#130574 = CARTESIAN_POINT ( 'NONE',  ( 15.72974639402176855, 15.80617190586768217, 26.87609039468567218 ) ) ;
#130575 = CARTESIAN_POINT ( 'NONE',  ( 22.44159573604009594, -16.30477369853687364, 142.1750000027311671 ) ) ;
#130576 = CARTESIAN_POINT ( 'NONE',  ( 8.224510206698742110, 14.34966873604972548, 107.0844237280190043 ) ) ;
#130577 = CARTESIAN_POINT ( 'NONE',  ( 16.55341960407611168, 4.379528057220329451, 113.9572429386477239 ) ) ;
#130578 = CARTESIAN_POINT ( 'NONE',  ( -19.02544592524342804, 5.153800228976336051, 76.04057627198102409 ) ) ;
#130579 = CARTESIAN_POINT ( 'NONE',  ( 16.20063489777861676, -7.373262058553140541, 22.00000000000000711 ) ) ;
#130580 = CARTESIAN_POINT ( 'NONE',  ( 37.99999999999999289, 12.34694845685046793, -10.64999999453762669 ) ) ;
#130581 = CARTESIAN_POINT ( 'NONE',  ( -16.52544592524342804, 4.483927247898546575, 31.04057627198102409 ) ) ;
#130582 = CARTESIAN_POINT ( 'NONE',  ( 21.53943276465977519, 0.05219959533937863772, 56.25109039468568284 ) ) ;
#130583 = CARTESIAN_POINT ( 'NONE',  ( 27.29882810768421919, -25.71095057349885948, -18.52182797988482221 ) ) ;
#130584 = CARTESIAN_POINT ( 'NONE',  ( -10.81492255796105439, 18.62759615963255655, 87.91775706135234714 ) ) ;
#130585 = CARTESIAN_POINT ( 'NONE',  ( -5.049401038298153566, 19.05341960407611168, 50.20724293864770260 ) ) ;
#130586 = CARTESIAN_POINT ( 'NONE',  ( -16.46253265017160317, 9.564922557960807481, 50.83224293864770260 ) ) ;
#130587 = ORIENTED_EDGE ( 'NONE', *, *, #181371, .F. ) ;
#130588 = CARTESIAN_POINT ( 'NONE',  ( 21.55341960407619695, -5.719274019375665929, 96.04275706135236135 ) ) ;
#130589 = CARTESIAN_POINT ( 'NONE',  ( 14.34966873604972726, -8.224510206698740333, 60.83442372801901854 ) ) ;
#130590 = CARTESIAN_POINT ( 'NONE',  ( -21.52544592524334988, -5.823673210054445271, 88.95942372801901854 ) ) ;
#130591 = CARTESIAN_POINT ( 'NONE',  ( 10.81492255796078972, 18.62759615963270932, 24.58224293864768839 ) ) ;
#130592 = CARTESIAN_POINT ( 'NONE',  ( 5.153800228976615827, -19.02544592524334988, 95.20942372801897591 ) ) ;
#130593 = CARTESIAN_POINT ( 'NONE',  ( 21.53943276465977519, 0.05219959533937863772, 66.25109039468567573 ) ) ;
#130594 = CARTESIAN_POINT ( 'NONE',  ( 4.483927247898790824, -16.52544592524335698, 35.20942372801901854 ) ) ;
#130595 = CARTESIAN_POINT ( 'NONE',  ( 21.55341960407610458, 5.719274019375980345, 88.95724293864769550 ) ) ;
#130596 = CARTESIAN_POINT ( 'NONE',  ( 13.97604488694548053, -13.89961937509957401, 80.62609039468567573 ) ) ;
#130597 = CARTESIAN_POINT ( 'NONE',  ( 13.97604488694527802, 13.89961937509977652, 64.37390960531436690 ) ) ;
#130598 = CARTESIAN_POINT ( 'NONE',  ( -9.564922557961040184, 16.46253265017147172, 97.91775706135233293 ) ) ;
#130599 = CIRCLE ( 'NONE', #182456, 40.00000000000002132 ) ;
#130600 = CARTESIAN_POINT ( 'NONE',  ( 5.049401038297881783, 19.05341960407617563, 107.2927570613523187 ) ) ;
#130601 = CARTESIAN_POINT ( 'NONE',  ( 14.29746914071049879, -8.314922557960816363, 53.33224293864769550 ) ) ;
#130602 = EDGE_CURVE ( 'NONE', #166806, #126933, #67622, .T. ) ;
#130603 = CARTESIAN_POINT ( 'NONE',  ( 16.51473224551083163, -9.474510206698727899, 75.83442372801900433 ) ) ;
#130604 = CARTESIAN_POINT ( 'NONE',  ( 4.483927247898790824, -16.52544592524335698, 65.20942372801901854 ) ) ;
#130605 = CARTESIAN_POINT ( 'NONE',  ( -13.89961937509977652, 13.97604488694528158, 35.62390960531435269 ) ) ;
#130606 = CARTESIAN_POINT ( 'NONE',  ( -0.05219959533909027116, -19.03943276465977164, 57.49890960531435979 ) ) ;
#130607 = CARTESIAN_POINT ( 'NONE',  ( 16.55341960407618274, -4.379528057220086978, 56.04275706135235424 ) ) ;
#130608 = CARTESIAN_POINT ( 'NONE',  ( -22.44159573604010305, 16.30477369853692338, 148.6750000027311671 ) ) ;
#130609 = CARTESIAN_POINT ( 'NONE',  ( -5.049401038298153566, 19.05341960407611168, 110.2072429386476671 ) ) ;
#130610 = CARTESIAN_POINT ( 'NONE',  ( 19.05341960407611168, 5.049401038298154454, 23.95724293864769194 ) ) ;
#130611 = ORIENTED_EDGE ( 'NONE', *, *, #18566, .T. ) ;
#130612 = CARTESIAN_POINT ( 'NONE',  ( 13.89961937509957401, 13.97604488694547697, 106.8760903946856757 ) ) ;
#130613 = CARTESIAN_POINT ( 'NONE',  ( -10.81492255796078084, -18.62759615963271287, 42.08224293864769550 ) ) ;
#130615 = CARTESIAN_POINT ( 'NONE',  ( -14.34966873604972548, 8.224510206698743886, 28.33442372801902209 ) ) ;
#130614 = CARTESIAN_POINT ( 'NONE',  ( 9.564922557961047289, -16.46253265017146816, 35.41775706135233293 ) ) ;
#130616 = CARTESIAN_POINT ( 'NONE',  ( 19.03943276465977164, -0.05219959533909143690, 23.74890960531435269 ) ) ;
#130617 = CARTESIAN_POINT ( 'NONE',  ( -9.474510206698964154, 16.51473224551069663, 45.41557627198103120 ) ) ;
#130618 = CARTESIAN_POINT ( 'NONE',  ( -15.72974639402197994, 15.80617190586746368, 75.62390960531439532 ) ) ;
#130619 = CARTESIAN_POINT ( 'NONE',  ( -16.51473224551069308, -9.474510206698971260, 101.6655762719810241 ) ) ;
#130620 = CARTESIAN_POINT ( 'NONE',  ( 19.05341960407611168, 5.049401038298154454, 53.95724293864770260 ) ) ;
#130621 = CARTESIAN_POINT ( 'NONE',  ( 27.73933785331498925, -9.013057229001034898, 144.2750000027311899 ) ) ;
#130622 = CARTESIAN_POINT ( 'NONE',  ( 5.153800228976615827, -19.02544592524334988, 80.20942372801901854 ) ) ;
#130623 = CARTESIAN_POINT ( 'NONE',  ( -16.52544592524342804, 4.483927247898546575, 71.04057627198103830 ) ) ;
#130624 = CARTESIAN_POINT ( 'NONE',  ( 21.52544592524344225, -5.823673210054117533, 48.54057627198103120 ) ) ;
#130625 = CARTESIAN_POINT ( 'NONE',  ( -18.62759615963255300, -10.81492255796106328, 109.1677570613523613 ) ) ;
#130626 = CARTESIAN_POINT ( 'NONE',  ( -5.823673210054116645, -21.52544592524344225, 97.29057627198105251 ) ) ;
#130627 = CARTESIAN_POINT ( 'NONE',  ( -10.72451020669870658, -18.67979575497194134, 69.58442372801900433 ) ) ;
#130628 = B_SPLINE_CURVE_WITH_KNOTS ( 'NONE', 3,
 ( #73957, #130862, #29435, #105270, #91066, #182119, #59753, #122414, #137589, #38870, #90095, #131873, #199272, #12292, #167936, #70206, #152753, #54036, #121423, #14243, #106253, #197296, #75915, #151777, #115710, #74933, #193558, #177398, #58759, #183115, #120428, #136596 ),
 .UNSPECIFIED., .F., .F.,
 ( 4, 2, 2, 2, 2, 2, 2, 2, 2, 2, 2, 2, 2, 2, 2, 4 ),
 ( 2.969368287472575283E-17, 0.0003712461730036904100, 0.0007424923460073511129, 0.001113738519011011653, 0.001484984692014672519, 0.002227477038022000321, 0.002598723211025682003, 0.002969969384029364119, 0.003341215557033045368, 0.003712461730036727917, 0.004083707903040409599, 0.004454954076044090848, 0.004826200249047772964, 0.005197446422051455080, 0.005568692595055137196, 0.005939938768058818444 ),
 .UNSPECIFIED. ) ;
#130629 = CARTESIAN_POINT ( 'NONE',  ( -21.52544592524334988, -5.823673210054445271, 78.95942372801901854 ) ) ;
#130630 = ADVANCED_FACE ( 'NONE', ( #74976 ), #73009, .F. ) ;
#130631 = CARTESIAN_POINT ( 'NONE',  ( 16.51473224551069308, 9.474510206698969483, 114.1655762719810241 ) ) ;
#130633 = CARTESIAN_POINT ( 'NONE',  ( 15.72974639402176855, 15.80617190586768217, 71.87609039468568994 ) ) ;
#130632 = CARTESIAN_POINT ( 'NONE',  ( -0.05219959533934338120, 16.53943276465976808, 112.5010903946857042 ) ) ;
#130634 = CARTESIAN_POINT ( 'NONE',  ( -19.03943276465977164, 0.05219959533909376836, 66.24890960531436690 ) ) ;
#130635 = CARTESIAN_POINT ( 'NONE',  ( -21.53943276465977519, -0.05219959533937600094, 28.75109039468567929 ) ) ;
#130636 = CARTESIAN_POINT ( 'NONE',  ( -5.049401038298153566, 19.05341960407611168, 65.20724293864765286 ) ) ;
#130637 = CARTESIAN_POINT ( 'NONE',  ( 12.14591786802309770, 12.06949235617756955, 74.37390960531436690 ) ) ;
#130638 = CARTESIAN_POINT ( 'NONE',  ( 12.06949235617757843, -12.14591786802309237, 43.12390960531435269 ) ) ;
#130639 = CARTESIAN_POINT ( 'NONE',  ( 15.72974639402199770, -15.80617190586745480, 53.12390960531436690 ) ) ;
#130640 = EDGE_CURVE ( 'NONE', #12139, #197947, #149834, .T. ) ;
#130641 = CARTESIAN_POINT ( 'NONE',  ( -19.05341960407611168, -5.049401038298163336, 61.45724293864769550 ) ) ;
#130642 = CARTESIAN_POINT ( 'NONE',  ( 21.55341960407610458, 5.719274019375980345, 68.95724293864769550 ) ) ;
#130643 = CARTESIAN_POINT ( 'NONE',  ( 19.05341960407617918, -5.049401038297876454, 66.04275706135233293 ) ) ;
#130645 = CARTESIAN_POINT ( 'NONE',  ( 4.483927247898545687, 16.52544592524342804, 64.79057627198103830 ) ) ;
#130644 = CARTESIAN_POINT ( 'NONE',  ( -16.46253265017146816, -9.564922557961047289, 19.16775706135233293 ) ) ;
#130646 = CARTESIAN_POINT ( 'NONE',  ( 18.62759615963271287, -10.81492255796078972, 43.33224293864769550 ) ) ;
#130647 = VERTEX_POINT ( 'NONE', #75959 ) ;
#130648 = LINE ( 'NONE', #126654, #133424 ) ;
#130650 = CARTESIAN_POINT ( 'NONE',  ( 27.73933785331498569, 2.768321779492822058E-14, 140.3750000027311842 ) ) ;
#130649 = CARTESIAN_POINT ( 'NONE',  ( 16.52544592524335698, 4.483927247898782831, 96.45942372801901854 ) ) ;
#130651 = CARTESIAN_POINT ( 'NONE',  ( -13.89961937509957401, -13.97604488694547875, 84.37609039468567573 ) ) ;
#130652 = CARTESIAN_POINT ( 'NONE',  ( 12.06949235617757843, -12.14591786802309237, 73.12390960531436690 ) ) ;
#130653 = CARTESIAN_POINT ( 'NONE',  ( -5.000000000000000000, -130.0000000000000000, 13.99999999999999822 ) ) ;
#130654 = CARTESIAN_POINT ( 'NONE',  ( -5.049401038298153566, 19.05341960407611168, 65.20724293864765286 ) ) ;
#130655 = CARTESIAN_POINT ( 'NONE',  ( -14.34966873604960291, -8.224510206698953496, 51.66557627198102409 ) ) ;
#130656 = CARTESIAN_POINT ( 'NONE',  ( -5.153800228976328057, -19.02544592524343514, 82.29057627198103830 ) ) ;
#130657 = AXIS2_PLACEMENT_3D ( 'NONE', #105058, #167724, #103066 ) ;
#130659 = CARTESIAN_POINT ( 'NONE',  ( 0.05219959533909260263, 19.03943276465977164, 49.99890960531435979 ) ) ;
#130658 = CARTESIAN_POINT ( 'NONE',  ( 13.97604488694548053, -13.89961937509957401, 75.62609039468564731 ) ) ;
#130660 = CARTESIAN_POINT ( 'NONE',  ( -9.474510206698964154, 16.51473224551069663, 80.41557627198103830 ) ) ;
#130661 = CARTESIAN_POINT ( 'NONE',  ( -16.51473224551069308, -9.474510206698971260, 21.66557627198102765 ) ) ;
#130662 = CARTESIAN_POINT ( 'NONE',  ( -19.05341960407611168, -5.049401038298163336, 66.45724293864769550 ) ) ;
#130663 = CARTESIAN_POINT ( 'NONE',  ( -21.53943276465977519, 0.05219959533907696930, 56.24890960531436690 ) ) ;
#130664 = CARTESIAN_POINT ( 'NONE',  ( -16.46253265017160317, 9.564922557960807481, 45.83224293864769550 ) ) ;
#130665 = CARTESIAN_POINT ( 'NONE',  ( 21.52544592524344225, -5.823673210054117533, 53.54057627198103120 ) ) ;
#130666 = CARTESIAN_POINT ( 'NONE',  ( 9.564922557961047289, -16.46253265017146816, 80.41775706135234714 ) ) ;
#130667 = CARTESIAN_POINT ( 'NONE',  ( -8.314922557961024197, 14.29746914071037800, 102.9177570613523756 ) ) ;
#130668 = CARTESIAN_POINT ( 'NONE',  ( 9.474510206698729675, 16.51473224551082808, 42.08442372801900433 ) ) ;
#130670 = CARTESIAN_POINT ( 'NONE',  ( -16.53943276465976808, -0.05219959533934237506, 98.75109039468568994 ) ) ;
#130669 = CARTESIAN_POINT ( 'NONE',  ( -0.05219959533934338120, 16.53943276465976808, 57.50109039468568994 ) ) ;
#130671 = CARTESIAN_POINT ( 'NONE',  ( 18.39443945427631277, -5.499999999999984013, 41.01745347608650860 ) ) ;
#130672 = CARTESIAN_POINT ( 'NONE',  ( 14.29746914071037800, 8.314922557961029526, 76.66775706135234714 ) ) ;
#130673 = CARTESIAN_POINT ( 'NONE',  ( -5.719274019375978568, 21.55341960407610458, 30.20724293864769550 ) ) ;
#130674 = CARTESIAN_POINT ( 'NONE',  ( -19.05341960407611168, -5.049401038298163336, 31.45724293864769550 ) ) ;
#130675 = CARTESIAN_POINT ( 'NONE',  ( -16.53943276465976808, -0.05219959533934237506, 33.75109039468568284 ) ) ;
#130676 = CARTESIAN_POINT ( 'NONE',  ( 9.564922557960805705, 16.46253265017160317, 44.58224293864769550 ) ) ;
#130677 = CARTESIAN_POINT ( 'NONE',  ( -18.67979575497193778, 10.72451020669871902, 43.33442372801901143 ) ) ;
#130678 = CARTESIAN_POINT ( 'NONE',  ( -16.52544592524335698, -4.483927247898792601, 43.95942372801902565 ) ) ;
#130679 = CARTESIAN_POINT ( 'NONE',  ( -8.314922557960811034, -14.29746914071050412, 22.08224293864769194 ) ) ;
#130680 = CARTESIAN_POINT ( 'NONE',  ( 5.153800228976335163, 19.02544592524342804, 24.79057627198102765 ) ) ;
#130681 = CARTESIAN_POINT ( 'NONE',  ( 16.46253265017146816, 9.564922557961045513, 21.66775706135233648 ) ) ;
#130682 = CARTESIAN_POINT ( 'NONE',  ( 13.97604488694548053, -13.89961937509957401, 110.6260903946856615 ) ) ;
#130683 = CARTESIAN_POINT ( 'NONE',  ( -9.564922557961040184, 16.46253265017147172, 67.91775706135233293 ) ) ;
#130684 = CARTESIAN_POINT ( 'NONE',  ( 14.34966873604960469, 8.224510206698951720, 69.16557627198102409 ) ) ;
#130685 = CARTESIAN_POINT ( 'NONE',  ( 5.049401038298161559, -19.05341960407611168, 42.70724293864767418 ) ) ;
#130687 = DIRECTION ( 'NONE',  ( 0.000000000000000000, 0.7071067811865466846, 0.7071067811865484609 ) ) ;
#130686 = CARTESIAN_POINT ( 'NONE',  ( 13.97604488694548053, -13.89961937509957401, 80.62609039468567573 ) ) ;
#130688 = CARTESIAN_POINT ( 'NONE',  ( 21.53943276465977519, 0.05219959533937863772, 66.25109039468567573 ) ) ;
#130689 = CARTESIAN_POINT ( 'NONE',  ( 16.52544592524335698, 4.483927247898782831, 46.45942372801901854 ) ) ;
#130690 = CARTESIAN_POINT ( 'NONE',  ( 19.52837319214028255, -5.499999999999890754, 57.10471352585541638 ) ) ;
#130691 = CARTESIAN_POINT ( 'NONE',  ( -21.55341960407610458, -5.719274019375992779, 31.45724293864769550 ) ) ;
#130692 = CARTESIAN_POINT ( 'NONE',  ( 16.53943276465976808, 0.05219959533934440121, 26.25109039468567573 ) ) ;
#130693 = CARTESIAN_POINT ( 'NONE',  ( -27.19095269391954517, -8.032454009542490780, 149.5864051666458181 ) ) ;
#130694 = CARTESIAN_POINT ( 'NONE',  ( -21.97054992548845576, 8.562709642470919036, 171.7904333278019351 ) ) ;
#130695 = CARTESIAN_POINT ( 'NONE',  ( 19.03943276465977164, -0.05219959533909143690, 43.74890960531435979 ) ) ;
#130696 = CARTESIAN_POINT ( 'NONE',  ( -0.05219959533937732626, 21.53943276465977519, 107.5010903946856899 ) ) ;
#130697 = CARTESIAN_POINT ( 'NONE',  ( -13.89961937509977652, 13.97604488694528158, 50.62390960531435979 ) ) ;
#130698 = CARTESIAN_POINT ( 'NONE',  ( -10.72451020669870658, -18.67979575497194134, 69.58442372801900433 ) ) ;
#130699 = CARTESIAN_POINT ( 'NONE',  ( 21.52544592524334988, 5.823673210054432836, 106.4594237280190328 ) ) ;
#130700 = CARTESIAN_POINT ( 'NONE',  ( -16.55341960407617563, 4.379528057220093196, 113.5427570613523756 ) ) ;
#130701 = CARTESIAN_POINT ( 'NONE',  ( -13.89961937509977652, 13.97604488694528158, 35.62390960531435269 ) ) ;
#130702 = CARTESIAN_POINT ( 'NONE',  ( -19.05341960407611168, -5.049401038298163336, 86.45724293864769550 ) ) ;
#130703 = CARTESIAN_POINT ( 'NONE',  ( 21.52544592524334988, 5.823673210054432836, 51.45942372801901854 ) ) ;
#130704 = CARTESIAN_POINT ( 'NONE',  ( -9.564922557960796823, -16.46253265017161027, 32.08224293864769550 ) ) ;
#130705 = B_SPLINE_CURVE_WITH_KNOTS ( 'NONE', 3,
 ( #130478, #191176, #98131, #176016, #128483, #178013, #7136, #131490, #66820, #52650, #192175, #175010, #177024, #117324, #36474, #39480 ),
 .UNSPECIFIED., .F., .F.,
 ( 4, 2, 2, 2, 2, 2, 2, 4 ),
 ( 0.001218919368246023033, 0.002217820489337911892, 0.002717271049883857731, 0.003216721610429803570, 0.003716172170975749409, 0.004215622731521694380, 0.004715073292067640219, 0.005214523852613586058 ),
 .UNSPECIFIED. ) ;
#130706 = CARTESIAN_POINT ( 'NONE',  ( -18.67979575497193778, 10.72451020669871902, 48.33442372801902565 ) ) ;
#130708 = CARTESIAN_POINT ( 'NONE',  ( -5.153800228976328057, -19.02544592524343514, 107.2905762719810383 ) ) ;
#130707 = CARTESIAN_POINT ( 'NONE',  ( -16.46253265017146816, -9.564922557961047289, 94.16775706135233293 ) ) ;
#130709 = CARTESIAN_POINT ( 'NONE',  ( 19.05341960407611168, 5.049401038298154454, 23.95724293864769194 ) ) ;
#130710 = CARTESIAN_POINT ( 'NONE',  ( -21.52544592524343514, 5.823673210054127303, 111.0405762719810525 ) ) ;
#130711 = CARTESIAN_POINT ( 'NONE',  ( 16.46253265017146816, 9.564922557961045513, 31.66775706135232937 ) ) ;
#130712 = CARTESIAN_POINT ( 'NONE',  ( 16.52544592524342804, -4.483927247898539470, 113.5405762719810383 ) ) ;
#130713 = CARTESIAN_POINT ( 'NONE',  ( -0.05219959533909027116, -19.03943276465977164, 62.49890960531435979 ) ) ;
#130715 = AXIS2_PLACEMENT_3D ( 'NONE', #60072, #2371, #48888 ) ;
#130714 = CARTESIAN_POINT ( 'NONE',  ( 13.89961937509957401, 13.97604488694547697, 91.87609039468567573 ) ) ;
#130716 = CARTESIAN_POINT ( 'NONE',  ( -4.379528057220328563, 16.55341960407611168, 65.20724293864768129 ) ) ;
#130717 = CARTESIAN_POINT ( 'NONE',  ( 5.049401038297881783, 19.05341960407617563, 27.29275706135232937 ) ) ;
#130718 = CARTESIAN_POINT ( 'NONE',  ( 5.049401038298161559, -19.05341960407611168, 112.7072429386476813 ) ) ;
#130719 = CARTESIAN_POINT ( 'NONE',  ( -9.474510206698720793, -16.51473224551083518, 94.58442372801900433 ) ) ;
#130720 = CARTESIAN_POINT ( 'NONE',  ( -21.53943276465977519, 0.05219959533907696930, 91.24890960531436690 ) ) ;
#130721 = CIRCLE ( 'NONE', #121057, 7.500000000000000000 ) ;
#130722 = CARTESIAN_POINT ( 'NONE',  ( 15.80617190586769283, -15.72974639402175789, 45.62609039468567573 ) ) ;
#130723 = CARTESIAN_POINT ( 'NONE',  ( -4.483927247898782831, 16.52544592524335698, 42.70942372801901854 ) ) ;
#130724 = CARTESIAN_POINT ( 'NONE',  ( -0.05219959533934338120, 16.53943276465976808, 102.5010903946856899 ) ) ;
#130726 = CARTESIAN_POINT ( 'NONE',  ( -10.72451020669870658, -18.67979575497194134, 49.58442372801901143 ) ) ;
#130725 = CARTESIAN_POINT ( 'NONE',  ( 4.483927247898790824, -16.52544592524335698, 45.20942372801901854 ) ) ;
#130727 = CARTESIAN_POINT ( 'NONE',  ( -21.55341960407610458, -5.719274019375992779, 51.45724293864770260 ) ) ;
#130728 = CARTESIAN_POINT ( 'NONE',  ( 13.89961937509977652, -13.97604488694527269, 28.12390960531435624 ) ) ;
#130729 = CARTESIAN_POINT ( 'NONE',  ( 38.00000000000000000, 12.34694845685046616, -6.649999994537624914 ) ) ;
#130730 = CARTESIAN_POINT ( 'NONE',  ( 0.05219959533934541429, -16.53943276465976808, 60.00109039468568284 ) ) ;
#130731 = CARTESIAN_POINT ( 'NONE',  ( 10.72451020669898902, -18.67979575497178502, 87.91557627198103830 ) ) ;
#130732 = CARTESIAN_POINT ( 'NONE',  ( 4.483927247898545687, 16.52544592524342804, 39.79057627198103830 ) ) ;
#130733 = CARTESIAN_POINT ( 'NONE',  ( -8.224510206698735004, -14.34966873604973081, 59.58442372801901854 ) ) ;
#130734 = CARTESIAN_POINT ( 'NONE',  ( -19.05341960407617563, 5.049401038297882671, 103.5427570613523329 ) ) ;
#130735 = CARTESIAN_POINT ( 'NONE',  ( 5.719274019375991003, -21.55341960407610458, 97.70724293864772392 ) ) ;
#130736 = CARTESIAN_POINT ( 'NONE',  ( 16.53943276465976808, -0.05219959533910856209, 33.74890960531436690 ) ) ;
#130737 = EDGE_LOOP ( 'NONE', ( #165681, #38569, #71952, #45156 ) ) ;
#130738 = CARTESIAN_POINT ( 'NONE',  ( -16.53943276465976808, -0.05219959533934237506, 73.75109039468567573 ) ) ;
#130739 = CARTESIAN_POINT ( 'NONE',  ( 23.03403192006594224, 14.65170476119024201, 169.9999999999999716 ) ) ;
#130740 = CARTESIAN_POINT ( 'NONE',  ( -18.62759615963270932, 10.81492255796079327, 70.83224293864770971 ) ) ;
#130741 = CARTESIAN_POINT ( 'NONE',  ( 16.52544592524335698, 4.483927247898782831, 101.4594237280190185 ) ) ;
#130742 = ORIENTED_EDGE ( 'NONE', *, *, #170510, .F. ) ;
#130743 = CARTESIAN_POINT ( 'NONE',  ( 19.20446147854527297, 5.499999999999894307, 86.88999695167679249 ) ) ;
#130744 = CARTESIAN_POINT ( 'NONE',  ( 21.55341960407610458, 5.719274019375980345, 93.95724293864770971 ) ) ;
#130745 = CARTESIAN_POINT ( 'NONE',  ( -18.62759615963270932, 10.81492255796079327, 105.8322429386476955 ) ) ;
#130746 = CARTESIAN_POINT ( 'NONE',  ( 12.14591786802309770, 12.06949235617756955, 39.37390960531436690 ) ) ;
#130748 = CARTESIAN_POINT ( 'NONE',  ( -14.29746914071037622, -8.314922557961029526, 39.16775706135235424 ) ) ;
#130747 = CIRCLE ( 'NONE', #108085, 4.000000000000000888 ) ;
#130749 = CARTESIAN_POINT ( 'NONE',  ( -19.05341960407611168, -5.049401038298163336, 46.45724293864768129 ) ) ;
#130750 = CARTESIAN_POINT ( 'NONE',  ( 19.03943276465977164, -0.05219959533909143690, 63.74890960531435979 ) ) ;
#130751 = CARTESIAN_POINT ( 'NONE',  ( 13.97604488694527802, 13.89961937509977652, 114.3739096053143669 ) ) ;
#130752 = CARTESIAN_POINT ( 'NONE',  ( -9.474510206698964154, 16.51473224551069663, 115.4155762719810241 ) ) ;
#130753 = CARTESIAN_POINT ( 'NONE',  ( -9.564922557961040184, 16.46253265017147172, 102.9177570613523329 ) ) ;
#130754 = CARTESIAN_POINT ( 'NONE',  ( -19.02544592524334988, -5.153800228976617603, 48.95942372801900433 ) ) ;
#130755 = CARTESIAN_POINT ( 'NONE',  ( 18.67979575497178502, 10.72451020669898547, 94.16557627198103830 ) ) ;
#130756 = CARTESIAN_POINT ( 'NONE',  ( -12.06949235617756955, 12.14591786802309770, 25.62390960531435624 ) ) ;
#130757 = CARTESIAN_POINT ( 'NONE',  ( 10.72451020669898902, -18.67979575497178502, 42.91557627198103120 ) ) ;
#130759 = CARTESIAN_POINT ( 'NONE',  ( -5.049401038297874678, -19.05341960407617918, 109.7927570613523187 ) ) ;
#130758 = CARTESIAN_POINT ( 'NONE',  ( 18.67979575497178502, 10.72451020669898547, 84.16557627198103830 ) ) ;
#130760 = CARTESIAN_POINT ( 'NONE',  ( -5.049401038298153566, 19.05341960407611168, 105.2072429386476671 ) ) ;
#130761 = CARTESIAN_POINT ( 'NONE',  ( 5.823673210054444382, -21.52544592524334988, 75.20942372801901854 ) ) ;
#130762 = CARTESIAN_POINT ( 'NONE',  ( 13.89961937509977652, -13.97604488694527269, 68.12390960531436690 ) ) ;
#130763 = DIRECTION ( 'NONE',  ( 0.000000000000000000, 0.000000000000000000, -1.000000000000000000 ) ) ;
#130764 = CARTESIAN_POINT ( 'NONE',  ( -5.049401038298153566, 19.05341960407611168, 70.20724293864769550 ) ) ;
#130765 = CARTESIAN_POINT ( 'NONE',  ( -8.224510206698948167, 14.34966873604960824, 85.41557627198102409 ) ) ;
#130766 = EDGE_LOOP ( 'NONE', ( #117109, #95511, #184232 ) ) ;
#130767 = CARTESIAN_POINT ( 'NONE',  ( -9.474510206698720793, -16.51473224551083518, 104.5844237280190043 ) ) ;
#130768 = CARTESIAN_POINT ( 'NONE',  ( 16.18388926212238488, -7.379444403734519931, 82.06046848633847901 ) ) ;
#130769 = CARTESIAN_POINT ( 'NONE',  ( 19.05341960407611168, 5.049401038298154454, 68.95724293864769550 ) ) ;
#130771 = CARTESIAN_POINT ( 'NONE',  ( -9.564922557960796823, -16.46253265017161027, 97.08224293864769550 ) ) ;
#130770 = CARTESIAN_POINT ( 'NONE',  ( -5.719274019375665041, -21.55341960407619695, 84.79275706135234714 ) ) ;
#130772 = CARTESIAN_POINT ( 'NONE',  ( 8.224510206698742110, 14.34966873604972548, 82.08442372801901854 ) ) ;
#130773 = CARTESIAN_POINT ( 'NONE',  ( -31.90000000000003411, 3.219216299777112361E-13, -45.64921306006598201 ) ) ;
#130774 = CARTESIAN_POINT ( 'NONE',  ( -5.153800228976607833, 19.02544592524334988, 62.70942372801899722 ) ) ;
#130775 = CARTESIAN_POINT ( 'NONE',  ( -15.72974639402176322, -15.80617190586768395, 94.37609039468568994 ) ) ;
#130776 = DIRECTION ( 'NONE',  ( 1.000000000000000000, 0.000000000000000000, 0.000000000000000000 ) ) ;
#130777 = LINE ( 'NONE', #113605, #198340 ) ;
#130778 = CARTESIAN_POINT ( 'NONE',  ( -11.40812507854755609, 35.11059874428196537, -5.524999997268813523 ) ) ;
#130779 = CARTESIAN_POINT ( 'NONE',  ( -4.379528057220086978, -16.55341960407618274, 109.7927570613523613 ) ) ;
#130780 = CARTESIAN_POINT ( 'NONE',  ( 0.05219959533936267826, -19.03943276465977164, 75.00109039468566152 ) ) ;
#130781 = CARTESIAN_POINT ( 'NONE',  ( 0.05219959533934541429, -16.53943276465976808, 90.00109039468567573 ) ) ;
#130782 = CARTESIAN_POINT ( 'NONE',  ( -0.3535533905929095222, 35.00000000000000000, 4.646446609406721606 ) ) ;
#130783 = CARTESIAN_POINT ( 'NONE',  ( -12.14591786802326823, 12.06949235617739902, 73.12609039468567573 ) ) ;
#130784 = CARTESIAN_POINT ( 'NONE',  ( 5.719274019375673035, 21.55341960407619339, 82.29275706135234714 ) ) ;
#130785 = CARTESIAN_POINT ( 'NONE',  ( 19.03943276465977164, 0.05219959533936151252, 86.25109039468567573 ) ) ;
#130786 = CARTESIAN_POINT ( 'NONE',  ( -19.05341960407617563, 5.049401038297882671, 33.54275706135231871 ) ) ;
#130787 = AXIS2_PLACEMENT_3D ( 'NONE', #5395, #20571, #124778 ) ;
#130788 = CARTESIAN_POINT ( 'NONE',  ( -19.03943276465977164, 0.05219959533909376836, 66.24890960531436690 ) ) ;
#130789 = CARTESIAN_POINT ( 'NONE',  ( -5.049401038298153566, 19.05341960407611168, 55.20724293864769550 ) ) ;
#130790 = CARTESIAN_POINT ( 'NONE',  ( -16.51473224551069308, -9.474510206698971260, 86.66557627198102409 ) ) ;
#130791 = CARTESIAN_POINT ( 'NONE',  ( 10.72451020669898902, -18.67979575497178502, 82.91557627198103830 ) ) ;
#130792 = CARTESIAN_POINT ( 'NONE',  ( -18.62759615963270932, 10.81492255796079327, 50.83224293864770971 ) ) ;
#130793 = CARTESIAN_POINT ( 'NONE',  ( 5.049401038298161559, -19.05341960407611168, 27.70724293864769550 ) ) ;
#130794 = CARTESIAN_POINT ( 'NONE',  ( 4.483927247898790824, -16.52544592524335698, 70.20942372801904696 ) ) ;
#130795 = UNCERTAINTY_MEASURE_WITH_UNIT (LENGTH_MEASURE( 1.000000000000000082E-05 ), #151754, 'distance_accuracy_value', 'NONE');
#130796 = VERTEX_POINT ( 'NONE', #196364 ) ;
#130797 = CARTESIAN_POINT ( 'NONE',  ( 18.67979575497194134, -10.72451020669871369, 45.83442372801901854 ) ) ;
#130798 = CONICAL_SURFACE ( 'NONE', #43654, 2.500000000000002220, 1.029744258676656754 ) ;
#130800 = CARTESIAN_POINT ( 'NONE',  ( -38.00000000000000711, 2.428612866367529932E-14, -2.000000000000000000 ) ) ;
#130799 = CARTESIAN_POINT ( 'NONE',  ( -8.224510206698948167, 14.34966873604960824, 60.41557627198102409 ) ) ;
#130801 = CARTESIAN_POINT ( 'NONE',  ( 12.06949235617739724, 12.14591786802326823, 41.87609039468568284 ) ) ;
#130802 = CARTESIAN_POINT ( 'NONE',  ( 5.049401038297881783, 19.05341960407617563, 57.29275706135231871 ) ) ;
#130803 = CARTESIAN_POINT ( 'NONE',  ( 16.55341960407611168, 4.379528057220329451, 53.95724293864770260 ) ) ;
#130804 = CARTESIAN_POINT ( 'NONE',  ( 18.62759615963255655, 10.81492255796105972, 36.66775706135234714 ) ) ;
#130806 = CARTESIAN_POINT ( 'NONE',  ( 5.719274019375991003, -21.55341960407610458, 87.70724293864769550 ) ) ;
#130805 = DIRECTION ( 'NONE',  ( 1.000000000000000000, 0.000000000000000000, -0.000000000000000000 ) ) ;
#130807 = CARTESIAN_POINT ( 'NONE',  ( 19.02544592524343514, -5.153800228976328945, 103.5405762719809957 ) ) ;
#130808 = CARTESIAN_POINT ( 'NONE',  ( 0.05219959533910956823, 16.53943276465976808, 79.99890960531435269 ) ) ;
#130809 = CARTESIAN_POINT ( 'NONE',  ( 29.21837264310193305, -26.94013878454481414, -20.44914777673364981 ) ) ;
#130810 = CARTESIAN_POINT ( 'NONE',  ( -29.86685920354755197, -21.69954338932560134, -6.424999997268812990 ) ) ;
#130811 = CARTESIAN_POINT ( 'NONE',  ( 16.46253265017146816, 9.564922557961045513, 66.66775706135233293 ) ) ;
#130812 = CARTESIAN_POINT ( 'NONE',  ( -21.53943276465977519, -0.05219959533937600094, 18.75109039468568639 ) ) ;
#130813 = CARTESIAN_POINT ( 'NONE',  ( -0.05219959533909027116, -19.03943276465977164, 57.49890960531435979 ) ) ;
#130814 = CARTESIAN_POINT ( 'NONE',  ( 19.03943276465977164, 0.05219959533936151252, 61.25109039468566863 ) ) ;
#130815 = CARTESIAN_POINT ( 'NONE',  ( 9.474510206698971260, -16.51473224551069308, 27.91557627198103120 ) ) ;
#130816 = CARTESIAN_POINT ( 'NONE',  ( 5.823673210054444382, -21.52544592524334988, 70.20942372801904696 ) ) ;
#130817 = CARTESIAN_POINT ( 'NONE',  ( -16.21995358207302829, -7.366697692864232039, 70.06448998487846325 ) ) ;
#130818 = CARTESIAN_POINT ( 'NONE',  ( -12.14591786802309592, -12.06949235617757132, 51.87390960531437401 ) ) ;
#130819 = CARTESIAN_POINT ( 'NONE',  ( -5.049401038298153566, 19.05341960407611168, 60.20724293864768129 ) ) ;
#130820 = CARTESIAN_POINT ( 'NONE',  ( -21.53943276465977519, 0.05219959533907696930, 91.24890960531436690 ) ) ;
#130821 = CARTESIAN_POINT ( 'NONE',  ( 9.474510206698971260, -16.51473224551069308, 52.91557627198102409 ) ) ;
#130822 = ORIENTED_EDGE ( 'NONE', *, *, #94296, .T. ) ;
#130823 = CARTESIAN_POINT ( 'NONE',  ( 5.823673210054125526, 21.52544592524343514, 79.79057627198102409 ) ) ;
#130824 = EDGE_LOOP ( 'NONE', ( #111963, #178898, #57395, #35131 ) ) ;
#130825 = CARTESIAN_POINT ( 'NONE',  ( -18.67979575497193778, 10.72451020669871902, 103.3344237280190043 ) ) ;
#130828 = CARTESIAN_POINT ( 'NONE',  ( 14.34966873604960469, 8.224510206698951720, 94.16557627198103830 ) ) ;
#130827 = CARTESIAN_POINT ( 'NONE',  ( -16.52544592524335698, -4.483927247898792601, 93.95942372801903275 ) ) ;
#130826 = CARTESIAN_POINT ( 'NONE',  ( 9.474510206698971260, -16.51473224551069308, 22.91557627198102765 ) ) ;
#130829 = CARTESIAN_POINT ( 'NONE',  ( -9.564922557961040184, 16.46253265017147172, 97.91775706135233293 ) ) ;
#130830 = ORIENTED_EDGE ( 'NONE', *, *, #131641, .F. ) ;
#130831 = CARTESIAN_POINT ( 'NONE',  ( 10.72451020669871369, 18.67979575497193778, 22.08442372801901143 ) ) ;
#130832 = CARTESIAN_POINT ( 'NONE',  ( -5.153800228976607833, 19.02544592524334988, 37.70942372801899722 ) ) ;
#130833 = CARTESIAN_POINT ( 'NONE',  ( -14.34966873604972548, 8.224510206698743886, 103.3344237280190043 ) ) ;
#130834 = CARTESIAN_POINT ( 'NONE',  ( -16.46253265017146816, -9.564922557961047289, 29.16775706135232937 ) ) ;
#130835 = CARTESIAN_POINT ( 'NONE',  ( -9.564922557960796823, -16.46253265017161027, 92.08224293864769550 ) ) ;
#130836 = CARTESIAN_POINT ( 'NONE',  ( -0.05219959533907301413, -21.53943276465977519, 67.49890960531436690 ) ) ;
#130837 = CARTESIAN_POINT ( 'NONE',  ( -19.01533133064921088, 5.499999999999432454, 48.76586590595736226 ) ) ;
#130838 = CARTESIAN_POINT ( 'NONE',  ( -19.05341960407611168, -5.049401038298163336, 21.45724293864768839 ) ) ;
#130839 = CARTESIAN_POINT ( 'NONE',  ( -16.46253265017146816, -9.564922557961047289, 19.16775706135233293 ) ) ;
#130840 = CARTESIAN_POINT ( 'NONE',  ( 16.55341960407618274, -4.379528057220086978, 81.04275706135236135 ) ) ;
#130841 = CARTESIAN_POINT ( 'NONE',  ( -0.05219959533937732626, 21.53943276465977519, 22.50109039468567573 ) ) ;
#130842 = CARTESIAN_POINT ( 'NONE',  ( -14.29746914071037622, -8.314922557961029526, 29.16775706135234003 ) ) ;
#130843 = CARTESIAN_POINT ( 'NONE',  ( 5.049401038298161559, -19.05341960407611168, 107.7072429386476955 ) ) ;
#130844 = CARTESIAN_POINT ( 'NONE',  ( -13.89961937509977652, 13.97604488694528158, 40.62390960531435979 ) ) ;
#130845 = CARTESIAN_POINT ( 'NONE',  ( -5.049401038298153566, 19.05341960407611168, 70.20724293864769550 ) ) ;
#130846 = CARTESIAN_POINT ( 'NONE',  ( 8.314922557961029526, -14.29746914071037800, 45.41775706135234003 ) ) ;
#130847 = CARTESIAN_POINT ( 'NONE',  ( -8.314922557960811034, -14.29746914071050412, 87.08224293864769550 ) ) ;
#130848 = CARTESIAN_POINT ( 'NONE',  ( 16.55341960407618274, -4.379528057220086978, 96.04275706135236135 ) ) ;
#130851 = CARTESIAN_POINT ( 'NONE',  ( -13.89961937509977652, 13.97604488694528158, 70.62390960531432427 ) ) ;
#130850 = CARTESIAN_POINT ( 'NONE',  ( -19.03943276465977164, 0.05219959533909376836, 76.24890960531435269 ) ) ;
#130849 = CARTESIAN_POINT ( 'NONE',  ( -15.80617190586768217, 15.72974639402176855, 58.12609039468568994 ) ) ;
#130852 = CARTESIAN_POINT ( 'NONE',  ( -19.02544592524342804, 5.153800228976336051, 101.0405762719810241 ) ) ;
#130853 = CARTESIAN_POINT ( 'NONE',  ( -16.55341960407611168, -4.379528057220339221, 46.45724293864769550 ) ) ;
#130854 = CARTESIAN_POINT ( 'NONE',  ( -4.379528057220086978, -16.55341960407618274, 94.79275706135234714 ) ) ;
#130855 = ORIENTED_EDGE ( 'NONE', *, *, #37807, .T. ) ;
#130856 = CARTESIAN_POINT ( 'NONE',  ( 13.89961937509957401, 13.97604488694547697, 46.87609039468565442 ) ) ;
#130858 = AXIS2_PLACEMENT_3D ( 'NONE', #103367, #149866, #150874 ) ;
#130857 = CARTESIAN_POINT ( 'NONE',  ( 9.564922557960805705, 16.46253265017160317, 114.5822429386476955 ) ) ;
#130859 = CARTESIAN_POINT ( 'NONE',  ( -9.564922557960796823, -16.46253265017161027, 62.08224293864769550 ) ) ;
#130860 = CARTESIAN_POINT ( 'NONE',  ( 0.05219959533936267826, -19.03943276465977164, 45.00109039468566863 ) ) ;
#130861 = CARTESIAN_POINT ( 'NONE',  ( -29.86685920354755197, -21.69954338932560134, -8.424999997268812990 ) ) ;
#130862 = CARTESIAN_POINT ( 'NONE',  ( -17.49999999999998934, -5.624438216177606087, 64.18329655085355512 ) ) ;
#130863 = CARTESIAN_POINT ( 'NONE',  ( -14.29746914071037622, -8.314922557961029526, 59.16775706135234714 ) ) ;
#130864 = VECTOR ( 'NONE', #97426, 1000.000000000000000 ) ;
#130866 = CARTESIAN_POINT ( 'NONE',  ( 12.06949235617739724, 12.14591786802326823, 71.87609039468568994 ) ) ;
#130865 = CARTESIAN_POINT ( 'NONE',  ( 0.05219959533936267826, -19.03943276465977164, 70.00109039468566152 ) ) ;
#130867 = CARTESIAN_POINT ( 'NONE',  ( 17.40805194822030799, 6.112264579159338851, 91.66628727489390371 ) ) ;
#130868 = CARTESIAN_POINT ( 'NONE',  ( 16.51473224551069308, 9.474510206698969483, 84.16557627198102409 ) ) ;
#130869 = CARTESIAN_POINT ( 'NONE',  ( -5.823673210054431948, 21.52544592524334988, 27.70942372801901854 ) ) ;
#130870 = CARTESIAN_POINT ( 'NONE',  ( -0.05219959533936034679, 19.03943276465977164, 77.50109039468566152 ) ) ;
#130872 = CARTESIAN_POINT ( 'NONE',  ( 16.51473224551069308, 9.474510206698969483, 39.16557627198103120 ) ) ;
#130871 = CARTESIAN_POINT ( 'NONE',  ( -16.51473224551069308, -9.474510206698971260, 106.6655762719810383 ) ) ;
#130873 = CARTESIAN_POINT ( 'NONE',  ( 9.564922557960805705, 16.46253265017160317, 94.58224293864769550 ) ) ;
#130875 = CARTESIAN_POINT ( 'NONE',  ( -19.02544592524342804, 5.153800228976336051, 41.04057627198103120 ) ) ;
#130874 = CARTESIAN_POINT ( 'NONE',  ( 8.224510206698953496, -14.34966873604960469, 47.91557627198102409 ) ) ;
#130876 = CARTESIAN_POINT ( 'NONE',  ( 9.564922557961047289, -16.46253265017146816, 45.41775706135232582 ) ) ;
#130877 = CARTESIAN_POINT ( 'NONE',  ( 14.34966873604960469, 8.224510206698951720, 94.16557627198103830 ) ) ;
#130878 = CARTESIAN_POINT ( 'NONE',  ( 18.67979575497194134, -10.72451020669871369, 110.8344237280190043 ) ) ;
#130879 = CARTESIAN_POINT ( 'NONE',  ( 19.05341960407611168, 5.049401038298154454, 53.95724293864770260 ) ) ;
#130880 = ADVANCED_FACE ( 'NONE', ( #121467, #148844 ), #103333, .T. ) ;
#130881 = CARTESIAN_POINT ( 'NONE',  ( 21.53943276465977519, -0.05219959533907433946, 58.74890960531436690 ) ) ;
#130883 = CARTESIAN_POINT ( 'NONE',  ( 16.51473224551083163, -9.474510206698727899, 20.83442372801899722 ) ) ;
#130882 = CARTESIAN_POINT ( 'NONE',  ( 14.34966873604960469, 8.224510206698951720, 49.16557627198102409 ) ) ;
#130884 = CARTESIAN_POINT ( 'NONE',  ( -5.049401038298153566, 19.05341960407611168, 105.2072429386476671 ) ) ;
#130885 = CARTESIAN_POINT ( 'NONE',  ( -5.049401038298153566, 19.05341960407611168, 110.2072429386476671 ) ) ;
#130886 = CARTESIAN_POINT ( 'NONE',  ( 5.049401038298161559, -19.05341960407611168, 52.70724293864767418 ) ) ;
#130887 = CARTESIAN_POINT ( 'NONE',  ( -13.89961937509977652, 13.97604488694528158, 25.62390960531434558 ) ) ;
#130888 = CARTESIAN_POINT ( 'NONE',  ( -14.34966873604960291, -8.224510206698953496, 91.66557627198103830 ) ) ;
#130889 = CARTESIAN_POINT ( 'NONE',  ( -5.719274019375978568, 21.55341960407610458, 100.2072429386476955 ) ) ;
#130890 = CARTESIAN_POINT ( 'NONE',  ( 13.89961937509977652, -13.97604488694527269, 98.12390960531433848 ) ) ;
#130891 = CARTESIAN_POINT ( 'NONE',  ( -10.72451020669870658, -18.67979575497194134, 19.58442372801901143 ) ) ;
#130892 = CARTESIAN_POINT ( 'NONE',  ( 5.153800228976335163, 19.02544592524342804, 109.7905762719810099 ) ) ;
#130893 = CARTESIAN_POINT ( 'NONE',  ( 16.51473224551069308, 9.474510206698969483, 24.16557627198102765 ) ) ;
#130894 = CARTESIAN_POINT ( 'NONE',  ( -10.81492255796105439, 18.62759615963255655, 77.91775706135231871 ) ) ;
#130895 = CARTESIAN_POINT ( 'NONE',  ( -21.53943276465977519, 0.05219959533907696930, 91.24890960531436690 ) ) ;
#130896 = CARTESIAN_POINT ( 'NONE',  ( 17.50000000000000355, -5.624438216177586547, 108.3167034491464591 ) ) ;
#130897 = DIRECTION ( 'NONE',  ( -0.000000000000000000, -0.000000000000000000, 1.000000000000000000 ) ) ;
#130898 = CARTESIAN_POINT ( 'NONE',  ( 31.49504140153652898, -1.029908246020218687, -49.63772645510939441 ) ) ;
#130899 = CARTESIAN_POINT ( 'NONE',  ( -14.34966873604972548, 8.224510206698743886, 33.33442372801900433 ) ) ;
#130900 = CARTESIAN_POINT ( 'NONE',  ( 14.34966873604960469, 8.224510206698951720, 104.1655762719810241 ) ) ;
#130901 = CARTESIAN_POINT ( 'NONE',  ( 28.82186960331498327, 2.781578969918950771E-14, 143.2500000054623683 ) ) ;
#130902 = CARTESIAN_POINT ( 'NONE',  ( -9.474510206698964154, 16.51473224551069663, 55.41557627198103120 ) ) ;
#130903 = CARTESIAN_POINT ( 'NONE',  ( 12.14591786802309770, 12.06949235617756955, 89.37390960531435269 ) ) ;
#130904 = CARTESIAN_POINT ( 'NONE',  ( 21.55341960407610458, 5.719274019375980345, 28.95724293864769905 ) ) ;
#130905 = CARTESIAN_POINT ( 'NONE',  ( 0.05219959533910956823, 16.53943276465976808, 59.99890960531436690 ) ) ;
#130906 = CARTESIAN_POINT ( 'NONE',  ( 16.51473224551083163, -9.474510206698727899, 110.8344237280190043 ) ) ;
#130907 = CARTESIAN_POINT ( 'NONE',  ( 15.72974639402176855, 15.80617190586768217, 66.87609039468568994 ) ) ;
#130908 = CARTESIAN_POINT ( 'NONE',  ( 16.29526858892876362, -7.335722546920109721, 76.70329402199793378 ) ) ;
#130909 = CARTESIAN_POINT ( 'NONE',  ( 16.46253265017160672, -9.564922557960803928, 108.3322429386476955 ) ) ;
#130910 = CARTESIAN_POINT ( 'NONE',  ( 14.29746914071037800, 8.314922557961029526, 96.66775706135234714 ) ) ;
#130911 = CARTESIAN_POINT ( 'NONE',  ( -19.03943276465977164, 0.05219959533909376836, 41.24890960531435269 ) ) ;
#130912 = CARTESIAN_POINT ( 'NONE',  ( 9.564922557960805705, 16.46253265017160317, 84.58224293864769550 ) ) ;
#130913 = CARTESIAN_POINT ( 'NONE',  ( -10.81492255796078084, -18.62759615963271287, 92.08224293864769550 ) ) ;
#130914 = CARTESIAN_POINT ( 'NONE',  ( 12.14591786802327356, -12.06949235617739191, 30.62609039468567929 ) ) ;
#130916 = CARTESIAN_POINT ( 'NONE',  ( 5.719274019375673035, 21.55341960407619339, 67.29275706135234714 ) ) ;
#130915 = CARTESIAN_POINT ( 'NONE',  ( 0.05219959533910956823, 16.53943276465976808, 59.99890960531436690 ) ) ;
#130917 = CARTESIAN_POINT ( 'NONE',  ( 16.55341960407618274, -4.379528057220086978, 101.0427570613523756 ) ) ;
#130918 = CARTESIAN_POINT ( 'NONE',  ( 16.19135201231369692, 7.376712067591807198, 27.68680854052031393 ) ) ;
#130919 = CARTESIAN_POINT ( 'NONE',  ( -17.49999999999999645, 5.624438216177592764, 80.81670344914644488 ) ) ;
#130920 = CARTESIAN_POINT ( 'NONE',  ( -16.52544592524342804, 4.483927247898546575, 31.04057627198102409 ) ) ;
#130921 = CARTESIAN_POINT ( 'NONE',  ( -4.483927247898782831, 16.52544592524335698, 67.70942372801901854 ) ) ;
#130922 = CARTESIAN_POINT ( 'NONE',  ( 5.153800228976335163, 19.02544592524342804, 74.79057627198103830 ) ) ;
#130923 = CARTESIAN_POINT ( 'NONE',  ( -16.51473224551069308, -9.474510206698971260, 91.66557627198103830 ) ) ;
#130924 = CARTESIAN_POINT ( 'NONE',  ( 15.72974639402176855, 15.80617190586768217, 91.87609039468568994 ) ) ;
#130925 = CARTESIAN_POINT ( 'NONE',  ( -16.53943276465976808, -0.05219959533934237506, 83.75109039468568994 ) ) ;
#130926 = CARTESIAN_POINT ( 'NONE',  ( 16.53943276465976808, -0.05219959533910856209, 63.74890960531435979 ) ) ;
#130927 = CARTESIAN_POINT ( 'NONE',  ( 9.564922557960805705, 16.46253265017160317, 74.58224293864769550 ) ) ;
#130928 = ORIENTED_EDGE ( 'NONE', *, *, #183592, .T. ) ;
#130929 = CARTESIAN_POINT ( 'NONE',  ( -5.153800228976607833, 19.02544592524334988, 112.7094237280190043 ) ) ;
#130930 = CARTESIAN_POINT ( 'NONE',  ( 0.05219959533910956823, 16.53943276465976808, 109.9989096053143527 ) ) ;
#130931 = CARTESIAN_POINT ( 'NONE',  ( -0.05219959533909027116, -19.03943276465977164, 77.49890960531435269 ) ) ;
#130933 = CARTESIAN_POINT ( 'NONE',  ( -11.40812507854755609, 35.11059874428196537, -7.024999997268813523 ) ) ;
#130932 = CARTESIAN_POINT ( 'NONE',  ( -9.564922557961040184, 16.46253265017147172, 107.9177570613523471 ) ) ;
#130934 = CARTESIAN_POINT ( 'NONE',  ( 13.97604488694548053, -13.89961937509957401, 20.62609039468567573 ) ) ;
#130935 = CARTESIAN_POINT ( 'NONE',  ( -12.06949235617739369, -12.14591786802326823, 79.37609039468567573 ) ) ;
#130936 = CARTESIAN_POINT ( 'NONE',  ( 5.049401038297881783, 19.05341960407617563, 87.29275706135234714 ) ) ;
#130937 = CARTESIAN_POINT ( 'NONE',  ( 14.34966873604960469, 8.224510206698951720, 109.1655762719810383 ) ) ;
#130938 = CARTESIAN_POINT ( 'NONE',  ( -16.55341960407617563, 4.379528057220093196, 68.54275706135234714 ) ) ;
#130939 = CARTESIAN_POINT ( 'NONE',  ( -7.656827144875921753, -71.74905178543390605, -4.999999999999999112 ) ) ;
#130940 = CARTESIAN_POINT ( 'NONE',  ( 0.05219959533936267826, -19.03943276465977164, 60.00109039468566863 ) ) ;
#130941 = AXIS2_PLACEMENT_3D ( 'NONE', #110309, #2136, #80957 ) ;
#130942 = CARTESIAN_POINT ( 'NONE',  ( 18.67979575497194134, -10.72451020669871369, 95.83442372801903275 ) ) ;
#130943 = CARTESIAN_POINT ( 'NONE',  ( -16.51473224551069308, -9.474510206698971260, 36.66557627198102409 ) ) ;
#130944 = CARTESIAN_POINT ( 'NONE',  ( -9.564922557960796823, -16.46253265017161027, 77.08224293864769550 ) ) ;
#130945 = CARTESIAN_POINT ( 'NONE',  ( -16.55341960407611168, -4.379528057220339221, 76.45724293864769550 ) ) ;
#130946 = CARTESIAN_POINT ( 'NONE',  ( -21.53943276465977519, -0.05219959533937600094, 83.75109039468568994 ) ) ;
#130947 = CARTESIAN_POINT ( 'NONE',  ( 16.46253265017146816, 9.564922557961045513, 61.66775706135234003 ) ) ;
#130948 = CARTESIAN_POINT ( 'NONE',  ( 19.03943276465977164, 0.05219959533936151252, 46.25109039468566863 ) ) ;
#130949 = CARTESIAN_POINT ( 'NONE',  ( -18.62759615963270932, 10.81492255796079327, 35.83224293864768839 ) ) ;
#130950 = CARTESIAN_POINT ( 'NONE',  ( 18.67979575497194134, -10.72451020669871369, 95.83442372801903275 ) ) ;
#130951 = CARTESIAN_POINT ( 'NONE',  ( -5.153800228976328057, -19.02544592524343514, 82.29057627198103830 ) ) ;
#130952 = CARTESIAN_POINT ( 'NONE',  ( 18.62759615963255655, 10.81492255796105972, 106.6677570613523756 ) ) ;
#130953 = CARTESIAN_POINT ( 'NONE',  ( -18.62759615963270932, 10.81492255796079327, 45.83224293864769550 ) ) ;
#130954 = CARTESIAN_POINT ( 'NONE',  ( -19.02544592524342804, 5.153800228976336051, 101.0405762719810241 ) ) ;
#130955 = CARTESIAN_POINT ( 'NONE',  ( -16.46253265017146816, -9.564922557961047289, 69.16775706135233293 ) ) ;
#130956 = CARTESIAN_POINT ( 'NONE',  ( -16.46253265017160317, 9.564922557960807481, 100.8322429386477097 ) ) ;
#130957 = CARTESIAN_POINT ( 'NONE',  ( -19.02544592524334988, -5.153800228976617603, 93.95942372801900433 ) ) ;
#130958 = CARTESIAN_POINT ( 'NONE',  ( 16.52544592524335698, 4.483927247898782831, 46.45942372801901854 ) ) ;
#130959 = CARTESIAN_POINT ( 'NONE',  ( -14.34966873604960291, -8.224510206698953496, 96.66557627198102409 ) ) ;
#130960 = CARTESIAN_POINT ( 'NONE',  ( 19.03943276465977164, -0.05219959533909143690, 83.74890960531436690 ) ) ;
#130961 = CARTESIAN_POINT ( 'NONE',  ( 21.53943276465977519, -0.05219959533907433946, 58.74890960531436690 ) ) ;
#130962 = CARTESIAN_POINT ( 'NONE',  ( -8.314922557961024197, 14.29746914071037800, 32.91775706135234714 ) ) ;
#130963 = CARTESIAN_POINT ( 'NONE',  ( 15.80617190586769283, -15.72974639402175789, 30.62609039468567929 ) ) ;
#130964 = CARTESIAN_POINT ( 'NONE',  ( -21.53943276465977519, -0.05219959533937600094, 88.75109039468567573 ) ) ;
#130965 = CARTESIAN_POINT ( 'NONE',  ( 16.55341960407618274, -4.379528057220086978, 81.04275706135236135 ) ) ;
#130966 = CARTESIAN_POINT ( 'NONE',  ( 19.03943276465977164, -0.05219959533909143690, 73.74890960531435269 ) ) ;
#130967 = CARTESIAN_POINT ( 'NONE',  ( -16.55341960407611168, -4.379528057220339221, 81.45724293864769550 ) ) ;
#130968 = CARTESIAN_POINT ( 'NONE',  ( -12.06949235617739369, -12.14591786802326823, 109.3760903946857042 ) ) ;
#130969 = CARTESIAN_POINT ( 'NONE',  ( 16.46253265017146816, 9.564922557961045513, 51.66775706135233293 ) ) ;
#130970 = CARTESIAN_POINT ( 'NONE',  ( -21.52544592524334988, -5.823673210054445271, 28.95942372801902209 ) ) ;
#130971 = CARTESIAN_POINT ( 'NONE',  ( 12.14591786802309770, 12.06949235617756955, 84.37390960531438111 ) ) ;
#130972 = CARTESIAN_POINT ( 'NONE',  ( 5.153800228976335163, 19.02544592524342804, 104.7905762719809957 ) ) ;
#130973 = CARTESIAN_POINT ( 'NONE',  ( -16.52544592524335698, -4.483927247898792601, 103.9594237280190185 ) ) ;
#130974 = CARTESIAN_POINT ( 'NONE',  ( 21.53943276465977519, 0.05219959533937863772, 76.25109039468568994 ) ) ;
#130975 = CARTESIAN_POINT ( 'NONE',  ( 8.314922557961029526, -14.29746914071037800, 50.41775706135235424 ) ) ;
#130976 = CARTESIAN_POINT ( 'NONE',  ( 10.72451020669871369, 18.67979575497193778, 47.08442372801901854 ) ) ;
#130977 = CARTESIAN_POINT ( 'NONE',  ( -16.53943276465976808, 0.05219959533911058130, 66.24890960531436690 ) ) ;
#130978 = ORIENTED_EDGE ( 'NONE', *, *, #4625, .F. ) ;
#130979 = CARTESIAN_POINT ( 'NONE',  ( 15.80617190586746368, 15.72974639402197994, 114.3739096053143527 ) ) ;
#130980 = CARTESIAN_POINT ( 'NONE',  ( -14.34966873604960291, -8.224510206698953496, 91.66557627198103830 ) ) ;
#130981 = CARTESIAN_POINT ( 'NONE',  ( 17.50000000000001776, -3.565345528327878100, 26.92494486806473120 ) ) ;
#130982 = CARTESIAN_POINT ( 'NONE',  ( 14.34966873604960469, 8.224510206698951720, 59.16557627198103120 ) ) ;
#130983 = CARTESIAN_POINT ( 'NONE',  ( -9.474510206698964154, 16.51473224551069663, 25.41557627198103120 ) ) ;
#130984 = CARTESIAN_POINT ( 'NONE',  ( -21.53943276465977519, 0.05219959533907696930, 41.24890960531435269 ) ) ;
#130985 = CARTESIAN_POINT ( 'NONE',  ( -12.14591786802309592, -12.06949235617757132, 81.87390960531435269 ) ) ;
#130986 = CARTESIAN_POINT ( 'NONE',  ( 18.62759615963271287, -10.81492255796078972, 78.33224293864770971 ) ) ;
#130987 = CARTESIAN_POINT ( 'NONE',  ( 16.51473224551069308, 9.474510206698969483, 84.16557627198102409 ) ) ;
#130989 = CARTESIAN_POINT ( 'NONE',  ( 5.153800228976615827, -19.02544592524334988, 85.20942372801900433 ) ) ;
#130988 = CARTESIAN_POINT ( 'NONE',  ( 5.049401038298161559, -19.05341960407611168, 37.70724293864768839 ) ) ;
#130991 = CARTESIAN_POINT ( 'NONE',  ( 5.719274019375991003, -21.55341960407610458, 67.70724293864769550 ) ) ;
#130990 = CARTESIAN_POINT ( 'NONE',  ( 0.05219959533937995610, -21.53943276465977519, 55.00109039468568284 ) ) ;
#130992 = CARTESIAN_POINT ( 'NONE',  ( -9.474510206698964154, 16.51473224551069663, 35.41557627198102409 ) ) ;
#130993 = CARTESIAN_POINT ( 'NONE',  ( -0.05219959533909027116, -19.03943276465977164, 77.49890960531435269 ) ) ;
#130994 = ORIENTED_EDGE ( 'NONE', *, *, #110091, .T. ) ;
#130995 = CARTESIAN_POINT ( 'NONE',  ( 16.55341960407618274, -4.379528057220086978, 46.04275706135234714 ) ) ;
#130996 = CARTESIAN_POINT ( 'NONE',  ( 15.72974639402176855, 15.80617190586768217, 31.87609039468567929 ) ) ;
#130997 = CARTESIAN_POINT ( 'NONE',  ( 21.52544592524334988, 5.823673210054432836, 76.45942372801901854 ) ) ;
#130998 = CARTESIAN_POINT ( 'NONE',  ( 15.80617190586746368, 15.72974639402197994, 24.37390960531435979 ) ) ;
#130999 = CARTESIAN_POINT ( 'NONE',  ( -15.72974639402197994, 15.80617190586746368, 90.62390960531436690 ) ) ;
#131001 = CARTESIAN_POINT ( 'NONE',  ( -16.55341960407617563, 4.379528057220093196, 48.54275706135234714 ) ) ;
#131000 = CARTESIAN_POINT ( 'NONE',  ( -21.53943276465977519, -0.05219959533937600094, 18.75109039468568639 ) ) ;
#131002 = CARTESIAN_POINT ( 'NONE',  ( -15.80617190586745835, -15.72974639402198527, 51.87390960531437401 ) ) ;
#131003 = CARTESIAN_POINT ( 'NONE',  ( -19.03943276465977164, -0.05219959533935918106, 23.75109039468566152 ) ) ;
#131004 = CARTESIAN_POINT ( 'NONE',  ( 19.03943276465977164, -0.05219959533909143690, 58.74890960531435979 ) ) ;
#131005 = CARTESIAN_POINT ( 'NONE',  ( -0.05219959533909027116, -19.03943276465977164, 112.4989096053143669 ) ) ;
#131006 = CARTESIAN_POINT ( 'NONE',  ( 16.51473224551069308, 9.474510206698969483, 89.16557627198103830 ) ) ;
#131007 = CARTESIAN_POINT ( 'NONE',  ( 9.474510206698729675, 16.51473224551082808, 52.08442372801900433 ) ) ;
#131008 = EDGE_CURVE ( 'NONE', #165007, #21338, #188507, .T. ) ;
#131009 = CARTESIAN_POINT ( 'NONE',  ( -9.564922557961040184, 16.46253265017147172, 62.91775706135233293 ) ) ;
#131010 = CARTESIAN_POINT ( 'NONE',  ( -5.823673210054116645, -21.52544592524344225, 42.29057627198103120 ) ) ;
#131011 = CARTESIAN_POINT ( 'NONE',  ( 14.34966873604960469, 8.224510206698951720, 29.16557627198103120 ) ) ;
#131012 = CARTESIAN_POINT ( 'NONE',  ( -9.564922557961040184, 16.46253265017147172, 97.91775706135233293 ) ) ;
#131013 = EDGE_CURVE ( 'NONE', #127046, #164406, #155783, .T. ) ;
#131014 = DIRECTION ( 'NONE',  ( 1.000000000000000000, 0.000000000000000000, 0.000000000000000000 ) ) ;
#131015 = CARTESIAN_POINT ( 'NONE',  ( 19.03943276465977164, 0.05219959533936151252, 21.25109039468565797 ) ) ;
#131016 = CARTESIAN_POINT ( 'NONE',  ( 16.51473224551083163, -9.474510206698727899, 100.8344237280190043 ) ) ;
#131018 = CARTESIAN_POINT ( 'NONE',  ( -16.51473224551082808, 9.474510206698731452, 53.33442372801900433 ) ) ;
#131017 = CARTESIAN_POINT ( 'NONE',  ( -21.55341960407610458, -5.719274019375992779, 86.45724293864770971 ) ) ;
#131019 = B_SPLINE_CURVE_WITH_KNOTS ( 'NONE', 3,
 ( #106154, #149691, #167836, #122309 ),
 .UNSPECIFIED., .F., .F.,
 ( 4, 4 ),
 ( 0.000000000000000000, 0.007966001190080656408 ),
 .UNSPECIFIED. ) ;
#131020 = CARTESIAN_POINT ( 'NONE',  ( 26.00011078373264795, -10.07146799416501359, 166.7325096689061752 ) ) ;
#131021 = CARTESIAN_POINT ( 'NONE',  ( -16.51473224551069308, -9.474510206698971260, 56.66557627198103120 ) ) ;
#131022 = CARTESIAN_POINT ( 'NONE',  ( -12.14591786802309592, -12.06949235617757132, 66.87390960531436690 ) ) ;
#131023 = CARTESIAN_POINT ( 'NONE',  ( -5.153800228976328057, -19.02544592524343514, 37.29057627198102409 ) ) ;
#131024 = CARTESIAN_POINT ( 'NONE',  ( -12.14591786802309592, -12.06949235617757132, 36.87390960531435979 ) ) ;
#131025 = FACE_OUTER_BOUND ( 'NONE', #7505, .T. ) ;
#131026 = CARTESIAN_POINT ( 'NONE',  ( -16.53943276465976808, -0.05219959533934237506, 103.7510903946857042 ) ) ;
#131027 = CARTESIAN_POINT ( 'NONE',  ( -13.89961937509977652, 13.97604488694528158, 65.62390960531436690 ) ) ;
#131028 = CARTESIAN_POINT ( 'NONE',  ( -13.97604488694547697, 13.89961937509957934, 23.12609039468565442 ) ) ;
#131029 = CARTESIAN_POINT ( 'NONE',  ( -4.379528057220086978, -16.55341960407618274, 39.79275706135235424 ) ) ;
#131030 = CARTESIAN_POINT ( 'NONE',  ( -5.719274019375978568, 21.55341960407610458, 55.20724293864770260 ) ) ;
#131032 = EDGE_LOOP ( 'NONE', ( #123245, #160459, #5632, #18952 ) ) ;
#131031 = CARTESIAN_POINT ( 'NONE',  ( -15.72974639402176322, -15.80617190586768395, 109.3760903946857042 ) ) ;
#131033 = CARTESIAN_POINT ( 'NONE',  ( -19.02544592524342804, 5.153800228976336051, 61.04057627198103120 ) ) ;
#131034 = CARTESIAN_POINT ( 'NONE',  ( 16.51473224551069308, 9.474510206698969483, 114.1655762719810241 ) ) ;
#131035 = CARTESIAN_POINT ( 'NONE',  ( -9.564922557960796823, -16.46253265017161027, 97.08224293864769550 ) ) ;
#131036 = CARTESIAN_POINT ( 'NONE',  ( 11.40812507854755253, -35.11059874428192273, -2.024999997268813079 ) ) ;
#131037 = CARTESIAN_POINT ( 'NONE',  ( 21.55341960407619695, -5.719274019375665929, 21.04275706135234714 ) ) ;
#131038 = VECTOR ( 'NONE', #83261, 1000.000000000000114 ) ;
#131039 = CARTESIAN_POINT ( 'NONE',  ( 14.34966873604960469, 8.224510206698951720, 94.16557627198103830 ) ) ;
#131041 = CARTESIAN_POINT ( 'NONE',  ( 9.564922557960805705, 16.46253265017160317, 64.58224293864769550 ) ) ;
#131040 = CARTESIAN_POINT ( 'NONE',  ( 10.81492255796078972, 18.62759615963270932, 94.58224293864769550 ) ) ;
#131042 = CARTESIAN_POINT ( 'NONE',  ( 16.46253265017160672, -9.564922557960803928, 68.33224293864770971 ) ) ;
#131043 = CARTESIAN_POINT ( 'NONE',  ( 15.80617190586746368, 15.72974639402197994, 104.3739096053143669 ) ) ;
#131044 = VERTEX_POINT ( 'NONE', #101 ) ;
#131045 = CARTESIAN_POINT ( 'NONE',  ( -0.05219959533909027116, -19.03943276465977164, 72.49890960531435269 ) ) ;
#131046 = CARTESIAN_POINT ( 'NONE',  ( 18.22780087662123805, -5.499999999999976019, 98.51763182126896368 ) ) ;
#131048 = CARTESIAN_POINT ( 'NONE',  ( 0.000000000000000000, 0.000000000000000000, -61.89430850415821794 ) ) ;
#131047 = CARTESIAN_POINT ( 'NONE',  ( -16.55341960407611168, -4.379528057220339221, 101.4572429386476955 ) ) ;
#131049 = CARTESIAN_POINT ( 'NONE',  ( 9.564922557961047289, -16.46253265017146816, 90.41775706135234714 ) ) ;
#131050 = CARTESIAN_POINT ( 'NONE',  ( -14.29746914071049879, 8.314922557960819915, 100.8322429386477097 ) ) ;
#131051 = CARTESIAN_POINT ( 'NONE',  ( 5.719274019375673035, 21.55341960407619339, 77.29275706135234714 ) ) ;
#131053 = CARTESIAN_POINT ( 'NONE',  ( 18.62759615963255655, 10.81492255796105972, 31.66775706135234358 ) ) ;
#131052 = CARTESIAN_POINT ( 'NONE',  ( 19.05341960407611168, 5.049401038298154454, 58.95724293864768129 ) ) ;
#131054 = CARTESIAN_POINT ( 'NONE',  ( 0.05219959533907565091, 21.53943276465977519, 109.9989096053143527 ) ) ;
#131055 = CARTESIAN_POINT ( 'NONE',  ( -28.82186960331499392, -9.364793116373526516, 142.0999999999999659 ) ) ;
#131056 = CARTESIAN_POINT ( 'NONE',  ( 5.049401038298161559, -19.05341960407611168, 72.70724293864768129 ) ) ;
#131057 = CARTESIAN_POINT ( 'NONE',  ( 21.30000000000002913, -7.567280135845077329E-14, -58.85720012050612837 ) ) ;
#131059 = CARTESIAN_POINT ( 'NONE',  ( 0.05219959533907565091, 21.53943276465977519, 24.99890960531435624 ) ) ;
#131058 = CARTESIAN_POINT ( 'NONE',  ( -16.53943276465976808, -0.05219959533934237506, 23.75109039468567929 ) ) ;
#131060 = CARTESIAN_POINT ( 'NONE',  ( -18.62759615963255300, -10.81492255796106328, 69.16775706135234714 ) ) ;
#131061 = CARTESIAN_POINT ( 'NONE',  ( 9.564922557960805705, 16.46253265017160317, 104.5822429386476955 ) ) ;
#131062 = CARTESIAN_POINT ( 'NONE',  ( -13.97604488694547697, 13.89961937509957934, 98.12609039468566152 ) ) ;
#131063 = CARTESIAN_POINT ( 'NONE',  ( 0.05219959533909260263, 19.03943276465977164, 44.99890960531435979 ) ) ;
#131064 = CARTESIAN_POINT ( 'NONE',  ( -19.03943276465977164, 0.05219959533909376836, 76.24890960531435269 ) ) ;
#131065 = CARTESIAN_POINT ( 'NONE',  ( 8.314922557960818139, 14.29746914071049879, 94.58224293864769550 ) ) ;
#131066 = CARTESIAN_POINT ( 'NONE',  ( -9.474510206698964154, 16.51473224551069663, 100.4155762719810241 ) ) ;
#131067 = CARTESIAN_POINT ( 'NONE',  ( 16.53943276465976808, -0.05219959533910856209, 88.74890960531436690 ) ) ;
#131068 = CARTESIAN_POINT ( 'NONE',  ( 13.97604488694527802, 13.89961937509977652, 104.3739096053143385 ) ) ;
#131070 = CARTESIAN_POINT ( 'NONE',  ( -0.05219959533909027116, -19.03943276465977164, 42.49890960531435269 ) ) ;
#131069 = CARTESIAN_POINT ( 'NONE',  ( 14.34966873604960469, 8.224510206698951720, 49.16557627198102409 ) ) ;
#131071 = CARTESIAN_POINT ( 'NONE',  ( -21.52544592524334988, -5.823673210054445271, 58.95942372801902565 ) ) ;
#131072 = CARTESIAN_POINT ( 'NONE',  ( -0.05219959533936034679, 19.03943276465977164, 92.50109039468566152 ) ) ;
#131073 = CARTESIAN_POINT ( 'NONE',  ( 12.14591786802309770, 12.06949235617756955, 49.37390960531436690 ) ) ;
#131074 = CARTESIAN_POINT ( 'NONE',  ( -10.81492255796078084, -18.62759615963271287, 102.0822429386476955 ) ) ;
#131075 = CARTESIAN_POINT ( 'NONE',  ( 10.72451020669898902, -18.67979575497178502, 42.91557627198103120 ) ) ;
#131077 = CARTESIAN_POINT ( 'NONE',  ( 8.224510206698953496, -14.34966873604960469, 82.91557627198103830 ) ) ;
#131076 = CARTESIAN_POINT ( 'NONE',  ( 9.474510206698971260, -16.51473224551069308, 107.9155762719810383 ) ) ;
#131078 = CARTESIAN_POINT ( 'NONE',  ( -5.049401038298153566, 19.05341960407611168, 60.20724293864768129 ) ) ;
#131079 = CARTESIAN_POINT ( 'NONE',  ( 4.483927247898545687, 16.52544592524342804, 29.79057627198102409 ) ) ;
#131080 = CARTESIAN_POINT ( 'NONE',  ( -0.05219959533934338120, 16.53943276465976808, 102.5010903946856899 ) ) ;
#131081 = CARTESIAN_POINT ( 'NONE',  ( -8.314922557961024197, 14.29746914071037800, 87.91775706135234714 ) ) ;
#131082 = CARTESIAN_POINT ( 'NONE',  ( 0.05219959533936267826, -19.03943276465977164, 35.00109039468566863 ) ) ;
#131084 = CARTESIAN_POINT ( 'NONE',  ( 19.05341960407611168, 5.049401038298154454, 103.9572429386476671 ) ) ;
#131083 = CARTESIAN_POINT ( 'NONE',  ( -24.79445753310783473, -6.337991946471490223, 168.1742925226654393 ) ) ;
#131085 = CARTESIAN_POINT ( 'NONE',  ( 16.46253265017160672, -9.564922557960803928, 73.33224293864769550 ) ) ;
#131086 = CARTESIAN_POINT ( 'NONE',  ( -5.153800228976328057, -19.02544592524343514, 32.29057627198102409 ) ) ;
#131087 = EDGE_CURVE ( 'NONE', #179813, #123998, #60648, .T. ) ;
#131088 = CARTESIAN_POINT ( 'NONE',  ( 16.55341960407611168, 4.379528057220329451, 53.95724293864770260 ) ) ;
#131090 = CARTESIAN_POINT ( 'NONE',  ( 19.05341960407611168, 5.049401038298154454, 108.9572429386477097 ) ) ;
#131089 = CARTESIAN_POINT ( 'NONE',  ( 16.46253265017160672, -9.564922557960803928, 113.3322429386476955 ) ) ;
#131091 = CARTESIAN_POINT ( 'NONE',  ( 15.80617190586746368, 15.72974639402197994, 44.37390960531435979 ) ) ;
#131092 = CARTESIAN_POINT ( 'NONE',  ( 12.06949235617757843, -12.14591786802309237, 88.12390960531436690 ) ) ;
#131093 = CARTESIAN_POINT ( 'NONE',  ( -4.379528057220086978, -16.55341960407618274, 34.79275706135235424 ) ) ;
#131094 = CARTESIAN_POINT ( 'NONE',  ( 14.34966873604960469, 8.224510206698951720, 59.16557627198103120 ) ) ;
#131095 = CARTESIAN_POINT ( 'NONE',  ( -4.000000000000000888, -165.0000000000000000, -23.00000000000000000 ) ) ;
#131096 = CARTESIAN_POINT ( 'NONE',  ( 16.51473224551083163, -9.474510206698727899, 70.83442372801900433 ) ) ;
#131097 = CARTESIAN_POINT ( 'NONE',  ( 19.02544592524343514, -5.153800228976328945, 108.5405762719810383 ) ) ;
#131099 = ADVANCED_FACE ( 'NONE', ( #93106 ), #185404, .F. ) ;
#131098 = CARTESIAN_POINT ( 'NONE',  ( 5.153800228976615827, -19.02544592524334988, 80.20942372801901854 ) ) ;
#131100 = CARTESIAN_POINT ( 'NONE',  ( 8.571926809382603096, -26.38167802310801235, 147.9750000027311785 ) ) ;
#131102 = CARTESIAN_POINT ( 'NONE',  ( -4.483927247898782831, 16.52544592524335698, 102.7094237280190185 ) ) ;
#131101 = CARTESIAN_POINT ( 'NONE',  ( -14.29746914071037622, -8.314922557961029526, 29.16775706135234003 ) ) ;
#131103 = CARTESIAN_POINT ( 'NONE',  ( -5.049401038297874678, -19.05341960407617918, 69.79275706135233293 ) ) ;
#131104 = CARTESIAN_POINT ( 'NONE',  ( -5.719274019375978568, 21.55341960407610458, 30.20724293864769550 ) ) ;
#131105 = CARTESIAN_POINT ( 'NONE',  ( -0.05219959533937732626, 21.53943276465977519, 67.50109039468568994 ) ) ;
#131106 = CARTESIAN_POINT ( 'NONE',  ( -23.46037622756033869, -10.21219847193828123, 168.3031241911537847 ) ) ;
#131107 = CARTESIAN_POINT ( 'NONE',  ( 16.51473224551083163, -9.474510206698727899, 110.8344237280190043 ) ) ;
#131109 = CARTESIAN_POINT ( 'NONE',  ( -19.02544592524342804, 5.153800228976336051, 71.04057627198099567 ) ) ;
#131108 = LINE ( 'NONE', #192796, #60450 ) ;
#131110 = CARTESIAN_POINT ( 'NONE',  ( -5.049401038298153566, 19.05341960407611168, 25.20724293864768484 ) ) ;
#131112 = CARTESIAN_POINT ( 'NONE',  ( -16.51473224551069308, -9.474510206698971260, 71.66557627198102409 ) ) ;
#131111 = CARTESIAN_POINT ( 'NONE',  ( -12.14591786802309592, -12.06949235617757132, 81.87390960531435269 ) ) ;
#131113 = CARTESIAN_POINT ( 'NONE',  ( 0.05219959533909260263, 19.03943276465977164, 89.99890960531436690 ) ) ;
#131114 = ORIENTED_EDGE ( 'NONE', *, *, #40503, .T. ) ;
#131115 = CARTESIAN_POINT ( 'NONE',  ( 13.89961937509957401, 13.97604488694547697, 86.87609039468567573 ) ) ;
#131116 = CARTESIAN_POINT ( 'NONE',  ( -18.62759615963270932, 10.81492255796079327, 75.83224293864769550 ) ) ;
#131117 = CARTESIAN_POINT ( 'NONE',  ( 19.02544592524343514, -5.153800228976328945, 28.54057627198102409 ) ) ;
#131119 = CARTESIAN_POINT ( 'NONE',  ( 21.55341960407610458, 5.719274019375980345, 108.9572429386476955 ) ) ;
#131118 = CARTESIAN_POINT ( 'NONE',  ( 19.05341960407617918, -5.049401038297876454, 66.04275706135233293 ) ) ;
#131120 = CARTESIAN_POINT ( 'NONE',  ( -5.153800228976328057, -19.02544592524343514, 67.29057627198102409 ) ) ;
#131121 = CARTESIAN_POINT ( 'NONE',  ( -9.474510206698964154, 16.51473224551069663, 105.4155762719810383 ) ) ;
#131122 = EDGE_LOOP ( 'NONE', ( #77575, #145782, #113357, #112669 ) ) ;
#131123 = CARTESIAN_POINT ( 'NONE',  ( 21.53943276465977519, -0.05219959533907433946, 98.74890960531438111 ) ) ;
#131126 = CARTESIAN_POINT ( 'NONE',  ( 13.89961937509957401, 13.97604488694547697, 66.87609039468567573 ) ) ;
#131125 = CARTESIAN_POINT ( 'NONE',  ( 5.153800228976335163, 19.02544592524342804, 84.79057627198099567 ) ) ;
#131124 = CARTESIAN_POINT ( 'NONE',  ( 16.53943276465976808, -0.05219959533910856209, 98.74890960531438111 ) ) ;
#131127 = CARTESIAN_POINT ( 'NONE',  ( 18.62759615963271287, -10.81492255796078972, 83.33224293864769550 ) ) ;
#131128 = CARTESIAN_POINT ( 'NONE',  ( 15.80617190586746368, 15.72974639402197994, 69.37390960531436690 ) ) ;
#131129 = CARTESIAN_POINT ( 'NONE',  ( -14.29746914071049879, 8.314922557960819915, 40.83224293864769550 ) ) ;
#131130 = CARTESIAN_POINT ( 'NONE',  ( 10.72451020669871369, 18.67979575497193778, 107.0844237280190043 ) ) ;
#131132 = AXIS2_PLACEMENT_3D ( 'NONE', #6543, #82380, #7543 ) ;
#131131 = CARTESIAN_POINT ( 'NONE',  ( 16.53943276465976808, 0.05219959533934440121, 66.25109039468567573 ) ) ;
#131133 = CARTESIAN_POINT ( 'NONE',  ( -19.02544592524342804, 5.153800228976336051, 96.04057627198103830 ) ) ;
#131134 = CARTESIAN_POINT ( 'NONE',  ( 19.02544592524343514, -5.153800228976328945, 33.54057627198102409 ) ) ;
#131135 = CARTESIAN_POINT ( 'NONE',  ( 21.53943276465977519, 0.05219959533937863772, 36.25109039468567573 ) ) ;
#131136 = CARTESIAN_POINT ( 'NONE',  ( 18.67979575497194134, -10.72451020669871369, 55.83442372801901854 ) ) ;
#131137 = CARTESIAN_POINT ( 'NONE',  ( -19.03943276465977164, 0.05219959533909376836, 61.24890960531436690 ) ) ;
#131138 = CARTESIAN_POINT ( 'NONE',  ( -18.67979575497193778, 10.72451020669871902, 33.33442372801900433 ) ) ;
#131139 = CARTESIAN_POINT ( 'NONE',  ( -9.474510206698720793, -16.51473224551083518, 79.58442372801899012 ) ) ;
#131140 = CARTESIAN_POINT ( 'NONE',  ( -19.02544592524334988, -5.153800228976617603, 73.95942372801900433 ) ) ;
#131141 = CARTESIAN_POINT ( 'NONE',  ( 16.46253265017160672, -9.564922557960803928, 43.33224293864769550 ) ) ;
#131142 = CARTESIAN_POINT ( 'NONE',  ( 12.14591786802327356, -12.06949235617739191, 90.62609039468567573 ) ) ;
#131143 = CARTESIAN_POINT ( 'NONE',  ( -19.05341960407611168, -5.049401038298163336, 51.45724293864770260 ) ) ;
#131144 = DIRECTION ( 'NONE',  ( 0.5150380749100522682, 1.049727191138620051E-16, 0.8571673007021134438 ) ) ;
#131145 = CARTESIAN_POINT ( 'NONE',  ( -16.46253265017160317, 9.564922557960807481, 95.83224293864769550 ) ) ;
#131146 = CARTESIAN_POINT ( 'NONE',  ( 16.51473224551069308, 9.474510206698969483, 44.16557627198103120 ) ) ;
#131147 = CARTESIAN_POINT ( 'NONE',  ( -5.719274019375978568, 21.55341960407610458, 70.20724293864769550 ) ) ;
#131148 = CARTESIAN_POINT ( 'NONE',  ( 12.14591786802327356, -12.06949235617739191, 60.62609039468567573 ) ) ;
#131149 = CARTESIAN_POINT ( 'NONE',  ( -15.80617190586768217, 15.72974639402176855, 113.1260903946856899 ) ) ;
#131150 = CARTESIAN_POINT ( 'NONE',  ( -16.51473224551069308, -9.474510206698971260, 56.66557627198103120 ) ) ;
#131151 = CARTESIAN_POINT ( 'NONE',  ( -4.379528057220328563, 16.55341960407611168, 40.20724293864769550 ) ) ;
#131152 = CARTESIAN_POINT ( 'NONE',  ( -0.05219959533910754901, -16.53943276465976808, 77.49890960531433848 ) ) ;
#131153 = CARTESIAN_POINT ( 'NONE',  ( 0.05219959533909260263, 19.03943276465977164, 79.99890960531436690 ) ) ;
#131154 = CARTESIAN_POINT ( 'NONE',  ( -5.823673210054431948, 21.52544592524334988, 37.70942372801900433 ) ) ;
#131155 = CARTESIAN_POINT ( 'NONE',  ( -9.564922557960796823, -16.46253265017161027, 92.08224293864769550 ) ) ;
#131156 = CARTESIAN_POINT ( 'NONE',  ( -18.67979575497193778, 10.72451020669871902, 103.3344237280190043 ) ) ;
#131157 = CARTESIAN_POINT ( 'NONE',  ( -4.483927247898782831, 16.52544592524335698, 62.70942372801902565 ) ) ;
#131158 = CARTESIAN_POINT ( 'NONE',  ( 5.719274019375673035, 21.55341960407619339, 32.29275706135235424 ) ) ;
#131159 = CARTESIAN_POINT ( 'NONE',  ( -5.153800228976328057, -19.02544592524343514, 102.2905762719810383 ) ) ;
#131160 = CARTESIAN_POINT ( 'NONE',  ( 21.53943276465977519, -0.05219959533907433946, 83.74890960531435269 ) ) ;
#131161 = CARTESIAN_POINT ( 'NONE',  ( -4.483927247898539470, -16.52544592524342804, 52.29057627198102409 ) ) ;
#131162 = CARTESIAN_POINT ( 'NONE',  ( -13.89961937509977652, 13.97604488694528158, 45.62390960531433848 ) ) ;
#131163 = CARTESIAN_POINT ( 'NONE',  ( 4.379528057220339221, -16.55341960407611168, 62.70724293864769550 ) ) ;
#131164 = CARTESIAN_POINT ( 'NONE',  ( 5.719274019375991003, -21.55341960407610458, 32.70724293864770260 ) ) ;
#131165 = CARTESIAN_POINT ( 'NONE',  ( 10.72451020669898902, -18.67979575497178502, 27.91557627198103830 ) ) ;
#131166 = CARTESIAN_POINT ( 'NONE',  ( 19.03943276465977164, 0.05219959533936151252, 26.25109039468566507 ) ) ;
#131167 = CARTESIAN_POINT ( 'NONE',  ( -12.06949235617756955, 12.14591786802309770, 95.62390960531436690 ) ) ;
#131168 = CARTESIAN_POINT ( 'NONE',  ( -13.89961937509977652, 13.97604488694528158, 105.6239096053143527 ) ) ;
#131169 = ORIENTED_EDGE ( 'NONE', *, *, #137592, .T. ) ;
#131170 = CARTESIAN_POINT ( 'NONE',  ( -12.14591786802326823, 12.06949235617739902, 53.12609039468568284 ) ) ;
#131171 = CARTESIAN_POINT ( 'NONE',  ( 19.03943276465977164, -0.05219959533909143690, 48.74890960531435979 ) ) ;
#131172 = CARTESIAN_POINT ( 'NONE',  ( -16.75229466661211930, -6.775384016297254952, 21.10007927763472679 ) ) ;
#131173 = CARTESIAN_POINT ( 'NONE',  ( 13.97604488694548053, -13.89961937509957401, 60.62609039468564731 ) ) ;
#131174 = CARTESIAN_POINT ( 'NONE',  ( 4.483927247898790824, -16.52544592524335698, 100.2094237280190043 ) ) ;
#131175 = CARTESIAN_POINT ( 'NONE',  ( 0.05219959533936267826, -19.03943276465977164, 95.00109039468567573 ) ) ;
#131176 = CARTESIAN_POINT ( 'NONE',  ( 0.05219959533937995610, -21.53943276465977519, 65.00109039468568994 ) ) ;
#131177 = CARTESIAN_POINT ( 'NONE',  ( -16.51473224551069308, -9.474510206698971260, 71.66557627198102409 ) ) ;
#131178 = CARTESIAN_POINT ( 'NONE',  ( 0.05219959533907565091, 21.53943276465977519, 89.99890960531438111 ) ) ;
#131179 = CARTESIAN_POINT ( 'NONE',  ( -4.483927247898782831, 16.52544592524335698, 47.70942372801902565 ) ) ;
#131180 = CARTESIAN_POINT ( 'NONE',  ( -8.314922557960811034, -14.29746914071050412, 112.0822429386477097 ) ) ;
#131181 = CARTESIAN_POINT ( 'NONE',  ( -13.97604488694547697, 13.89961937509957934, 78.12609039468567573 ) ) ;
#131182 = CARTESIAN_POINT ( 'NONE',  ( -5.823673210054116645, -21.52544592524344225, 72.29057627198102409 ) ) ;
#131183 = CARTESIAN_POINT ( 'NONE',  ( 5.153800228976615827, -19.02544592524334988, 45.20942372801901143 ) ) ;
#131184 = CARTESIAN_POINT ( 'NONE',  ( 13.97604488694527802, 13.89961937509977652, 114.3739096053143669 ) ) ;
#131185 = CARTESIAN_POINT ( 'NONE',  ( 21.55341960407610458, 5.719274019375980345, 88.95724293864769550 ) ) ;
#131186 = CARTESIAN_POINT ( 'NONE',  ( 17.50000000000001421, 3.189878218039106983, 27.62948562571252964 ) ) ;
#131187 = CARTESIAN_POINT ( 'NONE',  ( -13.89961937509977652, 13.97604488694528158, 70.62390960531432427 ) ) ;
#131188 = CARTESIAN_POINT ( 'NONE',  ( -11.69745301899430956, -11.91991347263640222, -59.13370768023892055 ) ) ;
#131189 = CARTESIAN_POINT ( 'NONE',  ( -19.05341960407617563, 5.049401038297882671, 113.5427570613523471 ) ) ;
#131190 = CARTESIAN_POINT ( 'NONE',  ( 23.27014042476076838, 11.64952740454485713, 165.7333935355015342 ) ) ;
#131191 = CARTESIAN_POINT ( 'NONE',  ( -9.474510206698964154, 16.51473224551069663, 50.41557627198102409 ) ) ;
#131193 = CARTESIAN_POINT ( 'NONE',  ( 12.14591786802309770, 12.06949235617756955, 54.37390960531435979 ) ) ;
#131192 = CARTESIAN_POINT ( 'NONE',  ( 5.823673210054125526, 21.52544592524343514, 104.7905762719810241 ) ) ;
#131194 = CARTESIAN_POINT ( 'NONE',  ( 5.049401038298161559, -19.05341960407611168, 52.70724293864767418 ) ) ;
#131195 = CARTESIAN_POINT ( 'NONE',  ( -10.81492255796105439, 18.62759615963255655, 72.91775706135234714 ) ) ;
#131197 = CARTESIAN_POINT ( 'NONE',  ( 0.05219959533936267826, -19.03943276465977164, 25.00109039468566152 ) ) ;
#131196 = CARTESIAN_POINT ( 'NONE',  ( -16.51473224551082808, 9.474510206698731452, 113.3344237280190043 ) ) ;
#131198 = CARTESIAN_POINT ( 'NONE',  ( -8.224510206698948167, 14.34966873604960824, 25.41557627198103120 ) ) ;
#131199 = CARTESIAN_POINT ( 'NONE',  ( -10.72451020669870658, -18.67979575497194134, 44.58442372801901854 ) ) ;
#131200 = CARTESIAN_POINT ( 'NONE',  ( -5.823673210054431948, 21.52544592524334988, 22.70942372801901499 ) ) ;
#131201 = CARTESIAN_POINT ( 'NONE',  ( 5.823673210054125526, 21.52544592524343514, 59.79057627198103120 ) ) ;
#131202 = CARTESIAN_POINT ( 'NONE',  ( -16.46253265017146816, -9.564922557961047289, 94.16775706135233293 ) ) ;
#131203 = CARTESIAN_POINT ( 'NONE',  ( 5.049401038297881783, 19.05341960407617563, 62.29275706135234003 ) ) ;
#131204 = CARTESIAN_POINT ( 'NONE',  ( 18.62759615963255655, 10.81492255796105972, 66.66775706135234714 ) ) ;
#131205 = CARTESIAN_POINT ( 'NONE',  ( -5.153800228976607833, 19.02544592524334988, 52.70942372801900433 ) ) ;
#131206 = CARTESIAN_POINT ( 'NONE',  ( -16.52544592524342804, 4.483927247898546575, 116.0405762719810383 ) ) ;
#131207 = CARTESIAN_POINT ( 'NONE',  ( -0.05219959533907301413, -21.53943276465977519, 52.49890960531435979 ) ) ;
#131208 = CARTESIAN_POINT ( 'NONE',  ( -8.224510206698948167, 14.34966873604960824, 45.41557627198103830 ) ) ;
#131209 = CARTESIAN_POINT ( 'NONE',  ( -11.74264578624800670, 36.14014761921585972, -2.149999994537626691 ) ) ;
#131210 = CARTESIAN_POINT ( 'NONE',  ( -10.72451020669870658, -18.67979575497194134, 109.5844237280190328 ) ) ;
#131211 = CARTESIAN_POINT ( 'NONE',  ( 12.14591786802327356, -12.06949235617739191, 85.62609039468568994 ) ) ;
#131212 = CARTESIAN_POINT ( 'NONE',  ( 12.06949235617757843, -12.14591786802309237, 38.12390960531436690 ) ) ;
#131213 = CARTESIAN_POINT ( 'NONE',  ( 15.80617190586769283, -15.72974639402175789, 75.62609039468567573 ) ) ;
#131214 = CARTESIAN_POINT ( 'NONE',  ( 5.823673210054444382, -21.52544592524334988, 75.20942372801901854 ) ) ;
#131215 = CARTESIAN_POINT ( 'NONE',  ( 21.55341960407610458, 5.719274019375980345, 83.95724293864770971 ) ) ;
#131216 = CARTESIAN_POINT ( 'NONE',  ( 13.97604488694527802, 13.89961937509977652, 34.37390960531436690 ) ) ;
#131217 = CARTESIAN_POINT ( 'NONE',  ( -10.72451020669870658, -18.67979575497194134, 59.58442372801901854 ) ) ;
#131218 = CARTESIAN_POINT ( 'NONE',  ( 5.049401038298161559, -19.05341960407611168, 42.70724293864767418 ) ) ;
#131219 = CARTESIAN_POINT ( 'NONE',  ( 13.97604488694527802, 13.89961937509977652, 54.37390960531435979 ) ) ;
#131220 = CARTESIAN_POINT ( 'NONE',  ( 16.55341960407611168, 4.379528057220329451, 98.95724293864770971 ) ) ;
#131221 = CARTESIAN_POINT ( 'NONE',  ( 9.474510206698971260, -16.51473224551069308, 97.91557627198102409 ) ) ;
#131222 = AXIS2_PLACEMENT_3D ( 'NONE', #41329, #102989, #89815 ) ;
#131223 = CARTESIAN_POINT ( 'NONE',  ( 12.14591786802309770, 12.06949235617756955, 34.37390960531435979 ) ) ;
#131224 = CARTESIAN_POINT ( 'NONE',  ( 8.224510206698953496, -14.34966873604960469, 107.9155762719810241 ) ) ;
#131225 = CARTESIAN_POINT ( 'NONE',  ( 21.52544592524344225, -5.823673210054117533, 78.54057627198103830 ) ) ;
#131226 = CIRCLE ( 'NONE', #2054, 10.00000000000000000 ) ;
#131227 = CARTESIAN_POINT ( 'NONE',  ( -21.55341960407619339, 5.719274019375674811, 23.54275706135235424 ) ) ;
#131228 = CARTESIAN_POINT ( 'NONE',  ( 27.83964505791056254, -7.578386611925591154, 161.1890226338703940 ) ) ;
#131229 = CARTESIAN_POINT ( 'NONE',  ( 8.314922557961029526, -14.29746914071037800, 25.41775706135235779 ) ) ;
#131230 = CARTESIAN_POINT ( 'NONE',  ( 18.67979575497178502, 10.72451020669898547, 74.16557627198102409 ) ) ;
#131231 = CARTESIAN_POINT ( 'NONE',  ( -21.53943276465977519, -0.05219959533937600094, 93.75109039468567573 ) ) ;
#131232 = B_SPLINE_CURVE_WITH_KNOTS ( 'NONE', 3,
 ( #54595, #115274, #85930, #129421, #71767, #131435 ),
 .UNSPECIFIED., .F., .F.,
 ( 4, 2, 4 ),
 ( 0.003239945802372248222, 0.003620412082092099547, 0.004000878361811951306 ),
 .UNSPECIFIED. ) ;
#131233 = CARTESIAN_POINT ( 'NONE',  ( -9.474510206698964154, 16.51473224551069663, 85.41557627198102409 ) ) ;
#131234 = CARTESIAN_POINT ( 'NONE',  ( -18.62759615963255300, -10.81492255796106328, 24.16775706135235424 ) ) ;
#131235 = CARTESIAN_POINT ( 'NONE',  ( 5.049401038298161559, -19.05341960407611168, 112.7072429386476813 ) ) ;
#131236 = CARTESIAN_POINT ( 'NONE',  ( -8.224510206698735004, -14.34966873604973081, 94.58442372801901854 ) ) ;
#131237 = CARTESIAN_POINT ( 'NONE',  ( 18.62759615963255655, 10.81492255796105972, 76.66775706135234714 ) ) ;
#131238 = CARTESIAN_POINT ( 'NONE',  ( 19.02544592524334988, 5.153800228976608722, 21.45942372801899012 ) ) ;
#131239 = CARTESIAN_POINT ( 'NONE',  ( 4.483927247898790824, -16.52544592524335698, 70.20942372801904696 ) ) ;
#131240 = CARTESIAN_POINT ( 'NONE',  ( 15.72974639402176855, 15.80617190586768217, 31.87609039468567929 ) ) ;
#131241 = CARTESIAN_POINT ( 'NONE',  ( 16.46253265017160672, -9.564922557960803928, 33.33224293864770260 ) ) ;
#131242 = CARTESIAN_POINT ( 'NONE',  ( -21.53943276465977519, -0.05219959533937600094, 88.75109039468567573 ) ) ;
#131243 = CARTESIAN_POINT ( 'NONE',  ( -19.05341960407611168, -5.049401038298163336, 91.45724293864766707 ) ) ;
#131244 = CARTESIAN_POINT ( 'NONE',  ( 0.05219959533907565091, 21.53943276465977519, 104.9989096053143669 ) ) ;
#131246 = CARTESIAN_POINT ( 'NONE',  ( 21.55341960407610458, 5.719274019375980345, 58.95724293864770971 ) ) ;
#131245 = CARTESIAN_POINT ( 'NONE',  ( 19.34837522270368027, 5.499999999999741540, 83.36337684832578532 ) ) ;
#131248 = CARTESIAN_POINT ( 'NONE',  ( 4.379528057220339221, -16.55341960407611168, 47.70724293864770260 ) ) ;
#131247 = CARTESIAN_POINT ( 'NONE',  ( 13.89961937509977652, -13.97604488694527269, 93.12390960531436690 ) ) ;
#131249 = PLANE ( 'NONE',  #153204 ) ;
#131250 = CARTESIAN_POINT ( 'NONE',  ( -0.05219959533936034679, 19.03943276465977164, 82.50109039468567573 ) ) ;
#131251 = CARTESIAN_POINT ( 'NONE',  ( -16.18388926212237777, 7.379444403734522595, 104.5604684863385216 ) ) ;
#131252 = EDGE_CURVE ( 'NONE', #22005, #114833, #18284, .T. ) ;
#131253 = CARTESIAN_POINT ( 'NONE',  ( 9.564922557961047289, -16.46253265017146816, 105.4177570613523471 ) ) ;
#131254 = CARTESIAN_POINT ( 'NONE',  ( -10.72451020669898014, 18.67979575497178502, 80.41557627198103830 ) ) ;
#131255 = CARTESIAN_POINT ( 'NONE',  ( -8.224510206698948167, 14.34966873604960824, 65.41557627198102409 ) ) ;
#131256 = CARTESIAN_POINT ( 'NONE',  ( -13.89961937509977652, 13.97604488694528158, 100.6239096053143669 ) ) ;
#131257 = CARTESIAN_POINT ( 'NONE',  ( -14.34966873604972548, 8.224510206698743886, 38.33442372801900433 ) ) ;
#131258 = CARTESIAN_POINT ( 'NONE',  ( 19.05341960407611168, 5.049401038298154454, 63.95724293864769550 ) ) ;
#131260 = CARTESIAN_POINT ( 'NONE',  ( -0.05219959533936034679, 19.03943276465977164, 97.50109039468567573 ) ) ;
#131259 = CARTESIAN_POINT ( 'NONE',  ( 21.52544592524334988, 5.823673210054432836, 26.45942372801901854 ) ) ;
#131261 = CARTESIAN_POINT ( 'NONE',  ( -19.02544592524342804, 5.153800228976336051, 101.0405762719810241 ) ) ;
#131262 = CARTESIAN_POINT ( 'NONE',  ( -19.03943276465977164, 0.05219959533909376836, 86.24890960531436690 ) ) ;
#131263 = CARTESIAN_POINT ( 'NONE',  ( -5.719274019375978568, 21.55341960407610458, 90.20724293864770971 ) ) ;
#131264 = CARTESIAN_POINT ( 'NONE',  ( -9.474510206698964154, 16.51473224551069663, 40.41557627198103120 ) ) ;
#131265 = CARTESIAN_POINT ( 'NONE',  ( -16.29526858892878494, -7.335722546920003140, 60.79670597800208753 ) ) ;
#131266 = CARTESIAN_POINT ( 'NONE',  ( -16.52544592524342804, 4.483927247898546575, 71.04057627198103830 ) ) ;
#131267 = CARTESIAN_POINT ( 'NONE',  ( 5.049401038298161559, -19.05341960407611168, 102.7072429386476955 ) ) ;
#131268 = CARTESIAN_POINT ( 'NONE',  ( -18.09805431107247031, 5.500000000000101252, 61.01606229291886763 ) ) ;
#131269 = CARTESIAN_POINT ( 'NONE',  ( -9.474510206698720793, -16.51473224551083518, 59.58442372801900433 ) ) ;
#131270 = CARTESIAN_POINT ( 'NONE',  ( 15.72974639402199770, -15.80617190586745480, 93.12390960531436690 ) ) ;
#131271 = CARTESIAN_POINT ( 'NONE',  ( 5.049401038297881783, 19.05341960407617563, 52.29275706135234003 ) ) ;
#131272 = CARTESIAN_POINT ( 'NONE',  ( -0.05219959533909027116, -19.03943276465977164, 97.49890960531436690 ) ) ;
#131273 = CARTESIAN_POINT ( 'NONE',  ( 5.719274019375991003, -21.55341960407610458, 47.70724293864770260 ) ) ;
#131274 = CARTESIAN_POINT ( 'NONE',  ( -13.97604488694527625, -13.89961937509977652, 91.87390960531432427 ) ) ;
#131275 = CARTESIAN_POINT ( 'NONE',  ( -10.72451020669870658, -18.67979575497194134, 69.58442372801900433 ) ) ;
#131276 = CARTESIAN_POINT ( 'NONE',  ( -19.03943276465977164, 0.05219959533909376836, 41.24890960531435269 ) ) ;
#131277 = ADVANCED_FACE ( 'NONE', ( #154791 ), #16289, .T. ) ;
#131278 = CARTESIAN_POINT ( 'NONE',  ( -8.224510206698948167, 14.34966873604960824, 75.41557627198102409 ) ) ;
#131279 = CARTESIAN_POINT ( 'NONE',  ( -8.224510206698735004, -14.34966873604973081, 24.58442372801901499 ) ) ;
#131280 = CARTESIAN_POINT ( 'NONE',  ( 5.823673210054444382, -21.52544592524334988, 50.20942372801901854 ) ) ;
#131281 = EDGE_LOOP ( 'NONE', ( #95856, #195692, #44066, #22869 ) ) ;
#131282 = CARTESIAN_POINT ( 'NONE',  ( 19.02544592524343514, -5.153800228976328945, 113.5405762719810241 ) ) ;
#131283 = CARTESIAN_POINT ( 'NONE',  ( 9.564922557961047289, -16.46253265017146816, 65.41775706135233293 ) ) ;
#131284 = CARTESIAN_POINT ( 'NONE',  ( -12.73749492396214578, -155.7167183371837496, -13.00000000000000000 ) ) ;
#131285 = CARTESIAN_POINT ( 'NONE',  ( 5.823673210054444382, -21.52544592524334988, 20.20942372801900788 ) ) ;
#131286 = CARTESIAN_POINT ( 'NONE',  ( -19.03943276465977164, 0.05219959533909376836, 56.24890960531435979 ) ) ;
#131287 = CARTESIAN_POINT ( 'NONE',  ( -30.74264578624800492, -22.33583958711396278, -7.549999994537627934 ) ) ;
#131288 = CARTESIAN_POINT ( 'NONE',  ( -16.51473224551082808, 9.474510206698731452, 23.33442372801900078 ) ) ;
#131289 = CARTESIAN_POINT ( 'NONE',  ( -5.049401038298153566, 19.05341960407611168, 55.20724293864769550 ) ) ;
#131290 = CARTESIAN_POINT ( 'NONE',  ( -18.67979575497193778, 10.72451020669871902, 108.3344237280190185 ) ) ;
#131291 = CARTESIAN_POINT ( 'NONE',  ( 0.05219959533934541429, -16.53943276465976808, 100.0010903946857042 ) ) ;
#131293 = CARTESIAN_POINT ( 'NONE',  ( 5.719274019375673035, 21.55341960407619339, 72.29275706135236135 ) ) ;
#131292 = CARTESIAN_POINT ( 'NONE',  ( -9.564922557960796823, -16.46253265017161027, 102.0822429386477097 ) ) ;
#131294 = CARTESIAN_POINT ( 'NONE',  ( 1.784210473542230573E-15, -29.16686587814331588, 147.8750000027311273 ) ) ;
#131295 = CARTESIAN_POINT ( 'NONE',  ( 16.51473224551069308, 9.474510206698969483, 114.1655762719810241 ) ) ;
#131296 = CARTESIAN_POINT ( 'NONE',  ( -17.49999999999999645, -5.499999999999992895, 94.20309617465827046 ) ) ;
#131298 = CARTESIAN_POINT ( 'NONE',  ( 10.81492255796106328, -18.62759615963255655, 75.41775706135233293 ) ) ;
#131297 = CARTESIAN_POINT ( 'NONE',  ( -4.379528057220086978, -16.55341960407618274, 59.79275706135234714 ) ) ;
#131299 = CARTESIAN_POINT ( 'NONE',  ( -15.80617190586768217, 15.72974639402176855, 103.1260903946856757 ) ) ;
#131300 = CARTESIAN_POINT ( 'NONE',  ( 11.45643923738960446, -4.999999999999992895, -18.00000000000000000 ) ) ;
#131301 = CARTESIAN_POINT ( 'NONE',  ( -19.02544592524342804, 5.153800228976336051, 81.04057627198103830 ) ) ;
#131302 = CARTESIAN_POINT ( 'NONE',  ( -5.049401038298153566, 19.05341960407611168, 105.2072429386476671 ) ) ;
#131303 = ORIENTED_EDGE ( 'NONE', *, *, #126809, .T. ) ;
#131304 = CARTESIAN_POINT ( 'NONE',  ( 16.52216118717209170, 7.221426719304526287, 43.57599021046996057 ) ) ;
#131305 = CARTESIAN_POINT ( 'NONE',  ( -5.049401038298153566, 19.05341960407611168, 45.20724293864769550 ) ) ;
#131306 = CARTESIAN_POINT ( 'NONE',  ( 5.719274019375991003, -21.55341960407610458, 47.70724293864770260 ) ) ;
#131307 = CARTESIAN_POINT ( 'NONE',  ( 14.29746914071037800, 8.314922557961029526, 111.6677570613523613 ) ) ;
#131309 = CARTESIAN_POINT ( 'NONE',  ( 5.153800228976335163, 19.02544592524342804, 84.79057627198099567 ) ) ;
#131308 = CARTESIAN_POINT ( 'NONE',  ( 16.55341960407611168, 4.379528057220329451, 83.95724293864770971 ) ) ;
#131310 = CARTESIAN_POINT ( 'NONE',  ( 21.53943276465977519, 0.05219959533937863772, 101.2510903946856757 ) ) ;
#131311 = CARTESIAN_POINT ( 'NONE',  ( -5.153800228976328057, -19.02544592524343514, 32.29057627198102409 ) ) ;
#131312 = CARTESIAN_POINT ( 'NONE',  ( -16.52544592524342804, 4.483927247898546575, 86.04057627198102409 ) ) ;
#131313 = CARTESIAN_POINT ( 'NONE',  ( -21.52544592524334988, -5.823673210054445271, 43.95942372801902565 ) ) ;
#131314 = CARTESIAN_POINT ( 'NONE',  ( 18.67979575497178502, 10.72451020669898547, 89.16557627198102409 ) ) ;
#131315 = CARTESIAN_POINT ( 'NONE',  ( 0.05219959533936267826, -19.03943276465977164, 45.00109039468566863 ) ) ;
#131316 = CARTESIAN_POINT ( 'NONE',  ( -34.40392893854400569, 6.519971432731296979, 48.73974290947565891 ) ) ;
#131317 = CARTESIAN_POINT ( 'NONE',  ( 5.153800228976335163, 19.02544592524342804, 89.79057627198102409 ) ) ;
#131318 = CARTESIAN_POINT ( 'NONE',  ( 14.34966873604960469, 8.224510206698951720, 64.16557627198102409 ) ) ;
#131319 = AXIS2_PLACEMENT_3D ( 'NONE', #134490, #165822, #24318 ) ;
#131320 = CARTESIAN_POINT ( 'NONE',  ( -16.53943276465976808, 0.05219959533911058130, 51.24890960531436690 ) ) ;
#131321 = CARTESIAN_POINT ( 'NONE',  ( -16.46253265017146816, -9.564922557961047289, 84.16775706135233293 ) ) ;
#131322 = CARTESIAN_POINT ( 'NONE',  ( -3.573655867282028392E-15, 2.428612866367529932E-14, 139.9999999999999716 ) ) ;
#131323 = CARTESIAN_POINT ( 'NONE',  ( -5.719274019375978568, 21.55341960407610458, 25.20724293864769550 ) ) ;
#131324 = EDGE_CURVE ( 'NONE', #16960, #99783, #120134, .T. ) ;
#131325 = CARTESIAN_POINT ( 'NONE',  ( -4.483927247898539470, -16.52544592524342804, 92.29057627198103830 ) ) ;
#131326 = CARTESIAN_POINT ( 'NONE',  ( -69.65682714487590488, -71.74905178543390605, -15.00000000000000000 ) ) ;
#131328 = CARTESIAN_POINT ( 'NONE',  ( -21.55341960407610458, -5.719274019375992779, 51.45724293864770260 ) ) ;
#131327 = CARTESIAN_POINT ( 'NONE',  ( 9.564922557960805705, 16.46253265017160317, 49.58224293864770260 ) ) ;
#131329 = CARTESIAN_POINT ( 'NONE',  ( -5.049401038298153566, 19.05341960407611168, 30.20724293864768839 ) ) ;
#131331 = CARTESIAN_POINT ( 'NONE',  ( -16.51473224551069308, -9.474510206698971260, 61.66557627198103120 ) ) ;
#131330 = CARTESIAN_POINT ( 'NONE',  ( -14.34966873604972548, 8.224510206698743886, 73.33442372801901854 ) ) ;
#131332 = CARTESIAN_POINT ( 'NONE',  ( -13.89961937509957401, -13.97604488694547875, 34.37609039468566863 ) ) ;
#131333 = CARTESIAN_POINT ( 'NONE',  ( 18.67979575497194134, -10.72451020669871369, 70.83442372801901854 ) ) ;
#131334 = CARTESIAN_POINT ( 'NONE',  ( 18.62759615963271287, -10.81492255796078972, 38.33224293864768839 ) ) ;
#131335 = CARTESIAN_POINT ( 'NONE',  ( 16.46253265017160672, -9.564922557960803928, 23.33224293864769194 ) ) ;
#131336 = CARTESIAN_POINT ( 'NONE',  ( 13.89961937509957401, 13.97604488694547697, 96.87609039468566152 ) ) ;
#131337 = CARTESIAN_POINT ( 'NONE',  ( -36.91746825000000598, 2.428612866367529932E-14, -5.124999997268813168 ) ) ;
#131339 = CARTESIAN_POINT ( 'NONE',  ( -0.05219959533907301413, -21.53943276465977519, 42.49890960531435979 ) ) ;
#131338 = CARTESIAN_POINT ( 'NONE',  ( -1.500431131851305500, -22.62413958104530920, -57.95367621771161737 ) ) ;
#131340 = CARTESIAN_POINT ( 'NONE',  ( 16.51473224551069308, 9.474510206698969483, 24.16557627198102765 ) ) ;
#131341 = CARTESIAN_POINT ( 'NONE',  ( -15.80617190586768217, 15.72974639402176855, 78.12609039468570415 ) ) ;
#131342 = CARTESIAN_POINT ( 'NONE',  ( -14.34966873604960291, -8.224510206698953496, 46.66557627198102409 ) ) ;
#131344 = CARTESIAN_POINT ( 'NONE',  ( 16.52544592524342804, -4.483927247898539470, 53.54057627198103120 ) ) ;
#131343 = CARTESIAN_POINT ( 'NONE',  ( -4.379528057220086978, -16.55341960407618274, 74.79275706135234714 ) ) ;
#131345 = CARTESIAN_POINT ( 'NONE',  ( 21.52544592524344225, -5.823673210054117533, 78.54057627198103830 ) ) ;
#131346 = CARTESIAN_POINT ( 'NONE',  ( 0.05219959533907565091, 21.53943276465977519, 74.99890960531435269 ) ) ;
#131347 = CARTESIAN_POINT ( 'NONE',  ( -28.47622644277399928, -25.16156846422451920, -16.68312038616162951 ) ) ;
#131348 = CARTESIAN_POINT ( 'NONE',  ( -10.81492255796078084, -18.62759615963271287, 37.08224293864768129 ) ) ;
#131349 = CARTESIAN_POINT ( 'NONE',  ( -0.05219959533934338120, 16.53943276465976808, 47.50109039468568994 ) ) ;
#131350 = CARTESIAN_POINT ( 'NONE',  ( 16.52544592524342804, -4.483927247898539470, 78.54057627198103830 ) ) ;
#131351 = CARTESIAN_POINT ( 'NONE',  ( 16.46253265017160672, -9.564922557960803928, 68.33224293864770971 ) ) ;
#131352 = CARTESIAN_POINT ( 'NONE',  ( -16.51473224551069308, -9.474510206698971260, 31.66557627198102054 ) ) ;
#131353 = CARTESIAN_POINT ( 'NONE',  ( -17.72517630440434289, 5.499999999999977796, 75.92175719257211597 ) ) ;
#131354 = CARTESIAN_POINT ( 'NONE',  ( 12.06949235617739724, 12.14591786802326823, 76.87609039468567573 ) ) ;
#131355 = CARTESIAN_POINT ( 'NONE',  ( 15.80617190586746368, 15.72974639402197994, 114.3739096053143527 ) ) ;
#131356 = CARTESIAN_POINT ( 'NONE',  ( -16.51473224551069308, -9.474510206698971260, 66.66557627198102409 ) ) ;
#131357 = CARTESIAN_POINT ( 'NONE',  ( -5.823673210054431948, 21.52544592524334988, 52.70942372801902565 ) ) ;
#131358 = CARTESIAN_POINT ( 'NONE',  ( -0.05219959533909027116, -19.03943276465977164, 112.4989096053143669 ) ) ;
#131359 = CARTESIAN_POINT ( 'NONE',  ( -8.543935154431821388, -46.31530851242288804, -24.25021605108518941 ) ) ;
#131360 = ORIENTED_EDGE ( 'NONE', *, *, #60782, .F. ) ;
#131361 = CARTESIAN_POINT ( 'NONE',  ( 0.05219959533937995610, -21.53943276465977519, 50.00109039468568994 ) ) ;
#131363 = CARTESIAN_POINT ( 'NONE',  ( 16.46253265017160672, -9.564922557960803928, 103.3322429386476955 ) ) ;
#131362 = CARTESIAN_POINT ( 'NONE',  ( -9.474510206698964154, 16.51473224551069663, 115.4155762719810241 ) ) ;
#131364 = CARTESIAN_POINT ( 'NONE',  ( 0.05219959533936267826, -19.03943276465977164, 55.00109039468566863 ) ) ;
#131365 = CARTESIAN_POINT ( 'NONE',  ( -21.52544592524343514, 5.823673210054127303, 111.0405762719810525 ) ) ;
#131366 = CARTESIAN_POINT ( 'NONE',  ( -9.564922557961040184, 16.46253265017147172, 42.91775706135234003 ) ) ;
#131367 = CARTESIAN_POINT ( 'NONE',  ( -19.03943276465977164, -0.05219959533935918106, 68.75109039468566152 ) ) ;
#131368 = CARTESIAN_POINT ( 'NONE',  ( 12.14591786802327356, -12.06949235617739191, 100.6260903946857184 ) ) ;
#131370 = ORIENTED_EDGE ( 'NONE', *, *, #42762, .T. ) ;
#131369 = CARTESIAN_POINT ( 'NONE',  ( 30.00000000000000000, -5.510910596163089556E-15, 42.49999999999999289 ) ) ;
#131371 = CARTESIAN_POINT ( 'NONE',  ( 16.51473224551069308, 9.474510206698969483, 84.16557627198102409 ) ) ;
#131372 = CIRCLE ( 'NONE', #199217, 61.99999999999998579 ) ;
#131373 = CARTESIAN_POINT ( 'NONE',  ( 18.62759615963255655, 10.81492255796105972, 91.66775706135234714 ) ) ;
#131374 = CARTESIAN_POINT ( 'NONE',  ( 10.81492255796106328, -18.62759615963255655, 90.41775706135236135 ) ) ;
#131375 = CARTESIAN_POINT ( 'NONE',  ( 21.31291730435230747, -0.2247805922399771505, -56.45983593933052447 ) ) ;
#131376 = CARTESIAN_POINT ( 'NONE',  ( -5.153800228976328057, -19.02544592524343514, 107.2905762719810383 ) ) ;
#131377 = CARTESIAN_POINT ( 'NONE',  ( 5.823673210054444382, -21.52544592524334988, 75.20942372801901854 ) ) ;
#131378 = CARTESIAN_POINT ( 'NONE',  ( -19.03943276465977164, -0.05219959533935918106, 108.7510903946856615 ) ) ;
#131379 = CARTESIAN_POINT ( 'NONE',  ( -19.05341960407611168, -5.049401038298163336, 81.45724293864769550 ) ) ;
#131380 = CARTESIAN_POINT ( 'NONE',  ( -5.823673210054116645, -21.52544592524344225, 27.29057627198103120 ) ) ;
#131381 = CARTESIAN_POINT ( 'NONE',  ( 19.02544592524343514, -5.153800228976328945, 98.54057627198100988 ) ) ;
#131382 = CARTESIAN_POINT ( 'NONE',  ( -17.05116617787826527, -6.768360034955815507, 91.34324446740806991 ) ) ;
#131383 = CARTESIAN_POINT ( 'NONE',  ( 13.97604488694527802, 13.89961937509977652, 79.37390960531435269 ) ) ;
#131384 = CARTESIAN_POINT ( 'NONE',  ( -19.05341960407611168, -5.049401038298163336, 66.45724293864769550 ) ) ;
#131385 = CARTESIAN_POINT ( 'NONE',  ( 0.05219959533907565091, 21.53943276465977519, 109.9989096053143527 ) ) ;
#131386 = CARTESIAN_POINT ( 'NONE',  ( -8.314922557961024197, 14.29746914071037800, 97.91775706135236135 ) ) ;
#131387 = FACE_OUTER_BOUND ( 'NONE', #40329, .T. ) ;
#131388 = CARTESIAN_POINT ( 'NONE',  ( -5.153800228976607833, 19.02544592524334988, 52.70942372801900433 ) ) ;
#131389 = CARTESIAN_POINT ( 'NONE',  ( -13.97604488694527625, -13.89961937509977652, 96.87390960531433848 ) ) ;
#131390 = CARTESIAN_POINT ( 'NONE',  ( -8.314922557960811034, -14.29746914071050412, 87.08224293864769550 ) ) ;
#131391 = B_SPLINE_CURVE_WITH_KNOTS ( 'NONE', 3,
 ( #44873, #27741, #89383, #182402, #169187, #12563, #14526, #74229, #75202, #106529, #168206, #76187, #199546, #61016, #144814, #156010, #17507, #173182, #159991, #79165 ),
 .UNSPECIFIED., .F., .F.,
 ( 4, 2, 2, 2, 2, 2, 2, 2, 2, 4 ),
 ( 0.000000000000000000, 0.0004987090165372591501, 0.0009974180330745183003, 0.001246772541343151670, 0.001496127049611785040, 0.001994836066149047443, 0.002493545082686309412, 0.002742899590954942565, 0.002992254099223575717, 0.003989672132298185958 ),
 .UNSPECIFIED. ) ;
#131392 = CARTESIAN_POINT ( 'NONE',  ( 21.53943276465977519, -0.05219959533907433946, 28.74890960531435624 ) ) ;
#131393 = CARTESIAN_POINT ( 'NONE',  ( -9.564922557960796823, -16.46253265017161027, 112.0822429386476955 ) ) ;
#131394 = CARTESIAN_POINT ( 'NONE',  ( -16.55341960407611168, -4.379528057220339221, 96.45724293864770971 ) ) ;
#131395 = CARTESIAN_POINT ( 'NONE',  ( -16.61371651742604172, 7.165104196376022472, 53.85415069992998127 ) ) ;
#131396 = CARTESIAN_POINT ( 'NONE',  ( 19.05341960407617918, -5.049401038297876454, 41.04275706135233293 ) ) ;
#131397 = CARTESIAN_POINT ( 'NONE',  ( -16.53943276465976808, -0.05219959533934237506, 108.7510903946857042 ) ) ;
#131398 = CARTESIAN_POINT ( 'NONE',  ( 9.564922557960805705, 16.46253265017160317, 84.58224293864769550 ) ) ;
#131399 = CARTESIAN_POINT ( 'NONE',  ( 21.53943276465977519, 0.05219959533937863772, 71.25109039468568994 ) ) ;
#131400 = CARTESIAN_POINT ( 'NONE',  ( -21.53943276465977519, 0.05219959533907696930, 51.24890960531436690 ) ) ;
#131401 = CARTESIAN_POINT ( 'NONE',  ( -15.72974639402176322, -15.80617190586768395, 34.37609039468568284 ) ) ;
#131402 = CARTESIAN_POINT ( 'NONE',  ( 21.53943276465977519, -0.05219959533907433946, 88.74890960531436690 ) ) ;
#131403 = CARTESIAN_POINT ( 'NONE',  ( 8.314922557960818139, 14.29746914071049879, 114.5822429386477097 ) ) ;
#131404 = CARTESIAN_POINT ( 'NONE',  ( -19.05341960407617563, 5.049401038297882671, 68.54275706135230450 ) ) ;
#131405 = CARTESIAN_POINT ( 'NONE',  ( 13.97604488694527802, 13.89961937509977652, 44.37390960531435269 ) ) ;
#131406 =( BOUNDED_SURFACE ( )  B_SPLINE_SURFACE ( 3, 2, ( 
 ( #39061, #142242, #20892, #96724, #173600, #129050, #18922, #53221, #130039, #127065, #191738, #190751, #21898, #6709, #38066, #143229, #189765, #114898, #82550, #83548, #176592, #80567, #36057, #99722, #144232, #37056, #51237, #97706, #5716, #175579, #4712, #65404, #84544, #3727, #174592, #145227, #66401, #67393, #128063, #52225, #35069, #146221, #161406, #22898, #188773, #112898, #50256, #68387, #98715, #111912, #54233, #158412, #7709, #69393, #115904, #160409, #131061, #192750, #177594, #157428, #19901, #81542, #193759, #133066, #102734, #164423, #178588, #59202, #23902, #179599, #89555, #150253, #40052, #120871, #25916, #58228, #57242, #55227, #181582, #182571, #103738, #117910, #104726, #74396, #101729, #88554, #165418, #9738, #27912, #26911, #135085, #163417, #11747, #196761, #119897, #87560, #24913, #132070, #162399, #134079, #10738, #73414, #43060, #194756, #116896, #166418, #149247, #151241, #195768, #86560, #118916, #180600, #12730, #41071, #42074, #136061, #85556, #100719, #147241, #8733, #72402, #197736, #70402, #148244, #71402, #56228, #183559, #155196, #47029, #106703, #125844, #185536, #44054, #105714, #502, #170365, #138039, #121867, #108687, #31857, #141011, #93510, #154204, #167401, #153196, #107682, #123838, #79341, #61186, #28897, #13703, #124854, #60197, #90537, #122858, #16685, #75370, #17683, #186554, #30869, #156184, #152219, #199720, #168376, #184546, #137040, #29872, #91509, #2498, #1497, #109683, #78335, #45045, #171364, #198731, #32852, #62174, #46026, #14700, #140008, #48026, #76362, #169359, #63175, #92515, #94502, #64179, #15694, #77355, #139022, #112655, #67151, #81302, #127816, #174346, #143988, #34826, #95497, #114646, #110668, #4464, #51982, #173355, #97462, #96481, #159148, #65161, #176344, #68143, #21652, #172348, #158169, #18677, #113640, #20644, #80323, #84301, #128809, #188526, #35816, #142986, #50003, #37816, #33837, #157183, #141996, #82297, #83305, #3484, #190508, #126820, #19661, #144982, #111668, #99477, #36802, #66153, #189521, #49013, #6462, #50994, #5469, #175335, #98467, #160161, #129794, #161158, #69146, #191491, #187546, #52969, #22654, #145980, #7462, #8481, #133827, #72151, #27670, #118665, #40818, #53988, #39806, #194508, #10491, #166169, #148003, #192504, #100479, #11499, #146994, #115661, #9493, #195518, #162158, #104485, #73170, #117658, #42822, #12494, #24665, #54984, #86314, #130813, #193507, #116653, #89310, #88305, #196519, #56991, #70156, #57990, #23654, #119661, #87318, #132822, #178344, #177351, #180356, #181343, #151003, #71156, #179355, #149002, #41825, #163162, #38821, #103492, #85302, #134840, #165170, #131826, #101472, #55981, #26663, #102488, #164175, #25673, #149993, #75128, #60941, #168132, #136796, #65667, #120632, #58964, #182329, #122616, #111176, #90292, #77109, #13464, #121621, #172866, #105471, #127329, #126346, #151976, #198482, #135827, #34347, #76113, #92271, #183316, #64684, #96008, #197497, #138779, #260, #184306, #45787, #59954, #44798, #107439, #43808, #152951, #169111, #49513, #3987, #189041, #153955, #50516, #188043, #157692, #167157, #30618, #106453, #19183, #28657, #137790, #29628, #15451, #80832, #142509, #74156, #112179, #35335, #91260, #173867, #96988, #158670, #14450, #199474, #159661, #193017, #145492, #6972, #55492, #161669, #81805, #146487, #117162, #143492, #176859, #84808, #102000, #4977, #22161, #21158, #36315, #192003, #66663, #116166, #54494, #190025, #177856, #53489, #7978, #69662, #100984, #5978, #52487, #39325, #68652, #131329, #162668, #128326, #98979, #24174, #130308, #99984, #114147, #160669, #115166, #38328, #67658, #51499, #147513, #113159, #37321, #85825, #129315, #23165, #191011, #9003, #97969, #83812, #70670, #132337, #175848, #174849, #194029, #82813, #178858, #40324, #20160, #144495, #149504, #73675, #41336, #90796, #44319, #198000, #148513, #72673, #195021, #28180, #135347 ),
 ( #197021, #58487, #59470, #42338, #43324, #13967, #10003, #183823, #122136, #71663, #120154, #12014, #25185, #118175, #136325, #181844, #86827, #11001, #182837, #121143, #45313, #104991, #163682, #133330, #166679, #89822, #57508, #102997, #151503, #12995, #60461, #74658, #105978, #56497, #134350, #27176, #167663, #198993, #180862, #179866, #164683, #29159, #26177, #87818, #103999, #152480, #196032, #137312, #75634, #150516, #119177, #165677, #88823, #31138, #62444, #188803, #169642, #92786, #65433, #64450, #172627, #186830, #123127, #34115, #76630, #95773, #63456, #108961, #154474, #168637, #33123, #157459, #3756, #774, #155467, #125132, #48298, #139296, #106963, #109955, #199989, #124118, #170641, #32129, #184812, #127094, #30137, #185818, #18953, #156461, #46298, #91780, #93787, #94780, #153474, #16958, #15967, #78612, #140286, #171634, #14970, #17960, #138308, #61456, #1777, #79615, #141284, #142274, #107955, #77627, #2774, #126120, #187815, #47305, #49284, #110942, #80598, #85586, #111943, #6739, #114930, #132098, #35100, #52254, #189795, #66430, #21928, #173630, #146253, #22929, #19930, #84575, #83579, #176623, #99753, #131092, #36086, #82579, #7739, #175610, #38098, #69425, #96752, #129078, #192780, #37086, #130070, #144260, #190779, #98745, #68417, #97736, #158442, #177625, #81571, #67423, #161437, #159425, #160438, #20921, #145258, #128091, #39093, #54263, #115935, #143257, #5747, #4741, #100749, #191769, #51266, #147272, #53252, #112926, #162430, #113911, #174621, #23931, #8763, #70432, #50286, #42105, #27945, #9767, #196791, #133095, #41101, #89586, #24944, #182603, #43091, #71431, #194785, #55257, #151272, #195800, #11780, #102766, #181613, #12762, #116925, #58259, #119928, #103769, #165448, #56258, #117941, #180632, #178618, #72435, #26943, #166448, #120904, #44088, #73444, #105747, #104759, #74427, #40081, #88585, #25947, #136093, #75403, #135115, #193788, #101759, #150284, #197768, #87590, #179630, #59234, #167433, #90569, #28929, #152251, #163447, #164453, #57272, #13736, #86592, #10769, #148275, #149276, #134111, #118947, #60230, #15728, #16721, #106735, #110706, #17721, #123872, #49051, #18716, #30902, #61219, #92549, #137075, #199752, #122890, #95536, #94540, #2536, #78370, #153231, #64217, #168409, #125883, #93546, #139057, #184578, #198764, #63212, #187583, #33877, #154238, #185571, #155231, #140044, #169394, #121899, #1534, #29904, #77388, #536, #62208, #14734, #157223, #183593, #47064, #172387, #186591, #76395, #45077, #108724, #156221, #124892, #91542, #79379, #138071, #48063, #170401, #141050, #46059, #107714, #109719, #171402, #31892, #32889, #145021, #114689, #158209, #6502, #176384, #37858, #144027, #4502, #111708, #142036, #113679, #190546, #53010, #161199, #112693, #173394, #99517, #5509, #68182, #175373, #143024, #36841, #98506, #22694, #159187, #160201, #130853, #65200, #100518, #38862, #126859, #52020, #128847, #3524, #34864, #84341, #21691, #188565, #127856, #146020, #69187, #50045, #96519, #19699, #83345, #7503, #81341, #129834, #66193, #189560, #192545, #51032, #54028, #191533, #174385, #35855, #97501, #115701, #82337, #177390, #20682, #162197, #80363, #67190, #57032, #118705, #164214, #25711, #39846, #116693, #87356, #147036, #56019, #149042, #165208, #196556, #119697, #133867, #181380, #41867, #180396, #85343, #102531, #71196, #103533, #8520, #117697, #148041, #10530, #72194, #195558, #23695, #26703, #70198, #163202, #88343, #150035, #11541, #131865, #193549, #132860, #58027, #73209, #134880, #55022, #42858, #101512, #104523, #178382, #86355, #166204, #27706, #24706, #194549, #89348, #9530, #179394, #40857, #65843, #100172, #177046, #174045, #38516, #176037, #68842, #53679, #84993, #190199, #36496, #161854, #129497, #130501, #23348, #127513, #83001, #146674, #191196, #83998, #98150, #144676, #52671, #160857, #51677, #112354, #131513, #189217, #21343, #192197 ),
 ( #35514, #101163, #145677, #5158, #114334, #159850, #66841, #37505, #7159, #4165, #115356, #162851, #97162, #99167, #22347, #8169, #39503, #24358, #143677, #69845, #193199, #54672, #86009, #116346, #50696, #178035, #158847, #20335, #81984, #128504, #113339, #175031, #6161, #67841, #163871, #119358, #9186, #43505, #120327, #117348, #182022, #181042, #12193, #197198, #28359, #133515, #180054, #105171, #72863, #73858, #166857, #70851, #26362, #89997, #134533, #27358, #41523, #88002, #196220, #104180, #195207, #55674, #74835, #132520, #164867, #135527, #56687, #57690, #118361, #42517, #25370, #136497, #151679, #13172, #194209, #103186, #179044, #58661, #165862, #40512, #44497, #89004, #148698, #150695, #149690, #10186, #198177, #102183, #87012, #71846, #59647, #121321, #11188, #183013, #106153, #167835, #29336, #147698, #99803, #7793, #34162, #159475, #97786, #110992, #3804, #21978, #20969, #172677, #96805, #68469, #6790, #131142, #190828, #49331, #95823, #5798, #175660, #143304, #127144, #52304, #113961, #146304, #37134, #82626, #157508, #158491, #112976, #129130, #84626, #66480, #19002, #80648, #130124, #65482, #142324, #67471, #81621, #188851, #98794, #50335, #4790, #51315, #174669, #111992, #69476, #173682, #128142, #38149, #160488, #35149, #19978, #36134, #191821, #83630, #189842, #53301, #144308, #145307, #114980, #176673, #22977, #161489, #180677, #195845, #101808, #119971, #57318, #26989, #70480, #118994, #88634, #150330, #56306, #116975, #23980, #54311, #25991, #102813, #165493, #73490, #24994, #85636, #11825, #117988, #42153, #87634, #55303, #149320, #10814, #135163, #71477, #134157, #133142, #72484, #43136, #151319, #177672, #164498, #41150, #115983, #147323, #196836, #103813, #39140, #40130, #58304, #181657, #74475, #104805, #192830, #100795, #166494, #27992, #86638, #132146, #89631, #12808, #162478, #8811, #193839, #178667, #163496, #179678, #148321, #9816, #194833, #197816, #105793, #16765, #152298, #59281, #14782, #15774, #167479, #109760, #78413, #122937, #48104, #17766, #29953, #60275, #91591, #136140, #198810, #121948, #94586, #93590, #1581, #77433, #13782, #63256, #28974, #124936, #92594, #138119, #183641, #120951, #62250, #186633, #32931, #153281, #184624, #154284, #168456, #123919, #182650, #199800, #45123, #46106, #169445, #139105, #44134, #185618, #156265, #90616, #30947, #579, #47108, #171444, #75449, #137123, #108767, #61267, #107760, #106781, #170445, #76442, #31936, #155276, #140089, #35898, #144071, #161243, #64260, #81382, #18760, #95579, #51074, #141093, #175418, #52065, #49095, #113722, #112735, #5552, #128889, #160246, #65243, #111750, #36886, #4545, #67231, #98552, #2580, #158251, #21735, #66239, #159231, #173438, #19741, #127899, #97544, #126903, #187625, #6546, #125926, #96563, #190589, #188609, #189601, #50090, #174428, #157264, #68225, #83388, #145065, #110752, #34907, #172433, #129878, #20726, #33922, #176429, #82383, #80407, #191577, #143067, #142079, #53055, #3565, #114735, #37903, #99561, #79422, #56063, #57077, #101558, #164260, #163250, #102576, #73251, #181422, #7546, #132904, #71241, #84385, #177433, #195604, #194592, #146062, #70243, #41912, #180440, #104565, #25755, #22737, #69232, #179437, #149086, #116737, #100561, #87401, #10574, #119739, #72237, #117742, #130899, #131911, #86399, #133913, #118751, #178427, #24752, #148084, #40903, #193595, #192589, #150079, #54072, #39891, #103578, #8568, #165253, #55066, #26747, #162241, #11584, #88385, #134921, #115746, #9575, #38904, #196598, #58069, #23741, #42900, #85390, #147084, #153033, #60036, #167238, #155028, #12570, #93343, #75209, #46861, #91342, #182409, #169194, #105552, #13543, #108522, #170201, #16524, #76194, #43888, #28736, #27748, #339, #168213, #184384, #136880, #154037, #123672, #89391, #30701, #92351, #14533, #137873, #90373, #152058, #199553, #151079, #44880, #61023, #138859, #78171 ),
 ( #74236, #106536, #45865, #135905, #139840, #31694, #122695, #1329, #47862, #121703, #198566, #183397, #166247, #29710, #107518, #124688, #185370, #63009, #15532, #77189, #186384, #197576, #59043, #62007, #120709, #172185, #171197, #35654, #36638, #6304, #3326, #158009, #65988, #127658, #141834, #191332, #189358, #2332, #64999, #111502, #173188, #187380, #67982, #32686, #188360, #98295, #158988, #48849, #129636, #110503, #159997, #190342, #143823, #94338, #18515, #140843, #174186, #19500, #64013, #109515, #50835, #33670, #96322, #126657, #95332, #21484, #156017, #83146, #80162, #51818, #34664, #125682, #112492, #157017, #49838, #113478, #175172, #144820, #81145, #142826, #4306, #17514, #5304, #97302, #20480, #82130, #66988, #128647, #79172, #55822, #117495, #101311, #163000, #192345, #68987, #39650, #37650, #131665, #24506, #25515, #180198, #103331, #132666, #165010, #102329, #40660, #114477, #86157, #85142, #164019, #176180, #54822, #161997, #147847, #9333, #194355, #52810, #179192, #11336, #145819, #70999, #87160, #148842, #88146, #73007, #53827, #10332, #178185, #71989, #149832, #133663, #99314, #195353, #134676, #160999, #56833, #118508, #22493, #84140, #116497, #115502, #130651, #41667, #7302, #26504, #177189, #38663, #100318, #23493, #146827, #8321, #69997, #193347, #28500, #153793, #121464, #60783, #15288, #119503, #74974, #76947, #183157, #75957, #90134, #136636, #44641, #152797, #43647, #104323, #123436, #181184, #13308, #122454, #182163, #106293, #105311, #167979, #151819, #120471, #198318, #77937, #58803, #166998, #154788, #138617, #61768, #137631, #12334, #185129, #166007, #46620, #14289, #59795, #29477, #57830, #184147, #108281, #93104, #91108, #199316, #45628, #107280, #168951, #196362, #30457, #89149, #92105, #99, #169959, #73998, #16287, #42661, #31451, #27508, #150838, #135668, #197340, #141607, #97074, #96094, #32448, #20244, #162511, #142596, #156789, #143585, #116013, #17278, #127423, #4076, #48620, #69507, #65753, #173954, #78932, #189131, #35421, #158755, #3094, #63779, #170955, #1090, #172956, #49602, #112262, #81892, #171953, #94102, #5068, #110271, #19273, #155781, #111265, #34434, #157783, #131173, #18282, #80920, #79937, #50603, #192863, #100828, #124447, #54342, #188130, #62766, #140608, #177703, #39170, #186143, #187147, #24012, #139604, #47622, #109276, #2098, #125451, #33441, #95100, #64771, #126433, #88670, #27025, #182685, #73527, #195881, #8843, #194865, #149352, #165529, #120987, #102844, #147355, #55336, #166530, #101838, #70511, #164529, #150366, #117006, #59318, #28027, #72518, #197851, #167516, #87667, #103848, #133175, #135198, #43172, #132179, #11862, #196871, #134193, #57354, #25025, #163525, #119029, #193870, #26022, #180712, #58338, #12844, #136176, #120006, #44170, #181691, #104839, #178701, #42188, #118020, #89668, #40163, #10849, #56338, #151355, #74510, #105829, #85668, #86669, #148352, #9848, #71507, #179709, #41181, #64296, #187661, #168492, #1617, #154320, #15809, #125963, #170482, #90651, #155313, #49132, #152333, #185653, #93628, #110790, #13819, #30981, #29990, #45162, #617, #75485, #124973, #63293, #198847, #186670, #62287, #16802, #78452, #109797, #14818, #61304, #48140, #77470, #140126, #171480, #137158, #107797, #32969, #139140, #108803, #122974, #169481, #123955, #47145, #76479, #60311, #156302, #121987, #46143, #94623, #138156, #31972, #199837, #17803, #106818, #79460, #141129, #2619, #183677, #184661, #91629, #29011, #153317, #92629, #69268, #52101, #173474, #159267, #66276, #34947, #161278, #18798, #99598, #81418, #53092, #97579, #188647, #175454, #111786, #19777, #114770, #176464, #22773, #82418, #50126, #96599, #33958, #6583, #20763, #127935, #158288, #84421, #80443, #146098, #143104, #37937, #144107, #4583, #36925, #189637, #51112, #7582, #130934, #192625, #5587, #112771, #174464, #95616, #68262, #35933, #190626, #67267 ),
 ( #145100, #54107, #172471, #113758, #157301, #21772, #160281, #142116, #128925, #98587, #83423, #3601, #129913, #191613, #65280, #126939, #57117, #115781, #41951, #74275, #8606, #10615, #72276, #133953, #151119, #135945, #55103, #88428, #40942, #102614, #12611, #118791, #177470, #103617, #197615, #38939, #195644, #180480, #100596, #162278, #117783, #116773, #131947, #87439, #23778, #11623, #150122, #85428, #73291, #149124, #165293, #26786, #196639, #101600, #148123, #134961, #164300, #58108, #119778, #147119, #194632, #181462, #25793, #42940, #9614, #56102, #104604, #166292, #163288, #70279, #27788, #193631, #132944, #89430, #24789, #178464, #86437, #39931, #71279, #179477, #139879, #93381, #43926, #168251, #90411, #123713, #169234, #152096, #156056, #138896, #60073, #185410, #153071, #136918, #62048, #376, #17553, #46901, #30740, #182446, #29747, #122732, #108561, #94376, #76231, #120747, #28773, #1368, #75247, #105588, #137911, #170239, #13580, #32724, #63047, #45903, #171235, #140882, #14573, #183433, #199593, #59080, #121741, #44918, #79213, #16562, #124726, #31733, #198605, #186424, #106574, #47900, #15569, #61060, #91382, #167274, #155067, #109554, #184423, #107556, #92388, #77227, #78209, #154075, #84176, #20520, #95372, #34703, #4344, #66029, #80202, #161035, #125722, #81183, #191370, #51858, #141873, #22529, #127696, #160036, #159027, #157057, #83184, #2372, #5343, #19538, #6341, #176218, #3364, #190383, #67027, #111542, #129672, #128686, #36677, #65039, #113518, #98337, #21523, #189396, #126695, #33710, #64052, #35694, #112531, #175212, #144858, #96360, #18554, #68021, #173227, #82168, #188399, #174225, #97341, #143864, #52846, #142865, #114517, #50873, #37687, #99352, #187421, #48889, #110544, #172225, #49877, #158048, #118544, #194390, #7338, #193383, #165046, #103368, #27542, #87197, #145856, #69023, #102365, #10369, #180234, #23531, #72026, #41703, #26539, #9369, #70033, #177227, #130688, #179229, #55857, #88183, #149867, #178221, #38699, #11372, #116533, #25553, #100356, #117531, #40695, #164054, #73042, #24543, #148878, #86193, #133699, #196397, #104358, #192382, #195391, #56869, #53865, #162035, #134714, #57866, #115539, #54859, #119538, #181221, #85177, #42697, #146866, #8358, #166042, #131702, #39685, #101347, #163036, #147883, #71034, #132701, #199351, #12369, #198354, #152832, #168987, #124483, #106327, #150875, #58839, #169996, #105344, #74032, #168013, #30491, #120506, #62801, #31487, #75991, #1127, #170991, #183192, #13343, #44674, #89183, #151852, #75007, #47661, #46657, #154824, #92142, #167031, #16322, #182197, #77972, #45663, #91143, #136672, #135703, #15324, #139639, #186179, #29509, #137664, #107314, #153829, #121498, #197374, #76983, #43682, #14326, #60816, #122490, #28533, #109312, #90169, #184181, #59828, #138654, #135, #61804, #123474, #108316, #185166, #93139, #113282, #52613, #35456, #49639, #36437, #6103, #110307, #20279, #97107, #141642, #159790, #34469, #171989, #48655, #4109, #94137, #128445, #5101, #2134, #66783, #65788, #158790, #81925, #174973, #18317, #64807, #190141, #157817, #143617, #51617, #155816, #111302, #98092, #19307, #112297, #126468, #172991, #80955, #189163, #79974, #140644, #21285, #17314, #96128, #82942, #3132, #142630, #188166, #127457, #33477, #144620, #67784, #129441, #78969, #50635, #63814, #191140, #173987, #125487, #114275, #32484, #95135, #187184, #156824, #176987, #164807, #22288, #103126, #84935, #56628, #101106, #192137, #178984, #115294, #23291, #118302, #179994, #26302, #85949, #53618, #38457, #37447, #10127, #177978, #194152, #146616, #163809, #133457, #99108, #40451, #102125, #24301, #147638, #100112, #161796, #162792, #160800, #54613, #9127, #148637, #87942, #149630, #55616, #11128, #25311, #86953, #83939, #70793, #8108, #71787, #145620, #39446, #69786, #132461, #117290, #195147, #175979, #131454, #41461, #72803, #134473 ),
 ( #7099, #196158, #57631, #68781, #130438, #193141, #116288, #197139, #45428, #15088, #153590, #182958, #43446, #150638, #180981, #152596, #29279, #91899, #200104, #151623, #12134, #76749, #89942, #199110, #73798, #90911, #14087, #75753, #138424, #198123, #60577, #59590, #122253, #169759, #77744, #104121, #137430, #167781, #42457, #135471, #61572, #183943, #165803, #166801, #123241, #184932, #892, #107081, #119298, #27300, #168753, #30256, #13116, #58606, #46417, #108075, #16086, #31254, #92904, #88947, #28302, #44441, #154590, #139410, #136442, #120272, #181964, #105115, #74780, #121264, #106095, #111066, #156588, #110077, #143375, #49403, #174741, #144382, #18083, #186950, #79738, #62567, #125252, #48421, #21045, #20050, #128216, #142399, #78733, #189913, #32248, #51388, #19073, #64574, #171757, #124244, #188930, #113049, #159547, #141407, #172754, #80721, #3878, #94904, #185939, #65557, #155584, #2895, #126239, #187934, #140409, #82698, #47424, #34235, #36204, #112068, #1898, #109080, #95897, #81693, #127216, #17079, #4867, #170759, #50408, #157580, #66552, #97858, #63578, #173756, #35224, #33246, #93906, #96877, #158560, #192906, #38219, #193912, #67545, #7864, #115054, #116055, #39213, #40204, #114034, #99875, #84697, #98866, #100869, #162551, #24055, #41222, #164568, #145380, #178741, #131215, #54383, #102883, #147397, #129203, #132220, #26062, #190901, #85711, #70553, #87705, #52377, #69551, #6862, #22051, #177744, #175731, #101884, #163566, #37210, #25066, #8885, #55376, #117046, #86709, #191892, #161559, #148394, #9888, #71548, #133214, #160561, #146377, #194905, #56379, #118062, #23052, #179752, #5869, #83702, #53376, #68541, #130196, #176746, #166567, #13856, #135237, #59357, #196909, #121026, #27063, #79249, #32760, #186459, #134234, #58376, #180749, #75523, #182723, #42225, #48923, #29049, #150405, #136213, #43211, #11901, #140920, #195919, #2407, #120043, #94411, #74548, #165566, #152371, #88709, #181730, #156092, #17589, #64086, #44208, #73564, #104878, #10886, #47935, #151393, #167554, #28067, #137198, #109589, #72557, #198884, #60351, #197888, #105867, #89707, #12883, #90689, #57394, #122025, #171272, #125755, #187455, #110577, #172258, #33746, #149390, #103886, #119067, #128721, #5379, #68056, #176255, #127730, #126730, #129710, #66063, #175247, #188433, #67063, #190418, #51894, #191406, #174261, #36712, #35729, #98374, #145892, #53901, #80235, #113553, #143898, #157092, #49911, #52883, #160072, #18588, #142897, #114557, #37726, #177263, #21559, #95406, #141906, #83219, #144894, #189432, #173261, #6376, #99388, #192419, #161071, #22566, #3397, #4379, #159062, #84212, #130727, #112566, #65072, #111577, #7375, #34736, #96394, #69060, #115576, #50908, #97376, #158081, #82206, #19572, #81216, #20556, #39719, #147917, #104395, #178258, #101382, #42733, #103402, #149901, #148913, #131738, #11408, #146905, #73077, #25587, #194423, #116569, #38735, #56904, #134749, #100393, #71069, #102401, #10403, #72060, #9403, #162071, #133734, #193420, #132735, #117566, #179266, #163073, #23567, #8395, #40731, #181256, #165080, #24578, #85215, #164088, #196431, #118578, #86227, #57901, #70070, #26574, #87231, #54895, #55893, #119573, #195427, #180268, #41738, #88217, #83862, #53540, #97038, #145544, #115217, #176910, #82868, #143544, #38381, #142560, #98018, #100037, #144546, #99031, #113212, #159713, #6031, #175902, #66715, #127383, #146538, #4038, #36366, #7022, #5030, #129368, #128376, #191064, #158718, #8032, #161723, #23218, #65716, #190072, #50567, #68704, #52537, #112227, #116217, #160721, #20208, #67710, #174901, #81854, #69713, #189094, #131380, #51548, #84861, #114197, #35386, #22213, #21211, #37373, #193068, #54544, #177908, #130360, #192058, #39376, #80883, #101035, #19235, #173917, #10052, #150564, #120202, #85877, #165727, #27223, #11049, #72725, #102051, #178909, #149554, #147565 ),
 ( #24226, #164732, #71712, #134398, #196085, #197069, #70720, #195070, #41385, #55544, #57555, #119225, #180909, #198049, #121192, #163736, #135398, #87866, #42384, #59515, #104047, #9050, #88871, #182885, #132388, #12063, #73725, #44368, #194081, #26226, #25236, #40377, #58536, #117216, #181892, #43370, #86877, #105042, #166726, #28230, #89870, #151552, #148561, #56550, #13042, #74709, #136372, #162720, #133380, #179918, #118227, #103050, #183875, #93833, #109009, #15018, #33172, #170688, #140335, #45360, #32177, #1825, #63507, #169688, #30186, #137359, #167712, #139342, #16016, #78660, #186878, #138355, #199038, #125182, #76679, #185868, #60508, #77673, #821, #62495, #48348, #184862, #47354, #46345, #155513, #156509, #64500, #90842, #124166, #154519, #29208, #122183, #110002, #17008, #152527, #153521, #171683, #94831, #187862, #18010, #106025, #14014, #79664, #141335, #200037, #107012, #2822, #126167, #75680, #168685, #91828, #61505, #123174, #31183, #108002, #92834, #189366, #4314, #20489, #127666, #128655, #51826, #52818, #126665, #50843, #97310, #111510, #113486, #175180, #36646, #53837, #177199, #158017, #191340, #143832, #5312, #115511, #160005, #80171, #144828, #38672, #141843, #98305, #83154, #100327, #3334, #82138, #19508, #34672, #190350, #65008, #114486, #176189, #188369, #37658, #21493, #6312, #67990, #99323, #65997, #112500, #161007, #66996, #129644, #22501, #49846, #158996, #84148, #145827, #7310, #174194, #68995, #130660, #192353, #173196, #18524, #96330, #35662, #81153, #142835, #71997, #147855, #133671, #39658, #89157, #42671, #196371, #146836, #71007, #193355, #26512, #195362, #54831, #58811, #41675, #163008, #148850, #55830, #24515, #150846, #8329, #12342, #132675, #104332, #87169, #178193, #165019, #101319, #9342, #166016, #27516, #74006, #56841, #86165, #194363, #23502, #57839, #164027, #180206, #117503, #149841, #119512, #85150, #88156, #11345, #10341, #118516, #179200, #40668, #103339, #70004, #102337, #73016, #134685, #135676, #197348, #181193, #120480, #182171, #43657, #131674, #162006, #116505, #25523, #91116, #107288, #14298, #15296, #138626, #139612, #13316, #137639, #184155, #198327, #107, #61777, #123445, #140616, #63787, #44649, #77945, #30465, #92113, #2106, #46629, #167006, #31460, #125459, #28508, #185138, #169967, #187156, #90142, #168959, #106301, #121473, #76956, #151827, #1098, #62774, #74982, #124455, #108289, #93112, #154797, #186151, #152806, #199326, #47630, #153802, #16295, #109285, #136644, #45636, #170963, #32457, #94110, #60791, #155789, #17286, #78940, #75966, #105319, #59803, #122462, #183165, #167987, #29485, #160769, #130408, #142604, #172964, #4083, #48628, #111273, #34442, #7069, #6076, #114243, #128419, #64780, #175950, #18290, #37419, #5075, #50610, #96101, #110280, #174946, #99079, #145591, #65761, #97081, #66758, #190115, #80927, #171961, #51590, #141615, #127430, #112269, #173961, #126441, #68751, #33449, #189138, #22259, #98063, #188139, #95108, #35428, #67754, #113255, #3102, #129412, #156797, #36408, #158762, #52584, #83908, #49610, #159762, #21257, #157790, #79945, #82912, #144590, #19280, #191109, #20253, #81899, #143592, #116259, #23263, #53589, #25280, #102094, #164777, #72773, #24271, #84907, #26271, #162762, #71757, #146586, #163779, #86923, #148605, #87913, #70763, #133427, #132431, #195115, #42429, #150609, #176958, #10097, #40423, #115265, #8080, #149600, #56598, #38427, #39418, #11097, #134443, #73768, #118272, #192106, #100083, #179962, #41429, #85920, #69756, #103095, #196128, #88917, #57599, #119268, #161768, #101077, #55586, #147608, #12105, #180951, #131426, #193112, #104091, #54586, #177950, #9096, #194123, #117261, #165774, #27268, #178953, #93877, #137400, #92874, #91869, #28273, #16057, #155555, #138395, #152568, #139381, #109051, #13085, #123213, #200076, #44412, #62538, #61544, #169730, #74750, #184903, #31225 ) ),
 .UNSPECIFIED., .T., .F., .T. ) 
 B_SPLINE_SURFACE_WITH_KNOTS ( ( 4, 3, 4 ),
 ( 3, 2, 2, 2, 2, 2, 2, 2, 2, 2, 2, 2, 2, 2, 2, 2, 2, 2, 2, 2, 2, 2, 2, 2, 2, 2, 2, 2, 2, 2, 2, 2, 2, 2, 2, 2, 2, 2, 2, 2, 2, 2, 2, 2, 2, 2, 2, 2, 2, 2, 2, 2, 2, 2, 2, 2, 2, 2, 2, 2, 2, 2, 2, 2, 2, 2, 2, 2, 2, 2, 2, 2, 2, 2, 2, 2, 2, 2, 2, 2, 2, 2, 2, 2, 2, 2, 2, 2, 2, 2, 2, 2, 2, 2, 2, 2, 2, 2, 2, 2, 2, 2, 2, 2, 2, 2, 2, 2, 2, 2, 2, 2, 2, 2, 2, 2, 2, 2, 2, 2, 2, 2, 2, 2, 2, 2, 2, 2, 2, 2, 2, 2, 2, 2, 2, 2, 2, 2, 2, 2, 2, 2, 2, 2, 2, 2, 2, 2, 2, 2, 2, 2, 2, 2, 2, 2, 2, 2, 2, 2, 2, 2, 2, 2, 2, 2, 2, 2, 2, 2, 2, 2, 2, 2, 2, 2, 2, 2, 2, 2, 2, 2, 2, 2, 2, 2, 2, 2, 2, 2, 2, 2, 2, 2, 2, 2, 2, 2, 2, 2, 2, 2, 2, 2, 2, 2, 2, 2, 2, 2, 2, 2, 2, 2, 2, 2, 2, 2, 2, 2, 2, 2, 2, 2, 2, 2, 2, 2, 3 ),
 ( 0.000000000000000000, 0.5000000000000000000, 1.000000000000000000 ),
 ( 0.000000000000000000, 0.004385964912280701511, 0.008771929824561403022, 0.01315789473684210453, 0.01754385964912280604, 0.02192982456140350755, 0.02631578947368420907, 0.03070175438596491058, 0.03508771929824561209, 0.03947368421052631360, 0.04385964912280701511, 0.04824561403508771662, 0.05263157894736841813, 0.05701754385964911964, 0.06140350877192982115, 0.06578947368421052266, 0.07017543859649122417, 0.07456140350877192569, 0.07894736842105262720, 0.08333333333333332871, 0.08771929824561403022, 0.09210526315789473173, 0.09649122807017543324, 0.1008771929824561348, 0.1052631578947368363, 0.1096491228070175378, 0.1140350877192982393, 0.1184210526315789408, 0.1228070175438596423, 0.1271929824561403577, 0.1315789473684210453, 0.1359649122807017607, 0.1403508771929824483, 0.1447368421052631637, 0.1491228070175438514, 0.1535087719298245668, 0.1578947368421052544, 0.1622807017543859698, 0.1666666666666666574, 0.1710526315789473728, 0.1754385964912280604, 0.1798245614035087758, 0.1842105263157894635, 0.1885964912280701788, 0.1929824561403508665, 0.1973684210526315819, 0.2017543859649122695, 0.2061403508771929849, 0.2105263157894736725, 0.2149122807017543879, 0.2192982456140350755, 0.2236842105263157909, 0.2280701754385964786, 0.2324561403508771940, 0.2368421052631578816, 0.2412280701754385970, 0.2456140350877192846, 0.2500000000000000000, 0.2543859649122807154, 0.2587719298245614308, 0.2631578947368420907, 0.2675438596491228060, 0.2719298245614035214, 0.2763157894736842368, 0.2807017543859648967, 0.2850877192982456121, 0.2894736842105263275, 0.2938596491228070429, 0.2982456140350877027, 0.3026315789473684181, 0.3070175438596491335, 0.3114035087719298489, 0.3157894736842105088, 0.3201754385964912242, 0.3245614035087719396, 0.3289473684210526550, 0.3333333333333333148, 0.3377192982456140302, 0.3421052631578947456, 0.3464912280701754610, 0.3508771929824561209, 0.3552631578947368363, 0.3596491228070175517, 0.3640350877192982670, 0.3684210526315789269, 0.3728070175438596423, 0.3771929824561403577, 0.3815789473684210731, 0.3859649122807017330, 0.3903508771929824483, 0.3947368421052631637, 0.3991228070175438791, 0.4035087719298245390, 0.4078947368421052544, 0.4122807017543859698, 0.4166666666666666852, 0.4210526315789473450, 0.4254385964912280604, 0.4298245614035087758, 0.4342105263157894912, 0.4385964912280701511, 0.4429824561403508665, 0.4473684210526315819, 0.4517543859649122973, 0.4561403508771929571, 0.4605263157894736725, 0.4649122807017543879, 0.4692982456140351033, 0.4736842105263157632, 0.4780701754385964786, 0.4824561403508771940, 0.4868421052631579093, 0.4912280701754385692, 0.4956140350877192846, 0.5000000000000000000, 0.5043859649122807154, 0.5087719298245614308, 0.5131578947368421462, 0.5175438596491228616, 0.5219298245614034659, 0.5263157894736841813, 0.5307017543859648967, 0.5350877192982456121, 0.5394736842105263275, 0.5438596491228070429, 0.5482456140350877583, 0.5526315789473684736, 0.5570175438596490780, 0.5614035087719297934, 0.5657894736842105088, 0.5701754385964912242, 0.5745614035087719396, 0.5789473684210526550, 0.5833333333333333703, 0.5877192982456140857, 0.5921052631578946901, 0.5964912280701754055, 0.6008771929824561209, 0.6052631578947368363, 0.6096491228070175517, 0.6140350877192982670, 0.6184210526315789824, 0.6228070175438596978, 0.6271929824561403022, 0.6315789473684210176, 0.6359649122807017330, 0.6403508771929824483, 0.6447368421052631637, 0.6491228070175438791, 0.6535087719298245945, 0.6578947368421053099, 0.6622807017543859143, 0.6666666666666666297, 0.6710526315789473450, 0.6754385964912280604, 0.6798245614035087758, 0.6842105263157894912, 0.6885964912280702066, 0.6929824561403509220, 0.6973684210526315264, 0.7017543859649122417, 0.7061403508771929571, 0.7105263157894736725, 0.7149122807017543879, 0.7192982456140351033, 0.7236842105263158187, 0.7280701754385965341, 0.7324561403508771384, 0.7368421052631578538, 0.7412280701754385692, 0.7456140350877192846, 0.7500000000000000000, 0.7543859649122807154, 0.7587719298245614308, 0.7631578947368421462, 0.7675438596491228616, 0.7719298245614034659, 0.7763157894736841813, 0.7807017543859648967, 0.7850877192982456121, 0.7894736842105263275, 0.7938596491228070429, 0.7982456140350877583, 0.8026315789473684736, 0.8070175438596490780, 0.8114035087719297934, 0.8157894736842105088, 0.8201754385964912242, 0.8245614035087719396, 0.8289473684210526550, 0.8333333333333333703, 0.8377192982456140857, 0.8421052631578946901, 0.8464912280701754055, 0.8508771929824561209, 0.8552631578947368363, 0.8596491228070175517, 0.8640350877192982670, 0.8684210526315789824, 0.8728070175438596978, 0.8771929824561403022, 0.8815789473684210176, 0.8859649122807017330, 0.8903508771929824483, 0.8947368421052631637, 0.8991228070175438791, 0.9035087719298245945, 0.9078947368421053099, 0.9122807017543859143, 0.9166666666666666297, 0.9210526315789473450, 0.9254385964912280604, 0.9298245614035087758, 0.9342105263157894912, 0.9385964912280702066, 0.9429824561403509220, 0.9473684210526315264, 0.9517543859649122417, 0.9561403508771929571, 0.9605263157894736725, 0.9649122807017543879, 0.9692982456140351033, 0.9736842105263158187, 0.9780701754385965341, 0.9824561403508771384, 0.9868421052631578538, 0.9912280701754385692, 0.9956140350877192846, 1.000000000000000000 ),
 .UNSPECIFIED. ) 
 GEOMETRIC_REPRESENTATION_ITEM ( )  RATIONAL_B_SPLINE_SURFACE ( (
 ( 1.000000000000000000, 0.9659258262890683122, 1.000000000000000000, 0.9659258262890683122, 1.000000000000000000, 0.9659258262890683122, 1.000000000000000000, 0.9659258262890683122, 1.000000000000000000, 0.9659258262890683122, 1.000000000000000000, 0.9659258262890683122, 1.000000000000000000, 0.9659258262890683122, 1.000000000000000000, 0.9659258262890683122, 1.000000000000000000, 0.9659258262890683122, 1.000000000000000000, 0.9659258262890683122, 1.000000000000000000, 0.9659258262890683122, 1.000000000000000000, 0.9659258262890683122, 1.000000000000000000, 0.9659258262890683122, 1.000000000000000000, 0.9659258262890683122, 1.000000000000000000, 0.9659258262890683122, 1.000000000000000000, 0.9659258262890683122, 1.000000000000000000, 0.9659258262890683122, 1.000000000000000000, 0.9659258262890683122, 1.000000000000000000, 0.9659258262890683122, 1.000000000000000000, 0.9659258262890683122, 1.000000000000000000, 0.9659258262890683122, 1.000000000000000000, 0.9659258262890683122, 1.000000000000000000, 0.9659258262890683122, 1.000000000000000000, 0.9659258262890683122, 1.000000000000000000, 0.9659258262890683122, 1.000000000000000000, 0.9659258262890683122, 1.000000000000000000, 0.9659258262890683122, 1.000000000000000000, 0.9659258262890683122, 1.000000000000000000, 0.9659258262890683122, 1.000000000000000000, 0.9659258262890683122, 1.000000000000000000, 0.9659258262890683122, 1.000000000000000000, 0.9659258262890683122, 1.000000000000000000, 0.9659258262890683122, 1.000000000000000000, 0.9659258262890683122, 1.000000000000000000, 0.9659258262890683122, 1.000000000000000000, 0.9659258262890683122, 1.000000000000000000, 0.9659258262890683122, 1.000000000000000000, 0.9659258262890683122, 1.000000000000000000, 0.9659258262890683122, 1.000000000000000000, 0.9659258262890683122, 1.000000000000000000, 0.9659258262890683122, 1.000000000000000000, 0.9659258262890683122, 1.000000000000000000, 0.9659258262890683122, 1.000000000000000000, 0.9659258262890683122, 1.000000000000000000, 0.9659258262890683122, 1.000000000000000000, 0.9659258262890683122, 1.000000000000000000, 0.9659258262890683122, 1.000000000000000000, 0.9659258262890683122, 1.000000000000000000, 0.9659258262890683122, 1.000000000000000000, 0.9659258262890683122, 1.000000000000000000, 0.9659258262890683122, 1.000000000000000000, 0.9659258262890683122, 1.000000000000000000, 0.9659258262890683122, 1.000000000000000000, 0.9659258262890683122, 1.000000000000000000, 0.9659258262890683122, 1.000000000000000000, 0.9659258262890683122, 1.000000000000000000, 0.9659258262890683122, 1.000000000000000000, 0.9659258262890683122, 1.000000000000000000, 0.9659258262890683122, 1.000000000000000000, 0.9659258262890683122, 1.000000000000000000, 0.9659258262890683122, 1.000000000000000000, 0.9659258262890683122, 1.000000000000000000, 0.9659258262890683122, 1.000000000000000000, 0.9659258262890683122, 1.000000000000000000, 0.9659258262890683122, 1.000000000000000000, 0.9659258262890683122, 1.000000000000000000, 0.9659258262890683122, 1.000000000000000000, 0.9659258262890683122, 1.000000000000000000, 0.9659258262890683122, 1.000000000000000000, 0.9659258262890683122, 1.000000000000000000, 0.9659258262890683122, 1.000000000000000000, 0.9659258262890683122, 1.000000000000000000, 0.9659258262890683122, 1.000000000000000000, 0.9659258262890683122, 1.000000000000000000, 0.9659258262890683122, 1.000000000000000000, 0.9659258262890683122, 1.000000000000000000, 0.9659258262890683122, 1.000000000000000000, 0.9659258262890683122, 1.000000000000000000, 0.9659258262890683122, 1.000000000000000000, 0.9659258262890683122, 1.000000000000000000, 0.9659258262890683122, 1.000000000000000000, 0.9659258262890683122, 1.000000000000000000, 0.9659258262890683122, 1.000000000000000000, 0.9659258262890683122, 1.000000000000000000, 0.9659258262890683122, 1.000000000000000000, 0.9659258262890683122, 1.000000000000000000, 0.9659258262890683122, 1.000000000000000000, 0.9659258262890683122, 1.000000000000000000, 0.9659258262890683122, 1.000000000000000000, 0.9659258262890683122, 1.000000000000000000, 0.9659258262890683122, 1.000000000000000000, 0.9659258262890683122, 1.000000000000000000, 0.9659258262890683122, 1.000000000000000000, 0.9659258262890683122, 1.000000000000000000, 0.9659258262890683122, 1.000000000000000000, 0.9659258262890683122, 1.000000000000000000, 0.9659258262890683122, 1.000000000000000000, 0.9659258262890683122, 1.000000000000000000, 0.9659258262890683122, 1.000000000000000000, 0.9659258262890683122, 1.000000000000000000, 0.9659258262890683122, 1.000000000000000000, 0.9659258262890683122, 1.000000000000000000, 0.9659258262890683122, 1.000000000000000000, 0.9659258262890683122, 1.000000000000000000, 0.9659258262890683122, 1.000000000000000000, 0.9659258262890683122, 1.000000000000000000, 0.9659258262890683122, 1.000000000000000000, 0.9659258262890683122, 1.000000000000000000, 0.9659258262890683122, 1.000000000000000000, 0.9659258262890683122, 1.000000000000000000, 0.9659258262890683122, 1.000000000000000000, 0.9659258262890683122, 1.000000000000000000, 0.9659258262890683122, 1.000000000000000000, 0.9659258262890683122, 1.000000000000000000, 0.9659258262890683122, 1.000000000000000000, 0.9659258262890683122, 1.000000000000000000, 0.9659258262890683122, 1.000000000000000000, 0.9659258262890683122, 1.000000000000000000, 0.9659258262890683122, 1.000000000000000000, 0.9659258262890683122, 1.000000000000000000, 0.9659258262890683122, 1.000000000000000000, 0.9659258262890683122, 1.000000000000000000, 0.9659258262890683122, 1.000000000000000000, 0.9659258262890683122, 1.000000000000000000, 0.9659258262890683122, 1.000000000000000000, 0.9659258262890683122, 1.000000000000000000, 0.9659258262890683122, 1.000000000000000000, 0.9659258262890683122, 1.000000000000000000, 0.9659258262890683122, 1.000000000000000000, 0.9659258262890683122, 1.000000000000000000, 0.9659258262890683122, 1.000000000000000000, 0.9659258262890683122, 1.000000000000000000, 0.9659258262890683122, 1.000000000000000000, 0.9659258262890683122, 1.000000000000000000, 0.9659258262890683122, 1.000000000000000000, 0.9659258262890683122, 1.000000000000000000, 0.9659258262890683122, 1.000000000000000000, 0.9659258262890683122, 1.000000000000000000, 0.9659258262890683122, 1.000000000000000000, 0.9659258262890683122, 1.000000000000000000, 0.9659258262890683122, 1.000000000000000000, 0.9659258262890683122, 1.000000000000000000, 0.9659258262890683122, 1.000000000000000000, 0.9659258262890683122, 1.000000000000000000, 0.9659258262890683122, 1.000000000000000000, 0.9659258262890683122, 1.000000000000000000, 0.9659258262890683122, 1.000000000000000000, 0.9659258262890683122, 1.000000000000000000, 0.9659258262890683122, 1.000000000000000000, 0.9659258262890683122, 1.000000000000000000, 0.9659258262890683122, 1.000000000000000000, 0.9659258262890683122, 1.000000000000000000, 0.9659258262890683122, 1.000000000000000000, 0.9659258262890683122, 1.000000000000000000, 0.9659258262890683122, 1.000000000000000000, 0.9659258262890683122, 1.000000000000000000, 0.9659258262890683122, 1.000000000000000000, 0.9659258262890683122, 1.000000000000000000, 0.9659258262890683122, 1.000000000000000000, 0.9659258262890683122, 1.000000000000000000, 0.9659258262890683122, 1.000000000000000000, 0.9659258262890683122, 1.000000000000000000, 0.9659258262890683122, 1.000000000000000000, 0.9659258262890683122, 1.000000000000000000, 0.9659258262890683122, 1.000000000000000000, 0.9659258262890683122, 1.000000000000000000, 0.9659258262890683122, 1.000000000000000000, 0.9659258262890683122, 1.000000000000000000, 0.9659258262890683122, 1.000000000000000000, 0.9659258262890683122, 1.000000000000000000, 0.9659258262890683122, 1.000000000000000000, 0.9659258262890683122, 1.000000000000000000, 0.9659258262890683122, 1.000000000000000000, 0.9659258262890683122, 1.000000000000000000, 0.9659258262890683122, 1.000000000000000000, 0.9659258262890683122, 1.000000000000000000, 0.9659258262890683122, 1.000000000000000000, 0.9659258262890683122, 1.000000000000000000, 0.9659258262890683122, 1.000000000000000000, 0.9659258262890683122, 1.000000000000000000, 0.9659258262890683122, 1.000000000000000000, 0.9659258262890683122, 1.000000000000000000, 0.9659258262890683122, 1.000000000000000000, 0.9659258262890683122, 1.000000000000000000, 0.9659258262890683122, 1.000000000000000000, 0.9659258262890683122, 1.000000000000000000, 0.9659258262890683122, 1.000000000000000000, 0.9659258262890683122, 1.000000000000000000, 0.9659258262890683122, 1.000000000000000000, 0.9659258262890683122, 1.000000000000000000, 0.9659258262890683122, 1.000000000000000000, 0.9659258262890683122, 1.000000000000000000, 0.9659258262890683122, 1.000000000000000000, 0.9659258262890683122, 1.000000000000000000, 0.9659258262890683122, 1.000000000000000000, 0.9659258262890683122, 1.000000000000000000, 0.9659258262890683122, 1.000000000000000000, 0.9659258262890683122, 1.000000000000000000, 0.9659258262890683122, 1.000000000000000000, 0.9659258262890683122, 1.000000000000000000, 0.9659258262890683122, 1.000000000000000000, 0.9659258262890683122, 1.000000000000000000, 0.9659258262890683122, 1.000000000000000000, 0.9659258262890683122, 1.000000000000000000, 0.9659258262890683122, 1.000000000000000000, 0.9659258262890683122, 1.000000000000000000, 0.9659258262890683122, 1.000000000000000000, 0.9659258262890683122, 1.000000000000000000, 0.9659258262890683122, 1.000000000000000000, 0.9659258262890683122, 1.000000000000000000, 0.9659258262890683122, 1.000000000000000000, 0.9659258262890683122, 1.000000000000000000, 0.9659258262890683122, 1.000000000000000000, 0.9659258262890683122, 1.000000000000000000, 0.9659258262890683122, 1.000000000000000000, 0.9659258262890683122, 1.000000000000000000, 0.9659258262890683122, 1.000000000000000000, 0.9659258262890683122, 1.000000000000000000, 0.9659258262890683122, 1.000000000000000000, 0.9659258262890683122, 1.000000000000000000, 0.9659258262890683122, 1.000000000000000000, 0.9659258262890683122, 1.000000000000000000, 0.9659258262890683122, 1.000000000000000000, 0.9659258262890683122, 1.000000000000000000, 0.9659258262890683122, 1.000000000000000000, 0.9659258262890683122, 1.000000000000000000, 0.9659258262890683122, 1.000000000000000000, 0.9659258262890683122, 1.000000000000000000),
 ( 0.3333333333333333703, 0.3219752754296894559, 0.3333333333333333703, 0.3219752754296894559, 0.3333333333333333703, 0.3219752754296894559, 0.3333333333333333703, 0.3219752754296894559, 0.3333333333333333703, 0.3219752754296894559, 0.3333333333333333703, 0.3219752754296894559, 0.3333333333333333703, 0.3219752754296894559, 0.3333333333333333703, 0.3219752754296894559, 0.3333333333333333703, 0.3219752754296894559, 0.3333333333333333703, 0.3219752754296894559, 0.3333333333333333703, 0.3219752754296894559, 0.3333333333333333703, 0.3219752754296894559, 0.3333333333333333703, 0.3219752754296894559, 0.3333333333333333703, 0.3219752754296894559, 0.3333333333333333703, 0.3219752754296894559, 0.3333333333333333703, 0.3219752754296894559, 0.3333333333333333703, 0.3219752754296894559, 0.3333333333333333703, 0.3219752754296894559, 0.3333333333333333703, 0.3219752754296894559, 0.3333333333333333703, 0.3219752754296894559, 0.3333333333333333703, 0.3219752754296894559, 0.3333333333333333703, 0.3219752754296894559, 0.3333333333333333703, 0.3219752754296894559, 0.3333333333333333703, 0.3219752754296894559, 0.3333333333333333703, 0.3219752754296894559, 0.3333333333333333703, 0.3219752754296894559, 0.3333333333333333703, 0.3219752754296894559, 0.3333333333333333703, 0.3219752754296894559, 0.3333333333333333703, 0.3219752754296894559, 0.3333333333333333703, 0.3219752754296894559, 0.3333333333333333703, 0.3219752754296894559, 0.3333333333333333703, 0.3219752754296894559, 0.3333333333333333703, 0.3219752754296894559, 0.3333333333333333703, 0.3219752754296894559, 0.3333333333333333703, 0.3219752754296894559, 0.3333333333333333703, 0.3219752754296894559, 0.3333333333333333703, 0.3219752754296894559, 0.3333333333333333703, 0.3219752754296894559, 0.3333333333333333703, 0.3219752754296894559, 0.3333333333333333703, 0.3219752754296894559, 0.3333333333333333703, 0.3219752754296894559, 0.3333333333333333703, 0.3219752754296894559, 0.3333333333333333703, 0.3219752754296894559, 0.3333333333333333703, 0.3219752754296894559, 0.3333333333333333703, 0.3219752754296894559, 0.3333333333333333703, 0.3219752754296894559, 0.3333333333333333703, 0.3219752754296894559, 0.3333333333333333703, 0.3219752754296894559, 0.3333333333333333703, 0.3219752754296894559, 0.3333333333333333703, 0.3219752754296894559, 0.3333333333333333703, 0.3219752754296894559, 0.3333333333333333703, 0.3219752754296894559, 0.3333333333333333703, 0.3219752754296894559, 0.3333333333333333703, 0.3219752754296894559, 0.3333333333333333703, 0.3219752754296894559, 0.3333333333333333703, 0.3219752754296894559, 0.3333333333333333703, 0.3219752754296894559, 0.3333333333333333703, 0.3219752754296894559, 0.3333333333333333703, 0.3219752754296894559, 0.3333333333333333703, 0.3219752754296894559, 0.3333333333333333703, 0.3219752754296894559, 0.3333333333333333703, 0.3219752754296894559, 0.3333333333333333703, 0.3219752754296894559, 0.3333333333333333703, 0.3219752754296894559, 0.3333333333333333703, 0.3219752754296894559, 0.3333333333333333703, 0.3219752754296894559, 0.3333333333333333703, 0.3219752754296894559, 0.3333333333333333703, 0.3219752754296894559, 0.3333333333333333703, 0.3219752754296894559, 0.3333333333333333703, 0.3219752754296894559, 0.3333333333333333703, 0.3219752754296894559, 0.3333333333333333703, 0.3219752754296894559, 0.3333333333333333703, 0.3219752754296894559, 0.3333333333333333703, 0.3219752754296894559, 0.3333333333333333703, 0.3219752754296894559, 0.3333333333333333703, 0.3219752754296894559, 0.3333333333333333703, 0.3219752754296894559, 0.3333333333333333703, 0.3219752754296894559, 0.3333333333333333703, 0.3219752754296894559, 0.3333333333333333703, 0.3219752754296894559, 0.3333333333333333703, 0.3219752754296894559, 0.3333333333333333703, 0.3219752754296894559, 0.3333333333333333703, 0.3219752754296894559, 0.3333333333333333703, 0.3219752754296894559, 0.3333333333333333703, 0.3219752754296894559, 0.3333333333333333703, 0.3219752754296894559, 0.3333333333333333703, 0.3219752754296894559, 0.3333333333333333703, 0.3219752754296894559, 0.3333333333333333703, 0.3219752754296894559, 0.3333333333333333703, 0.3219752754296894559, 0.3333333333333333703, 0.3219752754296894559, 0.3333333333333333703, 0.3219752754296894559, 0.3333333333333333703, 0.3219752754296894559, 0.3333333333333333703, 0.3219752754296894559, 0.3333333333333333703, 0.3219752754296894559, 0.3333333333333333703, 0.3219752754296894559, 0.3333333333333333703, 0.3219752754296894559, 0.3333333333333333703, 0.3219752754296894559, 0.3333333333333333703, 0.3219752754296894559, 0.3333333333333333703, 0.3219752754296894559, 0.3333333333333333703, 0.3219752754296894559, 0.3333333333333333703, 0.3219752754296894559, 0.3333333333333333703, 0.3219752754296894559, 0.3333333333333333703, 0.3219752754296894559, 0.3333333333333333703, 0.3219752754296894559, 0.3333333333333333703, 0.3219752754296894559, 0.3333333333333333703, 0.3219752754296894559, 0.3333333333333333703, 0.3219752754296894559, 0.3333333333333333703, 0.3219752754296894559, 0.3333333333333333703, 0.3219752754296894559, 0.3333333333333333703, 0.3219752754296894559, 0.3333333333333333703, 0.3219752754296894559, 0.3333333333333333703, 0.3219752754296894559, 0.3333333333333333703, 0.3219752754296894559, 0.3333333333333333703, 0.3219752754296894559, 0.3333333333333333703, 0.3219752754296894559, 0.3333333333333333703, 0.3219752754296894559, 0.3333333333333333703, 0.3219752754296894559, 0.3333333333333333703, 0.3219752754296894559, 0.3333333333333333703, 0.3219752754296894559, 0.3333333333333333703, 0.3219752754296894559, 0.3333333333333333703, 0.3219752754296894559, 0.3333333333333333703, 0.3219752754296894559, 0.3333333333333333703, 0.3219752754296894559, 0.3333333333333333703, 0.3219752754296894559, 0.3333333333333333703, 0.3219752754296894559, 0.3333333333333333703, 0.3219752754296894559, 0.3333333333333333703, 0.3219752754296894559, 0.3333333333333333703, 0.3219752754296894559, 0.3333333333333333703, 0.3219752754296894559, 0.3333333333333333703, 0.3219752754296894559, 0.3333333333333333703, 0.3219752754296894559, 0.3333333333333333703, 0.3219752754296894559, 0.3333333333333333703, 0.3219752754296894559, 0.3333333333333333703, 0.3219752754296894559, 0.3333333333333333703, 0.3219752754296894559, 0.3333333333333333703, 0.3219752754296894559, 0.3333333333333333703, 0.3219752754296894559, 0.3333333333333333703, 0.3219752754296894559, 0.3333333333333333703, 0.3219752754296894559, 0.3333333333333333703, 0.3219752754296894559, 0.3333333333333333703, 0.3219752754296894559, 0.3333333333333333703, 0.3219752754296894559, 0.3333333333333333703, 0.3219752754296894559, 0.3333333333333333703, 0.3219752754296894559, 0.3333333333333333703, 0.3219752754296894559, 0.3333333333333333703, 0.3219752754296894559, 0.3333333333333333703, 0.3219752754296894559, 0.3333333333333333703, 0.3219752754296894559, 0.3333333333333333703, 0.3219752754296894559, 0.3333333333333333703, 0.3219752754296894559, 0.3333333333333333703, 0.3219752754296894559, 0.3333333333333333703, 0.3219752754296894559, 0.3333333333333333703, 0.3219752754296894559, 0.3333333333333333703, 0.3219752754296894559, 0.3333333333333333703, 0.3219752754296894559, 0.3333333333333333703, 0.3219752754296894559, 0.3333333333333333703, 0.3219752754296894559, 0.3333333333333333703, 0.3219752754296894559, 0.3333333333333333703, 0.3219752754296894559, 0.3333333333333333703, 0.3219752754296894559, 0.3333333333333333703, 0.3219752754296894559, 0.3333333333333333703, 0.3219752754296894559, 0.3333333333333333703, 0.3219752754296894559, 0.3333333333333333703, 0.3219752754296894559, 0.3333333333333333703, 0.3219752754296894559, 0.3333333333333333703, 0.3219752754296894559, 0.3333333333333333703, 0.3219752754296894559, 0.3333333333333333703, 0.3219752754296894559, 0.3333333333333333703, 0.3219752754296894559, 0.3333333333333333703, 0.3219752754296894559, 0.3333333333333333703, 0.3219752754296894559, 0.3333333333333333703, 0.3219752754296894559, 0.3333333333333333703, 0.3219752754296894559, 0.3333333333333333703, 0.3219752754296894559, 0.3333333333333333703, 0.3219752754296894559, 0.3333333333333333703, 0.3219752754296894559, 0.3333333333333333703, 0.3219752754296894559, 0.3333333333333333703, 0.3219752754296894559, 0.3333333333333333703, 0.3219752754296894559, 0.3333333333333333703, 0.3219752754296894559, 0.3333333333333333703, 0.3219752754296894559, 0.3333333333333333703, 0.3219752754296894559, 0.3333333333333333703, 0.3219752754296894559, 0.3333333333333333703, 0.3219752754296894559, 0.3333333333333333703, 0.3219752754296894559, 0.3333333333333333703, 0.3219752754296894559, 0.3333333333333333703, 0.3219752754296894559, 0.3333333333333333703, 0.3219752754296894559, 0.3333333333333333703, 0.3219752754296894559, 0.3333333333333333703, 0.3219752754296894559, 0.3333333333333333703, 0.3219752754296894559, 0.3333333333333333703, 0.3219752754296894559, 0.3333333333333333703, 0.3219752754296894559, 0.3333333333333333703, 0.3219752754296894559, 0.3333333333333333703, 0.3219752754296894559, 0.3333333333333333703, 0.3219752754296894559, 0.3333333333333333703, 0.3219752754296894559, 0.3333333333333333703, 0.3219752754296894559, 0.3333333333333333703, 0.3219752754296894559, 0.3333333333333333703, 0.3219752754296894559, 0.3333333333333333703, 0.3219752754296894559, 0.3333333333333333703, 0.3219752754296894559, 0.3333333333333333703, 0.3219752754296894559, 0.3333333333333333703, 0.3219752754296894559, 0.3333333333333333703, 0.3219752754296894559, 0.3333333333333333703, 0.3219752754296894559, 0.3333333333333333703, 0.3219752754296894559, 0.3333333333333333703, 0.3219752754296894559, 0.3333333333333333703, 0.3219752754296894559, 0.3333333333333333703, 0.3219752754296894559, 0.3333333333333333703, 0.3219752754296894559, 0.3333333333333333703, 0.3219752754296894559, 0.3333333333333333703, 0.3219752754296894559, 0.3333333333333333703, 0.3219752754296894559, 0.3333333333333333703, 0.3219752754296894559, 0.3333333333333333703, 0.3219752754296894559, 0.3333333333333333703, 0.3219752754296894559, 0.3333333333333333703, 0.3219752754296894559, 0.3333333333333333703, 0.3219752754296894559, 0.3333333333333333703, 0.3219752754296894559, 0.3333333333333333703, 0.3219752754296894559, 0.3333333333333333703, 0.3219752754296894559, 0.3333333333333333703, 0.3219752754296894559, 0.3333333333333333703, 0.3219752754296894559, 0.3333333333333333703, 0.3219752754296894559, 0.3333333333333333703, 0.3219752754296894559, 0.3333333333333333703, 0.3219752754296894559, 0.3333333333333333703),
 ( 0.3333333333333333703, 0.3219752754296894559, 0.3333333333333333703, 0.3219752754296894559, 0.3333333333333333703, 0.3219752754296894559, 0.3333333333333333703, 0.3219752754296894559, 0.3333333333333333703, 0.3219752754296894559, 0.3333333333333333703, 0.3219752754296894559, 0.3333333333333333703, 0.3219752754296894559, 0.3333333333333333703, 0.3219752754296894559, 0.3333333333333333703, 0.3219752754296894559, 0.3333333333333333703, 0.3219752754296894559, 0.3333333333333333703, 0.3219752754296894559, 0.3333333333333333703, 0.3219752754296894559, 0.3333333333333333703, 0.3219752754296894559, 0.3333333333333333703, 0.3219752754296894559, 0.3333333333333333703, 0.3219752754296894559, 0.3333333333333333703, 0.3219752754296894559, 0.3333333333333333703, 0.3219752754296894559, 0.3333333333333333703, 0.3219752754296894559, 0.3333333333333333703, 0.3219752754296894559, 0.3333333333333333703, 0.3219752754296894559, 0.3333333333333333703, 0.3219752754296894559, 0.3333333333333333703, 0.3219752754296894559, 0.3333333333333333703, 0.3219752754296894559, 0.3333333333333333703, 0.3219752754296894559, 0.3333333333333333703, 0.3219752754296894559, 0.3333333333333333703, 0.3219752754296894559, 0.3333333333333333703, 0.3219752754296894559, 0.3333333333333333703, 0.3219752754296894559, 0.3333333333333333703, 0.3219752754296894559, 0.3333333333333333703, 0.3219752754296894559, 0.3333333333333333703, 0.3219752754296894559, 0.3333333333333333703, 0.3219752754296894559, 0.3333333333333333703, 0.3219752754296894559, 0.3333333333333333703, 0.3219752754296894559, 0.3333333333333333703, 0.3219752754296894559, 0.3333333333333333703, 0.3219752754296894559, 0.3333333333333333703, 0.3219752754296894559, 0.3333333333333333703, 0.3219752754296894559, 0.3333333333333333703, 0.3219752754296894559, 0.3333333333333333703, 0.3219752754296894559, 0.3333333333333333703, 0.3219752754296894559, 0.3333333333333333703, 0.3219752754296894559, 0.3333333333333333703, 0.3219752754296894559, 0.3333333333333333703, 0.3219752754296894559, 0.3333333333333333703, 0.3219752754296894559, 0.3333333333333333703, 0.3219752754296894559, 0.3333333333333333703, 0.3219752754296894559, 0.3333333333333333703, 0.3219752754296894559, 0.3333333333333333703, 0.3219752754296894559, 0.3333333333333333703, 0.3219752754296894559, 0.3333333333333333703, 0.3219752754296894559, 0.3333333333333333703, 0.3219752754296894559, 0.3333333333333333703, 0.3219752754296894559, 0.3333333333333333703, 0.3219752754296894559, 0.3333333333333333703, 0.3219752754296894559, 0.3333333333333333703, 0.3219752754296894559, 0.3333333333333333703, 0.3219752754296894559, 0.3333333333333333703, 0.3219752754296894559, 0.3333333333333333703, 0.3219752754296894559, 0.3333333333333333703, 0.3219752754296894559, 0.3333333333333333703, 0.3219752754296894559, 0.3333333333333333703, 0.3219752754296894559, 0.3333333333333333703, 0.3219752754296894559, 0.3333333333333333703, 0.3219752754296894559, 0.3333333333333333703, 0.3219752754296894559, 0.3333333333333333703, 0.3219752754296894559, 0.3333333333333333703, 0.3219752754296894559, 0.3333333333333333703, 0.3219752754296894559, 0.3333333333333333703, 0.3219752754296894559, 0.3333333333333333703, 0.3219752754296894559, 0.3333333333333333703, 0.3219752754296894559, 0.3333333333333333703, 0.3219752754296894559, 0.3333333333333333703, 0.3219752754296894559, 0.3333333333333333703, 0.3219752754296894559, 0.3333333333333333703, 0.3219752754296894559, 0.3333333333333333703, 0.3219752754296894559, 0.3333333333333333703, 0.3219752754296894559, 0.3333333333333333703, 0.3219752754296894559, 0.3333333333333333703, 0.3219752754296894559, 0.3333333333333333703, 0.3219752754296894559, 0.3333333333333333703, 0.3219752754296894559, 0.3333333333333333703, 0.3219752754296894559, 0.3333333333333333703, 0.3219752754296894559, 0.3333333333333333703, 0.3219752754296894559, 0.3333333333333333703, 0.3219752754296894559, 0.3333333333333333703, 0.3219752754296894559, 0.3333333333333333703, 0.3219752754296894559, 0.3333333333333333703, 0.3219752754296894559, 0.3333333333333333703, 0.3219752754296894559, 0.3333333333333333703, 0.3219752754296894559, 0.3333333333333333703, 0.3219752754296894559, 0.3333333333333333703, 0.3219752754296894559, 0.3333333333333333703, 0.3219752754296894559, 0.3333333333333333703, 0.3219752754296894559, 0.3333333333333333703, 0.3219752754296894559, 0.3333333333333333703, 0.3219752754296894559, 0.3333333333333333703, 0.3219752754296894559, 0.3333333333333333703, 0.3219752754296894559, 0.3333333333333333703, 0.3219752754296894559, 0.3333333333333333703, 0.3219752754296894559, 0.3333333333333333703, 0.3219752754296894559, 0.3333333333333333703, 0.3219752754296894559, 0.3333333333333333703, 0.3219752754296894559, 0.3333333333333333703, 0.3219752754296894559, 0.3333333333333333703, 0.3219752754296894559, 0.3333333333333333703, 0.3219752754296894559, 0.3333333333333333703, 0.3219752754296894559, 0.3333333333333333703, 0.3219752754296894559, 0.3333333333333333703, 0.3219752754296894559, 0.3333333333333333703, 0.3219752754296894559, 0.3333333333333333703, 0.3219752754296894559, 0.3333333333333333703, 0.3219752754296894559, 0.3333333333333333703, 0.3219752754296894559, 0.3333333333333333703, 0.3219752754296894559, 0.3333333333333333703, 0.3219752754296894559, 0.3333333333333333703, 0.3219752754296894559, 0.3333333333333333703, 0.3219752754296894559, 0.3333333333333333703, 0.3219752754296894559, 0.3333333333333333703, 0.3219752754296894559, 0.3333333333333333703, 0.3219752754296894559, 0.3333333333333333703, 0.3219752754296894559, 0.3333333333333333703, 0.3219752754296894559, 0.3333333333333333703, 0.3219752754296894559, 0.3333333333333333703, 0.3219752754296894559, 0.3333333333333333703, 0.3219752754296894559, 0.3333333333333333703, 0.3219752754296894559, 0.3333333333333333703, 0.3219752754296894559, 0.3333333333333333703, 0.3219752754296894559, 0.3333333333333333703, 0.3219752754296894559, 0.3333333333333333703, 0.3219752754296894559, 0.3333333333333333703, 0.3219752754296894559, 0.3333333333333333703, 0.3219752754296894559, 0.3333333333333333703, 0.3219752754296894559, 0.3333333333333333703, 0.3219752754296894559, 0.3333333333333333703, 0.3219752754296894559, 0.3333333333333333703, 0.3219752754296894559, 0.3333333333333333703, 0.3219752754296894559, 0.3333333333333333703, 0.3219752754296894559, 0.3333333333333333703, 0.3219752754296894559, 0.3333333333333333703, 0.3219752754296894559, 0.3333333333333333703, 0.3219752754296894559, 0.3333333333333333703, 0.3219752754296894559, 0.3333333333333333703, 0.3219752754296894559, 0.3333333333333333703, 0.3219752754296894559, 0.3333333333333333703, 0.3219752754296894559, 0.3333333333333333703, 0.3219752754296894559, 0.3333333333333333703, 0.3219752754296894559, 0.3333333333333333703, 0.3219752754296894559, 0.3333333333333333703, 0.3219752754296894559, 0.3333333333333333703, 0.3219752754296894559, 0.3333333333333333703, 0.3219752754296894559, 0.3333333333333333703, 0.3219752754296894559, 0.3333333333333333703, 0.3219752754296894559, 0.3333333333333333703, 0.3219752754296894559, 0.3333333333333333703, 0.3219752754296894559, 0.3333333333333333703, 0.3219752754296894559, 0.3333333333333333703, 0.3219752754296894559, 0.3333333333333333703, 0.3219752754296894559, 0.3333333333333333703, 0.3219752754296894559, 0.3333333333333333703, 0.3219752754296894559, 0.3333333333333333703, 0.3219752754296894559, 0.3333333333333333703, 0.3219752754296894559, 0.3333333333333333703, 0.3219752754296894559, 0.3333333333333333703, 0.3219752754296894559, 0.3333333333333333703, 0.3219752754296894559, 0.3333333333333333703, 0.3219752754296894559, 0.3333333333333333703, 0.3219752754296894559, 0.3333333333333333703, 0.3219752754296894559, 0.3333333333333333703, 0.3219752754296894559, 0.3333333333333333703, 0.3219752754296894559, 0.3333333333333333703, 0.3219752754296894559, 0.3333333333333333703, 0.3219752754296894559, 0.3333333333333333703, 0.3219752754296894559, 0.3333333333333333703, 0.3219752754296894559, 0.3333333333333333703, 0.3219752754296894559, 0.3333333333333333703, 0.3219752754296894559, 0.3333333333333333703, 0.3219752754296894559, 0.3333333333333333703, 0.3219752754296894559, 0.3333333333333333703, 0.3219752754296894559, 0.3333333333333333703, 0.3219752754296894559, 0.3333333333333333703, 0.3219752754296894559, 0.3333333333333333703, 0.3219752754296894559, 0.3333333333333333703, 0.3219752754296894559, 0.3333333333333333703, 0.3219752754296894559, 0.3333333333333333703, 0.3219752754296894559, 0.3333333333333333703, 0.3219752754296894559, 0.3333333333333333703, 0.3219752754296894559, 0.3333333333333333703, 0.3219752754296894559, 0.3333333333333333703, 0.3219752754296894559, 0.3333333333333333703, 0.3219752754296894559, 0.3333333333333333703, 0.3219752754296894559, 0.3333333333333333703, 0.3219752754296894559, 0.3333333333333333703, 0.3219752754296894559, 0.3333333333333333703, 0.3219752754296894559, 0.3333333333333333703, 0.3219752754296894559, 0.3333333333333333703, 0.3219752754296894559, 0.3333333333333333703, 0.3219752754296894559, 0.3333333333333333703, 0.3219752754296894559, 0.3333333333333333703, 0.3219752754296894559, 0.3333333333333333703, 0.3219752754296894559, 0.3333333333333333703, 0.3219752754296894559, 0.3333333333333333703, 0.3219752754296894559, 0.3333333333333333703, 0.3219752754296894559, 0.3333333333333333703, 0.3219752754296894559, 0.3333333333333333703, 0.3219752754296894559, 0.3333333333333333703, 0.3219752754296894559, 0.3333333333333333703, 0.3219752754296894559, 0.3333333333333333703, 0.3219752754296894559, 0.3333333333333333703, 0.3219752754296894559, 0.3333333333333333703, 0.3219752754296894559, 0.3333333333333333703, 0.3219752754296894559, 0.3333333333333333703, 0.3219752754296894559, 0.3333333333333333703, 0.3219752754296894559, 0.3333333333333333703, 0.3219752754296894559, 0.3333333333333333703, 0.3219752754296894559, 0.3333333333333333703, 0.3219752754296894559, 0.3333333333333333703, 0.3219752754296894559, 0.3333333333333333703, 0.3219752754296894559, 0.3333333333333333703, 0.3219752754296894559, 0.3333333333333333703, 0.3219752754296894559, 0.3333333333333333703, 0.3219752754296894559, 0.3333333333333333703, 0.3219752754296894559, 0.3333333333333333703, 0.3219752754296894559, 0.3333333333333333703, 0.3219752754296894559, 0.3333333333333333703, 0.3219752754296894559, 0.3333333333333333703, 0.3219752754296894559, 0.3333333333333333703, 0.3219752754296894559, 0.3333333333333333703, 0.3219752754296894559, 0.3333333333333333703),
 ( 1.000000000000000000, 0.9659258262890683122, 1.000000000000000000, 0.9659258262890683122, 1.000000000000000000, 0.9659258262890683122, 1.000000000000000000, 0.9659258262890683122, 1.000000000000000000, 0.9659258262890683122, 1.000000000000000000, 0.9659258262890683122, 1.000000000000000000, 0.9659258262890683122, 1.000000000000000000, 0.9659258262890683122, 1.000000000000000000, 0.9659258262890683122, 1.000000000000000000, 0.9659258262890683122, 1.000000000000000000, 0.9659258262890683122, 1.000000000000000000, 0.9659258262890683122, 1.000000000000000000, 0.9659258262890683122, 1.000000000000000000, 0.9659258262890683122, 1.000000000000000000, 0.9659258262890683122, 1.000000000000000000, 0.9659258262890683122, 1.000000000000000000, 0.9659258262890683122, 1.000000000000000000, 0.9659258262890683122, 1.000000000000000000, 0.9659258262890683122, 1.000000000000000000, 0.9659258262890683122, 1.000000000000000000, 0.9659258262890683122, 1.000000000000000000, 0.9659258262890683122, 1.000000000000000000, 0.9659258262890683122, 1.000000000000000000, 0.9659258262890683122, 1.000000000000000000, 0.9659258262890683122, 1.000000000000000000, 0.9659258262890683122, 1.000000000000000000, 0.9659258262890683122, 1.000000000000000000, 0.9659258262890683122, 1.000000000000000000, 0.9659258262890683122, 1.000000000000000000, 0.9659258262890683122, 1.000000000000000000, 0.9659258262890683122, 1.000000000000000000, 0.9659258262890683122, 1.000000000000000000, 0.9659258262890683122, 1.000000000000000000, 0.9659258262890683122, 1.000000000000000000, 0.9659258262890683122, 1.000000000000000000, 0.9659258262890683122, 1.000000000000000000, 0.9659258262890683122, 1.000000000000000000, 0.9659258262890683122, 1.000000000000000000, 0.9659258262890683122, 1.000000000000000000, 0.9659258262890683122, 1.000000000000000000, 0.9659258262890683122, 1.000000000000000000, 0.9659258262890683122, 1.000000000000000000, 0.9659258262890683122, 1.000000000000000000, 0.9659258262890683122, 1.000000000000000000, 0.9659258262890683122, 1.000000000000000000, 0.9659258262890683122, 1.000000000000000000, 0.9659258262890683122, 1.000000000000000000, 0.9659258262890683122, 1.000000000000000000, 0.9659258262890683122, 1.000000000000000000, 0.9659258262890683122, 1.000000000000000000, 0.9659258262890683122, 1.000000000000000000, 0.9659258262890683122, 1.000000000000000000, 0.9659258262890683122, 1.000000000000000000, 0.9659258262890683122, 1.000000000000000000, 0.9659258262890683122, 1.000000000000000000, 0.9659258262890683122, 1.000000000000000000, 0.9659258262890683122, 1.000000000000000000, 0.9659258262890683122, 1.000000000000000000, 0.9659258262890683122, 1.000000000000000000, 0.9659258262890683122, 1.000000000000000000, 0.9659258262890683122, 1.000000000000000000, 0.9659258262890683122, 1.000000000000000000, 0.9659258262890683122, 1.000000000000000000, 0.9659258262890683122, 1.000000000000000000, 0.9659258262890683122, 1.000000000000000000, 0.9659258262890683122, 1.000000000000000000, 0.9659258262890683122, 1.000000000000000000, 0.9659258262890683122, 1.000000000000000000, 0.9659258262890683122, 1.000000000000000000, 0.9659258262890683122, 1.000000000000000000, 0.9659258262890683122, 1.000000000000000000, 0.9659258262890683122, 1.000000000000000000, 0.9659258262890683122, 1.000000000000000000, 0.9659258262890683122, 1.000000000000000000, 0.9659258262890683122, 1.000000000000000000, 0.9659258262890683122, 1.000000000000000000, 0.9659258262890683122, 1.000000000000000000, 0.9659258262890683122, 1.000000000000000000, 0.9659258262890683122, 1.000000000000000000, 0.9659258262890683122, 1.000000000000000000, 0.9659258262890683122, 1.000000000000000000, 0.9659258262890683122, 1.000000000000000000, 0.9659258262890683122, 1.000000000000000000, 0.9659258262890683122, 1.000000000000000000, 0.9659258262890683122, 1.000000000000000000, 0.9659258262890683122, 1.000000000000000000, 0.9659258262890683122, 1.000000000000000000, 0.9659258262890683122, 1.000000000000000000, 0.9659258262890683122, 1.000000000000000000, 0.9659258262890683122, 1.000000000000000000, 0.9659258262890683122, 1.000000000000000000, 0.9659258262890683122, 1.000000000000000000, 0.9659258262890683122, 1.000000000000000000, 0.9659258262890683122, 1.000000000000000000, 0.9659258262890683122, 1.000000000000000000, 0.9659258262890683122, 1.000000000000000000, 0.9659258262890683122, 1.000000000000000000, 0.9659258262890683122, 1.000000000000000000, 0.9659258262890683122, 1.000000000000000000, 0.9659258262890683122, 1.000000000000000000, 0.9659258262890683122, 1.000000000000000000, 0.9659258262890683122, 1.000000000000000000, 0.9659258262890683122, 1.000000000000000000, 0.9659258262890683122, 1.000000000000000000, 0.9659258262890683122, 1.000000000000000000, 0.9659258262890683122, 1.000000000000000000, 0.9659258262890683122, 1.000000000000000000, 0.9659258262890683122, 1.000000000000000000, 0.9659258262890683122, 1.000000000000000000, 0.9659258262890683122, 1.000000000000000000, 0.9659258262890683122, 1.000000000000000000, 0.9659258262890683122, 1.000000000000000000, 0.9659258262890683122, 1.000000000000000000, 0.9659258262890683122, 1.000000000000000000, 0.9659258262890683122, 1.000000000000000000, 0.9659258262890683122, 1.000000000000000000, 0.9659258262890683122, 1.000000000000000000, 0.9659258262890683122, 1.000000000000000000, 0.9659258262890683122, 1.000000000000000000, 0.9659258262890683122, 1.000000000000000000, 0.9659258262890683122, 1.000000000000000000, 0.9659258262890683122, 1.000000000000000000, 0.9659258262890683122, 1.000000000000000000, 0.9659258262890683122, 1.000000000000000000, 0.9659258262890683122, 1.000000000000000000, 0.9659258262890683122, 1.000000000000000000, 0.9659258262890683122, 1.000000000000000000, 0.9659258262890683122, 1.000000000000000000, 0.9659258262890683122, 1.000000000000000000, 0.9659258262890683122, 1.000000000000000000, 0.9659258262890683122, 1.000000000000000000, 0.9659258262890683122, 1.000000000000000000, 0.9659258262890683122, 1.000000000000000000, 0.9659258262890683122, 1.000000000000000000, 0.9659258262890683122, 1.000000000000000000, 0.9659258262890683122, 1.000000000000000000, 0.9659258262890683122, 1.000000000000000000, 0.9659258262890683122, 1.000000000000000000, 0.9659258262890683122, 1.000000000000000000, 0.9659258262890683122, 1.000000000000000000, 0.9659258262890683122, 1.000000000000000000, 0.9659258262890683122, 1.000000000000000000, 0.9659258262890683122, 1.000000000000000000, 0.9659258262890683122, 1.000000000000000000, 0.9659258262890683122, 1.000000000000000000, 0.9659258262890683122, 1.000000000000000000, 0.9659258262890683122, 1.000000000000000000, 0.9659258262890683122, 1.000000000000000000, 0.9659258262890683122, 1.000000000000000000, 0.9659258262890683122, 1.000000000000000000, 0.9659258262890683122, 1.000000000000000000, 0.9659258262890683122, 1.000000000000000000, 0.9659258262890683122, 1.000000000000000000, 0.9659258262890683122, 1.000000000000000000, 0.9659258262890683122, 1.000000000000000000, 0.9659258262890683122, 1.000000000000000000, 0.9659258262890683122, 1.000000000000000000, 0.9659258262890683122, 1.000000000000000000, 0.9659258262890683122, 1.000000000000000000, 0.9659258262890683122, 1.000000000000000000, 0.9659258262890683122, 1.000000000000000000, 0.9659258262890683122, 1.000000000000000000, 0.9659258262890683122, 1.000000000000000000, 0.9659258262890683122, 1.000000000000000000, 0.9659258262890683122, 1.000000000000000000, 0.9659258262890683122, 1.000000000000000000, 0.9659258262890683122, 1.000000000000000000, 0.9659258262890683122, 1.000000000000000000, 0.9659258262890683122, 1.000000000000000000, 0.9659258262890683122, 1.000000000000000000, 0.9659258262890683122, 1.000000000000000000, 0.9659258262890683122, 1.000000000000000000, 0.9659258262890683122, 1.000000000000000000, 0.9659258262890683122, 1.000000000000000000, 0.9659258262890683122, 1.000000000000000000, 0.9659258262890683122, 1.000000000000000000, 0.9659258262890683122, 1.000000000000000000, 0.9659258262890683122, 1.000000000000000000, 0.9659258262890683122, 1.000000000000000000, 0.9659258262890683122, 1.000000000000000000, 0.9659258262890683122, 1.000000000000000000, 0.9659258262890683122, 1.000000000000000000, 0.9659258262890683122, 1.000000000000000000, 0.9659258262890683122, 1.000000000000000000, 0.9659258262890683122, 1.000000000000000000, 0.9659258262890683122, 1.000000000000000000, 0.9659258262890683122, 1.000000000000000000, 0.9659258262890683122, 1.000000000000000000, 0.9659258262890683122, 1.000000000000000000, 0.9659258262890683122, 1.000000000000000000, 0.9659258262890683122, 1.000000000000000000, 0.9659258262890683122, 1.000000000000000000, 0.9659258262890683122, 1.000000000000000000, 0.9659258262890683122, 1.000000000000000000, 0.9659258262890683122, 1.000000000000000000, 0.9659258262890683122, 1.000000000000000000, 0.9659258262890683122, 1.000000000000000000, 0.9659258262890683122, 1.000000000000000000, 0.9659258262890683122, 1.000000000000000000, 0.9659258262890683122, 1.000000000000000000, 0.9659258262890683122, 1.000000000000000000, 0.9659258262890683122, 1.000000000000000000, 0.9659258262890683122, 1.000000000000000000, 0.9659258262890683122, 1.000000000000000000, 0.9659258262890683122, 1.000000000000000000, 0.9659258262890683122, 1.000000000000000000, 0.9659258262890683122, 1.000000000000000000, 0.9659258262890683122, 1.000000000000000000, 0.9659258262890683122, 1.000000000000000000, 0.9659258262890683122, 1.000000000000000000, 0.9659258262890683122, 1.000000000000000000, 0.9659258262890683122, 1.000000000000000000, 0.9659258262890683122, 1.000000000000000000, 0.9659258262890683122, 1.000000000000000000, 0.9659258262890683122, 1.000000000000000000, 0.9659258262890683122, 1.000000000000000000, 0.9659258262890683122, 1.000000000000000000, 0.9659258262890683122, 1.000000000000000000, 0.9659258262890683122, 1.000000000000000000, 0.9659258262890683122, 1.000000000000000000, 0.9659258262890683122, 1.000000000000000000, 0.9659258262890683122, 1.000000000000000000, 0.9659258262890683122, 1.000000000000000000, 0.9659258262890683122, 1.000000000000000000, 0.9659258262890683122, 1.000000000000000000, 0.9659258262890683122, 1.000000000000000000, 0.9659258262890683122, 1.000000000000000000, 0.9659258262890683122, 1.000000000000000000),
 ( 0.3333333333333333703, 0.3219752754296894559, 0.3333333333333333703, 0.3219752754296894559, 0.3333333333333333703, 0.3219752754296894559, 0.3333333333333333703, 0.3219752754296894559, 0.3333333333333333703, 0.3219752754296894559, 0.3333333333333333703, 0.3219752754296894559, 0.3333333333333333703, 0.3219752754296894559, 0.3333333333333333703, 0.3219752754296894559, 0.3333333333333333703, 0.3219752754296894559, 0.3333333333333333703, 0.3219752754296894559, 0.3333333333333333703, 0.3219752754296894559, 0.3333333333333333703, 0.3219752754296894559, 0.3333333333333333703, 0.3219752754296894559, 0.3333333333333333703, 0.3219752754296894559, 0.3333333333333333703, 0.3219752754296894559, 0.3333333333333333703, 0.3219752754296894559, 0.3333333333333333703, 0.3219752754296894559, 0.3333333333333333703, 0.3219752754296894559, 0.3333333333333333703, 0.3219752754296894559, 0.3333333333333333703, 0.3219752754296894559, 0.3333333333333333703, 0.3219752754296894559, 0.3333333333333333703, 0.3219752754296894559, 0.3333333333333333703, 0.3219752754296894559, 0.3333333333333333703, 0.3219752754296894559, 0.3333333333333333703, 0.3219752754296894559, 0.3333333333333333703, 0.3219752754296894559, 0.3333333333333333703, 0.3219752754296894559, 0.3333333333333333703, 0.3219752754296894559, 0.3333333333333333703, 0.3219752754296894559, 0.3333333333333333703, 0.3219752754296894559, 0.3333333333333333703, 0.3219752754296894559, 0.3333333333333333703, 0.3219752754296894559, 0.3333333333333333703, 0.3219752754296894559, 0.3333333333333333703, 0.3219752754296894559, 0.3333333333333333703, 0.3219752754296894559, 0.3333333333333333703, 0.3219752754296894559, 0.3333333333333333703, 0.3219752754296894559, 0.3333333333333333703, 0.3219752754296894559, 0.3333333333333333703, 0.3219752754296894559, 0.3333333333333333703, 0.3219752754296894559, 0.3333333333333333703, 0.3219752754296894559, 0.3333333333333333703, 0.3219752754296894559, 0.3333333333333333703, 0.3219752754296894559, 0.3333333333333333703, 0.3219752754296894559, 0.3333333333333333703, 0.3219752754296894559, 0.3333333333333333703, 0.3219752754296894559, 0.3333333333333333703, 0.3219752754296894559, 0.3333333333333333703, 0.3219752754296894559, 0.3333333333333333703, 0.3219752754296894559, 0.3333333333333333703, 0.3219752754296894559, 0.3333333333333333703, 0.3219752754296894559, 0.3333333333333333703, 0.3219752754296894559, 0.3333333333333333703, 0.3219752754296894559, 0.3333333333333333703, 0.3219752754296894559, 0.3333333333333333703, 0.3219752754296894559, 0.3333333333333333703, 0.3219752754296894559, 0.3333333333333333703, 0.3219752754296894559, 0.3333333333333333703, 0.3219752754296894559, 0.3333333333333333703, 0.3219752754296894559, 0.3333333333333333703, 0.3219752754296894559, 0.3333333333333333703, 0.3219752754296894559, 0.3333333333333333703, 0.3219752754296894559, 0.3333333333333333703, 0.3219752754296894559, 0.3333333333333333703, 0.3219752754296894559, 0.3333333333333333703, 0.3219752754296894559, 0.3333333333333333703, 0.3219752754296894559, 0.3333333333333333703, 0.3219752754296894559, 0.3333333333333333703, 0.3219752754296894559, 0.3333333333333333703, 0.3219752754296894559, 0.3333333333333333703, 0.3219752754296894559, 0.3333333333333333703, 0.3219752754296894559, 0.3333333333333333703, 0.3219752754296894559, 0.3333333333333333703, 0.3219752754296894559, 0.3333333333333333703, 0.3219752754296894559, 0.3333333333333333703, 0.3219752754296894559, 0.3333333333333333703, 0.3219752754296894559, 0.3333333333333333703, 0.3219752754296894559, 0.3333333333333333703, 0.3219752754296894559, 0.3333333333333333703, 0.3219752754296894559, 0.3333333333333333703, 0.3219752754296894559, 0.3333333333333333703, 0.3219752754296894559, 0.3333333333333333703, 0.3219752754296894559, 0.3333333333333333703, 0.3219752754296894559, 0.3333333333333333703, 0.3219752754296894559, 0.3333333333333333703, 0.3219752754296894559, 0.3333333333333333703, 0.3219752754296894559, 0.3333333333333333703, 0.3219752754296894559, 0.3333333333333333703, 0.3219752754296894559, 0.3333333333333333703, 0.3219752754296894559, 0.3333333333333333703, 0.3219752754296894559, 0.3333333333333333703, 0.3219752754296894559, 0.3333333333333333703, 0.3219752754296894559, 0.3333333333333333703, 0.3219752754296894559, 0.3333333333333333703, 0.3219752754296894559, 0.3333333333333333703, 0.3219752754296894559, 0.3333333333333333703, 0.3219752754296894559, 0.3333333333333333703, 0.3219752754296894559, 0.3333333333333333703, 0.3219752754296894559, 0.3333333333333333703, 0.3219752754296894559, 0.3333333333333333703, 0.3219752754296894559, 0.3333333333333333703, 0.3219752754296894559, 0.3333333333333333703, 0.3219752754296894559, 0.3333333333333333703, 0.3219752754296894559, 0.3333333333333333703, 0.3219752754296894559, 0.3333333333333333703, 0.3219752754296894559, 0.3333333333333333703, 0.3219752754296894559, 0.3333333333333333703, 0.3219752754296894559, 0.3333333333333333703, 0.3219752754296894559, 0.3333333333333333703, 0.3219752754296894559, 0.3333333333333333703, 0.3219752754296894559, 0.3333333333333333703, 0.3219752754296894559, 0.3333333333333333703, 0.3219752754296894559, 0.3333333333333333703, 0.3219752754296894559, 0.3333333333333333703, 0.3219752754296894559, 0.3333333333333333703, 0.3219752754296894559, 0.3333333333333333703, 0.3219752754296894559, 0.3333333333333333703, 0.3219752754296894559, 0.3333333333333333703, 0.3219752754296894559, 0.3333333333333333703, 0.3219752754296894559, 0.3333333333333333703, 0.3219752754296894559, 0.3333333333333333703, 0.3219752754296894559, 0.3333333333333333703, 0.3219752754296894559, 0.3333333333333333703, 0.3219752754296894559, 0.3333333333333333703, 0.3219752754296894559, 0.3333333333333333703, 0.3219752754296894559, 0.3333333333333333703, 0.3219752754296894559, 0.3333333333333333703, 0.3219752754296894559, 0.3333333333333333703, 0.3219752754296894559, 0.3333333333333333703, 0.3219752754296894559, 0.3333333333333333703, 0.3219752754296894559, 0.3333333333333333703, 0.3219752754296894559, 0.3333333333333333703, 0.3219752754296894559, 0.3333333333333333703, 0.3219752754296894559, 0.3333333333333333703, 0.3219752754296894559, 0.3333333333333333703, 0.3219752754296894559, 0.3333333333333333703, 0.3219752754296894559, 0.3333333333333333703, 0.3219752754296894559, 0.3333333333333333703, 0.3219752754296894559, 0.3333333333333333703, 0.3219752754296894559, 0.3333333333333333703, 0.3219752754296894559, 0.3333333333333333703, 0.3219752754296894559, 0.3333333333333333703, 0.3219752754296894559, 0.3333333333333333703, 0.3219752754296894559, 0.3333333333333333703, 0.3219752754296894559, 0.3333333333333333703, 0.3219752754296894559, 0.3333333333333333703, 0.3219752754296894559, 0.3333333333333333703, 0.3219752754296894559, 0.3333333333333333703, 0.3219752754296894559, 0.3333333333333333703, 0.3219752754296894559, 0.3333333333333333703, 0.3219752754296894559, 0.3333333333333333703, 0.3219752754296894559, 0.3333333333333333703, 0.3219752754296894559, 0.3333333333333333703, 0.3219752754296894559, 0.3333333333333333703, 0.3219752754296894559, 0.3333333333333333703, 0.3219752754296894559, 0.3333333333333333703, 0.3219752754296894559, 0.3333333333333333703, 0.3219752754296894559, 0.3333333333333333703, 0.3219752754296894559, 0.3333333333333333703, 0.3219752754296894559, 0.3333333333333333703, 0.3219752754296894559, 0.3333333333333333703, 0.3219752754296894559, 0.3333333333333333703, 0.3219752754296894559, 0.3333333333333333703, 0.3219752754296894559, 0.3333333333333333703, 0.3219752754296894559, 0.3333333333333333703, 0.3219752754296894559, 0.3333333333333333703, 0.3219752754296894559, 0.3333333333333333703, 0.3219752754296894559, 0.3333333333333333703, 0.3219752754296894559, 0.3333333333333333703, 0.3219752754296894559, 0.3333333333333333703, 0.3219752754296894559, 0.3333333333333333703, 0.3219752754296894559, 0.3333333333333333703, 0.3219752754296894559, 0.3333333333333333703, 0.3219752754296894559, 0.3333333333333333703, 0.3219752754296894559, 0.3333333333333333703, 0.3219752754296894559, 0.3333333333333333703, 0.3219752754296894559, 0.3333333333333333703, 0.3219752754296894559, 0.3333333333333333703, 0.3219752754296894559, 0.3333333333333333703, 0.3219752754296894559, 0.3333333333333333703, 0.3219752754296894559, 0.3333333333333333703, 0.3219752754296894559, 0.3333333333333333703, 0.3219752754296894559, 0.3333333333333333703, 0.3219752754296894559, 0.3333333333333333703, 0.3219752754296894559, 0.3333333333333333703, 0.3219752754296894559, 0.3333333333333333703, 0.3219752754296894559, 0.3333333333333333703, 0.3219752754296894559, 0.3333333333333333703, 0.3219752754296894559, 0.3333333333333333703, 0.3219752754296894559, 0.3333333333333333703, 0.3219752754296894559, 0.3333333333333333703, 0.3219752754296894559, 0.3333333333333333703, 0.3219752754296894559, 0.3333333333333333703, 0.3219752754296894559, 0.3333333333333333703, 0.3219752754296894559, 0.3333333333333333703, 0.3219752754296894559, 0.3333333333333333703, 0.3219752754296894559, 0.3333333333333333703, 0.3219752754296894559, 0.3333333333333333703, 0.3219752754296894559, 0.3333333333333333703, 0.3219752754296894559, 0.3333333333333333703, 0.3219752754296894559, 0.3333333333333333703, 0.3219752754296894559, 0.3333333333333333703, 0.3219752754296894559, 0.3333333333333333703, 0.3219752754296894559, 0.3333333333333333703, 0.3219752754296894559, 0.3333333333333333703, 0.3219752754296894559, 0.3333333333333333703, 0.3219752754296894559, 0.3333333333333333703, 0.3219752754296894559, 0.3333333333333333703, 0.3219752754296894559, 0.3333333333333333703, 0.3219752754296894559, 0.3333333333333333703, 0.3219752754296894559, 0.3333333333333333703, 0.3219752754296894559, 0.3333333333333333703, 0.3219752754296894559, 0.3333333333333333703, 0.3219752754296894559, 0.3333333333333333703, 0.3219752754296894559, 0.3333333333333333703, 0.3219752754296894559, 0.3333333333333333703, 0.3219752754296894559, 0.3333333333333333703, 0.3219752754296894559, 0.3333333333333333703, 0.3219752754296894559, 0.3333333333333333703, 0.3219752754296894559, 0.3333333333333333703, 0.3219752754296894559, 0.3333333333333333703, 0.3219752754296894559, 0.3333333333333333703, 0.3219752754296894559, 0.3333333333333333703, 0.3219752754296894559, 0.3333333333333333703, 0.3219752754296894559, 0.3333333333333333703, 0.3219752754296894559, 0.3333333333333333703, 0.3219752754296894559, 0.3333333333333333703, 0.3219752754296894559, 0.3333333333333333703, 0.3219752754296894559, 0.3333333333333333703),
 ( 0.3333333333333333703, 0.3219752754296894559, 0.3333333333333333703, 0.3219752754296894559, 0.3333333333333333703, 0.3219752754296894559, 0.3333333333333333703, 0.3219752754296894559, 0.3333333333333333703, 0.3219752754296894559, 0.3333333333333333703, 0.3219752754296894559, 0.3333333333333333703, 0.3219752754296894559, 0.3333333333333333703, 0.3219752754296894559, 0.3333333333333333703, 0.3219752754296894559, 0.3333333333333333703, 0.3219752754296894559, 0.3333333333333333703, 0.3219752754296894559, 0.3333333333333333703, 0.3219752754296894559, 0.3333333333333333703, 0.3219752754296894559, 0.3333333333333333703, 0.3219752754296894559, 0.3333333333333333703, 0.3219752754296894559, 0.3333333333333333703, 0.3219752754296894559, 0.3333333333333333703, 0.3219752754296894559, 0.3333333333333333703, 0.3219752754296894559, 0.3333333333333333703, 0.3219752754296894559, 0.3333333333333333703, 0.3219752754296894559, 0.3333333333333333703, 0.3219752754296894559, 0.3333333333333333703, 0.3219752754296894559, 0.3333333333333333703, 0.3219752754296894559, 0.3333333333333333703, 0.3219752754296894559, 0.3333333333333333703, 0.3219752754296894559, 0.3333333333333333703, 0.3219752754296894559, 0.3333333333333333703, 0.3219752754296894559, 0.3333333333333333703, 0.3219752754296894559, 0.3333333333333333703, 0.3219752754296894559, 0.3333333333333333703, 0.3219752754296894559, 0.3333333333333333703, 0.3219752754296894559, 0.3333333333333333703, 0.3219752754296894559, 0.3333333333333333703, 0.3219752754296894559, 0.3333333333333333703, 0.3219752754296894559, 0.3333333333333333703, 0.3219752754296894559, 0.3333333333333333703, 0.3219752754296894559, 0.3333333333333333703, 0.3219752754296894559, 0.3333333333333333703, 0.3219752754296894559, 0.3333333333333333703, 0.3219752754296894559, 0.3333333333333333703, 0.3219752754296894559, 0.3333333333333333703, 0.3219752754296894559, 0.3333333333333333703, 0.3219752754296894559, 0.3333333333333333703, 0.3219752754296894559, 0.3333333333333333703, 0.3219752754296894559, 0.3333333333333333703, 0.3219752754296894559, 0.3333333333333333703, 0.3219752754296894559, 0.3333333333333333703, 0.3219752754296894559, 0.3333333333333333703, 0.3219752754296894559, 0.3333333333333333703, 0.3219752754296894559, 0.3333333333333333703, 0.3219752754296894559, 0.3333333333333333703, 0.3219752754296894559, 0.3333333333333333703, 0.3219752754296894559, 0.3333333333333333703, 0.3219752754296894559, 0.3333333333333333703, 0.3219752754296894559, 0.3333333333333333703, 0.3219752754296894559, 0.3333333333333333703, 0.3219752754296894559, 0.3333333333333333703, 0.3219752754296894559, 0.3333333333333333703, 0.3219752754296894559, 0.3333333333333333703, 0.3219752754296894559, 0.3333333333333333703, 0.3219752754296894559, 0.3333333333333333703, 0.3219752754296894559, 0.3333333333333333703, 0.3219752754296894559, 0.3333333333333333703, 0.3219752754296894559, 0.3333333333333333703, 0.3219752754296894559, 0.3333333333333333703, 0.3219752754296894559, 0.3333333333333333703, 0.3219752754296894559, 0.3333333333333333703, 0.3219752754296894559, 0.3333333333333333703, 0.3219752754296894559, 0.3333333333333333703, 0.3219752754296894559, 0.3333333333333333703, 0.3219752754296894559, 0.3333333333333333703, 0.3219752754296894559, 0.3333333333333333703, 0.3219752754296894559, 0.3333333333333333703, 0.3219752754296894559, 0.3333333333333333703, 0.3219752754296894559, 0.3333333333333333703, 0.3219752754296894559, 0.3333333333333333703, 0.3219752754296894559, 0.3333333333333333703, 0.3219752754296894559, 0.3333333333333333703, 0.3219752754296894559, 0.3333333333333333703, 0.3219752754296894559, 0.3333333333333333703, 0.3219752754296894559, 0.3333333333333333703, 0.3219752754296894559, 0.3333333333333333703, 0.3219752754296894559, 0.3333333333333333703, 0.3219752754296894559, 0.3333333333333333703, 0.3219752754296894559, 0.3333333333333333703, 0.3219752754296894559, 0.3333333333333333703, 0.3219752754296894559, 0.3333333333333333703, 0.3219752754296894559, 0.3333333333333333703, 0.3219752754296894559, 0.3333333333333333703, 0.3219752754296894559, 0.3333333333333333703, 0.3219752754296894559, 0.3333333333333333703, 0.3219752754296894559, 0.3333333333333333703, 0.3219752754296894559, 0.3333333333333333703, 0.3219752754296894559, 0.3333333333333333703, 0.3219752754296894559, 0.3333333333333333703, 0.3219752754296894559, 0.3333333333333333703, 0.3219752754296894559, 0.3333333333333333703, 0.3219752754296894559, 0.3333333333333333703, 0.3219752754296894559, 0.3333333333333333703, 0.3219752754296894559, 0.3333333333333333703, 0.3219752754296894559, 0.3333333333333333703, 0.3219752754296894559, 0.3333333333333333703, 0.3219752754296894559, 0.3333333333333333703, 0.3219752754296894559, 0.3333333333333333703, 0.3219752754296894559, 0.3333333333333333703, 0.3219752754296894559, 0.3333333333333333703, 0.3219752754296894559, 0.3333333333333333703, 0.3219752754296894559, 0.3333333333333333703, 0.3219752754296894559, 0.3333333333333333703, 0.3219752754296894559, 0.3333333333333333703, 0.3219752754296894559, 0.3333333333333333703, 0.3219752754296894559, 0.3333333333333333703, 0.3219752754296894559, 0.3333333333333333703, 0.3219752754296894559, 0.3333333333333333703, 0.3219752754296894559, 0.3333333333333333703, 0.3219752754296894559, 0.3333333333333333703, 0.3219752754296894559, 0.3333333333333333703, 0.3219752754296894559, 0.3333333333333333703, 0.3219752754296894559, 0.3333333333333333703, 0.3219752754296894559, 0.3333333333333333703, 0.3219752754296894559, 0.3333333333333333703, 0.3219752754296894559, 0.3333333333333333703, 0.3219752754296894559, 0.3333333333333333703, 0.3219752754296894559, 0.3333333333333333703, 0.3219752754296894559, 0.3333333333333333703, 0.3219752754296894559, 0.3333333333333333703, 0.3219752754296894559, 0.3333333333333333703, 0.3219752754296894559, 0.3333333333333333703, 0.3219752754296894559, 0.3333333333333333703, 0.3219752754296894559, 0.3333333333333333703, 0.3219752754296894559, 0.3333333333333333703, 0.3219752754296894559, 0.3333333333333333703, 0.3219752754296894559, 0.3333333333333333703, 0.3219752754296894559, 0.3333333333333333703, 0.3219752754296894559, 0.3333333333333333703, 0.3219752754296894559, 0.3333333333333333703, 0.3219752754296894559, 0.3333333333333333703, 0.3219752754296894559, 0.3333333333333333703, 0.3219752754296894559, 0.3333333333333333703, 0.3219752754296894559, 0.3333333333333333703, 0.3219752754296894559, 0.3333333333333333703, 0.3219752754296894559, 0.3333333333333333703, 0.3219752754296894559, 0.3333333333333333703, 0.3219752754296894559, 0.3333333333333333703, 0.3219752754296894559, 0.3333333333333333703, 0.3219752754296894559, 0.3333333333333333703, 0.3219752754296894559, 0.3333333333333333703, 0.3219752754296894559, 0.3333333333333333703, 0.3219752754296894559, 0.3333333333333333703, 0.3219752754296894559, 0.3333333333333333703, 0.3219752754296894559, 0.3333333333333333703, 0.3219752754296894559, 0.3333333333333333703, 0.3219752754296894559, 0.3333333333333333703, 0.3219752754296894559, 0.3333333333333333703, 0.3219752754296894559, 0.3333333333333333703, 0.3219752754296894559, 0.3333333333333333703, 0.3219752754296894559, 0.3333333333333333703, 0.3219752754296894559, 0.3333333333333333703, 0.3219752754296894559, 0.3333333333333333703, 0.3219752754296894559, 0.3333333333333333703, 0.3219752754296894559, 0.3333333333333333703, 0.3219752754296894559, 0.3333333333333333703, 0.3219752754296894559, 0.3333333333333333703, 0.3219752754296894559, 0.3333333333333333703, 0.3219752754296894559, 0.3333333333333333703, 0.3219752754296894559, 0.3333333333333333703, 0.3219752754296894559, 0.3333333333333333703, 0.3219752754296894559, 0.3333333333333333703, 0.3219752754296894559, 0.3333333333333333703, 0.3219752754296894559, 0.3333333333333333703, 0.3219752754296894559, 0.3333333333333333703, 0.3219752754296894559, 0.3333333333333333703, 0.3219752754296894559, 0.3333333333333333703, 0.3219752754296894559, 0.3333333333333333703, 0.3219752754296894559, 0.3333333333333333703, 0.3219752754296894559, 0.3333333333333333703, 0.3219752754296894559, 0.3333333333333333703, 0.3219752754296894559, 0.3333333333333333703, 0.3219752754296894559, 0.3333333333333333703, 0.3219752754296894559, 0.3333333333333333703, 0.3219752754296894559, 0.3333333333333333703, 0.3219752754296894559, 0.3333333333333333703, 0.3219752754296894559, 0.3333333333333333703, 0.3219752754296894559, 0.3333333333333333703, 0.3219752754296894559, 0.3333333333333333703, 0.3219752754296894559, 0.3333333333333333703, 0.3219752754296894559, 0.3333333333333333703, 0.3219752754296894559, 0.3333333333333333703, 0.3219752754296894559, 0.3333333333333333703, 0.3219752754296894559, 0.3333333333333333703, 0.3219752754296894559, 0.3333333333333333703, 0.3219752754296894559, 0.3333333333333333703, 0.3219752754296894559, 0.3333333333333333703, 0.3219752754296894559, 0.3333333333333333703, 0.3219752754296894559, 0.3333333333333333703, 0.3219752754296894559, 0.3333333333333333703, 0.3219752754296894559, 0.3333333333333333703, 0.3219752754296894559, 0.3333333333333333703, 0.3219752754296894559, 0.3333333333333333703, 0.3219752754296894559, 0.3333333333333333703, 0.3219752754296894559, 0.3333333333333333703, 0.3219752754296894559, 0.3333333333333333703, 0.3219752754296894559, 0.3333333333333333703, 0.3219752754296894559, 0.3333333333333333703, 0.3219752754296894559, 0.3333333333333333703, 0.3219752754296894559, 0.3333333333333333703, 0.3219752754296894559, 0.3333333333333333703, 0.3219752754296894559, 0.3333333333333333703, 0.3219752754296894559, 0.3333333333333333703, 0.3219752754296894559, 0.3333333333333333703, 0.3219752754296894559, 0.3333333333333333703, 0.3219752754296894559, 0.3333333333333333703, 0.3219752754296894559, 0.3333333333333333703, 0.3219752754296894559, 0.3333333333333333703, 0.3219752754296894559, 0.3333333333333333703, 0.3219752754296894559, 0.3333333333333333703, 0.3219752754296894559, 0.3333333333333333703, 0.3219752754296894559, 0.3333333333333333703, 0.3219752754296894559, 0.3333333333333333703, 0.3219752754296894559, 0.3333333333333333703, 0.3219752754296894559, 0.3333333333333333703, 0.3219752754296894559, 0.3333333333333333703, 0.3219752754296894559, 0.3333333333333333703, 0.3219752754296894559, 0.3333333333333333703, 0.3219752754296894559, 0.3333333333333333703, 0.3219752754296894559, 0.3333333333333333703, 0.3219752754296894559, 0.3333333333333333703, 0.3219752754296894559, 0.3333333333333333703, 0.3219752754296894559, 0.3333333333333333703),
 ( 1.000000000000000000, 0.9659258262890683122, 1.000000000000000000, 0.9659258262890683122, 1.000000000000000000, 0.9659258262890683122, 1.000000000000000000, 0.9659258262890683122, 1.000000000000000000, 0.9659258262890683122, 1.000000000000000000, 0.9659258262890683122, 1.000000000000000000, 0.9659258262890683122, 1.000000000000000000, 0.9659258262890683122, 1.000000000000000000, 0.9659258262890683122, 1.000000000000000000, 0.9659258262890683122, 1.000000000000000000, 0.9659258262890683122, 1.000000000000000000, 0.9659258262890683122, 1.000000000000000000, 0.9659258262890683122, 1.000000000000000000, 0.9659258262890683122, 1.000000000000000000, 0.9659258262890683122, 1.000000000000000000, 0.9659258262890683122, 1.000000000000000000, 0.9659258262890683122, 1.000000000000000000, 0.9659258262890683122, 1.000000000000000000, 0.9659258262890683122, 1.000000000000000000, 0.9659258262890683122, 1.000000000000000000, 0.9659258262890683122, 1.000000000000000000, 0.9659258262890683122, 1.000000000000000000, 0.9659258262890683122, 1.000000000000000000, 0.9659258262890683122, 1.000000000000000000, 0.9659258262890683122, 1.000000000000000000, 0.9659258262890683122, 1.000000000000000000, 0.9659258262890683122, 1.000000000000000000, 0.9659258262890683122, 1.000000000000000000, 0.9659258262890683122, 1.000000000000000000, 0.9659258262890683122, 1.000000000000000000, 0.9659258262890683122, 1.000000000000000000, 0.9659258262890683122, 1.000000000000000000, 0.9659258262890683122, 1.000000000000000000, 0.9659258262890683122, 1.000000000000000000, 0.9659258262890683122, 1.000000000000000000, 0.9659258262890683122, 1.000000000000000000, 0.9659258262890683122, 1.000000000000000000, 0.9659258262890683122, 1.000000000000000000, 0.9659258262890683122, 1.000000000000000000, 0.9659258262890683122, 1.000000000000000000, 0.9659258262890683122, 1.000000000000000000, 0.9659258262890683122, 1.000000000000000000, 0.9659258262890683122, 1.000000000000000000, 0.9659258262890683122, 1.000000000000000000, 0.9659258262890683122, 1.000000000000000000, 0.9659258262890683122, 1.000000000000000000, 0.9659258262890683122, 1.000000000000000000, 0.9659258262890683122, 1.000000000000000000, 0.9659258262890683122, 1.000000000000000000, 0.9659258262890683122, 1.000000000000000000, 0.9659258262890683122, 1.000000000000000000, 0.9659258262890683122, 1.000000000000000000, 0.9659258262890683122, 1.000000000000000000, 0.9659258262890683122, 1.000000000000000000, 0.9659258262890683122, 1.000000000000000000, 0.9659258262890683122, 1.000000000000000000, 0.9659258262890683122, 1.000000000000000000, 0.9659258262890683122, 1.000000000000000000, 0.9659258262890683122, 1.000000000000000000, 0.9659258262890683122, 1.000000000000000000, 0.9659258262890683122, 1.000000000000000000, 0.9659258262890683122, 1.000000000000000000, 0.9659258262890683122, 1.000000000000000000, 0.9659258262890683122, 1.000000000000000000, 0.9659258262890683122, 1.000000000000000000, 0.9659258262890683122, 1.000000000000000000, 0.9659258262890683122, 1.000000000000000000, 0.9659258262890683122, 1.000000000000000000, 0.9659258262890683122, 1.000000000000000000, 0.9659258262890683122, 1.000000000000000000, 0.9659258262890683122, 1.000000000000000000, 0.9659258262890683122, 1.000000000000000000, 0.9659258262890683122, 1.000000000000000000, 0.9659258262890683122, 1.000000000000000000, 0.9659258262890683122, 1.000000000000000000, 0.9659258262890683122, 1.000000000000000000, 0.9659258262890683122, 1.000000000000000000, 0.9659258262890683122, 1.000000000000000000, 0.9659258262890683122, 1.000000000000000000, 0.9659258262890683122, 1.000000000000000000, 0.9659258262890683122, 1.000000000000000000, 0.9659258262890683122, 1.000000000000000000, 0.9659258262890683122, 1.000000000000000000, 0.9659258262890683122, 1.000000000000000000, 0.9659258262890683122, 1.000000000000000000, 0.9659258262890683122, 1.000000000000000000, 0.9659258262890683122, 1.000000000000000000, 0.9659258262890683122, 1.000000000000000000, 0.9659258262890683122, 1.000000000000000000, 0.9659258262890683122, 1.000000000000000000, 0.9659258262890683122, 1.000000000000000000, 0.9659258262890683122, 1.000000000000000000, 0.9659258262890683122, 1.000000000000000000, 0.9659258262890683122, 1.000000000000000000, 0.9659258262890683122, 1.000000000000000000, 0.9659258262890683122, 1.000000000000000000, 0.9659258262890683122, 1.000000000000000000, 0.9659258262890683122, 1.000000000000000000, 0.9659258262890683122, 1.000000000000000000, 0.9659258262890683122, 1.000000000000000000, 0.9659258262890683122, 1.000000000000000000, 0.9659258262890683122, 1.000000000000000000, 0.9659258262890683122, 1.000000000000000000, 0.9659258262890683122, 1.000000000000000000, 0.9659258262890683122, 1.000000000000000000, 0.9659258262890683122, 1.000000000000000000, 0.9659258262890683122, 1.000000000000000000, 0.9659258262890683122, 1.000000000000000000, 0.9659258262890683122, 1.000000000000000000, 0.9659258262890683122, 1.000000000000000000, 0.9659258262890683122, 1.000000000000000000, 0.9659258262890683122, 1.000000000000000000, 0.9659258262890683122, 1.000000000000000000, 0.9659258262890683122, 1.000000000000000000, 0.9659258262890683122, 1.000000000000000000, 0.9659258262890683122, 1.000000000000000000, 0.9659258262890683122, 1.000000000000000000, 0.9659258262890683122, 1.000000000000000000, 0.9659258262890683122, 1.000000000000000000, 0.9659258262890683122, 1.000000000000000000, 0.9659258262890683122, 1.000000000000000000, 0.9659258262890683122, 1.000000000000000000, 0.9659258262890683122, 1.000000000000000000, 0.9659258262890683122, 1.000000000000000000, 0.9659258262890683122, 1.000000000000000000, 0.9659258262890683122, 1.000000000000000000, 0.9659258262890683122, 1.000000000000000000, 0.9659258262890683122, 1.000000000000000000, 0.9659258262890683122, 1.000000000000000000, 0.9659258262890683122, 1.000000000000000000, 0.9659258262890683122, 1.000000000000000000, 0.9659258262890683122, 1.000000000000000000, 0.9659258262890683122, 1.000000000000000000, 0.9659258262890683122, 1.000000000000000000, 0.9659258262890683122, 1.000000000000000000, 0.9659258262890683122, 1.000000000000000000, 0.9659258262890683122, 1.000000000000000000, 0.9659258262890683122, 1.000000000000000000, 0.9659258262890683122, 1.000000000000000000, 0.9659258262890683122, 1.000000000000000000, 0.9659258262890683122, 1.000000000000000000, 0.9659258262890683122, 1.000000000000000000, 0.9659258262890683122, 1.000000000000000000, 0.9659258262890683122, 1.000000000000000000, 0.9659258262890683122, 1.000000000000000000, 0.9659258262890683122, 1.000000000000000000, 0.9659258262890683122, 1.000000000000000000, 0.9659258262890683122, 1.000000000000000000, 0.9659258262890683122, 1.000000000000000000, 0.9659258262890683122, 1.000000000000000000, 0.9659258262890683122, 1.000000000000000000, 0.9659258262890683122, 1.000000000000000000, 0.9659258262890683122, 1.000000000000000000, 0.9659258262890683122, 1.000000000000000000, 0.9659258262890683122, 1.000000000000000000, 0.9659258262890683122, 1.000000000000000000, 0.9659258262890683122, 1.000000000000000000, 0.9659258262890683122, 1.000000000000000000, 0.9659258262890683122, 1.000000000000000000, 0.9659258262890683122, 1.000000000000000000, 0.9659258262890683122, 1.000000000000000000, 0.9659258262890683122, 1.000000000000000000, 0.9659258262890683122, 1.000000000000000000, 0.9659258262890683122, 1.000000000000000000, 0.9659258262890683122, 1.000000000000000000, 0.9659258262890683122, 1.000000000000000000, 0.9659258262890683122, 1.000000000000000000, 0.9659258262890683122, 1.000000000000000000, 0.9659258262890683122, 1.000000000000000000, 0.9659258262890683122, 1.000000000000000000, 0.9659258262890683122, 1.000000000000000000, 0.9659258262890683122, 1.000000000000000000, 0.9659258262890683122, 1.000000000000000000, 0.9659258262890683122, 1.000000000000000000, 0.9659258262890683122, 1.000000000000000000, 0.9659258262890683122, 1.000000000000000000, 0.9659258262890683122, 1.000000000000000000, 0.9659258262890683122, 1.000000000000000000, 0.9659258262890683122, 1.000000000000000000, 0.9659258262890683122, 1.000000000000000000, 0.9659258262890683122, 1.000000000000000000, 0.9659258262890683122, 1.000000000000000000, 0.9659258262890683122, 1.000000000000000000, 0.9659258262890683122, 1.000000000000000000, 0.9659258262890683122, 1.000000000000000000, 0.9659258262890683122, 1.000000000000000000, 0.9659258262890683122, 1.000000000000000000, 0.9659258262890683122, 1.000000000000000000, 0.9659258262890683122, 1.000000000000000000, 0.9659258262890683122, 1.000000000000000000, 0.9659258262890683122, 1.000000000000000000, 0.9659258262890683122, 1.000000000000000000, 0.9659258262890683122, 1.000000000000000000, 0.9659258262890683122, 1.000000000000000000, 0.9659258262890683122, 1.000000000000000000, 0.9659258262890683122, 1.000000000000000000, 0.9659258262890683122, 1.000000000000000000, 0.9659258262890683122, 1.000000000000000000, 0.9659258262890683122, 1.000000000000000000, 0.9659258262890683122, 1.000000000000000000, 0.9659258262890683122, 1.000000000000000000, 0.9659258262890683122, 1.000000000000000000, 0.9659258262890683122, 1.000000000000000000, 0.9659258262890683122, 1.000000000000000000, 0.9659258262890683122, 1.000000000000000000, 0.9659258262890683122, 1.000000000000000000, 0.9659258262890683122, 1.000000000000000000, 0.9659258262890683122, 1.000000000000000000, 0.9659258262890683122, 1.000000000000000000, 0.9659258262890683122, 1.000000000000000000, 0.9659258262890683122, 1.000000000000000000, 0.9659258262890683122, 1.000000000000000000, 0.9659258262890683122, 1.000000000000000000, 0.9659258262890683122, 1.000000000000000000, 0.9659258262890683122, 1.000000000000000000, 0.9659258262890683122, 1.000000000000000000, 0.9659258262890683122, 1.000000000000000000, 0.9659258262890683122, 1.000000000000000000, 0.9659258262890683122, 1.000000000000000000, 0.9659258262890683122, 1.000000000000000000, 0.9659258262890683122, 1.000000000000000000, 0.9659258262890683122, 1.000000000000000000, 0.9659258262890683122, 1.000000000000000000, 0.9659258262890683122, 1.000000000000000000, 0.9659258262890683122, 1.000000000000000000, 0.9659258262890683122, 1.000000000000000000, 0.9659258262890683122, 1.000000000000000000, 0.9659258262890683122, 1.000000000000000000) ) ) 
 REPRESENTATION_ITEM ( '' )  SURFACE ( )  );
#131407 = CARTESIAN_POINT ( 'NONE',  ( -9.474510206698964154, 16.51473224551069663, 100.4155762719810241 ) ) ;
#131408 = CARTESIAN_POINT ( 'NONE',  ( -19.03943276465977164, 0.05219959533909376836, 96.24890960531436690 ) ) ;
#131409 = CARTESIAN_POINT ( 'NONE',  ( 16.53943276465976808, -0.05219959533910856209, 108.7489096053143669 ) ) ;
#131410 = CARTESIAN_POINT ( 'NONE',  ( -12.06949235617756955, 12.14591786802309770, 45.62390960531436690 ) ) ;
#131411 = CARTESIAN_POINT ( 'NONE',  ( 14.29746914071037800, 8.314922557961029526, 46.66775706135234714 ) ) ;
#131412 = CARTESIAN_POINT ( 'NONE',  ( 5.049401038298161559, -19.05341960407611168, 22.70724293864769194 ) ) ;
#131413 = CARTESIAN_POINT ( 'NONE',  ( 5.823673210054444382, -21.52544592524334988, 100.2094237280190043 ) ) ;
#131415 = CARTESIAN_POINT ( 'NONE',  ( -8.224510206698735004, -14.34966873604973081, 109.5844237280190328 ) ) ;
#131414 = CARTESIAN_POINT ( 'NONE',  ( 19.02544592524343514, -5.153800228976328945, 108.5405762719810383 ) ) ;
#131416 = CARTESIAN_POINT ( 'NONE',  ( -0.05219959533937732626, 21.53943276465977519, 32.50109039468568284 ) ) ;
#131417 = CARTESIAN_POINT ( 'NONE',  ( -9.564922557960796823, -16.46253265017161027, 107.0822429386476955 ) ) ;
#131418 = CARTESIAN_POINT ( 'NONE',  ( 8.314922557961029526, -14.29746914071037800, 40.41775706135234714 ) ) ;
#131419 = CARTESIAN_POINT ( 'NONE',  ( 8.314922557961029526, -14.29746914071037800, 110.4177570613523756 ) ) ;
#131420 = CARTESIAN_POINT ( 'NONE',  ( 12.06949235617739724, 12.14591786802326823, 86.87609039468568994 ) ) ;
#131421 = CARTESIAN_POINT ( 'NONE',  ( 8.314922557961029526, -14.29746914071037800, 30.41775706135234358 ) ) ;
#131422 = EDGE_CURVE ( 'NONE', #90572, #185765, #46278, .T. ) ;
#131423 = CARTESIAN_POINT ( 'NONE',  ( 16.46253265017160672, -9.564922557960803928, 53.33224293864768839 ) ) ;
#131424 = CARTESIAN_POINT ( 'NONE',  ( 0.05219959533910956823, 16.53943276465976808, 109.9989096053143527 ) ) ;
#131425 = CARTESIAN_POINT ( 'NONE',  ( -18.67979575497178146, -10.72451020669898902, 111.6655762719810525 ) ) ;
#131426 = CARTESIAN_POINT ( 'NONE',  ( 5.049401038298161559, -19.05341960407611168, 27.70724293864769550 ) ) ;
#131427 = CARTESIAN_POINT ( 'NONE',  ( -19.05341960407611168, -5.049401038298163336, 101.4572429386476955 ) ) ;
#131428 = CARTESIAN_POINT ( 'NONE',  ( 16.46253265017160672, -9.564922557960803928, 38.33224293864768839 ) ) ;
#131429 = CARTESIAN_POINT ( 'NONE',  ( -16.46253265017160317, 9.564922557960807481, 105.8322429386476955 ) ) ;
#131430 = CARTESIAN_POINT ( 'NONE',  ( -17.50000000000000711, -5.624438216177558125, 34.18329655085356933 ) ) ;
#131431 = CARTESIAN_POINT ( 'NONE',  ( -19.02544592524342804, 5.153800228976336051, 96.04057627198103830 ) ) ;
#131433 = CARTESIAN_POINT ( 'NONE',  ( 12.14591786802309770, 12.06949235617756955, 94.37390960531436690 ) ) ;
#131432 = CARTESIAN_POINT ( 'NONE',  ( -0.05219959533937732626, 21.53943276465977519, 42.50109039468567573 ) ) ;
#131434 = CARTESIAN_POINT ( 'NONE',  ( -16.46253265017160317, 9.564922557960807481, 110.8322429386476955 ) ) ;
#131435 = CARTESIAN_POINT ( 'NONE',  ( 18.22780087662122384, -5.500000000000022204, 96.01540105326108687 ) ) ;
#131436 = CARTESIAN_POINT ( 'NONE',  ( 14.34966873604972726, -8.224510206698740333, 60.83442372801901854 ) ) ;
#131437 = CARTESIAN_POINT ( 'NONE',  ( -0.05219959533937732626, 21.53943276465977519, 72.50109039468568994 ) ) ;
#131438 = CARTESIAN_POINT ( 'NONE',  ( 16.55341960407618274, -4.379528057220086978, 41.04275706135236135 ) ) ;
#131439 = CARTESIAN_POINT ( 'NONE',  ( -16.46253265017160317, 9.564922557960807481, 75.83224293864769550 ) ) ;
#131440 = CARTESIAN_POINT ( 'NONE',  ( -19.02544592524334988, -5.153800228976617603, 108.9594237280189759 ) ) ;
#131441 = CARTESIAN_POINT ( 'NONE',  ( -12.06949235617739369, -12.14591786802326823, 89.37609039468568994 ) ) ;
#131442 = CARTESIAN_POINT ( 'NONE',  ( -13.89961937509957401, -13.97604488694547875, 89.37609039468563310 ) ) ;
#131443 = CARTESIAN_POINT ( 'NONE',  ( 16.46253265017160672, -9.564922557960803928, 58.33224293864769550 ) ) ;
#131444 = CARTESIAN_POINT ( 'NONE',  ( 10.81492255796078972, 18.62759615963270932, 94.58224293864769550 ) ) ;
#131446 = CARTESIAN_POINT ( 'NONE',  ( 16.46253265017146816, 9.564922557961045513, 91.66775706135234714 ) ) ;
#131445 = CARTESIAN_POINT ( 'NONE',  ( 8.314922557960818139, 14.29746914071049879, 94.58224293864769550 ) ) ;
#131447 = CARTESIAN_POINT ( 'NONE',  ( 0.05219959533934541429, -16.53943276465976808, 60.00109039468568284 ) ) ;
#131448 = CARTESIAN_POINT ( 'NONE',  ( 24.81886791266634162, 6.075537473402705224, 168.3989613422507432 ) ) ;
#131449 = CARTESIAN_POINT ( 'NONE',  ( -19.05341960407617563, 5.049401038297882671, 73.54275706135233293 ) ) ;
#131450 = CARTESIAN_POINT ( 'NONE',  ( -16.55341960407611168, -4.379528057220339221, 36.45724293864768839 ) ) ;
#131451 = CARTESIAN_POINT ( 'NONE',  ( 14.29746914071049879, -8.314922557960816363, 78.33224293864770971 ) ) ;
#131453 = CARTESIAN_POINT ( 'NONE',  ( -17.44270441346522560, 5.991230190322816895, 38.63664920735773478 ) ) ;
#131452 = CARTESIAN_POINT ( 'NONE',  ( -13.97604488694547697, 13.89961937509957934, 23.12609039468565442 ) ) ;
#131454 = CARTESIAN_POINT ( 'NONE',  ( -15.72974639402176322, -15.80617190586768395, 19.37609039468568639 ) ) ;
#131455 = CARTESIAN_POINT ( 'NONE',  ( 5.153800228976335163, 19.02544592524342804, 114.7905762719810241 ) ) ;
#131456 = CARTESIAN_POINT ( 'NONE',  ( -16.51473224551069308, -9.474510206698971260, 81.66557627198103830 ) ) ;
#131457 = CARTESIAN_POINT ( 'NONE',  ( -10.81492255796105439, 18.62759615963255655, 97.91775706135236135 ) ) ;
#131458 = CARTESIAN_POINT ( 'NONE',  ( -19.02544592524342804, 5.153800228976336051, 81.04057627198103830 ) ) ;
#131459 = CARTESIAN_POINT ( 'NONE',  ( 0.05219959533907565091, 21.53943276465977519, 39.99890960531436690 ) ) ;
#131460 = CARTESIAN_POINT ( 'NONE',  ( 14.34966873604960469, 8.224510206698951720, 79.16557627198103830 ) ) ;
#131461 = CARTESIAN_POINT ( 'NONE',  ( 0.05219959533909260263, 19.03943276465977164, 54.99890960531435979 ) ) ;
#131462 = CARTESIAN_POINT ( 'NONE',  ( -4.483927247898539470, -16.52544592524342804, 112.2905762719810241 ) ) ;
#131463 = VECTOR ( 'NONE', #49543, 1000.000000000000000 ) ;
#131464 = CARTESIAN_POINT ( 'NONE',  ( -5.823673210054431948, 21.52544592524334988, 27.70942372801901854 ) ) ;
#131465 = CARTESIAN_POINT ( 'NONE',  ( -0.05219959533937732626, 21.53943276465977519, 67.50109039468568994 ) ) ;
#131466 = CARTESIAN_POINT ( 'NONE',  ( -19.02544592524342804, 5.153800228976336051, 46.04057627198101699 ) ) ;
#131467 = CARTESIAN_POINT ( 'NONE',  ( 16.53943276465976808, 0.05219959533934440121, 71.25109039468568994 ) ) ;
#131468 = CARTESIAN_POINT ( 'NONE',  ( -18.62759615963270932, 10.81492255796079327, 110.8322429386476955 ) ) ;
#131469 = CARTESIAN_POINT ( 'NONE',  ( 5.719274019375991003, -21.55341960407610458, 112.7072429386476955 ) ) ;
#131471 = CARTESIAN_POINT ( 'NONE',  ( 0.05219959533909260263, 19.03943276465977164, 59.99890960531436690 ) ) ;
#131470 = CARTESIAN_POINT ( 'NONE',  ( -16.46253265017146816, -9.564922557961047289, 44.16775706135232582 ) ) ;
#131472 = CARTESIAN_POINT ( 'NONE',  ( 19.03943276465977164, 0.05219959533936151252, 31.25109039468566863 ) ) ;
#131473 = CARTESIAN_POINT ( 'NONE',  ( -18.67979575497193778, 10.72451020669871902, 68.33442372801900433 ) ) ;
#131474 = CARTESIAN_POINT ( 'NONE',  ( 15.72974639402199770, -15.80617190586745480, 68.12390960531436690 ) ) ;
#131475 = CARTESIAN_POINT ( 'NONE',  ( 4.379528057220339221, -16.55341960407611168, 32.70724293864770260 ) ) ;
#131477 = CARTESIAN_POINT ( 'NONE',  ( -10.81492255796105439, 18.62759615963255655, 107.9177570613523471 ) ) ;
#131476 = CARTESIAN_POINT ( 'NONE',  ( 0.05219959533937995610, -21.53943276465977519, 85.00109039468568994 ) ) ;
#131478 = CARTESIAN_POINT ( 'NONE',  ( 4.483927247898545687, 16.52544592524342804, 54.79057627198104541 ) ) ;
#131479 = CARTESIAN_POINT ( 'NONE',  ( -0.05219959533910754901, -16.53943276465976808, 102.4989096053143811 ) ) ;
#131480 = CARTESIAN_POINT ( 'NONE',  ( -5.049401038297874678, -19.05341960407617918, 54.79275706135234003 ) ) ;
#131481 = CARTESIAN_POINT ( 'NONE',  ( 8.224510206698953496, -14.34966873604960469, 22.91557627198102765 ) ) ;
#131482 = CARTESIAN_POINT ( 'NONE',  ( -10.81492255796105439, 18.62759615963255655, 62.91775706135236135 ) ) ;
#131483 = CARTESIAN_POINT ( 'NONE',  ( 16.46253265017160672, -9.564922557960803928, 73.33224293864769550 ) ) ;
#131484 = CARTESIAN_POINT ( 'NONE',  ( -19.03943276465977164, -0.05219959533935918106, 33.75109039468566863 ) ) ;
#131485 = CARTESIAN_POINT ( 'NONE',  ( 21.52544592524344225, -5.823673210054117533, 53.54057627198103120 ) ) ;
#131486 = CARTESIAN_POINT ( 'NONE',  ( 10.81492255796106328, -18.62759615963255655, 40.41775706135234714 ) ) ;
#131487 = CARTESIAN_POINT ( 'NONE',  ( 21.52544592524344225, -5.823673210054117533, 98.54057627198105251 ) ) ;
#131488 = CARTESIAN_POINT ( 'NONE',  ( 0.05219959533936267826, -19.03943276465977164, 95.00109039468567573 ) ) ;
#131489 = CARTESIAN_POINT ( 'NONE',  ( -14.29746914071037622, -8.314922557961029526, 69.16775706135234714 ) ) ;
#131491 = CARTESIAN_POINT ( 'NONE',  ( 5.823673210054125526, 21.52544592524343514, 99.79057627198103830 ) ) ;
#131490 = CARTESIAN_POINT ( 'NONE',  ( -15.60300394477387265, -17.53633401217249954, -57.38906433430459231 ) ) ;
#131492 = CARTESIAN_POINT ( 'NONE',  ( -14.34966873604960291, -8.224510206698953496, 86.66557627198102409 ) ) ;
#131493 = CARTESIAN_POINT ( 'NONE',  ( -27.77250826529492755, -25.57832283906995130, -20.68473525701014992 ) ) ;
#131494 = CARTESIAN_POINT ( 'NONE',  ( -16.55341960407617563, 4.379528057220093196, 28.54275706135234358 ) ) ;
#131495 = CARTESIAN_POINT ( 'NONE',  ( 18.62759615963271287, -10.81492255796078972, 48.33224293864770260 ) ) ;
#131496 = CARTESIAN_POINT ( 'NONE',  ( -14.29746914071037622, -8.314922557961029526, 94.16775706135237556 ) ) ;
#131497 = CARTESIAN_POINT ( 'NONE',  ( -16.51473224551069308, -9.474510206698971260, 21.66557627198102765 ) ) ;
#131498 = CARTESIAN_POINT ( 'NONE',  ( 12.06949235617739724, 12.14591786802326823, 56.87609039468568994 ) ) ;
#131499 = CARTESIAN_POINT ( 'NONE',  ( -15.80617190586768217, 15.72974639402176855, 28.12609039468568284 ) ) ;
#131500 = CARTESIAN_POINT ( 'NONE',  ( 5.719274019375991003, -21.55341960407610458, 47.70724293864770260 ) ) ;
#131501 = CARTESIAN_POINT ( 'NONE',  ( 4.483927247898790824, -16.52544592524335698, 85.20942372801901854 ) ) ;
#131502 = CARTESIAN_POINT ( 'NONE',  ( 13.89961937509977652, -13.97604488694527269, 98.12390960531433848 ) ) ;
#131503 = CARTESIAN_POINT ( 'NONE',  ( -10.81492255796105439, 18.62759615963255655, 72.91775706135234714 ) ) ;
#131504 = CARTESIAN_POINT ( 'NONE',  ( 5.823673210054125526, 21.52544592524343514, 44.79057627198103120 ) ) ;
#131505 = CARTESIAN_POINT ( 'NONE',  ( -15.72974639402197994, 15.80617190586746368, 25.62390960531435624 ) ) ;
#131506 = VERTEX_POINT ( 'NONE', #121123 ) ;
#131507 = CARTESIAN_POINT ( 'NONE',  ( 13.89961937509957401, 13.97604488694547697, 56.87609039468564731 ) ) ;
#131508 = CARTESIAN_POINT ( 'NONE',  ( -16.52544592524335698, -4.483927247898792601, 63.95942372801901854 ) ) ;
#131509 = CARTESIAN_POINT ( 'NONE',  ( -5.719274019375978568, 21.55341960407610458, 35.20724293864768839 ) ) ;
#131510 = ORIENTED_EDGE ( 'NONE', *, *, #199827, .T. ) ;
#131511 = EDGE_CURVE ( 'NONE', #159561, #168063, #106491, .T. ) ;
#131512 = CARTESIAN_POINT ( 'NONE',  ( -19.02544592524342804, 5.153800228976336051, 86.04057627198103830 ) ) ;
#131513 = CARTESIAN_POINT ( 'NONE',  ( -12.14591786802309592, -12.06949235617757132, 21.87390960531436690 ) ) ;
#131514 = CARTESIAN_POINT ( 'NONE',  ( -17.72560187377287022, -5.499999999999976019, 79.07814504131323474 ) ) ;
#131515 = CARTESIAN_POINT ( 'NONE',  ( 0.05219959533910956823, 16.53943276465976808, 104.9989096053143669 ) ) ;
#131516 = CARTESIAN_POINT ( 'NONE',  ( -10.81492255796078084, -18.62759615963271287, 42.08224293864769550 ) ) ;
#131517 = CARTESIAN_POINT ( 'NONE',  ( -13.89961937509977652, 13.97604488694528158, 50.62390960531435979 ) ) ;
#131518 = CARTESIAN_POINT ( 'NONE',  ( -12.14591786802326823, 12.06949235617739902, 78.12609039468570415 ) ) ;
#131519 = CARTESIAN_POINT ( 'NONE',  ( -0.05219959533937732626, 21.53943276465977519, 27.50109039468567929 ) ) ;
#131520 = CARTESIAN_POINT ( 'NONE',  ( 16.46253265017146816, 9.564922557961045513, 86.66775706135233293 ) ) ;
#131521 = CARTESIAN_POINT ( 'NONE',  ( 8.224510206698953496, -14.34966873604960469, 87.91557627198103830 ) ) ;
#131522 = CARTESIAN_POINT ( 'NONE',  ( 19.03943276465977164, -0.05219959533909143690, 58.74890960531435979 ) ) ;
#131523 = AXIS2_PLACEMENT_3D ( 'NONE', #48868, #199571, #15549 ) ;
#131524 = CARTESIAN_POINT ( 'NONE',  ( 5.049401038298161559, -19.05341960407611168, 27.70724293864769550 ) ) ;
#131525 = CARTESIAN_POINT ( 'NONE',  ( 21.52544592524334988, 5.823673210054432836, 101.4594237280190185 ) ) ;
#131526 = CARTESIAN_POINT ( 'NONE',  ( 16.46253265017160672, -9.564922557960803928, 83.33224293864768129 ) ) ;
#131527 = ADVANCED_FACE ( 'NONE', ( #198974 ), #138289, .F. ) ;
#131528 = CARTESIAN_POINT ( 'NONE',  ( -14.29746914071037622, -8.314922557961029526, 69.16775706135234714 ) ) ;
#131529 = CARTESIAN_POINT ( 'NONE',  ( -21.52544592524334988, -5.823673210054445271, 93.95942372801903275 ) ) ;
#131530 = CARTESIAN_POINT ( 'NONE',  ( -10.72451020669898014, 18.67979575497178502, 45.41557627198103830 ) ) ;
#131531 = CARTESIAN_POINT ( 'NONE',  ( -8.224510206698735004, -14.34966873604973081, 79.58442372801903275 ) ) ;
#131532 = CARTESIAN_POINT ( 'NONE',  ( 5.049401038297881783, 19.05341960407617563, 47.29275706135231161 ) ) ;
#131533 = CARTESIAN_POINT ( 'NONE',  ( 13.97604488694548053, -13.89961937509957401, 60.62609039468564731 ) ) ;
#131534 = ORIENTED_EDGE ( 'NONE', *, *, #27507, .F. ) ;
#131535 = CARTESIAN_POINT ( 'NONE',  ( -0.05219959533937732626, 21.53943276465977519, 67.50109039468568994 ) ) ;
#131536 = CARTESIAN_POINT ( 'NONE',  ( -9.564922557960796823, -16.46253265017161027, 62.08224293864769550 ) ) ;
#131537 = CARTESIAN_POINT ( 'NONE',  ( -18.22780087662123805, 5.499999999999981348, 91.01763182126894947 ) ) ;
#131538 = CARTESIAN_POINT ( 'NONE',  ( -13.97604488694547697, 13.89961937509957934, 63.12609039468566152 ) ) ;
#131539 = DIRECTION ( 'NONE',  ( 0.000000000000000000, 0.000000000000000000, -1.000000000000000000 ) ) ;
#131540 = CARTESIAN_POINT ( 'NONE',  ( -16.46253265017160317, 9.564922557960807481, 90.83224293864769550 ) ) ;
#131541 = CARTESIAN_POINT ( 'NONE',  ( -12.14591786802309592, -12.06949235617757132, 46.87390960531435979 ) ) ;
#131542 = CARTESIAN_POINT ( 'NONE',  ( 21.55341960407610458, 5.719274019375980345, 48.95724293864770971 ) ) ;
#131543 = DIRECTION ( 'NONE',  ( 0.000000000000000000, 0.000000000000000000, -1.000000000000000000 ) ) ;
#131544 = CARTESIAN_POINT ( 'NONE',  ( 21.53943276465977519, 0.05219959533937863772, 111.2510903946856899 ) ) ;
#131545 = CARTESIAN_POINT ( 'NONE',  ( -17.50000000000001421, -5.622605283950846911, 81.31207310596113302 ) ) ;
#131546 = CARTESIAN_POINT ( 'NONE',  ( -9.474510206698964154, 16.51473224551069663, 55.41557627198103120 ) ) ;
#131547 = CARTESIAN_POINT ( 'NONE',  ( 16.46253265017160672, -9.564922557960803928, 28.33224293864769550 ) ) ;
#131548 = CARTESIAN_POINT ( 'NONE',  ( -9.248023074035629065, -10.74802307403544077, -60.25555373585994090 ) ) ;
#131549 = CARTESIAN_POINT ( 'NONE',  ( -11.74149087413294623, -36.13659316521243881, -1.602157773949822950 ) ) ;
#131550 = CARTESIAN_POINT ( 'NONE',  ( -12.14591786802326823, 12.06949235617739902, 68.12609039468567573 ) ) ;
#131551 = CARTESIAN_POINT ( 'NONE',  ( -21.53943276465977519, 0.05219959533907696930, 86.24890960531436690 ) ) ;
#131552 = CARTESIAN_POINT ( 'NONE',  ( 4.483927247898545687, 16.52544592524342804, 59.79057627198103120 ) ) ;
#131554 = CARTESIAN_POINT ( 'NONE',  ( -19.02544592524342804, 5.153800228976336051, 116.0405762719810383 ) ) ;
#131553 = CARTESIAN_POINT ( 'NONE',  ( -13.89961937509977652, 13.97604488694528158, 45.62390960531433848 ) ) ;
#131555 = CARTESIAN_POINT ( 'NONE',  ( -5.719274019375665041, -21.55341960407619695, 34.79275706135235424 ) ) ;
#131556 = CARTESIAN_POINT ( 'NONE',  ( -9.474510206698720793, -16.51473224551083518, 54.58442372801899722 ) ) ;
#131557 = CARTESIAN_POINT ( 'NONE',  ( -0.05219959533909027116, -19.03943276465977164, 37.49890960531436690 ) ) ;
#131558 = CARTESIAN_POINT ( 'NONE',  ( -21.55341960407619339, 5.719274019375674811, 93.54275706135234714 ) ) ;
#131559 = CARTESIAN_POINT ( 'NONE',  ( -23.84755066337005758, -5.771293611162919390, 171.0999092862842303 ) ) ;
#131560 = ORIENTED_EDGE ( 'NONE', *, *, #67045, .F. ) ;
#131561 = CARTESIAN_POINT ( 'NONE',  ( 12.14591786802309770, 12.06949235617756955, 44.37390960531435979 ) ) ;
#131562 = CARTESIAN_POINT ( 'NONE',  ( -14.30620887846971279, 1.220661533321985903, -60.18359034246770989 ) ) ;
#131563 = CARTESIAN_POINT ( 'NONE',  ( -5.823673210054116645, -21.52544592524344225, 42.29057627198103120 ) ) ;
#131564 = FACE_OUTER_BOUND ( 'NONE', #96641, .T. ) ;
#131565 = CARTESIAN_POINT ( 'NONE',  ( -19.02544592524342804, 5.153800228976336051, 91.04057627198100988 ) ) ;
#131566 = CARTESIAN_POINT ( 'NONE',  ( -4.379528057220328563, 16.55341960407611168, 85.20724293864770971 ) ) ;
#131567 = CARTESIAN_POINT ( 'NONE',  ( 14.29746914071037800, 8.314922557961029526, 21.66775706135235069 ) ) ;
#131568 = CARTESIAN_POINT ( 'NONE',  ( 14.29746914071037800, 8.314922557961029526, 111.6677570613523613 ) ) ;
#131569 = VERTEX_POINT ( 'NONE', #122116 ) ;
#131570 = CARTESIAN_POINT ( 'NONE',  ( 16.51473224551069308, 9.474510206698969483, 44.16557627198103120 ) ) ;
#131572 = CARTESIAN_POINT ( 'NONE',  ( -10.72451020669898014, 18.67979575497178502, 85.41557627198102409 ) ) ;
#131571 = CARTESIAN_POINT ( 'NONE',  ( -19.03943276465977164, 0.05219959533909376836, 91.24890960531436690 ) ) ;
#131574 = CARTESIAN_POINT ( 'NONE',  ( 9.564922557960805705, 16.46253265017160317, 99.58224293864770971 ) ) ;
#131573 = CARTESIAN_POINT ( 'NONE',  ( -12.14591786802309592, -12.06949235617757132, 31.87390960531435979 ) ) ;
#131575 = CARTESIAN_POINT ( 'NONE',  ( -5.049401038297874678, -19.05341960407617918, 74.79275706135231871 ) ) ;
#131576 = CARTESIAN_POINT ( 'NONE',  ( -21.53943276465977519, -0.05219959533937600094, 103.7510903946857042 ) ) ;
#131577 = CARTESIAN_POINT ( 'NONE',  ( -15.72974639402197994, 15.80617190586746368, 95.62390960531436690 ) ) ;
#131578 = CARTESIAN_POINT ( 'NONE',  ( -0.05219959533907301413, -21.53943276465977519, 37.49890960531436690 ) ) ;
#131579 = CARTESIAN_POINT ( 'NONE',  ( -5.153800228976328057, -19.02544592524343514, 67.29057627198102409 ) ) ;
#131580 = CARTESIAN_POINT ( 'NONE',  ( -14.29746914071037622, -8.314922557961029526, 109.1677570613523613 ) ) ;
#131581 = CARTESIAN_POINT ( 'NONE',  ( -16.51473224551069308, -9.474510206698971260, 71.66557627198102409 ) ) ;
#131582 = EDGE_LOOP ( 'NONE', ( #68840, #67801 ) ) ;
#131583 = CARTESIAN_POINT ( 'NONE',  ( -193.3062444957834884, -155.7167183371838064, -15.00000000000000000 ) ) ;
#131584 = CARTESIAN_POINT ( 'NONE',  ( -9.564922557961040184, 16.46253265017147172, 22.91775706135233648 ) ) ;
#131585 = CARTESIAN_POINT ( 'NONE',  ( -14.29746914071049879, 8.314922557960819915, 85.83224293864768129 ) ) ;
#131586 = CARTESIAN_POINT ( 'NONE',  ( 10.72451020669871369, 18.67979575497193778, 22.08442372801901143 ) ) ;
#131587 = CARTESIAN_POINT ( 'NONE',  ( -5.359611314223446995E-15, 29.16686587814335496, 146.8750000027311273 ) ) ;
#131588 = CARTESIAN_POINT ( 'NONE',  ( 21.53943276465977519, -0.05219959533907433946, 68.74890960531435269 ) ) ;
#131589 = CARTESIAN_POINT ( 'NONE',  ( 4.379528057220092307, 16.55341960407617563, 97.29275706135234714 ) ) ;
#131590 = CARTESIAN_POINT ( 'NONE',  ( 19.02544592524343514, -5.153800228976328945, 23.54057627198102054 ) ) ;
#131591 = CARTESIAN_POINT ( 'NONE',  ( -0.05219959533909027116, -19.03943276465977164, 72.49890960531435269 ) ) ;
#131592 = CARTESIAN_POINT ( 'NONE',  ( 37.99999999999999289, 2.893978650043524126E-14, -10.74999999453762811 ) ) ;
#131593 = CARTESIAN_POINT ( 'NONE',  ( -16.55341960407611168, -4.379528057220339221, 36.45724293864768839 ) ) ;
#131594 = CARTESIAN_POINT ( 'NONE',  ( 18.62759615963255655, 10.81492255796105972, 66.66775706135234714 ) ) ;
#131595 = CARTESIAN_POINT ( 'NONE',  ( -13.97604488694527625, -13.89961937509977652, 106.8739096053143669 ) ) ;
#131596 = CARTESIAN_POINT ( 'NONE',  ( 10.81492255796106328, -18.62759615963255655, 90.41775706135236135 ) ) ;
#131597 = CARTESIAN_POINT ( 'NONE',  ( -19.02544592524342804, 5.153800228976336051, 41.04057627198103120 ) ) ;
#131598 = CARTESIAN_POINT ( 'NONE',  ( 16.46253265017160672, -9.564922557960803928, 48.33224293864769550 ) ) ;
#131599 = ORIENTED_EDGE ( 'NONE', *, *, #137500, .T. ) ;
#131600 = CARTESIAN_POINT ( 'NONE',  ( -21.52544592524334988, -5.823673210054445271, 98.95942372801903275 ) ) ;
#131601 = CARTESIAN_POINT ( 'NONE',  ( -0.05219959533934338120, 16.53943276465976808, 62.50109039468568284 ) ) ;
#131602 = CARTESIAN_POINT ( 'NONE',  ( -15.80617190586768217, 15.72974639402176855, 88.12609039468570415 ) ) ;
#131603 = CARTESIAN_POINT ( 'NONE',  ( -5.049401038298153566, 19.05341960407611168, 115.2072429386477097 ) ) ;
#131604 = CARTESIAN_POINT ( 'NONE',  ( 19.03943276465977164, 0.05219959533936151252, 91.25109039468566152 ) ) ;
#131605 = CARTESIAN_POINT ( 'NONE',  ( -21.52544592524334988, -5.823673210054445271, 58.95942372801902565 ) ) ;
#131606 = CARTESIAN_POINT ( 'NONE',  ( 0.05219959533934541429, -16.53943276465976808, 40.00109039468567573 ) ) ;
#131607 = CARTESIAN_POINT ( 'NONE',  ( -21.55341960407610458, -5.719274019375992779, 91.45724293864769550 ) ) ;
#131608 = CARTESIAN_POINT ( 'NONE',  ( 19.03943276465977164, 0.05219959533936151252, 86.25109039468567573 ) ) ;
#131609 = CARTESIAN_POINT ( 'NONE',  ( 0.05219959533909260263, 19.03943276465977164, 59.99890960531436690 ) ) ;
#131610 = CARTESIAN_POINT ( 'NONE',  ( -13.89961937509957401, -13.97604488694547875, 94.37609039468566152 ) ) ;
#131611 = CIRCLE ( 'NONE', #8944, 2.649999999999992806 ) ;
#131612 = CARTESIAN_POINT ( 'NONE',  ( -13.97604488694547697, 13.89961937509957934, 103.1260903946856473 ) ) ;
#131613 = CARTESIAN_POINT ( 'NONE',  ( -12.14591786802309592, -12.06949235617757132, 51.87390960531437401 ) ) ;
#131614 = CARTESIAN_POINT ( 'NONE',  ( -16.46253265017146816, -9.564922557961047289, 79.16775706135234714 ) ) ;
#131615 = CARTESIAN_POINT ( 'NONE',  ( 8.224510206698742110, 14.34966873604972548, 67.08442372801901854 ) ) ;
#131616 = CARTESIAN_POINT ( 'NONE',  ( -16.46253265017146816, -9.564922557961047289, 44.16775706135232582 ) ) ;
#131617 = CARTESIAN_POINT ( 'NONE',  ( -9.564922557960796823, -16.46253265017161027, 42.08224293864769550 ) ) ;
#131618 = CARTESIAN_POINT ( 'NONE',  ( -19.05341960407611168, -5.049401038298163336, 51.45724293864770260 ) ) ;
#131619 = CARTESIAN_POINT ( 'NONE',  ( 16.52544592524335698, 4.483927247898782831, 61.45942372801901854 ) ) ;
#131620 = DIRECTION ( 'NONE',  ( 0.000000000000000000, -0.7071067811865466846, 0.7071067811865484609 ) ) ;
#131621 = CARTESIAN_POINT ( 'NONE',  ( -8.906447517083053711, -27.41122689804191026, 140.6500000054623740 ) ) ;
#131622 = CARTESIAN_POINT ( 'NONE',  ( -5.049401038298153566, 19.05341960407611168, 105.2072429386476671 ) ) ;
#131623 = EDGE_CURVE ( 'NONE', #131044, #69189, #47565, .T. ) ;
#131624 = CARTESIAN_POINT ( 'NONE',  ( -9.564922557960796823, -16.46253265017161027, 22.08224293864768839 ) ) ;
#131625 = ORIENTED_EDGE ( 'NONE', *, *, #192484, .F. ) ;
#131626 = CARTESIAN_POINT ( 'NONE',  ( -19.05341960407617563, 5.049401038297882671, 98.54275706135233293 ) ) ;
#131627 = CARTESIAN_POINT ( 'NONE',  ( -18.67979575497178146, -10.72451020669898902, 36.66557627198103120 ) ) ;
#131629 = CARTESIAN_POINT ( 'NONE',  ( 8.224510206698742110, 14.34966873604972548, 22.08442372801901143 ) ) ;
#131628 = CARTESIAN_POINT ( 'NONE',  ( -13.97604488694547697, 13.89961937509957934, 28.12609039468565797 ) ) ;
#131630 = CARTESIAN_POINT ( 'NONE',  ( 19.02544592524343514, -5.153800228976328945, 33.54057627198102409 ) ) ;
#131631 = CARTESIAN_POINT ( 'NONE',  ( 5.153800228976335163, 19.02544592524342804, 44.79057627198103830 ) ) ;
#131632 = CARTESIAN_POINT ( 'NONE',  ( 5.823673210054125526, 21.52544592524343514, 69.79057627198102409 ) ) ;
#131633 = CARTESIAN_POINT ( 'NONE',  ( -19.05341960407611168, -5.049401038298163336, 101.4572429386476955 ) ) ;
#131634 = CARTESIAN_POINT ( 'NONE',  ( 16.51473224551069308, 9.474510206698969483, 34.16557627198102409 ) ) ;
#131635 = CARTESIAN_POINT ( 'NONE',  ( 27.73933785331498925, -9.013057229001034898, 142.2750000027311899 ) ) ;
#131636 = CARTESIAN_POINT ( 'NONE',  ( 0.05219959533936267826, -19.03943276465977164, 90.00109039468567573 ) ) ;
#131638 = VECTOR ( 'NONE', #199198, 1000.000000000000000 ) ;
#131637 = CARTESIAN_POINT ( 'NONE',  ( 4.379528057220339221, -16.55341960407611168, 52.70724293864769550 ) ) ;
#131639 = CARTESIAN_POINT ( 'NONE',  ( 10.72451020669898902, -18.67979575497178502, 42.91557627198103120 ) ) ;
#131640 = CARTESIAN_POINT ( 'NONE',  ( -5.823673210054431948, 21.52544592524334988, 107.7094237280190328 ) ) ;
#131641 = EDGE_CURVE ( 'NONE', #150038, #140047, #24508, .T. ) ;
#131642 = CARTESIAN_POINT ( 'NONE',  ( -18.62759615963270932, 10.81492255796079327, 95.83224293864770971 ) ) ;
#131643 = CARTESIAN_POINT ( 'NONE',  ( 21.53943276465977519, 0.05219959533937863772, 66.25109039468567573 ) ) ;
#131644 = CARTESIAN_POINT ( 'NONE',  ( -0.05219959533937732626, 21.53943276465977519, 72.50109039468568994 ) ) ;
#131645 = CARTESIAN_POINT ( 'NONE',  ( 9.474510206698971260, -16.51473224551069308, 112.9155762719810383 ) ) ;
#131647 = CARTESIAN_POINT ( 'NONE',  ( 21.52544592524334988, 5.823673210054432836, 66.45942372801903275 ) ) ;
#131646 = CARTESIAN_POINT ( 'NONE',  ( -16.55341960407617563, 4.379528057220093196, 108.5427570613523756 ) ) ;
#131648 = CARTESIAN_POINT ( 'NONE',  ( 9.474510206698971260, -16.51473224551069308, 62.91557627198102409 ) ) ;
#131649 = CARTESIAN_POINT ( 'NONE',  ( 13.89961937509957401, 13.97604488694547697, 31.87609039468566863 ) ) ;
#131650 = CARTESIAN_POINT ( 'NONE',  ( -15.72974639402176322, -15.80617190586768395, 29.37609039468568284 ) ) ;
#131651 = CARTESIAN_POINT ( 'NONE',  ( 19.05341960407611168, 5.049401038298154454, 68.95724293864769550 ) ) ;
#131652 = CARTESIAN_POINT ( 'NONE',  ( -4.379528057220328563, 16.55341960407611168, 85.20724293864770971 ) ) ;
#131653 = CARTESIAN_POINT ( 'NONE',  ( -14.34966873604960291, -8.224510206698953496, 41.66557627198103120 ) ) ;
#131654 = CARTESIAN_POINT ( 'NONE',  ( -18.67979575497178146, -10.72451020669898902, 56.66557627198103830 ) ) ;
#131655 = CARTESIAN_POINT ( 'NONE',  ( -0.05219959533909027116, -19.03943276465977164, 62.49890960531435979 ) ) ;
#131656 = CARTESIAN_POINT ( 'NONE',  ( -5.823673210054116645, -21.52544592524344225, 67.29057627198103830 ) ) ;
#131657 = CARTESIAN_POINT ( 'NONE',  ( 19.03943276465977164, 0.05219959533936151252, 66.25109039468567573 ) ) ;
#131659 = CARTESIAN_POINT ( 'NONE',  ( -0.05219959533910754901, -16.53943276465976808, 57.49890960531435979 ) ) ;
#131658 = CARTESIAN_POINT ( 'NONE',  ( 13.89961937509957579, 13.97604488694547520, 26.87609039468566507 ) ) ;
#131660 = CARTESIAN_POINT ( 'NONE',  ( -21.53943276465977519, 0.05219959533907696930, 36.24890960531435979 ) ) ;
#131661 = ORIENTED_EDGE ( 'NONE', *, *, #76859, .T. ) ;
#131662 = FACE_OUTER_BOUND ( 'NONE', #3002, .T. ) ;
#131664 = CARTESIAN_POINT ( 'NONE',  ( -27.73933785331498925, 2.428612866367529932E-14, 141.3750000027311842 ) ) ;
#131663 = CARTESIAN_POINT ( 'NONE',  ( 12.06949235617739724, 12.14591786802326823, 81.87609039468568994 ) ) ;
#131665 = CARTESIAN_POINT ( 'NONE',  ( -19.05341960407617563, 5.049401038297882671, 93.54275706135234714 ) ) ;
#131666 = CARTESIAN_POINT ( 'NONE',  ( -16.52544592524342804, 4.483927247898546575, 61.04057627198103120 ) ) ;
#131667 = CARTESIAN_POINT ( 'NONE',  ( 4.500000000000000888, -130.0000000000000000, 13.99999999999999822 ) ) ;
#131668 = CARTESIAN_POINT ( 'NONE',  ( -5.153800228976328057, -19.02544592524343514, 52.29057627198100988 ) ) ;
#131669 = CARTESIAN_POINT ( 'NONE',  ( 16.53943276465976808, -0.05219959533910856209, 43.74890960531435979 ) ) ;
#131670 = EDGE_CURVE ( 'NONE', #93910, #194492, #46561, .T. ) ;
#131671 = CARTESIAN_POINT ( 'NONE',  ( -9.564922557960796823, -16.46253265017161027, 87.08224293864769550 ) ) ;
#131672 = CARTESIAN_POINT ( 'NONE',  ( -13.97604488694527625, -13.89961937509977652, 46.87390960531435979 ) ) ;
#131673 = CARTESIAN_POINT ( 'NONE',  ( 10.72451020669871369, 18.67979575497193778, 62.08442372801901143 ) ) ;
#131674 = CARTESIAN_POINT ( 'NONE',  ( -19.03943276465977164, 0.05219959533909376836, 66.24890960531436690 ) ) ;
#131675 = CARTESIAN_POINT ( 'NONE',  ( -19.03943276465977164, 0.05219959533909376836, 21.24890960531436335 ) ) ;
#131676 = CARTESIAN_POINT ( 'NONE',  ( 19.02544592524343514, -5.153800228976328945, 78.54057627198099567 ) ) ;
#131677 = CARTESIAN_POINT ( 'NONE',  ( -5.823673210054116645, -21.52544592524344225, 47.29057627198103120 ) ) ;
#131678 = CARTESIAN_POINT ( 'NONE',  ( -13.97604488694527625, -13.89961937509977652, 51.87390960531436690 ) ) ;
#131679 = CARTESIAN_POINT ( 'NONE',  ( 21.55341960407610458, 5.719274019375980345, 58.95724293864770971 ) ) ;
#131680 = CARTESIAN_POINT ( 'NONE',  ( -19.05341960407617563, 5.049401038297882671, 78.54275706135233293 ) ) ;
#131681 = CARTESIAN_POINT ( 'NONE',  ( -16.52544592524335698, -4.483927247898792601, 103.9594237280190185 ) ) ;
#131682 = CARTESIAN_POINT ( 'NONE',  ( -5.153800228976607833, 19.02544592524334988, 27.70942372801899722 ) ) ;
#131684 = CARTESIAN_POINT ( 'NONE',  ( 14.34966873604972726, -8.224510206698740333, 85.83442372801901854 ) ) ;
#131683 = CARTESIAN_POINT ( 'NONE',  ( 4.483927247898790824, -16.52544592524335698, 65.20942372801901854 ) ) ;
#131685 = CARTESIAN_POINT ( 'NONE',  ( -17.97182807773871716, 5.500000000000050626, 68.53038844047289047 ) ) ;
#131686 = CARTESIAN_POINT ( 'NONE',  ( 0.05219959533934541429, -16.53943276465976808, 65.00109039468568994 ) ) ;
#131687 = CARTESIAN_POINT ( 'NONE',  ( -15.72974639402197994, 15.80617190586746368, 30.62390960531436335 ) ) ;
#131688 = CARTESIAN_POINT ( 'NONE',  ( 19.02544592524343514, -5.153800228976328945, 38.54057627198103120 ) ) ;
#131689 = CARTESIAN_POINT ( 'NONE',  ( -16.55341960407617563, 4.379528057220093196, 38.54275706135234714 ) ) ;
#131690 = CARTESIAN_POINT ( 'NONE',  ( 19.03943276465977164, -0.05219959533909143690, 48.74890960531435979 ) ) ;
#131691 = CARTESIAN_POINT ( 'NONE',  ( 15.80617190586769283, -15.72974639402175789, 40.62609039468567573 ) ) ;
#131692 = CARTESIAN_POINT ( 'NONE',  ( 4.379528057220092307, 16.55341960407617563, 32.29275706135235424 ) ) ;
#131693 = CARTESIAN_POINT ( 'NONE',  ( 12.14591786802327356, -12.06949235617739191, 100.6260903946857184 ) ) ;
#131694 = CARTESIAN_POINT ( 'NONE',  ( -28.79475375365586842, 2.428612866367529932E-14, 141.9843446568999923 ) ) ;
#131695 = CARTESIAN_POINT ( 'NONE',  ( -0.05219959533936034679, 19.03943276465977164, 22.50109039468566152 ) ) ;
#131696 = CARTESIAN_POINT ( 'NONE',  ( 19.02544592524334988, 5.153800228976608722, 106.4594237280190185 ) ) ;
#131697 = CARTESIAN_POINT ( 'NONE',  ( -9.474510206698720793, -16.51473224551083518, 64.58442372801900433 ) ) ;
#131698 = CARTESIAN_POINT ( 'NONE',  ( -4.483927247898539470, -16.52544592524342804, 72.29057627198102409 ) ) ;
#131699 = CARTESIAN_POINT ( 'NONE',  ( -9.564922557960796823, -16.46253265017161027, 22.08224293864768839 ) ) ;
#131701 = DIRECTION ( 'NONE',  ( 0.000000000000000000, 1.000000000000000000, -4.336808689942013299E-16 ) ) ;
#131700 = CARTESIAN_POINT ( 'NONE',  ( 16.46253265017146816, 9.564922557961045513, 61.66775706135234003 ) ) ;
#131702 = CARTESIAN_POINT ( 'NONE',  ( -21.55341960407619339, 5.719274019375674811, 58.54275706135235424 ) ) ;
#131703 = CARTESIAN_POINT ( 'NONE',  ( 0.05219959533934541429, -16.53943276465976808, 40.00109039468567573 ) ) ;
#131704 = CARTESIAN_POINT ( 'NONE',  ( -30.20036327792369235, -26.22857331006468229, -17.18026671435357500 ) ) ;
#131705 = CARTESIAN_POINT ( 'NONE',  ( -10.81492255796078084, -18.62759615963271287, 27.08224293864769550 ) ) ;
#131706 = CARTESIAN_POINT ( 'NONE',  ( -9.564922557961040184, 16.46253265017147172, 102.9177570613523329 ) ) ;
#131707 = LINE ( 'NONE', #114522, #121652 ) ;
#131708 = CARTESIAN_POINT ( 'NONE',  ( -25.41223161463592106, 11.66315983254869693, 166.2610598689586254 ) ) ;
#131709 = CARTESIAN_POINT ( 'NONE',  ( -9.564922557960796823, -16.46253265017161027, 27.08224293864769550 ) ) ;
#131710 = CARTESIAN_POINT ( 'NONE',  ( -21.52544592524334988, -5.823673210054445271, 103.9594237280190185 ) ) ;
#131711 = CARTESIAN_POINT ( 'NONE',  ( 5.049401038298161559, -19.05341960407611168, 52.70724293864767418 ) ) ;
#131712 = CARTESIAN_POINT ( 'NONE',  ( -21.53943276465977519, -0.05219959533937600094, 58.75109039468568994 ) ) ;
#131713 = CARTESIAN_POINT ( 'NONE',  ( 21.53943276465977519, 0.05219959533937863772, 96.25109039468568994 ) ) ;
#131714 = CARTESIAN_POINT ( 'NONE',  ( 12.06949235617757843, -12.14591786802309237, 23.12390960531436335 ) ) ;
#131715 = CARTESIAN_POINT ( 'NONE',  ( -9.474510206698964154, 16.51473224551069663, 35.41557627198102409 ) ) ;
#131716 = CARTESIAN_POINT ( 'NONE',  ( -19.02544592524342804, 5.153800228976336051, 76.04057627198102409 ) ) ;
#131717 = CARTESIAN_POINT ( 'NONE',  ( -10.81492255796105439, 18.62759615963255655, 57.91775706135234714 ) ) ;
#131718 = CARTESIAN_POINT ( 'NONE',  ( 13.89961937509977652, -13.97604488694527269, 43.12390960531434558 ) ) ;
#131719 = CARTESIAN_POINT ( 'NONE',  ( 10.72451020669871369, 18.67979575497193778, 57.08442372801901854 ) ) ;
#131721 = CARTESIAN_POINT ( 'NONE',  ( 19.02544592524343514, -5.153800228976328945, 108.5405762719810383 ) ) ;
#131720 = CARTESIAN_POINT ( 'NONE',  ( -19.05341960407617563, 5.049401038297882671, 78.54275706135233293 ) ) ;
#131722 = CARTESIAN_POINT ( 'NONE',  ( -19.02544592524342804, 5.153800228976336051, 26.04057627198103120 ) ) ;
#131723 = CARTESIAN_POINT ( 'NONE',  ( -18.67979575497178146, -10.72451020669898902, 111.6655762719810525 ) ) ;
#131724 = CARTESIAN_POINT ( 'NONE',  ( 16.51473224551083163, -9.474510206698727899, 40.83442372801900433 ) ) ;
#131725 = CARTESIAN_POINT ( 'NONE',  ( -12.14591786802309592, -12.06949235617757132, 96.87390960531436690 ) ) ;
#131726 = CARTESIAN_POINT ( 'NONE',  ( 9.564922557960805705, 16.46253265017160317, 54.58224293864769550 ) ) ;
#131727 = CARTESIAN_POINT ( 'NONE',  ( 0.05219959533936267826, -19.03943276465977164, 100.0010903946856757 ) ) ;
#131728 = CARTESIAN_POINT ( 'NONE',  ( -8.314922557960811034, -14.29746914071050412, 62.08224293864769550 ) ) ;
#131729 = CARTESIAN_POINT ( 'NONE',  ( -5.823673210054431948, 21.52544592524334988, 112.7094237280190328 ) ) ;
#131730 = CARTESIAN_POINT ( 'NONE',  ( -5.049401038298153566, 19.05341960407611168, 100.2072429386476955 ) ) ;
#131731 = CARTESIAN_POINT ( 'NONE',  ( 9.474510206698729675, 16.51473224551082808, 92.08442372801900433 ) ) ;
#131732 = CARTESIAN_POINT ( 'NONE',  ( -5.719274019375978568, 21.55341960407610458, 90.20724293864770971 ) ) ;
#131733 = CARTESIAN_POINT ( 'NONE',  ( -5.823673210054431948, 21.52544592524334988, 42.70942372801901854 ) ) ;
#131734 = CARTESIAN_POINT ( 'NONE',  ( -16.55341960407617563, 4.379528057220093196, 43.54275706135235424 ) ) ;
#131735 = CARTESIAN_POINT ( 'NONE',  ( -12.14591786802326823, 12.06949235617739902, 108.1260903946856757 ) ) ;
#131737 = CARTESIAN_POINT ( 'NONE',  ( -5.823673210054431948, 21.52544592524334988, 42.70942372801901854 ) ) ;
#131736 = CARTESIAN_POINT ( 'NONE',  ( 0.05219959533934541429, -16.53943276465976808, 40.00109039468567573 ) ) ;
#131738 = CARTESIAN_POINT ( 'NONE',  ( -21.53943276465977519, 0.05219959533907696930, 46.24890960531435979 ) ) ;
#131739 = CARTESIAN_POINT ( 'NONE',  ( -0.05219959533909027116, -19.03943276465977164, 32.49890960531435979 ) ) ;
#131740 = CARTESIAN_POINT ( 'NONE',  ( -38.00000000000001421, 12.34694845685046438, -5.849999994537627757 ) ) ;
#131741 = CARTESIAN_POINT ( 'NONE',  ( -12.14591786802326823, 12.06949235617739902, 68.12609039468567573 ) ) ;
#131742 = CARTESIAN_POINT ( 'NONE',  ( -5.823673210054116645, -21.52544592524344225, 92.29057627198103830 ) ) ;
#131743 = CARTESIAN_POINT ( 'NONE',  ( 16.52544592524342804, -4.483927247898539470, 43.54057627198103830 ) ) ;
#131744 = CARTESIAN_POINT ( 'NONE',  ( 12.06949235617739724, 12.14591786802326823, 56.87609039468568994 ) ) ;
#131745 = CARTESIAN_POINT ( 'NONE',  ( -5.153800228976328057, -19.02544592524343514, 62.29057627198100988 ) ) ;
#131746 = CARTESIAN_POINT ( 'NONE',  ( 9.564922557961047289, -16.46253265017146816, 95.41775706135233293 ) ) ;
#131747 = CARTESIAN_POINT ( 'NONE',  ( -10.72451020669898014, 18.67979575497178502, 90.41557627198103830 ) ) ;
#131748 = CARTESIAN_POINT ( 'NONE',  ( -16.52544592524342804, 4.483927247898546575, 31.04057627198102409 ) ) ;
#131749 = ORIENTED_EDGE ( 'NONE', *, *, #6444, .F. ) ;
#131750 = CARTESIAN_POINT ( 'NONE',  ( 26.13941622279051558, 9.616497135380347672, 166.9083969906205311 ) ) ;
#131751 = CARTESIAN_POINT ( 'NONE',  ( 21.53943276465977519, -0.05219959533907433946, 68.74890960531435269 ) ) ;
#131752 = VERTEX_POINT ( 'NONE', #166659 ) ;
#131753 = CARTESIAN_POINT ( 'NONE',  ( -16.53943276465976808, -0.05219959533934237506, 108.7510903946857042 ) ) ;
#131754 = EDGE_LOOP ( 'NONE', ( #176701, #114815, #82996 ) ) ;
#131755 = CARTESIAN_POINT ( 'NONE',  ( 17.50000000000000711, -4.703611302593163401, 103.1505057453771030 ) ) ;
#131756 = CARTESIAN_POINT ( 'NONE',  ( 15.80617190586746368, 15.72974639402197994, 89.37390960531435269 ) ) ;
#131757 = CARTESIAN_POINT ( 'NONE',  ( 15.80617190586746368, 15.72974639402197994, 114.3739096053143527 ) ) ;
#131758 = CARTESIAN_POINT ( 'NONE',  ( 4.483927247898545687, 16.52544592524342804, 24.79057627198103120 ) ) ;
#131759 = CARTESIAN_POINT ( 'NONE',  ( -14.34966873604972548, 8.224510206698743886, 28.33442372801902209 ) ) ;
#131760 = CARTESIAN_POINT ( 'NONE',  ( 19.03943276465977164, -0.05219959533909143690, 38.74890960531436690 ) ) ;
#131761 = CARTESIAN_POINT ( 'NONE',  ( 19.05341960407611168, 5.049401038298154454, 68.95724293864769550 ) ) ;
#131762 = CARTESIAN_POINT ( 'NONE',  ( -22.44159573604009950, -16.30477369853688430, 139.5750000027311728 ) ) ;
#131763 = CARTESIAN_POINT ( 'NONE',  ( 15.72974639402199770, -15.80617190586745480, 28.12390960531435979 ) ) ;
#131764 = CARTESIAN_POINT ( 'NONE',  ( -9.248023074035627289, -10.55727144485873126, -62.45740887555399468 ) ) ;
#131765 = CARTESIAN_POINT ( 'NONE',  ( 5.049401038297881783, 19.05341960407617563, 102.2927570613523045 ) ) ;
#131766 = CARTESIAN_POINT ( 'NONE',  ( -13.97604488694547697, 13.89961937509957934, 43.12609039468566152 ) ) ;
#131767 = CARTESIAN_POINT ( 'NONE',  ( -10.72451020669898014, 18.67979575497178502, 85.41557627198102409 ) ) ;
#131768 = CARTESIAN_POINT ( 'NONE',  ( -12.06949235617739369, -12.14591786802326823, 109.3760903946857042 ) ) ;
#131769 = CARTESIAN_POINT ( 'NONE',  ( -18.67979575497178146, -10.72451020669898902, 51.66557627198102409 ) ) ;
#131771 = CARTESIAN_POINT ( 'NONE',  ( 19.02544592524334988, 5.153800228976608722, 101.4594237280189759 ) ) ;
#131770 = CARTESIAN_POINT ( 'NONE',  ( -5.719274019375978568, 21.55341960407610458, 80.20724293864769550 ) ) ;
#131772 = CARTESIAN_POINT ( 'NONE',  ( 19.03943276465977164, -0.05219959533909143690, 98.74890960531436690 ) ) ;
#131773 = CARTESIAN_POINT ( 'NONE',  ( -18.62759615963255300, -10.81492255796106328, 74.16775706135231871 ) ) ;
#131774 = CARTESIAN_POINT ( 'NONE',  ( 5.153800228976335163, 19.02544592524342804, 79.79057627198102409 ) ) ;
#131775 = CARTESIAN_POINT ( 'NONE',  ( -0.05219959533910754901, -16.53943276465976808, 97.49890960531436690 ) ) ;
#131776 = CARTESIAN_POINT ( 'NONE',  ( 31.72709406046301339, 0.4964181571218307387, 102.5000000000000284 ) ) ;
#131777 = CARTESIAN_POINT ( 'NONE',  ( 19.03943276465977164, -0.05219959533909143690, 68.74890960531436690 ) ) ;
#131778 = CARTESIAN_POINT ( 'NONE',  ( 4.379528057220339221, -16.55341960407611168, 97.70724293864772392 ) ) ;
#131779 = ORIENTED_EDGE ( 'NONE', *, *, #27507, .T. ) ;
#131780 = CARTESIAN_POINT ( 'NONE',  ( 5.153800228976615827, -19.02544592524334988, 90.20942372801900433 ) ) ;
#131781 =( BOUNDED_CURVE ( )  B_SPLINE_CURVE ( 3, ( #80990, #80006, #142665, #4144 ),
 .UNSPECIFIED., .F., .T. ) 
 B_SPLINE_CURVE_WITH_KNOTS ( ( 4, 4 ),
 ( 2.008945357379066987, 2.115944711806982070 ),
 .UNSPECIFIED. ) 
 CURVE ( )  GEOMETRIC_REPRESENTATION_ITEM ( )  RATIONAL_B_SPLINE_CURVE ( ( 1.000000000000000000, 0.9990461557208837329, 0.9990461557208837329, 1.000000000000000000 ) ) 
 REPRESENTATION_ITEM ( '' )  );
#131782 = CARTESIAN_POINT ( 'NONE',  ( 1.300000000000000044, -1.443375672974063884, -3.691112476943992763E-18 ) ) ;
#131783 = CARTESIAN_POINT ( 'NONE',  ( 19.05341960407611168, 5.049401038298154454, 63.95724293864769550 ) ) ;
#131784 = CIRCLE ( 'NONE', #41310, 28.79475375365586487 ) ;
#131786 = CARTESIAN_POINT ( 'NONE',  ( 16.51473224551069308, 9.474510206698969483, 104.1655762719810241 ) ) ;
#131785 = CARTESIAN_POINT ( 'NONE',  ( -21.53943276465977519, -0.05219959533937600094, 83.75109039468568994 ) ) ;
#131787 = CARTESIAN_POINT ( 'NONE',  ( -12.14591786802326823, 12.06949235617739902, 83.12609039468568994 ) ) ;
#131788 = CARTESIAN_POINT ( 'NONE',  ( -29.87692619418718110, 1.408284774589867894, -48.43935853184042628 ) ) ;
#131789 = CARTESIAN_POINT ( 'NONE',  ( 19.03943276465977164, 0.05219959533936151252, 56.25109039468566863 ) ) ;
#131790 = CARTESIAN_POINT ( 'NONE',  ( -10.72451020669870658, -18.67979575497194134, 99.58442372801900433 ) ) ;
#131791 = CARTESIAN_POINT ( 'NONE',  ( 37.24189295061466964, 4.138848244557342682, 41.36027101465354150 ) ) ;
#131792 = CARTESIAN_POINT ( 'NONE',  ( 6.551653823223136719, 3.660253528765625486, 8.410814283099844246 ) ) ;
#131793 = CARTESIAN_POINT ( 'NONE',  ( 14.34966873604972726, -8.224510206698740333, 105.8344237280190328 ) ) ;
#131794 = ADVANCED_FACE ( 'NONE', ( #74639 ), #82738, .T. ) ;
#131795 = CARTESIAN_POINT ( 'NONE',  ( 16.64782025964803225, -0.4052355915353793581, -59.15693706287429876 ) ) ;
#131796 = CARTESIAN_POINT ( 'NONE',  ( -4.379528057220086978, -16.55341960407618274, 94.79275706135234714 ) ) ;
#131797 = DIRECTION ( 'NONE',  ( 0.000000000000000000, 0.000000000000000000, 1.000000000000000000 ) ) ;
#131798 = CARTESIAN_POINT ( 'NONE',  ( -16.52544592524335698, -4.483927247898792601, 73.95942372801901854 ) ) ;
#131799 = DIRECTION ( 'NONE',  ( -5.204170427930421283E-16, 0.000000000000000000, -1.000000000000000000 ) ) ;
#131800 = CARTESIAN_POINT ( 'NONE',  ( 21.55341960407619695, -5.719274019375665929, 81.04275706135236135 ) ) ;
#131801 = CARTESIAN_POINT ( 'NONE',  ( 0.05219959533936267826, -19.03943276465977164, 85.00109039468567573 ) ) ;
#131802 = CARTESIAN_POINT ( 'NONE',  ( 16.51473224551083163, -9.474510206698727899, 45.83442372801900433 ) ) ;
#131803 = CARTESIAN_POINT ( 'NONE',  ( 9.474510206698971260, -16.51473224551069308, 67.91557627198102409 ) ) ;
#131804 = CARTESIAN_POINT ( 'NONE',  ( -13.97604488694527625, -13.89961937509977652, 61.87390960531435979 ) ) ;
#131805 = DIRECTION ( 'NONE',  ( -0.000000000000000000, -0.000000000000000000, 1.000000000000000000 ) ) ;
#131806 = CARTESIAN_POINT ( 'NONE',  ( -21.52544592524343514, 5.823673210054127303, 76.04057627198102409 ) ) ;
#131807 = CARTESIAN_POINT ( 'NONE',  ( -21.52544592524343514, 5.823673210054127303, 41.04057627198103120 ) ) ;
#131808 = CARTESIAN_POINT ( 'NONE',  ( 9.474510206698971260, -16.51473224551069308, 27.91557627198103120 ) ) ;
#131809 = CARTESIAN_POINT ( 'NONE',  ( -4.379528057220086978, -16.55341960407618274, 64.79275706135234714 ) ) ;
#131810 = EDGE_LOOP ( 'NONE', ( #17474, #141367, #104940, #158105 ) ) ;
#131811 = CARTESIAN_POINT ( 'NONE',  ( 5.823673210054444382, -21.52544592524334988, 30.20942372801902565 ) ) ;
#131813 = CARTESIAN_POINT ( 'NONE',  ( 37.99999999999999289, 2.893978650043524126E-14, -1.000000000000000000 ) ) ;
#131812 = CARTESIAN_POINT ( 'NONE',  ( -14.29746914071049879, 8.314922557960819915, 70.83224293864770971 ) ) ;
#131814 = CARTESIAN_POINT ( 'NONE',  ( -8.314922557961024197, 14.29746914071037800, 22.91775706135235069 ) ) ;
#131815 = CARTESIAN_POINT ( 'NONE',  ( 5.153800228976615827, -19.02544592524334988, 55.20942372801899722 ) ) ;
#131816 = CARTESIAN_POINT ( 'NONE',  ( 4.483927247898545687, 16.52544592524342804, 54.79057627198104541 ) ) ;
#131817 = CARTESIAN_POINT ( 'NONE',  ( 21.55341960407619695, -5.719274019375665929, 26.04275706135235779 ) ) ;
#131819 = CARTESIAN_POINT ( 'NONE',  ( -21.53943276465977519, 0.05219959533907696930, 71.24890960531435269 ) ) ;
#131818 = DIRECTION ( 'NONE',  ( 1.000000000000000000, 0.000000000000000000, 0.000000000000000000 ) ) ;
#131820 = CARTESIAN_POINT ( 'NONE',  ( 5.153800228976335163, 19.02544592524342804, 99.79057627198102409 ) ) ;
#131821 = CARTESIAN_POINT ( 'NONE',  ( -16.52544592524342804, 4.483927247898546575, 81.04057627198102409 ) ) ;
#131822 = CARTESIAN_POINT ( 'NONE',  ( 29.51469970000643883, -26.64072072720820472, -20.60124869737700948 ) ) ;
#131823 = CARTESIAN_POINT ( 'NONE',  ( 36.91746824999999887, -11.99521256947793546, -7.724999997268813701 ) ) ;
#131824 = CARTESIAN_POINT ( 'NONE',  ( 16.51473224551083163, -9.474510206698727899, 65.83442372801900433 ) ) ;
#131825 = CARTESIAN_POINT ( 'NONE',  ( 10.81492255796106328, -18.62759615963255655, 25.41775706135235779 ) ) ;
#131826 = CARTESIAN_POINT ( 'NONE',  ( -16.51473224551069308, -9.474510206698971260, 51.66557627198102409 ) ) ;
#131827 = CARTESIAN_POINT ( 'NONE',  ( 19.02544592524334988, 5.153800228976608722, 41.45942372801900433 ) ) ;
#131828 = CARTESIAN_POINT ( 'NONE',  ( -16.46253265017160317, 9.564922557960807481, 25.83224293864769194 ) ) ;
#131829 = CARTESIAN_POINT ( 'NONE',  ( -15.80617190586768217, 15.72974639402176855, 58.12609039468568994 ) ) ;
#131830 = DIRECTION ( 'NONE',  ( -0.1039620511844979306, 0.1039620511844979306, -0.9891328443778538704 ) ) ;
#131831 = CARTESIAN_POINT ( 'NONE',  ( 16.53943276465976808, -0.05219959533910856209, 43.74890960531435979 ) ) ;
#131832 = CARTESIAN_POINT ( 'NONE',  ( 16.51473224551069308, 9.474510206698969483, 64.16557627198102409 ) ) ;
#131833 = CARTESIAN_POINT ( 'NONE',  ( 0.05219959533907565091, 21.53943276465977519, 84.99890960531436690 ) ) ;
#131834 = CARTESIAN_POINT ( 'NONE',  ( -19.02544592524342804, 5.153800228976336051, 61.04057627198103120 ) ) ;
#131835 = ORIENTED_EDGE ( 'NONE', *, *, #153999, .T. ) ;
#131836 = CARTESIAN_POINT ( 'NONE',  ( 10.81492255796078972, 18.62759615963270932, 69.58224293864769550 ) ) ;
#131837 = CARTESIAN_POINT ( 'NONE',  ( -21.53943276465977519, -0.05219959533937600094, 103.7510903946857042 ) ) ;
#131840 = CARTESIAN_POINT ( 'NONE',  ( 14.29746914071049879, -8.314922557960816363, 88.33224293864769550 ) ) ;
#131839 = CARTESIAN_POINT ( 'NONE',  ( 16.55341960407618274, -4.379528057220086978, 91.04275706135236135 ) ) ;
#131838 = CARTESIAN_POINT ( 'NONE',  ( -9.474510206698964154, 16.51473224551069663, 25.41557627198103120 ) ) ;
#131841 = CARTESIAN_POINT ( 'NONE',  ( 16.51473224551083163, -9.474510206698727899, 90.83442372801900433 ) ) ;
#131842 = ORIENTED_EDGE ( 'NONE', *, *, #172113, .T. ) ;
#131843 = CARTESIAN_POINT ( 'NONE',  ( 15.80617190586746368, 15.72974639402197994, 114.3739096053143527 ) ) ;
#131844 = CARTESIAN_POINT ( 'NONE',  ( 5.049401038297881783, 19.05341960407617563, 42.29275706135234003 ) ) ;
#131845 = CARTESIAN_POINT ( 'NONE',  ( 16.52544592524335698, 4.483927247898782831, 96.45942372801901854 ) ) ;
#131846 = CARTESIAN_POINT ( 'NONE',  ( -13.97604488694547697, 13.89961937509957934, 33.12609039468566863 ) ) ;
#131847 = CARTESIAN_POINT ( 'NONE',  ( -0.05219959533909027116, -19.03943276465977164, 87.49890960531436690 ) ) ;
#131848 = CARTESIAN_POINT ( 'NONE',  ( -15.80617190586745835, -15.72974639402198527, 61.87390960531436690 ) ) ;
#131849 = CARTESIAN_POINT ( 'NONE',  ( 5.049401038298161559, -19.05341960407611168, 22.70724293864769194 ) ) ;
#131850 = CARTESIAN_POINT ( 'NONE',  ( -0.05219959533910754901, -16.53943276465976808, 112.4989096053143669 ) ) ;
#131851 = CARTESIAN_POINT ( 'NONE',  ( 18.67979575497194134, -10.72451020669871369, 100.8344237280190185 ) ) ;
#131852 = CARTESIAN_POINT ( 'NONE',  ( 0.05219959533934541429, -16.53943276465976808, 75.00109039468568994 ) ) ;
#131853 = CARTESIAN_POINT ( 'NONE',  ( -10.72451020669870658, -18.67979575497194134, 34.58442372801900433 ) ) ;
#131854 = CARTESIAN_POINT ( 'NONE',  ( 8.224510206698742110, 14.34966873604972548, 32.08442372801901854 ) ) ;
#131855 = CARTESIAN_POINT ( 'NONE',  ( 9.474510206698971260, -16.51473224551069308, 102.9155762719810241 ) ) ;
#131856 = CARTESIAN_POINT ( 'NONE',  ( -13.89961937509977652, 13.97604488694528158, 35.62390960531435269 ) ) ;
#131857 = CARTESIAN_POINT ( 'NONE',  ( -19.02544592524342804, 5.153800228976336051, 61.04057627198103120 ) ) ;
#131858 = CARTESIAN_POINT ( 'NONE',  ( -4.483927247898782831, 16.52544592524335698, 52.70942372801902565 ) ) ;
#131859 = CARTESIAN_POINT ( 'NONE',  ( 4.379528057220339221, -16.55341960407611168, 97.70724293864772392 ) ) ;
#131860 = CARTESIAN_POINT ( 'NONE',  ( -4.379528057220086978, -16.55341960407618274, 94.79275706135234714 ) ) ;
#131863 = CARTESIAN_POINT ( 'NONE',  ( -16.51473224551069308, -9.474510206698971260, 66.66557627198102409 ) ) ;
#131862 = CARTESIAN_POINT ( 'NONE',  ( -5.049401038298153566, 19.05341960407611168, 80.20724293864769550 ) ) ;
#131861 = CARTESIAN_POINT ( 'NONE',  ( -18.62759615963255300, -10.81492255796106328, 44.16775706135234714 ) ) ;
#131864 = CARTESIAN_POINT ( 'NONE',  ( -16.46253265017160317, 9.564922557960807481, 100.8322429386477097 ) ) ;
#131865 = CARTESIAN_POINT ( 'NONE',  ( -16.55341960407611168, -4.379528057220339221, 31.45724293864769550 ) ) ;
#131866 = CARTESIAN_POINT ( 'NONE',  ( -0.05219959533934338120, 16.53943276465976808, 97.50109039468567573 ) ) ;
#131867 = ORIENTED_EDGE ( 'NONE', *, *, #181095, .T. ) ;
#131868 = CARTESIAN_POINT ( 'NONE',  ( -16.51473224551082808, 9.474510206698731452, 43.33442372801900433 ) ) ;
#131869 = CARTESIAN_POINT ( 'NONE',  ( 16.46253265017160672, -9.564922557960803928, 108.3322429386476955 ) ) ;
#131870 = CARTESIAN_POINT ( 'NONE',  ( 9.474510206698971260, -16.51473224551069308, 62.91557627198102409 ) ) ;
#131871 = CARTESIAN_POINT ( 'NONE',  ( -13.89961937509957401, -13.97604488694547875, 44.37609039468566863 ) ) ;
#131872 = CARTESIAN_POINT ( 'NONE',  ( -22.81625015709509441, -31.40387420917324590, -6.324999997268815122 ) ) ;
#131873 = CARTESIAN_POINT ( 'NONE',  ( -16.38665767535052353, -7.295008042176046814, 64.73599135785458714 ) ) ;
#131874 = CARTESIAN_POINT ( 'NONE',  ( -0.05219959533934338120, 16.53943276465976808, 42.50109039468567573 ) ) ;
#131876 = CARTESIAN_POINT ( 'NONE',  ( -8.314922557961024197, 14.29746914071037800, 52.91775706135235424 ) ) ;
#131875 = CARTESIAN_POINT ( 'NONE',  ( 0.05219959533936267826, -19.03943276465977164, 65.00109039468567573 ) ) ;
#131877 = CARTESIAN_POINT ( 'NONE',  ( -5.049401038298153566, 19.05341960407611168, 115.2072429386477097 ) ) ;
#131878 = CARTESIAN_POINT ( 'NONE',  ( -19.02544592524342804, 5.153800228976336051, 96.04057627198103830 ) ) ;
#131879 = CARTESIAN_POINT ( 'NONE',  ( 15.80617190586746368, 15.72974639402197994, 109.3739096053143811 ) ) ;
#131880 = CARTESIAN_POINT ( 'NONE',  ( 13.97604488694548053, -13.89961937509957401, 75.62609039468564731 ) ) ;
#131882 = CARTESIAN_POINT ( 'NONE',  ( 19.03943276465977164, -0.05219959533909143690, 28.74890960531435624 ) ) ;
#131881 = CARTESIAN_POINT ( 'NONE',  ( -5.153800228976328057, -19.02544592524343514, 102.2905762719810383 ) ) ;
#131883 = CARTESIAN_POINT ( 'NONE',  ( 19.02544592524343514, -5.153800228976328945, 78.54057627198099567 ) ) ;
#131885 = CARTESIAN_POINT ( 'NONE',  ( 5.049401038298161559, -19.05341960407611168, 42.70724293864767418 ) ) ;
#131884 = CARTESIAN_POINT ( 'NONE',  ( -0.05219959533910754901, -16.53943276465976808, 52.49890960531435979 ) ) ;
#131886 = CARTESIAN_POINT ( 'NONE',  ( 19.02544592524334988, 5.153800228976608722, 51.45942372801900433 ) ) ;
#131887 = B_SPLINE_CURVE_WITH_KNOTS ( 'NONE', 3,
 ( #183120, #88110, #148804, #26468, #11299, #72970, #15253, #139571 ),
 .UNSPECIFIED., .F., .F.,
 ( 4, 2, 2, 4 ),
 ( 0.002324770996991016962, 0.005594641632892926458, 0.007229576950843881640, 0.008864512268794836822 ),
 .UNSPECIFIED. ) ;
#131888 = CARTESIAN_POINT ( 'NONE',  ( 8.224510206698953496, -14.34966873604960469, 87.91557627198103830 ) ) ;
#131889 = CARTESIAN_POINT ( 'NONE',  ( 15.72974639402176855, 15.80617190586768217, 106.8760903946856899 ) ) ;
#131890 = CARTESIAN_POINT ( 'NONE',  ( -5.049401038298153566, 19.05341960407611168, 55.20724293864769550 ) ) ;
#131891 = CARTESIAN_POINT ( 'NONE',  ( -10.72451020669898014, 18.67979575497178502, 55.41557627198102409 ) ) ;
#131893 = CARTESIAN_POINT ( 'NONE',  ( -13.97604488694547697, 13.89961937509957934, 23.12609039468565442 ) ) ;
#131892 = CARTESIAN_POINT ( 'NONE',  ( -4.483927247898539470, -16.52544592524342804, 47.29057627198103120 ) ) ;
#131894 = CARTESIAN_POINT ( 'NONE',  ( 9.564922557960805705, 16.46253265017160317, 104.5822429386476955 ) ) ;
#131895 = CARTESIAN_POINT ( 'NONE',  ( 16.46253265017160672, -9.564922557960803928, 103.3322429386476955 ) ) ;
#131896 = CARTESIAN_POINT ( 'NONE',  ( -9.474510206698964154, 16.51473224551069663, 35.41557627198102409 ) ) ;
#131897 = CARTESIAN_POINT ( 'NONE',  ( -13.97604488694527625, -13.89961937509977652, 31.87390960531435979 ) ) ;
#131898 = CARTESIAN_POINT ( 'NONE',  ( 8.224510206698953496, -14.34966873604960469, 87.91557627198103830 ) ) ;
#131899 = CARTESIAN_POINT ( 'NONE',  ( -18.67979575497178146, -10.72451020669898902, 91.66557627198103830 ) ) ;
#131900 = CARTESIAN_POINT ( 'NONE',  ( -16.46253265017160317, 9.564922557960807481, 105.8322429386476955 ) ) ;
#131901 = CARTESIAN_POINT ( 'NONE',  ( -18.67979575497178146, -10.72451020669898902, 106.6655762719810383 ) ) ;
#131902 = CARTESIAN_POINT ( 'NONE',  ( 13.89961937509977652, -13.97604488694527269, 98.12390960531433848 ) ) ;
#131904 = CARTESIAN_POINT ( 'NONE',  ( 4.483927247898545687, 16.52544592524342804, 104.7905762719810241 ) ) ;
#131903 = FACE_OUTER_BOUND ( 'NONE', #102673, .T. ) ;
#131905 = CARTESIAN_POINT ( 'NONE',  ( 13.97604488694527802, 13.89961937509977652, 74.37390960531436690 ) ) ;
#131906 = CARTESIAN_POINT ( 'NONE',  ( -21.53943276465977519, 0.05219959533907696930, 86.24890960531436690 ) ) ;
#131907 = CARTESIAN_POINT ( 'NONE',  ( 17.50000000000001066, -5.622605283950885990, 106.1879268940388954 ) ) ;
#131908 = CARTESIAN_POINT ( 'NONE',  ( -21.97143472835162825, -7.273127645264535701, 170.2116391040481176 ) ) ;
#131910 = CARTESIAN_POINT ( 'NONE',  ( 19.49149378614658090, -5.499999999999772626, 66.93757513605362419 ) ) ;
#131909 = CARTESIAN_POINT ( 'NONE',  ( -15.72974639402197994, 15.80617190586746368, 25.62390960531435624 ) ) ;
#131911 = CARTESIAN_POINT ( 'NONE',  ( -12.14591786802326823, 12.06949235617739902, 33.12609039468569705 ) ) ;
#131912 = CARTESIAN_POINT ( 'NONE',  ( -16.53943276465976808, 0.05219959533911058130, 101.2489096053143669 ) ) ;
#131913 = CARTESIAN_POINT ( 'NONE',  ( 18.39443945427642291, -5.499999999999867661, 51.01745347608655123 ) ) ;
#131914 = CARTESIAN_POINT ( 'NONE',  ( -0.05219959533909027116, -19.03943276465977164, 52.49890960531436690 ) ) ;
#131915 = CARTESIAN_POINT ( 'NONE',  ( -4.379528057220328563, 16.55341960407611168, 75.20724293864769550 ) ) ;
#131916 = CARTESIAN_POINT ( 'NONE',  ( -18.67979575497178146, -10.72451020669898902, 26.66557627198103475 ) ) ;
#131917 = CARTESIAN_POINT ( 'NONE',  ( -16.52544592524342804, 4.483927247898546575, 66.04057627198103830 ) ) ;
#131918 = CARTESIAN_POINT ( 'NONE',  ( -16.53943276465976808, -0.05219959533934237506, 23.75109039468567929 ) ) ;
#131919 = CARTESIAN_POINT ( 'NONE',  ( -21.55341960407619339, 5.719274019375674811, 78.54275706135236135 ) ) ;
#131920 = CARTESIAN_POINT ( 'NONE',  ( 17.26058549869092573, -6.457015423128476428, 76.12254162523932166 ) ) ;
#131921 = CARTESIAN_POINT ( 'NONE',  ( 5.719274019375991003, -21.55341960407610458, 22.70724293864769194 ) ) ;
#131922 = CARTESIAN_POINT ( 'NONE',  ( 8.314922557961029526, -14.29746914071037800, 80.41775706135234714 ) ) ;
#131923 = CARTESIAN_POINT ( 'NONE',  ( 16.46253265017160672, -9.564922557960803928, 43.33224293864769550 ) ) ;
#131924 = CARTESIAN_POINT ( 'NONE',  ( -0.05219959533909027116, -19.03943276465977164, 92.49890960531436690 ) ) ;
#131925 = CARTESIAN_POINT ( 'NONE',  ( -18.67979575497178146, -10.72451020669898902, 96.66557627198102409 ) ) ;
#131926 = CARTESIAN_POINT ( 'NONE',  ( 16.52544592524335698, 4.483927247898782831, 21.45942372801901499 ) ) ;
#131928 = CARTESIAN_POINT ( 'NONE',  ( 18.67979575497194134, -10.72451020669871369, 70.83442372801901854 ) ) ;
#131927 = CARTESIAN_POINT ( 'NONE',  ( -8.314922557960811034, -14.29746914071050412, 57.08224293864769550 ) ) ;
#131929 = AXIS2_PLACEMENT_3D ( 'NONE', #108728, #74430, #136097 ) ;
#131930 = CARTESIAN_POINT ( 'NONE',  ( 4.379528057220092307, 16.55341960407617563, 102.2927570613523613 ) ) ;
#131931 = CARTESIAN_POINT ( 'NONE',  ( 24.84792715949108199, 12.91290060751520130, 166.0205615092970106 ) ) ;
#131932 = FACE_OUTER_BOUND ( 'NONE', #181273, .T. ) ;
#131933 = CARTESIAN_POINT ( 'NONE',  ( -16.55341960407611168, -4.379528057220339221, 21.45724293864769550 ) ) ;
#131934 = CARTESIAN_POINT ( 'NONE',  ( -14.34966873604972548, 8.224510206698743886, 63.33442372801900433 ) ) ;
#131935 = CARTESIAN_POINT ( 'NONE',  ( -9.474510206698964154, 16.51473224551069663, 75.41557627198103830 ) ) ;
#131936 = CARTESIAN_POINT ( 'NONE',  ( -13.97604488694527625, -13.89961937509977652, 81.87390960531436690 ) ) ;
#131937 = CARTESIAN_POINT ( 'NONE',  ( 21.53943276465977519, 0.05219959533937863772, 66.25109039468567573 ) ) ;
#131938 = CARTESIAN_POINT ( 'NONE',  ( 16.53943276465976808, 0.05219959533934440121, 71.25109039468568994 ) ) ;
#131939 = CARTESIAN_POINT ( 'NONE',  ( -16.55341960407611168, -4.379528057220339221, 56.45724293864768839 ) ) ;
#131940 = CARTESIAN_POINT ( 'NONE',  ( 0.05219959533909260263, 19.03943276465977164, 49.99890960531435979 ) ) ;
#131941 = ORIENTED_EDGE ( 'NONE', *, *, #57594, .T. ) ;
#131942 = CARTESIAN_POINT ( 'NONE',  ( -0.05219959533936034679, 19.03943276465977164, 102.5010903946856757 ) ) ;
#131943 = CARTESIAN_POINT ( 'NONE',  ( -16.52544592524342804, 4.483927247898546575, 106.0405762719810525 ) ) ;
#131944 = CARTESIAN_POINT ( 'NONE',  ( 9.564922557960805705, 16.46253265017160317, 84.58224293864769550 ) ) ;
#131946 = CARTESIAN_POINT ( 'NONE',  ( 30.74264578624799782, 22.33583958711400541, -4.800000000000000711 ) ) ;
#131945 = CARTESIAN_POINT ( 'NONE',  ( 8.314922557961029526, -14.29746914071037800, 20.41775706135234714 ) ) ;
#131947 = CARTESIAN_POINT ( 'NONE',  ( 0.05219959533937995610, -21.53943276465977519, 105.0010903946856757 ) ) ;
#131948 = CARTESIAN_POINT ( 'NONE',  ( 4.483927247898790824, -16.52544592524335698, 75.20942372801901854 ) ) ;
#131949 = CARTESIAN_POINT ( 'NONE',  ( -0.05219959533936034679, 19.03943276465977164, 92.50109039468566152 ) ) ;
#131950 = CARTESIAN_POINT ( 'NONE',  ( 10.72451020669898902, -18.67979575497178502, 57.91557627198103120 ) ) ;
#131951 = CARTESIAN_POINT ( 'NONE',  ( -16.52544592524335698, -4.483927247898792601, 68.95942372801901854 ) ) ;
#131952 = CARTESIAN_POINT ( 'NONE',  ( -31.74999999999995737, 0.000000000000000000, 2.500000000000000444 ) ) ;
#131953 = CARTESIAN_POINT ( 'NONE',  ( 5.153800228976615827, -19.02544592524334988, 50.20942372801897591 ) ) ;
#131954 = CARTESIAN_POINT ( 'NONE',  ( -18.67979575497193778, 10.72451020669871902, 93.33442372801901854 ) ) ;
#131955 = CARTESIAN_POINT ( 'NONE',  ( 13.97604488694527802, 13.89961937509977652, 39.37390960531435269 ) ) ;
#131956 = CARTESIAN_POINT ( 'NONE',  ( 9.474510206698971260, -16.51473224551069308, 77.91557627198103830 ) ) ;
#131957 = CARTESIAN_POINT ( 'NONE',  ( -12.06949235617756955, 12.14591786802309770, 70.62390960531436690 ) ) ;
#131958 = CARTESIAN_POINT ( 'NONE',  ( 10.81492255796106328, -18.62759615963255655, 90.41775706135236135 ) ) ;
#131959 = CARTESIAN_POINT ( 'NONE',  ( 13.89961937509957401, 13.97604488694547697, 51.87609039468566863 ) ) ;
#131960 = CARTESIAN_POINT ( 'NONE',  ( 19.02544592524334988, 5.153800228976608722, 36.45942372801900433 ) ) ;
#131961 = CARTESIAN_POINT ( 'NONE',  ( 21.53943276465977519, -0.05219959533907433946, 38.74890960531435979 ) ) ;
#131962 = CARTESIAN_POINT ( 'NONE',  ( -18.67979575497193778, 10.72451020669871902, 98.33442372801901854 ) ) ;
#131963 = CARTESIAN_POINT ( 'NONE',  ( 19.03943276465977164, -0.05219959533909143690, 78.74890960531436690 ) ) ;
#131964 = CARTESIAN_POINT ( 'NONE',  ( 10.72451020669871369, 18.67979575497193778, 97.08442372801904696 ) ) ;
#131965 = CARTESIAN_POINT ( 'NONE',  ( -0.05219959533907301413, -21.53943276465977519, 52.49890960531435979 ) ) ;
#131967 = B_SPLINE_CURVE_WITH_KNOTS ( 'NONE', 3,
 ( #128697, #51869, #173239, #113529, #66040, #127707, #16573, #172236, #157070, #18565, #34714, #175223, #50884, #174236, #35705, #159038, #196523, #102494, #195522, #101476 ),
 .UNSPECIFIED., .F., .F.,
 ( 4, 2, 2, 2, 2, 2, 2, 2, 2, 4 ),
 ( 0.004000878361811991205, 0.004499404418915995893, 0.004997930476019999714, 0.005496456533124003535, 0.005994982590228008223, 0.006244245618780010568, 0.006493508647332012912, 0.006992034704436012396, 0.007490560761540013615, 0.007989086818644013099 ),
 .UNSPECIFIED. ) ;
#131966 = CARTESIAN_POINT ( 'NONE',  ( 5.153800228976335163, 19.02544592524342804, 89.79057627198102409 ) ) ;
#131968 = CARTESIAN_POINT ( 'NONE',  ( -9.474510206698720793, -16.51473224551083518, 79.58442372801899012 ) ) ;
#131969 = CARTESIAN_POINT ( 'NONE',  ( 16.46253265017160672, -9.564922557960803928, 93.33224293864769550 ) ) ;
#131970 = CARTESIAN_POINT ( 'NONE',  ( 13.97604488694548053, -13.89961937509957401, 90.62609039468567573 ) ) ;
#131971 = CARTESIAN_POINT ( 'NONE',  ( 16.53943276465976808, 0.05219959533934440121, 36.25109039468567573 ) ) ;
#131972 = CARTESIAN_POINT ( 'NONE',  ( -14.29746914071049879, 8.314922557960819915, 95.83224293864770971 ) ) ;
#131973 = CARTESIAN_POINT ( 'NONE',  ( 9.564922557960805705, 16.46253265017160317, 69.58224293864770971 ) ) ;
#131974 = CARTESIAN_POINT ( 'NONE',  ( -21.52544592524343514, 5.823673210054127303, 66.04057627198103830 ) ) ;
#131975 = CARTESIAN_POINT ( 'NONE',  ( 0.05219959533934541429, -16.53943276465976808, 30.00109039468568284 ) ) ;
#131976 = CARTESIAN_POINT ( 'NONE',  ( 15.72974639402176855, 15.80617190586768217, 36.87609039468568994 ) ) ;
#131977 = CARTESIAN_POINT ( 'NONE',  ( -15.80617190586768217, 15.72974639402176855, 88.12609039468570415 ) ) ;
#131978 = CARTESIAN_POINT ( 'NONE',  ( -8.314922557961024197, 14.29746914071037800, 82.91775706135234714 ) ) ;
#131979 = CARTESIAN_POINT ( 'NONE',  ( 13.89961937509977652, -13.97604488694527269, 68.12390960531436690 ) ) ;
#131980 = CARTESIAN_POINT ( 'NONE',  ( 16.53943276465976808, -0.05219959533910856209, 78.74890960531436690 ) ) ;
#131981 = CARTESIAN_POINT ( 'NONE',  ( 16.52544592524335698, 4.483927247898782831, 96.45942372801901854 ) ) ;
#131982 = CARTESIAN_POINT ( 'NONE',  ( -5.049401038297874678, -19.05341960407617918, 59.79275706135231871 ) ) ;
#131983 = CARTESIAN_POINT ( 'NONE',  ( 21.53943276465977519, 0.05219959533937863772, 26.25109039468567573 ) ) ;
#131984 = CARTESIAN_POINT ( 'NONE',  ( 16.55341960407611168, 4.379528057220329451, 78.95724293864769550 ) ) ;
#131985 = CARTESIAN_POINT ( 'NONE',  ( -5.049401038298153566, 19.05341960407611168, 95.20724293864770971 ) ) ;
#131986 = CARTESIAN_POINT ( 'NONE',  ( 12.14591786802327356, -12.06949235617739191, 100.6260903946857184 ) ) ;
#131987 = CARTESIAN_POINT ( 'NONE',  ( 15.80617190586769283, -15.72974639402175789, 75.62609039468567573 ) ) ;
#131988 = CARTESIAN_POINT ( 'NONE',  ( 8.314922557961029526, -14.29746914071037800, 45.41775706135234003 ) ) ;
#131989 = CARTESIAN_POINT ( 'NONE',  ( -5.823673210054431948, 21.52544592524334988, 27.70942372801901854 ) ) ;
#131990 = CARTESIAN_POINT ( 'NONE',  ( -4.483927247898539470, -16.52544592524342804, 67.29057627198103830 ) ) ;
#131991 = ORIENTED_EDGE ( 'NONE', *, *, #121465, .F. ) ;
#131992 = CARTESIAN_POINT ( 'NONE',  ( 5.719274019375991003, -21.55341960407610458, 112.7072429386476955 ) ) ;
#131993 = DIRECTION ( 'NONE',  ( 1.000000000000000000, 0.000000000000000000, 3.709348145883536076E-20 ) ) ;
#131994 = CARTESIAN_POINT ( 'NONE',  ( -12.06949235617756955, 12.14591786802309770, 55.62390960531436690 ) ) ;
#131995 = CARTESIAN_POINT ( 'NONE',  ( -13.97604488694527625, -13.89961937509977652, 21.87390960531435979 ) ) ;
#131996 = CARTESIAN_POINT ( 'NONE',  ( -21.52544592524343514, 5.823673210054127303, 36.04057627198102409 ) ) ;
#131997 = CARTESIAN_POINT ( 'NONE',  ( 8.224510206698953496, -14.34966873604960469, 77.91557627198102409 ) ) ;
#131998 = CARTESIAN_POINT ( 'NONE',  ( 18.67979575497178502, 10.72451020669898547, 79.16557627198103830 ) ) ;
#131999 = CARTESIAN_POINT ( 'NONE',  ( 16.46253265017160672, -9.564922557960803928, 73.33224293864769550 ) ) ;
#132001 = CARTESIAN_POINT ( 'NONE',  ( 13.89961937509957401, 13.97604488694547697, 81.87609039468564731 ) ) ;
#132000 = CARTESIAN_POINT ( 'NONE',  ( -19.02544592524342804, 5.153800228976336051, 36.04057627198100988 ) ) ;
#132003 = CARTESIAN_POINT ( 'NONE',  ( 18.67979575497178502, 10.72451020669898547, 59.16557627198103120 ) ) ;
#132002 = CARTESIAN_POINT ( 'NONE',  ( -21.55341960407619339, 5.719274019375674811, 53.54275706135234714 ) ) ;
#132004 = CARTESIAN_POINT ( 'NONE',  ( 9.564922557960805705, 16.46253265017160317, 44.58224293864769550 ) ) ;
#132005 = CARTESIAN_POINT ( 'NONE',  ( 16.46253265017160672, -9.564922557960803928, 78.33224293864769550 ) ) ;
#132006 = ORIENTED_EDGE ( 'NONE', *, *, #199554, .F. ) ;
#132007 = CARTESIAN_POINT ( 'NONE',  ( -8.224510206698735004, -14.34966873604973081, 49.58442372801901143 ) ) ;
#132008 = CARTESIAN_POINT ( 'NONE',  ( 5.823673210054444382, -21.52544592524334988, 25.20942372801901854 ) ) ;
#132009 = CARTESIAN_POINT ( 'NONE',  ( -21.53943276465977519, -0.05219959533937600094, 58.75109039468568994 ) ) ;
#132010 = CARTESIAN_POINT ( 'NONE',  ( 0.05219959533909260263, 19.03943276465977164, 109.9989096053143669 ) ) ;
#132011 = CARTESIAN_POINT ( 'NONE',  ( 10.72451020669898902, -18.67979575497178502, 87.91557627198103830 ) ) ;
#132013 = CARTESIAN_POINT ( 'NONE',  ( 8.314922557961029526, -14.29746914071037800, 55.41775706135234714 ) ) ;
#132012 = CARTESIAN_POINT ( 'NONE',  ( 18.62759615963255655, 10.81492255796105972, 21.66775706135235069 ) ) ;
#132014 = CARTESIAN_POINT ( 'NONE',  ( 21.53943276465977519, -0.05219959533907433946, 48.74890960531435979 ) ) ;
#132015 = CARTESIAN_POINT ( 'NONE',  ( -21.55341960407619339, 5.719274019375674811, 113.5427570613523756 ) ) ;
#132016 = CARTESIAN_POINT ( 'NONE',  ( 13.97604488694527802, 13.89961937509977652, 59.37390960531434558 ) ) ;
#132017 = CARTESIAN_POINT ( 'NONE',  ( 19.05341960407611168, 5.049401038298154454, 108.9572429386477097 ) ) ;
#132018 = CARTESIAN_POINT ( 'NONE',  ( -19.05341960407611168, -5.049401038298163336, 86.45724293864769550 ) ) ;
#132019 = CARTESIAN_POINT ( 'NONE',  ( 16.46253265017146816, 9.564922557961045513, 51.66775706135233293 ) ) ;
#132020 = CARTESIAN_POINT ( 'NONE',  ( -5.049401038297874678, -19.05341960407617918, 69.79275706135233293 ) ) ;
#132021 = CARTESIAN_POINT ( 'NONE',  ( -10.72451020669898014, 18.67979575497178502, 45.41557627198103830 ) ) ;
#132022 = CARTESIAN_POINT ( 'NONE',  ( -8.224510206698948167, 14.34966873604960824, 30.41557627198101699 ) ) ;
#132023 = CARTESIAN_POINT ( 'NONE',  ( 19.05341960407617918, -5.049401038297876454, 81.04275706135231871 ) ) ;
#132024 = CARTESIAN_POINT ( 'NONE',  ( 0.000000000000000000, 0.000000000000000000, -10.00000000000000000 ) ) ;
#132025 = CARTESIAN_POINT ( 'NONE',  ( 21.55341960407619695, -5.719274019375665929, 111.0427570613523613 ) ) ;
#132026 = CARTESIAN_POINT ( 'NONE',  ( 5.153800228976615827, -19.02544592524334988, 95.20942372801897591 ) ) ;
#132027 = CARTESIAN_POINT ( 'NONE',  ( -5.153800228976607833, 19.02544592524334988, 47.70942372801900433 ) ) ;
#132028 = LINE ( 'NONE', #129997, #140377 ) ;
#132029 = CARTESIAN_POINT ( 'NONE',  ( -19.05341960407611168, -5.049401038298163336, 51.45724293864770260 ) ) ;
#132030 = CARTESIAN_POINT ( 'NONE',  ( 16.53943276465976808, -0.05219959533910856209, 68.74890960531435269 ) ) ;
#132031 = EDGE_CURVE ( 'NONE', #60180, #167889, #144744, .T. ) ;
#132032 = CARTESIAN_POINT ( 'NONE',  ( -19.02544592524342804, 5.153800228976336051, 31.04057627198102409 ) ) ;
#132033 = CARTESIAN_POINT ( 'NONE',  ( -4.483927247898539470, -16.52544592524342804, 37.29057627198102409 ) ) ;
#132034 = CARTESIAN_POINT ( 'NONE',  ( -33.40031027765337512, -22.02106105253704982, -24.45416078184958764 ) ) ;
#132035 = CARTESIAN_POINT ( 'NONE',  ( -0.05219959533934338120, 16.53943276465976808, 102.5010903946856899 ) ) ;
#132036 = CARTESIAN_POINT ( 'NONE',  ( 0.05219959533909260263, 19.03943276465977164, 64.99890960531436690 ) ) ;
#132037 = CARTESIAN_POINT ( 'NONE',  ( 5.153800228976615827, -19.02544592524334988, 20.20942372801899722 ) ) ;
#132038 = CARTESIAN_POINT ( 'NONE',  ( -0.05219959533934338120, 16.53943276465976808, 27.50109039468567929 ) ) ;
#132039 = CARTESIAN_POINT ( 'NONE',  ( 21.53943276465977519, -0.05219959533907433946, 48.74890960531435979 ) ) ;
#132041 = ORIENTED_EDGE ( 'NONE', *, *, #482, .F. ) ;
#132040 = CARTESIAN_POINT ( 'NONE',  ( -21.52544592524334988, -5.823673210054445271, 103.9594237280190185 ) ) ;
#132042 = CARTESIAN_POINT ( 'NONE',  ( 5.153800228976335163, 19.02544592524342804, 59.79057627198100988 ) ) ;
#132043 = CARTESIAN_POINT ( 'NONE',  ( 0.05219959533909260263, 19.03943276465977164, 109.9989096053143669 ) ) ;
#132044 = CARTESIAN_POINT ( 'NONE',  ( 9.564922557960805705, 16.46253265017160317, 99.58224293864770971 ) ) ;
#132045 = CARTESIAN_POINT ( 'NONE',  ( 11.40812507854755253, -35.11059874428192273, -4.024999997268814411 ) ) ;
#132046 = CARTESIAN_POINT ( 'NONE',  ( 10.81492255796106328, -18.62759615963255655, 20.41775706135234714 ) ) ;
#132047 = CARTESIAN_POINT ( 'NONE',  ( -8.224510206698948167, 14.34966873604960824, 90.41557627198103830 ) ) ;
#132049 = CARTESIAN_POINT ( 'NONE',  ( -9.564922557960796823, -16.46253265017161027, 62.08224293864769550 ) ) ;
#132048 = CARTESIAN_POINT ( 'NONE',  ( 5.719274019375991003, -21.55341960407610458, 82.70724293864770971 ) ) ;
#132050 = CARTESIAN_POINT ( 'NONE',  ( -5.153800228976328057, -19.02544592524343514, 67.29057627198102409 ) ) ;
#132051 = CARTESIAN_POINT ( 'NONE',  ( -21.52544592524334988, -5.823673210054445271, 18.95942372801901143 ) ) ;
#132052 = ORIENTED_EDGE ( 'NONE', *, *, #165213, .T. ) ;
#132053 = CARTESIAN_POINT ( 'NONE',  ( 16.46253265017160672, -9.564922557960803928, 68.33224293864770971 ) ) ;
#132054 = CARTESIAN_POINT ( 'NONE',  ( -37.45873412500000654, 2.428612866367529932E-14, -1.437499995903219974 ) ) ;
#132056 = FACE_OUTER_BOUND ( 'NONE', #93194, .T. ) ;
#132055 = CARTESIAN_POINT ( 'NONE',  ( -0.05219959533910754901, -16.53943276465976808, 107.4989096053143669 ) ) ;
#132057 = CARTESIAN_POINT ( 'NONE',  ( 9.564922557960805705, 16.46253265017160317, 64.58224293864769550 ) ) ;
#132058 = CARTESIAN_POINT ( 'NONE',  ( -5.049401038297874678, -19.05341960407617918, 94.79275706135230450 ) ) ;
#132059 = CARTESIAN_POINT ( 'NONE',  ( 16.53943276465976808, -0.05219959533910856209, 98.74890960531438111 ) ) ;
#132060 = CARTESIAN_POINT ( 'NONE',  ( -18.67979575497193778, 10.72451020669871902, 78.33442372801901854 ) ) ;
#132062 = CARTESIAN_POINT ( 'NONE',  ( -10.72451020669870658, -18.67979575497194134, 29.58442372801901854 ) ) ;
#132061 = CARTESIAN_POINT ( 'NONE',  ( 16.51473224551069308, 9.474510206698969483, 54.16557627198103120 ) ) ;
#132063 = CARTESIAN_POINT ( 'NONE',  ( -5.823673210054116645, -21.52544592524344225, 107.2905762719810525 ) ) ;
#132064 = CARTESIAN_POINT ( 'NONE',  ( 17.81289503416611453, -24.51734667627695785, 140.6999999999999602 ) ) ;
#132065 = CARTESIAN_POINT ( 'NONE',  ( -16.51473224551069308, -9.474510206698971260, 66.66557627198102409 ) ) ;
#132066 = CARTESIAN_POINT ( 'NONE',  ( -17.81289503416611097, -24.51734667627696496, 138.5500000054623229 ) ) ;
#132068 = CARTESIAN_POINT ( 'NONE',  ( -21.52544592524343514, 5.823673210054127303, 31.04057627198102409 ) ) ;
#132067 = CARTESIAN_POINT ( 'NONE',  ( -19.02544592524334988, -5.153800228976617603, 103.9594237280190043 ) ) ;
#132069 = CARTESIAN_POINT ( 'NONE',  ( 5.823673210054444382, -21.52544592524334988, 65.20942372801901854 ) ) ;
#132070 = CARTESIAN_POINT ( 'NONE',  ( -19.02544592524342804, 5.153800228976336051, 96.04057627198103830 ) ) ;
#132071 = CARTESIAN_POINT ( 'NONE',  ( 19.03943276465977164, 0.05219959533936151252, 86.25109039468567573 ) ) ;
#132072 = CARTESIAN_POINT ( 'NONE',  ( 16.46253265017160672, -9.564922557960803928, 48.33224293864769550 ) ) ;
#132073 = CARTESIAN_POINT ( 'NONE',  ( 9.474510206698971260, -16.51473224551069308, 77.91557627198103830 ) ) ;
#132074 = CARTESIAN_POINT ( 'NONE',  ( 8.224510206698953496, -14.34966873604960469, 82.91557627198103830 ) ) ;
#132075 = CARTESIAN_POINT ( 'NONE',  ( 9.564922557960805705, 16.46253265017160317, 99.58224293864770971 ) ) ;
#132076 = CARTESIAN_POINT ( 'NONE',  ( 14.29746914071049879, -8.314922557960816363, 93.33224293864769550 ) ) ;
#132077 = CARTESIAN_POINT ( 'NONE',  ( -16.46253265017160317, 9.564922557960807481, 95.83224293864769550 ) ) ;
#132079 = CARTESIAN_POINT ( 'NONE',  ( -13.89961937509977652, 13.97604488694528158, 25.62390960531434558 ) ) ;
#132078 = CARTESIAN_POINT ( 'NONE',  ( -0.05219959533910754901, -16.53943276465976808, 37.49890960531436690 ) ) ;
#132080 = ORIENTED_EDGE ( 'NONE', *, *, #99048, .F. ) ;
#132081 = CARTESIAN_POINT ( 'NONE',  ( 18.67979575497194134, -10.72451020669871369, 55.83442372801901854 ) ) ;
#132082 = CARTESIAN_POINT ( 'NONE',  ( -13.97604488694547697, 13.89961937509957934, 83.12609039468564731 ) ) ;
#132083 = CARTESIAN_POINT ( 'NONE',  ( 16.53943276465976808, -0.05219959533910856209, 43.74890960531435979 ) ) ;
#132084 = CARTESIAN_POINT ( 'NONE',  ( 5.823673210054125526, 21.52544592524343514, 94.79057627198105251 ) ) ;
#132085 = CARTESIAN_POINT ( 'NONE',  ( -0.05219959533907301413, -21.53943276465977519, 32.49890960531435979 ) ) ;
#132086 = CARTESIAN_POINT ( 'NONE',  ( 12.14591786802309770, 12.06949235617756955, 89.37390960531435269 ) ) ;
#132087 = CARTESIAN_POINT ( 'NONE',  ( 16.51473224551069308, 9.474510206698969483, 59.16557627198102409 ) ) ;
#132088 = CARTESIAN_POINT ( 'NONE',  ( -14.29746914071049879, 8.314922557960819915, 25.83224293864769194 ) ) ;
#132089 = CARTESIAN_POINT ( 'NONE',  ( -0.05219959533934338120, 16.53943276465976808, 97.50109039468567573 ) ) ;
#132090 = CARTESIAN_POINT ( 'NONE',  ( 12.06949235617739724, 12.14591786802326823, 71.87609039468568994 ) ) ;
#132091 = CARTESIAN_POINT ( 'NONE',  ( 0.05219959533936267826, -19.03943276465977164, 25.00109039468566152 ) ) ;
#132092 = CARTESIAN_POINT ( 'NONE',  ( -13.97604488694527625, -13.89961937509977652, 101.8739096053143811 ) ) ;
#132093 = CARTESIAN_POINT ( 'NONE',  ( -13.97604488694527625, -13.89961937509977652, 71.87390960531433848 ) ) ;
#132094 = CARTESIAN_POINT ( 'NONE',  ( -19.02544592524342804, 5.153800228976336051, 36.04057627198100988 ) ) ;
#132095 = CARTESIAN_POINT ( 'NONE',  ( -4.483927247898539470, -16.52544592524342804, 47.29057627198103120 ) ) ;
#132096 = CARTESIAN_POINT ( 'NONE',  ( 16.51473224551069308, 9.474510206698969483, 109.1655762719810383 ) ) ;
#132097 = CARTESIAN_POINT ( 'NONE',  ( 15.72974639402199770, -15.80617190586745480, 38.12390960531436690 ) ) ;
#132098 = CARTESIAN_POINT ( 'NONE',  ( -16.52544592524342804, 4.483927247898546575, 91.04057627198103830 ) ) ;
#132099 = CARTESIAN_POINT ( 'NONE',  ( -8.224510206698735004, -14.34966873604973081, 24.58442372801901499 ) ) ;
#132100 = CARTESIAN_POINT ( 'NONE',  ( -16.53943276465976808, 0.05219959533911058130, 66.24890960531436690 ) ) ;
#132101 = CARTESIAN_POINT ( 'NONE',  ( 28.90000000000002700, -0.1353689087803565394, -49.67367017693150189 ) ) ;
#132102 = CARTESIAN_POINT ( 'NONE',  ( 9.474510206698729675, 16.51473224551082808, 67.08442372801900433 ) ) ;
#132103 = CARTESIAN_POINT ( 'NONE',  ( 19.03943276465977164, -0.05219959533909143690, 108.7489096053143527 ) ) ;
#132104 = CARTESIAN_POINT ( 'NONE',  ( -9.474510206698720793, -16.51473224551083518, 84.58442372801900433 ) ) ;
#132105 = CARTESIAN_POINT ( 'NONE',  ( -8.571926809382601320, -26.38167802310801591, 147.7750000027311899 ) ) ;
#132107 = CARTESIAN_POINT ( 'NONE',  ( 12.14591786802327356, -12.06949235617739191, 110.6260903946857042 ) ) ;
#132106 = CARTESIAN_POINT ( 'NONE',  ( -19.02544592524334988, -5.153800228976617603, 108.9594237280189759 ) ) ;
#132108 = CARTESIAN_POINT ( 'NONE',  ( -9.474510206698964154, 16.51473224551069663, 45.41557627198103120 ) ) ;
#132109 = CARTESIAN_POINT ( 'NONE',  ( 21.53943276465977519, -0.05219959533907433946, 33.74890960531436690 ) ) ;
#132110 = CARTESIAN_POINT ( 'NONE',  ( -21.53943276465977519, -0.05219959533937600094, 53.75109039468568994 ) ) ;
#132111 = CARTESIAN_POINT ( 'NONE',  ( 19.15291303114474886, 5.500000000000047962, 38.60837706366875466 ) ) ;
#132112 = CARTESIAN_POINT ( 'NONE',  ( 8.314922557961029526, -14.29746914071037800, 25.41775706135235779 ) ) ;
#132114 = CARTESIAN_POINT ( 'NONE',  ( 5.153800228976335163, 19.02544592524342804, 69.79057627198103830 ) ) ;
#132113 = CARTESIAN_POINT ( 'NONE',  ( 17.50000000000000355, 3.201899417648170321, 22.70706107622752512 ) ) ;
#132115 = CARTESIAN_POINT ( 'NONE',  ( 15.85590801997753552, 17.61085972261885502, -57.22569728324523197 ) ) ;
#132117 = CARTESIAN_POINT ( 'NONE',  ( -13.97604488694527625, -13.89961937509977652, 76.87390960531433848 ) ) ;
#132116 = CARTESIAN_POINT ( 'NONE',  ( 16.55341960407611168, 4.379528057220329451, 83.95724293864770971 ) ) ;
#132118 = CARTESIAN_POINT ( 'NONE',  ( 9.474510206698971260, -16.51473224551069308, 87.91557627198102409 ) ) ;
#132119 = ORIENTED_EDGE ( 'NONE', *, *, #109656, .F. ) ;
#132120 = CARTESIAN_POINT ( 'NONE',  ( -13.89961937509957401, -13.97604488694547875, 94.37609039468566152 ) ) ;
#132121 = CARTESIAN_POINT ( 'NONE',  ( 0.05219959533907565091, 21.53943276465977519, 64.99890960531435269 ) ) ;
#132122 = CARTESIAN_POINT ( 'NONE',  ( 19.05341960407611168, 5.049401038298154454, 23.95724293864769194 ) ) ;
#132123 = CARTESIAN_POINT ( 'NONE',  ( -5.153800228976607833, 19.02544592524334988, 62.70942372801899722 ) ) ;
#132124 = CARTESIAN_POINT ( 'NONE',  ( -13.89961937509977652, 13.97604488694528158, 50.62390960531435979 ) ) ;
#132125 = CARTESIAN_POINT ( 'NONE',  ( -9.564922557960796823, -16.46253265017161027, 97.08224293864769550 ) ) ;
#132126 = ORIENTED_EDGE ( 'NONE', *, *, #192515, .T. ) ;
#132127 = CARTESIAN_POINT ( 'NONE',  ( -18.62759615963270932, 10.81492255796079327, 85.83224293864768129 ) ) ;
#132130 = CARTESIAN_POINT ( 'NONE',  ( -16.51473224551082808, 9.474510206698731452, 58.33442372801900433 ) ) ;
#132129 = CARTESIAN_POINT ( 'NONE',  ( -19.03943276465977164, 0.05219959533909376836, 86.24890960531436690 ) ) ;
#132128 = CARTESIAN_POINT ( 'NONE',  ( -8.314922557960811034, -14.29746914071050412, 87.08224293864769550 ) ) ;
#132132 = B_SPLINE_CURVE_WITH_KNOTS ( 'NONE', 3,
 ( #140050, #44092, #167436, #12766, #47068, #43095 ),
 .UNSPECIFIED., .F., .F.,
 ( 4, 2, 4 ),
 ( 0.007228050697041446017, 0.007608510107494925040, 0.007988969517948404930 ),
 .UNSPECIFIED. ) ;
#132131 = CARTESIAN_POINT ( 'NONE',  ( -18.62759615963270932, 10.81492255796079327, 90.83224293864769550 ) ) ;
#132133 = CARTESIAN_POINT ( 'NONE',  ( 10.72451020669898902, -18.67979575497178502, 72.91557627198103830 ) ) ;
#132134 = CARTESIAN_POINT ( 'NONE',  ( 16.55341960407611168, 4.379528057220329451, 38.95724293864768839 ) ) ;
#132135 = CARTESIAN_POINT ( 'NONE',  ( -10.81492255796105439, 18.62759615963255655, 97.91775706135236135 ) ) ;
#132136 = CARTESIAN_POINT ( 'NONE',  ( 0.05219959533934541429, -16.53943276465976808, 70.00109039468568994 ) ) ;
#132137 = CARTESIAN_POINT ( 'NONE',  ( -19.05341960407611168, -5.049401038298163336, 76.45724293864769550 ) ) ;
#132138 = CARTESIAN_POINT ( 'NONE',  ( 9.474510206698971260, -16.51473224551069308, 27.91557627198103120 ) ) ;
#132139 = CARTESIAN_POINT ( 'NONE',  ( -21.55341960407619339, 5.719274019375674811, 33.54275706135234714 ) ) ;
#132140 = CARTESIAN_POINT ( 'NONE',  ( -21.55341960407619339, 5.719274019375674811, 58.54275706135235424 ) ) ;
#132141 = CARTESIAN_POINT ( 'NONE',  ( 5.153800228976335163, 19.02544592524342804, 44.79057627198103830 ) ) ;
#132142 = CARTESIAN_POINT ( 'NONE',  ( -18.62759615963255300, -10.81492255796106328, 24.16775706135235424 ) ) ;
#132143 = CARTESIAN_POINT ( 'NONE',  ( -19.02544592524334988, -5.153800228976617603, 73.95942372801900433 ) ) ;
#132144 = CARTESIAN_POINT ( 'NONE',  ( 5.049401038297881783, 19.05341960407617563, 72.29275706135234714 ) ) ;
#132145 = CARTESIAN_POINT ( 'NONE',  ( -5.049401038298153566, 19.05341960407611168, 25.20724293864768484 ) ) ;
#132146 = CARTESIAN_POINT ( 'NONE',  ( -14.29746914071037622, -8.314922557961029526, 69.16775706135234714 ) ) ;
#132147 = CARTESIAN_POINT ( 'NONE',  ( -0.05219959533909027116, -19.03943276465977164, 47.49890960531435979 ) ) ;
#132148 = CARTESIAN_POINT ( 'NONE',  ( -69.65682714487590488, -71.74905178543390605, -4.999999999999999112 ) ) ;
#132149 = CARTESIAN_POINT ( 'NONE',  ( -19.03943276465977164, 0.05219959533909376836, 96.24890960531436690 ) ) ;
#132150 = CARTESIAN_POINT ( 'NONE',  ( 16.46253265017160672, -9.564922557960803928, 38.33224293864768839 ) ) ;
#132151 = CARTESIAN_POINT ( 'NONE',  ( -10.81492255796078084, -18.62759615963271287, 67.08224293864770971 ) ) ;
#132152 = CARTESIAN_POINT ( 'NONE',  ( 16.55341960407618274, -4.379528057220086978, 56.04275706135235424 ) ) ;
#132153 = CARTESIAN_POINT ( 'NONE',  ( -21.55341960407619339, 5.719274019375674811, 108.5427570613523756 ) ) ;
#132154 = CARTESIAN_POINT ( 'NONE',  ( -19.03943276465977164, 0.05219959533909376836, 51.24890960531436690 ) ) ;
#132155 = CARTESIAN_POINT ( 'NONE',  ( -16.52544592524342804, 4.483927247898546575, 26.04057627198103475 ) ) ;
#132156 = CARTESIAN_POINT ( 'NONE',  ( -8.224510206698948167, 14.34966873604960824, 70.41557627198102409 ) ) ;
#132157 = CIRCLE ( 'NONE', #25528, 0.5000000000000004441 ) ;
#132158 = CARTESIAN_POINT ( 'NONE',  ( -5.049401038298153566, 19.05341960407611168, 75.20724293864769550 ) ) ;
#132159 = CARTESIAN_POINT ( 'NONE',  ( -21.53943276465977519, -0.05219959533937600094, 33.75109039468568284 ) ) ;
#132160 = CARTESIAN_POINT ( 'NONE',  ( -9.564922557960796823, -16.46253265017161027, 97.08224293864769550 ) ) ;
#132161 = CARTESIAN_POINT ( 'NONE',  ( 18.62759615963255655, 10.81492255796105972, 96.66775706135234714 ) ) ;
#132162 = CARTESIAN_POINT ( 'NONE',  ( 8.224510206698742110, 14.34966873604972548, 67.08442372801901854 ) ) ;
#132163 = EDGE_CURVE ( 'NONE', #132746, #142969, #185860, .T. ) ;
#132164 = CARTESIAN_POINT ( 'NONE',  ( 13.97604488694527802, 13.89961937509977652, 109.3739096053143669 ) ) ;
#132165 = CARTESIAN_POINT ( 'NONE',  ( 18.62759615963271287, -10.81492255796078972, 93.33224293864769550 ) ) ;
#132166 = CARTESIAN_POINT ( 'NONE',  ( -16.53943276465976808, 0.05219959533911058130, 51.24890960531436690 ) ) ;
#132167 = CARTESIAN_POINT ( 'NONE',  ( 5.153800228976335163, 19.02544592524342804, 29.79057627198102409 ) ) ;
#132168 = CARTESIAN_POINT ( 'NONE',  ( 4.379528057220092307, 16.55341960407617563, 57.29275706135234714 ) ) ;
#132169 = CARTESIAN_POINT ( 'NONE',  ( -12.14591786802309592, -12.06949235617757132, 61.87390960531436690 ) ) ;
#132170 = CARTESIAN_POINT ( 'NONE',  ( -16.51473224551069308, -9.474510206698971260, 111.6655762719810383 ) ) ;
#132171 = CARTESIAN_POINT ( 'NONE',  ( -5.823673210054116645, -21.52544592524344225, 37.29057627198102409 ) ) ;
#132172 = CARTESIAN_POINT ( 'NONE',  ( 19.02544592524334988, 5.153800228976608722, 26.45942372801899722 ) ) ;
#132173 = CARTESIAN_POINT ( 'NONE',  ( 16.53943276465976808, -0.05219959533910856209, 98.74890960531438111 ) ) ;
#132174 = CARTESIAN_POINT ( 'NONE',  ( 13.89961937509977652, -13.97604488694527269, 108.1239096053143669 ) ) ;
#132175 = ORIENTED_EDGE ( 'NONE', *, *, #56209, .F. ) ;
#132176 = CARTESIAN_POINT ( 'NONE',  ( -0.05219959533934338120, 16.53943276465976808, 57.50109039468568994 ) ) ;
#132177 = CARTESIAN_POINT ( 'NONE',  ( -0.05219959533909027116, -19.03943276465977164, 57.49890960531435979 ) ) ;
#132178 = DIRECTION ( 'NONE',  ( -1.734723475976805517E-15, 0.3420201433256828127, 0.9396926207859033209 ) ) ;
#132179 = CARTESIAN_POINT ( 'NONE',  ( -16.46253265017146816, -9.564922557961047289, 49.16775706135233293 ) ) ;
#132180 = CARTESIAN_POINT ( 'NONE',  ( -16.52544592524335698, -4.483927247898792601, 98.95942372801903275 ) ) ;
#132181 = CARTESIAN_POINT ( 'NONE',  ( 16.51473224551083163, -9.474510206698727899, 90.83442372801900433 ) ) ;
#132182 = CARTESIAN_POINT ( 'NONE',  ( 18.62759615963255655, 10.81492255796105972, 61.66775706135235424 ) ) ;
#132183 = CARTESIAN_POINT ( 'NONE',  ( 5.153800228976335163, 19.02544592524342804, 69.79057627198103830 ) ) ;
#132184 = CARTESIAN_POINT ( 'NONE',  ( -10.72451020669898014, 18.67979575497178502, 90.41557627198103830 ) ) ;
#132185 = CARTESIAN_POINT ( 'NONE',  ( 8.314922557960818139, 14.29746914071049879, 109.5822429386476955 ) ) ;
#132186 = AXIS2_PLACEMENT_3D ( 'NONE', #38494, #100150, #101141 ) ;
#132187 = CARTESIAN_POINT ( 'NONE',  ( 16.51473224551083163, -9.474510206698727899, 85.83442372801900433 ) ) ;
#132188 = CARTESIAN_POINT ( 'NONE',  ( 18.62759615963271287, -10.81492255796078972, 83.33224293864769550 ) ) ;
#132189 = CARTESIAN_POINT ( 'NONE',  ( -9.564922557961040184, 16.46253265017147172, 37.91775706135233293 ) ) ;
#132190 = DIRECTION ( 'NONE',  ( -1.000000000000000000, -0.000000000000000000, -0.000000000000000000 ) ) ;
#132191 = CARTESIAN_POINT ( 'NONE',  ( -18.67979575497178146, -10.72451020669898902, 86.66557627198102409 ) ) ;
#132192 = CARTESIAN_POINT ( 'NONE',  ( -19.35633801406906684, 5.499999999999777955, 54.13373818172763663 ) ) ;
#132193 = CARTESIAN_POINT ( 'NONE',  ( -16.46253265017160317, 9.564922557960807481, 70.83224293864770971 ) ) ;
#132194 = CARTESIAN_POINT ( 'NONE',  ( -26.46959431505279881, -27.26463967846491698, -11.49588912907431393 ) ) ;
#132195 = CARTESIAN_POINT ( 'NONE',  ( 16.55341960407618274, -4.379528057220086978, 26.04275706135235779 ) ) ;
#132196 = CARTESIAN_POINT ( 'NONE',  ( 36.91128768240056246, 2.428612879436746321E-14, 50.50000000000002842 ) ) ;
#132197 = CARTESIAN_POINT ( 'NONE',  ( 13.89961937509977652, -13.97604488694527269, 48.12390960531435979 ) ) ;
#132198 = CARTESIAN_POINT ( 'NONE',  ( 5.049401038298161559, -19.05341960407611168, 107.7072429386476955 ) ) ;
#132200 = CARTESIAN_POINT ( 'NONE',  ( -12.06949235617756955, 12.14591786802309770, 45.62390960531436690 ) ) ;
#132199 = CARTESIAN_POINT ( 'NONE',  ( 21.55341960407610458, 5.719274019375980345, 108.9572429386476955 ) ) ;
#132201 = CARTESIAN_POINT ( 'NONE',  ( 10.72451020669871369, 18.67979575497193778, 77.08442372801901854 ) ) ;
#132203 = CARTESIAN_POINT ( 'NONE',  ( -19.03943276465977164, -0.05219959533935918106, 23.75109039468566152 ) ) ;
#132202 = CARTESIAN_POINT ( 'NONE',  ( -12.06949235617739369, -12.14591786802326823, 29.37609039468568284 ) ) ;
#132204 = CARTESIAN_POINT ( 'NONE',  ( 8.224510206698953496, -14.34966873604960469, 32.91557627198102409 ) ) ;
#132205 = CARTESIAN_POINT ( 'NONE',  ( -10.81492255796105439, 18.62759615963255655, 32.91775706135234714 ) ) ;
#132206 = CARTESIAN_POINT ( 'NONE',  ( -21.53943276465977519, 0.05219959533907696930, 116.2489096053143669 ) ) ;
#132207 = CARTESIAN_POINT ( 'NONE',  ( 14.34966873604960469, 8.224510206698951720, 44.16557627198103120 ) ) ;
#132208 = CARTESIAN_POINT ( 'NONE',  ( -19.03943276465977164, -0.05219959533935918106, 98.75109039468567573 ) ) ;
#132209 = CARTESIAN_POINT ( 'NONE',  ( 13.89961937509957401, 13.97604488694547697, 71.87609039468567573 ) ) ;
#132210 = CARTESIAN_POINT ( 'NONE',  ( -18.67979575497193778, 10.72451020669871902, 73.33442372801901854 ) ) ;
#132211 = CARTESIAN_POINT ( 'NONE',  ( 9.564922557961047289, -16.46253265017146816, 55.41775706135234003 ) ) ;
#132212 = CARTESIAN_POINT ( 'NONE',  ( -19.03943276465977164, 0.05219959533909376836, 26.24890960531435624 ) ) ;
#132213 = CARTESIAN_POINT ( 'NONE',  ( 15.72974639402199770, -15.80617190586745480, 48.12390960531436690 ) ) ;
#132214 = CARTESIAN_POINT ( 'NONE',  ( 14.29746914071049879, -8.314922557960816363, 48.33224293864770260 ) ) ;
#132215 = CARTESIAN_POINT ( 'NONE',  ( 5.049401038297881783, 19.05341960407617563, 22.29275706135233648 ) ) ;
#132216 = CARTESIAN_POINT ( 'NONE',  ( 16.53943276465976808, 0.05219959533934440121, 81.25109039468568994 ) ) ;
#132217 = CARTESIAN_POINT ( 'NONE',  ( 12.14591786802309770, 12.06949235617756955, 34.37390960531435979 ) ) ;
#132218 = CARTESIAN_POINT ( 'NONE',  ( 5.719274019375673035, 21.55341960407619339, 82.29275706135234714 ) ) ;
#132219 = CARTESIAN_POINT ( 'NONE',  ( -5.823673210054431948, 21.52544592524334988, 77.70942372801900433 ) ) ;
#132220 = CARTESIAN_POINT ( 'NONE',  ( 10.72451020669898902, -18.67979575497178502, 82.91557627198103830 ) ) ;
#132221 = CARTESIAN_POINT ( 'NONE',  ( -5.153800228976328057, -19.02544592524343514, 32.29057627198102409 ) ) ;
#132222 = CARTESIAN_POINT ( 'NONE',  ( -10.81492255796105439, 18.62759615963255655, 62.91775706135236135 ) ) ;
#132223 = CARTESIAN_POINT ( 'NONE',  ( 9.474510206698971260, -16.51473224551069308, 42.91557627198103120 ) ) ;
#132224 = CARTESIAN_POINT ( 'NONE',  ( -19.05341960407611168, -5.049401038298163336, 56.45724293864768129 ) ) ;
#132225 = CARTESIAN_POINT ( 'NONE',  ( -16.53943276465976808, 0.05219959533911058130, 86.24890960531436690 ) ) ;
#132226 = CARTESIAN_POINT ( 'NONE',  ( 16.46253265017160672, -9.564922557960803928, 98.33224293864769550 ) ) ;
#132227 = CARTESIAN_POINT ( 'NONE',  ( -8.314922557960811034, -14.29746914071050412, 37.08224293864768129 ) ) ;
#132228 = CARTESIAN_POINT ( 'NONE',  ( -16.53943276465976808, 0.05219959533911058130, 111.2489096053143669 ) ) ;
#132229 = CARTESIAN_POINT ( 'NONE',  ( -21.55341960407610458, -5.719274019375992779, 76.45724293864769550 ) ) ;
#132230 = CARTESIAN_POINT ( 'NONE',  ( -21.53943276465977519, -0.05219959533937600094, 28.75109039468567929 ) ) ;
#132231 = DIRECTION ( 'NONE',  ( 0.000000000000000000, 0.000000000000000000, -1.000000000000000000 ) ) ;
#132232 = EDGE_CURVE ( 'NONE', #89057, #18224, #38376, .T. ) ;
#132234 = CARTESIAN_POINT ( 'NONE',  ( 16.55341960407618274, -4.379528057220086978, 26.04275706135235779 ) ) ;
#132233 = CARTESIAN_POINT ( 'NONE',  ( -13.89961937509977652, 13.97604488694528158, 75.62390960531438111 ) ) ;
#132235 = CARTESIAN_POINT ( 'NONE',  ( 10.72451020669898902, -18.67979575497178502, 72.91557627198103830 ) ) ;
#132236 = CARTESIAN_POINT ( 'NONE',  ( 21.52544592524334988, 5.823673210054432836, 96.45942372801901854 ) ) ;
#132237 = CARTESIAN_POINT ( 'NONE',  ( -9.474510206698964154, 16.51473224551069663, 80.41557627198103830 ) ) ;
#132238 = CARTESIAN_POINT ( 'NONE',  ( 5.823673210054444382, -21.52544592524334988, 35.20942372801901854 ) ) ;
#132239 = CARTESIAN_POINT ( 'NONE',  ( 15.72974639402199770, -15.80617190586745480, 23.12390960531436335 ) ) ;
#132240 = CARTESIAN_POINT ( 'NONE',  ( -12.06949235617739369, -12.14591786802326823, 84.37609039468570415 ) ) ;
#132241 = CARTESIAN_POINT ( 'NONE',  ( -10.72451020669870658, -18.67979575497194134, 69.58442372801900433 ) ) ;
#132242 = CARTESIAN_POINT ( 'NONE',  ( -21.52544592524334988, -5.823673210054445271, 103.9594237280190185 ) ) ;
#132243 = CARTESIAN_POINT ( 'NONE',  ( 4.379528057220092307, 16.55341960407617563, 77.29275706135234714 ) ) ;
#132244 = CARTESIAN_POINT ( 'NONE',  ( -10.81492255796105439, 18.62759615963255655, 22.91775706135235069 ) ) ;
#132245 = CARTESIAN_POINT ( 'NONE',  ( -13.89961937509977652, 13.97604488694528158, 25.62390960531434558 ) ) ;
#132246 = CARTESIAN_POINT ( 'NONE',  ( -21.53943276465977519, -0.05219959533937600094, 93.75109039468567573 ) ) ;
#132247 = CARTESIAN_POINT ( 'NONE',  ( -0.05219959533909027116, -19.03943276465977164, 87.49890960531436690 ) ) ;
#132249 = CARTESIAN_POINT ( 'NONE',  ( 21.55341960407610458, 5.719274019375980345, 93.95724293864770971 ) ) ;
#132248 = B_SPLINE_CURVE_WITH_KNOTS ( 'NONE', 3,
 ( #7935, #69618, #179818, #39280, #102950, #100937, #101952, #9956, #194972, #164634, #11963, #73628, #198948, #60415, #106919, #12945, #151457, #59421, #165630, #27128, #150468, #72626 ),
 .UNSPECIFIED., .F., .F.,
 ( 4, 2, 2, 2, 2, 2, 2, 2, 2, 2, 4 ),
 ( 0.000000000000000000, 0.001361773908209231061, 0.002042660862313851362, 0.002723547816418472097, 0.004085321724627708796, 0.004766208678732329965, 0.005447095632836950266, 0.006808869541046243777, 0.008170643449255537288, 0.009532417357464831667, 0.01089419126567412605 ),
 .UNSPECIFIED. ) ;
#132250 = CARTESIAN_POINT ( 'NONE',  ( 19.05341960407617918, -5.049401038297876454, 61.04275706135232582 ) ) ;
#132252 = CARTESIAN_POINT ( 'NONE',  ( -15.80617190586745835, -15.72974639402198527, 51.87390960531437401 ) ) ;
#132251 = CARTESIAN_POINT ( 'NONE',  ( 18.39639308325437028, 5.500000000000035527, 83.98252246182197212 ) ) ;
#132254 = CARTESIAN_POINT ( 'NONE',  ( 8.314922557960818139, 14.29746914071049879, 54.58224293864769550 ) ) ;
#132253 = CARTESIAN_POINT ( 'NONE',  ( -0.05219959533909027116, -19.03943276465977164, 92.49890960531436690 ) ) ;
#132255 = CARTESIAN_POINT ( 'NONE',  ( -28.82186960331489445, 9.364793116373697046, 145.8999999999999773 ) ) ;
#132256 = CARTESIAN_POINT ( 'NONE',  ( 19.05341960407617918, -5.049401038297876454, 81.04275706135231871 ) ) ;
#132257 = LINE ( 'NONE', #54419, #76495 ) ;
#132258 = CARTESIAN_POINT ( 'NONE',  ( 13.89961937509957401, 13.97604488694547697, 101.8760903946856331 ) ) ;
#132259 = CARTESIAN_POINT ( 'NONE',  ( -21.55341960407610458, -5.719274019375992779, 86.45724293864770971 ) ) ;
#132260 = CARTESIAN_POINT ( 'NONE',  ( -16.52544592524342804, 4.483927247898546575, 71.04057627198103830 ) ) ;
#132261 = CARTESIAN_POINT ( 'NONE',  ( 16.46253265017160672, -9.564922557960803928, 103.3322429386476955 ) ) ;
#132262 = CARTESIAN_POINT ( 'NONE',  ( -12.14591786802326823, 12.06949235617739902, 48.12609039468568284 ) ) ;
#132263 = CARTESIAN_POINT ( 'NONE',  ( 5.049401038298161559, -19.05341960407611168, 52.70724293864767418 ) ) ;
#132265 = CARTESIAN_POINT ( 'NONE',  ( -13.97604488694547697, 13.89961937509957934, 83.12609039468564731 ) ) ;
#132264 = CARTESIAN_POINT ( 'NONE',  ( -5.823673210054431948, 21.52544592524334988, 22.70942372801901499 ) ) ;
#132266 = CARTESIAN_POINT ( 'NONE',  ( 16.46253265017160672, -9.564922557960803928, 93.33224293864769550 ) ) ;
#132267 = CARTESIAN_POINT ( 'NONE',  ( 9.474510206698971260, -16.51473224551069308, 72.91557627198102409 ) ) ;
#132268 = CARTESIAN_POINT ( 'NONE',  ( -15.72974639402197994, 15.80617190586746368, 80.62390960531438111 ) ) ;
#132269 = CARTESIAN_POINT ( 'NONE',  ( 19.02544592524343514, -5.153800228976328945, 43.54057627198103120 ) ) ;
#132270 = CARTESIAN_POINT ( 'NONE',  ( 30.62874253898671384, 20.86932501997322476, -8.000000000000003553 ) ) ;
#132271 = CARTESIAN_POINT ( 'NONE',  ( 16.52544592524342804, -4.483927247898539470, 53.54057627198103120 ) ) ;
#132272 = CARTESIAN_POINT ( 'NONE',  ( -19.03943276465977164, 0.05219959533909376836, 106.2489096053143669 ) ) ;
#132273 = DIRECTION ( 'NONE',  ( -1.000000000000000000, 0.000000000000000000, 0.000000000000000000 ) ) ;
#132274 = CARTESIAN_POINT ( 'NONE',  ( 13.97604488694548053, -13.89961937509957401, 70.62609039468567573 ) ) ;
#132275 = CARTESIAN_POINT ( 'NONE',  ( 0.05219959533907565091, 21.53943276465977519, 89.99890960531438111 ) ) ;
#132276 = CARTESIAN_POINT ( 'NONE',  ( -19.02544592524334988, -5.153800228976617603, 48.95942372801900433 ) ) ;
#132277 = CARTESIAN_POINT ( 'NONE',  ( 5.153800228976335163, 19.02544592524342804, 94.79057627198103830 ) ) ;
#132278 = CARTESIAN_POINT ( 'NONE',  ( 7.992609269207028790E-30, -165.0000000000000000, -15.00000000000000000 ) ) ;
#132279 = CARTESIAN_POINT ( 'NONE',  ( -15.80617190586745835, -15.72974639402198527, 41.87390960531435979 ) ) ;
#132280 = CARTESIAN_POINT ( 'NONE',  ( 19.03943276465977164, -0.05219959533909143690, 78.74890960531436690 ) ) ;
#132281 = CARTESIAN_POINT ( 'NONE',  ( 21.53943276465977519, 0.05219959533937863772, 71.25109039468568994 ) ) ;
#132282 = CARTESIAN_POINT ( 'NONE',  ( 9.564922557960805705, 16.46253265017160317, 39.58224293864768839 ) ) ;
#132284 = ORIENTED_EDGE ( 'NONE', *, *, #143733, .F. ) ;
#132283 = CARTESIAN_POINT ( 'NONE',  ( 16.52544592524342804, -4.483927247898539470, 73.54057627198102409 ) ) ;
#132285 = CARTESIAN_POINT ( 'NONE',  ( 12.06949235617739724, 12.14591786802326823, 26.87609039468567218 ) ) ;
#132286 = CARTESIAN_POINT ( 'NONE',  ( -10.81492255796105439, 18.62759615963255655, 57.91775706135234714 ) ) ;
#132287 = ORIENTED_EDGE ( 'NONE', *, *, #70955, .F. ) ;
#132288 = CARTESIAN_POINT ( 'NONE',  ( -28.67965155328242233, -2.583289564940497218, 139.9999999999999716 ) ) ;
#132289 = CARTESIAN_POINT ( 'NONE',  ( 13.97604488694548053, -13.89961937509957401, 70.62609039468567573 ) ) ;
#132290 = DIRECTION ( 'NONE',  ( 0.000000000000000000, 0.000000000000000000, 1.000000000000000000 ) ) ;
#132291 = CARTESIAN_POINT ( 'NONE',  ( 10.81492255796106328, -18.62759615963255655, 25.41775706135235779 ) ) ;
#132292 = CARTESIAN_POINT ( 'NONE',  ( 5.153800228976335163, 19.02544592524342804, 59.79057627198100988 ) ) ;
#132293 = CARTESIAN_POINT ( 'NONE',  ( -0.05219959533934338120, 16.53943276465976808, 42.50109039468567573 ) ) ;
#132294 = CARTESIAN_POINT ( 'NONE',  ( 38.00000000000000000, 12.34694845685046616, -8.649999994537624914 ) ) ;
#132295 = CARTESIAN_POINT ( 'NONE',  ( -9.564922557961040184, 16.46253265017147172, 22.91775706135233648 ) ) ;
#132296 = CARTESIAN_POINT ( 'NONE',  ( -13.97604488694527625, -13.89961937509977652, 41.87390960531435979 ) ) ;
#132297 = CARTESIAN_POINT ( 'NONE',  ( 5.823673210054444382, -21.52544592524334988, 110.2094237280190185 ) ) ;
#132298 = CARTESIAN_POINT ( 'NONE',  ( 16.52544592524335698, 4.483927247898782831, 96.45942372801901854 ) ) ;
#132300 = CARTESIAN_POINT ( 'NONE',  ( -21.55341960407619339, 5.719274019375674811, 68.54275706135234714 ) ) ;
#132299 = CARTESIAN_POINT ( 'NONE',  ( -16.46253265017160317, 9.564922557960807481, 105.8322429386476955 ) ) ;
#132301 = CARTESIAN_POINT ( 'NONE',  ( -36.91746825000000598, 2.428612866367529932E-14, -10.62499999726881406 ) ) ;
#132302 = CARTESIAN_POINT ( 'NONE',  ( -19.03943276465977164, 0.05219959533909376836, 111.2489096053143669 ) ) ;
#132303 = DIRECTION ( 'NONE',  ( 0.000000000000000000, 0.000000000000000000, -1.000000000000000000 ) ) ;
#132305 = CARTESIAN_POINT ( 'NONE',  ( 5.823673210054444382, -21.52544592524334988, 70.20942372801904696 ) ) ;
#132304 = CARTESIAN_POINT ( 'NONE',  ( -8.224510206698735004, -14.34966873604973081, 54.58442372801901143 ) ) ;
#132306 = CARTESIAN_POINT ( 'NONE',  ( -15.72974639402176322, -15.80617190586768395, 99.37609039468568994 ) ) ;
#132307 = CARTESIAN_POINT ( 'NONE',  ( -9.687362902255733488, 9.687362902255692632, -60.44446360152740993 ) ) ;
#132308 = CARTESIAN_POINT ( 'NONE',  ( 16.52544592524335698, 4.483927247898782831, 31.45942372801901854 ) ) ;
#132309 = CARTESIAN_POINT ( 'NONE',  ( 19.03943276465977164, -0.05219959533909143690, 83.74890960531436690 ) ) ;
#132310 = CARTESIAN_POINT ( 'NONE',  ( 19.05341960407611168, 5.049401038298154454, 108.9572429386477097 ) ) ;
#132311 = ORIENTED_EDGE ( 'NONE', *, *, #140339, .F. ) ;
#132312 = CARTESIAN_POINT ( 'NONE',  ( 16.21995358207306026, 7.366697692864113911, 42.56448998487845614 ) ) ;
#132313 = CARTESIAN_POINT ( 'NONE',  ( 19.05341960407611168, 5.049401038298154454, 33.95724293864769550 ) ) ;
#132314 = CARTESIAN_POINT ( 'NONE',  ( 18.62759615963271287, -10.81492255796078972, 48.33224293864770260 ) ) ;
#132315 = CARTESIAN_POINT ( 'NONE',  ( -16.55341960407617563, 4.379528057220093196, 108.5427570613523756 ) ) ;
#132317 = CARTESIAN_POINT ( 'NONE',  ( -19.02544592524342804, 5.153800228976336051, 66.04057627198103830 ) ) ;
#132316 = CARTESIAN_POINT ( 'NONE',  ( 14.34966873604960469, 8.224510206698951720, 89.16557627198102409 ) ) ;
#132318 = CARTESIAN_POINT ( 'NONE',  ( 5.823673210054444382, -21.52544592524334988, 100.2094237280190043 ) ) ;
#132319 = CARTESIAN_POINT ( 'NONE',  ( 12.06949235617739724, 12.14591786802326823, 26.87609039468567218 ) ) ;
#132320 = CARTESIAN_POINT ( 'NONE',  ( -12.06949235617756955, 12.14591786802309770, 85.62390960531436690 ) ) ;
#132321 = CARTESIAN_POINT ( 'NONE',  ( 5.823673210054444382, -21.52544592524334988, 35.20942372801901854 ) ) ;
#132322 = CARTESIAN_POINT ( 'NONE',  ( 15.80617190586746368, 15.72974639402197994, 69.37390960531436690 ) ) ;
#132323 = CARTESIAN_POINT ( 'NONE',  ( 19.02544592524334988, 5.153800228976608722, 56.45942372801898301 ) ) ;
#132324 = CARTESIAN_POINT ( 'NONE',  ( -34.67272174748971736, 7.108278434163710635, 42.55803597338269384 ) ) ;
#132325 = CARTESIAN_POINT ( 'NONE',  ( 5.049401038298161559, -19.05341960407611168, 102.7072429386476955 ) ) ;
#132326 = CARTESIAN_POINT ( 'NONE',  ( 4.483927247898545687, 16.52544592524342804, 69.79057627198102409 ) ) ;
#132327 = CIRCLE ( 'NONE', #35466, 3.799999999999999378 ) ;
#132328 = CARTESIAN_POINT ( 'NONE',  ( 14.29746914071049879, -8.314922557960816363, 48.33224293864770260 ) ) ;
#132329 = CARTESIAN_POINT ( 'NONE',  ( -4.483927247898782831, 16.52544592524335698, 112.7094237280190328 ) ) ;
#132330 = CARTESIAN_POINT ( 'NONE',  ( 9.474510206698729675, 16.51473224551082808, 72.08442372801900433 ) ) ;
#132331 = CARTESIAN_POINT ( 'NONE',  ( -19.26498983726237313, 5.499999999999802824, 85.55319577422001487 ) ) ;
#132332 = CARTESIAN_POINT ( 'NONE',  ( 21.55341960407610458, 5.719274019375980345, 23.95724293864769550 ) ) ;
#132333 = CARTESIAN_POINT ( 'NONE',  ( -14.34966873604960291, -8.224510206698953496, 86.66557627198102409 ) ) ;
#132334 = DIRECTION ( 'NONE',  ( -0.000000000000000000, -0.000000000000000000, 1.000000000000000000 ) ) ;
#132336 = CARTESIAN_POINT ( 'NONE',  ( -15.80617190586745835, -15.72974639402198527, 51.87390960531437401 ) ) ;
#132335 = CARTESIAN_POINT ( 'NONE',  ( -19.03943276465977164, 0.05219959533909376836, 51.24890960531436690 ) ) ;
#132337 = CARTESIAN_POINT ( 'NONE',  ( -5.049401038298153566, 19.05341960407611168, 25.20724293864768484 ) ) ;
#132339 = CARTESIAN_POINT ( 'NONE',  ( 19.05341960407611168, 5.049401038298154454, 58.95724293864768129 ) ) ;
#132338 = CARTESIAN_POINT ( 'NONE',  ( -0.05219959533934338120, 16.53943276465976808, 67.50109039468568994 ) ) ;
#132340 = CARTESIAN_POINT ( 'NONE',  ( 5.153800228976615827, -19.02544592524334988, 35.20942372801899722 ) ) ;
#132341 = CARTESIAN_POINT ( 'NONE',  ( -10.72451020669870658, -18.67979575497194134, 49.58442372801901143 ) ) ;
#132342 = CARTESIAN_POINT ( 'NONE',  ( 5.719274019375991003, -21.55341960407610458, 42.70724293864770260 ) ) ;
#132343 = CARTESIAN_POINT ( 'NONE',  ( 14.34966873604960469, 8.224510206698951720, 99.16557627198100988 ) ) ;
#132344 = CARTESIAN_POINT ( 'NONE',  ( -19.02544592524334988, -5.153800228976617603, 93.95942372801900433 ) ) ;
#132345 = CARTESIAN_POINT ( 'NONE',  ( 36.91746824999999177, 2.880721459617395097E-14, -6.124999997268813168 ) ) ;
#132347 = CARTESIAN_POINT ( 'NONE',  ( -15.80617190586745835, -15.72974639402198527, 46.87390960531435979 ) ) ;
#132346 = CARTESIAN_POINT ( 'NONE',  ( -40.00200000000003087, -1.163414459189985801E-14, 95.00000000000000000 ) ) ;
#132348 = CARTESIAN_POINT ( 'NONE',  ( -13.89961937509977652, 13.97604488694528158, 25.62390960531434558 ) ) ;
#132349 = CARTESIAN_POINT ( 'NONE',  ( -15.80617190586768217, 15.72974639402176855, 88.12609039468570415 ) ) ;
#132350 = CARTESIAN_POINT ( 'NONE',  ( 16.52544592524342804, -4.483927247898539470, 48.54057627198103120 ) ) ;
#132352 = CARTESIAN_POINT ( 'NONE',  ( 16.55341960407611168, 4.379528057220329451, 53.95724293864770260 ) ) ;
#132351 = CARTESIAN_POINT ( 'NONE',  ( -14.29746914071037622, -8.314922557961029526, 59.16775706135234714 ) ) ;
#132353 = CARTESIAN_POINT ( 'NONE',  ( 15.72974639402199770, -15.80617190586745480, 83.12390960531436690 ) ) ;
#132354 = CARTESIAN_POINT ( 'NONE',  ( -10.72451020669898014, 18.67979575497178502, 70.41557627198102409 ) ) ;
#132355 = DIRECTION ( 'NONE',  ( 1.000000000000000000, 0.000000000000000000, 3.709348145883536076E-20 ) ) ;
#132357 = CARTESIAN_POINT ( 'NONE',  ( -15.80617190586745835, -15.72974639402198527, 21.87390960531436690 ) ) ;
#132356 = CARTESIAN_POINT ( 'NONE',  ( 13.89961937509957401, 13.97604488694547697, 86.87609039468567573 ) ) ;
#132358 = EDGE_CURVE ( 'NONE', #19818, #31363, #82020, .T. ) ;
#132359 = CARTESIAN_POINT ( 'NONE',  ( 19.02544592524343514, -5.153800228976328945, 63.54057627198103830 ) ) ;
#132360 = CARTESIAN_POINT ( 'NONE',  ( 19.05341960407611168, 5.049401038298154454, 28.95724293864769550 ) ) ;
#132361 = CARTESIAN_POINT ( 'NONE',  ( 17.49999999999999289, 5.500000000000006217, 48.78230962303565121 ) ) ;
#132362 = ORIENTED_EDGE ( 'NONE', *, *, #98398, .T. ) ;
#132363 = CARTESIAN_POINT ( 'NONE',  ( -16.55341960407617563, 4.379528057220093196, 88.54275706135236135 ) ) ;
#132364 = CARTESIAN_POINT ( 'NONE',  ( -15.80617190586768217, 15.72974639402176855, 23.12609039468567573 ) ) ;
#132365 = CARTESIAN_POINT ( 'NONE',  ( 16.46253265017160672, -9.564922557960803928, 63.33224293864769550 ) ) ;
#132366 = CARTESIAN_POINT ( 'NONE',  ( 5.823673210054444382, -21.52544592524334988, 50.20942372801901854 ) ) ;
#132367 = CARTESIAN_POINT ( 'NONE',  ( -5.153800228976328057, -19.02544592524343514, 102.2905762719810383 ) ) ;
#132368 = CARTESIAN_POINT ( 'NONE',  ( -23.77862661291642610, -32.55609251395267734, -17.57696395782127752 ) ) ;
#132369 = ORIENTED_EDGE ( 'NONE', *, *, #52560, .F. ) ;
#132370 = CARTESIAN_POINT ( 'NONE',  ( -5.823673210054431948, 21.52544592524334988, 42.70942372801901854 ) ) ;
#132372 = CARTESIAN_POINT ( 'NONE',  ( 19.02544592524343514, -5.153800228976328945, 108.5405762719810383 ) ) ;
#132371 = CARTESIAN_POINT ( 'NONE',  ( -19.05341960407611168, -5.049401038298163336, 21.45724293864768839 ) ) ;
#132373 = CARTESIAN_POINT ( 'NONE',  ( -16.46253265017146816, -9.564922557961047289, 54.16775706135234003 ) ) ;
#132374 = CARTESIAN_POINT ( 'NONE',  ( 21.55341960407610458, 5.719274019375980345, 113.9572429386477239 ) ) ;
#132375 = CARTESIAN_POINT ( 'NONE',  ( -19.03943276465977164, -0.05219959533935918106, 43.75109039468566863 ) ) ;
#132376 = CARTESIAN_POINT ( 'NONE',  ( 13.97604488694548053, -13.89961937509957401, 45.62609039468566863 ) ) ;
#132377 = CARTESIAN_POINT ( 'NONE',  ( -14.34966873604972548, 8.224510206698743886, 108.3344237280190185 ) ) ;
#132379 = VERTEX_POINT ( 'NONE', #161718 ) ;
#132378 = CARTESIAN_POINT ( 'NONE',  ( 9.455153793104345894, 11.51446144058595422, -62.12179458070791327 ) ) ;
#132380 = CARTESIAN_POINT ( 'NONE',  ( 9.474510206698971260, -16.51473224551069308, 72.91557627198102409 ) ) ;
#132381 = CARTESIAN_POINT ( 'NONE',  ( -5.823673210054431948, 21.52544592524334988, 77.70942372801900433 ) ) ;
#132382 = CARTESIAN_POINT ( 'NONE',  ( 21.53943276465977519, 0.05219959533937863772, 91.25109039468568994 ) ) ;
#132383 = CARTESIAN_POINT ( 'NONE',  ( -1.203296689329353519, -8.516692751257727068, -64.06477955746662190 ) ) ;
#132384 = CARTESIAN_POINT ( 'NONE',  ( -5.049401038298153566, 19.05341960407611168, 85.20724293864766707 ) ) ;
#132385 = CARTESIAN_POINT ( 'NONE',  ( 10.72451020669871369, 18.67979575497193778, 82.08442372801901854 ) ) ;
#132386 = CARTESIAN_POINT ( 'NONE',  ( -0.05219959533936034679, 19.03943276465977164, 112.5010903946856757 ) ) ;
#132387 = CARTESIAN_POINT ( 'NONE',  ( 0.05219959533909260263, 19.03943276465977164, 74.99890960531435269 ) ) ;
#132388 = CARTESIAN_POINT ( 'NONE',  ( -19.03943276465977164, 0.05219959533909376836, 111.2489096053143669 ) ) ;
#132389 = CARTESIAN_POINT ( 'NONE',  ( 16.51473224551069308, 9.474510206698969483, 89.16557627198103830 ) ) ;
#132390 = DIRECTION ( 'NONE',  ( 1.000000000000000000, 0.000000000000000000, 0.000000000000000000 ) ) ;
#132391 = CARTESIAN_POINT ( 'NONE',  ( -5.153800228976328057, -19.02544592524343514, 82.29057627198103830 ) ) ;
#132392 = CARTESIAN_POINT ( 'NONE',  ( 19.02544592524343514, -5.153800228976328945, 63.54057627198103830 ) ) ;
#132393 = CARTESIAN_POINT ( 'NONE',  ( -15.80617190586745835, -15.72974639402198527, 106.8739096053143811 ) ) ;
#132394 = CARTESIAN_POINT ( 'NONE',  ( -14.34966873604972548, 8.224510206698743886, 98.33442372801901854 ) ) ;
#132395 = CARTESIAN_POINT ( 'NONE',  ( 0.000000000000000000, -105.0000000000000000, 5.497848452431111532 ) ) ;
#132396 = CARTESIAN_POINT ( 'NONE',  ( 19.02544592524334988, 5.153800228976608722, 51.45942372801900433 ) ) ;
#132397 = CARTESIAN_POINT ( 'NONE',  ( 19.02544592524343514, -5.153800228976328945, 93.54057627198102409 ) ) ;
#132398 = CARTESIAN_POINT ( 'NONE',  ( -8.224510206698948167, 14.34966873604960824, 85.41557627198102409 ) ) ;
#132399 = CARTESIAN_POINT ( 'NONE',  ( 13.97604488694527802, 13.89961937509977652, 24.37390960531435624 ) ) ;
#132400 = CARTESIAN_POINT ( 'NONE',  ( 5.719274019375991003, -21.55341960407610458, 27.70724293864769905 ) ) ;
#132401 = CARTESIAN_POINT ( 'NONE',  ( 18.62759615963271287, -10.81492255796078972, 23.33224293864769194 ) ) ;
#132402 = CARTESIAN_POINT ( 'NONE',  ( -4.379528057220328563, 16.55341960407611168, 95.20724293864769550 ) ) ;
#132403 = CARTESIAN_POINT ( 'NONE',  ( -3.573655867282028392E-15, 2.428612866367529932E-14, 167.9999999999999716 ) ) ;
#132404 = CARTESIAN_POINT ( 'NONE',  ( -19.03943276465977164, -0.05219959533935918106, 48.75109039468566863 ) ) ;
#132405 = CARTESIAN_POINT ( 'NONE',  ( 4.379528057220092307, 16.55341960407617563, 102.2927570613523613 ) ) ;
#132407 = EDGE_CURVE ( 'NONE', #171657, #65708, #98186, .T. ) ;
#132406 = CARTESIAN_POINT ( 'NONE',  ( -5.153800228976328057, -19.02544592524343514, 82.29057627198103830 ) ) ;
#132408 = CARTESIAN_POINT ( 'NONE',  ( -18.67979575497193778, 10.72451020669871902, 63.33442372801900433 ) ) ;
#132409 = CARTESIAN_POINT ( 'NONE',  ( 0.05219959533907565091, 21.53943276465977519, 44.99890960531435979 ) ) ;
#132410 = CARTESIAN_POINT ( 'NONE',  ( 18.62759615963255655, 10.81492255796105972, 36.66775706135234714 ) ) ;
#132411 = CARTESIAN_POINT ( 'NONE',  ( 0.05219959533907565091, 21.53943276465977519, 79.99890960531435269 ) ) ;
#132412 = CARTESIAN_POINT ( 'NONE',  ( 16.55341960407611168, 4.379528057220329451, 103.9572429386476813 ) ) ;
#132413 = CARTESIAN_POINT ( 'NONE',  ( 13.89961937509957401, 13.97604488694547697, 71.87609039468567573 ) ) ;
#132414 = CARTESIAN_POINT ( 'NONE',  ( -13.97604488694527625, -13.89961937509977652, 41.87390960531435979 ) ) ;
#132415 = CARTESIAN_POINT ( 'NONE',  ( 5.049401038298161559, -19.05341960407611168, 92.70724293864769550 ) ) ;
#132416 = CARTESIAN_POINT ( 'NONE',  ( -19.03943276465977164, 0.05219959533909376836, 101.2489096053143669 ) ) ;
#132417 = CARTESIAN_POINT ( 'NONE',  ( -9.564922557960796823, -16.46253265017161027, 22.08224293864768839 ) ) ;
#132418 = CARTESIAN_POINT ( 'NONE',  ( 4.379528057220339221, -16.55341960407611168, 42.70724293864770260 ) ) ;
#132419 = CARTESIAN_POINT ( 'NONE',  ( 12.06949235617739724, 12.14591786802326823, 36.87609039468568994 ) ) ;
#132420 = CARTESIAN_POINT ( 'NONE',  ( -10.81492255796105439, 18.62759615963255655, 112.9177570613523329 ) ) ;
#132422 = CARTESIAN_POINT ( 'NONE',  ( -16.55341960407611168, -4.379528057220339221, 21.45724293864769550 ) ) ;
#132421 = DIRECTION ( 'NONE',  ( 0.000000000000000000, 1.000000000000000000, 0.000000000000000000 ) ) ;
#132423 = CARTESIAN_POINT ( 'NONE',  ( -18.62759615963255300, -10.81492255796106328, 34.16775706135234714 ) ) ;
#132424 = CARTESIAN_POINT ( 'NONE',  ( 5.049401038298161559, -19.05341960407611168, 102.7072429386476955 ) ) ;
#132425 = CARTESIAN_POINT ( 'NONE',  ( -12.14591786802326823, 12.06949235617739902, 108.1260903946856757 ) ) ;
#132426 = CARTESIAN_POINT ( 'NONE',  ( 4.379528057220092307, 16.55341960407617563, 97.29275706135234714 ) ) ;
#132427 = CARTESIAN_POINT ( 'NONE',  ( 4.483927247898790824, -16.52544592524335698, 25.20942372801901854 ) ) ;
#132428 = CARTESIAN_POINT ( 'NONE',  ( 19.05341960407611168, 5.049401038298154454, 53.95724293864770260 ) ) ;
#132429 = CARTESIAN_POINT ( 'NONE',  ( -4.379528057220328563, 16.55341960407611168, 105.2072429386477097 ) ) ;
#132430 = CARTESIAN_POINT ( 'NONE',  ( 18.62759615963255655, 10.81492255796105972, 21.66775706135235069 ) ) ;
#132431 = CARTESIAN_POINT ( 'NONE',  ( 5.153800228976335163, 19.02544592524342804, 34.79057627198102409 ) ) ;
#132432 = CARTESIAN_POINT ( 'NONE',  ( 19.03943276465977164, -0.05219959533909143690, 108.7489096053143527 ) ) ;
#132433 = CARTESIAN_POINT ( 'NONE',  ( -18.67979575497193778, 10.72451020669871902, 38.33442372801900433 ) ) ;
#132434 = CARTESIAN_POINT ( 'NONE',  ( 19.03943276465977164, -0.05219959533909143690, 28.74890960531435624 ) ) ;
#132435 = CARTESIAN_POINT ( 'NONE',  ( -13.97604488694527625, -13.89961937509977652, 106.8739096053143669 ) ) ;
#132436 = CARTESIAN_POINT ( 'NONE',  ( -16.36317988757060604, -7.306389748694898323, 35.90210391636776421 ) ) ;
#132437 = AXIS2_PLACEMENT_3D ( 'NONE', #44639, #140606, #107278 ) ;
#132438 = CARTESIAN_POINT ( 'NONE',  ( -0.05219959533909027116, -19.03943276465977164, 97.49890960531436690 ) ) ;
#132440 = CARTESIAN_POINT ( 'NONE',  ( 12.06949235617757843, -12.14591786802309237, 88.12390960531436690 ) ) ;
#132439 = CARTESIAN_POINT ( 'NONE',  ( -21.52544592524334988, -5.823673210054445271, 48.95942372801902565 ) ) ;
#132441 = CARTESIAN_POINT ( 'NONE',  ( 19.05341960407611168, 5.049401038298154454, 98.95724293864766707 ) ) ;
#132442 = CARTESIAN_POINT ( 'NONE',  ( -27.95311704539973974, -7.352561457324001459, 160.8984504615040976 ) ) ;
#132443 = CARTESIAN_POINT ( 'NONE',  ( 12.06949235617739724, 12.14591786802326823, 66.87609039468568994 ) ) ;
#132444 = CARTESIAN_POINT ( 'NONE',  ( -21.52544592524334988, -5.823673210054445271, 78.95942372801901854 ) ) ;
#132445 = CARTESIAN_POINT ( 'NONE',  ( 14.34966873604972726, -8.224510206698740333, 35.83442372801901143 ) ) ;
#132446 = CARTESIAN_POINT ( 'NONE',  ( -13.97604488694527625, -13.89961937509977652, 76.87390960531433848 ) ) ;
#132447 = CARTESIAN_POINT ( 'NONE',  ( -12.06949235617739369, -12.14591786802326823, 19.37609039468568639 ) ) ;
#132448 = CARTESIAN_POINT ( 'NONE',  ( 12.06949235617739724, 12.14591786802326823, 71.87609039468568994 ) ) ;
#132449 = CARTESIAN_POINT ( 'NONE',  ( -19.05341960407617563, 5.049401038297882671, 88.54275706135230450 ) ) ;
#132450 = CARTESIAN_POINT ( 'NONE',  ( 5.153800228976335163, 19.02544592524342804, 64.79057627198100988 ) ) ;
#132451 = CARTESIAN_POINT ( 'NONE',  ( -18.62759615963270932, 10.81492255796079327, 90.83224293864769550 ) ) ;
#132453 = CARTESIAN_POINT ( 'NONE',  ( -16.46253265017146816, -9.564922557961047289, 94.16775706135233293 ) ) ;
#132452 = CARTESIAN_POINT ( 'NONE',  ( 12.06949235617757843, -12.14591786802309237, 93.12390960531436690 ) ) ;
#132454 = CARTESIAN_POINT ( 'NONE',  ( -14.34966873604972548, 8.224510206698743886, 53.33442372801901854 ) ) ;
#132455 = CARTESIAN_POINT ( 'NONE',  ( -19.48894818550246200, 5.499999999999919176, 80.10307310435239003 ) ) ;
#132456 = CARTESIAN_POINT ( 'NONE',  ( -5.153800228976607833, 19.02544592524334988, 62.70942372801899722 ) ) ;
#132457 = CARTESIAN_POINT ( 'NONE',  ( -12.06949235617756955, 12.14591786802309770, 35.62390960531437401 ) ) ;
#132458 = CARTESIAN_POINT ( 'NONE',  ( 16.53943276465976808, -0.05219959533910856209, 73.74890960531433848 ) ) ;
#132460 = CARTESIAN_POINT ( 'NONE',  ( -17.05116617787847844, 6.768360034955528626, 38.65675553259191588 ) ) ;
#132459 = CARTESIAN_POINT ( 'NONE',  ( 19.02544592524334988, 5.153800228976608722, 21.45942372801899012 ) ) ;
#132461 = CARTESIAN_POINT ( 'NONE',  ( 5.823673210054444382, -21.52544592524334988, 20.20942372801900788 ) ) ;
#132462 = CARTESIAN_POINT ( 'NONE',  ( -69.65682714487590488, -71.74905178543390605, 8.936314941956774358E-29 ) ) ;
#132463 = CARTESIAN_POINT ( 'NONE',  ( -19.03943276465977164, 0.05219959533909376836, 76.24890960531435269 ) ) ;
#132464 = CARTESIAN_POINT ( 'NONE',  ( 5.823673210054444382, -21.52544592524334988, 100.2094237280190043 ) ) ;
#132465 = CARTESIAN_POINT ( 'NONE',  ( -9.474510206698964154, 16.51473224551069663, 80.41557627198103830 ) ) ;
#132466 = CARTESIAN_POINT ( 'NONE',  ( 15.72974639402199770, -15.80617190586745480, 43.12390960531435269 ) ) ;
#132467 = CARTESIAN_POINT ( 'NONE',  ( -14.34966873604960291, -8.224510206698953496, 76.66557627198103830 ) ) ;
#132468 = CARTESIAN_POINT ( 'NONE',  ( 19.02544592524343514, -5.153800228976328945, 53.54057627198102409 ) ) ;
#132469 = CARTESIAN_POINT ( 'NONE',  ( 0.05219959533910956823, 16.53943276465976808, 109.9989096053143527 ) ) ;
#132470 = CARTESIAN_POINT ( 'NONE',  ( -18.62759615963255300, -10.81492255796106328, 19.16775706135234714 ) ) ;
#132471 = AXIS2_PLACEMENT_3D ( 'NONE', #77211, #185393, #78193 ) ;
#132472 = CARTESIAN_POINT ( 'NONE',  ( 21.52544592524334988, 5.823673210054432836, 66.45942372801903275 ) ) ;
#132473 = CARTESIAN_POINT ( 'NONE',  ( -19.05341960407611168, -5.049401038298163336, 46.45724293864768129 ) ) ;
#132474 = EDGE_CURVE ( 'NONE', #106381, #23056, #27032, .T. ) ;
#132475 = CARTESIAN_POINT ( 'NONE',  ( -16.55341960407617563, 4.379528057220093196, 63.54275706135234003 ) ) ;
#132476 = CARTESIAN_POINT ( 'NONE',  ( -5.823673210054431948, 21.52544592524334988, 22.70942372801901499 ) ) ;
#132477 = CARTESIAN_POINT ( 'NONE',  ( -18.62759615963255300, -10.81492255796106328, 19.16775706135234714 ) ) ;
#132479 = CARTESIAN_POINT ( 'NONE',  ( 16.51473224551069308, 9.474510206698969483, 69.16557627198102409 ) ) ;
#132478 = CARTESIAN_POINT ( 'NONE',  ( -5.049401038297874678, -19.05341960407617918, 44.79275706135232582 ) ) ;
#132480 = CARTESIAN_POINT ( 'NONE',  ( -18.22780087662119541, 5.500000000000102141, 41.01763182126894236 ) ) ;
#132481 = CARTESIAN_POINT ( 'NONE',  ( 0.05219959533937995610, -21.53943276465977519, 65.00109039468568994 ) ) ;
#132482 = CARTESIAN_POINT ( 'NONE',  ( -10.81492255796078084, -18.62759615963271287, 57.08224293864769550 ) ) ;
#132483 = CARTESIAN_POINT ( 'NONE',  ( -14.29746914071049879, 8.314922557960819915, 35.83224293864768839 ) ) ;
#132485 = CARTESIAN_POINT ( 'NONE',  ( 13.89961937509957401, 13.97604488694547697, 21.87609039468566152 ) ) ;
#132484 = CARTESIAN_POINT ( 'NONE',  ( -10.81492255796105439, 18.62759615963255655, 72.91775706135234714 ) ) ;
#132486 = CARTESIAN_POINT ( 'NONE',  ( 14.29746914071049879, -8.314922557960816363, 63.33224293864770260 ) ) ;
#132487 = CARTESIAN_POINT ( 'NONE',  ( -12.06949235617756955, 12.14591786802309770, 110.6239096053143669 ) ) ;
#132488 = CARTESIAN_POINT ( 'NONE',  ( -16.51473224551082808, 9.474510206698731452, 63.33442372801900433 ) ) ;
#132489 = CARTESIAN_POINT ( 'NONE',  ( 14.29746914071049879, -8.314922557960816363, 28.33224293864769550 ) ) ;
#132490 = CARTESIAN_POINT ( 'NONE',  ( 5.719274019375673035, 21.55341960407619339, 72.29275706135236135 ) ) ;
#132491 = CARTESIAN_POINT ( 'NONE',  ( -13.97604488694527625, -13.89961937509977652, 76.87390960531433848 ) ) ;
#132492 = CARTESIAN_POINT ( 'NONE',  ( 0.05219959533936267826, -19.03943276465977164, 30.00109039468566863 ) ) ;
#132493 = CARTESIAN_POINT ( 'NONE',  ( -18.67979575497178146, -10.72451020669898902, 41.66557627198103120 ) ) ;
#132494 = CARTESIAN_POINT ( 'NONE',  ( 18.67979575497194134, -10.72451020669871369, 30.83442372801902209 ) ) ;
#132495 = CARTESIAN_POINT ( 'NONE',  ( 15.72974639402199770, -15.80617190586745480, 93.12390960531436690 ) ) ;
#132496 = CARTESIAN_POINT ( 'NONE',  ( -5.153800228976607833, 19.02544592524334988, 102.7094237280189759 ) ) ;
#132497 = CARTESIAN_POINT ( 'NONE',  ( 16.52544592524335698, 4.483927247898782831, 51.45942372801901854 ) ) ;
#132499 = CARTESIAN_POINT ( 'NONE',  ( 15.72974639402199770, -15.80617190586745480, 93.12390960531436690 ) ) ;
#132498 = DIRECTION ( 'NONE',  ( 0.000000000000000000, 0.000000000000000000, 1.000000000000000000 ) ) ;
#132500 = CARTESIAN_POINT ( 'NONE',  ( 14.29746914071049879, -8.314922557960816363, 93.33224293864769550 ) ) ;
#132501 = CARTESIAN_POINT ( 'NONE',  ( -26.42731554605150635, -26.90581007260913537, -20.33945912742373707 ) ) ;
#132502 = CARTESIAN_POINT ( 'NONE',  ( 16.46253265017146816, 9.564922557961045513, 111.6677570613523329 ) ) ;
#132503 = CARTESIAN_POINT ( 'NONE',  ( -10.81492255796078084, -18.62759615963271287, 52.08224293864768839 ) ) ;
#132504 = CARTESIAN_POINT ( 'NONE',  ( 16.52544592524335698, 4.483927247898782831, 96.45942372801901854 ) ) ;
#132505 = CARTESIAN_POINT ( 'NONE',  ( 13.89961937509977652, -13.97604488694527269, 23.12390960531436335 ) ) ;
#132506 = CARTESIAN_POINT ( 'NONE',  ( 4.379528057220092307, 16.55341960407617563, 47.29275706135234003 ) ) ;
#132507 = CARTESIAN_POINT ( 'NONE',  ( -0.05219959533937732626, 21.53943276465977519, 27.50109039468567929 ) ) ;
#132508 = CARTESIAN_POINT ( 'NONE',  ( 18.62759615963271287, -10.81492255796078972, 48.33224293864770260 ) ) ;
#132509 = CARTESIAN_POINT ( 'NONE',  ( 16.52544592524335698, 4.483927247898782831, 86.45942372801901854 ) ) ;
#132510 = CARTESIAN_POINT ( 'NONE',  ( -9.564922557960796823, -16.46253265017161027, 97.08224293864769550 ) ) ;
#132511 = CARTESIAN_POINT ( 'NONE',  ( -15.80617190586768217, 15.72974639402176855, 68.12609039468567573 ) ) ;
#132512 = CARTESIAN_POINT ( 'NONE',  ( 15.72974639402199770, -15.80617190586745480, 43.12390960531435269 ) ) ;
#132513 = CARTESIAN_POINT ( 'NONE',  ( 13.89961937509977652, -13.97604488694527269, 113.1239096053143527 ) ) ;
#132514 = VERTEX_POINT ( 'NONE', #81850 ) ;
#132515 = CARTESIAN_POINT ( 'NONE',  ( -5.153800228976607833, 19.02544592524334988, 52.70942372801900433 ) ) ;
#132516 = CARTESIAN_POINT ( 'NONE',  ( -14.29746914071037622, -8.314922557961029526, 69.16775706135234714 ) ) ;
#132517 = CARTESIAN_POINT ( 'NONE',  ( -19.02544592524342804, 5.153800228976336051, 116.0405762719810383 ) ) ;
#132518 = ORIENTED_EDGE ( 'NONE', *, *, #48174, .F. ) ;
#132519 = CARTESIAN_POINT ( 'NONE',  ( 16.51473224551069308, 9.474510206698969483, 89.16557627198103830 ) ) ;
#132520 = CARTESIAN_POINT ( 'NONE',  ( 12.14591786802327356, -12.06949235617739191, 100.6260903946857184 ) ) ;
#132521 = CARTESIAN_POINT ( 'NONE',  ( 7.284589286804261654, -1.784589286804270980, 8.181980515339454030 ) ) ;
#132522 = CARTESIAN_POINT ( 'NONE',  ( 16.52544592524342804, -4.483927247898539470, 98.54057627198105251 ) ) ;
#132523 = CARTESIAN_POINT ( 'NONE',  ( -18.62759615963270932, 10.81492255796079327, 50.83224293864770971 ) ) ;
#132524 = CARTESIAN_POINT ( 'NONE',  ( 13.97604488694527802, 13.89961937509977652, 34.37390960531436690 ) ) ;
#132525 = CARTESIAN_POINT ( 'NONE',  ( 16.53943276465976808, 0.05219959533934440121, 71.25109039468568994 ) ) ;
#132526 = CARTESIAN_POINT ( 'NONE',  ( -15.72974639402176322, -15.80617190586768395, 34.37609039468568284 ) ) ;
#132527 = CARTESIAN_POINT ( 'NONE',  ( 19.02544592524334988, 5.153800228976608722, 86.45942372801900433 ) ) ;
#132528 = CARTESIAN_POINT ( 'NONE',  ( -14.34966873604960291, -8.224510206698953496, 91.66557627198103830 ) ) ;
#132529 = CARTESIAN_POINT ( 'NONE',  ( -16.46253265017160317, 9.564922557960807481, 55.83224293864769550 ) ) ;
#132530 = CARTESIAN_POINT ( 'NONE',  ( 0.05219959533909260263, 19.03943276465977164, 114.9989096053143669 ) ) ;
#132531 = CARTESIAN_POINT ( 'NONE',  ( -21.52544592524334988, -5.823673210054445271, 108.9594237280190185 ) ) ;
#132532 = CARTESIAN_POINT ( 'NONE',  ( -0.05219959533909027116, -19.03943276465977164, 77.49890960531435269 ) ) ;
#132533 = CARTESIAN_POINT ( 'NONE',  ( -16.53943276465976808, -0.05219959533934237506, 58.75109039468568994 ) ) ;
#132534 = CARTESIAN_POINT ( 'NONE',  ( -21.53943276465977519, -0.05219959533937600094, 98.75109039468568994 ) ) ;
#132535 = CARTESIAN_POINT ( 'NONE',  ( 8.314922557961029526, -14.29746914071037800, 75.41775706135233293 ) ) ;
#132536 = CARTESIAN_POINT ( 'NONE',  ( 0.05219959533936267826, -19.03943276465977164, 55.00109039468566863 ) ) ;
#132537 = CARTESIAN_POINT ( 'NONE',  ( -5.153800228976607833, 19.02544592524334988, 72.70942372801900433 ) ) ;
#132538 = ORIENTED_EDGE ( 'NONE', *, *, #73698, .T. ) ;
#132539 = CARTESIAN_POINT ( 'NONE',  ( -5.719274019375665041, -21.55341960407619695, 59.79275706135234714 ) ) ;
#132540 = CARTESIAN_POINT ( 'NONE',  ( 16.46253265017160672, -9.564922557960803928, 68.33224293864770971 ) ) ;
#132541 = DIRECTION ( 'NONE',  ( -0.000000000000000000, -0.000000000000000000, -1.000000000000000000 ) ) ;
#132542 = CARTESIAN_POINT ( 'NONE',  ( 0.05219959533936267826, -19.03943276465977164, 65.00109039468567573 ) ) ;
#132543 = CARTESIAN_POINT ( 'NONE',  ( 19.05341960407611168, 5.049401038298154454, 88.95724293864769550 ) ) ;
#132544 = CARTESIAN_POINT ( 'NONE',  ( -4.483927247898539470, -16.52544592524342804, 42.29057627198103120 ) ) ;
#132545 = CARTESIAN_POINT ( 'NONE',  ( 21.55341960407610458, 5.719274019375980345, 53.95724293864770260 ) ) ;
#132546 = CARTESIAN_POINT ( 'NONE',  ( 8.898068258721464119, 27.38543819252877398, 141.3843446568999980 ) ) ;
#132547 = B_SPLINE_CURVE_WITH_KNOTS ( 'NONE', 3,
 ( #71604, #90738, #43264, #167604, #74597, #70611, #133270, #194961, #56438, #118119, #164623, #78550 ),
 .UNSPECIFIED., .F., .F.,
 ( 4, 2, 2, 2, 2, 4 ),
 ( 2.787091001330594030E-07, 0.0009290869694426631643, 0.001857895229785193293, 0.002786703490127723313, 0.003251107620298992334, 0.003715511750470261790 ),
 .UNSPECIFIED. ) ;
#132548 = CARTESIAN_POINT ( 'NONE',  ( 19.02544592524334988, 5.153800228976608722, 21.45942372801899012 ) ) ;
#132549 = CARTESIAN_POINT ( 'NONE',  ( -17.44270441346519007, -5.991230190322953675, 81.36335079264232206 ) ) ;
#132550 = CARTESIAN_POINT ( 'NONE',  ( -19.03943276465977164, 0.05219959533909376836, 36.24890960531436690 ) ) ;
#132551 = CARTESIAN_POINT ( 'NONE',  ( 13.89961937509977652, -13.97604488694527269, 28.12390960531435624 ) ) ;
#132552 = CARTESIAN_POINT ( 'NONE',  ( -18.09805431107249518, 5.499999999999980460, 81.01606229291886052 ) ) ;
#132553 = CARTESIAN_POINT ( 'NONE',  ( 21.53943276465977519, 0.05219959533937863772, 66.25109039468567573 ) ) ;
#132554 = CARTESIAN_POINT ( 'NONE',  ( -23.64874990377911956, -15.04272038711346582, 165.8682408883346397 ) ) ;
#132555 = CARTESIAN_POINT ( 'NONE',  ( -4.483927247898782831, 16.52544592524335698, 62.70942372801902565 ) ) ;
#132556 = CARTESIAN_POINT ( 'NONE',  ( 15.80617190586746368, 15.72974639402197994, 84.37390960531438111 ) ) ;
#132557 = CARTESIAN_POINT ( 'NONE',  ( -8.314922557960811034, -14.29746914071050412, 57.08224293864769550 ) ) ;
#132558 = CARTESIAN_POINT ( 'NONE',  ( 19.02544592524343514, -5.153800228976328945, 33.54057627198102409 ) ) ;
#132559 = CARTESIAN_POINT ( 'NONE',  ( -5.719274019375665041, -21.55341960407619695, 44.79275706135234714 ) ) ;
#132560 = CARTESIAN_POINT ( 'NONE',  ( -9.474510206698720793, -16.51473224551083518, 44.58442372801900433 ) ) ;
#132561 = CARTESIAN_POINT ( 'NONE',  ( 9.474510206698971260, -16.51473224551069308, 27.91557627198103120 ) ) ;
#132562 = CARTESIAN_POINT ( 'NONE',  ( 5.823673210054444382, -21.52544592524334988, 85.20942372801901854 ) ) ;
#132563 = CARTESIAN_POINT ( 'NONE',  ( 16.18388926212238488, 7.379444403734537694, 97.93953151366152099 ) ) ;
#132564 = CARTESIAN_POINT ( 'NONE',  ( -8.314922557960811034, -14.29746914071050412, 37.08224293864768129 ) ) ;
#132565 = CARTESIAN_POINT ( 'NONE',  ( 17.50000000000000711, 3.237210098469639696, 112.7876301262046894 ) ) ;
#132566 = CARTESIAN_POINT ( 'NONE',  ( -0.05219959533907301413, -21.53943276465977519, 47.49890960531435979 ) ) ;
#132567 = CARTESIAN_POINT ( 'NONE',  ( 27.73933785331498925, -9.013057229001034898, 141.7750000027311899 ) ) ;
#132568 = CARTESIAN_POINT ( 'NONE',  ( 9.564922557960805705, 16.46253265017160317, 89.58224293864769550 ) ) ;
#132569 = CARTESIAN_POINT ( 'NONE',  ( -14.34966873604960291, -8.224510206698953496, 91.66557627198103830 ) ) ;
#132570 = CARTESIAN_POINT ( 'NONE',  ( 4.483927247898790824, -16.52544592524335698, 30.20942372801902565 ) ) ;
#132571 = CARTESIAN_POINT ( 'NONE',  ( -5.719274019375978568, 21.55341960407610458, 60.20724293864768839 ) ) ;
#132572 = VERTEX_POINT ( 'NONE', #99026 ) ;
#132573 = CARTESIAN_POINT ( 'NONE',  ( -13.97604488694527625, -13.89961937509977652, 31.87390960531435979 ) ) ;
#132574 = EDGE_CURVE ( 'NONE', #31363, #171664, #134200, .T. ) ;
#132576 = CARTESIAN_POINT ( 'NONE',  ( 21.52544592524344225, -5.823673210054117533, 83.54057627198102409 ) ) ;
#132575 = CARTESIAN_POINT ( 'NONE',  ( 13.97604488694527802, 13.89961937509977652, 79.37390960531435269 ) ) ;
#132578 = CARTESIAN_POINT ( 'NONE',  ( -13.89961937509977652, 13.97604488694528158, 95.62390960531436690 ) ) ;
#132577 = CARTESIAN_POINT ( 'NONE',  ( -8.314922557960811034, -14.29746914071050412, 32.08224293864769550 ) ) ;
#132579 = CARTESIAN_POINT ( 'NONE',  ( 13.89961937509957401, 13.97604488694547697, 76.87609039468566152 ) ) ;
#132580 = CARTESIAN_POINT ( 'NONE',  ( -16.46253265017146816, -9.564922557961047289, 19.16775706135233293 ) ) ;
#132581 = CARTESIAN_POINT ( 'NONE',  ( -0.05219959533907301413, -21.53943276465977519, 82.49890960531436690 ) ) ;
#132582 = CARTESIAN_POINT ( 'NONE',  ( -0.05219959533907301413, -21.53943276465977519, 42.49890960531435979 ) ) ;
#132583 = CARTESIAN_POINT ( 'NONE',  ( -13.97604488694527625, -13.89961937509977652, 51.87390960531436690 ) ) ;
#132584 = CARTESIAN_POINT ( 'NONE',  ( -14.34966873604972548, 8.224510206698743886, 113.3344237280190328 ) ) ;
#132585 = CARTESIAN_POINT ( 'NONE',  ( 16.51473224551069308, 9.474510206698969483, 79.16557627198103830 ) ) ;
#132586 = ORIENTED_EDGE ( 'NONE', *, *, #13873, .F. ) ;
#132587 = CARTESIAN_POINT ( 'NONE',  ( -19.02544592524334988, -5.153800228976617603, 28.95942372801900433 ) ) ;
#132588 = CARTESIAN_POINT ( 'NONE',  ( 12.06949235617757843, -12.14591786802309237, 83.12390960531436690 ) ) ;
#132589 = CARTESIAN_POINT ( 'NONE',  ( 10.81492255796106328, -18.62759615963255655, 30.41775706135234358 ) ) ;
#132590 = CARTESIAN_POINT ( 'NONE',  ( 17.14385361876520264, -23.59649016807271238, 144.0750000027311444 ) ) ;
#132591 = CARTESIAN_POINT ( 'NONE',  ( 10.81492255796078972, 18.62759615963270932, 64.58224293864769550 ) ) ;
#132592 = CARTESIAN_POINT ( 'NONE',  ( 4.379528057220092307, 16.55341960407617563, 87.29275706135236135 ) ) ;
#132593 = CARTESIAN_POINT ( 'NONE',  ( 0.05219959533909260263, 19.03943276465977164, 24.99890960531435269 ) ) ;
#132594 = CARTESIAN_POINT ( 'NONE',  ( -19.03943276465977164, 0.05219959533909376836, 76.24890960531435269 ) ) ;
#132595 = CARTESIAN_POINT ( 'NONE',  ( -19.03943276465977164, 0.05219959533909376836, 21.24890960531436335 ) ) ;
#132596 = CARTESIAN_POINT ( 'NONE',  ( 12.06949235617757843, -12.14591786802309237, 28.12390960531435979 ) ) ;
#132597 = CARTESIAN_POINT ( 'NONE',  ( 21.53943276465977519, 0.05219959533937863772, 61.25109039468567573 ) ) ;
#132598 = CARTESIAN_POINT ( 'NONE',  ( -19.02544592524342804, 5.153800228976336051, 111.0405762719810099 ) ) ;
#132599 = CARTESIAN_POINT ( 'NONE',  ( 5.823673210054444382, -21.52544592524334988, 95.20942372801903275 ) ) ;
#132600 = CARTESIAN_POINT ( 'NONE',  ( 16.51473224551069308, 9.474510206698969483, 39.16557627198103120 ) ) ;
#132601 = CARTESIAN_POINT ( 'NONE',  ( 9.474510206698971260, -16.51473224551069308, 42.91557627198103120 ) ) ;
#132602 =( BOUNDED_CURVE ( )  B_SPLINE_CURVE ( 2, ( #83749, #112116, #96928, #19122, #68589, #97907, #52426, #81744, #22099, #143431, #65608 ),
 .UNSPECIFIED., .F., .F. ) 
 B_SPLINE_CURVE_WITH_KNOTS ( ( 3, 2, 2, 2, 2, 3 ),
 ( 0.000000000000000000, 0.02000000000000000042, 0.04000000000000000083, 0.05999999999999999778, 0.08000000000000000167, 0.1000000000000000194 ),
 .UNSPECIFIED. ) 
 CURVE ( )  GEOMETRIC_REPRESENTATION_ITEM ( )  RATIONAL_B_SPLINE_CURVE ( ( 1.000000000000000000, 0.9510565162951535312, 1.000000000000000000, 0.9510565162951535312, 1.000000000000000000, 0.9510565162951535312, 1.000000000000000000, 0.9510565162951535312, 1.000000000000000000, 0.9510565162951535312, 1.000000000000000000 ) ) 
 REPRESENTATION_ITEM ( '' )  );
#132603 = VERTEX_POINT ( 'NONE', #20204 ) ;
#132604 = CARTESIAN_POINT ( 'NONE',  ( -10.72451020669870658, -18.67979575497194134, 94.58442372801901854 ) ) ;
#132605 = CARTESIAN_POINT ( 'NONE',  ( 12.14591786802327356, -12.06949235617739191, 60.62609039468567573 ) ) ;
#132606 = CARTESIAN_POINT ( 'NONE',  ( 21.55341960407619695, -5.719274019375665929, 81.04275706135236135 ) ) ;
#132607 = CARTESIAN_POINT ( 'NONE',  ( 15.72974639402199770, -15.80617190586745480, 23.12390960531436335 ) ) ;
#132608 = CARTESIAN_POINT ( 'NONE',  ( -19.05341960407617563, 5.049401038297882671, 93.54275706135234714 ) ) ;
#132609 = CARTESIAN_POINT ( 'NONE',  ( -10.72451020669870658, -18.67979575497194134, 59.58442372801901854 ) ) ;
#132610 = CARTESIAN_POINT ( 'NONE',  ( 16.55341960407618274, -4.379528057220086978, 36.04275706135234714 ) ) ;
#132611 = CARTESIAN_POINT ( 'NONE',  ( -0.05219959533936034679, 19.03943276465977164, 87.50109039468567573 ) ) ;
#132612 = CARTESIAN_POINT ( 'NONE',  ( -19.05341960407611168, -5.049401038298163336, 56.45724293864768129 ) ) ;
#132613 = CARTESIAN_POINT ( 'NONE',  ( 19.03943276465977164, 0.05219959533936151252, 96.25109039468567573 ) ) ;
#132614 = EDGE_CURVE ( 'NONE', #144758, #2854, #172855, .T. ) ;
#132615 = VECTOR ( 'NONE', #26276, 1000.000000000000000 ) ;
#132616 = CARTESIAN_POINT ( 'NONE',  ( -5.153800228976607833, 19.02544592524334988, 87.70942372801897591 ) ) ;
#132617 = CARTESIAN_POINT ( 'NONE',  ( 12.14591786802309770, 12.06949235617756955, 54.37390960531435979 ) ) ;
#132618 = CARTESIAN_POINT ( 'NONE',  ( -16.51473224551082808, 9.474510206698731452, 73.33442372801900433 ) ) ;
#132619 = CARTESIAN_POINT ( 'NONE',  ( -12.06949235617739369, -12.14591786802326823, 54.37609039468568994 ) ) ;
#132620 = CARTESIAN_POINT ( 'NONE',  ( 19.05341960407617918, -5.049401038297876454, 21.04275706135232582 ) ) ;
#132621 = CARTESIAN_POINT ( 'NONE',  ( 19.05341960407611168, 5.049401038298154454, 33.95724293864769550 ) ) ;
#132622 = CARTESIAN_POINT ( 'NONE',  ( 19.05341960407611168, 5.049401038298154454, 43.95724293864769550 ) ) ;
#132623 = CARTESIAN_POINT ( 'NONE',  ( 4.379528057220092307, 16.55341960407617563, 57.29275706135234714 ) ) ;
#132624 = CARTESIAN_POINT ( 'NONE',  ( 22.44159573604009239, 16.30477369853692693, 142.5750000027311728 ) ) ;
#132625 = CARTESIAN_POINT ( 'NONE',  ( 22.44159573604009239, 16.30477369853692693, 148.0750000027312012 ) ) ;
#132626 = CARTESIAN_POINT ( 'NONE',  ( -0.05219959533909027116, -19.03943276465977164, 102.4989096053143669 ) ) ;
#132627 = LINE ( 'NONE', #119463, #184630 ) ;
#132628 = VERTEX_POINT ( 'NONE', #83857 ) ;
#132629 = CARTESIAN_POINT ( 'NONE',  ( 19.03943276465977164, 0.05219959533936151252, 101.2510903946856757 ) ) ;
#132630 = CARTESIAN_POINT ( 'NONE',  ( 5.719274019375991003, -21.55341960407610458, 32.70724293864770260 ) ) ;
#132632 = CARTESIAN_POINT ( 'NONE',  ( 16.46253265017146816, 9.564922557961045513, 111.6677570613523329 ) ) ;
#132631 = CARTESIAN_POINT ( 'NONE',  ( 19.05341960407617918, -5.049401038297876454, 31.04275706135232227 ) ) ;
#132633 = CARTESIAN_POINT ( 'NONE',  ( -19.02544592524342804, 5.153800228976336051, 36.04057627198100988 ) ) ;
#132634 = CARTESIAN_POINT ( 'NONE',  ( -0.05219959533909027116, -19.03943276465977164, 37.49890960531436690 ) ) ;
#132635 = CARTESIAN_POINT ( 'NONE',  ( -15.80617190586745835, -15.72974639402198527, 71.87390960531438111 ) ) ;
#132636 = CARTESIAN_POINT ( 'NONE',  ( -0.05219959533909027116, -19.03943276465977164, 102.4989096053143669 ) ) ;
#132637 = CARTESIAN_POINT ( 'NONE',  ( -9.564922557960796823, -16.46253265017161027, 32.08224293864769550 ) ) ;
#132638 = CARTESIAN_POINT ( 'NONE',  ( -5.359611314223446995E-15, 29.16686587814335851, 142.8750000027311842 ) ) ;
#132639 = CARTESIAN_POINT ( 'NONE',  ( 5.049401038297881783, 19.05341960407617563, 87.29275706135234714 ) ) ;
#132640 = CARTESIAN_POINT ( 'NONE',  ( 14.29746914071049879, -8.314922557960816363, 48.33224293864770260 ) ) ;
#132641 = CARTESIAN_POINT ( 'NONE',  ( 0.05219959533907565091, 21.53943276465977519, 39.99890960531436690 ) ) ;
#132642 = CARTESIAN_POINT ( 'NONE',  ( -10.81492255796105439, 18.62759615963255655, 102.9177570613523756 ) ) ;
#132643 = CARTESIAN_POINT ( 'NONE',  ( 18.67979575497178502, 10.72451020669898547, 99.16557627198100988 ) ) ;
#132644 = CARTESIAN_POINT ( 'NONE',  ( 15.72974639402176855, 15.80617190586768217, 76.87609039468567573 ) ) ;
#132645 = CARTESIAN_POINT ( 'NONE',  ( -5.719274019375665041, -21.55341960407619695, 74.79275706135234714 ) ) ;
#132646 = CARTESIAN_POINT ( 'NONE',  ( 13.97604488694527802, 13.89961937509977652, 109.3739096053143669 ) ) ;
#132648 = CARTESIAN_POINT ( 'NONE',  ( 5.823673210054444382, -21.52544592524334988, 65.20942372801901854 ) ) ;
#132647 = CARTESIAN_POINT ( 'NONE',  ( 16.55341960407618274, -4.379528057220086978, 111.0427570613523613 ) ) ;
#132649 = CARTESIAN_POINT ( 'NONE',  ( 19.03943276465977164, -0.05219959533909143690, 58.74890960531435979 ) ) ;
#132650 = CARTESIAN_POINT ( 'NONE',  ( 5.049401038297881783, 19.05341960407617563, 37.29275706135232582 ) ) ;
#132651 = CARTESIAN_POINT ( 'NONE',  ( -0.05219959533937732626, 21.53943276465977519, 32.50109039468568284 ) ) ;
#132652 = CARTESIAN_POINT ( 'NONE',  ( -9.564922557960796823, -16.46253265017161027, 67.08224293864769550 ) ) ;
#132653 = CARTESIAN_POINT ( 'NONE',  ( -12.06949235617756955, 12.14591786802309770, 85.62390960531436690 ) ) ;
#132654 = CARTESIAN_POINT ( 'NONE',  ( -8.314922557960811034, -14.29746914071050412, 52.08224293864768839 ) ) ;
#132655 = CARTESIAN_POINT ( 'NONE',  ( -21.55341960407610458, -5.719274019375992779, 61.45724293864770260 ) ) ;
#132656 = CARTESIAN_POINT ( 'NONE',  ( 9.564922557960805705, 16.46253265017160317, 64.58224293864769550 ) ) ;
#132657 = CARTESIAN_POINT ( 'NONE',  ( 10.72451020669898902, -18.67979575497178502, 77.91557627198102409 ) ) ;
#132658 = CARTESIAN_POINT ( 'NONE',  ( 19.02544592524334988, 5.153800228976608722, 56.45942372801898301 ) ) ;
#132660 = CARTESIAN_POINT ( 'NONE',  ( 16.52544592524342804, -4.483927247898539470, 58.54057627198103120 ) ) ;
#132659 = DIRECTION ( 'NONE',  ( 0.000000000000000000, 0.000000000000000000, 1.000000000000000000 ) ) ;
#132661 = CARTESIAN_POINT ( 'NONE',  ( -15.72974639402197994, 15.80617190586746368, 35.62390960531437401 ) ) ;
#132662 = EDGE_LOOP ( 'NONE', ( #135631, #187655, #72170, #96705, #178806, #107422 ) ) ;
#132663 = CARTESIAN_POINT ( 'NONE',  ( 16.21995358207305316, 7.366697692864181413, 102.5644899848784348 ) ) ;
#132665 = CARTESIAN_POINT ( 'NONE',  ( 8.571926809382603096, -26.38167802310801235, 147.4750000027311785 ) ) ;
#132664 = CARTESIAN_POINT ( 'NONE',  ( 0.05219959533934541429, -16.53943276465976808, 85.00109039468568994 ) ) ;
#132666 = CARTESIAN_POINT ( 'NONE',  ( -0.05219959533936034679, 19.03943276465977164, 92.50109039468566152 ) ) ;
#132667 = ADVANCED_FACE ( 'NONE', ( #145538 ), #174895, .F. ) ;
#132668 = CARTESIAN_POINT ( 'NONE',  ( -14.34966873604960291, -8.224510206698953496, 56.66557627198103830 ) ) ;
#132669 = DIRECTION ( 'NONE',  ( 1.000000000000000000, 0.000000000000000000, 0.000000000000000000 ) ) ;
#132670 = CARTESIAN_POINT ( 'NONE',  ( 16.51473224551069308, 9.474510206698969483, 44.16557627198103120 ) ) ;
#132671 = CARTESIAN_POINT ( 'NONE',  ( 0.05219959533910956823, 16.53943276465976808, 44.99890960531435979 ) ) ;
#132672 = CARTESIAN_POINT ( 'NONE',  ( 13.97604488694527802, 13.89961937509977652, 84.37390960531433848 ) ) ;
#132673 = CARTESIAN_POINT ( 'NONE',  ( -16.46253265017160317, 9.564922557960807481, 50.83224293864770260 ) ) ;
#132674 = CARTESIAN_POINT ( 'NONE',  ( 15.80617190586769283, -15.72974639402175789, 55.62609039468568284 ) ) ;
#132675 = CARTESIAN_POINT ( 'NONE',  ( 16.51473224551069308, 9.474510206698969483, 74.16557627198103830 ) ) ;
#132676 = CARTESIAN_POINT ( 'NONE',  ( 13.97604488694527802, 13.89961937509977652, 24.37390960531435624 ) ) ;
#132677 = CARTESIAN_POINT ( 'NONE',  ( -19.05341960407611168, -5.049401038298163336, 71.45724293864766707 ) ) ;
#132678 = CARTESIAN_POINT ( 'NONE',  ( 18.67979575497178502, 10.72451020669898547, 44.16557627198103120 ) ) ;
#132679 = CARTESIAN_POINT ( 'NONE',  ( -13.89961937509977652, 13.97604488694528158, 40.62390960531435979 ) ) ;
#132680 = CARTESIAN_POINT ( 'NONE',  ( 18.62759615963271287, -10.81492255796078972, 38.33224293864768839 ) ) ;
#132681 = CARTESIAN_POINT ( 'NONE',  ( 8.224510206698742110, 14.34966873604972548, 107.0844237280190043 ) ) ;
#132682 = CARTESIAN_POINT ( 'NONE',  ( -13.89961937509957401, -13.97604488694547875, 29.37609039468565797 ) ) ;
#132684 = CARTESIAN_POINT ( 'NONE',  ( 14.34966873604972726, -8.224510206698740333, 80.83442372801901854 ) ) ;
#132683 = CARTESIAN_POINT ( 'NONE',  ( 8.314922557961029526, -14.29746914071037800, 45.41775706135234003 ) ) ;
#132685 = CARTESIAN_POINT ( 'NONE',  ( -19.02544592524342804, 5.153800228976336051, 116.0405762719810383 ) ) ;
#132686 = CARTESIAN_POINT ( 'NONE',  ( -8.314922557961024197, 14.29746914071037800, 62.91775706135236135 ) ) ;
#132687 = CARTESIAN_POINT ( 'NONE',  ( 21.55341960407610458, 5.719274019375980345, 28.95724293864769905 ) ) ;
#132688 = CARTESIAN_POINT ( 'NONE',  ( -5.049401038298153566, 19.05341960407611168, 30.20724293864768839 ) ) ;
#132689 = CARTESIAN_POINT ( 'NONE',  ( 16.55341960407618274, -4.379528057220086978, 36.04275706135234714 ) ) ;
#132690 = CARTESIAN_POINT ( 'NONE',  ( -9.474510206698964154, 16.51473224551069663, 45.41557627198103120 ) ) ;
#132691 = CARTESIAN_POINT ( 'NONE',  ( 10.81492255796106328, -18.62759615963255655, 20.41775706135234714 ) ) ;
#132692 = CARTESIAN_POINT ( 'NONE',  ( -12.14591786802326823, 12.06949235617739902, 33.12609039468569705 ) ) ;
#132693 = CARTESIAN_POINT ( 'NONE',  ( 14.34966873604972726, -8.224510206698740333, 105.8344237280190328 ) ) ;
#132694 = CARTESIAN_POINT ( 'NONE',  ( 5.719274019375673035, 21.55341960407619339, 107.2927570613523471 ) ) ;
#132695 = CARTESIAN_POINT ( 'NONE',  ( 5.049401038297881783, 19.05341960407617563, 102.2927570613523045 ) ) ;
#132696 = CARTESIAN_POINT ( 'NONE',  ( 9.474510206698729675, 16.51473224551082808, 52.08442372801900433 ) ) ;
#132697 = CARTESIAN_POINT ( 'NONE',  ( 16.55341960407611168, 4.379528057220329451, 73.95724293864769550 ) ) ;
#132698 = CARTESIAN_POINT ( 'NONE',  ( -8.224510206698948167, 14.34966873604960824, 115.4155762719810241 ) ) ;
#132700 = CARTESIAN_POINT ( 'NONE',  ( -23.48529157249599919, -32.32473071737749848, -3.449999994537626957 ) ) ;
#132699 = CARTESIAN_POINT ( 'NONE',  ( 5.153800228976615827, -19.02544592524334988, 55.20942372801899722 ) ) ;
#132701 = CARTESIAN_POINT ( 'NONE',  ( 5.719274019375673035, 21.55341960407619339, 57.29275706135234714 ) ) ;
#132702 = CARTESIAN_POINT ( 'NONE',  ( 14.34966873604972726, -8.224510206698740333, 30.83442372801902209 ) ) ;
#132703 = CARTESIAN_POINT ( 'NONE',  ( 19.49149378614658090, -5.499999999999769074, 56.93757513605362419 ) ) ;
#132704 = CARTESIAN_POINT ( 'NONE',  ( 15.72974639402199770, -15.80617190586745480, 28.12390960531435979 ) ) ;
#132705 = CARTESIAN_POINT ( 'NONE',  ( -5.049401038297874678, -19.05341960407617918, 109.7927570613523187 ) ) ;
#132706 = CARTESIAN_POINT ( 'NONE',  ( -1.022580077288041090E-15, -16.70000000000002061, -64.92279855667830191 ) ) ;
#132707 = CARTESIAN_POINT ( 'NONE',  ( -26.45594755429569034, 8.318738267476192050, 167.5492909577866385 ) ) ;
#132708 = CARTESIAN_POINT ( 'NONE',  ( 4.483927247898545687, 16.52544592524342804, 114.7905762719810383 ) ) ;
#132709 = CARTESIAN_POINT ( 'NONE',  ( 18.67979575497194134, -10.72451020669871369, 110.8344237280190043 ) ) ;
#132710 = CARTESIAN_POINT ( 'NONE',  ( -9.474510206698964154, 16.51473224551069663, 60.41557627198102409 ) ) ;
#132711 = CARTESIAN_POINT ( 'NONE',  ( 18.67979575497194134, -10.72451020669871369, 65.83442372801900433 ) ) ;
#132712 = CARTESIAN_POINT ( 'NONE',  ( 0.05219959533937995610, -21.53943276465977519, 100.0010903946857042 ) ) ;
#132713 = CARTESIAN_POINT ( 'NONE',  ( -14.34966873604972548, 8.224510206698743886, 98.33442372801901854 ) ) ;
#132714 = CARTESIAN_POINT ( 'NONE',  ( 19.02544592524343514, -5.153800228976328945, 73.54057627198103830 ) ) ;
#132715 = CARTESIAN_POINT ( 'NONE',  ( -5.823673210054431948, 21.52544592524334988, 52.70942372801902565 ) ) ;
#132716 = CARTESIAN_POINT ( 'NONE',  ( -18.67979575497193778, 10.72451020669871902, 53.33442372801901854 ) ) ;
#132718 = CARTESIAN_POINT ( 'NONE',  ( 16.51473224551069308, 9.474510206698969483, 109.1655762719810383 ) ) ;
#132717 = CARTESIAN_POINT ( 'NONE',  ( -13.89961937509957401, -13.97604488694547875, 84.37609039468567573 ) ) ;
#132719 = CARTESIAN_POINT ( 'NONE',  ( -19.03943276465977164, 0.05219959533909376836, 21.24890960531436335 ) ) ;
#132720 = CARTESIAN_POINT ( 'NONE',  ( 10.81492255796078972, 18.62759615963270932, 99.58224293864770971 ) ) ;
#132721 = CARTESIAN_POINT ( 'NONE',  ( -0.05219959533936034679, 19.03943276465977164, 27.50109039468566507 ) ) ;
#132722 = CARTESIAN_POINT ( 'NONE',  ( 14.34966873604960469, 8.224510206698951720, 99.16557627198100988 ) ) ;
#132723 = CARTESIAN_POINT ( 'NONE',  ( 5.049401038298161559, -19.05341960407611168, 47.70724293864770260 ) ) ;
#132724 = CARTESIAN_POINT ( 'NONE',  ( -0.05219959533936034679, 19.03943276465977164, 102.5010903946856757 ) ) ;
#132725 = CARTESIAN_POINT ( 'NONE',  ( 16.55341960407611168, 4.379528057220329451, 63.95724293864770260 ) ) ;
#132726 = CARTESIAN_POINT ( 'NONE',  ( -21.52544592524334988, -5.823673210054445271, 103.9594237280190185 ) ) ;
#132727 = CARTESIAN_POINT ( 'NONE',  ( 19.05341960407611168, 5.049401038298154454, 108.9572429386477097 ) ) ;
#132728 = CARTESIAN_POINT ( 'NONE',  ( -19.05341960407617563, 5.049401038297882671, 68.54275706135230450 ) ) ;
#132729 = CARTESIAN_POINT ( 'NONE',  ( -5.719274019375978568, 21.55341960407610458, 80.20724293864769550 ) ) ;
#132730 = CARTESIAN_POINT ( 'NONE',  ( -15.72974639402176322, -15.80617190586768395, 39.37609039468567573 ) ) ;
#132731 = CARTESIAN_POINT ( 'NONE',  ( 8.224510206698742110, 14.34966873604972548, 42.08442372801901854 ) ) ;
#132732 = CARTESIAN_POINT ( 'NONE',  ( -12.14591786802326823, 12.06949235617739902, 93.12609039468568994 ) ) ;
#132734 = CARTESIAN_POINT ( 'NONE',  ( 18.62759615963255655, 10.81492255796105972, 31.66775706135234358 ) ) ;
#132733 = CARTESIAN_POINT ( 'NONE',  ( 4.379528057220092307, 16.55341960407617563, 37.29275706135235424 ) ) ;
#132735 = CARTESIAN_POINT ( 'NONE',  ( -5.823673210054116645, -21.52544592524344225, 42.29057627198103120 ) ) ;
#132736 = CARTESIAN_POINT ( 'NONE',  ( 5.049401038298161559, -19.05341960407611168, 37.70724293864768839 ) ) ;
#132737 = CARTESIAN_POINT ( 'NONE',  ( 11.74264578624799427, 36.14014761921585972, -8.349999994537625980 ) ) ;
#132738 = CARTESIAN_POINT ( 'NONE',  ( 14.34966873604972726, -8.224510206698740333, 55.83442372801901854 ) ) ;
#132739 = CARTESIAN_POINT ( 'NONE',  ( 21.55341960407610458, 5.719274019375980345, 88.95724293864769550 ) ) ;
#132740 = CARTESIAN_POINT ( 'NONE',  ( -16.53943276465976808, 0.05219959533911058130, 36.24890960531435979 ) ) ;
#132741 = CARTESIAN_POINT ( 'NONE',  ( -4.379528057220086978, -16.55341960407618274, 44.79275706135234714 ) ) ;
#132742 = CARTESIAN_POINT ( 'NONE',  ( 5.153800228976335163, 19.02544592524342804, 59.79057627198100988 ) ) ;
#132743 = CARTESIAN_POINT ( 'NONE',  ( -16.46253265017146816, -9.564922557961047289, 89.16775706135234714 ) ) ;
#132744 = CARTESIAN_POINT ( 'NONE',  ( -18.62759615963270932, 10.81492255796079327, 80.83224293864769550 ) ) ;
#132745 = CARTESIAN_POINT ( 'NONE',  ( 4.379528057220339221, -16.55341960407611168, 32.70724293864770260 ) ) ;
#132746 = VERTEX_POINT ( 'NONE', #68699 ) ;
#132747 = CARTESIAN_POINT ( 'NONE',  ( 24.95262708931866058, 12.69764001896744432, 166.0532406165024497 ) ) ;
#132748 = CARTESIAN_POINT ( 'NONE',  ( -18.67979575497178146, -10.72451020669898902, 56.66557627198103830 ) ) ;
#132749 = ORIENTED_EDGE ( 'NONE', *, *, #196169, .F. ) ;
#132750 = CARTESIAN_POINT ( 'NONE',  ( 16.55341960407618274, -4.379528057220086978, 106.0427570613523471 ) ) ;
#132751 = EDGE_LOOP ( 'NONE', ( #174095, #152500, #43611, #69328, #13189, #24677 ) ) ;
#132752 = CARTESIAN_POINT ( 'NONE',  ( 19.49671883438228193, 5.499999999999968026, 87.39279849105679432 ) ) ;
#132753 = CARTESIAN_POINT ( 'NONE',  ( -10.72451020669898014, 18.67979575497178502, 85.41557627198102409 ) ) ;
#132754 = CARTESIAN_POINT ( 'NONE',  ( 16.52544592524342804, -4.483927247898539470, 28.54057627198103120 ) ) ;
#132755 = CARTESIAN_POINT ( 'NONE',  ( -14.34966873604972548, 8.224510206698743886, 38.33442372801900433 ) ) ;
#132756 = CARTESIAN_POINT ( 'NONE',  ( 13.97604488694527802, 13.89961937509977652, 39.37390960531435269 ) ) ;
#132757 = CARTESIAN_POINT ( 'NONE',  ( 13.97604488694527802, 13.89961937509977652, 64.37390960531436690 ) ) ;
#132758 = CARTESIAN_POINT ( 'NONE',  ( 8.906447517083050158, 27.41122689804195645, 149.4000000000000057 ) ) ;
#132759 = CARTESIAN_POINT ( 'NONE',  ( -16.46253265017160317, 9.564922557960807481, 115.8322429386477097 ) ) ;
#132760 = CARTESIAN_POINT ( 'NONE',  ( 0.1264748200299367631, 28.90000000000004832, -52.65483682830182488 ) ) ;
#132761 = CARTESIAN_POINT ( 'NONE',  ( -12.06949235617739369, -12.14591786802326823, 99.37609039468568994 ) ) ;
#132762 = CARTESIAN_POINT ( 'NONE',  ( 19.02544592524334988, 5.153800228976608722, 106.4594237280190185 ) ) ;
#132763 = CARTESIAN_POINT ( 'NONE',  ( 9.474510206698729675, 16.51473224551082808, 32.08442372801900433 ) ) ;
#132764 = CARTESIAN_POINT ( 'NONE',  ( 10.72451020669898902, -18.67979575497178502, 82.91557627198103830 ) ) ;
#132765 = CARTESIAN_POINT ( 'NONE',  ( 8.224510206698953496, -14.34966873604960469, 22.91557627198102765 ) ) ;
#132766 = CARTESIAN_POINT ( 'NONE',  ( 10.81492255796078972, 18.62759615963270932, 44.58224293864769550 ) ) ;
#132768 = CARTESIAN_POINT ( 'NONE',  ( 16.51473224551083163, -9.474510206698727899, 110.8344237280190043 ) ) ;
#132767 = CARTESIAN_POINT ( 'NONE',  ( 15.80617190586746368, 15.72974639402197994, 69.37390960531436690 ) ) ;
#132769 = CARTESIAN_POINT ( 'NONE',  ( -5.049401038298153566, 19.05341960407611168, 110.2072429386476671 ) ) ;
#132770 = CARTESIAN_POINT ( 'NONE',  ( -18.67979575497193778, 10.72451020669871902, 63.33442372801900433 ) ) ;
#132771 = CARTESIAN_POINT ( 'NONE',  ( 13.97604488694527802, 13.89961937509977652, 54.37390960531435979 ) ) ;
#132772 = CARTESIAN_POINT ( 'NONE',  ( -16.53943276465976808, 0.05219959533911058130, 96.24890960531435269 ) ) ;
#132773 = CARTESIAN_POINT ( 'NONE',  ( 32.42786921226272767, 3.325810949901237379, 88.27324663263311777 ) ) ;
#132774 = CARTESIAN_POINT ( 'NONE',  ( 16.51473224551069308, 9.474510206698969483, 69.16557627198102409 ) ) ;
#132775 = CARTESIAN_POINT ( 'NONE',  ( 12.14591786802309770, 12.06949235617756955, 79.37390960531436690 ) ) ;
#132776 = ORIENTED_EDGE ( 'NONE', *, *, #118723, .T. ) ;
#132777 = CARTESIAN_POINT ( 'NONE',  ( -19.05341960407617563, 5.049401038297882671, 93.54275706135234714 ) ) ;
#132778 = DIRECTION ( 'NONE',  ( -0.000000000000000000, -0.000000000000000000, -1.000000000000000000 ) ) ;
#132779 = CARTESIAN_POINT ( 'NONE',  ( 16.51473224551069308, 9.474510206698969483, 54.16557627198103120 ) ) ;
#132780 = CARTESIAN_POINT ( 'NONE',  ( 0.9976825729257744468, 8.724364686941823877, -61.97160884975856732 ) ) ;
#132782 = CARTESIAN_POINT ( 'NONE',  ( 5.153800228976335163, 19.02544592524342804, 104.7905762719809957 ) ) ;
#132781 = CARTESIAN_POINT ( 'NONE',  ( 21.52544592524334988, 5.823673210054432836, 86.45942372801901854 ) ) ;
#132783 = CARTESIAN_POINT ( 'NONE',  ( 8.314922557961029526, -14.29746914071037800, 70.41775706135236135 ) ) ;
#132784 = DIRECTION ( 'NONE',  ( -0.7071067811865561215, -0.7071067811865389130, -0.000000000000000000 ) ) ;
#132785 = CARTESIAN_POINT ( 'NONE',  ( 5.049401038297881783, 19.05341960407617563, 47.29275706135231161 ) ) ;
#132786 = CARTESIAN_POINT ( 'NONE',  ( -10.72451020669870658, -18.67979575497194134, 104.5844237280190185 ) ) ;
#132787 = CARTESIAN_POINT ( 'NONE',  ( 36.77234560139675779, 5.215770478161304347, 46.75454185840154508 ) ) ;
#132788 = CARTESIAN_POINT ( 'NONE',  ( -19.05341960407611168, -5.049401038298163336, 21.45724293864768839 ) ) ;
#132789 = CARTESIAN_POINT ( 'NONE',  ( -8.314922557961024197, 14.29746914071037800, 102.9177570613523756 ) ) ;
#132790 = DIRECTION ( 'NONE',  ( 1.000000000000000000, 0.000000000000000000, 0.000000000000000000 ) ) ;
#132791 = CARTESIAN_POINT ( 'NONE',  ( -8.314922557961024197, 14.29746914071037800, 97.91775706135236135 ) ) ;
#132792 = CARTESIAN_POINT ( 'NONE',  ( -28.79475375365501932, 9.355982642740395150, 146.1656553485623249 ) ) ;
#132793 = CARTESIAN_POINT ( 'NONE',  ( -14.29746914071037622, -8.314922557961029526, 74.16775706135231871 ) ) ;
#132794 = CARTESIAN_POINT ( 'NONE',  ( 17.60728821186566506, -5.500000000000022204, 68.36690927743006796 ) ) ;
#132795 = CARTESIAN_POINT ( 'NONE',  ( 15.80617190586769283, -15.72974639402175789, 75.62609039468567573 ) ) ;
#132796 = CARTESIAN_POINT ( 'NONE',  ( -9.474510206698720793, -16.51473224551083518, 94.58442372801900433 ) ) ;
#132797 = CARTESIAN_POINT ( 'NONE',  ( 19.02544592524334988, 5.153800228976608722, 21.45942372801899012 ) ) ;
#132798 = CARTESIAN_POINT ( 'NONE',  ( -9.474510206698964154, 16.51473224551069663, 65.41557627198102409 ) ) ;
#132799 = CARTESIAN_POINT ( 'NONE',  ( 5.049401038298161559, -19.05341960407611168, 62.70724293864769550 ) ) ;
#132800 = CARTESIAN_POINT ( 'NONE',  ( -19.11512514549023578, -35.13775691452683247, -7.538968404279507318 ) ) ;
#132801 = CARTESIAN_POINT ( 'NONE',  ( 18.62759615963271287, -10.81492255796078972, 83.33224293864769550 ) ) ;
#132802 = CARTESIAN_POINT ( 'NONE',  ( -21.52544592524343514, 5.823673210054127303, 31.04057627198102409 ) ) ;
#132803 = CARTESIAN_POINT ( 'NONE',  ( -16.46253265017160317, 9.564922557960807481, 35.83224293864768839 ) ) ;
#132804 = CARTESIAN_POINT ( 'NONE',  ( 12.14591786802327356, -12.06949235617739191, 65.62609039468568994 ) ) ;
#132805 = ORIENTED_EDGE ( 'NONE', *, *, #184390, .F. ) ;
#132806 = ADVANCED_FACE ( 'NONE', ( #130354 ), #107880, .T. ) ;
#132807 = CARTESIAN_POINT ( 'NONE',  ( -18.67979575497193778, 10.72451020669871902, 33.33442372801900433 ) ) ;
#132809 = CARTESIAN_POINT ( 'NONE',  ( -11.40812507854755609, 35.11059874428196537, -7.024999997268813523 ) ) ;
#132808 = CARTESIAN_POINT ( 'NONE',  ( 14.29746914071049879, -8.314922557960816363, 63.33224293864770260 ) ) ;
#132810 = CARTESIAN_POINT ( 'NONE',  ( -4.379528057220086978, -16.55341960407618274, 29.79275706135234358 ) ) ;
#132811 = CARTESIAN_POINT ( 'NONE',  ( -5.153800228976607833, 19.02544592524334988, 52.70942372801900433 ) ) ;
#132812 = CARTESIAN_POINT ( 'NONE',  ( -14.34966873604960291, -8.224510206698953496, 61.66557627198103120 ) ) ;
#132813 = CARTESIAN_POINT ( 'NONE',  ( 10.81492255796078972, 18.62759615963270932, 114.5822429386477097 ) ) ;
#132815 = CARTESIAN_POINT ( 'NONE',  ( -10.81492255796078084, -18.62759615963271287, 72.08224293864769550 ) ) ;
#132814 = CARTESIAN_POINT ( 'NONE',  ( -18.22780087662123805, 5.499999999999981348, 101.0176318212689495 ) ) ;
#132816 = CARTESIAN_POINT ( 'NONE',  ( 19.05341960407611168, 5.049401038298154454, 93.95724293864769550 ) ) ;
#132817 = CARTESIAN_POINT ( 'NONE',  ( 4.483927247898545687, 16.52544592524342804, 64.79057627198103830 ) ) ;
#132818 = CARTESIAN_POINT ( 'NONE',  ( -5.049401038298153566, 19.05341960407611168, 115.2072429386477097 ) ) ;
#132819 = DIRECTION ( 'NONE',  ( 0.06104853953485701173, 0.000000000000000000, -0.9981347984218670311 ) ) ;
#132820 = CARTESIAN_POINT ( 'NONE',  ( -5.153800228976607833, 19.02544592524334988, 62.70942372801899722 ) ) ;
#132821 = CARTESIAN_POINT ( 'NONE',  ( 21.52544592524344225, -5.823673210054117533, 113.5405762719810383 ) ) ;
#132822 = CARTESIAN_POINT ( 'NONE',  ( 0.05219959533909260263, 19.03943276465977164, 54.99890960531435979 ) ) ;
#132823 = CARTESIAN_POINT ( 'NONE',  ( -16.51473224551082808, 9.474510206698731452, 43.33442372801900433 ) ) ;
#132824 = CARTESIAN_POINT ( 'NONE',  ( -5.049401038298153566, 19.05341960407611168, 35.20724293864768839 ) ) ;
#132825 = CARTESIAN_POINT ( 'NONE',  ( -21.55341960407619339, 5.719274019375674811, 63.54275706135234003 ) ) ;
#132826 = CARTESIAN_POINT ( 'NONE',  ( -17.49999999999999645, -5.499999999999992895, 69.20309617465828467 ) ) ;
#132827 = CARTESIAN_POINT ( 'NONE',  ( -14.34966873604960291, -8.224510206698953496, 36.66557627198103120 ) ) ;
#132828 = CARTESIAN_POINT ( 'NONE',  ( -9.564922557960796823, -16.46253265017161027, 57.08224293864769550 ) ) ;
#132829 = CARTESIAN_POINT ( 'NONE',  ( -15.80617190586745835, -15.72974639402198527, 71.87390960531438111 ) ) ;
#132830 = CARTESIAN_POINT ( 'NONE',  ( 9.564922557960805705, 16.46253265017160317, 59.58224293864769550 ) ) ;
#132831 = ORIENTED_EDGE ( 'NONE', *, *, #11291, .T. ) ;
#132832 = CARTESIAN_POINT ( 'NONE',  ( 10.72451020669898902, -18.67979575497178502, 67.91557627198102409 ) ) ;
#132833 = CARTESIAN_POINT ( 'NONE',  ( 15.72974639402176855, 15.80617190586768217, 101.8760903946857042 ) ) ;
#132836 = CARTESIAN_POINT ( 'NONE',  ( 12.14591786802309770, 12.06949235617756955, 89.37390960531435269 ) ) ;
#132835 = CARTESIAN_POINT ( 'NONE',  ( -4.379528057220086978, -16.55341960407618274, 99.79275706135234714 ) ) ;
#132834 = LINE ( 'NONE', #103507, #76758 ) ;
#132837 = CARTESIAN_POINT ( 'NONE',  ( -9.474510206698720793, -16.51473224551083518, 89.58442372801900433 ) ) ;
#132838 = EDGE_LOOP ( 'NONE', ( #131991, #131360 ) ) ;
#132839 = CARTESIAN_POINT ( 'NONE',  ( 9.564922557961047289, -16.46253265017146816, 40.41775706135234003 ) ) ;
#132840 = CARTESIAN_POINT ( 'NONE',  ( -4.483927247898782831, 16.52544592524335698, 107.7094237280190328 ) ) ;
#132841 = CARTESIAN_POINT ( 'NONE',  ( -19.05341960407617563, 5.049401038297882671, 28.54275706135232937 ) ) ;
#132842 = CARTESIAN_POINT ( 'NONE',  ( 9.564922557960805705, 16.46253265017160317, 94.58224293864769550 ) ) ;
#132843 = CARTESIAN_POINT ( 'NONE',  ( -5.823673210054116645, -21.52544592524344225, 62.29057627198102409 ) ) ;
#132844 = CARTESIAN_POINT ( 'NONE',  ( -18.22780087662119541, 5.500000000000102141, 51.01763182126894947 ) ) ;
#132845 = CARTESIAN_POINT ( 'NONE',  ( -19.03943276465977164, 0.05219959533909376836, 21.24890960531436335 ) ) ;
#132846 = CARTESIAN_POINT ( 'NONE',  ( 21.53943276465977519, 0.05219959533937863772, 91.25109039468568994 ) ) ;
#132847 = CARTESIAN_POINT ( 'NONE',  ( 8.224510206698742110, 14.34966873604972548, 82.08442372801901854 ) ) ;
#132848 = CARTESIAN_POINT ( 'NONE',  ( -15.80617190586768217, 15.72974639402176855, 23.12609039468567573 ) ) ;
#132849 = CARTESIAN_POINT ( 'NONE',  ( 0.05219959533934541429, -16.53943276465976808, 35.00109039468568284 ) ) ;
#132850 = CARTESIAN_POINT ( 'NONE',  ( 9.564922557960805705, 16.46253265017160317, 109.5822429386476955 ) ) ;
#132851 = CARTESIAN_POINT ( 'NONE',  ( 16.51473224551069308, 9.474510206698969483, 34.16557627198102409 ) ) ;
#132852 = CARTESIAN_POINT ( 'NONE',  ( 19.02544592524343514, -5.153800228976328945, 58.54057627198102409 ) ) ;
#132853 = CARTESIAN_POINT ( 'NONE',  ( -16.55341960407617563, 4.379528057220093196, 33.54275706135234714 ) ) ;
#132854 = CARTESIAN_POINT ( 'NONE',  ( 14.29746914071049879, -8.314922557960816363, 98.33224293864769550 ) ) ;
#132855 = CARTESIAN_POINT ( 'NONE',  ( -12.14591786802326823, 12.06949235617739902, 103.1260903946856757 ) ) ;
#132858 = CARTESIAN_POINT ( 'NONE',  ( 0.05219959533909260263, 19.03943276465977164, 69.99890960531435269 ) ) ;
#132857 = CARTESIAN_POINT ( 'NONE',  ( -9.564922557960796823, -16.46253265017161027, 82.08224293864768129 ) ) ;
#132856 = CARTESIAN_POINT ( 'NONE',  ( 0.05219959533937995610, -21.53943276465977519, 45.00109039468568284 ) ) ;
#132859 = CARTESIAN_POINT ( 'NONE',  ( -16.51473224551069308, -9.474510206698971260, 86.66557627198102409 ) ) ;
#132860 = CARTESIAN_POINT ( 'NONE',  ( -16.52544592524342804, 4.483927247898546575, 31.04057627198102409 ) ) ;
#132861 = CARTESIAN_POINT ( 'NONE',  ( 16.55341960407618274, -4.379528057220086978, 96.04275706135236135 ) ) ;
#132862 = ORIENTED_EDGE ( 'NONE', *, *, #18488, .F. ) ;
#132863 = CARTESIAN_POINT ( 'NONE',  ( -19.02544592524334988, -5.153800228976617603, 38.95942372801900433 ) ) ;
#132864 = CARTESIAN_POINT ( 'NONE',  ( -9.564922557960796823, -16.46253265017161027, 107.0822429386476955 ) ) ;
#132865 = CARTESIAN_POINT ( 'NONE',  ( -19.05341960407611168, -5.049401038298163336, 56.45724293864768129 ) ) ;
#132866 = CARTESIAN_POINT ( 'NONE',  ( -19.05341960407617563, 5.049401038297882671, 43.54275706135232582 ) ) ;
#132867 = CARTESIAN_POINT ( 'NONE',  ( -29.86685920354755552, 21.69954338932564397, -8.824999997268815122 ) ) ;
#132868 = CARTESIAN_POINT ( 'NONE',  ( 4.483927247898790824, -16.52544592524335698, 40.20942372801901854 ) ) ;
#132870 = CARTESIAN_POINT ( 'NONE',  ( 14.29746914071037800, 8.314922557961029526, 51.66775706135234714 ) ) ;
#132869 = CARTESIAN_POINT ( 'NONE',  ( 19.05341960407617918, -5.049401038297876454, 76.04275706135230450 ) ) ;
#132871 = CARTESIAN_POINT ( 'NONE',  ( 16.51473224551069308, 9.474510206698969483, 114.1655762719810241 ) ) ;
#132872 = CARTESIAN_POINT ( 'NONE',  ( -19.05341960407611168, -5.049401038298163336, 86.45724293864769550 ) ) ;
#132873 = CARTESIAN_POINT ( 'NONE',  ( -18.67979575497178146, -10.72451020669898902, 106.6655762719810383 ) ) ;
#132874 = CARTESIAN_POINT ( 'NONE',  ( 19.03943276465977164, 0.05219959533936151252, 81.25109039468567573 ) ) ;
#132876 = CARTESIAN_POINT ( 'NONE',  ( -5.153800228976328057, -19.02544592524343514, 37.29057627198102409 ) ) ;
#132875 = CARTESIAN_POINT ( 'NONE',  ( -19.02544592524342804, 5.153800228976336051, 106.0405762719810241 ) ) ;
#132877 = CARTESIAN_POINT ( 'NONE',  ( 19.02544592524343514, -5.153800228976328945, 83.54057627198100988 ) ) ;
#132879 = CARTESIAN_POINT ( 'NONE',  ( 13.97604488694527802, 13.89961937509977652, 39.37390960531435269 ) ) ;
#132878 = CARTESIAN_POINT ( 'NONE',  ( -12.14591786802309592, -12.06949235617757132, 31.87390960531435979 ) ) ;
#132880 = CARTESIAN_POINT ( 'NONE',  ( 16.46253265017146816, 9.564922557961045513, 56.66775706135233293 ) ) ;
#132881 = CARTESIAN_POINT ( 'NONE',  ( 16.52544592524342804, -4.483927247898539470, 93.54057627198103830 ) ) ;
#132882 = CARTESIAN_POINT ( 'NONE',  ( 10.81492255796106328, -18.62759615963255655, 105.4177570613523613 ) ) ;
#132883 = CARTESIAN_POINT ( 'NONE',  ( -13.97604488694527625, -13.89961937509977652, 46.87390960531435979 ) ) ;
#132884 = CARTESIAN_POINT ( 'NONE',  ( -5.719274019375978568, 21.55341960407610458, 45.20724293864769550 ) ) ;
#132886 = CARTESIAN_POINT ( 'NONE',  ( -18.62759615963255300, -10.81492255796106328, 99.16775706135234714 ) ) ;
#132885 = CARTESIAN_POINT ( 'NONE',  ( 16.55341960407611168, 4.379528057220329451, 53.95724293864770260 ) ) ;
#132887 = CARTESIAN_POINT ( 'NONE',  ( -13.89961937509977652, 13.97604488694528158, 110.6239096053143243 ) ) ;
#132888 = CARTESIAN_POINT ( 'NONE',  ( 16.51473224551069308, 9.474510206698969483, 104.1655762719810241 ) ) ;
#132889 = CARTESIAN_POINT ( 'NONE',  ( 16.51473224551069308, 9.474510206698969483, 34.16557627198102409 ) ) ;
#132890 = CARTESIAN_POINT ( 'NONE',  ( 9.564922557960805705, 16.46253265017160317, 29.58224293864769550 ) ) ;
#132891 = CARTESIAN_POINT ( 'NONE',  ( -14.34966873604960291, -8.224510206698953496, 81.66557627198103830 ) ) ;
#132892 = CARTESIAN_POINT ( 'NONE',  ( -21.52544592524343514, 5.823673210054127303, 96.04057627198102409 ) ) ;
#132893 = CARTESIAN_POINT ( 'NONE',  ( 9.564922557960805705, 16.46253265017160317, 99.58224293864770971 ) ) ;
#132894 = CARTESIAN_POINT ( 'NONE',  ( -5.823673210054116645, -21.52544592524344225, 112.2905762719810241 ) ) ;
#132895 = CARTESIAN_POINT ( 'NONE',  ( 5.049401038298161559, -19.05341960407611168, 87.70724293864769550 ) ) ;
#132897 = CARTESIAN_POINT ( 'NONE',  ( -4.483927247898539470, -16.52544592524342804, 97.29057627198105251 ) ) ;
#132896 = CARTESIAN_POINT ( 'NONE',  ( 17.50000000000000000, 5.499999999999997335, 120.0000000000000142 ) ) ;
#132898 = CARTESIAN_POINT ( 'NONE',  ( -9.474510206698964154, 16.51473224551069663, 70.41557627198102409 ) ) ;
#132899 = CARTESIAN_POINT ( 'NONE',  ( -10.72451020669898014, 18.67979575497178502, 75.41557627198102409 ) ) ;
#132900 = CARTESIAN_POINT ( 'NONE',  ( -31.25711108810729755, 6.845500155895384076, 98.07395821223767030 ) ) ;
#132901 = CARTESIAN_POINT ( 'NONE',  ( -21.38418241377623374, -5.438282248597753110, 174.2683007571264113 ) ) ;
#132903 = PLANE ( 'NONE',  #33738 ) ;
#132902 = CARTESIAN_POINT ( 'NONE',  ( 21.52544592524344225, -5.823673210054117533, 33.54057627198102409 ) ) ;
#132904 = CARTESIAN_POINT ( 'NONE',  ( -12.14591786802326823, 12.06949235617739902, 38.12609039468567573 ) ) ;
#132905 = EDGE_CURVE ( 'NONE', #94779, #138821, #159548, .T. ) ;
#132906 = CARTESIAN_POINT ( 'NONE',  ( 4.483927247898545687, 16.52544592524342804, 94.79057627198105251 ) ) ;
#132907 = CARTESIAN_POINT ( 'NONE',  ( -17.50000000000000355, -3.189878218039142954, 110.1294856257124337 ) ) ;
#132908 = CARTESIAN_POINT ( 'NONE',  ( 19.02544592524343514, -5.153800228976328945, 93.54057627198102409 ) ) ;
#132909 = CARTESIAN_POINT ( 'NONE',  ( -19.02544592524342804, 5.153800228976336051, 51.04057627198103120 ) ) ;
#132910 = CARTESIAN_POINT ( 'NONE',  ( 16.52544592524342804, -4.483927247898539470, 83.54057627198102409 ) ) ;
#132911 = CARTESIAN_POINT ( 'NONE',  ( 15.80617190586746368, 15.72974639402197994, 34.37390960531435979 ) ) ;
#132912 = CARTESIAN_POINT ( 'NONE',  ( -16.55341960407611168, -4.379528057220339221, 51.45724293864770260 ) ) ;
#132913 = CARTESIAN_POINT ( 'NONE',  ( 8.314922557961029526, -14.29746914071037800, 25.41775706135235779 ) ) ;
#132914 = CARTESIAN_POINT ( 'NONE',  ( -21.53943276465977519, -0.05219959533937600094, 73.75109039468567573 ) ) ;
#132915 = CARTESIAN_POINT ( 'NONE',  ( -8.571926809382601320, -26.38167802310801591, 145.2750000027311899 ) ) ;
#132916 = CARTESIAN_POINT ( 'NONE',  ( -0.05219959533909027116, -19.03943276465977164, 112.4989096053143669 ) ) ;
#132917 = CARTESIAN_POINT ( 'NONE',  ( -16.55341960407617563, 4.379528057220093196, 83.54275706135234714 ) ) ;
#132918 = CARTESIAN_POINT ( 'NONE',  ( -16.46253265017160317, 9.564922557960807481, 25.83224293864769194 ) ) ;
#132919 = CARTESIAN_POINT ( 'NONE',  ( 19.05341960407611168, 5.049401038298154454, 78.95724293864769550 ) ) ;
#132920 = CARTESIAN_POINT ( 'NONE',  ( -15.80617190586745835, -15.72974639402198527, 81.87390960531435269 ) ) ;
#132921 = CARTESIAN_POINT ( 'NONE',  ( 8.224510206698742110, 14.34966873604972548, 32.08442372801901854 ) ) ;
#132923 = CARTESIAN_POINT ( 'NONE',  ( -10.81492255796105439, 18.62759615963255655, 72.91775706135234714 ) ) ;
#132922 = CARTESIAN_POINT ( 'NONE',  ( -8.224510206698948167, 14.34966873604960824, 55.41557627198102409 ) ) ;
#132925 = CARTESIAN_POINT ( 'NONE',  ( 16.46253265017160672, -9.564922557960803928, 113.3322429386476955 ) ) ;
#132924 = CARTESIAN_POINT ( 'NONE',  ( -8.314922557961024197, 14.29746914071037800, 92.91775706135236135 ) ) ;
#132926 = CARTESIAN_POINT ( 'NONE',  ( 17.05116617787826172, 6.768360034955700044, 28.84324446740803083 ) ) ;
#132927 = CARTESIAN_POINT ( 'NONE',  ( -24.95432927374998755, -4.974562764236790002, 190.0000000000000000 ) ) ;
#132928 = CARTESIAN_POINT ( 'NONE',  ( 8.224510206698742110, 14.34966873604972548, 102.0844237280190185 ) ) ;
#132929 = CARTESIAN_POINT ( 'NONE',  ( -4.379528057220086978, -16.55341960407618274, 59.79275706135234714 ) ) ;
#132930 = CARTESIAN_POINT ( 'NONE',  ( -19.03943276465977164, 0.05219959533909376836, 66.24890960531436690 ) ) ;
#132931 = CARTESIAN_POINT ( 'NONE',  ( -16.46253265017160317, 9.564922557960807481, 90.83224293864769550 ) ) ;
#132932 = CARTESIAN_POINT ( 'NONE',  ( -21.53943276465977519, -0.05219959533937600094, 73.75109039468567573 ) ) ;
#132933 = EDGE_CURVE ( 'NONE', #122157, #64689, #82470, .T. ) ;
#132934 = CARTESIAN_POINT ( 'NONE',  ( -14.34966873604972548, 8.224510206698743886, 78.33442372801901854 ) ) ;
#132935 = CARTESIAN_POINT ( 'NONE',  ( -16.55341960407611168, -4.379528057220339221, 41.45724293864769550 ) ) ;
#132936 = CARTESIAN_POINT ( 'NONE',  ( -16.46253265017160317, 9.564922557960807481, 50.83224293864770260 ) ) ;
#132937 = CARTESIAN_POINT ( 'NONE',  ( 16.46253265017160672, -9.564922557960803928, 48.33224293864769550 ) ) ;
#132938 = ORIENTED_EDGE ( 'NONE', *, *, #19810, .T. ) ;
#132939 = CARTESIAN_POINT ( 'NONE',  ( 5.049401038297881783, 19.05341960407617563, 112.2927570613523471 ) ) ;
#132940 = CARTESIAN_POINT ( 'NONE',  ( -16.52544592524342804, 4.483927247898546575, 111.0405762719810525 ) ) ;
#132941 = CARTESIAN_POINT ( 'NONE',  ( -16.51473224551069308, -9.474510206698971260, 66.66557627198102409 ) ) ;
#132943 = CARTESIAN_POINT ( 'NONE',  ( -23.48529157249599919, -32.32473071737750558, -1.699999999999999734 ) ) ;
#132942 = CARTESIAN_POINT ( 'NONE',  ( 9.474510206698729675, 16.51473224551082808, 97.08442372801900433 ) ) ;
#132944 = CARTESIAN_POINT ( 'NONE',  ( -21.53943276465977519, -0.05219959533937600094, 98.75109039468568994 ) ) ;
#132945 = CARTESIAN_POINT ( 'NONE',  ( 0.05219959533934541429, -16.53943276465976808, 70.00109039468568994 ) ) ;
#132946 = CARTESIAN_POINT ( 'NONE',  ( -9.474510206698720793, -16.51473224551083518, 94.58442372801900433 ) ) ;
#132947 = CARTESIAN_POINT ( 'NONE',  ( -15.72974639402197994, 15.80617190586746368, 60.62390960531437401 ) ) ;
#132948 = CARTESIAN_POINT ( 'NONE',  ( -8.314922557961024197, 14.29746914071037800, 57.91775706135234714 ) ) ;
#132949 = DIRECTION ( 'NONE',  ( 1.000000000000000000, 0.000000000000000000, 0.000000000000000000 ) ) ;
#132950 = CARTESIAN_POINT ( 'NONE',  ( 16.51473224551083163, -9.474510206698727899, 60.83442372801900433 ) ) ;
#132951 = CARTESIAN_POINT ( 'NONE',  ( -18.67979575497193778, 10.72451020669871902, 103.3344237280190043 ) ) ;
#132952 = CARTESIAN_POINT ( 'NONE',  ( -8.224510206698948167, 14.34966873604960824, 115.4155762719810241 ) ) ;
#132953 = CARTESIAN_POINT ( 'NONE',  ( -9.474510206698964154, 16.51473224551069663, 65.41557627198102409 ) ) ;
#132954 = CARTESIAN_POINT ( 'NONE',  ( 8.314922557960818139, 14.29746914071049879, 59.58224293864770260 ) ) ;
#132955 = CARTESIAN_POINT ( 'NONE',  ( 15.80617190586769283, -15.72974639402175789, 90.62609039468567573 ) ) ;
#132956 = CARTESIAN_POINT ( 'NONE',  ( -0.05219959533936034679, 19.03943276465977164, 42.50109039468566152 ) ) ;
#132957 = CARTESIAN_POINT ( 'NONE',  ( 16.46253265017146816, 9.564922557961045513, 21.66775706135233648 ) ) ;
#132958 = CARTESIAN_POINT ( 'NONE',  ( 18.62759615963271287, -10.81492255796078972, 23.33224293864769194 ) ) ;
#132959 = CARTESIAN_POINT ( 'NONE',  ( 10.81492255796106328, -18.62759615963255655, 95.41775706135234714 ) ) ;
#132960 = CARTESIAN_POINT ( 'NONE',  ( -9.474510206698964154, 16.51473224551069663, 75.41557627198103830 ) ) ;
#132961 = CARTESIAN_POINT ( 'NONE',  ( 0.05219959533937995610, -21.53943276465977519, 90.00109039468567573 ) ) ;
#132962 = CARTESIAN_POINT ( 'NONE',  ( -15.72974639402197994, 15.80617190586746368, 50.62390960531435979 ) ) ;
#132963 = CARTESIAN_POINT ( 'NONE',  ( 19.02544592524343514, -5.153800228976328945, 83.54057627198100988 ) ) ;
#132964 = CARTESIAN_POINT ( 'NONE',  ( 16.46253265017146816, 9.564922557961045513, 76.66775706135234714 ) ) ;
#132965 = CARTESIAN_POINT ( 'NONE',  ( 13.97604488694527802, 13.89961937509977652, 39.37390960531435269 ) ) ;
#132966 = CARTESIAN_POINT ( 'NONE',  ( 13.97604488694527802, 13.89961937509977652, 94.37390960531436690 ) ) ;
#132967 = CARTESIAN_POINT ( 'NONE',  ( 16.46253265017146816, 9.564922557961045513, 86.66775706135233293 ) ) ;
#132968 = CARTESIAN_POINT ( 'NONE',  ( -12.14591786802326823, 12.06949235617739902, 43.12609039468568284 ) ) ;
#132969 = CARTESIAN_POINT ( 'NONE',  ( 16.53943276465976808, -0.05219959533910856209, 108.7489096053143669 ) ) ;
#132970 = CARTESIAN_POINT ( 'NONE',  ( 9.474510206698971260, -16.51473224551069308, 67.91557627198102409 ) ) ;
#132971 = CARTESIAN_POINT ( 'NONE',  ( 15.80617190586746368, 15.72974639402197994, 44.37390960531435979 ) ) ;
#132972 = CARTESIAN_POINT ( 'NONE',  ( -8.314922557961024197, 14.29746914071037800, 22.91775706135235069 ) ) ;
#132973 = CARTESIAN_POINT ( 'NONE',  ( -10.81492255796105439, 18.62759615963255655, 32.91775706135234714 ) ) ;
#132974 = CARTESIAN_POINT ( 'NONE',  ( 5.719274019375673035, 21.55341960407619339, 87.29275706135236135 ) ) ;
#132975 = CARTESIAN_POINT ( 'NONE',  ( -0.05219959533934338120, 16.53943276465976808, 82.50109039468568994 ) ) ;
#132976 = CARTESIAN_POINT ( 'NONE',  ( -5.049401038298153566, 19.05341960407611168, 75.20724293864769550 ) ) ;
#132977 = CARTESIAN_POINT ( 'NONE',  ( 16.52544592524335698, 4.483927247898782831, 106.4594237280190328 ) ) ;
#132978 = CARTESIAN_POINT ( 'NONE',  ( 13.89961937509957401, 13.97604488694547697, 51.87609039468566863 ) ) ;
#132979 = CARTESIAN_POINT ( 'NONE',  ( -18.62759615963255300, -10.81492255796106328, 29.16775706135234003 ) ) ;
#132980 = CARTESIAN_POINT ( 'NONE',  ( -0.05219959533910754901, -16.53943276465976808, 77.49890960531433848 ) ) ;
#132981 = CARTESIAN_POINT ( 'NONE',  ( 16.51473224551069308, 9.474510206698969483, 94.16557627198103830 ) ) ;
#132982 = CARTESIAN_POINT ( 'NONE',  ( -4.379528057220086978, -16.55341960407618274, 104.7927570613523898 ) ) ;
#132983 = CARTESIAN_POINT ( 'NONE',  ( 5.719274019375673035, 21.55341960407619339, 77.29275706135234714 ) ) ;
#132984 = CARTESIAN_POINT ( 'NONE',  ( 16.55341960407618274, -4.379528057220086978, 36.04275706135234714 ) ) ;
#132985 = CARTESIAN_POINT ( 'NONE',  ( -18.67979575497193778, 10.72451020669871902, 28.33442372801902209 ) ) ;
#132986 = CARTESIAN_POINT ( 'NONE',  ( 16.52544592524342804, -4.483927247898539470, 68.54057627198103830 ) ) ;
#132987 = VERTEX_POINT ( 'NONE', #71707 ) ;
#132988 = CARTESIAN_POINT ( 'NONE',  ( 5.719274019375991003, -21.55341960407610458, 102.7072429386476955 ) ) ;
#132989 = CARTESIAN_POINT ( 'NONE',  ( 16.53943276465976808, -0.05219959533910856209, 53.74890960531437401 ) ) ;
#132990 = CARTESIAN_POINT ( 'NONE',  ( 13.89961937509977652, -13.97604488694527269, 23.12390960531436335 ) ) ;
#132991 = CARTESIAN_POINT ( 'NONE',  ( 5.719274019375991003, -21.55341960407610458, 27.70724293864769905 ) ) ;
#132992 = CARTESIAN_POINT ( 'NONE',  ( 18.62759615963255655, 10.81492255796105972, 51.66775706135234714 ) ) ;
#132993 = CARTESIAN_POINT ( 'NONE',  ( 8.224510206698953496, -14.34966873604960469, 67.91557627198102409 ) ) ;
#132994 = CARTESIAN_POINT ( 'NONE',  ( 21.53943276465977519, -0.05219959533907433946, 73.74890960531433848 ) ) ;
#132995 = CARTESIAN_POINT ( 'NONE',  ( -5.153800228976328057, -19.02544592524343514, 72.29057627198102409 ) ) ;
#132997 = CARTESIAN_POINT ( 'NONE',  ( -5.049401038297874678, -19.05341960407617918, 74.79275706135231871 ) ) ;
#132996 = CARTESIAN_POINT ( 'NONE',  ( -19.05341960407611168, -5.049401038298163336, 26.45724293864769550 ) ) ;
#132999 = CARTESIAN_POINT ( 'NONE',  ( -0.05219959533907301413, -21.53943276465977519, 62.49890960531436690 ) ) ;
#132998 = CARTESIAN_POINT ( 'NONE',  ( -5.719274019375665041, -21.55341960407619695, 59.79275706135234714 ) ) ;
#133000 = B_SPLINE_CURVE_WITH_KNOTS ( 'NONE', 3,
 ( #106020, #123169, #158235, #89865, #66222, #167707 ),
 .UNSPECIFIED., .F., .F.,
 ( 4, 2, 4 ),
 ( 0.003989672132298083609, 0.004372778065220518998, 0.004755883998142954386 ),
 .UNSPECIFIED. ) ;
#133001 = CARTESIAN_POINT ( 'NONE',  ( -5.049401038298153566, 19.05341960407611168, 40.20724293864768839 ) ) ;
#133002 = CARTESIAN_POINT ( 'NONE',  ( -13.89961937509977652, 13.97604488694528158, 70.62390960531432427 ) ) ;
#133003 = VERTEX_POINT ( 'NONE', #165722 ) ;
#133004 = CARTESIAN_POINT ( 'NONE',  ( 4.483927247898790824, -16.52544592524335698, 45.20942372801901854 ) ) ;
#133005 = CARTESIAN_POINT ( 'NONE',  ( -18.62759615963255300, -10.81492255796106328, 34.16775706135234714 ) ) ;
#133006 = CARTESIAN_POINT ( 'NONE',  ( -15.72974639402176322, -15.80617190586768395, 59.37609039468568284 ) ) ;
#133007 = CARTESIAN_POINT ( 'NONE',  ( 16.51473224551069308, 9.474510206698969483, 99.16557627198102409 ) ) ;
#133008 = CARTESIAN_POINT ( 'NONE',  ( -5.823673210054116645, -21.52544592524344225, 82.29057627198103830 ) ) ;
#133010 = CARTESIAN_POINT ( 'NONE',  ( 14.29746914071037800, 8.314922557961029526, 46.66775706135234714 ) ) ;
#133009 = CARTESIAN_POINT ( 'NONE',  ( -0.05219959533937732626, 21.53943276465977519, 22.50109039468567573 ) ) ;
#133011 = EDGE_CURVE ( 'NONE', #100403, #116458, #29523, .T. ) ;
#133012 = CARTESIAN_POINT ( 'NONE',  ( 0.05219959533907565091, 21.53943276465977519, 49.99890960531437401 ) ) ;
#133013 = CARTESIAN_POINT ( 'NONE',  ( 18.67979575497194134, -10.72451020669871369, 110.8344237280190043 ) ) ;
#133014 = CARTESIAN_POINT ( 'NONE',  ( 13.89961937509977652, -13.97604488694527269, 53.12390960531434558 ) ) ;
#133015 = CARTESIAN_POINT ( 'NONE',  ( -9.474510206698964154, 16.51473224551069663, 110.4155762719810383 ) ) ;
#133016 = CARTESIAN_POINT ( 'NONE',  ( 16.51473224551069308, 9.474510206698969483, 84.16557627198102409 ) ) ;
#133017 = CARTESIAN_POINT ( 'NONE',  ( 0.000000000000000000, 0.000000000000000000, -64.92279855667830191 ) ) ;
#133018 = CARTESIAN_POINT ( 'NONE',  ( 16.46253265017146816, 9.564922557961045513, 71.66775706135233293 ) ) ;
#133019 = CARTESIAN_POINT ( 'NONE',  ( 10.81492255796078972, 18.62759615963270932, 44.58224293864769550 ) ) ;
#133020 = CARTESIAN_POINT ( 'NONE',  ( -12.14591786802309592, -12.06949235617757132, 31.87390960531435979 ) ) ;
#133021 = CARTESIAN_POINT ( 'NONE',  ( -0.05219959533936034679, 19.03943276465977164, 87.50109039468567573 ) ) ;
#133022 = CARTESIAN_POINT ( 'NONE',  ( -17.44279575226822843, 5.990770900252466724, 60.83557567514318265 ) ) ;
#133023 = CARTESIAN_POINT ( 'NONE',  ( 5.719274019375673035, 21.55341960407619339, 112.2927570613523471 ) ) ;
#133024 = CARTESIAN_POINT ( 'NONE',  ( 16.46253265017146816, 9.564922557961045513, 81.66775706135233293 ) ) ;
#133025 = CARTESIAN_POINT ( 'NONE',  ( -5.049401038297874678, -19.05341960407617918, 49.79275706135231871 ) ) ;
#133026 = CARTESIAN_POINT ( 'NONE',  ( -15.06137443927361019, -15.06137443927335440, -56.46919128290398504 ) ) ;
#133027 = CARTESIAN_POINT ( 'NONE',  ( 5.049401038298161559, -19.05341960407611168, 57.70724293864769550 ) ) ;
#133028 = CARTESIAN_POINT ( 'NONE',  ( 14.29746914071049879, -8.314922557960816363, 48.33224293864770260 ) ) ;
#133029 = CARTESIAN_POINT ( 'NONE',  ( 5.153800228976335163, 19.02544592524342804, 34.79057627198102409 ) ) ;
#133030 = CARTESIAN_POINT ( 'NONE',  ( -8.314922557960811034, -14.29746914071050412, 42.08224293864769550 ) ) ;
#133031 = FACE_OUTER_BOUND ( 'NONE', #198500, .T. ) ;
#133032 = CARTESIAN_POINT ( 'NONE',  ( 16.52544592524335698, 4.483927247898782831, 111.4594237280190328 ) ) ;
#133033 = CARTESIAN_POINT ( 'NONE',  ( 9.564922557960805705, 16.46253265017160317, 44.58224293864769550 ) ) ;
#133034 = CARTESIAN_POINT ( 'NONE',  ( -19.03943276465977164, -0.05219959533935918106, 23.75109039468566152 ) ) ;
#133035 = CARTESIAN_POINT ( 'NONE',  ( -12.06949235617739369, -12.14591786802326823, 39.37609039468567573 ) ) ;
#133036 = CARTESIAN_POINT ( 'NONE',  ( 15.72974639402199770, -15.80617190586745480, 33.12390960531435979 ) ) ;
#133038 = ORIENTED_EDGE ( 'NONE', *, *, #43155, .F. ) ;
#133037 = CARTESIAN_POINT ( 'NONE',  ( 0.05219959533937995610, -21.53943276465977519, 90.00109039468567573 ) ) ;
#133039 = CARTESIAN_POINT ( 'NONE',  ( 0.05219959533909260263, 19.03943276465977164, 59.99890960531436690 ) ) ;
#133040 = CARTESIAN_POINT ( 'NONE',  ( -9.564922557960796823, -16.46253265017161027, 107.0822429386476955 ) ) ;
#133041 = CARTESIAN_POINT ( 'NONE',  ( 19.02544592524343514, -5.153800228976328945, 98.54057627198100988 ) ) ;
#133042 = CARTESIAN_POINT ( 'NONE',  ( -22.81625015709510507, 31.40387420917330275, -2.924999997268813434 ) ) ;
#133043 = CARTESIAN_POINT ( 'NONE',  ( 21.53943276465977519, 0.05219959533937863772, 26.25109039468567573 ) ) ;
#133044 = CARTESIAN_POINT ( 'NONE',  ( 8.224510206698953496, -14.34966873604960469, 82.91557627198103830 ) ) ;
#133046 = CARTESIAN_POINT ( 'NONE',  ( -9.474510206698964154, 16.51473224551069663, 70.41557627198102409 ) ) ;
#133045 = CARTESIAN_POINT ( 'NONE',  ( 10.72451020669898902, -18.67979575497178502, 72.91557627198103830 ) ) ;
#133047 = CARTESIAN_POINT ( 'NONE',  ( -5.049401038298153566, 19.05341960407611168, 70.20724293864769550 ) ) ;
#133048 = CARTESIAN_POINT ( 'NONE',  ( 5.823673210054125526, 21.52544592524343514, 109.7905762719810383 ) ) ;
#133049 = ORIENTED_EDGE ( 'NONE', *, *, #110780, .F. ) ;
#133050 = CARTESIAN_POINT ( 'NONE',  ( 13.97604488694527802, 13.89961937509977652, 69.37390960531436690 ) ) ;
#133052 = CARTESIAN_POINT ( 'NONE',  ( 2.973862142520697471, -93.04182470242776049, -15.00000000000000178 ) ) ;
#133051 = CARTESIAN_POINT ( 'NONE',  ( 12.06949235617757843, -12.14591786802309237, 103.1239096053143811 ) ) ;
#133053 = CARTESIAN_POINT ( 'NONE',  ( 9.564922557960805705, 16.46253265017160317, 59.58224293864769550 ) ) ;
#133054 = CARTESIAN_POINT ( 'NONE',  ( 19.02544592524334988, 5.153800228976608722, 96.45942372801897591 ) ) ;
#133055 = CARTESIAN_POINT ( 'NONE',  ( 12.06949235617757843, -12.14591786802309237, 103.1239096053143811 ) ) ;
#133056 = CARTESIAN_POINT ( 'NONE',  ( -5.719274019375665041, -21.55341960407619695, 74.79275706135234714 ) ) ;
#133058 = CARTESIAN_POINT ( 'NONE',  ( -15.72974639402176322, -15.80617190586768395, 24.37609039468567573 ) ) ;
#133057 = CARTESIAN_POINT ( 'NONE',  ( -19.03943276465977164, 0.05219959533909376836, 46.24890960531435979 ) ) ;
#133059 = CARTESIAN_POINT ( 'NONE',  ( -16.52544592524342804, 4.483927247898546575, 96.04057627198102409 ) ) ;
#133060 = CARTESIAN_POINT ( 'NONE',  ( -28.82186960331499392, 9.364793116373565596, 143.9000000000000057 ) ) ;
#133061 = CARTESIAN_POINT ( 'NONE',  ( 16.46253265017160672, -9.564922557960803928, 78.33224293864769550 ) ) ;
#133062 = CARTESIAN_POINT ( 'NONE',  ( 16.20579543436677739, 7.371946100355099674, 113.0652083417187441 ) ) ;
#133064 = CARTESIAN_POINT ( 'NONE',  ( 21.55341960407610458, 5.719274019375980345, 33.95724293864769550 ) ) ;
#133063 = CARTESIAN_POINT ( 'NONE',  ( -12.06949235617739369, -12.14591786802326823, 19.37609039468568639 ) ) ;
#133065 = CARTESIAN_POINT ( 'NONE',  ( 15.80617190586769283, -15.72974639402175789, 50.62609039468568994 ) ) ;
#133066 = CARTESIAN_POINT ( 'NONE',  ( 13.89961937509977652, -13.97604488694527269, 103.1239096053143527 ) ) ;
#133067 = CARTESIAN_POINT ( 'NONE',  ( -13.89961937509957401, -13.97604488694547875, 79.37609039468567573 ) ) ;
#133068 = CARTESIAN_POINT ( 'NONE',  ( -16.51473224551069308, -9.474510206698971260, 71.66557627198102409 ) ) ;
#133069 = CARTESIAN_POINT ( 'NONE',  ( -4.483927247898539470, -16.52544592524342804, 82.29057627198103830 ) ) ;
#133070 = CARTESIAN_POINT ( 'NONE',  ( -16.46253265017160317, 9.564922557960807481, 100.8322429386477097 ) ) ;
#133071 = CARTESIAN_POINT ( 'NONE',  ( -16.53943276465976808, 0.05219959533911058130, 91.24890960531436690 ) ) ;
#133072 = CARTESIAN_POINT ( 'NONE',  ( 5.049401038298161559, -19.05341960407611168, 92.70724293864769550 ) ) ;
#133074 = CARTESIAN_POINT ( 'NONE',  ( -19.05341960407611168, -5.049401038298163336, 31.45724293864769550 ) ) ;
#133073 = CARTESIAN_POINT ( 'NONE',  ( 16.52544592524342804, -4.483927247898539470, 43.54057627198103830 ) ) ;
#133075 = ORIENTED_EDGE ( 'NONE', *, *, #165138, .T. ) ;
#133076 = CARTESIAN_POINT ( 'NONE',  ( -10.81492255796105439, 18.62759615963255655, 57.91775706135234714 ) ) ;
#133077 = CARTESIAN_POINT ( 'NONE',  ( -9.564922557961040184, 16.46253265017147172, 82.91775706135233293 ) ) ;
#133078 = CARTESIAN_POINT ( 'NONE',  ( 16.52544592524342804, -4.483927247898539470, 43.54057627198103830 ) ) ;
#133079 = CARTESIAN_POINT ( 'NONE',  ( 21.52544592524344225, -5.823673210054117533, 98.54057627198105251 ) ) ;
#133080 = CARTESIAN_POINT ( 'NONE',  ( 18.62759615963271287, -10.81492255796078972, 33.33224293864769550 ) ) ;
#133081 = CARTESIAN_POINT ( 'NONE',  ( -8.314922557960811034, -14.29746914071050412, 87.08224293864769550 ) ) ;
#133082 = CARTESIAN_POINT ( 'NONE',  ( 19.05341960407611168, 5.049401038298154454, 53.95724293864770260 ) ) ;
#133083 = CARTESIAN_POINT ( 'NONE',  ( -12.14591786802309592, -12.06949235617757132, 21.87390960531436690 ) ) ;
#133084 = CARTESIAN_POINT ( 'NONE',  ( -14.34966873604972548, 8.224510206698743886, 88.33442372801901854 ) ) ;
#133085 = CARTESIAN_POINT ( 'NONE',  ( -16.52544592524335698, -4.483927247898792601, 73.95942372801901854 ) ) ;
#133086 = CARTESIAN_POINT ( 'NONE',  ( -9.474510206698720793, -16.51473224551083518, 19.58442372801899722 ) ) ;
#133087 = CARTESIAN_POINT ( 'NONE',  ( 19.02544592524343514, -5.153800228976328945, 88.54057627198102409 ) ) ;
#133088 = CARTESIAN_POINT ( 'NONE',  ( -9.564922557960796823, -16.46253265017161027, 82.08224293864768129 ) ) ;
#133089 = CARTESIAN_POINT ( 'NONE',  ( 16.52544592524335698, 4.483927247898782831, 91.45942372801901854 ) ) ;
#133090 = CARTESIAN_POINT ( 'NONE',  ( -19.03943276465977164, 0.05219959533909376836, 41.24890960531435269 ) ) ;
#133091 = CARTESIAN_POINT ( 'NONE',  ( 12.14591786802309770, 12.06949235617756955, 54.37390960531435979 ) ) ;
#133093 = CARTESIAN_POINT ( 'NONE',  ( 16.46253265017160672, -9.564922557960803928, 103.3322429386476955 ) ) ;
#133092 = DIRECTION ( 'NONE',  ( -7.855351589328939542E-15, 0.000000000000000000, 1.000000000000000000 ) ) ;
#133094 = CARTESIAN_POINT ( 'NONE',  ( -15.72974639402197994, 15.80617190586746368, 35.62390960531437401 ) ) ;
#133095 = CARTESIAN_POINT ( 'NONE',  ( 4.379528057220339221, -16.55341960407611168, 77.70724293864770971 ) ) ;
#133096 = CARTESIAN_POINT ( 'NONE',  ( 16.55341960407618274, -4.379528057220086978, 31.04275706135234714 ) ) ;
#133097 = ORIENTED_EDGE ( 'NONE', *, *, #133150, .F. ) ;
#133098 = CARTESIAN_POINT ( 'NONE',  ( 8.314922557960818139, 14.29746914071049879, 59.58224293864770260 ) ) ;
#133099 = CARTESIAN_POINT ( 'NONE',  ( 0.000000000000000000, -0.7216878364870318308, -1.250000000000000000 ) ) ;
#133100 = CARTESIAN_POINT ( 'NONE',  ( -5.153800228976607833, 19.02544592524334988, 57.70942372801899012 ) ) ;
#133101 = CARTESIAN_POINT ( 'NONE',  ( -5.049401038298153566, 19.05341960407611168, 100.2072429386476955 ) ) ;
#133102 = CARTESIAN_POINT ( 'NONE',  ( -5.049401038297874678, -19.05341960407617918, 74.79275706135231871 ) ) ;
#133103 = CARTESIAN_POINT ( 'NONE',  ( -22.44159573604009950, -16.30477369853688430, 147.5750000027312012 ) ) ;
#133105 = CARTESIAN_POINT ( 'NONE',  ( 16.53943276465976808, 0.05219959533934440121, 101.2510903946856757 ) ) ;
#133104 = CARTESIAN_POINT ( 'NONE',  ( 19.02544592524334988, 5.153800228976608722, 106.4594237280190185 ) ) ;
#133106 = CARTESIAN_POINT ( 'NONE',  ( 9.564922557960805705, 16.46253265017160317, 34.58224293864770260 ) ) ;
#133107 = CARTESIAN_POINT ( 'NONE',  ( 18.67979575497178502, 10.72451020669898547, 29.16557627198103120 ) ) ;
#133108 = CARTESIAN_POINT ( 'NONE',  ( 21.55341960407619695, -5.719274019375665929, 56.04275706135235424 ) ) ;
#133109 = CARTESIAN_POINT ( 'NONE',  ( -19.05341960407617563, 5.049401038297882671, 113.5427570613523471 ) ) ;
#133111 = CARTESIAN_POINT ( 'NONE',  ( -16.51473224551069308, -9.474510206698971260, 76.66557627198103830 ) ) ;
#133110 = LINE ( 'NONE', #11794, #163818 ) ;
#133112 = CARTESIAN_POINT ( 'NONE',  ( 27.86273085795036408, -28.69962071417356242, -25.00000000000000000 ) ) ;
#133114 = CARTESIAN_POINT ( 'NONE',  ( -13.97604488694527625, -13.89961937509977652, 71.87390960531433848 ) ) ;
#133113 = CARTESIAN_POINT ( 'NONE',  ( 16.53943276465976808, -0.05219959533910856209, 68.74890960531435269 ) ) ;
#133115 = CARTESIAN_POINT ( 'NONE',  ( -9.564922557960796823, -16.46253265017161027, 92.08224293864769550 ) ) ;
#133116 = ORIENTED_EDGE ( 'NONE', *, *, #93518, .F. ) ;
#133117 = CARTESIAN_POINT ( 'NONE',  ( 19.05341960407617918, -5.049401038297876454, 96.04275706135231871 ) ) ;
#133118 = CARTESIAN_POINT ( 'NONE',  ( 21.55341960407610458, 5.719274019375980345, 63.95724293864770260 ) ) ;
#133119 = CARTESIAN_POINT ( 'NONE',  ( -9.474510206698964154, 16.51473224551069663, 35.41557627198102409 ) ) ;
#133120 = CARTESIAN_POINT ( 'NONE',  ( -13.97604488694547697, 13.89961937509957934, 63.12609039468566152 ) ) ;
#133121 = CARTESIAN_POINT ( 'NONE',  ( -16.46253265017160317, 9.564922557960807481, 60.83224293864769550 ) ) ;
#133122 = CARTESIAN_POINT ( 'NONE',  ( 19.03943276465977164, -0.05219959533909143690, 88.74890960531436690 ) ) ;
#133123 = VERTEX_POINT ( 'NONE', #73720 ) ;
#133124 = CARTESIAN_POINT ( 'NONE',  ( -21.53943276465977519, 0.05219959533907696930, 96.24890960531435269 ) ) ;
#133126 = CARTESIAN_POINT ( 'NONE',  ( -19.05341960407617563, 5.049401038297882671, 53.54275706135231871 ) ) ;
#133125 = CARTESIAN_POINT ( 'NONE',  ( 16.55341960407611168, 4.379528057220329451, 93.95724293864770971 ) ) ;
#133127 = CARTESIAN_POINT ( 'NONE',  ( 0.05219959533907565091, 21.53943276465977519, 94.99890960531436690 ) ) ;
#133128 = CARTESIAN_POINT ( 'NONE',  ( -21.53943276465977519, 0.05219959533907696930, 76.24890960531435269 ) ) ;
#133129 = CARTESIAN_POINT ( 'NONE',  ( -12.14591786802309592, -12.06949235617757132, 31.87390960531435979 ) ) ;
#133130 = CARTESIAN_POINT ( 'NONE',  ( 18.67979575497194134, -10.72451020669871369, 105.8344237280190328 ) ) ;
#133131 = CARTESIAN_POINT ( 'NONE',  ( -12.06949235617739369, -12.14591786802326823, 49.37609039468569705 ) ) ;
#133132 = CARTESIAN_POINT ( 'NONE',  ( -13.97604488694527625, -13.89961937509977652, 81.87390960531436690 ) ) ;
#133133 = CARTESIAN_POINT ( 'NONE',  ( -19.02544592524342804, 5.153800228976336051, 26.04057627198103120 ) ) ;
#133134 = CARTESIAN_POINT ( 'NONE',  ( -10.81492255796105439, 18.62759615963255655, 37.91775706135235424 ) ) ;
#133135 = CARTESIAN_POINT ( 'NONE',  ( 10.81492255796106328, -18.62759615963255655, 60.41775706135235424 ) ) ;
#133136 = CARTESIAN_POINT ( 'NONE',  ( 0.05219959533909260263, 19.03943276465977164, 44.99890960531435979 ) ) ;
#133137 = CARTESIAN_POINT ( 'NONE',  ( -18.62759615963255300, -10.81492255796106328, 19.16775706135234714 ) ) ;
#133138 = CARTESIAN_POINT ( 'NONE',  ( -5.153800228976607833, 19.02544592524334988, 67.70942372801900433 ) ) ;
#133139 = CARTESIAN_POINT ( 'NONE',  ( 5.049401038297881783, 19.05341960407617563, 77.29275706135231871 ) ) ;
#133140 = CARTESIAN_POINT ( 'NONE',  ( -14.34966873604972548, 8.224510206698743886, 28.33442372801902209 ) ) ;
#133141 = CARTESIAN_POINT ( 'NONE',  ( -5.049401038298153566, 19.05341960407611168, 30.20724293864768839 ) ) ;
#133142 = CARTESIAN_POINT ( 'NONE',  ( -16.53943276465976808, -0.05219959533934237506, 73.75109039468567573 ) ) ;
#133143 = CARTESIAN_POINT ( 'NONE',  ( 13.97604488694527802, 13.89961937509977652, 44.37390960531435269 ) ) ;
#133144 = CARTESIAN_POINT ( 'NONE',  ( 24.51266705573319626, -8.027923408435217567, 167.0300397585817791 ) ) ;
#133145 = CARTESIAN_POINT ( 'NONE',  ( 5.153800228976335163, 19.02544592524342804, 104.7905762719809957 ) ) ;
#133146 = CARTESIAN_POINT ( 'NONE',  ( -19.05341960407611168, -5.049401038298163336, 31.45724293864769550 ) ) ;
#133147 = CARTESIAN_POINT ( 'NONE',  ( -21.52544592524343514, 5.823673210054127303, 71.04057627198103830 ) ) ;
#133148 = CARTESIAN_POINT ( 'NONE',  ( -12.06949235617739369, -12.14591786802326823, 59.37609039468568284 ) ) ;
#133149 = CARTESIAN_POINT ( 'NONE',  ( -21.53943276465977519, -0.05219959533937600094, 108.7510903946857042 ) ) ;
#133150 = EDGE_CURVE ( 'NONE', #112132, #86619, #143815, .T. ) ;
#133151 = CARTESIAN_POINT ( 'NONE',  ( -0.05219959533909027116, -19.03943276465977164, 42.49890960531435269 ) ) ;
#133152 = CARTESIAN_POINT ( 'NONE',  ( -12.06949235617756955, 12.14591786802309770, 25.62390960531435624 ) ) ;
#133153 = CARTESIAN_POINT ( 'NONE',  ( -8.314922557960811034, -14.29746914071050412, 62.08224293864769550 ) ) ;
#133154 = CARTESIAN_POINT ( 'NONE',  ( 19.02544592524343514, -5.153800228976328945, 68.54057627198103830 ) ) ;
#133155 = CARTESIAN_POINT ( 'NONE',  ( 18.62759615963255655, 10.81492255796105972, 41.66775706135235424 ) ) ;
#133156 = CARTESIAN_POINT ( 'NONE',  ( -13.97604488694527625, -13.89961937509977652, 81.87390960531436690 ) ) ;
#133157 = CARTESIAN_POINT ( 'NONE',  ( 15.80617190586769283, -15.72974639402175789, 85.62609039468568994 ) ) ;
#133158 = CARTESIAN_POINT ( 'NONE',  ( -14.29746914071037622, -8.314922557961029526, 69.16775706135234714 ) ) ;
#133159 = CARTESIAN_POINT ( 'NONE',  ( -5.049401038298153566, 19.05341960407611168, 105.2072429386476671 ) ) ;
#133160 = CARTESIAN_POINT ( 'NONE',  ( -16.52544592524342804, 4.483927247898546575, 46.04057627198103830 ) ) ;
#133161 = CARTESIAN_POINT ( 'NONE',  ( -16.51473224551069308, -9.474510206698971260, 21.66557627198102765 ) ) ;
#133162 = CARTESIAN_POINT ( 'NONE',  ( -14.29746914071037622, -8.314922557961029526, 49.16775706135234003 ) ) ;
#133163 = CARTESIAN_POINT ( 'NONE',  ( -8.224510206698948167, 14.34966873604960824, 60.41557627198102409 ) ) ;
#133164 = B_SPLINE_CURVE_WITH_KNOTS ( 'NONE', 3,
 ( #52371, #128210, #67539, #17073, #36198, #174735, #140403, #4861, #81687, #126233, #189907, #48415, #51382, #80714, #171751, #125246, #129197, #49397, #173749, #78727, #110071, #64568 ),
 .UNSPECIFIED., .F., .F.,
 ( 4, 2, 2, 2, 2, 2, 2, 2, 2, 2, 4 ),
 ( 0.000000000000000000, 0.001027542925581743189, 0.002055085851163486379, 0.002568857313954357648, 0.003082628776745229785, 0.004110171702327031738, 0.004623943165117908212, 0.005137714627908783818, 0.006165257553490564521, 0.007192800479072345224, 0.008220343404654125927 ),
 .UNSPECIFIED. ) ;
#133165 = CARTESIAN_POINT ( 'NONE',  ( -5.823673210054116645, -21.52544592524344225, 22.29057627198102765 ) ) ;
#133166 = CARTESIAN_POINT ( 'NONE',  ( -10.81492255796078084, -18.62759615963271287, 27.08224293864769550 ) ) ;
#133167 = CARTESIAN_POINT ( 'NONE',  ( 21.55341960407619695, -5.719274019375665929, 111.0427570613523613 ) ) ;
#133168 = EDGE_CURVE ( 'NONE', #62156, #193436, #25231, .T. ) ;
#133169 = CARTESIAN_POINT ( 'NONE',  ( -14.29746914071049879, 8.314922557960819915, 90.83224293864769550 ) ) ;
#133170 = CARTESIAN_POINT ( 'NONE',  ( -19.02544592524342804, 5.153800228976336051, 101.0405762719810241 ) ) ;
#133171 = VERTEX_POINT ( 'NONE', #87861 ) ;
#133172 = CARTESIAN_POINT ( 'NONE',  ( 4.483927247898790824, -16.52544592524335698, 60.20942372801902565 ) ) ;
#133173 = CARTESIAN_POINT ( 'NONE',  ( -5.049401038298153566, 19.05341960407611168, 55.20724293864769550 ) ) ;
#133174 = SURFACE_STYLE_FILL_AREA ( #90650 ) ;
#133175 = CARTESIAN_POINT ( 'NONE',  ( -5.049401038297874678, -19.05341960407617918, 49.79275706135231871 ) ) ;
#133176 = CARTESIAN_POINT ( 'NONE',  ( 14.34966873604972726, -8.224510206698740333, 80.83442372801901854 ) ) ;
#133177 = CARTESIAN_POINT ( 'NONE',  ( 5.049401038297881783, 19.05341960407617563, 102.2927570613523045 ) ) ;
#133178 = CARTESIAN_POINT ( 'NONE',  ( -21.53943276465977519, -0.05219959533937600094, 63.75109039468568284 ) ) ;
#133179 = CARTESIAN_POINT ( 'NONE',  ( 5.049401038298161559, -19.05341960407611168, 72.70724293864768129 ) ) ;
#133180 = CARTESIAN_POINT ( 'NONE',  ( 15.80617190586746368, 15.72974639402197994, 89.37390960531435269 ) ) ;
#133181 = CARTESIAN_POINT ( 'NONE',  ( 16.52544592524342804, -4.483927247898539470, 103.5405762719810383 ) ) ;
#133182 = CARTESIAN_POINT ( 'NONE',  ( -13.97604488694547697, 13.89961937509957934, 73.12609039468568994 ) ) ;
#133183 = CARTESIAN_POINT ( 'NONE',  ( 15.80617190586746368, 15.72974639402197994, 69.37390960531436690 ) ) ;
#133184 = CARTESIAN_POINT ( 'NONE',  ( 16.51473224551083163, -9.474510206698727899, 35.83442372801899722 ) ) ;
#133185 = CARTESIAN_POINT ( 'NONE',  ( -5.823673210054116645, -21.52544592524344225, 92.29057627198103830 ) ) ;
#133186 = CARTESIAN_POINT ( 'NONE',  ( 18.22780087662125226, -5.499999999999864997, 51.01540105326108687 ) ) ;
#133187 = CARTESIAN_POINT ( 'NONE',  ( -13.89961937509977652, 13.97604488694528158, 60.62390960531436690 ) ) ;
#133188 = LINE ( 'NONE', #76243, #195009 ) ;
#133189 = CARTESIAN_POINT ( 'NONE',  ( 5.153800228976615827, -19.02544592524334988, 110.2094237280189901 ) ) ;
#133190 = CARTESIAN_POINT ( 'NONE',  ( 37.47059448506524149, -2.437326220201137872, 40.06626038917661958 ) ) ;
#133191 = CARTESIAN_POINT ( 'NONE',  ( 19.02544592524343514, -5.153800228976328945, 53.54057627198102409 ) ) ;
#133192 = CARTESIAN_POINT ( 'NONE',  ( -13.89961937509977652, 13.97604488694528158, 105.6239096053143527 ) ) ;
#133194 = CARTESIAN_POINT ( 'NONE',  ( -4.379528057220328563, 16.55341960407611168, 45.20724293864769550 ) ) ;
#133193 = CARTESIAN_POINT ( 'NONE',  ( 5.823673210054125526, 21.52544592524343514, 84.79057627198102409 ) ) ;
#133195 = CARTESIAN_POINT ( 'NONE',  ( 21.55341960407619695, -5.719274019375665929, 76.04275706135237556 ) ) ;
#133197 = CARTESIAN_POINT ( 'NONE',  ( -9.474510206698720793, -16.51473224551083518, 24.58442372801900078 ) ) ;
#133196 = CARTESIAN_POINT ( 'NONE',  ( 8.314922557961029526, -14.29746914071037800, 25.41775706135235779 ) ) ;
#133198 = CARTESIAN_POINT ( 'NONE',  ( 16.52544592524342804, -4.483927247898539470, 28.54057627198103120 ) ) ;
#133199 = CARTESIAN_POINT ( 'NONE',  ( 10.81492255796078972, 18.62759615963270932, 109.5822429386476955 ) ) ;
#133200 = CARTESIAN_POINT ( 'NONE',  ( 14.29746914071049879, -8.314922557960816363, 48.33224293864770260 ) ) ;
#133201 = CARTESIAN_POINT ( 'NONE',  ( -19.02544592524334988, -5.153800228976617603, 98.95942372801900433 ) ) ;
#133202 = CARTESIAN_POINT ( 'NONE',  ( -5.153800228976607833, 19.02544592524334988, 72.70942372801900433 ) ) ;
#133203 = CARTESIAN_POINT ( 'NONE',  ( 10.72451020669871369, 18.67979575497193778, 67.08442372801901854 ) ) ;
#133204 = CARTESIAN_POINT ( 'NONE',  ( 5.049401038297881783, 19.05341960407617563, 57.29275706135231871 ) ) ;
#133205 = CARTESIAN_POINT ( 'NONE',  ( 9.564922557960805705, 16.46253265017160317, 29.58224293864769550 ) ) ;
#133206 = CARTESIAN_POINT ( 'NONE',  ( -5.719274019375978568, 21.55341960407610458, 45.20724293864769550 ) ) ;
#133207 = CARTESIAN_POINT ( 'NONE',  ( 16.53943276465976808, -0.05219959533910856209, 48.74890960531435979 ) ) ;
#133208 = CARTESIAN_POINT ( 'NONE',  ( -18.39635199886970440, 5.499999999999980460, 96.01967076360006104 ) ) ;
#133209 = CARTESIAN_POINT ( 'NONE',  ( 0.05219959533936267826, -19.03943276465977164, 20.00109039468567218 ) ) ;
#133210 = CARTESIAN_POINT ( 'NONE',  ( 16.55341960407618274, -4.379528057220086978, 86.04275706135236135 ) ) ;
#133211 = CARTESIAN_POINT ( 'NONE',  ( 4.483927247898545687, 16.52544592524342804, 44.79057627198103120 ) ) ;
#133212 = CARTESIAN_POINT ( 'NONE',  ( -5.719274019375665041, -21.55341960407619695, 74.79275706135234714 ) ) ;
#133213 = CARTESIAN_POINT ( 'NONE',  ( -21.55341960407619339, 5.719274019375674811, 73.54275706135234714 ) ) ;
#133214 = CARTESIAN_POINT ( 'NONE',  ( 5.719274019375991003, -21.55341960407610458, 77.70724293864770971 ) ) ;
#133215 = CARTESIAN_POINT ( 'NONE',  ( -19.03943276465977164, 0.05219959533909376836, 41.24890960531435269 ) ) ;
#133216 = CARTESIAN_POINT ( 'NONE',  ( -0.05219959533937732626, 21.53943276465977519, 52.50109039468567573 ) ) ;
#133217 = CARTESIAN_POINT ( 'NONE',  ( 16.46253265017160672, -9.564922557960803928, 33.33224293864770260 ) ) ;
#133218 = CARTESIAN_POINT ( 'NONE',  ( -9.564922557960796823, -16.46253265017161027, 47.08224293864769550 ) ) ;
#133219 = CARTESIAN_POINT ( 'NONE',  ( 14.29746914071049879, -8.314922557960816363, 93.33224293864769550 ) ) ;
#133220 = CARTESIAN_POINT ( 'NONE',  ( -19.05341960407611168, -5.049401038298163336, 81.45724293864769550 ) ) ;
#133221 = CARTESIAN_POINT ( 'NONE',  ( 0.05219959533910956823, 16.53943276465976808, 39.99890960531436690 ) ) ;
#133222 = CARTESIAN_POINT ( 'NONE',  ( 16.52544592524342804, -4.483927247898539470, 98.54057627198105251 ) ) ;
#133223 = CARTESIAN_POINT ( 'NONE',  ( -18.62759615963270932, 10.81492255796079327, 70.83224293864770971 ) ) ;
#133224 = CARTESIAN_POINT ( 'NONE',  ( -15.72974639402176322, -15.80617190586768395, 24.37609039468567573 ) ) ;
#133225 = CYLINDRICAL_SURFACE ( 'NONE', #18142, 1.500000000000001332 ) ;
#133227 = CARTESIAN_POINT ( 'NONE',  ( 8.314922557961029526, -14.29746914071037800, 30.41775706135234358 ) ) ;
#133226 = CARTESIAN_POINT ( 'NONE',  ( 5.049401038298161559, -19.05341960407611168, 82.70724293864770971 ) ) ;
#133228 = CARTESIAN_POINT ( 'NONE',  ( -10.72451020669898014, 18.67979575497178502, 75.41557627198102409 ) ) ;
#133229 = CARTESIAN_POINT ( 'NONE',  ( -5.823673210054431948, 21.52544592524334988, 92.70942372801901854 ) ) ;
#133230 = CARTESIAN_POINT ( 'NONE',  ( 19.02544592524343514, -5.153800228976328945, 83.54057627198100988 ) ) ;
#133231 = CARTESIAN_POINT ( 'NONE',  ( -18.62759615963270932, 10.81492255796079327, 110.8322429386476955 ) ) ;
#133232 = CARTESIAN_POINT ( 'NONE',  ( 13.97604488694527802, 13.89961937509977652, 109.3739096053143669 ) ) ;
#133233 = CARTESIAN_POINT ( 'NONE',  ( -12.06949235617739369, -12.14591786802326823, 94.37609039468568994 ) ) ;
#133234 = CARTESIAN_POINT ( 'NONE',  ( 21.55341960407619695, -5.719274019375665929, 76.04275706135237556 ) ) ;
#133235 = CARTESIAN_POINT ( 'NONE',  ( -21.53943276465977519, -0.05219959533937600094, 93.75109039468567573 ) ) ;
#133236 = CARTESIAN_POINT ( 'NONE',  ( -8.314922557961024197, 14.29746914071037800, 62.91775706135236135 ) ) ;
#133237 = CARTESIAN_POINT ( 'NONE',  ( 21.52544592524334988, 5.823673210054432836, 26.45942372801901854 ) ) ;
#133238 = CARTESIAN_POINT ( 'NONE',  ( 13.97604488694527802, 13.89961937509977652, 114.3739096053143669 ) ) ;
#133239 = CARTESIAN_POINT ( 'NONE',  ( -18.67979575497193778, 10.72451020669871902, 88.33442372801901854 ) ) ;
#133240 = CARTESIAN_POINT ( 'NONE',  ( -0.05219959533909027116, -19.03943276465977164, 97.49890960531436690 ) ) ;
#133241 = CARTESIAN_POINT ( 'NONE',  ( -15.72974639402197994, 15.80617190586746368, 95.62390960531436690 ) ) ;
#133242 = CARTESIAN_POINT ( 'NONE',  ( -19.05341960407617563, 5.049401038297882671, 58.54275706135234003 ) ) ;
#133244 = CARTESIAN_POINT ( 'NONE',  ( 21.53943276465977519, -0.05219959533907433946, 58.74890960531436690 ) ) ;
#133243 = CARTESIAN_POINT ( 'NONE',  ( -21.74014569710914202, -31.09693755439675300, -22.87366378656648536 ) ) ;
#133246 = CARTESIAN_POINT ( 'NONE',  ( 8.314922557960818139, 14.29746914071049879, 34.58224293864770260 ) ) ;
#133245 = CARTESIAN_POINT ( 'NONE',  ( 16.46253265017160672, -9.564922557960803928, 88.33224293864769550 ) ) ;
#133247 = CARTESIAN_POINT ( 'NONE',  ( 28.82186960331511827, 9.364793116373395065, 145.0999999999999943 ) ) ;
#133248 = CARTESIAN_POINT ( 'NONE',  ( 5.049401038297881783, 19.05341960407617563, 77.29275706135231871 ) ) ;
#133249 = DIRECTION ( 'NONE',  ( -0.000000000000000000, -0.9396926207859095381, 0.3420201433256656043 ) ) ;
#133250 = CARTESIAN_POINT ( 'NONE',  ( -13.97604488694547697, 13.89961937509957934, 113.1260903946856757 ) ) ;
#133251 = CARTESIAN_POINT ( 'NONE',  ( -15.80617190586745835, -15.72974639402198527, 86.87390960531438111 ) ) ;
#133252 = CARTESIAN_POINT ( 'NONE',  ( 16.55341960407611168, 4.379528057220329451, 63.95724293864770260 ) ) ;
#133253 = CARTESIAN_POINT ( 'NONE',  ( -5.049401038298153566, 19.05341960407611168, 95.20724293864770971 ) ) ;
#133254 = CARTESIAN_POINT ( 'NONE',  ( 16.53943276465976808, 0.05219959533934440121, 26.25109039468567573 ) ) ;
#133255 = CARTESIAN_POINT ( 'NONE',  ( 5.049401038298161559, -19.05341960407611168, 47.70724293864770260 ) ) ;
#133257 = CARTESIAN_POINT ( 'NONE',  ( 16.51473224551083163, -9.474510206698727899, 85.83442372801900433 ) ) ;
#133256 = CARTESIAN_POINT ( 'NONE',  ( -21.55341960407610458, -5.719274019375992779, 111.4572429386476813 ) ) ;
#133258 = CARTESIAN_POINT ( 'NONE',  ( -16.51473224551069308, -9.474510206698971260, 96.66557627198102409 ) ) ;
#133259 = CARTESIAN_POINT ( 'NONE',  ( -5.049401038298153566, 19.05341960407611168, 75.20724293864769550 ) ) ;
#133260 = CARTESIAN_POINT ( 'NONE',  ( -18.62759615963270932, 10.81492255796079327, 70.83224293864770971 ) ) ;
#133261 = CARTESIAN_POINT ( 'NONE',  ( 0.05219959533909260263, 19.03943276465977164, 49.99890960531435979 ) ) ;
#133262 = DIRECTION ( 'NONE',  ( 1.000000000000000000, 0.000000000000000000, 0.000000000000000000 ) ) ;
#133263 = CARTESIAN_POINT ( 'NONE',  ( 4.483927247898545687, 16.52544592524342804, 49.79057627198102409 ) ) ;
#133264 = CARTESIAN_POINT ( 'NONE',  ( 19.05341960407611168, 5.049401038298154454, 98.95724293864766707 ) ) ;
#133265 = CARTESIAN_POINT ( 'NONE',  ( -37.99626262588766679, 2.428612866367529932E-14, 6.432029388270255055E-14 ) ) ;
#133266 = CARTESIAN_POINT ( 'NONE',  ( -16.51473224551082808, 9.474510206698731452, 68.33442372801900433 ) ) ;
#133267 = CARTESIAN_POINT ( 'NONE',  ( 21.52544592524344225, -5.823673210054117533, 83.54057627198102409 ) ) ;
#133268 = CARTESIAN_POINT ( 'NONE',  ( -16.46253265017146816, -9.564922557961047289, 54.16775706135234003 ) ) ;
#133269 = CARTESIAN_POINT ( 'NONE',  ( -0.05219959533909027116, -19.03943276465977164, 102.4989096053143669 ) ) ;
#133270 = CARTESIAN_POINT ( 'NONE',  ( 11.84747491945383224, -9.688819730466811109, -59.78303737067794543 ) ) ;
#133271 = CARTESIAN_POINT ( 'NONE',  ( 21.52544592524344225, -5.823673210054117533, 43.54057627198103830 ) ) ;
#133272 = CARTESIAN_POINT ( 'NONE',  ( -0.05219959533909027116, -19.03943276465977164, 67.49890960531436690 ) ) ;
#133273 = CARTESIAN_POINT ( 'NONE',  ( 15.72974639402176855, 15.80617190586768217, 71.87609039468568994 ) ) ;
#133274 = CARTESIAN_POINT ( 'NONE',  ( 16.52544592524342804, -4.483927247898539470, 113.5405762719810383 ) ) ;
#133276 = ORIENTED_EDGE ( 'NONE', *, *, #73153, .T. ) ;
#133275 = CARTESIAN_POINT ( 'NONE',  ( 5.719274019375673035, 21.55341960407619339, 22.29275706135235069 ) ) ;
#133277 = CARTESIAN_POINT ( 'NONE',  ( 18.67979575497194134, -10.72451020669871369, 50.83442372801901143 ) ) ;
#133278 = ORIENTED_EDGE ( 'NONE', *, *, #11460, .T. ) ;
#133279 = CARTESIAN_POINT ( 'NONE',  ( -16.46253265017160317, 9.564922557960807481, 110.8322429386476955 ) ) ;
#133280 = CARTESIAN_POINT ( 'NONE',  ( 16.51473224551083163, -9.474510206698727899, 65.83442372801900433 ) ) ;
#133281 = AXIS2_PLACEMENT_3D ( 'NONE', #90127, #197333, #107274 ) ;
#133282 = CARTESIAN_POINT ( 'NONE',  ( 23.36741966814239646, -32.36690354120208468, -22.32433735814155540 ) ) ;
#133283 = CARTESIAN_POINT ( 'NONE',  ( 10.72451020669898902, -18.67979575497178502, 107.9155762719810241 ) ) ;
#133284 = CARTESIAN_POINT ( 'NONE',  ( -19.02544592524342804, 5.153800228976336051, 66.04057627198103830 ) ) ;
#133285 = CARTESIAN_POINT ( 'NONE',  ( -4.483927247898782831, 16.52544592524335698, 42.70942372801901854 ) ) ;
#133286 = CARTESIAN_POINT ( 'NONE',  ( 3.766062262543149401E-15, -39.95556452105413570, -9.249999994537628112 ) ) ;
#133287 = CARTESIAN_POINT ( 'NONE',  ( -0.05219959533937732626, 21.53943276465977519, 102.5010903946856899 ) ) ;
#133288 = CARTESIAN_POINT ( 'NONE',  ( -9.564922557960796823, -16.46253265017161027, 37.08224293864768839 ) ) ;
#133289 = CARTESIAN_POINT ( 'NONE',  ( 13.97604488694548053, -13.89961937509957401, 20.62609039468567573 ) ) ;
#133290 = CARTESIAN_POINT ( 'NONE',  ( 4.483927247898790824, -16.52544592524335698, 85.20942372801901854 ) ) ;
#133292 = CARTESIAN_POINT ( 'NONE',  ( -21.52544592524334988, -5.823673210054445271, 53.95942372801900433 ) ) ;
#133291 = CARTESIAN_POINT ( 'NONE',  ( -5.049401038298153566, 19.05341960407611168, 95.20724293864770971 ) ) ;
#133293 = CARTESIAN_POINT ( 'NONE',  ( 6.874011537017776341, -5.374011537017756801, -61.98469907122333922 ) ) ;
#133294 = CARTESIAN_POINT ( 'NONE',  ( -16.46253265017160317, 9.564922557960807481, 115.8322429386477097 ) ) ;
#133295 = CARTESIAN_POINT ( 'NONE',  ( 17.72560187377285601, 5.500000000000048850, 46.57814504131322053 ) ) ;
#133297 = CARTESIAN_POINT ( 'NONE',  ( 0.05219959533937995610, -21.53943276465977519, 70.00109039468568994 ) ) ;
#133296 = CARTESIAN_POINT ( 'NONE',  ( -16.53943276465976808, -0.05219959533934237506, 48.75109039468568284 ) ) ;
#133298 = CARTESIAN_POINT ( 'NONE',  ( -21.52544592524334988, -5.823673210054445271, 93.95942372801903275 ) ) ;
#133299 = CARTESIAN_POINT ( 'NONE',  ( -4.500000000000000888, -126.1226662136678272, 8.481152457036387204 ) ) ;
#133300 = CARTESIAN_POINT ( 'NONE',  ( 8.314922557961029526, -14.29746914071037800, 25.41775706135235779 ) ) ;
#133301 = CARTESIAN_POINT ( 'NONE',  ( -19.02544592524342804, 5.153800228976336051, 91.04057627198100988 ) ) ;
#133302 = EDGE_CURVE ( 'NONE', #34377, #90572, #124042, .T. ) ;
#133303 = CARTESIAN_POINT ( 'NONE',  ( 16.51473224551069308, 9.474510206698969483, 109.1655762719810383 ) ) ;
#133304 = ORIENTED_EDGE ( 'NONE', *, *, #31820, .T. ) ;
#133305 = CARTESIAN_POINT ( 'NONE',  ( 17.50000000000000355, 5.622605283950885990, 43.81207310596114013 ) ) ;
#133306 = CARTESIAN_POINT ( 'NONE',  ( -4.379528057220328563, 16.55341960407611168, 115.2072429386476955 ) ) ;
#133307 = CARTESIAN_POINT ( 'NONE',  ( 10.72451020669898902, -18.67979575497178502, 42.91557627198103120 ) ) ;
#133308 = CARTESIAN_POINT ( 'NONE',  ( -12.06949235617739369, -12.14591786802326823, 109.3760903946857042 ) ) ;
#133310 = CARTESIAN_POINT ( 'NONE',  ( 9.564922557960805705, 16.46253265017160317, 64.58224293864769550 ) ) ;
#133309 = CARTESIAN_POINT ( 'NONE',  ( -14.29746914071049879, 8.314922557960819915, 85.83224293864768129 ) ) ;
#133311 = CARTESIAN_POINT ( 'NONE',  ( 21.53943276465977519, 0.05219959533937863772, 86.25109039468568994 ) ) ;
#133312 = CARTESIAN_POINT ( 'NONE',  ( -4.379528057220086978, -16.55341960407618274, 29.79275706135234358 ) ) ;
#133313 = CARTESIAN_POINT ( 'NONE',  ( 12.14591786802309770, 12.06949235617756955, 84.37390960531438111 ) ) ;
#133314 = CARTESIAN_POINT ( 'NONE',  ( -21.55341960407619339, 5.719274019375674811, 38.54275706135234714 ) ) ;
#133315 = CARTESIAN_POINT ( 'NONE',  ( 21.52544592524344225, -5.823673210054117533, 73.54057627198102409 ) ) ;
#133316 = CARTESIAN_POINT ( 'NONE',  ( 13.89961937509957401, 13.97604488694547697, 31.87609039468566863 ) ) ;
#133317 = CARTESIAN_POINT ( 'NONE',  ( -34.37178856895487655, 7.314363934749350094, 46.67665261413968381 ) ) ;
#133318 = CARTESIAN_POINT ( 'NONE',  ( 16.46253265017160672, -9.564922557960803928, 98.33224293864769550 ) ) ;
#133319 = CARTESIAN_POINT ( 'NONE',  ( 12.14591786802309770, 12.06949235617756955, 64.37390960531435269 ) ) ;
#133320 = CARTESIAN_POINT ( 'NONE',  ( -4.379528057220328563, 16.55341960407611168, 55.20724293864770260 ) ) ;
#133321 = CARTESIAN_POINT ( 'NONE',  ( 16.52544592524335698, 4.483927247898782831, 111.4594237280190328 ) ) ;
#133322 = CARTESIAN_POINT ( 'NONE',  ( -19.02544592524334988, -5.153800228976617603, 63.95942372801899012 ) ) ;
#133323 = CARTESIAN_POINT ( 'NONE',  ( 18.22780087662126647, 5.499999999999818812, 51.48236817873107896 ) ) ;
#133324 = CARTESIAN_POINT ( 'NONE',  ( -5.153800228976328057, -19.02544592524343514, 112.2905762719810099 ) ) ;
#133325 = CARTESIAN_POINT ( 'NONE',  ( -0.05219959533910754901, -16.53943276465976808, 82.49890960531436690 ) ) ;
#133326 = CARTESIAN_POINT ( 'NONE',  ( 19.48255537605750831, -5.500000000000005329, 37.64712184717532750 ) ) ;
#133328 = CARTESIAN_POINT ( 'NONE',  ( 21.52544592524344225, -5.823673210054117533, 48.54057627198103120 ) ) ;
#133327 = CARTESIAN_POINT ( 'NONE',  ( 19.03943276465977164, -0.05219959533909143690, 48.74890960531435979 ) ) ;
#133329 = CARTESIAN_POINT ( 'NONE',  ( 0.05219959533907565091, 21.53943276465977519, 84.99890960531436690 ) ) ;
#133330 = CARTESIAN_POINT ( 'NONE',  ( -16.55341960407611168, -4.379528057220339221, 111.4572429386476813 ) ) ;
#133332 = CARTESIAN_POINT ( 'NONE',  ( -13.97604488694527625, -13.89961937509977652, 51.87390960531436690 ) ) ;
#133331 = CARTESIAN_POINT ( 'NONE',  ( 16.53943276465976808, 0.05219959533934440121, 71.25109039468568994 ) ) ;
#133333 = CARTESIAN_POINT ( 'NONE',  ( -19.05341960407617563, 5.049401038297882671, 38.54275706135233293 ) ) ;
#133334 = CARTESIAN_POINT ( 'NONE',  ( 18.67979575497194134, -10.72451020669871369, 55.83442372801901854 ) ) ;
#133335 = CARTESIAN_POINT ( 'NONE',  ( -14.29746914071049879, 8.314922557960819915, 105.8322429386476955 ) ) ;
#133336 = CARTESIAN_POINT ( 'NONE',  ( 9.474510206698729675, 16.51473224551082808, 97.08442372801900433 ) ) ;
#133337 = CARTESIAN_POINT ( 'NONE',  ( 29.86685920354754842, -21.69954338932559068, -2.324999997268813345 ) ) ;
#133339 = CARTESIAN_POINT ( 'NONE',  ( -21.52544592524343514, 5.823673210054127303, 46.04057627198103830 ) ) ;
#133338 = CARTESIAN_POINT ( 'NONE',  ( -18.22780087662123094, -5.499999999999984901, 91.48459894673894155 ) ) ;
#133340 = CARTESIAN_POINT ( 'NONE',  ( 19.05341960407611168, 5.049401038298154454, 23.95724293864769194 ) ) ;
#133341 = CARTESIAN_POINT ( 'NONE',  ( -18.67979575497193778, 10.72451020669871902, 83.33442372801903275 ) ) ;
#133342 = CARTESIAN_POINT ( 'NONE',  ( -8.314922557960811034, -14.29746914071050412, 37.08224293864768129 ) ) ;
#133344 = CARTESIAN_POINT ( 'NONE',  ( -0.05219959533910754901, -16.53943276465976808, 37.49890960531436690 ) ) ;
#133343 = CARTESIAN_POINT ( 'NONE',  ( 4.379528057220092307, 16.55341960407617563, 52.29275706135236135 ) ) ;
#133345 = CARTESIAN_POINT ( 'NONE',  ( -5.719274019375978568, 21.55341960407610458, 75.20724293864769550 ) ) ;
#133346 = CARTESIAN_POINT ( 'NONE',  ( -10.81492255796078084, -18.62759615963271287, 82.08224293864768129 ) ) ;
#133347 = CARTESIAN_POINT ( 'NONE',  ( -9.687362902255733488, 9.687362902255692632, -65.00100000000003320 ) ) ;
#133349 = CARTESIAN_POINT ( 'NONE',  ( 16.51473224551069308, 9.474510206698969483, 109.1655762719810383 ) ) ;
#133348 = CARTESIAN_POINT ( 'NONE',  ( -13.97604488694547697, 13.89961937509957934, 88.12609039468563310 ) ) ;
#133350 = CARTESIAN_POINT ( 'NONE',  ( 13.89961937509977652, -13.97604488694527269, 43.12390960531434558 ) ) ;
#133351 = CARTESIAN_POINT ( 'NONE',  ( 19.05341960407611168, 5.049401038298154454, 33.95724293864769550 ) ) ;
#133352 = CARTESIAN_POINT ( 'NONE',  ( 0.000000000000000000, 0.000000000000000000, 0.000000000000000000 ) ) ;
#133353 = FACE_OUTER_BOUND ( 'NONE', #158864, .T. ) ;
#133354 = ORIENTED_EDGE ( 'NONE', *, *, #112928, .F. ) ;
#133355 = CARTESIAN_POINT ( 'NONE',  ( 8.314922557961029526, -14.29746914071037800, 85.41775706135236135 ) ) ;
#133356 = CARTESIAN_POINT ( 'NONE',  ( 0.05219959533907565091, 21.53943276465977519, 109.9989096053143527 ) ) ;
#133357 = CARTESIAN_POINT ( 'NONE',  ( -13.89961937509977652, 13.97604488694528158, 75.62390960531438111 ) ) ;
#133358 = CARTESIAN_POINT ( 'NONE',  ( -10.72451020669870658, -18.67979575497194134, 44.58442372801901854 ) ) ;
#133359 = CARTESIAN_POINT ( 'NONE',  ( 13.89961937509977652, -13.97604488694527269, 98.12390960531433848 ) ) ;
#133360 = CARTESIAN_POINT ( 'NONE',  ( -29.18329815487601664, -27.17471096552342402, -17.01306446741856249 ) ) ;
#133361 = VERTEX_POINT ( 'NONE', #179913 ) ;
#133362 = CARTESIAN_POINT ( 'NONE',  ( 18.62759615963255655, 10.81492255796105972, 31.66775706135234358 ) ) ;
#133364 = CARTESIAN_POINT ( 'NONE',  ( -19.03943276465977164, 0.05219959533909376836, 101.2489096053143669 ) ) ;
#133363 = CARTESIAN_POINT ( 'NONE',  ( 19.03943276465977164, -0.05219959533909143690, 113.7489096053143669 ) ) ;
#133365 = CARTESIAN_POINT ( 'NONE',  ( 0.05219959533936267826, -19.03943276465977164, 35.00109039468566863 ) ) ;
#133366 = CARTESIAN_POINT ( 'NONE',  ( -21.52544592524334988, -5.823673210054445271, 18.95942372801901143 ) ) ;
#133367 = CARTESIAN_POINT ( 'NONE',  ( 19.03943276465977164, 0.05219959533936151252, 41.25109039468566152 ) ) ;
#133368 = CARTESIAN_POINT ( 'NONE',  ( 19.05341960407617918, -5.049401038297876454, 46.04275706135233293 ) ) ;
#133369 = CARTESIAN_POINT ( 'NONE',  ( 4.379528057220092307, 16.55341960407617563, 97.29275706135234714 ) ) ;
#133371 = EDGE_LOOP ( 'NONE', ( #59937, #141744, #8522, #10295 ) ) ;
#133370 = CARTESIAN_POINT ( 'NONE',  ( -28.79475375365571210, -9.355982642739411048, 146.0843446569000434 ) ) ;
#133372 = CARTESIAN_POINT ( 'NONE',  ( -19.03943276465977164, 0.05219959533909376836, 71.24890960531435269 ) ) ;
#133373 = CARTESIAN_POINT ( 'NONE',  ( -18.62759615963255300, -10.81492255796106328, 74.16775706135231871 ) ) ;
#133374 = CARTESIAN_POINT ( 'NONE',  ( -18.62759615963255300, -10.81492255796106328, 89.16775706135236135 ) ) ;
#133375 = LINE ( 'NONE', #150559, #11532 ) ;
#133376 = CARTESIAN_POINT ( 'NONE',  ( 9.474510206698971260, -16.51473224551069308, 82.91557627198103830 ) ) ;
#133377 = CARTESIAN_POINT ( 'NONE',  ( -21.53943276465977519, -0.05219959533937600094, 68.75109039468568994 ) ) ;
#133378 = CARTESIAN_POINT ( 'NONE',  ( -13.97604488694547697, 13.89961937509957934, 98.12609039468566152 ) ) ;
#133379 = CARTESIAN_POINT ( 'NONE',  ( -19.05341960407611168, -5.049401038298163336, 66.45724293864769550 ) ) ;
#133380 = CARTESIAN_POINT ( 'NONE',  ( -19.03943276465977164, 0.05219959533909376836, 106.2489096053143669 ) ) ;
#133381 = CARTESIAN_POINT ( 'NONE',  ( 0.05219959533909260263, 19.03943276465977164, 84.99890960531436690 ) ) ;
#133382 = CARTESIAN_POINT ( 'NONE',  ( -17.49999999999999645, -5.499999999999992895, 89.20309617465829888 ) ) ;
#133383 = CARTESIAN_POINT ( 'NONE',  ( -0.05219959533909027116, -19.03943276465977164, 67.49890960531436690 ) ) ;
#133384 = CARTESIAN_POINT ( 'NONE',  ( 19.03943276465977164, -0.05219959533909143690, 53.74890960531436690 ) ) ;
#133385 = CARTESIAN_POINT ( 'NONE',  ( -21.52544592524343514, 5.823673210054127303, 116.0405762719810383 ) ) ;
#133386 = CARTESIAN_POINT ( 'NONE',  ( -14.29746914071037622, -8.314922557961029526, 99.16775706135234714 ) ) ;
#133387 = FACE_OUTER_BOUND ( 'NONE', #119908, .T. ) ;
#133388 = DIRECTION ( 'NONE',  ( 1.000000000000000000, 0.000000000000000000, 0.000000000000000000 ) ) ;
#133389 = CARTESIAN_POINT ( 'NONE',  ( 16.46253265017146816, 9.564922557961045513, 56.66775706135233293 ) ) ;
#133390 = CARTESIAN_POINT ( 'NONE',  ( -13.89961937509977652, 13.97604488694528158, 85.62390960531433848 ) ) ;
#133391 = CARTESIAN_POINT ( 'NONE',  ( -14.34966873604960291, -8.224510206698953496, 66.66557627198102409 ) ) ;
#133392 = CARTESIAN_POINT ( 'NONE',  ( -0.05219959533910754901, -16.53943276465976808, 102.4989096053143811 ) ) ;
#133393 = CARTESIAN_POINT ( 'NONE',  ( 10.72451020669898902, -18.67979575497178502, 37.91557627198102409 ) ) ;
#133394 = CARTESIAN_POINT ( 'NONE',  ( 15.80617190586746368, 15.72974639402197994, 29.37390960531435269 ) ) ;
#133395 = AXIS2_PLACEMENT_3D ( 'NONE', #70388, #101712, #116882 ) ;
#133396 = CARTESIAN_POINT ( 'NONE',  ( 16.52544592524342804, -4.483927247898539470, 98.54057627198105251 ) ) ;
#133397 = CARTESIAN_POINT ( 'NONE',  ( -3.181980515339573046, -29.99999999999998934, 1.110912703473986074 ) ) ;
#133398 = CARTESIAN_POINT ( 'NONE',  ( -5.049401038297874678, -19.05341960407617918, 24.79275706135233648 ) ) ;
#133399 = CARTESIAN_POINT ( 'NONE',  ( 12.14591786802327356, -12.06949235617739191, 110.6260903946857042 ) ) ;
#133400 = CARTESIAN_POINT ( 'NONE',  ( 0.05219959533909260263, 19.03943276465977164, 89.99890960531436690 ) ) ;
#133401 = CARTESIAN_POINT ( 'NONE',  ( -18.67979575497193778, 10.72451020669871902, 58.33442372801901143 ) ) ;
#133402 = CARTESIAN_POINT ( 'NONE',  ( 5.823673210054125526, 21.52544592524343514, 49.79057627198102409 ) ) ;
#133403 = CARTESIAN_POINT ( 'NONE',  ( 5.719274019375673035, 21.55341960407619339, 27.29275706135234358 ) ) ;
#133404 = CARTESIAN_POINT ( 'NONE',  ( 18.62759615963271287, -10.81492255796078972, 78.33224293864770971 ) ) ;
#133405 = CARTESIAN_POINT ( 'NONE',  ( 8.224510206698953496, -14.34966873604960469, 97.91557627198103830 ) ) ;
#133406 = CARTESIAN_POINT ( 'NONE',  ( 9.474510206698729675, 16.51473224551082808, 62.08442372801899722 ) ) ;
#133407 = EDGE_CURVE ( 'NONE', #94299, #124967, #133375, .T. ) ;
#133408 = CARTESIAN_POINT ( 'NONE',  ( -9.474510206698964154, 16.51473224551069663, 40.41557627198103120 ) ) ;
#133409 = CARTESIAN_POINT ( 'NONE',  ( -0.05219959533909027116, -19.03943276465977164, 92.49890960531436690 ) ) ;
#133410 = CARTESIAN_POINT ( 'NONE',  ( -19.05341960407611168, -5.049401038298163336, 101.4572429386476955 ) ) ;
#133411 = CARTESIAN_POINT ( 'NONE',  ( -14.34966873604960291, -8.224510206698953496, 111.6655762719810525 ) ) ;
#133412 = CARTESIAN_POINT ( 'NONE',  ( -16.53943276465976808, 0.05219959533911058130, 41.24890960531435269 ) ) ;
#133413 = CARTESIAN_POINT ( 'NONE',  ( 16.53943276465976808, 0.05219959533934440121, 36.25109039468567573 ) ) ;
#133414 = CARTESIAN_POINT ( 'NONE',  ( -18.67979575497193778, 10.72451020669871902, 103.3344237280190043 ) ) ;
#133416 = CARTESIAN_POINT ( 'NONE',  ( -8.314922557961024197, 14.29746914071037800, 112.9177570613523329 ) ) ;
#133415 = CARTESIAN_POINT ( 'NONE',  ( -19.02544592524342804, 5.153800228976336051, 116.0405762719810383 ) ) ;
#133417 = CARTESIAN_POINT ( 'NONE',  ( -15.72974639402176322, -15.80617190586768395, 39.37609039468567573 ) ) ;
#133418 = CARTESIAN_POINT ( 'NONE',  ( -13.97604488694527625, -13.89961937509977652, 106.8739096053143669 ) ) ;
#133419 = CARTESIAN_POINT ( 'NONE',  ( -14.29746914071037622, -8.314922557961029526, 39.16775706135235424 ) ) ;
#133420 = CARTESIAN_POINT ( 'NONE',  ( -16.55341960407617563, 4.379528057220093196, 113.5427570613523756 ) ) ;
#133421 = CARTESIAN_POINT ( 'NONE',  ( 14.29746914071037800, 8.314922557961029526, 96.66775706135234714 ) ) ;
#133422 = CARTESIAN_POINT ( 'NONE',  ( 4.483927247898790824, -16.52544592524335698, 30.20942372801902565 ) ) ;
#133423 = CARTESIAN_POINT ( 'NONE',  ( -13.89961937509977652, 13.97604488694528158, 35.62390960531435269 ) ) ;
#133424 = VECTOR ( 'NONE', #114474, 1000.000000000000000 ) ;
#133425 = CARTESIAN_POINT ( 'NONE',  ( 4.379528057220339221, -16.55341960407611168, 107.7072429386476955 ) ) ;
#133426 = CARTESIAN_POINT ( 'NONE',  ( -0.05219959533907301413, -21.53943276465977519, 112.4989096053143669 ) ) ;
#133427 = CARTESIAN_POINT ( 'NONE',  ( 0.05219959533909260263, 19.03943276465977164, 34.99890960531435979 ) ) ;
#133428 = CARTESIAN_POINT ( 'NONE',  ( 5.153800228976335163, 19.02544592524342804, 104.7905762719809957 ) ) ;
#133429 = CARTESIAN_POINT ( 'NONE',  ( 5.719274019375673035, 21.55341960407619339, 32.29275706135235424 ) ) ;
#133430 = CARTESIAN_POINT ( 'NONE',  ( -16.46253265017160317, 9.564922557960807481, 25.83224293864769194 ) ) ;
#133431 = CARTESIAN_POINT ( 'NONE',  ( -0.05219959533909027116, -19.03943276465977164, 102.4989096053143669 ) ) ;
#133432 = CARTESIAN_POINT ( 'NONE',  ( 17.05587630539789146, -6.762274262135674618, 113.2418030903731534 ) ) ;
#133433 = CARTESIAN_POINT ( 'NONE',  ( 19.02544592524343514, -5.153800228976328945, 98.54057627198100988 ) ) ;
#133435 = CARTESIAN_POINT ( 'NONE',  ( -0.05219959533910754901, -16.53943276465976808, 92.49890960531436690 ) ) ;
#133434 = CARTESIAN_POINT ( 'NONE',  ( 10.72451020669871369, 18.67979575497193778, 47.08442372801901854 ) ) ;
#133436 = CARTESIAN_POINT ( 'NONE',  ( 9.474510206698971260, -16.51473224551069308, 102.9155762719810241 ) ) ;
#133437 = CARTESIAN_POINT ( 'NONE',  ( -27.67912082739735524, -7.698001346388012145, 161.8872396492397741 ) ) ;
#133438 = CARTESIAN_POINT ( 'NONE',  ( 8.224510206698742110, 14.34966873604972548, 62.08442372801901143 ) ) ;
#133439 = CARTESIAN_POINT ( 'NONE',  ( -5.719274019375665041, -21.55341960407619695, 84.79275706135234714 ) ) ;
#133440 = CARTESIAN_POINT ( 'NONE',  ( 12.06949235617739724, 12.14591786802326823, 46.87609039468568994 ) ) ;
#133441 = CARTESIAN_POINT ( 'NONE',  ( 19.03943276465977164, -0.05219959533909143690, 78.74890960531436690 ) ) ;
#133442 = CARTESIAN_POINT ( 'NONE',  ( -14.29746914071037622, -8.314922557961029526, 19.16775706135234714 ) ) ;
#133443 = CARTESIAN_POINT ( 'NONE',  ( -12.06949235617739369, -12.14591786802326823, 64.37609039468568994 ) ) ;
#133444 = CARTESIAN_POINT ( 'NONE',  ( -0.05219959533937732626, 21.53943276465977519, 112.5010903946857042 ) ) ;
#133445 = CARTESIAN_POINT ( 'NONE',  ( 5.049401038297881783, 19.05341960407617563, 87.29275706135234714 ) ) ;
#133446 = CARTESIAN_POINT ( 'NONE',  ( -5.153800228976328057, -19.02544592524343514, 57.29057627198103120 ) ) ;
#133447 = CARTESIAN_POINT ( 'NONE',  ( 5.823673210054125526, 21.52544592524343514, 79.79057627198102409 ) ) ;
#133449 = CARTESIAN_POINT ( 'NONE',  ( 5.153800228976615827, -19.02544592524334988, 95.20942372801897591 ) ) ;
#133448 = CARTESIAN_POINT ( 'NONE',  ( 12.06949235617757843, -12.14591786802309237, 88.12390960531436690 ) ) ;
#133450 = CARTESIAN_POINT ( 'NONE',  ( 12.14591786802327356, -12.06949235617739191, 60.62609039468567573 ) ) ;
#133451 = CARTESIAN_POINT ( 'NONE',  ( 21.94905633995363559, 7.481063542984161430, 170.0146117665088923 ) ) ;
#133452 = CARTESIAN_POINT ( 'NONE',  ( -16.51473224551082808, 9.474510206698731452, 63.33442372801900433 ) ) ;
#133453 = CARTESIAN_POINT ( 'NONE',  ( -16.52544592524342804, 4.483927247898546575, 36.04057627198102409 ) ) ;
#133454 = CARTESIAN_POINT ( 'NONE',  ( -16.52544592524342804, 4.483927247898546575, 76.04057627198102409 ) ) ;
#133456 = CARTESIAN_POINT ( 'NONE',  ( -17.48853670773248226, 5.747243402302952830, 38.66671299749993551 ) ) ;
#133455 = CARTESIAN_POINT ( 'NONE',  ( -13.89961937509957401, -13.97604488694547875, 19.37609039468566507 ) ) ;
#133457 = CARTESIAN_POINT ( 'NONE',  ( 15.80617190586769283, -15.72974639402175789, 25.62609039468567929 ) ) ;
#133458 = CARTESIAN_POINT ( 'NONE',  ( 9.564922557960805705, 16.46253265017160317, 104.5822429386476955 ) ) ;
#133459 = CARTESIAN_POINT ( 'NONE',  ( -19.05341960407611168, -5.049401038298163336, 76.45724293864769550 ) ) ;
#133460 = CARTESIAN_POINT ( 'NONE',  ( -5.823673210054431948, 21.52544592524334988, 92.70942372801901854 ) ) ;
#133461 = CARTESIAN_POINT ( 'NONE',  ( -16.46253265017160317, 9.564922557960807481, 75.83224293864769550 ) ) ;
#133462 = CARTESIAN_POINT ( 'NONE',  ( 10.72451020669898902, -18.67979575497178502, 37.91557627198102409 ) ) ;
#133463 = CARTESIAN_POINT ( 'NONE',  ( 8.314922557960818139, 14.29746914071049879, 74.58224293864768129 ) ) ;
#133464 = CARTESIAN_POINT ( 'NONE',  ( 19.02544592524343514, -5.153800228976328945, 38.54057627198103120 ) ) ;
#133465 = CARTESIAN_POINT ( 'NONE',  ( -14.34966873604960291, -8.224510206698953496, 91.66557627198103830 ) ) ;
#133466 = CARTESIAN_POINT ( 'NONE',  ( 18.62759615963271287, -10.81492255796078972, 108.3322429386477097 ) ) ;
#133467 = CARTESIAN_POINT ( 'NONE',  ( 15.72974639402176855, 15.80617190586768217, 61.87609039468568284 ) ) ;
#133468 = CARTESIAN_POINT ( 'NONE',  ( -0.05219959533909027116, -19.03943276465977164, 27.49890960531435624 ) ) ;
#133469 = CARTESIAN_POINT ( 'NONE',  ( 12.14591786802327356, -12.06949235617739191, 65.62609039468568994 ) ) ;
#133470 = CARTESIAN_POINT ( 'NONE',  ( 5.823673210054444382, -21.52544592524334988, 20.20942372801900788 ) ) ;
#133471 = CARTESIAN_POINT ( 'NONE',  ( -15.80617190586745835, -15.72974639402198527, 106.8739096053143811 ) ) ;
#133473 = CARTESIAN_POINT ( 'NONE',  ( 16.46253265017160672, -9.564922557960803928, 48.33224293864769550 ) ) ;
#133472 = CARTESIAN_POINT ( 'NONE',  ( -16.46253265017146816, -9.564922557961047289, 39.16775706135234003 ) ) ;
#133474 = CARTESIAN_POINT ( 'NONE',  ( -18.62759615963255300, -10.81492255796106328, 74.16775706135231871 ) ) ;
#133475 = CARTESIAN_POINT ( 'NONE',  ( -18.62759615963270932, 10.81492255796079327, 60.83224293864769550 ) ) ;
#133476 = CARTESIAN_POINT ( 'NONE',  ( -12.14591786802309592, -12.06949235617757132, 31.87390960531435979 ) ) ;
#133478 = CARTESIAN_POINT ( 'NONE',  ( 16.46253265017146816, 9.564922557961045513, 21.66775706135233648 ) ) ;
#133477 = CARTESIAN_POINT ( 'NONE',  ( 18.62759615963255655, 10.81492255796105972, 81.66775706135236135 ) ) ;
#133479 = CARTESIAN_POINT ( 'NONE',  ( 14.29746914071049879, -8.314922557960816363, 53.33224293864769550 ) ) ;
#133480 = CARTESIAN_POINT ( 'NONE',  ( -16.53943276465976808, 0.05219959533911058130, 106.2489096053143811 ) ) ;
#133481 = CARTESIAN_POINT ( 'NONE',  ( 19.03943276465977164, 0.05219959533936151252, 46.25109039468566863 ) ) ;
#133482 = CARTESIAN_POINT ( 'NONE',  ( 14.34966873604972726, -8.224510206698740333, 95.83442372801903275 ) ) ;
#133483 = CARTESIAN_POINT ( 'NONE',  ( 15.80617190586769283, -15.72974639402175789, 65.62609039468568994 ) ) ;
#133484 = CARTESIAN_POINT ( 'NONE',  ( -13.89961937509977652, 13.97604488694528158, 65.62390960531436690 ) ) ;
#133485 = CARTESIAN_POINT ( 'NONE',  ( 9.564922557961047289, -16.46253265017146816, 40.41775706135234003 ) ) ;
#133486 = CARTESIAN_POINT ( 'NONE',  ( 15.72974639402199770, -15.80617190586745480, 33.12390960531435979 ) ) ;
#133487 = CARTESIAN_POINT ( 'NONE',  ( 10.72451020669871369, 18.67979575497193778, 37.08442372801901143 ) ) ;
#133488 = CARTESIAN_POINT ( 'NONE',  ( 18.62759615963271287, -10.81492255796078972, 93.33224293864769550 ) ) ;
#133489 = CARTESIAN_POINT ( 'NONE',  ( -5.049401038297874678, -19.05341960407617918, 84.79275706135233293 ) ) ;
#133490 = CARTESIAN_POINT ( 'NONE',  ( -12.14591786802326823, 12.06949235617739902, 48.12609039468568284 ) ) ;
#133492 = CARTESIAN_POINT ( 'NONE',  ( -15.80617190586745835, -15.72974639402198527, 96.87390960531436690 ) ) ;
#133491 = CARTESIAN_POINT ( 'NONE',  ( -4.625078002628085549, 4.070616889113791714, -62.49731305256337066 ) ) ;
#133493 = CARTESIAN_POINT ( 'NONE',  ( -8.224510206698948167, 14.34966873604960824, 70.41557627198102409 ) ) ;
#133494 = CARTESIAN_POINT ( 'NONE',  ( -19.96964676835922248, -32.33678545050552344, -24.48363814647542114 ) ) ;
#133495 = CARTESIAN_POINT ( 'NONE',  ( 4.379528057220092307, 16.55341960407617563, 27.29275706135234358 ) ) ;
#133496 = CIRCLE ( 'NONE', #72154, 16.70000000000002061 ) ;
#133497 = CARTESIAN_POINT ( 'NONE',  ( -0.05219959533907301413, -21.53943276465977519, 47.49890960531435979 ) ) ;
#133498 = CARTESIAN_POINT ( 'NONE',  ( 14.29746914071037800, 8.314922557961029526, 76.66775706135234714 ) ) ;
#133499 = FACE_OUTER_BOUND ( 'NONE', #144288, .T. ) ;
#133500 = CARTESIAN_POINT ( 'NONE',  ( -8.314922557961024197, 14.29746914071037800, 57.91775706135234714 ) ) ;
#133501 = CARTESIAN_POINT ( 'NONE',  ( 15.72974639402176855, 15.80617190586768217, 26.87609039468567218 ) ) ;
#133502 = CARTESIAN_POINT ( 'NONE',  ( 15.80617190586746368, 15.72974639402197994, 44.37390960531435979 ) ) ;
#133503 = CARTESIAN_POINT ( 'NONE',  ( -0.05219959533934338120, 16.53943276465976808, 77.50109039468567573 ) ) ;
#133504 = CARTESIAN_POINT ( 'NONE',  ( 16.51473224551069308, 9.474510206698969483, 99.16557627198102409 ) ) ;
#133506 = CARTESIAN_POINT ( 'NONE',  ( 13.97604488694527802, 13.89961937509977652, 29.37390960531435979 ) ) ;
#133505 = CARTESIAN_POINT ( 'NONE',  ( -18.62759615963255300, -10.81492255796106328, 59.16775706135234714 ) ) ;
#133507 = CARTESIAN_POINT ( 'NONE',  ( -21.52544592524343514, 5.823673210054127303, 36.04057627198102409 ) ) ;
#133508 = CARTESIAN_POINT ( 'NONE',  ( -13.89961937509977652, 13.97604488694528158, 110.6239096053143243 ) ) ;
#133509 = VERTEX_POINT ( 'NONE', #85871 ) ;
#133510 = CARTESIAN_POINT ( 'NONE',  ( 19.02544592524334988, 5.153800228976608722, 36.45942372801900433 ) ) ;
#133511 = CARTESIAN_POINT ( 'NONE',  ( -16.53943276465976808, -0.05219959533934237506, 53.75109039468568994 ) ) ;
#133512 = CARTESIAN_POINT ( 'NONE',  ( 0.05219959533909260263, 19.03943276465977164, 109.9989096053143669 ) ) ;
#133513 = EDGE_LOOP ( 'NONE', ( #53390, #122661, #36845, #161378 ) ) ;
#133514 = CARTESIAN_POINT ( 'NONE',  ( -19.05341960407611168, -5.049401038298163336, 86.45724293864769550 ) ) ;
#133515 = CARTESIAN_POINT ( 'NONE',  ( -12.06949235617739369, -12.14591786802326823, 104.3760903946856899 ) ) ;
#133516 = CARTESIAN_POINT ( 'NONE',  ( 13.99740082693655019, -37.19577201402442057, -29.83961662117126323 ) ) ;
#133517 = CARTESIAN_POINT ( 'NONE',  ( -4.379528057220328563, 16.55341960407611168, 90.20724293864770971 ) ) ;
#133518 = CARTESIAN_POINT ( 'NONE',  ( 15.80617190586746368, 15.72974639402197994, 49.37390960531436690 ) ) ;
#133519 = CARTESIAN_POINT ( 'NONE',  ( -19.05341960407611168, -5.049401038298163336, 31.45724293864769550 ) ) ;
#133520 = CARTESIAN_POINT ( 'NONE',  ( -12.14591786802326823, 12.06949235617739902, 73.12609039468567573 ) ) ;
#133521 = CARTESIAN_POINT ( 'NONE',  ( 21.55341960407619695, -5.719274019375665929, 26.04275706135235779 ) ) ;
#133522 = CARTESIAN_POINT ( 'NONE',  ( 19.05341960407617918, -5.049401038297876454, 96.04275706135231871 ) ) ;
#133523 = CARTESIAN_POINT ( 'NONE',  ( -16.51473224551069308, -9.474510206698971260, 46.66557627198102409 ) ) ;
#133524 = CARTESIAN_POINT ( 'NONE',  ( -9.564922557960796823, -16.46253265017161027, 107.0822429386476955 ) ) ;
#133525 = CARTESIAN_POINT ( 'NONE',  ( 15.80617190586769283, -15.72974639402175789, 105.6260903946856899 ) ) ;
#133526 = CARTESIAN_POINT ( 'NONE',  ( 5.153800228976335163, 19.02544592524342804, 84.79057627198099567 ) ) ;
#133527 = CARTESIAN_POINT ( 'NONE',  ( 12.06949235617739724, 12.14591786802326823, 56.87609039468568994 ) ) ;
#133528 = CARTESIAN_POINT ( 'NONE',  ( -10.81492255796105439, 18.62759615963255655, 97.91775706135236135 ) ) ;
#133529 = CARTESIAN_POINT ( 'NONE',  ( -13.89961937509957401, -13.97604488694547875, 49.37609039468567573 ) ) ;
#133530 = CARTESIAN_POINT ( 'NONE',  ( -9.474510206698720793, -16.51473224551083518, 69.58442372801901854 ) ) ;
#133531 = ORIENTED_EDGE ( 'NONE', *, *, #160688, .T. ) ;
#133532 = CARTESIAN_POINT ( 'NONE',  ( 10.72451020669871369, 18.67979575497193778, 67.08442372801901854 ) ) ;
#133533 = DIRECTION ( 'NONE',  ( 0.000000000000000000, 0.000000000000000000, -1.000000000000000000 ) ) ;
#133534 = CARTESIAN_POINT ( 'NONE',  ( -13.89961937509957401, -13.97604488694547875, 54.37609039468565442 ) ) ;
#133535 = CARTESIAN_POINT ( 'NONE',  ( 4.999999999999997335, 0.000000000000000000, 0.000000000000000000 ) ) ;
#133536 = CARTESIAN_POINT ( 'NONE',  ( 19.05341960407611168, 5.049401038298154454, 83.95724293864766707 ) ) ;
#133537 = CARTESIAN_POINT ( 'NONE',  ( 16.55341960407611168, 4.379528057220329451, 43.95724293864769550 ) ) ;
#133538 = CARTESIAN_POINT ( 'NONE',  ( 21.52544592524344225, -5.823673210054117533, 33.54057627198102409 ) ) ;
#133539 = CARTESIAN_POINT ( 'NONE',  ( 17.49999999999999645, 5.624438216177602534, 56.68329655085356933 ) ) ;
#133540 =( BOUNDED_CURVE ( )  B_SPLINE_CURVE ( 2, ( #173236, #33719, #159036, #68030, #99360, #7346, #161043, #112540, #176227, #5352, #114526, #81192, #67036 ),
 .UNSPECIFIED., .F., .T. ) 
 B_SPLINE_CURVE_WITH_KNOTS ( ( 3, 2, 2, 2, 2, 2, 3 ),
 ( 0.5814234846701880066, 0.5833333333333333703, 0.5877192982456140857, 0.5921052631578946901, 0.5964912280701754055, 0.6008771929824561209, 0.6028327214676918455 ),
 .UNSPECIFIED. ) 
 CURVE ( )  GEOMETRIC_REPRESENTATION_ITEM ( )  RATIONAL_B_SPLINE_CURVE ( ( 0.9832469066685285419, 0.9851625545550100060, 1.000000000000000000, 0.9659258262890683122, 1.000000000000000000, 0.9659258262890683122, 1.000000000000000000, 0.9659258262890683122, 1.000000000000000000, 0.9659258262890683122, 1.000000000000000000, 0.9848076720550078544, 0.9831626618144001517 ) ) 
 REPRESENTATION_ITEM ( '' )  );
#133541 = CARTESIAN_POINT ( 'NONE',  ( -21.53943276465977519, -0.05219959533937600094, 113.7510903946856757 ) ) ;
#133542 = CARTESIAN_POINT ( 'NONE',  ( -27.94119071623633843, 7.398115196984048403, 160.8979257793639590 ) ) ;
#133543 = CARTESIAN_POINT ( 'NONE',  ( -16.46253265017160317, 9.564922557960807481, 40.83224293864769550 ) ) ;
#133544 = CARTESIAN_POINT ( 'NONE',  ( -17.58332526062529411, 7.635886036038502134, 85.92334959558466778 ) ) ;
#133545 = EDGE_CURVE ( 'NONE', #153939, #79638, #121184, .T. ) ;
#133546 = CARTESIAN_POINT ( 'NONE',  ( -18.22780087662123805, 5.499999999999981348, 81.01763182126896368 ) ) ;
#133547 = CARTESIAN_POINT ( 'NONE',  ( 21.52544592524334988, 5.823673210054432836, 66.45942372801903275 ) ) ;
#133548 = CARTESIAN_POINT ( 'NONE',  ( -30.34862450090452057, -22.29628711642643779, -7.999999999999994671 ) ) ;
#133549 = CARTESIAN_POINT ( 'NONE',  ( -14.34966873604972548, 8.224510206698743886, 63.33442372801900433 ) ) ;
#133550 = CARTESIAN_POINT ( 'NONE',  ( 18.67979575497178502, 10.72451020669898547, 84.16557627198103830 ) ) ;
#133551 = CARTESIAN_POINT ( 'NONE',  ( 16.52544592524342804, -4.483927247898539470, 53.54057627198103120 ) ) ;
#133553 = CARTESIAN_POINT ( 'NONE',  ( -13.97604488694527625, -13.89961937509977652, 106.8739096053143669 ) ) ;
#133552 = CARTESIAN_POINT ( 'NONE',  ( 16.46253265017160672, -9.564922557960803928, 23.33224293864769194 ) ) ;
#133554 = CARTESIAN_POINT ( 'NONE',  ( 18.62759615963255655, 10.81492255796105972, 31.66775706135234358 ) ) ;
#133555 = CARTESIAN_POINT ( 'NONE',  ( -19.02544592524334988, -5.153800228976617603, 53.95942372801898301 ) ) ;
#133556 = CARTESIAN_POINT ( 'NONE',  ( 16.51473224551069308, 9.474510206698969483, 39.16557627198103120 ) ) ;
#133557 = CARTESIAN_POINT ( 'NONE',  ( 15.72974639402176855, 15.80617190586768217, 81.87609039468568994 ) ) ;
#133558 = CARTESIAN_POINT ( 'NONE',  ( 16.18388926212234580, -7.379444403734662927, 32.06046848633847901 ) ) ;
#133559 = CARTESIAN_POINT ( 'NONE',  ( 16.53943276465976808, -0.05219959533910856209, 28.74890960531435624 ) ) ;
#133560 = CARTESIAN_POINT ( 'NONE',  ( 17.50000000000148148, 3.254303733634527074, 112.4760410692860830 ) ) ;
#133561 = CARTESIAN_POINT ( 'NONE',  ( -18.62759615963270932, 10.81492255796079327, 45.83224293864769550 ) ) ;
#133562 = CARTESIAN_POINT ( 'NONE',  ( 16.52544592524342804, -4.483927247898539470, 103.5405762719810383 ) ) ;
#133563 = CARTESIAN_POINT ( 'NONE',  ( 8.898962301217535398, -0.7565710328820663966, -63.99033069988504963 ) ) ;
#133564 = CARTESIAN_POINT ( 'NONE',  ( 9.474510206698971260, -16.51473224551069308, 87.91557627198102409 ) ) ;
#133565 = CARTESIAN_POINT ( 'NONE',  ( 0.05219959533910956823, 16.53943276465976808, 94.99890960531436690 ) ) ;
#133566 = CARTESIAN_POINT ( 'NONE',  ( 16.51473224551083163, -9.474510206698727899, 105.8344237280190043 ) ) ;
#133567 = CARTESIAN_POINT ( 'NONE',  ( -5.719274019375978568, 21.55341960407610458, 65.20724293864768129 ) ) ;
#133568 = VERTEX_POINT ( 'NONE', #149549 ) ;
#133569 = CARTESIAN_POINT ( 'NONE',  ( 19.03943276465977164, -0.05219959533909143690, 28.74890960531435624 ) ) ;
#133571 = CARTESIAN_POINT ( 'NONE',  ( 21.53943276465977519, -0.05219959533907433946, 93.74890960531436690 ) ) ;
#133570 = CARTESIAN_POINT ( 'NONE',  ( -0.05219959533909027116, -19.03943276465977164, 87.49890960531436690 ) ) ;
#133572 = CIRCLE ( 'NONE', #81856, 10.00000000000000000 ) ;
#133574 = CARTESIAN_POINT ( 'NONE',  ( 9.474510206698971260, -16.51473224551069308, 102.9155762719810241 ) ) ;
#133573 = CARTESIAN_POINT ( 'NONE',  ( 12.06949235617739724, 12.14591786802326823, 106.8760903946856899 ) ) ;
#133575 = CARTESIAN_POINT ( 'NONE',  ( 19.05341960407617918, -5.049401038297876454, 76.04275706135230450 ) ) ;
#133576 = CARTESIAN_POINT ( 'NONE',  ( -21.53943276465977519, -0.05219959533937600094, 98.75109039468568994 ) ) ;
#133577 = CARTESIAN_POINT ( 'NONE',  ( 18.67979575497178502, 10.72451020669898547, 74.16557627198102409 ) ) ;
#133578 = CARTESIAN_POINT ( 'NONE',  ( 21.53943276465977519, -0.05219959533907433946, 43.74890960531435979 ) ) ;
#133579 = CARTESIAN_POINT ( 'NONE',  ( -19.03943276465977164, 0.05219959533909376836, 56.24890960531435979 ) ) ;
#133580 = CARTESIAN_POINT ( 'NONE',  ( -8.224510206698735004, -14.34966873604973081, 109.5844237280190328 ) ) ;
#133581 = CARTESIAN_POINT ( 'NONE',  ( -19.05341960407611168, -5.049401038298163336, 66.45724293864769550 ) ) ;
#133582 = ORIENTED_EDGE ( 'NONE', *, *, #126480, .T. ) ;
#133583 = CARTESIAN_POINT ( 'NONE',  ( -31.24012740013092326, -7.112679799535561287, 97.39185870086456021 ) ) ;
#133584 = CARTESIAN_POINT ( 'NONE',  ( 16.51473224551083163, -9.474510206698727899, 25.83442372801900078 ) ) ;
#133585 = CARTESIAN_POINT ( 'NONE',  ( 16.52544592524342804, -4.483927247898539470, 78.54057627198103830 ) ) ;
#133586 = CARTESIAN_POINT ( 'NONE',  ( -21.52544592524343514, 5.823673210054127303, 116.0405762719810383 ) ) ;
#133587 = CARTESIAN_POINT ( 'NONE',  ( -22.44159573604010305, 16.30477369853692338, 141.1750000027311671 ) ) ;
#133588 = CARTESIAN_POINT ( 'NONE',  ( -18.67979575497178146, -10.72451020669898902, 56.66557627198103830 ) ) ;
#133589 = CARTESIAN_POINT ( 'NONE',  ( -8.224510206698735004, -14.34966873604973081, 94.58442372801901854 ) ) ;
#133590 = CARTESIAN_POINT ( 'NONE',  ( 4.483927247898545687, 16.52544592524342804, 109.7905762719810383 ) ) ;
#133591 = CARTESIAN_POINT ( 'NONE',  ( 13.89961937509977652, -13.97604488694527269, 73.12390960531436690 ) ) ;
#133592 = CARTESIAN_POINT ( 'NONE',  ( -14.34966873604960291, -8.224510206698953496, 31.66557627198102054 ) ) ;
#133593 = CARTESIAN_POINT ( 'NONE',  ( -0.05219959533937732626, 21.53943276465977519, 42.50109039468567573 ) ) ;
#133594 = CARTESIAN_POINT ( 'NONE',  ( -19.02544592524342804, 5.153800228976336051, 106.0405762719810241 ) ) ;
#133595 = CARTESIAN_POINT ( 'NONE',  ( 5.823673210054444382, -21.52544592524334988, 80.20942372801901854 ) ) ;
#133596 = CARTESIAN_POINT ( 'NONE',  ( 5.049401038298161559, -19.05341960407611168, 27.70724293864769550 ) ) ;
#133597 = CARTESIAN_POINT ( 'NONE',  ( -0.05219959533909027116, -19.03943276465977164, 32.49890960531435979 ) ) ;
#133598 = ORIENTED_EDGE ( 'NONE', *, *, #2819, .F. ) ;
#133599 = CARTESIAN_POINT ( 'NONE',  ( 18.62759615963255655, 10.81492255796105972, 101.6677570613523613 ) ) ;
#133600 = CARTESIAN_POINT ( 'NONE',  ( 14.34966873604972726, -8.224510206698740333, 45.83442372801901854 ) ) ;
#133601 = CARTESIAN_POINT ( 'NONE',  ( -15.72974639402176322, -15.80617190586768395, 74.37609039468568994 ) ) ;
#133602 = CARTESIAN_POINT ( 'NONE',  ( -16.51473224551069308, -9.474510206698971260, 106.6655762719810383 ) ) ;
#133603 = CARTESIAN_POINT ( 'NONE',  ( 19.05341960407617918, -5.049401038297876454, 76.04275706135230450 ) ) ;
#133604 = CARTESIAN_POINT ( 'NONE',  ( 10.72451020669871369, 18.67979575497193778, 52.08442372801901854 ) ) ;
#133605 = CARTESIAN_POINT ( 'NONE',  ( 4.483927247898790824, -16.52544592524335698, 25.20942372801901854 ) ) ;
#133606 = CARTESIAN_POINT ( 'NONE',  ( -9.474510206698720793, -16.51473224551083518, 79.58442372801899012 ) ) ;
#133607 = CARTESIAN_POINT ( 'NONE',  ( -13.97604488694527625, -13.89961937509977652, 46.87390960531435979 ) ) ;
#133608 = CARTESIAN_POINT ( 'NONE',  ( 9.564922557961047289, -16.46253265017146816, 100.4177570613523329 ) ) ;
#133609 = CARTESIAN_POINT ( 'NONE',  ( -16.55341960407617563, 4.379528057220093196, 113.5427570613523756 ) ) ;
#133610 = CARTESIAN_POINT ( 'NONE',  ( 16.51473224551083163, -9.474510206698727899, 90.83442372801900433 ) ) ;
#133611 = CARTESIAN_POINT ( 'NONE',  ( -4.379528057220328563, 16.55341960407611168, 50.20724293864769550 ) ) ;
#133612 = CARTESIAN_POINT ( 'NONE',  ( 13.97604488694548053, -13.89961937509957401, 60.62609039468564731 ) ) ;
#133613 = CARTESIAN_POINT ( 'NONE',  ( -14.29746914071037622, -8.314922557961029526, 64.16775706135234714 ) ) ;
#133614 = CARTESIAN_POINT ( 'NONE',  ( -18.67979575497193778, 10.72451020669871902, 113.3344237280190328 ) ) ;
#133615 = EDGE_CURVE ( 'NONE', #48307, #106382, #171681, .T. ) ;
#133616 = CARTESIAN_POINT ( 'NONE',  ( -19.03943276465977164, 0.05219959533909376836, 21.24890960531436335 ) ) ;
#133617 = CARTESIAN_POINT ( 'NONE',  ( -9.564922557960796823, -16.46253265017161027, 47.08224293864769550 ) ) ;
#133618 = CARTESIAN_POINT ( 'NONE',  ( 0.05219959533934541429, -16.53943276465976808, 55.00109039468568284 ) ) ;
#133619 = DIRECTION ( 'NONE',  ( 0.000000000000000000, 0.000000000000000000, 1.000000000000000000 ) ) ;
#133620 = CARTESIAN_POINT ( 'NONE',  ( -8.906447517083060816, 27.41122689804195645, 139.8500000054623911 ) ) ;
#133621 = CARTESIAN_POINT ( 'NONE',  ( -5.153800228976328057, -19.02544592524343514, 87.29057627198103830 ) ) ;
#133622 = CARTESIAN_POINT ( 'NONE',  ( 17.50000000000000000, 5.499999999999997335, 120.0000000000000142 ) ) ;
#133623 = EDGE_CURVE ( 'NONE', #77704, #156506, #195550, .T. ) ;
#133624 = ORIENTED_EDGE ( 'NONE', *, *, #56474, .T. ) ;
#133625 = CARTESIAN_POINT ( 'NONE',  ( 19.05341960407617918, -5.049401038297876454, 101.0427570613523045 ) ) ;
#133626 = ADVANCED_FACE ( 'NONE', ( #111735 ), #163194, .F. ) ;
#133627 = CARTESIAN_POINT ( 'NONE',  ( -21.55341960407610458, -5.719274019375992779, 36.45724293864768839 ) ) ;
#133629 = CARTESIAN_POINT ( 'NONE',  ( 16.51473224551083163, -9.474510206698727899, 110.8344237280190043 ) ) ;
#133628 = CARTESIAN_POINT ( 'NONE',  ( 16.46253265017146816, 9.564922557961045513, 36.66775706135233293 ) ) ;
#133630 = CARTESIAN_POINT ( 'NONE',  ( -16.55341960407611168, -4.379528057220339221, 111.4572429386476813 ) ) ;
#133631 = CARTESIAN_POINT ( 'NONE',  ( -5.153800228976328057, -19.02544592524343514, 42.29057627198101699 ) ) ;
#133632 = CARTESIAN_POINT ( 'NONE',  ( 21.53943276465977519, -0.05219959533907433946, 78.74890960531436690 ) ) ;
#133633 = AXIS2_PLACEMENT_3D ( 'NONE', #70133, #131805, #193484 ) ;
#133634 = CARTESIAN_POINT ( 'NONE',  ( -9.474510206698964154, 16.51473224551069663, 30.41557627198102054 ) ) ;
#133635 = CARTESIAN_POINT ( 'NONE',  ( 8.571926809382603096, -26.38167802310801235, 141.9750000027312069 ) ) ;
#133636 = CARTESIAN_POINT ( 'NONE',  ( 19.02544592524334988, 5.153800228976608722, 86.45942372801900433 ) ) ;
#133637 = CARTESIAN_POINT ( 'NONE',  ( 12.06949235617757843, -12.14591786802309237, 53.12390960531436690 ) ) ;
#133638 = CARTESIAN_POINT ( 'NONE',  ( -15.80617190586745835, -15.72974639402198527, 26.87390960531435979 ) ) ;
#133639 = CARTESIAN_POINT ( 'NONE',  ( -15.72974639402176322, -15.80617190586768395, 94.37609039468568994 ) ) ;
#133640 = CARTESIAN_POINT ( 'NONE',  ( 10.72451020669898902, -18.67979575497178502, 82.91557627198103830 ) ) ;
#133641 = CARTESIAN_POINT ( 'NONE',  ( 10.72451020669871369, 18.67979575497193778, 77.08442372801901854 ) ) ;
#133642 = CARTESIAN_POINT ( 'NONE',  ( 0.05219959533937995610, -21.53943276465977519, 60.00109039468568284 ) ) ;
#133643 = CARTESIAN_POINT ( 'NONE',  ( 5.153800228976335163, 19.02544592524342804, 99.79057627198102409 ) ) ;
#133645 = CARTESIAN_POINT ( 'NONE',  ( -21.52544592524334988, -5.823673210054445271, 63.95942372801901854 ) ) ;
#133644 = CARTESIAN_POINT ( 'NONE',  ( -4.483927247898782831, 16.52544592524335698, 112.7094237280190328 ) ) ;
#133646 = CARTESIAN_POINT ( 'NONE',  ( 19.05341960407611168, 5.049401038298154454, 53.95724293864770260 ) ) ;
#133647 = CARTESIAN_POINT ( 'NONE',  ( -18.67979575497193778, 10.72451020669871902, 33.33442372801900433 ) ) ;
#133648 = CARTESIAN_POINT ( 'NONE',  ( 19.05341960407611168, 5.049401038298154454, 63.95724293864769550 ) ) ;
#133649 = CARTESIAN_POINT ( 'NONE',  ( 16.52544592524342804, -4.483927247898539470, 83.54057627198102409 ) ) ;
#133650 = CARTESIAN_POINT ( 'NONE',  ( -14.29746914071049879, 8.314922557960819915, 45.83224293864769550 ) ) ;
#133651 = CARTESIAN_POINT ( 'NONE',  ( 10.72451020669898902, -18.67979575497178502, 62.91557627198102409 ) ) ;
#133652 = CARTESIAN_POINT ( 'NONE',  ( 19.05341960407611168, 5.049401038298154454, 43.95724293864769550 ) ) ;
#133653 = CARTESIAN_POINT ( 'NONE',  ( -5.719274019375978568, 21.55341960407610458, 65.20724293864768129 ) ) ;
#133655 = VECTOR ( 'NONE', #101002, 1000.000000000000000 ) ;
#133654 = CARTESIAN_POINT ( 'NONE',  ( -19.05341960407617563, 5.049401038297882671, 48.54275706135233293 ) ) ;
#133657 = CARTESIAN_POINT ( 'NONE',  ( -0.05219959533910754901, -16.53943276465976808, 62.49890960531436690 ) ) ;
#133656 = CARTESIAN_POINT ( 'NONE',  ( 9.564922557961047289, -16.46253265017146816, 20.41775706135233293 ) ) ;
#133658 = CARTESIAN_POINT ( 'NONE',  ( -10.72451020669898014, 18.67979575497178502, 40.41557627198103120 ) ) ;
#133659 = ORIENTED_EDGE ( 'NONE', *, *, #182855, .T. ) ;
#133660 = LINE ( 'NONE', #9330, #143212 ) ;
#133662 = CARTESIAN_POINT ( 'NONE',  ( 1.490379145827383622, 7.404560491896994279, -64.28054250939490544 ) ) ;
#133661 = CARTESIAN_POINT ( 'NONE',  ( -8.224510206698735004, -14.34966873604973081, 84.58442372801903275 ) ) ;
#133663 = CARTESIAN_POINT ( 'NONE',  ( 16.46253265017146816, 9.564922557961045513, 86.66775706135233293 ) ) ;
#133664 = CARTESIAN_POINT ( 'NONE',  ( 14.29746914071049879, -8.314922557960816363, 58.33224293864768839 ) ) ;
#133665 = CARTESIAN_POINT ( 'NONE',  ( -19.20446147854528718, -5.499999999999910294, 59.38999695167679960 ) ) ;
#133666 = CARTESIAN_POINT ( 'NONE',  ( -5.153800228976328057, -19.02544592524343514, 47.29057627198102409 ) ) ;
#133667 = CARTESIAN_POINT ( 'NONE',  ( 8.314922557960818139, 14.29746914071049879, 44.58224293864769550 ) ) ;
#133668 = CARTESIAN_POINT ( 'NONE',  ( -16.46253265017160317, 9.564922557960807481, 85.83224293864769550 ) ) ;
#133669 = CARTESIAN_POINT ( 'NONE',  ( 9.564922557960805705, 16.46253265017160317, 54.58224293864769550 ) ) ;
#133670 = CARTESIAN_POINT ( 'NONE',  ( -0.05219959533937732626, 21.53943276465977519, 62.50109039468568284 ) ) ;
#133671 = CARTESIAN_POINT ( 'NONE',  ( 16.46253265017160672, -9.564922557960803928, 78.33224293864769550 ) ) ;
#133672 = CARTESIAN_POINT ( 'NONE',  ( 16.51473224551069308, 9.474510206698969483, 24.16557627198102765 ) ) ;
#133673 = CARTESIAN_POINT ( 'NONE',  ( -13.89961937509977652, 13.97604488694528158, 65.62390960531436690 ) ) ;
#133674 = CARTESIAN_POINT ( 'NONE',  ( 15.72974639402199770, -15.80617190586745480, 43.12390960531435269 ) ) ;
#133675 = CARTESIAN_POINT ( 'NONE',  ( -5.049401038298153566, 19.05341960407611168, 30.20724293864768839 ) ) ;
#133676 = CARTESIAN_POINT ( 'NONE',  ( 5.823673210054125526, 21.52544592524343514, 39.79057627198103830 ) ) ;
#133677 = CARTESIAN_POINT ( 'NONE',  ( 4.379528057220092307, 16.55341960407617563, 102.2927570613523613 ) ) ;
#133678 = CARTESIAN_POINT ( 'NONE',  ( -13.89961937509957401, -13.97604488694547875, 24.37609039468565442 ) ) ;
#133680 = CARTESIAN_POINT ( 'NONE',  ( -12.14591786802326823, 12.06949235617739902, 78.12609039468570415 ) ) ;
#133679 = CARTESIAN_POINT ( 'NONE',  ( 16.52544592524335698, 4.483927247898782831, 41.45942372801901143 ) ) ;
#133681 = DIRECTION ( 'NONE',  ( -0.000000000000000000, -0.000000000000000000, 1.000000000000000000 ) ) ;
#133682 = CARTESIAN_POINT ( 'NONE',  ( 8.314922557961029526, -14.29746914071037800, 70.41775706135236135 ) ) ;
#133683 = CARTESIAN_POINT ( 'NONE',  ( -16.52544592524335698, -4.483927247898792601, 53.95942372801900433 ) ) ;
#133684 = CARTESIAN_POINT ( 'NONE',  ( 19.05341960407611168, 5.049401038298154454, 103.9572429386476671 ) ) ;
#133685 = CARTESIAN_POINT ( 'NONE',  ( -16.46253265017160317, 9.564922557960807481, 30.83224293864769550 ) ) ;
#133686 = CARTESIAN_POINT ( 'NONE',  ( -0.05219959533934338120, 16.53943276465976808, 32.50109039468568284 ) ) ;
#133687 = CARTESIAN_POINT ( 'NONE',  ( 13.97604488694527802, 13.89961937509977652, 49.37390960531434558 ) ) ;
#133688 = CARTESIAN_POINT ( 'NONE',  ( 5.719274019375673035, 21.55341960407619339, 27.29275706135234358 ) ) ;
#133689 = CARTESIAN_POINT ( 'NONE',  ( -14.34966873604972548, 8.224510206698743886, 38.33442372801900433 ) ) ;
#133690 = CARTESIAN_POINT ( 'NONE',  ( -16.53943276465976808, -0.05219959533934237506, 103.7510903946857042 ) ) ;
#133691 = PLANE ( 'NONE',  #150704 ) ;
#133692 = CARTESIAN_POINT ( 'NONE',  ( 10.81492255796106328, -18.62759615963255655, 105.4177570613523613 ) ) ;
#133693 = CARTESIAN_POINT ( 'NONE',  ( 9.474510206698729675, 16.51473224551082808, 92.08442372801900433 ) ) ;
#133694 = CARTESIAN_POINT ( 'NONE',  ( -16.46253265017146816, -9.564922557961047289, 59.16775706135233293 ) ) ;
#133695 = CARTESIAN_POINT ( 'NONE',  ( -4.379528057220328563, 16.55341960407611168, 60.20724293864768839 ) ) ;
#133696 = CARTESIAN_POINT ( 'NONE',  ( -9.474510206698964154, 16.51473224551069663, 30.41557627198102054 ) ) ;
#133698 = CARTESIAN_POINT ( 'NONE',  ( 38.00000000000000000, -12.34694845685040754, -2.849999994537626424 ) ) ;
#133697 = CARTESIAN_POINT ( 'NONE',  ( 5.049401038297881783, 19.05341960407617563, 67.29275706135234714 ) ) ;
#133699 = CARTESIAN_POINT ( 'NONE',  ( -0.05219959533937732626, 21.53943276465977519, 62.50109039468568284 ) ) ;
#133700 = CARTESIAN_POINT ( 'NONE',  ( 16.53943276465976808, 0.05219959533934440121, 31.25109039468568639 ) ) ;
#133701 = CARTESIAN_POINT ( 'NONE',  ( 17.50000000000000000, 5.499999999999992895, 81.70309617465829888 ) ) ;
#133702 = CARTESIAN_POINT ( 'NONE',  ( -5.049401038298153566, 19.05341960407611168, 115.2072429386477097 ) ) ;
#133703 = CARTESIAN_POINT ( 'NONE',  ( 19.05341960407617918, -5.049401038297876454, 111.0427570613523329 ) ) ;
#133704 = DIRECTION ( 'NONE',  ( -0.000000000000000000, -0.000000000000000000, 1.000000000000000000 ) ) ;
#133705 = CARTESIAN_POINT ( 'NONE',  ( -20.56371838171435584, 11.43208494587337043, 170.0924998638764976 ) ) ;
#133706 = CARTESIAN_POINT ( 'NONE',  ( 13.97604488694527802, 13.89961937509977652, 24.37390960531435624 ) ) ;
#133707 = CARTESIAN_POINT ( 'NONE',  ( 10.72451020669871369, 18.67979575497193778, 107.0844237280190043 ) ) ;
#133708 = CARTESIAN_POINT ( 'NONE',  ( -0.05219959533909027116, -19.03943276465977164, 42.49890960531435269 ) ) ;
#133709 = CARTESIAN_POINT ( 'NONE',  ( -21.53943276465977519, -0.05219959533937600094, 68.75109039468568994 ) ) ;
#133710 = CARTESIAN_POINT ( 'NONE',  ( 21.55341960407619695, -5.719274019375665929, 106.0427570613523471 ) ) ;
#133711 = CARTESIAN_POINT ( 'NONE',  ( -16.53943276465976808, -0.05219959533934237506, 103.7510903946857042 ) ) ;
#133712 = CARTESIAN_POINT ( 'NONE',  ( 19.05341960407611168, 5.049401038298154454, 78.95724293864769550 ) ) ;
#133713 = CARTESIAN_POINT ( 'NONE',  ( -21.55341960407619339, 5.719274019375674811, 53.54275706135234714 ) ) ;
#133714 = ADVANCED_FACE ( 'NONE', ( #127882 ), #108327, .T. ) ;
#133715 = CARTESIAN_POINT ( 'NONE',  ( -21.52544592524334988, -5.823673210054445271, 53.95942372801900433 ) ) ;
#133717 = CARTESIAN_POINT ( 'NONE',  ( 5.049401038298161559, -19.05341960407611168, 107.7072429386476955 ) ) ;
#133716 = CARTESIAN_POINT ( 'NONE',  ( 19.02544592524334988, 5.153800228976608722, 76.45942372801897591 ) ) ;
#133718 = CARTESIAN_POINT ( 'NONE',  ( 13.89961937509977652, -13.97604488694527269, 28.12390960531435624 ) ) ;
#133719 = CARTESIAN_POINT ( 'NONE',  ( -5.719274019375978568, 21.55341960407610458, 95.20724293864769550 ) ) ;
#133720 = CARTESIAN_POINT ( 'NONE',  ( -21.53943276465977519, -0.05219959533937600094, 113.7510903946856757 ) ) ;
#133721 = CARTESIAN_POINT ( 'NONE',  ( -8.314922557960811034, -14.29746914071050412, 97.08224293864770971 ) ) ;
#133722 = CARTESIAN_POINT ( 'NONE',  ( 19.03943276465977164, -0.05219959533909143690, 48.74890960531435979 ) ) ;
#133723 = CARTESIAN_POINT ( 'NONE',  ( 9.564922557961047289, -16.46253265017146816, 80.41775706135234714 ) ) ;
#133724 = CARTESIAN_POINT ( 'NONE',  ( -8.224510206698948167, 14.34966873604960824, 65.41557627198102409 ) ) ;
#133725 = CARTESIAN_POINT ( 'NONE',  ( -19.03943276465977164, -0.05219959533935918106, 18.75109039468567218 ) ) ;
#133726 = CARTESIAN_POINT ( 'NONE',  ( -19.05341960407611168, -5.049401038298163336, 106.4572429386476955 ) ) ;
#133727 = CARTESIAN_POINT ( 'NONE',  ( 16.46253265017146816, 9.564922557961045513, 76.66775706135234714 ) ) ;
#133728 = CARTESIAN_POINT ( 'NONE',  ( 10.81492255796078972, 18.62759615963270932, 74.58224293864768129 ) ) ;
#133729 = CARTESIAN_POINT ( 'NONE',  ( -10.81492255796105439, 18.62759615963255655, 32.91775706135234714 ) ) ;
#133730 = CARTESIAN_POINT ( 'NONE',  ( 8.314922557961029526, -14.29746914071037800, 30.41775706135234358 ) ) ;
#133731 = CARTESIAN_POINT ( 'NONE',  ( 4.379528057220092307, 16.55341960407617563, 87.29275706135236135 ) ) ;
#133733 = CARTESIAN_POINT ( 'NONE',  ( -10.72451020669870658, -18.67979575497194134, 34.58442372801900433 ) ) ;
#133732 = CARTESIAN_POINT ( 'NONE',  ( -4.379528057220086978, -16.55341960407618274, 44.79275706135234714 ) ) ;
#133734 = CARTESIAN_POINT ( 'NONE',  ( 5.719274019375991003, -21.55341960407610458, 42.70724293864770260 ) ) ;
#133735 = CARTESIAN_POINT ( 'NONE',  ( -9.474510206698964154, 16.51473224551069663, 30.41557627198102054 ) ) ;
#133736 = CARTESIAN_POINT ( 'NONE',  ( -38.00000000000001421, -12.34694845685042708, -7.649999994537626691 ) ) ;
#133737 = CARTESIAN_POINT ( 'NONE',  ( -16.53943276465976808, -0.05219959533934237506, 58.75109039468568994 ) ) ;
#133738 = CARTESIAN_POINT ( 'NONE',  ( 15.72974639402199770, -15.80617190586745480, 88.12390960531436690 ) ) ;
#133739 = CARTESIAN_POINT ( 'NONE',  ( 4.379528057220339221, -16.55341960407611168, 42.70724293864770260 ) ) ;
#133740 = CARTESIAN_POINT ( 'NONE',  ( 16.52544592524335698, 4.483927247898782831, 46.45942372801901854 ) ) ;
#133741 = CARTESIAN_POINT ( 'NONE',  ( 0.05219959533909260263, 19.03943276465977164, 64.99890960531436690 ) ) ;
#133742 = CARTESIAN_POINT ( 'NONE',  ( -16.52544592524335698, -4.483927247898792601, 98.95942372801903275 ) ) ;
#133743 = CARTESIAN_POINT ( 'NONE',  ( 9.564922557961047289, -16.46253265017146816, 90.41775706135234714 ) ) ;
#133744 = CARTESIAN_POINT ( 'NONE',  ( -5.823673210054116645, -21.52544592524344225, 87.29057627198103830 ) ) ;
#133745 = CARTESIAN_POINT ( 'NONE',  ( 14.29746914071049879, -8.314922557960816363, 33.33224293864769550 ) ) ;
#133746 = ORIENTED_EDGE ( 'NONE', *, *, #132163, .T. ) ;
#133747 = CARTESIAN_POINT ( 'NONE',  ( 9.100000000000001421, 0.000000000000000000, -63.95112321872120731 ) ) ;
#133748 = VECTOR ( 'NONE', #92107, 1000.000000000000000 ) ;
#133749 = CARTESIAN_POINT ( 'NONE',  ( 18.62759615963271287, -10.81492255796078972, 58.33224293864768839 ) ) ;
#133750 = ORIENTED_EDGE ( 'NONE', *, *, #6380, .T. ) ;
#133751 = CARTESIAN_POINT ( 'NONE',  ( 4.379528057220092307, 16.55341960407617563, 107.2927570613523471 ) ) ;
#133752 = VERTEX_POINT ( 'NONE', #168680 ) ;
#133753 = CARTESIAN_POINT ( 'NONE',  ( -5.719274019375978568, 21.55341960407610458, 30.20724293864769550 ) ) ;
#133754 = CARTESIAN_POINT ( 'NONE',  ( -38.00000000000000711, 2.428612866367529932E-14, -4.000000000000000000 ) ) ;
#133755 = CARTESIAN_POINT ( 'NONE',  ( 5.719274019375991003, -21.55341960407610458, 92.70724293864770971 ) ) ;
#133756 = CARTESIAN_POINT ( 'NONE',  ( 12.06949235617739724, 12.14591786802326823, 111.8760903946856615 ) ) ;
#133757 = CARTESIAN_POINT ( 'NONE',  ( -16.55341960407617563, 4.379528057220093196, 38.54275706135234714 ) ) ;
#133758 = CARTESIAN_POINT ( 'NONE',  ( 19.02544592524343514, -5.153800228976328945, 28.54057627198102409 ) ) ;
#133759 = CARTESIAN_POINT ( 'NONE',  ( 16.52544592524335698, 4.483927247898782831, 31.45942372801901854 ) ) ;
#133760 = CARTESIAN_POINT ( 'NONE',  ( 19.03943276465977164, -0.05219959533909143690, 53.74890960531436690 ) ) ;
#133761 = CARTESIAN_POINT ( 'NONE',  ( -8.906447517083060816, 27.41122689804195645, 147.5999999999999943 ) ) ;
#133762 = CARTESIAN_POINT ( 'NONE',  ( 13.97604488694527802, 13.89961937509977652, 109.3739096053143669 ) ) ;
#133763 = CARTESIAN_POINT ( 'NONE',  ( 19.03943276465977164, -0.05219959533909143690, 113.7489096053143669 ) ) ;
#133764 = CARTESIAN_POINT ( 'NONE',  ( 12.14591786802327356, -12.06949235617739191, 100.6260903946857184 ) ) ;
#133765 = CARTESIAN_POINT ( 'NONE',  ( 5.049401038297881783, 19.05341960407617563, 87.29275706135234714 ) ) ;
#133766 = CARTESIAN_POINT ( 'NONE',  ( 13.89961937509957401, 13.97604488694547697, 36.87609039468565442 ) ) ;
#133767 = CARTESIAN_POINT ( 'NONE',  ( 21.53943276465977519, -0.05219959533907433946, 88.74890960531436690 ) ) ;
#133768 = CARTESIAN_POINT ( 'NONE',  ( 0.05219959533934541429, -16.53943276465976808, 100.0010903946857042 ) ) ;
#133769 = CARTESIAN_POINT ( 'NONE',  ( -18.67979575497178146, -10.72451020669898902, 31.66557627198102054 ) ) ;
#133770 = CARTESIAN_POINT ( 'NONE',  ( -0.05219959533936034679, 19.03943276465977164, 102.5010903946856757 ) ) ;
#133772 = AXIS2_PLACEMENT_3D ( 'NONE', #120605, #105444, #13437 ) ;
#133771 = CARTESIAN_POINT ( 'NONE',  ( -13.97604488694527625, -13.89961937509977652, 106.8739096053143669 ) ) ;
#133773 = CARTESIAN_POINT ( 'NONE',  ( -18.62759615963255300, -10.81492255796106328, 59.16775706135234714 ) ) ;
#133774 = CARTESIAN_POINT ( 'NONE',  ( -5.153800228976328057, -19.02544592524343514, 57.29057627198103120 ) ) ;
#133775 = CARTESIAN_POINT ( 'NONE',  ( -4.379528057220328563, 16.55341960407611168, 95.20724293864769550 ) ) ;
#133776 = CARTESIAN_POINT ( 'NONE',  ( 32.33351994418282516, 3.967450966133691193, 88.63067128610951784 ) ) ;
#133777 = CARTESIAN_POINT ( 'NONE',  ( -14.34966873604960291, -8.224510206698953496, 71.66557627198100988 ) ) ;
#133778 = ORIENTED_EDGE ( 'NONE', *, *, #103351, .T. ) ;
#133779 = CARTESIAN_POINT ( 'NONE',  ( -0.05219959533936034679, 19.03943276465977164, 87.50109039468567573 ) ) ;
#133780 = DIRECTION ( 'NONE',  ( 0.000000000000000000, 0.000000000000000000, 1.000000000000000000 ) ) ;
#133781 = CARTESIAN_POINT ( 'NONE',  ( -5.049401038298153566, 19.05341960407611168, 65.20724293864765286 ) ) ;
#133782 = CARTESIAN_POINT ( 'NONE',  ( 10.20000000000000107, 0.000000000000000000, 1.610000000000000098 ) ) ;
#133784 = CARTESIAN_POINT ( 'NONE',  ( 19.05341960407611168, 5.049401038298154454, 88.95724293864769550 ) ) ;
#133783 = CARTESIAN_POINT ( 'NONE',  ( 16.51473224551069308, 9.474510206698969483, 79.16557627198103830 ) ) ;
#133785 = EDGE_CURVE ( 'NONE', #29612, #120193, #7751, .T. ) ;
#133786 = CARTESIAN_POINT ( 'NONE',  ( 8.314922557961029526, -14.29746914071037800, 65.41775706135234714 ) ) ;
#133787 = CARTESIAN_POINT ( 'NONE',  ( -16.21995358207306381, -7.366697692864125457, 50.06448998487844904 ) ) ;
#133788 = CARTESIAN_POINT ( 'NONE',  ( -9.474510206698720793, -16.51473224551083518, 44.58442372801900433 ) ) ;
#133789 = CARTESIAN_POINT ( 'NONE',  ( 21.53943276465977519, 0.05219959533937863772, 101.2510903946856757 ) ) ;
#133790 = CARTESIAN_POINT ( 'NONE',  ( 17.51956405198879807, -15.55922825390971731, -57.41917273836692459 ) ) ;
#133791 = CARTESIAN_POINT ( 'NONE',  ( -16.46253265017160317, 9.564922557960807481, 115.8322429386477097 ) ) ;
#133792 = CARTESIAN_POINT ( 'NONE',  ( 16.55341960407618274, -4.379528057220086978, 96.04275706135236135 ) ) ;
#133793 = CARTESIAN_POINT ( 'NONE',  ( 15.92681084339661268, -1.315686079477300874, -59.47631410104522587 ) ) ;
#133794 = CARTESIAN_POINT ( 'NONE',  ( 12.06949235617739724, 12.14591786802326823, 91.87609039468568994 ) ) ;
#133795 = CARTESIAN_POINT ( 'NONE',  ( -17.44279575226823198, 5.990770900252466724, 30.83557567514319331 ) ) ;
#133796 =( BOUNDED_CURVE ( )  B_SPLINE_CURVE ( 2, ( #164806, #134472, #163808, #179993, #100111, #68780, #42456, #130437, #192136, #53617, #176986, #41460, #117289 ),
 .UNSPECIFIED., .F., .T. ) 
 B_SPLINE_CURVE_WITH_KNOTS ( ( 3, 2, 2, 2, 2, 2, 3 ),
 ( 0.7130024320386090242, 0.7149122807017543879, 0.7192982456140351033, 0.7236842105263158187, 0.7280701754385965341, 0.7324561403508771384, 0.7344116688361128631 ),
 .UNSPECIFIED. ) 
 CURVE ( )  GEOMETRIC_REPRESENTATION_ITEM ( )  RATIONAL_B_SPLINE_CURVE ( ( 0.9832469066685285419, 0.9851625545550100060, 1.000000000000000000, 0.9659258262890683122, 1.000000000000000000, 0.9659258262890683122, 1.000000000000000000, 0.9659258262890683122, 1.000000000000000000, 0.9659258262890683122, 1.000000000000000000, 0.9848076720550078544, 0.9831626618144001517 ) ) 
 REPRESENTATION_ITEM ( '' )  );
#133797 = CARTESIAN_POINT ( 'NONE',  ( 16.52544592524335698, 4.483927247898782831, 66.45942372801903275 ) ) ;
#133798 = CARTESIAN_POINT ( 'NONE',  ( -17.60691670004651499, -5.500000000000069278, 59.13333313366439370 ) ) ;
#133799 = CARTESIAN_POINT ( 'NONE',  ( 5.719274019375673035, 21.55341960407619339, 87.29275706135236135 ) ) ;
#133800 = CARTESIAN_POINT ( 'NONE',  ( -19.05341960407617563, 5.049401038297882671, 93.54275706135234714 ) ) ;
#133801 = CARTESIAN_POINT ( 'NONE',  ( 13.97604488694548053, -13.89961937509957401, 30.62609039468566863 ) ) ;
#133802 = CARTESIAN_POINT ( 'NONE',  ( 13.97604488694527802, 13.89961937509977652, 64.37390960531436690 ) ) ;
#133803 = CARTESIAN_POINT ( 'NONE',  ( -9.474510206698964154, 16.51473224551069663, 45.41557627198103120 ) ) ;
#133804 = CARTESIAN_POINT ( 'NONE',  ( -3.503282210674349528, -48.86437366581481001, -23.00000000000000000 ) ) ;
#133805 = CARTESIAN_POINT ( 'NONE',  ( 10.72451020669898902, -18.67979575497178502, 77.91557627198102409 ) ) ;
#133806 = AXIS2_PLACEMENT_3D ( 'NONE', #33632, #97261, #191293 ) ;
#133807 = CARTESIAN_POINT ( 'NONE',  ( 21.55341960407610458, 5.719274019375980345, 33.95724293864769550 ) ) ;
#133808 = CARTESIAN_POINT ( 'NONE',  ( 5.153800228976335163, 19.02544592524342804, 29.79057627198102409 ) ) ;
#133809 = CARTESIAN_POINT ( 'NONE',  ( 16.55341960407618274, -4.379528057220086978, 56.04275706135235424 ) ) ;
#133810 = EDGE_CURVE ( 'NONE', #46248, #10418, #133000, .T. ) ;
#133811 = VERTEX_POINT ( 'NONE', #50074 ) ;
#133812 = CARTESIAN_POINT ( 'NONE',  ( 0.05219959533937995610, -21.53943276465977519, 30.00109039468568284 ) ) ;
#133814 = CARTESIAN_POINT ( 'NONE',  ( 36.91746824999999177, 2.880721459617395097E-14, -9.624999997268814056 ) ) ;
#133813 = CARTESIAN_POINT ( 'NONE',  ( -8.314922557960811034, -14.29746914071050412, 57.08224293864769550 ) ) ;
#133815 = CARTESIAN_POINT ( 'NONE',  ( -8.224510206698735004, -14.34966873604973081, 24.58442372801901499 ) ) ;
#133816 = CARTESIAN_POINT ( 'NONE',  ( 5.153800228976615827, -19.02544592524334988, 40.20942372801898301 ) ) ;
#133817 = CARTESIAN_POINT ( 'NONE',  ( 16.53943276465976808, -0.05219959533910856209, 58.74890960531436690 ) ) ;
#133818 = CARTESIAN_POINT ( 'NONE',  ( 21.53943276465977519, -0.05219959533907433946, 113.7489096053143527 ) ) ;
#133820 = CARTESIAN_POINT ( 'NONE',  ( -21.53943276465977519, 0.05219959533907696930, 76.24890960531435269 ) ) ;
#133819 = FACE_OUTER_BOUND ( 'NONE', #25478, .T. ) ;
#133821 = CARTESIAN_POINT ( 'NONE',  ( -5.049401038298153566, 19.05341960407611168, 90.20724293864766707 ) ) ;
#133822 = CARTESIAN_POINT ( 'NONE',  ( -8.314922557960811034, -14.29746914071050412, 67.08224293864770971 ) ) ;
#133823 = CARTESIAN_POINT ( 'NONE',  ( 13.89961937509977652, -13.97604488694527269, 98.12390960531433848 ) ) ;
#133824 = CARTESIAN_POINT ( 'NONE',  ( -37.58407650405590061, 0.3600258186295099971, 39.49999999999997868 ) ) ;
#133825 = CARTESIAN_POINT ( 'NONE',  ( 0.05219959533936267826, -19.03943276465977164, 70.00109039468566152 ) ) ;
#133826 = CARTESIAN_POINT ( 'NONE',  ( -0.05219959533907301413, -21.53943276465977519, 107.4989096053143669 ) ) ;
#133827 = CARTESIAN_POINT ( 'NONE',  ( 13.89961937509977652, -13.97604488694527269, 63.12390960531435979 ) ) ;
#133828 = CARTESIAN_POINT ( 'NONE',  ( -19.02544592524334988, -5.153800228976617603, 48.95942372801900433 ) ) ;
#133829 = CARTESIAN_POINT ( 'NONE',  ( 16.52544592524342804, -4.483927247898539470, 108.5405762719810241 ) ) ;
#133830 = CARTESIAN_POINT ( 'NONE',  ( 15.80617190586769283, -15.72974639402175789, 65.62609039468568994 ) ) ;
#133831 = CARTESIAN_POINT ( 'NONE',  ( -17.05116617787826172, -6.768360034955815507, 71.34324446740799885 ) ) ;
#133832 = CARTESIAN_POINT ( 'NONE',  ( 16.55341960407611168, 4.379528057220329451, 43.95724293864769550 ) ) ;
#133833 = CARTESIAN_POINT ( 'NONE',  ( -9.564922557960796823, -16.46253265017161027, 62.08224293864769550 ) ) ;
#133834 = CARTESIAN_POINT ( 'NONE',  ( -21.55341960407610458, -5.719274019375992779, 76.45724293864769550 ) ) ;
#133835 = CARTESIAN_POINT ( 'NONE',  ( 27.73933785331498569, 2.768321779492822058E-14, 145.8750000027311842 ) ) ;
#133836 = CARTESIAN_POINT ( 'NONE',  ( -5.049401038298153566, 19.05341960407611168, 55.20724293864769550 ) ) ;
#133837 = ORIENTED_EDGE ( 'NONE', *, *, #110611, .T. ) ;
#133838 = CARTESIAN_POINT ( 'NONE',  ( -10.81492255796078084, -18.62759615963271287, 67.08224293864770971 ) ) ;
#133839 = ORIENTED_EDGE ( 'NONE', *, *, #172288, .F. ) ;
#133840 = CARTESIAN_POINT ( 'NONE',  ( -10.81492255796105439, 18.62759615963255655, 102.9177570613523756 ) ) ;
#133843 = CARTESIAN_POINT ( 'NONE',  ( 4.379528057220339221, -16.55341960407611168, 87.70724293864769550 ) ) ;
#133842 = CARTESIAN_POINT ( 'NONE',  ( 12.14591786802327356, -12.06949235617739191, 95.62609039468568994 ) ) ;
#133841 = CARTESIAN_POINT ( 'NONE',  ( 17.60779699588839975, 5.500000000000012434, 53.84981316670104690 ) ) ;
#133844 = CARTESIAN_POINT ( 'NONE',  ( 0.05219959533909260263, 19.03943276465977164, 64.99890960531436690 ) ) ;
#133845 = EDGE_LOOP ( 'NONE', ( #135751, #74080, #183067, #28587 ) ) ;
#133846 = CARTESIAN_POINT ( 'NONE',  ( -19.03943276465977164, -0.05219959533935918106, 33.75109039468566863 ) ) ;
#133847 = CARTESIAN_POINT ( 'NONE',  ( -8.224510206698735004, -14.34966873604973081, 84.58442372801903275 ) ) ;
#133848 = CARTESIAN_POINT ( 'NONE',  ( -16.51473224551082808, 9.474510206698731452, 33.33442372801899722 ) ) ;
#133849 = CARTESIAN_POINT ( 'NONE',  ( 16.51473224551069308, 9.474510206698969483, 94.16557627198103830 ) ) ;
#133850 = CARTESIAN_POINT ( 'NONE',  ( 18.67979575497178502, 10.72451020669898547, 64.16557627198102409 ) ) ;
#133851 = DIRECTION ( 'NONE',  ( -1.000000000000000000, 0.000000000000000000, 0.000000000000000000 ) ) ;
#133852 = CARTESIAN_POINT ( 'NONE',  ( -5.153800228976328057, -19.02544592524343514, 22.29057627198102765 ) ) ;
#133853 = CARTESIAN_POINT ( 'NONE',  ( 5.823673210054444382, -21.52544592524334988, 100.2094237280190043 ) ) ;
#133854 = CARTESIAN_POINT ( 'NONE',  ( 16.52544592524335698, 4.483927247898782831, 61.45942372801901854 ) ) ;
#133855 = CARTESIAN_POINT ( 'NONE',  ( -18.67979575497193778, 10.72451020669871902, 28.33442372801902209 ) ) ;
#133856 = CARTESIAN_POINT ( 'NONE',  ( -0.05219959533934338120, 16.53943276465976808, 32.50109039468568284 ) ) ;
#133857 = CARTESIAN_POINT ( 'NONE',  ( -9.474510206698964154, 16.51473224551069663, 95.41557627198102409 ) ) ;
#133858 = CARTESIAN_POINT ( 'NONE',  ( -9.474510206698964154, 16.51473224551069663, 40.41557627198103120 ) ) ;
#133859 = CARTESIAN_POINT ( 'NONE',  ( 5.049401038298161559, -19.05341960407611168, 52.70724293864767418 ) ) ;
#133860 = CARTESIAN_POINT ( 'NONE',  ( -14.29746914071037622, -8.314922557961029526, 34.16775706135234714 ) ) ;
#133861 = CARTESIAN_POINT ( 'NONE',  ( 0.05219959533910956823, 16.53943276465976808, 94.99890960531436690 ) ) ;
#133862 = CARTESIAN_POINT ( 'NONE',  ( 4.379528057220092307, 16.55341960407617563, 107.2927570613523471 ) ) ;
#133865 = CARTESIAN_POINT ( 'NONE',  ( 13.97604488694527802, 13.89961937509977652, 49.37390960531434558 ) ) ;
#133864 = CARTESIAN_POINT ( 'NONE',  ( 13.89961937509977652, -13.97604488694527269, 78.12390960531433848 ) ) ;
#133863 = CARTESIAN_POINT ( 'NONE',  ( -5.719274019375665041, -21.55341960407619695, 49.79275706135234714 ) ) ;
#133866 = CARTESIAN_POINT ( 'NONE',  ( 5.153800228976335163, 19.02544592524342804, 84.79057627198099567 ) ) ;
#133867 = CARTESIAN_POINT ( 'NONE',  ( -14.29746914071049879, 8.314922557960819915, 35.83224293864768839 ) ) ;
#133868 = CARTESIAN_POINT ( 'NONE',  ( 8.314922557961029526, -14.29746914071037800, 95.41775706135234714 ) ) ;
#133869 = AXIS2_PLACEMENT_3D ( 'NONE', #165978, #167952, #122429 ) ;
#133870 = EDGE_LOOP ( 'NONE', ( #92317, #28128 ) ) ;
#133871 = CARTESIAN_POINT ( 'NONE',  ( 16.46253265017146816, 9.564922557961045513, 41.66775706135234003 ) ) ;
#133872 = CARTESIAN_POINT ( 'NONE',  ( 19.03943276465977164, -0.05219959533909143690, 113.7489096053143669 ) ) ;
#133873 = CARTESIAN_POINT ( 'NONE',  ( -5.049401038298153566, 19.05341960407611168, 50.20724293864770260 ) ) ;
#133874 = CARTESIAN_POINT ( 'NONE',  ( -9.474510206698720793, -16.51473224551083518, 19.58442372801899722 ) ) ;
#133875 = CARTESIAN_POINT ( 'NONE',  ( 29.86685920354754487, 21.69954338932564752, -7.424999997268813878 ) ) ;
#133876 = CARTESIAN_POINT ( 'NONE',  ( 8.224510206698742110, 14.34966873604972548, 37.08442372801901143 ) ) ;
#133878 = CARTESIAN_POINT ( 'NONE',  ( 16.55341960407618274, -4.379528057220086978, 61.04275706135234714 ) ) ;
#133877 = CARTESIAN_POINT ( 'NONE',  ( -9.564922557961040184, 16.46253265017147172, 72.91775706135233293 ) ) ;
#133879 = CARTESIAN_POINT ( 'NONE',  ( 5.153800228976335163, 19.02544592524342804, 114.7905762719810241 ) ) ;
#133880 = CARTESIAN_POINT ( 'NONE',  ( -13.97604488694527625, -13.89961937509977652, 76.87390960531433848 ) ) ;
#133881 = CARTESIAN_POINT ( 'NONE',  ( 18.67979575497194134, -10.72451020669871369, 20.83442372801901143 ) ) ;
#133882 = CARTESIAN_POINT ( 'NONE',  ( 19.05341960407617918, -5.049401038297876454, 81.04275706135231871 ) ) ;
#133884 = CARTESIAN_POINT ( 'NONE',  ( 9.564922557960805705, 16.46253265017160317, 29.58224293864769550 ) ) ;
#133883 = CARTESIAN_POINT ( 'NONE',  ( 16.51473224551069308, 9.474510206698969483, 109.1655762719810383 ) ) ;
#133885 = CARTESIAN_POINT ( 'NONE',  ( 9.564922557960805705, 16.46253265017160317, 74.58224293864769550 ) ) ;
#133887 = CARTESIAN_POINT ( 'NONE',  ( 13.89961937509977652, -13.97604488694527269, 33.12390960531434558 ) ) ;
#133886 = CARTESIAN_POINT ( 'NONE',  ( 16.52544592524342804, -4.483927247898539470, 28.54057627198103120 ) ) ;
#133888 = CARTESIAN_POINT ( 'NONE',  ( -5.153800228976607833, 19.02544592524334988, 52.70942372801900433 ) ) ;
#133889 = CARTESIAN_POINT ( 'NONE',  ( 14.29746914071049879, -8.314922557960816363, 78.33224293864770971 ) ) ;
#133890 = CARTESIAN_POINT ( 'NONE',  ( -9.474510206698720793, -16.51473224551083518, 19.58442372801899722 ) ) ;
#133891 = CARTESIAN_POINT ( 'NONE',  ( -13.97604488694527625, -13.89961937509977652, 56.87390960531434558 ) ) ;
#133892 = AXIS2_PLACEMENT_3D ( 'NONE', #16873, #153388, #170554 ) ;
#133893 = CARTESIAN_POINT ( 'NONE',  ( -0.05219959533907301413, -21.53943276465977519, 47.49890960531435979 ) ) ;
#133895 = CARTESIAN_POINT ( 'NONE',  ( 10.81492255796106328, -18.62759615963255655, 100.4177570613523471 ) ) ;
#133894 = CARTESIAN_POINT ( 'NONE',  ( -16.52544592524342804, 4.483927247898546575, 51.04057627198103120 ) ) ;
#133896 = CARTESIAN_POINT ( 'NONE',  ( -19.05341960407611168, -5.049401038298163336, 96.45724293864769550 ) ) ;
#133897 = CARTESIAN_POINT ( 'NONE',  ( 9.564922557960805705, 16.46253265017160317, 109.5822429386476955 ) ) ;
#133898 = CARTESIAN_POINT ( 'NONE',  ( 16.46253265017160672, -9.564922557960803928, 38.33224293864768839 ) ) ;
#133899 = CARTESIAN_POINT ( 'NONE',  ( 4.483927247898545687, 16.52544592524342804, 114.7905762719810383 ) ) ;
#133900 = CARTESIAN_POINT ( 'NONE',  ( 16.55341960407611168, 4.379528057220329451, 93.95724293864770971 ) ) ;
#133901 = CARTESIAN_POINT ( 'NONE',  ( -15.72974639402197994, 15.80617190586746368, 100.6239096053143811 ) ) ;
#133902 = CARTESIAN_POINT ( 'NONE',  ( 19.05341960407611168, 5.049401038298154454, 83.95724293864766707 ) ) ;
#133903 = CARTESIAN_POINT ( 'NONE',  ( -21.53943276465977519, -0.05219959533937600094, 18.75109039468568639 ) ) ;
#133904 = CARTESIAN_POINT ( 'NONE',  ( -19.03943276465977164, 0.05219959533909376836, 91.24890960531436690 ) ) ;
#133906 = CARTESIAN_POINT ( 'NONE',  ( 16.55341960407611168, 4.379528057220329451, 103.9572429386476813 ) ) ;
#133905 = FACE_OUTER_BOUND ( 'NONE', #11242, .T. ) ;
#133907 = CARTESIAN_POINT ( 'NONE',  ( 19.03943276465977164, -0.05219959533909143690, 73.74890960531435269 ) ) ;
#133908 = CARTESIAN_POINT ( 'NONE',  ( -21.53943276465977519, 0.05219959533907696930, 76.24890960531435269 ) ) ;
#133909 = CARTESIAN_POINT ( 'NONE',  ( -13.89961937509977652, 13.97604488694528158, 115.6239096053143669 ) ) ;
#133910 = DIRECTION ( 'NONE',  ( 1.000000000000000000, -0.000000000000000000, -0.000000000000000000 ) ) ;
#133912 = CARTESIAN_POINT ( 'NONE',  ( 18.22780087662119897, -5.500000000000096811, 68.51763182126893525 ) ) ;
#133911 = CARTESIAN_POINT ( 'NONE',  ( 18.62759615963271287, -10.81492255796078972, 33.33224293864769550 ) ) ;
#133913 = CARTESIAN_POINT ( 'NONE',  ( -4.483927247898782831, 16.52544592524335698, 32.70942372801900433 ) ) ;
#133915 =( GEOMETRIC_REPRESENTATION_CONTEXT ( 3 ) GLOBAL_UNCERTAINTY_ASSIGNED_CONTEXT ( ( #100462 ) ) GLOBAL_UNIT_ASSIGNED_CONTEXT ( ( #126467, #81924, #157816 ) ) REPRESENTATION_CONTEXT ( 'NONE', 'WORKASPACE' ) );
#133914 = CARTESIAN_POINT ( 'NONE',  ( -12.14591786802309592, -12.06949235617757132, 91.87390960531436690 ) ) ;
#133916 = CARTESIAN_POINT ( 'NONE',  ( -17.50000000000001066, -3.471454075611646317, 110.5166741885564505 ) ) ;
#133917 = CARTESIAN_POINT ( 'NONE',  ( -0.05219959533909027116, -19.03943276465977164, 82.49890960531436690 ) ) ;
#133918 = CARTESIAN_POINT ( 'NONE',  ( 5.049401038298161559, -19.05341960407611168, 42.70724293864767418 ) ) ;
#133919 = CARTESIAN_POINT ( 'NONE',  ( 16.52544592524342804, -4.483927247898539470, 78.54057627198103830 ) ) ;
#133920 = CARTESIAN_POINT ( 'NONE',  ( -0.05219959533907301413, -21.53943276465977519, 37.49890960531436690 ) ) ;
#133921 = CARTESIAN_POINT ( 'NONE',  ( -0.05219959533910754901, -16.53943276465976808, 57.49890960531435979 ) ) ;
#133922 = CARTESIAN_POINT ( 'NONE',  ( 13.97604488694548053, -13.89961937509957401, 105.6260903946856757 ) ) ;
#133923 = CARTESIAN_POINT ( 'NONE',  ( 15.80617190586769283, -15.72974639402175789, 65.62609039468568994 ) ) ;
#133924 = AXIS2_PLACEMENT_3D ( 'NONE', #12807, #151318, #163495 ) ;
#133925 = CARTESIAN_POINT ( 'NONE',  ( -8.571926809382608425, 26.38167802310805854, 148.4750000027311785 ) ) ;
#133926 = CARTESIAN_POINT ( 'NONE',  ( -5.049401038298153566, 19.05341960407611168, 115.2072429386477097 ) ) ;
#133927 = CARTESIAN_POINT ( 'NONE',  ( 12.14591786802327356, -12.06949235617739191, 85.62609039468568994 ) ) ;
#133928 = CARTESIAN_POINT ( 'NONE',  ( -17.31728774477212340, 6.344390552233681646, 95.81906651689308774 ) ) ;
#133929 = CARTESIAN_POINT ( 'NONE',  ( -0.05219959533909027116, -19.03943276465977164, 72.49890960531435269 ) ) ;
#133930 = CARTESIAN_POINT ( 'NONE',  ( 5.719274019375991003, -21.55341960407610458, 77.70724293864770971 ) ) ;
#133931 = CARTESIAN_POINT ( 'NONE',  ( -4.483927247898782831, 16.52544592524335698, 22.70942372801901499 ) ) ;
#133933 = CARTESIAN_POINT ( 'NONE',  ( -21.52544592524334988, -5.823673210054445271, 58.95942372801902565 ) ) ;
#133932 = CARTESIAN_POINT ( 'NONE',  ( -16.53943276465976808, 0.05219959533911058130, 51.24890960531436690 ) ) ;
#133935 = CARTESIAN_POINT ( 'NONE',  ( 18.67979575497178502, 10.72451020669898547, 24.16557627198103120 ) ) ;
#133934 = CARTESIAN_POINT ( 'NONE',  ( -16.52544592524335698, -4.483927247898792601, 83.95942372801900433 ) ) ;
#133936 = CARTESIAN_POINT ( 'NONE',  ( -13.89961937509977830, 13.97604488694528158, 115.6239096053143669 ) ) ;
#133937 = CARTESIAN_POINT ( 'NONE',  ( -17.48847506799967633, 5.747544572773789717, 80.82697437843280852 ) ) ;
#133938 = CARTESIAN_POINT ( 'NONE',  ( 16.55341960407618274, -4.379528057220086978, 101.0427570613523756 ) ) ;
#133939 = CARTESIAN_POINT ( 'NONE',  ( -8.224510206698735004, -14.34966873604973081, 54.58442372801901143 ) ) ;
#133940 = CARTESIAN_POINT ( 'NONE',  ( 16.46253265017160672, -9.564922557960803928, 78.33224293864769550 ) ) ;
#133941 = CARTESIAN_POINT ( 'NONE',  ( -19.02544592524342804, 5.153800228976336051, 91.04057627198100988 ) ) ;
#133942 = CARTESIAN_POINT ( 'NONE',  ( 5.719274019375673035, 21.55341960407619339, 77.29275706135234714 ) ) ;
#133943 = CARTESIAN_POINT ( 'NONE',  ( 16.52544592524335698, 4.483927247898782831, 71.45942372801901854 ) ) ;
#133944 = CARTESIAN_POINT ( 'NONE',  ( -4.483927247898539470, -16.52544592524342804, 47.29057627198103120 ) ) ;
#133945 = CARTESIAN_POINT ( 'NONE',  ( 19.02544592524343514, -5.153800228976328945, 48.54057627198103120 ) ) ;
#133946 = CARTESIAN_POINT ( 'NONE',  ( -13.97604488694527625, -13.89961937509977652, 41.87390960531435979 ) ) ;
#133947 = EDGE_LOOP ( 'NONE', ( #85536, #98649, #22489, #10532 ) ) ;
#133948 = CARTESIAN_POINT ( 'NONE',  ( 5.153800228976615827, -19.02544592524334988, 90.20942372801900433 ) ) ;
#133949 = CARTESIAN_POINT ( 'NONE',  ( 12.06949235617757843, -12.14591786802309237, 103.1239096053143811 ) ) ;
#133950 = CARTESIAN_POINT ( 'NONE',  ( -19.03943276465977164, 0.05219959533909376836, 61.24890960531436690 ) ) ;
#133952 = CARTESIAN_POINT ( 'NONE',  ( -11.74264578624800670, 36.14014761921585972, -4.400000000000000355 ) ) ;
#133951 = CARTESIAN_POINT ( 'NONE',  ( 5.049401038297881783, 19.05341960407617563, 107.2927570613523187 ) ) ;
#133953 = CARTESIAN_POINT ( 'NONE',  ( -21.52544592524334988, -5.823673210054445271, 108.9594237280190185 ) ) ;
#133954 = CARTESIAN_POINT ( 'NONE',  ( -4.379528057220086978, -16.55341960407618274, 69.79275706135234714 ) ) ;
#133955 = CARTESIAN_POINT ( 'NONE',  ( -19.05341960407617563, 5.049401038297882671, 93.54275706135234714 ) ) ;
#133956 = CARTESIAN_POINT ( 'NONE',  ( 15.80617190586746368, 15.72974639402197994, 59.37390960531436690 ) ) ;
#133957 = CARTESIAN_POINT ( 'NONE',  ( 16.55341960407618274, -4.379528057220086978, 56.04275706135235424 ) ) ;
#133958 = CARTESIAN_POINT ( 'NONE',  ( 4.500000000000000888, -139.5000000000000000, 21.32407087589995953 ) ) ;
#133959 = CARTESIAN_POINT ( 'NONE',  ( -5.153800228976607833, 19.02544592524334988, 52.70942372801900433 ) ) ;
#133960 = CARTESIAN_POINT ( 'NONE',  ( 0.05219959533909260263, 19.03943276465977164, 84.99890960531436690 ) ) ;
#133961 = CARTESIAN_POINT ( 'NONE',  ( -16.52544592524342804, 4.483927247898546575, 111.0405762719810525 ) ) ;
#133962 = CARTESIAN_POINT ( 'NONE',  ( -9.564922557960796823, -16.46253265017161027, 62.08224293864769550 ) ) ;
#133963 = CARTESIAN_POINT ( 'NONE',  ( -14.34966873604960291, -8.224510206698953496, 56.66557627198103830 ) ) ;
#133964 = AXIS2_PLACEMENT_3D ( 'NONE', #177822, #38297, #125575 ) ;
#133965 = CARTESIAN_POINT ( 'NONE',  ( -18.62759615963255300, -10.81492255796106328, 94.16775706135237556 ) ) ;
#133966 = CARTESIAN_POINT ( 'NONE',  ( -16.51473224551082808, 9.474510206698731452, 48.33442372801900433 ) ) ;
#133967 = CARTESIAN_POINT ( 'NONE',  ( -0.05219959533936034679, 19.03943276465977164, 27.50109039468566507 ) ) ;
#133968 = CARTESIAN_POINT ( 'NONE',  ( 21.52544592524344225, -5.823673210054117533, 23.54057627198102765 ) ) ;
#133969 = CARTESIAN_POINT ( 'NONE',  ( -21.55341960407619339, 5.719274019375674811, 93.54275706135234714 ) ) ;
#133970 = CARTESIAN_POINT ( 'NONE',  ( 16.46253265017160672, -9.564922557960803928, 78.33224293864769550 ) ) ;
#133971 = ADVANCED_FACE ( 'NONE', ( #184857 ), #189586, .F. ) ;
#133972 = CARTESIAN_POINT ( 'NONE',  ( -5.719274019375665041, -21.55341960407619695, 99.79275706135234714 ) ) ;
#133973 = CARTESIAN_POINT ( 'NONE',  ( -21.53943276465977519, 0.05219959533907696930, 46.24890960531435979 ) ) ;
#133974 = CARTESIAN_POINT ( 'NONE',  ( 5.153800228976335163, 19.02544592524342804, 84.79057627198099567 ) ) ;
#133975 = CARTESIAN_POINT ( 'NONE',  ( -0.05219959533936034679, 19.03943276465977164, 67.50109039468566152 ) ) ;
#133976 = CARTESIAN_POINT ( 'NONE',  ( -9.564922557960796823, -16.46253265017161027, 37.08224293864768839 ) ) ;
#133977 = CARTESIAN_POINT ( 'NONE',  ( 19.03943276465977164, -0.05219959533909143690, 93.74890960531435269 ) ) ;
#133978 = CARTESIAN_POINT ( 'NONE',  ( -9.564922557961040184, 16.46253265017147172, 87.91775706135233293 ) ) ;
#133979 = CARTESIAN_POINT ( 'NONE',  ( -16.52544592524335698, -4.483927247898792601, 43.95942372801902565 ) ) ;
#133980 = CARTESIAN_POINT ( 'NONE',  ( 14.34966873604960469, 8.224510206698951720, 99.16557627198100988 ) ) ;
#133981 = CARTESIAN_POINT ( 'NONE',  ( 19.02544592524343514, -5.153800228976328945, 68.54057627198103830 ) ) ;
#133982 = CARTESIAN_POINT ( 'NONE',  ( 10.81492255796078972, 18.62759615963270932, 54.58224293864769550 ) ) ;
#133983 = CARTESIAN_POINT ( 'NONE',  ( 5.153800228976615827, -19.02544592524334988, 110.2094237280189901 ) ) ;
#133984 = CARTESIAN_POINT ( 'NONE',  ( 5.823673210054125526, 21.52544592524343514, 114.7905762719810383 ) ) ;
#133985 = CARTESIAN_POINT ( 'NONE',  ( 18.62759615963255655, 10.81492255796105972, 71.66775706135234714 ) ) ;
#133986 = CARTESIAN_POINT ( 'NONE',  ( -8.314922557961024197, 14.29746914071037800, 77.91775706135231871 ) ) ;
#133987 = CARTESIAN_POINT ( 'NONE',  ( -9.564922557960796823, -16.46253265017161027, 72.08224293864770971 ) ) ;
#133988 = CARTESIAN_POINT ( 'NONE',  ( -0.05219959533934338120, 16.53943276465976808, 107.5010903946856899 ) ) ;
#133989 = CARTESIAN_POINT ( 'NONE',  ( -13.89961937509957401, -13.97604488694547875, 39.37609039468566152 ) ) ;
#133990 = CARTESIAN_POINT ( 'NONE',  ( 18.62759615963255655, 10.81492255796105972, 36.66775706135234714 ) ) ;
#133991 = CARTESIAN_POINT ( 'NONE',  ( -0.05219959533910754901, -16.53943276465976808, 82.49890960531436690 ) ) ;
#133992 = CARTESIAN_POINT ( 'NONE',  ( -19.03943276465977164, 0.05219959533909376836, 101.2489096053143669 ) ) ;
#133993 = CARTESIAN_POINT ( 'NONE',  ( -16.55341960407617563, 4.379528057220093196, 83.54275706135234714 ) ) ;
#133994 = CARTESIAN_POINT ( 'NONE',  ( 21.55341960407619695, -5.719274019375665929, 76.04275706135237556 ) ) ;
#133995 = CARTESIAN_POINT ( 'NONE',  ( -16.52544592524335698, -4.483927247898792601, 28.95942372801902209 ) ) ;
#133996 = CARTESIAN_POINT ( 'NONE',  ( 21.52544592524334988, 5.823673210054432836, 26.45942372801901854 ) ) ;
#133997 = CARTESIAN_POINT ( 'NONE',  ( 16.53943276465976808, -0.05219959533910856209, 73.74890960531433848 ) ) ;
#133998 = ORIENTED_EDGE ( 'NONE', *, *, #72679, .T. ) ;
#133999 = CARTESIAN_POINT ( 'NONE',  ( 5.823673210054125526, 21.52544592524343514, 94.79057627198105251 ) ) ;
#134000 = CARTESIAN_POINT ( 'NONE',  ( 0.05219959533910956823, 16.53943276465976808, 54.99890960531435269 ) ) ;
#134001 = ORIENTED_EDGE ( 'NONE', *, *, #195051, .T. ) ;
#134002 = CARTESIAN_POINT ( 'NONE',  ( -13.97604488694527625, -13.89961937509977652, 31.87390960531435979 ) ) ;
#134003 = CARTESIAN_POINT ( 'NONE',  ( 15.80617190586746368, 15.72974639402197994, 24.37390960531435979 ) ) ;
#134004 = CARTESIAN_POINT ( 'NONE',  ( 10.81492255796106328, -18.62759615963255655, 40.41775706135234714 ) ) ;
#134005 = CARTESIAN_POINT ( 'NONE',  ( 12.14591786802309770, 12.06949235617756955, 69.37390960531436690 ) ) ;
#134006 = CARTESIAN_POINT ( 'NONE',  ( -10.81492255796078084, -18.62759615963271287, 72.08224293864769550 ) ) ;
#134007 = CARTESIAN_POINT ( 'NONE',  ( 5.049401038298161559, -19.05341960407611168, 77.70724293864765286 ) ) ;
#134009 = CARTESIAN_POINT ( 'NONE',  ( 19.03943276465977164, 0.05219959533936151252, 76.25109039468566152 ) ) ;
#134008 = CARTESIAN_POINT ( 'NONE',  ( 9.564922557960805705, 16.46253265017160317, 24.58224293864769194 ) ) ;
#134010 = CARTESIAN_POINT ( 'NONE',  ( -18.62759615963270932, 10.81492255796079327, 60.83224293864769550 ) ) ;
#134011 = CARTESIAN_POINT ( 'NONE',  ( 9.474510206698971260, -16.51473224551069308, 37.91557627198102409 ) ) ;
#134012 = CARTESIAN_POINT ( 'NONE',  ( -13.97604488694527625, -13.89961937509977652, 66.87390960531436690 ) ) ;
#134013 = ORIENTED_EDGE ( 'NONE', *, *, #193512, .F. ) ;
#134014 = CARTESIAN_POINT ( 'NONE',  ( 12.14591786802327356, -12.06949235617739191, 50.62609039468568994 ) ) ;
#134015 = CARTESIAN_POINT ( 'NONE',  ( 18.67979575497194134, -10.72451020669871369, 25.83442372801901499 ) ) ;
#134016 = CARTESIAN_POINT ( 'NONE',  ( -21.52544592524334988, -5.823673210054445271, 53.95942372801900433 ) ) ;
#134017 = CARTESIAN_POINT ( 'NONE',  ( 13.97604488694527802, 13.89961937509977652, 104.3739096053143385 ) ) ;
#134018 = CARTESIAN_POINT ( 'NONE',  ( 15.80617190586746368, 15.72974639402197994, 69.37390960531436690 ) ) ;
#134020 = CARTESIAN_POINT ( 'NONE',  ( -16.53943276465976808, -0.05219959533934237506, 48.75109039468568284 ) ) ;
#134019 = CARTESIAN_POINT ( 'NONE',  ( 21.52544592524344225, -5.823673210054117533, 113.5405762719810383 ) ) ;
#134021 = CARTESIAN_POINT ( 'NONE',  ( 15.72974639402199770, -15.80617190586745480, 48.12390960531436690 ) ) ;
#134022 = CARTESIAN_POINT ( 'NONE',  ( 18.67979575497194134, -10.72451020669871369, 105.8344237280190328 ) ) ;
#134023 = CARTESIAN_POINT ( 'NONE',  ( 9.474510206698971260, -16.51473224551069308, 57.91557627198103120 ) ) ;
#134024 = CARTESIAN_POINT ( 'NONE',  ( -193.3062444957834884, -155.7167183371838064, -15.00000000000000000 ) ) ;
#134025 = CARTESIAN_POINT ( 'NONE',  ( 13.97604488694527802, 13.89961937509977652, 74.37390960531436690 ) ) ;
#134026 = CARTESIAN_POINT ( 'NONE',  ( -23.23284429171610910, -30.31406682163553867, -16.83429831496585649 ) ) ;
#134027 = CARTESIAN_POINT ( 'NONE',  ( -5.049401038297874678, -19.05341960407617918, 64.79275706135233293 ) ) ;
#134029 = CARTESIAN_POINT ( 'NONE',  ( -5.719274019375978568, 21.55341960407610458, 40.20724293864769550 ) ) ;
#134028 = CARTESIAN_POINT ( 'NONE',  ( 16.51473224551083163, -9.474510206698727899, 20.83442372801899722 ) ) ;
#134030 = CARTESIAN_POINT ( 'NONE',  ( -14.29746914071037622, -8.314922557961029526, 109.1677570613523613 ) ) ;
#134031 = CARTESIAN_POINT ( 'NONE',  ( -16.51473224551082808, 9.474510206698731452, 83.33442372801899012 ) ) ;
#134032 = CARTESIAN_POINT ( 'NONE',  ( -17.31728774477273802, 6.344390552232390235, 60.81906651689319432 ) ) ;
#134033 = CARTESIAN_POINT ( 'NONE',  ( 19.02544592524334988, 5.153800228976608722, 26.45942372801899722 ) ) ;
#134034 = CARTESIAN_POINT ( 'NONE',  ( -19.03943276465977164, -0.05219959533935918106, 78.75109039468567573 ) ) ;
#134035 = CARTESIAN_POINT ( 'NONE',  ( 5.049401038297881783, 19.05341960407617563, 47.29275706135231161 ) ) ;
#134036 = CARTESIAN_POINT ( 'NONE',  ( -17.44279575226823198, -5.990770900252489817, 44.16442432485681735 ) ) ;
#134037 = CARTESIAN_POINT ( 'NONE',  ( 5.153800228976335163, 19.02544592524342804, 39.79057627198100988 ) ) ;
#134038 = CARTESIAN_POINT ( 'NONE',  ( -8.314922557960811034, -14.29746914071050412, 52.08224293864768839 ) ) ;
#134039 = CARTESIAN_POINT ( 'NONE',  ( -19.02544592524342804, 5.153800228976336051, 36.04057627198100988 ) ) ;
#134040 = CARTESIAN_POINT ( 'NONE',  ( 4.483927247898545687, 16.52544592524342804, 44.79057627198103120 ) ) ;
#134041 = CARTESIAN_POINT ( 'NONE',  ( 7.052343178074679031, 2.552343178074557350, 1.110912703473986074 ) ) ;
#134042 = CARTESIAN_POINT ( 'NONE',  ( -14.34966873604972548, 8.224510206698743886, 108.3344237280190185 ) ) ;
#134043 = CARTESIAN_POINT ( 'NONE',  ( 19.02544592524343514, -5.153800228976328945, 48.54057627198103120 ) ) ;
#134044 = CARTESIAN_POINT ( 'NONE',  ( -5.153800228976607833, 19.02544592524334988, 27.70942372801899722 ) ) ;
#134045 = CARTESIAN_POINT ( 'NONE',  ( 12.14591786802327356, -12.06949235617739191, 30.62609039468567929 ) ) ;
#134046 = CARTESIAN_POINT ( 'NONE',  ( 15.80617190586746368, 15.72974639402197994, 39.37390960531436690 ) ) ;
#134048 = VERTEX_POINT ( 'NONE', #3549 ) ;
#134047 = CARTESIAN_POINT ( 'NONE',  ( -10.72451020669870658, -18.67979575497194134, 94.58442372801901854 ) ) ;
#134049 = CARTESIAN_POINT ( 'NONE',  ( -16.46253265017160317, 9.564922557960807481, 110.8322429386476955 ) ) ;
#134050 = CARTESIAN_POINT ( 'NONE',  ( 9.564922557960805705, 16.46253265017160317, 94.58224293864769550 ) ) ;
#134051 = CARTESIAN_POINT ( 'NONE',  ( -11.40812507854754720, -35.11059874428192273, -10.22499999726881548 ) ) ;
#134052 = CARTESIAN_POINT ( 'NONE',  ( 15.72974639402199770, -15.80617190586745480, 103.1239096053143811 ) ) ;
#134053 = AXIS2_PLACEMENT_3D ( 'NONE', #191766, #99750, #38095 ) ;
#134054 = CARTESIAN_POINT ( 'NONE',  ( 16.52544592524342804, -4.483927247898539470, 73.54057627198102409 ) ) ;
#134056 = CARTESIAN_POINT ( 'NONE',  ( -16.46253265017160317, 9.564922557960807481, 65.83224293864769550 ) ) ;
#134055 = CARTESIAN_POINT ( 'NONE',  ( 18.62759615963271287, -10.81492255796078972, 78.33224293864770971 ) ) ;
#134057 = CARTESIAN_POINT ( 'NONE',  ( -5.153800228976328057, -19.02544592524343514, 72.29057627198102409 ) ) ;
#134058 = CARTESIAN_POINT ( 'NONE',  ( 21.55341960407610458, 5.719274019375980345, 98.95724293864770971 ) ) ;
#134059 = EDGE_CURVE ( 'NONE', #152327, #125536, #96548, .T. ) ;
#134060 = ORIENTED_EDGE ( 'NONE', *, *, #78948, .T. ) ;
#134061 = CARTESIAN_POINT ( 'NONE',  ( -9.564922557960796823, -16.46253265017161027, 62.08224293864769550 ) ) ;
#134063 = CARTESIAN_POINT ( 'NONE',  ( -19.05341960407611168, -5.049401038298163336, 26.45724293864769550 ) ) ;
#134062 = CARTESIAN_POINT ( 'NONE',  ( -8.314922557960811034, -14.29746914071050412, 112.0822429386477097 ) ) ;
#134064 = CARTESIAN_POINT ( 'NONE',  ( 9.474510206698971260, -16.51473224551069308, 57.91557627198103120 ) ) ;
#134065 = CARTESIAN_POINT ( 'NONE',  ( 19.03943276465977164, 0.05219959533936151252, 86.25109039468567573 ) ) ;
#134066 = AXIS2_PLACEMENT_3D ( 'NONE', #44169, #42187, #167515 ) ;
#134067 = CARTESIAN_POINT ( 'NONE',  ( -12.06949235617756955, 12.14591786802309770, 100.6239096053143811 ) ) ;
#134068 = CARTESIAN_POINT ( 'NONE',  ( -18.67979575497193778, 10.72451020669871902, 53.33442372801901854 ) ) ;
#134070 = CARTESIAN_POINT ( 'NONE',  ( 10.72451020669898902, -18.67979575497178502, 112.9155762719810383 ) ) ;
#134069 = CARTESIAN_POINT ( 'NONE',  ( 13.89961937509977652, -13.97604488694527269, 48.12390960531435979 ) ) ;
#134071 = CARTESIAN_POINT ( 'NONE',  ( -8.224510206698948167, 14.34966873604960824, 95.41557627198102409 ) ) ;
#134072 = CARTESIAN_POINT ( 'NONE',  ( -8.906447517083053711, -27.41122689804191026, 140.4000000000000057 ) ) ;
#134073 = CARTESIAN_POINT ( 'NONE',  ( -9.564922557960796823, -16.46253265017161027, 77.08224293864769550 ) ) ;
#134074 = DIRECTION ( 'NONE',  ( -0.000000000000000000, -0.000000000000000000, 1.000000000000000000 ) ) ;
#134076 = CARTESIAN_POINT ( 'NONE',  ( 0.05219959533907565091, 21.53943276465977519, 29.99890960531435979 ) ) ;
#134075 = CARTESIAN_POINT ( 'NONE',  ( -8.224510206698735004, -14.34966873604973081, 19.58442372801901143 ) ) ;
#134077 = CARTESIAN_POINT ( 'NONE',  ( 10.72451020669871369, 18.67979575497193778, 52.08442372801901854 ) ) ;
#134078 = PRODUCT_DEFINITION_FORMATION_WITH_SPECIFIED_SOURCE ( 'ANY', '', #14587, .NOT_KNOWN. ) ;
#134079 = CARTESIAN_POINT ( 'NONE',  ( -13.89961937509977652, 13.97604488694528158, 95.62390960531436690 ) ) ;
#134080 = CARTESIAN_POINT ( 'NONE',  ( 13.89961937509957401, 13.97604488694547697, 86.87609039468567573 ) ) ;
#134081 = CARTESIAN_POINT ( 'NONE',  ( -16.46253265017160317, 9.564922557960807481, 65.83224293864769550 ) ) ;
#134082 = CARTESIAN_POINT ( 'NONE',  ( 0.05219959533910956823, 16.53943276465976808, 84.99890960531436690 ) ) ;
#134083 = CARTESIAN_POINT ( 'NONE',  ( 19.03943276465977164, -0.05219959533909143690, 108.7489096053143527 ) ) ;
#134084 = CARTESIAN_POINT ( 'NONE',  ( 4.483927247898545687, 16.52544592524342804, 79.79057627198102409 ) ) ;
#134085 = CARTESIAN_POINT ( 'NONE',  ( 9.474510206698971260, -16.51473224551069308, 92.91557627198103830 ) ) ;
#134086 = CARTESIAN_POINT ( 'NONE',  ( 16.51473224551083163, -9.474510206698727899, 40.83442372801900433 ) ) ;
#134089 = CARTESIAN_POINT ( 'NONE',  ( -19.03943276465977164, 0.05219959533909376836, 31.24890960531435979 ) ) ;
#134088 = CARTESIAN_POINT ( 'NONE',  ( 12.14591786802309770, 12.06949235617756955, 39.37390960531436690 ) ) ;
#134087 = CARTESIAN_POINT ( 'NONE',  ( -19.03943276465977164, 0.05219959533909376836, 46.24890960531435979 ) ) ;
#134090 = EDGE_LOOP ( 'NONE', ( #171895, #135117, #12655 ) ) ;
#134091 = CARTESIAN_POINT ( 'NONE',  ( -5.719274019375665041, -21.55341960407619695, 39.79275706135235424 ) ) ;
#134092 = CARTESIAN_POINT ( 'NONE',  ( 13.97604488694548053, -13.89961937509957401, 85.62609039468568994 ) ) ;
#134093 = CARTESIAN_POINT ( 'NONE',  ( 16.53943276465976808, -0.05219959533910856209, 53.74890960531437401 ) ) ;
#134094 = CARTESIAN_POINT ( 'NONE',  ( -21.52544592524343514, 5.823673210054127303, 106.0405762719810525 ) ) ;
#134095 = CARTESIAN_POINT ( 'NONE',  ( -21.53943276465977519, 0.05219959533907696930, 36.24890960531435979 ) ) ;
#134096 = CARTESIAN_POINT ( 'NONE',  ( 4.483927247898545687, 16.52544592524342804, 79.79057627198102409 ) ) ;
#134097 = CARTESIAN_POINT ( 'NONE',  ( 16.51473224551069308, 9.474510206698969483, 44.16557627198103120 ) ) ;
#134098 = CARTESIAN_POINT ( 'NONE',  ( -12.14591786802326823, 12.06949235617739902, 113.1260903946856899 ) ) ;
#134099 = VECTOR ( 'NONE', #41067, 1000.000000000000000 ) ;
#134100 = CARTESIAN_POINT ( 'NONE',  ( 12.14591786802327356, -12.06949235617739191, 90.62609039468567573 ) ) ;
#134101 = CARTESIAN_POINT ( 'NONE',  ( 16.52544592524335698, 4.483927247898782831, 76.45942372801901854 ) ) ;
#134102 = CARTESIAN_POINT ( 'NONE',  ( 5.153800228976615827, -19.02544592524334988, 30.20942372801900433 ) ) ;
#134103 = CARTESIAN_POINT ( 'NONE',  ( 19.05341960407611168, 5.049401038298154454, 88.95724293864769550 ) ) ;
#134104 = CARTESIAN_POINT ( 'NONE',  ( -13.89961937509977652, 13.97604488694528158, 75.62390960531438111 ) ) ;
#134105 = CARTESIAN_POINT ( 'NONE',  ( 8.224510206698742110, 14.34966873604972548, 72.08442372801899012 ) ) ;
#134106 = CARTESIAN_POINT ( 'NONE',  ( -0.05219959533909027116, -19.03943276465977164, 37.49890960531436690 ) ) ;
#134107 = CARTESIAN_POINT ( 'NONE',  ( 0.05219959533910956823, 16.53943276465976808, 49.99890960531437401 ) ) ;
#134109 = CARTESIAN_POINT ( 'NONE',  ( 19.02544592524343514, -5.153800228976328945, 98.54057627198100988 ) ) ;
#134108 = DIRECTION ( 'NONE',  ( -1.000000000000000000, 0.000000000000000000, 0.000000000000000000 ) ) ;
#134110 = CARTESIAN_POINT ( 'NONE',  ( -10.72451020669898014, 18.67979575497178502, 30.41557627198101699 ) ) ;
#134111 = CARTESIAN_POINT ( 'NONE',  ( -12.06949235617756955, 12.14591786802309770, 65.62390960531436690 ) ) ;
#134112 = ORIENTED_EDGE ( 'NONE', *, *, #66266, .F. ) ;
#134113 = CARTESIAN_POINT ( 'NONE',  ( -16.52544592524342804, 4.483927247898546575, 66.04057627198103830 ) ) ;
#134114 = CARTESIAN_POINT ( 'NONE',  ( 30.59399807301411656, -1.495846735942621297, -47.49088840515945265 ) ) ;
#134115 = CARTESIAN_POINT ( 'NONE',  ( -9.564922557961040184, 16.46253265017147172, 67.91775706135233293 ) ) ;
#134116 = CARTESIAN_POINT ( 'NONE',  ( 5.049401038298161559, -19.05341960407611168, 87.70724293864769550 ) ) ;
#134117 = CARTESIAN_POINT ( 'NONE',  ( -9.474510206698720793, -16.51473224551083518, 74.58442372801900433 ) ) ;
#134118 = CARTESIAN_POINT ( 'NONE',  ( -18.22780087662123805, -5.499999999999968026, 93.98236817873105053 ) ) ;
#134120 = CARTESIAN_POINT ( 'NONE',  ( 0.05219959533934541429, -16.53943276465976808, 100.0010903946857042 ) ) ;
#134119 = CARTESIAN_POINT ( 'NONE',  ( -4.379528057220086978, -16.55341960407618274, 19.79275706135235069 ) ) ;
#134121 = CARTESIAN_POINT ( 'NONE',  ( 9.564922557960805705, 16.46253265017160317, 44.58224293864769550 ) ) ;
#134122 = CARTESIAN_POINT ( 'NONE',  ( 21.52544592524344225, -5.823673210054117533, 28.54057627198103120 ) ) ;
#134123 = CARTESIAN_POINT ( 'NONE',  ( -18.62759615963255300, -10.81492255796106328, 54.16775706135235424 ) ) ;
#134124 = CARTESIAN_POINT ( 'NONE',  ( -4.483927247898782831, 16.52544592524335698, 22.70942372801901499 ) ) ;
#134126 = CARTESIAN_POINT ( 'NONE',  ( 0.05219959533909260263, 19.03943276465977164, 74.99890960531435269 ) ) ;
#134125 = CARTESIAN_POINT ( 'NONE',  ( -18.22780087662126647, -5.499999999999827693, 53.98236817873107185 ) ) ;
#134127 = CARTESIAN_POINT ( 'NONE',  ( -5.153800228976328057, -19.02544592524343514, 112.2905762719810099 ) ) ;
#134129 = CARTESIAN_POINT ( 'NONE',  ( -5.049401038298153566, 19.05341960407611168, 75.20724293864769550 ) ) ;
#134128 = CARTESIAN_POINT ( 'NONE',  ( -16.53943276465976808, 0.05219959533911058130, 76.24890960531435269 ) ) ;
#134130 = CARTESIAN_POINT ( 'NONE',  ( 0.05219959533909260263, 19.03943276465977164, 79.99890960531436690 ) ) ;
#134131 = ORIENTED_EDGE ( 'NONE', *, *, #122987, .F. ) ;
#134132 = CARTESIAN_POINT ( 'NONE',  ( 13.97604488694548053, -13.89961937509957401, 85.62609039468568994 ) ) ;
#134133 = CARTESIAN_POINT ( 'NONE',  ( -10.72451020669898014, 18.67979575497178502, 65.41557627198102409 ) ) ;
#134134 = CARTESIAN_POINT ( 'NONE',  ( 5.049401038298161559, -19.05341960407611168, 27.70724293864769550 ) ) ;
#134135 = CARTESIAN_POINT ( 'NONE',  ( 16.51473224551083163, -9.474510206698727899, 60.83442372801900433 ) ) ;
#134136 = CARTESIAN_POINT ( 'NONE',  ( 9.564922557960805705, 16.46253265017160317, 59.58224293864769550 ) ) ;
#134137 = CARTESIAN_POINT ( 'NONE',  ( -16.51473224551069308, -9.474510206698971260, 96.66557627198102409 ) ) ;
#134138 = ORIENTED_EDGE ( 'NONE', *, *, #121277, .F. ) ;
#134139 = CARTESIAN_POINT ( 'NONE',  ( -15.72974639402197994, 15.80617190586746368, 85.62390960531436690 ) ) ;
#134141 = CARTESIAN_POINT ( 'NONE',  ( 16.46253265017146816, 9.564922557961045513, 51.66775706135233293 ) ) ;
#134140 = CARTESIAN_POINT ( 'NONE',  ( -8.314922557960811034, -14.29746914071050412, 97.08224293864770971 ) ) ;
#134142 = CARTESIAN_POINT ( 'NONE',  ( -5.719274019375978568, 21.55341960407610458, 85.20724293864770971 ) ) ;
#134143 = CARTESIAN_POINT ( 'NONE',  ( 18.67979575497178502, 10.72451020669898547, 79.16557627198103830 ) ) ;
#134144 = VECTOR ( 'NONE', #96410, 1000.000000000000000 ) ;
#134145 = CARTESIAN_POINT ( 'NONE',  ( 16.53943276465976808, -0.05219959533910856209, 38.74890960531435979 ) ) ;
#134146 = CARTESIAN_POINT ( 'NONE',  ( -15.80617190586768217, 15.72974639402176855, 108.1260903946856757 ) ) ;
#134147 = CARTESIAN_POINT ( 'NONE',  ( 19.05341960407611168, 5.049401038298154454, 73.95724293864768129 ) ) ;
#134148 = CARTESIAN_POINT ( 'NONE',  ( -19.02544592524342804, 5.153800228976336051, 36.04057627198100988 ) ) ;
#134149 = CARTESIAN_POINT ( 'NONE',  ( 15.80617190586769283, -15.72974639402175789, 45.62609039468567573 ) ) ;
#134150 = CARTESIAN_POINT ( 'NONE',  ( 18.67979575497194134, -10.72451020669871369, 50.83442372801901143 ) ) ;
#134151 = CARTESIAN_POINT ( 'NONE',  ( 0.05219959533909260263, 19.03943276465977164, 49.99890960531435979 ) ) ;
#134152 = CARTESIAN_POINT ( 'NONE',  ( 5.719274019375673035, 21.55341960407619339, 22.29275706135235069 ) ) ;
#134153 = CARTESIAN_POINT ( 'NONE',  ( -9.474510206698720793, -16.51473224551083518, 54.58442372801899722 ) ) ;
#134154 = CARTESIAN_POINT ( 'NONE',  ( -9.564922557960796823, -16.46253265017161027, 42.08224293864769550 ) ) ;
#134155 = CARTESIAN_POINT ( 'NONE',  ( -14.34966873604972548, 8.224510206698743886, 23.33442372801901499 ) ) ;
#134156 = CARTESIAN_POINT ( 'NONE',  ( -0.05219959533909027116, -19.03943276465977164, 22.49890960531436690 ) ) ;
#134157 = CARTESIAN_POINT ( 'NONE',  ( -16.52544592524335698, -4.483927247898792601, 73.95942372801901854 ) ) ;
#134158 = CARTESIAN_POINT ( 'NONE',  ( -13.89961937509977652, 13.97604488694528158, 40.62390960531435979 ) ) ;
#134159 = CARTESIAN_POINT ( 'NONE',  ( 21.70479006154308621, -8.695791278452025708, 169.0563666577075423 ) ) ;
#134160 = CARTESIAN_POINT ( 'NONE',  ( -5.049401038298153566, 19.05341960407611168, 80.20724293864769550 ) ) ;
#134161 = CARTESIAN_POINT ( 'NONE',  ( -13.97604488694527625, -13.89961937509977652, 31.87390960531435979 ) ) ;
#134162 = CARTESIAN_POINT ( 'NONE',  ( 10.81492255796078972, 18.62759615963270932, 74.58224293864768129 ) ) ;
#134163 = CARTESIAN_POINT ( 'NONE',  ( -12.14591786802326823, 12.06949235617739902, 43.12609039468568284 ) ) ;
#134164 = CARTESIAN_POINT ( 'NONE',  ( -21.53943276465977519, -0.05219959533937600094, 113.7510903946856757 ) ) ;
#134165 = ADVANCED_FACE ( 'NONE', ( #65227 ), #136367, .F. ) ;
#134166 = CARTESIAN_POINT ( 'NONE',  ( 19.02544592524343514, -5.153800228976328945, 33.54057627198102409 ) ) ;
#134167 = CARTESIAN_POINT ( 'NONE',  ( -8.224510206698948167, 14.34966873604960824, 25.41557627198103120 ) ) ;
#134168 = CARTESIAN_POINT ( 'NONE',  ( 4.483927247898545687, 16.52544592524342804, 69.79057627198102409 ) ) ;
#134169 = CARTESIAN_POINT ( 'NONE',  ( 9.564922557960805705, 16.46253265017160317, 69.58224293864770971 ) ) ;
#134170 = CARTESIAN_POINT ( 'NONE',  ( -21.55341960407619339, 5.719274019375674811, 108.5427570613523756 ) ) ;
#134171 = CARTESIAN_POINT ( 'NONE',  ( -10.81492255796105439, 18.62759615963255655, 27.91775706135234358 ) ) ;
#134172 = CARTESIAN_POINT ( 'NONE',  ( -5.049401038298153566, 19.05341960407611168, 75.20724293864769550 ) ) ;
#134173 = CARTESIAN_POINT ( 'NONE',  ( -21.52544592524334988, -5.823673210054445271, 88.95942372801901854 ) ) ;
#134174 = CARTESIAN_POINT ( 'NONE',  ( 14.29746914071037800, 8.314922557961029526, 66.66775706135234714 ) ) ;
#134175 = CARTESIAN_POINT ( 'NONE',  ( 0.05219959533934541429, -16.53943276465976808, 35.00109039468568284 ) ) ;
#134177 = CARTESIAN_POINT ( 'NONE',  ( 9.474510206698971260, -16.51473224551069308, 102.9155762719810241 ) ) ;
#134176 = CARTESIAN_POINT ( 'NONE',  ( -14.34966873604960291, -8.224510206698953496, 91.66557627198103830 ) ) ;
#134178 = ADVANCED_FACE ( 'NONE', ( #90837 ), #47937, .T. ) ;
#134179 = CARTESIAN_POINT ( 'NONE',  ( 14.34966873604960469, 8.224510206698951720, 34.16557627198102409 ) ) ;
#134180 = CARTESIAN_POINT ( 'NONE',  ( -13.89961937509977652, 13.97604488694528158, 25.62390960531434558 ) ) ;
#134181 = CARTESIAN_POINT ( 'NONE',  ( -16.53943276465976808, -0.05219959533934237506, 48.75109039468568284 ) ) ;
#134182 = CARTESIAN_POINT ( 'NONE',  ( 0.05219959533910956823, 16.53943276465976808, 49.99890960531437401 ) ) ;
#134183 = CARTESIAN_POINT ( 'NONE',  ( -12.14591786802326823, 12.06949235617739902, 98.12609039468570415 ) ) ;
#134184 = CARTESIAN_POINT ( 'NONE',  ( -16.46253265017160317, 9.564922557960807481, 115.8322429386477097 ) ) ;
#134185 = CARTESIAN_POINT ( 'NONE',  ( -5.719274019375978568, 21.55341960407610458, 30.20724293864769550 ) ) ;
#134186 = CARTESIAN_POINT ( 'NONE',  ( 5.823673210054444382, -21.52544592524334988, 110.2094237280190185 ) ) ;
#134187 = CARTESIAN_POINT ( 'NONE',  ( -8.314922557960811034, -14.29746914071050412, 82.08224293864768129 ) ) ;
#134188 = CARTESIAN_POINT ( 'NONE',  ( 0.05219959533909260263, 19.03943276465977164, 89.99890960531436690 ) ) ;
#134189 = ORIENTED_EDGE ( 'NONE', *, *, #69472, .F. ) ;
#134190 = CARTESIAN_POINT ( 'NONE',  ( -8.224510206698735004, -14.34966873604973081, 39.58442372801901143 ) ) ;
#134191 = CARTESIAN_POINT ( 'NONE',  ( 0.05219959533909260263, 19.03943276465977164, 39.99890960531436690 ) ) ;
#134192 = CARTESIAN_POINT ( 'NONE',  ( -17.33423593373957772, -5.611347464745015223, 21.19882084351016971 ) ) ;
#134193 = CARTESIAN_POINT ( 'NONE',  ( -19.05341960407617563, 5.049401038297882671, 48.54275706135233293 ) ) ;
#134194 = CARTESIAN_POINT ( 'NONE',  ( 5.049401038298161559, -19.05341960407611168, 42.70724293864767418 ) ) ;
#134195 = CARTESIAN_POINT ( 'NONE',  ( -14.29746914071037622, -8.314922557961029526, 74.16775706135231871 ) ) ;
#134196 = CARTESIAN_POINT ( 'NONE',  ( 16.46253265017146816, 9.564922557961045513, 91.66775706135234714 ) ) ;
#134197 = CARTESIAN_POINT ( 'NONE',  ( 9.474510206698971260, -16.51473224551069308, 57.91557627198103120 ) ) ;
#134198 = CARTESIAN_POINT ( 'NONE',  ( 10.72451020669898902, -18.67979575497178502, 87.91557627198103830 ) ) ;
#134200 = CIRCLE ( 'NONE', #34012, 40.00000000000000000 ) ;
#134199 = CARTESIAN_POINT ( 'NONE',  ( -16.55341960407611168, -4.379528057220339221, 96.45724293864770971 ) ) ;
#134201 = CARTESIAN_POINT ( 'NONE',  ( -9.564922557961040184, 16.46253265017147172, 67.91775706135233293 ) ) ;
#134202 = CARTESIAN_POINT ( 'NONE',  ( 0.05219959533907565091, 21.53943276465977519, 59.99890960531436690 ) ) ;
#134203 = CARTESIAN_POINT ( 'NONE',  ( 16.46253265017146816, 9.564922557961045513, 46.66775706135233293 ) ) ;
#134204 = CARTESIAN_POINT ( 'NONE',  ( 5.049401038298161559, -19.05341960407611168, 112.7072429386476813 ) ) ;
#134205 = EDGE_CURVE ( 'NONE', #75891, #66692, #96803, .T. ) ;
#134206 = CARTESIAN_POINT ( 'NONE',  ( -10.81492255796078084, -18.62759615963271287, 92.08224293864769550 ) ) ;
#134207 = CARTESIAN_POINT ( 'NONE',  ( -18.56453257813361191, 5.500000000000043521, 55.99000423690686290 ) ) ;
#134208 = CARTESIAN_POINT ( 'NONE',  ( -9.474510206698720793, -16.51473224551083518, 104.5844237280190043 ) ) ;
#134209 = CARTESIAN_POINT ( 'NONE',  ( -18.39443945427639449, 5.500000000000033751, 58.51745347608655123 ) ) ;
#134210 = CARTESIAN_POINT ( 'NONE',  ( -14.29746914071037622, -8.314922557961029526, 29.16775706135234003 ) ) ;
#134211 = CARTESIAN_POINT ( 'NONE',  ( -16.46253265017160317, 9.564922557960807481, 45.83224293864769550 ) ) ;
#134212 = CARTESIAN_POINT ( 'NONE',  ( 13.89961937509977652, -13.97604488694527269, 113.1239096053143527 ) ) ;
#134213 = CARTESIAN_POINT ( 'NONE',  ( 21.53943276465977519, -0.05219959533907433946, 83.74890960531435269 ) ) ;
#134214 = VECTOR ( 'NONE', #154731, 1000.000000000000000 ) ;
#134215 = CARTESIAN_POINT ( 'NONE',  ( -15.72974639402176322, -15.80617190586768395, 64.37609039468568994 ) ) ;
#134217 = CARTESIAN_POINT ( 'NONE',  ( -13.97604488694547697, 13.89961937509957934, 33.12609039468566863 ) ) ;
#134216 = CARTESIAN_POINT ( 'NONE',  ( 9.564922557961047289, -16.46253265017146816, 110.4177570613523471 ) ) ;
#134218 = CARTESIAN_POINT ( 'NONE',  ( -14.29746914071049879, 8.314922557960819915, 35.83224293864768839 ) ) ;
#134219 = CARTESIAN_POINT ( 'NONE',  ( 10.72451020669898902, -18.67979575497178502, 97.91557627198103830 ) ) ;
#134220 = CARTESIAN_POINT ( 'NONE',  ( -16.53943276465976808, 0.05219959533911058130, 51.24890960531436690 ) ) ;
#134221 = CARTESIAN_POINT ( 'NONE',  ( 0.05219959533936267826, -19.03943276465977164, 100.0010903946856757 ) ) ;
#134222 = CARTESIAN_POINT ( 'NONE',  ( 16.51473224551083163, -9.474510206698727899, 55.83442372801899722 ) ) ;
#134223 = CONICAL_SURFACE ( 'NONE', #49752, 2.041999999999999815, 1.047197551196591858 ) ;
#134224 = CARTESIAN_POINT ( 'NONE',  ( -0.05219959533937732626, 21.53943276465977519, 77.50109039468567573 ) ) ;
#134225 = CARTESIAN_POINT ( 'NONE',  ( 0.05219959533936267826, -19.03943276465977164, 45.00109039468566863 ) ) ;
#134226 = CARTESIAN_POINT ( 'NONE',  ( -19.05341960407611168, -5.049401038298163336, 21.45724293864768839 ) ) ;
#134227 = CARTESIAN_POINT ( 'NONE',  ( 21.52544592524344225, -5.823673210054117533, 43.54057627198103830 ) ) ;
#134228 = CARTESIAN_POINT ( 'NONE',  ( -12.14591786802309592, -12.06949235617757132, 36.87390960531435979 ) ) ;
#134229 = CARTESIAN_POINT ( 'NONE',  ( -21.55341960407619339, 5.719274019375674811, 113.5427570613523756 ) ) ;
#134230 = CARTESIAN_POINT ( 'NONE',  ( 8.314922557961029526, -14.29746914071037800, 70.41775706135236135 ) ) ;
#134231 = CARTESIAN_POINT ( 'NONE',  ( -14.29746914071049879, 8.314922557960819915, 40.83224293864769550 ) ) ;
#134232 = CARTESIAN_POINT ( 'NONE',  ( 21.52544592524334988, 5.823673210054432836, 71.45942372801901854 ) ) ;
#134233 = CARTESIAN_POINT ( 'NONE',  ( -18.62759615963255300, -10.81492255796106328, 64.16775706135234714 ) ) ;
#134234 = CARTESIAN_POINT ( 'NONE',  ( 5.719274019375991003, -21.55341960407610458, 72.70724293864769550 ) ) ;
#134235 = CARTESIAN_POINT ( 'NONE',  ( 13.89961937509977652, -13.97604488694527269, 43.12390960531434558 ) ) ;
#134236 = CARTESIAN_POINT ( 'NONE',  ( -0.05219959533937732626, 21.53943276465977519, 47.50109039468568994 ) ) ;
#134237 = CARTESIAN_POINT ( 'NONE',  ( -16.52544592524342804, 4.483927247898546575, 116.0405762719810383 ) ) ;
#134238 = CARTESIAN_POINT ( 'NONE',  ( -9.474510206698964154, 16.51473224551069663, 40.41557627198103120 ) ) ;
#134239 = CARTESIAN_POINT ( 'NONE',  ( 16.55341960407611168, 4.379528057220329451, 88.95724293864769550 ) ) ;
#134240 = CARTESIAN_POINT ( 'NONE',  ( 19.03943276465977164, -0.05219959533909143690, 78.74890960531436690 ) ) ;
#134241 = CARTESIAN_POINT ( 'NONE',  ( -12.14591786802309592, -12.06949235617757132, 46.87390960531435979 ) ) ;
#134242 = CARTESIAN_POINT ( 'NONE',  ( 0.05219959533910956823, 16.53943276465976808, 94.99890960531436690 ) ) ;
#134243 = CARTESIAN_POINT ( 'NONE',  ( 21.53943276465977519, -0.05219959533907433946, 63.74890960531435979 ) ) ;
#134244 = CARTESIAN_POINT ( 'NONE',  ( -5.719274019375978568, 21.55341960407610458, 110.2072429386477239 ) ) ;
#134245 = CARTESIAN_POINT ( 'NONE',  ( -9.564922557960796823, -16.46253265017161027, 112.0822429386476955 ) ) ;
#134247 = CARTESIAN_POINT ( 'NONE',  ( -4.379528057220086978, -16.55341960407618274, 24.79275706135235779 ) ) ;
#134246 = CARTESIAN_POINT ( 'NONE',  ( 9.564922557960805705, 16.46253265017160317, 59.58224293864769550 ) ) ;
#134248 = CARTESIAN_POINT ( 'NONE',  ( -18.67979575497178146, -10.72451020669898902, 61.66557627198103120 ) ) ;
#134249 = CARTESIAN_POINT ( 'NONE',  ( -15.80617190586768217, 15.72974639402176855, 98.12609039468570415 ) ) ;
#134250 = CARTESIAN_POINT ( 'NONE',  ( 0.05219959533909260263, 19.03943276465977164, 74.99890960531435269 ) ) ;
#134251 = CARTESIAN_POINT ( 'NONE',  ( 18.62759615963255655, 10.81492255796105972, 21.66775706135235069 ) ) ;
#134252 = CARTESIAN_POINT ( 'NONE',  ( 19.03943276465977164, -0.05219959533909143690, 108.7489096053143527 ) ) ;
#134253 = CARTESIAN_POINT ( 'NONE',  ( -8.224510206698735004, -14.34966873604973081, 89.58442372801901854 ) ) ;
#134254 = CARTESIAN_POINT ( 'NONE',  ( 18.62759615963255655, 10.81492255796105972, 66.66775706135234714 ) ) ;
#134255 = CARTESIAN_POINT ( 'NONE',  ( 5.823673210054444382, -21.52544592524334988, 105.2094237280190328 ) ) ;
#134256 = CARTESIAN_POINT ( 'NONE',  ( 12.14591786802327356, -12.06949235617739191, 60.62609039468567573 ) ) ;
#134257 = CARTESIAN_POINT ( 'NONE',  ( 18.62759615963255655, 10.81492255796105972, 26.66775706135235424 ) ) ;
#134258 = CARTESIAN_POINT ( 'NONE',  ( -19.03943276465977164, 0.05219959533909376836, 111.2489096053143669 ) ) ;
#134259 = CARTESIAN_POINT ( 'NONE',  ( 21.55341960407619695, -5.719274019375665929, 86.04275706135236135 ) ) ;
#134260 = CARTESIAN_POINT ( 'NONE',  ( 9.474510206698971260, -16.51473224551069308, 92.91557627198103830 ) ) ;
#134261 = CARTESIAN_POINT ( 'NONE',  ( 10.72451020669898902, -18.67979575497178502, 87.91557627198103830 ) ) ;
#134262 = CARTESIAN_POINT ( 'NONE',  ( -0.05219959533936034679, 19.03943276465977164, 52.50109039468566863 ) ) ;
#134263 = CARTESIAN_POINT ( 'NONE',  ( -15.72974639402197994, 15.80617190586746368, 55.62390960531436690 ) ) ;
#134265 = CARTESIAN_POINT ( 'NONE',  ( -8.314922557960811034, -14.29746914071050412, 42.08224293864769550 ) ) ;
#134264 = CARTESIAN_POINT ( 'NONE',  ( 16.51473224551069308, 9.474510206698969483, 94.16557627198103830 ) ) ;
#134266 = CARTESIAN_POINT ( 'NONE',  ( 21.27717364736664152, 9.815017990598704500, 168.4818444780604523 ) ) ;
#134267 = CARTESIAN_POINT ( 'NONE',  ( 13.89961937509957401, 13.97604488694547697, 61.87609039468566863 ) ) ;
#134268 = CARTESIAN_POINT ( 'NONE',  ( 8.388830574159379737E-16, 13.70000000000001528, -60.44446360152740283 ) ) ;
#134269 = CARTESIAN_POINT ( 'NONE',  ( 0.05219959533936267826, -19.03943276465977164, 105.0010903946856615 ) ) ;
#134270 = CARTESIAN_POINT ( 'NONE',  ( 18.67979575497178502, 10.72451020669898547, 89.16557627198102409 ) ) ;
#134271 = CARTESIAN_POINT ( 'NONE',  ( -16.53943276465976808, 0.05219959533911058130, 56.24890960531436690 ) ) ;
#134272 = CARTESIAN_POINT ( 'NONE',  ( -16.52544592524335698, -4.483927247898792601, 33.95942372801901143 ) ) ;
#134273 = CARTESIAN_POINT ( 'NONE',  ( 19.02544592524343514, -5.153800228976328945, 48.54057627198103120 ) ) ;
#134275 = CARTESIAN_POINT ( 'NONE',  ( 5.153800228976615827, -19.02544592524334988, 90.20942372801900433 ) ) ;
#134274 = CARTESIAN_POINT ( 'NONE',  ( -15.72974639402176322, -15.80617190586768395, 19.37609039468568639 ) ) ;
#134276 = CARTESIAN_POINT ( 'NONE',  ( -19.02544592524342804, 5.153800228976336051, 91.04057627198100988 ) ) ;
#134277 = CARTESIAN_POINT ( 'NONE',  ( -19.02544592524342804, 5.153800228976336051, 81.04057627198103830 ) ) ;
#134278 = CARTESIAN_POINT ( 'NONE',  ( 10.72451020669898902, -18.67979575497178502, 82.91557627198103830 ) ) ;
#134279 = CARTESIAN_POINT ( 'NONE',  ( -13.97604488694527625, -13.89961937509977652, 46.87390960531435979 ) ) ;
#134280 = CARTESIAN_POINT ( 'NONE',  ( 8.704215515294519534, 36.44267296588056837, -7.999999999999996447 ) ) ;
#134281 = CARTESIAN_POINT ( 'NONE',  ( 4.483927247898545687, 16.52544592524342804, 59.79057627198103120 ) ) ;
#134282 = CARTESIAN_POINT ( 'NONE',  ( 9.474510206698971260, -16.51473224551069308, 92.91557627198103830 ) ) ;
#134283 = CARTESIAN_POINT ( 'NONE',  ( -32.00000000000000000, -5.510910596163089556E-15, 45.00000000000000000 ) ) ;
#134284 = CARTESIAN_POINT ( 'NONE',  ( -5.153800228976607833, 19.02544592524334988, 62.70942372801899722 ) ) ;
#134285 = AXIS2_PLACEMENT_3D ( 'NONE', #40697, #23533, #54861 ) ;
#134286 = CARTESIAN_POINT ( 'NONE',  ( -10.81492255796078084, -18.62759615963271287, 72.08224293864769550 ) ) ;
#134287 = CARTESIAN_POINT ( 'NONE',  ( -19.03943276465977164, -0.05219959533935918106, 33.75109039468566863 ) ) ;
#134288 = CARTESIAN_POINT ( 'NONE',  ( 9.564922557960805705, 16.46253265017160317, 99.58224293864770971 ) ) ;
#134289 = LINE ( 'NONE', #119121, #4830 ) ;
#134290 = CARTESIAN_POINT ( 'NONE',  ( 18.62759615963271287, -10.81492255796078972, 38.33224293864768839 ) ) ;
#134291 = CARTESIAN_POINT ( 'NONE',  ( 19.02544592524343514, -5.153800228976328945, 73.54057627198103830 ) ) ;
#134292 = EDGE_CURVE ( 'NONE', #87243, #185765, #40522, .T. ) ;
#134293 = CARTESIAN_POINT ( 'NONE',  ( -15.72974639402176322, -15.80617190586768395, 59.37609039468568284 ) ) ;
#134294 = CARTESIAN_POINT ( 'NONE',  ( -5.049401038298153566, 19.05341960407611168, 30.20724293864768839 ) ) ;
#134296 = ORIENTED_EDGE ( 'NONE', *, *, #80939, .F. ) ;
#134295 = CARTESIAN_POINT ( 'NONE',  ( -5.823673210054116645, -21.52544592524344225, 112.2905762719810241 ) ) ;
#134297 = CARTESIAN_POINT ( 'NONE',  ( -18.67979575497193778, 10.72451020669871902, 48.33442372801902565 ) ) ;
#134298 = VERTEX_POINT ( 'NONE', #86053 ) ;
#134299 = CARTESIAN_POINT ( 'NONE',  ( -19.02544592524342804, 5.153800228976336051, 96.04057627198103830 ) ) ;
#134300 = CARTESIAN_POINT ( 'NONE',  ( 9.474510206698729675, 16.51473224551082808, 72.08442372801900433 ) ) ;
#134301 = DIRECTION ( 'NONE',  ( -0.000000000000000000, -0.000000000000000000, 1.000000000000000000 ) ) ;
#134302 = CARTESIAN_POINT ( 'NONE',  ( 21.52544592524344225, -5.823673210054117533, 103.5405762719810383 ) ) ;
#134303 = CARTESIAN_POINT ( 'NONE',  ( -19.05341960407611168, -5.049401038298163336, 56.45724293864768129 ) ) ;
#134304 = CARTESIAN_POINT ( 'NONE',  ( -4.379528057220086978, -16.55341960407618274, 34.79275706135235424 ) ) ;
#134305 = CARTESIAN_POINT ( 'NONE',  ( -30.74264578624800492, 22.33583958711400186, -5.949999994537626513 ) ) ;
#134306 = CARTESIAN_POINT ( 'NONE',  ( 10.72451020669871369, 18.67979575497193778, 97.08442372801904696 ) ) ;
#134307 = CARTESIAN_POINT ( 'NONE',  ( 19.02544592524343514, -5.153800228976328945, 48.54057627198103120 ) ) ;
#134308 = CARTESIAN_POINT ( 'NONE',  ( -5.719274019375665041, -21.55341960407619695, 104.7927570613523898 ) ) ;
#134310 = CARTESIAN_POINT ( 'NONE',  ( 21.55341960407619695, -5.719274019375665929, 61.04275706135234714 ) ) ;
#134309 = CARTESIAN_POINT ( 'NONE',  ( 9.564922557960805705, 16.46253265017160317, 94.58224293864769550 ) ) ;
#134311 = CARTESIAN_POINT ( 'NONE',  ( 6.218960876731467913, -4.126125163602036849, -62.26018854728523166 ) ) ;
#134312 = CARTESIAN_POINT ( 'NONE',  ( -9.474510206698964154, 16.51473224551069663, 110.4155762719810383 ) ) ;
#134313 = DIRECTION ( 'NONE',  ( -1.000000000000000000, -0.000000000000000000, -0.000000000000000000 ) ) ;
#134315 = CARTESIAN_POINT ( 'NONE',  ( 15.72974639402176855, 15.80617190586768217, 66.87609039468568994 ) ) ;
#134314 = CARTESIAN_POINT ( 'NONE',  ( -16.55341960407617563, 4.379528057220093196, 48.54275706135234714 ) ) ;
#134316 = CARTESIAN_POINT ( 'NONE',  ( -0.05219959533937732626, 21.53943276465977519, 92.50109039468567573 ) ) ;
#134317 = CARTESIAN_POINT ( 'NONE',  ( -12.24338688535747721, 10.51869806896807802, -59.40202214942380721 ) ) ;
#134318 = CARTESIAN_POINT ( 'NONE',  ( 16.52544592524335698, 4.483927247898782831, 21.45942372801901499 ) ) ;
#134319 = CARTESIAN_POINT ( 'NONE',  ( 9.564922557960805705, 16.46253265017160317, 69.58224293864770971 ) ) ;
#134320 = CARTESIAN_POINT ( 'NONE',  ( -13.97604488694527625, -13.89961937509977652, 106.8739096053143669 ) ) ;
#134321 = CARTESIAN_POINT ( 'NONE',  ( -1.366177905283608052, -29.77433414031402137, -51.67655205196554391 ) ) ;
#134322 = CARTESIAN_POINT ( 'NONE',  ( 5.153800228976335163, 19.02544592524342804, 24.79057627198102765 ) ) ;
#134324 = EDGE_CURVE ( 'NONE', #135096, #59793, #169152, .T. ) ;
#134323 = CARTESIAN_POINT ( 'NONE',  ( 21.55341960407610458, 5.719274019375980345, 48.95724293864770971 ) ) ;
#134325 = CARTESIAN_POINT ( 'NONE',  ( -16.52544592524335698, -4.483927247898792601, 98.95942372801903275 ) ) ;
#134327 = CARTESIAN_POINT ( 'NONE',  ( 19.02544592524343514, -5.153800228976328945, 63.54057627198103830 ) ) ;
#134326 = CARTESIAN_POINT ( 'NONE',  ( -16.55341960407611168, -4.379528057220339221, 81.45724293864769550 ) ) ;
#134328 = CARTESIAN_POINT ( 'NONE',  ( 0.05219959533937995610, -21.53943276465977519, 85.00109039468568994 ) ) ;
#134329 = CARTESIAN_POINT ( 'NONE',  ( -24.24152472029835792, 0.4285070731210879891, -56.81472536503801507 ) ) ;
#134330 = CARTESIAN_POINT ( 'NONE',  ( -16.51473224551082808, 9.474510206698731452, 113.3344237280190043 ) ) ;
#134331 = CARTESIAN_POINT ( 'NONE',  ( 14.29746914071049879, -8.314922557960816363, 93.33224293864769550 ) ) ;
#134332 = CARTESIAN_POINT ( 'NONE',  ( -15.80617190586768217, 15.72974639402176855, 38.12609039468567573 ) ) ;
#134333 = CARTESIAN_POINT ( 'NONE',  ( -5.823673210054116645, -21.52544592524344225, 72.29057627198102409 ) ) ;
#134334 = CARTESIAN_POINT ( 'NONE',  ( 13.97604488694548053, -13.89961937509957401, 40.62609039468564731 ) ) ;
#134335 = DIRECTION ( 'NONE',  ( -0.8660254037844391517, -0.000000000000000000, -0.4999999999999991673 ) ) ;
#134336 = CARTESIAN_POINT ( 'NONE',  ( 16.51473224551069308, 9.474510206698969483, 89.16557627198103830 ) ) ;
#134337 = CARTESIAN_POINT ( 'NONE',  ( -16.55341960407611168, -4.379528057220339221, 66.45724293864768129 ) ) ;
#134338 = EDGE_CURVE ( 'NONE', #184472, #70081, #144778, .T. ) ;
#134339 = CARTESIAN_POINT ( 'NONE',  ( -0.05219959533910754901, -16.53943276465976808, 32.49890960531435979 ) ) ;
#134340 = CARTESIAN_POINT ( 'NONE',  ( 14.34966873604972726, -8.224510206698740333, 105.8344237280190328 ) ) ;
#134341 = CARTESIAN_POINT ( 'NONE',  ( -5.049401038297874678, -19.05341960407617918, 69.79275706135233293 ) ) ;
#134342 = B_SPLINE_CURVE_WITH_KNOTS ( 'NONE', 3,
 ( #53216, #188768, #7705, #20888, #113878, #177590, #143225, #142238, #190747, #189761, #144228, #68383, #176588, #3723, #159393, #99718, #52221, #98711, #66397, #130035, #38062, #4707, #192746, #115900, #18918, #22894, #39057, #128059 ),
 .UNSPECIFIED., .F., .F.,
 ( 4, 2, 2, 2, 2, 2, 2, 2, 2, 2, 2, 2, 2, 4 ),
 ( 0.000000000000000000, 0.002181393419099474963, 0.004362786838198949926, 0.005453483547748686974, 0.006544180257298424890, 0.006816854434685860019, 0.007089528612073295148, 0.007225865700767011846, 0.007294034245113868893, 0.007362202789460725941, 0.007498539878154482537, 0.007634876966848239133, 0.008180225321623478887, 0.008725573676398716907 ),
 .UNSPECIFIED. ) ;
#134343 = FACE_OUTER_BOUND ( 'NONE', #97415, .T. ) ;
#134344 = CARTESIAN_POINT ( 'NONE',  ( -18.67979575497178146, -10.72451020669898902, 26.66557627198103475 ) ) ;
#134345 = CARTESIAN_POINT ( 'NONE',  ( 4.483927247898545687, 16.52544592524342804, 89.79057627198103830 ) ) ;
#134346 = CYLINDRICAL_SURFACE ( 'NONE', #169059, 37.99626262588765968 ) ;
#134348 = CARTESIAN_POINT ( 'NONE',  ( -15.80617190586745835, -15.72974639402198527, 46.87390960531435979 ) ) ;
#134347 = CARTESIAN_POINT ( 'NONE',  ( 5.049401038298161559, -19.05341960407611168, 47.70724293864770260 ) ) ;
#134349 = CARTESIAN_POINT ( 'NONE',  ( 0.05219959533907565091, 21.53943276465977519, 69.99890960531435269 ) ) ;
#134350 = CARTESIAN_POINT ( 'NONE',  ( 14.34966873604960469, 8.224510206698951720, 109.1655762719810383 ) ) ;
#134352 = CARTESIAN_POINT ( 'NONE',  ( -19.05341960407611168, -5.049401038298163336, 41.45724293864769550 ) ) ;
#134351 = CARTESIAN_POINT ( 'NONE',  ( -8.224510206698735004, -14.34966873604973081, 59.58442372801901854 ) ) ;
#134353 = CARTESIAN_POINT ( 'NONE',  ( -15.80617190586768217, 15.72974639402176855, 53.12609039468568284 ) ) ;
#134354 = CARTESIAN_POINT ( 'NONE',  ( -12.06949235617756955, 12.14591786802309770, 105.6239096053143669 ) ) ;
#134355 = CARTESIAN_POINT ( 'NONE',  ( 16.46253265017146816, 9.564922557961045513, 91.66775706135234714 ) ) ;
#134356 = CARTESIAN_POINT ( 'NONE',  ( -22.81625015709510507, 31.40387420917330275, -3.424999997268813434 ) ) ;
#134358 = CARTESIAN_POINT ( 'NONE',  ( 18.67979575497178502, 10.72451020669898547, 49.16557627198102409 ) ) ;
#134357 = FACE_OUTER_BOUND ( 'NONE', #107369, .T. ) ;
#134359 = CARTESIAN_POINT ( 'NONE',  ( 16.19135201231363297, -7.376712067592068323, 67.31319145947966831 ) ) ;
#134360 = CARTESIAN_POINT ( 'NONE',  ( 21.53943276465977519, 0.05219959533937863772, 71.25109039468568994 ) ) ;
#134362 = CARTESIAN_POINT ( 'NONE',  ( -14.34966873604960291, -8.224510206698953496, 36.66557627198103120 ) ) ;
#134361 = CARTESIAN_POINT ( 'NONE',  ( -14.34966873604972548, 8.224510206698743886, 53.33442372801901854 ) ) ;
#134363 = CARTESIAN_POINT ( 'NONE',  ( 15.80617190586746368, 15.72974639402197994, 74.37390960531436690 ) ) ;
#134364 = CARTESIAN_POINT ( 'NONE',  ( 15.80617190586746368, 15.72974639402197994, 69.37390960531436690 ) ) ;
#134365 = CARTESIAN_POINT ( 'NONE',  ( 30.57569798415968876, -22.56501773984572168, -20.05394705607442063 ) ) ;
#134367 = CARTESIAN_POINT ( 'NONE',  ( -13.97604488694527625, -13.89961937509977652, 111.8739096053143243 ) ) ;
#134366 = CARTESIAN_POINT ( 'NONE',  ( 9.564922557961047289, -16.46253265017146816, 85.41775706135233293 ) ) ;
#134368 = CARTESIAN_POINT ( 'NONE',  ( 16.51473224551069308, 9.474510206698969483, 54.16557627198103120 ) ) ;
#134369 = CARTESIAN_POINT ( 'NONE',  ( -19.03943276465977164, 0.05219959533909376836, 21.24890960531436335 ) ) ;
#134370 = DIRECTION ( 'NONE',  ( -1.000000000000000000, 0.000000000000000000, 0.000000000000000000 ) ) ;
#134371 = ORIENTED_EDGE ( 'NONE', *, *, #29683, .F. ) ;
#134372 = CARTESIAN_POINT ( 'NONE',  ( 14.29746914071037800, 8.314922557961029526, 86.66775706135234714 ) ) ;
#134373 = CARTESIAN_POINT ( 'NONE',  ( 15.80617190586746368, 15.72974639402197994, 104.3739096053143669 ) ) ;
#134374 = CARTESIAN_POINT ( 'NONE',  ( -9.564922557960796823, -16.46253265017161027, 72.08224293864770971 ) ) ;
#134375 = CARTESIAN_POINT ( 'NONE',  ( -5.823673210054431948, 21.52544592524334988, 42.70942372801901854 ) ) ;
#134376 = CARTESIAN_POINT ( 'NONE',  ( 9.564922557960805705, 16.46253265017160317, 99.58224293864770971 ) ) ;
#134377 = CARTESIAN_POINT ( 'NONE',  ( -30.85002141292116917, -24.92539791875024946, -19.32025355658407761 ) ) ;
#134378 = ORIENTED_EDGE ( 'NONE', *, *, #130602, .T. ) ;
#134379 = CARTESIAN_POINT ( 'NONE',  ( 18.67979575497194134, -10.72451020669871369, 25.83442372801901499 ) ) ;
#134381 = CARTESIAN_POINT ( 'NONE',  ( 13.89961937509957401, 13.97604488694547697, 86.87609039468567573 ) ) ;
#134380 = CARTESIAN_POINT ( 'NONE',  ( -16.51473224551069308, -9.474510206698971260, 21.66557627198102765 ) ) ;
#134382 = CARTESIAN_POINT ( 'NONE',  ( -9.564922557961040184, 16.46253265017147172, 37.91775706135233293 ) ) ;
#134383 = CARTESIAN_POINT ( 'NONE',  ( -21.53943276465977519, 0.05219959533907696930, 116.2489096053143669 ) ) ;
#134384 = CARTESIAN_POINT ( 'NONE',  ( 19.02544592524334988, 5.153800228976608722, 36.45942372801900433 ) ) ;
#134385 = CARTESIAN_POINT ( 'NONE',  ( -19.02544592524334988, -5.153800228976617603, 43.95942372801899012 ) ) ;
#134386 = CARTESIAN_POINT ( 'NONE',  ( 14.34966873604972726, -8.224510206698740333, 95.83442372801903275 ) ) ;
#134388 = ORIENTED_EDGE ( 'NONE', *, *, #95674, .F. ) ;
#134387 = CARTESIAN_POINT ( 'NONE',  ( 19.05341960407611168, 5.049401038298154454, 113.9572429386477097 ) ) ;
#134389 = CARTESIAN_POINT ( 'NONE',  ( 13.89961937509977652, -13.97604488694527269, 68.12390960531436690 ) ) ;
#134390 = AXIS2_PLACEMENT_3D ( 'NONE', #162621, #115121, #54451 ) ;
#134391 = CARTESIAN_POINT ( 'NONE',  ( 0.05219959533937995610, -21.53943276465977519, 75.00109039468568994 ) ) ;
#134392 = CARTESIAN_POINT ( 'NONE',  ( -21.53943276465977519, -0.05219959533937600094, 98.75109039468568994 ) ) ;
#134393 = CARTESIAN_POINT ( 'NONE',  ( -0.3916721525565259876, -9.051314012904525086, -63.96062167512636876 ) ) ;
#134394 = CARTESIAN_POINT ( 'NONE',  ( 16.51473224551069308, 9.474510206698969483, 84.16557627198102409 ) ) ;
#134395 = CARTESIAN_POINT ( 'NONE',  ( -18.67979575497193778, 10.72451020669871902, 58.33442372801901143 ) ) ;
#134396 = CARTESIAN_POINT ( 'NONE',  ( 0.05219959533936267826, -19.03943276465977164, 95.00109039468567573 ) ) ;
#134397 = CARTESIAN_POINT ( 'NONE',  ( 13.97604488694527802, 13.89961937509977652, 64.37390960531436690 ) ) ;
#134398 = CARTESIAN_POINT ( 'NONE',  ( -13.89961937509977652, 13.97604488694528158, 115.6239096053143669 ) ) ;
#134399 = CARTESIAN_POINT ( 'NONE',  ( 13.97604488694527802, 13.89961937509977652, 74.37390960531436690 ) ) ;
#134400 = DIRECTION ( 'NONE',  ( -3.720488476448336339E-46, 1.000000000000000000, 7.149051953565418611E-31 ) ) ;
#134401 = CARTESIAN_POINT ( 'NONE',  ( 13.89961937509977652, -13.97604488694527269, 68.12390960531436690 ) ) ;
#134402 = CARTESIAN_POINT ( 'NONE',  ( -5.049401038298153566, 19.05341960407611168, 55.20724293864769550 ) ) ;
#134403 = CARTESIAN_POINT ( 'NONE',  ( 5.823673210054125526, 21.52544592524343514, 114.7905762719810383 ) ) ;
#134404 = CARTESIAN_POINT ( 'NONE',  ( -16.53943276465976808, -0.05219959533934237506, 83.75109039468568994 ) ) ;
#134405 = CARTESIAN_POINT ( 'NONE',  ( 7.052343178074640839, -2.552343178074650609, 8.889087296526001936 ) ) ;
#134406 = DIRECTION ( 'NONE',  ( -1.000000000000000000, -0.000000000000000000, -0.000000000000000000 ) ) ;
#134407 = CARTESIAN_POINT ( 'NONE',  ( 9.474510206698729675, 16.51473224551082808, 57.08442372801900433 ) ) ;
#134408 = B_SPLINE_CURVE_WITH_KNOTS ( 'NONE', 3,
 ( #179575, #41045, #102710, #195743, #42050, #103714, #27888, #89530, #165394, #26887, #88530, #151218 ),
 .UNSPECIFIED., .F., .F.,
 ( 4, 2, 2, 2, 2, 4 ),
 ( -6.183812803946990913E-05, 0.002421080454147832121, 0.004903999036335133718, 0.006145458327428788420, 0.007386917618522443121, 0.009869836200709747320 ),
 .UNSPECIFIED. ) ;
#134409 = CARTESIAN_POINT ( 'NONE',  ( -16.51473224551069308, -9.474510206698971260, 76.66557627198103830 ) ) ;
#134410 = CARTESIAN_POINT ( 'NONE',  ( -0.05219959533910754901, -16.53943276465976808, 67.49890960531436690 ) ) ;
#134411 = CARTESIAN_POINT ( 'NONE',  ( 14.29746914071049879, -8.314922557960816363, 103.3322429386476955 ) ) ;
#134412 = CARTESIAN_POINT ( 'NONE',  ( -21.53943276465977519, 0.05219959533907696930, 31.24890960531435979 ) ) ;
#134413 = CARTESIAN_POINT ( 'NONE',  ( -9.564922557960796823, -16.46253265017161027, 107.0822429386476955 ) ) ;
#134414 = CARTESIAN_POINT ( 'NONE',  ( 8.314922557960818139, 14.29746914071049879, 94.58224293864769550 ) ) ;
#134415 = CARTESIAN_POINT ( 'NONE',  ( -37.99626262588762415, -12.34573411038919311, -3.902157773949822772 ) ) ;
#134416 = CARTESIAN_POINT ( 'NONE',  ( 13.89961937509957401, 13.97604488694547697, 36.87609039468565442 ) ) ;
#134417 = CARTESIAN_POINT ( 'NONE',  ( -12.14591786802326823, 12.06949235617739902, 103.1260903946856757 ) ) ;
#134418 = CARTESIAN_POINT ( 'NONE',  ( 0.05219959533909260263, 19.03943276465977164, 84.99890960531436690 ) ) ;
#134419 = CARTESIAN_POINT ( 'NONE',  ( 18.62759615963255655, 10.81492255796105972, 56.66775706135235424 ) ) ;
#134420 = CARTESIAN_POINT ( 'NONE',  ( 21.55341960407610458, 5.719274019375980345, 43.95724293864769550 ) ) ;
#134421 = CARTESIAN_POINT ( 'NONE',  ( -21.55341960407610458, -5.719274019375992779, 111.4572429386476813 ) ) ;
#134422 = CARTESIAN_POINT ( 'NONE',  ( 10.72451020669898902, -18.67979575497178502, 72.91557627198103830 ) ) ;
#134423 = CARTESIAN_POINT ( 'NONE',  ( -4.379528057220328563, 16.55341960407611168, 90.20724293864770971 ) ) ;
#134424 = CARTESIAN_POINT ( 'NONE',  ( -13.97604488694547697, 13.89961937509957934, 63.12609039468566152 ) ) ;
#134425 = CARTESIAN_POINT ( 'NONE',  ( -9.474510206698964154, 16.51473224551069663, 30.41557627198102054 ) ) ;
#134426 = CARTESIAN_POINT ( 'NONE',  ( 0.05219959533909260263, 19.03943276465977164, 99.99890960531436690 ) ) ;
#134427 = CARTESIAN_POINT ( 'NONE',  ( -19.03943276465977164, 0.05219959533909376836, 91.24890960531436690 ) ) ;
#134428 = CARTESIAN_POINT ( 'NONE',  ( 12.06949235617757843, -12.14591786802309237, 108.1239096053143811 ) ) ;
#134429 = CARTESIAN_POINT ( 'NONE',  ( 14.34966873604960469, 8.224510206698951720, 24.16557627198103120 ) ) ;
#134430 = CARTESIAN_POINT ( 'NONE',  ( 4.483927247898790824, -16.52544592524335698, 40.20942372801901854 ) ) ;
#134431 = CARTESIAN_POINT ( 'NONE',  ( -15.80617190586768217, 15.72974639402176855, 113.1260903946856899 ) ) ;
#134433 = CARTESIAN_POINT ( 'NONE',  ( 16.52544592524342804, -4.483927247898539470, 28.54057627198103120 ) ) ;
#134432 = CARTESIAN_POINT ( 'NONE',  ( 0.05219959533909260263, 19.03943276465977164, 104.9989096053143669 ) ) ;
#134434 = CARTESIAN_POINT ( 'NONE',  ( -18.67979575497193778, 10.72451020669871902, 33.33442372801900433 ) ) ;
#134435 = CARTESIAN_POINT ( 'NONE',  ( 16.51473224551069308, 9.474510206698969483, 44.16557627198103120 ) ) ;
#134436 = CARTESIAN_POINT ( 'NONE',  ( -4.379528057220086978, -16.55341960407618274, 44.79275706135234714 ) ) ;
#134437 = CARTESIAN_POINT ( 'NONE',  ( 4.483927247898790824, -16.52544592524335698, 110.2094237280190185 ) ) ;
#134438 = CARTESIAN_POINT ( 'NONE',  ( 12.14591786802327356, -12.06949235617739191, 95.62609039468568994 ) ) ;
#134439 = CARTESIAN_POINT ( 'NONE',  ( -16.52544592524335698, -4.483927247898792601, 18.95942372801901143 ) ) ;
#134440 = CARTESIAN_POINT ( 'NONE',  ( 19.05341960407611168, 5.049401038298154454, 28.95724293864769550 ) ) ;
#134441 = CARTESIAN_POINT ( 'NONE',  ( -8.224510206698948167, 14.34966873604960824, 90.41557627198103830 ) ) ;
#134442 = CARTESIAN_POINT ( 'NONE',  ( 5.719274019375991003, -21.55341960407610458, 107.7072429386476955 ) ) ;
#134443 = CARTESIAN_POINT ( 'NONE',  ( -13.97604488694527625, -13.89961937509977652, 31.87390960531435979 ) ) ;
#134444 = CARTESIAN_POINT ( 'NONE',  ( -19.03943276465977164, 0.05219959533909376836, 101.2489096053143669 ) ) ;
#134445 = CARTESIAN_POINT ( 'NONE',  ( -5.823673210054431948, 21.52544592524334988, 37.70942372801900433 ) ) ;
#134446 = DIRECTION ( 'NONE',  ( -0.000000000000000000, -0.000000000000000000, 1.000000000000000000 ) ) ;
#134447 = CARTESIAN_POINT ( 'NONE',  ( -13.89961937509977652, 13.97604488694528158, 105.6239096053143527 ) ) ;
#134448 = CARTESIAN_POINT ( 'NONE',  ( 16.38665767535056261, -7.295008042176093888, 112.7640086421455123 ) ) ;
#134449 = CARTESIAN_POINT ( 'NONE',  ( -16.51473224551069308, -9.474510206698971260, 86.66557627198102409 ) ) ;
#134451 = CARTESIAN_POINT ( 'NONE',  ( 16.55341960407611168, 4.379528057220329451, 93.95724293864770971 ) ) ;
#134450 = CARTESIAN_POINT ( 'NONE',  ( -21.53943276465977519, -0.05219959533937600094, 28.75109039468567929 ) ) ;
#134452 = CARTESIAN_POINT ( 'NONE',  ( -5.153800228976328057, -19.02544592524343514, 92.29057627198099567 ) ) ;
#134453 = CARTESIAN_POINT ( 'NONE',  ( -16.51473224551082808, 9.474510206698731452, 28.33442372801900433 ) ) ;
#134454 = CARTESIAN_POINT ( 'NONE',  ( -14.29746914071037622, -8.314922557961029526, 59.16775706135234714 ) ) ;
#134455 = CARTESIAN_POINT ( 'NONE',  ( -21.55341960407619339, 5.719274019375674811, 73.54275706135234714 ) ) ;
#134456 = CARTESIAN_POINT ( 'NONE',  ( -14.34966873604972548, 8.224510206698743886, 38.33442372801900433 ) ) ;
#134457 = CARTESIAN_POINT ( 'NONE',  ( -16.51473224551069308, -9.474510206698971260, 76.66557627198103830 ) ) ;
#134458 = CARTESIAN_POINT ( 'NONE',  ( 13.97604488694548053, -13.89961937509957401, 100.6260903946856615 ) ) ;
#134459 = CARTESIAN_POINT ( 'NONE',  ( -8.314922557961024197, 14.29746914071037800, 62.91775706135236135 ) ) ;
#134460 = CARTESIAN_POINT ( 'NONE',  ( 21.53943276465977519, 0.05219959533937863772, 106.2510903946856757 ) ) ;
#134461 = CARTESIAN_POINT ( 'NONE',  ( 16.46253265017146816, 9.564922557961045513, 86.66775706135233293 ) ) ;
#134462 = CARTESIAN_POINT ( 'NONE',  ( -9.564922557960796823, -16.46253265017161027, 67.08224293864769550 ) ) ;
#134463 = CARTESIAN_POINT ( 'NONE',  ( 5.719274019375991003, -21.55341960407610458, 87.70724293864769550 ) ) ;
#134465 = CARTESIAN_POINT ( 'NONE',  ( 13.89961937509957401, 13.97604488694547697, 86.87609039468567573 ) ) ;
#134464 = CARTESIAN_POINT ( 'NONE',  ( -4.379528057220328563, 16.55341960407611168, 85.20724293864770971 ) ) ;
#134466 = CARTESIAN_POINT ( 'NONE',  ( 14.29746914071037800, 8.314922557961029526, 61.66775706135235424 ) ) ;
#134467 = CARTESIAN_POINT ( 'NONE',  ( -18.22780087662122028, 5.500000000000031086, 78.51540105326107266 ) ) ;
#134468 = CARTESIAN_POINT ( 'NONE',  ( -19.03943276465977164, -0.05219959533935918106, 53.75109039468566863 ) ) ;
#134469 = CARTESIAN_POINT ( 'NONE',  ( -16.55341960407611168, -4.379528057220339221, 21.45724293864769550 ) ) ;
#134470 = CARTESIAN_POINT ( 'NONE',  ( -0.05219959533910754901, -16.53943276465976808, 82.49890960531436690 ) ) ;
#134472 = CARTESIAN_POINT ( 'NONE',  ( 17.59860650958994555, -7.585241751806880650, 45.92337014262493966 ) ) ;
#134471 = CARTESIAN_POINT ( 'NONE',  ( 9.564922557961047289, -16.46253265017146816, 20.41775706135233293 ) ) ;
#134473 = CARTESIAN_POINT ( 'NONE',  ( -21.53943276465977519, -0.05219959533937600094, 18.75109039468568639 ) ) ;
#134474 = CARTESIAN_POINT ( 'NONE',  ( -16.51473224551069308, -9.474510206698971260, 101.6655762719810241 ) ) ;
#134475 = CARTESIAN_POINT ( 'NONE',  ( 0.05219959533909260263, 19.03943276465977164, 74.99890960531435269 ) ) ;
#134476 = CARTESIAN_POINT ( 'NONE',  ( -21.55341960407619339, 5.719274019375674811, 88.54275706135236135 ) ) ;
#134477 = CARTESIAN_POINT ( 'NONE',  ( 19.03943276465977164, -0.05219959533909143690, 58.74890960531435979 ) ) ;
#134478 = CARTESIAN_POINT ( 'NONE',  ( 15.80617190586746368, 15.72974639402197994, 29.37390960531435269 ) ) ;
#134479 = CARTESIAN_POINT ( 'NONE',  ( -12.06949235617756955, 12.14591786802309770, 80.62390960531438111 ) ) ;
#134480 = CARTESIAN_POINT ( 'NONE',  ( 19.05341960407611168, 5.049401038298154454, 38.95724293864767418 ) ) ;
#134481 = CARTESIAN_POINT ( 'NONE',  ( -4.379528057220328563, 16.55341960407611168, 95.20724293864769550 ) ) ;
#134482 = CARTESIAN_POINT ( 'NONE',  ( 10.81492255796078972, 18.62759615963270932, 104.5822429386477097 ) ) ;
#134483 = CARTESIAN_POINT ( 'NONE',  ( 0.05219959533937995610, -21.53943276465977519, 65.00109039468568994 ) ) ;
#134484 = CARTESIAN_POINT ( 'NONE',  ( -19.05341960407611168, -5.049401038298163336, 26.45724293864769550 ) ) ;
#134485 = CARTESIAN_POINT ( 'NONE',  ( 8.224510206698742110, 14.34966873604972548, 62.08442372801901143 ) ) ;
#134486 = CARTESIAN_POINT ( 'NONE',  ( -21.53943276465977519, 0.05219959533907696930, 101.2489096053143669 ) ) ;
#134487 = CARTESIAN_POINT ( 'NONE',  ( -18.67979575497178146, -10.72451020669898902, 111.6655762719810525 ) ) ;
#134489 = CARTESIAN_POINT ( 'NONE',  ( -0.05219959533909027116, -19.03943276465977164, 47.49890960531435979 ) ) ;
#134488 = CARTESIAN_POINT ( 'NONE',  ( 9.564922557961047289, -16.46253265017146816, 40.41775706135234003 ) ) ;
#134490 = CARTESIAN_POINT ( 'NONE',  ( -3.573655867282028392E-15, 2.428612866367529932E-14, -23.00000000000000000 ) ) ;
#134491 = CARTESIAN_POINT ( 'NONE',  ( -21.52544592524334988, -5.823673210054445271, 53.95942372801900433 ) ) ;
#134492 = CARTESIAN_POINT ( 'NONE',  ( -5.719274019375978568, 21.55341960407610458, 60.20724293864768839 ) ) ;
#134493 = CARTESIAN_POINT ( 'NONE',  ( 14.29746914071049879, -8.314922557960816363, 38.33224293864768839 ) ) ;
#134495 = CARTESIAN_POINT ( 'NONE',  ( 21.52544592524334988, 5.823673210054432836, 111.4594237280190328 ) ) ;
#134494 = CARTESIAN_POINT ( 'NONE',  ( 10.72451020669871369, 18.67979575497193778, 72.08442372801899012 ) ) ;
#134496 = CARTESIAN_POINT ( 'NONE',  ( 16.52544592524342804, -4.483927247898539470, 63.54057627198103830 ) ) ;
#134498 = B_SPLINE_CURVE_WITH_KNOTS ( 'NONE', 3,
 ( #158059, #124740, #189408, #95383, #97352, #17565 ),
 .UNSPECIFIED., .F., .F.,
 ( 4, 2, 4 ),
 ( 3.469446951953614189E-18, 0.0003837532665635036075, 0.0007675065331270037455 ),
 .UNSPECIFIED. ) ;
#134497 = CARTESIAN_POINT ( 'NONE',  ( 8.314922557960818139, 14.29746914071049879, 104.5822429386477097 ) ) ;
#134499 = CARTESIAN_POINT ( 'NONE',  ( 19.05341960407617918, -5.049401038297876454, 41.04275706135233293 ) ) ;
#134500 = CARTESIAN_POINT ( 'NONE',  ( 14.29746914071037800, 8.314922557961029526, 96.66775706135234714 ) ) ;
#134501 = CARTESIAN_POINT ( 'NONE',  ( 10.72451020669871369, 18.67979575497193778, 67.08442372801901854 ) ) ;
#134502 = CARTESIAN_POINT ( 'NONE',  ( 9.564922557960805705, 16.46253265017160317, 54.58224293864769550 ) ) ;
#134503 = CARTESIAN_POINT ( 'NONE',  ( 19.05341960407617918, -5.049401038297876454, 41.04275706135233293 ) ) ;
#134504 = CARTESIAN_POINT ( 'NONE',  ( 15.72974639402199770, -15.80617190586745480, 43.12390960531435269 ) ) ;
#134505 = CARTESIAN_POINT ( 'NONE',  ( 21.53943276465977519, 0.05219959533937863772, 31.25109039468568639 ) ) ;
#134506 = CARTESIAN_POINT ( 'NONE',  ( -15.80617190586745835, -15.72974639402198527, 81.87390960531435269 ) ) ;
#134507 = CARTESIAN_POINT ( 'NONE',  ( 9.564922557961047289, -16.46253265017146816, 85.41775706135233293 ) ) ;
#134508 = CARTESIAN_POINT ( 'NONE',  ( 16.55341960407618274, -4.379528057220086978, 51.04275706135234714 ) ) ;
#134510 = CARTESIAN_POINT ( 'NONE',  ( -21.52544592524343514, 5.823673210054127303, 91.04057627198103830 ) ) ;
#134509 = CARTESIAN_POINT ( 'NONE',  ( 38.00000000000002842, 12.34694845685041109, -6.899999999999999467 ) ) ;
#134512 = CARTESIAN_POINT ( 'NONE',  ( 12.14591786802309770, 12.06949235617756955, 74.37390960531436690 ) ) ;
#134511 = CARTESIAN_POINT ( 'NONE',  ( -12.14591786802326823, 12.06949235617739902, 83.12609039468568994 ) ) ;
#134513 = CARTESIAN_POINT ( 'NONE',  ( -17.48853670773243607, -5.747243402303094051, 101.3332870025000574 ) ) ;
#134514 = CARTESIAN_POINT ( 'NONE',  ( -0.05219959533934338120, 16.53943276465976808, 22.50109039468567573 ) ) ;
#134515 = CARTESIAN_POINT ( 'NONE',  ( 18.62759615963271287, -10.81492255796078972, 33.33224293864769550 ) ) ;
#134516 = CARTESIAN_POINT ( 'NONE',  ( 8.224510206698742110, 14.34966873604972548, 82.08442372801901854 ) ) ;
#134517 = FACE_OUTER_BOUND ( 'NONE', #129580, .T. ) ;
#134518 = CARTESIAN_POINT ( 'NONE',  ( 4.379528057220092307, 16.55341960407617563, 52.29275706135236135 ) ) ;
#134519 = CARTESIAN_POINT ( 'NONE',  ( -18.67979575497193778, 10.72451020669871902, 33.33442372801900433 ) ) ;
#134520 = CARTESIAN_POINT ( 'NONE',  ( 5.719274019375991003, -21.55341960407610458, 42.70724293864770260 ) ) ;
#134521 = CARTESIAN_POINT ( 'NONE',  ( -8.224510206698735004, -14.34966873604973081, 69.58442372801900433 ) ) ;
#134522 = CARTESIAN_POINT ( 'NONE',  ( 16.51473224551069308, 9.474510206698969483, 89.16557627198103830 ) ) ;
#134524 = CARTESIAN_POINT ( 'NONE',  ( 9.564922557960805705, 16.46253265017160317, 29.58224293864769550 ) ) ;
#134523 = CARTESIAN_POINT ( 'NONE',  ( -10.72451020669870658, -18.67979575497194134, 54.58442372801901143 ) ) ;
#134525 = CARTESIAN_POINT ( 'NONE',  ( -5.719274019375978568, 21.55341960407610458, 35.20724293864768839 ) ) ;
#134526 = CARTESIAN_POINT ( 'NONE',  ( -19.03943276465977164, 0.05219959533909376836, 116.2489096053143669 ) ) ;
#134527 = EDGE_LOOP ( 'NONE', ( #98698, #166739, #152372, #9796 ) ) ;
#134528 = CARTESIAN_POINT ( 'NONE',  ( -19.03943276465977164, -0.05219959533935918106, 38.75109039468566152 ) ) ;
#134529 = CARTESIAN_POINT ( 'NONE',  ( 8.314922557961029526, -14.29746914071037800, 55.41775706135234714 ) ) ;
#134530 = CARTESIAN_POINT ( 'NONE',  ( 9.474510206698971260, -16.51473224551069308, 107.9155762719810383 ) ) ;
#134531 = ORIENTED_EDGE ( 'NONE', *, *, #186207, .T. ) ;
#134532 = CARTESIAN_POINT ( 'NONE',  ( -9.564922557960796823, -16.46253265017161027, 82.08224293864768129 ) ) ;
#134533 = CARTESIAN_POINT ( 'NONE',  ( -0.05219959533934338120, 16.53943276465976808, 102.5010903946856899 ) ) ;
#134534 = CARTESIAN_POINT ( 'NONE',  ( -14.29746914071049879, 8.314922557960819915, 95.83224293864770971 ) ) ;
#134535 = CARTESIAN_POINT ( 'NONE',  ( 5.719274019375991003, -21.55341960407610458, 32.70724293864770260 ) ) ;
#134536 = CARTESIAN_POINT ( 'NONE',  ( 13.89961937509977652, -13.97604488694527269, 33.12390960531434558 ) ) ;
#134537 = CARTESIAN_POINT ( 'NONE',  ( -8.224510206698735004, -14.34966873604973081, 79.58442372801903275 ) ) ;
#134538 = CARTESIAN_POINT ( 'NONE',  ( 21.52544592524334988, 5.823673210054432836, 21.45942372801901499 ) ) ;
#134539 = CARTESIAN_POINT ( 'NONE',  ( 9.564922557961047289, -16.46253265017146816, 80.41775706135234714 ) ) ;
#134540 = CARTESIAN_POINT ( 'NONE',  ( 13.97604488694527802, 13.89961937509977652, 34.37390960531436690 ) ) ;
#134541 = CONICAL_SURFACE ( 'NONE', #173181, 28.85599147140294107, 0.1745329251994333364 ) ;
#134542 = CARTESIAN_POINT ( 'NONE',  ( 5.823673210054444382, -21.52544592524334988, 105.2094237280190328 ) ) ;
#134543 = CARTESIAN_POINT ( 'NONE',  ( -13.97604488694527625, -13.89961937509977652, 61.87390960531435979 ) ) ;
#134544 = CARTESIAN_POINT ( 'NONE',  ( 16.52544592524335698, 4.483927247898782831, 51.45942372801901854 ) ) ;
#134545 = CARTESIAN_POINT ( 'NONE',  ( 21.53943276465977519, 0.05219959533937863772, 86.25109039468568994 ) ) ;
#134546 = CARTESIAN_POINT ( 'NONE',  ( 9.474510206698729675, 16.51473224551082808, 47.08442372801900433 ) ) ;
#134547 = CARTESIAN_POINT ( 'NONE',  ( -19.05341960407617563, 5.049401038297882671, 58.54275706135234003 ) ) ;
#134548 = ORIENTED_EDGE ( 'NONE', *, *, #139988, .F. ) ;
#134549 = CARTESIAN_POINT ( 'NONE',  ( 15.80617190586769283, -15.72974639402175789, 55.62609039468568284 ) ) ;
#134550 = DIRECTION ( 'NONE',  ( -1.000000000000000000, -5.267352820763006950E-15, 0.000000000000000000 ) ) ;
#134552 = B_SPLINE_CURVE_WITH_KNOTS ( 'NONE', 3,
 ( #172578, #54955, #126069, #174570, #132794, #20871 ),
 .UNSPECIFIED., .F., .F.,
 ( 4, 2, 4 ),
 ( 0.000000000000000000, 0.0003837532665635039327, 0.0007675065331270078655 ),
 .UNSPECIFIED. ) ;
#134551 = CARTESIAN_POINT ( 'NONE',  ( 5.153800228976615827, -19.02544592524334988, 40.20942372801898301 ) ) ;
#134553 = CARTESIAN_POINT ( 'NONE',  ( -13.89961937509977652, 13.97604488694528158, 95.62390960531436690 ) ) ;
#134554 = CARTESIAN_POINT ( 'NONE',  ( -0.05219959533909027116, -19.03943276465977164, 77.49890960531435269 ) ) ;
#134555 = CARTESIAN_POINT ( 'NONE',  ( -12.14591786802309592, -12.06949235617757132, 31.87390960531435979 ) ) ;
#134556 = CARTESIAN_POINT ( 'NONE',  ( 21.53943276465977519, -0.05219959533907433946, 28.74890960531435624 ) ) ;
#134557 = CARTESIAN_POINT ( 'NONE',  ( 29.86685920354754842, -21.69954338932559068, -2.324999997268813345 ) ) ;
#134558 = CARTESIAN_POINT ( 'NONE',  ( 20.56805782000754590, 22.68575836265089762, -50.73663675503807013 ) ) ;
#134559 = CARTESIAN_POINT ( 'NONE',  ( -0.05219959533937732626, 21.53943276465977519, 112.5010903946857042 ) ) ;
#134560 = DIRECTION ( 'NONE',  ( -1.000000000000000000, -0.000000000000000000, -0.000000000000000000 ) ) ;
#134561 = CARTESIAN_POINT ( 'NONE',  ( -19.02544592524342804, 5.153800228976336051, 41.04057627198103120 ) ) ;
#134562 = CARTESIAN_POINT ( 'NONE',  ( 19.02544592524343514, -5.153800228976328945, 28.54057627198102409 ) ) ;
#134563 = CARTESIAN_POINT ( 'NONE',  ( -10.00792592295668548, -12.06067447007310101, -59.61799893849534016 ) ) ;
#134564 = CARTESIAN_POINT ( 'NONE',  ( -5.271334918318021145, -36.86995875308960535, -7.999999999999994671 ) ) ;
#134565 = CARTESIAN_POINT ( 'NONE',  ( 12.06949235617739724, 12.14591786802326823, 61.87609039468568284 ) ) ;
#134567 = EDGE_CURVE ( 'NONE', #141307, #46822, #120371, .T. ) ;
#134566 = CARTESIAN_POINT ( 'NONE',  ( 18.62759615963271287, -10.81492255796078972, 83.33224293864769550 ) ) ;
#134568 = CARTESIAN_POINT ( 'NONE',  ( -4.483927247898539470, -16.52544592524342804, 57.29057627198103120 ) ) ;
#134570 = CARTESIAN_POINT ( 'NONE',  ( -19.03943276465977164, 0.05219959533909376836, 111.2489096053143669 ) ) ;
#134569 = CARTESIAN_POINT ( 'NONE',  ( 19.02544592524343514, -5.153800228976328945, 28.54057627198102409 ) ) ;
#134571 = CARTESIAN_POINT ( 'NONE',  ( -15.72974639402176322, -15.80617190586768395, 29.37609039468568284 ) ) ;
#134572 = CARTESIAN_POINT ( 'NONE',  ( 13.97604488694548053, -13.89961937509957401, 40.62609039468564731 ) ) ;
#134573 = CARTESIAN_POINT ( 'NONE',  ( 9.474510206698971260, -16.51473224551069308, 37.91557627198102409 ) ) ;
#134574 = CARTESIAN_POINT ( 'NONE',  ( -10.81492255796105439, 18.62759615963255655, 87.91775706135234714 ) ) ;
#134575 = CARTESIAN_POINT ( 'NONE',  ( 16.61371651742598132, -7.165104196376269385, 31.35415069992996706 ) ) ;
#134576 = CARTESIAN_POINT ( 'NONE',  ( -4.483927247898539470, -16.52544592524342804, 22.29057627198102765 ) ) ;
#134577 = CARTESIAN_POINT ( 'NONE',  ( -36.91746825000000598, 11.99521256947798520, -3.224999997268813257 ) ) ;
#134578 = CARTESIAN_POINT ( 'NONE',  ( -18.67979575497178146, -10.72451020669898902, 26.66557627198103475 ) ) ;
#134579 = CARTESIAN_POINT ( 'NONE',  ( 12.14591786802309770, 12.06949235617756955, 104.3739096053143669 ) ) ;
#134580 = CARTESIAN_POINT ( 'NONE',  ( 8.343164238912780917, -45.63112023308525522, -22.26988597240829293 ) ) ;
#134581 = AXIS2_PLACEMENT_3D ( 'NONE', #125841, #170361, #30865 ) ;
#134582 = CARTESIAN_POINT ( 'NONE',  ( 19.02544592524343514, -5.153800228976328945, 93.54057627198102409 ) ) ;
#134583 = CARTESIAN_POINT ( 'NONE',  ( -16.53943276465976808, 0.05219959533911058130, 81.24890960531436690 ) ) ;
#134584 = CARTESIAN_POINT ( 'NONE',  ( 19.05341960407617918, -5.049401038297876454, 101.0427570613523045 ) ) ;
#134585 = CARTESIAN_POINT ( 'NONE',  ( 18.62759615963271287, -10.81492255796078972, 68.33224293864769550 ) ) ;
#134586 = EDGE_LOOP ( 'NONE', ( #170526, #66616, #157534, #121661 ) ) ;
#134587 = CARTESIAN_POINT ( 'NONE',  ( -5.153800228976328057, -19.02544592524343514, 27.29057627198103120 ) ) ;
#134589 = CARTESIAN_POINT ( 'NONE',  ( 15.72974639402199770, -15.80617190586745480, 93.12390960531436690 ) ) ;
#134588 = CARTESIAN_POINT ( 'NONE',  ( -16.46253265017160317, 9.564922557960807481, 90.83224293864769550 ) ) ;
#134591 = CARTESIAN_POINT ( 'NONE',  ( -0.05219959533909027116, -19.03943276465977164, 87.49890960531436690 ) ) ;
#134590 = CARTESIAN_POINT ( 'NONE',  ( 12.06949235617739724, 12.14591786802326823, 111.8760903946856615 ) ) ;
#134592 = CARTESIAN_POINT ( 'NONE',  ( 5.153800228976615827, -19.02544592524334988, 80.20942372801901854 ) ) ;
#134593 = CARTESIAN_POINT ( 'NONE',  ( 18.67979575497194134, -10.72451020669871369, 90.83442372801901854 ) ) ;
#134594 = CARTESIAN_POINT ( 'NONE',  ( -5.823673210054116645, -21.52544592524344225, 82.29057627198103830 ) ) ;
#134595 = CARTESIAN_POINT ( 'NONE',  ( 10.81492255796078972, 18.62759615963270932, 34.58224293864770260 ) ) ;
#134596 = CARTESIAN_POINT ( 'NONE',  ( 0.05219959533909260263, 19.03943276465977164, 49.99890960531435979 ) ) ;
#134597 = CARTESIAN_POINT ( 'NONE',  ( -16.52544592524342804, 4.483927247898546575, 26.04057627198103475 ) ) ;
#134598 = CARTESIAN_POINT ( 'NONE',  ( -19.02544592524342804, 5.153800228976336051, 61.04057627198103120 ) ) ;
#134599 = CARTESIAN_POINT ( 'NONE',  ( -69.65682714487590488, -71.74905178543390605, -15.00000000000000178 ) ) ;
#134600 = CARTESIAN_POINT ( 'NONE',  ( 5.153800228976615827, -19.02544592524334988, 25.20942372801900433 ) ) ;
#134601 = CARTESIAN_POINT ( 'NONE',  ( -4.483927247898539470, -16.52544592524342804, 67.29057627198103830 ) ) ;
#134602 = CARTESIAN_POINT ( 'NONE',  ( 21.52544592524344225, -5.823673210054117533, 113.5405762719810383 ) ) ;
#134603 = CARTESIAN_POINT ( 'NONE',  ( -6.875025434611812258, 5.563988007711742512, -64.01045944195826110 ) ) ;
#134604 = CARTESIAN_POINT ( 'NONE',  ( -5.719274019375978568, 21.55341960407610458, 55.20724293864770260 ) ) ;
#134605 = CARTESIAN_POINT ( 'NONE',  ( -12.14591786802326823, 12.06949235617739902, 93.12609039468568994 ) ) ;
#134606 = CARTESIAN_POINT ( 'NONE',  ( -12.14591786802309592, -12.06949235617757132, 106.8739096053143811 ) ) ;
#134607 = CARTESIAN_POINT ( 'NONE',  ( -16.46253265017160317, 9.564922557960807481, 65.83224293864769550 ) ) ;
#134608 =( NAMED_UNIT ( * ) PLANE_ANGLE_UNIT ( ) SI_UNIT ( $, .RADIAN. ) );
#134609 = CARTESIAN_POINT ( 'NONE',  ( -4.379528057220328563, 16.55341960407611168, 35.20724293864768839 ) ) ;
#134610 = ORIENTED_EDGE ( 'NONE', *, *, #43224, .F. ) ;
#134611 = CARTESIAN_POINT ( 'NONE',  ( 21.52544592524334988, 5.823673210054432836, 46.45942372801901854 ) ) ;
#134612 = CARTESIAN_POINT ( 'NONE',  ( 5.153800228976335163, 19.02544592524342804, 109.7905762719810099 ) ) ;
#134613 = CARTESIAN_POINT ( 'NONE',  ( -5.719274019375665041, -21.55341960407619695, 79.79275706135236135 ) ) ;
#134614 = CARTESIAN_POINT ( 'NONE',  ( -0.05219959533909027116, -19.03943276465977164, 27.49890960531435624 ) ) ;
#134615 = CARTESIAN_POINT ( 'NONE',  ( 19.03943276465977164, -0.05219959533909143690, 38.74890960531436690 ) ) ;
#134616 = ORIENTED_EDGE ( 'NONE', *, *, #145209, .T. ) ;
#134617 = CARTESIAN_POINT ( 'NONE',  ( 10.81492255796106328, -18.62759615963255655, 90.41775706135236135 ) ) ;
#134618 = CARTESIAN_POINT ( 'NONE',  ( -12.06949235617739369, -12.14591786802326823, 44.37609039468567573 ) ) ;
#134619 = CARTESIAN_POINT ( 'NONE',  ( 18.67979575497194134, -10.72451020669871369, 70.83442372801901854 ) ) ;
#134620 = CARTESIAN_POINT ( 'NONE',  ( -13.97604488694527625, -13.89961937509977652, 96.87390960531433848 ) ) ;
#134621 = CARTESIAN_POINT ( 'NONE',  ( 13.89961937509957401, 13.97604488694547697, 86.87609039468567573 ) ) ;
#134622 = CARTESIAN_POINT ( 'NONE',  ( 18.67979575497194134, -10.72451020669871369, 50.83442372801901143 ) ) ;
#134623 = CARTESIAN_POINT ( 'NONE',  ( -14.34966873604972548, 8.224510206698743886, 23.33442372801901499 ) ) ;
#134624 = CARTESIAN_POINT ( 'NONE',  ( 9.564922557961047289, -16.46253265017146816, 85.41775706135233293 ) ) ;
#134625 = CARTESIAN_POINT ( 'NONE',  ( 9.474510206698971260, -16.51473224551069308, 52.91557627198102409 ) ) ;
#134626 = CARTESIAN_POINT ( 'NONE',  ( -16.51473224551082808, 9.474510206698731452, 83.33442372801899012 ) ) ;
#134627 = CARTESIAN_POINT ( 'NONE',  ( -16.53943276465976808, 0.05219959533911058130, 21.24890960531436690 ) ) ;
#134628 = CARTESIAN_POINT ( 'NONE',  ( 0.05219959533936267826, -19.03943276465977164, 90.00109039468567573 ) ) ;
#134629 = CARTESIAN_POINT ( 'NONE',  ( -16.53943276465976808, 0.05219959533911058130, 36.24890960531435979 ) ) ;
#134630 = CARTESIAN_POINT ( 'NONE',  ( 13.97604488694548053, -13.89961937509957401, 65.62609039468567573 ) ) ;
#134631 = CARTESIAN_POINT ( 'NONE',  ( 12.14591786802327356, -12.06949235617739191, 45.62609039468567573 ) ) ;
#134632 = CARTESIAN_POINT ( 'NONE',  ( 13.97604488694548053, -13.89961937509957401, 25.62609039468566507 ) ) ;
#134633 = CARTESIAN_POINT ( 'NONE',  ( 8.314922557960818139, 14.29746914071049879, 114.5822429386477097 ) ) ;
#134634 = CARTESIAN_POINT ( 'NONE',  ( 5.153800228976335163, 19.02544592524342804, 39.79057627198100988 ) ) ;
#134635 = CARTESIAN_POINT ( 'NONE',  ( 8.224510206698742110, 14.34966873604972548, 52.08442372801901854 ) ) ;
#134636 = DIRECTION ( 'NONE',  ( 0.000000000000000000, 0.000000000000000000, -1.000000000000000000 ) ) ;
#134637 = CARTESIAN_POINT ( 'NONE',  ( 1.993301997531345292E-15, -30.30510711980685912, 140.7500000054623683 ) ) ;
#134638 = CARTESIAN_POINT ( 'NONE',  ( -19.03943276465977164, 0.05219959533909376836, 86.24890960531436690 ) ) ;
#134639 = CYLINDRICAL_SURFACE ( 'NONE', #584, 1.500000000000001332 ) ;
#134640 = ORIENTED_EDGE ( 'NONE', *, *, #59992, .F. ) ;
#134641 = CARTESIAN_POINT ( 'NONE',  ( -13.97604488694547697, 13.89961937509957934, 93.12609039468566152 ) ) ;
#134642 = CARTESIAN_POINT ( 'NONE',  ( -15.72974639402197994, 15.80617190586746368, 25.62390960531435624 ) ) ;
#134644 = CARTESIAN_POINT ( 'NONE',  ( -9.474510206698720793, -16.51473224551083518, 104.5844237280190043 ) ) ;
#134643 = CARTESIAN_POINT ( 'NONE',  ( 19.05341960407617918, -5.049401038297876454, 36.04275706135234003 ) ) ;
#134645 = CARTESIAN_POINT ( 'NONE',  ( -12.14591786802309592, -12.06949235617757132, 106.8739096053143811 ) ) ;
#134646 = CARTESIAN_POINT ( 'NONE',  ( 19.02544592524343514, -5.153800228976328945, 33.54057627198102409 ) ) ;
#134647 = CARTESIAN_POINT ( 'NONE',  ( -15.80617190586745835, -15.72974639402198527, 76.87390960531439532 ) ) ;
#134648 = CARTESIAN_POINT ( 'NONE',  ( -19.03943276465977164, 0.05219959533909376836, 36.24890960531436690 ) ) ;
#134649 = DIRECTION ( 'NONE',  ( 1.000000000000000000, -0.000000000000000000, -0.000000000000000000 ) ) ;
#134650 = CARTESIAN_POINT ( 'NONE',  ( 9.564922557961047289, -16.46253265017146816, 70.41775706135233293 ) ) ;
#134651 = CARTESIAN_POINT ( 'NONE',  ( 8.224510206698953496, -14.34966873604960469, 57.91557627198103120 ) ) ;
#134652 = CARTESIAN_POINT ( 'NONE',  ( 18.62759615963271287, -10.81492255796078972, 38.33224293864768839 ) ) ;
#134653 = CARTESIAN_POINT ( 'NONE',  ( -15.72974639402176322, -15.80617190586768395, 89.37609039468568994 ) ) ;
#134654 = CARTESIAN_POINT ( 'NONE',  ( 21.53943276465977519, -0.05219959533907433946, 78.74890960531436690 ) ) ;
#134655 = CARTESIAN_POINT ( 'NONE',  ( -18.67979575497193778, 10.72451020669871902, 73.33442372801901854 ) ) ;
#134656 = CARTESIAN_POINT ( 'NONE',  ( 18.67979575497194134, -10.72451020669871369, 60.83442372801901854 ) ) ;
#134657 = CARTESIAN_POINT ( 'NONE',  ( 13.97604488694527802, 13.89961937509977652, 94.37390960531436690 ) ) ;
#134659 = CARTESIAN_POINT ( 'NONE',  ( -18.62759615963255300, -10.81492255796106328, 59.16775706135234714 ) ) ;
#134658 = CARTESIAN_POINT ( 'NONE',  ( -12.06949235617739369, -12.14591786802326823, 99.37609039468568994 ) ) ;
#134660 = CARTESIAN_POINT ( 'NONE',  ( -13.89961937509977652, 13.97604488694528158, 55.62390960531434558 ) ) ;
#134661 = CARTESIAN_POINT ( 'NONE',  ( -21.52544592524334988, -5.823673210054445271, 33.95942372801901143 ) ) ;
#134662 = CARTESIAN_POINT ( 'NONE',  ( 13.97604488694527802, 13.89961937509977652, 69.37390960531436690 ) ) ;
#134663 = CARTESIAN_POINT ( 'NONE',  ( 0.05219959533910956823, 16.53943276465976808, 69.99890960531435269 ) ) ;
#134664 = CARTESIAN_POINT ( 'NONE',  ( -4.379528057220328563, 16.55341960407611168, 40.20724293864769550 ) ) ;
#134665 = CARTESIAN_POINT ( 'NONE',  ( 5.823673210054125526, 21.52544592524343514, 49.79057627198102409 ) ) ;
#134666 = CARTESIAN_POINT ( 'NONE',  ( -5.049401038298153566, 19.05341960407611168, 45.20724293864769550 ) ) ;
#134667 = CARTESIAN_POINT ( 'NONE',  ( 21.55341960407610458, 5.719274019375980345, 63.95724293864770260 ) ) ;
#134668 = CARTESIAN_POINT ( 'NONE',  ( 0.05219959533936267826, -19.03943276465977164, 55.00109039468566863 ) ) ;
#134671 = CARTESIAN_POINT ( 'NONE',  ( 8.224510206698953496, -14.34966873604960469, 67.91557627198102409 ) ) ;
#134670 = FACE_OUTER_BOUND ( 'NONE', #181969, .T. ) ;
#134669 = AXIS2_PLACEMENT_3D ( 'NONE', #104609, #10620, #117788 ) ;
#134672 = CARTESIAN_POINT ( 'NONE',  ( -15.80617190586745835, -15.72974639402198527, 36.87390960531435979 ) ) ;
#134673 = EDGE_LOOP ( 'NONE', ( #148696, #138619, #128220, #189824 ) ) ;
#134674 = LINE ( 'NONE', #57828, #26944 ) ;
#134675 = CARTESIAN_POINT ( 'NONE',  ( 0.05219959533934541429, -16.53943276465976808, 90.00109039468567573 ) ) ;
#134676 = CARTESIAN_POINT ( 'NONE',  ( 19.05341960407617918, -5.049401038297876454, 86.04275706135233293 ) ) ;
#134677 = CARTESIAN_POINT ( 'NONE',  ( 8.224510206698953496, -14.34966873604960469, 57.91557627198103120 ) ) ;
#134678 = CARTESIAN_POINT ( 'NONE',  ( 17.50000000000002132, -5.624438216177543026, 53.31670344914648041 ) ) ;
#134679 = CARTESIAN_POINT ( 'NONE',  ( -19.03943276465977164, 0.05219959533909376836, 51.24890960531436690 ) ) ;
#134680 = CARTESIAN_POINT ( 'NONE',  ( -14.29746914071049879, 8.314922557960819915, 35.83224293864768839 ) ) ;
#134681 = CARTESIAN_POINT ( 'NONE',  ( -13.89961937509977652, 13.97604488694528158, 50.62390960531435979 ) ) ;
#134682 = CARTESIAN_POINT ( 'NONE',  ( -9.474510206698964154, 16.51473224551069663, 70.41557627198102409 ) ) ;
#134683 = CARTESIAN_POINT ( 'NONE',  ( 19.03943276465977164, -0.05219959533909143690, 38.74890960531436690 ) ) ;
#134684 = CARTESIAN_POINT ( 'NONE',  ( 0.05219959533937995610, -21.53943276465977519, 50.00109039468568994 ) ) ;
#134685 = CARTESIAN_POINT ( 'NONE',  ( 5.049401038298161559, -19.05341960407611168, 67.70724293864769550 ) ) ;
#134686 = CARTESIAN_POINT ( 'NONE',  ( 5.153800228976335163, 19.02544592524342804, 24.79057627198102765 ) ) ;
#134687 = AXIS2_PLACEMENT_3D ( 'NONE', #24861, #39014, #161356 ) ;
#134688 = CARTESIAN_POINT ( 'NONE',  ( -19.02544592524342804, 5.153800228976336051, 56.04057627198100988 ) ) ;
#134689 = CARTESIAN_POINT ( 'NONE',  ( -15.72974639402197994, 15.80617190586746368, 45.62390960531436690 ) ) ;
#134690 = CARTESIAN_POINT ( 'NONE',  ( -19.02544592524342804, 5.153800228976336051, 41.04057627198103120 ) ) ;
#134691 = CARTESIAN_POINT ( 'NONE',  ( -15.72974639402197994, 15.80617190586746368, 45.62390960531436690 ) ) ;
#134692 = ADVANCED_FACE ( 'NONE', ( #75853 ), #137529, .T. ) ;
#134693 = CARTESIAN_POINT ( 'NONE',  ( -8.224510206698735004, -14.34966873604973081, 99.58442372801900433 ) ) ;
#134694 = EDGE_CURVE ( 'NONE', #42057, #120796, #102228, .T. ) ;
#134695 = CARTESIAN_POINT ( 'NONE',  ( 19.03943276465977164, 0.05219959533936151252, 21.25109039468565797 ) ) ;
#134697 = CARTESIAN_POINT ( 'NONE',  ( -14.29746914071037622, -8.314922557961029526, 79.16775706135234714 ) ) ;
#134696 = CARTESIAN_POINT ( 'NONE',  ( -16.55341960407617563, 4.379528057220093196, 43.54275706135235424 ) ) ;
#134698 = DIRECTION ( 'NONE',  ( 0.000000000000000000, 0.8660254037844387076, -0.4999999999999999445 ) ) ;
#134699 = CARTESIAN_POINT ( 'NONE',  ( -0.05219959533934338120, 16.53943276465976808, 67.50109039468568994 ) ) ;
#134700 = CARTESIAN_POINT ( 'NONE',  ( 16.53943276465976808, 0.05219959533934440121, 51.25109039468568994 ) ) ;
#134701 = CARTESIAN_POINT ( 'NONE',  ( 0.05219959533909260263, 19.03943276465977164, 104.9989096053143669 ) ) ;
#134702 = CARTESIAN_POINT ( 'NONE',  ( 14.29746914071037800, 8.314922557961029526, 41.66775706135235424 ) ) ;
#134703 = CARTESIAN_POINT ( 'NONE',  ( -5.049401038298153566, 19.05341960407611168, 35.20724293864768839 ) ) ;
#134704 = CARTESIAN_POINT ( 'NONE',  ( 21.52544592524334988, 5.823673210054432836, 31.45942372801901854 ) ) ;
#134705 = CARTESIAN_POINT ( 'NONE',  ( -8.224510206698735004, -14.34966873604973081, 34.58442372801900433 ) ) ;
#134706 = CARTESIAN_POINT ( 'NONE',  ( 14.29746914071037800, 8.314922557961029526, 101.6677570613523613 ) ) ;
#134707 = CARTESIAN_POINT ( 'NONE',  ( -17.97214573761834799, -5.500000000000021316, 71.46970049038654338 ) ) ;
#134708 = CARTESIAN_POINT ( 'NONE',  ( 21.52544592524334988, 5.823673210054432836, 106.4594237280190328 ) ) ;
#134709 = CARTESIAN_POINT ( 'NONE',  ( 9.564922557961047289, -16.46253265017146816, 100.4177570613523329 ) ) ;
#134710 = CARTESIAN_POINT ( 'NONE',  ( 8.224510206698953496, -14.34966873604960469, 62.91557627198102409 ) ) ;
#134711 = CARTESIAN_POINT ( 'NONE',  ( 9.474510206698971260, -16.51473224551069308, 22.91557627198102765 ) ) ;
#134713 = CARTESIAN_POINT ( 'NONE',  ( 17.50000000000001066, 5.622605283950888655, 78.81207310596111881 ) ) ;
#134712 = CARTESIAN_POINT ( 'NONE',  ( 19.03943276465977164, 0.05219959533936151252, 56.25109039468566863 ) ) ;
#134714 = CARTESIAN_POINT ( 'NONE',  ( 18.67979575497194134, -10.72451020669871369, 60.83442372801901854 ) ) ;
#134715 = CARTESIAN_POINT ( 'NONE',  ( -14.29746914071037622, -8.314922557961029526, 29.16775706135234003 ) ) ;
#134716 = CARTESIAN_POINT ( 'NONE',  ( 17.50000000000000000, 5.500000000000013323, 63.78230962303565832 ) ) ;
#134717 = CARTESIAN_POINT ( 'NONE',  ( 5.719274019375991003, -21.55341960407610458, 27.70724293864769905 ) ) ;
#134718 = CARTESIAN_POINT ( 'NONE',  ( 13.97604488694548053, -13.89961937509957401, 105.6260903946856757 ) ) ;
#134719 = CARTESIAN_POINT ( 'NONE',  ( 17.81289503416610742, 24.51734667627700404, 147.2999999999999545 ) ) ;
#134720 = CARTESIAN_POINT ( 'NONE',  ( 10.65970682939788716, -25.60940286011448919, 139.9999999999999716 ) ) ;
#134721 = CARTESIAN_POINT ( 'NONE',  ( -5.049401038298153566, 19.05341960407611168, 25.20724293864768484 ) ) ;
#134722 = CARTESIAN_POINT ( 'NONE',  ( 10.72451020669871369, 18.67979575497193778, 102.0844237280190185 ) ) ;
#134723 = CARTESIAN_POINT ( 'NONE',  ( -13.97604488694527625, -13.89961937509977652, 41.87390960531435979 ) ) ;
#134725 = CARTESIAN_POINT ( 'NONE',  ( 15.80617190586769283, -15.72974639402175789, 50.62609039468568994 ) ) ;
#134724 = CIRCLE ( 'NONE', #166906, 2.000000000000001776 ) ;
#134726 = CARTESIAN_POINT ( 'NONE',  ( 5.719274019375673035, 21.55341960407619339, 97.29275706135234714 ) ) ;
#134727 = CARTESIAN_POINT ( 'NONE',  ( -14.29746914071037622, -8.314922557961029526, 99.16775706135234714 ) ) ;
#134728 = CARTESIAN_POINT ( 'NONE',  ( 19.05341960407611168, 5.049401038298154454, 83.95724293864766707 ) ) ;
#134729 = CARTESIAN_POINT ( 'NONE',  ( -15.80617190586768217, 15.72974639402176855, 48.12609039468568284 ) ) ;
#134730 = CARTESIAN_POINT ( 'NONE',  ( -18.62759615963255300, -10.81492255796106328, 49.16775706135234003 ) ) ;
#134732 = CARTESIAN_POINT ( 'NONE',  ( -13.89961937509977652, 13.97604488694528158, 90.62390960531432427 ) ) ;
#134731 = CARTESIAN_POINT ( 'NONE',  ( -9.564922557961040184, 16.46253265017147172, 77.91775706135234714 ) ) ;
#134733 = CARTESIAN_POINT ( 'NONE',  ( -12.06949235617756955, 12.14591786802309770, 100.6239096053143811 ) ) ;
#134734 = CARTESIAN_POINT ( 'NONE',  ( -5.719274019375978568, 21.55341960407610458, 100.2072429386476955 ) ) ;
#134735 = CARTESIAN_POINT ( 'NONE',  ( 19.05341960407617918, -5.049401038297876454, 21.04275706135232582 ) ) ;
#134736 = CARTESIAN_POINT ( 'NONE',  ( 14.34966873604960469, 8.224510206698951720, 94.16557627198103830 ) ) ;
#134737 = CARTESIAN_POINT ( 'NONE',  ( -9.564922557960796823, -16.46253265017161027, 47.08224293864769550 ) ) ;
#134738 = CARTESIAN_POINT ( 'NONE',  ( 0.05219959533936267826, -19.03943276465977164, 80.00109039468567573 ) ) ;
#134739 = CARTESIAN_POINT ( 'NONE',  ( 16.52544592524342804, -4.483927247898539470, 43.54057627198103830 ) ) ;
#134740 = CARTESIAN_POINT ( 'NONE',  ( -5.049401038297874678, -19.05341960407617918, 19.79275706135233293 ) ) ;
#134741 = CARTESIAN_POINT ( 'NONE',  ( 13.89961937509977652, -13.97604488694527269, 108.1239096053143669 ) ) ;
#134742 = CARTESIAN_POINT ( 'NONE',  ( -0.05219959533936034679, 19.03943276465977164, 77.50109039468566152 ) ) ;
#134743 = CARTESIAN_POINT ( 'NONE',  ( -21.55341960407610458, -5.719274019375992779, 81.45724293864769550 ) ) ;
#134744 = CARTESIAN_POINT ( 'NONE',  ( 21.52544592524334988, 5.823673210054432836, 36.45942372801901143 ) ) ;
#134745 = CARTESIAN_POINT ( 'NONE',  ( -4.379528057220086978, -16.55341960407618274, 29.79275706135234358 ) ) ;
#134746 = CARTESIAN_POINT ( 'NONE',  ( 12.06949235617739724, 12.14591786802326823, 86.87609039468568994 ) ) ;
#134748 = CARTESIAN_POINT ( 'NONE',  ( 5.823673210054444382, -21.52544592524334988, 30.20942372801902565 ) ) ;
#134747 = CARTESIAN_POINT ( 'NONE',  ( 17.50000000000000000, 5.499999999999992895, 61.70309617465829177 ) ) ;
#134749 = CARTESIAN_POINT ( 'NONE',  ( 15.80617190586746368, 15.72974639402197994, 44.37390960531435979 ) ) ;
#134750 = CARTESIAN_POINT ( 'NONE',  ( 9.474510206698971260, -16.51473224551069308, 27.91557627198103120 ) ) ;
#134751 = CARTESIAN_POINT ( 'NONE',  ( 30.74264578624799782, 22.33583958711400541, -8.549999994537627046 ) ) ;
#134752 = CARTESIAN_POINT ( 'NONE',  ( 8.224510206698742110, 14.34966873604972548, 57.08442372801901854 ) ) ;
#134753 = CARTESIAN_POINT ( 'NONE',  ( 4.379528057220339221, -16.55341960407611168, 92.70724293864770971 ) ) ;
#134754 = CARTESIAN_POINT ( 'NONE',  ( 0.05219959533907565091, 21.53943276465977519, 79.99890960531435269 ) ) ;
#134755 = CARTESIAN_POINT ( 'NONE',  ( 14.29746914071037800, 8.314922557961029526, 111.6677570613523613 ) ) ;
#134756 = CARTESIAN_POINT ( 'NONE',  ( 0.05219959533934541429, -16.53943276465976808, 45.00109039468568284 ) ) ;
#134757 = CARTESIAN_POINT ( 'NONE',  ( -13.89961937509977652, 13.97604488694528158, 55.62390960531434558 ) ) ;
#134758 = CARTESIAN_POINT ( 'NONE',  ( 12.06949235617739724, 12.14591786802326823, 86.87609039468568994 ) ) ;
#134759 = CARTESIAN_POINT ( 'NONE',  ( -19.02544592524334988, -5.153800228976617603, 83.95942372801901854 ) ) ;
#134760 = CARTESIAN_POINT ( 'NONE',  ( 10.81492255796078972, 18.62759615963270932, 84.58224293864769550 ) ) ;
#134761 = CARTESIAN_POINT ( 'NONE',  ( 12.14591786802327356, -12.06949235617739191, 105.6260903946856899 ) ) ;
#134762 = EDGE_LOOP ( 'NONE', ( #181848, #13033, #163134, #62098 ) ) ;
#134763 = DIRECTION ( 'NONE',  ( -0.000000000000000000, -0.000000000000000000, 1.000000000000000000 ) ) ;
#134764 = CARTESIAN_POINT ( 'NONE',  ( 5.823673210054125526, 21.52544592524343514, 59.79057627198103120 ) ) ;
#134765 = CARTESIAN_POINT ( 'NONE',  ( 16.53943276465976808, 0.05219959533934440121, 96.25109039468568994 ) ) ;
#134766 = ORIENTED_EDGE ( 'NONE', *, *, #177434, .T. ) ;
#134767 = CARTESIAN_POINT ( 'NONE',  ( -21.53943276465977519, 0.05219959533907696930, 31.24890960531435979 ) ) ;
#134768 = CARTESIAN_POINT ( 'NONE',  ( -19.48894818550246200, 5.499999999999919176, 75.10307310435239003 ) ) ;
#134769 = CARTESIAN_POINT ( 'NONE',  ( 21.53943276465977519, -0.05219959533907433946, 83.74890960531435269 ) ) ;
#134770 = CARTESIAN_POINT ( 'NONE',  ( -0.05219959533910754901, -16.53943276465976808, 27.49890960531435269 ) ) ;
#134771 = CARTESIAN_POINT ( 'NONE',  ( 8.314922557961029526, -14.29746914071037800, 20.41775706135234714 ) ) ;
#134772 = CARTESIAN_POINT ( 'NONE',  ( -5.153800228976328057, -19.02544592524343514, 32.29057627198102409 ) ) ;
#134773 = CARTESIAN_POINT ( 'NONE',  ( -16.53943276465976808, -0.05219959533934237506, 23.75109039468567929 ) ) ;
#134774 = CARTESIAN_POINT ( 'NONE',  ( -13.97604488694527625, -13.89961937509977652, 51.87390960531436690 ) ) ;
#134775 = EDGE_CURVE ( 'NONE', #105306, #104760, #30844, .T. ) ;
#134776 = CARTESIAN_POINT ( 'NONE',  ( 17.14385361876520264, 23.59649016807275856, 140.6750000027311387 ) ) ;
#134777 = CARTESIAN_POINT ( 'NONE',  ( -5.049401038298153566, 19.05341960407611168, 105.2072429386476671 ) ) ;
#134778 = CARTESIAN_POINT ( 'NONE',  ( 9.564922557960805705, 16.46253265017160317, 109.5822429386476955 ) ) ;
#134779 = CARTESIAN_POINT ( 'NONE',  ( 16.52544592524335698, 4.483927247898782831, 86.45942372801901854 ) ) ;
#134780 = CARTESIAN_POINT ( 'NONE',  ( 9.474510206698729675, 16.51473224551082808, 97.08442372801900433 ) ) ;
#134781 = CARTESIAN_POINT ( 'NONE',  ( -19.05341960407617563, 5.049401038297882671, 33.54275706135231871 ) ) ;
#134782 = CARTESIAN_POINT ( 'NONE',  ( -15.72974639402197994, 15.80617190586746368, 75.62390960531439532 ) ) ;
#134783 = CARTESIAN_POINT ( 'NONE',  ( 16.53943276465976808, 0.05219959533934440121, 106.2510903946856757 ) ) ;
#134784 = CARTESIAN_POINT ( 'NONE',  ( -18.67979575497178146, -10.72451020669898902, 36.66557627198103120 ) ) ;
#134785 = CARTESIAN_POINT ( 'NONE',  ( -13.97604488694547697, 13.89961937509957934, 93.12609039468566152 ) ) ;
#134786 = CARTESIAN_POINT ( 'NONE',  ( 13.89961937509977652, -13.97604488694527269, 53.12390960531434558 ) ) ;
#134787 = CARTESIAN_POINT ( 'NONE',  ( -19.05341960407611168, -5.049401038298163336, 101.4572429386476955 ) ) ;
#134788 = CARTESIAN_POINT ( 'NONE',  ( 15.80617190586769283, -15.72974639402175789, 65.62609039468568994 ) ) ;
#134789 = CARTESIAN_POINT ( 'NONE',  ( -16.51473224551069308, -9.474510206698971260, 66.66557627198102409 ) ) ;
#134790 = CARTESIAN_POINT ( 'NONE',  ( 16.55341960407611168, 4.379528057220329451, 93.95724293864770971 ) ) ;
#134791 = DIRECTION ( 'NONE',  ( 1.000000000000000000, 0.000000000000000000, 0.000000000000000000 ) ) ;
#134792 = CARTESIAN_POINT ( 'NONE',  ( -12.06949235617756955, 12.14591786802309770, 75.62390960531439532 ) ) ;
#134793 = CARTESIAN_POINT ( 'NONE',  ( -5.719274019375978568, 21.55341960407610458, 80.20724293864769550 ) ) ;
#134794 = EDGE_LOOP ( 'NONE', ( #119411, #144739, #188824, #33527, #121546, #132586, #196744, #129110 ) ) ;
#134795 = CARTESIAN_POINT ( 'NONE',  ( 16.51473224551083163, -9.474510206698727899, 85.83442372801900433 ) ) ;
#134796 = CARTESIAN_POINT ( 'NONE',  ( 16.52216118717209881, -7.221426719304498754, 81.42400978953010338 ) ) ;
#134797 = CARTESIAN_POINT ( 'NONE',  ( 0.05219959533909260263, 19.03943276465977164, 64.99890960531436690 ) ) ;
#134798 = CARTESIAN_POINT ( 'NONE',  ( 17.31728774477215183, -6.344390552233685199, 73.31906651689308774 ) ) ;
#134800 = CARTESIAN_POINT ( 'NONE',  ( 9.474510206698971260, -16.51473224551069308, 82.91557627198103830 ) ) ;
#134799 = CARTESIAN_POINT ( 'NONE',  ( -19.05341960407611168, -5.049401038298163336, 81.45724293864769550 ) ) ;
#134801 = CARTESIAN_POINT ( 'NONE',  ( -12.14591786802326823, 12.06949235617739902, 58.12609039468568994 ) ) ;
#134802 = EDGE_CURVE ( 'NONE', #38745, #146788, #79610, .T. ) ;
#134803 = CARTESIAN_POINT ( 'NONE',  ( -16.18388926212241330, -7.379444403734411573, 50.43953151366153520 ) ) ;
#134804 = CARTESIAN_POINT ( 'NONE',  ( -5.049401038297874678, -19.05341960407617918, 39.79275706135232582 ) ) ;
#134805 = CARTESIAN_POINT ( 'NONE',  ( 17.31245056299218632, 6.303547735381235917, 21.68954763021610432 ) ) ;
#134806 = CARTESIAN_POINT ( 'NONE',  ( 19.03943276465977164, -0.05219959533909143690, 108.7489096053143527 ) ) ;
#134807 = CARTESIAN_POINT ( 'NONE',  ( -14.34966873604972548, 8.224510206698743886, 103.3344237280190043 ) ) ;
#134808 = CARTESIAN_POINT ( 'NONE',  ( -34.75592306271660448, -1.707766843171850679, 52.30709029423474021 ) ) ;
#134809 = CARTESIAN_POINT ( 'NONE',  ( -16.52544592524335698, -4.483927247898792601, 93.95942372801903275 ) ) ;
#134810 = CARTESIAN_POINT ( 'NONE',  ( -17.49999999999999645, 5.499999999999992006, 28.71769037696435234 ) ) ;
#134811 = CARTESIAN_POINT ( 'NONE',  ( 16.52544592524335698, 4.483927247898782831, 71.45942372801901854 ) ) ;
#134812 = CARTESIAN_POINT ( 'NONE',  ( 13.97604488694527802, 13.89961937509977830, 74.37390960531436690 ) ) ;
#134813 = CARTESIAN_POINT ( 'NONE',  ( -18.62759615963255300, -10.81492255796106328, 64.16775706135234714 ) ) ;
#134814 = CARTESIAN_POINT ( 'NONE',  ( 19.05341960407617918, -5.049401038297876454, 76.04275706135230450 ) ) ;
#134815 = CARTESIAN_POINT ( 'NONE',  ( -9.564922557961040184, 16.46253265017147172, 32.91775706135233293 ) ) ;
#134816 = CARTESIAN_POINT ( 'NONE',  ( -19.05341960407611168, -5.049401038298163336, 66.45724293864769550 ) ) ;
#134817 = CARTESIAN_POINT ( 'NONE',  ( 13.89961937509977652, -13.97604488694527269, 48.12390960531435979 ) ) ;
#134818 = CARTESIAN_POINT ( 'NONE',  ( -19.29520783494825409, -35.03893545922181119, -7.263628290518377106 ) ) ;
#134819 = CARTESIAN_POINT ( 'NONE',  ( -18.62759615963270932, 10.81492255796079327, 80.83224293864769550 ) ) ;
#134820 = AXIS2_PLACEMENT_3D ( 'NONE', #27960, #59252, #182620 ) ;
#134821 = CARTESIAN_POINT ( 'NONE',  ( -18.62759615963270932, 10.81492255796079327, 35.83224293864768839 ) ) ;
#134822 = CARTESIAN_POINT ( 'NONE',  ( 13.97604488694527802, 13.89961937509977652, 34.37390960531436690 ) ) ;
#134823 = CARTESIAN_POINT ( 'NONE',  ( -16.55341960407617563, 4.379528057220093196, 48.54275706135234714 ) ) ;
#134824 = VERTEX_POINT ( 'NONE', #117391 ) ;
#134825 = CARTESIAN_POINT ( 'NONE',  ( 15.80617190586769283, -15.72974639402175789, 35.62609039468568994 ) ) ;
#134827 = CARTESIAN_POINT ( 'NONE',  ( -23.48529157249600985, 32.32473071737754111, -8.300000000000000711 ) ) ;
#134826 = CARTESIAN_POINT ( 'NONE',  ( -12.06949235617756955, 12.14591786802309770, 50.62390960531435979 ) ) ;
#134828 = CARTESIAN_POINT ( 'NONE',  ( -14.34966873604972548, 8.224510206698743886, 23.33442372801901499 ) ) ;
#134829 = CARTESIAN_POINT ( 'NONE',  ( -0.05219959533936034679, 19.03943276465977164, 42.50109039468566152 ) ) ;
#134830 = CARTESIAN_POINT ( 'NONE',  ( -16.53943276465976808, 0.05219959533911058130, 61.24890960531435979 ) ) ;
#134831 = CARTESIAN_POINT ( 'NONE',  ( -18.67979575497193778, 10.72451020669871902, 23.33442372801901499 ) ) ;
#134833 = CARTESIAN_POINT ( 'NONE',  ( 18.62759615963271287, -10.81492255796078972, 73.33224293864769550 ) ) ;
#134832 = CARTESIAN_POINT ( 'NONE',  ( 1.151390856322186851, 16.16634691005189595, -59.37054012757567278 ) ) ;
#134834 = CARTESIAN_POINT ( 'NONE',  ( -0.05219959533909027116, -19.03943276465977164, 87.49890960531436690 ) ) ;
#134835 = CARTESIAN_POINT ( 'NONE',  ( -12.06949235617756955, 12.14591786802309770, 65.62390960531436690 ) ) ;
#134836 = CARTESIAN_POINT ( 'NONE',  ( 9.474510206698971260, -16.51473224551069308, 107.9155762719810383 ) ) ;
#134837 = CARTESIAN_POINT ( 'NONE',  ( 14.18669005401828187, -34.08280046153741694, -8.000000000000001776 ) ) ;
#134838 = CARTESIAN_POINT ( 'NONE',  ( -13.97604488694547697, 13.89961937509957934, 73.12609039468568994 ) ) ;
#134839 = CARTESIAN_POINT ( 'NONE',  ( -21.52544592524343514, 5.823673210054127303, 111.0405762719810525 ) ) ;
#134840 = CARTESIAN_POINT ( 'NONE',  ( -9.564922557960796823, -16.46253265017161027, 52.08224293864768839 ) ) ;
#134841 = CARTESIAN_POINT ( 'NONE',  ( -19.05341960407617563, 5.049401038297882671, 43.54275706135232582 ) ) ;
#134842 = CARTESIAN_POINT ( 'NONE',  ( 4.483927247898545687, 16.52544592524342804, 114.7905762719810383 ) ) ;
#134843 = CARTESIAN_POINT ( 'NONE',  ( -10.72451020669870658, -18.67979575497194134, 64.58442372801900433 ) ) ;
#134844 = AXIS2_PLACEMENT_3D ( 'NONE', #62652, #125338, #76834 ) ;
#134845 = CARTESIAN_POINT ( 'NONE',  ( -16.52216118717210591, -7.221426719304506747, 71.07599021046993926 ) ) ;
#134846 = CARTESIAN_POINT ( 'NONE',  ( -8.314922557960811034, -14.29746914071050412, 42.08224293864769550 ) ) ;
#134847 = CARTESIAN_POINT ( 'NONE',  ( -16.46253265017160317, 9.564922557960807481, 50.83224293864770260 ) ) ;
#134848 = CARTESIAN_POINT ( 'NONE',  ( 19.20446147854523389, 5.500000000000086153, 71.88999695167674986 ) ) ;
#134849 = CARTESIAN_POINT ( 'NONE',  ( -5.719274019375978568, 21.55341960407610458, 80.20724293864769550 ) ) ;
#134850 = CARTESIAN_POINT ( 'NONE',  ( 17.14385361876520264, 23.59649016807275856, 146.1750000027311387 ) ) ;
#134851 = CARTESIAN_POINT ( 'NONE',  ( 0.05219959533909260263, 19.03943276465977164, 44.99890960531435979 ) ) ;
#134852 = CARTESIAN_POINT ( 'NONE',  ( -0.05219959533907301413, -21.53943276465977519, 62.49890960531436690 ) ) ;
#134853 = EDGE_LOOP ( 'NONE', ( #123877, #26379, #54912, #125957 ) ) ;
#134854 = CARTESIAN_POINT ( 'NONE',  ( 18.67979575497194134, -10.72451020669871369, 80.83442372801901854 ) ) ;
#134857 = CARTESIAN_POINT ( 'NONE',  ( 12.14591786802309770, 12.06949235617756955, 84.37390960531438111 ) ) ;
#134856 = CARTESIAN_POINT ( 'NONE',  ( 16.53943276465976808, 0.05219959533934440121, 86.25109039468568994 ) ) ;
#134855 = DIRECTION ( 'NONE',  ( 1.000000000000000000, 0.000000000000000000, 0.000000000000000000 ) ) ;
#134858 = CARTESIAN_POINT ( 'NONE',  ( 16.46253265017160672, -9.564922557960803928, 73.33224293864769550 ) ) ;
#134859 = EDGE_LOOP ( 'NONE', ( #103503, #190433, #46709, #70200 ) ) ;
#134860 = CARTESIAN_POINT ( 'NONE',  ( -19.03943276465977164, -0.05219959533935918106, 38.75109039468566152 ) ) ;
#134861 = CARTESIAN_POINT ( 'NONE',  ( 12.06949235617739724, 12.14591786802326823, 81.87609039468568994 ) ) ;
#134862 = CARTESIAN_POINT ( 'NONE',  ( -13.97604488694547697, 13.89961937509957934, 23.12609039468565442 ) ) ;
#134863 = CARTESIAN_POINT ( 'NONE',  ( 9.474510206698971260, -16.51473224551069308, 82.91557627198103830 ) ) ;
#134864 = CARTESIAN_POINT ( 'NONE',  ( 21.53943276465977519, -0.05219959533907433946, 43.74890960531435979 ) ) ;
#134865 = CARTESIAN_POINT ( 'NONE',  ( 21.53943276465977519, 0.05219959533937863772, 96.25109039468568994 ) ) ;
#134866 = CARTESIAN_POINT ( 'NONE',  ( -12.14591786802326823, 12.06949235617739902, 58.12609039468568994 ) ) ;
#134867 = CARTESIAN_POINT ( 'NONE',  ( -15.80617190586745835, -15.72974639402198527, 106.8739096053143811 ) ) ;
#134868 = CARTESIAN_POINT ( 'NONE',  ( -16.53943276465976808, -0.05219959533934237506, 33.75109039468568284 ) ) ;
#134869 = CARTESIAN_POINT ( 'NONE',  ( 19.05341960407611168, 5.049401038298154454, 88.95724293864769550 ) ) ;
#134870 = CARTESIAN_POINT ( 'NONE',  ( 16.46253265017160672, -9.564922557960803928, 43.33224293864769550 ) ) ;
#134871 = CARTESIAN_POINT ( 'NONE',  ( -19.02544592524342804, 5.153800228976336051, 51.04057627198103120 ) ) ;
#134872 = CIRCLE ( 'NONE', #89532, 28.79475375365586487 ) ;
#134873 = CARTESIAN_POINT ( 'NONE',  ( -14.34966873604972548, 8.224510206698743886, 28.33442372801902209 ) ) ;
#134874 = CARTESIAN_POINT ( 'NONE',  ( 8.314922557960818139, 14.29746914071049879, 84.58224293864769550 ) ) ;
#134875 = CARTESIAN_POINT ( 'NONE',  ( 0.05219959533934541429, -16.53943276465976808, 90.00109039468567573 ) ) ;
#134878 = CARTESIAN_POINT ( 'NONE',  ( -9.474510206698964154, 16.51473224551069663, 55.41557627198103120 ) ) ;
#134877 = CARTESIAN_POINT ( 'NONE',  ( -5.049401038298153566, 19.05341960407611168, 70.20724293864769550 ) ) ;
#134876 = CARTESIAN_POINT ( 'NONE',  ( -10.81492255796105439, 18.62759615963255655, 47.91775706135234714 ) ) ;
#134879 = CARTESIAN_POINT ( 'NONE',  ( -19.03943276465977164, 0.05219959533909376836, 76.24890960531435269 ) ) ;
#134880 = CARTESIAN_POINT ( 'NONE',  ( -8.224510206698948167, 14.34966873604960824, 30.41557627198101699 ) ) ;
#134881 = CARTESIAN_POINT ( 'NONE',  ( 0.05219959533934541429, -16.53943276465976808, 90.00109039468567573 ) ) ;
#134882 = ORIENTED_EDGE ( 'NONE', *, *, #120075, .T. ) ;
#134883 = CARTESIAN_POINT ( 'NONE',  ( -5.049401038297874678, -19.05341960407617918, 29.79275706135232227 ) ) ;
#134884 = CARTESIAN_POINT ( 'NONE',  ( 13.97604488694527802, 13.89961937509977652, 104.3739096053143385 ) ) ;
#134885 = CARTESIAN_POINT ( 'NONE',  ( 19.03943276465977164, -0.05219959533909143690, 43.74890960531435979 ) ) ;
#134886 = CARTESIAN_POINT ( 'NONE',  ( -5.950531402560715689E-15, 38.81732327939063509, -7.124999997268814944 ) ) ;
#134887 = CARTESIAN_POINT ( 'NONE',  ( 16.55341960407618274, -4.379528057220086978, 41.04275706135236135 ) ) ;
#134889 = CARTESIAN_POINT ( 'NONE',  ( -16.52544592524335698, -4.483927247898792601, 58.95942372801902565 ) ) ;
#134888 = CARTESIAN_POINT ( 'NONE',  ( 5.049401038297881783, 19.05341960407617563, 72.29275706135234714 ) ) ;
#134890 = CARTESIAN_POINT ( 'NONE',  ( 6.874011537017777229, -5.225174246120010579, -64.05724122177205970 ) ) ;
#134891 = CARTESIAN_POINT ( 'NONE',  ( 16.46253265017160672, -9.564922557960803928, 83.33224293864768129 ) ) ;
#134892 = CARTESIAN_POINT ( 'NONE',  ( -18.62759615963255300, -10.81492255796106328, 19.16775706135234714 ) ) ;
#134893 = CARTESIAN_POINT ( 'NONE',  ( -9.564922557961040184, 16.46253265017147172, 62.91775706135233293 ) ) ;
#134895 = CARTESIAN_POINT ( 'NONE',  ( -13.97604488694527625, -13.89961937509977652, 36.87390960531436690 ) ) ;
#134894 = CARTESIAN_POINT ( 'NONE',  ( -19.05341960407611168, -5.049401038298163336, 111.4572429386476671 ) ) ;
#134896 = CARTESIAN_POINT ( 'NONE',  ( -19.02544592524342804, 5.153800228976336051, 81.04057627198103830 ) ) ;
#134898 = CARTESIAN_POINT ( 'NONE',  ( -13.89961937509977830, 13.97604488694528158, 70.62390960531435269 ) ) ;
#134897 = CARTESIAN_POINT ( 'NONE',  ( -0.05219959533910754901, -16.53943276465976808, 37.49890960531436690 ) ) ;
#134899 = CARTESIAN_POINT ( 'NONE',  ( -16.46253265017146816, -9.564922557961047289, 34.16775706135233293 ) ) ;
#134900 = CARTESIAN_POINT ( 'NONE',  ( -16.55341960407611168, -4.379528057220339221, 71.45724293864769550 ) ) ;
#134901 = CARTESIAN_POINT ( 'NONE',  ( -5.719274019375665041, -21.55341960407619695, 109.7927570613523613 ) ) ;
#134902 = CARTESIAN_POINT ( 'NONE',  ( 19.03943276465977164, -0.05219959533909143690, 53.74890960531436690 ) ) ;
#134904 = CARTESIAN_POINT ( 'NONE',  ( -10.72451020669870658, -18.67979575497194134, 104.5844237280190185 ) ) ;
#134903 = CARTESIAN_POINT ( 'NONE',  ( -12.06949235617756955, 12.14591786802309770, 35.62390960531437401 ) ) ;
#134905 = CARTESIAN_POINT ( 'NONE',  ( 13.89961937509977652, -13.97604488694527269, 93.12390960531436690 ) ) ;
#134906 = CARTESIAN_POINT ( 'NONE',  ( -13.89961937509977652, 13.97604488694528158, 105.6239096053143527 ) ) ;
#134907 = CARTESIAN_POINT ( 'NONE',  ( -9.564922557960796823, -16.46253265017161027, 42.08224293864769550 ) ) ;
#134908 = CARTESIAN_POINT ( 'NONE',  ( -12.06949235617756955, 12.14591786802309770, 110.6239096053143669 ) ) ;
#134909 = CARTESIAN_POINT ( 'NONE',  ( 8.224510206698953496, -14.34966873604960469, 92.91557627198103830 ) ) ;
#134910 = CARTESIAN_POINT ( 'NONE',  ( -21.55341960407610458, -5.719274019375992779, 101.4572429386476955 ) ) ;
#134911 = CARTESIAN_POINT ( 'NONE',  ( 19.02544592524343514, -5.153800228976328945, 93.54057627198102409 ) ) ;
#134912 = CARTESIAN_POINT ( 'NONE',  ( -18.67979575497178146, -10.72451020669898902, 96.66557627198102409 ) ) ;
#134913 = CARTESIAN_POINT ( 'NONE',  ( -13.97604488694527625, -13.89961937509977652, 91.87390960531432427 ) ) ;
#134915 = CARTESIAN_POINT ( 'NONE',  ( 14.34966873604960469, 8.224510206698951720, 104.1655762719810241 ) ) ;
#134914 = DIRECTION ( 'NONE',  ( 1.000000000000000000, 0.000000000000000000, 0.000000000000000000 ) ) ;
#134916 = CARTESIAN_POINT ( 'NONE',  ( -16.51473224551069308, -9.474510206698971260, 66.66557627198102409 ) ) ;
#134917 = CARTESIAN_POINT ( 'NONE',  ( 21.55341960407610458, 5.719274019375980345, 83.95724293864770971 ) ) ;
#134918 = DIRECTION ( 'NONE',  ( 0.000000000000000000, 0.000000000000000000, 1.000000000000000000 ) ) ;
#134920 = CARTESIAN_POINT ( 'NONE',  ( 17.50000000000000000, 5.499999999999997335, 120.0000000000000142 ) ) ;
#134919 = CARTESIAN_POINT ( 'NONE',  ( 10.72451020669898902, -18.67979575497178502, 32.91557627198102409 ) ) ;
#134921 = CARTESIAN_POINT ( 'NONE',  ( -16.53943276465976808, -0.05219959533934237506, 28.75109039468567929 ) ) ;
#134922 = CARTESIAN_POINT ( 'NONE',  ( 12.14591786802309770, 12.06949235617756955, 99.37390960531436690 ) ) ;
#134923 = CARTESIAN_POINT ( 'NONE',  ( 0.000000000000000000, 0.000000000000000000, -61.89430850415821794 ) ) ;
#134924 = CARTESIAN_POINT ( 'NONE',  ( -16.46253265017160317, 9.564922557960807481, 85.83224293864769550 ) ) ;
#134925 = CARTESIAN_POINT ( 'NONE',  ( 0.05219959533909260263, 19.03943276465977164, 44.99890960531435979 ) ) ;
#134926 = CARTESIAN_POINT ( 'NONE',  ( 16.55341960407611168, 4.379528057220329451, 78.95724293864769550 ) ) ;
#134927 = CARTESIAN_POINT ( 'NONE',  ( -5.719274019375978568, 21.55341960407610458, 25.20724293864769550 ) ) ;
#134928 = CARTESIAN_POINT ( 'NONE',  ( -16.52544592524342804, 4.483927247898546575, 56.04057627198102409 ) ) ;
#134929 = CARTESIAN_POINT ( 'NONE',  ( 9.564922557961047289, -16.46253265017146816, 105.4177570613523471 ) ) ;
#134930 = CARTESIAN_POINT ( 'NONE',  ( -0.05219959533937732626, 21.53943276465977519, 57.50109039468568994 ) ) ;
#134931 = CYLINDRICAL_SURFACE ( 'NONE', #172389, 40.00000000000000711 ) ;
#134932 = CARTESIAN_POINT ( 'NONE',  ( 0.05219959533909260263, 19.03943276465977164, 99.99890960531436690 ) ) ;
#134933 = CARTESIAN_POINT ( 'NONE',  ( 16.53943276465976808, 0.05219959533934440121, 81.25109039468568994 ) ) ;
#134934 = CARTESIAN_POINT ( 'NONE',  ( -17.13100169013222640, 6.664070546374242454, 95.76789835699824494 ) ) ;
#134935 = CARTESIAN_POINT ( 'NONE',  ( -16.51473224551069308, -9.474510206698971260, 76.66557627198103830 ) ) ;
#134936 = CARTESIAN_POINT ( 'NONE',  ( -5.823673210054116645, -21.52544592524344225, 87.29057627198103830 ) ) ;
#134937 = CARTESIAN_POINT ( 'NONE',  ( 16.51473224551083163, -9.474510206698727899, 105.8344237280190043 ) ) ;
#134939 = CARTESIAN_POINT ( 'NONE',  ( 21.55341960407619695, -5.719274019375665929, 61.04275706135234714 ) ) ;
#134938 = CARTESIAN_POINT ( 'NONE',  ( -12.14591786802309592, -12.06949235617757132, 51.87390960531437401 ) ) ;
#134940 = EDGE_CURVE ( 'NONE', #60353, #185073, #40559, .T. ) ;
#134942 = CARTESIAN_POINT ( 'NONE',  ( -9.474510206698964154, 16.51473224551069663, 115.4155762719810241 ) ) ;
#134941 = CARTESIAN_POINT ( 'NONE',  ( 8.224510206698742110, 14.34966873604972548, 82.08442372801901854 ) ) ;
#134943 = CARTESIAN_POINT ( 'NONE',  ( 16.46253265017160672, -9.564922557960803928, 113.3322429386476955 ) ) ;
#134944 = DIRECTION ( 'NONE',  ( -1.000000000000000000, 0.000000000000000000, -0.000000000000000000 ) ) ;
#134945 = CARTESIAN_POINT ( 'NONE',  ( 12.14591786802327356, -12.06949235617739191, 110.6260903946857042 ) ) ;
#134946 = CARTESIAN_POINT ( 'NONE',  ( -8.224510206698735004, -14.34966873604973081, 64.58442372801900433 ) ) ;
#134947 = CARTESIAN_POINT ( 'NONE',  ( 19.05341960407611168, 5.049401038298154454, 68.95724293864769550 ) ) ;
#134948 = CARTESIAN_POINT ( 'NONE',  ( -13.89961937509977652, 13.97604488694528158, 70.62390960531432427 ) ) ;
#134949 = CARTESIAN_POINT ( 'NONE',  ( -5.823673210054431948, 21.52544592524334988, 72.70942372801901854 ) ) ;
#134950 = CARTESIAN_POINT ( 'NONE',  ( -8.224510206698735004, -14.34966873604973081, 79.58442372801903275 ) ) ;
#134951 = CARTESIAN_POINT ( 'NONE',  ( 4.379528057220339221, -16.55341960407611168, 47.70724293864770260 ) ) ;
#134952 = CARTESIAN_POINT ( 'NONE',  ( -9.474510206698964154, 16.51473224551069663, 60.41557627198102409 ) ) ;
#134953 = CARTESIAN_POINT ( 'NONE',  ( 0.05219959533909260263, 19.03943276465977164, 49.99890960531435979 ) ) ;
#134955 = ORIENTED_EDGE ( 'NONE', *, *, #115825, .F. ) ;
#134954 = CARTESIAN_POINT ( 'NONE',  ( -14.34966873604972548, 8.224510206698743886, 48.33442372801902565 ) ) ;
#134956 = CARTESIAN_POINT ( 'NONE',  ( -13.89961937509957401, -13.97604488694547875, 99.37609039468567573 ) ) ;
#134957 = CARTESIAN_POINT ( 'NONE',  ( -16.52544592524342804, 4.483927247898546575, 101.0405762719810383 ) ) ;
#134958 = CARTESIAN_POINT ( 'NONE',  ( -13.89961937509977652, 13.97604488694528158, 70.62390960531432427 ) ) ;
#134960 = CARTESIAN_POINT ( 'NONE',  ( 37.99999999999999289, 2.893978650043524126E-14, -3.000000000000000000 ) ) ;
#134959 = CARTESIAN_POINT ( 'NONE',  ( -19.03943276465977164, -0.05219959533935918106, 103.7510903946856757 ) ) ;
#134961 = CARTESIAN_POINT ( 'NONE',  ( 5.719274019375673035, 21.55341960407619339, 102.2927570613523613 ) ) ;
#134962 = CARTESIAN_POINT ( 'NONE',  ( -16.55341960407617563, 4.379528057220093196, 73.54275706135234714 ) ) ;
#134963 = CARTESIAN_POINT ( 'NONE',  ( 4.500000000000000888, -125.7396439921083555, 8.159758652193113804 ) ) ;
#134964 = CARTESIAN_POINT ( 'NONE',  ( 15.72974639402199770, -15.80617190586745480, 68.12390960531436690 ) ) ;
#134965 = CARTESIAN_POINT ( 'NONE',  ( -14.34966873604972548, 8.224510206698743886, 58.33442372801901143 ) ) ;
#134966 = DIRECTION ( 'NONE',  ( 1.000000000000000000, 0.000000000000000000, 0.000000000000000000 ) ) ;
#134967 = CARTESIAN_POINT ( 'NONE',  ( -16.51473224551082808, 9.474510206698731452, 48.33442372801900433 ) ) ;
#134968 = CARTESIAN_POINT ( 'NONE',  ( -19.02544592524342804, 5.153800228976336051, 86.04057627198103830 ) ) ;
#134969 = CARTESIAN_POINT ( 'NONE',  ( -9.564922557960796823, -16.46253265017161027, 27.08224293864769550 ) ) ;
#134970 = CARTESIAN_POINT ( 'NONE',  ( -0.05219959533909027116, -19.03943276465977164, 67.49890960531436690 ) ) ;
#134971 = CARTESIAN_POINT ( 'NONE',  ( 0.05219959533910956823, 16.53943276465976808, 59.99890960531436690 ) ) ;
#134972 = AXIS2_PLACEMENT_3D ( 'NONE', #8493, #191505, #128819 ) ;
#134973 = CARTESIAN_POINT ( 'NONE',  ( -0.05219959533937732626, 21.53943276465977519, 72.50109039468568994 ) ) ;
#134974 = CARTESIAN_POINT ( 'NONE',  ( 19.05341960407617918, -5.049401038297876454, 41.04275706135233293 ) ) ;
#134975 = CARTESIAN_POINT ( 'NONE',  ( 9.474510206698729675, 16.51473224551082808, 32.08442372801900433 ) ) ;
#134976 = CARTESIAN_POINT ( 'NONE',  ( -13.89961937509977652, 13.97604488694528158, 50.62390960531435979 ) ) ;
#134977 = CARTESIAN_POINT ( 'NONE',  ( 18.62759615963271287, -10.81492255796078972, 28.33224293864769550 ) ) ;
#134978 = CARTESIAN_POINT ( 'NONE',  ( 18.62759615963255655, 10.81492255796105972, 101.6677570613523613 ) ) ;
#134979 = CARTESIAN_POINT ( 'NONE',  ( 0.05219959533909260263, 19.03943276465977164, 64.99890960531436690 ) ) ;
#134980 = CARTESIAN_POINT ( 'NONE',  ( -18.62759615963255300, -10.81492255796106328, 94.16775706135237556 ) ) ;
#134981 = CARTESIAN_POINT ( 'NONE',  ( 15.72974639402199770, -15.80617190586745480, 33.12390960531435979 ) ) ;
#134982 = CARTESIAN_POINT ( 'NONE',  ( -9.474510206698964154, 16.51473224551069663, 80.41557627198103830 ) ) ;
#134983 = CARTESIAN_POINT ( 'NONE',  ( -5.153800228976607833, 19.02544592524334988, 62.70942372801899722 ) ) ;
#134984 = CARTESIAN_POINT ( 'NONE',  ( 19.02544592524343514, -5.153800228976328945, 43.54057627198103120 ) ) ;
#134985 = CARTESIAN_POINT ( 'NONE',  ( 0.05219959533909260263, 19.03943276465977164, 89.99890960531436690 ) ) ;
#134986 = CARTESIAN_POINT ( 'NONE',  ( 8.314922557961029526, -14.29746914071037800, 30.41775706135234358 ) ) ;
#134987 = CARTESIAN_POINT ( 'NONE',  ( -14.34966873604960291, -8.224510206698953496, 91.66557627198103830 ) ) ;
#134988 = CARTESIAN_POINT ( 'NONE',  ( -19.05341960407611168, -5.049401038298163336, 76.45724293864769550 ) ) ;
#134989 = CARTESIAN_POINT ( 'NONE',  ( -5.719274019375978568, 21.55341960407610458, 50.20724293864769550 ) ) ;
#134990 = CARTESIAN_POINT ( 'NONE',  ( -16.51473224551082808, 9.474510206698731452, 108.3344237280190043 ) ) ;
#134991 = CARTESIAN_POINT ( 'NONE',  ( 15.72974639402199770, -15.80617190586745480, 113.1239096053143953 ) ) ;
#134992 = CARTESIAN_POINT ( 'NONE',  ( -15.72974639402176322, -15.80617190586768395, 64.37609039468568994 ) ) ;
#134993 = CARTESIAN_POINT ( 'NONE',  ( -8.224510206698735004, -14.34966873604973081, 69.58442372801900433 ) ) ;
#134994 = CARTESIAN_POINT ( 'NONE',  ( 4.483927247898790824, -16.52544592524335698, 65.20942372801901854 ) ) ;
#134995 = CARTESIAN_POINT ( 'NONE',  ( -19.02544592524342804, 5.153800228976336051, 56.04057627198100988 ) ) ;
#134996 = CARTESIAN_POINT ( 'NONE',  ( -4.483927247898782831, 16.52544592524335698, 97.70942372801904696 ) ) ;
#134997 = CARTESIAN_POINT ( 'NONE',  ( -16.46253265017146816, -9.564922557961047289, 44.16775706135232582 ) ) ;
#134998 = AXIS2_PLACEMENT_3D ( 'NONE', #22132, #84780, #113130 ) ;
#134999 = CARTESIAN_POINT ( 'NONE',  ( -18.67979575497193778, 10.72451020669871902, 28.33442372801902209 ) ) ;
#135000 = CARTESIAN_POINT ( 'NONE',  ( -12.14591786802309592, -12.06949235617757132, 61.87390960531436690 ) ) ;
#135001 = CARTESIAN_POINT ( 'NONE',  ( 9.564922557960805705, 16.46253265017160317, 104.5822429386476955 ) ) ;
#135002 = CARTESIAN_POINT ( 'NONE',  ( -14.29746914071037622, -8.314922557961029526, 89.16775706135236135 ) ) ;
#135003 = CARTESIAN_POINT ( 'NONE',  ( -5.823673210054431948, 21.52544592524334988, 72.70942372801901854 ) ) ;
#135004 = CARTESIAN_POINT ( 'NONE',  ( 12.14591786802327356, -12.06949235617739191, 30.62609039468567929 ) ) ;
#135005 = CARTESIAN_POINT ( 'NONE',  ( -18.62759615963255300, -10.81492255796106328, 29.16775706135234003 ) ) ;
#135006 = CARTESIAN_POINT ( 'NONE',  ( 16.52544592524342804, -4.483927247898539470, 63.54057627198103830 ) ) ;
#135007 = ORIENTED_EDGE ( 'NONE', *, *, #187359, .T. ) ;
#135008 =( BOUNDED_SURFACE ( )  B_SPLINE_SURFACE ( 1, 2, ( 
 ( #150637, #89941, #138423, #170758, #62566, #14086, #139409, #154589, #182957, #137429, #29278, #151622, #200103, #15087, #135470, #891, #167780, #109079, #122252, #124243, #181963, #59589, #32247, #76748, #197138, #13115, #61571, #123240, #185938, #44440, #47423, #184931, #43445, #46416, #121263, #153589, #106094, #12133, #16085, #73797, #90910, #45427, #108074, #199109, #105114, #58605, #92903, #120271, #152595, #183942, #136441, #169758, #166800, #75752, #28301, #60576, #107080, #74779, #168752, #198122, #30255, #91898, #31253, #77743, #18082, #156587, #96875, #49402, #2894, #93905, #48420, #187933, #112066, #80719, #188928, #155583, #111065, #17078, #186949, #110076, #50406, #79737, #141406, #64573, #171756, #140408, #157579, #173754, #126238, #35222, #172753, #65555, #34234, #78732, #1897, #63577, #95896, #33245, #125251, #19072, #127214 ),
 ( #142397, #94903, #3876, #50795, #14747, #45090, #15741, #29917, #1547, #199765, #63223, #123887, #74438, #189318, #76408, #91557, #97260, #30914, #61232, #158948, #137088, #46073, #124903, #108735, #140057, #136105, #169408, #197781, #28941, #13748, #78381, #106747, #153244, #168422, #75416, #59247, #77400, #112454, #138084, #16733, #107727, #170412, #121913, #120916, #155243, #174143, #122903, #44100, #182615, #90582, #92562, #167444, #152263, #35615, #184592, #154250, #139070, #548, #105758, #62219, #185585, #47075, #31904, #198776, #93557, #60242, #183606, #20437, #132624, #82088, #99270, #54779, #102288, #23451, #85098, #5263, #176138, #51777, #143781, #159955, #8277, #40618, #194312, #84099, #9289, #24463, #52768, #7259, #160957, #21443, #69955, #146784, #66945, #70954, #37607, #179150, #192303, #55778, #113437, #129596, #128607 ) ),
 .UNSPECIFIED., .F., .F., .T. ) 
 B_SPLINE_SURFACE_WITH_KNOTS ( ( 2, 2 ),
 ( 3, 2, 2, 2, 2, 2, 2, 2, 2, 2, 2, 2, 2, 2, 2, 2, 2, 2, 2, 2, 2, 2, 2, 2, 2, 2, 2, 2, 2, 2, 2, 2, 2, 2, 2, 2, 2, 2, 2, 2, 2, 2, 2, 2, 2, 2, 2, 2, 2, 2, 3 ),
 ( 0.000000000000000000, 1.000000000000000000 ),
 ( 0.000000000000000000, 0.02000000000000000042, 0.04000000000000000083, 0.05999999999999999778, 0.08000000000000000167, 0.1000000000000000056, 0.1199999999999999956, 0.1400000000000000133, 0.1600000000000000033, 0.1799999999999999933, 0.2000000000000000111, 0.2200000000000000011, 0.2399999999999999911, 0.2600000000000000089, 0.2800000000000000266, 0.2999999999999999889, 0.3200000000000000067, 0.3400000000000000244, 0.3599999999999999867, 0.3800000000000000044, 0.4000000000000000222, 0.4199999999999999845, 0.4400000000000000022, 0.4600000000000000200, 0.4799999999999999822, 0.5000000000000000000, 0.5200000000000000178, 0.5400000000000000355, 0.5600000000000000533, 0.5799999999999999600, 0.5999999999999999778, 0.6199999999999999956, 0.6400000000000000133, 0.6600000000000000311, 0.6800000000000000488, 0.6999999999999999556, 0.7199999999999999734, 0.7399999999999999911, 0.7600000000000000089, 0.7800000000000000266, 0.8000000000000000444, 0.8199999999999999512, 0.8399999999999999689, 0.8599999999999999867, 0.8800000000000000044, 0.9000000000000000222, 0.9200000000000000400, 0.9399999999999999467, 0.9599999999999999645, 0.9799999999999999822, 1.000000000000000000 ),
 .UNSPECIFIED. ) 
 GEOMETRIC_REPRESENTATION_ITEM ( )  RATIONAL_B_SPLINE_SURFACE ( (
 ( 1.000000000000000000, 0.9510565162951535312, 1.000000000000000000, 0.9510565162951535312, 1.000000000000000000, 0.9510565162951535312, 1.000000000000000000, 0.9510565162951535312, 1.000000000000000000, 0.9510565162951535312, 1.000000000000000000, 0.9510565162951535312, 1.000000000000000000, 0.9510565162951535312, 1.000000000000000000, 0.9510565162951535312, 1.000000000000000000, 0.9510565162951535312, 1.000000000000000000, 0.9510565162951535312, 1.000000000000000000, 0.9510565162951535312, 1.000000000000000000, 0.9510565162951535312, 1.000000000000000000, 0.9510565162951535312, 1.000000000000000000, 0.9510565162951535312, 1.000000000000000000, 0.9510565162951535312, 1.000000000000000000, 0.9510565162951535312, 1.000000000000000000, 0.9510565162951535312, 1.000000000000000000, 0.9510565162951535312, 1.000000000000000000, 0.9510565162951535312, 1.000000000000000000, 0.9510565162951535312, 1.000000000000000000, 0.9510565162951535312, 1.000000000000000000, 0.9510565162951535312, 1.000000000000000000, 0.9510565162951535312, 1.000000000000000000, 0.9510565162951535312, 1.000000000000000000, 0.9510565162951535312, 1.000000000000000000, 0.9510565162951535312, 1.000000000000000000, 0.9510565162951535312, 1.000000000000000000, 0.9510565162951535312, 1.000000000000000000, 0.9510565162951535312, 1.000000000000000000, 0.9510565162951535312, 1.000000000000000000, 0.9510565162951535312, 1.000000000000000000, 0.9510565162951535312, 1.000000000000000000, 0.9510565162951535312, 1.000000000000000000, 0.9510565162951535312, 1.000000000000000000, 0.9510565162951535312, 1.000000000000000000, 0.9510565162951535312, 1.000000000000000000, 0.9510565162951535312, 1.000000000000000000, 0.9510565162951535312, 1.000000000000000000, 0.9510565162951535312, 1.000000000000000000, 0.9510565162951535312, 1.000000000000000000, 0.9510565162951535312, 1.000000000000000000, 0.9510565162951535312, 1.000000000000000000, 0.9510565162951535312, 1.000000000000000000, 0.9510565162951535312, 1.000000000000000000, 0.9510565162951535312, 1.000000000000000000, 0.9510565162951535312, 1.000000000000000000, 0.9510565162951535312, 1.000000000000000000, 0.9510565162951535312, 1.000000000000000000, 0.9510565162951535312, 1.000000000000000000, 0.9510565162951535312, 1.000000000000000000),
 ( 1.000000000000000000, 0.9510565162951535312, 1.000000000000000000, 0.9510565162951535312, 1.000000000000000000, 0.9510565162951535312, 1.000000000000000000, 0.9510565162951535312, 1.000000000000000000, 0.9510565162951535312, 1.000000000000000000, 0.9510565162951535312, 1.000000000000000000, 0.9510565162951535312, 1.000000000000000000, 0.9510565162951535312, 1.000000000000000000, 0.9510565162951535312, 1.000000000000000000, 0.9510565162951535312, 1.000000000000000000, 0.9510565162951535312, 1.000000000000000000, 0.9510565162951535312, 1.000000000000000000, 0.9510565162951535312, 1.000000000000000000, 0.9510565162951535312, 1.000000000000000000, 0.9510565162951535312, 1.000000000000000000, 0.9510565162951535312, 1.000000000000000000, 0.9510565162951535312, 1.000000000000000000, 0.9510565162951535312, 1.000000000000000000, 0.9510565162951535312, 1.000000000000000000, 0.9510565162951535312, 1.000000000000000000, 0.9510565162951535312, 1.000000000000000000, 0.9510565162951535312, 1.000000000000000000, 0.9510565162951535312, 1.000000000000000000, 0.9510565162951535312, 1.000000000000000000, 0.9510565162951535312, 1.000000000000000000, 0.9510565162951535312, 1.000000000000000000, 0.9510565162951535312, 1.000000000000000000, 0.9510565162951535312, 1.000000000000000000, 0.9510565162951535312, 1.000000000000000000, 0.9510565162951535312, 1.000000000000000000, 0.9510565162951535312, 1.000000000000000000, 0.9510565162951535312, 1.000000000000000000, 0.9510565162951535312, 1.000000000000000000, 0.9510565162951535312, 1.000000000000000000, 0.9510565162951535312, 1.000000000000000000, 0.9510565162951535312, 1.000000000000000000, 0.9510565162951535312, 1.000000000000000000, 0.9510565162951535312, 1.000000000000000000, 0.9510565162951535312, 1.000000000000000000, 0.9510565162951535312, 1.000000000000000000, 0.9510565162951535312, 1.000000000000000000, 0.9510565162951535312, 1.000000000000000000, 0.9510565162951535312, 1.000000000000000000, 0.9510565162951535312, 1.000000000000000000, 0.9510565162951535312, 1.000000000000000000, 0.9510565162951535312, 1.000000000000000000, 0.9510565162951535312, 1.000000000000000000, 0.9510565162951535312, 1.000000000000000000, 0.9510565162951535312, 1.000000000000000000, 0.9510565162951535312, 1.000000000000000000) ) ) 
 REPRESENTATION_ITEM ( '' )  SURFACE ( )  );
#135009 = CARTESIAN_POINT ( 'NONE',  ( -10.72451020669898014, 18.67979575497178502, 105.4155762719810383 ) ) ;
#135010 = CARTESIAN_POINT ( 'NONE',  ( -12.14591786802309592, -12.06949235617757132, 41.87390960531435979 ) ) ;
#135011 = EDGE_LOOP ( 'NONE', ( #11961, #22607, #130103, #104738 ) ) ;
#135012 = CARTESIAN_POINT ( 'NONE',  ( 5.049401038298161559, -19.05341960407611168, 22.70724293864769194 ) ) ;
#135013 = CARTESIAN_POINT ( 'NONE',  ( 15.72974639402199770, -15.80617190586745480, 33.12390960531435979 ) ) ;
#135014 = CARTESIAN_POINT ( 'NONE',  ( -10.72451020669870658, -18.67979575497194134, 39.58442372801901143 ) ) ;
#135015 = CARTESIAN_POINT ( 'NONE',  ( -4.379528057220328563, 16.55341960407611168, 65.20724293864768129 ) ) ;
#135016 = CARTESIAN_POINT ( 'NONE',  ( 18.62759615963271287, -10.81492255796078972, 68.33224293864769550 ) ) ;
#135017 = CARTESIAN_POINT ( 'NONE',  ( 0.05219959533909260263, 19.03943276465977164, 69.99890960531435269 ) ) ;
#135019 = CARTESIAN_POINT ( 'NONE',  ( 19.05341960407617918, -5.049401038297876454, 81.04275706135231871 ) ) ;
#135018 = CARTESIAN_POINT ( 'NONE',  ( -9.474510206698964154, 16.51473224551069663, 30.41557627198102054 ) ) ;
#135020 = EDGE_CURVE ( 'NONE', #108375, #136724, #42559, .T. ) ;
#135021 = CARTESIAN_POINT ( 'NONE',  ( 18.67979575497178502, 10.72451020669898547, 44.16557627198103120 ) ) ;
#135022 = CARTESIAN_POINT ( 'NONE',  ( 13.97604488694527802, 13.89961937509977652, 39.37390960531435269 ) ) ;
#135023 = CARTESIAN_POINT ( 'NONE',  ( 19.02544592524343514, -5.153800228976328945, 68.54057627198103830 ) ) ;
#135024 = VERTEX_POINT ( 'NONE', #118403 ) ;
#135025 = CARTESIAN_POINT ( 'NONE',  ( 14.34966873604972726, -8.224510206698740333, 40.83442372801901854 ) ) ;
#135026 = CARTESIAN_POINT ( 'NONE',  ( 5.719274019375673035, 21.55341960407619339, 22.29275706135235069 ) ) ;
#135027 = CARTESIAN_POINT ( 'NONE',  ( -14.34966873604960291, -8.224510206698953496, 41.66557627198103120 ) ) ;
#135028 = CARTESIAN_POINT ( 'NONE',  ( 19.02544592524343514, -5.153800228976328945, 108.5405762719810383 ) ) ;
#135029 = CARTESIAN_POINT ( 'NONE',  ( -21.52544592524343514, 5.823673210054127303, 76.04057627198102409 ) ) ;
#135031 = CARTESIAN_POINT ( 'NONE',  ( 4.379528057220092307, 16.55341960407617563, 52.29275706135236135 ) ) ;
#135030 = CARTESIAN_POINT ( 'NONE',  ( 18.67979575497178502, 10.72451020669898547, 104.1655762719810241 ) ) ;
#135032 = CARTESIAN_POINT ( 'NONE',  ( -5.823673210054116645, -21.52544592524344225, 47.29057627198103120 ) ) ;
#135033 = CARTESIAN_POINT ( 'NONE',  ( -10.81492255796105439, 18.62759615963255655, 97.91775706135236135 ) ) ;
#135034 = CARTESIAN_POINT ( 'NONE',  ( 13.89961937509977652, -13.97604488694527269, 43.12390960531434558 ) ) ;
#135035 = CARTESIAN_POINT ( 'NONE',  ( 13.89961937509977652, -13.97604488694527269, 103.1239096053143527 ) ) ;
#135036 = CARTESIAN_POINT ( 'NONE',  ( 0.05219959533909260263, 19.03943276465977164, 69.99890960531435269 ) ) ;
#135037 = CARTESIAN_POINT ( 'NONE',  ( -15.49673173449292563, -38.75597260390001964, -19.54956558032594671 ) ) ;
#135038 = CARTESIAN_POINT ( 'NONE',  ( -5.049401038297874678, -19.05341960407617918, 59.79275706135231871 ) ) ;
#135040 = CARTESIAN_POINT ( 'NONE',  ( 21.53943276465977519, -0.05219959533907433946, 33.74890960531436690 ) ) ;
#135039 = CARTESIAN_POINT ( 'NONE',  ( -15.72974639402176322, -15.80617190586768395, 109.3760903946857042 ) ) ;
#135041 = CARTESIAN_POINT ( 'NONE',  ( -16.52544592524335698, -4.483927247898792601, 98.95942372801903275 ) ) ;
#135042 = CARTESIAN_POINT ( 'NONE',  ( -16.46253265017146816, -9.564922557961047289, 84.16775706135233293 ) ) ;
#135043 = CARTESIAN_POINT ( 'NONE',  ( -14.76659222988139675, -15.47206428619941398, -58.80197253718059613 ) ) ;
#135044 = CARTESIAN_POINT ( 'NONE',  ( 13.89961937509977652, -13.97604488694527269, 103.1239096053143527 ) ) ;
#135045 = CARTESIAN_POINT ( 'NONE',  ( -9.564922557961040184, 16.46253265017147172, 82.91775706135233293 ) ) ;
#135046 = CARTESIAN_POINT ( 'NONE',  ( -16.46253265017146816, -9.564922557961047289, 49.16775706135233293 ) ) ;
#135047 = CARTESIAN_POINT ( 'NONE',  ( -17.13100169013299023, -6.664070546373169535, 44.23210164300152059 ) ) ;
#135048 = CARTESIAN_POINT ( 'NONE',  ( 5.049401038298161559, -19.05341960407611168, 47.70724293864770260 ) ) ;
#135049 = CARTESIAN_POINT ( 'NONE',  ( -16.55341960407611168, -4.379528057220339221, 51.45724293864770260 ) ) ;
#135050 = CARTESIAN_POINT ( 'NONE',  ( 13.97604488694527802, 13.89961937509977652, 39.37390960531435269 ) ) ;
#135051 = CARTESIAN_POINT ( 'NONE',  ( -4.379528057220328563, 16.55341960407611168, 45.20724293864769550 ) ) ;
#135052 = DIRECTION ( 'NONE',  ( -0.8660254037844391517, 0.000000000000000000, 0.4999999999999989453 ) ) ;
#135053 = CARTESIAN_POINT ( 'NONE',  ( 0.05219959533934541429, -16.53943276465976808, 105.0010903946856757 ) ) ;
#135054 = CARTESIAN_POINT ( 'NONE',  ( -19.02544592524342804, 5.153800228976336051, 51.04057627198103120 ) ) ;
#135055 = CARTESIAN_POINT ( 'NONE',  ( 10.72451020669871369, 18.67979575497193778, 107.0844237280190043 ) ) ;
#135056 = CARTESIAN_POINT ( 'NONE',  ( -14.34966873604972548, 8.224510206698743886, 38.33442372801900433 ) ) ;
#135057 = CARTESIAN_POINT ( 'NONE',  ( 0.05219959533907565091, 21.53943276465977519, 39.99890960531436690 ) ) ;
#135059 = ORIENTED_EDGE ( 'NONE', *, *, #124207, .F. ) ;
#135058 = CARTESIAN_POINT ( 'NONE',  ( -5.823673210054431948, 21.52544592524334988, 97.70942372801904696 ) ) ;
#135060 = CARTESIAN_POINT ( 'NONE',  ( -19.03943276465977164, 0.05219959533909376836, 111.2489096053143669 ) ) ;
#135061 = CARTESIAN_POINT ( 'NONE',  ( 19.05341960407611168, 5.049401038298154454, 83.95724293864766707 ) ) ;
#135062 = CARTESIAN_POINT ( 'NONE',  ( 36.91746824999999887, -11.99521256947793546, -7.724999997268813701 ) ) ;
#135063 = CARTESIAN_POINT ( 'NONE',  ( 5.719274019375991003, -21.55341960407610458, 107.7072429386476955 ) ) ;
#135064 = CARTESIAN_POINT ( 'NONE',  ( 0.05219959533910956823, 16.53943276465976808, 74.99890960531435269 ) ) ;
#135065 = CARTESIAN_POINT ( 'NONE',  ( -10.81492255796078084, -18.62759615963271287, 72.08224293864769550 ) ) ;
#135066 = CARTESIAN_POINT ( 'NONE',  ( -16.46253265017160317, 9.564922557960807481, 75.83224293864769550 ) ) ;
#135067 = CARTESIAN_POINT ( 'NONE',  ( 5.719274019375991003, -21.55341960407610458, 92.70724293864770971 ) ) ;
#135068 = EDGE_LOOP ( 'NONE', ( #44209, #161081, #5242 ) ) ;
#135069 = CARTESIAN_POINT ( 'NONE',  ( -16.51473224551069308, -9.474510206698971260, 66.66557627198102409 ) ) ;
#135071 = CARTESIAN_POINT ( 'NONE',  ( 13.97604488694527802, 13.89961937509977652, 24.37390960531435624 ) ) ;
#135070 = CARTESIAN_POINT ( 'NONE',  ( 4.379528057220339221, -16.55341960407611168, 92.70724293864770971 ) ) ;
#135072 = CARTESIAN_POINT ( 'NONE',  ( -9.474510206698964154, 16.51473224551069663, 65.41557627198102409 ) ) ;
#135073 = CARTESIAN_POINT ( 'NONE',  ( -13.89961937509957401, -13.97604488694547875, 74.37609039468566152 ) ) ;
#135074 = CARTESIAN_POINT ( 'NONE',  ( -14.34966873604960291, -8.224510206698953496, 96.66557627198102409 ) ) ;
#135075 = CARTESIAN_POINT ( 'NONE',  ( 18.67979575497194134, -10.72451020669871369, 60.83442372801901854 ) ) ;
#135077 = CARTESIAN_POINT ( 'NONE',  ( 21.55341960407610458, 5.719274019375980345, 113.9572429386477239 ) ) ;
#135076 = CARTESIAN_POINT ( 'NONE',  ( 5.049401038298161559, -19.05341960407611168, 52.70724293864767418 ) ) ;
#135078 = CARTESIAN_POINT ( 'NONE',  ( -4.483927247898539470, -16.52544592524342804, 97.29057627198105251 ) ) ;
#135079 = CARTESIAN_POINT ( 'NONE',  ( -8.906447517083060816, 27.41122689804195645, 147.8500000054623627 ) ) ;
#135080 = CARTESIAN_POINT ( 'NONE',  ( 19.05341960407611168, 5.049401038298154454, 58.95724293864768129 ) ) ;
#135081 = CARTESIAN_POINT ( 'NONE',  ( -28.82186960331499037, 2.428612866367529932E-14, 138.2500000054623683 ) ) ;
#135083 = CARTESIAN_POINT ( 'NONE',  ( -13.97604488694527625, -13.89961937509977652, 111.8739096053143243 ) ) ;
#135082 = CARTESIAN_POINT ( 'NONE',  ( -19.05341960407617563, 5.049401038297882671, 108.5427570613523187 ) ) ;
#135084 = CARTESIAN_POINT ( 'NONE',  ( -18.67979575497193778, 10.72451020669871902, 43.33442372801901143 ) ) ;
#135085 = CARTESIAN_POINT ( 'NONE',  ( -0.05219959533909027116, -19.03943276465977164, 97.49890960531436690 ) ) ;
#135086 = CARTESIAN_POINT ( 'NONE',  ( 5.153800228976615827, -19.02544592524334988, 85.20942372801900433 ) ) ;
#135087 = CARTESIAN_POINT ( 'NONE',  ( 16.51473224551069308, 9.474510206698969483, 59.16557627198102409 ) ) ;
#135088 = CARTESIAN_POINT ( 'NONE',  ( -4.379528057220328563, 16.55341960407611168, 75.20724293864769550 ) ) ;
#135089 = CARTESIAN_POINT ( 'NONE',  ( 5.049401038298161559, -19.05341960407611168, 92.70724293864769550 ) ) ;
#135090 = CARTESIAN_POINT ( 'NONE',  ( -0.05219959533910754901, -16.53943276465976808, 72.49890960531435269 ) ) ;
#135091 = CARTESIAN_POINT ( 'NONE',  ( 16.46253265017160672, -9.564922557960803928, 78.33224293864769550 ) ) ;
#135092 = CARTESIAN_POINT ( 'NONE',  ( 16.46253265017146816, 9.564922557961045513, 31.66775706135232937 ) ) ;
#135095 = CARTESIAN_POINT ( 'NONE',  ( 13.89961937509977652, -13.97604488694527269, 23.12390960531436335 ) ) ;
#135094 = CARTESIAN_POINT ( 'NONE',  ( -4.483927247898539470, -16.52544592524342804, 42.29057627198103120 ) ) ;
#135093 = CARTESIAN_POINT ( 'NONE',  ( -9.474510206698964154, 16.51473224551069663, 55.41557627198103120 ) ) ;
#135096 = VERTEX_POINT ( 'NONE', #103228 ) ;
#135097 = CARTESIAN_POINT ( 'NONE',  ( 21.52544592524334988, 5.823673210054432836, 41.45942372801901143 ) ) ;
#135098 = CARTESIAN_POINT ( 'NONE',  ( 13.97604488694548053, -13.89961937509957401, 75.62609039468564731 ) ) ;
#135099 = CARTESIAN_POINT ( 'NONE',  ( 0.05219959533910956823, 16.53943276465976808, 29.99890960531435979 ) ) ;
#135100 = CARTESIAN_POINT ( 'NONE',  ( -5.719274019375978568, 21.55341960407610458, 105.2072429386477097 ) ) ;
#135101 = CARTESIAN_POINT ( 'NONE',  ( 15.80617190586746368, 15.72974639402197994, 39.37390960531436690 ) ) ;
#135102 = CARTESIAN_POINT ( 'NONE',  ( 14.34966873604960469, 8.224510206698951720, 69.16557627198102409 ) ) ;
#135103 = CARTESIAN_POINT ( 'NONE',  ( -9.564922557960796823, -16.46253265017161027, 47.08224293864769550 ) ) ;
#135104 = CARTESIAN_POINT ( 'NONE',  ( 14.34966873604972726, -8.224510206698740333, 100.8344237280190185 ) ) ;
#135105 = CARTESIAN_POINT ( 'NONE',  ( -12.06949235617739369, -12.14591786802326823, 64.37609039468568994 ) ) ;
#135106 = CARTESIAN_POINT ( 'NONE',  ( -19.03943276465977164, -0.05219959533935918106, 23.75109039468566152 ) ) ;
#135107 = CARTESIAN_POINT ( 'NONE',  ( 19.03943276465977164, -0.05219959533909143690, 98.74890960531436690 ) ) ;
#135108 = CARTESIAN_POINT ( 'NONE',  ( -16.51473224551069308, -9.474510206698971260, 81.66557627198103830 ) ) ;
#135109 = CARTESIAN_POINT ( 'NONE',  ( -16.55341960407617563, 4.379528057220093196, 68.54275706135234714 ) ) ;
#135110 = CARTESIAN_POINT ( 'NONE',  ( 19.03943276465977164, -0.05219959533909143690, 23.74890960531435269 ) ) ;
#135111 = CARTESIAN_POINT ( 'NONE',  ( -12.14591786802309592, -12.06949235617757132, 46.87390960531435979 ) ) ;
#135113 = CARTESIAN_POINT ( 'NONE',  ( -9.564922557960796823, -16.46253265017161027, 87.08224293864769550 ) ) ;
#135112 = CARTESIAN_POINT ( 'NONE',  ( -16.51473224551069308, -9.474510206698971260, 101.6655762719810241 ) ) ;
#135114 = CARTESIAN_POINT ( 'NONE',  ( 0.05219959533907565091, 21.53943276465977519, 24.99890960531435624 ) ) ;
#135115 = CARTESIAN_POINT ( 'NONE',  ( 4.483927247898545687, 16.52544592524342804, 69.79057627198102409 ) ) ;
#135116 = EDGE_CURVE ( 'NONE', #163891, #54169, #164910, .T. ) ;
#135117 = ORIENTED_EDGE ( 'NONE', *, *, #45131, .F. ) ;
#135118 = CARTESIAN_POINT ( 'NONE',  ( 14.34966873604960469, 8.224510206698951720, 69.16557627198102409 ) ) ;
#135120 = CARTESIAN_POINT ( 'NONE',  ( 31.88110949919180470, -0.2682394567895525772, -45.67705988491094615 ) ) ;
#135119 = CARTESIAN_POINT ( 'NONE',  ( 16.55341960407618274, -4.379528057220086978, 56.04275706135235424 ) ) ;
#135121 = CARTESIAN_POINT ( 'NONE',  ( 16.46253265017146816, 9.564922557961045513, 61.66775706135234003 ) ) ;
#135122 = CARTESIAN_POINT ( 'NONE',  ( 19.02544592524343514, -5.153800228976328945, 83.54057627198100988 ) ) ;
#135123 = CARTESIAN_POINT ( 'NONE',  ( 0.05219959533936267826, -19.03943276465977164, 60.00109039468566863 ) ) ;
#135124 = CARTESIAN_POINT ( 'NONE',  ( -27.73933785331498925, 9.013057229001089965, 149.2750000027311330 ) ) ;
#135126 = CARTESIAN_POINT ( 'NONE',  ( -14.29746914071037622, -8.314922557961029526, 94.16775706135237556 ) ) ;
#135125 = CARTESIAN_POINT ( 'NONE',  ( 16.46253265017146816, 9.564922557961045513, 111.6677570613523329 ) ) ;
#135127 = CARTESIAN_POINT ( 'NONE',  ( 19.02544592524343514, -5.153800228976328945, 38.54057627198103120 ) ) ;
#135128 = CARTESIAN_POINT ( 'NONE',  ( 21.55341960407610458, 5.719274019375980345, 23.95724293864769550 ) ) ;
#135129 = CARTESIAN_POINT ( 'NONE',  ( -5.719274019375665041, -21.55341960407619695, 49.79275706135234714 ) ) ;
#135130 = CARTESIAN_POINT ( 'NONE',  ( -16.46253265017146816, -9.564922557961047289, 109.1677570613523471 ) ) ;
#135132 = CARTESIAN_POINT ( 'NONE',  ( -13.89961937509977652, 13.97604488694528158, 80.62390960531436690 ) ) ;
#135131 = LINE ( 'NONE', #57286, #108949 ) ;
#135133 = AXIS2_PLACEMENT_3D ( 'NONE', #27949, #155236, #540 ) ;
#135134 = CARTESIAN_POINT ( 'NONE',  ( -30.73962218707678673, 22.33364281372846705, -0.2021577739498228998 ) ) ;
#135136 = CARTESIAN_POINT ( 'NONE',  ( 5.049401038298161559, -19.05341960407611168, 77.70724293864765286 ) ) ;
#135135 = CARTESIAN_POINT ( 'NONE',  ( 4.483927247898545687, 16.52544592524342804, 74.79057627198105251 ) ) ;
#135137 = CARTESIAN_POINT ( 'NONE',  ( 5.049401038298161559, -19.05341960407611168, 72.70724293864768129 ) ) ;
#135138 = CARTESIAN_POINT ( 'NONE',  ( -5.049401038297874678, -19.05341960407617918, 74.79275706135231871 ) ) ;
#135139 = CARTESIAN_POINT ( 'NONE',  ( 10.72451020669898902, -18.67979575497178502, 62.91557627198102409 ) ) ;
#135140 = CARTESIAN_POINT ( 'NONE',  ( -16.55341960407611168, -4.379528057220339221, 111.4572429386476813 ) ) ;
#135141 = CARTESIAN_POINT ( 'NONE',  ( -5.049401038297874678, -19.05341960407617918, 54.79275706135234003 ) ) ;
#135142 = CARTESIAN_POINT ( 'NONE',  ( -19.03943276465977164, 0.05219959533909376836, 51.24890960531436690 ) ) ;
#135143 = CARTESIAN_POINT ( 'NONE',  ( -5.049401038298153566, 19.05341960407611168, 90.20724293864766707 ) ) ;
#135144 = VERTEX_POINT ( 'NONE', #165903 ) ;
#135145 = CARTESIAN_POINT ( 'NONE',  ( 21.52544592524344225, -5.823673210054117533, 83.54057627198102409 ) ) ;
#135147 = CARTESIAN_POINT ( 'NONE',  ( 13.89961937509957401, 13.97604488694547697, 41.87609039468566152 ) ) ;
#135146 = CARTESIAN_POINT ( 'NONE',  ( 0.05219959533910956823, 16.53943276465976808, 89.99890960531438111 ) ) ;
#135148 = CARTESIAN_POINT ( 'NONE',  ( -5.719274019375978568, 21.55341960407610458, 80.20724293864769550 ) ) ;
#135149 = CARTESIAN_POINT ( 'NONE',  ( -10.81492255796078084, -18.62759615963271287, 57.08224293864769550 ) ) ;
#135150 = CARTESIAN_POINT ( 'NONE',  ( -12.06949235617756955, 12.14591786802309770, 35.62390960531437401 ) ) ;
#135151 = CARTESIAN_POINT ( 'NONE',  ( 21.55341960407619695, -5.719274019375665929, 101.0427570613523756 ) ) ;
#135152 = CARTESIAN_POINT ( 'NONE',  ( 9.474510206698971260, -16.51473224551069308, 77.91557627198103830 ) ) ;
#135153 = CARTESIAN_POINT ( 'NONE',  ( -0.05219959533909027116, -19.03943276465977164, 37.49890960531436690 ) ) ;
#135154 = CARTESIAN_POINT ( 'NONE',  ( 5.719274019375673035, 21.55341960407619339, 42.29275706135235424 ) ) ;
#135155 = CARTESIAN_POINT ( 'NONE',  ( 18.67979575497194134, -10.72451020669871369, 35.83442372801901143 ) ) ;
#135156 = CARTESIAN_POINT ( 'NONE',  ( -5.049401038298153566, 19.05341960407611168, 50.20724293864770260 ) ) ;
#135157 = CARTESIAN_POINT ( 'NONE',  ( -5.823673210054431948, 21.52544592524334988, 22.70942372801901499 ) ) ;
#135158 = CARTESIAN_POINT ( 'NONE',  ( 0.05219959533936267826, -19.03943276465977164, 65.00109039468567573 ) ) ;
#135160 = CARTESIAN_POINT ( 'NONE',  ( 16.46253265017160672, -9.564922557960803928, 33.33224293864770260 ) ) ;
#135159 = B_SPLINE_CURVE_WITH_KNOTS ( 'NONE', 3,
 ( #65593, #4902, #98900, #145413, #50442, #96912, #6895, #68573, #20084, #173791, #158595, #143414 ),
 .UNSPECIFIED., .F., .F.,
 ( 4, 2, 2, 2, 2, 4 ),
 ( 0.002244533994399153676, 0.002800305961463194111, 0.003078191944995206306, 0.003356077928527217633, 0.003911849895591248093, 0.004467621862655278553 ),
 .UNSPECIFIED. ) ;
#135161 = CARTESIAN_POINT ( 'NONE',  ( 16.53943276465976808, 0.05219959533934440121, 31.25109039468568639 ) ) ;
#135162 = CARTESIAN_POINT ( 'NONE',  ( 19.05341960407611168, 5.049401038298154454, 28.95724293864769550 ) ) ;
#135163 = CARTESIAN_POINT ( 'NONE',  ( -12.06949235617739369, -12.14591786802326823, 74.37609039468568994 ) ) ;
#135164 = CARTESIAN_POINT ( 'NONE',  ( 0.05219959533909260263, 19.03943276465977164, 39.99890960531436690 ) ) ;
#135165 = CARTESIAN_POINT ( 'NONE',  ( -24.54404792736193386, -12.06373989673657654, 169.8487138613016896 ) ) ;
#135166 = CARTESIAN_POINT ( 'NONE',  ( -16.46253265017160317, 9.564922557960807481, 90.83224293864769550 ) ) ;
#135167 = CARTESIAN_POINT ( 'NONE',  ( -13.89961937509977652, 13.97604488694528158, 30.62390960531435269 ) ) ;
#135168 = CARTESIAN_POINT ( 'NONE',  ( -21.55341960407610458, -5.719274019375992779, 71.45724293864769550 ) ) ;
#135169 = CARTESIAN_POINT ( 'NONE',  ( -16.53943276465976808, -0.05219959533934237506, 53.75109039468568994 ) ) ;
#135170 = CARTESIAN_POINT ( 'NONE',  ( 21.52544592524334988, 5.823673210054432836, 96.45942372801901854 ) ) ;
#135171 = CARTESIAN_POINT ( 'NONE',  ( 9.474510206698971260, -16.51473224551069308, 42.91557627198103120 ) ) ;
#135172 = CARTESIAN_POINT ( 'NONE',  ( -4.379528057220328563, 16.55341960407611168, 35.20724293864768839 ) ) ;
#135173 = CARTESIAN_POINT ( 'NONE',  ( 8.314922557960818139, 14.29746914071049879, 74.58224293864768129 ) ) ;
#135174 = CARTESIAN_POINT ( 'NONE',  ( 19.05341960407611168, 5.049401038298154454, 68.95724293864769550 ) ) ;
#135175 = CARTESIAN_POINT ( 'NONE',  ( 5.153800228976615827, -19.02544592524334988, 20.20942372801899722 ) ) ;
#135176 = CARTESIAN_POINT ( 'NONE',  ( 10.72451020669871369, 18.67979575497193778, 22.08442372801901143 ) ) ;
#135177 = CARTESIAN_POINT ( 'NONE',  ( 19.02544592524343514, -5.153800228976328945, 83.54057627198100988 ) ) ;
#135178 = CARTESIAN_POINT ( 'NONE',  ( -10.72451020669870658, -18.67979575497194134, 89.58442372801901854 ) ) ;
#135179 = CARTESIAN_POINT ( 'NONE',  ( 4.379528057220092307, 16.55341960407617563, 47.29275706135234003 ) ) ;
#135180 = CARTESIAN_POINT ( 'NONE',  ( -4.379528057220086978, -16.55341960407618274, 24.79275706135235779 ) ) ;
#135182 = CARTESIAN_POINT ( 'NONE',  ( 10.72451020669871369, 18.67979575497193778, 97.08442372801904696 ) ) ;
#135181 = CARTESIAN_POINT ( 'NONE',  ( -0.05219959533910754901, -16.53943276465976808, 92.49890960531436690 ) ) ;
#135183 = CARTESIAN_POINT ( 'NONE',  ( 4.483927247898545687, 16.52544592524342804, 34.79057627198103120 ) ) ;
#135184 = CARTESIAN_POINT ( 'NONE',  ( -16.46253265017160317, 9.564922557960807481, 25.83224293864769194 ) ) ;
#135185 = CARTESIAN_POINT ( 'NONE',  ( -8.314922557961024197, 14.29746914071037800, 57.91775706135234714 ) ) ;
#135186 = CARTESIAN_POINT ( 'NONE',  ( -4.483927247898539470, -16.52544592524342804, 52.29057627198102409 ) ) ;
#135187 = CARTESIAN_POINT ( 'NONE',  ( 16.55341960407618274, -4.379528057220086978, 96.04275706135236135 ) ) ;
#135188 = CARTESIAN_POINT ( 'NONE',  ( -10.81492255796078084, -18.62759615963271287, 22.08224293864769194 ) ) ;
#135189 = CARTESIAN_POINT ( 'NONE',  ( 5.719274019375991003, -21.55341960407610458, 37.70724293864769550 ) ) ;
#135190 = CARTESIAN_POINT ( 'NONE',  ( 15.72974639402176855, 15.80617190586768217, 111.8760903946856615 ) ) ;
#135191 = CARTESIAN_POINT ( 'NONE',  ( 8.224510206698953496, -14.34966873604960469, 92.91557627198103830 ) ) ;
#135192 = CARTESIAN_POINT ( 'NONE',  ( 5.049401038298161559, -19.05341960407611168, 92.70724293864769550 ) ) ;
#135193 = ORIENTED_EDGE ( 'NONE', *, *, #38432, .F. ) ;
#135194 = CARTESIAN_POINT ( 'NONE',  ( -8.314922557961024197, 14.29746914071037800, 37.91775706135235424 ) ) ;
#135195 = CARTESIAN_POINT ( 'NONE',  ( -16.46253265017160317, 9.564922557960807481, 35.83224293864768839 ) ) ;
#135197 = DIRECTION ( 'NONE',  ( -1.000000000000000000, -0.000000000000000000, -0.000000000000000000 ) ) ;
#135196 = CARTESIAN_POINT ( 'NONE',  ( 16.55341960407618274, -4.379528057220086978, 46.04275706135234714 ) ) ;
#135198 = CARTESIAN_POINT ( 'NONE',  ( -9.474510206698720793, -16.51473224551083518, 49.58442372801899722 ) ) ;
#135199 = EDGE_CURVE ( 'NONE', #42057, #76374, #176171, .T. ) ;
#135200 = CARTESIAN_POINT ( 'NONE',  ( -13.89961937509977652, 13.97604488694528158, 40.62390960531435979 ) ) ;
#135201 = CARTESIAN_POINT ( 'NONE',  ( 4.483927247898790824, -16.52544592524335698, 85.20942372801901854 ) ) ;
#135202 = CARTESIAN_POINT ( 'NONE',  ( 19.05341960407617918, -5.049401038297876454, 96.04275706135231871 ) ) ;
#135203 = CARTESIAN_POINT ( 'NONE',  ( 19.02544592524334988, 5.153800228976608722, 31.45942372801900433 ) ) ;
#135204 = CARTESIAN_POINT ( 'NONE',  ( 13.97604488694527802, 13.89961937509977652, 59.37390960531434558 ) ) ;
#135205 = CARTESIAN_POINT ( 'NONE',  ( 14.29746914071049879, -8.314922557960816363, 93.33224293864769550 ) ) ;
#135206 = EDGE_CURVE ( 'NONE', #160176, #161389, #56235, .T. ) ;
#135207 = CARTESIAN_POINT ( 'NONE',  ( -5.049401038297874678, -19.05341960407617918, 64.79275706135233293 ) ) ;
#135208 = CARTESIAN_POINT ( 'NONE',  ( 10.81492255796078972, 18.62759615963270932, 64.58224293864769550 ) ) ;
#135209 = CARTESIAN_POINT ( 'NONE',  ( -5.049401038297874678, -19.05341960407617918, 34.79275706135233293 ) ) ;
#135210 = CARTESIAN_POINT ( 'NONE',  ( -13.89961937509977652, 13.97604488694528158, 100.6239096053143669 ) ) ;
#135211 = CARTESIAN_POINT ( 'NONE',  ( -15.80617190586745835, -15.72974639402198527, 86.87390960531438111 ) ) ;
#135212 = CARTESIAN_POINT ( 'NONE',  ( -16.18388926212237777, 7.379444403734523483, 84.56046848633847901 ) ) ;
#135213 = CARTESIAN_POINT ( 'NONE',  ( -0.05219959533936034679, 19.03943276465977164, 97.50109039468567573 ) ) ;
#135214 = CARTESIAN_POINT ( 'NONE',  ( -18.22780087662122028, 5.500000000000031086, 98.51540105326105845 ) ) ;
#135215 = CARTESIAN_POINT ( 'NONE',  ( -14.29746914071037622, -8.314922557961029526, 24.16775706135235424 ) ) ;
#135216 = CARTESIAN_POINT ( 'NONE',  ( -9.474510206698964154, 16.51473224551069663, 45.41557627198103120 ) ) ;
#135217 = CARTESIAN_POINT ( 'NONE',  ( 19.03943276465977164, -0.05219959533909143690, 113.7489096053143669 ) ) ;
#135218 = CARTESIAN_POINT ( 'NONE',  ( 21.52544592524344225, -5.823673210054117533, 93.54057627198103830 ) ) ;
#135219 = CARTESIAN_POINT ( 'NONE',  ( -15.72974639402176322, -15.80617190586768395, 59.37609039468568284 ) ) ;
#135221 = CARTESIAN_POINT ( 'NONE',  ( -10.81492255796105439, 18.62759615963255655, 112.9177570613523329 ) ) ;
#135220 = CARTESIAN_POINT ( 'NONE',  ( 16.46253265017146816, 9.564922557961045513, 111.6677570613523329 ) ) ;
#135222 = CARTESIAN_POINT ( 'NONE',  ( -4.483927247898539470, -16.52544592524342804, 22.29057627198102765 ) ) ;
#135223 = CARTESIAN_POINT ( 'NONE',  ( 21.53943276465977519, -0.05219959533907433946, 103.7489096053143669 ) ) ;
#135224 = CARTESIAN_POINT ( 'NONE',  ( 0.05219959533910956823, 16.53943276465976808, 49.99890960531437401 ) ) ;
#135225 = CARTESIAN_POINT ( 'NONE',  ( -0.05219959533936034679, 19.03943276465977164, 82.50109039468567573 ) ) ;
#135226 = CARTESIAN_POINT ( 'NONE',  ( 19.03943276465977164, 0.05219959533936151252, 51.25109039468567573 ) ) ;
#135227 = CARTESIAN_POINT ( 'NONE',  ( 10.72451020669871369, 18.67979575497193778, 72.08442372801899012 ) ) ;
#135228 = CARTESIAN_POINT ( 'NONE',  ( -16.51473224551082808, 9.474510206698731452, 33.33442372801899722 ) ) ;
#135229 = CARTESIAN_POINT ( 'NONE',  ( 5.153800228976335163, 19.02544592524342804, 24.79057627198102765 ) ) ;
#135230 = CARTESIAN_POINT ( 'NONE',  ( -15.72974639402197994, 15.80617190586746368, 40.62390960531435269 ) ) ;
#135231 = CARTESIAN_POINT ( 'NONE',  ( 16.55341960407611168, 4.379528057220329451, 38.95724293864768839 ) ) ;
#135232 = CARTESIAN_POINT ( 'NONE',  ( 21.53943276465977519, 0.05219959533937863772, 106.2510903946856757 ) ) ;
#135233 = CARTESIAN_POINT ( 'NONE',  ( 4.379528057220092307, 16.55341960407617563, 77.29275706135234714 ) ) ;
#135234 = CARTESIAN_POINT ( 'NONE',  ( 8.314922557960818139, 14.29746914071049879, 24.58224293864768839 ) ) ;
#135235 = CARTESIAN_POINT ( 'NONE',  ( -21.52544592524334988, -5.823673210054445271, 63.95942372801901854 ) ) ;
#135236 = CARTESIAN_POINT ( 'NONE',  ( 5.719274019375673035, 21.55341960407619339, 72.29275706135236135 ) ) ;
#135237 = CARTESIAN_POINT ( 'NONE',  ( 15.80617190586746368, 15.72974639402197994, 74.37390960531436690 ) ) ;
#135238 = ORIENTED_EDGE ( 'NONE', *, *, #57626, .T. ) ;
#135239 = CARTESIAN_POINT ( 'NONE',  ( -0.05219959533909027116, -19.03943276465977164, 22.49890960531436690 ) ) ;
#135240 = CARTESIAN_POINT ( 'NONE',  ( -10.72451020669870658, -18.67979575497194134, 49.58442372801901143 ) ) ;
#135241 = CARTESIAN_POINT ( 'NONE',  ( -0.05219959533909027116, -19.03943276465977164, 27.49890960531435624 ) ) ;
#135242 = CARTESIAN_POINT ( 'NONE',  ( 5.049401038298161559, -19.05341960407611168, 42.70724293864767418 ) ) ;
#135243 = CARTESIAN_POINT ( 'NONE',  ( -14.29746914071049879, 8.314922557960819915, 90.83224293864769550 ) ) ;
#135244 = CARTESIAN_POINT ( 'NONE',  ( 5.049401038298161559, -19.05341960407611168, 87.70724293864769550 ) ) ;
#135245 = CARTESIAN_POINT ( 'NONE',  ( 4.483927247898545687, 16.52544592524342804, 29.79057627198102409 ) ) ;
#135246 = CARTESIAN_POINT ( 'NONE',  ( -8.224510206698948167, 14.34966873604960824, 100.4155762719810241 ) ) ;
#135247 = CARTESIAN_POINT ( 'NONE',  ( -15.72974639402197994, 15.80617190586746368, 70.62390960531436690 ) ) ;
#135248 = CARTESIAN_POINT ( 'NONE',  ( -5.823673210054116645, -21.52544592524344225, 102.2905762719810383 ) ) ;
#135249 = CARTESIAN_POINT ( 'NONE',  ( -13.97604488694527625, -13.89961937509977652, 111.8739096053143243 ) ) ;
#135251 = CARTESIAN_POINT ( 'NONE',  ( -16.52544592524335698, -4.483927247898792601, 23.95942372801901143 ) ) ;
#135250 = CARTESIAN_POINT ( 'NONE',  ( 0.05219959533909260263, 19.03943276465977164, 64.99890960531436690 ) ) ;
#135252 = CARTESIAN_POINT ( 'NONE',  ( 10.72451020669898902, -18.67979575497178502, 57.91557627198103120 ) ) ;
#135253 = CARTESIAN_POINT ( 'NONE',  ( 21.53943276465977519, 0.05219959533937863772, 86.25109039468568994 ) ) ;
#135254 = CARTESIAN_POINT ( 'NONE',  ( 5.049401038298161559, -19.05341960407611168, 77.70724293864765286 ) ) ;
#135255 = CARTESIAN_POINT ( 'NONE',  ( -5.049401038298153566, 19.05341960407611168, 115.2072429386477097 ) ) ;
#135256 = CARTESIAN_POINT ( 'NONE',  ( 14.29746914071037800, 8.314922557961029526, 81.66775706135236135 ) ) ;
#135257 = CARTESIAN_POINT ( 'NONE',  ( 5.823673210054444382, -21.52544592524334988, 60.20942372801902565 ) ) ;
#135258 = CARTESIAN_POINT ( 'NONE',  ( 10.81492255796106328, -18.62759615963255655, 95.41775706135234714 ) ) ;
#135259 = CARTESIAN_POINT ( 'NONE',  ( 14.29746914071037800, 8.314922557961029526, 61.66775706135235424 ) ) ;
#135260 = CARTESIAN_POINT ( 'NONE',  ( 21.55341960407610458, 5.719274019375980345, 108.9572429386476955 ) ) ;
#135261 = CARTESIAN_POINT ( 'NONE',  ( -0.05219959533909027116, -19.03943276465977164, 22.49890960531436690 ) ) ;
#135262 = VERTEX_POINT ( 'NONE', #154688 ) ;
#135263 = CARTESIAN_POINT ( 'NONE',  ( 21.53943276465977519, -0.05219959533907433946, 93.74890960531436690 ) ) ;
#135264 = CARTESIAN_POINT ( 'NONE',  ( 9.474510206698729675, 16.51473224551082808, 52.08442372801900433 ) ) ;
#135265 = CARTESIAN_POINT ( 'NONE',  ( -15.80617190586745835, -15.72974639402198527, 56.87390960531436690 ) ) ;
#135267 = CARTESIAN_POINT ( 'NONE',  ( -4.483927247898539470, -16.52544592524342804, 32.29057627198102409 ) ) ;
#135266 = CARTESIAN_POINT ( 'NONE',  ( -5.049401038298153566, 19.05341960407611168, 95.20724293864770971 ) ) ;
#135268 = CARTESIAN_POINT ( 'NONE',  ( 37.99999999999999289, 2.428612866367529932E-14, -24.99999999999997868 ) ) ;
#135269 = CARTESIAN_POINT ( 'NONE',  ( 9.564922557961047289, -16.46253265017146816, 110.4177570613523471 ) ) ;
#135270 = CARTESIAN_POINT ( 'NONE',  ( 10.81492255796078972, 18.62759615963270932, 74.58224293864768129 ) ) ;
#135271 = CARTESIAN_POINT ( 'NONE',  ( -8.314922557960811034, -14.29746914071050412, 57.08224293864769550 ) ) ;
#135272 = CARTESIAN_POINT ( 'NONE',  ( -8.314922557961024197, 14.29746914071037800, 27.91775706135234358 ) ) ;
#135273 = CARTESIAN_POINT ( 'NONE',  ( -9.474510206698964154, 16.51473224551069663, 45.41557627198103120 ) ) ;
#135275 = CARTESIAN_POINT ( 'NONE',  ( 16.46253265017146816, 9.564922557961045513, 81.66775706135233293 ) ) ;
#135274 = CARTESIAN_POINT ( 'NONE',  ( -15.72974639402197994, 15.80617190586746368, 115.6239096053143669 ) ) ;
#135276 = CARTESIAN_POINT ( 'NONE',  ( 9.564922557960805705, 16.46253265017160317, 79.58224293864769550 ) ) ;
#135277 = CARTESIAN_POINT ( 'NONE',  ( 16.51473224551069308, 9.474510206698969483, 79.16557627198103830 ) ) ;
#135278 = CARTESIAN_POINT ( 'NONE',  ( 18.67979575497178502, 10.72451020669898547, 79.16557627198103830 ) ) ;
#135279 = CARTESIAN_POINT ( 'NONE',  ( -19.02544592524342804, 5.153800228976336051, 36.04057627198100988 ) ) ;
#135280 = DIRECTION ( 'NONE',  ( -1.000000000000000000, 0.000000000000000000, 0.000000000000000000 ) ) ;
#135281 = CARTESIAN_POINT ( 'NONE',  ( 12.06949235617757843, -12.14591786802309237, 53.12390960531436690 ) ) ;
#135282 = CARTESIAN_POINT ( 'NONE',  ( 19.03943276465977164, -0.05219959533909143690, 83.74890960531436690 ) ) ;
#135283 = DIRECTION ( 'NONE',  ( 1.000000000000000000, -0.000000000000000000, -0.000000000000000000 ) ) ;
#135284 = CARTESIAN_POINT ( 'NONE',  ( 19.03943276465977164, 0.05219959533936151252, 71.25109039468566152 ) ) ;
#135285 = CARTESIAN_POINT ( 'NONE',  ( -15.80617190586745835, -15.72974639402198527, 76.87390960531439532 ) ) ;
#135286 = CARTESIAN_POINT ( 'NONE',  ( 9.564922557961047289, -16.46253265017146816, 40.41775706135234003 ) ) ;
#135287 = CARTESIAN_POINT ( 'NONE',  ( 13.97604488694527802, 13.89961937509977652, 84.37390960531433848 ) ) ;
#135288 = DIRECTION ( 'NONE',  ( -0.000000000000000000, -0.000000000000000000, 1.000000000000000000 ) ) ;
#135289 = CARTESIAN_POINT ( 'NONE',  ( 5.719274019375991003, -21.55341960407610458, 32.70724293864770260 ) ) ;
#135290 = CARTESIAN_POINT ( 'NONE',  ( 16.46253265017160672, -9.564922557960803928, 78.33224293864769550 ) ) ;
#135291 = CARTESIAN_POINT ( 'NONE',  ( 10.81492255796106328, -18.62759615963255655, 50.41775706135235424 ) ) ;
#135292 = CARTESIAN_POINT ( 'NONE',  ( -19.05341960407611168, -5.049401038298163336, 26.45724293864769550 ) ) ;
#135294 = ORIENTED_EDGE ( 'NONE', *, *, #40745, .T. ) ;
#135293 = CARTESIAN_POINT ( 'NONE',  ( 21.52544592524344225, -5.823673210054117533, 113.5405762719810383 ) ) ;
#135295 = CARTESIAN_POINT ( 'NONE',  ( -21.52544592524334988, -5.823673210054445271, 43.95942372801902565 ) ) ;
#135296 = ORIENTED_EDGE ( 'NONE', *, *, #102991, .T. ) ;
#135297 = CARTESIAN_POINT ( 'NONE',  ( -19.02544592524342804, 5.153800228976336051, 106.0405762719810241 ) ) ;
#135298 = CARTESIAN_POINT ( 'NONE',  ( -30.00000000000000000, 40.00100000000004741, 37.49999999999999289 ) ) ;
#135299 = CARTESIAN_POINT ( 'NONE',  ( 10.81492255796078972, 18.62759615963270932, 109.5822429386476955 ) ) ;
#135300 = CARTESIAN_POINT ( 'NONE',  ( -13.97604488694527625, -13.89961937509977652, 61.87390960531435979 ) ) ;
#135302 = EDGE_CURVE ( 'NONE', #132379, #88260, #144383, .T. ) ;
#135301 = CARTESIAN_POINT ( 'NONE',  ( -16.52544592524335698, -4.483927247898792601, 18.95942372801901143 ) ) ;
#135303 = CARTESIAN_POINT ( 'NONE',  ( 37.99999999999999289, 2.893978650043524126E-14, -6.749999994537627224 ) ) ;
#135304 = CARTESIAN_POINT ( 'NONE',  ( -21.52544592524334988, -5.823673210054445271, 103.9594237280190185 ) ) ;
#135305 = CARTESIAN_POINT ( 'NONE',  ( 9.564922557960805705, 16.46253265017160317, 44.58224293864769550 ) ) ;
#135306 = CARTESIAN_POINT ( 'NONE',  ( 10.72451020669871369, 18.67979575497193778, 97.08442372801904696 ) ) ;
#135308 = CARTESIAN_POINT ( 'NONE',  ( 10.81492255796106328, -18.62759615963255655, 60.41775706135235424 ) ) ;
#135307 = CARTESIAN_POINT ( 'NONE',  ( -5.049401038298153566, 19.05341960407611168, 90.20724293864766707 ) ) ;
#135309 = CARTESIAN_POINT ( 'NONE',  ( -17.14385361876520264, -23.59649016807271593, 143.6750000027311671 ) ) ;
#135310 = CARTESIAN_POINT ( 'NONE',  ( -5.153800228976328057, -19.02544592524343514, 97.29057627198099567 ) ) ;
#135311 = CARTESIAN_POINT ( 'NONE',  ( -24.49873734152895111, 24.99873734152937743, 5.353553390593268624 ) ) ;
#135314 = CARTESIAN_POINT ( 'NONE',  ( 21.53943276465977519, 0.05219959533937863772, 61.25109039468567573 ) ) ;
#135313 = CARTESIAN_POINT ( 'NONE',  ( -16.52544592524335698, -4.483927247898792601, 63.95942372801901854 ) ) ;
#135312 = CARTESIAN_POINT ( 'NONE',  ( 16.55341960407618274, -4.379528057220086978, 56.04275706135235424 ) ) ;
#135315 = CARTESIAN_POINT ( 'NONE',  ( -21.53943276465977519, -0.05219959533937600094, 83.75109039468568994 ) ) ;
#135316 = CARTESIAN_POINT ( 'NONE',  ( 31.79999999999968807, 4.791014396527177230E-13, 45.00000000000022027 ) ) ;
#135317 = CARTESIAN_POINT ( 'NONE',  ( 8.224510206698742110, 14.34966873604972548, 27.08442372801901854 ) ) ;
#135318 = CARTESIAN_POINT ( 'NONE',  ( 16.51473224551069308, 9.474510206698969483, 74.16557627198103830 ) ) ;
#135319 = CARTESIAN_POINT ( 'NONE',  ( -16.46253265017160317, 9.564922557960807481, 100.8322429386477097 ) ) ;
#135320 = EDGE_CURVE ( 'NONE', #15137, #114628, #171850, .T. ) ;
#135321 = CARTESIAN_POINT ( 'NONE',  ( 16.79531203550650176, 7.028104445595485750, 43.75244988220443787 ) ) ;
#135322 = CARTESIAN_POINT ( 'NONE',  ( 5.153800228976335163, 19.02544592524342804, 29.79057627198102409 ) ) ;
#135323 = CARTESIAN_POINT ( 'NONE',  ( -15.72974639402197994, 15.80617190586746368, 40.62390960531435269 ) ) ;
#135324 = CARTESIAN_POINT ( 'NONE',  ( -16.53943276465976808, -0.05219959533934237506, 88.75109039468567573 ) ) ;
#135326 = CARTESIAN_POINT ( 'NONE',  ( -16.51473224551069308, -9.474510206698971260, 61.66557627198103120 ) ) ;
#135325 = CARTESIAN_POINT ( 'NONE',  ( 8.314922557960818139, 14.29746914071049879, 89.58224293864768129 ) ) ;
#135327 = CARTESIAN_POINT ( 'NONE',  ( -15.80617190586768217, 15.72974639402176855, 88.12609039468570415 ) ) ;
#135328 = CARTESIAN_POINT ( 'NONE',  ( -24.28797299941338039, 0.2180554607495331365, -56.78142080721297447 ) ) ;
#135329 = CARTESIAN_POINT ( 'NONE',  ( 8.224510206698742110, 14.34966873604972548, 22.08442372801901143 ) ) ;
#135330 = CARTESIAN_POINT ( 'NONE',  ( 12.14591786802309770, 12.06949235617756955, 79.37390960531436690 ) ) ;
#135331 = CARTESIAN_POINT ( 'NONE',  ( -10.81492255796105439, 18.62759615963255655, 47.91775706135234714 ) ) ;
#135332 = CARTESIAN_POINT ( 'NONE',  ( -15.80617190586745835, -15.72974639402198527, 71.87390960531438111 ) ) ;
#135333 = CARTESIAN_POINT ( 'NONE',  ( -13.89961937509957401, -13.97604488694547875, 34.37609039468566863 ) ) ;
#135334 = CARTESIAN_POINT ( 'NONE',  ( 18.22780087662121673, 5.500000000000056843, 43.98459894673892734 ) ) ;
#135335 = CARTESIAN_POINT ( 'NONE',  ( -9.564922557960796823, -16.46253265017161027, 77.08224293864769550 ) ) ;
#135336 = CARTESIAN_POINT ( 'NONE',  ( -8.224510206698948167, 14.34966873604960824, 45.41557627198103830 ) ) ;
#135337 = CARTESIAN_POINT ( 'NONE',  ( 16.55341960407611168, 4.379528057220329451, 33.95724293864769550 ) ) ;
#135338 = CARTESIAN_POINT ( 'NONE',  ( -16.53943276465976808, 0.05219959533911058130, 21.24890960531436690 ) ) ;
#135339 = CARTESIAN_POINT ( 'NONE',  ( 19.02544592524334988, 5.153800228976608722, 66.45942372801899012 ) ) ;
#135340 = CARTESIAN_POINT ( 'NONE',  ( 18.87255363501902394, 5.499999999999941380, 53.82513748171829349 ) ) ;
#135341 = CARTESIAN_POINT ( 'NONE',  ( 15.80617190586746368, 15.72974639402197994, 29.37390960531435269 ) ) ;
#135342 = CARTESIAN_POINT ( 'NONE',  ( 16.55341960407611168, 4.379528057220329451, 93.95724293864770971 ) ) ;
#135343 = DIRECTION ( 'NONE',  ( 0.000000000000000000, 0.000000000000000000, -1.000000000000000000 ) ) ;
#135345 = CARTESIAN_POINT ( 'NONE',  ( -18.62759615963270932, 10.81492255796079327, 30.83224293864770260 ) ) ;
#135344 = CARTESIAN_POINT ( 'NONE',  ( 13.97604488694527802, 13.89961937509977652, 39.37390960531435269 ) ) ;
#135346 = CARTESIAN_POINT ( 'NONE',  ( 5.719274019375991003, -21.55341960407610458, 62.70724293864769550 ) ) ;
#135347 = CARTESIAN_POINT ( 'NONE',  ( -19.03943276465977164, 0.05219959533909376836, 21.24890960531436335 ) ) ;
#135349 = CARTESIAN_POINT ( 'NONE',  ( 5.049401038298161559, -19.05341960407611168, 52.70724293864767418 ) ) ;
#135348 = CARTESIAN_POINT ( 'NONE',  ( -14.29746914071037622, -8.314922557961029526, 69.16775706135234714 ) ) ;
#135350 = EDGE_CURVE ( 'NONE', #80087, #165429, #168850, .T. ) ;
#135351 = CARTESIAN_POINT ( 'NONE',  ( 10.72451020669871369, 18.67979575497193778, 52.08442372801901854 ) ) ;
#135352 = VERTEX_POINT ( 'NONE', #184042 ) ;
#135353 = CARTESIAN_POINT ( 'NONE',  ( -12.14591786802309592, -12.06949235617757132, 101.8739096053143811 ) ) ;
#135354 = CARTESIAN_POINT ( 'NONE',  ( 9.564922557961047289, -16.46253265017146816, 90.41775706135234714 ) ) ;
#135355 = CARTESIAN_POINT ( 'NONE',  ( -36.91746825000000598, -11.99521256947794789, -5.024999997268813523 ) ) ;
#135357 = CARTESIAN_POINT ( 'NONE',  ( -15.80617190586745835, -15.72974639402198527, 36.87390960531435979 ) ) ;
#135356 = LINE ( 'NONE', #124887, #170195 ) ;
#135358 = CARTESIAN_POINT ( 'NONE',  ( 17.49999999999998934, -5.500000000000023981, 78.29690382534170112 ) ) ;
#135359 = CARTESIAN_POINT ( 'NONE',  ( -21.55341960407619339, 5.719274019375674811, 73.54275706135234714 ) ) ;
#135360 = VECTOR ( 'NONE', #33556, 1000.000000000000000 ) ;
#135362 = CARTESIAN_POINT ( 'NONE',  ( -0.05219959533910754901, -16.53943276465976808, 42.49890960531435979 ) ) ;
#135361 = CARTESIAN_POINT ( 'NONE',  ( 4.483927247898790824, -16.52544592524335698, 50.20942372801901854 ) ) ;
#135363 = CARTESIAN_POINT ( 'NONE',  ( 21.53943276465977519, -0.05219959533907433946, 68.74890960531435269 ) ) ;
#135364 = CARTESIAN_POINT ( 'NONE',  ( -15.80617190586745835, -15.72974639402198527, 66.87390960531436690 ) ) ;
#135365 = CARTESIAN_POINT ( 'NONE',  ( -21.81018892176227553, -9.477090470496813523, 170.9397748289982246 ) ) ;
#135367 = CARTESIAN_POINT ( 'NONE',  ( -18.62759615963270932, 10.81492255796079327, 25.83224293864769194 ) ) ;
#135366 = CARTESIAN_POINT ( 'NONE',  ( -13.97604488694547697, 13.89961937509957934, 83.12609039468564731 ) ) ;
#135368 = CARTESIAN_POINT ( 'NONE',  ( 9.474510206698971260, -16.51473224551069308, 47.91557627198102409 ) ) ;
#135369 = CARTESIAN_POINT ( 'NONE',  ( 8.314922557960818139, 14.29746914071049879, 109.5822429386476955 ) ) ;
#135370 =( NAMED_UNIT ( * ) SI_UNIT ( $, .STERADIAN. ) SOLID_ANGLE_UNIT ( ) );
#135371 = CARTESIAN_POINT ( 'NONE',  ( -19.02544592524342804, 5.153800228976336051, 116.0405762719810383 ) ) ;
#135372 = EDGE_LOOP ( 'NONE', ( #184079, #73182 ) ) ;
#135373 = CARTESIAN_POINT ( 'NONE',  ( 12.06949235617739724, 12.14591786802326823, 71.87609039468568994 ) ) ;
#135374 = CARTESIAN_POINT ( 'NONE',  ( 10.72451020669898902, -18.67979575497178502, 102.9155762719810383 ) ) ;
#135375 = CARTESIAN_POINT ( 'NONE',  ( -13.97604488694527625, -13.89961937509977652, 66.87390960531436690 ) ) ;
#135376 = CARTESIAN_POINT ( 'NONE',  ( -15.72974639402176322, -15.80617190586768395, 39.37609039468567573 ) ) ;
#135377 = CARTESIAN_POINT ( 'NONE',  ( -13.97604488694527625, -13.89961937509977652, 101.8739096053143811 ) ) ;
#135378 = CARTESIAN_POINT ( 'NONE',  ( -26.35664240927071944, -29.91691629194321322, -17.00538226201434711 ) ) ;
#135379 = EDGE_LOOP ( 'NONE', ( #169124, #165287 ) ) ;
#135380 = CARTESIAN_POINT ( 'NONE',  ( 5.719274019375673035, 21.55341960407619339, 32.29275706135235424 ) ) ;
#135382 = CARTESIAN_POINT ( 'NONE',  ( -19.05341960407617563, 5.049401038297882671, 93.54275706135234714 ) ) ;
#135381 = CARTESIAN_POINT ( 'NONE',  ( 5.153800228976335163, 19.02544592524342804, 24.79057627198102765 ) ) ;
#135383 = CARTESIAN_POINT ( 'NONE',  ( 9.474510206698729675, 16.51473224551082808, 47.08442372801900433 ) ) ;
#135384 = CARTESIAN_POINT ( 'NONE',  ( -18.62759615963270932, 10.81492255796079327, 100.8322429386477097 ) ) ;
#135385 = CARTESIAN_POINT ( 'NONE',  ( 5.049401038297881783, 19.05341960407617563, 37.29275706135232582 ) ) ;
#135386 = CARTESIAN_POINT ( 'NONE',  ( 19.03943276465977164, 0.05219959533936151252, 46.25109039468566863 ) ) ;
#135387 = CARTESIAN_POINT ( 'NONE',  ( 4.483927247898790824, -16.52544592524335698, 95.20942372801903275 ) ) ;
#135389 = EDGE_LOOP ( 'NONE', ( #90331, #68836, #102269, #58711 ) ) ;
#135388 = CARTESIAN_POINT ( 'NONE',  ( -16.46253265017160317, 9.564922557960807481, 115.8322429386477097 ) ) ;
#135390 = CARTESIAN_POINT ( 'NONE',  ( -5.153800228976328057, -19.02544592524343514, 67.29057627198102409 ) ) ;
#135391 = CARTESIAN_POINT ( 'NONE',  ( -0.05219959533937732626, 21.53943276465977519, 82.50109039468568994 ) ) ;
#135392 = CARTESIAN_POINT ( 'NONE',  ( 15.80617190586769283, -15.72974639402175789, 90.62609039468567573 ) ) ;
#135393 = CARTESIAN_POINT ( 'NONE',  ( -1.351053078614605107, -6.941067294099600105, -64.37011660792194334 ) ) ;
#135394 = CARTESIAN_POINT ( 'NONE',  ( 9.564922557960805705, 16.46253265017160317, 89.58224293864769550 ) ) ;
#135395 = CARTESIAN_POINT ( 'NONE',  ( 5.823673210054444382, -21.52544592524334988, 60.20942372801902565 ) ) ;
#135396 = CARTESIAN_POINT ( 'NONE',  ( 9.474510206698729675, 16.51473224551082808, 107.0844237280190043 ) ) ;
#135397 = CARTESIAN_POINT ( 'NONE',  ( -13.97604488694527625, -13.89961937509977652, 61.87390960531435979 ) ) ;
#135398 = CARTESIAN_POINT ( 'NONE',  ( 9.474510206698971260, -16.51473224551069308, 112.9155762719810383 ) ) ;
#135399 = CARTESIAN_POINT ( 'NONE',  ( 13.97604488694527802, 13.89961937509977652, 84.37390960531433848 ) ) ;
#135400 = CARTESIAN_POINT ( 'NONE',  ( -17.44270441346520073, -5.991230190322948346, 91.36335079264229364 ) ) ;
#135401 = CARTESIAN_POINT ( 'NONE',  ( 13.97604488694527802, 13.89961937509977652, 64.37390960531436690 ) ) ;
#135402 = CARTESIAN_POINT ( 'NONE',  ( -19.02544592524342804, 5.153800228976336051, 46.04057627198101699 ) ) ;
#135403 = CARTESIAN_POINT ( 'NONE',  ( -10.72451020669898014, 18.67979575497178502, 110.4155762719810383 ) ) ;
#135404 = CARTESIAN_POINT ( 'NONE',  ( -12.14591786802326823, 12.06949235617739902, 88.12609039468570415 ) ) ;
#135405 = FACE_OUTER_BOUND ( 'NONE', #159261, .T. ) ;
#135406 = CARTESIAN_POINT ( 'NONE',  ( -16.46253265017146816, -9.564922557961047289, 49.16775706135233293 ) ) ;
#135407 = CARTESIAN_POINT ( 'NONE',  ( 13.89961937509977652, -13.97604488694527269, 73.12390960531436690 ) ) ;
#135408 = CARTESIAN_POINT ( 'NONE',  ( -12.06949235617756955, 12.14591786802309770, 65.62390960531436690 ) ) ;
#135409 = CARTESIAN_POINT ( 'NONE',  ( -14.34966873604960291, -8.224510206698953496, 106.6655762719810383 ) ) ;
#135410 = CARTESIAN_POINT ( 'NONE',  ( -16.46253265017160317, 9.564922557960807481, 110.8322429386476955 ) ) ;
#135411 = CARTESIAN_POINT ( 'NONE',  ( -13.97604488694527625, -13.89961937509977652, 111.8739096053143243 ) ) ;
#135412 = CARTESIAN_POINT ( 'NONE',  ( -14.29746914071049879, 8.314922557960819915, 75.83224293864769550 ) ) ;
#135413 = CARTESIAN_POINT ( 'NONE',  ( 19.97888994334924817, -34.65319547504296338, -7.500000000000000000 ) ) ;
#135414 = CARTESIAN_POINT ( 'NONE',  ( -16.46253265017146816, -9.564922557961047289, 29.16775706135232937 ) ) ;
#135415 = CARTESIAN_POINT ( 'NONE',  ( 12.14591786802327356, -12.06949235617739191, 100.6260903946857184 ) ) ;
#135416 = CARTESIAN_POINT ( 'NONE',  ( -9.474510206698964154, 16.51473224551069663, 85.41557627198102409 ) ) ;
#135417 = CARTESIAN_POINT ( 'NONE',  ( 10.81492255796106328, -18.62759615963255655, 55.41775706135234714 ) ) ;
#135418 = CARTESIAN_POINT ( 'NONE',  ( -21.55341960407610458, -5.719274019375992779, 46.45724293864769550 ) ) ;
#135419 = CARTESIAN_POINT ( 'NONE',  ( -21.53943276465977519, 0.05219959533907696930, 111.2489096053143669 ) ) ;
#135420 = CARTESIAN_POINT ( 'NONE',  ( 21.52544592524344225, -5.823673210054117533, 63.54057627198103830 ) ) ;
#135421 = CARTESIAN_POINT ( 'NONE',  ( 8.314922557960818139, 14.29746914071049879, 94.58224293864769550 ) ) ;
#135422 = CARTESIAN_POINT ( 'NONE',  ( -16.51473224551082808, 9.474510206698731452, 58.33442372801900433 ) ) ;
#135423 = CARTESIAN_POINT ( 'NONE',  ( -9.474510206698964154, 16.51473224551069663, 25.41557627198103120 ) ) ;
#135424 = CARTESIAN_POINT ( 'NONE',  ( 9.564922557960805705, 16.46253265017160317, 84.58224293864769550 ) ) ;
#135425 = CARTESIAN_POINT ( 'NONE',  ( 19.03943276465977164, -0.05219959533909143690, 83.74890960531436690 ) ) ;
#135426 = CARTESIAN_POINT ( 'NONE',  ( -8.314922557960811034, -14.29746914071050412, 107.0822429386476955 ) ) ;
#135427 = ORIENTED_EDGE ( 'NONE', *, *, #172537, .F. ) ;
#135428 = CARTESIAN_POINT ( 'NONE',  ( -8.224510206698948167, 14.34966873604960824, 30.41557627198101699 ) ) ;
#135429 = CARTESIAN_POINT ( 'NONE',  ( -16.52544592524335698, -4.483927247898792601, 38.95942372801901854 ) ) ;
#135430 = CARTESIAN_POINT ( 'NONE',  ( 0.05219959533937995610, -21.53943276465977519, 105.0010903946856757 ) ) ;
#135431 = CARTESIAN_POINT ( 'NONE',  ( -16.46253265017160317, 9.564922557960807481, 95.83224293864769550 ) ) ;
#135432 = CARTESIAN_POINT ( 'NONE',  ( -5.719274019375665041, -21.55341960407619695, 34.79275706135235424 ) ) ;
#135433 = CARTESIAN_POINT ( 'NONE',  ( 9.564922557960805705, 16.46253265017160317, 49.58224293864770260 ) ) ;
#135434 = CARTESIAN_POINT ( 'NONE',  ( 8.314922557961029526, -14.29746914071037800, 45.41775706135234003 ) ) ;
#135435 = EDGE_CURVE ( 'NONE', #84987, #171876, #62850, .T. ) ;
#135436 = CARTESIAN_POINT ( 'NONE',  ( -13.97604488694547697, 13.89961937509957934, 108.1260903946856331 ) ) ;
#135437 = CARTESIAN_POINT ( 'NONE',  ( 0.05219959533909260263, 19.03943276465977164, 39.99890960531436690 ) ) ;
#135438 = CARTESIAN_POINT ( 'NONE',  ( 4.379528057220339221, -16.55341960407611168, 97.70724293864772392 ) ) ;
#135439 = CARTESIAN_POINT ( 'NONE',  ( 18.67979575497178502, 10.72451020669898547, 99.16557627198100988 ) ) ;
#135440 = CARTESIAN_POINT ( 'NONE',  ( -5.153800228976607833, 19.02544592524334988, 77.70942372801900433 ) ) ;
#135441 = FILL_AREA_STYLE ('',( #182929 ) ) ;
#135442 = CARTESIAN_POINT ( 'NONE',  ( 16.51473224551069308, 9.474510206698969483, 89.16557627198103830 ) ) ;
#135443 = CARTESIAN_POINT ( 'NONE',  ( 18.67979575497194134, -10.72451020669871369, 35.83442372801901143 ) ) ;
#135444 = CARTESIAN_POINT ( 'NONE',  ( -19.03943276465977164, 0.05219959533909376836, 21.24890960531436335 ) ) ;
#135445 = CARTESIAN_POINT ( 'NONE',  ( -16.51473224551069308, -9.474510206698971260, 91.66557627198103830 ) ) ;
#135446 = CARTESIAN_POINT ( 'NONE',  ( 17.31728774477275223, -6.344390552232368030, 113.3190665168932014 ) ) ;
#135447 = CARTESIAN_POINT ( 'NONE',  ( -13.89961937509977652, 13.97604488694528158, 85.62390960531433848 ) ) ;
#135449 = CARTESIAN_POINT ( 'NONE',  ( -4.379528057220328563, 16.55341960407611168, 85.20724293864770971 ) ) ;
#135448 = CARTESIAN_POINT ( 'NONE',  ( -18.62759615963255300, -10.81492255796106328, 34.16775706135234714 ) ) ;
#135450 = CARTESIAN_POINT ( 'NONE',  ( -13.97604488694527625, -13.89961937509977652, 96.87390960531433848 ) ) ;
#135451 = CARTESIAN_POINT ( 'NONE',  ( -21.55341960407619339, 5.719274019375674811, 113.5427570613523756 ) ) ;
#135452 = CARTESIAN_POINT ( 'NONE',  ( 12.06949235617739724, 12.14591786802326823, 51.87609039468568284 ) ) ;
#135453 = CARTESIAN_POINT ( 'NONE',  ( -18.62759615963255300, -10.81492255796106328, 74.16775706135231871 ) ) ;
#135454 = CARTESIAN_POINT ( 'NONE',  ( -16.55341960407617563, 4.379528057220093196, 28.54275706135234358 ) ) ;
#135455 = CARTESIAN_POINT ( 'NONE',  ( -19.03943276465977164, 0.05219959533909376836, 66.24890960531436690 ) ) ;
#135456 = CARTESIAN_POINT ( 'NONE',  ( 13.97604488694548053, -13.89961937509957401, 90.62609039468567573 ) ) ;
#135457 = CARTESIAN_POINT ( 'NONE',  ( -16.52544592524335698, -4.483927247898792601, 68.95942372801901854 ) ) ;
#135458 = CARTESIAN_POINT ( 'NONE',  ( 16.46253265017146816, 9.564922557961045513, 21.66775706135233648 ) ) ;
#135459 = CARTESIAN_POINT ( 'NONE',  ( 9.474510206698729675, 16.51473224551082808, 82.08442372801899012 ) ) ;
#135460 = CARTESIAN_POINT ( 'NONE',  ( 19.05341960407611168, 5.049401038298154454, 58.95724293864768129 ) ) ;
#135461 = CARTESIAN_POINT ( 'NONE',  ( 15.80617190586746368, 15.72974639402197994, 89.37390960531435269 ) ) ;
#135463 = CARTESIAN_POINT ( 'NONE',  ( -19.03943276465977164, -0.05219959533935918106, 78.75109039468567573 ) ) ;
#135462 = CARTESIAN_POINT ( 'NONE',  ( -8.224510206698948167, 14.34966873604960824, 75.41557627198102409 ) ) ;
#135464 = CARTESIAN_POINT ( 'NONE',  ( -17.49999999999999645, -5.499999999999992895, 74.20309617465828467 ) ) ;
#135466 = ADVANCED_FACE ( 'NONE', ( #16183 ), #28473, .T. ) ;
#135465 = CARTESIAN_POINT ( 'NONE',  ( 19.03943276465977164, 0.05219959533936151252, 51.25109039468567573 ) ) ;
#135467 = CARTESIAN_POINT ( 'NONE',  ( 8.314922557960818139, 14.29746914071049879, 24.58224293864768839 ) ) ;
#135468 = CARTESIAN_POINT ( 'NONE',  ( -14.34966873604960291, -8.224510206698953496, 81.66557627198103830 ) ) ;
#135470 = CARTESIAN_POINT ( 'NONE',  ( 8.571926809382603096, -26.38167802310801235, 147.4750000027311785 ) ) ;
#135469 = CARTESIAN_POINT ( 'NONE',  ( -15.80617190586768217, 15.72974639402176855, 113.1260903946856899 ) ) ;
#135471 = CARTESIAN_POINT ( 'NONE',  ( 15.72974639402199770, -15.80617190586745480, 108.1239096053143811 ) ) ;
#135472 = CARTESIAN_POINT ( 'NONE',  ( -9.474510206698964154, 16.51473224551069663, 100.4155762719810241 ) ) ;
#135473 = CARTESIAN_POINT ( 'NONE',  ( 13.89961937509977652, -13.97604488694527269, 68.12390960531436690 ) ) ;
#135474 = CARTESIAN_POINT ( 'NONE',  ( -15.72974639402176322, -15.80617190586768395, 79.37609039468567573 ) ) ;
#135475 = CARTESIAN_POINT ( 'NONE',  ( -19.05341960407611168, -5.049401038298163336, 66.45724293864769550 ) ) ;
#135476 = CARTESIAN_POINT ( 'NONE',  ( -16.46253265017160317, 9.564922557960807481, 35.83224293864768839 ) ) ;
#135477 = CARTESIAN_POINT ( 'NONE',  ( -5.719274019375978568, 21.55341960407610458, 25.20724293864769550 ) ) ;
#135478 = CARTESIAN_POINT ( 'NONE',  ( -14.29746914071049879, 8.314922557960819915, 85.83224293864768129 ) ) ;
#135479 = CARTESIAN_POINT ( 'NONE',  ( 5.153800228976335163, 19.02544592524342804, 44.79057627198103830 ) ) ;
#135480 = CARTESIAN_POINT ( 'NONE',  ( -12.14591786802309592, -12.06949235617757132, 101.8739096053143811 ) ) ;
#135481 = CARTESIAN_POINT ( 'NONE',  ( 18.67979575497178502, 10.72451020669898547, 109.1655762719810383 ) ) ;
#135482 = CARTESIAN_POINT ( 'NONE',  ( -10.72451020669870658, -18.67979575497194134, 44.58442372801901854 ) ) ;
#135483 = CARTESIAN_POINT ( 'NONE',  ( 16.51473224551069308, 9.474510206698969483, 34.16557627198102409 ) ) ;
#135484 = CARTESIAN_POINT ( 'NONE',  ( 4.483927247898790824, -16.52544592524335698, 70.20942372801904696 ) ) ;
#135485 = CARTESIAN_POINT ( 'NONE',  ( -15.80617190586745835, -15.72974639402198527, 96.87390960531436690 ) ) ;
#135486 = CARTESIAN_POINT ( 'NONE',  ( -21.52544592524343514, 5.823673210054127303, 96.04057627198102409 ) ) ;
#135488 = CARTESIAN_POINT ( 'NONE',  ( 19.02544592524343514, -5.153800228976328945, 58.54057627198102409 ) ) ;
#135487 = CARTESIAN_POINT ( 'NONE',  ( -19.02544592524334988, -5.153800228976617603, 23.95942372801900078 ) ) ;
#135489 = CARTESIAN_POINT ( 'NONE',  ( -17.97161686094258215, 5.499999999999976019, 40.99637206859248550 ) ) ;
#135490 = CARTESIAN_POINT ( 'NONE',  ( -10.72451020669870658, -18.67979575497194134, 59.58442372801901854 ) ) ;
#135491 = CARTESIAN_POINT ( 'NONE',  ( -15.72974639402197994, 15.80617190586746368, 60.62390960531437401 ) ) ;
#135492 = CARTESIAN_POINT ( 'NONE',  ( 0.05219959533910956823, 16.53943276465976808, 24.99890960531435624 ) ) ;
#135494 = CARTESIAN_POINT ( 'NONE',  ( 9.474510206698729675, 16.51473224551082808, 22.08442372801899722 ) ) ;
#135493 = CARTESIAN_POINT ( 'NONE',  ( -21.55341960407619339, 5.719274019375674811, 73.54275706135234714 ) ) ;
#135495 = CARTESIAN_POINT ( 'NONE',  ( 5.049401038297881783, 19.05341960407617563, 47.29275706135231161 ) ) ;
#135496 = CARTESIAN_POINT ( 'NONE',  ( 16.53943276465976808, 0.05219959533934440121, 96.25109039468568994 ) ) ;
#135497 = CARTESIAN_POINT ( 'NONE',  ( -10.81492255796105439, 18.62759615963255655, 52.91775706135235424 ) ) ;
#135498 = CARTESIAN_POINT ( 'NONE',  ( 9.474510206698971260, -16.51473224551069308, 52.91557627198102409 ) ) ;
#135499 = CARTESIAN_POINT ( 'NONE',  ( 5.153800228976615827, -19.02544592524334988, 40.20942372801898301 ) ) ;
#135500 = CARTESIAN_POINT ( 'NONE',  ( -5.719274019375978568, 21.55341960407610458, 35.20724293864768839 ) ) ;
#135501 = CARTESIAN_POINT ( 'NONE',  ( -21.53943276465977519, -0.05219959533937600094, 33.75109039468568284 ) ) ;
#135502 = VECTOR ( 'NONE', #114479, 999.9999999999998863 ) ;
#135503 = CARTESIAN_POINT ( 'NONE',  ( -21.52544592524343514, 5.823673210054127303, 86.04057627198102409 ) ) ;
#135504 = CARTESIAN_POINT ( 'NONE',  ( -5.153800228976607833, 19.02544592524334988, 82.70942372801897591 ) ) ;
#135505 = CARTESIAN_POINT ( 'NONE',  ( 14.34966873604972726, -8.224510206698740333, 50.83442372801901143 ) ) ;
#135507 = CARTESIAN_POINT ( 'NONE',  ( 0.05219959533907565091, 21.53943276465977519, 94.99890960531436690 ) ) ;
#135506 = CARTESIAN_POINT ( 'NONE',  ( -6.875118674992797274, 5.563226388833924396, -61.95704554880759218 ) ) ;
#135509 = CARTESIAN_POINT ( 'NONE',  ( -8.224510206698948167, 14.34966873604960824, 80.41557627198103830 ) ) ;
#135508 = CARTESIAN_POINT ( 'NONE',  ( 12.06949235617739724, 12.14591786802326823, 81.87609039468568994 ) ) ;
#135510 = DIRECTION ( 'NONE',  ( 0.5000000000000037748, 0.4999999999999950595, 0.7071067811865484609 ) ) ;
#135511 = CARTESIAN_POINT ( 'NONE',  ( 13.89961937509957401, 13.97604488694547697, 101.8760903946856331 ) ) ;
#135512 = CARTESIAN_POINT ( 'NONE',  ( 15.80617190586746368, 15.72974639402197994, 34.37390960531435979 ) ) ;
#135513 = CARTESIAN_POINT ( 'NONE',  ( -18.22780087662123805, 5.499999999999981348, 96.01763182126897789 ) ) ;
#135514 = CARTESIAN_POINT ( 'NONE',  ( -8.224510206698735004, -14.34966873604973081, 49.58442372801901143 ) ) ;
#135515 = CARTESIAN_POINT ( 'NONE',  ( -15.80617190586768217, 15.72974639402176855, 33.12609039468569705 ) ) ;
#135516 = CARTESIAN_POINT ( 'NONE',  ( 21.52544592524344225, -5.823673210054117533, 33.54057627198102409 ) ) ;
#135517 = CARTESIAN_POINT ( 'NONE',  ( -16.55341960407617563, 4.379528057220093196, 68.54275706135234714 ) ) ;
#135518 = CARTESIAN_POINT ( 'NONE',  ( -0.05219959533909027116, -19.03943276465977164, 87.49890960531436690 ) ) ;
#135520 = CARTESIAN_POINT ( 'NONE',  ( 13.89961937509977652, -13.97604488694527269, 28.12390960531435624 ) ) ;
#135519 = CARTESIAN_POINT ( 'NONE',  ( -15.80617190586768217, 15.72974639402176855, 58.12609039468568994 ) ) ;
#135521 = CARTESIAN_POINT ( 'NONE',  ( 5.719274019375991003, -21.55341960407610458, 27.70724293864769905 ) ) ;
#135522 = ORIENTED_EDGE ( 'NONE', *, *, #74471, .T. ) ;
#135523 = CARTESIAN_POINT ( 'NONE',  ( 13.89961937509957401, 13.97604488694547697, 36.87609039468565442 ) ) ;
#135524 = CARTESIAN_POINT ( 'NONE',  ( 8.224510206698742110, 14.34966873604972548, 57.08442372801901854 ) ) ;
#135525 = CARTESIAN_POINT ( 'NONE',  ( 5.823673210054125526, 21.52544592524343514, 24.79057627198103120 ) ) ;
#135526 = CARTESIAN_POINT ( 'NONE',  ( 19.05341960407611168, 5.049401038298154454, 68.95724293864769550 ) ) ;
#135527 = CARTESIAN_POINT ( 'NONE',  ( 4.483927247898790824, -16.52544592524335698, 100.2094237280190043 ) ) ;
#135528 = CYLINDRICAL_SURFACE ( 'NONE', #153839, 7.500000000000000000 ) ;
#135529 = CARTESIAN_POINT ( 'NONE',  ( -14.34966873604960291, -8.224510206698953496, 96.66557627198102409 ) ) ;
#135530 = CARTESIAN_POINT ( 'NONE',  ( 0.05219959533907565091, 21.53943276465977519, 34.99890960531435979 ) ) ;
#135531 = CARTESIAN_POINT ( 'NONE',  ( -13.97604488694527625, -13.89961937509977652, 36.87390960531436690 ) ) ;
#135532 = CARTESIAN_POINT ( 'NONE',  ( -8.224510206698735004, -14.34966873604973081, 74.58442372801901854 ) ) ;
#135533 = CARTESIAN_POINT ( 'NONE',  ( -5.719274019375665041, -21.55341960407619695, 19.79275706135235069 ) ) ;
#135534 = CARTESIAN_POINT ( 'NONE',  ( -16.46253265017146816, -9.564922557961047289, 74.16775706135234714 ) ) ;
#135535 = CARTESIAN_POINT ( 'NONE',  ( 13.89961937509977652, -13.97604488694527269, 43.12390960531434558 ) ) ;
#135536 = VECTOR ( 'NONE', #65589, 1000.000000000000000 ) ;
#135537 = CARTESIAN_POINT ( 'NONE',  ( -13.89961937509977652, 13.97604488694528158, 110.6239096053143243 ) ) ;
#135538 = CARTESIAN_POINT ( 'NONE',  ( 5.719274019375673035, 21.55341960407619339, 97.29275706135234714 ) ) ;
#135539 = CARTESIAN_POINT ( 'NONE',  ( 19.02544592524343514, -5.153800228976328945, 58.54057627198102409 ) ) ;
#135540 = CARTESIAN_POINT ( 'NONE',  ( -12.14591786802326823, 12.06949235617739902, 53.12609039468568284 ) ) ;
#135541 = CARTESIAN_POINT ( 'NONE',  ( -21.52544592524334988, -5.823673210054445271, 83.95942372801900433 ) ) ;
#135542 = CARTESIAN_POINT ( 'NONE',  ( 19.05341960407617918, -5.049401038297876454, 36.04275706135234003 ) ) ;
#135543 = CARTESIAN_POINT ( 'NONE',  ( 0.05219959533936267826, -19.03943276465977164, 55.00109039468566863 ) ) ;
#135544 = CARTESIAN_POINT ( 'NONE',  ( -21.55341960407619339, 5.719274019375674811, 53.54275706135234714 ) ) ;
#135545 = EDGE_CURVE ( 'NONE', #91305, #199831, #49110, .T. ) ;
#135546 = CARTESIAN_POINT ( 'NONE',  ( -5.049401038298153566, 19.05341960407611168, 25.20724293864768484 ) ) ;
#135547 = CARTESIAN_POINT ( 'NONE',  ( 19.05341960407617918, -5.049401038297876454, 51.04275706135231871 ) ) ;
#135548 = CARTESIAN_POINT ( 'NONE',  ( 13.89961937509977652, -13.97604488694527269, 98.12390960531433848 ) ) ;
#135549 = CARTESIAN_POINT ( 'NONE',  ( 16.51473224551069308, 9.474510206698969483, 79.16557627198103830 ) ) ;
#135550 = CARTESIAN_POINT ( 'NONE',  ( 14.29746914071049879, -8.314922557960816363, 38.33224293864768839 ) ) ;
#135551 = CARTESIAN_POINT ( 'NONE',  ( -21.55341960407610458, -5.719274019375992779, 36.45724293864768839 ) ) ;
#135552 = CARTESIAN_POINT ( 'NONE',  ( -11.40812507854754720, -35.11059874428192273, -4.724999997268812812 ) ) ;
#135553 = CARTESIAN_POINT ( 'NONE',  ( 28.79475375365586132, 2.781246896534039337E-14, 140.9843446568999923 ) ) ;
#135554 = CARTESIAN_POINT ( 'NONE',  ( 10.81492255796106328, -18.62759615963255655, 95.41775706135234714 ) ) ;
#135555 = CARTESIAN_POINT ( 'NONE',  ( -27.89903062892789620, 7.496893268503697527, 160.9845644947731387 ) ) ;
#135556 = CARTESIAN_POINT ( 'NONE',  ( 19.03943276465977164, -0.05219959533909143690, 38.74890960531436690 ) ) ;
#135557 = FACE_OUTER_BOUND ( 'NONE', #181040, .T. ) ;
#135558 = CARTESIAN_POINT ( 'NONE',  ( 0.05219959533934541429, -16.53943276465976808, 65.00109039468568994 ) ) ;
#135559 = EDGE_CURVE ( 'NONE', #164346, #138197, #53036, .T. ) ;
#135560 = CARTESIAN_POINT ( 'NONE',  ( -5.823673210054116645, -21.52544592524344225, 77.29057627198102409 ) ) ;
#135561 = CARTESIAN_POINT ( 'NONE',  ( 12.06949235617757843, -12.14591786802309237, 38.12390960531436690 ) ) ;
#135563 = CARTESIAN_POINT ( 'NONE',  ( 13.89961937509977652, -13.97604488694527269, 108.1239096053143669 ) ) ;
#135562 = CARTESIAN_POINT ( 'NONE',  ( -9.474510206698964154, 16.51473224551069663, 30.41557627198102054 ) ) ;
#135564 = CARTESIAN_POINT ( 'NONE',  ( -21.53943276465977519, -0.05219959533937600094, 23.75109039468567929 ) ) ;
#135565 = CARTESIAN_POINT ( 'NONE',  ( -9.474510206698720793, -16.51473224551083518, 29.58442372801900433 ) ) ;
#135566 = CARTESIAN_POINT ( 'NONE',  ( -19.03943276465977164, 0.05219959533909376836, 21.24890960531436335 ) ) ;
#135567 = CARTESIAN_POINT ( 'NONE',  ( 21.53943276465977519, 0.05219959533937863772, 81.25109039468568994 ) ) ;
#135568 = DIRECTION ( 'NONE',  ( 1.000000000000000000, 0.000000000000000000, 0.000000000000000000 ) ) ;
#135569 = CARTESIAN_POINT ( 'NONE',  ( -14.34966873604960291, -8.224510206698953496, 21.66557627198102409 ) ) ;
#135570 = CARTESIAN_POINT ( 'NONE',  ( -22.81625015709510507, 31.40387420917330275, -1.424999997268813212 ) ) ;
#135571 = CARTESIAN_POINT ( 'NONE',  ( 10.72451020669898902, -18.67979575497178502, 22.91557627198102765 ) ) ;
#135572 = CARTESIAN_POINT ( 'NONE',  ( -0.05219959533910754901, -16.53943276465976808, 102.4989096053143811 ) ) ;
#135573 = CARTESIAN_POINT ( 'NONE',  ( 21.25171708481321176, -32.43382446246057071, -17.33145006470355654 ) ) ;
#135574 = CARTESIAN_POINT ( 'NONE',  ( 0.05219959533909260263, 19.03943276465977164, 84.99890960531436690 ) ) ;
#135575 = CARTESIAN_POINT ( 'NONE',  ( -12.06949235617756955, 12.14591786802309770, 70.62390960531436690 ) ) ;
#135576 = CARTESIAN_POINT ( 'NONE',  ( -9.474510206698720793, -16.51473224551083518, 99.58442372801900433 ) ) ;
#135577 = CARTESIAN_POINT ( 'NONE',  ( -5.823673210054116645, -21.52544592524344225, 62.29057627198102409 ) ) ;
#135578 = ORIENTED_EDGE ( 'NONE', *, *, #184713, .F. ) ;
#135579 = CARTESIAN_POINT ( 'NONE',  ( 19.02544592524343514, -5.153800228976328945, 33.54057627198102409 ) ) ;
#135581 = CARTESIAN_POINT ( 'NONE',  ( -18.67979575497178146, -10.72451020669898902, 86.66557627198102409 ) ) ;
#135580 = CARTESIAN_POINT ( 'NONE',  ( -16.51473224551069308, -9.474510206698971260, 91.66557627198103830 ) ) ;
#135583 = CARTESIAN_POINT ( 'NONE',  ( -19.02544592524342804, 5.153800228976336051, 81.04057627198103830 ) ) ;
#135582 = CARTESIAN_POINT ( 'NONE',  ( -16.52544592524335698, -4.483927247898792601, 98.95942372801903275 ) ) ;
#135584 = CARTESIAN_POINT ( 'NONE',  ( -5.153800228976607833, 19.02544592524334988, 67.70942372801900433 ) ) ;
#135585 = CARTESIAN_POINT ( 'NONE',  ( 10.72451020669871369, 18.67979575497193778, 92.08442372801901854 ) ) ;
#135586 = CARTESIAN_POINT ( 'NONE',  ( -18.62759615963270932, 10.81492255796079327, 70.83224293864770971 ) ) ;
#135587 = CARTESIAN_POINT ( 'NONE',  ( 21.55341960407610458, 5.719274019375980345, 38.95724293864768839 ) ) ;
#135588 = CARTESIAN_POINT ( 'NONE',  ( -16.51473224551069308, -9.474510206698971260, 56.66557627198103120 ) ) ;
#135589 = CARTESIAN_POINT ( 'NONE',  ( -14.34966873604960291, -8.224510206698953496, 21.66557627198102409 ) ) ;
#135590 = CARTESIAN_POINT ( 'NONE',  ( 9.474510206698971260, -16.51473224551069308, 62.91557627198102409 ) ) ;
#135591 = CARTESIAN_POINT ( 'NONE',  ( 17.50000000000000000, 5.624438216177601646, 51.68329655085358354 ) ) ;
#135592 = CARTESIAN_POINT ( 'NONE',  ( 18.67979575497194134, -10.72451020669871369, 105.8344237280190328 ) ) ;
#135593 = CARTESIAN_POINT ( 'NONE',  ( -14.29746914071049879, 8.314922557960819915, 75.83224293864769550 ) ) ;
#135594 = CARTESIAN_POINT ( 'NONE',  ( 15.72974639402199770, -15.80617190586745480, 108.1239096053143811 ) ) ;
#135595 = CARTESIAN_POINT ( 'NONE',  ( -15.72974639402197994, 15.80617190586746368, 105.6239096053143669 ) ) ;
#135596 = CARTESIAN_POINT ( 'NONE',  ( 0.000000000000000000, 0.000000000000000000, -10.00000000000000000 ) ) ;
#135597 = CARTESIAN_POINT ( 'NONE',  ( 15.80617190586746368, 15.72974639402197994, 64.37390960531435269 ) ) ;
#135598 = CARTESIAN_POINT ( 'NONE',  ( 8.314922557961029526, -14.29746914071037800, 85.41775706135236135 ) ) ;
#135599 = CARTESIAN_POINT ( 'NONE',  ( -16.52544592524342804, 4.483927247898546575, 106.0405762719810525 ) ) ;
#135600 = CARTESIAN_POINT ( 'NONE',  ( -9.474510206698964154, 16.51473224551069663, 65.41557627198102409 ) ) ;
#135601 = FILL_AREA_STYLE_COLOUR ( '', #136953 ) ;
#135602 = CARTESIAN_POINT ( 'NONE',  ( -4.379528057220086978, -16.55341960407618274, 104.7927570613523898 ) ) ;
#135603 = CARTESIAN_POINT ( 'NONE',  ( -21.53943276465977519, -0.05219959533937600094, 48.75109039468568284 ) ) ;
#135604 = CARTESIAN_POINT ( 'NONE',  ( 16.46253265017160672, -9.564922557960803928, 103.3322429386476955 ) ) ;
#135605 = CARTESIAN_POINT ( 'NONE',  ( 18.67979575497194134, -10.72451020669871369, 85.83442372801901854 ) ) ;
#135606 = CARTESIAN_POINT ( 'NONE',  ( -9.474510206698964154, 16.51473224551069663, 25.41557627198103120 ) ) ;
#135607 = CARTESIAN_POINT ( 'NONE',  ( -13.97604488694527625, -13.89961937509977652, 36.87390960531436690 ) ) ;
#135608 = ORIENTED_EDGE ( 'NONE', *, *, #53169, .F. ) ;
#135609 = CARTESIAN_POINT ( 'NONE',  ( 10.81492255796106328, -18.62759615963255655, 80.41775706135234714 ) ) ;
#135610 = CARTESIAN_POINT ( 'NONE',  ( -15.80617190586768217, 15.72974639402176855, 73.12609039468567573 ) ) ;
#135611 = CARTESIAN_POINT ( 'NONE',  ( 9.564922557960805705, 16.46253265017160317, 104.5822429386476955 ) ) ;
#135612 = CARTESIAN_POINT ( 'NONE',  ( 9.474510206698729675, 16.51473224551082808, 77.08442372801900433 ) ) ;
#135613 = CARTESIAN_POINT ( 'NONE',  ( 5.823673210054444382, -21.52544592524334988, 50.20942372801901854 ) ) ;
#135614 = CARTESIAN_POINT ( 'NONE',  ( -12.06949235617739369, -12.14591786802326823, 24.37609039468567573 ) ) ;
#135615 = CARTESIAN_POINT ( 'NONE',  ( -13.89961937509957401, -13.97604488694547875, 74.37609039468566152 ) ) ;
#135616 = CARTESIAN_POINT ( 'NONE',  ( 16.46253265017160672, -9.564922557960803928, 48.33224293864769550 ) ) ;
#135617 = CARTESIAN_POINT ( 'NONE',  ( -0.05219959533936034679, 19.03943276465977164, 77.50109039468566152 ) ) ;
#135618 = CARTESIAN_POINT ( 'NONE',  ( 0.05219959533910956823, 16.53943276465976808, 24.99890960531435624 ) ) ;
#135619 = CARTESIAN_POINT ( 'NONE',  ( 0.05219959533936267826, -19.03943276465977164, 95.00109039468567573 ) ) ;
#135620 = CARTESIAN_POINT ( 'NONE',  ( 0.05219959533910956823, 16.53943276465976808, 39.99890960531436690 ) ) ;
#135621 = CARTESIAN_POINT ( 'NONE',  ( -13.89961937509957401, -13.97604488694547875, 64.37609039468567573 ) ) ;
#135622 = CARTESIAN_POINT ( 'NONE',  ( -8.314922557961024197, 14.29746914071037800, 42.91775706135235424 ) ) ;
#135623 = CARTESIAN_POINT ( 'NONE',  ( 5.049401038297881783, 19.05341960407617563, 27.29275706135232937 ) ) ;
#135624 = CARTESIAN_POINT ( 'NONE',  ( -9.564922557960796823, -16.46253265017161027, 37.08224293864768839 ) ) ;
#135625 = CARTESIAN_POINT ( 'NONE',  ( -17.59860650958989936, -7.585241751807033417, 66.57662985737508166 ) ) ;
#135626 = CARTESIAN_POINT ( 'NONE',  ( 16.55341960407618274, -4.379528057220086978, 46.04275706135234714 ) ) ;
#135627 = FACE_OUTER_BOUND ( 'NONE', #104835, .T. ) ;
#135628 = CARTESIAN_POINT ( 'NONE',  ( 22.44159573604009594, -16.30477369853687364, 141.6750000027311671 ) ) ;
#135629 = CARTESIAN_POINT ( 'NONE',  ( -16.46253265017160317, 9.564922557960807481, 95.83224293864769550 ) ) ;
#135630 = CARTESIAN_POINT ( 'NONE',  ( -17.58332526062526213, -7.635886036038624702, 84.07665040441537485 ) ) ;
#135631 = ORIENTED_EDGE ( 'NONE', *, *, #101975, .T. ) ;
#135632 = CARTESIAN_POINT ( 'NONE',  ( 0.05219959533936267826, -19.03943276465977164, 95.00109039468567573 ) ) ;
#135634 = CARTESIAN_POINT ( 'NONE',  ( -15.80617190586745835, -15.72974639402198527, 21.87390960531436690 ) ) ;
#135633 = CIRCLE ( 'NONE', #132437, 2.700000000000001066 ) ;
#135636 = CARTESIAN_POINT ( 'NONE',  ( 13.89961937509957401, 13.97604488694547697, 106.8760903946856757 ) ) ;
#135635 = CARTESIAN_POINT ( 'NONE',  ( 21.53943276465977519, 0.05219959533937863772, 111.2510903946856899 ) ) ;
#135637 = CARTESIAN_POINT ( 'NONE',  ( -16.51473224551069308, -9.474510206698971260, 21.66557627198102765 ) ) ;
#135638 = CARTESIAN_POINT ( 'NONE',  ( -5.153800228976328057, -19.02544592524343514, 37.29057627198102409 ) ) ;
#135639 = CARTESIAN_POINT ( 'NONE',  ( -21.52544592524343514, 5.823673210054127303, 56.04057627198102409 ) ) ;
#135640 = CARTESIAN_POINT ( 'NONE',  ( -13.89961937509977652, 13.97604488694528158, 35.62390960531435269 ) ) ;
#135641 = CARTESIAN_POINT ( 'NONE',  ( 1.993301997531345686E-15, -30.30510711980685556, 142.7500000054623683 ) ) ;
#135642 = CARTESIAN_POINT ( 'NONE',  ( -19.05341960407617563, 5.049401038297882671, 68.54275706135230450 ) ) ;
#135643 = CARTESIAN_POINT ( 'NONE',  ( -16.53943276465976808, 0.05219959533911058130, 56.24890960531436690 ) ) ;
#135644 = CARTESIAN_POINT ( 'NONE',  ( 21.52544592524344225, -5.823673210054117533, 28.54057627198103120 ) ) ;
#135645 = CARTESIAN_POINT ( 'NONE',  ( -21.55341960407619339, 5.719274019375674811, 93.54275706135234714 ) ) ;
#135646 = CARTESIAN_POINT ( 'NONE',  ( 21.53943276465977519, -0.05219959533907433946, 83.74890960531435269 ) ) ;
#135647 = CARTESIAN_POINT ( 'NONE',  ( 21.55341960407619695, -5.719274019375665929, 61.04275706135234714 ) ) ;
#135648 = CARTESIAN_POINT ( 'NONE',  ( 0.05219959533937995610, -21.53943276465977519, 70.00109039468568994 ) ) ;
#135649 = CARTESIAN_POINT ( 'NONE',  ( -19.02544592524342804, 5.153800228976336051, 96.04057627198103830 ) ) ;
#135651 = CARTESIAN_POINT ( 'NONE',  ( -10.72451020669870658, -18.67979575497194134, 64.58442372801900433 ) ) ;
#135650 = CARTESIAN_POINT ( 'NONE',  ( -16.52544592524335698, -4.483927247898792601, 88.95942372801901854 ) ) ;
#135652 = CARTESIAN_POINT ( 'NONE',  ( 19.03943276465977164, -0.05219959533909143690, 53.74890960531436690 ) ) ;
#135653 = CARTESIAN_POINT ( 'NONE',  ( -9.564922557960796823, -16.46253265017161027, 22.08224293864768839 ) ) ;
#135654 = CARTESIAN_POINT ( 'NONE',  ( 16.51473224551069308, 9.474510206698969483, 49.16557627198102409 ) ) ;
#135655 = CARTESIAN_POINT ( 'NONE',  ( 16.52544592524342804, -4.483927247898539470, 68.54057627198103830 ) ) ;
#135656 = CARTESIAN_POINT ( 'NONE',  ( 16.53943276465976808, -0.05219959533910856209, 33.74890960531436690 ) ) ;
#135657 = CARTESIAN_POINT ( 'NONE',  ( 21.53943276465977519, -0.05219959533907433946, 48.74890960531435979 ) ) ;
#135658 = CARTESIAN_POINT ( 'NONE',  ( 19.05341960407611168, 5.049401038298154454, 53.95724293864770260 ) ) ;
#135659 = CARTESIAN_POINT ( 'NONE',  ( 10.81492255796078972, 18.62759615963270932, 59.58224293864770260 ) ) ;
#135660 = CARTESIAN_POINT ( 'NONE',  ( -9.564922557961040184, 16.46253265017147172, 47.91775706135233293 ) ) ;
#135662 = CARTESIAN_POINT ( 'NONE',  ( 16.55341960407611168, 4.379528057220329451, 53.95724293864770260 ) ) ;
#135661 = DIRECTION ( 'NONE',  ( -0.000000000000000000, -0.000000000000000000, 1.000000000000000000 ) ) ;
#135663 = CARTESIAN_POINT ( 'NONE',  ( -0.05219959533907301413, -21.53943276465977519, 27.49890960531435269 ) ) ;
#135664 = ORIENTED_EDGE ( 'NONE', *, *, #95255, .T. ) ;
#135665 = EDGE_LOOP ( 'NONE', ( #171162, #131625, #152428, #28022 ) ) ;
#135666 = CARTESIAN_POINT ( 'NONE',  ( 17.26058549869091152, 6.457015423128542153, 103.8774583747606783 ) ) ;
#135667 = CARTESIAN_POINT ( 'NONE',  ( 12.14591786802327356, -12.06949235617739191, 65.62609039468568994 ) ) ;
#135668 = CARTESIAN_POINT ( 'NONE',  ( -19.02544592524334988, -5.153800228976617603, 68.95942372801896170 ) ) ;
#135669 = CARTESIAN_POINT ( 'NONE',  ( -8.224510206698948167, 14.34966873604960824, 55.41557627198102409 ) ) ;
#135670 = DIRECTION ( 'NONE',  ( 0.000000000000000000, 0.000000000000000000, 1.000000000000000000 ) ) ;
#135671 = CARTESIAN_POINT ( 'NONE',  ( -14.29746914071049879, 8.314922557960819915, 40.83224293864769550 ) ) ;
#135672 = CARTESIAN_POINT ( 'NONE',  ( 5.049401038298161559, -19.05341960407611168, 47.70724293864770260 ) ) ;
#135673 = CARTESIAN_POINT ( 'NONE',  ( 9.564922557960805705, 16.46253265017160317, 69.58224293864770971 ) ) ;
#135674 = CARTESIAN_POINT ( 'NONE',  ( -19.02544592524342804, 5.153800228976336051, 41.04057627198103120 ) ) ;
#135675 = CARTESIAN_POINT ( 'NONE',  ( 15.72974639402176855, 15.80617190586768217, 41.87609039468568284 ) ) ;
#135676 = CARTESIAN_POINT ( 'NONE',  ( -0.05219959533909027116, -19.03943276465977164, 67.49890960531436690 ) ) ;
#135677 = CARTESIAN_POINT ( 'NONE',  ( 17.97182807773871005, -5.500000000000040856, 81.03038844047284783 ) ) ;
#135678 = CARTESIAN_POINT ( 'NONE',  ( -5.153800228976328057, -19.02544592524343514, 57.29057627198103120 ) ) ;
#135679 = CARTESIAN_POINT ( 'NONE',  ( 15.80617190586746368, 15.72974639402197994, 39.37390960531436690 ) ) ;
#135680 = CARTESIAN_POINT ( 'NONE',  ( 16.46253265017160672, -9.564922557960803928, 33.33224293864770260 ) ) ;
#135681 = CARTESIAN_POINT ( 'NONE',  ( 15.72974639402199770, -15.80617190586745480, 43.12390960531435269 ) ) ;
#135682 = CARTESIAN_POINT ( 'NONE',  ( 12.14591786802327356, -12.06949235617739191, 95.62609039468568994 ) ) ;
#135683 = CARTESIAN_POINT ( 'NONE',  ( 19.05341960407617918, -5.049401038297876454, 21.04275706135232582 ) ) ;
#135685 = CARTESIAN_POINT ( 'NONE',  ( 12.14591786802327356, -12.06949235617739191, 75.62609039468567573 ) ) ;
#135684 = CARTESIAN_POINT ( 'NONE',  ( -0.05219959533934338120, 16.53943276465976808, 52.50109039468567573 ) ) ;
#135686 = CARTESIAN_POINT ( 'NONE',  ( 5.153800228976335163, 19.02544592524342804, 104.7905762719809957 ) ) ;
#135687 = CARTESIAN_POINT ( 'NONE',  ( -12.14591786802326823, 12.06949235617739902, 68.12609039468567573 ) ) ;
#135688 = CARTESIAN_POINT ( 'NONE',  ( -4.379528057220086978, -16.55341960407618274, 44.79275706135234714 ) ) ;
#135689 = CARTESIAN_POINT ( 'NONE',  ( 5.153800228976335163, 19.02544592524342804, 109.7905762719810099 ) ) ;
#135690 = CARTESIAN_POINT ( 'NONE',  ( 12.14591786802327356, -12.06949235617739191, 20.62609039468568639 ) ) ;
#135691 = CARTESIAN_POINT ( 'NONE',  ( 5.153800228976335163, 19.02544592524342804, 34.79057627198102409 ) ) ;
#135692 = CARTESIAN_POINT ( 'NONE',  ( 15.80617190586769283, -15.72974639402175789, 30.62609039468567929 ) ) ;
#135693 = CARTESIAN_POINT ( 'NONE',  ( -8.314922557961024197, 14.29746914071037800, 32.91775706135234714 ) ) ;
#135694 = CARTESIAN_POINT ( 'NONE',  ( 12.06949235617739724, 12.14591786802326823, 101.8760903946857042 ) ) ;
#135695 = CARTESIAN_POINT ( 'NONE',  ( 27.29906736325804673, 2.428612866367529932E-14, 169.9999999999999716 ) ) ;
#135696 = CARTESIAN_POINT ( 'NONE',  ( -10.81492255796105439, 18.62759615963255655, 97.91775706135236135 ) ) ;
#135698 = ADVANCED_FACE ( 'NONE', ( #98377 ), #165095, .T. ) ;
#135697 = CARTESIAN_POINT ( 'NONE',  ( -9.474510206698720793, -16.51473224551083518, 94.58442372801900433 ) ) ;
#135699 = CARTESIAN_POINT ( 'NONE',  ( 4.379528057220339221, -16.55341960407611168, 62.70724293864769550 ) ) ;
#135700 = CARTESIAN_POINT ( 'NONE',  ( -16.46253265017160317, 9.564922557960807481, 30.83224293864769550 ) ) ;
#135702 = CARTESIAN_POINT ( 'NONE',  ( 17.50000000001358202, -5.500000000000038192, 58.29690382535058291 ) ) ;
#135701 = CARTESIAN_POINT ( 'NONE',  ( 9.564922557961047289, -16.46253265017146816, 55.41775706135234003 ) ) ;
#135703 = CARTESIAN_POINT ( 'NONE',  ( -15.72974639402176322, -15.80617190586768395, 49.37609039468569705 ) ) ;
#135704 = CARTESIAN_POINT ( 'NONE',  ( 14.29746914071037800, 8.314922557961029526, 31.66775706135234358 ) ) ;
#135705 = CARTESIAN_POINT ( 'NONE',  ( 17.13100169013299734, 6.664070546373167758, 81.73210164300149927 ) ) ;
#135706 = CARTESIAN_POINT ( 'NONE',  ( 13.89961937509977652, -13.97604488694527269, 113.1239096053143527 ) ) ;
#135707 = CARTESIAN_POINT ( 'NONE',  ( -15.72974639402197994, 15.80617190586746368, 75.62390960531439532 ) ) ;
#135708 = CARTESIAN_POINT ( 'NONE',  ( -13.97604488694547697, 13.89961937509957934, 113.1260903946856757 ) ) ;
#135709 = CARTESIAN_POINT ( 'NONE',  ( -19.05341960407611168, -5.049401038298163336, 106.4572429386476955 ) ) ;
#135710 = CARTESIAN_POINT ( 'NONE',  ( -10.24465944170948895, -26.23679381505269959, 139.9999999999999716 ) ) ;
#135711 = CARTESIAN_POINT ( 'NONE',  ( 9.474510206698971260, -16.51473224551069308, 22.91557627198102765 ) ) ;
#135712 = CARTESIAN_POINT ( 'NONE',  ( -10.81492255796105439, 18.62759615963255655, 87.91775706135234714 ) ) ;
#135713 = CARTESIAN_POINT ( 'NONE',  ( 19.02544592524343514, -5.153800228976328945, 43.54057627198103120 ) ) ;
#135714 = CARTESIAN_POINT ( 'NONE',  ( -21.55341960407619339, 5.719274019375674811, 48.54275706135234714 ) ) ;
#135715 = CARTESIAN_POINT ( 'NONE',  ( -18.67979575497193778, 10.72451020669871902, 88.33442372801901854 ) ) ;
#135716 = CARTESIAN_POINT ( 'NONE',  ( 8.314922557961029526, -14.29746914071037800, 100.4177570613523471 ) ) ;
#135717 = CARTESIAN_POINT ( 'NONE',  ( -19.03943276465977164, 0.05219959533909376836, 81.24890960531436690 ) ) ;
#135718 = CARTESIAN_POINT ( 'NONE',  ( 21.53943276465977519, 0.05219959533937863772, 46.25109039468567573 ) ) ;
#135719 = CARTESIAN_POINT ( 'NONE',  ( 10.72451020669871369, 18.67979575497193778, 37.08442372801901143 ) ) ;
#135721 = CARTESIAN_POINT ( 'NONE',  ( -5.049401038298153566, 19.05341960407611168, 90.20724293864766707 ) ) ;
#135720 = CARTESIAN_POINT ( 'NONE',  ( -19.02544592524334988, -5.153800228976617603, 73.95942372801900433 ) ) ;
#135722 = CARTESIAN_POINT ( 'NONE',  ( -8.224510206698948167, 14.34966873604960824, 110.4155762719810383 ) ) ;
#135723 = CARTESIAN_POINT ( 'NONE',  ( 18.62759615963271287, -10.81492255796078972, 93.33224293864769550 ) ) ;
#135724 = CARTESIAN_POINT ( 'NONE',  ( 12.14591786802309770, 12.06949235617756955, 79.37390960531436690 ) ) ;
#135725 = CARTESIAN_POINT ( 'NONE',  ( 5.049401038297881783, 19.05341960407617563, 22.29275706135233648 ) ) ;
#135726 = CARTESIAN_POINT ( 'NONE',  ( -14.29746914071049879, 8.314922557960819915, 95.83224293864770971 ) ) ;
#135727 = CARTESIAN_POINT ( 'NONE',  ( -9.564922557960796823, -16.46253265017161027, 52.08224293864768839 ) ) ;
#135728 = CARTESIAN_POINT ( 'NONE',  ( 19.03943276465977164, 0.05219959533936151252, 86.25109039468567573 ) ) ;
#135729 = CARTESIAN_POINT ( 'NONE',  ( -16.52544592524342804, 4.483927247898546575, 46.04057627198103830 ) ) ;
#135730 = CARTESIAN_POINT ( 'NONE',  ( 5.719274019375673035, 21.55341960407619339, 112.2927570613523471 ) ) ;
#135731 = CARTESIAN_POINT ( 'NONE',  ( 19.02544592524343514, -5.153800228976328945, 108.5405762719810383 ) ) ;
#135732 = CARTESIAN_POINT ( 'NONE',  ( -19.02544592524334988, -5.153800228976617603, 73.95942372801900433 ) ) ;
#135733 = CARTESIAN_POINT ( 'NONE',  ( -0.05219959533907301413, -21.53943276465977519, 77.49890960531433848 ) ) ;
#135734 = CARTESIAN_POINT ( 'NONE',  ( 5.823673210054444382, -21.52544592524334988, 35.20942372801901854 ) ) ;
#135735 = CARTESIAN_POINT ( 'NONE',  ( -16.55341960407617563, 4.379528057220093196, 33.54275706135234714 ) ) ;
#135736 = CARTESIAN_POINT ( 'NONE',  ( -8.314922557961024197, 14.29746914071037800, 97.91775706135236135 ) ) ;
#135738 = CARTESIAN_POINT ( 'NONE',  ( -21.53943276465977519, -0.05219959533937600094, 38.75109039468567573 ) ) ;
#135737 = CARTESIAN_POINT ( 'NONE',  ( -9.564922557960796823, -16.46253265017161027, 22.08224293864768839 ) ) ;
#135739 = CARTESIAN_POINT ( 'NONE',  ( -19.02544592524342804, 5.153800228976336051, 26.04057627198103120 ) ) ;
#135740 = CARTESIAN_POINT ( 'NONE',  ( 36.91746825000000598, -11.99521256947793546, -2.224999997268813701 ) ) ;
#135741 = CARTESIAN_POINT ( 'NONE',  ( 0.05219959533934541429, -16.53943276465976808, 50.00109039468568994 ) ) ;
#135742 = CARTESIAN_POINT ( 'NONE',  ( 16.55341960407611168, 4.379528057220329451, 83.95724293864770971 ) ) ;
#135743 = CARTESIAN_POINT ( 'NONE',  ( 21.55341960407610458, 5.719274019375980345, 78.95724293864769550 ) ) ;
#135744 = CARTESIAN_POINT ( 'NONE',  ( -4.483927247898539470, -16.52544592524342804, 22.29057627198102765 ) ) ;
#135745 = CARTESIAN_POINT ( 'NONE',  ( -4.483927247898782831, 16.52544592524335698, 52.70942372801902565 ) ) ;
#135746 = CARTESIAN_POINT ( 'NONE',  ( 16.51473224551069308, 9.474510206698969483, 44.16557627198103120 ) ) ;
#135747 = CARTESIAN_POINT ( 'NONE',  ( -14.34966873604972548, 8.224510206698743886, 93.33442372801901854 ) ) ;
#135748 = CARTESIAN_POINT ( 'NONE',  ( 13.89961937509957401, 13.97604488694547697, 86.87609039468567573 ) ) ;
#135749 = CARTESIAN_POINT ( 'NONE',  ( -21.55341960407610458, -5.719274019375992779, 81.45724293864769550 ) ) ;
#135750 = CARTESIAN_POINT ( 'NONE',  ( -8.314922557961024197, 14.29746914071037800, 112.9177570613523329 ) ) ;
#135751 = ORIENTED_EDGE ( 'NONE', *, *, #142962, .F. ) ;
#135752 = CARTESIAN_POINT ( 'NONE',  ( 9.474510206698971260, -16.51473224551069308, 112.9155762719810383 ) ) ;
#135753 = CARTESIAN_POINT ( 'NONE',  ( -5.823673210054116645, -21.52544592524344225, 67.29057627198103830 ) ) ;
#135754 = ORIENTED_EDGE ( 'NONE', *, *, #41891, .T. ) ;
#135755 = CARTESIAN_POINT ( 'NONE',  ( 8.314922557961029526, -14.29746914071037800, 95.41775706135234714 ) ) ;
#135756 = ORIENTED_EDGE ( 'NONE', *, *, #109880, .T. ) ;
#135757 = CARTESIAN_POINT ( 'NONE',  ( 21.53943276465977519, -0.05219959533907433946, 33.74890960531436690 ) ) ;
#135758 = CARTESIAN_POINT ( 'NONE',  ( 17.50000000000014566, 3.417042746626903771, 107.3261960376752455 ) ) ;
#135759 = CARTESIAN_POINT ( 'NONE',  ( 21.55341960407610458, 5.719274019375980345, 78.95724293864769550 ) ) ;
#135760 = CARTESIAN_POINT ( 'NONE',  ( 8.224510206698953496, -14.34966873604960469, 22.91557627198102765 ) ) ;
#135761 = CARTESIAN_POINT ( 'NONE',  ( 9.474510206698729675, 16.51473224551082808, 112.0844237280190043 ) ) ;
#135762 = CARTESIAN_POINT ( 'NONE',  ( -19.02544592524342804, 5.153800228976336051, 31.04057627198102409 ) ) ;
#135763 = CARTESIAN_POINT ( 'NONE',  ( -4.379528057220086978, -16.55341960407618274, 29.79275706135234358 ) ) ;
#135764 = CARTESIAN_POINT ( 'NONE',  ( -9.564922557960796823, -16.46253265017161027, 52.08224293864768839 ) ) ;
#135765 = CARTESIAN_POINT ( 'NONE',  ( 22.44159573604009594, -16.30477369853687364, 140.1750000027311955 ) ) ;
#135766 = CARTESIAN_POINT ( 'NONE',  ( -13.97604488694527625, -13.89961937509977652, 106.8739096053143669 ) ) ;
#135767 = CARTESIAN_POINT ( 'NONE',  ( -16.51473224551069308, -9.474510206698971260, 101.6655762719810241 ) ) ;
#135768 = CARTESIAN_POINT ( 'NONE',  ( 4.379528057220092307, 16.55341960407617563, 87.29275706135236135 ) ) ;
#135769 = CARTESIAN_POINT ( 'NONE',  ( 19.03943276465977164, 0.05219959533936151252, 86.25109039468567573 ) ) ;
#135770 = CARTESIAN_POINT ( 'NONE',  ( 19.05341960407617918, -5.049401038297876454, 31.04275706135232227 ) ) ;
#135771 = CARTESIAN_POINT ( 'NONE',  ( -18.62759615963270932, 10.81492255796079327, 80.83224293864769550 ) ) ;
#135772 = CARTESIAN_POINT ( 'NONE',  ( 14.29746914071037800, 8.314922557961029526, 96.66775706135234714 ) ) ;
#135773 = CARTESIAN_POINT ( 'NONE',  ( -10.81492255796078084, -18.62759615963271287, 32.08224293864769550 ) ) ;
#135774 = CARTESIAN_POINT ( 'NONE',  ( -19.02544592524334988, -5.153800228976617603, 98.95942372801900433 ) ) ;
#135775 = CARTESIAN_POINT ( 'NONE',  ( -5.049401038298153566, 19.05341960407611168, 45.20724293864769550 ) ) ;
#135776 = CARTESIAN_POINT ( 'NONE',  ( 13.89961937509977652, -13.97604488694527269, 93.12390960531436690 ) ) ;
#135777 = CARTESIAN_POINT ( 'NONE',  ( 21.55341960407619695, -5.719274019375665929, 66.04275706135236135 ) ) ;
#135778 = CARTESIAN_POINT ( 'NONE',  ( 9.564922557960805705, 16.46253265017160317, 54.58224293864769550 ) ) ;
#135779 = CARTESIAN_POINT ( 'NONE',  ( -16.52544592524342804, 4.483927247898546575, 106.0405762719810525 ) ) ;
#135780 = CARTESIAN_POINT ( 'NONE',  ( 20.14845677604719754, -11.85354687992394496, 170.0217845860066745 ) ) ;
#135781 = CARTESIAN_POINT ( 'NONE',  ( 4.379528057220339221, -16.55341960407611168, 82.70724293864770971 ) ) ;
#135782 = CARTESIAN_POINT ( 'NONE',  ( 0.05219959533907565091, 21.53943276465977519, 79.99890960531435269 ) ) ;
#135783 = CARTESIAN_POINT ( 'NONE',  ( 13.97604488694548053, -13.89961937509957401, 90.62609039468567573 ) ) ;
#135784 = CARTESIAN_POINT ( 'NONE',  ( 16.36317988757059894, -7.306389748694929409, 81.59789608363225000 ) ) ;
#135785 = CARTESIAN_POINT ( 'NONE',  ( 13.97604488694548053, -13.89961937509957401, 40.62609039468564731 ) ) ;
#135786 = CARTESIAN_POINT ( 'NONE',  ( 17.48847506799950224, -5.747544572775296068, 73.32697437843290800 ) ) ;
#135788 = CARTESIAN_POINT ( 'NONE',  ( -13.89961937509977652, 13.97604488694528158, 85.62390960531433848 ) ) ;
#135787 = CARTESIAN_POINT ( 'NONE',  ( -19.05341960407611168, -5.049401038298163336, 76.45724293864769550 ) ) ;
#135789 = CARTESIAN_POINT ( 'NONE',  ( -14.34966873604972548, 8.224510206698743886, 68.33442372801900433 ) ) ;
#135790 = CARTESIAN_POINT ( 'NONE',  ( -10.74802307403555268, 10.74802307403551715, -65.00100000000003320 ) ) ;
#135791 = CARTESIAN_POINT ( 'NONE',  ( 13.89961937509957401, 13.97604488694547697, 46.87609039468565442 ) ) ;
#135792 = CARTESIAN_POINT ( 'NONE',  ( 16.22700747346227246, -14.59405422056926938, -58.52327065384329075 ) ) ;
#135793 = CARTESIAN_POINT ( 'NONE',  ( 13.97604488694527802, 13.89961937509977652, 109.3739096053143669 ) ) ;
#135794 = CARTESIAN_POINT ( 'NONE',  ( -12.06949235617739369, -12.14591786802326823, 99.37609039468568994 ) ) ;
#135795 = CARTESIAN_POINT ( 'NONE',  ( -0.9928668394654698304, -21.65895526037597563, -56.20821996642036567 ) ) ;
#135796 = CARTESIAN_POINT ( 'NONE',  ( 16.55341960407618274, -4.379528057220086978, 76.04275706135237556 ) ) ;
#135797 = CYLINDRICAL_SURFACE ( 'NONE', #77156, 2.500000000000000000 ) ;
#135798 = CARTESIAN_POINT ( 'NONE',  ( -4.379528057220086978, -16.55341960407618274, 59.79275706135234714 ) ) ;
#135799 = CARTESIAN_POINT ( 'NONE',  ( -18.22780087662124160, -5.499999999999927169, 78.98236817873106475 ) ) ;
#135800 = CARTESIAN_POINT ( 'NONE',  ( -21.53943276465977519, -0.05219959533937600094, 68.75109039468568994 ) ) ;
#135801 = CARTESIAN_POINT ( 'NONE',  ( 9.564922557961047289, -16.46253265017146816, 70.41775706135233293 ) ) ;
#135802 = CARTESIAN_POINT ( 'NONE',  ( 5.049401038297881783, 19.05341960407617563, 22.29275706135233648 ) ) ;
#135803 = CARTESIAN_POINT ( 'NONE',  ( 19.02544592524343514, -5.153800228976328945, 53.54057627198102409 ) ) ;
#135804 = CARTESIAN_POINT ( 'NONE',  ( -9.474510206698964154, 16.51473224551069663, 40.41557627198103120 ) ) ;
#135805 = DIRECTION ( 'NONE',  ( 0.000000000000000000, 0.000000000000000000, -1.000000000000000000 ) ) ;
#135806 = CARTESIAN_POINT ( 'NONE',  ( 15.72974639402199770, -15.80617190586745480, 73.12390960531436690 ) ) ;
#135807 = CIRCLE ( 'NONE', #16283, 10.00000000000000000 ) ;
#135808 = CARTESIAN_POINT ( 'NONE',  ( -15.80617190586745835, -15.72974639402198527, 36.87390960531435979 ) ) ;
#135809 = CARTESIAN_POINT ( 'NONE',  ( -16.52544592524342804, 4.483927247898546575, 116.0405762719810383 ) ) ;
#135810 = CARTESIAN_POINT ( 'NONE',  ( -16.53943276465976808, -0.05219959533934237506, 48.75109039468568284 ) ) ;
#135811 = VERTEX_POINT ( 'NONE', #111338 ) ;
#135812 = CARTESIAN_POINT ( 'NONE',  ( -5.823673210054431948, 21.52544592524334988, 32.70942372801900433 ) ) ;
#135814 = CARTESIAN_POINT ( 'NONE',  ( 23.48529157249599919, 32.32473071737754111, -4.699999999999999289 ) ) ;
#135813 = CARTESIAN_POINT ( 'NONE',  ( 12.06949235617757843, -12.14591786802309237, 48.12390960531436690 ) ) ;
#135815 = CARTESIAN_POINT ( 'NONE',  ( 8.314922557961029526, -14.29746914071037800, 30.41775706135234358 ) ) ;
#135816 = CARTESIAN_POINT ( 'NONE',  ( 9.474510206698729675, 16.51473224551082808, 42.08442372801900433 ) ) ;
#135817 = CARTESIAN_POINT ( 'NONE',  ( 16.55341960407611168, 4.379528057220329451, 43.95724293864769550 ) ) ;
#135818 = CARTESIAN_POINT ( 'NONE',  ( -21.52544592524334988, -5.823673210054445271, 18.95942372801901143 ) ) ;
#135820 = CARTESIAN_POINT ( 'NONE',  ( 21.53943276465977519, -0.05219959533907433946, 73.74890960531433848 ) ) ;
#135819 = CARTESIAN_POINT ( 'NONE',  ( -9.474510206698964154, 16.51473224551069663, 100.4155762719810241 ) ) ;
#135821 = CARTESIAN_POINT ( 'NONE',  ( 0.05219959533909260263, 19.03943276465977164, 89.99890960531436690 ) ) ;
#135822 = CARTESIAN_POINT ( 'NONE',  ( -16.52544592524342804, 4.483927247898546575, 66.04057627198103830 ) ) ;
#135823 = CARTESIAN_POINT ( 'NONE',  ( 19.02544592524343514, -5.153800228976328945, 103.5405762719809957 ) ) ;
#135824 = DIRECTION ( 'NONE',  ( 0.000000000000000000, -0.4999999999999998890, 0.8660254037844387076 ) ) ;
#135825 = CARTESIAN_POINT ( 'NONE',  ( -9.564922557961040184, 16.46253265017147172, 57.91775706135233293 ) ) ;
#135826 = CARTESIAN_POINT ( 'NONE',  ( -18.62759615963270932, 10.81492255796079327, 100.8322429386477097 ) ) ;
#135827 = CARTESIAN_POINT ( 'NONE',  ( -16.46253265017160317, 9.564922557960807481, 45.83224293864769550 ) ) ;
#135828 = CARTESIAN_POINT ( 'NONE',  ( -0.05219959533909027116, -19.03943276465977164, 22.49890960531436690 ) ) ;
#135829 = ADVANCED_FACE ( 'NONE', ( #112335 ), #35496, .F. ) ;
#135830 = CARTESIAN_POINT ( 'NONE',  ( 15.72974639402176855, 15.80617190586768217, 51.87609039468568284 ) ) ;
#135831 = CARTESIAN_POINT ( 'NONE',  ( -27.73933785331498925, 2.428612866367529932E-14, 148.8750000027311842 ) ) ;
#135832 = CARTESIAN_POINT ( 'NONE',  ( -8.224510206698948167, 14.34966873604960824, 35.41557627198102409 ) ) ;
#135833 = CARTESIAN_POINT ( 'NONE',  ( 9.564922557960805705, 16.46253265017160317, 44.58224293864769550 ) ) ;
#135834 = CARTESIAN_POINT ( 'NONE',  ( 9.474510206698971260, -16.51473224551069308, 97.91557627198102409 ) ) ;
#135835 = CARTESIAN_POINT ( 'NONE',  ( -15.72974639402197994, 15.80617190586746368, 75.62390960531439532 ) ) ;
#135836 = CARTESIAN_POINT ( 'NONE',  ( -17.14385361876520619, 23.59649016807275856, 146.5750000027311444 ) ) ;
#135837 = CARTESIAN_POINT ( 'NONE',  ( 19.03943276465977164, -0.05219959533909143690, 48.74890960531435979 ) ) ;
#135838 = CARTESIAN_POINT ( 'NONE',  ( 5.719274019375991003, -21.55341960407610458, 72.70724293864769550 ) ) ;
#135839 = CARTESIAN_POINT ( 'NONE',  ( 10.81492255796106328, -18.62759615963255655, 90.41775706135236135 ) ) ;
#135842 = CARTESIAN_POINT ( 'NONE',  ( -0.05219959533910754901, -16.53943276465976808, 67.49890960531436690 ) ) ;
#135841 = CARTESIAN_POINT ( 'NONE',  ( 12.14591786802327356, -12.06949235617739191, 80.62609039468567573 ) ) ;
#135840 = DIRECTION ( 'NONE',  ( 0.000000000000000000, -0.8164965809277234809, -0.5773502691896292838 ) ) ;
#135843 = CARTESIAN_POINT ( 'NONE',  ( -9.564922557960796823, -16.46253265017161027, 67.08224293864769550 ) ) ;
#135844 = ORIENTED_EDGE ( 'NONE', *, *, #64962, .F. ) ;
#135845 = CARTESIAN_POINT ( 'NONE',  ( 13.89961937509957401, 13.97604488694547697, 31.87609039468566863 ) ) ;
#135846 = CARTESIAN_POINT ( 'NONE',  ( 14.34966873604972726, -8.224510206698740333, 90.83442372801901854 ) ) ;
#135847 = CARTESIAN_POINT ( 'NONE',  ( -10.72451020669870658, -18.67979575497194134, 109.5844237280190328 ) ) ;
#135848 = CARTESIAN_POINT ( 'NONE',  ( -9.564922557960796823, -16.46253265017161027, 82.08224293864768129 ) ) ;
#135849 = CARTESIAN_POINT ( 'NONE',  ( 5.823673210054125526, 21.52544592524343514, 44.79057627198103120 ) ) ;
#135850 = CARTESIAN_POINT ( 'NONE',  ( -10.72451020669870658, -18.67979575497194134, 99.58442372801900433 ) ) ;
#135851 = CARTESIAN_POINT ( 'NONE',  ( 0.05219959533934541429, -16.53943276465976808, 65.00109039468568994 ) ) ;
#135852 = CARTESIAN_POINT ( 'NONE',  ( 18.62759615963271287, -10.81492255796078972, 108.3322429386477097 ) ) ;
#135853 = CARTESIAN_POINT ( 'NONE',  ( 13.97604488694548053, -13.89961937509957401, 110.6260903946856615 ) ) ;
#135854 = CARTESIAN_POINT ( 'NONE',  ( 19.03943276465977164, -0.05219959533909143690, 88.74890960531436690 ) ) ;
#135855 = CARTESIAN_POINT ( 'NONE',  ( 16.52544592524335698, 4.483927247898782831, 31.45942372801901854 ) ) ;
#135856 = CARTESIAN_POINT ( 'NONE',  ( -16.46253265017160317, 9.564922557960807481, 50.83224293864770260 ) ) ;
#135857 = CARTESIAN_POINT ( 'NONE',  ( 16.55341960407618274, -4.379528057220086978, 36.04275706135234714 ) ) ;
#135858 = CARTESIAN_POINT ( 'NONE',  ( -12.14591786802309592, -12.06949235617757132, 81.87390960531435269 ) ) ;
#135859 = CARTESIAN_POINT ( 'NONE',  ( -14.29746914071037622, -8.314922557961029526, 89.16775706135236135 ) ) ;
#135861 = CARTESIAN_POINT ( 'NONE',  ( 16.51473224551069308, 9.474510206698969483, 59.16557627198102409 ) ) ;
#135860 = CARTESIAN_POINT ( 'NONE',  ( -10.72451020669870658, -18.67979575497194134, 39.58442372801901143 ) ) ;
#135862 = CARTESIAN_POINT ( 'NONE',  ( 19.05341960407611168, 5.049401038298154454, 78.95724293864769550 ) ) ;
#135863 = CARTESIAN_POINT ( 'NONE',  ( -16.55341960407617563, 4.379528057220093196, 88.54275706135236135 ) ) ;
#135864 = DIRECTION ( 'NONE',  ( -1.000000000000000000, -0.000000000000000000, -0.000000000000000000 ) ) ;
#135865 = EDGE_LOOP ( 'NONE', ( #138257, #133582, #120183, #102533 ) ) ;
#135866 = CARTESIAN_POINT ( 'NONE',  ( 5.049401038297881783, 19.05341960407617563, 37.29275706135232582 ) ) ;
#135867 = CARTESIAN_POINT ( 'NONE',  ( -19.05341960407611168, -5.049401038298163336, 101.4572429386476955 ) ) ;
#135868 = CARTESIAN_POINT ( 'NONE',  ( -19.03943276465977164, 0.05219959533909376836, 51.24890960531436690 ) ) ;
#135869 = CARTESIAN_POINT ( 'NONE',  ( 5.153800228976335163, 19.02544592524342804, 109.7905762719810099 ) ) ;
#135870 = CARTESIAN_POINT ( 'NONE',  ( -16.53943276465976808, -0.05219959533934237506, 48.75109039468568284 ) ) ;
#135872 = CARTESIAN_POINT ( 'NONE',  ( -12.06949235617739369, -12.14591786802326823, 59.37609039468568284 ) ) ;
#135871 = CARTESIAN_POINT ( 'NONE',  ( -9.474510206698720793, -16.51473224551083518, 59.58442372801900433 ) ) ;
#135873 = CARTESIAN_POINT ( 'NONE',  ( 5.686924398124309832, -3.878244659966709307, -64.40439148883940845 ) ) ;
#135874 = CARTESIAN_POINT ( 'NONE',  ( -16.46253265017160317, 9.564922557960807481, 80.83224293864769550 ) ) ;
#135875 = CARTESIAN_POINT ( 'NONE',  ( -5.719274019375665041, -21.55341960407619695, 19.79275706135235069 ) ) ;
#135876 = CARTESIAN_POINT ( 'NONE',  ( -19.02544592524334988, -5.153800228976617603, 68.95942372801896170 ) ) ;
#135878 = CARTESIAN_POINT ( 'NONE',  ( -13.97604488694527625, -13.89961937509977652, 26.87390960531434558 ) ) ;
#135877 = CARTESIAN_POINT ( 'NONE',  ( 13.97604488694527802, 13.89961937509977652, 89.37390960531436690 ) ) ;
#135879 = CARTESIAN_POINT ( 'NONE',  ( 9.474510206698971260, -16.51473224551069308, 72.91557627198102409 ) ) ;
#135881 = CARTESIAN_POINT ( 'NONE',  ( 19.03943276465977164, -0.05219959533909143690, 28.74890960531435624 ) ) ;
#135880 = CARTESIAN_POINT ( 'NONE',  ( -14.29746914071049879, 8.314922557960819915, 30.83224293864770260 ) ) ;
#135882 = CARTESIAN_POINT ( 'NONE',  ( 16.51473224551083163, -9.474510206698727899, 40.83442372801900433 ) ) ;
#135883 = CARTESIAN_POINT ( 'NONE',  ( 12.14591786802309770, 12.06949235617756955, 69.37390960531436690 ) ) ;
#135884 = CARTESIAN_POINT ( 'NONE',  ( -15.72974639402176322, -15.80617190586768395, 99.37609039468568994 ) ) ;
#135885 = CARTESIAN_POINT ( 'NONE',  ( 13.97604488694527802, 13.89961937509977652, 39.37390960531435269 ) ) ;
#135887 = CARTESIAN_POINT ( 'NONE',  ( -21.55341960407619339, 5.719274019375674811, 98.54275706135234714 ) ) ;
#135886 = CARTESIAN_POINT ( 'NONE',  ( 4.483927247898545687, 16.52544592524342804, 44.79057627198103120 ) ) ;
#135888 = CARTESIAN_POINT ( 'NONE',  ( -9.564922557960796823, -16.46253265017161027, 97.08224293864769550 ) ) ;
#135889 = CARTESIAN_POINT ( 'NONE',  ( -5.049401038298153566, 19.05341960407611168, 90.20724293864766707 ) ) ;
#135890 = CARTESIAN_POINT ( 'NONE',  ( 5.153800228976335163, 19.02544592524342804, 39.79057627198100988 ) ) ;
#135891 = CARTESIAN_POINT ( 'NONE',  ( -16.52544592524342804, 4.483927247898546575, 106.0405762719810525 ) ) ;
#135892 = CARTESIAN_POINT ( 'NONE',  ( -8.314922557960811034, -14.29746914071050412, 72.08224293864769550 ) ) ;
#135893 = CARTESIAN_POINT ( 'NONE',  ( 21.55341960407610458, 5.719274019375980345, 83.95724293864770971 ) ) ;
#135894 = CARTESIAN_POINT ( 'NONE',  ( 13.97604488694527802, 13.89961937509977652, 84.37390960531433848 ) ) ;
#135895 = CARTESIAN_POINT ( 'NONE',  ( 18.62759615963271287, -10.81492255796078972, 93.33224293864769550 ) ) ;
#135896 = CARTESIAN_POINT ( 'NONE',  ( 13.97604488694527802, 13.89961937509977652, 89.37390960531436690 ) ) ;
#135898 = CARTESIAN_POINT ( 'NONE',  ( 4.483927247898545687, 16.52544592524342804, 89.79057627198103830 ) ) ;
#135897 = CARTESIAN_POINT ( 'NONE',  ( 17.50000000001358202, -5.500000000000038192, 88.29690382535061133 ) ) ;
#135899 = CARTESIAN_POINT ( 'NONE',  ( 9.564922557960805705, 16.46253265017160317, 69.58224293864770971 ) ) ;
#135900 = CARTESIAN_POINT ( 'NONE',  ( 18.67979575497178502, 10.72451020669898547, 79.16557627198103830 ) ) ;
#135901 = EDGE_CURVE ( 'NONE', #167324, #197337, #26645, .T. ) ;
#135902 = CYLINDRICAL_SURFACE ( 'NONE', #85051, 7.500000000000007105 ) ;
#135904 = CARTESIAN_POINT ( 'NONE',  ( 19.35633801406907750, -5.499999999999773515, 66.63373818172765084 ) ) ;
#135903 = CARTESIAN_POINT ( 'NONE',  ( 21.53943276465977519, -0.05219959533907433946, 33.74890960531436690 ) ) ;
#135905 = CARTESIAN_POINT ( 'NONE',  ( -13.97604488694547697, 13.89961937509957934, 113.1260903946856757 ) ) ;
#135906 = CARTESIAN_POINT ( 'NONE',  ( 16.55341960407611168, 4.379528057220329451, 93.95724293864770971 ) ) ;
#135907 = CARTESIAN_POINT ( 'NONE',  ( -17.05116617787827238, -6.768360034955764881, 96.34324446740805570 ) ) ;
#135908 = CARTESIAN_POINT ( 'NONE',  ( 16.51473224551069308, 9.474510206698969483, 89.16557627198103830 ) ) ;
#135909 = CARTESIAN_POINT ( 'NONE',  ( -5.153800228976328057, -19.02544592524343514, 52.29057627198100988 ) ) ;
#135910 = CARTESIAN_POINT ( 'NONE',  ( -12.14591786802309592, -12.06949235617757132, 81.87390960531435269 ) ) ;
#135911 = CARTESIAN_POINT ( 'NONE',  ( -19.02544592524342804, 5.153800228976336051, 111.0405762719810099 ) ) ;
#135912 = CARTESIAN_POINT ( 'NONE',  ( -8.224510206698948167, 14.34966873604960824, 55.41557627198102409 ) ) ;
#135913 = CARTESIAN_POINT ( 'NONE',  ( -13.97604488694547697, 13.89961937509957934, 108.1260903946856331 ) ) ;
#135914 = CARTESIAN_POINT ( 'NONE',  ( 0.05219959533937995610, -21.53943276465977519, 55.00109039468568284 ) ) ;
#135915 = CARTESIAN_POINT ( 'NONE',  ( 27.73933785331498569, 9.013057229001093518, 145.9750000027311785 ) ) ;
#135916 = CARTESIAN_POINT ( 'NONE',  ( 19.03943276465977164, -0.05219959533909143690, 93.74890960531435269 ) ) ;
#135917 = CARTESIAN_POINT ( 'NONE',  ( -0.05219959533907301413, -21.53943276465977519, 92.49890960531436690 ) ) ;
#135918 = CARTESIAN_POINT ( 'NONE',  ( -16.52544592524335698, -4.483927247898792601, 83.95942372801900433 ) ) ;
#135919 = CARTESIAN_POINT ( 'NONE',  ( 9.564922557960805705, 16.46253265017160317, 24.58224293864769194 ) ) ;
#135920 = CARTESIAN_POINT ( 'NONE',  ( -13.89961937509977652, 13.97604488694528158, 80.62390960531436690 ) ) ;
#135921 = CARTESIAN_POINT ( 'NONE',  ( 5.823673210054125526, 21.52544592524343514, 84.79057627198102409 ) ) ;
#135922 =( BOUNDED_CURVE ( )  B_SPLINE_CURVE ( 3, ( #125489, #142633, #187186, #19309 ),
 .UNSPECIFIED., .F., .F. ) 
 B_SPLINE_CURVE_WITH_KNOTS ( ( 4, 4 ),
 ( 1.025647941782811046, 2.008945357379067431 ),
 .UNSPECIFIED. ) 
 CURVE ( )  GEOMETRIC_REPRESENTATION_ITEM ( )  RATIONAL_B_SPLINE_CURVE ( ( 1.000000000000000000, 0.9210371567966664230, 0.9210371567966664230, 1.000000000000000000 ) ) 
 REPRESENTATION_ITEM ( '' )  );
#135923 = CARTESIAN_POINT ( 'NONE',  ( -19.02544592524334988, -5.153800228976617603, 103.9594237280190043 ) ) ;
#135925 = CARTESIAN_POINT ( 'NONE',  ( 10.81492255796106328, -18.62759615963255655, 65.41775706135234714 ) ) ;
#135924 = CARTESIAN_POINT ( 'NONE',  ( -4.483927247898539470, -16.52544592524342804, 47.29057627198103120 ) ) ;
#135927 = CARTESIAN_POINT ( 'NONE',  ( 19.05341960407611168, 5.049401038298154454, 113.9572429386477097 ) ) ;
#135926 = CARTESIAN_POINT ( 'NONE',  ( 4.379528057220092307, 16.55341960407617563, 92.29275706135236135 ) ) ;
#135928 = CARTESIAN_POINT ( 'NONE',  ( 16.51473224551069308, 9.474510206698969483, 109.1655762719810383 ) ) ;
#135929 = CARTESIAN_POINT ( 'NONE',  ( -16.29526858892876717, 7.335722546920118603, 79.20329402199793378 ) ) ;
#135930 = CARTESIAN_POINT ( 'NONE',  ( -4.483927247898782831, 16.52544592524335698, 102.7094237280190185 ) ) ;
#135931 = CARTESIAN_POINT ( 'NONE',  ( -14.34966873604972548, 8.224510206698743886, 53.33442372801901854 ) ) ;
#135932 = CARTESIAN_POINT ( 'NONE',  ( -19.03943276465977164, 0.05219959533909376836, 61.24890960531436690 ) ) ;
#135933 = CARTESIAN_POINT ( 'NONE',  ( 19.02544592524343514, -5.153800228976328945, 73.54057627198103830 ) ) ;
#135934 = CARTESIAN_POINT ( 'NONE',  ( 0.05219959533934541429, -16.53943276465976808, 80.00109039468568994 ) ) ;
#135935 = CARTESIAN_POINT ( 'NONE',  ( 16.52544592524342804, -4.483927247898539470, 43.54057627198103830 ) ) ;
#135936 = CARTESIAN_POINT ( 'NONE',  ( 13.97604488694527802, 13.89961937509977652, 54.37390960531435979 ) ) ;
#135937 = CARTESIAN_POINT ( 'NONE',  ( -9.564922557960796823, -16.46253265017161027, 47.08224293864769550 ) ) ;
#135939 = VERTEX_POINT ( 'NONE', #143657 ) ;
#135938 = CARTESIAN_POINT ( 'NONE',  ( -8.314922557961024197, 14.29746914071037800, 47.91775706135234714 ) ) ;
#135940 = CARTESIAN_POINT ( 'NONE',  ( 19.02544592524334988, 5.153800228976608722, 91.45942372801900433 ) ) ;
#135941 = CARTESIAN_POINT ( 'NONE',  ( 14.29746914071049879, -8.314922557960816363, 93.33224293864769550 ) ) ;
#135942 = CARTESIAN_POINT ( 'NONE',  ( 9.474510206698971260, -16.51473224551069308, 67.91557627198102409 ) ) ;
#135944 = CARTESIAN_POINT ( 'NONE',  ( 30.74264578624799782, 22.33583958711400541, -6.800000000000000711 ) ) ;
#135943 = CARTESIAN_POINT ( 'NONE',  ( -9.474510206698720793, -16.51473224551083518, 104.5844237280190043 ) ) ;
#135945 = CARTESIAN_POINT ( 'NONE',  ( -21.55341960407619339, 5.719274019375674811, 108.5427570613523756 ) ) ;
#135946 = CARTESIAN_POINT ( 'NONE',  ( 16.55341960407618274, -4.379528057220086978, 71.04275706135234714 ) ) ;
#135947 = CARTESIAN_POINT ( 'NONE',  ( 30.00000000000000000, -5.499999999999992895, 102.5000000000000142 ) ) ;
#135948 = CARTESIAN_POINT ( 'NONE',  ( 0.05219959533907565091, 21.53943276465977519, 59.99890960531436690 ) ) ;
#135949 = CARTESIAN_POINT ( 'NONE',  ( -16.55341960407617563, 4.379528057220093196, 58.54275706135235424 ) ) ;
#135950 = CARTESIAN_POINT ( 'NONE',  ( -19.05341960407611168, -5.049401038298164224, 31.45724293864769905 ) ) ;
#135951 = CARTESIAN_POINT ( 'NONE',  ( -5.153800228976607833, 19.02544592524334988, 37.70942372801899722 ) ) ;
#135952 = CARTESIAN_POINT ( 'NONE',  ( -0.05219959533909027116, -19.03943276465977164, 92.49890960531436690 ) ) ;
#135953 = CARTESIAN_POINT ( 'NONE',  ( 16.52544592524342804, -4.483927247898539470, 113.5405762719810383 ) ) ;
#135954 = CARTESIAN_POINT ( 'NONE',  ( -16.51473224551069308, -9.474510206698971260, 61.66557627198103120 ) ) ;
#135955 = CARTESIAN_POINT ( 'NONE',  ( -10.81492255796105439, 18.62759615963255655, 82.91775706135234714 ) ) ;
#135956 = CARTESIAN_POINT ( 'NONE',  ( -16.51473224551082808, 9.474510206698731452, 38.33442372801899722 ) ) ;
#135957 = CARTESIAN_POINT ( 'NONE',  ( -0.05219959533936034679, 19.03943276465977164, 32.50109039468566863 ) ) ;
#135958 = CARTESIAN_POINT ( 'NONE',  ( -16.46253265017160317, 9.564922557960807481, 55.83224293864769550 ) ) ;
#135959 = CARTESIAN_POINT ( 'NONE',  ( 5.823673210054125526, 21.52544592524343514, 29.79057627198102409 ) ) ;
#135960 = CARTESIAN_POINT ( 'NONE',  ( 10.72451020669871369, 18.67979575497193778, 82.08442372801901854 ) ) ;
#135961 = CARTESIAN_POINT ( 'NONE',  ( -13.89961937509977652, 13.97604488694528158, 60.62390960531436690 ) ) ;
#135962 = CARTESIAN_POINT ( 'NONE',  ( -5.823673210054431948, 21.52544592524334988, 92.70942372801901854 ) ) ;
#135963 = CARTESIAN_POINT ( 'NONE',  ( -15.80617190586745835, -15.72974639402198527, 41.87390960531435979 ) ) ;
#135964 = CARTESIAN_POINT ( 'NONE',  ( -13.97604488694527625, -13.89961937509977652, 81.87390960531436690 ) ) ;
#135965 = CARTESIAN_POINT ( 'NONE',  ( 0.05219959533937995610, -21.53943276465977519, 40.00109039468567573 ) ) ;
#135966 = CARTESIAN_POINT ( 'NONE',  ( 16.51473224551083163, -9.474510206698727899, 55.83442372801899722 ) ) ;
#135967 = CARTESIAN_POINT ( 'NONE',  ( -16.46253265017160317, 9.564922557960807481, 35.83224293864768839 ) ) ;
#135968 = CARTESIAN_POINT ( 'NONE',  ( -16.46253265017160317, 9.564922557960807481, 85.83224293864769550 ) ) ;
#135969 = CARTESIAN_POINT ( 'NONE',  ( -12.14591786802326823, 12.06949235617739902, 23.12609039468567573 ) ) ;
#135970 = CARTESIAN_POINT ( 'NONE',  ( 14.34966873604960469, 8.224510206698951720, 94.16557627198103830 ) ) ;
#135971 = CARTESIAN_POINT ( 'NONE',  ( -19.02544592524342804, 5.153800228976336051, 71.04057627198099567 ) ) ;
#135972 = CARTESIAN_POINT ( 'NONE',  ( -5.823673210054116645, -21.52544592524344225, 47.29057627198103120 ) ) ;
#135973 = CARTESIAN_POINT ( 'NONE',  ( 14.34966873604972726, -8.224510206698740333, 25.83442372801901499 ) ) ;
#135974 = CARTESIAN_POINT ( 'NONE',  ( 5.719274019375991003, -21.55341960407610458, 112.7072429386476955 ) ) ;
#135975 = CARTESIAN_POINT ( 'NONE',  ( 21.55341960407619695, -5.719274019375665929, 76.04275706135237556 ) ) ;
#135976 = CARTESIAN_POINT ( 'NONE',  ( -8.314922557961024197, 14.29746914071037800, 72.91775706135234714 ) ) ;
#135977 = CARTESIAN_POINT ( 'NONE',  ( 4.379528057220092307, 16.55341960407617563, 62.29275706135236845 ) ) ;
#135978 = CARTESIAN_POINT ( 'NONE',  ( -19.05341960407611168, -5.049401038298163336, 66.45724293864769550 ) ) ;
#135979 = CARTESIAN_POINT ( 'NONE',  ( -12.06949235617739369, -12.14591786802326823, 99.37609039468568994 ) ) ;
#135980 = CARTESIAN_POINT ( 'NONE',  ( 5.049401038297881783, 19.05341960407617563, 47.29275706135231161 ) ) ;
#135981 = CARTESIAN_POINT ( 'NONE',  ( 15.72974639402199770, -15.80617190586745480, 113.1239096053143953 ) ) ;
#135982 = CARTESIAN_POINT ( 'NONE',  ( -4.379528057220328563, 16.55341960407611168, 60.20724293864768839 ) ) ;
#135983 = CARTESIAN_POINT ( 'NONE',  ( 5.049401038298161559, -19.05341960407611168, 92.70724293864769550 ) ) ;
#135984 = CARTESIAN_POINT ( 'NONE',  ( -12.06949235617739369, -12.14591786802326823, 94.37609039468568994 ) ) ;
#135985 = CARTESIAN_POINT ( 'NONE',  ( 21.52544592524334988, 5.823673210054432836, 56.45942372801902565 ) ) ;
#135986 = CARTESIAN_POINT ( 'NONE',  ( -4.379528057220086978, -16.55341960407618274, 29.79275706135234358 ) ) ;
#135987 = CARTESIAN_POINT ( 'NONE',  ( -21.55341960407619339, 5.719274019375674811, 33.54275706135234714 ) ) ;
#135988 = CARTESIAN_POINT ( 'NONE',  ( -8.314922557960811034, -14.29746914071050412, 62.08224293864769550 ) ) ;
#135989 = VERTEX_POINT ( 'NONE', #50675 ) ;
#135990 = CARTESIAN_POINT ( 'NONE',  ( -21.52544592524343514, 5.823673210054127303, 101.0405762719810383 ) ) ;
#135991 = CARTESIAN_POINT ( 'NONE',  ( -12.14591786802309592, -12.06949235617757132, 36.87390960531435979 ) ) ;
#135992 = ORIENTED_EDGE ( 'NONE', *, *, #20851, .F. ) ;
#135993 = DIRECTION ( 'NONE',  ( 0.8164965809277261455, 0.000000000000000000, 0.5773502691896257311 ) ) ;
#135994 = CARTESIAN_POINT ( 'NONE',  ( 0.05219959533907565091, 21.53943276465977519, 34.99890960531435979 ) ) ;
#135995 = CARTESIAN_POINT ( 'NONE',  ( -10.81492255796105439, 18.62759615963255655, 37.91775706135235424 ) ) ;
#135996 = CARTESIAN_POINT ( 'NONE',  ( -16.52544592524342804, 4.483927247898546575, 61.04057627198103120 ) ) ;
#135997 = CARTESIAN_POINT ( 'NONE',  ( -5.823673210054116645, -21.52544592524344225, 67.29057627198103830 ) ) ;
#135998 = CARTESIAN_POINT ( 'NONE',  ( -9.474510206698964154, 16.51473224551069663, 70.41557627198102409 ) ) ;
#136000 = CARTESIAN_POINT ( 'NONE',  ( -16.46253265017146816, -9.564922557961047289, 69.16775706135233293 ) ) ;
#135999 = CARTESIAN_POINT ( 'NONE',  ( -5.049401038298153566, 19.05341960407611168, 30.20724293864768839 ) ) ;
#136001 = CARTESIAN_POINT ( 'NONE',  ( -18.67979575497178146, -10.72451020669898902, 46.66557627198102409 ) ) ;
#136002 = CARTESIAN_POINT ( 'NONE',  ( 5.153800228976335163, 19.02544592524342804, 59.79057627198100988 ) ) ;
#136003 = CARTESIAN_POINT ( 'NONE',  ( 12.06949235617739724, 12.14591786802326823, 41.87609039468568284 ) ) ;
#136004 = CARTESIAN_POINT ( 'NONE',  ( 18.67979575497194134, -10.72451020669871369, 20.83442372801901143 ) ) ;
#136005 = CARTESIAN_POINT ( 'NONE',  ( 16.55341960407611168, 4.379528057220329451, 53.95724293864770260 ) ) ;
#136006 = CARTESIAN_POINT ( 'NONE',  ( -16.46253265017160317, 9.564922557960807481, 85.83224293864769550 ) ) ;
#136007 = CARTESIAN_POINT ( 'NONE',  ( -10.81492255796078084, -18.62759615963271287, 77.08224293864769550 ) ) ;
#136009 = CARTESIAN_POINT ( 'NONE',  ( -12.14591786802326823, 12.06949235617739902, 38.12609039468567573 ) ) ;
#136008 = CARTESIAN_POINT ( 'NONE',  ( -18.62759615963270932, 10.81492255796079327, 110.8322429386476955 ) ) ;
#136010 = CARTESIAN_POINT ( 'NONE',  ( -10.81492255796078084, -18.62759615963271287, 37.08224293864768129 ) ) ;
#136011 = CARTESIAN_POINT ( 'NONE',  ( -18.67979575497193778, 10.72451020669871902, 98.33442372801901854 ) ) ;
#136012 = CARTESIAN_POINT ( 'NONE',  ( 13.89961937509977652, -13.97604488694527269, 48.12390960531435979 ) ) ;
#136013 = CARTESIAN_POINT ( 'NONE',  ( -9.564922557960796823, -16.46253265017161027, 102.0822429386477097 ) ) ;
#136014 = CARTESIAN_POINT ( 'NONE',  ( -19.02544592524342804, 5.153800228976336051, 76.04057627198102409 ) ) ;
#136015 = CARTESIAN_POINT ( 'NONE',  ( -25.80819889657188781, -27.69677943096050043, -16.54815200935615493 ) ) ;
#136016 = CARTESIAN_POINT ( 'NONE',  ( 19.02544592524334988, 5.153800228976608722, 51.45942372801900433 ) ) ;
#136018 = CARTESIAN_POINT ( 'NONE',  ( 10.81492255796078972, 18.62759615963270932, 29.58224293864769905 ) ) ;
#136017 = CARTESIAN_POINT ( 'NONE',  ( 21.53943276465977519, 0.05219959533937863772, 106.2510903946856757 ) ) ;
#136019 = CARTESIAN_POINT ( 'NONE',  ( 8.224510206698742110, 14.34966873604972548, 102.0844237280190185 ) ) ;
#136020 = CARTESIAN_POINT ( 'NONE',  ( -5.049401038297874678, -19.05341960407617918, 89.79275706135230450 ) ) ;
#136021 = CARTESIAN_POINT ( 'NONE',  ( -16.81555441253552274, 7.025013491695479395, 60.63685445334257906 ) ) ;
#136022 = CARTESIAN_POINT ( 'NONE',  ( 5.153800228976615827, -19.02544592524334988, 90.20942372801900433 ) ) ;
#136023 = CARTESIAN_POINT ( 'NONE',  ( 0.05219959533936267826, -19.03943276465977164, 50.00109039468566863 ) ) ;
#136024 = CARTESIAN_POINT ( 'NONE',  ( -16.21995358207306026, -7.366697692864121016, 45.06448998487843483 ) ) ;
#136025 = CARTESIAN_POINT ( 'NONE',  ( 19.03943276465977164, -0.05219959533909143690, 38.74890960531436690 ) ) ;
#136026 = CARTESIAN_POINT ( 'NONE',  ( 0.05219959533910956823, 16.53943276465976808, 54.99890960531435269 ) ) ;
#136027 = CARTESIAN_POINT ( 'NONE',  ( 5.153800228976335163, 19.02544592524342804, 24.79057627198102765 ) ) ;
#136028 = CARTESIAN_POINT ( 'NONE',  ( 14.29746914071049879, -8.314922557960816363, 23.33224293864769194 ) ) ;
#136029 = DIRECTION ( 'NONE',  ( -1.000000000000000000, -0.000000000000000000, -0.000000000000000000 ) ) ;
#136030 = CARTESIAN_POINT ( 'NONE',  ( 8.314922557961029526, -14.29746914071037800, 90.41775706135236135 ) ) ;
#136031 = CARTESIAN_POINT ( 'NONE',  ( -13.89961937509977652, 13.97604488694528158, 50.62390960531435979 ) ) ;
#136032 = CARTESIAN_POINT ( 'NONE',  ( -10.81492255796105439, 18.62759615963255655, 102.9177570613523756 ) ) ;
#136033 = CARTESIAN_POINT ( 'NONE',  ( 14.29746914071037800, 8.314922557961029526, 21.66775706135235069 ) ) ;
#136034 = CARTESIAN_POINT ( 'NONE',  ( 15.80617190586746368, 15.72974639402197994, 34.37390960531435979 ) ) ;
#136035 = CARTESIAN_POINT ( 'NONE',  ( -21.53943276465977519, -0.05219959533937600094, 93.75109039468567573 ) ) ;
#136036 = CARTESIAN_POINT ( 'NONE',  ( 16.46253265017160672, -9.564922557960803928, 103.3322429386476955 ) ) ;
#136037 = CARTESIAN_POINT ( 'NONE',  ( 19.05341960407611168, 5.049401038298154454, 88.95724293864769550 ) ) ;
#136038 = CARTESIAN_POINT ( 'NONE',  ( -22.81625015709509441, -31.40387420917324590, -10.32499999726881157 ) ) ;
#136039 = CARTESIAN_POINT ( 'NONE',  ( 21.53943276465977519, -0.05219959533907433946, 103.7489096053143669 ) ) ;
#136040 = CARTESIAN_POINT ( 'NONE',  ( 16.53943276465976808, -0.05219959533910856209, 78.74890960531436690 ) ) ;
#136041 = CARTESIAN_POINT ( 'NONE',  ( 5.823673210054125526, 21.52544592524343514, 79.79057627198102409 ) ) ;
#136042 = CARTESIAN_POINT ( 'NONE',  ( -19.05341960407611168, -5.049401038298163336, 66.45724293864769550 ) ) ;
#136043 = CARTESIAN_POINT ( 'NONE',  ( 21.52544592524344225, -5.823673210054117533, 103.5405762719810383 ) ) ;
#136044 = EDGE_LOOP ( 'NONE', ( #151224, #164713, #1807, #91019, #104598, #5394, #131842, #123527 ) ) ;
#136045 = CARTESIAN_POINT ( 'NONE',  ( 19.03943276465977164, -0.05219959533909143690, 63.74890960531435979 ) ) ;
#136047 = CYLINDRICAL_SURFACE ( 'NONE', #17061, 1.499999999999997780 ) ;
#136046 = CARTESIAN_POINT ( 'NONE',  ( 16.55341960407611168, 4.379528057220329451, 88.95724293864769550 ) ) ;
#136048 = CARTESIAN_POINT ( 'NONE',  ( 16.51473224551069308, 9.474510206698969483, 64.16557627198102409 ) ) ;
#136049 = CARTESIAN_POINT ( 'NONE',  ( 19.03943276465977164, 0.05219959533936151252, 81.25109039468567573 ) ) ;
#136050 = CARTESIAN_POINT ( 'NONE',  ( -8.224510206698948167, 14.34966873604960824, 90.41557627198103830 ) ) ;
#136051 = CARTESIAN_POINT ( 'NONE',  ( -18.67979575497193778, 10.72451020669871902, 58.33442372801901143 ) ) ;
#136053 = CARTESIAN_POINT ( 'NONE',  ( 5.823673210054444382, -21.52544592524334988, 25.20942372801901854 ) ) ;
#136052 = CARTESIAN_POINT ( 'NONE',  ( -19.05341960407611168, -5.049401038298163336, 51.45724293864770260 ) ) ;
#136054 = CARTESIAN_POINT ( 'NONE',  ( 14.34966873604960469, 8.224510206698951720, 99.16557627198100988 ) ) ;
#136055 = CARTESIAN_POINT ( 'NONE',  ( 0.000000000000000000, -5.500000000000000888, 118.0000000000000142 ) ) ;
#136056 = CARTESIAN_POINT ( 'NONE',  ( -16.51473224551069308, -9.474510206698971260, 61.66557627198103120 ) ) ;
#136057 = DIRECTION ( 'NONE',  ( 0.000000000000000000, -1.734723475976807489E-15, 1.000000000000000000 ) ) ;
#136059 = CARTESIAN_POINT ( 'NONE',  ( 19.05341960407611168, 5.049401038298154454, 113.9572429386477097 ) ) ;
#136058 = CARTESIAN_POINT ( 'NONE',  ( 13.97604488694548053, -13.89961937509957401, 110.6260903946856615 ) ) ;
#136060 = CARTESIAN_POINT ( 'NONE',  ( -21.55341960407619339, 5.719274019375674811, 53.54275706135234714 ) ) ;
#136061 = CARTESIAN_POINT ( 'NONE',  ( -5.153800228976328057, -19.02544592524343514, 92.29057627198099567 ) ) ;
#136062 = CARTESIAN_POINT ( 'NONE',  ( 5.049401038297881783, 19.05341960407617563, 82.29275706135229029 ) ) ;
#136063 = CARTESIAN_POINT ( 'NONE',  ( 9.474510206698971260, -16.51473224551069308, 62.91557627198102409 ) ) ;
#136064 = EDGE_CURVE ( 'NONE', #129907, #115190, #6143, .T. ) ;
#136065 = CARTESIAN_POINT ( 'NONE',  ( -16.55341960407611168, -4.379528057220339221, 76.45724293864769550 ) ) ;
#136066 = CARTESIAN_POINT ( 'NONE',  ( -16.53943276465976808, 0.05219959533911058130, 86.24890960531436690 ) ) ;
#136067 = CARTESIAN_POINT ( 'NONE',  ( -13.97604488694527625, -13.89961937509977652, 86.87390960531436690 ) ) ;
#136068 = CARTESIAN_POINT ( 'NONE',  ( 4.379528057220339221, -16.55341960407611168, 82.70724293864770971 ) ) ;
#136069 = CARTESIAN_POINT ( 'NONE',  ( 5.049401038298161559, -19.05341960407611168, 82.70724293864770971 ) ) ;
#136070 = CARTESIAN_POINT ( 'NONE',  ( 13.97604488694548053, -13.89961937509957401, 25.62609039468566507 ) ) ;
#136073 = CARTESIAN_POINT ( 'NONE',  ( -16.51473224551069308, -9.474510206698971260, 31.66557627198102054 ) ) ;
#136072 = CARTESIAN_POINT ( 'NONE',  ( 12.14591786802309770, 12.06949235617756955, 24.37390960531435979 ) ) ;
#136071 = CARTESIAN_POINT ( 'NONE',  ( -0.05219959533909027116, -19.03943276465977164, 52.49890960531436690 ) ) ;
#136074 = ORIENTED_EDGE ( 'NONE', *, *, #96295, .T. ) ;
#136075 = CARTESIAN_POINT ( 'NONE',  ( 21.53943276465977519, 0.05219959533937863772, 46.25109039468567573 ) ) ;
#136076 = CARTESIAN_POINT ( 'NONE',  ( 5.153800228976615827, -19.02544592524334988, 60.20942372801899012 ) ) ;
#136077 = CARTESIAN_POINT ( 'NONE',  ( 16.53943276465976808, -0.05219959533910856209, 38.74890960531435979 ) ) ;
#136078 = CARTESIAN_POINT ( 'NONE',  ( -15.72974639402197994, 15.80617190586746368, 90.62390960531436690 ) ) ;
#136079 = CARTESIAN_POINT ( 'NONE',  ( -18.62759615963270932, 10.81492255796079327, 30.83224293864770260 ) ) ;
#136080 = CARTESIAN_POINT ( 'NONE',  ( -14.29746914071049879, 8.314922557960819915, 70.83224293864770971 ) ) ;
#136081 = CARTESIAN_POINT ( 'NONE',  ( -9.474510206698964154, 16.51473224551069663, 40.41557627198103120 ) ) ;
#136082 = CARTESIAN_POINT ( 'NONE',  ( 16.53943276465976808, 0.05219959533934440121, 96.25109039468568994 ) ) ;
#136083 = CARTESIAN_POINT ( 'NONE',  ( -12.14591786802326823, 12.06949235617739902, 73.12609039468567573 ) ) ;
#136084 = CARTESIAN_POINT ( 'NONE',  ( -15.80617190586745835, -15.72974639402198527, 31.87390960531435979 ) ) ;
#136085 = CARTESIAN_POINT ( 'NONE',  ( -0.05219959533936034679, 19.03943276465977164, 32.50109039468566863 ) ) ;
#136086 = CARTESIAN_POINT ( 'NONE',  ( -19.03943276465977164, 0.05219959533909376836, 91.24890960531436690 ) ) ;
#136087 = CARTESIAN_POINT ( 'NONE',  ( -12.06949235617739369, -12.14591786802326823, 74.37609039468568994 ) ) ;
#136088 = CARTESIAN_POINT ( 'NONE',  ( -14.29746914071049879, 8.314922557960819915, 115.8322429386477097 ) ) ;
#136089 = CARTESIAN_POINT ( 'NONE',  ( 16.55341960407611168, 4.379528057220329451, 33.95724293864769550 ) ) ;
#136091 = CARTESIAN_POINT ( 'NONE',  ( -16.51473224551069308, -9.474510206698971260, 86.66557627198102409 ) ) ;
#136090 = CARTESIAN_POINT ( 'NONE',  ( -9.474510206698964154, 16.51473224551069663, 100.4155762719810241 ) ) ;
#136092 = CARTESIAN_POINT ( 'NONE',  ( -15.80617190586745835, -15.72974639402198527, 26.87390960531435979 ) ) ;
#136093 = CARTESIAN_POINT ( 'NONE',  ( -4.379528057220328563, 16.55341960407611168, 70.20724293864769550 ) ) ;
#136094 = EDGE_LOOP ( 'NONE', ( #109478, #49470, #157584, #175686, #35349, #184558, #114952, #23873, #3836, #65623, #93046, #19137, #160113, #130210, #136780, #23823, #94303, #188215, #12940, #28354, #168177, #186232, #165856, #181507, #68982, #185332, #103476, #25898, #60413, #157197, #25599, #71922, #41540, #108371, #181180, #804, #132287, #143522, #134112, #197042, #14921, #126620, #119677, #193519, #199020, #151527, #132175, #113184, #147059, #185460, #147486, #176387, #175513, #194967, #166096, #5581 ) ) ;
#136095 = CARTESIAN_POINT ( 'NONE',  ( 16.53943276465976808, -0.05219959533910856209, 53.74890960531437401 ) ) ;
#136097 = DIRECTION ( 'NONE',  ( -1.000000000000000000, 0.000000000000000000, 0.000000000000000000 ) ) ;
#136096 = CARTESIAN_POINT ( 'NONE',  ( -8.314922557961024197, 14.29746914071037800, 52.91775706135235424 ) ) ;
#136098 = CARTESIAN_POINT ( 'NONE',  ( 5.153800228976615827, -19.02544592524334988, 50.20942372801897591 ) ) ;
#136099 = CARTESIAN_POINT ( 'NONE',  ( -19.02544592524342804, 5.153800228976336051, 86.04057627198103830 ) ) ;
#136100 = CARTESIAN_POINT ( 'NONE',  ( -16.51473224551082808, 9.474510206698731452, 68.33442372801900433 ) ) ;
#136101 = CARTESIAN_POINT ( 'NONE',  ( -5.359611314223446995E-15, 29.16686587814335496, 144.8750000027311557 ) ) ;
#136102 = CARTESIAN_POINT ( 'NONE',  ( 5.153800228976615827, -19.02544592524334988, 60.20942372801899012 ) ) ;
#136104 = CARTESIAN_POINT ( 'NONE',  ( -4.379528057220086978, -16.55341960407618274, 89.79275706135236135 ) ) ;
#136103 = CARTESIAN_POINT ( 'NONE',  ( 5.049401038297881783, 19.05341960407617563, 112.2927570613523471 ) ) ;
#136105 = CARTESIAN_POINT ( 'NONE',  ( -5.359611314223446995E-15, 29.16686587814335496, 146.8750000027311273 ) ) ;
#136106 = CARTESIAN_POINT ( 'NONE',  ( -9.564922557960796823, -16.46253265017161027, 37.08224293864768839 ) ) ;
#136107 = CARTESIAN_POINT ( 'NONE',  ( -15.80617190586745835, -15.72974639402198527, 21.87390960531436690 ) ) ;
#136108 = CARTESIAN_POINT ( 'NONE',  ( -21.53943276465977519, -0.05219959533937600094, 58.75109039468568994 ) ) ;
#136109 = CARTESIAN_POINT ( 'NONE',  ( -5.153800228976607833, 19.02544592524334988, 97.70942372801900433 ) ) ;
#136111 = CARTESIAN_POINT ( 'NONE',  ( 19.02544592524343514, -5.153800228976328945, 63.54057627198103830 ) ) ;
#136110 = CARTESIAN_POINT ( 'NONE',  ( 19.49401214000076621, 12.39993551617566681, 167.9999999999999716 ) ) ;
#136112 = CARTESIAN_POINT ( 'NONE',  ( 5.153800228976335163, 19.02544592524342804, 114.7905762719810241 ) ) ;
#136114 = CARTESIAN_POINT ( 'NONE',  ( 9.564922557960805705, 16.46253265017160317, 69.58224293864770971 ) ) ;
#136113 = CARTESIAN_POINT ( 'NONE',  ( -16.52544592524342804, 4.483927247898546575, 76.04057627198102409 ) ) ;
#136115 = CARTESIAN_POINT ( 'NONE',  ( -19.03943276465977164, 0.05219959533909376836, 71.24890960531435269 ) ) ;
#136116 = CARTESIAN_POINT ( 'NONE',  ( -13.97604488694547697, 13.89961937509957934, 78.12609039468567573 ) ) ;
#136117 = CARTESIAN_POINT ( 'NONE',  ( -10.72451020669898014, 18.67979575497178502, 70.41557627198102409 ) ) ;
#136118 = CARTESIAN_POINT ( 'NONE',  ( 8.314922557960818139, 14.29746914071049879, 109.5822429386476955 ) ) ;
#136119 = CARTESIAN_POINT ( 'NONE',  ( 13.97604488694548053, -13.89961937509957401, 60.62609039468564731 ) ) ;
#136120 = CARTESIAN_POINT ( 'NONE',  ( -19.02544592524342804, 5.153800228976336051, 51.04057627198103120 ) ) ;
#136121 = CARTESIAN_POINT ( 'NONE',  ( -13.97604488694527625, -13.89961937509977652, 81.87390960531436690 ) ) ;
#136122 = CARTESIAN_POINT ( 'NONE',  ( -10.81492255796078084, -18.62759615963271287, 92.08224293864769550 ) ) ;
#136124 = CARTESIAN_POINT ( 'NONE',  ( 13.89961937509957401, 13.97604488694547697, 46.87609039468565442 ) ) ;
#136123 = CARTESIAN_POINT ( 'NONE',  ( 14.29746914071049879, -8.314922557960816363, 83.33224293864769550 ) ) ;
#136125 = CARTESIAN_POINT ( 'NONE',  ( -5.823673210054116645, -21.52544592524344225, 82.29057627198103830 ) ) ;
#136126 = CARTESIAN_POINT ( 'NONE',  ( -10.72451020669898014, 18.67979575497178502, 55.41557627198102409 ) ) ;
#136127 = CARTESIAN_POINT ( 'NONE',  ( -12.14591786802309592, -12.06949235617757132, 36.87390960531435979 ) ) ;
#136128 = CARTESIAN_POINT ( 'NONE',  ( 5.823673210054444382, -21.52544592524334988, 90.20942372801903275 ) ) ;
#136129 = CARTESIAN_POINT ( 'NONE',  ( 9.564922557960805705, 16.46253265017160317, 84.58224293864769550 ) ) ;
#136130 = CARTESIAN_POINT ( 'NONE',  ( 12.06949235617757843, -12.14591786802309237, 113.1239096053143953 ) ) ;
#136131 = CARTESIAN_POINT ( 'NONE',  ( 15.72974639402176855, 15.80617190586768217, 26.87609039468567218 ) ) ;
#136132 = CARTESIAN_POINT ( 'NONE',  ( 21.55341960407619695, -5.719274019375665929, 41.04275706135236135 ) ) ;
#136133 = CARTESIAN_POINT ( 'NONE',  ( -16.46253265017160317, 9.564922557960807481, 45.83224293864769550 ) ) ;
#136134 = CARTESIAN_POINT ( 'NONE',  ( 21.55341960407619695, -5.719274019375665929, 26.04275706135235779 ) ) ;
#136135 = EDGE_CURVE ( 'NONE', #99274, #91848, #130453, .T. ) ;
#136136 = CARTESIAN_POINT ( 'NONE',  ( 16.51473224551083163, -9.474510206698727899, 60.83442372801900433 ) ) ;
#136137 = CARTESIAN_POINT ( 'NONE',  ( -13.97604488694527625, -13.89961937509977652, 41.87390960531435979 ) ) ;
#136138 = CARTESIAN_POINT ( 'NONE',  ( 4.379528057220092307, 16.55341960407617563, 32.29275706135235424 ) ) ;
#136139 = CARTESIAN_POINT ( 'NONE',  ( -13.89961937509977652, 13.97604488694528158, 30.62390960531435269 ) ) ;
#136140 = CARTESIAN_POINT ( 'NONE',  ( -14.34966873604972548, 8.224510206698743886, 63.33442372801900433 ) ) ;
#136141 = CARTESIAN_POINT ( 'NONE',  ( 19.05341960407611168, 5.049401038298154454, 38.95724293864767418 ) ) ;
#136142 = CARTESIAN_POINT ( 'NONE',  ( -20.56371838171433097, -11.43208494587363688, 170.0924998638764691 ) ) ;
#136143 = CARTESIAN_POINT ( 'NONE',  ( -5.049401038298153566, 19.05341960407611168, 85.20724293864766707 ) ) ;
#136144 = CARTESIAN_POINT ( 'NONE',  ( -9.564922557960796823, -16.46253265017161027, 27.08224293864769550 ) ) ;
#136145 = CARTESIAN_POINT ( 'NONE',  ( 18.62759615963271287, -10.81492255796078972, 58.33224293864768839 ) ) ;
#136146 = CARTESIAN_POINT ( 'NONE',  ( 14.34966873604972726, -8.224510206698740333, 45.83442372801901854 ) ) ;
#136147 = CARTESIAN_POINT ( 'NONE',  ( 18.67979575497194134, -10.72451020669871369, 95.83442372801903275 ) ) ;
#136148 = CARTESIAN_POINT ( 'NONE',  ( 13.89961937509977652, -13.97604488694527269, 43.12390960531434558 ) ) ;
#136149 = EDGE_CURVE ( 'NONE', #13391, #20566, #19460, .T. ) ;
#136150 = CARTESIAN_POINT ( 'NONE',  ( 0.05219959533910956823, 16.53943276465976808, 29.99890960531435979 ) ) ;
#136151 = CARTESIAN_POINT ( 'NONE',  ( -12.06949235617756955, 12.14591786802309770, 65.62390960531436690 ) ) ;
#136152 = CARTESIAN_POINT ( 'NONE',  ( 5.049401038298161559, -19.05341960407611168, 62.70724293864769550 ) ) ;
#136153 = CARTESIAN_POINT ( 'NONE',  ( 13.97604488694548053, -13.89961937509957401, 20.62609039468567573 ) ) ;
#136154 = CARTESIAN_POINT ( 'NONE',  ( -15.72974639402176322, -15.80617190586768395, 24.37609039468567573 ) ) ;
#136155 = CARTESIAN_POINT ( 'NONE',  ( 19.02544592524343514, -5.153800228976328945, 78.54057627198099567 ) ) ;
#136156 = CARTESIAN_POINT ( 'NONE',  ( 18.62759615963255655, 10.81492255796105972, 86.66775706135234714 ) ) ;
#136157 = CARTESIAN_POINT ( 'NONE',  ( -12.06949235617739369, -12.14591786802326823, 49.37609039468569705 ) ) ;
#136158 = CARTESIAN_POINT ( 'NONE',  ( 0.05219959533934541429, -16.53943276465976808, 25.00109039468567218 ) ) ;
#136160 = CARTESIAN_POINT ( 'NONE',  ( 15.80617190586769283, -15.72974639402175789, 95.62609039468568994 ) ) ;
#136159 = CARTESIAN_POINT ( 'NONE',  ( 12.06949235617757843, -12.14591786802309237, 98.12390960531436690 ) ) ;
#136161 = CARTESIAN_POINT ( 'NONE',  ( -0.05219959533910754901, -16.53943276465976808, 32.49890960531435979 ) ) ;
#136162 = CARTESIAN_POINT ( 'NONE',  ( 16.46253265017160672, -9.564922557960803928, 33.33224293864770260 ) ) ;
#136163 = CARTESIAN_POINT ( 'NONE',  ( -8.314922557961024197, 14.29746914071037800, 47.91775706135234714 ) ) ;
#136164 = CARTESIAN_POINT ( 'NONE',  ( -8.314922557960811034, -14.29746914071050412, 57.08224293864769550 ) ) ;
#136165 = CARTESIAN_POINT ( 'NONE',  ( 12.14591786802327356, -12.06949235617739191, 100.6260903946857184 ) ) ;
#136166 = CARTESIAN_POINT ( 'NONE',  ( -19.02544592524342804, 5.153800228976336051, 111.0405762719810099 ) ) ;
#136167 = CARTESIAN_POINT ( 'NONE',  ( 9.474510206698971260, -16.51473224551069308, 107.9155762719810383 ) ) ;
#136168 = CARTESIAN_POINT ( 'NONE',  ( -19.03943276465977164, -0.05219959533935918106, 23.75109039468566152 ) ) ;
#136169 = CARTESIAN_POINT ( 'NONE',  ( -14.34966873604960291, -8.224510206698953496, 86.66557627198102409 ) ) ;
#136170 = CARTESIAN_POINT ( 'NONE',  ( -16.51473224551069308, -9.474510206698971260, 101.6655762719810241 ) ) ;
#136171 = ORIENTED_EDGE ( 'NONE', *, *, #63061, .F. ) ;
#136172 = CARTESIAN_POINT ( 'NONE',  ( -14.29746914071037622, -8.314922557961029526, 39.16775706135235424 ) ) ;
#136173 = CARTESIAN_POINT ( 'NONE',  ( -9.474510206698964154, 16.51473224551069663, 35.41557627198102409 ) ) ;
#136175 = DIRECTION ( 'NONE',  ( 1.000000000000000000, -4.336808689942017120E-17, 0.000000000000000000 ) ) ;
#136174 = CARTESIAN_POINT ( 'NONE',  ( -16.55341960407617563, 4.379528057220093196, 48.54275706135234714 ) ) ;
#136176 = CARTESIAN_POINT ( 'NONE',  ( 19.02544592524334988, 5.153800228976608722, 46.45942372801899012 ) ) ;
#136177 = CARTESIAN_POINT ( 'NONE',  ( -13.89961937509977652, 13.97604488694528158, 50.62390960531435979 ) ) ;
#136178 = CARTESIAN_POINT ( 'NONE',  ( 16.55341960407618274, -4.379528057220086978, 81.04275706135236135 ) ) ;
#136179 = CARTESIAN_POINT ( 'NONE',  ( 13.89961937509957401, 13.97604488694547697, 81.87609039468564731 ) ) ;
#136180 = CARTESIAN_POINT ( 'NONE',  ( -9.474510206698720793, -16.51473224551083518, 29.58442372801900433 ) ) ;
#136181 = CARTESIAN_POINT ( 'NONE',  ( -13.97604488694527625, -13.89961937509977652, 61.87390960531435979 ) ) ;
#136182 = CARTESIAN_POINT ( 'NONE',  ( -12.14591786802309592, -12.06949235617757132, 101.8739096053143811 ) ) ;
#136183 = CARTESIAN_POINT ( 'NONE',  ( 19.03943276465977164, 0.05219959533936151252, 66.25109039468567573 ) ) ;
#136184 = CARTESIAN_POINT ( 'NONE',  ( 21.52544592524344225, -5.823673210054117533, 63.54057627198103830 ) ) ;
#136185 = CARTESIAN_POINT ( 'NONE',  ( -9.474510206698720793, -16.51473224551083518, 24.58442372801900078 ) ) ;
#136186 = CARTESIAN_POINT ( 'NONE',  ( -16.46253265017160317, 9.564922557960807481, 105.8322429386476955 ) ) ;
#136187 = CARTESIAN_POINT ( 'NONE',  ( -18.67979575497178146, -10.72451020669898902, 81.66557627198103830 ) ) ;
#136188 = CARTESIAN_POINT ( 'NONE',  ( -17.05587630539787014, 6.762274262135701264, 85.74180309037315340 ) ) ;
#136189 = CARTESIAN_POINT ( 'NONE',  ( -5.049401038297874678, -19.05341960407617918, 99.79275706135234714 ) ) ;
#136190 = CARTESIAN_POINT ( 'NONE',  ( -17.59860650958993844, 7.585241751806885979, 98.42337014262494677 ) ) ;
#136191 = CARTESIAN_POINT ( 'NONE',  ( 4.379528057220092307, 16.55341960407617563, 32.29275706135235424 ) ) ;
#136192 = CARTESIAN_POINT ( 'NONE',  ( 5.049401038298161559, -19.05341960407611168, 32.70724293864768129 ) ) ;
#136193 = CARTESIAN_POINT ( 'NONE',  ( -5.153800228976328057, -19.02544592524343514, 107.2905762719810383 ) ) ;
#136194 = CARTESIAN_POINT ( 'NONE',  ( -21.53943276465977519, 0.05219959533907696930, 96.24890960531435269 ) ) ;
#136195 = CARTESIAN_POINT ( 'NONE',  ( -0.05219959533937732626, 21.53943276465977519, 62.50109039468568284 ) ) ;
#136197 = CARTESIAN_POINT ( 'NONE',  ( -15.80617190586768217, 15.72974639402176855, 113.1260903946856899 ) ) ;
#136196 = CARTESIAN_POINT ( 'NONE',  ( 5.049401038297881783, 19.05341960407617563, 107.2927570613523187 ) ) ;
#136198 = CARTESIAN_POINT ( 'NONE',  ( -14.34966873604972548, 8.224510206698743886, 103.3344237280190043 ) ) ;
#136199 = CARTESIAN_POINT ( 'NONE',  ( -21.55341960407610458, -5.719274019375992779, 106.4572429386477097 ) ) ;
#136200 = CARTESIAN_POINT ( 'NONE',  ( 4.379528057220339221, -16.55341960407611168, 47.70724293864770260 ) ) ;
#136201 = CARTESIAN_POINT ( 'NONE',  ( 5.049401038297881783, 19.05341960407617563, 87.29275706135234714 ) ) ;
#136202 = CARTESIAN_POINT ( 'NONE',  ( -9.474510206698720793, -16.51473224551083518, 54.58442372801899722 ) ) ;
#136203 = CARTESIAN_POINT ( 'NONE',  ( -18.67979575497193778, 10.72451020669871902, 53.33442372801901854 ) ) ;
#136204 = CARTESIAN_POINT ( 'NONE',  ( 19.03943276465977164, 0.05219959533936151252, 46.25109039468566863 ) ) ;
#136205 = CARTESIAN_POINT ( 'NONE',  ( 8.314922557960818139, 14.29746914071049879, 104.5822429386477097 ) ) ;
#136206 = CARTESIAN_POINT ( 'NONE',  ( 10.81492255796078972, 18.62759615963270932, 24.58224293864768839 ) ) ;
#136207 = CARTESIAN_POINT ( 'NONE',  ( -14.34966873604960291, -8.224510206698953496, 36.66557627198103120 ) ) ;
#136208 = CARTESIAN_POINT ( 'NONE',  ( 21.52544592524334988, 5.823673210054432836, 101.4594237280190185 ) ) ;
#136209 = CARTESIAN_POINT ( 'NONE',  ( 8.314922557961029526, -14.29746914071037800, 75.41775706135233293 ) ) ;
#136210 = CARTESIAN_POINT ( 'NONE',  ( -0.05219959533910754901, -16.53943276465976808, 22.49890960531436335 ) ) ;
#136211 = CARTESIAN_POINT ( 'NONE',  ( 18.62759615963255655, 10.81492255796105972, 56.66775706135235424 ) ) ;
#136212 = CARTESIAN_POINT ( 'NONE',  ( -5.823673210054431948, 21.52544592524334988, 62.70942372801902565 ) ) ;
#136213 = CARTESIAN_POINT ( 'NONE',  ( -18.62759615963270932, 10.81492255796079327, 70.83224293864770971 ) ) ;
#136214 = VERTEX_POINT ( 'NONE', #101144 ) ;
#136215 = CARTESIAN_POINT ( 'NONE',  ( 5.153800228976335163, 19.02544592524342804, 29.79057627198102409 ) ) ;
#136216 = CARTESIAN_POINT ( 'NONE',  ( -18.62759615963255300, -10.81492255796106328, 44.16775706135234714 ) ) ;
#136217 = CARTESIAN_POINT ( 'NONE',  ( -8.224510206698948167, 14.34966873604960824, 115.4155762719810241 ) ) ;
#136218 = CARTESIAN_POINT ( 'NONE',  ( -5.049401038298153566, 19.05341960407611168, 45.20724293864769550 ) ) ;
#136219 = CARTESIAN_POINT ( 'NONE',  ( 16.53943276465976808, -0.05219959533910856209, 78.74890960531436690 ) ) ;
#136220 = CARTESIAN_POINT ( 'NONE',  ( -19.02544592524342804, 5.153800228976336051, 86.04057627198103830 ) ) ;
#136221 = CARTESIAN_POINT ( 'NONE',  ( -14.34966873604972548, 8.224510206698743886, 113.3344237280190328 ) ) ;
#136222 = CARTESIAN_POINT ( 'NONE',  ( -12.14591786802309592, -12.06949235617757132, 96.87390960531436690 ) ) ;
#136223 = CARTESIAN_POINT ( 'NONE',  ( -21.53943276465977519, 0.05219959533907696930, 71.24890960531435269 ) ) ;
#136224 = CARTESIAN_POINT ( 'NONE',  ( -15.80617190586745835, -15.72974639402198527, 111.8739096053143669 ) ) ;
#136225 = CARTESIAN_POINT ( 'NONE',  ( 9.474510206698971260, -16.51473224551069308, 112.9155762719810383 ) ) ;
#136227 = CARTESIAN_POINT ( 'NONE',  ( 19.05341960407617918, -5.049401038297876454, 101.0427570613523045 ) ) ;
#136226 = CARTESIAN_POINT ( 'NONE',  ( -19.02544592524342804, 5.153800228976336051, 66.04057627198103830 ) ) ;
#136228 = CARTESIAN_POINT ( 'NONE',  ( -21.52544592524343514, 5.823673210054127303, 61.04057627198103120 ) ) ;
#136229 = CARTESIAN_POINT ( 'NONE',  ( -21.52544592524334988, -5.823673210054445271, 83.95942372801900433 ) ) ;
#136230 = CARTESIAN_POINT ( 'NONE',  ( 5.049401038298161559, -19.05341960407611168, 62.70724293864769550 ) ) ;
#136231 = EDGE_CURVE ( 'NONE', #37612, #89057, #166092, .T. ) ;
#136232 = CARTESIAN_POINT ( 'NONE',  ( -19.05341960407611168, -5.049401038298163336, 96.45724293864769550 ) ) ;
#136233 = CARTESIAN_POINT ( 'NONE',  ( 4.483927247898790824, -16.52544592524335698, 80.20942372801901854 ) ) ;
#136234 = CARTESIAN_POINT ( 'NONE',  ( -10.81492255796105439, 18.62759615963255655, 57.91775706135234714 ) ) ;
#136235 = CARTESIAN_POINT ( 'NONE',  ( -10.81492255796105439, 18.62759615963255655, 102.9177570613523756 ) ) ;
#136236 = CARTESIAN_POINT ( 'NONE',  ( 18.62759615963271287, -10.81492255796078972, 113.3322429386476955 ) ) ;
#136237 = CARTESIAN_POINT ( 'NONE',  ( -21.53943276465977519, 0.05219959533907696930, 86.24890960531436690 ) ) ;
#136238 = CARTESIAN_POINT ( 'NONE',  ( 16.46253265017146816, 9.564922557961045513, 51.66775706135233293 ) ) ;
#136239 = CARTESIAN_POINT ( 'NONE',  ( -21.55341960407610458, -5.719274019375992779, 46.45724293864769550 ) ) ;
#136241 = CARTESIAN_POINT ( 'NONE',  ( -16.52544592524342804, 4.483927247898546575, 31.04057627198102409 ) ) ;
#136240 = CARTESIAN_POINT ( 'NONE',  ( -5.049401038298153566, 19.05341960407611168, 80.20724293864769550 ) ) ;
#136242 = PLANE ( 'NONE',  #27248 ) ;
#136243 = CARTESIAN_POINT ( 'NONE',  ( -18.56101223717333326, -5.500000000000065725, 81.44978406935680937 ) ) ;
#136244 = CARTESIAN_POINT ( 'NONE',  ( 16.51473224551083163, -9.474510206698727899, 95.83442372801900433 ) ) ;
#136245 = CARTESIAN_POINT ( 'NONE',  ( -21.52544592524343514, 5.823673210054127303, 66.04057627198103830 ) ) ;
#136246 = CARTESIAN_POINT ( 'NONE',  ( 4.483927247898545687, 16.52544592524342804, 49.79057627198102409 ) ) ;
#136247 = CARTESIAN_POINT ( 'NONE',  ( 16.53943276465976808, 0.05219959533934440121, 31.25109039468568639 ) ) ;
#136248 = CARTESIAN_POINT ( 'NONE',  ( -16.51473224551069308, -9.474510206698971260, 46.66557627198102409 ) ) ;
#136250 = CARTESIAN_POINT ( 'NONE',  ( 0.05219959533936267826, -19.03943276465977164, 85.00109039468567573 ) ) ;
#136249 = CARTESIAN_POINT ( 'NONE',  ( 10.72451020669898902, -18.67979575497178502, 107.9155762719810241 ) ) ;
#136251 = CARTESIAN_POINT ( 'NONE',  ( -9.474510206698964154, 16.51473224551069663, 75.41557627198103830 ) ) ;
#136252 = CARTESIAN_POINT ( 'NONE',  ( -16.52544592524342804, 4.483927247898546575, 86.04057627198102409 ) ) ;
#136253 = CARTESIAN_POINT ( 'NONE',  ( -13.89961937509977652, 13.97604488694528158, 80.62390960531436690 ) ) ;
#136254 = CARTESIAN_POINT ( 'NONE',  ( -0.05219959533907301413, -21.53943276465977519, 77.49890960531433848 ) ) ;
#136255 = CARTESIAN_POINT ( 'NONE',  ( 9.474510206698971260, -16.51473224551069308, 27.91557627198103120 ) ) ;
#136256 = CARTESIAN_POINT ( 'NONE',  ( 12.34766581223309245, 35.29190279822739740, -8.000000000000007105 ) ) ;
#136257 = CARTESIAN_POINT ( 'NONE',  ( 14.34966873604960469, 8.224510206698951720, 54.16557627198103120 ) ) ;
#136258 = CARTESIAN_POINT ( 'NONE',  ( -13.97604488694527625, -13.89961937509977652, 91.87390960531432427 ) ) ;
#136259 = CARTESIAN_POINT ( 'NONE',  ( 25.62086810090348976, 2.428612866367529932E-14, 167.9999999999999716 ) ) ;
#136260 = CARTESIAN_POINT ( 'NONE',  ( -16.46253265017146816, -9.564922557961047289, 49.16775706135233293 ) ) ;
#136261 = CARTESIAN_POINT ( 'NONE',  ( -8.224510206698735004, -14.34966873604973081, 54.58442372801901143 ) ) ;
#136262 = CARTESIAN_POINT ( 'NONE',  ( -18.67979575497178146, -10.72451020669898902, 76.66557627198103830 ) ) ;
#136263 = CARTESIAN_POINT ( 'NONE',  ( -9.564922557961040184, 16.46253265017147172, 37.91775706135233293 ) ) ;
#136264 = CARTESIAN_POINT ( 'NONE',  ( 9.564922557960805705, 16.46253265017160317, 84.58224293864769550 ) ) ;
#136265 = CARTESIAN_POINT ( 'NONE',  ( -17.49999999999999645, 3.209263204892610410, 114.7619682560627297 ) ) ;
#136266 = CARTESIAN_POINT ( 'NONE',  ( 21.52544592524344225, -5.823673210054117533, 23.54057627198102765 ) ) ;
#136267 = CARTESIAN_POINT ( 'NONE',  ( -9.564922557960796823, -16.46253265017161027, 72.08224293864770971 ) ) ;
#136268 = CARTESIAN_POINT ( 'NONE',  ( -18.62759615963255300, -10.81492255796106328, 49.16775706135234003 ) ) ;
#136269 = CARTESIAN_POINT ( 'NONE',  ( 16.51473224551069308, 9.474510206698969483, 24.16557627198102765 ) ) ;
#136272 = ORIENTED_EDGE ( 'NONE', *, *, #57708, .T. ) ;
#136271 = CARTESIAN_POINT ( 'NONE',  ( 16.46253265017160672, -9.564922557960803928, 93.33224293864769550 ) ) ;
#136270 = CARTESIAN_POINT ( 'NONE',  ( -18.62759615963270932, 10.81492255796079327, 110.8322429386476955 ) ) ;
#136273 = CARTESIAN_POINT ( 'NONE',  ( -5.823673210054431948, 21.52544592524334988, 42.70942372801901854 ) ) ;
#136274 = ORIENTED_EDGE ( 'NONE', *, *, #108101, .T. ) ;
#136275 = CARTESIAN_POINT ( 'NONE',  ( 13.97604488694527802, 13.89961937509977652, 99.37390960531436690 ) ) ;
#136276 = CARTESIAN_POINT ( 'NONE',  ( 16.51473224551069308, 9.474510206698969483, 89.16557627198103830 ) ) ;
#136277 = CARTESIAN_POINT ( 'NONE',  ( 10.72451020669898902, -18.67979575497178502, 112.9155762719810383 ) ) ;
#136278 = CARTESIAN_POINT ( 'NONE',  ( 13.89961937509977652, -13.97604488694527269, 48.12390960531435979 ) ) ;
#136279 = CARTESIAN_POINT ( 'NONE',  ( -16.53943276465976808, -0.05219959533934237506, 28.75109039468567929 ) ) ;
#136280 = CARTESIAN_POINT ( 'NONE',  ( 22.81625015709510151, -31.40387420917324590, -4.424999997268812990 ) ) ;
#136281 = CARTESIAN_POINT ( 'NONE',  ( -10.72451020669870658, -18.67979575497194134, 99.58442372801900433 ) ) ;
#136282 = CARTESIAN_POINT ( 'NONE',  ( -9.564922557960796823, -16.46253265017161027, 32.08224293864769550 ) ) ;
#136283 = CARTESIAN_POINT ( 'NONE',  ( -5.823673210054431948, 21.52544592524334988, 92.70942372801901854 ) ) ;
#136285 = CARTESIAN_POINT ( 'NONE',  ( 10.72451020669871369, 18.67979575497193778, 62.08442372801901143 ) ) ;
#136284 = CARTESIAN_POINT ( 'NONE',  ( 16.51473224551069308, 9.474510206698969483, 89.16557627198103830 ) ) ;
#136286 = CARTESIAN_POINT ( 'NONE',  ( -22.44159573604009950, -16.30477369853688430, 141.5750000027311728 ) ) ;
#136287 = CARTESIAN_POINT ( 'NONE',  ( -9.474510206698964154, 16.51473224551069663, 105.4155762719810383 ) ) ;
#136288 = CARTESIAN_POINT ( 'NONE',  ( 15.50000000000000178, -5.500000000000000888, 22.00000000000000711 ) ) ;
#136291 = CARTESIAN_POINT ( 'NONE',  ( 21.55341960407619695, -5.719274019375665929, 56.04275706135235424 ) ) ;
#136290 = CARTESIAN_POINT ( 'NONE',  ( 16.52544592524335698, 4.483927247898782831, 71.45942372801901854 ) ) ;
#136289 = CARTESIAN_POINT ( 'NONE',  ( 14.29746914071037800, 8.314922557961029526, 51.66775706135234714 ) ) ;
#136292 = CARTESIAN_POINT ( 'NONE',  ( 5.719274019375673035, 21.55341960407619339, 92.29275706135236135 ) ) ;
#136293 = CARTESIAN_POINT ( 'NONE',  ( -18.22780087662124160, -5.499999999999927169, 68.98236817873106475 ) ) ;
#136294 = CARTESIAN_POINT ( 'NONE',  ( -16.53943276465976808, -0.05219959533934237506, 28.75109039468567929 ) ) ;
#136295 = CARTESIAN_POINT ( 'NONE',  ( 5.049401038298161559, -19.05341960407611168, 72.70724293864768129 ) ) ;
#136296 = CARTESIAN_POINT ( 'NONE',  ( -19.02544592524342804, 5.153800228976336051, 96.04057627198103830 ) ) ;
#136297 = EDGE_CURVE ( 'NONE', #186567, #24637, #180996, .T. ) ;
#136298 = LINE ( 'NONE', #78327, #118042 ) ;
#136299 = CARTESIAN_POINT ( 'NONE',  ( -9.564922557960796823, -16.46253265017161027, 22.08224293864768839 ) ) ;
#136300 = CARTESIAN_POINT ( 'NONE',  ( 15.80617190586746368, 15.72974639402197994, 24.37390960531435979 ) ) ;
#136301 = CARTESIAN_POINT ( 'NONE',  ( -12.06949235617739369, -12.14591786802326823, 89.37609039468568994 ) ) ;
#136303 = CARTESIAN_POINT ( 'NONE',  ( 16.46253265017160672, -9.564922557960803928, 68.33224293864770971 ) ) ;
#136302 = CARTESIAN_POINT ( 'NONE',  ( -14.34966873604960291, -8.224510206698953496, 76.66557627198103830 ) ) ;
#136304 = CARTESIAN_POINT ( 'NONE',  ( 5.719274019375673035, 21.55341960407619339, 97.29275706135234714 ) ) ;
#136305 = DIRECTION ( 'NONE',  ( 1.000000000000000000, 0.000000000000000000, 0.000000000000000000 ) ) ;
#136306 = CARTESIAN_POINT ( 'NONE',  ( 14.34966873604972726, -8.224510206698740333, 25.83442372801901499 ) ) ;
#136307 = CARTESIAN_POINT ( 'NONE',  ( 12.14591786802309770, 12.06949235617756955, 69.37390960531436690 ) ) ;
#136308 = CARTESIAN_POINT ( 'NONE',  ( 0.05219959533937995610, -21.53943276465977519, 25.00109039468567218 ) ) ;
#136309 = CARTESIAN_POINT ( 'NONE',  ( 0.05219959533907565091, 21.53943276465977519, 79.99890960531435269 ) ) ;
#136310 = CARTESIAN_POINT ( 'NONE',  ( -19.05341960407617563, 5.049401038297882671, 38.54275706135233293 ) ) ;
#136311 = CARTESIAN_POINT ( 'NONE',  ( -23.31738231874055245, -16.94106989632524574, 144.4500000054623854 ) ) ;
#136312 = CARTESIAN_POINT ( 'NONE',  ( 9.474510206698971260, -16.51473224551069308, 82.91557627198103830 ) ) ;
#136313 = CARTESIAN_POINT ( 'NONE',  ( -16.53943276465976808, 0.05219959533911058130, 46.24890960531435979 ) ) ;
#136314 = CARTESIAN_POINT ( 'NONE',  ( 14.29746914071049879, -8.314922557960816363, 33.33224293864769550 ) ) ;
#136315 = CARTESIAN_POINT ( 'NONE',  ( -12.14591786802326823, 12.06949235617739902, 113.1260903946856899 ) ) ;
#136316 = CARTESIAN_POINT ( 'NONE',  ( 16.51473224551083163, -9.474510206698727899, 60.83442372801900433 ) ) ;
#136317 = CARTESIAN_POINT ( 'NONE',  ( 19.35543954521082455, 5.499999999999579892, 52.08901960356453742 ) ) ;
#136318 = CARTESIAN_POINT ( 'NONE',  ( -13.89961937509977652, 13.97604488694528158, 110.6239096053143243 ) ) ;
#136319 = EDGE_CURVE ( 'NONE', #182913, #191214, #169368, .T. ) ;
#136320 = CARTESIAN_POINT ( 'NONE',  ( -4.379528057220328563, 16.55341960407611168, 75.20724293864769550 ) ) ;
#136321 = CARTESIAN_POINT ( 'NONE',  ( -1.221313414957698099E-14, 31.90000000000003411, -49.13275782002545355 ) ) ;
#136323 = CARTESIAN_POINT ( 'NONE',  ( -21.55341960407610458, -5.719274019375992779, 41.45724293864769550 ) ) ;
#136322 = CARTESIAN_POINT ( 'NONE',  ( -19.03943276465977164, 0.05219959533909376836, 31.24890960531435979 ) ) ;
#136324 = CARTESIAN_POINT ( 'NONE',  ( -0.05219959533907301413, -21.53943276465977519, 67.49890960531436690 ) ) ;
#136325 = CARTESIAN_POINT ( 'NONE',  ( 14.29746914071049879, -8.314922557960816363, 113.3322429386476955 ) ) ;
#136327 = CARTESIAN_POINT ( 'NONE',  ( 19.02544592524343514, -5.153800228976328945, 53.54057627198102409 ) ) ;
#136326 = CARTESIAN_POINT ( 'NONE',  ( 14.29746914071037800, 8.314922557961029526, 61.66775706135235424 ) ) ;
#136328 = CARTESIAN_POINT ( 'NONE',  ( 15.80617190586769283, -15.72974639402175789, 50.62609039468568994 ) ) ;
#136329 = ORIENTED_EDGE ( 'NONE', *, *, #70955, .T. ) ;
#136330 = CARTESIAN_POINT ( 'NONE',  ( -8.224510206698948167, 14.34966873604960824, 95.41557627198102409 ) ) ;
#136331 = CARTESIAN_POINT ( 'NONE',  ( -17.50000000001356781, 5.500000000000039968, 40.79690382535057580 ) ) ;
#136332 = CARTESIAN_POINT ( 'NONE',  ( -17.49999999999999645, 5.624438216177593652, 50.81670344914645909 ) ) ;
#136333 = CARTESIAN_POINT ( 'NONE',  ( 21.55341960407610458, 5.719274019375980345, 38.95724293864768839 ) ) ;
#136334 = CARTESIAN_POINT ( 'NONE',  ( 22.73749492396215288, -155.7167183371838064, -15.00000000000000000 ) ) ;
#136336 = DIRECTION ( 'NONE',  ( 0.000000000000000000, 0.000000000000000000, -1.000000000000000000 ) ) ;
#136335 = CARTESIAN_POINT ( 'NONE',  ( -21.52544592524334988, -5.823673210054445271, 73.95942372801901854 ) ) ;
#136338 = CARTESIAN_POINT ( 'NONE',  ( 8.224510206698953496, -14.34966873604960469, 37.91557627198102409 ) ) ;
#136337 = CARTESIAN_POINT ( 'NONE',  ( 14.29746914071037800, 8.314922557961029526, 61.66775706135235424 ) ) ;
#136339 = CARTESIAN_POINT ( 'NONE',  ( 5.823673210054125526, 21.52544592524343514, 74.79057627198105251 ) ) ;
#136340 = CARTESIAN_POINT ( 'NONE',  ( 15.72974639402199770, -15.80617190586745480, 58.12390960531435979 ) ) ;
#136341 = CARTESIAN_POINT ( 'NONE',  ( -21.83923006935332367, -7.858462611068593340, 172.8812894384829519 ) ) ;
#136343 = CARTESIAN_POINT ( 'NONE',  ( 19.02544592524343514, -5.153800228976328945, 113.5405762719810241 ) ) ;
#136342 = CARTESIAN_POINT ( 'NONE',  ( -19.02544592524334988, -5.153800228976617603, 78.95942372801900433 ) ) ;
#136344 = CARTESIAN_POINT ( 'NONE',  ( 9.564922557960805705, 16.46253265017160317, 54.58224293864769550 ) ) ;
#136345 = CARTESIAN_POINT ( 'NONE',  ( -9.564922557960796823, -16.46253265017161027, 22.08224293864768839 ) ) ;
#136346 = LINE ( 'NONE', #105998, #18609 ) ;
#136347 = ORIENTED_EDGE ( 'NONE', *, *, #157667, .F. ) ;
#136348 = CARTESIAN_POINT ( 'NONE',  ( -16.53943276465976808, -0.05219959533934237506, 63.75109039468568284 ) ) ;
#136349 = CARTESIAN_POINT ( 'NONE',  ( -15.80617190586745835, -15.72974639402198527, 101.8739096053143811 ) ) ;
#136350 = CARTESIAN_POINT ( 'NONE',  ( -19.02544592524342804, 5.153800228976336051, 51.04057627198103120 ) ) ;
#136351 = CARTESIAN_POINT ( 'NONE',  ( 21.55341960407619695, -5.719274019375665929, 41.04275706135236135 ) ) ;
#136352 = CARTESIAN_POINT ( 'NONE',  ( -16.46253265017160317, 9.564922557960807481, 95.83224293864769550 ) ) ;
#136353 = CARTESIAN_POINT ( 'NONE',  ( -31.83877234781512655, -24.10177343596587107, -22.51708424455619451 ) ) ;
#136354 = ORIENTED_EDGE ( 'NONE', *, *, #26797, .F. ) ;
#136355 = CARTESIAN_POINT ( 'NONE',  ( -10.72451020669870658, -18.67979575497194134, 29.58442372801901854 ) ) ;
#136357 = CARTESIAN_POINT ( 'NONE',  ( -16.46253265017146816, -9.564922557961047289, 84.16775706135233293 ) ) ;
#136356 = CARTESIAN_POINT ( 'NONE',  ( -19.03943276465977164, 0.05219959533909376836, 106.2489096053143669 ) ) ;
#136358 = CARTESIAN_POINT ( 'NONE',  ( 16.46253265017146816, 9.564922557961045513, 41.66775706135234003 ) ) ;
#136359 = CARTESIAN_POINT ( 'NONE',  ( 15.80617190586746368, 15.72974639402197994, 104.3739096053143669 ) ) ;
#136360 = CARTESIAN_POINT ( 'NONE',  ( 16.51473224551083163, -9.474510206698727899, 35.83442372801899722 ) ) ;
#136361 = CARTESIAN_POINT ( 'NONE',  ( 5.153800228976615827, -19.02544592524334988, 40.20942372801898301 ) ) ;
#136362 = CARTESIAN_POINT ( 'NONE',  ( -16.52544592524335698, -4.483927247898792601, 88.95942372801901854 ) ) ;
#136363 = FACE_OUTER_BOUND ( 'NONE', #102840, .T. ) ;
#136364 = CARTESIAN_POINT ( 'NONE',  ( -19.03943276465977164, 0.05219959533909376836, 66.24890960531436690 ) ) ;
#136365 = CARTESIAN_POINT ( 'NONE',  ( -18.67979575497193778, 10.72451020669871902, 78.33442372801901854 ) ) ;
#136366 = CARTESIAN_POINT ( 'NONE',  ( 5.823673210054444382, -21.52544592524334988, 75.20942372801901854 ) ) ;
#136367 = PLANE ( 'NONE',  #127650 ) ;
#136368 = CARTESIAN_POINT ( 'NONE',  ( 5.049401038298161559, -19.05341960407611168, 87.70724293864769550 ) ) ;
#136369 = CARTESIAN_POINT ( 'NONE',  ( 18.67979575497194134, -10.72451020669871369, 65.83442372801900433 ) ) ;
#136370 = CARTESIAN_POINT ( 'NONE',  ( -19.05341960407617563, 5.049401038297882671, 98.54275706135233293 ) ) ;
#136371 = CARTESIAN_POINT ( 'NONE',  ( -9.564922557960796823, -16.46253265017161027, 67.08224293864769550 ) ) ;
#136372 = CARTESIAN_POINT ( 'NONE',  ( -16.51473224551069308, -9.474510206698971260, 106.6655762719810383 ) ) ;
#136373 = CARTESIAN_POINT ( 'NONE',  ( -16.46253265017160317, 9.564922557960807481, 75.83224293864769550 ) ) ;
#136374 = DIRECTION ( 'NONE',  ( -1.000000000000000000, 6.391086490440866478E-16, 0.000000000000000000 ) ) ;
#136375 = CARTESIAN_POINT ( 'NONE',  ( -13.97604488694527625, -13.89961937509977652, 71.87390960531433848 ) ) ;
#136376 = CARTESIAN_POINT ( 'NONE',  ( -19.05341960407611168, -5.049401038298163336, 51.45724293864770260 ) ) ;
#136377 = CARTESIAN_POINT ( 'NONE',  ( -21.52544592524343514, 5.823673210054127303, 101.0405762719810383 ) ) ;
#136378 = CARTESIAN_POINT ( 'NONE',  ( 14.34966873604972726, -8.224510206698740333, 80.83442372801901854 ) ) ;
#136379 = CARTESIAN_POINT ( 'NONE',  ( -15.49999999999999822, 5.499999999999998224, 22.00000000000000000 ) ) ;
#136380 = CARTESIAN_POINT ( 'NONE',  ( 19.02544592524334988, 5.153800228976608722, 41.45942372801900433 ) ) ;
#136381 = CARTESIAN_POINT ( 'NONE',  ( 16.51473224551069308, 9.474510206698969483, 79.16557627198103830 ) ) ;
#136382 = CARTESIAN_POINT ( 'NONE',  ( 0.05219959533910956823, 16.53943276465976808, 74.99890960531435269 ) ) ;
#136383 = CARTESIAN_POINT ( 'NONE',  ( 12.14591786802309770, 12.06949235617756955, 114.3739096053143527 ) ) ;
#136384 = CARTESIAN_POINT ( 'NONE',  ( 5.823673210054125526, 21.52544592524343514, 24.79057627198103120 ) ) ;
#136385 = CARTESIAN_POINT ( 'NONE',  ( -19.02544592524342804, 5.153800228976336051, 101.0405762719810241 ) ) ;
#136386 = CARTESIAN_POINT ( 'NONE',  ( -14.29746914071049879, 8.314922557960819915, 80.83224293864769550 ) ) ;
#136387 = CARTESIAN_POINT ( 'NONE',  ( -11.74149087413294623, -36.13659316521243881, -3.602157773949823394 ) ) ;
#136388 = CARTESIAN_POINT ( 'NONE',  ( 13.97604488694548053, -13.89961937509957401, 25.62609039468566507 ) ) ;
#136389 = CARTESIAN_POINT ( 'NONE',  ( -8.314922557961024197, 14.29746914071037800, 97.91775706135236135 ) ) ;
#136390 = CARTESIAN_POINT ( 'NONE',  ( 16.46253265017160672, -9.564922557960803928, 78.33224293864769550 ) ) ;
#136391 = CARTESIAN_POINT ( 'NONE',  ( 15.80617190586769283, -15.72974639402175789, 50.62609039468568994 ) ) ;
#136392 = CARTESIAN_POINT ( 'NONE',  ( 15.80617190586746368, 15.72974639402197994, 39.37390960531436690 ) ) ;
#136393 = CARTESIAN_POINT ( 'NONE',  ( 18.62759615963271287, -10.81492255796078972, 113.3322429386476955 ) ) ;
#136394 = CARTESIAN_POINT ( 'NONE',  ( 18.62759615963271287, -10.81492255796078972, 73.33224293864769550 ) ) ;
#136395 = CARTESIAN_POINT ( 'NONE',  ( 16.52544592524342804, -4.483927247898539470, 93.54057627198103830 ) ) ;
#136396 = CARTESIAN_POINT ( 'NONE',  ( 13.89961937509957401, 13.97604488694547697, 61.87609039468566863 ) ) ;
#136397 = CARTESIAN_POINT ( 'NONE',  ( -9.474510206698964154, 16.51473224551069663, 35.41557627198102409 ) ) ;
#136398 = CARTESIAN_POINT ( 'NONE',  ( 13.97604488694527802, 13.89961937509977652, 79.37390960531435269 ) ) ;
#136399 = CARTESIAN_POINT ( 'NONE',  ( 5.049401038298161559, -19.05341960407611168, 82.70724293864770971 ) ) ;
#136400 = CARTESIAN_POINT ( 'NONE',  ( 14.29746914071049879, -8.314922557960816363, 98.33224293864769550 ) ) ;
#136401 = CARTESIAN_POINT ( 'NONE',  ( 8.224510206698953496, -14.34966873604960469, 27.91557627198103830 ) ) ;
#136402 = CARTESIAN_POINT ( 'NONE',  ( 16.52544592524335698, 4.483927247898782831, 21.45942372801901499 ) ) ;
#136403 = CARTESIAN_POINT ( 'NONE',  ( -10.81492255796105439, 18.62759615963255655, 97.91775706135236135 ) ) ;
#136404 = CARTESIAN_POINT ( 'NONE',  ( -19.02544592524342804, 5.153800228976336051, 101.0405762719810241 ) ) ;
#136405 = CARTESIAN_POINT ( 'NONE',  ( 21.52544592524344225, -5.823673210054117533, 113.5405762719810383 ) ) ;
#136406 = CARTESIAN_POINT ( 'NONE',  ( -16.51473224551069308, -9.474510206698971260, 41.66557627198103120 ) ) ;
#136407 = CARTESIAN_POINT ( 'NONE',  ( -16.52544592524335698, -4.483927247898792601, 43.95942372801902565 ) ) ;
#136408 = CARTESIAN_POINT ( 'NONE',  ( -19.05341960407617563, 5.049401038297882671, 103.5427570613523329 ) ) ;
#136409 = CARTESIAN_POINT ( 'NONE',  ( -5.153800228976328057, -19.02544592524343514, 37.29057627198102409 ) ) ;
#136410 = CARTESIAN_POINT ( 'NONE',  ( 16.53943276465976808, -0.05219959533910856209, 98.74890960531438111 ) ) ;
#136411 = CARTESIAN_POINT ( 'NONE',  ( 15.72974639402199770, -15.80617190586745480, 103.1239096053143811 ) ) ;
#136412 = CARTESIAN_POINT ( 'NONE',  ( 19.02544592524334988, 5.153800228976608722, 66.45942372801899012 ) ) ;
#136413 = CARTESIAN_POINT ( 'NONE',  ( -17.60691670004651499, -5.500000000000069278, 64.13333313366436528 ) ) ;
#136414 = CARTESIAN_POINT ( 'NONE',  ( 5.153800228976335163, 19.02544592524342804, 94.79057627198103830 ) ) ;
#136415 = CARTESIAN_POINT ( 'NONE',  ( 18.62759615963255655, 10.81492255796105972, 21.66775706135235069 ) ) ;
#136416 = DIRECTION ( 'NONE',  ( 0.000000000000000000, 0.000000000000000000, -1.000000000000000000 ) ) ;
#136417 = CARTESIAN_POINT ( 'NONE',  ( -19.05341960407611168, -5.049401038298163336, 86.45724293864769550 ) ) ;
#136418 = CARTESIAN_POINT ( 'NONE',  ( 17.05116617787824396, -6.768360034955819060, 111.1567555325920011 ) ) ;
#136419 = CARTESIAN_POINT ( 'NONE',  ( 13.89961937509977652, -13.97604488694527269, 83.12390960531436690 ) ) ;
#136421 = CARTESIAN_POINT ( 'NONE',  ( 16.53943276465976808, -0.05219959533910856209, 78.74890960531436690 ) ) ;
#136420 = CARTESIAN_POINT ( 'NONE',  ( -15.80617190586768217, 15.72974639402176855, 38.12609039468567573 ) ) ;
#136422 = CARTESIAN_POINT ( 'NONE',  ( -19.02544592524342804, 5.153800228976336051, 86.04057627198103830 ) ) ;
#136423 = CARTESIAN_POINT ( 'NONE',  ( 9.564922557961047289, -16.46253265017146816, 25.41775706135234003 ) ) ;
#136424 = CARTESIAN_POINT ( 'NONE',  ( 14.34966873604972726, -8.224510206698740333, 55.83442372801901854 ) ) ;
#136425 = CARTESIAN_POINT ( 'NONE',  ( 21.53943276465977519, 0.05219959533937863772, 71.25109039468568994 ) ) ;
#136426 = CARTESIAN_POINT ( 'NONE',  ( 16.52544592524335698, 4.483927247898782831, 21.45942372801901499 ) ) ;
#136427 = CARTESIAN_POINT ( 'NONE',  ( 9.564922557960805705, 16.46253265017160317, 64.58224293864769550 ) ) ;
#136428 = CARTESIAN_POINT ( 'NONE',  ( -5.049401038297874678, -19.05341960407617918, 94.79275706135230450 ) ) ;
#136429 = CARTESIAN_POINT ( 'NONE',  ( 14.34966873604972726, -8.224510206698740333, 65.83442372801900433 ) ) ;
#136430 = CARTESIAN_POINT ( 'NONE',  ( -10.81492255796105439, 18.62759615963255655, 107.9177570613523471 ) ) ;
#136431 = CARTESIAN_POINT ( 'NONE',  ( -19.03943276465977164, -0.05219959533935918106, 73.75109039468566152 ) ) ;
#136432 = CARTESIAN_POINT ( 'NONE',  ( 13.89961937509977652, -13.97604488694527269, 53.12390960531434558 ) ) ;
#136433 = CARTESIAN_POINT ( 'NONE',  ( 0.05219959533907565091, 21.53943276465977519, 79.99890960531435269 ) ) ;
#136435 = CARTESIAN_POINT ( 'NONE',  ( 13.89961937509957401, 13.97604488694547697, 81.87609039468564731 ) ) ;
#136434 = CARTESIAN_POINT ( 'NONE',  ( 16.53943276465976808, -0.05219959533910856209, 73.74890960531433848 ) ) ;
#136436 = CARTESIAN_POINT ( 'NONE',  ( -2.500000000000000000, 3.061616997868383141E-16, -65.00100000000003320 ) ) ;
#136437 = CARTESIAN_POINT ( 'NONE',  ( -9.474510206698720793, -16.51473224551083518, 44.58442372801900433 ) ) ;
#136438 = CARTESIAN_POINT ( 'NONE',  ( 16.53943276465976808, 0.05219959533934440121, 106.2510903946856757 ) ) ;
#136439 = CARTESIAN_POINT ( 'NONE',  ( 14.29746914071049879, -8.314922557960816363, 63.33224293864770260 ) ) ;
#136441 = CARTESIAN_POINT ( 'NONE',  ( 27.73933785331498569, 2.768321779492822058E-14, 143.8750000027311842 ) ) ;
#136440 = CARTESIAN_POINT ( 'NONE',  ( -0.05219959533937732626, 21.53943276465977519, 97.50109039468567573 ) ) ;
#136442 = CARTESIAN_POINT ( 'NONE',  ( 10.72451020669898902, -18.67979575497178502, 102.9155762719810383 ) ) ;
#136443 = CARTESIAN_POINT ( 'NONE',  ( -13.89961937509977652, 13.97604488694528158, 60.62390960531436690 ) ) ;
#136444 = CARTESIAN_POINT ( 'NONE',  ( -10.81492255796105439, 18.62759615963255655, 77.91775706135231871 ) ) ;
#136445 = CARTESIAN_POINT ( 'NONE',  ( -0.05219959533909027116, -19.03943276465977164, 67.49890960531436690 ) ) ;
#136446 = CARTESIAN_POINT ( 'NONE',  ( -5.049401038298153566, 19.05341960407611168, 25.20724293864768484 ) ) ;
#136447 = CARTESIAN_POINT ( 'NONE',  ( -15.72974639402197994, 15.80617190586746368, 25.62390960531435624 ) ) ;
#136448 = CARTESIAN_POINT ( 'NONE',  ( 4.483927247898545687, 16.52544592524342804, 64.79057627198103830 ) ) ;
#136449 = CARTESIAN_POINT ( 'NONE',  ( 19.03943276465977164, -0.05219959533909143690, 38.74890960531436690 ) ) ;
#136450 = CARTESIAN_POINT ( 'NONE',  ( 16.53943276465976808, -0.05219959533910856209, 93.74890960531436690 ) ) ;
#136451 = CARTESIAN_POINT ( 'NONE',  ( 15.72974639402199770, -15.80617190586745480, 108.1239096053143811 ) ) ;
#136452 = CARTESIAN_POINT ( 'NONE',  ( -18.67979575497193778, 10.72451020669871902, 53.33442372801901854 ) ) ;
#136453 = CARTESIAN_POINT ( 'NONE',  ( 16.46253265017160672, -9.564922557960803928, 28.33224293864769550 ) ) ;
#136454 = CARTESIAN_POINT ( 'NONE',  ( -14.29746914071037622, -8.314922557961029526, 69.16775706135234714 ) ) ;
#136455 = CARTESIAN_POINT ( 'NONE',  ( -21.53943276465977519, 0.05219959533907696930, 106.2489096053143811 ) ) ;
#136456 = CARTESIAN_POINT ( 'NONE',  ( -18.67979575497178146, -10.72451020669898902, 101.6655762719810383 ) ) ;
#136458 = CARTESIAN_POINT ( 'NONE',  ( -13.89961937509977652, 13.97604488694528158, 55.62390960531434558 ) ) ;
#136457 = CARTESIAN_POINT ( 'NONE',  ( -9.474510206698720793, -16.51473224551083518, 24.58442372801900078 ) ) ;
#136459 = CARTESIAN_POINT ( 'NONE',  ( -18.10062525802553424, 5.500000000000031086, 83.51383468041922242 ) ) ;
#136460 = CARTESIAN_POINT ( 'NONE',  ( -15.72974639402176322, -15.80617190586768395, 54.37609039468568994 ) ) ;
#136461 = EDGE_CURVE ( 'NONE', #89236, #140310, #147320, .T. ) ;
#136462 = CARTESIAN_POINT ( 'NONE',  ( -15.72974639402197994, 15.80617190586746368, 50.62390960531435979 ) ) ;
#136463 = CARTESIAN_POINT ( 'NONE',  ( 4.379528057220339221, -16.55341960407611168, 22.70724293864769194 ) ) ;
#136465 = CARTESIAN_POINT ( 'NONE',  ( 18.62759615963255655, 10.81492255796105972, 101.6677570613523613 ) ) ;
#136464 = CARTESIAN_POINT ( 'NONE',  ( 21.53943276465977519, 0.05219959533937863772, 76.25109039468568994 ) ) ;
#136466 = CARTESIAN_POINT ( 'NONE',  ( 16.46253265017146816, 9.564922557961045513, 46.66775706135233293 ) ) ;
#136467 = CARTESIAN_POINT ( 'NONE',  ( 0.05219959533934541429, -16.53943276465976808, 105.0010903946856757 ) ) ;
#136468 = CARTESIAN_POINT ( 'NONE',  ( -5.719274019375665041, -21.55341960407619695, 59.79275706135234714 ) ) ;
#136469 = CARTESIAN_POINT ( 'NONE',  ( 0.05219959533909260263, 19.03943276465977164, 64.99890960531436690 ) ) ;
#136470 = CARTESIAN_POINT ( 'NONE',  ( 19.03943276465977164, 0.05219959533936151252, 26.25109039468566507 ) ) ;
#136471 = CARTESIAN_POINT ( 'NONE',  ( -10.72451020669898014, 18.67979575497178502, 40.41557627198103120 ) ) ;
#136472 = CARTESIAN_POINT ( 'NONE',  ( 15.72974639402176855, 15.80617190586768217, 26.87609039468567218 ) ) ;
#136473 = CARTESIAN_POINT ( 'NONE',  ( 21.52544592524344225, -5.823673210054117533, 83.54057627198102409 ) ) ;
#136474 = CARTESIAN_POINT ( 'NONE',  ( -19.02544592524334988, -5.153800228976617603, 88.95942372801897591 ) ) ;
#136475 = CARTESIAN_POINT ( 'NONE',  ( -16.52544592524335698, -4.483927247898792601, 53.95942372801900433 ) ) ;
#136477 = CARTESIAN_POINT ( 'NONE',  ( 5.719274019375991003, -21.55341960407610458, 82.70724293864770971 ) ) ;
#136476 = CARTESIAN_POINT ( 'NONE',  ( 18.22780087662121673, 5.500000000000056843, 63.98459894673894155 ) ) ;
#136479 = CARTESIAN_POINT ( 'NONE',  ( 4.379528057220339221, -16.55341960407611168, 77.70724293864770971 ) ) ;
#136478 = CARTESIAN_POINT ( 'NONE',  ( 8.314922557961029526, -14.29746914071037800, 70.41775706135236135 ) ) ;
#136480 = CARTESIAN_POINT ( 'NONE',  ( -20.85937581585705658, 20.13181022538182674, -49.56857446948050949 ) ) ;
#136481 = CARTESIAN_POINT ( 'NONE',  ( -13.97604488694547697, 13.89961937509957934, 98.12609039468566152 ) ) ;
#136482 = CARTESIAN_POINT ( 'NONE',  ( 5.719274019375991003, -21.55341960407610458, 37.70724293864769550 ) ) ;
#136483 = CARTESIAN_POINT ( 'NONE',  ( -17.58332526062529411, 7.635886036038502134, 95.92334959558468199 ) ) ;
#136484 = CARTESIAN_POINT ( 'NONE',  ( 14.29746914071037800, 8.314922557961029526, 41.66775706135235424 ) ) ;
#136485 = CARTESIAN_POINT ( 'NONE',  ( 5.719274019375991003, -21.55341960407610458, 107.7072429386476955 ) ) ;
#136486 = CARTESIAN_POINT ( 'NONE',  ( 21.52544592524344225, -5.823673210054117533, 38.54057627198103120 ) ) ;
#136487 = CARTESIAN_POINT ( 'NONE',  ( 16.55341960407618274, -4.379528057220086978, 66.04275706135236135 ) ) ;
#136488 = CARTESIAN_POINT ( 'NONE',  ( 19.03943276465977164, -0.05219959533909143690, 83.74890960531436690 ) ) ;
#136490 = CARTESIAN_POINT ( 'NONE',  ( -16.51473224551069308, -9.474510206698971260, 31.66557627198102054 ) ) ;
#136489 = CARTESIAN_POINT ( 'NONE',  ( 15.80617190586769283, -15.72974639402175789, 50.62609039468568994 ) ) ;
#136491 = CARTESIAN_POINT ( 'NONE',  ( -18.67979575497178146, -10.72451020669898902, 21.66557627198102409 ) ) ;
#136492 = ORIENTED_EDGE ( 'NONE', *, *, #122945, .T. ) ;
#136493 = CARTESIAN_POINT ( 'NONE',  ( 5.153800228976615827, -19.02544592524334988, 40.20942372801898301 ) ) ;
#136494 = CARTESIAN_POINT ( 'NONE',  ( 4.379528057220092307, 16.55341960407617563, 47.29275706135234003 ) ) ;
#136495 = CARTESIAN_POINT ( 'NONE',  ( -16.46253265017160317, 9.564922557960807481, 110.8322429386476955 ) ) ;
#136496 = CARTESIAN_POINT ( 'NONE',  ( 9.474510206698971260, -16.51473224551069308, 72.91557627198102409 ) ) ;
#136497 = CARTESIAN_POINT ( 'NONE',  ( -16.52544592524335698, -4.483927247898792601, 98.95942372801903275 ) ) ;
#136498 = DIRECTION ( 'NONE',  ( -1.000000000000000000, 0.000000000000000000, 0.000000000000000000 ) ) ;
#136499 = CARTESIAN_POINT ( 'NONE',  ( 4.483927247898545687, 16.52544592524342804, 99.79057627198103830 ) ) ;
#136500 = CARTESIAN_POINT ( 'NONE',  ( 18.67979575497178502, 10.72451020669898547, 29.16557627198103120 ) ) ;
#136501 = CARTESIAN_POINT ( 'NONE',  ( 5.153800228976335163, 19.02544592524342804, 29.79057627198102409 ) ) ;
#136502 = CARTESIAN_POINT ( 'NONE',  ( -16.55341960407617563, 4.379528057220093196, 63.54275706135234003 ) ) ;
#136503 = CARTESIAN_POINT ( 'NONE',  ( 10.81492255796078972, 18.62759615963270932, 114.5822429386477097 ) ) ;
#136504 = CARTESIAN_POINT ( 'NONE',  ( 13.89961937509957401, 13.97604488694547697, 81.87609039468564731 ) ) ;
#136505 = CARTESIAN_POINT ( 'NONE',  ( -5.049401038298153566, 19.05341960407611168, 45.20724293864769550 ) ) ;
#136506 = CARTESIAN_POINT ( 'NONE',  ( -0.05219959533907301413, -21.53943276465977519, 67.49890960531436690 ) ) ;
#136507 = CARTESIAN_POINT ( 'NONE',  ( 19.05341960407611168, 5.049401038298154454, 108.9572429386477097 ) ) ;
#136508 = CARTESIAN_POINT ( 'NONE',  ( 5.719274019375673035, 21.55341960407619339, 87.29275706135236135 ) ) ;
#136509 = CARTESIAN_POINT ( 'NONE',  ( 0.05219959533909260263, 19.03943276465977164, 69.99890960531435269 ) ) ;
#136510 = CARTESIAN_POINT ( 'NONE',  ( 8.314922557961029526, -14.29746914071037800, 50.41775706135235424 ) ) ;
#136511 = CARTESIAN_POINT ( 'NONE',  ( -19.03943276465977164, 0.05219959533909376836, 66.24890960531436690 ) ) ;
#136512 = CARTESIAN_POINT ( 'NONE',  ( 21.52544592524334988, 5.823673210054432836, 81.45942372801900433 ) ) ;
#136513 = CARTESIAN_POINT ( 'NONE',  ( 0.05219959533936267826, -19.03943276465977164, 35.00109039468566863 ) ) ;
#136514 = CARTESIAN_POINT ( 'NONE',  ( -19.03943276465977164, -0.05219959533935918106, 53.75109039468566863 ) ) ;
#136515 = ORIENTED_EDGE ( 'NONE', *, *, #137830, .F. ) ;
#136516 = CARTESIAN_POINT ( 'NONE',  ( 15.80617190586769283, -15.72974639402175789, 45.62609039468567573 ) ) ;
#136517 = DIRECTION ( 'NONE',  ( 1.186620743768021534E-15, -0.9396926207859040980, 0.3420201433256805368 ) ) ;
#136518 = CARTESIAN_POINT ( 'NONE',  ( -5.049401038297874678, -19.05341960407617918, 49.79275706135231871 ) ) ;
#136519 = CARTESIAN_POINT ( 'NONE',  ( 5.153800228976335163, 19.02544592524342804, 99.79057627198102409 ) ) ;
#136520 = CARTESIAN_POINT ( 'NONE',  ( 16.46253265017160672, -9.564922557960803928, 83.33224293864768129 ) ) ;
#136521 = CARTESIAN_POINT ( 'NONE',  ( 12.14591786802309770, 12.06949235617756955, 34.37390960531435979 ) ) ;
#136522 = CARTESIAN_POINT ( 'NONE',  ( -10.81492255796078084, -18.62759615963271287, 32.08224293864769550 ) ) ;
#136523 = CARTESIAN_POINT ( 'NONE',  ( -36.91746825000001309, 11.99521256947798342, -0.7249999972688133676 ) ) ;
#136524 = CYLINDRICAL_SURFACE ( 'NONE', #170841, 38.00000000000000000 ) ;
#136525 = CARTESIAN_POINT ( 'NONE',  ( -10.72451020669870658, -18.67979575497194134, 94.58442372801901854 ) ) ;
#136526 = CARTESIAN_POINT ( 'NONE',  ( -27.94727395831376882, 6.976223361892389896, 161.4607800657733492 ) ) ;
#136527 = CARTESIAN_POINT ( 'NONE',  ( 5.049401038298161559, -19.05341960407611168, 32.70724293864768129 ) ) ;
#136528 = CARTESIAN_POINT ( 'NONE',  ( 0.05219959533909260263, 19.03943276465977164, 109.9989096053143669 ) ) ;
#136529 = DIRECTION ( 'NONE',  ( 1.000000000000000000, -0.000000000000000000, -0.000000000000000000 ) ) ;
#136530 = CARTESIAN_POINT ( 'NONE',  ( -14.34966873604972548, 8.224510206698743886, 48.33442372801902565 ) ) ;
#136531 = CARTESIAN_POINT ( 'NONE',  ( -18.62759615963270932, 10.81492255796079327, 75.83224293864769550 ) ) ;
#136532 = CARTESIAN_POINT ( 'NONE',  ( 16.53943276465976808, -0.05219959533910856209, 33.74890960531436690 ) ) ;
#136534 = CARTESIAN_POINT ( 'NONE',  ( 5.049401038298161559, -19.05341960407611168, 107.7072429386476955 ) ) ;
#136533 = CARTESIAN_POINT ( 'NONE',  ( -19.02544592524342804, 5.153800228976336051, 26.04057627198103120 ) ) ;
#136535 = CARTESIAN_POINT ( 'NONE',  ( 15.72974639402176855, 15.80617190586768217, 26.87609039468567218 ) ) ;
#136536 = CARTESIAN_POINT ( 'NONE',  ( 19.05341960407617918, -5.049401038297876454, 41.04275706135233293 ) ) ;
#136537 = CARTESIAN_POINT ( 'NONE',  ( -8.224510206698948167, 14.34966873604960824, 110.4155762719810383 ) ) ;
#136538 = CARTESIAN_POINT ( 'NONE',  ( -0.05219959533937732626, 21.53943276465977519, 87.50109039468568994 ) ) ;
#136539 = CARTESIAN_POINT ( 'NONE',  ( 17.31747979337950483, -6.344076630960993946, 31.12055131934817354 ) ) ;
#136540 = CARTESIAN_POINT ( 'NONE',  ( -12.14591786802309592, -12.06949235617757132, 26.87390960531435979 ) ) ;
#136541 = PLANE ( 'NONE',  #194989 ) ;
#136542 = CARTESIAN_POINT ( 'NONE',  ( -15.80617190586745835, -15.72974639402198527, 31.87390960531435979 ) ) ;
#136543 = CARTESIAN_POINT ( 'NONE',  ( -16.53943276465976808, 0.05219959533911058130, 91.24890960531436690 ) ) ;
#136544 = DIRECTION ( 'NONE',  ( -1.000000000000000000, 0.000000000000000000, 0.000000000000000000 ) ) ;
#136545 = CARTESIAN_POINT ( 'NONE',  ( -19.02544592524342804, 5.153800228976336051, 76.04057627198102409 ) ) ;
#136546 = CARTESIAN_POINT ( 'NONE',  ( -12.06949235617756955, 12.14591786802309770, 80.62390960531438111 ) ) ;
#136547 = CARTESIAN_POINT ( 'NONE',  ( 5.049401038297881783, 19.05341960407617563, 112.2927570613523471 ) ) ;
#136548 = CARTESIAN_POINT ( 'NONE',  ( -10.72451020669898014, 18.67979575497178502, 60.41557627198102409 ) ) ;
#136549 = ORIENTED_EDGE ( 'NONE', *, *, #181095, .F. ) ;
#136550 = EDGE_CURVE ( 'NONE', #26587, #80788, #127361, .T. ) ;
#136551 = CARTESIAN_POINT ( 'NONE',  ( -5.049401038298153566, 19.05341960407611168, 35.20724293864768839 ) ) ;
#136553 = CARTESIAN_POINT ( 'NONE',  ( 10.81492255796078972, 18.62759615963270932, 69.58224293864769550 ) ) ;
#136552 = CARTESIAN_POINT ( 'NONE',  ( -5.049401038298153566, 19.05341960407611168, 70.20724293864769550 ) ) ;
#136555 = CARTESIAN_POINT ( 'NONE',  ( 5.049401038298161559, -19.05341960407611168, 82.70724293864770971 ) ) ;
#136554 = CARTESIAN_POINT ( 'NONE',  ( 14.34966873604972726, -8.224510206698740333, 105.8344237280190328 ) ) ;
#136556 = CARTESIAN_POINT ( 'NONE',  ( -13.89961937509957401, -13.97604488694547875, 64.37609039468567573 ) ) ;
#136557 = CARTESIAN_POINT ( 'NONE',  ( -15.72974639402176322, -15.80617190586768395, 99.37609039468568994 ) ) ;
#136558 = CARTESIAN_POINT ( 'NONE',  ( -10.81492255796078084, -18.62759615963271287, 77.08224293864769550 ) ) ;
#136559 = CARTESIAN_POINT ( 'NONE',  ( -15.80617190586745835, -15.72974639402198527, 21.87390960531436690 ) ) ;
#136560 = CARTESIAN_POINT ( 'NONE',  ( 9.564922557960805705, 16.46253265017160317, 49.58224293864770260 ) ) ;
#136561 = CARTESIAN_POINT ( 'NONE',  ( 8.224510206698742110, 14.34966873604972548, 97.08442372801904696 ) ) ;
#136562 = CARTESIAN_POINT ( 'NONE',  ( 13.97604488694527802, 13.89961937509977652, 64.37390960531436690 ) ) ;
#136563 = CARTESIAN_POINT ( 'NONE',  ( 27.05641397906351386, 3.631740835637567333, 169.9999999999999716 ) ) ;
#136564 = CARTESIAN_POINT ( 'NONE',  ( -21.55341960407619339, 5.719274019375674811, 103.5427570613523613 ) ) ;
#136565 = CARTESIAN_POINT ( 'NONE',  ( -12.14591786802309592, -12.06949235617757132, 66.87390960531436690 ) ) ;
#136566 = VECTOR ( 'NONE', #160960, 1000.000000000000000 ) ;
#136567 = CARTESIAN_POINT ( 'NONE',  ( -21.55341960407610458, -5.719274019375992779, 111.4572429386476813 ) ) ;
#136568 = CARTESIAN_POINT ( 'NONE',  ( 15.72974639402199770, -15.80617190586745480, 98.12390960531436690 ) ) ;
#136569 = LINE ( 'NONE', #150766, #62630 ) ;
#136570 = CARTESIAN_POINT ( 'NONE',  ( -15.80617190586745835, -15.72974639402198527, 61.87390960531436690 ) ) ;
#136571 = CARTESIAN_POINT ( 'NONE',  ( -4.379528057220086978, -16.55341960407618274, 79.79275706135236135 ) ) ;
#136572 = CARTESIAN_POINT ( 'NONE',  ( -4.379528057220328563, 16.55341960407611168, 100.2072429386476955 ) ) ;
#136573 = CARTESIAN_POINT ( 'NONE',  ( 13.89961937509977652, -13.97604488694527269, 58.12390960531436690 ) ) ;
#136574 = CARTESIAN_POINT ( 'NONE',  ( 16.52544592524335698, 4.483927247898782831, 111.4594237280190328 ) ) ;
#136575 = CARTESIAN_POINT ( 'NONE',  ( 5.719274019375673035, 21.55341960407619339, 47.29275706135234003 ) ) ;
#136576 = CARTESIAN_POINT ( 'NONE',  ( -19.05341960407611168, -5.049401038298163336, 96.45724293864769550 ) ) ;
#136577 = CARTESIAN_POINT ( 'NONE',  ( -0.05219959533937732626, 21.53943276465977519, 77.50109039468567573 ) ) ;
#136578 = CARTESIAN_POINT ( 'NONE',  ( 13.97604488694527802, 13.89961937509977652, 24.37390960531435624 ) ) ;
#136579 = CARTESIAN_POINT ( 'NONE',  ( 13.97604488694527802, 13.89961937509977652, 34.37390960531436690 ) ) ;
#136580 = ORIENTED_EDGE ( 'NONE', *, *, #117330, .T. ) ;
#136581 = CARTESIAN_POINT ( 'NONE',  ( -10.81492255796105439, 18.62759615963255655, 77.91775706135231871 ) ) ;
#136582 = CARTESIAN_POINT ( 'NONE',  ( -16.46253265017160317, 9.564922557960807481, 105.8322429386476955 ) ) ;
#136583 = CARTESIAN_POINT ( 'NONE',  ( 13.97604488694548053, -13.89961937509957401, 85.62609039468568994 ) ) ;
#136584 = CARTESIAN_POINT ( 'NONE',  ( 10.81492255796106328, -18.62759615963255655, 40.41775706135234714 ) ) ;
#136585 = CARTESIAN_POINT ( 'NONE',  ( 0.05219959533934541429, -16.53943276465976808, 20.00109039468568639 ) ) ;
#136586 = CARTESIAN_POINT ( 'NONE',  ( -16.51473224551082808, 9.474510206698731452, 68.33442372801900433 ) ) ;
#136587 = CARTESIAN_POINT ( 'NONE',  ( 16.46253265017160672, -9.564922557960803928, 53.33224293864768839 ) ) ;
#136588 = CARTESIAN_POINT ( 'NONE',  ( -19.05341960407617563, 5.049401038297882671, 83.54275706135233293 ) ) ;
#136589 = CARTESIAN_POINT ( 'NONE',  ( 0.05219959533910956823, 16.53943276465976808, 29.99890960531435979 ) ) ;
#136590 = CARTESIAN_POINT ( 'NONE',  ( 9.564922557961047289, -16.46253265017146816, 85.41775706135233293 ) ) ;
#136591 = CARTESIAN_POINT ( 'NONE',  ( 8.314922557960818139, 14.29746914071049879, 39.58224293864769550 ) ) ;
#136592 = CARTESIAN_POINT ( 'NONE',  ( 0.05219959533936267826, -19.03943276465977164, 60.00109039468566863 ) ) ;
#136593 = CARTESIAN_POINT ( 'NONE',  ( 12.06949235617739724, 12.14591786802326823, 46.87609039468568994 ) ) ;
#136594 = CARTESIAN_POINT ( 'NONE',  ( 9.474510206698729675, 16.51473224551082808, 27.08442372801900433 ) ) ;
#136595 = CARTESIAN_POINT ( 'NONE',  ( 19.03943276465977164, -0.05219959533909143690, 38.74890960531436690 ) ) ;
#136596 = CARTESIAN_POINT ( 'NONE',  ( -17.50000000000000355, -5.500000000000022204, 66.28230962303567253 ) ) ;
#136597 = CARTESIAN_POINT ( 'NONE',  ( 4.379528057220092307, 16.55341960407617563, 47.29275706135234003 ) ) ;
#136598 = FACE_OUTER_BOUND ( 'NONE', #37861, .T. ) ;
#136599 = CARTESIAN_POINT ( 'NONE',  ( 8.571926809382597767, 26.38167802310806209, 144.2750000027311899 ) ) ;
#136600 = CARTESIAN_POINT ( 'NONE',  ( 13.89961937509977652, -13.97604488694527269, 93.12390960531436690 ) ) ;
#136601 = CARTESIAN_POINT ( 'NONE',  ( -18.22780087662124160, -5.499999999999927169, 68.98236817873106475 ) ) ;
#136602 = ORIENTED_EDGE ( 'NONE', *, *, #85875, .F. ) ;
#136603 = CARTESIAN_POINT ( 'NONE',  ( -16.51473224551082808, 9.474510206698731452, 88.33442372801900433 ) ) ;
#136604 = CARTESIAN_POINT ( 'NONE',  ( 18.62759615963271287, -10.81492255796078972, 23.33224293864769194 ) ) ;
#136606 = CARTESIAN_POINT ( 'NONE',  ( -5.153800228976607833, 19.02544592524334988, 102.7094237280189759 ) ) ;
#136605 = CARTESIAN_POINT ( 'NONE',  ( -13.97604488694547697, 13.89961937509957934, 23.12609039468565442 ) ) ;
#136607 = CARTESIAN_POINT ( 'NONE',  ( -19.05341960407611168, -5.049401038298163336, 21.45724293864768839 ) ) ;
#136608 = CARTESIAN_POINT ( 'NONE',  ( -19.05341960407611168, -5.049401038298163336, 36.45724293864766707 ) ) ;
#136609 = CARTESIAN_POINT ( 'NONE',  ( 18.62759615963271287, -10.81492255796078972, 58.33224293864768839 ) ) ;
#136610 = CARTESIAN_POINT ( 'NONE',  ( -5.153800228976328057, -19.02544592524343514, 22.29057627198102765 ) ) ;
#136611 = CARTESIAN_POINT ( 'NONE',  ( 18.22780087662121673, 5.500000000000056843, 78.98459894673892734 ) ) ;
#136612 = CARTESIAN_POINT ( 'NONE',  ( 5.049401038297881783, 19.05341960407617563, 72.29275706135234714 ) ) ;
#136613 = CARTESIAN_POINT ( 'NONE',  ( 0.05219959533910956823, 16.53943276465976808, 34.99890960531435979 ) ) ;
#136614 = CARTESIAN_POINT ( 'NONE',  ( 18.62759615963271287, -10.81492255796078972, 28.33224293864769550 ) ) ;
#136615 = CARTESIAN_POINT ( 'NONE',  ( -18.67979575497193778, 10.72451020669871902, 98.33442372801901854 ) ) ;
#136616 = CARTESIAN_POINT ( 'NONE',  ( -10.81492255796078084, -18.62759615963271287, 87.08224293864769550 ) ) ;
#136617 = CARTESIAN_POINT ( 'NONE',  ( 5.719274019375673035, 21.55341960407619339, 52.29275706135236135 ) ) ;
#136618 = CARTESIAN_POINT ( 'NONE',  ( 10.72451020669871369, 18.67979575497193778, 67.08442372801901854 ) ) ;
#136619 = CARTESIAN_POINT ( 'NONE',  ( -5.049401038298153566, 19.05341960407611168, 95.20724293864770971 ) ) ;
#136621 = CARTESIAN_POINT ( 'NONE',  ( 5.823673210054444382, -21.52544592524334988, 55.20942372801902565 ) ) ;
#136620 = CARTESIAN_POINT ( 'NONE',  ( 16.52544592524335698, 4.483927247898782831, 91.45942372801901854 ) ) ;
#136622 = CARTESIAN_POINT ( 'NONE',  ( 16.55341960407611168, 4.379528057220329451, 113.9572429386477239 ) ) ;
#136623 = CARTESIAN_POINT ( 'NONE',  ( -16.53943276465976808, 0.05219959533911058130, 61.24890960531435979 ) ) ;
#136624 = CARTESIAN_POINT ( 'NONE',  ( -16.55341960407611168, -4.379528057220339221, 36.45724293864768839 ) ) ;
#136625 = CARTESIAN_POINT ( 'NONE',  ( 5.719274019375991003, -21.55341960407610458, 37.70724293864769550 ) ) ;
#136626 = CARTESIAN_POINT ( 'NONE',  ( 19.05341960407611168, 5.049401038298154454, 48.95724293864768129 ) ) ;
#136627 = CARTESIAN_POINT ( 'NONE',  ( 21.53943276465977519, -0.05219959533907433946, 53.74890960531437401 ) ) ;
#136628 = CARTESIAN_POINT ( 'NONE',  ( 5.153800228976615827, -19.02544592524334988, 45.20942372801901143 ) ) ;
#136630 = CARTESIAN_POINT ( 'NONE',  ( -16.53943276465976808, 0.05219959533911058130, 51.24890960531436690 ) ) ;
#136629 = DIRECTION ( 'NONE',  ( 1.000000000000000000, 0.000000000000000000, 0.000000000000000000 ) ) ;
#136631 = CARTESIAN_POINT ( 'NONE',  ( 15.72974639402199770, -15.80617190586745480, 33.12390960531435979 ) ) ;
#136632 = VERTEX_POINT ( 'NONE', #14124 ) ;
#136633 = ORIENTED_EDGE ( 'NONE', *, *, #185965, .F. ) ;
#136634 = CARTESIAN_POINT ( 'NONE',  ( -22.00000000000000000, -5.510910596163089556E-15, 45.00000000000000000 ) ) ;
#136635 = CARTESIAN_POINT ( 'NONE',  ( 4.379528057220092307, 16.55341960407617563, 72.29275706135236135 ) ) ;
#136636 = CARTESIAN_POINT ( 'NONE',  ( -9.474510206698720793, -16.51473224551083518, 79.58442372801899012 ) ) ;
#136637 = CARTESIAN_POINT ( 'NONE',  ( 12.14591786802309770, 12.06949235617756955, 44.37390960531435979 ) ) ;
#136638 = CARTESIAN_POINT ( 'NONE',  ( 8.673617379884035472E-16, 0.000000000000000000, 0.000000000000000000 ) ) ;
#136639 = CARTESIAN_POINT ( 'NONE',  ( -0.05219959533910754901, -16.53943276465976808, 32.49890960531435979 ) ) ;
#136640 = CARTESIAN_POINT ( 'NONE',  ( 13.89961937509977652, -13.97604488694527269, 53.12390960531434558 ) ) ;
#136641 = CARTESIAN_POINT ( 'NONE',  ( 13.97604488694527802, 13.89961937509977652, 79.37390960531435269 ) ) ;
#136642 = CARTESIAN_POINT ( 'NONE',  ( -0.05219959533909027116, -19.03943276465977164, 42.49890960531435269 ) ) ;
#136643 = CARTESIAN_POINT ( 'NONE',  ( 18.62759615963255655, 10.81492255796105972, 46.66775706135234714 ) ) ;
#136644 = CARTESIAN_POINT ( 'NONE',  ( -9.474510206698964154, 16.51473224551069663, 55.41557627198103120 ) ) ;
#136645 = DIRECTION ( 'NONE',  ( -1.000000000000000000, 0.000000000000000000, 0.000000000000000000 ) ) ;
#136646 = CARTESIAN_POINT ( 'NONE',  ( 19.03943276465977164, -0.05219959533909143690, 58.74890960531435979 ) ) ;
#136647 = EDGE_CURVE ( 'NONE', #24637, #44838, #166674, .T. ) ;
#136648 = CARTESIAN_POINT ( 'NONE',  ( 15.80617190586746368, 15.72974639402197994, 34.37390960531435979 ) ) ;
#136649 = CARTESIAN_POINT ( 'NONE',  ( -9.564922557960796823, -16.46253265017161027, 42.08224293864769550 ) ) ;
#136650 = CARTESIAN_POINT ( 'NONE',  ( -21.53943276465977519, 0.05219959533907696930, 46.24890960531435979 ) ) ;
#136651 = AXIS2_PLACEMENT_3D ( 'NONE', #1729, #63407, #186780 ) ;
#136652 = CARTESIAN_POINT ( 'NONE',  ( 8.224510206698742110, 14.34966873604972548, 87.08442372801901854 ) ) ;
#136653 = CARTESIAN_POINT ( 'NONE',  ( 10.72451020669871369, 18.67979575497193778, 112.0844237280190185 ) ) ;
#136654 = CARTESIAN_POINT ( 'NONE',  ( -4.483927247898782831, 16.52544592524335698, 62.70942372801902565 ) ) ;
#136655 = CARTESIAN_POINT ( 'NONE',  ( -5.153800228976328057, -19.02544592524343514, 102.2905762719810383 ) ) ;
#136656 = EDGE_CURVE ( 'NONE', #146461, #119499, #91852, .T. ) ;
#136657 = CARTESIAN_POINT ( 'NONE',  ( 0.05219959533934541429, -16.53943276465976808, 55.00109039468568284 ) ) ;
#136658 = CARTESIAN_POINT ( 'NONE',  ( -12.14591786802326823, 12.06949235617739902, 43.12609039468568284 ) ) ;
#136659 = CARTESIAN_POINT ( 'NONE',  ( 19.03943276465977164, -0.05219959533909143690, 113.7489096053143669 ) ) ;
#136660 = CARTESIAN_POINT ( 'NONE',  ( -14.29746914071037622, -8.314922557961029526, 29.16775706135234003 ) ) ;
#136661 = CARTESIAN_POINT ( 'NONE',  ( -5.049401038298153566, 19.05341960407611168, 40.20724293864768839 ) ) ;
#136662 = CARTESIAN_POINT ( 'NONE',  ( 15.72974639402176855, 15.80617190586768217, 26.87609039468567218 ) ) ;
#136663 = CARTESIAN_POINT ( 'NONE',  ( 19.03943276465977164, 0.05219959533936151252, 111.2510903946856757 ) ) ;
#136664 = CARTESIAN_POINT ( 'NONE',  ( -8.224510206698735004, -14.34966873604973081, 89.58442372801901854 ) ) ;
#136665 = CARTESIAN_POINT ( 'NONE',  ( -3.573655867282028392E-15, 2.428612866367529932E-14, 0.000000000000000000 ) ) ;
#136666 = CARTESIAN_POINT ( 'NONE',  ( -15.80617190586768217, 15.72974639402176855, 98.12609039468570415 ) ) ;
#136667 = CARTESIAN_POINT ( 'NONE',  ( -13.89961937509957401, -13.97604488694547875, 94.37609039468566152 ) ) ;
#136668 = CARTESIAN_POINT ( 'NONE',  ( -16.53943276465976808, 0.05219959533911058130, 51.24890960531436690 ) ) ;
#136669 = CARTESIAN_POINT ( 'NONE',  ( 4.379528057220339221, -16.55341960407611168, 102.7072429386476955 ) ) ;
#136671 = CARTESIAN_POINT ( 'NONE',  ( -6.615299585309108110, 1.135848680322218751, -64.43295106733367561 ) ) ;
#136670 = CARTESIAN_POINT ( 'NONE',  ( 5.153800228976615827, -19.02544592524334988, 45.20942372801901143 ) ) ;
#136672 = CARTESIAN_POINT ( 'NONE',  ( -10.72451020669870658, -18.67979575497194134, 49.58442372801901143 ) ) ;
#136673 = CARTESIAN_POINT ( 'NONE',  ( -0.05219959533936034679, 19.03943276465977164, 107.5010903946856615 ) ) ;
#136674 = CARTESIAN_POINT ( 'NONE',  ( -17.49999999999999645, 5.499999999999992895, 63.71769037696435589 ) ) ;
#136675 = CARTESIAN_POINT ( 'NONE',  ( 16.51473224551069308, 9.474510206698969483, 104.1655762719810241 ) ) ;
#136676 = CARTESIAN_POINT ( 'NONE',  ( -15.80617190586745835, -15.72974639402198527, 71.87390960531438111 ) ) ;
#136677 = CARTESIAN_POINT ( 'NONE',  ( 9.564922557961047289, -16.46253265017146816, 95.41775706135233293 ) ) ;
#136678 = CARTESIAN_POINT ( 'NONE',  ( 9.564922557960805705, 16.46253265017160317, 109.5822429386476955 ) ) ;
#136679 = CARTESIAN_POINT ( 'NONE',  ( -26.79623349963135581, 5.044589688426436069, 170.2051123914324080 ) ) ;
#136680 = CARTESIAN_POINT ( 'NONE',  ( 4.379528057220339221, -16.55341960407611168, 102.7072429386476955 ) ) ;
#136681 = CARTESIAN_POINT ( 'NONE',  ( -18.62759615963255300, -10.81492255796106328, 94.16775706135237556 ) ) ;
#136682 = CARTESIAN_POINT ( 'NONE',  ( 5.153800228976335163, 19.02544592524342804, 39.79057627198100988 ) ) ;
#136683 = CARTESIAN_POINT ( 'NONE',  ( -21.53943276465977519, -0.05219959533937600094, 53.75109039468568994 ) ) ;
#136684 = CARTESIAN_POINT ( 'NONE',  ( 10.72451020669871369, 18.67979575497193778, 92.08442372801901854 ) ) ;
#136685 = CARTESIAN_POINT ( 'NONE',  ( -8.224510206698735004, -14.34966873604973081, 109.5844237280190328 ) ) ;
#136686 = CARTESIAN_POINT ( 'NONE',  ( -16.51473224551069308, -9.474510206698971260, 61.66557627198103120 ) ) ;
#136687 = CARTESIAN_POINT ( 'NONE',  ( -10.81492255796105439, 18.62759615963255655, 37.91775706135235424 ) ) ;
#136688 = CARTESIAN_POINT ( 'NONE',  ( -10.72451020669870658, -18.67979575497194134, 44.58442372801901854 ) ) ;
#136690 = CARTESIAN_POINT ( 'NONE',  ( 5.153800228976335163, 19.02544592524342804, 94.79057627198103830 ) ) ;
#136689 = CARTESIAN_POINT ( 'NONE',  ( 0.05219959533936267826, -19.03943276465977164, 70.00109039468566152 ) ) ;
#136691 = CARTESIAN_POINT ( 'NONE',  ( 0.05219959533910956823, 16.53943276465976808, 104.9989096053143669 ) ) ;
#136692 = EDGE_CURVE ( 'NONE', #69503, #42366, #84623, .T. ) ;
#136693 = CARTESIAN_POINT ( 'NONE',  ( 10.81492255796078972, 18.62759615963270932, 94.58224293864769550 ) ) ;
#136694 = CARTESIAN_POINT ( 'NONE',  ( 14.34966873604960469, 8.224510206698951720, 69.16557627198102409 ) ) ;
#136695 = CARTESIAN_POINT ( 'NONE',  ( -16.51473224551082808, 9.474510206698731452, 23.33442372801900078 ) ) ;
#136696 = CARTESIAN_POINT ( 'NONE',  ( -12.14591786802309592, -12.06949235617757132, 86.87390960531438111 ) ) ;
#136697 = CARTESIAN_POINT ( 'NONE',  ( 19.03943276465977164, -0.05219959533909143690, 38.74890960531436690 ) ) ;
#136698 = CARTESIAN_POINT ( 'NONE',  ( 0.05219959533936267826, -19.03943276465977164, 90.00109039468567573 ) ) ;
#136699 = CARTESIAN_POINT ( 'NONE',  ( -12.14591786802309592, -12.06949235617757132, 51.87390960531437401 ) ) ;
#136700 = CARTESIAN_POINT ( 'NONE',  ( -18.67979575497193778, 10.72451020669871902, 93.33442372801901854 ) ) ;
#136701 = CARTESIAN_POINT ( 'NONE',  ( 5.049401038298161559, -19.05341960407611168, 87.70724293864769550 ) ) ;
#136702 = CARTESIAN_POINT ( 'NONE',  ( -19.02544592524334988, -5.153800228976617603, 78.95942372801900433 ) ) ;
#136703 = CARTESIAN_POINT ( 'NONE',  ( -5.719274019375978568, 21.55341960407610458, 75.20724293864769550 ) ) ;
#136704 = CARTESIAN_POINT ( 'NONE',  ( 21.53943276465977519, 0.05219959533937863772, 26.25109039468567573 ) ) ;
#136705 = CARTESIAN_POINT ( 'NONE',  ( -4.379528057220086978, -16.55341960407618274, 34.79275706135235424 ) ) ;
#136706 = CARTESIAN_POINT ( 'NONE',  ( -16.52544592524335698, -4.483927247898792601, 88.95942372801901854 ) ) ;
#136708 = CARTESIAN_POINT ( 'NONE',  ( -21.52544592524334988, -5.823673210054445271, 38.95942372801901854 ) ) ;
#136707 = CARTESIAN_POINT ( 'NONE',  ( -16.51473224551069308, -9.474510206698971260, 26.66557627198103120 ) ) ;
#136709 = CARTESIAN_POINT ( 'NONE',  ( 19.03943276465977164, -0.05219959533909143690, 23.74890960531435269 ) ) ;
#136710 = CARTESIAN_POINT ( 'NONE',  ( 23.48529157249600630, -32.32473071737749137, -9.049999994537627046 ) ) ;
#136711 = CARTESIAN_POINT ( 'NONE',  ( 0.05219959533934541429, -16.53943276465976808, 55.00109039468568284 ) ) ;
#136712 = CARTESIAN_POINT ( 'NONE',  ( 8.314922557960818139, 14.29746914071049879, 74.58224293864768129 ) ) ;
#136713 = CARTESIAN_POINT ( 'NONE',  ( -10.72451020669898014, 18.67979575497178502, 80.41557627198103830 ) ) ;
#136714 = CARTESIAN_POINT ( 'NONE',  ( 12.06949235617757843, -12.14591786802309237, 28.12390960531435979 ) ) ;
#136715 = CARTESIAN_POINT ( 'NONE',  ( -0.05219959533934338120, 16.53943276465976808, 52.50109039468567573 ) ) ;
#136716 = CARTESIAN_POINT ( 'NONE',  ( -13.97604488694527625, -13.89961937509977652, 41.87390960531435979 ) ) ;
#136717 = CARTESIAN_POINT ( 'NONE',  ( -14.34966873604972548, 8.224510206698743886, 98.33442372801901854 ) ) ;
#136718 = CARTESIAN_POINT ( 'NONE',  ( 13.97604488694548053, -13.89961937509957401, 80.62609039468567573 ) ) ;
#136719 = CARTESIAN_POINT ( 'NONE',  ( 18.62759615963271287, -10.81492255796078972, 78.33224293864770971 ) ) ;
#136720 = CARTESIAN_POINT ( 'NONE',  ( 14.34966873604972726, -8.224510206698740333, 110.8344237280190043 ) ) ;
#136721 = EDGE_LOOP ( 'NONE', ( #71273, #131661, #94857, #121268 ) ) ;
#136722 = CARTESIAN_POINT ( 'NONE',  ( 0.000000000000000000, 0.000000000000000000, -62.50719930893269805 ) ) ;
#136723 = CARTESIAN_POINT ( 'NONE',  ( 18.67979575497178502, 10.72451020669898547, 59.16557627198103120 ) ) ;
#136724 = VERTEX_POINT ( 'NONE', #89980 ) ;
#136725 = CARTESIAN_POINT ( 'NONE',  ( 16.53943276465976808, 0.05219959533934440121, 86.25109039468568994 ) ) ;
#136726 = ORIENTED_EDGE ( 'NONE', *, *, #160293, .F. ) ;
#136727 = CARTESIAN_POINT ( 'NONE',  ( -5.153800228976328057, -19.02544592524343514, 107.2905762719810383 ) ) ;
#136728 = CARTESIAN_POINT ( 'NONE',  ( 17.49999999999999289, 4.640572885337564735, 106.8621183545116082 ) ) ;
#136729 = CARTESIAN_POINT ( 'NONE',  ( 18.67979575497178502, 10.72451020669898547, 79.16557627198103830 ) ) ;
#136730 = CARTESIAN_POINT ( 'NONE',  ( -8.224510206698735004, -14.34966873604973081, 109.5844237280190328 ) ) ;
#136731 = CARTESIAN_POINT ( 'NONE',  ( -19.05341960407617563, 5.049401038297882671, 113.5427570613523471 ) ) ;
#136732 = CARTESIAN_POINT ( 'NONE',  ( 0.05219959533909260263, 19.03943276465977164, 24.99890960531435269 ) ) ;
#136733 = CARTESIAN_POINT ( 'NONE',  ( 16.53943276465976808, 0.05219959533934440121, 26.25109039468567573 ) ) ;
#136734 = CARTESIAN_POINT ( 'NONE',  ( -13.97604488694527625, -13.89961937509977652, 56.87390960531434558 ) ) ;
#136735 = CARTESIAN_POINT ( 'NONE',  ( 8.906447517083057264, -27.41122689804191026, 140.5999999999999943 ) ) ;
#136736 = CARTESIAN_POINT ( 'NONE',  ( 19.02544592524343514, -5.153800228976328945, 103.5405762719809957 ) ) ;
#136737 = CARTESIAN_POINT ( 'NONE',  ( -14.34966873604972548, 8.224510206698743886, 93.33442372801901854 ) ) ;
#136738 = CARTESIAN_POINT ( 'NONE',  ( 13.89961937509957401, 13.97604488694547697, 96.87609039468566152 ) ) ;
#136739 = CARTESIAN_POINT ( 'NONE',  ( -16.51473224551082808, 9.474510206698731452, 23.33442372801900078 ) ) ;
#136740 = CARTESIAN_POINT ( 'NONE',  ( 15.80617190586746368, 15.72974639402197994, 79.37390960531436690 ) ) ;
#136741 = CARTESIAN_POINT ( 'NONE',  ( 16.52544592524335698, 4.483927247898782831, 106.4594237280190328 ) ) ;
#136742 = VECTOR ( 'NONE', #133910, 1000.000000000000000 ) ;
#136743 = CARTESIAN_POINT ( 'NONE',  ( -19.02544592524334988, -5.153800228976617603, 93.95942372801900433 ) ) ;
#136744 = CARTESIAN_POINT ( 'NONE',  ( -9.474510206698964154, 16.51473224551069663, 55.41557627198103120 ) ) ;
#136745 = CARTESIAN_POINT ( 'NONE',  ( -0.05219959533909027116, -19.03943276465977164, 92.49890960531436690 ) ) ;
#136746 = CARTESIAN_POINT ( 'NONE',  ( 21.52544592524334988, 5.823673210054432836, 56.45942372801902565 ) ) ;
#136747 = CARTESIAN_POINT ( 'NONE',  ( 19.05341960407611168, 5.049401038298154454, 63.95724293864769550 ) ) ;
#136748 = CARTESIAN_POINT ( 'NONE',  ( -0.05219959533910754901, -16.53943276465976808, 92.49890960531436690 ) ) ;
#136749 = CARTESIAN_POINT ( 'NONE',  ( 24.95262708931878493, -12.69764001896723116, 166.0532406165022508 ) ) ;
#136750 = CARTESIAN_POINT ( 'NONE',  ( -16.55341960407611168, -4.379528057220339221, 76.45724293864769550 ) ) ;
#136751 = CARTESIAN_POINT ( 'NONE',  ( -15.72974639402197994, 15.80617190586746368, 80.62390960531438111 ) ) ;
#136752 = CARTESIAN_POINT ( 'NONE',  ( -28.79475375365586842, 2.428612866367529932E-14, 144.2656553485623760 ) ) ;
#136753 = CARTESIAN_POINT ( 'NONE',  ( 16.61371651742602396, -7.165104196376141488, 81.35415069992998838 ) ) ;
#136754 = CARTESIAN_POINT ( 'NONE',  ( 19.05341960407617918, -5.049401038297876454, 46.04275706135233293 ) ) ;
#136755 = CARTESIAN_POINT ( 'NONE',  ( 17.26172910966714724, -6.454744622557085698, 73.30646908649207205 ) ) ;
#136757 = CARTESIAN_POINT ( 'NONE',  ( -19.02544592524342804, 5.153800228976336051, 86.04057627198103830 ) ) ;
#136756 = CARTESIAN_POINT ( 'NONE',  ( 16.51473224551069308, 9.474510206698969483, 74.16557627198103830 ) ) ;
#136758 = CARTESIAN_POINT ( 'NONE',  ( 8.224510206698742110, 14.34966873604972548, 62.08442372801901143 ) ) ;
#136759 = CARTESIAN_POINT ( 'NONE',  ( 18.70878831527338093, -37.83292004501380035, -19.76830273372893387 ) ) ;
#136760 = CARTESIAN_POINT ( 'NONE',  ( -16.46253265017146816, -9.564922557961047289, 49.16775706135233293 ) ) ;
#136761 = DIRECTION ( 'NONE',  ( 0.000000000000000000, 0.000000000000000000, -1.000000000000000000 ) ) ;
#136762 = CARTESIAN_POINT ( 'NONE',  ( 19.02544592524343514, -5.153800228976328945, 108.5405762719810383 ) ) ;
#136763 = CARTESIAN_POINT ( 'NONE',  ( 14.29746914071037800, 8.314922557961029526, 86.66775706135234714 ) ) ;
#136764 = CARTESIAN_POINT ( 'NONE',  ( -0.4379334789936237260, -21.36119649488922789, -56.42482690868973094 ) ) ;
#136765 = CARTESIAN_POINT ( 'NONE',  ( -14.29746914071037622, -8.314922557961029526, 74.16775706135231871 ) ) ;
#136766 = DIRECTION ( 'NONE',  ( 0.000000000000000000, -1.000000000000000000, 0.000000000000000000 ) ) ;
#136767 = CARTESIAN_POINT ( 'NONE',  ( 12.14591786802327356, -12.06949235617739191, 55.62609039468568284 ) ) ;
#136768 = CARTESIAN_POINT ( 'NONE',  ( -16.46253265017160317, 9.564922557960807481, 75.83224293864769550 ) ) ;
#136769 = CARTESIAN_POINT ( 'NONE',  ( 21.53943276465977519, 0.05219959533937863772, 61.25109039468567573 ) ) ;
#136770 = CARTESIAN_POINT ( 'NONE',  ( -9.474510206698720793, -16.51473224551083518, 79.58442372801899012 ) ) ;
#136771 = CARTESIAN_POINT ( 'NONE',  ( 5.153800228976615827, -19.02544592524334988, 20.20942372801899722 ) ) ;
#136772 = CARTESIAN_POINT ( 'NONE',  ( -5.049401038298153566, 19.05341960407611168, 50.20724293864770260 ) ) ;
#136773 = CARTESIAN_POINT ( 'NONE',  ( 5.153800228976335163, 19.02544592524342804, 44.79057627198103830 ) ) ;
#136774 = CARTESIAN_POINT ( 'NONE',  ( 16.62544781628812274, 7.153289815129877383, 22.00000000000000000 ) ) ;
#136775 = CARTESIAN_POINT ( 'NONE',  ( 5.719274019375991003, -21.55341960407610458, 62.70724293864769550 ) ) ;
#136776 = EDGE_CURVE ( 'NONE', #31087, #46062, #2631, .T. ) ;
#136777 = CARTESIAN_POINT ( 'NONE',  ( 19.05341960407611168, 5.049401038298154454, 113.9572429386477097 ) ) ;
#136778 = CARTESIAN_POINT ( 'NONE',  ( 4.379528057220339221, -16.55341960407611168, 112.7072429386476955 ) ) ;
#136779 = CARTESIAN_POINT ( 'NONE',  ( -14.29746914071037622, -8.314922557961029526, 54.16775706135235424 ) ) ;
#136780 = ORIENTED_EDGE ( 'NONE', *, *, #87285, .F. ) ;
#136781 = CARTESIAN_POINT ( 'NONE',  ( -21.53943276465977519, -0.05219959533937600094, 23.75109039468567929 ) ) ;
#136783 = CARTESIAN_POINT ( 'NONE',  ( 37.99999999999999289, 2.893978650043524126E-14, -5.000000000000000000 ) ) ;
#136782 = CARTESIAN_POINT ( 'NONE',  ( -16.53943276465976808, 0.05219959533911058130, 51.24890960531436690 ) ) ;
#136784 = CARTESIAN_POINT ( 'NONE',  ( -0.05219959533936034679, 19.03943276465977164, 107.5010903946856615 ) ) ;
#136785 = CARTESIAN_POINT ( 'NONE',  ( 5.049401038297881783, 19.05341960407617563, 37.29275706135232582 ) ) ;
#136786 = CARTESIAN_POINT ( 'NONE',  ( 12.14591786802309770, 12.06949235617756955, 39.37390960531436690 ) ) ;
#136787 = CARTESIAN_POINT ( 'NONE',  ( -10.81492255796105439, 18.62759615963255655, 22.91775706135235069 ) ) ;
#136789 = CARTESIAN_POINT ( 'NONE',  ( 10.72451020669898902, -18.67979575497178502, 57.91557627198103120 ) ) ;
#136788 = CARTESIAN_POINT ( 'NONE',  ( 17.12812012977024878, 6.668231424566067211, 33.85948759323144941 ) ) ;
#136790 = CARTESIAN_POINT ( 'NONE',  ( 19.02544592524343514, -5.153800228976328945, 93.54057627198102409 ) ) ;
#136791 = CARTESIAN_POINT ( 'NONE',  ( -16.53943276465976808, 0.05219959533911058130, 56.24890960531436690 ) ) ;
#136792 = CARTESIAN_POINT ( 'NONE',  ( 5.049401038298161559, -19.05341960407611168, 107.7072429386476955 ) ) ;
#136793 = CARTESIAN_POINT ( 'NONE',  ( -36.81592377195798349, 3.639597414954541144, 49.13916779353752418 ) ) ;
#136794 = CARTESIAN_POINT ( 'NONE',  ( -19.03943276465977164, -0.05219959533935918106, 48.75109039468566863 ) ) ;
#136795 = CARTESIAN_POINT ( 'NONE',  ( -18.67979575497178146, -10.72451020669898902, 91.66557627198103830 ) ) ;
#136796 = CARTESIAN_POINT ( 'NONE',  ( 13.97604488694527802, 13.89961937509977652, 49.37390960531434558 ) ) ;
#136797 = B_SPLINE_CURVE_WITH_KNOTS ( 'NONE', 3,
 ( #81462, #92675, #32019, #66319, #187706, #49178, #46188, #154363 ),
 .UNSPECIFIED., .F., .F.,
 ( 4, 2, 2, 4 ),
 ( 2.110382192020081086E-17, 0.002784256700436093385, 0.005568513400872164218, 0.01113702680174430762 ),
 .UNSPECIFIED. ) ;
#136798 = CARTESIAN_POINT ( 'NONE',  ( -4.379528057220328563, 16.55341960407611168, 110.2072429386477239 ) ) ;
#136799 = VECTOR ( 'NONE', #48988, 1000.000000000000000 ) ;
#136800 = CARTESIAN_POINT ( 'NONE',  ( 5.823673210054444382, -21.52544592524334988, 45.20942372801901854 ) ) ;
#136801 = DIRECTION ( 'NONE',  ( 1.000000000000000000, 0.000000000000000000, 0.000000000000000000 ) ) ;
#136802 = CARTESIAN_POINT ( 'NONE',  ( 14.34966873604960469, 8.224510206698951720, 24.16557627198103120 ) ) ;
#136803 = CARTESIAN_POINT ( 'NONE',  ( -16.46253265017160317, 9.564922557960807481, 55.83224293864769550 ) ) ;
#136804 = CARTESIAN_POINT ( 'NONE',  ( 19.05341960407611168, 5.049401038298154454, 93.95724293864769550 ) ) ;
#136805 = CARTESIAN_POINT ( 'NONE',  ( 5.719274019375991003, -21.55341960407610458, 72.70724293864769550 ) ) ;
#136806 = CARTESIAN_POINT ( 'NONE',  ( 8.571926809382603096, -26.38167802310801235, 141.4750000027312069 ) ) ;
#136807 = CARTESIAN_POINT ( 'NONE',  ( 5.153800228976335163, 19.02544592524342804, 49.79057627198100988 ) ) ;
#136808 = CARTESIAN_POINT ( 'NONE',  ( 21.52544592524344225, -5.823673210054117533, 48.54057627198103120 ) ) ;
#136809 = ADVANCED_FACE ( 'NONE', ( #124280, #151661 ), #13155, .T. ) ;
#136810 = ORIENTED_EDGE ( 'NONE', *, *, #53259, .T. ) ;
#136811 = CARTESIAN_POINT ( 'NONE',  ( -15.72974639402176322, -15.80617190586768395, 89.37609039468568994 ) ) ;
#136814 = CARTESIAN_POINT ( 'NONE',  ( 12.14591786802309770, 12.06949235617756955, 64.37390960531435269 ) ) ;
#136813 = CARTESIAN_POINT ( 'NONE',  ( 14.29746914071037800, 8.314922557961029526, 76.66775706135234714 ) ) ;
#136812 = CARTESIAN_POINT ( 'NONE',  ( 2.662494480112517437, -37.13692398601924793, -32.60000000000000142 ) ) ;
#136815 = CARTESIAN_POINT ( 'NONE',  ( 9.564922557960805705, 16.46253265017160317, 74.58224293864769550 ) ) ;
#136816 = ORIENTED_EDGE ( 'NONE', *, *, #131324, .T. ) ;
#136817 = CARTESIAN_POINT ( 'NONE',  ( -13.89961937509957401, -13.97604488694547875, 29.37609039468565797 ) ) ;
#136818 = CARTESIAN_POINT ( 'NONE',  ( -14.29746914071037622, -8.314922557961029526, 89.16775706135236135 ) ) ;
#136819 = CARTESIAN_POINT ( 'NONE',  ( 10.81492255796106328, -18.62759615963255655, 110.4177570613523756 ) ) ;
#136820 = CARTESIAN_POINT ( 'NONE',  ( -5.049401038298153566, 19.05341960407611168, 75.20724293864769550 ) ) ;
#136821 = CARTESIAN_POINT ( 'NONE',  ( -5.823673210054116645, -21.52544592524344225, 47.29057627198103120 ) ) ;
#136822 = CARTESIAN_POINT ( 'NONE',  ( -16.55341960407617563, 4.379528057220093196, 28.54275706135234358 ) ) ;
#136823 = CARTESIAN_POINT ( 'NONE',  ( -21.53943276465977519, -0.05219959533937600094, 88.75109039468567573 ) ) ;
#136824 = CARTESIAN_POINT ( 'NONE',  ( -16.55341960407617563, 4.379528057220093196, 68.54275706135234714 ) ) ;
#136825 = CARTESIAN_POINT ( 'NONE',  ( -18.62759615963270932, 10.81492255796079327, 110.8322429386476955 ) ) ;
#136826 = CARTESIAN_POINT ( 'NONE',  ( 19.03943276465977164, 0.05219959533936151252, 111.2510903946856757 ) ) ;
#136828 = EDGE_CURVE ( 'NONE', #107664, #60981, #120806, .T. ) ;
#136827 = CARTESIAN_POINT ( 'NONE',  ( -9.474510206698964154, 16.51473224551069663, 85.41557627198102409 ) ) ;
#136829 = CARTESIAN_POINT ( 'NONE',  ( -14.34966873604972548, 8.224510206698743886, 33.33442372801900433 ) ) ;
#136830 = CARTESIAN_POINT ( 'NONE',  ( 16.51473224551069308, 9.474510206698969483, 59.16557627198102409 ) ) ;
#136831 = CARTESIAN_POINT ( 'NONE',  ( 12.14591786802327356, -12.06949235617739191, 30.62609039468567929 ) ) ;
#136832 = CARTESIAN_POINT ( 'NONE',  ( -12.06949235617756955, 12.14591786802309770, 85.62390960531436690 ) ) ;
#136833 = CARTESIAN_POINT ( 'NONE',  ( -8.224510206698735004, -14.34966873604973081, 89.58442372801901854 ) ) ;
#136835 = CARTESIAN_POINT ( 'NONE',  ( 13.97604488694527802, 13.89961937509977652, 69.37390960531436690 ) ) ;
#136834 = CARTESIAN_POINT ( 'NONE',  ( -5.719274019375665041, -21.55341960407619695, 24.79275706135235779 ) ) ;
#136836 = CARTESIAN_POINT ( 'NONE',  ( 19.03943276465977164, -0.05219959533909143690, 78.74890960531436690 ) ) ;
#136837 = CARTESIAN_POINT ( 'NONE',  ( -0.05219959533934338120, 16.53943276465976808, 87.50109039468568994 ) ) ;
#136839 = ORIENTED_EDGE ( 'NONE', *, *, #95776, .F. ) ;
#136838 = CARTESIAN_POINT ( 'NONE',  ( -24.66578506923897152, -3.377805382906099219, 172.1149105766467926 ) ) ;
#136840 = ORIENTED_EDGE ( 'NONE', *, *, #37272, .F. ) ;
#136841 = CARTESIAN_POINT ( 'NONE',  ( 5.153800228976615827, -19.02544592524334988, 30.20942372801900433 ) ) ;
#136842 = CARTESIAN_POINT ( 'NONE',  ( 9.564922557960805705, 16.46253265017160317, 104.5822429386476955 ) ) ;
#136843 = CARTESIAN_POINT ( 'NONE',  ( -19.03943276465977164, 0.05219959533909376836, 46.24890960531435979 ) ) ;
#136844 = CARTESIAN_POINT ( 'NONE',  ( 16.51473224551069308, 9.474510206698969483, 114.1655762719810241 ) ) ;
#136845 = CARTESIAN_POINT ( 'NONE',  ( 12.06949235617739724, 12.14591786802326823, 31.87609039468567929 ) ) ;
#136847 = CARTESIAN_POINT ( 'NONE',  ( -14.29746914071037622, -8.314922557961029526, 39.16775706135235424 ) ) ;
#136846 = CARTESIAN_POINT ( 'NONE',  ( -16.46253265017146816, -9.564922557961047289, 54.16775706135234003 ) ) ;
#136848 = CARTESIAN_POINT ( 'NONE',  ( -16.51473224551069308, -9.474510206698971260, 111.6655762719810383 ) ) ;
#136849 = CARTESIAN_POINT ( 'NONE',  ( 19.02544592524343514, -5.153800228976328945, 78.54057627198099567 ) ) ;
#136850 = CARTESIAN_POINT ( 'NONE',  ( 18.67979575497178502, 10.72451020669898547, 99.16557627198100988 ) ) ;
#136851 = CARTESIAN_POINT ( 'NONE',  ( -5.049401038297874678, -19.05341960407617918, 69.79275706135233293 ) ) ;
#136853 = CARTESIAN_POINT ( 'NONE',  ( 17.49809244619821413, -3.610541912967066835, 21.90429107297349987 ) ) ;
#136852 = CARTESIAN_POINT ( 'NONE',  ( -19.05341960407611168, -5.049401038298163336, 86.45724293864769550 ) ) ;
#136854 = CARTESIAN_POINT ( 'NONE',  ( 5.049401038298161559, -19.05341960407611168, 67.70724293864769550 ) ) ;
#136856 = CARTESIAN_POINT ( 'NONE',  ( 0.05219959533909260263, 19.03943276465977164, 24.99890960531435269 ) ) ;
#136855 = CARTESIAN_POINT ( 'NONE',  ( -8.224510206698948167, 14.34966873604960824, 35.41557627198102409 ) ) ;
#136857 = CARTESIAN_POINT ( 'NONE',  ( -0.05219959533936034679, 19.03943276465977164, 37.50109039468567573 ) ) ;
#136858 = CARTESIAN_POINT ( 'NONE',  ( 12.06949235617757843, -12.14591786802309237, 78.12390960531436690 ) ) ;
#136859 = CARTESIAN_POINT ( 'NONE',  ( 15.80617190586769283, -15.72974639402175789, 95.62609039468568994 ) ) ;
#136860 = CARTESIAN_POINT ( 'NONE',  ( 19.02544592524343514, -5.153800228976328945, 33.54057627198102409 ) ) ;
#136861 = CARTESIAN_POINT ( 'NONE',  ( -0.05219959533934338120, 16.53943276465976808, 57.50109039468568994 ) ) ;
#136863 = CARTESIAN_POINT ( 'NONE',  ( 18.67979575497194134, -10.72451020669871369, 100.8344237280190185 ) ) ;
#136862 = CARTESIAN_POINT ( 'NONE',  ( -4.483927247898539470, -16.52544592524342804, 42.29057627198103120 ) ) ;
#136864 = CARTESIAN_POINT ( 'NONE',  ( -19.05341960407611168, -5.049401038298163336, 91.45724293864766707 ) ) ;
#136865 = CARTESIAN_POINT ( 'NONE',  ( -19.02544592524342804, 5.153800228976336051, 96.04057627198103830 ) ) ;
#136866 = CARTESIAN_POINT ( 'NONE',  ( 0.05219959533909260263, 19.03943276465977164, 24.99890960531435269 ) ) ;
#136867 = CARTESIAN_POINT ( 'NONE',  ( 14.29746914071049879, -8.314922557960816363, 103.3322429386476955 ) ) ;
#136868 = CARTESIAN_POINT ( 'NONE',  ( 0.05219959533910956823, 16.53943276465976808, 79.99890960531435269 ) ) ;
#136869 = CARTESIAN_POINT ( 'NONE',  ( 21.55341960407610458, 5.719274019375980345, 78.95724293864769550 ) ) ;
#136870 = CARTESIAN_POINT ( 'NONE',  ( -16.46253265017160317, 9.564922557960807481, 85.83224293864769550 ) ) ;
#136871 = CARTESIAN_POINT ( 'NONE',  ( 5.823673210054125526, 21.52544592524343514, 99.79057627198103830 ) ) ;
#136872 = CARTESIAN_POINT ( 'NONE',  ( -13.97604488694527625, -13.89961937509977652, 86.87390960531436690 ) ) ;
#136874 = CARTESIAN_POINT ( 'NONE',  ( -12.14591786802309592, -12.06949235617757132, 86.87390960531438111 ) ) ;
#136873 = DIRECTION ( 'NONE',  ( -0.000000000000000000, -0.000000000000000000, 1.000000000000000000 ) ) ;
#136875 = CARTESIAN_POINT ( 'NONE',  ( -5.153800228976328057, -19.02544592524343514, 57.29057627198103120 ) ) ;
#136876 = CARTESIAN_POINT ( 'NONE',  ( -21.55341960407610458, -5.719274019375992779, 71.45724293864769550 ) ) ;
#136877 = FACE_OUTER_BOUND ( 'NONE', #14624, .T. ) ;
#136879 = CARTESIAN_POINT ( 'NONE',  ( -22.44159573604010305, 16.30477369853692338, 149.1750000027311671 ) ) ;
#136878 = CARTESIAN_POINT ( 'NONE',  ( 8.314922557960818139, 14.29746914071049879, 24.58224293864768839 ) ) ;
#136880 = CARTESIAN_POINT ( 'NONE',  ( 12.06949235617739724, 12.14591786802326823, 21.87609039468567573 ) ) ;
#136881 = CARTESIAN_POINT ( 'NONE',  ( 4.379528057220339221, -16.55341960407611168, 77.70724293864770971 ) ) ;
#136882 = CARTESIAN_POINT ( 'NONE',  ( -17.44270441346516165, -5.991230190323025617, 96.36335079264230785 ) ) ;
#136883 = CARTESIAN_POINT ( 'NONE',  ( -16.46253265017160317, 9.564922557960807481, 80.83224293864769550 ) ) ;
#136884 = CARTESIAN_POINT ( 'NONE',  ( 0.05219959533909260263, 19.03943276465977164, 49.99890960531435979 ) ) ;
#136885 = CARTESIAN_POINT ( 'NONE',  ( -16.55341960407611168, -4.379528057220339221, 66.45724293864768129 ) ) ;
#136886 = AXIS2_PLACEMENT_3D ( 'NONE', #182833, #44315, #56493 ) ;
#136887 = CARTESIAN_POINT ( 'NONE',  ( -19.03943276465977164, 0.05219959533909376836, 111.2489096053143669 ) ) ;
#136888 = CARTESIAN_POINT ( 'NONE',  ( -19.03943276465977164, -0.05219959533935918106, 98.75109039468567573 ) ) ;
#136889 = CARTESIAN_POINT ( 'NONE',  ( 5.719274019375673035, 21.55341960407619339, 57.29275706135234714 ) ) ;
#136890 = CARTESIAN_POINT ( 'NONE',  ( -5.049401038298153566, 19.05341960407611168, 105.2072429386476671 ) ) ;
#136891 = CARTESIAN_POINT ( 'NONE',  ( 21.55341960407610458, 5.719274019375980345, 78.95724293864769550 ) ) ;
#136892 = CARTESIAN_POINT ( 'NONE',  ( 8.224510206698742110, 14.34966873604972548, 67.08442372801901854 ) ) ;
#136893 = CARTESIAN_POINT ( 'NONE',  ( 5.153800228976335163, 19.02544592524342804, 29.79057627198102409 ) ) ;
#136894 = CARTESIAN_POINT ( 'NONE',  ( -16.46253265017160317, 9.564922557960807481, 75.83224293864769550 ) ) ;
#136895 = CARTESIAN_POINT ( 'NONE',  ( 21.53943276465977519, -0.05219959533907433946, 83.74890960531435269 ) ) ;
#136896 = CARTESIAN_POINT ( 'NONE',  ( -13.97604488694547697, 13.89961937509957934, 113.1260903946856757 ) ) ;
#136898 = CARTESIAN_POINT ( 'NONE',  ( 0.05219959533937995610, -21.53943276465977519, 60.00109039468568284 ) ) ;
#136897 = CARTESIAN_POINT ( 'NONE',  ( -16.53943276465976808, 0.05219959533911058130, 41.24890960531435269 ) ) ;
#136900 = CARTESIAN_POINT ( 'NONE',  ( -9.564922557960796823, -16.46253265017161027, 102.0822429386477097 ) ) ;
#136899 = CARTESIAN_POINT ( 'NONE',  ( 16.52544592524335698, 4.483927247898782831, 91.45942372801901854 ) ) ;
#136901 = CARTESIAN_POINT ( 'NONE',  ( -16.51473224551069308, -9.474510206698971260, 106.6655762719810383 ) ) ;
#136902 = CARTESIAN_POINT ( 'NONE',  ( 0.7993202289070840960, 31.67416946171545433, -49.41566550377648070 ) ) ;
#136903 = CARTESIAN_POINT ( 'NONE',  ( 16.52544592524335698, 4.483927247898782831, 91.45942372801901854 ) ) ;
#136904 = CARTESIAN_POINT ( 'NONE',  ( -14.29746914071037622, -8.314922557961029526, 49.16775706135234003 ) ) ;
#136905 = CARTESIAN_POINT ( 'NONE',  ( -13.89961937509977652, 13.97604488694528158, 55.62390960531434558 ) ) ;
#136906 = CARTESIAN_POINT ( 'NONE',  ( 16.46253265017160672, -9.564922557960803928, 68.33224293864770971 ) ) ;
#136907 = CARTESIAN_POINT ( 'NONE',  ( 10.81492255796106328, -18.62759615963255655, 65.41775706135234714 ) ) ;
#136908 = CARTESIAN_POINT ( 'NONE',  ( 8.314922557961029526, -14.29746914071037800, 65.41775706135234714 ) ) ;
#136909 = CARTESIAN_POINT ( 'NONE',  ( -16.52544592524342804, 4.483927247898546575, 51.04057627198103120 ) ) ;
#136910 = CARTESIAN_POINT ( 'NONE',  ( -9.474510206698964154, 16.51473224551069663, 45.41557627198103120 ) ) ;
#136911 = CARTESIAN_POINT ( 'NONE',  ( -9.564922557960796823, -16.46253265017161027, 52.08224293864768839 ) ) ;
#136912 = CARTESIAN_POINT ( 'NONE',  ( 12.06949235617739724, 12.14591786802326823, 46.87609039468568994 ) ) ;
#136913 = CARTESIAN_POINT ( 'NONE',  ( -16.51473224551082808, 9.474510206698731452, 93.33442372801900433 ) ) ;
#136914 = CARTESIAN_POINT ( 'NONE',  ( -14.29746914071049879, 8.314922557960819915, 90.83224293864769550 ) ) ;
#136915 = CARTESIAN_POINT ( 'NONE',  ( -19.02544592524342804, 5.153800228976336051, 66.04057627198103830 ) ) ;
#136917 = CARTESIAN_POINT ( 'NONE',  ( 30.00000000000000000, 5.499999999999992895, 102.5000000000000142 ) ) ;
#136916 = CARTESIAN_POINT ( 'NONE',  ( -19.02544592524334988, -5.153800228976617603, 103.9594237280190043 ) ) ;
#136918 = CARTESIAN_POINT ( 'NONE',  ( -15.72974639402176322, -15.80617190586768395, 94.37609039468568994 ) ) ;
#136919 = CARTESIAN_POINT ( 'NONE',  ( 8.224510206698742110, 14.34966873604972548, 67.08442372801901854 ) ) ;
#136920 = CARTESIAN_POINT ( 'NONE',  ( -28.28060372831499336, 2.428612866367529932E-14, 139.6875000013656063 ) ) ;
#136921 = CARTESIAN_POINT ( 'NONE',  ( 5.719274019375991003, -21.55341960407610458, 52.70724293864769550 ) ) ;
#136922 = CARTESIAN_POINT ( 'NONE',  ( -16.53943276465976808, -0.05219959533934237506, 48.75109039468568284 ) ) ;
#136923 = CARTESIAN_POINT ( 'NONE',  ( -19.53037848336980886, 5.499999999999899636, 69.85532783611442653 ) ) ;
#136924 = CARTESIAN_POINT ( 'NONE',  ( 0.05219959533936267826, -19.03943276465977164, 45.00109039468566863 ) ) ;
#136925 = CARTESIAN_POINT ( 'NONE',  ( -19.03943276465977164, 0.05219959533909376836, 96.24890960531436690 ) ) ;
#136926 = CARTESIAN_POINT ( 'NONE',  ( 5.153800228976335163, 19.02544592524342804, 24.79057627198102765 ) ) ;
#136927 = CARTESIAN_POINT ( 'NONE',  ( -19.02544592524342804, 5.153800228976336051, 46.04057627198101699 ) ) ;
#136928 = DIRECTION ( 'NONE',  ( 1.000000000000000000, -0.000000000000000000, -0.000000000000000000 ) ) ;
#136929 = CARTESIAN_POINT ( 'NONE',  ( -5.719274019375665041, -21.55341960407619695, 74.79275706135234714 ) ) ;
#136930 = CARTESIAN_POINT ( 'NONE',  ( -3.573655867282028392E-15, 2.428612866367529932E-14, 155.0000000000000000 ) ) ;
#136931 = CARTESIAN_POINT ( 'NONE',  ( -19.02544592524334988, -5.153800228976617603, 28.95942372801900433 ) ) ;
#136932 = CARTESIAN_POINT ( 'NONE',  ( -0.05219959533936034679, 19.03943276465977164, 22.50109039468566152 ) ) ;
#136933 = CARTESIAN_POINT ( 'NONE',  ( 0.05219959533910956823, 16.53943276465976808, 54.99890960531435269 ) ) ;
#136934 = CARTESIAN_POINT ( 'NONE',  ( -13.89961937509977652, 13.97604488694528158, 55.62390960531434558 ) ) ;
#136935 = CARTESIAN_POINT ( 'NONE',  ( 10.72451020669898902, -18.67979575497178502, 22.91557627198102765 ) ) ;
#136936 = CARTESIAN_POINT ( 'NONE',  ( 18.67979575497194134, -10.72451020669871369, 80.83442372801901854 ) ) ;
#136937 = CARTESIAN_POINT ( 'NONE',  ( -5.153800228976328057, -19.02544592524343514, 62.29057627198100988 ) ) ;
#136938 = CARTESIAN_POINT ( 'NONE',  ( 10.81492255796106328, -18.62759615963255655, 75.41775706135233293 ) ) ;
#136939 = CARTESIAN_POINT ( 'NONE',  ( -18.62759615963270932, 10.81492255796079327, 30.83224293864770260 ) ) ;
#136940 = CARTESIAN_POINT ( 'NONE',  ( 18.62759615963255655, 10.81492255796105972, 36.66775706135234714 ) ) ;
#136941 = CARTESIAN_POINT ( 'NONE',  ( -5.153800228976607833, 19.02544592524334988, 67.70942372801900433 ) ) ;
#136942 = CARTESIAN_POINT ( 'NONE',  ( 13.97604488694527802, 13.89961937509977652, 44.37390960531435269 ) ) ;
#136943 = CARTESIAN_POINT ( 'NONE',  ( -9.564922557960796823, -16.46253265017161027, 82.08224293864768129 ) ) ;
#136944 = CARTESIAN_POINT ( 'NONE',  ( -12.06949235617739369, -12.14591786802326823, 34.37609039468568284 ) ) ;
#136945 = CARTESIAN_POINT ( 'NONE',  ( 16.53943276465976808, -0.05219959533910856209, 88.74890960531436690 ) ) ;
#136946 = CARTESIAN_POINT ( 'NONE',  ( 13.97604488694527802, 13.89961937509977652, 54.37390960531435979 ) ) ;
#136947 = CARTESIAN_POINT ( 'NONE',  ( -10.72451020669898014, 18.67979575497178502, 45.41557627198103830 ) ) ;
#136948 = CARTESIAN_POINT ( 'NONE',  ( -8.224510206698735004, -14.34966873604973081, 19.58442372801901143 ) ) ;
#136949 = CARTESIAN_POINT ( 'NONE',  ( 5.719274019375673035, 21.55341960407619339, 22.29275706135235069 ) ) ;
#136950 = CARTESIAN_POINT ( 'NONE',  ( 10.72451020669871369, 18.67979575497193778, 72.08442372801899012 ) ) ;
#136951 = CARTESIAN_POINT ( 'NONE',  ( -12.14591786802326823, 12.06949235617739902, 73.12609039468567573 ) ) ;
#136952 = CARTESIAN_POINT ( 'NONE',  ( -8.224510206698735004, -14.34966873604973081, 74.58442372801901854 ) ) ;
#136953 = COLOUR_RGB ( '', 0.66274510, 0.83137255, 0.94901961) ;
#136954 = CARTESIAN_POINT ( 'NONE',  ( 0.05219959533909260263, 19.03943276465977164, 54.99890960531435979 ) ) ;
#136955 = CARTESIAN_POINT ( 'NONE',  ( -12.14591786802326823, 12.06949235617739902, 88.12609039468570415 ) ) ;
#136956 = CARTESIAN_POINT ( 'NONE',  ( 16.51473224551083163, -9.474510206698727899, 40.83442372801900433 ) ) ;
#136957 = CARTESIAN_POINT ( 'NONE',  ( -5.719274019375665041, -21.55341960407619695, 19.79275706135235069 ) ) ;
#136958 = CARTESIAN_POINT ( 'NONE',  ( 14.34966873604960469, 8.224510206698951720, 59.16557627198103120 ) ) ;
#136959 = CARTESIAN_POINT ( 'NONE',  ( -16.51473224551069308, -9.474510206698971260, 81.66557627198103830 ) ) ;
#136960 = CARTESIAN_POINT ( 'NONE',  ( -16.55341960407617563, 4.379528057220093196, 93.54275706135234714 ) ) ;
#136961 = CARTESIAN_POINT ( 'NONE',  ( 18.62759615963255655, 10.81492255796105972, 61.66775706135235424 ) ) ;
#136962 = CARTESIAN_POINT ( 'NONE',  ( -12.14591786802326823, 12.06949235617739902, 38.12609039468567573 ) ) ;
#136963 = CARTESIAN_POINT ( 'NONE',  ( -10.72451020669898014, 18.67979575497178502, 105.4155762719810383 ) ) ;
#136964 = CARTESIAN_POINT ( 'NONE',  ( -4.483927247898539470, -16.52544592524342804, 62.29057627198102409 ) ) ;
#136965 = ORIENTED_EDGE ( 'NONE', *, *, #32058, .T. ) ;
#136966 = CARTESIAN_POINT ( 'NONE',  ( 21.53943276465977519, -0.05219959533907433946, 103.7489096053143669 ) ) ;
#136967 = CARTESIAN_POINT ( 'NONE',  ( 12.06949235617757843, -12.14591786802309237, 38.12390960531436690 ) ) ;
#136968 = ORIENTED_EDGE ( 'NONE', *, *, #132232, .T. ) ;
#136969 = CARTESIAN_POINT ( 'NONE',  ( 34.61352925372422362, 7.251504142776767026, 43.02394063628852194 ) ) ;
#136970 = CARTESIAN_POINT ( 'NONE',  ( 16.46253265017160672, -9.564922557960803928, 108.3322429386476955 ) ) ;
#136971 = CARTESIAN_POINT ( 'NONE',  ( -21.53943276465977519, -0.05219959533937600094, 38.75109039468567573 ) ) ;
#136972 = CARTESIAN_POINT ( 'NONE',  ( -16.55341960407611168, -4.379528057220339221, 71.45724293864769550 ) ) ;
#136973 = VECTOR ( 'NONE', #191866, 1000.000000000000000 ) ;
#136974 = CARTESIAN_POINT ( 'NONE',  ( 19.02544592524343514, -5.153800228976328945, 63.54057627198103830 ) ) ;
#136975 = CARTESIAN_POINT ( 'NONE',  ( 16.46253265017146816, 9.564922557961045513, 61.66775706135234003 ) ) ;
#136976 = CARTESIAN_POINT ( 'NONE',  ( 21.52544592524344225, -5.823673210054117533, 53.54057627198103120 ) ) ;
#136977 = CARTESIAN_POINT ( 'NONE',  ( -14.93382465614873666, -34.77343615282673994, -28.53315611748318759 ) ) ;
#136978 = CARTESIAN_POINT ( 'NONE',  ( -0.05219959533909027116, -19.03943276465977164, 57.49890960531435979 ) ) ;
#136979 = CARTESIAN_POINT ( 'NONE',  ( 4.483927247898790824, -16.52544592524335698, 40.20942372801901854 ) ) ;
#136980 = CARTESIAN_POINT ( 'NONE',  ( -18.67979575497193778, 10.72451020669871902, 23.33442372801901499 ) ) ;
#136981 = CARTESIAN_POINT ( 'NONE',  ( -16.55341960407611168, -4.379528057220339221, 51.45724293864770260 ) ) ;
#136982 = ORIENTED_EDGE ( 'NONE', *, *, #143563, .T. ) ;
#136983 = CARTESIAN_POINT ( 'NONE',  ( -13.97604488694527625, -13.89961937509977652, 86.87390960531436690 ) ) ;
#136984 = CARTESIAN_POINT ( 'NONE',  ( 21.53943276465977519, -0.05219959533907433946, 68.74890960531435269 ) ) ;
#136986 = CARTESIAN_POINT ( 'NONE',  ( -16.53943276465976808, -0.05219959533934237506, 38.75109039468567573 ) ) ;
#136985 = CARTESIAN_POINT ( 'NONE',  ( -21.53943276465977519, 0.05219959533907696930, 111.2489096053143669 ) ) ;
#136987 = CARTESIAN_POINT ( 'NONE',  ( -10.81492255796078084, -18.62759615963271287, 32.08224293864769550 ) ) ;
#136988 = CARTESIAN_POINT ( 'NONE',  ( -21.53943276465977519, -0.05219959533937600094, 103.7510903946857042 ) ) ;
#136989 = CARTESIAN_POINT ( 'NONE',  ( -5.153800228976328057, -19.02544592524343514, 102.2905762719810383 ) ) ;
#136990 = CARTESIAN_POINT ( 'NONE',  ( -19.05341960407611168, -5.049401038298163336, 46.45724293864768129 ) ) ;
#136991 = CARTESIAN_POINT ( 'NONE',  ( 5.049401038298161559, -19.05341960407611168, 92.70724293864769550 ) ) ;
#136992 = CARTESIAN_POINT ( 'NONE',  ( -9.474510206698964154, 16.51473224551069663, 75.41557627198103830 ) ) ;
#136993 = CARTESIAN_POINT ( 'NONE',  ( -7.776400214313161641, -46.08030136692367051, -22.42299576004354833 ) ) ;
#136994 = CARTESIAN_POINT ( 'NONE',  ( -19.02544592524334988, -5.153800228976617603, 53.95942372801898301 ) ) ;
#136996 = CARTESIAN_POINT ( 'NONE',  ( 18.67979575497178502, 10.72451020669898547, 29.16557627198103120 ) ) ;
#136995 = CARTESIAN_POINT ( 'NONE',  ( -21.55341960407619339, 5.719274019375674811, 108.5427570613523756 ) ) ;
#136997 = CARTESIAN_POINT ( 'NONE',  ( 12.06949235617739724, 12.14591786802326823, 101.8760903946857042 ) ) ;
#136998 = CARTESIAN_POINT ( 'NONE',  ( -9.564922557961040184, 16.46253265017147172, 72.91775706135233293 ) ) ;
#136999 = AXIS2_PLACEMENT_3D ( 'NONE', #145946, #8448, #163128 ) ;
#137000 = CARTESIAN_POINT ( 'NONE',  ( 17.59860650958989936, 7.585241751807028088, 39.07662985737508166 ) ) ;
#137001 = CARTESIAN_POINT ( 'NONE',  ( -0.05219959533936034679, 19.03943276465977164, 82.50109039468567573 ) ) ;
#137002 = CARTESIAN_POINT ( 'NONE',  ( -13.89961937509957401, -13.97604488694547875, 34.37609039468566863 ) ) ;
#137003 = CARTESIAN_POINT ( 'NONE',  ( 13.97604488694527802, 13.89961937509977652, 39.37390960531435269 ) ) ;
#137004 = CARTESIAN_POINT ( 'NONE',  ( 12.14591786802309770, 12.06949235617756955, 44.37390960531435979 ) ) ;
#137005 = CARTESIAN_POINT ( 'NONE',  ( -17.44279575226825685, -5.990770900252416098, 109.1644243248568387 ) ) ;
#137006 = CARTESIAN_POINT ( 'NONE',  ( 8.314922557960818139, 14.29746914071049879, 29.58224293864769905 ) ) ;
#137007 = CARTESIAN_POINT ( 'NONE',  ( 6.874011537017776341, -5.374011537017756801, -61.98469907122333922 ) ) ;
#137008 = CARTESIAN_POINT ( 'NONE',  ( -14.34966873604972548, 8.224510206698743886, 88.33442372801901854 ) ) ;
#137009 = CARTESIAN_POINT ( 'NONE',  ( 5.153800228976335163, 19.02544592524342804, 54.79057627198103120 ) ) ;
#137010 = CARTESIAN_POINT ( 'NONE',  ( 15.72974639402176855, 15.80617190586768217, 106.8760903946856899 ) ) ;
#137011 = CARTESIAN_POINT ( 'NONE',  ( -8.314922557961024197, 14.29746914071037800, 22.91775706135235069 ) ) ;
#137012 = CARTESIAN_POINT ( 'NONE',  ( 18.67979575497194134, -10.72451020669871369, 90.83442372801901854 ) ) ;
#137013 = CARTESIAN_POINT ( 'NONE',  ( -19.02544592524342804, 5.153800228976336051, 91.04057627198100988 ) ) ;
#137014 = CARTESIAN_POINT ( 'NONE',  ( -19.05341960407611168, -5.049401038298163336, 86.45724293864769550 ) ) ;
#137015 = CARTESIAN_POINT ( 'NONE',  ( 36.91746824999999177, 11.99521256947799230, -5.524999997268812635 ) ) ;
#137016 = CARTESIAN_POINT ( 'NONE',  ( -10.72451020669898014, 18.67979575497178502, 105.4155762719810383 ) ) ;
#137018 = EDGE_CURVE ( 'NONE', #171133, #130796, #159583, .T. ) ;
#137017 = CARTESIAN_POINT ( 'NONE',  ( -16.55341960407611168, -4.379528057220339221, 81.45724293864769550 ) ) ;
#137019 = CARTESIAN_POINT ( 'NONE',  ( -0.05219959533907301413, -21.53943276465977519, 72.49890960531435269 ) ) ;
#137020 = CARTESIAN_POINT ( 'NONE',  ( 5.049401038298161559, -19.05341960407611168, 62.70724293864769550 ) ) ;
#137022 = CARTESIAN_POINT ( 'NONE',  ( 12.14591786802327356, -12.06949235617739191, 85.62609039468568994 ) ) ;
#137021 = CARTESIAN_POINT ( 'NONE',  ( -10.81492255796078084, -18.62759615963271287, 97.08224293864770971 ) ) ;
#137023 = ORIENTED_EDGE ( 'NONE', *, *, #66474, .T. ) ;
#137024 = CARTESIAN_POINT ( 'NONE',  ( 16.46253265017160672, -9.564922557960803928, 58.33224293864769550 ) ) ;
#137026 = LINE ( 'NONE', #198716, #175387 ) ;
#137025 = CARTESIAN_POINT ( 'NONE',  ( -16.52544592524342804, 4.483927247898546575, 86.04057627198102409 ) ) ;
#137027 = CARTESIAN_POINT ( 'NONE',  ( 5.049401038298161559, -19.05341960407611168, 47.70724293864770260 ) ) ;
#137028 = CARTESIAN_POINT ( 'NONE',  ( 0.05219959533936267826, -19.03943276465977164, 85.00109039468567573 ) ) ;
#137029 = CARTESIAN_POINT ( 'NONE',  ( -16.53943276465976808, 0.05219959533911058130, 86.24890960531436690 ) ) ;
#137030 = CARTESIAN_POINT ( 'NONE',  ( 15.72974639402176855, 15.80617190586768217, 61.87609039468568284 ) ) ;
#137032 = CARTESIAN_POINT ( 'NONE',  ( 18.67979575497178502, 10.72451020669898547, 99.16557627198100988 ) ) ;
#137031 = CARTESIAN_POINT ( 'NONE',  ( -0.05219959533909027116, -19.03943276465977164, 32.49890960531435979 ) ) ;
#137033 = CARTESIAN_POINT ( 'NONE',  ( -4.483927247898539470, -16.52544592524342804, 102.2905762719810383 ) ) ;
#137034 = CARTESIAN_POINT ( 'NONE',  ( 13.59403193627403539, -42.61206874333516481, -22.32444481402548675 ) ) ;
#137035 = CARTESIAN_POINT ( 'NONE',  ( 19.03943276465977164, -0.05219959533909143690, 63.74890960531435979 ) ) ;
#137036 = CARTESIAN_POINT ( 'NONE',  ( 17.40861289039003879, 6.110651285853319514, 113.8723247082744052 ) ) ;
#137038 = CARTESIAN_POINT ( 'NONE',  ( -13.97604488694527625, -13.89961937509977652, 106.8739096053143669 ) ) ;
#137037 = CARTESIAN_POINT ( 'NONE',  ( 19.02544592524334988, 5.153800228976608722, 101.4594237280189759 ) ) ;
#137039 = CARTESIAN_POINT ( 'NONE',  ( -21.52544592524334988, -5.823673210054445271, 43.95942372801902565 ) ) ;
#137040 = CARTESIAN_POINT ( 'NONE',  ( -13.97604488694527625, -13.89961937509977652, 81.87390960531436690 ) ) ;
#137041 = CARTESIAN_POINT ( 'NONE',  ( -0.05219959533936034679, 19.03943276465977164, 72.50109039468566152 ) ) ;
#137042 = CARTESIAN_POINT ( 'NONE',  ( 19.02544592524343514, -5.153800228976328945, 63.54057627198103830 ) ) ;
#137043 = CARTESIAN_POINT ( 'NONE',  ( 14.29746914071049879, -8.314922557960816363, 73.33224293864769550 ) ) ;
#137044 = CARTESIAN_POINT ( 'NONE',  ( -8.314922557960811034, -14.29746914071050412, 67.08224293864770971 ) ) ;
#137045 = CARTESIAN_POINT ( 'NONE',  ( 13.97604488694527802, 13.89961937509977652, 84.37390960531433848 ) ) ;
#137046 = CARTESIAN_POINT ( 'NONE',  ( -8.224510206698948167, 14.34966873604960824, 80.41557627198103830 ) ) ;
#137047 = CARTESIAN_POINT ( 'NONE',  ( -16.51473224551069308, -9.474510206698971260, 86.66557627198102409 ) ) ;
#137048 = EDGE_CURVE ( 'NONE', #176832, #106856, #97891, .T. ) ;
#137049 = AXIS2_PLACEMENT_3D ( 'NONE', #94878, #122226, #30230 ) ;
#137050 = CARTESIAN_POINT ( 'NONE',  ( -13.89961937509957401, -13.97604488694547875, 29.37609039468565797 ) ) ;
#137053 = CARTESIAN_POINT ( 'NONE',  ( 8.224510206698953496, -14.34966873604960469, 112.9155762719810383 ) ) ;
#137052 = CARTESIAN_POINT ( 'NONE',  ( -14.34966873604960291, -8.224510206698953496, 26.66557627198103475 ) ) ;
#137051 = CARTESIAN_POINT ( 'NONE',  ( -16.51473224551069308, -9.474510206698971260, 46.66557627198102409 ) ) ;
#137054 = ORIENTED_EDGE ( 'NONE', *, *, #79191, .T. ) ;
#137055 = CARTESIAN_POINT ( 'NONE',  ( -15.72974639402176322, -15.80617190586768395, 39.37609039468567573 ) ) ;
#137056 = CARTESIAN_POINT ( 'NONE',  ( 19.05341960407617918, -5.049401038297876454, 71.04275706135234714 ) ) ;
#137057 = CARTESIAN_POINT ( 'NONE',  ( 14.29746914071049879, -8.314922557960816363, 38.33224293864768839 ) ) ;
#137058 = CARTESIAN_POINT ( 'NONE',  ( 0.05219959533907565091, 21.53943276465977519, 79.99890960531435269 ) ) ;
#137059 = CARTESIAN_POINT ( 'NONE',  ( -5.823673210054116645, -21.52544592524344225, 22.29057627198102765 ) ) ;
#137060 = CARTESIAN_POINT ( 'NONE',  ( 8.314922557960818139, 14.29746914071049879, 74.58224293864768129 ) ) ;
#137061 = CARTESIAN_POINT ( 'NONE',  ( 9.564922557960805705, 16.46253265017160317, 39.58224293864768839 ) ) ;
#137062 = CARTESIAN_POINT ( 'NONE',  ( -0.05219959533936034679, 19.03943276465977164, 37.50109039468567573 ) ) ;
#137063 = CARTESIAN_POINT ( 'NONE',  ( 14.29746914071037800, 8.314922557961029526, 101.6677570613523613 ) ) ;
#137064 = CARTESIAN_POINT ( 'NONE',  ( 14.34966873604972726, -8.224510206698740333, 60.83442372801901854 ) ) ;
#137065 = CARTESIAN_POINT ( 'NONE',  ( -10.72451020669898014, 18.67979575497178502, 35.41557627198102409 ) ) ;
#137066 = CARTESIAN_POINT ( 'NONE',  ( 5.719274019375673035, 21.55341960407619339, 102.2927570613523613 ) ) ;
#137067 = CARTESIAN_POINT ( 'NONE',  ( -19.05341960407611168, -5.049401038298163336, 91.45724293864766707 ) ) ;
#137068 = CARTESIAN_POINT ( 'NONE',  ( 16.55341960407618274, -4.379528057220086978, 76.04275706135237556 ) ) ;
#137069 = CARTESIAN_POINT ( 'NONE',  ( 12.06949235617757843, -12.14591786802309237, 113.1239096053143953 ) ) ;
#137070 = CARTESIAN_POINT ( 'NONE',  ( 14.34966873604960469, 8.224510206698951720, 29.16557627198103120 ) ) ;
#137072 = CARTESIAN_POINT ( 'NONE',  ( -16.46253265017160317, 9.564922557960807481, 85.83224293864769550 ) ) ;
#137071 = CARTESIAN_POINT ( 'NONE',  ( -16.46253265017160317, 9.564922557960807481, 110.8322429386476955 ) ) ;
#137073 = CARTESIAN_POINT ( 'NONE',  ( -19.02544592524342804, 5.153800228976336051, 116.0405762719810383 ) ) ;
#137074 = AXIS2_PLACEMENT_3D ( 'NONE', #128444, #99107, #4108 ) ;
#137075 = CARTESIAN_POINT ( 'NONE',  ( 4.379528057220339221, -16.55341960407611168, 62.70724293864769550 ) ) ;
#137076 = CARTESIAN_POINT ( 'NONE',  ( -16.53943276465976808, 0.05219959533911058130, 36.24890960531435979 ) ) ;
#137077 = CARTESIAN_POINT ( 'NONE',  ( 4.483927247898545687, 16.52544592524342804, 54.79057627198104541 ) ) ;
#137080 = VECTOR ( 'NONE', #90589, 1000.000000000000000 ) ;
#137079 = CARTESIAN_POINT ( 'NONE',  ( -13.89961937509957401, -13.97604488694547697, 59.37609039468566863 ) ) ;
#137078 = CARTESIAN_POINT ( 'NONE',  ( -12.14591786802326823, 12.06949235617739902, 53.12609039468568284 ) ) ;
#137081 = CARTESIAN_POINT ( 'NONE',  ( 9.564922557961047289, -16.46253265017146816, 50.41775706135233293 ) ) ;
#137082 = CARTESIAN_POINT ( 'NONE',  ( 9.564922557960805705, 16.46253265017160317, 94.58224293864769550 ) ) ;
#137083 = CARTESIAN_POINT ( 'NONE',  ( 16.46253265017146816, 9.564922557961045513, 71.66775706135233293 ) ) ;
#137084 = CARTESIAN_POINT ( 'NONE',  ( -27.73933785331498925, 9.013057229001089965, 141.2750000027311614 ) ) ;
#137085 = CARTESIAN_POINT ( 'NONE',  ( 13.97604488694548053, -13.89961937509957401, 50.62609039468566152 ) ) ;
#137087 = CARTESIAN_POINT ( 'NONE',  ( -0.05219959533934338120, 16.53943276465976808, 97.50109039468567573 ) ) ;
#137086 = CARTESIAN_POINT ( 'NONE',  ( -19.02544592524334988, -5.153800228976617603, 93.95942372801900433 ) ) ;
#137088 = CARTESIAN_POINT ( 'NONE',  ( -27.73933785331498925, 2.428612866367529932E-14, 147.3750000027311842 ) ) ;
#137090 = CARTESIAN_POINT ( 'NONE',  ( -16.51473224551069308, -9.474510206698971260, 21.66557627198102765 ) ) ;
#137089 = COLOUR_RGB ( '', 0.08235294, 0.09019608, 0.10196078) ;
#137091 =( BOUNDED_CURVE ( )  B_SPLINE_CURVE ( 2, ( #35838, #70181, #143007, #128830, #55006 ),
 .UNSPECIFIED., .F., .T. ) 
 B_SPLINE_CURVE_WITH_KNOTS ( ( 3, 2, 3 ),
 ( 0.8000000000000035971, 0.8200000000000008393, 0.8266400941232673327 ),
 .UNSPECIFIED. ) 
 CURVE ( )  GEOMETRIC_REPRESENTATION_ITEM ( )  RATIONAL_B_SPLINE_CURVE ( ( 0.9999999999999913403, 0.9510565162951621909, 1.000000000000000000, 0.9837505330739607645, 0.9782908651321036153 ) ) 
 REPRESENTATION_ITEM ( '' )  );
#137092 = CARTESIAN_POINT ( 'NONE',  ( 13.89961937509977652, -13.97604488694527269, 113.1239096053143527 ) ) ;
#137093 = CARTESIAN_POINT ( 'NONE',  ( 10.81492255796106328, -18.62759615963255655, 40.41775706135234714 ) ) ;
#137094 = CARTESIAN_POINT ( 'NONE',  ( 13.97604488694548053, -13.89961937509957401, 105.6260903946856757 ) ) ;
#137096 = CARTESIAN_POINT ( 'NONE',  ( 0.05219959533909260263, 19.03943276465977164, 54.99890960531435979 ) ) ;
#137095 = CARTESIAN_POINT ( 'NONE',  ( 17.50000000000147793, -3.254303733634592799, 107.5239589307140591 ) ) ;
#137097 = CARTESIAN_POINT ( 'NONE',  ( 0.05219959533909260263, 19.03943276465977164, 99.99890960531436690 ) ) ;
#137099 = CARTESIAN_POINT ( 'NONE',  ( 5.153800228976335163, 19.02544592524342804, 59.79057627198100988 ) ) ;
#137098 = CARTESIAN_POINT ( 'NONE',  ( -4.379528057220328563, 16.55341960407611168, 75.20724293864769550 ) ) ;
#137100 = CARTESIAN_POINT ( 'NONE',  ( -16.46253265017160317, 9.564922557960807481, 75.83224293864769550 ) ) ;
#137101 = CARTESIAN_POINT ( 'NONE',  ( 5.153800228976615827, -19.02544592524334988, 80.20942372801901854 ) ) ;
#137102 = CARTESIAN_POINT ( 'NONE',  ( -21.52544592524343514, 5.823673210054127303, 51.04057627198103120 ) ) ;
#137103 = CARTESIAN_POINT ( 'NONE',  ( 12.06949235617757843, -12.14591786802309237, 108.1239096053143811 ) ) ;
#137104 = CARTESIAN_POINT ( 'NONE',  ( -13.89961937509957401, -13.97604488694547875, 49.37609039468567573 ) ) ;
#137105 = CARTESIAN_POINT ( 'NONE',  ( 13.89961937509977652, -13.97604488694527269, 73.12390960531436690 ) ) ;
#137106 = CARTESIAN_POINT ( 'NONE',  ( -10.81492255796078084, -18.62759615963271287, 72.08224293864769550 ) ) ;
#137108 = CARTESIAN_POINT ( 'NONE',  ( -5.049401038297874678, -19.05341960407617918, 54.79275706135234003 ) ) ;
#137107 = CARTESIAN_POINT ( 'NONE',  ( -8.224510206698948167, 14.34966873604960824, 80.41557627198103830 ) ) ;
#137109 = CARTESIAN_POINT ( 'NONE',  ( 15.80617190586746368, 15.72974639402197994, 74.37390960531436690 ) ) ;
#137110 = CARTESIAN_POINT ( 'NONE',  ( 15.72974639402199770, -15.80617190586745480, 58.12390960531435979 ) ) ;
#137111 = CARTESIAN_POINT ( 'NONE',  ( -21.52544592524343514, 5.823673210054127303, 46.04057627198103830 ) ) ;
#137112 = CARTESIAN_POINT ( 'NONE',  ( 10.81492255796106328, -18.62759615963255655, 90.41775706135236135 ) ) ;
#137113 = CARTESIAN_POINT ( 'NONE',  ( 16.51473224551069308, 9.474510206698969483, 69.16557627198102409 ) ) ;
#137114 = CARTESIAN_POINT ( 'NONE',  ( 16.51473224551069308, 9.474510206698969483, 24.16557627198102765 ) ) ;
#137115 = CIRCLE ( 'NONE', #179141, 5.000000000000000000 ) ;
#137116 = CARTESIAN_POINT ( 'NONE',  ( 21.55341960407619695, -5.719274019375665929, 21.04275706135234714 ) ) ;
#137117 = CARTESIAN_POINT ( 'NONE',  ( -21.53943276465977519, -0.05219959533937600094, 38.75109039468567573 ) ) ;
#137118 = CARTESIAN_POINT ( 'NONE',  ( 9.564922557960805705, 16.46253265017160317, 29.58224293864769550 ) ) ;
#137119 = CARTESIAN_POINT ( 'NONE',  ( -15.80617190586745835, -15.72974639402198527, 106.8739096053143811 ) ) ;
#137120 = CARTESIAN_POINT ( 'NONE',  ( 16.51473224551083163, -9.474510206698727899, 55.83442372801899722 ) ) ;
#137121 = CARTESIAN_POINT ( 'NONE',  ( 9.564922557960805705, 16.46253265017160317, 34.58224293864770260 ) ) ;
#137122 = CARTESIAN_POINT ( 'NONE',  ( 14.34966873604972726, -8.224510206698740333, 25.83442372801901499 ) ) ;
#137123 = CARTESIAN_POINT ( 'NONE',  ( 8.314922557961029526, -14.29746914071037800, 55.41775706135234714 ) ) ;
#137124 = CARTESIAN_POINT ( 'NONE',  ( 16.51473224551069308, 9.474510206698969483, 34.16557627198102409 ) ) ;
#137125 = CARTESIAN_POINT ( 'NONE',  ( -21.97054992548789087, -8.562709642470920812, 171.7904333278019351 ) ) ;
#137126 = CARTESIAN_POINT ( 'NONE',  ( 16.51473224551069308, 9.474510206698969483, 89.16557627198103830 ) ) ;
#137127 = CARTESIAN_POINT ( 'NONE',  ( 12.14591786802309770, 12.06949235617756955, 104.3739096053143669 ) ) ;
#137128 = CARTESIAN_POINT ( 'NONE',  ( -18.62759615963270932, 10.81492255796079327, 60.83224293864769550 ) ) ;
#137129 = CARTESIAN_POINT ( 'NONE',  ( 16.55341960407618274, -4.379528057220086978, 46.04275706135234714 ) ) ;
#137130 = CARTESIAN_POINT ( 'NONE',  ( -15.72974639402176322, -15.80617190586768395, 99.37609039468568994 ) ) ;
#137131 = CARTESIAN_POINT ( 'NONE',  ( -16.51473224551069308, -9.474510206698971260, 41.66557627198103120 ) ) ;
#137132 = CARTESIAN_POINT ( 'NONE',  ( 4.483927247898790824, -16.52544592524335698, 105.2094237280190328 ) ) ;
#137133 = CARTESIAN_POINT ( 'NONE',  ( 8.224510206698953496, -14.34966873604960469, 57.91557627198103120 ) ) ;
#137134 = CARTESIAN_POINT ( 'NONE',  ( 0.05219959533909260263, 19.03943276465977164, 64.99890960531436690 ) ) ;
#137135 = CARTESIAN_POINT ( 'NONE',  ( 15.72974639402176855, 15.80617190586768217, 106.8760903946856899 ) ) ;
#137136 = CARTESIAN_POINT ( 'NONE',  ( 18.62759615963255655, 10.81492255796105972, 21.66775706135235069 ) ) ;
#137137 = CARTESIAN_POINT ( 'NONE',  ( 5.823673210054444382, -21.52544592524334988, 80.20942372801901854 ) ) ;
#137138 = CARTESIAN_POINT ( 'NONE',  ( 16.53943276465976808, 0.05219959533934440121, 46.25109039468567573 ) ) ;
#137139 = CARTESIAN_POINT ( 'NONE',  ( -16.53943276465976808, -0.05219959533934237506, 33.75109039468568284 ) ) ;
#137141 = CARTESIAN_POINT ( 'NONE',  ( 21.55341960407619695, -5.719274019375665929, 106.0427570613523471 ) ) ;
#137140 = CARTESIAN_POINT ( 'NONE',  ( 14.34966873604960469, 8.224510206698951720, 74.16557627198102409 ) ) ;
#137142 = CARTESIAN_POINT ( 'NONE',  ( -8.224510206698948167, 14.34966873604960824, 30.41557627198101699 ) ) ;
#137143 = CARTESIAN_POINT ( 'NONE',  ( -16.18388926212238133, 7.379444403734517266, 114.5604684863385359 ) ) ;
#137144 = CARTESIAN_POINT ( 'NONE',  ( 14.34966873604972726, -8.224510206698740333, 40.83442372801901854 ) ) ;
#137145 = CARTESIAN_POINT ( 'NONE',  ( 8.224510206698953496, -14.34966873604960469, 52.91557627198103830 ) ) ;
#137146 = CARTESIAN_POINT ( 'NONE',  ( 12.06949235617739724, 12.14591786802326823, 91.87609039468568994 ) ) ;
#137147 = CARTESIAN_POINT ( 'NONE',  ( -0.05219959533909027116, -19.03943276465977164, 97.49890960531436690 ) ) ;
#137148 = CARTESIAN_POINT ( 'NONE',  ( 0.05219959533907565091, 21.53943276465977519, 24.99890960531435624 ) ) ;
#137149 = CARTESIAN_POINT ( 'NONE',  ( -21.52544592524334988, -5.823673210054445271, 98.95942372801903275 ) ) ;
#137150 = CARTESIAN_POINT ( 'NONE',  ( -4.483927247898539470, -16.52544592524342804, 82.29057627198103830 ) ) ;
#137151 = CARTESIAN_POINT ( 'NONE',  ( 19.02544592524343514, -5.153800228976328945, 98.54057627198100988 ) ) ;
#137152 = ORIENTED_EDGE ( 'NONE', *, *, #188131, .F. ) ;
#137153 = CARTESIAN_POINT ( 'NONE',  ( 8.314922557961029526, -14.29746914071037800, 35.41775706135234003 ) ) ;
#137154 = CARTESIAN_POINT ( 'NONE',  ( 19.03943276465977164, -0.05219959533909143690, 38.74890960531436690 ) ) ;
#137155 = CARTESIAN_POINT ( 'NONE',  ( -19.05341960407611168, -5.049401038298163336, 106.4572429386476955 ) ) ;
#137157 = CARTESIAN_POINT ( 'NONE',  ( 18.09873248133752810, 5.499999999999960032, 101.4839295033382882 ) ) ;
#137156 = CARTESIAN_POINT ( 'NONE',  ( 12.14591786802327356, -12.06949235617739191, 40.62609039468567573 ) ) ;
#137158 = CARTESIAN_POINT ( 'NONE',  ( -9.474510206698720793, -16.51473224551083518, 34.58442372801899722 ) ) ;
#137159 = CARTESIAN_POINT ( 'NONE',  ( -5.049401038298153566, 19.05341960407611168, 45.20724293864769550 ) ) ;
#137160 = CARTESIAN_POINT ( 'NONE',  ( -16.55341960407617563, 4.379528057220093196, 78.54275706135236135 ) ) ;
#137161 = CARTESIAN_POINT ( 'NONE',  ( -5.153800228976607833, 19.02544592524334988, 77.70942372801900433 ) ) ;
#137162 = CARTESIAN_POINT ( 'NONE',  ( 9.564922557961047289, -16.46253265017146816, 25.41775706135234003 ) ) ;
#137163 = CARTESIAN_POINT ( 'NONE',  ( -13.97604488694527625, -13.89961937509977652, 66.87390960531436690 ) ) ;
#137164 = CARTESIAN_POINT ( 'NONE',  ( -4.483927247898539470, -16.52544592524342804, 102.2905762719810383 ) ) ;
#137165 = CARTESIAN_POINT ( 'NONE',  ( 0.05219959533936267826, -19.03943276465977164, 65.00109039468567573 ) ) ;
#137166 = CARTESIAN_POINT ( 'NONE',  ( 21.52544592524344225, -5.823673210054117533, 58.54057627198103120 ) ) ;
#137167 = CARTESIAN_POINT ( 'NONE',  ( -0.05219959533936034679, 19.03943276465977164, 32.50109039468566863 ) ) ;
#137168 = CARTESIAN_POINT ( 'NONE',  ( 13.89961937509977652, -13.97604488694527269, 108.1239096053143669 ) ) ;
#137169 = CONICAL_SURFACE ( 'NONE', #20826, 2.500000000000002220, 1.029744260000000189 ) ;
#137170 = CARTESIAN_POINT ( 'NONE',  ( -10.81492255796078084, -18.62759615963271287, 72.08224293864769550 ) ) ;
#137171 = CARTESIAN_POINT ( 'NONE',  ( -16.51473224551069308, -9.474510206698971260, 106.6655762719810383 ) ) ;
#137172 = CARTESIAN_POINT ( 'NONE',  ( 16.51473224551083163, -9.474510206698727899, 95.83442372801900433 ) ) ;
#137173 = CARTESIAN_POINT ( 'NONE',  ( -9.474510206698964154, 16.51473224551069663, 110.4155762719810383 ) ) ;
#137174 = CARTESIAN_POINT ( 'NONE',  ( 16.52544592524335698, 4.483927247898782831, 21.45942372801901499 ) ) ;
#137175 = CARTESIAN_POINT ( 'NONE',  ( 19.02544592524343514, -5.153800228976328945, 33.54057627198102409 ) ) ;
#137176 = CARTESIAN_POINT ( 'NONE',  ( 16.46253265017160672, -9.564922557960803928, 93.33224293864769550 ) ) ;
#137177 = CARTESIAN_POINT ( 'NONE',  ( -5.719274019375978568, 21.55341960407610458, 95.20724293864769550 ) ) ;
#137178 = CARTESIAN_POINT ( 'NONE',  ( 10.81492255796106328, -18.62759615963255655, 60.41775706135235424 ) ) ;
#137180 = CARTESIAN_POINT ( 'NONE',  ( -5.823673210054431948, 21.52544592524334988, 112.7094237280190328 ) ) ;
#137179 = CARTESIAN_POINT ( 'NONE',  ( -0.05219959533936034679, 19.03943276465977164, 102.5010903946856757 ) ) ;
#137181 = CARTESIAN_POINT ( 'NONE',  ( 12.06949235617739724, 12.14591786802326823, 111.8760903946856615 ) ) ;
#137182 = CARTESIAN_POINT ( 'NONE',  ( -10.72451020669898014, 18.67979575497178502, 100.4155762719810241 ) ) ;
#137183 = CARTESIAN_POINT ( 'NONE',  ( -16.52544592524342804, 4.483927247898546575, 36.04057627198102409 ) ) ;
#137184 = CARTESIAN_POINT ( 'NONE',  ( 19.03943276465977164, 0.05219959533936151252, 86.25109039468567573 ) ) ;
#137185 = EDGE_CURVE ( 'NONE', #90049, #109599, #185741, .T. ) ;
#137186 = CARTESIAN_POINT ( 'NONE',  ( 5.049401038297881783, 19.05341960407617563, 57.29275706135231871 ) ) ;
#137187 = CARTESIAN_POINT ( 'NONE',  ( 21.53943276465977519, 0.05219959533937863772, 56.25109039468568284 ) ) ;
#137188 = CARTESIAN_POINT ( 'NONE',  ( 9.564922557961047289, -16.46253265017146816, 40.41775706135234003 ) ) ;
#137189 = CARTESIAN_POINT ( 'NONE',  ( 16.55341960407611168, 4.379528057220329451, 103.9572429386476813 ) ) ;
#137190 = CARTESIAN_POINT ( 'NONE',  ( 18.62759615963271287, -10.81492255796078972, 33.33224293864769550 ) ) ;
#137192 = EDGE_CURVE ( 'NONE', #93735, #145198, #188966, .T. ) ;
#137191 = CARTESIAN_POINT ( 'NONE',  ( 8.224510206698953496, -14.34966873604960469, 37.91557627198102409 ) ) ;
#137193 = CARTESIAN_POINT ( 'NONE',  ( 15.72974639402176855, 15.80617190586768217, 96.87609039468568994 ) ) ;
#137194 = CARTESIAN_POINT ( 'NONE',  ( -16.52544592524335698, -4.483927247898792601, 68.95942372801901854 ) ) ;
#137195 = CARTESIAN_POINT ( 'NONE',  ( 16.52544592524342804, -4.483927247898539470, 28.54057627198103120 ) ) ;
#137196 = CARTESIAN_POINT ( 'NONE',  ( 15.72974639402176855, 15.80617190586768217, 61.87609039468568284 ) ) ;
#137197 = CARTESIAN_POINT ( 'NONE',  ( -21.53943276465977519, -0.05219959533937600094, 68.75109039468568994 ) ) ;
#137198 = CARTESIAN_POINT ( 'NONE',  ( -18.62759615963270932, 10.81492255796079327, 65.83224293864769550 ) ) ;
#137199 = ORIENTED_EDGE ( 'NONE', *, *, #79032, .T. ) ;
#137200 = CARTESIAN_POINT ( 'NONE',  ( 5.049401038298161559, -19.05341960407611168, 22.70724293864769194 ) ) ;
#137201 = CARTESIAN_POINT ( 'NONE',  ( -15.80617190586768217, 15.72974639402176855, 43.12609039468568284 ) ) ;
#137202 = CARTESIAN_POINT ( 'NONE',  ( 4.483927247898545687, 16.52544592524342804, 114.7905762719810383 ) ) ;
#137203 = CARTESIAN_POINT ( 'NONE',  ( 16.46253265017160672, -9.564922557960803928, 33.33224293864770260 ) ) ;
#137204 = CARTESIAN_POINT ( 'NONE',  ( -8.224510206698948167, 14.34966873604960824, 85.41557627198102409 ) ) ;
#137205 = CARTESIAN_POINT ( 'NONE',  ( -19.02544592524342804, 5.153800228976336051, 81.04057627198103830 ) ) ;
#137206 = CARTESIAN_POINT ( 'NONE',  ( 16.53943276465976808, -0.05219959533910856209, 28.74890960531435624 ) ) ;
#137207 = CARTESIAN_POINT ( 'NONE',  ( -21.52544592524343514, 5.823673210054127303, 71.04057627198103830 ) ) ;
#137208 = CARTESIAN_POINT ( 'NONE',  ( -0.05219959533907301413, -21.53943276465977519, 107.4989096053143669 ) ) ;
#137209 = CARTESIAN_POINT ( 'NONE',  ( -5.153800228976328057, -19.02544592524343514, 112.2905762719810099 ) ) ;
#137211 = CARTESIAN_POINT ( 'NONE',  ( 5.153800228976615827, -19.02544592524334988, 105.2094237280190185 ) ) ;
#137210 = CARTESIAN_POINT ( 'NONE',  ( -19.05341960407611168, -5.049401038298163336, 71.45724293864766707 ) ) ;
#137212 = CARTESIAN_POINT ( 'NONE',  ( 21.55341960407610458, 5.719274019375980345, 63.95724293864770260 ) ) ;
#137213 = CARTESIAN_POINT ( 'NONE',  ( 21.55341960407619695, -5.719274019375665929, 76.04275706135237556 ) ) ;
#137214 = CARTESIAN_POINT ( 'NONE',  ( -13.89961937509977652, 13.97604488694528158, 60.62390960531436690 ) ) ;
#137215 = CARTESIAN_POINT ( 'NONE',  ( -9.474510206698964154, 16.51473224551069663, 100.4155762719810241 ) ) ;
#137216 = CARTESIAN_POINT ( 'NONE',  ( 8.224510206698742110, 14.34966873604972548, 77.08442372801901854 ) ) ;
#137217 = CARTESIAN_POINT ( 'NONE',  ( 15.72974639402176855, 15.80617190586768217, 51.87609039468568284 ) ) ;
#137218 = CARTESIAN_POINT ( 'NONE',  ( -0.05219959533937732626, 21.53943276465977519, 82.50109039468568994 ) ) ;
#137219 = CARTESIAN_POINT ( 'NONE',  ( -5.719274019375978568, 21.55341960407610458, 115.2072429386476955 ) ) ;
#137220 = COLOUR_RGB ( '', 0.31764706, 0.68627451, 0.89019608) ;
#137221 = CARTESIAN_POINT ( 'NONE',  ( -5.823673210054116645, -21.52544592524344225, 72.29057627198102409 ) ) ;
#137222 = CARTESIAN_POINT ( 'NONE',  ( -13.89961937509957401, -13.97604488694547875, 49.37609039468567573 ) ) ;
#137223 = CARTESIAN_POINT ( 'NONE',  ( -18.62759615963270932, 10.81492255796079327, 35.83224293864768839 ) ) ;
#137224 = VECTOR ( 'NONE', #111630, 1000.000000000000000 ) ;
#137226 = CARTESIAN_POINT ( 'NONE',  ( -0.05219959533910754901, -16.53943276465976808, 32.49890960531435979 ) ) ;
#137225 = CARTESIAN_POINT ( 'NONE',  ( 5.153800228976335163, 19.02544592524342804, 84.79057627198099567 ) ) ;
#137227 = FACE_OUTER_BOUND ( 'NONE', #25368, .T. ) ;
#137228 = AXIS2_PLACEMENT_3D ( 'NONE', #138329, #108982, #125152 ) ;
#137229 = DIRECTION ( 'NONE',  ( -0.000000000000000000, -0.000000000000000000, 1.000000000000000000 ) ) ;
#137230 = CARTESIAN_POINT ( 'NONE',  ( 19.05341960407617918, -5.049401038297876454, 91.04275706135234714 ) ) ;
#137231 = CARTESIAN_POINT ( 'NONE',  ( -5.719274019375978568, 21.55341960407610458, 65.20724293864768129 ) ) ;
#137232 = CARTESIAN_POINT ( 'NONE',  ( -12.14591786802309592, -12.06949235617757132, 56.87390960531436690 ) ) ;
#137233 = CARTESIAN_POINT ( 'NONE',  ( -4.483927247898782831, 16.52544592524335698, 32.70942372801900433 ) ) ;
#137234 = CARTESIAN_POINT ( 'NONE',  ( 5.153800228976335163, 19.02544592524342804, 44.79057627198103830 ) ) ;
#137236 = CARTESIAN_POINT ( 'NONE',  ( -16.51473224551082808, 9.474510206698731452, 68.33442372801900433 ) ) ;
#137235 = CARTESIAN_POINT ( 'NONE',  ( -18.62759615963270932, 10.81492255796079327, 100.8322429386477097 ) ) ;
#137237 = CARTESIAN_POINT ( 'NONE',  ( -9.564922557960796823, -16.46253265017161027, 87.08224293864769550 ) ) ;
#137238 = CARTESIAN_POINT ( 'NONE',  ( 4.483927247898545687, 16.52544592524342804, 89.79057627198103830 ) ) ;
#137239 = CARTESIAN_POINT ( 'NONE',  ( -19.03943276465977164, 0.05219959533909376836, 61.24890960531436690 ) ) ;
#137240 = CARTESIAN_POINT ( 'NONE',  ( -8.224510206698948167, 14.34966873604960824, 70.41557627198102409 ) ) ;
#137241 = CARTESIAN_POINT ( 'NONE',  ( 19.05341960407611168, 5.049401038298154454, 38.95724293864767418 ) ) ;
#137242 = CARTESIAN_POINT ( 'NONE',  ( -17.10208260729133301, -5.355177916403385474, 20.80190055885774569 ) ) ;
#137243 = CARTESIAN_POINT ( 'NONE',  ( 14.34966873604960469, 8.224510206698951720, 44.16557627198103120 ) ) ;
#137244 = CARTESIAN_POINT ( 'NONE',  ( -19.03943276465977164, 0.05219959533909376836, 86.24890960531436690 ) ) ;
#137245 = FACE_BOUND ( 'NONE', #53676, .T. ) ;
#137246 = CARTESIAN_POINT ( 'NONE',  ( -16.51473224551082808, 9.474510206698731452, 53.33442372801900433 ) ) ;
#137247 = CARTESIAN_POINT ( 'NONE',  ( -12.06949235617739369, -12.14591786802326823, 59.37609039468568284 ) ) ;
#137248 = CARTESIAN_POINT ( 'NONE',  ( -21.55341960407610458, -5.719274019375992779, 81.45724293864769550 ) ) ;
#137249 = CARTESIAN_POINT ( 'NONE',  ( 19.05341960407617918, -5.049401038297876454, 41.04275706135233293 ) ) ;
#137250 = CARTESIAN_POINT ( 'NONE',  ( -19.05341960407611168, -5.049401038298163336, 91.45724293864766707 ) ) ;
#137251 = CARTESIAN_POINT ( 'NONE',  ( -19.99604614807126524, -21.49604614807087799, -49.12629558063592583 ) ) ;
#137252 = CARTESIAN_POINT ( 'NONE',  ( 15.72974639402199770, -15.80617190586745480, 33.12390960531435979 ) ) ;
#137253 = AXIS2_PLACEMENT_3D ( 'NONE', #162127, #179323, #23623 ) ;
#137254 = CARTESIAN_POINT ( 'NONE',  ( 19.05341960407611168, 5.049401038298154454, 58.95724293864768129 ) ) ;
#137255 = CARTESIAN_POINT ( 'NONE',  ( 15.72974639402176855, 15.80617190586768217, 51.87609039468568284 ) ) ;
#137257 = CARTESIAN_POINT ( 'NONE',  ( 12.14591786802309770, 12.06949235617756955, 114.3739096053143527 ) ) ;
#137256 = PRODUCT_DEFINITION_SHAPE ( 'NONE', 'NONE',  #189524 ) ;
#137258 = ADVANCED_FACE ( 'NONE', ( #35258 ), #34272, .F. ) ;
#137261 = ORIENTED_EDGE ( 'NONE', *, *, #14195, .T. ) ;
#137260 = CARTESIAN_POINT ( 'NONE',  ( -13.97604488694527625, -13.89961937509977652, 96.87390960531433848 ) ) ;
#137259 = CARTESIAN_POINT ( 'NONE',  ( -21.55341960407610458, -5.719274019375992779, 111.4572429386476813 ) ) ;
#137262 = CARTESIAN_POINT ( 'NONE',  ( -21.55341960407619339, 5.719274019375674811, 43.54275706135235424 ) ) ;
#137263 = ORIENTED_EDGE ( 'NONE', *, *, #110504, .T. ) ;
#137264 = CARTESIAN_POINT ( 'NONE',  ( -5.153800228976328057, -19.02544592524343514, 102.2905762719810383 ) ) ;
#137265 = DIRECTION ( 'NONE',  ( -1.000000000000000000, -0.000000000000000000, -0.000000000000000000 ) ) ;
#137266 = CARTESIAN_POINT ( 'NONE',  ( 21.53943276465977519, -0.05219959533907433946, 108.7489096053143669 ) ) ;
#137267 = CARTESIAN_POINT ( 'NONE',  ( -9.474510206698964154, 16.51473224551069663, 50.41557627198102409 ) ) ;
#137268 = CARTESIAN_POINT ( 'NONE',  ( -8.314922557961024197, 14.29746914071037800, 22.91775706135235069 ) ) ;
#137269 = CARTESIAN_POINT ( 'NONE',  ( 36.91746825000000598, -11.99521256947793546, -4.224999997268812812 ) ) ;
#137270 = CARTESIAN_POINT ( 'NONE',  ( -15.80617190586768217, 15.72974639402176855, 98.12609039468570415 ) ) ;
#137271 = CARTESIAN_POINT ( 'NONE',  ( -13.89961937509977652, 13.97604488694528158, 30.62390960531435269 ) ) ;
#137272 = CARTESIAN_POINT ( 'NONE',  ( -15.72974639402176322, -15.80617190586768395, 94.37609039468568994 ) ) ;
#137274 = CARTESIAN_POINT ( 'NONE',  ( 18.67979575497194134, -10.72451020669871369, 65.83442372801900433 ) ) ;
#137273 = CARTESIAN_POINT ( 'NONE',  ( 19.05341960407611168, 5.049401038298154454, 93.95724293864769550 ) ) ;
#137275 = CARTESIAN_POINT ( 'NONE',  ( -8.571926809382601320, -26.38167802310801591, 143.7750000027311899 ) ) ;
#137276 = CARTESIAN_POINT ( 'NONE',  ( 19.05341960407611168, 5.049401038298154454, 93.95724293864769550 ) ) ;
#137277 = CARTESIAN_POINT ( 'NONE',  ( 18.87255363501903105, 5.499999999999943157, 63.82513748171827928 ) ) ;
#137280 = CARTESIAN_POINT ( 'NONE',  ( -15.80617190586768217, 15.72974639402176855, 53.12609039468568284 ) ) ;
#137279 = CARTESIAN_POINT ( 'NONE',  ( 16.53943276465976808, 0.05219959533934440121, 66.25109039468567573 ) ) ;
#137278 = CARTESIAN_POINT ( 'NONE',  ( 14.34966873604972726, -8.224510206698740333, 40.83442372801901854 ) ) ;
#137281 = CARTESIAN_POINT ( 'NONE',  ( -18.67979575497193778, 10.72451020669871902, 93.33442372801901854 ) ) ;
#137282 = CARTESIAN_POINT ( 'NONE',  ( -17.49999999999999645, -5.500000000000000888, 39.20309617465829177 ) ) ;
#137283 = CARTESIAN_POINT ( 'NONE',  ( -0.05219959533936034679, 19.03943276465977164, 112.5010903946856757 ) ) ;
#137284 = CARTESIAN_POINT ( 'NONE',  ( 9.564922557960805705, 16.46253265017160317, 74.58224293864769550 ) ) ;
#137285 = CARTESIAN_POINT ( 'NONE',  ( -19.05341960407611168, -5.049401038298163336, 101.4572429386476955 ) ) ;
#137286 = CARTESIAN_POINT ( 'NONE',  ( 13.97604488694527802, 13.89961937509977652, 24.37390960531435624 ) ) ;
#137287 = CARTESIAN_POINT ( 'NONE',  ( 21.52544592524344225, -5.823673210054117533, 23.54057627198102765 ) ) ;
#137288 = CARTESIAN_POINT ( 'NONE',  ( -0.05219959533934338120, 16.53943276465976808, 92.50109039468567573 ) ) ;
#137290 = CARTESIAN_POINT ( 'NONE',  ( 5.153800228976335163, 19.02544592524342804, 54.79057627198103120 ) ) ;
#137289 = CARTESIAN_POINT ( 'NONE',  ( 14.34966873604960469, 8.224510206698951720, 64.16557627198102409 ) ) ;
#137291 = CARTESIAN_POINT ( 'NONE',  ( -15.72974639402176322, -15.80617190586768395, 89.37609039468568994 ) ) ;
#137292 = CARTESIAN_POINT ( 'NONE',  ( 17.50000000000000000, 4.189786006557876696, 22.00000000000000711 ) ) ;
#137293 = CARTESIAN_POINT ( 'NONE',  ( -16.46253265017146816, -9.564922557961047289, 104.1677570613523329 ) ) ;
#137294 = CARTESIAN_POINT ( 'NONE',  ( 14.34966873604960469, 8.224510206698951720, 79.16557627198103830 ) ) ;
#137295 = CARTESIAN_POINT ( 'NONE',  ( -10.72451020669870658, -18.67979575497194134, 29.58442372801901854 ) ) ;
#137296 = CARTESIAN_POINT ( 'NONE',  ( -15.72974639402197994, 15.80617190586746368, 65.62390960531436690 ) ) ;
#137298 = CARTESIAN_POINT ( 'NONE',  ( 5.153800228976615827, -19.02544592524334988, 40.20942372801898301 ) ) ;
#137297 = AXIS2_PLACEMENT_3D ( 'NONE', #143678, #109366, #127514 ) ;
#137299 = CARTESIAN_POINT ( 'NONE',  ( -23.31738231874055600, 16.94106989632528837, 144.0500000054623513 ) ) ;
#137300 = CARTESIAN_POINT ( 'NONE',  ( -5.153800228976328057, -19.02544592524343514, 82.29057627198103830 ) ) ;
#137301 = CARTESIAN_POINT ( 'NONE',  ( -16.55341960407611168, -4.379528057220339221, 51.45724293864770260 ) ) ;
#137302 = CARTESIAN_POINT ( 'NONE',  ( -12.14591786802309592, -12.06949235617757132, 41.87390960531435979 ) ) ;
#137303 = CARTESIAN_POINT ( 'NONE',  ( -16.55341960407617563, 4.379528057220093196, 98.54275706135234714 ) ) ;
#137304 = CARTESIAN_POINT ( 'NONE',  ( -19.03943276465977164, -0.05219959533935918106, 48.75109039468566863 ) ) ;
#137305 = CARTESIAN_POINT ( 'NONE',  ( 18.56399227203345959, 5.499999999999819700, 51.47830131249905605 ) ) ;
#137306 = CARTESIAN_POINT ( 'NONE',  ( 13.97604488694527802, 13.89961937509977652, 99.37390960531436690 ) ) ;
#137307 = CARTESIAN_POINT ( 'NONE',  ( 4.483927247898545687, 16.52544592524342804, 74.79057627198105251 ) ) ;
#137308 = CARTESIAN_POINT ( 'NONE',  ( 16.51473224551083163, -9.474510206698727899, 45.83442372801900433 ) ) ;
#137310 = CARTESIAN_POINT ( 'NONE',  ( -18.62759615963270932, 10.81492255796079327, 35.83224293864768839 ) ) ;
#137309 = CARTESIAN_POINT ( 'NONE',  ( -9.474510206698964154, 16.51473224551069663, 30.41557627198102054 ) ) ;
#137311 = CARTESIAN_POINT ( 'NONE',  ( 15.80617190586746368, 15.72974639402197994, 69.37390960531436690 ) ) ;
#137312 = CARTESIAN_POINT ( 'NONE',  ( -16.55341960407611168, -4.379528057220339221, 106.4572429386477097 ) ) ;
#137314 = CARTESIAN_POINT ( 'NONE',  ( 19.03943276465977164, -0.05219959533909143690, 53.74890960531436690 ) ) ;
#137313 = CARTESIAN_POINT ( 'NONE',  ( -16.53943276465976808, -0.05219959533934237506, 53.75109039468568994 ) ) ;
#137315 = CARTESIAN_POINT ( 'NONE',  ( 21.53943276465977519, 0.05219959533937863772, 41.25109039468568284 ) ) ;
#137316 = CARTESIAN_POINT ( 'NONE',  ( 16.55341960407611168, 4.379528057220329451, 93.95724293864770971 ) ) ;
#137317 = DIRECTION ( 'NONE',  ( 0.000000000000000000, -1.000000000000000000, 0.000000000000000000 ) ) ;
#137318 = CARTESIAN_POINT ( 'NONE',  ( 36.91746824999999177, 11.99521256947799230, -8.024999997268814411 ) ) ;
#137319 = CARTESIAN_POINT ( 'NONE',  ( 21.52544592524344225, -5.823673210054117533, 28.54057627198103120 ) ) ;
#137320 = CARTESIAN_POINT ( 'NONE',  ( 17.40861289039004944, -6.110651285853255565, 66.12767529172569425 ) ) ;
#137321 = CARTESIAN_POINT ( 'NONE',  ( 1.242190437790102076, 23.66305621013599136, -57.22677643647746493 ) ) ;
#137323 = CARTESIAN_POINT ( 'NONE',  ( -14.29746914071049879, 8.314922557960819915, 45.83224293864769550 ) ) ;
#137322 = CARTESIAN_POINT ( 'NONE',  ( 14.29746914071037800, 8.314922557961029526, 46.66775706135234714 ) ) ;
#137324 = CARTESIAN_POINT ( 'NONE',  ( -10.81492255796078084, -18.62759615963271287, 67.08224293864770971 ) ) ;
#137325 = CARTESIAN_POINT ( 'NONE',  ( -21.52544592524343514, 5.823673210054127303, 56.04057627198102409 ) ) ;
#137326 = CARTESIAN_POINT ( 'NONE',  ( -20.02446474427092937, -11.96320450740733676, 170.0134183209140133 ) ) ;
#137328 = CARTESIAN_POINT ( 'NONE',  ( -5.049401038298153566, 19.05341960407611168, 105.2072429386476671 ) ) ;
#137327 = CARTESIAN_POINT ( 'NONE',  ( 16.46253265017160672, -9.564922557960803928, 38.33224293864768839 ) ) ;
#137329 = CARTESIAN_POINT ( 'NONE',  ( -5.049401038298153566, 19.05341960407611168, 50.20724293864770260 ) ) ;
#137330 = CARTESIAN_POINT ( 'NONE',  ( -19.05341960407611168, -5.049401038298163336, 21.45724293864768839 ) ) ;
#137331 = DIRECTION ( 'NONE',  ( 5.551115123125774690E-17, 9.714451465470120961E-17, -1.000000000000000000 ) ) ;
#137332 = CARTESIAN_POINT ( 'NONE',  ( 16.51473224551069308, 9.474510206698969483, 114.1655762719810241 ) ) ;
#137333 = ORIENTED_EDGE ( 'NONE', *, *, #176321, .T. ) ;
#137334 = CARTESIAN_POINT ( 'NONE',  ( -12.14591786802326823, 12.06949235617739902, 68.12609039468567573 ) ) ;
#137335 = CARTESIAN_POINT ( 'NONE',  ( 5.823673210054125526, 21.52544592524343514, 99.79057627198103830 ) ) ;
#137336 = CARTESIAN_POINT ( 'NONE',  ( -5.153800228976328057, -19.02544592524343514, 57.29057627198103120 ) ) ;
#137337 = CARTESIAN_POINT ( 'NONE',  ( 18.67979575497194134, -10.72451020669871369, 45.83442372801901854 ) ) ;
#137338 = CARTESIAN_POINT ( 'NONE',  ( -5.153800228976328057, -19.02544592524343514, 87.29057627198103830 ) ) ;
#137339 = CARTESIAN_POINT ( 'NONE',  ( 13.97604488694527802, 13.89961937509977652, 114.3739096053143669 ) ) ;
#137340 = ORIENTED_EDGE ( 'NONE', *, *, #98904, .T. ) ;
#137341 = CARTESIAN_POINT ( 'NONE',  ( -21.53943276465977519, -0.05219959533937600094, 28.75109039468567929 ) ) ;
#137343 = CARTESIAN_POINT ( 'NONE',  ( 19.03943276465977164, 0.05219959533936151252, 86.25109039468567573 ) ) ;
#137342 = CARTESIAN_POINT ( 'NONE',  ( -19.05341960407611168, -5.049401038298163336, 111.4572429386476671 ) ) ;
#137344 = CARTESIAN_POINT ( 'NONE',  ( 16.51473224551083163, -9.474510206698727899, 40.83442372801900433 ) ) ;
#137345 = CARTESIAN_POINT ( 'NONE',  ( 21.52544592524344225, -5.823673210054117533, 103.5405762719810383 ) ) ;
#137346 = CARTESIAN_POINT ( 'NONE',  ( -13.97604488694547697, 13.89961937509957934, 38.12609039468566152 ) ) ;
#137347 = CARTESIAN_POINT ( 'NONE',  ( 0.05219959533936267826, -19.03943276465977164, 35.00109039468566863 ) ) ;
#137348 = CARTESIAN_POINT ( 'NONE',  ( 0.05219959533934541429, -16.53943276465976808, 90.00109039468567573 ) ) ;
#137349 = CARTESIAN_POINT ( 'NONE',  ( 23.29544513554940366, -16.92513159979222337, 146.7843446569000037 ) ) ;
#137350 = CARTESIAN_POINT ( 'NONE',  ( 0.05219959533909260263, 19.03943276465977164, 54.99890960531435979 ) ) ;
#137351 = AXIS2_PLACEMENT_3D ( 'NONE', #72654, #149485, #103979 ) ;
#137352 = CARTESIAN_POINT ( 'NONE',  ( -15.80617190586768217, 15.72974639402176855, 63.12609039468568994 ) ) ;
#137353 = CARTESIAN_POINT ( 'NONE',  ( 18.62759615963255655, 10.81492255796105972, 81.66775706135236135 ) ) ;
#137354 = DIRECTION ( 'NONE',  ( 0.000000000000000000, -0.7071067811865483499, -0.7071067811865465735 ) ) ;
#137355 = CARTESIAN_POINT ( 'NONE',  ( -0.05219959533909027116, -19.03943276465977164, 72.49890960531435269 ) ) ;
#137356 = CARTESIAN_POINT ( 'NONE',  ( 5.823673210054444382, -21.52544592524334988, 65.20942372801901854 ) ) ;
#137357 = CARTESIAN_POINT ( 'NONE',  ( 0.05219959533936267826, -19.03943276465977164, 105.0010903946856615 ) ) ;
#137358 = CARTESIAN_POINT ( 'NONE',  ( 19.02544592524343514, -5.153800228976328945, 58.54057627198102409 ) ) ;
#137359 = CARTESIAN_POINT ( 'NONE',  ( 5.049401038298161559, -19.05341960407611168, 102.7072429386476955 ) ) ;
#137360 = CARTESIAN_POINT ( 'NONE',  ( -0.05219959533909027116, -19.03943276465977164, 77.49890960531435269 ) ) ;
#137361 = DIRECTION ( 'NONE',  ( -1.000000000000000000, 0.000000000000000000, 0.000000000000000000 ) ) ;
#137362 = CARTESIAN_POINT ( 'NONE',  ( -9.474510206698964154, 16.51473224551069663, 60.41557627198102409 ) ) ;
#137363 = CARTESIAN_POINT ( 'NONE',  ( 21.53943276465977519, -0.05219959533907433946, 93.74890960531436690 ) ) ;
#137364 = CARTESIAN_POINT ( 'NONE',  ( -8.314922557961024197, 14.29746914071037800, 92.91775706135236135 ) ) ;
#137365 = CARTESIAN_POINT ( 'NONE',  ( 7.405238625847253786, -1.490470117976223863, -64.28041130758167299 ) ) ;
#137366 = CARTESIAN_POINT ( 'NONE',  ( 13.89961937509957401, 13.97604488694547697, 41.87609039468566152 ) ) ;
#137367 = CARTESIAN_POINT ( 'NONE',  ( 16.51473224551069308, 9.474510206698969483, 84.16557627198102409 ) ) ;
#137368 = CARTESIAN_POINT ( 'NONE',  ( 12.14591786802309770, 12.06949235617756955, 69.37390960531436690 ) ) ;
#137369 = CARTESIAN_POINT ( 'NONE',  ( 8.224510206698953496, -14.34966873604960469, 107.9155762719810241 ) ) ;
#137370 = AXIS2_PLACEMENT_3D ( 'NONE', #172896, #96035, #157722 ) ;
#137371 = CARTESIAN_POINT ( 'NONE',  ( 5.719274019375991003, -21.55341960407610458, 22.70724293864769194 ) ) ;
#137372 = CARTESIAN_POINT ( 'NONE',  ( -0.05219959533909027116, -19.03943276465977164, 102.4989096053143669 ) ) ;
#137373 = CARTESIAN_POINT ( 'NONE',  ( 30.00000000000000711, -5.510910596163089556E-15, 45.00000000000000000 ) ) ;
#137374 = CARTESIAN_POINT ( 'NONE',  ( 0.05219959533936267826, -19.03943276465977164, 25.00109039468566152 ) ) ;
#137375 = CARTESIAN_POINT ( 'NONE',  ( 8.224510206698742110, 14.34966873604972548, 92.08442372801901854 ) ) ;
#137376 = CARTESIAN_POINT ( 'NONE',  ( -19.05341960407611168, -5.049401038298163336, 81.45724293864769550 ) ) ;
#137377 = CARTESIAN_POINT ( 'NONE',  ( 15.72974639402176855, 15.80617190586768217, 51.87609039468568284 ) ) ;
#137378 = CARTESIAN_POINT ( 'NONE',  ( 18.62759615963271287, -10.81492255796078972, 33.33224293864769550 ) ) ;
#137379 = CARTESIAN_POINT ( 'NONE',  ( 5.823673210054444382, -21.52544592524334988, 25.20942372801901854 ) ) ;
#137380 = CARTESIAN_POINT ( 'NONE',  ( -18.67979575497178146, -10.72451020669898902, 66.66557627198102409 ) ) ;
#137381 = CARTESIAN_POINT ( 'NONE',  ( -4.379528057220328563, 16.55341960407611168, 100.2072429386476955 ) ) ;
#137382 = CARTESIAN_POINT ( 'NONE',  ( -5.153800228976607833, 19.02544592524334988, 52.70942372801900433 ) ) ;
#137383 = CARTESIAN_POINT ( 'NONE',  ( 16.46253265017160672, -9.564922557960803928, 28.33224293864769550 ) ) ;
#137384 = CARTESIAN_POINT ( 'NONE',  ( -13.97604488694527625, -13.89961937509977652, 86.87390960531436690 ) ) ;
#137385 = CARTESIAN_POINT ( 'NONE',  ( -0.05219959533909027116, -19.03943276465977164, 82.49890960531436690 ) ) ;
#137386 = CARTESIAN_POINT ( 'NONE',  ( 16.53943276465976808, -0.05219959533910856209, 98.74890960531438111 ) ) ;
#137387 = ORIENTED_EDGE ( 'NONE', *, *, #21229, .T. ) ;
#137388 = CARTESIAN_POINT ( 'NONE',  ( -12.14591786802309592, -12.06949235617757132, 31.87390960531435979 ) ) ;
#137389 = CARTESIAN_POINT ( 'NONE',  ( -4.483927247898782831, 16.52544592524335698, 22.70942372801901499 ) ) ;
#137390 = CARTESIAN_POINT ( 'NONE',  ( -21.53943276465977519, -0.05219959533937600094, 88.75109039468567573 ) ) ;
#137391 = CARTESIAN_POINT ( 'NONE',  ( 9.564922557960805705, 16.46253265017160317, 99.58224293864770971 ) ) ;
#137392 = CARTESIAN_POINT ( 'NONE',  ( -18.62759615963255300, -10.81492255796106328, 24.16775706135235424 ) ) ;
#137393 = CARTESIAN_POINT ( 'NONE',  ( 13.89961937509977652, -13.97604488694527269, 48.12390960531435979 ) ) ;
#137394 = CARTESIAN_POINT ( 'NONE',  ( -16.53943276465976808, -0.05219959533934237506, 38.75109039468567573 ) ) ;
#137395 = CARTESIAN_POINT ( 'NONE',  ( -19.02544592524334988, -5.153800228976617603, 103.9594237280190043 ) ) ;
#137396 = CARTESIAN_POINT ( 'NONE',  ( -19.02544592524342804, 5.153800228976336051, 31.04057627198102409 ) ) ;
#137397 = CARTESIAN_POINT ( 'NONE',  ( 0.05219959533910956823, 16.53943276465976808, 99.99890960531436690 ) ) ;
#137398 = CARTESIAN_POINT ( 'NONE',  ( 18.62759615963271287, -10.81492255796078972, 108.3322429386477097 ) ) ;
#137399 = CARTESIAN_POINT ( 'NONE',  ( 9.474510206698729675, 16.51473224551082808, 62.08442372801899722 ) ) ;
#137400 = CARTESIAN_POINT ( 'NONE',  ( -5.049401038298153566, 19.05341960407611168, 25.20724293864768484 ) ) ;
#137401 = CARTESIAN_POINT ( 'NONE',  ( 5.823673210054444382, -21.52544592524334988, 20.20942372801900788 ) ) ;
#137402 = CARTESIAN_POINT ( 'NONE',  ( 1.022580077288041090E-15, 16.70000000000002061, -65.00100000000003320 ) ) ;
#137403 = CARTESIAN_POINT ( 'NONE',  ( -13.89961937509977652, 13.97604488694528158, 85.62390960531433848 ) ) ;
#137404 = CARTESIAN_POINT ( 'NONE',  ( 16.88567814943161594, -6.947325034625701612, 111.2099887734741799 ) ) ;
#137405 = B_SPLINE_CURVE_WITH_KNOTS ( 'NONE', 3,
 ( #198691, #105675, #9697, #183521, #41029, #73375 ),
 .UNSPECIFIED., .F., .F.,
 ( 4, 2, 4 ),
 ( 0.003989672132298154733, 0.004372778065220565835, 0.004755883998142976937 ),
 .UNSPECIFIED. ) ;
#137406 = CARTESIAN_POINT ( 'NONE',  ( 5.153800228976335163, 19.02544592524342804, 79.79057627198102409 ) ) ;
#137408 = CARTESIAN_POINT ( 'NONE',  ( -16.52544592524342804, 4.483927247898546575, 76.04057627198102409 ) ) ;
#137407 = CARTESIAN_POINT ( 'NONE',  ( 10.81492255796106328, -18.62759615963255655, 35.41775706135234003 ) ) ;
#137409 = CARTESIAN_POINT ( 'NONE',  ( 13.97604488694527802, 13.89961937509977652, 89.37390960531436690 ) ) ;
#137411 = CARTESIAN_POINT ( 'NONE',  ( 13.97604488694548053, -13.89961937509957401, 50.62609039468566152 ) ) ;
#137410 = CARTESIAN_POINT ( 'NONE',  ( 16.55341960407618274, -4.379528057220086978, 51.04275706135234714 ) ) ;
#137412 = CARTESIAN_POINT ( 'NONE',  ( 0.05219959533937995610, -21.53943276465977519, 70.00109039468568994 ) ) ;
#137413 = CARTESIAN_POINT ( 'NONE',  ( 16.53943276465976808, 0.05219959533934440121, 26.25109039468567573 ) ) ;
#137415 = ADVANCED_FACE ( 'NONE', ( #129238 ), #144417, .F. ) ;
#137414 = CARTESIAN_POINT ( 'NONE',  ( -16.46253265017160317, 9.564922557960807481, 70.83224293864770971 ) ) ;
#137416 = CARTESIAN_POINT ( 'NONE',  ( -9.564922557961040184, 16.46253265017147172, 92.91775706135233293 ) ) ;
#137417 = CARTESIAN_POINT ( 'NONE',  ( 0.05219959533934541429, -16.53943276465976808, 55.00109039468568284 ) ) ;
#137418 = CARTESIAN_POINT ( 'NONE',  ( -21.53943276465977519, -0.05219959533937600094, 98.75109039468568994 ) ) ;
#137419 = CARTESIAN_POINT ( 'NONE',  ( 19.02544592524334988, 5.153800228976608722, 86.45942372801900433 ) ) ;
#137420 = CARTESIAN_POINT ( 'NONE',  ( 16.51473224551069308, 9.474510206698969483, 49.16557627198102409 ) ) ;
#137421 = CARTESIAN_POINT ( 'NONE',  ( 18.62759615963271287, -10.81492255796078972, 73.33224293864769550 ) ) ;
#137423 = CARTESIAN_POINT ( 'NONE',  ( 19.02544592524334988, 5.153800228976608722, 71.45942372801900433 ) ) ;
#137422 = CARTESIAN_POINT ( 'NONE',  ( -8.314922557960811034, -14.29746914071050412, 72.08224293864769550 ) ) ;
#137424 = CARTESIAN_POINT ( 'NONE',  ( 17.48853670773246805, -5.747243402303059412, 61.16671299749989288 ) ) ;
#137425 = CARTESIAN_POINT ( 'NONE',  ( -16.46253265017146816, -9.564922557961047289, 44.16775706135232582 ) ) ;
#137426 = CARTESIAN_POINT ( 'NONE',  ( 16.55341960407611168, 4.379528057220329451, 23.95724293864769550 ) ) ;
#137427 = CARTESIAN_POINT ( 'NONE',  ( -8.224510206698948167, 14.34966873604960824, 70.41557627198102409 ) ) ;
#137429 = CARTESIAN_POINT ( 'NONE',  ( 27.73933785331498214, 9.013057229001095294, 147.9750000027311501 ) ) ;
#137428 = CARTESIAN_POINT ( 'NONE',  ( 21.52544592524334988, 5.823673210054432836, 96.45942372801901854 ) ) ;
#137430 = CARTESIAN_POINT ( 'NONE',  ( 21.53943276465977519, -0.05219959533907433946, 108.7489096053143669 ) ) ;
#137431 = CARTESIAN_POINT ( 'NONE',  ( -19.03943276465977164, 0.05219959533909376836, 71.24890960531435269 ) ) ;
#137432 = CARTESIAN_POINT ( 'NONE',  ( 10.81492255796106328, -18.62759615963255655, 85.41775706135236135 ) ) ;
#137433 = CARTESIAN_POINT ( 'NONE',  ( 13.89961937509977652, -13.97604488694527269, 63.12390960531435979 ) ) ;
#137434 = ORIENTED_EDGE ( 'NONE', *, *, #47812, .F. ) ;
#137435 = CARTESIAN_POINT ( 'NONE',  ( -19.02544592524342804, 5.153800228976336051, 26.04057627198103120 ) ) ;
#137436 = CARTESIAN_POINT ( 'NONE',  ( -21.55341960407610458, -5.719274019375992779, 36.45724293864768839 ) ) ;
#137437 = VECTOR ( 'NONE', #137, 1000.000000000000000 ) ;
#137438 = CARTESIAN_POINT ( 'NONE',  ( -0.05219959533910754901, -16.53943276465976808, 72.49890960531435269 ) ) ;
#137439 = CARTESIAN_POINT ( 'NONE',  ( 5.049401038298161559, -19.05341960407611168, 42.70724293864767418 ) ) ;
#137440 = CARTESIAN_POINT ( 'NONE',  ( 12.06949235617757843, -12.14591786802309237, 93.12390960531436690 ) ) ;
#137441 = CARTESIAN_POINT ( 'NONE',  ( 5.823673210054125526, 21.52544592524343514, 114.7905762719810383 ) ) ;
#137442 = CARTESIAN_POINT ( 'NONE',  ( -10.81492255796105439, 18.62759615963255655, 52.91775706135235424 ) ) ;
#137443 = CARTESIAN_POINT ( 'NONE',  ( -5.049401038298153566, 19.05341960407611168, 35.20724293864768839 ) ) ;
#137444 = CARTESIAN_POINT ( 'NONE',  ( -4.483927247898782831, 16.52544592524335698, 47.70942372801902565 ) ) ;
#137445 = EDGE_CURVE ( 'NONE', #138583, #196688, #68207, .T. ) ;
#137446 = CARTESIAN_POINT ( 'NONE',  ( 15.72974639402199770, -15.80617190586745480, 98.12390960531436690 ) ) ;
#137447 = CARTESIAN_POINT ( 'NONE',  ( 21.55341960407610458, 5.719274019375980345, 103.9572429386476813 ) ) ;
#137449 = CARTESIAN_POINT ( 'NONE',  ( 5.153800228976335163, 19.02544592524342804, 49.79057627198100988 ) ) ;
#137448 = CARTESIAN_POINT ( 'NONE',  ( 19.02544592524334988, 5.153800228976608722, 26.45942372801899722 ) ) ;
#137450 = CARTESIAN_POINT ( 'NONE',  ( 0.05219959533909260263, 19.03943276465977164, 104.9989096053143669 ) ) ;
#137451 = CARTESIAN_POINT ( 'NONE',  ( 21.55341960407619695, -5.719274019375665929, 56.04275706135235424 ) ) ;
#137452 = CARTESIAN_POINT ( 'NONE',  ( 0.05219959533907565091, 21.53943276465977519, 49.99890960531437401 ) ) ;
#137453 = CARTESIAN_POINT ( 'NONE',  ( 16.53943276465976808, 0.05219959533934440121, 111.2510903946856899 ) ) ;
#137455 = CARTESIAN_POINT ( 'NONE',  ( 10.81492255796106328, -18.62759615963255655, 95.41775706135234714 ) ) ;
#137454 = CARTESIAN_POINT ( 'NONE',  ( 15.80617190586769283, -15.72974639402175789, 65.62609039468568994 ) ) ;
#137456 = CARTESIAN_POINT ( 'NONE',  ( 5.153800228976615827, -19.02544592524334988, 50.20942372801897591 ) ) ;
#137457 = CARTESIAN_POINT ( 'NONE',  ( 14.29746914071037800, 8.314922557961029526, 106.6677570613523756 ) ) ;
#137458 = CARTESIAN_POINT ( 'NONE',  ( 18.62759615963255655, 10.81492255796105972, 61.66775706135235424 ) ) ;
#137459 = CARTESIAN_POINT ( 'NONE',  ( -19.02544592524342804, 5.153800228976336051, 56.04057627198100988 ) ) ;
#137460 = CARTESIAN_POINT ( 'NONE',  ( -16.51473224551082808, 9.474510206698731452, 23.33442372801900078 ) ) ;
#137461 = CARTESIAN_POINT ( 'NONE',  ( 5.719274019375991003, -21.55341960407610458, 22.70724293864769194 ) ) ;
#137462 = CARTESIAN_POINT ( 'NONE',  ( 15.80617190586769283, -15.72974639402175789, 20.62609039468568639 ) ) ;
#137463 = CARTESIAN_POINT ( 'NONE',  ( -0.05219959533907301413, -21.53943276465977519, 72.49890960531435269 ) ) ;
#137464 = CARTESIAN_POINT ( 'NONE',  ( 16.53943276465976808, 0.05219959533934440121, 46.25109039468567573 ) ) ;
#137466 = CARTESIAN_POINT ( 'NONE',  ( 21.55341960407610458, 5.719274019375980345, 83.95724293864770971 ) ) ;
#137465 = LINE ( 'NONE', #41499, #106339 ) ;
#137468 = CARTESIAN_POINT ( 'NONE',  ( 16.55341960407611168, 4.379528057220329451, 73.95724293864769550 ) ) ;
#137467 = CARTESIAN_POINT ( 'NONE',  ( 14.29746914071037800, 8.314922557961029526, 71.66775706135234714 ) ) ;
#137469 = CARTESIAN_POINT ( 'NONE',  ( 1.285635531079530436, 29.62244251375079784, -48.76710130854527137 ) ) ;
#137470 = CARTESIAN_POINT ( 'NONE',  ( -9.564922557961040184, 16.46253265017147172, 102.9177570613523329 ) ) ;
#137471 = CARTESIAN_POINT ( 'NONE',  ( -15.80617190586745835, -15.72974639402198527, 36.87390960531435979 ) ) ;
#137472 = CARTESIAN_POINT ( 'NONE',  ( 16.51473224551069308, 9.474510206698969483, 94.16557627198103830 ) ) ;
#137473 = CARTESIAN_POINT ( 'NONE',  ( -4.379528057220086978, -16.55341960407618274, 34.79275706135235424 ) ) ;
#137474 = CARTESIAN_POINT ( 'NONE',  ( -5.719274019375978568, 21.55341960407610458, 105.2072429386477097 ) ) ;
#137475 = CARTESIAN_POINT ( 'NONE',  ( 10.72451020669898902, -18.67979575497178502, 37.91557627198102409 ) ) ;
#137476 = CARTESIAN_POINT ( 'NONE',  ( -16.55341960407617563, 4.379528057220093196, 73.54275706135234714 ) ) ;
#137477 = CARTESIAN_POINT ( 'NONE',  ( -9.564922557960796823, -16.46253265017161027, 87.08224293864769550 ) ) ;
#137479 = CARTESIAN_POINT ( 'NONE',  ( 9.474510206698971260, -16.51473224551069308, 22.91557627198102765 ) ) ;
#137478 = CARTESIAN_POINT ( 'NONE',  ( -0.05219959533937732626, 21.53943276465977519, 37.50109039468568284 ) ) ;
#137480 = CARTESIAN_POINT ( 'NONE',  ( 0.05219959533907565091, 21.53943276465977519, 24.99890960531435624 ) ) ;
#137481 = EDGE_LOOP ( 'NONE', ( #55668, #37985, #61968, #39791 ) ) ;
#137482 = CARTESIAN_POINT ( 'NONE',  ( 16.51473224551083163, -9.474510206698727899, 25.83442372801900078 ) ) ;
#137483 = CARTESIAN_POINT ( 'NONE',  ( -14.29746914071037622, -8.314922557961029526, 54.16775706135235424 ) ) ;
#137484 = CARTESIAN_POINT ( 'NONE',  ( -19.02544592524342804, 5.153800228976336051, 106.0405762719810241 ) ) ;
#137485 = CARTESIAN_POINT ( 'NONE',  ( -5.823673210054116645, -21.52544592524344225, 97.29057627198105251 ) ) ;
#137486 = CARTESIAN_POINT ( 'NONE',  ( 19.02544592524343514, -5.153800228976328945, 73.54057627198103830 ) ) ;
#137487 = CARTESIAN_POINT ( 'NONE',  ( -3.874011537017815421, -5.374011537017722162, -62.41807096325323556 ) ) ;
#137488 = CARTESIAN_POINT ( 'NONE',  ( -6.856101608890801443E-16, -71.74905178543389184, -22.99263613531268291 ) ) ;
#137489 = CARTESIAN_POINT ( 'NONE',  ( 8.224510206698953496, -14.34966873604960469, 87.91557627198103830 ) ) ;
#137490 = CARTESIAN_POINT ( 'NONE',  ( -15.72974639402197994, 15.80617190586746368, 30.62390960531436335 ) ) ;
#137491 = CARTESIAN_POINT ( 'NONE',  ( -17.31747979337949417, 6.344076630960994834, 33.62055131934815932 ) ) ;
#137492 = CARTESIAN_POINT ( 'NONE',  ( 14.34966873604972726, -8.224510206698740333, 65.83442372801900433 ) ) ;
#137493 = CARTESIAN_POINT ( 'NONE',  ( 15.72974639402199770, -15.80617190586745480, 113.1239096053143953 ) ) ;
#137494 = CARTESIAN_POINT ( 'NONE',  ( -9.564922557961040184, 16.46253265017147172, 72.91775706135233293 ) ) ;
#137495 = CARTESIAN_POINT ( 'NONE',  ( 16.51473224551069308, 9.474510206698969483, 44.16557627198103120 ) ) ;
#137496 = CARTESIAN_POINT ( 'NONE',  ( 21.53943276465977519, -0.05219959533907433946, 63.74890960531435979 ) ) ;
#137497 = CARTESIAN_POINT ( 'NONE',  ( 5.153800228976335163, 19.02544592524342804, 99.79057627198102409 ) ) ;
#137498 = CARTESIAN_POINT ( 'NONE',  ( 21.55341960407619695, -5.719274019375665929, 91.04275706135236135 ) ) ;
#137499 = CARTESIAN_POINT ( 'NONE',  ( 9.564922557960805705, 16.46253265017160317, 69.58224293864770971 ) ) ;
#137500 = EDGE_CURVE ( 'NONE', #62281, #123348, #135159, .T. ) ;
#137501 = CARTESIAN_POINT ( 'NONE',  ( -16.52544592524335698, -4.483927247898792601, 43.95942372801902565 ) ) ;
#137502 = CARTESIAN_POINT ( 'NONE',  ( -19.02544592524342804, 5.153800228976336051, 61.04057627198103120 ) ) ;
#137503 = CARTESIAN_POINT ( 'NONE',  ( -15.72974639402176322, -15.80617190586768395, 74.37609039468568994 ) ) ;
#137504 = CARTESIAN_POINT ( 'NONE',  ( 19.03943276465977164, 0.05219959533936151252, 41.25109039468566152 ) ) ;
#137505 = CARTESIAN_POINT ( 'NONE',  ( -16.51473224551082808, 9.474510206698731452, 48.33442372801900433 ) ) ;
#137506 = CARTESIAN_POINT ( 'NONE',  ( -21.53943276465977519, -0.05219959533937600094, 48.75109039468568284 ) ) ;
#137507 = CARTESIAN_POINT ( 'NONE',  ( -18.56101223717332971, -5.499999999999953815, 46.44978406935678805 ) ) ;
#137508 = CARTESIAN_POINT ( 'NONE',  ( 5.049401038297881783, 19.05341960407617563, 47.29275706135231161 ) ) ;
#137509 = CARTESIAN_POINT ( 'NONE',  ( 19.02544592524343514, -5.153800228976328945, 103.5405762719809957 ) ) ;
#137510 = CARTESIAN_POINT ( 'NONE',  ( 16.51473224551069308, 9.474510206698969483, 69.16557627198102409 ) ) ;
#137511 = CARTESIAN_POINT ( 'NONE',  ( -16.53943276465976808, -0.05219959533934237506, 113.7510903946856757 ) ) ;
#137513 = CARTESIAN_POINT ( 'NONE',  ( 18.67979575497194134, -10.72451020669871369, 100.8344237280190185 ) ) ;
#137512 = CARTESIAN_POINT ( 'NONE',  ( 21.52544592524344225, -5.823673210054117533, 28.54057627198103120 ) ) ;
#137514 = CARTESIAN_POINT ( 'NONE',  ( -36.91746825000001309, -11.99521256947794789, -2.524999997268813523 ) ) ;
#137515 = CARTESIAN_POINT ( 'NONE',  ( 16.21995358207306026, 7.366697692864117464, 57.56448998487844904 ) ) ;
#137516 = CARTESIAN_POINT ( 'NONE',  ( -18.62759615963255300, -10.81492255796106328, 99.16775706135234714 ) ) ;
#137517 = CARTESIAN_POINT ( 'NONE',  ( 9.100000000000001421, 0.000000000000000000, -61.89430850415821794 ) ) ;
#137518 = CARTESIAN_POINT ( 'NONE',  ( 5.153800228976335163, 19.02544592524342804, 24.79057627198102765 ) ) ;
#137519 = CARTESIAN_POINT ( 'NONE',  ( 19.05341960407611168, 5.049401038298154454, 108.9572429386477097 ) ) ;
#137520 = CARTESIAN_POINT ( 'NONE',  ( 34.25194412823101686, 3.632597792548375448, 90.85486465461555383 ) ) ;
#137521 = CARTESIAN_POINT ( 'NONE',  ( 4.379528057220092307, 16.55341960407617563, 52.29275706135236135 ) ) ;
#137522 = CARTESIAN_POINT ( 'NONE',  ( 21.53943276465977519, -0.05219959533907433946, 73.74890960531433848 ) ) ;
#137523 = CARTESIAN_POINT ( 'NONE',  ( 14.29746914071049879, -8.314922557960816363, 43.33224293864769550 ) ) ;
#137525 = CARTESIAN_POINT ( 'NONE',  ( 5.153800228976335163, 19.02544592524342804, 104.7905762719809957 ) ) ;
#137524 = CARTESIAN_POINT ( 'NONE',  ( -16.52544592524342804, 4.483927247898546575, 111.0405762719810525 ) ) ;
#137526 = CARTESIAN_POINT ( 'NONE',  ( 9.474510206698729675, 16.51473224551082808, 37.08442372801899722 ) ) ;
#137527 = CARTESIAN_POINT ( 'NONE',  ( -16.53943276465976808, 0.05219959533911058130, 111.2489096053143669 ) ) ;
#137528 = CARTESIAN_POINT ( 'NONE',  ( -18.62759615963255300, -10.81492255796106328, 74.16775706135231871 ) ) ;
#137529 = CYLINDRICAL_SURFACE ( 'NONE', #4965, 28.90000000000004476 ) ;
#137530 = CARTESIAN_POINT ( 'NONE',  ( -16.55341960407611168, -4.379528057220339221, 31.45724293864769550 ) ) ;
#137531 = CARTESIAN_POINT ( 'NONE',  ( -17.59860650958993844, 7.585241751806885979, 68.42337014262493256 ) ) ;
#137532 = CARTESIAN_POINT ( 'NONE',  ( 18.67979575497178502, 10.72451020669898547, 29.16557627198103120 ) ) ;
#137533 = CARTESIAN_POINT ( 'NONE',  ( 16.53943276465976808, -0.05219959533910856209, 83.74890960531435269 ) ) ;
#137535 = CARTESIAN_POINT ( 'NONE',  ( -5.362406601429247743, -6.881127002625603062, -64.03737582163388709 ) ) ;
#137534 = AXIS2_PLACEMENT_3D ( 'NONE', #88262, #132778, #194465 ) ;
#137536 = CARTESIAN_POINT ( 'NONE',  ( 16.51473224551069308, 9.474510206698969483, 74.16557627198103830 ) ) ;
#137537 = CARTESIAN_POINT ( 'NONE',  ( 0.05219959533910956823, 16.53943276465976808, 79.99890960531435269 ) ) ;
#137538 = CARTESIAN_POINT ( 'NONE',  ( 5.153800228976615827, -19.02544592524334988, 110.2094237280189901 ) ) ;
#137539 = CARTESIAN_POINT ( 'NONE',  ( -18.62759615963270932, 10.81492255796079327, 50.83224293864770971 ) ) ;
#137540 = ORIENTED_EDGE ( 'NONE', *, *, #103145, .F. ) ;
#137541 = CARTESIAN_POINT ( 'NONE',  ( -9.474510206698964154, 16.51473224551069663, 25.41557627198103120 ) ) ;
#137543 = CARTESIAN_POINT ( 'NONE',  ( -18.67979575497178146, -10.72451020669898902, 71.66557627198100988 ) ) ;
#137542 = CARTESIAN_POINT ( 'NONE',  ( -9.474510206698964154, 16.51473224551069663, 75.41557627198103830 ) ) ;
#137545 = CARTESIAN_POINT ( 'NONE',  ( -19.02544592524342804, 5.153800228976336051, 91.04057627198100988 ) ) ;
#137544 = CARTESIAN_POINT ( 'NONE',  ( 8.314922557961029526, -14.29746914071037800, 100.4177570613523471 ) ) ;
#137546 = CARTESIAN_POINT ( 'NONE',  ( -5.049401038297874678, -19.05341960407617918, 64.79275706135233293 ) ) ;
#137547 = CARTESIAN_POINT ( 'NONE',  ( -18.67979575497193778, 10.72451020669871902, 83.33442372801903275 ) ) ;
#137548 = CARTESIAN_POINT ( 'NONE',  ( 5.719274019375991003, -21.55341960407610458, 62.70724293864769550 ) ) ;
#137549 = CARTESIAN_POINT ( 'NONE',  ( -10.72451020669898014, 18.67979575497178502, 25.41557627198103120 ) ) ;
#137550 = CARTESIAN_POINT ( 'NONE',  ( 16.46253265017160672, -9.564922557960803928, 43.33224293864769550 ) ) ;
#137551 = CARTESIAN_POINT ( 'NONE',  ( 14.29746914071037800, 8.314922557961029526, 96.66775706135234714 ) ) ;
#137552 = CARTESIAN_POINT ( 'NONE',  ( 19.02544592524343514, -5.153800228976328945, 58.54057627198102409 ) ) ;
#137553 = CARTESIAN_POINT ( 'NONE',  ( -16.53943276465976808, -0.05219959533934237506, 28.75109039468567929 ) ) ;
#137554 = CARTESIAN_POINT ( 'NONE',  ( 18.22780087662122739, 5.500000000000000888, 81.48236817873103632 ) ) ;
#137555 = CARTESIAN_POINT ( 'NONE',  ( 16.51473224551083163, -9.474510206698727899, 20.83442372801899722 ) ) ;
#137556 = CARTESIAN_POINT ( 'NONE',  ( 16.53943276465976808, -0.05219959533910856209, 68.74890960531435269 ) ) ;
#137557 = CARTESIAN_POINT ( 'NONE',  ( 21.55341960407610458, 5.719274019375980345, 108.9572429386476955 ) ) ;
#137558 = CARTESIAN_POINT ( 'NONE',  ( -18.67979575497178146, -10.72451020669898902, 101.6655762719810383 ) ) ;
#137559 = DIRECTION ( 'NONE',  ( 0.000000000000000000, 0.000000000000000000, 1.000000000000000000 ) ) ;
#137560 = CARTESIAN_POINT ( 'NONE',  ( 10.81492255796078972, 18.62759615963270932, 39.58224293864769550 ) ) ;
#137561 = CARTESIAN_POINT ( 'NONE',  ( 8.224510206698742110, 14.34966873604972548, 82.08442372801901854 ) ) ;
#137562 = CARTESIAN_POINT ( 'NONE',  ( 12.14591786802309770, 12.06949235617756955, 99.37390960531436690 ) ) ;
#137563 = CARTESIAN_POINT ( 'NONE',  ( -19.03943276465977164, 0.05219959533909376836, 56.24890960531435979 ) ) ;
#137564 = LINE ( 'NONE', #138553, #167284 ) ;
#137565 = CARTESIAN_POINT ( 'NONE',  ( 12.06949235617739724, 12.14591786802326823, 111.8760903946856615 ) ) ;
#137566 = VERTEX_POINT ( 'NONE', #81729 ) ;
#137567 = CARTESIAN_POINT ( 'NONE',  ( 21.52544592524334988, 5.823673210054432836, 41.45942372801901143 ) ) ;
#137568 = CARTESIAN_POINT ( 'NONE',  ( 16.51473224551069308, 9.474510206698969483, 94.16557627198103830 ) ) ;
#137569 = CARTESIAN_POINT ( 'NONE',  ( -21.53943276465977519, -0.05219959533937600094, 83.75109039468568994 ) ) ;
#137570 = CARTESIAN_POINT ( 'NONE',  ( -9.564922557960796823, -16.46253265017161027, 32.08224293864769550 ) ) ;
#137571 = CARTESIAN_POINT ( 'NONE',  ( 13.89961937509977652, -13.97604488694527269, 23.12390960531436335 ) ) ;
#137572 = VERTEX_POINT ( 'NONE', #130230 ) ;
#137573 = CARTESIAN_POINT ( 'NONE',  ( 5.823673210054444382, -21.52544592524334988, 75.20942372801901854 ) ) ;
#137574 = CARTESIAN_POINT ( 'NONE',  ( -9.474510206698964154, 16.51473224551069663, 100.4155762719810241 ) ) ;
#137575 = CARTESIAN_POINT ( 'NONE',  ( 16.46253265017146816, 9.564922557961045513, 86.66775706135233293 ) ) ;
#137576 = CARTESIAN_POINT ( 'NONE',  ( 15.72974639402176855, 15.80617190586768217, 36.87609039468568994 ) ) ;
#137577 = CARTESIAN_POINT ( 'NONE',  ( -16.51473224551082808, 9.474510206698731452, 113.3344237280190043 ) ) ;
#137578 = VECTOR ( 'NONE', #194022, 1000.000000000000114 ) ;
#137579 = CARTESIAN_POINT ( 'NONE',  ( -19.03943276465977164, -0.05219959533935918106, 73.75109039468566152 ) ) ;
#137580 = CARTESIAN_POINT ( 'NONE',  ( -5.153800228976328057, -19.02544592524343514, 42.29057627198101699 ) ) ;
#137581 = CARTESIAN_POINT ( 'NONE',  ( 5.049401038297881783, 19.05341960407617563, 77.29275706135231871 ) ) ;
#137582 = CARTESIAN_POINT ( 'NONE',  ( 8.224510206698953496, -14.34966873604960469, 22.91557627198102765 ) ) ;
#137583 = CARTESIAN_POINT ( 'NONE',  ( -16.46253265017146816, -9.564922557961047289, 79.16775706135234714 ) ) ;
#137584 = CARTESIAN_POINT ( 'NONE',  ( 16.53943276465976808, -0.05219959533910856209, 33.74890960531436690 ) ) ;
#137585 = CARTESIAN_POINT ( 'NONE',  ( 0.05219959533936267826, -19.03943276465977164, 65.00109039468567573 ) ) ;
#137586 = CARTESIAN_POINT ( 'NONE',  ( -21.55341960407619339, 5.719274019375674811, 108.5427570613523756 ) ) ;
#137587 = CARTESIAN_POINT ( 'NONE',  ( -5.049401038297874678, -19.05341960407617918, 29.79275706135232227 ) ) ;
#137588 = CARTESIAN_POINT ( 'NONE',  ( 13.89961937509977652, -13.97604488694527269, 28.12390960531435624 ) ) ;
#137589 = CARTESIAN_POINT ( 'NONE',  ( -17.05587630539784527, -6.762274262135712810, 64.25819690962687503 ) ) ;
#137590 = CARTESIAN_POINT ( 'NONE',  ( -14.34966873604972548, 8.224510206698743886, 48.33442372801902565 ) ) ;
#137591 = CARTESIAN_POINT ( 'NONE',  ( -17.49999999999999645, 5.499999999999992895, 120.0000000000000142 ) ) ;
#137592 = EDGE_CURVE ( 'NONE', #92102, #170830, #191925, .T. ) ;
#137593 = CARTESIAN_POINT ( 'NONE',  ( -27.73933785331498925, 9.013057229001089965, 144.7750000027311614 ) ) ;
#137594 = CARTESIAN_POINT ( 'NONE',  ( 5.049401038298161559, -19.05341960407611168, 87.70724293864769550 ) ) ;
#137595 = CARTESIAN_POINT ( 'NONE',  ( 11.30153831258470731, -188.0000000000000000, -1.787262988391354872E-28 ) ) ;
#137596 = VERTEX_POINT ( 'NONE', #171792 ) ;
#137597 = CARTESIAN_POINT ( 'NONE',  ( 16.51473224551083163, -9.474510206698727899, 90.83442372801900433 ) ) ;
#137598 = CARTESIAN_POINT ( 'NONE',  ( -13.89961937509977652, 13.97604488694528158, 115.6239096053143669 ) ) ;
#137600 = CARTESIAN_POINT ( 'NONE',  ( 9.474510206698729675, 16.51473224551082808, 97.08442372801900433 ) ) ;
#137599 = CARTESIAN_POINT ( 'NONE',  ( 5.153800228976615827, -19.02544592524334988, 20.20942372801899722 ) ) ;
#137601 = CARTESIAN_POINT ( 'NONE',  ( -8.314922557960811034, -14.29746914071050412, 107.0822429386476955 ) ) ;
#137602 = CARTESIAN_POINT ( 'NONE',  ( 16.46253265017160672, -9.564922557960803928, 28.33224293864769550 ) ) ;
#137603 = CARTESIAN_POINT ( 'NONE',  ( -21.55341960407610458, -5.719274019375992779, 56.45724293864768839 ) ) ;
#137604 = CARTESIAN_POINT ( 'NONE',  ( 18.67979575497178502, 10.72451020669898547, 49.16557627198102409 ) ) ;
#137605 = CARTESIAN_POINT ( 'NONE',  ( -9.474510206698964154, 16.51473224551069663, 25.41557627198103120 ) ) ;
#137606 = CARTESIAN_POINT ( 'NONE',  ( 17.85839625232364014, -22.61300660583702538, 140.0884876851766876 ) ) ;
#137607 = CARTESIAN_POINT ( 'NONE',  ( -19.05341960407617563, 5.049401038297882671, 73.54275706135233293 ) ) ;
#137608 = CARTESIAN_POINT ( 'NONE',  ( 12.14591786802309770, 12.06949235617756955, 34.37390960531435979 ) ) ;
#137609 = CARTESIAN_POINT ( 'NONE',  ( -21.55341960407610458, -5.719274019375992779, 26.45724293864768839 ) ) ;
#137610 = CARTESIAN_POINT ( 'NONE',  ( -5.823673210054431948, 21.52544592524334988, 87.70942372801901854 ) ) ;
#137611 = CARTESIAN_POINT ( 'NONE',  ( -5.823673210054116645, -21.52544592524344225, 82.29057627198103830 ) ) ;
#137612 = CARTESIAN_POINT ( 'NONE',  ( -10.72451020669870658, -18.67979575497194134, 54.58442372801901143 ) ) ;
#137613 = CARTESIAN_POINT ( 'NONE',  ( -10.72451020669870658, -18.67979575497194134, 69.58442372801900433 ) ) ;
#137614 = CARTESIAN_POINT ( 'NONE',  ( -19.03943276465977164, 0.05219959533909376836, 101.2489096053143669 ) ) ;
#137616 = CARTESIAN_POINT ( 'NONE',  ( -18.67979575497193778, 10.72451020669871902, 53.33442372801901854 ) ) ;
#137615 = CARTESIAN_POINT ( 'NONE',  ( -4.483927247898782831, 16.52544592524335698, 92.70942372801901854 ) ) ;
#137617 = CARTESIAN_POINT ( 'NONE',  ( 4.483927247898545687, 16.52544592524342804, 114.7905762719810383 ) ) ;
#137618 = CARTESIAN_POINT ( 'NONE',  ( -32.53418548917481701, 2.421649558188280427, 87.88477275112326481 ) ) ;
#137619 = CARTESIAN_POINT ( 'NONE',  ( -0.05219959533910754901, -16.53943276465976808, 72.49890960531435269 ) ) ;
#137620 = CARTESIAN_POINT ( 'NONE',  ( 16.53943276465976808, -0.05219959533910856209, 38.74890960531435979 ) ) ;
#137621 = CARTESIAN_POINT ( 'NONE',  ( 9.564922557960805705, 16.46253265017160317, 64.58224293864769550 ) ) ;
#137622 = CARTESIAN_POINT ( 'NONE',  ( -0.05219959533909027116, -19.03943276465977164, 52.49890960531436690 ) ) ;
#137623 = CARTESIAN_POINT ( 'NONE',  ( 18.62759615963271287, -10.81492255796078972, 63.33224293864770260 ) ) ;
#137624 = CARTESIAN_POINT ( 'NONE',  ( -5.049401038297874678, -19.05341960407617918, 39.79275706135232582 ) ) ;
#137626 = CARTESIAN_POINT ( 'NONE',  ( -8.224510206698948167, 14.34966873604960824, 55.41557627198102409 ) ) ;
#137625 = CARTESIAN_POINT ( 'NONE',  ( 22.71484980649369945, -22.39856283320808217, -49.13275782002545355 ) ) ;
#137627 = CARTESIAN_POINT ( 'NONE',  ( 21.55341960407610458, 5.719274019375980345, 23.95724293864769550 ) ) ;
#137628 = ORIENTED_EDGE ( 'NONE', *, *, #1893, .T. ) ;
#137629 = DIRECTION ( 'NONE',  ( 0.000000000000000000, 0.4999999999999991118, -0.8660254037844391517 ) ) ;
#137630 = CARTESIAN_POINT ( 'NONE',  ( -16.55341960407617563, 4.379528057220093196, 68.54275706135234714 ) ) ;
#137631 = CARTESIAN_POINT ( 'NONE',  ( 0.05219959533936267826, -19.03943276465977164, 75.00109039468566152 ) ) ;
#137632 = CARTESIAN_POINT ( 'NONE',  ( -14.34966873604960291, -8.224510206698953496, 46.66557627198102409 ) ) ;
#137633 = DIRECTION ( 'NONE',  ( 1.000000000000000000, 0.000000000000000000, -0.000000000000000000 ) ) ;
#137634 = CARTESIAN_POINT ( 'NONE',  ( -14.34966873604960291, -8.224510206698953496, 26.66557627198103475 ) ) ;
#137635 = CARTESIAN_POINT ( 'NONE',  ( 19.03943276465977164, -0.05219959533909143690, 53.74890960531436690 ) ) ;
#137636 = CARTESIAN_POINT ( 'NONE',  ( -5.153800228976328057, -19.02544592524343514, 77.29057627198099567 ) ) ;
#137637 = CARTESIAN_POINT ( 'NONE',  ( -13.89961937509977652, 13.97604488694528158, 45.62390960531433848 ) ) ;
#137638 = CARTESIAN_POINT ( 'NONE',  ( -18.62759615963255300, -10.81492255796106328, 44.16775706135234714 ) ) ;
#137639 = CARTESIAN_POINT ( 'NONE',  ( 19.05341960407611168, 5.049401038298154454, 63.95724293864769550 ) ) ;
#137640 = DIRECTION ( 'NONE',  ( 0.000000000000000000, 0.000000000000000000, -1.000000000000000000 ) ) ;
#137641 = CARTESIAN_POINT ( 'NONE',  ( 13.97604488694527802, 13.89961937509977652, 64.37390960531436690 ) ) ;
#137642 = CARTESIAN_POINT ( 'NONE',  ( -5.823673210054116645, -21.52544592524344225, 42.29057627198103120 ) ) ;
#137643 = CARTESIAN_POINT ( 'NONE',  ( 16.51473224551069308, 9.474510206698969483, 24.16557627198102765 ) ) ;
#137644 = CARTESIAN_POINT ( 'NONE',  ( -10.81492255796078084, -18.62759615963271287, 32.08224293864769550 ) ) ;
#137645 = CARTESIAN_POINT ( 'NONE',  ( -16.55341960407617563, 4.379528057220093196, 93.54275706135234714 ) ) ;
#137646 = CARTESIAN_POINT ( 'NONE',  ( -5.719274019375665041, -21.55341960407619695, 109.7927570613523613 ) ) ;
#137647 = CARTESIAN_POINT ( 'NONE',  ( 12.06949235617739724, 12.14591786802326823, 71.87609039468568994 ) ) ;
#137648 = CARTESIAN_POINT ( 'NONE',  ( -5.153800228976328057, -19.02544592524343514, 112.2905762719810099 ) ) ;
#137649 = CARTESIAN_POINT ( 'NONE',  ( -4.379528057220086978, -16.55341960407618274, 59.79275706135234714 ) ) ;
#137650 = CARTESIAN_POINT ( 'NONE',  ( 8.314922557961029526, -14.29746914071037800, 45.41775706135234003 ) ) ;
#137651 = CARTESIAN_POINT ( 'NONE',  ( -5.153800228976328057, -19.02544592524343514, 107.2905762719810383 ) ) ;
#137652 = CARTESIAN_POINT ( 'NONE',  ( -12.14591786802326823, 12.06949235617739902, 23.12609039468567573 ) ) ;
#137653 = CARTESIAN_POINT ( 'NONE',  ( 5.153800228976335163, 19.02544592524342804, 39.79057627198100988 ) ) ;
#137654 = CARTESIAN_POINT ( 'NONE',  ( 18.67979575497178502, 10.72451020669898547, 109.1655762719810383 ) ) ;
#137655 = CARTESIAN_POINT ( 'NONE',  ( -16.53943276465976808, -0.05219959533934237506, 18.75109039468568639 ) ) ;
#137656 = CARTESIAN_POINT ( 'NONE',  ( 8.314922557961029526, -14.29746914071037800, 85.41775706135236135 ) ) ;
#137657 = CARTESIAN_POINT ( 'NONE',  ( -17.31728774477213051, 6.344390552233684311, 45.81906651689308063 ) ) ;
#137658 = CARTESIAN_POINT ( 'NONE',  ( 10.81492255796106328, -18.62759615963255655, 85.41775706135236135 ) ) ;
#137659 = CARTESIAN_POINT ( 'NONE',  ( -13.97604488694547697, 13.89961937509957934, 88.12609039468563310 ) ) ;
#137660 = CARTESIAN_POINT ( 'NONE',  ( 16.53943276465976808, -0.05219959533910856209, 48.74890960531435979 ) ) ;
#137661 = CARTESIAN_POINT ( 'NONE',  ( 12.14591786802309770, 12.06949235617756955, 104.3739096053143669 ) ) ;
#137663 = PLANE ( 'NONE',  #166405 ) ;
#137662 = CARTESIAN_POINT ( 'NONE',  ( -9.564922557961040184, 16.46253265017147172, 42.91775706135234003 ) ) ;
#137664 = CARTESIAN_POINT ( 'NONE',  ( -18.67979575497193778, 10.72451020669871902, 48.33442372801902565 ) ) ;
#137665 = CARTESIAN_POINT ( 'NONE',  ( -19.02544592524334988, -5.153800228976617603, 103.9594237280190043 ) ) ;
#137666 = CARTESIAN_POINT ( 'NONE',  ( 16.19135201231366494, 7.376712067591956412, 82.68680854052030327 ) ) ;
#137667 = CARTESIAN_POINT ( 'NONE',  ( -19.03943276465977164, 0.05219959533909376836, 101.2489096053143669 ) ) ;
#137668 = CARTESIAN_POINT ( 'NONE',  ( 10.81492255796078972, 18.62759615963270932, 74.58224293864768129 ) ) ;
#137669 = CARTESIAN_POINT ( 'NONE',  ( 19.02544592524334988, 5.153800228976608722, 101.4594237280189759 ) ) ;
#137670 = EDGE_CURVE ( 'NONE', #188934, #113441, #197812, .T. ) ;
#137671 = CARTESIAN_POINT ( 'NONE',  ( 13.97604488694527802, 13.89961937509977652, 104.3739096053143385 ) ) ;
#137672 = CARTESIAN_POINT ( 'NONE',  ( 9.564922557961047289, -16.46253265017146816, 50.41775706135233293 ) ) ;
#137673 = CARTESIAN_POINT ( 'NONE',  ( -14.29746914071049879, 8.314922557960819915, 100.8322429386477097 ) ) ;
#137674 = CARTESIAN_POINT ( 'NONE',  ( -21.53943276465977519, -0.05219959533937600094, 88.75109039468567573 ) ) ;
#137675 = CARTESIAN_POINT ( 'NONE',  ( -5.049401038298153566, 19.05341960407611168, 45.20724293864769550 ) ) ;
#137676 = CIRCLE ( 'NONE', #50504, 0.5000000000000004441 ) ;
#137677 = CARTESIAN_POINT ( 'NONE',  ( 18.67979575497194134, -10.72451020669871369, 50.83442372801901143 ) ) ;
#137678 = CARTESIAN_POINT ( 'NONE',  ( -18.62759615963255300, -10.81492255796106328, 89.16775706135236135 ) ) ;
#137679 = CARTESIAN_POINT ( 'NONE',  ( 0.05219959533934541429, -16.53943276465976808, 85.00109039468568994 ) ) ;
#137680 = EDGE_CURVE ( 'NONE', #83313, #16981, #41254, .T. ) ;
#137681 = CARTESIAN_POINT ( 'NONE',  ( 5.823673210054444382, -21.52544592524334988, 40.20942372801901854 ) ) ;
#137682 = CARTESIAN_POINT ( 'NONE',  ( -0.05219959533937732626, 21.53943276465977519, 42.50109039468567573 ) ) ;
#137684 = CARTESIAN_POINT ( 'NONE',  ( -16.51473224551069308, -9.474510206698971260, 96.66557627198102409 ) ) ;
#137683 = CARTESIAN_POINT ( 'NONE',  ( -19.05341960407617563, 5.049401038297882671, 63.54275706135234003 ) ) ;
#137685 = CARTESIAN_POINT ( 'NONE',  ( 16.52544592524342804, -4.483927247898539470, 103.5405762719810383 ) ) ;
#137686 = CARTESIAN_POINT ( 'NONE',  ( -15.80617190586745835, -15.72974639402198527, 81.87390960531435269 ) ) ;
#137687 = CARTESIAN_POINT ( 'NONE',  ( 14.29746914071049879, -8.314922557960816363, 68.33224293864769550 ) ) ;
#137688 = CARTESIAN_POINT ( 'NONE',  ( -10.72451020669870658, -18.67979575497194134, 109.5844237280190328 ) ) ;
#137689 = CARTESIAN_POINT ( 'NONE',  ( 14.29746914071049879, -8.314922557960816363, 78.33224293864770971 ) ) ;
#137690 = CARTESIAN_POINT ( 'NONE',  ( -16.51473224551069308, -9.474510206698971260, 36.66557627198102409 ) ) ;
#137691 = CARTESIAN_POINT ( 'NONE',  ( 19.05341960407617918, -5.049401038297876454, 91.04275706135234714 ) ) ;
#137692 = CARTESIAN_POINT ( 'NONE',  ( 14.34966873604960469, 8.224510206698951720, 49.16557627198102409 ) ) ;
#137693 = CARTESIAN_POINT ( 'NONE',  ( -15.72974639402176322, -15.80617190586768395, 89.37609039468568994 ) ) ;
#137694 = CARTESIAN_POINT ( 'NONE',  ( -13.89961937509977652, 13.97604488694528158, 85.62390960531433848 ) ) ;
#137695 = CARTESIAN_POINT ( 'NONE',  ( 16.51473224551083163, -9.474510206698727899, 65.83442372801900433 ) ) ;
#137696 = CARTESIAN_POINT ( 'NONE',  ( -5.719274019375978568, 21.55341960407610458, 60.20724293864768839 ) ) ;
#137697 = CARTESIAN_POINT ( 'NONE',  ( -15.80617190586768217, 15.72974639402176855, 28.12609039468568284 ) ) ;
#137698 = CARTESIAN_POINT ( 'NONE',  ( 12.06949235617739724, 12.14591786802326823, 26.87609039468567218 ) ) ;
#137699 = CARTESIAN_POINT ( 'NONE',  ( 16.53943276465976808, 0.05219959533934440121, 81.25109039468568994 ) ) ;
#137701 = CARTESIAN_POINT ( 'NONE',  ( -21.52544592524334988, -5.823673210054445271, 18.95942372801901143 ) ) ;
#137700 = CARTESIAN_POINT ( 'NONE',  ( 16.51473224551069308, 9.474510206698969483, 29.16557627198103475 ) ) ;
#137702 = CARTESIAN_POINT ( 'NONE',  ( -16.55341960407611168, -4.379528057220339221, 111.4572429386476813 ) ) ;
#137703 = CARTESIAN_POINT ( 'NONE',  ( 3.556970738554033499E-15, -38.81732327939057825, -8.624999997268814056 ) ) ;
#137704 = CARTESIAN_POINT ( 'NONE',  ( -14.29746914071037622, -8.314922557961029526, 54.16775706135235424 ) ) ;
#137705 = B_SPLINE_CURVE_WITH_KNOTS ( 'NONE', 3,
 ( #162881, #51705, #129525, #160886, #145706, #36525, #55703, #143708, #68872, #147727, #146704, #98179, #117376, #130531, #9214, #115387, #113368, #70881, #179073, #100202, #192229, #177075, #23378, #83030, #38546, #144704, #85024, #159883, #132549, #194237, #131545, #5188 ),
 .UNSPECIFIED., .F., .F.,
 ( 4, 2, 2, 2, 2, 2, 2, 2, 2, 2, 2, 2, 2, 2, 2, 4 ),
 ( 4.336808689942017736E-18, 0.0003712461730036830374, 0.0007424923460073617381, 0.001113738519011040493, 0.001484984692014719139, 0.002227477038022076649, 0.002598723211025741418, 0.002969969384029406186, 0.003341215557033070955, 0.003712461730036735724, 0.004083707903040400058, 0.004454954076044064827, 0.004826200249047730463, 0.005197446422051395232, 0.005568692595055060000, 0.005939938768058724769 ),
 .UNSPECIFIED. ) ;
#137706 = CARTESIAN_POINT ( 'NONE',  ( 12.14591786802309770, 12.06949235617756955, 79.37390960531436690 ) ) ;
#137707 = CARTESIAN_POINT ( 'NONE',  ( 15.72974639402199770, -15.80617190586745480, 78.12390960531436690 ) ) ;
#137708 = CARTESIAN_POINT ( 'NONE',  ( 16.53943276465976808, -0.05219959533910856209, 23.74890960531435269 ) ) ;
#137709 = CARTESIAN_POINT ( 'NONE',  ( 0.05219959533934541429, -16.53943276465976808, 35.00109039468568284 ) ) ;
#137710 = CARTESIAN_POINT ( 'NONE',  ( -13.89961937509977652, 13.97604488694528158, 40.62390960531435979 ) ) ;
#137711 = CARTESIAN_POINT ( 'NONE',  ( -16.55341960407617563, 4.379528057220093196, 78.54275706135236135 ) ) ;
#137712 = CARTESIAN_POINT ( 'NONE',  ( 16.46253265017146816, 9.564922557961045513, 71.66775706135233293 ) ) ;
#137713 = CARTESIAN_POINT ( 'NONE',  ( -18.62759615963270932, 10.81492255796079327, 65.83224293864769550 ) ) ;
#137714 = CARTESIAN_POINT ( 'NONE',  ( -12.14591786802309592, -12.06949235617757132, 21.87390960531436690 ) ) ;
#137715 = ORIENTED_EDGE ( 'NONE', *, *, #70168, .F. ) ;
#137716 = CARTESIAN_POINT ( 'NONE',  ( 26.68407921138447847, 3.932373394472265193, 171.8653659962753295 ) ) ;
#137717 = CARTESIAN_POINT ( 'NONE',  ( 21.52544592524344225, -5.823673210054117533, 43.54057627198103830 ) ) ;
#137718 = ORIENTED_EDGE ( 'NONE', *, *, #187478, .T. ) ;
#137719 = ORIENTED_EDGE ( 'NONE', *, *, #55537, .F. ) ;
#137720 = CARTESIAN_POINT ( 'NONE',  ( -14.29746914071037622, -8.314922557961029526, 89.16775706135236135 ) ) ;
#137721 = VERTEX_POINT ( 'NONE', #180781 ) ;
#137722 = CARTESIAN_POINT ( 'NONE',  ( 16.46253265017160672, -9.564922557960803928, 113.3322429386476955 ) ) ;
#137723 = CARTESIAN_POINT ( 'NONE',  ( -38.00000000000000711, 2.428612866367529932E-14, -1.749999994537626558 ) ) ;
#137724 = CARTESIAN_POINT ( 'NONE',  ( 21.53943276465977519, -0.05219959533907433946, 78.74890960531436690 ) ) ;
#137725 = CARTESIAN_POINT ( 'NONE',  ( -16.53943276465976808, -0.05219959533934237506, 108.7510903946857042 ) ) ;
#137726 = CARTESIAN_POINT ( 'NONE',  ( 18.67979575497194134, -10.72451020669871369, 65.83442372801900433 ) ) ;
#137727 = CARTESIAN_POINT ( 'NONE',  ( -4.379528057220086978, -16.55341960407618274, 24.79275706135235779 ) ) ;
#137728 = CARTESIAN_POINT ( 'NONE',  ( -12.06949235617756955, 12.14591786802309770, 110.6239096053143669 ) ) ;
#137729 = CARTESIAN_POINT ( 'NONE',  ( -12.14591786802326823, 12.06949235617739902, 23.12609039468567573 ) ) ;
#137730 = CARTESIAN_POINT ( 'NONE',  ( 16.51473224551069308, 9.474510206698969483, 59.16557627198102409 ) ) ;
#137731 = CARTESIAN_POINT ( 'NONE',  ( -17.81289503416611808, 24.51734667627700404, 141.6999999999999602 ) ) ;
#137732 = CARTESIAN_POINT ( 'NONE',  ( 16.46253265017160672, -9.564922557960803928, 108.3322429386476955 ) ) ;
#137733 = CARTESIAN_POINT ( 'NONE',  ( -14.29746914071037622, -8.314922557961029526, 94.16775706135237556 ) ) ;
#137734 = CARTESIAN_POINT ( 'NONE',  ( 0.05219959533936267826, -19.03943276465977164, 90.00109039468567573 ) ) ;
#137735 = CARTESIAN_POINT ( 'NONE',  ( -21.55341960407619339, 5.719274019375674811, 113.5427570613523756 ) ) ;
#137736 = CARTESIAN_POINT ( 'NONE',  ( 18.67979575497178502, 10.72451020669898547, 69.16557627198102409 ) ) ;
#137737 = CARTESIAN_POINT ( 'NONE',  ( 8.314922557961029526, -14.29746914071037800, 105.4177570613523613 ) ) ;
#137738 = CARTESIAN_POINT ( 'NONE',  ( -9.474510206698720793, -16.51473224551083518, 94.58442372801900433 ) ) ;
#137739 = CARTESIAN_POINT ( 'NONE',  ( -0.05219959533909027116, -19.03943276465977164, 52.49890960531436690 ) ) ;
#137740 = CARTESIAN_POINT ( 'NONE',  ( -0.05219959533909027116, -19.03943276465977164, 97.49890960531436690 ) ) ;
#137741 = CARTESIAN_POINT ( 'NONE',  ( 18.62759615963255655, 10.81492255796105972, 46.66775706135234714 ) ) ;
#137742 = CARTESIAN_POINT ( 'NONE',  ( 0.05219959533909260263, 19.03943276465977164, 44.99890960531435979 ) ) ;
#137743 = DIRECTION ( 'NONE',  ( -1.000000000000000000, 0.000000000000000000, 5.204170427930421283E-16 ) ) ;
#137744 = CARTESIAN_POINT ( 'NONE',  ( 16.52544592524342804, -4.483927247898539470, 58.54057627198103120 ) ) ;
#137745 = CARTESIAN_POINT ( 'NONE',  ( 10.72451020669898902, -18.67979575497178502, 72.91557627198103830 ) ) ;
#137746 = CARTESIAN_POINT ( 'NONE',  ( -4.500000000000001776, -120.9970989573719038, 14.58956564881029827 ) ) ;
#137747 = CARTESIAN_POINT ( 'NONE',  ( 5.049401038297881783, 19.05341960407617563, 37.29275706135232582 ) ) ;
#137748 = DIRECTION ( 'NONE',  ( -0.7071067811865492381, 0.000000000000000000, 0.7071067811865457964 ) ) ;
#137750 = CARTESIAN_POINT ( 'NONE',  ( 16.46253265017160672, -9.564922557960803928, 88.33224293864769550 ) ) ;
#137749 = CARTESIAN_POINT ( 'NONE',  ( 19.02544592524343514, -5.153800228976328945, 73.54057627198103830 ) ) ;
#137751 = CARTESIAN_POINT ( 'NONE',  ( 16.55341960407618274, -4.379528057220086978, 56.04275706135235424 ) ) ;
#137752 = CARTESIAN_POINT ( 'NONE',  ( -23.31738231874055600, 16.94106989632528837, 143.7999999999999829 ) ) ;
#137753 = CARTESIAN_POINT ( 'NONE',  ( 19.02544592524334988, 5.153800228976608722, 31.45942372801900433 ) ) ;
#137754 = DIRECTION ( 'NONE',  ( -0.000000000000000000, -0.000000000000000000, -1.000000000000000000 ) ) ;
#137755 = CARTESIAN_POINT ( 'NONE',  ( 16.53943276465976808, 0.05219959533934440121, 91.25109039468568994 ) ) ;
#137756 = CARTESIAN_POINT ( 'NONE',  ( -19.99999999999998224, -190.0000000000000000, -15.00000000000000000 ) ) ;
#137757 = CARTESIAN_POINT ( 'NONE',  ( 16.53943276465976808, 0.05219959533934440121, 86.25109039468568994 ) ) ;
#137758 = CARTESIAN_POINT ( 'NONE',  ( -12.06949235617739369, -12.14591786802326823, 54.37609039468568994 ) ) ;
#137760 = DIRECTION ( 'NONE',  ( 0.000000000000000000, -1.000000000000000000, 0.000000000000000000 ) ) ;
#137759 = CARTESIAN_POINT ( 'NONE',  ( -19.05341960407611168, -5.049401038298163336, 61.45724293864769550 ) ) ;
#137761 = CARTESIAN_POINT ( 'NONE',  ( -5.823673210054431948, 21.52544592524334988, 62.70942372801902565 ) ) ;
#137762 = CARTESIAN_POINT ( 'NONE',  ( 16.51473224551083163, -9.474510206698727899, 75.83442372801900433 ) ) ;
#137763 = CARTESIAN_POINT ( 'NONE',  ( -16.46253265017146816, -9.564922557961047289, 19.16775706135233293 ) ) ;
#137764 = CARTESIAN_POINT ( 'NONE',  ( 0.05219959533909260263, 19.03943276465977164, 49.99890960531435979 ) ) ;
#137765 = CARTESIAN_POINT ( 'NONE',  ( -5.153800228976328057, -19.02544592524343514, 37.29057627198102409 ) ) ;
#137766 = CARTESIAN_POINT ( 'NONE',  ( 19.24578484527059175, -180.9428398739492820, -25.00000000000000000 ) ) ;
#137767 = CARTESIAN_POINT ( 'NONE',  ( 18.62759615963271287, -10.81492255796078972, 68.33224293864769550 ) ) ;
#137768 = CARTESIAN_POINT ( 'NONE',  ( -9.474510206698964154, 16.51473224551069663, 110.4155762719810383 ) ) ;
#137769 = CARTESIAN_POINT ( 'NONE',  ( -14.29746914071049879, 8.314922557960819915, 110.8322429386476955 ) ) ;
#137770 = CARTESIAN_POINT ( 'NONE',  ( -4.379528057220086978, -16.55341960407618274, 44.79275706135234714 ) ) ;
#137771 = CARTESIAN_POINT ( 'NONE',  ( -12.06949235617756955, 12.14591786802309770, 30.62390960531436335 ) ) ;
#137772 = ORIENTED_EDGE ( 'NONE', *, *, #57273, .F. ) ;
#137773 = CARTESIAN_POINT ( 'NONE',  ( 15.80617190586746368, 15.72974639402197994, 109.3739096053143811 ) ) ;
#137775 = CARTESIAN_POINT ( 'NONE',  ( 3.766062262543149401E-15, -39.95556452105413570, -3.499999999999999556 ) ) ;
#137774 = CARTESIAN_POINT ( 'NONE',  ( 16.55341960407611168, 4.379528057220329451, 58.95724293864770971 ) ) ;
#137776 = CARTESIAN_POINT ( 'NONE',  ( -19.02544592524334988, -5.153800228976617603, 103.9594237280190043 ) ) ;
#137777 = CARTESIAN_POINT ( 'NONE',  ( -5.049401038297874678, -19.05341960407617918, 39.79275706135232582 ) ) ;
#137778 = CARTESIAN_POINT ( 'NONE',  ( -12.06949235617756955, 12.14591786802309770, 50.62390960531435979 ) ) ;
#137780 = EDGE_CURVE ( 'NONE', #38003, #59237, #163075, .T. ) ;
#137779 = CARTESIAN_POINT ( 'NONE',  ( -5.719274019375978568, 21.55341960407610458, 105.2072429386477097 ) ) ;
#137782 = CARTESIAN_POINT ( 'NONE',  ( 18.67979575497178502, 10.72451020669898547, 59.16557627198103120 ) ) ;
#137781 = CARTESIAN_POINT ( 'NONE',  ( 17.40861289039003879, 6.110651285853275994, 33.87232470827431996 ) ) ;
#137783 = CARTESIAN_POINT ( 'NONE',  ( 9.474510206698971260, -16.51473224551069308, 72.91557627198102409 ) ) ;
#137784 = CARTESIAN_POINT ( 'NONE',  ( 14.29746914071049879, -8.314922557960816363, 48.33224293864770260 ) ) ;
#137785 = CARTESIAN_POINT ( 'NONE',  ( -5.153800228976328057, -19.02544592524343514, 107.2905762719810383 ) ) ;
#137786 = B_SPLINE_CURVE_WITH_KNOTS ( 'NONE', 3,
 ( #146826, #10331, #133662, #60534, #116495, #183901, #148841, #100317, #195352, #54821, #71987, #178184, #115501, #90868 ),
 .UNSPECIFIED., .F., .F.,
 ( 4, 2, 2, 2, 2, 2, 4 ),
 ( 0.002367542108447648688, 0.002663271933649134175, 0.002959001758850619661, 0.003254731584052104713, 0.003550461409253590200, 0.004141921059656562473, 0.004733380710059535181 ),
 .UNSPECIFIED. ) ;
#137787 = FACE_OUTER_BOUND ( 'NONE', #168713, .T. ) ;
#137788 = CARTESIAN_POINT ( 'NONE',  ( 5.153800228976615827, -19.02544592524334988, 55.20942372801899722 ) ) ;
#137789 = CARTESIAN_POINT ( 'NONE',  ( 5.719274019375991003, -21.55341960407610458, 92.70724293864770971 ) ) ;
#137790 = CARTESIAN_POINT ( 'NONE',  ( 9.564922557960805705, 16.46253265017160317, 39.58224293864768839 ) ) ;
#137791 = CARTESIAN_POINT ( 'NONE',  ( -16.52544592524342804, 4.483927247898546575, 116.0405762719810383 ) ) ;
#137792 = CARTESIAN_POINT ( 'NONE',  ( 10.81492255796106328, -18.62759615963255655, 50.41775706135235424 ) ) ;
#137793 = CARTESIAN_POINT ( 'NONE',  ( -22.44159573604009950, -16.30477369853688430, 145.0750000027311728 ) ) ;
#137794 = ADVANCED_FACE ( 'NONE', ( #115087 ), #131249, .T. ) ;
#137795 = CARTESIAN_POINT ( 'NONE',  ( 14.29746914071049879, -8.314922557960816363, 33.33224293864769550 ) ) ;
#137796 = CARTESIAN_POINT ( 'NONE',  ( 9.474510206698971260, -16.51473224551069308, 47.91557627198102409 ) ) ;
#137797 = CARTESIAN_POINT ( 'NONE',  ( 5.153800228976335163, 19.02544592524342804, 104.7905762719809957 ) ) ;
#137798 = CARTESIAN_POINT ( 'NONE',  ( -15.72974639402197994, 15.80617190586746368, 65.62390960531436690 ) ) ;
#137799 = CARTESIAN_POINT ( 'NONE',  ( 17.14385361876520264, -23.59649016807271238, 141.5750000027312012 ) ) ;
#137800 = CARTESIAN_POINT ( 'NONE',  ( -19.03943276465977164, 0.05219959533909376836, 46.24890960531435979 ) ) ;
#137801 = CARTESIAN_POINT ( 'NONE',  ( -10.72451020669898014, 18.67979575497178502, 50.41557627198103120 ) ) ;
#137802 = CARTESIAN_POINT ( 'NONE',  ( 18.62759615963255655, 10.81492255796105972, 81.66775706135236135 ) ) ;
#137805 = CARTESIAN_POINT ( 'NONE',  ( -14.29746914071049879, 8.314922557960819915, 70.83224293864770971 ) ) ;
#137804 = CARTESIAN_POINT ( 'NONE',  ( -14.29746914071037622, -8.314922557961029526, 84.16775706135234714 ) ) ;
#137803 = CARTESIAN_POINT ( 'NONE',  ( 12.88217944815845684, -35.43691452638582717, -29.79217952741381836 ) ) ;
#137806 = CARTESIAN_POINT ( 'NONE',  ( 12.14591786802327356, -12.06949235617739191, 85.62609039468568994 ) ) ;
#137807 = CARTESIAN_POINT ( 'NONE',  ( 0.05219959533909260263, 19.03943276465977164, 74.99890960531435269 ) ) ;
#137808 = VERTEX_POINT ( 'NONE', #73595 ) ;
#137809 = CARTESIAN_POINT ( 'NONE',  ( 13.97604488694548053, -13.89961937509957401, 25.62609039468566507 ) ) ;
#137810 = CARTESIAN_POINT ( 'NONE',  ( -0.05219959533934338120, 16.53943276465976808, 92.50109039468567573 ) ) ;
#137811 = CARTESIAN_POINT ( 'NONE',  ( -21.53943276465977519, -0.05219959533937600094, 113.7510903946856757 ) ) ;
#137812 = CARTESIAN_POINT ( 'NONE',  ( 16.46253265017160672, -9.564922557960803928, 78.33224293864769550 ) ) ;
#137813 = CARTESIAN_POINT ( 'NONE',  ( 21.52544592524344225, -5.823673210054117533, 53.54057627198103120 ) ) ;
#137814 = CARTESIAN_POINT ( 'NONE',  ( 16.53943276465976808, 0.05219959533934440121, 26.25109039468567573 ) ) ;
#137815 = CARTESIAN_POINT ( 'NONE',  ( 5.719274019375673035, 21.55341960407619339, 77.29275706135234714 ) ) ;
#137816 = CARTESIAN_POINT ( 'NONE',  ( 4.379528057220092307, 16.55341960407617563, 67.29275706135234714 ) ) ;
#137817 = CARTESIAN_POINT ( 'NONE',  ( -15.72974639402176322, -15.80617190586768395, 19.37609039468568639 ) ) ;
#137818 = CARTESIAN_POINT ( 'NONE',  ( 16.46253265017146816, 9.564922557961045513, 111.6677570613523329 ) ) ;
#137819 = CARTESIAN_POINT ( 'NONE',  ( -19.05341960407611168, -5.049401038298163336, 96.45724293864769550 ) ) ;
#137820 = CARTESIAN_POINT ( 'NONE',  ( 14.29746914071037800, 8.314922557961029526, 26.66775706135235424 ) ) ;
#137821 = CARTESIAN_POINT ( 'NONE',  ( -0.05219959533909027116, -19.03943276465977164, 37.49890960531436690 ) ) ;
#137822 = AXIS2_PLACEMENT_3D ( 'NONE', #43605, #13270, #192553 ) ;
#137823 = CARTESIAN_POINT ( 'NONE',  ( 16.52544592524335698, 4.483927247898782831, 21.45942372801901499 ) ) ;
#137824 = CARTESIAN_POINT ( 'NONE',  ( -14.29746914071049879, 8.314922557960819915, 85.83224293864768129 ) ) ;
#137825 = CARTESIAN_POINT ( 'NONE',  ( 16.53943276465976808, 0.05219959533934440121, 91.25109039468568994 ) ) ;
#137827 = CARTESIAN_POINT ( 'NONE',  ( 16.46253265017160672, -9.564922557960803928, 68.33224293864770971 ) ) ;
#137826 = CARTESIAN_POINT ( 'NONE',  ( 5.719274019375673035, 21.55341960407619339, 27.29275706135234358 ) ) ;
#137828 = CARTESIAN_POINT ( 'NONE',  ( -13.97604488694527625, -13.89961937509977652, 71.87390960531433848 ) ) ;
#137829 = CARTESIAN_POINT ( 'NONE',  ( -4.379528057220086978, -16.55341960407618274, 84.79275706135234714 ) ) ;
#137830 = EDGE_CURVE ( 'NONE', #123524, #146762, #8918, .T. ) ;
#137832 = ORIENTED_EDGE ( 'NONE', *, *, #113277, .F. ) ;
#137831 = CARTESIAN_POINT ( 'NONE',  ( -21.93180397000192272, -7.641141194970263228, 169.8616410530808878 ) ) ;
#137833 = VERTEX_POINT ( 'NONE', #87738 ) ;
#137834 = CARTESIAN_POINT ( 'NONE',  ( 9.564922557961047289, -16.46253265017146816, 30.41775706135232937 ) ) ;
#137835 = AXIS2_PLACEMENT_3D ( 'NONE', #92701, #1694, #18872 ) ;
#137836 = CARTESIAN_POINT ( 'NONE',  ( 13.89961937509977652, -13.97604488694527269, 48.12390960531435979 ) ) ;
#137838 = ORIENTED_EDGE ( 'NONE', *, *, #143824, .F. ) ;
#137837 = CARTESIAN_POINT ( 'NONE',  ( -5.049401038298153566, 19.05341960407611168, 110.2072429386476671 ) ) ;
#137839 = CARTESIAN_POINT ( 'NONE',  ( -8.224510206698735004, -14.34966873604973081, 24.58442372801901499 ) ) ;
#137841 = CARTESIAN_POINT ( 'NONE',  ( -8.224510206698735004, -14.34966873604973081, 44.58442372801901854 ) ) ;
#137840 = CARTESIAN_POINT ( 'NONE',  ( 13.89961937509957401, 13.97604488694547697, 56.87609039468564731 ) ) ;
#137842 = CARTESIAN_POINT ( 'NONE',  ( 5.153800228976335163, 19.02544592524342804, 99.79057627198102409 ) ) ;
#137843 = CARTESIAN_POINT ( 'NONE',  ( 19.03943276465977164, -0.05219959533909143690, 78.74890960531436690 ) ) ;
#137844 = CARTESIAN_POINT ( 'NONE',  ( 18.67979575497178502, 10.72451020669898547, 104.1655762719810241 ) ) ;
#137845 = CARTESIAN_POINT ( 'NONE',  ( 9.474510206698729675, 16.51473224551082808, 67.08442372801900433 ) ) ;
#137847 = CARTESIAN_POINT ( 'NONE',  ( -9.564922557960796823, -16.46253265017161027, 22.08224293864768839 ) ) ;
#137846 = CARTESIAN_POINT ( 'NONE',  ( 9.474510206698971260, -16.51473224551069308, 92.91557627198103830 ) ) ;
#137848 = CARTESIAN_POINT ( 'NONE',  ( 0.05219959533909260263, 19.03943276465977164, 64.99890960531436690 ) ) ;
#137850 = CARTESIAN_POINT ( 'NONE',  ( -0.05219959533909027116, -19.03943276465977164, 22.49890960531436690 ) ) ;
#137849 = CARTESIAN_POINT ( 'NONE',  ( 4.379528057220339221, -16.55341960407611168, 22.70724293864769194 ) ) ;
#137851 = CARTESIAN_POINT ( 'NONE',  ( -13.97604488694547697, 13.89961937509957934, 43.12609039468566152 ) ) ;
#137852 = CARTESIAN_POINT ( 'NONE',  ( 12.14591786802309770, 12.06949235617756955, 74.37390960531436690 ) ) ;
#137853 = CARTESIAN_POINT ( 'NONE',  ( -10.81492255796105439, 18.62759615963255655, 92.91775706135236135 ) ) ;
#137854 = CARTESIAN_POINT ( 'NONE',  ( -13.89961937509977652, 13.97604488694528158, 40.62390960531435979 ) ) ;
#137855 = CARTESIAN_POINT ( 'NONE',  ( 16.55341960407618274, -4.379528057220086978, 56.04275706135235424 ) ) ;
#137857 = CARTESIAN_POINT ( 'NONE',  ( -0.05219959533937732626, 21.53943276465977519, 87.50109039468568994 ) ) ;
#137856 = CARTESIAN_POINT ( 'NONE',  ( 8.314922557960818139, 14.29746914071049879, 44.58224293864769550 ) ) ;
#137858 = CARTESIAN_POINT ( 'NONE',  ( -5.153800228976328057, -19.02544592524343514, 97.29057627198099567 ) ) ;
#137859 = CARTESIAN_POINT ( 'NONE',  ( 16.46253265017160672, -9.564922557960803928, 93.33224293864769550 ) ) ;
#137860 = CARTESIAN_POINT ( 'NONE',  ( -4.483927247898539470, -16.52544592524342804, 107.2905762719810525 ) ) ;
#137861 = CARTESIAN_POINT ( 'NONE',  ( 12.06949235617757843, -12.14591786802309237, 68.12390960531436690 ) ) ;
#137862 = CARTESIAN_POINT ( 'NONE',  ( 5.823673210054125526, 21.52544592524343514, 89.79057627198103830 ) ) ;
#137863 = CARTESIAN_POINT ( 'NONE',  ( -16.51473224551069308, -9.474510206698971260, 91.66557627198103830 ) ) ;
#137864 = CARTESIAN_POINT ( 'NONE',  ( -15.80617190586745835, -15.72974639402198527, 96.87390960531436690 ) ) ;
#137865 = CARTESIAN_POINT ( 'NONE',  ( -16.51473224551082808, 9.474510206698731452, 73.33442372801900433 ) ) ;
#137867 = CARTESIAN_POINT ( 'NONE',  ( 0.05219959533910956823, 16.53943276465976808, 84.99890960531436690 ) ) ;
#137866 = DIRECTION ( 'NONE',  ( -0.000000000000000000, 0.7071067811865483499, 0.7071067811865467956 ) ) ;
#137869 = CARTESIAN_POINT ( 'NONE',  ( 16.46253265017160672, -9.564922557960803928, 53.33224293864768839 ) ) ;
#137868 = AXIS2_PLACEMENT_3D ( 'NONE', #128367, #190063, #175892 ) ;
#137870 = CARTESIAN_POINT ( 'NONE',  ( 0.05219959533907565091, 21.53943276465977519, 69.99890960531435269 ) ) ;
#137871 = CARTESIAN_POINT ( 'NONE',  ( 17.31728774477274158, -6.344390552232384906, 28.31906651689320142 ) ) ;
#137872 = CARTESIAN_POINT ( 'NONE',  ( 4.483927247898545687, 16.52544592524342804, 24.79057627198103120 ) ) ;
#137873 = CARTESIAN_POINT ( 'NONE',  ( 8.314922557961029526, -14.29746914071037800, 20.41775706135234714 ) ) ;
#137874 = CARTESIAN_POINT ( 'NONE',  ( -4.483927247898539470, -16.52544592524342804, 87.29057627198103830 ) ) ;
#137875 = CARTESIAN_POINT ( 'NONE',  ( -17.31747979337947285, -6.344076630961057006, 96.37944868065184778 ) ) ;
#137876 = CARTESIAN_POINT ( 'NONE',  ( 5.153800228976335163, 19.02544592524342804, 69.79057627198103830 ) ) ;
#137877 = CARTESIAN_POINT ( 'NONE',  ( -19.02544592524342804, 5.153800228976336051, 36.04057627198100988 ) ) ;
#137878 = CARTESIAN_POINT ( 'NONE',  ( -12.06949235617756955, 12.14591786802309770, 65.62390960531436690 ) ) ;
#137879 = CARTESIAN_POINT ( 'NONE',  ( -18.62759615963270932, 10.81492255796079327, 25.83224293864769194 ) ) ;
#137880 = CARTESIAN_POINT ( 'NONE',  ( 5.153800228976615827, -19.02544592524334988, 90.20942372801900433 ) ) ;
#137881 = CARTESIAN_POINT ( 'NONE',  ( 5.049401038298161559, -19.05341960407611168, 102.7072429386476955 ) ) ;
#137882 = CARTESIAN_POINT ( 'NONE',  ( -15.80617190586745835, -15.72974639402198527, 71.87390960531438111 ) ) ;
#137883 = CARTESIAN_POINT ( 'NONE',  ( -14.34966873604972548, 8.224510206698743886, 68.33442372801900433 ) ) ;
#137884 = CARTESIAN_POINT ( 'NONE',  ( 13.89961937509957579, 13.97604488694547520, 106.8760903946856615 ) ) ;
#137885 = CARTESIAN_POINT ( 'NONE',  ( -9.474510206698964154, 16.51473224551069663, 65.41557627198102409 ) ) ;
#137886 = CARTESIAN_POINT ( 'NONE',  ( -15.80617190586745835, -15.72974639402198527, 71.87390960531438111 ) ) ;
#137887 = CARTESIAN_POINT ( 'NONE',  ( -5.153800228976607833, 19.02544592524334988, 107.7094237280189759 ) ) ;
#137889 = CARTESIAN_POINT ( 'NONE',  ( -21.55341960407619339, 5.719274019375674811, 58.54275706135235424 ) ) ;
#137888 = CARTESIAN_POINT ( 'NONE',  ( 8.314922557960818139, 14.29746914071049879, 39.58224293864769550 ) ) ;
#137890 = CARTESIAN_POINT ( 'NONE',  ( 17.81289503416611453, -24.51734667627695785, 144.9500000054623854 ) ) ;
#137892 = CARTESIAN_POINT ( 'NONE',  ( -13.89961937509977652, 13.97604488694528158, 100.6239096053143669 ) ) ;
#137891 = CARTESIAN_POINT ( 'NONE',  ( -14.34966873604972548, 8.224510206698743886, 78.33442372801901854 ) ) ;
#137893 = CARTESIAN_POINT ( 'NONE',  ( -13.89961937509977830, 13.97604488694528158, 105.6239096053143527 ) ) ;
#137894 = CARTESIAN_POINT ( 'NONE',  ( -16.61371651742601685, 7.165104196376145040, 78.85415069992998838 ) ) ;
#137895 = CARTESIAN_POINT ( 'NONE',  ( -12.14591786802326823, 12.06949235617739902, 98.12609039468570415 ) ) ;
#137896 = CARTESIAN_POINT ( 'NONE',  ( 12.14591786802327356, -12.06949235617739191, 40.62609039468567573 ) ) ;
#137897 = CARTESIAN_POINT ( 'NONE',  ( 0.05219959533909260263, 19.03943276465977164, 59.99890960531436690 ) ) ;
#137898 = CARTESIAN_POINT ( 'NONE',  ( -5.153800228976328057, -19.02544592524343514, 72.29057627198102409 ) ) ;
#137899 = CARTESIAN_POINT ( 'NONE',  ( 21.53943276465977519, 0.05219959533937863772, 66.25109039468567573 ) ) ;
#137900 = CARTESIAN_POINT ( 'NONE',  ( -4.379528057220086978, -16.55341960407618274, 59.79275706135234714 ) ) ;
#137901 = CARTESIAN_POINT ( 'NONE',  ( 12.06949235617757843, -12.14591786802309237, 33.12390960531435979 ) ) ;
#137902 = CARTESIAN_POINT ( 'NONE',  ( 19.03943276465977164, -0.05219959533909143690, 38.74890960531436690 ) ) ;
#137903 = CARTESIAN_POINT ( 'NONE',  ( -16.46253265017160317, 9.564922557960807481, 35.83224293864768839 ) ) ;
#137904 = CARTESIAN_POINT ( 'NONE',  ( 12.06949235617739724, 12.14591786802326823, 31.87609039468567929 ) ) ;
#137906 = CARTESIAN_POINT ( 'NONE',  ( -16.46253265017146816, -9.564922557961047289, 99.16775706135233293 ) ) ;
#137905 =( BOUNDED_CURVE ( )  B_SPLINE_CURVE ( 2, ( #79899, #51550, #174903, #141570, #64735, #98021, #159716, #21213, #126397, #188093, #191066 ),
 .UNSPECIFIED., .F., .T. ) 
 B_SPLINE_CURVE_WITH_KNOTS ( ( 3, 2, 2, 2, 2, 3 ),
 ( 0.7000000000000001776, 0.7200000000000001954, 0.7400000000000001021, 0.7600000000000001199, 0.7800000000000000266, 0.8000000000000000444 ),
 .UNSPECIFIED. ) 
 CURVE ( )  GEOMETRIC_REPRESENTATION_ITEM ( )  RATIONAL_B_SPLINE_CURVE ( ( 0.9999999999999994449, 0.9510565162951540863, 1.000000000000000000, 0.9510565162951535312, 1.000000000000000000, 0.9510565162951535312, 1.000000000000000000, 0.9510565162951535312, 1.000000000000000000, 0.9510565162951535312, 1.000000000000000000 ) ) 
 REPRESENTATION_ITEM ( '' )  );
#137907 = CARTESIAN_POINT ( 'NONE',  ( -16.53943276465976808, 0.05219959533911058130, 96.24890960531435269 ) ) ;
#137908 = CARTESIAN_POINT ( 'NONE',  ( 13.97604488694527802, 13.89961937509977652, 54.37390960531435979 ) ) ;
#137910 = CARTESIAN_POINT ( 'NONE',  ( -38.00000000000000711, 2.428612866367529932E-14, -10.00000000000000000 ) ) ;
#137909 = CARTESIAN_POINT ( 'NONE',  ( -19.03943276465977164, -0.05219959533935918106, 83.75109039468567573 ) ) ;
#137911 = CARTESIAN_POINT ( 'NONE',  ( 18.67979575497194134, -10.72451020669871369, 90.83442372801901854 ) ) ;
#137912 = CARTESIAN_POINT ( 'NONE',  ( 0.05219959533934541429, -16.53943276465976808, 60.00109039468568284 ) ) ;
#137913 = SPHERICAL_SURFACE ( 'NONE', #8263, 0.5000000000000000000 ) ;
#137914 = CARTESIAN_POINT ( 'NONE',  ( -5.719274019375978568, 21.55341960407610458, 45.20724293864769550 ) ) ;
#137915 = CARTESIAN_POINT ( 'NONE',  ( -4.379528057220086978, -16.55341960407618274, 34.79275706135235424 ) ) ;
#137916 = CARTESIAN_POINT ( 'NONE',  ( -19.02544592524334988, -5.153800228976617603, 38.95942372801900433 ) ) ;
#137917 = CARTESIAN_POINT ( 'NONE',  ( -13.89961937509977652, 13.97604488694528158, 95.62390960531436690 ) ) ;
#137918 = CARTESIAN_POINT ( 'NONE',  ( -13.89961937509977652, 13.97604488694528158, 50.62390960531435979 ) ) ;
#137919 = CARTESIAN_POINT ( 'NONE',  ( -21.74947994262150175, -22.98248435370785714, -49.47049204653305310 ) ) ;
#137920 = CARTESIAN_POINT ( 'NONE',  ( -21.55341960407619339, 5.719274019375674811, 78.54275706135236135 ) ) ;
#137921 = CARTESIAN_POINT ( 'NONE',  ( 0.000000000000000000, -1.443375672974063884, -3.691112476943992763E-18 ) ) ;
#137922 = CARTESIAN_POINT ( 'NONE',  ( 5.049401038297881783, 19.05341960407617563, 27.29275706135232937 ) ) ;
#137923 = CARTESIAN_POINT ( 'NONE',  ( -15.80617190586768217, 15.72974639402176855, 108.1260903946856757 ) ) ;
#137924 = CARTESIAN_POINT ( 'NONE',  ( -4.483927247898539470, -16.52544592524342804, 47.29057627198103120 ) ) ;
#137925 = CARTESIAN_POINT ( 'NONE',  ( -19.02544592524342804, 5.153800228976336051, 61.04057627198103120 ) ) ;
#137926 = CARTESIAN_POINT ( 'NONE',  ( -5.049401038298153566, 19.05341960407611168, 110.2072429386476671 ) ) ;
#137927 = CARTESIAN_POINT ( 'NONE',  ( -18.67979575497193778, 10.72451020669871902, 78.33442372801901854 ) ) ;
#137928 = CARTESIAN_POINT ( 'NONE',  ( 5.153800228976335163, 19.02544592524342804, 69.79057627198103830 ) ) ;
#137929 = CARTESIAN_POINT ( 'NONE',  ( -18.67979575497193778, 10.72451020669871902, 73.33442372801901854 ) ) ;
#137930 = CARTESIAN_POINT ( 'NONE',  ( 21.52544592524344225, -5.823673210054117533, 43.54057627198103830 ) ) ;
#137931 = CARTESIAN_POINT ( 'NONE',  ( -18.62759615963255300, -10.81492255796106328, 24.16775706135235424 ) ) ;
#137932 = CARTESIAN_POINT ( 'NONE',  ( -9.564922557961040184, 16.46253265017147172, 62.91775706135233293 ) ) ;
#137933 = CARTESIAN_POINT ( 'NONE',  ( 16.46253265017160672, -9.564922557960803928, 33.33224293864770260 ) ) ;
#137934 = CARTESIAN_POINT ( 'NONE',  ( -0.05219959533909027116, -19.03943276465977164, 72.49890960531435269 ) ) ;
#137935 = CARTESIAN_POINT ( 'NONE',  ( -4.379528057220086978, -16.55341960407618274, 24.79275706135235779 ) ) ;
#137936 = CARTESIAN_POINT ( 'NONE',  ( 12.06949235617757843, -12.14591786802309237, 88.12390960531436690 ) ) ;
#137937 = CARTESIAN_POINT ( 'NONE',  ( 9.564922557960805705, 16.46253265017160317, 54.58224293864769550 ) ) ;
#137938 = CARTESIAN_POINT ( 'NONE',  ( 15.80617190586746368, 15.72974639402197994, 39.37390960531436690 ) ) ;
#137939 = CARTESIAN_POINT ( 'NONE',  ( -13.89961937509957401, -13.97604488694547875, 99.37609039468567573 ) ) ;
#137940 = CARTESIAN_POINT ( 'NONE',  ( -15.80617190586768217, 15.72974639402176855, 23.12609039468567573 ) ) ;
#137941 = CARTESIAN_POINT ( 'NONE',  ( -18.62759615963255300, -10.81492255796106328, 74.16775706135231871 ) ) ;
#137942 = CARTESIAN_POINT ( 'NONE',  ( -8.224510206698735004, -14.34966873604973081, 74.58442372801901854 ) ) ;
#137943 = CARTESIAN_POINT ( 'NONE',  ( 4.379528057220092307, 16.55341960407617563, 67.29275706135234714 ) ) ;
#137944 = ORIENTED_EDGE ( 'NONE', *, *, #115458, .T. ) ;
#137945 = CARTESIAN_POINT ( 'NONE',  ( 5.049401038298161559, -19.05341960407611168, 62.70724293864769550 ) ) ;
#137946 = CARTESIAN_POINT ( 'NONE',  ( -12.06949235617739369, -12.14591786802326823, 84.37609039468570415 ) ) ;
#137947 = CARTESIAN_POINT ( 'NONE',  ( -16.51473224551082808, 9.474510206698731452, 43.33442372801900433 ) ) ;
#137948 = CARTESIAN_POINT ( 'NONE',  ( -21.55341960407610458, -5.719274019375992779, 111.4572429386476813 ) ) ;
#137949 = CARTESIAN_POINT ( 'NONE',  ( 8.314922557960818139, 14.29746914071049879, 69.58224293864769550 ) ) ;
#137950 = CARTESIAN_POINT ( 'NONE',  ( 9.564922557960805705, 16.46253265017160317, 89.58224293864769550 ) ) ;
#137951 = CARTESIAN_POINT ( 'NONE',  ( 0.05219959533934541429, -16.53943276465976808, 85.00109039468568994 ) ) ;
#137952 = CARTESIAN_POINT ( 'NONE',  ( -18.62759615963255300, -10.81492255796106328, 59.16775706135234714 ) ) ;
#137953 = CARTESIAN_POINT ( 'NONE',  ( 5.049401038297881783, 19.05341960407617563, 112.2927570613523471 ) ) ;
#137954 = CARTESIAN_POINT ( 'NONE',  ( -5.719274019375978568, 21.55341960407610458, 115.2072429386476955 ) ) ;
#137955 = CARTESIAN_POINT ( 'NONE',  ( 8.314922557960818139, 14.29746914071049879, 54.58224293864769550 ) ) ;
#137956 = EDGE_CURVE ( 'NONE', #101739, #172658, #106109, .T. ) ;
#137957 = ORIENTED_EDGE ( 'NONE', *, *, #118820, .F. ) ;
#137958 = CARTESIAN_POINT ( 'NONE',  ( -5.823673210054116645, -21.52544592524344225, 92.29057627198103830 ) ) ;
#137959 = CARTESIAN_POINT ( 'NONE',  ( -8.224510206698948167, 14.34966873604960824, 40.41557627198103120 ) ) ;
#137960 = VERTEX_POINT ( 'NONE', #195953 ) ;
#137961 = PLANE ( 'NONE',  #108269 ) ;
#137962 = CARTESIAN_POINT ( 'NONE',  ( -21.53943276465977519, -0.05219959533937600094, 23.75109039468567929 ) ) ;
#137963 = CARTESIAN_POINT ( 'NONE',  ( 19.03943276465977164, -0.05219959533909143690, 108.7489096053143527 ) ) ;
#137964 = CARTESIAN_POINT ( 'NONE',  ( 15.80617190586769283, -15.72974639402175789, 30.62609039468567929 ) ) ;
#137965 = CARTESIAN_POINT ( 'NONE',  ( 12.06949235617757843, -12.14591786802309237, 58.12390960531435979 ) ) ;
#137966 = AXIS2_PLACEMENT_3D ( 'NONE', #133535, #193223, #98173 ) ;
#137967 = CARTESIAN_POINT ( 'NONE',  ( -19.03943276465977164, 0.05219959533909376836, 56.24890960531435979 ) ) ;
#137968 = CARTESIAN_POINT ( 'NONE',  ( -9.564922557961040184, 16.46253265017147172, 62.91775706135233293 ) ) ;
#137969 = CARTESIAN_POINT ( 'NONE',  ( 13.97604488694527802, 13.89961937509977652, 89.37390960531436690 ) ) ;
#137970 = CARTESIAN_POINT ( 'NONE',  ( 0.05219959533907565091, 21.53943276465977519, 44.99890960531435979 ) ) ;
#137971 = CARTESIAN_POINT ( 'NONE',  ( -23.65597376185835898, -29.51279439667934668, -21.31698521574488225 ) ) ;
#137972 = CARTESIAN_POINT ( 'NONE',  ( -5.049401038298153566, 19.05341960407611168, 65.20724293864765286 ) ) ;
#137973 = CARTESIAN_POINT ( 'NONE',  ( -12.14591786802326823, 12.06949235617739902, 43.12609039468568284 ) ) ;
#137974 = CARTESIAN_POINT ( 'NONE',  ( 19.05341960407617918, -5.049401038297876454, 66.04275706135233293 ) ) ;
#137975 = CARTESIAN_POINT ( 'NONE',  ( -5.719274019375978568, 21.55341960407610458, 110.2072429386477239 ) ) ;
#137976 = CARTESIAN_POINT ( 'NONE',  ( 16.55341960407611168, 4.379528057220329451, 48.95724293864770971 ) ) ;
#137977 = ORIENTED_EDGE ( 'NONE', *, *, #20816, .T. ) ;
#137978 = CARTESIAN_POINT ( 'NONE',  ( -5.153800228976328057, -19.02544592524343514, 97.29057627198099567 ) ) ;
#137979 = CARTESIAN_POINT ( 'NONE',  ( 21.53943276465977519, -0.05219959533907433946, 73.74890960531433848 ) ) ;
#137981 = CARTESIAN_POINT ( 'NONE',  ( 12.14591786802327356, -12.06949235617739191, 35.62609039468568994 ) ) ;
#137980 = CARTESIAN_POINT ( 'NONE',  ( 21.53943276465977519, -0.05219959533907433946, 103.7489096053143669 ) ) ;
#137982 = CARTESIAN_POINT ( 'NONE',  ( -21.55341960407610458, -5.719274019375992779, 31.45724293864769550 ) ) ;
#137983 = CARTESIAN_POINT ( 'NONE',  ( -21.55341960407619339, 5.719274019375674811, 98.54275706135234714 ) ) ;
#137984 = CARTESIAN_POINT ( 'NONE',  ( -16.51473224551069308, -9.474510206698971260, 91.66557627198103830 ) ) ;
#137985 = CARTESIAN_POINT ( 'NONE',  ( -13.89961937509977652, 13.97604488694528158, 40.62390960531435979 ) ) ;
#137986 = CARTESIAN_POINT ( 'NONE',  ( 13.97604488694527802, 13.89961937509977652, 99.37390960531436690 ) ) ;
#137987 = CARTESIAN_POINT ( 'NONE',  ( -16.51473224551069308, -9.474510206698971260, 71.66557627198102409 ) ) ;
#137988 = CARTESIAN_POINT ( 'NONE',  ( 4.483927247898790824, -16.52544592524335698, 20.20942372801900788 ) ) ;
#137989 = CARTESIAN_POINT ( 'NONE',  ( 0.05219959533936267826, -19.03943276465977164, 55.00109039468566863 ) ) ;
#137990 = AXIS2_PLACEMENT_3D ( 'NONE', #181070, #120357, #90996 ) ;
#137992 = CARTESIAN_POINT ( 'NONE',  ( -21.53943276465977519, 0.05219959533907696930, 31.24890960531435979 ) ) ;
#137991 = CARTESIAN_POINT ( 'NONE',  ( -21.52544592524334988, -5.823673210054445271, 108.9594237280190185 ) ) ;
#137993 = CARTESIAN_POINT ( 'NONE',  ( -16.55341960407617563, 4.379528057220093196, 103.5427570613523613 ) ) ;
#137994 = CARTESIAN_POINT ( 'NONE',  ( 20.85174543112844603, -20.13817253549177977, -49.56969272635731727 ) ) ;
#137995 = CARTESIAN_POINT ( 'NONE',  ( -19.02544592524334988, -5.153800228976617603, 73.95942372801900433 ) ) ;
#137996 = CARTESIAN_POINT ( 'NONE',  ( 9.564922557961047289, -16.46253265017146816, 35.41775706135233293 ) ) ;
#137997 = CARTESIAN_POINT ( 'NONE',  ( 24.07993927064490336, -13.88935938516710777, 140.0000000000000853 ) ) ;
#137998 = CARTESIAN_POINT ( 'NONE',  ( -9.474510206698964154, 16.51473224551069663, 45.41557627198103120 ) ) ;
#137999 = CARTESIAN_POINT ( 'NONE',  ( -16.53943276465976808, 0.05219959533911058130, 41.24890960531435269 ) ) ;
#138000 = CARTESIAN_POINT ( 'NONE',  ( -0.05219959533909027116, -19.03943276465977164, 22.49890960531436690 ) ) ;
#138001 = CARTESIAN_POINT ( 'NONE',  ( -0.05219959533910754901, -16.53943276465976808, 32.49890960531435979 ) ) ;
#138002 = LINE ( 'NONE', #153163, #145266 ) ;
#138003 = CARTESIAN_POINT ( 'NONE',  ( 0.05219959533934541429, -16.53943276465976808, 100.0010903946857042 ) ) ;
#138004 = CARTESIAN_POINT ( 'NONE',  ( -19.05341960407611168, -5.049401038298163336, 36.45724293864766707 ) ) ;
#138005 = CARTESIAN_POINT ( 'NONE',  ( 5.719274019375673035, 21.55341960407619339, 107.2927570613523471 ) ) ;
#138006 = CARTESIAN_POINT ( 'NONE',  ( -19.03943276465977164, -0.05219959533935918106, 113.7510903946856757 ) ) ;
#138008 = EDGE_LOOP ( 'NONE', ( #100237, #84415, #157411, #115586 ) ) ;
#138007 = CARTESIAN_POINT ( 'NONE',  ( -21.53943276465977519, -0.05219959533937600094, 83.75109039468568994 ) ) ;
#138009 = CARTESIAN_POINT ( 'NONE',  ( 19.02544592524334988, 5.153800228976608722, 56.45942372801898301 ) ) ;
#138010 = CARTESIAN_POINT ( 'NONE',  ( 13.97604488694527802, 13.89961937509977652, 94.37390960531436690 ) ) ;
#138011 = CARTESIAN_POINT ( 'NONE',  ( -0.05219959533909027116, -19.03943276465977164, 82.49890960531436690 ) ) ;
#138012 = CARTESIAN_POINT ( 'NONE',  ( -11.40812507854755609, 35.11059874428196537, -7.024999997268813523 ) ) ;
#138013 = CARTESIAN_POINT ( 'NONE',  ( 21.53943276465977519, -0.05219959533907433946, 108.7489096053143669 ) ) ;
#138014 = AXIS2_PLACEMENT_3D ( 'NONE', #171215, #138876, #45883 ) ;
#138015 = CARTESIAN_POINT ( 'NONE',  ( -16.52544592524342804, 4.483927247898546575, 66.04057627198103830 ) ) ;
#138016 = CARTESIAN_POINT ( 'NONE',  ( -0.05219959533907301413, -21.53943276465977519, 67.49890960531436690 ) ) ;
#138017 = CARTESIAN_POINT ( 'NONE',  ( -9.474510206698964154, 16.51473224551069663, 65.41557627198102409 ) ) ;
#138019 = CARTESIAN_POINT ( 'NONE',  ( 16.53943276465976808, 0.05219959533934440121, 96.25109039468568994 ) ) ;
#138018 = CARTESIAN_POINT ( 'NONE',  ( -5.823673210054116645, -21.52544592524344225, 92.29057627198103830 ) ) ;
#138021 = VERTEX_POINT ( 'NONE', #165598 ) ;
#138020 = B_SPLINE_CURVE_WITH_KNOTS ( 'NONE', 3,
 ( #86159, #40662, #37652, #22495, #145821, #53829, #38665, #100320, #161999, #89151, #195355, #44643, #56835, #90136, #10335, #150840, #133665, #183159, #165012, #12336 ),
 .UNSPECIFIED., .F., .F.,
 ( 4, 2, 2, 2, 2, 2, 2, 2, 2, 4 ),
 ( 0.000000000000000000, 0.0004987090165372568733, 0.0009974180330745137466, 0.001246772541343134973, 0.001496127049611756417, 0.001994836066149022289, 0.002493545082686287728, 0.002742899590954930421, 0.002992254099223572682, 0.003989672132298142590 ),
 .UNSPECIFIED. ) ;
#138022 = CARTESIAN_POINT ( 'NONE',  ( -16.51473224551069308, -9.474510206698971260, 56.66557627198103120 ) ) ;
#138024 = DIRECTION ( 'NONE',  ( -0.000000000000000000, -0.000000000000000000, -1.000000000000000000 ) ) ;
#138023 = CARTESIAN_POINT ( 'NONE',  ( 8.224510206698953496, -14.34966873604960469, 97.91557627198103830 ) ) ;
#138025 = CARTESIAN_POINT ( 'NONE',  ( 13.97604488694527802, 13.89961937509977652, 44.37390960531435269 ) ) ;
#138026 = CARTESIAN_POINT ( 'NONE',  ( -16.51473224551082808, 9.474510206698731452, 83.33442372801899012 ) ) ;
#138027 = CARTESIAN_POINT ( 'NONE',  ( 14.29746914071049879, -8.314922557960816363, 78.33224293864770971 ) ) ;
#138028 = CARTESIAN_POINT ( 'NONE',  ( -0.05219959533937732626, 21.53943276465977519, 62.50109039468568284 ) ) ;
#138030 = CARTESIAN_POINT ( 'NONE',  ( 10.81492255796078972, 18.62759615963270932, 104.5822429386477097 ) ) ;
#138029 = CARTESIAN_POINT ( 'NONE',  ( -9.474510206698964154, 16.51473224551069663, 30.41557627198102054 ) ) ;
#138031 = CARTESIAN_POINT ( 'NONE',  ( -14.34966873604960291, -8.224510206698953496, 86.66557627198102409 ) ) ;
#138032 = CARTESIAN_POINT ( 'NONE',  ( -40.00200000000003087, -4.592425496802575156E-15, 52.50000000000000000 ) ) ;
#138033 = B_SPLINE_CURVE_WITH_KNOTS ( 'NONE', 3,
 ( #40097, #24960, #26959, #88602, #119942, #164466, #25960 ),
 .UNSPECIFIED., .F., .F.,
 ( 4, 3, 4 ),
 ( -4.508036450095025827E-05, 0.000000000000000000, 0.006877813788783031929 ),
 .UNSPECIFIED. ) ;
#138034 = CARTESIAN_POINT ( 'NONE',  ( 13.97604488694527802, 13.89961937509977652, 59.37390960531434558 ) ) ;
#138035 = CARTESIAN_POINT ( 'NONE',  ( 19.52851543214741881, 5.500000000000026645, 47.89357721762581122 ) ) ;
#138037 = CARTESIAN_POINT ( 'NONE',  ( -19.03943276465977164, 0.05219959533909376836, 111.2489096053143669 ) ) ;
#138036 = CARTESIAN_POINT ( 'NONE',  ( 5.153800228976615827, -19.02544592524334988, 95.20942372801897591 ) ) ;
#138038 = CARTESIAN_POINT ( 'NONE',  ( -15.72974639402176322, -15.80617190586768395, 34.37609039468568284 ) ) ;
#138039 = CARTESIAN_POINT ( 'NONE',  ( 9.474510206698971260, -16.51473224551069308, 87.91557627198102409 ) ) ;
#138040 = CARTESIAN_POINT ( 'NONE',  ( -13.97604488694547697, 13.89961937509957934, 73.12609039468568994 ) ) ;
#138041 = CARTESIAN_POINT ( 'NONE',  ( 16.46253265017160672, -9.564922557960803928, 63.33224293864769550 ) ) ;
#138042 = CARTESIAN_POINT ( 'NONE',  ( -16.53943276465976808, 0.05219959533911058130, 76.24890960531435269 ) ) ;
#138043 = CARTESIAN_POINT ( 'NONE',  ( 16.52544592524342804, -4.483927247898539470, 63.54057627198103830 ) ) ;
#138044 = CARTESIAN_POINT ( 'NONE',  ( -0.05219959533909027116, -19.03943276465977164, 92.49890960531436690 ) ) ;
#138045 = CARTESIAN_POINT ( 'NONE',  ( 10.72451020669898902, -18.67979575497178502, 102.9155762719810383 ) ) ;
#138046 = CARTESIAN_POINT ( 'NONE',  ( 16.46253265017160672, -9.564922557960803928, 88.33224293864769550 ) ) ;
#138047 = CARTESIAN_POINT ( 'NONE',  ( -19.05341960407617563, 5.049401038297882671, 33.54275706135231871 ) ) ;
#138050 = CARTESIAN_POINT ( 'NONE',  ( 12.14591786802309770, 12.06949235617756955, 104.3739096053143669 ) ) ;
#138049 = CARTESIAN_POINT ( 'NONE',  ( 4.483927247898545687, 16.52544592524342804, 34.79057627198103120 ) ) ;
#138048 = CARTESIAN_POINT ( 'NONE',  ( -16.46253265017160317, 9.564922557960807481, 30.83224293864769550 ) ) ;
#138051 = ORIENTED_EDGE ( 'NONE', *, *, #135206, .F. ) ;
#138052 = CARTESIAN_POINT ( 'NONE',  ( -10.81492255796105439, 18.62759615963255655, 37.91775706135235424 ) ) ;
#138053 = CARTESIAN_POINT ( 'NONE',  ( 19.02544592524334988, 5.153800228976608722, 66.45942372801899012 ) ) ;
#138054 = CARTESIAN_POINT ( 'NONE',  ( 4.483927247898545687, 16.52544592524342804, 34.79057627198103120 ) ) ;
#138055 = CARTESIAN_POINT ( 'NONE',  ( 21.55341960407610458, 5.719274019375980345, 88.95724293864769550 ) ) ;
#138056 = CARTESIAN_POINT ( 'NONE',  ( -9.474510206698964154, 16.51473224551069663, 110.4155762719810383 ) ) ;
#138057 = CARTESIAN_POINT ( 'NONE',  ( 0.05219959533910956823, 16.53943276465976808, 69.99890960531435269 ) ) ;
#138058 = CARTESIAN_POINT ( 'NONE',  ( -0.05219959533909027116, -19.03943276465977164, 27.49890960531435624 ) ) ;
#138059 = CARTESIAN_POINT ( 'NONE',  ( -13.97604488694547697, 13.89961937509957934, 23.12609039468565442 ) ) ;
#138060 = CARTESIAN_POINT ( 'NONE',  ( 12.06949235617739724, 12.14591786802326823, 96.87609039468568994 ) ) ;
#138061 = CARTESIAN_POINT ( 'NONE',  ( -16.53943276465976808, -0.05219959533934237506, 58.75109039468568994 ) ) ;
#138062 = CARTESIAN_POINT ( 'NONE',  ( 10.72451020669898902, -18.67979575497178502, 37.91557627198102409 ) ) ;
#138063 = CARTESIAN_POINT ( 'NONE',  ( 21.52544592524334988, 5.823673210054432836, 101.4594237280190185 ) ) ;
#138064 = CARTESIAN_POINT ( 'NONE',  ( 13.89961937509977652, -13.97604488694527269, 78.12390960531433848 ) ) ;
#138065 = CARTESIAN_POINT ( 'NONE',  ( -12.06949235617739369, -12.14591786802326823, 79.37609039468567573 ) ) ;
#138066 = CARTESIAN_POINT ( 'NONE',  ( 16.51473224551069308, 9.474510206698969483, 24.16557627198102765 ) ) ;
#138067 = CARTESIAN_POINT ( 'NONE',  ( 14.34966873604960469, 8.224510206698951720, 34.16557627198102409 ) ) ;
#138069 = CARTESIAN_POINT ( 'NONE',  ( -13.89961937509977652, 13.97604488694528158, 90.62390960531432427 ) ) ;
#138068 = CARTESIAN_POINT ( 'NONE',  ( 19.03943276465977164, -0.05219959533909143690, 103.7489096053143669 ) ) ;
#138070 = CARTESIAN_POINT ( 'NONE',  ( 21.53943276465977519, -0.05219959533907433946, 28.74890960531435624 ) ) ;
#138071 = CARTESIAN_POINT ( 'NONE',  ( 16.55341960407611168, 4.379528057220329451, 53.95724293864770260 ) ) ;
#138072 = CARTESIAN_POINT ( 'NONE',  ( -4.379528057220328563, 16.55341960407611168, 35.20724293864768839 ) ) ;
#138073 = ORIENTED_EDGE ( 'NONE', *, *, #145930, .T. ) ;
#138074 = CARTESIAN_POINT ( 'NONE',  ( -4.379528057220328563, 16.55341960407611168, 50.20724293864769550 ) ) ;
#138076 = DIRECTION ( 'NONE',  ( 0.000000000000000000, -0.7071067811865466846, 0.7071067811865484609 ) ) ;
#138075 = CARTESIAN_POINT ( 'NONE',  ( -16.52544592524335698, -4.483927247898792601, 43.95942372801902565 ) ) ;
#138077 = CARTESIAN_POINT ( 'NONE',  ( -9.474510206698720793, -16.51473224551083518, 54.58442372801899722 ) ) ;
#138078 = CARTESIAN_POINT ( 'NONE',  ( 19.05341960407611168, 5.049401038298154454, 88.95724293864769550 ) ) ;
#138079 = CARTESIAN_POINT ( 'NONE',  ( 13.97604488694548053, -13.89961937509957401, 60.62609039468564731 ) ) ;
#138080 = CARTESIAN_POINT ( 'NONE',  ( 22.44159573604009594, -16.30477369853687364, 146.1750000027311671 ) ) ;
#138081 = CARTESIAN_POINT ( 'NONE',  ( 19.02544592524334988, 5.153800228976608722, 61.45942372801900433 ) ) ;
#138083 = CARTESIAN_POINT ( 'NONE',  ( -14.29746914071037622, -8.314922557961029526, 84.16775706135234714 ) ) ;
#138082 = CARTESIAN_POINT ( 'NONE',  ( 5.153800228976615827, -19.02544592524334988, 95.20942372801897591 ) ) ;
#138084 = CARTESIAN_POINT ( 'NONE',  ( -22.44159573604009950, -16.30477369853688430, 145.5750000027311728 ) ) ;
#138085 = CARTESIAN_POINT ( 'NONE',  ( 9.474510206698971260, -16.51473224551069308, 27.91557627198103120 ) ) ;
#138086 = CARTESIAN_POINT ( 'NONE',  ( 18.62759615963271287, -10.81492255796078972, 23.33224293864769194 ) ) ;
#138087 = CARTESIAN_POINT ( 'NONE',  ( 5.719274019375673035, 21.55341960407619339, 37.29275706135235424 ) ) ;
#138088 = CARTESIAN_POINT ( 'NONE',  ( 5.153800228976615827, -19.02544592524334988, 110.2094237280189901 ) ) ;
#138090 = CARTESIAN_POINT ( 'NONE',  ( 16.46253265017160672, -9.564922557960803928, 63.33224293864769550 ) ) ;
#138089 = CARTESIAN_POINT ( 'NONE',  ( 17.50000000000001066, 3.604700896430133472, 23.09746379124990767 ) ) ;
#138091 = CARTESIAN_POINT ( 'NONE',  ( -13.97604488694527625, -13.89961937509977652, 106.8739096053143669 ) ) ;
#138093 = CARTESIAN_POINT ( 'NONE',  ( 9.564922557960805705, 16.46253265017160317, 59.58224293864769550 ) ) ;
#138092 = CARTESIAN_POINT ( 'NONE',  ( -14.29746914071049879, 8.314922557960819915, 55.83224293864770260 ) ) ;
#138094 = CARTESIAN_POINT ( 'NONE',  ( 19.02544592524343514, -5.153800228976328945, 73.54057627198103830 ) ) ;
#138095 = CARTESIAN_POINT ( 'NONE',  ( -0.05219959533936034679, 19.03943276465977164, 77.50109039468566152 ) ) ;
#138096 = CARTESIAN_POINT ( 'NONE',  ( 10.81492255796078972, 18.62759615963270932, 54.58224293864769550 ) ) ;
#138097 = CARTESIAN_POINT ( 'NONE',  ( -14.29746914071049879, 8.314922557960819915, 110.8322429386476955 ) ) ;
#138098 = CARTESIAN_POINT ( 'NONE',  ( -16.51473224551082808, 9.474510206698731452, 48.33442372801900433 ) ) ;
#138099 = CARTESIAN_POINT ( 'NONE',  ( -5.049401038298153566, 19.05341960407611168, 85.20724293864766707 ) ) ;
#138100 = CARTESIAN_POINT ( 'NONE',  ( -21.52544592524343514, 5.823673210054127303, 71.04057627198103830 ) ) ;
#138102 = CARTESIAN_POINT ( 'NONE',  ( 5.153800228976615827, -19.02544592524334988, 30.20942372801900433 ) ) ;
#138101 = CARTESIAN_POINT ( 'NONE',  ( 14.34966873604960469, 8.224510206698951720, 79.16557627198103830 ) ) ;
#138103 = CARTESIAN_POINT ( 'NONE',  ( -15.80617190586745835, -15.72974639402198527, 71.87390960531438111 ) ) ;
#138104 = CARTESIAN_POINT ( 'NONE',  ( 21.55341960407610458, 5.719274019375980345, 58.95724293864770971 ) ) ;
#138105 = CARTESIAN_POINT ( 'NONE',  ( 5.719274019375991003, -21.55341960407610458, 42.70724293864770260 ) ) ;
#138106 = CARTESIAN_POINT ( 'NONE',  ( 5.823673210054444382, -21.52544592524334988, 85.20942372801901854 ) ) ;
#138107 = CARTESIAN_POINT ( 'NONE',  ( -9.564922557960796823, -16.46253265017161027, 62.08224293864769550 ) ) ;
#138108 = CARTESIAN_POINT ( 'NONE',  ( 0.05219959533910956823, 16.53943276465976808, 114.9989096053143669 ) ) ;
#138109 = AXIS2_PLACEMENT_3D ( 'NONE', #90304, #9504, #150008 ) ;
#138110 = CARTESIAN_POINT ( 'NONE',  ( -10.81492255796105439, 18.62759615963255655, 27.91775706135234358 ) ) ;
#138111 = FACE_OUTER_BOUND ( 'NONE', #156050, .T. ) ;
#138112 = CARTESIAN_POINT ( 'NONE',  ( 15.72974639402176855, 15.80617190586768217, 36.87609039468568994 ) ) ;
#138113 = CARTESIAN_POINT ( 'NONE',  ( 5.153800228976335163, 19.02544592524342804, 34.79057627198102409 ) ) ;
#138114 = CARTESIAN_POINT ( 'NONE',  ( 15.72974639402199770, -15.80617190586745480, 103.1239096053143811 ) ) ;
#138115 = CARTESIAN_POINT ( 'NONE',  ( -13.89961937509957401, -13.97604488694547875, 44.37609039468566863 ) ) ;
#138116 = CARTESIAN_POINT ( 'NONE',  ( 0.05219959533909260263, 19.03943276465977164, 39.99890960531436690 ) ) ;
#138117 = CARTESIAN_POINT ( 'NONE',  ( -9.474510206698964154, 16.51473224551069663, 25.41557627198103120 ) ) ;
#138118 = CARTESIAN_POINT ( 'NONE',  ( -3.573655867282028392E-15, 2.428612866367529932E-14, -24.99999999999997868 ) ) ;
#138119 = CARTESIAN_POINT ( 'NONE',  ( 14.34966873604972726, -8.224510206698740333, 60.83442372801901854 ) ) ;
#138120 = CARTESIAN_POINT ( 'NONE',  ( -5.153800228976328057, -19.02544592524343514, 27.29057627198103120 ) ) ;
#138121 = CARTESIAN_POINT ( 'NONE',  ( -23.35043118190795042, -14.19381810412062883, 169.8796877288296798 ) ) ;
#138122 = CARTESIAN_POINT ( 'NONE',  ( -19.02544592524342804, 5.153800228976336051, 91.04057627198100988 ) ) ;
#138123 = CARTESIAN_POINT ( 'NONE',  ( 14.34966873604960469, 8.224510206698951720, 104.1655762719810241 ) ) ;
#138124 = CARTESIAN_POINT ( 'NONE',  ( 21.52544592524344225, -5.823673210054117533, 58.54057627198103120 ) ) ;
#138125 = CARTESIAN_POINT ( 'NONE',  ( 12.14591786802327356, -12.06949235617739191, 45.62609039468567573 ) ) ;
#138126 = CARTESIAN_POINT ( 'NONE',  ( 0.05219959533937995610, -21.53943276465977519, 95.00109039468568994 ) ) ;
#138127 = CARTESIAN_POINT ( 'NONE',  ( -9.564922557960796823, -16.46253265017161027, 27.08224293864769550 ) ) ;
#138128 = CARTESIAN_POINT ( 'NONE',  ( 12.06949235617757843, -12.14591786802309237, 23.12390960531436335 ) ) ;
#138129 = CARTESIAN_POINT ( 'NONE',  ( 14.34966873604960469, 8.224510206698951720, 59.16557627198103120 ) ) ;
#138130 = CARTESIAN_POINT ( 'NONE',  ( -9.474510206698964154, 16.51473224551069663, 55.41557627198103120 ) ) ;
#138131 = CARTESIAN_POINT ( 'NONE',  ( -19.02544592524334988, -5.153800228976617603, 18.95942372801899722 ) ) ;
#138132 = CARTESIAN_POINT ( 'NONE',  ( 10.72451020669871369, 18.67979575497193778, 27.08442372801901854 ) ) ;
#138133 = CARTESIAN_POINT ( 'NONE',  ( 0.05219959533937995610, -21.53943276465977519, 75.00109039468568994 ) ) ;
#138134 = CARTESIAN_POINT ( 'NONE',  ( -0.05219959533934338120, 16.53943276465976808, 57.50109039468568994 ) ) ;
#138135 = CARTESIAN_POINT ( 'NONE',  ( -14.34966873604972548, 8.224510206698743886, 28.33442372801902209 ) ) ;
#138137 = CARTESIAN_POINT ( 'NONE',  ( -15.80617190586768217, 15.72974639402176855, 93.12609039468568994 ) ) ;
#138136 = CARTESIAN_POINT ( 'NONE',  ( 4.379528057220339221, -16.55341960407611168, 82.70724293864770971 ) ) ;
#138138 = AXIS2_PLACEMENT_3D ( 'NONE', #42307, #43293, #197969 ) ;
#138139 = CARTESIAN_POINT ( 'NONE',  ( -8.224510206698948167, 14.34966873604960824, 25.41557627198103120 ) ) ;
#138140 = CARTESIAN_POINT ( 'NONE',  ( -17.49999999999999645, 5.499999999999996447, 113.7176903769643417 ) ) ;
#138141 = CARTESIAN_POINT ( 'NONE',  ( 12.06949235617739724, 12.14591786802326823, 36.87609039468568994 ) ) ;
#138142 = CARTESIAN_POINT ( 'NONE',  ( 16.52544592524342804, -4.483927247898539470, 38.54057627198103120 ) ) ;
#138143 = CARTESIAN_POINT ( 'NONE',  ( -12.14591786802326823, 12.06949235617739902, 88.12609039468570415 ) ) ;
#138144 = CARTESIAN_POINT ( 'NONE',  ( 5.049401038298161559, -19.05341960407611168, 97.70724293864766707 ) ) ;
#138145 = CARTESIAN_POINT ( 'NONE',  ( 13.97604488694527802, 13.89961937509977652, 114.3739096053143669 ) ) ;
#138146 = CARTESIAN_POINT ( 'NONE',  ( 18.67979575497194134, -10.72451020669871369, 95.83442372801903275 ) ) ;
#138147 = CARTESIAN_POINT ( 'NONE',  ( -4.483927247898782831, 16.52544592524335698, 97.70942372801904696 ) ) ;
#138148 = CARTESIAN_POINT ( 'NONE',  ( -16.53943276465976808, 0.05219959533911058130, 71.24890960531435269 ) ) ;
#138149 = CARTESIAN_POINT ( 'NONE',  ( -16.46253265017160317, 9.564922557960807481, 85.83224293864769550 ) ) ;
#138150 = ORIENTED_EDGE ( 'NONE', *, *, #85603, .F. ) ;
#138151 = CARTESIAN_POINT ( 'NONE',  ( 4.483927247898790824, -16.52544592524335698, 40.20942372801901854 ) ) ;
#138152 = CARTESIAN_POINT ( 'NONE',  ( 16.51473224551069308, 9.474510206698969483, 44.16557627198103120 ) ) ;
#138153 = CARTESIAN_POINT ( 'NONE',  ( -0.05219959533909027116, -19.03943276465977164, 97.49890960531436690 ) ) ;
#138155 = CARTESIAN_POINT ( 'NONE',  ( -36.91746825000000598, 2.428612866367529932E-14, -4.624999997268814056 ) ) ;
#138154 = CARTESIAN_POINT ( 'NONE',  ( -14.29746914071037622, -8.314922557961029526, 34.16775706135234714 ) ) ;
#138156 = CARTESIAN_POINT ( 'NONE',  ( 19.02544592524334988, 5.153800228976608722, 31.45942372801900433 ) ) ;
#138157 = CARTESIAN_POINT ( 'NONE',  ( -0.05219959533934338120, 16.53943276465976808, 92.50109039468567573 ) ) ;
#138158 = CARTESIAN_POINT ( 'NONE',  ( 13.89961937509977652, -13.97604488694527269, 38.12390960531436690 ) ) ;
#138159 = CARTESIAN_POINT ( 'NONE',  ( 8.314922557961029526, -14.29746914071037800, 85.41775706135236135 ) ) ;
#138160 = CARTESIAN_POINT ( 'NONE',  ( 16.55341960407618274, -4.379528057220086978, 66.04275706135236135 ) ) ;
#138161 = CARTESIAN_POINT ( 'NONE',  ( -13.97604488694547697, 13.89961937509957934, 88.12609039468563310 ) ) ;
#138162 = CARTESIAN_POINT ( 'NONE',  ( -16.46253265017146816, -9.564922557961047289, 29.16775706135232937 ) ) ;
#138163 = CARTESIAN_POINT ( 'NONE',  ( 13.89961937509977652, -13.97604488694527269, 63.12390960531435979 ) ) ;
#138164 = CARTESIAN_POINT ( 'NONE',  ( -14.34966873604960291, -8.224510206698953496, 86.66557627198102409 ) ) ;
#138165 = EDGE_CURVE ( 'NONE', #115190, #22576, #103994, .T. ) ;
#138166 = CARTESIAN_POINT ( 'NONE',  ( 19.03943276465977164, 0.05219959533936151252, 56.25109039468566863 ) ) ;
#138167 = CARTESIAN_POINT ( 'NONE',  ( -21.55341960407610458, -5.719274019375992779, 56.45724293864768839 ) ) ;
#138168 = CARTESIAN_POINT ( 'NONE',  ( 16.46253265017146816, 9.564922557961045513, 21.66775706135233648 ) ) ;
#138169 = CARTESIAN_POINT ( 'NONE',  ( 9.474510206698971260, -16.51473224551069308, 107.9155762719810383 ) ) ;
#138170 = CARTESIAN_POINT ( 'NONE',  ( 21.52544592524344225, -5.823673210054117533, 83.54057627198102409 ) ) ;
#138171 = CARTESIAN_POINT ( 'NONE',  ( 19.05341960407611168, 5.049401038298154454, 103.9572429386476671 ) ) ;
#138172 = CARTESIAN_POINT ( 'NONE',  ( 9.474510206698729675, 16.51473224551082808, 97.08442372801900433 ) ) ;
#138173 = CARTESIAN_POINT ( 'NONE',  ( -9.564922557960796823, -16.46253265017161027, 112.0822429386476955 ) ) ;
#138174 = CARTESIAN_POINT ( 'NONE',  ( -13.97604488694547697, 13.89961937509957934, 108.1260903946856331 ) ) ;
#138175 = CARTESIAN_POINT ( 'NONE',  ( 19.03943276465977164, -0.05219959533909143690, 33.74890960531435979 ) ) ;
#138176 = CARTESIAN_POINT ( 'NONE',  ( -5.153800228976328057, -19.02544592524343514, 102.2905762719810383 ) ) ;
#138177 = CARTESIAN_POINT ( 'NONE',  ( -0.05219959533907301413, -21.53943276465977519, 82.49890960531436690 ) ) ;
#138178 = CARTESIAN_POINT ( 'NONE',  ( -16.52544592524335698, -4.483927247898792601, 63.95942372801901854 ) ) ;
#138179 = CARTESIAN_POINT ( 'NONE',  ( 21.53943276465977519, 0.05219959533937863772, 66.25109039468567573 ) ) ;
#138181 = CARTESIAN_POINT ( 'NONE',  ( 10.72451020669871369, 18.67979575497193778, 112.0844237280190185 ) ) ;
#138180 = CARTESIAN_POINT ( 'NONE',  ( 0.05219959533936267826, -19.03943276465977164, 100.0010903946856757 ) ) ;
#138182 = CARTESIAN_POINT ( 'NONE',  ( -12.14591786802309592, -12.06949235617757132, 21.87390960531436690 ) ) ;
#138183 = CARTESIAN_POINT ( 'NONE',  ( 10.72451020669898902, -18.67979575497178502, 102.9155762719810383 ) ) ;
#138184 = CARTESIAN_POINT ( 'NONE',  ( -12.06949235617756955, 12.14591786802309770, 35.62390960531437401 ) ) ;
#138185 = CARTESIAN_POINT ( 'NONE',  ( 13.89961937509957401, 13.97604488694547697, 76.87609039468566152 ) ) ;
#138186 = CARTESIAN_POINT ( 'NONE',  ( -21.52544592524334988, -5.823673210054445271, 58.95942372801902565 ) ) ;
#138187 = CARTESIAN_POINT ( 'NONE',  ( 5.153800228976615827, -19.02544592524334988, 35.20942372801899722 ) ) ;
#138188 = CARTESIAN_POINT ( 'NONE',  ( -16.55341960407611168, -4.379528057220339221, 101.4572429386476955 ) ) ;
#138189 = CARTESIAN_POINT ( 'NONE',  ( -21.52544592524343514, 5.823673210054127303, 26.04057627198103475 ) ) ;
#138190 = CARTESIAN_POINT ( 'NONE',  ( 12.06949235617757843, -12.14591786802309237, 38.12390960531436690 ) ) ;
#138191 = CARTESIAN_POINT ( 'NONE',  ( 5.719274019375673035, 21.55341960407619339, 97.29275706135234714 ) ) ;
#138192 = CARTESIAN_POINT ( 'NONE',  ( -0.05219959533934338120, 16.53943276465976808, 72.50109039468568994 ) ) ;
#138193 = CARTESIAN_POINT ( 'NONE',  ( 4.379528057220339221, -16.55341960407611168, 32.70724293864770260 ) ) ;
#138194 = CARTESIAN_POINT ( 'NONE',  ( -18.67979575497193778, 10.72451020669871902, 58.33442372801901143 ) ) ;
#138195 = CARTESIAN_POINT ( 'NONE',  ( 10.72451020669871369, 18.67979575497193778, 52.08442372801901854 ) ) ;
#138196 = ADVANCED_FACE ( 'NONE', ( #104911 ), #199907, .F. ) ;
#138197 = VERTEX_POINT ( 'NONE', #107866 ) ;
#138198 = CARTESIAN_POINT ( 'NONE',  ( 19.05341960407611168, 5.049401038298154454, 23.95724293864769194 ) ) ;
#138199 = CARTESIAN_POINT ( 'NONE',  ( -18.62759615963255300, -10.81492255796106328, 49.16775706135234003 ) ) ;
#138200 = CARTESIAN_POINT ( 'NONE',  ( 19.03943276465977164, -0.05219959533909143690, 23.74890960531435269 ) ) ;
#138201 = CARTESIAN_POINT ( 'NONE',  ( 16.46253265017160672, -9.564922557960803928, 38.33224293864768839 ) ) ;
#138202 = CARTESIAN_POINT ( 'NONE',  ( 4.483927247898545687, 16.52544592524342804, 84.79057627198102409 ) ) ;
#138203 = CARTESIAN_POINT ( 'NONE',  ( 5.153800228976335163, 19.02544592524342804, 74.79057627198103830 ) ) ;
#138204 = CARTESIAN_POINT ( 'NONE',  ( 8.224510206698953496, -14.34966873604960469, 27.91557627198103830 ) ) ;
#138205 = CARTESIAN_POINT ( 'NONE',  ( -21.55341960407610458, -5.719274019375992779, 61.45724293864770260 ) ) ;
#138206 = CARTESIAN_POINT ( 'NONE',  ( 16.52544592524342804, -4.483927247898539470, 93.54057627198103830 ) ) ;
#138207 = CARTESIAN_POINT ( 'NONE',  ( -18.62759615963270932, 10.81492255796079327, 105.8322429386476955 ) ) ;
#138208 = CARTESIAN_POINT ( 'NONE',  ( 16.46253265017160672, -9.564922557960803928, 103.3322429386476955 ) ) ;
#138210 = CARTESIAN_POINT ( 'NONE',  ( -9.474510206698720793, -16.51473224551083518, 99.58442372801900433 ) ) ;
#138209 = CARTESIAN_POINT ( 'NONE',  ( -13.97604488694527625, -13.89961937509977652, 71.87390960531433848 ) ) ;
#138211 = CARTESIAN_POINT ( 'NONE',  ( -10.72451020669898014, 18.67979575497178502, 55.41557627198102409 ) ) ;
#138212 = CARTESIAN_POINT ( 'NONE',  ( -0.05219959533937732626, 21.53943276465977519, 77.50109039468567573 ) ) ;
#138213 = CARTESIAN_POINT ( 'NONE',  ( 0.05219959533909260263, 19.03943276465977164, 69.99890960531435269 ) ) ;
#138214 = CARTESIAN_POINT ( 'NONE',  ( 9.564922557960805705, 16.46253265017160317, 104.5822429386476955 ) ) ;
#138215 = CARTESIAN_POINT ( 'NONE',  ( -0.05219959533934338120, 16.53943276465976808, 72.50109039468568994 ) ) ;
#138216 = CARTESIAN_POINT ( 'NONE',  ( -5.719274019375665041, -21.55341960407619695, 54.79275706135235424 ) ) ;
#138217 = CARTESIAN_POINT ( 'NONE',  ( 21.52544592524334988, 5.823673210054432836, 81.45942372801900433 ) ) ;
#138218 = CARTESIAN_POINT ( 'NONE',  ( 5.719274019375991003, -21.55341960407610458, 107.7072429386476955 ) ) ;
#138219 = CARTESIAN_POINT ( 'NONE',  ( -4.483927247898782831, 16.52544592524335698, 72.70942372801901854 ) ) ;
#138220 = CARTESIAN_POINT ( 'NONE',  ( 0.05219959533907565091, 21.53943276465977519, 69.99890960531435269 ) ) ;
#138221 = CARTESIAN_POINT ( 'NONE',  ( -5.049401038297874678, -19.05341960407617918, 44.79275706135232582 ) ) ;
#138222 = CARTESIAN_POINT ( 'NONE',  ( 10.72451020669898902, -18.67979575497178502, 37.91557627198102409 ) ) ;
#138224 = CARTESIAN_POINT ( 'NONE',  ( -14.34966873604972548, 8.224510206698743886, 113.3344237280190328 ) ) ;
#138223 = CARTESIAN_POINT ( 'NONE',  ( -19.02544592524342804, 5.153800228976336051, 86.04057627198103830 ) ) ;
#138225 = CARTESIAN_POINT ( 'NONE',  ( -17.40861289039003168, 6.110651285853254677, 63.62767529172569425 ) ) ;
#138226 = CARTESIAN_POINT ( 'NONE',  ( 19.02544592524343514, -5.153800228976328945, 113.5405762719810241 ) ) ;
#138227 = LINE ( 'NONE', #89738, #70145 ) ;
#138228 = CARTESIAN_POINT ( 'NONE',  ( -16.46253265017146816, -9.564922557961047289, 89.16775706135234714 ) ) ;
#138229 = CARTESIAN_POINT ( 'NONE',  ( -15.80617190586745835, -15.72974639402198527, 71.87390960531438111 ) ) ;
#138230 = CARTESIAN_POINT ( 'NONE',  ( -16.52544592524342804, 4.483927247898546575, 56.04057627198102409 ) ) ;
#138231 = CARTESIAN_POINT ( 'NONE',  ( -5.049401038297874678, -19.05341960407617918, 109.7927570613523187 ) ) ;
#138232 = CARTESIAN_POINT ( 'NONE',  ( 5.049401038298161559, -19.05341960407611168, 32.70724293864768129 ) ) ;
#138234 = CARTESIAN_POINT ( 'NONE',  ( -19.03943276465977164, -0.05219959533935918106, 73.75109039468566152 ) ) ;
#138233 = CARTESIAN_POINT ( 'NONE',  ( -21.52544592524343514, 5.823673210054127303, 96.04057627198102409 ) ) ;
#138235 = CARTESIAN_POINT ( 'NONE',  ( 9.474510206698971260, -16.51473224551069308, 77.91557627198103830 ) ) ;
#138236 = CARTESIAN_POINT ( 'NONE',  ( -16.55341960407611168, -4.379528057220339221, 81.45724293864769550 ) ) ;
#138237 = CARTESIAN_POINT ( 'NONE',  ( -0.05219959533909027116, -19.03943276465977164, 57.49890960531435979 ) ) ;
#138238 = CARTESIAN_POINT ( 'NONE',  ( -12.06949235617756955, 12.14591786802309770, 60.62390960531437401 ) ) ;
#138239 = CARTESIAN_POINT ( 'NONE',  ( 5.049401038298161559, -19.05341960407611168, 27.70724293864769550 ) ) ;
#138240 = CARTESIAN_POINT ( 'NONE',  ( 0.1001742010324345455, 9.100000000000003197, -61.89430850415824636 ) ) ;
#138241 = CARTESIAN_POINT ( 'NONE',  ( 4.483927247898545687, 16.52544592524342804, 44.79057627198103120 ) ) ;
#138242 = CARTESIAN_POINT ( 'NONE',  ( 16.51473224551069308, 9.474510206698969483, 89.16557627198103830 ) ) ;
#138243 = CARTESIAN_POINT ( 'NONE',  ( -9.656827144875922642, -71.74905178543390605, 0.000000000000000000 ) ) ;
#138244 = CARTESIAN_POINT ( 'NONE',  ( -5.153800228976607833, 19.02544592524334988, 47.70942372801900433 ) ) ;
#138245 = CARTESIAN_POINT ( 'NONE',  ( -4.483927247898782831, 16.52544592524335698, 57.70942372801901143 ) ) ;
#138246 = CARTESIAN_POINT ( 'NONE',  ( -10.72451020669898014, 18.67979575497178502, 60.41557627198102409 ) ) ;
#138247 = CARTESIAN_POINT ( 'NONE',  ( -0.05219959533937732626, 21.53943276465977519, 112.5010903946857042 ) ) ;
#138248 = CARTESIAN_POINT ( 'NONE',  ( -13.89961937509977652, 13.97604488694528158, 90.62390960531432427 ) ) ;
#138249 = CARTESIAN_POINT ( 'NONE',  ( -21.88302055210221297, -22.95674879174745087, -45.93240442770092358 ) ) ;
#138250 = CARTESIAN_POINT ( 'NONE',  ( -0.05219959533907301413, -21.53943276465977519, 27.49890960531435269 ) ) ;
#138251 = AXIS2_PLACEMENT_3D ( 'NONE', #167821, #105157, #29320 ) ;
#138252 = CARTESIAN_POINT ( 'NONE',  ( -16.46253265017160317, 9.564922557960807481, 55.83224293864769550 ) ) ;
#138253 = CARTESIAN_POINT ( 'NONE',  ( 10.81492255796106328, -18.62759615963255655, 45.41775706135234003 ) ) ;
#138254 = CARTESIAN_POINT ( 'NONE',  ( 0.05219959533910956823, 16.53943276465976808, 104.9989096053143669 ) ) ;
#138257 = ORIENTED_EDGE ( 'NONE', *, *, #106636, .F. ) ;
#138256 = CARTESIAN_POINT ( 'NONE',  ( -5.049401038298153566, 19.05341960407611168, 100.2072429386476955 ) ) ;
#138255 = CARTESIAN_POINT ( 'NONE',  ( 15.72974639402199770, -15.80617190586745480, 98.12390960531436690 ) ) ;
#138258 = CARTESIAN_POINT ( 'NONE',  ( -10.72451020669870658, -18.67979575497194134, 44.58442372801901854 ) ) ;
#138259 = ORIENTED_EDGE ( 'NONE', *, *, #5261, .T. ) ;
#138260 = CARTESIAN_POINT ( 'NONE',  ( -16.46253265017160317, 9.564922557960807481, 95.83224293864769550 ) ) ;
#138261 = LINE ( 'NONE', #28132, #69705 ) ;
#138262 = CARTESIAN_POINT ( 'NONE',  ( -10.81492255796078084, -18.62759615963271287, 92.08224293864769550 ) ) ;
#138263 = CARTESIAN_POINT ( 'NONE',  ( 16.51473224551069308, 9.474510206698969483, 44.16557627198103120 ) ) ;
#138264 = CARTESIAN_POINT ( 'NONE',  ( 14.34966873604972726, -8.224510206698740333, 20.83442372801901143 ) ) ;
#138265 = CARTESIAN_POINT ( 'NONE',  ( -38.00000000000000711, 2.428612866367529932E-14, -11.74999999453762634 ) ) ;
#138266 = CARTESIAN_POINT ( 'NONE',  ( 9.474510206698971260, -16.51473224551069308, 22.91557627198102765 ) ) ;
#138267 = CARTESIAN_POINT ( 'NONE',  ( -21.55341960407619339, 5.719274019375674811, 103.5427570613523613 ) ) ;
#138269 = CARTESIAN_POINT ( 'NONE',  ( 18.67979575497194134, -10.72451020669871369, 50.83442372801901143 ) ) ;
#138268 = CARTESIAN_POINT ( 'NONE',  ( -13.89961937509977652, 13.97604488694528158, 75.62390960531438111 ) ) ;
#138270 = CARTESIAN_POINT ( 'NONE',  ( 17.14385361876520264, 23.59649016807275856, 144.6750000027311671 ) ) ;
#138271 = CARTESIAN_POINT ( 'NONE',  ( 13.89961937509977652, -13.97604488694527269, 93.12390960531436690 ) ) ;
#138272 = CARTESIAN_POINT ( 'NONE',  ( 19.35543954521082455, 5.499999999999579892, 62.08901960356454452 ) ) ;
#138275 = CARTESIAN_POINT ( 'NONE',  ( -18.67979575497193778, 10.72451020669871902, 63.33442372801900433 ) ) ;
#138274 = CARTESIAN_POINT ( 'NONE',  ( -4.483927247898782831, 16.52544592524335698, 67.70942372801901854 ) ) ;
#138273 = CARTESIAN_POINT ( 'NONE',  ( 14.34966873604972726, -8.224510206698740333, 35.83442372801901143 ) ) ;
#138276 = CARTESIAN_POINT ( 'NONE',  ( 21.53943276465977519, 0.05219959533937863772, 81.25109039468568994 ) ) ;
#138277 = CARTESIAN_POINT ( 'NONE',  ( 12.24802307403557577, -10.74802307403608737, -59.32879157176802920 ) ) ;
#138278 =( BOUNDED_SURFACE ( )  B_SPLINE_SURFACE ( 3, 2, ( 
 ( #41765, #22591, #115601, #69085, #130752, #99414, #25612, #24605, #148941, #177290, #10431, #72089, #133763, #161096, #56933, #103430, #165109, #149930, #84239, #129734, #192444, #53926, #100418, #45729, #201, #123540, #152894, #183257, #92211, #170064, #184247, #14390, #134778, #30559, #196460, #31554, #90234, #107381, #137732, #93206, #154891, #27609, #76056, #181284, #199416, #60880, #150941, #42761, #169053, #122557, #15392, #138720, #121562, #104424, #153896, #57930, #77049, #108387, #119601, #166107, #43748, #136736, #73108, #61870, #89249, #12435, #105411, #74097, #185233, #46724, #135767, #197438, #44738, #58904, #120570, #182264, #167095, #28596, #151917, #13406, #106394, #75070, #198418, #59895, #168076, #29573, #91204, #140709, #109376, #126531, #187247, #63880, #124550, #143688, #139705, #17378, #66853, #175043, #33539, #142696, #172052, #173058, #36508, #1192, #188230, #64869, #78036, #171058, #189229, #49703, #34535, #157883, #158858, #62868, #186247, #97173, #3196, #18385, #96194, #4176, #110370, #94201, #19372, #81021, #113351, #65854, #98162, #5170, #47725, #111369, #127525, #32548, #80036, #155881, #50707, #112365, #79034, #2199, #174056, #48717, #190210, #35525, #20346, #81995, #125551, #128515, #51689, #16389, #95202, #156889, #141705, #133526, #146686, #10197, #25381, #39515, #176050, #87023, #131526, #70864, #38528, #177058, #193211, #101175, #53691, #148709, #56699, #115369, #8182, #116358, #178047, #192209, #41534, #162863, #69858, #195218, #6173, #67853, #23360, #71857, #129508, #147711, #118372, #9198, #37518, #180066, #132532, #159863, #21356, #54685, #40525, #83013, #24371, #100184, #85005, #84011, #144688, #191208, #52683, #99180, #161866, #194221, #55686, #160869, #86022, #117360, #179056, #102196, #145689, #114346, #68854, #22359, #163884, #7171, #130513, #103198, #26373, #58673, #120339, #88013, #57701, #153659, #136509, #198189, #137499, #182034, #90009, #14154, #199180, #60646, #59659, #149701, #107149, #43517, #122320, #105183, #119370, #151693, #11199, #166870, #13183, #75821, #30324, #15155, #183026, #74846, #184012, #200169, #45494, #44509, #164878, #168819, #72875, #61638, #28371, #91966, #167848, #123306, #184999, #181053, #106165, #134543, #29348, #90977, #42528, #196232, #76816, #152664, #138487, #104191, #121333, #165873, #27369, #89016, #150707, #12206, #73869, #135539, #197210, #110141, #66612, #19133, #46483, #128276, #78798, #108143, #142461, #80784, #16153, #3939, #18148, #111129, #95960, #139476, #20111, #77807, #169827, #157644, #79802, #172818, #109145, #125319, #127279, #171820, #126299, #170824, #957, #156652, #17145, #93970, #154657, #173819, #31319, #47489, #96940, #4929, #63644, #34298, #1964, #143443, #140476, #188992, #65619, #92971, #155650, #62633, #50468, #141474, #124309, #186007, #35284, #48486, #112128, #2958, #187015, #64637, #158621, #33308, #32317, #94968, #187996, #49466, #81755, #129267, #37271, #162613, #40272, #82764, #175798, #67606, #190961, #51448, #24118, #191953, #7927, #98929, #177803, #9949, #71608, #144445, #131276, #97919, #192964, #39272, #52438, #159612, #85771, #54444, #132282, #55436, #38279, #21109, #147458, #113109, #116114, #25129, #174799, #5930, #160620, #53438, #189973, #8947, #36265, #114096, #22111, #83761, #70615, #193974, #145441, #117107, #161619, #100929, #178802, #6923, #163626, #68601, #130257, #101945, #23113, #86771, #115113, #176807, #148454, #99933, #69611, #84758, #146436, #43268, #103943, #180806, #41281, #60408, #56444, #134294, #183772, #91724, #150462, #59413, #88769, #30083, #165623, #13913, #167608, #118123, #42285, #164627, #197944, #104937, #26121, #102943, #122081, #135292, #152425, #89765, #27122, #151450, #90742, #196964, #87764, #11957, #73622, #149449, #136269, #72619, #58432, #105923, #45258, #10945, #119125, #195980, #57453, #194965, #29104, #120099, #12937, #181787, #121088 ),
 ( #106912, #168585, #74602, #166623, #75579, #153420, #44265, #182782, #179811, #137257, #28125, #14917, #198941, #133274, #141229, #48242, #2720, #126065, #169584, #50233, #46243, #158389, #187762, #109897, #64397, #139242, #155413, #157406, #1722, #156402, #717, #31082, #186772, #47248, #124059, #184758, #3702, #199937, #77570, #127041, #35046, #93732, #49232, #32075, #173577, #110890, #154418, #172575, #34061, #95720, #140229, #62389, #107897, #185760, #138254, #18899, #16903, #17906, #76578, #61401, #78554, #63398, #123072, #92729, #188748, #171581, #33069, #80545, #125075, #94724, #142219, #65381, #79562, #96700, #15912, #111888, #108905, #170584, #174567, #192728, #68365, #38044, #161384, #162377, #81518, #189740, #100696, #6687, #21876, #176570, #146199, #113860, #97682, #22875, #84522, #116873, #7685, #178564, #8710, #128039, #130016, #69369, #4686, #83526, #51213, #191715, #131039, #159371, #112874, #53199, #190729, #193736, #115882, #54211, #177572, #66378, #99700, #114875, #39039, #36033, #37031, #70379, #55204, #23879, #132047, #85531, #147219, #20868, #40029, #101703, #19878, #98693, #160387, #143205, #82526, #175556, #144208, #5693, #145204, #67369, #129028, #52202, #195746, #104705, #57220, #28875, #60175, #118893, #11725, #119876, #181561, #180578, #45022, #43039, #150229, #198708, #9716, #71380, #26889, #13681, #133044, #151220, #152197, #12709, #41048, #121844, #74375, #137017, #183537, #196740, #44031, #163393, #166395, #42052, #88532, #87538, #24890, #86538, #75348, #105692, #136040, #167378, #197715, #102712, #89533, #59180, #120849, #73393, #149225, #194734, #72379, #148222, #182549, #103716, #27891, #56204, #117887, #165396, #135064, #179577, #164401, #25893, #58207, #90515, #10716, #134054, #93485, #17657, #140987, #63151, #65139, #91487, #16662, #155171, #168354, #61164, #79317, #78310, #124830, #48003, #48989, #29850, #76339, #187524, #139983, #108664, #186530, #32827, #477, #184524, #109659, #171339, #3462, #94478, #126796, #95474, #14677, #1472, #156159, #153174, #170342, #138015, #2475, #64156, #46004, #199698, #125820, #77331, #80301, #110644, #172325, #33814, #122835, #157161, #18655, #141974, #107659, #123815, #188502, #106681, #169336, #30845, #92492, #154181, #15671, #138998, #62151, #185513, #47005, #31834, #24397, #131552, #69883, #86046, #194245, #146712, #118396, #149724, #8208, #101198, #9222, #70889, #85031, #134568, #132557, #39539, #88036, #99204, #160892, #116382, #103221, #22384, #40552, #41558, #102221, #130538, #11225, #163910, #26397, #72899, #147735, #133551, #49981, #55712, #193237, #178072, #177081, #111645, #173331, #164903, #195242, #25406, #56726, #87048, #192236, #179083, #148733, #10221, #162888, #38552, #84034, #161889, #37540, #71881, #54710, #117384, #145713, #7194, #180090, #68878, #53716, #115393, #100209, #23385, #29371, #30349, #74870, #183049, #107173, #91991, #152688, #154682, #181077, #106188, #44533, #57724, #150729, #168844, #167872, #14177, #137523, #138511, #119394, #165896, #76840, #91002, #198213, #75847, #122347, #90032, #73891, #199205, #60672, #92996, #184036, #16177, #185024, #104215, #45519, #153685, #42552, #59685, #27394, #15181, #153389, #135561, #89039, #61662, #166893, #169851, #123331, #46511, #108170, #12229, #31345, #77832, #196255, #197233, #13207, #58694, #120364, #182057, #43540, #105206, #28393, #151714, #136532, #121356, #50492, #187041, #157671, #96965, #2983, #109170, #33332, #18172, #155674, #142487, #78823, #48511, #112156, #190001, #32340, #125343, #17169, #140501, #982, #173845, #141499, #19160, #110165, #127307, #35311, #34325, #62657, #143469, #79829, #158645, #156678, #93993, #126324, #124336, #64662, #49493, #20137, #66638, #51475, #80808, #111155, #81782, #36291, #4953, #3965, #186032, #128301, #47514, #97947, #188021, #113137, #65645, #159639, #21135, #1990, #189018, #170849, #174827, #139499 ),
 ( #172844, #63669, #95986, #171844, #94992, #24153, #176837, #148490, #179843, #38308, #131307, #39303, #100962, #115144, #164659, #162647, #69641, #118153, #129293, #190989, #146466, #133308, #52465, #70649, #71641, #132315, #160647, #41314, #194007, #56475, #102974, #116144, #163659, #82790, #85804, #99963, #7958, #6950, #144472, #5956, #194997, #25162, #55470, #86804, #117140, #22139, #8981, #178835, #40303, #192997, #68630, #114123, #191980, #67634, #101979, #23143, #147490, #175825, #9981, #37298, #98957, #83789, #145469, #130286, #161647, #53467, #84787, #54474, #177835, #180837, #167640, #134325, #29136, #13943, #103975, #196010, #60437, #90773, #168614, #91755, #74635, #57485, #198970, #87796, #152457, #61431, #149481, #119155, #196996, #89798, #46274, #122112, #26154, #107930, #58463, #10977, #183801, #45289, #42314, #106941, #197976, #75609, #137288, #165654, #199966, #27152, #72650, #30114, #59446, #153449, #88799, #104968, #14947, #151480, #105955, #150492, #11989, #136301, #120130, #73652, #135324, #76607, #181821, #43300, #138285, #184788, #166655, #123103, #28156, #12971, #121119, #182813, #44296, #154450, #93763, #77602, #64426, #171612, #139273, #15943, #142249, #63431, #95750, #156438, #32106, #17937, #34092, #125107, #750, #16934, #1753, #62421, #141260, #185792, #155444, #110919, #65411, #124093, #170617, #47280, #108936, #31113, #172605, #186805, #79591, #78588, #126095, #157435, #94756, #92761, #18930, #48275, #80575, #140261, #109930, #33100, #2750, #187792, #49261, #3734, #127072, #188780, #50263, #111920, #173607, #35077, #169616, #106610, #136952, #198641, #58142, #167311, #409, #123746, #60107, #62081, #15602, #29782, #166325, #77260, #121775, #61094, #28807, #90447, #183468, #91418, #43961, #138929, #46935, #105623, #44954, #168285, #153105, #182480, #31765, #14609, #76265, #185445, #196673, #119810, #13615, #108594, #181495, #137943, #170271, #199627, #27822, #150156, #122767, #11657, #73323, #184456, #30775, #134994, #45936, #152132, #75282, #74310, #42973, #104636, #89464, #92422, #107591, #154108, #169269, #151153, #12643, #135977, #197648, #59114, #120779, #124762, #2406, #155100, #81215, #33745, #34735, #93414, #16594, #48922, #110576, #78242, #47934, #143896, #126729, #188432, #127729, #172257, #80234, #4378, #189431, #49910, #51892, #139913, #3396, #141905, #1404, #109588, #66062, #65071, #111576, #96393, #35727, #63083, #186458, #174259, #173260, #95405, #158080, #19571, #187454, #171271, #142896, #50906, #190416, #112564, #113551, #82204, #32759, #97374, #159060, #94410, #157091, #156091, #20554, #5377, #17588, #79248, #67061, #64085, #128719, #175245, #140919, #125754, #18587, #87229, #10401, #23565, #148911, #102399, #116567, #52881, #164086, #8393, #147915, #115574, #53899, #70068, #178256, #130725, #25585, #133732, #192417, #85213, #193418, #54893, #69058, #118576, #39717, #146903, #72058, #83217, #144892, #100391, #195425, #6374, #24576, #56902, #86225, #114555, #36710, #9401, #98372, #160070, #131736, #117564, #21557, #101380, #177261, #162069, #161069, #68054, #129708, #191404, #179264, #71067, #40729, #132733, #176253, #163071, #194421, #55891, #37724, #22564, #99386, #145890, #84210, #7373, #38733, #199504, #27697, #60970, #46811, #121650, #89338, #152006, #136829, #74185, #122644, #197525, #105500, #30648, #108470, #151030, #43836, #135855, #58994, #119688, #92302, #59983, #76142, #167186, #45816, #153985, #152981, #181372, #61958, #198512, #15482, #75157, #12521, #44827, #42850, #183345, #168161, #77139, #185320, #170148, #137820, #29658, #138808, #154976, #169143, #184334, #104515, #289, #166196, #16472, #106482, #123625, #107467, #78121, #139790, #120660, #31642, #182358, #93291, #58018, #28685, #90320, #13492, #91290, #14480, #111455, #20429, #98243, #112446, #142778, #62955, #158940, #124636, #159946, #18466, #174135, #65938, #21433, #83093 ),
 ( #35606, #186330, #127610, #36588, #47813, #171145, #172137, #64951, #1278, #97252, #109462, #32634, #33623, #94288, #82079, #143772, #155966, #5253, #173141, #189309, #50786, #17463, #175120, #79120, #140793, #66934, #34616, #128597, #63964, #80117, #190291, #126610, #81100, #125634, #2281, #96275, #95286, #48802, #187331, #51767, #110456, #156970, #113428, #141785, #3279, #188312, #49789, #157961, #19452, #4259, #179140, #129587, #53774, #176129, #9280, #54769, #37599, #52758, #71938, #146773, #163967, #86103, #114427, #147794, #133608, #8267, #99261, #38610, #23442, #160948, #70945, #84090, #192295, #117442, #195301, #22441, #130598, #145769, #7251, #6254, #40609, #69946, #162947, #115448, #132613, #102279, #39599, #67933, #148790, #85089, #25465, #161947, #68936, #131610, #191283, #193295, #116443, #87105, #56783, #118455, #180146, #178132, #10279, #164960, #194302, #101258, #24454, #177139, #26453, #41615, #103280, #144769, #55768, #100266, #122405, #165955, #14235, #184095, #45578, #151769, #12283, #119450, #197288, #149781, #75906, #28451, #61722, #138569, #104273, #182111, #43596, #11283, #42609, #47, #121414, #183107, #107231, #166948, #74925, #199264, #168902, #44588, #46571, #72957, #198268, #136588, #134626, #27455, #196310, #123390, #30408, #106245, #57780, #92054, #90087, #153744, #105262, #89097, #59744, #181135, #13262, #167927, #60731, #15239, #185082, #29427, #91058, #76898, #110969, #172653, #152745, #150788, #88095, #73948, #135617, #137581, #58751, #120420, #54289, #115961, #188828, #175636, #142302, #37110, #21954, #111968, #3782, #68445, #98769, #176649, #99779, #82603, #65459, #6766, #95800, #160463, #69451, #157486, #127122, #4768, #97763, #34141, #130099, #18979, #80625, #66455, #50312, #191796, #53277, #173660, #114956, #5773, #83604, #145283, #35127, #7768, #96779, #158468, #38125, #67448, #161464, #19956, #112953, #22954, #159450, #113937, #84602, #146281, #81598, #131118, #192807, #143282, #20946, #128117, #189820, #51292, #174646, #36111, #144284, #129106, #190805, #52279, #71455, #133120, #100773, #132123, #27970, #10793, #72461, #11804, #56283, #164476, #88611, #73468, #134135, #136119, #162456, #87613, #25970, #40107, #42131, #194809, #43116, #195824, #118972, #119951, #39117, #147299, #58282, #149299, #179656, #57295, #103792, #117965, #55281, #180655, #165472, #74453, #26968, #197795, #166472, #85612, #150307, #135141, #23957, #41126, #8788, #196815, #181636, #116952, #70458, #104784, #148299, #151299, #89610, #12788, #59261, #193816, #177649, #178644, #101785, #163473, #102790, #24970, #86616, #9793, #171425, #186613, #561, #137104, #48085, #92576, #31917, #199779, #138098, #154264, #62232, #14761, #109741, #17747, #76422, #169423, #77414, #139084, #153259, #2559, #123900, #107742, #156245, #167459, #28955, #184606, #32912, #90596, #108749, #94566, #170425, #198790, #79403, #93571, #141074, #120930, #15755, #1561, #182629, #185599, #61246, #46087, #45104, #44114, #105772, #152278, #63236, #155256, #122918, #13762, #75430, #30928, #60256, #121927, #47088, #183621, #106761, #16745, #78394, #140070, #124915, #168436, #29932, #91571, #129858, #161223, #158230, #112715, #20705, #82361, #96542, #146042, #144050, #51053, #99541, #110731, #172413, #127877, #114715, #33901, #52045, #53033, #113701, #142058, #22717, #175397, #37883, #84365, #97523, #145045, #64241, #67211, #81362, #189581, #188588, #125908, #187606, #176407, #6526, #36865, #68205, #98531, #3544, #190569, #160224, #21715, #174408, #50069, #95558, #173417, #49075, #83368, #4524, #157245, #18739, #80386, #19720, #143046, #65222, #126882, #111730, #159211, #5532, #191556, #66217, #35877, #34887, #128869, #164237, #166226, #192568, #117719, #56041, #70221, #72216, #24728, #73230, #25733, #149064, #150058, #69210, #177413, #88365, #194571, #9553, #87379, #133890, #101535, #85367, #10552, #195582 ),
 ( #180417, #57054, #27727, #89370, #162220, #118729, #115726, #41889, #103556, #147061, #38884, #165231, #26726, #196578, #130878, #42880, #11564, #102553, #54051, #134901, #86377, #58048, #148062, #23719, #179415, #100541, #71219, #40880, #119718, #181402, #104545, #7526, #8543, #131889, #193573, #55045, #116716, #178405, #39869, #163228, #132882, #168193, #123653, #15512, #171178, #32666, #105532, #92331, #59023, #154017, #138839, #28715, #120690, #185351, #77169, #93324, #16505, #199533, #182389, #46842, #12550, #319, #186363, #74216, #43867, #121682, #14512, #151059, #108501, #135884, #197555, #183378, #167218, #170181, #31675, #90352, #155008, #122675, #61987, #78153, #152037, #124667, #13522, #75187, #139821, #184364, #1310, #136859, #29690, #62989, #76173, #30679, #198545, #60015, #61003, #44860, #106515, #91321, #47843, #153012, #137853, #109496, #45845, #107498, #169174, #3306, #63992, #21462, #175149, #128627, #79151, #64979, #125663, #158968, #4286, #187361, #2311, #83124, #96302, #113456, #35635, #48830, #97280, #144800, #157988, #110483, #188339, #173167, #172166, #20460, #33651, #141813, #66967, #6283, #95312, #80143, #156997, #18495, #155997, #190320, #142806, #51797, #140822, #126637, #49818, #82110, #65967, #111482, #34643, #67961, #19479, #36617, #143801, #81125, #5284, #129616, #127637, #189337, #50815, #112472, #174165, #98274, #159975, #191311, #52787, #114456, #176158, #94319, #17493, #115479, #99291, #71967, #86133, #26484, #160977, #72986, #133641, #132644, #22471, #41645, #116474, #195332, #54799, #192323, #24483, #84119, #178163, #147825, #10310, #164990, #88126, #117472, #9311, #56812, #134655, #148820, #179170, #145798, #118486, #7281, #196341, #39628, #180177, #102307, #57809, #119480, #53804, #40638, #68965, #163996, #25493, #177167, #130627, #103310, #87136, #149810, #11316, #70976, #38640, #37628, #100297, #161975, #23471, #85120, #146804, #8297, #101288, #69975, #131643, #193325, #162978, #194332, #55800, #76930, #153775, #150816, #15270, #152776, #45610, #30439, #73978, #154771, #12313, #62746, #92086, #14268, #107262, #43627, #59775, #61751, #106273, #60763, #105290, #135647, #91089, #151799, #28481, #89128, #108262, #104302, #182143, #31433, #139586, #198298, #16268, #90115, #197317, #169942, #123419, #29457, #93087, #165985, #77919, #138599, #75937, #27485, #185112, #121444, #81, #183136, #58781, #167958, #120450, #44620, #137612, #46602, #1071, #181163, #122435, #199296, #42640, #166978, #13290, #184127, #74954, #136617, #168933, #82887, #141587, #97054, #189111, #144565, #6051, #78911, #65734, #32427, #127402, #112244, #2078, #94081, #158737, #50584, #66734, #190091, #172936, #155760, #20226, #186122, #173935, #159735, #47602, #17258, #95080, #188110, #124426, #81874, #109256, #170935, #156768, #140588, #143566, #5048, #63757, #128394, #96074, #35403, #51566, #125431, #98038, #187127, #48599, #113230, #157763, #174920, #110251, #3075, #36384, #49582, #4056, #171932, #33421, #34415, #18262, #79915, #64751, #21232, #126413, #111245, #19253, #80900, #142577, #41407, #176930, #37393, #195092, #148583, #102072, #52556, #38400, #99051, #132410, #177928, #160740, #175922, #56575, #69733, #86899, #9072, #22232, #70742, #118249, #131401, #83881, #161742, #146559, #145563, #194102, #7041, #115238, #40401, #179940, #68723, #53560, #130380, #192078, #129387, #163757, #191083, #100056, #103072, #101056, #162741, #25257, #8054, #54565, #178931, #10074, #24249, #26249, #114217, #39396, #116237, #23237, #55564, #84881, #133403, #85898, #117238, #71733, #193089, #147586, #164754, #87889, #149576, #67729, #137379, #105064, #88893, #14034, #152546, #108022, #199058, #169709, #200055, #119247, #121215, #75699, #196107, #74729, #180931, #182905, #60527, #150585, #42406, #59536, #181913, #184882, #107032, #122202, #168704, #57577, #167730, #198070, #44389, #104069, #28251, #61524 ),
 ( #166748, #76699, #31202, #89891, #106044, #29228, #90861, #43393, #92853, #183894, #45379, #46364, #165751, #27244, #136393, #123193, #12084, #30206, #11072, #91847, #73747, #72750, #153541, #134421, #135419, #15038, #138375, #197090, #58557, #151574, #120223, #13063, #36153, #128161, #4810, #96825, #3823, #35170, #188871, #32197, #80667, #50354, #112013, #18030, #78679, #185888, #63525, #16035, #142343, #94850, #189861, #66498, #170707, #48367, #110023, #65502, #126186, #19021, #17026, #33191, #158509, #79684, #34182, #140355, #47373, #64519, #125200, #1843, #62515, #81640, #77693, #155531, #51335, #112995, #171702, #174689, #186896, #124187, #143323, #19996, #173702, #139361, #156531, #109028, #127163, #187882, #93854, #141354, #154539, #2841, #842, #95843, #49349, #157527, #111011, #172697, #67492, #191839, #176693, #113980, #100814, #37152, #145327, #70497, #151092, #190846, #83649, #175678, #98812, #159494, #132165, #146322, #89403, #20989, #135917, #193856, #192850, #82644, #101825, #38167, #55321, #114999, #52323, #84645, #144327, #99822, #7811, #116992, #27760, #12583, #177689, #69495, #178687, #197588, #8829, #39157, #5816, #40148, #129149, #59054, #161507, #166261, #162497, #120721, #182420, #160506, #23997, #21996, #85654, #147341, #6809, #68487, #74248, #97805, #130142, #53320, #131160, #22999, #54329, #116000, #170211, #79183, #105562, #13553, #14543, #107527, #64023, #16534, #43899, #125693, #76203, #167248, #139850, #78181, #75219, #1339, #15541, #108532, #93353, #136891, #17524, #198577, #28747, #155039, #140853, #2342, #77199, #124698, #90383, #46872, #61032, #169204, #168222, #152068, #60046, #94348, #186395, #63019, #47872, #109525, #121713, #31704, #171207, #32697, #30711, #29719, #183406, #153043, #44889, #156027, #184394, #106546, #91351, #137882, #199563, #122704, #45874, #92360, #154046, #138868, #348, #62018, #123682, #185381, #98307, #21495, #143834, #145829, #172196, #97312, #35664, #49848, #51829, #4316, #52820, #5314, #128657, #129646, #48860, #157028, #67993, #174196, #189368, #66998, #113488, #81155, #65010, #190352, #175182, #84150, #36649, #37660, #160007, #80173, #50845, #83156, #110515, #144830, #33681, #7312, #65999, #6314, #191342, #68997, #187392, #141845, #114489, #95343, #176191, #99325, #126667, #18526, #161009, #22503, #3336, #188371, #158998, #111512, #173198, #34674, #96332, #158019, #19510, #142837, #127668, #112502, #20491, #82140, #130663, #150850, #163011, #192357, #26515, #103343, #100330, #165022, #102341, #195365, #180209, #23505, #104335, #162009, #12345, #41678, #164030, #56844, #193358, #9345, #11348, #55833, #88159, #85153, #166019, #146839, #53840, #149844, #25527, #118520, #54834, #71010, #73019, #117506, #10344, #116508, #8332, #40671, #101322, #178196, #38675, #57842, #115514, #131677, #181197, #89160, #147859, #27519, #39661, #70008, #119515, #134689, #196374, #177202, #24518, #86169, #42674, #87172, #132678, #194366, #179203, #148853, #72000, #133674, #43660, #15299, #62777, #137642, #105322, #167990, #152809, #90145, #76959, #13319, #121476, #46632, #124458, #167010, #59806, #151830, #74985, #135679, #108292, #122465, #186154, #197351, #109288, #169971, #168962, #58815, #77948, #14302, #31463, #91120, #28511, #60794, #120483, #75969, #184158, #93115, #1101, #47634, #153805, #170966, #61780, #136648, #199329, #138629, #182174, #154800, #198330, #32460, #45639, #16298, #110, #94113, #155792, #183169, #123448, #44652, #185141, #139615, #106304, #29487, #74008, #107291, #30468, #92117, #65764, #187159, #190118, #78943, #143595, #52587, #140619, #48631, #188142, #80931, #37422, #51593, #17289, #99082, #49613, #2109, #113258, #174950, #110283, #36412, #189140, #81902, #97084, #141618, #171964, #127433, #111276, #64783, #125463, #144593, #63790, #18293, #67757, #175953, #34445, #191113, #126444, #33452, #6079, #98066, #159765 ),
 ( #172967, #96104, #95111, #156800, #129415, #50613, #112272, #21260, #157793, #4086, #128422, #82915, #173964, #79948, #3106, #35431, #158767, #19283, #5078, #142607, #114247, #20256, #66761, #103100, #22262, #130411, #41433, #147613, #162765, #117265, #86927, #54589, #38430, #163783, #102098, #57603, #148609, #164781, #24275, #85924, #83911, #25284, #145594, #9100, #68754, #132435, #10101, #100086, #192110, #70767, #131429, #134447, #56602, #71761, #118276, #7073, #178957, #194127, #55590, #53592, #177953, #11101, #196132, #40427, #72777, #26275, #133431, #176961, #87917, #195119, #179967, #39421, #101080, #149604, #119272, #116262, #180955, #42432, #160772, #115268, #161771, #23266, #193115, #84910, #146589, #8083, #69760, #150613, #12109, #167755, #154564, #73772, #91872, #92877, #153565, #181938, #62541, #27272, #108048, #182932, #138398, #121238, #58581, #90885, #88921, #44415, #14060, #76722, #31228, #16060, #183918, #77718, #15062, #197114, #29253, #45403, #165778, #61547, #135445, #124215, #106069, #200079, #168727, #185913, #104095, #120247, #107056, #43420, #30231, #123216, #105090, #166776, #184906, #46390, #169733, #139384, #152571, #28277, #866, #89916, #151598, #13089, #74754, #136417, #198097, #75727, #59562, #137403, #199084, #60552, #122227, #109054, #143351, #20026, #17052, #81668, #19048, #112042, #96852, #140383, #21016, #78707, #129176, #158536, #80695, #173730, #110051, #126213, #128189, #172727, #127190, #171731, #1871, #157555, #18058, #94879, #155558, #174715, #170731, #48394, #97832, #5843, #64548, #82672, #156559, #63552, #36179, #189887, #4839, #32222, #79713, #125226, #35199, #142372, #186924, #33219, #159520, #49378, #66526, #188901, #141382, #50382, #144356, #111041, #2870, #187909, #34209, #95872, #51362, #3851, #65530, #113023, #67519, #47398, #93880, #145353, #6835, #52350, #132193, #131187, #86682, #114006, #71520, #55349, #116027, #194878, #38192, #175704, #193884, #117019, #98839, #178714, #54355, #24027, #8857, #22023, #9861, #160534, #56352, #70524, #177716, #85681, #68514, #23025, #40176, #69522, #100842, #191865, #83675, #192877, #176719, #53347, #37180, #163539, #130168, #115026, #148366, #190874, #101855, #99848, #147368, #39184, #161532, #84670, #146349, #162524, #25039, #133187, #7836, #81331, #2525, #79367, #98497, #173384, #190536, #112683, #141038, #174375, #160190, #34854, #64205, #65189, #50032, #187572, #35845, #110695, #18705, #144016, #21680, #125872, #157211, #49040, #172375, #32878, #5497, #19689, #83334, #94528, #6492, #67180, #66182, #156210, #175363, #111697, #128837, #188554, #33865, #158199, #17710, #96509, #143014, #52010, #145011, #68172, #51022, #129824, #159177, #95525, #4492, #97491, #80352, #113669, #142024, #191523, #127844, #36831, #20672, #53000, #171391, #3513, #82326, #126848, #189550, #102521, #192535, #84331, #149033, #179385, #57022, #180387, #163192, #146010, #87347, #176374, #40847, #150025, #37847, #7493, #85334, #178373, #134870, #10521, #114678, #11530, #99507, #69178, #147026, #39837, #196548, #72184, #161188, #22684, #8510, #130844, #133858, #195548, #54018, #118695, #86345, #164204, #25702, #115692, #88334, #177380, #38852, #41857, #148032, #103524, #100509, #193539, #165199, #101503, #194539, #162188, #23686, #24696, #70188, #131856, #55013, #26694, #116683, #9521, #73200, #71187, #132851, #56010, #117688, #25524, #165020, #8330, #56842, #26513, #88157, #194364, #54832, #162007, #39659, #192354, #118517, #71008, #104333, #181194, #146837, #24516, #86166, #53838, #85151, #42672, #164028, #87170, #149842, #9343, #117504, #41676, #11346, #148851, #89158, #115512, #40669, #179201, #193356, #195363, #147856, #196372, #10342, #71998, #73017, #177200, #100328, #134686, #102338, #132676, #133672, #180207, #55831, #70005, #103340, #57840, #27517, #119513, #166017, #150847, #12343, #38673, #130661, #23503, #131675 ) ),
 .UNSPECIFIED., .T., .F., .F. ) 
 B_SPLINE_SURFACE_WITH_KNOTS ( ( 4, 3, 4 ),
 ( 3, 2, 2, 2, 2, 2, 2, 2, 2, 2, 2, 2, 2, 2, 2, 2, 2, 2, 2, 2, 2, 2, 2, 2, 2, 2, 2, 2, 2, 2, 2, 2, 2, 2, 2, 2, 2, 2, 2, 2, 2, 2, 2, 2, 2, 2, 2, 2, 2, 2, 2, 2, 2, 2, 2, 2, 2, 2, 2, 2, 2, 2, 2, 2, 2, 2, 2, 2, 2, 2, 2, 2, 2, 2, 2, 2, 2, 2, 2, 2, 2, 2, 2, 2, 2, 2, 2, 2, 2, 2, 2, 2, 2, 2, 2, 2, 2, 2, 2, 2, 2, 2, 2, 2, 2, 2, 2, 2, 2, 2, 2, 2, 2, 2, 2, 2, 2, 2, 2, 2, 2, 2, 2, 2, 2, 2, 2, 2, 2, 2, 2, 2, 2, 2, 2, 2, 2, 2, 2, 2, 2, 2, 2, 2, 2, 2, 2, 2, 2, 2, 2, 2, 2, 2, 2, 2, 2, 2, 2, 2, 2, 2, 2, 2, 2, 2, 2, 2, 2, 2, 2, 2, 2, 2, 2, 2, 2, 2, 2, 2, 2, 2, 2, 2, 2, 2, 2, 2, 2, 2, 2, 2, 2, 2, 2, 2, 2, 2, 2, 2, 2, 2, 2, 2, 2, 2, 2, 2, 2, 2, 2, 2, 2, 2, 2, 2, 2, 2, 2, 2, 2, 2, 2, 2, 2, 2, 2, 2, 3 ),
 ( 0.000000000000000000, 0.5000000000000000000, 1.000000000000000000 ),
 ( 0.000000000000000000, 0.004385964912280701511, 0.008771929824561403022, 0.01315789473684210453, 0.01754385964912280604, 0.02192982456140350755, 0.02631578947368420907, 0.03070175438596491058, 0.03508771929824561209, 0.03947368421052631360, 0.04385964912280701511, 0.04824561403508771662, 0.05263157894736841813, 0.05701754385964911964, 0.06140350877192982115, 0.06578947368421052266, 0.07017543859649122417, 0.07456140350877192569, 0.07894736842105262720, 0.08333333333333332871, 0.08771929824561403022, 0.09210526315789473173, 0.09649122807017543324, 0.1008771929824561348, 0.1052631578947368363, 0.1096491228070175378, 0.1140350877192982393, 0.1184210526315789408, 0.1228070175438596423, 0.1271929824561403577, 0.1315789473684210453, 0.1359649122807017607, 0.1403508771929824483, 0.1447368421052631637, 0.1491228070175438514, 0.1535087719298245668, 0.1578947368421052544, 0.1622807017543859698, 0.1666666666666666574, 0.1710526315789473728, 0.1754385964912280604, 0.1798245614035087758, 0.1842105263157894635, 0.1885964912280701788, 0.1929824561403508665, 0.1973684210526315819, 0.2017543859649122695, 0.2061403508771929849, 0.2105263157894736725, 0.2149122807017543879, 0.2192982456140350755, 0.2236842105263157909, 0.2280701754385964786, 0.2324561403508771940, 0.2368421052631578816, 0.2412280701754385970, 0.2456140350877192846, 0.2500000000000000000, 0.2543859649122807154, 0.2587719298245614308, 0.2631578947368420907, 0.2675438596491228060, 0.2719298245614035214, 0.2763157894736842368, 0.2807017543859648967, 0.2850877192982456121, 0.2894736842105263275, 0.2938596491228070429, 0.2982456140350877027, 0.3026315789473684181, 0.3070175438596491335, 0.3114035087719298489, 0.3157894736842105088, 0.3201754385964912242, 0.3245614035087719396, 0.3289473684210526550, 0.3333333333333333148, 0.3377192982456140302, 0.3421052631578947456, 0.3464912280701754610, 0.3508771929824561209, 0.3552631578947368363, 0.3596491228070175517, 0.3640350877192982670, 0.3684210526315789269, 0.3728070175438596423, 0.3771929824561403577, 0.3815789473684210731, 0.3859649122807017330, 0.3903508771929824483, 0.3947368421052631637, 0.3991228070175438791, 0.4035087719298245390, 0.4078947368421052544, 0.4122807017543859698, 0.4166666666666666852, 0.4210526315789473450, 0.4254385964912280604, 0.4298245614035087758, 0.4342105263157894912, 0.4385964912280701511, 0.4429824561403508665, 0.4473684210526315819, 0.4517543859649122973, 0.4561403508771929571, 0.4605263157894736725, 0.4649122807017543879, 0.4692982456140351033, 0.4736842105263157632, 0.4780701754385964786, 0.4824561403508771940, 0.4868421052631579093, 0.4912280701754385692, 0.4956140350877192846, 0.5000000000000000000, 0.5043859649122807154, 0.5087719298245614308, 0.5131578947368421462, 0.5175438596491228616, 0.5219298245614034659, 0.5263157894736841813, 0.5307017543859648967, 0.5350877192982456121, 0.5394736842105263275, 0.5438596491228070429, 0.5482456140350877583, 0.5526315789473684736, 0.5570175438596490780, 0.5614035087719297934, 0.5657894736842105088, 0.5701754385964912242, 0.5745614035087719396, 0.5789473684210526550, 0.5833333333333333703, 0.5877192982456140857, 0.5921052631578946901, 0.5964912280701754055, 0.6008771929824561209, 0.6052631578947368363, 0.6096491228070175517, 0.6140350877192982670, 0.6184210526315789824, 0.6228070175438596978, 0.6271929824561403022, 0.6315789473684210176, 0.6359649122807017330, 0.6403508771929824483, 0.6447368421052631637, 0.6491228070175438791, 0.6535087719298245945, 0.6578947368421053099, 0.6622807017543859143, 0.6666666666666666297, 0.6710526315789473450, 0.6754385964912280604, 0.6798245614035087758, 0.6842105263157894912, 0.6885964912280702066, 0.6929824561403509220, 0.6973684210526315264, 0.7017543859649122417, 0.7061403508771929571, 0.7105263157894736725, 0.7149122807017543879, 0.7192982456140351033, 0.7236842105263158187, 0.7280701754385965341, 0.7324561403508771384, 0.7368421052631578538, 0.7412280701754385692, 0.7456140350877192846, 0.7500000000000000000, 0.7543859649122807154, 0.7587719298245614308, 0.7631578947368421462, 0.7675438596491228616, 0.7719298245614034659, 0.7763157894736841813, 0.7807017543859648967, 0.7850877192982456121, 0.7894736842105263275, 0.7938596491228070429, 0.7982456140350877583, 0.8026315789473684736, 0.8070175438596490780, 0.8114035087719297934, 0.8157894736842105088, 0.8201754385964912242, 0.8245614035087719396, 0.8289473684210526550, 0.8333333333333333703, 0.8377192982456140857, 0.8421052631578946901, 0.8464912280701754055, 0.8508771929824561209, 0.8552631578947368363, 0.8596491228070175517, 0.8640350877192982670, 0.8684210526315789824, 0.8728070175438596978, 0.8771929824561403022, 0.8815789473684210176, 0.8859649122807017330, 0.8903508771929824483, 0.8947368421052631637, 0.8991228070175438791, 0.9035087719298245945, 0.9078947368421053099, 0.9122807017543859143, 0.9166666666666666297, 0.9210526315789473450, 0.9254385964912280604, 0.9298245614035087758, 0.9342105263157894912, 0.9385964912280702066, 0.9429824561403509220, 0.9473684210526315264, 0.9517543859649122417, 0.9561403508771929571, 0.9605263157894736725, 0.9649122807017543879, 0.9692982456140351033, 0.9736842105263158187, 0.9780701754385965341, 0.9824561403508771384, 0.9868421052631578538, 0.9912280701754385692, 0.9956140350877192846, 1.000000000000000000 ),
 .UNSPECIFIED. ) 
 GEOMETRIC_REPRESENTATION_ITEM ( )  RATIONAL_B_SPLINE_SURFACE ( (
 ( 1.000000000000000000, 0.9659258262890683122, 1.000000000000000000, 0.9659258262890683122, 1.000000000000000000, 0.9659258262890683122, 1.000000000000000000, 0.9659258262890683122, 1.000000000000000000, 0.9659258262890683122, 1.000000000000000000, 0.9659258262890683122, 1.000000000000000000, 0.9659258262890683122, 1.000000000000000000, 0.9659258262890683122, 1.000000000000000000, 0.9659258262890683122, 1.000000000000000000, 0.9659258262890683122, 1.000000000000000000, 0.9659258262890683122, 1.000000000000000000, 0.9659258262890683122, 1.000000000000000000, 0.9659258262890683122, 1.000000000000000000, 0.9659258262890683122, 1.000000000000000000, 0.9659258262890683122, 1.000000000000000000, 0.9659258262890683122, 1.000000000000000000, 0.9659258262890683122, 1.000000000000000000, 0.9659258262890683122, 1.000000000000000000, 0.9659258262890683122, 1.000000000000000000, 0.9659258262890683122, 1.000000000000000000, 0.9659258262890683122, 1.000000000000000000, 0.9659258262890683122, 1.000000000000000000, 0.9659258262890683122, 1.000000000000000000, 0.9659258262890683122, 1.000000000000000000, 0.9659258262890683122, 1.000000000000000000, 0.9659258262890683122, 1.000000000000000000, 0.9659258262890683122, 1.000000000000000000, 0.9659258262890683122, 1.000000000000000000, 0.9659258262890683122, 1.000000000000000000, 0.9659258262890683122, 1.000000000000000000, 0.9659258262890683122, 1.000000000000000000, 0.9659258262890683122, 1.000000000000000000, 0.9659258262890683122, 1.000000000000000000, 0.9659258262890683122, 1.000000000000000000, 0.9659258262890683122, 1.000000000000000000, 0.9659258262890683122, 1.000000000000000000, 0.9659258262890683122, 1.000000000000000000, 0.9659258262890683122, 1.000000000000000000, 0.9659258262890683122, 1.000000000000000000, 0.9659258262890683122, 1.000000000000000000, 0.9659258262890683122, 1.000000000000000000, 0.9659258262890683122, 1.000000000000000000, 0.9659258262890683122, 1.000000000000000000, 0.9659258262890683122, 1.000000000000000000, 0.9659258262890683122, 1.000000000000000000, 0.9659258262890683122, 1.000000000000000000, 0.9659258262890683122, 1.000000000000000000, 0.9659258262890683122, 1.000000000000000000, 0.9659258262890683122, 1.000000000000000000, 0.9659258262890683122, 1.000000000000000000, 0.9659258262890683122, 1.000000000000000000, 0.9659258262890683122, 1.000000000000000000, 0.9659258262890683122, 1.000000000000000000, 0.9659258262890683122, 1.000000000000000000, 0.9659258262890683122, 1.000000000000000000, 0.9659258262890683122, 1.000000000000000000, 0.9659258262890683122, 1.000000000000000000, 0.9659258262890683122, 1.000000000000000000, 0.9659258262890683122, 1.000000000000000000, 0.9659258262890683122, 1.000000000000000000, 0.9659258262890683122, 1.000000000000000000, 0.9659258262890683122, 1.000000000000000000, 0.9659258262890683122, 1.000000000000000000, 0.9659258262890683122, 1.000000000000000000, 0.9659258262890683122, 1.000000000000000000, 0.9659258262890683122, 1.000000000000000000, 0.9659258262890683122, 1.000000000000000000, 0.9659258262890683122, 1.000000000000000000, 0.9659258262890683122, 1.000000000000000000, 0.9659258262890683122, 1.000000000000000000, 0.9659258262890683122, 1.000000000000000000, 0.9659258262890683122, 1.000000000000000000, 0.9659258262890683122, 1.000000000000000000, 0.9659258262890683122, 1.000000000000000000, 0.9659258262890683122, 1.000000000000000000, 0.9659258262890683122, 1.000000000000000000, 0.9659258262890683122, 1.000000000000000000, 0.9659258262890683122, 1.000000000000000000, 0.9659258262890683122, 1.000000000000000000, 0.9659258262890683122, 1.000000000000000000, 0.9659258262890683122, 1.000000000000000000, 0.9659258262890683122, 1.000000000000000000, 0.9659258262890683122, 1.000000000000000000, 0.9659258262890683122, 1.000000000000000000, 0.9659258262890683122, 1.000000000000000000, 0.9659258262890683122, 1.000000000000000000, 0.9659258262890683122, 1.000000000000000000, 0.9659258262890683122, 1.000000000000000000, 0.9659258262890683122, 1.000000000000000000, 0.9659258262890683122, 1.000000000000000000, 0.9659258262890683122, 1.000000000000000000, 0.9659258262890683122, 1.000000000000000000, 0.9659258262890683122, 1.000000000000000000, 0.9659258262890683122, 1.000000000000000000, 0.9659258262890683122, 1.000000000000000000, 0.9659258262890683122, 1.000000000000000000, 0.9659258262890683122, 1.000000000000000000, 0.9659258262890683122, 1.000000000000000000, 0.9659258262890683122, 1.000000000000000000, 0.9659258262890683122, 1.000000000000000000, 0.9659258262890683122, 1.000000000000000000, 0.9659258262890683122, 1.000000000000000000, 0.9659258262890683122, 1.000000000000000000, 0.9659258262890683122, 1.000000000000000000, 0.9659258262890683122, 1.000000000000000000, 0.9659258262890683122, 1.000000000000000000, 0.9659258262890683122, 1.000000000000000000, 0.9659258262890683122, 1.000000000000000000, 0.9659258262890683122, 1.000000000000000000, 0.9659258262890683122, 1.000000000000000000, 0.9659258262890683122, 1.000000000000000000, 0.9659258262890683122, 1.000000000000000000, 0.9659258262890683122, 1.000000000000000000, 0.9659258262890683122, 1.000000000000000000, 0.9659258262890683122, 1.000000000000000000, 0.9659258262890683122, 1.000000000000000000, 0.9659258262890683122, 1.000000000000000000, 0.9659258262890683122, 1.000000000000000000, 0.9659258262890683122, 1.000000000000000000, 0.9659258262890683122, 1.000000000000000000, 0.9659258262890683122, 1.000000000000000000, 0.9659258262890683122, 1.000000000000000000, 0.9659258262890683122, 1.000000000000000000, 0.9659258262890683122, 1.000000000000000000, 0.9659258262890683122, 1.000000000000000000, 0.9659258262890683122, 1.000000000000000000, 0.9659258262890683122, 1.000000000000000000, 0.9659258262890683122, 1.000000000000000000, 0.9659258262890683122, 1.000000000000000000, 0.9659258262890683122, 1.000000000000000000, 0.9659258262890683122, 1.000000000000000000, 0.9659258262890683122, 1.000000000000000000, 0.9659258262890683122, 1.000000000000000000, 0.9659258262890683122, 1.000000000000000000, 0.9659258262890683122, 1.000000000000000000, 0.9659258262890683122, 1.000000000000000000, 0.9659258262890683122, 1.000000000000000000, 0.9659258262890683122, 1.000000000000000000, 0.9659258262890683122, 1.000000000000000000, 0.9659258262890683122, 1.000000000000000000, 0.9659258262890683122, 1.000000000000000000, 0.9659258262890683122, 1.000000000000000000, 0.9659258262890683122, 1.000000000000000000, 0.9659258262890683122, 1.000000000000000000, 0.9659258262890683122, 1.000000000000000000, 0.9659258262890683122, 1.000000000000000000, 0.9659258262890683122, 1.000000000000000000, 0.9659258262890683122, 1.000000000000000000, 0.9659258262890683122, 1.000000000000000000, 0.9659258262890683122, 1.000000000000000000, 0.9659258262890683122, 1.000000000000000000, 0.9659258262890683122, 1.000000000000000000, 0.9659258262890683122, 1.000000000000000000, 0.9659258262890683122, 1.000000000000000000, 0.9659258262890683122, 1.000000000000000000, 0.9659258262890683122, 1.000000000000000000, 0.9659258262890683122, 1.000000000000000000, 0.9659258262890683122, 1.000000000000000000, 0.9659258262890683122, 1.000000000000000000, 0.9659258262890683122, 1.000000000000000000, 0.9659258262890683122, 1.000000000000000000, 0.9659258262890683122, 1.000000000000000000, 0.9659258262890683122, 1.000000000000000000, 0.9659258262890683122, 1.000000000000000000, 0.9659258262890683122, 1.000000000000000000, 0.9659258262890683122, 1.000000000000000000, 0.9659258262890683122, 1.000000000000000000, 0.9659258262890683122, 1.000000000000000000, 0.9659258262890683122, 1.000000000000000000, 0.9659258262890683122, 1.000000000000000000, 0.9659258262890683122, 1.000000000000000000, 0.9659258262890683122, 1.000000000000000000, 0.9659258262890683122, 1.000000000000000000, 0.9659258262890683122, 1.000000000000000000, 0.9659258262890683122, 1.000000000000000000, 0.9659258262890683122, 1.000000000000000000, 0.9659258262890683122, 1.000000000000000000, 0.9659258262890683122, 1.000000000000000000, 0.9659258262890683122, 1.000000000000000000, 0.9659258262890683122, 1.000000000000000000, 0.9659258262890683122, 1.000000000000000000, 0.9659258262890683122, 1.000000000000000000, 0.9659258262890683122, 1.000000000000000000, 0.9659258262890683122, 1.000000000000000000, 0.9659258262890683122, 1.000000000000000000, 0.9659258262890683122, 1.000000000000000000, 0.9659258262890683122, 1.000000000000000000, 0.9659258262890683122, 1.000000000000000000, 0.9659258262890683122, 1.000000000000000000, 0.9659258262890683122, 1.000000000000000000, 0.9659258262890683122, 1.000000000000000000, 0.9659258262890683122, 1.000000000000000000, 0.9659258262890683122, 1.000000000000000000, 0.9659258262890683122, 1.000000000000000000, 0.9659258262890683122, 1.000000000000000000, 0.9659258262890683122, 1.000000000000000000, 0.9659258262890683122, 1.000000000000000000, 0.9659258262890683122, 1.000000000000000000, 0.9659258262890683122, 1.000000000000000000, 0.9659258262890683122, 1.000000000000000000, 0.9659258262890683122, 1.000000000000000000, 0.9659258262890683122, 1.000000000000000000, 0.9659258262890683122, 1.000000000000000000, 0.9659258262890683122, 1.000000000000000000, 0.9659258262890683122, 1.000000000000000000, 0.9659258262890683122, 1.000000000000000000, 0.9659258262890683122, 1.000000000000000000, 0.9659258262890683122, 1.000000000000000000, 0.9659258262890683122, 1.000000000000000000, 0.9659258262890683122, 1.000000000000000000, 0.9659258262890683122, 1.000000000000000000, 0.9659258262890683122, 1.000000000000000000, 0.9659258262890683122, 1.000000000000000000, 0.9659258262890683122, 1.000000000000000000, 0.9659258262890683122, 1.000000000000000000, 0.9659258262890683122, 1.000000000000000000, 0.9659258262890683122, 1.000000000000000000, 0.9659258262890683122, 1.000000000000000000, 0.9659258262890683122, 1.000000000000000000, 0.9659258262890683122, 1.000000000000000000, 0.9659258262890683122, 1.000000000000000000, 0.9659258262890683122, 1.000000000000000000, 0.9659258262890683122, 1.000000000000000000, 0.9659258262890683122, 1.000000000000000000, 0.9659258262890683122, 1.000000000000000000, 0.9659258262890683122, 1.000000000000000000, 0.9659258262890683122, 1.000000000000000000, 0.9659258262890683122, 1.000000000000000000),
 ( 0.3333333333333333703, 0.3219752754296894559, 0.3333333333333333703, 0.3219752754296894559, 0.3333333333333333703, 0.3219752754296894559, 0.3333333333333333703, 0.3219752754296894559, 0.3333333333333333703, 0.3219752754296894559, 0.3333333333333333703, 0.3219752754296894559, 0.3333333333333333703, 0.3219752754296894559, 0.3333333333333333703, 0.3219752754296894559, 0.3333333333333333703, 0.3219752754296894559, 0.3333333333333333703, 0.3219752754296894559, 0.3333333333333333703, 0.3219752754296894559, 0.3333333333333333703, 0.3219752754296894559, 0.3333333333333333703, 0.3219752754296894559, 0.3333333333333333703, 0.3219752754296894559, 0.3333333333333333703, 0.3219752754296894559, 0.3333333333333333703, 0.3219752754296894559, 0.3333333333333333703, 0.3219752754296894559, 0.3333333333333333703, 0.3219752754296894559, 0.3333333333333333703, 0.3219752754296894559, 0.3333333333333333703, 0.3219752754296894559, 0.3333333333333333703, 0.3219752754296894559, 0.3333333333333333703, 0.3219752754296894559, 0.3333333333333333703, 0.3219752754296894559, 0.3333333333333333703, 0.3219752754296894559, 0.3333333333333333703, 0.3219752754296894559, 0.3333333333333333703, 0.3219752754296894559, 0.3333333333333333703, 0.3219752754296894559, 0.3333333333333333703, 0.3219752754296894559, 0.3333333333333333703, 0.3219752754296894559, 0.3333333333333333703, 0.3219752754296894559, 0.3333333333333333703, 0.3219752754296894559, 0.3333333333333333703, 0.3219752754296894559, 0.3333333333333333703, 0.3219752754296894559, 0.3333333333333333703, 0.3219752754296894559, 0.3333333333333333703, 0.3219752754296894559, 0.3333333333333333703, 0.3219752754296894559, 0.3333333333333333703, 0.3219752754296894559, 0.3333333333333333703, 0.3219752754296894559, 0.3333333333333333703, 0.3219752754296894559, 0.3333333333333333703, 0.3219752754296894559, 0.3333333333333333703, 0.3219752754296894559, 0.3333333333333333703, 0.3219752754296894559, 0.3333333333333333703, 0.3219752754296894559, 0.3333333333333333703, 0.3219752754296894559, 0.3333333333333333703, 0.3219752754296894559, 0.3333333333333333703, 0.3219752754296894559, 0.3333333333333333703, 0.3219752754296894559, 0.3333333333333333703, 0.3219752754296894559, 0.3333333333333333703, 0.3219752754296894559, 0.3333333333333333703, 0.3219752754296894559, 0.3333333333333333703, 0.3219752754296894559, 0.3333333333333333703, 0.3219752754296894559, 0.3333333333333333703, 0.3219752754296894559, 0.3333333333333333703, 0.3219752754296894559, 0.3333333333333333703, 0.3219752754296894559, 0.3333333333333333703, 0.3219752754296894559, 0.3333333333333333703, 0.3219752754296894559, 0.3333333333333333703, 0.3219752754296894559, 0.3333333333333333703, 0.3219752754296894559, 0.3333333333333333703, 0.3219752754296894559, 0.3333333333333333703, 0.3219752754296894559, 0.3333333333333333703, 0.3219752754296894559, 0.3333333333333333703, 0.3219752754296894559, 0.3333333333333333703, 0.3219752754296894559, 0.3333333333333333703, 0.3219752754296894559, 0.3333333333333333703, 0.3219752754296894559, 0.3333333333333333703, 0.3219752754296894559, 0.3333333333333333703, 0.3219752754296894559, 0.3333333333333333703, 0.3219752754296894559, 0.3333333333333333703, 0.3219752754296894559, 0.3333333333333333703, 0.3219752754296894559, 0.3333333333333333703, 0.3219752754296894559, 0.3333333333333333703, 0.3219752754296894559, 0.3333333333333333703, 0.3219752754296894559, 0.3333333333333333703, 0.3219752754296894559, 0.3333333333333333703, 0.3219752754296894559, 0.3333333333333333703, 0.3219752754296894559, 0.3333333333333333703, 0.3219752754296894559, 0.3333333333333333703, 0.3219752754296894559, 0.3333333333333333703, 0.3219752754296894559, 0.3333333333333333703, 0.3219752754296894559, 0.3333333333333333703, 0.3219752754296894559, 0.3333333333333333703, 0.3219752754296894559, 0.3333333333333333703, 0.3219752754296894559, 0.3333333333333333703, 0.3219752754296894559, 0.3333333333333333703, 0.3219752754296894559, 0.3333333333333333703, 0.3219752754296894559, 0.3333333333333333703, 0.3219752754296894559, 0.3333333333333333703, 0.3219752754296894559, 0.3333333333333333703, 0.3219752754296894559, 0.3333333333333333703, 0.3219752754296894559, 0.3333333333333333703, 0.3219752754296894559, 0.3333333333333333703, 0.3219752754296894559, 0.3333333333333333703, 0.3219752754296894559, 0.3333333333333333703, 0.3219752754296894559, 0.3333333333333333703, 0.3219752754296894559, 0.3333333333333333703, 0.3219752754296894559, 0.3333333333333333703, 0.3219752754296894559, 0.3333333333333333703, 0.3219752754296894559, 0.3333333333333333703, 0.3219752754296894559, 0.3333333333333333703, 0.3219752754296894559, 0.3333333333333333703, 0.3219752754296894559, 0.3333333333333333703, 0.3219752754296894559, 0.3333333333333333703, 0.3219752754296894559, 0.3333333333333333703, 0.3219752754296894559, 0.3333333333333333703, 0.3219752754296894559, 0.3333333333333333703, 0.3219752754296894559, 0.3333333333333333703, 0.3219752754296894559, 0.3333333333333333703, 0.3219752754296894559, 0.3333333333333333703, 0.3219752754296894559, 0.3333333333333333703, 0.3219752754296894559, 0.3333333333333333703, 0.3219752754296894559, 0.3333333333333333703, 0.3219752754296894559, 0.3333333333333333703, 0.3219752754296894559, 0.3333333333333333703, 0.3219752754296894559, 0.3333333333333333703, 0.3219752754296894559, 0.3333333333333333703, 0.3219752754296894559, 0.3333333333333333703, 0.3219752754296894559, 0.3333333333333333703, 0.3219752754296894559, 0.3333333333333333703, 0.3219752754296894559, 0.3333333333333333703, 0.3219752754296894559, 0.3333333333333333703, 0.3219752754296894559, 0.3333333333333333703, 0.3219752754296894559, 0.3333333333333333703, 0.3219752754296894559, 0.3333333333333333703, 0.3219752754296894559, 0.3333333333333333703, 0.3219752754296894559, 0.3333333333333333703, 0.3219752754296894559, 0.3333333333333333703, 0.3219752754296894559, 0.3333333333333333703, 0.3219752754296894559, 0.3333333333333333703, 0.3219752754296894559, 0.3333333333333333703, 0.3219752754296894559, 0.3333333333333333703, 0.3219752754296894559, 0.3333333333333333703, 0.3219752754296894559, 0.3333333333333333703, 0.3219752754296894559, 0.3333333333333333703, 0.3219752754296894559, 0.3333333333333333703, 0.3219752754296894559, 0.3333333333333333703, 0.3219752754296894559, 0.3333333333333333703, 0.3219752754296894559, 0.3333333333333333703, 0.3219752754296894559, 0.3333333333333333703, 0.3219752754296894559, 0.3333333333333333703, 0.3219752754296894559, 0.3333333333333333703, 0.3219752754296894559, 0.3333333333333333703, 0.3219752754296894559, 0.3333333333333333703, 0.3219752754296894559, 0.3333333333333333703, 0.3219752754296894559, 0.3333333333333333703, 0.3219752754296894559, 0.3333333333333333703, 0.3219752754296894559, 0.3333333333333333703, 0.3219752754296894559, 0.3333333333333333703, 0.3219752754296894559, 0.3333333333333333703, 0.3219752754296894559, 0.3333333333333333703, 0.3219752754296894559, 0.3333333333333333703, 0.3219752754296894559, 0.3333333333333333703, 0.3219752754296894559, 0.3333333333333333703, 0.3219752754296894559, 0.3333333333333333703, 0.3219752754296894559, 0.3333333333333333703, 0.3219752754296894559, 0.3333333333333333703, 0.3219752754296894559, 0.3333333333333333703, 0.3219752754296894559, 0.3333333333333333703, 0.3219752754296894559, 0.3333333333333333703, 0.3219752754296894559, 0.3333333333333333703, 0.3219752754296894559, 0.3333333333333333703, 0.3219752754296894559, 0.3333333333333333703, 0.3219752754296894559, 0.3333333333333333703, 0.3219752754296894559, 0.3333333333333333703, 0.3219752754296894559, 0.3333333333333333703, 0.3219752754296894559, 0.3333333333333333703, 0.3219752754296894559, 0.3333333333333333703, 0.3219752754296894559, 0.3333333333333333703, 0.3219752754296894559, 0.3333333333333333703, 0.3219752754296894559, 0.3333333333333333703, 0.3219752754296894559, 0.3333333333333333703, 0.3219752754296894559, 0.3333333333333333703, 0.3219752754296894559, 0.3333333333333333703, 0.3219752754296894559, 0.3333333333333333703, 0.3219752754296894559, 0.3333333333333333703, 0.3219752754296894559, 0.3333333333333333703, 0.3219752754296894559, 0.3333333333333333703, 0.3219752754296894559, 0.3333333333333333703, 0.3219752754296894559, 0.3333333333333333703, 0.3219752754296894559, 0.3333333333333333703, 0.3219752754296894559, 0.3333333333333333703, 0.3219752754296894559, 0.3333333333333333703, 0.3219752754296894559, 0.3333333333333333703, 0.3219752754296894559, 0.3333333333333333703, 0.3219752754296894559, 0.3333333333333333703, 0.3219752754296894559, 0.3333333333333333703, 0.3219752754296894559, 0.3333333333333333703, 0.3219752754296894559, 0.3333333333333333703, 0.3219752754296894559, 0.3333333333333333703, 0.3219752754296894559, 0.3333333333333333703, 0.3219752754296894559, 0.3333333333333333703, 0.3219752754296894559, 0.3333333333333333703, 0.3219752754296894559, 0.3333333333333333703, 0.3219752754296894559, 0.3333333333333333703, 0.3219752754296894559, 0.3333333333333333703, 0.3219752754296894559, 0.3333333333333333703, 0.3219752754296894559, 0.3333333333333333703, 0.3219752754296894559, 0.3333333333333333703, 0.3219752754296894559, 0.3333333333333333703, 0.3219752754296894559, 0.3333333333333333703, 0.3219752754296894559, 0.3333333333333333703, 0.3219752754296894559, 0.3333333333333333703, 0.3219752754296894559, 0.3333333333333333703, 0.3219752754296894559, 0.3333333333333333703, 0.3219752754296894559, 0.3333333333333333703, 0.3219752754296894559, 0.3333333333333333703, 0.3219752754296894559, 0.3333333333333333703, 0.3219752754296894559, 0.3333333333333333703, 0.3219752754296894559, 0.3333333333333333703, 0.3219752754296894559, 0.3333333333333333703, 0.3219752754296894559, 0.3333333333333333703, 0.3219752754296894559, 0.3333333333333333703, 0.3219752754296894559, 0.3333333333333333703, 0.3219752754296894559, 0.3333333333333333703, 0.3219752754296894559, 0.3333333333333333703, 0.3219752754296894559, 0.3333333333333333703, 0.3219752754296894559, 0.3333333333333333703, 0.3219752754296894559, 0.3333333333333333703, 0.3219752754296894559, 0.3333333333333333703, 0.3219752754296894559, 0.3333333333333333703, 0.3219752754296894559, 0.3333333333333333703, 0.3219752754296894559, 0.3333333333333333703, 0.3219752754296894559, 0.3333333333333333703, 0.3219752754296894559, 0.3333333333333333703, 0.3219752754296894559, 0.3333333333333333703, 0.3219752754296894559, 0.3333333333333333703, 0.3219752754296894559, 0.3333333333333333703, 0.3219752754296894559, 0.3333333333333333703),
 ( 0.3333333333333333703, 0.3219752754296894559, 0.3333333333333333703, 0.3219752754296894559, 0.3333333333333333703, 0.3219752754296894559, 0.3333333333333333703, 0.3219752754296894559, 0.3333333333333333703, 0.3219752754296894559, 0.3333333333333333703, 0.3219752754296894559, 0.3333333333333333703, 0.3219752754296894559, 0.3333333333333333703, 0.3219752754296894559, 0.3333333333333333703, 0.3219752754296894559, 0.3333333333333333703, 0.3219752754296894559, 0.3333333333333333703, 0.3219752754296894559, 0.3333333333333333703, 0.3219752754296894559, 0.3333333333333333703, 0.3219752754296894559, 0.3333333333333333703, 0.3219752754296894559, 0.3333333333333333703, 0.3219752754296894559, 0.3333333333333333703, 0.3219752754296894559, 0.3333333333333333703, 0.3219752754296894559, 0.3333333333333333703, 0.3219752754296894559, 0.3333333333333333703, 0.3219752754296894559, 0.3333333333333333703, 0.3219752754296894559, 0.3333333333333333703, 0.3219752754296894559, 0.3333333333333333703, 0.3219752754296894559, 0.3333333333333333703, 0.3219752754296894559, 0.3333333333333333703, 0.3219752754296894559, 0.3333333333333333703, 0.3219752754296894559, 0.3333333333333333703, 0.3219752754296894559, 0.3333333333333333703, 0.3219752754296894559, 0.3333333333333333703, 0.3219752754296894559, 0.3333333333333333703, 0.3219752754296894559, 0.3333333333333333703, 0.3219752754296894559, 0.3333333333333333703, 0.3219752754296894559, 0.3333333333333333703, 0.3219752754296894559, 0.3333333333333333703, 0.3219752754296894559, 0.3333333333333333703, 0.3219752754296894559, 0.3333333333333333703, 0.3219752754296894559, 0.3333333333333333703, 0.3219752754296894559, 0.3333333333333333703, 0.3219752754296894559, 0.3333333333333333703, 0.3219752754296894559, 0.3333333333333333703, 0.3219752754296894559, 0.3333333333333333703, 0.3219752754296894559, 0.3333333333333333703, 0.3219752754296894559, 0.3333333333333333703, 0.3219752754296894559, 0.3333333333333333703, 0.3219752754296894559, 0.3333333333333333703, 0.3219752754296894559, 0.3333333333333333703, 0.3219752754296894559, 0.3333333333333333703, 0.3219752754296894559, 0.3333333333333333703, 0.3219752754296894559, 0.3333333333333333703, 0.3219752754296894559, 0.3333333333333333703, 0.3219752754296894559, 0.3333333333333333703, 0.3219752754296894559, 0.3333333333333333703, 0.3219752754296894559, 0.3333333333333333703, 0.3219752754296894559, 0.3333333333333333703, 0.3219752754296894559, 0.3333333333333333703, 0.3219752754296894559, 0.3333333333333333703, 0.3219752754296894559, 0.3333333333333333703, 0.3219752754296894559, 0.3333333333333333703, 0.3219752754296894559, 0.3333333333333333703, 0.3219752754296894559, 0.3333333333333333703, 0.3219752754296894559, 0.3333333333333333703, 0.3219752754296894559, 0.3333333333333333703, 0.3219752754296894559, 0.3333333333333333703, 0.3219752754296894559, 0.3333333333333333703, 0.3219752754296894559, 0.3333333333333333703, 0.3219752754296894559, 0.3333333333333333703, 0.3219752754296894559, 0.3333333333333333703, 0.3219752754296894559, 0.3333333333333333703, 0.3219752754296894559, 0.3333333333333333703, 0.3219752754296894559, 0.3333333333333333703, 0.3219752754296894559, 0.3333333333333333703, 0.3219752754296894559, 0.3333333333333333703, 0.3219752754296894559, 0.3333333333333333703, 0.3219752754296894559, 0.3333333333333333703, 0.3219752754296894559, 0.3333333333333333703, 0.3219752754296894559, 0.3333333333333333703, 0.3219752754296894559, 0.3333333333333333703, 0.3219752754296894559, 0.3333333333333333703, 0.3219752754296894559, 0.3333333333333333703, 0.3219752754296894559, 0.3333333333333333703, 0.3219752754296894559, 0.3333333333333333703, 0.3219752754296894559, 0.3333333333333333703, 0.3219752754296894559, 0.3333333333333333703, 0.3219752754296894559, 0.3333333333333333703, 0.3219752754296894559, 0.3333333333333333703, 0.3219752754296894559, 0.3333333333333333703, 0.3219752754296894559, 0.3333333333333333703, 0.3219752754296894559, 0.3333333333333333703, 0.3219752754296894559, 0.3333333333333333703, 0.3219752754296894559, 0.3333333333333333703, 0.3219752754296894559, 0.3333333333333333703, 0.3219752754296894559, 0.3333333333333333703, 0.3219752754296894559, 0.3333333333333333703, 0.3219752754296894559, 0.3333333333333333703, 0.3219752754296894559, 0.3333333333333333703, 0.3219752754296894559, 0.3333333333333333703, 0.3219752754296894559, 0.3333333333333333703, 0.3219752754296894559, 0.3333333333333333703, 0.3219752754296894559, 0.3333333333333333703, 0.3219752754296894559, 0.3333333333333333703, 0.3219752754296894559, 0.3333333333333333703, 0.3219752754296894559, 0.3333333333333333703, 0.3219752754296894559, 0.3333333333333333703, 0.3219752754296894559, 0.3333333333333333703, 0.3219752754296894559, 0.3333333333333333703, 0.3219752754296894559, 0.3333333333333333703, 0.3219752754296894559, 0.3333333333333333703, 0.3219752754296894559, 0.3333333333333333703, 0.3219752754296894559, 0.3333333333333333703, 0.3219752754296894559, 0.3333333333333333703, 0.3219752754296894559, 0.3333333333333333703, 0.3219752754296894559, 0.3333333333333333703, 0.3219752754296894559, 0.3333333333333333703, 0.3219752754296894559, 0.3333333333333333703, 0.3219752754296894559, 0.3333333333333333703, 0.3219752754296894559, 0.3333333333333333703, 0.3219752754296894559, 0.3333333333333333703, 0.3219752754296894559, 0.3333333333333333703, 0.3219752754296894559, 0.3333333333333333703, 0.3219752754296894559, 0.3333333333333333703, 0.3219752754296894559, 0.3333333333333333703, 0.3219752754296894559, 0.3333333333333333703, 0.3219752754296894559, 0.3333333333333333703, 0.3219752754296894559, 0.3333333333333333703, 0.3219752754296894559, 0.3333333333333333703, 0.3219752754296894559, 0.3333333333333333703, 0.3219752754296894559, 0.3333333333333333703, 0.3219752754296894559, 0.3333333333333333703, 0.3219752754296894559, 0.3333333333333333703, 0.3219752754296894559, 0.3333333333333333703, 0.3219752754296894559, 0.3333333333333333703, 0.3219752754296894559, 0.3333333333333333703, 0.3219752754296894559, 0.3333333333333333703, 0.3219752754296894559, 0.3333333333333333703, 0.3219752754296894559, 0.3333333333333333703, 0.3219752754296894559, 0.3333333333333333703, 0.3219752754296894559, 0.3333333333333333703, 0.3219752754296894559, 0.3333333333333333703, 0.3219752754296894559, 0.3333333333333333703, 0.3219752754296894559, 0.3333333333333333703, 0.3219752754296894559, 0.3333333333333333703, 0.3219752754296894559, 0.3333333333333333703, 0.3219752754296894559, 0.3333333333333333703, 0.3219752754296894559, 0.3333333333333333703, 0.3219752754296894559, 0.3333333333333333703, 0.3219752754296894559, 0.3333333333333333703, 0.3219752754296894559, 0.3333333333333333703, 0.3219752754296894559, 0.3333333333333333703, 0.3219752754296894559, 0.3333333333333333703, 0.3219752754296894559, 0.3333333333333333703, 0.3219752754296894559, 0.3333333333333333703, 0.3219752754296894559, 0.3333333333333333703, 0.3219752754296894559, 0.3333333333333333703, 0.3219752754296894559, 0.3333333333333333703, 0.3219752754296894559, 0.3333333333333333703, 0.3219752754296894559, 0.3333333333333333703, 0.3219752754296894559, 0.3333333333333333703, 0.3219752754296894559, 0.3333333333333333703, 0.3219752754296894559, 0.3333333333333333703, 0.3219752754296894559, 0.3333333333333333703, 0.3219752754296894559, 0.3333333333333333703, 0.3219752754296894559, 0.3333333333333333703, 0.3219752754296894559, 0.3333333333333333703, 0.3219752754296894559, 0.3333333333333333703, 0.3219752754296894559, 0.3333333333333333703, 0.3219752754296894559, 0.3333333333333333703, 0.3219752754296894559, 0.3333333333333333703, 0.3219752754296894559, 0.3333333333333333703, 0.3219752754296894559, 0.3333333333333333703, 0.3219752754296894559, 0.3333333333333333703, 0.3219752754296894559, 0.3333333333333333703, 0.3219752754296894559, 0.3333333333333333703, 0.3219752754296894559, 0.3333333333333333703, 0.3219752754296894559, 0.3333333333333333703, 0.3219752754296894559, 0.3333333333333333703, 0.3219752754296894559, 0.3333333333333333703, 0.3219752754296894559, 0.3333333333333333703, 0.3219752754296894559, 0.3333333333333333703, 0.3219752754296894559, 0.3333333333333333703, 0.3219752754296894559, 0.3333333333333333703, 0.3219752754296894559, 0.3333333333333333703, 0.3219752754296894559, 0.3333333333333333703, 0.3219752754296894559, 0.3333333333333333703, 0.3219752754296894559, 0.3333333333333333703, 0.3219752754296894559, 0.3333333333333333703, 0.3219752754296894559, 0.3333333333333333703, 0.3219752754296894559, 0.3333333333333333703, 0.3219752754296894559, 0.3333333333333333703, 0.3219752754296894559, 0.3333333333333333703, 0.3219752754296894559, 0.3333333333333333703, 0.3219752754296894559, 0.3333333333333333703, 0.3219752754296894559, 0.3333333333333333703, 0.3219752754296894559, 0.3333333333333333703, 0.3219752754296894559, 0.3333333333333333703, 0.3219752754296894559, 0.3333333333333333703, 0.3219752754296894559, 0.3333333333333333703, 0.3219752754296894559, 0.3333333333333333703, 0.3219752754296894559, 0.3333333333333333703, 0.3219752754296894559, 0.3333333333333333703, 0.3219752754296894559, 0.3333333333333333703, 0.3219752754296894559, 0.3333333333333333703, 0.3219752754296894559, 0.3333333333333333703, 0.3219752754296894559, 0.3333333333333333703, 0.3219752754296894559, 0.3333333333333333703, 0.3219752754296894559, 0.3333333333333333703, 0.3219752754296894559, 0.3333333333333333703, 0.3219752754296894559, 0.3333333333333333703, 0.3219752754296894559, 0.3333333333333333703, 0.3219752754296894559, 0.3333333333333333703, 0.3219752754296894559, 0.3333333333333333703, 0.3219752754296894559, 0.3333333333333333703, 0.3219752754296894559, 0.3333333333333333703, 0.3219752754296894559, 0.3333333333333333703, 0.3219752754296894559, 0.3333333333333333703, 0.3219752754296894559, 0.3333333333333333703, 0.3219752754296894559, 0.3333333333333333703, 0.3219752754296894559, 0.3333333333333333703, 0.3219752754296894559, 0.3333333333333333703, 0.3219752754296894559, 0.3333333333333333703, 0.3219752754296894559, 0.3333333333333333703, 0.3219752754296894559, 0.3333333333333333703, 0.3219752754296894559, 0.3333333333333333703, 0.3219752754296894559, 0.3333333333333333703, 0.3219752754296894559, 0.3333333333333333703, 0.3219752754296894559, 0.3333333333333333703, 0.3219752754296894559, 0.3333333333333333703, 0.3219752754296894559, 0.3333333333333333703, 0.3219752754296894559, 0.3333333333333333703, 0.3219752754296894559, 0.3333333333333333703, 0.3219752754296894559, 0.3333333333333333703),
 ( 1.000000000000000000, 0.9659258262890683122, 1.000000000000000000, 0.9659258262890683122, 1.000000000000000000, 0.9659258262890683122, 1.000000000000000000, 0.9659258262890683122, 1.000000000000000000, 0.9659258262890683122, 1.000000000000000000, 0.9659258262890683122, 1.000000000000000000, 0.9659258262890683122, 1.000000000000000000, 0.9659258262890683122, 1.000000000000000000, 0.9659258262890683122, 1.000000000000000000, 0.9659258262890683122, 1.000000000000000000, 0.9659258262890683122, 1.000000000000000000, 0.9659258262890683122, 1.000000000000000000, 0.9659258262890683122, 1.000000000000000000, 0.9659258262890683122, 1.000000000000000000, 0.9659258262890683122, 1.000000000000000000, 0.9659258262890683122, 1.000000000000000000, 0.9659258262890683122, 1.000000000000000000, 0.9659258262890683122, 1.000000000000000000, 0.9659258262890683122, 1.000000000000000000, 0.9659258262890683122, 1.000000000000000000, 0.9659258262890683122, 1.000000000000000000, 0.9659258262890683122, 1.000000000000000000, 0.9659258262890683122, 1.000000000000000000, 0.9659258262890683122, 1.000000000000000000, 0.9659258262890683122, 1.000000000000000000, 0.9659258262890683122, 1.000000000000000000, 0.9659258262890683122, 1.000000000000000000, 0.9659258262890683122, 1.000000000000000000, 0.9659258262890683122, 1.000000000000000000, 0.9659258262890683122, 1.000000000000000000, 0.9659258262890683122, 1.000000000000000000, 0.9659258262890683122, 1.000000000000000000, 0.9659258262890683122, 1.000000000000000000, 0.9659258262890683122, 1.000000000000000000, 0.9659258262890683122, 1.000000000000000000, 0.9659258262890683122, 1.000000000000000000, 0.9659258262890683122, 1.000000000000000000, 0.9659258262890683122, 1.000000000000000000, 0.9659258262890683122, 1.000000000000000000, 0.9659258262890683122, 1.000000000000000000, 0.9659258262890683122, 1.000000000000000000, 0.9659258262890683122, 1.000000000000000000, 0.9659258262890683122, 1.000000000000000000, 0.9659258262890683122, 1.000000000000000000, 0.9659258262890683122, 1.000000000000000000, 0.9659258262890683122, 1.000000000000000000, 0.9659258262890683122, 1.000000000000000000, 0.9659258262890683122, 1.000000000000000000, 0.9659258262890683122, 1.000000000000000000, 0.9659258262890683122, 1.000000000000000000, 0.9659258262890683122, 1.000000000000000000, 0.9659258262890683122, 1.000000000000000000, 0.9659258262890683122, 1.000000000000000000, 0.9659258262890683122, 1.000000000000000000, 0.9659258262890683122, 1.000000000000000000, 0.9659258262890683122, 1.000000000000000000, 0.9659258262890683122, 1.000000000000000000, 0.9659258262890683122, 1.000000000000000000, 0.9659258262890683122, 1.000000000000000000, 0.9659258262890683122, 1.000000000000000000, 0.9659258262890683122, 1.000000000000000000, 0.9659258262890683122, 1.000000000000000000, 0.9659258262890683122, 1.000000000000000000, 0.9659258262890683122, 1.000000000000000000, 0.9659258262890683122, 1.000000000000000000, 0.9659258262890683122, 1.000000000000000000, 0.9659258262890683122, 1.000000000000000000, 0.9659258262890683122, 1.000000000000000000, 0.9659258262890683122, 1.000000000000000000, 0.9659258262890683122, 1.000000000000000000, 0.9659258262890683122, 1.000000000000000000, 0.9659258262890683122, 1.000000000000000000, 0.9659258262890683122, 1.000000000000000000, 0.9659258262890683122, 1.000000000000000000, 0.9659258262890683122, 1.000000000000000000, 0.9659258262890683122, 1.000000000000000000, 0.9659258262890683122, 1.000000000000000000, 0.9659258262890683122, 1.000000000000000000, 0.9659258262890683122, 1.000000000000000000, 0.9659258262890683122, 1.000000000000000000, 0.9659258262890683122, 1.000000000000000000, 0.9659258262890683122, 1.000000000000000000, 0.9659258262890683122, 1.000000000000000000, 0.9659258262890683122, 1.000000000000000000, 0.9659258262890683122, 1.000000000000000000, 0.9659258262890683122, 1.000000000000000000, 0.9659258262890683122, 1.000000000000000000, 0.9659258262890683122, 1.000000000000000000, 0.9659258262890683122, 1.000000000000000000, 0.9659258262890683122, 1.000000000000000000, 0.9659258262890683122, 1.000000000000000000, 0.9659258262890683122, 1.000000000000000000, 0.9659258262890683122, 1.000000000000000000, 0.9659258262890683122, 1.000000000000000000, 0.9659258262890683122, 1.000000000000000000, 0.9659258262890683122, 1.000000000000000000, 0.9659258262890683122, 1.000000000000000000, 0.9659258262890683122, 1.000000000000000000, 0.9659258262890683122, 1.000000000000000000, 0.9659258262890683122, 1.000000000000000000, 0.9659258262890683122, 1.000000000000000000, 0.9659258262890683122, 1.000000000000000000, 0.9659258262890683122, 1.000000000000000000, 0.9659258262890683122, 1.000000000000000000, 0.9659258262890683122, 1.000000000000000000, 0.9659258262890683122, 1.000000000000000000, 0.9659258262890683122, 1.000000000000000000, 0.9659258262890683122, 1.000000000000000000, 0.9659258262890683122, 1.000000000000000000, 0.9659258262890683122, 1.000000000000000000, 0.9659258262890683122, 1.000000000000000000, 0.9659258262890683122, 1.000000000000000000, 0.9659258262890683122, 1.000000000000000000, 0.9659258262890683122, 1.000000000000000000, 0.9659258262890683122, 1.000000000000000000, 0.9659258262890683122, 1.000000000000000000, 0.9659258262890683122, 1.000000000000000000, 0.9659258262890683122, 1.000000000000000000, 0.9659258262890683122, 1.000000000000000000, 0.9659258262890683122, 1.000000000000000000, 0.9659258262890683122, 1.000000000000000000, 0.9659258262890683122, 1.000000000000000000, 0.9659258262890683122, 1.000000000000000000, 0.9659258262890683122, 1.000000000000000000, 0.9659258262890683122, 1.000000000000000000, 0.9659258262890683122, 1.000000000000000000, 0.9659258262890683122, 1.000000000000000000, 0.9659258262890683122, 1.000000000000000000, 0.9659258262890683122, 1.000000000000000000, 0.9659258262890683122, 1.000000000000000000, 0.9659258262890683122, 1.000000000000000000, 0.9659258262890683122, 1.000000000000000000, 0.9659258262890683122, 1.000000000000000000, 0.9659258262890683122, 1.000000000000000000, 0.9659258262890683122, 1.000000000000000000, 0.9659258262890683122, 1.000000000000000000, 0.9659258262890683122, 1.000000000000000000, 0.9659258262890683122, 1.000000000000000000, 0.9659258262890683122, 1.000000000000000000, 0.9659258262890683122, 1.000000000000000000, 0.9659258262890683122, 1.000000000000000000, 0.9659258262890683122, 1.000000000000000000, 0.9659258262890683122, 1.000000000000000000, 0.9659258262890683122, 1.000000000000000000, 0.9659258262890683122, 1.000000000000000000, 0.9659258262890683122, 1.000000000000000000, 0.9659258262890683122, 1.000000000000000000, 0.9659258262890683122, 1.000000000000000000, 0.9659258262890683122, 1.000000000000000000, 0.9659258262890683122, 1.000000000000000000, 0.9659258262890683122, 1.000000000000000000, 0.9659258262890683122, 1.000000000000000000, 0.9659258262890683122, 1.000000000000000000, 0.9659258262890683122, 1.000000000000000000, 0.9659258262890683122, 1.000000000000000000, 0.9659258262890683122, 1.000000000000000000, 0.9659258262890683122, 1.000000000000000000, 0.9659258262890683122, 1.000000000000000000, 0.9659258262890683122, 1.000000000000000000, 0.9659258262890683122, 1.000000000000000000, 0.9659258262890683122, 1.000000000000000000, 0.9659258262890683122, 1.000000000000000000, 0.9659258262890683122, 1.000000000000000000, 0.9659258262890683122, 1.000000000000000000, 0.9659258262890683122, 1.000000000000000000, 0.9659258262890683122, 1.000000000000000000, 0.9659258262890683122, 1.000000000000000000, 0.9659258262890683122, 1.000000000000000000, 0.9659258262890683122, 1.000000000000000000, 0.9659258262890683122, 1.000000000000000000, 0.9659258262890683122, 1.000000000000000000, 0.9659258262890683122, 1.000000000000000000, 0.9659258262890683122, 1.000000000000000000, 0.9659258262890683122, 1.000000000000000000, 0.9659258262890683122, 1.000000000000000000, 0.9659258262890683122, 1.000000000000000000, 0.9659258262890683122, 1.000000000000000000, 0.9659258262890683122, 1.000000000000000000, 0.9659258262890683122, 1.000000000000000000, 0.9659258262890683122, 1.000000000000000000, 0.9659258262890683122, 1.000000000000000000, 0.9659258262890683122, 1.000000000000000000, 0.9659258262890683122, 1.000000000000000000, 0.9659258262890683122, 1.000000000000000000, 0.9659258262890683122, 1.000000000000000000, 0.9659258262890683122, 1.000000000000000000, 0.9659258262890683122, 1.000000000000000000, 0.9659258262890683122, 1.000000000000000000, 0.9659258262890683122, 1.000000000000000000, 0.9659258262890683122, 1.000000000000000000, 0.9659258262890683122, 1.000000000000000000, 0.9659258262890683122, 1.000000000000000000, 0.9659258262890683122, 1.000000000000000000, 0.9659258262890683122, 1.000000000000000000, 0.9659258262890683122, 1.000000000000000000, 0.9659258262890683122, 1.000000000000000000, 0.9659258262890683122, 1.000000000000000000, 0.9659258262890683122, 1.000000000000000000, 0.9659258262890683122, 1.000000000000000000, 0.9659258262890683122, 1.000000000000000000, 0.9659258262890683122, 1.000000000000000000, 0.9659258262890683122, 1.000000000000000000, 0.9659258262890683122, 1.000000000000000000, 0.9659258262890683122, 1.000000000000000000, 0.9659258262890683122, 1.000000000000000000, 0.9659258262890683122, 1.000000000000000000, 0.9659258262890683122, 1.000000000000000000, 0.9659258262890683122, 1.000000000000000000, 0.9659258262890683122, 1.000000000000000000, 0.9659258262890683122, 1.000000000000000000, 0.9659258262890683122, 1.000000000000000000, 0.9659258262890683122, 1.000000000000000000, 0.9659258262890683122, 1.000000000000000000, 0.9659258262890683122, 1.000000000000000000, 0.9659258262890683122, 1.000000000000000000, 0.9659258262890683122, 1.000000000000000000, 0.9659258262890683122, 1.000000000000000000, 0.9659258262890683122, 1.000000000000000000, 0.9659258262890683122, 1.000000000000000000, 0.9659258262890683122, 1.000000000000000000, 0.9659258262890683122, 1.000000000000000000, 0.9659258262890683122, 1.000000000000000000, 0.9659258262890683122, 1.000000000000000000, 0.9659258262890683122, 1.000000000000000000, 0.9659258262890683122, 1.000000000000000000, 0.9659258262890683122, 1.000000000000000000, 0.9659258262890683122, 1.000000000000000000, 0.9659258262890683122, 1.000000000000000000),
 ( 0.3333333333333333703, 0.3219752754296894559, 0.3333333333333333703, 0.3219752754296894559, 0.3333333333333333703, 0.3219752754296894559, 0.3333333333333333703, 0.3219752754296894559, 0.3333333333333333703, 0.3219752754296894559, 0.3333333333333333703, 0.3219752754296894559, 0.3333333333333333703, 0.3219752754296894559, 0.3333333333333333703, 0.3219752754296894559, 0.3333333333333333703, 0.3219752754296894559, 0.3333333333333333703, 0.3219752754296894559, 0.3333333333333333703, 0.3219752754296894559, 0.3333333333333333703, 0.3219752754296894559, 0.3333333333333333703, 0.3219752754296894559, 0.3333333333333333703, 0.3219752754296894559, 0.3333333333333333703, 0.3219752754296894559, 0.3333333333333333703, 0.3219752754296894559, 0.3333333333333333703, 0.3219752754296894559, 0.3333333333333333703, 0.3219752754296894559, 0.3333333333333333703, 0.3219752754296894559, 0.3333333333333333703, 0.3219752754296894559, 0.3333333333333333703, 0.3219752754296894559, 0.3333333333333333703, 0.3219752754296894559, 0.3333333333333333703, 0.3219752754296894559, 0.3333333333333333703, 0.3219752754296894559, 0.3333333333333333703, 0.3219752754296894559, 0.3333333333333333703, 0.3219752754296894559, 0.3333333333333333703, 0.3219752754296894559, 0.3333333333333333703, 0.3219752754296894559, 0.3333333333333333703, 0.3219752754296894559, 0.3333333333333333703, 0.3219752754296894559, 0.3333333333333333703, 0.3219752754296894559, 0.3333333333333333703, 0.3219752754296894559, 0.3333333333333333703, 0.3219752754296894559, 0.3333333333333333703, 0.3219752754296894559, 0.3333333333333333703, 0.3219752754296894559, 0.3333333333333333703, 0.3219752754296894559, 0.3333333333333333703, 0.3219752754296894559, 0.3333333333333333703, 0.3219752754296894559, 0.3333333333333333703, 0.3219752754296894559, 0.3333333333333333703, 0.3219752754296894559, 0.3333333333333333703, 0.3219752754296894559, 0.3333333333333333703, 0.3219752754296894559, 0.3333333333333333703, 0.3219752754296894559, 0.3333333333333333703, 0.3219752754296894559, 0.3333333333333333703, 0.3219752754296894559, 0.3333333333333333703, 0.3219752754296894559, 0.3333333333333333703, 0.3219752754296894559, 0.3333333333333333703, 0.3219752754296894559, 0.3333333333333333703, 0.3219752754296894559, 0.3333333333333333703, 0.3219752754296894559, 0.3333333333333333703, 0.3219752754296894559, 0.3333333333333333703, 0.3219752754296894559, 0.3333333333333333703, 0.3219752754296894559, 0.3333333333333333703, 0.3219752754296894559, 0.3333333333333333703, 0.3219752754296894559, 0.3333333333333333703, 0.3219752754296894559, 0.3333333333333333703, 0.3219752754296894559, 0.3333333333333333703, 0.3219752754296894559, 0.3333333333333333703, 0.3219752754296894559, 0.3333333333333333703, 0.3219752754296894559, 0.3333333333333333703, 0.3219752754296894559, 0.3333333333333333703, 0.3219752754296894559, 0.3333333333333333703, 0.3219752754296894559, 0.3333333333333333703, 0.3219752754296894559, 0.3333333333333333703, 0.3219752754296894559, 0.3333333333333333703, 0.3219752754296894559, 0.3333333333333333703, 0.3219752754296894559, 0.3333333333333333703, 0.3219752754296894559, 0.3333333333333333703, 0.3219752754296894559, 0.3333333333333333703, 0.3219752754296894559, 0.3333333333333333703, 0.3219752754296894559, 0.3333333333333333703, 0.3219752754296894559, 0.3333333333333333703, 0.3219752754296894559, 0.3333333333333333703, 0.3219752754296894559, 0.3333333333333333703, 0.3219752754296894559, 0.3333333333333333703, 0.3219752754296894559, 0.3333333333333333703, 0.3219752754296894559, 0.3333333333333333703, 0.3219752754296894559, 0.3333333333333333703, 0.3219752754296894559, 0.3333333333333333703, 0.3219752754296894559, 0.3333333333333333703, 0.3219752754296894559, 0.3333333333333333703, 0.3219752754296894559, 0.3333333333333333703, 0.3219752754296894559, 0.3333333333333333703, 0.3219752754296894559, 0.3333333333333333703, 0.3219752754296894559, 0.3333333333333333703, 0.3219752754296894559, 0.3333333333333333703, 0.3219752754296894559, 0.3333333333333333703, 0.3219752754296894559, 0.3333333333333333703, 0.3219752754296894559, 0.3333333333333333703, 0.3219752754296894559, 0.3333333333333333703, 0.3219752754296894559, 0.3333333333333333703, 0.3219752754296894559, 0.3333333333333333703, 0.3219752754296894559, 0.3333333333333333703, 0.3219752754296894559, 0.3333333333333333703, 0.3219752754296894559, 0.3333333333333333703, 0.3219752754296894559, 0.3333333333333333703, 0.3219752754296894559, 0.3333333333333333703, 0.3219752754296894559, 0.3333333333333333703, 0.3219752754296894559, 0.3333333333333333703, 0.3219752754296894559, 0.3333333333333333703, 0.3219752754296894559, 0.3333333333333333703, 0.3219752754296894559, 0.3333333333333333703, 0.3219752754296894559, 0.3333333333333333703, 0.3219752754296894559, 0.3333333333333333703, 0.3219752754296894559, 0.3333333333333333703, 0.3219752754296894559, 0.3333333333333333703, 0.3219752754296894559, 0.3333333333333333703, 0.3219752754296894559, 0.3333333333333333703, 0.3219752754296894559, 0.3333333333333333703, 0.3219752754296894559, 0.3333333333333333703, 0.3219752754296894559, 0.3333333333333333703, 0.3219752754296894559, 0.3333333333333333703, 0.3219752754296894559, 0.3333333333333333703, 0.3219752754296894559, 0.3333333333333333703, 0.3219752754296894559, 0.3333333333333333703, 0.3219752754296894559, 0.3333333333333333703, 0.3219752754296894559, 0.3333333333333333703, 0.3219752754296894559, 0.3333333333333333703, 0.3219752754296894559, 0.3333333333333333703, 0.3219752754296894559, 0.3333333333333333703, 0.3219752754296894559, 0.3333333333333333703, 0.3219752754296894559, 0.3333333333333333703, 0.3219752754296894559, 0.3333333333333333703, 0.3219752754296894559, 0.3333333333333333703, 0.3219752754296894559, 0.3333333333333333703, 0.3219752754296894559, 0.3333333333333333703, 0.3219752754296894559, 0.3333333333333333703, 0.3219752754296894559, 0.3333333333333333703, 0.3219752754296894559, 0.3333333333333333703, 0.3219752754296894559, 0.3333333333333333703, 0.3219752754296894559, 0.3333333333333333703, 0.3219752754296894559, 0.3333333333333333703, 0.3219752754296894559, 0.3333333333333333703, 0.3219752754296894559, 0.3333333333333333703, 0.3219752754296894559, 0.3333333333333333703, 0.3219752754296894559, 0.3333333333333333703, 0.3219752754296894559, 0.3333333333333333703, 0.3219752754296894559, 0.3333333333333333703, 0.3219752754296894559, 0.3333333333333333703, 0.3219752754296894559, 0.3333333333333333703, 0.3219752754296894559, 0.3333333333333333703, 0.3219752754296894559, 0.3333333333333333703, 0.3219752754296894559, 0.3333333333333333703, 0.3219752754296894559, 0.3333333333333333703, 0.3219752754296894559, 0.3333333333333333703, 0.3219752754296894559, 0.3333333333333333703, 0.3219752754296894559, 0.3333333333333333703, 0.3219752754296894559, 0.3333333333333333703, 0.3219752754296894559, 0.3333333333333333703, 0.3219752754296894559, 0.3333333333333333703, 0.3219752754296894559, 0.3333333333333333703, 0.3219752754296894559, 0.3333333333333333703, 0.3219752754296894559, 0.3333333333333333703, 0.3219752754296894559, 0.3333333333333333703, 0.3219752754296894559, 0.3333333333333333703, 0.3219752754296894559, 0.3333333333333333703, 0.3219752754296894559, 0.3333333333333333703, 0.3219752754296894559, 0.3333333333333333703, 0.3219752754296894559, 0.3333333333333333703, 0.3219752754296894559, 0.3333333333333333703, 0.3219752754296894559, 0.3333333333333333703, 0.3219752754296894559, 0.3333333333333333703, 0.3219752754296894559, 0.3333333333333333703, 0.3219752754296894559, 0.3333333333333333703, 0.3219752754296894559, 0.3333333333333333703, 0.3219752754296894559, 0.3333333333333333703, 0.3219752754296894559, 0.3333333333333333703, 0.3219752754296894559, 0.3333333333333333703, 0.3219752754296894559, 0.3333333333333333703, 0.3219752754296894559, 0.3333333333333333703, 0.3219752754296894559, 0.3333333333333333703, 0.3219752754296894559, 0.3333333333333333703, 0.3219752754296894559, 0.3333333333333333703, 0.3219752754296894559, 0.3333333333333333703, 0.3219752754296894559, 0.3333333333333333703, 0.3219752754296894559, 0.3333333333333333703, 0.3219752754296894559, 0.3333333333333333703, 0.3219752754296894559, 0.3333333333333333703, 0.3219752754296894559, 0.3333333333333333703, 0.3219752754296894559, 0.3333333333333333703, 0.3219752754296894559, 0.3333333333333333703, 0.3219752754296894559, 0.3333333333333333703, 0.3219752754296894559, 0.3333333333333333703, 0.3219752754296894559, 0.3333333333333333703, 0.3219752754296894559, 0.3333333333333333703, 0.3219752754296894559, 0.3333333333333333703, 0.3219752754296894559, 0.3333333333333333703, 0.3219752754296894559, 0.3333333333333333703, 0.3219752754296894559, 0.3333333333333333703, 0.3219752754296894559, 0.3333333333333333703, 0.3219752754296894559, 0.3333333333333333703, 0.3219752754296894559, 0.3333333333333333703, 0.3219752754296894559, 0.3333333333333333703, 0.3219752754296894559, 0.3333333333333333703, 0.3219752754296894559, 0.3333333333333333703, 0.3219752754296894559, 0.3333333333333333703, 0.3219752754296894559, 0.3333333333333333703, 0.3219752754296894559, 0.3333333333333333703, 0.3219752754296894559, 0.3333333333333333703, 0.3219752754296894559, 0.3333333333333333703, 0.3219752754296894559, 0.3333333333333333703, 0.3219752754296894559, 0.3333333333333333703, 0.3219752754296894559, 0.3333333333333333703, 0.3219752754296894559, 0.3333333333333333703, 0.3219752754296894559, 0.3333333333333333703, 0.3219752754296894559, 0.3333333333333333703, 0.3219752754296894559, 0.3333333333333333703, 0.3219752754296894559, 0.3333333333333333703, 0.3219752754296894559, 0.3333333333333333703, 0.3219752754296894559, 0.3333333333333333703, 0.3219752754296894559, 0.3333333333333333703, 0.3219752754296894559, 0.3333333333333333703, 0.3219752754296894559, 0.3333333333333333703, 0.3219752754296894559, 0.3333333333333333703, 0.3219752754296894559, 0.3333333333333333703, 0.3219752754296894559, 0.3333333333333333703, 0.3219752754296894559, 0.3333333333333333703, 0.3219752754296894559, 0.3333333333333333703, 0.3219752754296894559, 0.3333333333333333703, 0.3219752754296894559, 0.3333333333333333703, 0.3219752754296894559, 0.3333333333333333703, 0.3219752754296894559, 0.3333333333333333703, 0.3219752754296894559, 0.3333333333333333703, 0.3219752754296894559, 0.3333333333333333703, 0.3219752754296894559, 0.3333333333333333703, 0.3219752754296894559, 0.3333333333333333703, 0.3219752754296894559, 0.3333333333333333703, 0.3219752754296894559, 0.3333333333333333703),
 ( 0.3333333333333333703, 0.3219752754296894559, 0.3333333333333333703, 0.3219752754296894559, 0.3333333333333333703, 0.3219752754296894559, 0.3333333333333333703, 0.3219752754296894559, 0.3333333333333333703, 0.3219752754296894559, 0.3333333333333333703, 0.3219752754296894559, 0.3333333333333333703, 0.3219752754296894559, 0.3333333333333333703, 0.3219752754296894559, 0.3333333333333333703, 0.3219752754296894559, 0.3333333333333333703, 0.3219752754296894559, 0.3333333333333333703, 0.3219752754296894559, 0.3333333333333333703, 0.3219752754296894559, 0.3333333333333333703, 0.3219752754296894559, 0.3333333333333333703, 0.3219752754296894559, 0.3333333333333333703, 0.3219752754296894559, 0.3333333333333333703, 0.3219752754296894559, 0.3333333333333333703, 0.3219752754296894559, 0.3333333333333333703, 0.3219752754296894559, 0.3333333333333333703, 0.3219752754296894559, 0.3333333333333333703, 0.3219752754296894559, 0.3333333333333333703, 0.3219752754296894559, 0.3333333333333333703, 0.3219752754296894559, 0.3333333333333333703, 0.3219752754296894559, 0.3333333333333333703, 0.3219752754296894559, 0.3333333333333333703, 0.3219752754296894559, 0.3333333333333333703, 0.3219752754296894559, 0.3333333333333333703, 0.3219752754296894559, 0.3333333333333333703, 0.3219752754296894559, 0.3333333333333333703, 0.3219752754296894559, 0.3333333333333333703, 0.3219752754296894559, 0.3333333333333333703, 0.3219752754296894559, 0.3333333333333333703, 0.3219752754296894559, 0.3333333333333333703, 0.3219752754296894559, 0.3333333333333333703, 0.3219752754296894559, 0.3333333333333333703, 0.3219752754296894559, 0.3333333333333333703, 0.3219752754296894559, 0.3333333333333333703, 0.3219752754296894559, 0.3333333333333333703, 0.3219752754296894559, 0.3333333333333333703, 0.3219752754296894559, 0.3333333333333333703, 0.3219752754296894559, 0.3333333333333333703, 0.3219752754296894559, 0.3333333333333333703, 0.3219752754296894559, 0.3333333333333333703, 0.3219752754296894559, 0.3333333333333333703, 0.3219752754296894559, 0.3333333333333333703, 0.3219752754296894559, 0.3333333333333333703, 0.3219752754296894559, 0.3333333333333333703, 0.3219752754296894559, 0.3333333333333333703, 0.3219752754296894559, 0.3333333333333333703, 0.3219752754296894559, 0.3333333333333333703, 0.3219752754296894559, 0.3333333333333333703, 0.3219752754296894559, 0.3333333333333333703, 0.3219752754296894559, 0.3333333333333333703, 0.3219752754296894559, 0.3333333333333333703, 0.3219752754296894559, 0.3333333333333333703, 0.3219752754296894559, 0.3333333333333333703, 0.3219752754296894559, 0.3333333333333333703, 0.3219752754296894559, 0.3333333333333333703, 0.3219752754296894559, 0.3333333333333333703, 0.3219752754296894559, 0.3333333333333333703, 0.3219752754296894559, 0.3333333333333333703, 0.3219752754296894559, 0.3333333333333333703, 0.3219752754296894559, 0.3333333333333333703, 0.3219752754296894559, 0.3333333333333333703, 0.3219752754296894559, 0.3333333333333333703, 0.3219752754296894559, 0.3333333333333333703, 0.3219752754296894559, 0.3333333333333333703, 0.3219752754296894559, 0.3333333333333333703, 0.3219752754296894559, 0.3333333333333333703, 0.3219752754296894559, 0.3333333333333333703, 0.3219752754296894559, 0.3333333333333333703, 0.3219752754296894559, 0.3333333333333333703, 0.3219752754296894559, 0.3333333333333333703, 0.3219752754296894559, 0.3333333333333333703, 0.3219752754296894559, 0.3333333333333333703, 0.3219752754296894559, 0.3333333333333333703, 0.3219752754296894559, 0.3333333333333333703, 0.3219752754296894559, 0.3333333333333333703, 0.3219752754296894559, 0.3333333333333333703, 0.3219752754296894559, 0.3333333333333333703, 0.3219752754296894559, 0.3333333333333333703, 0.3219752754296894559, 0.3333333333333333703, 0.3219752754296894559, 0.3333333333333333703, 0.3219752754296894559, 0.3333333333333333703, 0.3219752754296894559, 0.3333333333333333703, 0.3219752754296894559, 0.3333333333333333703, 0.3219752754296894559, 0.3333333333333333703, 0.3219752754296894559, 0.3333333333333333703, 0.3219752754296894559, 0.3333333333333333703, 0.3219752754296894559, 0.3333333333333333703, 0.3219752754296894559, 0.3333333333333333703, 0.3219752754296894559, 0.3333333333333333703, 0.3219752754296894559, 0.3333333333333333703, 0.3219752754296894559, 0.3333333333333333703, 0.3219752754296894559, 0.3333333333333333703, 0.3219752754296894559, 0.3333333333333333703, 0.3219752754296894559, 0.3333333333333333703, 0.3219752754296894559, 0.3333333333333333703, 0.3219752754296894559, 0.3333333333333333703, 0.3219752754296894559, 0.3333333333333333703, 0.3219752754296894559, 0.3333333333333333703, 0.3219752754296894559, 0.3333333333333333703, 0.3219752754296894559, 0.3333333333333333703, 0.3219752754296894559, 0.3333333333333333703, 0.3219752754296894559, 0.3333333333333333703, 0.3219752754296894559, 0.3333333333333333703, 0.3219752754296894559, 0.3333333333333333703, 0.3219752754296894559, 0.3333333333333333703, 0.3219752754296894559, 0.3333333333333333703, 0.3219752754296894559, 0.3333333333333333703, 0.3219752754296894559, 0.3333333333333333703, 0.3219752754296894559, 0.3333333333333333703, 0.3219752754296894559, 0.3333333333333333703, 0.3219752754296894559, 0.3333333333333333703, 0.3219752754296894559, 0.3333333333333333703, 0.3219752754296894559, 0.3333333333333333703, 0.3219752754296894559, 0.3333333333333333703, 0.3219752754296894559, 0.3333333333333333703, 0.3219752754296894559, 0.3333333333333333703, 0.3219752754296894559, 0.3333333333333333703, 0.3219752754296894559, 0.3333333333333333703, 0.3219752754296894559, 0.3333333333333333703, 0.3219752754296894559, 0.3333333333333333703, 0.3219752754296894559, 0.3333333333333333703, 0.3219752754296894559, 0.3333333333333333703, 0.3219752754296894559, 0.3333333333333333703, 0.3219752754296894559, 0.3333333333333333703, 0.3219752754296894559, 0.3333333333333333703, 0.3219752754296894559, 0.3333333333333333703, 0.3219752754296894559, 0.3333333333333333703, 0.3219752754296894559, 0.3333333333333333703, 0.3219752754296894559, 0.3333333333333333703, 0.3219752754296894559, 0.3333333333333333703, 0.3219752754296894559, 0.3333333333333333703, 0.3219752754296894559, 0.3333333333333333703, 0.3219752754296894559, 0.3333333333333333703, 0.3219752754296894559, 0.3333333333333333703, 0.3219752754296894559, 0.3333333333333333703, 0.3219752754296894559, 0.3333333333333333703, 0.3219752754296894559, 0.3333333333333333703, 0.3219752754296894559, 0.3333333333333333703, 0.3219752754296894559, 0.3333333333333333703, 0.3219752754296894559, 0.3333333333333333703, 0.3219752754296894559, 0.3333333333333333703, 0.3219752754296894559, 0.3333333333333333703, 0.3219752754296894559, 0.3333333333333333703, 0.3219752754296894559, 0.3333333333333333703, 0.3219752754296894559, 0.3333333333333333703, 0.3219752754296894559, 0.3333333333333333703, 0.3219752754296894559, 0.3333333333333333703, 0.3219752754296894559, 0.3333333333333333703, 0.3219752754296894559, 0.3333333333333333703, 0.3219752754296894559, 0.3333333333333333703, 0.3219752754296894559, 0.3333333333333333703, 0.3219752754296894559, 0.3333333333333333703, 0.3219752754296894559, 0.3333333333333333703, 0.3219752754296894559, 0.3333333333333333703, 0.3219752754296894559, 0.3333333333333333703, 0.3219752754296894559, 0.3333333333333333703, 0.3219752754296894559, 0.3333333333333333703, 0.3219752754296894559, 0.3333333333333333703, 0.3219752754296894559, 0.3333333333333333703, 0.3219752754296894559, 0.3333333333333333703, 0.3219752754296894559, 0.3333333333333333703, 0.3219752754296894559, 0.3333333333333333703, 0.3219752754296894559, 0.3333333333333333703, 0.3219752754296894559, 0.3333333333333333703, 0.3219752754296894559, 0.3333333333333333703, 0.3219752754296894559, 0.3333333333333333703, 0.3219752754296894559, 0.3333333333333333703, 0.3219752754296894559, 0.3333333333333333703, 0.3219752754296894559, 0.3333333333333333703, 0.3219752754296894559, 0.3333333333333333703, 0.3219752754296894559, 0.3333333333333333703, 0.3219752754296894559, 0.3333333333333333703, 0.3219752754296894559, 0.3333333333333333703, 0.3219752754296894559, 0.3333333333333333703, 0.3219752754296894559, 0.3333333333333333703, 0.3219752754296894559, 0.3333333333333333703, 0.3219752754296894559, 0.3333333333333333703, 0.3219752754296894559, 0.3333333333333333703, 0.3219752754296894559, 0.3333333333333333703, 0.3219752754296894559, 0.3333333333333333703, 0.3219752754296894559, 0.3333333333333333703, 0.3219752754296894559, 0.3333333333333333703, 0.3219752754296894559, 0.3333333333333333703, 0.3219752754296894559, 0.3333333333333333703, 0.3219752754296894559, 0.3333333333333333703, 0.3219752754296894559, 0.3333333333333333703, 0.3219752754296894559, 0.3333333333333333703, 0.3219752754296894559, 0.3333333333333333703, 0.3219752754296894559, 0.3333333333333333703, 0.3219752754296894559, 0.3333333333333333703, 0.3219752754296894559, 0.3333333333333333703, 0.3219752754296894559, 0.3333333333333333703, 0.3219752754296894559, 0.3333333333333333703, 0.3219752754296894559, 0.3333333333333333703, 0.3219752754296894559, 0.3333333333333333703, 0.3219752754296894559, 0.3333333333333333703, 0.3219752754296894559, 0.3333333333333333703, 0.3219752754296894559, 0.3333333333333333703, 0.3219752754296894559, 0.3333333333333333703, 0.3219752754296894559, 0.3333333333333333703, 0.3219752754296894559, 0.3333333333333333703, 0.3219752754296894559, 0.3333333333333333703, 0.3219752754296894559, 0.3333333333333333703, 0.3219752754296894559, 0.3333333333333333703, 0.3219752754296894559, 0.3333333333333333703, 0.3219752754296894559, 0.3333333333333333703, 0.3219752754296894559, 0.3333333333333333703, 0.3219752754296894559, 0.3333333333333333703, 0.3219752754296894559, 0.3333333333333333703, 0.3219752754296894559, 0.3333333333333333703, 0.3219752754296894559, 0.3333333333333333703, 0.3219752754296894559, 0.3333333333333333703, 0.3219752754296894559, 0.3333333333333333703, 0.3219752754296894559, 0.3333333333333333703, 0.3219752754296894559, 0.3333333333333333703, 0.3219752754296894559, 0.3333333333333333703, 0.3219752754296894559, 0.3333333333333333703, 0.3219752754296894559, 0.3333333333333333703, 0.3219752754296894559, 0.3333333333333333703, 0.3219752754296894559, 0.3333333333333333703, 0.3219752754296894559, 0.3333333333333333703, 0.3219752754296894559, 0.3333333333333333703, 0.3219752754296894559, 0.3333333333333333703, 0.3219752754296894559, 0.3333333333333333703, 0.3219752754296894559, 0.3333333333333333703, 0.3219752754296894559, 0.3333333333333333703),
 ( 1.000000000000000000, 0.9659258262890683122, 1.000000000000000000, 0.9659258262890683122, 1.000000000000000000, 0.9659258262890683122, 1.000000000000000000, 0.9659258262890683122, 1.000000000000000000, 0.9659258262890683122, 1.000000000000000000, 0.9659258262890683122, 1.000000000000000000, 0.9659258262890683122, 1.000000000000000000, 0.9659258262890683122, 1.000000000000000000, 0.9659258262890683122, 1.000000000000000000, 0.9659258262890683122, 1.000000000000000000, 0.9659258262890683122, 1.000000000000000000, 0.9659258262890683122, 1.000000000000000000, 0.9659258262890683122, 1.000000000000000000, 0.9659258262890683122, 1.000000000000000000, 0.9659258262890683122, 1.000000000000000000, 0.9659258262890683122, 1.000000000000000000, 0.9659258262890683122, 1.000000000000000000, 0.9659258262890683122, 1.000000000000000000, 0.9659258262890683122, 1.000000000000000000, 0.9659258262890683122, 1.000000000000000000, 0.9659258262890683122, 1.000000000000000000, 0.9659258262890683122, 1.000000000000000000, 0.9659258262890683122, 1.000000000000000000, 0.9659258262890683122, 1.000000000000000000, 0.9659258262890683122, 1.000000000000000000, 0.9659258262890683122, 1.000000000000000000, 0.9659258262890683122, 1.000000000000000000, 0.9659258262890683122, 1.000000000000000000, 0.9659258262890683122, 1.000000000000000000, 0.9659258262890683122, 1.000000000000000000, 0.9659258262890683122, 1.000000000000000000, 0.9659258262890683122, 1.000000000000000000, 0.9659258262890683122, 1.000000000000000000, 0.9659258262890683122, 1.000000000000000000, 0.9659258262890683122, 1.000000000000000000, 0.9659258262890683122, 1.000000000000000000, 0.9659258262890683122, 1.000000000000000000, 0.9659258262890683122, 1.000000000000000000, 0.9659258262890683122, 1.000000000000000000, 0.9659258262890683122, 1.000000000000000000, 0.9659258262890683122, 1.000000000000000000, 0.9659258262890683122, 1.000000000000000000, 0.9659258262890683122, 1.000000000000000000, 0.9659258262890683122, 1.000000000000000000, 0.9659258262890683122, 1.000000000000000000, 0.9659258262890683122, 1.000000000000000000, 0.9659258262890683122, 1.000000000000000000, 0.9659258262890683122, 1.000000000000000000, 0.9659258262890683122, 1.000000000000000000, 0.9659258262890683122, 1.000000000000000000, 0.9659258262890683122, 1.000000000000000000, 0.9659258262890683122, 1.000000000000000000, 0.9659258262890683122, 1.000000000000000000, 0.9659258262890683122, 1.000000000000000000, 0.9659258262890683122, 1.000000000000000000, 0.9659258262890683122, 1.000000000000000000, 0.9659258262890683122, 1.000000000000000000, 0.9659258262890683122, 1.000000000000000000, 0.9659258262890683122, 1.000000000000000000, 0.9659258262890683122, 1.000000000000000000, 0.9659258262890683122, 1.000000000000000000, 0.9659258262890683122, 1.000000000000000000, 0.9659258262890683122, 1.000000000000000000, 0.9659258262890683122, 1.000000000000000000, 0.9659258262890683122, 1.000000000000000000, 0.9659258262890683122, 1.000000000000000000, 0.9659258262890683122, 1.000000000000000000, 0.9659258262890683122, 1.000000000000000000, 0.9659258262890683122, 1.000000000000000000, 0.9659258262890683122, 1.000000000000000000, 0.9659258262890683122, 1.000000000000000000, 0.9659258262890683122, 1.000000000000000000, 0.9659258262890683122, 1.000000000000000000, 0.9659258262890683122, 1.000000000000000000, 0.9659258262890683122, 1.000000000000000000, 0.9659258262890683122, 1.000000000000000000, 0.9659258262890683122, 1.000000000000000000, 0.9659258262890683122, 1.000000000000000000, 0.9659258262890683122, 1.000000000000000000, 0.9659258262890683122, 1.000000000000000000, 0.9659258262890683122, 1.000000000000000000, 0.9659258262890683122, 1.000000000000000000, 0.9659258262890683122, 1.000000000000000000, 0.9659258262890683122, 1.000000000000000000, 0.9659258262890683122, 1.000000000000000000, 0.9659258262890683122, 1.000000000000000000, 0.9659258262890683122, 1.000000000000000000, 0.9659258262890683122, 1.000000000000000000, 0.9659258262890683122, 1.000000000000000000, 0.9659258262890683122, 1.000000000000000000, 0.9659258262890683122, 1.000000000000000000, 0.9659258262890683122, 1.000000000000000000, 0.9659258262890683122, 1.000000000000000000, 0.9659258262890683122, 1.000000000000000000, 0.9659258262890683122, 1.000000000000000000, 0.9659258262890683122, 1.000000000000000000, 0.9659258262890683122, 1.000000000000000000, 0.9659258262890683122, 1.000000000000000000, 0.9659258262890683122, 1.000000000000000000, 0.9659258262890683122, 1.000000000000000000, 0.9659258262890683122, 1.000000000000000000, 0.9659258262890683122, 1.000000000000000000, 0.9659258262890683122, 1.000000000000000000, 0.9659258262890683122, 1.000000000000000000, 0.9659258262890683122, 1.000000000000000000, 0.9659258262890683122, 1.000000000000000000, 0.9659258262890683122, 1.000000000000000000, 0.9659258262890683122, 1.000000000000000000, 0.9659258262890683122, 1.000000000000000000, 0.9659258262890683122, 1.000000000000000000, 0.9659258262890683122, 1.000000000000000000, 0.9659258262890683122, 1.000000000000000000, 0.9659258262890683122, 1.000000000000000000, 0.9659258262890683122, 1.000000000000000000, 0.9659258262890683122, 1.000000000000000000, 0.9659258262890683122, 1.000000000000000000, 0.9659258262890683122, 1.000000000000000000, 0.9659258262890683122, 1.000000000000000000, 0.9659258262890683122, 1.000000000000000000, 0.9659258262890683122, 1.000000000000000000, 0.9659258262890683122, 1.000000000000000000, 0.9659258262890683122, 1.000000000000000000, 0.9659258262890683122, 1.000000000000000000, 0.9659258262890683122, 1.000000000000000000, 0.9659258262890683122, 1.000000000000000000, 0.9659258262890683122, 1.000000000000000000, 0.9659258262890683122, 1.000000000000000000, 0.9659258262890683122, 1.000000000000000000, 0.9659258262890683122, 1.000000000000000000, 0.9659258262890683122, 1.000000000000000000, 0.9659258262890683122, 1.000000000000000000, 0.9659258262890683122, 1.000000000000000000, 0.9659258262890683122, 1.000000000000000000, 0.9659258262890683122, 1.000000000000000000, 0.9659258262890683122, 1.000000000000000000, 0.9659258262890683122, 1.000000000000000000, 0.9659258262890683122, 1.000000000000000000, 0.9659258262890683122, 1.000000000000000000, 0.9659258262890683122, 1.000000000000000000, 0.9659258262890683122, 1.000000000000000000, 0.9659258262890683122, 1.000000000000000000, 0.9659258262890683122, 1.000000000000000000, 0.9659258262890683122, 1.000000000000000000, 0.9659258262890683122, 1.000000000000000000, 0.9659258262890683122, 1.000000000000000000, 0.9659258262890683122, 1.000000000000000000, 0.9659258262890683122, 1.000000000000000000, 0.9659258262890683122, 1.000000000000000000, 0.9659258262890683122, 1.000000000000000000, 0.9659258262890683122, 1.000000000000000000, 0.9659258262890683122, 1.000000000000000000, 0.9659258262890683122, 1.000000000000000000, 0.9659258262890683122, 1.000000000000000000, 0.9659258262890683122, 1.000000000000000000, 0.9659258262890683122, 1.000000000000000000, 0.9659258262890683122, 1.000000000000000000, 0.9659258262890683122, 1.000000000000000000, 0.9659258262890683122, 1.000000000000000000, 0.9659258262890683122, 1.000000000000000000, 0.9659258262890683122, 1.000000000000000000, 0.9659258262890683122, 1.000000000000000000, 0.9659258262890683122, 1.000000000000000000, 0.9659258262890683122, 1.000000000000000000, 0.9659258262890683122, 1.000000000000000000, 0.9659258262890683122, 1.000000000000000000, 0.9659258262890683122, 1.000000000000000000, 0.9659258262890683122, 1.000000000000000000, 0.9659258262890683122, 1.000000000000000000, 0.9659258262890683122, 1.000000000000000000, 0.9659258262890683122, 1.000000000000000000, 0.9659258262890683122, 1.000000000000000000, 0.9659258262890683122, 1.000000000000000000, 0.9659258262890683122, 1.000000000000000000, 0.9659258262890683122, 1.000000000000000000, 0.9659258262890683122, 1.000000000000000000, 0.9659258262890683122, 1.000000000000000000, 0.9659258262890683122, 1.000000000000000000, 0.9659258262890683122, 1.000000000000000000, 0.9659258262890683122, 1.000000000000000000, 0.9659258262890683122, 1.000000000000000000, 0.9659258262890683122, 1.000000000000000000, 0.9659258262890683122, 1.000000000000000000, 0.9659258262890683122, 1.000000000000000000, 0.9659258262890683122, 1.000000000000000000, 0.9659258262890683122, 1.000000000000000000, 0.9659258262890683122, 1.000000000000000000, 0.9659258262890683122, 1.000000000000000000, 0.9659258262890683122, 1.000000000000000000, 0.9659258262890683122, 1.000000000000000000, 0.9659258262890683122, 1.000000000000000000, 0.9659258262890683122, 1.000000000000000000, 0.9659258262890683122, 1.000000000000000000, 0.9659258262890683122, 1.000000000000000000, 0.9659258262890683122, 1.000000000000000000, 0.9659258262890683122, 1.000000000000000000, 0.9659258262890683122, 1.000000000000000000, 0.9659258262890683122, 1.000000000000000000, 0.9659258262890683122, 1.000000000000000000, 0.9659258262890683122, 1.000000000000000000, 0.9659258262890683122, 1.000000000000000000, 0.9659258262890683122, 1.000000000000000000, 0.9659258262890683122, 1.000000000000000000, 0.9659258262890683122, 1.000000000000000000, 0.9659258262890683122, 1.000000000000000000, 0.9659258262890683122, 1.000000000000000000, 0.9659258262890683122, 1.000000000000000000, 0.9659258262890683122, 1.000000000000000000, 0.9659258262890683122, 1.000000000000000000, 0.9659258262890683122, 1.000000000000000000, 0.9659258262890683122, 1.000000000000000000, 0.9659258262890683122, 1.000000000000000000, 0.9659258262890683122, 1.000000000000000000, 0.9659258262890683122, 1.000000000000000000, 0.9659258262890683122, 1.000000000000000000, 0.9659258262890683122, 1.000000000000000000, 0.9659258262890683122, 1.000000000000000000, 0.9659258262890683122, 1.000000000000000000, 0.9659258262890683122, 1.000000000000000000, 0.9659258262890683122, 1.000000000000000000, 0.9659258262890683122, 1.000000000000000000, 0.9659258262890683122, 1.000000000000000000, 0.9659258262890683122, 1.000000000000000000, 0.9659258262890683122, 1.000000000000000000, 0.9659258262890683122, 1.000000000000000000, 0.9659258262890683122, 1.000000000000000000, 0.9659258262890683122, 1.000000000000000000, 0.9659258262890683122, 1.000000000000000000, 0.9659258262890683122, 1.000000000000000000) ) ) 
 REPRESENTATION_ITEM ( '' )  SURFACE ( )  );
#138279 = CARTESIAN_POINT ( 'NONE',  ( -16.46253265017146816, -9.564922557961047289, 104.1677570613523329 ) ) ;
#138280 = CARTESIAN_POINT ( 'NONE',  ( 5.153800228976335163, 19.02544592524342804, 69.79057627198103830 ) ) ;
#138281 = CARTESIAN_POINT ( 'NONE',  ( -9.564922557960796823, -16.46253265017161027, 97.08224293864769550 ) ) ;
#138282 = VECTOR ( 'NONE', #160441, 1000.000000000000000 ) ;
#138283 = CARTESIAN_POINT ( 'NONE',  ( -14.34966873604960291, -8.224510206698953496, 106.6655762719810383 ) ) ;
#138284 = CARTESIAN_POINT ( 'NONE',  ( -21.53943276465977519, 0.05219959533907696930, 36.24890960531435979 ) ) ;
#138285 = CARTESIAN_POINT ( 'NONE',  ( -8.314922557961024197, 14.29746914071037800, 87.91775706135234714 ) ) ;
#138287 = CARTESIAN_POINT ( 'NONE',  ( -9.474510206698964154, 16.51473224551069663, 55.41557627198103120 ) ) ;
#138286 = CARTESIAN_POINT ( 'NONE',  ( 16.53943276465976808, -0.05219959533910856209, 73.74890960531433848 ) ) ;
#138288 = CARTESIAN_POINT ( 'NONE',  ( -0.05219959533937732626, 21.53943276465977519, 77.50109039468567573 ) ) ;
#138289 = CYLINDRICAL_SURFACE ( 'NONE', #117580, 59.99999999999998579 ) ;
#138290 = CARTESIAN_POINT ( 'NONE',  ( 9.564922557961047289, -16.46253265017146816, 100.4177570613523329 ) ) ;
#138291 = CARTESIAN_POINT ( 'NONE',  ( 16.55341960407611168, 4.379528057220329451, 78.95724293864769550 ) ) ;
#138292 = CARTESIAN_POINT ( 'NONE',  ( 15.80617190586769283, -15.72974639402175789, 30.62609039468567929 ) ) ;
#138293 = CARTESIAN_POINT ( 'NONE',  ( -15.72974639402197994, 15.80617190586746368, 55.62390960531436690 ) ) ;
#138294 = CARTESIAN_POINT ( 'NONE',  ( -17.26172910966779739, -6.454744622555836919, 104.1935309135077574 ) ) ;
#138295 = CARTESIAN_POINT ( 'NONE',  ( 8.906447517083050158, 27.41122689804195645, 145.6500000054623740 ) ) ;
#138296 = CARTESIAN_POINT ( 'NONE',  ( -9.564922557960796823, -16.46253265017161027, 87.08224293864769550 ) ) ;
#138297 = CARTESIAN_POINT ( 'NONE',  ( 14.34966873604960469, 8.224510206698951720, 49.16557627198102409 ) ) ;
#138298 = CARTESIAN_POINT ( 'NONE',  ( -16.55341960407611168, -4.379528057220339221, 36.45724293864768839 ) ) ;
#138299 = CARTESIAN_POINT ( 'NONE',  ( -14.29746914071037622, -8.314922557961029526, 99.16775706135234714 ) ) ;
#138300 = CARTESIAN_POINT ( 'NONE',  ( 13.89961937509957401, 13.97604488694547697, 46.87609039468565442 ) ) ;
#138301 = CARTESIAN_POINT ( 'NONE',  ( 16.20579543436682002, 7.371946100354975329, 48.06520834171878676 ) ) ;
#138302 = CARTESIAN_POINT ( 'NONE',  ( 19.02544592524343514, -5.153800228976328945, 108.5405762719810383 ) ) ;
#138303 = CARTESIAN_POINT ( 'NONE',  ( -0.05219959533910754901, -16.53943276465976808, 77.49890960531433848 ) ) ;
#138304 = CARTESIAN_POINT ( 'NONE',  ( -9.564922557961040184, 16.46253265017147172, 37.91775706135233293 ) ) ;
#138306 = CARTESIAN_POINT ( 'NONE',  ( 21.53943276465977519, -0.05219959533907433946, 33.74890960531436690 ) ) ;
#138305 = CARTESIAN_POINT ( 'NONE',  ( 19.05341960407611168, 5.049401038298154454, 33.95724293864769550 ) ) ;
#138307 = CARTESIAN_POINT ( 'NONE',  ( -18.62759615963270932, 10.81492255796079327, 60.83224293864769550 ) ) ;
#138308 = CARTESIAN_POINT ( 'NONE',  ( 0.05219959533910956823, 16.53943276465976808, 94.99890960531436690 ) ) ;
#138309 = CARTESIAN_POINT ( 'NONE',  ( 16.55341960407618274, -4.379528057220086978, 56.04275706135235424 ) ) ;
#138310 = CARTESIAN_POINT ( 'NONE',  ( -15.80617190586768217, 15.72974639402176855, 48.12609039468568284 ) ) ;
#138311 = CARTESIAN_POINT ( 'NONE',  ( 4.483927247898545687, 16.52544592524342804, 89.79057627198103830 ) ) ;
#138312 = CARTESIAN_POINT ( 'NONE',  ( 17.40861289039004944, -6.110651285853252901, 36.12767529172568715 ) ) ;
#138313 = CARTESIAN_POINT ( 'NONE',  ( -17.40861289039003523, 6.110651285853255565, 48.62767529172570136 ) ) ;
#138314 = CARTESIAN_POINT ( 'NONE',  ( 0.05219959533907565091, 21.53943276465977519, 29.99890960531435979 ) ) ;
#138315 = CARTESIAN_POINT ( 'NONE',  ( -17.49999999999999645, 5.499999999999992895, 63.71769037696435589 ) ) ;
#138316 = CARTESIAN_POINT ( 'NONE',  ( -23.48298174826589602, -32.32155151706771790, -7.447842220587802764 ) ) ;
#138318 = CARTESIAN_POINT ( 'NONE',  ( -12.14591786802309592, -12.06949235617757132, 31.87390960531435979 ) ) ;
#138317 = CARTESIAN_POINT ( 'NONE',  ( -4.379528057220086978, -16.55341960407618274, 39.79275706135235424 ) ) ;
#138319 = CARTESIAN_POINT ( 'NONE',  ( -21.55341960407610458, -5.719274019375992779, 66.45724293864768129 ) ) ;
#138320 = CARTESIAN_POINT ( 'NONE',  ( -16.51473224551082808, 9.474510206698731452, 83.33442372801899012 ) ) ;
#138321 = CARTESIAN_POINT ( 'NONE',  ( 5.719274019375991003, -21.55341960407610458, 62.70724293864769550 ) ) ;
#138322 = CARTESIAN_POINT ( 'NONE',  ( -20.51334883519573182, 11.49142661404780696, 170.0774692710818101 ) ) ;
#138323 = CARTESIAN_POINT ( 'NONE',  ( -14.34966873604972548, 8.224510206698743886, 53.33442372801901854 ) ) ;
#138326 = EDGE_CURVE ( 'NONE', #190734, #45261, #32044, .T. ) ;
#138325 = CARTESIAN_POINT ( 'NONE',  ( -19.02544592524342804, 5.153800228976336051, 106.0405762719810241 ) ) ;
#138324 = CARTESIAN_POINT ( 'NONE',  ( 9.474510206698971260, -16.51473224551069308, 32.91557627198102409 ) ) ;
#138327 = CARTESIAN_POINT ( 'NONE',  ( -5.153800228976328057, -19.02544592524343514, 42.29057627198101699 ) ) ;
#138328 = CARTESIAN_POINT ( 'NONE',  ( -16.46253265017160317, 9.564922557960807481, 25.83224293864769194 ) ) ;
#138329 = CARTESIAN_POINT ( 'NONE',  ( 0.000000000000000000, 0.000000000000000000, 0.000000000000000000 ) ) ;
#138330 = CARTESIAN_POINT ( 'NONE',  ( 13.97604488694527802, 13.89961937509977652, 114.3739096053143669 ) ) ;
#138331 = VERTEX_POINT ( 'NONE', #91696 ) ;
#138332 = CARTESIAN_POINT ( 'NONE',  ( 16.55341960407618274, -4.379528057220086978, 76.04275706135237556 ) ) ;
#138333 = CARTESIAN_POINT ( 'NONE',  ( 21.55341960407610458, 5.719274019375980345, 88.95724293864769550 ) ) ;
#138334 = CARTESIAN_POINT ( 'NONE',  ( 16.51473224551069308, 9.474510206698969483, 59.16557627198102409 ) ) ;
#138335 = CARTESIAN_POINT ( 'NONE',  ( 5.823673210054444382, -21.52544592524334988, 30.20942372801902565 ) ) ;
#138336 = CARTESIAN_POINT ( 'NONE',  ( -19.02544592524342804, 5.153800228976336051, 86.04057627198103830 ) ) ;
#138337 = CARTESIAN_POINT ( 'NONE',  ( 13.89961937509977652, -13.97604488694527269, 113.1239096053143527 ) ) ;
#138338 = EDGE_LOOP ( 'NONE', ( #196444, #69455, #85866, #95256 ) ) ;
#138339 = CARTESIAN_POINT ( 'NONE',  ( -21.53943276465977519, -0.05219959533937600094, 18.75109039468568639 ) ) ;
#138342 = CARTESIAN_POINT ( 'NONE',  ( 16.46253265017146816, 9.564922557961045513, 91.66775706135234714 ) ) ;
#138341 = CARTESIAN_POINT ( 'NONE',  ( 0.05219959533909260263, 19.03943276465977164, 104.9989096053143669 ) ) ;
#138340 = CARTESIAN_POINT ( 'NONE',  ( -8.224510206698948167, 14.34966873604960824, 115.4155762719810241 ) ) ;
#138343 = CARTESIAN_POINT ( 'NONE',  ( 5.049401038297881783, 19.05341960407617563, 27.29275706135232937 ) ) ;
#138344 = CARTESIAN_POINT ( 'NONE',  ( -10.72451020669898014, 18.67979575497178502, 100.4155762719810241 ) ) ;
#138345 = CARTESIAN_POINT ( 'NONE',  ( 9.564922557961047289, -16.46253265017146816, 30.41775706135232937 ) ) ;
#138346 = CARTESIAN_POINT ( 'NONE',  ( 16.53943276465976808, 0.05219959533934440121, 81.25109039468568994 ) ) ;
#138347 = CARTESIAN_POINT ( 'NONE',  ( -0.05219959533909027116, -19.03943276465977164, 112.4989096053143669 ) ) ;
#138348 = CARTESIAN_POINT ( 'NONE',  ( 19.05341960407611168, 5.049401038298154454, 53.95724293864770260 ) ) ;
#138349 = CARTESIAN_POINT ( 'NONE',  ( 18.67979575497194134, -10.72451020669871369, 70.83442372801901854 ) ) ;
#138350 = CARTESIAN_POINT ( 'NONE',  ( 21.55341960407619695, -5.719274019375665929, 86.04275706135236135 ) ) ;
#138351 = CARTESIAN_POINT ( 'NONE',  ( 5.049401038298161559, -19.05341960407611168, 72.70724293864768129 ) ) ;
#138352 = CARTESIAN_POINT ( 'NONE',  ( 15.72974639402176855, 15.80617190586768217, 46.87609039468568994 ) ) ;
#138353 = CARTESIAN_POINT ( 'NONE',  ( 5.153800228976615827, -19.02544592524334988, 90.20942372801900433 ) ) ;
#138354 = CARTESIAN_POINT ( 'NONE',  ( -19.03943276465977164, 0.05219959533909376836, 46.24890960531435979 ) ) ;
#138355 = CARTESIAN_POINT ( 'NONE',  ( -19.05341960407611168, -5.049401038298163336, 101.4572429386476955 ) ) ;
#138356 = CARTESIAN_POINT ( 'NONE',  ( -13.97604488694527625, -13.89961937509977652, 71.87390960531433848 ) ) ;
#138357 = CARTESIAN_POINT ( 'NONE',  ( 16.70000000000002061, 0.000000000000000000, -61.34707691135562868 ) ) ;
#138358 = CARTESIAN_POINT ( 'NONE',  ( 13.97604488694527802, 13.89961937509977652, 49.37390960531434558 ) ) ;
#138359 = CARTESIAN_POINT ( 'NONE',  ( 21.55341960407610458, 5.719274019375980345, 98.95724293864770971 ) ) ;
#138360 = CARTESIAN_POINT ( 'NONE',  ( -16.55341960407617563, 4.379528057220093196, 93.54275706135234714 ) ) ;
#138361 = CARTESIAN_POINT ( 'NONE',  ( -24.10884208241213500, 5.471882726981272427, 173.8287385965644489 ) ) ;
#138362 = CARTESIAN_POINT ( 'NONE',  ( 19.03943276465977164, 0.05219959533936151252, 51.25109039468567573 ) ) ;
#138363 = CARTESIAN_POINT ( 'NONE',  ( -19.03943276465977164, 0.05219959533909376836, 66.24890960531436690 ) ) ;
#138364 = CARTESIAN_POINT ( 'NONE',  ( -12.06949235617756955, 12.14591786802309770, 60.62390960531437401 ) ) ;
#138365 = CARTESIAN_POINT ( 'NONE',  ( 8.224510206698953496, -14.34966873604960469, 92.91557627198103830 ) ) ;
#138366 = CARTESIAN_POINT ( 'NONE',  ( 16.51473224551069308, 9.474510206698969483, 114.1655762719810241 ) ) ;
#138367 = CARTESIAN_POINT ( 'NONE',  ( -0.05219959533909027116, -19.03943276465977164, 87.49890960531436690 ) ) ;
#138368 = CARTESIAN_POINT ( 'NONE',  ( 5.049401038298161559, -19.05341960407611168, 112.7072429386476813 ) ) ;
#138369 = APPLICATION_CONTEXT ( 'automotive_design' ) ;
#138370 = CARTESIAN_POINT ( 'NONE',  ( -5.823673210054431948, 21.52544592524334988, 112.7094237280190328 ) ) ;
#138371 = CARTESIAN_POINT ( 'NONE',  ( 16.52544592524335698, 4.483927247898782831, 86.45942372801901854 ) ) ;
#138372 = CARTESIAN_POINT ( 'NONE',  ( -13.89961937509977652, 13.97604488694528158, 80.62390960531436690 ) ) ;
#138373 = CARTESIAN_POINT ( 'NONE',  ( 21.53943276465977519, 0.05219959533937863772, 46.25109039468567573 ) ) ;
#138374 = CARTESIAN_POINT ( 'NONE',  ( -15.80617190586745835, -15.72974639402198527, 26.87390960531435979 ) ) ;
#138375 = CARTESIAN_POINT ( 'NONE',  ( -18.62759615963270932, 10.81492255796079327, 110.8322429386476955 ) ) ;
#138376 = CARTESIAN_POINT ( 'NONE',  ( 5.823673210054125526, 21.52544592524343514, 64.79057627198103830 ) ) ;
#138377 = CARTESIAN_POINT ( 'NONE',  ( -12.06949235617756955, 12.14591786802309770, 85.62390960531436690 ) ) ;
#138378 = CARTESIAN_POINT ( 'NONE',  ( 13.89961937509957401, 13.97604488694547697, 46.87609039468565442 ) ) ;
#138379 = CARTESIAN_POINT ( 'NONE',  ( -0.05219959533909027116, -19.03943276465977164, 27.49890960531435624 ) ) ;
#138380 = CARTESIAN_POINT ( 'NONE',  ( 13.97604488694527802, 13.89961937509977652, 84.37390960531433848 ) ) ;
#138381 = CARTESIAN_POINT ( 'NONE',  ( -19.03943276465977164, 0.05219959533909376836, 76.24890960531435269 ) ) ;
#138382 = CARTESIAN_POINT ( 'NONE',  ( -27.73933785331498925, 2.428612866367529932E-14, 140.8750000027311842 ) ) ;
#138383 = CARTESIAN_POINT ( 'NONE',  ( -4.379528057220328563, 16.55341960407611168, 100.2072429386476955 ) ) ;
#138384 = CARTESIAN_POINT ( 'NONE',  ( -8.314922557961024197, 14.29746914071037800, 107.9177570613523471 ) ) ;
#138385 = CARTESIAN_POINT ( 'NONE',  ( -16.52544592524335698, -4.483927247898792601, 33.95942372801901143 ) ) ;
#138386 = CARTESIAN_POINT ( 'NONE',  ( 5.719274019375673035, 21.55341960407619339, 87.29275706135236135 ) ) ;
#138387 = CARTESIAN_POINT ( 'NONE',  ( -16.46253265017160317, 9.564922557960807481, 100.8322429386477097 ) ) ;
#138388 = CARTESIAN_POINT ( 'NONE',  ( -18.67979575497193778, 10.72451020669871902, 23.33442372801901499 ) ) ;
#138389 = CARTESIAN_POINT ( 'NONE',  ( -9.564922557960796823, -16.46253265017161027, 47.08224293864769550 ) ) ;
#138390 = ADVANCED_FACE ( 'NONE', ( #77540, #105895 ), #136242, .T. ) ;
#138391 = CARTESIAN_POINT ( 'NONE',  ( -0.05219959533934338120, 16.53943276465976808, 27.50109039468567929 ) ) ;
#138392 = CARTESIAN_POINT ( 'NONE',  ( -16.51473224551082808, 9.474510206698731452, 108.3344237280190043 ) ) ;
#138393 = CARTESIAN_POINT ( 'NONE',  ( 18.62759615963271287, -10.81492255796078972, 98.33224293864769550 ) ) ;
#138394 = CARTESIAN_POINT ( 'NONE',  ( -0.05219959533936034679, 19.03943276465977164, 67.50109039468566152 ) ) ;
#138395 = CARTESIAN_POINT ( 'NONE',  ( 19.05341960407611168, 5.049401038298154454, 23.95724293864769194 ) ) ;
#138396 = CARTESIAN_POINT ( 'NONE',  ( -21.52544592524343514, 5.823673210054127303, 111.0405762719810525 ) ) ;
#138397 = CARTESIAN_POINT ( 'NONE',  ( 17.81289503416610742, 24.51734667627700404, 141.5500000054623513 ) ) ;
#138398 = CARTESIAN_POINT ( 'NONE',  ( -9.474510206698964154, 16.51473224551069663, 95.41557627198102409 ) ) ;
#138399 = CARTESIAN_POINT ( 'NONE',  ( -17.50000000001358202, 5.499999999999951150, 100.7969038253505687 ) ) ;
#138400 = CARTESIAN_POINT ( 'NONE',  ( 16.46253265017160672, -9.564922557960803928, 78.33224293864769550 ) ) ;
#138402 = CARTESIAN_POINT ( 'NONE',  ( 14.34966873604960469, 8.224510206698951720, 84.16557627198103830 ) ) ;
#138401 = CARTESIAN_POINT ( 'NONE',  ( 15.72974639402176855, 15.80617190586768217, 26.87609039468567218 ) ) ;
#138403 = CARTESIAN_POINT ( 'NONE',  ( -9.474510206698964154, 16.51473224551069663, 80.41557627198103830 ) ) ;
#138405 = CARTESIAN_POINT ( 'NONE',  ( 9.564922557961047289, -16.46253265017146816, 60.41775706135233293 ) ) ;
#138404 = CARTESIAN_POINT ( 'NONE',  ( 16.53943276465976808, 0.05219959533934440121, 51.25109039468568994 ) ) ;
#138406 = CARTESIAN_POINT ( 'NONE',  ( 18.67979575497194134, -10.72451020669871369, 70.83442372801901854 ) ) ;
#138407 = VECTOR ( 'NONE', #79385, 1000.000000000000000 ) ;
#138408 = CARTESIAN_POINT ( 'NONE',  ( -8.314922557961024197, 14.29746914071037800, 22.91775706135235069 ) ) ;
#138409 = CARTESIAN_POINT ( 'NONE',  ( 9.474510206698971260, -16.51473224551069308, 62.91557627198102409 ) ) ;
#138410 = CARTESIAN_POINT ( 'NONE',  ( 0.05219959533936267826, -19.03943276465977164, 90.00109039468567573 ) ) ;
#138411 = CARTESIAN_POINT ( 'NONE',  ( 16.55341960407618274, -4.379528057220086978, 51.04275706135234714 ) ) ;
#138412 = CARTESIAN_POINT ( 'NONE',  ( -0.05219959533937732626, 21.53943276465977519, 92.50109039468567573 ) ) ;
#138413 = CARTESIAN_POINT ( 'NONE',  ( -9.564922557961040184, 16.46253265017147172, 77.91775706135234714 ) ) ;
#138414 = CARTESIAN_POINT ( 'NONE',  ( 5.153800228976335163, 19.02544592524342804, 54.79057627198103120 ) ) ;
#138415 = CARTESIAN_POINT ( 'NONE',  ( 5.823673210054125526, 21.52544592524343514, 69.79057627198102409 ) ) ;
#138417 = CARTESIAN_POINT ( 'NONE',  ( -16.46253265017146816, -9.564922557961047289, 84.16775706135233293 ) ) ;
#138416 = CARTESIAN_POINT ( 'NONE',  ( 0.05219959533910956823, 16.53943276465976808, 79.99890960531435269 ) ) ;
#138418 = CARTESIAN_POINT ( 'NONE',  ( 16.38665767535056617, -7.295008042175987306, 62.76400864214551234 ) ) ;
#138419 = CARTESIAN_POINT ( 'NONE',  ( -16.46253265017146816, -9.564922557961047289, 49.16775706135233293 ) ) ;
#138420 = CARTESIAN_POINT ( 'NONE',  ( -12.14591786802326823, 12.06949235617739902, 113.1260903946856899 ) ) ;
#138421 = CARTESIAN_POINT ( 'NONE',  ( -14.34966873604960291, -8.224510206698953496, 61.66557627198103120 ) ) ;
#138423 = CARTESIAN_POINT ( 'NONE',  ( -22.44159573604010305, 16.30477369853692338, 148.6750000027311671 ) ) ;
#138422 = CARTESIAN_POINT ( 'NONE',  ( -21.53943276465977519, -0.05219959533937600094, 108.7510903946857042 ) ) ;
#138424 = CARTESIAN_POINT ( 'NONE',  ( -10.72451020669898014, 18.67979575497178502, 110.4155762719810383 ) ) ;
#138425 = CARTESIAN_POINT ( 'NONE',  ( -16.51473224551069308, -9.474510206698971260, 66.66557627198102409 ) ) ;
#138426 = CARTESIAN_POINT ( 'NONE',  ( -0.05219959533937732626, 21.53943276465977519, 82.50109039468568994 ) ) ;
#138427 = CARTESIAN_POINT ( 'NONE',  ( 19.03943276465977164, -0.05219959533909143690, 68.74890960531436690 ) ) ;
#138428 = CARTESIAN_POINT ( 'NONE',  ( -5.049401038298153566, 19.05341960407611168, 30.20724293864768839 ) ) ;
#138429 = CARTESIAN_POINT ( 'NONE',  ( -21.53943276465977519, 0.05219959533907696930, 31.24890960531435979 ) ) ;
#138430 = CARTESIAN_POINT ( 'NONE',  ( -8.224510206698948167, 14.34966873604960824, 70.41557627198102409 ) ) ;
#138431 = CARTESIAN_POINT ( 'NONE',  ( -13.89961937509977652, 13.97604488694528158, 25.62390960531434558 ) ) ;
#138432 = CARTESIAN_POINT ( 'NONE',  ( 0.05219959533910956823, 16.53943276465976808, 89.99890960531438111 ) ) ;
#138433 = CARTESIAN_POINT ( 'NONE',  ( -0.05219959533907301413, -21.53943276465977519, 102.4989096053143811 ) ) ;
#138434 = CARTESIAN_POINT ( 'NONE',  ( -15.72974639402176322, -15.80617190586768395, 54.37609039468568994 ) ) ;
#138435 = CARTESIAN_POINT ( 'NONE',  ( -17.81289503416611808, 24.51734667627700404, 149.6999999999999602 ) ) ;
#138436 = CARTESIAN_POINT ( 'NONE',  ( 12.14591786802327356, -12.06949235617739191, 55.62609039468568284 ) ) ;
#138437 = CARTESIAN_POINT ( 'NONE',  ( -10.81492255796078084, -18.62759615963271287, 102.0822429386476955 ) ) ;
#138438 = CARTESIAN_POINT ( 'NONE',  ( -16.51473224551082808, 9.474510206698731452, 23.33442372801900078 ) ) ;
#138439 = CARTESIAN_POINT ( 'NONE',  ( -19.05341960407611168, -5.049401038298163336, 101.4572429386476955 ) ) ;
#138440 = CARTESIAN_POINT ( 'NONE',  ( -18.62759615963255300, -10.81492255796106328, 59.16775706135234714 ) ) ;
#138441 = CARTESIAN_POINT ( 'NONE',  ( 5.823673210054125526, 21.52544592524343514, 39.79057627198103830 ) ) ;
#138442 = CARTESIAN_POINT ( 'NONE',  ( 16.55341960407618274, -4.379528057220086978, 111.0427570613523613 ) ) ;
#138444 = CARTESIAN_POINT ( 'NONE',  ( 15.72974639402176855, 15.80617190586768217, 91.87609039468568994 ) ) ;
#138443 = CARTESIAN_POINT ( 'NONE',  ( -21.52544592524334988, -5.823673210054445271, 63.95942372801901854 ) ) ;
#138445 = CARTESIAN_POINT ( 'NONE',  ( -19.05341960407617563, 5.049401038297882671, 28.54275706135232937 ) ) ;
#138446 = CARTESIAN_POINT ( 'NONE',  ( 14.34966873604972726, -8.224510206698740333, 90.83442372801901854 ) ) ;
#138447 = CARTESIAN_POINT ( 'NONE',  ( -21.55341960407619339, 5.719274019375674811, 53.54275706135234714 ) ) ;
#138448 = CARTESIAN_POINT ( 'NONE',  ( 13.89961937509977652, -13.97604488694527269, 43.12390960531434558 ) ) ;
#138449 = CARTESIAN_POINT ( 'NONE',  ( -21.53943276465977519, -0.05219959533937600094, 113.7510903946856757 ) ) ;
#138450 = CARTESIAN_POINT ( 'NONE',  ( 15.80617190586746368, 15.72974639402197994, 29.37390960531435269 ) ) ;
#138451 = CARTESIAN_POINT ( 'NONE',  ( 0.05219959533907565091, 21.53943276465977519, 109.9989096053143527 ) ) ;
#138452 = CARTESIAN_POINT ( 'NONE',  ( 21.53943276465977519, -0.05219959533907433946, 68.74890960531435269 ) ) ;
#138453 = CARTESIAN_POINT ( 'NONE',  ( -12.06949235617739369, -12.14591786802326823, 39.37609039468567573 ) ) ;
#138455 = CARTESIAN_POINT ( 'NONE',  ( -10.72451020669898014, 18.67979575497178502, 85.41557627198102409 ) ) ;
#138454 = CARTESIAN_POINT ( 'NONE',  ( -18.09918380851992836, -5.500000000000039968, 61.48618307335612343 ) ) ;
#138457 = CARTESIAN_POINT ( 'NONE',  ( 16.52544592524342804, -4.483927247898539470, 68.54057627198103830 ) ) ;
#138456 = CARTESIAN_POINT ( 'NONE',  ( 16.52544592524335698, 4.483927247898782831, 66.45942372801903275 ) ) ;
#138458 = CARTESIAN_POINT ( 'NONE',  ( -27.18966431762779834, -4.276553394869433866, 168.7322077152509507 ) ) ;
#138459 = CARTESIAN_POINT ( 'NONE',  ( -9.564922557961040184, 16.46253265017147172, 107.9177570613523471 ) ) ;
#138460 = CARTESIAN_POINT ( 'NONE',  ( 21.55341960407610458, 5.719274019375980345, 38.95724293864768839 ) ) ;
#138461 = CARTESIAN_POINT ( 'NONE',  ( -5.049401038298153566, 19.05341960407611168, 95.20724293864769550 ) ) ;
#138462 = CARTESIAN_POINT ( 'NONE',  ( -14.34966873604972548, 8.224510206698743886, 43.33442372801901143 ) ) ;
#138463 = CARTESIAN_POINT ( 'NONE',  ( 10.81492255796078972, 18.62759615963270932, 109.5822429386476955 ) ) ;
#138464 = CARTESIAN_POINT ( 'NONE',  ( 10.81492255796078972, 18.62759615963270932, 34.58224293864770260 ) ) ;
#138465 = CARTESIAN_POINT ( 'NONE',  ( -8.224510206698735004, -14.34966873604973081, 54.58442372801901143 ) ) ;
#138466 = CARTESIAN_POINT ( 'NONE',  ( 19.05341960407611168, 5.049401038298154454, 88.95724293864769550 ) ) ;
#138468 = CARTESIAN_POINT ( 'NONE',  ( 14.34966873604972726, -8.224510206698740333, 20.83442372801901143 ) ) ;
#138467 = CARTESIAN_POINT ( 'NONE',  ( -10.81492255796105439, 18.62759615963255655, 47.91775706135234714 ) ) ;
#138469 = CARTESIAN_POINT ( 'NONE',  ( -5.719274019375978568, 21.55341960407610458, 25.20724293864769550 ) ) ;
#138470 = ORIENTED_EDGE ( 'NONE', *, *, #181979, .T. ) ;
#138471 = CARTESIAN_POINT ( 'NONE',  ( 16.46253265017146816, 9.564922557961045513, 26.66775706135234003 ) ) ;
#138472 = CARTESIAN_POINT ( 'NONE',  ( 12.14591786802327356, -12.06949235617739191, 40.62609039468567573 ) ) ;
#138473 = CARTESIAN_POINT ( 'NONE',  ( 13.89961937509977652, -13.97604488694527269, 103.1239096053143527 ) ) ;
#138474 = CARTESIAN_POINT ( 'NONE',  ( -10.81492255796078084, -18.62759615963271287, 107.0822429386476955 ) ) ;
#138475 = CARTESIAN_POINT ( 'NONE',  ( 5.049401038298161559, -19.05341960407611168, 77.70724293864765286 ) ) ;
#138476 = DIRECTION ( 'NONE',  ( -1.000000000000000000, -0.000000000000000000, -0.000000000000000000 ) ) ;
#138477 = CARTESIAN_POINT ( 'NONE',  ( -12.06949235617756955, 12.14591786802309770, 80.62390960531438111 ) ) ;
#138478 = CARTESIAN_POINT ( 'NONE',  ( -0.05219959533907301413, -21.53943276465977519, 37.49890960531436690 ) ) ;
#138479 = CARTESIAN_POINT ( 'NONE',  ( -16.20579543436675252, 7.371946100355235565, 34.43479165828124877 ) ) ;
#138480 = CARTESIAN_POINT ( 'NONE',  ( -8.224510206698735004, -14.34966873604973081, 64.58442372801900433 ) ) ;
#138481 = CARTESIAN_POINT ( 'NONE',  ( 10.81492255796078972, 18.62759615963270932, 99.58224293864770971 ) ) ;
#138482 = CARTESIAN_POINT ( 'NONE',  ( 9.474510206698729675, 16.51473224551082808, 77.08442372801900433 ) ) ;
#138483 = CARTESIAN_POINT ( 'NONE',  ( -5.153800228976328057, -19.02544592524343514, 27.29057627198103120 ) ) ;
#138484 = CARTESIAN_POINT ( 'NONE',  ( 18.67979575497178502, 10.72451020669898547, 64.16557627198102409 ) ) ;
#138485 = CARTESIAN_POINT ( 'NONE',  ( -16.46253265017160317, 9.564922557960807481, 95.83224293864769550 ) ) ;
#138486 = CARTESIAN_POINT ( 'NONE',  ( 10.81492255796106328, -18.62759615963255655, 95.41775706135234714 ) ) ;
#138487 = CARTESIAN_POINT ( 'NONE',  ( -9.474510206698964154, 16.51473224551069663, 60.41557627198102409 ) ) ;
#138488 = CARTESIAN_POINT ( 'NONE',  ( 16.53943276465976808, 0.05219959533934440121, 51.25109039468568994 ) ) ;
#138489 = CARTESIAN_POINT ( 'NONE',  ( 19.02544592524343514, -5.153800228976328945, 53.54057627198102409 ) ) ;
#138490 = CARTESIAN_POINT ( 'NONE',  ( 18.62759615963255655, 10.81492255796105972, 76.66775706135234714 ) ) ;
#138491 = ORIENTED_EDGE ( 'NONE', *, *, #13540, .F. ) ;
#138492 = CARTESIAN_POINT ( 'NONE',  ( -9.564922557961040184, 16.46253265017147172, 32.91775706135233293 ) ) ;
#138493 = CARTESIAN_POINT ( 'NONE',  ( 13.89961937509957401, 13.97604488694547697, 56.87609039468564731 ) ) ;
#138494 = CARTESIAN_POINT ( 'NONE',  ( 21.55341960407619695, -5.719274019375665929, 51.04275706135234714 ) ) ;
#138495 = CARTESIAN_POINT ( 'NONE',  ( -9.051216217265920960, 0.3920586954752999786, -61.90435651123958394 ) ) ;
#138496 = CARTESIAN_POINT ( 'NONE',  ( 19.05341960407617918, -5.049401038297876454, 41.04275706135233293 ) ) ;
#138497 = CARTESIAN_POINT ( 'NONE',  ( 0.05219959533909260263, 19.03943276465977164, 84.99890960531436690 ) ) ;
#138498 = CARTESIAN_POINT ( 'NONE',  ( -9.564922557960796823, -16.46253265017161027, 72.08224293864770971 ) ) ;
#138499 = CARTESIAN_POINT ( 'NONE',  ( 12.06949235617757843, -12.14591786802309237, 28.12390960531435979 ) ) ;
#138501 = CARTESIAN_POINT ( 'NONE',  ( -0.05219959533937732626, 21.53943276465977519, 92.50109039468567573 ) ) ;
#138500 = CARTESIAN_POINT ( 'NONE',  ( 5.823673210054125526, 21.52544592524343514, 24.79057627198103120 ) ) ;
#138502 = VECTOR ( 'NONE', #101087, 1000.000000000000000 ) ;
#138503 = CARTESIAN_POINT ( 'NONE',  ( -36.91746825000001309, 11.99521256947798342, -9.224999997268813701 ) ) ;
#138504 = CARTESIAN_POINT ( 'NONE',  ( 5.000000000000000888, -130.0000000000000000, -12.99999999999999822 ) ) ;
#138505 = CARTESIAN_POINT ( 'NONE',  ( 15.72974639402176855, 15.80617190586768217, 96.87609039468568994 ) ) ;
#138506 = CARTESIAN_POINT ( 'NONE',  ( 19.05341960407611168, 5.049401038298154454, 23.95724293864769194 ) ) ;
#138507 = CARTESIAN_POINT ( 'NONE',  ( 19.05341960407611168, 5.049401038298154454, 113.9572429386477097 ) ) ;
#138508 = CARTESIAN_POINT ( 'NONE',  ( 33.78659134798514430, 2.758747016945830133, 99.77194732211482631 ) ) ;
#138509 = CARTESIAN_POINT ( 'NONE',  ( -12.06949235617739369, -12.14591786802326823, 49.37609039468569705 ) ) ;
#138510 = CARTESIAN_POINT ( 'NONE',  ( -10.72451020669898014, 18.67979575497178502, 75.41557627198102409 ) ) ;
#138511 = CARTESIAN_POINT ( 'NONE',  ( 12.06949235617757843, -12.14591786802309237, 43.12390960531435269 ) ) ;
#138513 = CARTESIAN_POINT ( 'NONE',  ( -5.153800228976328057, -19.02544592524343514, 92.29057627198099567 ) ) ;
#138512 = CARTESIAN_POINT ( 'NONE',  ( 14.34966873604960469, 8.224510206698951720, 114.1655762719810383 ) ) ;
#138514 = CARTESIAN_POINT ( 'NONE',  ( -5.049401038297874678, -19.05341960407617918, 34.79275706135233293 ) ) ;
#138515 = CARTESIAN_POINT ( 'NONE',  ( 4.379528057220339221, -16.55341960407611168, 112.7072429386476955 ) ) ;
#138516 = CARTESIAN_POINT ( 'NONE',  ( 0.05219959533937995610, -21.53943276465977519, 75.00109039468568994 ) ) ;
#138517 = CARTESIAN_POINT ( 'NONE',  ( -19.03943276465977164, 0.05219959533909376836, 116.2489096053143669 ) ) ;
#138518 = CARTESIAN_POINT ( 'NONE',  ( 8.314922557961029526, -14.29746914071037800, 110.4177570613523756 ) ) ;
#138519 = CARTESIAN_POINT ( 'NONE',  ( 36.91746824999999887, -11.99521256947793546, -6.224999997268814589 ) ) ;
#138520 = CARTESIAN_POINT ( 'NONE',  ( -21.55341960407610458, -5.719274019375992779, 26.45724293864768839 ) ) ;
#138521 = CARTESIAN_POINT ( 'NONE',  ( -12.14591786802309592, -12.06949235617757132, 91.87390960531436690 ) ) ;
#138522 = CARTESIAN_POINT ( 'NONE',  ( -5.049401038297874678, -19.05341960407617918, 59.79275706135231871 ) ) ;
#138523 = CARTESIAN_POINT ( 'NONE',  ( 13.97604488694527802, 13.89961937509977652, 74.37390960531436690 ) ) ;
#138524 = CARTESIAN_POINT ( 'NONE',  ( -16.53943276465976808, 0.05219959533911058130, 71.24890960531435269 ) ) ;
#138525 = CARTESIAN_POINT ( 'NONE',  ( -19.05341960407617563, 5.049401038297882671, 88.54275706135230450 ) ) ;
#138526 = CARTESIAN_POINT ( 'NONE',  ( 0.05219959533907565091, 21.53943276465977519, 54.99890960531435269 ) ) ;
#138527 = ORIENTED_EDGE ( 'NONE', *, *, #86587, .F. ) ;
#138528 = CARTESIAN_POINT ( 'NONE',  ( 0.05219959533910956823, 16.53943276465976808, 114.9989096053143669 ) ) ;
#138529 = CARTESIAN_POINT ( 'NONE',  ( -3.573655867282025236E-15, -180.0000000000000000, -13.00000000000000000 ) ) ;
#138531 = CARTESIAN_POINT ( 'NONE',  ( -5.719274019375978568, 21.55341960407610458, 75.20724293864769550 ) ) ;
#138530 = CARTESIAN_POINT ( 'NONE',  ( -19.02544592524342804, 5.153800228976336051, 66.04057627198103830 ) ) ;
#138533 = CARTESIAN_POINT ( 'NONE',  ( 19.05341960407611168, 5.049401038298154454, 88.95724293864769550 ) ) ;
#138532 = CARTESIAN_POINT ( 'NONE',  ( 0.05219959533934541429, -16.53943276465976808, 90.00109039468567573 ) ) ;
#138534 = CARTESIAN_POINT ( 'NONE',  ( 9.564922557961047289, -16.46253265017146816, 70.41775706135233293 ) ) ;
#138535 = CARTESIAN_POINT ( 'NONE',  ( -18.67979575497193778, 10.72451020669871902, 78.33442372801901854 ) ) ;
#138536 = CARTESIAN_POINT ( 'NONE',  ( -10.81492255796078084, -18.62759615963271287, 57.08224293864769550 ) ) ;
#138537 = CARTESIAN_POINT ( 'NONE',  ( -18.67979575497178146, -10.72451020669898902, 26.66557627198103475 ) ) ;
#138538 = CARTESIAN_POINT ( 'NONE',  ( 9.564922557960805705, 16.46253265017160317, 34.58224293864770260 ) ) ;
#138539 = CARTESIAN_POINT ( 'NONE',  ( -12.14591786802326823, 12.06949235617739902, 98.12609039468570415 ) ) ;
#138540 = CARTESIAN_POINT ( 'NONE',  ( 16.51473224551069308, 9.474510206698969483, 49.16557627198102409 ) ) ;
#138541 = CARTESIAN_POINT ( 'NONE',  ( -14.29746914071037622, -8.314922557961029526, 24.16775706135235424 ) ) ;
#138542 = CARTESIAN_POINT ( 'NONE',  ( 17.50000000000000000, 5.499999999999992895, 51.70309617465830598 ) ) ;
#138543 = CARTESIAN_POINT ( 'NONE',  ( -19.03943276465977164, -0.05219959533935918106, 18.75109039468567218 ) ) ;
#138544 = CARTESIAN_POINT ( 'NONE',  ( -16.55341960407611168, -4.379528057220339221, 56.45724293864768839 ) ) ;
#138545 = CARTESIAN_POINT ( 'NONE',  ( -21.55341960407610458, -5.719274019375992779, 106.4572429386477097 ) ) ;
#138546 = CARTESIAN_POINT ( 'NONE',  ( 10.72451020669898902, -18.67979575497178502, 97.91557627198103830 ) ) ;
#138547 = CARTESIAN_POINT ( 'NONE',  ( -6.502961151143344942, 4.381597987324907351, -64.22400872216478263 ) ) ;
#138549 = EDGE_CURVE ( 'NONE', #17000, #88586, #13884, .T. ) ;
#138548 = CARTESIAN_POINT ( 'NONE',  ( 18.62759615963271287, -10.81492255796078972, 43.33224293864769550 ) ) ;
#138550 = CARTESIAN_POINT ( 'NONE',  ( -4.379528057220086978, -16.55341960407618274, 74.79275706135234714 ) ) ;
#138551 = CARTESIAN_POINT ( 'NONE',  ( 4.483927247898545687, 16.52544592524342804, 89.79057627198103830 ) ) ;
#138552 = CARTESIAN_POINT ( 'NONE',  ( -19.05341960407611168, -5.049401038298163336, 61.45724293864769550 ) ) ;
#138553 = CARTESIAN_POINT ( 'NONE',  ( 22.49873734152911453, -26.99873734152921045, 1.110912703473986074 ) ) ;
#138554 = CARTESIAN_POINT ( 'NONE',  ( -0.05219959533934338120, 16.53943276465976808, 107.5010903946856899 ) ) ;
#138555 = CARTESIAN_POINT ( 'NONE',  ( 18.67979575497194134, -10.72451020669871369, 35.83442372801901143 ) ) ;
#138556 = CARTESIAN_POINT ( 'NONE',  ( -9.564922557960796823, -16.46253265017161027, 92.08224293864769550 ) ) ;
#138557 = CARTESIAN_POINT ( 'NONE',  ( 21.53943276465977519, 0.05219959533937863772, 71.25109039468568994 ) ) ;
#138558 = FACE_OUTER_BOUND ( 'NONE', #81593, .T. ) ;
#138559 = LINE ( 'NONE', #37, #176804 ) ;
#138560 = ORIENTED_EDGE ( 'NONE', *, *, #72464, .F. ) ;
#138561 = CARTESIAN_POINT ( 'NONE',  ( -15.72974639402176322, -15.80617190586768395, 59.37609039468568284 ) ) ;
#138562 = CARTESIAN_POINT ( 'NONE',  ( -16.46253265017160317, 9.564922557960807481, 55.83224293864769550 ) ) ;
#138563 = CARTESIAN_POINT ( 'NONE',  ( -19.03943276465977164, 0.05219959533909376836, 91.24890960531436690 ) ) ;
#138564 = CARTESIAN_POINT ( 'NONE',  ( -19.03943276465977164, -0.05219959533935918106, 63.75109039468566863 ) ) ;
#138565 = CARTESIAN_POINT ( 'NONE',  ( 18.67979575497194134, -10.72451020669871369, 45.83442372801901854 ) ) ;
#138566 = CARTESIAN_POINT ( 'NONE',  ( -9.474510206698720793, -16.51473224551083518, 104.5844237280190043 ) ) ;
#138567 = CARTESIAN_POINT ( 'NONE',  ( 9.564922557961047289, -16.46253265017146816, 70.41775706135233293 ) ) ;
#138568 = CARTESIAN_POINT ( 'NONE',  ( 16.51473224551069308, 9.474510206698969483, 39.16557627198103120 ) ) ;
#138569 = CARTESIAN_POINT ( 'NONE',  ( 5.049401038297881783, 19.05341960407617563, 87.29275706135234714 ) ) ;
#138570 = CARTESIAN_POINT ( 'NONE',  ( -14.29746914071037622, -8.314922557961029526, 99.16775706135234714 ) ) ;
#138571 = CARTESIAN_POINT ( 'NONE',  ( 9.474510206698729675, 16.51473224551082808, 72.08442372801900433 ) ) ;
#138572 = CARTESIAN_POINT ( 'NONE',  ( -8.314922557960811034, -14.29746914071050412, 27.08224293864769550 ) ) ;
#138573 = CARTESIAN_POINT ( 'NONE',  ( -13.97604488694547697, 13.89961937509957934, 48.12609039468566863 ) ) ;
#138574 = CARTESIAN_POINT ( 'NONE',  ( -18.62759615963255300, -10.81492255796106328, 109.1677570613523613 ) ) ;
#138575 = CARTESIAN_POINT ( 'NONE',  ( -9.474510206698720793, -16.51473224551083518, 24.58442372801900078 ) ) ;
#138576 = CARTESIAN_POINT ( 'NONE',  ( 0.05219959533909260263, 19.03943276465977164, 34.99890960531435979 ) ) ;
#138577 = CARTESIAN_POINT ( 'NONE',  ( 15.80617190586769283, -15.72974639402175789, 85.62609039468568994 ) ) ;
#138578 = CARTESIAN_POINT ( 'NONE',  ( -0.05219959533934338120, 16.53943276465976808, 42.50109039468567573 ) ) ;
#138579 = CARTESIAN_POINT ( 'NONE',  ( 13.97604488694527802, 13.89961937509977652, 99.37390960531436690 ) ) ;
#138580 = CARTESIAN_POINT ( 'NONE',  ( 22.44159573604009594, -16.30477369853687364, 145.6750000027311671 ) ) ;
#138581 = CARTESIAN_POINT ( 'NONE',  ( -5.049401038298153566, 19.05341960407611168, 80.20724293864769550 ) ) ;
#138582 = CARTESIAN_POINT ( 'NONE',  ( -17.60728821187772297, 5.500000000000019540, 95.86690927743606494 ) ) ;
#138583 = VERTEX_POINT ( 'NONE', #75551 ) ;
#138584 = CARTESIAN_POINT ( 'NONE',  ( -19.03943276465977164, -0.05219959533935918106, 88.75109039468567573 ) ) ;
#138585 = CARTESIAN_POINT ( 'NONE',  ( -19.03943276465977164, 0.05219959533909376836, 116.2489096053143669 ) ) ;
#138587 = CARTESIAN_POINT ( 'NONE',  ( -16.51473224551082808, 9.474510206698731452, 103.3344237280190043 ) ) ;
#138586 = CARTESIAN_POINT ( 'NONE',  ( -5.719274019375665041, -21.55341960407619695, 109.7927570613523613 ) ) ;
#138588 = CARTESIAN_POINT ( 'NONE',  ( 8.224510206698953496, -14.34966873604960469, 97.91557627198103830 ) ) ;
#138589 = CARTESIAN_POINT ( 'NONE',  ( 19.03943276465977164, -0.05219959533909143690, 28.74890960531435624 ) ) ;
#138590 = CARTESIAN_POINT ( 'NONE',  ( -5.719274019375978568, 21.55341960407610458, 55.20724293864770260 ) ) ;
#138591 = CARTESIAN_POINT ( 'NONE',  ( 18.62759615963271287, -10.81492255796078972, 48.33224293864770260 ) ) ;
#138592 = CARTESIAN_POINT ( 'NONE',  ( 0.05219959533910956823, 16.53943276465976808, 114.9989096053143669 ) ) ;
#138593 = DIRECTION ( 'NONE',  ( 0.000000000000000000, 0.000000000000000000, -1.000000000000000000 ) ) ;
#138594 = CARTESIAN_POINT ( 'NONE',  ( -0.05219959533936034679, 19.03943276465977164, 72.50109039468566152 ) ) ;
#138595 = CARTESIAN_POINT ( 'NONE',  ( -12.06949235617756955, 12.14591786802309770, 45.62390960531436690 ) ) ;
#138596 = CARTESIAN_POINT ( 'NONE',  ( -9.474510206698964154, 16.51473224551069663, 115.4155762719810241 ) ) ;
#138597 = CARTESIAN_POINT ( 'NONE',  ( 21.55341960407619695, -5.719274019375665929, 76.04275706135237556 ) ) ;
#138598 = CARTESIAN_POINT ( 'NONE',  ( -21.53943276465977519, 0.05219959533907696930, 66.24890960531436690 ) ) ;
#138599 = CARTESIAN_POINT ( 'NONE',  ( 15.72974639402176855, 15.80617190586768217, 56.87609039468568994 ) ) ;
#138600 = CARTESIAN_POINT ( 'NONE',  ( 21.55341960407619695, -5.719274019375665929, 46.04275706135234714 ) ) ;
#138601 = CARTESIAN_POINT ( 'NONE',  ( 9.564922557960805705, 16.46253265017160317, 79.58224293864769550 ) ) ;
#138602 = CARTESIAN_POINT ( 'NONE',  ( 4.483927247898790824, -16.52544592524335698, 90.20942372801903275 ) ) ;
#138603 = CARTESIAN_POINT ( 'NONE',  ( 5.049401038298161559, -19.05341960407611168, 27.70724293864769550 ) ) ;
#138604 = CARTESIAN_POINT ( 'NONE',  ( -31.24009710442677701, 7.113574878955727598, 97.38907943302068304 ) ) ;
#138605 = CARTESIAN_POINT ( 'NONE',  ( 0.05219959533910956823, 16.53943276465976808, 64.99890960531435269 ) ) ;
#138606 = CARTESIAN_POINT ( 'NONE',  ( 4.483927247898545687, 16.52544592524342804, 29.79057627198102409 ) ) ;
#138607 = CARTESIAN_POINT ( 'NONE',  ( -5.049401038298153566, 19.05341960407611168, 65.20724293864765286 ) ) ;
#138608 = CARTESIAN_POINT ( 'NONE',  ( -13.97604488694527625, -13.89961937509977652, 36.87390960531436690 ) ) ;
#138609 = CARTESIAN_POINT ( 'NONE',  ( 18.62759615963271287, -10.81492255796078972, 48.33224293864770260 ) ) ;
#138610 = CARTESIAN_POINT ( 'NONE',  ( -0.05219959533936034679, 19.03943276465977164, 32.50109039468566863 ) ) ;
#138612 = CARTESIAN_POINT ( 'NONE',  ( 14.29746914071049879, -8.314922557960816363, 48.33224293864770260 ) ) ;
#138611 = CARTESIAN_POINT ( 'NONE',  ( 9.809999999999998721, 0.000000000000000000, 0.000000000000000000 ) ) ;
#138613 = CARTESIAN_POINT ( 'NONE',  ( -0.05219959533907301413, -21.53943276465977519, 32.49890960531435979 ) ) ;
#138614 = LINE ( 'NONE', #123434, #25846 ) ;
#138615 = CARTESIAN_POINT ( 'NONE',  ( -14.29746914071037622, -8.314922557961029526, 74.16775706135231871 ) ) ;
#138616 = ADVANCED_FACE ( 'NONE', ( #93701 ), #108874, .T. ) ;
#138617 = CARTESIAN_POINT ( 'NONE',  ( 9.564922557961047289, -16.46253265017146816, 75.41775706135234714 ) ) ;
#138618 = CARTESIAN_POINT ( 'NONE',  ( -8.224510206698948167, 14.34966873604960824, 45.41557627198103830 ) ) ;
#138619 = ORIENTED_EDGE ( 'NONE', *, *, #9338, .T. ) ;
#138620 = CARTESIAN_POINT ( 'NONE',  ( 17.50000000000006040, -5.622605283950772304, 51.18792689403892382 ) ) ;
#138621 = CARTESIAN_POINT ( 'NONE',  ( -8.314922557960811034, -14.29746914071050412, 32.08224293864769550 ) ) ;
#138622 = CARTESIAN_POINT ( 'NONE',  ( 19.02544592524343514, -5.153800228976328945, 48.54057627198103120 ) ) ;
#138623 = CARTESIAN_POINT ( 'NONE',  ( 13.97604488694527802, 13.89961937509977652, 74.37390960531436690 ) ) ;
#138624 = CARTESIAN_POINT ( 'NONE',  ( -9.474510206698964154, 16.51473224551069663, 40.41557627198103120 ) ) ;
#138625 = CARTESIAN_POINT ( 'NONE',  ( 21.53943276465977519, 0.05219959533937863772, 41.25109039468568284 ) ) ;
#138626 = CARTESIAN_POINT ( 'NONE',  ( 9.564922557960805705, 16.46253265017160317, 64.58224293864769550 ) ) ;
#138627 = CARTESIAN_POINT ( 'NONE',  ( -24.95432927374998044, 3.806786798636383917, 190.0000000000000000 ) ) ;
#138628 = CARTESIAN_POINT ( 'NONE',  ( 9.474510206698971260, -16.51473224551069308, 47.91557627198102409 ) ) ;
#138629 = CARTESIAN_POINT ( 'NONE',  ( 21.55341960407610458, 5.719274019375980345, 33.95724293864769550 ) ) ;
#138630 = AXIS2_PLACEMENT_3D ( 'NONE', #77192, #122697, #150082 ) ;
#138632 = CARTESIAN_POINT ( 'NONE',  ( 19.03943276465977164, -0.05219959533909143690, 28.74890960531435624 ) ) ;
#138631 = CARTESIAN_POINT ( 'NONE',  ( 21.55341960407619695, -5.719274019375665929, 76.04275706135237556 ) ) ;
#138633 = CARTESIAN_POINT ( 'NONE',  ( 18.62759615963271287, -10.81492255796078972, 33.33224293864769550 ) ) ;
#138634 = CARTESIAN_POINT ( 'NONE',  ( 0.05219959533934541429, -16.53943276465976808, 95.00109039468568994 ) ) ;
#138635 = CARTESIAN_POINT ( 'NONE',  ( -18.62759615963255300, -10.81492255796106328, 99.16775706135234714 ) ) ;
#138636 = CARTESIAN_POINT ( 'NONE',  ( -14.29746914071037622, -8.314922557961029526, 64.16775706135234714 ) ) ;
#138637 = CARTESIAN_POINT ( 'NONE',  ( 5.049401038298161559, -19.05341960407611168, 107.7072429386476955 ) ) ;
#138638 = CARTESIAN_POINT ( 'NONE',  ( -4.483927247898782831, 16.52544592524335698, 52.70942372801902565 ) ) ;
#138639 = CARTESIAN_POINT ( 'NONE',  ( 8.314922557961029526, -14.29746914071037800, 40.41775706135234714 ) ) ;
#138640 = CARTESIAN_POINT ( 'NONE',  ( -16.53943276465976808, -0.05219959533934237506, 93.75109039468567573 ) ) ;
#138641 = CARTESIAN_POINT ( 'NONE',  ( 21.52544592524334988, 5.823673210054432836, 56.45942372801902565 ) ) ;
#138642 = CARTESIAN_POINT ( 'NONE',  ( -14.34966873604972548, 8.224510206698743886, 23.33442372801901499 ) ) ;
#138643 = CARTESIAN_POINT ( 'NONE',  ( 21.53943276465977519, -0.05219959533907433946, 113.7489096053143527 ) ) ;
#138644 = CARTESIAN_POINT ( 'NONE',  ( -0.05219959533934338120, 16.53943276465976808, 27.50109039468567929 ) ) ;
#138645 = CARTESIAN_POINT ( 'NONE',  ( 8.224510206698742110, 14.34966873604972548, 87.08442372801901854 ) ) ;
#138646 = CARTESIAN_POINT ( 'NONE',  ( -16.81555441253465943, 7.025013491696272538, 45.63685445334211011 ) ) ;
#138647 = CARTESIAN_POINT ( 'NONE',  ( 21.53943276465977519, 0.05219959533937863772, 81.25109039468568994 ) ) ;
#138648 = CARTESIAN_POINT ( 'NONE',  ( -5.049401038297874678, -19.05341960407617918, 79.79275706135233293 ) ) ;
#138649 = CARTESIAN_POINT ( 'NONE',  ( 12.06949235617757843, -12.14591786802309237, 58.12390960531435979 ) ) ;
#138650 = CARTESIAN_POINT ( 'NONE',  ( 16.52544592524342804, -4.483927247898539470, 43.54057627198103830 ) ) ;
#138651 = CARTESIAN_POINT ( 'NONE',  ( 12.06949235617757843, -12.14591786802309237, 113.1239096053143953 ) ) ;
#138653 = CARTESIAN_POINT ( 'NONE',  ( -19.03943276465977164, 0.05219959533909376836, 21.24890960531436335 ) ) ;
#138652 = CARTESIAN_POINT ( 'NONE',  ( -19.02544592524334988, -5.153800228976617603, 53.95942372801898301 ) ) ;
#138654 = CARTESIAN_POINT ( 'NONE',  ( 5.823673210054444382, -21.52544592524334988, 45.20942372801901854 ) ) ;
#138655 = CARTESIAN_POINT ( 'NONE',  ( 13.89961937509957401, 13.97604488694547697, 106.8760903946856757 ) ) ;
#138656 = LINE ( 'NONE', #32486, #137437 ) ;
#138657 = CARTESIAN_POINT ( 'NONE',  ( -16.51473224551069308, -9.474510206698971260, 106.6655762719810383 ) ) ;
#138658 = CARTESIAN_POINT ( 'NONE',  ( 21.52544592524344225, -5.823673210054117533, 73.54057627198102409 ) ) ;
#138659 = CARTESIAN_POINT ( 'NONE',  ( -16.51473224551082808, 9.474510206698731452, 98.33442372801900433 ) ) ;
#138660 = CARTESIAN_POINT ( 'NONE',  ( -19.03943276465977164, 0.05219959533909376836, 106.2489096053143669 ) ) ;
#138661 = CARTESIAN_POINT ( 'NONE',  ( -20.73749492396214933, -155.7167183371837496, -4.999999999999999112 ) ) ;
#138662 = CARTESIAN_POINT ( 'NONE',  ( -0.05219959533910754901, -16.53943276465976808, 102.4989096053143811 ) ) ;
#138663 = CARTESIAN_POINT ( 'NONE',  ( -18.62759615963255300, -10.81492255796106328, 99.16775706135234714 ) ) ;
#138664 = CARTESIAN_POINT ( 'NONE',  ( 13.97604488694527802, 13.89961937509977652, 24.37390960531435624 ) ) ;
#138665 = CARTESIAN_POINT ( 'NONE',  ( 21.53943276465977519, 0.05219959533937863772, 46.25109039468567573 ) ) ;
#138666 = VECTOR ( 'NONE', #97887, 1000.000000000000000 ) ;
#138667 = CARTESIAN_POINT ( 'NONE',  ( -5.823673210054431948, 21.52544592524334988, 87.70942372801901854 ) ) ;
#138668 = CARTESIAN_POINT ( 'NONE',  ( -0.05219959533934338120, 16.53943276465976808, 87.50109039468568994 ) ) ;
#138669 = CARTESIAN_POINT ( 'NONE',  ( 10.72451020669871369, 18.67979575497193778, 42.08442372801901854 ) ) ;
#138670 = CARTESIAN_POINT ( 'NONE',  ( -0.05219959533937732626, 21.53943276465977519, 37.50109039468568284 ) ) ;
#138672 = CARTESIAN_POINT ( 'NONE',  ( -5.153800228976328057, -19.02544592524343514, 97.29057627198099567 ) ) ;
#138671 = CARTESIAN_POINT ( 'NONE',  ( -5.153800228976607833, 19.02544592524334988, 72.70942372801900433 ) ) ;
#138673 = CARTESIAN_POINT ( 'NONE',  ( 4.379528057220339221, -16.55341960407611168, 107.7072429386476955 ) ) ;
#138674 = CARTESIAN_POINT ( 'NONE',  ( 21.53943276465977519, -0.05219959533907433946, 88.74890960531436690 ) ) ;
#138675 = CARTESIAN_POINT ( 'NONE',  ( -16.55341960407611168, -4.379528057220339221, 66.45724293864768129 ) ) ;
#138676 = CARTESIAN_POINT ( 'NONE',  ( -0.05219959533937732626, 21.53943276465977519, 97.50109039468567573 ) ) ;
#138677 = CARTESIAN_POINT ( 'NONE',  ( 0.05219959533910956823, 16.53943276465976808, 79.99890960531435269 ) ) ;
#138678 = CARTESIAN_POINT ( 'NONE',  ( -0.05219959533909027116, -19.03943276465977164, 32.49890960531435979 ) ) ;
#138679 = CARTESIAN_POINT ( 'NONE',  ( 19.05341960407617918, -5.049401038297876454, 66.04275706135233293 ) ) ;
#138680 = CARTESIAN_POINT ( 'NONE',  ( 14.29746914071049879, -8.314922557960816363, 53.33224293864769550 ) ) ;
#138681 = CARTESIAN_POINT ( 'NONE',  ( 5.823673210054444382, -21.52544592524334988, 90.20942372801903275 ) ) ;
#138682 = CARTESIAN_POINT ( 'NONE',  ( 5.153800228976335163, 19.02544592524342804, 89.79057627198102409 ) ) ;
#138683 = CARTESIAN_POINT ( 'NONE',  ( 9.564922557961047289, -16.46253265017146816, 55.41775706135234003 ) ) ;
#138684 = CARTESIAN_POINT ( 'NONE',  ( 21.55341960407610458, 5.719274019375980345, 58.95724293864770971 ) ) ;
#138685 = CARTESIAN_POINT ( 'NONE',  ( 15.80617190586746368, 15.72974639402197994, 109.3739096053143811 ) ) ;
#138686 = CARTESIAN_POINT ( 'NONE',  ( 16.46253265017146816, 9.564922557961045513, 111.6677570613523329 ) ) ;
#138687 = CARTESIAN_POINT ( 'NONE',  ( -14.29746914071037622, -8.314922557961029526, 84.16775706135234714 ) ) ;
#138689 = CARTESIAN_POINT ( 'NONE',  ( 5.823673210054444382, -21.52544592524334988, 20.20942372801900788 ) ) ;
#138688 = CARTESIAN_POINT ( 'NONE',  ( 19.03943276465977164, -0.05219959533909143690, 28.74890960531435624 ) ) ;
#138690 = CARTESIAN_POINT ( 'NONE',  ( -16.53943276465976808, 0.05219959533911058130, 111.2489096053143669 ) ) ;
#138691 = CARTESIAN_POINT ( 'NONE',  ( -5.950531402560715689E-15, 38.81732327939063509, -5.624999997268812280 ) ) ;
#138692 = CARTESIAN_POINT ( 'NONE',  ( 12.06949235617739724, 12.14591786802326823, 46.87609039468568994 ) ) ;
#138693 = CARTESIAN_POINT ( 'NONE',  ( 0.05219959533910956823, 16.53943276465976808, 79.99890960531435269 ) ) ;
#138694 = CARTESIAN_POINT ( 'NONE',  ( -21.52544592524343514, 5.823673210054127303, 76.04057627198102409 ) ) ;
#138695 = CARTESIAN_POINT ( 'NONE',  ( -12.14591786802326823, 12.06949235617739902, 113.1260903946856899 ) ) ;
#138696 = CARTESIAN_POINT ( 'NONE',  ( -8.314922557961024197, 14.29746914071037800, 32.91775706135234714 ) ) ;
#138697 = CARTESIAN_POINT ( 'NONE',  ( 19.05341960407611168, 5.049401038298154454, 38.95724293864767418 ) ) ;
#138698 = CARTESIAN_POINT ( 'NONE',  ( 0.05219959533934541429, -16.53943276465976808, 85.00109039468568994 ) ) ;
#138699 = CARTESIAN_POINT ( 'NONE',  ( -16.46253265017146816, -9.564922557961047289, 74.16775706135234714 ) ) ;
#138700 = CARTESIAN_POINT ( 'NONE',  ( -10.72451020669898014, 18.67979575497178502, 65.41557627198102409 ) ) ;
#138701 = CARTESIAN_POINT ( 'NONE',  ( -12.14591786802326823, 12.06949235617739902, 113.1260903946856899 ) ) ;
#138702 = ORIENTED_EDGE ( 'NONE', *, *, #148381, .F. ) ;
#138703 = CARTESIAN_POINT ( 'NONE',  ( 5.823673210054444382, -21.52544592524334988, 85.20942372801901854 ) ) ;
#138704 = CARTESIAN_POINT ( 'NONE',  ( 21.52544592524344225, -5.823673210054117533, 48.54057627198103120 ) ) ;
#138705 = ORIENTED_EDGE ( 'NONE', *, *, #114259, .F. ) ;
#138706 = CARTESIAN_POINT ( 'NONE',  ( 8.224510206698742110, 14.34966873604972548, 87.08442372801901854 ) ) ;
#138707 = CARTESIAN_POINT ( 'NONE',  ( 5.719274019375991003, -21.55341960407610458, 47.70724293864770260 ) ) ;
#138708 = ORIENTED_EDGE ( 'NONE', *, *, #125504, .F. ) ;
#138709 = CARTESIAN_POINT ( 'NONE',  ( -5.049401038298153566, 19.05341960407611168, 115.2072429386477097 ) ) ;
#138710 = CARTESIAN_POINT ( 'NONE',  ( -18.56197773271726703, 5.500000000000080824, 73.55066217314454491 ) ) ;
#138711 = CARTESIAN_POINT ( 'NONE',  ( 16.46253265017160672, -9.564922557960803928, 28.33224293864769550 ) ) ;
#138712 = CARTESIAN_POINT ( 'NONE',  ( 18.62759615963271287, -10.81492255796078972, 78.33224293864770971 ) ) ;
#138713 = CARTESIAN_POINT ( 'NONE',  ( 14.34966873604972726, -8.224510206698740333, 100.8344237280190185 ) ) ;
#138714 = CARTESIAN_POINT ( 'NONE',  ( -10.81492255796105439, 18.62759615963255655, 62.91775706135236135 ) ) ;
#138715 = CARTESIAN_POINT ( 'NONE',  ( -4.483927247898782831, 16.52544592524335698, 22.70942372801901499 ) ) ;
#138716 = CARTESIAN_POINT ( 'NONE',  ( 8.314922557960818139, 14.29746914071049879, 114.5822429386477097 ) ) ;
#138717 = CARTESIAN_POINT ( 'NONE',  ( 13.97604488694548053, -13.89961937509957401, 105.6260903946856757 ) ) ;
#138718 = CARTESIAN_POINT ( 'NONE',  ( -9.474510206698964154, 16.51473224551069663, 35.41557627198102409 ) ) ;
#138719 = CARTESIAN_POINT ( 'NONE',  ( -17.81289503416611097, -24.51734667627696496, 144.2999999999999829 ) ) ;
#138720 = CARTESIAN_POINT ( 'NONE',  ( -13.89961937509977652, 13.97604488694528158, 105.6239096053143527 ) ) ;
#138721 = CARTESIAN_POINT ( 'NONE',  ( -16.52544592524335698, -4.483927247898792601, 88.95942372801901854 ) ) ;
#138722 = CARTESIAN_POINT ( 'NONE',  ( 0.05219959533936267826, -19.03943276465977164, 80.00109039468567573 ) ) ;
#138723 = CARTESIAN_POINT ( 'NONE',  ( -13.97604488694547697, 13.89961937509957934, 23.12609039468565442 ) ) ;
#138724 = CARTESIAN_POINT ( 'NONE',  ( -21.53943276465977519, 0.05219959533907696930, 66.24890960531436690 ) ) ;
#138725 = ADVANCED_FACE ( 'NONE', ( #137227 ), #183743, .T. ) ;
#138726 = CARTESIAN_POINT ( 'NONE',  ( -16.55341960407617563, 4.379528057220093196, 83.54275706135234714 ) ) ;
#138727 = CARTESIAN_POINT ( 'NONE',  ( -19.02544592524334988, -5.153800228976617603, 88.95942372801897591 ) ) ;
#138728 = CARTESIAN_POINT ( 'NONE',  ( -19.03943276465977164, 0.05219959533909376836, 46.24890960531435979 ) ) ;
#138729 = CARTESIAN_POINT ( 'NONE',  ( -19.02544592524342804, 5.153800228976336051, 86.04057627198103830 ) ) ;
#138730 = CARTESIAN_POINT ( 'NONE',  ( -18.67979575497193778, 10.72451020669871902, 48.33442372801902565 ) ) ;
#138731 = CARTESIAN_POINT ( 'NONE',  ( -9.564922557960796823, -16.46253265017161027, 42.08224293864769550 ) ) ;
#138732 = CARTESIAN_POINT ( 'NONE',  ( -17.50000000000001421, -5.622605283950843358, 86.31207310596114723 ) ) ;
#138733 = CARTESIAN_POINT ( 'NONE',  ( 0.05219959533909260263, 19.03943276465977164, 114.9989096053143669 ) ) ;
#138734 = CARTESIAN_POINT ( 'NONE',  ( 12.14591786802309770, 12.06949235617756955, 59.37390960531436690 ) ) ;
#138735 = CARTESIAN_POINT ( 'NONE',  ( -18.67979575497178146, -10.72451020669898902, 76.66557627198103830 ) ) ;
#138736 = CARTESIAN_POINT ( 'NONE',  ( -13.89961937509957401, -13.97604488694547875, 49.37609039468567573 ) ) ;
#138737 = CARTESIAN_POINT ( 'NONE',  ( 19.49401214000073779, -12.39993551617566503, 169.9999999999999716 ) ) ;
#138739 = CARTESIAN_POINT ( 'NONE',  ( 16.51473224551069308, 9.474510206698969483, 69.16557627198102409 ) ) ;
#138738 = CARTESIAN_POINT ( 'NONE',  ( 19.05341960407611168, 5.049401038298154454, 63.95724293864769550 ) ) ;
#138740 = CARTESIAN_POINT ( 'NONE',  ( -12.06949235617739369, -12.14591786802326823, 49.37609039468569705 ) ) ;
#138741 = DIRECTION ( 'NONE',  ( 1.000000000000000000, 0.000000000000000000, 0.000000000000000000 ) ) ;
#138742 = CARTESIAN_POINT ( 'NONE',  ( -9.564922557961040184, 16.46253265017147172, 32.91775706135233293 ) ) ;
#138743 = CARTESIAN_POINT ( 'NONE',  ( -17.49999999999999645, 5.624438216177580330, 110.8167034491464449 ) ) ;
#138744 = CARTESIAN_POINT ( 'NONE',  ( 0.05219959533934541429, -16.53943276465976808, 85.00109039468568994 ) ) ;
#138745 = CARTESIAN_POINT ( 'NONE',  ( 13.70000000000001528, 0.000000000000000000, -60.44446360152740283 ) ) ;
#138746 = CARTESIAN_POINT ( 'NONE',  ( -14.34966873604972548, 8.224510206698743886, 83.33442372801903275 ) ) ;
#138747 = CARTESIAN_POINT ( 'NONE',  ( 4.379528057220092307, 16.55341960407617563, 52.29275706135236135 ) ) ;
#138748 = CARTESIAN_POINT ( 'NONE',  ( -10.81492255796105439, 18.62759615963255655, 112.9177570613523329 ) ) ;
#138750 = FACE_BOUND ( 'NONE', #150116, .T. ) ;
#138749 = CARTESIAN_POINT ( 'NONE',  ( 5.049401038298161559, -19.05341960407611168, 57.70724293864769550 ) ) ;
#138751 = CARTESIAN_POINT ( 'NONE',  ( 15.80617190586769283, -15.72974639402175789, 70.62609039468567573 ) ) ;
#138752 = CARTESIAN_POINT ( 'NONE',  ( 19.03943276465977164, 0.05219959533936151252, 76.25109039468566152 ) ) ;
#138753 = CARTESIAN_POINT ( 'NONE',  ( -21.53943276465977519, -0.05219959533937600094, 113.7510903946856757 ) ) ;
#138754 = CARTESIAN_POINT ( 'NONE',  ( 9.564922557960805705, 16.46253265017160317, 29.58224293864769550 ) ) ;
#138755 = CARTESIAN_POINT ( 'NONE',  ( -17.41603567004575837, 15.34147874640864906, -57.57865799245708871 ) ) ;
#138756 = CARTESIAN_POINT ( 'NONE',  ( -18.67979575497178146, -10.72451020669898902, 61.66557627198103120 ) ) ;
#138757 = CARTESIAN_POINT ( 'NONE',  ( 21.53943276465977519, -0.05219959533907433946, 23.74890960531435269 ) ) ;
#138758 = CARTESIAN_POINT ( 'NONE',  ( 8.224510206698953496, -14.34966873604960469, 112.9155762719810383 ) ) ;
#138759 = CARTESIAN_POINT ( 'NONE',  ( 8.314922557961029526, -14.29746914071037800, 35.41775706135234003 ) ) ;
#138760 = CARTESIAN_POINT ( 'NONE',  ( 4.483927247898545687, 16.52544592524342804, 24.79057627198103120 ) ) ;
#138761 = VERTEX_POINT ( 'NONE', #45230 ) ;
#138762 = B_SPLINE_CURVE_WITH_KNOTS ( 'NONE', 3,
 ( #98292, #128644, #97299, #20477, #82127, #190339, #51815, #191329, #87157, #27505, #161994, #73996, #117492, #132663, #8318, #42659, #196360, #40657, #10329, #54819, #25512, #194351, #116493, #41665, #180195, #135666, #26502, #104321, #102326, #164016, #23490, #103329 ),
 .UNSPECIFIED., .F., .F.,
 ( 4, 2, 2, 2, 2, 2, 2, 2, 2, 2, 2, 2, 2, 2, 2, 4 ),
 ( 1.430489624538199204E-17, 0.0003712461730036792969, 0.0007424923460073442824, 0.001113738519011009268, 0.001484984692014674253, 0.002227477038022005959, 0.002598723211025686340, 0.002969969384029366288, 0.003341215557033046235, 0.003712461730036726616, 0.004083707903040406130, 0.004454954076044086511, 0.004826200249047766025, 0.005197446422051446406, 0.005568692595055126787, 0.005939938768058806301 ),
 .UNSPECIFIED. ) ;
#138763 = CARTESIAN_POINT ( 'NONE',  ( 10.72451020669898902, -18.67979575497178502, 112.9155762719810383 ) ) ;
#138765 = CARTESIAN_POINT ( 'NONE',  ( -11.74264578624799782, -36.14014761921581709, -7.599999999999999645 ) ) ;
#138764 = CARTESIAN_POINT ( 'NONE',  ( 12.06949235617757843, -12.14591786802309237, 38.12390960531436690 ) ) ;
#138766 = CARTESIAN_POINT ( 'NONE',  ( -16.46253265017146816, -9.564922557961047289, 104.1677570613523329 ) ) ;
#138767 = CARTESIAN_POINT ( 'NONE',  ( -19.02544592524334988, -5.153800228976617603, 23.95942372801900078 ) ) ;
#138768 = CARTESIAN_POINT ( 'NONE',  ( -14.34966873604960291, -8.224510206698953496, 46.66557627198102409 ) ) ;
#138769 = CARTESIAN_POINT ( 'NONE',  ( 15.80617190586746368, 15.72974639402197994, 99.37390960531436690 ) ) ;
#138771 = CARTESIAN_POINT ( 'NONE',  ( 5.823673210054125526, 21.52544592524343514, 59.79057627198103120 ) ) ;
#138770 = CARTESIAN_POINT ( 'NONE',  ( -28.82186960331499037, 2.428612866367529932E-14, 139.9999999999999716 ) ) ;
#138772 = CARTESIAN_POINT ( 'NONE',  ( -13.97604488694527625, -13.89961937509977652, 71.87390960531433848 ) ) ;
#138773 = CARTESIAN_POINT ( 'NONE',  ( -8.224510206698948167, 14.34966873604960824, 50.41557627198103120 ) ) ;
#138774 = CARTESIAN_POINT ( 'NONE',  ( 9.474510206698971260, -16.51473224551069308, 87.91557627198102409 ) ) ;
#138775 = AXIS2_PLACEMENT_3D ( 'NONE', #136634, #106291, #76945 ) ;
#138776 = CARTESIAN_POINT ( 'NONE',  ( -36.77035430826401097, 5.154579508995667858, 46.92692430510570034 ) ) ;
#138777 = CARTESIAN_POINT ( 'NONE',  ( -16.51473224551082808, 9.474510206698731452, 53.33442372801900433 ) ) ;
#138778 = CARTESIAN_POINT ( 'NONE',  ( 21.52544592524344225, -5.823673210054117533, 88.54057627198103830 ) ) ;
#138779 = CARTESIAN_POINT ( 'NONE',  ( 16.51473224551069308, 9.474510206698969483, 44.16557627198103120 ) ) ;
#138780 = CARTESIAN_POINT ( 'NONE',  ( -8.224510206698948167, 14.34966873604960824, 105.4155762719810383 ) ) ;
#138781 = CARTESIAN_POINT ( 'NONE',  ( 5.719274019375673035, 21.55341960407619339, 57.29275706135234714 ) ) ;
#138782 = DIRECTION ( 'NONE',  ( -0.000000000000000000, -0.000000000000000000, 1.000000000000000000 ) ) ;
#138783 = CARTESIAN_POINT ( 'NONE',  ( -4.483927247898539470, -16.52544592524342804, 27.29057627198103120 ) ) ;
#138784 = CARTESIAN_POINT ( 'NONE',  ( -5.153800228976328057, -19.02544592524343514, 52.29057627198100988 ) ) ;
#138785 = CARTESIAN_POINT ( 'NONE',  ( -13.97604488694527625, -13.89961937509977652, 101.8739096053143811 ) ) ;
#138786 = CARTESIAN_POINT ( 'NONE',  ( -21.55341960407610458, -5.719274019375992779, 66.45724293864768129 ) ) ;
#138787 = CARTESIAN_POINT ( 'NONE',  ( -0.05219959533936034679, 19.03943276465977164, 92.50109039468566152 ) ) ;
#138788 = CARTESIAN_POINT ( 'NONE',  ( -16.51473224551069308, -9.474510206698971260, 46.66557627198102409 ) ) ;
#138789 = CARTESIAN_POINT ( 'NONE',  ( -0.05219959533907301413, -21.53943276465977519, 52.49890960531435979 ) ) ;
#138790 = CARTESIAN_POINT ( 'NONE',  ( 5.719274019375673035, 21.55341960407619339, 82.29275706135234714 ) ) ;
#138792 = CARTESIAN_POINT ( 'NONE',  ( 14.34966873604972726, -8.224510206698740333, 85.83442372801901854 ) ) ;
#138791 = CARTESIAN_POINT ( 'NONE',  ( 17.48462780208548750, -33.70920939566803298, -26.63509803227954720 ) ) ;
#138793 = CARTESIAN_POINT ( 'NONE',  ( -12.14591786802326823, 12.06949235617739902, 93.12609039468568994 ) ) ;
#138794 = CARTESIAN_POINT ( 'NONE',  ( -19.05341960407611168, -5.049401038298163336, 56.45724293864768129 ) ) ;
#138795 = CARTESIAN_POINT ( 'NONE',  ( 9.474510206698971260, -16.51473224551069308, 67.91557627198102409 ) ) ;
#138796 = ORIENTED_EDGE ( 'NONE', *, *, #96295, .F. ) ;
#138797 = CARTESIAN_POINT ( 'NONE',  ( 13.97604488694548053, -13.89961937509957401, 30.62609039468566863 ) ) ;
#138798 = CARTESIAN_POINT ( 'NONE',  ( -16.53943276465976808, -0.05219959533934237506, 78.75109039468568994 ) ) ;
#138799 = CARTESIAN_POINT ( 'NONE',  ( -21.53943276465977519, -0.05219959533937600094, 108.7510903946857042 ) ) ;
#138800 = CARTESIAN_POINT ( 'NONE',  ( -13.97604488694527625, -13.89961937509977652, 71.87390960531433848 ) ) ;
#138801 = CARTESIAN_POINT ( 'NONE',  ( -21.53943276465977519, 0.05219959533907696930, 46.24890960531435979 ) ) ;
#138802 = CARTESIAN_POINT ( 'NONE',  ( 16.52544592524335698, 4.483927247898782831, 26.45942372801901854 ) ) ;
#138803 = CARTESIAN_POINT ( 'NONE',  ( 5.719274019375673035, 21.55341960407619339, 82.29275706135234714 ) ) ;
#138804 = CARTESIAN_POINT ( 'NONE',  ( -16.52544592524335698, -4.483927247898792601, 43.95942372801902565 ) ) ;
#138805 = CARTESIAN_POINT ( 'NONE',  ( -10.81492255796078084, -18.62759615963271287, 107.0822429386476955 ) ) ;
#138806 = CARTESIAN_POINT ( 'NONE',  ( 16.55341960407618274, -4.379528057220086978, 21.04275706135234714 ) ) ;
#138807 = CARTESIAN_POINT ( 'NONE',  ( 9.474510206698971260, -16.51473224551069308, 82.91557627198103830 ) ) ;
#138808 = CARTESIAN_POINT ( 'NONE',  ( 16.53943276465976808, 0.05219959533934440121, 26.25109039468567573 ) ) ;
#138809 = CARTESIAN_POINT ( 'NONE',  ( 16.51473224551069308, 9.474510206698969483, 39.16557627198103120 ) ) ;
#138810 = AXIS2_PLACEMENT_3D ( 'NONE', #5975, #39322, #116163 ) ;
#138811 = CARTESIAN_POINT ( 'NONE',  ( -12.06949235617739369, -12.14591786802326823, 19.37609039468568639 ) ) ;
#138812 = CARTESIAN_POINT ( 'NONE',  ( 4.483927247898545687, 16.52544592524342804, 84.79057627198102409 ) ) ;
#138813 = CARTESIAN_POINT ( 'NONE',  ( -16.53943276465976808, -0.05219959533934237506, 88.75109039468567573 ) ) ;
#138815 = CARTESIAN_POINT ( 'NONE',  ( 9.564922557960805705, 16.46253265017160317, 59.58224293864769550 ) ) ;
#138814 = CARTESIAN_POINT ( 'NONE',  ( -18.67979575497193778, 10.72451020669871902, 28.33442372801902209 ) ) ;
#138817 = EDGE_CURVE ( 'NONE', #172040, #39588, #86890, .T. ) ;
#138816 = CARTESIAN_POINT ( 'NONE',  ( 16.46253265017160672, -9.564922557960803928, 63.33224293864769550 ) ) ;
#138818 = CARTESIAN_POINT ( 'NONE',  ( -8.314922557961024197, 14.29746914071037800, 87.91775706135234714 ) ) ;
#138820 = ORIENTED_EDGE ( 'NONE', *, *, #79148, .F. ) ;
#138819 = DIRECTION ( 'NONE',  ( 0.000000000000000000, 0.000000000000000000, -1.000000000000000000 ) ) ;
#138821 = VERTEX_POINT ( 'NONE', #66347 ) ;
#138822 = CARTESIAN_POINT ( 'NONE',  ( -13.89961937509957401, -13.97604488694547875, 29.37609039468565797 ) ) ;
#138823 = CARTESIAN_POINT ( 'NONE',  ( -19.02544592524342804, 5.153800228976336051, 31.04057627198102409 ) ) ;
#138825 = VERTEX_POINT ( 'NONE', #156373 ) ;
#138824 = CARTESIAN_POINT ( 'NONE',  ( -13.89961937509977652, 13.97604488694528158, 110.6239096053143243 ) ) ;
#138826 = CARTESIAN_POINT ( 'NONE',  ( -14.34966873604972548, 8.224510206698743886, 33.33442372801900433 ) ) ;
#138828 = CARTESIAN_POINT ( 'NONE',  ( 4.483927247898790824, -16.52544592524335698, 45.20942372801901854 ) ) ;
#138827 = CARTESIAN_POINT ( 'NONE',  ( 13.89961937509957401, 13.97604488694547697, 61.87609039468566863 ) ) ;
#138829 = CARTESIAN_POINT ( 'NONE',  ( 19.05341960407611168, 5.049401038298154454, 103.9572429386476671 ) ) ;
#138830 = CARTESIAN_POINT ( 'NONE',  ( 16.46253265017160672, -9.564922557960803928, 68.33224293864770971 ) ) ;
#138831 = CARTESIAN_POINT ( 'NONE',  ( -15.72974639402197994, 15.80617190586746368, 95.62390960531436690 ) ) ;
#138833 = FACE_OUTER_BOUND ( 'NONE', #32389, .T. ) ;
#138832 = CARTESIAN_POINT ( 'NONE',  ( -19.03943276465977164, 0.05219959533909376836, 91.24890960531436690 ) ) ;
#138834 = CARTESIAN_POINT ( 'NONE',  ( 16.51473224551069308, 9.474510206698969483, 69.16557627198102409 ) ) ;
#138836 = CARTESIAN_POINT ( 'NONE',  ( -16.51473224551069308, -9.474510206698971260, 21.66557627198102765 ) ) ;
#138835 = CARTESIAN_POINT ( 'NONE',  ( 12.06949235617739724, 12.14591786802326823, 111.8760903946856615 ) ) ;
#138837 = CARTESIAN_POINT ( 'NONE',  ( 19.03943276465977164, 0.05219959533936151252, 36.25109039468567573 ) ) ;
#138838 = CARTESIAN_POINT ( 'NONE',  ( -12.06949235617756955, 12.14591786802309770, 60.62390960531437401 ) ) ;
#138839 = CARTESIAN_POINT ( 'NONE',  ( -18.67979575497193778, 10.72451020669871902, 103.3344237280190043 ) ) ;
#138840 = CARTESIAN_POINT ( 'NONE',  ( -9.474510206698964154, 16.51473224551069663, 40.41557627198103120 ) ) ;
#138841 = CARTESIAN_POINT ( 'NONE',  ( -4.483927247898782831, 16.52544592524335698, 57.70942372801901143 ) ) ;
#138843 = CARTESIAN_POINT ( 'NONE',  ( 0.05219959533937995610, -21.53943276465977519, 90.00109039468567573 ) ) ;
#138842 = CARTESIAN_POINT ( 'NONE',  ( -16.52544592524342804, 4.483927247898546575, 36.04057627198102409 ) ) ;
#138844 = CARTESIAN_POINT ( 'NONE',  ( 9.564922557960805705, 16.46253265017160317, 84.58224293864769550 ) ) ;
#138845 = CARTESIAN_POINT ( 'NONE',  ( 0.05219959533909260263, 19.03943276465977164, 99.99890960531436690 ) ) ;
#138846 = CARTESIAN_POINT ( 'NONE',  ( 8.224510206698953496, -14.34966873604960469, 107.9155762719810241 ) ) ;
#138847 = CARTESIAN_POINT ( 'NONE',  ( 12.06949235617757843, -12.14591786802309237, 78.12390960531436690 ) ) ;
#138848 = CARTESIAN_POINT ( 'NONE',  ( 5.823673210054125526, 21.52544592524343514, 84.79057627198102409 ) ) ;
#138849 = CARTESIAN_POINT ( 'NONE',  ( -16.51473224551069308, -9.474510206698971260, 71.66557627198102409 ) ) ;
#138850 = CARTESIAN_POINT ( 'NONE',  ( 18.67979575497178502, 10.72451020669898547, 99.16557627198100988 ) ) ;
#138851 = CARTESIAN_POINT ( 'NONE',  ( 13.89961937509957401, 13.97604488694547697, 71.87609039468567573 ) ) ;
#138853 = CARTESIAN_POINT ( 'NONE',  ( 14.34966873604960469, 8.224510206698951720, 94.16557627198103830 ) ) ;
#138852 = CARTESIAN_POINT ( 'NONE',  ( 19.26498983726237668, -5.499999999999590550, 48.05319577422005040 ) ) ;
#138854 = CARTESIAN_POINT ( 'NONE',  ( -5.049401038298153566, 19.05341960407611168, 60.20724293864768129 ) ) ;
#138855 = CARTESIAN_POINT ( 'NONE',  ( 10.72451020669898902, -18.67979575497178502, 67.91557627198102409 ) ) ;
#138856 = CARTESIAN_POINT ( 'NONE',  ( -18.22780087662124160, -5.499999999999927169, 83.98236817873107896 ) ) ;
#138858 = DIRECTION ( 'NONE',  ( 1.000000000000000000, 0.000000000000000000, 0.000000000000000000 ) ) ;
#138857 = CARTESIAN_POINT ( 'NONE',  ( -14.34966873604960291, -8.224510206698953496, 21.66557627198102409 ) ) ;
#138859 = CARTESIAN_POINT ( 'NONE',  ( -16.52544592524335698, -4.483927247898792601, 18.95942372801901143 ) ) ;
#138860 = CARTESIAN_POINT ( 'NONE',  ( 8.224510206698953496, -14.34966873604960469, 77.91557627198102409 ) ) ;
#138861 = CARTESIAN_POINT ( 'NONE',  ( -19.49190055781012276, -5.500000000000019540, 95.56116087098779133 ) ) ;
#138862 = CARTESIAN_POINT ( 'NONE',  ( -19.02544592524342804, 5.153800228976336051, 81.04057627198103830 ) ) ;
#138863 = CARTESIAN_POINT ( 'NONE',  ( 5.049401038298161559, -19.05341960407611168, 32.70724293864768129 ) ) ;
#138864 = CARTESIAN_POINT ( 'NONE',  ( -16.53943276465976808, 0.05219959533911058130, 66.24890960531436690 ) ) ;
#138865 = CARTESIAN_POINT ( 'NONE',  ( 21.55341960407610458, 5.719274019375980345, 23.95724293864769550 ) ) ;
#138866 = CARTESIAN_POINT ( 'NONE',  ( 16.46253265017146816, 9.564922557961045513, 86.66775706135233293 ) ) ;
#138867 = CARTESIAN_POINT ( 'NONE',  ( -19.05341960407611168, -5.049401038298163336, 96.45724293864769550 ) ) ;
#138868 = CARTESIAN_POINT ( 'NONE',  ( -15.72974639402197994, 15.80617190586746368, 70.62390960531436690 ) ) ;
#138869 = CARTESIAN_POINT ( 'NONE',  ( -8.314922557961024197, 14.29746914071037800, 72.91775706135234714 ) ) ;
#138870 = CARTESIAN_POINT ( 'NONE',  ( -0.05219959533936034679, 19.03943276465977164, 112.5010903946856757 ) ) ;
#138871 = CARTESIAN_POINT ( 'NONE',  ( -5.153800228976328057, -19.02544592524343514, 57.29057627198103120 ) ) ;
#138872 = CARTESIAN_POINT ( 'NONE',  ( 15.80617190586746368, 15.72974639402197994, 74.37390960531436690 ) ) ;
#138873 = CARTESIAN_POINT ( 'NONE',  ( 19.05341960407617918, -5.049401038297876454, 111.0427570613523329 ) ) ;
#138875 = CARTESIAN_POINT ( 'NONE',  ( 5.719274019375673035, 21.55341960407619339, 47.29275706135234003 ) ) ;
#138874 = CARTESIAN_POINT ( 'NONE',  ( -12.14591786802309592, -12.06949235617757132, 36.87390960531435979 ) ) ;
#138876 = DIRECTION ( 'NONE',  ( -0.000000000000000000, -0.000000000000000000, 1.000000000000000000 ) ) ;
#138878 = CARTESIAN_POINT ( 'NONE',  ( 19.03943276465977164, -0.05219959533909143690, 103.7489096053143669 ) ) ;
#138877 = CARTESIAN_POINT ( 'NONE',  ( -14.29746914071037622, -8.314922557961029526, 74.16775706135231871 ) ) ;
#138879 = DIRECTION ( 'NONE',  ( -1.000000000000000000, 0.000000000000000000, 0.000000000000000000 ) ) ;
#138880 = CARTESIAN_POINT ( 'NONE',  ( -16.88567814943162659, 6.947325034625691842, 78.70998877347415146 ) ) ;
#138881 = CARTESIAN_POINT ( 'NONE',  ( 16.55341960407618274, -4.379528057220086978, 91.04275706135236135 ) ) ;
#138882 = CARTESIAN_POINT ( 'NONE',  ( 8.224510206698742110, 14.34966873604972548, 52.08442372801901854 ) ) ;
#138883 = CARTESIAN_POINT ( 'NONE',  ( 13.89961937509977652, -13.97604488694527269, 63.12390960531435979 ) ) ;
#138884 = CARTESIAN_POINT ( 'NONE',  ( 16.46253265017160672, -9.564922557960803928, 78.33224293864769550 ) ) ;
#138885 = CARTESIAN_POINT ( 'NONE',  ( 5.823673210054444382, -21.52544592524334988, 55.20942372801902565 ) ) ;
#138886 = CARTESIAN_POINT ( 'NONE',  ( 12.14591786802327356, -12.06949235617739191, 65.62609039468568994 ) ) ;
#138887 = CARTESIAN_POINT ( 'NONE',  ( -0.05219959533910754901, -16.53943276465976808, 27.49890960531435269 ) ) ;
#138888 = CARTESIAN_POINT ( 'NONE',  ( 13.89961937509977652, -13.97604488694527269, 43.12390960531434558 ) ) ;
#138889 = CARTESIAN_POINT ( 'NONE',  ( -9.564922557960796823, -16.46253265017161027, 37.08224293864768839 ) ) ;
#138890 = CARTESIAN_POINT ( 'NONE',  ( -0.05219959533934338120, 16.53943276465976808, 27.50109039468567929 ) ) ;
#138891 = CARTESIAN_POINT ( 'NONE',  ( -16.51473224551082808, 9.474510206698731452, 78.33442372801900433 ) ) ;
#138892 = CARTESIAN_POINT ( 'NONE',  ( 16.55341960407611168, 4.379528057220329451, 83.95724293864770971 ) ) ;
#138893 = CARTESIAN_POINT ( 'NONE',  ( 5.049401038298161559, -19.05341960407611168, 57.70724293864769550 ) ) ;
#138895 = CARTESIAN_POINT ( 'NONE',  ( 23.29544513554940366, -16.92513159979222337, 148.7843446569000037 ) ) ;
#138894 = CARTESIAN_POINT ( 'NONE',  ( 9.564922557961047289, -16.46253265017146816, 90.41775706135234714 ) ) ;
#138896 = CARTESIAN_POINT ( 'NONE',  ( 5.823673210054444382, -21.52544592524334988, 95.20942372801903275 ) ) ;
#138897 = CARTESIAN_POINT ( 'NONE',  ( -16.55341960407617563, 4.379528057220093196, 48.54275706135234714 ) ) ;
#138898 = CARTESIAN_POINT ( 'NONE',  ( 0.3535533905936371069, 34.99999999999999289, 5.353553390593268624 ) ) ;
#138899 = CARTESIAN_POINT ( 'NONE',  ( 15.72974639402199770, -15.80617190586745480, 53.12390960531436690 ) ) ;
#138900 = CARTESIAN_POINT ( 'NONE',  ( -16.55341960407617563, 4.379528057220093196, 33.54275706135234714 ) ) ;
#138901 = CARTESIAN_POINT ( 'NONE',  ( 16.46253265017160672, -9.564922557960803928, 33.33224293864770260 ) ) ;
#138902 = CARTESIAN_POINT ( 'NONE',  ( 19.05341960407617918, -5.049401038297876454, 36.04275706135234003 ) ) ;
#138903 = CARTESIAN_POINT ( 'NONE',  ( -13.97604488694527625, -13.89961937509977652, 76.87390960531433848 ) ) ;
#138904 = CARTESIAN_POINT ( 'NONE',  ( -13.97604488694527625, -13.89961937509977652, 46.87390960531435979 ) ) ;
#138905 = CARTESIAN_POINT ( 'NONE',  ( -18.22780087662123805, 5.499999999999981348, 81.01763182126896368 ) ) ;
#138906 = CARTESIAN_POINT ( 'NONE',  ( 0.05219959533909260263, 19.03943276465977164, 74.99890960531435269 ) ) ;
#138907 = CARTESIAN_POINT ( 'NONE',  ( 5.153800228976615827, -19.02544592524334988, 30.20942372801900433 ) ) ;
#138908 = CARTESIAN_POINT ( 'NONE',  ( 19.03943276465977164, 0.05219959533936151252, 21.25109039468565797 ) ) ;
#138909 = CARTESIAN_POINT ( 'NONE',  ( -12.14591786802309592, -12.06949235617757132, 41.87390960531435979 ) ) ;
#138910 = CARTESIAN_POINT ( 'NONE',  ( 16.46253265017160672, -9.564922557960803928, 38.33224293864768839 ) ) ;
#138911 = CARTESIAN_POINT ( 'NONE',  ( 13.97604488694527802, 13.89961937509977652, 109.3739096053143669 ) ) ;
#138912 = CARTESIAN_POINT ( 'NONE',  ( -10.72451020669870658, -18.67979575497194134, 84.58442372801903275 ) ) ;
#138913 = CARTESIAN_POINT ( 'NONE',  ( -9.564922557960796823, -16.46253265017161027, 57.08224293864769550 ) ) ;
#138914 = CARTESIAN_POINT ( 'NONE',  ( -10.81492255796105439, 18.62759615963255655, 77.91775706135231871 ) ) ;
#138915 = CARTESIAN_POINT ( 'NONE',  ( -10.72451020669898014, 18.67979575497178502, 40.41557627198103120 ) ) ;
#138916 = CARTESIAN_POINT ( 'NONE',  ( 15.80617190586769283, -15.72974639402175789, 25.62609039468567929 ) ) ;
#138917 = CARTESIAN_POINT ( 'NONE',  ( -19.02544592524334988, -5.153800228976617603, 48.95942372801900433 ) ) ;
#138918 = CARTESIAN_POINT ( 'NONE',  ( 5.049401038298161559, -19.05341960407611168, 22.70724293864769194 ) ) ;
#138919 = CARTESIAN_POINT ( 'NONE',  ( 5.049401038298161559, -19.05341960407611168, 82.70724293864770971 ) ) ;
#138920 = CARTESIAN_POINT ( 'NONE',  ( 14.34966873604972726, -8.224510206698740333, 35.83442372801901143 ) ) ;
#138921 = CARTESIAN_POINT ( 'NONE',  ( -16.52544592524342804, 4.483927247898546575, 91.04057627198103830 ) ) ;
#138922 = CARTESIAN_POINT ( 'NONE',  ( -19.05341960407611168, -5.049401038298163336, 61.45724293864769550 ) ) ;
#138923 = CARTESIAN_POINT ( 'NONE',  ( 21.53943276465977519, -0.05219959533907433946, 38.74890960531435979 ) ) ;
#138924 = AXIS2_PLACEMENT_3D ( 'NONE', #85273, #131797, #144950 ) ;
#138925 = CARTESIAN_POINT ( 'NONE',  ( -9.564922557961040184, 16.46253265017147172, 97.91775706135233293 ) ) ;
#138926 = CARTESIAN_POINT ( 'NONE',  ( 18.67979575497178502, 10.72451020669898547, 104.1655762719810241 ) ) ;
#138927 = CARTESIAN_POINT ( 'NONE',  ( -10.72451020669870658, -18.67979575497194134, 54.58442372801901143 ) ) ;
#138928 = CARTESIAN_POINT ( 'NONE',  ( 8.314922557961029526, -14.29746914071037800, 70.41775706135236135 ) ) ;
#138929 = CARTESIAN_POINT ( 'NONE',  ( 12.14591786802327356, -12.06949235617739191, 70.62609039468567573 ) ) ;
#138930 = CARTESIAN_POINT ( 'NONE',  ( 16.51473224551069308, 9.474510206698969483, 59.16557627198102409 ) ) ;
#138931 = CARTESIAN_POINT ( 'NONE',  ( 8.224510206698742110, 14.34966873604972548, 87.08442372801901854 ) ) ;
#138932 = CARTESIAN_POINT ( 'NONE',  ( -10.81492255796078084, -18.62759615963271287, 112.0822429386477097 ) ) ;
#138933 = CARTESIAN_POINT ( 'NONE',  ( 8.224510206698953496, -14.34966873604960469, 67.91557627198102409 ) ) ;
#138934 = CARTESIAN_POINT ( 'NONE',  ( -19.03943276465977164, 0.05219959533909376836, 91.24890960531436690 ) ) ;
#138935 = CARTESIAN_POINT ( 'NONE',  ( 8.224510206698742110, 14.34966873604972548, 77.08442372801901854 ) ) ;
#138936 = CARTESIAN_POINT ( 'NONE',  ( -15.80617190586768217, 15.72974639402176855, 63.12609039468568994 ) ) ;
#138937 = CARTESIAN_POINT ( 'NONE',  ( -14.29746914071037622, -8.314922557961029526, 24.16775706135235424 ) ) ;
#138938 = CARTESIAN_POINT ( 'NONE',  ( 21.52544592524344225, -5.823673210054117533, 108.5405762719810241 ) ) ;
#138939 = CARTESIAN_POINT ( 'NONE',  ( -0.05219959533910754901, -16.53943276465976808, 57.49890960531435979 ) ) ;
#138940 = VERTEX_POINT ( 'NONE', #109866 ) ;
#138941 = CARTESIAN_POINT ( 'NONE',  ( -16.18388926212238133, 7.379444403734531477, 74.56046848633853585 ) ) ;
#138942 = CARTESIAN_POINT ( 'NONE',  ( 0.05219959533907565091, 21.53943276465977519, 84.99890960531436690 ) ) ;
#138943 = CARTESIAN_POINT ( 'NONE',  ( 8.314922557960818139, 14.29746914071049879, 34.58224293864770260 ) ) ;
#138944 = ORIENTED_EDGE ( 'NONE', *, *, #166279, .F. ) ;
#138945 = CARTESIAN_POINT ( 'NONE',  ( 34.74703179323498148, 1.946018278951714198, 52.24735473369668171 ) ) ;
#138946 = CARTESIAN_POINT ( 'NONE',  ( -21.52544592524334988, -5.823673210054445271, 18.95942372801901143 ) ) ;
#138947 = CARTESIAN_POINT ( 'NONE',  ( -19.02544592524342804, 5.153800228976336051, 116.0405762719810383 ) ) ;
#138948 = CARTESIAN_POINT ( 'NONE',  ( 21.53943276465977519, 0.05219959533937863772, 21.25109039468567218 ) ) ;
#138949 = CARTESIAN_POINT ( 'NONE',  ( 16.52544592524342804, -4.483927247898539470, 53.54057627198103120 ) ) ;
#138950 = CARTESIAN_POINT ( 'NONE',  ( 4.379528057220092307, 16.55341960407617563, 57.29275706135234714 ) ) ;
#138951 = CIRCLE ( 'NONE', #184143, 2.000000000000001776 ) ;
#138952 = CARTESIAN_POINT ( 'NONE',  ( 0.05219959533909260263, 19.03943276465977164, 59.99890960531436690 ) ) ;
#138953 = CARTESIAN_POINT ( 'NONE',  ( -0.05219959533936034679, 19.03943276465977164, 67.50109039468566152 ) ) ;
#138954 = CARTESIAN_POINT ( 'NONE',  ( -19.05341960407611168, -5.049401038298163336, 76.45724293864769550 ) ) ;
#138955 = CARTESIAN_POINT ( 'NONE',  ( -15.80617190586745835, -15.72974639402198527, 41.87390960531435979 ) ) ;
#138956 = CARTESIAN_POINT ( 'NONE',  ( -8.122171662652368340, -45.80197342711005604, -22.32604245071853555 ) ) ;
#138957 = CARTESIAN_POINT ( 'NONE',  ( 16.51473224551069308, 9.474510206698969483, 64.16557627198102409 ) ) ;
#138958 = CARTESIAN_POINT ( 'NONE',  ( -12.06949235617739369, -12.14591786802326823, 24.37609039468567573 ) ) ;
#138959 = CARTESIAN_POINT ( 'NONE',  ( -9.474510206698720793, -16.51473224551083518, 69.58442372801901854 ) ) ;
#138960 = CARTESIAN_POINT ( 'NONE',  ( -21.52544592524343514, 5.823673210054127303, 116.0405762719810383 ) ) ;
#138961 = EDGE_CURVE ( 'NONE', #141234, #61486, #173822, .T. ) ;
#138962 = CARTESIAN_POINT ( 'NONE',  ( -4.483927247898539470, -16.52544592524342804, 52.29057627198102409 ) ) ;
#138963 = CARTESIAN_POINT ( 'NONE',  ( 19.05341960407611168, 5.049401038298154454, 93.95724293864769550 ) ) ;
#138964 = CARTESIAN_POINT ( 'NONE',  ( 18.67979575497178502, 10.72451020669898547, 59.16557627198103120 ) ) ;
#138966 = CARTESIAN_POINT ( 'NONE',  ( -4.379528057220086978, -16.55341960407618274, 34.79275706135235424 ) ) ;
#138965 = CARTESIAN_POINT ( 'NONE',  ( 15.72974639402199770, -15.80617190586745480, 93.12390960531436690 ) ) ;
#138967 = CARTESIAN_POINT ( 'NONE',  ( -10.72451020669898014, 18.67979575497178502, 30.41557627198101699 ) ) ;
#138968 = CARTESIAN_POINT ( 'NONE',  ( 5.823673210054444382, -21.52544592524334988, 90.20942372801903275 ) ) ;
#138969 = CARTESIAN_POINT ( 'NONE',  ( 9.474510206698971260, -16.51473224551069308, 82.91557627198103830 ) ) ;
#138970 = CARTESIAN_POINT ( 'NONE',  ( 13.97604488694527802, 13.89961937509977652, 39.37390960531435269 ) ) ;
#138971 = CARTESIAN_POINT ( 'NONE',  ( 16.46253265017160672, -9.564922557960803928, 98.33224293864769550 ) ) ;
#138972 = CARTESIAN_POINT ( 'NONE',  ( 16.55341960407611168, 4.379528057220329451, 103.9572429386476813 ) ) ;
#138973 = CARTESIAN_POINT ( 'NONE',  ( -9.474510206698964154, 16.51473224551069663, 60.41557627198102409 ) ) ;
#138974 = CARTESIAN_POINT ( 'NONE',  ( 12.14591786802327356, -12.06949235617739191, 25.62609039468567929 ) ) ;
#138975 = CARTESIAN_POINT ( 'NONE',  ( 17.50000000000003197, 4.049696124445839374, 33.31960329334057747 ) ) ;
#138977 = CARTESIAN_POINT ( 'NONE',  ( 15.72974639402199770, -15.80617190586745480, 28.12390960531435979 ) ) ;
#138976 = CARTESIAN_POINT ( 'NONE',  ( 15.80617190586769283, -15.72974639402175789, 100.6260903946857184 ) ) ;
#138978 = CARTESIAN_POINT ( 'NONE',  ( -12.14591786802326823, 12.06949235617739902, 88.12609039468570415 ) ) ;
#138979 = CARTESIAN_POINT ( 'NONE',  ( 37.99999999999999289, 2.893978650043524126E-14, -9.000000000000001776 ) ) ;
#138980 = CARTESIAN_POINT ( 'NONE',  ( -19.02544592524334988, -5.153800228976617603, 63.95942372801899012 ) ) ;
#138981 = CARTESIAN_POINT ( 'NONE',  ( -16.46253265017146816, -9.564922557961047289, 34.16775706135233293 ) ) ;
#138982 = CARTESIAN_POINT ( 'NONE',  ( 26.33251596241889914, 8.908286433081562095, 140.0000000000000000 ) ) ;
#138983 = CARTESIAN_POINT ( 'NONE',  ( 19.03943276465977164, -0.05219959533909143690, 28.74890960531435624 ) ) ;
#138984 = CARTESIAN_POINT ( 'NONE',  ( -12.14591786802309592, -12.06949235617757132, 41.87390960531435979 ) ) ;
#138985 = CARTESIAN_POINT ( 'NONE',  ( -16.20579543436677383, -7.371946100355105003, 110.5652083417187157 ) ) ;
#138986 = CARTESIAN_POINT ( 'NONE',  ( -4.483927247898539470, -16.52544592524342804, 27.29057627198103120 ) ) ;
#138987 = CARTESIAN_POINT ( 'NONE',  ( 17.50000000000000000, 5.499999999999992895, 66.70309617465828467 ) ) ;
#138988 = CARTESIAN_POINT ( 'NONE',  ( 4.379528057220092307, 16.55341960407617563, 97.29275706135234714 ) ) ;
#138989 = CARTESIAN_POINT ( 'NONE',  ( -9.564922557960796823, -16.46253265017161027, 32.08224293864769550 ) ) ;
#138990 = CARTESIAN_POINT ( 'NONE',  ( 5.823673210054444382, -21.52544592524334988, 105.2094237280190328 ) ) ;
#138991 = CARTESIAN_POINT ( 'NONE',  ( 16.53943276465976808, 0.05219959533934440121, 26.25109039468567573 ) ) ;
#138992 = CARTESIAN_POINT ( 'NONE',  ( -15.72974639402176322, -15.80617190586768395, 74.37609039468568994 ) ) ;
#138993 = CARTESIAN_POINT ( 'NONE',  ( 16.51473224551083163, -9.474510206698727899, 55.83442372801899722 ) ) ;
#138994 = CARTESIAN_POINT ( 'NONE',  ( 0.05219959533909260263, 19.03943276465977164, 94.99890960531436690 ) ) ;
#138995 = CARTESIAN_POINT ( 'NONE',  ( -16.51473224551069308, -9.474510206698971260, 71.66557627198102409 ) ) ;
#138996 = CARTESIAN_POINT ( 'NONE',  ( -19.25663599770061296, 5.499999999999452882, 38.99419308057201050 ) ) ;
#138997 = CARTESIAN_POINT ( 'NONE',  ( 15.72974639402199770, -15.80617190586745480, 93.12390960531436690 ) ) ;
#138998 = CARTESIAN_POINT ( 'NONE',  ( -16.52544592524342804, 4.483927247898546575, 61.04057627198103120 ) ) ;
#138999 = CARTESIAN_POINT ( 'NONE',  ( -15.72974639402197994, 15.80617190586746368, 55.62390960531436690 ) ) ;
#139000 = CARTESIAN_POINT ( 'NONE',  ( 13.97604488694527802, 13.89961937509977652, 54.37390960531435979 ) ) ;
#139002 = CARTESIAN_POINT ( 'NONE',  ( 8.224510206698742110, 14.34966873604972548, 77.08442372801901854 ) ) ;
#139001 = CARTESIAN_POINT ( 'NONE',  ( 18.67979575497178502, 10.72451020669898547, 89.16557627198102409 ) ) ;
#139003 = VERTEX_POINT ( 'NONE', #128009 ) ;
#139004 = CARTESIAN_POINT ( 'NONE',  ( -0.05219959533909027116, -19.03943276465977164, 42.49890960531435269 ) ) ;
#139006 = DIRECTION ( 'NONE',  ( 0.000000000000000000, 0.000000000000000000, 1.000000000000000000 ) ) ;
#139005 = CARTESIAN_POINT ( 'NONE',  ( 8.224510206698953496, -14.34966873604960469, 87.91557627198103830 ) ) ;
#139007 = CARTESIAN_POINT ( 'NONE',  ( 9.564922557960805705, 16.46253265017160317, 44.58224293864769550 ) ) ;
#139008 = CARTESIAN_POINT ( 'NONE',  ( -4.379528057220328563, 16.55341960407611168, 115.2072429386476955 ) ) ;
#139009 = CARTESIAN_POINT ( 'NONE',  ( 16.46253265017146816, 9.564922557961045513, 66.66775706135233293 ) ) ;
#139010 = CARTESIAN_POINT ( 'NONE',  ( -4.379528057220328563, 16.55341960407611168, 90.20724293864770971 ) ) ;
#139011 = CARTESIAN_POINT ( 'NONE',  ( 18.67979575497194134, -10.72451020669871369, 50.83442372801901143 ) ) ;
#139013 = CARTESIAN_POINT ( 'NONE',  ( 10.81492255796078972, 18.62759615963270932, 109.5822429386476955 ) ) ;
#139012 = CARTESIAN_POINT ( 'NONE',  ( -9.474510206698964154, 16.51473224551069663, 35.41557627198102409 ) ) ;
#139014 = B_SPLINE_CURVE_WITH_KNOTS ( 'NONE', 3,
 ( #144720, #7204, #53726, #19404, #66885, #146721, #190243, #161899, #158891, #68888, #176081, #20381, #96225, #82028, #67886, #37550, #54719, #51720, #6206, #130548 ),
 .UNSPECIFIED., .F., .F.,
 ( 4, 2, 2, 2, 2, 2, 2, 2, 2, 4 ),
 ( 0.000000000000000000, 0.0004987090165372665227, 0.0009974180330745330454, 0.001246772541343162946, 0.001496127049611792846, 0.001994836066149056984, 0.002493545082686320687, 0.002742899590954941264, 0.002992254099223561406, 0.003989672132298042843 ),
 .UNSPECIFIED. ) ;
#139015 = CARTESIAN_POINT ( 'NONE',  ( 16.55341960407611168, 4.379528057220329451, 83.95724293864770971 ) ) ;
#139016 = CARTESIAN_POINT ( 'NONE',  ( 17.72662750342728444, 5.499999999999958256, 93.90179492283741070 ) ) ;
#139017 = CARTESIAN_POINT ( 'NONE',  ( -5.049401038298153566, 19.05341960407611168, 65.20724293864765286 ) ) ;
#139018 = CARTESIAN_POINT ( 'NONE',  ( -11.57166747000293228, -12.01093693996313405, -61.35735997286332122 ) ) ;
#139020 = CARTESIAN_POINT ( 'NONE',  ( -0.05219959533909027116, -19.03943276465977164, 97.49890960531436690 ) ) ;
#139019 = CARTESIAN_POINT ( 'NONE',  ( -19.05341960407617563, 5.049401038297882671, 93.54275706135234714 ) ) ;
#139021 = CARTESIAN_POINT ( 'NONE',  ( 18.67979575497194134, -10.72451020669871369, 40.83442372801901854 ) ) ;
#139022 = CARTESIAN_POINT ( 'NONE',  ( -13.97604488694527625, -13.89961937509977652, 76.87390960531433848 ) ) ;
#139023 = CARTESIAN_POINT ( 'NONE',  ( 13.97604488694548053, -13.89961937509957401, 65.62609039468567573 ) ) ;
#139024 = CARTESIAN_POINT ( 'NONE',  ( -9.474510206698964154, 16.51473224551069663, 60.41557627198102409 ) ) ;
#139025 = CARTESIAN_POINT ( 'NONE',  ( 8.224510206698953496, -14.34966873604960469, 77.91557627198102409 ) ) ;
#139026 = B_SPLINE_CURVE_WITH_KNOTS ( 'NONE', 3,
 ( #154304, #186654, #48124, #171464, #15793, #2602 ),
 .UNSPECIFIED., .F., .F.,
 ( 4, 2, 4 ),
 ( 0.003239945802372271207, 0.003620412082092145951, 0.004000878361812020695 ),
 .UNSPECIFIED. ) ;
#139027 = CARTESIAN_POINT ( 'NONE',  ( -14.34966873604960291, -8.224510206698953496, 66.66557627198102409 ) ) ;
#139028 = CARTESIAN_POINT ( 'NONE',  ( -19.05341960407611168, -5.049401038298163336, 91.45724293864766707 ) ) ;
#139029 = CARTESIAN_POINT ( 'NONE',  ( 0.05219959533907565091, 21.53943276465977519, 94.99890960531436690 ) ) ;
#139030 = CARTESIAN_POINT ( 'NONE',  ( -19.03943276465977164, 0.05219959533909376836, 81.24890960531436690 ) ) ;
#139031 = CARTESIAN_POINT ( 'NONE',  ( 19.02544592524334988, 5.153800228976608722, 36.45942372801900433 ) ) ;
#139034 = CARTESIAN_POINT ( 'NONE',  ( 8.314922557960818139, 14.29746914071049879, 104.5822429386477097 ) ) ;
#139033 = CARTESIAN_POINT ( 'NONE',  ( 16.52544592524342804, -4.483927247898539470, 33.54057627198102409 ) ) ;
#139032 = CARTESIAN_POINT ( 'NONE',  ( -13.89961937509977652, 13.97604488694528158, 30.62390960531435269 ) ) ;
#139035 = ORIENTED_EDGE ( 'NONE', *, *, #77093, .T. ) ;
#139036 = CARTESIAN_POINT ( 'NONE',  ( -5.823673210054431948, 21.52544592524334988, 32.70942372801900433 ) ) ;
#139037 = CARTESIAN_POINT ( 'NONE',  ( -5.153800228976607833, 19.02544592524334988, 72.70942372801900433 ) ) ;
#139038 = CARTESIAN_POINT ( 'NONE',  ( 4.379528057220339221, -16.55341960407611168, 27.70724293864769905 ) ) ;
#139039 = CARTESIAN_POINT ( 'NONE',  ( 15.72974639402199770, -15.80617190586745480, 83.12390960531436690 ) ) ;
#139040 = CARTESIAN_POINT ( 'NONE',  ( -21.53943276465977519, 0.05219959533907696930, 21.24890960531436690 ) ) ;
#139041 = CARTESIAN_POINT ( 'NONE',  ( -12.06949235617756955, 12.14591786802309770, 65.62390960531436690 ) ) ;
#139042 = CARTESIAN_POINT ( 'NONE',  ( 19.05341960407611168, 5.049401038298154454, 23.95724293864769194 ) ) ;
#139043 = CARTESIAN_POINT ( 'NONE',  ( 16.51473224551083163, -9.474510206698727899, 30.83442372801900433 ) ) ;
#139044 = CARTESIAN_POINT ( 'NONE',  ( -4.379528057220086978, -16.55341960407618274, 99.79275706135234714 ) ) ;
#139045 = CARTESIAN_POINT ( 'NONE',  ( 4.379528057220092307, 16.55341960407617563, 52.29275706135236135 ) ) ;
#139046 = CARTESIAN_POINT ( 'NONE',  ( 0.05219959533907565091, 21.53943276465977519, 24.99890960531435624 ) ) ;
#139047 = CARTESIAN_POINT ( 'NONE',  ( 21.55341960407619695, -5.719274019375665929, 106.0427570613523471 ) ) ;
#139048 = CARTESIAN_POINT ( 'NONE',  ( 19.05341960407611168, 5.049401038298154454, 78.95724293864769550 ) ) ;
#139049 = CARTESIAN_POINT ( 'NONE',  ( -8.224510206698735004, -14.34966873604973081, 64.58442372801900433 ) ) ;
#139050 = CARTESIAN_POINT ( 'NONE',  ( 4.379528057220339221, -16.55341960407611168, 112.7072429386476955 ) ) ;
#139051 = CARTESIAN_POINT ( 'NONE',  ( -12.06949235617756955, 12.14591786802309770, 35.62390960531437401 ) ) ;
#139052 = CARTESIAN_POINT ( 'NONE',  ( -18.09805431107249873, 5.499999999999980460, 71.01606229291884631 ) ) ;
#139054 = CARTESIAN_POINT ( 'NONE',  ( 19.02544592524343514, -5.153800228976328945, 93.54057627198102409 ) ) ;
#139053 = CARTESIAN_POINT ( 'NONE',  ( -5.049401038298153566, 19.05341960407611168, 110.2072429386476671 ) ) ;
#139056 = EDGE_CURVE ( 'NONE', #27352, #166707, #78871, .T. ) ;
#139055 = CARTESIAN_POINT ( 'NONE',  ( -19.03943276465977164, 0.05219959533909376836, 111.2489096053143669 ) ) ;
#139057 = CARTESIAN_POINT ( 'NONE',  ( -4.379528057220328563, 16.55341960407611168, 60.20724293864768839 ) ) ;
#139058 = CARTESIAN_POINT ( 'NONE',  ( 12.14591786802309770, 12.06949235617756955, 34.37390960531435979 ) ) ;
#139059 = CARTESIAN_POINT ( 'NONE',  ( -4.379528057220328563, 16.55341960407611168, 55.20724293864770260 ) ) ;
#139060 = ORIENTED_EDGE ( 'NONE', *, *, #3105, .T. ) ;
#139062 = CARTESIAN_POINT ( 'NONE',  ( 17.59860650958997397, -7.585241751806833577, 60.92337014262493966 ) ) ;
#139061 = CARTESIAN_POINT ( 'NONE',  ( 0.05219959533934541429, -16.53943276465976808, 45.00109039468568284 ) ) ;
#139063 = CARTESIAN_POINT ( 'NONE',  ( 0.05219959533936267826, -19.03943276465977164, 55.00109039468566863 ) ) ;
#139064 = CARTESIAN_POINT ( 'NONE',  ( -13.97604488694527625, -13.89961937509977652, 81.87390960531436690 ) ) ;
#139065 = CARTESIAN_POINT ( 'NONE',  ( 19.03943276465977164, 0.05219959533936151252, 71.25109039468566152 ) ) ;
#139066 = CARTESIAN_POINT ( 'NONE',  ( -22.44159573604010305, 16.30477369853692338, 143.1750000027311671 ) ) ;
#139067 = CARTESIAN_POINT ( 'NONE',  ( 16.51473224551083163, -9.474510206698727899, 60.83442372801900433 ) ) ;
#139069 = CARTESIAN_POINT ( 'NONE',  ( 4.483927247898790824, -16.52544592524335698, 85.20942372801901854 ) ) ;
#139068 = CARTESIAN_POINT ( 'NONE',  ( -5.049401038297874678, -19.05341960407617918, 104.7927570613523471 ) ) ;
#139070 = CARTESIAN_POINT ( 'NONE',  ( -8.571926809382601320, -26.38167802310801591, 143.7750000027311899 ) ) ;
#139071 = CARTESIAN_POINT ( 'NONE',  ( -19.03943276465977164, 0.05219959533909376836, 31.24890960531435979 ) ) ;
#139072 = CARTESIAN_POINT ( 'NONE',  ( 13.89961937509977652, -13.97604488694527269, 98.12390960531433848 ) ) ;
#139073 = CARTESIAN_POINT ( 'NONE',  ( -15.72974639402176322, -15.80617190586768395, 39.37609039468567573 ) ) ;
#139074 = CARTESIAN_POINT ( 'NONE',  ( 13.89961937509957401, 13.97604488694547697, 101.8760903946856331 ) ) ;
#139076 = CARTESIAN_POINT ( 'NONE',  ( 13.89961937509977652, -13.97604488694527269, 58.12390960531436690 ) ) ;
#139075 = CARTESIAN_POINT ( 'NONE',  ( 17.50000000000000711, 4.873317850230757031, 23.61681730595545758 ) ) ;
#139077 = CARTESIAN_POINT ( 'NONE',  ( -9.474510206698964154, 16.51473224551069663, 105.4155762719810383 ) ) ;
#139079 = CARTESIAN_POINT ( 'NONE',  ( -9.564922557960796823, -16.46253265017161027, 57.08224293864769550 ) ) ;
#139078 = CARTESIAN_POINT ( 'NONE',  ( -16.53943276465976808, 0.05219959533911058130, 61.24890960531435979 ) ) ;
#139080 = CARTESIAN_POINT ( 'NONE',  ( 16.46253265017160672, -9.564922557960803928, 63.33224293864769550 ) ) ;
#139081 = CARTESIAN_POINT ( 'NONE',  ( 5.049401038297881783, 19.05341960407617563, 82.29275706135229029 ) ) ;
#139082 = CARTESIAN_POINT ( 'NONE',  ( -18.62759615963270932, 10.81492255796079327, 45.83224293864769550 ) ) ;
#139083 = CARTESIAN_POINT ( 'NONE',  ( -0.05219959533909027116, -19.03943276465977164, 22.49890960531436690 ) ) ;
#139084 = CARTESIAN_POINT ( 'NONE',  ( 19.02544592524334988, 5.153800228976608722, 46.45942372801899012 ) ) ;
#139086 = EDGE_CURVE ( 'NONE', #161460, #130499, #5662, .T. ) ;
#139085 = CARTESIAN_POINT ( 'NONE',  ( 13.97604488694527802, 13.89961937509977652, 79.37390960531435269 ) ) ;
#139087 =( BOUNDED_CURVE ( )  B_SPLINE_CURVE ( 2, ( #176636, #144273, #163460, #128104, #145272, #193804, #115949, #5760, #24958, #66443, #4754 ),
 .UNSPECIFIED., .F., .F. ) 
 B_SPLINE_CURVE_WITH_KNOTS ( ( 3, 2, 2, 2, 2, 3 ),
 ( 0.1000000000000000888, 0.1200000000000000927, 0.1400000000000001243, 0.1600000000000001421, 0.1800000000000001321, 0.2000000000000001776 ),
 .UNSPECIFIED. ) 
 CURVE ( )  GEOMETRIC_REPRESENTATION_ITEM ( )  RATIONAL_B_SPLINE_CURVE ( ( 0.9999999999999997780, 0.9510565162951537532, 1.000000000000000000, 0.9510565162951535312, 1.000000000000000000, 0.9510565162951535312, 1.000000000000000000, 0.9510565162951535312, 1.000000000000000000, 0.9510565162951530871, 1.000000000000000444 ) ) 
 REPRESENTATION_ITEM ( '' )  );
#139088 = CARTESIAN_POINT ( 'NONE',  ( -21.52544592524343514, 5.823673210054127303, 81.04057627198102409 ) ) ;
#139090 = CARTESIAN_POINT ( 'NONE',  ( -0.05219959533936034679, 19.03943276465977164, 32.50109039468566863 ) ) ;
#139089 = CARTESIAN_POINT ( 'NONE',  ( 16.52544592524342804, -4.483927247898539470, 78.54057627198103830 ) ) ;
#139091 = CARTESIAN_POINT ( 'NONE',  ( -15.72974639402197994, 15.80617190586746368, 55.62390960531436690 ) ) ;
#139092 = CARTESIAN_POINT ( 'NONE',  ( 21.52544592524344225, -5.823673210054117533, 43.54057627198103830 ) ) ;
#139093 = CARTESIAN_POINT ( 'NONE',  ( 21.53943276465977519, 0.05219959533937863772, 91.25109039468568994 ) ) ;
#139094 = CARTESIAN_POINT ( 'NONE',  ( -9.474510206698964154, 16.51473224551069663, 70.41557627198102409 ) ) ;
#139095 = CARTESIAN_POINT ( 'NONE',  ( -4.379528057220328563, 16.55341960407611168, 110.2072429386477239 ) ) ;
#139096 = CARTESIAN_POINT ( 'NONE',  ( 18.67979575497194134, -10.72451020669871369, 30.83442372801902209 ) ) ;
#139097 = CARTESIAN_POINT ( 'NONE',  ( -19.25918095147780917, -5.499999999999586997, 39.45284276293936188 ) ) ;
#139098 = CARTESIAN_POINT ( 'NONE',  ( -5.719274019375665041, -21.55341960407619695, 39.79275706135235424 ) ) ;
#139099 = CARTESIAN_POINT ( 'NONE',  ( 16.46253265017160672, -9.564922557960803928, 33.33224293864770260 ) ) ;
#139100 = CARTESIAN_POINT ( 'NONE',  ( -18.67979575497178146, -10.72451020669898902, 101.6655762719810383 ) ) ;
#139101 = CARTESIAN_POINT ( 'NONE',  ( -13.89961937509957401, -13.97604488694547875, 49.37609039468567573 ) ) ;
#139102 = CARTESIAN_POINT ( 'NONE',  ( 4.999999999999997335, 5.204748896376250699E-16, -4.250000000000000000 ) ) ;
#139103 = CARTESIAN_POINT ( 'NONE',  ( 18.39443945427639449, -5.500000000000023093, 76.01745347608652992 ) ) ;
#139104 = DIRECTION ( 'NONE',  ( 0.000000000000000000, 0.000000000000000000, 1.000000000000000000 ) ) ;
#139105 = CARTESIAN_POINT ( 'NONE',  ( -0.05219959533934338120, 16.53943276465976808, 57.50109039468568994 ) ) ;
#139106 = CARTESIAN_POINT ( 'NONE',  ( -0.05219959533909027116, -19.03943276465977164, 22.49890960531436690 ) ) ;
#139107 = CARTESIAN_POINT ( 'NONE',  ( -26.57611637973506546, -7.696099174151179056, 167.9177021574075468 ) ) ;
#139108 = CARTESIAN_POINT ( 'NONE',  ( -5.153800228976328057, -19.02544592524343514, 72.29057627198102409 ) ) ;
#139109 = CARTESIAN_POINT ( 'NONE',  ( 8.314922557960818139, 14.29746914071049879, 104.5822429386477097 ) ) ;
#139110 = CARTESIAN_POINT ( 'NONE',  ( -10.72451020669898014, 18.67979575497178502, 60.41557627198102409 ) ) ;
#139111 = CARTESIAN_POINT ( 'NONE',  ( -16.55341960407617563, 4.379528057220093196, 33.54275706135234714 ) ) ;
#139112 = CARTESIAN_POINT ( 'NONE',  ( 10.72451020669871369, 18.67979575497193778, 97.08442372801904696 ) ) ;
#139113 = FACE_OUTER_BOUND ( 'NONE', #134859, .T. ) ;
#139114 = CARTESIAN_POINT ( 'NONE',  ( 8.224510206698742110, 14.34966873604972548, 107.0844237280190043 ) ) ;
#139115 = CARTESIAN_POINT ( 'NONE',  ( 16.55341960407611168, 4.379528057220329451, 48.95724293864770971 ) ) ;
#139116 = CARTESIAN_POINT ( 'NONE',  ( 0.05219959533909260263, 19.03943276465977164, 54.99890960531435979 ) ) ;
#139117 = CARTESIAN_POINT ( 'NONE',  ( 0.05219959533937995610, -21.53943276465977519, 95.00109039468568994 ) ) ;
#139118 = CARTESIAN_POINT ( 'NONE',  ( -0.05219959533907301413, -21.53943276465977519, 112.4989096053143669 ) ) ;
#139119 = CARTESIAN_POINT ( 'NONE',  ( 21.53943276465977519, 0.05219959533937863772, 66.25109039468567573 ) ) ;
#139120 = CARTESIAN_POINT ( 'NONE',  ( -12.06949235617739369, -12.14591786802326823, 54.37609039468568994 ) ) ;
#139122 = CARTESIAN_POINT ( 'NONE',  ( 15.80617190586769283, -15.72974639402175789, 105.6260903946856899 ) ) ;
#139121 = CARTESIAN_POINT ( 'NONE',  ( -4.379528057220328563, 16.55341960407611168, 80.20724293864769550 ) ) ;
#139123 = CARTESIAN_POINT ( 'NONE',  ( 4.483927247898545687, 16.52544592524342804, 24.79057627198103120 ) ) ;
#139124 = CARTESIAN_POINT ( 'NONE',  ( -8.898068258721469448, -27.38543819252872069, 140.6656553485623817 ) ) ;
#139125 = CARTESIAN_POINT ( 'NONE',  ( -16.55341960407617563, 4.379528057220093196, 33.54275706135234714 ) ) ;
#139126 = CARTESIAN_POINT ( 'NONE',  ( -16.52544592524342804, 4.483927247898546575, 41.04057627198103120 ) ) ;
#139127 = CARTESIAN_POINT ( 'NONE',  ( 16.52544592524335698, 4.483927247898782831, 81.45942372801900433 ) ) ;
#139128 = CARTESIAN_POINT ( 'NONE',  ( -19.02544592524342804, 5.153800228976336051, 96.04057627198103830 ) ) ;
#139129 = CARTESIAN_POINT ( 'NONE',  ( -19.05341960407611168, -5.049401038298163336, 111.4572429386476671 ) ) ;
#139130 = CARTESIAN_POINT ( 'NONE',  ( 18.62759615963255655, 10.81492255796105972, 96.66775706135234714 ) ) ;
#139131 = CARTESIAN_POINT ( 'NONE',  ( -12.06949235617739369, -12.14591786802326823, 104.3760903946856899 ) ) ;
#139132 = CARTESIAN_POINT ( 'NONE',  ( -0.05219959533910754901, -16.53943276465976808, 77.49890960531433848 ) ) ;
#139133 = CARTESIAN_POINT ( 'NONE',  ( -16.51473224551069308, -9.474510206698971260, 76.66557627198103830 ) ) ;
#139134 = ORIENTED_EDGE ( 'NONE', *, *, #189500, .F. ) ;
#139135 = CARTESIAN_POINT ( 'NONE',  ( 0.05219959533934541429, -16.53943276465976808, 30.00109039468568284 ) ) ;
#139136 = CARTESIAN_POINT ( 'NONE',  ( -19.02544592524342804, 5.153800228976336051, 26.04057627198103120 ) ) ;
#139137 = CARTESIAN_POINT ( 'NONE',  ( 16.46253265017160672, -9.564922557960803928, 88.33224293864769550 ) ) ;
#139139 = CARTESIAN_POINT ( 'NONE',  ( 18.09918380851992481, 5.500000000000035527, 68.98618307335613054 ) ) ;
#139138 = CARTESIAN_POINT ( 'NONE',  ( -16.55341960407617563, 4.379528057220093196, 38.54275706135234714 ) ) ;
#139140 = CARTESIAN_POINT ( 'NONE',  ( -19.02544592524334988, -5.153800228976617603, 33.95942372801897591 ) ) ;
#139141 = CARTESIAN_POINT ( 'NONE',  ( -4.483927247898782831, 16.52544592524335698, 97.70942372801904696 ) ) ;
#139142 = CARTESIAN_POINT ( 'NONE',  ( -19.05341960407611168, -5.049401038298163336, 31.45724293864769550 ) ) ;
#139143 = CARTESIAN_POINT ( 'NONE',  ( -12.06949235617739369, -12.14591786802326823, 74.37609039468568994 ) ) ;
#139144 = CARTESIAN_POINT ( 'NONE',  ( 8.224510206698742110, 14.34966873604972548, 62.08442372801901143 ) ) ;
#139145 = CARTESIAN_POINT ( 'NONE',  ( -19.02544592524334988, -5.153800228976617603, 83.95942372801901854 ) ) ;
#139146 = CARTESIAN_POINT ( 'NONE',  ( -5.049401038297874678, -19.05341960407617918, 29.79275706135232227 ) ) ;
#139147 = CARTESIAN_POINT ( 'NONE',  ( 19.02544592524343514, -5.153800228976328945, 43.54057627198103120 ) ) ;
#139148 = CARTESIAN_POINT ( 'NONE',  ( -4.379528057220328563, 16.55341960407611168, 85.20724293864770971 ) ) ;
#139149 = CARTESIAN_POINT ( 'NONE',  ( 9.564922557961047289, -16.46253265017146816, 50.41775706135233293 ) ) ;
#139150 = CARTESIAN_POINT ( 'NONE',  ( 18.62759615963271287, -10.81492255796078972, 48.33224293864770260 ) ) ;
#139151 = CARTESIAN_POINT ( 'NONE',  ( -19.02544592524334988, -5.153800228976617603, 33.95942372801897591 ) ) ;
#139152 = CARTESIAN_POINT ( 'NONE',  ( 19.05341960407611168, 5.049401038298154454, 98.95724293864766707 ) ) ;
#139153 = CARTESIAN_POINT ( 'NONE',  ( -18.67979575497178146, -10.72451020669898902, 76.66557627198103830 ) ) ;
#139154 = FACE_OUTER_BOUND ( 'NONE', #89946, .T. ) ;
#139155 = CARTESIAN_POINT ( 'NONE',  ( -16.51473224551082808, 9.474510206698731452, 93.33442372801900433 ) ) ;
#139156 = CARTESIAN_POINT ( 'NONE',  ( -2.044528755335720316, -7.220908937440006170, 8.410814283099840694 ) ) ;
#139157 = EDGE_CURVE ( 'NONE', #91492, #147765, #24122, .T. ) ;
#139158 = CARTESIAN_POINT ( 'NONE',  ( 16.46253265017146816, 9.564922557961045513, 111.6677570613523329 ) ) ;
#139159 = CARTESIAN_POINT ( 'NONE',  ( 5.153800228976335163, 19.02544592524342804, 39.79057627198100988 ) ) ;
#139160 = CARTESIAN_POINT ( 'NONE',  ( -9.564922557960796823, -16.46253265017161027, 102.0822429386477097 ) ) ;
#139161 = CARTESIAN_POINT ( 'NONE',  ( -15.80617190586745835, -15.72974639402198527, 71.87390960531438111 ) ) ;
#139162 = CARTESIAN_POINT ( 'NONE',  ( 14.34966873604972726, -8.224510206698740333, 50.83442372801901143 ) ) ;
#139163 = CARTESIAN_POINT ( 'NONE',  ( -21.55341960407619339, 5.719274019375674811, 43.54275706135235424 ) ) ;
#139165 = CARTESIAN_POINT ( 'NONE',  ( -15.80617190586768217, 15.72974639402176855, 108.1260903946856757 ) ) ;
#139164 = CARTESIAN_POINT ( 'NONE',  ( -5.049401038297874678, -19.05341960407617918, 94.79275706135230450 ) ) ;
#139166 = CARTESIAN_POINT ( 'NONE',  ( 16.55341960407618274, -4.379528057220086978, 106.0427570613523471 ) ) ;
#139167 = CARTESIAN_POINT ( 'NONE',  ( 5.153800228976335163, 19.02544592524342804, 99.79057627198102409 ) ) ;
#139168 = CARTESIAN_POINT ( 'NONE',  ( 8.224510206698953496, -14.34966873604960469, 92.91557627198103830 ) ) ;
#139169 = CARTESIAN_POINT ( 'NONE',  ( 14.34966873604960469, 8.224510206698951720, 39.16557627198102409 ) ) ;
#139170 = CARTESIAN_POINT ( 'NONE',  ( 16.46253265017146816, 9.564922557961045513, 86.66775706135233293 ) ) ;
#139171 = CARTESIAN_POINT ( 'NONE',  ( -15.80617190586768217, 15.72974639402176855, 58.12609039468568994 ) ) ;
#139173 = ADVANCED_FACE ( 'NONE', ( #80516 ), #113830, .T. ) ;
#139172 = CARTESIAN_POINT ( 'NONE',  ( 9.474510206698729675, 16.51473224551082808, 32.08442372801900433 ) ) ;
#139174 = CARTESIAN_POINT ( 'NONE',  ( -16.55341960407611168, -4.379528057220339221, 111.4572429386476813 ) ) ;
#139175 = CARTESIAN_POINT ( 'NONE',  ( -5.719274019375978568, 21.55341960407610458, 25.20724293864769550 ) ) ;
#139176 = CARTESIAN_POINT ( 'NONE',  ( 12.06949235617757843, -12.14591786802309237, 28.12390960531435979 ) ) ;
#139177 = CARTESIAN_POINT ( 'NONE',  ( 0.05219959533937995610, -21.53943276465977519, 105.0010903946856757 ) ) ;
#139178 = CARTESIAN_POINT ( 'NONE',  ( 12.06949235617739724, 12.14591786802326823, 56.87609039468568994 ) ) ;
#139179 = CARTESIAN_POINT ( 'NONE',  ( 16.55341960407611168, 4.379528057220329451, 28.95724293864769905 ) ) ;
#139180 = CARTESIAN_POINT ( 'NONE',  ( -0.05219959533937732626, 21.53943276465977519, 57.50109039468568994 ) ) ;
#139182 = EDGE_CURVE ( 'NONE', #45563, #89527, #66023, .T. ) ;
#139181 = CARTESIAN_POINT ( 'NONE',  ( 15.72974639402176855, 15.80617190586768217, 51.87609039468568284 ) ) ;
#139183 = EDGE_LOOP ( 'NONE', ( #135294, #41309, #121667, #68605, #164343, #116610, #56975, #110468 ) ) ;
#139184 = CARTESIAN_POINT ( 'NONE',  ( -17.59860650958989936, -7.585241751807033417, 61.57662985737508876 ) ) ;
#139185 = CARTESIAN_POINT ( 'NONE',  ( 21.52544592524334988, 5.823673210054432836, 26.45942372801901854 ) ) ;
#139186 = CARTESIAN_POINT ( 'NONE',  ( -4.483927247898539470, -16.52544592524342804, 102.2905762719810383 ) ) ;
#139187 = CARTESIAN_POINT ( 'NONE',  ( 19.03943276465977164, -0.05219959533909143690, 23.74890960531435269 ) ) ;
#139188 = CARTESIAN_POINT ( 'NONE',  ( -12.06949235617756955, 12.14591786802309770, 85.62390960531436690 ) ) ;
#139189 = CARTESIAN_POINT ( 'NONE',  ( 13.89961937509977652, -13.97604488694527269, 68.12390960531436690 ) ) ;
#139190 = CARTESIAN_POINT ( 'NONE',  ( -12.06949235617756955, 12.14591786802309770, 25.62390960531435624 ) ) ;
#139191 = CARTESIAN_POINT ( 'NONE',  ( -0.05219959533907301413, -21.53943276465977519, 52.49890960531435979 ) ) ;
#139192 = CARTESIAN_POINT ( 'NONE',  ( -16.53943276465976808, 0.05219959533911058130, 91.24890960531436690 ) ) ;
#139193 = CARTESIAN_POINT ( 'NONE',  ( -5.823673210054116645, -21.52544592524344225, 92.29057627198103830 ) ) ;
#139194 = CARTESIAN_POINT ( 'NONE',  ( 0.05219959533909260263, 19.03943276465977164, 104.9989096053143669 ) ) ;
#139196 = CARTESIAN_POINT ( 'NONE',  ( 9.474510206698729675, 16.51473224551082808, 112.0844237280190043 ) ) ;
#139195 = CARTESIAN_POINT ( 'NONE',  ( -5.153800228976328057, -19.02544592524343514, 47.29057627198102409 ) ) ;
#139197 = CARTESIAN_POINT ( 'NONE',  ( -5.823673210054116645, -21.52544592524344225, 42.29057627198103120 ) ) ;
#139198 = CARTESIAN_POINT ( 'NONE',  ( 18.62759615963255655, 10.81492255796105972, 76.66775706135234714 ) ) ;
#139199 = CARTESIAN_POINT ( 'NONE',  ( 19.05341960407611168, 5.049401038298154454, 63.95724293864769550 ) ) ;
#139200 = CARTESIAN_POINT ( 'NONE',  ( -19.02544592524342804, 5.153800228976336051, 101.0405762719810241 ) ) ;
#139201 = CARTESIAN_POINT ( 'NONE',  ( 16.55341960407618274, -4.379528057220086978, 81.04275706135236135 ) ) ;
#139202 = CARTESIAN_POINT ( 'NONE',  ( -0.05219959533937732626, 21.53943276465977519, 62.50109039468568284 ) ) ;
#139203 = CARTESIAN_POINT ( 'NONE',  ( 15.80617190586769283, -15.72974639402175789, 90.62609039468567573 ) ) ;
#139204 = CARTESIAN_POINT ( 'NONE',  ( -5.719274019375978568, 21.55341960407610458, 110.2072429386477239 ) ) ;
#139206 = CARTESIAN_POINT ( 'NONE',  ( -12.06949235617739369, -12.14591786802326823, 84.37609039468570415 ) ) ;
#139205 = CARTESIAN_POINT ( 'NONE',  ( -18.62759615963255300, -10.81492255796106328, 39.16775706135235424 ) ) ;
#139207 = CARTESIAN_POINT ( 'NONE',  ( -10.72451020669898014, 18.67979575497178502, 80.41557627198103830 ) ) ;
#139208 = CARTESIAN_POINT ( 'NONE',  ( -13.89961937509957401, -13.97604488694547875, 34.37609039468566863 ) ) ;
#139209 = CARTESIAN_POINT ( 'NONE',  ( 21.53943276465977519, -0.05219959533907433946, 43.74890960531435979 ) ) ;
#139211 = CARTESIAN_POINT ( 'NONE',  ( -14.29746914071049879, 8.314922557960819915, 25.83224293864769194 ) ) ;
#139210 = CARTESIAN_POINT ( 'NONE',  ( 16.46253265017160672, -9.564922557960803928, 83.33224293864768129 ) ) ;
#139212 = CARTESIAN_POINT ( 'NONE',  ( -17.48847506799968343, 5.747544572773785276, 65.82697437843285115 ) ) ;
#139213 = CARTESIAN_POINT ( 'NONE',  ( -0.05219959533909027116, -19.03943276465977164, 107.4989096053143527 ) ) ;
#139214 = CARTESIAN_POINT ( 'NONE',  ( -3.573655867282028392E-15, 2.428612866367529932E-14, 139.9999999999999716 ) ) ;
#139215 = CARTESIAN_POINT ( 'NONE',  ( 9.474510206698729675, 16.51473224551082808, 97.08442372801900433 ) ) ;
#139216 = CARTESIAN_POINT ( 'NONE',  ( 0.05219959533907565091, 21.53943276465977519, 69.99890960531435269 ) ) ;
#139217 = CARTESIAN_POINT ( 'NONE',  ( -14.29746914071049879, 8.314922557960819915, 40.83224293864769550 ) ) ;
#139218 = CARTESIAN_POINT ( 'NONE',  ( 5.049401038297881783, 19.05341960407617563, 112.2927570613523471 ) ) ;
#139219 = CARTESIAN_POINT ( 'NONE',  ( 9.474510206698971260, -16.51473224551069308, 32.91557627198102409 ) ) ;
#139220 = CARTESIAN_POINT ( 'NONE',  ( 5.049401038297881783, 19.05341960407617563, 107.2927570613523187 ) ) ;
#139222 = CARTESIAN_POINT ( 'NONE',  ( 0.05219959533936267826, -19.03943276465977164, 65.00109039468567573 ) ) ;
#139221 = CARTESIAN_POINT ( 'NONE',  ( -21.52544592524343514, 5.823673210054127303, 101.0405762719810383 ) ) ;
#139223 = CARTESIAN_POINT ( 'NONE',  ( 14.29746914071037800, 8.314922557961029526, 76.66775706135234714 ) ) ;
#139224 = CARTESIAN_POINT ( 'NONE',  ( -19.03943276465977164, 0.05219959533909376836, 81.24890960531436690 ) ) ;
#139225 = CARTESIAN_POINT ( 'NONE',  ( 16.53943276465976808, -0.05219959533910856209, 78.74890960531436690 ) ) ;
#139226 = CARTESIAN_POINT ( 'NONE',  ( -5.153800228976328057, -19.02544592524343514, 67.29057627198102409 ) ) ;
#139227 = CARTESIAN_POINT ( 'NONE',  ( 8.314922557960818139, 14.29746914071049879, 69.58224293864769550 ) ) ;
#139228 = CARTESIAN_POINT ( 'NONE',  ( -19.05341960407611168, -5.049401038298163336, 31.45724293864769550 ) ) ;
#139229 = CARTESIAN_POINT ( 'NONE',  ( -36.89003987753539349, -5.463308683677073674, 44.27017301194418764 ) ) ;
#139230 = CARTESIAN_POINT ( 'NONE',  ( -14.29746914071049879, 8.314922557960819915, 40.83224293864769550 ) ) ;
#139231 = CARTESIAN_POINT ( 'NONE',  ( 13.89961937509977652, -13.97604488694527269, 78.12390960531433848 ) ) ;
#139232 = CARTESIAN_POINT ( 'NONE',  ( 9.310586156219267749E-15, -64.87124026077280803, -14.99999901254159873 ) ) ;
#139233 = CARTESIAN_POINT ( 'NONE',  ( 19.05341960407617918, -5.049401038297876454, 46.04275706135233293 ) ) ;
#139234 = CARTESIAN_POINT ( 'NONE',  ( 14.34966873604972726, -8.224510206698740333, 60.83442372801901854 ) ) ;
#139235 = CARTESIAN_POINT ( 'NONE',  ( 5.719274019375991003, -21.55341960407610458, 57.70724293864770260 ) ) ;
#139236 = CARTESIAN_POINT ( 'NONE',  ( -16.51473224551082808, 9.474510206698731452, 23.33442372801900078 ) ) ;
#139237 = CARTESIAN_POINT ( 'NONE',  ( -5.049401038298153566, 19.05341960407611168, 90.20724293864766707 ) ) ;
#139238 = DIRECTION ( 'NONE',  ( 0.000000000000000000, 0.000000000000000000, 1.000000000000000000 ) ) ;
#139239 = CARTESIAN_POINT ( 'NONE',  ( -21.55341960407610458, -5.719274019375992779, 26.45724293864768839 ) ) ;
#139240 = CARTESIAN_POINT ( 'NONE',  ( -16.46253265017160317, 9.564922557960807481, 60.83224293864769550 ) ) ;
#139241 = CARTESIAN_POINT ( 'NONE',  ( 18.62759615963255655, 10.81492255796105972, 56.66775706135235424 ) ) ;
#139242 = CARTESIAN_POINT ( 'NONE',  ( -16.52544592524342804, 4.483927247898546575, 111.0405762719810525 ) ) ;
#139245 = VERTEX_POINT ( 'NONE', #187732 ) ;
#139244 = CARTESIAN_POINT ( 'NONE',  ( 9.474510206698971260, -16.51473224551069308, 92.91557627198103830 ) ) ;
#139243 = CARTESIAN_POINT ( 'NONE',  ( 21.55341960407610458, 5.719274019375980345, 103.9572429386476813 ) ) ;
#139246 = CARTESIAN_POINT ( 'NONE',  ( 0.05219959533937995610, -21.53943276465977519, 40.00109039468567573 ) ) ;
#139247 = VERTEX_POINT ( 'NONE', #125045 ) ;
#139248 = CARTESIAN_POINT ( 'NONE',  ( -13.89961937509977652, 13.97604488694528158, 90.62390960531432427 ) ) ;
#139249 = CARTESIAN_POINT ( 'NONE',  ( 18.56197773271728479, -5.500000000000079048, 81.05066217314454491 ) ) ;
#139250 = CARTESIAN_POINT ( 'NONE',  ( 18.62759615963271287, -10.81492255796078972, 88.33224293864769550 ) ) ;
#139251 = CARTESIAN_POINT ( 'NONE',  ( -19.02544592524342804, 5.153800228976336051, 51.04057627198103120 ) ) ;
#139252 = CARTESIAN_POINT ( 'NONE',  ( 0.05219959533934541429, -16.53943276465976808, 20.00109039468568639 ) ) ;
#139253 = CARTESIAN_POINT ( 'NONE',  ( 3.766062262543149401E-15, -39.95556452105413570, -11.24999999453762278 ) ) ;
#139254 = CARTESIAN_POINT ( 'NONE',  ( -9.474510206698964154, 16.51473224551069663, 30.41557627198102054 ) ) ;
#139255 = CARTESIAN_POINT ( 'NONE',  ( -21.53943276465977519, -0.05219959533937600094, 83.75109039468568994 ) ) ;
#139257 = CARTESIAN_POINT ( 'NONE',  ( -15.80617190586768217, 15.72974639402176855, 48.12609039468568284 ) ) ;
#139256 = CARTESIAN_POINT ( 'NONE',  ( -5.153800228976328057, -19.02544592524343514, 72.29057627198102409 ) ) ;
#139258 = CARTESIAN_POINT ( 'NONE',  ( 0.05219959533937995610, -21.53943276465977519, 25.00109039468567218 ) ) ;
#139259 = CARTESIAN_POINT ( 'NONE',  ( 8.571926809382597767, 26.38167802310806209, 142.7750000027311899 ) ) ;
#139260 = CARTESIAN_POINT ( 'NONE',  ( 9.474510206698971260, -16.51473224551069308, 92.91557627198103830 ) ) ;
#139261 = CARTESIAN_POINT ( 'NONE',  ( 18.22780087662121673, 5.500000000000056843, 63.98459894673894155 ) ) ;
#139264 = CARTESIAN_POINT ( 'NONE',  ( 0.05219959533937995610, -21.53943276465977519, 45.00109039468568284 ) ) ;
#139263 = CARTESIAN_POINT ( 'NONE',  ( 14.29746914071037800, 8.314922557961029526, 66.66775706135234714 ) ) ;
#139262 = CARTESIAN_POINT ( 'NONE',  ( -12.14591786802326823, 12.06949235617739902, 33.12609039468569705 ) ) ;
#139265 = CARTESIAN_POINT ( 'NONE',  ( 18.67979575497194134, -10.72451020669871369, 80.83442372801901854 ) ) ;
#139266 = CARTESIAN_POINT ( 'NONE',  ( 2.500000000000000000, 2.357898499370431722, -2.818925648462311528E-15 ) ) ;
#139267 = CARTESIAN_POINT ( 'NONE',  ( 9.564922557961047289, -16.46253265017146816, 110.4177570613523471 ) ) ;
#139268 = CARTESIAN_POINT ( 'NONE',  ( -5.049401038298153566, 19.05341960407611168, 60.20724293864768129 ) ) ;
#139269 = CARTESIAN_POINT ( 'NONE',  ( 19.05341960407611168, 5.049401038298154454, 98.95724293864766707 ) ) ;
#139270 = CARTESIAN_POINT ( 'NONE',  ( 4.379528057220339221, -16.55341960407611168, 112.7072429386476955 ) ) ;
#139271 = CARTESIAN_POINT ( 'NONE',  ( 0.05219959533910956823, 16.53943276465976808, 99.99890960531436690 ) ) ;
#139272 = CARTESIAN_POINT ( 'NONE',  ( 15.72974639402199770, -15.80617190586745480, 33.12390960531435979 ) ) ;
#139273 = CARTESIAN_POINT ( 'NONE',  ( 0.05219959533934541429, -16.53943276465976808, 85.00109039468568994 ) ) ;
#139275 = CARTESIAN_POINT ( 'NONE',  ( 9.564922557960805705, 16.46253265017160317, 59.58224293864769550 ) ) ;
#139274 = CARTESIAN_POINT ( 'NONE',  ( 14.34966873604960469, 8.224510206698951720, 69.16557627198102409 ) ) ;
#139276 = CARTESIAN_POINT ( 'NONE',  ( -5.823673210054431948, 21.52544592524334988, 72.70942372801901854 ) ) ;
#139277 = CARTESIAN_POINT ( 'NONE',  ( 21.53943276465977519, 0.05219959533937863772, 71.25109039468568994 ) ) ;
#139278 = CARTESIAN_POINT ( 'NONE',  ( -13.89961937509957401, -13.97604488694547875, 109.3760903946856331 ) ) ;
#139279 = CARTESIAN_POINT ( 'NONE',  ( -12.14591786802309592, -12.06949235617757132, 71.87390960531438111 ) ) ;
#139280 = CARTESIAN_POINT ( 'NONE',  ( -18.67979575497193778, 10.72451020669871902, 23.33442372801901499 ) ) ;
#139281 = CARTESIAN_POINT ( 'NONE',  ( -21.52544592524343514, 5.823673210054127303, 56.04057627198102409 ) ) ;
#139282 = CARTESIAN_POINT ( 'NONE',  ( -17.40861289039000326, -6.110651285853326620, 106.3723247082743057 ) ) ;
#139283 = CARTESIAN_POINT ( 'NONE',  ( 8.906447517083057264, -27.41122689804191026, 146.8500000054623627 ) ) ;
#139284 = CARTESIAN_POINT ( 'NONE',  ( 9.564922557960805705, 16.46253265017160317, 74.58224293864769550 ) ) ;
#139285 = CARTESIAN_POINT ( 'NONE',  ( 4.379528057220339221, -16.55341960407611168, 52.70724293864769550 ) ) ;
#139286 = CARTESIAN_POINT ( 'NONE',  ( -12.14591786802309592, -12.06949235617757132, 26.87390960531435979 ) ) ;
#139287 = CARTESIAN_POINT ( 'NONE',  ( 16.55341960407618274, -4.379528057220086978, 91.04275706135236135 ) ) ;
#139288 = CARTESIAN_POINT ( 'NONE',  ( -19.05341960407617563, 5.049401038297882671, 53.54275706135231871 ) ) ;
#139289 = CARTESIAN_POINT ( 'NONE',  ( -23.84689744903970876, -10.26551614244695720, 166.0764362378396868 ) ) ;
#139290 = CARTESIAN_POINT ( 'NONE',  ( -19.05341960407611168, -5.049401038298163336, 106.4572429386476955 ) ) ;
#139291 = CARTESIAN_POINT ( 'NONE',  ( 8.314922557960818139, 14.29746914071049879, 79.58224293864769550 ) ) ;
#139292 = CARTESIAN_POINT ( 'NONE',  ( -13.89961937509957401, -13.97604488694547875, 44.37609039468566863 ) ) ;
#139294 = CARTESIAN_POINT ( 'NONE',  ( 21.52544592524344225, -5.823673210054117533, 33.54057627198102409 ) ) ;
#139293 = CARTESIAN_POINT ( 'NONE',  ( -5.049401038298153566, 19.05341960407611168, 35.20724293864768839 ) ) ;
#139295 = CARTESIAN_POINT ( 'NONE',  ( 0.05219959533907565091, 21.53943276465977519, 54.99890960531435269 ) ) ;
#139296 = CARTESIAN_POINT ( 'NONE',  ( -4.379528057220328563, 16.55341960407611168, 100.2072429386476955 ) ) ;
#139297 = CARTESIAN_POINT ( 'NONE',  ( 8.224510206698742110, 14.34966873604972548, 57.08442372801901854 ) ) ;
#139298 = CARTESIAN_POINT ( 'NONE',  ( 16.52544592524342804, -4.483927247898539470, 93.54057627198103830 ) ) ;
#139299 = CARTESIAN_POINT ( 'NONE',  ( -38.00000000000000711, 2.893978650043524126E-14, -25.00000000000000000 ) ) ;
#139300 = CARTESIAN_POINT ( 'NONE',  ( -17.05587630539785948, 6.762274262135695047, 50.74180309037313208 ) ) ;
#139301 = CARTESIAN_POINT ( 'NONE',  ( -15.80617190586745835, -15.72974639402198527, 31.87390960531435979 ) ) ;
#139302 = LINE ( 'NONE', #136334, #42917 ) ;
#139303 = CARTESIAN_POINT ( 'NONE',  ( 17.81289503416611453, -24.51734667627695785, 142.6999999999999886 ) ) ;
#139305 = CARTESIAN_POINT ( 'NONE',  ( -14.29746914071049879, 8.314922557960819915, 25.83224293864769194 ) ) ;
#139304 = CARTESIAN_POINT ( 'NONE',  ( 16.52544592524335698, 4.483927247898782831, 41.45942372801901143 ) ) ;
#139306 = CARTESIAN_POINT ( 'NONE',  ( 10.72451020669898902, -18.67979575497178502, 52.91557627198103830 ) ) ;
#139307 = CARTESIAN_POINT ( 'NONE',  ( 13.89961937509957401, 13.97604488694547697, 86.87609039468567573 ) ) ;
#139308 = CARTESIAN_POINT ( 'NONE',  ( 21.53943276465977519, -0.05219959533907433946, 58.74890960531436690 ) ) ;
#139309 = CARTESIAN_POINT ( 'NONE',  ( -15.80617190586768217, 15.72974639402176855, 83.12609039468568994 ) ) ;
#139310 = CARTESIAN_POINT ( 'NONE',  ( -9.760382078682885876, 9.614343725828547349, -62.58071313852360618 ) ) ;
#139311 = CARTESIAN_POINT ( 'NONE',  ( 8.224510206698742110, 14.34966873604972548, 42.08442372801901854 ) ) ;
#139313 = CARTESIAN_POINT ( 'NONE',  ( 19.02544592524343514, -5.153800228976328945, 103.5405762719809957 ) ) ;
#139312 = CARTESIAN_POINT ( 'NONE',  ( -19.02544592524342804, 5.153800228976336051, 31.04057627198102409 ) ) ;
#139314 = CARTESIAN_POINT ( 'NONE',  ( -9.474510206698964154, 16.51473224551069663, 30.41557627198102054 ) ) ;
#139315 = CARTESIAN_POINT ( 'NONE',  ( -8.224510206698948167, 14.34966873604960824, 95.41557627198102409 ) ) ;
#139316 = DIRECTION ( 'NONE',  ( -1.000000000000000000, 0.000000000000000000, 0.000000000000000000 ) ) ;
#139317 = EDGE_LOOP ( 'NONE', ( #114960, #57225, #159935, #157687, #5156 ) ) ;
#139318 = CARTESIAN_POINT ( 'NONE',  ( 12.14591786802327356, -12.06949235617739191, 75.62609039468567573 ) ) ;
#139319 = CARTESIAN_POINT ( 'NONE',  ( 5.823673210054125526, 21.52544592524343514, 89.79057627198103830 ) ) ;
#139320 = CARTESIAN_POINT ( 'NONE',  ( -19.05341960407611168, -5.049401038298163336, 56.45724293864768129 ) ) ;
#139321 = CARTESIAN_POINT ( 'NONE',  ( 5.719274019375673035, 21.55341960407619339, 22.29275706135235069 ) ) ;
#139322 = CARTESIAN_POINT ( 'NONE',  ( -9.564922557960796823, -16.46253265017161027, 87.08224293864769550 ) ) ;
#139324 = ADVANCED_FACE ( 'NONE', ( #48212 ), #49203, .F. ) ;
#139323 = PLANE ( 'NONE',  #157313 ) ;
#139325 = EDGE_LOOP ( 'NONE', ( #49777, #40827, #10502, #121460 ) ) ;
#139326 = CARTESIAN_POINT ( 'NONE',  ( 10.81492255796106328, -18.62759615963255655, 25.41775706135235779 ) ) ;
#139329 = CARTESIAN_POINT ( 'NONE',  ( 13.97604488694548053, -13.89961937509957401, 75.62609039468564731 ) ) ;
#139328 = CARTESIAN_POINT ( 'NONE',  ( -5.153800228976328057, -19.02544592524343514, 107.2905762719810383 ) ) ;
#139327 = CARTESIAN_POINT ( 'NONE',  ( -13.89961937509977652, 13.97604488694528158, 30.62390960531435269 ) ) ;
#139330 = CARTESIAN_POINT ( 'NONE',  ( -5.153800228976607833, 19.02544592524334988, 32.70942372801899722 ) ) ;
#139331 = CARTESIAN_POINT ( 'NONE',  ( -18.67979575497178146, -10.72451020669898902, 106.6655762719810383 ) ) ;
#139332 = CARTESIAN_POINT ( 'NONE',  ( 5.153800228976615827, -19.02544592524334988, 35.20942372801899722 ) ) ;
#139333 = CARTESIAN_POINT ( 'NONE',  ( -16.53943276465976808, -0.05219959533934237506, 78.75109039468568994 ) ) ;
#139334 = CARTESIAN_POINT ( 'NONE',  ( 19.05341960407611168, 5.049401038298154454, 103.9572429386476671 ) ) ;
#139335 = CARTESIAN_POINT ( 'NONE',  ( 9.474510206698971260, -16.51473224551069308, 52.91557627198102409 ) ) ;
#139336 = CARTESIAN_POINT ( 'NONE',  ( -5.719274019375665041, -21.55341960407619695, 59.79275706135234714 ) ) ;
#139337 = CARTESIAN_POINT ( 'NONE',  ( 21.53943276465977519, 0.05219959533937863772, 76.25109039468568994 ) ) ;
#139338 = CARTESIAN_POINT ( 'NONE',  ( 19.05341960407611168, 5.049401038298154454, 68.95724293864769550 ) ) ;
#139339 = CARTESIAN_POINT ( 'NONE',  ( 18.67979575497194134, -10.72451020669871369, 50.83442372801901143 ) ) ;
#139340 = CARTESIAN_POINT ( 'NONE',  ( -16.51473224551082808, 9.474510206698731452, 88.33442372801900433 ) ) ;
#139341 = CARTESIAN_POINT ( 'NONE',  ( 9.474510206698971260, -16.51473224551069308, 47.91557627198102409 ) ) ;
#139342 = CARTESIAN_POINT ( 'NONE',  ( -5.153800228976328057, -19.02544592524343514, 102.2905762719810383 ) ) ;
#139343 = CARTESIAN_POINT ( 'NONE',  ( -5.153800228976328057, -19.02544592524343514, 62.29057627198100988 ) ) ;
#139344 = CARTESIAN_POINT ( 'NONE',  ( 5.153800228976335163, 19.02544592524342804, 109.7905762719810099 ) ) ;
#139345 = CARTESIAN_POINT ( 'NONE',  ( -5.049401038298153566, 19.05341960407611168, 55.20724293864769550 ) ) ;
#139346 = CARTESIAN_POINT ( 'NONE',  ( -10.72451020669898014, 18.67979575497178502, 100.4155762719810241 ) ) ;
#139347 = CARTESIAN_POINT ( 'NONE',  ( 4.379528057220092307, 16.55341960407617563, 77.29275706135234714 ) ) ;
#139348 = CARTESIAN_POINT ( 'NONE',  ( -23.19706360625338704, 11.80427776162510689, 165.7059442611694067 ) ) ;
#139349 = CARTESIAN_POINT ( 'NONE',  ( 9.564922557961047289, -16.46253265017146816, 40.41775706135234003 ) ) ;
#139350 = CARTESIAN_POINT ( 'NONE',  ( 13.97604488694527802, 13.89961937509977652, 64.37390960531436690 ) ) ;
#139351 = CARTESIAN_POINT ( 'NONE',  ( -14.29746914071049879, 8.314922557960819915, 60.83224293864769550 ) ) ;
#139352 = CARTESIAN_POINT ( 'NONE',  ( 8.314922557960818139, 14.29746914071049879, 89.58224293864768129 ) ) ;
#139353 = CARTESIAN_POINT ( 'NONE',  ( 5.153800228976335163, 19.02544592524342804, 114.7905762719810241 ) ) ;
#139354 = CARTESIAN_POINT ( 'NONE',  ( -9.564922557960796823, -16.46253265017161027, 87.08224293864769550 ) ) ;
#139355 = CARTESIAN_POINT ( 'NONE',  ( 9.564922557960805705, 16.46253265017160317, 109.5822429386476955 ) ) ;
#139356 = CARTESIAN_POINT ( 'NONE',  ( 10.72451020669871369, 18.67979575497193778, 107.0844237280190043 ) ) ;
#139357 = CARTESIAN_POINT ( 'NONE',  ( 12.06949235617739724, 12.14591786802326823, 91.87609039468568994 ) ) ;
#139358 = CARTESIAN_POINT ( 'NONE',  ( -13.97604488694527625, -13.89961937509977652, 81.87390960531436690 ) ) ;
#139359 = CARTESIAN_POINT ( 'NONE',  ( -21.53943276465977519, -0.05219959533937600094, 33.75109039468568284 ) ) ;
#139360 = CARTESIAN_POINT ( 'NONE',  ( -15.72974639402197994, 15.80617190586746368, 35.62390960531437401 ) ) ;
#139361 = CARTESIAN_POINT ( 'NONE',  ( 15.80617190586746368, 15.72974639402197994, 99.37390960531436690 ) ) ;
#139362 = CARTESIAN_POINT ( 'NONE',  ( 0.05219959533910956823, 16.53943276465976808, 59.99890960531436690 ) ) ;
#139363 = CARTESIAN_POINT ( 'NONE',  ( 5.049401038298161559, -19.05341960407611168, 52.70724293864767418 ) ) ;
#139364 = CARTESIAN_POINT ( 'NONE',  ( 0.05219959533910956823, 16.53943276465976808, 84.99890960531436690 ) ) ;
#139365 = CARTESIAN_POINT ( 'NONE',  ( -9.474510206698720793, -16.51473224551083518, 39.58442372801899722 ) ) ;
#139366 = CARTESIAN_POINT ( 'NONE',  ( 13.97604488694527802, 13.89961937509977652, 24.37390960531435624 ) ) ;
#139367 = CARTESIAN_POINT ( 'NONE',  ( 4.379528057220092307, 16.55341960407617563, 67.29275706135234714 ) ) ;
#139368 = CARTESIAN_POINT ( 'NONE',  ( -5.049401038298153566, 19.05341960407611168, 75.20724293864769550 ) ) ;
#139369 = CARTESIAN_POINT ( 'NONE',  ( -17.14385361876520975, 23.59649016807275856, 144.5750000027311728 ) ) ;
#139370 = CARTESIAN_POINT ( 'NONE',  ( 4.379528057220339221, -16.55341960407611168, 102.7072429386476955 ) ) ;
#139371 = CARTESIAN_POINT ( 'NONE',  ( 16.55341960407618274, -4.379528057220086978, 101.0427570613523756 ) ) ;
#139372 = CARTESIAN_POINT ( 'NONE',  ( -12.14591786802326823, 12.06949235617739902, 28.12609039468568284 ) ) ;
#139373 = CARTESIAN_POINT ( 'NONE',  ( -5.719274019375665041, -21.55341960407619695, 89.79275706135236135 ) ) ;
#139374 = CARTESIAN_POINT ( 'NONE',  ( 9.564922557960805705, 16.46253265017160317, 84.58224293864769550 ) ) ;
#139375 = CARTESIAN_POINT ( 'NONE',  ( -18.62759615963255300, -10.81492255796106328, 19.16775706135234714 ) ) ;
#139376 = CARTESIAN_POINT ( 'NONE',  ( -13.97604488694527625, -13.89961937509977652, 36.87390960531436690 ) ) ;
#139377 = CARTESIAN_POINT ( 'NONE',  ( 4.483927247898790824, -16.52544592524335698, 25.20942372801901854 ) ) ;
#139378 = CARTESIAN_POINT ( 'NONE',  ( 13.97604488694548053, -13.89961937509957401, 95.62609039468563310 ) ) ;
#139379 = CARTESIAN_POINT ( 'NONE',  ( 15.80617190586746368, 15.72974639402197994, 94.37390960531436690 ) ) ;
#139380 = CARTESIAN_POINT ( 'NONE',  ( 16.46253265017146816, 9.564922557961045513, 66.66775706135233293 ) ) ;
#139381 = CARTESIAN_POINT ( 'NONE',  ( 19.02544592524343514, -5.153800228976328945, 23.54057627198102054 ) ) ;
#139382 = CARTESIAN_POINT ( 'NONE',  ( 21.55341960407619695, -5.719274019375665929, 26.04275706135235779 ) ) ;
#139383 = CARTESIAN_POINT ( 'NONE',  ( -32.09281931051391012, -20.34824190692417289, -24.99999999999999289 ) ) ;
#139384 = CARTESIAN_POINT ( 'NONE',  ( 13.89961937509977652, -13.97604488694527269, 88.12390960531438111 ) ) ;
#139385 = CARTESIAN_POINT ( 'NONE',  ( 4.379528057220092307, 16.55341960407617563, 47.29275706135234003 ) ) ;
#139386 = CARTESIAN_POINT ( 'NONE',  ( -3.573655867282028392E-15, 2.428612866367529932E-14, 165.5209445330007441 ) ) ;
#139387 = CARTESIAN_POINT ( 'NONE',  ( -19.02544592524334988, -5.153800228976617603, 53.95942372801898301 ) ) ;
#139389 = CARTESIAN_POINT ( 'NONE',  ( 8.314922557960818139, 14.29746914071049879, 74.58224293864768129 ) ) ;
#139388 = CARTESIAN_POINT ( 'NONE',  ( -10.72451020669870658, -18.67979575497194134, 19.58442372801901143 ) ) ;
#139390 = CARTESIAN_POINT ( 'NONE',  ( 5.153800228976335163, 19.02544592524342804, 89.79057627198102409 ) ) ;
#139392 = CARTESIAN_POINT ( 'NONE',  ( 16.51473224551083163, -9.474510206698727899, 60.83442372801900433 ) ) ;
#139391 = CARTESIAN_POINT ( 'NONE',  ( 16.52544592524335698, 4.483927247898782831, 56.45942372801902565 ) ) ;
#139393 = CARTESIAN_POINT ( 'NONE',  ( 15.72974639402176855, 15.80617190586768217, 71.87609039468568994 ) ) ;
#139394 = CARTESIAN_POINT ( 'NONE',  ( -12.14591786802326823, 12.06949235617739902, 28.12609039468568284 ) ) ;
#139395 = CARTESIAN_POINT ( 'NONE',  ( 9.564922557960805705, 16.46253265017160317, 69.58224293864770971 ) ) ;
#139396 = CARTESIAN_POINT ( 'NONE',  ( -19.03943276465977164, -0.05219959533935918106, 78.75109039468567573 ) ) ;
#139397 = CARTESIAN_POINT ( 'NONE',  ( -4.379528057220086978, -16.55341960407618274, 59.79275706135234714 ) ) ;
#139398 = CARTESIAN_POINT ( 'NONE',  ( -5.823673210054431948, 21.52544592524334988, 92.70942372801901854 ) ) ;
#139399 = CARTESIAN_POINT ( 'NONE',  ( -19.02544592524334988, -5.153800228976617603, 68.95942372801896170 ) ) ;
#139400 = CARTESIAN_POINT ( 'NONE',  ( 9.564922557960805705, 16.46253265017160317, 54.58224293864769550 ) ) ;
#139401 = CARTESIAN_POINT ( 'NONE',  ( -10.81492255796078084, -18.62759615963271287, 72.08224293864769550 ) ) ;
#139403 = CARTESIAN_POINT ( 'NONE',  ( 9.564922557961047289, -16.46253265017146816, 80.41775706135234714 ) ) ;
#139402 = CARTESIAN_POINT ( 'NONE',  ( -8.314922557960811034, -14.29746914071050412, 82.08224293864768129 ) ) ;
#139404 = CARTESIAN_POINT ( 'NONE',  ( -19.49671883438224640, -5.500000000000076383, 69.89279849105676590 ) ) ;
#139405 = CARTESIAN_POINT ( 'NONE',  ( -13.89961937509957401, -13.97604488694547875, 44.37609039468566863 ) ) ;
#139406 = CARTESIAN_POINT ( 'NONE',  ( -12.14591786802326823, 12.06949235617739902, 103.1260903946856757 ) ) ;
#139407 = CARTESIAN_POINT ( 'NONE',  ( 8.224510206698953496, -14.34966873604960469, 67.91557627198102409 ) ) ;
#139409 = CARTESIAN_POINT ( 'NONE',  ( 8.571926809382597767, 26.38167802310806209, 148.2750000027311899 ) ) ;
#139408 = CARTESIAN_POINT ( 'NONE',  ( -15.72974639402176322, -15.80617190586768395, 104.3760903946856899 ) ) ;
#139410 = CARTESIAN_POINT ( 'NONE',  ( 15.72974639402199770, -15.80617190586745480, 103.1239096053143811 ) ) ;
#139411 = CARTESIAN_POINT ( 'NONE',  ( 16.51473224551069308, 9.474510206698969483, 64.16557627198102409 ) ) ;
#139412 = CARTESIAN_POINT ( 'NONE',  ( -21.53943276465977519, -0.05219959533937600094, 73.75109039468567573 ) ) ;
#139413 = CARTESIAN_POINT ( 'NONE',  ( 0.05219959533909260263, 19.03943276465977164, 54.99890960531435979 ) ) ;
#139414 = ORIENTED_EDGE ( 'NONE', *, *, #5777, .T. ) ;
#139415 = CARTESIAN_POINT ( 'NONE',  ( -5.153800228976328057, -19.02544592524343514, 22.29057627198102765 ) ) ;
#139416 = CARTESIAN_POINT ( 'NONE',  ( 9.474510206698971260, -16.51473224551069308, 112.9155762719810383 ) ) ;
#139417 = CARTESIAN_POINT ( 'NONE',  ( -16.55341960407611168, -4.379528057220339221, 66.45724293864768129 ) ) ;
#139418 = CARTESIAN_POINT ( 'NONE',  ( 16.51473224551069308, 9.474510206698969483, 24.16557627198102765 ) ) ;
#139419 = CARTESIAN_POINT ( 'NONE',  ( -12.06949235617756955, 12.14591786802309770, 90.62390960531436690 ) ) ;
#139420 = CARTESIAN_POINT ( 'NONE',  ( -0.05219959533907301413, -21.53943276465977519, 92.49890960531436690 ) ) ;
#139421 = CARTESIAN_POINT ( 'NONE',  ( 21.55341960407619695, -5.719274019375665929, 36.04275706135234714 ) ) ;
#139422 = CARTESIAN_POINT ( 'NONE',  ( -5.429308488886486681E-15, 30.30510711980690175, 149.5000000000000000 ) ) ;
#139423 = CARTESIAN_POINT ( 'NONE',  ( 0.05219959533934541429, -16.53943276465976808, 50.00109039468568994 ) ) ;
#139424 = CARTESIAN_POINT ( 'NONE',  ( -15.72974639402197994, 15.80617190586746368, 100.6239096053143811 ) ) ;
#139425 = CARTESIAN_POINT ( 'NONE',  ( -13.89961937509957401, -13.97604488694547875, 29.37609039468565797 ) ) ;
#139426 = CARTESIAN_POINT ( 'NONE',  ( 5.153800228976335163, 19.02544592524342804, 109.7905762719810099 ) ) ;
#139427 = CARTESIAN_POINT ( 'NONE',  ( -0.05219959533937732626, 21.53943276465977519, 47.50109039468568994 ) ) ;
#139428 = CARTESIAN_POINT ( 'NONE',  ( -10.72451020669898014, 18.67979575497178502, 45.41557627198103830 ) ) ;
#139429 = CARTESIAN_POINT ( 'NONE',  ( -4.483927247898539470, -16.52544592524342804, 27.29057627198103120 ) ) ;
#139430 = CIRCLE ( 'NONE', #10292, 7.500000000000000000 ) ;
#139432 = CARTESIAN_POINT ( 'NONE',  ( -10.81492255796105439, 18.62759615963255655, 102.9177570613523756 ) ) ;
#139431 = CARTESIAN_POINT ( 'NONE',  ( 15.80617190586769283, -15.72974639402175789, 60.62609039468567573 ) ) ;
#139433 = CARTESIAN_POINT ( 'NONE',  ( 13.97604488694548053, -13.89961937509957401, 30.62609039468566863 ) ) ;
#139434 = CARTESIAN_POINT ( 'NONE',  ( -8.314922557961024197, 14.29746914071037800, 92.91775706135236135 ) ) ;
#139435 = CARTESIAN_POINT ( 'NONE',  ( 18.67979575497194134, -10.72451020669871369, 50.83442372801901143 ) ) ;
#139436 = CARTESIAN_POINT ( 'NONE',  ( 16.51473224551069308, 9.474510206698969483, 49.16557627198102409 ) ) ;
#139437 = CARTESIAN_POINT ( 'NONE',  ( -0.05219959533936034679, 19.03943276465977164, 27.50109039468566507 ) ) ;
#139438 = CARTESIAN_POINT ( 'NONE',  ( 0.05219959533907565091, 21.53943276465977519, 24.99890960531435624 ) ) ;
#139439 = CARTESIAN_POINT ( 'NONE',  ( -18.62759615963255300, -10.81492255796106328, 24.16775706135235424 ) ) ;
#139440 = CARTESIAN_POINT ( 'NONE',  ( 15.80617190586746368, 15.72974639402197994, 74.37390960531436690 ) ) ;
#139441 = CARTESIAN_POINT ( 'NONE',  ( 8.314922557961029526, -14.29746914071037800, 40.41775706135234714 ) ) ;
#139443 = CARTESIAN_POINT ( 'NONE',  ( -15.72974639402197994, 15.80617190586746368, 75.62390960531439532 ) ) ;
#139442 = CYLINDRICAL_SURFACE ( 'NONE', #122502, 216.0437394197456342 ) ;
#139445 = CARTESIAN_POINT ( 'NONE',  ( 14.34966873604960469, 8.224510206698951720, 59.16557627198103120 ) ) ;
#139444 = CARTESIAN_POINT ( 'NONE',  ( -14.29746914071037622, -8.314922557961029526, 64.16775706135234714 ) ) ;
#139446 = CARTESIAN_POINT ( 'NONE',  ( 1.236971479055096745, 29.54649313627097840, -48.86402641782576239 ) ) ;
#139447 = CARTESIAN_POINT ( 'NONE',  ( -13.89961937509957401, -13.97604488694547875, 109.3760903946856331 ) ) ;
#139448 =( BOUNDED_CURVE ( )  B_SPLINE_CURVE ( 2, ( #34657, #143817, #65982, #128641, #66981, #64993, #140836, #96316, #6297, #2324, #64006, #158002, #21478, #125676, #97296, #67976, #50829, #187374, #112486, #20474, #83138, #19494, #80156, #142820, #48843, #174179, #110497, #81139, #171190, #172179, #109508, #32679, #18508, #111496, #141827, #190335, #51812, #94332, #3320, #82124, #36632, #33664, #113471, #189352, #175166, #127652, #129630, #191325, #95326, #126651, #157011, #4300, #158982, #98289, #188354, #49832, #87152, #131658, #146819, #52803, #145812, #115494, #176173, #39643, #177182, #161990, #101304, #41661, #37643, #88140, #193340, #8314, #22485, #56826, #10325, #54814, #24498, #68979, #162993, #99306, #116489, #147840, #160991, #149825, #178178, #148835, #9326, #71981, #133656, #69990, #84133, #86150, #11330, #7295, #130644, #70991, #103324 ),
 .UNSPECIFIED., .F., .F. ) 
 B_SPLINE_CURVE_WITH_KNOTS ( ( 3, 2, 2, 2, 2, 2, 2, 2, 2, 2, 2, 2, 2, 2, 2, 2, 2, 2, 2, 2, 2, 2, 2, 2, 2, 2, 2, 2, 2, 2, 2, 2, 2, 2, 2, 2, 2, 2, 2, 2, 2, 2, 2, 2, 2, 2, 2, 2, 3 ),
 ( 0.7919498004596616791, 0.7938596491228070429, 0.7982456140350877583, 0.8026315789473684736, 0.8070175438596490780, 0.8114035087719297934, 0.8157894736842105088, 0.8201754385964912242, 0.8245614035087719396, 0.8289473684210526550, 0.8333333333333333703, 0.8377192982456140857, 0.8421052631578946901, 0.8464912280701754055, 0.8508771929824561209, 0.8552631578947368363, 0.8596491228070175517, 0.8640350877192982670, 0.8684210526315789824, 0.8728070175438596978, 0.8771929824561403022, 0.8815789473684210176, 0.8859649122807017330, 0.8903508771929824483, 0.8947368421052631637, 0.8991228070175438791, 0.9035087719298245945, 0.9078947368421053099, 0.9122807017543859143, 0.9166666666666666297, 0.9210526315789473450, 0.9254385964912280604, 0.9298245614035087758, 0.9342105263157894912, 0.9385964912280702066, 0.9429824561403509220, 0.9473684210526315264, 0.9517543859649122417, 0.9561403508771929571, 0.9605263157894736725, 0.9649122807017543879, 0.9692982456140351033, 0.9736842105263158187, 0.9780701754385965341, 0.9824561403508771384, 0.9868421052631578538, 0.9912280701754385692, 0.9956140350877192846, 1.000000000000000000 ),
 .UNSPECIFIED. ) 
 CURVE ( )  GEOMETRIC_REPRESENTATION_ITEM ( )  RATIONAL_B_SPLINE_CURVE ( ( 0.9832469066685285419, 0.9851625545550100060, 1.000000000000000000, 0.9659258262890683122, 1.000000000000000000, 0.9659258262890683122, 1.000000000000000000, 0.9659258262890683122, 1.000000000000000000, 0.9659258262890683122, 1.000000000000000000, 0.9659258262890683122, 1.000000000000000000, 0.9659258262890683122, 1.000000000000000000, 0.9659258262890683122, 1.000000000000000000, 0.9659258262890683122, 1.000000000000000000, 0.9659258262890683122, 1.000000000000000000, 0.9659258262890683122, 1.000000000000000000, 0.9659258262890683122, 1.000000000000000000, 0.9659258262890683122, 1.000000000000000000, 0.9659258262890683122, 1.000000000000000000, 0.9659258262890683122, 1.000000000000000000, 0.9659258262890683122, 1.000000000000000000, 0.9659258262890683122, 1.000000000000000000, 0.9659258262890683122, 1.000000000000000000, 0.9659258262890683122, 1.000000000000000000, 0.9659258262890683122, 1.000000000000000000, 0.9659258262890683122, 1.000000000000000000, 0.9659258262890683122, 1.000000000000000000, 0.9659258262890683122, 1.000000000000000000, 0.9659258262890683122, 1.000000000000000000, 0.9659258262890683122, 1.000000000000000000, 0.9659258262890683122, 1.000000000000000000, 0.9659258262890683122, 1.000000000000000000, 0.9659258262890683122, 1.000000000000000000, 0.9659258262890683122, 1.000000000000000000, 0.9659258262890683122, 1.000000000000000000, 0.9659258262890683122, 1.000000000000000000, 0.9659258262890683122, 1.000000000000000000, 0.9659258262890683122, 1.000000000000000000, 0.9659258262890683122, 1.000000000000000000, 0.9659258262890683122, 1.000000000000000000, 0.9659258262890683122, 1.000000000000000000, 0.9659258262890683122, 1.000000000000000000, 0.9659258262890683122, 1.000000000000000000, 0.9659258262890683122, 1.000000000000000000, 0.9659258262890683122, 1.000000000000000000, 0.9659258262890683122, 1.000000000000000000, 0.9659258262890683122, 1.000000000000000000, 0.9659258262890683122, 1.000000000000000000, 0.9659258262890683122, 1.000000000000000000, 0.9659258262890683122, 1.000000000000000000, 0.9659258262890683122, 1.000000000000000000, 0.9659258262890683122, 1.000000000000000000, 0.9659258262890683122, 1.000000000000000000 ) ) 
 REPRESENTATION_ITEM ( '' )  );
#139449 = CARTESIAN_POINT ( 'NONE',  ( 6.835670873143622650, -5.764277696854612998, -61.93353089080586216 ) ) ;
#139450 = CARTESIAN_POINT ( 'NONE',  ( -14.34966873604972548, 8.224510206698743886, 38.33442372801900433 ) ) ;
#139451 = CARTESIAN_POINT ( 'NONE',  ( -5.823673210054116645, -21.52544592524344225, 112.2905762719810241 ) ) ;
#139452 = CARTESIAN_POINT ( 'NONE',  ( 5.719274019375991003, -21.55341960407610458, 32.70724293864770260 ) ) ;
#139453 = CARTESIAN_POINT ( 'NONE',  ( 16.53943276465976808, 0.05219959533934440121, 51.25109039468568994 ) ) ;
#139454 = CARTESIAN_POINT ( 'NONE',  ( -19.05341960407611168, -5.049401038298163336, 71.45724293864766707 ) ) ;
#139456 = CARTESIAN_POINT ( 'NONE',  ( 8.224510206698742110, 14.34966873604972548, 22.08442372801901143 ) ) ;
#139455 = CARTESIAN_POINT ( 'NONE',  ( -10.81492255796105439, 18.62759615963255655, 42.91775706135235424 ) ) ;
#139457 = CARTESIAN_POINT ( 'NONE',  ( 21.53943276465977519, -0.05219959533907433946, 23.74890960531435269 ) ) ;
#139458 = ORIENTED_EDGE ( 'NONE', *, *, #176553, .F. ) ;
#139459 = CARTESIAN_POINT ( 'NONE',  ( -5.153800228976607833, 19.02544592524334988, 27.70942372801899722 ) ) ;
#139460 = CARTESIAN_POINT ( 'NONE',  ( -8.224510206698735004, -14.34966873604973081, 44.58442372801901854 ) ) ;
#139461 = CARTESIAN_POINT ( 'NONE',  ( -19.03943276465977164, 0.05219959533909376836, 106.2489096053143669 ) ) ;
#139462 = CARTESIAN_POINT ( 'NONE',  ( -10.81492255796078084, -18.62759615963271287, 97.08224293864770971 ) ) ;
#139463 = CARTESIAN_POINT ( 'NONE',  ( 16.51473224551069308, 9.474510206698969483, 69.16557627198102409 ) ) ;
#139464 = CARTESIAN_POINT ( 'NONE',  ( -3.949974356353050720, -4.892573799038928861, -62.47626111183155473 ) ) ;
#139465 = CARTESIAN_POINT ( 'NONE',  ( 12.14591786802309770, 12.06949235617756955, 79.37390960531436690 ) ) ;
#139466 = CARTESIAN_POINT ( 'NONE',  ( -13.97604488694527625, -13.89961937509977652, 111.8739096053143243 ) ) ;
#139467 = CARTESIAN_POINT ( 'NONE',  ( -17.49999999999999645, 5.499999999999997335, 35.79690382534171533 ) ) ;
#139468 = CARTESIAN_POINT ( 'NONE',  ( 0.05219959533934541429, -16.53943276465976808, 60.00109039468568284 ) ) ;
#139469 = CARTESIAN_POINT ( 'NONE',  ( -15.80617190586745835, -15.72974639402198527, 101.8739096053143811 ) ) ;
#139470 = CARTESIAN_POINT ( 'NONE',  ( -9.564922557961040184, 16.46253265017147172, 57.91775706135233293 ) ) ;
#139471 = CARTESIAN_POINT ( 'NONE',  ( -10.81492255796078084, -18.62759615963271287, 27.08224293864769550 ) ) ;
#139472 = CARTESIAN_POINT ( 'NONE',  ( 5.153800228976335163, 19.02544592524342804, 29.79057627198102409 ) ) ;
#139473 = CARTESIAN_POINT ( 'NONE',  ( 5.719274019375991003, -21.55341960407610458, 72.70724293864769550 ) ) ;
#139474 = CARTESIAN_POINT ( 'NONE',  ( -13.89961937509977652, 13.97604488694528158, 105.6239096053143527 ) ) ;
#139475 = CARTESIAN_POINT ( 'NONE',  ( 15.72974639402176855, 15.80617190586768217, 91.87609039468568994 ) ) ;
#139476 = CARTESIAN_POINT ( 'NONE',  ( -5.049401038298153566, 19.05341960407611168, 55.20724293864769550 ) ) ;
#139477 = CARTESIAN_POINT ( 'NONE',  ( 14.29746914071037800, 8.314922557961029526, 31.66775706135234358 ) ) ;
#139478 = CARTESIAN_POINT ( 'NONE',  ( -5.049401038298153566, 19.05341960407611168, 55.20724293864769550 ) ) ;
#139479 = CARTESIAN_POINT ( 'NONE',  ( -10.72451020669870658, -18.67979575497194134, 74.58442372801901854 ) ) ;
#139480 = EDGE_LOOP ( 'NONE', ( #131835, #176527, #187889, #23584, #103180, #120554, #70384, #11133, #189269, #106205, #61946, #164015 ) ) ;
#139481 = CARTESIAN_POINT ( 'NONE',  ( 9.564922557961047289, -16.46253265017146816, 40.41775706135234003 ) ) ;
#139482 = CARTESIAN_POINT ( 'NONE',  ( -5.049401038297874678, -19.05341960407617918, 44.79275706135232582 ) ) ;
#139483 = CARTESIAN_POINT ( 'NONE',  ( 21.53943276465977519, 0.05219959533937863772, 41.25109039468568284 ) ) ;
#139484 = CARTESIAN_POINT ( 'NONE',  ( 8.898068258721464119, 27.38543819252877398, 143.3843446568999980 ) ) ;
#139485 = CARTESIAN_POINT ( 'NONE',  ( 9.474510206698729675, 16.51473224551082808, 37.08442372801899722 ) ) ;
#139486 = CARTESIAN_POINT ( 'NONE',  ( -5.153800228976328057, -19.02544592524343514, 82.29057627198103830 ) ) ;
#139487 = CARTESIAN_POINT ( 'NONE',  ( -9.474510206698964154, 16.51473224551069663, 75.41557627198103830 ) ) ;
#139488 = CARTESIAN_POINT ( 'NONE',  ( 12.14591786802309770, 12.06949235617756955, 24.37390960531435979 ) ) ;
#139490 = CARTESIAN_POINT ( 'NONE',  ( -18.67979575497193778, 10.72451020669871902, 83.33442372801903275 ) ) ;
#139489 = CARTESIAN_POINT ( 'NONE',  ( -19.05341960407611168, -5.049401038298163336, 111.4572429386476671 ) ) ;
#139491 = CARTESIAN_POINT ( 'NONE',  ( 36.91746825000000598, -11.99521256947793546, -1.724999997268813479 ) ) ;
#139492 = CARTESIAN_POINT ( 'NONE',  ( 17.48847506799968343, 5.747544572773806593, 56.67302562156723411 ) ) ;
#139493 = CARTESIAN_POINT ( 'NONE',  ( -15.80617190586768217, 15.72974639402176855, 98.12609039468570415 ) ) ;
#139494 = CARTESIAN_POINT ( 'NONE',  ( 24.30000000000003268, 0.000000000000000000, -56.77278709839600879 ) ) ;
#139495 = CARTESIAN_POINT ( 'NONE',  ( -5.049401038298153566, 19.05341960407611168, 115.2072429386477097 ) ) ;
#139496 = DIRECTION ( 'NONE',  ( -0.5150380737757255245, 1.049727191973305394E-16, -0.8571673013836856869 ) ) ;
#139497 = CARTESIAN_POINT ( 'NONE',  ( -16.52544592524335698, -4.483927247898792601, 53.95942372801900433 ) ) ;
#139498 = CARTESIAN_POINT ( 'NONE',  ( -21.52544592524343514, 5.823673210054127303, 76.04057627198102409 ) ) ;
#139499 = CARTESIAN_POINT ( 'NONE',  ( -16.53943276465976808, 0.05219959533911058130, 21.24890960531436690 ) ) ;
#139501 = CARTESIAN_POINT ( 'NONE',  ( 19.03943276465977164, -0.05219959533909143690, 88.74890960531436690 ) ) ;
#139500 = CARTESIAN_POINT ( 'NONE',  ( 0.05219959533910956823, 16.53943276465976808, 114.9989096053143669 ) ) ;
#139502 = CARTESIAN_POINT ( 'NONE',  ( -5.153800228976607833, 19.02544592524334988, 22.70942372801899012 ) ) ;
#139503 = CARTESIAN_POINT ( 'NONE',  ( 19.02544592524343514, -5.153800228976328945, 23.54057627198102054 ) ) ;
#139504 = CARTESIAN_POINT ( 'NONE',  ( 18.67979575497194134, -10.72451020669871369, 65.83442372801900433 ) ) ;
#139505 = CARTESIAN_POINT ( 'NONE',  ( 18.46320343559671429, 23.96320343559620625, 8.181980515339455806 ) ) ;
#139506 = CARTESIAN_POINT ( 'NONE',  ( -8.224510206698735004, -14.34966873604973081, 109.5844237280190328 ) ) ;
#139507 = CARTESIAN_POINT ( 'NONE',  ( 19.03943276465977164, 0.05219959533936151252, 66.25109039468567573 ) ) ;
#139508 = CARTESIAN_POINT ( 'NONE',  ( -36.91746825000000598, 2.428612866367529932E-14, -7.124999997268813168 ) ) ;
#139509 = CARTESIAN_POINT ( 'NONE',  ( -19.03943276465977164, 0.05219959533909376836, 106.2489096053143669 ) ) ;
#139510 = CARTESIAN_POINT ( 'NONE',  ( 12.06949235617757843, -12.14591786802309237, 88.12390960531436690 ) ) ;
#139511 = CARTESIAN_POINT ( 'NONE',  ( 16.46253265017146816, 9.564922557961045513, 51.66775706135233293 ) ) ;
#139512 = CARTESIAN_POINT ( 'NONE',  ( 19.03943276465977164, -0.05219959533909143690, 78.74890960531436690 ) ) ;
#139513 = CARTESIAN_POINT ( 'NONE',  ( 12.06949235617757843, -12.14591786802309237, 68.12390960531436690 ) ) ;
#139514 = CARTESIAN_POINT ( 'NONE',  ( -16.51473224551082808, 9.474510206698731452, 88.33442372801900433 ) ) ;
#139515 = CARTESIAN_POINT ( 'NONE',  ( 15.72974639402199770, -15.80617190586745480, 53.12390960531436690 ) ) ;
#139516 = ORIENTED_EDGE ( 'NONE', *, *, #10280, .T. ) ;
#139517 = CARTESIAN_POINT ( 'NONE',  ( 12.14591786802309770, 12.06949235617756955, 109.3739096053143811 ) ) ;
#139518 = CARTESIAN_POINT ( 'NONE',  ( 0.05219959533936267826, -19.03943276465977164, 100.0010903946856757 ) ) ;
#139520 = CARTESIAN_POINT ( 'NONE',  ( -10.72451020669898014, 18.67979575497178502, 70.41557627198102409 ) ) ;
#139519 = CARTESIAN_POINT ( 'NONE',  ( -19.03943276465977164, 0.05219959533909376836, 76.24890960531435269 ) ) ;
#139522 = CARTESIAN_POINT ( 'NONE',  ( -9.564922557960796823, -16.46253265017161027, 72.08224293864770971 ) ) ;
#139521 = CARTESIAN_POINT ( 'NONE',  ( -0.05219959533934338120, 16.53943276465976808, 92.50109039468567573 ) ) ;
#139523 = CARTESIAN_POINT ( 'NONE',  ( 9.474510206698729675, 16.51473224551082808, 67.08442372801900433 ) ) ;
#139524 = CARTESIAN_POINT ( 'NONE',  ( -15.80617190586768217, 15.72974639402176855, 78.12609039468570415 ) ) ;
#139525 = CARTESIAN_POINT ( 'NONE',  ( -0.05219959533907301413, -21.53943276465977519, 67.49890960531436690 ) ) ;
#139526 = CARTESIAN_POINT ( 'NONE',  ( 21.53943276465977519, -0.05219959533907433946, 23.74890960531435269 ) ) ;
#139527 = CARTESIAN_POINT ( 'NONE',  ( -9.564922557960796823, -16.46253265017161027, 32.08224293864769550 ) ) ;
#139528 = CARTESIAN_POINT ( 'NONE',  ( -0.05219959533934338120, 16.53943276465976808, 97.50109039468567573 ) ) ;
#139529 = CARTESIAN_POINT ( 'NONE',  ( -13.89961937509977652, 13.97604488694528158, 45.62390960531433848 ) ) ;
#139530 = CARTESIAN_POINT ( 'NONE',  ( -4.379528057220086978, -16.55341960407618274, 19.79275706135235069 ) ) ;
#139531 = CARTESIAN_POINT ( 'NONE',  ( -31.43434485161624536, -5.140865793513094140, 100.4663950908259409 ) ) ;
#139532 = CARTESIAN_POINT ( 'NONE',  ( 15.72974639402176855, 15.80617190586768217, 111.8760903946856615 ) ) ;
#139533 = CARTESIAN_POINT ( 'NONE',  ( 0.05219959533910956823, 16.53943276465976808, 64.99890960531435269 ) ) ;
#139534 = CARTESIAN_POINT ( 'NONE',  ( 10.81492255796078972, 18.62759615963270932, 99.58224293864770971 ) ) ;
#139535 = CARTESIAN_POINT ( 'NONE',  ( 15.80617190586746368, 15.72974639402197994, 104.3739096053143669 ) ) ;
#139536 = CARTESIAN_POINT ( 'NONE',  ( 16.19135201231366494, -7.376712067591922661, 97.31319145947975358 ) ) ;
#139537 = CARTESIAN_POINT ( 'NONE',  ( -21.55341960407610458, -5.719274019375992779, 51.45724293864770260 ) ) ;
#139538 = CARTESIAN_POINT ( 'NONE',  ( -14.34966873604972548, 8.224510206698743886, 83.33442372801903275 ) ) ;
#139539 = CARTESIAN_POINT ( 'NONE',  ( 16.55341960407611168, 4.379528057220329451, 88.95724293864769550 ) ) ;
#139540 = CARTESIAN_POINT ( 'NONE',  ( 19.03943276465977164, -0.05219959533909143690, 48.74890960531435979 ) ) ;
#139541 = CARTESIAN_POINT ( 'NONE',  ( -29.09442113371788352, -27.25731168736310295, -16.99878707713624948 ) ) ;
#139542 = CARTESIAN_POINT ( 'NONE',  ( -16.55341960407617563, 4.379528057220093196, 103.5427570613523613 ) ) ;
#139543 = CARTESIAN_POINT ( 'NONE',  ( -5.823673210054431948, 21.52544592524334988, 27.70942372801901854 ) ) ;
#139544 = CARTESIAN_POINT ( 'NONE',  ( 16.46253265017160672, -9.564922557960803928, 98.33224293864769550 ) ) ;
#139545 = CARTESIAN_POINT ( 'NONE',  ( -21.52544592524334988, -5.823673210054445271, 68.95942372801901854 ) ) ;
#139546 = CYLINDRICAL_SURFACE ( 'NONE', #169699, 214.0437394197456911 ) ;
#139548 = EDGE_CURVE ( 'NONE', #97924, #142920, #75703, .T. ) ;
#139547 = CARTESIAN_POINT ( 'NONE',  ( 16.51473224551069308, 9.474510206698969483, 29.16557627198103475 ) ) ;
#139549 = ORIENTED_EDGE ( 'NONE', *, *, #102120, .F. ) ;
#139550 = CARTESIAN_POINT ( 'NONE',  ( -0.05219959533937732626, 21.53943276465977519, 57.50109039468568994 ) ) ;
#139552 = CARTESIAN_POINT ( 'NONE',  ( 0.05219959533909260263, 19.03943276465977164, 24.99890960531435269 ) ) ;
#139551 = CARTESIAN_POINT ( 'NONE',  ( -5.049401038298153566, 19.05341960407611168, 45.20724293864769550 ) ) ;
#139553 = CARTESIAN_POINT ( 'NONE',  ( 5.153800228976335163, 19.02544592524342804, 89.79057627198102409 ) ) ;
#139554 = CARTESIAN_POINT ( 'NONE',  ( 5.153800228976615827, -19.02544592524334988, 70.20942372801899012 ) ) ;
#139555 = CARTESIAN_POINT ( 'NONE',  ( 5.823673210054444382, -21.52544592524334988, 40.20942372801901854 ) ) ;
#139556 = CARTESIAN_POINT ( 'NONE',  ( -0.05219959533936034679, 19.03943276465977164, 107.5010903946856615 ) ) ;
#139557 = CARTESIAN_POINT ( 'NONE',  ( 13.97604488694548053, -13.89961937509957401, 75.62609039468564731 ) ) ;
#139558 = CARTESIAN_POINT ( 'NONE',  ( -9.564922557960796823, -16.46253265017161027, 32.08224293864769550 ) ) ;
#139559 = CARTESIAN_POINT ( 'NONE',  ( -8.314922557961024197, 14.29746914071037800, 102.9177570613523756 ) ) ;
#139560 = CARTESIAN_POINT ( 'NONE',  ( 5.153800228976615827, -19.02544592524334988, 75.20942372801896170 ) ) ;
#139561 = CARTESIAN_POINT ( 'NONE',  ( -16.53943276465976808, 0.05219959533911058130, 21.24890960531436690 ) ) ;
#139562 = CARTESIAN_POINT ( 'NONE',  ( 16.46253265017146816, 9.564922557961045513, 56.66775706135233293 ) ) ;
#139563 = CARTESIAN_POINT ( 'NONE',  ( 15.72974639402176855, 15.80617190586768217, 106.8760903946856899 ) ) ;
#139564 = CARTESIAN_POINT ( 'NONE',  ( 19.05341960407617918, -5.049401038297876454, 31.04275706135232227 ) ) ;
#139565 = CARTESIAN_POINT ( 'NONE',  ( -13.97604488694527625, -13.89961937509977652, 31.87390960531435979 ) ) ;
#139566 = CARTESIAN_POINT ( 'NONE',  ( 10.81492255796106328, -18.62759615963255655, 95.41775706135234714 ) ) ;
#139567 = CARTESIAN_POINT ( 'NONE',  ( 8.224510206698742110, 14.34966873604972548, 27.08442372801901854 ) ) ;
#139568 = CARTESIAN_POINT ( 'NONE',  ( -16.46253265017160317, 9.564922557960807481, 90.83224293864769550 ) ) ;
#139569 = CARTESIAN_POINT ( 'NONE',  ( -8.571926809382601320, -26.38167802310801591, 141.2750000027311899 ) ) ;
#139570 = CARTESIAN_POINT ( 'NONE',  ( 5.153800228976335163, 19.02544592524342804, 74.79057627198103830 ) ) ;
#139571 = CARTESIAN_POINT ( 'NONE',  ( 17.50000000000001066, -3.242565516153302241, 102.5000000000090807 ) ) ;
#139572 = CARTESIAN_POINT ( 'NONE',  ( -9.474510206698720793, -16.51473224551083518, 89.58442372801900433 ) ) ;
#139573 = CARTESIAN_POINT ( 'NONE',  ( -16.51473224551069308, -9.474510206698971260, 111.6655762719810383 ) ) ;
#139574 = CARTESIAN_POINT ( 'NONE',  ( 9.564922557961047289, -16.46253265017146816, 20.41775706135233293 ) ) ;
#139575 = CARTESIAN_POINT ( 'NONE',  ( -12.14591786802309592, -12.06949235617757132, 91.87390960531436690 ) ) ;
#139576 = CARTESIAN_POINT ( 'NONE',  ( 22.78714015946003002, -11.73760554535578748, 167.9671921004704700 ) ) ;
#139577 = CARTESIAN_POINT ( 'NONE',  ( -21.52544592524343514, 5.823673210054127303, 61.04057627198103120 ) ) ;
#139578 = CARTESIAN_POINT ( 'NONE',  ( -0.05219959533907301413, -21.53943276465977519, 32.49890960531435979 ) ) ;
#139579 = CARTESIAN_POINT ( 'NONE',  ( 16.51473224551069308, 9.474510206698969483, 29.16557627198103475 ) ) ;
#139580 = CARTESIAN_POINT ( 'NONE',  ( -3.573655867282028392E-15, 2.428612866367529932E-14, -25.00000000000000000 ) ) ;
#139581 = CARTESIAN_POINT ( 'NONE',  ( -5.049401038297874678, -19.05341960407617918, 59.79275706135231871 ) ) ;
#139582 = CARTESIAN_POINT ( 'NONE',  ( -4.483927247898539470, -16.52544592524342804, 42.29057627198103120 ) ) ;
#139583 = CARTESIAN_POINT ( 'NONE',  ( -5.153800228976328057, -19.02544592524343514, 112.2905762719810099 ) ) ;
#139584 = CARTESIAN_POINT ( 'NONE',  ( -5.719274019375665041, -21.55341960407619695, 74.79275706135234714 ) ) ;
#139585 = CARTESIAN_POINT ( 'NONE',  ( -10.81492255796078084, -18.62759615963271287, 77.08224293864769550 ) ) ;
#139586 = CARTESIAN_POINT ( 'NONE',  ( -18.62759615963255300, -10.81492255796106328, 59.16775706135234714 ) ) ;
#139587 = CARTESIAN_POINT ( 'NONE',  ( 10.72451020669898902, -18.67979575497178502, 97.91557627198103830 ) ) ;
#139588 = CARTESIAN_POINT ( 'NONE',  ( 0.05219959533937995610, -21.53943276465977519, 55.00109039468568284 ) ) ;
#139589 = CARTESIAN_POINT ( 'NONE',  ( -9.564922557960796823, -16.46253265017161027, 77.08224293864769550 ) ) ;
#139590 = CARTESIAN_POINT ( 'NONE',  ( 8.314922557961029526, -14.29746914071037800, 85.41775706135236135 ) ) ;
#139591 = CARTESIAN_POINT ( 'NONE',  ( -5.153800228976328057, -19.02544592524343514, 22.29057627198102765 ) ) ;
#139592 = CARTESIAN_POINT ( 'NONE',  ( -31.76179951907201371, 6.484602924383671585, 91.22381659560100786 ) ) ;
#139593 = CARTESIAN_POINT ( 'NONE',  ( -4.379528057220328563, 16.55341960407611168, 60.20724293864768839 ) ) ;
#139594 = CARTESIAN_POINT ( 'NONE',  ( -4.483927247898539470, -16.52544592524342804, 22.29057627198102765 ) ) ;
#139595 = CARTESIAN_POINT ( 'NONE',  ( 19.02544592524343514, -5.153800228976328945, 68.54057627198103830 ) ) ;
#139596 = CARTESIAN_POINT ( 'NONE',  ( -19.05341960407611168, -5.049401038298163336, 31.45724293864769550 ) ) ;
#139597 = CARTESIAN_POINT ( 'NONE',  ( 21.53943276465977519, -0.05219959533907433946, 43.74890960531435979 ) ) ;
#139598 = CARTESIAN_POINT ( 'NONE',  ( 5.153800228976615827, -19.02544592524334988, 40.20942372801898301 ) ) ;
#139600 = CARTESIAN_POINT ( 'NONE',  ( -14.34966873604960291, -8.224510206698953496, 51.66557627198102409 ) ) ;
#139599 = CARTESIAN_POINT ( 'NONE',  ( -18.22780087662123094, -5.499999999999984901, 86.48459894673892734 ) ) ;
#139601 = CARTESIAN_POINT ( 'NONE',  ( -5.823673210054116645, -21.52544592524344225, 32.29057627198102409 ) ) ;
#139602 = CARTESIAN_POINT ( 'NONE',  ( -3.573655867282028392E-15, 2.428612866367529932E-14, 155.0000000000000000 ) ) ;
#139603 = CARTESIAN_POINT ( 'NONE',  ( -8.314922557961024197, 14.29746914071037800, 77.91775706135231871 ) ) ;
#139604 = CARTESIAN_POINT ( 'NONE',  ( 9.474510206698729675, 16.51473224551082808, 57.08442372801900433 ) ) ;
#139605 = CARTESIAN_POINT ( 'NONE',  ( 12.06949235617757843, -12.14591786802309237, 38.12390960531436690 ) ) ;
#139606 = CARTESIAN_POINT ( 'NONE',  ( -19.25918095147780562, -5.499999999999489297, 74.45284276293934056 ) ) ;
#139607 = CARTESIAN_POINT ( 'NONE',  ( 8.224510206698953496, -14.34966873604960469, 22.91557627198102765 ) ) ;
#139608 = CARTESIAN_POINT ( 'NONE',  ( 5.153800228976335163, 19.02544592524342804, 44.79057627198103830 ) ) ;
#139609 = CARTESIAN_POINT ( 'NONE',  ( -13.89961937509977652, 13.97604488694528158, 65.62390960531436690 ) ) ;
#139610 = CARTESIAN_POINT ( 'NONE',  ( 19.02544592524343514, -5.153800228976328945, 23.54057627198102054 ) ) ;
#139611 = CARTESIAN_POINT ( 'NONE',  ( 15.72974639402176855, 15.80617190586768217, 26.87609039468567218 ) ) ;
#139612 = CARTESIAN_POINT ( 'NONE',  ( 13.97604488694527802, 13.89961937509977652, 64.37390960531436690 ) ) ;
#139613 = FACE_OUTER_BOUND ( 'NONE', #154876, .T. ) ;
#139614 = CARTESIAN_POINT ( 'NONE',  ( -19.03943276465977164, 0.05219959533909376836, 41.24890960531435269 ) ) ;
#139615 = CARTESIAN_POINT ( 'NONE',  ( -21.52544592524343514, 5.823673210054127303, 31.04057627198102409 ) ) ;
#139617 = CARTESIAN_POINT ( 'NONE',  ( -14.29746914071049879, 8.314922557960819915, 115.8322429386477097 ) ) ;
#139616 = CARTESIAN_POINT ( 'NONE',  ( -21.52544592524334988, -5.823673210054445271, 58.95942372801902565 ) ) ;
#139618 = CARTESIAN_POINT ( 'NONE',  ( 21.53943276465977519, -0.05219959533907433946, 33.74890960531436690 ) ) ;
#139619 = CARTESIAN_POINT ( 'NONE',  ( -0.05219959533934338120, 16.53943276465976808, 87.50109039468568994 ) ) ;
#139620 = CARTESIAN_POINT ( 'NONE',  ( 5.823673210054444382, -21.52544592524334988, 110.2094237280190185 ) ) ;
#139621 = CARTESIAN_POINT ( 'NONE',  ( 16.53943276465976808, 0.05219959533934440121, 66.25109039468567573 ) ) ;
#139622 = CARTESIAN_POINT ( 'NONE',  ( -16.46253265017160317, 9.564922557960807481, 110.8322429386476955 ) ) ;
#139623 = CARTESIAN_POINT ( 'NONE',  ( -0.05219959533934338120, 16.53943276465976808, 52.50109039468567573 ) ) ;
#139624 = CARTESIAN_POINT ( 'NONE',  ( 16.55341960407618274, -4.379528057220086978, 41.04275706135236135 ) ) ;
#139625 = CARTESIAN_POINT ( 'NONE',  ( 12.14591786802327356, -12.06949235617739191, 90.62609039468567573 ) ) ;
#139626 = CARTESIAN_POINT ( 'NONE',  ( 0.05219959533937995610, -21.53943276465977519, 50.00109039468568994 ) ) ;
#139627 = CARTESIAN_POINT ( 'NONE',  ( -16.51473224551082808, 9.474510206698731452, 113.3344237280190043 ) ) ;
#139628 = CARTESIAN_POINT ( 'NONE',  ( -5.719274019375978568, 21.55341960407610458, 105.2072429386477097 ) ) ;
#139629 = CARTESIAN_POINT ( 'NONE',  ( 12.14591786802327356, -12.06949235617739191, 20.62609039468568639 ) ) ;
#139630 = CARTESIAN_POINT ( 'NONE',  ( 14.34966873604972726, -8.224510206698740333, 90.83442372801901854 ) ) ;
#139631 = CARTESIAN_POINT ( 'NONE',  ( -38.00000000000000711, 12.34694845685046438, -3.849999994537626424 ) ) ;
#139632 = CARTESIAN_POINT ( 'NONE',  ( 18.67979575497194134, -10.72451020669871369, 90.83442372801901854 ) ) ;
#139633 = CARTESIAN_POINT ( 'NONE',  ( -19.03943276465977164, -0.05219959533935918106, 88.75109039468567573 ) ) ;
#139634 = CARTESIAN_POINT ( 'NONE',  ( 14.29746914071049879, -8.314922557960816363, 63.33224293864770260 ) ) ;
#139635 = CARTESIAN_POINT ( 'NONE',  ( -0.05219959533910754901, -16.53943276465976808, 37.49890960531436690 ) ) ;
#139636 = CARTESIAN_POINT ( 'NONE',  ( 16.52544592524342804, -4.483927247898539470, 113.5405762719810383 ) ) ;
#139638 = SURFACE_STYLE_USAGE ( .BOTH. , #77971 ) ;
#139637 = CARTESIAN_POINT ( 'NONE',  ( 13.97604488694548053, -13.89961937509957401, 50.62609039468566152 ) ) ;
#139639 = CARTESIAN_POINT ( 'NONE',  ( -21.52544592524334988, -5.823673210054445271, 48.95942372801902565 ) ) ;
#139640 = CARTESIAN_POINT ( 'NONE',  ( 9.474510206698729675, 16.51473224551082808, 107.0844237280190043 ) ) ;
#139641 = DIRECTION ( 'NONE',  ( 0.000000000000000000, 0.000000000000000000, 1.000000000000000000 ) ) ;
#139642 = CARTESIAN_POINT ( 'NONE',  ( -13.97604488694527625, -13.89961937509977652, 106.8739096053143669 ) ) ;
#139643 = CARTESIAN_POINT ( 'NONE',  ( 10.81492255796078972, 18.62759615963270932, 69.58224293864769550 ) ) ;
#139644 = CARTESIAN_POINT ( 'NONE',  ( -0.05219959533936034679, 19.03943276465977164, 92.50109039468566152 ) ) ;
#139645 = CARTESIAN_POINT ( 'NONE',  ( -19.05341960407611168, -5.049401038298163336, 86.45724293864769550 ) ) ;
#139646 = CARTESIAN_POINT ( 'NONE',  ( -15.72974639402197994, 15.80617190586746368, 60.62390960531437401 ) ) ;
#139647 = CARTESIAN_POINT ( 'NONE',  ( -16.55341960407611168, -4.379528057220339221, 101.4572429386476955 ) ) ;
#139648 = CARTESIAN_POINT ( 'NONE',  ( -5.153800228976328057, -19.02544592524343514, 67.29057627198102409 ) ) ;
#139649 = CARTESIAN_POINT ( 'NONE',  ( -16.51473224551069308, -9.474510206698971260, 31.66557627198102054 ) ) ;
#139650 = CARTESIAN_POINT ( 'NONE',  ( -15.80617190586768217, 15.72974639402176855, 43.12609039468568284 ) ) ;
#139651 = CARTESIAN_POINT ( 'NONE',  ( -21.52544592524334988, -5.823673210054445271, 83.95942372801900433 ) ) ;
#139652 = CARTESIAN_POINT ( 'NONE',  ( 16.55341960407618274, -4.379528057220086978, 96.04275706135236135 ) ) ;
#139653 = CARTESIAN_POINT ( 'NONE',  ( 5.823673210054444382, -21.52544592524334988, 35.20942372801901854 ) ) ;
#139654 = CARTESIAN_POINT ( 'NONE',  ( 10.72451020669871369, 18.67979575497193778, 42.08442372801901854 ) ) ;
#139656 = CARTESIAN_POINT ( 'NONE',  ( 19.02544592524343514, -5.153800228976328945, 78.54057627198099567 ) ) ;
#139655 = CARTESIAN_POINT ( 'NONE',  ( -19.03943276465977164, -0.05219959533935918106, 63.75109039468566863 ) ) ;
#139657 = CARTESIAN_POINT ( 'NONE',  ( -21.52544592524334988, -5.823673210054445271, 83.95942372801900433 ) ) ;
#139658 = CARTESIAN_POINT ( 'NONE',  ( 10.81492255796078972, 18.62759615963270932, 84.58224293864769550 ) ) ;
#139659 = CARTESIAN_POINT ( 'NONE',  ( 0.05219959533910956823, 16.53943276465976808, 69.99890960531435269 ) ) ;
#139660 = CARTESIAN_POINT ( 'NONE',  ( 21.55341960407619695, -5.719274019375665929, 106.0427570613523471 ) ) ;
#139661 = CARTESIAN_POINT ( 'NONE',  ( -12.06949235617756955, 12.14591786802309770, 90.62390960531436690 ) ) ;
#139662 = CARTESIAN_POINT ( 'NONE',  ( 19.02544592524343514, -5.153800228976328945, 33.54057627198102409 ) ) ;
#139663 = CARTESIAN_POINT ( 'NONE',  ( -19.03943276465977164, -0.05219959533935918106, 68.75109039468566152 ) ) ;
#139664 = CARTESIAN_POINT ( 'NONE',  ( -14.34966873604960291, -8.224510206698953496, 36.66557627198103120 ) ) ;
#139665 = CARTESIAN_POINT ( 'NONE',  ( 15.80617190586769283, -15.72974639402175789, 100.6260903946857184 ) ) ;
#139666 = CARTESIAN_POINT ( 'NONE',  ( -9.474510206698964154, 16.51473224551069663, 90.41557627198103830 ) ) ;
#139667 = CARTESIAN_POINT ( 'NONE',  ( 13.97604488694548053, -13.89961937509957401, 65.62609039468567573 ) ) ;
#139668 = CARTESIAN_POINT ( 'NONE',  ( -15.80617190586745835, -15.72974639402198527, 61.87390960531436690 ) ) ;
#139669 = CARTESIAN_POINT ( 'NONE',  ( 15.80617190586769283, -15.72974639402175789, 20.62609039468568639 ) ) ;
#139670 = CARTESIAN_POINT ( 'NONE',  ( 19.03943276465977164, 0.05219959533936151252, 106.2510903946856615 ) ) ;
#139671 = CARTESIAN_POINT ( 'NONE',  ( -16.53943276465976808, -0.05219959533934237506, 78.75109039468568994 ) ) ;
#139673 = CARTESIAN_POINT ( 'NONE',  ( 18.62759615963255655, 10.81492255796105972, 26.66775706135235424 ) ) ;
#139672 = CARTESIAN_POINT ( 'NONE',  ( 16.88567814943165146, 6.947325034625595030, 63.79001122652589117 ) ) ;
#139674 = CARTESIAN_POINT ( 'NONE',  ( -4.483927247898539470, -16.52544592524342804, 102.2905762719810383 ) ) ;
#139675 = CARTESIAN_POINT ( 'NONE',  ( 36.91746824999999177, 2.880721459617395097E-14, -6.124999997268813168 ) ) ;
#139676 = CARTESIAN_POINT ( 'NONE',  ( -16.55341960407617563, 4.379528057220093196, 43.54275706135235424 ) ) ;
#139677 = ADVANCED_FACE ( 'NONE', ( #178534 ), #128198, .T. ) ;
#139678 = CARTESIAN_POINT ( 'NONE',  ( 0.05219959533907565091, 21.53943276465977519, 64.99890960531435269 ) ) ;
#139679 = CARTESIAN_POINT ( 'NONE',  ( -16.52544592524335698, -4.483927247898792601, 98.95942372801903275 ) ) ;
#139680 = CARTESIAN_POINT ( 'NONE',  ( -16.53943276465976808, -0.05219959533934237506, 38.75109039468567573 ) ) ;
#139681 = CARTESIAN_POINT ( 'NONE',  ( 19.02544592524343514, -5.153800228976328945, 48.54057627198103120 ) ) ;
#139682 = CARTESIAN_POINT ( 'NONE',  ( -4.483927247898782831, 16.52544592524335698, 82.70942372801900433 ) ) ;
#139683 = CARTESIAN_POINT ( 'NONE',  ( -13.97604488694547697, 13.89961937509957934, 78.12609039468567573 ) ) ;
#139684 = EDGE_CURVE ( 'NONE', #46374, #189055, #54417, .T. ) ;
#139685 = CARTESIAN_POINT ( 'NONE',  ( -21.53943276465977519, 0.05219959533907696930, 66.24890960531436690 ) ) ;
#139686 = CARTESIAN_POINT ( 'NONE',  ( 14.29746914071037800, 8.314922557961029526, 91.66775706135234714 ) ) ;
#139687 = CARTESIAN_POINT ( 'NONE',  ( -21.55341960407619339, 5.719274019375674811, 83.54275706135234714 ) ) ;
#139688 = CARTESIAN_POINT ( 'NONE',  ( 0.05219959533907565091, 21.53943276465977519, 69.99890960531435269 ) ) ;
#139689 = CARTESIAN_POINT ( 'NONE',  ( 21.53943276465977519, -0.05219959533907433946, 53.74890960531437401 ) ) ;
#139690 = ORIENTED_EDGE ( 'NONE', *, *, #158172, .T. ) ;
#139691 = CARTESIAN_POINT ( 'NONE',  ( 14.29746914071037800, 8.314922557961029526, 76.66775706135234714 ) ) ;
#139692 = CARTESIAN_POINT ( 'NONE',  ( 0.05219959533907565091, 21.53943276465977519, 44.99890960531435979 ) ) ;
#139693 = VERTEX_POINT ( 'NONE', #121237 ) ;
#139694 = CARTESIAN_POINT ( 'NONE',  ( -5.049401038298153566, 19.05341960407611168, 110.2072429386476671 ) ) ;
#139695 = CARTESIAN_POINT ( 'NONE',  ( -18.46320343559621691, 23.96320343559658994, 1.818019484660534424 ) ) ;
#139696 = CARTESIAN_POINT ( 'NONE',  ( 9.474510206698971260, -16.51473224551069308, 22.91557627198102765 ) ) ;
#139697 = CARTESIAN_POINT ( 'NONE',  ( -10.81492255796078084, -18.62759615963271287, 72.08224293864769550 ) ) ;
#139698 = CARTESIAN_POINT ( 'NONE',  ( -14.29746914071037622, -8.314922557961029526, 99.16775706135234714 ) ) ;
#139699 = CARTESIAN_POINT ( 'NONE',  ( 15.72974639402176855, 15.80617190586768217, 51.87609039468568284 ) ) ;
#139700 = CARTESIAN_POINT ( 'NONE',  ( 19.05341960407617918, -5.049401038297876454, 106.0427570613523471 ) ) ;
#139701 = CARTESIAN_POINT ( 'NONE',  ( 14.29746914071049879, -8.314922557960816363, 113.3322429386476955 ) ) ;
#139702 = CARTESIAN_POINT ( 'NONE',  ( 5.153800228976615827, -19.02544592524334988, 105.2094237280190185 ) ) ;
#139703 = CARTESIAN_POINT ( 'NONE',  ( -19.02544592524342804, 5.153800228976336051, 46.04057627198101699 ) ) ;
#139704 = CARTESIAN_POINT ( 'NONE',  ( -28.82186960331499392, -9.364793116373526516, 144.0999999999999659 ) ) ;
#139705 = CARTESIAN_POINT ( 'NONE',  ( -16.51473224551069308, -9.474510206698971260, 96.66557627198102409 ) ) ;
#139706 = CARTESIAN_POINT ( 'NONE',  ( 12.14591786802327356, -12.06949235617739191, 80.62609039468567573 ) ) ;
#139707 = CARTESIAN_POINT ( 'NONE',  ( 19.05341960407617918, -5.049401038297876454, 76.04275706135230450 ) ) ;
#139708 = CARTESIAN_POINT ( 'NONE',  ( 13.97604488694548053, -13.89961937509957401, 20.62609039468567573 ) ) ;
#139709 = CARTESIAN_POINT ( 'NONE',  ( 21.55341960407610458, 5.719274019375980345, 63.95724293864770260 ) ) ;
#139710 = CARTESIAN_POINT ( 'NONE',  ( 4.379528057220092307, 16.55341960407617563, 82.29275706135234714 ) ) ;
#139711 = CARTESIAN_POINT ( 'NONE',  ( 16.46253265017146816, 9.564922557961045513, 81.66775706135233293 ) ) ;
#139712 = CARTESIAN_POINT ( 'NONE',  ( 16.46253265017160672, -9.564922557960803928, 33.33224293864770260 ) ) ;
#139713 = CARTESIAN_POINT ( 'NONE',  ( -5.049401038298153566, 19.05341960407611168, 90.20724293864766707 ) ) ;
#139714 = CARTESIAN_POINT ( 'NONE',  ( 5.823673210054444382, -21.52544592524334988, 45.20942372801901854 ) ) ;
#139715 = CARTESIAN_POINT ( 'NONE',  ( 16.51473224551069308, 9.474510206698969483, 49.16557627198102409 ) ) ;
#139716 = CARTESIAN_POINT ( 'NONE',  ( 26.26139018963107219, -3.005588016160671838, 174.9127113745526287 ) ) ;
#139717 = CARTESIAN_POINT ( 'NONE',  ( 19.03943276465977164, -0.05219959533909143690, 113.7489096053143669 ) ) ;
#139718 = CARTESIAN_POINT ( 'NONE',  ( 12.06949235617757843, -12.14591786802309237, 58.12390960531435979 ) ) ;
#139719 = CARTESIAN_POINT ( 'NONE',  ( 0.05219959533907565091, 21.53943276465977519, 59.99890960531436690 ) ) ;
#139720 = DIRECTION ( 'NONE',  ( 0.000000000000000000, 1.000000000000000000, 0.000000000000000000 ) ) ;
#139721 = CARTESIAN_POINT ( 'NONE',  ( -5.153800228976607833, 19.02544592524334988, 47.70942372801900433 ) ) ;
#139723 = CARTESIAN_POINT ( 'NONE',  ( 9.474510206698971260, -16.51473224551069308, 77.91557627198103830 ) ) ;
#139722 = CARTESIAN_POINT ( 'NONE',  ( 13.97604488694527802, 13.89961937509977652, 59.37390960531434558 ) ) ;
#139724 = CARTESIAN_POINT ( 'NONE',  ( 12.14591786802327356, -12.06949235617739191, 55.62609039468568284 ) ) ;
#139725 = CARTESIAN_POINT ( 'NONE',  ( -17.81289503416611808, 24.51734667627700404, 143.6999999999999886 ) ) ;
#139726 = CARTESIAN_POINT ( 'NONE',  ( 28.82186960331498327, 2.781578969918950771E-14, 145.2500000054623683 ) ) ;
#139727 = CARTESIAN_POINT ( 'NONE',  ( -8.314922557961024197, 14.29746914071037800, 87.91775706135234714 ) ) ;
#139728 = CARTESIAN_POINT ( 'NONE',  ( -4.072063699643443613, -4.622657777628663922, -64.52289142388788434 ) ) ;
#139729 = CARTESIAN_POINT ( 'NONE',  ( 16.52544592524335698, 4.483927247898782831, 76.45942372801901854 ) ) ;
#139730 = CARTESIAN_POINT ( 'NONE',  ( 14.34966873604972726, -8.224510206698740333, 50.83442372801901143 ) ) ;
#139731 = CARTESIAN_POINT ( 'NONE',  ( 13.89961937509957401, 13.97604488694547697, 26.87609039468566507 ) ) ;
#139733 = DIRECTION ( 'NONE',  ( -1.000000000000000000, 0.000000000000000000, -0.000000000000000000 ) ) ;
#139732 = CARTESIAN_POINT ( 'NONE',  ( 19.02544592524343514, -5.153800228976328945, 58.54057627198102409 ) ) ;
#139734 = CARTESIAN_POINT ( 'NONE',  ( 10.72451020669871369, 18.67979575497193778, 52.08442372801901854 ) ) ;
#139735 = CARTESIAN_POINT ( 'NONE',  ( -0.05219959533936034679, 19.03943276465977164, 67.50109039468566152 ) ) ;
#139736 = CARTESIAN_POINT ( 'NONE',  ( 5.719274019375673035, 21.55341960407619339, 112.2927570613523471 ) ) ;
#139737 = CARTESIAN_POINT ( 'NONE',  ( 16.51473224551069308, 9.474510206698969483, 24.16557627198102765 ) ) ;
#139738 = CARTESIAN_POINT ( 'NONE',  ( -17.60164288208769889, 16.44579809102482670, -56.93377352129066082 ) ) ;
#139739 = CARTESIAN_POINT ( 'NONE',  ( -10.81492255796078084, -18.62759615963271287, 67.08224293864770971 ) ) ;
#139740 = CARTESIAN_POINT ( 'NONE',  ( -10.81492255796078084, -18.62759615963271287, 22.08224293864769194 ) ) ;
#139741 = CARTESIAN_POINT ( 'NONE',  ( 4.483927247898545687, 16.52544592524342804, 114.7905762719810383 ) ) ;
#139742 = CARTESIAN_POINT ( 'NONE',  ( -14.34966873604972548, 8.224510206698743886, 38.33442372801900433 ) ) ;
#139743 = EDGE_CURVE ( 'NONE', #149545, #45716, #140212, .T. ) ;
#139744 = CARTESIAN_POINT ( 'NONE',  ( -14.34966873604960291, -8.224510206698953496, 36.66557627198103120 ) ) ;
#139745 = ORIENTED_EDGE ( 'NONE', *, *, #166522, .T. ) ;
#139746 = CARTESIAN_POINT ( 'NONE',  ( 10.81492255796078972, 18.62759615963270932, 114.5822429386477097 ) ) ;
#139747 = AXIS2_PLACEMENT_3D ( 'NONE', #185124, #152791, #91103 ) ;
#139749 = CARTESIAN_POINT ( 'NONE',  ( -19.03943276465977164, 0.05219959533909376836, 116.2489096053143669 ) ) ;
#139748 = CARTESIAN_POINT ( 'NONE',  ( 16.55341960407611168, 4.379528057220329451, 43.95724293864769550 ) ) ;
#139750 = CARTESIAN_POINT ( 'NONE',  ( -9.474510206698720793, -16.51473224551083518, 109.5844237280190043 ) ) ;
#139751 = CARTESIAN_POINT ( 'NONE',  ( 9.564922557961047289, -16.46253265017146816, 20.41775706135233293 ) ) ;
#139752 = CARTESIAN_POINT ( 'NONE',  ( -0.05219959533910754901, -16.53943276465976808, 27.49890960531435269 ) ) ;
#139753 = CARTESIAN_POINT ( 'NONE',  ( -15.80617190586745835, -15.72974639402198527, 96.87390960531436690 ) ) ;
#139755 = CARTESIAN_POINT ( 'NONE',  ( -5.719274019375978568, 21.55341960407610458, 60.20724293864768839 ) ) ;
#139754 = CARTESIAN_POINT ( 'NONE',  ( 17.05587630539785593, 6.762274262135710146, 31.75819690962688924 ) ) ;
#139756 = CARTESIAN_POINT ( 'NONE',  ( -13.89961937509977652, 13.97604488694528158, 80.62390960531436690 ) ) ;
#139757 = CARTESIAN_POINT ( 'NONE',  ( 12.14591786802309770, 12.06949235617756955, 54.37390960531435979 ) ) ;
#139758 = CARTESIAN_POINT ( 'NONE',  ( 0.05219959533909260263, 19.03943276465977164, 84.99890960531436690 ) ) ;
#139759 = EDGE_CURVE ( 'NONE', #178146, #85226, #105089, .T. ) ;
#139760 = LINE ( 'NONE', #61926, #160386 ) ;
#139761 = CARTESIAN_POINT ( 'NONE',  ( 16.51473224551083163, -9.474510206698727899, 50.83442372801899722 ) ) ;
#139762 = CARTESIAN_POINT ( 'NONE',  ( 0.05219959533907565091, 21.53943276465977519, 94.99890960531436690 ) ) ;
#139763 = CARTESIAN_POINT ( 'NONE',  ( 16.52544592524342804, -4.483927247898539470, 98.54057627198105251 ) ) ;
#139764 = CARTESIAN_POINT ( 'NONE',  ( 21.52544592524334988, 5.823673210054432836, 56.45942372801902565 ) ) ;
#139765 = CARTESIAN_POINT ( 'NONE',  ( -17.14385361876520264, -23.59649016807271593, 143.1750000027311671 ) ) ;
#139766 = CARTESIAN_POINT ( 'NONE',  ( 8.314922557960818139, 14.29746914071049879, 29.58224293864769905 ) ) ;
#139767 = CARTESIAN_POINT ( 'NONE',  ( -16.46253265017160317, 9.564922557960807481, 35.83224293864768839 ) ) ;
#139768 = CARTESIAN_POINT ( 'NONE',  ( -0.05219959533909027116, -19.03943276465977164, 97.49890960531436690 ) ) ;
#139769 = CARTESIAN_POINT ( 'NONE',  ( -15.72974639402197994, 15.80617190586746368, 60.62390960531437401 ) ) ;
#139770 = CARTESIAN_POINT ( 'NONE',  ( -18.39443945427639449, 5.500000000000030198, 43.51745347608652281 ) ) ;
#139771 = CARTESIAN_POINT ( 'NONE',  ( 5.049401038298161559, -19.05341960407611168, 32.70724293864768129 ) ) ;
#139772 = CARTESIAN_POINT ( 'NONE',  ( -10.81492255796078084, -18.62759615963271287, 47.08224293864770260 ) ) ;
#139773 = CARTESIAN_POINT ( 'NONE',  ( -15.72974639402176322, -15.80617190586768395, 79.37609039468567573 ) ) ;
#139775 = CARTESIAN_POINT ( 'NONE',  ( 8.314922557961029526, -14.29746914071037800, 70.41775706135236135 ) ) ;
#139774 = CARTESIAN_POINT ( 'NONE',  ( 14.93382465614801902, -34.77343615282724443, -28.53315611748132241 ) ) ;
#139776 = CARTESIAN_POINT ( 'NONE',  ( 5.153800228976335163, 19.02544592524342804, 59.79057627198100988 ) ) ;
#139777 = CARTESIAN_POINT ( 'NONE',  ( 5.153800228976335163, 19.02544592524342804, 59.79057627198100988 ) ) ;
#139778 = VERTEX_POINT ( 'NONE', #164780 ) ;
#139779 = CARTESIAN_POINT ( 'NONE',  ( 16.46253265017146816, 9.564922557961045513, 26.66775706135234003 ) ) ;
#139780 = CARTESIAN_POINT ( 'NONE',  ( 12.06949235617739724, 12.14591786802326823, 76.87609039468567573 ) ) ;
#139781 = CARTESIAN_POINT ( 'NONE',  ( -18.62759615963255300, -10.81492255796106328, 94.16775706135237556 ) ) ;
#139782 = CARTESIAN_POINT ( 'NONE',  ( 13.97604488694527802, 13.89961937509977652, 74.37390960531436690 ) ) ;
#139783 = CARTESIAN_POINT ( 'NONE',  ( 15.80617190586746368, 15.72974639402197994, 39.37390960531436690 ) ) ;
#139784 = CARTESIAN_POINT ( 'NONE',  ( -9.474510206698720793, -16.51473224551083518, 109.5844237280190043 ) ) ;
#139785 = CARTESIAN_POINT ( 'NONE',  ( -5.823673210054431948, 21.52544592524334988, 77.70942372801900433 ) ) ;
#139786 = CARTESIAN_POINT ( 'NONE',  ( -12.06949235617739369, -12.14591786802326823, 49.37609039468569705 ) ) ;
#139787 = CARTESIAN_POINT ( 'NONE',  ( 10.81492255796078972, 18.62759615963270932, 94.58224293864769550 ) ) ;
#139788 = CARTESIAN_POINT ( 'NONE',  ( -4.379528057220086978, -16.55341960407618274, 19.79275706135235069 ) ) ;
#139789 = CARTESIAN_POINT ( 'NONE',  ( -5.153800228976328057, -19.02544592524343514, 82.29057627198103830 ) ) ;
#139790 = CARTESIAN_POINT ( 'NONE',  ( -16.53943276465976808, -0.05219959533934237506, 23.75109039468567929 ) ) ;
#139791 = CARTESIAN_POINT ( 'NONE',  ( -16.46253265017160317, 9.564922557960807481, 45.83224293864769550 ) ) ;
#139792 = CARTESIAN_POINT ( 'NONE',  ( -9.474510206698720793, -16.51473224551083518, 109.5844237280190043 ) ) ;
#139793 = CARTESIAN_POINT ( 'NONE',  ( -4.483927247898539470, -16.52544592524342804, 72.29057627198102409 ) ) ;
#139794 = CARTESIAN_POINT ( 'NONE',  ( 16.53943276465976808, 0.05219959533934440121, 71.25109039468568994 ) ) ;
#139796 = CARTESIAN_POINT ( 'NONE',  ( 19.02544592524343514, -5.153800228976328945, 53.54057627198102409 ) ) ;
#139795 = CARTESIAN_POINT ( 'NONE',  ( 10.72451020669871369, 18.67979575497193778, 27.08442372801901854 ) ) ;
#139797 = CARTESIAN_POINT ( 'NONE',  ( 19.05341960407611168, 5.049401038298154454, 68.95724293864769550 ) ) ;
#139798 = CARTESIAN_POINT ( 'NONE',  ( -0.05219959533934338120, 16.53943276465976808, 77.50109039468567573 ) ) ;
#139800 = ORIENTED_EDGE ( 'NONE', *, *, #53832, .F. ) ;
#139799 = CARTESIAN_POINT ( 'NONE',  ( -18.09918380851993902, -5.499999999999988454, 81.48618307335611632 ) ) ;
#139801 = ORIENTED_EDGE ( 'NONE', *, *, #132614, .T. ) ;
#139802 = CARTESIAN_POINT ( 'NONE',  ( 21.53943276465977519, 0.05219959533937863772, 111.2510903946856899 ) ) ;
#139803 = CARTESIAN_POINT ( 'NONE',  ( 5.049401038298161559, -19.05341960407611168, 42.70724293864767418 ) ) ;
#139805 = VERTEX_POINT ( 'NONE', #198096 ) ;
#139804 = CARTESIAN_POINT ( 'NONE',  ( 3.556970738554033499E-15, -38.81732327939057825, -10.12499999726881228 ) ) ;
#139806 = CARTESIAN_POINT ( 'NONE',  ( 4.379528057220092307, 16.55341960407617563, 32.29275706135235424 ) ) ;
#139808 = CARTESIAN_POINT ( 'NONE',  ( -12.14591786802326823, 12.06949235617739902, 38.12609039468567573 ) ) ;
#139807 = CARTESIAN_POINT ( 'NONE',  ( -16.46253265017146816, -9.564922557961047289, 64.16775706135233293 ) ) ;
#139809 = CARTESIAN_POINT ( 'NONE',  ( 16.51473224551069308, 9.474510206698969483, 39.16557627198103120 ) ) ;
#139810 = CARTESIAN_POINT ( 'NONE',  ( -5.153800228976328057, -19.02544592524343514, 112.2905762719810099 ) ) ;
#139811 = CARTESIAN_POINT ( 'NONE',  ( 9.564922557960805705, 16.46253265017160317, 59.58224293864769550 ) ) ;
#139812 = CARTESIAN_POINT ( 'NONE',  ( 5.823673210054125526, 21.52544592524343514, 94.79057627198105251 ) ) ;
#139814 = CARTESIAN_POINT ( 'NONE',  ( -19.03943276465977164, 0.05219959533909376836, 21.24890960531436335 ) ) ;
#139813 = CARTESIAN_POINT ( 'NONE',  ( 19.05341960407611168, 5.049401038298154454, 88.95724293864769550 ) ) ;
#139815 =( REPRESENTATION_RELATIONSHIP ('NONE','NONE', #154205, #31381 ) REPRESENTATION_RELATIONSHIP_WITH_TRANSFORMATION ( #34135 )SHAPE_REPRESENTATION_RELATIONSHIP( ) );
#139816 = CARTESIAN_POINT ( 'NONE',  ( 16.51473224551069308, 9.474510206698969483, 59.16557627198102409 ) ) ;
#139817 = CARTESIAN_POINT ( 'NONE',  ( -16.53943276465976808, 0.05219959533911058130, 21.24890960531436690 ) ) ;
#139818 = CARTESIAN_POINT ( 'NONE',  ( 19.03943276465977164, 0.05219959533936151252, 101.2510903946856757 ) ) ;
#139819 = CARTESIAN_POINT ( 'NONE',  ( -9.564922557961040184, 16.46253265017147172, 22.91775706135233648 ) ) ;
#139820 = CARTESIAN_POINT ( 'NONE',  ( -12.06949235617756955, 12.14591786802309770, 55.62390960531436690 ) ) ;
#139821 = CARTESIAN_POINT ( 'NONE',  ( 21.53943276465977519, 0.05219959533937863772, 96.25109039468568994 ) ) ;
#139822 = CARTESIAN_POINT ( 'NONE',  ( -5.049401038298153566, 19.05341960407611168, 45.20724293864769550 ) ) ;
#139824 = CARTESIAN_POINT ( 'NONE',  ( -10.72451020669870658, -18.67979575497194134, 84.58442372801903275 ) ) ;
#139823 = CARTESIAN_POINT ( 'NONE',  ( -8.224510206698948167, 14.34966873604960824, 30.41557627198101699 ) ) ;
#139825 = CARTESIAN_POINT ( 'NONE',  ( -5.049401038298153566, 19.05341960407611168, 80.20724293864769550 ) ) ;
#139826 = CARTESIAN_POINT ( 'NONE',  ( 13.97604488694527802, 13.89961937509977652, 94.37390960531436690 ) ) ;
#139827 = CARTESIAN_POINT ( 'NONE',  ( -8.224510206698948167, 14.34966873604960824, 95.41557627198102409 ) ) ;
#139828 = CARTESIAN_POINT ( 'NONE',  ( -0.05219959533910754901, -16.53943276465976808, 72.49890960531435269 ) ) ;
#139829 = CARTESIAN_POINT ( 'NONE',  ( -21.52544592524343514, 5.823673210054127303, 81.04057627198102409 ) ) ;
#139830 = CARTESIAN_POINT ( 'NONE',  ( -19.02544592524342804, 5.153800228976336051, 76.04057627198102409 ) ) ;
#139831 = CARTESIAN_POINT ( 'NONE',  ( 15.80617190586746368, 15.72974639402197994, 79.37390960531436690 ) ) ;
#139832 = CARTESIAN_POINT ( 'NONE',  ( -13.89961937509957401, -13.97604488694547875, 74.37609039468566152 ) ) ;
#139834 = CARTESIAN_POINT ( 'NONE',  ( -8.314922557960811034, -14.29746914071050412, 92.08224293864769550 ) ) ;
#139833 = DIRECTION ( 'NONE',  ( 0.7071067811865483499, 0.000000000000000000, -0.7071067811865465735 ) ) ;
#139835 = CARTESIAN_POINT ( 'NONE',  ( 13.97604488694527802, 13.89961937509977652, 64.37390960531436690 ) ) ;
#139836 = CARTESIAN_POINT ( 'NONE',  ( 21.53943276465977519, -0.05219959533907433946, 68.74890960531435269 ) ) ;
#139837 = CARTESIAN_POINT ( 'NONE',  ( -28.82186960331499037, 2.428612866367529932E-14, 146.0000000000000000 ) ) ;
#139839 = CARTESIAN_POINT ( 'NONE',  ( -69.65682714487590488, -71.74905178543390605, -15.00000000000000178 ) ) ;
#139838 = CARTESIAN_POINT ( 'NONE',  ( 12.14591786802309770, 12.06949235617756955, 24.37390960531435979 ) ) ;
#139840 = CARTESIAN_POINT ( 'NONE',  ( -9.564922557961040184, 16.46253265017147172, 112.9177570613523329 ) ) ;
#139841 = CARTESIAN_POINT ( 'NONE',  ( 12.06949235617757843, -12.14591786802309237, 83.12390960531436690 ) ) ;
#139842 = CARTESIAN_POINT ( 'NONE',  ( 9.100000000000001421, 0.000000000000000000, -61.89430850415821794 ) ) ;
#139843 = CARTESIAN_POINT ( 'NONE',  ( 16.51473224551069308, 9.474510206698969483, 79.16557627198103830 ) ) ;
#139844 = CARTESIAN_POINT ( 'NONE',  ( -9.564922557960796823, -16.46253265017161027, 27.08224293864769550 ) ) ;
#139845 = CARTESIAN_POINT ( 'NONE',  ( 8.224510206698953496, -14.34966873604960469, 62.91557627198102409 ) ) ;
#139846 = CARTESIAN_POINT ( 'NONE',  ( -0.05219959533909027116, -19.03943276465977164, 102.4989096053143669 ) ) ;
#139848 = CARTESIAN_POINT ( 'NONE',  ( 0.05219959533909260263, 19.03943276465977164, 84.99890960531436690 ) ) ;
#139847 = CARTESIAN_POINT ( 'NONE',  ( 16.46253265017146816, 9.564922557961045513, 91.66775706135234714 ) ) ;
#139849 = CARTESIAN_POINT ( 'NONE',  ( 16.46253265017160672, -9.564922557960803928, 88.33224293864769550 ) ) ;
#139850 = CARTESIAN_POINT ( 'NONE',  ( -10.72451020669898014, 18.67979575497178502, 80.41557627198103830 ) ) ;
#139851 = CARTESIAN_POINT ( 'NONE',  ( -16.55341960407617563, 4.379528057220093196, 68.54275706135234714 ) ) ;
#139852 = CARTESIAN_POINT ( 'NONE',  ( -16.52216118717250737, 7.221426719304233188, 93.92400978952976232 ) ) ;
#139853 = CARTESIAN_POINT ( 'NONE',  ( -5.153800228976328057, -19.02544592524343514, 67.29057627198102409 ) ) ;
#139854 = CARTESIAN_POINT ( 'NONE',  ( -5.823673210054116645, -21.52544592524344225, 67.29057627198103830 ) ) ;
#139855 = CARTESIAN_POINT ( 'NONE',  ( 19.03943276465977164, 0.05219959533936151252, 96.25109039468567573 ) ) ;
#139856 = VECTOR ( 'NONE', #140753, 1000.000000000000000 ) ;
#139858 = CARTESIAN_POINT ( 'NONE',  ( -5.719274019375665041, -21.55341960407619695, 49.79275706135234714 ) ) ;
#139857 = CARTESIAN_POINT ( 'NONE',  ( -8.314922557960811034, -14.29746914071050412, 32.08224293864769550 ) ) ;
#139859 = CARTESIAN_POINT ( 'NONE',  ( 18.09918380851992126, 5.500000000000036415, 83.98618307335611632 ) ) ;
#139861 = CARTESIAN_POINT ( 'NONE',  ( -16.51473224551069308, -9.474510206698971260, 101.6655762719810241 ) ) ;
#139860 = CARTESIAN_POINT ( 'NONE',  ( -12.14591786802326823, 12.06949235617739902, 78.12609039468570415 ) ) ;
#139862 = CARTESIAN_POINT ( 'NONE',  ( -0.05219959533909027116, -19.03943276465977164, 107.4989096053143527 ) ) ;
#139863 = CARTESIAN_POINT ( 'NONE',  ( 15.06137443927350361, 15.06137443927346098, -56.46919128290398504 ) ) ;
#139864 = CARTESIAN_POINT ( 'NONE',  ( -8.224510206698735004, -14.34966873604973081, 94.58442372801901854 ) ) ;
#139865 = CARTESIAN_POINT ( 'NONE',  ( 4.379528057220092307, 16.55341960407617563, 42.29275706135235424 ) ) ;
#139866 = CARTESIAN_POINT ( 'NONE',  ( -9.564922557960796823, -16.46253265017161027, 62.08224293864769550 ) ) ;
#139867 = CARTESIAN_POINT ( 'NONE',  ( -19.03943276465977164, 0.05219959533909376836, 66.24890960531436690 ) ) ;
#139868 = CARTESIAN_POINT ( 'NONE',  ( -21.52544592524334988, -5.823673210054445271, 48.95942372801902565 ) ) ;
#139869 = CARTESIAN_POINT ( 'NONE',  ( -14.29746914071037622, -8.314922557961029526, 69.16775706135234714 ) ) ;
#139870 = CARTESIAN_POINT ( 'NONE',  ( 4.483927247898545687, 16.52544592524342804, 29.79057627198102409 ) ) ;
#139871 = CARTESIAN_POINT ( 'NONE',  ( 0.05219959533909260263, 19.03943276465977164, 44.99890960531435979 ) ) ;
#139872 = CARTESIAN_POINT ( 'NONE',  ( 19.03943276465977164, -0.05219959533909143690, 28.74890960531435624 ) ) ;
#139873 = CARTESIAN_POINT ( 'NONE',  ( 8.224510206698742110, 14.34966873604972548, 22.08442372801901143 ) ) ;
#139874 = CARTESIAN_POINT ( 'NONE',  ( 13.89961937509957401, 13.97604488694547697, 76.87609039468566152 ) ) ;
#139875 = CARTESIAN_POINT ( 'NONE',  ( 16.55341960407611168, 4.379528057220329451, 88.95724293864769550 ) ) ;
#139876 = CARTESIAN_POINT ( 'NONE',  ( -19.05341960407611168, -5.049401038298163336, 56.45724293864768129 ) ) ;
#139878 = DIRECTION ( 'NONE',  ( 0.000000000000000000, 1.000000000000000000, 0.000000000000000000 ) ) ;
#139877 = CARTESIAN_POINT ( 'NONE',  ( 19.05341960407617918, -5.049401038297876454, 86.04275706135233293 ) ) ;
#139879 = CARTESIAN_POINT ( 'NONE',  ( 10.72451020669871369, 18.67979575497193778, 97.08442372801904696 ) ) ;
#139880 = CARTESIAN_POINT ( 'NONE',  ( -4.483927247898782831, 16.52544592524335698, 52.70942372801902565 ) ) ;
#139881 = CARTESIAN_POINT ( 'NONE',  ( 17.50000000000000000, -5.499999999999992895, 81.21769037696435589 ) ) ;
#139882 = CARTESIAN_POINT ( 'NONE',  ( -5.719274019375978568, 21.55341960407610458, 50.20724293864769550 ) ) ;
#139883 = CARTESIAN_POINT ( 'NONE',  ( 16.53943276465976808, 0.05219959533934440121, 46.25109039468567573 ) ) ;
#139884 = CARTESIAN_POINT ( 'NONE',  ( -13.97604488694527625, -13.89961937509977830, 36.87390960531436690 ) ) ;
#139885 = CARTESIAN_POINT ( 'NONE',  ( -0.05219959533936034679, 19.03943276465977164, 32.50109039468566863 ) ) ;
#139886 = CARTESIAN_POINT ( 'NONE',  ( 19.05341960407611168, 5.049401038298154454, 73.95724293864768129 ) ) ;
#139887 = CARTESIAN_POINT ( 'NONE',  ( -30.74264578624800492, -22.33583958711396278, -7.800000000000000711 ) ) ;
#139888 = CARTESIAN_POINT ( 'NONE',  ( -19.05341960407611168, -5.049401038298163336, 46.45724293864768129 ) ) ;
#139889 = CARTESIAN_POINT ( 'NONE',  ( -19.99604614807123326, -21.65269601533040245, -52.04364612718746486 ) ) ;
#139890 = CARTESIAN_POINT ( 'NONE',  ( -13.89961937509977652, 13.97604488694528158, 70.62390960531432427 ) ) ;
#139891 = CARTESIAN_POINT ( 'NONE',  ( 17.50000000000001066, -4.658240926743199672, 111.4447041781679957 ) ) ;
#139892 = CARTESIAN_POINT ( 'NONE',  ( 9.474510206698729675, 16.51473224551082808, 32.08442372801900433 ) ) ;
#139893 = CARTESIAN_POINT ( 'NONE',  ( -21.55341960407619339, 5.719274019375674811, 103.5427570613523613 ) ) ;
#139894 = CARTESIAN_POINT ( 'NONE',  ( 16.55341960407611168, 4.379528057220329451, 33.95724293864769550 ) ) ;
#139895 = CARTESIAN_POINT ( 'NONE',  ( 16.51473224551069308, 9.474510206698969483, 44.16557627198103120 ) ) ;
#139896 = CARTESIAN_POINT ( 'NONE',  ( 13.89961937509977652, -13.97604488694527269, 108.1239096053143669 ) ) ;
#139897 = CARTESIAN_POINT ( 'NONE',  ( 5.719274019375673035, 21.55341960407619339, 67.29275706135234714 ) ) ;
#139898 = CARTESIAN_POINT ( 'NONE',  ( -16.51473224551069308, -9.474510206698971260, 46.66557627198102409 ) ) ;
#139899 = CIRCLE ( 'NONE', #156076, 214.0437394197456342 ) ;
#139900 = CARTESIAN_POINT ( 'NONE',  ( 0.05219959533937995610, -21.53943276465977519, 75.00109039468568994 ) ) ;
#139901 = CARTESIAN_POINT ( 'NONE',  ( 21.55341960407610458, 5.719274019375980345, 28.95724293864769905 ) ) ;
#139902 = CARTESIAN_POINT ( 'NONE',  ( 5.719274019375673035, 21.55341960407619339, 32.29275706135235424 ) ) ;
#139903 = CARTESIAN_POINT ( 'NONE',  ( -0.05219959533936034679, 19.03943276465977164, 52.50109039468566863 ) ) ;
#139904 = CARTESIAN_POINT ( 'NONE',  ( -16.51473224551069308, -9.474510206698971260, 31.66557627198102054 ) ) ;
#139905 = CARTESIAN_POINT ( 'NONE',  ( 16.51473224551069308, 9.474510206698969483, 79.16557627198103830 ) ) ;
#139906 = CARTESIAN_POINT ( 'NONE',  ( 0.05219959533936267826, -19.03943276465977164, 110.0010903946856757 ) ) ;
#139907 = CARTESIAN_POINT ( 'NONE',  ( -8.314922557960811034, -14.29746914071050412, 77.08224293864769550 ) ) ;
#139908 = CARTESIAN_POINT ( 'NONE',  ( 18.62759615963271287, -10.81492255796078972, 38.33224293864768839 ) ) ;
#139909 = CARTESIAN_POINT ( 'NONE',  ( -5.049401038297874678, -19.05341960407617918, 94.79275706135230450 ) ) ;
#139910 = CARTESIAN_POINT ( 'NONE',  ( 5.719274019375991003, -21.55341960407610458, 102.7072429386476955 ) ) ;
#139911 = CARTESIAN_POINT ( 'NONE',  ( 15.80617190586769283, -15.72974639402175789, 60.62609039468567573 ) ) ;
#139912 = CARTESIAN_POINT ( 'NONE',  ( -4.379528057220086978, -16.55341960407618274, 59.79275706135234714 ) ) ;
#139913 = CARTESIAN_POINT ( 'NONE',  ( 12.06949235617739724, 12.14591786802326823, 56.87609039468568994 ) ) ;
#139914 = ORIENTED_EDGE ( 'NONE', *, *, #68656, .T. ) ;
#139915 = CARTESIAN_POINT ( 'NONE',  ( 19.03943276465977164, -0.05219959533909143690, 43.74890960531435979 ) ) ;
#139916 = CARTESIAN_POINT ( 'NONE',  ( -16.55341960407617563, 4.379528057220093196, 83.54275706135234714 ) ) ;
#139917 = EDGE_CURVE ( 'NONE', #141361, #51904, #14059, .T. ) ;
#139918 = CARTESIAN_POINT ( 'NONE',  ( -21.52544592524334988, -5.823673210054445271, 18.95942372801901143 ) ) ;
#139919 = CARTESIAN_POINT ( 'NONE',  ( -4.483927247898539470, -16.52544592524342804, 47.29057627198103120 ) ) ;
#139920 = CARTESIAN_POINT ( 'NONE',  ( -13.97604488694527625, -13.89961937509977652, 81.87390960531436690 ) ) ;
#139921 = CARTESIAN_POINT ( 'NONE',  ( -8.224510206698735004, -14.34966873604973081, 69.58442372801900433 ) ) ;
#139922 = CARTESIAN_POINT ( 'NONE',  ( -21.52544592524334988, -5.823673210054445271, 48.95942372801902565 ) ) ;
#139923 = CARTESIAN_POINT ( 'NONE',  ( -14.34966873604972548, 8.224510206698743886, 23.33442372801901499 ) ) ;
#139924 = CARTESIAN_POINT ( 'NONE',  ( -21.55341960407610458, -5.719274019375992779, 111.4572429386476813 ) ) ;
#139925 = CARTESIAN_POINT ( 'NONE',  ( 0.05219959533910956823, 16.53943276465976808, 49.99890960531437401 ) ) ;
#139926 = VERTEX_POINT ( 'NONE', #75726 ) ;
#139927 = CARTESIAN_POINT ( 'NONE',  ( -17.44270441346519362, 5.991230190322974103, 73.63664920735772057 ) ) ;
#139928 = CARTESIAN_POINT ( 'NONE',  ( -21.53943276465977519, 0.05219959533907696930, 81.24890960531436690 ) ) ;
#139929 = CARTESIAN_POINT ( 'NONE',  ( -4.483927247898782831, 16.52544592524335698, 112.7094237280190328 ) ) ;
#139930 = ORIENTED_EDGE ( 'NONE', *, *, #13078, .T. ) ;
#139931 = FACE_BOUND ( 'NONE', #52667, .T. ) ;
#139932 = CARTESIAN_POINT ( 'NONE',  ( -15.80617190586768217, 15.72974639402176855, 23.12609039468567573 ) ) ;
#139933 = CARTESIAN_POINT ( 'NONE',  ( -5.049401038298153566, 19.05341960407611168, 110.2072429386476671 ) ) ;
#139934 = CARTESIAN_POINT ( 'NONE',  ( 5.823673210054444382, -21.52544592524334988, 20.20942372801900788 ) ) ;
#139935 = CARTESIAN_POINT ( 'NONE',  ( -14.29746914071049879, 8.314922557960819915, 50.83224293864770971 ) ) ;
#139936 = CARTESIAN_POINT ( 'NONE',  ( -14.34966873604972548, 8.224510206698743886, 63.33442372801900433 ) ) ;
#139937 = CARTESIAN_POINT ( 'NONE',  ( -5.049401038298153566, 19.05341960407611168, 65.20724293864765286 ) ) ;
#139938 = CARTESIAN_POINT ( 'NONE',  ( 13.89961937509957401, 13.97604488694547697, 71.87609039468567573 ) ) ;
#139939 = CARTESIAN_POINT ( 'NONE',  ( 13.97604488694527802, 13.89961937509977652, 74.37390960531436690 ) ) ;
#139940 = EDGE_CURVE ( 'NONE', #23953, #63287, #11224, .T. ) ;
#139941 = CARTESIAN_POINT ( 'NONE',  ( -21.53943276465977519, 0.05219959533907696930, 41.24890960531435269 ) ) ;
#139942 = CARTESIAN_POINT ( 'NONE',  ( -14.16830335033896660, -40.16376294012538040, -20.11902964094489121 ) ) ;
#139943 = CARTESIAN_POINT ( 'NONE',  ( 13.89961937509977652, -13.97604488694527269, 63.12390960531435979 ) ) ;
#139944 = CARTESIAN_POINT ( 'NONE',  ( 16.52544592524335698, 4.483927247898782831, 21.45942372801901499 ) ) ;
#139945 = CARTESIAN_POINT ( 'NONE',  ( -19.03943276465977164, -0.05219959533935918106, 63.75109039468566863 ) ) ;
#139946 = CARTESIAN_POINT ( 'NONE',  ( 5.719274019375991003, -21.55341960407610458, 107.7072429386476955 ) ) ;
#139947 = CARTESIAN_POINT ( 'NONE',  ( 16.53943276465976808, -0.05219959533910856209, 38.74890960531435979 ) ) ;
#139948 = CARTESIAN_POINT ( 'NONE',  ( 13.89961937509977652, -13.97604488694527269, 93.12390960531436690 ) ) ;
#139949 = CARTESIAN_POINT ( 'NONE',  ( -18.62759615963270932, 10.81492255796079327, 60.83224293864769550 ) ) ;
#139951 = CARTESIAN_POINT ( 'NONE',  ( -8.224510206698735004, -14.34966873604973081, 39.58442372801901143 ) ) ;
#139950 = CARTESIAN_POINT ( 'NONE',  ( -5.719274019375978568, 21.55341960407610458, 90.20724293864770971 ) ) ;
#139952 = CARTESIAN_POINT ( 'NONE',  ( -18.62759615963270932, 10.81492255796079327, 30.83224293864770260 ) ) ;
#139953 = CARTESIAN_POINT ( 'NONE',  ( 15.80617190586769283, -15.72974639402175789, 85.62609039468568994 ) ) ;
#139954 = CARTESIAN_POINT ( 'NONE',  ( -9.564922557960796823, -16.46253265017161027, 82.08224293864768129 ) ) ;
#139955 = CARTESIAN_POINT ( 'NONE',  ( -19.02544592524342804, 5.153800228976336051, 26.04057627198103120 ) ) ;
#139956 = CARTESIAN_POINT ( 'NONE',  ( -19.05341960407611168, -5.049401038298163336, 86.45724293864769550 ) ) ;
#139957 = CARTESIAN_POINT ( 'NONE',  ( 16.53943276465976808, -0.05219959533910856209, 108.7489096053143669 ) ) ;
#139958 = CARTESIAN_POINT ( 'NONE',  ( 9.564922557960805705, 16.46253265017160317, 64.58224293864769550 ) ) ;
#139959 = CARTESIAN_POINT ( 'NONE',  ( 19.02544592524334988, 5.153800228976608722, 111.4594237280190043 ) ) ;
#139960 = CIRCLE ( 'NONE', #13980, 2.500000000000000444 ) ;
#139961 = CARTESIAN_POINT ( 'NONE',  ( 17.58332526062528345, 7.635886036038587399, 41.57665040441534643 ) ) ;
#139963 = CARTESIAN_POINT ( 'NONE',  ( 10.81492255796078972, 18.62759615963270932, 24.58224293864768839 ) ) ;
#139962 = CARTESIAN_POINT ( 'NONE',  ( -15.72974639402176322, -15.80617190586768395, 94.37609039468568994 ) ) ;
#139964 = CARTESIAN_POINT ( 'NONE',  ( 14.34966873604972726, -8.224510206698740333, 85.83442372801901854 ) ) ;
#139965 = DIRECTION ( 'NONE',  ( 1.000000000000000000, 0.000000000000000000, 0.000000000000000000 ) ) ;
#139966 = CARTESIAN_POINT ( 'NONE',  ( 5.049401038297881783, 19.05341960407617563, 67.29275706135234714 ) ) ;
#139967 = CARTESIAN_POINT ( 'NONE',  ( -16.46253265017146816, -9.564922557961047289, 29.16775706135232937 ) ) ;
#139968 = CARTESIAN_POINT ( 'NONE',  ( 3.873560230149206252, 5.283393095647500814, -64.45999282322711110 ) ) ;
#139969 = CARTESIAN_POINT ( 'NONE',  ( 13.97604488694527802, 13.89961937509977652, 24.37390960531435624 ) ) ;
#139970 = CARTESIAN_POINT ( 'NONE',  ( -8.224510206698948167, 14.34966873604960824, 30.41557627198101699 ) ) ;
#139971 = CARTESIAN_POINT ( 'NONE',  ( -31.90000000000003411, 3.219216299777112361E-13, -49.13275782002545355 ) ) ;
#139972 = CARTESIAN_POINT ( 'NONE',  ( -16.55341960407611168, -4.379528057220339221, 26.45724293864768839 ) ) ;
#139973 = DIRECTION ( 'NONE',  ( 0.000000000000000000, 0.000000000000000000, -1.000000000000000000 ) ) ;
#139974 = CARTESIAN_POINT ( 'NONE',  ( 16.53943276465976808, 0.05219959533934440121, 96.25109039468568994 ) ) ;
#139975 = CARTESIAN_POINT ( 'NONE',  ( -19.03943276465977164, 0.05219959533909376836, 41.24890960531435269 ) ) ;
#139976 = CARTESIAN_POINT ( 'NONE',  ( 10.72451020669871369, 18.67979575497193778, 97.08442372801904696 ) ) ;
#139977 = CARTESIAN_POINT ( 'NONE',  ( -9.564922557961040184, 16.46253265017147172, 102.9177570613523329 ) ) ;
#139978 = CARTESIAN_POINT ( 'NONE',  ( -5.719274019375665041, -21.55341960407619695, 84.79275706135234714 ) ) ;
#139979 = CARTESIAN_POINT ( 'NONE',  ( -19.05341960407617563, 5.049401038297882671, 58.54275706135234003 ) ) ;
#139980 = CARTESIAN_POINT ( 'NONE',  ( -9.564922557960796823, -16.46253265017161027, 87.08224293864769550 ) ) ;
#139981 = CARTESIAN_POINT ( 'NONE',  ( 13.89961937509977652, -13.97604488694527269, 68.12390960531436690 ) ) ;
#139982 = DIRECTION ( 'NONE',  ( -1.000000000000000000, 0.000000000000000000, 0.000000000000000000 ) ) ;
#139983 = CARTESIAN_POINT ( 'NONE',  ( 8.314922557960818139, 14.29746914071049879, 69.58224293864769550 ) ) ;
#139984 = CARTESIAN_POINT ( 'NONE',  ( 5.719274019375991003, -21.55341960407610458, 57.70724293864770260 ) ) ;
#139985 = CARTESIAN_POINT ( 'NONE',  ( -9.474510206698964154, 16.51473224551069663, 60.41557627198102409 ) ) ;
#139987 = CARTESIAN_POINT ( 'NONE',  ( -0.05219959533934338120, 16.53943276465976808, 72.50109039468568994 ) ) ;
#139986 = CARTESIAN_POINT ( 'NONE',  ( 5.823673210054125526, 21.52544592524343514, 84.79057627198102409 ) ) ;
#139988 = EDGE_CURVE ( 'NONE', #126376, #154964, #149603, .T. ) ;
#139989 = VERTEX_POINT ( 'NONE', #196131 ) ;
#139990 = CARTESIAN_POINT ( 'NONE',  ( -19.05341960407611168, -5.049401038298163336, 51.45724293864770260 ) ) ;
#139992 = CARTESIAN_POINT ( 'NONE',  ( -11.40812507854755609, 35.11059874428196537, -1.024999997268813301 ) ) ;
#139991 = CARTESIAN_POINT ( 'NONE',  ( -12.06949235617756955, 12.14591786802309770, 80.62390960531438111 ) ) ;
#139993 = CARTESIAN_POINT ( 'NONE',  ( 9.474510206698971260, -16.51473224551069308, 52.91557627198102409 ) ) ;
#139994 = CARTESIAN_POINT ( 'NONE',  ( 5.153800228976335163, 19.02544592524342804, 24.79057627198102765 ) ) ;
#139995 = CARTESIAN_POINT ( 'NONE',  ( 5.153800228976615827, -19.02544592524334988, 70.20942372801899012 ) ) ;
#139996 = CARTESIAN_POINT ( 'NONE',  ( 14.29746914071049879, -8.314922557960816363, 83.33224293864769550 ) ) ;
#139997 = CARTESIAN_POINT ( 'NONE',  ( 21.53943276465977519, 0.05219959533937863772, 41.25109039468568284 ) ) ;
#139999 = CARTESIAN_POINT ( 'NONE',  ( -21.53943276465977519, 0.05219959533907696930, 106.2489096053143811 ) ) ;
#139998 = CARTESIAN_POINT ( 'NONE',  ( 13.89961937509977652, -13.97604488694527269, 33.12390960531434558 ) ) ;
#140000 = CARTESIAN_POINT ( 'NONE',  ( 13.89961937509977652, -13.97604488694527269, 113.1239096053143527 ) ) ;
#140001 = CARTESIAN_POINT ( 'NONE',  ( 14.29746914071049879, -8.314922557960816363, 88.33224293864769550 ) ) ;
#140002 = CARTESIAN_POINT ( 'NONE',  ( 22.96436041962737207, -32.42578188301177988, -19.82561655440861514 ) ) ;
#140003 = CARTESIAN_POINT ( 'NONE',  ( 5.153800228976335163, 19.02544592524342804, 44.79057627198103830 ) ) ;
#140004 = CARTESIAN_POINT ( 'NONE',  ( -9.574954286947731319, -11.69376568609066958, -62.03511740007206043 ) ) ;
#140006 = CARTESIAN_POINT ( 'NONE',  ( 13.97604488694527802, 13.89961937509977652, 94.37390960531436690 ) ) ;
#140005 = CARTESIAN_POINT ( 'NONE',  ( -9.474510206698720793, -16.51473224551083518, 89.58442372801900433 ) ) ;
#140007 = CARTESIAN_POINT ( 'NONE',  ( -18.67979575497193778, 10.72451020669871902, 38.33442372801900433 ) ) ;
#140008 = CARTESIAN_POINT ( 'NONE',  ( 19.05341960407611168, 5.049401038298154454, 78.95724293864769550 ) ) ;
#140009 =( BOUNDED_SURFACE ( )  B_SPLINE_SURFACE ( 3, 2, ( 
 ( #85183, #38705, #8364 ),
 ( #115545, #164060, #54865 ),
 ( #52853, #193389, #72032 ),
 ( #24549, #180240, #133705 ),
 ( #86199, #177233, #178227 ),
 ( #131708, #165052, #53871 ),
 ( #6348, #87203, #102371 ),
 ( #39691, #114524, #41709 ),
 ( #100362, #163042, #9375 ),
 ( #71040, #162041, #144865 ),
 ( #132707, #10375, #83191 ),
 ( #55863, #103374, #117537 ),
 ( #179235, #40701, #25559 ),
 ( #148884, #195397, #176225 ),
 ( #161041, #56875, #69029 ),
 ( #129679, #37694, #99358 ),
 ( #145862, #7344, #130694 ),
 ( #136679, #166049, #75014 ),
 ( #46664, #15332, #197381 ),
 ( #57873, #60823, #183199 ),
 ( #108323, #27549, #59836 ),
 ( #90176, #11378, #13350 ),
 ( #92149, #26545, #91150 ),
 ( #119545, #30498, #73048 ) ),
 .UNSPECIFIED., .F., .F., .F. ) 
 B_SPLINE_SURFACE_WITH_KNOTS ( ( 4, 2, 2, 2, 2, 2, 2, 2, 2, 2, 2, 4 ),
 ( 3, 3 ),
 ( -8.673617379884035472E-19, 0.001899702839891689908, 0.002849554259837535405, 0.003799405679783380684, 0.005699108519675071677, 0.006648959939620916956, 0.007598811359566762236, 0.008548662779512607515, 0.009498514199458452795, 0.01139821703935014335, 0.01329791987924183391, 0.01519762271913352447 ),
 ( 0.000000000000000000, 1.000000000000000000 ),
 .UNSPECIFIED. ) 
 GEOMETRIC_REPRESENTATION_ITEM ( )  RATIONAL_B_SPLINE_SURFACE ( (
 ( 1.000000000000000000, 0.7660444431189777914, 1.000000000000000000),
 ( 1.000000000000000000, 0.7753720600381861505, 1.000000000000000000),
 ( 1.000000000000000000, 0.7832595754286625356, 1.000000000000000000),
 ( 1.000000000000000000, 0.7928595458705119947, 1.000000000000000000),
 ( 1.000000000000000000, 0.7956872332516092827, 1.000000000000000000),
 ( 1.000000000000000000, 0.8005750596157589216, 1.000000000000000000),
 ( 1.000000000000000000, 0.8026302056541514407, 1.000000000000000000),
 ( 1.000000000000000000, 0.8075080643848788764, 1.000000000000000000),
 ( 1.000000000000000000, 0.8091143015810093875, 1.000000000000000000),
 ( 1.000000000000000000, 0.8093067629632906268, 1.000000000000000000),
 ( 1.000000000000000000, 0.8089952915731616345, 1.000000000000000000),
 ( 1.000000000000000000, 0.8076919994862351571, 1.000000000000000000),
 ( 1.000000000000000000, 0.8067078407648706762, 1.000000000000000000),
 ( 1.000000000000000000, 0.8041786842467621987, 1.000000000000000000),
 ( 1.000000000000000000, 0.8026334674877082520, 1.000000000000000000),
 ( 1.000000000000000000, 0.7990747329469325422, 1.000000000000000000),
 ( 1.000000000000000000, 0.7970509760941956179, 1.000000000000000000),
 ( 1.000000000000000000, 0.7904793850863031102, 1.000000000000000000),
 ( 1.000000000000000000, 0.7855040224313080133, 1.000000000000000000),
 ( 1.000000000000000000, 0.7751942650508213406, 1.000000000000000000),
 ( 1.000000000000000000, 0.7698260778211012401, 1.000000000000000000),
 ( 1.000000000000000000, 0.7598259884961471311, 1.000000000000000000),
 ( 1.000000000000000000, 0.7551428682219897270, 1.000000000000000000),
 ( 1.000000000000000000, 0.7510191126010854479, 1.000000000000000000) ) ) 
 REPRESENTATION_ITEM ( '' )  SURFACE ( )  );
#140010 = CARTESIAN_POINT ( 'NONE',  ( -16.46253265017146816, -9.564922557961047289, 74.16775706135234714 ) ) ;
#140011 = CARTESIAN_POINT ( 'NONE',  ( 19.02544592524343514, -5.153800228976328945, 48.54057627198103120 ) ) ;
#140012 = CARTESIAN_POINT ( 'NONE',  ( -14.29746914071049879, 8.314922557960819915, 70.83224293864770971 ) ) ;
#140013 = CARTESIAN_POINT ( 'NONE',  ( 16.53943276465976808, -0.05219959533910856209, 73.74890960531433848 ) ) ;
#140014 = CARTESIAN_POINT ( 'NONE',  ( 9.564922557960805705, 16.46253265017160317, 79.58224293864769550 ) ) ;
#140015 = CARTESIAN_POINT ( 'NONE',  ( -15.72974639402197994, 15.80617190586746368, 100.6239096053143811 ) ) ;
#140016 = CARTESIAN_POINT ( 'NONE',  ( 19.03943276465977164, -0.05219959533909143690, 73.74890960531435269 ) ) ;
#140017 = CARTESIAN_POINT ( 'NONE',  ( -9.564922557961040184, 16.46253265017147172, 22.91775706135233648 ) ) ;
#140020 = CARTESIAN_POINT ( 'NONE',  ( -8.314922557960811034, -14.29746914071050412, 107.0822429386476955 ) ) ;
#140019 = CARTESIAN_POINT ( 'NONE',  ( -4.379528057220328563, 16.55341960407611168, 30.20724293864769550 ) ) ;
#140018 = CARTESIAN_POINT ( 'NONE',  ( 19.03943276465977164, -0.05219959533909143690, 38.74890960531436690 ) ) ;
#140021 = CARTESIAN_POINT ( 'NONE',  ( -13.97604488694547697, 13.89961937509957934, 108.1260903946856331 ) ) ;
#140022 = ORIENTED_EDGE ( 'NONE', *, *, #61909, .T. ) ;
#140023 = CARTESIAN_POINT ( 'NONE',  ( 21.53943276465977519, 0.05219959533937863772, 26.25109039468567573 ) ) ;
#140024 = CARTESIAN_POINT ( 'NONE',  ( -5.049401038297874678, -19.05341960407617918, 64.79275706135233293 ) ) ;
#140025 = CARTESIAN_POINT ( 'NONE',  ( -8.314922557960811034, -14.29746914071050412, 27.08224293864769550 ) ) ;
#140026 = CARTESIAN_POINT ( 'NONE',  ( -18.67979575497178146, -10.72451020669898902, 91.66557627198103830 ) ) ;
#140027 = CARTESIAN_POINT ( 'NONE',  ( -10.81492255796078084, -18.62759615963271287, 27.08224293864769550 ) ) ;
#140028 = CARTESIAN_POINT ( 'NONE',  ( -4.379528057220328563, 16.55341960407611168, 55.20724293864770260 ) ) ;
#140029 = CARTESIAN_POINT ( 'NONE',  ( 5.049401038298161559, -19.05341960407611168, 32.70724293864768129 ) ) ;
#140030 = CARTESIAN_POINT ( 'NONE',  ( 16.51473224551083163, -9.474510206698727899, 20.83442372801899722 ) ) ;
#140031 = CARTESIAN_POINT ( 'NONE',  ( -16.52544592524335698, -4.483927247898792601, 83.95942372801900433 ) ) ;
#140032 = CARTESIAN_POINT ( 'NONE',  ( 12.14591786802327356, -12.06949235617739191, 50.62609039468568994 ) ) ;
#140033 = CARTESIAN_POINT ( 'NONE',  ( 10.81492255796078972, 18.62759615963270932, 29.58224293864769905 ) ) ;
#140034 = CARTESIAN_POINT ( 'NONE',  ( -18.62759615963255300, -10.81492255796106328, 104.1677570613523471 ) ) ;
#140035 = CARTESIAN_POINT ( 'NONE',  ( 13.89961937509977652, -13.97604488694527269, 83.12390960531436690 ) ) ;
#140036 = CARTESIAN_POINT ( 'NONE',  ( 12.14591786802327356, -12.06949235617739191, 65.62609039468568994 ) ) ;
#140037 = CARTESIAN_POINT ( 'NONE',  ( -4.483927247898539470, -16.52544592524342804, 107.2905762719810525 ) ) ;
#140038 = CARTESIAN_POINT ( 'NONE',  ( 12.14591786802309770, 12.06949235617756955, 39.37390960531436690 ) ) ;
#140039 = PLANE ( 'NONE',  #73245 ) ;
#140042 = CARTESIAN_POINT ( 'NONE',  ( 5.049401038298161559, -19.05341960407611168, 72.70724293864768129 ) ) ;
#140041 = CARTESIAN_POINT ( 'NONE',  ( 5.049401038298161559, -19.05341960407611168, 92.70724293864769550 ) ) ;
#140040 = CARTESIAN_POINT ( 'NONE',  ( -15.72974639402176322, -15.80617190586768395, 69.37609039468567573 ) ) ;
#140043 = CARTESIAN_POINT ( 'NONE',  ( -16.51473224551069308, -9.474510206698971260, 111.6655762719810383 ) ) ;
#140044 = CARTESIAN_POINT ( 'NONE',  ( 14.29746914071049879, -8.314922557960816363, 58.33224293864768839 ) ) ;
#140045 = CARTESIAN_POINT ( 'NONE',  ( -14.34966873604960291, -8.224510206698953496, 21.66557627198102409 ) ) ;
#140046 = AXIS2_PLACEMENT_3D ( 'NONE', #53728, #39552, #128548 ) ;
#140047 = VERTEX_POINT ( 'NONE', #180954 ) ;
#140048 = CARTESIAN_POINT ( 'NONE',  ( -14.29746914071049879, 8.314922557960819915, 50.83224293864770971 ) ) ;
#140050 = CARTESIAN_POINT ( 'NONE',  ( -17.49999999999998934, -5.500000000000015987, 56.28230962303566542 ) ) ;
#140049 = CARTESIAN_POINT ( 'NONE',  ( 12.14591786802327356, -12.06949235617739191, 40.62609039468567573 ) ) ;
#140051 = CARTESIAN_POINT ( 'NONE',  ( -9.474510206698720793, -16.51473224551083518, 44.58442372801900433 ) ) ;
#140052 = CARTESIAN_POINT ( 'NONE',  ( -0.05219959533909027116, -19.03943276465977164, 72.49890960531435269 ) ) ;
#140053 = CARTESIAN_POINT ( 'NONE',  ( 19.05341960407617918, -5.049401038297876454, 46.04275706135233293 ) ) ;
#140054 = CARTESIAN_POINT ( 'NONE',  ( 0.05219959533936267826, -19.03943276465977164, 60.00109039468566863 ) ) ;
#140056 = CARTESIAN_POINT ( 'NONE',  ( -16.55341960407617563, 4.379528057220093196, 83.54275706135234714 ) ) ;
#140055 = CARTESIAN_POINT ( 'NONE',  ( -16.46253265017146816, -9.564922557961047289, 104.1677570613523329 ) ) ;
#140057 = CARTESIAN_POINT ( 'NONE',  ( -8.571926809382608425, 26.38167802310805854, 146.9750000027311785 ) ) ;
#140058 = CARTESIAN_POINT ( 'NONE',  ( -9.474510206698964154, 16.51473224551069663, 30.41557627198102054 ) ) ;
#140059 = CARTESIAN_POINT ( 'NONE',  ( -9.564922557960796823, -16.46253265017161027, 107.0822429386476955 ) ) ;
#140060 = CARTESIAN_POINT ( 'NONE',  ( -18.67979575497193778, 10.72451020669871902, 43.33442372801901143 ) ) ;
#140061 = CARTESIAN_POINT ( 'NONE',  ( -16.46253265017146816, -9.564922557961047289, 89.16775706135234714 ) ) ;
#140063 = CARTESIAN_POINT ( 'NONE',  ( 13.89961937509977652, -13.97604488694527269, 63.12390960531435979 ) ) ;
#140062 = CARTESIAN_POINT ( 'NONE',  ( 17.49999999999999645, -3.305555262949659401, 107.1251715215659317 ) ) ;
#140064 = CARTESIAN_POINT ( 'NONE',  ( -19.05341960407611168, -5.049401038298163336, 106.4572429386476955 ) ) ;
#140066 = CARTESIAN_POINT ( 'NONE',  ( 19.05341960407611168, 5.049401038298154454, 68.95724293864769550 ) ) ;
#140065 = CARTESIAN_POINT ( 'NONE',  ( -12.14591786802309592, -12.06949235617757132, 66.87390960531436690 ) ) ;
#140067 = CARTESIAN_POINT ( 'NONE',  ( 5.153800228976335163, 19.02544592524342804, 64.79057627198100988 ) ) ;
#140068 = CARTESIAN_POINT ( 'NONE',  ( -13.89961937509957401, -13.97604488694547875, 59.37609039468566863 ) ) ;
#140069 = CARTESIAN_POINT ( 'NONE',  ( -5.823673210054116645, -21.52544592524344225, 52.29057627198102409 ) ) ;
#140070 = CARTESIAN_POINT ( 'NONE',  ( -5.153800228976607833, 19.02544592524334988, 37.70942372801899722 ) ) ;
#140071 = CARTESIAN_POINT ( 'NONE',  ( 13.89961937509977652, -13.97604488694527269, 78.12390960531433848 ) ) ;
#140072 = CARTESIAN_POINT ( 'NONE',  ( -10.72451020669898014, 18.67979575497178502, 80.41557627198103830 ) ) ;
#140074 = CARTESIAN_POINT ( 'NONE',  ( -19.02544592524334988, -5.153800228976617603, 38.95942372801900433 ) ) ;
#140073 = CARTESIAN_POINT ( 'NONE',  ( -14.34966873604960291, -8.224510206698953496, 76.66557627198103830 ) ) ;
#140075 = CARTESIAN_POINT ( 'NONE',  ( -18.62759615963270932, 10.81492255796079327, 45.83224293864769550 ) ) ;
#140076 = CARTESIAN_POINT ( 'NONE',  ( 0.05219959533907565091, 21.53943276465977519, 34.99890960531435979 ) ) ;
#140077 = CARTESIAN_POINT ( 'NONE',  ( -0.05219959533909027116, -19.03943276465977164, 67.49890960531436690 ) ) ;
#140078 = CARTESIAN_POINT ( 'NONE',  ( 9.474510206698971260, -16.51473224551069308, 57.91557627198103120 ) ) ;
#140079 = CARTESIAN_POINT ( 'NONE',  ( 9.474510206698971260, -16.51473224551069308, 22.91557627198102765 ) ) ;
#140080 = CARTESIAN_POINT ( 'NONE',  ( 21.52544592524334988, 5.823673210054432836, 21.45942372801901499 ) ) ;
#140081 = DIRECTION ( 'NONE',  ( 0.000000000000000000, 0.000000000000000000, 1.000000000000000000 ) ) ;
#140082 = CARTESIAN_POINT ( 'NONE',  ( -21.52544592524334988, -5.823673210054445271, 33.95942372801901143 ) ) ;
#140083 = CARTESIAN_POINT ( 'NONE',  ( -13.97604488694527625, -13.89961937509977652, 36.87390960531436690 ) ) ;
#140084 = CARTESIAN_POINT ( 'NONE',  ( 5.823673210054125526, 21.52544592524343514, 104.7905762719810241 ) ) ;
#140085 = CARTESIAN_POINT ( 'NONE',  ( -19.03943276465977164, -0.05219959533935918106, 48.75109039468566863 ) ) ;
#140086 = CARTESIAN_POINT ( 'NONE',  ( 19.03943276465977164, -0.05219959533909143690, 28.74890960531435624 ) ) ;
#140087 = FACE_OUTER_BOUND ( 'NONE', #5778, .T. ) ;
#140088 = CARTESIAN_POINT ( 'NONE',  ( 16.65483384399521682, -7.017357588706441440, 21.38698616505659444 ) ) ;
#140089 = CARTESIAN_POINT ( 'NONE',  ( -16.55341960407617563, 4.379528057220093196, 53.54275706135234714 ) ) ;
#140090 = CARTESIAN_POINT ( 'NONE',  ( -9.474510206698964154, 16.51473224551069663, 25.41557627198103120 ) ) ;
#140091 = CARTESIAN_POINT ( 'NONE',  ( 33.70061762759713986, -5.431516297171046226, 95.88384366041691464 ) ) ;
#140092 = CARTESIAN_POINT ( 'NONE',  ( 19.05341960407611168, 5.049401038298154454, 78.95724293864769550 ) ) ;
#140094 = EDGE_CURVE ( 'NONE', #120101, #162507, #178442, .T. ) ;
#140093 = CARTESIAN_POINT ( 'NONE',  ( -14.29746914071049879, 8.314922557960819915, 110.8322429386476955 ) ) ;
#140095 = CARTESIAN_POINT ( 'NONE',  ( -5.823673210054116645, -21.52544592524344225, 57.29057627198103120 ) ) ;
#140096 = CARTESIAN_POINT ( 'NONE',  ( 12.06949235617757843, -12.14591786802309237, 73.12390960531436690 ) ) ;
#140097 = CARTESIAN_POINT ( 'NONE',  ( -12.06949235617739369, -12.14591786802326823, 29.37609039468568284 ) ) ;
#140098 = CARTESIAN_POINT ( 'NONE',  ( -10.81492255796105439, 18.62759615963255655, 87.91775706135234714 ) ) ;
#140099 = CARTESIAN_POINT ( 'NONE',  ( 19.05341960407611168, 5.049401038298154454, 28.95724293864769550 ) ) ;
#140100 = CARTESIAN_POINT ( 'NONE',  ( 0.05219959533910956823, 16.53943276465976808, 24.99890960531435624 ) ) ;
#140101 = CARTESIAN_POINT ( 'NONE',  ( -14.29746914071049879, 8.314922557960819915, 60.83224293864769550 ) ) ;
#140102 = CARTESIAN_POINT ( 'NONE',  ( -19.02544592524342804, 5.153800228976336051, 56.04057627198100988 ) ) ;
#140103 = CARTESIAN_POINT ( 'NONE',  ( -0.05219959533937732626, 21.53943276465977519, 102.5010903946856899 ) ) ;
#140104 = CARTESIAN_POINT ( 'NONE',  ( -18.67979575497178146, -10.72451020669898902, 101.6655762719810383 ) ) ;
#140105 = CARTESIAN_POINT ( 'NONE',  ( 21.55341960407619695, -5.719274019375665929, 76.04275706135237556 ) ) ;
#140106 = CARTESIAN_POINT ( 'NONE',  ( -14.29746914071037622, -8.314922557961029526, 44.16775706135234714 ) ) ;
#140108 = CARTESIAN_POINT ( 'NONE',  ( -10.72451020669870658, -18.67979575497194134, 89.58442372801901854 ) ) ;
#140107 = CARTESIAN_POINT ( 'NONE',  ( -16.52544592524342804, 4.483927247898546575, 81.04057627198102409 ) ) ;
#140109 = CARTESIAN_POINT ( 'NONE',  ( -16.53943276465976808, 0.05219959533911058130, 21.24890960531436690 ) ) ;
#140110 = CARTESIAN_POINT ( 'NONE',  ( -31.80000000000000782, -5.180255960393304182E-15, 47.70000000000000284 ) ) ;
#140111 = CARTESIAN_POINT ( 'NONE',  ( 14.29746914071037800, 8.314922557961029526, 41.66775706135235424 ) ) ;
#140112 = CARTESIAN_POINT ( 'NONE',  ( -12.14591786802309592, -12.06949235617757132, 46.87390960531435979 ) ) ;
#140113 = CARTESIAN_POINT ( 'NONE',  ( 12.14591786802327356, -12.06949235617739191, 90.62609039468567573 ) ) ;
#140114 = CARTESIAN_POINT ( 'NONE',  ( 5.153800228976335163, 19.02544592524342804, 99.79057627198102409 ) ) ;
#140115 = CARTESIAN_POINT ( 'NONE',  ( -19.02544592524342804, 5.153800228976336051, 116.0405762719810383 ) ) ;
#140116 = CARTESIAN_POINT ( 'NONE',  ( -21.55341960407619339, 5.719274019375674811, 103.5427570613523613 ) ) ;
#140117 = CARTESIAN_POINT ( 'NONE',  ( 12.06949235617739724, 12.14591786802326823, 101.8760903946857042 ) ) ;
#140118 = CARTESIAN_POINT ( 'NONE',  ( -16.55341960407611168, -4.379528057220339221, 76.45724293864769550 ) ) ;
#140119 = CARTESIAN_POINT ( 'NONE',  ( 0.05219959533909260263, 19.03943276465977164, 84.99890960531436690 ) ) ;
#140120 = ORIENTED_EDGE ( 'NONE', *, *, #174667, .T. ) ;
#140121 = CARTESIAN_POINT ( 'NONE',  ( -16.52544592524335698, -4.483927247898792601, 23.95942372801901143 ) ) ;
#140122 = CARTESIAN_POINT ( 'NONE',  ( 5.153800228976335163, 19.02544592524342804, 34.79057627198102409 ) ) ;
#140123 = CARTESIAN_POINT ( 'NONE',  ( -9.564922557960796823, -16.46253265017161027, 92.08224293864769550 ) ) ;
#140125 = CARTESIAN_POINT ( 'NONE',  ( 1.499999999999996891, 7.600000000000007638, -65.00100000000003320 ) ) ;
#140124 = CARTESIAN_POINT ( 'NONE',  ( 12.06949235617739724, 12.14591786802326823, 31.87609039468567929 ) ) ;
#140126 = CARTESIAN_POINT ( 'NONE',  ( 0.05219959533936267826, -19.03943276465977164, 35.00109039468566863 ) ) ;
#140127 = CARTESIAN_POINT ( 'NONE',  ( -4.379528057220086978, -16.55341960407618274, 99.79275706135234714 ) ) ;
#140128 = CARTESIAN_POINT ( 'NONE',  ( 0.05219959533936267826, -19.03943276465977164, 110.0010903946856757 ) ) ;
#140129 = CARTESIAN_POINT ( 'NONE',  ( 13.89961937509977652, -13.97604488694527269, 28.12390960531435624 ) ) ;
#140130 = CARTESIAN_POINT ( 'NONE',  ( -8.224510206698735004, -14.34966873604973081, 74.58442372801901854 ) ) ;
#140131 = CARTESIAN_POINT ( 'NONE',  ( -4.379528057220086978, -16.55341960407618274, 69.79275706135234714 ) ) ;
#140132 = CARTESIAN_POINT ( 'NONE',  ( 19.03943276465977164, 0.05219959533936151252, 86.25109039468567573 ) ) ;
#140133 = CARTESIAN_POINT ( 'NONE',  ( -15.80617190586768217, 15.72974639402176855, 113.1260903946856899 ) ) ;
#140134 = CARTESIAN_POINT ( 'NONE',  ( 13.89961937509977652, -13.97604488694527269, 43.12390960531434558 ) ) ;
#140135 = CARTESIAN_POINT ( 'NONE',  ( -16.51473224551069308, -9.474510206698971260, 96.66557627198102409 ) ) ;
#140136 = CARTESIAN_POINT ( 'NONE',  ( 16.55341960407611168, 4.379528057220329451, 88.95724293864769550 ) ) ;
#140137 = VECTOR ( 'NONE', #66527, 1000.000000000000114 ) ;
#140138 = CARTESIAN_POINT ( 'NONE',  ( -0.05219959533936034679, 19.03943276465977164, 57.50109039468566863 ) ) ;
#140139 = CARTESIAN_POINT ( 'NONE',  ( 21.55341960407610458, 5.719274019375980345, 48.95724293864770971 ) ) ;
#140140 = CARTESIAN_POINT ( 'NONE',  ( -13.89961937509957401, -13.97604488694547875, 24.37609039468565442 ) ) ;
#140141 = CARTESIAN_POINT ( 'NONE',  ( -9.474510206698964154, 16.51473224551069663, 90.41557627198103830 ) ) ;
#140142 = CARTESIAN_POINT ( 'NONE',  ( 5.153800228976615827, -19.02544592524334988, 25.20942372801900433 ) ) ;
#140143 = CARTESIAN_POINT ( 'NONE',  ( 15.80617190586746368, 15.72974639402197994, 69.37390960531436690 ) ) ;
#140144 = CARTESIAN_POINT ( 'NONE',  ( 9.474510206698971260, -16.51473224551069308, 107.9155762719810383 ) ) ;
#140145 = CARTESIAN_POINT ( 'NONE',  ( 13.97604488694548053, -13.89961937509957401, 85.62609039468568994 ) ) ;
#140146 = CARTESIAN_POINT ( 'NONE',  ( 19.05341960407611168, 5.049401038298154454, 113.9572429386477097 ) ) ;
#140147 = CARTESIAN_POINT ( 'NONE',  ( 9.564922557961047289, -16.46253265017146816, 105.4177570613523471 ) ) ;
#140148 = CARTESIAN_POINT ( 'NONE',  ( -0.05219959533909027116, -19.03943276465977164, 32.49890960531435979 ) ) ;
#140149 = CARTESIAN_POINT ( 'NONE',  ( -16.51473224551069308, -9.474510206698971260, 101.6655762719810241 ) ) ;
#140150 = CARTESIAN_POINT ( 'NONE',  ( 18.67979575497178502, 10.72451020669898547, 74.16557627198102409 ) ) ;
#140151 = CARTESIAN_POINT ( 'NONE',  ( 12.06949235617739724, 12.14591786802326823, 46.87609039468568994 ) ) ;
#140152 = CARTESIAN_POINT ( 'NONE',  ( 5.823673210054444382, -21.52544592524334988, 50.20942372801901854 ) ) ;
#140154 = CARTESIAN_POINT ( 'NONE',  ( -5.823673210054431948, 21.52544592524334988, 92.70942372801901854 ) ) ;
#140153 = CARTESIAN_POINT ( 'NONE',  ( 16.46253265017146816, 9.564922557961045513, 86.66775706135233293 ) ) ;
#140155 = CARTESIAN_POINT ( 'NONE',  ( -12.14591786802326823, 12.06949235617739902, 98.12609039468570415 ) ) ;
#140156 = CARTESIAN_POINT ( 'NONE',  ( 0.05219959533909260263, 19.03943276465977164, 94.99890960531436690 ) ) ;
#140157 = CARTESIAN_POINT ( 'NONE',  ( -8.224510206698948167, 14.34966873604960824, 85.41557627198102409 ) ) ;
#140158 = CARTESIAN_POINT ( 'NONE',  ( -16.55341960407611168, -4.379528057220339221, 36.45724293864768839 ) ) ;
#140159 = CARTESIAN_POINT ( 'NONE',  ( -19.05341960407617563, 5.049401038297882671, 73.54275706135233293 ) ) ;
#140160 = CARTESIAN_POINT ( 'NONE',  ( 21.55341960407619695, -5.719274019375665929, 56.04275706135235424 ) ) ;
#140161 = CARTESIAN_POINT ( 'NONE',  ( -0.05219959533936034679, 19.03943276465977164, 32.50109039468566863 ) ) ;
#140162 = CARTESIAN_POINT ( 'NONE',  ( 12.14591786802309770, 12.06949235617756955, 94.37390960531436690 ) ) ;
#140163 = CARTESIAN_POINT ( 'NONE',  ( -0.05219959533907301413, -21.53943276465977519, 27.49890960531435269 ) ) ;
#140164 = CARTESIAN_POINT ( 'NONE',  ( 16.53943276465976808, -0.05219959533910856209, 23.74890960531435269 ) ) ;
#140165 = CARTESIAN_POINT ( 'NONE',  ( 10.81492255796106328, -18.62759615963255655, 95.41775706135234714 ) ) ;
#140166 = CARTESIAN_POINT ( 'NONE',  ( 14.34966873604972726, -8.224510206698740333, 60.83442372801901854 ) ) ;
#140167 = CARTESIAN_POINT ( 'NONE',  ( -12.14591786802326823, 12.06949235617739902, 103.1260903946856757 ) ) ;
#140168 = CARTESIAN_POINT ( 'NONE',  ( -5.823673210054431948, 21.52544592524334988, 47.70942372801902565 ) ) ;
#140169 = CARTESIAN_POINT ( 'NONE',  ( -15.80617190586768217, 15.72974639402176855, 58.12609039468568994 ) ) ;
#140170 = ORIENTED_EDGE ( 'NONE', *, *, #102515, .F. ) ;
#140171 = CARTESIAN_POINT ( 'NONE',  ( -18.62759615963255300, -10.81492255796106328, 29.16775706135234003 ) ) ;
#140172 = CARTESIAN_POINT ( 'NONE',  ( 12.14591786802309770, 12.06949235617756955, 99.37390960531436690 ) ) ;
#140173 = CARTESIAN_POINT ( 'NONE',  ( 13.97604488694527802, 13.89961937509977652, 24.37390960531435624 ) ) ;
#140174 = CARTESIAN_POINT ( 'NONE',  ( 14.34966873604960469, 8.224510206698951720, 74.16557627198102409 ) ) ;
#140175 = CARTESIAN_POINT ( 'NONE',  ( -19.02544592524342804, 5.153800228976336051, 66.04057627198103830 ) ) ;
#140176 = CARTESIAN_POINT ( 'NONE',  ( -16.52544592524335698, -4.483927247898792601, 108.9594237280190185 ) ) ;
#140177 = CARTESIAN_POINT ( 'NONE',  ( -21.52544592524343514, 5.823673210054127303, 56.04057627198102409 ) ) ;
#140178 = CARTESIAN_POINT ( 'NONE',  ( 14.34966873604960469, 8.224510206698951720, 89.16557627198102409 ) ) ;
#140179 = CARTESIAN_POINT ( 'NONE',  ( -0.05219959533907301413, -21.53943276465977519, 87.49890960531436690 ) ) ;
#140180 = CARTESIAN_POINT ( 'NONE',  ( -5.153800228976328057, -19.02544592524343514, 102.2905762719810383 ) ) ;
#140182 = CARTESIAN_POINT ( 'NONE',  ( 5.049401038297881783, 19.05341960407617563, 112.2927570613523471 ) ) ;
#140181 = CARTESIAN_POINT ( 'NONE',  ( -16.51473224551069308, -9.474510206698971260, 46.66557627198102409 ) ) ;
#140183 = ADVANCED_FACE ( 'NONE', ( #15061 ), #77717, .T. ) ;
#140184 = CARTESIAN_POINT ( 'NONE',  ( 5.823673210054125526, 21.52544592524343514, 49.79057627198102409 ) ) ;
#140185 = CARTESIAN_POINT ( 'NONE',  ( -10.72451020669870658, -18.67979575497194134, 69.58442372801900433 ) ) ;
#140186 = CARTESIAN_POINT ( 'NONE',  ( 13.89961937509977652, -13.97604488694527269, 68.12390960531436690 ) ) ;
#140187 = CARTESIAN_POINT ( 'NONE',  ( -5.153800228976328057, -19.02544592524343514, 102.2905762719810383 ) ) ;
#140188 = CARTESIAN_POINT ( 'NONE',  ( -16.52544592524335698, -4.483927247898792601, 58.95942372801902565 ) ) ;
#140189 = CARTESIAN_POINT ( 'NONE',  ( -10.81492255796105439, 18.62759615963255655, 47.91775706135234714 ) ) ;
#140190 = CARTESIAN_POINT ( 'NONE',  ( -5.719274019375665041, -21.55341960407619695, 84.79275706135234714 ) ) ;
#140191 = CARTESIAN_POINT ( 'NONE',  ( 18.62759615963271287, -10.81492255796078972, 93.33224293864769550 ) ) ;
#140193 = CARTESIAN_POINT ( 'NONE',  ( -16.55341960407617563, 4.379528057220093196, 78.54275706135236135 ) ) ;
#140192 = CARTESIAN_POINT ( 'NONE',  ( -5.719274019375665041, -21.55341960407619695, 34.79275706135235424 ) ) ;
#140194 = CARTESIAN_POINT ( 'NONE',  ( -10.72451020669898014, 18.67979575497178502, 75.41557627198102409 ) ) ;
#140195 = CARTESIAN_POINT ( 'NONE',  ( 5.153800228976615827, -19.02544592524334988, 40.20942372801898301 ) ) ;
#140197 = CARTESIAN_POINT ( 'NONE',  ( 16.52544592524342804, -4.483927247898539470, 23.54057627198102765 ) ) ;
#140196 = CARTESIAN_POINT ( 'NONE',  ( -13.89961937509977652, 13.97604488694528158, 85.62390960531433848 ) ) ;
#140198 = CARTESIAN_POINT ( 'NONE',  ( -17.13100169013298668, 6.664070546373142889, 65.76789835699850073 ) ) ;
#140199 = CARTESIAN_POINT ( 'NONE',  ( 19.03943276465977164, -0.05219959533909143690, 98.74890960531436690 ) ) ;
#140200 = CARTESIAN_POINT ( 'NONE',  ( 28.79475375365586132, 2.781246896534039337E-14, 143.2656553485623760 ) ) ;
#140201 = CARTESIAN_POINT ( 'NONE',  ( -19.05341960407617563, 5.049401038297882671, 98.54275706135233293 ) ) ;
#140202 = CARTESIAN_POINT ( 'NONE',  ( 10.72451020669898902, -18.67979575497178502, 52.91557627198103830 ) ) ;
#140203 = CARTESIAN_POINT ( 'NONE',  ( -16.52544592524342804, 4.483927247898546575, 41.04057627198103120 ) ) ;
#140204 = CARTESIAN_POINT ( 'NONE',  ( -5.153800228976607833, 19.02544592524334988, 112.7094237280190043 ) ) ;
#140205 = CARTESIAN_POINT ( 'NONE',  ( -5.049401038298153566, 19.05341960407611168, 25.20724293864768484 ) ) ;
#140206 = CARTESIAN_POINT ( 'NONE',  ( 8.314922557961029526, -14.29746914071037800, 20.41775706135234714 ) ) ;
#140208 = CARTESIAN_POINT ( 'NONE',  ( -9.474510206698720793, -16.51473224551083518, 74.58442372801900433 ) ) ;
#140207 = CARTESIAN_POINT ( 'NONE',  ( -10.81492255796078084, -18.62759615963271287, 107.0822429386476955 ) ) ;
#140209 = CARTESIAN_POINT ( 'NONE',  ( -12.14591786802326823, 12.06949235617739902, 78.12609039468570415 ) ) ;
#140210 = CARTESIAN_POINT ( 'NONE',  ( -5.049401038298153566, 19.05341960407611168, 65.20724293864765286 ) ) ;
#140211 = CARTESIAN_POINT ( 'NONE',  ( -16.53943276465976808, 0.05219959533911058130, 81.24890960531436690 ) ) ;
#140212 = CIRCLE ( 'NONE', #111206, 2.500000000000000000 ) ;
#140213 = CARTESIAN_POINT ( 'NONE',  ( 5.049401038298161559, -19.05341960407611168, 62.70724293864769550 ) ) ;
#140214 = CARTESIAN_POINT ( 'NONE',  ( 8.314922557960818139, 14.29746914071049879, 64.58224293864769550 ) ) ;
#140215 = CARTESIAN_POINT ( 'NONE',  ( 5.000000000000000888, -140.0000000000000000, 0.0009999999999992653654 ) ) ;
#140216 = CARTESIAN_POINT ( 'NONE',  ( -37.11169547541891234, -4.770708601134445281, 42.23953901806350331 ) ) ;
#140217 = CARTESIAN_POINT ( 'NONE',  ( -8.314922557960811034, -14.29746914071050412, 42.08224293864769550 ) ) ;
#140218 = CARTESIAN_POINT ( 'NONE',  ( -5.153800228976328057, -19.02544592524343514, 77.29057627198099567 ) ) ;
#140219 = CARTESIAN_POINT ( 'NONE',  ( 1.348150961071065097E-30, -64.82615989628266107, -15.00000000000000000 ) ) ;
#140220 = CARTESIAN_POINT ( 'NONE',  ( 13.89961937509957401, 13.97604488694547697, 51.87609039468566863 ) ) ;
#140221 = CARTESIAN_POINT ( 'NONE',  ( -12.06949235617739369, -12.14591786802326823, 64.37609039468568994 ) ) ;
#140222 = CARTESIAN_POINT ( 'NONE',  ( -15.72974639402197994, 15.80617190586746368, 70.62390960531436690 ) ) ;
#140223 = CARTESIAN_POINT ( 'NONE',  ( -19.02544592524334988, -5.153800228976617603, 18.95942372801899722 ) ) ;
#140224 = CARTESIAN_POINT ( 'NONE',  ( -0.05219959533909027116, -19.03943276465977164, 77.49890960531435269 ) ) ;
#140225 = CARTESIAN_POINT ( 'NONE',  ( -21.00974791550152432, -22.92140990621084384, -46.84590699842355832 ) ) ;
#140226 = CARTESIAN_POINT ( 'NONE',  ( -16.46253265017160317, 9.564922557960807481, 110.8322429386476955 ) ) ;
#140227 = CARTESIAN_POINT ( 'NONE',  ( -19.05341960407611168, -5.049401038298163336, 61.45724293864769550 ) ) ;
#140228 = CARTESIAN_POINT ( 'NONE',  ( -5.719274019375665041, -21.55341960407619695, 39.79275706135235424 ) ) ;
#140229 = CARTESIAN_POINT ( 'NONE',  ( -14.29746914071049879, 8.314922557960819915, 105.8322429386476955 ) ) ;
#140232 = VERTEX_POINT ( 'NONE', #95871 ) ;
#140231 = CARTESIAN_POINT ( 'NONE',  ( 5.153800228976335163, 19.02544592524342804, 94.79057627198103830 ) ) ;
#140230 = CARTESIAN_POINT ( 'NONE',  ( 10.72451020669898902, -18.67979575497178502, 107.9155762719810241 ) ) ;
#140233 = CARTESIAN_POINT ( 'NONE',  ( 15.72974639402176855, 15.80617190586768217, 31.87609039468567929 ) ) ;
#140234 = ORIENTED_EDGE ( 'NONE', *, *, #24149, .F. ) ;
#140235 = CARTESIAN_POINT ( 'NONE',  ( 13.89961937509977652, -13.97604488694527269, 83.12390960531436690 ) ) ;
#140236 = FACE_OUTER_BOUND ( 'NONE', #102325, .T. ) ;
#140237 = CARTESIAN_POINT ( 'NONE',  ( 5.823673210054125526, 21.52544592524343514, 99.79057627198103830 ) ) ;
#140238 = CARTESIAN_POINT ( 'NONE',  ( 13.97604488694527802, 13.89961937509977652, 44.37390960531435269 ) ) ;
#140239 = CARTESIAN_POINT ( 'NONE',  ( 5.049401038297881783, 19.05341960407617563, 102.2927570613523045 ) ) ;
#140240 = CARTESIAN_POINT ( 'NONE',  ( 30.74264578624800137, -22.33583958711395212, -10.94999999453762562 ) ) ;
#140241 = AXIS2_PLACEMENT_3D ( 'NONE', #193594, #115745, #10573 ) ;
#140242 = CARTESIAN_POINT ( 'NONE',  ( -19.05341960407611168, -5.049401038298163336, 31.45724293864769550 ) ) ;
#140243 = CARTESIAN_POINT ( 'NONE',  ( 15.80617190586769283, -15.72974639402175789, 80.62609039468567573 ) ) ;
#140245 = CARTESIAN_POINT ( 'NONE',  ( -0.05219959533937732626, 21.53943276465977519, 42.50109039468567573 ) ) ;
#140244 = CARTESIAN_POINT ( 'NONE',  ( 9.474510206698971260, -16.51473224551069308, 72.91557627198102409 ) ) ;
#140246 = CARTESIAN_POINT ( 'NONE',  ( 10.81492255796106328, -18.62759615963255655, 20.41775706135234714 ) ) ;
#140247 = CARTESIAN_POINT ( 'NONE',  ( 17.81289503416611453, -24.51734667627695785, 146.6999999999999886 ) ) ;
#140248 = CARTESIAN_POINT ( 'NONE',  ( -16.51473224551069308, -9.474510206698971260, 91.66557627198103830 ) ) ;
#140249 = DIRECTION ( 'NONE',  ( 0.000000000000000000, 0.000000000000000000, 1.000000000000000000 ) ) ;
#140252 = CARTESIAN_POINT ( 'NONE',  ( 5.719274019375673035, 21.55341960407619339, 42.29275706135235424 ) ) ;
#140251 = CARTESIAN_POINT ( 'NONE',  ( 18.67979575497178502, 10.72451020669898547, 44.16557627198103120 ) ) ;
#140250 = CARTESIAN_POINT ( 'NONE',  ( -14.34966873604972548, 8.224510206698743886, 38.33442372801900433 ) ) ;
#140253 = CARTESIAN_POINT ( 'NONE',  ( 10.81492255796106328, -18.62759615963255655, 80.41775706135234714 ) ) ;
#140254 = LINE ( 'NONE', #184782, #118830 ) ;
#140255 = CARTESIAN_POINT ( 'NONE',  ( -19.03943276465977164, -0.05219959533935918106, 108.7510903946856615 ) ) ;
#140256 = CARTESIAN_POINT ( 'NONE',  ( 19.02544592524343514, -5.153800228976328945, 58.54057627198102409 ) ) ;
#140257 = CARTESIAN_POINT ( 'NONE',  ( -9.474510206698964154, 16.51473224551069663, 90.41557627198103830 ) ) ;
#140258 = CARTESIAN_POINT ( 'NONE',  ( -4.483927247898539470, -16.52544592524342804, 102.2905762719810383 ) ) ;
#140259 = CARTESIAN_POINT ( 'NONE',  ( -4.379528057220328563, 16.55341960407611168, 105.2072429386477097 ) ) ;
#140260 = CARTESIAN_POINT ( 'NONE',  ( -10.81492255796078084, -18.62759615963271287, 22.08224293864769194 ) ) ;
#140261 = CARTESIAN_POINT ( 'NONE',  ( -4.483927247898782831, 16.52544592524335698, 77.70942372801900433 ) ) ;
#140263 = CARTESIAN_POINT ( 'NONE',  ( 5.049401038298161559, -19.05341960407611168, 57.70724293864769550 ) ) ;
#140262 = CARTESIAN_POINT ( 'NONE',  ( 12.14591786802309770, 12.06949235617756955, 64.37390960531435269 ) ) ;
#140264 = CARTESIAN_POINT ( 'NONE',  ( 21.55341960407619695, -5.719274019375665929, 81.04275706135236135 ) ) ;
#140265 = CARTESIAN_POINT ( 'NONE',  ( -18.67979575497193778, 10.72451020669871902, 73.33442372801901854 ) ) ;
#140266 = CARTESIAN_POINT ( 'NONE',  ( 16.46253265017146816, 9.564922557961045513, 106.6677570613523471 ) ) ;
#140267 = CARTESIAN_POINT ( 'NONE',  ( 12.06949235617757843, -12.14591786802309237, 68.12390960531436690 ) ) ;
#140268 = CARTESIAN_POINT ( 'NONE',  ( 5.719274019375673035, 21.55341960407619339, 22.29275706135235069 ) ) ;
#140269 = CARTESIAN_POINT ( 'NONE',  ( 5.719274019375991003, -21.55341960407610458, 62.70724293864769550 ) ) ;
#140270 = CARTESIAN_POINT ( 'NONE',  ( 19.19724070472095789, 5.499999999999971578, 73.56193348274379673 ) ) ;
#140271 = CARTESIAN_POINT ( 'NONE',  ( 28.82186960331499392, -9.364793116373510529, 147.1500000054623456 ) ) ;
#140272 = CARTESIAN_POINT ( 'NONE',  ( 19.02544592524343514, -5.153800228976328945, 63.54057627198103830 ) ) ;
#140273 = CARTESIAN_POINT ( 'NONE',  ( -8.314922557960811034, -14.29746914071050412, 42.08224293864769550 ) ) ;
#140274 = AXIS2_PLACEMENT_3D ( 'NONE', #148530, #83828, #159680 ) ;
#140275 = CARTESIAN_POINT ( 'NONE',  ( 16.52544592524342804, -4.483927247898539470, 23.54057627198102765 ) ) ;
#140276 = CARTESIAN_POINT ( 'NONE',  ( -8.314922557961024197, 14.29746914071037800, 97.91775706135236135 ) ) ;
#140277 = CARTESIAN_POINT ( 'NONE',  ( -19.05341960407617563, 5.049401038297882671, 58.54275706135234003 ) ) ;
#140278 = DIRECTION ( 'NONE',  ( -1.000000000000000000, 0.000000000000000000, 0.000000000000000000 ) ) ;
#140279 = CARTESIAN_POINT ( 'NONE',  ( -19.05341960407611168, -5.049401038298163336, 111.4572429386476671 ) ) ;
#140280 = CARTESIAN_POINT ( 'NONE',  ( -4.379528057220328563, 16.55341960407611168, 80.20724293864769550 ) ) ;
#140281 = CARTESIAN_POINT ( 'NONE',  ( 5.049401038297881783, 19.05341960407617563, 47.29275706135231161 ) ) ;
#140283 = CARTESIAN_POINT ( 'NONE',  ( 0.05219959533909260263, 19.03943276465977164, 114.9989096053143669 ) ) ;
#140282 = CARTESIAN_POINT ( 'NONE',  ( -16.46253265017160317, 9.564922557960807481, 35.83224293864768839 ) ) ;
#140285 = EDGE_LOOP ( 'NONE', ( #108700, #63538, #154121, #197481 ) ) ;
#140284 = CARTESIAN_POINT ( 'NONE',  ( 18.67979575497178502, 10.72451020669898547, 49.16557627198102409 ) ) ;
#140286 = CARTESIAN_POINT ( 'NONE',  ( -14.29746914071049879, 8.314922557960819915, 95.83224293864770971 ) ) ;
#140287 = CARTESIAN_POINT ( 'NONE',  ( -8.224510206698735004, -14.34966873604973081, 54.58442372801901143 ) ) ;
#140288 = CARTESIAN_POINT ( 'NONE',  ( -16.55341960407611168, -4.379528057220339221, 86.45724293864770971 ) ) ;
#140289 = EDGE_CURVE ( 'NONE', #185003, #117197, #124192, .T. ) ;
#140290 = DIRECTION ( 'NONE',  ( 1.000000000000000000, 0.000000000000000000, 0.000000000000000000 ) ) ;
#140291 = CARTESIAN_POINT ( 'NONE',  ( 11.40812507854754365, 35.11059874428196537, -9.724999997268813701 ) ) ;
#140292 = CARTESIAN_POINT ( 'NONE',  ( -18.67979575497178146, -10.72451020669898902, 26.66557627198103475 ) ) ;
#140293 = CARTESIAN_POINT ( 'NONE',  ( 29.86685920354754842, -21.69954338932559068, -6.324999997268814234 ) ) ;
#140294 = CARTESIAN_POINT ( 'NONE',  ( -4.999999999999999112, -140.0000000000000000, 0.0009999999999992653654 ) ) ;
#140295 = ORIENTED_EDGE ( 'NONE', *, *, #37951, .F. ) ;
#140297 = CARTESIAN_POINT ( 'NONE',  ( -8.224510206698948167, 14.34966873604960824, 30.41557627198101699 ) ) ;
#140296 = CARTESIAN_POINT ( 'NONE',  ( 12.14591786802327356, -12.06949235617739191, 45.62609039468567573 ) ) ;
#140298 = CARTESIAN_POINT ( 'NONE',  ( -15.72974639402197994, 15.80617190586746368, 55.62390960531436690 ) ) ;
#140299 = CARTESIAN_POINT ( 'NONE',  ( -16.46253265017146816, -9.564922557961047289, 79.16775706135234714 ) ) ;
#140300 = CARTESIAN_POINT ( 'NONE',  ( -10.72451020669898014, 18.67979575497178502, 45.41557627198103830 ) ) ;
#140301 = CARTESIAN_POINT ( 'NONE',  ( -10.72451020669870658, -18.67979575497194134, 84.58442372801903275 ) ) ;
#140302 = CARTESIAN_POINT ( 'NONE',  ( -21.76480897080537602, 7.725232727579774306, 173.1951875983968137 ) ) ;
#140303 = CARTESIAN_POINT ( 'NONE',  ( -4.379528057220086978, -16.55341960407618274, 54.79275706135235424 ) ) ;
#140305 = CARTESIAN_POINT ( 'NONE',  ( -0.05219959533909027116, -19.03943276465977164, 102.4989096053143669 ) ) ;
#140304 = CARTESIAN_POINT ( 'NONE',  ( 5.049401038298161559, -19.05341960407611168, 37.70724293864768839 ) ) ;
#140306 = CARTESIAN_POINT ( 'NONE',  ( 9.564922557960805705, 16.46253265017160317, 34.58224293864770260 ) ) ;
#140308 = EDGE_CURVE ( 'NONE', #112403, #152017, #18401, .T. ) ;
#140307 = CARTESIAN_POINT ( 'NONE',  ( 12.06949235617757843, -12.14591786802309237, 103.1239096053143811 ) ) ;
#140309 = CARTESIAN_POINT ( 'NONE',  ( -13.89961937509977652, 13.97604488694528158, 95.62390960531436690 ) ) ;
#140310 = VERTEX_POINT ( 'NONE', #139383 ) ;
#140311 = CARTESIAN_POINT ( 'NONE',  ( 4.379528057220092307, 16.55341960407617563, 52.29275706135236135 ) ) ;
#140312 = CARTESIAN_POINT ( 'NONE',  ( -10.72451020669898014, 18.67979575497178502, 90.41557627198103830 ) ) ;
#140313 = CARTESIAN_POINT ( 'NONE',  ( 13.97604488694527802, 13.89961937509977652, 59.37390960531434558 ) ) ;
#140314 = CARTESIAN_POINT ( 'NONE',  ( 21.52544592524334988, 5.823673210054432836, 26.45942372801901854 ) ) ;
#140315 = CARTESIAN_POINT ( 'NONE',  ( 19.03943276465977164, -0.05219959533909143690, 88.74890960531436690 ) ) ;
#140316 = CARTESIAN_POINT ( 'NONE',  ( -17.49999999999999645, -5.499999999999992895, 84.20309617465829888 ) ) ;
#140317 = EDGE_LOOP ( 'NONE', ( #37741, #65951 ) ) ;
#140318 = CARTESIAN_POINT ( 'NONE',  ( 16.52544592524335698, 4.483927247898782831, 51.45942372801901854 ) ) ;
#140319 = CARTESIAN_POINT ( 'NONE',  ( -10.81492255796078084, -18.62759615963271287, 112.0822429386477097 ) ) ;
#140322 = CARTESIAN_POINT ( 'NONE',  ( 5.153800228976615827, -19.02544592524334988, 70.20942372801899012 ) ) ;
#140321 = CARTESIAN_POINT ( 'NONE',  ( 13.89961937509977652, -13.97604488694527269, 103.1239096053143527 ) ) ;
#140320 = CARTESIAN_POINT ( 'NONE',  ( -16.46253265017160317, 9.564922557960807481, 25.83224293864769194 ) ) ;
#140323 = CARTESIAN_POINT ( 'NONE',  ( 19.02544592524334988, 5.153800228976608722, 26.45942372801899722 ) ) ;
#140324 = CARTESIAN_POINT ( 'NONE',  ( -5.719274019375978568, 21.55341960407610458, 90.20724293864770971 ) ) ;
#140325 = CARTESIAN_POINT ( 'NONE',  ( -16.46253265017146816, -9.564922557961047289, 34.16775706135233293 ) ) ;
#140326 = CARTESIAN_POINT ( 'NONE',  ( 16.53943276465976808, 0.05219959533934440121, 76.25109039468568994 ) ) ;
#140327 = CARTESIAN_POINT ( 'NONE',  ( 5.153800228976335163, 19.02544592524342804, 109.7905762719810099 ) ) ;
#140328 = CARTESIAN_POINT ( 'NONE',  ( -0.05219959533909027116, -19.03943276465977164, 62.49890960531435979 ) ) ;
#140329 = CARTESIAN_POINT ( 'NONE',  ( 15.80617190586769283, -15.72974639402175789, 70.62609039468567573 ) ) ;
#140330 = CARTESIAN_POINT ( 'NONE',  ( 21.52544592524334988, 5.823673210054432836, 76.45942372801901854 ) ) ;
#140331 = CARTESIAN_POINT ( 'NONE',  ( 9.474510206698971260, -16.51473224551069308, 77.91557627198103830 ) ) ;
#140332 = CARTESIAN_POINT ( 'NONE',  ( -21.52544592524334988, -5.823673210054445271, 53.95942372801900433 ) ) ;
#140333 = CARTESIAN_POINT ( 'NONE',  ( -13.97604488694547697, 13.89961937509957934, 88.12609039468563310 ) ) ;
#140334 = CARTESIAN_POINT ( 'NONE',  ( -19.03943276465977164, 0.05219959533909376836, 51.24890960531436690 ) ) ;
#140335 = CARTESIAN_POINT ( 'NONE',  ( 16.51473224551069308, 9.474510206698969483, 104.1655762719810241 ) ) ;
#140336 = CARTESIAN_POINT ( 'NONE',  ( 19.03943276465977164, -0.05219959533909143690, 68.74890960531436690 ) ) ;
#140337 = CARTESIAN_POINT ( 'NONE',  ( -9.474510206698964154, 16.51473224551069663, 115.4155762719810241 ) ) ;
#140339 = EDGE_CURVE ( 'NONE', #158522, #182127, #124214, .T. ) ;
#140338 = CARTESIAN_POINT ( 'NONE',  ( -19.05341960407611168, -5.049401038298163336, 56.45724293864768129 ) ) ;
#140340 = AXIS2_PLACEMENT_3D ( 'NONE', #137373, #13057, #166742 ) ;
#140341 = CARTESIAN_POINT ( 'NONE',  ( -10.72451020669898014, 18.67979575497178502, 105.4155762719810383 ) ) ;
#140342 = CARTESIAN_POINT ( 'NONE',  ( -14.29746914071037622, -8.314922557961029526, 74.16775706135231871 ) ) ;
#140343 = CARTESIAN_POINT ( 'NONE',  ( -21.51693143705273670, 9.260949364272581974, 168.7281092719940432 ) ) ;
#140344 = CARTESIAN_POINT ( 'NONE',  ( -5.153800228976607833, 19.02544592524334988, 32.70942372801899722 ) ) ;
#140345 = CARTESIAN_POINT ( 'NONE',  ( -5.153800228976328057, -19.02544592524343514, 72.29057627198102409 ) ) ;
#140346 = CARTESIAN_POINT ( 'NONE',  ( -16.53943276465976808, 0.05219959533911058130, 61.24890960531435979 ) ) ;
#140347 = CARTESIAN_POINT ( 'NONE',  ( 12.14591786802309770, 12.06949235617756955, 94.37390960531436690 ) ) ;
#140348 = CARTESIAN_POINT ( 'NONE',  ( 13.89961937509977652, -13.97604488694527269, 98.12390960531433848 ) ) ;
#140349 = CARTESIAN_POINT ( 'NONE',  ( -16.46253265017160317, 9.564922557960807481, 85.83224293864769550 ) ) ;
#140350 = CARTESIAN_POINT ( 'NONE',  ( -19.02544592524342804, 5.153800228976336051, 111.0405762719810099 ) ) ;
#140351 = CARTESIAN_POINT ( 'NONE',  ( 9.564922557961047289, -16.46253265017146816, 20.41775706135233293 ) ) ;
#140352 = CARTESIAN_POINT ( 'NONE',  ( 16.53943276465976808, 0.05219959533934440121, 86.25109039468568994 ) ) ;
#140353 = CARTESIAN_POINT ( 'NONE',  ( -15.72974639402176322, -15.80617190586768395, 39.37609039468567573 ) ) ;
#140354 = CARTESIAN_POINT ( 'NONE',  ( 15.72974639402199770, -15.80617190586745480, 33.12390960531435979 ) ) ;
#140355 = CARTESIAN_POINT ( 'NONE',  ( 15.72974639402199770, -15.80617190586745480, 103.1239096053143811 ) ) ;
#140356 = CARTESIAN_POINT ( 'NONE',  ( 8.314922557960818139, 14.29746914071049879, 54.58224293864769550 ) ) ;
#140357 = CARTESIAN_POINT ( 'NONE',  ( -13.97604488694527625, -13.89961937509977652, 51.87390960531436690 ) ) ;
#140358 = CARTESIAN_POINT ( 'NONE',  ( -14.34966873604960291, -8.224510206698953496, 86.66557627198102409 ) ) ;
#140359 = CARTESIAN_POINT ( 'NONE',  ( -15.80617190586745835, -15.72974639402198527, 46.87390960531435979 ) ) ;
#140360 = CARTESIAN_POINT ( 'NONE',  ( 19.02544592524334988, 5.153800228976608722, 41.45942372801900433 ) ) ;
#140361 = VECTOR ( 'NONE', #134108, 1000.000000000000000 ) ;
#140362 = CARTESIAN_POINT ( 'NONE',  ( 12.06949235617757843, -12.14591786802309237, 108.1239096053143811 ) ) ;
#140363 = ORIENTED_EDGE ( 'NONE', *, *, #162333, .F. ) ;
#140364 = CARTESIAN_POINT ( 'NONE',  ( -14.29746914071037622, -8.314922557961029526, 64.16775706135234714 ) ) ;
#140365 = CARTESIAN_POINT ( 'NONE',  ( 19.02544592524343514, -5.153800228976328945, 68.54057627198103830 ) ) ;
#140366 = CARTESIAN_POINT ( 'NONE',  ( -22.44159573604009950, -16.30477369853688430, 143.0750000027311728 ) ) ;
#140367 = CARTESIAN_POINT ( 'NONE',  ( -4.483927247898539470, -16.52544592524342804, 87.29057627198103830 ) ) ;
#140368 = CARTESIAN_POINT ( 'NONE',  ( 10.81492255796078972, 18.62759615963270932, 34.58224293864770260 ) ) ;
#140369 = ORIENTED_EDGE ( 'NONE', *, *, #12998, .T. ) ;
#140370 = CARTESIAN_POINT ( 'NONE',  ( 16.53943276465976808, 0.05219959533934440121, 106.2510903946856757 ) ) ;
#140371 = CARTESIAN_POINT ( 'NONE',  ( 14.29746914071037800, 8.314922557961029526, 31.66775706135234358 ) ) ;
#140372 = CARTESIAN_POINT ( 'NONE',  ( 18.62759615963255655, 10.81492255796105972, 96.66775706135234714 ) ) ;
#140373 = CARTESIAN_POINT ( 'NONE',  ( -16.51473224551069308, -9.474510206698971260, 86.66557627198102409 ) ) ;
#140374 = CARTESIAN_POINT ( 'NONE',  ( 10.81492255796078972, 18.62759615963270932, 114.5822429386477097 ) ) ;
#140375 = CARTESIAN_POINT ( 'NONE',  ( -16.46253265017160317, 9.564922557960807481, 35.83224293864768839 ) ) ;
#140376 = CARTESIAN_POINT ( 'NONE',  ( -4.379528057220086978, -16.55341960407618274, 24.79275706135235779 ) ) ;
#140377 = VECTOR ( 'NONE', #161366, 1000.000000000000000 ) ;
#140378 = CARTESIAN_POINT ( 'NONE',  ( 16.51473224551083163, -9.474510206698727899, 100.8344237280190043 ) ) ;
#140379 = CARTESIAN_POINT ( 'NONE',  ( -10.81492255796078084, -18.62759615963271287, 97.08224293864770971 ) ) ;
#140380 = CARTESIAN_POINT ( 'NONE',  ( 16.51473224551083163, -9.474510206698727899, 65.83442372801900433 ) ) ;
#140381 = CARTESIAN_POINT ( 'NONE',  ( 4.500000000000000888, -132.8113331068338425, 10.91562811307058389 ) ) ;
#140382 = CARTESIAN_POINT ( 'NONE',  ( -15.80617190586768217, 15.72974639402176855, 23.12609039468567573 ) ) ;
#140383 = CARTESIAN_POINT ( 'NONE',  ( 13.89961937509977652, -13.97604488694527269, 83.12390960531436690 ) ) ;
#140384 = VECTOR ( 'NONE', #71506, 1000.000000000000000 ) ;
#140385 = CARTESIAN_POINT ( 'NONE',  ( -0.05219959533934338120, 16.53943276465976808, 37.50109039468568284 ) ) ;
#140386 = CARTESIAN_POINT ( 'NONE',  ( 13.89961937509957401, 13.97604488694547697, 66.87609039468567573 ) ) ;
#140388 = CARTESIAN_POINT ( 'NONE',  ( -14.34966873604960291, -8.224510206698953496, 71.66557627198100988 ) ) ;
#140387 = CARTESIAN_POINT ( 'NONE',  ( 0.05219959533907565091, 21.53943276465977519, 114.9989096053143669 ) ) ;
#140389 = CARTESIAN_POINT ( 'NONE',  ( -5.049401038298153566, 19.05341960407611168, 80.20724293864769550 ) ) ;
#140391 = CARTESIAN_POINT ( 'NONE',  ( -9.474510206698720793, -16.51473224551083518, 39.58442372801899722 ) ) ;
#140390 = CARTESIAN_POINT ( 'NONE',  ( -12.06949235617739369, -12.14591786802326823, 34.37609039468568284 ) ) ;
#140392 = CARTESIAN_POINT ( 'NONE',  ( 5.719274019375673035, 21.55341960407619339, 67.29275706135234714 ) ) ;
#140393 = CARTESIAN_POINT ( 'NONE',  ( 4.483927247898790824, -16.52544592524335698, 20.20942372801900788 ) ) ;
#140394 = CARTESIAN_POINT ( 'NONE',  ( -5.153800228976328057, -19.02544592524343514, 57.29057627198103120 ) ) ;
#140395 = CARTESIAN_POINT ( 'NONE',  ( -16.46253265017146816, -9.564922557961047289, 84.16775706135233293 ) ) ;
#140396 = CARTESIAN_POINT ( 'NONE',  ( -14.29746914071037622, -8.314922557961029526, 59.16775706135234714 ) ) ;
#140397 = CARTESIAN_POINT ( 'NONE',  ( -21.53943276465977519, -0.05219959533937600094, 103.7510903946857042 ) ) ;
#140398 = CARTESIAN_POINT ( 'NONE',  ( 5.153800228976615827, -19.02544592524334988, 65.20942372801900433 ) ) ;
#140399 = CARTESIAN_POINT ( 'NONE',  ( 0.05219959533909260263, 19.03943276465977164, 49.99890960531435979 ) ) ;
#140400 = CARTESIAN_POINT ( 'NONE',  ( -5.823673210054116645, -21.52544592524344225, 67.29057627198103830 ) ) ;
#140402 = CARTESIAN_POINT ( 'NONE',  ( -13.89961937509957401, -13.97604488694547875, 69.37609039468564731 ) ) ;
#140401 = CARTESIAN_POINT ( 'NONE',  ( 8.314922557960818139, 14.29746914071049879, 64.58224293864769550 ) ) ;
#140403 = CARTESIAN_POINT ( 'NONE',  ( 21.93653645885849457, 8.192071713419744938, 172.2938920027118570 ) ) ;
#140404 = CARTESIAN_POINT ( 'NONE',  ( -16.51473224551082808, 9.474510206698731452, 43.33442372801900433 ) ) ;
#140405 = CARTESIAN_POINT ( 'NONE',  ( 12.14591786802327356, -12.06949235617739191, 95.62609039468568994 ) ) ;
#140406 = CARTESIAN_POINT ( 'NONE',  ( -12.06949235617756955, 12.14591786802309770, 70.62390960531436690 ) ) ;
#140408 = CARTESIAN_POINT ( 'NONE',  ( -5.359611314223446995E-15, 29.16686587814335496, 140.3750000027311842 ) ) ;
#140407 = CARTESIAN_POINT ( 'NONE',  ( 18.62759615963255655, 10.81492255796105972, 101.6677570613523613 ) ) ;
#140409 = CARTESIAN_POINT ( 'NONE',  ( 18.62759615963271287, -10.81492255796078972, 93.33224293864769550 ) ) ;
#140410 = CARTESIAN_POINT ( 'NONE',  ( 13.89961937509977652, -13.97604488694527269, 58.12390960531436690 ) ) ;
#140411 = CARTESIAN_POINT ( 'NONE',  ( -5.719274019375665041, -21.55341960407619695, 69.79275706135234714 ) ) ;
#140412 = CARTESIAN_POINT ( 'NONE',  ( 16.46253265017160672, -9.564922557960803928, 48.33224293864769550 ) ) ;
#140413 = CARTESIAN_POINT ( 'NONE',  ( 0.05219959533909260263, 19.03943276465977164, 64.99890960531436690 ) ) ;
#140414 = CARTESIAN_POINT ( 'NONE',  ( 9.474510206698971260, -16.51473224551069308, 27.91557627198103120 ) ) ;
#140415 = CARTESIAN_POINT ( 'NONE',  ( -16.51473224551069308, -9.474510206698971260, 106.6655762719810383 ) ) ;
#140416 = CARTESIAN_POINT ( 'NONE',  ( 4.379528057220339221, -16.55341960407611168, 47.70724293864770260 ) ) ;
#140417 = CARTESIAN_POINT ( 'NONE',  ( 19.05341960407611168, 5.049401038298154454, 28.95724293864769550 ) ) ;
#140418 = CARTESIAN_POINT ( 'NONE',  ( 8.224510206698953496, -14.34966873604960469, 82.91557627198103830 ) ) ;
#140419 = VECTOR ( 'NONE', #122185, 1000.000000000000000 ) ;
#140420 = CARTESIAN_POINT ( 'NONE',  ( -10.72451020669898014, 18.67979575497178502, 100.4155762719810241 ) ) ;
#140421 = CARTESIAN_POINT ( 'NONE',  ( 21.52544592524334988, 5.823673210054432836, 31.45942372801901854 ) ) ;
#140422 = CARTESIAN_POINT ( 'NONE',  ( 17.81289503416610742, 24.51734667627700404, 149.2999999999999261 ) ) ;
#140423 = CARTESIAN_POINT ( 'NONE',  ( 4.483927247898790824, -16.52544592524335698, 45.20942372801901854 ) ) ;
#140424 = CARTESIAN_POINT ( 'NONE',  ( 5.823673210054125526, 21.52544592524343514, 84.79057627198102409 ) ) ;
#140425 = CARTESIAN_POINT ( 'NONE',  ( -5.719274019375665041, -21.55341960407619695, 109.7927570613523613 ) ) ;
#140426 = CARTESIAN_POINT ( 'NONE',  ( -0.05219959533909027116, -19.03943276465977164, 107.4989096053143527 ) ) ;
#140427 = CARTESIAN_POINT ( 'NONE',  ( -10.81492255796105439, 18.62759615963255655, 42.91775706135235424 ) ) ;
#140428 = CARTESIAN_POINT ( 'NONE',  ( -5.823673210054116645, -21.52544592524344225, 47.29057627198103120 ) ) ;
#140429 = CARTESIAN_POINT ( 'NONE',  ( 0.05219959533934541429, -16.53943276465976808, 110.0010903946856757 ) ) ;
#140431 = CARTESIAN_POINT ( 'NONE',  ( -18.67979575497193778, 10.72451020669871902, 98.33442372801901854 ) ) ;
#140430 = CARTESIAN_POINT ( 'NONE',  ( -10.72451020669870658, -18.67979575497194134, 59.58442372801901854 ) ) ;
#140432 = CARTESIAN_POINT ( 'NONE',  ( -19.03943276465977164, -0.05219959533935918106, 28.75109039468566507 ) ) ;
#140433 = CARTESIAN_POINT ( 'NONE',  ( 0.05219959533934541429, -16.53943276465976808, 90.00109039468567573 ) ) ;
#140434 = CARTESIAN_POINT ( 'NONE',  ( 21.55341960407619695, -5.719274019375665929, 46.04275706135234714 ) ) ;
#140435 = CARTESIAN_POINT ( 'NONE',  ( 5.153800228976335163, 19.02544592524342804, 44.79057627198103830 ) ) ;
#140436 = CARTESIAN_POINT ( 'NONE',  ( 9.564922557961047289, -16.46253265017146816, 20.41775706135233293 ) ) ;
#140437 = CARTESIAN_POINT ( 'NONE',  ( -18.67979575497178146, -10.72451020669898902, 31.66557627198102054 ) ) ;
#140438 = CARTESIAN_POINT ( 'NONE',  ( 10.81492255796106328, -18.62759615963255655, 20.41775706135234714 ) ) ;
#140439 = CARTESIAN_POINT ( 'NONE',  ( -10.72451020669898014, 18.67979575497178502, 70.41557627198102409 ) ) ;
#140440 = CARTESIAN_POINT ( 'NONE',  ( -0.05219959533934338120, 16.53943276465976808, 42.50109039468567573 ) ) ;
#140442 = CARTESIAN_POINT ( 'NONE',  ( -5.823673210054116645, -21.52544592524344225, 77.29057627198102409 ) ) ;
#140441 = DIRECTION ( 'NONE',  ( 0.000000000000000000, 0.000000000000000000, 1.000000000000000000 ) ) ;
#140444 = CARTESIAN_POINT ( 'NONE',  ( -16.53943276465976808, 0.05219959533911058130, 66.24890960531436690 ) ) ;
#140443 = CARTESIAN_POINT ( 'NONE',  ( 16.53943276465976808, 0.05219959533934440121, 61.25109039468567573 ) ) ;
#140445 = CARTESIAN_POINT ( 'NONE',  ( -22.47021661561681327, 20.34442274205735046, -47.91864530057669924 ) ) ;
#140446 = CARTESIAN_POINT ( 'NONE',  ( -13.89961937509957401, -13.97604488694547875, 94.37609039468566152 ) ) ;
#140447 = CARTESIAN_POINT ( 'NONE',  ( -21.31291730435233234, 0.2247805922401949763, -56.45983593933052447 ) ) ;
#140448 = CARTESIAN_POINT ( 'NONE',  ( 16.52544592524335698, 4.483927247898782831, 46.45942372801901854 ) ) ;
#140449 = CARTESIAN_POINT ( 'NONE',  ( 0.05219959533937995610, -21.53943276465977519, 20.00109039468568639 ) ) ;
#140450 = CARTESIAN_POINT ( 'NONE',  ( -10.72451020669898014, 18.67979575497178502, 70.41557627198102409 ) ) ;
#140451 = CARTESIAN_POINT ( 'NONE',  ( 16.51473224551069308, 9.474510206698969483, 114.1655762719810241 ) ) ;
#140452 = CARTESIAN_POINT ( 'NONE',  ( -16.52544592524335698, -4.483927247898792601, 63.95942372801901854 ) ) ;
#140453 = CARTESIAN_POINT ( 'NONE',  ( 5.153800228976335163, 19.02544592524342804, 69.79057627198103830 ) ) ;
#140455 = CARTESIAN_POINT ( 'NONE',  ( -5.153800228976607833, 19.02544592524334988, 107.7094237280189759 ) ) ;
#140454 = CARTESIAN_POINT ( 'NONE',  ( -18.67979575497193778, 10.72451020669871902, 43.33442372801901143 ) ) ;
#140456 = EDGE_CURVE ( 'NONE', #172412, #116580, #199091, .T. ) ;
#140457 = CARTESIAN_POINT ( 'NONE',  ( 0.05219959533909260263, 19.03943276465977164, 109.9989096053143669 ) ) ;
#140458 = CARTESIAN_POINT ( 'NONE',  ( -9.564922557961040184, 16.46253265017147172, 27.91775706135232582 ) ) ;
#140459 = CARTESIAN_POINT ( 'NONE',  ( -12.14591786802326823, 12.06949235617739902, 43.12609039468568284 ) ) ;
#140460 = CARTESIAN_POINT ( 'NONE',  ( 16.51473224551069308, 9.474510206698969483, 104.1655762719810241 ) ) ;
#140461 = CARTESIAN_POINT ( 'NONE',  ( 18.62759615963271287, -10.81492255796078972, 103.3322429386476955 ) ) ;
#140462 = CARTESIAN_POINT ( 'NONE',  ( 5.049401038298161559, -19.05341960407611168, 57.70724293864769550 ) ) ;
#140463 = CARTESIAN_POINT ( 'NONE',  ( -16.18388926212242751, 7.379444403734384039, 24.56046848633850033 ) ) ;
#140464 = CARTESIAN_POINT ( 'NONE',  ( 14.29746914071049879, -8.314922557960816363, 78.33224293864770971 ) ) ;
#140465 = CARTESIAN_POINT ( 'NONE',  ( -5.153800228976328057, -19.02544592524343514, 112.2905762719810099 ) ) ;
#140466 = CARTESIAN_POINT ( 'NONE',  ( 5.153800228976335163, 19.02544592524342804, 24.79057627198102765 ) ) ;
#140467 = CIRCLE ( 'NONE', #130787, 0.5000000000000004441 ) ;
#140468 = CARTESIAN_POINT ( 'NONE',  ( 15.72974639402199770, -15.80617190586745480, 98.12390960531436690 ) ) ;
#140469 = CARTESIAN_POINT ( 'NONE',  ( -19.02544592524334988, -5.153800228976617603, 63.95942372801899012 ) ) ;
#140471 = ADVANCED_FACE ( 'NONE', ( #32221 ), #170730, .F. ) ;
#140470 = CARTESIAN_POINT ( 'NONE',  ( 5.719274019375991003, -21.55341960407610458, 32.70724293864770260 ) ) ;
#140472 = CARTESIAN_POINT ( 'NONE',  ( -9.474510206698964154, 16.51473224551069663, 30.41557627198102054 ) ) ;
#140473 = CARTESIAN_POINT ( 'NONE',  ( 0.05219959533907565091, 21.53943276465977519, 49.99890960531437401 ) ) ;
#140474 = CARTESIAN_POINT ( 'NONE',  ( 9.474510206698971260, -16.51473224551069308, 102.9155762719810241 ) ) ;
#140475 = CARTESIAN_POINT ( 'NONE',  ( -21.53943276465977519, -0.05219959533937600094, 83.75109039468568994 ) ) ;
#140476 = CARTESIAN_POINT ( 'NONE',  ( 9.564922557960805705, 16.46253265017160317, 49.58224293864770260 ) ) ;
#140477 = CARTESIAN_POINT ( 'NONE',  ( -16.55341960407611168, -4.379528057220339221, 91.45724293864769550 ) ) ;
#140478 = CARTESIAN_POINT ( 'NONE',  ( -4.379528057220086978, -16.55341960407618274, 39.79275706135235424 ) ) ;
#140479 = CARTESIAN_POINT ( 'NONE',  ( -19.03943276465977164, 0.05219959533909376836, 56.24890960531435979 ) ) ;
#140480 = CARTESIAN_POINT ( 'NONE',  ( -21.53943276465977519, -0.05219959533937600094, 68.75109039468568994 ) ) ;
#140481 = ORIENTED_EDGE ( 'NONE', *, *, #163492, .F. ) ;
#140482 = CARTESIAN_POINT ( 'NONE',  ( -0.05219959533936034679, 19.03943276465977164, 27.50109039468566507 ) ) ;
#140483 = AXIS2_PLACEMENT_3D ( 'NONE', #155267, #140081, #141085 ) ;
#140484 = CARTESIAN_POINT ( 'NONE',  ( -16.51473224551082808, 9.474510206698731452, 43.33442372801900433 ) ) ;
#140485 = DIRECTION ( 'NONE',  ( -0.000000000000000000, 0.000000000000000000, 1.000000000000000000 ) ) ;
#140486 = CARTESIAN_POINT ( 'NONE',  ( -18.67979575497193778, 10.72451020669871902, 33.33442372801900433 ) ) ;
#140487 = CARTESIAN_POINT ( 'NONE',  ( 4.500000000000000888, -139.5000000000000000, 13.35010376910484275 ) ) ;
#140488 = CARTESIAN_POINT ( 'NONE',  ( -9.564922557961040184, 16.46253265017147172, 37.91775706135233293 ) ) ;
#140489 = CARTESIAN_POINT ( 'NONE',  ( -9.564922557960796823, -16.46253265017161027, 87.08224293864769550 ) ) ;
#140490 = CARTESIAN_POINT ( 'NONE',  ( -13.97604488694527625, -13.89961937509977652, 66.87390960531436690 ) ) ;
#140491 = CARTESIAN_POINT ( 'NONE',  ( -16.53943276465976808, 0.05219959533911058130, 31.24890960531435979 ) ) ;
#140493 = CARTESIAN_POINT ( 'NONE',  ( -5.823673210054431948, 21.52544592524334988, 87.70942372801901854 ) ) ;
#140492 = CARTESIAN_POINT ( 'NONE',  ( -19.03943276465977164, 0.05219959533909376836, 116.2489096053143669 ) ) ;
#140494 = CARTESIAN_POINT ( 'NONE',  ( 36.91746825000000598, -11.99521256947793546, -10.22499999726881548 ) ) ;
#140495 = CARTESIAN_POINT ( 'NONE',  ( 17.40805194822031510, 6.112264579159357503, 56.66628727489389661 ) ) ;
#140496 = CARTESIAN_POINT ( 'NONE',  ( -10.81492255796105439, 18.62759615963255655, 82.91775706135234714 ) ) ;
#140497 = CARTESIAN_POINT ( 'NONE',  ( 22.98313974082799405, -1.499560036715175126, -57.70434786042491737 ) ) ;
#140498 = CARTESIAN_POINT ( 'NONE',  ( 16.46253265017160672, -9.564922557960803928, 98.33224293864769550 ) ) ;
#140499 = CARTESIAN_POINT ( 'NONE',  ( 33.84581411518096417, 5.355620490906737530, 93.73536670833321693 ) ) ;
#140500 = CARTESIAN_POINT ( 'NONE',  ( 10.81492255796078972, 18.62759615963270932, 64.58224293864769550 ) ) ;
#140501 = CARTESIAN_POINT ( 'NONE',  ( 4.483927247898545687, 16.52544592524342804, 29.79057627198102409 ) ) ;
#140503 = CARTESIAN_POINT ( 'NONE',  ( -19.03943276465977164, 0.05219959533909376836, 101.2489096053143669 ) ) ;
#140502 = CARTESIAN_POINT ( 'NONE',  ( 8.314922557960818139, 14.29746914071049879, 109.5822429386476955 ) ) ;
#140504 = CARTESIAN_POINT ( 'NONE',  ( -19.02544592524334988, -5.153800228976617603, 23.95942372801900078 ) ) ;
#140505 = CARTESIAN_POINT ( 'NONE',  ( -12.14591786802309592, -12.06949235617757132, 96.87390960531436690 ) ) ;
#140506 = CARTESIAN_POINT ( 'NONE',  ( 15.72974639402176855, 15.80617190586768217, 66.87609039468568994 ) ) ;
#140507 = CARTESIAN_POINT ( 'NONE',  ( 19.05341960407611168, 5.049401038298154454, 113.9572429386477097 ) ) ;
#140508 = CARTESIAN_POINT ( 'NONE',  ( 12.14591786802327356, -12.06949235617739191, 105.6260903946856899 ) ) ;
#140509 = CARTESIAN_POINT ( 'NONE',  ( -16.46253265017146816, -9.564922557961047289, 69.16775706135233293 ) ) ;
#140510 = CARTESIAN_POINT ( 'NONE',  ( 36.91746824999999887, -11.99521256947793546, -4.224999997268813701 ) ) ;
#140511 = CARTESIAN_POINT ( 'NONE',  ( -5.153800228976328057, -19.02544592524343514, 107.2905762719810383 ) ) ;
#140512 = CARTESIAN_POINT ( 'NONE',  ( 12.06949235617757843, -12.14591786802309237, 83.12390960531436690 ) ) ;
#140513 = CARTESIAN_POINT ( 'NONE',  ( 16.51473224551083163, -9.474510206698727899, 55.83442372801899722 ) ) ;
#140514 = CARTESIAN_POINT ( 'NONE',  ( 9.564922557960805705, 16.46253265017160317, 74.58224293864769550 ) ) ;
#140515 = CARTESIAN_POINT ( 'NONE',  ( -14.29746914071049879, 8.314922557960819915, 55.83224293864770260 ) ) ;
#140516 = CARTESIAN_POINT ( 'NONE',  ( -19.02544592524334988, -5.153800228976617603, 88.95942372801897591 ) ) ;
#140517 = CARTESIAN_POINT ( 'NONE',  ( 15.80617190586746368, 15.72974639402197994, 49.37390960531436690 ) ) ;
#140518 = ORIENTED_EDGE ( 'NONE', *, *, #164973, .T. ) ;
#140519 = CARTESIAN_POINT ( 'NONE',  ( -4.379528057220328563, 16.55341960407611168, 110.2072429386477239 ) ) ;
#140520 = CARTESIAN_POINT ( 'NONE',  ( 13.97604488694548053, -13.89961937509957401, 100.6260903946856757 ) ) ;
#140522 = CARTESIAN_POINT ( 'NONE',  ( -5.823673210054116645, -21.52544592524344225, 82.29057627198103830 ) ) ;
#140521 = CARTESIAN_POINT ( 'NONE',  ( -19.02544592524342804, 5.153800228976336051, 71.04057627198099567 ) ) ;
#140524 = CARTESIAN_POINT ( 'NONE',  ( 16.46253265017160672, -9.564922557960803928, 68.33224293864770971 ) ) ;
#140523 = CARTESIAN_POINT ( 'NONE',  ( 16.52544592524335698, 4.483927247898782831, 96.45942372801901854 ) ) ;
#140525 = CARTESIAN_POINT ( 'NONE',  ( 9.564922557961047289, -16.46253265017146816, 50.41775706135233293 ) ) ;
#140526 = CARTESIAN_POINT ( 'NONE',  ( 21.55341960407619695, -5.719274019375665929, 86.04275706135236135 ) ) ;
#140527 = CARTESIAN_POINT ( 'NONE',  ( 21.52544592524344225, -5.823673210054117533, 68.54057627198103830 ) ) ;
#140528 = CARTESIAN_POINT ( 'NONE',  ( -5.049401038298153566, 19.05341960407611168, 105.2072429386476671 ) ) ;
#140529 = VECTOR ( 'NONE', #161034, 1000.000000000000000 ) ;
#140530 = CARTESIAN_POINT ( 'NONE',  ( 16.51473224551069308, 9.474510206698969483, 34.16557627198102409 ) ) ;
#140531 = CARTESIAN_POINT ( 'NONE',  ( -12.06949235617739369, -12.14591786802326823, 104.3760903946856899 ) ) ;
#140532 = CARTESIAN_POINT ( 'NONE',  ( 16.52544592524335698, 4.483927247898782831, 26.45942372801901854 ) ) ;
#140533 = CARTESIAN_POINT ( 'NONE',  ( 17.72517630440429670, -5.500000000000135891, 43.42175719257209465 ) ) ;
#140534 = CARTESIAN_POINT ( 'NONE',  ( -15.80617190586768217, 15.72974639402176855, 103.1260903946856757 ) ) ;
#140535 = AXIS2_PLACEMENT_3D ( 'NONE', #81266, #142947, #130776 ) ;
#140536 = CARTESIAN_POINT ( 'NONE',  ( -8.224510206698948167, 14.34966873604960824, 55.41557627198102409 ) ) ;
#140537 = CARTESIAN_POINT ( 'NONE',  ( 0.05219959533907565091, 21.53943276465977519, 89.99890960531438111 ) ) ;
#140538 = CARTESIAN_POINT ( 'NONE',  ( 10.72451020669898902, -18.67979575497178502, 87.91557627198103830 ) ) ;
#140539 = CARTESIAN_POINT ( 'NONE',  ( 17.05116617787824396, -6.768360034955806626, 96.15675553259195851 ) ) ;
#140540 = CARTESIAN_POINT ( 'NONE',  ( -5.719274019375978568, 21.55341960407610458, 40.20724293864769550 ) ) ;
#140541 = CARTESIAN_POINT ( 'NONE',  ( 12.06949235617739724, 12.14591786802326823, 61.87609039468568284 ) ) ;
#140542 = CARTESIAN_POINT ( 'NONE',  ( -16.52544592524342804, 4.483927247898546575, 91.04057627198103830 ) ) ;
#140543 = CARTESIAN_POINT ( 'NONE',  ( 5.049401038298161559, -19.05341960407611168, 52.70724293864767418 ) ) ;
#140544 = CARTESIAN_POINT ( 'NONE',  ( 15.50000000000000178, -5.500000000000000888, 120.0000000000000142 ) ) ;
#140545 = CARTESIAN_POINT ( 'NONE',  ( -4.483927247898782831, 16.52544592524335698, 102.7094237280190185 ) ) ;
#140546 = CARTESIAN_POINT ( 'NONE',  ( -21.55341960407619339, 5.719274019375674811, 33.54275706135234714 ) ) ;
#140547 = CARTESIAN_POINT ( 'NONE',  ( -0.05219959533909027116, -19.03943276465977164, 97.49890960531436690 ) ) ;
#140548 = CARTESIAN_POINT ( 'NONE',  ( -18.67979575497193778, 10.72451020669871902, 68.33442372801900433 ) ) ;
#140549 = CARTESIAN_POINT ( 'NONE',  ( -31.90000000000003411, 3.219216299777112361E-13, -45.64921306006598201 ) ) ;
#140550 = CARTESIAN_POINT ( 'NONE',  ( 9.474510206698971260, -16.51473224551069308, 27.91557627198103120 ) ) ;
#140551 = EDGE_LOOP ( 'NONE', ( #152879, #125539, #146560, #113818, #35577 ) ) ;
#140552 = CARTESIAN_POINT ( 'NONE',  ( 15.72974639402176855, 15.80617190586768217, 56.87609039468568994 ) ) ;
#140554 = CARTESIAN_POINT ( 'NONE',  ( -16.46253265017160317, 9.564922557960807481, 115.8322429386477097 ) ) ;
#140553 = CARTESIAN_POINT ( 'NONE',  ( 16.46253265017160672, -9.564922557960803928, 53.33224293864768839 ) ) ;
#140555 = CARTESIAN_POINT ( 'NONE',  ( -19.05341960407611168, -5.049401038298163336, 91.45724293864766707 ) ) ;
#140556 = CARTESIAN_POINT ( 'NONE',  ( 13.89961937509957401, 13.97604488694547697, 61.87609039468566863 ) ) ;
#140557 = CARTESIAN_POINT ( 'NONE',  ( 10.72451020669871369, 18.67979575497193778, 42.08442372801901854 ) ) ;
#140558 = CARTESIAN_POINT ( 'NONE',  ( -5.153800228976607833, 19.02544592524334988, 57.70942372801899012 ) ) ;
#140559 = CARTESIAN_POINT ( 'NONE',  ( 16.51473224551069308, 9.474510206698969483, 44.16557627198103120 ) ) ;
#140560 = CARTESIAN_POINT ( 'NONE',  ( -14.29746914071037622, -8.314922557961029526, 109.1677570613523613 ) ) ;
#140561 = CARTESIAN_POINT ( 'NONE',  ( -5.049401038297874678, -19.05341960407617918, 79.79275706135233293 ) ) ;
#140562 = CARTESIAN_POINT ( 'NONE',  ( -16.55341960407617563, 4.379528057220093196, 113.5427570613523756 ) ) ;
#140563 = CARTESIAN_POINT ( 'NONE',  ( -19.02544592524334988, -5.153800228976617603, 53.95942372801898301 ) ) ;
#140564 = CARTESIAN_POINT ( 'NONE',  ( 16.51473224551069308, 9.474510206698969483, 99.16557627198102409 ) ) ;
#140565 = CARTESIAN_POINT ( 'NONE',  ( 0.05219959533937995610, -21.53943276465977519, 110.0010903946856757 ) ) ;
#140566 = CARTESIAN_POINT ( 'NONE',  ( -0.05219959533936034679, 19.03943276465977164, 27.50109039468566507 ) ) ;
#140567 = CARTESIAN_POINT ( 'NONE',  ( -5.153800228976328057, -19.02544592524343514, 27.29057627198103120 ) ) ;
#140568 = CARTESIAN_POINT ( 'NONE',  ( 10.81492255796106328, -18.62759615963255655, 90.41775706135236135 ) ) ;
#140569 = CARTESIAN_POINT ( 'NONE',  ( -4.483927247898782831, 16.52544592524335698, 32.70942372801900433 ) ) ;
#140570 = CARTESIAN_POINT ( 'NONE',  ( 16.51473224551069308, 9.474510206698969483, 99.16557627198102409 ) ) ;
#140571 = CARTESIAN_POINT ( 'NONE',  ( 3.889087296525912674, -30.00000000000002132, 8.181980515339454030 ) ) ;
#140572 = CARTESIAN_POINT ( 'NONE',  ( -0.05219959533909027116, -19.03943276465977164, 82.49890960531436690 ) ) ;
#140573 = DIRECTION ( 'NONE',  ( 1.000000000000000000, 0.000000000000000000, 0.000000000000000000 ) ) ;
#140574 = CARTESIAN_POINT ( 'NONE',  ( -16.46253265017146816, -9.564922557961047289, 84.16775706135233293 ) ) ;
#140575 = CARTESIAN_POINT ( 'NONE',  ( 9.474510206698971260, -16.51473224551069308, 107.9155762719810383 ) ) ;
#140576 = CARTESIAN_POINT ( 'NONE',  ( 5.719274019375673035, 21.55341960407619339, 97.29275706135234714 ) ) ;
#140577 = CARTESIAN_POINT ( 'NONE',  ( -14.34966873604960291, -8.224510206698953496, 101.6655762719810383 ) ) ;
#140578 = CARTESIAN_POINT ( 'NONE',  ( 9.474510206698971260, -16.51473224551069308, 27.91557627198103120 ) ) ;
#140579 = CARTESIAN_POINT ( 'NONE',  ( -21.53943276465977519, 0.05219959533907696930, 51.24890960531436690 ) ) ;
#140580 = CARTESIAN_POINT ( 'NONE',  ( -18.62759615963270932, 10.81492255796079327, 30.83224293864770260 ) ) ;
#140581 = CARTESIAN_POINT ( 'NONE',  ( 0.05219959533910956823, 16.53943276465976808, 109.9989096053143527 ) ) ;
#140582 = CARTESIAN_POINT ( 'NONE',  ( -13.74234921310041813, 0.4081324879002323769, -62.56359473395610138 ) ) ;
#140583 = CARTESIAN_POINT ( 'NONE',  ( -16.46253265017146816, -9.564922557961047289, 64.16775706135233293 ) ) ;
#140584 = CARTESIAN_POINT ( 'NONE',  ( 8.224510206698953496, -14.34966873604960469, 37.91557627198102409 ) ) ;
#140585 = CARTESIAN_POINT ( 'NONE',  ( -15.72974639402197994, 15.80617190586746368, 25.62390960531435624 ) ) ;
#140586 = CARTESIAN_POINT ( 'NONE',  ( -18.67979575497193778, 10.72451020669871902, 73.33442372801901854 ) ) ;
#140587 = CARTESIAN_POINT ( 'NONE',  ( 10.81492255796078972, 18.62759615963270932, 74.58224293864768129 ) ) ;
#140588 = CARTESIAN_POINT ( 'NONE',  ( 5.823673210054444382, -21.52544592524334988, 45.20942372801901854 ) ) ;
#140589 = CARTESIAN_POINT ( 'NONE',  ( -5.719274019375978568, 21.55341960407610458, 95.20724293864769550 ) ) ;
#140590 = CARTESIAN_POINT ( 'NONE',  ( -21.52544592524334988, -5.823673210054445271, 53.95942372801900433 ) ) ;
#140591 = CARTESIAN_POINT ( 'NONE',  ( -16.51473224551069308, -9.474510206698971260, 26.66557627198103120 ) ) ;
#140592 = CARTESIAN_POINT ( 'NONE',  ( 13.97604488694527802, 13.89961937509977652, 84.37390960531433848 ) ) ;
#140593 = CARTESIAN_POINT ( 'NONE',  ( -12.06949235617739369, -12.14591786802326823, 79.37609039468567573 ) ) ;
#140594 = CARTESIAN_POINT ( 'NONE',  ( 4.483927247898545687, 16.52544592524342804, 104.7905762719810241 ) ) ;
#140595 = CARTESIAN_POINT ( 'NONE',  ( 0.05219959533909260263, 19.03943276465977164, 114.9989096053143669 ) ) ;
#140596 = CARTESIAN_POINT ( 'NONE',  ( 14.29746914071049879, -8.314922557960816363, 53.33224293864769550 ) ) ;
#140597 = CARTESIAN_POINT ( 'NONE',  ( -16.55341960407611168, -4.379528057220339221, 26.45724293864768839 ) ) ;
#140598 = CARTESIAN_POINT ( 'NONE',  ( -13.89961937509977652, 13.97604488694528158, 60.62390960531436690 ) ) ;
#140599 = CARTESIAN_POINT ( 'NONE',  ( 16.46253265017160672, -9.564922557960803928, 33.33224293864770260 ) ) ;
#140600 = CARTESIAN_POINT ( 'NONE',  ( -15.80617190586745835, -15.72974639402198527, 41.87390960531435979 ) ) ;
#140601 = CARTESIAN_POINT ( 'NONE',  ( 19.03943276465977164, 0.05219959533936151252, 41.25109039468566152 ) ) ;
#140603 = CARTESIAN_POINT ( 'NONE',  ( 14.29746914071049879, -8.314922557960816363, 33.33224293864769550 ) ) ;
#140602 = DIRECTION ( 'NONE',  ( 1.000000000000000000, 0.000000000000000000, 0.000000000000000000 ) ) ;
#140604 = CARTESIAN_POINT ( 'NONE',  ( -5.153800228976328057, -19.02544592524343514, 107.2905762719810383 ) ) ;
#140605 = CARTESIAN_POINT ( 'NONE',  ( 21.55341960407619695, -5.719274019375665929, 61.04275706135234714 ) ) ;
#140606 = DIRECTION ( 'NONE',  ( -1.000000000000000000, -0.000000000000000000, -0.000000000000000000 ) ) ;
#140607 = CARTESIAN_POINT ( 'NONE',  ( -16.52544592524335698, -4.483927247898792601, 63.95942372801901854 ) ) ;
#140608 = CARTESIAN_POINT ( 'NONE',  ( -16.51473224551082808, 9.474510206698731452, 58.33442372801900433 ) ) ;
#140609 = CARTESIAN_POINT ( 'NONE',  ( 12.14591786802309770, 12.06949235617756955, 39.37390960531436690 ) ) ;
#140610 = CARTESIAN_POINT ( 'NONE',  ( 17.40861289039001036, -6.110651285853410108, 51.12767529172567293 ) ) ;
#140611 = CARTESIAN_POINT ( 'NONE',  ( -14.34966873604972548, 8.224510206698743886, 108.3344237280190185 ) ) ;
#140612 = CARTESIAN_POINT ( 'NONE',  ( -13.97604488694527625, -13.89961937509977652, 41.87390960531435979 ) ) ;
#140613 = CARTESIAN_POINT ( 'NONE',  ( -13.89961937509977652, 13.97604488694528158, 55.62390960531434558 ) ) ;
#140614 = CARTESIAN_POINT ( 'NONE',  ( 13.97604488694527802, 13.89961937509977652, 29.37390960531435979 ) ) ;
#140615 = CARTESIAN_POINT ( 'NONE',  ( 21.52544592524334988, 5.823673210054432836, 26.45942372801901854 ) ) ;
#140616 = CARTESIAN_POINT ( 'NONE',  ( 5.049401038298161559, -19.05341960407611168, 62.70724293864769550 ) ) ;
#140617 = CARTESIAN_POINT ( 'NONE',  ( -16.46253265017160317, 9.564922557960807481, 115.8322429386477097 ) ) ;
#140618 = CARTESIAN_POINT ( 'NONE',  ( 16.46253265017160672, -9.564922557960803928, 43.33224293864769550 ) ) ;
#140619 = CARTESIAN_POINT ( 'NONE',  ( 18.62759615963271287, -10.81492255796078972, 28.33224293864769550 ) ) ;
#140621 = CARTESIAN_POINT ( 'NONE',  ( 13.89961937509977652, -13.97604488694527269, 28.12390960531435624 ) ) ;
#140620 = CARTESIAN_POINT ( 'NONE',  ( 5.719274019375673035, 21.55341960407619339, 57.29275706135234714 ) ) ;
#140622 = CARTESIAN_POINT ( 'NONE',  ( -21.53943276465977519, 0.05219959533907696930, 26.24890960531435624 ) ) ;
#140623 = CARTESIAN_POINT ( 'NONE',  ( -8.314922557961024197, 14.29746914071037800, 72.91775706135234714 ) ) ;
#140624 = CARTESIAN_POINT ( 'NONE',  ( -15.72974639402176322, -15.80617190586768395, 104.3760903946856899 ) ) ;
#140625 = CARTESIAN_POINT ( 'NONE',  ( -16.53943276465976808, -0.05219959533934237506, 63.75109039468568284 ) ) ;
#140626 = CARTESIAN_POINT ( 'NONE',  ( -19.05341960407611168, -5.049401038298163336, 101.4572429386476955 ) ) ;
#140627 = CARTESIAN_POINT ( 'NONE',  ( -4.379528057220086978, -16.55341960407618274, 54.79275706135235424 ) ) ;
#140628 = CARTESIAN_POINT ( 'NONE',  ( 12.06949235617739724, 12.14591786802326823, 21.87609039468567573 ) ) ;
#140629 = CARTESIAN_POINT ( 'NONE',  ( 4.483927247898790824, -16.52544592524335698, 95.20942372801903275 ) ) ;
#140630 = CARTESIAN_POINT ( 'NONE',  ( -10.72451020669870658, -18.67979575497194134, 49.58442372801901143 ) ) ;
#140631 = CARTESIAN_POINT ( 'NONE',  ( -5.049401038297874678, -19.05341960407617918, 104.7927570613523471 ) ) ;
#140632 = CARTESIAN_POINT ( 'NONE',  ( 21.55341960407610458, 5.719274019375980345, 113.9572429386477239 ) ) ;
#140634 = CARTESIAN_POINT ( 'NONE',  ( -16.51473224551082808, 9.474510206698731452, 113.3344237280190043 ) ) ;
#140633 = CARTESIAN_POINT ( 'NONE',  ( -4.379528057220328563, 16.55341960407611168, 105.2072429386477097 ) ) ;
#140635 = CARTESIAN_POINT ( 'NONE',  ( -14.29746914071037622, -8.314922557961029526, 84.16775706135234714 ) ) ;
#140636 = CARTESIAN_POINT ( 'NONE',  ( 37.99999999999999289, 2.893978650043524126E-14, -4.749999994537627224 ) ) ;
#140637 = CARTESIAN_POINT ( 'NONE',  ( -21.55341960407619339, 5.719274019375674811, 88.54275706135236135 ) ) ;
#140638 = CARTESIAN_POINT ( 'NONE',  ( -19.05341960407617563, 5.049401038297882671, 78.54275706135233293 ) ) ;
#140639 = CARTESIAN_POINT ( 'NONE',  ( -16.55341960407611168, -4.379528057220339221, 41.45724293864769550 ) ) ;
#140640 = CARTESIAN_POINT ( 'NONE',  ( -0.05219959533910754901, -16.53943276465976808, 47.49890960531435979 ) ) ;
#140641 = CARTESIAN_POINT ( 'NONE',  ( -8.314922557960811034, -14.29746914071050412, 112.0822429386477097 ) ) ;
#140643 = DIRECTION ( 'NONE',  ( -1.000000000000000000, -0.000000000000000000, -0.000000000000000000 ) ) ;
#140642 = CARTESIAN_POINT ( 'NONE',  ( 19.02544592524334988, 5.153800228976608722, 41.45942372801900433 ) ) ;
#140644 = CARTESIAN_POINT ( 'NONE',  ( 10.81492255796106328, -18.62759615963255655, 35.41775706135234003 ) ) ;
#140645 = CARTESIAN_POINT ( 'NONE',  ( 13.97604488694548053, -13.89961937509957401, 110.6260903946856615 ) ) ;
#140646 = FACE_OUTER_BOUND ( 'NONE', #52207, .T. ) ;
#140647 = CARTESIAN_POINT ( 'NONE',  ( -5.049401038298153566, 19.05341960407611168, 110.2072429386476671 ) ) ;
#140648 = CARTESIAN_POINT ( 'NONE',  ( 10.81492255796078972, 18.62759615963270932, 64.58224293864769550 ) ) ;
#140649 = CARTESIAN_POINT ( 'NONE',  ( 13.97604488694527802, 13.89961937509977652, 84.37390960531433848 ) ) ;
#140650 = CARTESIAN_POINT ( 'NONE',  ( -21.55341960407610458, -5.719274019375992779, 51.45724293864770260 ) ) ;
#140651 = CARTESIAN_POINT ( 'NONE',  ( 16.53943276465976808, -0.05219959533910856209, 113.7489096053143527 ) ) ;
#140652 = CARTESIAN_POINT ( 'NONE',  ( 16.46253265017160672, -9.564922557960803928, 73.33224293864769550 ) ) ;
#140653 = CARTESIAN_POINT ( 'NONE',  ( 5.049401038298161559, -19.05341960407611168, 27.70724293864769550 ) ) ;
#140654 = CARTESIAN_POINT ( 'NONE',  ( 5.719274019375673035, 21.55341960407619339, 32.29275706135235424 ) ) ;
#140655 = CARTESIAN_POINT ( 'NONE',  ( -15.72974639402176322, -15.80617190586768395, 79.37609039468567573 ) ) ;
#140656 = CARTESIAN_POINT ( 'NONE',  ( -16.53943276465976808, -0.05219959533934237506, 93.75109039468567573 ) ) ;
#140657 = CARTESIAN_POINT ( 'NONE',  ( 15.72974639402176855, 15.80617190586768217, 31.87609039468567929 ) ) ;
#140658 = CARTESIAN_POINT ( 'NONE',  ( 21.53943276465977519, 0.05219959533937863772, 31.25109039468568639 ) ) ;
#140660 = CARTESIAN_POINT ( 'NONE',  ( -5.049401038298153566, 19.05341960407611168, 80.20724293864769550 ) ) ;
#140659 = CARTESIAN_POINT ( 'NONE',  ( 19.02544592524334988, 5.153800228976608722, 71.45942372801900433 ) ) ;
#140661 = CARTESIAN_POINT ( 'NONE',  ( -21.52544592524334988, -5.823673210054445271, 88.95942372801901854 ) ) ;
#140662 = CARTESIAN_POINT ( 'NONE',  ( 5.823673210054125526, 21.52544592524343514, 89.79057627198103830 ) ) ;
#140663 = CARTESIAN_POINT ( 'NONE',  ( 4.379528057220339221, -16.55341960407611168, 62.70724293864769550 ) ) ;
#140664 = CARTESIAN_POINT ( 'NONE',  ( -21.52544592524334988, -5.823673210054445271, 108.9594237280190185 ) ) ;
#140665 = CARTESIAN_POINT ( 'NONE',  ( 4.483927247898545687, 16.52544592524342804, 79.79057627198102409 ) ) ;
#140666 = CARTESIAN_POINT ( 'NONE',  ( 16.52544592524342804, -4.483927247898539470, 113.5405762719810383 ) ) ;
#140667 = CARTESIAN_POINT ( 'NONE',  ( -5.153800228976607833, 19.02544592524334988, 67.70942372801900433 ) ) ;
#140668 = CARTESIAN_POINT ( 'NONE',  ( 8.314922557960818139, 14.29746914071049879, 34.58224293864770260 ) ) ;
#140669 = CARTESIAN_POINT ( 'NONE',  ( 21.55341960407619695, -5.719274019375665929, 91.04275706135236135 ) ) ;
#140670 = CARTESIAN_POINT ( 'NONE',  ( -19.05341960407611168, -5.049401038298163336, 91.45724293864766707 ) ) ;
#140671 = CARTESIAN_POINT ( 'NONE',  ( -9.474510206698720793, -16.51473224551083518, 64.58442372801900433 ) ) ;
#140672 = CARTESIAN_POINT ( 'NONE',  ( -21.52544592524343514, 5.823673210054127303, 66.04057627198103830 ) ) ;
#140673 = CARTESIAN_POINT ( 'NONE',  ( -5.823673210054116645, -21.52544592524344225, 112.2905762719810241 ) ) ;
#140674 = CARTESIAN_POINT ( 'NONE',  ( 13.97604488694548053, -13.89961937509957401, 110.6260903946856615 ) ) ;
#140675 = CARTESIAN_POINT ( 'NONE',  ( -14.29746914071037622, -8.314922557961029526, 74.16775706135231871 ) ) ;
#140677 = CARTESIAN_POINT ( 'NONE',  ( -21.52544592524334988, -5.823673210054445271, 23.95942372801901143 ) ) ;
#140676 = CARTESIAN_POINT ( 'NONE',  ( 17.40861289039003523, 6.110651285853275994, 63.87232470827430575 ) ) ;
#140678 = CARTESIAN_POINT ( 'NONE',  ( 16.53943276465976808, -0.05219959533910856209, 108.7489096053143669 ) ) ;
#140679 = CARTESIAN_POINT ( 'NONE',  ( -36.91746825000001309, 11.99521256947798342, -7.224999997268814589 ) ) ;
#140680 = CARTESIAN_POINT ( 'NONE',  ( -16.52544592524335698, -4.483927247898792601, 33.95942372801901143 ) ) ;
#140681 = CARTESIAN_POINT ( 'NONE',  ( -5.823673210054116645, -21.52544592524344225, 62.29057627198102409 ) ) ;
#140682 = CARTESIAN_POINT ( 'NONE',  ( 8.224510206698742110, 14.34966873604972548, 102.0844237280190185 ) ) ;
#140683 = CARTESIAN_POINT ( 'NONE',  ( 16.53943276465976808, 0.05219959533934440121, 36.25109039468567573 ) ) ;
#140684 = CARTESIAN_POINT ( 'NONE',  ( 5.049401038298161559, -19.05341960407611168, 37.70724293864768839 ) ) ;
#140685 = CARTESIAN_POINT ( 'NONE',  ( -12.14591786802326823, 12.06949235617739902, 78.12609039468570415 ) ) ;
#140686 = CARTESIAN_POINT ( 'NONE',  ( 5.153800228976615827, -19.02544592524334988, 70.20942372801899012 ) ) ;
#140687 = CARTESIAN_POINT ( 'NONE',  ( -21.52544592524343514, 5.823673210054127303, 66.04057627198103830 ) ) ;
#140688 = CARTESIAN_POINT ( 'NONE',  ( -0.05219959533934338120, 16.53943276465976808, 102.5010903946856899 ) ) ;
#140689 = B_SPLINE_CURVE_WITH_KNOTS ( 'NONE', 3,
 ( #58832, #163028, #23523, #55849, #85169, #24534 ),
 .UNSPECIFIED., .F., .F.,
 ( 4, 2, 4 ),
 ( 0.0003734705499802213453, 0.004296280022383715952, 0.008219089494787211805 ),
 .UNSPECIFIED. ) ;
#140690 = CARTESIAN_POINT ( 'NONE',  ( -0.05219959533937732626, 21.53943276465977519, 87.50109039468568994 ) ) ;
#140691 = EDGE_CURVE ( 'NONE', #103031, #36560, #111040, .T. ) ;
#140692 = CARTESIAN_POINT ( 'NONE',  ( -18.62759615963270932, 10.81492255796079327, 65.83224293864769550 ) ) ;
#140693 = CARTESIAN_POINT ( 'NONE',  ( 5.719274019375991003, -21.55341960407610458, 52.70724293864769550 ) ) ;
#140694 = CARTESIAN_POINT ( 'NONE',  ( -16.53943276465976808, -0.05219959533934237506, 73.75109039468567573 ) ) ;
#140695 = CARTESIAN_POINT ( 'NONE',  ( -18.67979575497178146, -10.72451020669898902, 41.66557627198103120 ) ) ;
#140696 = ORIENTED_EDGE ( 'NONE', *, *, #183353, .F. ) ;
#140697 = CARTESIAN_POINT ( 'NONE',  ( -21.55341960407610458, -5.719274019375992779, 21.45724293864769550 ) ) ;
#140698 = CYLINDRICAL_SURFACE ( 'NONE', #27493, 5.000000000000000888 ) ;
#140699 = CARTESIAN_POINT ( 'NONE',  ( 13.89961937509977652, -13.97604488694527269, 33.12390960531434558 ) ) ;
#140700 = CARTESIAN_POINT ( 'NONE',  ( -5.823673210054116645, -21.52544592524344225, 62.29057627198102409 ) ) ;
#140701 = CARTESIAN_POINT ( 'NONE',  ( -4.483927247898782831, 16.52544592524335698, 107.7094237280190328 ) ) ;
#140702 = CARTESIAN_POINT ( 'NONE',  ( -15.72974639402176322, -15.80617190586768395, 44.37609039468567573 ) ) ;
#140703 = CARTESIAN_POINT ( 'NONE',  ( -19.05341960407617563, 5.049401038297882671, 98.54275706135233293 ) ) ;
#140704 = CARTESIAN_POINT ( 'NONE',  ( 13.97604488694527802, 13.89961937509977652, 24.37390960531435624 ) ) ;
#140705 = CARTESIAN_POINT ( 'NONE',  ( 5.153800228976615827, -19.02544592524334988, 110.2094237280189901 ) ) ;
#140706 = AXIS2_PLACEMENT_3D ( 'NONE', #68608, #190968, #130265 ) ;
#140707 = CARTESIAN_POINT ( 'NONE',  ( 5.153800228976335163, 19.02544592524342804, 44.79057627198103830 ) ) ;
#140708 = CARTESIAN_POINT ( 'NONE',  ( 17.81289503416610742, 24.51734667627700404, 141.2999999999999829 ) ) ;
#140709 = CARTESIAN_POINT ( 'NONE',  ( 13.89961937509977652, -13.97604488694527269, 98.12390960531433848 ) ) ;
#140710 = CARTESIAN_POINT ( 'NONE',  ( 0.05219959533934541429, -16.53943276465976808, 75.00109039468568994 ) ) ;
#140711 = CARTESIAN_POINT ( 'NONE',  ( 16.46253265017146816, 9.564922557961045513, 81.66775706135233293 ) ) ;
#140712 = CARTESIAN_POINT ( 'NONE',  ( 19.03943276465977164, 0.05219959533936151252, 21.25109039468565797 ) ) ;
#140713 = CARTESIAN_POINT ( 'NONE',  ( -10.81492255796078084, -18.62759615963271287, 57.08224293864769550 ) ) ;
#140714 = CARTESIAN_POINT ( 'NONE',  ( 8.314922557961029526, -14.29746914071037800, 80.41775706135234714 ) ) ;
#140715 = CARTESIAN_POINT ( 'NONE',  ( 0.05219959533936267826, -19.03943276465977164, 80.00109039468567573 ) ) ;
#140716 = CARTESIAN_POINT ( 'NONE',  ( -0.05219959533909027116, -19.03943276465977164, 32.49890960531435979 ) ) ;
#140717 = CARTESIAN_POINT ( 'NONE',  ( -13.97604488694527625, -13.89961937509977652, 76.87390960531433848 ) ) ;
#140718 = CARTESIAN_POINT ( 'NONE',  ( 0.05219959533937995610, -21.53943276465977519, 55.00109039468568284 ) ) ;
#140719 = CARTESIAN_POINT ( 'NONE',  ( -5.153800228976328057, -19.02544592524343514, 47.29057627198102409 ) ) ;
#140720 = CARTESIAN_POINT ( 'NONE',  ( -16.51473224551082808, 9.474510206698731452, 68.33442372801900433 ) ) ;
#140721 = CARTESIAN_POINT ( 'NONE',  ( 26.77293948118372313, -6.014770499723137931, 169.2063755025577336 ) ) ;
#140722 = CARTESIAN_POINT ( 'NONE',  ( 9.474510206698971260, -16.51473224551069308, 112.9155762719810383 ) ) ;
#140723 = CARTESIAN_POINT ( 'NONE',  ( 4.379528057220339221, -16.55341960407611168, 67.70724293864769550 ) ) ;
#140724 = CARTESIAN_POINT ( 'NONE',  ( -5.719274019375978568, 21.55341960407610458, 65.20724293864768129 ) ) ;
#140725 = CARTESIAN_POINT ( 'NONE',  ( 4.500000000000000888, -120.9970989573719038, 14.58956564881029649 ) ) ;
#140726 = CARTESIAN_POINT ( 'NONE',  ( -9.564922557961040184, 16.46253265017147172, 27.91775706135232582 ) ) ;
#140727 = CARTESIAN_POINT ( 'NONE',  ( -18.10062525802553424, 5.500000000000031974, 88.51383468041920821 ) ) ;
#140729 = CARTESIAN_POINT ( 'NONE',  ( -13.89961937509977652, 13.97604488694528158, 70.62390960531432427 ) ) ;
#140728 = CARTESIAN_POINT ( 'NONE',  ( 16.46253265017160672, -9.564922557960803928, 58.33224293864769550 ) ) ;
#140730 = CARTESIAN_POINT ( 'NONE',  ( 14.29746914071037800, 8.314922557961029526, 51.66775706135234714 ) ) ;
#140731 = CARTESIAN_POINT ( 'NONE',  ( -18.22780087662124160, -5.499999999999927169, 78.98236817873106475 ) ) ;
#140732 = CARTESIAN_POINT ( 'NONE',  ( 23.31738231874054534, 16.94106989632529192, 145.4500000054623854 ) ) ;
#140733 = CARTESIAN_POINT ( 'NONE',  ( -8.224510206698735004, -14.34966873604973081, 89.58442372801901854 ) ) ;
#140734 = CARTESIAN_POINT ( 'NONE',  ( 22.97079825734836689, -21.83149972758499402, -45.97092040041037109 ) ) ;
#140735 = CARTESIAN_POINT ( 'NONE',  ( -12.06949235617739369, -12.14591786802326823, 69.37609039468567573 ) ) ;
#140736 = CARTESIAN_POINT ( 'NONE',  ( 4.483927247898790824, -16.52544592524335698, 45.20942372801901854 ) ) ;
#140738 = FACE_BOUND ( 'NONE', #53911, .T. ) ;
#140737 = CARTESIAN_POINT ( 'NONE',  ( 13.89961937509977652, -13.97604488694527269, 58.12390960531436690 ) ) ;
#140739 = CARTESIAN_POINT ( 'NONE',  ( 0.05219959533937995610, -21.53943276465977519, 60.00109039468568284 ) ) ;
#140740 = CARTESIAN_POINT ( 'NONE',  ( -13.89961937509957401, -13.97604488694547875, 59.37609039468566863 ) ) ;
#140741 = CARTESIAN_POINT ( 'NONE',  ( 10.72451020669871369, 18.67979575497193778, 107.0844237280190043 ) ) ;
#140742 = AXIS2_PLACEMENT_3D ( 'NONE', #131322, #24168, #117155 ) ;
#140743 = CARTESIAN_POINT ( 'NONE',  ( -19.05341960407611168, -5.049401038298163336, 26.45724293864769550 ) ) ;
#140744 = CARTESIAN_POINT ( 'NONE',  ( -30.73962218707678318, -22.33364281372842441, -7.802157773949823572 ) ) ;
#140745 = CARTESIAN_POINT ( 'NONE',  ( 5.719274019375991003, -21.55341960407610458, 52.70724293864769550 ) ) ;
#140746 = CARTESIAN_POINT ( 'NONE',  ( -16.51473224551069308, -9.474510206698971260, 111.6655762719810383 ) ) ;
#140747 = CARTESIAN_POINT ( 'NONE',  ( -8.224510206698948167, 14.34966873604960824, 105.4155762719810383 ) ) ;
#140748 = CARTESIAN_POINT ( 'NONE',  ( -14.29746914071037622, -8.314922557961029526, 39.16775706135235424 ) ) ;
#140749 = CARTESIAN_POINT ( 'NONE',  ( 4.379528057220339221, -16.55341960407611168, 27.70724293864769905 ) ) ;
#140750 = ORIENTED_EDGE ( 'NONE', *, *, #125272, .F. ) ;
#140751 = CARTESIAN_POINT ( 'NONE',  ( 21.53943276465977519, -0.05219959533907433946, 113.7489096053143527 ) ) ;
#140753 = DIRECTION ( 'NONE',  ( 4.336808689942017120E-17, 1.000000000000000000, 0.000000000000000000 ) ) ;
#140752 = CARTESIAN_POINT ( 'NONE',  ( 8.224510206698953496, -14.34966873604960469, 42.91557627198103120 ) ) ;
#140754 = CARTESIAN_POINT ( 'NONE',  ( 19.03943276465977164, 0.05219959533936151252, 101.2510903946856757 ) ) ;
#140755 = CARTESIAN_POINT ( 'NONE',  ( -5.049401038297874678, -19.05341960407617918, 24.79275706135233648 ) ) ;
#140756 = CARTESIAN_POINT ( 'NONE',  ( 4.379528057220339221, -16.55341960407611168, 37.70724293864769550 ) ) ;
#140757 = CARTESIAN_POINT ( 'NONE',  ( -21.55341960407610458, -5.719274019375992779, 106.4572429386477097 ) ) ;
#140758 = CARTESIAN_POINT ( 'NONE',  ( 21.55341960407610458, 5.719274019375980345, 63.95724293864770260 ) ) ;
#140759 = CARTESIAN_POINT ( 'NONE',  ( -9.564922557960796823, -16.46253265017161027, 72.08224293864770971 ) ) ;
#140760 = CARTESIAN_POINT ( 'NONE',  ( 16.53943276465976808, -0.05219959533910856209, 43.74890960531435979 ) ) ;
#140761 = CARTESIAN_POINT ( 'NONE',  ( 9.474510206698971260, -16.51473224551069308, 92.91557627198103830 ) ) ;
#140762 = CARTESIAN_POINT ( 'NONE',  ( 19.49190055781009789, 5.500000000000041744, 58.06116087098783396 ) ) ;
#140763 = CARTESIAN_POINT ( 'NONE',  ( 5.049401038297881783, 19.05341960407617563, 47.29275706135231161 ) ) ;
#140764 = CARTESIAN_POINT ( 'NONE',  ( -21.52544592524343514, 5.823673210054127303, 91.04057627198103830 ) ) ;
#140765 = CARTESIAN_POINT ( 'NONE',  ( 16.52544592524342804, -4.483927247898539470, 93.54057627198103830 ) ) ;
#140766 = CARTESIAN_POINT ( 'NONE',  ( -15.80617190586768217, 15.72974639402176855, 33.12609039468569705 ) ) ;
#140767 = CARTESIAN_POINT ( 'NONE',  ( -27.73933785331498925, 9.013057229001089965, 140.7750000027311899 ) ) ;
#140768 = CARTESIAN_POINT ( 'NONE',  ( -12.14591786802309592, -12.06949235617757132, 31.87390960531435979 ) ) ;
#140769 = CARTESIAN_POINT ( 'NONE',  ( -16.51473224551069308, -9.474510206698971260, 31.66557627198102054 ) ) ;
#140770 = CARTESIAN_POINT ( 'NONE',  ( 16.51473224551069308, 9.474510206698969483, 89.16557627198103830 ) ) ;
#140771 = CARTESIAN_POINT ( 'NONE',  ( 21.52544592524344225, -5.823673210054117533, 58.54057627198103120 ) ) ;
#140772 = CARTESIAN_POINT ( 'NONE',  ( 8.571926809382597767, 26.38167802310806209, 140.2750000027311899 ) ) ;
#140773 = CARTESIAN_POINT ( 'NONE',  ( -13.89961937509977652, 13.97604488694528158, 25.62390960531434558 ) ) ;
#140774 = CARTESIAN_POINT ( 'NONE',  ( 15.80617190586746368, 15.72974639402197994, 49.37390960531436690 ) ) ;
#140775 = CARTESIAN_POINT ( 'NONE',  ( 21.53943276465977519, 0.05219959533937863772, 76.25109039468568994 ) ) ;
#140777 = CARTESIAN_POINT ( 'NONE',  ( -8.314922557961024197, 14.29746914071037800, 72.91775706135234714 ) ) ;
#140776 = CARTESIAN_POINT ( 'NONE',  ( 14.90098780496084885, -35.24605353401756247, -22.56189394118873892 ) ) ;
#140778 = CARTESIAN_POINT ( 'NONE',  ( 5.049401038298161559, -19.05341960407611168, 52.70724293864767418 ) ) ;
#140779 = CARTESIAN_POINT ( 'NONE',  ( 19.05341960407611168, 5.049401038298154454, 63.95724293864769550 ) ) ;
#140780 = VERTEX_POINT ( 'NONE', #125225 ) ;
#140781 = CARTESIAN_POINT ( 'NONE',  ( 10.81492255796106328, -18.62759615963255655, 105.4177570613523613 ) ) ;
#140782 = CARTESIAN_POINT ( 'NONE',  ( 16.52544592524335698, 4.483927247898782831, 71.45942372801901854 ) ) ;
#140783 = CARTESIAN_POINT ( 'NONE',  ( -5.719274019375665041, -21.55341960407619695, 99.79275706135234714 ) ) ;
#140784 = CARTESIAN_POINT ( 'NONE',  ( -13.89961937509977652, 13.97604488694528158, 60.62390960531436690 ) ) ;
#140785 = CARTESIAN_POINT ( 'NONE',  ( 18.62759615963271287, -10.81492255796078972, 28.33224293864769550 ) ) ;
#140786 = CARTESIAN_POINT ( 'NONE',  ( -13.97604488694547697, 13.89961937509957934, 103.1260903946856473 ) ) ;
#140787 = CARTESIAN_POINT ( 'NONE',  ( -0.05219959533937732626, 21.53943276465977519, 87.50109039468568994 ) ) ;
#140788 = CARTESIAN_POINT ( 'NONE',  ( 0.05219959533934541429, -16.53943276465976808, 45.00109039468568284 ) ) ;
#140789 = CARTESIAN_POINT ( 'NONE',  ( 10.72451020669898902, -18.67979575497178502, 92.91557627198103830 ) ) ;
#140791 = VECTOR ( 'NONE', #123916, 1000.000000000000000 ) ;
#140790 = CARTESIAN_POINT ( 'NONE',  ( -16.46253265017146816, -9.564922557961047289, 104.1677570613523329 ) ) ;
#140792 = CARTESIAN_POINT ( 'NONE',  ( -0.05219959533909027116, -19.03943276465977164, 72.49890960531435269 ) ) ;
#140793 = CARTESIAN_POINT ( 'NONE',  ( -19.03943276465977164, -0.05219959533935918106, 108.7510903946856615 ) ) ;
#140794 = CARTESIAN_POINT ( 'NONE',  ( -5.049401038298153566, 19.05341960407611168, 35.20724293864768839 ) ) ;
#140795 = CARTESIAN_POINT ( 'NONE',  ( 14.29746914071037800, 8.314922557961029526, 26.66775706135235424 ) ) ;
#140796 = CARTESIAN_POINT ( 'NONE',  ( 8.224510206698953496, -14.34966873604960469, 62.91557627198102409 ) ) ;
#140797 = CARTESIAN_POINT ( 'NONE',  ( -14.29746914071037622, -8.314922557961029526, 69.16775706135234714 ) ) ;
#140799 = CARTESIAN_POINT ( 'NONE',  ( -19.05341960407611168, -5.049401038298163336, 51.45724293864770260 ) ) ;
#140798 = CARTESIAN_POINT ( 'NONE',  ( 10.72451020669871369, 18.67979575497193778, 32.08442372801901854 ) ) ;
#140800 = CARTESIAN_POINT ( 'NONE',  ( 19.03943276465977164, -0.05219959533909143690, 68.74890960531436690 ) ) ;
#140801 = CARTESIAN_POINT ( 'NONE',  ( 4.379528057220092307, 16.55341960407617563, 77.29275706135234714 ) ) ;
#140802 = CARTESIAN_POINT ( 'NONE',  ( -23.31738231874055600, 16.94106989632528837, 148.0500000054623797 ) ) ;
#140803 = ORIENTED_EDGE ( 'NONE', *, *, #128488, .F. ) ;
#140804 = CARTESIAN_POINT ( 'NONE',  ( -10.72451020669870658, -18.67979575497194134, 109.5844237280190328 ) ) ;
#140805 = CARTESIAN_POINT ( 'NONE',  ( 13.89961937509977652, -13.97604488694527269, 38.12390960531436690 ) ) ;
#140806 = EDGE_LOOP ( 'NONE', ( #192152, #147931, #192488, #62853, #39274, #38, #183572, #121223, #77154, #113113, #146949, #29109, #12658, #25838, #32209, #29797 ) ) ;
#140807 = CARTESIAN_POINT ( 'NONE',  ( 16.52544592524335698, 4.483927247898782831, 26.45942372801901854 ) ) ;
#140809 = CARTESIAN_POINT ( 'NONE',  ( 8.314922557961029526, -14.29746914071037800, 45.41775706135234003 ) ) ;
#140808 = CARTESIAN_POINT ( 'NONE',  ( 19.05341960407617918, -5.049401038297876454, 51.04275706135231871 ) ) ;
#140810 = CARTESIAN_POINT ( 'NONE',  ( 5.153800228976335163, 19.02544592524342804, 39.79057627198100988 ) ) ;
#140811 = CARTESIAN_POINT ( 'NONE',  ( -0.05219959533909027116, -19.03943276465977164, 102.4989096053143669 ) ) ;
#140812 = CARTESIAN_POINT ( 'NONE',  ( 5.049401038298161559, -19.05341960407611168, 57.70724293864769550 ) ) ;
#140813 = CARTESIAN_POINT ( 'NONE',  ( 5.823673210054125526, 21.52544592524343514, 104.7905762719810241 ) ) ;
#140815 = DIRECTION ( 'NONE',  ( 0.000000000000000000, 0.000000000000000000, -1.000000000000000000 ) ) ;
#140814 = CARTESIAN_POINT ( 'NONE',  ( -0.05219959533909027116, -19.03943276465977164, 77.49890960531435269 ) ) ;
#140816 = EDGE_CURVE ( 'NONE', #196237, #193343, #33218, .T. ) ;
#140817 = CARTESIAN_POINT ( 'NONE',  ( -9.474510206698964154, 16.51473224551069663, 65.41557627198102409 ) ) ;
#140818 = CARTESIAN_POINT ( 'NONE',  ( -17.14385361876520975, 23.59649016807275856, 147.0750000027312012 ) ) ;
#140819 = CARTESIAN_POINT ( 'NONE',  ( -13.97604488694547697, 13.89961937509957934, 93.12609039468566152 ) ) ;
#140820 = CARTESIAN_POINT ( 'NONE',  ( -13.89961937509957401, -13.97604488694547875, 19.37609039468566507 ) ) ;
#140821 = CARTESIAN_POINT ( 'NONE',  ( -14.29746914071049879, 8.314922557960819915, 65.83224293864769550 ) ) ;
#140822 = CARTESIAN_POINT ( 'NONE',  ( -18.62759615963255300, -10.81492255796106328, 84.16775706135234714 ) ) ;
#140823 = CARTESIAN_POINT ( 'NONE',  ( -16.51473224551069308, -9.474510206698971260, 21.66557627198102765 ) ) ;
#140825 = CARTESIAN_POINT ( 'NONE',  ( -15.72974639402176322, -15.80617190586768395, 94.37609039468568994 ) ) ;
#140824 = CARTESIAN_POINT ( 'NONE',  ( -0.05219959533910754901, -16.53943276465976808, 27.49890960531435269 ) ) ;
#140826 = CARTESIAN_POINT ( 'NONE',  ( -16.46253265017160317, 9.564922557960807481, 80.83224293864769550 ) ) ;
#140827 = CARTESIAN_POINT ( 'NONE',  ( -15.80617190586768217, 15.72974639402176855, 48.12609039468568284 ) ) ;
#140828 = CARTESIAN_POINT ( 'NONE',  ( -5.049401038298153566, 19.05341960407611168, 80.20724293864769550 ) ) ;
#140829 = CARTESIAN_POINT ( 'NONE',  ( 0.05219959533910956823, 16.53943276465976808, 89.99890960531438111 ) ) ;
#140830 = CARTESIAN_POINT ( 'NONE',  ( -16.53943276465976808, 0.05219959533911058130, 61.24890960531435979 ) ) ;
#140831 = CARTESIAN_POINT ( 'NONE',  ( 10.72451020669898902, -18.67979575497178502, 72.91557627198103830 ) ) ;
#140832 = CARTESIAN_POINT ( 'NONE',  ( 5.153800228976335163, 19.02544592524342804, 74.79057627198103830 ) ) ;
#140833 = CARTESIAN_POINT ( 'NONE',  ( 0.05219959533907565091, 21.53943276465977519, 84.99890960531436690 ) ) ;
#140834 = CARTESIAN_POINT ( 'NONE',  ( -13.97604488694547697, 13.89961937509957934, 83.12609039468564731 ) ) ;
#140837 = CARTESIAN_POINT ( 'NONE',  ( 4.379528057220339221, -16.55341960407611168, 82.70724293864770971 ) ) ;
#140836 = CARTESIAN_POINT ( 'NONE',  ( -0.05219959533936034679, 19.03943276465977164, 37.50109039468567573 ) ) ;
#140835 = AXIS2_PLACEMENT_3D ( 'NONE', #34229, #127209, #82692 ) ;
#140838 = CARTESIAN_POINT ( 'NONE',  ( 19.03943276465977164, -0.05219959533909143690, 63.74890960531435979 ) ) ;
#140839 = CARTESIAN_POINT ( 'NONE',  ( -5.719274019375978568, 21.55341960407610458, 70.20724293864769550 ) ) ;
#140840 = CARTESIAN_POINT ( 'NONE',  ( -193.3062444957834884, -155.7167183371838064, -15.00000000000000000 ) ) ;
#140842 = CARTESIAN_POINT ( 'NONE',  ( -27.73933785331498925, 2.428612866367529932E-14, 147.3750000027311842 ) ) ;
#140841 = CARTESIAN_POINT ( 'NONE',  ( -8.314922557960811034, -14.29746914071050412, 22.08224293864769194 ) ) ;
#140843 = CARTESIAN_POINT ( 'NONE',  ( 5.049401038297881783, 19.05341960407617563, 102.2927570613523045 ) ) ;
#140844 = CARTESIAN_POINT ( 'NONE',  ( -12.14591786802309592, -12.06949235617757132, 81.87390960531435269 ) ) ;
#140845 = CARTESIAN_POINT ( 'NONE',  ( 6.100000000000006750, 0.000000000000000000, -62.50719930893269805 ) ) ;
#140846 = CARTESIAN_POINT ( 'NONE',  ( -5.153800228976328057, -19.02544592524343514, 77.29057627198099567 ) ) ;
#140847 = CARTESIAN_POINT ( 'NONE',  ( 13.89961937509977652, -13.97604488694527269, 33.12390960531434558 ) ) ;
#140848 = CARTESIAN_POINT ( 'NONE',  ( -4.483927247898539470, -16.52544592524342804, 62.29057627198102409 ) ) ;
#140849 = CARTESIAN_POINT ( 'NONE',  ( -19.05341960407611168, -5.049401038298163336, 96.45724293864769550 ) ) ;
#140851 = CARTESIAN_POINT ( 'NONE',  ( -13.97604488694527625, -13.89961937509977652, 61.87390960531435979 ) ) ;
#140850 = CARTESIAN_POINT ( 'NONE',  ( 19.02544592524334988, 5.153800228976608722, 86.45942372801900433 ) ) ;
#140852 = CARTESIAN_POINT ( 'NONE',  ( -16.46253265017160317, 9.564922557960807481, 90.83224293864769550 ) ) ;
#140853 = CARTESIAN_POINT ( 'NONE',  ( 10.72451020669898902, -18.67979575497178502, 77.91557627198102409 ) ) ;
#140854 = CARTESIAN_POINT ( 'NONE',  ( 0.05219959533934541429, -16.53943276465976808, 75.00109039468568994 ) ) ;
#140855 = CARTESIAN_POINT ( 'NONE',  ( -19.03943276465977164, -0.05219959533935918106, 108.7510903946856615 ) ) ;
#140856 = CARTESIAN_POINT ( 'NONE',  ( -19.05341960407611168, -5.049401038298163336, 66.45724293864769550 ) ) ;
#140857 = CARTESIAN_POINT ( 'NONE',  ( -21.55341960407610458, -5.719274019375992779, 71.45724293864769550 ) ) ;
#140858 = CARTESIAN_POINT ( 'NONE',  ( 5.049401038297881783, 19.05341960407617563, 97.29275706135233293 ) ) ;
#140860 = CARTESIAN_POINT ( 'NONE',  ( 21.53943276465977519, 0.05219959533937863772, 46.25109039468567573 ) ) ;
#140859 = CARTESIAN_POINT ( 'NONE',  ( 16.52544592524342804, -4.483927247898539470, 43.54057627198103830 ) ) ;
#140861 = DIRECTION ( 'NONE',  ( -0.000000000000000000, -0.000000000000000000, 1.000000000000000000 ) ) ;
#140863 = CARTESIAN_POINT ( 'NONE',  ( 19.05341960407611168, 5.049401038298154454, 103.9572429386476671 ) ) ;
#140862 = CARTESIAN_POINT ( 'NONE',  ( -8.314922557961024197, 14.29746914071037800, 77.91775706135231871 ) ) ;
#140864 = CARTESIAN_POINT ( 'NONE',  ( -16.46253265017160317, 9.564922557960807481, 105.8322429386476955 ) ) ;
#140865 = CARTESIAN_POINT ( 'NONE',  ( -17.13100169013302221, -6.664070546373105586, 34.23210164300150637 ) ) ;
#140866 = CARTESIAN_POINT ( 'NONE',  ( 16.55341960407618274, -4.379528057220086978, 96.04275706135236135 ) ) ;
#140867 = CARTESIAN_POINT ( 'NONE',  ( 12.06949235617739724, 12.14591786802326823, 36.87609039468568994 ) ) ;
#140868 = CARTESIAN_POINT ( 'NONE',  ( 0.05219959533909260263, 19.03943276465977164, 44.99890960531435979 ) ) ;
#140869 = CARTESIAN_POINT ( 'NONE',  ( -16.46253265017160317, 9.564922557960807481, 55.83224293864769550 ) ) ;
#140870 = CARTESIAN_POINT ( 'NONE',  ( -13.89961937509977652, 13.97604488694528158, 60.62390960531436690 ) ) ;
#140871 = CARTESIAN_POINT ( 'NONE',  ( 21.55341960407619695, -5.719274019375665929, 56.04275706135235424 ) ) ;
#140872 = CARTESIAN_POINT ( 'NONE',  ( -12.14591786802326823, 12.06949235617739902, 68.12609039468567573 ) ) ;
#140873 = CARTESIAN_POINT ( 'NONE',  ( 12.14591786802309770, 12.06949235617756955, 34.37390960531435979 ) ) ;
#140874 = CARTESIAN_POINT ( 'NONE',  ( 0.05219959533909260263, 19.03943276465977164, 39.99890960531436690 ) ) ;
#140875 = CARTESIAN_POINT ( 'NONE',  ( 19.03943276465977164, -0.05219959533909143690, 38.74890960531436690 ) ) ;
#140876 = CARTESIAN_POINT ( 'NONE',  ( -14.34966873604972548, 8.224510206698743886, 28.33442372801902209 ) ) ;
#140877 = CARTESIAN_POINT ( 'NONE',  ( 16.51473224551083163, -9.474510206698727899, 85.83442372801900433 ) ) ;
#140878 = CARTESIAN_POINT ( 'NONE',  ( -8.224510206698948167, 14.34966873604960824, 80.41557627198103830 ) ) ;
#140879 = CARTESIAN_POINT ( 'NONE',  ( -16.51473224551069308, -9.474510206698971260, 46.66557627198102409 ) ) ;
#140881 = CARTESIAN_POINT ( 'NONE',  ( -38.00000000000000711, 2.428612866367529932E-14, -8.000000000000000000 ) ) ;
#140880 = CARTESIAN_POINT ( 'NONE',  ( -9.564922557961040184, 16.46253265017147172, 82.91775706135233293 ) ) ;
#140882 = CARTESIAN_POINT ( 'NONE',  ( -15.72974639402176322, -15.80617190586768395, 89.37609039468568994 ) ) ;
#140883 = CARTESIAN_POINT ( 'NONE',  ( 12.14591786802327356, -12.06949235617739191, 60.62609039468567573 ) ) ;
#140884 = CARTESIAN_POINT ( 'NONE',  ( 17.31747979337949772, 6.344076630961017038, 38.87944868065184778 ) ) ;
#140885 = CARTESIAN_POINT ( 'NONE',  ( -21.53943276465977519, 0.05219959533907696930, 56.24890960531436690 ) ) ;
#140886 = CARTESIAN_POINT ( 'NONE',  ( 16.52544592524335698, 4.483927247898782831, 46.45942372801901854 ) ) ;
#140887 = CARTESIAN_POINT ( 'NONE',  ( 5.153800228976335163, 19.02544592524342804, 24.79057627198102765 ) ) ;
#140888 = CARTESIAN_POINT ( 'NONE',  ( -16.51473224551082808, 9.474510206698731452, 23.33442372801900078 ) ) ;
#140889 = AXIS2_PLACEMENT_3D ( 'NONE', #180348, #42814, #177342 ) ;
#140890 = CARTESIAN_POINT ( 'NONE',  ( -13.89961937509977652, 13.97604488694528158, 80.62390960531436690 ) ) ;
#140891 = CARTESIAN_POINT ( 'NONE',  ( 9.333912919581869971, 11.25730316407965503, -60.07366171483953110 ) ) ;
#140892 = CARTESIAN_POINT ( 'NONE',  ( 19.03943276465977164, -0.05219959533909143690, 48.74890960531435979 ) ) ;
#140893 = CARTESIAN_POINT ( 'NONE',  ( 14.81572341150385341, 16.93990830356618460, -55.62237631978510422 ) ) ;
#140894 = CARTESIAN_POINT ( 'NONE',  ( 13.97604488694527802, 13.89961937509977652, 74.37390960531436690 ) ) ;
#140896 = CARTESIAN_POINT ( 'NONE',  ( 17.49999999999999645, -3.305555262949672279, 112.1251715215659743 ) ) ;
#140895 = CIRCLE ( 'NONE', #176423, 1.249999999999999778 ) ;
#140897 = EDGE_CURVE ( 'NONE', #164148, #145515, #123215, .T. ) ;
#140898 = CARTESIAN_POINT ( 'NONE',  ( -21.53943276465977519, -0.05219959533937600094, 113.7510903946856757 ) ) ;
#140899 = CARTESIAN_POINT ( 'NONE',  ( -5.823673210054431948, 21.52544592524334988, 112.7094237280190328 ) ) ;
#140900 = CARTESIAN_POINT ( 'NONE',  ( 8.224510206698953496, -14.34966873604960469, 37.91557627198102409 ) ) ;
#140901 = CARTESIAN_POINT ( 'NONE',  ( 5.049401038298161559, -19.05341960407611168, 47.70724293864770260 ) ) ;
#140902 = CARTESIAN_POINT ( 'NONE',  ( -0.05219959533909027116, -19.03943276465977164, 107.4989096053143527 ) ) ;
#140903 = CARTESIAN_POINT ( 'NONE',  ( -21.52544592524334988, -5.823673210054445271, 68.95942372801901854 ) ) ;
#140904 = CARTESIAN_POINT ( 'NONE',  ( 5.049401038298161559, -19.05341960407611168, 47.70724293864770260 ) ) ;
#140905 = CARTESIAN_POINT ( 'NONE',  ( -21.53943276465977519, -0.05219959533937600094, 78.75109039468568994 ) ) ;
#140906 = CARTESIAN_POINT ( 'NONE',  ( -10.72451020669898014, 18.67979575497178502, 25.41557627198103120 ) ) ;
#140907 = CARTESIAN_POINT ( 'NONE',  ( 19.02544592524343514, -5.153800228976328945, 33.54057627198102409 ) ) ;
#140908 = CARTESIAN_POINT ( 'NONE',  ( -21.52544592524334988, -5.823673210054445271, 23.95942372801901143 ) ) ;
#140909 = CARTESIAN_POINT ( 'NONE',  ( -16.51473224551082808, 9.474510206698731452, 53.33442372801900433 ) ) ;
#140910 = CARTESIAN_POINT ( 'NONE',  ( -9.564922557960796823, -16.46253265017161027, 27.08224293864769550 ) ) ;
#140911 = CARTESIAN_POINT ( 'NONE',  ( -13.97604488694527625, -13.89961937509977652, 71.87390960531433848 ) ) ;
#140912 = CARTESIAN_POINT ( 'NONE',  ( 13.97604488694548053, -13.89961937509957401, 105.6260903946856757 ) ) ;
#140913 = CARTESIAN_POINT ( 'NONE',  ( -4.483927247898539470, -16.52544592524342804, 72.29057627198102409 ) ) ;
#140914 = CARTESIAN_POINT ( 'NONE',  ( -15.80617190586745835, -15.72974639402198527, 31.87390960531435979 ) ) ;
#140915 = CARTESIAN_POINT ( 'NONE',  ( 19.02544592524334988, 5.153800228976608722, 96.45942372801897591 ) ) ;
#140916 = CARTESIAN_POINT ( 'NONE',  ( -21.55341960407610458, -5.719274019375992779, 106.4572429386477097 ) ) ;
#140917 = CARTESIAN_POINT ( 'NONE',  ( -15.80617190586768217, 15.72974639402176855, 58.12609039468568994 ) ) ;
#140918 = CARTESIAN_POINT ( 'NONE',  ( 0.05219959533934541429, -16.53943276465976808, 50.00109039468568994 ) ) ;
#140919 = CARTESIAN_POINT ( 'NONE',  ( -16.53943276465976808, -0.05219959533934237506, 48.75109039468568284 ) ) ;
#140920 = CARTESIAN_POINT ( 'NONE',  ( -5.719274019375978568, 21.55341960407610458, 70.20724293864769550 ) ) ;
#140921 = EDGE_LOOP ( 'NONE', ( #191272, #5402, #84598, #157706 ) ) ;
#140922 = CARTESIAN_POINT ( 'NONE',  ( 16.51473224551069308, 9.474510206698969483, 44.16557627198103120 ) ) ;
#140923 = CARTESIAN_POINT ( 'NONE',  ( -8.314922557961024197, 14.29746914071037800, 87.91775706135234714 ) ) ;
#140924 = CARTESIAN_POINT ( 'NONE',  ( -5.823673210054116645, -21.52544592524344225, 97.29057627198105251 ) ) ;
#140925 = CARTESIAN_POINT ( 'NONE',  ( -16.52544592524342804, 4.483927247898546575, 56.04057627198102409 ) ) ;
#140926 = CARTESIAN_POINT ( 'NONE',  ( 0.05219959533909260263, 19.03943276465977164, 69.99890960531435269 ) ) ;
#140927 = CARTESIAN_POINT ( 'NONE',  ( 8.314922557961029526, -14.29746914071037800, 80.41775706135234714 ) ) ;
#140928 = CARTESIAN_POINT ( 'NONE',  ( -16.51473224551082808, 9.474510206698731452, 113.3344237280190043 ) ) ;
#140929 = CARTESIAN_POINT ( 'NONE',  ( -21.53943276465977519, 0.05219959533907696930, 106.2489096053143811 ) ) ;
#140930 = CARTESIAN_POINT ( 'NONE',  ( 0.05219959533910956823, 16.53943276465976808, 39.99890960531436690 ) ) ;
#140931 = VERTEX_POINT ( 'NONE', #80694 ) ;
#140932 = CARTESIAN_POINT ( 'NONE',  ( -17.31747979337945154, 6.344076630961109409, 73.62055131934816643 ) ) ;
#140933 = CARTESIAN_POINT ( 'NONE',  ( 15.72974639402199770, -15.80617190586745480, 88.12390960531436690 ) ) ;
#140934 = CARTESIAN_POINT ( 'NONE',  ( -14.29746914071049879, 8.314922557960819915, 30.83224293864770260 ) ) ;
#140935 = VERTEX_POINT ( 'NONE', #107055 ) ;
#140936 = CARTESIAN_POINT ( 'NONE',  ( -17.05587630539787014, -6.762274262135727021, 54.25819690962693187 ) ) ;
#140937 = CARTESIAN_POINT ( 'NONE',  ( 18.62759615963271287, -10.81492255796078972, 103.3322429386476955 ) ) ;
#140938 = CARTESIAN_POINT ( 'NONE',  ( 16.51473224551069308, 9.474510206698969483, 114.1655762719810241 ) ) ;
#140939 = CARTESIAN_POINT ( 'NONE',  ( -18.62759615963270932, 10.81492255796079327, 115.8322429386477097 ) ) ;
#140940 = CARTESIAN_POINT ( 'NONE',  ( 4.483927247898545687, 16.52544592524342804, 49.79057627198102409 ) ) ;
#140941 = CARTESIAN_POINT ( 'NONE',  ( -14.29746914071037622, -8.314922557961029526, 54.16775706135235424 ) ) ;
#140942 = CARTESIAN_POINT ( 'NONE',  ( -16.46253265017160317, 9.564922557960807481, 60.83224293864769550 ) ) ;
#140943 = CARTESIAN_POINT ( 'NONE',  ( -16.51473224551082808, 9.474510206698731452, 53.33442372801900433 ) ) ;
#140944 = CARTESIAN_POINT ( 'NONE',  ( 0.05219959533909260263, 19.03943276465977164, 79.99890960531436690 ) ) ;
#140945 = CARTESIAN_POINT ( 'NONE',  ( 5.719274019375991003, -21.55341960407610458, 37.70724293864769550 ) ) ;
#140946 = CARTESIAN_POINT ( 'NONE',  ( -28.84224951681783367, -24.48020638810389826, -21.31946643861265400 ) ) ;
#140947 = CARTESIAN_POINT ( 'NONE',  ( 0.05219959533909260263, 19.03943276465977164, 49.99890960531435979 ) ) ;
#140948 = CARTESIAN_POINT ( 'NONE',  ( -16.52544592524335698, -4.483927247898792601, 18.95942372801901143 ) ) ;
#140949 = CARTESIAN_POINT ( 'NONE',  ( -5.153800228976607833, 19.02544592524334988, 67.70942372801900433 ) ) ;
#140950 = CARTESIAN_POINT ( 'NONE',  ( -18.62759615963270932, 10.81492255796079327, 105.8322429386476955 ) ) ;
#140951 = CARTESIAN_POINT ( 'NONE',  ( -16.55341960407611168, -4.379528057220339221, 36.45724293864768839 ) ) ;
#140952 = CARTESIAN_POINT ( 'NONE',  ( 19.03943276465977164, -0.05219959533909143690, 78.74890960531436690 ) ) ;
#140953 = CARTESIAN_POINT ( 'NONE',  ( 21.52544592524344225, -5.823673210054117533, 63.54057627198103830 ) ) ;
#140955 = CARTESIAN_POINT ( 'NONE',  ( 14.29746914071037800, 8.314922557961029526, 26.66775706135235424 ) ) ;
#140954 = CARTESIAN_POINT ( 'NONE',  ( -5.823673210054116645, -21.52544592524344225, 97.29057627198105251 ) ) ;
#140956 = CARTESIAN_POINT ( 'NONE',  ( 13.89961937509977652, -13.97604488694527269, 113.1239096053143527 ) ) ;
#140957 = CARTESIAN_POINT ( 'NONE',  ( -21.53943276465977519, -0.05219959533937600094, 88.75109039468567573 ) ) ;
#140958 = CARTESIAN_POINT ( 'NONE',  ( -19.03943276465977164, 0.05219959533909376836, 81.24890960531436690 ) ) ;
#140959 = CARTESIAN_POINT ( 'NONE',  ( 0.05219959533909260263, 19.03943276465977164, 29.99890960531435979 ) ) ;
#140960 = CARTESIAN_POINT ( 'NONE',  ( -19.05341960407611168, -5.049401038298163336, 81.45724293864769550 ) ) ;
#140961 = CARTESIAN_POINT ( 'NONE',  ( 12.14591786802309770, 12.06949235617756955, 99.37390960531436690 ) ) ;
#140962 = CARTESIAN_POINT ( 'NONE',  ( 5.049401038298161559, -19.05341960407611168, 62.70724293864769550 ) ) ;
#140963 = CARTESIAN_POINT ( 'NONE',  ( -5.153800228976607833, 19.02544592524334988, 112.7094237280190043 ) ) ;
#140964 = CARTESIAN_POINT ( 'NONE',  ( -0.05219959533936034679, 19.03943276465977164, 42.50109039468566152 ) ) ;
#140966 = CARTESIAN_POINT ( 'NONE',  ( 21.55341960407610458, 5.719274019375980345, 23.95724293864769550 ) ) ;
#140965 = CARTESIAN_POINT ( 'NONE',  ( 21.52544592524334988, 5.823673210054432836, 91.45942372801901854 ) ) ;
#140967 = CARTESIAN_POINT ( 'NONE',  ( 16.55341960407618274, -4.379528057220086978, 86.04275706135236135 ) ) ;
#140968 = DIRECTION ( 'NONE',  ( 1.000000000000000000, 0.000000000000000000, -0.000000000000000000 ) ) ;
#140969 = CARTESIAN_POINT ( 'NONE',  ( -19.03943276465977164, -0.05219959533935918106, 73.75109039468566152 ) ) ;
#140970 = CARTESIAN_POINT ( 'NONE',  ( 19.02544592524334988, 5.153800228976608722, 31.45942372801900433 ) ) ;
#140971 = CARTESIAN_POINT ( 'NONE',  ( 24.93761727085874469, -12.28292609113013256, 139.9999999999999716 ) ) ;
#140972 = CARTESIAN_POINT ( 'NONE',  ( 0.05219959533909260263, 19.03943276465977164, 29.99890960531435979 ) ) ;
#140973 = CARTESIAN_POINT ( 'NONE',  ( 4.483927247898545687, 16.52544592524342804, 34.79057627198103120 ) ) ;
#140974 = CARTESIAN_POINT ( 'NONE',  ( 0.000000000000000000, 0.000000000000000000, -15.00000000000000000 ) ) ;
#140975 = CARTESIAN_POINT ( 'NONE',  ( -16.55341960407617563, 4.379528057220093196, 108.5427570613523756 ) ) ;
#140976 = CARTESIAN_POINT ( 'NONE',  ( 16.81555441253552274, 7.025013491695498047, 66.86314554665746357 ) ) ;
#140977 = CARTESIAN_POINT ( 'NONE',  ( -8.224510206698735004, -14.34966873604973081, 84.58442372801903275 ) ) ;
#140978 = CARTESIAN_POINT ( 'NONE',  ( 16.51473224551069308, 9.474510206698969483, 39.16557627198103120 ) ) ;
#140979 = CARTESIAN_POINT ( 'NONE',  ( -0.05219959533937732626, 21.53943276465977519, 87.50109039468568994 ) ) ;
#140980 = CARTESIAN_POINT ( 'NONE',  ( -5.153800228976607833, 19.02544592524334988, 97.70942372801900433 ) ) ;
#140981 = CARTESIAN_POINT ( 'NONE',  ( -5.823673210054431948, 21.52544592524334988, 77.70942372801900433 ) ) ;
#140982 = CARTESIAN_POINT ( 'NONE',  ( -19.03943276465977164, -0.05219959533935918106, 48.75109039468566863 ) ) ;
#140983 = CARTESIAN_POINT ( 'NONE',  ( 16.46253265017160672, -9.564922557960803928, 88.33224293864769550 ) ) ;
#140984 = CARTESIAN_POINT ( 'NONE',  ( 19.05341960407611168, 5.049401038298154454, 73.95724293864768129 ) ) ;
#140985 = DIRECTION ( 'NONE',  ( 0.000000000000000000, 0.000000000000000000, -1.000000000000000000 ) ) ;
#140986 = CIRCLE ( 'NONE', #21628, 2.649999999999999467 ) ;
#140987 = CARTESIAN_POINT ( 'NONE',  ( 8.224510206698953496, -14.34966873604960469, 72.91557627198103830 ) ) ;
#140988 = CARTESIAN_POINT ( 'NONE',  ( -0.05219959533907301413, -21.53943276465977519, 62.49890960531436690 ) ) ;
#140989 = CARTESIAN_POINT ( 'NONE',  ( 9.474510206698971260, -16.51473224551069308, 52.91557627198102409 ) ) ;
#140991 = CARTESIAN_POINT ( 'NONE',  ( 12.06949235617739724, 12.14591786802326823, 76.87609039468567573 ) ) ;
#140990 = CARTESIAN_POINT ( 'NONE',  ( -15.80617190586745835, -15.72974639402198527, 86.87390960531438111 ) ) ;
#140992 = ORIENTED_EDGE ( 'NONE', *, *, #36780, .T. ) ;
#140993 = CARTESIAN_POINT ( 'NONE',  ( -9.474510206698964154, 16.51473224551069663, 45.41557627198103120 ) ) ;
#140995 = CARTESIAN_POINT ( 'NONE',  ( -22.81625015709509441, -31.40387420917324590, -6.324999997268815122 ) ) ;
#140994 = CARTESIAN_POINT ( 'NONE',  ( 16.52544592524342804, -4.483927247898539470, 73.54057627198102409 ) ) ;
#140996 = CARTESIAN_POINT ( 'NONE',  ( -0.05219959533909027116, -19.03943276465977164, 47.49890960531435979 ) ) ;
#140997 = CARTESIAN_POINT ( 'NONE',  ( 9.564922557960805705, 16.46253265017160317, 24.58224293864769194 ) ) ;
#140998 = CARTESIAN_POINT ( 'NONE',  ( 13.89961937509957401, 13.97604488694547697, 71.87609039468567573 ) ) ;
#140999 = CARTESIAN_POINT ( 'NONE',  ( -16.52544592524342804, 4.483927247898546575, 76.04057627198102409 ) ) ;
#141000 = CARTESIAN_POINT ( 'NONE',  ( 10.72451020669871369, 18.67979575497193778, 52.08442372801901854 ) ) ;
#141002 = CARTESIAN_POINT ( 'NONE',  ( -18.62759615963270932, 10.81492255796079327, 105.8322429386476955 ) ) ;
#141001 = CARTESIAN_POINT ( 'NONE',  ( 0.05219959533909260263, 19.03943276465977164, 29.99890960531435979 ) ) ;
#141003 = CARTESIAN_POINT ( 'NONE',  ( -19.02544592524342804, 5.153800228976336051, 116.0405762719810383 ) ) ;
#141004 = CARTESIAN_POINT ( 'NONE',  ( 4.379528057220339221, -16.55341960407611168, 87.70724293864769550 ) ) ;
#141005 = CARTESIAN_POINT ( 'NONE',  ( 24.61032826407981844, -31.32210114170771220, -21.33226357150231678 ) ) ;
#141006 = CARTESIAN_POINT ( 'NONE',  ( -19.05341960407611168, -5.049401038298163336, 41.45724293864769550 ) ) ;
#141007 = CARTESIAN_POINT ( 'NONE',  ( 16.79531203550646623, 7.028104445595634076, 113.7524498822045302 ) ) ;
#141009 = CARTESIAN_POINT ( 'NONE',  ( 19.05341960407611168, 5.049401038298154454, 103.9572429386476671 ) ) ;
#141008 = CARTESIAN_POINT ( 'NONE',  ( 9.474510206698729675, 16.51473224551082808, 92.08442372801900433 ) ) ;
#141010 = CARTESIAN_POINT ( 'NONE',  ( -10.81492255796105439, 18.62759615963255655, 32.91775706135234714 ) ) ;
#141011 = CARTESIAN_POINT ( 'NONE',  ( -9.564922557960796823, -16.46253265017161027, 87.08224293864769550 ) ) ;
#141012 = CARTESIAN_POINT ( 'NONE',  ( -19.05341960407617563, 5.049401038297882671, 68.54275706135230450 ) ) ;
#141013 = CARTESIAN_POINT ( 'NONE',  ( -0.05219959533909027116, -19.03943276465977164, 47.49890960531435979 ) ) ;
#141014 =( REPRESENTATION_RELATIONSHIP ('NONE','NONE', #154205, #92179 ) REPRESENTATION_RELATIONSHIP_WITH_TRANSFORMATION ( #159445 )SHAPE_REPRESENTATION_RELATIONSHIP( ) );
#141015 = CARTESIAN_POINT ( 'NONE',  ( -16.52544592524342804, 4.483927247898546575, 61.04057627198103120 ) ) ;
#141016 = CARTESIAN_POINT ( 'NONE',  ( 16.55341960407611168, 4.379528057220329451, 73.95724293864769550 ) ) ;
#141017 = CARTESIAN_POINT ( 'NONE',  ( -16.51473224551069308, -9.474510206698971260, 71.66557627198102409 ) ) ;
#141018 = CARTESIAN_POINT ( 'NONE',  ( 21.53943276465977519, -0.05219959533907433946, 103.7489096053143669 ) ) ;
#141019 = CARTESIAN_POINT ( 'NONE',  ( -16.51473224551069308, -9.474510206698971260, 76.66557627198103830 ) ) ;
#141020 = CARTESIAN_POINT ( 'NONE',  ( -5.719274019375665041, -21.55341960407619695, 109.7927570613523613 ) ) ;
#141023 = CARTESIAN_POINT ( 'NONE',  ( 0.05219959533910956823, 16.53943276465976808, 109.9989096053143527 ) ) ;
#141022 = CARTESIAN_POINT ( 'NONE',  ( 16.55341960407618274, -4.379528057220086978, 111.0427570613523613 ) ) ;
#141021 = CARTESIAN_POINT ( 'NONE',  ( 16.46253265017160672, -9.564922557960803928, 33.33224293864770260 ) ) ;
#141024 = CARTESIAN_POINT ( 'NONE',  ( 19.05341960407617918, -5.049401038297876454, 106.0427570613523471 ) ) ;
#141025 = ORIENTED_EDGE ( 'NONE', *, *, #8030, .F. ) ;
#141026 = CARTESIAN_POINT ( 'NONE',  ( 21.52544592524334988, 5.823673210054432836, 36.45942372801901143 ) ) ;
#141027 = CARTESIAN_POINT ( 'NONE',  ( -16.46253265017146816, -9.564922557961047289, 49.16775706135233293 ) ) ;
#141028 = CARTESIAN_POINT ( 'NONE',  ( -14.34966873604972548, 8.224510206698743886, 113.3344237280190328 ) ) ;
#141029 = CARTESIAN_POINT ( 'NONE',  ( 18.62759615963271287, -10.81492255796078972, 78.33224293864770971 ) ) ;
#141030 = CARTESIAN_POINT ( 'NONE',  ( -0.05219959533909027116, -19.03943276465977164, 112.4989096053143669 ) ) ;
#141031 = CARTESIAN_POINT ( 'NONE',  ( 12.06949235617757843, -12.14591786802309237, 58.12390960531435979 ) ) ;
#141032 = CARTESIAN_POINT ( 'NONE',  ( 0.05219959533909260263, 19.03943276465977164, 29.99890960531435979 ) ) ;
#141033 = CARTESIAN_POINT ( 'NONE',  ( 19.02544592524343514, -5.153800228976328945, 38.54057627198103120 ) ) ;
#141034 = CARTESIAN_POINT ( 'NONE',  ( -0.05219959533936034679, 19.03943276465977164, 27.50109039468566507 ) ) ;
#141035 = CARTESIAN_POINT ( 'NONE',  ( 14.29746914071037800, 8.314922557961029526, 91.66775706135234714 ) ) ;
#141036 = CARTESIAN_POINT ( 'NONE',  ( -16.53943276465976808, -0.05219959533934237506, 63.75109039468568284 ) ) ;
#141037 = CARTESIAN_POINT ( 'NONE',  ( -13.97604488694527625, -13.89961937509977652, 111.8739096053143243 ) ) ;
#141039 = CARTESIAN_POINT ( 'NONE',  ( -15.80617190586768217, 15.72974639402176855, 103.1260903946856757 ) ) ;
#141038 = CARTESIAN_POINT ( 'NONE',  ( 19.03943276465977164, -0.05219959533909143690, 58.74890960531435979 ) ) ;
#141040 = CARTESIAN_POINT ( 'NONE',  ( -9.474510206698964154, 16.51473224551069663, 80.41557627198103830 ) ) ;
#141041 = AXIS2_PLACEMENT_3D ( 'NONE', #163691, #52497, #70680 ) ;
#141042 = CARTESIAN_POINT ( 'NONE',  ( 16.52544592524335698, 4.483927247898782831, 61.45942372801901854 ) ) ;
#141043 = CARTESIAN_POINT ( 'NONE',  ( 0.05219959533910956823, 16.53943276465976808, 109.9989096053143527 ) ) ;
#141044 = CARTESIAN_POINT ( 'NONE',  ( -16.53943276465976808, -0.05219959533934237506, 113.7510903946856757 ) ) ;
#141045 = CARTESIAN_POINT ( 'NONE',  ( -0.1105695005018468569, -21.30000000000002558, -58.85720012050614969 ) ) ;
#141048 = CARTESIAN_POINT ( 'NONE',  ( -19.05341960407611168, -5.049401038298163336, 81.45724293864769550 ) ) ;
#141047 = CARTESIAN_POINT ( 'NONE',  ( -19.05341960407611168, -5.049401038298163336, 86.45724293864769550 ) ) ;
#141046 = CARTESIAN_POINT ( 'NONE',  ( 21.55341960407619695, -5.719274019375665929, 76.04275706135237556 ) ) ;
#141049 = CARTESIAN_POINT ( 'NONE',  ( 5.153800228976335163, 19.02544592524342804, 104.7905762719809957 ) ) ;
#141050 = CARTESIAN_POINT ( 'NONE',  ( 14.29746914071049879, -8.314922557960816363, 53.33224293864769550 ) ) ;
#141051 = CARTESIAN_POINT ( 'NONE',  ( -0.05219959533934338120, 16.53943276465976808, 112.5010903946857042 ) ) ;
#141052 = CARTESIAN_POINT ( 'NONE',  ( -12.14591786802309592, -12.06949235617757132, 41.87390960531435979 ) ) ;
#141054 = CARTESIAN_POINT ( 'NONE',  ( -14.62203461105329438, -16.42507781964516766, -55.99240808130958413 ) ) ;
#141053 = CARTESIAN_POINT ( 'NONE',  ( 16.52544592524335698, 4.483927247898782831, 46.45942372801901854 ) ) ;
#141055 = CARTESIAN_POINT ( 'NONE',  ( -13.89961937509957401, -13.97604488694547875, 34.37609039468566863 ) ) ;
#141056 = CARTESIAN_POINT ( 'NONE',  ( -19.03943276465977164, 0.05219959533909376836, 76.24890960531435269 ) ) ;
#141057 = CARTESIAN_POINT ( 'NONE',  ( 19.02544592524334988, 5.153800228976608722, 51.45942372801900433 ) ) ;
#141058 = CARTESIAN_POINT ( 'NONE',  ( 22.81625015709510151, -31.40387420917324590, -8.424999997268812990 ) ) ;
#141059 = CARTESIAN_POINT ( 'NONE',  ( 37.99999999999999289, 12.34694845685046793, -2.649999994537626247 ) ) ;
#141061 = CARTESIAN_POINT ( 'NONE',  ( 16.52544592524335698, 4.483927247898782831, 86.45942372801901854 ) ) ;
#141060 = CARTESIAN_POINT ( 'NONE',  ( 13.97604488694548053, -13.89961937509957401, 80.62609039468567573 ) ) ;
#141062 = CARTESIAN_POINT ( 'NONE',  ( 5.049401038298161559, -19.05341960407611168, 22.70724293864769194 ) ) ;
#141063 = CARTESIAN_POINT ( 'NONE',  ( 5.049401038298161559, -19.05341960407611168, 107.7072429386476955 ) ) ;
#141064 = CARTESIAN_POINT ( 'NONE',  ( 5.823673210054444382, -21.52544592524334988, 45.20942372801901854 ) ) ;
#141065 = CARTESIAN_POINT ( 'NONE',  ( -19.03943276465977164, -0.05219959533935918106, 83.75109039468567573 ) ) ;
#141067 = CARTESIAN_POINT ( 'NONE',  ( -16.51473224551069308, -9.474510206698971260, 41.66557627198103120 ) ) ;
#141066 = CARTESIAN_POINT ( 'NONE',  ( 17.50000000000001066, -3.189878218039145175, 107.3705143742875947 ) ) ;
#141068 = EDGE_CURVE ( 'NONE', #84463, #23611, #109923, .T. ) ;
#141069 = CARTESIAN_POINT ( 'NONE',  ( 5.049401038298161559, -19.05341960407611168, 107.7072429386476955 ) ) ;
#141071 = CARTESIAN_POINT ( 'NONE',  ( 0.05219959533909260263, 19.03943276465977164, 44.99890960531435979 ) ) ;
#141070 = CARTESIAN_POINT ( 'NONE',  ( -16.52544592524342804, 4.483927247898546575, 66.04057627198103830 ) ) ;
#141072 = CARTESIAN_POINT ( 'NONE',  ( 13.89961937509977652, -13.97604488694527269, 63.12390960531435979 ) ) ;
#141073 = CARTESIAN_POINT ( 'NONE',  ( 0.05219959533936267826, -19.03943276465977164, 70.00109039468566152 ) ) ;
#141074 = CARTESIAN_POINT ( 'NONE',  ( -9.564922557961040184, 16.46253265017147172, 42.91775706135234003 ) ) ;
#141075 = CARTESIAN_POINT ( 'NONE',  ( 9.564922557960805705, 16.46253265017160317, 64.58224293864769550 ) ) ;
#141076 = CARTESIAN_POINT ( 'NONE',  ( -10.72451020669898014, 18.67979575497178502, 75.41557627198102409 ) ) ;
#141078 = CARTESIAN_POINT ( 'NONE',  ( -9.564922557961040184, 16.46253265017147172, 32.91775706135233293 ) ) ;
#141077 = CARTESIAN_POINT ( 'NONE',  ( 8.224510206698953496, -14.34966873604960469, 62.91557627198102409 ) ) ;
#141079 = CARTESIAN_POINT ( 'NONE',  ( -10.72451020669898014, 18.67979575497178502, 50.41557627198103120 ) ) ;
#141080 = CARTESIAN_POINT ( 'NONE',  ( 0.05219959533907565091, 21.53943276465977519, 44.99890960531435979 ) ) ;
#141081 = CARTESIAN_POINT ( 'NONE',  ( -16.51473224551069308, -9.474510206698971260, 71.66557627198102409 ) ) ;
#141082 = CARTESIAN_POINT ( 'NONE',  ( -0.05219959533909027116, -19.03943276465977164, 42.49890960531435269 ) ) ;
#141083 = CARTESIAN_POINT ( 'NONE',  ( 4.483927247898545687, 16.52544592524342804, 99.79057627198103830 ) ) ;
#141084 = CARTESIAN_POINT ( 'NONE',  ( -21.55341960407610458, -5.719274019375992779, 106.4572429386477097 ) ) ;
#141085 = DIRECTION ( 'NONE',  ( -1.000000000000000000, 0.000000000000000000, 0.000000000000000000 ) ) ;
#141086 = CARTESIAN_POINT ( 'NONE',  ( -5.823673210054431948, 21.52544592524334988, 27.70942372801901854 ) ) ;
#141087 = CARTESIAN_POINT ( 'NONE',  ( -5.153800228976328057, -19.02544592524343514, 32.29057627198102409 ) ) ;
#141088 = CARTESIAN_POINT ( 'NONE',  ( -5.823673210054116645, -21.52544592524344225, 112.2905762719810241 ) ) ;
#141089 = CARTESIAN_POINT ( 'NONE',  ( 19.05341960407617918, -5.049401038297876454, 51.04275706135231871 ) ) ;
#141090 = CARTESIAN_POINT ( 'NONE',  ( 16.46253265017160672, -9.564922557960803928, 23.33224293864769194 ) ) ;
#141091 = CARTESIAN_POINT ( 'NONE',  ( 9.474510206698971260, -16.51473224551069308, 27.91557627198103120 ) ) ;
#141092 = CARTESIAN_POINT ( 'NONE',  ( 17.05217265608910537, -6.523264755457947928, 21.23078202051969399 ) ) ;
#141093 = CARTESIAN_POINT ( 'NONE',  ( 14.29746914071037800, 8.314922557961029526, 51.66775706135234714 ) ) ;
#141094 = CARTESIAN_POINT ( 'NONE',  ( -13.97604488694527625, -13.89961937509977652, 26.87390960531434558 ) ) ;
#141095 = CARTESIAN_POINT ( 'NONE',  ( 33.71409597518591283, -4.151718627496498115, 98.62556914322648538 ) ) ;
#141096 = CARTESIAN_POINT ( 'NONE',  ( -9.564922557960796823, -16.46253265017161027, 77.08224293864769550 ) ) ;
#141097 = CARTESIAN_POINT ( 'NONE',  ( 12.06949235617757843, -12.14591786802309237, 113.1239096053143953 ) ) ;
#141098 = CARTESIAN_POINT ( 'NONE',  ( -5.719274019375978568, 21.55341960407610458, 50.20724293864769550 ) ) ;
#141099 = CARTESIAN_POINT ( 'NONE',  ( 0.05219959533910956823, 16.53943276465976808, 84.99890960531436690 ) ) ;
#141100 = CARTESIAN_POINT ( 'NONE',  ( 12.14591786802327356, -12.06949235617739191, 35.62609039468568994 ) ) ;
#141101 = CARTESIAN_POINT ( 'NONE',  ( -18.67979575497193778, 10.72451020669871902, 83.33442372801903275 ) ) ;
#141102 = CARTESIAN_POINT ( 'NONE',  ( -5.153800228976328057, -19.02544592524343514, 27.29057627198103120 ) ) ;
#141103 = CARTESIAN_POINT ( 'NONE',  ( -12.14591786802326823, 12.06949235617739902, 108.1260903946856757 ) ) ;
#141104 = CARTESIAN_POINT ( 'NONE',  ( 4.379528057220339221, -16.55341960407611168, 57.70724293864770260 ) ) ;
#141105 = CARTESIAN_POINT ( 'NONE',  ( -5.153800228976328057, -19.02544592524343514, 57.29057627198103120 ) ) ;
#141106 = CARTESIAN_POINT ( 'NONE',  ( 15.80617190586769283, -15.72974639402175789, 95.62609039468568994 ) ) ;
#141107 = CARTESIAN_POINT ( 'NONE',  ( -15.80617190586745835, -15.72974639402198527, 111.8739096053143669 ) ) ;
#141108 = CARTESIAN_POINT ( 'NONE',  ( 21.52544592524334988, 5.823673210054432836, 71.45942372801901854 ) ) ;
#141109 = CARTESIAN_POINT ( 'NONE',  ( 0.05219959533934541429, -16.53943276465976808, 35.00109039468568284 ) ) ;
#141111 = CARTESIAN_POINT ( 'NONE',  ( -5.823673210054431948, 21.52544592524334988, 87.70942372801901854 ) ) ;
#141110 = CARTESIAN_POINT ( 'NONE',  ( -4.483927247898539470, -16.52544592524342804, 82.29057627198103830 ) ) ;
#141112 = CARTESIAN_POINT ( 'NONE',  ( -16.52544592524342804, 4.483927247898546575, 26.04057627198103475 ) ) ;
#141113 = CARTESIAN_POINT ( 'NONE',  ( 23.29544513554940366, -16.92513159979222337, 141.0656553485623590 ) ) ;
#141114 = CARTESIAN_POINT ( 'NONE',  ( 16.52544592524335698, 4.483927247898782831, 36.45942372801901143 ) ) ;
#141115 = CARTESIAN_POINT ( 'NONE',  ( 8.314922557960818139, 14.29746914071049879, 39.58224293864769550 ) ) ;
#141116 = CARTESIAN_POINT ( 'NONE',  ( 4.379528057220092307, 16.55341960407617563, 92.29275706135236135 ) ) ;
#141117 = CARTESIAN_POINT ( 'NONE',  ( 0.05219959533909260263, 19.03943276465977164, 94.99890960531436690 ) ) ;
#141118 = CARTESIAN_POINT ( 'NONE',  ( -13.89961937509977652, 13.97604488694528158, 95.62390960531436690 ) ) ;
#141119 = CARTESIAN_POINT ( 'NONE',  ( 10.72451020669871369, 18.67979575497193778, 102.0844237280190185 ) ) ;
#141120 = CARTESIAN_POINT ( 'NONE',  ( -4.379528057220086978, -16.55341960407618274, 99.79275706135234714 ) ) ;
#141121 = CARTESIAN_POINT ( 'NONE',  ( -4.379528057220328563, 16.55341960407611168, 70.20724293864769550 ) ) ;
#141122 = CARTESIAN_POINT ( 'NONE',  ( 13.89961937509977652, -13.97604488694527269, 78.12390960531433848 ) ) ;
#141123 = EDGE_LOOP ( 'NONE', ( #49803, #109900, #156197, #83715 ) ) ;
#141124 = CARTESIAN_POINT ( 'NONE',  ( -12.14591786802326823, 12.06949235617739902, 28.12609039468568284 ) ) ;
#141125 = CARTESIAN_POINT ( 'NONE',  ( -9.474510206698964154, 16.51473224551069663, 30.41557627198102054 ) ) ;
#141126 = CARTESIAN_POINT ( 'NONE',  ( 5.153800228976335163, 19.02544592524342804, 89.79057627198102409 ) ) ;
#141128 = CARTESIAN_POINT ( 'NONE',  ( -22.81625015709510507, 31.40387420917330275, -2.924999997268813434 ) ) ;
#141127 = CARTESIAN_POINT ( 'NONE',  ( -8.224510206698735004, -14.34966873604973081, 29.58442372801901854 ) ) ;
#141129 = CARTESIAN_POINT ( 'NONE',  ( 5.153800228976615827, -19.02544592524334988, 30.20942372801900433 ) ) ;
#141130 = CARTESIAN_POINT ( 'NONE',  ( -8.224510206698735004, -14.34966873604973081, 94.58442372801901854 ) ) ;
#141131 = CARTESIAN_POINT ( 'NONE',  ( 16.51473224551083163, -9.474510206698727899, 100.8344237280190043 ) ) ;
#141132 = CARTESIAN_POINT ( 'NONE',  ( -19.05341960407611168, -5.049401038298163336, 36.45724293864766707 ) ) ;
#141133 = CARTESIAN_POINT ( 'NONE',  ( -8.224510206698735004, -14.34966873604973081, 84.58442372801903275 ) ) ;
#141134 = CARTESIAN_POINT ( 'NONE',  ( -4.483927247898782831, 16.52544592524335698, 67.70942372801901854 ) ) ;
#141135 = DIRECTION ( 'NONE',  ( 0.000000000000000000, 0.000000000000000000, -1.000000000000000000 ) ) ;
#141136 = CARTESIAN_POINT ( 'NONE',  ( 0.05219959533936267826, -19.03943276465977164, 75.00109039468566152 ) ) ;
#141137 = CARTESIAN_POINT ( 'NONE',  ( 18.62759615963255655, 10.81492255796105972, 106.6677570613523756 ) ) ;
#141138 = CARTESIAN_POINT ( 'NONE',  ( 9.474510206698971260, -16.51473224551069308, 47.91557627198102409 ) ) ;
#141139 = CARTESIAN_POINT ( 'NONE',  ( 19.02544592524343514, -5.153800228976328945, 88.54057627198102409 ) ) ;
#141140 = CARTESIAN_POINT ( 'NONE',  ( -16.55341960407611168, -4.379528057220339221, 86.45724293864770971 ) ) ;
#141141 = EDGE_CURVE ( 'NONE', #146788, #82599, #184905, .T. ) ;
#141142 = CARTESIAN_POINT ( 'NONE',  ( 16.46253265017146816, 9.564922557961045513, 56.66775706135233293 ) ) ;
#141143 = CARTESIAN_POINT ( 'NONE',  ( -18.62759615963270932, 10.81492255796079327, 55.83224293864770260 ) ) ;
#141144 = CARTESIAN_POINT ( 'NONE',  ( -10.72451020669870658, -18.67979575497194134, 109.5844237280190328 ) ) ;
#141145 = CARTESIAN_POINT ( 'NONE',  ( -16.51473224551069308, -9.474510206698971260, 96.66557627198102409 ) ) ;
#141146 = CARTESIAN_POINT ( 'NONE',  ( -19.05341960407617563, 5.049401038297882671, 23.54275706135233648 ) ) ;
#141147 = CARTESIAN_POINT ( 'NONE',  ( 5.823673210054125526, 21.52544592524343514, 64.79057627198103830 ) ) ;
#141148 = CARTESIAN_POINT ( 'NONE',  ( -18.22780087662119541, 5.500000000000102141, 56.01763182126894947 ) ) ;
#141149 = AXIS2_PLACEMENT_3D ( 'NONE', #139214, #31052, #186743 ) ;
#141150 = CARTESIAN_POINT ( 'NONE',  ( -19.05341960407617563, 5.049401038297882671, 88.54275706135230450 ) ) ;
#141151 = CARTESIAN_POINT ( 'NONE',  ( 13.97604488694527802, 13.89961937509977652, 114.3739096053143669 ) ) ;
#141152 = CARTESIAN_POINT ( 'NONE',  ( -16.51473224551082808, 9.474510206698731452, 113.3344237280190043 ) ) ;
#141153 = CARTESIAN_POINT ( 'NONE',  ( -12.06949235617756955, 12.14591786802309770, 110.6239096053143669 ) ) ;
#141154 = CARTESIAN_POINT ( 'NONE',  ( -0.05219959533909027116, -19.03943276465977164, 102.4989096053143669 ) ) ;
#141155 = CARTESIAN_POINT ( 'NONE',  ( -10.72451020669898014, 18.67979575497178502, 75.41557627198102409 ) ) ;
#141156 = CARTESIAN_POINT ( 'NONE',  ( 8.314922557961029526, -14.29746914071037800, 45.41775706135234003 ) ) ;
#141157 = CARTESIAN_POINT ( 'NONE',  ( -5.719274019375665041, -21.55341960407619695, 44.79275706135234714 ) ) ;
#141158 = CARTESIAN_POINT ( 'NONE',  ( -15.80617190586768217, 15.72974639402176855, 103.1260903946856757 ) ) ;
#141159 = CARTESIAN_POINT ( 'NONE',  ( 16.55341960407618274, -4.379528057220086978, 96.04275706135236135 ) ) ;
#141160 = CARTESIAN_POINT ( 'NONE',  ( -13.97604488694527625, -13.89961937509977652, 86.87390960531436690 ) ) ;
#141161 = CARTESIAN_POINT ( 'NONE',  ( -12.06949235617756955, 12.14591786802309770, 90.62390960531436690 ) ) ;
#141162 = CARTESIAN_POINT ( 'NONE',  ( -8.314922557960811034, -14.29746914071050412, 37.08224293864768129 ) ) ;
#141163 = CARTESIAN_POINT ( 'NONE',  ( 19.02544592524334988, 5.153800228976608722, 71.45942372801900433 ) ) ;
#141164 = CARTESIAN_POINT ( 'NONE',  ( -18.62759615963255300, -10.81492255796106328, 49.16775706135234003 ) ) ;
#141165 = CARTESIAN_POINT ( 'NONE',  ( -5.049401038297874678, -19.05341960407617918, 24.79275706135233648 ) ) ;
#141166 = CARTESIAN_POINT ( 'NONE',  ( 8.314922557960818139, 14.29746914071049879, 89.58224293864768129 ) ) ;
#141167 = CARTESIAN_POINT ( 'NONE',  ( -5.153800228976328057, -19.02544592524343514, 112.2905762719810099 ) ) ;
#141168 = CARTESIAN_POINT ( 'NONE',  ( 8.224510206698953496, -14.34966873604960469, 22.91557627198102765 ) ) ;
#141169 = CARTESIAN_POINT ( 'NONE',  ( -10.81492255796105439, 18.62759615963255655, 87.91775706135234714 ) ) ;
#141170 = CARTESIAN_POINT ( 'NONE',  ( -14.34966873604972548, 8.224510206698743886, 63.33442372801900433 ) ) ;
#141171 = CARTESIAN_POINT ( 'NONE',  ( -4.379528057220086978, -16.55341960407618274, 104.7927570613523898 ) ) ;
#141172 = CARTESIAN_POINT ( 'NONE',  ( -18.67979575497193778, 10.72451020669871902, 48.33442372801902565 ) ) ;
#141173 = CARTESIAN_POINT ( 'NONE',  ( -21.53943276465977519, -0.05219959533937600094, 33.75109039468568284 ) ) ;
#141174 = CARTESIAN_POINT ( 'NONE',  ( -8.224510206698948167, 14.34966873604960824, 105.4155762719810383 ) ) ;
#141175 = CARTESIAN_POINT ( 'NONE',  ( -19.05341960407611168, -5.049401038298163336, 21.45724293864768839 ) ) ;
#141176 = CARTESIAN_POINT ( 'NONE',  ( 14.34966873604960469, 8.224510206698951720, 69.16557627198102409 ) ) ;
#141177 = CARTESIAN_POINT ( 'NONE',  ( 5.049401038298161559, -19.05341960407611168, 77.70724293864765286 ) ) ;
#141178 = CARTESIAN_POINT ( 'NONE',  ( 4.379528057220092307, 16.55341960407617563, 102.2927570613523613 ) ) ;
#141179 = CARTESIAN_POINT ( 'NONE',  ( 13.89961937509977652, -13.97604488694527269, 43.12390960531434558 ) ) ;
#141180 = CARTESIAN_POINT ( 'NONE',  ( 10.72451020669898902, -18.67979575497178502, 62.91557627198102409 ) ) ;
#141181 = CARTESIAN_POINT ( 'NONE',  ( -8.224510206698948167, 14.34966873604960824, 95.41557627198102409 ) ) ;
#141182 = AXIS2_PLACEMENT_3D ( 'NONE', #172566, #98682, #51204 ) ;
#141183 = CARTESIAN_POINT ( 'NONE',  ( 5.719274019375991003, -21.55341960407610458, 97.70724293864772392 ) ) ;
#141184 = CARTESIAN_POINT ( 'NONE',  ( -16.46253265017160317, 9.564922557960807481, 95.83224293864769550 ) ) ;
#141186 = CARTESIAN_POINT ( 'NONE',  ( 5.049401038297881783, 19.05341960407617563, 87.29275706135234714 ) ) ;
#141185 = CARTESIAN_POINT ( 'NONE',  ( 19.03943276465977164, -0.05219959533909143690, 48.74890960531435979 ) ) ;
#141187 = CARTESIAN_POINT ( 'NONE',  ( 5.719274019375991003, -21.55341960407610458, 47.70724293864770260 ) ) ;
#141188 = CARTESIAN_POINT ( 'NONE',  ( 18.62759615963255655, 10.81492255796105972, 61.66775706135235424 ) ) ;
#141189 = CARTESIAN_POINT ( 'NONE',  ( -13.97604488694527625, -13.89961937509977652, 46.87390960531435979 ) ) ;
#141190 = CARTESIAN_POINT ( 'NONE',  ( -9.474510206698964154, 16.51473224551069663, 80.41557627198103830 ) ) ;
#141191 = CARTESIAN_POINT ( 'NONE',  ( -16.52544592524335698, -4.483927247898792601, 68.95942372801901854 ) ) ;
#141192 = CARTESIAN_POINT ( 'NONE',  ( -21.52544592524334988, -5.823673210054445271, 38.95942372801901854 ) ) ;
#141193 = CARTESIAN_POINT ( 'NONE',  ( 21.52544592524334988, 5.823673210054432836, 86.45942372801901854 ) ) ;
#141194 = CARTESIAN_POINT ( 'NONE',  ( 21.52544592524344225, -5.823673210054117533, 103.5405762719810383 ) ) ;
#141196 = CARTESIAN_POINT ( 'NONE',  ( -16.52544592524335698, -4.483927247898792601, 58.95942372801902565 ) ) ;
#141195 = CARTESIAN_POINT ( 'NONE',  ( 10.72451020669871369, 18.67979575497193778, 32.08442372801901854 ) ) ;
#141197 = CARTESIAN_POINT ( 'NONE',  ( -15.80617190586745835, -15.72974639402198527, 81.87390960531435269 ) ) ;
#141198 = CARTESIAN_POINT ( 'NONE',  ( -0.05219959533936034679, 19.03943276465977164, 32.50109039468566863 ) ) ;
#141200 = CARTESIAN_POINT ( 'NONE',  ( 14.29746914071037800, 8.314922557961029526, 111.6677570613523613 ) ) ;
#141199 = CARTESIAN_POINT ( 'NONE',  ( -5.153800228976328057, -19.02544592524343514, 62.29057627198100988 ) ) ;
#141201 = CARTESIAN_POINT ( 'NONE',  ( 30.74264578624800137, -22.33583958711395212, -5.200000000000001066 ) ) ;
#141202 = CARTESIAN_POINT ( 'NONE',  ( -9.564922557960796823, -16.46253265017161027, 102.0822429386477097 ) ) ;
#141203 = DIRECTION ( 'NONE',  ( 0.000000000000000000, 0.000000000000000000, 1.000000000000000000 ) ) ;
#141204 = CARTESIAN_POINT ( 'NONE',  ( -16.46253265017146816, -9.564922557961047289, 84.16775706135233293 ) ) ;
#141205 = CARTESIAN_POINT ( 'NONE',  ( -0.05219959533907301413, -21.53943276465977519, 57.49890960531435979 ) ) ;
#141206 = CARTESIAN_POINT ( 'NONE',  ( 12.14591786802309770, 12.06949235617756955, 39.37390960531436690 ) ) ;
#141207 = CARTESIAN_POINT ( 'NONE',  ( -16.52544592524335698, -4.483927247898792601, 23.95942372801901143 ) ) ;
#141208 = CARTESIAN_POINT ( 'NONE',  ( 16.46253265017160672, -9.564922557960803928, 28.33224293864769550 ) ) ;
#141209 = CARTESIAN_POINT ( 'NONE',  ( 19.03943276465977164, 0.05219959533936151252, 106.2510903946856615 ) ) ;
#141211 = CARTESIAN_POINT ( 'NONE',  ( -9.564922557961040184, 16.46253265017147172, 67.91775706135233293 ) ) ;
#141210 = CARTESIAN_POINT ( 'NONE',  ( 0.05219959533907565091, 21.53943276465977519, 94.99890960531436690 ) ) ;
#141212 = CARTESIAN_POINT ( 'NONE',  ( 12.14591786802327356, -12.06949235617739191, 75.62609039468567573 ) ) ;
#141213 = CARTESIAN_POINT ( 'NONE',  ( 19.05341960407611168, 5.049401038298154454, 63.95724293864769550 ) ) ;
#141214 = CARTESIAN_POINT ( 'NONE',  ( -0.05219959533910754901, -16.53943276465976808, 72.49890960531435269 ) ) ;
#141215 = CARTESIAN_POINT ( 'NONE',  ( 16.51473224551069308, 9.474510206698969483, 64.16557627198102409 ) ) ;
#141216 = CARTESIAN_POINT ( 'NONE',  ( 4.379528057220339221, -16.55341960407611168, 67.70724293864769550 ) ) ;
#141217 = CARTESIAN_POINT ( 'NONE',  ( -36.76875311564131721, -5.017346702420296900, 47.26027925686760511 ) ) ;
#141218 = CARTESIAN_POINT ( 'NONE',  ( -14.34966873604960291, -8.224510206698953496, 36.66557627198103120 ) ) ;
#141219 = CARTESIAN_POINT ( 'NONE',  ( -16.46253265017160317, 9.564922557960807481, 70.83224293864770971 ) ) ;
#141220 = FACE_BOUND ( 'NONE', #34809, .T. ) ;
#141221 = CARTESIAN_POINT ( 'NONE',  ( 5.153800228976615827, -19.02544592524334988, 45.20942372801901143 ) ) ;
#141222 = CARTESIAN_POINT ( 'NONE',  ( 16.55341960407618274, -4.379528057220086978, 51.04275706135234714 ) ) ;
#141223 = CARTESIAN_POINT ( 'NONE',  ( -5.719274019375978568, 21.55341960407610458, 65.20724293864768129 ) ) ;
#141224 = CARTESIAN_POINT ( 'NONE',  ( 13.89961937509957401, 13.97604488694547697, 21.87609039468566152 ) ) ;
#141225 = CARTESIAN_POINT ( 'NONE',  ( 5.153800228976335163, 19.02544592524342804, 69.79057627198103830 ) ) ;
#141226 = CARTESIAN_POINT ( 'NONE',  ( -8.388830574159379737E-16, -13.70000000000001528, -62.58071313852362039 ) ) ;
#141227 = CARTESIAN_POINT ( 'NONE',  ( -5.049401038298153566, 19.05341960407611168, 105.2072429386476671 ) ) ;
#141228 = CARTESIAN_POINT ( 'NONE',  ( -5.719274019375665041, -21.55341960407619695, 34.79275706135235424 ) ) ;
#141229 = CARTESIAN_POINT ( 'NONE',  ( 14.29746914071049879, -8.314922557960816363, 113.3322429386476955 ) ) ;
#141232 = ORIENTED_EDGE ( 'NONE', *, *, #80827, .F. ) ;
#141231 = CARTESIAN_POINT ( 'NONE',  ( -5.153800228976328057, -19.02544592524343514, 82.29057627198103830 ) ) ;
#141230 = CARTESIAN_POINT ( 'NONE',  ( -21.53943276465977519, 0.05219959533907696930, 101.2489096053143669 ) ) ;
#141233 = CARTESIAN_POINT ( 'NONE',  ( 10.81492255796106328, -18.62759615963255655, 30.41775706135234358 ) ) ;
#141234 = VERTEX_POINT ( 'NONE', #147367 ) ;
#141235 = CARTESIAN_POINT ( 'NONE',  ( -9.474510206698964154, 16.51473224551069663, 90.41557627198103830 ) ) ;
#141236 = EDGE_CURVE ( 'NONE', #106384, #76130, #173356, .T. ) ;
#141237 = DIRECTION ( 'NONE',  ( 0.000000000000000000, -0.000000000000000000, -1.000000000000000000 ) ) ;
#141238 = B_SPLINE_CURVE_WITH_KNOTS ( 'NONE', 3,
 ( #8450, #70123, #193474, #131795, #54951, #163130, #24633, #86281, #147972, #133793, #108411, #122584, #58932, #170086, #12464, #31580, #199440, #44766, #106419, #90261, #182295, #104453, #166136, #138745 ),
 .UNSPECIFIED., .F., .F.,
 ( 4, 2, 2, 2, 2, 2, 2, 2, 2, 2, 2, 4 ),
 ( 1.970462153819272771E-07, 0.0003069708713090705718, 0.0006137446964027592957, 0.001227292346590132732, 0.001534066171683819233, 0.001840839996777505734, 0.002147613821871192236, 0.002454387646964878520, 0.003067935297152264533, 0.003681482947339650546, 0.004295030597527036559, 0.004908578247714422138 ),
 .UNSPECIFIED. ) ;
#141239 = CARTESIAN_POINT ( 'NONE',  ( 16.51473224551069308, 9.474510206698969483, 29.16557627198103475 ) ) ;
#141240 = CARTESIAN_POINT ( 'NONE',  ( -9.474510206698720793, -16.51473224551083518, 104.5844237280190043 ) ) ;
#141241 = CARTESIAN_POINT ( 'NONE',  ( 29.86685920354754842, -21.69954338932559068, -8.324999997268813345 ) ) ;
#141242 = CARTESIAN_POINT ( 'NONE',  ( -8.314922557960811034, -14.29746914071050412, 112.0822429386477097 ) ) ;
#141243 = CARTESIAN_POINT ( 'NONE',  ( 0.05219959533937995610, -21.53943276465977519, 85.00109039468568994 ) ) ;
#141245 = CARTESIAN_POINT ( 'NONE',  ( 21.52544592524334988, 5.823673210054432836, 51.45942372801901854 ) ) ;
#141244 = CARTESIAN_POINT ( 'NONE',  ( 5.153800228976335163, 19.02544592524342804, 74.79057627198103830 ) ) ;
#141246 = CARTESIAN_POINT ( 'NONE',  ( 21.52544592524334988, 5.823673210054432836, 31.45942372801901854 ) ) ;
#141247 = CARTESIAN_POINT ( 'NONE',  ( 1.993301997531345292E-15, -30.30510711980685912, 148.5000000000000000 ) ) ;
#141248 = CARTESIAN_POINT ( 'NONE',  ( -19.03943276465977164, 0.05219959533909376836, 91.24890960531436690 ) ) ;
#141249 = DIRECTION ( 'NONE',  ( 0.5000000000000036637, 0.4999999999999949485, 0.7071067811865484609 ) ) ;
#141251 = CARTESIAN_POINT ( 'NONE',  ( 18.67979575497178502, 10.72451020669898547, 39.16557627198102409 ) ) ;
#141250 = CARTESIAN_POINT ( 'NONE',  ( 8.314922557961029526, -14.29746914071037800, 40.41775706135234714 ) ) ;
#141252 = CARTESIAN_POINT ( 'NONE',  ( -15.80617190586768217, 15.72974639402176855, 78.12609039468570415 ) ) ;
#141253 = LINE ( 'NONE', #187784, #31615 ) ;
#141254 = CARTESIAN_POINT ( 'NONE',  ( 16.51473224551083163, -9.474510206698727899, 105.8344237280190043 ) ) ;
#141255 = CARTESIAN_POINT ( 'NONE',  ( -19.05341960407611168, -5.049401038298163336, 66.45724293864769550 ) ) ;
#141256 = CARTESIAN_POINT ( 'NONE',  ( 19.02544592524343514, -5.153800228976328945, 78.54057627198099567 ) ) ;
#141257 = CARTESIAN_POINT ( 'NONE',  ( -4.483927247898539470, -16.52544592524342804, 107.2905762719810525 ) ) ;
#141258 = CARTESIAN_POINT ( 'NONE',  ( 16.55341960407611168, 4.379528057220329451, 103.9572429386476813 ) ) ;
#141259 = CARTESIAN_POINT ( 'NONE',  ( -16.46253265017160317, 9.564922557960807481, 105.8322429386476955 ) ) ;
#141260 = CARTESIAN_POINT ( 'NONE',  ( 8.224510206698742110, 14.34966873604972548, 82.08442372801901854 ) ) ;
#141262 = CARTESIAN_POINT ( 'NONE',  ( 5.049401038298161559, -19.05341960407611168, 52.70724293864767418 ) ) ;
#141261 = CARTESIAN_POINT ( 'NONE',  ( -12.14591786802309592, -12.06949235617757132, 56.87390960531436690 ) ) ;
#141263 = CARTESIAN_POINT ( 'NONE',  ( 5.719274019375673035, 21.55341960407619339, 77.29275706135234714 ) ) ;
#141264 = CARTESIAN_POINT ( 'NONE',  ( -5.719274019375665041, -21.55341960407619695, 64.79275706135234714 ) ) ;
#141265 = CARTESIAN_POINT ( 'NONE',  ( 13.97604488694548053, -13.89961937509957401, 110.6260903946856615 ) ) ;
#141266 = CARTESIAN_POINT ( 'NONE',  ( 16.53943276465976808, -0.05219959533910856209, 63.74890960531435979 ) ) ;
#141267 = CARTESIAN_POINT ( 'NONE',  ( 5.719274019375991003, -21.55341960407610458, 107.7072429386476955 ) ) ;
#141268 = CARTESIAN_POINT ( 'NONE',  ( 21.55341960407610458, 5.719274019375980345, 53.95724293864770260 ) ) ;
#141269 = CARTESIAN_POINT ( 'NONE',  ( 18.56101223717333326, 5.499999999999950262, 73.94978406935678095 ) ) ;
#141270 = CARTESIAN_POINT ( 'NONE',  ( 28.82186960331499392, -9.364793116373510529, 139.1500000054623456 ) ) ;
#141271 = CARTESIAN_POINT ( 'NONE',  ( -19.03943276465977164, 0.05219959533909376836, 76.24890960531435269 ) ) ;
#141272 = CARTESIAN_POINT ( 'NONE',  ( 8.224510206698953496, -14.34966873604960469, 37.91557627198102409 ) ) ;
#141273 = CIRCLE ( 'NONE', #137966, 4.250000000000000000 ) ;
#141274 = CARTESIAN_POINT ( 'NONE',  ( -0.05219959533910754901, -16.53943276465976808, 27.49890960531435269 ) ) ;
#141275 = CARTESIAN_POINT ( 'NONE',  ( 14.34966873604972726, -8.224510206698740333, 90.83442372801901854 ) ) ;
#141276 = CARTESIAN_POINT ( 'NONE',  ( -16.46253265017146816, -9.564922557961047289, 49.16775706135233293 ) ) ;
#141277 = DIRECTION ( 'NONE',  ( 1.000000000000000000, 0.000000000000000000, 0.000000000000000000 ) ) ;
#141278 = CARTESIAN_POINT ( 'NONE',  ( -13.97604488694527625, -13.89961937509977652, 86.87390960531436690 ) ) ;
#141279 = CARTESIAN_POINT ( 'NONE',  ( -14.34966873604960291, -8.224510206698953496, 66.66557627198102409 ) ) ;
#141281 = CARTESIAN_POINT ( 'NONE',  ( -18.67979575497178146, -10.72451020669898902, 26.66557627198103475 ) ) ;
#141280 = CARTESIAN_POINT ( 'NONE',  ( 17.44270441346516520, -5.991230190323024729, 101.1366492073577206 ) ) ;
#141283 = ORIENTED_EDGE ( 'NONE', *, *, #130264, .T. ) ;
#141282 = CARTESIAN_POINT ( 'NONE',  ( -15.80617190586745835, -15.72974639402198527, 51.87390960531437401 ) ) ;
#141284 = CARTESIAN_POINT ( 'NONE',  ( 14.34966873604960469, 8.224510206698951720, 94.16557627198103830 ) ) ;
#141285 = CARTESIAN_POINT ( 'NONE',  ( -0.05219959533934338120, 16.53943276465976808, 52.50109039468567573 ) ) ;
#141286 = CARTESIAN_POINT ( 'NONE',  ( -4.483927247898539470, -16.52544592524342804, 72.29057627198102409 ) ) ;
#141287 = CARTESIAN_POINT ( 'NONE',  ( 1.300000000000000044, -1.082531754730548412, 0.6249999999999998890 ) ) ;
#141288 = CARTESIAN_POINT ( 'NONE',  ( 9.474510206698729675, 16.51473224551082808, 82.08442372801899012 ) ) ;
#141289 = CARTESIAN_POINT ( 'NONE',  ( -21.55341960407610458, -5.719274019375992779, 26.45724293864768839 ) ) ;
#141290 = CARTESIAN_POINT ( 'NONE',  ( 3.556970738554033499E-15, -38.81732327939057825, -4.624999997268814056 ) ) ;
#141291 = CARTESIAN_POINT ( 'NONE',  ( -23.31738231874055245, -16.94106989632524574, 142.1999999999999886 ) ) ;
#141293 = CARTESIAN_POINT ( 'NONE',  ( 16.53943276465976808, -0.05219959533910856209, 28.74890960531435624 ) ) ;
#141292 = CARTESIAN_POINT ( 'NONE',  ( -4.483927247898782831, 16.52544592524335698, 42.70942372801901854 ) ) ;
#141294 = CARTESIAN_POINT ( 'NONE',  ( 0.05219959533907565091, 21.53943276465977519, 54.99890960531435269 ) ) ;
#141295 = CARTESIAN_POINT ( 'NONE',  ( 19.02544592524334988, 5.153800228976608722, 81.45942372801897591 ) ) ;
#141296 = CARTESIAN_POINT ( 'NONE',  ( 21.53943276465977519, -0.05219959533907433946, 43.74890960531435979 ) ) ;
#141297 = CARTESIAN_POINT ( 'NONE',  ( -21.52544592524334988, -5.823673210054445271, 78.95942372801901854 ) ) ;
#141298 = CARTESIAN_POINT ( 'NONE',  ( -12.05108236997114446, 9.980772036771131894, -61.81300923031701444 ) ) ;
#141299 = CARTESIAN_POINT ( 'NONE',  ( 16.55341960407618274, -4.379528057220086978, 31.04275706135234714 ) ) ;
#141301 = CARTESIAN_POINT ( 'NONE',  ( -19.05341960407611168, -5.049401038298163336, 96.45724293864769550 ) ) ;
#141300 = CARTESIAN_POINT ( 'NONE',  ( 9.474510206698971260, -16.51473224551069308, 37.91557627198102409 ) ) ;
#141302 = VECTOR ( 'NONE', #37292, 1000.000000000000000 ) ;
#141303 = CARTESIAN_POINT ( 'NONE',  ( 16.51473224551069308, 9.474510206698969483, 39.16557627198103120 ) ) ;
#141304 = CARTESIAN_POINT ( 'NONE',  ( -14.34966873604960291, -8.224510206698953496, 101.6655762719810383 ) ) ;
#141305 = CARTESIAN_POINT ( 'NONE',  ( 0.000000000000000000, 0.000000000000000000, 0.000000000000000000 ) ) ;
#141306 = CARTESIAN_POINT ( 'NONE',  ( -16.51473224551069308, -9.474510206698971260, 106.6655762719810383 ) ) ;
#141307 = VERTEX_POINT ( 'NONE', #65529 ) ;
#141308 = CARTESIAN_POINT ( 'NONE',  ( 0.05219959533934541429, -16.53943276465976808, 50.00109039468568994 ) ) ;
#141309 = CARTESIAN_POINT ( 'NONE',  ( -18.62759615963270932, 10.81492255796079327, 95.83224293864770971 ) ) ;
#141310 = CARTESIAN_POINT ( 'NONE',  ( 19.05341960407611168, 5.049401038298154454, 43.95724293864769550 ) ) ;
#141311 = CARTESIAN_POINT ( 'NONE',  ( -18.62759615963255300, -10.81492255796106328, 24.16775706135235424 ) ) ;
#141312 = CARTESIAN_POINT ( 'NONE',  ( 9.474510206698971260, -16.51473224551069308, 87.91557627198102409 ) ) ;
#141313 = CARTESIAN_POINT ( 'NONE',  ( 32.00000000000000000, -5.510910596163089556E-15, 39.49999999999996447 ) ) ;
#141314 = ORIENTED_EDGE ( 'NONE', *, *, #45175, .T. ) ;
#141315 = CARTESIAN_POINT ( 'NONE',  ( -16.52544592524335698, -4.483927247898792601, 48.95942372801902565 ) ) ;
#141316 = CARTESIAN_POINT ( 'NONE',  ( -15.72974639402176322, -15.80617190586768395, 19.37609039468568639 ) ) ;
#141319 = CARTESIAN_POINT ( 'NONE',  ( -19.02544592524334988, -5.153800228976617603, 68.95942372801896170 ) ) ;
#141318 = CARTESIAN_POINT ( 'NONE',  ( 9.564922557960805705, 16.46253265017160317, 94.58224293864769550 ) ) ;
#141317 = CARTESIAN_POINT ( 'NONE',  ( -4.483927247898539470, -16.52544592524342804, 107.2905762719810525 ) ) ;
#141320 = CARTESIAN_POINT ( 'NONE',  ( 19.03943276465977164, 0.05219959533936151252, 31.25109039468566863 ) ) ;
#141321 = CARTESIAN_POINT ( 'NONE',  ( -21.53943276465977519, 0.05219959533907696930, 91.24890960531436690 ) ) ;
#141322 = CARTESIAN_POINT ( 'NONE',  ( -16.46253265017146816, -9.564922557961047289, 19.16775706135233293 ) ) ;
#141323 = CARTESIAN_POINT ( 'NONE',  ( 0.05219959533934541429, -16.53943276465976808, 80.00109039468568994 ) ) ;
#141324 = CARTESIAN_POINT ( 'NONE',  ( 13.89961937509977652, -13.97604488694527269, 108.1239096053143669 ) ) ;
#141325 = CARTESIAN_POINT ( 'NONE',  ( -19.03943276465977164, 0.05219959533909376836, 61.24890960531436690 ) ) ;
#141326 = CIRCLE ( 'NONE', #18633, 10.00000000000000178 ) ;
#141327 = CARTESIAN_POINT ( 'NONE',  ( 10.81492255796106328, -18.62759615963255655, 65.41775706135234714 ) ) ;
#141328 = CARTESIAN_POINT ( 'NONE',  ( -18.62759615963255300, -10.81492255796106328, 64.16775706135234714 ) ) ;
#141329 = CARTESIAN_POINT ( 'NONE',  ( -9.474510206698964154, 16.51473224551069663, 70.41557627198102409 ) ) ;
#141330 = CARTESIAN_POINT ( 'NONE',  ( 10.81492255796106328, -18.62759615963255655, 55.41775706135234714 ) ) ;
#141331 = ORIENTED_EDGE ( 'NONE', *, *, #53585, .T. ) ;
#141332 = CARTESIAN_POINT ( 'NONE',  ( -0.05219959533936034679, 19.03943276465977164, 87.50109039468567573 ) ) ;
#141333 = ADVANCED_FACE ( 'NONE', ( #5842 ), #175880, .F. ) ;
#141334 = CARTESIAN_POINT ( 'NONE',  ( -9.474510206698964154, 16.51473224551069663, 55.41557627198103120 ) ) ;
#141335 = CARTESIAN_POINT ( 'NONE',  ( 5.153800228976335163, 19.02544592524342804, 94.79057627198103830 ) ) ;
#141336 = CARTESIAN_POINT ( 'NONE',  ( 9.474510206698971260, -16.51473224551069308, 62.91557627198102409 ) ) ;
#141337 = CARTESIAN_POINT ( 'NONE',  ( 19.03943276465977164, -0.05219959533909143690, 113.7489096053143669 ) ) ;
#141338 = CARTESIAN_POINT ( 'NONE',  ( -9.474510206698964154, 16.51473224551069663, 55.41557627198103120 ) ) ;
#141339 = CARTESIAN_POINT ( 'NONE',  ( -5.823673210054116645, -21.52544592524344225, 82.29057627198103830 ) ) ;
#141340 = CARTESIAN_POINT ( 'NONE',  ( -4.379528057220086978, -16.55341960407618274, 69.79275706135234714 ) ) ;
#141341 = CARTESIAN_POINT ( 'NONE',  ( -22.65770943308888619, 11.99324031494455589, 167.9410816520763206 ) ) ;
#141342 = CARTESIAN_POINT ( 'NONE',  ( 19.02544592524334988, 5.153800228976608722, 26.45942372801899722 ) ) ;
#141343 = CARTESIAN_POINT ( 'NONE',  ( 0.05219959533909260263, 19.03943276465977164, 64.99890960531436690 ) ) ;
#141344 = CARTESIAN_POINT ( 'NONE',  ( 0.05219959533910956823, 16.53943276465976808, 59.99890960531436690 ) ) ;
#141345 = CARTESIAN_POINT ( 'NONE',  ( 0.05219959533910956823, 16.53943276465976808, 94.99890960531436690 ) ) ;
#141346 = CARTESIAN_POINT ( 'NONE',  ( -13.97604488694527625, -13.89961937509977652, 96.87390960531433848 ) ) ;
#141347 = CARTESIAN_POINT ( 'NONE',  ( -19.05341960407611168, -5.049401038298163336, 91.45724293864766707 ) ) ;
#141348 = CARTESIAN_POINT ( 'NONE',  ( 5.823673210054444382, -21.52544592524334988, 45.20942372801901854 ) ) ;
#141349 = CARTESIAN_POINT ( 'NONE',  ( 5.049401038298161559, -19.05341960407611168, 107.7072429386476955 ) ) ;
#141350 = CARTESIAN_POINT ( 'NONE',  ( -0.05219959533937732626, 21.53943276465977519, 112.5010903946857042 ) ) ;
#141351 = CARTESIAN_POINT ( 'NONE',  ( 14.29746914071037800, 8.314922557961029526, 81.66775706135236135 ) ) ;
#141352 = CARTESIAN_POINT ( 'NONE',  ( 15.80617190586769283, -15.72974639402175789, 35.62609039468568994 ) ) ;
#141353 = CARTESIAN_POINT ( 'NONE',  ( -15.72974639402197994, 15.80617190586746368, 30.62390960531436335 ) ) ;
#141354 = CARTESIAN_POINT ( 'NONE',  ( 15.72974639402199770, -15.80617190586745480, 98.12390960531436690 ) ) ;
#141355 = CARTESIAN_POINT ( 'NONE',  ( -16.53943276465976808, 0.05219959533911058130, 66.24890960531436690 ) ) ;
#141356 = CARTESIAN_POINT ( 'NONE',  ( -19.05341960407611168, -5.049401038298163336, 61.45724293864769550 ) ) ;
#141357 = CARTESIAN_POINT ( 'NONE',  ( 8.314922557960818139, 14.29746914071049879, 79.58224293864769550 ) ) ;
#141358 = CARTESIAN_POINT ( 'NONE',  ( 0.05219959533907565091, 21.53943276465977519, 49.99890960531437401 ) ) ;
#141359 = CARTESIAN_POINT ( 'NONE',  ( -13.97604488694547697, 13.89961937509957934, 48.12609039468566863 ) ) ;
#141360 = CARTESIAN_POINT ( 'NONE',  ( -16.52544592524342804, 4.483927247898546575, 111.0405762719810525 ) ) ;
#141361 = VERTEX_POINT ( 'NONE', #127189 ) ;
#141362 = CARTESIAN_POINT ( 'NONE',  ( 12.14591786802327356, -12.06949235617739191, 70.62609039468567573 ) ) ;
#141363 = CARTESIAN_POINT ( 'NONE',  ( -5.153800228976328057, -19.02544592524343514, 72.29057627198102409 ) ) ;
#141364 = CARTESIAN_POINT ( 'NONE',  ( -22.44159573604010305, 16.30477369853692338, 144.6750000027311671 ) ) ;
#141365 = CARTESIAN_POINT ( 'NONE',  ( 16.55341960407611168, 4.379528057220329451, 93.95724293864770971 ) ) ;
#141366 = CARTESIAN_POINT ( 'NONE',  ( 18.67979575497178502, 10.72451020669898547, 39.16557627198102409 ) ) ;
#141367 = ORIENTED_EDGE ( 'NONE', *, *, #630, .F. ) ;
#141368 = CARTESIAN_POINT ( 'NONE',  ( -16.53943276465976808, -0.05219959533934237506, 103.7510903946857042 ) ) ;
#141369 = CARTESIAN_POINT ( 'NONE',  ( 5.153800228976615827, -19.02544592524334988, 105.2094237280190185 ) ) ;
#141370 = CARTESIAN_POINT ( 'NONE',  ( -18.62759615963255300, -10.81492255796106328, 84.16775706135234714 ) ) ;
#141371 = CARTESIAN_POINT ( 'NONE',  ( -0.05219959533909027116, -19.03943276465977164, 92.49890960531436690 ) ) ;
#141372 = CARTESIAN_POINT ( 'NONE',  ( -10.72451020669898014, 18.67979575497178502, 100.4155762719810241 ) ) ;
#141373 = CARTESIAN_POINT ( 'NONE',  ( 16.52544592524335698, 4.483927247898782831, 56.45942372801902565 ) ) ;
#141374 = CARTESIAN_POINT ( 'NONE',  ( 13.97604488694527802, 13.89961937509977652, 29.37390960531435979 ) ) ;
#141375 = CARTESIAN_POINT ( 'NONE',  ( 14.29746914071037800, 8.314922557961029526, 36.66775706135234714 ) ) ;
#141376 = CARTESIAN_POINT ( 'NONE',  ( -5.049401038297874678, -19.05341960407617918, 99.79275706135234714 ) ) ;
#141377 = CARTESIAN_POINT ( 'NONE',  ( -0.05219959533907301413, -21.53943276465977519, 92.49890960531436690 ) ) ;
#141378 = CARTESIAN_POINT ( 'NONE',  ( -13.97604488694547697, 13.89961937509957934, 48.12609039468566863 ) ) ;
#141379 = LINE ( 'NONE', #3848, #109118 ) ;
#141380 = CARTESIAN_POINT ( 'NONE',  ( 18.62759615963271287, -10.81492255796078972, 108.3322429386477097 ) ) ;
#141381 = CARTESIAN_POINT ( 'NONE',  ( -18.22780087662123094, -5.499999999999984901, 71.48459894673891313 ) ) ;
#141382 = CARTESIAN_POINT ( 'NONE',  ( 9.564922557960805705, 16.46253265017160317, 74.58224293864769550 ) ) ;
#141383 = CARTESIAN_POINT ( 'NONE',  ( -12.14591786802326823, 12.06949235617739902, 38.12609039468567573 ) ) ;
#141384 = CARTESIAN_POINT ( 'NONE',  ( -4.500000000000001776, -116.8122400552013431, 54.87277500418469600 ) ) ;
#141385 = CARTESIAN_POINT ( 'NONE',  ( 13.97604488694548053, -13.89961937509957401, 55.62609039468566863 ) ) ;
#141387 = CARTESIAN_POINT ( 'NONE',  ( 0.05219959533910956823, 16.53943276465976808, 64.99890960531435269 ) ) ;
#141386 = CARTESIAN_POINT ( 'NONE',  ( 21.53943276465977519, -0.05219959533907433946, 113.7489096053143527 ) ) ;
#141388 = CARTESIAN_POINT ( 'NONE',  ( -19.02544592524342804, 5.153800228976336051, 71.04057627198099567 ) ) ;
#141390 = CARTESIAN_POINT ( 'NONE',  ( -0.05219959533936034679, 19.03943276465977164, 42.50109039468566152 ) ) ;
#141389 = CARTESIAN_POINT ( 'NONE',  ( 0.05219959533934541429, -16.53943276465976808, 35.00109039468568284 ) ) ;
#141391 = CARTESIAN_POINT ( 'NONE',  ( -18.62759615963255300, -10.81492255796106328, 49.16775706135234003 ) ) ;
#141392 = CARTESIAN_POINT ( 'NONE',  ( 19.02544592524334988, 5.153800228976608722, 111.4594237280190043 ) ) ;
#141393 = CARTESIAN_POINT ( 'NONE',  ( 19.02544592524343514, -5.153800228976328945, 58.54057627198102409 ) ) ;
#141394 = CARTESIAN_POINT ( 'NONE',  ( 19.05341960407617918, -5.049401038297876454, 76.04275706135230450 ) ) ;
#141395 = CARTESIAN_POINT ( 'NONE',  ( -10.81492255796105439, 18.62759615963255655, 92.91775706135236135 ) ) ;
#141396 = CARTESIAN_POINT ( 'NONE',  ( 16.51473224551083163, -9.474510206698727899, 70.83442372801900433 ) ) ;
#141397 = CARTESIAN_POINT ( 'NONE',  ( 19.05341960407611168, 5.049401038298154454, 38.95724293864767418 ) ) ;
#141398 = CARTESIAN_POINT ( 'NONE',  ( 0.05219959533907565091, 21.53943276465977519, 74.99890960531435269 ) ) ;
#141400 = CARTESIAN_POINT ( 'NONE',  ( 5.049401038297881783, 19.05341960407617563, 67.29275706135234714 ) ) ;
#141399 = CARTESIAN_POINT ( 'NONE',  ( -16.52544592524342804, 4.483927247898546575, 66.04057627198103830 ) ) ;
#141401 = CARTESIAN_POINT ( 'NONE',  ( -16.62475595723697097, -7.163666690055194408, 24.47286648189534830 ) ) ;
#141402 = CARTESIAN_POINT ( 'NONE',  ( 19.05341960407617918, -5.049401038297876454, 36.04275706135234003 ) ) ;
#141403 = CARTESIAN_POINT ( 'NONE',  ( -12.06949235617739369, -12.14591786802326823, 94.37609039468568994 ) ) ;
#141404 = CARTESIAN_POINT ( 'NONE',  ( -16.53943276465976808, 0.05219959533911058130, 51.24890960531436690 ) ) ;
#141406 = CARTESIAN_POINT ( 'NONE',  ( -22.44159573604010305, 16.30477369853692338, 140.6750000027311671 ) ) ;
#141405 = CARTESIAN_POINT ( 'NONE',  ( -21.53943276465977519, -0.05219959533937600094, 83.75109039468568994 ) ) ;
#141407 = CARTESIAN_POINT ( 'NONE',  ( -15.72974639402197994, 15.80617190586746368, 95.62390960531436690 ) ) ;
#141408 = CARTESIAN_POINT ( 'NONE',  ( 5.049401038298161559, -19.05341960407611168, 47.70724293864770260 ) ) ;
#141409 = CARTESIAN_POINT ( 'NONE',  ( 5.719274019375673035, 21.55341960407619339, 67.29275706135234714 ) ) ;
#141410 = CARTESIAN_POINT ( 'NONE',  ( 16.46253265017160672, -9.564922557960803928, 43.33224293864769550 ) ) ;
#141411 = VERTEX_POINT ( 'NONE', #24026 ) ;
#141412 = CARTESIAN_POINT ( 'NONE',  ( 19.02544592524343514, -5.153800228976328945, 63.54057627198103830 ) ) ;
#141413 = CARTESIAN_POINT ( 'NONE',  ( 8.314922557960818139, 14.29746914071049879, 99.58224293864770971 ) ) ;
#141414 = CARTESIAN_POINT ( 'NONE',  ( 13.89961937509977652, -13.97604488694527269, 113.1239096053143527 ) ) ;
#141415 = CARTESIAN_POINT ( 'NONE',  ( -8.314922557960811034, -14.29746914071050412, 57.08224293864769550 ) ) ;
#141416 = CARTESIAN_POINT ( 'NONE',  ( 19.02544592524343514, -5.153800228976328945, 33.54057627198102409 ) ) ;
#141417 = CARTESIAN_POINT ( 'NONE',  ( 14.34966873604960469, 8.224510206698951720, 89.16557627198102409 ) ) ;
#141418 = AXIS2_PLACEMENT_3D ( 'NONE', #33375, #187084, #21183 ) ;
#141419 = CARTESIAN_POINT ( 'NONE',  ( 10.72451020669898902, -18.67979575497178502, 97.91557627198103830 ) ) ;
#141420 = CARTESIAN_POINT ( 'NONE',  ( -21.53943276465977519, -0.05219959533937600094, 33.75109039468568284 ) ) ;
#141421 = CARTESIAN_POINT ( 'NONE',  ( 27.96813078753324078, -7.160245613315928459, 161.0900052257271966 ) ) ;
#141422 = CARTESIAN_POINT ( 'NONE',  ( -4.379528057220086978, -16.55341960407618274, 49.79275706135234714 ) ) ;
#141423 = CARTESIAN_POINT ( 'NONE',  ( 10.72451020669898902, -18.67979575497178502, 87.91557627198103830 ) ) ;
#141425 = CARTESIAN_POINT ( 'NONE',  ( -19.02544592524334988, -5.153800228976617603, 18.95942372801899722 ) ) ;
#141424 = UNCERTAINTY_MEASURE_WITH_UNIT (LENGTH_MEASURE( 1.000000000000000082E-05 ), #198021, 'distance_accuracy_value', 'NONE');
#141426 = CARTESIAN_POINT ( 'NONE',  ( -13.89961937509977652, 13.97604488694528158, 105.6239096053143527 ) ) ;
#141427 = CARTESIAN_POINT ( 'NONE',  ( 21.53943276465977519, 0.05219959533937863772, 46.25109039468567573 ) ) ;
#141428 = CARTESIAN_POINT ( 'NONE',  ( 21.55341960407610458, 5.719274019375980345, 33.95724293864769550 ) ) ;
#141429 = CARTESIAN_POINT ( 'NONE',  ( -16.53943276465976808, -0.05219959533934237506, 108.7510903946857042 ) ) ;
#141431 = CARTESIAN_POINT ( 'NONE',  ( -18.62759615963255300, -10.81492255796106328, 89.16775706135236135 ) ) ;
#141430 = CARTESIAN_POINT ( 'NONE',  ( 0.05219959533937995610, -21.53943276465977519, 65.00109039468568994 ) ) ;
#141432 = CARTESIAN_POINT ( 'NONE',  ( 13.89961937509957401, 13.97604488694547697, 36.87609039468565442 ) ) ;
#141433 = CARTESIAN_POINT ( 'NONE',  ( -12.14591786802326823, 12.06949235617739902, 88.12609039468570415 ) ) ;
#141434 = CARTESIAN_POINT ( 'NONE',  ( 5.823673210054444382, -21.52544592524334988, 35.20942372801901854 ) ) ;
#141435 = CARTESIAN_POINT ( 'NONE',  ( 9.564922557960805705, 16.46253265017160317, 44.58224293864769550 ) ) ;
#141436 = CARTESIAN_POINT ( 'NONE',  ( -18.67979575497193778, 10.72451020669871902, 103.3344237280190043 ) ) ;
#141437 = CARTESIAN_POINT ( 'NONE',  ( -5.823673210054116645, -21.52544592524344225, 22.29057627198102765 ) ) ;
#141438 = CARTESIAN_POINT ( 'NONE',  ( 18.67979575497194134, -10.72451020669871369, 20.83442372801901143 ) ) ;
#141439 = CARTESIAN_POINT ( 'NONE',  ( 5.823673210054125526, 21.52544592524343514, 79.79057627198102409 ) ) ;
#141441 = CARTESIAN_POINT ( 'NONE',  ( 10.72451020669898902, -18.67979575497178502, 72.91557627198103830 ) ) ;
#141440 = DIRECTION ( 'NONE',  ( 0.000000000000000000, 0.000000000000000000, 1.000000000000000000 ) ) ;
#141443 = CARTESIAN_POINT ( 'NONE',  ( 16.52544592524342804, -4.483927247898539470, 58.54057627198103120 ) ) ;
#141442 = CARTESIAN_POINT ( 'NONE',  ( -8.224510206698735004, -14.34966873604973081, 54.58442372801901143 ) ) ;
#141444 = DIRECTION ( 'NONE',  ( -0.000000000000000000, -0.000000000000000000, -1.000000000000000000 ) ) ;
#141445 = CARTESIAN_POINT ( 'NONE',  ( 16.46253265017146816, 9.564922557961045513, 91.66775706135234714 ) ) ;
#141446 = CIRCLE ( 'NONE', #15454, 5.500000000001017852 ) ;
#141447 = CARTESIAN_POINT ( 'NONE',  ( -21.65895526037597207, 0.9928668394656959828, -56.20821996642037988 ) ) ;
#141448 = EDGE_CURVE ( 'NONE', #133123, #126008, #120355, .T. ) ;
#141449 = CARTESIAN_POINT ( 'NONE',  ( -12.14591786802326823, 12.06949235617739902, 23.12609039468567573 ) ) ;
#141450 = CARTESIAN_POINT ( 'NONE',  ( 21.53943276465977519, -0.05219959533907433946, 98.74890960531438111 ) ) ;
#141451 = CARTESIAN_POINT ( 'NONE',  ( 21.52544592524344225, -5.823673210054117533, 73.54057627198102409 ) ) ;
#141452 = CARTESIAN_POINT ( 'NONE',  ( 15.72974639402199770, -15.80617190586745480, 23.12390960531436335 ) ) ;
#141453 = CARTESIAN_POINT ( 'NONE',  ( -14.34966873604972548, 8.224510206698743886, 63.33442372801900433 ) ) ;
#141454 = CARTESIAN_POINT ( 'NONE',  ( 19.03943276465977164, -0.05219959533909143690, 68.74890960531436690 ) ) ;
#141456 = CARTESIAN_POINT ( 'NONE',  ( -8.224510206698735004, -14.34966873604973081, 19.58442372801901143 ) ) ;
#141455 = CARTESIAN_POINT ( 'NONE',  ( -21.55341960407619339, 5.719274019375674811, 38.54275706135234714 ) ) ;
#141457 = CARTESIAN_POINT ( 'NONE',  ( 9.474510206698971260, -16.51473224551069308, 102.9155762719810241 ) ) ;
#141458 = CARTESIAN_POINT ( 'NONE',  ( 0.05219959533936267826, -19.03943276465977164, 25.00109039468566152 ) ) ;
#141459 =( BOUNDED_CURVE ( )  B_SPLINE_CURVE ( 2, ( #30433, #61745, #198292, #41639, #121437, #135641, #168927, #59769, #92080, #14262, #180170 ),
 .UNSPECIFIED., .F., .F. ) 
 B_SPLINE_CURVE_WITH_KNOTS ( ( 3, 2, 2, 2, 2, 3 ),
 ( 0.5000000000000004441, 0.5200000000000004619, 0.5400000000000004796, 0.5600000000000006084, 0.5800000000000005151, 0.6000000000000005329 ),
 .UNSPECIFIED. ) 
 CURVE ( )  GEOMETRIC_REPRESENTATION_ITEM ( )  RATIONAL_B_SPLINE_CURVE ( ( 0.9999999999999988898, 0.9510565162951546414, 1.000000000000000000, 0.9510565162951535312, 1.000000000000000000, 0.9510565162951535312, 1.000000000000000000, 0.9510565162951535312, 1.000000000000000000, 0.9510565162951521989, 1.000000000000001332 ) ) 
 REPRESENTATION_ITEM ( '' )  );
#141460 = CARTESIAN_POINT ( 'NONE',  ( -16.46253265017160317, 9.564922557960807481, 95.83224293864769550 ) ) ;
#141461 = CARTESIAN_POINT ( 'NONE',  ( 15.72974639402199770, -15.80617190586745480, 108.1239096053143811 ) ) ;
#141462 = CARTESIAN_POINT ( 'NONE',  ( 5.153800228976335163, 19.02544592524342804, 54.79057627198103120 ) ) ;
#141463 = CARTESIAN_POINT ( 'NONE',  ( -16.31925111598458855, 7.325300261831456439, 25.16424538967252644 ) ) ;
#141464 = CARTESIAN_POINT ( 'NONE',  ( -14.34966873604960291, -8.224510206698953496, 81.66557627198103830 ) ) ;
#141465 = CARTESIAN_POINT ( 'NONE',  ( -5.823673210054116645, -21.52544592524344225, 22.29057627198102765 ) ) ;
#141466 = CARTESIAN_POINT ( 'NONE',  ( -16.19135201231370047, 7.376712067591781441, 34.81319145947970384 ) ) ;
#141467 = CARTESIAN_POINT ( 'NONE',  ( -15.72974639402197994, 15.80617190586746368, 105.6239096053143669 ) ) ;
#141468 = CARTESIAN_POINT ( 'NONE',  ( 5.153800228976615827, -19.02544592524334988, 65.20942372801900433 ) ) ;
#141469 = CARTESIAN_POINT ( 'NONE',  ( -21.55341960407610458, -5.719274019375992779, 21.45724293864769550 ) ) ;
#141470 = CARTESIAN_POINT ( 'NONE',  ( -16.51473224551069308, -9.474510206698971260, 26.66557627198103120 ) ) ;
#141471 = CARTESIAN_POINT ( 'NONE',  ( 5.719274019375991003, -21.55341960407610458, 52.70724293864769550 ) ) ;
#141472 = CARTESIAN_POINT ( 'NONE',  ( -13.89961937509977652, 13.97604488694528158, 95.62390960531436690 ) ) ;
#141473 = CARTESIAN_POINT ( 'NONE',  ( -0.05219959533937732626, 21.53943276465977519, 72.50109039468568994 ) ) ;
#141474 = CARTESIAN_POINT ( 'NONE',  ( 13.89961937509977652, -13.97604488694527269, 48.12390960531435979 ) ) ;
#141475 = CARTESIAN_POINT ( 'NONE',  ( -4.379528057220328563, 16.55341960407611168, 90.20724293864770971 ) ) ;
#141476 = CARTESIAN_POINT ( 'NONE',  ( 16.52544592524335698, 4.483927247898782831, 41.45942372801901143 ) ) ;
#141477 = CARTESIAN_POINT ( 'NONE',  ( 21.52544592524334988, 5.823673210054432836, 61.45942372801901854 ) ) ;
#141478 = ORIENTED_EDGE ( 'NONE', *, *, #124946, .T. ) ;
#141479 = CARTESIAN_POINT ( 'NONE',  ( -19.05341960407617563, 5.049401038297882671, 28.54275706135232937 ) ) ;
#141481 = EDGE_CURVE ( 'NONE', #175318, #11483, #156570, .T. ) ;
#141480 = CARTESIAN_POINT ( 'NONE',  ( 5.153800228976615827, -19.02544592524334988, 85.20942372801900433 ) ) ;
#141482 = CARTESIAN_POINT ( 'NONE',  ( -16.51473224551082808, 9.474510206698731452, 38.33442372801899722 ) ) ;
#141483 = CARTESIAN_POINT ( 'NONE',  ( -17.97214573761834799, -5.500000000000021316, 91.46970049038660022 ) ) ;
#141484 = CARTESIAN_POINT ( 'NONE',  ( -5.719274019375665041, -21.55341960407619695, 34.79275706135235424 ) ) ;
#141485 = DIRECTION ( 'NONE',  ( -0.000000000000000000, -0.000000000000000000, 1.000000000000000000 ) ) ;
#141486 = CARTESIAN_POINT ( 'NONE',  ( -19.03943276465977164, -0.05219959533935918106, 38.75109039468566152 ) ) ;
#141487 = CARTESIAN_POINT ( 'NONE',  ( -5.049401038298153566, 19.05341960407611168, 75.20724293864769550 ) ) ;
#141488 = CARTESIAN_POINT ( 'NONE',  ( 8.314922557960818139, 14.29746914071049879, 24.58224293864768839 ) ) ;
#141490 = CARTESIAN_POINT ( 'NONE',  ( -21.52544592524334988, -5.823673210054445271, 88.95942372801901854 ) ) ;
#141489 = CARTESIAN_POINT ( 'NONE',  ( 16.51473224551069308, 9.474510206698969483, 114.1655762719810241 ) ) ;
#141491 = CARTESIAN_POINT ( 'NONE',  ( 36.91746824999999177, 2.880721459617395097E-14, -3.624999997268813168 ) ) ;
#141492 = DIRECTION ( 'NONE',  ( 1.000000000000000000, -0.000000000000000000, -0.000000000000000000 ) ) ;
#141493 = CARTESIAN_POINT ( 'NONE',  ( -18.62759615963255300, -10.81492255796106328, 84.16775706135234714 ) ) ;
#141494 = CARTESIAN_POINT ( 'NONE',  ( 24.11964846217548342, -0.7207009035786856588, -56.90195918390940477 ) ) ;
#141495 = CARTESIAN_POINT ( 'NONE',  ( 5.049401038298161559, -19.05341960407611168, 97.70724293864766707 ) ) ;
#141496 = CARTESIAN_POINT ( 'NONE',  ( 23.31485601308175148, -29.82028178162995147, -21.55021174911959747 ) ) ;
#141497 = CARTESIAN_POINT ( 'NONE',  ( 19.05341960407611168, 5.049401038298154454, 48.95724293864768129 ) ) ;
#141498 = CARTESIAN_POINT ( 'NONE',  ( 18.67979575497178502, 10.72451020669898547, 54.16557627198103120 ) ) ;
#141499 = CARTESIAN_POINT ( 'NONE',  ( 14.34966873604960469, 8.224510206698951720, 29.16557627198103120 ) ) ;
#141501 = CARTESIAN_POINT ( 'NONE',  ( 19.05341960407611168, 5.049401038298154454, 88.95724293864769550 ) ) ;
#141500 = CARTESIAN_POINT ( 'NONE',  ( 8.314922557960818139, 14.29746914071049879, 114.5822429386477097 ) ) ;
#141502 = CARTESIAN_POINT ( 'NONE',  ( -5.049401038297874678, -19.05341960407617918, 19.79275706135233293 ) ) ;
#141503 = CARTESIAN_POINT ( 'NONE',  ( -16.55341960407611168, -4.379528057220339221, 101.4572429386476955 ) ) ;
#141504 = CARTESIAN_POINT ( 'NONE',  ( 21.52544592524334988, 5.823673210054432836, 51.45942372801901854 ) ) ;
#141505 = CARTESIAN_POINT ( 'NONE',  ( -16.46253265017160317, 9.564922557960807481, 115.8322429386477097 ) ) ;
#141506 = CARTESIAN_POINT ( 'NONE',  ( 14.29746914071037800, 8.314922557961029526, 101.6677570613523613 ) ) ;
#141507 = CARTESIAN_POINT ( 'NONE',  ( 5.153800228976615827, -19.02544592524334988, 60.20942372801899012 ) ) ;
#141508 = CARTESIAN_POINT ( 'NONE',  ( 36.91746824999999177, 2.880721459617395097E-14, -6.124999997268813168 ) ) ;
#141509 = CARTESIAN_POINT ( 'NONE',  ( 9.564922557960805705, 16.46253265017160317, 114.5822429386476955 ) ) ;
#141510 = CARTESIAN_POINT ( 'NONE',  ( 14.29746914071049879, -8.314922557960816363, 78.33224293864770971 ) ) ;
#141511 = CARTESIAN_POINT ( 'NONE',  ( -19.03943276465977164, -0.05219959533935918106, 63.75109039468566863 ) ) ;
#141512 = CARTESIAN_POINT ( 'NONE',  ( -19.05341960407611168, -5.049401038298163336, 66.45724293864769550 ) ) ;
#141513 = CARTESIAN_POINT ( 'NONE',  ( -16.55341960407611168, -4.379528057220339221, 66.45724293864768129 ) ) ;
#141514 = CARTESIAN_POINT ( 'NONE',  ( -19.05341960407617563, 5.049401038297882671, 98.54275706135233293 ) ) ;
#141515 = CARTESIAN_POINT ( 'NONE',  ( -21.52544592524343514, 5.823673210054127303, 56.04057627198102409 ) ) ;
#141516 = ORIENTED_EDGE ( 'NONE', *, *, #142804, .T. ) ;
#141517 = CARTESIAN_POINT ( 'NONE',  ( -14.34966873604960291, -8.224510206698953496, 101.6655762719810383 ) ) ;
#141518 = CARTESIAN_POINT ( 'NONE',  ( -16.29526858892880625, -7.335722546920006693, 30.79670597800208398 ) ) ;
#141520 = CARTESIAN_POINT ( 'NONE',  ( 18.62759615963271287, -10.81492255796078972, 63.33224293864770260 ) ) ;
#141519 = CARTESIAN_POINT ( 'NONE',  ( -19.02544592524342804, 5.153800228976336051, 56.04057627198100988 ) ) ;
#141522 = CARTESIAN_POINT ( 'NONE',  ( -0.05219959533909027116, -19.03943276465977164, 72.49890960531435269 ) ) ;
#141521 = CARTESIAN_POINT ( 'NONE',  ( -12.14591786802326823, 12.06949235617739902, 98.12609039468570415 ) ) ;
#141523 = CARTESIAN_POINT ( 'NONE',  ( 9.564922557961047289, -16.46253265017146816, 55.41775706135234003 ) ) ;
#141524 = CARTESIAN_POINT ( 'NONE',  ( 21.55341960407619695, -5.719274019375665929, 81.04275706135236135 ) ) ;
#141525 = CARTESIAN_POINT ( 'NONE',  ( 15.72974639402199770, -15.80617190586745480, 58.12390960531435979 ) ) ;
#141526 = CARTESIAN_POINT ( 'NONE',  ( -19.05341960407611168, -5.049401038298163336, 101.4572429386476955 ) ) ;
#141527 = CARTESIAN_POINT ( 'NONE',  ( 13.97604488694527802, 13.89961937509977652, 34.37390960531436690 ) ) ;
#141528 = CARTESIAN_POINT ( 'NONE',  ( 12.06949235617739724, 12.14591786802326823, 91.87609039468568994 ) ) ;
#141529 = CARTESIAN_POINT ( 'NONE',  ( 12.14591786802327356, -12.06949235617739191, 20.62609039468568639 ) ) ;
#141530 = CARTESIAN_POINT ( 'NONE',  ( 27.88129983271499768, 6.733757357597986548, 162.1517353552272880 ) ) ;
#141531 = CARTESIAN_POINT ( 'NONE',  ( 18.22780087662119897, -5.500000000000096811, 43.51763182126894236 ) ) ;
#141532 = CARTESIAN_POINT ( 'NONE',  ( 5.719274019375673035, 21.55341960407619339, 92.29275706135236135 ) ) ;
#141533 = CARTESIAN_POINT ( 'NONE',  ( 12.14591786802309770, 12.06949235617756955, 64.37390960531435269 ) ) ;
#141534 = CARTESIAN_POINT ( 'NONE',  ( 8.314922557960818139, 14.29746914071049879, 74.58224293864768129 ) ) ;
#141535 = CARTESIAN_POINT ( 'NONE',  ( -15.72974639402197994, 15.80617190586746368, 95.62390960531436690 ) ) ;
#141536 = CARTESIAN_POINT ( 'NONE',  ( 21.53943276465977519, -0.05219959533907433946, 93.74890960531436690 ) ) ;
#141537 = CARTESIAN_POINT ( 'NONE',  ( -37.87393738558670009, 1.964790904463869577E-14, 2.000000000000000000 ) ) ;
#141538 = CARTESIAN_POINT ( 'NONE',  ( -18.62759615963270932, 10.81492255796079327, 50.83224293864770971 ) ) ;
#141539 = CARTESIAN_POINT ( 'NONE',  ( 16.52544592524335698, 4.483927247898782831, 61.45942372801901854 ) ) ;
#141540 = CARTESIAN_POINT ( 'NONE',  ( 16.55341960407611168, 4.379528057220329451, 93.95724293864770971 ) ) ;
#141541 = CARTESIAN_POINT ( 'NONE',  ( 13.89961937509977652, -13.97604488694527269, 48.12390960531435979 ) ) ;
#141542 = CARTESIAN_POINT ( 'NONE',  ( 25.63014048727049854, -6.600871414792749192, 163.2070037194164911 ) ) ;
#141543 = CARTESIAN_POINT ( 'NONE',  ( -12.14591786802326823, 12.06949235617739902, 93.12609039468568994 ) ) ;
#141544 = CARTESIAN_POINT ( 'NONE',  ( 10.72451020669871369, 18.67979575497193778, 37.08442372801901143 ) ) ;
#141545 = CARTESIAN_POINT ( 'NONE',  ( -13.89961937509977652, 13.97604488694528158, 80.62390960531436690 ) ) ;
#141546 = CARTESIAN_POINT ( 'NONE',  ( -15.80617190586768217, 15.72974639402176855, 73.12609039468567573 ) ) ;
#141547 = CYLINDRICAL_SURFACE ( 'NONE', #92173, 37.99626262588765968 ) ;
#141548 = CARTESIAN_POINT ( 'NONE',  ( -13.97604488694527625, -13.89961937509977652, 21.87390960531435979 ) ) ;
#141549 = VERTEX_POINT ( 'NONE', #129175 ) ;
#141550 = CARTESIAN_POINT ( 'NONE',  ( 10.72451020669871369, 18.67979575497193778, 62.08442372801901143 ) ) ;
#141552 = CARTESIAN_POINT ( 'NONE',  ( 13.89961937509977652, -13.97604488694527269, 113.1239096053143527 ) ) ;
#141551 = CARTESIAN_POINT ( 'NONE',  ( -5.153800228976328057, -19.02544592524343514, 32.29057627198102409 ) ) ;
#141553 = CARTESIAN_POINT ( 'NONE',  ( -13.89961937509977652, 13.97604488694528158, 90.62390960531432427 ) ) ;
#141554 = CARTESIAN_POINT ( 'NONE',  ( -19.05341960407617563, 5.049401038297882671, 63.54275706135234003 ) ) ;
#141555 = CARTESIAN_POINT ( 'NONE',  ( 21.55341960407619695, -5.719274019375665929, 31.04275706135234714 ) ) ;
#141556 = CARTESIAN_POINT ( 'NONE',  ( -13.89961937509957401, -13.97604488694547875, 54.37609039468565442 ) ) ;
#141557 = CARTESIAN_POINT ( 'NONE',  ( -13.97604488694527625, -13.89961937509977652, 41.87390960531435979 ) ) ;
#141558 = CARTESIAN_POINT ( 'NONE',  ( 8.314922557961029526, -14.29746914071037800, 105.4177570613523613 ) ) ;
#141559 = CARTESIAN_POINT ( 'NONE',  ( -9.474510206698720793, -16.51473224551083518, 69.58442372801901854 ) ) ;
#141560 = CARTESIAN_POINT ( 'NONE',  ( -12.14591786802326823, 12.06949235617739902, 113.1260903946856899 ) ) ;
#141561 = CARTESIAN_POINT ( 'NONE',  ( 19.03943276465977164, 0.05219959533936151252, 51.25109039468567573 ) ) ;
#141562 = CARTESIAN_POINT ( 'NONE',  ( 13.89961937509977652, -13.97604488694527269, 98.12390960531433848 ) ) ;
#141563 = CARTESIAN_POINT ( 'NONE',  ( 0.05219959533937995610, -21.53943276465977519, 105.0010903946856757 ) ) ;
#141564 = CARTESIAN_POINT ( 'NONE',  ( -19.02544592524334988, -5.153800228976617603, 18.95942372801899722 ) ) ;
#141565 = CARTESIAN_POINT ( 'NONE',  ( -19.02544592524342804, 5.153800228976336051, 31.04057627198102409 ) ) ;
#141566 = CARTESIAN_POINT ( 'NONE',  ( 5.719274019375673035, 21.55341960407619339, 87.29275706135236135 ) ) ;
#141567 = CARTESIAN_POINT ( 'NONE',  ( 4.483927247898790824, -16.52544592524335698, 30.20942372801902565 ) ) ;
#141568 = EDGE_CURVE ( 'NONE', #40349, #179309, #52349, .T. ) ;
#141569 = CARTESIAN_POINT ( 'NONE',  ( -16.46253265017160317, 9.564922557960807481, 95.83224293864769550 ) ) ;
#141570 = CARTESIAN_POINT ( 'NONE',  ( 23.48529157249600630, -32.32473071737748427, -9.049999994537627046 ) ) ;
#141571 = CARTESIAN_POINT ( 'NONE',  ( 19.02544592524343514, -5.153800228976328945, 73.54057627198103830 ) ) ;
#141572 = CARTESIAN_POINT ( 'NONE',  ( -30.00000000000000000, -1.132798289211302014E-14, 92.50000000000000000 ) ) ;
#141573 = CARTESIAN_POINT ( 'NONE',  ( 0.05219959533936267826, -19.03943276465977164, 65.00109039468567573 ) ) ;
#141574 = CARTESIAN_POINT ( 'NONE',  ( 16.46253265017160672, -9.564922557960803928, 103.3322429386476955 ) ) ;
#141575 = CARTESIAN_POINT ( 'NONE',  ( 15.80617190586769283, -15.72974639402175789, 105.6260903946856899 ) ) ;
#141576 = CARTESIAN_POINT ( 'NONE',  ( 4.379528057220339221, -16.55341960407611168, 97.70724293864772392 ) ) ;
#141577 = CARTESIAN_POINT ( 'NONE',  ( 5.719274019375991003, -21.55341960407610458, 47.70724293864770260 ) ) ;
#141578 = CARTESIAN_POINT ( 'NONE',  ( 15.72974639402199770, -15.80617190586745480, 33.12390960531435979 ) ) ;
#141579 = CARTESIAN_POINT ( 'NONE',  ( 4.379528057220339221, -16.55341960407611168, 107.7072429386476955 ) ) ;
#141580 = CARTESIAN_POINT ( 'NONE',  ( -1.500046863536438568, -7.503800738396990688, -62.22166870076608092 ) ) ;
#141581 = CARTESIAN_POINT ( 'NONE',  ( -19.03943276465977164, -0.05219959533935918106, 58.75109039468566863 ) ) ;
#141583 = VECTOR ( 'NONE', #156468, 1000.000000000000000 ) ;
#141582 = CARTESIAN_POINT ( 'NONE',  ( 12.06949235617757843, -12.14591786802309237, 33.12390960531435979 ) ) ;
#141584 = CARTESIAN_POINT ( 'NONE',  ( -19.05341960407611168, -5.049401038298163336, 101.4572429386476955 ) ) ;
#141585 = CARTESIAN_POINT ( 'NONE',  ( -15.80617190586768217, 15.72974639402176855, 78.12609039468570415 ) ) ;
#141586 = CARTESIAN_POINT ( 'NONE',  ( 15.80617190586746368, 15.72974639402197994, 69.37390960531436690 ) ) ;
#141587 = CARTESIAN_POINT ( 'NONE',  ( 18.62759615963255655, 10.81492255796105972, 51.66775706135234714 ) ) ;
#141588 = CARTESIAN_POINT ( 'NONE',  ( 5.823673210054125526, 21.52544592524343514, 99.79057627198103830 ) ) ;
#141589 = CARTESIAN_POINT ( 'NONE',  ( 18.62759615963255655, 10.81492255796105972, 51.66775706135234714 ) ) ;
#141590 = CARTESIAN_POINT ( 'NONE',  ( 16.51473224551069308, 9.474510206698969483, 24.16557627198102765 ) ) ;
#141591 = EDGE_CURVE ( 'NONE', #88085, #163981, #17691, .T. ) ;
#141592 = CARTESIAN_POINT ( 'NONE',  ( 16.51473224551069308, 9.474510206698969483, 79.16557627198103830 ) ) ;
#141593 = CARTESIAN_POINT ( 'NONE',  ( 16.55341960407618274, -4.379528057220086978, 81.04275706135236135 ) ) ;
#141594 = CARTESIAN_POINT ( 'NONE',  ( -16.52544592524342804, 4.483927247898546575, 106.0405762719810525 ) ) ;
#141595 = CARTESIAN_POINT ( 'NONE',  ( 9.564922557960805705, 16.46253265017160317, 104.5822429386476955 ) ) ;
#141596 = CARTESIAN_POINT ( 'NONE',  ( -14.34966873604960291, -8.224510206698953496, 56.66557627198103830 ) ) ;
#141597 = CARTESIAN_POINT ( 'NONE',  ( 14.34966873604972726, -8.224510206698740333, 110.8344237280190043 ) ) ;
#141598 = CARTESIAN_POINT ( 'NONE',  ( 9.564922557960805705, 16.46253265017160317, 59.58224293864769550 ) ) ;
#141599 = CARTESIAN_POINT ( 'NONE',  ( 16.51473224551069308, 9.474510206698969483, 34.16557627198102409 ) ) ;
#141600 = CARTESIAN_POINT ( 'NONE',  ( 15.80617190586746368, 15.72974639402197994, 44.37390960531435979 ) ) ;
#141601 = CARTESIAN_POINT ( 'NONE',  ( 5.153800228976615827, -19.02544592524334988, 35.20942372801899722 ) ) ;
#141603 = CARTESIAN_POINT ( 'NONE',  ( -4.379528057220328563, 16.55341960407611168, 30.20724293864769550 ) ) ;
#141602 = CARTESIAN_POINT ( 'NONE',  ( -9.687362902255733488, 9.687362902255692632, -60.44446360152740993 ) ) ;
#141604 = CARTESIAN_POINT ( 'NONE',  ( -5.823673210054431948, 21.52544592524334988, 42.70942372801901854 ) ) ;
#141605 = CARTESIAN_POINT ( 'NONE',  ( -13.97604488694527625, -13.89961937509977652, 111.8739096053143243 ) ) ;
#141606 = CARTESIAN_POINT ( 'NONE',  ( -12.06949235617739369, -12.14591786802326823, 54.37609039468568994 ) ) ;
#141607 = CARTESIAN_POINT ( 'NONE',  ( -19.05341960407617563, 5.049401038297882671, 68.54275706135230450 ) ) ;
#141608 = CARTESIAN_POINT ( 'NONE',  ( -12.14591786802309592, -12.06949235617757132, 26.87390960531435979 ) ) ;
#141609 = CARTESIAN_POINT ( 'NONE',  ( 16.18388926212236356, -7.379444403734617630, 52.06046848633854296 ) ) ;
#141610 = CARTESIAN_POINT ( 'NONE',  ( -14.34966873604972548, 8.224510206698743886, 103.3344237280190043 ) ) ;
#141611 = CARTESIAN_POINT ( 'NONE',  ( -19.03943276465977164, 0.05219959533909376836, 41.24890960531435269 ) ) ;
#141612 = CARTESIAN_POINT ( 'NONE',  ( -19.02544592524342804, 5.153800228976336051, 61.04057627198103120 ) ) ;
#141613 = CARTESIAN_POINT ( 'NONE',  ( -16.51473224551069308, -9.474510206698971260, 26.66557627198103120 ) ) ;
#141614 = CARTESIAN_POINT ( 'NONE',  ( -15.72974639402176322, -15.80617190586768395, 39.37609039468567573 ) ) ;
#141615 = CARTESIAN_POINT ( 'NONE',  ( -16.46253265017160317, 9.564922557960807481, 45.83224293864769550 ) ) ;
#141616 = CARTESIAN_POINT ( 'NONE',  ( -38.00000000000000711, 2.893978650043524126E-14, -25.00000000000000000 ) ) ;
#141617 = CARTESIAN_POINT ( 'NONE',  ( -0.05219959533909027116, -19.03943276465977164, 47.49890960531435979 ) ) ;
#141618 = CARTESIAN_POINT ( 'NONE',  ( 5.823673210054125526, 21.52544592524343514, 24.79057627198103120 ) ) ;
#141620 = CARTESIAN_POINT ( 'NONE',  ( -5.153800228976328057, -19.02544592524343514, 27.29057627198103120 ) ) ;
#141619 = CARTESIAN_POINT ( 'NONE',  ( -15.72974639402176322, -15.80617190586768395, 59.37609039468568284 ) ) ;
#141621 = CARTESIAN_POINT ( 'NONE',  ( -0.05219959533907301413, -21.53943276465977519, 32.49890960531435979 ) ) ;
#141622 = CARTESIAN_POINT ( 'NONE',  ( 12.06949235617739724, 12.14591786802326823, 71.87609039468568994 ) ) ;
#141623 = CARTESIAN_POINT ( 'NONE',  ( -18.67979575497193778, 10.72451020669871902, 98.33442372801901854 ) ) ;
#141624 = CARTESIAN_POINT ( 'NONE',  ( 14.34966873604972726, -8.224510206698740333, 50.83442372801901143 ) ) ;
#141625 = CARTESIAN_POINT ( 'NONE',  ( 19.05341960407611168, 5.049401038298154454, 93.95724293864769550 ) ) ;
#141626 = CARTESIAN_POINT ( 'NONE',  ( -12.06949235617739369, -12.14591786802326823, 39.37609039468567573 ) ) ;
#141627 = CARTESIAN_POINT ( 'NONE',  ( -4.379528057220086978, -16.55341960407618274, 29.79275706135234358 ) ) ;
#141628 = CARTESIAN_POINT ( 'NONE',  ( -16.52544592524335698, -4.483927247898792601, 98.95942372801903275 ) ) ;
#141629 = CARTESIAN_POINT ( 'NONE',  ( 5.719274019375673035, 21.55341960407619339, 57.29275706135234714 ) ) ;
#141630 = CARTESIAN_POINT ( 'NONE',  ( 19.02544592524334988, 5.153800228976608722, 101.4594237280189759 ) ) ;
#141631 = CARTESIAN_POINT ( 'NONE',  ( -21.53943276465977519, -0.05219959533937600094, 18.75109039468568639 ) ) ;
#141633 = CARTESIAN_POINT ( 'NONE',  ( 13.89961937509957401, 13.97604488694547697, 106.8760903946856757 ) ) ;
#141632 = CARTESIAN_POINT ( 'NONE',  ( 4.379528057220339221, -16.55341960407611168, 97.70724293864772392 ) ) ;
#141634 = CARTESIAN_POINT ( 'NONE',  ( -0.05219959533934338120, 16.53943276465976808, 77.50109039468567573 ) ) ;
#141635 = CARTESIAN_POINT ( 'NONE',  ( -16.61371651742640410, 7.165104196375925660, 43.85415069992968995 ) ) ;
#141636 = CARTESIAN_POINT ( 'NONE',  ( -5.049401038297874678, -19.05341960407617918, 84.79275706135233293 ) ) ;
#141637 = CARTESIAN_POINT ( 'NONE',  ( -14.34966873604960291, -8.224510206698953496, 51.66557627198102409 ) ) ;
#141638 = CARTESIAN_POINT ( 'NONE',  ( 0.05219959533910956823, 16.53943276465976808, 49.99890960531437401 ) ) ;
#141639 = CARTESIAN_POINT ( 'NONE',  ( 14.29746914071049879, -8.314922557960816363, 98.33224293864769550 ) ) ;
#141641 = CARTESIAN_POINT ( 'NONE',  ( -18.56197773271727769, 5.500000000000086153, 88.55066217314450228 ) ) ;
#141640 = CARTESIAN_POINT ( 'NONE',  ( 16.46253265017146816, 9.564922557961045513, 31.66775706135232937 ) ) ;
#141642 = CARTESIAN_POINT ( 'NONE',  ( 15.72974639402176855, 15.80617190586768217, 41.87609039468568284 ) ) ;
#141643 = CARTESIAN_POINT ( 'NONE',  ( 9.564922557961047289, -16.46253265017146816, 95.41775706135233293 ) ) ;
#141644 = CARTESIAN_POINT ( 'NONE',  ( -5.000000000000000888, 11.45643923738960090, -18.00000000000000000 ) ) ;
#141645 = CARTESIAN_POINT ( 'NONE',  ( -16.51473224551069308, -9.474510206698971260, 91.66557627198103830 ) ) ;
#141646 = CARTESIAN_POINT ( 'NONE',  ( 0.05219959533909260263, 19.03943276465977164, 94.99890960531436690 ) ) ;
#141647 = CARTESIAN_POINT ( 'NONE',  ( -10.81492255796078084, -18.62759615963271287, 52.08224293864768839 ) ) ;
#141648 = CARTESIAN_POINT ( 'NONE',  ( -16.52544592524342804, 4.483927247898546575, 91.04057627198103830 ) ) ;
#141649 = CARTESIAN_POINT ( 'NONE',  ( -19.05341960407611168, -5.049401038298163336, 71.45724293864766707 ) ) ;
#141650 = CARTESIAN_POINT ( 'NONE',  ( 0.05219959533909260263, 19.03943276465977164, 34.99890960531435979 ) ) ;
#141651 = CARTESIAN_POINT ( 'NONE',  ( -21.53943276465977519, -0.05219959533937600094, 43.75109039468568284 ) ) ;
#141652 = CARTESIAN_POINT ( 'NONE',  ( 0.05219959533937995610, -21.53943276465977519, 70.00109039468568994 ) ) ;
#141653 = CARTESIAN_POINT ( 'NONE',  ( 12.06949235617739724, 12.14591786802326823, 91.87609039468568994 ) ) ;
#141654 = CARTESIAN_POINT ( 'NONE',  ( 18.62759615963255655, 10.81492255796105972, 31.66775706135234358 ) ) ;
#141655 = CARTESIAN_POINT ( 'NONE',  ( 18.67979575497194134, -10.72451020669871369, 20.83442372801901143 ) ) ;
#141657 = CARTESIAN_POINT ( 'NONE',  ( 19.02544592524343514, -5.153800228976328945, 73.54057627198103830 ) ) ;
#141656 = CARTESIAN_POINT ( 'NONE',  ( 16.46253265017146816, 9.564922557961045513, 51.66775706135233293 ) ) ;
#141658 = CARTESIAN_POINT ( 'NONE',  ( 15.80617190586769283, -15.72974639402175789, 80.62609039468567573 ) ) ;
#141659 = CARTESIAN_POINT ( 'NONE',  ( 21.52544592524344225, -5.823673210054117533, 83.54057627198102409 ) ) ;
#141660 = CARTESIAN_POINT ( 'NONE',  ( 16.52544592524342804, -4.483927247898539470, 53.54057627198103120 ) ) ;
#141662 = CARTESIAN_POINT ( 'NONE',  ( -19.03943276465977164, -0.05219959533935918106, 33.75109039468566863 ) ) ;
#141661 = CARTESIAN_POINT ( 'NONE',  ( -10.81492255796105439, 18.62759615963255655, 102.9177570613523756 ) ) ;
#141663 = CARTESIAN_POINT ( 'NONE',  ( 12.06949235617757843, -12.14591786802309237, 73.12390960531436690 ) ) ;
#141664 = CARTESIAN_POINT ( 'NONE',  ( 4.379528057220339221, -16.55341960407611168, 112.7072429386476955 ) ) ;
#141665 = CARTESIAN_POINT ( 'NONE',  ( 19.02544592524334988, 5.153800228976608722, 71.45942372801900433 ) ) ;
#141666 = CARTESIAN_POINT ( 'NONE',  ( 4.483927247898545687, 16.52544592524342804, 39.79057627198103830 ) ) ;
#141668 = EDGE_CURVE ( 'NONE', #50018, #116638, #55175, .T. ) ;
#141667 = CARTESIAN_POINT ( 'NONE',  ( -18.67979575497193778, 10.72451020669871902, 78.33442372801901854 ) ) ;
#141669 = CARTESIAN_POINT ( 'NONE',  ( -19.03943276465977164, 0.05219959533909376836, 81.24890960531436690 ) ) ;
#141670 = CARTESIAN_POINT ( 'NONE',  ( -19.03943276465977164, -0.05219959533935918106, 63.75109039468566863 ) ) ;
#141671 = CARTESIAN_POINT ( 'NONE',  ( 15.72974639402199770, -15.80617190586745480, 63.12390960531435979 ) ) ;
#141672 = CARTESIAN_POINT ( 'NONE',  ( 5.823673210054125526, 21.52544592524343514, 109.7905762719810383 ) ) ;
#141673 = CARTESIAN_POINT ( 'NONE',  ( 16.51473224551083163, -9.474510206698727899, 110.8344237280190043 ) ) ;
#141674 = CARTESIAN_POINT ( 'NONE',  ( 12.14591786802327356, -12.06949235617739191, 80.62609039468567573 ) ) ;
#141676 = CARTESIAN_POINT ( 'NONE',  ( -5.719274019375665041, -21.55341960407619695, 19.79275706135235069 ) ) ;
#141675 = CARTESIAN_POINT ( 'NONE',  ( 30.40000000000003766, -9.573269184497053765E-14, -64.92279855667830191 ) ) ;
#141677 = CARTESIAN_POINT ( 'NONE',  ( -8.314922557960811034, -14.29746914071050412, 102.0822429386476955 ) ) ;
#141678 = CARTESIAN_POINT ( 'NONE',  ( 29.86685920354754842, -21.69954338932559068, -10.32499999726881335 ) ) ;
#141679 = CARTESIAN_POINT ( 'NONE',  ( -12.06949235617739369, -12.14591786802326823, 34.37609039468568284 ) ) ;
#141680 = CARTESIAN_POINT ( 'NONE',  ( -15.72974639402197994, 15.80617190586746368, 55.62390960531436690 ) ) ;
#141681 = CARTESIAN_POINT ( 'NONE',  ( 8.314922557961029526, -14.29746914071037800, 105.4177570613523613 ) ) ;
#141682 = CARTESIAN_POINT ( 'NONE',  ( 19.02544592524343514, -5.153800228976328945, 38.54057627198103120 ) ) ;
#141683 = CARTESIAN_POINT ( 'NONE',  ( -4.379528057220086978, -16.55341960407618274, 79.79275706135236135 ) ) ;
#141684 = CARTESIAN_POINT ( 'NONE',  ( 19.05341960407617918, -5.049401038297876454, 76.04275706135230450 ) ) ;
#141685 = CARTESIAN_POINT ( 'NONE',  ( -21.53943276465977519, -0.05219959533937600094, 43.75109039468568284 ) ) ;
#141686 = CARTESIAN_POINT ( 'NONE',  ( -21.53943276465977519, 0.05219959533907696930, 61.24890960531435979 ) ) ;
#141687 = CARTESIAN_POINT ( 'NONE',  ( 16.52544592524335698, 4.483927247898782831, 101.4594237280190185 ) ) ;
#141688 = CARTESIAN_POINT ( 'NONE',  ( 15.80617190586769283, -15.72974639402175789, 85.62609039468568994 ) ) ;
#141689 = CARTESIAN_POINT ( 'NONE',  ( 21.55341960407610458, 5.719274019375980345, 48.95724293864770971 ) ) ;
#141690 = CARTESIAN_POINT ( 'NONE',  ( 5.719274019375991003, -21.55341960407610458, 47.70724293864770260 ) ) ;
#141691 = CARTESIAN_POINT ( 'NONE',  ( 12.14591786802327356, -12.06949235617739191, 80.62609039468567573 ) ) ;
#141692 = CARTESIAN_POINT ( 'NONE',  ( 21.55341960407610458, 5.719274019375980345, 48.95724293864770971 ) ) ;
#141693 = ORIENTED_EDGE ( 'NONE', *, *, #148381, .T. ) ;
#141694 = CARTESIAN_POINT ( 'NONE',  ( 16.51473224551069308, 9.474510206698969483, 94.16557627198103830 ) ) ;
#141695 = LINE ( 'NONE', #3186, #188985 ) ;
#141696 = CARTESIAN_POINT ( 'NONE',  ( 9.564922557960805705, 16.46253265017160317, 29.58224293864769550 ) ) ;
#141697 = CARTESIAN_POINT ( 'NONE',  ( 18.67979575497178502, 10.72451020669898547, 64.16557627198102409 ) ) ;
#141698 = CARTESIAN_POINT ( 'NONE',  ( 8.224510206698742110, 14.34966873604972548, 92.08442372801901854 ) ) ;
#141699 = CARTESIAN_POINT ( 'NONE',  ( -10.81492255796105439, 18.62759615963255655, 52.91775706135235424 ) ) ;
#141700 = CARTESIAN_POINT ( 'NONE',  ( 13.89961937509957401, 13.97604488694547697, 96.87609039468566152 ) ) ;
#141701 = CARTESIAN_POINT ( 'NONE',  ( -8.314922557960811034, -14.29746914071050412, 102.0822429386476955 ) ) ;
#141702 = CARTESIAN_POINT ( 'NONE',  ( 13.89961937509957401, 13.97604488694547697, 111.8760903946856757 ) ) ;
#141703 = CARTESIAN_POINT ( 'NONE',  ( 9.474510206698971260, -16.51473224551069308, 37.91557627198102409 ) ) ;
#141704 = CARTESIAN_POINT ( 'NONE',  ( 0.7300717321527865344, 24.11456854404507411, -54.35927238525124494 ) ) ;
#141705 = CARTESIAN_POINT ( 'NONE',  ( 0.05219959533909260263, 19.03943276465977164, 84.99890960531436690 ) ) ;
#141706 = CARTESIAN_POINT ( 'NONE',  ( 12.06949235617739724, 12.14591786802326823, 76.87609039468567573 ) ) ;
#141707 = CARTESIAN_POINT ( 'NONE',  ( 21.53943276465977519, 0.05219959533937863772, 101.2510903946856757 ) ) ;
#141708 = CARTESIAN_POINT ( 'NONE',  ( 21.55341960407610458, 5.719274019375980345, 58.95724293864770971 ) ) ;
#141709 = CARTESIAN_POINT ( 'NONE',  ( -16.55341960407617563, 4.379528057220093196, 88.54275706135236135 ) ) ;
#141710 = CARTESIAN_POINT ( 'NONE',  ( -19.03943276465977164, -0.05219959533935918106, 73.75109039468566152 ) ) ;
#141711 = CARTESIAN_POINT ( 'NONE',  ( 9.474510206698971260, -16.51473224551069308, 32.91557627198102409 ) ) ;
#141712 = CARTESIAN_POINT ( 'NONE',  ( 19.02544592524343514, -5.153800228976328945, 78.54057627198099567 ) ) ;
#141713 = CARTESIAN_POINT ( 'NONE',  ( -5.719274019375665041, -21.55341960407619695, 49.79275706135234714 ) ) ;
#141714 = CARTESIAN_POINT ( 'NONE',  ( 5.153800228976335163, 19.02544592524342804, 29.79057627198102409 ) ) ;
#141715 = CARTESIAN_POINT ( 'NONE',  ( -0.05219959533936034679, 19.03943276465977164, 67.50109039468566152 ) ) ;
#141716 = CARTESIAN_POINT ( 'NONE',  ( 25.75939503182788926, -8.559839547495068146, 171.7912139782359588 ) ) ;
#141717 = CARTESIAN_POINT ( 'NONE',  ( -5.049401038298153566, 19.05341960407611168, 115.2072429386477097 ) ) ;
#141718 = CARTESIAN_POINT ( 'NONE',  ( 12.14591786802309770, 12.06949235617756955, 69.37390960531436690 ) ) ;
#141719 = CARTESIAN_POINT ( 'NONE',  ( -10.72451020669898014, 18.67979575497178502, 60.41557627198102409 ) ) ;
#141720 = DIRECTION ( 'NONE',  ( -0.1039620511844979306, -0.1039620511844979306, 0.9891328443778538704 ) ) ;
#141721 = CARTESIAN_POINT ( 'NONE',  ( -19.03943276465977164, -0.05219959533935918106, 33.75109039468566863 ) ) ;
#141722 = CARTESIAN_POINT ( 'NONE',  ( -17.60769864724391809, 5.499999999999989342, 88.65024842019164453 ) ) ;
#141724 = CARTESIAN_POINT ( 'NONE',  ( 16.46253265017160672, -9.564922557960803928, 78.33224293864769550 ) ) ;
#141723 = CARTESIAN_POINT ( 'NONE',  ( -16.51473224551069308, -9.474510206698971260, 61.66557627198103120 ) ) ;
#141725 = CARTESIAN_POINT ( 'NONE',  ( 0.05219959533934541429, -16.53943276465976808, 55.00109039468568284 ) ) ;
#141726 = LINE ( 'NONE', #97193, #104660 ) ;
#141727 = CARTESIAN_POINT ( 'NONE',  ( -17.44279575226824619, 5.990770900252421427, 110.8355756751432040 ) ) ;
#141728 = CARTESIAN_POINT ( 'NONE',  ( -16.52544592524335698, -4.483927247898792601, 73.95942372801901854 ) ) ;
#141729 = DIRECTION ( 'NONE',  ( 0.000000000000000000, -1.000000000000000000, 1.471414886128461471E-15 ) ) ;
#141730 = CARTESIAN_POINT ( 'NONE',  ( 16.53943276465976808, 0.05219959533934440121, 61.25109039468567573 ) ) ;
#141731 = CARTESIAN_POINT ( 'NONE',  ( 16.55341960407618274, -4.379528057220086978, 36.04275706135234714 ) ) ;
#141733 = CARTESIAN_POINT ( 'NONE',  ( 17.32164067428065835, -17.02822768543988019, -56.78066529741710156 ) ) ;
#141732 = CARTESIAN_POINT ( 'NONE',  ( 5.049401038298161559, -19.05341960407611168, 52.70724293864767418 ) ) ;
#141734 = CARTESIAN_POINT ( 'NONE',  ( -18.62759615963255300, -10.81492255796106328, 54.16775706135235424 ) ) ;
#141735 = CARTESIAN_POINT ( 'NONE',  ( 13.97604488694548053, -13.89961937509957401, 65.62609039468567573 ) ) ;
#141736 = CARTESIAN_POINT ( 'NONE',  ( -19.02544592524334988, -5.153800228976617603, 18.95942372801899722 ) ) ;
#141737 = CARTESIAN_POINT ( 'NONE',  ( 0.05219959533909260263, 19.03943276465977164, 29.99890960531435979 ) ) ;
#141738 = CARTESIAN_POINT ( 'NONE',  ( 16.18414358144004694, 7.379350812367110102, 22.98974271850655526 ) ) ;
#141739 = CARTESIAN_POINT ( 'NONE',  ( -21.52544592524343514, 5.823673210054127303, 61.04057627198103120 ) ) ;
#141740 = CARTESIAN_POINT ( 'NONE',  ( 19.03943276465977164, -0.05219959533909143690, 108.7489096053143527 ) ) ;
#141741 = CARTESIAN_POINT ( 'NONE',  ( 12.14591786802309770, 12.06949235617756955, 104.3739096053143669 ) ) ;
#141742 = CARTESIAN_POINT ( 'NONE',  ( 16.53943276465976808, 0.05219959533934440121, 41.25109039468568284 ) ) ;
#141743 = CARTESIAN_POINT ( 'NONE',  ( -12.06949235617756955, 12.14591786802309770, 25.62390960531435624 ) ) ;
#141744 = ORIENTED_EDGE ( 'NONE', *, *, #170515, .F. ) ;
#141745 = CARTESIAN_POINT ( 'NONE',  ( 10.81492255796078972, 18.62759615963270932, 99.58224293864770971 ) ) ;
#141747 = CARTESIAN_POINT ( 'NONE',  ( -9.474510206698964154, 16.51473224551069663, 115.4155762719810241 ) ) ;
#141746 = CARTESIAN_POINT ( 'NONE',  ( -0.05219959533910754901, -16.53943276465976808, 42.49890960531435979 ) ) ;
#141748 = CARTESIAN_POINT ( 'NONE',  ( -19.03943276465977164, -0.05219959533935918106, 93.75109039468566152 ) ) ;
#141749 = CARTESIAN_POINT ( 'NONE',  ( 0.05219959533936267826, -19.03943276465977164, 25.00109039468566152 ) ) ;
#141750 = CARTESIAN_POINT ( 'NONE',  ( 8.224510206698953496, -14.34966873604960469, 27.91557627198103830 ) ) ;
#141751 = CARTESIAN_POINT ( 'NONE',  ( 15.72974639402199770, -15.80617190586745480, 103.1239096053143811 ) ) ;
#141752 = CARTESIAN_POINT ( 'NONE',  ( 0.05219959533907565091, 21.53943276465977519, 49.99890960531437401 ) ) ;
#141753 = CARTESIAN_POINT ( 'NONE',  ( -16.51473224551069308, -9.474510206698971260, 81.66557627198103830 ) ) ;
#141754 = CARTESIAN_POINT ( 'NONE',  ( -4.483927247898539470, -16.52544592524342804, 52.29057627198102409 ) ) ;
#141755 = CARTESIAN_POINT ( 'NONE',  ( -5.049401038298153566, 19.05341960407611168, 90.20724293864766707 ) ) ;
#141756 = ORIENTED_EDGE ( 'NONE', *, *, #60885, .T. ) ;
#141757 = CARTESIAN_POINT ( 'NONE',  ( 5.153800228976615827, -19.02544592524334988, 35.20942372801899722 ) ) ;
#141758 = CARTESIAN_POINT ( 'NONE',  ( 10.72451020669898902, -18.67979575497178502, 77.91557627198102409 ) ) ;
#141759 = CARTESIAN_POINT ( 'NONE',  ( 14.34966873604960469, 8.224510206698951720, 104.1655762719810241 ) ) ;
#141760 = CARTESIAN_POINT ( 'NONE',  ( 21.53943276465977519, 0.05219959533937863772, 31.25109039468568639 ) ) ;
#141761 = CARTESIAN_POINT ( 'NONE',  ( 8.571926809382597767, 26.38167802310806209, 148.7750000027311899 ) ) ;
#141762 = CARTESIAN_POINT ( 'NONE',  ( -12.06949235617739369, -12.14591786802326823, 109.3760903946857042 ) ) ;
#141763 = CARTESIAN_POINT ( 'NONE',  ( -16.51473224551069308, -9.474510206698971260, 36.66557627198102409 ) ) ;
#141764 = CARTESIAN_POINT ( 'NONE',  ( -19.05341960407611168, -5.049401038298163336, 91.45724293864766707 ) ) ;
#141765 = CARTESIAN_POINT ( 'NONE',  ( -22.44159573604009950, -16.30477369853688430, 141.0750000027311728 ) ) ;
#141766 = CARTESIAN_POINT ( 'NONE',  ( -5.049401038298153566, 19.05341960407611168, 35.20724293864768839 ) ) ;
#141767 = CARTESIAN_POINT ( 'NONE',  ( 16.52544592524342804, -4.483927247898539470, 43.54057627198103830 ) ) ;
#141768 = CARTESIAN_POINT ( 'NONE',  ( 15.80617190586769283, -15.72974639402175789, 75.62609039468567573 ) ) ;
#141770 = CARTESIAN_POINT ( 'NONE',  ( -12.06949235617739369, -12.14591786802326823, 69.37609039468567573 ) ) ;
#141769 = CARTESIAN_POINT ( 'NONE',  ( 23.14280555631448877, -30.41650385747942664, -16.87365452858796999 ) ) ;
#141771 = CARTESIAN_POINT ( 'NONE',  ( 19.03943276465977164, -0.05219959533909143690, 58.74890960531435979 ) ) ;
#141772 = CARTESIAN_POINT ( 'NONE',  ( -19.05341960407611168, -5.049401038298163336, 61.45724293864769550 ) ) ;
#141773 = EDGE_LOOP ( 'NONE', ( #1289, #9329, #26682, #22663 ) ) ;
#141774 = CARTESIAN_POINT ( 'NONE',  ( -18.62759615963255300, -10.81492255796106328, 104.1677570613523471 ) ) ;
#141775 = CARTESIAN_POINT ( 'NONE',  ( -8.224510206698735004, -14.34966873604973081, 69.58442372801900433 ) ) ;
#141776 = CARTESIAN_POINT ( 'NONE',  ( -15.72974639402176322, -15.80617190586768395, 104.3760903946856899 ) ) ;
#141777 = CARTESIAN_POINT ( 'NONE',  ( 9.474510206698971260, -16.51473224551069308, 62.91557627198102409 ) ) ;
#141778 = CARTESIAN_POINT ( 'NONE',  ( 21.53943276465977519, -0.05219959533907433946, 38.74890960531435979 ) ) ;
#141779 = CARTESIAN_POINT ( 'NONE',  ( 16.51473224551083163, -9.474510206698727899, 100.8344237280190043 ) ) ;
#141780 = CARTESIAN_POINT ( 'NONE',  ( 5.719274019375673035, 21.55341960407619339, 67.29275706135234714 ) ) ;
#141781 = CARTESIAN_POINT ( 'NONE',  ( 14.34966873604972726, -8.224510206698740333, 55.83442372801901854 ) ) ;
#141782 = CARTESIAN_POINT ( 'NONE',  ( -15.72974639402197994, 15.80617190586746368, 100.6239096053143811 ) ) ;
#141783 = CARTESIAN_POINT ( 'NONE',  ( -0.05219959533936034679, 19.03943276465977164, 102.5010903946856757 ) ) ;
#141784 = CARTESIAN_POINT ( 'NONE',  ( 13.89961937509977652, -13.97604488694527269, 78.12390960531433848 ) ) ;
#141785 = CARTESIAN_POINT ( 'NONE',  ( -5.049401038297874678, -19.05341960407617918, 104.7927570613523471 ) ) ;
#141786 = CARTESIAN_POINT ( 'NONE',  ( 12.06949235617739724, 12.14591786802326823, 26.87609039468567218 ) ) ;
#141787 = CARTESIAN_POINT ( 'NONE',  ( -0.05219959533910754901, -16.53943276465976808, 72.49890960531435269 ) ) ;
#141788 = EDGE_CURVE ( 'NONE', #108375, #103711, #95743, .T. ) ;
#141789 = CARTESIAN_POINT ( 'NONE',  ( -4.483927247898782831, 16.52544592524335698, 67.70942372801901854 ) ) ;
#141791 = CARTESIAN_POINT ( 'NONE',  ( 9.564922557960805705, 16.46253265017160317, 49.58224293864770260 ) ) ;
#141790 = CARTESIAN_POINT ( 'NONE',  ( 10.81492255796106328, -18.62759615963255655, 20.41775706135234714 ) ) ;
#141792 = CARTESIAN_POINT ( 'NONE',  ( 16.51473224551069308, 9.474510206698969483, 69.16557627198102409 ) ) ;
#141793 = CARTESIAN_POINT ( 'NONE',  ( 16.55341960407618274, -4.379528057220086978, 76.04275706135237556 ) ) ;
#141794 = CARTESIAN_POINT ( 'NONE',  ( 23.31738231874054534, 16.94106989632529192, 147.4500000054623854 ) ) ;
#141795 = ORIENTED_EDGE ( 'NONE', *, *, #169539, .F. ) ;
#141796 = CARTESIAN_POINT ( 'NONE',  ( 18.62759615963255655, 10.81492255796105972, 111.6677570613523613 ) ) ;
#141797 = CARTESIAN_POINT ( 'NONE',  ( 0.05219959533909260263, 19.03943276465977164, 39.99890960531436690 ) ) ;
#141798 = ORIENTED_EDGE ( 'NONE', *, *, #115652, .T. ) ;
#141799 = CARTESIAN_POINT ( 'NONE',  ( -19.03943276465977164, -0.05219959533935918106, 108.7510903946856615 ) ) ;
#141800 = VECTOR ( 'NONE', #131144, 1000.000000000000000 ) ;
#141802 = CARTESIAN_POINT ( 'NONE',  ( -16.55341960407617563, 4.379528057220093196, 28.54275706135234358 ) ) ;
#141801 = CARTESIAN_POINT ( 'NONE',  ( -5.049401038297874678, -19.05341960407617918, 44.79275706135232582 ) ) ;
#141803 = CARTESIAN_POINT ( 'NONE',  ( -16.51473224551069308, -9.474510206698971260, 46.66557627198102409 ) ) ;
#141804 = CARTESIAN_POINT ( 'NONE',  ( 16.51473224551069308, 9.474510206698969483, 64.16557627198102409 ) ) ;
#141805 = CARTESIAN_POINT ( 'NONE',  ( -15.80617190586745835, -15.72974639402198527, 86.87390960531438111 ) ) ;
#141806 = CARTESIAN_POINT ( 'NONE',  ( 19.02544592524343514, -5.153800228976328945, 108.5405762719810383 ) ) ;
#141807 = CARTESIAN_POINT ( 'NONE',  ( -16.46253265017160317, 9.564922557960807481, 45.83224293864769550 ) ) ;
#141808 = DIRECTION ( 'NONE',  ( -0.000000000000000000, -0.000000000000000000, 1.000000000000000000 ) ) ;
#141809 = CARTESIAN_POINT ( 'NONE',  ( 5.049401038297881783, 19.05341960407617563, 97.29275706135233293 ) ) ;
#141810 = CARTESIAN_POINT ( 'NONE',  ( -15.72974639402197994, 15.80617190586746368, 70.62390960531436690 ) ) ;
#141811 = CARTESIAN_POINT ( 'NONE',  ( -19.02544592524334988, -5.153800228976617603, 23.95942372801900078 ) ) ;
#141812 = CARTESIAN_POINT ( 'NONE',  ( 14.34966873604960469, 8.224510206698951720, 64.16557627198102409 ) ) ;
#141813 = CARTESIAN_POINT ( 'NONE',  ( 21.52544592524334988, 5.823673210054432836, 86.45942372801901854 ) ) ;
#141814 = CARTESIAN_POINT ( 'NONE',  ( -16.51473224551069308, -9.474510206698971260, 31.66557627198102054 ) ) ;
#141815 = EDGE_CURVE ( 'NONE', #147006, #199732, #150379, .T. ) ;
#141817 = CARTESIAN_POINT ( 'NONE',  ( 18.67979575497194134, -10.72451020669871369, 90.83442372801901854 ) ) ;
#141816 = CARTESIAN_POINT ( 'NONE',  ( 16.53943276465976808, -0.05219959533910856209, 28.74890960531435624 ) ) ;
#141818 = CARTESIAN_POINT ( 'NONE',  ( 13.89961937509977652, -13.97604488694527269, 78.12390960531433848 ) ) ;
#141819 = CARTESIAN_POINT ( 'NONE',  ( -10.72451020669870658, -18.67979575497194134, 39.58442372801901143 ) ) ;
#141820 = CARTESIAN_POINT ( 'NONE',  ( -19.05341960407611168, -5.049401038298163336, 76.45724293864769550 ) ) ;
#141821 = CARTESIAN_POINT ( 'NONE',  ( 16.53943276465976808, -0.05219959533910856209, 88.74890960531436690 ) ) ;
#141822 = CARTESIAN_POINT ( 'NONE',  ( 14.34966873604960469, 8.224510206698951720, 59.16557627198103120 ) ) ;
#141823 = CARTESIAN_POINT ( 'NONE',  ( 18.67979575497178502, 10.72451020669898547, 69.16557627198102409 ) ) ;
#141824 = CARTESIAN_POINT ( 'NONE',  ( -19.03943276465977164, 0.05219959533909376836, 76.24890960531435269 ) ) ;
#141825 = CARTESIAN_POINT ( 'NONE',  ( 15.80617190586746368, 15.72974639402197994, 89.37390960531435269 ) ) ;
#141826 = CARTESIAN_POINT ( 'NONE',  ( -9.474510206698720793, -16.51473224551083518, 74.58442372801900433 ) ) ;
#141828 = CARTESIAN_POINT ( 'NONE',  ( 12.06949235617757843, -12.14591786802309237, 78.12390960531436690 ) ) ;
#141827 = CARTESIAN_POINT ( 'NONE',  ( 16.46253265017146816, 9.564922557961045513, 31.66775706135232937 ) ) ;
#141830 = VECTOR ( 'NONE', #69525, 1000.000000000000000 ) ;
#141829 = CARTESIAN_POINT ( 'NONE',  ( -10.81492255796078084, -18.62759615963271287, 52.08224293864768839 ) ) ;
#141831 = CARTESIAN_POINT ( 'NONE',  ( -17.49999999999999645, 5.499999999999997335, 115.7969038253417438 ) ) ;
#141833 = CARTESIAN_POINT ( 'NONE',  ( 8.571926809382597767, 26.38167802310806209, 142.7750000027311899 ) ) ;
#141832 = CARTESIAN_POINT ( 'NONE',  ( -8.314922557961024197, 14.29746914071037800, 97.91775706135236135 ) ) ;
#141834 = CARTESIAN_POINT ( 'NONE',  ( 16.46253265017146816, 9.564922557961045513, 106.6677570613523471 ) ) ;
#141835 = CARTESIAN_POINT ( 'NONE',  ( 16.53943276465976808, -0.05219959533910856209, 73.74890960531433848 ) ) ;
#141836 = CARTESIAN_POINT ( 'NONE',  ( -18.56399227203342051, -5.499999999999968026, 93.97830131249902763 ) ) ;
#141837 = CARTESIAN_POINT ( 'NONE',  ( -5.153800228976328057, -19.02544592524343514, 67.29057627198102409 ) ) ;
#141838 = CARTESIAN_POINT ( 'NONE',  ( -16.51473224551069308, -9.474510206698971260, 26.66557627198103120 ) ) ;
#141839 = CARTESIAN_POINT ( 'NONE',  ( -16.52544592524342804, 4.483927247898546575, 56.04057627198102409 ) ) ;
#141840 = CARTESIAN_POINT ( 'NONE',  ( 16.46253265017160672, -9.564922557960803928, 98.33224293864769550 ) ) ;
#141842 = CARTESIAN_POINT ( 'NONE',  ( 5.049401038298161559, -19.05341960407611168, 62.70724293864769550 ) ) ;
#141841 = CARTESIAN_POINT ( 'NONE',  ( 5.049401038297881783, 19.05341960407617563, 92.29275706135234714 ) ) ;
#141843 = CARTESIAN_POINT ( 'NONE',  ( -13.97604488694527625, -13.89961937509977652, 86.87390960531436690 ) ) ;
#141844 = CARTESIAN_POINT ( 'NONE',  ( 9.474510206698971260, -16.51473224551069308, 87.91557627198102409 ) ) ;
#141845 = CARTESIAN_POINT ( 'NONE',  ( -21.52544592524343514, 5.823673210054127303, 61.04057627198103120 ) ) ;
#141846 = CARTESIAN_POINT ( 'NONE',  ( -14.34966873604972548, 8.224510206698743886, 63.33442372801900433 ) ) ;
#141847 = DIRECTION ( 'NONE',  ( -1.000000000000000000, -0.000000000000000000, -0.000000000000000000 ) ) ;
#141848 = CARTESIAN_POINT ( 'NONE',  ( -19.05341960407611168, -5.049401038298163336, 61.45724293864769550 ) ) ;
#141849 = CARTESIAN_POINT ( 'NONE',  ( -10.72451020669898014, 18.67979575497178502, 65.41557627198102409 ) ) ;
#141850 = CARTESIAN_POINT ( 'NONE',  ( -19.03943276465977164, -0.05219959533935918106, 88.75109039468567573 ) ) ;
#141852 = CARTESIAN_POINT ( 'NONE',  ( -15.72974639402176322, -15.80617190586768395, 44.37609039468567573 ) ) ;
#141851 = CARTESIAN_POINT ( 'NONE',  ( 16.52544592524342804, -4.483927247898539470, 23.54057627198102765 ) ) ;
#141853 = CARTESIAN_POINT ( 'NONE',  ( 8.906447517083057264, -27.41122689804191026, 144.8500000054623911 ) ) ;
#141855 = CARTESIAN_POINT ( 'NONE',  ( -12.14591786802326823, 12.06949235617739902, 98.12609039468570415 ) ) ;
#141854 = CARTESIAN_POINT ( 'NONE',  ( 12.06949235617739724, 12.14591786802326823, 66.87609039468568994 ) ) ;
#141856 = CARTESIAN_POINT ( 'NONE',  ( -8.898068258721474777, 27.38543819252877398, 147.8656553485623704 ) ) ;
#141857 = CARTESIAN_POINT ( 'NONE',  ( 12.14591786802327356, -12.06949235617739191, 80.62609039468567573 ) ) ;
#141858 = CARTESIAN_POINT ( 'NONE',  ( 0.05219959533934541429, -16.53943276465976808, 30.00109039468568284 ) ) ;
#141859 = CARTESIAN_POINT ( 'NONE',  ( -9.564922557960796823, -16.46253265017161027, 52.08224293864768839 ) ) ;
#141860 = CARTESIAN_POINT ( 'NONE',  ( -5.153800228976328057, -19.02544592524343514, 52.29057627198100988 ) ) ;
#141861 = CARTESIAN_POINT ( 'NONE',  ( 16.46253265017160672, -9.564922557960803928, 63.33224293864769550 ) ) ;
#141862 = CARTESIAN_POINT ( 'NONE',  ( 10.81492255796106328, -18.62759615963255655, 55.41775706135234714 ) ) ;
#141863 = CARTESIAN_POINT ( 'NONE',  ( -14.34966873604972548, 8.224510206698743886, 48.33442372801902565 ) ) ;
#141864 = CARTESIAN_POINT ( 'NONE',  ( 0.05219959533910956823, 16.53943276465976808, 34.99890960531435979 ) ) ;
#141865 = CARTESIAN_POINT ( 'NONE',  ( 9.474510206698971260, -16.51473224551069308, 22.91557627198102765 ) ) ;
#141866 = CARTESIAN_POINT ( 'NONE',  ( -13.89961937509977652, 13.97604488694528158, 35.62390960531435269 ) ) ;
#141867 = CARTESIAN_POINT ( 'NONE',  ( 16.53943276465976808, 0.05219959533934440121, 26.25109039468567573 ) ) ;
#141868 = CARTESIAN_POINT ( 'NONE',  ( 19.05341960407617918, -5.049401038297876454, 86.04275706135233293 ) ) ;
#141869 = CARTESIAN_POINT ( 'NONE',  ( -4.483927247898539470, -16.52544592524342804, 77.29057627198102409 ) ) ;
#141870 = CARTESIAN_POINT ( 'NONE',  ( 9.474510206698971260, -16.51473224551069308, 52.91557627198102409 ) ) ;
#141872 = CARTESIAN_POINT ( 'NONE',  ( -17.49999999999999645, -5.499999999999992895, 54.20309617465830598 ) ) ;
#141871 = CARTESIAN_POINT ( 'NONE',  ( 5.049401038297881783, 19.05341960407617563, 72.29275706135234714 ) ) ;
#141873 = CARTESIAN_POINT ( 'NONE',  ( 21.53943276465977519, 0.05219959533937863772, 81.25109039468568994 ) ) ;
#141874 = CARTESIAN_POINT ( 'NONE',  ( -16.52544592524335698, -4.483927247898792601, 53.95942372801900433 ) ) ;
#141875 = DIRECTION ( 'NONE',  ( 0.000000000000000000, 0.7660444431189601389, -0.6427876096865606792 ) ) ;
#141876 = CARTESIAN_POINT ( 'NONE',  ( 5.719274019375991003, -21.55341960407610458, 37.70724293864769550 ) ) ;
#141877 = CARTESIAN_POINT ( 'NONE',  ( 16.52544592524335698, 4.483927247898782831, 36.45942372801901143 ) ) ;
#141878 = CARTESIAN_POINT ( 'NONE',  ( -13.89961937509977830, 13.97604488694528158, 25.62390960531435269 ) ) ;
#141879 = CARTESIAN_POINT ( 'NONE',  ( -5.153800228976607833, 19.02544592524334988, 27.70942372801899722 ) ) ;
#141880 = CYLINDRICAL_SURFACE ( 'NONE', #23657, 13.70000000000001528 ) ;
#141881 = CARTESIAN_POINT ( 'NONE',  ( 5.049401038298161559, -19.05341960407611168, 42.70724293864767418 ) ) ;
#141882 = PLANE ( 'NONE',  #91606 ) ;
#141883 = CARTESIAN_POINT ( 'NONE',  ( -13.97604488694527625, -13.89961937509977652, 66.87390960531436690 ) ) ;
#141884 = CARTESIAN_POINT ( 'NONE',  ( 17.50000000000000711, -3.512728167236853771, 112.7280999518112310 ) ) ;
#141885 = CARTESIAN_POINT ( 'NONE',  ( -9.474510206698720793, -16.51473224551083518, 19.58442372801899722 ) ) ;
#141886 = CARTESIAN_POINT ( 'NONE',  ( 4.483927247898545687, 16.52544592524342804, 39.79057627198103830 ) ) ;
#141887 = CARTESIAN_POINT ( 'NONE',  ( -19.02544592524342804, 5.153800228976336051, 41.04057627198103120 ) ) ;
#141888 = CARTESIAN_POINT ( 'NONE',  ( -13.89961937509977652, 13.97604488694528158, 105.6239096053143527 ) ) ;
#141889 = CARTESIAN_POINT ( 'NONE',  ( 21.52544592524334988, 5.823673210054432836, 66.45942372801903275 ) ) ;
#141890 = CARTESIAN_POINT ( 'NONE',  ( -16.46253265017160317, 9.564922557960807481, 55.83224293864769550 ) ) ;
#141891 = CARTESIAN_POINT ( 'NONE',  ( -15.80617190586768217, 15.72974639402176855, 63.12609039468568994 ) ) ;
#141892 = CARTESIAN_POINT ( 'NONE',  ( 5.153800228976335163, 19.02544592524342804, 114.7905762719810241 ) ) ;
#141893 = CARTESIAN_POINT ( 'NONE',  ( -5.153800228976328057, -19.02544592524343514, 37.29057627198102409 ) ) ;
#141894 = CARTESIAN_POINT ( 'NONE',  ( 10.72451020669871369, 18.67979575497193778, 27.08442372801901854 ) ) ;
#141895 = CARTESIAN_POINT ( 'NONE',  ( -0.05219959533936034679, 19.03943276465977164, 42.50109039468566152 ) ) ;
#141896 = CARTESIAN_POINT ( 'NONE',  ( -4.379528057220328563, 16.55341960407611168, 115.2072429386476955 ) ) ;
#141897 = CARTESIAN_POINT ( 'NONE',  ( -5.153800228976328057, -19.02544592524343514, 67.29057627198102409 ) ) ;
#141898 = CARTESIAN_POINT ( 'NONE',  ( 16.53943276465976808, 0.05219959533934440121, 21.25109039468567218 ) ) ;
#141899 = CARTESIAN_POINT ( 'NONE',  ( 8.314922557960818139, 14.29746914071049879, 79.58224293864769550 ) ) ;
#141900 = CARTESIAN_POINT ( 'NONE',  ( 10.81492255796078972, 18.62759615963270932, 34.58224293864770260 ) ) ;
#141901 = CARTESIAN_POINT ( 'NONE',  ( 13.97604488694548053, -13.89961937509957401, 100.6260903946856615 ) ) ;
#141902 = CARTESIAN_POINT ( 'NONE',  ( -21.52544592524343514, 5.823673210054127303, 111.0405762719810525 ) ) ;
#141903 = CARTESIAN_POINT ( 'NONE',  ( -10.81492255796105439, 18.62759615963255655, 57.91775706135234714 ) ) ;
#141904 = CARTESIAN_POINT ( 'NONE',  ( -8.314922557961024197, 14.29746914071037800, 57.91775706135234714 ) ) ;
#141905 = CARTESIAN_POINT ( 'NONE',  ( 16.52544592524335698, 4.483927247898782831, 56.45942372801902565 ) ) ;
#141906 = CARTESIAN_POINT ( 'NONE',  ( 15.80617190586746368, 15.72974639402197994, 54.37390960531435979 ) ) ;
#141907 = CARTESIAN_POINT ( 'NONE',  ( 19.05341960407611168, 5.049401038298154454, 53.95724293864770260 ) ) ;
#141908 = CARTESIAN_POINT ( 'NONE',  ( -12.14591786802326823, 12.06949235617739902, 78.12609039468570415 ) ) ;
#141909 = CARTESIAN_POINT ( 'NONE',  ( -21.53943276465977519, 0.05219959533907696930, 96.24890960531435269 ) ) ;
#141910 = CARTESIAN_POINT ( 'NONE',  ( 8.224510206698953496, -14.34966873604960469, 52.91557627198103830 ) ) ;
#141911 = CARTESIAN_POINT ( 'NONE',  ( 19.05341960407611168, 5.049401038298154454, 68.95724293864769550 ) ) ;
#141912 = CARTESIAN_POINT ( 'NONE',  ( -8.314922557961024197, 14.29746914071037800, 77.91775706135231871 ) ) ;
#141913 = CARTESIAN_POINT ( 'NONE',  ( -13.97604488694547697, 13.89961937509957934, 113.1260903946856757 ) ) ;
#141914 = CARTESIAN_POINT ( 'NONE',  ( -21.53943276465977519, 0.05219959533907696930, 101.2489096053143669 ) ) ;
#141915 = CARTESIAN_POINT ( 'NONE',  ( 14.34966873604960469, 8.224510206698951720, 39.16557627198102409 ) ) ;
#141916 = ORIENTED_EDGE ( 'NONE', *, *, #55568, .F. ) ;
#141917 = CARTESIAN_POINT ( 'NONE',  ( -17.13100169013299734, 6.664070546373147330, 75.76789835699851494 ) ) ;
#141918 = CARTESIAN_POINT ( 'NONE',  ( -21.52544592524343514, 5.823673210054127303, 86.04057627198102409 ) ) ;
#141919 = CARTESIAN_POINT ( 'NONE',  ( 16.53943276465976808, -0.05219959533910856209, 28.74890960531435624 ) ) ;
#141920 = VERTEX_POINT ( 'NONE', #133186 ) ;
#141921 = FACE_OUTER_BOUND ( 'NONE', #63485, .T. ) ;
#141922 = CARTESIAN_POINT ( 'NONE',  ( -18.67979575497178146, -10.72451020669898902, 96.66557627198102409 ) ) ;
#141923 = CARTESIAN_POINT ( 'NONE',  ( 19.03943276465977164, -0.05219959533909143690, 98.74890960531436690 ) ) ;
#141924 = CARTESIAN_POINT ( 'NONE',  ( 15.80617190586769283, -15.72974639402175789, 25.62609039468567929 ) ) ;
#141925 = CARTESIAN_POINT ( 'NONE',  ( -14.34966873604960291, -8.224510206698953496, 46.66557627198102409 ) ) ;
#141926 = CARTESIAN_POINT ( 'NONE',  ( 0.05219959533934541429, -16.53943276465976808, 45.00109039468568284 ) ) ;
#141927 = CARTESIAN_POINT ( 'NONE',  ( 13.97604488694527802, 13.89961937509977652, 54.37390960531435979 ) ) ;
#141928 = CARTESIAN_POINT ( 'NONE',  ( -5.153800228976607833, 19.02544592524334988, 57.70942372801899012 ) ) ;
#141929 = CARTESIAN_POINT ( 'NONE',  ( 5.153800228976335163, 19.02544592524342804, 84.79057627198099567 ) ) ;
#141930 = CARTESIAN_POINT ( 'NONE',  ( -21.55341960407610458, -5.719274019375992779, 36.45724293864768839 ) ) ;
#141931 = CARTESIAN_POINT ( 'NONE',  ( -28.40128899756798120, -24.57310642926549349, -18.78835905295398589 ) ) ;
#141932 = CARTESIAN_POINT ( 'NONE',  ( -12.06949235617739369, -12.14591786802326823, 19.37609039468568639 ) ) ;
#141933 = CARTESIAN_POINT ( 'NONE',  ( 9.474510206698729675, 16.51473224551082808, 52.08442372801900433 ) ) ;
#141934 = CARTESIAN_POINT ( 'NONE',  ( -18.67979575497178146, -10.72451020669898902, 101.6655762719810383 ) ) ;
#141935 = CARTESIAN_POINT ( 'NONE',  ( -4.379528057220328563, 16.55341960407611168, 40.20724293864769550 ) ) ;
#141936 = CARTESIAN_POINT ( 'NONE',  ( -9.474510206698964154, 16.51473224551069663, 75.41557627198103830 ) ) ;
#141937 = CARTESIAN_POINT ( 'NONE',  ( -15.80617190586745835, -15.72974639402198527, 56.87390960531436690 ) ) ;
#141939 = CARTESIAN_POINT ( 'NONE',  ( -12.06949235617739369, -12.14591786802326823, 19.37609039468568639 ) ) ;
#141938 = CARTESIAN_POINT ( 'NONE',  ( -18.62759615963270932, 10.81492255796079327, 90.83224293864769550 ) ) ;
#141940 = CARTESIAN_POINT ( 'NONE',  ( -13.97604488694527625, -13.89961937509977652, 111.8739096053143243 ) ) ;
#141941 = CARTESIAN_POINT ( 'NONE',  ( -10.81492255796105439, 18.62759615963255655, 92.91775706135236135 ) ) ;
#141942 = CARTESIAN_POINT ( 'NONE',  ( 16.46253265017160672, -9.564922557960803928, 83.33224293864768129 ) ) ;
#141943 = AXIS2_PLACEMENT_3D ( 'NONE', #101313, #179194, #24509 ) ;
#141944 = CARTESIAN_POINT ( 'NONE',  ( -9.564922557960796823, -16.46253265017161027, 27.08224293864769550 ) ) ;
#141945 = CARTESIAN_POINT ( 'NONE',  ( 5.049401038298161559, -19.05341960407611168, 87.70724293864769550 ) ) ;
#141946 = CARTESIAN_POINT ( 'NONE',  ( -16.53943276465976808, 0.05219959533911058130, 106.2489096053143811 ) ) ;
#141947 = CARTESIAN_POINT ( 'NONE',  ( 19.02544592524343514, -5.153800228976328945, 63.54057627198103830 ) ) ;
#141948 = CARTESIAN_POINT ( 'NONE',  ( 14.34966873604972726, -8.224510206698740333, 20.83442372801901143 ) ) ;
#141949 = CYLINDRICAL_SURFACE ( 'NONE', #186043, 21.30000000000002913 ) ;
#141950 = EDGE_CURVE ( 'NONE', #56021, #184472, #149365, .T. ) ;
#141951 = CARTESIAN_POINT ( 'NONE',  ( 5.153800228976335163, 19.02544592524342804, 79.79057627198102409 ) ) ;
#141953 = CARTESIAN_POINT ( 'NONE',  ( 19.03943276465977164, -0.05219959533909143690, 113.7489096053143669 ) ) ;
#141952 = CARTESIAN_POINT ( 'NONE',  ( -10.81492255796105439, 18.62759615963255655, 97.91775706135236135 ) ) ;
#141954 = CARTESIAN_POINT ( 'NONE',  ( -14.29746914071037622, -8.314922557961029526, 94.16775706135237556 ) ) ;
#141955 = DIRECTION ( 'NONE',  ( 0.000000000000000000, 0.000000000000000000, 1.000000000000000000 ) ) ;
#141956 = CARTESIAN_POINT ( 'NONE',  ( -0.05219959533936034679, 19.03943276465977164, 67.50109039468566152 ) ) ;
#141957 = CARTESIAN_POINT ( 'NONE',  ( 10.81492255796106328, -18.62759615963255655, 110.4177570613523756 ) ) ;
#141958 = CARTESIAN_POINT ( 'NONE',  ( -27.49873734152928151, -21.99873734152901861, 1.818019484660534424 ) ) ;
#141959 = CARTESIAN_POINT ( 'NONE',  ( 13.97604488694527802, 13.89961937509977652, 29.37390960531435979 ) ) ;
#141960 = CARTESIAN_POINT ( 'NONE',  ( 16.52544592524342804, -4.483927247898539470, 33.54057627198102409 ) ) ;
#141961 = DIRECTION ( 'NONE',  ( 0.000000000000000000, -0.6427876096865404731, -0.7660444431189771253 ) ) ;
#141962 = CARTESIAN_POINT ( 'NONE',  ( 16.53943276465976808, 0.05219959533934440121, 101.2510903946856757 ) ) ;
#141963 = CARTESIAN_POINT ( 'NONE',  ( 22.63233124262814044, -20.50857827831517355, -50.83049096057695238 ) ) ;
#141964 = CARTESIAN_POINT ( 'NONE',  ( -8.224510206698735004, -14.34966873604973081, 79.58442372801903275 ) ) ;
#141965 = CARTESIAN_POINT ( 'NONE',  ( -19.05341960407611168, -5.049401038298163336, 41.45724293864769550 ) ) ;
#141966 = CARTESIAN_POINT ( 'NONE',  ( -15.80617190586768217, 15.72974639402176855, 93.12609039468568994 ) ) ;
#141967 = CARTESIAN_POINT ( 'NONE',  ( -9.564922557961040184, 16.46253265017147172, 107.9177570613523471 ) ) ;
#141968 = CARTESIAN_POINT ( 'NONE',  ( 0.05219959533937995610, -21.53943276465977519, 75.00109039468568994 ) ) ;
#141969 = CARTESIAN_POINT ( 'NONE',  ( -5.049401038297874678, -19.05341960407617918, 49.79275706135231871 ) ) ;
#141970 = CARTESIAN_POINT ( 'NONE',  ( 13.97604488694527802, 13.89961937509977652, 84.37390960531433848 ) ) ;
#141971 = CARTESIAN_POINT ( 'NONE',  ( 13.97604488694527802, 13.89961937509977652, 74.37390960531436690 ) ) ;
#141972 = CARTESIAN_POINT ( 'NONE',  ( -19.99999999999998224, -188.0000000000000000, -15.00000000000000178 ) ) ;
#141973 = AXIS2_PLACEMENT_3D ( 'NONE', #101320, #163009, #137640 ) ;
#141974 = CARTESIAN_POINT ( 'NONE',  ( 12.06949235617757843, -12.14591786802309237, 63.12390960531435979 ) ) ;
#141975 = CARTESIAN_POINT ( 'NONE',  ( 10.72451020669898902, -18.67979575497178502, 67.91557627198102409 ) ) ;
#141976 = CARTESIAN_POINT ( 'NONE',  ( -16.46253265017160317, 9.564922557960807481, 40.83224293864769550 ) ) ;
#141978 = CARTESIAN_POINT ( 'NONE',  ( 4.379528057220092307, 16.55341960407617563, 77.29275706135234714 ) ) ;
#141977 = CARTESIAN_POINT ( 'NONE',  ( -21.52544592524343514, 5.823673210054127303, 86.04057627198102409 ) ) ;
#141979 = ORIENTED_EDGE ( 'NONE', *, *, #57708, .F. ) ;
#141981 = CARTESIAN_POINT ( 'NONE',  ( 29.86685920354754487, 21.69954338932564752, -3.424999997268813434 ) ) ;
#141980 = CARTESIAN_POINT ( 'NONE',  ( -4.379528057220328563, 16.55341960407611168, 80.20724293864769550 ) ) ;
#141982 = CARTESIAN_POINT ( 'NONE',  ( -4.483927247898782831, 16.52544592524335698, 32.70942372801900433 ) ) ;
#141983 = CARTESIAN_POINT ( 'NONE',  ( 16.46253265017160672, -9.564922557960803928, 23.33224293864769194 ) ) ;
#141984 = CARTESIAN_POINT ( 'NONE',  ( 16.46253265017146816, 9.564922557961045513, 71.66775706135233293 ) ) ;
#141985 = CARTESIAN_POINT ( 'NONE',  ( 12.06949235617757843, -12.14591786802309237, 73.12390960531436690 ) ) ;
#141986 = CARTESIAN_POINT ( 'NONE',  ( 18.67979575497194134, -10.72451020669871369, 45.83442372801901854 ) ) ;
#141988 = CARTESIAN_POINT ( 'NONE',  ( -0.05219959533907301413, -21.53943276465977519, 97.49890960531436690 ) ) ;
#141987 = CARTESIAN_POINT ( 'NONE',  ( 19.03943276465977164, -0.05219959533909143690, 23.74890960531435269 ) ) ;
#141989 = CARTESIAN_POINT ( 'NONE',  ( 19.03943276465977164, -0.05219959533909143690, 113.7489096053143669 ) ) ;
#141990 = CARTESIAN_POINT ( 'NONE',  ( -12.06949235617756955, 12.14591786802309770, 90.62390960531436690 ) ) ;
#141991 = CARTESIAN_POINT ( 'NONE',  ( 21.14397880779448968, -35.31393329058613517, -18.60109459635480889 ) ) ;
#141992 = CARTESIAN_POINT ( 'NONE',  ( 19.02544592524343514, -5.153800228976328945, 43.54057627198103120 ) ) ;
#141993 = CARTESIAN_POINT ( 'NONE',  ( 29.86685920354754842, -21.69954338932559068, -1.824999997268813345 ) ) ;
#141994 = CARTESIAN_POINT ( 'NONE',  ( -0.05219959533936034679, 19.03943276465977164, 82.50109039468567573 ) ) ;
#141995 = CARTESIAN_POINT ( 'NONE',  ( 21.53943276465977519, 0.05219959533937863772, 36.25109039468567573 ) ) ;
#141996 = CARTESIAN_POINT ( 'NONE',  ( 13.97604488694527802, 13.89961937509977652, 69.37390960531436690 ) ) ;
#141997 = CARTESIAN_POINT ( 'NONE',  ( 13.89961937509957401, 13.97604488694547697, 61.87609039468566863 ) ) ;
#141998 = CARTESIAN_POINT ( 'NONE',  ( 5.049401038298161559, -19.05341960407611168, 42.70724293864767418 ) ) ;
#141999 = CARTESIAN_POINT ( 'NONE',  ( -4.483927247898539470, -16.52544592524342804, 67.29057627198103830 ) ) ;
#142000 = CARTESIAN_POINT ( 'NONE',  ( -12.06949235617756955, 12.14591786802309770, 50.62390960531435979 ) ) ;
#142001 = CARTESIAN_POINT ( 'NONE',  ( -16.46253265017160317, 9.564922557960807481, 70.83224293864770971 ) ) ;
#142002 = CARTESIAN_POINT ( 'NONE',  ( -18.67979575497178146, -10.72451020669898902, 96.66557627198102409 ) ) ;
#142003 = CARTESIAN_POINT ( 'NONE',  ( -0.05219959533909027116, -19.03943276465977164, 67.49890960531436690 ) ) ;
#142004 = CARTESIAN_POINT ( 'NONE',  ( -18.62759615963270932, 10.81492255796079327, 80.83224293864769550 ) ) ;
#142005 = CARTESIAN_POINT ( 'NONE',  ( -21.53943276465977519, -0.05219959533937600094, 108.7510903946857042 ) ) ;
#142008 = CARTESIAN_POINT ( 'NONE',  ( -16.52544592524342804, 4.483927247898546575, 91.04057627198103830 ) ) ;
#142007 = CARTESIAN_POINT ( 'NONE',  ( -8.224510206698735004, -14.34966873604973081, 104.5844237280190185 ) ) ;
#142006 = CARTESIAN_POINT ( 'NONE',  ( 13.89961937509977652, -13.97604488694527269, 33.12390960531434558 ) ) ;
#142009 = CARTESIAN_POINT ( 'NONE',  ( 13.89961937509957401, 13.97604488694547697, 106.8760903946856757 ) ) ;
#142010 = ORIENTED_EDGE ( 'NONE', *, *, #71748, .F. ) ;
#142011 = CARTESIAN_POINT ( 'NONE',  ( 15.72974639402176855, 15.80617190586768217, 31.87609039468567929 ) ) ;
#142012 = CARTESIAN_POINT ( 'NONE',  ( 9.564922557961047289, -16.46253265017146816, 55.41775706135234003 ) ) ;
#142013 = CARTESIAN_POINT ( 'NONE',  ( -12.06949235617756955, 12.14591786802309770, 25.62390960531435624 ) ) ;
#142014 = CARTESIAN_POINT ( 'NONE',  ( 21.55341960407610458, 5.719274019375980345, 78.95724293864769550 ) ) ;
#142015 = CARTESIAN_POINT ( 'NONE',  ( -9.564922557960796823, -16.46253265017161027, 102.0822429386477097 ) ) ;
#142016 = CARTESIAN_POINT ( 'NONE',  ( -0.05219959533910754901, -16.53943276465976808, 57.49890960531435979 ) ) ;
#142017 = CARTESIAN_POINT ( 'NONE',  ( -16.46253265017160317, 9.564922557960807481, 35.83224293864768839 ) ) ;
#142018 = CARTESIAN_POINT ( 'NONE',  ( -13.97604488694527625, -13.89961937509977652, 31.87390960531435979 ) ) ;
#142019 = CARTESIAN_POINT ( 'NONE',  ( -16.51473224551082808, 9.474510206698731452, 28.33442372801900433 ) ) ;
#142020 = CARTESIAN_POINT ( 'NONE',  ( -12.06949235617739369, -12.14591786802326823, 94.37609039468568994 ) ) ;
#142021 = CARTESIAN_POINT ( 'NONE',  ( 10.81492255796106328, -18.62759615963255655, 35.41775706135234003 ) ) ;
#142022 = CARTESIAN_POINT ( 'NONE',  ( 8.224510206698742110, 14.34966873604972548, 42.08442372801901854 ) ) ;
#142023 = CARTESIAN_POINT ( 'NONE',  ( -9.474510206698964154, 16.51473224551069663, 115.4155762719810241 ) ) ;
#142025 = CARTESIAN_POINT ( 'NONE',  ( -10.72451020669870658, -18.67979575497194134, 99.58442372801900433 ) ) ;
#142024 = CARTESIAN_POINT ( 'NONE',  ( 16.51473224551069308, 9.474510206698969483, 49.16557627198102409 ) ) ;
#142026 = CARTESIAN_POINT ( 'NONE',  ( -16.46253265017160317, 9.564922557960807481, 80.83224293864769550 ) ) ;
#142027 = CARTESIAN_POINT ( 'NONE',  ( -16.52544592524335698, -4.483927247898792601, 58.95942372801902565 ) ) ;
#142028 = CARTESIAN_POINT ( 'NONE',  ( 16.53943276465976808, -0.05219959533910856209, 103.7489096053143669 ) ) ;
#142029 = EDGE_CURVE ( 'NONE', #173841, #135262, #105841, .T. ) ;
#142030 = CARTESIAN_POINT ( 'NONE',  ( 12.14591786802327356, -12.06949235617739191, 110.6260903946857042 ) ) ;
#142031 = CARTESIAN_POINT ( 'NONE',  ( -17.58332526062525858, 7.635886036038558977, 50.92334959558467489 ) ) ;
#142034 = CARTESIAN_POINT ( 'NONE',  ( -5.049401038298153566, 19.05341960407611168, 75.20724293864769550 ) ) ;
#142033 = CARTESIAN_POINT ( 'NONE',  ( -9.564922557960796823, -16.46253265017161027, 97.08224293864769550 ) ) ;
#142032 = CARTESIAN_POINT ( 'NONE',  ( 15.72974639402176855, 15.80617190586768217, 56.87609039468568994 ) ) ;
#142035 = CARTESIAN_POINT ( 'NONE',  ( 16.51473224551069308, 9.474510206698969483, 104.1655762719810241 ) ) ;
#142036 = CARTESIAN_POINT ( 'NONE',  ( 0.05219959533910956823, 16.53943276465976808, 49.99890960531437401 ) ) ;
#142037 = CARTESIAN_POINT ( 'NONE',  ( 4.483927247898545687, 16.52544592524342804, 24.79057627198103120 ) ) ;
#142038 = CARTESIAN_POINT ( 'NONE',  ( -16.53943276465976808, 0.05219959533911058130, 36.24890960531435979 ) ) ;
#142039 = CARTESIAN_POINT ( 'NONE',  ( -7.284589286804255437, 1.784589286804319386, 8.181980515339454030 ) ) ;
#142040 = CARTESIAN_POINT ( 'NONE',  ( -9.564922557961040184, 16.46253265017147172, 32.91775706135233293 ) ) ;
#142041 = CARTESIAN_POINT ( 'NONE',  ( -19.03943276465977164, 0.05219959533909376836, 81.24890960531436690 ) ) ;
#142042 = CARTESIAN_POINT ( 'NONE',  ( -19.03943276465977164, -0.05219959533935918106, 48.75109039468566863 ) ) ;
#142043 = CARTESIAN_POINT ( 'NONE',  ( -22.81625015709510507, 31.40387420917330275, -0.9249999972688132122 ) ) ;
#142044 = DIRECTION ( 'NONE',  ( -1.000000000000000000, -0.000000000000000000, -0.000000000000000000 ) ) ;
#142046 = CARTESIAN_POINT ( 'NONE',  ( -14.34966873604972548, 8.224510206698743886, 68.33442372801900433 ) ) ;
#142045 = CARTESIAN_POINT ( 'NONE',  ( -19.02544592524334988, -5.153800228976617603, 83.95942372801901854 ) ) ;
#142047 = CARTESIAN_POINT ( 'NONE',  ( 16.29526858892874941, 7.335722546920129261, 93.29670597800205201 ) ) ;
#142048 = CARTESIAN_POINT ( 'NONE',  ( 19.03943276465977164, -0.05219959533909143690, 103.7489096053143669 ) ) ;
#142049 = CARTESIAN_POINT ( 'NONE',  ( 15.72974639402176855, 15.80617190586768217, 31.87609039468567929 ) ) ;
#142050 = CARTESIAN_POINT ( 'NONE',  ( 5.153800228976615827, -19.02544592524334988, 90.20942372801900433 ) ) ;
#142052 = CARTESIAN_POINT ( 'NONE',  ( -9.474510206698964154, 16.51473224551069663, 45.41557627198103120 ) ) ;
#142051 = CARTESIAN_POINT ( 'NONE',  ( 16.79531203550646978, 7.028104445595628746, 88.75244988220444498 ) ) ;
#142053 = CARTESIAN_POINT ( 'NONE',  ( 0.05219959533909260263, 19.03943276465977164, 89.99890960531436690 ) ) ;
#142055 = CARTESIAN_POINT ( 'NONE',  ( 19.02544592524343514, -5.153800228976328945, 43.54057627198103120 ) ) ;
#142054 = CARTESIAN_POINT ( 'NONE',  ( -16.55341960407611168, -4.379528057220339221, 66.45724293864768129 ) ) ;
#142056 = CARTESIAN_POINT ( 'NONE',  ( -9.564922557960796823, -16.46253265017161027, 62.08224293864769550 ) ) ;
#142057 = CARTESIAN_POINT ( 'NONE',  ( -9.474510206698720793, -16.51473224551083518, 64.58442372801900433 ) ) ;
#142058 = CARTESIAN_POINT ( 'NONE',  ( -5.153800228976607833, 19.02544592524334988, 32.70942372801899722 ) ) ;
#142059 = CARTESIAN_POINT ( 'NONE',  ( -13.97604488694527625, -13.89961937509977652, 66.87390960531436690 ) ) ;
#142060 = CARTESIAN_POINT ( 'NONE',  ( 21.52544592524344225, -5.823673210054117533, 63.54057627198103830 ) ) ;
#142062 = CARTESIAN_POINT ( 'NONE',  ( -19.02544592524334988, -5.153800228976617603, 33.95942372801897591 ) ) ;
#142061 = CARTESIAN_POINT ( 'NONE',  ( -4.483927247898539470, -16.52544592524342804, 67.29057627198103830 ) ) ;
#142063 = CARTESIAN_POINT ( 'NONE',  ( -29.15849868437705439, -8.010956209263452976, 149.7909430734646890 ) ) ;
#142064 = CARTESIAN_POINT ( 'NONE',  ( -5.719274019375978568, 21.55341960407610458, 50.20724293864769550 ) ) ;
#142065 = CARTESIAN_POINT ( 'NONE',  ( -21.55341960407610458, -5.719274019375992779, 26.45724293864768839 ) ) ;
#142066 = CARTESIAN_POINT ( 'NONE',  ( -0.05219959533909027116, -19.03943276465977164, 47.49890960531435979 ) ) ;
#142067 = CARTESIAN_POINT ( 'NONE',  ( -5.049401038298153566, 19.05341960407611168, 35.20724293864768839 ) ) ;
#142068 = CARTESIAN_POINT ( 'NONE',  ( 16.52544592524342804, -4.483927247898539470, 103.5405762719810383 ) ) ;
#142069 = CARTESIAN_POINT ( 'NONE',  ( -5.719274019375978568, 21.55341960407610458, 115.2072429386476955 ) ) ;
#142070 = CARTESIAN_POINT ( 'NONE',  ( 19.05341960407611168, 5.049401038298154454, 108.9572429386477097 ) ) ;
#142071 = CARTESIAN_POINT ( 'NONE',  ( -15.72974639402176322, -15.80617190586768395, 29.37609039468568284 ) ) ;
#142072 = CARTESIAN_POINT ( 'NONE',  ( 14.34966873604960469, 8.224510206698951720, 114.1655762719810383 ) ) ;
#142073 = CARTESIAN_POINT ( 'NONE',  ( 5.719274019375673035, 21.55341960407619339, 82.29275706135234714 ) ) ;
#142074 = CARTESIAN_POINT ( 'NONE',  ( 18.62759615963271287, -10.81492255796078972, 88.33224293864769550 ) ) ;
#142075 = CARTESIAN_POINT ( 'NONE',  ( -5.049401038297874678, -19.05341960407617918, 49.79275706135231871 ) ) ;
#142076 = CARTESIAN_POINT ( 'NONE',  ( 16.51473224551069308, 9.474510206698969483, 24.16557627198102765 ) ) ;
#142077 = CARTESIAN_POINT ( 'NONE',  ( 5.153800228976335163, 19.02544592524342804, 24.79057627198102765 ) ) ;
#142078 = CARTESIAN_POINT ( 'NONE',  ( 31.67901979315914573, -0.7913989229878923837, -49.40962234820030829 ) ) ;
#142079 = CARTESIAN_POINT ( 'NONE',  ( 16.52544592524335698, 4.483927247898782831, 41.45942372801901143 ) ) ;
#142080 = CARTESIAN_POINT ( 'NONE',  ( 4.483927247898545687, 16.52544592524342804, 114.7905762719810383 ) ) ;
#142081 = CARTESIAN_POINT ( 'NONE',  ( 33.75684350552030821, -3.359699206722003062, 99.36933870599243335 ) ) ;
#142082 = CARTESIAN_POINT ( 'NONE',  ( 16.46253265017160672, -9.564922557960803928, 73.33224293864769550 ) ) ;
#142083 = CARTESIAN_POINT ( 'NONE',  ( 8.224510206698953496, -14.34966873604960469, 87.91557627198103830 ) ) ;
#142084 = CARTESIAN_POINT ( 'NONE',  ( 5.823673210054125526, 21.52544592524343514, 44.79057627198103120 ) ) ;
#142085 = CARTESIAN_POINT ( 'NONE',  ( 16.55341960407611168, 4.379528057220329451, 73.95724293864769550 ) ) ;
#142086 = CARTESIAN_POINT ( 'NONE',  ( 4.483927247898790824, -16.52544592524335698, 30.20942372801902565 ) ) ;
#142087 = CARTESIAN_POINT ( 'NONE',  ( 18.62759615963255655, 10.81492255796105972, 86.66775706135234714 ) ) ;
#142088 = CARTESIAN_POINT ( 'NONE',  ( -5.049401038298153566, 19.05341960407611168, 30.20724293864768839 ) ) ;
#142089 = CARTESIAN_POINT ( 'NONE',  ( -16.55341960407617563, 4.379528057220093196, 103.5427570613523613 ) ) ;
#142090 = CARTESIAN_POINT ( 'NONE',  ( -14.29746914071049879, 8.314922557960819915, 45.83224293864769550 ) ) ;
#142091 = CIRCLE ( 'NONE', #193797, 1.000000000000000888 ) ;
#142092 = CARTESIAN_POINT ( 'NONE',  ( 5.153800228976335163, 19.02544592524342804, 54.79057627198103120 ) ) ;
#142093 = CARTESIAN_POINT ( 'NONE',  ( -15.80617190586768217, 15.72974639402176855, 98.12609039468570415 ) ) ;
#142094 = CARTESIAN_POINT ( 'NONE',  ( 15.72974639402199770, -15.80617190586745480, 103.1239096053143811 ) ) ;
#142095 = CARTESIAN_POINT ( 'NONE',  ( -0.05219959533937732626, 21.53943276465977519, 77.50109039468567573 ) ) ;
#142096 = CARTESIAN_POINT ( 'NONE',  ( -14.29746914071037622, -8.314922557961029526, 34.16775706135234714 ) ) ;
#142098 = CARTESIAN_POINT ( 'NONE',  ( 10.81492255796106328, -18.62759615963255655, 90.41775706135236135 ) ) ;
#142097 = CARTESIAN_POINT ( 'NONE',  ( -4.379528057220328563, 16.55341960407611168, 70.20724293864769550 ) ) ;
#142099 = CARTESIAN_POINT ( 'NONE',  ( 16.52544592524342804, -4.483927247898539470, 23.54057627198102765 ) ) ;
#142100 = CARTESIAN_POINT ( 'NONE',  ( 16.38665767534995865, -7.295008042176399421, 47.76400864214470232 ) ) ;
#142101 = CARTESIAN_POINT ( 'NONE',  ( 0.000000000000000000, 0.000000000000000000, -25.00000000000000000 ) ) ;
#142102 = CARTESIAN_POINT ( 'NONE',  ( 14.34966873604960469, 8.224510206698951720, 44.16557627198103120 ) ) ;
#142103 = CARTESIAN_POINT ( 'NONE',  ( 4.379528057220092307, 16.55341960407617563, 77.29275706135234714 ) ) ;
#142104 = CARTESIAN_POINT ( 'NONE',  ( 9.564922557960805705, 16.46253265017160317, 84.58224293864769550 ) ) ;
#142105 = CARTESIAN_POINT ( 'NONE',  ( -19.03943276465977164, 0.05219959533909376836, 96.24890960531436690 ) ) ;
#142106 = CARTESIAN_POINT ( 'NONE',  ( -15.80617190586768217, 15.72974639402176855, 88.12609039468570415 ) ) ;
#142107 = CARTESIAN_POINT ( 'NONE',  ( 12.06949235617739724, 12.14591786802326823, 86.87609039468568994 ) ) ;
#142108 = CARTESIAN_POINT ( 'NONE',  ( 4.483927247898545687, 16.52544592524342804, 69.79057627198102409 ) ) ;
#142109 = CARTESIAN_POINT ( 'NONE',  ( 5.049401038298161559, -19.05341960407611168, 82.70724293864770971 ) ) ;
#142110 = VERTEX_POINT ( 'NONE', #41195 ) ;
#142111 = CARTESIAN_POINT ( 'NONE',  ( -12.14591786802326823, 12.06949235617739902, 33.12609039468569705 ) ) ;
#142112 = CARTESIAN_POINT ( 'NONE',  ( -5.153800228976328057, -19.02544592524343514, 27.29057627198103120 ) ) ;
#142113 = CARTESIAN_POINT ( 'NONE',  ( -19.03943276465977164, 0.05219959533909376836, 96.24890960531436690 ) ) ;
#142115 = CARTESIAN_POINT ( 'NONE',  ( -6.412877669190332419, -3.889087296526017479, 8.181980515339454030 ) ) ;
#142114 = CARTESIAN_POINT ( 'NONE',  ( 16.52544592524335698, 4.483927247898782831, 26.45942372801901854 ) ) ;
#142116 = CARTESIAN_POINT ( 'NONE',  ( 5.719274019375673035, 21.55341960407619339, 112.2927570613523471 ) ) ;
#142117 = CARTESIAN_POINT ( 'NONE',  ( 4.483927247898790824, -16.52544592524335698, 100.2094237280190043 ) ) ;
#142118 = CARTESIAN_POINT ( 'NONE',  ( 19.05341960407617918, -5.049401038297876454, 106.0427570613523471 ) ) ;
#142119 = CARTESIAN_POINT ( 'NONE',  ( -19.03943276465977164, 0.05219959533909376836, 26.24890960531435624 ) ) ;
#142120 = CARTESIAN_POINT ( 'NONE',  ( -16.52544592524335698, -4.483927247898792601, 83.95942372801900433 ) ) ;
#142121 = CARTESIAN_POINT ( 'NONE',  ( -0.05219959533934338120, 16.53943276465976808, 67.50109039468568994 ) ) ;
#142122 = CARTESIAN_POINT ( 'NONE',  ( 25.19119763768592790, -31.08384082485095590, -7.296079031154174110 ) ) ;
#142123 = CARTESIAN_POINT ( 'NONE',  ( 13.89961937509957401, 13.97604488694547697, 66.87609039468567573 ) ) ;
#142124 = CARTESIAN_POINT ( 'NONE',  ( -5.719274019375665041, -21.55341960407619695, 104.7927570613523898 ) ) ;
#142125 = CARTESIAN_POINT ( 'NONE',  ( -13.97604488694527625, -13.89961937509977652, 51.87390960531436690 ) ) ;
#142126 = CARTESIAN_POINT ( 'NONE',  ( 19.05341960407611168, 5.049401038298154454, 93.95724293864769550 ) ) ;
#142127 = CARTESIAN_POINT ( 'NONE',  ( -0.05219959533910754901, -16.53943276465976808, 82.49890960531436690 ) ) ;
#142128 = CIRCLE ( 'NONE', #132471, 1.250000000000006439 ) ;
#142129 = CARTESIAN_POINT ( 'NONE',  ( -9.564922557961040184, 16.46253265017147172, 52.91775706135233293 ) ) ;
#142130 = CARTESIAN_POINT ( 'NONE',  ( -15.72974639402197994, 15.80617190586746368, 55.62390960531436690 ) ) ;
#142131 = CARTESIAN_POINT ( 'NONE',  ( 19.03943276465977164, 0.05219959533936151252, 21.25109039468565797 ) ) ;
#142132 = CARTESIAN_POINT ( 'NONE',  ( 5.049401038298161559, -19.05341960407611168, 87.70724293864769550 ) ) ;
#142133 = CARTESIAN_POINT ( 'NONE',  ( 10.81492255796106328, -18.62759615963255655, 110.4177570613523756 ) ) ;
#142134 = CARTESIAN_POINT ( 'NONE',  ( -15.80617190586745835, -15.72974639402198527, 61.87390960531436690 ) ) ;
#142135 = CARTESIAN_POINT ( 'NONE',  ( -13.89961937509977652, 13.97604488694528158, 95.62390960531436690 ) ) ;
#142136 = CARTESIAN_POINT ( 'NONE',  ( -9.474510206698720793, -16.51473224551083518, 84.58442372801900433 ) ) ;
#142137 = CARTESIAN_POINT ( 'NONE',  ( 0.05219959533909260263, 19.03943276465977164, 104.9989096053143669 ) ) ;
#142138 = CARTESIAN_POINT ( 'NONE',  ( -16.51473224551082808, 9.474510206698731452, 103.3344237280190043 ) ) ;
#142139 = CARTESIAN_POINT ( 'NONE',  ( 4.483927247898545687, 16.52544592524342804, 114.7905762719810383 ) ) ;
#142140 = CARTESIAN_POINT ( 'NONE',  ( -19.03943276465977164, 0.05219959533909376836, 86.24890960531436690 ) ) ;
#142141 = CARTESIAN_POINT ( 'NONE',  ( -10.72451020669898014, 18.67979575497178502, 80.41557627198103830 ) ) ;
#142142 = CARTESIAN_POINT ( 'NONE',  ( -16.53943276465976808, -0.05219959533934237506, 43.75109039468568284 ) ) ;
#142143 = CARTESIAN_POINT ( 'NONE',  ( 18.67979575497194134, -10.72451020669871369, 45.83442372801901854 ) ) ;
#142144 = CARTESIAN_POINT ( 'NONE',  ( 10.72451020669871369, 18.67979575497193778, 92.08442372801901854 ) ) ;
#142145 = CARTESIAN_POINT ( 'NONE',  ( 0.05219959533934541429, -16.53943276465976808, 90.00109039468567573 ) ) ;
#142146 = CARTESIAN_POINT ( 'NONE',  ( -5.049401038298153566, 19.05341960407611168, 90.20724293864766707 ) ) ;
#142147 = CARTESIAN_POINT ( 'NONE',  ( -4.483927247898539470, -16.52544592524342804, 87.29057627198103830 ) ) ;
#142148 = CARTESIAN_POINT ( 'NONE',  ( -4.379528057220328563, 16.55341960407611168, 25.20724293864769550 ) ) ;
#142149 = CARTESIAN_POINT ( 'NONE',  ( -13.89961937509957401, -13.97604488694547875, 64.37609039468567573 ) ) ;
#142150 = EDGE_CURVE ( 'NONE', #23884, #10184, #93846, .T. ) ;
#142151 = CARTESIAN_POINT ( 'NONE',  ( -0.05219959533937732626, 21.53943276465977519, 42.50109039468567573 ) ) ;
#142152 = CARTESIAN_POINT ( 'NONE',  ( 16.46253265017146816, 9.564922557961045513, 26.66775706135234003 ) ) ;
#142153 = CARTESIAN_POINT ( 'NONE',  ( -16.55341960407611168, -4.379528057220339221, 86.45724293864770971 ) ) ;
#142154 = CARTESIAN_POINT ( 'NONE',  ( 19.03943276465977164, -0.05219959533909143690, 113.7489096053143669 ) ) ;
#142155 = CARTESIAN_POINT ( 'NONE',  ( -8.314922557961024197, 14.29746914071037800, 112.9177570613523329 ) ) ;
#142156 = CARTESIAN_POINT ( 'NONE',  ( 10.81492255796106328, -18.62759615963255655, 90.41775706135236135 ) ) ;
#142157 = CARTESIAN_POINT ( 'NONE',  ( -14.34966873604972548, 8.224510206698743886, 58.33442372801901143 ) ) ;
#142158 = CARTESIAN_POINT ( 'NONE',  ( -16.52544592524335698, -4.483927247898792601, 103.9594237280190185 ) ) ;
#142159 = CARTESIAN_POINT ( 'NONE',  ( 5.719274019375673035, 21.55341960407619339, 57.29275706135234714 ) ) ;
#142160 = ORIENTED_EDGE ( 'NONE', *, *, #111650, .T. ) ;
#142161 = CARTESIAN_POINT ( 'NONE',  ( -18.62759615963255300, -10.81492255796106328, 34.16775706135234714 ) ) ;
#142162 = CARTESIAN_POINT ( 'NONE',  ( -0.05219959533910754901, -16.53943276465976808, 102.4989096053143811 ) ) ;
#142163 = CARTESIAN_POINT ( 'NONE',  ( 13.97604488694527802, 13.89961937509977652, 29.37390960531435979 ) ) ;
#142164 = CARTESIAN_POINT ( 'NONE',  ( -8.314922557960811034, -14.29746914071050412, 62.08224293864769550 ) ) ;
#142165 = CARTESIAN_POINT ( 'NONE',  ( 16.46253265017160672, -9.564922557960803928, 73.33224293864769550 ) ) ;
#142166 = CARTESIAN_POINT ( 'NONE',  ( -16.55341960407617563, 4.379528057220093196, 103.5427570613523613 ) ) ;
#142167 = CARTESIAN_POINT ( 'NONE',  ( 5.153800228976335163, 19.02544592524342804, 34.79057627198102409 ) ) ;
#142168 = CARTESIAN_POINT ( 'NONE',  ( 0.05219959533907565091, 21.53943276465977519, 49.99890960531437401 ) ) ;
#142169 = CARTESIAN_POINT ( 'NONE',  ( 16.52544592524342804, -4.483927247898539470, 88.54057627198103830 ) ) ;
#142170 = CARTESIAN_POINT ( 'NONE',  ( 10.81492255796078972, 18.62759615963270932, 89.58224293864768129 ) ) ;
#142171 = CARTESIAN_POINT ( 'NONE',  ( -19.05341960407611168, -5.049401038298163336, 101.4572429386476955 ) ) ;
#142173 = CARTESIAN_POINT ( 'NONE',  ( 16.46253265017146816, 9.564922557961045513, 86.66775706135233293 ) ) ;
#142172 = CARTESIAN_POINT ( 'NONE',  ( 16.51473224551069308, 9.474510206698969483, 49.16557627198102409 ) ) ;
#142174 = CARTESIAN_POINT ( 'NONE',  ( 10.81492255796078972, 18.62759615963270932, 39.58224293864769550 ) ) ;
#142175 = CARTESIAN_POINT ( 'NONE',  ( 5.719274019375673035, 21.55341960407619339, 72.29275706135236135 ) ) ;
#142176 = CARTESIAN_POINT ( 'NONE',  ( -19.03943276465977164, 0.05219959533909376836, 56.24890960531435979 ) ) ;
#142177 = CARTESIAN_POINT ( 'NONE',  ( 0.05219959533909260263, 19.03943276465977164, 79.99890960531436690 ) ) ;
#142178 = CARTESIAN_POINT ( 'NONE',  ( 16.52544592524335698, 4.483927247898782831, 61.45942372801901854 ) ) ;
#142179 = CARTESIAN_POINT ( 'NONE',  ( -15.80617190586768217, 15.72974639402176855, 38.12609039468567573 ) ) ;
#142180 = CARTESIAN_POINT ( 'NONE',  ( 5.823673210054444382, -21.52544592524334988, 70.20942372801904696 ) ) ;
#142181 = CARTESIAN_POINT ( 'NONE',  ( -0.05219959533907301413, -21.53943276465977519, 22.49890960531436335 ) ) ;
#142182 = CARTESIAN_POINT ( 'NONE',  ( 0.05219959533907565091, 21.53943276465977519, 99.99890960531436690 ) ) ;
#142184 = CARTESIAN_POINT ( 'NONE',  ( -14.34966873604972548, 8.224510206698743886, 58.33442372801901143 ) ) ;
#142183 = CARTESIAN_POINT ( 'NONE',  ( -21.53943276465977519, -0.05219959533937600094, 33.75109039468568284 ) ) ;
#142185 = CARTESIAN_POINT ( 'NONE',  ( 21.55341960407610458, 5.719274019375980345, 58.95724293864770971 ) ) ;
#142186 = CARTESIAN_POINT ( 'NONE',  ( 13.89961937509957401, 13.97604488694547697, 36.87609039468565442 ) ) ;
#142188 = CARTESIAN_POINT ( 'NONE',  ( 12.14591786802309770, 12.06949235617756955, 29.37390960531435269 ) ) ;
#142187 = CARTESIAN_POINT ( 'NONE',  ( -0.05219959533909027116, -19.03943276465977164, 72.49890960531435269 ) ) ;
#142189 = CARTESIAN_POINT ( 'NONE',  ( -17.49999999999998934, -4.640572885337569176, 104.3621183545115940 ) ) ;
#142190 = CARTESIAN_POINT ( 'NONE',  ( 16.51473224551069308, 9.474510206698969483, 104.1655762719810241 ) ) ;
#142191 = DIRECTION ( 'NONE',  ( -1.000000000000000000, -0.000000000000000000, 0.000000000000000000 ) ) ;
#142192 = ADVANCED_FACE ( 'NONE', ( #139154 ), #142380, .T. ) ;
#142193 = CARTESIAN_POINT ( 'NONE',  ( 19.05341960407617918, -5.049401038297876454, 86.04275706135233293 ) ) ;
#142194 = CARTESIAN_POINT ( 'NONE',  ( 21.53943276465977519, -0.05219959533907433946, 63.74890960531435979 ) ) ;
#142195 = CARTESIAN_POINT ( 'NONE',  ( 16.53943276465976808, -0.05219959533910856209, 33.74890960531436690 ) ) ;
#142196 = CARTESIAN_POINT ( 'NONE',  ( -19.02544592524334988, -5.153800228976617603, 108.9594237280189759 ) ) ;
#142197 = CARTESIAN_POINT ( 'NONE',  ( 5.049401038298161559, -19.05341960407611168, 27.70724293864769550 ) ) ;
#142198 = CARTESIAN_POINT ( 'NONE',  ( -0.05219959533936034679, 19.03943276465977164, 107.5010903946856615 ) ) ;
#142200 = CARTESIAN_POINT ( 'NONE',  ( 13.89961937509957401, 13.97604488694547697, 61.87609039468566863 ) ) ;
#142199 = CARTESIAN_POINT ( 'NONE',  ( 15.80617190586746368, 15.72974639402197994, 84.37390960531438111 ) ) ;
#142201 = CARTESIAN_POINT ( 'NONE',  ( 8.314922557961029526, -14.29746914071037800, 80.41775706135234714 ) ) ;
#142202 = CARTESIAN_POINT ( 'NONE',  ( -16.46253265017160317, 9.564922557960807481, 65.83224293864769550 ) ) ;
#142203 = CARTESIAN_POINT ( 'NONE',  ( 4.379528057220339221, -16.55341960407611168, 72.70724293864769550 ) ) ;
#142204 = CARTESIAN_POINT ( 'NONE',  ( -13.97604488694527625, -13.89961937509977652, 41.87390960531435979 ) ) ;
#142205 = CARTESIAN_POINT ( 'NONE',  ( -14.34966873604960291, -8.224510206698953496, 51.66557627198102409 ) ) ;
#142206 = CARTESIAN_POINT ( 'NONE',  ( -1.784589286804201480, 7.284589286804282970, 1.818019484660534424 ) ) ;
#142207 = CARTESIAN_POINT ( 'NONE',  ( 1.249015985346455970, 21.94700952099570301, -55.99705856128547765 ) ) ;
#142208 = CARTESIAN_POINT ( 'NONE',  ( 16.52544592524342804, -4.483927247898539470, 23.54057627198102765 ) ) ;
#142209 = CARTESIAN_POINT ( 'NONE',  ( 19.05341960407611168, 5.049401038298154454, 73.95724293864768129 ) ) ;
#142210 = CARTESIAN_POINT ( 'NONE',  ( -18.22780087662119541, 5.500000000000102141, 51.01763182126894947 ) ) ;
#142211 = CARTESIAN_POINT ( 'NONE',  ( -19.03943276465977164, -0.05219959533935918106, 33.75109039468566863 ) ) ;
#142212 = CARTESIAN_POINT ( 'NONE',  ( 4.379528057220092307, 16.55341960407617563, 47.29275706135234003 ) ) ;
#142213 = CARTESIAN_POINT ( 'NONE',  ( -5.823673210054116645, -21.52544592524344225, 67.29057627198103830 ) ) ;
#142214 = CARTESIAN_POINT ( 'NONE',  ( 5.049401038297881783, 19.05341960407617563, 27.29275706135232937 ) ) ;
#142215 = CARTESIAN_POINT ( 'NONE',  ( -19.02544592524342804, 5.153800228976336051, 76.04057627198102409 ) ) ;
#142216 = CARTESIAN_POINT ( 'NONE',  ( -19.03943276465977164, 0.05219959533909376836, 116.2489096053143669 ) ) ;
#142217 = CARTESIAN_POINT ( 'NONE',  ( 16.51473224551069308, 9.474510206698969483, 104.1655762719810241 ) ) ;
#142218 = CARTESIAN_POINT ( 'NONE',  ( -21.55341960407619339, 5.719274019375674811, 38.54275706135234714 ) ) ;
#142219 = CARTESIAN_POINT ( 'NONE',  ( -14.34966873604960291, -8.224510206698953496, 101.6655762719810383 ) ) ;
#142222 = ORIENTED_EDGE ( 'NONE', *, *, #54562, .T. ) ;
#142221 = CARTESIAN_POINT ( 'NONE',  ( -16.46253265017160317, 9.564922557960807481, 80.83224293864769550 ) ) ;
#142220 = CARTESIAN_POINT ( 'NONE',  ( 5.823673210054125526, 21.52544592524343514, 104.7905762719810241 ) ) ;
#142223 = CARTESIAN_POINT ( 'NONE',  ( -10.81492255796105439, 18.62759615963255655, 22.91775706135235069 ) ) ;
#142224 = VERTEX_POINT ( 'NONE', #81568 ) ;
#142225 = CARTESIAN_POINT ( 'NONE',  ( 19.03943276465977164, -0.05219959533909143690, 83.74890960531436690 ) ) ;
#142226 = DIRECTION ( 'NONE',  ( 0.000000000000000000, 0.000000000000000000, -1.000000000000000000 ) ) ;
#142228 = CARTESIAN_POINT ( 'NONE',  ( -16.46253265017160317, 9.564922557960807481, 30.83224293864769550 ) ) ;
#142227 = CARTESIAN_POINT ( 'NONE',  ( 13.97604488694527802, 13.89961937509977652, 24.37390960531435624 ) ) ;
#142229 = CARTESIAN_POINT ( 'NONE',  ( -5.049401038297874678, -19.05341960407617918, 104.7927570613523471 ) ) ;
#142230 = CARTESIAN_POINT ( 'NONE',  ( 36.91746825000000598, -11.99521256947793546, -6.224999997268814589 ) ) ;
#142231 = CARTESIAN_POINT ( 'NONE',  ( 8.224510206698953496, -14.34966873604960469, 112.9155762719810383 ) ) ;
#142232 = CARTESIAN_POINT ( 'NONE',  ( -10.81492255796105439, 18.62759615963255655, 87.91775706135234714 ) ) ;
#142234 = CARTESIAN_POINT ( 'NONE',  ( 15.80617190586769283, -15.72974639402175789, 40.62609039468567573 ) ) ;
#142233 = CARTESIAN_POINT ( 'NONE',  ( -19.02544592524342804, 5.153800228976336051, 71.04057627198099567 ) ) ;
#142235 = CARTESIAN_POINT ( 'NONE',  ( 21.53943276465977519, 0.05219959533937863772, 21.25109039468567218 ) ) ;
#142236 = CARTESIAN_POINT ( 'NONE',  ( -8.906447517083053711, -27.41122689804191026, 148.4000000000000057 ) ) ;
#142237 = CARTESIAN_POINT ( 'NONE',  ( -16.46253265017160317, 9.564922557960807481, 90.83224293864769550 ) ) ;
#142238 = CARTESIAN_POINT ( 'NONE',  ( 27.60805440473492567, 7.718125693463445458, 162.2444234560357756 ) ) ;
#142240 = CARTESIAN_POINT ( 'NONE',  ( -5.823673210054116645, -21.52544592524344225, 42.29057627198103120 ) ) ;
#142239 = CARTESIAN_POINT ( 'NONE',  ( 12.06949235617739724, 12.14591786802326823, 31.87609039468567929 ) ) ;
#142241 = CARTESIAN_POINT ( 'NONE',  ( -21.55341960407619339, 5.719274019375674811, 73.54275706135234714 ) ) ;
#142242 = CARTESIAN_POINT ( 'NONE',  ( -19.02544592524342804, 5.153800228976336051, 116.0405762719810383 ) ) ;
#142243 = CARTESIAN_POINT ( 'NONE',  ( 16.46253265017146816, 9.564922557961045513, 91.66775706135234714 ) ) ;
#142244 = CARTESIAN_POINT ( 'NONE',  ( 9.564922557960805705, 16.46253265017160317, 64.58224293864769550 ) ) ;
#142245 = CARTESIAN_POINT ( 'NONE',  ( -5.153800228976328057, -19.02544592524343514, 82.29057627198103830 ) ) ;
#142246 = CARTESIAN_POINT ( 'NONE',  ( -16.53943276465976808, 0.05219959533911058130, 101.2489096053143669 ) ) ;
#142247 = CARTESIAN_POINT ( 'NONE',  ( -8.224510206698948167, 14.34966873604960824, 105.4155762719810383 ) ) ;
#142248 = CARTESIAN_POINT ( 'NONE',  ( -19.02544592524342804, 5.153800228976336051, 116.0405762719810383 ) ) ;
#142249 = CARTESIAN_POINT ( 'NONE',  ( -8.224510206698735004, -14.34966873604973081, 84.58442372801903275 ) ) ;
#142251 = CARTESIAN_POINT ( 'NONE',  ( 9.474510206698971260, -16.51473224551069308, 42.91557627198103120 ) ) ;
#142250 = CARTESIAN_POINT ( 'NONE',  ( 4.379528057220339221, -16.55341960407611168, 52.70724293864769550 ) ) ;
#142252 = CARTESIAN_POINT ( 'NONE',  ( -5.823673210054431948, 21.52544592524334988, 77.70942372801900433 ) ) ;
#142253 = CARTESIAN_POINT ( 'NONE',  ( 5.719274019375673035, 21.55341960407619339, 67.29275706135234714 ) ) ;
#142254 = CARTESIAN_POINT ( 'NONE',  ( 9.564922557961047289, -16.46253265017146816, 90.41775706135234714 ) ) ;
#142255 = CARTESIAN_POINT ( 'NONE',  ( -4.379528057220328563, 16.55341960407611168, 65.20724293864768129 ) ) ;
#142256 = CARTESIAN_POINT ( 'NONE',  ( -10.72451020669870658, -18.67979575497194134, 19.58442372801901143 ) ) ;
#142257 = CARTESIAN_POINT ( 'NONE',  ( 0.05219959533907565091, 21.53943276465977519, 49.99890960531437401 ) ) ;
#142258 = CARTESIAN_POINT ( 'NONE',  ( -16.20579543436677739, -7.371946100355105891, 105.5652083417187299 ) ) ;
#142259 = CARTESIAN_POINT ( 'NONE',  ( 27.73933785331498214, 9.013057229001095294, 147.9750000027311501 ) ) ;
#142260 = CARTESIAN_POINT ( 'NONE',  ( -5.049401038298153566, 19.05341960407611168, 75.20724293864769550 ) ) ;
#142261 = CARTESIAN_POINT ( 'NONE',  ( -4.379528057220328563, 16.55341960407611168, 30.20724293864769550 ) ) ;
#142262 = AXIS2_PLACEMENT_3D ( 'NONE', #35918, #97564, #126924 ) ;
#142263 = CARTESIAN_POINT ( 'NONE',  ( 4.483927247898545687, 16.52544592524342804, 24.79057627198103120 ) ) ;
#142264 = CARTESIAN_POINT ( 'NONE',  ( 0.05219959533934541429, -16.53943276465976808, 90.00109039468567573 ) ) ;
#142265 = CARTESIAN_POINT ( 'NONE',  ( -9.564922557961040184, 16.46253265017147172, 42.91775706135234003 ) ) ;
#142266 = FACE_OUTER_BOUND ( 'NONE', #198492, .T. ) ;
#142267 = CARTESIAN_POINT ( 'NONE',  ( -9.564922557960796823, -16.46253265017161027, 87.08224293864769550 ) ) ;
#142268 = EDGE_CURVE ( 'NONE', #154217, #190522, #163698, .T. ) ;
#142269 = CARTESIAN_POINT ( 'NONE',  ( -12.06949235617756955, 12.14591786802309770, 60.62390960531437401 ) ) ;
#142271 = CARTESIAN_POINT ( 'NONE',  ( 5.719274019375991003, -21.55341960407610458, 27.70724293864769905 ) ) ;
#142270 = CARTESIAN_POINT ( 'NONE',  ( 9.564922557960805705, 16.46253265017160317, 24.58224293864769194 ) ) ;
#142273 = ORIENTED_EDGE ( 'NONE', *, *, #176999, .T. ) ;
#142272 = CARTESIAN_POINT ( 'NONE',  ( -0.05219959533907301413, -21.53943276465977519, 52.49890960531435979 ) ) ;
#142274 = CARTESIAN_POINT ( 'NONE',  ( 16.55341960407611168, 4.379528057220329451, 93.95724293864770971 ) ) ;
#142275 = CARTESIAN_POINT ( 'NONE',  ( 8.224510206698742110, 14.34966873604972548, 42.08442372801901854 ) ) ;
#142276 = ORIENTED_EDGE ( 'NONE', *, *, #155303, .T. ) ;
#142277 = CARTESIAN_POINT ( 'NONE',  ( -4.379528057220328563, 16.55341960407611168, 75.20724293864769550 ) ) ;
#142278 = CARTESIAN_POINT ( 'NONE',  ( -19.36337904590691750, 5.499999999999950262, 65.41494137495624273 ) ) ;
#142279 = CARTESIAN_POINT ( 'NONE',  ( -16.46253265017146816, -9.564922557961047289, 79.16775706135234714 ) ) ;
#142280 = CARTESIAN_POINT ( 'NONE',  ( -10.81492255796078084, -18.62759615963271287, 27.08224293864769550 ) ) ;
#142282 = EDGE_CURVE ( 'NONE', #12092, #198282, #156523, .T. ) ;
#142281 = CARTESIAN_POINT ( 'NONE',  ( -5.950531402560715689E-15, 38.81732327939063509, -1.624999997268813612 ) ) ;
#142283 = DIRECTION ( 'NONE',  ( 0.000000000000000000, -0.5000000000000011102, -0.8660254037844379305 ) ) ;
#142285 = CARTESIAN_POINT ( 'NONE',  ( -4.379528057220328563, 16.55341960407611168, 30.20724293864769550 ) ) ;
#142284 = CARTESIAN_POINT ( 'NONE',  ( -8.314922557961024197, 14.29746914071037800, 32.91775706135234714 ) ) ;
#142286 = CARTESIAN_POINT ( 'NONE',  ( -10.81492255796078084, -18.62759615963271287, 52.08224293864768839 ) ) ;
#142287 = CARTESIAN_POINT ( 'NONE',  ( -0.05219959533936034679, 19.03943276465977164, 87.50109039468567573 ) ) ;
#142288 = CARTESIAN_POINT ( 'NONE',  ( 21.52544592524344225, -5.823673210054117533, 53.54057627198103120 ) ) ;
#142289 = CARTESIAN_POINT ( 'NONE',  ( -18.67979575497193778, 10.72451020669871902, 63.33442372801900433 ) ) ;
#142290 = CARTESIAN_POINT ( 'NONE',  ( 193.3062444957835453, -155.7167183371837496, 0.000000000000000000 ) ) ;
#142291 = CARTESIAN_POINT ( 'NONE',  ( 14.34966873604972726, -8.224510206698740333, 40.83442372801901854 ) ) ;
#142293 = CARTESIAN_POINT ( 'NONE',  ( 9.564922557960805705, 16.46253265017160317, 84.58224293864769550 ) ) ;
#142292 = CARTESIAN_POINT ( 'NONE',  ( 16.51473224551083163, -9.474510206698727899, 55.83442372801899722 ) ) ;
#142294 = CARTESIAN_POINT ( 'NONE',  ( -5.049401038298153566, 19.05341960407611168, 40.20724293864768839 ) ) ;
#142295 = CARTESIAN_POINT ( 'NONE',  ( -4.379528057220328563, 16.55341960407611168, 105.2072429386477097 ) ) ;
#142296 = APPLICATION_PROTOCOL_DEFINITION ( 'draft international standard', 'automotive_design', 1998, #151378 ) ;
#142297 = CARTESIAN_POINT ( 'NONE',  ( -9.564922557960796823, -16.46253265017161027, 102.0822429386477097 ) ) ;
#142298 = EDGE_LOOP ( 'NONE', ( #85899, #4763, #85138, #113941, #190686, #167976, #170866 ) ) ;
#142299 = CARTESIAN_POINT ( 'NONE',  ( 0.05219959533934541429, -16.53943276465976808, 60.00109039468568284 ) ) ;
#142300 = CARTESIAN_POINT ( 'NONE',  ( -15.80617190586745835, -15.72974639402198527, 91.87390960531436690 ) ) ;
#142301 = CARTESIAN_POINT ( 'NONE',  ( 5.153800228976335163, 19.02544592524342804, 49.79057627198100988 ) ) ;
#142303 = CARTESIAN_POINT ( 'NONE',  ( -21.55341960407619339, 5.719274019375674811, 28.54275706135234358 ) ) ;
#142302 = CARTESIAN_POINT ( 'NONE',  ( 16.51473224551083163, -9.474510206698727899, 75.83442372801900433 ) ) ;
#142304 = CARTESIAN_POINT ( 'NONE',  ( 9.564922557960805705, 16.46253265017160317, 74.58224293864769550 ) ) ;
#142305 = CARTESIAN_POINT ( 'NONE',  ( -13.89961937509977652, 13.97604488694528158, 110.6239096053143243 ) ) ;
#142306 = VERTEX_POINT ( 'NONE', #98742 ) ;
#142307 = CARTESIAN_POINT ( 'NONE',  ( 12.14591786802327356, -12.06949235617739191, 40.62609039468567573 ) ) ;
#142308 = CARTESIAN_POINT ( 'NONE',  ( 15.80617190586769283, -15.72974639402175789, 25.62609039468567929 ) ) ;
#142311 = CARTESIAN_POINT ( 'NONE',  ( -13.89961937509957401, -13.97604488694547875, 74.37609039468566152 ) ) ;
#142310 = CARTESIAN_POINT ( 'NONE',  ( 16.51473224551069308, 9.474510206698969483, 99.16557627198102409 ) ) ;
#142309 = CARTESIAN_POINT ( 'NONE',  ( -8.224510206698948167, 14.34966873604960824, 100.4155762719810241 ) ) ;
#142312 = CARTESIAN_POINT ( 'NONE',  ( 18.67979575497178502, 10.72451020669898547, 84.16557627198103830 ) ) ;
#142313 = CARTESIAN_POINT ( 'NONE',  ( -14.34966873604960291, -8.224510206698953496, 51.66557627198102409 ) ) ;
#142314 = CARTESIAN_POINT ( 'NONE',  ( 16.46253265017146816, 9.564922557961045513, 26.66775706135234003 ) ) ;
#142315 = CARTESIAN_POINT ( 'NONE',  ( 8.314922557961029526, -14.29746914071037800, 75.41775706135233293 ) ) ;
#142316 = CARTESIAN_POINT ( 'NONE',  ( 19.02544592524343514, -5.153800228976328945, 108.5405762719810383 ) ) ;
#142317 = CARTESIAN_POINT ( 'NONE',  ( -13.89961937509977652, 13.97604488694528158, 45.62390960531433848 ) ) ;
#142318 = CARTESIAN_POINT ( 'NONE',  ( 21.52544592524334988, 5.823673210054432836, 51.45942372801901854 ) ) ;
#142319 = CARTESIAN_POINT ( 'NONE',  ( 18.62759615963255655, 10.81492255796105972, 61.66775706135235424 ) ) ;
#142320 = CARTESIAN_POINT ( 'NONE',  ( -13.89961937509977652, 13.97604488694528158, 55.62390960531434558 ) ) ;
#142321 = CARTESIAN_POINT ( 'NONE',  ( 21.55341960407619695, -5.719274019375665929, 51.04275706135234714 ) ) ;
#142322 = CARTESIAN_POINT ( 'NONE',  ( -16.46253265017146816, -9.564922557961047289, 84.16775706135233293 ) ) ;
#142323 = CARTESIAN_POINT ( 'NONE',  ( -5.153800228976328057, -19.02544592524343514, 37.29057627198102409 ) ) ;
#142324 = CARTESIAN_POINT ( 'NONE',  ( 14.34966873604972726, -8.224510206698740333, 85.83442372801901854 ) ) ;
#142325 = CARTESIAN_POINT ( 'NONE',  ( -19.02544592524342804, 5.153800228976336051, 61.04057627198103120 ) ) ;
#142326 = CARTESIAN_POINT ( 'NONE',  ( -19.02544592524342804, 5.153800228976336051, 111.0405762719810099 ) ) ;
#142327 = CARTESIAN_POINT ( 'NONE',  ( -0.05219959533909027116, -19.03943276465977164, 52.49890960531436690 ) ) ;
#142328 = CARTESIAN_POINT ( 'NONE',  ( -18.67979575497178146, -10.72451020669898902, 81.66557627198103830 ) ) ;
#142329 = CARTESIAN_POINT ( 'NONE',  ( -14.29746914071037622, -8.314922557961029526, 79.16775706135234714 ) ) ;
#142330 = CARTESIAN_POINT ( 'NONE',  ( -21.84611564451296672, 8.148379233837022895, 169.4346228884802485 ) ) ;
#142331 = CARTESIAN_POINT ( 'NONE',  ( -5.049401038297874678, -19.05341960407617918, 29.79275706135232227 ) ) ;
#142332 = CARTESIAN_POINT ( 'NONE',  ( 19.05341960407611168, 5.049401038298154454, 63.95724293864769550 ) ) ;
#142333 = CARTESIAN_POINT ( 'NONE',  ( 4.379528057220339221, -16.55341960407611168, 52.70724293864769550 ) ) ;
#142334 = CARTESIAN_POINT ( 'NONE',  ( -12.06949235617756955, 12.14591786802309770, 75.62390960531439532 ) ) ;
#142335 = CARTESIAN_POINT ( 'NONE',  ( -19.05341960407611168, -5.049401038298163336, 101.4572429386476955 ) ) ;
#142336 = CARTESIAN_POINT ( 'NONE',  ( -13.97604488694527625, -13.89961937509977652, 86.87390960531436690 ) ) ;
#142337 = CARTESIAN_POINT ( 'NONE',  ( -21.53943276465977519, -0.05219959533937600094, 43.75109039468568284 ) ) ;
#142338 = CARTESIAN_POINT ( 'NONE',  ( -0.05219959533909027116, -19.03943276465977164, 102.4989096053143669 ) ) ;
#142339 = CARTESIAN_POINT ( 'NONE',  ( 10.81492255796106328, -18.62759615963255655, 110.4177570613523756 ) ) ;
#142340 = CARTESIAN_POINT ( 'NONE',  ( 12.14591786802327356, -12.06949235617739191, 80.62609039468567573 ) ) ;
#142341 = CARTESIAN_POINT ( 'NONE',  ( -5.719274019375665041, -21.55341960407619695, 39.79275706135235424 ) ) ;
#142342 = CARTESIAN_POINT ( 'NONE',  ( 19.03943276465977164, -0.05219959533909143690, 108.7489096053143527 ) ) ;
#142343 = CARTESIAN_POINT ( 'NONE',  ( -21.53943276465977519, 0.05219959533907696930, 106.2489096053143811 ) ) ;
#142344 = CARTESIAN_POINT ( 'NONE',  ( -4.483927247898539470, -16.52544592524342804, 57.29057627198103120 ) ) ;
#142345 = CARTESIAN_POINT ( 'NONE',  ( -5.153800228976328057, -19.02544592524343514, 57.29057627198103120 ) ) ;
#142346 = CARTESIAN_POINT ( 'NONE',  ( 16.55341960407611168, 4.379528057220329451, 83.95724293864770971 ) ) ;
#142347 = CARTESIAN_POINT ( 'NONE',  ( -15.72974639402197994, 15.80617190586746368, 25.62390960531435624 ) ) ;
#142348 = CARTESIAN_POINT ( 'NONE',  ( 19.05341960407617918, -5.049401038297876454, 41.04275706135233293 ) ) ;
#142349 = CARTESIAN_POINT ( 'NONE',  ( -4.379528057220328563, 16.55341960407611168, 110.2072429386477239 ) ) ;
#142350 = VERTEX_POINT ( 'NONE', #49280 ) ;
#142351 = CARTESIAN_POINT ( 'NONE',  ( 16.55341960407618274, -4.379528057220086978, 71.04275706135234714 ) ) ;
#142352 = CARTESIAN_POINT ( 'NONE',  ( 19.05341960407611168, 5.049401038298154454, 68.95724293864769550 ) ) ;
#142353 = CARTESIAN_POINT ( 'NONE',  ( -27.73933785331498925, -9.013057229001049109, 144.9750000027312069 ) ) ;
#142354 = CARTESIAN_POINT ( 'NONE',  ( 16.53943276465976808, -0.05219959533910856209, 93.74890960531436690 ) ) ;
#142355 = CARTESIAN_POINT ( 'NONE',  ( -18.67979575497178146, -10.72451020669898902, 31.66557627198102054 ) ) ;
#142356 = ORIENTED_EDGE ( 'NONE', *, *, #20816, .F. ) ;
#142357 = CARTESIAN_POINT ( 'NONE',  ( -4.379528057220086978, -16.55341960407618274, 109.7927570613523613 ) ) ;
#142358 = CARTESIAN_POINT ( 'NONE',  ( 9.564922557961047289, -16.46253265017146816, 110.4177570613523471 ) ) ;
#142359 = CARTESIAN_POINT ( 'NONE',  ( -15.72974639402176322, -15.80617190586768395, 79.37609039468567573 ) ) ;
#142360 = CARTESIAN_POINT ( 'NONE',  ( -16.51473224551069308, -9.474510206698971260, 91.66557627198103830 ) ) ;
#142361 = CARTESIAN_POINT ( 'NONE',  ( 10.72451020669898902, -18.67979575497178502, 102.9155762719810383 ) ) ;
#142362 = CARTESIAN_POINT ( 'NONE',  ( -12.06949235617739369, -12.14591786802326823, 59.37609039468568284 ) ) ;
#142363 = CARTESIAN_POINT ( 'NONE',  ( 19.05341960407611168, 5.049401038298154454, 23.95724293864769194 ) ) ;
#142364 = CARTESIAN_POINT ( 'NONE',  ( 16.52544592524335698, 4.483927247898782831, 31.45942372801901854 ) ) ;
#142365 = CARTESIAN_POINT ( 'NONE',  ( -0.05219959533936034679, 19.03943276465977164, 97.50109039468567573 ) ) ;
#142366 = EDGE_CURVE ( 'NONE', #108481, #26617, #166228, .T. ) ;
#142367 = CARTESIAN_POINT ( 'NONE',  ( 0.05219959533907565091, 21.53943276465977519, 94.99890960531436690 ) ) ;
#142368 = CARTESIAN_POINT ( 'NONE',  ( -5.153800228976607833, 19.02544592524334988, 57.70942372801899012 ) ) ;
#142369 = DIRECTION ( 'NONE',  ( 0.000000000000000000, 0.3420201433256804813, 0.9396926207859040980 ) ) ;
#142370 = CARTESIAN_POINT ( 'NONE',  ( 5.823673210054125526, 21.52544592524343514, 109.7905762719810383 ) ) ;
#142371 = CARTESIAN_POINT ( 'NONE',  ( -16.51473224551069308, -9.474510206698971260, 71.66557627198102409 ) ) ;
#142372 = CARTESIAN_POINT ( 'NONE',  ( -19.02544592524342804, 5.153800228976336051, 76.04057627198102409 ) ) ;
#142373 = CARTESIAN_POINT ( 'NONE',  ( -16.53943276465976808, -0.05219959533934237506, 33.75109039468568284 ) ) ;
#142374 = CARTESIAN_POINT ( 'NONE',  ( -11.74149087413295511, 36.13659316521247433, -6.402157773949824104 ) ) ;
#142375 = CARTESIAN_POINT ( 'NONE',  ( -13.97604488694547697, 13.89961937509957934, 63.12609039468566152 ) ) ;
#142377 = CARTESIAN_POINT ( 'NONE',  ( 8.224510206698953496, -14.34966873604960469, 57.91557627198103120 ) ) ;
#142376 = CARTESIAN_POINT ( 'NONE',  ( 5.823673210054444382, -21.52544592524334988, 25.20942372801901854 ) ) ;
#142378 = CARTESIAN_POINT ( 'NONE',  ( 16.51473224551069308, 9.474510206698969483, 69.16557627198102409 ) ) ;
#142381 = CARTESIAN_POINT ( 'NONE',  ( 19.02544592524334988, 5.153800228976608722, 46.45942372801899012 ) ) ;
#142380 =( BOUNDED_SURFACE ( )  B_SPLINE_SURFACE ( 3, 2, ( 
 ( #33978, #45177, #16819, #15824, #187680, #108819, #92644, #77485, #632, #122989, #184675, #2638, #62302, #107813, #153331, #185669, #46158, #48158, #183690, #47160, #64314, #75497, #109816, #106831, #170498, #17822, #152346, #30995, #123972, #198859, #168506, #110808, #31988, #169496, #49150, #93646, #155331, #91642, #78470, #61318, #140144, #1636, #13831, #63313, #172490, #94641, #137171, #124992, #186688, #171499, #32988, #60325, #30004, #156322, #79480, #125982, #122000, #14832, #76494, #138171, #199852, #50145, #69288, #143122, #6604, #54127, #128944, #175473, #4602, #177490, #188666, #160301, #159285, #130954, #52121, #35951, #20782, #115800, #129934, #68283, #36945, #176484, #113777, #157321, #111805, #191633, #66294, #97597, #95634, #114791, #53113, #37960, #21791, #190645, #82437, #98607, #83442, #146118, #51130, #142135, #189657, #145120, #99618, #161298, #192644, #173493, #22794, #84440, #34966, #18817, #127953, #7602, #112790, #80461, #3619, #65298, #126957, #96618, #144125, #174484, #158307, #19795, #5606, #67286, #81436, #58128, #70298, #131966, #8626, #72295, #88448, #119797, #150143, #181482, #27809, #11645, #149145, #85448, #55123, #197635, #179497, #194652, #74295, #118812, #41970, #178484, #40962, #148142, #102634, #57136, #100616, #133974, #59101, #42960, #23798, #180498, #164319, #132963, #10635, #162298, #116792, #104623, #25812, #73311, #12630, #135964, #195665, #147138, #24808, #193651, #120766, #86457, #134982, #38959, #103637, #165315, #9633, #39950, #101621, #26808, #87458, #163310, #196659, #166312, #89450, #71300, #151139, #56122, #117804, #65795, #3139, #43948, #1136, #19314, #155825, #187191, #66790, #4116, #80962, #127464, #49646, #18324, #125494, #64814, #188173, #35463, #140652, #28794, #78977, #34476, #172998, #189170, #81932, #77981, #126475, #141649, #62810, #20286, #17322, #96135, #2142, #111309, #112304, #157824, #158797, #142638, #48662, #63821, #79981, #50642, #95142, #110314, #152119, #173994, #16331, #139648, #124492, #97114, #143624, #5109, #182467, #105610, #167298, #90433, #33484, #171996, #156831, #186188, #47669, #109321, #171001, #32493, #94146, #24308, #159798, #23298, #117296, #51625, #85957, #21293, #161803, #194159, #10134, #7107, #148645, #70800, #113290, #146623, #68788, #22296, #38464, #174981, #6111, #9134, #130446, #39452, #102132, #163816, #84942, #36445, #114284, #82950, #25318, #175987, #101113, #86960, #8116, #69793, #37455, #128454, #144628, #193148, #192145, #190150, #131461, #53625, #115301, #98100, #162799, #147645, #54620, #132468, #116295, #67793, #129449, #55623, #99116, #176994, #191148, #178991, #40459, #52622, #177985, #160808, #100120, #83947, #145627, #122261, #27308, #118309, #165811, #121272, #59598, #90918, #168760, #164814, #151630, #28310, #149639, #107089, #104129, #182966, #88956, #89950, #199118, #44449, #45436, #106103, #12143, #42466, #166810, #167788, #181973, #135479, #41469, #152604, #103133, #26310, #87950, #105124, #29287, #14094, #75761, #137439, #60585, #183950, #120281, #150646, #73807, #30263, #197148, #58614, #72811, #13124, #43455, #91907, #11136, #74787, #153600, #195154, #71795, #134480, #136449, #133464, #56636, #198130, #180001, #196165, #57639, #119305, #180989, #170768, #50417, #94912, #18092, #154598, #155593, #124252, #17088, #33254, #76756, #110086, #34245, #79747, #48430, #78741, #156597, #141416, #65565, #32257, #61580, #109088, #64582, #2904, #95905, #112076, #108083, #126247, #171765, #92912, #173765, #47432, #187943, #93915, #49412, #142408, #111075, #188939, #172764, #140417, #185948, #157589, #19081, #125261, #1908, #184940, #80729, #46425, #169768, #31261, #3886, #127225, #35232, #96886, #15097, #138431, #200112, #63587, #186959, #123249, #16094, #77752, #139418, #900, #62574, #129211, #54391, #189922, #53385, #147405, #81702, #116064, #51397, #191900, #24064, #40213, #37218 ),
 ( #39221, #85719, #23061, #177752, #115063, #8893, #6870, #162559, #100877, #70561, #176755, #68549, #178749, #190909, #38228, #82709, #113057, #130205, #52386, #158569, #161568, #159556, #143385, #174749, #132228, #193921, #84706, #55384, #66560, #69559, #144392, #146385, #98874, #36213, #97866, #4877, #7873, #21053, #5877, #117054, #131224, #20058, #192914, #160570, #99883, #128225, #67554, #114043, #175741, #22059, #83710, #145388, #164576, #11909, #59366, #120052, #197897, #150414, #167563, #194913, #165574, #56388, #28076, #166576, #103894, #181739, #71557, #73573, #43220, #101892, #9896, #121035, #119075, #163574, #104888, #72567, #135246, #27073, #196918, #148402, #118070, #179760, #105876, #58385, #89717, #133222, #151402, #42233, #88719, #41230, #74555, #102891, #12892, #136222, #26070, #182733, #25074, #44217, #86717, #87713, #149399, #10894, #134242, #195927, #57403, #180757, #130877, #86376, #101534, #132881, #177412, #192567, #102552, #53032, #115725, #6525, #175396, #54050, #114714, #164236, #85366, #83367, #67210, #36864, #178404, #148061, #147060, #71218, #190568, #193572, #68204, #8542, #22716, #160223, #98530, #128868, #131888, #21714, #145044, #9552, #70220, #194570, #116715, #161222, #100540, #38883, #55044, #56040, #39868, #117718, #52044, #82360, #162219, #113700, #129857, #40879, #146041, #163227, #24727, #5531, #69209, #191555, #176406, #37882, #99540, #84364, #179414, #7525, #23718, #144049, #29689, #10551, #152036, #42879, #180416, #26725, #11563, #73229, #121681, #91320, #90351, #14511, #133889, #136858, #150057, #28714, #166225, #103555, #41888, #72215, #75186, #118728, #165230, #153011, #13521, #76172, #60014, #104544, #43866, #182388, #198544, #137852, #183377, #199532, #195581, #107497, #197554, #57053, #88364, #184363, #89369, #44859, #106514, #149063, #12549, #134900, #196577, #58047, #181401, #119717, #168192, #27726, #151058, #74215, #61002, #135883, #122674, #59022, #120689, #105531, #167217, #45844, #25732, #87378, #16504, #48829, #81124, #156996, #157987, #187360, #50814, #185350, #140821, #123652, #188338, #64978, #79150, #18494, #61986, #172165, #141812, #169173, #77168, #96301, #171177, #127636, #3305, #1309, #110482, #17492, #125662, #154016, #46841, #108500, #4285, #33650, #80142, #138838, #95311, #94318, #155996, #15511, #111481, #318, #126636, #49817, #155007, #173166, #30678, #34642, #19478, #142805, #65966, #189336, #92330, #170180, #2310, #31674, #63991, #93323, #78152, #139820, #62988, #124666, #186362, #47842, #109495, #32665, #105652, #136005, #150188, #89494, #58172, #77291, #151184, #14639, #119839, #138962, #12672, #76298, #62115, #136981, #183500, #74339, #185477, #196702, #168316, #167340, #440, #60137, #43990, #28837, #123778, #137976, #199658, #44983, #184488, #121805, #165357, #181524, #61125, #197676, #90478, #103678, #122798, #45967, #107621, #29812, #198670, #152160, #106643, #91448, #154142, #59141, #11688, #120811, #153136, #169299, #30805, #26851, #43003, #92454, #15634, #104670, #88492, #182510, #73354, #13643, #135027, #166355, #27854, #75310, #19603, #187487, #17622, #141935, #81245, #157122, #110606, #16627, #66093, #78274, #139947, #1437, #80265, #96425, #127760, #158111, #189460, #35758, #142926, #95438, #79281, #140951, #97403, #48953, #2438, #47968, #3426, #64120, #4408, #63115, #65102, #159090, #170304, #50938, #124793, #126760, #112596, #128751, #125785, #18618, #93446, #186492, #5409, #172289, #33778, #82237, #188463, #49945, #109620, #111609, #156123, #173294, #34768, #108626, #174288, #67092, #20585, #31797, #143927, #46967, #155133, #171304, #32790, #94443, #71098, #192448, #191435, #102432, #53930, #22595, #36742, #176285, #163105, #130756, #161101, #85246, #24609, #100422, #115605, #160102, #9433, #21589, #83248, #144923, #23599, #39750, #132765, #101413, #194453, #179299, #86257, #38765, #72095, #129738, #117598 ),
 ( #98406, #54926, #177294, #162103, #6405, #55923, #68086, #116599, #147947, #37757, #8427, #190448, #178287, #40763, #146937, #164119, #25617, #87261, #148946, #70099, #10436, #131768, #51923, #113582, #175276, #193450, #52912, #114588, #84243, #99418, #145922, #7405, #69089, #105417, #15397, #136741, #134783, #118612, #88250, #29578, #137737, #198425, #122562, #41770, #44743, #57935, #59900, #74102, #11442, #149936, #180302, #183263, #26607, #73113, #60886, #121568, #184252, #168081, #12440, #151922, #90239, #106399, #199421, #91209, #45734, #103435, #133768, #167100, #165115, #196465, #92216, #197443, #152899, #14396, #56938, #120576, #119606, #42767, #181289, #89254, #27615, #76062, #135772, #150946, #104429, #107386, #166112, #169058, #58909, #182270, #43753, #30565, #13411, #195463, #28601, #75075, #153902, #96198, #173062, #187253, #126535, #170069, #110375, #34539, #158862, #16395, #4180, #79039, #35529, #49708, #109383, #156893, #125556, #33544, #61875, #31560, #93211, #112369, #95206, #188234, #185238, #141709, #2204, #63885, #123545, #19376, #46730, #3200, #111373, #62874, #18389, #77054, #64874, #157887, #80040, #81025, #142701, #65858, #127530, #172058, #189233, #48722, #50711, #174060, #97177, #138726, #206, #108392, #47730, #154896, #78041, #139710, #171063, #1197, #124555, #186252, #32553, #94207, #155886, #17383, #140714, #85010, #9202, #128519, #131531, #144692, #23364, #160873, #98167, #36512, #5175, #69862, #113355, #159867, #147714, #8186, #70867, #54689, #99184, #38532, #177062, #146690, #24375, #193215, #132535, #66857, #102199, #192213, #190214, #51693, #179059, #84015, #39519, #116362, #143692, #7175, #83018, #129512, #6177, #176055, #114350, #178051, #22363, #37522, #175047, #86025, #21360, #101179, #145693, #67857, #191212, #52687, #68858, #53696, #130517, #115373, #100188, #194224, #162867, #40528, #55689, #161870, #117363, #20351, #81999, #76570, #89756, #44257, #47238, #168577, #167600, #78546, #30075, #198932, #12929, #152417, #121079, #140221, #13905, #77562, #125067, #199929, #46235, #75571, #48234, #59405, #31073, #91716, #1714, #123064, #106904, #153410, #186764, #709, #139234, #107889, #108897, #184750, #25384, #182773, #62381, #137247, #14908, #163887, #185750, #124051, #170576, #92721, #61392, #138245, #169576, #154410, #16895, #122072, #74593, #60400, #15904, #32067, #93723, #63390, #105914, #155405, #151442, #29095, #136261, #183764, #197936, #45250, #90734, #37023, #82517, #83518, #144199, #50226, #80538, #4679, #5685, #19871, #173570, #79553, #129020, #141222, #2713, #64390, #143198, #159363, #190721, #20860, #52194, #98684, #174558, #191706, #128031, #158382, #160377, #111880, #65374, #110883, #66371, #142212, #67361, #126058, #189733, #21868, #33062, #113852, #187755, #51206, #175548, #109889, #188741, #81511, #156395, #49225, #68356, #35039, #127034, #145195, #112867, #36025, #172568, #96693, #18892, #97674, #6678, #171573, #130007, #94717, #17899, #34054, #95711, #157399, #3695, #100687, #24880, #131029, #162369, #133035, #165388, #41038, #42044, #71371, #135056, #69360, #86529, #7676, #72371, #149217, #163383, #102704, #146191, #148213, #10708, #53190, #192718, #180570, #55195, #11717, #25885, #85521, #194725, #101694, #9707, #38035, #54202, #115874, #88524, #56195, #164392, #161375, #117878, #178555, #40021, #99691, #195738, #22866, #179568, #87530, #39032, #134045, #114865, #57211, #118886, #103708, #26881, #150220, #73384, #176560, #84513, #177563, #23870, #147209, #8700, #70370, #132038, #193727, #116864, #167371, #29842, #91479, #138991, #90508, #168346, #78304, #199690, #197707, #181553, #151213, #92484, #470, #61155, #185506, #104698, #107652, #120842, #122828, #137011, #74367, #12701, #43032, #45997, #89524, #136033, #123808, #184517, #46997, #30836, #75341, #14668, #153167, #169329, #62144, #154173, #108656, #166386, #196732, #76329 ),
 ( #138006, #15664, #59173, #31827, #28868, #77323, #170334, #182541, #44023, #93477, #155164, #16656, #58200, #119868, #27882, #105684, #152190, #13674, #198701, #60167, #106673, #121836, #183530, #45014, #97436, #21621, #79311, #67123, #141967, #98438, #112627, #172319, #19633, #188496, #96454, #124823, #94472, #32821, #175307, #158141, #189490, #47997, #4437, #65133, #126790, #186523, #82267, #109651, #66125, #174319, #125814, #81275, #139977, #127790, #50968, #142957, #20617, #5439, #35789, #159121, #173324, #128781, #49975, #143959, #190481, #51953, #34799, #111639, #160133, #110638, #113613, #36773, #1466, #33808, #63144, #171333, #156153, #140980, #17651, #2468, #64150, #187517, #48983, #95468, #157154, #18649, #80295, #3456, #23628, #161130, #99450, #68116, #132796, #176316, #22626, #10465, #71130, #133800, #117631, #162132, #101445, #39781, #9467, #87292, #194483, #195491, #129768, #165145, #54957, #191464, #52942, #41799, #146967, #102462, #86288, #6434, #70129, #145954, #192477, #7435, #38795, #177324, #179329, #85276, #100452, #114616, #148976, #37786, #55955, #8456, #84273, #69119, #130785, #53960, #115635, #118639, #163136, #40793, #131801, #147978, #193480, #116629, #178318, #25647, #24640, #164150, #72126, #56966, #180331, #83278, #103466, #144953, #183290, #107413, #92244, #91235, #122590, #59927, #15424, #75103, #30592, #45761, #77083, #121595, #136770, #46759, #197472, #44772, #106425, #169086, #120607, #198456, #108417, #29603, #27644, #11473, #181318, #184278, #153930, #152925, #138752, #134814, #137762, #150975, #14422, #167130, #104459, #42797, #73144, #76086, #119635, #166142, #234, #199446, #61901, #60914, #105446, #168106, #123572, #185267, #26636, #88279, #149967, #196494, #57964, #89284, #12469, #74130, #135801, #90267, #58938, #182301, #43781, #13439, #28630, #151950, #94234, #125581, #63911, #4206, #48749, #187279, #139735, #174085, #154922, #96222, #110402, #124582, #171090, #155915, #17410, #141735, #47757, #79067, #49734, #82024, #157911, #158887, #188260, #51716, #186278, #3225, #109411, #189259, #65884, #80065, #19401, #62902, #64899, #127558, #170093, #32581, #97201, #172084, #128542, #142726, #2229, #111402, #18416, #126560, #16420, #140740, #173087, #20377, #93237, #50735, #33571, #34566, #35554, #31587, #95233, #81050, #78067, #156919, #190239, #112394, #143720, #5199, #66881, #1224, #52708, #53720, #22388, #115397, #131556, #175069, #8212, #133555, #55716, #98190, #193241, #177085, #7198, #23389, #36534, #191234, #194249, #38556, #114372, #25410, #100213, #145717, #159893, #99208, #67881, #87052, #160896, #24401, #71885, #146716, #54714, #84038, #195246, #6201, #178076, #161893, #148737, #69887, #85035, #116386, #113379, #147739, #86050, #39543, #117388, #101202, #21381, #129534, #9226, #68882, #162892, #83040, #132560, #70893, #179087, #40556, #102225, #163914, #10225, #144715, #176076, #130542, #37544, #192240, #106192, #44537, #75850, #153688, #149728, #136536, #13211, #134572, #91994, #89043, #167876, #150733, #74874, #184039, #29375, #30352, #91006, #197237, #27398, #151718, #152692, #166897, #120368, #26401, #137526, #88040, #11229, #72903, #90036, #14181, #199208, #60675, #122350, #45522, #121360, #138514, #198217, #105210, #107176, #58698, #12233, #57728, #59689, #73895, #168847, #196259, #164907, #183053, #15184, #42556, #76843, #56730, #118400, #180094, #41562, #103225, #119398, #181081, #104219, #165900, #135565, #28397, #182061, #43544, #50495, #94995, #48514, #20140, #170852, #33335, #156681, #142490, #93996, #171847, #81785, #2986, #985, #185027, #154685, #95989, #3968, #64665, #189021, #108173, #111158, #124339, #126327, #140504, #77835, #16180, #46514, #49496, #92999, #139502, #127310, #188024, #112159, #34328, #78826, #18175, #79832, #172847, #65648, #157674, #173848, #169854, #66205, #141502, #31348, #62660, #158648, #63672, #19163 ),
 ( #186035, #80811, #17172, #47517, #109173, #32343, #155677, #35314, #1993, #125346, #96968, #61665, #123334, #187044, #110168, #25165, #159642, #115147, #97950, #162650, #39306, #53470, #193000, #36294, #176840, #100965, #143472, #82793, #70652, #145472, #101982, #116147, #175828, #23146, #191983, #99966, #128304, #21138, #144475, #178838, #161650, #54477, #51478, #7961, #68633, #130289, #190004, #85807, #5959, #69644, #6953, #40306, #84790, #83792, #38311, #163662, #177838, #24156, #146469, #147493, #131310, #4956, #67637, #8984, #114126, #132318, #66641, #194010, #55473, #117143, #113140, #174830, #129296, #190992, #52468, #37301, #98960, #160650, #22142, #136304, #74638, #105958, #183804, #179846, #166658, #43303, #164662, #122115, #119158, #197979, #180840, #104971, #13946, #59449, #60440, #121122, #27155, #57488, #181824, #182817, #168617, #44299, #75612, #28159, #86807, #102977, #58466, #41317, #167643, #29139, #197000, #90776, #26157, #120133, #152460, #148493, #87799, #137291, #88802, #45292, #198973, #42317, #89801, #135327, #151483, #71644, #149484, #10980, #106944, #12974, #9984, #195000, #133311, #11992, #73655, #56478, #118156, #72653, #134328, #196013, #103978, #165657, #150495, #17940, #156441, #186808, #110922, #95753, #94759, #126099, #63434, #18933, #78591, #34095, #49264, #80578, #125110, #140264, #52972, #753, #48278, #109933, #172608, #124096, #1756, #114649, #33103, #31116, #14950, #184791, #187795, #157438, #79594, #142252, #138288, #141263, #6465, #64429, #108939, #171615, #2753, #68146, #129797, #191496, #30117, #76610, #91758, #153452, #199969, #61434, #123106, #93766, #46277, #107933, #169619, #16937, #92764, #139276, #154454, #185795, #47283, #15946, #170620, #32109, #77605, #62424, #155447, #102492, #193510, #130816, #177354, #162161, #23658, #148006, #7465, #161161, #192507, #57993, #164178, #165173, #194511, #176347, #53991, #9496, #115664, #195521, #72155, #86318, #25676, #69150, #71159, #133830, #37819, #38824, #103495, #178347, #134843, #149005, #8484, #55985, #24669, #132825, #22657, #100482, #85305, #11502, #117661, #87321, #84304, #40821, #101475, #163165, #145983, #118668, #146998, #10494, #56994, #70159, #179358, #99480, #180360, #41828, #26666, #88308, #149996, #73173, #196522, #131829, #54987, #116656, #39810, #138781, #170120, #14452, #168134, #139764, #90294, #152954, #76115, #61930, #13467, #91263, #1252, #122618, #120635, #104488, #74158, #15453, #123599, #184308, #108444, #27672, #30620, #43810, #45789, #59956, #197499, #135830, #166171, #169115, #12496, #58966, #46785, #167159, #137792, #151005, #89312, #182331, #119663, #107441, #31614, #199476, #181345, #105473, #60943, #28659, #262, #77111, #29630, #92273, #151978, #153957, #185294, #42824, #75130, #93264, #121623, #78095, #154950, #136800, #16446, #198484, #183318, #44800, #106455, #155941, #98220, #81074, #112420, #171118, #127585, #188287, #49763, #109436, #5228, #32608, #189285, #35582, #48775, #142753, #62929, #50763, #174112, #19427, #143749, #128573, #97228, #158916, #96248, #51745, #111429, #66910, #82055, #113406, #157936, #173116, #83069, #33598, #4233, #65913, #190268, #156944, #34591, #144745, #20406, #63937, #47784, #17437, #175097, #36565, #159923, #21412, #94261, #124609, #187305, #186304, #3252, #140766, #79093, #2255, #125606, #110430, #172111, #95261, #18441, #80092, #141760, #64925, #126585, #162922, #132589, #10255, #117419, #118431, #191261, #88072, #178106, #114403, #176104, #164938, #69920, #25440, #9255, #129563, #193270, #68912, #115425, #130574, #161923, #100241, #40585, #85065, #23417, #37574, #71914, #52736, #194278, #146747, #160924, #7227, #192269, #177114, #8242, #24430, #67910, #101233, #26431, #148766, #99237, #86078, #131586, #54744, #116417, #22417, #84067, #87081, #39574, #53751, #180124, #147769, #38585, #145746, #70922, #55745, #41592, #179117, #102256 ),
 ( #163943, #133586, #195277, #56759, #103256, #6231, #28428, #167906, #106222, #75882, #153720, #60705, #61697, #134602, #31382, #121392, #57757, #119427, #108209, #13240, #168878, #152723, #72933, #136567, #12261, #58728, #73925, #105239, #43575, #184070, #90065, #166927, #181111, #15216, #196288, #137557, #151747, #104248, #150764, #135594, #197266, #183084, #42585, #165931, #27429, #149757, #199240, #138545, #29406, #11261, #89073, #44567, #120398, #30383, #45554, #59722, #122381, #182091, #91036, #107208, #74903, #198247, #76875, #14213, #169888, #92030, #23, #123366, #185059, #46547, #77867, #47551, #186068, #128340, #111191, #142525, #1018, #157709, #18208, #79866, #139534, #35352, #62691, #19199, #65682, #78857, #172882, #93031, #80848, #4003, #127345, #189059, #49528, #173882, #158685, #50531, #112193, #126362, #81820, #141535, #97003, #20174, #143507, #188058, #3024, #113175, #63705, #34362, #96023, #4993, #187077, #64700, #174865, #66678, #94028, #124373, #109204, #190039, #51513, #154719, #16212, #170884, #32375, #17204, #155708, #33368, #140537, #2025, #125380, #48546, #110200, #171879, #95026, #156716, #86843, #70687, #115181, #54510, #193033, #162685, #40341, #147531, #148528, #21174, #118191, #7994, #144510, #5995, #195036, #99999, #55509, #39341, #159678, #23181, #98995, #145507, #160684, #192020, #130323, #132353, #176874, #53504, #67674, #102016, #82829, #24191, #38343, #191027, #37337, #22176, #83826, #69678, #129332, #52502, #114162, #36331, #85841, #25200, #116182, #97984, #175864, #131345, #6988, #117179, #194045, #146504, #9019, #68668, #177873, #178874, #161684, #84824, #163699, #101000, #56513, #10019, #71678, #133345, #28194, #136339, #164697, #134363, #72688, #14981, #198013, #29173, #87832, #44333, #105005, #166691, #26192, #122147, #149518, #105990, #152492, #165691, #59483, #179882, #61467, #199005, #13979, #60471, #167676, #13008, #120167, #121157, #182850, #30148, #135363, #11015, #73691, #90809, #75646, #183836, #76641, #196047, #137324, #45325, #57522, #138319, #12028, #106975, #197034, #168649, #91791, #153485, #200001, #41350, #181858, #43337, #119191, #103013, #180875, #89836, #42351, #104013, #27189, #88836, #150529, #74672, #58501, #151517, #2784, #110952, #18963, #17972, #188812, #171644, #63467, #157470, #16969, #32140, #785, #48310, #108971, #187825, #92796, #109965, #80609, #184824, #126130, #154484, #33134, #34125, #123138, #78622, #94791, #31148, #62456, #46309, #1789, #140298, #127104, #79626, #141294, #124130, #125142, #93797, #186841, #156471, #169652, #64463, #107965, #65443, #139306, #49294, #172637, #95784, #142286, #185829, #170652, #3766, #15978, #155477, #77637, #47316, #110910, #190749, #111910, #109919, #93753, #63421, #4709, #112896, #173598, #97704, #16924, #19899, #33090, #35067, #49252, #186794, #125096, #155434, #158410, #1743, #48265, #36055, #96722, #159395, #143227, #187782, #127063, #65402, #81540, #80565, #140251, #78577, #171602, #108926, #66399, #20890, #188770, #170606, #94746, #142240, #156426, #128061, #189763, #18920, #51235, #17927, #3725, #174590, #32096, #79582, #82548, #172596, #67391, #144230, #141251, #50254, #157426, #5714, #2740, #64417, #126086, #129048, #34082, #95740, #160407, #116894, #177592, #39059, #98713, #194754, #21896, #178586, #24911, #38064, #70400, #52223, #40050, #101726, #8731, #133064, #117908, #163415, #148242, #85553, #41069, #100717, #56226, #71400, #102732, #147239, #162397, #72400, #22896, #132068, #9736, #84542, #192748, #54231, #134076, #55225, #53218, #37054, #6707, #179597, #164421, #86558, #25914, #83546, #87558, #176590, #149245, #115902, #130037, #68385, #145225, #10736, #191736, #114896, #113880, #175577, #99720, #161404, #131059, #193757, #146219, #7707, #69390, #23900, #107680, #180598, #77353, #167399, #103736, #165416, #154202, #59200, #14698, #198729, #118914, #182569, #58226 ),
 ( #196759, #181580, #43058, #27910, #183557, #89553, #13701, #122856, #168374, #169357, #29870, #136059, #197734, #26909, #15692, #88552, #120869, #150251, #76360, #11745, #73412, #135083, #28895, #45043, #138037, #106701, #199718, #184544, #60195, #195766, #75368, #44052, #46024, #105712, #151239, #119895, #90535, #166416, #91507, #104724, #152217, #30867, #42072, #153194, #12728, #137038, #61184, #57240, #74394, #121865, #92513, #155194, #100226, #79339, #94500, #177099, #21396, #144728, #78333, #141009, #48024, #5212, #159907, #500, #36548, #161908, #84053, #123836, #83054, #66893, #32850, #51728, #62172, #16683, #22402, #128555, #17681, #67894, #113391, #171362, #185534, #124852, #93508, #115410, #186552, #52721, #23402, #175081, #6215, #109681, #139020, #31855, #129547, #190251, #38570, #98203, #191247, #114387, #47027, #176089, #37559, #99222, #145731, #160909, #108685, #140006, #7212, #156182, #68896, #170363, #130556, #192254, #53735, #1495, #63173, #25425, #164923, #88056, #135580, #40570, #131571, #179101, #134588, #72919, #104234, #182076, #178090, #26416, #41577, #162907, #120383, #165916, #196274, #27413, #73910, #149743, #166913, #103241, #133570, #197252, #87066, #102240, #86064, #118416, #55730, #181097, #116401, #180109, #58714, #8227, #42571, #39560, #11245, #150750, #85049, #163928, #195261, #193255, #101217, #43560, #148751, #10240, #105225, #57743, #119413, #24415, #71899, #194263, #56745, #89059, #146731, #12248, #69905, #54729, #147754, #9240, #70907, #132575, #117403, #151733, #106207, #109190, #30368, #107192, #154703, #8, #60690, #74889, #14197, #183069, #2011, #75866, #139519, #187061, #61682, #108191, #137542, #110185, #121377, #93016, #92012, #63690, #185044, #167891, #186052, #125365, #123351, #155694, #16197, #78843, #62676, #168863, #46531, #169873, #77852, #32360, #1002, #140521, #13226, #28414, #31366, #136552, #198232, #48531, #153705, #47536, #124357, #59704, #15201, #91021, #199225, #152707, #184055, #122366, #170869, #76860, #45538, #44552, #94013, #29390, #17189, #138530, #90051, #172864, #157690, #19181, #143490, #3006, #156699, #126344, #53487, #159659, #160667, #190023, #171863, #188041, #4975, #49511, #191009, #174847, #34345, #18193, #111174, #67656, #175846, #36313, #22159, #79850, #82811, #96006, #97967, #112177, #80830, #142507, #3985, #129313, #6970, #66661, #98977, #21156, #83810, #5976, #50514, #51497, #128324, #144493, #37319, #52485, #145490, #141519, #33352, #113157, #64682, #65665, #130306, #35333, #114145, #68650, #95011, #158668, #127327, #189039, #173865, #96986, #20158, #192001, #81803, #9001, #84806, #119174, #99982, #41333, #132335, #69660, #116164, #100982, #162666, #86824, #146485, #161667, #131327, #197018, #102994, #103996, #133327, #115164, #193015, #148510, #54492, #134347, #10998, #25182, #164680, #7976, #10000, #72670, #176857, #177854, #42335, #117159, #73672, #87815, #147511, #195018, #163679, #71660, #23163, #39323, #24172, #150513, #56494, #26174, #85823, #179863, #40321, #101997, #70668, #57505, #194026, #149501, #196029, #55489, #118172, #38326, #180859, #165674, #27173, #88820, #12011, #135344, #178855, #91777, #47301, #106960, #62440, #77623, #108958, #153471, #168634, #78608, #29156, #14967, #154471, #90793, #198990, #60458, #140282, #122133, #58484, #139293, #92782, #770, #123123, #76627, #183820, #138305, #61453, #170637, #13964, #104988, #152477, #107951, #46294, #124114, #155464, #151500, #199986, #184808, #136322, #93783, #75631, #169638, #137309, #31134, #185814, #15963, #32126, #16954, #45310, #30134, #166676, #120151, #28177, #181841, #89819, #43321, #12992, #74655, #197997, #59467, #121140, #182834, #44316, #105975, #167660, #66427, #83576, #19927, #50282, #190776, #142270, #157455, #2770, #35097, #172624, #97733, #33119, #96749, #52251, #125129, #159422, #94776, #158439, #67420, #1774, #80595, #111940 ) ),
 .UNSPECIFIED., .T., .F., .T. ) 
 B_SPLINE_SURFACE_WITH_KNOTS ( ( 4, 3, 4 ),
 ( 3, 2, 2, 2, 2, 2, 2, 2, 2, 2, 2, 2, 2, 2, 2, 2, 2, 2, 2, 2, 2, 2, 2, 2, 2, 2, 2, 2, 2, 2, 2, 2, 2, 2, 2, 2, 2, 2, 2, 2, 2, 2, 2, 2, 2, 2, 2, 2, 2, 2, 2, 2, 2, 2, 2, 2, 2, 2, 2, 2, 2, 2, 2, 2, 2, 2, 2, 2, 2, 2, 2, 2, 2, 2, 2, 2, 2, 2, 2, 2, 2, 2, 2, 2, 2, 2, 2, 2, 2, 2, 2, 2, 2, 2, 2, 2, 2, 2, 2, 2, 2, 2, 2, 2, 2, 2, 2, 2, 2, 2, 2, 2, 2, 2, 2, 2, 2, 2, 2, 2, 2, 2, 2, 2, 2, 2, 2, 2, 2, 2, 2, 2, 2, 2, 2, 2, 2, 2, 2, 2, 2, 2, 2, 2, 2, 2, 2, 2, 2, 2, 2, 2, 2, 2, 2, 2, 2, 2, 2, 2, 2, 2, 2, 2, 2, 2, 2, 2, 2, 2, 2, 2, 2, 2, 2, 2, 2, 2, 2, 2, 2, 2, 2, 2, 2, 2, 2, 2, 2, 2, 2, 2, 2, 2, 2, 2, 2, 2, 2, 2, 2, 2, 2, 2, 2, 2, 2, 2, 2, 2, 2, 2, 2, 2, 2, 2, 2, 2, 2, 2, 2, 2, 2, 2, 2, 2, 2, 2, 3 ),
 ( 0.000000000000000000, 0.5000000000000000000, 1.000000000000000000 ),
 ( 0.000000000000000000, 0.004385964912280701511, 0.008771929824561403022, 0.01315789473684210453, 0.01754385964912280604, 0.02192982456140350755, 0.02631578947368420907, 0.03070175438596491058, 0.03508771929824561209, 0.03947368421052631360, 0.04385964912280701511, 0.04824561403508771662, 0.05263157894736841813, 0.05701754385964911964, 0.06140350877192982115, 0.06578947368421052266, 0.07017543859649122417, 0.07456140350877192569, 0.07894736842105262720, 0.08333333333333332871, 0.08771929824561403022, 0.09210526315789473173, 0.09649122807017543324, 0.1008771929824561348, 0.1052631578947368363, 0.1096491228070175378, 0.1140350877192982393, 0.1184210526315789408, 0.1228070175438596423, 0.1271929824561403577, 0.1315789473684210453, 0.1359649122807017607, 0.1403508771929824483, 0.1447368421052631637, 0.1491228070175438514, 0.1535087719298245668, 0.1578947368421052544, 0.1622807017543859698, 0.1666666666666666574, 0.1710526315789473728, 0.1754385964912280604, 0.1798245614035087758, 0.1842105263157894635, 0.1885964912280701788, 0.1929824561403508665, 0.1973684210526315819, 0.2017543859649122695, 0.2061403508771929849, 0.2105263157894736725, 0.2149122807017543879, 0.2192982456140350755, 0.2236842105263157909, 0.2280701754385964786, 0.2324561403508771940, 0.2368421052631578816, 0.2412280701754385970, 0.2456140350877192846, 0.2500000000000000000, 0.2543859649122807154, 0.2587719298245614308, 0.2631578947368420907, 0.2675438596491228060, 0.2719298245614035214, 0.2763157894736842368, 0.2807017543859648967, 0.2850877192982456121, 0.2894736842105263275, 0.2938596491228070429, 0.2982456140350877027, 0.3026315789473684181, 0.3070175438596491335, 0.3114035087719298489, 0.3157894736842105088, 0.3201754385964912242, 0.3245614035087719396, 0.3289473684210526550, 0.3333333333333333148, 0.3377192982456140302, 0.3421052631578947456, 0.3464912280701754610, 0.3508771929824561209, 0.3552631578947368363, 0.3596491228070175517, 0.3640350877192982670, 0.3684210526315789269, 0.3728070175438596423, 0.3771929824561403577, 0.3815789473684210731, 0.3859649122807017330, 0.3903508771929824483, 0.3947368421052631637, 0.3991228070175438791, 0.4035087719298245390, 0.4078947368421052544, 0.4122807017543859698, 0.4166666666666666852, 0.4210526315789473450, 0.4254385964912280604, 0.4298245614035087758, 0.4342105263157894912, 0.4385964912280701511, 0.4429824561403508665, 0.4473684210526315819, 0.4517543859649122973, 0.4561403508771929571, 0.4605263157894736725, 0.4649122807017543879, 0.4692982456140351033, 0.4736842105263157632, 0.4780701754385964786, 0.4824561403508771940, 0.4868421052631579093, 0.4912280701754385692, 0.4956140350877192846, 0.5000000000000000000, 0.5043859649122807154, 0.5087719298245614308, 0.5131578947368421462, 0.5175438596491228616, 0.5219298245614034659, 0.5263157894736841813, 0.5307017543859648967, 0.5350877192982456121, 0.5394736842105263275, 0.5438596491228070429, 0.5482456140350877583, 0.5526315789473684736, 0.5570175438596490780, 0.5614035087719297934, 0.5657894736842105088, 0.5701754385964912242, 0.5745614035087719396, 0.5789473684210526550, 0.5833333333333333703, 0.5877192982456140857, 0.5921052631578946901, 0.5964912280701754055, 0.6008771929824561209, 0.6052631578947368363, 0.6096491228070175517, 0.6140350877192982670, 0.6184210526315789824, 0.6228070175438596978, 0.6271929824561403022, 0.6315789473684210176, 0.6359649122807017330, 0.6403508771929824483, 0.6447368421052631637, 0.6491228070175438791, 0.6535087719298245945, 0.6578947368421053099, 0.6622807017543859143, 0.6666666666666666297, 0.6710526315789473450, 0.6754385964912280604, 0.6798245614035087758, 0.6842105263157894912, 0.6885964912280702066, 0.6929824561403509220, 0.6973684210526315264, 0.7017543859649122417, 0.7061403508771929571, 0.7105263157894736725, 0.7149122807017543879, 0.7192982456140351033, 0.7236842105263158187, 0.7280701754385965341, 0.7324561403508771384, 0.7368421052631578538, 0.7412280701754385692, 0.7456140350877192846, 0.7500000000000000000, 0.7543859649122807154, 0.7587719298245614308, 0.7631578947368421462, 0.7675438596491228616, 0.7719298245614034659, 0.7763157894736841813, 0.7807017543859648967, 0.7850877192982456121, 0.7894736842105263275, 0.7938596491228070429, 0.7982456140350877583, 0.8026315789473684736, 0.8070175438596490780, 0.8114035087719297934, 0.8157894736842105088, 0.8201754385964912242, 0.8245614035087719396, 0.8289473684210526550, 0.8333333333333333703, 0.8377192982456140857, 0.8421052631578946901, 0.8464912280701754055, 0.8508771929824561209, 0.8552631578947368363, 0.8596491228070175517, 0.8640350877192982670, 0.8684210526315789824, 0.8728070175438596978, 0.8771929824561403022, 0.8815789473684210176, 0.8859649122807017330, 0.8903508771929824483, 0.8947368421052631637, 0.8991228070175438791, 0.9035087719298245945, 0.9078947368421053099, 0.9122807017543859143, 0.9166666666666666297, 0.9210526315789473450, 0.9254385964912280604, 0.9298245614035087758, 0.9342105263157894912, 0.9385964912280702066, 0.9429824561403509220, 0.9473684210526315264, 0.9517543859649122417, 0.9561403508771929571, 0.9605263157894736725, 0.9649122807017543879, 0.9692982456140351033, 0.9736842105263158187, 0.9780701754385965341, 0.9824561403508771384, 0.9868421052631578538, 0.9912280701754385692, 0.9956140350877192846, 1.000000000000000000 ),
 .UNSPECIFIED. ) 
 GEOMETRIC_REPRESENTATION_ITEM ( )  RATIONAL_B_SPLINE_SURFACE ( (
 ( 1.000000000000000000, 0.9659258262890683122, 1.000000000000000000, 0.9659258262890683122, 1.000000000000000000, 0.9659258262890683122, 1.000000000000000000, 0.9659258262890683122, 1.000000000000000000, 0.9659258262890683122, 1.000000000000000000, 0.9659258262890683122, 1.000000000000000000, 0.9659258262890683122, 1.000000000000000000, 0.9659258262890683122, 1.000000000000000000, 0.9659258262890683122, 1.000000000000000000, 0.9659258262890683122, 1.000000000000000000, 0.9659258262890683122, 1.000000000000000000, 0.9659258262890683122, 1.000000000000000000, 0.9659258262890683122, 1.000000000000000000, 0.9659258262890683122, 1.000000000000000000, 0.9659258262890683122, 1.000000000000000000, 0.9659258262890683122, 1.000000000000000000, 0.9659258262890683122, 1.000000000000000000, 0.9659258262890683122, 1.000000000000000000, 0.9659258262890683122, 1.000000000000000000, 0.9659258262890683122, 1.000000000000000000, 0.9659258262890683122, 1.000000000000000000, 0.9659258262890683122, 1.000000000000000000, 0.9659258262890683122, 1.000000000000000000, 0.9659258262890683122, 1.000000000000000000, 0.9659258262890683122, 1.000000000000000000, 0.9659258262890683122, 1.000000000000000000, 0.9659258262890683122, 1.000000000000000000, 0.9659258262890683122, 1.000000000000000000, 0.9659258262890683122, 1.000000000000000000, 0.9659258262890683122, 1.000000000000000000, 0.9659258262890683122, 1.000000000000000000, 0.9659258262890683122, 1.000000000000000000, 0.9659258262890683122, 1.000000000000000000, 0.9659258262890683122, 1.000000000000000000, 0.9659258262890683122, 1.000000000000000000, 0.9659258262890683122, 1.000000000000000000, 0.9659258262890683122, 1.000000000000000000, 0.9659258262890683122, 1.000000000000000000, 0.9659258262890683122, 1.000000000000000000, 0.9659258262890683122, 1.000000000000000000, 0.9659258262890683122, 1.000000000000000000, 0.9659258262890683122, 1.000000000000000000, 0.9659258262890683122, 1.000000000000000000, 0.9659258262890683122, 1.000000000000000000, 0.9659258262890683122, 1.000000000000000000, 0.9659258262890683122, 1.000000000000000000, 0.9659258262890683122, 1.000000000000000000, 0.9659258262890683122, 1.000000000000000000, 0.9659258262890683122, 1.000000000000000000, 0.9659258262890683122, 1.000000000000000000, 0.9659258262890683122, 1.000000000000000000, 0.9659258262890683122, 1.000000000000000000, 0.9659258262890683122, 1.000000000000000000, 0.9659258262890683122, 1.000000000000000000, 0.9659258262890683122, 1.000000000000000000, 0.9659258262890683122, 1.000000000000000000, 0.9659258262890683122, 1.000000000000000000, 0.9659258262890683122, 1.000000000000000000, 0.9659258262890683122, 1.000000000000000000, 0.9659258262890683122, 1.000000000000000000, 0.9659258262890683122, 1.000000000000000000, 0.9659258262890683122, 1.000000000000000000, 0.9659258262890683122, 1.000000000000000000, 0.9659258262890683122, 1.000000000000000000, 0.9659258262890683122, 1.000000000000000000, 0.9659258262890683122, 1.000000000000000000, 0.9659258262890683122, 1.000000000000000000, 0.9659258262890683122, 1.000000000000000000, 0.9659258262890683122, 1.000000000000000000, 0.9659258262890683122, 1.000000000000000000, 0.9659258262890683122, 1.000000000000000000, 0.9659258262890683122, 1.000000000000000000, 0.9659258262890683122, 1.000000000000000000, 0.9659258262890683122, 1.000000000000000000, 0.9659258262890683122, 1.000000000000000000, 0.9659258262890683122, 1.000000000000000000, 0.9659258262890683122, 1.000000000000000000, 0.9659258262890683122, 1.000000000000000000, 0.9659258262890683122, 1.000000000000000000, 0.9659258262890683122, 1.000000000000000000, 0.9659258262890683122, 1.000000000000000000, 0.9659258262890683122, 1.000000000000000000, 0.9659258262890683122, 1.000000000000000000, 0.9659258262890683122, 1.000000000000000000, 0.9659258262890683122, 1.000000000000000000, 0.9659258262890683122, 1.000000000000000000, 0.9659258262890683122, 1.000000000000000000, 0.9659258262890683122, 1.000000000000000000, 0.9659258262890683122, 1.000000000000000000, 0.9659258262890683122, 1.000000000000000000, 0.9659258262890683122, 1.000000000000000000, 0.9659258262890683122, 1.000000000000000000, 0.9659258262890683122, 1.000000000000000000, 0.9659258262890683122, 1.000000000000000000, 0.9659258262890683122, 1.000000000000000000, 0.9659258262890683122, 1.000000000000000000, 0.9659258262890683122, 1.000000000000000000, 0.9659258262890683122, 1.000000000000000000, 0.9659258262890683122, 1.000000000000000000, 0.9659258262890683122, 1.000000000000000000, 0.9659258262890683122, 1.000000000000000000, 0.9659258262890683122, 1.000000000000000000, 0.9659258262890683122, 1.000000000000000000, 0.9659258262890683122, 1.000000000000000000, 0.9659258262890683122, 1.000000000000000000, 0.9659258262890683122, 1.000000000000000000, 0.9659258262890683122, 1.000000000000000000, 0.9659258262890683122, 1.000000000000000000, 0.9659258262890683122, 1.000000000000000000, 0.9659258262890683122, 1.000000000000000000, 0.9659258262890683122, 1.000000000000000000, 0.9659258262890683122, 1.000000000000000000, 0.9659258262890683122, 1.000000000000000000, 0.9659258262890683122, 1.000000000000000000, 0.9659258262890683122, 1.000000000000000000, 0.9659258262890683122, 1.000000000000000000, 0.9659258262890683122, 1.000000000000000000, 0.9659258262890683122, 1.000000000000000000, 0.9659258262890683122, 1.000000000000000000, 0.9659258262890683122, 1.000000000000000000, 0.9659258262890683122, 1.000000000000000000, 0.9659258262890683122, 1.000000000000000000, 0.9659258262890683122, 1.000000000000000000, 0.9659258262890683122, 1.000000000000000000, 0.9659258262890683122, 1.000000000000000000, 0.9659258262890683122, 1.000000000000000000, 0.9659258262890683122, 1.000000000000000000, 0.9659258262890683122, 1.000000000000000000, 0.9659258262890683122, 1.000000000000000000, 0.9659258262890683122, 1.000000000000000000, 0.9659258262890683122, 1.000000000000000000, 0.9659258262890683122, 1.000000000000000000, 0.9659258262890683122, 1.000000000000000000, 0.9659258262890683122, 1.000000000000000000, 0.9659258262890683122, 1.000000000000000000, 0.9659258262890683122, 1.000000000000000000, 0.9659258262890683122, 1.000000000000000000, 0.9659258262890683122, 1.000000000000000000, 0.9659258262890683122, 1.000000000000000000, 0.9659258262890683122, 1.000000000000000000, 0.9659258262890683122, 1.000000000000000000, 0.9659258262890683122, 1.000000000000000000, 0.9659258262890683122, 1.000000000000000000, 0.9659258262890683122, 1.000000000000000000, 0.9659258262890683122, 1.000000000000000000, 0.9659258262890683122, 1.000000000000000000, 0.9659258262890683122, 1.000000000000000000, 0.9659258262890683122, 1.000000000000000000, 0.9659258262890683122, 1.000000000000000000, 0.9659258262890683122, 1.000000000000000000, 0.9659258262890683122, 1.000000000000000000, 0.9659258262890683122, 1.000000000000000000, 0.9659258262890683122, 1.000000000000000000, 0.9659258262890683122, 1.000000000000000000, 0.9659258262890683122, 1.000000000000000000, 0.9659258262890683122, 1.000000000000000000, 0.9659258262890683122, 1.000000000000000000, 0.9659258262890683122, 1.000000000000000000, 0.9659258262890683122, 1.000000000000000000, 0.9659258262890683122, 1.000000000000000000, 0.9659258262890683122, 1.000000000000000000, 0.9659258262890683122, 1.000000000000000000, 0.9659258262890683122, 1.000000000000000000, 0.9659258262890683122, 1.000000000000000000, 0.9659258262890683122, 1.000000000000000000, 0.9659258262890683122, 1.000000000000000000, 0.9659258262890683122, 1.000000000000000000, 0.9659258262890683122, 1.000000000000000000, 0.9659258262890683122, 1.000000000000000000, 0.9659258262890683122, 1.000000000000000000, 0.9659258262890683122, 1.000000000000000000, 0.9659258262890683122, 1.000000000000000000, 0.9659258262890683122, 1.000000000000000000, 0.9659258262890683122, 1.000000000000000000, 0.9659258262890683122, 1.000000000000000000, 0.9659258262890683122, 1.000000000000000000, 0.9659258262890683122, 1.000000000000000000, 0.9659258262890683122, 1.000000000000000000, 0.9659258262890683122, 1.000000000000000000, 0.9659258262890683122, 1.000000000000000000, 0.9659258262890683122, 1.000000000000000000, 0.9659258262890683122, 1.000000000000000000, 0.9659258262890683122, 1.000000000000000000, 0.9659258262890683122, 1.000000000000000000, 0.9659258262890683122, 1.000000000000000000, 0.9659258262890683122, 1.000000000000000000, 0.9659258262890683122, 1.000000000000000000, 0.9659258262890683122, 1.000000000000000000, 0.9659258262890683122, 1.000000000000000000, 0.9659258262890683122, 1.000000000000000000, 0.9659258262890683122, 1.000000000000000000, 0.9659258262890683122, 1.000000000000000000, 0.9659258262890683122, 1.000000000000000000, 0.9659258262890683122, 1.000000000000000000, 0.9659258262890683122, 1.000000000000000000, 0.9659258262890683122, 1.000000000000000000, 0.9659258262890683122, 1.000000000000000000, 0.9659258262890683122, 1.000000000000000000, 0.9659258262890683122, 1.000000000000000000, 0.9659258262890683122, 1.000000000000000000, 0.9659258262890683122, 1.000000000000000000, 0.9659258262890683122, 1.000000000000000000, 0.9659258262890683122, 1.000000000000000000, 0.9659258262890683122, 1.000000000000000000, 0.9659258262890683122, 1.000000000000000000, 0.9659258262890683122, 1.000000000000000000, 0.9659258262890683122, 1.000000000000000000, 0.9659258262890683122, 1.000000000000000000, 0.9659258262890683122, 1.000000000000000000, 0.9659258262890683122, 1.000000000000000000, 0.9659258262890683122, 1.000000000000000000, 0.9659258262890683122, 1.000000000000000000, 0.9659258262890683122, 1.000000000000000000, 0.9659258262890683122, 1.000000000000000000, 0.9659258262890683122, 1.000000000000000000, 0.9659258262890683122, 1.000000000000000000, 0.9659258262890683122, 1.000000000000000000, 0.9659258262890683122, 1.000000000000000000, 0.9659258262890683122, 1.000000000000000000, 0.9659258262890683122, 1.000000000000000000, 0.9659258262890683122, 1.000000000000000000, 0.9659258262890683122, 1.000000000000000000, 0.9659258262890683122, 1.000000000000000000, 0.9659258262890683122, 1.000000000000000000, 0.9659258262890683122, 1.000000000000000000, 0.9659258262890683122, 1.000000000000000000, 0.9659258262890683122, 1.000000000000000000, 0.9659258262890683122, 1.000000000000000000),
 ( 0.3333333333333333703, 0.3219752754296894559, 0.3333333333333333703, 0.3219752754296894559, 0.3333333333333333703, 0.3219752754296894559, 0.3333333333333333703, 0.3219752754296894559, 0.3333333333333333703, 0.3219752754296894559, 0.3333333333333333703, 0.3219752754296894559, 0.3333333333333333703, 0.3219752754296894559, 0.3333333333333333703, 0.3219752754296894559, 0.3333333333333333703, 0.3219752754296894559, 0.3333333333333333703, 0.3219752754296894559, 0.3333333333333333703, 0.3219752754296894559, 0.3333333333333333703, 0.3219752754296894559, 0.3333333333333333703, 0.3219752754296894559, 0.3333333333333333703, 0.3219752754296894559, 0.3333333333333333703, 0.3219752754296894559, 0.3333333333333333703, 0.3219752754296894559, 0.3333333333333333703, 0.3219752754296894559, 0.3333333333333333703, 0.3219752754296894559, 0.3333333333333333703, 0.3219752754296894559, 0.3333333333333333703, 0.3219752754296894559, 0.3333333333333333703, 0.3219752754296894559, 0.3333333333333333703, 0.3219752754296894559, 0.3333333333333333703, 0.3219752754296894559, 0.3333333333333333703, 0.3219752754296894559, 0.3333333333333333703, 0.3219752754296894559, 0.3333333333333333703, 0.3219752754296894559, 0.3333333333333333703, 0.3219752754296894559, 0.3333333333333333703, 0.3219752754296894559, 0.3333333333333333703, 0.3219752754296894559, 0.3333333333333333703, 0.3219752754296894559, 0.3333333333333333703, 0.3219752754296894559, 0.3333333333333333703, 0.3219752754296894559, 0.3333333333333333703, 0.3219752754296894559, 0.3333333333333333703, 0.3219752754296894559, 0.3333333333333333703, 0.3219752754296894559, 0.3333333333333333703, 0.3219752754296894559, 0.3333333333333333703, 0.3219752754296894559, 0.3333333333333333703, 0.3219752754296894559, 0.3333333333333333703, 0.3219752754296894559, 0.3333333333333333703, 0.3219752754296894559, 0.3333333333333333703, 0.3219752754296894559, 0.3333333333333333703, 0.3219752754296894559, 0.3333333333333333703, 0.3219752754296894559, 0.3333333333333333703, 0.3219752754296894559, 0.3333333333333333703, 0.3219752754296894559, 0.3333333333333333703, 0.3219752754296894559, 0.3333333333333333703, 0.3219752754296894559, 0.3333333333333333703, 0.3219752754296894559, 0.3333333333333333703, 0.3219752754296894559, 0.3333333333333333703, 0.3219752754296894559, 0.3333333333333333703, 0.3219752754296894559, 0.3333333333333333703, 0.3219752754296894559, 0.3333333333333333703, 0.3219752754296894559, 0.3333333333333333703, 0.3219752754296894559, 0.3333333333333333703, 0.3219752754296894559, 0.3333333333333333703, 0.3219752754296894559, 0.3333333333333333703, 0.3219752754296894559, 0.3333333333333333703, 0.3219752754296894559, 0.3333333333333333703, 0.3219752754296894559, 0.3333333333333333703, 0.3219752754296894559, 0.3333333333333333703, 0.3219752754296894559, 0.3333333333333333703, 0.3219752754296894559, 0.3333333333333333703, 0.3219752754296894559, 0.3333333333333333703, 0.3219752754296894559, 0.3333333333333333703, 0.3219752754296894559, 0.3333333333333333703, 0.3219752754296894559, 0.3333333333333333703, 0.3219752754296894559, 0.3333333333333333703, 0.3219752754296894559, 0.3333333333333333703, 0.3219752754296894559, 0.3333333333333333703, 0.3219752754296894559, 0.3333333333333333703, 0.3219752754296894559, 0.3333333333333333703, 0.3219752754296894559, 0.3333333333333333703, 0.3219752754296894559, 0.3333333333333333703, 0.3219752754296894559, 0.3333333333333333703, 0.3219752754296894559, 0.3333333333333333703, 0.3219752754296894559, 0.3333333333333333703, 0.3219752754296894559, 0.3333333333333333703, 0.3219752754296894559, 0.3333333333333333703, 0.3219752754296894559, 0.3333333333333333703, 0.3219752754296894559, 0.3333333333333333703, 0.3219752754296894559, 0.3333333333333333703, 0.3219752754296894559, 0.3333333333333333703, 0.3219752754296894559, 0.3333333333333333703, 0.3219752754296894559, 0.3333333333333333703, 0.3219752754296894559, 0.3333333333333333703, 0.3219752754296894559, 0.3333333333333333703, 0.3219752754296894559, 0.3333333333333333703, 0.3219752754296894559, 0.3333333333333333703, 0.3219752754296894559, 0.3333333333333333703, 0.3219752754296894559, 0.3333333333333333703, 0.3219752754296894559, 0.3333333333333333703, 0.3219752754296894559, 0.3333333333333333703, 0.3219752754296894559, 0.3333333333333333703, 0.3219752754296894559, 0.3333333333333333703, 0.3219752754296894559, 0.3333333333333333703, 0.3219752754296894559, 0.3333333333333333703, 0.3219752754296894559, 0.3333333333333333703, 0.3219752754296894559, 0.3333333333333333703, 0.3219752754296894559, 0.3333333333333333703, 0.3219752754296894559, 0.3333333333333333703, 0.3219752754296894559, 0.3333333333333333703, 0.3219752754296894559, 0.3333333333333333703, 0.3219752754296894559, 0.3333333333333333703, 0.3219752754296894559, 0.3333333333333333703, 0.3219752754296894559, 0.3333333333333333703, 0.3219752754296894559, 0.3333333333333333703, 0.3219752754296894559, 0.3333333333333333703, 0.3219752754296894559, 0.3333333333333333703, 0.3219752754296894559, 0.3333333333333333703, 0.3219752754296894559, 0.3333333333333333703, 0.3219752754296894559, 0.3333333333333333703, 0.3219752754296894559, 0.3333333333333333703, 0.3219752754296894559, 0.3333333333333333703, 0.3219752754296894559, 0.3333333333333333703, 0.3219752754296894559, 0.3333333333333333703, 0.3219752754296894559, 0.3333333333333333703, 0.3219752754296894559, 0.3333333333333333703, 0.3219752754296894559, 0.3333333333333333703, 0.3219752754296894559, 0.3333333333333333703, 0.3219752754296894559, 0.3333333333333333703, 0.3219752754296894559, 0.3333333333333333703, 0.3219752754296894559, 0.3333333333333333703, 0.3219752754296894559, 0.3333333333333333703, 0.3219752754296894559, 0.3333333333333333703, 0.3219752754296894559, 0.3333333333333333703, 0.3219752754296894559, 0.3333333333333333703, 0.3219752754296894559, 0.3333333333333333703, 0.3219752754296894559, 0.3333333333333333703, 0.3219752754296894559, 0.3333333333333333703, 0.3219752754296894559, 0.3333333333333333703, 0.3219752754296894559, 0.3333333333333333703, 0.3219752754296894559, 0.3333333333333333703, 0.3219752754296894559, 0.3333333333333333703, 0.3219752754296894559, 0.3333333333333333703, 0.3219752754296894559, 0.3333333333333333703, 0.3219752754296894559, 0.3333333333333333703, 0.3219752754296894559, 0.3333333333333333703, 0.3219752754296894559, 0.3333333333333333703, 0.3219752754296894559, 0.3333333333333333703, 0.3219752754296894559, 0.3333333333333333703, 0.3219752754296894559, 0.3333333333333333703, 0.3219752754296894559, 0.3333333333333333703, 0.3219752754296894559, 0.3333333333333333703, 0.3219752754296894559, 0.3333333333333333703, 0.3219752754296894559, 0.3333333333333333703, 0.3219752754296894559, 0.3333333333333333703, 0.3219752754296894559, 0.3333333333333333703, 0.3219752754296894559, 0.3333333333333333703, 0.3219752754296894559, 0.3333333333333333703, 0.3219752754296894559, 0.3333333333333333703, 0.3219752754296894559, 0.3333333333333333703, 0.3219752754296894559, 0.3333333333333333703, 0.3219752754296894559, 0.3333333333333333703, 0.3219752754296894559, 0.3333333333333333703, 0.3219752754296894559, 0.3333333333333333703, 0.3219752754296894559, 0.3333333333333333703, 0.3219752754296894559, 0.3333333333333333703, 0.3219752754296894559, 0.3333333333333333703, 0.3219752754296894559, 0.3333333333333333703, 0.3219752754296894559, 0.3333333333333333703, 0.3219752754296894559, 0.3333333333333333703, 0.3219752754296894559, 0.3333333333333333703, 0.3219752754296894559, 0.3333333333333333703, 0.3219752754296894559, 0.3333333333333333703, 0.3219752754296894559, 0.3333333333333333703, 0.3219752754296894559, 0.3333333333333333703, 0.3219752754296894559, 0.3333333333333333703, 0.3219752754296894559, 0.3333333333333333703, 0.3219752754296894559, 0.3333333333333333703, 0.3219752754296894559, 0.3333333333333333703, 0.3219752754296894559, 0.3333333333333333703, 0.3219752754296894559, 0.3333333333333333703, 0.3219752754296894559, 0.3333333333333333703, 0.3219752754296894559, 0.3333333333333333703, 0.3219752754296894559, 0.3333333333333333703, 0.3219752754296894559, 0.3333333333333333703, 0.3219752754296894559, 0.3333333333333333703, 0.3219752754296894559, 0.3333333333333333703, 0.3219752754296894559, 0.3333333333333333703, 0.3219752754296894559, 0.3333333333333333703, 0.3219752754296894559, 0.3333333333333333703, 0.3219752754296894559, 0.3333333333333333703, 0.3219752754296894559, 0.3333333333333333703, 0.3219752754296894559, 0.3333333333333333703, 0.3219752754296894559, 0.3333333333333333703, 0.3219752754296894559, 0.3333333333333333703, 0.3219752754296894559, 0.3333333333333333703, 0.3219752754296894559, 0.3333333333333333703, 0.3219752754296894559, 0.3333333333333333703, 0.3219752754296894559, 0.3333333333333333703, 0.3219752754296894559, 0.3333333333333333703, 0.3219752754296894559, 0.3333333333333333703, 0.3219752754296894559, 0.3333333333333333703, 0.3219752754296894559, 0.3333333333333333703, 0.3219752754296894559, 0.3333333333333333703, 0.3219752754296894559, 0.3333333333333333703, 0.3219752754296894559, 0.3333333333333333703, 0.3219752754296894559, 0.3333333333333333703, 0.3219752754296894559, 0.3333333333333333703, 0.3219752754296894559, 0.3333333333333333703, 0.3219752754296894559, 0.3333333333333333703, 0.3219752754296894559, 0.3333333333333333703, 0.3219752754296894559, 0.3333333333333333703, 0.3219752754296894559, 0.3333333333333333703, 0.3219752754296894559, 0.3333333333333333703, 0.3219752754296894559, 0.3333333333333333703, 0.3219752754296894559, 0.3333333333333333703, 0.3219752754296894559, 0.3333333333333333703, 0.3219752754296894559, 0.3333333333333333703, 0.3219752754296894559, 0.3333333333333333703, 0.3219752754296894559, 0.3333333333333333703, 0.3219752754296894559, 0.3333333333333333703, 0.3219752754296894559, 0.3333333333333333703, 0.3219752754296894559, 0.3333333333333333703, 0.3219752754296894559, 0.3333333333333333703, 0.3219752754296894559, 0.3333333333333333703, 0.3219752754296894559, 0.3333333333333333703, 0.3219752754296894559, 0.3333333333333333703, 0.3219752754296894559, 0.3333333333333333703, 0.3219752754296894559, 0.3333333333333333703, 0.3219752754296894559, 0.3333333333333333703, 0.3219752754296894559, 0.3333333333333333703, 0.3219752754296894559, 0.3333333333333333703, 0.3219752754296894559, 0.3333333333333333703, 0.3219752754296894559, 0.3333333333333333703, 0.3219752754296894559, 0.3333333333333333703, 0.3219752754296894559, 0.3333333333333333703, 0.3219752754296894559, 0.3333333333333333703),
 ( 0.3333333333333333703, 0.3219752754296894559, 0.3333333333333333703, 0.3219752754296894559, 0.3333333333333333703, 0.3219752754296894559, 0.3333333333333333703, 0.3219752754296894559, 0.3333333333333333703, 0.3219752754296894559, 0.3333333333333333703, 0.3219752754296894559, 0.3333333333333333703, 0.3219752754296894559, 0.3333333333333333703, 0.3219752754296894559, 0.3333333333333333703, 0.3219752754296894559, 0.3333333333333333703, 0.3219752754296894559, 0.3333333333333333703, 0.3219752754296894559, 0.3333333333333333703, 0.3219752754296894559, 0.3333333333333333703, 0.3219752754296894559, 0.3333333333333333703, 0.3219752754296894559, 0.3333333333333333703, 0.3219752754296894559, 0.3333333333333333703, 0.3219752754296894559, 0.3333333333333333703, 0.3219752754296894559, 0.3333333333333333703, 0.3219752754296894559, 0.3333333333333333703, 0.3219752754296894559, 0.3333333333333333703, 0.3219752754296894559, 0.3333333333333333703, 0.3219752754296894559, 0.3333333333333333703, 0.3219752754296894559, 0.3333333333333333703, 0.3219752754296894559, 0.3333333333333333703, 0.3219752754296894559, 0.3333333333333333703, 0.3219752754296894559, 0.3333333333333333703, 0.3219752754296894559, 0.3333333333333333703, 0.3219752754296894559, 0.3333333333333333703, 0.3219752754296894559, 0.3333333333333333703, 0.3219752754296894559, 0.3333333333333333703, 0.3219752754296894559, 0.3333333333333333703, 0.3219752754296894559, 0.3333333333333333703, 0.3219752754296894559, 0.3333333333333333703, 0.3219752754296894559, 0.3333333333333333703, 0.3219752754296894559, 0.3333333333333333703, 0.3219752754296894559, 0.3333333333333333703, 0.3219752754296894559, 0.3333333333333333703, 0.3219752754296894559, 0.3333333333333333703, 0.3219752754296894559, 0.3333333333333333703, 0.3219752754296894559, 0.3333333333333333703, 0.3219752754296894559, 0.3333333333333333703, 0.3219752754296894559, 0.3333333333333333703, 0.3219752754296894559, 0.3333333333333333703, 0.3219752754296894559, 0.3333333333333333703, 0.3219752754296894559, 0.3333333333333333703, 0.3219752754296894559, 0.3333333333333333703, 0.3219752754296894559, 0.3333333333333333703, 0.3219752754296894559, 0.3333333333333333703, 0.3219752754296894559, 0.3333333333333333703, 0.3219752754296894559, 0.3333333333333333703, 0.3219752754296894559, 0.3333333333333333703, 0.3219752754296894559, 0.3333333333333333703, 0.3219752754296894559, 0.3333333333333333703, 0.3219752754296894559, 0.3333333333333333703, 0.3219752754296894559, 0.3333333333333333703, 0.3219752754296894559, 0.3333333333333333703, 0.3219752754296894559, 0.3333333333333333703, 0.3219752754296894559, 0.3333333333333333703, 0.3219752754296894559, 0.3333333333333333703, 0.3219752754296894559, 0.3333333333333333703, 0.3219752754296894559, 0.3333333333333333703, 0.3219752754296894559, 0.3333333333333333703, 0.3219752754296894559, 0.3333333333333333703, 0.3219752754296894559, 0.3333333333333333703, 0.3219752754296894559, 0.3333333333333333703, 0.3219752754296894559, 0.3333333333333333703, 0.3219752754296894559, 0.3333333333333333703, 0.3219752754296894559, 0.3333333333333333703, 0.3219752754296894559, 0.3333333333333333703, 0.3219752754296894559, 0.3333333333333333703, 0.3219752754296894559, 0.3333333333333333703, 0.3219752754296894559, 0.3333333333333333703, 0.3219752754296894559, 0.3333333333333333703, 0.3219752754296894559, 0.3333333333333333703, 0.3219752754296894559, 0.3333333333333333703, 0.3219752754296894559, 0.3333333333333333703, 0.3219752754296894559, 0.3333333333333333703, 0.3219752754296894559, 0.3333333333333333703, 0.3219752754296894559, 0.3333333333333333703, 0.3219752754296894559, 0.3333333333333333703, 0.3219752754296894559, 0.3333333333333333703, 0.3219752754296894559, 0.3333333333333333703, 0.3219752754296894559, 0.3333333333333333703, 0.3219752754296894559, 0.3333333333333333703, 0.3219752754296894559, 0.3333333333333333703, 0.3219752754296894559, 0.3333333333333333703, 0.3219752754296894559, 0.3333333333333333703, 0.3219752754296894559, 0.3333333333333333703, 0.3219752754296894559, 0.3333333333333333703, 0.3219752754296894559, 0.3333333333333333703, 0.3219752754296894559, 0.3333333333333333703, 0.3219752754296894559, 0.3333333333333333703, 0.3219752754296894559, 0.3333333333333333703, 0.3219752754296894559, 0.3333333333333333703, 0.3219752754296894559, 0.3333333333333333703, 0.3219752754296894559, 0.3333333333333333703, 0.3219752754296894559, 0.3333333333333333703, 0.3219752754296894559, 0.3333333333333333703, 0.3219752754296894559, 0.3333333333333333703, 0.3219752754296894559, 0.3333333333333333703, 0.3219752754296894559, 0.3333333333333333703, 0.3219752754296894559, 0.3333333333333333703, 0.3219752754296894559, 0.3333333333333333703, 0.3219752754296894559, 0.3333333333333333703, 0.3219752754296894559, 0.3333333333333333703, 0.3219752754296894559, 0.3333333333333333703, 0.3219752754296894559, 0.3333333333333333703, 0.3219752754296894559, 0.3333333333333333703, 0.3219752754296894559, 0.3333333333333333703, 0.3219752754296894559, 0.3333333333333333703, 0.3219752754296894559, 0.3333333333333333703, 0.3219752754296894559, 0.3333333333333333703, 0.3219752754296894559, 0.3333333333333333703, 0.3219752754296894559, 0.3333333333333333703, 0.3219752754296894559, 0.3333333333333333703, 0.3219752754296894559, 0.3333333333333333703, 0.3219752754296894559, 0.3333333333333333703, 0.3219752754296894559, 0.3333333333333333703, 0.3219752754296894559, 0.3333333333333333703, 0.3219752754296894559, 0.3333333333333333703, 0.3219752754296894559, 0.3333333333333333703, 0.3219752754296894559, 0.3333333333333333703, 0.3219752754296894559, 0.3333333333333333703, 0.3219752754296894559, 0.3333333333333333703, 0.3219752754296894559, 0.3333333333333333703, 0.3219752754296894559, 0.3333333333333333703, 0.3219752754296894559, 0.3333333333333333703, 0.3219752754296894559, 0.3333333333333333703, 0.3219752754296894559, 0.3333333333333333703, 0.3219752754296894559, 0.3333333333333333703, 0.3219752754296894559, 0.3333333333333333703, 0.3219752754296894559, 0.3333333333333333703, 0.3219752754296894559, 0.3333333333333333703, 0.3219752754296894559, 0.3333333333333333703, 0.3219752754296894559, 0.3333333333333333703, 0.3219752754296894559, 0.3333333333333333703, 0.3219752754296894559, 0.3333333333333333703, 0.3219752754296894559, 0.3333333333333333703, 0.3219752754296894559, 0.3333333333333333703, 0.3219752754296894559, 0.3333333333333333703, 0.3219752754296894559, 0.3333333333333333703, 0.3219752754296894559, 0.3333333333333333703, 0.3219752754296894559, 0.3333333333333333703, 0.3219752754296894559, 0.3333333333333333703, 0.3219752754296894559, 0.3333333333333333703, 0.3219752754296894559, 0.3333333333333333703, 0.3219752754296894559, 0.3333333333333333703, 0.3219752754296894559, 0.3333333333333333703, 0.3219752754296894559, 0.3333333333333333703, 0.3219752754296894559, 0.3333333333333333703, 0.3219752754296894559, 0.3333333333333333703, 0.3219752754296894559, 0.3333333333333333703, 0.3219752754296894559, 0.3333333333333333703, 0.3219752754296894559, 0.3333333333333333703, 0.3219752754296894559, 0.3333333333333333703, 0.3219752754296894559, 0.3333333333333333703, 0.3219752754296894559, 0.3333333333333333703, 0.3219752754296894559, 0.3333333333333333703, 0.3219752754296894559, 0.3333333333333333703, 0.3219752754296894559, 0.3333333333333333703, 0.3219752754296894559, 0.3333333333333333703, 0.3219752754296894559, 0.3333333333333333703, 0.3219752754296894559, 0.3333333333333333703, 0.3219752754296894559, 0.3333333333333333703, 0.3219752754296894559, 0.3333333333333333703, 0.3219752754296894559, 0.3333333333333333703, 0.3219752754296894559, 0.3333333333333333703, 0.3219752754296894559, 0.3333333333333333703, 0.3219752754296894559, 0.3333333333333333703, 0.3219752754296894559, 0.3333333333333333703, 0.3219752754296894559, 0.3333333333333333703, 0.3219752754296894559, 0.3333333333333333703, 0.3219752754296894559, 0.3333333333333333703, 0.3219752754296894559, 0.3333333333333333703, 0.3219752754296894559, 0.3333333333333333703, 0.3219752754296894559, 0.3333333333333333703, 0.3219752754296894559, 0.3333333333333333703, 0.3219752754296894559, 0.3333333333333333703, 0.3219752754296894559, 0.3333333333333333703, 0.3219752754296894559, 0.3333333333333333703, 0.3219752754296894559, 0.3333333333333333703, 0.3219752754296894559, 0.3333333333333333703, 0.3219752754296894559, 0.3333333333333333703, 0.3219752754296894559, 0.3333333333333333703, 0.3219752754296894559, 0.3333333333333333703, 0.3219752754296894559, 0.3333333333333333703, 0.3219752754296894559, 0.3333333333333333703, 0.3219752754296894559, 0.3333333333333333703, 0.3219752754296894559, 0.3333333333333333703, 0.3219752754296894559, 0.3333333333333333703, 0.3219752754296894559, 0.3333333333333333703, 0.3219752754296894559, 0.3333333333333333703, 0.3219752754296894559, 0.3333333333333333703, 0.3219752754296894559, 0.3333333333333333703, 0.3219752754296894559, 0.3333333333333333703, 0.3219752754296894559, 0.3333333333333333703, 0.3219752754296894559, 0.3333333333333333703, 0.3219752754296894559, 0.3333333333333333703, 0.3219752754296894559, 0.3333333333333333703, 0.3219752754296894559, 0.3333333333333333703, 0.3219752754296894559, 0.3333333333333333703, 0.3219752754296894559, 0.3333333333333333703, 0.3219752754296894559, 0.3333333333333333703, 0.3219752754296894559, 0.3333333333333333703, 0.3219752754296894559, 0.3333333333333333703, 0.3219752754296894559, 0.3333333333333333703, 0.3219752754296894559, 0.3333333333333333703, 0.3219752754296894559, 0.3333333333333333703, 0.3219752754296894559, 0.3333333333333333703, 0.3219752754296894559, 0.3333333333333333703, 0.3219752754296894559, 0.3333333333333333703, 0.3219752754296894559, 0.3333333333333333703, 0.3219752754296894559, 0.3333333333333333703, 0.3219752754296894559, 0.3333333333333333703, 0.3219752754296894559, 0.3333333333333333703, 0.3219752754296894559, 0.3333333333333333703, 0.3219752754296894559, 0.3333333333333333703, 0.3219752754296894559, 0.3333333333333333703, 0.3219752754296894559, 0.3333333333333333703, 0.3219752754296894559, 0.3333333333333333703, 0.3219752754296894559, 0.3333333333333333703, 0.3219752754296894559, 0.3333333333333333703, 0.3219752754296894559, 0.3333333333333333703, 0.3219752754296894559, 0.3333333333333333703, 0.3219752754296894559, 0.3333333333333333703, 0.3219752754296894559, 0.3333333333333333703, 0.3219752754296894559, 0.3333333333333333703, 0.3219752754296894559, 0.3333333333333333703, 0.3219752754296894559, 0.3333333333333333703),
 ( 1.000000000000000000, 0.9659258262890683122, 1.000000000000000000, 0.9659258262890683122, 1.000000000000000000, 0.9659258262890683122, 1.000000000000000000, 0.9659258262890683122, 1.000000000000000000, 0.9659258262890683122, 1.000000000000000000, 0.9659258262890683122, 1.000000000000000000, 0.9659258262890683122, 1.000000000000000000, 0.9659258262890683122, 1.000000000000000000, 0.9659258262890683122, 1.000000000000000000, 0.9659258262890683122, 1.000000000000000000, 0.9659258262890683122, 1.000000000000000000, 0.9659258262890683122, 1.000000000000000000, 0.9659258262890683122, 1.000000000000000000, 0.9659258262890683122, 1.000000000000000000, 0.9659258262890683122, 1.000000000000000000, 0.9659258262890683122, 1.000000000000000000, 0.9659258262890683122, 1.000000000000000000, 0.9659258262890683122, 1.000000000000000000, 0.9659258262890683122, 1.000000000000000000, 0.9659258262890683122, 1.000000000000000000, 0.9659258262890683122, 1.000000000000000000, 0.9659258262890683122, 1.000000000000000000, 0.9659258262890683122, 1.000000000000000000, 0.9659258262890683122, 1.000000000000000000, 0.9659258262890683122, 1.000000000000000000, 0.9659258262890683122, 1.000000000000000000, 0.9659258262890683122, 1.000000000000000000, 0.9659258262890683122, 1.000000000000000000, 0.9659258262890683122, 1.000000000000000000, 0.9659258262890683122, 1.000000000000000000, 0.9659258262890683122, 1.000000000000000000, 0.9659258262890683122, 1.000000000000000000, 0.9659258262890683122, 1.000000000000000000, 0.9659258262890683122, 1.000000000000000000, 0.9659258262890683122, 1.000000000000000000, 0.9659258262890683122, 1.000000000000000000, 0.9659258262890683122, 1.000000000000000000, 0.9659258262890683122, 1.000000000000000000, 0.9659258262890683122, 1.000000000000000000, 0.9659258262890683122, 1.000000000000000000, 0.9659258262890683122, 1.000000000000000000, 0.9659258262890683122, 1.000000000000000000, 0.9659258262890683122, 1.000000000000000000, 0.9659258262890683122, 1.000000000000000000, 0.9659258262890683122, 1.000000000000000000, 0.9659258262890683122, 1.000000000000000000, 0.9659258262890683122, 1.000000000000000000, 0.9659258262890683122, 1.000000000000000000, 0.9659258262890683122, 1.000000000000000000, 0.9659258262890683122, 1.000000000000000000, 0.9659258262890683122, 1.000000000000000000, 0.9659258262890683122, 1.000000000000000000, 0.9659258262890683122, 1.000000000000000000, 0.9659258262890683122, 1.000000000000000000, 0.9659258262890683122, 1.000000000000000000, 0.9659258262890683122, 1.000000000000000000, 0.9659258262890683122, 1.000000000000000000, 0.9659258262890683122, 1.000000000000000000, 0.9659258262890683122, 1.000000000000000000, 0.9659258262890683122, 1.000000000000000000, 0.9659258262890683122, 1.000000000000000000, 0.9659258262890683122, 1.000000000000000000, 0.9659258262890683122, 1.000000000000000000, 0.9659258262890683122, 1.000000000000000000, 0.9659258262890683122, 1.000000000000000000, 0.9659258262890683122, 1.000000000000000000, 0.9659258262890683122, 1.000000000000000000, 0.9659258262890683122, 1.000000000000000000, 0.9659258262890683122, 1.000000000000000000, 0.9659258262890683122, 1.000000000000000000, 0.9659258262890683122, 1.000000000000000000, 0.9659258262890683122, 1.000000000000000000, 0.9659258262890683122, 1.000000000000000000, 0.9659258262890683122, 1.000000000000000000, 0.9659258262890683122, 1.000000000000000000, 0.9659258262890683122, 1.000000000000000000, 0.9659258262890683122, 1.000000000000000000, 0.9659258262890683122, 1.000000000000000000, 0.9659258262890683122, 1.000000000000000000, 0.9659258262890683122, 1.000000000000000000, 0.9659258262890683122, 1.000000000000000000, 0.9659258262890683122, 1.000000000000000000, 0.9659258262890683122, 1.000000000000000000, 0.9659258262890683122, 1.000000000000000000, 0.9659258262890683122, 1.000000000000000000, 0.9659258262890683122, 1.000000000000000000, 0.9659258262890683122, 1.000000000000000000, 0.9659258262890683122, 1.000000000000000000, 0.9659258262890683122, 1.000000000000000000, 0.9659258262890683122, 1.000000000000000000, 0.9659258262890683122, 1.000000000000000000, 0.9659258262890683122, 1.000000000000000000, 0.9659258262890683122, 1.000000000000000000, 0.9659258262890683122, 1.000000000000000000, 0.9659258262890683122, 1.000000000000000000, 0.9659258262890683122, 1.000000000000000000, 0.9659258262890683122, 1.000000000000000000, 0.9659258262890683122, 1.000000000000000000, 0.9659258262890683122, 1.000000000000000000, 0.9659258262890683122, 1.000000000000000000, 0.9659258262890683122, 1.000000000000000000, 0.9659258262890683122, 1.000000000000000000, 0.9659258262890683122, 1.000000000000000000, 0.9659258262890683122, 1.000000000000000000, 0.9659258262890683122, 1.000000000000000000, 0.9659258262890683122, 1.000000000000000000, 0.9659258262890683122, 1.000000000000000000, 0.9659258262890683122, 1.000000000000000000, 0.9659258262890683122, 1.000000000000000000, 0.9659258262890683122, 1.000000000000000000, 0.9659258262890683122, 1.000000000000000000, 0.9659258262890683122, 1.000000000000000000, 0.9659258262890683122, 1.000000000000000000, 0.9659258262890683122, 1.000000000000000000, 0.9659258262890683122, 1.000000000000000000, 0.9659258262890683122, 1.000000000000000000, 0.9659258262890683122, 1.000000000000000000, 0.9659258262890683122, 1.000000000000000000, 0.9659258262890683122, 1.000000000000000000, 0.9659258262890683122, 1.000000000000000000, 0.9659258262890683122, 1.000000000000000000, 0.9659258262890683122, 1.000000000000000000, 0.9659258262890683122, 1.000000000000000000, 0.9659258262890683122, 1.000000000000000000, 0.9659258262890683122, 1.000000000000000000, 0.9659258262890683122, 1.000000000000000000, 0.9659258262890683122, 1.000000000000000000, 0.9659258262890683122, 1.000000000000000000, 0.9659258262890683122, 1.000000000000000000, 0.9659258262890683122, 1.000000000000000000, 0.9659258262890683122, 1.000000000000000000, 0.9659258262890683122, 1.000000000000000000, 0.9659258262890683122, 1.000000000000000000, 0.9659258262890683122, 1.000000000000000000, 0.9659258262890683122, 1.000000000000000000, 0.9659258262890683122, 1.000000000000000000, 0.9659258262890683122, 1.000000000000000000, 0.9659258262890683122, 1.000000000000000000, 0.9659258262890683122, 1.000000000000000000, 0.9659258262890683122, 1.000000000000000000, 0.9659258262890683122, 1.000000000000000000, 0.9659258262890683122, 1.000000000000000000, 0.9659258262890683122, 1.000000000000000000, 0.9659258262890683122, 1.000000000000000000, 0.9659258262890683122, 1.000000000000000000, 0.9659258262890683122, 1.000000000000000000, 0.9659258262890683122, 1.000000000000000000, 0.9659258262890683122, 1.000000000000000000, 0.9659258262890683122, 1.000000000000000000, 0.9659258262890683122, 1.000000000000000000, 0.9659258262890683122, 1.000000000000000000, 0.9659258262890683122, 1.000000000000000000, 0.9659258262890683122, 1.000000000000000000, 0.9659258262890683122, 1.000000000000000000, 0.9659258262890683122, 1.000000000000000000, 0.9659258262890683122, 1.000000000000000000, 0.9659258262890683122, 1.000000000000000000, 0.9659258262890683122, 1.000000000000000000, 0.9659258262890683122, 1.000000000000000000, 0.9659258262890683122, 1.000000000000000000, 0.9659258262890683122, 1.000000000000000000, 0.9659258262890683122, 1.000000000000000000, 0.9659258262890683122, 1.000000000000000000, 0.9659258262890683122, 1.000000000000000000, 0.9659258262890683122, 1.000000000000000000, 0.9659258262890683122, 1.000000000000000000, 0.9659258262890683122, 1.000000000000000000, 0.9659258262890683122, 1.000000000000000000, 0.9659258262890683122, 1.000000000000000000, 0.9659258262890683122, 1.000000000000000000, 0.9659258262890683122, 1.000000000000000000, 0.9659258262890683122, 1.000000000000000000, 0.9659258262890683122, 1.000000000000000000, 0.9659258262890683122, 1.000000000000000000, 0.9659258262890683122, 1.000000000000000000, 0.9659258262890683122, 1.000000000000000000, 0.9659258262890683122, 1.000000000000000000, 0.9659258262890683122, 1.000000000000000000, 0.9659258262890683122, 1.000000000000000000, 0.9659258262890683122, 1.000000000000000000, 0.9659258262890683122, 1.000000000000000000, 0.9659258262890683122, 1.000000000000000000, 0.9659258262890683122, 1.000000000000000000, 0.9659258262890683122, 1.000000000000000000, 0.9659258262890683122, 1.000000000000000000, 0.9659258262890683122, 1.000000000000000000, 0.9659258262890683122, 1.000000000000000000, 0.9659258262890683122, 1.000000000000000000, 0.9659258262890683122, 1.000000000000000000, 0.9659258262890683122, 1.000000000000000000, 0.9659258262890683122, 1.000000000000000000, 0.9659258262890683122, 1.000000000000000000, 0.9659258262890683122, 1.000000000000000000, 0.9659258262890683122, 1.000000000000000000, 0.9659258262890683122, 1.000000000000000000, 0.9659258262890683122, 1.000000000000000000, 0.9659258262890683122, 1.000000000000000000, 0.9659258262890683122, 1.000000000000000000, 0.9659258262890683122, 1.000000000000000000, 0.9659258262890683122, 1.000000000000000000, 0.9659258262890683122, 1.000000000000000000, 0.9659258262890683122, 1.000000000000000000, 0.9659258262890683122, 1.000000000000000000, 0.9659258262890683122, 1.000000000000000000, 0.9659258262890683122, 1.000000000000000000, 0.9659258262890683122, 1.000000000000000000, 0.9659258262890683122, 1.000000000000000000, 0.9659258262890683122, 1.000000000000000000, 0.9659258262890683122, 1.000000000000000000, 0.9659258262890683122, 1.000000000000000000, 0.9659258262890683122, 1.000000000000000000, 0.9659258262890683122, 1.000000000000000000, 0.9659258262890683122, 1.000000000000000000, 0.9659258262890683122, 1.000000000000000000, 0.9659258262890683122, 1.000000000000000000, 0.9659258262890683122, 1.000000000000000000, 0.9659258262890683122, 1.000000000000000000, 0.9659258262890683122, 1.000000000000000000, 0.9659258262890683122, 1.000000000000000000, 0.9659258262890683122, 1.000000000000000000, 0.9659258262890683122, 1.000000000000000000, 0.9659258262890683122, 1.000000000000000000, 0.9659258262890683122, 1.000000000000000000, 0.9659258262890683122, 1.000000000000000000, 0.9659258262890683122, 1.000000000000000000, 0.9659258262890683122, 1.000000000000000000, 0.9659258262890683122, 1.000000000000000000, 0.9659258262890683122, 1.000000000000000000),
 ( 0.3333333333333333703, 0.3219752754296894559, 0.3333333333333333703, 0.3219752754296894559, 0.3333333333333333703, 0.3219752754296894559, 0.3333333333333333703, 0.3219752754296894559, 0.3333333333333333703, 0.3219752754296894559, 0.3333333333333333703, 0.3219752754296894559, 0.3333333333333333703, 0.3219752754296894559, 0.3333333333333333703, 0.3219752754296894559, 0.3333333333333333703, 0.3219752754296894559, 0.3333333333333333703, 0.3219752754296894559, 0.3333333333333333703, 0.3219752754296894559, 0.3333333333333333703, 0.3219752754296894559, 0.3333333333333333703, 0.3219752754296894559, 0.3333333333333333703, 0.3219752754296894559, 0.3333333333333333703, 0.3219752754296894559, 0.3333333333333333703, 0.3219752754296894559, 0.3333333333333333703, 0.3219752754296894559, 0.3333333333333333703, 0.3219752754296894559, 0.3333333333333333703, 0.3219752754296894559, 0.3333333333333333703, 0.3219752754296894559, 0.3333333333333333703, 0.3219752754296894559, 0.3333333333333333703, 0.3219752754296894559, 0.3333333333333333703, 0.3219752754296894559, 0.3333333333333333703, 0.3219752754296894559, 0.3333333333333333703, 0.3219752754296894559, 0.3333333333333333703, 0.3219752754296894559, 0.3333333333333333703, 0.3219752754296894559, 0.3333333333333333703, 0.3219752754296894559, 0.3333333333333333703, 0.3219752754296894559, 0.3333333333333333703, 0.3219752754296894559, 0.3333333333333333703, 0.3219752754296894559, 0.3333333333333333703, 0.3219752754296894559, 0.3333333333333333703, 0.3219752754296894559, 0.3333333333333333703, 0.3219752754296894559, 0.3333333333333333703, 0.3219752754296894559, 0.3333333333333333703, 0.3219752754296894559, 0.3333333333333333703, 0.3219752754296894559, 0.3333333333333333703, 0.3219752754296894559, 0.3333333333333333703, 0.3219752754296894559, 0.3333333333333333703, 0.3219752754296894559, 0.3333333333333333703, 0.3219752754296894559, 0.3333333333333333703, 0.3219752754296894559, 0.3333333333333333703, 0.3219752754296894559, 0.3333333333333333703, 0.3219752754296894559, 0.3333333333333333703, 0.3219752754296894559, 0.3333333333333333703, 0.3219752754296894559, 0.3333333333333333703, 0.3219752754296894559, 0.3333333333333333703, 0.3219752754296894559, 0.3333333333333333703, 0.3219752754296894559, 0.3333333333333333703, 0.3219752754296894559, 0.3333333333333333703, 0.3219752754296894559, 0.3333333333333333703, 0.3219752754296894559, 0.3333333333333333703, 0.3219752754296894559, 0.3333333333333333703, 0.3219752754296894559, 0.3333333333333333703, 0.3219752754296894559, 0.3333333333333333703, 0.3219752754296894559, 0.3333333333333333703, 0.3219752754296894559, 0.3333333333333333703, 0.3219752754296894559, 0.3333333333333333703, 0.3219752754296894559, 0.3333333333333333703, 0.3219752754296894559, 0.3333333333333333703, 0.3219752754296894559, 0.3333333333333333703, 0.3219752754296894559, 0.3333333333333333703, 0.3219752754296894559, 0.3333333333333333703, 0.3219752754296894559, 0.3333333333333333703, 0.3219752754296894559, 0.3333333333333333703, 0.3219752754296894559, 0.3333333333333333703, 0.3219752754296894559, 0.3333333333333333703, 0.3219752754296894559, 0.3333333333333333703, 0.3219752754296894559, 0.3333333333333333703, 0.3219752754296894559, 0.3333333333333333703, 0.3219752754296894559, 0.3333333333333333703, 0.3219752754296894559, 0.3333333333333333703, 0.3219752754296894559, 0.3333333333333333703, 0.3219752754296894559, 0.3333333333333333703, 0.3219752754296894559, 0.3333333333333333703, 0.3219752754296894559, 0.3333333333333333703, 0.3219752754296894559, 0.3333333333333333703, 0.3219752754296894559, 0.3333333333333333703, 0.3219752754296894559, 0.3333333333333333703, 0.3219752754296894559, 0.3333333333333333703, 0.3219752754296894559, 0.3333333333333333703, 0.3219752754296894559, 0.3333333333333333703, 0.3219752754296894559, 0.3333333333333333703, 0.3219752754296894559, 0.3333333333333333703, 0.3219752754296894559, 0.3333333333333333703, 0.3219752754296894559, 0.3333333333333333703, 0.3219752754296894559, 0.3333333333333333703, 0.3219752754296894559, 0.3333333333333333703, 0.3219752754296894559, 0.3333333333333333703, 0.3219752754296894559, 0.3333333333333333703, 0.3219752754296894559, 0.3333333333333333703, 0.3219752754296894559, 0.3333333333333333703, 0.3219752754296894559, 0.3333333333333333703, 0.3219752754296894559, 0.3333333333333333703, 0.3219752754296894559, 0.3333333333333333703, 0.3219752754296894559, 0.3333333333333333703, 0.3219752754296894559, 0.3333333333333333703, 0.3219752754296894559, 0.3333333333333333703, 0.3219752754296894559, 0.3333333333333333703, 0.3219752754296894559, 0.3333333333333333703, 0.3219752754296894559, 0.3333333333333333703, 0.3219752754296894559, 0.3333333333333333703, 0.3219752754296894559, 0.3333333333333333703, 0.3219752754296894559, 0.3333333333333333703, 0.3219752754296894559, 0.3333333333333333703, 0.3219752754296894559, 0.3333333333333333703, 0.3219752754296894559, 0.3333333333333333703, 0.3219752754296894559, 0.3333333333333333703, 0.3219752754296894559, 0.3333333333333333703, 0.3219752754296894559, 0.3333333333333333703, 0.3219752754296894559, 0.3333333333333333703, 0.3219752754296894559, 0.3333333333333333703, 0.3219752754296894559, 0.3333333333333333703, 0.3219752754296894559, 0.3333333333333333703, 0.3219752754296894559, 0.3333333333333333703, 0.3219752754296894559, 0.3333333333333333703, 0.3219752754296894559, 0.3333333333333333703, 0.3219752754296894559, 0.3333333333333333703, 0.3219752754296894559, 0.3333333333333333703, 0.3219752754296894559, 0.3333333333333333703, 0.3219752754296894559, 0.3333333333333333703, 0.3219752754296894559, 0.3333333333333333703, 0.3219752754296894559, 0.3333333333333333703, 0.3219752754296894559, 0.3333333333333333703, 0.3219752754296894559, 0.3333333333333333703, 0.3219752754296894559, 0.3333333333333333703, 0.3219752754296894559, 0.3333333333333333703, 0.3219752754296894559, 0.3333333333333333703, 0.3219752754296894559, 0.3333333333333333703, 0.3219752754296894559, 0.3333333333333333703, 0.3219752754296894559, 0.3333333333333333703, 0.3219752754296894559, 0.3333333333333333703, 0.3219752754296894559, 0.3333333333333333703, 0.3219752754296894559, 0.3333333333333333703, 0.3219752754296894559, 0.3333333333333333703, 0.3219752754296894559, 0.3333333333333333703, 0.3219752754296894559, 0.3333333333333333703, 0.3219752754296894559, 0.3333333333333333703, 0.3219752754296894559, 0.3333333333333333703, 0.3219752754296894559, 0.3333333333333333703, 0.3219752754296894559, 0.3333333333333333703, 0.3219752754296894559, 0.3333333333333333703, 0.3219752754296894559, 0.3333333333333333703, 0.3219752754296894559, 0.3333333333333333703, 0.3219752754296894559, 0.3333333333333333703, 0.3219752754296894559, 0.3333333333333333703, 0.3219752754296894559, 0.3333333333333333703, 0.3219752754296894559, 0.3333333333333333703, 0.3219752754296894559, 0.3333333333333333703, 0.3219752754296894559, 0.3333333333333333703, 0.3219752754296894559, 0.3333333333333333703, 0.3219752754296894559, 0.3333333333333333703, 0.3219752754296894559, 0.3333333333333333703, 0.3219752754296894559, 0.3333333333333333703, 0.3219752754296894559, 0.3333333333333333703, 0.3219752754296894559, 0.3333333333333333703, 0.3219752754296894559, 0.3333333333333333703, 0.3219752754296894559, 0.3333333333333333703, 0.3219752754296894559, 0.3333333333333333703, 0.3219752754296894559, 0.3333333333333333703, 0.3219752754296894559, 0.3333333333333333703, 0.3219752754296894559, 0.3333333333333333703, 0.3219752754296894559, 0.3333333333333333703, 0.3219752754296894559, 0.3333333333333333703, 0.3219752754296894559, 0.3333333333333333703, 0.3219752754296894559, 0.3333333333333333703, 0.3219752754296894559, 0.3333333333333333703, 0.3219752754296894559, 0.3333333333333333703, 0.3219752754296894559, 0.3333333333333333703, 0.3219752754296894559, 0.3333333333333333703, 0.3219752754296894559, 0.3333333333333333703, 0.3219752754296894559, 0.3333333333333333703, 0.3219752754296894559, 0.3333333333333333703, 0.3219752754296894559, 0.3333333333333333703, 0.3219752754296894559, 0.3333333333333333703, 0.3219752754296894559, 0.3333333333333333703, 0.3219752754296894559, 0.3333333333333333703, 0.3219752754296894559, 0.3333333333333333703, 0.3219752754296894559, 0.3333333333333333703, 0.3219752754296894559, 0.3333333333333333703, 0.3219752754296894559, 0.3333333333333333703, 0.3219752754296894559, 0.3333333333333333703, 0.3219752754296894559, 0.3333333333333333703, 0.3219752754296894559, 0.3333333333333333703, 0.3219752754296894559, 0.3333333333333333703, 0.3219752754296894559, 0.3333333333333333703, 0.3219752754296894559, 0.3333333333333333703, 0.3219752754296894559, 0.3333333333333333703, 0.3219752754296894559, 0.3333333333333333703, 0.3219752754296894559, 0.3333333333333333703, 0.3219752754296894559, 0.3333333333333333703, 0.3219752754296894559, 0.3333333333333333703, 0.3219752754296894559, 0.3333333333333333703, 0.3219752754296894559, 0.3333333333333333703, 0.3219752754296894559, 0.3333333333333333703, 0.3219752754296894559, 0.3333333333333333703, 0.3219752754296894559, 0.3333333333333333703, 0.3219752754296894559, 0.3333333333333333703, 0.3219752754296894559, 0.3333333333333333703, 0.3219752754296894559, 0.3333333333333333703, 0.3219752754296894559, 0.3333333333333333703, 0.3219752754296894559, 0.3333333333333333703, 0.3219752754296894559, 0.3333333333333333703, 0.3219752754296894559, 0.3333333333333333703, 0.3219752754296894559, 0.3333333333333333703, 0.3219752754296894559, 0.3333333333333333703, 0.3219752754296894559, 0.3333333333333333703, 0.3219752754296894559, 0.3333333333333333703, 0.3219752754296894559, 0.3333333333333333703, 0.3219752754296894559, 0.3333333333333333703, 0.3219752754296894559, 0.3333333333333333703, 0.3219752754296894559, 0.3333333333333333703, 0.3219752754296894559, 0.3333333333333333703, 0.3219752754296894559, 0.3333333333333333703, 0.3219752754296894559, 0.3333333333333333703, 0.3219752754296894559, 0.3333333333333333703, 0.3219752754296894559, 0.3333333333333333703, 0.3219752754296894559, 0.3333333333333333703, 0.3219752754296894559, 0.3333333333333333703, 0.3219752754296894559, 0.3333333333333333703, 0.3219752754296894559, 0.3333333333333333703, 0.3219752754296894559, 0.3333333333333333703, 0.3219752754296894559, 0.3333333333333333703, 0.3219752754296894559, 0.3333333333333333703, 0.3219752754296894559, 0.3333333333333333703, 0.3219752754296894559, 0.3333333333333333703, 0.3219752754296894559, 0.3333333333333333703, 0.3219752754296894559, 0.3333333333333333703),
 ( 0.3333333333333333703, 0.3219752754296894559, 0.3333333333333333703, 0.3219752754296894559, 0.3333333333333333703, 0.3219752754296894559, 0.3333333333333333703, 0.3219752754296894559, 0.3333333333333333703, 0.3219752754296894559, 0.3333333333333333703, 0.3219752754296894559, 0.3333333333333333703, 0.3219752754296894559, 0.3333333333333333703, 0.3219752754296894559, 0.3333333333333333703, 0.3219752754296894559, 0.3333333333333333703, 0.3219752754296894559, 0.3333333333333333703, 0.3219752754296894559, 0.3333333333333333703, 0.3219752754296894559, 0.3333333333333333703, 0.3219752754296894559, 0.3333333333333333703, 0.3219752754296894559, 0.3333333333333333703, 0.3219752754296894559, 0.3333333333333333703, 0.3219752754296894559, 0.3333333333333333703, 0.3219752754296894559, 0.3333333333333333703, 0.3219752754296894559, 0.3333333333333333703, 0.3219752754296894559, 0.3333333333333333703, 0.3219752754296894559, 0.3333333333333333703, 0.3219752754296894559, 0.3333333333333333703, 0.3219752754296894559, 0.3333333333333333703, 0.3219752754296894559, 0.3333333333333333703, 0.3219752754296894559, 0.3333333333333333703, 0.3219752754296894559, 0.3333333333333333703, 0.3219752754296894559, 0.3333333333333333703, 0.3219752754296894559, 0.3333333333333333703, 0.3219752754296894559, 0.3333333333333333703, 0.3219752754296894559, 0.3333333333333333703, 0.3219752754296894559, 0.3333333333333333703, 0.3219752754296894559, 0.3333333333333333703, 0.3219752754296894559, 0.3333333333333333703, 0.3219752754296894559, 0.3333333333333333703, 0.3219752754296894559, 0.3333333333333333703, 0.3219752754296894559, 0.3333333333333333703, 0.3219752754296894559, 0.3333333333333333703, 0.3219752754296894559, 0.3333333333333333703, 0.3219752754296894559, 0.3333333333333333703, 0.3219752754296894559, 0.3333333333333333703, 0.3219752754296894559, 0.3333333333333333703, 0.3219752754296894559, 0.3333333333333333703, 0.3219752754296894559, 0.3333333333333333703, 0.3219752754296894559, 0.3333333333333333703, 0.3219752754296894559, 0.3333333333333333703, 0.3219752754296894559, 0.3333333333333333703, 0.3219752754296894559, 0.3333333333333333703, 0.3219752754296894559, 0.3333333333333333703, 0.3219752754296894559, 0.3333333333333333703, 0.3219752754296894559, 0.3333333333333333703, 0.3219752754296894559, 0.3333333333333333703, 0.3219752754296894559, 0.3333333333333333703, 0.3219752754296894559, 0.3333333333333333703, 0.3219752754296894559, 0.3333333333333333703, 0.3219752754296894559, 0.3333333333333333703, 0.3219752754296894559, 0.3333333333333333703, 0.3219752754296894559, 0.3333333333333333703, 0.3219752754296894559, 0.3333333333333333703, 0.3219752754296894559, 0.3333333333333333703, 0.3219752754296894559, 0.3333333333333333703, 0.3219752754296894559, 0.3333333333333333703, 0.3219752754296894559, 0.3333333333333333703, 0.3219752754296894559, 0.3333333333333333703, 0.3219752754296894559, 0.3333333333333333703, 0.3219752754296894559, 0.3333333333333333703, 0.3219752754296894559, 0.3333333333333333703, 0.3219752754296894559, 0.3333333333333333703, 0.3219752754296894559, 0.3333333333333333703, 0.3219752754296894559, 0.3333333333333333703, 0.3219752754296894559, 0.3333333333333333703, 0.3219752754296894559, 0.3333333333333333703, 0.3219752754296894559, 0.3333333333333333703, 0.3219752754296894559, 0.3333333333333333703, 0.3219752754296894559, 0.3333333333333333703, 0.3219752754296894559, 0.3333333333333333703, 0.3219752754296894559, 0.3333333333333333703, 0.3219752754296894559, 0.3333333333333333703, 0.3219752754296894559, 0.3333333333333333703, 0.3219752754296894559, 0.3333333333333333703, 0.3219752754296894559, 0.3333333333333333703, 0.3219752754296894559, 0.3333333333333333703, 0.3219752754296894559, 0.3333333333333333703, 0.3219752754296894559, 0.3333333333333333703, 0.3219752754296894559, 0.3333333333333333703, 0.3219752754296894559, 0.3333333333333333703, 0.3219752754296894559, 0.3333333333333333703, 0.3219752754296894559, 0.3333333333333333703, 0.3219752754296894559, 0.3333333333333333703, 0.3219752754296894559, 0.3333333333333333703, 0.3219752754296894559, 0.3333333333333333703, 0.3219752754296894559, 0.3333333333333333703, 0.3219752754296894559, 0.3333333333333333703, 0.3219752754296894559, 0.3333333333333333703, 0.3219752754296894559, 0.3333333333333333703, 0.3219752754296894559, 0.3333333333333333703, 0.3219752754296894559, 0.3333333333333333703, 0.3219752754296894559, 0.3333333333333333703, 0.3219752754296894559, 0.3333333333333333703, 0.3219752754296894559, 0.3333333333333333703, 0.3219752754296894559, 0.3333333333333333703, 0.3219752754296894559, 0.3333333333333333703, 0.3219752754296894559, 0.3333333333333333703, 0.3219752754296894559, 0.3333333333333333703, 0.3219752754296894559, 0.3333333333333333703, 0.3219752754296894559, 0.3333333333333333703, 0.3219752754296894559, 0.3333333333333333703, 0.3219752754296894559, 0.3333333333333333703, 0.3219752754296894559, 0.3333333333333333703, 0.3219752754296894559, 0.3333333333333333703, 0.3219752754296894559, 0.3333333333333333703, 0.3219752754296894559, 0.3333333333333333703, 0.3219752754296894559, 0.3333333333333333703, 0.3219752754296894559, 0.3333333333333333703, 0.3219752754296894559, 0.3333333333333333703, 0.3219752754296894559, 0.3333333333333333703, 0.3219752754296894559, 0.3333333333333333703, 0.3219752754296894559, 0.3333333333333333703, 0.3219752754296894559, 0.3333333333333333703, 0.3219752754296894559, 0.3333333333333333703, 0.3219752754296894559, 0.3333333333333333703, 0.3219752754296894559, 0.3333333333333333703, 0.3219752754296894559, 0.3333333333333333703, 0.3219752754296894559, 0.3333333333333333703, 0.3219752754296894559, 0.3333333333333333703, 0.3219752754296894559, 0.3333333333333333703, 0.3219752754296894559, 0.3333333333333333703, 0.3219752754296894559, 0.3333333333333333703, 0.3219752754296894559, 0.3333333333333333703, 0.3219752754296894559, 0.3333333333333333703, 0.3219752754296894559, 0.3333333333333333703, 0.3219752754296894559, 0.3333333333333333703, 0.3219752754296894559, 0.3333333333333333703, 0.3219752754296894559, 0.3333333333333333703, 0.3219752754296894559, 0.3333333333333333703, 0.3219752754296894559, 0.3333333333333333703, 0.3219752754296894559, 0.3333333333333333703, 0.3219752754296894559, 0.3333333333333333703, 0.3219752754296894559, 0.3333333333333333703, 0.3219752754296894559, 0.3333333333333333703, 0.3219752754296894559, 0.3333333333333333703, 0.3219752754296894559, 0.3333333333333333703, 0.3219752754296894559, 0.3333333333333333703, 0.3219752754296894559, 0.3333333333333333703, 0.3219752754296894559, 0.3333333333333333703, 0.3219752754296894559, 0.3333333333333333703, 0.3219752754296894559, 0.3333333333333333703, 0.3219752754296894559, 0.3333333333333333703, 0.3219752754296894559, 0.3333333333333333703, 0.3219752754296894559, 0.3333333333333333703, 0.3219752754296894559, 0.3333333333333333703, 0.3219752754296894559, 0.3333333333333333703, 0.3219752754296894559, 0.3333333333333333703, 0.3219752754296894559, 0.3333333333333333703, 0.3219752754296894559, 0.3333333333333333703, 0.3219752754296894559, 0.3333333333333333703, 0.3219752754296894559, 0.3333333333333333703, 0.3219752754296894559, 0.3333333333333333703, 0.3219752754296894559, 0.3333333333333333703, 0.3219752754296894559, 0.3333333333333333703, 0.3219752754296894559, 0.3333333333333333703, 0.3219752754296894559, 0.3333333333333333703, 0.3219752754296894559, 0.3333333333333333703, 0.3219752754296894559, 0.3333333333333333703, 0.3219752754296894559, 0.3333333333333333703, 0.3219752754296894559, 0.3333333333333333703, 0.3219752754296894559, 0.3333333333333333703, 0.3219752754296894559, 0.3333333333333333703, 0.3219752754296894559, 0.3333333333333333703, 0.3219752754296894559, 0.3333333333333333703, 0.3219752754296894559, 0.3333333333333333703, 0.3219752754296894559, 0.3333333333333333703, 0.3219752754296894559, 0.3333333333333333703, 0.3219752754296894559, 0.3333333333333333703, 0.3219752754296894559, 0.3333333333333333703, 0.3219752754296894559, 0.3333333333333333703, 0.3219752754296894559, 0.3333333333333333703, 0.3219752754296894559, 0.3333333333333333703, 0.3219752754296894559, 0.3333333333333333703, 0.3219752754296894559, 0.3333333333333333703, 0.3219752754296894559, 0.3333333333333333703, 0.3219752754296894559, 0.3333333333333333703, 0.3219752754296894559, 0.3333333333333333703, 0.3219752754296894559, 0.3333333333333333703, 0.3219752754296894559, 0.3333333333333333703, 0.3219752754296894559, 0.3333333333333333703, 0.3219752754296894559, 0.3333333333333333703, 0.3219752754296894559, 0.3333333333333333703, 0.3219752754296894559, 0.3333333333333333703, 0.3219752754296894559, 0.3333333333333333703, 0.3219752754296894559, 0.3333333333333333703, 0.3219752754296894559, 0.3333333333333333703, 0.3219752754296894559, 0.3333333333333333703, 0.3219752754296894559, 0.3333333333333333703, 0.3219752754296894559, 0.3333333333333333703, 0.3219752754296894559, 0.3333333333333333703, 0.3219752754296894559, 0.3333333333333333703, 0.3219752754296894559, 0.3333333333333333703, 0.3219752754296894559, 0.3333333333333333703, 0.3219752754296894559, 0.3333333333333333703, 0.3219752754296894559, 0.3333333333333333703, 0.3219752754296894559, 0.3333333333333333703, 0.3219752754296894559, 0.3333333333333333703, 0.3219752754296894559, 0.3333333333333333703, 0.3219752754296894559, 0.3333333333333333703, 0.3219752754296894559, 0.3333333333333333703, 0.3219752754296894559, 0.3333333333333333703, 0.3219752754296894559, 0.3333333333333333703, 0.3219752754296894559, 0.3333333333333333703, 0.3219752754296894559, 0.3333333333333333703, 0.3219752754296894559, 0.3333333333333333703, 0.3219752754296894559, 0.3333333333333333703, 0.3219752754296894559, 0.3333333333333333703, 0.3219752754296894559, 0.3333333333333333703, 0.3219752754296894559, 0.3333333333333333703, 0.3219752754296894559, 0.3333333333333333703, 0.3219752754296894559, 0.3333333333333333703, 0.3219752754296894559, 0.3333333333333333703, 0.3219752754296894559, 0.3333333333333333703, 0.3219752754296894559, 0.3333333333333333703, 0.3219752754296894559, 0.3333333333333333703, 0.3219752754296894559, 0.3333333333333333703, 0.3219752754296894559, 0.3333333333333333703, 0.3219752754296894559, 0.3333333333333333703, 0.3219752754296894559, 0.3333333333333333703, 0.3219752754296894559, 0.3333333333333333703, 0.3219752754296894559, 0.3333333333333333703, 0.3219752754296894559, 0.3333333333333333703, 0.3219752754296894559, 0.3333333333333333703, 0.3219752754296894559, 0.3333333333333333703),
 ( 1.000000000000000000, 0.9659258262890683122, 1.000000000000000000, 0.9659258262890683122, 1.000000000000000000, 0.9659258262890683122, 1.000000000000000000, 0.9659258262890683122, 1.000000000000000000, 0.9659258262890683122, 1.000000000000000000, 0.9659258262890683122, 1.000000000000000000, 0.9659258262890683122, 1.000000000000000000, 0.9659258262890683122, 1.000000000000000000, 0.9659258262890683122, 1.000000000000000000, 0.9659258262890683122, 1.000000000000000000, 0.9659258262890683122, 1.000000000000000000, 0.9659258262890683122, 1.000000000000000000, 0.9659258262890683122, 1.000000000000000000, 0.9659258262890683122, 1.000000000000000000, 0.9659258262890683122, 1.000000000000000000, 0.9659258262890683122, 1.000000000000000000, 0.9659258262890683122, 1.000000000000000000, 0.9659258262890683122, 1.000000000000000000, 0.9659258262890683122, 1.000000000000000000, 0.9659258262890683122, 1.000000000000000000, 0.9659258262890683122, 1.000000000000000000, 0.9659258262890683122, 1.000000000000000000, 0.9659258262890683122, 1.000000000000000000, 0.9659258262890683122, 1.000000000000000000, 0.9659258262890683122, 1.000000000000000000, 0.9659258262890683122, 1.000000000000000000, 0.9659258262890683122, 1.000000000000000000, 0.9659258262890683122, 1.000000000000000000, 0.9659258262890683122, 1.000000000000000000, 0.9659258262890683122, 1.000000000000000000, 0.9659258262890683122, 1.000000000000000000, 0.9659258262890683122, 1.000000000000000000, 0.9659258262890683122, 1.000000000000000000, 0.9659258262890683122, 1.000000000000000000, 0.9659258262890683122, 1.000000000000000000, 0.9659258262890683122, 1.000000000000000000, 0.9659258262890683122, 1.000000000000000000, 0.9659258262890683122, 1.000000000000000000, 0.9659258262890683122, 1.000000000000000000, 0.9659258262890683122, 1.000000000000000000, 0.9659258262890683122, 1.000000000000000000, 0.9659258262890683122, 1.000000000000000000, 0.9659258262890683122, 1.000000000000000000, 0.9659258262890683122, 1.000000000000000000, 0.9659258262890683122, 1.000000000000000000, 0.9659258262890683122, 1.000000000000000000, 0.9659258262890683122, 1.000000000000000000, 0.9659258262890683122, 1.000000000000000000, 0.9659258262890683122, 1.000000000000000000, 0.9659258262890683122, 1.000000000000000000, 0.9659258262890683122, 1.000000000000000000, 0.9659258262890683122, 1.000000000000000000, 0.9659258262890683122, 1.000000000000000000, 0.9659258262890683122, 1.000000000000000000, 0.9659258262890683122, 1.000000000000000000, 0.9659258262890683122, 1.000000000000000000, 0.9659258262890683122, 1.000000000000000000, 0.9659258262890683122, 1.000000000000000000, 0.9659258262890683122, 1.000000000000000000, 0.9659258262890683122, 1.000000000000000000, 0.9659258262890683122, 1.000000000000000000, 0.9659258262890683122, 1.000000000000000000, 0.9659258262890683122, 1.000000000000000000, 0.9659258262890683122, 1.000000000000000000, 0.9659258262890683122, 1.000000000000000000, 0.9659258262890683122, 1.000000000000000000, 0.9659258262890683122, 1.000000000000000000, 0.9659258262890683122, 1.000000000000000000, 0.9659258262890683122, 1.000000000000000000, 0.9659258262890683122, 1.000000000000000000, 0.9659258262890683122, 1.000000000000000000, 0.9659258262890683122, 1.000000000000000000, 0.9659258262890683122, 1.000000000000000000, 0.9659258262890683122, 1.000000000000000000, 0.9659258262890683122, 1.000000000000000000, 0.9659258262890683122, 1.000000000000000000, 0.9659258262890683122, 1.000000000000000000, 0.9659258262890683122, 1.000000000000000000, 0.9659258262890683122, 1.000000000000000000, 0.9659258262890683122, 1.000000000000000000, 0.9659258262890683122, 1.000000000000000000, 0.9659258262890683122, 1.000000000000000000, 0.9659258262890683122, 1.000000000000000000, 0.9659258262890683122, 1.000000000000000000, 0.9659258262890683122, 1.000000000000000000, 0.9659258262890683122, 1.000000000000000000, 0.9659258262890683122, 1.000000000000000000, 0.9659258262890683122, 1.000000000000000000, 0.9659258262890683122, 1.000000000000000000, 0.9659258262890683122, 1.000000000000000000, 0.9659258262890683122, 1.000000000000000000, 0.9659258262890683122, 1.000000000000000000, 0.9659258262890683122, 1.000000000000000000, 0.9659258262890683122, 1.000000000000000000, 0.9659258262890683122, 1.000000000000000000, 0.9659258262890683122, 1.000000000000000000, 0.9659258262890683122, 1.000000000000000000, 0.9659258262890683122, 1.000000000000000000, 0.9659258262890683122, 1.000000000000000000, 0.9659258262890683122, 1.000000000000000000, 0.9659258262890683122, 1.000000000000000000, 0.9659258262890683122, 1.000000000000000000, 0.9659258262890683122, 1.000000000000000000, 0.9659258262890683122, 1.000000000000000000, 0.9659258262890683122, 1.000000000000000000, 0.9659258262890683122, 1.000000000000000000, 0.9659258262890683122, 1.000000000000000000, 0.9659258262890683122, 1.000000000000000000, 0.9659258262890683122, 1.000000000000000000, 0.9659258262890683122, 1.000000000000000000, 0.9659258262890683122, 1.000000000000000000, 0.9659258262890683122, 1.000000000000000000, 0.9659258262890683122, 1.000000000000000000, 0.9659258262890683122, 1.000000000000000000, 0.9659258262890683122, 1.000000000000000000, 0.9659258262890683122, 1.000000000000000000, 0.9659258262890683122, 1.000000000000000000, 0.9659258262890683122, 1.000000000000000000, 0.9659258262890683122, 1.000000000000000000, 0.9659258262890683122, 1.000000000000000000, 0.9659258262890683122, 1.000000000000000000, 0.9659258262890683122, 1.000000000000000000, 0.9659258262890683122, 1.000000000000000000, 0.9659258262890683122, 1.000000000000000000, 0.9659258262890683122, 1.000000000000000000, 0.9659258262890683122, 1.000000000000000000, 0.9659258262890683122, 1.000000000000000000, 0.9659258262890683122, 1.000000000000000000, 0.9659258262890683122, 1.000000000000000000, 0.9659258262890683122, 1.000000000000000000, 0.9659258262890683122, 1.000000000000000000, 0.9659258262890683122, 1.000000000000000000, 0.9659258262890683122, 1.000000000000000000, 0.9659258262890683122, 1.000000000000000000, 0.9659258262890683122, 1.000000000000000000, 0.9659258262890683122, 1.000000000000000000, 0.9659258262890683122, 1.000000000000000000, 0.9659258262890683122, 1.000000000000000000, 0.9659258262890683122, 1.000000000000000000, 0.9659258262890683122, 1.000000000000000000, 0.9659258262890683122, 1.000000000000000000, 0.9659258262890683122, 1.000000000000000000, 0.9659258262890683122, 1.000000000000000000, 0.9659258262890683122, 1.000000000000000000, 0.9659258262890683122, 1.000000000000000000, 0.9659258262890683122, 1.000000000000000000, 0.9659258262890683122, 1.000000000000000000, 0.9659258262890683122, 1.000000000000000000, 0.9659258262890683122, 1.000000000000000000, 0.9659258262890683122, 1.000000000000000000, 0.9659258262890683122, 1.000000000000000000, 0.9659258262890683122, 1.000000000000000000, 0.9659258262890683122, 1.000000000000000000, 0.9659258262890683122, 1.000000000000000000, 0.9659258262890683122, 1.000000000000000000, 0.9659258262890683122, 1.000000000000000000, 0.9659258262890683122, 1.000000000000000000, 0.9659258262890683122, 1.000000000000000000, 0.9659258262890683122, 1.000000000000000000, 0.9659258262890683122, 1.000000000000000000, 0.9659258262890683122, 1.000000000000000000, 0.9659258262890683122, 1.000000000000000000, 0.9659258262890683122, 1.000000000000000000, 0.9659258262890683122, 1.000000000000000000, 0.9659258262890683122, 1.000000000000000000, 0.9659258262890683122, 1.000000000000000000, 0.9659258262890683122, 1.000000000000000000, 0.9659258262890683122, 1.000000000000000000, 0.9659258262890683122, 1.000000000000000000, 0.9659258262890683122, 1.000000000000000000, 0.9659258262890683122, 1.000000000000000000, 0.9659258262890683122, 1.000000000000000000, 0.9659258262890683122, 1.000000000000000000, 0.9659258262890683122, 1.000000000000000000, 0.9659258262890683122, 1.000000000000000000, 0.9659258262890683122, 1.000000000000000000, 0.9659258262890683122, 1.000000000000000000, 0.9659258262890683122, 1.000000000000000000, 0.9659258262890683122, 1.000000000000000000, 0.9659258262890683122, 1.000000000000000000, 0.9659258262890683122, 1.000000000000000000, 0.9659258262890683122, 1.000000000000000000, 0.9659258262890683122, 1.000000000000000000, 0.9659258262890683122, 1.000000000000000000, 0.9659258262890683122, 1.000000000000000000, 0.9659258262890683122, 1.000000000000000000, 0.9659258262890683122, 1.000000000000000000, 0.9659258262890683122, 1.000000000000000000, 0.9659258262890683122, 1.000000000000000000, 0.9659258262890683122, 1.000000000000000000, 0.9659258262890683122, 1.000000000000000000, 0.9659258262890683122, 1.000000000000000000, 0.9659258262890683122, 1.000000000000000000, 0.9659258262890683122, 1.000000000000000000, 0.9659258262890683122, 1.000000000000000000, 0.9659258262890683122, 1.000000000000000000, 0.9659258262890683122, 1.000000000000000000, 0.9659258262890683122, 1.000000000000000000, 0.9659258262890683122, 1.000000000000000000, 0.9659258262890683122, 1.000000000000000000, 0.9659258262890683122, 1.000000000000000000, 0.9659258262890683122, 1.000000000000000000, 0.9659258262890683122, 1.000000000000000000, 0.9659258262890683122, 1.000000000000000000, 0.9659258262890683122, 1.000000000000000000, 0.9659258262890683122, 1.000000000000000000, 0.9659258262890683122, 1.000000000000000000, 0.9659258262890683122, 1.000000000000000000, 0.9659258262890683122, 1.000000000000000000, 0.9659258262890683122, 1.000000000000000000, 0.9659258262890683122, 1.000000000000000000, 0.9659258262890683122, 1.000000000000000000, 0.9659258262890683122, 1.000000000000000000, 0.9659258262890683122, 1.000000000000000000, 0.9659258262890683122, 1.000000000000000000, 0.9659258262890683122, 1.000000000000000000, 0.9659258262890683122, 1.000000000000000000, 0.9659258262890683122, 1.000000000000000000, 0.9659258262890683122, 1.000000000000000000, 0.9659258262890683122, 1.000000000000000000, 0.9659258262890683122, 1.000000000000000000, 0.9659258262890683122, 1.000000000000000000, 0.9659258262890683122, 1.000000000000000000, 0.9659258262890683122, 1.000000000000000000, 0.9659258262890683122, 1.000000000000000000, 0.9659258262890683122, 1.000000000000000000, 0.9659258262890683122, 1.000000000000000000, 0.9659258262890683122, 1.000000000000000000) ) ) 
 REPRESENTATION_ITEM ( '' )  SURFACE ( )  );
#142379 = CARTESIAN_POINT ( 'NONE',  ( -4.483927247898782831, 16.52544592524335698, 42.70942372801901854 ) ) ;
#142382 = CARTESIAN_POINT ( 'NONE',  ( -5.823673210054431948, 21.52544592524334988, 57.70942372801901143 ) ) ;
#142383 = CARTESIAN_POINT ( 'NONE',  ( 13.89961937509957401, 13.97604488694547697, 111.8760903946856757 ) ) ;
#142384 = CARTESIAN_POINT ( 'NONE',  ( 0.05219959533909260263, 19.03943276465977164, 59.99890960531436690 ) ) ;
#142385 = CARTESIAN_POINT ( 'NONE',  ( 16.51473224551083163, -9.474510206698727899, 85.83442372801900433 ) ) ;
#142386 = CARTESIAN_POINT ( 'NONE',  ( 21.52544592524334988, 5.823673210054432836, 86.45942372801901854 ) ) ;
#142387 = CARTESIAN_POINT ( 'NONE',  ( 5.153800228976615827, -19.02544592524334988, 70.20942372801899012 ) ) ;
#142388 = CARTESIAN_POINT ( 'NONE',  ( -19.03943276465977164, 0.05219959533909376836, 41.24890960531435269 ) ) ;
#142389 = CARTESIAN_POINT ( 'NONE',  ( -0.05219959533907301413, -21.53943276465977519, 57.49890960531435979 ) ) ;
#142391 = CARTESIAN_POINT ( 'NONE',  ( 5.153800228976615827, -19.02544592524334988, 65.20942372801900433 ) ) ;
#142390 = CARTESIAN_POINT ( 'NONE',  ( 16.52544592524342804, -4.483927247898539470, 68.54057627198103830 ) ) ;
#142392 = CARTESIAN_POINT ( 'NONE',  ( -16.19135201231362942, -7.376712067592052335, 25.18680854052033169 ) ) ;
#142393 = CARTESIAN_POINT ( 'NONE',  ( 16.46253265017146816, 9.564922557961045513, 26.66775706135234003 ) ) ;
#142394 = CARTESIAN_POINT ( 'NONE',  ( 16.52544592524335698, 4.483927247898782831, 101.4594237280190185 ) ) ;
#142395 = CARTESIAN_POINT ( 'NONE',  ( 16.53943276465976808, -0.05219959533910856209, 48.74890960531435979 ) ) ;
#142397 = CARTESIAN_POINT ( 'NONE',  ( -27.73933785331498925, 2.428612866367529932E-14, 149.3750000027311842 ) ) ;
#142396 = CARTESIAN_POINT ( 'NONE',  ( 0.05219959533937995610, -21.53943276465977519, 90.00109039468567573 ) ) ;
#142398 = CARTESIAN_POINT ( 'NONE',  ( -10.81492255796105439, 18.62759615963255655, 92.91775706135236135 ) ) ;
#142399 = CARTESIAN_POINT ( 'NONE',  ( 15.72974639402199770, -15.80617190586745480, 98.12390960531436690 ) ) ;
#142400 = CARTESIAN_POINT ( 'NONE',  ( -13.89961937509977652, 13.97604488694528158, 45.62390960531433848 ) ) ;
#142401 = CARTESIAN_POINT ( 'NONE',  ( -10.81492255796105439, 18.62759615963255655, 67.91775706135234714 ) ) ;
#142402 = CARTESIAN_POINT ( 'NONE',  ( -16.51473224551069308, -9.474510206698971260, 51.66557627198102409 ) ) ;
#142403 = EDGE_LOOP ( 'NONE', ( #52806, #6646 ) ) ;
#142404 = CARTESIAN_POINT ( 'NONE',  ( -19.03943276465977164, 0.05219959533909376836, 71.24890960531435269 ) ) ;
#142405 = CARTESIAN_POINT ( 'NONE',  ( 12.14591786802309770, 12.06949235617756955, 104.3739096053143669 ) ) ;
#142406 = CARTESIAN_POINT ( 'NONE',  ( -13.97604488694527625, -13.89961937509977652, 111.8739096053143243 ) ) ;
#142407 = CARTESIAN_POINT ( 'NONE',  ( 14.29746914071049879, -8.314922557960816363, 53.33224293864769550 ) ) ;
#142408 = CARTESIAN_POINT ( 'NONE',  ( 5.153800228976335163, 19.02544592524342804, 29.79057627198102409 ) ) ;
#142409 = CARTESIAN_POINT ( 'NONE',  ( -8.224510206698948167, 14.34966873604960824, 75.41557627198102409 ) ) ;
#142410 = CARTESIAN_POINT ( 'NONE',  ( -15.80617190586745835, -15.72974639402198527, 91.87390960531436690 ) ) ;
#142411 = CARTESIAN_POINT ( 'NONE',  ( 21.52544592524334988, 5.823673210054432836, 36.45942372801901143 ) ) ;
#142412 = CARTESIAN_POINT ( 'NONE',  ( 13.89961937509977652, -13.97604488694527269, 23.12390960531436335 ) ) ;
#142413 = CARTESIAN_POINT ( 'NONE',  ( 14.34966873604972726, -8.224510206698740333, 35.83442372801901143 ) ) ;
#142414 = CARTESIAN_POINT ( 'NONE',  ( -10.72451020669898014, 18.67979575497178502, 90.41557627198103830 ) ) ;
#142415 = CARTESIAN_POINT ( 'NONE',  ( 21.53943276465977519, 0.05219959533937863772, 106.2510903946856757 ) ) ;
#142416 = CARTESIAN_POINT ( 'NONE',  ( 9.474510206698971260, -16.51473224551069308, 87.91557627198102409 ) ) ;
#142417 = CARTESIAN_POINT ( 'NONE',  ( -21.55341960407619339, 5.719274019375674811, 38.54275706135234714 ) ) ;
#142418 = CARTESIAN_POINT ( 'NONE',  ( 21.53943276465977519, -0.05219959533907433946, 28.74890960531435624 ) ) ;
#142419 = CARTESIAN_POINT ( 'NONE',  ( -12.06949235617739369, -12.14591786802326823, 104.3760903946856899 ) ) ;
#142421 = CARTESIAN_POINT ( 'NONE',  ( -18.62759615963255300, -10.81492255796106328, 84.16775706135234714 ) ) ;
#142420 = CARTESIAN_POINT ( 'NONE',  ( -15.80617190586768217, 15.72974639402176855, 53.12609039468568284 ) ) ;
#142422 = CARTESIAN_POINT ( 'NONE',  ( 16.46253265017146816, 9.564922557961045513, 31.66775706135232937 ) ) ;
#142423 = CARTESIAN_POINT ( 'NONE',  ( 4.483927247898790824, -16.52544592524335698, 90.20942372801903275 ) ) ;
#142424 = CARTESIAN_POINT ( 'NONE',  ( -10.72451020669870658, -18.67979575497194134, 39.58442372801901143 ) ) ;
#142425 = CARTESIAN_POINT ( 'NONE',  ( 19.02544592524343514, -5.153800228976328945, 28.54057627198102409 ) ) ;
#142426 = CARTESIAN_POINT ( 'NONE',  ( -15.72974639402176322, -15.80617190586768395, 109.3760903946857042 ) ) ;
#142427 = CARTESIAN_POINT ( 'NONE',  ( -13.89961937509977652, 13.97604488694528158, 105.6239096053143527 ) ) ;
#142428 = CARTESIAN_POINT ( 'NONE',  ( 18.67979575497178502, 10.72451020669898547, 99.16557627198100988 ) ) ;
#142429 = CARTESIAN_POINT ( 'NONE',  ( 15.80617190586746368, 15.72974639402197994, 64.37390960531435269 ) ) ;
#142431 = CARTESIAN_POINT ( 'NONE',  ( 15.72974639402199770, -15.80617190586745480, 63.12390960531435979 ) ) ;
#142430 = CARTESIAN_POINT ( 'NONE',  ( -6.677994727576217926, -3.424326230466338661, 8.646741581399133736 ) ) ;
#142433 = CARTESIAN_POINT ( 'NONE',  ( 4.379528057220339221, -16.55341960407611168, 57.70724293864770260 ) ) ;
#142432 = CARTESIAN_POINT ( 'NONE',  ( 8.224510206698742110, 14.34966873604972548, 47.08442372801901854 ) ) ;
#142434 = CARTESIAN_POINT ( 'NONE',  ( 1.988064558232696151E-15, -30.27659582821216588, 146.7656553485623760 ) ) ;
#142435 = CARTESIAN_POINT ( 'NONE',  ( -5.049401038297874678, -19.05341960407617918, 89.79275706135230450 ) ) ;
#142436 = CARTESIAN_POINT ( 'NONE',  ( -24.20415418211123537, 0.5379555815581192890, -54.28961862586981368 ) ) ;
#142437 = EDGE_CURVE ( 'NONE', #39277, #12274, #163444, .T. ) ;
#142438 = CARTESIAN_POINT ( 'NONE',  ( 4.483927247898790824, -16.52544592524335698, 20.20942372801900788 ) ) ;
#142439 = CARTESIAN_POINT ( 'NONE',  ( 0.05219959533907565091, 21.53943276465977519, 104.9989096053143669 ) ) ;
#142440 = CARTESIAN_POINT ( 'NONE',  ( -0.05219959533907301413, -21.53943276465977519, 77.49890960531433848 ) ) ;
#142441 = CARTESIAN_POINT ( 'NONE',  ( 10.81492255796078972, 18.62759615963270932, 24.58224293864768839 ) ) ;
#142442 = CARTESIAN_POINT ( 'NONE',  ( 4.379528057220092307, 16.55341960407617563, 62.29275706135236845 ) ) ;
#142443 = CARTESIAN_POINT ( 'NONE',  ( -13.97604488694527625, -13.89961937509977652, 76.87390960531433848 ) ) ;
#142445 = CARTESIAN_POINT ( 'NONE',  ( 12.06949235617739724, 12.14591786802326823, 21.87609039468567573 ) ) ;
#142444 = CARTESIAN_POINT ( 'NONE',  ( -21.55341960407619339, 5.719274019375674811, 33.54275706135234714 ) ) ;
#142446 = CARTESIAN_POINT ( 'NONE',  ( -16.51473224551069308, -9.474510206698971260, 111.6655762719810383 ) ) ;
#142447 = CARTESIAN_POINT ( 'NONE',  ( -0.05219959533909027116, -19.03943276465977164, 82.49890960531436690 ) ) ;
#142448 = CARTESIAN_POINT ( 'NONE',  ( -18.62759615963270932, 10.81492255796079327, 85.83224293864768129 ) ) ;
#142449 = CARTESIAN_POINT ( 'NONE',  ( 19.02544592524343514, -5.153800228976328945, 63.54057627198103830 ) ) ;
#142450 = CARTESIAN_POINT ( 'NONE',  ( -16.61371651742604527, -7.165104196376050893, 61.14584930007005426 ) ) ;
#142451 = CARTESIAN_POINT ( 'NONE',  ( 8.314922557960818139, 14.29746914071049879, 64.58224293864769550 ) ) ;
#142452 = CARTESIAN_POINT ( 'NONE',  ( -15.72974639402197994, 15.80617190586746368, 25.62390960531435624 ) ) ;
#142453 = CARTESIAN_POINT ( 'NONE',  ( -31.82351365011400901, 0.4884129450686308105, -49.22894560581806900 ) ) ;
#142454 = CARTESIAN_POINT ( 'NONE',  ( -18.62759615963270932, 10.81492255796079327, 110.8322429386476955 ) ) ;
#142455 = CARTESIAN_POINT ( 'NONE',  ( 9.474510206698729675, 16.51473224551082808, 62.08442372801899722 ) ) ;
#142456 = CARTESIAN_POINT ( 'NONE',  ( 19.05341960407611168, 5.049401038298154454, 108.9572429386477097 ) ) ;
#142457 = CARTESIAN_POINT ( 'NONE',  ( 11.30153831258469843, -180.0000000000000000, -15.00000000000000000 ) ) ;
#142458 = CARTESIAN_POINT ( 'NONE',  ( -18.62759615963270932, 10.81492255796079327, 50.83224293864770971 ) ) ;
#142459 = CARTESIAN_POINT ( 'NONE',  ( -5.049401038298153566, 19.05341960407611168, 90.20724293864766707 ) ) ;
#142460 = CARTESIAN_POINT ( 'NONE',  ( -21.53943276465977519, -0.05219959533937600094, 78.75109039468568994 ) ) ;
#142461 = CARTESIAN_POINT ( 'NONE',  ( -16.51473224551069308, -9.474510206698971260, 56.66557627198103120 ) ) ;
#142462 = EDGE_CURVE ( 'NONE', #57160, #155489, #194782, .T. ) ;
#142463 = CARTESIAN_POINT ( 'NONE',  ( -12.14591786802309592, -12.06949235617757132, 81.87390960531435269 ) ) ;
#142464 = CARTESIAN_POINT ( 'NONE',  ( -4.379528057220086978, -16.55341960407618274, 34.79275706135235424 ) ) ;
#142465 = CARTESIAN_POINT ( 'NONE',  ( 18.62759615963255655, 10.81492255796105972, 66.66775706135234714 ) ) ;
#142466 = ORIENTED_EDGE ( 'NONE', *, *, #130384, .T. ) ;
#142467 = CARTESIAN_POINT ( 'NONE',  ( 19.03943276465977164, 0.05219959533936151252, 26.25109039468566507 ) ) ;
#142468 = CARTESIAN_POINT ( 'NONE',  ( -19.05341960407617563, 5.049401038297882671, 78.54275706135233293 ) ) ;
#142469 = CARTESIAN_POINT ( 'NONE',  ( 16.51473224551083163, -9.474510206698727899, 40.83442372801900433 ) ) ;
#142470 = CARTESIAN_POINT ( 'NONE',  ( -6.020228577223754586E-15, 39.95556452105416412, -6.249999994537626336 ) ) ;
#142471 = CARTESIAN_POINT ( 'NONE',  ( -5.719274019375665041, -21.55341960407619695, 39.79275706135235424 ) ) ;
#142472 = CARTESIAN_POINT ( 'NONE',  ( -30.74264578624800492, 22.33583958711400186, -1.949999994537626735 ) ) ;
#142473 = CARTESIAN_POINT ( 'NONE',  ( -16.46253265017146816, -9.564922557961047289, 39.16775706135234003 ) ) ;
#142474 = CARTESIAN_POINT ( 'NONE',  ( -13.97604488694527625, -13.89961937509977652, 51.87390960531436690 ) ) ;
#142475 = CARTESIAN_POINT ( 'NONE',  ( 9.564922557961047289, -16.46253265017146816, 35.41775706135233293 ) ) ;
#142476 = CARTESIAN_POINT ( 'NONE',  ( -14.29746914071037622, -8.314922557961029526, 99.16775706135234714 ) ) ;
#142478 = CARTESIAN_POINT ( 'NONE',  ( -5.823673210054431948, 21.52544592524334988, 82.70942372801900433 ) ) ;
#142477 = CARTESIAN_POINT ( 'NONE',  ( 9.564922557960805705, 16.46253265017160317, 109.5822429386476955 ) ) ;
#142479 = CARTESIAN_POINT ( 'NONE',  ( -22.81625015709510507, 31.40387420917330275, -6.924999997268812990 ) ) ;
#142480 = CARTESIAN_POINT ( 'NONE',  ( -33.68482864984028424, 4.779698632210292786, 97.74495643025990432 ) ) ;
#142481 = CARTESIAN_POINT ( 'NONE',  ( 18.62759615963255655, 10.81492255796105972, 81.66775706135236135 ) ) ;
#142482 = CARTESIAN_POINT ( 'NONE',  ( 24.20670376297029236, -0.5310992180246828509, -56.83968087238904587 ) ) ;
#142483 = CARTESIAN_POINT ( 'NONE',  ( 16.51473224551069308, 9.474510206698969483, 104.1655762719810241 ) ) ;
#142484 = FACE_OUTER_BOUND ( 'NONE', #98933, .T. ) ;
#142485 = CARTESIAN_POINT ( 'NONE',  ( -13.97604488694527625, -13.89961937509977652, 46.87390960531435979 ) ) ;
#142486 = CARTESIAN_POINT ( 'NONE',  ( 10.72451020669898902, -18.67979575497178502, 52.91557627198103830 ) ) ;
#142487 = CARTESIAN_POINT ( 'NONE',  ( -16.55341960407611168, -4.379528057220339221, 31.45724293864769550 ) ) ;
#142489 = CARTESIAN_POINT ( 'NONE',  ( 5.153800228976335163, 19.02544592524342804, 94.79057627198103830 ) ) ;
#142488 = CARTESIAN_POINT ( 'NONE',  ( 16.52544592524342804, -4.483927247898539470, 98.54057627198105251 ) ) ;
#142490 = CARTESIAN_POINT ( 'NONE',  ( 5.049401038297881783, 19.05341960407617563, 27.29275706135232937 ) ) ;
#142491 = CARTESIAN_POINT ( 'NONE',  ( -16.51473224551069308, -9.474510206698971260, 36.66557627198102409 ) ) ;
#142492 = CARTESIAN_POINT ( 'NONE',  ( 16.55341960407611168, 4.379528057220329451, 103.9572429386476813 ) ) ;
#142493 = CARTESIAN_POINT ( 'NONE',  ( -21.52544592524334988, -5.823673210054445271, 53.95942372801900433 ) ) ;
#142494 = CARTESIAN_POINT ( 'NONE',  ( -4.379528057220086978, -16.55341960407618274, 109.7927570613523613 ) ) ;
#142495 = CARTESIAN_POINT ( 'NONE',  ( 13.97604488694548053, -13.89961937509957401, 65.62609039468567573 ) ) ;
#142496 = CARTESIAN_POINT ( 'NONE',  ( -27.21294631871472802, -29.31732793098551682, -5.578473613576554690 ) ) ;
#142497 = CARTESIAN_POINT ( 'NONE',  ( 16.46253265017160672, -9.564922557960803928, 108.3322429386476955 ) ) ;
#142498 = CARTESIAN_POINT ( 'NONE',  ( -16.52544592524342804, 4.483927247898546575, 81.04057627198102409 ) ) ;
#142499 = CARTESIAN_POINT ( 'NONE',  ( 16.46253265017146816, 9.564922557961045513, 61.66775706135234003 ) ) ;
#142500 = CARTESIAN_POINT ( 'NONE',  ( -16.51473224551069308, -9.474510206698971260, 61.66557627198103120 ) ) ;
#142501 = CARTESIAN_POINT ( 'NONE',  ( -16.52544592524342804, 4.483927247898546575, 61.04057627198103120 ) ) ;
#142502 = CARTESIAN_POINT ( 'NONE',  ( -19.03943276465977164, -0.05219959533935918106, 83.75109039468567573 ) ) ;
#142503 = CARTESIAN_POINT ( 'NONE',  ( 18.62759615963271287, -10.81492255796078972, 38.33224293864768839 ) ) ;
#142504 = VERTEX_POINT ( 'NONE', #147269 ) ;
#142505 = CARTESIAN_POINT ( 'NONE',  ( -12.06949235617756955, 12.14591786802309770, 95.62390960531436690 ) ) ;
#142506 = CARTESIAN_POINT ( 'NONE',  ( -17.13100169013300089, -6.664070546373174864, 29.23210164300154190 ) ) ;
#142508 = CARTESIAN_POINT ( 'NONE',  ( -5.823673210054116645, -21.52544592524344225, 67.29057627198103830 ) ) ;
#142507 = CARTESIAN_POINT ( 'NONE',  ( 13.97604488694527802, 13.89961937509977652, 59.37390960531434558 ) ) ;
#142509 = CARTESIAN_POINT ( 'NONE',  ( 19.03943276465977164, -0.05219959533909143690, 38.74890960531436690 ) ) ;
#142511 = CARTESIAN_POINT ( 'NONE',  ( 13.89961937509977652, -13.97604488694527269, 73.12390960531436690 ) ) ;
#142510 = CARTESIAN_POINT ( 'NONE',  ( 8.224510206698742110, 14.34966873604972548, 92.08442372801901854 ) ) ;
#142512 = CARTESIAN_POINT ( 'NONE',  ( 16.46253265017146816, 9.564922557961045513, 56.66775706135233293 ) ) ;
#142513 = CARTESIAN_POINT ( 'NONE',  ( 0.05219959533937995610, -21.53943276465977519, 75.00109039468568994 ) ) ;
#142514 = CARTESIAN_POINT ( 'NONE',  ( 18.62759615963271287, -10.81492255796078972, 48.33224293864770260 ) ) ;
#142515 = CARTESIAN_POINT ( 'NONE',  ( -16.46253265017160317, 9.564922557960807481, 100.8322429386477097 ) ) ;
#142516 = CARTESIAN_POINT ( 'NONE',  ( 13.89961937509977652, -13.97604488694527269, 23.12390960531436335 ) ) ;
#142517 = CARTESIAN_POINT ( 'NONE',  ( -16.52544592524335698, -4.483927247898792601, 88.95942372801901854 ) ) ;
#142518 = CARTESIAN_POINT ( 'NONE',  ( 9.474510206698729675, 16.51473224551082808, 102.0844237280190043 ) ) ;
#142519 = CARTESIAN_POINT ( 'NONE',  ( -11.30153831258472508, -180.0000000000000000, -4.999999999999999112 ) ) ;
#142520 = DIRECTION ( 'NONE',  ( 0.000000000000000000, -1.000000000000000000, 0.000000000000000000 ) ) ;
#142521 = CARTESIAN_POINT ( 'NONE',  ( 10.72451020669871369, 18.67979575497193778, 97.08442372801904696 ) ) ;
#142522 = ORIENTED_EDGE ( 'NONE', *, *, #34865, .F. ) ;
#142523 = CARTESIAN_POINT ( 'NONE',  ( -4.379528057220328563, 16.55341960407611168, 65.20724293864768129 ) ) ;
#142524 = CARTESIAN_POINT ( 'NONE',  ( 16.55341960407611168, 4.379528057220329451, 73.95724293864769550 ) ) ;
#142525 = CARTESIAN_POINT ( 'NONE',  ( -15.72974639402197994, 15.80617190586746368, 100.6239096053143811 ) ) ;
#142526 = CARTESIAN_POINT ( 'NONE',  ( 18.67979575497178502, 10.72451020669898547, 89.16557627198102409 ) ) ;
#142527 = CARTESIAN_POINT ( 'NONE',  ( 16.20579543436678449, -7.371946100355080134, 96.93479165828125588 ) ) ;
#142528 = CARTESIAN_POINT ( 'NONE',  ( 18.62759615963271287, -10.81492255796078972, 28.33224293864769550 ) ) ;
#142529 = CARTESIAN_POINT ( 'NONE',  ( 4.483927247898790824, -16.52544592524335698, 65.20942372801901854 ) ) ;
#142530 = CARTESIAN_POINT ( 'NONE',  ( -8.224510206698948167, 14.34966873604960824, 95.41557627198102409 ) ) ;
#142531 = CARTESIAN_POINT ( 'NONE',  ( -16.51473224551069308, -9.474510206698971260, 41.66557627198103120 ) ) ;
#142532 = CARTESIAN_POINT ( 'NONE',  ( 34.51183469268315207, -7.447092774749549449, 43.98515247788456151 ) ) ;
#142533 = CARTESIAN_POINT ( 'NONE',  ( -14.29746914071037622, -8.314922557961029526, 99.16775706135234714 ) ) ;
#142534 = CARTESIAN_POINT ( 'NONE',  ( 15.80617190586769283, -15.72974639402175789, 30.62609039468567929 ) ) ;
#142535 = CARTESIAN_POINT ( 'NONE',  ( -13.97604488694527625, -13.89961937509977652, 86.87390960531436690 ) ) ;
#142536 = CARTESIAN_POINT ( 'NONE',  ( 21.53943276465977519, 0.05219959533937863772, 66.25109039468567573 ) ) ;
#142537 = DIRECTION ( 'NONE',  ( -0.07151044867601363819, 0.9974398506828144884, 0.000000000000000000 ) ) ;
#142538 = DIRECTION ( 'NONE',  ( -1.000000000000000000, -0.000000000000000000, -0.000000000000000000 ) ) ;
#142539 = ORIENTED_EDGE ( 'NONE', *, *, #6876, .F. ) ;
#142540 = CARTESIAN_POINT ( 'NONE',  ( -10.72451020669870658, -18.67979575497194134, 64.58442372801900433 ) ) ;
#142542 = CARTESIAN_POINT ( 'NONE',  ( -19.02544592524342804, 5.153800228976336051, 116.0405762719810383 ) ) ;
#142541 = CARTESIAN_POINT ( 'NONE',  ( -0.05219959533909027116, -19.03943276465977164, 42.49890960531435269 ) ) ;
#142543 = CARTESIAN_POINT ( 'NONE',  ( -16.51473224551069308, -9.474510206698971260, 86.66557627198102409 ) ) ;
#142544 = CARTESIAN_POINT ( 'NONE',  ( 13.97604488694548053, -13.89961937509957401, 65.62609039468567573 ) ) ;
#142545 = CARTESIAN_POINT ( 'NONE',  ( 18.67979575497194134, -10.72451020669871369, 25.83442372801901499 ) ) ;
#142546 = CARTESIAN_POINT ( 'NONE',  ( 19.02544592524334988, 5.153800228976608722, 56.45942372801898301 ) ) ;
#142547 = CARTESIAN_POINT ( 'NONE',  ( -0.05219959533909027116, -19.03943276465977164, 22.49890960531436690 ) ) ;
#142548 = CARTESIAN_POINT ( 'NONE',  ( 14.34966873604972726, -8.224510206698740333, 90.83442372801901854 ) ) ;
#142549 = CARTESIAN_POINT ( 'NONE',  ( -5.049401038297874678, -19.05341960407617918, 59.79275706135231871 ) ) ;
#142550 = CARTESIAN_POINT ( 'NONE',  ( 12.06949235617757843, -12.14591786802309237, 23.12390960531436335 ) ) ;
#142552 = EDGE_LOOP ( 'NONE', ( #56279, #21060, #183485 ) ) ;
#142551 = CARTESIAN_POINT ( 'NONE',  ( -19.05341960407617563, 5.049401038297882671, 48.54275706135233293 ) ) ;
#142553 = CARTESIAN_POINT ( 'NONE',  ( -9.474510206698964154, 16.51473224551069663, 90.41557627198103830 ) ) ;
#142554 = CARTESIAN_POINT ( 'NONE',  ( -15.80617190586768217, 15.72974639402176855, 93.12609039468568994 ) ) ;
#142555 = CARTESIAN_POINT ( 'NONE',  ( 21.53943276465977519, 0.05219959533937863772, 101.2510903946856757 ) ) ;
#142556 = CARTESIAN_POINT ( 'NONE',  ( 18.09867054820431065, 5.500000000000001776, 66.48393025253587041 ) ) ;
#142557 = CARTESIAN_POINT ( 'NONE',  ( 10.72451020669871369, 18.67979575497193778, 92.08442372801901854 ) ) ;
#142558 = CARTESIAN_POINT ( 'NONE',  ( -0.05219959533934338120, 16.53943276465976808, 37.50109039468568284 ) ) ;
#142559 = CARTESIAN_POINT ( 'NONE',  ( 13.89961937509977652, -13.97604488694527269, 88.12390960531438111 ) ) ;
#142560 = CARTESIAN_POINT ( 'NONE',  ( 0.05219959533907565091, 21.53943276465977519, 34.99890960531435979 ) ) ;
#142561 = LINE ( 'NONE', #6033, #198462 ) ;
#142562 = CARTESIAN_POINT ( 'NONE',  ( 13.97604488694527802, 13.89961937509977652, 84.37390960531433848 ) ) ;
#142563 = FACE_BOUND ( 'NONE', #179396, .T. ) ;
#142564 = CARTESIAN_POINT ( 'NONE',  ( -9.474510206698720793, -16.51473224551083518, 74.58442372801900433 ) ) ;
#142565 = CARTESIAN_POINT ( 'NONE',  ( -19.03943276465977164, 0.05219959533909376836, 106.2489096053143669 ) ) ;
#142566 = CARTESIAN_POINT ( 'NONE',  ( 10.81492255796106328, -18.62759615963255655, 105.4177570613523613 ) ) ;
#142567 = CARTESIAN_POINT ( 'NONE',  ( 4.483927247898545687, 16.52544592524342804, 99.79057627198103830 ) ) ;
#142568 = CARTESIAN_POINT ( 'NONE',  ( -15.80617190586745835, -15.72974639402198527, 46.87390960531435979 ) ) ;
#142569 = CARTESIAN_POINT ( 'NONE',  ( 10.72451020669898902, -18.67979575497178502, 37.91557627198102409 ) ) ;
#142570 = CARTESIAN_POINT ( 'NONE',  ( -16.55341960407611168, -4.379528057220339221, 106.4572429386477097 ) ) ;
#142571 = CARTESIAN_POINT ( 'NONE',  ( -1.452998035947202560, -7.215019197202739321, -62.28058590214430268 ) ) ;
#142572 = CARTESIAN_POINT ( 'NONE',  ( 9.564922557961047289, -16.46253265017146816, 55.41775706135234003 ) ) ;
#142573 = CARTESIAN_POINT ( 'NONE',  ( -14.34966873604960291, -8.224510206698953496, 21.66557627198102409 ) ) ;
#142574 = CARTESIAN_POINT ( 'NONE',  ( -16.51473224551069308, -9.474510206698971260, 96.66557627198102409 ) ) ;
#142575 = CARTESIAN_POINT ( 'NONE',  ( 18.62759615963255655, 10.81492255796105972, 76.66775706135234714 ) ) ;
#142576 = CARTESIAN_POINT ( 'NONE',  ( -21.55341960407610458, -5.719274019375992779, 56.45724293864768839 ) ) ;
#142577 = CARTESIAN_POINT ( 'NONE',  ( -21.53943276465977519, -0.05219959533937600094, 38.75109039468567573 ) ) ;
#142578 = CARTESIAN_POINT ( 'NONE',  ( -18.67979575497178146, -10.72451020669898902, 96.66557627198102409 ) ) ;
#142579 = CARTESIAN_POINT ( 'NONE',  ( -21.53943276465977519, -0.05219959533937600094, 33.75109039468568284 ) ) ;
#142580 = CARTESIAN_POINT ( 'NONE',  ( -14.29746914071049879, 8.314922557960819915, 115.8322429386477097 ) ) ;
#142581 = CARTESIAN_POINT ( 'NONE',  ( 19.02544592524343514, -5.153800228976328945, 88.54057627198102409 ) ) ;
#142582 = CARTESIAN_POINT ( 'NONE',  ( 8.224510206698742110, 14.34966873604972548, 82.08442372801901854 ) ) ;
#142583 = CARTESIAN_POINT ( 'NONE',  ( 12.06949235617757843, -12.14591786802309237, 103.1239096053143811 ) ) ;
#142584 = CARTESIAN_POINT ( 'NONE',  ( -9.474510206698964154, 16.51473224551069663, 110.4155762719810383 ) ) ;
#142585 = CARTESIAN_POINT ( 'NONE',  ( -4.379528057220328563, 16.55341960407611168, 50.20724293864769550 ) ) ;
#142586 = CARTESIAN_POINT ( 'NONE',  ( -0.05219959533934338120, 16.53943276465976808, 112.5010903946857042 ) ) ;
#142587 = CARTESIAN_POINT ( 'NONE',  ( -19.02544592524342804, 5.153800228976336051, 56.04057627198100988 ) ) ;
#142588 = CARTESIAN_POINT ( 'NONE',  ( -19.03943276465977164, 0.05219959533909376836, 31.24890960531435979 ) ) ;
#142589 = CARTESIAN_POINT ( 'NONE',  ( -10.81492255796078084, -18.62759615963271287, 42.08224293864769550 ) ) ;
#142590 = CARTESIAN_POINT ( 'NONE',  ( -16.51473224551082808, 9.474510206698731452, 28.33442372801900433 ) ) ;
#142592 = CARTESIAN_POINT ( 'NONE',  ( 12.06949235617757843, -12.14591786802309237, 33.12390960531435979 ) ) ;
#142591 = DIRECTION ( 'NONE',  ( 0.000000000000000000, 0.000000000000000000, -1.000000000000000000 ) ) ;
#142593 = CARTESIAN_POINT ( 'NONE',  ( 21.52544592524334988, 5.823673210054432836, 51.45942372801901854 ) ) ;
#142594 = CARTESIAN_POINT ( 'NONE',  ( -8.204442743001470362, -36.48291145135368652, -31.77125895174630443 ) ) ;
#142595 = CARTESIAN_POINT ( 'NONE',  ( 12.14591786802327356, -12.06949235617739191, 55.62609039468568284 ) ) ;
#142596 = CARTESIAN_POINT ( 'NONE',  ( 5.049401038297881783, 19.05341960407617563, 67.29275706135234714 ) ) ;
#142597 = CARTESIAN_POINT ( 'NONE',  ( 16.55341960407611168, 4.379528057220329451, 23.95724293864769550 ) ) ;
#142598 = CARTESIAN_POINT ( 'NONE',  ( -8.224510206698735004, -14.34966873604973081, 104.5844237280190185 ) ) ;
#142599 = CARTESIAN_POINT ( 'NONE',  ( 9.474510206698971260, -16.51473224551069308, 32.91557627198102409 ) ) ;
#142600 = EDGE_CURVE ( 'NONE', #97477, #26617, #22926, .T. ) ;
#142601 = CARTESIAN_POINT ( 'NONE',  ( -19.03943276465977164, 0.05219959533909376836, 66.24890960531436690 ) ) ;
#142602 = CARTESIAN_POINT ( 'NONE',  ( -13.89961937509977652, 13.97604488694528158, 25.62390960531434558 ) ) ;
#142603 = CARTESIAN_POINT ( 'NONE',  ( 10.72451020669871369, 18.67979575497193778, 27.08442372801901854 ) ) ;
#142604 = CARTESIAN_POINT ( 'NONE',  ( -16.51473224551069308, -9.474510206698971260, 51.66557627198102409 ) ) ;
#142605 = CARTESIAN_POINT ( 'NONE',  ( -5.511913701082267636, -6.874908499604756251, -61.96452946383318050 ) ) ;
#142606 = CARTESIAN_POINT ( 'NONE',  ( 16.46253265017160672, -9.564922557960803928, 48.33224293864769550 ) ) ;
#142607 = CARTESIAN_POINT ( 'NONE',  ( -5.153800228976328057, -19.02544592524343514, 112.2905762719810099 ) ) ;
#142609 = CARTESIAN_POINT ( 'NONE',  ( 14.34966873604960469, 8.224510206698951720, 104.1655762719810241 ) ) ;
#142608 = CARTESIAN_POINT ( 'NONE',  ( 15.80617190586769283, -15.72974639402175789, 60.62609039468567573 ) ) ;
#142610 = CARTESIAN_POINT ( 'NONE',  ( -19.03943276465977164, 0.05219959533909376836, 111.2489096053143669 ) ) ;
#142611 = CARTESIAN_POINT ( 'NONE',  ( -16.55341960407617563, 4.379528057220093196, 83.54275706135234714 ) ) ;
#142612 = CARTESIAN_POINT ( 'NONE',  ( -21.55341960407619339, 5.719274019375674811, 88.54275706135236135 ) ) ;
#142613 = CARTESIAN_POINT ( 'NONE',  ( -16.55341960407617563, 4.379528057220093196, 48.54275706135234714 ) ) ;
#142614 = CARTESIAN_POINT ( 'NONE',  ( 19.05341960407611168, 5.049401038298154454, 88.95724293864769550 ) ) ;
#142615 = CARTESIAN_POINT ( 'NONE',  ( -4.379528057220086978, -16.55341960407618274, 34.79275706135235424 ) ) ;
#142616 = CARTESIAN_POINT ( 'NONE',  ( 4.379528057220092307, 16.55341960407617563, 27.29275706135234358 ) ) ;
#142617 = CARTESIAN_POINT ( 'NONE',  ( -16.52544592524335698, -4.483927247898792601, 93.95942372801903275 ) ) ;
#142618 = CARTESIAN_POINT ( 'NONE',  ( -13.97604488694547697, 13.89961937509957934, 108.1260903946856331 ) ) ;
#142619 = CARTESIAN_POINT ( 'NONE',  ( -21.53943276465977519, 0.05219959533907696930, 96.24890960531435269 ) ) ;
#142621 = CARTESIAN_POINT ( 'NONE',  ( -5.049401038297874678, -19.05341960407617918, 99.79275706135234714 ) ) ;
#142620 = CARTESIAN_POINT ( 'NONE',  ( -14.34966873604960291, -8.224510206698953496, 96.66557627198102409 ) ) ;
#142622 = CARTESIAN_POINT ( 'NONE',  ( -14.34966873604972548, 8.224510206698743886, 68.33442372801900433 ) ) ;
#142623 = CARTESIAN_POINT ( 'NONE',  ( 21.88033147701376890, 7.974798826777440119, 169.5716465351766260 ) ) ;
#142624 = CARTESIAN_POINT ( 'NONE',  ( 9.564922557961047289, -16.46253265017146816, 65.41775706135233293 ) ) ;
#142625 = CARTESIAN_POINT ( 'NONE',  ( 16.52544592524342804, -4.483927247898539470, 43.54057627198103830 ) ) ;
#142626 = CARTESIAN_POINT ( 'NONE',  ( 8.314922557960818139, 14.29746914071049879, 29.58224293864769905 ) ) ;
#142627 = CARTESIAN_POINT ( 'NONE',  ( -16.53943276465976808, 0.05219959533911058130, 91.24890960531436690 ) ) ;
#142629 = CARTESIAN_POINT ( 'NONE',  ( -17.40805194822031154, 6.112264579159341515, 90.83371272510612471 ) ) ;
#142628 = CARTESIAN_POINT ( 'NONE',  ( -9.564922557961040184, 16.46253265017147172, 27.91775706135232582 ) ) ;
#142630 = CARTESIAN_POINT ( 'NONE',  ( -18.62759615963255300, -10.81492255796106328, 34.16775706135234714 ) ) ;
#142631 = CARTESIAN_POINT ( 'NONE',  ( -13.97604488694547697, 13.89961937509957934, 93.12609039468566152 ) ) ;
#142632 =( BOUNDED_CURVE ( )  B_SPLINE_CURVE ( 2, ( #106573, #198604, #79212, #64051, #184422, #46900, #76230, #108560, #138895, #75246, #199592 ),
 .UNSPECIFIED., .F., .T. ) 
 B_SPLINE_CURVE_WITH_KNOTS ( ( 3, 2, 2, 2, 2, 3 ),
 ( 0.8000000000000007105, 0.8200000000000007283, 0.8400000000000006350, 0.8600000000000007638, 0.8800000000000007816, 0.9000000000000007994 ),
 .UNSPECIFIED. ) 
 CURVE ( )  GEOMETRIC_REPRESENTATION_ITEM ( )  RATIONAL_B_SPLINE_CURVE ( ( 0.9999999999999983347, 0.9510565162951551965, 1.000000000000000000, 0.9510565162951535312, 1.000000000000000000, 0.9510565162951535312, 1.000000000000000000, 0.9510565162951535312, 1.000000000000000000, 0.9510565162951516438, 1.000000000000001998 ) ) 
 REPRESENTATION_ITEM ( '' )  );
#142633 = CARTESIAN_POINT ( 'NONE',  ( 1.697796032038806358, 7.741785448087941113, 4.009310749147818598 ) ) ;
#142634 = CARTESIAN_POINT ( 'NONE',  ( -9.474510206698964154, 16.51473224551069663, 85.41557627198102409 ) ) ;
#142635 = CARTESIAN_POINT ( 'NONE',  ( -5.049401038298153566, 19.05341960407611168, 90.20724293864766707 ) ) ;
#142636 = CARTESIAN_POINT ( 'NONE',  ( -21.53943276465977519, 0.05219959533907696930, 51.24890960531436690 ) ) ;
#142637 = CARTESIAN_POINT ( 'NONE',  ( 16.52544592524342804, -4.483927247898539470, 88.54057627198103830 ) ) ;
#142638 = CARTESIAN_POINT ( 'NONE',  ( 13.97604488694527802, 13.89961937509977652, 69.37390960531436690 ) ) ;
#142639 = CARTESIAN_POINT ( 'NONE',  ( 16.51473224551069308, 9.474510206698969483, 29.16557627198103475 ) ) ;
#142640 = CARTESIAN_POINT ( 'NONE',  ( 21.52544592524334988, 5.823673210054432836, 36.45942372801901143 ) ) ;
#142641 = CARTESIAN_POINT ( 'NONE',  ( -15.80617190586768217, 15.72974639402176855, 73.12609039468567573 ) ) ;
#142642 = CARTESIAN_POINT ( 'NONE',  ( 16.46253265017160672, -9.564922557960803928, 63.33224293864769550 ) ) ;
#142643 = CARTESIAN_POINT ( 'NONE',  ( -8.314922557961024197, 14.29746914071037800, 82.91775706135234714 ) ) ;
#142644 = CARTESIAN_POINT ( 'NONE',  ( -21.52544592524334988, -5.823673210054445271, 33.95942372801901143 ) ) ;
#142645 = CARTESIAN_POINT ( 'NONE',  ( 5.823673210054444382, -21.52544592524334988, 20.20942372801900788 ) ) ;
#142647 = CARTESIAN_POINT ( 'NONE',  ( -13.97604488694527625, -13.89961937509977652, 76.87390960531433848 ) ) ;
#142646 = CARTESIAN_POINT ( 'NONE',  ( -19.05341960407617563, 5.049401038297882671, 58.54275706135234003 ) ) ;
#142648 = CARTESIAN_POINT ( 'NONE',  ( 13.97604488694548053, -13.89961937509957401, 30.62609039468566863 ) ) ;
#142649 = CARTESIAN_POINT ( 'NONE',  ( 21.52544592524334988, 5.823673210054432836, 86.45942372801901854 ) ) ;
#142650 = CARTESIAN_POINT ( 'NONE',  ( 10.81492255796078972, 18.62759615963270932, 69.58224293864769550 ) ) ;
#142651 = CARTESIAN_POINT ( 'NONE',  ( 12.14591786802309770, 12.06949235617756955, 44.37390960531435979 ) ) ;
#142653 = CARTESIAN_POINT ( 'NONE',  ( 19.05341960407617918, -5.049401038297876454, 26.04275706135233293 ) ) ;
#142652 = CARTESIAN_POINT ( 'NONE',  ( -15.72974639402176322, -15.80617190586768395, 94.37609039468568994 ) ) ;
#142654 = CARTESIAN_POINT ( 'NONE',  ( 16.52544592524342804, -4.483927247898539470, 73.54057627198102409 ) ) ;
#142655 = CARTESIAN_POINT ( 'NONE',  ( -19.03943276465977164, 0.05219959533909376836, 26.24890960531435624 ) ) ;
#142656 = CARTESIAN_POINT ( 'NONE',  ( -9.564922557961040184, 16.46253265017147172, 72.91775706135233293 ) ) ;
#142657 = CARTESIAN_POINT ( 'NONE',  ( 4.379528057220339221, -16.55341960407611168, 37.70724293864769550 ) ) ;
#142658 = CARTESIAN_POINT ( 'NONE',  ( -10.81492255796105439, 18.62759615963255655, 87.91775706135234714 ) ) ;
#142659 = CARTESIAN_POINT ( 'NONE',  ( 19.03943276465977164, -0.05219959533909143690, 73.74890960531435269 ) ) ;
#142660 = CARTESIAN_POINT ( 'NONE',  ( -9.564922557961040184, 16.46253265017147172, 47.91775706135233293 ) ) ;
#142661 = CARTESIAN_POINT ( 'NONE',  ( -21.53943276465977519, 0.05219959533907696930, 51.24890960531436690 ) ) ;
#142662 = CARTESIAN_POINT ( 'NONE',  ( 5.823673210054444382, -21.52544592524334988, 20.20942372801900788 ) ) ;
#142663 = CARTESIAN_POINT ( 'NONE',  ( -0.05219959533936034679, 19.03943276465977164, 112.5010903946856757 ) ) ;
#142664 = CARTESIAN_POINT ( 'NONE',  ( 12.06949235617739724, 12.14591786802326823, 66.87609039468568994 ) ) ;
#142666 = CARTESIAN_POINT ( 'NONE',  ( -0.05219959533907301413, -21.53943276465977519, 112.4989096053143669 ) ) ;
#142665 = CARTESIAN_POINT ( 'NONE',  ( -6.551653823223139383, 3.660253528765621045, 1.589185716900141543 ) ) ;
#142667 = CARTESIAN_POINT ( 'NONE',  ( -16.55341960407611168, -4.379528057220339221, 101.4572429386476955 ) ) ;
#142668 = CARTESIAN_POINT ( 'NONE',  ( -11.40812507854754720, -35.11059874428192273, -10.72499999726881548 ) ) ;
#142669 = CARTESIAN_POINT ( 'NONE',  ( 0.05219959533934541429, -16.53943276465976808, 40.00109039468567573 ) ) ;
#142670 = CARTESIAN_POINT ( 'NONE',  ( 18.67979575497178502, 10.72451020669898547, 64.16557627198102409 ) ) ;
#142671 = CARTESIAN_POINT ( 'NONE',  ( -4.379528057220086978, -16.55341960407618274, 109.7927570613523613 ) ) ;
#142672 = CARTESIAN_POINT ( 'NONE',  ( -13.89961937509977652, 13.97604488694528158, 30.62390960531435269 ) ) ;
#142673 = CARTESIAN_POINT ( 'NONE',  ( 0.05219959533934541429, -16.53943276465976808, 65.00109039468568994 ) ) ;
#142674 = CARTESIAN_POINT ( 'NONE',  ( -19.03943276465977164, -0.05219959533935918106, 58.75109039468566863 ) ) ;
#142675 = CARTESIAN_POINT ( 'NONE',  ( -21.52544592524334988, -5.823673210054445271, 43.95942372801902565 ) ) ;
#142676 = CARTESIAN_POINT ( 'NONE',  ( -5.719274019375978568, 21.55341960407610458, 65.20724293864768129 ) ) ;
#142677 = CARTESIAN_POINT ( 'NONE',  ( 8.314922557961029526, -14.29746914071037800, 100.4177570613523471 ) ) ;
#142678 = CARTESIAN_POINT ( 'NONE',  ( -5.823673210054431948, 21.52544592524334988, 82.70942372801900433 ) ) ;
#142679 = CARTESIAN_POINT ( 'NONE',  ( -5.719274019375978568, 21.55341960407610458, 55.20724293864770260 ) ) ;
#142680 = CARTESIAN_POINT ( 'NONE',  ( 18.67979575497178502, 10.72451020669898547, 29.16557627198103120 ) ) ;
#142681 = ORIENTED_EDGE ( 'NONE', *, *, #32687, .T. ) ;
#142682 = CARTESIAN_POINT ( 'NONE',  ( -0.05219959533934338120, 16.53943276465976808, 82.50109039468568994 ) ) ;
#142683 = CARTESIAN_POINT ( 'NONE',  ( -5.719274019375978568, 21.55341960407610458, 40.20724293864769550 ) ) ;
#142684 = ORIENTED_EDGE ( 'NONE', *, *, #3940, .F. ) ;
#142685 = CARTESIAN_POINT ( 'NONE',  ( -19.03943276465977164, 0.05219959533909376836, 101.2489096053143669 ) ) ;
#142686 = CARTESIAN_POINT ( 'NONE',  ( -24.93942350307309752, 7.769968609432599926, 171.2173313942149946 ) ) ;
#142687 = CARTESIAN_POINT ( 'NONE',  ( 19.05341960407611168, 5.049401038298154454, 28.95724293864769550 ) ) ;
#142688 = CARTESIAN_POINT ( 'NONE',  ( 15.72974639402199770, -15.80617190586745480, 68.12390960531436690 ) ) ;
#142689 = CARTESIAN_POINT ( 'NONE',  ( 16.52544592524335698, 4.483927247898782831, 86.45942372801901854 ) ) ;
#142690 = CARTESIAN_POINT ( 'NONE',  ( 5.719274019375673035, 21.55341960407619339, 52.29275706135236135 ) ) ;
#142691 = CARTESIAN_POINT ( 'NONE',  ( 16.51473224551083163, -9.474510206698727899, 105.8344237280190043 ) ) ;
#142692 = CARTESIAN_POINT ( 'NONE',  ( 16.55341960407611168, 4.379528057220329451, 98.95724293864770971 ) ) ;
#142693 = CARTESIAN_POINT ( 'NONE',  ( 16.52544592524335698, 4.483927247898782831, 21.45942372801901499 ) ) ;
#142694 = CARTESIAN_POINT ( 'NONE',  ( -13.89961937509977652, 13.97604488694528158, 40.62390960531435979 ) ) ;
#142695 = DIRECTION ( 'NONE',  ( 1.000000000000000000, 0.000000000000000000, 0.000000000000000000 ) ) ;
#142696 = CARTESIAN_POINT ( 'NONE',  ( -13.89961937509977652, 13.97604488694528158, 95.62390960531436690 ) ) ;
#142697 = EDGE_CURVE ( 'NONE', #88111, #43212, #24941, .T. ) ;
#142698 = CARTESIAN_POINT ( 'NONE',  ( -16.55341960407617563, 4.379528057220093196, 73.54275706135234714 ) ) ;
#142699 = CARTESIAN_POINT ( 'NONE',  ( -21.53943276465977519, -0.05219959533937600094, 108.7510903946857042 ) ) ;
#142700 = CARTESIAN_POINT ( 'NONE',  ( 15.72974639402199770, -15.80617190586745480, 63.12390960531435979 ) ) ;
#142701 = CARTESIAN_POINT ( 'NONE',  ( 8.314922557961029526, -14.29746914071037800, 85.41775706135236135 ) ) ;
#142702 = CARTESIAN_POINT ( 'NONE',  ( -5.049401038297874678, -19.05341960407617918, 84.79275706135233293 ) ) ;
#142703 = CARTESIAN_POINT ( 'NONE',  ( -16.51473224551069308, -9.474510206698971260, 31.66557627198102054 ) ) ;
#142704 = CARTESIAN_POINT ( 'NONE',  ( 9.564922557960805705, 16.46253265017160317, 84.58224293864769550 ) ) ;
#142705 = CARTESIAN_POINT ( 'NONE',  ( -19.05341960407611168, -5.049401038298163336, 31.45724293864769550 ) ) ;
#142706 = CARTESIAN_POINT ( 'NONE',  ( 9.564922557961047289, -16.46253265017146816, 70.41775706135233293 ) ) ;
#142707 = CARTESIAN_POINT ( 'NONE',  ( 21.56952297831669441, -7.512152360717372801, 173.9007003117368697 ) ) ;
#142708 = CARTESIAN_POINT ( 'NONE',  ( -13.89961937509977652, 13.97604488694528158, 90.62390960531432427 ) ) ;
#142709 = CARTESIAN_POINT ( 'NONE',  ( 8.224510206698953496, -14.34966873604960469, 47.91557627198102409 ) ) ;
#142710 = CARTESIAN_POINT ( 'NONE',  ( -18.67979575497178146, -10.72451020669898902, 66.66557627198102409 ) ) ;
#142711 = CARTESIAN_POINT ( 'NONE',  ( -17.50000000000147438, 3.202012800152229666, 104.9282241602725634 ) ) ;
#142712 = CARTESIAN_POINT ( 'NONE',  ( 0.05219959533936267826, -19.03943276465977164, 25.00109039468566152 ) ) ;
#142713 = SURFACE_SIDE_STYLE ('',( #18403 ) ) ;
#142715 = CARTESIAN_POINT ( 'NONE',  ( -9.564922557960796823, -16.46253265017161027, 72.08224293864770971 ) ) ;
#142714 = CARTESIAN_POINT ( 'NONE',  ( -16.46253265017160317, 9.564922557960807481, 65.83224293864769550 ) ) ;
#142716 = CARTESIAN_POINT ( 'NONE',  ( 4.379528057220092307, 16.55341960407617563, 37.29275706135235424 ) ) ;
#142717 = CARTESIAN_POINT ( 'NONE',  ( 27.44803035730394924, -28.83687526680896696, -16.92468093647911331 ) ) ;
#142718 = LINE ( 'NONE', #52702, #21024 ) ;
#142719 = CARTESIAN_POINT ( 'NONE',  ( -0.05219959533934338120, 16.53943276465976808, 72.50109039468568994 ) ) ;
#142721 = CARTESIAN_POINT ( 'NONE',  ( -10.72451020669898014, 18.67979575497178502, 90.41557627198103830 ) ) ;
#142720 = CARTESIAN_POINT ( 'NONE',  ( 8.224510206698742110, 14.34966873604972548, 67.08442372801901854 ) ) ;
#142722 = CARTESIAN_POINT ( 'NONE',  ( -0.05219959533934338120, 16.53943276465976808, 47.50109039468568994 ) ) ;
#142724 = FACE_OUTER_BOUND ( 'NONE', #59642, .T. ) ;
#142723 = CARTESIAN_POINT ( 'NONE',  ( -5.153800228976328057, -19.02544592524343514, 42.29057627198101699 ) ) ;
#142725 = CARTESIAN_POINT ( 'NONE',  ( 10.81492255796106328, -18.62759615963255655, 55.41775706135234714 ) ) ;
#142726 = CARTESIAN_POINT ( 'NONE',  ( 13.97604488694548053, -13.89961937509957401, 60.62609039468564731 ) ) ;
#142727 = CARTESIAN_POINT ( 'NONE',  ( -21.52544592524334988, -5.823673210054445271, 98.95942372801903275 ) ) ;
#142728 = CARTESIAN_POINT ( 'NONE',  ( -19.02544592524342804, 5.153800228976336051, 26.04057627198103120 ) ) ;
#142729 = CARTESIAN_POINT ( 'NONE',  ( -16.68934465457932603, 0.2055526423336037911, -59.13845350790285949 ) ) ;
#142730 = CARTESIAN_POINT ( 'NONE',  ( -21.55341960407610458, -5.719274019375992779, 51.45724293864770260 ) ) ;
#142731 = MANIFOLD_SOLID_BREP ( 'Cavity2', #4555 ) ;
#142732 = CARTESIAN_POINT ( 'NONE',  ( -5.049401038298153566, 19.05341960407611168, 100.2072429386476955 ) ) ;
#142733 = CARTESIAN_POINT ( 'NONE',  ( 16.53943276465976808, -0.05219959533910856209, 103.7489096053143669 ) ) ;
#142734 = CARTESIAN_POINT ( 'NONE',  ( -16.53943276465976808, -0.05219959533934237506, 33.75109039468568284 ) ) ;
#142735 = CARTESIAN_POINT ( 'NONE',  ( 4.379528057220092307, 16.55341960407617563, 107.2927570613523471 ) ) ;
#142736 = VERTEX_POINT ( 'NONE', #165445 ) ;
#142737 = CARTESIAN_POINT ( 'NONE',  ( -18.62759615963270932, 10.81492255796079327, 100.8322429386477097 ) ) ;
#142739 = DIRECTION ( 'NONE',  ( 1.000000000000000000, -5.392603844284257652E-33, 0.000000000000000000 ) ) ;
#142738 = CARTESIAN_POINT ( 'NONE',  ( -8.314922557960811034, -14.29746914071050412, 37.08224293864768129 ) ) ;
#142740 = CARTESIAN_POINT ( 'NONE',  ( 9.564922557961047289, -16.46253265017146816, 100.4177570613523329 ) ) ;
#142741 = CARTESIAN_POINT ( 'NONE',  ( 19.02544592524334988, 5.153800228976608722, 26.45942372801899722 ) ) ;
#142742 = CARTESIAN_POINT ( 'NONE',  ( -12.06949235617756955, 12.14591786802309770, 35.62390960531437401 ) ) ;
#142743 = CARTESIAN_POINT ( 'NONE',  ( -21.55341960407610458, -5.719274019375992779, 96.45724293864770971 ) ) ;
#142744 = CARTESIAN_POINT ( 'NONE',  ( 21.52544592524344225, -5.823673210054117533, 48.54057627198103120 ) ) ;
#142745 = CARTESIAN_POINT ( 'NONE',  ( 19.03943276465977164, -0.05219959533909143690, 68.74890960531436690 ) ) ;
#142746 = CARTESIAN_POINT ( 'NONE',  ( -12.06949235617756955, 12.14591786802309770, 35.62390960531437401 ) ) ;
#142747 = CARTESIAN_POINT ( 'NONE',  ( 13.97604488694527802, 13.89961937509977652, 89.37390960531436690 ) ) ;
#142748 = ORIENTED_EDGE ( 'NONE', *, *, #71161, .T. ) ;
#142749 = CARTESIAN_POINT ( 'NONE',  ( 9.564922557960805705, 16.46253265017160317, 79.58224293864769550 ) ) ;
#142750 = CARTESIAN_POINT ( 'NONE',  ( -9.474510206698720793, -16.51473224551083518, 39.58442372801899722 ) ) ;
#142751 = CARTESIAN_POINT ( 'NONE',  ( -10.72451020669898014, 18.67979575497178502, 75.41557627198102409 ) ) ;
#142752 = CARTESIAN_POINT ( 'NONE',  ( 8.224510206698953496, -14.34966873604960469, 97.91557627198103830 ) ) ;
#142753 = CARTESIAN_POINT ( 'NONE',  ( 21.55341960407619695, -5.719274019375665929, 41.04275706135236135 ) ) ;
#142754 = CARTESIAN_POINT ( 'NONE',  ( 8.571926809382603096, -26.38167802310801235, 141.4750000027312069 ) ) ;
#142755 = CARTESIAN_POINT ( 'NONE',  ( -14.29746914071037622, -8.314922557961029526, 104.1677570613523471 ) ) ;
#142756 = CARTESIAN_POINT ( 'NONE',  ( 9.564922557960805705, 16.46253265017160317, 34.58224293864770260 ) ) ;
#142757 = CARTESIAN_POINT ( 'NONE',  ( -16.51473224551069308, -9.474510206698971260, 86.66557627198102409 ) ) ;
#142758 = CARTESIAN_POINT ( 'NONE',  ( -24.81835880841865816, 6.052260367207988878, 168.4265213779230521 ) ) ;
#142759 = CARTESIAN_POINT ( 'NONE',  ( -9.474510206698964154, 16.51473224551069663, 30.41557627198102054 ) ) ;
#142760 = CARTESIAN_POINT ( 'NONE',  ( -4.483927247898539470, -16.52544592524342804, 37.29057627198102409 ) ) ;
#142761 = CARTESIAN_POINT ( 'NONE',  ( -18.62759615963255300, -10.81492255796106328, 74.16775706135231871 ) ) ;
#142763 = CARTESIAN_POINT ( 'NONE',  ( -14.34966873604972548, 8.224510206698743886, 73.33442372801901854 ) ) ;
#142762 = CARTESIAN_POINT ( 'NONE',  ( 30.04893132686963853, -22.76590847478654211, -19.45433810172651334 ) ) ;
#142764 = CARTESIAN_POINT ( 'NONE',  ( 16.46253265017160672, -9.564922557960803928, 63.33224293864769550 ) ) ;
#142765 = CARTESIAN_POINT ( 'NONE',  ( 5.049401038298161559, -19.05341960407611168, 67.70724293864769550 ) ) ;
#142766 = ORIENTED_EDGE ( 'NONE', *, *, #176553, .T. ) ;
#142767 = CARTESIAN_POINT ( 'NONE',  ( -21.55341960407619339, 5.719274019375674811, 113.5427570613523756 ) ) ;
#142768 = CARTESIAN_POINT ( 'NONE',  ( -4.379528057220086978, -16.55341960407618274, 69.79275706135234714 ) ) ;
#142769 = CARTESIAN_POINT ( 'NONE',  ( -5.719274019375665041, -21.55341960407619695, 104.7927570613523898 ) ) ;
#142770 = CARTESIAN_POINT ( 'NONE',  ( -5.153800228976328057, -19.02544592524343514, 57.29057627198103120 ) ) ;
#142771 = CARTESIAN_POINT ( 'NONE',  ( 21.55341960407610458, 5.719274019375980345, 33.95724293864769550 ) ) ;
#142772 = CARTESIAN_POINT ( 'NONE',  ( -19.05341960407617563, 5.049401038297882671, 108.5427570613523187 ) ) ;
#142773 = CARTESIAN_POINT ( 'NONE',  ( -10.81492255796105439, 18.62759615963255655, 62.91775706135236135 ) ) ;
#142774 = CARTESIAN_POINT ( 'NONE',  ( 14.29746914071037800, 8.314922557961029526, 51.66775706135234714 ) ) ;
#142775 = CARTESIAN_POINT ( 'NONE',  ( 10.72451020669898902, -18.67979575497178502, 102.9155762719810383 ) ) ;
#142776 = CARTESIAN_POINT ( 'NONE',  ( 19.05341960407617918, -5.049401038297876454, 96.04275706135231871 ) ) ;
#142777 = CARTESIAN_POINT ( 'NONE',  ( 9.474510206698971260, -16.51473224551069308, 77.91557627198103830 ) ) ;
#142778 = CARTESIAN_POINT ( 'NONE',  ( 12.14591786802327356, -12.06949235617739191, 20.62609039468568639 ) ) ;
#142779 = CARTESIAN_POINT ( 'NONE',  ( 19.05341960407617918, -5.049401038297876454, 101.0427570613523045 ) ) ;
#142780 = CARTESIAN_POINT ( 'NONE',  ( 4.483927247898545687, 16.52544592524342804, 69.79057627198102409 ) ) ;
#142781 = CARTESIAN_POINT ( 'NONE',  ( 14.29746914071037800, 8.314922557961029526, 76.66775706135234714 ) ) ;
#142783 = CARTESIAN_POINT ( 'NONE',  ( 19.02544592524343514, -5.153800228976328945, 48.54057627198103120 ) ) ;
#142782 = CARTESIAN_POINT ( 'NONE',  ( -5.719274019375978568, 21.55341960407610458, 110.2072429386477239 ) ) ;
#142784 = CARTESIAN_POINT ( 'NONE',  ( -16.51473224551069308, -9.474510206698971260, 61.66557627198103120 ) ) ;
#142785 = CARTESIAN_POINT ( 'NONE',  ( 8.314922557961029526, -14.29746914071037800, 75.41775706135233293 ) ) ;
#142786 = CARTESIAN_POINT ( 'NONE',  ( -23.31738231874055245, -16.94106989632524574, 146.4500000054623854 ) ) ;
#142787 = ORIENTED_EDGE ( 'NONE', *, *, #129491, .T. ) ;
#142788 = CARTESIAN_POINT ( 'NONE',  ( -19.02544592524334988, -5.153800228976617603, 18.95942372801899722 ) ) ;
#142789 = EDGE_CURVE ( 'NONE', #118785, #125859, #159860, .T. ) ;
#142790 = CARTESIAN_POINT ( 'NONE',  ( -9.474510206698964154, 16.51473224551069663, 30.41557627198102054 ) ) ;
#142791 = EDGE_LOOP ( 'NONE', ( #21301, #114598, #69074, #17797 ) ) ;
#142792 = CARTESIAN_POINT ( 'NONE',  ( 19.02544592524334988, 5.153800228976608722, 106.4594237280190185 ) ) ;
#142794 = CARTESIAN_POINT ( 'NONE',  ( -14.29746914071037622, -8.314922557961029526, 24.16775706135235424 ) ) ;
#142793 = CARTESIAN_POINT ( 'NONE',  ( -13.89961937509957401, -13.97604488694547875, 44.37609039468566863 ) ) ;
#142795 = CARTESIAN_POINT ( 'NONE',  ( 9.474510206698971260, -16.51473224551069308, 37.91557627198102409 ) ) ;
#142796 = CARTESIAN_POINT ( 'NONE',  ( -5.049401038298153566, 19.05341960407611168, 60.20724293864768129 ) ) ;
#142797 = CARTESIAN_POINT ( 'NONE',  ( 18.62759615963271287, -10.81492255796078972, 88.33224293864769550 ) ) ;
#142798 = CARTESIAN_POINT ( 'NONE',  ( 19.05341960407611168, 5.049401038298154454, 113.9572429386477097 ) ) ;
#142799 = CARTESIAN_POINT ( 'NONE',  ( 5.049401038298161559, -19.05341960407611168, 47.70724293864770260 ) ) ;
#142800 = DIRECTION ( 'NONE',  ( -1.000000000000000000, -0.000000000000000000, -0.000000000000000000 ) ) ;
#142801 = CARTESIAN_POINT ( 'NONE',  ( 19.03943276465977164, 0.05219959533936151252, 96.25109039468567573 ) ) ;
#142802 = CARTESIAN_POINT ( 'NONE',  ( 4.379528057220339221, -16.55341960407611168, 67.70724293864769550 ) ) ;
#142803 = CARTESIAN_POINT ( 'NONE',  ( -16.51473224551082808, 9.474510206698731452, 28.33442372801900433 ) ) ;
#142804 = EDGE_CURVE ( 'NONE', #140780, #9769, #193785, .T. ) ;
#142805 = CARTESIAN_POINT ( 'NONE',  ( 4.379528057220339221, -16.55341960407611168, 57.70724293864770260 ) ) ;
#142806 = CARTESIAN_POINT ( 'NONE',  ( -10.72451020669870658, -18.67979575497194134, 84.58442372801903275 ) ) ;
#142807 = CARTESIAN_POINT ( 'NONE',  ( 0.05219959533909260263, 19.03943276465977164, 29.99890960531435979 ) ) ;
#142808 = CARTESIAN_POINT ( 'NONE',  ( -10.72451020669870658, -18.67979575497194134, 94.58442372801901854 ) ) ;
#142810 = CARTESIAN_POINT ( 'NONE',  ( 15.80617190586769283, -15.72974639402175789, 70.62609039468567573 ) ) ;
#142809 = CARTESIAN_POINT ( 'NONE',  ( -4.379528057220328563, 16.55341960407611168, 25.20724293864769550 ) ) ;
#142811 = CARTESIAN_POINT ( 'NONE',  ( 5.153800228976335163, 19.02544592524342804, 79.79057627198102409 ) ) ;
#142812 = CARTESIAN_POINT ( 'NONE',  ( -5.719274019375665041, -21.55341960407619695, 39.79275706135235424 ) ) ;
#142813 = CARTESIAN_POINT ( 'NONE',  ( -5.049401038298153566, 19.05341960407611168, 85.20724293864766707 ) ) ;
#142814 = CARTESIAN_POINT ( 'NONE',  ( -14.34966873604960291, -8.224510206698953496, 96.66557627198102409 ) ) ;
#142815 = CARTESIAN_POINT ( 'NONE',  ( -14.34966873604960291, -8.224510206698953496, 56.66557627198103830 ) ) ;
#142816 = CARTESIAN_POINT ( 'NONE',  ( 5.719274019375991003, -21.55341960407610458, 67.70724293864769550 ) ) ;
#142817 = CARTESIAN_POINT ( 'NONE',  ( 0.05219959533909260263, 19.03943276465977164, 74.99890960531435269 ) ) ;
#142818 = CARTESIAN_POINT ( 'NONE',  ( -10.72451020669898014, 18.67979575497178502, 80.41557627198103830 ) ) ;
#142819 = CARTESIAN_POINT ( 'NONE',  ( 13.97604488694548053, -13.89961937509957401, 65.62609039468567573 ) ) ;
#142821 = CARTESIAN_POINT ( 'NONE',  ( 4.379528057220339221, -16.55341960407611168, 72.70724293864769550 ) ) ;
#142820 = CARTESIAN_POINT ( 'NONE',  ( -19.02544592524335343, -5.153800228976618492, 33.95942372801899012 ) ) ;
#142822 = CARTESIAN_POINT ( 'NONE',  ( 18.62759615963271287, -10.81492255796078972, 48.33224293864770260 ) ) ;
#142823 = CARTESIAN_POINT ( 'NONE',  ( 20.43538597629128262, -20.43538597629122222, -52.65483682830183199 ) ) ;
#142825 = CARTESIAN_POINT ( 'NONE',  ( 17.14385361876520264, 23.59649016807275856, 144.6750000027311671 ) ) ;
#142824 = CARTESIAN_POINT ( 'NONE',  ( 16.52544592524335698, 4.483927247898782831, 101.4594237280190185 ) ) ;
#142826 = CARTESIAN_POINT ( 'NONE',  ( 5.049401038297881783, 19.05341960407617563, 97.29275706135233293 ) ) ;
#142827 = CARTESIAN_POINT ( 'NONE',  ( -4.483927247898539470, -16.52544592524342804, 62.29057627198102409 ) ) ;
#142828 = CARTESIAN_POINT ( 'NONE',  ( 9.051216217265929842, -0.3920586954752088293, -61.90435651123959104 ) ) ;
#142829 = CARTESIAN_POINT ( 'NONE',  ( -19.05341960407611168, -5.049401038298163336, 56.45724293864768129 ) ) ;
#142830 = CARTESIAN_POINT ( 'NONE',  ( 14.34966873604960469, 8.224510206698951720, 54.16557627198103120 ) ) ;
#142831 = ADVANCED_FACE ( 'NONE', ( #10766 ), #13097, .T. ) ;
#142832 = CARTESIAN_POINT ( 'NONE',  ( 16.46253265017160672, -9.564922557960803928, 103.3322429386476955 ) ) ;
#142834 = CARTESIAN_POINT ( 'NONE',  ( -16.46253265017160317, 9.564922557960807481, 70.83224293864770971 ) ) ;
#142833 = CARTESIAN_POINT ( 'NONE',  ( -16.51473224551082808, 9.474510206698731452, 78.33442372801900433 ) ) ;
#142835 = CARTESIAN_POINT ( 'NONE',  ( 19.05341960407611168, 5.049401038298154454, 78.95724293864769550 ) ) ;
#142836 = CARTESIAN_POINT ( 'NONE',  ( -19.02544592524342804, 5.153800228976336051, 81.04057627198103830 ) ) ;
#142837 = CARTESIAN_POINT ( 'NONE',  ( -5.823673210054116645, -21.52544592524344225, 57.29057627198103120 ) ) ;
#142838 = CARTESIAN_POINT ( 'NONE',  ( -16.55341960407617563, 4.379528057220093196, 63.54275706135234003 ) ) ;
#142839 = CARTESIAN_POINT ( 'NONE',  ( -2.285367203649865752E-16, -64.83960026421343059, -23.00000000000000000 ) ) ;
#142840 = CARTESIAN_POINT ( 'NONE',  ( -5.153800228976328057, -19.02544592524343514, 52.29057627198100988 ) ) ;
#142841 = CARTESIAN_POINT ( 'NONE',  ( -21.52544592524343514, 5.823673210054127303, 61.04057627198103120 ) ) ;
#142842 = CARTESIAN_POINT ( 'NONE',  ( -19.03943276465977164, -0.05219959533935918106, 93.75109039468566152 ) ) ;
#142844 = CARTESIAN_POINT ( 'NONE',  ( -18.67979575497193778, 10.72451020669871902, 48.33442372801902565 ) ) ;
#142843 = CARTESIAN_POINT ( 'NONE',  ( 14.34966873604960469, 8.224510206698951720, 29.16557627198103120 ) ) ;
#142845 = CARTESIAN_POINT ( 'NONE',  ( 16.46253265017146816, 9.564922557961045513, 36.66775706135233293 ) ) ;
#142847 = CARTESIAN_POINT ( 'NONE',  ( 8.314922557961029526, -14.29746914071037800, 90.41775706135236135 ) ) ;
#142846 = CARTESIAN_POINT ( 'NONE',  ( -8.224510206698735004, -14.34966873604973081, 59.58442372801901854 ) ) ;
#142848 = DIRECTION ( 'NONE',  ( -1.000000000000000000, -0.000000000000000000, -0.000000000000000000 ) ) ;
#142849 = CARTESIAN_POINT ( 'NONE',  ( 14.29746914071037800, 8.314922557961029526, 81.66775706135236135 ) ) ;
#142850 = CARTESIAN_POINT ( 'NONE',  ( -12.14591786802326823, 12.06949235617739902, 38.12609039468567573 ) ) ;
#142851 = CARTESIAN_POINT ( 'NONE',  ( 9.564922557960805705, 16.46253265017160317, 44.58224293864769550 ) ) ;
#142852 = CARTESIAN_POINT ( 'NONE',  ( 5.153800228976335163, 19.02544592524342804, 44.79057627198103830 ) ) ;
#142853 = CARTESIAN_POINT ( 'NONE',  ( -5.049401038298153566, 19.05341960407611168, 65.20724293864765286 ) ) ;
#142854 = CARTESIAN_POINT ( 'NONE',  ( -18.67979575497193778, 10.72451020669871902, 58.33442372801901143 ) ) ;
#142855 = CARTESIAN_POINT ( 'NONE',  ( -4.483927247898782831, 16.52544592524335698, 52.70942372801902565 ) ) ;
#142856 = CARTESIAN_POINT ( 'NONE',  ( -16.55341960407617563, 4.379528057220093196, 113.5427570613523756 ) ) ;
#142857 = CARTESIAN_POINT ( 'NONE',  ( 16.46253265017160672, -9.564922557960803928, 23.33224293864769194 ) ) ;
#142858 = CARTESIAN_POINT ( 'NONE',  ( -13.89961937509957401, -13.97604488694547875, 24.37609039468565442 ) ) ;
#142859 = CARTESIAN_POINT ( 'NONE',  ( -9.474510206698720793, -16.51473224551083518, 104.5844237280190043 ) ) ;
#142860 = CARTESIAN_POINT ( 'NONE',  ( -19.05341960407617563, 5.049401038297882671, 68.54275706135230450 ) ) ;
#142861 = CARTESIAN_POINT ( 'NONE',  ( 16.55341960407611168, 4.379528057220329451, 78.95724293864769550 ) ) ;
#142862 = CARTESIAN_POINT ( 'NONE',  ( -16.46253265017160317, 9.564922557960807481, 40.83224293864769550 ) ) ;
#142864 = DIRECTION ( 'NONE',  ( 0.000000000000000000, -0.9396926207859049862, 0.3420201433256783163 ) ) ;
#142863 = CARTESIAN_POINT ( 'NONE',  ( -19.05341960407617563, 5.049401038297882671, 68.54275706135230450 ) ) ;
#142865 = CARTESIAN_POINT ( 'NONE',  ( -5.823673210054431948, 21.52544592524334988, 72.70942372801901854 ) ) ;
#142866 = CARTESIAN_POINT ( 'NONE',  ( -8.314922557961024197, 14.29746914071037800, 37.91775706135235424 ) ) ;
#142867 = CARTESIAN_POINT ( 'NONE',  ( -17.49999999999999289, 3.565345528327877211, 24.42494486806482712 ) ) ;
#142868 = CARTESIAN_POINT ( 'NONE',  ( -18.62759615963270932, 10.81492255796079327, 30.83224293864770260 ) ) ;
#142869 = CARTESIAN_POINT ( 'NONE',  ( 0.05219959533934541429, -16.53943276465976808, 25.00109039468567218 ) ) ;
#142870 = CARTESIAN_POINT ( 'NONE',  ( 16.46253265017160672, -9.564922557960803928, 23.33224293864769194 ) ) ;
#142871 = CARTESIAN_POINT ( 'NONE',  ( -5.049401038297874678, -19.05341960407617918, 24.79275706135233648 ) ) ;
#142872 = CARTESIAN_POINT ( 'NONE',  ( 5.049401038298161559, -19.05341960407611168, 37.70724293864768839 ) ) ;
#142873 = CARTESIAN_POINT ( 'NONE',  ( -20.29110136410554333, -20.59644990402605558, -52.64180230391848170 ) ) ;
#142874 = CARTESIAN_POINT ( 'NONE',  ( 19.03943276465977164, -0.05219959533909143690, 73.74890960531435269 ) ) ;
#142875 = CARTESIAN_POINT ( 'NONE',  ( 17.50000000000147793, -3.202012800152233218, 112.4282241602725634 ) ) ;
#142876 = CARTESIAN_POINT ( 'NONE',  ( -18.62759615963255300, -10.81492255796106328, 109.1677570613523613 ) ) ;
#142877 = CARTESIAN_POINT ( 'NONE',  ( -16.55341960407611168, -4.379528057220339221, 31.45724293864769550 ) ) ;
#142878 = CARTESIAN_POINT ( 'NONE',  ( 16.46253265017160672, -9.564922557960803928, 48.33224293864769550 ) ) ;
#142879 = CARTESIAN_POINT ( 'NONE',  ( 9.564922557960805705, 16.46253265017160317, 94.58224293864769550 ) ) ;
#142880 = CARTESIAN_POINT ( 'NONE',  ( 10.81492255796106328, -18.62759615963255655, 75.41775706135233293 ) ) ;
#142881 = CARTESIAN_POINT ( 'NONE',  ( -16.51473224551069308, -9.474510206698971260, 51.66557627198102409 ) ) ;
#142882 = CARTESIAN_POINT ( 'NONE',  ( 15.72974639402176855, 15.80617190586768217, 71.87609039468568994 ) ) ;
#142883 = CARTESIAN_POINT ( 'NONE',  ( 5.823673210054125526, 21.52544592524343514, 24.79057627198103120 ) ) ;
#142884 = CARTESIAN_POINT ( 'NONE',  ( -13.89961937509977652, 13.97604488694528158, 40.62390960531435979 ) ) ;
#142885 = CARTESIAN_POINT ( 'NONE',  ( -18.62759615963270932, 10.81492255796079327, 115.8322429386477097 ) ) ;
#142886 = CARTESIAN_POINT ( 'NONE',  ( 9.474510206698729675, 16.51473224551082808, 52.08442372801900433 ) ) ;
#142887 = CARTESIAN_POINT ( 'NONE',  ( -12.06949235617756955, 12.14591786802309770, 110.6239096053143669 ) ) ;
#142888 = CARTESIAN_POINT ( 'NONE',  ( -19.02544592524342804, 5.153800228976336051, 66.04057627198103830 ) ) ;
#142889 = CARTESIAN_POINT ( 'NONE',  ( 12.06949235617739724, 12.14591786802326823, 21.87609039468567573 ) ) ;
#142890 = CARTESIAN_POINT ( 'NONE',  ( -14.34966873604960291, -8.224510206698953496, 76.66557627198103830 ) ) ;
#142891 = CARTESIAN_POINT ( 'NONE',  ( 0.05219959533907565091, 21.53943276465977519, 29.99890960531435979 ) ) ;
#142892 = CARTESIAN_POINT ( 'NONE',  ( 5.049401038297881783, 19.05341960407617563, 87.29275706135234714 ) ) ;
#142893 = CARTESIAN_POINT ( 'NONE',  ( 10.72451020669898902, -18.67979575497178502, 102.9155762719810383 ) ) ;
#142894 = CARTESIAN_POINT ( 'NONE',  ( -5.719274019375665041, -21.55341960407619695, 59.79275706135234714 ) ) ;
#142895 = CARTESIAN_POINT ( 'NONE',  ( -4.379528057220086978, -16.55341960407618274, 54.79275706135235424 ) ) ;
#142896 = CARTESIAN_POINT ( 'NONE',  ( -8.314922557961024197, 14.29746914071037800, 52.91775706135235424 ) ) ;
#142897 = CARTESIAN_POINT ( 'NONE',  ( -15.72974639402197994, 15.80617190586746368, 55.62390960531436690 ) ) ;
#142898 = CARTESIAN_POINT ( 'NONE',  ( -9.564922557960796823, -16.46253265017161027, 52.08224293864768839 ) ) ;
#142899 = CARTESIAN_POINT ( 'NONE',  ( -6.020228577223754586E-15, 39.95556452105416412, -2.249999994537625891 ) ) ;
#142900 = CARTESIAN_POINT ( 'NONE',  ( -4.379528057220086978, -16.55341960407618274, 79.79275706135236135 ) ) ;
#142901 = CARTESIAN_POINT ( 'NONE',  ( 18.62759615963271287, -10.81492255796078972, 103.3322429386476955 ) ) ;
#142902 = CARTESIAN_POINT ( 'NONE',  ( 12.14591786802309770, 12.06949235617756955, 54.37390960531435979 ) ) ;
#142903 = CARTESIAN_POINT ( 'NONE',  ( 9.474510206698971260, -16.51473224551069308, 72.91557627198102409 ) ) ;
#142904 = CARTESIAN_POINT ( 'NONE',  ( -14.29746914071037622, -8.314922557961029526, 74.16775706135231871 ) ) ;
#142905 = CARTESIAN_POINT ( 'NONE',  ( -13.89961937509957401, -13.97604488694547875, 99.37609039468567573 ) ) ;
#142906 = CARTESIAN_POINT ( 'NONE',  ( -21.53943276465977519, 0.05219959533907696930, 96.24890960531435269 ) ) ;
#142907 = CARTESIAN_POINT ( 'NONE',  ( 14.34966873604960469, 8.224510206698951720, 49.16557627198102409 ) ) ;
#142908 = ORIENTED_EDGE ( 'NONE', *, *, #177312, .T. ) ;
#142909 = CARTESIAN_POINT ( 'NONE',  ( -16.18388926212238843, 7.379444403734526148, 69.56046848633849322 ) ) ;
#142910 = CARTESIAN_POINT ( 'NONE',  ( -10.72451020669898014, 18.67979575497178502, 75.41557627198102409 ) ) ;
#142911 = CARTESIAN_POINT ( 'NONE',  ( -16.55341960407617563, 4.379528057220093196, 113.5427570613523756 ) ) ;
#142912 = VERTEX_POINT ( 'NONE', #19129 ) ;
#142913 = CARTESIAN_POINT ( 'NONE',  ( -17.40861289039003523, -6.110651285853283099, 56.37232470827432707 ) ) ;
#142914 = CARTESIAN_POINT ( 'NONE',  ( -5.823673210054116645, -21.52544592524344225, 97.29057627198105251 ) ) ;
#142915 = CARTESIAN_POINT ( 'NONE',  ( 0.05219959533937995610, -21.53943276465977519, 25.00109039468567218 ) ) ;
#142916 = CARTESIAN_POINT ( 'NONE',  ( 16.52544592524342804, -4.483927247898539470, 43.54057627198103830 ) ) ;
#142917 = CARTESIAN_POINT ( 'NONE',  ( -14.29746914071037622, -8.314922557961029526, 49.16775706135234003 ) ) ;
#142918 = CARTESIAN_POINT ( 'NONE',  ( 16.51473224551069308, 9.474510206698969483, 49.16557627198102409 ) ) ;
#142919 = CARTESIAN_POINT ( 'NONE',  ( 19.03943276465977164, -0.05219959533909143690, 83.74890960531436690 ) ) ;
#142920 = VERTEX_POINT ( 'NONE', #142457 ) ;
#142921 = CARTESIAN_POINT ( 'NONE',  ( 18.67979575497178502, 10.72451020669898547, 29.16557627198103120 ) ) ;
#142922 = CARTESIAN_POINT ( 'NONE',  ( -31.20004872165591436, -21.37828431676506113, -20.08970689225503392 ) ) ;
#142923 = CARTESIAN_POINT ( 'NONE',  ( 14.29746914071037800, 8.314922557961029526, 26.66775706135235424 ) ) ;
#142924 = CARTESIAN_POINT ( 'NONE',  ( -19.02544592524334988, -5.153800228976617603, 53.95942372801898301 ) ) ;
#142925 = CARTESIAN_POINT ( 'NONE',  ( -21.53943276465977519, 0.05219959533907696930, 101.2489096053143669 ) ) ;
#142926 = CARTESIAN_POINT ( 'NONE',  ( -8.314922557960811034, -14.29746914071050412, 37.08224293864768129 ) ) ;
#142927 = CIRCLE ( 'NONE', #197951, 4.250000000000000000 ) ;
#142928 = CARTESIAN_POINT ( 'NONE',  ( -5.049401038298153566, 19.05341960407611168, 75.20724293864769550 ) ) ;
#142929 = CARTESIAN_POINT ( 'NONE',  ( 10.81492255796078972, 18.62759615963270932, 64.58224293864769550 ) ) ;
#142931 = CARTESIAN_POINT ( 'NONE',  ( -14.29746914071037622, -8.314922557961029526, 19.16775706135234714 ) ) ;
#142930 = CARTESIAN_POINT ( 'NONE',  ( 10.81492255796078972, 18.62759615963270932, 94.58224293864769550 ) ) ;
#142932 = CARTESIAN_POINT ( 'NONE',  ( -21.55341960407610458, -5.719274019375992779, 26.45724293864768839 ) ) ;
#142933 = CARTESIAN_POINT ( 'NONE',  ( -21.55341960407619339, 5.719274019375674811, 83.54275706135234714 ) ) ;
#142934 = CARTESIAN_POINT ( 'NONE',  ( -9.474510206698964154, 16.51473224551069663, 75.41557627198103830 ) ) ;
#142935 = CARTESIAN_POINT ( 'NONE',  ( 19.03943276465977164, -0.05219959533909143690, 33.74890960531435979 ) ) ;
#142936 = CARTESIAN_POINT ( 'NONE',  ( 19.02544592524343514, -5.153800228976328945, 83.54057627198100988 ) ) ;
#142937 = CARTESIAN_POINT ( 'NONE',  ( -14.29746914071049879, 8.314922557960819915, 100.8322429386477097 ) ) ;
#142938 = CARTESIAN_POINT ( 'NONE',  ( -9.474510206698720793, -16.51473224551083518, 99.58442372801900433 ) ) ;
#142939 = CARTESIAN_POINT ( 'NONE',  ( 17.50000000000000355, 5.076555817581247076, 33.67951492049776618 ) ) ;
#142940 = CARTESIAN_POINT ( 'NONE',  ( -0.05219959533909027116, -19.03943276465977164, 77.49890960531435269 ) ) ;
#142942 = CARTESIAN_POINT ( 'NONE',  ( 21.52544592524344225, -5.823673210054117533, 23.54057627198102765 ) ) ;
#142941 = CARTESIAN_POINT ( 'NONE',  ( 15.72974639402176855, 15.80617190586768217, 96.87609039468568994 ) ) ;
#142943 = CARTESIAN_POINT ( 'NONE',  ( -12.14591786802326823, 12.06949235617739902, 93.12609039468568994 ) ) ;
#142944 = CARTESIAN_POINT ( 'NONE',  ( -16.36317988757059894, -7.306389748694932962, 75.90210391636779264 ) ) ;
#142945 = CARTESIAN_POINT ( 'NONE',  ( -9.474510206698720793, -16.51473224551083518, 59.58442372801900433 ) ) ;
#142946 = CARTESIAN_POINT ( 'NONE',  ( -0.05219959533937732626, 21.53943276465977519, 107.5010903946856899 ) ) ;
#142947 = DIRECTION ( 'NONE',  ( -0.000000000000000000, -0.000000000000000000, 1.000000000000000000 ) ) ;
#142948 = CARTESIAN_POINT ( 'NONE',  ( -19.03943276465977164, 0.05219959533909376836, 31.24890960531435979 ) ) ;
#142949 = CARTESIAN_POINT ( 'NONE',  ( 16.55341960407618274, -4.379528057220086978, 111.0427570613523613 ) ) ;
#142950 = ADVANCED_FACE ( 'NONE', ( #45490 ), #69607, .T. ) ;
#142951 = CARTESIAN_POINT ( 'NONE',  ( 18.22780087662121673, 5.500000000000056843, 83.98459894673892734 ) ) ;
#142952 = CARTESIAN_POINT ( 'NONE',  ( -4.483927247898782831, 16.52544592524335698, 102.7094237280190185 ) ) ;
#142953 = CARTESIAN_POINT ( 'NONE',  ( 22.71303993882839833, -20.60981468104613512, -50.67862666510512781 ) ) ;
#142954 = CARTESIAN_POINT ( 'NONE',  ( -4.483927247898782831, 16.52544592524335698, 82.70942372801900433 ) ) ;
#142955 = CARTESIAN_POINT ( 'NONE',  ( 17.59860650958989936, 7.585241751807028088, 84.07662985737508166 ) ) ;
#142956 = CARTESIAN_POINT ( 'NONE',  ( -5.823673210054431948, 21.52544592524334988, 97.70942372801904696 ) ) ;
#142957 = CARTESIAN_POINT ( 'NONE',  ( 5.049401038297881783, 19.05341960407617563, 102.2927570613523045 ) ) ;
#142958 = CARTESIAN_POINT ( 'NONE',  ( 0.05219959533937995610, -21.53943276465977519, 65.00109039468568994 ) ) ;
#142959 = CARTESIAN_POINT ( 'NONE',  ( 19.03943276465977164, 0.05219959533936151252, 36.25109039468567573 ) ) ;
#142960 = CARTESIAN_POINT ( 'NONE',  ( -16.46253265017160317, 9.564922557960807481, 80.83224293864769550 ) ) ;
#142961 = CARTESIAN_POINT ( 'NONE',  ( 9.564922557960805705, 16.46253265017160317, 64.58224293864769550 ) ) ;
#142962 = EDGE_CURVE ( 'NONE', #142350, #184761, #175793, .T. ) ;
#142963 = CARTESIAN_POINT ( 'NONE',  ( 17.05587630539786304, 6.762274262135722580, 71.75819690962690345 ) ) ;
#142964 = CARTESIAN_POINT ( 'NONE',  ( -5.823673210054116645, -21.52544592524344225, 47.29057627198103120 ) ) ;
#142965 = CARTESIAN_POINT ( 'NONE',  ( 13.89961937509977652, -13.97604488694527269, 43.12390960531434558 ) ) ;
#142967 = CARTESIAN_POINT ( 'NONE',  ( -16.53943276465976808, -0.05219959533934237506, 83.75109039468568994 ) ) ;
#142966 = CARTESIAN_POINT ( 'NONE',  ( -5.719274019375978568, 21.55341960407610458, 90.20724293864770971 ) ) ;
#142968 = UNCERTAINTY_MEASURE_WITH_UNIT (LENGTH_MEASURE( 1.000000000000000082E-05 ), #28026, 'distance_accuracy_value', 'NONE');
#142969 = VERTEX_POINT ( 'NONE', #83757 ) ;
#142971 = CARTESIAN_POINT ( 'NONE',  ( 36.91746824999999177, 2.880721459617395097E-14, -1.624999997268813390 ) ) ;
#142970 = CARTESIAN_POINT ( 'NONE',  ( -4.483927247898539470, -16.52544592524342804, 77.29057627198102409 ) ) ;
#142972 = CARTESIAN_POINT ( 'NONE',  ( 12.14591786802327356, -12.06949235617739191, 40.62609039468567573 ) ) ;
#142973 = CARTESIAN_POINT ( 'NONE',  ( -13.89961937509977652, 13.97604488694528158, 25.62390960531434558 ) ) ;
#142974 = CARTESIAN_POINT ( 'NONE',  ( 19.02544592524334988, 5.153800228976608722, 66.45942372801899012 ) ) ;
#142975 = CARTESIAN_POINT ( 'NONE',  ( -12.06949235617756955, 12.14591786802309770, 70.62390960531436690 ) ) ;
#142976 = CARTESIAN_POINT ( 'NONE',  ( 18.67979575497194134, -10.72451020669871369, 40.83442372801901854 ) ) ;
#142978 = CARTESIAN_POINT ( 'NONE',  ( 18.67979575497178502, 10.72451020669898547, 89.16557627198102409 ) ) ;
#142977 = DIRECTION ( 'NONE',  ( -1.000000000000000000, 0.000000000000000000, 0.000000000000000000 ) ) ;
#142979 = CARTESIAN_POINT ( 'NONE',  ( 9.564922557960805705, 16.46253265017160317, 114.5822429386476955 ) ) ;
#142980 = CARTESIAN_POINT ( 'NONE',  ( -12.06949235617756955, 12.14591786802309770, 75.62390960531439532 ) ) ;
#142981 = CARTESIAN_POINT ( 'NONE',  ( 15.71981542752503103, -36.60361700297598730, -28.71911170260956681 ) ) ;
#142982 = CARTESIAN_POINT ( 'NONE',  ( -5.049401038298153566, 19.05341960407611168, 45.20724293864769550 ) ) ;
#142983 = CARTESIAN_POINT ( 'NONE',  ( -11.40812507854754720, -35.11059874428192273, -4.224999997268813701 ) ) ;
#142984 = CARTESIAN_POINT ( 'NONE',  ( 16.46253265017146816, 9.564922557961045513, 86.66775706135233293 ) ) ;
#142985 = CARTESIAN_POINT ( 'NONE',  ( 15.72974639402176855, 15.80617190586768217, 21.87609039468567573 ) ) ;
#142986 = CARTESIAN_POINT ( 'NONE',  ( -9.474510206698964154, 16.51473224551069663, 70.41557627198102409 ) ) ;
#142987 = CARTESIAN_POINT ( 'NONE',  ( 19.02544592524334988, 5.153800228976608722, 56.45942372801898301 ) ) ;
#142988 = CARTESIAN_POINT ( 'NONE',  ( -5.153800228976328057, -19.02544592524343514, 42.29057627198101699 ) ) ;
#142989 = CARTESIAN_POINT ( 'NONE',  ( 16.53943276465976808, -0.05219959533910856209, 58.74890960531436690 ) ) ;
#142990 = CARTESIAN_POINT ( 'NONE',  ( 16.53943276465976808, -0.05219959533910856209, 48.74890960531435979 ) ) ;
#142991 = CARTESIAN_POINT ( 'NONE',  ( -19.02544592524342804, 5.153800228976336051, 81.04057627198103830 ) ) ;
#142992 = CARTESIAN_POINT ( 'NONE',  ( 21.53943276465977519, -0.05219959533907433946, 88.74890960531436690 ) ) ;
#142993 = CARTESIAN_POINT ( 'NONE',  ( 5.049401038298161559, -19.05341960407611168, 77.70724293864765286 ) ) ;
#142994 = CARTESIAN_POINT ( 'NONE',  ( 21.52544592524344225, -5.823673210054117533, 83.54057627198102409 ) ) ;
#142995 = CARTESIAN_POINT ( 'NONE',  ( -5.823673210054431948, 21.52544592524334988, 112.7094237280190328 ) ) ;
#142998 = CARTESIAN_POINT ( 'NONE',  ( 8.314922557960818139, 14.29746914071049879, 94.58224293864769550 ) ) ;
#142997 = CARTESIAN_POINT ( 'NONE',  ( 16.55341960407618274, -4.379528057220086978, 106.0427570613523471 ) ) ;
#142996 = CARTESIAN_POINT ( 'NONE',  ( -0.05219959533909027116, -19.03943276465977164, 27.49890960531435624 ) ) ;
#142999 = CARTESIAN_POINT ( 'NONE',  ( -19.03943276465977164, -0.05219959533935918106, 108.7510903946856615 ) ) ;
#143000 = ORIENTED_EDGE ( 'NONE', *, *, #2819, .T. ) ;
#143001 = CARTESIAN_POINT ( 'NONE',  ( 18.67979575497194134, -10.72451020669871369, 30.83442372801902209 ) ) ;
#143002 = CARTESIAN_POINT ( 'NONE',  ( -9.474510206698720793, -16.51473224551083518, 49.58442372801899722 ) ) ;
#143003 = CARTESIAN_POINT ( 'NONE',  ( 8.314922557960818139, 14.29746914071049879, 24.58224293864768839 ) ) ;
#143004 = CARTESIAN_POINT ( 'NONE',  ( -21.52544592524343514, 5.823673210054127303, 71.04057627198103830 ) ) ;
#143005 = CARTESIAN_POINT ( 'NONE',  ( -19.05341960407611168, -5.049401038298163336, 106.4572429386476955 ) ) ;
#143006 = CARTESIAN_POINT ( 'NONE',  ( 16.55341960407611168, 4.379528057220329451, 53.95724293864770260 ) ) ;
#143007 = CARTESIAN_POINT ( 'NONE',  ( -23.29544513554941076, 16.92513159979227666, 140.0656553485623590 ) ) ;
#143008 = CARTESIAN_POINT ( 'NONE',  ( -19.05341960407611168, -5.049401038298163336, 36.45724293864766707 ) ) ;
#143009 = CARTESIAN_POINT ( 'NONE',  ( -21.53943276465977519, -0.05219959533937600094, 103.7510903946857042 ) ) ;
#143010 = CARTESIAN_POINT ( 'NONE',  ( 16.55341960407618274, -4.379528057220086978, 86.04275706135236135 ) ) ;
#143011 = CARTESIAN_POINT ( 'NONE',  ( -18.62759615963255300, -10.81492255796106328, 44.16775706135234714 ) ) ;
#143012 = CARTESIAN_POINT ( 'NONE',  ( 14.34966873604972726, -8.224510206698740333, 40.83442372801901854 ) ) ;
#143013 = CARTESIAN_POINT ( 'NONE',  ( 5.823673210054125526, 21.52544592524343514, 29.79057627198102409 ) ) ;
#143014 = CARTESIAN_POINT ( 'NONE',  ( -16.51473224551069308, -9.474510206698971260, 51.66557627198102409 ) ) ;
#143015 = CARTESIAN_POINT ( 'NONE',  ( -13.97604488694527625, -13.89961937509977652, 71.87390960531433848 ) ) ;
#143016 = CARTESIAN_POINT ( 'NONE',  ( -4.379528057220086978, -16.55341960407618274, 64.79275706135234714 ) ) ;
#143017 = CARTESIAN_POINT ( 'NONE',  ( 4.483927247898545687, 16.52544592524342804, 104.7905762719810241 ) ) ;
#143018 = CARTESIAN_POINT ( 'NONE',  ( -4.483927247898782831, 16.52544592524335698, 112.7094237280190328 ) ) ;
#143019 = DIRECTION ( 'NONE',  ( -1.000000000000000000, -0.000000000000000000, -3.709348145883536076E-20 ) ) ;
#143022 = CARTESIAN_POINT ( 'NONE',  ( -16.51473224551069308, -9.474510206698971260, 76.66557627198103830 ) ) ;
#143021 = CARTESIAN_POINT ( 'NONE',  ( 9.474510206698971260, -16.51473224551069308, 92.91557627198103830 ) ) ;
#143020 = CARTESIAN_POINT ( 'NONE',  ( 15.80617190586769283, -15.72974639402175789, 50.62609039468568994 ) ) ;
#143023 = CARTESIAN_POINT ( 'NONE',  ( 19.02544592524343514, -5.153800228976328945, 93.54057627198102409 ) ) ;
#143024 = CARTESIAN_POINT ( 'NONE',  ( 4.379528057220339221, -16.55341960407611168, 47.70724293864770260 ) ) ;
#143025 = B_SPLINE_CURVE_WITH_KNOTS ( 'NONE', 3,
 ( #112737, #143069, #109762, #63258, #144073, #172436, #159233, #155278, #96565, #142081, #78415, #141095, #127901, #81384, #82385, #5554, #3567, #140091, #94588, #186635, #67233, #126905, #174430, #188611, #171446, #20728, #1583, #4548, #32933, #111752, #49097, #17768, #2582, #64262, #125928, #158253, #187627, #170447, #66241, #110754 ),
 .UNSPECIFIED., .F., .F.,
 ( 4, 2, 2, 2, 2, 2, 2, 2, 2, 2, 2, 2, 2, 2, 2, 2, 2, 2, 2, 4 ),
 ( 0.02158449572284441148, 0.02266158837400314083, 0.02373868102516187018, 0.02427722735074124005, 0.02481577367632061340, 0.02589286632747935663, 0.02696995897863810332, 0.02804705162979684654, 0.02912414428095558977, 0.02966269060653496312, 0.03020123693211433646, 0.03127832958327311785, 0.03235542223443189924, 0.03343251488559068757, 0.03450960753674947590, 0.03558670018790825729, 0.03612524651348765492, 0.03666379283906703868, 0.03774088549022582006, 0.03881797814138458758 ),
 .UNSPECIFIED. ) ;
#143026 = CARTESIAN_POINT ( 'NONE',  ( -16.55341960407611168, -4.379528057220339221, 21.45724293864769550 ) ) ;
#143027 = CARTESIAN_POINT ( 'NONE',  ( 16.53943276465976808, -0.05219959533910856209, 33.74890960531436690 ) ) ;
#143028 = CARTESIAN_POINT ( 'NONE',  ( -4.500000000000001776, -140.0000000000000000, 21.32407087589996308 ) ) ;
#143029 = CARTESIAN_POINT ( 'NONE',  ( 19.05341960407617918, -5.049401038297876454, 31.04275706135232227 ) ) ;
#143030 = CARTESIAN_POINT ( 'NONE',  ( -5.153800228976328057, -19.02544592524343514, 72.29057627198102409 ) ) ;
#143031 = CARTESIAN_POINT ( 'NONE',  ( 16.46253265017146816, 9.564922557961045513, 46.66775706135233293 ) ) ;
#143032 = CARTESIAN_POINT ( 'NONE',  ( 3.556970738554033499E-15, -38.81732327939057825, -10.62499999726881050 ) ) ;
#143033 = CARTESIAN_POINT ( 'NONE',  ( 16.46253265017160672, -9.564922557960803928, 68.33224293864770971 ) ) ;
#143035 = CARTESIAN_POINT ( 'NONE',  ( -12.06949235617739369, -12.14591786802326823, 64.37609039468568994 ) ) ;
#143034 = CARTESIAN_POINT ( 'NONE',  ( 9.564922557961047289, -16.46253265017146816, 85.41775706135233293 ) ) ;
#143036 = CARTESIAN_POINT ( 'NONE',  ( -19.03943276465977164, -0.05219959533935918106, 113.7510903946856757 ) ) ;
#143037 = CARTESIAN_POINT ( 'NONE',  ( -9.564922557960796823, -16.46253265017161027, 102.0822429386477097 ) ) ;
#143038 = CARTESIAN_POINT ( 'NONE',  ( -21.52544592524334988, -5.823673210054445271, 33.95942372801901143 ) ) ;
#143039 = CARTESIAN_POINT ( 'NONE',  ( -16.51473224551082808, 9.474510206698731452, 93.33442372801900433 ) ) ;
#143041 = CARTESIAN_POINT ( 'NONE',  ( 19.02544592524343514, -5.153800228976328945, 53.54057627198102409 ) ) ;
#143040 = CARTESIAN_POINT ( 'NONE',  ( -0.05219959533909027116, -19.03943276465977164, 112.4989096053143669 ) ) ;
#143042 = CARTESIAN_POINT ( 'NONE',  ( -0.05219959533909027116, -19.03943276465977164, 92.49890960531436690 ) ) ;
#143044 = CARTESIAN_POINT ( 'NONE',  ( -16.46253265017160317, 9.564922557960807481, 55.83224293864769550 ) ) ;
#143043 = CARTESIAN_POINT ( 'NONE',  ( 16.52544592524342804, -4.483927247898539470, 48.54057627198103120 ) ) ;
#143045 = CARTESIAN_POINT ( 'NONE',  ( 5.153800228976615827, -19.02544592524334988, 70.20942372801899012 ) ) ;
#143046 = CARTESIAN_POINT ( 'NONE',  ( 13.97604488694548053, -13.89961937509957401, 25.62609039468566507 ) ) ;
#143047 = CARTESIAN_POINT ( 'NONE',  ( -13.97604488694527625, -13.89961937509977652, 61.87390960531435979 ) ) ;
#143048 = CARTESIAN_POINT ( 'NONE',  ( 0.05219959533907565091, 21.53943276465977519, 59.99890960531436690 ) ) ;
#143050 = CARTESIAN_POINT ( 'NONE',  ( -0.05219959533937732626, 21.53943276465977519, 112.5010903946857042 ) ) ;
#143049 = CARTESIAN_POINT ( 'NONE',  ( 14.29746914071049879, -8.314922557960816363, 73.33224293864769550 ) ) ;
#143051 = CARTESIAN_POINT ( 'NONE',  ( -0.7621229312825035240, -6.292920404648720378, -64.49503546857650349 ) ) ;
#143052 = CARTESIAN_POINT ( 'NONE',  ( -19.02544592524342804, 5.153800228976336051, 116.0405762719810383 ) ) ;
#143053 = CARTESIAN_POINT ( 'NONE',  ( -16.46253265017160317, 9.564922557960807481, 55.83224293864769550 ) ) ;
#143054 = CARTESIAN_POINT ( 'NONE',  ( 19.05341960407611168, 5.049401038298154454, 43.95724293864769550 ) ) ;
#143055 = CARTESIAN_POINT ( 'NONE',  ( 0.05219959533910956823, 16.53943276465976808, 99.99890960531436690 ) ) ;
#143056 = MANIFOLD_SOLID_BREP ( 'AdvancedHole2', #20735 ) ;
#143057 = CARTESIAN_POINT ( 'NONE',  ( -18.67979575497178146, -10.72451020669898902, 111.6655762719810525 ) ) ;
#143058 = CARTESIAN_POINT ( 'NONE',  ( 5.153800228976335163, 19.02544592524342804, 114.7905762719810241 ) ) ;
#143059 = CARTESIAN_POINT ( 'NONE',  ( -5.719274019375665041, -21.55341960407619695, 24.79275706135235779 ) ) ;
#143060 = CARTESIAN_POINT ( 'NONE',  ( 0.05219959533910956823, 16.53943276465976808, 109.9989096053143527 ) ) ;
#143061 = CARTESIAN_POINT ( 'NONE',  ( 21.53943276465977519, 0.05219959533937863772, 76.25109039468568994 ) ) ;
#143062 = CARTESIAN_POINT ( 'NONE',  ( 0.05219959533907565091, 21.53943276465977519, 94.99890960531436690 ) ) ;
#143063 = CARTESIAN_POINT ( 'NONE',  ( -13.97604488694547697, 13.89961937509957934, 38.12609039468566152 ) ) ;
#143064 = CARTESIAN_POINT ( 'NONE',  ( -9.564922557960796823, -16.46253265017161027, 27.08224293864769550 ) ) ;
#143065 = CARTESIAN_POINT ( 'NONE',  ( -18.22780087662126647, -5.499999999999827693, 58.98236817873108606 ) ) ;
#143066 = CARTESIAN_POINT ( 'NONE',  ( 30.09553654342099094, -1.478515647795636490, -51.30846887466859130 ) ) ;
#143067 = CARTESIAN_POINT ( 'NONE',  ( 14.29746914071037800, 8.314922557961029526, 41.66775706135235424 ) ) ;
#143068 = CARTESIAN_POINT ( 'NONE',  ( -14.29746914071049879, 8.314922557960819915, 110.8322429386476955 ) ) ;
#143069 = CARTESIAN_POINT ( 'NONE',  ( 33.85315667487628843, -0.3599896029658087859, 100.5000000000010374 ) ) ;
#143070 = CARTESIAN_POINT ( 'NONE',  ( 13.89961937509977652, -13.97604488694527269, 73.12390960531436690 ) ) ;
#143071 = CARTESIAN_POINT ( 'NONE',  ( 16.53943276465976808, -0.05219959533910856209, 98.74890960531438111 ) ) ;
#143072 = AXIS2_PLACEMENT_3D ( 'NONE', #195350, #39647, #101308 ) ;
#143073 = CARTESIAN_POINT ( 'NONE',  ( -15.80617190586745835, -15.72974639402198527, 51.87390960531437401 ) ) ;
#143074 = CARTESIAN_POINT ( 'NONE',  ( 12.14591786802309770, 12.06949235617756955, 69.37390960531436690 ) ) ;
#143075 = CARTESIAN_POINT ( 'NONE',  ( -8.224510206698735004, -14.34966873604973081, 34.58442372801900433 ) ) ;
#143076 = CARTESIAN_POINT ( 'NONE',  ( 5.823673210054444382, -21.52544592524334988, 90.20942372801903275 ) ) ;
#143077 = DIRECTION ( 'NONE',  ( 0.000000000000000000, -0.7071067811865483499, 0.7071067811865465735 ) ) ;
#143078 = CARTESIAN_POINT ( 'NONE',  ( 16.55341960407618274, -4.379528057220086978, 96.04275706135236135 ) ) ;
#143079 = CARTESIAN_POINT ( 'NONE',  ( -8.224510206698948167, 14.34966873604960824, 40.41557627198103120 ) ) ;
#143080 = CARTESIAN_POINT ( 'NONE',  ( -9.474510206698964154, 16.51473224551069663, 40.41557627198103120 ) ) ;
#143081 = CARTESIAN_POINT ( 'NONE',  ( -18.67979575497193778, 10.72451020669871902, 93.33442372801901854 ) ) ;
#143082 = CARTESIAN_POINT ( 'NONE',  ( 21.53943276465977519, -0.05219959533907433946, 108.7489096053143669 ) ) ;
#143083 = CARTESIAN_POINT ( 'NONE',  ( -10.72451020669870658, -18.67979575497194134, 59.58442372801901854 ) ) ;
#143084 = CARTESIAN_POINT ( 'NONE',  ( 16.55341960407618274, -4.379528057220086978, 41.04275706135236135 ) ) ;
#143086 = CARTESIAN_POINT ( 'NONE',  ( -5.719274019375665041, -21.55341960407619695, 89.79275706135236135 ) ) ;
#143085 = CARTESIAN_POINT ( 'NONE',  ( -14.34966873604960291, -8.224510206698953496, 61.66557627198103120 ) ) ;
#143087 = CARTESIAN_POINT ( 'NONE',  ( 4.379528057220092307, 16.55341960407617563, 97.29275706135234714 ) ) ;
#143088 = CARTESIAN_POINT ( 'NONE',  ( 16.61371651742603461, 7.165104196376042012, 28.64584930007005781 ) ) ;
#143089 = CARTESIAN_POINT ( 'NONE',  ( -15.49999999999999822, 5.499999999999998224, 118.0000000000000142 ) ) ;
#143090 = CARTESIAN_POINT ( 'NONE',  ( -0.05219959533910754901, -16.53943276465976808, 27.49890960531435269 ) ) ;
#143091 = CARTESIAN_POINT ( 'NONE',  ( 4.483927247898790824, -16.52544592524335698, 80.20942372801901854 ) ) ;
#143092 = CARTESIAN_POINT ( 'NONE',  ( -13.89961937509977652, 13.97604488694528158, 85.62390960531433848 ) ) ;
#143093 = CARTESIAN_POINT ( 'NONE',  ( -5.049401038298153566, 19.05341960407611168, 95.20724293864770971 ) ) ;
#143094 = CARTESIAN_POINT ( 'NONE',  ( -18.62759615963255300, -10.81492255796106328, 89.16775706135236135 ) ) ;
#143095 = CARTESIAN_POINT ( 'NONE',  ( -14.34966873604972548, 8.224510206698743886, 88.33442372801901854 ) ) ;
#143096 = CARTESIAN_POINT ( 'NONE',  ( 16.53943276465976808, -0.05219959533910856209, 58.74890960531436690 ) ) ;
#143097 = CARTESIAN_POINT ( 'NONE',  ( 13.89961937509977652, -13.97604488694527269, 68.12390960531436690 ) ) ;
#143098 = ORIENTED_EDGE ( 'NONE', *, *, #121993, .F. ) ;
#143099 = CARTESIAN_POINT ( 'NONE',  ( -4.483927247898782831, 16.52544592524335698, 27.70942372801901854 ) ) ;
#143100 = CARTESIAN_POINT ( 'NONE',  ( -9.564922557960796823, -16.46253265017161027, 32.08224293864769550 ) ) ;
#143101 = CARTESIAN_POINT ( 'NONE',  ( -13.89961937509977652, 13.97604488694528158, 75.62390960531438111 ) ) ;
#143103 = CARTESIAN_POINT ( 'NONE',  ( -11.40812507854754720, -35.11059874428192273, -6.224999997268812812 ) ) ;
#143102 = CARTESIAN_POINT ( 'NONE',  ( 12.06949235617739724, 12.14591786802326823, 21.87609039468567573 ) ) ;
#143104 = CARTESIAN_POINT ( 'NONE',  ( 5.049401038297881783, 19.05341960407617563, 22.29275706135233648 ) ) ;
#143105 = CARTESIAN_POINT ( 'NONE',  ( -8.224510206698735004, -14.34966873604973081, 79.58442372801903275 ) ) ;
#143106 = CARTESIAN_POINT ( 'NONE',  ( -9.474510206698720793, -16.51473224551083518, 104.5844237280190043 ) ) ;
#143107 = CARTESIAN_POINT ( 'NONE',  ( -19.02544592524342804, 5.153800228976336051, 26.04057627198103120 ) ) ;
#143108 = CARTESIAN_POINT ( 'NONE',  ( 14.34966873604972726, -8.224510206698740333, 70.83442372801901854 ) ) ;
#143109 = CARTESIAN_POINT ( 'NONE',  ( -4.379528057220086978, -16.55341960407618274, 49.79275706135234714 ) ) ;
#143110 = CARTESIAN_POINT ( 'NONE',  ( -19.03943276465977164, 0.05219959533909376836, 26.24890960531435624 ) ) ;
#143111 = CARTESIAN_POINT ( 'NONE',  ( 0.05219959533936267826, -19.03943276465977164, 70.00109039468566152 ) ) ;
#143112 = CARTESIAN_POINT ( 'NONE',  ( 9.474510206698729675, 16.51473224551082808, 22.08442372801899722 ) ) ;
#143113 = CARTESIAN_POINT ( 'NONE',  ( -9.474510206698964154, 16.51473224551069663, 35.41557627198102409 ) ) ;
#143114 = CARTESIAN_POINT ( 'NONE',  ( 16.51473224551069308, 9.474510206698969483, 79.16557627198103830 ) ) ;
#143115 = CARTESIAN_POINT ( 'NONE',  ( 8.224510206698953496, -14.34966873604960469, 77.91557627198102409 ) ) ;
#143116 = CARTESIAN_POINT ( 'NONE',  ( 5.153800228976615827, -19.02544592524334988, 40.20942372801898301 ) ) ;
#143117 = CARTESIAN_POINT ( 'NONE',  ( 5.719274019375991003, -21.55341960407610458, 32.70724293864770260 ) ) ;
#143118 = CARTESIAN_POINT ( 'NONE',  ( -19.03943276465977164, -0.05219959533935918106, 18.75109039468567218 ) ) ;
#143119 = CARTESIAN_POINT ( 'NONE',  ( -19.02544592524342804, 5.153800228976336051, 91.04057627198100988 ) ) ;
#143120 = CARTESIAN_POINT ( 'NONE',  ( -21.52544592524334988, -5.823673210054445271, 103.9594237280190185 ) ) ;
#143121 = CARTESIAN_POINT ( 'NONE',  ( -10.72451020669898014, 18.67979575497178502, 60.41557627198102409 ) ) ;
#143122 = CARTESIAN_POINT ( 'NONE',  ( 13.89961937509977652, -13.97604488694527269, 103.1239096053143527 ) ) ;
#143123 = CARTESIAN_POINT ( 'NONE',  ( -19.05341960407617563, 5.049401038297882671, 83.54275706135233293 ) ) ;
#143124 = CARTESIAN_POINT ( 'NONE',  ( -0.05219959533909027116, -19.03943276465977164, 102.4989096053143669 ) ) ;
#143125 = CARTESIAN_POINT ( 'NONE',  ( 13.97604488694548053, -13.89961937509957401, 100.6260903946856615 ) ) ;
#143126 = CARTESIAN_POINT ( 'NONE',  ( 19.05341960407611168, 5.049401038298154454, 23.95724293864769194 ) ) ;
#143127 = CARTESIAN_POINT ( 'NONE',  ( 5.153800228976335163, 19.02544592524342804, 84.79057627198099567 ) ) ;
#143128 = CARTESIAN_POINT ( 'NONE',  ( -5.823673210054116645, -21.52544592524344225, 67.29057627198103830 ) ) ;
#143129 = CARTESIAN_POINT ( 'NONE',  ( 12.14591786802327356, -12.06949235617739191, 40.62609039468567573 ) ) ;
#143130 = CARTESIAN_POINT ( 'NONE',  ( -21.52544592524334988, -5.823673210054445271, 53.95942372801900433 ) ) ;
#143131 = CARTESIAN_POINT ( 'NONE',  ( 21.53943276465977519, 0.05219959533937863772, 91.25109039468568994 ) ) ;
#143132 = CARTESIAN_POINT ( 'NONE',  ( 8.314922557961029526, -14.29746914071037800, 100.4177570613523471 ) ) ;
#143133 = AXIS2_PLACEMENT_3D ( 'NONE', #24897, #146206, #69376 ) ;
#143134 = CARTESIAN_POINT ( 'NONE',  ( 9.564922557960805705, 16.46253265017160317, 94.58224293864769550 ) ) ;
#143135 = CARTESIAN_POINT ( 'NONE',  ( -0.05219959533910754901, -16.53943276465976808, 92.49890960531436690 ) ) ;
#143136 = CARTESIAN_POINT ( 'NONE',  ( 16.53943276465976808, 0.05219959533934440121, 111.2510903946856899 ) ) ;
#143137 = CARTESIAN_POINT ( 'NONE',  ( -16.51473224551082808, 9.474510206698731452, 63.33442372801900433 ) ) ;
#143138 = CARTESIAN_POINT ( 'NONE',  ( 15.72974639402176855, 15.80617190586768217, 46.87609039468568994 ) ) ;
#143139 = CARTESIAN_POINT ( 'NONE',  ( -8.224510206698948167, 14.34966873604960824, 95.41557627198102409 ) ) ;
#143140 = CARTESIAN_POINT ( 'NONE',  ( -19.05341960407611168, -5.049401038298163336, 111.4572429386476671 ) ) ;
#143141 = CARTESIAN_POINT ( 'NONE',  ( -12.14591786802309592, -12.06949235617757132, 26.87390960531435979 ) ) ;
#143142 = CARTESIAN_POINT ( 'NONE',  ( 15.72974639402176855, 15.80617190586768217, 86.87609039468568994 ) ) ;
#143143 = CARTESIAN_POINT ( 'NONE',  ( 8.314922557961029526, -14.29746914071037800, 60.41775706135235424 ) ) ;
#143144 = CARTESIAN_POINT ( 'NONE',  ( -10.72451020669870658, -18.67979575497194134, 44.58442372801901854 ) ) ;
#143145 = ORIENTED_EDGE ( 'NONE', *, *, #32058, .F. ) ;
#143146 = CARTESIAN_POINT ( 'NONE',  ( -5.823673210054431948, 21.52544592524334988, 27.70942372801901854 ) ) ;
#143147 = CARTESIAN_POINT ( 'NONE',  ( 0.05219959533910956823, 16.53943276465976808, 94.99890960531436690 ) ) ;
#143148 = CARTESIAN_POINT ( 'NONE',  ( -16.51473224551069308, -9.474510206698971260, 31.66557627198102054 ) ) ;
#143149 = CARTESIAN_POINT ( 'NONE',  ( 12.06949235617757843, -12.14591786802309237, 68.12390960531436690 ) ) ;
#143150 = CARTESIAN_POINT ( 'NONE',  ( -19.02544592524342804, 5.153800228976336051, 56.04057627198100988 ) ) ;
#143151 = CARTESIAN_POINT ( 'NONE',  ( 14.29746914071037800, 8.314922557961029526, 106.6677570613523756 ) ) ;
#143152 = CARTESIAN_POINT ( 'NONE',  ( -9.474510206698964154, 16.51473224551069663, 40.41557627198103120 ) ) ;
#143153 = CARTESIAN_POINT ( 'NONE',  ( -21.52544592524343514, 5.823673210054127303, 46.04057627198103830 ) ) ;
#143154 = CARTESIAN_POINT ( 'NONE',  ( -12.14591786802309592, -12.06949235617757132, 76.87390960531439532 ) ) ;
#143155 = CARTESIAN_POINT ( 'NONE',  ( 21.55341960407610458, 5.719274019375980345, 88.95724293864769550 ) ) ;
#143157 = EDGE_CURVE ( 'NONE', #73939, #106381, #199864, .T. ) ;
#143156 = CARTESIAN_POINT ( 'NONE',  ( 19.02544592524343514, -5.153800228976328945, 83.54057627198100988 ) ) ;
#143159 = CARTESIAN_POINT ( 'NONE',  ( -13.97604488694547697, 13.89961937509957934, 98.12609039468566152 ) ) ;
#143158 = CARTESIAN_POINT ( 'NONE',  ( 19.05341960407611168, 5.049401038298154454, 48.95724293864768129 ) ) ;
#143160 = CARTESIAN_POINT ( 'NONE',  ( -5.823673210054116645, -21.52544592524344225, 47.29057627198103120 ) ) ;
#143161 = CARTESIAN_POINT ( 'NONE',  ( -18.67979575497193778, 10.72451020669871902, 63.33442372801900433 ) ) ;
#143162 = CARTESIAN_POINT ( 'NONE',  ( -13.97604488694527625, -13.89961937509977652, 51.87390960531436690 ) ) ;
#143163 = CARTESIAN_POINT ( 'NONE',  ( 16.51473224551069308, 9.474510206698969483, 84.16557627198102409 ) ) ;
#143164 = EDGE_LOOP ( 'NONE', ( #184229, #178599, #133778, #85608, #63865 ) ) ;
#143165 = CARTESIAN_POINT ( 'NONE',  ( -12.06949235617739369, -12.14591786802326823, 64.37609039468568994 ) ) ;
#143166 = CARTESIAN_POINT ( 'NONE',  ( -10.72451020669870658, -18.67979575497194134, 44.58442372801901854 ) ) ;
#143167 = CARTESIAN_POINT ( 'NONE',  ( -18.67979575497193778, 10.72451020669871902, 68.33442372801900433 ) ) ;
#143168 = CARTESIAN_POINT ( 'NONE',  ( 5.823673210054125526, 21.52544592524343514, 24.79057627198103120 ) ) ;
#143169 = CARTESIAN_POINT ( 'NONE',  ( 21.53943276465977519, -0.05219959533907433946, 103.7489096053143669 ) ) ;
#143171 = CARTESIAN_POINT ( 'NONE',  ( -4.483927247898782831, 16.52544592524335698, 62.70942372801902565 ) ) ;
#143170 = CARTESIAN_POINT ( 'NONE',  ( -10.81492255796105439, 18.62759615963255655, 32.91775706135234714 ) ) ;
#143172 = CARTESIAN_POINT ( 'NONE',  ( -21.55341960407610458, -5.719274019375992779, 61.45724293864770260 ) ) ;
#143173 = CARTESIAN_POINT ( 'NONE',  ( -16.51473224551082808, 9.474510206698731452, 38.33442372801899722 ) ) ;
#143175 = CARTESIAN_POINT ( 'NONE',  ( 8.224510206698742110, 14.34966873604972548, 102.0844237280190185 ) ) ;
#143174 = CARTESIAN_POINT ( 'NONE',  ( -19.03943276465977164, 0.05219959533909376836, 71.24890960531435269 ) ) ;
#143176 = CARTESIAN_POINT ( 'NONE',  ( -17.49999999999999645, -3.850315288878843223, 105.7337086939655535 ) ) ;
#143177 = CARTESIAN_POINT ( 'NONE',  ( 9.564922557960805705, 16.46253265017160317, 109.5822429386476955 ) ) ;
#143178 = CARTESIAN_POINT ( 'NONE',  ( -4.500000000000001776, -130.0000000000000000, 13.99999999999999822 ) ) ;
#143179 = CARTESIAN_POINT ( 'NONE',  ( 19.05341960407617918, -5.049401038297876454, 76.04275706135230450 ) ) ;
#143180 = CARTESIAN_POINT ( 'NONE',  ( 5.823673210054125526, 21.52544592524343514, 59.79057627198103120 ) ) ;
#143181 = CARTESIAN_POINT ( 'NONE',  ( 4.483927247898545687, 16.52544592524342804, 44.79057627198103120 ) ) ;
#143182 = CARTESIAN_POINT ( 'NONE',  ( -19.05341960407617563, 5.049401038297882671, 93.54275706135234714 ) ) ;
#143183 = CARTESIAN_POINT ( 'NONE',  ( -16.51473224551069308, -9.474510206698971260, 21.66557627198102765 ) ) ;
#143184 = CARTESIAN_POINT ( 'NONE',  ( 9.474510206698729675, 16.51473224551082808, 97.08442372801900433 ) ) ;
#143186 = CARTESIAN_POINT ( 'NONE',  ( -0.05219959533936034679, 19.03943276465977164, 57.50109039468566863 ) ) ;
#143185 = CARTESIAN_POINT ( 'NONE',  ( -5.823673210054116645, -21.52544592524344225, 82.29057627198103830 ) ) ;
#143187 = CARTESIAN_POINT ( 'NONE',  ( 16.55341960407618274, -4.379528057220086978, 81.04275706135236135 ) ) ;
#143188 = CARTESIAN_POINT ( 'NONE',  ( -0.05219959533909027116, -19.03943276465977164, 72.49890960531435269 ) ) ;
#143189 = CARTESIAN_POINT ( 'NONE',  ( 12.06949235617757843, -12.14591786802309237, 63.12390960531435979 ) ) ;
#143190 = EDGE_CURVE ( 'NONE', #119352, #181556, #113104, .T. ) ;
#143191 = CARTESIAN_POINT ( 'NONE',  ( -9.564922557960796823, -16.46253265017161027, 52.08224293864768839 ) ) ;
#143192 = CARTESIAN_POINT ( 'NONE',  ( 16.52544592524342804, -4.483927247898539470, 48.54057627198103120 ) ) ;
#143193 = CARTESIAN_POINT ( 'NONE',  ( -9.564922557960796823, -16.46253265017161027, 22.08224293864768839 ) ) ;
#143194 = CARTESIAN_POINT ( 'NONE',  ( 32.58888545195122077, -1.708444646721647420, 87.69298048441147841 ) ) ;
#143195 = CARTESIAN_POINT ( 'NONE',  ( -4.379528057220328563, 16.55341960407611168, 35.20724293864768839 ) ) ;
#143196 = CARTESIAN_POINT ( 'NONE',  ( 5.049401038298161559, -19.05341960407611168, 82.70724293864770971 ) ) ;
#143197 = CARTESIAN_POINT ( 'NONE',  ( -0.05219959533936034679, 19.03943276465977164, 37.50109039468567573 ) ) ;
#143198 = CARTESIAN_POINT ( 'NONE',  ( 8.314922557961029526, -14.29746914071037800, 50.41775706135235424 ) ) ;
#143199 = CARTESIAN_POINT ( 'NONE',  ( -0.05219959533907301413, -21.53943276465977519, 57.49890960531435979 ) ) ;
#143200 = CARTESIAN_POINT ( 'NONE',  ( 5.823673210054444382, -21.52544592524334988, 100.2094237280190043 ) ) ;
#143201 = CARTESIAN_POINT ( 'NONE',  ( 19.05341960407611168, 5.049401038298154454, 73.95724293864768129 ) ) ;
#143202 = CARTESIAN_POINT ( 'NONE',  ( 19.02544592524343514, -5.153800228976328945, 113.5405762719810241 ) ) ;
#143203 = CARTESIAN_POINT ( 'NONE',  ( -19.05341960407611168, -5.049401038298163336, 111.4572429386476671 ) ) ;
#143204 = CARTESIAN_POINT ( 'NONE',  ( 10.72451020669871369, 18.67979575497193778, 42.08442372801901854 ) ) ;
#143205 = CARTESIAN_POINT ( 'NONE',  ( 16.52544592524342804, -4.483927247898539470, 88.54057627198103830 ) ) ;
#143208 = ORIENTED_EDGE ( 'NONE', *, *, #4389, .T. ) ;
#143207 = CARTESIAN_POINT ( 'NONE',  ( 9.564922557960805705, 16.46253265017160317, 84.58224293864769550 ) ) ;
#143206 = CARTESIAN_POINT ( 'NONE',  ( -0.05219959533907301413, -21.53943276465977519, 87.49890960531436690 ) ) ;
#143209 = CARTESIAN_POINT ( 'NONE',  ( -15.72974639402176322, -15.80617190586768395, 24.37609039468567573 ) ) ;
#143210 = VERTEX_POINT ( 'NONE', #84754 ) ;
#143211 = CARTESIAN_POINT ( 'NONE',  ( 19.02544592524343514, -5.153800228976328945, 88.54057627198102409 ) ) ;
#143212 = VECTOR ( 'NONE', #149829, 1000.000000000000000 ) ;
#143213 = CARTESIAN_POINT ( 'NONE',  ( 18.39443945427639093, -5.500000000000021316, 81.01745347608652992 ) ) ;
#143215 = CARTESIAN_POINT ( 'NONE',  ( 0.05219959533909260263, 19.03943276465977164, 29.99890960531435979 ) ) ;
#143214 = CARTESIAN_POINT ( 'NONE',  ( -19.02544592524342804, 5.153800228976336051, 26.04057627198103120 ) ) ;
#143216 = CARTESIAN_POINT ( 'NONE',  ( -16.51473224551082808, 9.474510206698731452, 108.3344237280190043 ) ) ;
#143217 = CARTESIAN_POINT ( 'NONE',  ( 29.86685920354754842, -21.69954338932559068, -6.324999997268814234 ) ) ;
#143218 = CARTESIAN_POINT ( 'NONE',  ( -16.55341960407611168, -4.379528057220339221, 106.4572429386477097 ) ) ;
#143219 = CARTESIAN_POINT ( 'NONE',  ( -0.05219959533937732626, 21.53943276465977519, 82.50109039468568994 ) ) ;
#143221 = CARTESIAN_POINT ( 'NONE',  ( -0.05219959533937732626, 21.53943276465977519, 37.50109039468568284 ) ) ;
#143220 = CARTESIAN_POINT ( 'NONE',  ( -5.049401038298153566, 19.05341960407611168, 65.20724293864765286 ) ) ;
#143222 = CARTESIAN_POINT ( 'NONE',  ( -21.55341960407619339, 5.719274019375674811, 28.54275706135234358 ) ) ;
#143223 = CARTESIAN_POINT ( 'NONE',  ( -8.906447517083060816, 27.41122689804195645, 149.5999999999999943 ) ) ;
#143224 = CARTESIAN_POINT ( 'NONE',  ( 19.02544592524343514, -5.153800228976328945, 88.54057627198102409 ) ) ;
#143225 = CARTESIAN_POINT ( 'NONE',  ( 27.46944729267101337, 7.746537029272661634, 162.9576794167388130 ) ) ;
#143227 = CARTESIAN_POINT ( 'NONE',  ( -10.72451020669898014, 18.67979575497178502, 45.41557627198103830 ) ) ;
#143226 = CARTESIAN_POINT ( 'NONE',  ( 8.314922557961029526, -14.29746914071037800, 25.41775706135235779 ) ) ;
#143228 = CARTESIAN_POINT ( 'NONE',  ( -10.81492255796105439, 18.62759615963255655, 62.91775706135236135 ) ) ;
#143229 = CARTESIAN_POINT ( 'NONE',  ( 13.89961937509977652, -13.97604488694527269, 113.1239096053143527 ) ) ;
#143230 = CARTESIAN_POINT ( 'NONE',  ( -5.153800228976607833, 19.02544592524334988, 92.70942372801901854 ) ) ;
#143231 = CARTESIAN_POINT ( 'NONE',  ( -16.46253265017160317, 9.564922557960807481, 55.83224293864769550 ) ) ;
#143232 = CARTESIAN_POINT ( 'NONE',  ( 16.46253265017160672, -9.564922557960803928, 83.33224293864768129 ) ) ;
#143233 = CARTESIAN_POINT ( 'NONE',  ( -16.52544592524342804, 4.483927247898546575, 96.04057627198102409 ) ) ;
#143234 = CARTESIAN_POINT ( 'NONE',  ( -16.52544592524342804, 4.483927247898546575, 101.0405762719810383 ) ) ;
#143235 = CARTESIAN_POINT ( 'NONE',  ( -9.564922557960796823, -16.46253265017161027, 112.0822429386476955 ) ) ;
#143237 = CARTESIAN_POINT ( 'NONE',  ( -19.05341960407611168, -5.049401038298163336, 36.45724293864766707 ) ) ;
#143236 = CARTESIAN_POINT ( 'NONE',  ( -8.314922557960811034, -14.29746914071050412, 62.08224293864769550 ) ) ;
#143238 = CARTESIAN_POINT ( 'NONE',  ( 21.55341960407619695, -5.719274019375665929, 76.04275706135237556 ) ) ;
#143239 = CARTESIAN_POINT ( 'NONE',  ( -5.153800228976607833, 19.02544592524334988, 92.70942372801901854 ) ) ;
#143240 = CARTESIAN_POINT ( 'NONE',  ( -16.52544592524342804, 4.483927247898546575, 66.04057627198103830 ) ) ;
#143241 = CARTESIAN_POINT ( 'NONE',  ( -21.52544592524343514, 5.823673210054127303, 116.0405762719810383 ) ) ;
#143242 = CARTESIAN_POINT ( 'NONE',  ( -18.67979575497178146, -10.72451020669898902, 41.66557627198103120 ) ) ;
#143243 = CARTESIAN_POINT ( 'NONE',  ( -19.03943276465977164, 0.05219959533909376836, 116.2489096053143669 ) ) ;
#143244 = CARTESIAN_POINT ( 'NONE',  ( 27.73933785331498925, -9.013057229001033122, 147.7750000027311899 ) ) ;
#143245 = CARTESIAN_POINT ( 'NONE',  ( -5.153800228976328057, -19.02544592524343514, 72.29057627198102409 ) ) ;
#143246 = CARTESIAN_POINT ( 'NONE',  ( -12.14591786802309592, -12.06949235617757132, 41.87390960531435979 ) ) ;
#143247 = CARTESIAN_POINT ( 'NONE',  ( -14.34966873604972548, 8.224510206698743886, 108.3344237280190185 ) ) ;
#143248 = CARTESIAN_POINT ( 'NONE',  ( -16.52544592524335698, -4.483927247898792601, 78.95942372801901854 ) ) ;
#143249 = CARTESIAN_POINT ( 'NONE',  ( 16.51473224551083163, -9.474510206698727899, 45.83442372801900433 ) ) ;
#143250 = CARTESIAN_POINT ( 'NONE',  ( -23.27014359241646702, 11.64952062020055479, 165.7333947824558322 ) ) ;
#143251 = CARTESIAN_POINT ( 'NONE',  ( 13.97604488694527802, 13.89961937509977652, 89.37390960531436690 ) ) ;
#143252 = CARTESIAN_POINT ( 'NONE',  ( 9.474510206698971260, -16.51473224551069308, 47.91557627198102409 ) ) ;
#143253 = CARTESIAN_POINT ( 'NONE',  ( -14.29746914071049879, 8.314922557960819915, 65.83224293864769550 ) ) ;
#143255 = CARTESIAN_POINT ( 'NONE',  ( 18.62759615963271287, -10.81492255796078972, 23.33224293864769194 ) ) ;
#143254 = CARTESIAN_POINT ( 'NONE',  ( 17.50000000000000000, -5.624438216177590988, 103.3167034491464733 ) ) ;
#143256 = CARTESIAN_POINT ( 'NONE',  ( -21.52544592524343514, 5.823673210054127303, 51.04057627198103120 ) ) ;
#143257 = CARTESIAN_POINT ( 'NONE',  ( -12.14591786802309592, -12.06949235617757132, 81.87390960531435269 ) ) ;
#143258 = CARTESIAN_POINT ( 'NONE',  ( 14.29746914071037800, 8.314922557961029526, 36.66775706135234714 ) ) ;
#143259 = CARTESIAN_POINT ( 'NONE',  ( 12.06949235617757843, -12.14591786802309237, 73.12390960531436690 ) ) ;
#143260 = CARTESIAN_POINT ( 'NONE',  ( 25.31005825231498108, 7.802036135343648482, 170.7258689498729609 ) ) ;
#143261 = CARTESIAN_POINT ( 'NONE',  ( -19.05341960407617563, 5.049401038297882671, 78.54275706135233293 ) ) ;
#143262 = CARTESIAN_POINT ( 'NONE',  ( 18.67979575497178502, 10.72451020669898547, 24.16557627198103120 ) ) ;
#143263 = CARTESIAN_POINT ( 'NONE',  ( 11.40812507854754365, 35.11059874428196537, -5.724999997268812812 ) ) ;
#143264 = CARTESIAN_POINT ( 'NONE',  ( -32.64453336272028139, 2.028832619897439204E-14, 87.50000000000000000 ) ) ;
#143266 = CARTESIAN_POINT ( 'NONE',  ( -16.55341960407617563, 4.379528057220093196, 108.5427570613523756 ) ) ;
#143265 = CARTESIAN_POINT ( 'NONE',  ( -12.06949235617739369, -12.14591786802326823, 34.37609039468568284 ) ) ;
#143268 = CARTESIAN_POINT ( 'NONE',  ( -9.474510206698720793, -16.51473224551083518, 69.58442372801901854 ) ) ;
#143267 = AXIS2_PLACEMENT_3D ( 'NONE', #21387, #83045, #115402 ) ;
#143269 = CARTESIAN_POINT ( 'NONE',  ( 21.55341960407610458, 5.719274019375980345, 53.95724293864770260 ) ) ;
#143270 = CARTESIAN_POINT ( 'NONE',  ( 15.72974639402176855, 15.80617190586768217, 71.87609039468568994 ) ) ;
#143271 = CARTESIAN_POINT ( 'NONE',  ( 5.883457575057182254, -36.84471599068518799, -32.38015766500865311 ) ) ;
#143272 = CARTESIAN_POINT ( 'NONE',  ( 4.379528057220092307, 16.55341960407617563, 37.29275706135235424 ) ) ;
#143274 = CARTESIAN_POINT ( 'NONE',  ( -9.564922557960796823, -16.46253265017161027, 82.08224293864768129 ) ) ;
#143273 = CARTESIAN_POINT ( 'NONE',  ( -24.99873734152929217, -24.49873734152903282, 5.353553390593268624 ) ) ;
#143275 = CARTESIAN_POINT ( 'NONE',  ( 16.74109322108054343, 17.49235657833704138, -56.83968056806632774 ) ) ;
#143276 = CARTESIAN_POINT ( 'NONE',  ( -14.29746914071049879, 8.314922557960819915, 105.8322429386476955 ) ) ;
#143277 = CARTESIAN_POINT ( 'NONE',  ( 19.05341960407611168, 5.049401038298154454, 98.95724293864766707 ) ) ;
#143278 = CARTESIAN_POINT ( 'NONE',  ( -4.483927247898782831, 16.52544592524335698, 52.70942372801902565 ) ) ;
#143279 = CARTESIAN_POINT ( 'NONE',  ( -16.51473224551082808, 9.474510206698731452, 103.3344237280190043 ) ) ;
#143280 = CARTESIAN_POINT ( 'NONE',  ( -15.72974639402197994, 15.80617190586746368, 80.62390960531438111 ) ) ;
#143281 = CARTESIAN_POINT ( 'NONE',  ( -16.51473224551069308, -9.474510206698971260, 36.66557627198102409 ) ) ;
#143283 = CARTESIAN_POINT ( 'NONE',  ( -5.719274019375665041, -21.55341960407619695, 19.79275706135235069 ) ) ;
#143282 = CARTESIAN_POINT ( 'NONE',  ( 13.97604488694548053, -13.89961937509957401, 65.62609039468567573 ) ) ;
#143284 = CARTESIAN_POINT ( 'NONE',  ( 0.05219959533909260263, 19.03943276465977164, 74.99890960531435269 ) ) ;
#143285 = CARTESIAN_POINT ( 'NONE',  ( -16.51473224551069308, -9.474510206698971260, 111.6655762719810383 ) ) ;
#143286 = ORIENTED_EDGE ( 'NONE', *, *, #75190, .F. ) ;
#143287 = CARTESIAN_POINT ( 'NONE',  ( 4.379528057220092307, 16.55341960407617563, 37.29275706135235424 ) ) ;
#143288 = CARTESIAN_POINT ( 'NONE',  ( 10.81492255796078972, 18.62759615963270932, 99.58224293864770971 ) ) ;
#143291 = CARTESIAN_POINT ( 'NONE',  ( -5.049401038297874678, -19.05341960407617918, 74.79275706135231871 ) ) ;
#143290 = CARTESIAN_POINT ( 'NONE',  ( 19.02544592524343514, -5.153800228976328945, 93.54057627198102409 ) ) ;
#143289 = CARTESIAN_POINT ( 'NONE',  ( -16.53943276465976808, 0.05219959533911058130, 111.2489096053143669 ) ) ;
#143292 = CARTESIAN_POINT ( 'NONE',  ( -0.05219959533907301413, -21.53943276465977519, 87.49890960531436690 ) ) ;
#143293 = CARTESIAN_POINT ( 'NONE',  ( 16.52544592524342804, -4.483927247898539470, 43.54057627198103830 ) ) ;
#143294 = CARTESIAN_POINT ( 'NONE',  ( -5.153800228976607833, 19.02544592524334988, 27.70942372801899722 ) ) ;
#143295 = CARTESIAN_POINT ( 'NONE',  ( 14.29746914071037800, 8.314922557961029526, 71.66775706135234714 ) ) ;
#143296 = CARTESIAN_POINT ( 'NONE',  ( -13.97604488694527625, -13.89961937509977652, 96.87390960531433848 ) ) ;
#143297 = CARTESIAN_POINT ( 'NONE',  ( -16.46253265017160317, 9.564922557960807481, 50.83224293864770260 ) ) ;
#143298 = CARTESIAN_POINT ( 'NONE',  ( -10.81492255796105439, 18.62759615963255655, 52.91775706135235424 ) ) ;
#143299 = CARTESIAN_POINT ( 'NONE',  ( -15.80617190586768217, 15.72974639402176855, 73.12609039468567573 ) ) ;
#143300 = CARTESIAN_POINT ( 'NONE',  ( -9.474510206698964154, 16.51473224551069663, 60.41557627198102409 ) ) ;
#143301 = CARTESIAN_POINT ( 'NONE',  ( 18.62759615963255655, 10.81492255796105972, 31.66775706135234358 ) ) ;
#143302 = CARTESIAN_POINT ( 'NONE',  ( 9.474510206698729675, 16.51473224551082808, 72.08442372801900433 ) ) ;
#143303 = CARTESIAN_POINT ( 'NONE',  ( 5.153800228976335163, 19.02544592524342804, 34.79057627198102409 ) ) ;
#143304 = CARTESIAN_POINT ( 'NONE',  ( -12.06949235617739369, -12.14591786802326823, 89.37609039468568994 ) ) ;
#143305 = CARTESIAN_POINT ( 'NONE',  ( 13.89961937509977652, -13.97604488694527269, 53.12390960531434558 ) ) ;
#143306 = CARTESIAN_POINT ( 'NONE',  ( -16.51473224551069308, -9.474510206698971260, 106.6655762719810383 ) ) ;
#143307 = CARTESIAN_POINT ( 'NONE',  ( -19.05341960407611168, -5.049401038298163336, 41.45724293864769550 ) ) ;
#143308 = CARTESIAN_POINT ( 'NONE',  ( 15.80617190586746368, 15.72974639402197994, 84.37390960531438111 ) ) ;
#143309 = CARTESIAN_POINT ( 'NONE',  ( 12.06949235617739724, 12.14591786802326823, 76.87609039468567573 ) ) ;
#143310 = CARTESIAN_POINT ( 'NONE',  ( -7.656827144875921753, -71.74905178543390605, 0.000000000000000000 ) ) ;
#143311 = CARTESIAN_POINT ( 'NONE',  ( -16.51473224551082808, 9.474510206698731452, 33.33442372801899722 ) ) ;
#143312 = CARTESIAN_POINT ( 'NONE',  ( 16.46253265017160672, -9.564922557960803928, 58.33224293864769550 ) ) ;
#143313 = CARTESIAN_POINT ( 'NONE',  ( 16.55341960407611168, 4.379528057220329451, 43.95724293864769550 ) ) ;
#143314 = CARTESIAN_POINT ( 'NONE',  ( 0.05219959533910956823, 16.53943276465976808, 79.99890960531435269 ) ) ;
#143315 = CARTESIAN_POINT ( 'NONE',  ( 9.474510206698971260, -16.51473224551069308, 102.9155762719810241 ) ) ;
#143316 = CARTESIAN_POINT ( 'NONE',  ( -5.049401038298153566, 19.05341960407611168, 80.20724293864769550 ) ) ;
#143317 = CARTESIAN_POINT ( 'NONE',  ( 21.52544592524334988, 5.823673210054432836, 56.45942372801902565 ) ) ;
#143318 = CARTESIAN_POINT ( 'NONE',  ( -16.46253265017160317, 9.564922557960807481, 95.83224293864769550 ) ) ;
#143319 = CARTESIAN_POINT ( 'NONE',  ( -21.53943276465977519, -0.05219959533937600094, 103.7510903946857042 ) ) ;
#143320 = CARTESIAN_POINT ( 'NONE',  ( -16.55341960407617563, 4.379528057220093196, 78.54275706135236135 ) ) ;
#143321 = ADVANCED_FACE ( 'NONE', ( #98925 ), #174795, .F. ) ;
#143322 = CARTESIAN_POINT ( 'NONE',  ( 0.05219959533937995610, -21.53943276465977519, 25.00109039468567218 ) ) ;
#143323 = CARTESIAN_POINT ( 'NONE',  ( 0.05219959533907565091, 21.53943276465977519, 99.99890960531436690 ) ) ;
#143324 = EDGE_CURVE ( 'NONE', #142920, #178033, #79163, .T. ) ;
#143325 = CARTESIAN_POINT ( 'NONE',  ( 12.06949235617757843, -12.14591786802309237, 63.12390960531435979 ) ) ;
#143326 = CARTESIAN_POINT ( 'NONE',  ( 5.153800228976335163, 19.02544592524342804, 44.79057627198103830 ) ) ;
#143327 = CARTESIAN_POINT ( 'NONE',  ( -14.29746914071049879, 8.314922557960819915, 65.83224293864769550 ) ) ;
#143328 = CARTESIAN_POINT ( 'NONE',  ( 15.80617190586746368, 15.72974639402197994, 24.37390960531435979 ) ) ;
#143329 = CARTESIAN_POINT ( 'NONE',  ( -5.049401038297874678, -19.05341960407617918, 24.79275706135233648 ) ) ;
#143330 = CARTESIAN_POINT ( 'NONE',  ( -0.05219959533910754901, -16.53943276465976808, 107.4989096053143669 ) ) ;
#143331 = EDGE_LOOP ( 'NONE', ( #162701, #24413, #31777, #13630 ) ) ;
#143332 = CARTESIAN_POINT ( 'NONE',  ( 8.224510206698742110, 14.34966873604972548, 72.08442372801899012 ) ) ;
#143333 = CARTESIAN_POINT ( 'NONE',  ( -0.05219959533909027116, -19.03943276465977164, 67.49890960531436690 ) ) ;
#143334 = CARTESIAN_POINT ( 'NONE',  ( -16.63122886436918435, -6.465204090714604668, 20.66090433330151654 ) ) ;
#143335 = CARTESIAN_POINT ( 'NONE',  ( -8.314922557960811034, -14.29746914071050412, 87.08224293864769550 ) ) ;
#143336 = CARTESIAN_POINT ( 'NONE',  ( -15.80617190586745835, -15.72974639402198527, 31.87390960531435979 ) ) ;
#143337 = CARTESIAN_POINT ( 'NONE',  ( -8.224510206698735004, -14.34966873604973081, 94.58442372801901854 ) ) ;
#143338 = CARTESIAN_POINT ( 'NONE',  ( 0.05219959533936267826, -19.03943276465977164, 105.0010903946856615 ) ) ;
#143339 = CARTESIAN_POINT ( 'NONE',  ( -21.55341960407619339, 5.719274019375674811, 73.54275706135234714 ) ) ;
#143340 = CARTESIAN_POINT ( 'NONE',  ( 19.05341960407611168, 5.049401038298154454, 93.95724293864769550 ) ) ;
#143341 = CARTESIAN_POINT ( 'NONE',  ( -21.52544592524343514, 5.823673210054127303, 101.0405762719810383 ) ) ;
#143342 = CARTESIAN_POINT ( 'NONE',  ( 8.314922557961029526, -14.29746914071037800, 60.41775706135235424 ) ) ;
#143343 = CARTESIAN_POINT ( 'NONE',  ( 14.34966873604960469, 8.224510206698951720, 109.1655762719810383 ) ) ;
#143344 = CARTESIAN_POINT ( 'NONE',  ( 4.483927247898790824, -16.52544592524335698, 20.20942372801900788 ) ) ;
#143345 = CARTESIAN_POINT ( 'NONE',  ( 16.46253265017146816, 9.564922557961045513, 91.66775706135234714 ) ) ;
#143346 = CARTESIAN_POINT ( 'NONE',  ( -18.62759615963270932, 10.81492255796079327, 95.83224293864770971 ) ) ;
#143347 = CARTESIAN_POINT ( 'NONE',  ( -19.02544592524334988, -5.153800228976617603, 53.95942372801898301 ) ) ;
#143348 = CARTESIAN_POINT ( 'NONE',  ( 18.87075004821566537, -5.500000000000075495, 86.17408112101047379 ) ) ;
#143349 = CARTESIAN_POINT ( 'NONE',  ( -21.55341960407610458, -5.719274019375992779, 101.4572429386476955 ) ) ;
#143350 = DIRECTION ( 'NONE',  ( 0.8437662581494472791, 0.5367108174878539861, 0.000000000000000000 ) ) ;
#143351 = CARTESIAN_POINT ( 'NONE',  ( 9.564922557960805705, 16.46253265017160317, 84.58224293864769550 ) ) ;
#143352 = DIRECTION ( 'NONE',  ( 0.000000000000000000, 0.000000000000000000, -1.000000000000000000 ) ) ;
#143353 = CARTESIAN_POINT ( 'NONE',  ( -12.06949235617739369, -12.14591786802326823, 29.37609039468568284 ) ) ;
#143354 = DIRECTION ( 'NONE',  ( 0.4999999999999932832, -0.5000000000000055511, 0.7071067811865483499 ) ) ;
#143356 = CARTESIAN_POINT ( 'NONE',  ( 8.314922557960818139, 14.29746914071049879, 59.58224293864770260 ) ) ;
#143355 = CARTESIAN_POINT ( 'NONE',  ( -15.72974639402197994, 15.80617190586746368, 100.6239096053143811 ) ) ;
#143357 = CARTESIAN_POINT ( 'NONE',  ( -19.03943276465977164, 0.05219959533909376836, 76.24890960531435269 ) ) ;
#143359 = CARTESIAN_POINT ( 'NONE',  ( -13.97604488694547697, 13.89961937509957934, 43.12609039468566152 ) ) ;
#143358 = CARTESIAN_POINT ( 'NONE',  ( -16.55341960407617563, 4.379528057220093196, 43.54275706135235424 ) ) ;
#143360 = CARTESIAN_POINT ( 'NONE',  ( -18.67979575497193778, 10.72451020669871902, 48.33442372801902565 ) ) ;
#143361 = CARTESIAN_POINT ( 'NONE',  ( -14.29746914071037622, -8.314922557961029526, 19.16775706135234714 ) ) ;
#143362 = CARTESIAN_POINT ( 'NONE',  ( -19.02544592524342804, 5.153800228976336051, 61.04057627198103120 ) ) ;
#143363 = CARTESIAN_POINT ( 'NONE',  ( -5.153800228976607833, 19.02544592524334988, 82.70942372801897591 ) ) ;
#143364 = CARTESIAN_POINT ( 'NONE',  ( 10.81492255796106328, -18.62759615963255655, 80.41775706135234714 ) ) ;
#143365 = CARTESIAN_POINT ( 'NONE',  ( 0.05219959533936267826, -19.03943276465977164, 60.00109039468566863 ) ) ;
#143366 = CARTESIAN_POINT ( 'NONE',  ( -19.03943276465977164, 0.05219959533909376836, 36.24890960531436690 ) ) ;
#143367 = CARTESIAN_POINT ( 'NONE',  ( -5.719274019375978568, 21.55341960407610458, 60.20724293864768839 ) ) ;
#143368 = CARTESIAN_POINT ( 'NONE',  ( 16.55341960407611168, 4.379528057220329451, 58.95724293864770971 ) ) ;
#143369 = CARTESIAN_POINT ( 'NONE',  ( -17.31728774477276289, -6.344390552232334279, 24.18093348310682700 ) ) ;
#143370 = CARTESIAN_POINT ( 'NONE',  ( 19.02544592524334988, 5.153800228976608722, 31.45942372801900433 ) ) ;
#143371 = CARTESIAN_POINT ( 'NONE',  ( 12.06949235617739724, 12.14591786802326823, 101.8760903946857042 ) ) ;
#143372 = CARTESIAN_POINT ( 'NONE',  ( -4.483927247898539470, -16.52544592524342804, 57.29057627198103120 ) ) ;
#143373 = CARTESIAN_POINT ( 'NONE',  ( -10.72451020669870658, -18.67979575497194134, 89.58442372801901854 ) ) ;
#143374 = CARTESIAN_POINT ( 'NONE',  ( -0.05219959533937732626, 21.53943276465977519, 77.50109039468567573 ) ) ;
#143375 = CARTESIAN_POINT ( 'NONE',  ( -18.62759615963270932, 10.81492255796079327, 100.8322429386477097 ) ) ;
#143376 = VECTOR ( 'NONE', #72906, 1000.000000000000000 ) ;
#143377 = CARTESIAN_POINT ( 'NONE',  ( 0.05219959533909260263, 19.03943276465977164, 54.99890960531435979 ) ) ;
#143378 = CARTESIAN_POINT ( 'NONE',  ( 5.719274019375673035, 21.55341960407619339, 72.29275706135236135 ) ) ;
#143379 = CARTESIAN_POINT ( 'NONE',  ( 5.049401038298161559, -19.05341960407611168, 52.70724293864767418 ) ) ;
#143380 = ORIENTED_EDGE ( 'NONE', *, *, #122956, .F. ) ;
#143381 = CARTESIAN_POINT ( 'NONE',  ( -13.97604488694527625, -13.89961937509977652, 66.87390960531436690 ) ) ;
#143382 = CARTESIAN_POINT ( 'NONE',  ( -14.34966873604960291, -8.224510206698953496, 106.6655762719810383 ) ) ;
#143383 = CARTESIAN_POINT ( 'NONE',  ( 13.89961937509977652, -13.97604488694527269, 93.12390960531436690 ) ) ;
#143384 = CARTESIAN_POINT ( 'NONE',  ( -0.05219959533910754901, -16.53943276465976808, 52.49890960531435979 ) ) ;
#143385 = CARTESIAN_POINT ( 'NONE',  ( -14.34966873604960291, -8.224510206698953496, 111.6655762719810525 ) ) ;
#143386 = CARTESIAN_POINT ( 'NONE',  ( 12.06949235617757843, -12.14591786802309237, 68.12390960531436690 ) ) ;
#143387 = CARTESIAN_POINT ( 'NONE',  ( 21.52544592524344225, -5.823673210054117533, 83.54057627198102409 ) ) ;
#143388 = CARTESIAN_POINT ( 'NONE',  ( -21.55341960407619339, 5.719274019375674811, 38.54275706135234714 ) ) ;
#143389 = CARTESIAN_POINT ( 'NONE',  ( -7.500000000000000000, 0.000000000000000000, 10.00000000000000000 ) ) ;
#143390 = EDGE_CURVE ( 'NONE', #61770, #82999, #117856, .T. ) ;
#143391 = CARTESIAN_POINT ( 'NONE',  ( -8.314922557961024197, 14.29746914071037800, 37.91775706135235424 ) ) ;
#143392 = CARTESIAN_POINT ( 'NONE',  ( 18.67979575497178502, 10.72451020669898547, 84.16557627198103830 ) ) ;
#143393 = AXIS2_PLACEMENT_3D ( 'NONE', #36, #107220, #93044 ) ;
#143395 = CARTESIAN_POINT ( 'NONE',  ( -15.80617190586768217, 15.72974639402176855, 113.1260903946856899 ) ) ;
#143394 = PRODUCT_DEFINITION_CONTEXT ( 'detailed design', #174, 'design' ) ;
#143396 = CARTESIAN_POINT ( 'NONE',  ( -5.049401038298153566, 19.05341960407611168, 95.20724293864770971 ) ) ;
#143397 = CARTESIAN_POINT ( 'NONE',  ( -15.72974639402176322, -15.80617190586768395, 44.37609039468567573 ) ) ;
#143398 = CARTESIAN_POINT ( 'NONE',  ( 5.823673210054125526, 21.52544592524343514, 34.79057627198103120 ) ) ;
#143399 = CARTESIAN_POINT ( 'NONE',  ( 12.14591786802327356, -12.06949235617739191, 100.6260903946857184 ) ) ;
#143401 = CARTESIAN_POINT ( 'NONE',  ( 21.52544592524334988, 5.823673210054432836, 81.45942372801900433 ) ) ;
#143400 = CARTESIAN_POINT ( 'NONE',  ( -18.62759615963255300, -10.81492255796106328, 44.16775706135234714 ) ) ;
#143402 = CARTESIAN_POINT ( 'NONE',  ( 21.55341960407619695, -5.719274019375665929, 111.0427570613523613 ) ) ;
#143403 = CARTESIAN_POINT ( 'NONE',  ( -4.379528057220086978, -16.55341960407618274, 79.79275706135236135 ) ) ;
#143404 = CARTESIAN_POINT ( 'NONE',  ( 15.80617190586769283, -15.72974639402175789, 45.62609039468567573 ) ) ;
#143405 = AXIS2_PLACEMENT_3D ( 'NONE', #73142, #152923, #11471 ) ;
#143406 = CARTESIAN_POINT ( 'NONE',  ( -0.05219959533909027116, -19.03943276465977164, 32.49890960531435979 ) ) ;
#143407 = CARTESIAN_POINT ( 'NONE',  ( 10.72451020669871369, 18.67979575497193778, 97.08442372801904696 ) ) ;
#143408 = CARTESIAN_POINT ( 'NONE',  ( -0.05219959533909027116, -19.03943276465977164, 102.4989096053143669 ) ) ;
#143409 = CARTESIAN_POINT ( 'NONE',  ( 15.72974639402199770, -15.80617190586745480, 108.1239096053143811 ) ) ;
#143411 = CARTESIAN_POINT ( 'NONE',  ( 15.80617190586746368, 15.72974639402197994, 69.37390960531436690 ) ) ;
#143410 = CARTESIAN_POINT ( 'NONE',  ( 7.600000000000007638, -2.566789643721943520E-14, -64.92279855667830191 ) ) ;
#143413 = CARTESIAN_POINT ( 'NONE',  ( 16.55341960407611168, 4.379528057220329451, 43.95724293864769550 ) ) ;
#143412 = CARTESIAN_POINT ( 'NONE',  ( -0.05219959533934338120, 16.53943276465976808, 57.50109039468568994 ) ) ;
#143414 = CARTESIAN_POINT ( 'NONE',  ( 19.50973618000807264, -5.499999999999992895, 102.5000000000000142 ) ) ;
#143415 = CARTESIAN_POINT ( 'NONE',  ( 13.97604488694548053, -13.89961937509957401, 95.62609039468563310 ) ) ;
#143416 = COLOUR_RGB ( '', 0.09019608, 0.27058824, 0.51372549) ;
#143417 = CARTESIAN_POINT ( 'NONE',  ( -24.93942350307309752, -7.769968609432603479, 171.2173313942149662 ) ) ;
#143418 = CARTESIAN_POINT ( 'NONE',  ( -16.53943276465976808, -0.05219959533934237506, 28.75109039468567929 ) ) ;
#143419 = CARTESIAN_POINT ( 'NONE',  ( 10.81492255796078972, 18.62759615963270932, 104.5822429386477097 ) ) ;
#143420 = CARTESIAN_POINT ( 'NONE',  ( 10.72451020669898902, -18.67979575497178502, 77.91557627198102409 ) ) ;
#143421 = CARTESIAN_POINT ( 'NONE',  ( 9.564922557960805705, 16.46253265017160317, 114.5822429386476955 ) ) ;
#143422 = CARTESIAN_POINT ( 'NONE',  ( -8.224510206698735004, -14.34966873604973081, 49.58442372801901143 ) ) ;
#143423 = CARTESIAN_POINT ( 'NONE',  ( 9.564922557960805705, 16.46253265017160317, 74.58224293864769550 ) ) ;
#143425 = CARTESIAN_POINT ( 'NONE',  ( -19.03943276465977164, -0.05219959533935918106, 98.75109039468567573 ) ) ;
#143424 = CARTESIAN_POINT ( 'NONE',  ( 5.823673210054444382, -21.52544592524334988, 35.20942372801901854 ) ) ;
#143426 = CARTESIAN_POINT ( 'NONE',  ( 5.049401038298161559, -19.05341960407611168, 107.7072429386476955 ) ) ;
#143427 = VERTEX_POINT ( 'NONE', #88765 ) ;
#143428 = CARTESIAN_POINT ( 'NONE',  ( -9.564922557960796823, -16.46253265017161027, 92.08224293864769550 ) ) ;
#143429 = CARTESIAN_POINT ( 'NONE',  ( 21.55341960407610458, 5.719274019375980345, 83.95724293864770971 ) ) ;
#143430 = CARTESIAN_POINT ( 'NONE',  ( 19.02544592524343514, -5.153800228976328945, 58.54057627198102409 ) ) ;
#143431 = CARTESIAN_POINT ( 'NONE',  ( 37.99999999999999289, 12.34694845685046793, -0.9000000000000000222 ) ) ;
#143432 = CARTESIAN_POINT ( 'NONE',  ( -0.05219959533910754901, -16.53943276465976808, 62.49890960531436690 ) ) ;
#143433 = CARTESIAN_POINT ( 'NONE',  ( 15.80617190586746368, 15.72974639402197994, 24.37390960531435979 ) ) ;
#143434 = CARTESIAN_POINT ( 'NONE',  ( -29.53952216915896400, 1.232294487434969499, -51.94279119241696918 ) ) ;
#143435 = CARTESIAN_POINT ( 'NONE',  ( 5.719274019375991003, -21.55341960407610458, 92.70724293864770971 ) ) ;
#143436 = CARTESIAN_POINT ( 'NONE',  ( 9.564922557961047289, -16.46253265017146816, 65.41775706135233293 ) ) ;
#143437 = CARTESIAN_POINT ( 'NONE',  ( -10.72451020669898014, 18.67979575497178502, 25.41557627198103120 ) ) ;
#143438 = CARTESIAN_POINT ( 'NONE',  ( 19.52851543214744012, 5.500000000000030198, 67.89357721762580411 ) ) ;
#143439 = CARTESIAN_POINT ( 'NONE',  ( -5.719274019375978568, 21.55341960407610458, 60.20724293864768839 ) ) ;
#143440 = VECTOR ( 'NONE', #15492, 1000.000000000000114 ) ;
#143441 = CARTESIAN_POINT ( 'NONE',  ( -13.97604488694527625, -13.89961937509977652, 81.87390960531436690 ) ) ;
#143442 = CARTESIAN_POINT ( 'NONE',  ( -21.55341960407619339, 5.719274019375674811, 78.54275706135236135 ) ) ;
#143443 = CARTESIAN_POINT ( 'NONE',  ( 5.153800228976335163, 19.02544592524342804, 49.79057627198100988 ) ) ;
#143444 = CARTESIAN_POINT ( 'NONE',  ( 16.53943276465976808, -0.05219959533910856209, 78.74890960531436690 ) ) ;
#143445 = CARTESIAN_POINT ( 'NONE',  ( -14.34966873604972548, 8.224510206698743886, 38.33442372801900433 ) ) ;
#143446 = CARTESIAN_POINT ( 'NONE',  ( 15.80617190586769283, -15.72974639402175789, 65.62609039468568994 ) ) ;
#143447 = ORIENTED_EDGE ( 'NONE', *, *, #190013, .T. ) ;
#143448 = CARTESIAN_POINT ( 'NONE',  ( 13.89961937509957401, 13.97604488694547697, 21.87609039468566152 ) ) ;
#143449 = CARTESIAN_POINT ( 'NONE',  ( 19.02544592524334988, 5.153800228976608722, 76.45942372801897591 ) ) ;
#143450 = FACE_OUTER_BOUND ( 'NONE', #46562, .T. ) ;
#143451 = CARTESIAN_POINT ( 'NONE',  ( 5.823673210054444382, -21.52544592524334988, 40.20942372801901854 ) ) ;
#143452 = CARTESIAN_POINT ( 'NONE',  ( -23.48529157249600985, 32.32473071737754111, -4.049999994537626158 ) ) ;
#143453 = CARTESIAN_POINT ( 'NONE',  ( 19.05341960407617918, -5.049401038297876454, 36.04275706135234003 ) ) ;
#143454 = CARTESIAN_POINT ( 'NONE',  ( 13.89961937509977652, -13.97604488694527269, 53.12390960531434558 ) ) ;
#143455 = CARTESIAN_POINT ( 'NONE',  ( 9.474510206698729675, 16.51473224551082808, 32.08442372801900433 ) ) ;
#143456 = CARTESIAN_POINT ( 'NONE',  ( 8.314922557961029526, -14.29746914071037800, 100.4177570613523471 ) ) ;
#143458 = CARTESIAN_POINT ( 'NONE',  ( -21.55341960407619339, 5.719274019375674811, 73.54275706135234714 ) ) ;
#143457 = CARTESIAN_POINT ( 'NONE',  ( 5.049401038298161559, -19.05341960407611168, 97.70724293864766707 ) ) ;
#143459 = CARTESIAN_POINT ( 'NONE',  ( 29.86685920354754487, 21.69954338932564752, -7.424999997268813878 ) ) ;
#143460 = CARTESIAN_POINT ( 'NONE',  ( -33.68458106784984096, 5.328653173427194467, 96.40873914273848300 ) ) ;
#143461 = CARTESIAN_POINT ( 'NONE',  ( 21.52544592524334988, 5.823673210054432836, 81.45942372801900433 ) ) ;
#143462 = CARTESIAN_POINT ( 'NONE',  ( 17.40861289039005300, -6.110651285853256454, 41.12767529172569425 ) ) ;
#143463 = CARTESIAN_POINT ( 'NONE',  ( -19.02544592524342804, 5.153800228976336051, 101.0405762719810241 ) ) ;
#143464 = CARTESIAN_POINT ( 'NONE',  ( -13.97604488694547697, 13.89961937509957934, 28.12609039468565797 ) ) ;
#143465 = AXIS2_PLACEMENT_3D ( 'NONE', #162125, #35780, #20607 ) ;
#143466 = DIRECTION ( 'NONE',  ( 0.7071067811865467956, -7.406550393246788537E-15, 0.7071067811865483499 ) ) ;
#143467 = CARTESIAN_POINT ( 'NONE',  ( 16.51473224551069308, 9.474510206698969483, 39.16557627198103120 ) ) ;
#143468 = CARTESIAN_POINT ( 'NONE',  ( -15.72974639402197994, 15.80617190586746368, 55.62390960531436690 ) ) ;
#143469 = CARTESIAN_POINT ( 'NONE',  ( 4.379528057220339221, -16.55341960407611168, 27.70724293864769905 ) ) ;
#143471 = CARTESIAN_POINT ( 'NONE',  ( -13.89961937509977652, 13.97604488694528158, 75.62390960531438111 ) ) ;
#143470 = CARTESIAN_POINT ( 'NONE',  ( -4.483927247898539470, -16.52544592524342804, 92.29057627198103830 ) ) ;
#143472 = CARTESIAN_POINT ( 'NONE',  ( -18.67979575497193778, 10.72451020669871902, 108.3344237280190185 ) ) ;
#143473 = CARTESIAN_POINT ( 'NONE',  ( 16.46253265017160672, -9.564922557960803928, 38.33224293864768839 ) ) ;
#143474 = CARTESIAN_POINT ( 'NONE',  ( -4.483927247898539470, -16.52544592524342804, 107.2905762719810525 ) ) ;
#143475 = CARTESIAN_POINT ( 'NONE',  ( -18.62759615963255300, -10.81492255796106328, 59.16775706135234714 ) ) ;
#143476 = CARTESIAN_POINT ( 'NONE',  ( -18.62759615963270932, 10.81492255796079327, 80.83224293864769550 ) ) ;
#143477 = CARTESIAN_POINT ( 'NONE',  ( -13.89961937509957401, -13.97604488694547875, 59.37609039468566863 ) ) ;
#143478 = CARTESIAN_POINT ( 'NONE',  ( -11.73768782171584313, -38.24263654170160720, -14.51834023846848254 ) ) ;
#143479 = CARTESIAN_POINT ( 'NONE',  ( -16.46253265017160317, 9.564922557960807481, 105.8322429386476955 ) ) ;
#143480 = CARTESIAN_POINT ( 'NONE',  ( -14.34966873604960291, -8.224510206698953496, 76.66557627198103830 ) ) ;
#143481 = CARTESIAN_POINT ( 'NONE',  ( 0.05219959533936267826, -19.03943276465977164, 40.00109039468566152 ) ) ;
#143482 = CARTESIAN_POINT ( 'NONE',  ( 5.049401038298161559, -19.05341960407611168, 62.70724293864769550 ) ) ;
#143483 = CARTESIAN_POINT ( 'NONE',  ( -14.34966873604960291, -8.224510206698953496, 56.66557627198103830 ) ) ;
#143484 = CARTESIAN_POINT ( 'NONE',  ( -19.02544592524334988, -5.153800228976617603, 73.95942372801900433 ) ) ;
#143485 = CARTESIAN_POINT ( 'NONE',  ( 16.31925111598457079, 7.325300261831479531, 32.33575461032751974 ) ) ;
#143486 = CARTESIAN_POINT ( 'NONE',  ( 10.81492255796078972, 18.62759615963270932, 34.58224293864770260 ) ) ;
#143487 = VERTEX_POINT ( 'NONE', #40267 ) ;
#143488 = CARTESIAN_POINT ( 'NONE',  ( 14.34966873604960469, 8.224510206698951720, 99.16557627198100988 ) ) ;
#143489 = DIRECTION ( 'NONE',  ( -0.000000000000000000, -0.000000000000000000, 1.000000000000000000 ) ) ;
#143491 = CARTESIAN_POINT ( 'NONE',  ( 21.55341960407610458, 5.719274019375980345, 68.95724293864769550 ) ) ;
#143490 = CARTESIAN_POINT ( 'NONE',  ( 0.05219959533909260263, 19.03943276465977164, 64.99890960531436690 ) ) ;
#143492 = CARTESIAN_POINT ( 'NONE',  ( 5.153800228976335163, 19.02544592524342804, 34.79057627198102409 ) ) ;
#143494 = CARTESIAN_POINT ( 'NONE',  ( -5.153800228976328057, -19.02544592524343514, 67.29057627198102409 ) ) ;
#143493 = CARTESIAN_POINT ( 'NONE',  ( -14.29746914071037622, -8.314922557961029526, 79.16775706135234714 ) ) ;
#143495 = CARTESIAN_POINT ( 'NONE',  ( -5.153800228976607833, 19.02544592524334988, 52.70942372801900433 ) ) ;
#143496 = CARTESIAN_POINT ( 'NONE',  ( -0.05219959533937732626, 21.53943276465977519, 67.50109039468568994 ) ) ;
#143497 = ORIENTED_EDGE ( 'NONE', *, *, #47680, .T. ) ;
#143498 = CARTESIAN_POINT ( 'NONE',  ( 15.80617190586746368, 15.72974639402197994, 44.37390960531435979 ) ) ;
#143499 = CARTESIAN_POINT ( 'NONE',  ( 16.55341960407611168, 4.379528057220329451, 113.9572429386477239 ) ) ;
#143500 = CARTESIAN_POINT ( 'NONE',  ( 14.34966873604972726, -8.224510206698740333, 85.83442372801901854 ) ) ;
#143501 = CARTESIAN_POINT ( 'NONE',  ( 5.049401038297881783, 19.05341960407617563, 102.2927570613523045 ) ) ;
#143502 = CARTESIAN_POINT ( 'NONE',  ( -36.91746825000000598, 11.99521256947798520, -1.224999997268813257 ) ) ;
#143503 = CARTESIAN_POINT ( 'NONE',  ( -15.49999999999999822, 5.499999999999998224, 22.00000000000000711 ) ) ;
#143504 = CARTESIAN_POINT ( 'NONE',  ( 18.62759615963255655, 10.81492255796105972, 91.66775706135234714 ) ) ;
#143505 = CARTESIAN_POINT ( 'NONE',  ( 12.06949235617757843, -12.14591786802309237, 48.12390960531436690 ) ) ;
#143506 = CARTESIAN_POINT ( 'NONE',  ( 0.05219959533910956823, 16.53943276465976808, 59.99890960531436690 ) ) ;
#143507 = CARTESIAN_POINT ( 'NONE',  ( 0.05219959533907565091, 21.53943276465977519, 94.99890960531436690 ) ) ;
#143508 = CARTESIAN_POINT ( 'NONE',  ( 21.55341960407610458, 5.719274019375980345, 93.95724293864770971 ) ) ;
#143509 = CARTESIAN_POINT ( 'NONE',  ( -28.79475375365586487, 2.428612866367529932E-14, 149.9843446568999923 ) ) ;
#143510 = CARTESIAN_POINT ( 'NONE',  ( -18.62759615963270932, 10.81492255796079327, 30.83224293864770260 ) ) ;
#143511 = CARTESIAN_POINT ( 'NONE',  ( 14.34966873604972726, -8.224510206698740333, 70.83442372801901854 ) ) ;
#143512 = CARTESIAN_POINT ( 'NONE',  ( 12.06949235617757843, -12.14591786802309237, 78.12390960531436690 ) ) ;
#143513 = CARTESIAN_POINT ( 'NONE',  ( -0.05219959533909027116, -19.03943276465977164, 47.49890960531435979 ) ) ;
#143514 = CARTESIAN_POINT ( 'NONE',  ( 34.46950536905809059, -7.498137530812974738, 44.48224578455059941 ) ) ;
#143515 = CARTESIAN_POINT ( 'NONE',  ( 12.06949235617739724, 12.14591786802326823, 96.87609039468568994 ) ) ;
#143516 = CARTESIAN_POINT ( 'NONE',  ( -21.52544592524343514, 5.823673210054127303, 116.0405762719810383 ) ) ;
#143517 = CARTESIAN_POINT ( 'NONE',  ( 13.89961937509977652, -13.97604488694527269, 78.12390960531433848 ) ) ;
#143518 = CARTESIAN_POINT ( 'NONE',  ( -18.62759615963255300, -10.81492255796106328, 49.16775706135234003 ) ) ;
#143519 = CARTESIAN_POINT ( 'NONE',  ( 19.03943276465977164, -0.05219959533909143690, 103.7489096053143669 ) ) ;
#143520 = CARTESIAN_POINT ( 'NONE',  ( -17.43506102071591357, -39.09281690107973617, -20.41854293744172821 ) ) ;
#143521 = AXIS2_PLACEMENT_3D ( 'NONE', #162830, #135510, #196199 ) ;
#143522 = ORIENTED_EDGE ( 'NONE', *, *, #6444, .T. ) ;
#143523 = CARTESIAN_POINT ( 'NONE',  ( 5.719274019375673035, 21.55341960407619339, 47.29275706135234003 ) ) ;
#143525 = CARTESIAN_POINT ( 'NONE',  ( -5.049401038298153566, 19.05341960407611168, 115.2072429386477097 ) ) ;
#143524 = CARTESIAN_POINT ( 'NONE',  ( -13.89961937509977652, 13.97604488694528158, 40.62390960531435979 ) ) ;
#143526 = CARTESIAN_POINT ( 'NONE',  ( 19.05341960407617918, -5.049401038297876454, 51.04275706135231871 ) ) ;
#143527 = CARTESIAN_POINT ( 'NONE',  ( -10.72451020669870658, -18.67979575497194134, 34.58442372801900433 ) ) ;
#143528 = CARTESIAN_POINT ( 'NONE',  ( -19.03943276465977164, -0.05219959533935918106, 53.75109039468566863 ) ) ;
#143529 = CARTESIAN_POINT ( 'NONE',  ( -9.564922557960796823, -16.46253265017161027, 22.08224293864768839 ) ) ;
#143530 = CARTESIAN_POINT ( 'NONE',  ( -0.05219959533934338120, 16.53943276465976808, 87.50109039468568994 ) ) ;
#143531 = CARTESIAN_POINT ( 'NONE',  ( 16.51473224551083163, -9.474510206698727899, 65.83442372801900433 ) ) ;
#143532 = CARTESIAN_POINT ( 'NONE',  ( -0.05219959533934338120, 16.53943276465976808, 102.5010903946856899 ) ) ;
#143534 = EDGE_LOOP ( 'NONE', ( #183992, #57688, #43383, #120411 ) ) ;
#143533 = FACE_OUTER_BOUND ( 'NONE', #37503, .T. ) ;
#143535 = CARTESIAN_POINT ( 'NONE',  ( 9.564922557960805705, 16.46253265017160317, 89.58224293864769550 ) ) ;
#143536 = CARTESIAN_POINT ( 'NONE',  ( -10.81492255796105439, 18.62759615963255655, 87.91775706135234714 ) ) ;
#143537 = CARTESIAN_POINT ( 'NONE',  ( -19.03943276465977164, -0.05219959533935918106, 18.75109039468567218 ) ) ;
#143538 = DIRECTION ( 'NONE',  ( -1.000000000000000000, -0.000000000000000000, -0.000000000000000000 ) ) ;
#143539 = CARTESIAN_POINT ( 'NONE',  ( -5.049401038298153566, 19.05341960407611168, 95.20724293864770971 ) ) ;
#143540 = CARTESIAN_POINT ( 'NONE',  ( -10.72451020669870658, -18.67979575497194134, 79.58442372801903275 ) ) ;
#143541 = CARTESIAN_POINT ( 'NONE',  ( -9.564922557961040184, 16.46253265017147172, 107.9177570613523471 ) ) ;
#143542 = CIRCLE ( 'NONE', #185570, 40.00000000000002132 ) ;
#143543 = CARTESIAN_POINT ( 'NONE',  ( 16.46253265017160672, -9.564922557960803928, 73.33224293864769550 ) ) ;
#143544 = CARTESIAN_POINT ( 'NONE',  ( -10.72451020669898014, 18.67979575497178502, 35.41557627198102409 ) ) ;
#143545 = CARTESIAN_POINT ( 'NONE',  ( -27.88129983271662837, 6.733757357602863536, 162.1517353552117982 ) ) ;
#143546 = CARTESIAN_POINT ( 'NONE',  ( 9.564922557960805705, 16.46253265017160317, 59.58224293864769550 ) ) ;
#143547 = CARTESIAN_POINT ( 'NONE',  ( 8.224510206698742110, 14.34966873604972548, 112.0844237280190185 ) ) ;
#143548 = DIRECTION ( 'NONE',  ( 0.000000000000000000, 0.000000000000000000, 1.000000000000000000 ) ) ;
#143549 = COLOUR_RGB ( '', 0.66274510, 0.83137255, 0.94901961) ;
#143550 = CARTESIAN_POINT ( 'NONE',  ( 5.153800228976615827, -19.02544592524334988, 70.20942372801899012 ) ) ;
#143551 = CARTESIAN_POINT ( 'NONE',  ( -16.51473224551069308, -9.474510206698971260, 101.6655762719810241 ) ) ;
#143552 = CARTESIAN_POINT ( 'NONE',  ( -21.52544592524334988, -5.823673210054445271, 103.9594237280190185 ) ) ;
#143553 = CARTESIAN_POINT ( 'NONE',  ( 16.55341960407611168, 4.379528057220329451, 88.95724293864769550 ) ) ;
#143554 = B_SPLINE_CURVE_WITH_KNOTS ( 'NONE', 3,
 ( #28729, #13536, #186376, #62000, #91334, #29703, #166240, #121695, #184377, #332, #90366, #154030, #123666, #151072, #138852, #155021, #152051, #185363, #45858, #108515 ),
 .UNSPECIFIED., .F., .F.,
 ( 4, 2, 2, 2, 2, 2, 2, 2, 2, 4 ),
 ( 0.004000878361811896662, 0.004499404418915904820, 0.004997930476019913845, 0.005496456533123922003, 0.005994982590227930161, 0.006244245618779934240, 0.006493508647331939186, 0.006992034704435923925, 0.007490560761539909532, 0.007989086818643895138 ),
 .UNSPECIFIED. ) ;
#143555 = CARTESIAN_POINT ( 'NONE',  ( -18.67979575497178146, -10.72451020669898902, 46.66557627198102409 ) ) ;
#143556 =( BOUNDED_CURVE ( )  B_SPLINE_CURVE ( 2, ( #135513, #136483, #181027, #57675, #14127, #138461, #75794, #59633, #121307, #182999, #137472, #30296, #108115 ),
 .UNSPECIFIED., .F., .T. ) 
 B_SPLINE_CURVE_WITH_KNOTS ( ( 3, 2, 2, 2, 2, 2, 3 ),
 ( 0.2129567522165188298, 0.2149122807017543879, 0.2192982456140350755, 0.2236842105263157909, 0.2280701754385964786, 0.2324561403508771940, 0.2343659890140226687 ),
 .UNSPECIFIED. ) 
 CURVE ( )  GEOMETRIC_REPRESENTATION_ITEM ( )  RATIONAL_B_SPLINE_CURVE ( ( 0.9831626618144004848, 0.9848076720550091867, 1.000000000000000000, 0.9659258262890683122, 1.000000000000000000, 0.9659258262890683122, 1.000000000000000000, 0.9659258262890683122, 1.000000000000000000, 0.9659258262890683122, 1.000000000000000000, 0.9851625545550090068, 0.9832469066685280978 ) ) 
 REPRESENTATION_ITEM ( '' )  );
#143557 = CARTESIAN_POINT ( 'NONE',  ( -18.67979575497178146, -10.72451020669898902, 36.66557627198103120 ) ) ;
#143558 = CARTESIAN_POINT ( 'NONE',  ( -16.52544592524342804, 4.483927247898546575, 111.0405762719810525 ) ) ;
#143559 = CARTESIAN_POINT ( 'NONE',  ( -1.425225664899842037, -7.122238460089386436, -62.29949481927936716 ) ) ;
#143560 = CARTESIAN_POINT ( 'NONE',  ( -9.474510206698720793, -16.51473224551083518, 44.58442372801900433 ) ) ;
#143561 = CARTESIAN_POINT ( 'NONE',  ( 16.52544592524342804, -4.483927247898539470, 23.54057627198102765 ) ) ;
#143563 = EDGE_CURVE ( 'NONE', #80087, #52906, #134289, .T. ) ;
#143562 = CARTESIAN_POINT ( 'NONE',  ( -16.46253265017160317, 9.564922557960807481, 100.8322429386477097 ) ) ;
#143564 = CARTESIAN_POINT ( 'NONE',  ( -0.05219959533937732626, 21.53943276465977519, 67.50109039468568994 ) ) ;
#143565 = CARTESIAN_POINT ( 'NONE',  ( 10.81492255796078972, 18.62759615963270932, 54.58224293864769550 ) ) ;
#143566 = CARTESIAN_POINT ( 'NONE',  ( 0.05219959533937995610, -21.53943276465977519, 45.00109039468568284 ) ) ;
#143567 = CARTESIAN_POINT ( 'NONE',  ( -18.67979575497178146, -10.72451020669898902, 101.6655762719810383 ) ) ;
#143568 = CARTESIAN_POINT ( 'NONE',  ( -21.52544592524334988, -5.823673210054445271, 33.95942372801901143 ) ) ;
#143569 = CARTESIAN_POINT ( 'NONE',  ( -16.46253265017160317, 9.564922557960807481, 25.83224293864769194 ) ) ;
#143570 = CARTESIAN_POINT ( 'NONE',  ( 16.46253265017146816, 9.564922557961045513, 71.66775706135233293 ) ) ;
#143571 = CARTESIAN_POINT ( 'NONE',  ( 16.52544592524342804, -4.483927247898539470, 98.54057627198105251 ) ) ;
#143572 = CARTESIAN_POINT ( 'NONE',  ( 13.97604488694527802, 13.89961937509977652, 109.3739096053143669 ) ) ;
#143573 = CARTESIAN_POINT ( 'NONE',  ( 14.34966873604960469, 8.224510206698951720, 49.16557627198102409 ) ) ;
#143574 = CARTESIAN_POINT ( 'NONE',  ( 4.483927247898790824, -16.52544592524335698, 110.2094237280190185 ) ) ;
#143575 = CARTESIAN_POINT ( 'NONE',  ( -19.02544592524342804, 5.153800228976336051, 51.04057627198103120 ) ) ;
#143576 = CARTESIAN_POINT ( 'NONE',  ( 5.049401038298161559, -19.05341960407611168, 27.70724293864769550 ) ) ;
#143577 = CARTESIAN_POINT ( 'NONE',  ( 18.67979575497178502, 10.72451020669898547, 34.16557627198102409 ) ) ;
#143579 = AXIS2_PLACEMENT_3D ( 'NONE', #144512, #168652, #104015 ) ;
#143578 = CARTESIAN_POINT ( 'NONE',  ( -16.46253265017146816, -9.564922557961047289, 19.16775706135233293 ) ) ;
#143581 = CARTESIAN_POINT ( 'NONE',  ( 4.379528057220339221, -16.55341960407611168, 37.70724293864769550 ) ) ;
#143580 = DIRECTION ( 'NONE',  ( -0.000000000000000000, -0.000000000000000000, 1.000000000000000000 ) ) ;
#143582 = CARTESIAN_POINT ( 'NONE',  ( 15.72974639402176855, 15.80617190586768217, 51.87609039468568284 ) ) ;
#143583 = CARTESIAN_POINT ( 'NONE',  ( -18.83841601638275520, -33.00795687112476173, -25.49111855720881792 ) ) ;
#143584 = CARTESIAN_POINT ( 'NONE',  ( -4.483927247898782831, 16.52544592524335698, 57.70942372801901143 ) ) ;
#143585 = CARTESIAN_POINT ( 'NONE',  ( 13.89961937509957401, 13.97604488694547697, 66.87609039468567573 ) ) ;
#143586 = CARTESIAN_POINT ( 'NONE',  ( 0.05219959533910956823, 16.53943276465976808, 29.99890960531435979 ) ) ;
#143587 = CARTESIAN_POINT ( 'NONE',  ( 14.29746914071037800, 8.314922557961029526, 111.6677570613523613 ) ) ;
#143588 = CARTESIAN_POINT ( 'NONE',  ( -5.153800228976328057, -19.02544592524343514, 37.29057627198102409 ) ) ;
#143589 = CARTESIAN_POINT ( 'NONE',  ( -5.153800228976328057, -19.02544592524343514, 62.29057627198100988 ) ) ;
#143590 = CARTESIAN_POINT ( 'NONE',  ( 5.049401038298161559, -19.05341960407611168, 27.70724293864769550 ) ) ;
#143591 = CARTESIAN_POINT ( 'NONE',  ( -21.53943276465977519, -0.05219959533937600094, 38.75109039468567573 ) ) ;
#143592 = CARTESIAN_POINT ( 'NONE',  ( 19.05341960407611168, 5.049401038298154454, 38.95724293864767418 ) ) ;
#143593 = CARTESIAN_POINT ( 'NONE',  ( -6.434671708797631950, -6.434671708797536027, -61.89430850415821794 ) ) ;
#143594 = CARTESIAN_POINT ( 'NONE',  ( -13.97604488694527625, -13.89961937509977652, 36.87390960531436690 ) ) ;
#143595 = CARTESIAN_POINT ( 'NONE',  ( 21.53943276465977519, -0.05219959533907433946, 28.74890960531435624 ) ) ;
#143597 = CARTESIAN_POINT ( 'NONE',  ( 8.314922557960818139, 14.29746914071049879, 109.5822429386476955 ) ) ;
#143596 = CARTESIAN_POINT ( 'NONE',  ( 15.72974639402176855, 15.80617190586768217, 56.87609039468568994 ) ) ;
#143598 = CARTESIAN_POINT ( 'NONE',  ( 9.474510206698971260, -16.51473224551069308, 107.9155762719810383 ) ) ;
#143599 = CARTESIAN_POINT ( 'NONE',  ( 16.55341960407618274, -4.379528057220086978, 76.04275706135237556 ) ) ;
#143600 = CARTESIAN_POINT ( 'NONE',  ( 0.05219959533937995610, -21.53943276465977519, 95.00109039468568994 ) ) ;
#143601 = CARTESIAN_POINT ( 'NONE',  ( -14.29746914071037622, -8.314922557961029526, 49.16775706135234003 ) ) ;
#143602 = CARTESIAN_POINT ( 'NONE',  ( -16.46253265017160317, 9.564922557960807481, 100.8322429386477097 ) ) ;
#143603 = CARTESIAN_POINT ( 'NONE',  ( 4.483927247898790824, -16.52544592524335698, 45.20942372801901854 ) ) ;
#143604 = CARTESIAN_POINT ( 'NONE',  ( -8.314922557961024197, 14.29746914071037800, 32.91775706135234714 ) ) ;
#143605 = CARTESIAN_POINT ( 'NONE',  ( 14.29746914071037800, 8.314922557961029526, 81.66775706135236135 ) ) ;
#143606 = CARTESIAN_POINT ( 'NONE',  ( -9.474510206698720793, -16.51473224551083518, 109.5844237280190043 ) ) ;
#143607 = CARTESIAN_POINT ( 'NONE',  ( 18.67979575497178502, 10.72451020669898547, 94.16557627198103830 ) ) ;
#143609 = CARTESIAN_POINT ( 'NONE',  ( -9.474510206698720793, -16.51473224551083518, 99.58442372801900433 ) ) ;
#143608 = CARTESIAN_POINT ( 'NONE',  ( 8.314922557960818139, 14.29746914071049879, 109.5822429386476955 ) ) ;
#143610 = CARTESIAN_POINT ( 'NONE',  ( -16.53943276465976808, -0.05219959533934237506, 78.75109039468568994 ) ) ;
#143611 = CARTESIAN_POINT ( 'NONE',  ( 23.03120525563286236, 11.22467059994808558, 168.0473679553712429 ) ) ;
#143612 = CARTESIAN_POINT ( 'NONE',  ( 16.46253265017146816, 9.564922557961045513, 66.66775706135233293 ) ) ;
#143613 = CARTESIAN_POINT ( 'NONE',  ( -14.34966873604960291, -8.224510206698953496, 41.66557627198103120 ) ) ;
#143614 = CARTESIAN_POINT ( 'NONE',  ( -8.314922557960811034, -14.29746914071050412, 97.08224293864770971 ) ) ;
#143616 = CARTESIAN_POINT ( 'NONE',  ( -19.35633801406908461, 5.499999999999578115, 89.13373818172762242 ) ) ;
#143615 = CARTESIAN_POINT ( 'NONE',  ( -9.564922557961040184, 16.46253265017147172, 37.91775706135233293 ) ) ;
#143617 = CARTESIAN_POINT ( 'NONE',  ( -10.81492255796105439, 18.62759615963255655, 37.91775706135235424 ) ) ;
#143618 = CARTESIAN_POINT ( 'NONE',  ( -9.564922557961040184, 16.46253265017147172, 97.91775706135233293 ) ) ;
#143619 = DIRECTION ( 'NONE',  ( 0.000000000000000000, 0.000000000000000000, 1.000000000000000000 ) ) ;
#143620 = CARTESIAN_POINT ( 'NONE',  ( -13.89961937509977652, 13.97604488694528158, 95.62390960531436690 ) ) ;
#143621 = CARTESIAN_POINT ( 'NONE',  ( -16.46253265017160317, 9.564922557960807481, 85.83224293864769550 ) ) ;
#143622 = CARTESIAN_POINT ( 'NONE',  ( 21.52544592524344225, -5.823673210054117533, 53.54057627198103120 ) ) ;
#143623 = CARTESIAN_POINT ( 'NONE',  ( 8.224510206698953496, -14.34966873604960469, 87.91557627198103830 ) ) ;
#143624 = CARTESIAN_POINT ( 'NONE',  ( -16.51473224551069308, -9.474510206698971260, 66.66557627198102409 ) ) ;
#143625 = CARTESIAN_POINT ( 'NONE',  ( 16.55341960407611168, 4.379528057220329451, 113.9572429386477239 ) ) ;
#143626 = CARTESIAN_POINT ( 'NONE',  ( -21.52544592524334988, -5.823673210054445271, 38.95942372801901854 ) ) ;
#143627 = CARTESIAN_POINT ( 'NONE',  ( -18.67979575497193778, 10.72451020669871902, 73.33442372801901854 ) ) ;
#143628 = CARTESIAN_POINT ( 'NONE',  ( 13.89961937509977652, -13.97604488694527269, 48.12390960531435979 ) ) ;
#143629 = EDGE_CURVE ( 'NONE', #161460, #93860, #101941, .T. ) ;
#143630 = CARTESIAN_POINT ( 'NONE',  ( -16.53943276465976808, -0.05219959533934237506, 73.75109039468567573 ) ) ;
#143631 = CARTESIAN_POINT ( 'NONE',  ( 10.81492255796106328, -18.62759615963255655, 25.41775706135235779 ) ) ;
#143632 = CARTESIAN_POINT ( 'NONE',  ( 0.05219959533937995610, -21.53943276465977519, 30.00109039468568284 ) ) ;
#143634 = CARTESIAN_POINT ( 'NONE',  ( -9.564922557960796823, -16.46253265017161027, 72.08224293864770971 ) ) ;
#143633 = CARTESIAN_POINT ( 'NONE',  ( -19.03943276465977164, -0.05219959533935918106, 53.75109039468566863 ) ) ;
#143635 = CARTESIAN_POINT ( 'NONE',  ( 13.89961937509957401, 13.97604488694547697, 26.87609039468566507 ) ) ;
#143636 = CARTESIAN_POINT ( 'NONE',  ( -15.72974639402176322, -15.80617190586768395, 89.37609039468568994 ) ) ;
#143637 = CIRCLE ( 'NONE', #14489, 31.90000000000003411 ) ;
#143638 = CARTESIAN_POINT ( 'NONE',  ( -5.719274019375978568, 21.55341960407610458, 65.20724293864768129 ) ) ;
#143639 = CARTESIAN_POINT ( 'NONE',  ( -0.05219959533910754901, -16.53943276465976808, 52.49890960531435979 ) ) ;
#143641 = CARTESIAN_POINT ( 'NONE',  ( 0.05219959533936267826, -19.03943276465977164, 35.00109039468566863 ) ) ;
#143640 = CARTESIAN_POINT ( 'NONE',  ( 18.67979575497194134, -10.72451020669871369, 85.83442372801901854 ) ) ;
#143642 = CARTESIAN_POINT ( 'NONE',  ( -14.29746914071049879, 8.314922557960819915, 70.83224293864770971 ) ) ;
#143643 = CARTESIAN_POINT ( 'NONE',  ( 19.05341960407611168, 5.049401038298154454, 28.95724293864769550 ) ) ;
#143644 = CARTESIAN_POINT ( 'NONE',  ( 13.97604488694548053, -13.89961937509957401, 55.62609039468566863 ) ) ;
#143645 = CARTESIAN_POINT ( 'NONE',  ( -8.314922557960811034, -14.29746914071050412, 32.08224293864769550 ) ) ;
#143646 = CARTESIAN_POINT ( 'NONE',  ( -0.05219959533937732626, 21.53943276465977519, 87.50109039468568994 ) ) ;
#143647 = CARTESIAN_POINT ( 'NONE',  ( -5.153800228976328057, -19.02544592524343514, 72.29057627198102409 ) ) ;
#143648 = CARTESIAN_POINT ( 'NONE',  ( -0.05219959533936034679, 19.03943276465977164, 52.50109039468566863 ) ) ;
#143649 = CARTESIAN_POINT ( 'NONE',  ( 18.67979575497178502, 10.72451020669898547, 49.16557627198102409 ) ) ;
#143650 = CARTESIAN_POINT ( 'NONE',  ( -18.62759615963255300, -10.81492255796106328, 39.16775706135235424 ) ) ;
#143651 = CARTESIAN_POINT ( 'NONE',  ( -18.67979575497178146, -10.72451020669898902, 96.66557627198102409 ) ) ;
#143652 = CARTESIAN_POINT ( 'NONE',  ( -9.474510206698720793, -16.51473224551083518, 94.58442372801900433 ) ) ;
#143653 = CARTESIAN_POINT ( 'NONE',  ( -0.05219959533934338120, 16.53943276465976808, 62.50109039468568284 ) ) ;
#143655 = CARTESIAN_POINT ( 'NONE',  ( -21.52544592524343514, 5.823673210054127303, 101.0405762719810383 ) ) ;
#143654 = DIRECTION ( 'NONE',  ( -1.000000000000000000, 0.000000000000000000, 0.000000000000000000 ) ) ;
#143656 = CARTESIAN_POINT ( 'NONE',  ( -14.34966873604960291, -8.224510206698953496, 96.66557627198102409 ) ) ;
#143657 = CARTESIAN_POINT ( 'NONE',  ( -24.93942350307309752, 7.769968609432599926, 171.2173313942149946 ) ) ;
#143658 = CARTESIAN_POINT ( 'NONE',  ( 12.06949235617739724, 12.14591786802326823, 36.87609039468568994 ) ) ;
#143659 = APPLICATION_CONTEXT ( 'automotive_design' ) ;
#143660 = CARTESIAN_POINT ( 'NONE',  ( -15.80617190586745835, -15.72974639402198527, 66.87390960531436690 ) ) ;
#143661 = CARTESIAN_POINT ( 'NONE',  ( -4.483927247898782831, 16.52544592524335698, 92.70942372801901854 ) ) ;
#143662 = CARTESIAN_POINT ( 'NONE',  ( -19.05341960407611168, -5.049401038298163336, 36.45724293864766707 ) ) ;
#143663 = B_SPLINE_CURVE_WITH_KNOTS ( 'NONE', 3,
 ( #112755, #83407, #66259, #191597, #159251, #84405, #20747, #129897, #114754, #176448, #82402, #69252, #100580, #67251, #130918, #34930, #96583, #158272, #81402, #19761, #143088, #127919, #41933, #132926, #148106, #86420, #24773, #9597, #120731, #119760, #27770, #103599 ),
 .UNSPECIFIED., .F., .F.,
 ( 4, 2, 2, 2, 2, 2, 2, 2, 2, 2, 2, 2, 2, 2, 2, 4 ),
 ( 2.281672496420497865E-17, 0.0003712461730036942047, 0.0007424923460073655328, 0.001113738519011037023, 0.001484984692014708297, 0.002227477038022051496, 0.002598723211025726239, 0.002969969384029401416, 0.003341215557033076159, 0.003712461730036750469, 0.004083707903040425212, 0.004454954076044099522, 0.004826200249047774699, 0.005197446422051449008, 0.005568692595055124185, 0.005939938768058799362 ),
 .UNSPECIFIED. ) ;
#143664 = CARTESIAN_POINT ( 'NONE',  ( 16.53943276465976808, 0.05219959533934440121, 61.25109039468567573 ) ) ;
#143665 = CARTESIAN_POINT ( 'NONE',  ( -19.02544592524334988, -5.153800228976617603, 58.95942372801900433 ) ) ;
#143666 = CARTESIAN_POINT ( 'NONE',  ( -10.81492255796105439, 18.62759615963255655, 37.91775706135235424 ) ) ;
#143667 = VECTOR ( 'NONE', #43910, 1000.000000000000000 ) ;
#143668 = CARTESIAN_POINT ( 'NONE',  ( -5.823673210054116645, -21.52544592524344225, 57.29057627198103120 ) ) ;
#143669 = CARTESIAN_POINT ( 'NONE',  ( -14.29746914071037622, -8.314922557961029526, 94.16775706135237556 ) ) ;
#143670 = CARTESIAN_POINT ( 'NONE',  ( -21.52544592524334988, -5.823673210054445271, 73.95942372801901854 ) ) ;
#143671 = CARTESIAN_POINT ( 'NONE',  ( 5.823673210054125526, 21.52544592524343514, 54.79057627198104541 ) ) ;
#143672 = CARTESIAN_POINT ( 'NONE',  ( 21.53943276465977519, -0.05219959533907433946, 38.74890960531435979 ) ) ;
#143673 = CARTESIAN_POINT ( 'NONE',  ( -0.05219959533934338120, 16.53943276465976808, 72.50109039468568994 ) ) ;
#143674 = CARTESIAN_POINT ( 'NONE',  ( -10.81492255796078084, -18.62759615963271287, 37.08224293864768129 ) ) ;
#143675 = ORIENTED_EDGE ( 'NONE', *, *, #32497, .F. ) ;
#143676 = CARTESIAN_POINT ( 'NONE',  ( -9.564922557960796823, -16.46253265017161027, 97.08224293864769550 ) ) ;
#143677 = CARTESIAN_POINT ( 'NONE',  ( 0.05219959533934541429, -16.53943276465976808, 110.0010903946856757 ) ) ;
#143678 = CARTESIAN_POINT ( 'NONE',  ( 4.999999999999999112, 0.000000000000000000, 0.000000000000000000 ) ) ;
#143679 = CARTESIAN_POINT ( 'NONE',  ( 14.29746914071049879, -8.314922557960816363, 103.3322429386476955 ) ) ;
#143680 = CARTESIAN_POINT ( 'NONE',  ( 21.53943276465977519, -0.05219959533907433946, 58.74890960531436690 ) ) ;
#143681 = CARTESIAN_POINT ( 'NONE',  ( 16.52544592524335698, 4.483927247898782831, 96.45942372801901854 ) ) ;
#143682 = CARTESIAN_POINT ( 'NONE',  ( 18.62759615963255655, 10.81492255796105972, 51.66775706135234714 ) ) ;
#143683 = CARTESIAN_POINT ( 'NONE',  ( 16.46253265017146816, 9.564922557961045513, 101.6677570613523329 ) ) ;
#143684 = CARTESIAN_POINT ( 'NONE',  ( 8.224510206698953496, -14.34966873604960469, 97.91557627198103830 ) ) ;
#143685 = CARTESIAN_POINT ( 'NONE',  ( -0.05219959533909027116, -19.03943276465977164, 52.49890960531436690 ) ) ;
#143686 = CARTESIAN_POINT ( 'NONE',  ( 5.153800228976335163, 19.02544592524342804, 29.79057627198102409 ) ) ;
#143687 = CARTESIAN_POINT ( 'NONE',  ( 1.500000000001896261, 23.15496181198761150, -55.09642484015217434 ) ) ;
#143688 = CARTESIAN_POINT ( 'NONE',  ( -13.97604488694527625, -13.89961937509977652, 96.87390960531433848 ) ) ;
#143689 = CARTESIAN_POINT ( 'NONE',  ( 0.05219959533934541429, -16.53943276465976808, 70.00109039468568994 ) ) ;
#143690 = CARTESIAN_POINT ( 'NONE',  ( 0.05219959533937995610, -21.53943276465977519, 105.0010903946856757 ) ) ;
#143691 = CARTESIAN_POINT ( 'NONE',  ( 18.67979575497178502, 10.72451020669898547, 49.16557627198102409 ) ) ;
#143692 = CARTESIAN_POINT ( 'NONE',  ( -14.34966873604972548, 8.224510206698743886, 73.33442372801901854 ) ) ;
#143693 = CARTESIAN_POINT ( 'NONE',  ( 5.153800228976615827, -19.02544592524334988, 85.20942372801900433 ) ) ;
#143694 = ORIENTED_EDGE ( 'NONE', *, *, #163998, .F. ) ;
#143695 = CARTESIAN_POINT ( 'NONE',  ( -5.153800228976328057, -19.02544592524343514, 42.29057627198101699 ) ) ;
#143697 = AXIS2_PLACEMENT_3D ( 'NONE', #178700, #135197, #166529 ) ;
#143696 = CARTESIAN_POINT ( 'NONE',  ( -16.46253265017160317, 9.564922557960807481, 80.83224293864769550 ) ) ;
#143698 = CARTESIAN_POINT ( 'NONE',  ( 16.46253265017160672, -9.564922557960803928, 38.33224293864768839 ) ) ;
#143699 = CARTESIAN_POINT ( 'NONE',  ( 16.46253265017146816, 9.564922557961045513, 76.66775706135234714 ) ) ;
#143700 = CARTESIAN_POINT ( 'NONE',  ( 25.76143648876522718, -7.343476467571410815, 174.8772314887141306 ) ) ;
#143701 = CARTESIAN_POINT ( 'NONE',  ( 9.474510206698971260, -16.51473224551069308, 92.91557627198103830 ) ) ;
#143702 = CARTESIAN_POINT ( 'NONE',  ( 8.224510206698953496, -14.34966873604960469, 57.91557627198103120 ) ) ;
#143703 = CARTESIAN_POINT ( 'NONE',  ( 18.67979575497178502, 10.72451020669898547, 49.16557627198102409 ) ) ;
#143704 = CIRCLE ( 'NONE', #156567, 5.000000000000000888 ) ;
#143705 = CARTESIAN_POINT ( 'NONE',  ( 5.000000000000000888, -140.0000000000000000, 0.0009999999999992653654 ) ) ;
#143706 = PRODUCT_DEFINITION_FORMATION_WITH_SPECIFIED_SOURCE ( 'ANY', '', #98692, .NOT_KNOWN. ) ;
#143707 = CARTESIAN_POINT ( 'NONE',  ( 19.05341960407617918, -5.049401038297876454, 36.04275706135234003 ) ) ;
#143708 = CARTESIAN_POINT ( 'NONE',  ( -17.13100169013301866, -6.664070546373139337, 79.23210164300157032 ) ) ;
#143710 = CARTESIAN_POINT ( 'NONE',  ( -9.474510206698964154, 16.51473224551069663, 60.41557627198102409 ) ) ;
#143709 = CARTESIAN_POINT ( 'NONE',  ( -0.05219959533909027116, -19.03943276465977164, 52.49890960531436690 ) ) ;
#143711 = CARTESIAN_POINT ( 'NONE',  ( -16.52544592524335698, -4.483927247898792601, 43.95942372801902565 ) ) ;
#143712 = CARTESIAN_POINT ( 'NONE',  ( -33.68444218968560477, -5.327119193238887718, 96.41491933019771920 ) ) ;
#143713 = CARTESIAN_POINT ( 'NONE',  ( -16.20579543436678094, 7.371946100355097897, 109.4347916582812985 ) ) ;
#143714 = CARTESIAN_POINT ( 'NONE',  ( 16.52544592524335698, 4.483927247898782831, 81.45942372801900433 ) ) ;
#143715 = CARTESIAN_POINT ( 'NONE',  ( -10.81492255796078084, -18.62759615963271287, 97.08224293864770971 ) ) ;
#143716 = CARTESIAN_POINT ( 'NONE',  ( 8.224510206698742110, 14.34966873604972548, 42.08442372801901854 ) ) ;
#143718 = DIRECTION ( 'NONE',  ( 1.000000000000000000, 0.000000000000000000, 0.000000000000000000 ) ) ;
#143717 = CARTESIAN_POINT ( 'NONE',  ( 19.05341960407611168, 5.049401038298154454, 38.95724293864767418 ) ) ;
#143719 = CARTESIAN_POINT ( 'NONE',  ( 21.55341960407619695, -5.719274019375665929, 51.04275706135234714 ) ) ;
#143720 = CARTESIAN_POINT ( 'NONE',  ( 19.03943276465977164, 0.05219959533936151252, 56.25109039468566863 ) ) ;
#143721 = CARTESIAN_POINT ( 'NONE',  ( 21.53943276465977519, 0.05219959533937863772, 96.25109039468568994 ) ) ;
#143722 = CARTESIAN_POINT ( 'NONE',  ( -24.12203661075782790, -5.823883908176388680, 170.5995460337422855 ) ) ;
#143723 = CARTESIAN_POINT ( 'NONE',  ( 14.29746914071049879, -8.314922557960816363, 43.33224293864769550 ) ) ;
#143724 = CARTESIAN_POINT ( 'NONE',  ( -15.66521691804237015, 1.429200727443527663, -59.59145728475412795 ) ) ;
#143725 = CARTESIAN_POINT ( 'NONE',  ( -5.719274019375978568, 21.55341960407610458, 60.20724293864768839 ) ) ;
#143726 = AXIS2_PLACEMENT_3D ( 'NONE', #125094, #157424, #60426 ) ;
#143727 = CARTESIAN_POINT ( 'NONE',  ( -17.14385361876520975, 23.59649016807275856, 144.5750000027311728 ) ) ;
#143728 = CARTESIAN_POINT ( 'NONE',  ( 9.474510206698971260, -16.51473224551069308, 97.91557627198102409 ) ) ;
#143729 = CARTESIAN_POINT ( 'NONE',  ( 14.29746914071049879, -8.314922557960816363, 98.33224293864769550 ) ) ;
#143730 = CARTESIAN_POINT ( 'NONE',  ( -8.224510206698735004, -14.34966873604973081, 19.58442372801901143 ) ) ;
#143731 = CARTESIAN_POINT ( 'NONE',  ( 8.224510206698953496, -14.34966873604960469, 22.91557627198102765 ) ) ;
#143732 = ORIENTED_EDGE ( 'NONE', *, *, #110412, .F. ) ;
#143733 = EDGE_CURVE ( 'NONE', #145279, #6627, #195401, .T. ) ;
#143734 = CARTESIAN_POINT ( 'NONE',  ( 21.55341960407610458, 5.719274019375980345, 103.9572429386476813 ) ) ;
#143736 = CARTESIAN_POINT ( 'NONE',  ( -9.564922557960796823, -16.46253265017161027, 112.0822429386476955 ) ) ;
#143735 = CARTESIAN_POINT ( 'NONE',  ( 16.55341960407611168, 4.379528057220329451, 28.95724293864769905 ) ) ;
#143737 = CARTESIAN_POINT ( 'NONE',  ( 9.474510206698729675, 16.51473224551082808, 97.08442372801900433 ) ) ;
#143738 = CARTESIAN_POINT ( 'NONE',  ( -0.05219959533937732626, 21.53943276465977519, 102.5010903946856899 ) ) ;
#143739 = CARTESIAN_POINT ( 'NONE',  ( -8.314922557960811034, -14.29746914071050412, 37.08224293864768129 ) ) ;
#143740 = CARTESIAN_POINT ( 'NONE',  ( -5.823673210054116645, -21.52544592524344225, 87.29057627198103830 ) ) ;
#143741 = CARTESIAN_POINT ( 'NONE',  ( -18.67979575497178146, -10.72451020669898902, 51.66557627198102409 ) ) ;
#143742 = CARTESIAN_POINT ( 'NONE',  ( 19.05341960407611168, 5.049401038298154454, 68.95724293864769550 ) ) ;
#143743 = CARTESIAN_POINT ( 'NONE',  ( 16.53943276465976808, -0.05219959533910856209, 28.74890960531435624 ) ) ;
#143744 = CARTESIAN_POINT ( 'NONE',  ( 19.03943276465977164, -0.05219959533909143690, 83.74890960531436690 ) ) ;
#143745 = LINE ( 'NONE', #187300, #69897 ) ;
#143746 = CARTESIAN_POINT ( 'NONE',  ( -16.46253265017146816, -9.564922557961047289, 44.16775706135232582 ) ) ;
#143747 = CARTESIAN_POINT ( 'NONE',  ( 15.80617190586746368, 15.72974639402197994, 74.37390960531436690 ) ) ;
#143748 = CARTESIAN_POINT ( 'NONE',  ( 4.379528057220339221, -16.55341960407611168, 92.70724293864770971 ) ) ;
#143749 = CARTESIAN_POINT ( 'NONE',  ( 0.05219959533937995610, -21.53943276465977519, 40.00109039468567573 ) ) ;
#143750 = CARTESIAN_POINT ( 'NONE',  ( 27.73933785331498925, -9.013057229001033122, 139.7750000027311899 ) ) ;
#143751 = CARTESIAN_POINT ( 'NONE',  ( 12.06949235617739724, 12.14591786802326823, 101.8760903946857042 ) ) ;
#143752 = CARTESIAN_POINT ( 'NONE',  ( -13.97604488694527625, -13.89961937509977652, 41.87390960531435979 ) ) ;
#143753 = CARTESIAN_POINT ( 'NONE',  ( 19.02544592524343514, -5.153800228976328945, 83.54057627198100988 ) ) ;
#143754 = PLANE ( 'NONE',  #57612 ) ;
#143755 = CARTESIAN_POINT ( 'NONE',  ( 12.06949235617757843, -12.14591786802309237, 43.12390960531435269 ) ) ;
#143756 = CARTESIAN_POINT ( 'NONE',  ( 15.72974639402176855, 15.80617190586768217, 66.87609039468568994 ) ) ;
#143758 = CARTESIAN_POINT ( 'NONE',  ( 16.52544592524335698, 4.483927247898782831, 71.45942372801901854 ) ) ;
#143757 = CARTESIAN_POINT ( 'NONE',  ( 37.02045864137332387, -17.72559658019842743, -19.07609595512616707 ) ) ;
#143759 = CARTESIAN_POINT ( 'NONE',  ( 19.05341960407611168, 5.049401038298154454, 43.95724293864769550 ) ) ;
#143760 = CARTESIAN_POINT ( 'NONE',  ( 13.97604488694527802, 13.89961937509977652, 49.37390960531434558 ) ) ;
#143761 = ORIENTED_EDGE ( 'NONE', *, *, #94032, .F. ) ;
#143762 = CARTESIAN_POINT ( 'NONE',  ( 18.67979575497194134, -10.72451020669871369, 110.8344237280190043 ) ) ;
#143763 = CARTESIAN_POINT ( 'NONE',  ( -12.14591786802326823, 12.06949235617739902, 68.12609039468567573 ) ) ;
#143764 = CARTESIAN_POINT ( 'NONE',  ( 18.62759615963255655, 10.81492255796105972, 96.66775706135234714 ) ) ;
#143765 = CARTESIAN_POINT ( 'NONE',  ( 10.72451020669898902, -18.67979575497178502, 22.91557627198102765 ) ) ;
#143766 = CARTESIAN_POINT ( 'NONE',  ( -16.46253265017146816, -9.564922557961047289, 104.1677570613523329 ) ) ;
#143767 = CARTESIAN_POINT ( 'NONE',  ( -21.52544592524334988, -5.823673210054445271, 73.95942372801901854 ) ) ;
#143768 = CARTESIAN_POINT ( 'NONE',  ( 14.29746914071037800, 8.314922557961029526, 31.66775706135234358 ) ) ;
#143769 = CARTESIAN_POINT ( 'NONE',  ( 5.823673210054125526, 21.52544592524343514, 84.79057627198102409 ) ) ;
#143770 = CARTESIAN_POINT ( 'NONE',  ( -19.05341960407617563, 5.049401038297882671, 103.5427570613523329 ) ) ;
#143771 = CARTESIAN_POINT ( 'NONE',  ( -13.89961937509977652, 13.97604488694528158, 70.62390960531432427 ) ) ;
#143772 = CARTESIAN_POINT ( 'NONE',  ( 13.97604488694548053, -13.89961937509957401, 110.6260903946856615 ) ) ;
#143773 = CARTESIAN_POINT ( 'NONE',  ( 9.474510206698729675, 16.51473224551082808, 107.0844237280190043 ) ) ;
#143774 = CARTESIAN_POINT ( 'NONE',  ( 4.379528057220339221, -16.55341960407611168, 62.70724293864769550 ) ) ;
#143775 = CARTESIAN_POINT ( 'NONE',  ( 5.153800228976615827, -19.02544592524334988, 75.20942372801896170 ) ) ;
#143776 = CARTESIAN_POINT ( 'NONE',  ( -8.314922557961024197, 14.29746914071037800, 72.91775706135234714 ) ) ;
#143778 = CARTESIAN_POINT ( 'NONE',  ( -19.05341960407611168, -5.049401038298163336, 56.45724293864768129 ) ) ;
#143777 = CARTESIAN_POINT ( 'NONE',  ( -10.72451020669898014, 18.67979575497178502, 115.4155762719810241 ) ) ;
#143779 = CARTESIAN_POINT ( 'NONE',  ( -13.89961937509977652, 13.97604488694528158, 55.62390960531434558 ) ) ;
#143780 = CARTESIAN_POINT ( 'NONE',  ( 16.55341960407618274, -4.379528057220086978, 66.04275706135236135 ) ) ;
#143781 = CARTESIAN_POINT ( 'NONE',  ( -22.44159573604009950, -16.30477369853688430, 141.5750000027311728 ) ) ;
#143782 = CARTESIAN_POINT ( 'NONE',  ( -8.906447517083053711, -27.41122689804191026, 146.6500000054623740 ) ) ;
#143783 = EDGE_LOOP ( 'NONE', ( #151113, #41837, #164104, #7104 ) ) ;
#143784 = CARTESIAN_POINT ( 'NONE',  ( 18.67979575497194134, -10.72451020669871369, 110.8344237280190043 ) ) ;
#143785 = CARTESIAN_POINT ( 'NONE',  ( -2.500000000000000000, -105.0000000000000000, 12.00000000000000355 ) ) ;
#143786 = ORIENTED_EDGE ( 'NONE', *, *, #50192, .T. ) ;
#143787 = CARTESIAN_POINT ( 'NONE',  ( 16.46253265017146816, 9.564922557961045513, 111.6677570613523329 ) ) ;
#143788 = CARTESIAN_POINT ( 'NONE',  ( 21.52544592524344225, -5.823673210054117533, 48.54057627198103120 ) ) ;
#143790 = CARTESIAN_POINT ( 'NONE',  ( 14.34966873604972726, -8.224510206698740333, 35.83442372801901143 ) ) ;
#143789 = CARTESIAN_POINT ( 'NONE',  ( 13.97604488694548053, -13.89961937509957401, 50.62609039468566152 ) ) ;
#143791 = CARTESIAN_POINT ( 'NONE',  ( -19.03943276465977164, 0.05219959533909376836, 46.24890960531435979 ) ) ;
#143792 = CARTESIAN_POINT ( 'NONE',  ( 9.564922557960805705, 16.46253265017160317, 44.58224293864769550 ) ) ;
#143793 = CARTESIAN_POINT ( 'NONE',  ( -5.719274019375978568, 21.55341960407610458, 85.20724293864770971 ) ) ;
#143794 = CARTESIAN_POINT ( 'NONE',  ( -13.89961937509977652, 13.97604488694528158, 115.6239096053143669 ) ) ;
#143795 = CARTESIAN_POINT ( 'NONE',  ( 9.564922557960805705, 16.46253265017160317, 49.58224293864770260 ) ) ;
#143796 = FACE_OUTER_BOUND ( 'NONE', #69703, .T. ) ;
#143797 = CARTESIAN_POINT ( 'NONE',  ( 19.02544592524334988, 5.153800228976608722, 91.45942372801900433 ) ) ;
#143798 = CARTESIAN_POINT ( 'NONE',  ( -16.55341960407611168, -4.379528057220339221, 61.45724293864770260 ) ) ;
#143799 = CARTESIAN_POINT ( 'NONE',  ( 0.05219959533936267826, -19.03943276465977164, 20.00109039468567218 ) ) ;
#143800 = CARTESIAN_POINT ( 'NONE',  ( -5.823673210054116645, -21.52544592524344225, 92.29057627198103830 ) ) ;
#143801 = CARTESIAN_POINT ( 'NONE',  ( 10.72451020669871369, 18.67979575497193778, 82.08442372801901854 ) ) ;
#143802 = CARTESIAN_POINT ( 'NONE',  ( -19.05341960407611168, -5.049401038298163336, 26.45724293864769550 ) ) ;
#143803 = CARTESIAN_POINT ( 'NONE',  ( -15.72974639402176322, -15.80617190586768395, 84.37609039468570415 ) ) ;
#143805 = CARTESIAN_POINT ( 'NONE',  ( 15.80617190586769283, -15.72974639402175789, 80.62609039468567573 ) ) ;
#143804 = CARTESIAN_POINT ( 'NONE',  ( -16.53943276465976808, 0.05219959533911058130, 21.24890960531436690 ) ) ;
#143806 = CARTESIAN_POINT ( 'NONE',  ( -5.153800228976328057, -19.02544592524343514, 67.29057627198102409 ) ) ;
#143807 = EDGE_CURVE ( 'NONE', #96182, #11730, #114680, .T. ) ;
#143808 = CARTESIAN_POINT ( 'NONE',  ( 0.05219959533937995610, -21.53943276465977519, 50.00109039468568994 ) ) ;
#143809 = CARTESIAN_POINT ( 'NONE',  ( 9.564922557960805705, 16.46253265017160317, 84.58224293864769550 ) ) ;
#143810 = CARTESIAN_POINT ( 'NONE',  ( 14.29746914071049879, -8.314922557960816363, 93.33224293864769550 ) ) ;
#143811 = CARTESIAN_POINT ( 'NONE',  ( -8.224510206698948167, 14.34966873604960824, 55.41557627198102409 ) ) ;
#143812 = CARTESIAN_POINT ( 'NONE',  ( 5.823673210054125526, 21.52544592524343514, 74.79057627198105251 ) ) ;
#143813 = CARTESIAN_POINT ( 'NONE',  ( 19.03943276465977164, -0.05219959533909143690, 58.74890960531435979 ) ) ;
#143814 = CARTESIAN_POINT ( 'NONE',  ( 10.81492255796078972, 18.62759615963270932, 79.58224293864769550 ) ) ;
#143815 = CIRCLE ( 'NONE', #4526, 13.70000000000001528 ) ;
#143816 = CARTESIAN_POINT ( 'NONE',  ( -9.474510206698720793, -16.51473224551083518, 69.58442372801901854 ) ) ;
#143818 = CARTESIAN_POINT ( 'NONE',  ( 16.55341960407611168, 4.379528057220329451, 78.95724293864769550 ) ) ;
#143817 = CARTESIAN_POINT ( 'NONE',  ( -17.59860650958993844, 7.585241751806885979, 38.42337014262493256 ) ) ;
#143819 = CARTESIAN_POINT ( 'NONE',  ( -10.81492255796078084, -18.62759615963271287, 47.08224293864770260 ) ) ;
#143820 = FACE_OUTER_BOUND ( 'NONE', #162693, .T. ) ;
#143822 = CARTESIAN_POINT ( 'NONE',  ( -27.73933785331498925, 2.428612866367529932E-14, 145.3750000027311842 ) ) ;
#143821 = CARTESIAN_POINT ( 'NONE',  ( 4.379528057220092307, 16.55341960407617563, 102.2927570613523613 ) ) ;
#143823 = CARTESIAN_POINT ( 'NONE',  ( -9.564922557961040184, 16.46253265017147172, 102.9177570613523329 ) ) ;
#143824 = EDGE_CURVE ( 'NONE', #115197, #33312, #72003, .T. ) ;
#143825 = CARTESIAN_POINT ( 'NONE',  ( 8.224510206698953496, -14.34966873604960469, 72.91557627198103830 ) ) ;
#143826 = FACE_OUTER_BOUND ( 'NONE', #41664, .T. ) ;
#143827 = CARTESIAN_POINT ( 'NONE',  ( 9.564922557960805705, 16.46253265017160317, 59.58224293864769550 ) ) ;
#143828 = CARTESIAN_POINT ( 'NONE',  ( -8.224510206698948167, 14.34966873604960824, 60.41557627198102409 ) ) ;
#143829 = CARTESIAN_POINT ( 'NONE',  ( -0.05219959533909027116, -19.03943276465977164, 107.4989096053143527 ) ) ;
#143831 = CARTESIAN_POINT ( 'NONE',  ( -0.05219959533909027116, -19.03943276465977164, 72.49890960531435269 ) ) ;
#143830 = CARTESIAN_POINT ( 'NONE',  ( 19.03943276465977164, 0.05219959533936151252, 76.25109039468566152 ) ) ;
#143832 = CARTESIAN_POINT ( 'NONE',  ( 16.46253265017160672, -9.564922557960803928, 88.33224293864769550 ) ) ;
#143833 = CARTESIAN_POINT ( 'NONE',  ( -13.97604488694527625, -13.89961937509977652, 86.87390960531436690 ) ) ;
#143834 = CARTESIAN_POINT ( 'NONE',  ( 18.67979575497178502, 10.72451020669898547, 69.16557627198102409 ) ) ;
#143835 = CARTESIAN_POINT ( 'NONE',  ( -16.52544592524335698, -4.483927247898792601, 63.95942372801901854 ) ) ;
#143836 = CONICAL_SURFACE ( 'NONE', #163212, 2.500000000000002220, 1.029744260000000189 ) ;
#143837 = CARTESIAN_POINT ( 'NONE',  ( -15.49999999999999822, -5.500000000000000888, 22.00000000000000000 ) ) ;
#143838 = CARTESIAN_POINT ( 'NONE',  ( 0.05219959533909260263, 19.03943276465977164, 44.99890960531435979 ) ) ;
#143839 = CARTESIAN_POINT ( 'NONE',  ( -5.719274019375978568, 21.55341960407610458, 50.20724293864769550 ) ) ;
#143840 = CARTESIAN_POINT ( 'NONE',  ( 19.02544592524334988, 5.153800228976608722, 96.45942372801897591 ) ) ;
#143842 = CARTESIAN_POINT ( 'NONE',  ( -21.53943276465977519, -0.05219959533937600094, 33.75109039468568284 ) ) ;
#143841 = CARTESIAN_POINT ( 'NONE',  ( 4.483927247898545687, 16.52544592524342804, 24.79057627198103120 ) ) ;
#143843 = CARTESIAN_POINT ( 'NONE',  ( 9.474510206698729675, 16.51473224551082808, 32.08442372801900433 ) ) ;
#143845 = CARTESIAN_POINT ( 'NONE',  ( -12.14591786802326823, 12.06949235617739902, 88.12609039468570415 ) ) ;
#143844 = CARTESIAN_POINT ( 'NONE',  ( -16.52544592524335698, -4.483927247898792601, 58.95942372801902565 ) ) ;
#143846 = DIRECTION ( 'NONE',  ( 0.000000000000000000, 0.000000000000000000, 1.000000000000000000 ) ) ;
#143847 = CARTESIAN_POINT ( 'NONE',  ( -16.55341960407617563, 4.379528057220093196, 78.54275706135236135 ) ) ;
#143849 = CARTESIAN_POINT ( 'NONE',  ( -16.55341960407617563, 4.379528057220093196, 33.54275706135234714 ) ) ;
#143848 = CARTESIAN_POINT ( 'NONE',  ( -15.80617190586745835, -15.72974639402198527, 26.87390960531435979 ) ) ;
#143850 = CARTESIAN_POINT ( 'NONE',  ( -19.05341960407611168, -5.049401038298163336, 41.45724293864769550 ) ) ;
#143851 = CARTESIAN_POINT ( 'NONE',  ( 5.049401038298161559, -19.05341960407611168, 52.70724293864767418 ) ) ;
#143852 = CARTESIAN_POINT ( 'NONE',  ( -19.05341960407611168, -5.049401038298163336, 56.45724293864768129 ) ) ;
#143853 = CARTESIAN_POINT ( 'NONE',  ( -10.72451020669870658, -18.67979575497194134, 34.58442372801900433 ) ) ;
#143854 = CARTESIAN_POINT ( 'NONE',  ( 16.52544592524335698, 4.483927247898782831, 46.45942372801901854 ) ) ;
#143855 = CARTESIAN_POINT ( 'NONE',  ( 16.52544592524335698, 4.483927247898782831, 106.4594237280190328 ) ) ;
#143856 = CARTESIAN_POINT ( 'NONE',  ( -0.05219959533909027116, -19.03943276465977164, 32.49890960531435979 ) ) ;
#143857 = CARTESIAN_POINT ( 'NONE',  ( -5.719274019375665041, -21.55341960407619695, 109.7927570613523613 ) ) ;
#143858 = CARTESIAN_POINT ( 'NONE',  ( 9.564922557961047289, -16.46253265017146816, 110.4177570613523471 ) ) ;
#143859 = CARTESIAN_POINT ( 'NONE',  ( 0.05219959533936267826, -19.03943276465977164, 70.00109039468566152 ) ) ;
#143860 = CARTESIAN_POINT ( 'NONE',  ( -14.34966873604960291, -8.224510206698953496, 66.66557627198102409 ) ) ;
#143861 = CARTESIAN_POINT ( 'NONE',  ( 16.51473224551069308, 9.474510206698969483, 34.16557627198102409 ) ) ;
#143863 = FACE_OUTER_BOUND ( 'NONE', #104413, .T. ) ;
#143862 = CARTESIAN_POINT ( 'NONE',  ( -16.46253265017146816, -9.564922557961047289, 69.16775706135233293 ) ) ;
#143864 = CARTESIAN_POINT ( 'NONE',  ( -15.80617190586768217, 15.72974639402176855, 73.12609039468567573 ) ) ;
#143865 = CARTESIAN_POINT ( 'NONE',  ( 16.53943276465976808, 0.05219959533934440121, 36.25109039468567573 ) ) ;
#143866 = CARTESIAN_POINT ( 'NONE',  ( 6.100000000000006750, -2.167155344068307965E-14, -64.53213882399991519 ) ) ;
#143867 = CARTESIAN_POINT ( 'NONE',  ( -10.81492255796078084, -18.62759615963271287, 37.08224293864768129 ) ) ;
#143868 = CARTESIAN_POINT ( 'NONE',  ( 16.52544592524335698, 4.483927247898782831, 26.45942372801901854 ) ) ;
#143869 = CARTESIAN_POINT ( 'NONE',  ( 9.474510206698971260, -16.51473224551069308, 27.91557627198103120 ) ) ;
#143870 = CARTESIAN_POINT ( 'NONE',  ( 19.03943276465977164, 0.05219959533936151252, 31.25109039468566863 ) ) ;
#143871 = CARTESIAN_POINT ( 'NONE',  ( 23.48529157249600630, -32.32473071737748427, -7.299999999999998934 ) ) ;
#143872 = CARTESIAN_POINT ( 'NONE',  ( -0.05219959533909027116, -19.03943276465977164, 37.49890960531436690 ) ) ;
#143873 = CARTESIAN_POINT ( 'NONE',  ( -13.97604488694527625, -13.89961937509977652, 56.87390960531434558 ) ) ;
#143874 = CARTESIAN_POINT ( 'NONE',  ( -19.34837522270365895, -5.499999999999741540, 55.86337684832579953 ) ) ;
#143875 = CARTESIAN_POINT ( 'NONE',  ( 0.05219959533936267826, -19.03943276465977164, 25.00109039468566152 ) ) ;
#143876 = CARTESIAN_POINT ( 'NONE',  ( 12.14591786802309770, 12.06949235617756955, 24.37390960531435979 ) ) ;
#143877 = CARTESIAN_POINT ( 'NONE',  ( 13.97604488694527802, 13.89961937509977652, 29.37390960531435979 ) ) ;
#143878 = CARTESIAN_POINT ( 'NONE',  ( 9.474510206698971260, -16.51473224551069308, 97.91557627198102409 ) ) ;
#143879 = CARTESIAN_POINT ( 'NONE',  ( -10.81492255796105439, 18.62759615963255655, 72.91775706135234714 ) ) ;
#143880 = CARTESIAN_POINT ( 'NONE',  ( -0.05219959533909027116, -19.03943276465977164, 37.49890960531436690 ) ) ;
#143881 = CARTESIAN_POINT ( 'NONE',  ( 10.81492255796106328, -18.62759615963255655, 65.41775706135234714 ) ) ;
#143883 = CARTESIAN_POINT ( 'NONE',  ( -18.67979575497178146, -10.72451020669898902, 26.66557627198103475 ) ) ;
#143882 = CARTESIAN_POINT ( 'NONE',  ( -13.89961937509957401, -13.97604488694547875, 99.37609039468567573 ) ) ;
#143884 = CARTESIAN_POINT ( 'NONE',  ( -9.474510206698964154, 16.51473224551069663, 40.41557627198103120 ) ) ;
#143885 = CARTESIAN_POINT ( 'NONE',  ( 18.62759615963271287, -10.81492255796078972, 113.3322429386476955 ) ) ;
#143886 = CARTESIAN_POINT ( 'NONE',  ( -5.049401038297874678, -19.05341960407617918, 34.79275706135233293 ) ) ;
#143887 = CARTESIAN_POINT ( 'NONE',  ( -13.97604488694527625, -13.89961937509977652, 21.87390960531435979 ) ) ;
#143888 = CARTESIAN_POINT ( 'NONE',  ( -19.05341960407611168, -5.049401038298163336, 61.45724293864769550 ) ) ;
#143889 = CARTESIAN_POINT ( 'NONE',  ( 19.05341960407617918, -5.049401038297876454, 111.0427570613523329 ) ) ;
#143890 = CARTESIAN_POINT ( 'NONE',  ( 12.14591786802309770, 12.06949235617756955, 74.37390960531436690 ) ) ;
#143891 = CARTESIAN_POINT ( 'NONE',  ( -13.89961937509977652, 13.97604488694528158, 115.6239096053143669 ) ) ;
#143892 = CARTESIAN_POINT ( 'NONE',  ( 13.89961937509957401, 13.97604488694547697, 91.87609039468567573 ) ) ;
#143893 = CARTESIAN_POINT ( 'NONE',  ( -0.05219959533907301413, -21.53943276465977519, 97.49890960531436690 ) ) ;
#143894 = CARTESIAN_POINT ( 'NONE',  ( -18.62759615963255300, -10.81492255796106328, 44.16775706135234714 ) ) ;
#143895 = CARTESIAN_POINT ( 'NONE',  ( 4.483927247898790824, -16.52544592524335698, 45.20942372801901854 ) ) ;
#143897 = CARTESIAN_POINT ( 'NONE',  ( -18.67979575497193778, 10.72451020669871902, 43.33442372801901143 ) ) ;
#143896 = CARTESIAN_POINT ( 'NONE',  ( -16.52544592524335698, -4.483927247898792601, 58.95942372801902565 ) ) ;
#143898 = CARTESIAN_POINT ( 'NONE',  ( -15.80617190586745835, -15.72974639402198527, 56.87390960531436690 ) ) ;
#143899 = CARTESIAN_POINT ( 'NONE',  ( -9.474510206698964154, 16.51473224551069663, 50.41557627198102409 ) ) ;
#143900 = CARTESIAN_POINT ( 'NONE',  ( -38.00000000000000711, 2.428612866367529932E-14, -5.749999994537626336 ) ) ;
#143901 = CARTESIAN_POINT ( 'NONE',  ( 12.14591786802327356, -12.06949235617739191, 75.62609039468567573 ) ) ;
#143902 = CARTESIAN_POINT ( 'NONE',  ( -0.05219959533907301413, -21.53943276465977519, 102.4989096053143811 ) ) ;
#143903 = CARTESIAN_POINT ( 'NONE',  ( -4.483927247898539470, -16.52544592524342804, 57.29057627198103120 ) ) ;
#143904 = CARTESIAN_POINT ( 'NONE',  ( 8.224510206698742110, 14.34966873604972548, 67.08442372801901854 ) ) ;
#143905 = CARTESIAN_POINT ( 'NONE',  ( -5.153800228976607833, 19.02544592524334988, 97.70942372801900433 ) ) ;
#143906 = CARTESIAN_POINT ( 'NONE',  ( 10.81492255796078972, 18.62759615963270932, 99.58224293864770971 ) ) ;
#143907 = CARTESIAN_POINT ( 'NONE',  ( 16.52544592524342804, -4.483927247898539470, 48.54057627198103120 ) ) ;
#143908 = ORIENTED_EDGE ( 'NONE', *, *, #184085, .T. ) ;
#143909 = CARTESIAN_POINT ( 'NONE',  ( -18.67979575497178146, -10.72451020669898902, 76.66557627198103830 ) ) ;
#143910 = B_SPLINE_CURVE_WITH_KNOTS ( 'NONE', 3,
 ( #192013, #53497, #115174, #21167, #38336, #99992, #23173, #141530 ),
 .UNSPECIFIED., .F., .F.,
 ( 4, 2, 2, 4 ),
 ( 2.244678719550583187E-07, 0.002115167047686612300, 0.004230109627501268954, 0.008459994787130583130 ),
 .UNSPECIFIED. ) ;
#143911 = CARTESIAN_POINT ( 'NONE',  ( -14.34966873604960291, -8.224510206698953496, 26.66557627198103475 ) ) ;
#143912 = ORIENTED_EDGE ( 'NONE', *, *, #74692, .F. ) ;
#143913 = CARTESIAN_POINT ( 'NONE',  ( -17.49999999999999289, -5.622605283950892208, 56.31207310596111171 ) ) ;
#143914 = CARTESIAN_POINT ( 'NONE',  ( 21.53943276465977519, -0.05219959533907433946, 103.7489096053143669 ) ) ;
#143915 = AXIS2_PLACEMENT_3D ( 'NONE', #14575, #12613, #45905 ) ;
#143916 = CARTESIAN_POINT ( 'NONE',  ( -18.62759615963270932, 10.81492255796079327, 110.8322429386476955 ) ) ;
#143917 = CARTESIAN_POINT ( 'NONE',  ( 0.05219959533910956823, 16.53943276465976808, 39.99890960531436690 ) ) ;
#143918 = CARTESIAN_POINT ( 'NONE',  ( 0.05219959533934541429, -16.53943276465976808, 50.00109039468568994 ) ) ;
#143919 = CARTESIAN_POINT ( 'NONE',  ( -19.03943276465977164, 0.05219959533909376836, 46.24890960531435979 ) ) ;
#143920 = CARTESIAN_POINT ( 'NONE',  ( -9.564922557960796823, -16.46253265017161027, 72.08224293864770971 ) ) ;
#143921 = ORIENTED_EDGE ( 'NONE', *, *, #65570, .F. ) ;
#143922 = CARTESIAN_POINT ( 'NONE',  ( 21.52544592524344225, -5.823673210054117533, 28.54057627198103120 ) ) ;
#143923 = CARTESIAN_POINT ( 'NONE',  ( -26.91739389983944264, -26.09363094301675901, -18.46721497145169977 ) ) ;
#143924 = CARTESIAN_POINT ( 'NONE',  ( -5.153800228976607833, 19.02544592524334988, 102.7094237280189759 ) ) ;
#143925 = CARTESIAN_POINT ( 'NONE',  ( 16.46253265017146816, 9.564922557961045513, 56.66775706135233293 ) ) ;
#143926 = CARTESIAN_POINT ( 'NONE',  ( -15.72974639402197994, 15.80617190586746368, 105.6239096053143669 ) ) ;
#143927 = CARTESIAN_POINT ( 'NONE',  ( 16.53943276465976808, -0.05219959533910856209, 28.74890960531435624 ) ) ;
#143928 = CARTESIAN_POINT ( 'NONE',  ( 9.564922557960805705, 16.46253265017160317, 79.58224293864769550 ) ) ;
#143929 = CARTESIAN_POINT ( 'NONE',  ( 15.80617190586746368, 15.72974639402197994, 49.37390960531436690 ) ) ;
#143931 = CARTESIAN_POINT ( 'NONE',  ( -12.14591786802326823, 12.06949235617739902, 28.12609039468568284 ) ) ;
#143930 = CARTESIAN_POINT ( 'NONE',  ( 10.81492255796078972, 18.62759615963270932, 79.58224293864769550 ) ) ;
#143932 = ADVANCED_FACE ( 'NONE', ( #193969, #58428, #59409, #11953 ), #9945, .F. ) ;
#143933 = CARTESIAN_POINT ( 'NONE',  ( 0.05219959533909260263, 19.03943276465977164, 114.9989096053143669 ) ) ;
#143934 = CARTESIAN_POINT ( 'NONE',  ( 10.72451020669871369, 18.67979575497193778, 72.08442372801899012 ) ) ;
#143935 = CARTESIAN_POINT ( 'NONE',  ( 16.46253265017160672, -9.564922557960803928, 68.33224293864770971 ) ) ;
#143936 = CARTESIAN_POINT ( 'NONE',  ( -19.05341960407611168, -5.049401038298163336, 26.45724293864769550 ) ) ;
#143937 = CARTESIAN_POINT ( 'NONE',  ( 5.153800228976335163, 19.02544592524342804, 89.79057627198102409 ) ) ;
#143938 = CARTESIAN_POINT ( 'NONE',  ( 8.224510206698953496, -14.34966873604960469, 97.91557627198103830 ) ) ;
#143939 = ORIENTED_EDGE ( 'NONE', *, *, #79274, .T. ) ;
#143940 = CARTESIAN_POINT ( 'NONE',  ( -5.049401038297874678, -19.05341960407617918, 104.7927570613523471 ) ) ;
#143941 = CARTESIAN_POINT ( 'NONE',  ( 17.48847506799968698, -5.747544572773781724, 83.32697437843280852 ) ) ;
#143942 = CARTESIAN_POINT ( 'NONE',  ( 16.46253265017160672, -9.564922557960803928, 68.33224293864770971 ) ) ;
#143944 = CARTESIAN_POINT ( 'NONE',  ( 18.67979575497178502, 10.72451020669898547, 24.16557627198103120 ) ) ;
#143943 = CARTESIAN_POINT ( 'NONE',  ( -21.52544592524334988, -5.823673210054445271, 83.95942372801900433 ) ) ;
#143946 = EDGE_CURVE ( 'NONE', #150536, #127511, #92002, .T. ) ;
#143945 = CARTESIAN_POINT ( 'NONE',  ( 12.06949235617739724, 12.14591786802326823, 76.87609039468567573 ) ) ;
#143947 = CARTESIAN_POINT ( 'NONE',  ( -17.12812012977029497, -6.668231424565920662, 76.35948759323146362 ) ) ;
#143948 = CARTESIAN_POINT ( 'NONE',  ( -9.564922557961040184, 16.46253265017147172, 52.91775706135233293 ) ) ;
#143949 = CARTESIAN_POINT ( 'NONE',  ( -9.474510206698720793, -16.51473224551083518, 24.58442372801900078 ) ) ;
#143950 = CARTESIAN_POINT ( 'NONE',  ( 4.381597987324926002, 6.502961151143325402, -64.22400872216481105 ) ) ;
#143951 = CARTESIAN_POINT ( 'NONE',  ( -16.51473224551069308, -9.474510206698971260, 21.66557627198102765 ) ) ;
#143952 = CARTESIAN_POINT ( 'NONE',  ( -5.950531402560715689E-15, 38.81732327939063509, -5.624999997268812280 ) ) ;
#143953 = CARTESIAN_POINT ( 'NONE',  ( 12.14591786802327356, -12.06949235617739191, 110.6260903946857042 ) ) ;
#143954 = DIRECTION ( 'NONE',  ( 0.000000000000000000, 0.000000000000000000, 1.000000000000000000 ) ) ;
#143955 = CARTESIAN_POINT ( 'NONE',  ( 8.224510206698742110, 14.34966873604972548, 102.0844237280190185 ) ) ;
#143956 = CARTESIAN_POINT ( 'NONE',  ( 31.75360176573013860, -24.33155002292239288, -19.38334379417544184 ) ) ;
#143957 = CARTESIAN_POINT ( 'NONE',  ( 12.14591786802327356, -12.06949235617739191, 80.62609039468567573 ) ) ;
#143958 = CARTESIAN_POINT ( 'NONE',  ( 21.52544592524334988, 5.823673210054432836, 91.45942372801901854 ) ) ;
#143959 = CARTESIAN_POINT ( 'NONE',  ( 13.97604488694548053, -13.89961937509957401, 100.6260903946856615 ) ) ;
#143960 = CARTESIAN_POINT ( 'NONE',  ( 21.53943276465977519, 0.05219959533937863772, 61.25109039468567573 ) ) ;
#143961 = CARTESIAN_POINT ( 'NONE',  ( 9.564922557961047289, -16.46253265017146816, 40.41775706135234003 ) ) ;
#143962 = CARTESIAN_POINT ( 'NONE',  ( -9.564922557960796823, -16.46253265017161027, 82.08224293864768129 ) ) ;
#143963 = CARTESIAN_POINT ( 'NONE',  ( -19.02544592524342804, 5.153800228976336051, 51.04057627198103120 ) ) ;
#143964 = CARTESIAN_POINT ( 'NONE',  ( -19.26498983726237313, 5.499999999999599432, 40.55319577422005040 ) ) ;
#143965 = CARTESIAN_POINT ( 'NONE',  ( -21.55341960407610458, -5.719274019375992779, 96.45724293864770971 ) ) ;
#143966 = B_SPLINE_CURVE_WITH_KNOTS ( 'NONE', 3,
 ( #193995, #165642, #42303, #104956, #12958, #164647, #163647, #166642, #57472, #196984, #27140, #194985, #29124, #148478, #74622, #120118, #56463, #182801, #167627, #28144, #90762, #9969 ),
 .UNSPECIFIED., .F., .F.,
 ( 4, 2, 2, 2, 2, 2, 2, 2, 2, 2, 4 ),
 ( 1.262897753262583006E-17, 0.001309639967555230192, 0.001964459951332838891, 0.002291869943221642916, 0.002455574939166047747, 0.002619279935110452578, 0.002782984931054856975, 0.002946689926999261806, 0.003274099918888071035, 0.003928919902665695130, 0.005238559870220941585 ),
 .UNSPECIFIED. ) ;
#143967 = CARTESIAN_POINT ( 'NONE',  ( 10.72451020669898902, -18.67979575497178502, 47.91557627198102409 ) ) ;
#143968 = CARTESIAN_POINT ( 'NONE',  ( 5.049401038298161559, -19.05341960407611168, 52.70724293864767418 ) ) ;
#143969 = CARTESIAN_POINT ( 'NONE',  ( 0.05219959533934541429, -16.53943276465976808, 65.00109039468568994 ) ) ;
#143970 = ORIENTED_EDGE ( 'NONE', *, *, #6551, .F. ) ;
#143971 = EDGE_CURVE ( 'NONE', #123998, #163715, #52653, .T. ) ;
#143972 = CARTESIAN_POINT ( 'NONE',  ( 21.52544592524334988, 5.823673210054432836, 41.45942372801901143 ) ) ;
#143974 = CARTESIAN_POINT ( 'NONE',  ( -29.86685920354755197, -21.69954338932560134, -2.424999997268813434 ) ) ;
#143973 = CARTESIAN_POINT ( 'NONE',  ( 4.379528057220339221, -16.55341960407611168, 77.70724293864770971 ) ) ;
#143975 = CARTESIAN_POINT ( 'NONE',  ( 8.314922557961029526, -14.29746914071037800, 40.41775706135234714 ) ) ;
#143976 = CARTESIAN_POINT ( 'NONE',  ( 14.29746914071049879, -8.314922557960816363, 108.3322429386477097 ) ) ;
#143977 = CARTESIAN_POINT ( 'NONE',  ( 0.05219959533936267826, -19.03943276465977164, 55.00109039468566863 ) ) ;
#143978 = CARTESIAN_POINT ( 'NONE',  ( 14.29746914071049879, -8.314922557960816363, 68.33224293864769550 ) ) ;
#143979 = CARTESIAN_POINT ( 'NONE',  ( 10.72451020669871369, 18.67979575497193778, 32.08442372801901854 ) ) ;
#143981 = CARTESIAN_POINT ( 'NONE',  ( 21.52544592524344225, -5.823673210054117533, 93.54057627198103830 ) ) ;
#143980 = CARTESIAN_POINT ( 'NONE',  ( 13.89961937509977652, -13.97604488694527269, 28.12390960531435624 ) ) ;
#143982 = CARTESIAN_POINT ( 'NONE',  ( -5.049401038298153566, 19.05341960407611168, 100.2072429386476955 ) ) ;
#143983 = CARTESIAN_POINT ( 'NONE',  ( 16.52544592524342804, -4.483927247898539470, 68.54057627198103830 ) ) ;
#143984 = CARTESIAN_POINT ( 'NONE',  ( 23.77862661291771929, -32.55609251395039649, -17.57696395782325283 ) ) ;
#143985 = CARTESIAN_POINT ( 'NONE',  ( 22.81625015709510151, -31.40387420917324590, -1.924999997268813212 ) ) ;
#143986 = CARTESIAN_POINT ( 'NONE',  ( -5.049401038297874678, -19.05341960407617918, 84.79275706135233293 ) ) ;
#143987 = CARTESIAN_POINT ( 'NONE',  ( -5.719274019375978568, 21.55341960407610458, 115.2072429386476955 ) ) ;
#143988 = CARTESIAN_POINT ( 'NONE',  ( -13.89961937509977652, 13.97604488694528158, 75.62390960531438111 ) ) ;
#143989 = CARTESIAN_POINT ( 'NONE',  ( -5.153800228976607833, 19.02544592524334988, 62.70942372801899722 ) ) ;
#143990 = CARTESIAN_POINT ( 'NONE',  ( 16.46253265017160672, -9.564922557960803928, 48.33224293864769550 ) ) ;
#143991 = CARTESIAN_POINT ( 'NONE',  ( 12.14591786802309770, 12.06949235617756955, 64.37390960531435269 ) ) ;
#143992 = CARTESIAN_POINT ( 'NONE',  ( -12.06949235617756955, 12.14591786802309770, 55.62390960531436690 ) ) ;
#143993 = CARTESIAN_POINT ( 'NONE',  ( 16.46253265017160672, -9.564922557960803928, 73.33224293864769550 ) ) ;
#143994 = CARTESIAN_POINT ( 'NONE',  ( -0.05219959533907301413, -21.53943276465977519, 87.49890960531436690 ) ) ;
#143995 = CARTESIAN_POINT ( 'NONE',  ( 9.474510206698971260, -16.51473224551069308, 77.91557627198103830 ) ) ;
#143996 = CARTESIAN_POINT ( 'NONE',  ( 10.81492255796078972, 18.62759615963270932, 84.58224293864769550 ) ) ;
#143997 = CARTESIAN_POINT ( 'NONE',  ( 16.46253265017146816, 9.564922557961045513, 21.66775706135233648 ) ) ;
#144000 = CARTESIAN_POINT ( 'NONE',  ( -16.53943276465976808, 0.05219959533911058130, 91.24890960531436690 ) ) ;
#143999 = CARTESIAN_POINT ( 'NONE',  ( -16.53943276465976808, -0.05219959533934237506, 108.7510903946857042 ) ) ;
#143998 = PLANE ( 'NONE',  #134972 ) ;
#144001 = CARTESIAN_POINT ( 'NONE',  ( 16.46253265017146816, 9.564922557961045513, 86.66775706135233293 ) ) ;
#144002 = ORIENTED_EDGE ( 'NONE', *, *, #44938, .T. ) ;
#144003 = CARTESIAN_POINT ( 'NONE',  ( 18.62759615963255655, 10.81492255796105972, 21.66775706135235069 ) ) ;
#144004 = CARTESIAN_POINT ( 'NONE',  ( 16.46253265017146816, 9.564922557961045513, 56.66775706135233293 ) ) ;
#144005 = CARTESIAN_POINT ( 'NONE',  ( 12.14591786802327356, -12.06949235617739191, 100.6260903946857184 ) ) ;
#144006 = CARTESIAN_POINT ( 'NONE',  ( 16.51473224551083163, -9.474510206698727899, 40.83442372801900433 ) ) ;
#144007 = CARTESIAN_POINT ( 'NONE',  ( 19.05341960407611168, 5.049401038298154454, 103.9572429386476671 ) ) ;
#144008 = CARTESIAN_POINT ( 'NONE',  ( -8.224510206698948167, 14.34966873604960824, 60.41557627198102409 ) ) ;
#144009 = CARTESIAN_POINT ( 'NONE',  ( -19.52837319214026834, 5.499999999999896971, 49.60471352585536664 ) ) ;
#144010 = CARTESIAN_POINT ( 'NONE',  ( 0.05219959533909260263, 19.03943276465977164, 39.99890960531436690 ) ) ;
#144011 = CARTESIAN_POINT ( 'NONE',  ( -21.52544592524334988, -5.823673210054445271, 103.9594237280190185 ) ) ;
#144012 = CARTESIAN_POINT ( 'NONE',  ( -0.05219959533934338120, 16.53943276465976808, 72.50109039468568994 ) ) ;
#144013 = CARTESIAN_POINT ( 'NONE',  ( -21.53943276465977519, -0.05219959533937600094, 38.75109039468567573 ) ) ;
#144014 = CARTESIAN_POINT ( 'NONE',  ( -8.224510206698735004, -14.34966873604973081, 49.58442372801901143 ) ) ;
#144015 = CARTESIAN_POINT ( 'NONE',  ( 19.02544592524343514, -5.153800228976328945, 103.5405762719809957 ) ) ;
#144016 = CARTESIAN_POINT ( 'NONE',  ( -19.05341960407611168, -5.049401038298163336, 56.45724293864768129 ) ) ;
#144017 = CARTESIAN_POINT ( 'NONE',  ( 5.153800228976335163, 19.02544592524342804, 69.79057627198103830 ) ) ;
#144018 = VECTOR ( 'NONE', #188004, 1000.000000000000000 ) ;
#144019 = CARTESIAN_POINT ( 'NONE',  ( -16.52544592524335698, -4.483927247898792601, 53.95942372801900433 ) ) ;
#144020 = CARTESIAN_POINT ( 'NONE',  ( 16.53943276465976808, -0.05219959533910856209, 108.7489096053143669 ) ) ;
#144021 = CARTESIAN_POINT ( 'NONE',  ( -4.483927247898782831, 16.52544592524335698, 107.7094237280190328 ) ) ;
#144022 = CARTESIAN_POINT ( 'NONE',  ( 0.000000000000000000, 0.000000000000000000, 0.000000000000000000 ) ) ;
#144025 = CARTESIAN_POINT ( 'NONE',  ( -5.153800228976328057, -19.02544592524343514, 77.29057627198099567 ) ) ;
#144024 = CARTESIAN_POINT ( 'NONE',  ( 19.02544592524343514, -5.153800228976328945, 88.54057627198102409 ) ) ;
#144023 = CARTESIAN_POINT ( 'NONE',  ( 18.67979575497194134, -10.72451020669871369, 55.83442372801901854 ) ) ;
#144026 = CARTESIAN_POINT ( 'NONE',  ( 19.02544592524343514, -5.153800228976328945, 98.54057627198100988 ) ) ;
#144027 = CARTESIAN_POINT ( 'NONE',  ( -12.06949235617756955, 12.14591786802309770, 50.62390960531435979 ) ) ;
#144028 = CARTESIAN_POINT ( 'NONE',  ( 14.34966873604972726, -8.224510206698740333, 110.8344237280190043 ) ) ;
#144029 = CARTESIAN_POINT ( 'NONE',  ( -14.29746914071049879, 8.314922557960819915, 35.83224293864768839 ) ) ;
#144030 = ORIENTED_EDGE ( 'NONE', *, *, #117641, .T. ) ;
#144031 = CARTESIAN_POINT ( 'NONE',  ( -16.62134038107351230, -17.54604082932918274, -54.32399035855149805 ) ) ;
#144032 = CARTESIAN_POINT ( 'NONE',  ( -16.51473224551069308, -9.474510206698971260, 66.66557627198102409 ) ) ;
#144033 = CARTESIAN_POINT ( 'NONE',  ( 19.03943276465977164, 0.05219959533936151252, 51.25109039468567573 ) ) ;
#144034 = CARTESIAN_POINT ( 'NONE',  ( 11.40812507854754365, 35.11059874428196537, -1.224999997268813479 ) ) ;
#144035 = CARTESIAN_POINT ( 'NONE',  ( 18.46320343559671429, 23.96320343559620625, 8.181980515339454030 ) ) ;
#144037 = CARTESIAN_POINT ( 'NONE',  ( -12.14591786802326823, 12.06949235617739902, 63.12609039468568994 ) ) ;
#144036 = CARTESIAN_POINT ( 'NONE',  ( -13.97604488694547697, 13.89961937509957934, 83.12609039468564731 ) ) ;
#144038 = DIRECTION ( 'NONE',  ( 0.000000000000000000, -0.8164965809277251463, 0.5773502691896268413 ) ) ;
#144039 = CARTESIAN_POINT ( 'NONE',  ( 13.97604488694527802, 13.89961937509977652, 94.37390960531436690 ) ) ;
#144040 = CARTESIAN_POINT ( 'NONE',  ( -15.72974639402176322, -15.80617190586768395, 29.37609039468568284 ) ) ;
#144041 = CARTESIAN_POINT ( 'NONE',  ( -5.049401038297874678, -19.05341960407617918, 89.79275706135230450 ) ) ;
#144043 = CARTESIAN_POINT ( 'NONE',  ( -5.153800228976328057, -19.02544592524343514, 42.29057627198101699 ) ) ;
#144042 = CARTESIAN_POINT ( 'NONE',  ( 9.564922557960805705, 16.46253265017160317, 114.5822429386476955 ) ) ;
#144044 = CARTESIAN_POINT ( 'NONE',  ( -16.51473224551069308, -9.474510206698971260, 96.66557627198102409 ) ) ;
#144046 = CARTESIAN_POINT ( 'NONE',  ( -16.51473224551069308, -9.474510206698971260, 46.66557627198102409 ) ) ;
#144045 = CARTESIAN_POINT ( 'NONE',  ( -8.314922557960811034, -14.29746914071050412, 42.08224293864769550 ) ) ;
#144047 = CARTESIAN_POINT ( 'NONE',  ( -5.153800228976607833, 19.02544592524334988, 62.70942372801899722 ) ) ;
#144048 = ORIENTED_EDGE ( 'NONE', *, *, #189746, .F. ) ;
#144049 = CARTESIAN_POINT ( 'NONE',  ( -16.52544592524342804, 4.483927247898546575, 81.04057627198102409 ) ) ;
#144050 = CARTESIAN_POINT ( 'NONE',  ( 0.05219959533936267826, -19.03943276465977164, 35.00109039468566863 ) ) ;
#144051 = CARTESIAN_POINT ( 'NONE',  ( -13.89961937509977652, 13.97604488694528158, 70.62390960531432427 ) ) ;
#144052 = CARTESIAN_POINT ( 'NONE',  ( -21.55341960407610458, -5.719274019375992779, 66.45724293864768129 ) ) ;
#144054 = CARTESIAN_POINT ( 'NONE',  ( 16.51473224551083163, -9.474510206698727899, 25.83442372801900078 ) ) ;
#144053 = CARTESIAN_POINT ( 'NONE',  ( -14.29746914071049879, 8.314922557960819915, 65.83224293864769550 ) ) ;
#144055 = CARTESIAN_POINT ( 'NONE',  ( 19.03943276465977164, -0.05219959533909143690, 108.7489096053143527 ) ) ;
#144056 = AXIS2_PLACEMENT_3D ( 'NONE', #114638, #130805, #145972 ) ;
#144057 = CARTESIAN_POINT ( 'NONE',  ( 21.52544592524344225, -5.823673210054117533, 28.54057627198103120 ) ) ;
#144058 = CARTESIAN_POINT ( 'NONE',  ( 19.05341960407611168, 5.049401038298154454, 48.95724293864768129 ) ) ;
#144059 = CARTESIAN_POINT ( 'NONE',  ( 5.049401038298161559, -19.05341960407611168, 32.70724293864768129 ) ) ;
#144060 = CARTESIAN_POINT ( 'NONE',  ( -12.14591786802309592, -12.06949235617757132, 101.8739096053143811 ) ) ;
#144061 = CARTESIAN_POINT ( 'NONE',  ( -15.72974639402197994, 15.80617190586746368, 105.6239096053143669 ) ) ;
#144062 = CARTESIAN_POINT ( 'NONE',  ( -16.51473224551069308, -9.474510206698971260, 111.6655762719810383 ) ) ;
#144063 = CARTESIAN_POINT ( 'NONE',  ( -18.67979575497193778, 10.72451020669871902, 23.33442372801901499 ) ) ;
#144064 = CARTESIAN_POINT ( 'NONE',  ( -19.03943276465977164, 0.05219959533909376836, 106.2489096053143669 ) ) ;
#144065 = CARTESIAN_POINT ( 'NONE',  ( 4.483927247898545687, 16.52544592524342804, 114.7905762719810383 ) ) ;
#144066 = CARTESIAN_POINT ( 'NONE',  ( -15.80617190586768217, 15.72974639402176855, 78.12609039468570415 ) ) ;
#144067 = CARTESIAN_POINT ( 'NONE',  ( 10.72451020669898902, -18.67979575497178502, 92.91557627198103830 ) ) ;
#144068 = CARTESIAN_POINT ( 'NONE',  ( -27.86273085795036408, -28.69962071417357663, -15.00000000000000000 ) ) ;
#144069 = CARTESIAN_POINT ( 'NONE',  ( 18.56453257813364743, -5.500000000000051514, 78.49000423690682737 ) ) ;
#144070 = CARTESIAN_POINT ( 'NONE',  ( 28.97745891950394537, -0.4911207797135175301, -52.56957762865169315 ) ) ;
#144071 = CARTESIAN_POINT ( 'NONE',  ( -12.14591786802326823, 12.06949235617739902, 53.12609039468568284 ) ) ;
#144072 = CARTESIAN_POINT ( 'NONE',  ( -12.14591786802309592, -12.06949235617757132, 101.8739096053143811 ) ) ;
#144073 = CARTESIAN_POINT ( 'NONE',  ( 33.82551795724113930, -1.774401534882015241, 100.2184796937738582 ) ) ;
#144074 = CARTESIAN_POINT ( 'NONE',  ( -13.97604488694527625, -13.89961937509977652, 61.87390960531435979 ) ) ;
#144075 = CARTESIAN_POINT ( 'NONE',  ( -12.06949235617756955, 12.14591786802309770, 90.62390960531436690 ) ) ;
#144076 = CARTESIAN_POINT ( 'NONE',  ( -10.81492255796078084, -18.62759615963271287, 47.08224293864770260 ) ) ;
#144077 = CARTESIAN_POINT ( 'NONE',  ( 8.224510206698953496, -14.34966873604960469, 67.91557627198102409 ) ) ;
#144078 = CARTESIAN_POINT ( 'NONE',  ( -14.34966873604972548, 8.224510206698743886, 23.33442372801901499 ) ) ;
#144079 = CARTESIAN_POINT ( 'NONE',  ( 10.72451020669871369, 18.67979575497193778, 82.08442372801901854 ) ) ;
#144080 = SPHERICAL_SURFACE ( 'NONE', #59375, 0.5000000000000000000 ) ;
#144081 = CARTESIAN_POINT ( 'NONE',  ( -14.29746914071037622, -8.314922557961029526, 99.16775706135234714 ) ) ;
#144082 = CARTESIAN_POINT ( 'NONE',  ( -4.483927247898539470, -16.52544592524342804, 37.29057627198102409 ) ) ;
#144083 = CARTESIAN_POINT ( 'NONE',  ( -9.564922557960796823, -16.46253265017161027, 32.08224293864769550 ) ) ;
#144084 = CARTESIAN_POINT ( 'NONE',  ( 9.564922557960805705, 16.46253265017160317, 89.58224293864769550 ) ) ;
#144085 = CARTESIAN_POINT ( 'NONE',  ( -10.81492255796078084, -18.62759615963271287, 97.08224293864770971 ) ) ;
#144086 = CARTESIAN_POINT ( 'NONE',  ( -8.314922557961024197, 14.29746914071037800, 42.91775706135235424 ) ) ;
#144088 = CARTESIAN_POINT ( 'NONE',  ( -0.05219959533937732626, 21.53943276465977519, 92.50109039468567573 ) ) ;
#144087 = CARTESIAN_POINT ( 'NONE',  ( 4.379528057220339221, -16.55341960407611168, 62.70724293864769550 ) ) ;
#144089 = CARTESIAN_POINT ( 'NONE',  ( -4.379528057220086978, -16.55341960407618274, 94.79275706135234714 ) ) ;
#144090 = CARTESIAN_POINT ( 'NONE',  ( 17.40805194821983903, -6.112264579160780364, 48.33371272510606786 ) ) ;
#144091 = CYLINDRICAL_SURFACE ( 'NONE', #103472, 1.499999999999997780 ) ;
#144092 = CARTESIAN_POINT ( 'NONE',  ( -16.53943276465976808, 0.05219959533911058130, 31.24890960531435979 ) ) ;
#144093 = CARTESIAN_POINT ( 'NONE',  ( 0.05219959533934541429, -16.53943276465976808, 75.00109039468568994 ) ) ;
#144094 = CARTESIAN_POINT ( 'NONE',  ( -19.03943276465977164, 0.05219959533909376836, 91.24890960531436690 ) ) ;
#144095 = CARTESIAN_POINT ( 'NONE',  ( -13.89961937509977652, 13.97604488694528158, 105.6239096053143527 ) ) ;
#144096 = CARTESIAN_POINT ( 'NONE',  ( 21.55341960407619695, -5.719274019375665929, 86.04275706135236135 ) ) ;
#144097 = EDGE_CURVE ( 'NONE', #102970, #194207, #132547, .T. ) ;
#144098 = CARTESIAN_POINT ( 'NONE',  ( -4.379528057220086978, -16.55341960407618274, 94.79275706135234714 ) ) ;
#144099 = CARTESIAN_POINT ( 'NONE',  ( -0.05219959533910754901, -16.53943276465976808, 57.49890960531435979 ) ) ;
#144100 = CARTESIAN_POINT ( 'NONE',  ( 0.05219959533909260263, 19.03943276465977164, 74.99890960531435269 ) ) ;
#144101 = EDGE_LOOP ( 'NONE', ( #121173, #16698 ) ) ;
#144102 = CARTESIAN_POINT ( 'NONE',  ( -19.03943276465977164, -0.05219959533935918106, 108.7510903946856615 ) ) ;
#144103 = CARTESIAN_POINT ( 'NONE',  ( -0.05219959533910754901, -16.53943276465976808, 107.4989096053143669 ) ) ;
#144104 = CARTESIAN_POINT ( 'NONE',  ( 5.153800228976335163, 19.02544592524342804, 74.79057627198103830 ) ) ;
#144106 = CARTESIAN_POINT ( 'NONE',  ( -36.91746825000001309, 11.99521256947798342, -8.724999997268813701 ) ) ;
#144105 = CARTESIAN_POINT ( 'NONE',  ( 14.34966873604972726, -8.224510206698740333, 20.83442372801901143 ) ) ;
#144107 = CARTESIAN_POINT ( 'NONE',  ( 13.89961937509957401, 13.97604488694547697, 21.87609039468566152 ) ) ;
#144108 = CARTESIAN_POINT ( 'NONE',  ( 12.14591786802327356, -12.06949235617739191, 75.62609039468567573 ) ) ;
#144109 = CARTESIAN_POINT ( 'NONE',  ( -5.049401038297874678, -19.05341960407617918, 104.7927570613523471 ) ) ;
#144110 = CARTESIAN_POINT ( 'NONE',  ( -12.06949235617756955, 12.14591786802309770, 110.6239096053143669 ) ) ;
#144111 = CARTESIAN_POINT ( 'NONE',  ( -16.52544592524335698, -4.483927247898792601, 63.95942372801901854 ) ) ;
#144112 = CARTESIAN_POINT ( 'NONE',  ( 4.379528057220092307, 16.55341960407617563, 57.29275706135234714 ) ) ;
#144113 = CARTESIAN_POINT ( 'NONE',  ( -0.05219959533909027116, -19.03943276465977164, 22.49890960531436690 ) ) ;
#144114 = CARTESIAN_POINT ( 'NONE',  ( -5.049401038297874678, -19.05341960407617918, 64.79275706135233293 ) ) ;
#144115 = CARTESIAN_POINT ( 'NONE',  ( 21.52544592524334988, 5.823673210054432836, 111.4594237280190328 ) ) ;
#144116 = CARTESIAN_POINT ( 'NONE',  ( 9.474510206698971260, -16.51473224551069308, 32.91557627198102409 ) ) ;
#144117 = CARTESIAN_POINT ( 'NONE',  ( -5.049401038298153566, 19.05341960407611168, 85.20724293864766707 ) ) ;
#144118 = CARTESIAN_POINT ( 'NONE',  ( 4.379528057220339221, -16.55341960407611168, 67.70724293864769550 ) ) ;
#144119 = CARTESIAN_POINT ( 'NONE',  ( 5.153800228976615827, -19.02544592524334988, 45.20942372801901143 ) ) ;
#144120 = CARTESIAN_POINT ( 'NONE',  ( 21.52544592524344225, -5.823673210054117533, 33.54057627198102409 ) ) ;
#144121 = CARTESIAN_POINT ( 'NONE',  ( 10.72451020669871369, 18.67979575497193778, 107.0844237280190043 ) ) ;
#144122 = CARTESIAN_POINT ( 'NONE',  ( -19.05341960407611168, -5.049401038298163336, 86.45724293864769550 ) ) ;
#144123 = CARTESIAN_POINT ( 'NONE',  ( 21.55341960407619695, -5.719274019375665929, 106.0427570613523471 ) ) ;
#144124 = CARTESIAN_POINT ( 'NONE',  ( 15.80617190586746368, 15.72974639402197994, 64.37390960531435269 ) ) ;
#144125 = CARTESIAN_POINT ( 'NONE',  ( -16.51473224551069308, -9.474510206698971260, 91.66557627198103830 ) ) ;
#144126 = CARTESIAN_POINT ( 'NONE',  ( -16.51473224551082808, 9.474510206698731452, 73.33442372801900433 ) ) ;
#144127 = CARTESIAN_POINT ( 'NONE',  ( 19.03943276465977164, -0.05219959533909143690, 103.7489096053143669 ) ) ;
#144128 = CARTESIAN_POINT ( 'NONE',  ( 0.05219959533936267826, -19.03943276465977164, 90.00109039468567573 ) ) ;
#144129 = CARTESIAN_POINT ( 'NONE',  ( 4.483927247898790824, -16.52544592524335698, 60.20942372801902565 ) ) ;
#144130 = CARTESIAN_POINT ( 'NONE',  ( 8.224510206698953496, -14.34966873604960469, 112.9155762719810383 ) ) ;
#144131 = CARTESIAN_POINT ( 'NONE',  ( 9.564922557960805705, 16.46253265017160317, 84.58224293864769550 ) ) ;
#144132 = CARTESIAN_POINT ( 'NONE',  ( 5.719274019375991003, -21.55341960407610458, 62.70724293864769550 ) ) ;
#144133 = CARTESIAN_POINT ( 'NONE',  ( -16.53943276465976808, -0.05219959533934237506, 38.75109039468567573 ) ) ;
#144134 = CARTESIAN_POINT ( 'NONE',  ( 5.719274019375673035, 21.55341960407619339, 32.29275706135235424 ) ) ;
#144135 = CARTESIAN_POINT ( 'NONE',  ( 21.53943276465977519, 0.05219959533937863772, 96.25109039468568994 ) ) ;
#144136 = CARTESIAN_POINT ( 'NONE',  ( 14.29746914071037800, 8.314922557961029526, 96.66775706135234714 ) ) ;
#144137 = CARTESIAN_POINT ( 'NONE',  ( 9.474510206698971260, -16.51473224551069308, 87.91557627198102409 ) ) ;
#144138 = CARTESIAN_POINT ( 'NONE',  ( -4.483927247898539470, -16.52544592524342804, 82.29057627198103830 ) ) ;
#144139 = CARTESIAN_POINT ( 'NONE',  ( 16.55341960407611168, 4.379528057220329451, 28.95724293864769905 ) ) ;
#144140 = CARTESIAN_POINT ( 'NONE',  ( 13.89961937509957401, 13.97604488694547697, 66.87609039468567573 ) ) ;
#144141 = CARTESIAN_POINT ( 'NONE',  ( -18.62759615963255300, -10.81492255796106328, 44.16775706135234714 ) ) ;
#144142 = CARTESIAN_POINT ( 'NONE',  ( 16.52544592524342804, -4.483927247898539470, 98.54057627198105251 ) ) ;
#144143 = CARTESIAN_POINT ( 'NONE',  ( 16.51473224551069308, 9.474510206698969483, 114.1655762719810241 ) ) ;
#144144 = CARTESIAN_POINT ( 'NONE',  ( 4.483927247898790824, -16.52544592524335698, 100.2094237280190043 ) ) ;
#144145 = CARTESIAN_POINT ( 'NONE',  ( -15.72974639402176322, -15.80617190586768395, 89.37609039468568994 ) ) ;
#144146 = CARTESIAN_POINT ( 'NONE',  ( 8.224510206698742110, 14.34966873604972548, 47.08442372801901854 ) ) ;
#144147 = CARTESIAN_POINT ( 'NONE',  ( -21.53943276465977519, -0.05219959533937600094, 43.75109039468568284 ) ) ;
#144148 = CARTESIAN_POINT ( 'NONE',  ( 0.05219959533907565091, 21.53943276465977519, 109.9989096053143527 ) ) ;
#144149 = CARTESIAN_POINT ( 'NONE',  ( -4.379528057220328563, 16.55341960407611168, 95.20724293864769550 ) ) ;
#144150 = DIRECTION ( 'NONE',  ( 0.000000000000000000, 0.000000000000000000, -1.000000000000000000 ) ) ;
#144151 = CARTESIAN_POINT ( 'NONE',  ( 16.53943276465976808, -0.05219959533910856209, 63.74890960531435979 ) ) ;
#144152 = CARTESIAN_POINT ( 'NONE',  ( 16.52544592524335698, 4.483927247898782831, 106.4594237280190328 ) ) ;
#144153 = CARTESIAN_POINT ( 'NONE',  ( -9.474510206698964154, 16.51473224551069663, 45.41557627198103120 ) ) ;
#144154 = CARTESIAN_POINT ( 'NONE',  ( -15.80617190586745835, -15.72974639402198527, 36.87390960531435979 ) ) ;
#144155 = CARTESIAN_POINT ( 'NONE',  ( 8.224510206698953496, -14.34966873604960469, 72.91557627198103830 ) ) ;
#144156 = CARTESIAN_POINT ( 'NONE',  ( -21.53943276465977519, 0.05219959533907696930, 86.24890960531436690 ) ) ;
#144157 = CARTESIAN_POINT ( 'NONE',  ( -9.474510206698964154, 16.51473224551069663, 85.41557627198102409 ) ) ;
#144159 = CARTESIAN_POINT ( 'NONE',  ( -0.05219959533936034679, 19.03943276465977164, 97.50109039468567573 ) ) ;
#144158 = CARTESIAN_POINT ( 'NONE',  ( -13.89961937509977652, 13.97604488694528158, 40.62390960531435979 ) ) ;
#144160 = CARTESIAN_POINT ( 'NONE',  ( -0.05219959533907301413, -21.53943276465977519, 37.49890960531436690 ) ) ;
#144161 = CARTESIAN_POINT ( 'NONE',  ( 21.55341960407619695, -5.719274019375665929, 71.04275706135234714 ) ) ;
#144162 = CARTESIAN_POINT ( 'NONE',  ( -5.153800228976328057, -19.02544592524343514, 52.29057627198100988 ) ) ;
#144163 = CARTESIAN_POINT ( 'NONE',  ( 13.89961937509977652, -13.97604488694527269, 88.12390960531438111 ) ) ;
#144164 = ORIENTED_EDGE ( 'NONE', *, *, #91586, .T. ) ;
#144165 = CARTESIAN_POINT ( 'NONE',  ( -16.53943276465976808, -0.05219959533934237506, 68.75109039468568994 ) ) ;
#144166 = CARTESIAN_POINT ( 'NONE',  ( -15.72974639402176322, -15.80617190586768395, 39.37609039468567573 ) ) ;
#144167 = CARTESIAN_POINT ( 'NONE',  ( 18.62759615963255655, 10.81492255796105972, 66.66775706135234714 ) ) ;
#144168 = CARTESIAN_POINT ( 'NONE',  ( 21.52544592524344225, -5.823673210054117533, 23.54057627198102765 ) ) ;
#144169 = CARTESIAN_POINT ( 'NONE',  ( -5.719274019375978568, 21.55341960407610458, 100.2072429386476955 ) ) ;
#144171 = CARTESIAN_POINT ( 'NONE',  ( -8.224510206698735004, -14.34966873604973081, 59.58442372801901854 ) ) ;
#144170 = CARTESIAN_POINT ( 'NONE',  ( -5.719274019375665041, -21.55341960407619695, 19.79275706135235069 ) ) ;
#144172 = CARTESIAN_POINT ( 'NONE',  ( 18.67979575497178502, 10.72451020669898547, 59.16557627198103120 ) ) ;
#144173 = CARTESIAN_POINT ( 'NONE',  ( -21.53943276465977519, -0.05219959533937600094, 113.7510903946856757 ) ) ;
#144175 = CARTESIAN_POINT ( 'NONE',  ( 8.314922557961029526, -14.29746914071037800, 105.4177570613523613 ) ) ;
#144174 = CARTESIAN_POINT ( 'NONE',  ( 9.564922557960805705, 16.46253265017160317, 64.58224293864769550 ) ) ;
#144176 = CARTESIAN_POINT ( 'NONE',  ( -17.49999999999999645, -3.237210098469652131, 105.2876301262046468 ) ) ;
#144177 = CARTESIAN_POINT ( 'NONE',  ( 19.03943276465977164, -0.05219959533909143690, 88.74890960531436690 ) ) ;
#144178 = CARTESIAN_POINT ( 'NONE',  ( -4.483927247898782831, 16.52544592524335698, 37.70942372801900433 ) ) ;
#144179 = CARTESIAN_POINT ( 'NONE',  ( 22.13519047554794739, 22.85886502250322039, -45.77314885760243612 ) ) ;
#144180 = CARTESIAN_POINT ( 'NONE',  ( 9.564922557961047289, -16.46253265017146816, 80.41775706135234714 ) ) ;
#144181 = CARTESIAN_POINT ( 'NONE',  ( 5.823673210054125526, 21.52544592524343514, 64.79057627198103830 ) ) ;
#144182 = CARTESIAN_POINT ( 'NONE',  ( -4.483927247898539470, -16.52544592524342804, 22.29057627198102765 ) ) ;
#144183 = CARTESIAN_POINT ( 'NONE',  ( -19.03943276465977164, -0.05219959533935918106, 93.75109039468566152 ) ) ;
#144184 = CARTESIAN_POINT ( 'NONE',  ( -18.22780087662119897, 5.500000000000102141, 41.01763182126894236 ) ) ;
#144185 = CARTESIAN_POINT ( 'NONE',  ( -16.51473224551082808, 9.474510206698731452, 98.33442372801900433 ) ) ;
#144187 = CARTESIAN_POINT ( 'NONE',  ( 16.51473224551083163, -9.474510206698727899, 60.83442372801900433 ) ) ;
#144186 = CARTESIAN_POINT ( 'NONE',  ( -21.52544592524343514, 5.823673210054127303, 86.04057627198102409 ) ) ;
#144188 = DIRECTION ( 'NONE',  ( -0.000000000000000000, -0.000000000000000000, -1.000000000000000000 ) ) ;
#144189 = CARTESIAN_POINT ( 'NONE',  ( 16.51473224551069308, 9.474510206698969483, 69.16557627198102409 ) ) ;
#144190 = CARTESIAN_POINT ( 'NONE',  ( 12.06949235617757843, -12.14591786802309237, 58.12390960531435979 ) ) ;
#144191 = CARTESIAN_POINT ( 'NONE',  ( 13.97604488694527802, 13.89961937509977652, 44.37390960531435269 ) ) ;
#144192 = CARTESIAN_POINT ( 'NONE',  ( 8.224510206698953496, -14.34966873604960469, 47.91557627198102409 ) ) ;
#144193 = CARTESIAN_POINT ( 'NONE',  ( 5.049401038298161559, -19.05341960407611168, 22.70724293864769194 ) ) ;
#144194 = CARTESIAN_POINT ( 'NONE',  ( 1.204023950788500885, 8.515746792609135696, -62.01447643120975783 ) ) ;
#144195 = CARTESIAN_POINT ( 'NONE',  ( -12.14591786802309592, -12.06949235617757132, 31.87390960531435979 ) ) ;
#144196 = CARTESIAN_POINT ( 'NONE',  ( -13.89961937509977652, 13.97604488694528158, 60.62390960531436690 ) ) ;
#144197 = CARTESIAN_POINT ( 'NONE',  ( -16.51473224551082808, 9.474510206698731452, 73.33442372801900433 ) ) ;
#144198 = CARTESIAN_POINT ( 'NONE',  ( -13.97604488694547697, 13.89961937509957934, 43.12609039468566152 ) ) ;
#144199 = CARTESIAN_POINT ( 'NONE',  ( -8.314922557961024197, 14.29746914071037800, 52.91775706135235424 ) ) ;
#144200 = CARTESIAN_POINT ( 'NONE',  ( 15.80617190586746368, 15.72974639402197994, 49.37390960531436690 ) ) ;
#144201 = CARTESIAN_POINT ( 'NONE',  ( -10.72451020669870658, -18.67979575497194134, 99.58442372801900433 ) ) ;
#144202 = CARTESIAN_POINT ( 'NONE',  ( -19.03943276465977164, 0.05219959533909376836, 71.24890960531435269 ) ) ;
#144203 = CARTESIAN_POINT ( 'NONE',  ( 5.049401038298161559, -19.05341960407611168, 112.7072429386476813 ) ) ;
#144204 = CARTESIAN_POINT ( 'NONE',  ( 5.049401038298161559, -19.05341960407611168, 107.7072429386476955 ) ) ;
#144205 = CARTESIAN_POINT ( 'NONE',  ( 36.91746824999999887, -11.99521256947793546, -3.724999997268813257 ) ) ;
#144206 = CARTESIAN_POINT ( 'NONE',  ( -21.52544592524334988, -5.823673210054445271, 33.95942372801901143 ) ) ;
#144207 = CIRCLE ( 'NONE', #170061, 0.5000000000000006661 ) ;
#144208 = CARTESIAN_POINT ( 'NONE',  ( 8.224510206698953496, -14.34966873604960469, 87.91557627198103830 ) ) ;
#144211 = DIRECTION ( 'NONE',  ( 0.000000000000000000, 0.000000000000000000, -1.000000000000000000 ) ) ;
#144210 = CARTESIAN_POINT ( 'NONE',  ( -5.049401038298153566, 19.05341960407611168, 85.20724293864766707 ) ) ;
#144209 = CARTESIAN_POINT ( 'NONE',  ( 10.81492255796078972, 18.62759615963270932, 84.58224293864769550 ) ) ;
#144212 = CARTESIAN_POINT ( 'NONE',  ( -9.474510206698964154, 16.51473224551069663, 80.41557627198103830 ) ) ;
#144213 = CARTESIAN_POINT ( 'NONE',  ( 21.53943276465977519, 0.05219959533937863772, 26.25109039468567573 ) ) ;
#144214 = ORIENTED_EDGE ( 'NONE', *, *, #94032, .T. ) ;
#144215 = CARTESIAN_POINT ( 'NONE',  ( -19.03943276465977164, 0.05219959533909376836, 76.24890960531435269 ) ) ;
#144216 = CARTESIAN_POINT ( 'NONE',  ( 18.39635199886969730, -5.499999999999974243, 98.51967076360000419 ) ) ;
#144218 = CARTESIAN_POINT ( 'NONE',  ( -16.46253265017160317, 9.564922557960807481, 35.83224293864768839 ) ) ;
#144217 = CARTESIAN_POINT ( 'NONE',  ( 9.564922557960805705, 16.46253265017160317, 24.58224293864769194 ) ) ;
#144219 = CARTESIAN_POINT ( 'NONE',  ( -9.474510206698720793, -16.51473224551083518, 109.5844237280190043 ) ) ;
#144220 = CARTESIAN_POINT ( 'NONE',  ( -29.86685920354755197, -21.69954338932560134, -6.924999997268813878 ) ) ;
#144221 = CARTESIAN_POINT ( 'NONE',  ( 8.314922557960818139, 14.29746914071049879, 109.5822429386476955 ) ) ;
#144222 = CARTESIAN_POINT ( 'NONE',  ( -21.53943276465977519, -0.05219959533937600094, 78.75109039468568994 ) ) ;
#144224 = CARTESIAN_POINT ( 'NONE',  ( -21.52544592524334988, -5.823673210054445271, 33.95942372801901143 ) ) ;
#144223 = CARTESIAN_POINT ( 'NONE',  ( -16.46253265017160317, 9.564922557960807481, 65.83224293864769550 ) ) ;
#144225 = CARTESIAN_POINT ( 'NONE',  ( -15.72974639402197994, 15.80617190586746368, 115.6239096053143669 ) ) ;
#144226 = CARTESIAN_POINT ( 'NONE',  ( -28.82186960331499392, -9.364793116373526516, 148.0999999999999943 ) ) ;
#144227 = CARTESIAN_POINT ( 'NONE',  ( -19.03943276465977164, 0.05219959533909376836, 86.24890960531436690 ) ) ;
#144228 = CARTESIAN_POINT ( 'NONE',  ( 27.79720911488089641, 7.618197028328711262, 161.3616953378221410 ) ) ;
#144230 = CARTESIAN_POINT ( 'NONE',  ( 15.80617190586746368, 15.72974639402197994, 39.37390960531436690 ) ) ;
#144229 = CARTESIAN_POINT ( 'NONE',  ( -16.52544592524335698, -4.483927247898792601, 28.95942372801902209 ) ) ;
#144231 = CARTESIAN_POINT ( 'NONE',  ( -21.52544592524334988, -5.823673210054445271, 68.95942372801901854 ) ) ;
#144232 = CARTESIAN_POINT ( 'NONE',  ( -19.03943276465977164, 0.05219959533909376836, 111.2489096053143669 ) ) ;
#144233 = CARTESIAN_POINT ( 'NONE',  ( 16.51473224551083163, -9.474510206698727899, 100.8344237280190043 ) ) ;
#144234 = CARTESIAN_POINT ( 'NONE',  ( -13.97604488694527625, -13.89961937509977652, 51.87390960531436690 ) ) ;
#144235 = CARTESIAN_POINT ( 'NONE',  ( 9.474510206698971260, -16.51473224551069308, 87.91557627198102409 ) ) ;
#144236 = CARTESIAN_POINT ( 'NONE',  ( 4.379528057220339221, -16.55341960407611168, 87.70724293864769550 ) ) ;
#144237 = CARTESIAN_POINT ( 'NONE',  ( -4.483927247898539470, -16.52544592524342804, 92.29057627198103830 ) ) ;
#144238 = CARTESIAN_POINT ( 'NONE',  ( 16.51473224551069308, 9.474510206698969483, 109.1655762719810383 ) ) ;
#144240 = CARTESIAN_POINT ( 'NONE',  ( -13.89961937509977652, 13.97604488694528158, 40.62390960531435979 ) ) ;
#144239 = CARTESIAN_POINT ( 'NONE',  ( -14.29746914071049879, 8.314922557960819915, 55.83224293864770260 ) ) ;
#144241 = CARTESIAN_POINT ( 'NONE',  ( 21.55341960407619695, -5.719274019375665929, 61.04275706135234714 ) ) ;
#144242 = CARTESIAN_POINT ( 'NONE',  ( 19.02544592524334988, 5.153800228976608722, 91.45942372801900433 ) ) ;
#144243 = CARTESIAN_POINT ( 'NONE',  ( -14.29746914071049879, 8.314922557960819915, 60.83224293864769550 ) ) ;
#144244 = CARTESIAN_POINT ( 'NONE',  ( 15.72974639402199770, -15.80617190586745480, 113.1239096053143953 ) ) ;
#144245 = CARTESIAN_POINT ( 'NONE',  ( 18.62759615963271287, -10.81492255796078972, 53.33224293864769550 ) ) ;
#144246 = CARTESIAN_POINT ( 'NONE',  ( -16.51473224551069308, -9.474510206698971260, 106.6655762719810383 ) ) ;
#144247 = CARTESIAN_POINT ( 'NONE',  ( 8.906447517083050158, 27.41122689804195645, 141.6500000054623740 ) ) ;
#144248 = CARTESIAN_POINT ( 'NONE',  ( 9.564922557960805705, 16.46253265017160317, 54.58224293864769550 ) ) ;
#144249 = CARTESIAN_POINT ( 'NONE',  ( 4.379528057220339221, -16.55341960407611168, 32.70724293864770260 ) ) ;
#144250 = CARTESIAN_POINT ( 'NONE',  ( -4.483927247898782831, 16.52544592524335698, 97.70942372801904696 ) ) ;
#144251 = CARTESIAN_POINT ( 'NONE',  ( 8.314922557961029526, -14.29746914071037800, 80.41775706135234714 ) ) ;
#144252 = CARTESIAN_POINT ( 'NONE',  ( -19.02544592524334988, -5.153800228976617603, 33.95942372801897591 ) ) ;
#144253 = CARTESIAN_POINT ( 'NONE',  ( -24.66672740160584354, -7.254147403784508619, 167.4978451254145000 ) ) ;
#144254 = CARTESIAN_POINT ( 'NONE',  ( -16.51473224551069308, -9.474510206698971260, 96.66557627198102409 ) ) ;
#144255 = CARTESIAN_POINT ( 'NONE',  ( -16.46253265017160317, 9.564922557960807481, 45.83224293864769550 ) ) ;
#144256 = CARTESIAN_POINT ( 'NONE',  ( 8.314922557960818139, 14.29746914071049879, 64.58224293864769550 ) ) ;
#144258 = CARTESIAN_POINT ( 'NONE',  ( 21.53943276465977519, -0.05219959533907433946, 28.74890960531435624 ) ) ;
#144257 = CARTESIAN_POINT ( 'NONE',  ( 17.26058549869091507, -6.457015423128539489, 101.1225416252393217 ) ) ;
#144259 = CARTESIAN_POINT ( 'NONE',  ( -18.62759615963270932, 10.81492255796079327, 45.83224293864769550 ) ) ;
#144260 = CARTESIAN_POINT ( 'NONE',  ( -12.06949235617756955, 12.14591786802309770, 85.62390960531436690 ) ) ;
#144261 = CARTESIAN_POINT ( 'NONE',  ( -4.483927247898782831, 16.52544592524335698, 32.70942372801900433 ) ) ;
#144262 = CARTESIAN_POINT ( 'NONE',  ( -4.379528057220328563, 16.55341960407611168, 80.20724293864769550 ) ) ;
#144263 = CARTESIAN_POINT ( 'NONE',  ( 3.503282210674363295, -48.86437366581479580, -25.00000000000000000 ) ) ;
#144264 = CARTESIAN_POINT ( 'NONE',  ( -5.049401038297874678, -19.05341960407617918, 74.79275706135231871 ) ) ;
#144265 = CARTESIAN_POINT ( 'NONE',  ( -19.03943276465977164, 0.05219959533909376836, 101.2489096053143669 ) ) ;
#144266 = CARTESIAN_POINT ( 'NONE',  ( -5.950531402560715689E-15, 38.81732327939063509, -3.624999997268813168 ) ) ;
#144267 = CARTESIAN_POINT ( 'NONE',  ( -22.99799039501310105, 21.44473182883388773, -49.72310555961293943 ) ) ;
#144269 = CARTESIAN_POINT ( 'NONE',  ( 4.379528057220339221, -16.55341960407611168, 22.70724293864769194 ) ) ;
#144268 = CARTESIAN_POINT ( 'NONE',  ( -14.34966873604972548, 8.224510206698743886, 28.33442372801902209 ) ) ;
#144270 = CARTESIAN_POINT ( 'NONE',  ( 0.05219959533936267826, -19.03943276465977164, 70.00109039468566152 ) ) ;
#144271 = CARTESIAN_POINT ( 'NONE',  ( -5.823673210054116645, -21.52544592524344225, 47.29057627198103120 ) ) ;
#144272 = CARTESIAN_POINT ( 'NONE',  ( -10.72451020669870658, -18.67979575497194134, 69.58442372801900433 ) ) ;
#144273 = CARTESIAN_POINT ( 'NONE',  ( 28.82186960331496905, -9.364793116373544279, 147.1500000054623456 ) ) ;
#144274 = CARTESIAN_POINT ( 'NONE',  ( 14.29746914071037800, 8.314922557961029526, 41.66775706135235424 ) ) ;
#144276 = CARTESIAN_POINT ( 'NONE',  ( -5.153800228976328057, -19.02544592524343514, 82.29057627198103830 ) ) ;
#144275 = CARTESIAN_POINT ( 'NONE',  ( 0.05219959533909260263, 19.03943276465977164, 24.99890960531435269 ) ) ;
#144277 = CARTESIAN_POINT ( 'NONE',  ( 16.83584321579687781, 17.44568526726159874, -56.81531555676559009 ) ) ;
#144278 = CARTESIAN_POINT ( 'NONE',  ( -4.379528057220328563, 16.55341960407611168, 85.20724293864770971 ) ) ;
#144279 = CARTESIAN_POINT ( 'NONE',  ( -0.05219959533909027116, -19.03943276465977164, 87.49890960531436690 ) ) ;
#144280 = VERTEX_POINT ( 'NONE', #48238 ) ;
#144281 = CARTESIAN_POINT ( 'NONE',  ( -16.46253265017146816, -9.564922557961047289, 104.1677570613523329 ) ) ;
#144282 = CARTESIAN_POINT ( 'NONE',  ( 5.719274019375991003, -21.55341960407610458, 77.70724293864770971 ) ) ;
#144283 = CARTESIAN_POINT ( 'NONE',  ( -16.46253265017160317, 9.564922557960807481, 45.83224293864769550 ) ) ;
#144285 = CARTESIAN_POINT ( 'NONE',  ( 18.62759615963271287, -10.81492255796078972, 113.3322429386476955 ) ) ;
#144284 = CARTESIAN_POINT ( 'NONE',  ( -16.46253265017146816, -9.564922557961047289, 64.16775706135233293 ) ) ;
#144286 = CARTESIAN_POINT ( 'NONE',  ( 9.564922557960805705, 16.46253265017160317, 64.58224293864769550 ) ) ;
#144287 = CARTESIAN_POINT ( 'NONE',  ( -9.564922557960796823, -16.46253265017161027, 107.0822429386476955 ) ) ;
#144288 = EDGE_LOOP ( 'NONE', ( #158516, #90549, #84783, #144048 ) ) ;
#144289 = CARTESIAN_POINT ( 'NONE',  ( -14.34966873604972548, 8.224510206698743886, 38.33442372801900433 ) ) ;
#144290 = CARTESIAN_POINT ( 'NONE',  ( -18.67979575497178146, -10.72451020669898902, 101.6655762719810383 ) ) ;
#144293 = CARTESIAN_POINT ( 'NONE',  ( 9.564922557961047289, -16.46253265017146816, 55.41775706135234003 ) ) ;
#144292 = CARTESIAN_POINT ( 'NONE',  ( -19.05341960407611168, -5.049401038298163336, 91.45724293864766707 ) ) ;
#144291 = CARTESIAN_POINT ( 'NONE',  ( 8.224510206698953496, -14.34966873604960469, 112.9155762719810383 ) ) ;
#144294 = CARTESIAN_POINT ( 'NONE',  ( -21.52544592524343514, 5.823673210054127303, 86.04057627198102409 ) ) ;
#144295 = CARTESIAN_POINT ( 'NONE',  ( 12.14591786802309770, 12.06949235617756955, 49.37390960531436690 ) ) ;
#144296 = CARTESIAN_POINT ( 'NONE',  ( -9.474510206698720793, -16.51473224551083518, 19.58442372801899722 ) ) ;
#144297 = CARTESIAN_POINT ( 'NONE',  ( -8.314922557961024197, 14.29746914071037800, 67.91775706135234714 ) ) ;
#144298 = CARTESIAN_POINT ( 'NONE',  ( -0.05219959533909027116, -19.03943276465977164, 87.49890960531436690 ) ) ;
#144299 = CARTESIAN_POINT ( 'NONE',  ( -5.153800228976328057, -19.02544592524343514, 42.29057627198101699 ) ) ;
#144300 = CIRCLE ( 'NONE', #137822, 35.99626262588765258 ) ;
#144301 = CARTESIAN_POINT ( 'NONE',  ( 10.72451020669871369, 18.67979575497193778, 57.08442372801901854 ) ) ;
#144302 = CARTESIAN_POINT ( 'NONE',  ( 21.55341960407619695, -5.719274019375665929, 61.04275706135234714 ) ) ;
#144303 = CARTESIAN_POINT ( 'NONE',  ( 13.89961937509977652, -13.97604488694527269, 58.12390960531436690 ) ) ;
#144304 = CARTESIAN_POINT ( 'NONE',  ( 21.53943276465977519, 0.05219959533937863772, 31.25109039468568639 ) ) ;
#144305 = CARTESIAN_POINT ( 'NONE',  ( 0.05219959533936267826, -19.03943276465977164, 75.00109039468566152 ) ) ;
#144306 = CARTESIAN_POINT ( 'NONE',  ( 19.05341960407617918, -5.049401038297876454, 76.04275706135230450 ) ) ;
#144307 = CARTESIAN_POINT ( 'NONE',  ( -0.05219959533909027116, -19.03943276465977164, 42.49890960531435269 ) ) ;
#144308 = CARTESIAN_POINT ( 'NONE',  ( 16.53943276465976808, 0.05219959533934440121, 81.25109039468568994 ) ) ;
#144309 = CARTESIAN_POINT ( 'NONE',  ( 16.46253265017160672, -9.564922557960803928, 53.33224293864768839 ) ) ;
#144310 = CARTESIAN_POINT ( 'NONE',  ( -9.474510206698964154, 16.51473224551069663, 25.41557627198103120 ) ) ;
#144311 = CARTESIAN_POINT ( 'NONE',  ( -0.05219959533909027116, -19.03943276465977164, 102.4989096053143669 ) ) ;
#144312 = CARTESIAN_POINT ( 'NONE',  ( 0.05219959533909260263, 19.03943276465977164, 34.99890960531435979 ) ) ;
#144313 = CARTESIAN_POINT ( 'NONE',  ( -15.72974639402197994, 15.80617190586746368, 85.62390960531436690 ) ) ;
#144314 = CARTESIAN_POINT ( 'NONE',  ( -16.52544592524335698, -4.483927247898792601, 63.95942372801901854 ) ) ;
#144315 = AXIS2_PLACEMENT_3D ( 'NONE', #189949, #19109, #111104 ) ;
#144316 = CARTESIAN_POINT ( 'NONE',  ( 13.89961937509957401, 13.97604488694547697, 36.87609039468565442 ) ) ;
#144317 = CARTESIAN_POINT ( 'NONE',  ( 9.474510206698971260, -16.51473224551069308, 47.91557627198102409 ) ) ;
#144318 = CARTESIAN_POINT ( 'NONE',  ( 12.14591786802309770, 12.06949235617756955, 44.37390960531435979 ) ) ;
#144319 = CARTESIAN_POINT ( 'NONE',  ( -16.52544592524342804, 4.483927247898546575, 86.04057627198102409 ) ) ;
#144320 = CARTESIAN_POINT ( 'NONE',  ( -19.02544592524342804, 5.153800228976336051, 96.04057627198103830 ) ) ;
#144321 = CARTESIAN_POINT ( 'NONE',  ( 5.049401038298161559, -19.05341960407611168, 77.70724293864765286 ) ) ;
#144322 = CARTESIAN_POINT ( 'NONE',  ( -21.55341960407619339, 5.719274019375674811, 33.54275706135234714 ) ) ;
#144323 = CARTESIAN_POINT ( 'NONE',  ( -5.153800228976328057, -19.02544592524343514, 87.29057627198103830 ) ) ;
#144324 = CARTESIAN_POINT ( 'NONE',  ( 0.05219959533937995610, -21.53943276465977519, 95.00109039468568994 ) ) ;
#144325 = CARTESIAN_POINT ( 'NONE',  ( -4.379528057220086978, -16.55341960407618274, 74.79275706135234714 ) ) ;
#144326 = CARTESIAN_POINT ( 'NONE',  ( -0.05219959533937732626, 21.53943276465977519, 22.50109039468567573 ) ) ;
#144327 = CARTESIAN_POINT ( 'NONE',  ( -10.72451020669898014, 18.67979575497178502, 90.41557627198103830 ) ) ;
#144328 = CARTESIAN_POINT ( 'NONE',  ( -14.34966873604960291, -8.224510206698953496, 46.66557627198102409 ) ) ;
#144329 = CARTESIAN_POINT ( 'NONE',  ( -16.51473224551069308, -9.474510206698971260, 41.66557627198103120 ) ) ;
#144330 = CARTESIAN_POINT ( 'NONE',  ( -8.314922557960811034, -14.29746914071050412, 72.08224293864769550 ) ) ;
#144331 = CARTESIAN_POINT ( 'NONE',  ( 21.53943276465977519, -0.05219959533907433946, 33.74890960531436690 ) ) ;
#144332 = CARTESIAN_POINT ( 'NONE',  ( 9.564922557961047289, -16.46253265017146816, 30.41775706135232937 ) ) ;
#144333 = ADVANCED_FACE ( 'NONE', ( #106908 ), #184754, .F. ) ;
#144334 = CARTESIAN_POINT ( 'NONE',  ( 8.224510206698953496, -14.34966873604960469, 102.9155762719810383 ) ) ;
#144335 = CARTESIAN_POINT ( 'NONE',  ( 0.05219959533909260263, 19.03943276465977164, 114.9989096053143669 ) ) ;
#144336 = ORIENTED_EDGE ( 'NONE', *, *, #87651, .T. ) ;
#144337 = CARTESIAN_POINT ( 'NONE',  ( 12.06949235617739724, 12.14591786802326823, 56.87609039468568994 ) ) ;
#144338 = CARTESIAN_POINT ( 'NONE',  ( -0.05219959533909027116, -19.03943276465977164, 62.49890960531435979 ) ) ;
#144339 = CARTESIAN_POINT ( 'NONE',  ( -17.14385361876520975, 23.59649016807275856, 140.5750000027311444 ) ) ;
#144340 = CARTESIAN_POINT ( 'NONE',  ( 21.53943276465977519, -0.05219959533907433946, 38.74890960531435979 ) ) ;
#144341 = CARTESIAN_POINT ( 'NONE',  ( 0.05219959533934541429, -16.53943276465976808, 90.00109039468567573 ) ) ;
#144342 = CARTESIAN_POINT ( 'NONE',  ( 8.314922557961029526, -14.29746914071037800, 20.41775706135234714 ) ) ;
#144343 = CARTESIAN_POINT ( 'NONE',  ( 5.719274019375673035, 21.55341960407619339, 77.29275706135234714 ) ) ;
#144344 = CARTESIAN_POINT ( 'NONE',  ( 5.153800228976335163, 19.02544592524342804, 79.79057627198102409 ) ) ;
#144345 = CARTESIAN_POINT ( 'NONE',  ( 18.62759615963271287, -10.81492255796078972, 98.33224293864769550 ) ) ;
#144346 = CARTESIAN_POINT ( 'NONE',  ( -4.483927247898782831, 16.52544592524335698, 52.70942372801902565 ) ) ;
#144347 = CARTESIAN_POINT ( 'NONE',  ( -14.29746914071049879, 8.314922557960819915, 110.8322429386476955 ) ) ;
#144348 = CIRCLE ( 'NONE', #141041, 59.99999999999998579 ) ;
#144349 = CARTESIAN_POINT ( 'NONE',  ( -12.14591786802326823, 12.06949235617739902, 23.12609039468567573 ) ) ;
#144350 = CARTESIAN_POINT ( 'NONE',  ( 13.89961937509957401, 13.97604488694547697, 76.87609039468566152 ) ) ;
#144351 = CARTESIAN_POINT ( 'NONE',  ( 15.72974639402199770, -15.80617190586745480, 78.12390960531436690 ) ) ;
#144352 = CARTESIAN_POINT ( 'NONE',  ( -19.05341960407617563, 5.049401038297882671, 53.54275706135231871 ) ) ;
#144353 = CARTESIAN_POINT ( 'NONE',  ( 24.99873734152912519, -24.49873734152920690, 4.646446609406722494 ) ) ;
#144354 = CARTESIAN_POINT ( 'NONE',  ( -15.72974639402197994, 15.80617190586746368, 105.6239096053143669 ) ) ;
#144355 = CARTESIAN_POINT ( 'NONE',  ( 7.260022482700430935, -2.182060888568182033, 2.110832330245268729 ) ) ;
#144356 = CARTESIAN_POINT ( 'NONE',  ( 16.51473224551069308, 9.474510206698969483, 74.16557627198103830 ) ) ;
#144357 = CARTESIAN_POINT ( 'NONE',  ( -19.99604614807126524, -21.49604614807087799, -52.16759353428663104 ) ) ;
#144358 = CARTESIAN_POINT ( 'NONE',  ( -12.14591786802326823, 12.06949235617739902, 23.12609039468567573 ) ) ;
#144359 = CARTESIAN_POINT ( 'NONE',  ( 12.23969591940464952, -38.08276121122112556, -12.22614352002200100 ) ) ;
#144361 = CARTESIAN_POINT ( 'NONE',  ( -12.06949235617756955, 12.14591786802309770, 70.62390960531436690 ) ) ;
#144360 = CARTESIAN_POINT ( 'NONE',  ( 18.67979575497178502, 10.72451020669898547, 99.16557627198100988 ) ) ;
#144362 = CARTESIAN_POINT ( 'NONE',  ( 19.05341960407611168, 5.049401038298154454, 68.95724293864769550 ) ) ;
#144363 = CARTESIAN_POINT ( 'NONE',  ( -15.72974639402176322, -15.80617190586768395, 84.37609039468570415 ) ) ;
#144365 = CARTESIAN_POINT ( 'NONE',  ( -5.049401038297874678, -19.05341960407617918, 39.79275706135232582 ) ) ;
#144364 = CARTESIAN_POINT ( 'NONE',  ( -14.29746914071037622, -8.314922557961029526, 44.16775706135234714 ) ) ;
#144366 = CARTESIAN_POINT ( 'NONE',  ( 18.62759615963255655, 10.81492255796105972, 46.66775706135234714 ) ) ;
#144367 = CARTESIAN_POINT ( 'NONE',  ( -21.52544592524343514, 5.823673210054127303, 61.04057627198103120 ) ) ;
#144368 = CARTESIAN_POINT ( 'NONE',  ( 13.89961937509957401, 13.97604488694547697, 106.8760903946856757 ) ) ;
#144369 = CARTESIAN_POINT ( 'NONE',  ( 5.049401038298161559, -19.05341960407611168, 52.70724293864767418 ) ) ;
#144370 = CARTESIAN_POINT ( 'NONE',  ( 5.153800228976615827, -19.02544592524334988, 75.20942372801896170 ) ) ;
#144371 = CARTESIAN_POINT ( 'NONE',  ( -21.53943276465977519, -0.05219959533937600094, 78.75109039468568994 ) ) ;
#144372 = CARTESIAN_POINT ( 'NONE',  ( -19.05341960407617563, 5.049401038297882671, 53.54275706135231871 ) ) ;
#144373 = CARTESIAN_POINT ( 'NONE',  ( 5.153800228976335163, 19.02544592524342804, 39.79057627198100988 ) ) ;
#144374 = CARTESIAN_POINT ( 'NONE',  ( 21.55341960407610458, 5.719274019375980345, 53.95724293864770260 ) ) ;
#144375 = CARTESIAN_POINT ( 'NONE',  ( 4.483927247898545687, 16.52544592524342804, 69.79057627198102409 ) ) ;
#144376 = CARTESIAN_POINT ( 'NONE',  ( 193.3062444957835453, -155.7167183371837496, -4.999999999999999112 ) ) ;
#144377 = CARTESIAN_POINT ( 'NONE',  ( -19.02544592524334988, -5.153800228976617603, 28.95942372801900433 ) ) ;
#144378 = CARTESIAN_POINT ( 'NONE',  ( 12.06949235617739724, 12.14591786802326823, 86.87609039468568994 ) ) ;
#144379 = CARTESIAN_POINT ( 'NONE',  ( 14.29746914071049879, -8.314922557960816363, 58.33224293864768839 ) ) ;
#144380 = CARTESIAN_POINT ( 'NONE',  ( 0.05219959533937995610, -21.53943276465977519, 95.00109039468568994 ) ) ;
#144381 = CARTESIAN_POINT ( 'NONE',  ( 21.53943276465977519, 0.05219959533937863772, 86.25109039468568994 ) ) ;
#144382 = CARTESIAN_POINT ( 'NONE',  ( -5.719274019375978568, 21.55341960407610458, 100.2072429386476955 ) ) ;
#144383 =( BOUNDED_CURVE ( )  B_SPLINE_CURVE ( 2, ( #45525, #93002, #48517, #187047, #18178, #98720, #91997, #78829, #155680, #76846, #37061, #31351, #199211 ),
 .UNSPECIFIED., .F., .T. ) 
 B_SPLINE_CURVE_WITH_KNOTS ( ( 3, 2, 2, 2, 2, 2, 3 ),
 ( 0.1866409627428346207, 0.1885964912280701788, 0.1929824561403508665, 0.1973684210526315819, 0.2017543859649122695, 0.2061403508771929849, 0.2080501995403384596 ),
 .UNSPECIFIED. ) 
 CURVE ( )  GEOMETRIC_REPRESENTATION_ITEM ( )  RATIONAL_B_SPLINE_CURVE ( ( 0.9831626618144004848, 0.9848076720550091867, 1.000000000000000000, 0.9659258262890683122, 1.000000000000000000, 0.9659258262890683122, 1.000000000000000000, 0.9659258262890683122, 1.000000000000000000, 0.9659258262890683122, 1.000000000000000000, 0.9851625545550090068, 0.9832469066685280978 ) ) 
 REPRESENTATION_ITEM ( '' )  );
#144384 = CARTESIAN_POINT ( 'NONE',  ( -13.97604488694527625, -13.89961937509977652, 51.87390960531436690 ) ) ;
#144385 = CARTESIAN_POINT ( 'NONE',  ( 21.52544592524334988, 5.823673210054432836, 56.45942372801902565 ) ) ;
#144386 = CARTESIAN_POINT ( 'NONE',  ( 0.05219959533909260263, 19.03943276465977164, 34.99890960531435979 ) ) ;
#144387 = VERTEX_POINT ( 'NONE', #124055 ) ;
#144388 = CARTESIAN_POINT ( 'NONE',  ( -19.02544592524342804, 5.153800228976336051, 56.04057627198100988 ) ) ;
#144389 = CARTESIAN_POINT ( 'NONE',  ( 4.379528057220339221, -16.55341960407611168, 107.7072429386476955 ) ) ;
#144390 = CARTESIAN_POINT ( 'NONE',  ( -0.05219959533909027116, -19.03943276465977164, 92.49890960531436690 ) ) ;
#144391 = CARTESIAN_POINT ( 'NONE',  ( 8.224510206698953496, -14.34966873604960469, 47.91557627198102409 ) ) ;
#144392 = CARTESIAN_POINT ( 'NONE',  ( 0.05219959533910956823, 16.53943276465976808, 109.9989096053143527 ) ) ;
#144393 = CARTESIAN_POINT ( 'NONE',  ( 5.719274019375991003, -21.55341960407610458, 87.70724293864769550 ) ) ;
#144394 = CARTESIAN_POINT ( 'NONE',  ( 21.55341960407619695, -5.719274019375665929, 21.04275706135234714 ) ) ;
#144395 = FACE_OUTER_BOUND ( 'NONE', #144909, .T. ) ;
#144396 = CARTESIAN_POINT ( 'NONE',  ( 12.06949235617739724, 12.14591786802326823, 41.87609039468568284 ) ) ;
#144397 = ORIENTED_EDGE ( 'NONE', *, *, #19482, .T. ) ;
#144398 = CARTESIAN_POINT ( 'NONE',  ( -18.67979575497178146, -10.72451020669898902, 86.66557627198102409 ) ) ;
#144399 = CARTESIAN_POINT ( 'NONE',  ( -0.05219959533937732626, 21.53943276465977519, 107.5010903946856899 ) ) ;
#144400 = CARTESIAN_POINT ( 'NONE',  ( 9.474510206698971260, -16.51473224551069308, 97.91557627198102409 ) ) ;
#144401 = CARTESIAN_POINT ( 'NONE',  ( -0.05219959533937732626, 21.53943276465977519, 27.50109039468567929 ) ) ;
#144402 = CARTESIAN_POINT ( 'NONE',  ( -18.62759615963270932, 10.81492255796079327, 30.83224293864770260 ) ) ;
#144403 = CARTESIAN_POINT ( 'NONE',  ( -12.14591786802326823, 12.06949235617739902, 108.1260903946856757 ) ) ;
#144405 = CARTESIAN_POINT ( 'NONE',  ( -0.05219959533937732626, 21.53943276465977519, 82.50109039468568994 ) ) ;
#144404 = CARTESIAN_POINT ( 'NONE',  ( 10.72451020669871369, 18.67979575497193778, 47.08442372801901854 ) ) ;
#144406 = CARTESIAN_POINT ( 'NONE',  ( -0.05219959533937732626, 21.53943276465977519, 107.5010903946856899 ) ) ;
#144407 = CARTESIAN_POINT ( 'NONE',  ( 14.29746914071037800, 8.314922557961029526, 76.66775706135234714 ) ) ;
#144408 = CARTESIAN_POINT ( 'NONE',  ( 10.72451020669871369, 18.67979575497193778, 37.08442372801901143 ) ) ;
#144409 = CARTESIAN_POINT ( 'NONE',  ( 16.51473224551069308, 9.474510206698969483, 29.16557627198103475 ) ) ;
#144410 = CARTESIAN_POINT ( 'NONE',  ( 0.05219959533937995610, -21.53943276465977519, 105.0010903946856757 ) ) ;
#144411 = CARTESIAN_POINT ( 'NONE',  ( 19.05341960407611168, 5.049401038298154454, 103.9572429386476671 ) ) ;
#144412 = CARTESIAN_POINT ( 'NONE',  ( -21.52544592524343514, 5.823673210054127303, 101.0405762719810383 ) ) ;
#144414 = CARTESIAN_POINT ( 'NONE',  ( -21.52544592524343514, 5.823673210054127303, 66.04057627198103830 ) ) ;
#144413 = CARTESIAN_POINT ( 'NONE',  ( -4.595912276383594453, -38.76652190272483267, -23.69787631201921840 ) ) ;
#144416 = CARTESIAN_POINT ( 'NONE',  ( 4.483927247898545687, 16.52544592524342804, 44.79057627198103120 ) ) ;
#144415 = CARTESIAN_POINT ( 'NONE',  ( -14.34966873604972548, 8.224510206698743886, 53.33442372801901854 ) ) ;
#144417 = CYLINDRICAL_SURFACE ( 'NONE', #149916, 1.499999999999997780 ) ;
#144418 = CARTESIAN_POINT ( 'NONE',  ( 19.03943276465977164, 0.05219959533936151252, 86.25109039468567573 ) ) ;
#144419 = CARTESIAN_POINT ( 'NONE',  ( -17.05116617787824040, 6.768360034955803073, 103.6567555325919585 ) ) ;
#144420 = CARTESIAN_POINT ( 'NONE',  ( -4.379528057220086978, -16.55341960407618274, 29.79275706135234358 ) ) ;
#144421 = CARTESIAN_POINT ( 'NONE',  ( 21.55341960407610458, 5.719274019375980345, 93.95724293864770971 ) ) ;
#144422 = CARTESIAN_POINT ( 'NONE',  ( 5.823673210054125526, 21.52544592524343514, 79.79057627198102409 ) ) ;
#144423 = CARTESIAN_POINT ( 'NONE',  ( -5.153800228976328057, -19.02544592524343514, 112.2905762719810099 ) ) ;
#144424 = CARTESIAN_POINT ( 'NONE',  ( -14.29746914071037622, -8.314922557961029526, 39.16775706135235424 ) ) ;
#144425 = CARTESIAN_POINT ( 'NONE',  ( 16.46253265017160672, -9.564922557960803928, 53.33224293864768839 ) ) ;
#144427 = CARTESIAN_POINT ( 'NONE',  ( 19.05341960407617918, -5.049401038297876454, 96.04275706135231871 ) ) ;
#144426 = CARTESIAN_POINT ( 'NONE',  ( 15.80617190586769283, -15.72974639402175789, 30.62609039468567929 ) ) ;
#144428 = CARTESIAN_POINT ( 'NONE',  ( 19.02544592524343514, -5.153800228976328945, 103.5405762719809957 ) ) ;
#144429 = CARTESIAN_POINT ( 'NONE',  ( -13.97604488694527625, -13.89961937509977652, 91.87390960531432427 ) ) ;
#144430 = CARTESIAN_POINT ( 'NONE',  ( -21.53943276465977519, 0.05219959533907696930, 91.24890960531436690 ) ) ;
#144431 = CARTESIAN_POINT ( 'NONE',  ( -16.51473224551069308, -9.474510206698971260, 56.66557627198103120 ) ) ;
#144432 = DIRECTION ( 'NONE',  ( 0.000000000000000000, -0.8660254037844390407, -0.4999999999999994449 ) ) ;
#144433 = CARTESIAN_POINT ( 'NONE',  ( 16.55341960407611168, 4.379528057220329451, 73.95724293864769550 ) ) ;
#144434 = CARTESIAN_POINT ( 'NONE',  ( -5.049401038298153566, 19.05341960407611168, 105.2072429386476671 ) ) ;
#144435 = DIRECTION ( 'NONE',  ( -1.000000000000000000, 0.000000000000000000, 0.000000000000000000 ) ) ;
#144436 = CARTESIAN_POINT ( 'NONE',  ( 19.02544592524334988, 5.153800228976608722, 81.45942372801897591 ) ) ;
#144437 = CARTESIAN_POINT ( 'NONE',  ( -10.81492255796078084, -18.62759615963271287, 87.08224293864769550 ) ) ;
#144438 = CARTESIAN_POINT ( 'NONE',  ( 19.02544592524334988, 5.153800228976608722, 46.45942372801899012 ) ) ;
#144439 = CARTESIAN_POINT ( 'NONE',  ( 13.97604488694527802, 13.89961937509977652, 114.3739096053143669 ) ) ;
#144440 = CARTESIAN_POINT ( 'NONE',  ( 18.22780087662121673, 5.500000000000056843, 68.98459894673892734 ) ) ;
#144441 = CARTESIAN_POINT ( 'NONE',  ( -10.72451020669898014, 18.67979575497178502, 60.41557627198102409 ) ) ;
#144442 = AXIS2_PLACEMENT_3D ( 'NONE', #130693, #103373, #195396 ) ;
#144443 = CARTESIAN_POINT ( 'NONE',  ( 9.564922557960805705, 16.46253265017160317, 79.58224293864769550 ) ) ;
#144444 = CARTESIAN_POINT ( 'NONE',  ( 21.53943276465977519, 0.05219959533937863772, 81.25109039468568994 ) ) ;
#144445 = CARTESIAN_POINT ( 'NONE',  ( -19.05341960407611168, -5.049401038298163336, 41.45724293864769550 ) ) ;
#144446 = CARTESIAN_POINT ( 'NONE',  ( -14.34966873604960291, -8.224510206698953496, 76.66557627198103830 ) ) ;
#144447 = CARTESIAN_POINT ( 'NONE',  ( -16.52544592524335698, -4.483927247898792601, 18.95942372801901143 ) ) ;
#144448 = CARTESIAN_POINT ( 'NONE',  ( 5.719274019375673035, 21.55341960407619339, 72.29275706135236135 ) ) ;
#144449 = VERTEX_POINT ( 'NONE', #33066 ) ;
#144450 = CARTESIAN_POINT ( 'NONE',  ( 13.97604488694548053, -13.89961937509957401, 30.62609039468566863 ) ) ;
#144451 = CARTESIAN_POINT ( 'NONE',  ( -19.05341960407617563, 5.049401038297882671, 83.54275706135233293 ) ) ;
#144452 = CARTESIAN_POINT ( 'NONE',  ( -17.49999999999999645, 5.499999999999997335, 120.0000000000000142 ) ) ;
#144453 = CARTESIAN_POINT ( 'NONE',  ( -18.62759615963255300, -10.81492255796106328, 29.16775706135234003 ) ) ;
#144454 = CARTESIAN_POINT ( 'NONE',  ( -15.49999999999999822, 5.499999999999998224, 22.00000000000000000 ) ) ;
#144455 = CARTESIAN_POINT ( 'NONE',  ( 5.719274019375673035, 21.55341960407619339, 112.2927570613523471 ) ) ;
#144456 = CARTESIAN_POINT ( 'NONE',  ( -19.05341960407611168, -5.049401038298163336, 61.45724293864769550 ) ) ;
#144457 = CARTESIAN_POINT ( 'NONE',  ( 13.89961937509957401, 13.97604488694547697, 26.87609039468566507 ) ) ;
#144458 = CARTESIAN_POINT ( 'NONE',  ( 16.52544592524335698, 4.483927247898782831, 101.4594237280190185 ) ) ;
#144460 = CARTESIAN_POINT ( 'NONE',  ( 15.72974639402176855, 15.80617190586768217, 66.87609039468568994 ) ) ;
#144459 = CARTESIAN_POINT ( 'NONE',  ( 5.153800228976335163, 19.02544592524342804, 99.79057627198102409 ) ) ;
#144461 = CARTESIAN_POINT ( 'NONE',  ( 36.91746824999999177, 2.880721459617395097E-14, -5.624999997268813168 ) ) ;
#144462 = CARTESIAN_POINT ( 'NONE',  ( -17.50000000000002132, -5.076555817581204444, 36.17951492049775197 ) ) ;
#144463 = CARTESIAN_POINT ( 'NONE',  ( 0.05219959533937995610, -21.53943276465977519, 90.00109039468567573 ) ) ;
#144464 = CARTESIAN_POINT ( 'NONE',  ( -15.72974639402176322, -15.80617190586768395, 104.3760903946856899 ) ) ;
#144465 = CARTESIAN_POINT ( 'NONE',  ( 0.000000000000000000, -1.178949249685214307, 2.042000000000002036 ) ) ;
#144466 = CARTESIAN_POINT ( 'NONE',  ( -19.03943276465977164, 0.05219959533909376836, 106.2489096053143669 ) ) ;
#144467 = EDGE_CURVE ( 'NONE', #47952, #73471, #31194, .T. ) ;
#144468 = CARTESIAN_POINT ( 'NONE',  ( 16.51473224551083163, -9.474510206698727899, 25.83442372801900078 ) ) ;
#144469 = CARTESIAN_POINT ( 'NONE',  ( -36.91746825000000598, 2.428612866367529932E-14, -1.124999997268813390 ) ) ;
#144470 = CARTESIAN_POINT ( 'NONE',  ( 9.474510206698971260, -16.51473224551069308, 37.91557627198102409 ) ) ;
#144471 = CARTESIAN_POINT ( 'NONE',  ( -0.05219959533907301413, -21.53943276465977519, 62.49890960531436690 ) ) ;
#144472 = CARTESIAN_POINT ( 'NONE',  ( 14.34966873604972726, -8.224510206698740333, 105.8344237280190328 ) ) ;
#144474 = CARTESIAN_POINT ( 'NONE',  ( 16.51473224551069308, 9.474510206698969483, 84.16557627198102409 ) ) ;
#144473 = CARTESIAN_POINT ( 'NONE',  ( 0.05219959533910956823, 16.53943276465976808, 99.99890960531436690 ) ) ;
#144475 = CARTESIAN_POINT ( 'NONE',  ( 18.67979575497194134, -10.72451020669871369, 105.8344237280190328 ) ) ;
#144476 = CARTESIAN_POINT ( 'NONE',  ( -19.02544592524342804, 5.153800228976336051, 36.04057627198100988 ) ) ;
#144477 = CARTESIAN_POINT ( 'NONE',  ( 16.53943276465976808, -0.05219959533910856209, 98.74890960531438111 ) ) ;
#144478 = CARTESIAN_POINT ( 'NONE',  ( 0.05219959533937995610, -21.53943276465977519, 60.00109039468568284 ) ) ;
#144479 = CARTESIAN_POINT ( 'NONE',  ( -5.823673210054116645, -21.52544592524344225, 87.29057627198103830 ) ) ;
#144480 = CARTESIAN_POINT ( 'NONE',  ( -9.564922557961040184, 16.46253265017147172, 47.91775706135233293 ) ) ;
#144481 = CARTESIAN_POINT ( 'NONE',  ( 18.22780087662119897, -5.500000000000096811, 48.51763182126894236 ) ) ;
#144482 = CARTESIAN_POINT ( 'NONE',  ( -16.51473224551069308, -9.474510206698971260, 101.6655762719810241 ) ) ;
#144483 = CARTESIAN_POINT ( 'NONE',  ( -14.34966873604960291, -8.224510206698953496, 71.66557627198100988 ) ) ;
#144484 = CARTESIAN_POINT ( 'NONE',  ( 9.564922557961047289, -16.46253265017146816, 45.41775706135232582 ) ) ;
#144485 = VECTOR ( 'NONE', #19869, 1000.000000000000000 ) ;
#144486 = CARTESIAN_POINT ( 'NONE',  ( -16.46253265017160317, 9.564922557960807481, 65.83224293864769550 ) ) ;
#144487 = CARTESIAN_POINT ( 'NONE',  ( -16.55341960407611168, -4.379528057220339221, 51.45724293864770260 ) ) ;
#144488 = CARTESIAN_POINT ( 'NONE',  ( -19.03943276465977164, -0.05219959533935918106, 78.75109039468567573 ) ) ;
#144489 = CARTESIAN_POINT ( 'NONE',  ( 16.51473224551083163, -9.474510206698727899, 90.83442372801900433 ) ) ;
#144490 = CARTESIAN_POINT ( 'NONE',  ( -0.05219959533907301413, -21.53943276465977519, 37.49890960531436690 ) ) ;
#144491 = CARTESIAN_POINT ( 'NONE',  ( -4.483927247898539470, -16.52544592524342804, 102.2905762719810383 ) ) ;
#144492 = FACE_BOUND ( 'NONE', #128554, .T. ) ;
#144494 = CARTESIAN_POINT ( 'NONE',  ( 10.72451020669898902, -18.67979575497178502, 67.91557627198102409 ) ) ;
#144493 = CARTESIAN_POINT ( 'NONE',  ( -13.97604488694527625, -13.89961937509977652, 56.87390960531434558 ) ) ;
#144495 = CARTESIAN_POINT ( 'NONE',  ( 19.02544592524343514, -5.153800228976328945, 23.54057627198102054 ) ) ;
#144497 = CARTESIAN_POINT ( 'NONE',  ( -13.89961937509977652, 13.97604488694528158, 55.62390960531434558 ) ) ;
#144496 = CARTESIAN_POINT ( 'NONE',  ( -8.314922557961024197, 14.29746914071037800, 72.91775706135234714 ) ) ;
#144498 = CARTESIAN_POINT ( 'NONE',  ( -19.03943276465977164, -0.05219959533935918106, 58.75109039468566863 ) ) ;
#144499 = CARTESIAN_POINT ( 'NONE',  ( 15.72974639402176855, 15.80617190586768217, 61.87609039468568284 ) ) ;
#144500 = CARTESIAN_POINT ( 'NONE',  ( -21.52544592524343514, 5.823673210054127303, 51.04057627198103120 ) ) ;
#144501 = CARTESIAN_POINT ( 'NONE',  ( 12.14591786802309770, 12.06949235617756955, 114.3739096053143527 ) ) ;
#144502 = CARTESIAN_POINT ( 'NONE',  ( -12.06949235617739369, -12.14591786802326823, 84.37609039468570415 ) ) ;
#144503 = CARTESIAN_POINT ( 'NONE',  ( 19.02544592524334988, 5.153800228976608722, 106.4594237280190185 ) ) ;
#144504 = CARTESIAN_POINT ( 'NONE',  ( -19.05341960407611168, -5.049401038298163336, 26.45724293864769550 ) ) ;
#144506 = CARTESIAN_POINT ( 'NONE',  ( 21.52544592524344225, -5.823673210054117533, 63.54057627198103830 ) ) ;
#144505 = DIRECTION ( 'NONE',  ( 1.000000000000000000, 0.000000000000000000, 0.000000000000000000 ) ) ;
#144507 = CARTESIAN_POINT ( 'NONE',  ( 5.823673210054444382, -21.52544592524334988, 100.2094237280190043 ) ) ;
#144508 = CARTESIAN_POINT ( 'NONE',  ( 8.314922557960818139, 14.29746914071049879, 49.58224293864769550 ) ) ;
#144509 = CARTESIAN_POINT ( 'NONE',  ( -14.34966873604960291, -8.224510206698953496, 51.66557627198102409 ) ) ;
#144510 = CARTESIAN_POINT ( 'NONE',  ( -18.62759615963270932, 10.81492255796079327, 85.83224293864768129 ) ) ;
#144511 = CARTESIAN_POINT ( 'NONE',  ( -21.53943276465977519, 0.05219959533907696930, 91.24890960531436690 ) ) ;
#144512 = CARTESIAN_POINT ( 'NONE',  ( 2.500000000000000000, 2.357898499370431722, -2.818925648462311528E-15 ) ) ;
#144513 = CARTESIAN_POINT ( 'NONE',  ( 15.72974639402199770, -15.80617190586745480, 33.12390960531435979 ) ) ;
#144514 = CARTESIAN_POINT ( 'NONE',  ( 16.55341960407618274, -4.379528057220086978, 71.04275706135234714 ) ) ;
#144515 = CARTESIAN_POINT ( 'NONE',  ( 14.29746914071049879, -8.314922557960816363, 78.33224293864770971 ) ) ;
#144516 = CARTESIAN_POINT ( 'NONE',  ( -0.05219959533909027116, -19.03943276465977164, 32.49890960531435979 ) ) ;
#144517 = CARTESIAN_POINT ( 'NONE',  ( 34.72618186072386948, -2.417897188208078418, 52.10384489098236571 ) ) ;
#144518 = ORIENTED_EDGE ( 'NONE', *, *, #173803, .T. ) ;
#144519 = CARTESIAN_POINT ( 'NONE',  ( 16.53943276465976808, 0.05219959533934440121, 91.25109039468568994 ) ) ;
#144520 = CARTESIAN_POINT ( 'NONE',  ( 15.80617190586769283, -15.72974639402175789, 25.62609039468567929 ) ) ;
#144521 = CARTESIAN_POINT ( 'NONE',  ( 9.564922557960805705, 16.46253265017160317, 79.58224293864769550 ) ) ;
#144522 = CARTESIAN_POINT ( 'NONE',  ( -21.55341960407619339, 5.719274019375674811, 58.54275706135235424 ) ) ;
#144523 = CARTESIAN_POINT ( 'NONE',  ( -19.03943276465977164, 0.05219959533909376836, 111.2489096053143669 ) ) ;
#144524 = CARTESIAN_POINT ( 'NONE',  ( -16.41350681615411489, -36.34403388527378098, -28.23867313180392458 ) ) ;
#144525 = VERTEX_POINT ( 'NONE', #123068 ) ;
#144526 = CARTESIAN_POINT ( 'NONE',  ( 15.72974639402176855, 15.80617190586768217, 41.87609039468568284 ) ) ;
#144528 = CARTESIAN_POINT ( 'NONE',  ( 13.89961937509977652, -13.97604488694527269, 98.12390960531433848 ) ) ;
#144527 = CARTESIAN_POINT ( 'NONE',  ( 19.03943276465977164, -0.05219959533909143690, 43.74890960531435979 ) ) ;
#144529 = CARTESIAN_POINT ( 'NONE',  ( 13.89961937509957401, 13.97604488694547697, 51.87609039468566863 ) ) ;
#144530 = CARTESIAN_POINT ( 'NONE',  ( 0.05219959533937995610, -21.53943276465977519, 25.00109039468567218 ) ) ;
#144531 = CARTESIAN_POINT ( 'NONE',  ( -19.03943276465977164, -0.05219959533935918106, 58.75109039468566863 ) ) ;
#144532 = CARTESIAN_POINT ( 'NONE',  ( -9.564922557960796823, -16.46253265017161027, 27.08224293864769550 ) ) ;
#144533 = CARTESIAN_POINT ( 'NONE',  ( -12.06949235617739369, -12.14591786802326823, 94.37609039468568994 ) ) ;
#144534 = CARTESIAN_POINT ( 'NONE',  ( 19.05341960407617918, -5.049401038297876454, 61.04275706135232582 ) ) ;
#144535 = CARTESIAN_POINT ( 'NONE',  ( -14.29746914071037622, -8.314922557961029526, 109.1677570613523613 ) ) ;
#144536 = CARTESIAN_POINT ( 'NONE',  ( 17.97058386085786807, 5.500000000000046185, 86.50390968646220813 ) ) ;
#144537 = CARTESIAN_POINT ( 'NONE',  ( 13.97604488694527802, 13.89961937509977652, 84.37390960531433848 ) ) ;
#144538 = CARTESIAN_POINT ( 'NONE',  ( 18.67979575497194134, -10.72451020669871369, 95.83442372801903275 ) ) ;
#144540 = EDGE_CURVE ( 'NONE', #185826, #60353, #67339, .T. ) ;
#144539 = CARTESIAN_POINT ( 'NONE',  ( 18.67979575497194134, -10.72451020669871369, 110.8344237280190043 ) ) ;
#144541 = CARTESIAN_POINT ( 'NONE',  ( -23.48298174826590667, 32.32155151706776053, -4.302157773949822683 ) ) ;
#144542 = CARTESIAN_POINT ( 'NONE',  ( -0.05219959533909027116, -19.03943276465977164, 107.4989096053143527 ) ) ;
#144543 = CARTESIAN_POINT ( 'NONE',  ( -21.55341960407619339, 5.719274019375674811, 78.54275706135236135 ) ) ;
#144544 = CARTESIAN_POINT ( 'NONE',  ( -16.51473224551082808, 9.474510206698731452, 113.3344237280190043 ) ) ;
#144545 = CARTESIAN_POINT ( 'NONE',  ( 19.03943276465977164, -0.05219959533909143690, 73.74890960531435269 ) ) ;
#144546 = CARTESIAN_POINT ( 'NONE',  ( 15.80617190586746368, 15.72974639402197994, 34.37390960531435979 ) ) ;
#144547 = CARTESIAN_POINT ( 'NONE',  ( 13.89961937509977652, -13.97604488694527269, 93.12390960531436690 ) ) ;
#144548 = CARTESIAN_POINT ( 'NONE',  ( 17.14385361876520264, -23.59649016807271238, 139.5750000027311444 ) ) ;
#144549 = CARTESIAN_POINT ( 'NONE',  ( 9.564922557960805705, 16.46253265017160317, 74.58224293864769550 ) ) ;
#144550 = CARTESIAN_POINT ( 'NONE',  ( -9.474510206698964154, 16.51473224551069663, 70.41557627198102409 ) ) ;
#144551 = CARTESIAN_POINT ( 'NONE',  ( -8.224510206698948167, 14.34966873604960824, 25.41557627198103120 ) ) ;
#144552 = CARTESIAN_POINT ( 'NONE',  ( 0.3535533905936372179, 34.99999999999999289, 5.353553390593270400 ) ) ;
#144553 = CARTESIAN_POINT ( 'NONE',  ( -13.97604488694547697, 13.89961937509957934, 68.12609039468563310 ) ) ;
#144554 = CARTESIAN_POINT ( 'NONE',  ( 5.049401038298161559, -19.05341960407611168, 87.70724293864769550 ) ) ;
#144555 = CARTESIAN_POINT ( 'NONE',  ( -14.34966873604960291, -8.224510206698953496, 81.66557627198103830 ) ) ;
#144556 = CARTESIAN_POINT ( 'NONE',  ( -21.55341960407610458, -5.719274019375992779, 41.45724293864769550 ) ) ;
#144557 = CARTESIAN_POINT ( 'NONE',  ( -10.72451020669898014, 18.67979575497178502, 25.41557627198103120 ) ) ;
#144558 = CARTESIAN_POINT ( 'NONE',  ( 4.483927247898545687, 16.52544592524342804, 99.79057627198103830 ) ) ;
#144559 = CARTESIAN_POINT ( 'NONE',  ( -17.31747979337950127, 6.344076630960999275, 53.62055131934816643 ) ) ;
#144560 = CARTESIAN_POINT ( 'NONE',  ( 9.474510206698729675, 16.51473224551082808, 47.08442372801900433 ) ) ;
#144561 = CARTESIAN_POINT ( 'NONE',  ( 0.05219959533910956823, 16.53943276465976808, 29.99890960531435979 ) ) ;
#144562 = CARTESIAN_POINT ( 'NONE',  ( 5.049401038298161559, -19.05341960407611168, 107.7072429386476955 ) ) ;
#144563 = CARTESIAN_POINT ( 'NONE',  ( -15.80617190586768217, 15.72974639402176855, 63.12609039468568994 ) ) ;
#144564 = CARTESIAN_POINT ( 'NONE',  ( -10.81492255796078084, -18.62759615963271287, 62.08224293864769550 ) ) ;
#144565 = CARTESIAN_POINT ( 'NONE',  ( 21.55341960407619695, -5.719274019375665929, 51.04275706135234714 ) ) ;
#144566 = CARTESIAN_POINT ( 'NONE',  ( -10.81492255796078084, -18.62759615963271287, 82.08224293864768129 ) ) ;
#144567 = CARTESIAN_POINT ( 'NONE',  ( -15.72974639402176322, -15.80617190586768395, 34.37609039468568284 ) ) ;
#144568 = CARTESIAN_POINT ( 'NONE',  ( 16.52544592524342804, -4.483927247898539470, 113.5405762719810383 ) ) ;
#144569 = CARTESIAN_POINT ( 'NONE',  ( -9.474510206698720793, -16.51473224551083518, 64.58442372801900433 ) ) ;
#144570 = CARTESIAN_POINT ( 'NONE',  ( 19.02544592524343514, -5.153800228976328945, 43.54057627198103120 ) ) ;
#144571 = CARTESIAN_POINT ( 'NONE',  ( -12.14591786802309592, -12.06949235617757132, 101.8739096053143811 ) ) ;
#144572 = CARTESIAN_POINT ( 'NONE',  ( 5.153800228976335163, 19.02544592524342804, 104.7905762719809957 ) ) ;
#144573 = CARTESIAN_POINT ( 'NONE',  ( -16.55341960407611168, -4.379528057220339221, 46.45724293864769550 ) ) ;
#144574 = CARTESIAN_POINT ( 'NONE',  ( 4.379528057220092307, 16.55341960407617563, 97.29275706135234714 ) ) ;
#144575 = CARTESIAN_POINT ( 'NONE',  ( 13.89961937509977652, -13.97604488694527269, 58.12390960531436690 ) ) ;
#144576 = CARTESIAN_POINT ( 'NONE',  ( -4.483927247898539470, -16.52544592524342804, 112.2905762719810241 ) ) ;
#144577 = CARTESIAN_POINT ( 'NONE',  ( 19.05341960407617918, -5.049401038297876454, 26.04275706135233293 ) ) ;
#144580 = CARTESIAN_POINT ( 'NONE',  ( 14.29746914071049879, -8.314922557960816363, 38.33224293864768839 ) ) ;
#144579 = CARTESIAN_POINT ( 'NONE',  ( -9.474510206698964154, 16.51473224551069663, 110.4155762719810383 ) ) ;
#144578 = VECTOR ( 'NONE', #115189, 1000.000000000000000 ) ;
#144581 = CARTESIAN_POINT ( 'NONE',  ( -10.81492255796105439, 18.62759615963255655, 52.91775706135235424 ) ) ;
#144582 = CARTESIAN_POINT ( 'NONE',  ( -11.30153831258472508, -180.0000000000000000, -15.00000000000000178 ) ) ;
#144583 = CARTESIAN_POINT ( 'NONE',  ( -4.483927247898782831, 16.52544592524335698, 62.70942372801902565 ) ) ;
#144584 = CARTESIAN_POINT ( 'NONE',  ( 16.52544592524342804, -4.483927247898539470, 23.54057627198102765 ) ) ;
#144585 = CARTESIAN_POINT ( 'NONE',  ( 8.314922557961029526, -14.29746914071037800, 110.4177570613523756 ) ) ;
#144586 = CARTESIAN_POINT ( 'NONE',  ( -4.483927247898782831, 16.52544592524335698, 27.70942372801901854 ) ) ;
#144587 = CARTESIAN_POINT ( 'NONE',  ( -13.89961937509977652, 13.97604488694528158, 50.62390960531435979 ) ) ;
#144588 = CARTESIAN_POINT ( 'NONE',  ( -4.379528057220328563, 16.55341960407611168, 110.2072429386477239 ) ) ;
#144589 = CARTESIAN_POINT ( 'NONE',  ( -15.72974639402197994, 15.80617190586746368, 115.6239096053143669 ) ) ;
#144590 = CARTESIAN_POINT ( 'NONE',  ( 0.05219959533909260263, 19.03943276465977164, 39.99890960531436690 ) ) ;
#144591 = DIRECTION ( 'NONE',  ( -1.000000000000000000, -0.000000000000000000, -0.000000000000000000 ) ) ;
#144592 = CARTESIAN_POINT ( 'NONE',  ( 13.89961937509977652, -13.97604488694527269, 28.12390960531435624 ) ) ;
#144593 = CARTESIAN_POINT ( 'NONE',  ( 21.52544592524344225, -5.823673210054117533, 23.54057627198102765 ) ) ;
#144594 = CARTESIAN_POINT ( 'NONE',  ( -17.31747979337952614, -6.344076630960945984, 36.37944868065184068 ) ) ;
#144595 = CARTESIAN_POINT ( 'NONE',  ( -19.03943276465977164, 0.05219959533909376836, 101.2489096053143669 ) ) ;
#144597 = CARTESIAN_POINT ( 'NONE',  ( 14.29746914071049879, -8.314922557960816363, 108.3322429386477097 ) ) ;
#144596 = CARTESIAN_POINT ( 'NONE',  ( -15.80617190586768217, 15.72974639402176855, 43.12609039468568284 ) ) ;
#144598 = CARTESIAN_POINT ( 'NONE',  ( -13.97604488694527625, -13.89961937509977652, 106.8739096053143669 ) ) ;
#144599 = CARTESIAN_POINT ( 'NONE',  ( -30.00000000000000000, -5.499999999999992895, 102.5000000000000142 ) ) ;
#144600 = CARTESIAN_POINT ( 'NONE',  ( -12.06949235617739369, -12.14591786802326823, 74.37609039468568994 ) ) ;
#144601 = CARTESIAN_POINT ( 'NONE',  ( -21.52544592524334988, -5.823673210054445271, 93.95942372801903275 ) ) ;
#144602 = AXIS2_PLACEMENT_3D ( 'NONE', #135316, #180829, #101970 ) ;
#144603 = CARTESIAN_POINT ( 'NONE',  ( 0.05219959533934541429, -16.53943276465976808, 55.00109039468568284 ) ) ;
#144604 = CARTESIAN_POINT ( 'NONE',  ( 16.46253265017160672, -9.564922557960803928, 93.33224293864769550 ) ) ;
#144605 = CARTESIAN_POINT ( 'NONE',  ( 16.52544592524335698, 4.483927247898782831, 41.45942372801901143 ) ) ;
#144606 = CARTESIAN_POINT ( 'NONE',  ( 16.51473224551083163, -9.474510206698727899, 110.8344237280190043 ) ) ;
#144607 = CARTESIAN_POINT ( 'NONE',  ( -14.29746914071037622, -8.314922557961029526, 89.16775706135236135 ) ) ;
#144608 = CARTESIAN_POINT ( 'NONE',  ( 19.02544592524334988, 5.153800228976608722, 111.4594237280190043 ) ) ;
#144609 = CARTESIAN_POINT ( 'NONE',  ( 5.049401038298161559, -19.05341960407611168, 77.70724293864765286 ) ) ;
#144610 = CARTESIAN_POINT ( 'NONE',  ( -18.67979575497178146, -10.72451020669898902, 91.66557627198103830 ) ) ;
#144612 = CARTESIAN_POINT ( 'NONE',  ( -19.02544592524334988, -5.153800228976617603, 108.9594237280189759 ) ) ;
#144611 = CARTESIAN_POINT ( 'NONE',  ( 16.55341960407611168, 4.379528057220329451, 108.9572429386476955 ) ) ;
#144613 = CARTESIAN_POINT ( 'NONE',  ( 0.05219959533934541429, -16.53943276465976808, 70.00109039468568994 ) ) ;
#144614 = CARTESIAN_POINT ( 'NONE',  ( -17.44270441346521849, 5.991230190322816007, 43.63664920735774899 ) ) ;
#144615 = CARTESIAN_POINT ( 'NONE',  ( -9.564922557961040184, 16.46253265017147172, 67.91775706135233293 ) ) ;
#144616 = CARTESIAN_POINT ( 'NONE',  ( 0.05219959533910956823, 16.53943276465976808, 49.99890960531437401 ) ) ;
#144617 = CARTESIAN_POINT ( 'NONE',  ( -14.34966873604960291, -8.224510206698953496, 91.66557627198103830 ) ) ;
#144619 = CARTESIAN_POINT ( 'NONE',  ( -16.79531203550646978, 7.028104445595602989, 88.74755011779558345 ) ) ;
#144618 = CARTESIAN_POINT ( 'NONE',  ( -13.97604488694547697, 13.89961937509957934, 38.12609039468566152 ) ) ;
#144620 = CARTESIAN_POINT ( 'NONE',  ( -18.67979575497193778, 10.72451020669871902, 33.33442372801900433 ) ) ;
#144621 = CARTESIAN_POINT ( 'NONE',  ( -16.51473224551082808, 9.474510206698731452, 98.33442372801900433 ) ) ;
#144622 = CARTESIAN_POINT ( 'NONE',  ( -13.89961937509977652, 13.97604488694528158, 110.6239096053143243 ) ) ;
#144623 = CARTESIAN_POINT ( 'NONE',  ( 0.05219959533909260263, 19.03943276465977164, 89.99890960531436690 ) ) ;
#144624 = CARTESIAN_POINT ( 'NONE',  ( -5.719274019375665041, -21.55341960407619695, 109.7927570613523613 ) ) ;
#144625 = CARTESIAN_POINT ( 'NONE',  ( -19.02544592524342804, 5.153800228976336051, 76.04057627198102409 ) ) ;
#144626 = CARTESIAN_POINT ( 'NONE',  ( 0.05219959533907565091, 21.53943276465977519, 49.99890960531437401 ) ) ;
#144627 = CARTESIAN_POINT ( 'NONE',  ( 16.53943276465976808, -0.05219959533910856209, 98.74890960531438111 ) ) ;
#144628 = CARTESIAN_POINT ( 'NONE',  ( -16.46253265017160317, 9.564922557960807481, 55.83224293864769550 ) ) ;
#144629 = CARTESIAN_POINT ( 'NONE',  ( 5.049401038298161559, -19.05341960407611168, 22.70724293864769194 ) ) ;
#144630 = CARTESIAN_POINT ( 'NONE',  ( -5.719274019375665041, -21.55341960407619695, 29.79275706135234358 ) ) ;
#144631 = CARTESIAN_POINT ( 'NONE',  ( 21.52544592524334988, 5.823673210054432836, 81.45942372801900433 ) ) ;
#144632 = CARTESIAN_POINT ( 'NONE',  ( 9.564922557960805705, 16.46253265017160317, 39.58224293864768839 ) ) ;
#144633 = CARTESIAN_POINT ( 'NONE',  ( -4.483927247898782831, 16.52544592524335698, 82.70942372801900433 ) ) ;
#144634 = CARTESIAN_POINT ( 'NONE',  ( 21.53943276465977519, -0.05219959533907433946, 113.7489096053143527 ) ) ;
#144635 = VERTEX_POINT ( 'NONE', #16899 ) ;
#144636 = CARTESIAN_POINT ( 'NONE',  ( 10.72451020669871369, 18.67979575497193778, 27.08442372801901854 ) ) ;
#144638 = CARTESIAN_POINT ( 'NONE',  ( -0.05219959533909027116, -19.03943276465977164, 67.49890960531436690 ) ) ;
#144637 = CARTESIAN_POINT ( 'NONE',  ( -19.02544592524334988, -5.153800228976617603, 53.95942372801898301 ) ) ;
#144639 = CARTESIAN_POINT ( 'NONE',  ( 0.05219959533936267826, -19.03943276465977164, 35.00109039468566863 ) ) ;
#144640 = CARTESIAN_POINT ( 'NONE',  ( -15.80617190586768217, 15.72974639402176855, 73.12609039468567573 ) ) ;
#144641 = CARTESIAN_POINT ( 'NONE',  ( -5.719274019375978568, 21.55341960407610458, 70.20724293864769550 ) ) ;
#144642 = CARTESIAN_POINT ( 'NONE',  ( -12.14591786802309592, -12.06949235617757132, 46.87390960531435979 ) ) ;
#144644 = CARTESIAN_POINT ( 'NONE',  ( 5.153800228976615827, -19.02544592524334988, 30.20942372801900433 ) ) ;
#144643 = CARTESIAN_POINT ( 'NONE',  ( -21.52544592524334988, -5.823673210054445271, 93.95942372801903275 ) ) ;
#144645 = CARTESIAN_POINT ( 'NONE',  ( 16.52544592524342804, -4.483927247898539470, 68.54057627198103830 ) ) ;
#144646 = CARTESIAN_POINT ( 'NONE',  ( -8.224510206698948167, 14.34966873604960824, 115.4155762719810241 ) ) ;
#144647 = CARTESIAN_POINT ( 'NONE',  ( -19.05341960407617563, 5.049401038297882671, 58.54275706135234003 ) ) ;
#144648 = CARTESIAN_POINT ( 'NONE',  ( -8.314922557961024197, 14.29746914071037800, 112.9177570613523329 ) ) ;
#144649 = CARTESIAN_POINT ( 'NONE',  ( 10.72451020669871369, 18.67979575497193778, 77.08442372801901854 ) ) ;
#144650 = CARTESIAN_POINT ( 'NONE',  ( 16.51473224551069308, 9.474510206698969483, 84.16557627198102409 ) ) ;
#144651 = CARTESIAN_POINT ( 'NONE',  ( 0.05219959533936267826, -19.03943276465977164, 45.00109039468566863 ) ) ;
#144652 = CARTESIAN_POINT ( 'NONE',  ( 21.53943276465977519, -0.05219959533907433946, 48.74890960531435979 ) ) ;
#144653 = CARTESIAN_POINT ( 'NONE',  ( 21.55341960407619695, -5.719274019375665929, 46.04275706135234714 ) ) ;
#144654 = CARTESIAN_POINT ( 'NONE',  ( 15.72974639402199770, -15.80617190586745480, 108.1239096053143811 ) ) ;
#144655 = CARTESIAN_POINT ( 'NONE',  ( 19.03943276465977164, 0.05219959533936151252, 96.25109039468567573 ) ) ;
#144656 = CARTESIAN_POINT ( 'NONE',  ( -4.379528057220086978, -16.55341960407618274, 59.79275706135234714 ) ) ;
#144658 = CARTESIAN_POINT ( 'NONE',  ( -5.823673210054116645, -21.52544592524344225, 112.2905762719810241 ) ) ;
#144657 = CARTESIAN_POINT ( 'NONE',  ( 23.48298174826590667, -32.32155151706770368, -5.302157773949822683 ) ) ;
#144659 = CARTESIAN_POINT ( 'NONE',  ( 14.34966873604960469, 8.224510206698951720, 89.16557627198102409 ) ) ;
#144660 = CARTESIAN_POINT ( 'NONE',  ( 36.91746824999999177, 2.880721459617395097E-14, -10.12499999726881583 ) ) ;
#144661 = CARTESIAN_POINT ( 'NONE',  ( 14.29746914071037800, 8.314922557961029526, 41.66775706135235424 ) ) ;
#144662 = CARTESIAN_POINT ( 'NONE',  ( 21.53943276465977519, -0.05219959533907433946, 43.74890960531435979 ) ) ;
#144663 = CARTESIAN_POINT ( 'NONE',  ( 8.314922557961029526, -14.29746914071037800, 90.41775706135236135 ) ) ;
#144664 = CARTESIAN_POINT ( 'NONE',  ( -19.02544592524342804, 5.153800228976336051, 26.04057627198103120 ) ) ;
#144665 = CARTESIAN_POINT ( 'NONE',  ( -14.29746914071037622, -8.314922557961029526, 64.16775706135234714 ) ) ;
#144666 = CARTESIAN_POINT ( 'NONE',  ( 18.62759615963255655, 10.81492255796105972, 36.66775706135234714 ) ) ;
#144667 = CARTESIAN_POINT ( 'NONE',  ( -0.05219959533907301413, -21.53943276465977519, 57.49890960531435979 ) ) ;
#144668 = CARTESIAN_POINT ( 'NONE',  ( 12.14591786802327356, -12.06949235617739191, 80.62609039468567573 ) ) ;
#144669 = CARTESIAN_POINT ( 'NONE',  ( 15.72974639402176855, 15.80617190586768217, 66.87609039468568994 ) ) ;
#144670 = CARTESIAN_POINT ( 'NONE',  ( -21.53943276465977519, 0.05219959533907696930, 56.24890960531436690 ) ) ;
#144671 = CARTESIAN_POINT ( 'NONE',  ( 18.62759615963271287, -10.81492255796078972, 38.33224293864768839 ) ) ;
#144672 = CARTESIAN_POINT ( 'NONE',  ( 4.379528057220092307, 16.55341960407617563, 62.29275706135236845 ) ) ;
#144673 = CARTESIAN_POINT ( 'NONE',  ( 21.53943276465977519, -0.05219959533907433946, 38.74890960531435979 ) ) ;
#144674 = EDGE_LOOP ( 'NONE', ( #73154, #123875, #145445, #57455, #96832 ) ) ;
#144675 = CARTESIAN_POINT ( 'NONE',  ( 16.51473224551069308, 9.474510206698969483, 104.1655762719810241 ) ) ;
#144676 = CARTESIAN_POINT ( 'NONE',  ( 8.224510206698953496, -14.34966873604960469, 22.91557627198102765 ) ) ;
#144677 = CARTESIAN_POINT ( 'NONE',  ( -17.49999999999999645, -5.499999999999992895, 79.20309617465829888 ) ) ;
#144678 = CARTESIAN_POINT ( 'NONE',  ( 16.53943276465976808, -0.05219959533910856209, 113.7489096053143527 ) ) ;
#144679 = CARTESIAN_POINT ( 'NONE',  ( -10.81492255796078084, -18.62759615963271287, 62.08224293864769550 ) ) ;
#144680 = CARTESIAN_POINT ( 'NONE',  ( 13.89961937509977652, -13.97604488694527269, 43.12390960531434558 ) ) ;
#144681 = CARTESIAN_POINT ( 'NONE',  ( -8.314922557961024197, 14.29746914071037800, 92.91775706135236135 ) ) ;
#144682 = CARTESIAN_POINT ( 'NONE',  ( 21.55341960407619695, -5.719274019375665929, 31.04275706135234714 ) ) ;
#144683 = CARTESIAN_POINT ( 'NONE',  ( 19.03943276465977164, 0.05219959533936151252, 86.25109039468567573 ) ) ;
#144684 = CARTESIAN_POINT ( 'NONE',  ( 4.379528057220339221, -16.55341960407611168, 97.70724293864772392 ) ) ;
#144685 = CARTESIAN_POINT ( 'NONE',  ( -5.153800228976328057, -19.02544592524343514, 47.29057627198102409 ) ) ;
#144686 = CARTESIAN_POINT ( 'NONE',  ( -17.49999999999999645, -5.500000000000000888, 29.20309617465828467 ) ) ;
#144687 = CARTESIAN_POINT ( 'NONE',  ( 18.09805431107249518, -5.499999999999988454, 63.51606229291888184 ) ) ;
#144688 = CARTESIAN_POINT ( 'NONE',  ( -9.474510206698964154, 16.51473224551069663, 75.41557627198103830 ) ) ;
#144689 = CARTESIAN_POINT ( 'NONE',  ( 14.29746914071037800, 8.314922557961029526, 66.66775706135234714 ) ) ;
#144690 = CARTESIAN_POINT ( 'NONE',  ( -15.80617190586768217, 15.72974639402176855, 103.1260903946856757 ) ) ;
#144691 = CARTESIAN_POINT ( 'NONE',  ( 15.80617190586746368, 15.72974639402197994, 54.37390960531435979 ) ) ;
#144692 = CARTESIAN_POINT ( 'NONE',  ( -12.06949235617739369, -12.14591786802326823, 79.37609039468567573 ) ) ;
#144693 = CARTESIAN_POINT ( 'NONE',  ( -5.049401038297874678, -19.05341960407617918, 64.79275706135233293 ) ) ;
#144694 = CARTESIAN_POINT ( 'NONE',  ( -5.823673210054431948, 21.52544592524334988, 57.70942372801901143 ) ) ;
#144695 = CARTESIAN_POINT ( 'NONE',  ( 0.05219959533909260263, 19.03943276465977164, 84.99890960531436690 ) ) ;
#144696 = CARTESIAN_POINT ( 'NONE',  ( 5.049401038298161559, -19.05341960407611168, 32.70724293864768129 ) ) ;
#144697 = CARTESIAN_POINT ( 'NONE',  ( 0.05219959533936267826, -19.03943276465977164, 55.00109039468566863 ) ) ;
#144698 = CARTESIAN_POINT ( 'NONE',  ( 9.564922557960805705, 16.46253265017160317, 109.5822429386476955 ) ) ;
#144699 = CARTESIAN_POINT ( 'NONE',  ( 9.564922557960805705, 16.46253265017160317, 89.58224293864769550 ) ) ;
#144700 = CARTESIAN_POINT ( 'NONE',  ( 12.14591786802309770, 12.06949235617756955, 49.37390960531436690 ) ) ;
#144701 = CARTESIAN_POINT ( 'NONE',  ( 5.823673210054125526, 21.52544592524343514, 44.79057627198103120 ) ) ;
#144702 = CARTESIAN_POINT ( 'NONE',  ( -30.00000000000000000, -5.510910596163089556E-15, 45.00000000000000000 ) ) ;
#144703 = CARTESIAN_POINT ( 'NONE',  ( -9.564922557961040184, 16.46253265017147172, 32.91775706135233293 ) ) ;
#144704 = CARTESIAN_POINT ( 'NONE',  ( -17.26058549869093994, -6.457015423128468434, 81.37745837476070676 ) ) ;
#144705 = CARTESIAN_POINT ( 'NONE',  ( -19.05341960407611168, -5.049401038298163336, 56.45724293864768129 ) ) ;
#144706 = EDGE_CURVE ( 'NONE', #56681, #153137, #150228, .T. ) ;
#144707 = CARTESIAN_POINT ( 'NONE',  ( 8.224510206698742110, 14.34966873604972548, 42.08442372801901854 ) ) ;
#144708 = CARTESIAN_POINT ( 'NONE',  ( 26.36902008128207697, -29.90370362120039971, -17.00062383490519835 ) ) ;
#144709 = CARTESIAN_POINT ( 'NONE',  ( -16.88567814943162304, 6.947325034625684737, 108.7099887734741799 ) ) ;
#144710 = CARTESIAN_POINT ( 'NONE',  ( -8.224510206698735004, -14.34966873604973081, 74.58442372801901854 ) ) ;
#144711 = CARTESIAN_POINT ( 'NONE',  ( -18.67979575497178146, -10.72451020669898902, 101.6655762719810383 ) ) ;
#144713 = DIRECTION ( 'NONE',  ( 0.000000000000000000, 0.000000000000000000, 1.000000000000000000 ) ) ;
#144712 = CARTESIAN_POINT ( 'NONE',  ( 9.474510206698971260, -16.51473224551069308, 37.91557627198102409 ) ) ;
#144714 = CARTESIAN_POINT ( 'NONE',  ( 5.823673210054444382, -21.52544592524334988, 40.20942372801901854 ) ) ;
#144715 = CARTESIAN_POINT ( 'NONE',  ( -13.97604488694547697, 13.89961937509957934, 43.12609039468566152 ) ) ;
#144716 = CARTESIAN_POINT ( 'NONE',  ( -19.03943276465977164, 0.05219959533909376836, 46.24890960531435979 ) ) ;
#144717 = CARTESIAN_POINT ( 'NONE',  ( -10.72451020669870658, -18.67979575497194134, 99.58442372801900433 ) ) ;
#144718 = CARTESIAN_POINT ( 'NONE',  ( 16.88567814943163015, 6.947325034625698947, 98.79001122652587696 ) ) ;
#144719 = CARTESIAN_POINT ( 'NONE',  ( 4.483927247898545687, 16.52544592524342804, 34.79057627198103120 ) ) ;
#144720 = CARTESIAN_POINT ( 'NONE',  ( 18.22780087662121673, 5.500000000000056843, 43.98459894673892734 ) ) ;
#144721 = CARTESIAN_POINT ( 'NONE',  ( -18.62759615963270932, 10.81492255796079327, 55.83224293864770260 ) ) ;
#144722 = CARTESIAN_POINT ( 'NONE',  ( -8.571926809382608425, 26.38167802310805854, 144.4750000027312069 ) ) ;
#144723 = CARTESIAN_POINT ( 'NONE',  ( 13.89961937509977652, -13.97604488694527269, 108.1239096053143669 ) ) ;
#144724 = CARTESIAN_POINT ( 'NONE',  ( 14.34966873604960469, 8.224510206698951720, 94.16557627198103830 ) ) ;
#144725 = CARTESIAN_POINT ( 'NONE',  ( -16.53943276465976808, -0.05219959533934237506, 18.75109039468568639 ) ) ;
#144726 = CARTESIAN_POINT ( 'NONE',  ( -16.52544592524335698, -4.483927247898792601, 103.9594237280190185 ) ) ;
#144727 = VERTEX_POINT ( 'NONE', #14913 ) ;
#144729 = CARTESIAN_POINT ( 'NONE',  ( -21.55341960407610458, -5.719274019375992779, 101.4572429386476955 ) ) ;
#144728 = CARTESIAN_POINT ( 'NONE',  ( 13.97604488694527802, 13.89961937509977652, 104.3739096053143385 ) ) ;
#144731 = CARTESIAN_POINT ( 'NONE',  ( 19.02544592524343514, -5.153800228976328945, 98.54057627198100988 ) ) ;
#144730 = CARTESIAN_POINT ( 'NONE',  ( 0.05219959533910956823, 16.53943276465976808, 24.99890960531435624 ) ) ;
#144732 = CARTESIAN_POINT ( 'NONE',  ( -16.51473224551082808, 9.474510206698731452, 98.33442372801900433 ) ) ;
#144733 = CARTESIAN_POINT ( 'NONE',  ( 10.72451020669871369, 18.67979575497193778, 112.0844237280190185 ) ) ;
#144734 = CARTESIAN_POINT ( 'NONE',  ( 10.81492255796078972, 18.62759615963270932, 84.58224293864769550 ) ) ;
#144735 = CARTESIAN_POINT ( 'NONE',  ( -15.72974639402197994, 15.80617190586746368, 45.62390960531436690 ) ) ;
#144736 = CARTESIAN_POINT ( 'NONE',  ( -19.02544592524342804, 5.153800228976336051, 61.04057627198103120 ) ) ;
#144737 = CARTESIAN_POINT ( 'NONE',  ( -12.06949235617756955, 12.14591786802309770, 40.62390960531435269 ) ) ;
#144738 = CARTESIAN_POINT ( 'NONE',  ( -19.03943276465977164, 0.05219959533909376836, 76.24890960531435269 ) ) ;
#144739 = ORIENTED_EDGE ( 'NONE', *, *, #89447, .T. ) ;
#144740 = CARTESIAN_POINT ( 'NONE',  ( 18.87580814761077619, -5.499999999999873879, 63.37172394265759579 ) ) ;
#144741 = CARTESIAN_POINT ( 'NONE',  ( -13.97604488694547697, 13.89961937509957934, 43.12609039468566152 ) ) ;
#144742 = CARTESIAN_POINT ( 'NONE',  ( 10.81492255796078972, 18.62759615963270932, 84.58224293864769550 ) ) ;
#144743 = CARTESIAN_POINT ( 'NONE',  ( 4.483927247898545687, 16.52544592524342804, 89.79057627198103830 ) ) ;
#144744 =( BOUNDED_CURVE ( )  B_SPLINE_CURVE ( 2, ( #111224, #160716, #19230, #113207, #82863, #172916, #36361, #144541, #6026, #53535, #158714 ),
 .UNSPECIFIED., .F., .T. ) 
 B_SPLINE_CURVE_WITH_KNOTS ( ( 3, 2, 2, 2, 2, 3 ),
 ( 0.5000000000000000000, 0.5200000000000000178, 0.5400000000000000355, 0.5600000000000001643, 0.5800000000000001821, 0.6000000000000000888 ),
 .UNSPECIFIED. ) 
 CURVE ( )  GEOMETRIC_REPRESENTATION_ITEM ( )  RATIONAL_B_SPLINE_CURVE ( ( 1.000000000000000000, 0.9510565162951535312, 1.000000000000000000, 0.9510565162951535312, 1.000000000000000000, 0.9510565162951535312, 1.000000000000000000, 0.9510565162951535312, 1.000000000000000000, 0.9510565162951533091, 1.000000000000000222 ) ) 
 REPRESENTATION_ITEM ( '' )  );
#144745 = CARTESIAN_POINT ( 'NONE',  ( 21.55341960407619695, -5.719274019375665929, 36.04275706135234714 ) ) ;
#144746 = VECTOR ( 'NONE', #73447, 1000.000000000000000 ) ;
#144747 = CARTESIAN_POINT ( 'NONE',  ( -27.73933785331498925, 2.428612866367529932E-14, 143.3750000027311842 ) ) ;
#144748 = CARTESIAN_POINT ( 'NONE',  ( -16.55341960407617563, 4.379528057220093196, 113.5427570613523756 ) ) ;
#144749 = CARTESIAN_POINT ( 'NONE',  ( -19.02544592524342804, 5.153800228976336051, 26.04057627198103120 ) ) ;
#144750 = CARTESIAN_POINT ( 'NONE',  ( -13.97604488694527625, -13.89961937509977652, 81.87390960531436690 ) ) ;
#144751 =( NAMED_UNIT ( * ) PLANE_ANGLE_UNIT ( ) SI_UNIT ( $, .RADIAN. ) );
#144752 = DIRECTION ( 'NONE',  ( 1.000000000000000000, 0.000000000000000000, 0.000000000000000000 ) ) ;
#144753 = CARTESIAN_POINT ( 'NONE',  ( 14.29746914071049879, -8.314922557960816363, 38.33224293864768839 ) ) ;
#144754 = CARTESIAN_POINT ( 'NONE',  ( -21.53943276465977519, -0.05219959533937600094, 58.75109039468568994 ) ) ;
#144755 = CARTESIAN_POINT ( 'NONE',  ( 25.98457697381383369, -27.33515243881158341, -20.34861096990326246 ) ) ;
#144756 = CARTESIAN_POINT ( 'NONE',  ( -13.97604488694527625, -13.89961937509977652, 46.87390960531435979 ) ) ;
#144757 = CARTESIAN_POINT ( 'NONE',  ( 16.51473224551069308, 9.474510206698969483, 54.16557627198103120 ) ) ;
#144758 = VERTEX_POINT ( 'NONE', #1718 ) ;
#144759 = CARTESIAN_POINT ( 'NONE',  ( -21.55341960407619339, 5.719274019375674811, 108.5427570613523756 ) ) ;
#144760 = CARTESIAN_POINT ( 'NONE',  ( -16.53943276465976808, -0.05219959533934237506, 58.75109039468568994 ) ) ;
#144761 = CARTESIAN_POINT ( 'NONE',  ( -0.05219959533937732626, 21.53943276465977519, 87.50109039468568994 ) ) ;
#144762 = CARTESIAN_POINT ( 'NONE',  ( -16.46253265017160317, 9.564922557960807481, 115.8322429386477097 ) ) ;
#144763 = CARTESIAN_POINT ( 'NONE',  ( -5.049401038297874678, -19.05341960407617918, 89.79275706135230450 ) ) ;
#144764 = CARTESIAN_POINT ( 'NONE',  ( 15.80617190586769283, -15.72974639402175789, 65.62609039468568994 ) ) ;
#144765 = CARTESIAN_POINT ( 'NONE',  ( -8.314922557961024197, 14.29746914071037800, 37.91775706135235424 ) ) ;
#144766 = CARTESIAN_POINT ( 'NONE',  ( -0.05219959533907301413, -21.53943276465977519, 82.49890960531436690 ) ) ;
#144767 = CARTESIAN_POINT ( 'NONE',  ( -0.05219959533936034679, 19.03943276465977164, 92.50109039468566152 ) ) ;
#144768 = CARTESIAN_POINT ( 'NONE',  ( 9.474510206698971260, -16.51473224551069308, 67.91557627198102409 ) ) ;
#144769 = CARTESIAN_POINT ( 'NONE',  ( 13.97604488694548053, -13.89961937509957401, 90.62609039468567573 ) ) ;
#144770 = CARTESIAN_POINT ( 'NONE',  ( -13.97604488694547697, 13.89961937509957934, 98.12609039468566152 ) ) ;
#144771 = CARTESIAN_POINT ( 'NONE',  ( 16.53943276465976808, -0.05219959533910856209, 58.74890960531436690 ) ) ;
#144772 = CARTESIAN_POINT ( 'NONE',  ( 5.049401038297881783, 19.05341960407617563, 72.29275706135234714 ) ) ;
#144773 = CARTESIAN_POINT ( 'NONE',  ( -16.55341960407617563, 4.379528057220093196, 63.54275706135234003 ) ) ;
#144774 = EDGE_CURVE ( 'NONE', #87243, #34377, #183768, .T. ) ;
#144776 = CARTESIAN_POINT ( 'NONE',  ( -5.153800228976328057, -19.02544592524343514, 32.29057627198102409 ) ) ;
#144775 = CARTESIAN_POINT ( 'NONE',  ( -10.81492255796105439, 18.62759615963255655, 22.91775706135235069 ) ) ;
#144777 = CARTESIAN_POINT ( 'NONE',  ( 5.153800228976335163, 19.02544592524342804, 49.79057627198100988 ) ) ;
#144778 = B_SPLINE_CURVE_WITH_KNOTS ( 'NONE', 3,
 ( #54717, #146719, #174087, #113381, #8215, #83043, #175071, #36537, #116389, #98193, #101205, #162895, #7201, #114375, #24404, #132563, #112396, #129537, #159896, #6204, #35556, #21385, #144718, #191237, #99211, #160899, #22391, #84041, #68885, #59692, #148740, #43547 ),
 .UNSPECIFIED., .F., .F.,
 ( 4, 2, 2, 2, 2, 2, 2, 2, 2, 2, 2, 2, 2, 2, 2, 4 ),
 ( 1.430489624538199204E-17, 0.0003712461730036907895, 0.0007424923460073672675, 0.001113738519011043746, 0.001484984692014720224, 0.002227477038022073180, 0.002598723211025749658, 0.002969969384029426136, 0.003341215557033102614, 0.003712461730036779092, 0.004083707903040455570, 0.004454954076044131614, 0.004826200249047807658, 0.005197446422051484570, 0.005568692595055161482, 0.005939938768058837526 ),
 .UNSPECIFIED. ) ;
#144779 = CARTESIAN_POINT ( 'NONE',  ( -4.483927247898782831, 16.52544592524335698, 52.70942372801902565 ) ) ;
#144780 = CARTESIAN_POINT ( 'NONE',  ( -17.50000000001357847, 5.500000000000046185, 45.79690382535059001 ) ) ;
#144781 = CARTESIAN_POINT ( 'NONE',  ( 8.906447517083057264, -27.41122689804191026, 144.8500000054623911 ) ) ;
#144782 = CARTESIAN_POINT ( 'NONE',  ( 19.02544592524343514, -5.153800228976328945, 103.5405762719809957 ) ) ;
#144783 = CARTESIAN_POINT ( 'NONE',  ( 5.049401038298161559, -19.05341960407611168, 27.70724293864769550 ) ) ;
#144784 = EDGE_LOOP ( 'NONE', ( #138491, #67103, #114416, #1477, #2186, #86003, #182962, #26360, #29331, #126193, #39072, #189680, #8784, #15493, #92423, #10659, #122396, #197748, #140481, #137719, #72325, #98450, #153642, #53328, #59545, #154992, #152705, #29473, #48934, #185276, #168065, #197059, #169131, #41365, #40531, #154988, #177097, #192265, #68370, #160961, #62394, #101393, #178360, #59491, #101398, #117629, #195529, #72078, #54101, #72880, #82340, #81846, #80246, #142276, #51996, #152507 ) ) ;
#144785 = CARTESIAN_POINT ( 'NONE',  ( -16.52544592524335698, -4.483927247898792601, 18.95942372801901143 ) ) ;
#144786 = B_SPLINE_CURVE_WITH_KNOTS ( 'NONE', 3,
 ( #119673, #133841, #101486, #28669, #118678, #167170 ),
 .UNSPECIFIED., .F., .F.,
 ( 4, 2, 4 ),
 ( 0.007228050697041362750, 0.007608510107494831365, 0.007988969517948299112 ),
 .UNSPECIFIED. ) ;
#144787 = CARTESIAN_POINT ( 'NONE',  ( -21.55341960407610458, -5.719274019375992779, 41.45724293864769550 ) ) ;
#144789 = CARTESIAN_POINT ( 'NONE',  ( 16.53943276465976808, 0.05219959533934440121, 26.25109039468567573 ) ) ;
#144788 = CARTESIAN_POINT ( 'NONE',  ( -5.153800228976607833, 19.02544592524334988, 47.70942372801900433 ) ) ;
#144790 = CARTESIAN_POINT ( 'NONE',  ( 16.51473224551069308, 9.474510206698969483, 24.16557627198102765 ) ) ;
#144791 = CARTESIAN_POINT ( 'NONE',  ( 13.89961937509977652, -13.97604488694527269, 48.12390960531435979 ) ) ;
#144792 = CARTESIAN_POINT ( 'NONE',  ( 10.72451020669898902, -18.67979575497178502, 82.91557627198103830 ) ) ;
#144793 = CARTESIAN_POINT ( 'NONE',  ( 19.03943276465977164, -0.05219959533909143690, 108.7489096053143527 ) ) ;
#144794 = CARTESIAN_POINT ( 'NONE',  ( 5.049401038298161559, -19.05341960407611168, 52.70724293864767418 ) ) ;
#144795 = CARTESIAN_POINT ( 'NONE',  ( -8.571926809382608425, 26.38167802310805854, 140.9750000027312069 ) ) ;
#144796 = CARTESIAN_POINT ( 'NONE',  ( -13.89961937509957401, -13.97604488694547875, 84.37609039468567573 ) ) ;
#144797 = CARTESIAN_POINT ( 'NONE',  ( 4.379528057220339221, -16.55341960407611168, 72.70724293864769550 ) ) ;
#144798 = CARTESIAN_POINT ( 'NONE',  ( 21.52544592524334988, 5.823673210054432836, 101.4594237280190185 ) ) ;
#144799 = CARTESIAN_POINT ( 'NONE',  ( -21.55341960407610458, -5.719274019375992779, 91.45724293864769550 ) ) ;
#144800 = CARTESIAN_POINT ( 'NONE',  ( -15.80617190586768217, 15.72974639402176855, 88.12609039468570415 ) ) ;
#144801 = CARTESIAN_POINT ( 'NONE',  ( 15.72974639402176855, 15.80617190586768217, 81.87609039468568994 ) ) ;
#144802 = CARTESIAN_POINT ( 'NONE',  ( 19.02544592524343514, -5.153800228976328945, 103.5405762719809957 ) ) ;
#144804 = CARTESIAN_POINT ( 'NONE',  ( 18.67979575497194134, -10.72451020669871369, 75.83442372801900433 ) ) ;
#144803 = CARTESIAN_POINT ( 'NONE',  ( -14.29746914071037622, -8.314922557961029526, 104.1677570613523471 ) ) ;
#144805 = CARTESIAN_POINT ( 'NONE',  ( 19.02544592524343514, -5.153800228976328945, 63.54057627198103830 ) ) ;
#144806 = CARTESIAN_POINT ( 'NONE',  ( -18.62759615963255300, -10.81492255796106328, 49.16775706135234003 ) ) ;
#144807 = CARTESIAN_POINT ( 'NONE',  ( 0.05219959533909260263, 19.03943276465977164, 84.99890960531436690 ) ) ;
#144808 = CARTESIAN_POINT ( 'NONE',  ( -4.483927247898539470, -16.52544592524342804, 87.29057627198103830 ) ) ;
#144809 = CARTESIAN_POINT ( 'NONE',  ( -14.29746914071049879, 8.314922557960819915, 65.83224293864769550 ) ) ;
#144810 = CARTESIAN_POINT ( 'NONE',  ( 15.80617190586746368, 15.72974639402197994, 64.37390960531435269 ) ) ;
#144811 = CARTESIAN_POINT ( 'NONE',  ( -13.97604488694527625, -13.89961937509977652, 56.87390960531434558 ) ) ;
#144812 = CARTESIAN_POINT ( 'NONE',  ( 15.80617190586746368, 15.72974639402197994, 69.37390960531436690 ) ) ;
#144813 = CARTESIAN_POINT ( 'NONE',  ( 0.05219959533936267826, -19.03943276465977164, 70.00109039468566152 ) ) ;
#144815 = CARTESIAN_POINT ( 'NONE',  ( 16.55341960407611168, 4.379528057220329451, 73.95724293864769550 ) ) ;
#144814 = CARTESIAN_POINT ( 'NONE',  ( -19.35543954521082455, -5.499999999999490186, 89.58901960356449479 ) ) ;
#144816 = CARTESIAN_POINT ( 'NONE',  ( -0.05219959533907301413, -21.53943276465977519, 57.49890960531435979 ) ) ;
#144817 = CARTESIAN_POINT ( 'NONE',  ( 16.70000000000002061, -5.933031843596843873E-14, -64.92279855667830191 ) ) ;
#144819 = CARTESIAN_POINT ( 'NONE',  ( 17.14385361876520264, 23.59649016807275856, 146.6750000027311671 ) ) ;
#144818 = CARTESIAN_POINT ( 'NONE',  ( 4.379528057220092307, 16.55341960407617563, 97.29275706135234714 ) ) ;
#144820 = CARTESIAN_POINT ( 'NONE',  ( -5.153800228976607833, 19.02544592524334988, 97.70942372801900433 ) ) ;
#144821 = CARTESIAN_POINT ( 'NONE',  ( -12.14591786802309592, -12.06949235617757132, 66.87390960531436690 ) ) ;
#144822 = DIRECTION ( 'NONE',  ( 0.000000000000000000, 0.000000000000000000, 1.000000000000000000 ) ) ;
#144823 = CARTESIAN_POINT ( 'NONE',  ( -13.97604488694527625, -13.89961937509977652, 66.87390960531436690 ) ) ;
#144824 = CARTESIAN_POINT ( 'NONE',  ( 4.379528057220339221, -16.55341960407611168, 52.70724293864769550 ) ) ;
#144825 = CARTESIAN_POINT ( 'NONE',  ( -13.97604488694527625, -13.89961937509977652, 86.87390960531436690 ) ) ;
#144827 = CARTESIAN_POINT ( 'NONE',  ( 16.46253265017160672, -9.564922557960803928, 68.33224293864770971 ) ) ;
#144826 = CARTESIAN_POINT ( 'NONE',  ( 9.474510206698729675, 16.51473224551082808, 82.08442372801899012 ) ) ;
#144828 = CARTESIAN_POINT ( 'NONE',  ( -5.153800228976328057, -19.02544592524343514, 87.29057627198103830 ) ) ;
#144829 = CARTESIAN_POINT ( 'NONE',  ( 19.02544592524343514, -5.153800228976328945, 68.54057627198103830 ) ) ;
#144830 = CARTESIAN_POINT ( 'NONE',  ( 5.719274019375991003, -21.55341960407610458, 62.70724293864769550 ) ) ;
#144831 = CARTESIAN_POINT ( 'NONE',  ( -4.483927247898782831, 16.52544592524335698, 62.70942372801902565 ) ) ;
#144832 = CARTESIAN_POINT ( 'NONE',  ( 5.153800228976617603, -19.02544592524335343, 105.2094237280189901 ) ) ;
#144833 = CARTESIAN_POINT ( 'NONE',  ( 9.564922557960805705, 16.46253265017160317, 54.58224293864769550 ) ) ;
#144834 = CARTESIAN_POINT ( 'NONE',  ( 21.53943276465977519, -0.05219959533907433946, 58.74890960531436690 ) ) ;
#144835 = CARTESIAN_POINT ( 'NONE',  ( 9.474510206698729675, 16.51473224551082808, 87.08442372801900433 ) ) ;
#144836 = CARTESIAN_POINT ( 'NONE',  ( -14.34966873604972548, 8.224510206698743886, 113.3344237280190328 ) ) ;
#144837 = CARTESIAN_POINT ( 'NONE',  ( 19.02544592524334988, 5.153800228976608722, 41.45942372801900433 ) ) ;
#144839 = CARTESIAN_POINT ( 'NONE',  ( 12.14591786802327356, -12.06949235617739191, 95.62609039468568994 ) ) ;
#144838 = CARTESIAN_POINT ( 'NONE',  ( 12.06949235617739724, 12.14591786802326823, 61.87609039468568284 ) ) ;
#144840 = LINE ( 'NONE', #6324, #179214 ) ;
#144841 = CARTESIAN_POINT ( 'NONE',  ( -12.14591786802326823, 12.06949235617739902, 83.12609039468568994 ) ) ;
#144843 = CARTESIAN_POINT ( 'NONE',  ( 4.483927247898790824, -16.52544592524335698, 35.20942372801901854 ) ) ;
#144842 = CARTESIAN_POINT ( 'NONE',  ( -5.823673210054116645, -21.52544592524344225, 27.29057627198103120 ) ) ;
#144844 = CARTESIAN_POINT ( 'NONE',  ( 13.97604488694527802, 13.89961937509977652, 49.37390960531434558 ) ) ;
#144845 = CARTESIAN_POINT ( 'NONE',  ( 19.03943276465977164, -0.05219959533909143690, 48.74890960531435979 ) ) ;
#144846 = CARTESIAN_POINT ( 'NONE',  ( -0.05219959533909027116, -19.03943276465977164, 52.49890960531436690 ) ) ;
#144847 = CARTESIAN_POINT ( 'NONE',  ( 10.72451020669871369, 18.67979575497193778, 37.08442372801901143 ) ) ;
#144848 = CARTESIAN_POINT ( 'NONE',  ( -12.14591786802326823, 12.06949235617739902, 53.12609039468568284 ) ) ;
#144849 = CARTESIAN_POINT ( 'NONE',  ( -14.34966873604972548, 8.224510206698743886, 113.3344237280190328 ) ) ;
#144850 = CARTESIAN_POINT ( 'NONE',  ( 19.02544592524343514, -5.153800228976328945, 28.54057627198102409 ) ) ;
#144851 = CARTESIAN_POINT ( 'NONE',  ( -15.72974639402176322, -15.80617190586768395, 109.3760903946857042 ) ) ;
#144852 = CARTESIAN_POINT ( 'NONE',  ( -13.97604488694547697, 13.89961937509957934, 113.1260903946856757 ) ) ;
#144853 = CARTESIAN_POINT ( 'NONE',  ( -16.51473224551082808, 9.474510206698731452, 63.33442372801900433 ) ) ;
#144854 = CARTESIAN_POINT ( 'NONE',  ( 12.06949235617757843, -12.14591786802309237, 68.12390960531436690 ) ) ;
#144855 = CARTESIAN_POINT ( 'NONE',  ( -0.05219959533909027116, -19.03943276465977164, 42.49890960531435269 ) ) ;
#144857 = DIRECTION ( 'NONE',  ( 0.000000000000000000, -0.3420201433256828127, -0.9396926207859033209 ) ) ;
#144856 = CARTESIAN_POINT ( 'NONE',  ( 5.153800228976615827, -19.02544592524334988, 70.20942372801899012 ) ) ;
#144858 = CARTESIAN_POINT ( 'NONE',  ( 0.05219959533937995610, -21.53943276465977519, 75.00109039468568994 ) ) ;
#144859 = CARTESIAN_POINT ( 'NONE',  ( 4.483927247898790824, -16.52544592524335698, 35.20942372801901854 ) ) ;
#144860 = CARTESIAN_POINT ( 'NONE',  ( 19.02130022317638236, -5.499999999999594102, 58.28188669246577547 ) ) ;
#144861 = CARTESIAN_POINT ( 'NONE',  ( 21.53943276465977519, -0.05219959533907433946, 33.74890960531436690 ) ) ;
#144862 = CARTESIAN_POINT ( 'NONE',  ( 4.379528057220092307, 16.55341960407617563, 27.29275706135234358 ) ) ;
#144863 = CARTESIAN_POINT ( 'NONE',  ( -13.89961937509977830, 13.97604488694528158, 30.62390960531435624 ) ) ;
#144864 = CARTESIAN_POINT ( 'NONE',  ( 21.55341960407619695, -5.719274019375665929, 106.0427570613523471 ) ) ;
#144865 = CARTESIAN_POINT ( 'NONE',  ( -21.70479006154311108, 9.754118203517286645, 170.7545476126474284 ) ) ;
#144866 = CARTESIAN_POINT ( 'NONE',  ( -16.46253265017160317, 9.564922557960807481, 35.83224293864768839 ) ) ;
#144867 = CARTESIAN_POINT ( 'NONE',  ( 1.820000000000000062, 3.799999999999999378, 0.000000000000000000 ) ) ;
#144868 = CARTESIAN_POINT ( 'NONE',  ( -9.564922557960796823, -16.46253265017161027, 52.08224293864768839 ) ) ;
#144869 = CARTESIAN_POINT ( 'NONE',  ( 5.719274019375673035, 21.55341960407619339, 67.29275706135234714 ) ) ;
#144870 = CARTESIAN_POINT ( 'NONE',  ( 18.62759615963255655, 10.81492255796105972, 111.6677570613523613 ) ) ;
#144871 = CARTESIAN_POINT ( 'NONE',  ( -12.14591786802309592, -12.06949235617757132, 26.87390960531435979 ) ) ;
#144872 = CARTESIAN_POINT ( 'NONE',  ( -19.03943276465977164, 0.05219959533909376836, 31.24890960531435979 ) ) ;
#144873 = CARTESIAN_POINT ( 'NONE',  ( 19.02544592524343514, -5.153800228976328945, 88.54057627198102409 ) ) ;
#144874 = CARTESIAN_POINT ( 'NONE',  ( 15.80617190586769283, -15.72974639402175789, 60.62609039468567573 ) ) ;
#144875 = CARTESIAN_POINT ( 'NONE',  ( 19.05341960407611168, 5.049401038298154454, 38.95724293864767418 ) ) ;
#144876 = ADVANCED_FACE ( 'NONE', ( #171577 ), #153414, .T. ) ;
#144877 = CARTESIAN_POINT ( 'NONE',  ( 21.55341960407619695, -5.719274019375665929, 66.04275706135236135 ) ) ;
#144879 = CARTESIAN_POINT ( 'NONE',  ( -19.05341960407611168, -5.049401038298163336, 111.4572429386476671 ) ) ;
#144878 = CARTESIAN_POINT ( 'NONE',  ( 19.02544592524334988, 5.153800228976608722, 91.45942372801900433 ) ) ;
#144880 = CARTESIAN_POINT ( 'NONE',  ( 9.474510206698971260, -16.51473224551069308, 27.91557627198103120 ) ) ;
#144881 = CARTESIAN_POINT ( 'NONE',  ( 21.52544592524344225, -5.823673210054117533, 103.5405762719810383 ) ) ;
#144882 = CARTESIAN_POINT ( 'NONE',  ( 9.564922557961047289, -16.46253265017146816, 35.41775706135233293 ) ) ;
#144883 = CARTESIAN_POINT ( 'NONE',  ( 0.05219959533910956823, 16.53943276465976808, 114.9989096053143669 ) ) ;
#144884 = CARTESIAN_POINT ( 'NONE',  ( 9.474510206698971260, -16.51473224551069308, 67.91557627198102409 ) ) ;
#144885 = CARTESIAN_POINT ( 'NONE',  ( 13.97604488694548053, -13.89961937509957401, 95.62609039468563310 ) ) ;
#144886 = CARTESIAN_POINT ( 'NONE',  ( 12.14591786802309770, 12.06949235617756955, 64.37390960531435269 ) ) ;
#144887 = CARTESIAN_POINT ( 'NONE',  ( -18.62759615963270932, 10.81492255796079327, 25.83224293864769194 ) ) ;
#144888 = CARTESIAN_POINT ( 'NONE',  ( 19.02544592524334988, 5.153800228976608722, 91.45942372801900433 ) ) ;
#144889 = CARTESIAN_POINT ( 'NONE',  ( -18.62759615963270932, 10.81492255796079327, 85.83224293864768129 ) ) ;
#144890 = CARTESIAN_POINT ( 'NONE',  ( -5.719274019375665041, -21.55341960407619695, 44.79275706135234714 ) ) ;
#144891 = CARTESIAN_POINT ( 'NONE',  ( -14.29746914071037622, -8.314922557961029526, 39.16775706135235424 ) ) ;
#144893 = CARTESIAN_POINT ( 'NONE',  ( 0.05219959533937995610, -21.53943276465977519, 45.00109039468568284 ) ) ;
#144892 = CARTESIAN_POINT ( 'NONE',  ( -0.05219959533934338120, 16.53943276465976808, 42.50109039468567573 ) ) ;
#144894 = CARTESIAN_POINT ( 'NONE',  ( 21.55341960407610458, 5.719274019375980345, 53.95724293864770260 ) ) ;
#144895 = CARTESIAN_POINT ( 'NONE',  ( -16.51473224551069308, -9.474510206698971260, 36.66557627198102409 ) ) ;
#144896 = CARTESIAN_POINT ( 'NONE',  ( -11.74264578624800670, 36.14014761921585972, -6.149999994537627579 ) ) ;
#144897 = CARTESIAN_POINT ( 'NONE',  ( 12.14591786802327356, -12.06949235617739191, 70.62609039468567573 ) ) ;
#144898 = CARTESIAN_POINT ( 'NONE',  ( -21.52544592524343514, 5.823673210054127303, 106.0405762719810525 ) ) ;
#144899 = CARTESIAN_POINT ( 'NONE',  ( 8.224510206698953496, -14.34966873604960469, 37.91557627198102409 ) ) ;
#144900 = CARTESIAN_POINT ( 'NONE',  ( -16.53943276465976808, -0.05219959533934237506, 63.75109039468568284 ) ) ;
#144901 = CARTESIAN_POINT ( 'NONE',  ( -5.153800228976607833, 19.02544592524334988, 102.7094237280189759 ) ) ;
#144902 = CARTESIAN_POINT ( 'NONE',  ( 15.80617190586746368, 15.72974639402197994, 94.37390960531436690 ) ) ;
#144903 = CARTESIAN_POINT ( 'NONE',  ( -8.224510206698948167, 14.34966873604960824, 35.41557627198102409 ) ) ;
#144904 = VERTEX_POINT ( 'NONE', #141226 ) ;
#144905 = CARTESIAN_POINT ( 'NONE',  ( -4.379528057220086978, -16.55341960407618274, 74.79275706135234714 ) ) ;
#144906 = CARTESIAN_POINT ( 'NONE',  ( 25.55222625260933356, 11.31436996698904629, 166.3494238031456405 ) ) ;
#144907 = CARTESIAN_POINT ( 'NONE',  ( -10.72451020669898014, 18.67979575497178502, 70.41557627198102409 ) ) ;
#144908 = CARTESIAN_POINT ( 'NONE',  ( 8.224510206698742110, 14.34966873604972548, 102.0844237280190185 ) ) ;
#144909 = EDGE_LOOP ( 'NONE', ( #102507, #72971 ) ) ;
#144910 = CARTESIAN_POINT ( 'NONE',  ( -21.23184647844206197, -181.1785498424364675, 0.000000000000000000 ) ) ;
#144911 = CARTESIAN_POINT ( 'NONE',  ( 15.72974639402199770, -15.80617190586745480, 103.1239096053143811 ) ) ;
#144912 = CARTESIAN_POINT ( 'NONE',  ( -15.80617190586745835, -15.72974639402198527, 106.8739096053143811 ) ) ;
#144913 = CARTESIAN_POINT ( 'NONE',  ( 8.224510206698953496, -14.34966873604960469, 37.91557627198102409 ) ) ;
#144914 = CARTESIAN_POINT ( 'NONE',  ( -14.29746914071037622, -8.314922557961029526, 44.16775706135234714 ) ) ;
#144915 = CARTESIAN_POINT ( 'NONE',  ( -13.97604488694527625, -13.89961937509977652, 46.87390960531435979 ) ) ;
#144916 = CARTESIAN_POINT ( 'NONE',  ( -9.564922557960796823, -16.46253265017161027, 67.08224293864769550 ) ) ;
#144917 = ORIENTED_EDGE ( 'NONE', *, *, #101613, .T. ) ;
#144918 = CARTESIAN_POINT ( 'NONE',  ( -19.03943276465977164, 0.05219959533909376836, 111.2489096053143669 ) ) ;
#144919 = CARTESIAN_POINT ( 'NONE',  ( -24.94736998983943366, -28.55544918295244372, -16.60430580961714142 ) ) ;
#144920 = CARTESIAN_POINT ( 'NONE',  ( -0.05219959533936034679, 19.03943276465977164, 102.5010903946856757 ) ) ;
#144921 = CARTESIAN_POINT ( 'NONE',  ( 5.153800228976615827, -19.02544592524334988, 50.20942372801897591 ) ) ;
#144922 = CARTESIAN_POINT ( 'NONE',  ( -5.719274019375978568, 21.55341960407610458, 90.20724293864770971 ) ) ;
#144923 = CARTESIAN_POINT ( 'NONE',  ( 16.52544592524342804, -4.483927247898539470, 23.54057627198102765 ) ) ;
#144924 = CARTESIAN_POINT ( 'NONE',  ( -19.05341960407611168, -5.049401038298163336, 81.45724293864769550 ) ) ;
#144925 = CARTESIAN_POINT ( 'NONE',  ( -15.80617190586745835, -15.72974639402198527, 41.87390960531435979 ) ) ;
#144927 = CARTESIAN_POINT ( 'NONE',  ( 14.34966873604972726, -8.224510206698740333, 20.83442372801901143 ) ) ;
#144926 = CARTESIAN_POINT ( 'NONE',  ( -18.62759615963270932, 10.81492255796079327, 85.83224293864768129 ) ) ;
#144928 = CARTESIAN_POINT ( 'NONE',  ( -19.02544592524342804, 5.153800228976336051, 116.0405762719810383 ) ) ;
#144929 = CARTESIAN_POINT ( 'NONE',  ( 5.823673210054444382, -21.52544592524334988, 80.20942372801901854 ) ) ;
#144930 = CARTESIAN_POINT ( 'NONE',  ( 16.51473224551069308, 9.474510206698969483, 79.16557627198103830 ) ) ;
#144931 = CARTESIAN_POINT ( 'NONE',  ( 31.24420449012917089, 7.031618440654747282, 97.62038805904606420 ) ) ;
#144932 = CARTESIAN_POINT ( 'NONE',  ( 5.049401038298161559, -19.05341960407611168, 72.70724293864768129 ) ) ;
#144933 = CARTESIAN_POINT ( 'NONE',  ( -4.483927247898539470, -16.52544592524342804, 92.29057627198103830 ) ) ;
#144934 = VERTEX_POINT ( 'NONE', #2717 ) ;
#144935 = CARTESIAN_POINT ( 'NONE',  ( -0.05219959533936034679, 19.03943276465977164, 107.5010903946856615 ) ) ;
#144936 = LINE ( 'NONE', #189473, #131038 ) ;
#144937 = CARTESIAN_POINT ( 'NONE',  ( 0.05219959533909260263, 19.03943276465977164, 74.99890960531435269 ) ) ;
#144939 = CARTESIAN_POINT ( 'NONE',  ( -19.03943276465977164, 0.05219959533909376836, 96.24890960531436690 ) ) ;
#144938 = CARTESIAN_POINT ( 'NONE',  ( 15.72974639402176855, 15.80617190586768217, 81.87609039468568994 ) ) ;
#144940 = CARTESIAN_POINT ( 'NONE',  ( -14.29746914071037622, -8.314922557961029526, 79.16775706135234714 ) ) ;
#144941 = CARTESIAN_POINT ( 'NONE',  ( -16.52216118717209170, -7.221426719304500530, 76.07599021046995347 ) ) ;
#144942 = CARTESIAN_POINT ( 'NONE',  ( -13.97604488694547697, 13.89961937509957934, 53.12609039468565442 ) ) ;
#144943 = CARTESIAN_POINT ( 'NONE',  ( 5.719274019375673035, 21.55341960407619339, 112.2927570613523471 ) ) ;
#144944 = CARTESIAN_POINT ( 'NONE',  ( 0.2500000000000002220, 5.204748896376250699E-16, -4.250000000000000000 ) ) ;
#144945 = DIRECTION ( 'NONE',  ( -0.000000000000000000, 0.000000000000000000, 1.000000000000000000 ) ) ;
#144946 = CARTESIAN_POINT ( 'NONE',  ( -11.40812507854754720, -35.11059874428192273, -6.724999997268813701 ) ) ;
#144947 = CARTESIAN_POINT ( 'NONE',  ( 4.379528057220092307, 16.55341960407617563, 112.2927570613523471 ) ) ;
#144948 = DIRECTION ( 'NONE',  ( 0.000000000000000000, -1.000000000000000000, 0.000000000000000000 ) ) ;
#144949 = CARTESIAN_POINT ( 'NONE',  ( 8.314922557961029526, -14.29746914071037800, 110.4177570613523756 ) ) ;
#144950 = DIRECTION ( 'NONE',  ( -1.000000000000000000, 0.000000000000000000, 0.000000000000000000 ) ) ;
#144951 = CARTESIAN_POINT ( 'NONE',  ( 16.52544592524335698, 4.483927247898782831, 86.45942372801901854 ) ) ;
#144952 = CARTESIAN_POINT ( 'NONE',  ( 21.53943276465977519, 0.05219959533937863772, 86.25109039468568994 ) ) ;
#144953 = CARTESIAN_POINT ( 'NONE',  ( 5.049401038297881783, 19.05341960407617563, 82.29275706135229029 ) ) ;
#144954 = CARTESIAN_POINT ( 'NONE',  ( -5.049401038297874678, -19.05341960407617918, 34.79275706135233293 ) ) ;
#144955 = CARTESIAN_POINT ( 'NONE',  ( 0.05219959533909260263, 19.03943276465977164, 74.99890960531435269 ) ) ;
#144956 = CARTESIAN_POINT ( 'NONE',  ( 19.02544592524343514, -5.153800228976328945, 58.54057627198102409 ) ) ;
#144957 = CARTESIAN_POINT ( 'NONE',  ( 17.97182807773870294, -5.499999999999849010, 41.03038844047290468 ) ) ;
#144958 = CARTESIAN_POINT ( 'NONE',  ( 0.05219959533907565091, 21.53943276465977519, 89.99890960531438111 ) ) ;
#144959 = CARTESIAN_POINT ( 'NONE',  ( -15.72974639402197994, 15.80617190586746368, 45.62390960531436690 ) ) ;
#144960 = CARTESIAN_POINT ( 'NONE',  ( -19.03943276465977164, 0.05219959533909376836, 46.24890960531435979 ) ) ;
#144961 = CARTESIAN_POINT ( 'NONE',  ( -12.14591786802326823, 12.06949235617739902, 58.12609039468568994 ) ) ;
#144962 = ADVANCED_FACE ( 'NONE', ( #76574 ), #64394, .T. ) ;
#144963 = UNCERTAINTY_MEASURE_WITH_UNIT (LENGTH_MEASURE( 1.000000000000000082E-05 ), #183092, 'distance_accuracy_value', 'NONE');
#144964 = VERTEX_POINT ( 'NONE', #13909 ) ;
#144965 = CARTESIAN_POINT ( 'NONE',  ( 21.52544592524334988, 5.823673210054432836, 51.45942372801901854 ) ) ;
#144967 = CARTESIAN_POINT ( 'NONE',  ( 38.00000000000000711, -12.34694845685040754, -1.099999999999999645 ) ) ;
#144966 = CARTESIAN_POINT ( 'NONE',  ( -16.52544592524342804, 4.483927247898546575, 71.04057627198103830 ) ) ;
#144968 = CARTESIAN_POINT ( 'NONE',  ( -16.55341960407617563, 4.379528057220093196, 33.54275706135234714 ) ) ;
#144969 = CARTESIAN_POINT ( 'NONE',  ( 12.06949235617757843, -12.14591786802309237, 103.1239096053143811 ) ) ;
#144970 = CARTESIAN_POINT ( 'NONE',  ( 16.51473224551083163, -9.474510206698727899, 55.83442372801899722 ) ) ;
#144971 = CARTESIAN_POINT ( 'NONE',  ( 16.52544592524342804, -4.483927247898539470, 68.54057627198103830 ) ) ;
#144972 = CARTESIAN_POINT ( 'NONE',  ( -21.55341960407619339, 5.719274019375674811, 33.54275706135234714 ) ) ;
#144974 = CARTESIAN_POINT ( 'NONE',  ( 5.823673210054125526, 21.52544592524343514, 94.79057627198105251 ) ) ;
#144973 = CARTESIAN_POINT ( 'NONE',  ( 19.05341960407611168, 5.049401038298154454, 23.95724293864769194 ) ) ;
#144975 = CARTESIAN_POINT ( 'NONE',  ( 5.153800228976335163, 19.02544592524342804, 109.7905762719810099 ) ) ;
#144976 = CARTESIAN_POINT ( 'NONE',  ( -12.06949235617756955, 12.14591786802309770, 70.62390960531436690 ) ) ;
#144977 = CARTESIAN_POINT ( 'NONE',  ( 33.88770617168000854, -21.25088722958024334, -25.15219191025233769 ) ) ;
#144978 = AXIS2_PLACEMENT_3D ( 'NONE', #102961, #148477, #115132 ) ;
#144979 = CARTESIAN_POINT ( 'NONE',  ( -11.40812507854754720, -35.11059874428192273, -6.224999997268812812 ) ) ;
#144980 = CARTESIAN_POINT ( 'NONE',  ( -9.564922557961040184, 16.46253265017147172, 77.91775706135234714 ) ) ;
#144981 = CARTESIAN_POINT ( 'NONE',  ( 21.53943276465977519, 0.05219959533937863772, 26.25109039468567573 ) ) ;
#144982 = CARTESIAN_POINT ( 'NONE',  ( 9.474510206698971260, -16.51473224551069308, 67.91557627198102409 ) ) ;
#144983 = CARTESIAN_POINT ( 'NONE',  ( 9.474510206698729675, 16.51473224551082808, 62.08442372801899722 ) ) ;
#144984 = CARTESIAN_POINT ( 'NONE',  ( 9.564922557960805705, 16.46253265017160317, 29.58224293864769550 ) ) ;
#144985 = CARTESIAN_POINT ( 'NONE',  ( -0.05219959533910754901, -16.53943276465976808, 67.49890960531436690 ) ) ;
#144986 = CARTESIAN_POINT ( 'NONE',  ( 8.314922557960818139, 14.29746914071049879, 54.58224293864769550 ) ) ;
#144987 = CARTESIAN_POINT ( 'NONE',  ( -0.05219959533909027116, -19.03943276465977164, 62.49890960531435979 ) ) ;
#144988 = CARTESIAN_POINT ( 'NONE',  ( 15.72974639402199770, -15.80617190586745480, 83.12390960531436690 ) ) ;
#144989 = CARTESIAN_POINT ( 'NONE',  ( 19.03943276465977164, -0.05219959533909143690, 63.74890960531435979 ) ) ;
#144990 = ORIENTED_EDGE ( 'NONE', *, *, #174403, .F. ) ;
#144991 = CARTESIAN_POINT ( 'NONE',  ( -5.719274019375978568, 21.55341960407610458, 80.20724293864769550 ) ) ;
#144992 = CARTESIAN_POINT ( 'NONE',  ( 18.67979575497194134, -10.72451020669871369, 100.8344237280190185 ) ) ;
#144995 = CARTESIAN_POINT ( 'NONE',  ( 12.14591786802309770, 12.06949235617756955, 94.37390960531436690 ) ) ;
#144994 = CARTESIAN_POINT ( 'NONE',  ( 14.29746914071037800, 8.314922557961029526, 106.6677570613523756 ) ) ;
#144993 = DIRECTION ( 'NONE',  ( 0.000000000000000000, 0.000000000000000000, -1.000000000000000000 ) ) ;
#144996 = CARTESIAN_POINT ( 'NONE',  ( -16.51473224551082808, 9.474510206698731452, 98.33442372801900433 ) ) ;
#144997 = ORIENTED_EDGE ( 'NONE', *, *, #78423, .T. ) ;
#144998 = CARTESIAN_POINT ( 'NONE',  ( -10.72451020669870658, -18.67979575497194134, 19.58442372801901143 ) ) ;
#144999 = CARTESIAN_POINT ( 'NONE',  ( 9.474510206698729675, 16.51473224551082808, 47.08442372801900433 ) ) ;
#145000 = CARTESIAN_POINT ( 'NONE',  ( -14.29746914071037622, -8.314922557961029526, 99.16775706135234714 ) ) ;
#145001 = CARTESIAN_POINT ( 'NONE',  ( -5.049401038297874678, -19.05341960407617918, 34.79275706135233293 ) ) ;
#145002 = CARTESIAN_POINT ( 'NONE',  ( 19.02544592524343514, -5.153800228976328945, 98.54057627198100988 ) ) ;
#145003 = CARTESIAN_POINT ( 'NONE',  ( 10.72451020669898902, -18.67979575497178502, 67.91557627198102409 ) ) ;
#145004 = CARTESIAN_POINT ( 'NONE',  ( -2.973862142520655727, -93.04182470242767522, -15.00000000000000178 ) ) ;
#145005 = CARTESIAN_POINT ( 'NONE',  ( 9.564922557960805705, 16.46253265017160317, 29.58224293864769550 ) ) ;
#145006 = CARTESIAN_POINT ( 'NONE',  ( 18.67979575497194134, -10.72451020669871369, 110.8344237280190043 ) ) ;
#145007 = CARTESIAN_POINT ( 'NONE',  ( 14.29746914071037800, 8.314922557961029526, 71.66775706135234714 ) ) ;
#145008 = CARTESIAN_POINT ( 'NONE',  ( 15.80617190586769283, -15.72974639402175789, 25.62609039468567929 ) ) ;
#145009 = CARTESIAN_POINT ( 'NONE',  ( -14.29746914071037622, -8.314922557961029526, 39.16775706135235424 ) ) ;
#145010 = CARTESIAN_POINT ( 'NONE',  ( -9.474510206698964154, 16.51473224551069663, 100.4155762719810241 ) ) ;
#145011 = CARTESIAN_POINT ( 'NONE',  ( -19.03943276465977164, 0.05219959533909376836, 51.24890960531436690 ) ) ;
#145012 = CARTESIAN_POINT ( 'NONE',  ( 5.049401038298161559, -19.05341960407611168, 72.70724293864768129 ) ) ;
#145013 = CARTESIAN_POINT ( 'NONE',  ( 14.29746914071037800, 8.314922557961029526, 41.66775706135235424 ) ) ;
#145014 = CARTESIAN_POINT ( 'NONE',  ( 16.53943276465976808, -0.05219959533910856209, 98.74890960531438111 ) ) ;
#145015 = CARTESIAN_POINT ( 'NONE',  ( 14.34966873604972726, -8.224510206698740333, 105.8344237280190328 ) ) ;
#145016 = CYLINDRICAL_SURFACE ( 'NONE', #89385, 3.799999999999999378 ) ;
#145019 = CARTESIAN_POINT ( 'NONE',  ( -5.153800228976328057, -19.02544592524343514, 67.29057627198102409 ) ) ;
#145018 = CARTESIAN_POINT ( 'NONE',  ( 19.02544592524343514, -5.153800228976328945, 78.54057627198099567 ) ) ;
#145017 = CARTESIAN_POINT ( 'NONE',  ( 5.823673210054444382, -21.52544592524334988, 55.20942372801902565 ) ) ;
#145020 = CARTESIAN_POINT ( 'NONE',  ( 0.05219959533909260263, 19.03943276465977164, 89.99890960531436690 ) ) ;
#145021 = CARTESIAN_POINT ( 'NONE',  ( -12.14591786802309592, -12.06949235617757132, 51.87390960531437401 ) ) ;
#145022 = CARTESIAN_POINT ( 'NONE',  ( 14.34966873604972726, -8.224510206698740333, 100.8344237280190185 ) ) ;
#145023 = CARTESIAN_POINT ( 'NONE',  ( -16.52544592524342804, 4.483927247898546575, 36.04057627198102409 ) ) ;
#145024 = EDGE_LOOP ( 'NONE', ( #18218, #86799, #85855, #78557 ) ) ;
#145025 = CARTESIAN_POINT ( 'NONE',  ( -9.564922557961040184, 16.46253265017147172, 42.91775706135234003 ) ) ;
#145026 = CARTESIAN_POINT ( 'NONE',  ( -15.23006821330878502, -17.33560778597399477, -55.19189381068117228 ) ) ;
#145027 = CARTESIAN_POINT ( 'NONE',  ( 19.05341960407611168, 5.049401038298154454, 68.95724293864769550 ) ) ;
#145028 = CARTESIAN_POINT ( 'NONE',  ( -13.89961937509957401, -13.97604488694547875, 39.37609039468566152 ) ) ;
#145029 = CARTESIAN_POINT ( 'NONE',  ( -29.86685920354755197, -21.69954338932560134, -2.424999997268813434 ) ) ;
#145030 = CARTESIAN_POINT ( 'NONE',  ( 17.49999999999999645, 5.500000000000007994, 73.78230962303568674 ) ) ;
#145032 = CARTESIAN_POINT ( 'NONE',  ( -16.53943276465976808, -0.05219959533934237506, 63.75109039468568284 ) ) ;
#145031 = CARTESIAN_POINT ( 'NONE',  ( 19.02544592524334988, 5.153800228976608722, 91.45942372801900433 ) ) ;
#145033 = FACE_OUTER_BOUND ( 'NONE', #120792, .T. ) ;
#145034 = CARTESIAN_POINT ( 'NONE',  ( 13.89961937509977652, -13.97604488694527269, 88.12390960531438111 ) ) ;
#145035 = CARTESIAN_POINT ( 'NONE',  ( -10.72451020669870658, -18.67979575497194134, 24.58442372801901499 ) ) ;
#145036 = CARTESIAN_POINT ( 'NONE',  ( 13.97604488694548053, -13.89961937509957401, 80.62609039468567573 ) ) ;
#145038 = CARTESIAN_POINT ( 'NONE',  ( 5.049401038298161559, -19.05341960407611168, 42.70724293864767418 ) ) ;
#145037 = CARTESIAN_POINT ( 'NONE',  ( 16.19135201231366139, 7.376712067591958188, 87.68680854052034590 ) ) ;
#145039 = CARTESIAN_POINT ( 'NONE',  ( 0.05219959533909260263, 19.03943276465977164, 94.99890960531436690 ) ) ;
#145041 = CARTESIAN_POINT ( 'NONE',  ( 9.474510206698971260, -16.51473224551069308, 47.91557627198102409 ) ) ;
#145040 = CARTESIAN_POINT ( 'NONE',  ( -12.14591786802309592, -12.06949235617757132, 51.87390960531437401 ) ) ;
#145042 = CARTESIAN_POINT ( 'NONE',  ( 13.89961937509957401, 13.97604488694547697, 46.87609039468565442 ) ) ;
#145043 = EDGE_LOOP ( 'NONE', ( #147976, #57706, #55909, #39925, #51105, #34750, #174524, #23672, #57001, #86332, #144990, #131749, #178088, #103664, #66451, #29855, #1800, #190492, #176563, #40773, #178523, #74379, #37114, #109151, #159918, #198172, #124354, #127118, #122656, #134013, #138702, #48008, #96179, #195201, #55532, #137540, #26884, #19360, #163469, #194203, #47304 ) ) ;
#145044 = CARTESIAN_POINT ( 'NONE',  ( -0.05219959533910754901, -16.53943276465976808, 87.49890960531436690 ) ) ;
#145045 = CARTESIAN_POINT ( 'NONE',  ( 19.02544592524334988, 5.153800228976608722, 31.45942372801900433 ) ) ;
#145046 = CARTESIAN_POINT ( 'NONE',  ( 0.05219959533909260263, 19.03943276465977164, 59.99890960531436690 ) ) ;
#145047 = CARTESIAN_POINT ( 'NONE',  ( -10.72451020669898014, 18.67979575497178502, 65.41557627198102409 ) ) ;
#145049 = CARTESIAN_POINT ( 'NONE',  ( -9.564922557961040184, 16.46253265017147172, 22.91775706135233648 ) ) ;
#145048 = CARTESIAN_POINT ( 'NONE',  ( -14.29746914071049879, 8.314922557960819915, 60.83224293864769550 ) ) ;
#145050 = CARTESIAN_POINT ( 'NONE',  ( -5.049401038298153566, 19.05341960407611168, 100.2072429386476955 ) ) ;
#145051 = CARTESIAN_POINT ( 'NONE',  ( 0.05219959533907565091, 21.53943276465977519, 24.99890960531435624 ) ) ;
#145052 = CARTESIAN_POINT ( 'NONE',  ( 19.02544592524343514, -5.153800228976328945, 58.54057627198102409 ) ) ;
#145053 = CARTESIAN_POINT ( 'NONE',  ( -16.46253265017160317, 9.564922557960807481, 35.83224293864768839 ) ) ;
#145054 = CARTESIAN_POINT ( 'NONE',  ( -0.05219959533910754901, -16.53943276465976808, 97.49890960531436690 ) ) ;
#145055 = CARTESIAN_POINT ( 'NONE',  ( 5.823673210054125526, 21.52544592524343514, 114.7905762719810383 ) ) ;
#145056 = CARTESIAN_POINT ( 'NONE',  ( 0.05219959533909260263, 19.03943276465977164, 99.99890960531436690 ) ) ;
#145057 = CARTESIAN_POINT ( 'NONE',  ( 0.05219959533907565091, 21.53943276465977519, 109.9989096053143527 ) ) ;
#145058 = CARTESIAN_POINT ( 'NONE',  ( 5.049401038298161559, -19.05341960407611168, 102.7072429386476955 ) ) ;
#145059 = CARTESIAN_POINT ( 'NONE',  ( -12.06949235617756955, 12.14591786802309770, 115.6239096053143669 ) ) ;
#145060 = CARTESIAN_POINT ( 'NONE',  ( -15.72974639402176322, -15.80617190586768395, 84.37609039468570415 ) ) ;
#145061 = CARTESIAN_POINT ( 'NONE',  ( -15.72974639402197994, 15.80617190586746368, 90.62390960531436690 ) ) ;
#145062 = CARTESIAN_POINT ( 'NONE',  ( 16.36317988757058117, -7.306389748694945396, 106.5978960836322642 ) ) ;
#145063 = DIRECTION ( 'NONE',  ( 1.000000000000000000, 6.391086490440868450E-16, 0.000000000000000000 ) ) ;
#145064 = CARTESIAN_POINT ( 'NONE',  ( 28.91687668646898146, -0.2552802045322939972, -52.63629878241255255 ) ) ;
#145065 = CARTESIAN_POINT ( 'NONE',  ( -16.52544592524335698, -4.483927247898792601, 43.95942372801902565 ) ) ;
#145066 = CARTESIAN_POINT ( 'NONE',  ( -12.14591786802309592, -12.06949235617757132, 106.8739096053143811 ) ) ;
#145067 = DIRECTION ( 'NONE',  ( 0.000000000000000000, 0.000000000000000000, -1.000000000000000000 ) ) ;
#145068 = CARTESIAN_POINT ( 'NONE',  ( 16.46253265017160672, -9.564922557960803928, 58.33224293864769550 ) ) ;
#145069 = CARTESIAN_POINT ( 'NONE',  ( 14.29746914071049879, -8.314922557960816363, 98.33224293864769550 ) ) ;
#145070 = CARTESIAN_POINT ( 'NONE',  ( 21.52544592524344225, -5.823673210054117533, 43.54057627198103830 ) ) ;
#145071 = CARTESIAN_POINT ( 'NONE',  ( -8.224510206698948167, 14.34966873604960824, 70.41557627198102409 ) ) ;
#145072 = CARTESIAN_POINT ( 'NONE',  ( -16.52544592524335698, -4.483927247898792601, 18.95942372801901143 ) ) ;
#145073 = CARTESIAN_POINT ( 'NONE',  ( 0.05219959533937995610, -21.53943276465977519, 70.00109039468568994 ) ) ;
#145074 = DIRECTION ( 'NONE',  ( -0.000000000000000000, -0.9946471445771456477, 0.1033298494363113634 ) ) ;
#145075 = CARTESIAN_POINT ( 'NONE',  ( 14.29746914071037800, 8.314922557961029526, 101.6677570613523613 ) ) ;
#145076 = CARTESIAN_POINT ( 'NONE',  ( 12.06949235617757843, -12.14591786802309237, 43.12390960531435269 ) ) ;
#145077 = CARTESIAN_POINT ( 'NONE',  ( 9.564922557960805705, 16.46253265017160317, 44.58224293864769550 ) ) ;
#145078 = CARTESIAN_POINT ( 'NONE',  ( 0.05219959533909260263, 19.03943276465977164, 94.99890960531436690 ) ) ;
#145079 = CARTESIAN_POINT ( 'NONE',  ( 10.81492255796078972, 18.62759615963270932, 94.58224293864769550 ) ) ;
#145080 = CARTESIAN_POINT ( 'NONE',  ( 8.314922557961029526, -14.29746914071037800, 30.41775706135234358 ) ) ;
#145082 = CARTESIAN_POINT ( 'NONE',  ( 21.52544592524334988, 5.823673210054432836, 71.45942372801901854 ) ) ;
#145081 = CARTESIAN_POINT ( 'NONE',  ( -16.52544592524342804, 4.483927247898546575, 66.04057627198103830 ) ) ;
#145083 = CARTESIAN_POINT ( 'NONE',  ( -16.53943276465976808, -0.05219959533934237506, 93.75109039468567573 ) ) ;
#145084 = CARTESIAN_POINT ( 'NONE',  ( 16.81555441253467365, -7.025013491696276091, 48.13685445334212432 ) ) ;
#145085 = CARTESIAN_POINT ( 'NONE',  ( -18.89770734986050016, -5.499999999999905853, 64.10214472496640781 ) ) ;
#145086 = CARTESIAN_POINT ( 'NONE',  ( -14.29746914071049879, 8.314922557960819915, 25.83224293864769194 ) ) ;
#145087 = CARTESIAN_POINT ( 'NONE',  ( 4.483927247898790824, -16.52544592524335698, 75.20942372801901854 ) ) ;
#145088 = CARTESIAN_POINT ( 'NONE',  ( 5.049401038298161559, -19.05341960407611168, 87.70724293864769550 ) ) ;
#145089 = CARTESIAN_POINT ( 'NONE',  ( 19.05341960407611168, 5.049401038298154454, 98.95724293864766707 ) ) ;
#145090 = CARTESIAN_POINT ( 'NONE',  ( 10.81492255796106328, -18.62759615963255655, 85.41775706135236135 ) ) ;
#145091 = CARTESIAN_POINT ( 'NONE',  ( 4.483927247898790824, -16.52544592524335698, 95.20942372801903275 ) ) ;
#145092 = CARTESIAN_POINT ( 'NONE',  ( 12.06949235617757843, -12.14591786802309237, 63.12390960531435979 ) ) ;
#145093 = CARTESIAN_POINT ( 'NONE',  ( 9.474510206698971260, -16.51473224551069308, 72.91557627198102409 ) ) ;
#145094 = ORIENTED_EDGE ( 'NONE', *, *, #38977, .F. ) ;
#145095 = CARTESIAN_POINT ( 'NONE',  ( 19.03943276465977164, 0.05219959533936151252, 111.2510903946856757 ) ) ;
#145096 = CARTESIAN_POINT ( 'NONE',  ( 4.483927247898545687, 16.52544592524342804, 114.7905762719810383 ) ) ;
#145097 = CARTESIAN_POINT ( 'NONE',  ( 9.564922557960805705, 16.46253265017160317, 74.58224293864769550 ) ) ;
#145099 = CARTESIAN_POINT ( 'NONE',  ( 29.86685920354754487, 21.69954338932564752, -9.424999997268814766 ) ) ;
#145098 = CARTESIAN_POINT ( 'NONE',  ( 4.483927247898790824, -16.52544592524335698, 25.20942372801901854 ) ) ;
#145100 = CARTESIAN_POINT ( 'NONE',  ( -21.53943276465977519, -0.05219959533937600094, 113.7510903946856757 ) ) ;
#145101 = CARTESIAN_POINT ( 'NONE',  ( -16.52544592524335698, -4.483927247898792601, 78.95942372801901854 ) ) ;
#145102 = CARTESIAN_POINT ( 'NONE',  ( 19.05341960407617918, -5.049401038297876454, 91.04275706135234714 ) ) ;
#145103 = CARTESIAN_POINT ( 'NONE',  ( 16.55341960407611168, 4.379528057220329451, 113.9572429386477239 ) ) ;
#145104 = CARTESIAN_POINT ( 'NONE',  ( -0.05219959533934338120, 16.53943276465976808, 67.50109039468568994 ) ) ;
#145105 = CARTESIAN_POINT ( 'NONE',  ( 4.379528057220092307, 16.55341960407617563, 47.29275706135234003 ) ) ;
#145106 = DIRECTION ( 'NONE',  ( -0.000000000000000000, -0.9396926207858838920, 0.3420201433257362145 ) ) ;
#145107 = CARTESIAN_POINT ( 'NONE',  ( -0.05219959533936034679, 19.03943276465977164, 67.50109039468566152 ) ) ;
#145108 = CARTESIAN_POINT ( 'NONE',  ( -21.53943276465977519, -0.05219959533937600094, 103.7510903946857042 ) ) ;
#145109 = CARTESIAN_POINT ( 'NONE',  ( -0.05219959533909027116, -19.03943276465977164, 32.49890960531435979 ) ) ;
#145110 = CARTESIAN_POINT ( 'NONE',  ( 19.05341960407611168, 5.049401038298154454, 83.95724293864766707 ) ) ;
#145111 = CARTESIAN_POINT ( 'NONE',  ( 4.483927247898545687, 16.52544592524342804, 74.79057627198105251 ) ) ;
#145112 = CARTESIAN_POINT ( 'NONE',  ( -5.719274019375665041, -21.55341960407619695, 89.79275706135236135 ) ) ;
#145113 = CARTESIAN_POINT ( 'NONE',  ( 5.049401038297881783, 19.05341960407617563, 47.29275706135231161 ) ) ;
#145114 = CARTESIAN_POINT ( 'NONE',  ( -5.719274019375978568, 21.55341960407610458, 35.20724293864768839 ) ) ;
#145115 = CARTESIAN_POINT ( 'NONE',  ( 18.62759615963255655, 10.81492255796105972, 106.6677570613523756 ) ) ;
#145116 = CARTESIAN_POINT ( 'NONE',  ( -9.564922557960796823, -16.46253265017161027, 82.08224293864768129 ) ) ;
#145117 = EDGE_CURVE ( 'NONE', #44838, #69503, #156690, .T. ) ;
#145118 = CARTESIAN_POINT ( 'NONE',  ( -18.62759615963255300, -10.81492255796106328, 109.1677570613523613 ) ) ;
#145119 = CARTESIAN_POINT ( 'NONE',  ( -10.81492255796078084, -18.62759615963271287, 47.08224293864770260 ) ) ;
#145120 = CARTESIAN_POINT ( 'NONE',  ( -5.049401038298153566, 19.05341960407611168, 95.20724293864770971 ) ) ;
#145121 = CARTESIAN_POINT ( 'NONE',  ( 19.03943276465977164, 0.05219959533936151252, 81.25109039468567573 ) ) ;
#145122 = CARTESIAN_POINT ( 'NONE',  ( 13.97604488694527802, 13.89961937509977652, 109.3739096053143669 ) ) ;
#145123 = CARTESIAN_POINT ( 'NONE',  ( -19.05341960407617563, 5.049401038297882671, 98.54275706135233293 ) ) ;
#145124 = CARTESIAN_POINT ( 'NONE',  ( -0.05219959533934338120, 16.53943276465976808, 42.50109039468567573 ) ) ;
#145125 = CARTESIAN_POINT ( 'NONE',  ( 14.34966873604960469, 8.224510206698951720, 114.1655762719810383 ) ) ;
#145126 = CARTESIAN_POINT ( 'NONE',  ( 16.46253265017160672, -9.564922557960803928, 78.33224293864769550 ) ) ;
#145127 = CARTESIAN_POINT ( 'NONE',  ( 21.52544592524344225, -5.823673210054117533, 63.54057627198103830 ) ) ;
#145128 = AXIS2_PLACEMENT_3D ( 'NONE', #25517, #41669, #198320 ) ;
#145129 = CARTESIAN_POINT ( 'NONE',  ( 16.52544592524335698, 4.483927247898782831, 26.45942372801901854 ) ) ;
#145130 = CARTESIAN_POINT ( 'NONE',  ( -21.55341960407619339, 5.719274019375674811, 28.54275706135234358 ) ) ;
#145131 = CARTESIAN_POINT ( 'NONE',  ( -15.80617190586768217, 15.72974639402176855, 78.12609039468570415 ) ) ;
#145132 = CARTESIAN_POINT ( 'NONE',  ( 4.379528057220092307, 16.55341960407617563, 82.29275706135234714 ) ) ;
#145133 = CARTESIAN_POINT ( 'NONE',  ( -5.153800228976328057, -19.02544592524343514, 92.29057627198099567 ) ) ;
#145134 = CARTESIAN_POINT ( 'NONE',  ( 4.483927247898545687, 16.52544592524342804, 74.79057627198105251 ) ) ;
#145135 = CARTESIAN_POINT ( 'NONE',  ( -16.55341960407611168, -4.379528057220339221, 21.45724293864769550 ) ) ;
#145136 = CARTESIAN_POINT ( 'NONE',  ( -16.46253265017146816, -9.564922557961047289, 54.16775706135234003 ) ) ;
#145137 = CARTESIAN_POINT ( 'NONE',  ( 10.72451020669871369, 18.67979575497193778, 42.08442372801901854 ) ) ;
#145138 = CARTESIAN_POINT ( 'NONE',  ( 16.53943276465976808, -0.05219959533910856209, 78.74890960531436690 ) ) ;
#145139 = CARTESIAN_POINT ( 'NONE',  ( 21.52544592524344225, -5.823673210054117533, 23.54057627198102765 ) ) ;
#145140 = CARTESIAN_POINT ( 'NONE',  ( 8.224510206698742110, 14.34966873604972548, 97.08442372801904696 ) ) ;
#145141 = CARTESIAN_POINT ( 'NONE',  ( 15.72974639402176855, 15.80617190586768217, 91.87609039468568994 ) ) ;
#145142 = CARTESIAN_POINT ( 'NONE',  ( 16.55341960407618274, -4.379528057220086978, 46.04275706135234714 ) ) ;
#145143 = CARTESIAN_POINT ( 'NONE',  ( 21.52544592524334988, 5.823673210054432836, 46.45942372801901854 ) ) ;
#145144 = ORIENTED_EDGE ( 'NONE', *, *, #42515, .T. ) ;
#145145 = CARTESIAN_POINT ( 'NONE',  ( -21.55341960407610458, -5.719274019375992779, 111.4572429386476813 ) ) ;
#145146 = CARTESIAN_POINT ( 'NONE',  ( -8.314922557960811034, -14.29746914071050412, 97.08224293864770971 ) ) ;
#145147 = CARTESIAN_POINT ( 'NONE',  ( 17.50000000000000711, -3.305555262949588791, 27.12517152156594591 ) ) ;
#145148 = CARTESIAN_POINT ( 'NONE',  ( 4.379528057220339221, -16.55341960407611168, 47.70724293864770260 ) ) ;
#145149 = CARTESIAN_POINT ( 'NONE',  ( 8.314922557961029526, -14.29746914071037800, 95.41775706135234714 ) ) ;
#145150 = CARTESIAN_POINT ( 'NONE',  ( 19.05341960407611168, 5.049401038298154454, 43.95724293864769550 ) ) ;
#145151 = CARTESIAN_POINT ( 'NONE',  ( 5.719274019375991003, -21.55341960407610458, 42.70724293864770260 ) ) ;
#145152 = CARTESIAN_POINT ( 'NONE',  ( -0.05219959533910754901, -16.53943276465976808, 72.49890960531435269 ) ) ;
#145153 = VECTOR ( 'NONE', #19050, 1000.000000000000000 ) ;
#145154 = CARTESIAN_POINT ( 'NONE',  ( -18.67979575497178146, -10.72451020669898902, 76.66557627198103830 ) ) ;
#145155 = CARTESIAN_POINT ( 'NONE',  ( 5.153800228976335163, 19.02544592524342804, 89.79057627198102409 ) ) ;
#145157 = CARTESIAN_POINT ( 'NONE',  ( -0.05219959533936034679, 19.03943276465977164, 92.50109039468566152 ) ) ;
#145156 = CARTESIAN_POINT ( 'NONE',  ( -13.97604488694527625, -13.89961937509977652, 41.87390960531435979 ) ) ;
#145158 = CARTESIAN_POINT ( 'NONE',  ( 21.55341960407610458, 5.719274019375980345, 33.95724293864769550 ) ) ;
#145159 = CARTESIAN_POINT ( 'NONE',  ( 10.81492255796106328, -18.62759615963255655, 60.41775706135235424 ) ) ;
#145160 = CARTESIAN_POINT ( 'NONE',  ( 9.564922557960805705, 16.46253265017160317, 54.58224293864769550 ) ) ;
#145161 = CARTESIAN_POINT ( 'NONE',  ( -13.97604488694527625, -13.89961937509977652, 91.87390960531432427 ) ) ;
#145162 = ORIENTED_EDGE ( 'NONE', *, *, #22998, .T. ) ;
#145163 = CARTESIAN_POINT ( 'NONE',  ( -16.52544592524335698, -4.483927247898792601, 53.95942372801900433 ) ) ;
#145164 = CARTESIAN_POINT ( 'NONE',  ( 15.80617190586769283, -15.72974639402175789, 35.62609039468568994 ) ) ;
#145165 = CARTESIAN_POINT ( 'NONE',  ( 18.67979575497194134, -10.72451020669871369, 70.83442372801901854 ) ) ;
#145166 = CARTESIAN_POINT ( 'NONE',  ( -5.823673210054116645, -21.52544592524344225, 27.29057627198103120 ) ) ;
#145167 = CARTESIAN_POINT ( 'NONE',  ( -10.72451020669898014, 18.67979575497178502, 90.41557627198103830 ) ) ;
#145169 = CARTESIAN_POINT ( 'NONE',  ( 14.29746914071037800, 8.314922557961029526, 66.66775706135234714 ) ) ;
#145168 = CARTESIAN_POINT ( 'NONE',  ( 15.72974639402176855, 15.80617190586768217, 21.87609039468567573 ) ) ;
#145170 = CARTESIAN_POINT ( 'NONE',  ( -5.823673210054116645, -21.52544592524344225, 57.29057627198103120 ) ) ;
#145171 = CARTESIAN_POINT ( 'NONE',  ( 16.46253265017146816, 9.564922557961045513, 26.66775706135234003 ) ) ;
#145172 = CARTESIAN_POINT ( 'NONE',  ( 16.46253265017160672, -9.564922557960803928, 63.33224293864769550 ) ) ;
#145173 = CARTESIAN_POINT ( 'NONE',  ( 13.89961937509977652, -13.97604488694527269, 108.1239096053143669 ) ) ;
#145174 = CARTESIAN_POINT ( 'NONE',  ( 13.89961937509977652, -13.97604488694527269, 93.12390960531436690 ) ) ;
#145175 = DIRECTION ( 'NONE',  ( -6.938893903907227392E-16, -0.7071067811865483499, -0.7071067811865465735 ) ) ;
#145176 = CARTESIAN_POINT ( 'NONE',  ( 13.97604488694548053, -13.89961937509957401, 75.62609039468564731 ) ) ;
#145177 = CARTESIAN_POINT ( 'NONE',  ( -10.72451020669898014, 18.67979575497178502, 40.41557627198103120 ) ) ;
#145178 = CARTESIAN_POINT ( 'NONE',  ( 14.29746914071037800, 8.314922557961029526, 111.6677570613523613 ) ) ;
#145179 = CARTESIAN_POINT ( 'NONE',  ( 16.46253265017146816, 9.564922557961045513, 96.66775706135233293 ) ) ;
#145180 = CARTESIAN_POINT ( 'NONE',  ( 13.89961937509977652, -13.97604488694527269, 23.12390960531436335 ) ) ;
#145181 = CARTESIAN_POINT ( 'NONE',  ( 19.05341960407617918, -5.049401038297876454, 96.04275706135231871 ) ) ;
#145183 = CARTESIAN_POINT ( 'NONE',  ( -13.89961937509957401, -13.97604488694547875, 64.37609039468567573 ) ) ;
#145182 = CARTESIAN_POINT ( 'NONE',  ( 18.67979575497178502, 10.72451020669898547, 84.16557627198103830 ) ) ;
#145184 = CARTESIAN_POINT ( 'NONE',  ( -32.00000000000000711, -1.163414459189985801E-14, 95.00000000000000000 ) ) ;
#145185 = CARTESIAN_POINT ( 'NONE',  ( -19.03943276465977164, 0.05219959533909376836, 56.24890960531435979 ) ) ;
#145186 = CARTESIAN_POINT ( 'NONE',  ( -8.314922557960811034, -14.29746914071050412, 67.08224293864770971 ) ) ;
#145187 = CARTESIAN_POINT ( 'NONE',  ( 13.89961937509977652, -13.97604488694527269, 43.12390960531434558 ) ) ;
#145188 = CARTESIAN_POINT ( 'NONE',  ( 14.29746914071049879, -8.314922557960816363, 58.33224293864768839 ) ) ;
#145189 = CARTESIAN_POINT ( 'NONE',  ( -28.30127546286004403, -27.84967942650712303, -20.15398247455540215 ) ) ;
#145190 = CARTESIAN_POINT ( 'NONE',  ( 32.15403441185031141, -4.954129643790904147, 89.34785441345067625 ) ) ;
#145191 = CARTESIAN_POINT ( 'NONE',  ( -4.483927247898539470, -16.52544592524342804, 27.29057627198103120 ) ) ;
#145192 = CARTESIAN_POINT ( 'NONE',  ( 9.564922557960805705, 16.46253265017160317, 69.58224293864770971 ) ) ;
#145193 = DIRECTION ( 'NONE',  ( 0.000000000000000000, -1.000000000000000000, 0.000000000000000000 ) ) ;
#145194 = CARTESIAN_POINT ( 'NONE',  ( -19.02544592524334988, -5.153800228976617603, 23.95942372801900078 ) ) ;
#145195 = CARTESIAN_POINT ( 'NONE',  ( -16.55341960407617563, 4.379528057220093196, 43.54275706135235424 ) ) ;
#145196 = CARTESIAN_POINT ( 'NONE',  ( 21.52544592524344225, -5.823673210054117533, 53.54057627198103120 ) ) ;
#145198 = VERTEX_POINT ( 'NONE', #177568 ) ;
#145197 = CARTESIAN_POINT ( 'NONE',  ( 10.81492255796106328, -18.62759615963255655, 100.4177570613523471 ) ) ;
#145199 = CARTESIAN_POINT ( 'NONE',  ( 5.049401038298161559, -19.05341960407611168, 57.70724293864769550 ) ) ;
#145200 = CARTESIAN_POINT ( 'NONE',  ( 0.000000000000000000, 0.000000000000000000, -49.67367017693150189 ) ) ;
#145201 = CARTESIAN_POINT ( 'NONE',  ( -0.05219959533909027116, -19.03943276465977164, 102.4989096053143669 ) ) ;
#145202 = FACE_OUTER_BOUND ( 'NONE', #150544, .T. ) ;
#145203 = CARTESIAN_POINT ( 'NONE',  ( -10.72451020669870658, -18.67979575497194134, 24.58442372801901499 ) ) ;
#145204 = CARTESIAN_POINT ( 'NONE',  ( -0.05219959533910754901, -16.53943276465976808, 87.49890960531436690 ) ) ;
#145206 = CARTESIAN_POINT ( 'NONE',  ( -19.02544592524342804, 5.153800228976336051, 81.04057627198103830 ) ) ;
#145205 = CARTESIAN_POINT ( 'NONE',  ( 10.72451020669898902, -18.67979575497178502, 87.91557627198103830 ) ) ;
#145207 = CARTESIAN_POINT ( 'NONE',  ( 19.03943276465977164, -0.05219959533909143690, 88.74890960531436690 ) ) ;
#145208 = CARTESIAN_POINT ( 'NONE',  ( -10.72451020669898014, 18.67979575497178502, 105.4155762719810383 ) ) ;
#145209 = EDGE_CURVE ( 'NONE', #20330, #29984, #4683, .T. ) ;
#145210 = VERTEX_POINT ( 'NONE', #67365 ) ;
#145211 = CARTESIAN_POINT ( 'NONE',  ( 16.51473224551069308, 9.474510206698969483, 69.16557627198102409 ) ) ;
#145212 = CARTESIAN_POINT ( 'NONE',  ( 19.25663599770060586, -5.499999999999437783, 96.49419308057204603 ) ) ;
#145214 = CARTESIAN_POINT ( 'NONE',  ( 5.049401038298161559, -19.05341960407611168, 37.70724293864768839 ) ) ;
#145213 = CARTESIAN_POINT ( 'NONE',  ( -12.14591786802309592, -12.06949235617757132, 106.8739096053143811 ) ) ;
#145215 = CARTESIAN_POINT ( 'NONE',  ( 19.03943276465977164, 0.05219959533936151252, 96.25109039468567573 ) ) ;
#145216 = CARTESIAN_POINT ( 'NONE',  ( -4.483927247898539470, -16.52544592524342804, 107.2905762719810525 ) ) ;
#145217 = CARTESIAN_POINT ( 'NONE',  ( 21.52544592524334988, 5.823673210054432836, 66.45942372801903275 ) ) ;
#145219 = CARTESIAN_POINT ( 'NONE',  ( 5.719274019375673035, 21.55341960407619339, 37.29275706135235424 ) ) ;
#145218 = CARTESIAN_POINT ( 'NONE',  ( 16.46253265017160672, -9.564922557960803928, 58.33224293864769550 ) ) ;
#145220 = CARTESIAN_POINT ( 'NONE',  ( -10.72451020669898014, 18.67979575497178502, 105.4155762719810383 ) ) ;
#145221 = FACE_OUTER_BOUND ( 'NONE', #20388, .T. ) ;
#145222 = CARTESIAN_POINT ( 'NONE',  ( 16.46253265017160672, -9.564922557960803928, 73.33224293864769550 ) ) ;
#145223 = CARTESIAN_POINT ( 'NONE',  ( -19.99999999999998224, -190.0000000000000000, -15.00000000000000178 ) ) ;
#145225 = CARTESIAN_POINT ( 'NONE',  ( -18.67979575497178146, -10.72451020669898902, 26.66557627198103475 ) ) ;
#145224 = CARTESIAN_POINT ( 'NONE',  ( 12.06949235617739724, 12.14591786802326823, 26.87609039468567218 ) ) ;
#145226 = CARTESIAN_POINT ( 'NONE',  ( -15.72974639402176322, -15.80617190586768395, 64.37609039468568994 ) ) ;
#145227 = CARTESIAN_POINT ( 'NONE',  ( 19.05341960407611168, 5.049401038298154454, 108.9572429386477097 ) ) ;
#145228 = CARTESIAN_POINT ( 'NONE',  ( -16.46253265017146816, -9.564922557961047289, 94.16775706135233293 ) ) ;
#145229 = CARTESIAN_POINT ( 'NONE',  ( -0.05219959533909027116, -19.03943276465977164, 42.49890960531435269 ) ) ;
#145230 = CARTESIAN_POINT ( 'NONE',  ( 19.05341960407611168, 5.049401038298154454, 68.95724293864769550 ) ) ;
#145231 = CARTESIAN_POINT ( 'NONE',  ( -16.55341960407611168, -4.379528057220339221, 91.45724293864769550 ) ) ;
#145232 = CARTESIAN_POINT ( 'NONE',  ( 5.049401038298161559, -19.05341960407611168, 102.7072429386476955 ) ) ;
#145233 = CARTESIAN_POINT ( 'NONE',  ( 4.483927247898545687, 16.52544592524342804, 94.79057627198105251 ) ) ;
#145235 = EDGE_CURVE ( 'NONE', #46465, #104408, #95716, .T. ) ;
#145234 = CARTESIAN_POINT ( 'NONE',  ( -16.51473224551069308, -9.474510206698971260, 96.66557627198102409 ) ) ;
#145237 = CARTESIAN_POINT ( 'NONE',  ( 16.51473224551069308, 9.474510206698969483, 39.16557627198103120 ) ) ;
#145236 = CARTESIAN_POINT ( 'NONE',  ( 12.14591786802309770, 12.06949235617756955, 54.37390960531435979 ) ) ;
#145238 = CARTESIAN_POINT ( 'NONE',  ( 10.81492255796106328, -18.62759615963255655, 55.41775706135234714 ) ) ;
#145239 = CARTESIAN_POINT ( 'NONE',  ( -19.02544592524334988, -5.153800228976617603, 98.95942372801900433 ) ) ;
#145240 = CARTESIAN_POINT ( 'NONE',  ( -14.29746914071049879, 8.314922557960819915, 50.83224293864770971 ) ) ;
#145241 = CARTESIAN_POINT ( 'NONE',  ( 21.53943276465977519, -0.05219959533907433946, 113.7489096053143527 ) ) ;
#145242 = CARTESIAN_POINT ( 'NONE',  ( 15.72974639402199770, -15.80617190586745480, 43.12390960531435269 ) ) ;
#145244 = CARTESIAN_POINT ( 'NONE',  ( -16.55341960407611168, -4.379528057220339221, 86.45724293864770971 ) ) ;
#145243 = CARTESIAN_POINT ( 'NONE',  ( -5.153800228976328057, -19.02544592524343514, 107.2905762719810383 ) ) ;
#145245 = CARTESIAN_POINT ( 'NONE',  ( 1.993301997531345292E-15, -30.30510711980685912, 142.7500000054623683 ) ) ;
#145246 = CARTESIAN_POINT ( 'NONE',  ( 9.564922557960805705, 16.46253265017160317, 59.58224293864769550 ) ) ;
#145247 = CARTESIAN_POINT ( 'NONE',  ( 14.34966873604972726, -8.224510206698740333, 110.8344237280190043 ) ) ;
#145248 = CARTESIAN_POINT ( 'NONE',  ( 12.14591786802327356, -12.06949235617739191, 100.6260903946857184 ) ) ;
#145249 = CARTESIAN_POINT ( 'NONE',  ( -8.314922557961024197, 14.29746914071037800, 82.91775706135234714 ) ) ;
#145250 = CARTESIAN_POINT ( 'NONE',  ( 13.97604488694548053, -13.89961937509957401, 40.62609039468564731 ) ) ;
#145251 = CARTESIAN_POINT ( 'NONE',  ( -24.75981411741738469, -6.635778407390994893, 167.9383864321132762 ) ) ;
#145252 = CARTESIAN_POINT ( 'NONE',  ( -19.03943276465977164, 0.05219959533909376836, 91.24890960531436690 ) ) ;
#145253 = CARTESIAN_POINT ( 'NONE',  ( 5.049401038298161559, -19.05341960407611168, 52.70724293864767418 ) ) ;
#145254 = CARTESIAN_POINT ( 'NONE',  ( -12.14591786802309592, -12.06949235617757132, 61.87390960531436690 ) ) ;
#145256 = CARTESIAN_POINT ( 'NONE',  ( -19.05341960407611168, -5.049401038298163336, 106.4572429386476955 ) ) ;
#145255 = DIRECTION ( 'NONE',  ( -1.000000000000000000, 0.000000000000000000, -6.982962677686266711E-15 ) ) ;
#145257 = CARTESIAN_POINT ( 'NONE',  ( -5.823673210054116645, -21.52544592524344225, 37.29057627198102409 ) ) ;
#145258 = CARTESIAN_POINT ( 'NONE',  ( 8.224510206698953496, -14.34966873604960469, 82.91557627198103830 ) ) ;
#145259 = CARTESIAN_POINT ( 'NONE',  ( 4.483927247898790824, -16.52544592524335698, 40.20942372801901854 ) ) ;
#145260 = CARTESIAN_POINT ( 'NONE',  ( -4.483927247898539470, -16.52544592524342804, 77.29057627198102409 ) ) ;
#145261 = PLANE ( 'NONE',  #102781 ) ;
#145262 = CARTESIAN_POINT ( 'NONE',  ( 9.474510206698729675, 16.51473224551082808, 72.08442372801900433 ) ) ;
#145263 = CARTESIAN_POINT ( 'NONE',  ( -9.564922557960796823, -16.46253265017161027, 97.08224293864769550 ) ) ;
#145264 = CARTESIAN_POINT ( 'NONE',  ( -16.51473224551082808, 9.474510206698731452, 78.33442372801900433 ) ) ;
#145265 = CARTESIAN_POINT ( 'NONE',  ( -22.45862007004993188, 20.33413869251830164, -51.11888769873471006 ) ) ;
#145266 = VECTOR ( 'NONE', #136029, 1000.000000000000000 ) ;
#145268 = CARTESIAN_POINT ( 'NONE',  ( 0.05219959533934541429, -16.53943276465976808, 105.0010903946856757 ) ) ;
#145267 = CARTESIAN_POINT ( 'NONE',  ( 16.55341960407618274, -4.379528057220086978, 26.04275706135235779 ) ) ;
#145269 = CARTESIAN_POINT ( 'NONE',  ( 13.89961937509957401, 13.97604488694547697, 71.87609039468567573 ) ) ;
#145270 = CARTESIAN_POINT ( 'NONE',  ( 0.05219959533907565091, 21.53943276465977519, 34.99890960531435979 ) ) ;
#145271 = CARTESIAN_POINT ( 'NONE',  ( 0.05219959533937995610, -21.53943276465977519, 75.00109039468568994 ) ) ;
#145272 = CARTESIAN_POINT ( 'NONE',  ( 8.906447517083057264, -27.41122689804191026, 146.8500000054623627 ) ) ;
#145273 = CARTESIAN_POINT ( 'NONE',  ( 4.379528057220092307, 16.55341960407617563, 22.29275706135235069 ) ) ;
#145275 = CARTESIAN_POINT ( 'NONE',  ( 9.564922557960805705, 16.46253265017160317, 94.58224293864769550 ) ) ;
#145274 = CYLINDRICAL_SURFACE ( 'NONE', #95957, 0.5000000000000017764 ) ;
#145276 = CARTESIAN_POINT ( 'NONE',  ( -19.05341960407611168, -5.049401038298163336, 21.45724293864768839 ) ) ;
#145277 = CARTESIAN_POINT ( 'NONE',  ( -4.483927247898539470, -16.52544592524342804, 92.29057627198103830 ) ) ;
#145278 = CARTESIAN_POINT ( 'NONE',  ( 16.46253265017160672, -9.564922557960803928, 83.33224293864768129 ) ) ;
#145279 = VERTEX_POINT ( 'NONE', #114870 ) ;
#145280 = CARTESIAN_POINT ( 'NONE',  ( 0.05219959533936267826, -19.03943276465977164, 105.0010903946856615 ) ) ;
#145281 = CARTESIAN_POINT ( 'NONE',  ( -21.53943276465977519, 0.05219959533907696930, 81.24890960531436690 ) ) ;
#145282 = CARTESIAN_POINT ( 'NONE',  ( -9.564922557960796823, -16.46253265017161027, 47.08224293864769550 ) ) ;
#145284 = CARTESIAN_POINT ( 'NONE',  ( 5.823673210054125526, 21.52544592524343514, 114.7905762719810383 ) ) ;
#145283 = CARTESIAN_POINT ( 'NONE',  ( -13.89961937509957401, -13.97604488694547875, 69.37609039468564731 ) ) ;
#145285 = CARTESIAN_POINT ( 'NONE',  ( -16.46253265017160317, 9.564922557960807481, 75.83224293864769550 ) ) ;
#145286 = CARTESIAN_POINT ( 'NONE',  ( 13.89961937509977652, -13.97604488694527269, 103.1239096053143527 ) ) ;
#145287 = ORIENTED_EDGE ( 'NONE', *, *, #34066, .T. ) ;
#145288 = CARTESIAN_POINT ( 'NONE',  ( -14.29746914071037622, -8.314922557961029526, 39.16775706135235424 ) ) ;
#145289 = CARTESIAN_POINT ( 'NONE',  ( -21.53943276465977519, 0.05219959533907696930, 106.2489096053143811 ) ) ;
#145292 = CARTESIAN_POINT ( 'NONE',  ( -16.51473224551082808, 9.474510206698731452, 68.33442372801900433 ) ) ;
#145291 = CARTESIAN_POINT ( 'NONE',  ( -0.05219959533909027116, -19.03943276465977164, 87.49890960531436690 ) ) ;
#145290 = CARTESIAN_POINT ( 'NONE',  ( -16.52544592524342804, 4.483927247898546575, 111.0405762719810525 ) ) ;
#145293 = CARTESIAN_POINT ( 'NONE',  ( 5.823673210054125526, 21.52544592524343514, 89.79057627198103830 ) ) ;
#145294 = CARTESIAN_POINT ( 'NONE',  ( -21.55341960407610458, -5.719274019375992779, 71.45724293864769550 ) ) ;
#145295 = CARTESIAN_POINT ( 'NONE',  ( -16.52544592524342804, 4.483927247898546575, 46.04057627198103830 ) ) ;
#145296 = CARTESIAN_POINT ( 'NONE',  ( -21.55341960407619339, 5.719274019375674811, 113.5427570613523756 ) ) ;
#145297 = CARTESIAN_POINT ( 'NONE',  ( -12.06949235617739369, -12.14591786802326823, 69.37609039468567573 ) ) ;
#145298 = CARTESIAN_POINT ( 'NONE',  ( -16.51473224551069308, -9.474510206698971260, 86.66557627198102409 ) ) ;
#145299 = CARTESIAN_POINT ( 'NONE',  ( -13.97604488694527625, -13.89961937509977652, 46.87390960531435979 ) ) ;
#145300 = CARTESIAN_POINT ( 'NONE',  ( -0.05219959533937732626, 21.53943276465977519, 57.50109039468568994 ) ) ;
#145301 = CARTESIAN_POINT ( 'NONE',  ( -5.823673210054431948, 21.52544592524334988, 72.70942372801901854 ) ) ;
#145302 = CARTESIAN_POINT ( 'NONE',  ( -19.03943276465977164, 0.05219959533909376836, 56.24890960531435979 ) ) ;
#145303 = CARTESIAN_POINT ( 'NONE',  ( -15.72974639402176322, -15.80617190586768395, 39.37609039468567573 ) ) ;
#145304 = CARTESIAN_POINT ( 'NONE',  ( 5.049401038297881783, 19.05341960407617563, 77.29275706135231871 ) ) ;
#145305 = CARTESIAN_POINT ( 'NONE',  ( -19.02544592524334988, -5.153800228976617603, 68.95942372801896170 ) ) ;
#145306 = CARTESIAN_POINT ( 'NONE',  ( -9.474510206698964154, 16.51473224551069663, 35.41557627198102409 ) ) ;
#145307 = CARTESIAN_POINT ( 'NONE',  ( 16.55341960407618274, -4.379528057220086978, 81.04275706135236135 ) ) ;
#145308 = CARTESIAN_POINT ( 'NONE',  ( -9.474510206698964154, 16.51473224551069663, 55.41557627198103120 ) ) ;
#145309 = CARTESIAN_POINT ( 'NONE',  ( 24.20757866959953120, -5.698759791481386117, 172.9004493943156433 ) ) ;
#145310 = CARTESIAN_POINT ( 'NONE',  ( 9.474510206698971260, -16.51473224551069308, 97.91557627198102409 ) ) ;
#145311 = CARTESIAN_POINT ( 'NONE',  ( 0.05219959533909260263, 19.03943276465977164, 44.99890960531435979 ) ) ;
#145312 = CARTESIAN_POINT ( 'NONE',  ( -5.823673210054116645, -21.52544592524344225, 92.29057627198103830 ) ) ;
#145313 = CARTESIAN_POINT ( 'NONE',  ( -16.55341960407617563, 4.379528057220093196, 63.54275706135234003 ) ) ;
#145314 = CARTESIAN_POINT ( 'NONE',  ( 18.67979575497194134, -10.72451020669871369, 110.8344237280190043 ) ) ;
#145315 = EDGE_CURVE ( 'NONE', #148642, #57253, #192723, .T. ) ;
#145316 = CARTESIAN_POINT ( 'NONE',  ( 13.89961937509977652, -13.97604488694527269, 48.12390960531435979 ) ) ;
#145317 = CARTESIAN_POINT ( 'NONE',  ( 4.483927247898545687, 16.52544592524342804, 49.79057627198102409 ) ) ;
#145318 = CARTESIAN_POINT ( 'NONE',  ( 4.379528057220339221, -16.55341960407611168, 77.70724293864770971 ) ) ;
#145319 = CARTESIAN_POINT ( 'NONE',  ( 19.05341960407611168, 5.049401038298154454, 78.95724293864769550 ) ) ;
#145320 = CARTESIAN_POINT ( 'NONE',  ( 21.52544592524334988, 5.823673210054432836, 36.45942372801901143 ) ) ;
#145321 = CARTESIAN_POINT ( 'NONE',  ( -5.153800228976328057, -19.02544592524343514, 92.29057627198099567 ) ) ;
#145322 = CARTESIAN_POINT ( 'NONE',  ( -10.81492255796105439, 18.62759615963255655, 102.9177570613523756 ) ) ;
#145323 = CARTESIAN_POINT ( 'NONE',  ( 16.55341960407618274, -4.379528057220086978, 81.04275706135236135 ) ) ;
#145324 = CARTESIAN_POINT ( 'NONE',  ( -10.81492255796105439, 18.62759615963255655, 32.91775706135234714 ) ) ;
#145325 = CARTESIAN_POINT ( 'NONE',  ( 9.474510206698971260, -16.51473224551069308, 107.9155762719810383 ) ) ;
#145326 = EDGE_CURVE ( 'NONE', #177515, #86241, #3699, .T. ) ;
#145327 = CARTESIAN_POINT ( 'NONE',  ( 0.05219959533907565091, 21.53943276465977519, 94.99890960531436690 ) ) ;
#145328 = CARTESIAN_POINT ( 'NONE',  ( -14.34966873604960291, -8.224510206698953496, 51.66557627198102409 ) ) ;
#145329 = CARTESIAN_POINT ( 'NONE',  ( -5.153800228976328057, -19.02544592524343514, 42.29057627198101699 ) ) ;
#145330 = CARTESIAN_POINT ( 'NONE',  ( 4.483927247898545687, 16.52544592524342804, 64.79057627198103830 ) ) ;
#145331 = CARTESIAN_POINT ( 'NONE',  ( -10.72451020669898014, 18.67979575497178502, 35.41557627198102409 ) ) ;
#145332 = CARTESIAN_POINT ( 'NONE',  ( -16.51473224551082808, 9.474510206698731452, 33.33442372801899722 ) ) ;
#145333 = CARTESIAN_POINT ( 'NONE',  ( 14.34966873604960469, 8.224510206698951720, 94.16557627198103830 ) ) ;
#145334 = CARTESIAN_POINT ( 'NONE',  ( -9.474510206698964154, 16.51473224551069663, 105.4155762719810383 ) ) ;
#145335 = VERTEX_POINT ( 'NONE', #36029 ) ;
#145336 = CARTESIAN_POINT ( 'NONE',  ( 16.53943276465976808, 0.05219959533934440121, 51.25109039468568994 ) ) ;
#145337 = CARTESIAN_POINT ( 'NONE',  ( 13.97604488694527802, 13.89961937509977652, 54.37390960531435979 ) ) ;
#145338 = CARTESIAN_POINT ( 'NONE',  ( -22.44159573604009950, -16.30477369853688430, 139.0750000027311728 ) ) ;
#145339 = CARTESIAN_POINT ( 'NONE',  ( -8.314922557961024197, 14.29746914071037800, 87.91775706135234714 ) ) ;
#145340 = CARTESIAN_POINT ( 'NONE',  ( 9.564922557961047289, -16.46253265017146816, 105.4177570613523471 ) ) ;
#145341 = CARTESIAN_POINT ( 'NONE',  ( 0.05219959533937995610, -21.53943276465977519, 80.00109039468568994 ) ) ;
#145342 = CARTESIAN_POINT ( 'NONE',  ( -5.049401038298153566, 19.05341960407611168, 70.20724293864769550 ) ) ;
#145343 = CARTESIAN_POINT ( 'NONE',  ( 18.62759615963271287, -10.81492255796078972, 103.3322429386476955 ) ) ;
#145344 = CARTESIAN_POINT ( 'NONE',  ( 12.06949235617739724, 12.14591786802326823, 51.87609039468568284 ) ) ;
#145345 = CARTESIAN_POINT ( 'NONE',  ( -16.55341960407611168, -4.379528057220339221, 106.4572429386477097 ) ) ;
#145346 = CARTESIAN_POINT ( 'NONE',  ( -12.06949235617739369, -12.14591786802326823, 19.37609039468568639 ) ) ;
#145347 = CARTESIAN_POINT ( 'NONE',  ( -5.049401038297874678, -19.05341960407617918, 79.79275706135233293 ) ) ;
#145348 = CARTESIAN_POINT ( 'NONE',  ( 10.81492255796078972, 18.62759615963270932, 79.58224293864769550 ) ) ;
#145349 = CARTESIAN_POINT ( 'NONE',  ( 19.05341960407617918, -5.049401038297876454, 51.04275706135231871 ) ) ;
#145350 = CARTESIAN_POINT ( 'NONE',  ( -19.03943276465977164, 0.05219959533909376836, 116.2489096053143669 ) ) ;
#145351 = CARTESIAN_POINT ( 'NONE',  ( 18.67979575497178502, 10.72451020669898547, 104.1655762719810241 ) ) ;
#145352 = CARTESIAN_POINT ( 'NONE',  ( 17.50000000000003553, 4.658240926743142829, 28.55529582183200077 ) ) ;
#145353 = CARTESIAN_POINT ( 'NONE',  ( -19.05341960407611168, -5.049401038298163336, 71.45724293864766707 ) ) ;
#145354 = CARTESIAN_POINT ( 'NONE',  ( -17.49999999999999645, -5.500000000000020428, 61.28230962303567964 ) ) ;
#145355 = CARTESIAN_POINT ( 'NONE',  ( -0.05219959533934338120, 16.53943276465976808, 22.50109039468567573 ) ) ;
#145356 = CARTESIAN_POINT ( 'NONE',  ( 22.77340731150488651, 12.66915506687109350, 165.5704399981227368 ) ) ;
#145357 = CARTESIAN_POINT ( 'NONE',  ( -0.05219959533937732626, 21.53943276465977519, 52.50109039468567573 ) ) ;
#145359 = CARTESIAN_POINT ( 'NONE',  ( 16.55341960407611168, 4.379528057220329451, 68.95724293864769550 ) ) ;
#145358 = CARTESIAN_POINT ( 'NONE',  ( 0.05219959533907565091, 21.53943276465977519, 99.99890960531436690 ) ) ;
#145360 = CARTESIAN_POINT ( 'NONE',  ( -9.474510206698964154, 16.51473224551069663, 75.41557627198103830 ) ) ;
#145361 = CARTESIAN_POINT ( 'NONE',  ( -21.52544592524334988, -5.823673210054445271, 78.95942372801901854 ) ) ;
#145363 = CARTESIAN_POINT ( 'NONE',  ( -16.51473224551082808, 9.474510206698731452, 28.33442372801900433 ) ) ;
#145362 = CARTESIAN_POINT ( 'NONE',  ( 14.29746914071037800, 8.314922557961029526, 21.66775706135235069 ) ) ;
#145364 = CARTESIAN_POINT ( 'NONE',  ( -21.52544592524334988, -5.823673210054445271, 48.95942372801902565 ) ) ;
#145365 = CARTESIAN_POINT ( 'NONE',  ( 21.52544592524344225, -5.823673210054117533, 113.5405762719810383 ) ) ;
#145366 = CARTESIAN_POINT ( 'NONE',  ( 15.80617190586746368, 15.72974639402197994, 59.37390960531436690 ) ) ;
#145367 = CARTESIAN_POINT ( 'NONE',  ( -13.89961937509957401, -13.97604488694547875, 99.37609039468567573 ) ) ;
#145368 = CARTESIAN_POINT ( 'NONE',  ( -19.03943276465977164, -0.05219959533935918106, 73.75109039468566152 ) ) ;
#145369 = CARTESIAN_POINT ( 'NONE',  ( 15.80617190586769283, -15.72974639402175789, 80.62609039468567573 ) ) ;
#145370 = CARTESIAN_POINT ( 'NONE',  ( -19.05341960407617563, 5.049401038297882671, 58.54275706135234003 ) ) ;
#145371 = CARTESIAN_POINT ( 'NONE',  ( -0.05219959533909027116, -19.03943276465977164, 32.49890960531435979 ) ) ;
#145372 = CARTESIAN_POINT ( 'NONE',  ( 18.62759615963271287, -10.81492255796078972, 53.33224293864769550 ) ) ;
#145373 = CARTESIAN_POINT ( 'NONE',  ( 12.14591786802309770, 12.06949235617756955, 54.37390960531435979 ) ) ;
#145374 = CARTESIAN_POINT ( 'NONE',  ( -17.44270441346514389, -5.991230190323014071, 26.36335079264227588 ) ) ;
#145375 = CARTESIAN_POINT ( 'NONE',  ( 5.153800228976615827, -19.02544592524334988, 25.20942372801900433 ) ) ;
#145376 = CARTESIAN_POINT ( 'NONE',  ( 4.483927247898790824, -16.52544592524335698, 80.20942372801901854 ) ) ;
#145377 = CARTESIAN_POINT ( 'NONE',  ( -8.314922557960811034, -14.29746914071050412, 57.08224293864769550 ) ) ;
#145378 = CARTESIAN_POINT ( 'NONE',  ( 18.67979575497194134, -10.72451020669871369, 70.83442372801901854 ) ) ;
#145379 = CARTESIAN_POINT ( 'NONE',  ( 0.05219959533937995610, -21.53943276465977519, 80.00109039468568994 ) ) ;
#145380 = CARTESIAN_POINT ( 'NONE',  ( 15.80617190586746368, 15.72974639402197994, 84.37390960531438111 ) ) ;
#145381 = CARTESIAN_POINT ( 'NONE',  ( 19.05341960407611168, 5.049401038298154454, 38.95724293864767418 ) ) ;
#145382 = CARTESIAN_POINT ( 'NONE',  ( 21.52544592524334988, 5.823673210054432836, 51.45942372801901854 ) ) ;
#145383 = CARTESIAN_POINT ( 'NONE',  ( -13.89961937509977652, 13.97604488694528158, 35.62390960531435269 ) ) ;
#145384 = CARTESIAN_POINT ( 'NONE',  ( 9.474510206698971260, -16.51473224551069308, 47.91557627198102409 ) ) ;
#145385 = CARTESIAN_POINT ( 'NONE',  ( -16.55341960407611168, -4.379528057220339221, 111.4572429386476813 ) ) ;
#145386 = CARTESIAN_POINT ( 'NONE',  ( 5.153800228976335163, 19.02544592524342804, 104.7905762719809957 ) ) ;
#145387 = CARTESIAN_POINT ( 'NONE',  ( -0.05219959533910754901, -16.53943276465976808, 42.49890960531435979 ) ) ;
#145388 = CARTESIAN_POINT ( 'NONE',  ( -12.06949235617756955, 12.14591786802309770, 105.6239096053143669 ) ) ;
#145389 = CARTESIAN_POINT ( 'NONE',  ( 21.55341960407610458, 5.719274019375980345, 88.95724293864769550 ) ) ;
#145390 = CARTESIAN_POINT ( 'NONE',  ( 18.62759615963255655, 10.81492255796105972, 26.66775706135235424 ) ) ;
#145391 = PLANE ( 'NONE',  #56523 ) ;
#145392 = CARTESIAN_POINT ( 'NONE',  ( -16.53943276465976808, -0.05219959533934237506, 43.75109039468568284 ) ) ;
#145393 = ORIENTED_EDGE ( 'NONE', *, *, #175772, .T. ) ;
#145394 = CARTESIAN_POINT ( 'NONE',  ( -0.05219959533907301413, -21.53943276465977519, 77.49890960531433848 ) ) ;
#145395 = CARTESIAN_POINT ( 'NONE',  ( -21.55341960407619339, 5.719274019375674811, 88.54275706135236135 ) ) ;
#145396 = CARTESIAN_POINT ( 'NONE',  ( 0.05219959533909260263, 19.03943276465977164, 89.99890960531436690 ) ) ;
#145397 = CARTESIAN_POINT ( 'NONE',  ( 0.05219959533937995610, -21.53943276465977519, 35.00109039468568284 ) ) ;
#145398 = B_SPLINE_CURVE_WITH_KNOTS ( 'NONE', 3,
 ( #13151, #149667, #57667, #182992, #60611, #103163, #196195, #11165, #72839, #71823, #106130, #12170, #28337, #119334 ),
 .UNSPECIFIED., .F., .F.,
 ( 4, 2, 2, 2, 2, 2, 4 ),
 ( 0.002427643230453598207, 0.002603325520439036134, 0.002779007810424474062, 0.003130372390395366397, 0.003833101550337150200, 0.004535830710278934003, 0.005238559870220718673 ),
 .UNSPECIFIED. ) ;
#145399 = CARTESIAN_POINT ( 'NONE',  ( -21.55341960407610458, -5.719274019375992779, 26.45724293864768839 ) ) ;
#145400 = CARTESIAN_POINT ( 'NONE',  ( -0.05219959533934338120, 16.53943276465976808, 87.50109039468568994 ) ) ;
#145401 = CARTESIAN_POINT ( 'NONE',  ( 15.80617190586769283, -15.72974639402175789, 90.62609039468567573 ) ) ;
#145402 = CARTESIAN_POINT ( 'NONE',  ( 5.153800228976615827, -19.02544592524334988, 20.20942372801899722 ) ) ;
#145403 = CARTESIAN_POINT ( 'NONE',  ( -12.14591786802326823, 12.06949235617739902, 78.12609039468570415 ) ) ;
#145404 = CARTESIAN_POINT ( 'NONE',  ( -5.719274019375665041, -21.55341960407619695, 24.79275706135235779 ) ) ;
#145405 = CARTESIAN_POINT ( 'NONE',  ( 5.153800228976335163, 19.02544592524342804, 29.79057627198102409 ) ) ;
#145406 = CARTESIAN_POINT ( 'NONE',  ( 15.72974639402176855, 15.80617190586768217, 106.8760903946856899 ) ) ;
#145407 = CARTESIAN_POINT ( 'NONE',  ( -19.02544592524342804, 5.153800228976336051, 111.0405762719810099 ) ) ;
#145408 = CARTESIAN_POINT ( 'NONE',  ( 10.81492255796078972, 18.62759615963270932, 99.58224293864770971 ) ) ;
#145410 = CARTESIAN_POINT ( 'NONE',  ( -18.67979575497178146, -10.72451020669898902, 61.66557627198103120 ) ) ;
#145409 = DIRECTION ( 'NONE',  ( 0.000000000000000000, 0.000000000000000000, 1.000000000000000000 ) ) ;
#145412 = CARTESIAN_POINT ( 'NONE',  ( -16.52544592524342804, 4.483927247898546575, 51.04057627198103120 ) ) ;
#145411 = CARTESIAN_POINT ( 'NONE',  ( 4.379528057220092307, 16.55341960407617563, 47.29275706135234003 ) ) ;
#145413 = CARTESIAN_POINT ( 'NONE',  ( 18.85284094683698086, -5.499999999999990230, 101.1723727239295414 ) ) ;
#145414 = CARTESIAN_POINT ( 'NONE',  ( -16.46253265017146816, -9.564922557961047289, 84.16775706135233293 ) ) ;
#145415 = CARTESIAN_POINT ( 'NONE',  ( -0.4081324879000859940, -13.74234921310041280, -62.56359473395608717 ) ) ;
#145416 = CARTESIAN_POINT ( 'NONE',  ( 16.55341960407618274, -4.379528057220086978, 31.04275706135234714 ) ) ;
#145417 = CARTESIAN_POINT ( 'NONE',  ( -18.67979575497178146, -10.72451020669898902, 96.66557627198102409 ) ) ;
#145418 = CARTESIAN_POINT ( 'NONE',  ( 8.314922557960818139, 14.29746914071049879, 59.58224293864770260 ) ) ;
#145419 = CARTESIAN_POINT ( 'NONE',  ( -5.049401038298153566, 19.05341960407611168, 100.2072429386476955 ) ) ;
#145420 = CARTESIAN_POINT ( 'NONE',  ( 16.52544592524335698, 4.483927247898782831, 41.45942372801901143 ) ) ;
#145421 = CARTESIAN_POINT ( 'NONE',  ( -9.564922557960796823, -16.46253265017161027, 57.08224293864769550 ) ) ;
#145423 = CARTESIAN_POINT ( 'NONE',  ( -19.03943276465977164, -0.05219959533935918106, 93.75109039468566152 ) ) ;
#145422 = CARTESIAN_POINT ( 'NONE',  ( 15.72974639402176855, 15.80617190586768217, 31.87609039468567929 ) ) ;
#145424 = CARTESIAN_POINT ( 'NONE',  ( -0.05219959533909027116, -19.03943276465977164, 92.49890960531436690 ) ) ;
#145425 = CARTESIAN_POINT ( 'NONE',  ( -5.153800228976328057, -19.02544592524343514, 87.29057627198103830 ) ) ;
#145426 = CARTESIAN_POINT ( 'NONE',  ( 5.823673210054125526, 21.52544592524343514, 89.79057627198103830 ) ) ;
#145427 = CARTESIAN_POINT ( 'NONE',  ( -9.564922557960796823, -16.46253265017161027, 42.08224293864769550 ) ) ;
#145428 = CARTESIAN_POINT ( 'NONE',  ( -17.40805194822029378, -6.112264579159359279, 59.16628727489389661 ) ) ;
#145429 = CARTESIAN_POINT ( 'NONE',  ( -14.34966873604960291, -8.224510206698953496, 66.66557627198102409 ) ) ;
#145430 = CARTESIAN_POINT ( 'NONE',  ( 5.049401038298161559, -19.05341960407611168, 97.70724293864766707 ) ) ;
#145431 = CARTESIAN_POINT ( 'NONE',  ( -29.39134536520996122, 1.114265510929974390, -52.10946600208640689 ) ) ;
#145432 = CARTESIAN_POINT ( 'NONE',  ( 13.89961937509957401, 13.97604488694547697, 76.87609039468566152 ) ) ;
#145433 = CARTESIAN_POINT ( 'NONE',  ( -15.72974639402197994, 15.80617190586746368, 95.62390960531436690 ) ) ;
#145434 = CARTESIAN_POINT ( 'NONE',  ( -16.46253265017146816, -9.564922557961047289, 44.16775706135232582 ) ) ;
#145435 = CARTESIAN_POINT ( 'NONE',  ( -16.46253265017160317, 9.564922557960807481, 115.8322429386477097 ) ) ;
#145436 = CARTESIAN_POINT ( 'NONE',  ( 18.56399227203340985, 5.500000000000002665, 66.47830131249901342 ) ) ;
#145437 = CARTESIAN_POINT ( 'NONE',  ( 18.62759615963271287, -10.81492255796078972, 48.33224293864770260 ) ) ;
#145438 = VECTOR ( 'NONE', #8084, 1000.000000000000000 ) ;
#145439 = CARTESIAN_POINT ( 'NONE',  ( 19.03943276465977164, -0.05219959533909143690, 83.74890960531436690 ) ) ;
#145440 = CARTESIAN_POINT ( 'NONE',  ( -15.72974639402176322, -15.80617190586768395, 64.37609039468568994 ) ) ;
#145441 = CARTESIAN_POINT ( 'NONE',  ( -9.474510206698964154, 16.51473224551069663, 35.41557627198102409 ) ) ;
#145442 = CARTESIAN_POINT ( 'NONE',  ( -12.14591786802309592, -12.06949235617757132, 71.87390960531438111 ) ) ;
#145443 = CARTESIAN_POINT ( 'NONE',  ( -16.55341960407617563, 4.379528057220093196, 28.54275706135234358 ) ) ;
#145444 = CARTESIAN_POINT ( 'NONE',  ( -0.05219959533937732626, 21.53943276465977519, 52.50109039468567573 ) ) ;
#145445 = ORIENTED_EDGE ( 'NONE', *, *, #136647, .T. ) ;
#145446 = CARTESIAN_POINT ( 'NONE',  ( -13.89961937509977652, 13.97604488694528158, 110.6239096053143243 ) ) ;
#145447 = CARTESIAN_POINT ( 'NONE',  ( 16.51473224551083163, -9.474510206698727899, 85.83442372801900433 ) ) ;
#145448 = DIRECTION ( 'NONE',  ( 1.000000000000000000, 0.000000000000000000, 0.000000000000000000 ) ) ;
#145449 = CARTESIAN_POINT ( 'NONE',  ( -21.55341960407619339, 5.719274019375674811, 28.54275706135234358 ) ) ;
#145450 = CARTESIAN_POINT ( 'NONE',  ( -38.00000000000000711, 2.428612866367529932E-14, -3.749999994537626780 ) ) ;
#145451 = CARTESIAN_POINT ( 'NONE',  ( 18.62759615963255655, 10.81492255796105972, 111.6677570613523613 ) ) ;
#145452 = CARTESIAN_POINT ( 'NONE',  ( -16.51473224551069308, -9.474510206698971260, 51.66557627198102409 ) ) ;
#145453 = CARTESIAN_POINT ( 'NONE',  ( 15.72974639402176855, 15.80617190586768217, 111.8760903946856615 ) ) ;
#145454 = CARTESIAN_POINT ( 'NONE',  ( 16.53943276465976808, 0.05219959533934440121, 101.2510903946856757 ) ) ;
#145456 = CARTESIAN_POINT ( 'NONE',  ( 0.05219959533937995610, -21.53943276465977519, 75.00109039468568994 ) ) ;
#145455 = CARTESIAN_POINT ( 'NONE',  ( 19.02544592524343514, -5.153800228976328945, 108.5405762719810383 ) ) ;
#145457 = CARTESIAN_POINT ( 'NONE',  ( -36.91746825000000598, 2.428612866367529932E-14, -4.624999997268814056 ) ) ;
#145458 = CARTESIAN_POINT ( 'NONE',  ( -33.83483822987809475, 1.427510505796699025, 100.3145928531379241 ) ) ;
#145459 = DIRECTION ( 'NONE',  ( 0.000000000000000000, -1.000000000000000000, 0.000000000000000000 ) ) ;
#145460 = CARTESIAN_POINT ( 'NONE',  ( -18.62759615963255300, -10.81492255796106328, 74.16775706135231871 ) ) ;
#145461 = CARTESIAN_POINT ( 'NONE',  ( 21.55341960407619695, -5.719274019375665929, 101.0427570613523756 ) ) ;
#145462 = CARTESIAN_POINT ( 'NONE',  ( -21.30000000000002913, 2.244099063931684814E-13, -64.92279855667830191 ) ) ;
#145463 = CARTESIAN_POINT ( 'NONE',  ( -9.564922557960796823, -16.46253265017161027, 92.08224293864769550 ) ) ;
#145464 = CARTESIAN_POINT ( 'NONE',  ( -5.049401038297874678, -19.05341960407617918, 24.79275706135233648 ) ) ;
#145465 = CARTESIAN_POINT ( 'NONE',  ( -0.8768460684518564197, -31.62105185743270397, -49.48175094143205399 ) ) ;
#145466 = CARTESIAN_POINT ( 'NONE',  ( -16.51473224551069308, -9.474510206698971260, 36.66557627198102409 ) ) ;
#145468 = EDGE_CURVE ( 'NONE', #124967, #197216, #101702, .T. ) ;
#145467 = CARTESIAN_POINT ( 'NONE',  ( -21.53943276465977519, 0.05219959533907696930, 51.24890960531436690 ) ) ;
#145469 = CARTESIAN_POINT ( 'NONE',  ( 14.34966873604972726, -8.224510206698740333, 100.8344237280190185 ) ) ;
#145471 = CARTESIAN_POINT ( 'NONE',  ( 16.46253265017160672, -9.564922557960803928, 83.33224293864768129 ) ) ;
#145470 = CARTESIAN_POINT ( 'NONE',  ( 4.379528057220339221, -16.55341960407611168, 92.70724293864770971 ) ) ;
#145472 = CARTESIAN_POINT ( 'NONE',  ( -5.823673210054431948, 21.52544592524334988, 107.7094237280190328 ) ) ;
#145473 = CARTESIAN_POINT ( 'NONE',  ( 19.03943276465977164, -0.05219959533909143690, 38.74890960531436690 ) ) ;
#145474 = CARTESIAN_POINT ( 'NONE',  ( -14.29746914071049879, 8.314922557960819915, 90.83224293864769550 ) ) ;
#145475 = CARTESIAN_POINT ( 'NONE',  ( -5.719274019375665041, -21.55341960407619695, 54.79275706135235424 ) ) ;
#145476 = CARTESIAN_POINT ( 'NONE',  ( -21.53943276465977519, 0.05219959533907696930, 91.24890960531436690 ) ) ;
#145477 = CARTESIAN_POINT ( 'NONE',  ( 9.564922557961047289, -16.46253265017146816, 55.41775706135234003 ) ) ;
#145478 = CARTESIAN_POINT ( 'NONE',  ( -19.99604614807126524, -21.49604614807087799, -49.12629558063592583 ) ) ;
#145479 = CARTESIAN_POINT ( 'NONE',  ( -5.153800228976328057, -19.02544592524343514, 92.29057627198099567 ) ) ;
#145480 = CARTESIAN_POINT ( 'NONE',  ( 12.06949235617757843, -12.14591786802309237, 58.12390960531435979 ) ) ;
#145481 = EDGE_CURVE ( 'NONE', #45951, #26587, #121037, .T. ) ;
#145482 = CARTESIAN_POINT ( 'NONE',  ( 19.05341960407617918, -5.049401038297876454, 51.04275706135231871 ) ) ;
#145483 = CARTESIAN_POINT ( 'NONE',  ( -13.97604488694527625, -13.89961937509977652, 66.87390960531436690 ) ) ;
#145484 = CARTESIAN_POINT ( 'NONE',  ( 16.55341960407611168, 4.379528057220329451, 53.95724293864770260 ) ) ;
#145485 = CARTESIAN_POINT ( 'NONE',  ( -0.05219959533936034679, 19.03943276465977164, 82.50109039468567573 ) ) ;
#145486 = CARTESIAN_POINT ( 'NONE',  ( -19.49149378614661643, 5.499999999999580780, 84.43757513605359577 ) ) ;
#145487 = CARTESIAN_POINT ( 'NONE',  ( 21.52544592524344225, -5.823673210054117533, 33.54057627198102409 ) ) ;
#145488 = CARTESIAN_POINT ( 'NONE',  ( 16.52544592524342804, -4.483927247898539470, 98.54057627198105251 ) ) ;
#145489 = CARTESIAN_POINT ( 'NONE',  ( -17.50000000000003908, -5.076555817581120067, 26.17951492049773776 ) ) ;
#145491 = CARTESIAN_POINT ( 'NONE',  ( 10.72451020669898902, -18.67979575497178502, 47.91557627198102409 ) ) ;
#145490 = CARTESIAN_POINT ( 'NONE',  ( -19.03943276465977164, 0.05219959533909376836, 56.24890960531435979 ) ) ;
#145492 = CARTESIAN_POINT ( 'NONE',  ( -19.03943276465977164, 0.05219959533909376836, 36.24890960531436690 ) ) ;
#145494 = CARTESIAN_POINT ( 'NONE',  ( -5.153800228976328057, -19.02544592524343514, 62.29057627198100988 ) ) ;
#145493 = CARTESIAN_POINT ( 'NONE',  ( -16.53943276465976808, -0.05219959533934237506, 83.75109039468568994 ) ) ;
#145495 = CARTESIAN_POINT ( 'NONE',  ( -13.89961937509957401, -13.97604488694547875, 39.37609039468566152 ) ) ;
#145496 = CARTESIAN_POINT ( 'NONE',  ( 10.72451020669871369, 18.67979575497193778, 72.08442372801899012 ) ) ;
#145497 = CARTESIAN_POINT ( 'NONE',  ( 0.05219959533907565091, 21.53943276465977519, 54.99890960531435269 ) ) ;
#145498 = CARTESIAN_POINT ( 'NONE',  ( -5.049401038298153566, 19.05341960407611168, 25.20724293864768484 ) ) ;
#145499 = CARTESIAN_POINT ( 'NONE',  ( 5.153800228976615827, -19.02544592524334988, 110.2094237280189901 ) ) ;
#145500 = DIRECTION ( 'NONE',  ( 0.000000000000000000, 1.000000000000000000, 0.000000000000000000 ) ) ;
#145502 = CARTESIAN_POINT ( 'NONE',  ( -10.81492255796078084, -18.62759615963271287, 47.08224293864770260 ) ) ;
#145501 = CARTESIAN_POINT ( 'NONE',  ( -1.467328942210815335, -23.16108095314130466, -57.58004187413776265 ) ) ;
#145503 = CARTESIAN_POINT ( 'NONE',  ( 16.29526858892872099, -7.335722546920259823, 66.70329402199793378 ) ) ;
#145504 = CARTESIAN_POINT ( 'NONE',  ( 10.81492255796106328, -18.62759615963255655, 85.41775706135236135 ) ) ;
#145505 = CARTESIAN_POINT ( 'NONE',  ( -16.53943276465976808, 0.05219959533911058130, 41.24890960531435269 ) ) ;
#145506 = CARTESIAN_POINT ( 'NONE',  ( 8.224510206698953496, -14.34966873604960469, 57.91557627198103120 ) ) ;
#145507 = CARTESIAN_POINT ( 'NONE',  ( 21.55341960407610458, 5.719274019375980345, 83.95724293864770971 ) ) ;
#145508 = CARTESIAN_POINT ( 'NONE',  ( -18.62759615963270932, 10.81492255796079327, 80.83224293864769550 ) ) ;
#145509 = DIRECTION ( 'NONE',  ( 1.000000000000000000, 0.000000000000000000, 0.000000000000000000 ) ) ;
#145510 = CARTESIAN_POINT ( 'NONE',  ( 15.72974639402199770, -15.80617190586745480, 38.12390960531436690 ) ) ;
#145511 = CARTESIAN_POINT ( 'NONE',  ( -16.55341960407617563, 4.379528057220093196, 48.54275706135234714 ) ) ;
#145512 = CARTESIAN_POINT ( 'NONE',  ( -8.314922557960811034, -14.29746914071050412, 82.08224293864768129 ) ) ;
#145513 = CARTESIAN_POINT ( 'NONE',  ( -0.05219959533909027116, -19.03943276465977164, 27.49890960531435624 ) ) ;
#145514 = CARTESIAN_POINT ( 'NONE',  ( -22.00000000000000000, -5.204748896376250896E-15, 42.49999999999999289 ) ) ;
#145515 = VERTEX_POINT ( 'NONE', #97678 ) ;
#145516 = CARTESIAN_POINT ( 'NONE',  ( -4.379528057220086978, -16.55341960407618274, 79.79275706135236135 ) ) ;
#145517 = CARTESIAN_POINT ( 'NONE',  ( -21.53943276465977519, -0.05219959533937600094, 23.75109039468567929 ) ) ;
#145518 = CARTESIAN_POINT ( 'NONE',  ( 19.03943276465977164, -0.05219959533909143690, 88.74890960531436690 ) ) ;
#145519 = CARTESIAN_POINT ( 'NONE',  ( -10.72451020669870658, -18.67979575497194134, 59.58442372801901854 ) ) ;
#145520 = CARTESIAN_POINT ( 'NONE',  ( 9.474510206698971260, -16.51473224551069308, 112.9155762719810383 ) ) ;
#145521 = CARTESIAN_POINT ( 'NONE',  ( -10.05780954200478305, -38.14163830725842530, -31.65208490131487551 ) ) ;
#145522 = AXIS2_PLACEMENT_3D ( 'NONE', #106415, #32571, #138741 ) ;
#145523 = ORIENTED_EDGE ( 'NONE', *, *, #196211, .F. ) ;
#145524 = CARTESIAN_POINT ( 'NONE',  ( 0.05219959533937995610, -21.53943276465977519, 40.00109039468567573 ) ) ;
#145526 = CARTESIAN_POINT ( 'NONE',  ( -0.05219959533909027116, -19.03943276465977164, 107.4989096053143527 ) ) ;
#145525 = CARTESIAN_POINT ( 'NONE',  ( 9.474510206698971260, -16.51473224551069308, 37.91557627198102409 ) ) ;
#145527 = CARTESIAN_POINT ( 'NONE',  ( -0.05219959533936034679, 19.03943276465977164, 57.50109039468566863 ) ) ;
#145528 = CARTESIAN_POINT ( 'NONE',  ( 0.05219959533937995610, -21.53943276465977519, 35.00109039468568284 ) ) ;
#145529 = CARTESIAN_POINT ( 'NONE',  ( 19.02544592524334988, 5.153800228976608722, 46.45942372801899012 ) ) ;
#145530 = CARTESIAN_POINT ( 'NONE',  ( 16.46253265017160672, -9.564922557960803928, 28.33224293864769550 ) ) ;
#145531 = CARTESIAN_POINT ( 'NONE',  ( -14.34966873604972548, 8.224510206698743886, 88.33442372801901854 ) ) ;
#145532 = CARTESIAN_POINT ( 'NONE',  ( 9.564922557961047289, -16.46253265017146816, 60.41775706135233293 ) ) ;
#145533 = CARTESIAN_POINT ( 'NONE',  ( -8.314922557961024197, 14.29746914071037800, 102.9177570613523756 ) ) ;
#145534 = CARTESIAN_POINT ( 'NONE',  ( 9.980772036771176303, 12.05108236997111071, -61.81300923031701444 ) ) ;
#145535 = CARTESIAN_POINT ( 'NONE',  ( -16.46253265017160317, 9.564922557960807481, 85.83224293864769550 ) ) ;
#145536 = CARTESIAN_POINT ( 'NONE',  ( 15.72974639402176855, 15.80617190586768217, 96.87609039468568994 ) ) ;
#145537 = CARTESIAN_POINT ( 'NONE',  ( -21.53943276465977519, -0.05219959533937600094, 113.7510903946856757 ) ) ;
#145538 = FACE_OUTER_BOUND ( 'NONE', #125907, .T. ) ;
#145539 = CARTESIAN_POINT ( 'NONE',  ( -16.46253265017160317, 9.564922557960807481, 100.8322429386477097 ) ) ;
#145540 = CARTESIAN_POINT ( 'NONE',  ( 0.05219959533937995610, -21.53943276465977519, 75.00109039468568994 ) ) ;
#145541 = CARTESIAN_POINT ( 'NONE',  ( 14.34966873604972726, -8.224510206698740333, 25.83442372801901499 ) ) ;
#145542 = B_SPLINE_CURVE_WITH_KNOTS ( 'NONE', 3,
 ( #170843, #44524, #974, #78816, #29363, #169843, #167863, #90993, #75837, #122337, #45510, #31337, #30341, #91982, #153676, #15173, #5947, #19153, #64655, #51466, #188014, #83779, #36282, #143460, #130275, #94985, #142480, #97937, #159630, #67624, #80802, #157663, #160637, #4945, #126317, #145458, #3958, #129284, #49484, #111147 ),
 .UNSPECIFIED., .F., .F.,
 ( 4, 2, 2, 2, 2, 2, 2, 2, 2, 2, 2, 2, 2, 2, 2, 2, 2, 2, 2, 4 ),
 ( 0.004339806180219608206, 0.005417599276633671204, 0.006495392373047733335, 0.007034288921254771773, 0.007573185469461809344, 0.008650978565875887955, 0.009728771662289966565, 0.01080656475870404344, 0.01134546130691106366, 0.01188435785511808215, 0.01296215095153212260, 0.01403994404794616131, 0.01511773714436020176, 0.01619553024077424047, 0.01727332333718828092, 0.01835111643360232137, 0.01942890953001635834, 0.01996780607822337336, 0.02050670262643038491, 0.02158449572284441495 ),
 .UNSPECIFIED. ) ;
#145543 = CARTESIAN_POINT ( 'NONE',  ( -13.97604488694527625, -13.89961937509977652, 81.87390960531436690 ) ) ;
#145544 = CARTESIAN_POINT ( 'NONE',  ( -21.53943276465977519, 0.05219959533907696930, 36.24890960531435979 ) ) ;
#145545 = CARTESIAN_POINT ( 'NONE',  ( 9.474510206698971260, -16.51473224551069308, 87.91557627198102409 ) ) ;
#145546 = CARTESIAN_POINT ( 'NONE',  ( 0.000000000000000000, -5.500000000000000888, 120.0000000000000142 ) ) ;
#145547 = CARTESIAN_POINT ( 'NONE',  ( -5.153800228976328057, -19.02544592524343514, 72.29057627198102409 ) ) ;
#145548 = CARTESIAN_POINT ( 'NONE',  ( -19.03943276465977164, 0.05219959533909376836, 71.24890960531435269 ) ) ;
#145549 = CARTESIAN_POINT ( 'NONE',  ( 0.05219959533934541429, -16.53943276465976808, 95.00109039468568994 ) ) ;
#145550 = CARTESIAN_POINT ( 'NONE',  ( -16.88567814943197831, 6.947325034625352558, 98.70998877347405198 ) ) ;
#145551 = CARTESIAN_POINT ( 'NONE',  ( -19.05341960407617563, 5.049401038297882671, 73.54275706135233293 ) ) ;
#145552 = CARTESIAN_POINT ( 'NONE',  ( -19.05341960407611168, -5.049401038298163336, 86.45724293864769550 ) ) ;
#145553 = CARTESIAN_POINT ( 'NONE',  ( -16.52544592524342804, 4.483927247898546575, 81.04057627198102409 ) ) ;
#145554 = CARTESIAN_POINT ( 'NONE',  ( 21.55341960407610458, 5.719274019375980345, 38.95724293864768839 ) ) ;
#145555 = CARTESIAN_POINT ( 'NONE',  ( -13.89961937509977652, 13.97604488694528158, 115.6239096053143669 ) ) ;
#145556 = CARTESIAN_POINT ( 'NONE',  ( -14.29746914071049879, 8.314922557960819915, 90.83224293864769550 ) ) ;
#145557 = CARTESIAN_POINT ( 'NONE',  ( -3.573655867282028392E-15, 2.428612866367529932E-14, -18.00000000000000000 ) ) ;
#145558 = CARTESIAN_POINT ( 'NONE',  ( -16.51473224551082808, 9.474510206698731452, 43.33442372801900433 ) ) ;
#145559 = CARTESIAN_POINT ( 'NONE',  ( 14.29746914071049879, -8.314922557960816363, 23.33224293864769194 ) ) ;
#145560 = CARTESIAN_POINT ( 'NONE',  ( -13.89961937509977652, 13.97604488694528158, 105.6239096053143527 ) ) ;
#145561 = CARTESIAN_POINT ( 'NONE',  ( 21.52544592524334988, 5.823673210054432836, 61.45942372801901854 ) ) ;
#145562 = CARTESIAN_POINT ( 'NONE',  ( -0.05219959533907301413, -21.53943276465977519, 62.49890960531436690 ) ) ;
#145563 = CARTESIAN_POINT ( 'NONE',  ( -21.55341960407619339, 5.719274019375674811, 33.54275706135234714 ) ) ;
#145564 = CARTESIAN_POINT ( 'NONE',  ( -21.53943276465977519, 0.05219959533907696930, 81.24890960531436690 ) ) ;
#145565 = CARTESIAN_POINT ( 'NONE',  ( -15.72974639402176322, -15.80617190586768395, 39.37609039468567573 ) ) ;
#145566 = CARTESIAN_POINT ( 'NONE',  ( 4.483927247898545687, 16.52544592524342804, 104.7905762719810241 ) ) ;
#145567 = CARTESIAN_POINT ( 'NONE',  ( -19.03943276465977164, -0.05219959533935918106, 68.75109039468566152 ) ) ;
#145568 = CARTESIAN_POINT ( 'NONE',  ( 19.02544592524343514, -5.153800228976328945, 48.54057627198103120 ) ) ;
#145569 =( BOUNDED_CURVE ( )  B_SPLINE_CURVE ( 2, ( #154912, #76076, #137752, #139725, #121584, #15413, #186268, #94224, #125572, #172075, #155905 ),
 .UNSPECIFIED., .F., .F. ) 
 B_SPLINE_CURVE_WITH_KNOTS ( ( 3, 2, 2, 2, 2, 3 ),
 ( 0.6000000000000005329, 0.6200000000000005507, 0.6400000000000005684, 0.6600000000000006972, 0.6800000000000007150, 0.7000000000000006217 ),
 .UNSPECIFIED. ) 
 CURVE ( )  GEOMETRIC_REPRESENTATION_ITEM ( )  RATIONAL_B_SPLINE_CURVE ( ( 0.9999999999999986677, 0.9510565162951548634, 1.000000000000000000, 0.9510565162951535312, 1.000000000000000000, 0.9510565162951535312, 1.000000000000000000, 0.9510565162951535312, 1.000000000000000000, 0.9510565162951518658, 1.000000000000001554 ) ) 
 REPRESENTATION_ITEM ( '' )  );
#145571 = CARTESIAN_POINT ( 'NONE',  ( 16.46253265017160672, -9.564922557960803928, 93.33224293864769550 ) ) ;
#145570 = CARTESIAN_POINT ( 'NONE',  ( -4.483927247898539470, -16.52544592524342804, 97.29057627198105251 ) ) ;
#145572 = CARTESIAN_POINT ( 'NONE',  ( -0.05219959533909027116, -19.03943276465977164, 97.49890960531436690 ) ) ;
#145573 = CARTESIAN_POINT ( 'NONE',  ( 8.224510206698953496, -14.34966873604960469, 107.9155762719810241 ) ) ;
#145574 = CARTESIAN_POINT ( 'NONE',  ( 4.483927247898545687, 16.52544592524342804, 39.79057627198103830 ) ) ;
#145575 = CARTESIAN_POINT ( 'NONE',  ( -14.29746914071037622, -8.314922557961029526, 94.16775706135237556 ) ) ;
#145576 = CARTESIAN_POINT ( 'NONE',  ( -5.153800228976328057, -19.02544592524343514, 57.29057627198103120 ) ) ;
#145577 = CARTESIAN_POINT ( 'NONE',  ( -16.51473224551069308, -9.474510206698971260, 26.66557627198103120 ) ) ;
#145578 = CARTESIAN_POINT ( 'NONE',  ( 5.153800228976615827, -19.02544592524334988, 30.20942372801900433 ) ) ;
#145580 = CARTESIAN_POINT ( 'NONE',  ( 8.314922557960818139, 14.29746914071049879, 29.58224293864769905 ) ) ;
#145579 = DIRECTION ( 'NONE',  ( -0.000000000000000000, -0.5000000000000002220, 0.8660254037844384856 ) ) ;
#145581 = CARTESIAN_POINT ( 'NONE',  ( -21.53943276465977519, -0.05219959533937600094, 48.75109039468568284 ) ) ;
#145582 = CARTESIAN_POINT ( 'NONE',  ( 21.87067081123542778, -5.494950430485622483, 173.7269556299024202 ) ) ;
#145583 = CARTESIAN_POINT ( 'NONE',  ( 14.34966873604972726, -8.224510206698740333, 50.83442372801901143 ) ) ;
#145584 = CARTESIAN_POINT ( 'NONE',  ( -12.14591786802309592, -12.06949235617757132, 21.87390960531436690 ) ) ;
#145585 = CARTESIAN_POINT ( 'NONE',  ( 19.03943276465977164, -0.05219959533909143690, 48.74890960531435979 ) ) ;
#145586 = CARTESIAN_POINT ( 'NONE',  ( -16.52544592524335698, -4.483927247898792601, 98.95942372801903275 ) ) ;
#145587 = CARTESIAN_POINT ( 'NONE',  ( 4.379528057220092307, 16.55341960407617563, 22.29275706135235069 ) ) ;
#145588 = CARTESIAN_POINT ( 'NONE',  ( 13.89961937509977652, -13.97604488694527269, 43.12390960531434558 ) ) ;
#145589 = CARTESIAN_POINT ( 'NONE',  ( -8.314922557960811034, -14.29746914071050412, 107.0822429386476955 ) ) ;
#145590 = CARTESIAN_POINT ( 'NONE',  ( -15.80617190586745835, -15.72974639402198527, 111.8739096053143669 ) ) ;
#145591 = CARTESIAN_POINT ( 'NONE',  ( -0.05219959533909027116, -19.03943276465977164, 47.49890960531435979 ) ) ;
#145592 = CARTESIAN_POINT ( 'NONE',  ( -16.51473224551069308, -9.474510206698971260, 111.6655762719810383 ) ) ;
#145593 = CARTESIAN_POINT ( 'NONE',  ( 13.89961937509977652, -13.97604488694527269, 38.12390960531436690 ) ) ;
#145594 = CARTESIAN_POINT ( 'NONE',  ( -0.05219959533909027116, -19.03943276465977164, 107.4989096053143527 ) ) ;
#145595 = LINE ( 'NONE', #7074, #197151 ) ;
#145596 = CARTESIAN_POINT ( 'NONE',  ( -5.153800228976328057, -19.02544592524343514, 92.29057627198099567 ) ) ;
#145598 = CARTESIAN_POINT ( 'NONE',  ( 8.224510206698953496, -14.34966873604960469, 107.9155762719810241 ) ) ;
#145597 = CARTESIAN_POINT ( 'NONE',  ( -10.72451020669870658, -18.67979575497194134, 39.58442372801901143 ) ) ;
#145599 = CARTESIAN_POINT ( 'NONE',  ( 13.89961937509977652, -13.97604488694527269, 108.1239096053143669 ) ) ;
#145600 = CARTESIAN_POINT ( 'NONE',  ( -16.46253265017146816, -9.564922557961047289, 69.16775706135233293 ) ) ;
#145601 = CARTESIAN_POINT ( 'NONE',  ( 4.483927247898790824, -16.52544592524335698, 60.20942372801902565 ) ) ;
#145602 = CARTESIAN_POINT ( 'NONE',  ( 5.823673210054444382, -21.52544592524334988, 90.20942372801903275 ) ) ;
#145603 = CARTESIAN_POINT ( 'NONE',  ( -16.53943276465976808, -0.05219959533934237506, 53.75109039468568994 ) ) ;
#145604 = CARTESIAN_POINT ( 'NONE',  ( -5.153800228976328057, -19.02544592524343514, 82.29057627198103830 ) ) ;
#145605 = CARTESIAN_POINT ( 'NONE',  ( -4.483927247898782831, 16.52544592524335698, 37.70942372801900433 ) ) ;
#145606 = CARTESIAN_POINT ( 'NONE',  ( -16.51473224551082808, 9.474510206698731452, 113.3344237280190043 ) ) ;
#145607 = CARTESIAN_POINT ( 'NONE',  ( -4.379528057220086978, -16.55341960407618274, 84.79275706135234714 ) ) ;
#145608 = CARTESIAN_POINT ( 'NONE',  ( -9.564922557961040184, 16.46253265017147172, 97.91775706135233293 ) ) ;
#145609 = CARTESIAN_POINT ( 'NONE',  ( -5.153800228976328057, -19.02544592524343514, 72.29057627198102409 ) ) ;
#145610 = CARTESIAN_POINT ( 'NONE',  ( -15.80617190586745835, -15.72974639402198527, 101.8739096053143811 ) ) ;
#145612 = CARTESIAN_POINT ( 'NONE',  ( -19.02544592524334988, -5.153800228976617603, 88.95942372801897591 ) ) ;
#145611 = CARTESIAN_POINT ( 'NONE',  ( -8.224510206698948167, 14.34966873604960824, 85.41557627198102409 ) ) ;
#145613 = CARTESIAN_POINT ( 'NONE',  ( 12.14591786802327356, -12.06949235617739191, 70.62609039468567573 ) ) ;
#145614 = CARTESIAN_POINT ( 'NONE',  ( 23.46037622755597951, 10.21219847193880703, 168.3031241911625386 ) ) ;
#145615 = CARTESIAN_POINT ( 'NONE',  ( 13.97604488694548053, -13.89961937509957401, 75.62609039468564731 ) ) ;
#145616 = CARTESIAN_POINT ( 'NONE',  ( 12.14591786802309770, 12.06949235617756955, 29.37390960531435269 ) ) ;
#145617 = CARTESIAN_POINT ( 'NONE',  ( -0.05219959533910754901, -16.53943276465976808, 92.49890960531436690 ) ) ;
#145619 = DIRECTION ( 'NONE',  ( 1.000000000000000000, 0.000000000000000000, 0.000000000000000000 ) ) ;
#145618 = CARTESIAN_POINT ( 'NONE',  ( -0.05219959533936034679, 19.03943276465977164, 32.50109039468566863 ) ) ;
#145620 = CARTESIAN_POINT ( 'NONE',  ( 18.67979575497194134, -10.72451020669871369, 20.83442372801901143 ) ) ;
#145621 = CARTESIAN_POINT ( 'NONE',  ( -16.51473224551069308, -9.474510206698971260, 111.6655762719810383 ) ) ;
#145622 = CARTESIAN_POINT ( 'NONE',  ( 13.97604488694527802, 13.89961937509977652, 94.37390960531436690 ) ) ;
#145623 = CARTESIAN_POINT ( 'NONE',  ( 10.81492255796106328, -18.62759615963255655, 95.41775706135234714 ) ) ;
#145624 = CARTESIAN_POINT ( 'NONE',  ( -16.51473224551069308, -9.474510206698971260, 71.66557627198102409 ) ) ;
#145625 = CARTESIAN_POINT ( 'NONE',  ( -18.67979575497178146, -10.72451020669898902, 46.66557627198102409 ) ) ;
#145626 = CARTESIAN_POINT ( 'NONE',  ( 0.05219959533910956823, 16.53943276465976808, 99.99890960531436690 ) ) ;
#145627 = CARTESIAN_POINT ( 'NONE',  ( -9.474510206698964154, 16.51473224551069663, 50.41557627198102409 ) ) ;
#145628 = CARTESIAN_POINT ( 'NONE',  ( 8.314922557960818139, 14.29746914071049879, 109.5822429386476955 ) ) ;
#145629 = CARTESIAN_POINT ( 'NONE',  ( 21.52544592524334988, 5.823673210054432836, 31.45942372801901854 ) ) ;
#145630 = CARTESIAN_POINT ( 'NONE',  ( -10.81492255796105439, 18.62759615963255655, 62.91775706135236135 ) ) ;
#145631 = CARTESIAN_POINT ( 'NONE',  ( 16.46253265017160672, -9.564922557960803928, 38.33224293864768839 ) ) ;
#145632 = CARTESIAN_POINT ( 'NONE',  ( -14.34966873604972548, 8.224510206698743886, 78.33442372801901854 ) ) ;
#145633 = CARTESIAN_POINT ( 'NONE',  ( -21.55341960407610458, -5.719274019375992779, 111.4572429386476813 ) ) ;
#145634 = ORIENTED_EDGE ( 'NONE', *, *, #187016, .F. ) ;
#145635 = CARTESIAN_POINT ( 'NONE',  ( -5.719274019375978568, 21.55341960407610458, 110.2072429386477239 ) ) ;
#145637 = CARTESIAN_POINT ( 'NONE',  ( 5.049401038298161559, -19.05341960407611168, 62.70724293864769550 ) ) ;
#145636 = CARTESIAN_POINT ( 'NONE',  ( -16.46253265017146816, -9.564922557961047289, 59.16775706135233293 ) ) ;
#145638 = CARTESIAN_POINT ( 'NONE',  ( 5.049401038297881783, 19.05341960407617563, 32.29275706135233293 ) ) ;
#145639 = CARTESIAN_POINT ( 'NONE',  ( 21.55341960407619695, -5.719274019375665929, 76.04275706135237556 ) ) ;
#145640 = CARTESIAN_POINT ( 'NONE',  ( 21.53943276465977519, -0.05219959533907433946, 68.74890960531435269 ) ) ;
#145641 = CARTESIAN_POINT ( 'NONE',  ( 4.483927247898545687, 16.52544592524342804, 49.79057627198102409 ) ) ;
#145643 = CARTESIAN_POINT ( 'NONE',  ( 5.153800228976615827, -19.02544592524334988, 35.20942372801899722 ) ) ;
#145642 = CARTESIAN_POINT ( 'NONE',  ( 0.05219959533937995610, -21.53943276465977519, 90.00109039468567573 ) ) ;
#145644 = CARTESIAN_POINT ( 'NONE',  ( -8.224510206698948167, 14.34966873604960824, 65.41557627198102409 ) ) ;
#145645 = CARTESIAN_POINT ( 'NONE',  ( 0.05219959533910956823, 16.53943276465976808, 109.9989096053143527 ) ) ;
#145646 = CARTESIAN_POINT ( 'NONE',  ( -9.474510206698720793, -16.51473224551083518, 64.58442372801900433 ) ) ;
#145647 = CARTESIAN_POINT ( 'NONE',  ( -16.55341960407611168, -4.379528057220339221, 26.45724293864768839 ) ) ;
#145648 = CARTESIAN_POINT ( 'NONE',  ( 15.72974639402176855, 15.80617190586768217, 71.87609039468568994 ) ) ;
#145649 = CARTESIAN_POINT ( 'NONE',  ( -13.97604488694547697, 13.89961937509957934, 48.12609039468566863 ) ) ;
#145650 = CARTESIAN_POINT ( 'NONE',  ( -21.53943276465977519, 0.05219959533907696930, 56.24890960531436690 ) ) ;
#145651 = CARTESIAN_POINT ( 'NONE',  ( -21.53943276465977519, -0.05219959533937600094, 48.75109039468568284 ) ) ;
#145652 = CARTESIAN_POINT ( 'NONE',  ( 18.67979575497178502, 10.72451020669898547, 99.16557627198100988 ) ) ;
#145653 = CARTESIAN_POINT ( 'NONE',  ( 19.03943276465977164, 0.05219959533936151252, 101.2510903946856757 ) ) ;
#145654 = CARTESIAN_POINT ( 'NONE',  ( 12.14591786802327356, -12.06949235617739191, 60.62609039468567573 ) ) ;
#145656 = CARTESIAN_POINT ( 'NONE',  ( -5.823673210054116645, -21.52544592524344225, 107.2905762719810525 ) ) ;
#145655 = DIRECTION ( 'NONE',  ( -1.000000000000000000, -0.000000000000000000, -0.000000000000000000 ) ) ;
#145657 = CARTESIAN_POINT ( 'NONE',  ( -12.14591786802309592, -12.06949235617757132, 91.87390960531436690 ) ) ;
#145658 = CARTESIAN_POINT ( 'NONE',  ( 29.86685920354754487, 21.69954338932564752, -9.924999997268812990 ) ) ;
#145659 = CARTESIAN_POINT ( 'NONE',  ( 0.05219959533934541429, -16.53943276465976808, 25.00109039468567218 ) ) ;
#145660 = CARTESIAN_POINT ( 'NONE',  ( -5.823673210054116645, -21.52544592524344225, 47.29057627198103120 ) ) ;
#145661 = CARTESIAN_POINT ( 'NONE',  ( 12.14591786802327356, -12.06949235617739191, 85.62609039468568994 ) ) ;
#145662 = CARTESIAN_POINT ( 'NONE',  ( 35.04522399272636335, 11.85564638482192557, -8.000000000000001776 ) ) ;
#145663 = CARTESIAN_POINT ( 'NONE',  ( 8.314922557961029526, -14.29746914071037800, 70.41775706135236135 ) ) ;
#145664 = CARTESIAN_POINT ( 'NONE',  ( 15.80617190586769283, -15.72974639402175789, 35.62609039468568994 ) ) ;
#145665 = CARTESIAN_POINT ( 'NONE',  ( 5.719274019375991003, -21.55341960407610458, 62.70724293864769550 ) ) ;
#145666 = CARTESIAN_POINT ( 'NONE',  ( 16.53943276465976808, 0.05219959533934440121, 86.25109039468568994 ) ) ;
#145667 = CARTESIAN_POINT ( 'NONE',  ( 16.46253265017160672, -9.564922557960803928, 93.33224293864769550 ) ) ;
#145668 = CARTESIAN_POINT ( 'NONE',  ( 10.72451020669871369, 18.67979575497193778, 72.08442372801899012 ) ) ;
#145669 = CARTESIAN_POINT ( 'NONE',  ( -18.62759615963270932, 10.81492255796079327, 35.83224293864768839 ) ) ;
#145670 = CARTESIAN_POINT ( 'NONE',  ( -5.823673210054116645, -21.52544592524344225, 32.29057627198102409 ) ) ;
#145671 = EDGE_LOOP ( 'NONE', ( #69363, #186318, #65841, #141798, #20658, #55024, #57349, #102947, #26646, #17969, #95243, #44966, #100270, #173287 ) ) ;
#145672 = CARTESIAN_POINT ( 'NONE',  ( 13.97604488694548053, -13.89961937509957401, 55.62609039468566863 ) ) ;
#145673 = CARTESIAN_POINT ( 'NONE',  ( -16.52544592524335698, -4.483927247898792601, 58.95942372801902565 ) ) ;
#145674 = CARTESIAN_POINT ( 'NONE',  ( 10.81492255796078972, 18.62759615963270932, 34.58224293864770260 ) ) ;
#145675 = ORIENTED_EDGE ( 'NONE', *, *, #93145, .T. ) ;
#145676 = CARTESIAN_POINT ( 'NONE',  ( -13.97604488694527625, -13.89961937509977652, 96.87390960531433848 ) ) ;
#145677 = CARTESIAN_POINT ( 'NONE',  ( -14.34966873604972548, 8.224510206698743886, 113.3344237280190328 ) ) ;
#145678 = CARTESIAN_POINT ( 'NONE',  ( 18.09918380851992836, 5.500000000000035527, 73.98618307335611632 ) ) ;
#145679 = CARTESIAN_POINT ( 'NONE',  ( -16.52544592524342804, 4.483927247898546575, 111.0405762719810525 ) ) ;
#145680 = CARTESIAN_POINT ( 'NONE',  ( 5.719274019375991003, -21.55341960407610458, 42.70724293864770260 ) ) ;
#145681 = CARTESIAN_POINT ( 'NONE',  ( -16.51473224551069308, -9.474510206698971260, 41.66557627198103120 ) ) ;
#145682 = CARTESIAN_POINT ( 'NONE',  ( -4.483927247898782831, 16.52544592524335698, 87.70942372801901854 ) ) ;
#145683 = CARTESIAN_POINT ( 'NONE',  ( 18.62759615963255655, 10.81492255796105972, 31.66775706135234358 ) ) ;
#145684 = CARTESIAN_POINT ( 'NONE',  ( -5.153800228976607833, 19.02544592524334988, 87.70942372801897591 ) ) ;
#145685 = CARTESIAN_POINT ( 'NONE',  ( -16.53943276465976808, 0.05219959533911058130, 101.2489096053143669 ) ) ;
#145686 = CARTESIAN_POINT ( 'NONE',  ( -13.97604488694527625, -13.89961937509977652, 56.87390960531434558 ) ) ;
#145687 = CARTESIAN_POINT ( 'NONE',  ( -9.564922557960796823, -16.46253265017161027, 32.08224293864769550 ) ) ;
#145688 = CARTESIAN_POINT ( 'NONE',  ( 1.500000000000020872, 22.80000000000002913, -55.36297086913598520 ) ) ;
#145689 = CARTESIAN_POINT ( 'NONE',  ( 9.474510206698971260, -16.51473224551069308, 72.91557627198102409 ) ) ;
#145690 = CARTESIAN_POINT ( 'NONE',  ( 14.29746914071037800, 8.314922557961029526, 56.66775706135235424 ) ) ;
#145691 = CARTESIAN_POINT ( 'NONE',  ( 5.719274019375673035, 21.55341960407619339, 112.2927570613523471 ) ) ;
#145692 = CARTESIAN_POINT ( 'NONE',  ( -15.80617190586745835, -15.72974639402198527, 51.87390960531437401 ) ) ;
#145693 = CARTESIAN_POINT ( 'NONE',  ( 8.314922557961029526, -14.29746914071037800, 70.41775706135236135 ) ) ;
#145694 = CARTESIAN_POINT ( 'NONE',  ( -16.46253265017146816, -9.564922557961047289, 54.16775706135234003 ) ) ;
#145695 = CARTESIAN_POINT ( 'NONE',  ( -16.51473224551082808, 9.474510206698731452, 63.33442372801900433 ) ) ;
#145696 = CARTESIAN_POINT ( 'NONE',  ( -21.53943276465977519, -0.05219959533937600094, 68.75109039468568994 ) ) ;
#145697 = CARTESIAN_POINT ( 'NONE',  ( -13.97604488694527625, -13.89961937509977652, 61.87390960531435979 ) ) ;
#145698 = CARTESIAN_POINT ( 'NONE',  ( 0.05219959533909260263, 19.03943276465977164, 39.99890960531436690 ) ) ;
#145699 = CARTESIAN_POINT ( 'NONE',  ( -0.05219959533936034679, 19.03943276465977164, 57.50109039468566863 ) ) ;
#145700 = CARTESIAN_POINT ( 'NONE',  ( 19.02544592524343514, -5.153800228976328945, 113.5405762719810241 ) ) ;
#145701 = CARTESIAN_POINT ( 'NONE',  ( -5.153800228976328057, -19.02544592524343514, 92.29057627198099567 ) ) ;
#145702 = CARTESIAN_POINT ( 'NONE',  ( 14.34966873604960469, 8.224510206698951720, 49.16557627198102409 ) ) ;
#145703 = CARTESIAN_POINT ( 'NONE',  ( 10.81492255796078972, 18.62759615963270932, 49.58224293864769550 ) ) ;
#145704 = DIRECTION ( 'NONE',  ( 0.000000000000000000, 0.000000000000000000, -1.000000000000000000 ) ) ;
#145705 = CARTESIAN_POINT ( 'NONE',  ( 0.05219959533937995610, -21.53943276465977519, 105.0010903946856757 ) ) ;
#145706 = CARTESIAN_POINT ( 'NONE',  ( -17.40805194822031510, -6.112264579159320199, 79.16628727489391792 ) ) ;
#145707 = CARTESIAN_POINT ( 'NONE',  ( -19.05341960407611168, -5.049401038298163336, 51.45724293864770260 ) ) ;
#145708 = CYLINDRICAL_SURFACE ( 'NONE', #123965, 1.500000000000001332 ) ;
#145709 = CARTESIAN_POINT ( 'NONE',  ( 14.18669005401828187, -34.08280046153741694, -8.000000000000001776 ) ) ;
#145710 = CARTESIAN_POINT ( 'NONE',  ( 12.06949235617739724, 12.14591786802326823, 71.87609039468568994 ) ) ;
#145712 = EDGE_CURVE ( 'NONE', #57684, #70174, #198557, .T. ) ;
#145711 = CARTESIAN_POINT ( 'NONE',  ( 15.72974639402199770, -15.80617190586745480, 98.12390960531436690 ) ) ;
#145713 = CARTESIAN_POINT ( 'NONE',  ( 14.29746914071049879, -8.314922557960816363, 48.33224293864770260 ) ) ;
#145715 = DIRECTION ( 'NONE',  ( -1.000000000000000000, -0.000000000000000000, 0.000000000000000000 ) ) ;
#145714 = CARTESIAN_POINT ( 'NONE',  ( 5.049401038298161559, -19.05341960407611168, 47.70724293864770260 ) ) ;
#145716 = CARTESIAN_POINT ( 'NONE',  ( -18.67979575497193778, 10.72451020669871902, 38.33442372801900433 ) ) ;
#145717 = CARTESIAN_POINT ( 'NONE',  ( 19.05341960407617918, -5.049401038297876454, 51.04275706135231871 ) ) ;
#145718 = CARTESIAN_POINT ( 'NONE',  ( 19.05341960407611168, 5.049401038298154454, 43.95724293864769550 ) ) ;
#145719 = CARTESIAN_POINT ( 'NONE',  ( 10.81492255796106328, -18.62759615963255655, 90.41775706135236135 ) ) ;
#145720 = CARTESIAN_POINT ( 'NONE',  ( 19.03943276465977164, -0.05219959533909143690, 23.74890960531435269 ) ) ;
#145721 = EDGE_LOOP ( 'NONE', ( #103446, #78109, #107837, #153502, #15374 ) ) ;
#145722 = CARTESIAN_POINT ( 'NONE',  ( -8.224510206698948167, 14.34966873604960824, 45.41557627198103830 ) ) ;
#145723 = CARTESIAN_POINT ( 'NONE',  ( -13.70000000000001528, 0.2077008434175769414, -60.44446360152740993 ) ) ;
#145724 = CARTESIAN_POINT ( 'NONE',  ( -0.05219959533907301413, -21.53943276465977519, 42.49890960531435979 ) ) ;
#145725 = CARTESIAN_POINT ( 'NONE',  ( -27.73933785331498925, 2.428612866367529932E-14, 138.8750000027311842 ) ) ;
#145726 = CARTESIAN_POINT ( 'NONE',  ( -5.153800228976328057, -19.02544592524343514, 107.2905762719810383 ) ) ;
#145727 = CARTESIAN_POINT ( 'NONE',  ( -16.52544592524342804, 4.483927247898546575, 86.04057627198102409 ) ) ;
#145728 = CARTESIAN_POINT ( 'NONE',  ( 14.34966873604972726, -8.224510206698740333, 25.83442372801901499 ) ) ;
#145729 = CARTESIAN_POINT ( 'NONE',  ( 4.483927247898790824, -16.52544592524335698, 110.2094237280190185 ) ) ;
#145730 = ORIENTED_EDGE ( 'NONE', *, *, #60319, .F. ) ;
#145732 = CARTESIAN_POINT ( 'NONE',  ( 10.72451020669898902, -18.67979575497178502, 102.9155762719810383 ) ) ;
#145731 = CARTESIAN_POINT ( 'NONE',  ( 0.05219959533909260263, 19.03943276465977164, 94.99890960531436690 ) ) ;
#145734 = CARTESIAN_POINT ( 'NONE',  ( 13.97604488694527802, 13.89961937509977652, 94.37390960531436690 ) ) ;
#145733 = CARTESIAN_POINT ( 'NONE',  ( -16.55341960407617563, 4.379528057220093196, 113.5427570613523756 ) ) ;
#145735 = CARTESIAN_POINT ( 'NONE',  ( 16.51473224551083163, -9.474510206698727899, 95.83442372801900433 ) ) ;
#145736 = CARTESIAN_POINT ( 'NONE',  ( 18.67979575497194134, -10.72451020669871369, 105.8344237280190328 ) ) ;
#145737 = CARTESIAN_POINT ( 'NONE',  ( -10.72451020669898014, 18.67979575497178502, 90.41557627198103830 ) ) ;
#145738 = CARTESIAN_POINT ( 'NONE',  ( 15.80617190586746368, 15.72974639402197994, 44.37390960531435979 ) ) ;
#145739 = CARTESIAN_POINT ( 'NONE',  ( -9.564922557960796823, -16.46253265017161027, 57.08224293864769550 ) ) ;
#145740 = CARTESIAN_POINT ( 'NONE',  ( -0.05219959533910754901, -16.53943276465976808, 32.49890960531435979 ) ) ;
#145741 = CARTESIAN_POINT ( 'NONE',  ( 9.474510206698971260, -16.51473224551069308, 72.91557627198102409 ) ) ;
#145742 = ORIENTED_EDGE ( 'NONE', *, *, #68093, .T. ) ;
#145743 = CYLINDRICAL_SURFACE ( 'NONE', #102233, 214.0437394197456342 ) ;
#145744 = CARTESIAN_POINT ( 'NONE',  ( 19.02544592524334988, 5.153800228976608722, 31.45942372801900433 ) ) ;
#145745 = CARTESIAN_POINT ( 'NONE',  ( 0.05219959533910956823, 16.53943276465976808, 89.99890960531438111 ) ) ;
#145746 = CARTESIAN_POINT ( 'NONE',  ( -5.719274019375665041, -21.55341960407619695, 19.79275706135235069 ) ) ;
#145747 = CARTESIAN_POINT ( 'NONE',  ( 17.14385361876520264, 23.59649016807275856, 142.6750000027311103 ) ) ;
#145748 = CARTESIAN_POINT ( 'NONE',  ( 16.52544592524335698, 4.483927247898782831, 101.4594237280190185 ) ) ;
#145749 = CARTESIAN_POINT ( 'NONE',  ( -19.05341960407611168, -5.049401038298163336, 26.45724293864769550 ) ) ;
#145750 = CARTESIAN_POINT ( 'NONE',  ( 19.02544592524343514, -5.153800228976328945, 73.54057627198103830 ) ) ;
#145751 = CARTESIAN_POINT ( 'NONE',  ( -0.05219959533909027116, -19.03943276465977164, 22.49890960531436690 ) ) ;
#145752 = CARTESIAN_POINT ( 'NONE',  ( -12.14591786802309592, -12.06949235617757132, 46.87390960531435979 ) ) ;
#145753 = CARTESIAN_POINT ( 'NONE',  ( -15.80617190586768217, 15.72974639402176855, 58.12609039468568994 ) ) ;
#145754 = LINE ( 'NONE', #4242, #67083 ) ;
#145755 = CARTESIAN_POINT ( 'NONE',  ( 18.62759615963255655, 10.81492255796105972, 91.66775706135234714 ) ) ;
#145756 = CARTESIAN_POINT ( 'NONE',  ( 13.97604488694527802, 13.89961937509977652, 49.37390960531434558 ) ) ;
#145757 = CARTESIAN_POINT ( 'NONE',  ( -5.049401038298153566, 19.05341960407611168, 55.20724293864769550 ) ) ;
#145758 = ORIENTED_EDGE ( 'NONE', *, *, #181804, .F. ) ;
#145759 = CARTESIAN_POINT ( 'NONE',  ( -18.67979575497193778, 10.72451020669871902, 98.33442372801901854 ) ) ;
#145760 = CARTESIAN_POINT ( 'NONE',  ( 4.483927247898790824, -16.52544592524335698, 60.20942372801902565 ) ) ;
#145761 = CARTESIAN_POINT ( 'NONE',  ( 5.719274019375673035, 21.55341960407619339, 82.29275706135234714 ) ) ;
#145762 = CARTESIAN_POINT ( 'NONE',  ( 16.51473224551069308, 9.474510206698969483, 114.1655762719810241 ) ) ;
#145763 = CARTESIAN_POINT ( 'NONE',  ( -19.05341960407617563, 5.049401038297882671, 88.54275706135230450 ) ) ;
#145764 = CARTESIAN_POINT ( 'NONE',  ( 21.52544592524334988, 5.823673210054432836, 66.45942372801903275 ) ) ;
#145765 = CARTESIAN_POINT ( 'NONE',  ( 4.379528057220092307, 16.55341960407617563, 37.29275706135235424 ) ) ;
#145766 = CARTESIAN_POINT ( 'NONE',  ( -0.05219959533907301413, -21.53943276465977519, 92.49890960531436690 ) ) ;
#145767 = CARTESIAN_POINT ( 'NONE',  ( -0.05219959533936034679, 19.03943276465977164, 82.50109039468567573 ) ) ;
#145768 = CARTESIAN_POINT ( 'NONE',  ( 13.97604488694527802, 13.89961937509977652, 69.37390960531436690 ) ) ;
#145769 = CARTESIAN_POINT ( 'NONE',  ( -5.153800228976607833, 19.02544592524334988, 97.70942372801900433 ) ) ;
#145770 = CARTESIAN_POINT ( 'NONE',  ( 13.89961937509957401, 13.97604488694547697, 106.8760903946856757 ) ) ;
#145771 = CARTESIAN_POINT ( 'NONE',  ( 16.52544592524342804, -4.483927247898539470, 48.54057627198103120 ) ) ;
#145773 = VERTEX_POINT ( 'NONE', #115878 ) ;
#145772 = CARTESIAN_POINT ( 'NONE',  ( 13.97604488694548053, -13.89961937509957401, 70.62609039468567573 ) ) ;
#145774 = CARTESIAN_POINT ( 'NONE',  ( 0.05219959533934541429, -16.53943276465976808, 55.00109039468568284 ) ) ;
#145775 = CARTESIAN_POINT ( 'NONE',  ( 19.03943276465977164, -0.05219959533909143690, 43.74890960531435979 ) ) ;
#145776 = CARTESIAN_POINT ( 'NONE',  ( 9.564922557960805705, 16.46253265017160317, 59.58224293864769550 ) ) ;
#145777 = CARTESIAN_POINT ( 'NONE',  ( -12.06949235617739369, -12.14591786802326823, 59.37609039468568284 ) ) ;
#145778 = LINE ( 'NONE', #114437, #120903 ) ;
#145779 = CARTESIAN_POINT ( 'NONE',  ( -8.906447517083053711, -27.41122689804191026, 138.6500000054623740 ) ) ;
#145780 = CARTESIAN_POINT ( 'NONE',  ( -13.97604488694527625, -13.89961937509977652, 111.8739096053143243 ) ) ;
#145781 = CARTESIAN_POINT ( 'NONE',  ( 19.02544592524343514, -5.153800228976328945, 28.54057627198102409 ) ) ;
#145782 = ORIENTED_EDGE ( 'NONE', *, *, #167192, .T. ) ;
#145783 = CARTESIAN_POINT ( 'NONE',  ( 19.02544592524334988, 5.153800228976608722, 111.4594237280190043 ) ) ;
#145784 = CARTESIAN_POINT ( 'NONE',  ( -15.72974639402197994, 15.80617190586746368, 35.62390960531437401 ) ) ;
#145786 = CARTESIAN_POINT ( 'NONE',  ( -14.29746914071037622, -8.314922557961029526, 34.16775706135234714 ) ) ;
#145785 = CARTESIAN_POINT ( 'NONE',  ( -19.02544592524334988, -5.153800228976617603, 33.95942372801897591 ) ) ;
#145787 = CARTESIAN_POINT ( 'NONE',  ( -19.05341960407611168, -5.049401038298163336, 26.45724293864769550 ) ) ;
#145788 = CARTESIAN_POINT ( 'NONE',  ( -19.05341960407611168, -5.049401038298163336, 51.45724293864770260 ) ) ;
#145789 = CARTESIAN_POINT ( 'NONE',  ( -5.823673210054116645, -21.52544592524344225, 77.29057627198102409 ) ) ;
#145790 = CARTESIAN_POINT ( 'NONE',  ( 5.049401038298161559, -19.05341960407611168, 97.70724293864766707 ) ) ;
#145791 = CARTESIAN_POINT ( 'NONE',  ( 5.153800228976335163, 19.02544592524342804, 44.79057627198103830 ) ) ;
#145792 = CARTESIAN_POINT ( 'NONE',  ( 22.44159573604009239, 16.30477369853692693, 144.5750000027311728 ) ) ;
#145793 = CARTESIAN_POINT ( 'NONE',  ( 13.97604488694548053, -13.89961937509957401, 85.62609039468568994 ) ) ;
#145794 = CARTESIAN_POINT ( 'NONE',  ( -4.379528057220328563, 16.55341960407611168, 65.20724293864768129 ) ) ;
#145795 = CARTESIAN_POINT ( 'NONE',  ( 21.55341960407610458, 5.719274019375980345, 48.95724293864770971 ) ) ;
#145796 = CARTESIAN_POINT ( 'NONE',  ( 10.72451020669871369, 18.67979575497193778, 112.0844237280190185 ) ) ;
#145797 = CARTESIAN_POINT ( 'NONE',  ( -5.823673210054116645, -21.52544592524344225, 102.2905762719810383 ) ) ;
#145798 = CARTESIAN_POINT ( 'NONE',  ( -5.823673210054431948, 21.52544592524334988, 72.70942372801901854 ) ) ;
#145799 = CARTESIAN_POINT ( 'NONE',  ( -21.53943276465977519, -0.05219959533937600094, 83.75109039468568994 ) ) ;
#145800 = CARTESIAN_POINT ( 'NONE',  ( -19.02544592524342804, 5.153800228976336051, 111.0405762719810099 ) ) ;
#145802 = CARTESIAN_POINT ( 'NONE',  ( -5.823673210054431948, 21.52544592524334988, 77.70942372801900433 ) ) ;
#145801 = CARTESIAN_POINT ( 'NONE',  ( -14.34966873604972548, 8.224510206698743886, 103.3344237280190043 ) ) ;
#145803 = CARTESIAN_POINT ( 'NONE',  ( 9.474510206698971260, -16.51473224551069308, 72.91557627198102409 ) ) ;
#145804 = CARTESIAN_POINT ( 'NONE',  ( 21.55341960407619695, -5.719274019375665929, 36.04275706135234714 ) ) ;
#145805 = CARTESIAN_POINT ( 'NONE',  ( -19.05341960407611168, -5.049401038298163336, 66.45724293864769550 ) ) ;
#145806 = CARTESIAN_POINT ( 'NONE',  ( -12.06949235617756955, 12.14591786802309770, 80.62390960531438111 ) ) ;
#145807 = CARTESIAN_POINT ( 'NONE',  ( 16.55341960407611168, 4.379528057220329451, 53.95724293864770260 ) ) ;
#145808 = CARTESIAN_POINT ( 'NONE',  ( 5.823673210054125526, 21.52544592524343514, 59.79057627198103120 ) ) ;
#145809 = CARTESIAN_POINT ( 'NONE',  ( -16.51473224551069308, -9.474510206698971260, 61.66557627198103120 ) ) ;
#145810 = CARTESIAN_POINT ( 'NONE',  ( -18.62759615963270932, 10.81492255796079327, 70.83224293864770971 ) ) ;
#145811 = CARTESIAN_POINT ( 'NONE',  ( -13.97604488694547697, 13.89961937509957934, 63.12609039468566152 ) ) ;
#145813 = CARTESIAN_POINT ( 'NONE',  ( 4.483927247898545687, 16.52544592524342804, 59.79057627198103120 ) ) ;
#145812 = CARTESIAN_POINT ( 'NONE',  ( 19.03943276465977164, 0.05219959533936151252, 26.25109039468566507 ) ) ;
#145814 = CARTESIAN_POINT ( 'NONE',  ( 15.72974639402199770, -15.80617190586745480, 58.12390960531435979 ) ) ;
#145815 = ORIENTED_EDGE ( 'NONE', *, *, #180229, .F. ) ;
#145816 = CARTESIAN_POINT ( 'NONE',  ( -17.97214573761831247, -5.500000000000087930, 41.46970049038657180 ) ) ;
#145818 = CARTESIAN_POINT ( 'NONE',  ( 17.14385361876520264, 23.59649016807275856, 140.6750000027311387 ) ) ;
#145817 = CARTESIAN_POINT ( 'NONE',  ( -8.314922557961024197, 14.29746914071037800, 102.9177570613523756 ) ) ;
#145819 = CARTESIAN_POINT ( 'NONE',  ( -19.02544592524334988, -5.153800228976617603, 88.95942372801897591 ) ) ;
#145820 = CARTESIAN_POINT ( 'NONE',  ( -8.314922557960811034, -14.29746914071050412, 62.08224293864769550 ) ) ;
#145821 = CARTESIAN_POINT ( 'NONE',  ( -19.01529144963332385, -5.500000000000167866, 61.23431955728440812 ) ) ;
#145822 = CARTESIAN_POINT ( 'NONE',  ( 16.51473224551069308, 9.474510206698969483, 59.16557627198102409 ) ) ;
#145823 = CARTESIAN_POINT ( 'NONE',  ( 0.05219959533910956823, 16.53943276465976808, 54.99890960531435269 ) ) ;
#145824 = CARTESIAN_POINT ( 'NONE',  ( 9.474510206698971260, -16.51473224551069308, 82.91557627198103830 ) ) ;
#145826 = CARTESIAN_POINT ( 'NONE',  ( 16.46253265017160672, -9.564922557960803928, 53.33224293864768839 ) ) ;
#145825 = CARTESIAN_POINT ( 'NONE',  ( -19.02544592524334988, -5.153800228976617603, 73.95942372801900433 ) ) ;
#145827 = CARTESIAN_POINT ( 'NONE',  ( -19.03943276465977164, 0.05219959533909376836, 81.24890960531436690 ) ) ;
#145828 = CARTESIAN_POINT ( 'NONE',  ( -13.89961937509977652, 13.97604488694528158, 70.62390960531432427 ) ) ;
#145829 = CARTESIAN_POINT ( 'NONE',  ( 21.55341960407610458, 5.719274019375980345, 68.95724293864769550 ) ) ;
#145830 = FACE_OUTER_BOUND ( 'NONE', #114664, .T. ) ;
#145831 = CARTESIAN_POINT ( 'NONE',  ( 13.89961937509977652, -13.97604488694527269, 53.12390960531434558 ) ) ;
#145832 = CARTESIAN_POINT ( 'NONE',  ( 15.72974639402199770, -15.80617190586745480, 53.12390960531436690 ) ) ;
#145833 = CARTESIAN_POINT ( 'NONE',  ( 5.153800228976615827, -19.02544592524334988, 80.20942372801901854 ) ) ;
#145834 = CARTESIAN_POINT ( 'NONE',  ( 14.29746914071049879, -8.314922557960816363, 23.33224293864769194 ) ) ;
#145835 = EDGE_CURVE ( 'NONE', #58799, #137572, #93458, .T. ) ;
#145836 = CARTESIAN_POINT ( 'NONE',  ( -13.97604488694547697, 13.89961937509957934, 33.12609039468566863 ) ) ;
#145838 = CARTESIAN_POINT ( 'NONE',  ( 0.05219959533934541429, -16.53943276465976808, 95.00109039468568994 ) ) ;
#145837 = CARTESIAN_POINT ( 'NONE',  ( -14.29746914071037622, -8.314922557961029526, 59.16775706135234714 ) ) ;
#145839 = CARTESIAN_POINT ( 'NONE',  ( -18.09867054820431420, -5.499999999999968026, 93.98393025253582778 ) ) ;
#145840 = CARTESIAN_POINT ( 'NONE',  ( -14.29746914071037622, -8.314922557961029526, 79.16775706135234714 ) ) ;
#145841 = CARTESIAN_POINT ( 'NONE',  ( -5.049401038298153566, 19.05341960407611168, 115.2072429386477097 ) ) ;
#145842 = CARTESIAN_POINT ( 'NONE',  ( 9.474510206698971260, -16.51473224551069308, 32.91557627198102409 ) ) ;
#145843 = CARTESIAN_POINT ( 'NONE',  ( -12.06949235617739369, -12.14591786802326823, 34.37609039468568284 ) ) ;
#145844 = CARTESIAN_POINT ( 'NONE',  ( 9.474510206698971260, -16.51473224551069308, 47.91557627198102409 ) ) ;
#145845 = CARTESIAN_POINT ( 'NONE',  ( -5.719274019375665041, -21.55341960407619695, 39.79275706135235424 ) ) ;
#145846 = CARTESIAN_POINT ( 'NONE',  ( -16.53943276465976808, -0.05219959533934237506, 48.75109039468568284 ) ) ;
#145847 = CARTESIAN_POINT ( 'NONE',  ( -16.55341960407617563, 4.379528057220093196, 108.5427570613523756 ) ) ;
#145848 = CARTESIAN_POINT ( 'NONE',  ( 16.51473224551069308, 9.474510206698969483, 29.16557627198103475 ) ) ;
#145849 = CARTESIAN_POINT ( 'NONE',  ( 9.564922557961047289, -16.46253265017146816, 25.41775706135234003 ) ) ;
#145850 = CARTESIAN_POINT ( 'NONE',  ( 19.03943276465977164, 0.05219959533936151252, 111.2510903946856757 ) ) ;
#145851 = CARTESIAN_POINT ( 'NONE',  ( -5.049401038297874678, -19.05341960407617918, 69.79275706135233293 ) ) ;
#145852 = CARTESIAN_POINT ( 'NONE',  ( -14.29746914071049879, 8.314922557960819915, 65.83224293864769550 ) ) ;
#145853 = CARTESIAN_POINT ( 'NONE',  ( 19.03943276465977164, -0.05219959533909143690, 38.74890960531436690 ) ) ;
#145855 = CARTESIAN_POINT ( 'NONE',  ( 16.20579543436678804, -7.371946100355086351, 91.93479165828122746 ) ) ;
#145854 = CARTESIAN_POINT ( 'NONE',  ( 19.05341960407617918, -5.049401038297876454, 76.04275706135230450 ) ) ;
#145856 = CARTESIAN_POINT ( 'NONE',  ( -21.53943276465977519, -0.05219959533937600094, 68.75109039468568994 ) ) ;
#145857 = CARTESIAN_POINT ( 'NONE',  ( 12.14591786802327356, -12.06949235617739191, 40.62609039468567573 ) ) ;
#145858 = CARTESIAN_POINT ( 'NONE',  ( 22.99604614807110181, -21.49604614807104142, -49.67998909148434450 ) ) ;
#145859 = CARTESIAN_POINT ( 'NONE',  ( -15.80617190586745835, -15.72974639402198527, 31.87390960531435979 ) ) ;
#145860 = CARTESIAN_POINT ( 'NONE',  ( 16.52544592524335698, 4.483927247898782831, 31.45942372801901854 ) ) ;
#145861 = CARTESIAN_POINT ( 'NONE',  ( 9.564922557960805705, 16.46253265017160317, 114.5822429386476955 ) ) ;
#145862 = CARTESIAN_POINT ( 'NONE',  ( -26.78465914369783007, 5.761000505272440897, 169.4491075441771670 ) ) ;
#145863 = CARTESIAN_POINT ( 'NONE',  ( 19.03943276465977164, -0.05219959533909143690, 33.74890960531435979 ) ) ;
#145864 = FACE_OUTER_BOUND ( 'NONE', #75757, .T. ) ;
#145865 = CARTESIAN_POINT ( 'NONE',  ( 19.03943276465977164, -0.05219959533909143690, 53.74890960531436690 ) ) ;
#145866 = CARTESIAN_POINT ( 'NONE',  ( -10.81492255796105439, 18.62759615963255655, 67.91775706135234714 ) ) ;
#145867 = CARTESIAN_POINT ( 'NONE',  ( -15.80617190586768217, 15.72974639402176855, 108.1260903946856757 ) ) ;
#145868 = CARTESIAN_POINT ( 'NONE',  ( -4.483927247898539470, -16.52544592524342804, 27.29057627198103120 ) ) ;
#145869 = CARTESIAN_POINT ( 'NONE',  ( 5.049401038298161559, -19.05341960407611168, 32.70724293864768129 ) ) ;
#145870 = CARTESIAN_POINT ( 'NONE',  ( 19.02544592524343514, -5.153800228976328945, 93.54057627198102409 ) ) ;
#145871 = CARTESIAN_POINT ( 'NONE',  ( 10.72451020669871369, 18.67979575497193778, 52.08442372801901854 ) ) ;
#145872 = CARTESIAN_POINT ( 'NONE',  ( 13.89961937509977652, -13.97604488694527269, 38.12390960531436690 ) ) ;
#145873 = CARTESIAN_POINT ( 'NONE',  ( -5.719274019375665041, -21.55341960407619695, 49.79275706135234714 ) ) ;
#145875 = CARTESIAN_POINT ( 'NONE',  ( -9.474510206698964154, 16.51473224551069663, 105.4155762719810383 ) ) ;
#145874 = CARTESIAN_POINT ( 'NONE',  ( -16.51473224551082808, 9.474510206698731452, 98.33442372801900433 ) ) ;
#145876 = CARTESIAN_POINT ( 'NONE',  ( -13.89961937509977652, 13.97604488694528158, 25.62390960531434558 ) ) ;
#145877 = CARTESIAN_POINT ( 'NONE',  ( -0.05219959533907301413, -21.53943276465977519, 107.4989096053143669 ) ) ;
#145878 = CARTESIAN_POINT ( 'NONE',  ( -5.049401038297874678, -19.05341960407617918, 39.79275706135232582 ) ) ;
#145879 = CARTESIAN_POINT ( 'NONE',  ( 14.34966873604960469, 8.224510206698951720, 109.1655762719810383 ) ) ;
#145880 = CARTESIAN_POINT ( 'NONE',  ( 19.02544592524343514, -5.153800228976328945, 58.54057627198102409 ) ) ;
#145881 = CARTESIAN_POINT ( 'NONE',  ( 0.05219959533936267826, -19.03943276465977164, 95.00109039468567573 ) ) ;
#145882 = CARTESIAN_POINT ( 'NONE',  ( 8.224510206698953496, -14.34966873604960469, 57.91557627198103120 ) ) ;
#145883 = CARTESIAN_POINT ( 'NONE',  ( 13.89961937509957401, 13.97604488694547697, 21.87609039468566152 ) ) ;
#145884 = CARTESIAN_POINT ( 'NONE',  ( 5.719274019375991003, -21.55341960407610458, 27.70724293864769905 ) ) ;
#145885 = CARTESIAN_POINT ( 'NONE',  ( -16.51473224551082808, 9.474510206698731452, 93.33442372801900433 ) ) ;
#145886 = CARTESIAN_POINT ( 'NONE',  ( 10.72451020669898902, -18.67979575497178502, 92.91557627198103830 ) ) ;
#145887 = CARTESIAN_POINT ( 'NONE',  ( -5.823673210054431948, 21.52544592524334988, 37.70942372801900433 ) ) ;
#145888 = CARTESIAN_POINT ( 'NONE',  ( -14.34966873604972548, 8.224510206698743886, 48.33442372801902565 ) ) ;
#145889 = CARTESIAN_POINT ( 'NONE',  ( 4.379528057220092307, 16.55341960407617563, 112.2927570613523471 ) ) ;
#145891 = CARTESIAN_POINT ( 'NONE',  ( -18.62759615963255300, -10.81492255796106328, 54.16775706135235424 ) ) ;
#145890 = CARTESIAN_POINT ( 'NONE',  ( 12.14591786802327356, -12.06949235617739191, 35.62609039468568994 ) ) ;
#145892 = CARTESIAN_POINT ( 'NONE',  ( 5.719274019375991003, -21.55341960407610458, 57.70724293864770260 ) ) ;
#145893 = CARTESIAN_POINT ( 'NONE',  ( 19.02544592524343514, -5.153800228976328945, 28.54057627198102409 ) ) ;
#145894 = CARTESIAN_POINT ( 'NONE',  ( 11.74264578624800315, -36.14014761921581709, -5.149999994537626691 ) ) ;
#145895 = CARTESIAN_POINT ( 'NONE',  ( 0.05219959533934541429, -16.53943276465976808, 75.00109039468568994 ) ) ;
#145896 = CARTESIAN_POINT ( 'NONE',  ( -21.52544592524343514, 5.823673210054127303, 91.04057627198103830 ) ) ;
#145897 = CARTESIAN_POINT ( 'NONE',  ( 16.52544592524342804, -4.483927247898539470, 33.54057627198102409 ) ) ;
#145898 = CARTESIAN_POINT ( 'NONE',  ( 16.53943276465976808, 0.05219959533934440121, 66.25109039468567573 ) ) ;
#145899 = CARTESIAN_POINT ( 'NONE',  ( -13.89961937509957401, -13.97604488694547875, 104.3760903946856757 ) ) ;
#145900 = CARTESIAN_POINT ( 'NONE',  ( 0.05219959533907565091, 21.53943276465977519, 99.99890960531436690 ) ) ;
#145901 = CARTESIAN_POINT ( 'NONE',  ( -16.53943276465976808, 0.05219959533911058130, 31.24890960531435979 ) ) ;
#145902 = ORIENTED_EDGE ( 'NONE', *, *, #122956, .T. ) ;
#145903 = CARTESIAN_POINT ( 'NONE',  ( 16.52544592524335698, 4.483927247898782831, 76.45942372801901854 ) ) ;
#145904 = CARTESIAN_POINT ( 'NONE',  ( 21.94905633995363559, 8.886455535323596777, 171.4390084046502523 ) ) ;
#145905 = CARTESIAN_POINT ( 'NONE',  ( 10.81492255796078972, 18.62759615963270932, 69.58224293864769550 ) ) ;
#145906 = CARTESIAN_POINT ( 'NONE',  ( -4.379528057220086978, -16.55341960407618274, 109.7927570613523613 ) ) ;
#145907 = EDGE_LOOP ( 'NONE', ( #86482, #145963, #69637, #177305 ) ) ;
#145908 = DIRECTION ( 'NONE',  ( 0.000000000000000000, 0.000000000000000000, 1.000000000000000000 ) ) ;
#145909 = CARTESIAN_POINT ( 'NONE',  ( -5.823673210054116645, -21.52544592524344225, 82.29057627198103830 ) ) ;
#145910 = CARTESIAN_POINT ( 'NONE',  ( -15.72974639402197994, 15.80617190586746368, 105.6239096053143669 ) ) ;
#145911 = CARTESIAN_POINT ( 'NONE',  ( 14.29746914071049879, -8.314922557960816363, 38.33224293864768839 ) ) ;
#145912 = CARTESIAN_POINT ( 'NONE',  ( 0.05219959533934541429, -16.53943276465976808, 35.00109039468568284 ) ) ;
#145913 = CARTESIAN_POINT ( 'NONE',  ( -9.474510206698964154, 16.51473224551069663, 45.41557627198103120 ) ) ;
#145914 = CARTESIAN_POINT ( 'NONE',  ( -5.049401038298153566, 19.05341960407611168, 70.20724293864769550 ) ) ;
#145915 = ORIENTED_EDGE ( 'NONE', *, *, #88289, .F. ) ;
#145916 = EDGE_CURVE ( 'NONE', #2296, #36039, #169531, .T. ) ;
#145917 = CARTESIAN_POINT ( 'NONE',  ( 15.72974639402199770, -15.80617190586745480, 23.12390960531436335 ) ) ;
#145918 = DIRECTION ( 'NONE',  ( 0.000000000000000000, 0.000000000000000000, 1.000000000000000000 ) ) ;
#145919 = CARTESIAN_POINT ( 'NONE',  ( -16.46253265017146816, -9.564922557961047289, 99.16775706135233293 ) ) ;
#145920 = CARTESIAN_POINT ( 'NONE',  ( 16.51473224551083163, -9.474510206698727899, 45.83442372801900433 ) ) ;
#145921 = CARTESIAN_POINT ( 'NONE',  ( 0.05219959533907565091, 21.53943276465977519, 94.99890960531436690 ) ) ;
#145922 = CARTESIAN_POINT ( 'NONE',  ( -0.05219959533934338120, 16.53943276465976808, 107.5010903946856899 ) ) ;
#145923 = CIRCLE ( 'NONE', #158763, 38.00000000000002132 ) ;
#145924 = CARTESIAN_POINT ( 'NONE',  ( -21.52544592524343514, 5.823673210054127303, 51.04057627198103120 ) ) ;
#145926 = CARTESIAN_POINT ( 'NONE',  ( 5.049401038297881783, 19.05341960407617563, 107.2927570613523187 ) ) ;
#145925 = CARTESIAN_POINT ( 'NONE',  ( 21.55341960407610458, 5.719274019375980345, 83.95724293864770971 ) ) ;
#145927 = CARTESIAN_POINT ( 'NONE',  ( 9.474510206698971260, -16.51473224551069308, 102.9155762719810241 ) ) ;
#145928 = CARTESIAN_POINT ( 'NONE',  ( -10.81492255796105439, 18.62759615963255655, 77.91775706135231871 ) ) ;
#145930 = EDGE_CURVE ( 'NONE', #4626, #45713, #14524, .T. ) ;
#145929 = CARTESIAN_POINT ( 'NONE',  ( 16.51473224551069308, 9.474510206698969483, 69.16557627198102409 ) ) ;
#145931 = CARTESIAN_POINT ( 'NONE',  ( 31.27056374934903715, 7.502136971886772976, 95.45648825569141138 ) ) ;
#145932 = CARTESIAN_POINT ( 'NONE',  ( -19.05341960407611168, -5.049401038298163336, 76.45724293864769550 ) ) ;
#145933 = CARTESIAN_POINT ( 'NONE',  ( 4.483927247898545687, 16.52544592524342804, 89.79057627198103830 ) ) ;
#145934 = ORIENTED_EDGE ( 'NONE', *, *, #99437, .T. ) ;
#145935 = CARTESIAN_POINT ( 'NONE',  ( -19.02544592524334988, -5.153800228976617603, 108.9594237280189759 ) ) ;
#145936 =( BOUNDED_CURVE ( )  B_SPLINE_CURVE ( 2, ( #64025, #78183, #14546, #187394, #170213, #171209, #138870, #15543, #155041, #1341, #123684, #110517, #95346, #16536, #156029, #124700, #186397, #30714, #80175, #47874, #79185, #172198, #76205, #198580, #140855, #2344, #33683, #61034, #157030, #44891, #18528, #60048, #122706, #137884, #199565, #169206, #184396, #45876, #175185, #111515, #20493, #144832, #159000, #188373, #6316, #3338, #67000, #83158, #96334, #36651, #67995, #129648, #97314, #81157, #173200, #66001, #65012, #98309, #174198, #99327, #176193 ),
 .UNSPECIFIED., .F., .F. ) 
 B_SPLINE_CURVE_WITH_KNOTS ( ( 3, 2, 2, 2, 2, 2, 2, 2, 2, 2, 2, 2, 2, 2, 2, 2, 2, 2, 2, 2, 2, 2, 2, 2, 2, 2, 2, 2, 2, 2, 3 ),
 ( 0.000000000000000000, 0.004385964912280701511, 0.008771929824561403022, 0.01315789473684210453, 0.01754385964912280604, 0.02192982456140350755, 0.02631578947368420907, 0.03070175438596491058, 0.03508771929824561209, 0.03947368421052631360, 0.04385964912280701511, 0.04824561403508771662, 0.05263157894736841813, 0.05701754385964911964, 0.06140350877192982115, 0.06578947368421052266, 0.07017543859649122417, 0.07456140350877192569, 0.07894736842105262720, 0.08333333333333332871, 0.08771929824561403022, 0.09210526315789473173, 0.09649122807017543324, 0.1008771929824561348, 0.1052631578947368363, 0.1096491228070175378, 0.1140350877192982393, 0.1184210526315789408, 0.1228070175438596423, 0.1271929824561403577, 0.1291485109413760268 ),
 .UNSPECIFIED. ) 
 CURVE ( )  GEOMETRIC_REPRESENTATION_ITEM ( )  RATIONAL_B_SPLINE_CURVE ( ( 1.000000000000000000, 0.9659258262890683122, 1.000000000000000000, 0.9659258262890683122, 1.000000000000000000, 0.9659258262890683122, 1.000000000000000000, 0.9659258262890683122, 1.000000000000000000, 0.9659258262890683122, 1.000000000000000000, 0.9659258262890683122, 1.000000000000000000, 0.9659258262890683122, 1.000000000000000000, 0.9659258262890683122, 1.000000000000000000, 0.9659258262890683122, 1.000000000000000000, 0.9659258262890683122, 1.000000000000000000, 0.9659258262890683122, 1.000000000000000000, 0.9659258262890683122, 1.000000000000000000, 0.9659258262890683122, 1.000000000000000000, 0.9659258262890683122, 1.000000000000000000, 0.9659258262890683122, 1.000000000000000000, 0.9659258262890683122, 1.000000000000000000, 0.9659258262890683122, 1.000000000000000000, 0.9659258262890683122, 1.000000000000000000, 0.9659258262890683122, 1.000000000000000000, 0.9659258262890683122, 1.000000000000000000, 0.9659258262890683122, 1.000000000000000000, 0.9659258262890683122, 1.000000000000000000, 0.9659258262890683122, 1.000000000000000000, 0.9659258262890683122, 1.000000000000000000, 0.9659258262890683122, 1.000000000000000000, 0.9659258262890683122, 1.000000000000000000, 0.9659258262890683122, 1.000000000000000000, 0.9659258262890683122, 1.000000000000000000, 0.9659258262890683122, 1.000000000000000000, 0.9848076720550082985, 0.9831626618144004848 ) ) 
 REPRESENTATION_ITEM ( '' )  );
#145937 = CARTESIAN_POINT ( 'NONE',  ( 16.31925111598454947, -7.325300261831590554, 82.66424538967253000 ) ) ;
#145938 = CARTESIAN_POINT ( 'NONE',  ( -13.89961937509977652, 13.97604488694528158, 70.62390960531432427 ) ) ;
#145940 = CARTESIAN_POINT ( 'NONE',  ( 0.05219959533909260263, 19.03943276465977164, 104.9989096053143669 ) ) ;
#145939 = CARTESIAN_POINT ( 'NONE',  ( 0.05219959533937995610, -21.53943276465977519, 90.00109039468567573 ) ) ;
#145941 = CARTESIAN_POINT ( 'NONE',  ( -16.55341960407617563, 4.379528057220093196, 73.54275706135234714 ) ) ;
#145942 = CARTESIAN_POINT ( 'NONE',  ( -17.44270441346519718, -5.991230190322950122, 76.36335079264230785 ) ) ;
#145943 = CARTESIAN_POINT ( 'NONE',  ( 19.02544592524334988, 5.153800228976608722, 56.45942372801898301 ) ) ;
#145944 = CARTESIAN_POINT ( 'NONE',  ( -21.55341960407619339, 5.719274019375674811, 108.5427570613523756 ) ) ;
#145945 = CARTESIAN_POINT ( 'NONE',  ( 2.500000000000000000, 1.178949249685212974, -2.042000000000001148 ) ) ;
#145946 = CARTESIAN_POINT ( 'NONE',  ( -69.65682714487590488, -71.74905178543390605, -15.00000000000000178 ) ) ;
#145947 = CARTESIAN_POINT ( 'NONE',  ( 29.86685920354754487, 21.69954338932564752, -3.924999997268812990 ) ) ;
#145948 = CARTESIAN_POINT ( 'NONE',  ( 16.52544592524342804, -4.483927247898539470, 28.54057627198103120 ) ) ;
#145949 = CARTESIAN_POINT ( 'NONE',  ( -31.99364916731038022, -5.510910596163089556E-15, 45.00000000000000000 ) ) ;
#145950 = CARTESIAN_POINT ( 'NONE',  ( 14.34966873604972726, -8.224510206698740333, 90.83442372801901854 ) ) ;
#145951 = CARTESIAN_POINT ( 'NONE',  ( 16.36317988757057051, 7.306389748694940067, 68.40210391636775000 ) ) ;
#145952 = CARTESIAN_POINT ( 'NONE',  ( 0.05219959533934541429, -16.53943276465976808, 70.00109039468568994 ) ) ;
#145953 = CARTESIAN_POINT ( 'NONE',  ( -18.67979575497193778, 10.72451020669871902, 83.33442372801903275 ) ) ;
#145954 = CARTESIAN_POINT ( 'NONE',  ( -13.89961937509957401, -13.97604488694547875, 89.37609039468563310 ) ) ;
#145955 = CARTESIAN_POINT ( 'NONE',  ( 19.05341960407617918, -5.049401038297876454, 36.04275706135234003 ) ) ;
#145956 = CARTESIAN_POINT ( 'NONE',  ( -9.564922557960796823, -16.46253265017161027, 77.08224293864769550 ) ) ;
#145957 = CARTESIAN_POINT ( 'NONE',  ( 9.564922557960805705, 16.46253265017160317, 59.58224293864769550 ) ) ;
#145958 = CARTESIAN_POINT ( 'NONE',  ( -0.05219959533909027116, -19.03943276465977164, 87.49890960531436690 ) ) ;
#145959 = CARTESIAN_POINT ( 'NONE',  ( 21.55341960407610458, 5.719274019375980345, 78.95724293864769550 ) ) ;
#145960 = CARTESIAN_POINT ( 'NONE',  ( 21.52544592524344225, -5.823673210054117533, 43.54057627198103830 ) ) ;
#145961 = CARTESIAN_POINT ( 'NONE',  ( 19.02544592524343514, -5.153800228976328945, 28.54057627198102409 ) ) ;
#145962 = CARTESIAN_POINT ( 'NONE',  ( -0.05219959533934338120, 16.53943276465976808, 57.50109039468568994 ) ) ;
#145963 = ORIENTED_EDGE ( 'NONE', *, *, #5408, .T. ) ;
#145964 = CARTESIAN_POINT ( 'NONE',  ( 5.719274019375673035, 21.55341960407619339, 47.29275706135234003 ) ) ;
#145966 = CARTESIAN_POINT ( 'NONE',  ( -23.48529157249599919, -32.32473071737750558, -1.699999999999999734 ) ) ;
#145965 = CARTESIAN_POINT ( 'NONE',  ( -12.14591786802309592, -12.06949235617757132, 66.87390960531436690 ) ) ;
#145967 = CARTESIAN_POINT ( 'NONE',  ( 14.29746914071037800, 8.314922557961029526, 41.66775706135235424 ) ) ;
#145968 = CARTESIAN_POINT ( 'NONE',  ( 12.14591786802309770, 12.06949235617756955, 109.3739096053143811 ) ) ;
#145969 = CARTESIAN_POINT ( 'NONE',  ( -0.05219959533936034679, 19.03943276465977164, 52.50109039468566863 ) ) ;
#145970 = CARTESIAN_POINT ( 'NONE',  ( -16.52544592524342804, 4.483927247898546575, 61.04057627198103120 ) ) ;
#145971 = CARTESIAN_POINT ( 'NONE',  ( 21.55341960407619695, -5.719274019375665929, 36.04275706135234714 ) ) ;
#145973 = CARTESIAN_POINT ( 'NONE',  ( 21.52544592524344225, -5.823673210054117533, 88.54057627198103830 ) ) ;
#145972 = DIRECTION ( 'NONE',  ( 0.000000000000000000, 0.000000000000000000, -1.000000000000000000 ) ) ;
#145974 = CARTESIAN_POINT ( 'NONE',  ( 13.97604488694527802, 13.89961937509977652, 109.3739096053143669 ) ) ;
#145975 = CARTESIAN_POINT ( 'NONE',  ( -4.379528057220328563, 16.55341960407611168, 75.20724293864769550 ) ) ;
#145976 = CARTESIAN_POINT ( 'NONE',  ( 35.06017246933186726, -19.40171014085571954, -22.29041292151832820 ) ) ;
#145977 = CARTESIAN_POINT ( 'NONE',  ( 3.556970738554034288E-15, -38.81732327939057114, -4.124999997268813168 ) ) ;
#145978 = CARTESIAN_POINT ( 'NONE',  ( -5.153800228976607833, 19.02544592524334988, 87.70942372801897591 ) ) ;
#145979 = CARTESIAN_POINT ( 'NONE',  ( -18.62759615963255300, -10.81492255796106328, 19.16775706135234714 ) ) ;
#145980 = CARTESIAN_POINT ( 'NONE',  ( 19.03943276465977164, -0.05219959533909143690, 63.74890960531435979 ) ) ;
#145981 = CARTESIAN_POINT ( 'NONE',  ( 16.46253265017146816, 9.564922557961045513, 51.66775706135233293 ) ) ;
#145982 = CARTESIAN_POINT ( 'NONE',  ( 13.97604488694527802, 13.89961937509977652, 29.37390960531435979 ) ) ;
#145983 = CARTESIAN_POINT ( 'NONE',  ( 21.53943276465977519, 0.05219959533937863772, 61.25109039468567573 ) ) ;
#145984 = CARTESIAN_POINT ( 'NONE',  ( -18.22780087662123805, 5.499999999999981348, 76.01763182126894947 ) ) ;
#145985 = CARTESIAN_POINT ( 'NONE',  ( 16.55341960407611168, 4.379528057220329451, 58.95724293864770971 ) ) ;
#145986 = CARTESIAN_POINT ( 'NONE',  ( 19.03943276465977164, -0.05219959533909143690, 58.74890960531435979 ) ) ;
#145987 = CARTESIAN_POINT ( 'NONE',  ( -15.80617190586745835, -15.72974639402198527, 91.87390960531436690 ) ) ;
#145988 = CARTESIAN_POINT ( 'NONE',  ( 19.05341960407611168, 5.049401038298154454, 63.95724293864769550 ) ) ;
#145989 = ORIENTED_EDGE ( 'NONE', *, *, #105310, .F. ) ;
#145990 = CARTESIAN_POINT ( 'NONE',  ( 15.72974639402199770, -15.80617190586745480, 83.12390960531436690 ) ) ;
#145991 = CARTESIAN_POINT ( 'NONE',  ( -21.52544592524334988, -5.823673210054445271, 93.95942372801903275 ) ) ;
#145994 = CARTESIAN_POINT ( 'NONE',  ( -8.224510206698948167, 14.34966873604960824, 95.41557627198102409 ) ) ;
#145993 = CARTESIAN_POINT ( 'NONE',  ( 0.05219959533934541429, -16.53943276465976808, 100.0010903946857042 ) ) ;
#145992 = CARTESIAN_POINT ( 'NONE',  ( 1.022580077288041090E-15, 16.70000000000002061, -61.34707691135562868 ) ) ;
#145995 = CARTESIAN_POINT ( 'NONE',  ( -5.153800228976607833, 19.02544592524334988, 87.70942372801897591 ) ) ;
#145996 = EDGE_LOOP ( 'NONE', ( #35512, #51675, #39497, #185518, #29844, #31324 ) ) ;
#145997 = CARTESIAN_POINT ( 'NONE',  ( 21.53943276465977519, -0.05219959533907433946, 113.7489096053143527 ) ) ;
#145998 = CARTESIAN_POINT ( 'NONE',  ( 19.03943276465977164, 0.05219959533936151252, 41.25109039468566152 ) ) ;
#145999 = CARTESIAN_POINT ( 'NONE',  ( -12.06949235617739369, -12.14591786802326823, 104.3760903946856899 ) ) ;
#146000 = CARTESIAN_POINT ( 'NONE',  ( -5.049401038297874678, -19.05341960407617918, 24.79275706135233648 ) ) ;
#146001 = CARTESIAN_POINT ( 'NONE',  ( -5.049401038298153566, 19.05341960407611168, 100.2072429386476955 ) ) ;
#146002 = CARTESIAN_POINT ( 'NONE',  ( 15.72974639402199770, -15.80617190586745480, 63.12390960531435979 ) ) ;
#146003 = CARTESIAN_POINT ( 'NONE',  ( -24.37407968765138833, 13.84118768211350492, 165.9040744261181430 ) ) ;
#146004 = CARTESIAN_POINT ( 'NONE',  ( 14.29746914071049879, -8.314922557960816363, 113.3322429386476955 ) ) ;
#146005 = CARTESIAN_POINT ( 'NONE',  ( 5.719274019375673035, 21.55341960407619339, 112.2927570613523471 ) ) ;
#146006 = CARTESIAN_POINT ( 'NONE',  ( -8.224510206698735004, -14.34966873604973081, 74.58442372801901854 ) ) ;
#146007 = CARTESIAN_POINT ( 'NONE',  ( -10.81492255796105439, 18.62759615963255655, 22.91775706135235069 ) ) ;
#146008 = CARTESIAN_POINT ( 'NONE',  ( -8.224510206698735004, -14.34966873604973081, 24.58442372801901499 ) ) ;
#146009 = CARTESIAN_POINT ( 'NONE',  ( -13.97604488694527625, -13.89961937509977652, 106.8739096053143669 ) ) ;
#146010 = CARTESIAN_POINT ( 'NONE',  ( -5.049401038298153566, 19.05341960407611168, 45.20724293864769550 ) ) ;
#146011 = CARTESIAN_POINT ( 'NONE',  ( -9.564922557960796823, -16.46253265017161027, 72.08224293864770971 ) ) ;
#146012 = CARTESIAN_POINT ( 'NONE',  ( 14.29746914071037800, 8.314922557961029526, 46.66775706135234714 ) ) ;
#146013 = CARTESIAN_POINT ( 'NONE',  ( 4.379528057220339221, -16.55341960407611168, 92.70724293864770971 ) ) ;
#146014 = CARTESIAN_POINT ( 'NONE',  ( 0.05219959533934541429, -16.53943276465976808, 105.0010903946856757 ) ) ;
#146015 = PLANE ( 'NONE',  #47527 ) ;
#146018 = CARTESIAN_POINT ( 'NONE',  ( -13.89961937509977652, 13.97604488694528158, 60.62390960531436690 ) ) ;
#146017 = CARTESIAN_POINT ( 'NONE',  ( -13.97604488694527625, -13.89961937509977652, 76.87390960531433848 ) ) ;
#146016 = CARTESIAN_POINT ( 'NONE',  ( 10.72451020669871369, 18.67979575497193778, 52.08442372801901854 ) ) ;
#146019 = CARTESIAN_POINT ( 'NONE',  ( -5.049401038298153566, 19.05341960407611168, 95.20724293864770971 ) ) ;
#146020 = CARTESIAN_POINT ( 'NONE',  ( 16.53943276465976808, -0.05219959533910856209, 43.74890960531435979 ) ) ;
#146021 = CARTESIAN_POINT ( 'NONE',  ( -16.53943276465976808, -0.05219959533934237506, 93.75109039468567573 ) ) ;
#146022 = ORIENTED_EDGE ( 'NONE', *, *, #26122, .T. ) ;
#146023 = CARTESIAN_POINT ( 'NONE',  ( -19.03943276465977164, -0.05219959533935918106, 43.75109039468566863 ) ) ;
#146024 = CARTESIAN_POINT ( 'NONE',  ( 9.564922557960805705, 16.46253265017160317, 109.5822429386476955 ) ) ;
#146025 = CARTESIAN_POINT ( 'NONE',  ( 19.05341960407611168, 5.049401038298154454, 58.95724293864768129 ) ) ;
#146026 = CARTESIAN_POINT ( 'NONE',  ( -9.564922557961040184, 16.46253265017147172, 42.91775706135234003 ) ) ;
#146027 = CARTESIAN_POINT ( 'NONE',  ( 36.91746824999999887, 11.99521256947799053, -7.524999997268814411 ) ) ;
#146028 = CARTESIAN_POINT ( 'NONE',  ( 18.39443945427639093, -5.500000000000021316, 71.01745347608650150 ) ) ;
#146030 = CARTESIAN_POINT ( 'NONE',  ( 0.05219959533934541429, -16.53943276465976808, 70.00109039468568994 ) ) ;
#146029 = CARTESIAN_POINT ( 'NONE',  ( 16.51473224551083163, -9.474510206698727899, 65.83442372801900433 ) ) ;
#146031 = CARTESIAN_POINT ( 'NONE',  ( -21.38418241377624085, 7.427326039334300134, 174.4773576836617224 ) ) ;
#146032 = CARTESIAN_POINT ( 'NONE',  ( 5.153800228976335163, 19.02544592524342804, 84.79057627198099567 ) ) ;
#146033 = CARTESIAN_POINT ( 'NONE',  ( 21.53943276465977519, 0.05219959533937863772, 31.25109039468568639 ) ) ;
#146034 = CARTESIAN_POINT ( 'NONE',  ( 19.02544592524334988, 5.153800228976608722, 76.45942372801897591 ) ) ;
#146036 = CARTESIAN_POINT ( 'NONE',  ( -9.474510206698964154, 16.51473224551069663, 40.41557627198103120 ) ) ;
#146035 = CARTESIAN_POINT ( 'NONE',  ( 5.153800228976335163, 19.02544592524342804, 114.7905762719810241 ) ) ;
#146037 = CARTESIAN_POINT ( 'NONE',  ( -19.03943276465977164, 0.05219959533909376836, 86.24890960531436690 ) ) ;
#146039 = CARTESIAN_POINT ( 'NONE',  ( -19.03943276465977164, 0.05219959533909376836, 36.24890960531436690 ) ) ;
#146038 = CARTESIAN_POINT ( 'NONE',  ( -12.14591786802309592, -12.06949235617757132, 46.87390960531435979 ) ) ;
#146040 = CARTESIAN_POINT ( 'NONE',  ( 9.474510206698729675, 16.51473224551082808, 52.08442372801900433 ) ) ;
#146041 = CARTESIAN_POINT ( 'NONE',  ( 16.53943276465976808, -0.05219959533910856209, 83.74890960531435269 ) ) ;
#146042 = CARTESIAN_POINT ( 'NONE',  ( 5.153800228976615827, -19.02544592524334988, 35.20942372801899722 ) ) ;
#146043 = CARTESIAN_POINT ( 'NONE',  ( -16.46253265017160317, 9.564922557960807481, 55.83224293864769550 ) ) ;
#146044 = CARTESIAN_POINT ( 'NONE',  ( -10.72451020669898014, 18.67979575497178502, 60.41557627198102409 ) ) ;
#146046 = CARTESIAN_POINT ( 'NONE',  ( -13.97604488694547697, 13.89961937509957934, 28.12609039468565797 ) ) ;
#146045 = CARTESIAN_POINT ( 'NONE',  ( -4.379528057220328563, 16.55341960407611168, 55.20724293864770260 ) ) ;
#146047 = CARTESIAN_POINT ( 'NONE',  ( -16.46253265017160317, 9.564922557960807481, 105.8322429386476955 ) ) ;
#146048 = CARTESIAN_POINT ( 'NONE',  ( -18.62759615963270932, 10.81492255796079327, 30.83224293864770260 ) ) ;
#146049 = CARTESIAN_POINT ( 'NONE',  ( -5.153800228976328057, -19.02544592524343514, 57.29057627198103120 ) ) ;
#146050 = CARTESIAN_POINT ( 'NONE',  ( -13.89961937509977652, 13.97604488694528158, 30.62390960531435269 ) ) ;
#146051 = CARTESIAN_POINT ( 'NONE',  ( -14.29746914071049879, 8.314922557960819915, 85.83224293864768129 ) ) ;
#146052 = CARTESIAN_POINT ( 'NONE',  ( 15.80617190586746368, 15.72974639402197994, 94.37390960531436690 ) ) ;
#146053 = CARTESIAN_POINT ( 'NONE',  ( 5.153800228976335163, 19.02544592524342804, 94.79057627198103830 ) ) ;
#146054 = CARTESIAN_POINT ( 'NONE',  ( -21.52544592524343514, 5.823673210054127303, 111.0405762719810525 ) ) ;
#146055 = CARTESIAN_POINT ( 'NONE',  ( 5.153800228976335163, 19.02544592524342804, 104.7905762719809957 ) ) ;
#146056 = CARTESIAN_POINT ( 'NONE',  ( -9.564922557960796823, -16.46253265017161027, 22.08224293864768839 ) ) ;
#146057 = CARTESIAN_POINT ( 'NONE',  ( -5.719274019375665041, -21.55341960407619695, 84.79275706135234714 ) ) ;
#146058 = CARTESIAN_POINT ( 'NONE',  ( 15.72974639402199770, -15.80617190586745480, 98.12390960531436690 ) ) ;
#146059 = CARTESIAN_POINT ( 'NONE',  ( 16.38665767535054485, -7.295008042176105434, 107.7640086421454839 ) ) ;
#146060 = FACE_OUTER_BOUND ( 'NONE', #44268, .T. ) ;
#146061 = CARTESIAN_POINT ( 'NONE',  ( 29.85394078251576744, -1.399641368455794899, -51.58569050288883062 ) ) ;
#146062 = CARTESIAN_POINT ( 'NONE',  ( 12.06949235617739724, 12.14591786802326823, 36.87609039468568994 ) ) ;
#146063 = CARTESIAN_POINT ( 'NONE',  ( -16.55341960407611168, -4.379528057220339221, 111.4572429386476813 ) ) ;
#146064 = CARTESIAN_POINT ( 'NONE',  ( 18.56197773271729545, -5.500000000000105693, 51.05066217314452359 ) ) ;
#146065 = CARTESIAN_POINT ( 'NONE',  ( -19.05341960407611168, -5.049401038298163336, 56.45724293864768129 ) ) ;
#146066 = CARTESIAN_POINT ( 'NONE',  ( 14.34966873604960469, 8.224510206698951720, 89.16557627198102409 ) ) ;
#146067 = CARTESIAN_POINT ( 'NONE',  ( 10.81492255796078972, 18.62759615963270932, 34.58224293864770260 ) ) ;
#146068 = CARTESIAN_POINT ( 'NONE',  ( -4.379528057220328563, 16.55341960407611168, 60.20724293864768839 ) ) ;
#146069 = CARTESIAN_POINT ( 'NONE',  ( 12.06949235617739724, 12.14591786802326823, 21.87609039468567573 ) ) ;
#146070 = CARTESIAN_POINT ( 'NONE',  ( -15.80617190586768217, 15.72974639402176855, 78.12609039468570415 ) ) ;
#146071 = FACE_OUTER_BOUND ( 'NONE', #13394, .T. ) ;
#146072 = CARTESIAN_POINT ( 'NONE',  ( 9.564922557960805705, 16.46253265017160317, 114.5822429386476955 ) ) ;
#146073 = CARTESIAN_POINT ( 'NONE',  ( 16.53943276465976808, 0.05219959533934440121, 91.25109039468568994 ) ) ;
#146074 = CARTESIAN_POINT ( 'NONE',  ( -13.97604488694527625, -13.89961937509977652, 41.87390960531435979 ) ) ;
#146075 = CARTESIAN_POINT ( 'NONE',  ( 5.049401038298161559, -19.05341960407611168, 92.70724293864769550 ) ) ;
#146076 = CARTESIAN_POINT ( 'NONE',  ( -0.05219959533907301413, -21.53943276465977519, 92.49890960531436690 ) ) ;
#146077 = CARTESIAN_POINT ( 'NONE',  ( 4.379528057220092307, 16.55341960407617563, 22.29275706135235069 ) ) ;
#146079 = CARTESIAN_POINT ( 'NONE',  ( 5.823673210054444382, -21.52544592524334988, 70.20942372801904696 ) ) ;
#146078 = CARTESIAN_POINT ( 'NONE',  ( 16.53943276465976808, -0.05219959533910856209, 63.74890960531435979 ) ) ;
#146080 = ADVANCED_FACE ( 'NONE', ( #54207 ), #169554, .T. ) ;
#146081 = CARTESIAN_POINT ( 'NONE',  ( -12.06949235617739369, -12.14591786802326823, 104.3760903946856899 ) ) ;
#146082 = CARTESIAN_POINT ( 'NONE',  ( 17.50000000000000000, -5.499999999999992895, 46.21769037696434168 ) ) ;
#146083 = CARTESIAN_POINT ( 'NONE',  ( 20.41037832431316090, -34.40082058117813801, -24.99999999999991829 ) ) ;
#146084 = CARTESIAN_POINT ( 'NONE',  ( 4.379528057220339221, -16.55341960407611168, 27.70724293864769905 ) ) ;
#146085 = CARTESIAN_POINT ( 'NONE',  ( -4.379528057220086978, -16.55341960407618274, 69.79275706135234714 ) ) ;
#146086 = CARTESIAN_POINT ( 'NONE',  ( -0.05219959533909027116, -19.03943276465977164, 82.49890960531436690 ) ) ;
#146087 = CARTESIAN_POINT ( 'NONE',  ( -13.97604488694527625, -13.89961937509977652, 86.87390960531436690 ) ) ;
#146088 = CARTESIAN_POINT ( 'NONE',  ( -21.52544592524334988, -5.823673210054445271, 83.95942372801900433 ) ) ;
#146089 = CARTESIAN_POINT ( 'NONE',  ( -16.52544592524335698, -4.483927247898792601, 83.95942372801900433 ) ) ;
#146090 = CARTESIAN_POINT ( 'NONE',  ( 12.06949235617757843, -12.14591786802309237, 58.12390960531435979 ) ) ;
#146091 = CARTESIAN_POINT ( 'NONE',  ( 19.03943276465977164, -0.05219959533909143690, 73.74890960531435269 ) ) ;
#146092 = ORIENTED_EDGE ( 'NONE', *, *, #144774, .F. ) ;
#146093 = CARTESIAN_POINT ( 'NONE',  ( -9.564922557961040184, 16.46253265017147172, 102.9177570613523329 ) ) ;
#146094 = CARTESIAN_POINT ( 'NONE',  ( 8.224510206698953496, -14.34966873604960469, 112.9155762719810383 ) ) ;
#146095 = CARTESIAN_POINT ( 'NONE',  ( -19.02544592524342804, 5.153800228976336051, 81.04057627198103830 ) ) ;
#146097 = CARTESIAN_POINT ( 'NONE',  ( 11.40812507854754365, 35.11059874428196537, -7.224999997268813701 ) ) ;
#146096 = CARTESIAN_POINT ( 'NONE',  ( -4.483927247898782831, 16.52544592524335698, 22.70942372801901499 ) ) ;
#146098 = CARTESIAN_POINT ( 'NONE',  ( -0.05219959533936034679, 19.03943276465977164, 22.50109039468566152 ) ) ;
#146099 = CARTESIAN_POINT ( 'NONE',  ( 14.29746914071037800, 8.314922557961029526, 81.66775706135236135 ) ) ;
#146100 = CARTESIAN_POINT ( 'NONE',  ( -16.46253265017146816, -9.564922557961047289, 89.16775706135234714 ) ) ;
#146101 = CARTESIAN_POINT ( 'NONE',  ( -0.05219959533910754901, -16.53943276465976808, 112.4989096053143669 ) ) ;
#146102 = CARTESIAN_POINT ( 'NONE',  ( 12.06949235617739724, 12.14591786802326823, 71.87609039468568994 ) ) ;
#146103 = DIRECTION ( 'NONE',  ( -1.000000000000000000, 0.000000000000000000, 0.000000000000000000 ) ) ;
#146104 = CARTESIAN_POINT ( 'NONE',  ( 19.02544592524334988, 5.153800228976608722, 51.45942372801900433 ) ) ;
#146105 = CARTESIAN_POINT ( 'NONE',  ( 5.823673210054444382, -21.52544592524334988, 100.2094237280190043 ) ) ;
#146106 = CARTESIAN_POINT ( 'NONE',  ( -19.03943276465977164, 0.05219959533909376836, 36.24890960531436690 ) ) ;
#146107 = CARTESIAN_POINT ( 'NONE',  ( -19.05341960407611168, -5.049401038298163336, 81.45724293864769550 ) ) ;
#146108 = CARTESIAN_POINT ( 'NONE',  ( 8.314922557960818139, 14.29746914071049879, 69.58224293864769550 ) ) ;
#146109 = CARTESIAN_POINT ( 'NONE',  ( 18.62759615963255655, 10.81492255796105972, 96.66775706135234714 ) ) ;
#146110 = EDGE_CURVE ( 'NONE', #43212, #22958, #136797, .T. ) ;
#146111 = CARTESIAN_POINT ( 'NONE',  ( 19.05341960407617918, -5.049401038297876454, 66.04275706135233293 ) ) ;
#146112 = CARTESIAN_POINT ( 'NONE',  ( 16.46253265017146816, 9.564922557961045513, 41.66775706135234003 ) ) ;
#146113 = CARTESIAN_POINT ( 'NONE',  ( 5.719274019375991003, -21.55341960407610458, 37.70724293864769550 ) ) ;
#146114 = CARTESIAN_POINT ( 'NONE',  ( 21.52544592524334988, 5.823673210054432836, 96.45942372801901854 ) ) ;
#146115 = CARTESIAN_POINT ( 'NONE',  ( 0.05219959533909260263, 19.03943276465977164, 74.99890960531435269 ) ) ;
#146116 = CARTESIAN_POINT ( 'NONE',  ( -0.05219959533937732626, 21.53943276465977519, 107.5010903946856899 ) ) ;
#146117 = CARTESIAN_POINT ( 'NONE',  ( 21.53943276465977519, -0.05219959533907433946, 48.74890960531435979 ) ) ;
#146118 = CARTESIAN_POINT ( 'NONE',  ( -19.02544592524342804, 5.153800228976336051, 96.04057627198103830 ) ) ;
#146119 = CARTESIAN_POINT ( 'NONE',  ( 19.03943276465977164, 0.05219959533936151252, 71.25109039468566152 ) ) ;
#146120 = CARTESIAN_POINT ( 'NONE',  ( -16.46253265017160317, 9.564922557960807481, 105.8322429386476955 ) ) ;
#146121 = CARTESIAN_POINT ( 'NONE',  ( -0.05219959533936034679, 19.03943276465977164, 97.50109039468567573 ) ) ;
#146122 = CARTESIAN_POINT ( 'NONE',  ( -0.05219959533934338120, 16.53943276465976808, 37.50109039468568284 ) ) ;
#146123 = CARTESIAN_POINT ( 'NONE',  ( -0.05219959533910754901, -16.53943276465976808, 107.4989096053143669 ) ) ;
#146124 = CARTESIAN_POINT ( 'NONE',  ( 19.05341960407611168, 5.049401038298154454, 78.95724293864769550 ) ) ;
#146125 = CARTESIAN_POINT ( 'NONE',  ( -10.81492255796078084, -18.62759615963271287, 67.08224293864770971 ) ) ;
#146126 = CARTESIAN_POINT ( 'NONE',  ( 8.314922557961029526, -14.29746914071037800, 35.41775706135234003 ) ) ;
#146127 = CARTESIAN_POINT ( 'NONE',  ( 10.72451020669871369, 18.67979575497193778, 37.08442372801901143 ) ) ;
#146128 = CARTESIAN_POINT ( 'NONE',  ( 21.55341960407619695, -5.719274019375665929, 86.04275706135236135 ) ) ;
#146129 = CARTESIAN_POINT ( 'NONE',  ( 16.53943276465976808, 0.05219959533934440121, 81.25109039468568994 ) ) ;
#146130 = CARTESIAN_POINT ( 'NONE',  ( -19.05341960407611168, -5.049401038298163336, 76.45724293864769550 ) ) ;
#146131 = CARTESIAN_POINT ( 'NONE',  ( -16.53943276465976808, 0.05219959533911058130, 76.24890960531435269 ) ) ;
#146132 = CARTESIAN_POINT ( 'NONE',  ( 4.483927247898790824, -16.52544592524335698, 110.2094237280190185 ) ) ;
#146133 = CARTESIAN_POINT ( 'NONE',  ( 9.564922557961047289, -16.46253265017146816, 55.41775706135234003 ) ) ;
#146134 = CARTESIAN_POINT ( 'NONE',  ( 21.55341960407619695, -5.719274019375665929, 26.04275706135235779 ) ) ;
#146135 = CARTESIAN_POINT ( 'NONE',  ( 16.52544592524342804, -4.483927247898539470, 78.54057627198103830 ) ) ;
#146136 = CARTESIAN_POINT ( 'NONE',  ( -13.89961937509977652, 13.97604488694528158, 95.62390960531436690 ) ) ;
#146137 = CARTESIAN_POINT ( 'NONE',  ( -0.05219959533934338120, 16.53943276465976808, 107.5010903946856899 ) ) ;
#146138 = CARTESIAN_POINT ( 'NONE',  ( -0.05219959533937732626, 21.53943276465977519, 72.50109039468568994 ) ) ;
#146139 = CARTESIAN_POINT ( 'NONE',  ( -4.379528057220086978, -16.55341960407618274, 49.79275706135234714 ) ) ;
#146140 = CARTESIAN_POINT ( 'NONE',  ( -5.719274019375665041, -21.55341960407619695, 34.79275706135235424 ) ) ;
#146141 = VERTEX_POINT ( 'NONE', #110836 ) ;
#146142 = CARTESIAN_POINT ( 'NONE',  ( 21.53943276465977519, -0.05219959533907433946, 108.7489096053143669 ) ) ;
#146143 = CARTESIAN_POINT ( 'NONE',  ( 0.05219959533910956823, 16.53943276465976808, 84.99890960531436690 ) ) ;
#146144 = CARTESIAN_POINT ( 'NONE',  ( -19.49190055781009789, -5.500000000000052403, 50.56116087098784107 ) ) ;
#146145 = CARTESIAN_POINT ( 'NONE',  ( -14.29746914071049879, 8.314922557960819915, 55.83224293864770260 ) ) ;
#146146 = CARTESIAN_POINT ( 'NONE',  ( 5.153800228976335163, 19.02544592524342804, 29.79057627198102409 ) ) ;
#146147 = CARTESIAN_POINT ( 'NONE',  ( -5.823673210054116645, -21.52544592524344225, 47.29057627198103120 ) ) ;
#146148 = CARTESIAN_POINT ( 'NONE',  ( -8.224510206698948167, 14.34966873604960824, 80.41557627198103830 ) ) ;
#146149 = CARTESIAN_POINT ( 'NONE',  ( -0.05219959533907301413, -21.53943276465977519, 77.49890960531433848 ) ) ;
#146150 = CARTESIAN_POINT ( 'NONE',  ( 19.02544592524343514, -5.153800228976328945, 88.54057627198102409 ) ) ;
#146152 = CARTESIAN_POINT ( 'NONE',  ( 16.51473224551083163, -9.474510206698727899, 75.83442372801900433 ) ) ;
#146151 = CARTESIAN_POINT ( 'NONE',  ( -19.05341960407611168, -5.049401038298163336, 41.45724293864769550 ) ) ;
#146153 = EDGE_CURVE ( 'NONE', #82599, #9179, #21126, .T. ) ;
#146155 = CARTESIAN_POINT ( 'NONE',  ( 21.55341960407610458, 5.719274019375980345, 58.95724293864770971 ) ) ;
#146154 = CARTESIAN_POINT ( 'NONE',  ( 21.53943276465977519, 0.05219959533937863772, 56.25109039468568284 ) ) ;
#146156 = CARTESIAN_POINT ( 'NONE',  ( -5.153800228976328057, -19.02544592524343514, 37.29057627198102409 ) ) ;
#146157 = CARTESIAN_POINT ( 'NONE',  ( 9.474510206698971260, -16.51473224551069308, 72.91557627198102409 ) ) ;
#146158 = ORIENTED_EDGE ( 'NONE', *, *, #124684, .T. ) ;
#146159 = CARTESIAN_POINT ( 'NONE',  ( -16.53943276465976808, -0.05219959533934237506, 43.75109039468568284 ) ) ;
#146160 = CARTESIAN_POINT ( 'NONE',  ( -5.719274019375665041, -21.55341960407619695, 34.79275706135235424 ) ) ;
#146161 = CARTESIAN_POINT ( 'NONE',  ( -21.52544592524334988, -5.823673210054445271, 68.95942372801901854 ) ) ;
#146162 = CARTESIAN_POINT ( 'NONE',  ( -16.46253265017160317, 9.564922557960807481, 115.8322429386477097 ) ) ;
#146163 = CARTESIAN_POINT ( 'NONE',  ( -21.53943276465977519, 0.05219959533907696930, 81.24890960531436690 ) ) ;
#146165 = CARTESIAN_POINT ( 'NONE',  ( -16.52544592524335698, -4.483927247898792601, 48.95942372801902565 ) ) ;
#146164 = CARTESIAN_POINT ( 'NONE',  ( -15.80617190586768217, 15.72974639402176855, 23.12609039468567573 ) ) ;
#146167 = CARTESIAN_POINT ( 'NONE',  ( 21.55341960407610458, 5.719274019375980345, 53.95724293864770260 ) ) ;
#146166 = ADVANCED_BREP_SHAPE_REPRESENTATION ( '', ( #143056, #82054 ), #78902 ) ;
#146168 = CARTESIAN_POINT ( 'NONE',  ( 9.474510206698729675, 16.51473224551082808, 22.08442372801899722 ) ) ;
#146169 = CARTESIAN_POINT ( 'NONE',  ( 9.564922557960805705, 16.46253265017160317, 54.58224293864769550 ) ) ;
#146170 = CARTESIAN_POINT ( 'NONE',  ( 13.97604488694527802, 13.89961937509977652, 114.3739096053143669 ) ) ;
#146171 = CARTESIAN_POINT ( 'NONE',  ( 13.97604488694527802, 13.89961937509977652, 89.37390960531436690 ) ) ;
#146172 = CARTESIAN_POINT ( 'NONE',  ( 17.50000000000000355, 3.242565516147348337, 102.5000000000000142 ) ) ;
#146173 = CARTESIAN_POINT ( 'NONE',  ( -13.97604488694547697, 13.89961937509957934, 68.12609039468563310 ) ) ;
#146174 = CARTESIAN_POINT ( 'NONE',  ( 21.52544592524344225, -5.823673210054117533, 48.54057627198103120 ) ) ;
#146175 = CARTESIAN_POINT ( 'NONE',  ( -14.29746914071049879, 8.314922557960819915, 30.83224293864770260 ) ) ;
#146176 = CARTESIAN_POINT ( 'NONE',  ( -9.474510206698720793, -16.51473224551083518, 94.58442372801900433 ) ) ;
#146177 = CARTESIAN_POINT ( 'NONE',  ( -9.564922557960796823, -16.46253265017161027, 22.08224293864768839 ) ) ;
#146178 = CARTESIAN_POINT ( 'NONE',  ( 19.05341960407617918, -5.049401038297876454, 21.04275706135232582 ) ) ;
#146179 = CARTESIAN_POINT ( 'NONE',  ( 5.049401038297881783, 19.05341960407617563, 92.29275706135234714 ) ) ;
#146181 = CARTESIAN_POINT ( 'NONE',  ( -9.564922557961040184, 16.46253265017147172, 62.91775706135233293 ) ) ;
#146180 = CARTESIAN_POINT ( 'NONE',  ( 5.719274019375991003, -21.55341960407610458, 92.70724293864770971 ) ) ;
#146182 = DIRECTION ( 'NONE',  ( 1.000000000000000000, 0.000000000000000000, 0.000000000000000000 ) ) ;
#146183 = CARTESIAN_POINT ( 'NONE',  ( 16.46253265017160672, -9.564922557960803928, 53.33224293864768839 ) ) ;
#146184 = CARTESIAN_POINT ( 'NONE',  ( 14.34966873604960469, 8.224510206698951720, 59.16557627198103120 ) ) ;
#146185 = CARTESIAN_POINT ( 'NONE',  ( 5.153800228976335163, 19.02544592524342804, 49.79057627198100988 ) ) ;
#146186 = CARTESIAN_POINT ( 'NONE',  ( 12.14591786802309770, 12.06949235617756955, 59.37390960531436690 ) ) ;
#146187 = LINE ( 'NONE', #115870, #6412 ) ;
#146188 = CARTESIAN_POINT ( 'NONE',  ( 0.05219959533910956823, 16.53943276465976808, 24.99890960531435624 ) ) ;
#146189 = CARTESIAN_POINT ( 'NONE',  ( 19.05341960407611168, 5.049401038298154454, 58.95724293864768129 ) ) ;
#146190 = CARTESIAN_POINT ( 'NONE',  ( -5.153800228976607833, 19.02544592524334988, 22.70942372801899012 ) ) ;
#146191 = CARTESIAN_POINT ( 'NONE',  ( 14.29746914071037800, 8.314922557961029526, 36.66775706135234714 ) ) ;
#146192 = CARTESIAN_POINT ( 'NONE',  ( 5.823673210054125526, 21.52544592524343514, 44.79057627198103120 ) ) ;
#146194 = ORIENTED_EDGE ( 'NONE', *, *, #119036, .F. ) ;
#146193 = CARTESIAN_POINT ( 'NONE',  ( 18.67979575497194134, -10.72451020669871369, 105.8344237280190328 ) ) ;
#146195 = CARTESIAN_POINT ( 'NONE',  ( -9.564922557960796823, -16.46253265017161027, 57.08224293864769550 ) ) ;
#146196 = CARTESIAN_POINT ( 'NONE',  ( -19.02544592524342804, 5.153800228976336051, 91.04057627198100988 ) ) ;
#146197 = CARTESIAN_POINT ( 'NONE',  ( -18.22780087662126647, -5.499999999999827693, 43.98236817873107185 ) ) ;
#146198 = CARTESIAN_POINT ( 'NONE',  ( -10.81492255796105439, 18.62759615963255655, 22.91775706135235069 ) ) ;
#146199 = CARTESIAN_POINT ( 'NONE',  ( -0.05219959533910754901, -16.53943276465976808, 97.49890960531436690 ) ) ;
#146201 = CARTESIAN_POINT ( 'NONE',  ( 0.05219959533909260263, 19.03943276465977164, 69.99890960531435269 ) ) ;
#146200 = CARTESIAN_POINT ( 'NONE',  ( -5.719274019375978568, 21.55341960407610458, 85.20724293864770971 ) ) ;
#146202 = CARTESIAN_POINT ( 'NONE',  ( 9.564922557960805705, 16.46253265017160317, 74.58224293864769550 ) ) ;
#146203 = CARTESIAN_POINT ( 'NONE',  ( -15.72974639402197994, 15.80617190586746368, 115.6239096053143669 ) ) ;
#146204 = ORIENTED_EDGE ( 'NONE', *, *, #6795, .F. ) ;
#146205 = CARTESIAN_POINT ( 'NONE',  ( -19.02544592524342804, 5.153800228976336051, 76.04057627198102409 ) ) ;
#146206 = DIRECTION ( 'NONE',  ( -0.000000000000000000, -0.000000000000000000, 1.000000000000000000 ) ) ;
#146208 = CARTESIAN_POINT ( 'NONE',  ( -9.474510206698964154, 16.51473224551069663, 25.41557627198103120 ) ) ;
#146207 = CARTESIAN_POINT ( 'NONE',  ( -4.379528057220328563, 16.55341960407611168, 105.2072429386477097 ) ) ;
#146209 = CARTESIAN_POINT ( 'NONE',  ( -16.51473224551082808, 9.474510206698731452, 93.33442372801900433 ) ) ;
#146210 = CARTESIAN_POINT ( 'NONE',  ( 0.05219959533910956823, 16.53943276465976808, 94.99890960531436690 ) ) ;
#146211 = CARTESIAN_POINT ( 'NONE',  ( 18.62759615963255655, 10.81492255796105972, 71.66775706135234714 ) ) ;
#146213 = CARTESIAN_POINT ( 'NONE',  ( -18.67979575497193778, 10.72451020669871902, 38.33442372801900433 ) ) ;
#146212 = CARTESIAN_POINT ( 'NONE',  ( 5.049401038298161559, -19.05341960407611168, 62.70724293864769550 ) ) ;
#146214 = CARTESIAN_POINT ( 'NONE',  ( -21.52544592524343514, 5.823673210054127303, 116.0405762719810383 ) ) ;
#146215 = CARTESIAN_POINT ( 'NONE',  ( -28.82186960331499392, 9.364793116373565596, 141.9000000000000057 ) ) ;
#146216 = CARTESIAN_POINT ( 'NONE',  ( 13.97604488694527802, 13.89961937509977652, 79.37390960531435269 ) ) ;
#146217 = CARTESIAN_POINT ( 'NONE',  ( 20.71617105148682469, 18.73729486426113766, 139.9999999999999716 ) ) ;
#146219 = CARTESIAN_POINT ( 'NONE',  ( 10.81492255796078972, 18.62759615963270932, 24.58224293864768839 ) ) ;
#146218 = CARTESIAN_POINT ( 'NONE',  ( -4.379528057220086978, -16.55341960407618274, 24.79275706135235779 ) ) ;
#146220 = CARTESIAN_POINT ( 'NONE',  ( 15.80617190586769283, -15.72974639402175789, 65.62609039468568994 ) ) ;
#146221 = CARTESIAN_POINT ( 'NONE',  ( 5.049401038298161559, -19.05341960407611168, 107.7072429386476955 ) ) ;
#146222 = CARTESIAN_POINT ( 'NONE',  ( 16.46253265017146816, 9.564922557961045513, 96.66775706135233293 ) ) ;
#146223 = CIRCLE ( 'NONE', #55897, 2.699999999999993960 ) ;
#146224 = CARTESIAN_POINT ( 'NONE',  ( 19.05341960407611168, 5.049401038298154454, 48.95724293864768129 ) ) ;
#146225 = CARTESIAN_POINT ( 'NONE',  ( -9.564922557960796823, -16.46253265017161027, 77.08224293864769550 ) ) ;
#146226 = CARTESIAN_POINT ( 'NONE',  ( -14.34966873604960291, -8.224510206698953496, 96.66557627198102409 ) ) ;
#146227 = CARTESIAN_POINT ( 'NONE',  ( 5.153800228976335163, 19.02544592524342804, 99.79057627198102409 ) ) ;
#146228 = CARTESIAN_POINT ( 'NONE',  ( -8.224510206698948167, 14.34966873604960824, 95.41557627198102409 ) ) ;
#146229 = CARTESIAN_POINT ( 'NONE',  ( 9.564922557960805705, 16.46253265017160317, 99.58224293864770971 ) ) ;
#146231 = CARTESIAN_POINT ( 'NONE',  ( 5.049401038298161559, -19.05341960407611168, 47.70724293864770260 ) ) ;
#146230 = CARTESIAN_POINT ( 'NONE',  ( -8.314922557960811034, -14.29746914071050412, 42.08224293864769550 ) ) ;
#146232 = CARTESIAN_POINT ( 'NONE',  ( -15.72974639402176322, -15.80617190586768395, 54.37609039468568994 ) ) ;
#146233 = CARTESIAN_POINT ( 'NONE',  ( 19.03943276465977164, 0.05219959533936151252, 91.25109039468566152 ) ) ;
#146234 = CARTESIAN_POINT ( 'NONE',  ( -16.55341960407611168, -4.379528057220339221, 51.45724293864770260 ) ) ;
#146235 = CARTESIAN_POINT ( 'NONE',  ( -0.05219959533907301413, -21.53943276465977519, 102.4989096053143811 ) ) ;
#146236 = CARTESIAN_POINT ( 'NONE',  ( -5.719274019375978568, 21.55341960407610458, 45.20724293864769550 ) ) ;
#146238 = CARTESIAN_POINT ( 'NONE',  ( -12.14591786802309592, -12.06949235617757132, 81.87390960531435269 ) ) ;
#146237 = CARTESIAN_POINT ( 'NONE',  ( -13.89961937509977652, 13.97604488694528158, 115.6239096053143669 ) ) ;
#146239 = CARTESIAN_POINT ( 'NONE',  ( -22.44159573604009950, -16.30477369853688430, 147.0750000027312012 ) ) ;
#146240 = CARTESIAN_POINT ( 'NONE',  ( -16.51473224551069308, -9.474510206698971260, 51.66557627198102409 ) ) ;
#146241 = CARTESIAN_POINT ( 'NONE',  ( -0.05219959533934338120, 16.53943276465976808, 112.5010903946857042 ) ) ;
#146242 = CARTESIAN_POINT ( 'NONE',  ( 4.379528057220092307, 16.55341960407617563, 102.2927570613523613 ) ) ;
#146243 = CARTESIAN_POINT ( 'NONE',  ( -8.224510206698735004, -14.34966873604973081, 79.58442372801903275 ) ) ;
#146244 = CARTESIAN_POINT ( 'NONE',  ( 16.46253265017146816, 9.564922557961045513, 36.66775706135233293 ) ) ;
#146246 = CARTESIAN_POINT ( 'NONE',  ( -9.474510206698964154, 16.51473224551069663, 105.4155762719810383 ) ) ;
#146245 = DIRECTION ( 'NONE',  ( 0.000000000000000000, 0.000000000000000000, 1.000000000000000000 ) ) ;
#146247 = CARTESIAN_POINT ( 'NONE',  ( 5.153800228976335163, 19.02544592524342804, 84.79057627198099567 ) ) ;
#146248 = CARTESIAN_POINT ( 'NONE',  ( -13.97604488694527625, -13.89961937509977652, 36.87390960531436690 ) ) ;
#146249 = CARTESIAN_POINT ( 'NONE',  ( -4.379528057220328563, 16.55341960407611168, 45.20724293864769550 ) ) ;
#146251 = CARTESIAN_POINT ( 'NONE',  ( -19.03943276465977164, 0.05219959533909376836, 106.2489096053143669 ) ) ;
#146250 = CARTESIAN_POINT ( 'NONE',  ( -19.02544592524342804, 5.153800228976336051, 116.0405762719810383 ) ) ;
#146252 = CARTESIAN_POINT ( 'NONE',  ( -15.80617190586745835, -15.72974639402198527, 41.87390960531435979 ) ) ;
#146253 = CARTESIAN_POINT ( 'NONE',  ( 8.314922557960818139, 14.29746914071049879, 89.58224293864768129 ) ) ;
#146254 = CARTESIAN_POINT ( 'NONE',  ( -16.55341960407617563, 4.379528057220093196, 38.54275706135234714 ) ) ;
#146255 = EDGE_CURVE ( 'NONE', #34840, #35595, #27646, .T. ) ;
#146256 = AXIS2_PLACEMENT_3D ( 'NONE', #49596, #78926, #140602 ) ;
#146257 = CARTESIAN_POINT ( 'NONE',  ( 4.379528057220339221, -16.55341960407611168, 67.70724293864769550 ) ) ;
#146258 = CARTESIAN_POINT ( 'NONE',  ( 28.91886483090991433, -0.2690448904508166983, -49.65045026909250936 ) ) ;
#146259 = CARTESIAN_POINT ( 'NONE',  ( -19.05341960407617563, 5.049401038297882671, 63.54275706135234003 ) ) ;
#146260 = CARTESIAN_POINT ( 'NONE',  ( 19.05341960407611168, 5.049401038298154454, 98.95724293864766707 ) ) ;
#146261 = CARTESIAN_POINT ( 'NONE',  ( 19.03943276465977164, 0.05219959533936151252, 81.25109039468567573 ) ) ;
#146262 = CARTESIAN_POINT ( 'NONE',  ( 27.73933785331498925, -9.013057229001033122, 148.2750000027311330 ) ) ;
#146264 = CARTESIAN_POINT ( 'NONE',  ( -16.55341960407617563, 4.379528057220093196, 103.5427570613523613 ) ) ;
#146263 = CARTESIAN_POINT ( 'NONE',  ( -4.483927247898782831, 16.52544592524335698, 27.70942372801901854 ) ) ;
#146265 = CARTESIAN_POINT ( 'NONE',  ( 13.97604488694548053, -13.89961937509957401, 70.62609039468567573 ) ) ;
#146266 = CARTESIAN_POINT ( 'NONE',  ( -21.53943276465977519, 0.05219959533907696930, 31.24890960531435979 ) ) ;
#146267 = CARTESIAN_POINT ( 'NONE',  ( 18.62759615963255655, 10.81492255796105972, 71.66775706135234714 ) ) ;
#146268 = CARTESIAN_POINT ( 'NONE',  ( -21.98685479826776756, -13.98560643873834586, 165.5209445330007725 ) ) ;
#146269 = CARTESIAN_POINT ( 'NONE',  ( -14.29746914071037622, -8.314922557961029526, 19.16775706135234714 ) ) ;
#146271 = CARTESIAN_POINT ( 'NONE',  ( 16.46253265017160672, -9.564922557960803928, 88.33224293864769550 ) ) ;
#146270 = CARTESIAN_POINT ( 'NONE',  ( 4.500000000000000888, -99.43240762267087973, 40.28936402012540441 ) ) ;
#146272 = CARTESIAN_POINT ( 'NONE',  ( 14.83455351965412561, 16.91340028822891384, -58.07447375877295315 ) ) ;
#146274 = CARTESIAN_POINT ( 'NONE',  ( 9.474510206698971260, -16.51473224551069308, 72.91557627198102409 ) ) ;
#146273 = CARTESIAN_POINT ( 'NONE',  ( 8.314922557960818139, 14.29746914071049879, 94.58224293864769550 ) ) ;
#146275 = PRODUCT_CONTEXT ( 'NONE', #124181, 'mechanical' ) ;
#146276 = CARTESIAN_POINT ( 'NONE',  ( 19.03943276465977164, -0.05219959533909143690, 83.74890960531436690 ) ) ;
#146277 = EDGE_LOOP ( 'NONE', ( #50691, #105254, #117831, #41605 ) ) ;
#146278 = CARTESIAN_POINT ( 'NONE',  ( 19.05341960407617918, -5.049401038297876454, 91.04275706135234714 ) ) ;
#146279 = CARTESIAN_POINT ( 'NONE',  ( 21.55341960407610458, 5.719274019375980345, 78.95724293864769550 ) ) ;
#146280 = CARTESIAN_POINT ( 'NONE',  ( 9.474510206698971260, -16.51473224551069308, 27.91557627198103120 ) ) ;
#146282 = CARTESIAN_POINT ( 'NONE',  ( -15.72974639402197994, 15.80617190586746368, 110.6239096053143669 ) ) ;
#146281 = CARTESIAN_POINT ( 'NONE',  ( 19.02544592524334988, 5.153800228976608722, 66.45942372801899012 ) ) ;
#146283 = CARTESIAN_POINT ( 'NONE',  ( 9.474510206698971260, -16.51473224551069308, 72.91557627198102409 ) ) ;
#146284 = CARTESIAN_POINT ( 'NONE',  ( -13.89961937509977652, 13.97604488694528158, 105.6239096053143527 ) ) ;
#146285 = ORIENTED_EDGE ( 'NONE', *, *, #136776, .F. ) ;
#146286 = CARTESIAN_POINT ( 'NONE',  ( -18.67979575497178146, -10.72451020669898902, 106.6655762719810383 ) ) ;
#146289 = CARTESIAN_POINT ( 'NONE',  ( -13.97604488694547697, 13.89961937509957934, 63.12609039468566152 ) ) ;
#146288 = CARTESIAN_POINT ( 'NONE',  ( 5.049401038298161559, -19.05341960407611168, 82.70724293864770971 ) ) ;
#146287 = CARTESIAN_POINT ( 'NONE',  ( 16.53943276465976808, -0.05219959533910856209, 88.74890960531436690 ) ) ;
#146290 = CARTESIAN_POINT ( 'NONE',  ( 15.80617190586746368, 15.72974639402197994, 84.37390960531438111 ) ) ;
#146291 = CARTESIAN_POINT ( 'NONE',  ( 5.719274019375991003, -21.55341960407610458, 67.70724293864769550 ) ) ;
#146292 = CARTESIAN_POINT ( 'NONE',  ( -12.06949235617756955, 12.14591786802309770, 40.62390960531435269 ) ) ;
#146293 = CARTESIAN_POINT ( 'NONE',  ( 5.823673210054444382, -21.52544592524334988, 100.2094237280190043 ) ) ;
#146294 = CARTESIAN_POINT ( 'NONE',  ( -8.224510206698735004, -14.34966873604973081, 69.58442372801900433 ) ) ;
#146295 = CARTESIAN_POINT ( 'NONE',  ( 13.89961937509977652, -13.97604488694527269, 93.12390960531436690 ) ) ;
#146296 = CARTESIAN_POINT ( 'NONE',  ( 9.564922557960805705, 16.46253265017160317, 39.58224293864768839 ) ) ;
#146297 = CARTESIAN_POINT ( 'NONE',  ( -5.823673210054431948, 21.52544592524334988, 47.70942372801902565 ) ) ;
#146298 = CARTESIAN_POINT ( 'NONE',  ( -5.823673210054431948, 21.52544592524334988, 47.70942372801902565 ) ) ;
#146299 = CARTESIAN_POINT ( 'NONE',  ( 9.564922557960805705, 16.46253265017160317, 64.58224293864769550 ) ) ;
#146300 = CARTESIAN_POINT ( 'NONE',  ( -15.72974639402176322, -15.80617190586768395, 34.37609039468568284 ) ) ;
#146301 = CARTESIAN_POINT ( 'NONE',  ( 9.474510206698729675, 16.51473224551082808, 77.08442372801900433 ) ) ;
#146302 = CARTESIAN_POINT ( 'NONE',  ( -0.05219959533936034679, 19.03943276465977164, 72.50109039468566152 ) ) ;
#146303 = CARTESIAN_POINT ( 'NONE',  ( 19.02544592524343514, -5.153800228976328945, 43.54057627198103120 ) ) ;
#146304 = CARTESIAN_POINT ( 'NONE',  ( -16.55341960407617563, 4.379528057220093196, 88.54275706135236135 ) ) ;
#146305 = CARTESIAN_POINT ( 'NONE',  ( 19.05341960407611168, 5.049401038298154454, 53.95724293864770260 ) ) ;
#146306 = CARTESIAN_POINT ( 'NONE',  ( 24.86035471869044500, -4.680034064337648125, 169.8578160361101084 ) ) ;
#146307 = CARTESIAN_POINT ( 'NONE',  ( 19.03943276465977164, -0.05219959533909143690, 103.7489096053143669 ) ) ;
#146308 = CARTESIAN_POINT ( 'NONE',  ( -0.05219959533909027116, -19.03943276465977164, 32.49890960531435979 ) ) ;
#146309 = CARTESIAN_POINT ( 'NONE',  ( -10.72451020669898014, 18.67979575497178502, 75.41557627198102409 ) ) ;
#146310 = CARTESIAN_POINT ( 'NONE',  ( -14.34966873604972548, 8.224510206698743886, 58.33442372801901143 ) ) ;
#146311 = CARTESIAN_POINT ( 'NONE',  ( -16.46253265017146816, -9.564922557961047289, 19.16775706135233293 ) ) ;
#146312 = CARTESIAN_POINT ( 'NONE',  ( -16.46253265017160317, 9.564922557960807481, 50.83224293864770260 ) ) ;
#146313 = CARTESIAN_POINT ( 'NONE',  ( -16.55341960407611168, -4.379528057220339221, 41.45724293864769550 ) ) ;
#146314 = CARTESIAN_POINT ( 'NONE',  ( -12.14591786802309592, -12.06949235617757132, 81.87390960531435269 ) ) ;
#146315 = CARTESIAN_POINT ( 'NONE',  ( 19.03943276465977164, -0.05219959533909143690, 83.74890960531436690 ) ) ;
#146316 = CARTESIAN_POINT ( 'NONE',  ( -21.55341960407619339, 5.719274019375674811, 38.54275706135234714 ) ) ;
#146317 = CARTESIAN_POINT ( 'NONE',  ( -0.05219959533909027116, -19.03943276465977164, 97.49890960531436690 ) ) ;
#146318 = CARTESIAN_POINT ( 'NONE',  ( -15.80617190586768217, 15.72974639402176855, 98.12609039468570415 ) ) ;
#146319 = CARTESIAN_POINT ( 'NONE',  ( 0.05219959533934541429, -16.53943276465976808, 65.00109039468568994 ) ) ;
#146320 = CARTESIAN_POINT ( 'NONE',  ( -5.823673210054431948, 21.52544592524334988, 32.70942372801900433 ) ) ;
#146321 = CARTESIAN_POINT ( 'NONE',  ( 19.05341960407611168, 5.049401038298154454, 103.9572429386476671 ) ) ;
#146322 = CARTESIAN_POINT ( 'NONE',  ( 15.72974639402199770, -15.80617190586745480, 93.12390960531436690 ) ) ;
#146323 = CARTESIAN_POINT ( 'NONE',  ( 16.53943276465976808, -0.05219959533910856209, 43.74890960531435979 ) ) ;
#146324 = CARTESIAN_POINT ( 'NONE',  ( 5.049401038298161559, -19.05341960407611168, 37.70724293864768839 ) ) ;
#146325 = CARTESIAN_POINT ( 'NONE',  ( -8.224510206698948167, 14.34966873604960824, 70.41557627198102409 ) ) ;
#146326 = CARTESIAN_POINT ( 'NONE',  ( -18.67979575497178146, -10.72451020669898902, 36.66557627198103120 ) ) ;
#146327 = CARTESIAN_POINT ( 'NONE',  ( -19.02544592524334988, -5.153800228976617603, 33.95942372801897591 ) ) ;
#146328 = CARTESIAN_POINT ( 'NONE',  ( 8.314922557960818139, 14.29746914071049879, 104.5822429386477097 ) ) ;
#146329 = CARTESIAN_POINT ( 'NONE',  ( 19.03943276465977164, -0.05219959533909143690, 108.7489096053143527 ) ) ;
#146330 = ORIENTED_EDGE ( 'NONE', *, *, #88897, .F. ) ;
#146331 = CARTESIAN_POINT ( 'NONE',  ( -16.52544592524335698, -4.483927247898792601, 58.95942372801902565 ) ) ;
#146332 = CARTESIAN_POINT ( 'NONE',  ( 16.51473224551069308, 9.474510206698969483, 49.16557627198102409 ) ) ;
#146333 = LINE ( 'NONE', #193869, #17727 ) ;
#146334 = EDGE_CURVE ( 'NONE', #27708, #127799, #172944, .T. ) ;
#146335 = CARTESIAN_POINT ( 'NONE',  ( 14.34966873604972726, -8.224510206698740333, 95.83442372801903275 ) ) ;
#146336 = CARTESIAN_POINT ( 'NONE',  ( 13.89961937509957401, 13.97604488694547697, 101.8760903946856331 ) ) ;
#146337 = CARTESIAN_POINT ( 'NONE',  ( 15.72974639402176855, 15.80617190586768217, 66.87609039468568994 ) ) ;
#146338 = CARTESIAN_POINT ( 'NONE',  ( 9.564922557960805705, 16.46253265017160317, 74.58224293864769550 ) ) ;
#146339 = CARTESIAN_POINT ( 'NONE',  ( -18.67979575497178146, -10.72451020669898902, 91.66557627198103830 ) ) ;
#146340 = CARTESIAN_POINT ( 'NONE',  ( 0.05219959533934541429, -16.53943276465976808, 45.00109039468568284 ) ) ;
#146341 = CARTESIAN_POINT ( 'NONE',  ( 0.05219959533910956823, 16.53943276465976808, 114.9989096053143669 ) ) ;
#146342 = EDGE_CURVE ( 'NONE', #139003, #83841, #69603, .T. ) ;
#146343 = CARTESIAN_POINT ( 'NONE',  ( -19.02544592524334988, -5.153800228976617603, 83.95942372801901854 ) ) ;
#146344 = CARTESIAN_POINT ( 'NONE',  ( 18.62759615963271287, -10.81492255796078972, 78.33224293864770971 ) ) ;
#146345 = CARTESIAN_POINT ( 'NONE',  ( 19.03943276465977164, 0.05219959533936151252, 41.25109039468566152 ) ) ;
#146346 = CARTESIAN_POINT ( 'NONE',  ( -5.049401038298153566, 19.05341960407611168, 115.2072429386477097 ) ) ;
#146347 = CARTESIAN_POINT ( 'NONE',  ( 15.72974639402199770, -15.80617190586745480, 93.12390960531436690 ) ) ;
#146348 = CARTESIAN_POINT ( 'NONE',  ( 17.72560187377285956, 5.500000000000053291, 61.57814504131322764 ) ) ;
#146349 = CARTESIAN_POINT ( 'NONE',  ( -19.03943276465977164, 0.05219959533909376836, 61.24890960531436690 ) ) ;
#146350 = DIRECTION ( 'NONE',  ( -0.000000000000000000, 0.5000000000000001110, 0.8660254037844385966 ) ) ;
#146351 = CARTESIAN_POINT ( 'NONE',  ( -19.03943276465977164, -0.05219959533935918106, 113.7510903946856757 ) ) ;
#146352 = CARTESIAN_POINT ( 'NONE',  ( 23.96320343559665389, 18.46320343559613164, 1.818019484660535090 ) ) ;
#146353 = CARTESIAN_POINT ( 'NONE',  ( 16.51473224551069308, 9.474510206698969483, 44.16557627198103120 ) ) ;
#146355 = CARTESIAN_POINT ( 'NONE',  ( -8.224510206698948167, 14.34966873604960824, 50.41557627198103120 ) ) ;
#146354 = CARTESIAN_POINT ( 'NONE',  ( -0.05219959533907301413, -21.53943276465977519, 107.4989096053143669 ) ) ;
#146356 = CARTESIAN_POINT ( 'NONE',  ( 16.51473224551069308, 9.474510206698969483, 54.16557627198103120 ) ) ;
#146357 = CARTESIAN_POINT ( 'NONE',  ( -5.719274019375665041, -21.55341960407619695, 79.79275706135236135 ) ) ;
#146359 = CARTESIAN_POINT ( 'NONE',  ( 13.97604488694548053, -13.89961937509957401, 30.62609039468566863 ) ) ;
#146358 = CARTESIAN_POINT ( 'NONE',  ( -16.55341960407617563, 4.379528057220093196, 23.54275706135235424 ) ) ;
#146360 = CARTESIAN_POINT ( 'NONE',  ( -14.29746914071049879, 8.314922557960819915, 25.83224293864769194 ) ) ;
#146361 = CARTESIAN_POINT ( 'NONE',  ( 21.52544592524334988, 5.823673210054432836, 36.45942372801901143 ) ) ;
#146362 = CARTESIAN_POINT ( 'NONE',  ( 18.62759615963255655, 10.81492255796105972, 21.66775706135235069 ) ) ;
#146363 = CARTESIAN_POINT ( 'NONE',  ( 18.67979575497178502, 10.72451020669898547, 54.16557627198103120 ) ) ;
#146364 = CARTESIAN_POINT ( 'NONE',  ( 19.02544592524334988, 5.153800228976608722, 101.4594237280189759 ) ) ;
#146365 = CARTESIAN_POINT ( 'NONE',  ( -5.153800228976607833, 19.02544592524334988, 62.70942372801899722 ) ) ;
#146366 = CARTESIAN_POINT ( 'NONE',  ( -21.55341960407619339, 5.719274019375674811, 78.54275706135236135 ) ) ;
#146367 = CARTESIAN_POINT ( 'NONE',  ( 16.46253265017146816, 9.564922557961045513, 46.66775706135233293 ) ) ;
#146368 = CARTESIAN_POINT ( 'NONE',  ( 16.51473224551069308, 9.474510206698969483, 24.16557627198102765 ) ) ;
#146369 = CARTESIAN_POINT ( 'NONE',  ( 0.05219959533907565091, 21.53943276465977519, 59.99890960531436690 ) ) ;
#146370 = CARTESIAN_POINT ( 'NONE',  ( 12.14591786802309770, 12.06949235617756955, 49.37390960531436690 ) ) ;
#146371 = DIRECTION ( 'NONE',  ( 1.000000000000000000, -5.392603844284257652E-33, 0.000000000000000000 ) ) ;
#146372 = CARTESIAN_POINT ( 'NONE',  ( -5.049401038297874678, -19.05341960407617918, 19.79275706135233293 ) ) ;
#146373 = CARTESIAN_POINT ( 'NONE',  ( 14.29746914071037800, 8.314922557961029526, 81.66775706135236135 ) ) ;
#146374 = CARTESIAN_POINT ( 'NONE',  ( 12.14591786802309770, 12.06949235617756955, 39.37390960531436690 ) ) ;
#146375 = CARTESIAN_POINT ( 'NONE',  ( -15.80617190586768217, 15.72974639402176855, 73.12609039468567573 ) ) ;
#146376 = CARTESIAN_POINT ( 'NONE',  ( 18.67979575497194134, -10.72451020669871369, 75.83442372801900433 ) ) ;
#146377 = CARTESIAN_POINT ( 'NONE',  ( -5.823673210054116645, -21.52544592524344225, 77.29057627198102409 ) ) ;
#146378 = CARTESIAN_POINT ( 'NONE',  ( -9.474510206698964154, 16.51473224551069663, 35.41557627198102409 ) ) ;
#146379 = CARTESIAN_POINT ( 'NONE',  ( 15.72974639402176855, 15.80617190586768217, 61.87609039468568284 ) ) ;
#146380 = CARTESIAN_POINT ( 'NONE',  ( 5.153800228976335163, 19.02544592524342804, 29.79057627198102409 ) ) ;
#146381 = CARTESIAN_POINT ( 'NONE',  ( 19.02544592524343514, -5.153800228976328945, 48.54057627198103120 ) ) ;
#146382 = CARTESIAN_POINT ( 'NONE',  ( 16.53943276465976808, -0.05219959533910856209, 88.74890960531436690 ) ) ;
#146383 = CARTESIAN_POINT ( 'NONE',  ( 19.05341960407611168, 5.049401038298154454, 98.95724293864766707 ) ) ;
#146384 = CARTESIAN_POINT ( 'NONE',  ( -8.224510206698948167, 14.34966873604960824, 35.41557627198102409 ) ) ;
#146385 = CARTESIAN_POINT ( 'NONE',  ( 4.483927247898545687, 16.52544592524342804, 109.7905762719810383 ) ) ;
#146386 = CARTESIAN_POINT ( 'NONE',  ( -10.81492255796078084, -18.62759615963271287, 82.08224293864768129 ) ) ;
#146387 = CARTESIAN_POINT ( 'NONE',  ( -10.72451020669898014, 18.67979575497178502, 115.4155762719810241 ) ) ;
#146388 = CYLINDRICAL_SURFACE ( 'NONE', #62987, 35.99626262588765258 ) ;
#146389 = CARTESIAN_POINT ( 'NONE',  ( 16.52544592524335698, 4.483927247898782831, 31.45942372801901854 ) ) ;
#146390 = CARTESIAN_POINT ( 'NONE',  ( 18.62759615963271287, -10.81492255796078972, 73.33224293864769550 ) ) ;
#146391 = CARTESIAN_POINT ( 'NONE',  ( 21.53943276465977519, 0.05219959533937863772, 96.25109039468568994 ) ) ;
#146392 = CARTESIAN_POINT ( 'NONE',  ( 19.03943276465977164, -0.05219959533909143690, 78.74890960531436690 ) ) ;
#146393 = CARTESIAN_POINT ( 'NONE',  ( 10.72451020669871369, 18.67979575497193778, 32.08442372801901854 ) ) ;
#146394 = CARTESIAN_POINT ( 'NONE',  ( -13.97604488694527625, -13.89961937509977652, 106.8739096053143669 ) ) ;
#146395 = CARTESIAN_POINT ( 'NONE',  ( 16.52544592524335698, 4.483927247898782831, 96.45942372801901854 ) ) ;
#146396 = CARTESIAN_POINT ( 'NONE',  ( -21.52544592524334988, -5.823673210054445271, 73.95942372801901854 ) ) ;
#146397 = CARTESIAN_POINT ( 'NONE',  ( -16.46253265017146816, -9.564922557961047289, 24.16775706135233648 ) ) ;
#146398 = CARTESIAN_POINT ( 'NONE',  ( -4.379528057220086978, -16.55341960407618274, 74.79275706135234714 ) ) ;
#146399 = CARTESIAN_POINT ( 'NONE',  ( -5.823673210054431948, 21.52544592524334988, 32.70942372801900433 ) ) ;
#146400 = CARTESIAN_POINT ( 'NONE',  ( 19.05341960407611168, 5.049401038298154454, 33.95724293864769550 ) ) ;
#146401 = CARTESIAN_POINT ( 'NONE',  ( 18.67979575497194134, -10.72451020669871369, 90.83442372801901854 ) ) ;
#146402 = CARTESIAN_POINT ( 'NONE',  ( -9.564922557960796823, -16.46253265017161027, 102.0822429386477097 ) ) ;
#146403 = CARTESIAN_POINT ( 'NONE',  ( 21.52544592524344225, -5.823673210054117533, 98.54057627198105251 ) ) ;
#146405 = CARTESIAN_POINT ( 'NONE',  ( -0.05219959533907301413, -21.53943276465977519, 52.49890960531435979 ) ) ;
#146404 = CARTESIAN_POINT ( 'NONE',  ( 18.56399227203341340, 5.500000000000001776, 81.47830131249899921 ) ) ;
#146407 = CARTESIAN_POINT ( 'NONE',  ( -16.52544592524342804, 4.483927247898546575, 56.04057627198102409 ) ) ;
#146406 = CARTESIAN_POINT ( 'NONE',  ( -9.474510206698964154, 16.51473224551069663, 95.41557627198102409 ) ) ;
#146408 = CARTESIAN_POINT ( 'NONE',  ( 20.96339774546123635, 10.39907118706507028, 168.2889211417203228 ) ) ;
#146409 = CARTESIAN_POINT ( 'NONE',  ( -9.474510206698720793, -16.51473224551083518, 74.58442372801900433 ) ) ;
#146410 = CARTESIAN_POINT ( 'NONE',  ( -17.44270441346517586, 5.991230190323018512, 103.6366492073577490 ) ) ;
#146411 = CARTESIAN_POINT ( 'NONE',  ( 19.02544592524334988, 5.153800228976608722, 111.4594237280190043 ) ) ;
#146412 = CARTESIAN_POINT ( 'NONE',  ( 18.62759615963271287, -10.81492255796078972, 88.33224293864769550 ) ) ;
#146413 = CARTESIAN_POINT ( 'NONE',  ( -12.14591786802309592, -12.06949235617757132, 61.87390960531436690 ) ) ;
#146414 = CARTESIAN_POINT ( 'NONE',  ( -9.564922557960796823, -16.46253265017161027, 97.08224293864769550 ) ) ;
#146415 = CARTESIAN_POINT ( 'NONE',  ( 14.34966873604972726, -8.224510206698740333, 40.83442372801901854 ) ) ;
#146416 = CARTESIAN_POINT ( 'NONE',  ( 16.46253265017160672, -9.564922557960803928, 63.33224293864769550 ) ) ;
#146418 = CARTESIAN_POINT ( 'NONE',  ( -19.03943276465977164, -0.05219959533935918106, 103.7510903946856757 ) ) ;
#146417 = CARTESIAN_POINT ( 'NONE',  ( -5.823673210054431948, 21.52544592524334988, 27.70942372801901854 ) ) ;
#146419 = CARTESIAN_POINT ( 'NONE',  ( -16.46253265017160317, 9.564922557960807481, 100.8322429386477097 ) ) ;
#146420 = CARTESIAN_POINT ( 'NONE',  ( 19.05341960407611168, 5.049401038298154454, 83.95724293864766707 ) ) ;
#146421 = CARTESIAN_POINT ( 'NONE',  ( -21.52544592524343514, 5.823673210054127303, 96.04057627198102409 ) ) ;
#146422 = CARTESIAN_POINT ( 'NONE',  ( -0.05219959533909027116, -19.03943276465977164, 47.49890960531435979 ) ) ;
#146423 = CARTESIAN_POINT ( 'NONE',  ( -17.40861289039003879, -6.110651285853285763, 61.37232470827434838 ) ) ;
#146425 = B_SPLINE_CURVE_WITH_KNOTS ( 'NONE', 3,
 ( #126127, #128098, #189802, #51274, #2781, #67430, #97745, #175618 ),
 .UNSPECIFIED., .F., .F.,
 ( 4, 2, 2, 4 ),
 ( 0.000000000000000000, 0.0004423531491111584095, 0.0008847062982223168190, 0.001769412596444650985 ),
 .UNSPECIFIED. ) ;
#146424 = CARTESIAN_POINT ( 'NONE',  ( -8.314922557960811034, -14.29746914071050412, 72.08224293864769550 ) ) ;
#146426 = CARTESIAN_POINT ( 'NONE',  ( -5.153800228976328057, -19.02544592524343514, 107.2905762719810383 ) ) ;
#146427 = CARTESIAN_POINT ( 'NONE',  ( -31.21487366219223603, 1.272595016298921244, -49.98150452412669154 ) ) ;
#146428 = CARTESIAN_POINT ( 'NONE',  ( 13.89961937509957401, 13.97604488694547697, 61.87609039468566863 ) ) ;
#146429 = CARTESIAN_POINT ( 'NONE',  ( -21.55341960407610458, -5.719274019375992779, 91.45724293864769550 ) ) ;
#146430 = CARTESIAN_POINT ( 'NONE',  ( -5.049401038297874678, -19.05341960407617918, 49.79275706135231871 ) ) ;
#146431 = CARTESIAN_POINT ( 'NONE',  ( 9.474510206698971260, -16.51473224551069308, 107.9155762719810383 ) ) ;
#146432 = CARTESIAN_POINT ( 'NONE',  ( 20.73749492396215288, -155.7167183371838064, -15.00000000000000000 ) ) ;
#146433 = CARTESIAN_POINT ( 'NONE',  ( -0.05219959533907301413, -21.53943276465977519, 47.49890960531435979 ) ) ;
#146434 = CARTESIAN_POINT ( 'NONE',  ( -5.049401038298153566, 19.05341960407611168, 85.20724293864766707 ) ) ;
#146435 = CARTESIAN_POINT ( 'NONE',  ( 10.81492255796106328, -18.62759615963255655, 70.41775706135236135 ) ) ;
#146436 = CARTESIAN_POINT ( 'NONE',  ( -16.51473224551069308, -9.474510206698971260, 31.66557627198102054 ) ) ;
#146437 = CARTESIAN_POINT ( 'NONE',  ( -16.53943276465976808, 0.05219959533911058130, 76.24890960531435269 ) ) ;
#146438 = CARTESIAN_POINT ( 'NONE',  ( 0.05219959533934541429, -16.53943276465976808, 25.00109039468567218 ) ) ;
#146439 = CARTESIAN_POINT ( 'NONE',  ( 10.72451020669871369, 18.67979575497193778, 57.08442372801901854 ) ) ;
#146440 = VERTEX_POINT ( 'NONE', #55149 ) ;
#146441 = CARTESIAN_POINT ( 'NONE',  ( 19.05341960407617918, -5.049401038297876454, 66.04275706135233293 ) ) ;
#146442 = CARTESIAN_POINT ( 'NONE',  ( 17.50000000000000000, -5.499999999999992895, 46.21769037696434168 ) ) ;
#146443 = CARTESIAN_POINT ( 'NONE',  ( -5.823673210054431948, 21.52544592524334988, 22.70942372801901499 ) ) ;
#146444 = EDGE_CURVE ( 'NONE', #28673, #14377, #118115, .T. ) ;
#146445 = CARTESIAN_POINT ( 'NONE',  ( 3.766062262543149401E-15, -39.95556452105413570, -7.249999994537627224 ) ) ;
#146446 = CARTESIAN_POINT ( 'NONE',  ( -0.05219959533937732626, 21.53943276465977519, 112.5010903946857042 ) ) ;
#146447 = CARTESIAN_POINT ( 'NONE',  ( -13.89961937509977652, 13.97604488694528158, 50.62390960531435979 ) ) ;
#146448 = CARTESIAN_POINT ( 'NONE',  ( 18.62759615963255655, 10.81492255796105972, 106.6677570613523756 ) ) ;
#146449 = CARTESIAN_POINT ( 'NONE',  ( 4.483927247898790824, -16.52544592524335698, 100.2094237280190043 ) ) ;
#146451 = CARTESIAN_POINT ( 'NONE',  ( -21.52544592524334988, -5.823673210054445271, 73.95942372801901854 ) ) ;
#146450 = CARTESIAN_POINT ( 'NONE',  ( -13.89961937509977652, 13.97604488694528158, 105.6239096053143527 ) ) ;
#146452 = CARTESIAN_POINT ( 'NONE',  ( 11.40812507854755253, -35.11059874428192273, -10.02499999726881441 ) ) ;
#146453 = CARTESIAN_POINT ( 'NONE',  ( -20.73749492396214933, -155.7167183371837496, -15.00000000000000178 ) ) ;
#146454 = CARTESIAN_POINT ( 'NONE',  ( 18.22780087662123805, 5.499999999999960032, 96.48236817873105053 ) ) ;
#146456 = CARTESIAN_POINT ( 'NONE',  ( -15.80617190586768217, 15.72974639402176855, 68.12609039468567573 ) ) ;
#146455 = CARTESIAN_POINT ( 'NONE',  ( -16.52544592524335698, -4.483927247898792601, 68.95942372801901854 ) ) ;
#146457 = CARTESIAN_POINT ( 'NONE',  ( 0.05219959533937995610, -21.53943276465977519, 105.0010903946856757 ) ) ;
#146458 = CARTESIAN_POINT ( 'NONE',  ( -3.573655867282028392E-15, 2.428612866367529932E-14, 165.5209445330007441 ) ) ;
#146459 = CARTESIAN_POINT ( 'NONE',  ( -5.153800228976328057, -19.02544592524343514, 92.29057627198099567 ) ) ;
#146460 = CARTESIAN_POINT ( 'NONE',  ( -19.03943276465977164, 0.05219959533909376836, 116.2489096053143669 ) ) ;
#146461 = VERTEX_POINT ( 'NONE', #53139 ) ;
#146462 = EDGE_CURVE ( 'NONE', #85061, #170763, #105664, .T. ) ;
#146463 = CARTESIAN_POINT ( 'NONE',  ( -0.8004727011103912604, -29.12650189376887866, -52.40478149256038165 ) ) ;
#146464 = CARTESIAN_POINT ( 'NONE',  ( 13.89961937509977652, -13.97604488694527269, 38.12390960531436690 ) ) ;
#146465 = CARTESIAN_POINT ( 'NONE',  ( 21.52544592524344225, -5.823673210054117533, 43.54057627198103830 ) ) ;
#146466 = CARTESIAN_POINT ( 'NONE',  ( -8.224510206698735004, -14.34966873604973081, 109.5844237280190328 ) ) ;
#146468 = CARTESIAN_POINT ( 'NONE',  ( 19.03943276465977164, -0.05219959533909143690, 78.74890960531436690 ) ) ;
#146467 = CARTESIAN_POINT ( 'NONE',  ( 4.379528057220339221, -16.55341960407611168, 97.70724293864772392 ) ) ;
#146469 = CARTESIAN_POINT ( 'NONE',  ( 18.62759615963255655, 10.81492255796105972, 101.6677570613523613 ) ) ;
#146470 = CARTESIAN_POINT ( 'NONE',  ( -5.153800228976328057, -19.02544592524343514, 37.29057627198102409 ) ) ;
#146471 = CARTESIAN_POINT ( 'NONE',  ( -12.14591786802309592, -12.06949235617757132, 86.87390960531438111 ) ) ;
#146472 = CARTESIAN_POINT ( 'NONE',  ( 21.53943276465977519, 0.05219959533937863772, 41.25109039468568284 ) ) ;
#146473 = CARTESIAN_POINT ( 'NONE',  ( 18.62759615963271287, -10.81492255796078972, 83.33224293864769550 ) ) ;
#146474 = CARTESIAN_POINT ( 'NONE',  ( 9.564922557961047289, -16.46253265017146816, 45.41775706135232582 ) ) ;
#146475 = CARTESIAN_POINT ( 'NONE',  ( -13.21949426486139423, -37.75586497602908764, -14.12003558585129426 ) ) ;
#146476 = CARTESIAN_POINT ( 'NONE',  ( -5.049401038298153566, 19.05341960407611168, 90.20724293864766707 ) ) ;
#146477 = CARTESIAN_POINT ( 'NONE',  ( 0.05219959533910956823, 16.53943276465976808, 59.99890960531436690 ) ) ;
#146478 = CARTESIAN_POINT ( 'NONE',  ( 5.049401038297881783, 19.05341960407617563, 42.29275706135234003 ) ) ;
#146479 = CARTESIAN_POINT ( 'NONE',  ( -8.314922557960811034, -14.29746914071050412, 42.08224293864769550 ) ) ;
#146480 = CARTESIAN_POINT ( 'NONE',  ( 16.51473224551083163, -9.474510206698727899, 80.83442372801899012 ) ) ;
#146481 = SPHERICAL_SURFACE ( 'NONE', #89240, 38.00000000000002132 ) ;
#146482 = CARTESIAN_POINT ( 'NONE',  ( -18.67979575497178146, -10.72451020669898902, 31.66557627198102054 ) ) ;
#146483 = CARTESIAN_POINT ( 'NONE',  ( -0.05219959533910754901, -16.53943276465976808, 92.49890960531436690 ) ) ;
#146484 = CARTESIAN_POINT ( 'NONE',  ( -4.814824860968089633E-30, -78.67194367458512261, -15.00000000000000000 ) ) ;
#146486 = CARTESIAN_POINT ( 'NONE',  ( 0.05219959533907565091, 21.53943276465977519, 44.99890960531435979 ) ) ;
#146485 = CARTESIAN_POINT ( 'NONE',  ( 0.05219959533909260263, 19.03943276465977164, 49.99890960531435979 ) ) ;
#146487 = CARTESIAN_POINT ( 'NONE',  ( -5.049401038298153566, 19.05341960407611168, 35.20724293864768839 ) ) ;
#146489 = CARTESIAN_POINT ( 'NONE',  ( -19.02544592524342804, 5.153800228976336051, 66.04057627198103830 ) ) ;
#146488 = CARTESIAN_POINT ( 'NONE',  ( -16.53943276465976808, -0.05219959533934237506, 78.75109039468568994 ) ) ;
#146491 = ADVANCED_FACE ( 'NONE', ( #378 ), #137913, .T. ) ;
#146490 = CARTESIAN_POINT ( 'NONE',  ( 9.564922557961047289, -16.46253265017146816, 35.41775706135233293 ) ) ;
#146492 = CARTESIAN_POINT ( 'NONE',  ( 15.72974639402176855, 15.80617190586768217, 66.87609039468568994 ) ) ;
#146493 = CARTESIAN_POINT ( 'NONE',  ( 0.05219959533907565091, 21.53943276465977519, 49.99890960531437401 ) ) ;
#146494 = CARTESIAN_POINT ( 'NONE',  ( 0.05219959533910956823, 16.53943276465976808, 114.9989096053143669 ) ) ;
#146495 = CARTESIAN_POINT ( 'NONE',  ( -0.05219959533936034679, 19.03943276465977164, 87.50109039468567573 ) ) ;
#146496 = CARTESIAN_POINT ( 'NONE',  ( 3.556970738554034288E-15, -38.81732327939057114, -2.624999997268812724 ) ) ;
#146498 = CARTESIAN_POINT ( 'NONE',  ( -21.53943276465977519, 0.05219959533907696930, 46.24890960531435979 ) ) ;
#146497 = CARTESIAN_POINT ( 'NONE',  ( -0.1103568551766080236, -24.30000000000002913, -56.77278709839600168 ) ) ;
#146499 = CARTESIAN_POINT ( 'NONE',  ( 17.40805194822030799, -6.112264579159333522, 68.33371272510613892 ) ) ;
#146500 = CARTESIAN_POINT ( 'NONE',  ( -10.72451020669870658, -18.67979575497194134, 89.58442372801901854 ) ) ;
#146501 = CARTESIAN_POINT ( 'NONE',  ( -14.34966873604960291, -8.224510206698953496, 41.66557627198103120 ) ) ;
#146503 = CARTESIAN_POINT ( 'NONE',  ( -16.53943276465976808, 0.05219959533911058130, 56.24890960531436690 ) ) ;
#146502 =( BOUNDED_CURVE ( )  B_SPLINE_CURVE ( 2, ( #154665, #167855, #29355, #16161, #139484, #44516, #185007, #125329, #59668, #61646, #168828 ),
 .UNSPECIFIED., .F., .F. ) 
 B_SPLINE_CURVE_WITH_KNOTS ( ( 3, 2, 2, 2, 2, 3 ),
 ( 0.2999999999999974909, 0.3199999999999979527, 0.3399999999999985811, 0.3599999999999991540, 0.3799999999999997824, 0.4000000000000003553 ),
 .UNSPECIFIED. ) 
 CURVE ( )  GEOMETRIC_REPRESENTATION_ITEM ( )  RATIONAL_B_SPLINE_CURVE ( ( 1.000000000000006217, 0.9510565162951473139, 1.000000000000000000, 0.9510565162951535312, 1.000000000000000000, 0.9510565162951535312, 1.000000000000000000, 0.9510565162951535312, 1.000000000000000000, 0.9510565162951527540, 1.000000000000000888 ) ) 
 REPRESENTATION_ITEM ( '' )  );
#146504 = CARTESIAN_POINT ( 'NONE',  ( 5.719274019375991003, -21.55341960407610458, 77.70724293864770971 ) ) ;
#146505 = CARTESIAN_POINT ( 'NONE',  ( 15.72974639402199770, -15.80617190586745480, 78.12390960531436690 ) ) ;
#146506 = CARTESIAN_POINT ( 'NONE',  ( -1.297617798568277969, -29.64248797448947315, -48.74145669546047088 ) ) ;
#146507 = CARTESIAN_POINT ( 'NONE',  ( -18.67979575497178146, -10.72451020669898902, 36.66557627198103120 ) ) ;
#146508 = CARTESIAN_POINT ( 'NONE',  ( -0.05219959533934338120, 16.53943276465976808, 52.50109039468567573 ) ) ;
#146509 = CARTESIAN_POINT ( 'NONE',  ( -4.483927247898539470, -16.52544592524342804, 77.29057627198102409 ) ) ;
#146510 = CARTESIAN_POINT ( 'NONE',  ( -16.46253265017160317, 9.564922557960807481, 55.83224293864769550 ) ) ;
#146511 = CARTESIAN_POINT ( 'NONE',  ( 5.049401038298161559, -19.05341960407611168, 32.70724293864768129 ) ) ;
#146512 = CARTESIAN_POINT ( 'NONE',  ( -31.99364916731038022, -5.186379194389042044E-15, 42.35000000000000853 ) ) ;
#146513 = ORIENTED_EDGE ( 'NONE', *, *, #164239, .T. ) ;
#146514 = CARTESIAN_POINT ( 'NONE',  ( -14.29746914071037622, -8.314922557961029526, 79.16775706135234714 ) ) ;
#146515 = CARTESIAN_POINT ( 'NONE',  ( 21.55341960407610458, 5.719274019375980345, 113.9572429386477239 ) ) ;
#146516 = CARTESIAN_POINT ( 'NONE',  ( 19.03943276465977164, -0.05219959533909143690, 63.74890960531435979 ) ) ;
#146517 = CARTESIAN_POINT ( 'NONE',  ( 5.823673210054444382, -21.52544592524334988, 55.20942372801902565 ) ) ;
#146518 = CARTESIAN_POINT ( 'NONE',  ( -9.474510206698964154, 16.51473224551069663, 115.4155762719810241 ) ) ;
#146519 = CARTESIAN_POINT ( 'NONE',  ( -31.74999999999995737, 3.061616997868383634E-16, -2.500000000000000444 ) ) ;
#146520 = EDGE_LOOP ( 'NONE', ( #113594, #60536, #129271, #171043 ) ) ;
#146521 = CARTESIAN_POINT ( 'NONE',  ( 15.72974639402176855, 15.80617190586768217, 51.87609039468568284 ) ) ;
#146522 = CARTESIAN_POINT ( 'NONE',  ( 0.05219959533909260263, 19.03943276465977164, 109.9989096053143669 ) ) ;
#146523 = CARTESIAN_POINT ( 'NONE',  ( 16.46253265017146816, 9.564922557961045513, 56.66775706135233293 ) ) ;
#146524 = CARTESIAN_POINT ( 'NONE',  ( 18.67979575497178502, 10.72451020669898547, 114.1655762719810383 ) ) ;
#146525 = CARTESIAN_POINT ( 'NONE',  ( 19.05341960407617918, -5.049401038297876454, 41.04275706135233293 ) ) ;
#146526 = CARTESIAN_POINT ( 'NONE',  ( 14.34966873604972726, -8.224510206698740333, 95.83442372801903275 ) ) ;
#146527 = CARTESIAN_POINT ( 'NONE',  ( 19.05341960407617918, -5.049401038297876454, 56.04275706135234714 ) ) ;
#146528 = CARTESIAN_POINT ( 'NONE',  ( 0.05219959533934541429, -16.53943276465976808, 110.0010903946856757 ) ) ;
#146529 = DIRECTION ( 'NONE',  ( 1.000000000000000000, 0.000000000000000000, 0.000000000000000000 ) ) ;
#146530 = CARTESIAN_POINT ( 'NONE',  ( -16.46253265017160317, 9.564922557960807481, 80.83224293864769550 ) ) ;
#146531 = CARTESIAN_POINT ( 'NONE',  ( -15.80617190586768217, 15.72974639402176855, 88.12609039468570415 ) ) ;
#146532 = CARTESIAN_POINT ( 'NONE',  ( 5.719274019375673035, 21.55341960407619339, 92.29275706135236135 ) ) ;
#146533 = DIRECTION ( 'NONE',  ( 0.8164965809277261455, 0.000000000000000000, 0.5773502691896257311 ) ) ;
#146534 = CARTESIAN_POINT ( 'NONE',  ( -13.97604488694527625, -13.89961937509977652, 106.8739096053143669 ) ) ;
#146535 = CARTESIAN_POINT ( 'NONE',  ( -5.719274019375665041, -21.55341960407619695, 79.79275706135236135 ) ) ;
#146536 = CARTESIAN_POINT ( 'NONE',  ( 19.05341960407617918, -5.049401038297876454, 111.0427570613523329 ) ) ;
#146537 = CARTESIAN_POINT ( 'NONE',  ( -13.97604488694527625, -13.89961937509977652, 76.87390960531433848 ) ) ;
#146538 = CARTESIAN_POINT ( 'NONE',  ( 5.719274019375991003, -21.55341960407610458, 32.70724293864770260 ) ) ;
#146539 = VECTOR ( 'NONE', #29155, 1000.000000000000000 ) ;
#146540 = CARTESIAN_POINT ( 'NONE',  ( -5.049401038298153566, 19.05341960407611168, 90.20724293864766707 ) ) ;
#146541 = CARTESIAN_POINT ( 'NONE',  ( -9.564922557961040184, 16.46253265017147172, 87.91775706135233293 ) ) ;
#146542 = CARTESIAN_POINT ( 'NONE',  ( 5.153800228976335163, 19.02544592524342804, 79.79057627198102409 ) ) ;
#146543 = CARTESIAN_POINT ( 'NONE',  ( -5.153800228976328057, -19.02544592524343514, 67.29057627198102409 ) ) ;
#146544 = CARTESIAN_POINT ( 'NONE',  ( 16.52544592524335698, 4.483927247898782831, 101.4594237280190185 ) ) ;
#146545 = DIRECTION ( 'NONE',  ( -0.000000000000000000, -0.000000000000000000, 1.000000000000000000 ) ) ;
#146546 = CARTESIAN_POINT ( 'NONE',  ( -19.03943276465977164, -0.05219959533935918106, 53.75109039468566863 ) ) ;
#146547 = CARTESIAN_POINT ( 'NONE',  ( 5.153800228976335163, 19.02544592524342804, 94.79057627198103830 ) ) ;
#146548 = CARTESIAN_POINT ( 'NONE',  ( 4.483927247898545687, 16.52544592524342804, 89.79057627198103830 ) ) ;
#146549 = CARTESIAN_POINT ( 'NONE',  ( 5.719274019375991003, -21.55341960407610458, 37.70724293864769550 ) ) ;
#146550 = CARTESIAN_POINT ( 'NONE',  ( 13.97604488694527802, 13.89961937509977652, 114.3739096053143669 ) ) ;
#146551 = CARTESIAN_POINT ( 'NONE',  ( -12.06949235617756955, 12.14591786802309770, 90.62390960531436690 ) ) ;
#146552 = CARTESIAN_POINT ( 'NONE',  ( -16.29526858892873165, 7.335722546920266041, 54.20329402199794089 ) ) ;
#146553 = CARTESIAN_POINT ( 'NONE',  ( -0.05219959533936034679, 19.03943276465977164, 42.50109039468566152 ) ) ;
#146554 = CARTESIAN_POINT ( 'NONE',  ( 12.06949235617739724, 12.14591786802326823, 106.8760903946856899 ) ) ;
#146555 = CARTESIAN_POINT ( 'NONE',  ( -5.153800228976328057, -19.02544592524343514, 92.29057627198099567 ) ) ;
#146556 = CARTESIAN_POINT ( 'NONE',  ( -21.55341960407619339, 5.719274019375674811, 63.54275706135234003 ) ) ;
#146557 = CARTESIAN_POINT ( 'NONE',  ( -21.52544592524343514, 5.823673210054127303, 56.04057627198102409 ) ) ;
#146558 = B_SPLINE_CURVE_WITH_KNOTS ( 'NONE', 3,
 ( #154755, #199278, #60745, #77904, #107245, #168916, #30421, #92069, #1056, #62729, #124412, #99037, #127386, #83868, #5034, #19238, #6037, #116224, #193076, #52543, #161729, #174907, #145550, #21217, #115224, #158721, #173920, #96059, #81860, #175908, #191070, #190077 ),
 .UNSPECIFIED., .F., .F.,
 ( 4, 2, 2, 2, 2, 2, 2, 2, 2, 2, 2, 2, 2, 2, 2, 4 ),
 ( 1.734980196055371455E-15, 0.0003712461730053016971, 0.0007424923460088683454, 0.001113738519012435211, 0.001484984692016001750, 0.002227477038023130494, 0.002598723211026691612, 0.002969969384030252298, 0.003341215557033814284, 0.003712461730037374535, 0.004083707903040936088, 0.004454954076044496773, 0.004826200249048058326, 0.005197446422051619878, 0.005568692595055181431, 0.005939938768058742984 ),
 .UNSPECIFIED. ) ;
#146560 = ORIENTED_EDGE ( 'NONE', *, *, #50546, .F. ) ;
#146559 = CARTESIAN_POINT ( 'NONE',  ( -21.53943276465977519, -0.05219959533937600094, 33.75109039468568284 ) ) ;
#146561 = CARTESIAN_POINT ( 'NONE',  ( 10.81492255796078972, 18.62759615963270932, 89.58224293864768129 ) ) ;
#146562 = CARTESIAN_POINT ( 'NONE',  ( -18.62759615963255300, -10.81492255796106328, 34.16775706135234714 ) ) ;
#146563 = CARTESIAN_POINT ( 'NONE',  ( 16.52544592524342804, -4.483927247898539470, 108.5405762719810241 ) ) ;
#146564 = CARTESIAN_POINT ( 'NONE',  ( 19.02544592524334988, 5.153800228976608722, 76.45942372801897591 ) ) ;
#146565 = CARTESIAN_POINT ( 'NONE',  ( 16.51473224551069308, 9.474510206698969483, 49.16557627198102409 ) ) ;
#146567 = CARTESIAN_POINT ( 'NONE',  ( 9.474510206698971260, -16.51473224551069308, 92.91557627198103830 ) ) ;
#146566 = CARTESIAN_POINT ( 'NONE',  ( 12.06949235617757843, -12.14591786802309237, 88.12390960531436690 ) ) ;
#146568 = CARTESIAN_POINT ( 'NONE',  ( 9.564922557960805705, 16.46253265017160317, 89.58224293864769550 ) ) ;
#146569 = CARTESIAN_POINT ( 'NONE',  ( 4.483927247898545687, 16.52544592524342804, 109.7905762719810383 ) ) ;
#146570 = CARTESIAN_POINT ( 'NONE',  ( 12.14591786802309770, 12.06949235617756955, 34.37390960531435979 ) ) ;
#146571 = CARTESIAN_POINT ( 'NONE',  ( -4.379528057220086978, -16.55341960407618274, 34.79275706135235424 ) ) ;
#146572 = CARTESIAN_POINT ( 'NONE',  ( -16.52544592524342804, 4.483927247898546575, 116.0405762719810383 ) ) ;
#146573 = CARTESIAN_POINT ( 'NONE',  ( -0.05219959533936034679, 19.03943276465977164, 22.50109039468566152 ) ) ;
#146575 = CARTESIAN_POINT ( 'NONE',  ( 16.52544592524342804, -4.483927247898539470, 23.54057627198102765 ) ) ;
#146574 = CARTESIAN_POINT ( 'NONE',  ( -5.049401038298153566, 19.05341960407611168, 110.2072429386476671 ) ) ;
#146576 = CARTESIAN_POINT ( 'NONE',  ( 18.62759615963255655, 10.81492255796105972, 31.66775706135234358 ) ) ;
#146577 = CARTESIAN_POINT ( 'NONE',  ( -19.02544592524342804, 5.153800228976336051, 106.0405762719810241 ) ) ;
#146578 = CARTESIAN_POINT ( 'NONE',  ( 16.53943276465976808, 0.05219959533934440121, 41.25109039468568284 ) ) ;
#146579 = CARTESIAN_POINT ( 'NONE',  ( -14.29746914071037622, -8.314922557961029526, 104.1677570613523471 ) ) ;
#146580 = B_SPLINE_CURVE_WITH_KNOTS ( 'NONE', 3,
 ( #82403, #110774, #53077, #20748, #5572, #188631, #3586, #174449, #172456, #66260, #128910, #21756, #114755, #99582, #190611, #161263, #83408, #145085, #6568, #176449 ),
 .UNSPECIFIED., .F., .F.,
 ( 4, 2, 2, 2, 2, 2, 2, 2, 2, 4 ),
 ( 0.000000000000000000, 0.0004987090165372665227, 0.0009974180330745330454, 0.001246772541343162512, 0.001496127049611791979, 0.001994836066149054815, 0.002493545082686318519, 0.002742899590954949503, 0.002992254099223581355, 0.003989672132298100089 ),
 .UNSPECIFIED. ) ;
#146581 = CARTESIAN_POINT ( 'NONE',  ( -8.314922557961024197, 14.29746914071037800, 92.91775706135236135 ) ) ;
#146582 = CARTESIAN_POINT ( 'NONE',  ( -16.53943276465976808, -0.05219959533934237506, 28.75109039468567929 ) ) ;
#146583 = CARTESIAN_POINT ( 'NONE',  ( 5.153800228976335163, 19.02544592524342804, 49.79057627198100988 ) ) ;
#146584 = CARTESIAN_POINT ( 'NONE',  ( 16.52544592524342804, -4.483927247898539470, 108.5405762719810241 ) ) ;
#146585 = CARTESIAN_POINT ( 'NONE',  ( 21.52544592524334988, 5.823673210054432836, 21.45942372801901499 ) ) ;
#146586 = CARTESIAN_POINT ( 'NONE',  ( -19.03943276465977164, 0.05219959533909376836, 36.24890960531436690 ) ) ;
#146587 = CARTESIAN_POINT ( 'NONE',  ( 5.153800228976335163, 19.02544592524342804, 99.79057627198102409 ) ) ;
#146588 = CARTESIAN_POINT ( 'NONE',  ( 19.05341960407611168, 5.049401038298154454, 33.95724293864769550 ) ) ;
#146589 = CARTESIAN_POINT ( 'NONE',  ( 19.03943276465977164, -0.05219959533909143690, 98.74890960531436690 ) ) ;
#146590 = DIRECTION ( 'NONE',  ( 0.000000000000000000, 0.000000000000000000, -1.000000000000000000 ) ) ;
#146591 = CARTESIAN_POINT ( 'NONE',  ( 19.03943276465977164, -0.05219959533909143690, 98.74890960531436690 ) ) ;
#146593 = CARTESIAN_POINT ( 'NONE',  ( 4.379528057220339221, -16.55341960407611168, 107.7072429386476955 ) ) ;
#146592 = CARTESIAN_POINT ( 'NONE',  ( -15.72974639402176322, -15.80617190586768395, 49.37609039468569705 ) ) ;
#146594 = CARTESIAN_POINT ( 'NONE',  ( 19.05341960407611168, 5.049401038298154454, 113.9572429386477097 ) ) ;
#146595 = DIRECTION ( 'NONE',  ( -0.7071067811865561215, -0.7071067811865389130, -0.000000000000000000 ) ) ;
#146596 = AXIS2_PLACEMENT_3D ( 'NONE', #194732, #115880, #190727 ) ;
#146597 = CARTESIAN_POINT ( 'NONE',  ( -8.314922557961024197, 14.29746914071037800, 57.91775706135234714 ) ) ;
#146598 = CARTESIAN_POINT ( 'NONE',  ( -21.53943276465977519, -0.05219959533937600094, 83.75109039468568994 ) ) ;
#146599 = CARTESIAN_POINT ( 'NONE',  ( 8.224510206698742110, 14.34966873604972548, 37.08442372801901143 ) ) ;
#146600 = CARTESIAN_POINT ( 'NONE',  ( -19.03943276465977164, 0.05219959533909376836, 86.24890960531436690 ) ) ;
#146601 = CARTESIAN_POINT ( 'NONE',  ( 5.049401038297881783, 19.05341960407617563, 107.2927570613523187 ) ) ;
#146602 = CARTESIAN_POINT ( 'NONE',  ( 12.06949235617739724, 12.14591786802326823, 81.87609039468568994 ) ) ;
#146603 = CARTESIAN_POINT ( 'NONE',  ( -9.474510206698720793, -16.51473224551083518, 94.58442372801900433 ) ) ;
#146604 = CARTESIAN_POINT ( 'NONE',  ( 19.02544592524343514, -5.153800228976328945, 68.54057627198103830 ) ) ;
#146605 = CARTESIAN_POINT ( 'NONE',  ( 21.52544592524344225, -5.823673210054117533, 93.54057627198103830 ) ) ;
#146607 = CARTESIAN_POINT ( 'NONE',  ( 16.51473224551083163, -9.474510206698727899, 90.83442372801900433 ) ) ;
#146606 = CARTESIAN_POINT ( 'NONE',  ( 16.52544592524342804, -4.483927247898539470, 83.54057627198102409 ) ) ;
#146608 = CARTESIAN_POINT ( 'NONE',  ( 12.06949235617739724, 12.14591786802326823, 61.87609039468568284 ) ) ;
#146609 = CARTESIAN_POINT ( 'NONE',  ( -19.46398650005390962, 5.499999999999953815, 80.18269651486369298 ) ) ;
#146611 = ADVANCED_FACE ( 'NONE', ( #26788 ), #184425, .T. ) ;
#146610 = CARTESIAN_POINT ( 'NONE',  ( -19.05341960407617563, 5.049401038297882671, 68.54275706135230450 ) ) ;
#146612 = CARTESIAN_POINT ( 'NONE',  ( -4.483927247898539470, -16.52544592524342804, 27.29057627198103120 ) ) ;
#146613 = CARTESIAN_POINT ( 'NONE',  ( -16.53943276465976808, 0.05219959533911058130, 86.24890960531436690 ) ) ;
#146615 = CARTESIAN_POINT ( 'NONE',  ( -16.88567814943193568, 6.947325034625406737, 38.70998877347406619 ) ) ;
#146614 = CARTESIAN_POINT ( 'NONE',  ( -21.55341960407619339, 5.719274019375674811, 113.5427570613523756 ) ) ;
#146616 = CARTESIAN_POINT ( 'NONE',  ( 21.55341960407619695, -5.719274019375665929, 26.04275706135235779 ) ) ;
#146617 = CARTESIAN_POINT ( 'NONE',  ( 13.89961937509977652, -13.97604488694527269, 108.1239096053143669 ) ) ;
#146618 = CARTESIAN_POINT ( 'NONE',  ( 5.153800228976335163, 19.02544592524342804, 79.79057627198102409 ) ) ;
#146619 = CARTESIAN_POINT ( 'NONE',  ( 15.72974639402176855, 15.80617190586768217, 96.87609039468568994 ) ) ;
#146620 = CARTESIAN_POINT ( 'NONE',  ( 5.153800228976335163, 19.02544592524342804, 69.79057627198103830 ) ) ;
#146621 = CARTESIAN_POINT ( 'NONE',  ( 21.53943276465977519, -0.05219959533907433946, 48.74890960531435979 ) ) ;
#146622 = CARTESIAN_POINT ( 'NONE',  ( -16.55341960407611168, -4.379528057220339221, 86.45724293864770971 ) ) ;
#146623 = CARTESIAN_POINT ( 'NONE',  ( -13.89961937509977652, 13.97604488694528158, 60.62390960531436690 ) ) ;
#146624 = CARTESIAN_POINT ( 'NONE',  ( -12.06949235617756955, 12.14591786802309770, 115.6239096053143669 ) ) ;
#146625 = AXIS2_PLACEMENT_3D ( 'NONE', #4841, #53349, #189888 ) ;
#146626 = CARTESIAN_POINT ( 'NONE',  ( 5.719274019375673035, 21.55341960407619339, 27.29275706135234358 ) ) ;
#146627 = CARTESIAN_POINT ( 'NONE',  ( 21.52544592524334988, 5.823673210054432836, 56.45942372801902565 ) ) ;
#146628 = CARTESIAN_POINT ( 'NONE',  ( -13.89961937509977652, 13.97604488694528158, 40.62390960531435979 ) ) ;
#146629 = CARTESIAN_POINT ( 'NONE',  ( 14.34966873604972726, -8.224510206698740333, 75.83442372801900433 ) ) ;
#146630 = CARTESIAN_POINT ( 'NONE',  ( 15.72974639402176855, 15.80617190586768217, 21.87609039468567573 ) ) ;
#146631 = CARTESIAN_POINT ( 'NONE',  ( 10.81492255796078972, 18.62759615963270932, 104.5822429386477097 ) ) ;
#146633 = CARTESIAN_POINT ( 'NONE',  ( -19.03943276465977164, 0.05219959533909376836, 61.24890960531436690 ) ) ;
#146632 = CARTESIAN_POINT ( 'NONE',  ( -16.51473224551082808, 9.474510206698731452, 38.33442372801899722 ) ) ;
#146634 = CARTESIAN_POINT ( 'NONE',  ( -16.46253265017146816, -9.564922557961047289, 29.16775706135232937 ) ) ;
#146635 = CARTESIAN_POINT ( 'NONE',  ( -10.72451020669870658, -18.67979575497194134, 74.58442372801901854 ) ) ;
#146636 = CARTESIAN_POINT ( 'NONE',  ( -21.55341960407610458, -5.719274019375992779, 71.45724293864769550 ) ) ;
#146637 = CARTESIAN_POINT ( 'NONE',  ( 16.53943276465976808, -0.05219959533910856209, 38.74890960531435979 ) ) ;
#146639 = CARTESIAN_POINT ( 'NONE',  ( -21.55341960407619339, 5.719274019375674811, 108.5427570613523756 ) ) ;
#146638 = CARTESIAN_POINT ( 'NONE',  ( -10.81492255796105439, 18.62759615963255655, 87.91775706135234714 ) ) ;
#146640 = CARTESIAN_POINT ( 'NONE',  ( -12.14591786802309592, -12.06949235617757132, 56.87390960531436690 ) ) ;
#146641 = CARTESIAN_POINT ( 'NONE',  ( 12.14591786802309770, 12.06949235617756955, 104.3739096053143669 ) ) ;
#146642 = CARTESIAN_POINT ( 'NONE',  ( -19.05341960407617563, 5.049401038297882671, 53.54275706135231871 ) ) ;
#146643 = CARTESIAN_POINT ( 'NONE',  ( 16.55341960407611168, 4.379528057220329451, 23.95724293864769550 ) ) ;
#146644 = CARTESIAN_POINT ( 'NONE',  ( -21.52544592524334988, -5.823673210054445271, 73.95942372801901854 ) ) ;
#146645 = CARTESIAN_POINT ( 'NONE',  ( -9.474510206698964154, 16.51473224551069663, 75.41557627198103830 ) ) ;
#146646 = CARTESIAN_POINT ( 'NONE',  ( 19.03943276465977164, 0.05219959533936151252, 46.25109039468566863 ) ) ;
#146647 = CARTESIAN_POINT ( 'NONE',  ( -5.719274019375978568, 21.55341960407610458, 55.20724293864770260 ) ) ;
#146648 = CARTESIAN_POINT ( 'NONE',  ( 5.823673210054444382, -21.52544592524334988, 45.20942372801901854 ) ) ;
#146649 = CARTESIAN_POINT ( 'NONE',  ( 18.67979575497178502, 10.72451020669898547, 104.1655762719810241 ) ) ;
#146650 = CARTESIAN_POINT ( 'NONE',  ( 19.02544592524334988, 5.153800228976608722, 101.4594237280189759 ) ) ;
#146651 = CARTESIAN_POINT ( 'NONE',  ( -0.05219959533934338120, 16.53943276465976808, 67.50109039468568994 ) ) ;
#146653 = CARTESIAN_POINT ( 'NONE',  ( 10.72451020669898902, -18.67979575497178502, 112.9155762719810383 ) ) ;
#146652 = CYLINDRICAL_SURFACE ( 'NONE', #6300, 40.00000000000000000 ) ;
#146654 = CARTESIAN_POINT ( 'NONE',  ( -16.53943276465976808, 0.05219959533911058130, 96.24890960531435269 ) ) ;
#146655 = CARTESIAN_POINT ( 'NONE',  ( 17.49999999999999289, 5.500000000000063061, 41.70309617465829177 ) ) ;
#146656 = CARTESIAN_POINT ( 'NONE',  ( 14.29746914071037800, 8.314922557961029526, 21.66775706135235069 ) ) ;
#146657 = CARTESIAN_POINT ( 'NONE',  ( -18.62759615963270932, 10.81492255796079327, 45.83224293864769550 ) ) ;
#146658 = CARTESIAN_POINT ( 'NONE',  ( 8.314922557961029526, -14.29746914071037800, 85.41775706135236135 ) ) ;
#146659 = CARTESIAN_POINT ( 'NONE',  ( 30.03989666729983199, -21.49319168150500303, -7.999999999999994671 ) ) ;
#146660 = CARTESIAN_POINT ( 'NONE',  ( -12.14591786802326823, 12.06949235617739902, 48.12609039468568284 ) ) ;
#146661 = CARTESIAN_POINT ( 'NONE',  ( 5.823673210054444382, -21.52544592524334988, 30.20942372801902565 ) ) ;
#146662 = CARTESIAN_POINT ( 'NONE',  ( 10.72451020669898902, -18.67979575497178502, 42.91557627198103120 ) ) ;
#146663 = CARTESIAN_POINT ( 'NONE',  ( 16.52544592524335698, 4.483927247898782831, 81.45942372801900433 ) ) ;
#146664 = CARTESIAN_POINT ( 'NONE',  ( 13.97604488694527802, 13.89961937509977652, 99.37390960531436690 ) ) ;
#146665 = CARTESIAN_POINT ( 'NONE',  ( 0.05219959533937995610, -21.53943276465977519, 70.00109039468568994 ) ) ;
#146666 = CARTESIAN_POINT ( 'NONE',  ( 21.52544592524344225, -5.823673210054117533, 43.54057627198103830 ) ) ;
#146667 = CARTESIAN_POINT ( 'NONE',  ( -18.62759615963270932, 10.81492255796079327, 35.83224293864768839 ) ) ;
#146668 = ORIENTED_EDGE ( 'NONE', *, *, #200190, .F. ) ;
#146669 = CARTESIAN_POINT ( 'NONE',  ( 16.46253265017146816, 9.564922557961045513, 51.66775706135233293 ) ) ;
#146670 = CARTESIAN_POINT ( 'NONE',  ( -12.06949235617739369, -12.14591786802326823, 64.37609039468568994 ) ) ;
#146671 = CARTESIAN_POINT ( 'NONE',  ( 10.81492255796078972, 18.62759615963270932, 29.58224293864769905 ) ) ;
#146672 = EDGE_LOOP ( 'NONE', ( #182583, #141331 ) ) ;
#146673 = CARTESIAN_POINT ( 'NONE',  ( 5.049401038298161559, -19.05341960407611168, 82.70724293864770971 ) ) ;
#146674 = CARTESIAN_POINT ( 'NONE',  ( 16.53943276465976808, -0.05219959533910856209, 23.74890960531435269 ) ) ;
#146675 = CARTESIAN_POINT ( 'NONE',  ( 9.441188956457336801, -38.26011958722975947, -31.87100816096936384 ) ) ;
#146676 = CARTESIAN_POINT ( 'NONE',  ( -12.06949235617756955, 12.14591786802309770, 105.6239096053143669 ) ) ;
#146677 = CARTESIAN_POINT ( 'NONE',  ( -5.823673210054116645, -21.52544592524344225, 52.29057627198102409 ) ) ;
#146678 = CARTESIAN_POINT ( 'NONE',  ( -13.89961937509977652, 13.97604488694528158, 45.62390960531433848 ) ) ;
#146679 = CARTESIAN_POINT ( 'NONE',  ( -16.55341960407617563, 4.379528057220093196, 83.54275706135234714 ) ) ;
#146680 = CARTESIAN_POINT ( 'NONE',  ( 5.823673210054444382, -21.52544592524334988, 30.20942372801902565 ) ) ;
#146681 = CARTESIAN_POINT ( 'NONE',  ( -19.05341960407617563, 5.049401038297882671, 83.54275706135233293 ) ) ;
#146682 = CARTESIAN_POINT ( 'NONE',  ( -8.314922557960811034, -14.29746914071050412, 92.08224293864769550 ) ) ;
#146683 = CARTESIAN_POINT ( 'NONE',  ( 0.05219959533909260263, 19.03943276465977164, 49.99890960531435979 ) ) ;
#146684 = CARTESIAN_POINT ( 'NONE',  ( 13.97604488694527802, 13.89961937509977652, 24.37390960531435624 ) ) ;
#146685 = CARTESIAN_POINT ( 'NONE',  ( 10.72451020669871369, 18.67979575497193778, 102.0844237280190185 ) ) ;
#146686 = CARTESIAN_POINT ( 'NONE',  ( 9.564922557960805705, 16.46253265017160317, 84.58224293864769550 ) ) ;
#146687 = CARTESIAN_POINT ( 'NONE',  ( 16.55341960407618274, -4.379528057220086978, 61.04275706135234714 ) ) ;
#146688 = CARTESIAN_POINT ( 'NONE',  ( 18.62759615963255655, 10.81492255796105972, 86.66775706135234714 ) ) ;
#146689 = CARTESIAN_POINT ( 'NONE',  ( 18.62759615963271287, -10.81492255796078972, 48.33224293864770260 ) ) ;
#146690 = CARTESIAN_POINT ( 'NONE',  ( 16.55341960407618274, -4.379528057220086978, 76.04275706135237556 ) ) ;
#146691 = CARTESIAN_POINT ( 'NONE',  ( 19.03943276465977164, 0.05219959533936151252, 46.25109039468566863 ) ) ;
#146692 = CARTESIAN_POINT ( 'NONE',  ( 16.51473224551083163, -9.474510206698727899, 60.83442372801900433 ) ) ;
#146693 = ORIENTED_EDGE ( 'NONE', *, *, #194310, .F. ) ;
#146694 = CARTESIAN_POINT ( 'NONE',  ( 0.05219959533937995610, -21.53943276465977519, 70.00109039468568994 ) ) ;
#146695 = CARTESIAN_POINT ( 'NONE',  ( -5.049401038298153566, 19.05341960407611168, 65.20724293864765286 ) ) ;
#146696 = CARTESIAN_POINT ( 'NONE',  ( 9.474510206698971260, -16.51473224551069308, 57.91557627198103120 ) ) ;
#146697 = CARTESIAN_POINT ( 'NONE',  ( -16.46253265017146816, -9.564922557961047289, 54.16775706135234003 ) ) ;
#146698 = CARTESIAN_POINT ( 'NONE',  ( -25.38323934330066933, 4.814940836774129096, 166.7856488131976676 ) ) ;
#146699 = CARTESIAN_POINT ( 'NONE',  ( 5.153800228976335163, 19.02544592524342804, 89.79057627198102409 ) ) ;
#146700 = CARTESIAN_POINT ( 'NONE',  ( 4.379528057220339221, -16.55341960407611168, 47.70724293864770260 ) ) ;
#146701 = CARTESIAN_POINT ( 'NONE',  ( -21.55341960407610458, -5.719274019375992779, 41.45724293864769550 ) ) ;
#146702 = CARTESIAN_POINT ( 'NONE',  ( 20.70421334297370919, 22.78074831271776191, -50.54281738342969987 ) ) ;
#146703 = CARTESIAN_POINT ( 'NONE',  ( 13.89961937509957401, 13.97604488694547697, 21.87609039468566152 ) ) ;
#146704 = CARTESIAN_POINT ( 'NONE',  ( -16.62475595723700650, -7.163666690055230823, 79.47286648189529501 ) ) ;
#146705 = CARTESIAN_POINT ( 'NONE',  ( -9.474510206698964154, 16.51473224551069663, 45.41557627198103120 ) ) ;
#146706 = CARTESIAN_POINT ( 'NONE',  ( 9.474510206698971260, -16.51473224551069308, 27.91557627198103120 ) ) ;
#146707 = CARTESIAN_POINT ( 'NONE',  ( -30.74264578624800492, 22.33583958711400186, -4.200000000000000178 ) ) ;
#146708 = CARTESIAN_POINT ( 'NONE',  ( -16.36317988757058828, 7.306389748694926745, 109.0978960836322358 ) ) ;
#146709 = CARTESIAN_POINT ( 'NONE',  ( -16.53943276465976808, -0.05219959533934237506, 63.75109039468568284 ) ) ;
#146710 = CARTESIAN_POINT ( 'NONE',  ( 0.05219959533907565091, 21.53943276465977519, 84.99890960531436690 ) ) ;
#146711 = VECTOR ( 'NONE', #51184, 1000.000000000000000 ) ;
#146712 = CARTESIAN_POINT ( 'NONE',  ( 16.55341960407611168, 4.379528057220329451, 58.95724293864770971 ) ) ;
#146714 = CARTESIAN_POINT ( 'NONE',  ( 7.500000000000000000, 9.184850993605147944E-16, 5.707106781186540800 ) ) ;
#146713 = CARTESIAN_POINT ( 'NONE',  ( -19.02544592524342804, 5.153800228976336051, 41.04057627198103120 ) ) ;
#146715 = CARTESIAN_POINT ( 'NONE',  ( 0.05219959533937995610, -21.53943276465977519, 45.00109039468568284 ) ) ;
#146716 = CARTESIAN_POINT ( 'NONE',  ( -13.89961937509957401, -13.97604488694547875, 49.37609039468567573 ) ) ;
#146717 = CARTESIAN_POINT ( 'NONE',  ( 13.89961937509977652, -13.97604488694527269, 33.12390960531434558 ) ) ;
#146718 = CARTESIAN_POINT ( 'NONE',  ( 5.823673210054444382, -21.52544592524334988, 90.20942372801903275 ) ) ;
#146719 = CARTESIAN_POINT ( 'NONE',  ( 17.49999999999999289, 5.624438216177591876, 96.68329655085355512 ) ) ;
#146720 = CARTESIAN_POINT ( 'NONE',  ( -12.14591786802309592, -12.06949235617757132, 36.87390960531435979 ) ) ;
#146721 = CARTESIAN_POINT ( 'NONE',  ( 19.19724070472090816, 5.500000000000156319, 43.56193348274383226 ) ) ;
#146722 = CARTESIAN_POINT ( 'NONE',  ( 5.823673210054125526, 21.52544592524343514, 34.79057627198103120 ) ) ;
#146723 = CARTESIAN_POINT ( 'NONE',  ( 25.64061671795035124, 10.58440545630783269, 139.9999999999999716 ) ) ;
#146724 = CARTESIAN_POINT ( 'NONE',  ( -19.05341960407611168, -5.049401038298163336, 86.45724293864769550 ) ) ;
#146725 = CARTESIAN_POINT ( 'NONE',  ( 16.53943276465976808, -0.05219959533910856209, 83.74890960531435269 ) ) ;
#146726 = CARTESIAN_POINT ( 'NONE',  ( 16.55341960407618274, -4.379528057220086978, 21.04275706135234714 ) ) ;
#146727 = CARTESIAN_POINT ( 'NONE',  ( 14.29746914071037800, 8.314922557961029526, 106.6677570613523756 ) ) ;
#146728 = VERTEX_POINT ( 'NONE', #88430 ) ;
#146729 = CARTESIAN_POINT ( 'NONE',  ( -19.02544592524342804, 5.153800228976336051, 46.04057627198101699 ) ) ;
#146730 = CIRCLE ( 'NONE', #14391, 23.10356920737165254 ) ;
#146732 = CARTESIAN_POINT ( 'NONE',  ( 10.81492255796078972, 18.62759615963270932, 84.58224293864769550 ) ) ;
#146731 = CARTESIAN_POINT ( 'NONE',  ( -16.46253265017160317, 9.564922557960807481, 80.83224293864769550 ) ) ;
#146734 = CARTESIAN_POINT ( 'NONE',  ( -0.05219959533909027116, -19.03943276465977164, 102.4989096053143669 ) ) ;
#146733 = CARTESIAN_POINT ( 'NONE',  ( 8.224510206698953496, -14.34966873604960469, 22.91557627198102765 ) ) ;
#146735 = CARTESIAN_POINT ( 'NONE',  ( -9.474510206698720793, -16.51473224551083518, 84.58442372801900433 ) ) ;
#146736 = CARTESIAN_POINT ( 'NONE',  ( 18.62759615963255655, 10.81492255796105972, 111.6677570613523613 ) ) ;
#146737 = CARTESIAN_POINT ( 'NONE',  ( -5.719274019375978568, 21.55341960407610458, 95.20724293864769550 ) ) ;
#146738 = CARTESIAN_POINT ( 'NONE',  ( 5.823673210054125526, 21.52544592524343514, 34.79057627198103120 ) ) ;
#146739 = AXIS2_PLACEMENT_3D ( 'NONE', #187624, #62249, #45122 ) ;
#146740 = CARTESIAN_POINT ( 'NONE',  ( -9.564922557960796823, -16.46253265017161027, 62.08224293864769550 ) ) ;
#146741 = CARTESIAN_POINT ( 'NONE',  ( 12.14591786802309770, 12.06949235617756955, 39.37390960531436690 ) ) ;
#146742 = CARTESIAN_POINT ( 'NONE',  ( 9.564922557960805705, 16.46253265017160317, 79.58224293864769550 ) ) ;
#146743 = EDGE_LOOP ( 'NONE', ( #159378, #194055, #28376, #164216, #196074 ) ) ;
#146744 = CARTESIAN_POINT ( 'NONE',  ( -32.36699822888682831, -3.753862658156239096, 88.50241378327223174 ) ) ;
#146745 = CARTESIAN_POINT ( 'NONE',  ( 13.89961937509957401, 13.97604488694547697, 26.87609039468566507 ) ) ;
#146746 = CARTESIAN_POINT ( 'NONE',  ( -12.14591786802309592, -12.06949235617757132, 81.87390960531435269 ) ) ;
#146747 = CARTESIAN_POINT ( 'NONE',  ( -5.719274019375665041, -21.55341960407619695, 24.79275706135235779 ) ) ;
#146748 = CARTESIAN_POINT ( 'NONE',  ( -5.359611314223446995E-15, 29.16686587814335496, 144.8750000027311557 ) ) ;
#146749 = CARTESIAN_POINT ( 'NONE',  ( -18.62759615963270932, 10.81492255796079327, 75.83224293864769550 ) ) ;
#146750 = CARTESIAN_POINT ( 'NONE',  ( -14.29746914071037622, -8.314922557961029526, 99.16775706135234714 ) ) ;
#146751 = CARTESIAN_POINT ( 'NONE',  ( 8.314922557960818139, 14.29746914071049879, 114.5822429386477097 ) ) ;
#146752 = CARTESIAN_POINT ( 'NONE',  ( 5.049401038298161559, -19.05341960407611168, 77.70724293864765286 ) ) ;
#146753 = CARTESIAN_POINT ( 'NONE',  ( 17.50000000000000000, -5.499999999999992895, 71.21769037696435589 ) ) ;
#146754 = CARTESIAN_POINT ( 'NONE',  ( 37.99626262588760994, -12.34573411038917357, -4.847842220587804007 ) ) ;
#146755 = CARTESIAN_POINT ( 'NONE',  ( 16.53943276465976808, -0.05219959533910856209, 33.74890960531436690 ) ) ;
#146756 = CARTESIAN_POINT ( 'NONE',  ( -5.823673210054431948, 21.52544592524334988, 62.70942372801902565 ) ) ;
#146757 = CARTESIAN_POINT ( 'NONE',  ( 28.84224951681686377, -24.48020638810656280, -21.31946643862243462 ) ) ;
#146758 = CARTESIAN_POINT ( 'NONE',  ( -21.55341960407619339, 5.719274019375674811, 93.54275706135234714 ) ) ;
#146759 = CARTESIAN_POINT ( 'NONE',  ( -5.153800228976328057, -19.02544592524343514, 47.29057627198102409 ) ) ;
#146760 = CARTESIAN_POINT ( 'NONE',  ( -19.05341960407611168, -5.049401038298163336, 56.45724293864768129 ) ) ;
#146761 =( BOUNDED_CURVE ( )  B_SPLINE_CURVE ( 2, ( #68918, #146754, #53756, #54751, #86085, #178113, #128580, #52741, #98226, #8248, #115430 ),
 .UNSPECIFIED., .F., .F. ) 
 B_SPLINE_CURVE_WITH_KNOTS ( ( 3, 2, 2, 2, 2, 3 ),
 ( 0.3000000000000000999, 0.3200000000000001177, 0.3400000000000000799, 0.3600000000000000422, 0.3800000000000000044, 0.4000000000000000222 ),
 .UNSPECIFIED. ) 
 CURVE ( )  GEOMETRIC_REPRESENTATION_ITEM ( )  RATIONAL_B_SPLINE_CURVE ( ( 0.9999999999999997780, 0.9510565162951537532, 1.000000000000000000, 0.9510565162951535312, 1.000000000000000000, 0.9510565162951535312, 1.000000000000000000, 0.9510565162951535312, 1.000000000000000000, 0.9510565162951535312, 1.000000000000000000 ) ) 
 REPRESENTATION_ITEM ( '' )  );
#146762 = VERTEX_POINT ( 'NONE', #134963 ) ;
#146763 = CARTESIAN_POINT ( 'NONE',  ( 15.80617190586769283, -15.72974639402175789, 100.6260903946857184 ) ) ;
#146764 = CARTESIAN_POINT ( 'NONE',  ( 16.53943276465976808, 0.05219959533934440121, 61.25109039468567573 ) ) ;
#146765 = CARTESIAN_POINT ( 'NONE',  ( -18.62759615963255300, -10.81492255796106328, 79.16775706135234714 ) ) ;
#146766 = CARTESIAN_POINT ( 'NONE',  ( -5.823673210054116645, -21.52544592524344225, 27.29057627198103120 ) ) ;
#146767 = CARTESIAN_POINT ( 'NONE',  ( 19.02544592524334988, 5.153800228976608722, 91.45942372801900433 ) ) ;
#146768 = CARTESIAN_POINT ( 'NONE',  ( -21.55341960407619339, 5.719274019375674811, 53.54275706135234714 ) ) ;
#146769 = CARTESIAN_POINT ( 'NONE',  ( -14.29746914071037622, -8.314922557961029526, 34.16775706135234714 ) ) ;
#146770 = CARTESIAN_POINT ( 'NONE',  ( -18.67979575497178146, -10.72451020669898902, 91.66557627198103830 ) ) ;
#146771 = CARTESIAN_POINT ( 'NONE',  ( -16.51473224551082808, 9.474510206698731452, 83.33442372801899012 ) ) ;
#146772 = CARTESIAN_POINT ( 'NONE',  ( -5.153800228976328057, -19.02544592524343514, 67.29057627198102409 ) ) ;
#146773 = CARTESIAN_POINT ( 'NONE',  ( 19.02544592524334988, 5.153800228976608722, 101.4594237280189759 ) ) ;
#146774 = AXIS2_PLACEMENT_3D ( 'NONE', #142290, #3770, #123141 ) ;
#146775 = CARTESIAN_POINT ( 'NONE',  ( 5.153800228976615827, -19.02544592524334988, 105.2094237280190185 ) ) ;
#146776 = CARTESIAN_POINT ( 'NONE',  ( 16.53943276465976808, -0.05219959533910856209, 53.74890960531437401 ) ) ;
#146777 = CARTESIAN_POINT ( 'NONE',  ( -19.02544592524334988, -5.153800228976617603, 73.95942372801900433 ) ) ;
#146778 = CARTESIAN_POINT ( 'NONE',  ( 8.314922557961029526, -14.29746914071037800, 60.41775706135235424 ) ) ;
#146779 = CARTESIAN_POINT ( 'NONE',  ( -19.03943276465977164, -0.05219959533935918106, 38.75109039468566152 ) ) ;
#146780 = PRODUCT_DEFINITION_SHAPE ( 'NONE', 'NONE',  #103014 ) ;
#146781 = CARTESIAN_POINT ( 'NONE',  ( -9.564922557960796823, -16.46253265017161027, 37.08224293864768839 ) ) ;
#146782 = CARTESIAN_POINT ( 'NONE',  ( 19.05341960407611168, 5.049401038298154454, 53.95724293864770260 ) ) ;
#146783 = CARTESIAN_POINT ( 'NONE',  ( 12.14591786802327356, -12.06949235617739191, 55.62609039468568284 ) ) ;
#146784 = CARTESIAN_POINT ( 'NONE',  ( 27.73933785331498925, -9.013057229001033122, 140.2750000027311330 ) ) ;
#146785 = CARTESIAN_POINT ( 'NONE',  ( -27.73933785331498925, 2.428612866367529932E-14, 148.8750000027311842 ) ) ;
#146786 = CARTESIAN_POINT ( 'NONE',  ( 19.02544592524343514, -5.153800228976328945, 108.5405762719810383 ) ) ;
#146787 = CARTESIAN_POINT ( 'NONE',  ( 13.97604488694527802, 13.89961937509977652, 24.37390960531435624 ) ) ;
#146788 = VERTEX_POINT ( 'NONE', #152098 ) ;
#146789 = CARTESIAN_POINT ( 'NONE',  ( 9.564922557961047289, -16.46253265017146816, 100.4177570613523329 ) ) ;
#146790 = CARTESIAN_POINT ( 'NONE',  ( 21.52544592524344225, -5.823673210054117533, 43.54057627198103830 ) ) ;
#146792 = CARTESIAN_POINT ( 'NONE',  ( 4.379528057220092307, 16.55341960407617563, 22.29275706135235069 ) ) ;
#146791 = CARTESIAN_POINT ( 'NONE',  ( 9.474510206698729675, 16.51473224551082808, 32.08442372801900433 ) ) ;
#146793 = CARTESIAN_POINT ( 'NONE',  ( 9.564922557960805705, 16.46253265017160317, 24.58224293864769194 ) ) ;
#146794 = CARTESIAN_POINT ( 'NONE',  ( -5.153800228976328057, -19.02544592524343514, 47.29057627198102409 ) ) ;
#146795 = CARTESIAN_POINT ( 'NONE',  ( -5.719274019375978568, 21.55341960407610458, 75.20724293864769550 ) ) ;
#146796 = CARTESIAN_POINT ( 'NONE',  ( -19.02544592524342804, 5.153800228976336051, 101.0405762719810241 ) ) ;
#146797 = CARTESIAN_POINT ( 'NONE',  ( -5.153800228976328057, -19.02544592524343514, 37.29057627198102409 ) ) ;
#146798 = CARTESIAN_POINT ( 'NONE',  ( 17.14385361876520264, -23.59649016807270883, 146.0750000027311728 ) ) ;
#146799 = CARTESIAN_POINT ( 'NONE',  ( -13.97604488694547697, 13.89961937509957934, 88.12609039468563310 ) ) ;
#146800 = CARTESIAN_POINT ( 'NONE',  ( 14.34966873604960469, 8.224510206698951720, 69.16557627198102409 ) ) ;
#146801 = CARTESIAN_POINT ( 'NONE',  ( -21.53943276465977519, 0.05219959533907696930, 51.24890960531436690 ) ) ;
#146802 = CARTESIAN_POINT ( 'NONE',  ( -15.72974639402176322, -15.80617190586768395, 109.3760903946857042 ) ) ;
#146803 = CARTESIAN_POINT ( 'NONE',  ( 15.72974639402199770, -15.80617190586745480, 98.12390960531436690 ) ) ;
#146804 = CARTESIAN_POINT ( 'NONE',  ( 10.72451020669871369, 18.67979575497193778, 67.08442372801901854 ) ) ;
#146805 = CARTESIAN_POINT ( 'NONE',  ( -21.55341960407619339, 5.719274019375674811, 73.54275706135234714 ) ) ;
#146806 = CARTESIAN_POINT ( 'NONE',  ( 0.05219959533909260263, 19.03943276465977164, 104.9989096053143669 ) ) ;
#146808 = CARTESIAN_POINT ( 'NONE',  ( 21.53943276465977519, 0.05219959533937863772, 81.25109039468568994 ) ) ;
#146807 = CARTESIAN_POINT ( 'NONE',  ( -16.53943276465976808, -0.05219959533934237506, 103.7510903946857042 ) ) ;
#146809 = CARTESIAN_POINT ( 'NONE',  ( 19.03943276465977164, -0.05219959533909143690, 63.74890960531435979 ) ) ;
#146810 = CARTESIAN_POINT ( 'NONE',  ( 13.97604488694548053, -13.89961937509957401, 40.62609039468564731 ) ) ;
#146811 = CARTESIAN_POINT ( 'NONE',  ( 15.72974639402176855, 15.80617190586768217, 31.87609039468567929 ) ) ;
#146812 = CARTESIAN_POINT ( 'NONE',  ( -9.564922557960796823, -16.46253265017161027, 62.08224293864769550 ) ) ;
#146813 = CARTESIAN_POINT ( 'NONE',  ( 8.314922557960818139, 14.29746914071049879, 79.58224293864769550 ) ) ;
#146814 = CARTESIAN_POINT ( 'NONE',  ( -12.14591786802309592, -12.06949235617757132, 41.87390960531435979 ) ) ;
#146815 = CARTESIAN_POINT ( 'NONE',  ( -0.05219959533907301413, -21.53943276465977519, 52.49890960531435979 ) ) ;
#146816 = CARTESIAN_POINT ( 'NONE',  ( 9.474510206698971260, -16.51473224551069308, 62.91557627198102409 ) ) ;
#146817 = CARTESIAN_POINT ( 'NONE',  ( 18.67979575497178502, 10.72451020669898547, 69.16557627198102409 ) ) ;
#146818 = CARTESIAN_POINT ( 'NONE',  ( -16.46253265017146816, -9.564922557961047289, 69.16775706135233293 ) ) ;
#146820 = CARTESIAN_POINT ( 'NONE',  ( 8.314922557960818139, 14.29746914071049879, 59.58224293864770260 ) ) ;
#146819 = CARTESIAN_POINT ( 'NONE',  ( 16.46253265017146816, 9.564922557961045513, 26.66775706135234003 ) ) ;
#146821 = CARTESIAN_POINT ( 'NONE',  ( -21.52544592524343514, 5.823673210054127303, 46.04057627198103830 ) ) ;
#146822 = ORIENTED_EDGE ( 'NONE', *, *, #53035, .T. ) ;
#146823 = ADVANCED_FACE ( 'NONE', ( #199595 ), #5055, .T. ) ;
#146824 = LINE ( 'NONE', #120469, #91544 ) ;
#146826 = CARTESIAN_POINT ( 'NONE',  ( 1.500000000004810818, 7.599999999999482725, -64.24270632869257724 ) ) ;
#146825 = CARTESIAN_POINT ( 'NONE',  ( -14.29746914071037622, -8.314922557961029526, 89.16775706135236135 ) ) ;
#146827 = CARTESIAN_POINT ( 'NONE',  ( -5.153800228976607833, 19.02544592524334988, 82.70942372801897591 ) ) ;
#146828 = CARTESIAN_POINT ( 'NONE',  ( -4.379528057220328563, 16.55341960407611168, 55.20724293864770260 ) ) ;
#146829 = CARTESIAN_POINT ( 'NONE',  ( -3.573655867282028392E-15, 2.428612866367529932E-14, -18.00000000000000000 ) ) ;
#146830 = CARTESIAN_POINT ( 'NONE',  ( -19.02544592524342804, 5.153800228976336051, 51.04057627198103120 ) ) ;
#146831 = CARTESIAN_POINT ( 'NONE',  ( -8.314922557960811034, -14.29746914071050412, 47.08224293864770260 ) ) ;
#146832 = CARTESIAN_POINT ( 'NONE',  ( 5.049401038298161559, -19.05341960407611168, 92.70724293864769550 ) ) ;
#146834 = CARTESIAN_POINT ( 'NONE',  ( -0.05219959533909027116, -19.03943276465977164, 57.49890960531435979 ) ) ;
#146833 = CARTESIAN_POINT ( 'NONE',  ( -16.51473224551082808, 9.474510206698731452, 73.33442372801900433 ) ) ;
#146835 = CARTESIAN_POINT ( 'NONE',  ( 10.72451020669871369, 18.67979575497193778, 57.08442372801901854 ) ) ;
#146836 = CARTESIAN_POINT ( 'NONE',  ( -5.153800228976328057, -19.02544592524343514, 77.29057627198099567 ) ) ;
#146837 = CARTESIAN_POINT ( 'NONE',  ( -9.474510206698964154, 16.51473224551069663, 30.41557627198102054 ) ) ;
#146838 = CARTESIAN_POINT ( 'NONE',  ( 13.89961937509977652, -13.97604488694527269, 73.12390960531436690 ) ) ;
#146839 = CARTESIAN_POINT ( 'NONE',  ( -21.52544592524343514, 5.823673210054127303, 51.04057627198103120 ) ) ;
#146840 = CARTESIAN_POINT ( 'NONE',  ( 9.474510206698971260, -16.51473224551069308, 52.91557627198102409 ) ) ;
#146841 = CARTESIAN_POINT ( 'NONE',  ( -5.719274019375978568, 21.55341960407610458, 55.20724293864770260 ) ) ;
#146842 = CARTESIAN_POINT ( 'NONE',  ( 9.474510206698729675, 16.51473224551082808, 82.08442372801899012 ) ) ;
#146843 = CARTESIAN_POINT ( 'NONE',  ( -8.224510206698735004, -14.34966873604973081, 109.5844237280190328 ) ) ;
#146844 = CARTESIAN_POINT ( 'NONE',  ( 16.51473224551083163, -9.474510206698727899, 40.83442372801900433 ) ) ;
#146846 = CARTESIAN_POINT ( 'NONE',  ( -4.483927247898782831, 16.52544592524335698, 77.70942372801900433 ) ) ;
#146845 = CARTESIAN_POINT ( 'NONE',  ( -16.52544592524335698, -4.483927247898792601, 53.95942372801900433 ) ) ;
#146847 = CARTESIAN_POINT ( 'NONE',  ( 30.00000000000000355, 3.889087296526017479, 8.181980515339454030 ) ) ;
#146848 = CARTESIAN_POINT ( 'NONE',  ( 16.52544592524335698, 4.483927247898782831, 66.45942372801903275 ) ) ;
#146849 = CARTESIAN_POINT ( 'NONE',  ( -10.72451020669898014, 18.67979575497178502, 30.41557627198101699 ) ) ;
#146850 = AXIS2_PLACEMENT_3D ( 'NONE', #113499, #143846, #111525 ) ;
#146851 = CARTESIAN_POINT ( 'NONE',  ( 19.03943276465977164, -0.05219959533909143690, 33.74890960531435979 ) ) ;
#146852 = CARTESIAN_POINT ( 'NONE',  ( -14.34966873604972548, 8.224510206698743886, 38.33442372801900433 ) ) ;
#146853 = CARTESIAN_POINT ( 'NONE',  ( 19.05341960407611168, 5.049401038298154454, 43.95724293864769550 ) ) ;
#146854 = CARTESIAN_POINT ( 'NONE',  ( 5.719274019375673035, 21.55341960407619339, 42.29275706135235424 ) ) ;
#146855 = CARTESIAN_POINT ( 'NONE',  ( -4.379528057220086978, -16.55341960407618274, 29.79275706135234358 ) ) ;
#146856 = CARTESIAN_POINT ( 'NONE',  ( 14.34966873604960469, 8.224510206698951720, 24.16557627198103120 ) ) ;
#146857 = FACE_OUTER_BOUND ( 'NONE', #11543, .T. ) ;
#146858 = CARTESIAN_POINT ( 'NONE',  ( 19.05341960407617918, -5.049401038297876454, 21.04275706135232582 ) ) ;
#146860 = ADVANCED_FACE ( 'NONE', ( #103619 ), #73293, .T. ) ;
#146859 = CARTESIAN_POINT ( 'NONE',  ( 16.51473224551083163, -9.474510206698727899, 105.8344237280190043 ) ) ;
#146861 = CARTESIAN_POINT ( 'NONE',  ( -16.51473224551082808, 9.474510206698731452, 73.33442372801900433 ) ) ;
#146862 = CARTESIAN_POINT ( 'NONE',  ( -14.29746914071049879, 8.314922557960819915, 70.83224293864770971 ) ) ;
#146863 = CARTESIAN_POINT ( 'NONE',  ( -13.89961937509977652, 13.97604488694528158, 35.62390960531435269 ) ) ;
#146865 = CARTESIAN_POINT ( 'NONE',  ( 16.18388926212244883, -7.379444403734566116, 57.06046848633770452 ) ) ;
#146864 = CARTESIAN_POINT ( 'NONE',  ( -19.02544592524334988, -5.153800228976617603, 63.95942372801899012 ) ) ;
#146866 = CARTESIAN_POINT ( 'NONE',  ( -18.62759615963255300, -10.81492255796106328, 59.16775706135234714 ) ) ;
#146867 = CARTESIAN_POINT ( 'NONE',  ( 4.379528057220092307, 16.55341960407617563, 42.29275706135235424 ) ) ;
#146868 = CARTESIAN_POINT ( 'NONE',  ( -17.97161686093726729, 5.499999999999973355, 90.99637206859165417 ) ) ;
#146869 = CARTESIAN_POINT ( 'NONE',  ( 10.72451020669898902, -18.67979575497178502, 22.91557627198102765 ) ) ;
#146870 = CARTESIAN_POINT ( 'NONE',  ( -4.379528057220086978, -16.55341960407618274, 19.79275706135235069 ) ) ;
#146871 = CARTESIAN_POINT ( 'NONE',  ( 28.82186960331498327, 2.781578969918950771E-14, 147.0000000000000000 ) ) ;
#146872 = CARTESIAN_POINT ( 'NONE',  ( -17.49999999999999645, -7.500000000000000888, 120.0000000000000142 ) ) ;
#146873 = CARTESIAN_POINT ( 'NONE',  ( 5.153800228976335163, 19.02544592524342804, 29.79057627198102409 ) ) ;
#146874 = CARTESIAN_POINT ( 'NONE',  ( -18.62759615963255300, -10.81492255796106328, 104.1677570613523471 ) ) ;
#146875 = CARTESIAN_POINT ( 'NONE',  ( 16.46253265017160672, -9.564922557960803928, 58.33224293864769550 ) ) ;
#146876 = AXIS2_PLACEMENT_3D ( 'NONE', #152421, #49229, #61396 ) ;
#146877 = CARTESIAN_POINT ( 'NONE',  ( -18.67979575497193778, 10.72451020669871902, 68.33442372801900433 ) ) ;
#146878 = CARTESIAN_POINT ( 'NONE',  ( -0.05219959533937732626, 21.53943276465977519, 97.50109039468567573 ) ) ;
#146879 = CARTESIAN_POINT ( 'NONE',  ( 12.14591786802309770, 12.06949235617756955, 29.37390960531435269 ) ) ;
#146880 = CARTESIAN_POINT ( 'NONE',  ( -9.474510206698964154, 16.51473224551069663, 25.41557627198103120 ) ) ;
#146881 = CARTESIAN_POINT ( 'NONE',  ( -9.474510206698964154, 16.51473224551069663, 90.41557627198103830 ) ) ;
#146882 = CARTESIAN_POINT ( 'NONE',  ( 21.55341960407619695, -5.719274019375665929, 61.04275706135234714 ) ) ;
#146883 = CARTESIAN_POINT ( 'NONE',  ( 13.97604488694527802, 13.89961937509977652, 34.37390960531436690 ) ) ;
#146884 = CARTESIAN_POINT ( 'NONE',  ( 18.62759615963255655, 10.81492255796105972, 56.66775706135235424 ) ) ;
#146886 = CARTESIAN_POINT ( 'NONE',  ( -5.049401038298153566, 19.05341960407611168, 100.2072429386476955 ) ) ;
#146885 = CARTESIAN_POINT ( 'NONE',  ( 9.564922557961047289, -16.46253265017146816, 85.41775706135233293 ) ) ;
#146887 = CARTESIAN_POINT ( 'NONE',  ( 14.34966873604960469, 8.224510206698951720, 114.1655762719810383 ) ) ;
#146888 = CARTESIAN_POINT ( 'NONE',  ( -21.55341960407610458, -5.719274019375992779, 106.4572429386477097 ) ) ;
#146889 = CARTESIAN_POINT ( 'NONE',  ( -5.049401038297874678, -19.05341960407617918, 29.79275706135232227 ) ) ;
#146890 = CARTESIAN_POINT ( 'NONE',  ( 8.224510206698953496, -14.34966873604960469, 92.91557627198103830 ) ) ;
#146891 = CARTESIAN_POINT ( 'NONE',  ( -16.51473224551069308, -9.474510206698971260, 46.66557627198102409 ) ) ;
#146893 = VECTOR ( 'NONE', #182408, 1000.000000000000000 ) ;
#146892 = CARTESIAN_POINT ( 'NONE',  ( 5.153800228976615827, -19.02544592524334988, 95.20942372801897591 ) ) ;
#146894 = CARTESIAN_POINT ( 'NONE',  ( -12.06949235617756955, 12.14591786802309770, 60.62390960531437401 ) ) ;
#146895 = CARTESIAN_POINT ( 'NONE',  ( 0.05219959533937995610, -21.53943276465977519, 110.0010903946856757 ) ) ;
#146896 = CARTESIAN_POINT ( 'NONE',  ( -19.02544592524342804, 5.153800228976336051, 101.0405762719810241 ) ) ;
#146897 = CARTESIAN_POINT ( 'NONE',  ( -16.46253265017146816, -9.564922557961047289, 84.16775706135233293 ) ) ;
#146898 = CARTESIAN_POINT ( 'NONE',  ( 15.72974639402199770, -15.80617190586745480, 93.12390960531436690 ) ) ;
#146899 = AXIS2_PLACEMENT_3D ( 'NONE', #129528, #191228, #114365 ) ;
#146900 = CARTESIAN_POINT ( 'NONE',  ( -15.72974639402176322, -15.80617190586768395, 44.37609039468567573 ) ) ;
#146901 = CARTESIAN_POINT ( 'NONE',  ( 4.379528057220092307, 16.55341960407617563, 47.29275706135234003 ) ) ;
#146902 = CARTESIAN_POINT ( 'NONE',  ( -0.05219959533934338120, 16.53943276465976808, 112.5010903946857042 ) ) ;
#146904 = CARTESIAN_POINT ( 'NONE',  ( -10.81492255796105439, 18.62759615963255655, 42.91775706135235424 ) ) ;
#146903 = CARTESIAN_POINT ( 'NONE',  ( -12.14591786802326823, 12.06949235617739902, 43.12609039468568284 ) ) ;
#146905 = CARTESIAN_POINT ( 'NONE',  ( -18.62759615963270932, 10.81492255796079327, 45.83224293864769550 ) ) ;
#146906 = PRESENTATION_LAYER_ASSIGNMENT (  '', '', ( #91879 ) ) ;
#146907 = CARTESIAN_POINT ( 'NONE',  ( 9.564922557960805705, 16.46253265017160317, 34.58224293864770260 ) ) ;
#146908 = DIRECTION ( 'NONE',  ( 1.000000000000000000, 0.000000000000000000, 0.000000000000000000 ) ) ;
#146909 = CARTESIAN_POINT ( 'NONE',  ( 16.52544592524335698, 4.483927247898782831, 61.45942372801901854 ) ) ;
#146910 = CARTESIAN_POINT ( 'NONE',  ( -15.72974639402197994, 15.80617190586746368, 85.62390960531436690 ) ) ;
#146911 = CARTESIAN_POINT ( 'NONE',  ( -4.483927247898539470, -16.52544592524342804, 42.29057627198103120 ) ) ;
#146912 = CARTESIAN_POINT ( 'NONE',  ( -14.29746914071037622, -8.314922557961029526, 69.16775706135234714 ) ) ;
#146913 = CARTESIAN_POINT ( 'NONE',  ( -13.89961937509977652, 13.97604488694528158, 60.62390960531436690 ) ) ;
#146914 = CARTESIAN_POINT ( 'NONE',  ( -16.51473224551082808, 9.474510206698731452, 98.33442372801900433 ) ) ;
#146915 = CARTESIAN_POINT ( 'NONE',  ( -15.72974639402197994, 15.80617190586746368, 80.62390960531438111 ) ) ;
#146916 = CARTESIAN_POINT ( 'NONE',  ( 16.55341960407611168, 4.379528057220329451, 33.95724293864769550 ) ) ;
#146917 = EDGE_LOOP ( 'NONE', ( #29906, #162615, #77275, #92623, #84284 ) ) ;
#146918 = CARTESIAN_POINT ( 'NONE',  ( 0.05219959533934541429, -16.53943276465976808, 80.00109039468568994 ) ) ;
#146919 = CARTESIAN_POINT ( 'NONE',  ( 21.88033147701376890, 9.239123595177357373, 171.1226046679828983 ) ) ;
#146920 = CARTESIAN_POINT ( 'NONE',  ( 21.55341960407610458, 5.719274019375980345, 73.95724293864769550 ) ) ;
#146921 = CARTESIAN_POINT ( 'NONE',  ( -14.29746914071037622, -8.314922557961029526, 109.1677570613523613 ) ) ;
#146922 = ORIENTED_EDGE ( 'NONE', *, *, #89104, .T. ) ;
#146923 = LINE ( 'NONE', #26593, #69462 ) ;
#146924 = CARTESIAN_POINT ( 'NONE',  ( -0.05219959533907301413, -21.53943276465977519, 82.49890960531436690 ) ) ;
#146925 = CARTESIAN_POINT ( 'NONE',  ( 10.81492255796078972, 18.62759615963270932, 109.5822429386476955 ) ) ;
#146926 = CARTESIAN_POINT ( 'NONE',  ( -0.05219959533934338120, 16.53943276465976808, 112.5010903946857042 ) ) ;
#146928 = CARTESIAN_POINT ( 'NONE',  ( 14.34966873604972726, -8.224510206698740333, 35.83442372801901143 ) ) ;
#146927 = VECTOR ( 'NONE', #17645, 1000.000000000000000 ) ;
#146929 = CARTESIAN_POINT ( 'NONE',  ( 9.564922557960805705, 16.46253265017160317, 39.58224293864768839 ) ) ;
#146930 = CARTESIAN_POINT ( 'NONE',  ( 9.564922557960805705, 16.46253265017160317, 64.58224293864769550 ) ) ;
#146931 = CARTESIAN_POINT ( 'NONE',  ( 17.81289503416611453, -24.51734667627695785, 148.6999999999999602 ) ) ;
#146932 = CARTESIAN_POINT ( 'NONE',  ( -0.05219959533909027116, -19.03943276465977164, 112.4989096053143669 ) ) ;
#146933 = CARTESIAN_POINT ( 'NONE',  ( 1.473961946532198919, 30.07508824747824150, -51.33206735129527942 ) ) ;
#146934 = CARTESIAN_POINT ( 'NONE',  ( 5.049401038297881783, 19.05341960407617563, 107.2927570613523187 ) ) ;
#146935 = CARTESIAN_POINT ( 'NONE',  ( 5.049401038297881783, 19.05341960407617563, 42.29275706135234003 ) ) ;
#146936 = CARTESIAN_POINT ( 'NONE',  ( 21.55341960407610458, 5.719274019375980345, 93.95724293864770971 ) ) ;
#146937 = CARTESIAN_POINT ( 'NONE',  ( 14.34966873604972726, -8.224510206698740333, 110.8344237280190043 ) ) ;
#146938 = CARTESIAN_POINT ( 'NONE',  ( 5.823673210054125526, 21.52544592524343514, 39.79057627198103830 ) ) ;
#146940 = CARTESIAN_POINT ( 'NONE',  ( -16.51473224551082808, 9.474510206698731452, 108.3344237280190043 ) ) ;
#146939 = CARTESIAN_POINT ( 'NONE',  ( 5.719274019375991003, -21.55341960407610458, 87.70724293864769550 ) ) ;
#146941 = CARTESIAN_POINT ( 'NONE',  ( -5.153800228976328057, -19.02544592524343514, 107.2905762719810383 ) ) ;
#146942 = CARTESIAN_POINT ( 'NONE',  ( -10.81492255796105439, 18.62759615963255655, 72.91775706135234714 ) ) ;
#146943 = CARTESIAN_POINT ( 'NONE',  ( -5.153800228976328057, -19.02544592524343514, 67.29057627198102409 ) ) ;
#146944 = B_SPLINE_CURVE_WITH_KNOTS ( 'NONE', 3,
 ( #182008, #172793, #110116, #18121, #186988, #157619, #173794, #51423 ),
 .UNSPECIFIED., .F., .F.,
 ( 4, 2, 2, 4 ),
 ( 2.787091001330594030E-07, 0.0002981295844663114534, 0.0005959804598324898710, 0.001191682210564843237 ),
 .UNSPECIFIED. ) ;
#146945 = CARTESIAN_POINT ( 'NONE',  ( 12.06949235617757843, -12.14591786802309237, 103.1239096053143811 ) ) ;
#146946 = CARTESIAN_POINT ( 'NONE',  ( 31.26591117326540115, 6.741338443544413472, 98.29621977100282493 ) ) ;
#146947 = CARTESIAN_POINT ( 'NONE',  ( -9.474510206698964154, 16.51473224551069663, 70.41557627198102409 ) ) ;
#146948 = CARTESIAN_POINT ( 'NONE',  ( 16.52544592524342804, -4.483927247898539470, 88.54057627198103830 ) ) ;
#146949 = ORIENTED_EDGE ( 'NONE', *, *, #101761, .T. ) ;
#146950 = CARTESIAN_POINT ( 'NONE',  ( -9.474510206698720793, -16.51473224551083518, 109.5844237280190043 ) ) ;
#146951 = DIRECTION ( 'NONE',  ( -0.000000000000000000, -0.000000000000000000, 1.000000000000000000 ) ) ;
#146952 = CARTESIAN_POINT ( 'NONE',  ( -9.564922557960796823, -16.46253265017161027, 62.08224293864769550 ) ) ;
#146954 = CARTESIAN_POINT ( 'NONE',  ( 9.564922557960805705, 16.46253265017160317, 99.58224293864770971 ) ) ;
#146953 = CARTESIAN_POINT ( 'NONE',  ( 18.67979575497194134, -10.72451020669871369, 80.83442372801901854 ) ) ;
#146955 = CARTESIAN_POINT ( 'NONE',  ( -16.55341960407617563, 4.379528057220093196, 83.54275706135234714 ) ) ;
#146956 = CARTESIAN_POINT ( 'NONE',  ( -16.79531203550648399, -7.028104445595611871, 76.25244988220444498 ) ) ;
#146957 = CARTESIAN_POINT ( 'NONE',  ( -13.89961937509957401, -13.97604488694547875, 54.37609039468565442 ) ) ;
#146958 = CARTESIAN_POINT ( 'NONE',  ( 21.53943276465977519, 0.05219959533937863772, 96.25109039468568994 ) ) ;
#146959 = CARTESIAN_POINT ( 'NONE',  ( -27.88129983271662837, 6.733757357602863536, 162.1517353552117982 ) ) ;
#146960 = CARTESIAN_POINT ( 'NONE',  ( 37.99999999999996447, -12.34694845685046793, -6.849999994537626868 ) ) ;
#146961 = CARTESIAN_POINT ( 'NONE',  ( 14.29746914071049879, -8.314922557960816363, 23.33224293864769194 ) ) ;
#146962 = CARTESIAN_POINT ( 'NONE',  ( 30.00000000000000711, -4.592425496802575156E-15, 52.50000000000000000 ) ) ;
#146963 = CARTESIAN_POINT ( 'NONE',  ( 8.224510206698742110, 14.34966873604972548, 92.08442372801901854 ) ) ;
#146964 = CARTESIAN_POINT ( 'NONE',  ( -28.79475375365586842, 2.428612866367529932E-14, 146.2656553485623760 ) ) ;
#146965 = CARTESIAN_POINT ( 'NONE',  ( -8.224510206698735004, -14.34966873604973081, 74.58442372801901854 ) ) ;
#146966 = CARTESIAN_POINT ( 'NONE',  ( 5.823673210054444382, -21.52544592524334988, 80.20942372801901854 ) ) ;
#146967 = CARTESIAN_POINT ( 'NONE',  ( 9.564922557961047289, -16.46253265017146816, 90.41775706135234714 ) ) ;
#146968 = CARTESIAN_POINT ( 'NONE',  ( -9.564922557961040184, 16.46253265017147172, 37.91775706135233293 ) ) ;
#146969 = VECTOR ( 'NONE', #101648, 1000.000000000000000 ) ;
#146970 = CARTESIAN_POINT ( 'NONE',  ( -19.02544592524342804, 5.153800228976336051, 66.04057627198103830 ) ) ;
#146971 = CARTESIAN_POINT ( 'NONE',  ( 19.03943276465977164, -0.05219959533909143690, 63.74890960531435979 ) ) ;
#146972 = CARTESIAN_POINT ( 'NONE',  ( -18.22780087662119541, 5.500000000000102141, 41.01763182126894236 ) ) ;
#146973 = CARTESIAN_POINT ( 'NONE',  ( -18.67979575497178146, -10.72451020669898902, 76.66557627198103830 ) ) ;
#146974 = CARTESIAN_POINT ( 'NONE',  ( -18.67979575497178146, -10.72451020669898902, 36.66557627198103120 ) ) ;
#146975 = CARTESIAN_POINT ( 'NONE',  ( 13.97604488694527802, 13.89961937509977652, 29.37390960531435979 ) ) ;
#146976 = CARTESIAN_POINT ( 'NONE',  ( -16.55341960407617563, 4.379528057220093196, 68.54275706135234714 ) ) ;
#146977 = UNCERTAINTY_MEASURE_WITH_UNIT (LENGTH_MEASURE( 1.000000000000000082E-05 ), #89080, 'distance_accuracy_value', 'NONE');
#146978 = ORIENTED_EDGE ( 'NONE', *, *, #97036, .T. ) ;
#146979 = CARTESIAN_POINT ( 'NONE',  ( 0.05219959533937995610, -21.53943276465977519, 35.00109039468568284 ) ) ;
#146981 = CARTESIAN_POINT ( 'NONE',  ( -23.48529157249600985, 32.32473071737754111, -2.299999999999999822 ) ) ;
#146980 = CARTESIAN_POINT ( 'NONE',  ( -0.05219959533910754901, -16.53943276465976808, 72.49890960531435269 ) ) ;
#146982 = CARTESIAN_POINT ( 'NONE',  ( -16.52544592524335698, -4.483927247898792601, 28.95942372801902209 ) ) ;
#146983 = CARTESIAN_POINT ( 'NONE',  ( 13.89961937509957401, 13.97604488694547697, 56.87609039468564731 ) ) ;
#146984 = CARTESIAN_POINT ( 'NONE',  ( 8.314922557960818139, 14.29746914071049879, 54.58224293864769550 ) ) ;
#146985 = CARTESIAN_POINT ( 'NONE',  ( -5.823673210054431948, 21.52544592524334988, 32.70942372801900433 ) ) ;
#146987 = CARTESIAN_POINT ( 'NONE',  ( 18.62759615963271287, -10.81492255796078972, 83.33224293864769550 ) ) ;
#146986 = DIRECTION ( 'NONE',  ( -1.000000000000000000, 0.000000000000000000, -0.000000000000000000 ) ) ;
#146988 = CARTESIAN_POINT ( 'NONE',  ( -16.46253265017160317, 9.564922557960807481, 100.8322429386477097 ) ) ;
#146989 = CARTESIAN_POINT ( 'NONE',  ( -16.52544592524342804, 4.483927247898546575, 76.04057627198102409 ) ) ;
#146990 = CARTESIAN_POINT ( 'NONE',  ( -16.46253265017160317, 9.564922557960807481, 110.8322429386476955 ) ) ;
#146991 = CARTESIAN_POINT ( 'NONE',  ( 29.86685920354754842, -21.69954338932559068, -7.824999997268813345 ) ) ;
#146992 = CARTESIAN_POINT ( 'NONE',  ( 5.153800228976615827, -19.02544592524334988, 70.20942372801899012 ) ) ;
#146993 = CARTESIAN_POINT ( 'NONE',  ( 21.55341960407619695, -5.719274019375665929, 26.04275706135235779 ) ) ;
#146994 = CARTESIAN_POINT ( 'NONE',  ( -5.049401038298153566, 19.05341960407611168, 60.20724293864768129 ) ) ;
#146995 = CARTESIAN_POINT ( 'NONE',  ( -13.97604488694547697, 13.89961937509957934, 48.12609039468566863 ) ) ;
#146996 = CARTESIAN_POINT ( 'NONE',  ( -13.89961937509977652, 13.97604488694528158, 35.62390960531435269 ) ) ;
#146997 = ADVANCED_FACE ( 'NONE', ( #13582 ), #196641, .T. ) ;
#146998 = CARTESIAN_POINT ( 'NONE',  ( 18.67979575497194134, -10.72451020669871369, 60.83442372801901854 ) ) ;
#146999 = LINE ( 'NONE', #178348, #40121 ) ;
#147000 = CARTESIAN_POINT ( 'NONE',  ( 12.14591786802309770, 12.06949235617756955, 44.37390960531435979 ) ) ;
#147001 = CARTESIAN_POINT ( 'NONE',  ( 5.049401038298161559, -19.05341960407611168, 62.70724293864769550 ) ) ;
#147002 = CARTESIAN_POINT ( 'NONE',  ( 21.52544592524344225, -5.823673210054117533, 93.54057627198103830 ) ) ;
#147003 = CARTESIAN_POINT ( 'NONE',  ( 5.153800228976335163, 19.02544592524342804, 64.79057627198100988 ) ) ;
#147004 = ORIENTED_EDGE ( 'NONE', *, *, #100613, .T. ) ;
#147005 = CARTESIAN_POINT ( 'NONE',  ( 5.719274019375991003, -21.55341960407610458, 62.70724293864769550 ) ) ;
#147006 = VERTEX_POINT ( 'NONE', #41953 ) ;
#147007 = CARTESIAN_POINT ( 'NONE',  ( 21.52544592524334988, 5.823673210054432836, 96.45942372801901854 ) ) ;
#147010 = CARTESIAN_POINT ( 'NONE',  ( 4.379528057220339221, -16.55341960407611168, 77.70724293864770971 ) ) ;
#147009 = CARTESIAN_POINT ( 'NONE',  ( 12.06949235617739724, 12.14591786802326823, 91.87609039468568994 ) ) ;
#147008 = DIRECTION ( 'NONE',  ( -1.000000000000000000, 0.000000000000000000, 0.000000000000000000 ) ) ;
#147011 = CARTESIAN_POINT ( 'NONE',  ( -19.05341960407617563, 5.049401038297882671, 93.54275706135234714 ) ) ;
#147012 = ORIENTED_EDGE ( 'NONE', *, *, #75822, .T. ) ;
#147013 = CARTESIAN_POINT ( 'NONE',  ( -18.62759615963270932, 10.81492255796079327, 110.8322429386476955 ) ) ;
#147014 = CARTESIAN_POINT ( 'NONE',  ( 16.51473224551083163, -9.474510206698727899, 40.83442372801900433 ) ) ;
#147015 = CARTESIAN_POINT ( 'NONE',  ( 12.14591786802327356, -12.06949235617739191, 105.6260903946856899 ) ) ;
#147016 = CARTESIAN_POINT ( 'NONE',  ( 19.05341960407617918, -5.049401038297876454, 36.04275706135234003 ) ) ;
#147017 = CARTESIAN_POINT ( 'NONE',  ( -19.03943276465977164, 0.05219959533909376836, 86.24890960531436690 ) ) ;
#147018 = CARTESIAN_POINT ( 'NONE',  ( -21.55341960407610458, -5.719274019375992779, 66.45724293864768129 ) ) ;
#147019 = CARTESIAN_POINT ( 'NONE',  ( 5.000000000000000000, -139.5000000000000000, 21.32407087589996308 ) ) ;
#147020 = CARTESIAN_POINT ( 'NONE',  ( 8.224510206698953496, -14.34966873604960469, 112.9155762719810383 ) ) ;
#147021 = CARTESIAN_POINT ( 'NONE',  ( -5.823673210054431948, 21.52544592524334988, 112.7094237280190328 ) ) ;
#147022 = CARTESIAN_POINT ( 'NONE',  ( 12.14591786802327356, -12.06949235617739191, 80.62609039468567573 ) ) ;
#147023 = CARTESIAN_POINT ( 'NONE',  ( -5.823673210054431948, 21.52544592524334988, 27.70942372801901854 ) ) ;
#147024 = CARTESIAN_POINT ( 'NONE',  ( -4.483927247898782831, 16.52544592524335698, 27.70942372801901854 ) ) ;
#147025 = CARTESIAN_POINT ( 'NONE',  ( -13.97604488694527625, -13.89961937509977652, 101.8739096053143811 ) ) ;
#147026 = CARTESIAN_POINT ( 'NONE',  ( -9.564922557960796823, -16.46253265017161027, 42.08224293864769550 ) ) ;
#147027 = CARTESIAN_POINT ( 'NONE',  ( -9.564922557960796823, -16.46253265017161027, 62.08224293864769550 ) ) ;
#147028 = AXIS2_PLACEMENT_3D ( 'NONE', #86872, #120197, #146533 ) ;
#147029 = CARTESIAN_POINT ( 'NONE',  ( 12.14591786802327356, -12.06949235617739191, 45.62609039468567573 ) ) ;
#147030 = CARTESIAN_POINT ( 'NONE',  ( 8.224510206698953496, -14.34966873604960469, 87.91557627198103830 ) ) ;
#147031 = CARTESIAN_POINT ( 'NONE',  ( 4.483927247898790824, -16.52544592524335698, 95.20942372801903275 ) ) ;
#147034 = CARTESIAN_POINT ( 'NONE',  ( 0.05219959533909260263, 19.03943276465977164, 59.99890960531436690 ) ) ;
#147033 = CARTESIAN_POINT ( 'NONE',  ( -16.51473224551069308, -9.474510206698971260, 81.66557627198103830 ) ) ;
#147032 = CARTESIAN_POINT ( 'NONE',  ( 5.719274019375673035, 21.55341960407619339, 47.29275706135234003 ) ) ;
#147035 = CARTESIAN_POINT ( 'NONE',  ( 19.05341960407611168, 5.049401038298154454, 98.95724293864766707 ) ) ;
#147036 = CARTESIAN_POINT ( 'NONE',  ( -8.314922557960811034, -14.29746914071050412, 37.08224293864768129 ) ) ;
#147037 = CARTESIAN_POINT ( 'NONE',  ( 16.52544592524335698, 4.483927247898782831, 101.4594237280190185 ) ) ;
#147038 = ORIENTED_EDGE ( 'NONE', *, *, #163855, .F. ) ;
#147039 = CARTESIAN_POINT ( 'NONE',  ( -16.46253265017146816, -9.564922557961047289, 39.16775706135234003 ) ) ;
#147040 = CARTESIAN_POINT ( 'NONE',  ( 19.05341960407611168, 5.049401038298154454, 108.9572429386477097 ) ) ;
#147041 = CARTESIAN_POINT ( 'NONE',  ( 5.049401038298161559, -19.05341960407611168, 67.70724293864769550 ) ) ;
#147042 = CARTESIAN_POINT ( 'NONE',  ( -19.02544592524334988, -5.153800228976617603, 43.95942372801899012 ) ) ;
#147043 = CARTESIAN_POINT ( 'NONE',  ( -36.91746825000001309, -11.99521256947794789, -4.524999997268813523 ) ) ;
#147044 = CARTESIAN_POINT ( 'NONE',  ( 19.52837319214027900, -5.499999999999891642, 72.10471352585544480 ) ) ;
#147045 = CARTESIAN_POINT ( 'NONE',  ( -0.05219959533934338120, 16.53943276465976808, 57.50109039468568994 ) ) ;
#147047 = CARTESIAN_POINT ( 'NONE',  ( -14.34966873604972548, 8.224510206698743886, 53.33442372801901854 ) ) ;
#147046 = CARTESIAN_POINT ( 'NONE',  ( 9.564922557961047289, -16.46253265017146816, 65.41775706135233293 ) ) ;
#147048 = FACE_OUTER_BOUND ( 'NONE', #149947, .T. ) ;
#147049 = CARTESIAN_POINT ( 'NONE',  ( -0.05219959533909027116, -19.03943276465977164, 92.49890960531436690 ) ) ;
#147050 = CARTESIAN_POINT ( 'NONE',  ( -15.72974639402197994, 15.80617190586746368, 110.6239096053143669 ) ) ;
#147051 = CARTESIAN_POINT ( 'NONE',  ( 9.564922557961047289, -16.46253265017146816, 80.41775706135234714 ) ) ;
#147053 = CARTESIAN_POINT ( 'NONE',  ( 16.51473224551069308, 9.474510206698969483, 29.16557627198103475 ) ) ;
#147052 = CARTESIAN_POINT ( 'NONE',  ( 16.46253265017160672, -9.564922557960803928, 108.3322429386476955 ) ) ;
#147054 = CARTESIAN_POINT ( 'NONE',  ( -19.02544592524342804, 5.153800228976336051, 76.04057627198102409 ) ) ;
#147056 = CARTESIAN_POINT ( 'NONE',  ( 13.89961937509977652, -13.97604488694527269, 43.12390960531434558 ) ) ;
#147055 = CARTESIAN_POINT ( 'NONE',  ( 4.379528057220339221, -16.55341960407611168, 47.70724293864770260 ) ) ;
#147057 = CIRCLE ( 'NONE', #91736, 8.000000000000000000 ) ;
#147058 = CARTESIAN_POINT ( 'NONE',  ( 13.89961937509957401, 13.97604488694547697, 56.87609039468564731 ) ) ;
#147059 = ORIENTED_EDGE ( 'NONE', *, *, #100803, .F. ) ;
#147060 = CARTESIAN_POINT ( 'NONE',  ( 0.05219959533910956823, 16.53943276465976808, 89.99890960531438111 ) ) ;
#147061 = CARTESIAN_POINT ( 'NONE',  ( 15.72974639402176855, 15.80617190586768217, 111.8760903946856615 ) ) ;
#147062 = CARTESIAN_POINT ( 'NONE',  ( 13.97604488694527802, 13.89961937509977652, 49.37390960531434558 ) ) ;
#147063 = CARTESIAN_POINT ( 'NONE',  ( 21.53943276465977519, -0.05219959533907433946, 53.74890960531437401 ) ) ;
#147065 = CARTESIAN_POINT ( 'NONE',  ( 19.03943276465977164, 0.05219959533936151252, 21.25109039468565797 ) ) ;
#147064 = CARTESIAN_POINT ( 'NONE',  ( -8.314922557960811034, -14.29746914071050412, 47.08224293864770260 ) ) ;
#147066 = CARTESIAN_POINT ( 'NONE',  ( -13.89961937509977652, 13.97604488694528158, 105.6239096053143527 ) ) ;
#147067 = CARTESIAN_POINT ( 'NONE',  ( 13.97604488694527802, 13.89961937509977652, 109.3739096053143669 ) ) ;
#147068 = CARTESIAN_POINT ( 'NONE',  ( -5.049401038298153566, 19.05341960407611168, 35.20724293864768839 ) ) ;
#147069 = CARTESIAN_POINT ( 'NONE',  ( -5.049401038298153566, 19.05341960407611168, 30.20724293864768839 ) ) ;
#147070 = CARTESIAN_POINT ( 'NONE',  ( 12.06949235617757843, -12.14591786802309237, 88.12390960531436690 ) ) ;
#147071 = CARTESIAN_POINT ( 'NONE',  ( -18.67979575497178146, -10.72451020669898902, 96.66557627198102409 ) ) ;
#147072 = CARTESIAN_POINT ( 'NONE',  ( 19.05341960407611168, 5.049401038298154454, 98.95724293864766707 ) ) ;
#147073 = CARTESIAN_POINT ( 'NONE',  ( 21.55341960407610458, 5.719274019375980345, 108.9572429386476955 ) ) ;
#147074 = CARTESIAN_POINT ( 'NONE',  ( 19.03943276465977164, -0.05219959533909143690, 108.7489096053143527 ) ) ;
#147076 = CARTESIAN_POINT ( 'NONE',  ( -4.379528057220328563, 16.55341960407611168, 100.2072429386476955 ) ) ;
#147075 = CARTESIAN_POINT ( 'NONE',  ( 31.99364916731003916, -5.186379194429593439E-15, 47.65000000000021885 ) ) ;
#147077 = CARTESIAN_POINT ( 'NONE',  ( -19.03943276465977164, 0.05219959533909376836, 71.24890960531435269 ) ) ;
#147078 = CARTESIAN_POINT ( 'NONE',  ( -21.52544592524343514, 5.823673210054127303, 81.04057627198102409 ) ) ;
#147079 = EDGE_CURVE ( 'NONE', #46465, #42359, #176274, .T. ) ;
#147080 = DIRECTION ( 'NONE',  ( -1.000000000000000000, 0.000000000000000000, -3.709348145883536076E-20 ) ) ;
#147081 = DIRECTION ( 'NONE',  ( -0.000000000000000000, 0.000000000000000000, 1.000000000000000000 ) ) ;
#147083 = CARTESIAN_POINT ( 'NONE',  ( 37.99626262588765258, 2.893932880411085066E-14, 2.000000000000000000 ) ) ;
#147082 = CARTESIAN_POINT ( 'NONE',  ( 21.55341960407610458, 5.719274019375980345, 28.95724293864769905 ) ) ;
#147084 = CARTESIAN_POINT ( 'NONE',  ( 12.06949235617739724, 12.14591786802326823, 26.87609039468567218 ) ) ;
#147085 = CARTESIAN_POINT ( 'NONE',  ( 16.55341960407611168, 4.379528057220329451, 108.9572429386476955 ) ) ;
#147086 = CARTESIAN_POINT ( 'NONE',  ( -17.49999999999999289, -5.068104630630392293, 109.2718159465996877 ) ) ;
#147087 = CARTESIAN_POINT ( 'NONE',  ( 13.89961937509977652, -13.97604488694527269, 53.12390960531434558 ) ) ;
#147088 = CARTESIAN_POINT ( 'NONE',  ( 0.05219959533910956823, 16.53943276465976808, 79.99890960531435269 ) ) ;
#147089 = CARTESIAN_POINT ( 'NONE',  ( 5.719274019375991003, -21.55341960407610458, 27.70724293864769905 ) ) ;
#147090 = CARTESIAN_POINT ( 'NONE',  ( 16.53943276465976808, -0.05219959533910856209, 63.74890960531435979 ) ) ;
#147091 = CARTESIAN_POINT ( 'NONE',  ( -16.53943276465976808, -0.05219959533934237506, 18.75109039468568639 ) ) ;
#147092 = CARTESIAN_POINT ( 'NONE',  ( -18.67979575497193778, 10.72451020669871902, 78.33442372801901854 ) ) ;
#147093 = CARTESIAN_POINT ( 'NONE',  ( 5.049401038297881783, 19.05341960407617918, 62.29275706135234003 ) ) ;
#147094 = CARTESIAN_POINT ( 'NONE',  ( -19.03943276465977164, 0.05219959533909376836, 106.2489096053143669 ) ) ;
#147095 = CARTESIAN_POINT ( 'NONE',  ( 4.483927247898790824, -16.52544592524335698, 85.20942372801901854 ) ) ;
#147096 = CARTESIAN_POINT ( 'NONE',  ( 5.153800228976335163, 19.02544592524342804, 44.79057627198103830 ) ) ;
#147097 = CARTESIAN_POINT ( 'NONE',  ( 19.05341960407611168, 5.049401038298154454, 88.95724293864769550 ) ) ;
#147098 = CARTESIAN_POINT ( 'NONE',  ( 18.67979575497178502, 10.72451020669898547, 89.16557627198102409 ) ) ;
#147099 = CARTESIAN_POINT ( 'NONE',  ( 16.53943276465976808, 0.05219959533934440121, 21.25109039468567218 ) ) ;
#147101 = CARTESIAN_POINT ( 'NONE',  ( 0.05219959533937995610, -21.53943276465977519, 70.00109039468568994 ) ) ;
#147100 = CARTESIAN_POINT ( 'NONE',  ( 12.06949235617757843, -12.14591786802309237, 53.12390960531436690 ) ) ;
#147102 = CARTESIAN_POINT ( 'NONE',  ( -8.224510206698735004, -14.34966873604973081, 94.58442372801901854 ) ) ;
#147103 = CARTESIAN_POINT ( 'NONE',  ( 5.153800228976335163, 19.02544592524342804, 114.7905762719810241 ) ) ;
#147104 = FACE_OUTER_BOUND ( 'NONE', #144101, .T. ) ;
#147105 = CARTESIAN_POINT ( 'NONE',  ( 8.224510206698953496, -14.34966873604960469, 32.91557627198102409 ) ) ;
#147106 = CARTESIAN_POINT ( 'NONE',  ( -14.34966873604972548, 8.224510206698743886, 58.33442372801901143 ) ) ;
#147107 = CARTESIAN_POINT ( 'NONE',  ( -19.03943276465977164, 0.05219959533909376836, 71.24890960531435269 ) ) ;
#147108 = CARTESIAN_POINT ( 'NONE',  ( -5.049401038298153566, 19.05341960407611168, 85.20724293864766707 ) ) ;
#147109 = CARTESIAN_POINT ( 'NONE',  ( 18.67979575497194134, -10.72451020669871369, 75.83442372801900433 ) ) ;
#147110 = CARTESIAN_POINT ( 'NONE',  ( -8.224510206698735004, -14.34966873604973081, 69.58442372801900433 ) ) ;
#147111 = CARTESIAN_POINT ( 'NONE',  ( -16.52544592524342804, 4.483927247898546575, 61.04057627198103120 ) ) ;
#147112 = CARTESIAN_POINT ( 'NONE',  ( -9.474510206698964154, 16.51473224551069663, 65.41557627198102409 ) ) ;
#147113 = ORIENTED_EDGE ( 'NONE', *, *, #160526, .T. ) ;
#147114 = CARTESIAN_POINT ( 'NONE',  ( 19.02544592524334988, 5.153800228976608722, 106.4594237280190185 ) ) ;
#147115 = CARTESIAN_POINT ( 'NONE',  ( 8.314922557960818139, 14.29746914071049879, 109.5822429386476955 ) ) ;
#147116 = CARTESIAN_POINT ( 'NONE',  ( -16.51473224551069308, -9.474510206698971260, 76.66557627198103830 ) ) ;
#147118 = CARTESIAN_POINT ( 'NONE',  ( 30.74264578624799782, 22.33583958711400541, -2.799999999999999822 ) ) ;
#147117 = CARTESIAN_POINT ( 'NONE',  ( -16.52544592524335698, -4.483927247898792601, 23.95942372801901143 ) ) ;
#147119 = CARTESIAN_POINT ( 'NONE',  ( 21.52544592524334988, 5.823673210054432836, 101.4594237280190185 ) ) ;
#147120 = CARTESIAN_POINT ( 'NONE',  ( 4.483927247898790824, -16.52544592524335698, 80.20942372801901854 ) ) ;
#147121 = CARTESIAN_POINT ( 'NONE',  ( 19.03943276465977164, 0.05219959533936151252, 96.25109039468567573 ) ) ;
#147122 = CARTESIAN_POINT ( 'NONE',  ( 14.29746914071049879, -8.314922557960816363, 108.3322429386477097 ) ) ;
#147123 = CARTESIAN_POINT ( 'NONE',  ( -8.224510206698735004, -14.34966873604973081, 69.58442372801900433 ) ) ;
#147124 = DIRECTION ( 'NONE',  ( -1.000000000000000000, 0.000000000000000000, 0.000000000000000000 ) ) ;
#147125 = CARTESIAN_POINT ( 'NONE',  ( -13.97604488694547697, 13.89961937509957934, 53.12609039468565442 ) ) ;
#147126 = CARTESIAN_POINT ( 'NONE',  ( -21.52544592524334988, -5.823673210054445271, 98.95942372801903275 ) ) ;
#147127 = CARTESIAN_POINT ( 'NONE',  ( 13.89961937509977652, -13.97604488694527269, 33.12390960531434558 ) ) ;
#147128 = CARTESIAN_POINT ( 'NONE',  ( 16.51473224551069308, 9.474510206698969483, 74.16557627198103830 ) ) ;
#147129 = CARTESIAN_POINT ( 'NONE',  ( -8.314922557960811034, -14.29746914071050412, 67.08224293864770971 ) ) ;
#147130 = CARTESIAN_POINT ( 'NONE',  ( 21.52544592524334988, 5.823673210054432836, 91.45942372801901854 ) ) ;
#147131 = CARTESIAN_POINT ( 'NONE',  ( 9.564922557961047289, -16.46253265017146816, 40.41775706135234003 ) ) ;
#147132 = CARTESIAN_POINT ( 'NONE',  ( 16.46253265017146816, 9.564922557961045513, 36.66775706135233293 ) ) ;
#147133 = CARTESIAN_POINT ( 'NONE',  ( -10.81492255796078084, -18.62759615963271287, 37.08224293864768129 ) ) ;
#147134 = CARTESIAN_POINT ( 'NONE',  ( -21.53943276465977519, -0.05219959533937600094, 98.75109039468568994 ) ) ;
#147135 = CARTESIAN_POINT ( 'NONE',  ( -13.97604488694527625, -13.89961937509977652, 81.87390960531436690 ) ) ;
#147136 = CARTESIAN_POINT ( 'NONE',  ( 15.72974639402176855, 15.80617190586768217, 86.87609039468568994 ) ) ;
#147137 = CARTESIAN_POINT ( 'NONE',  ( 18.67979575497178502, 10.72451020669898547, 44.16557627198103120 ) ) ;
#147138 = CARTESIAN_POINT ( 'NONE',  ( -19.05341960407611168, -5.049401038298163336, 81.45724293864769550 ) ) ;
#147139 = CARTESIAN_POINT ( 'NONE',  ( -5.153800228976607833, 19.02544592524334988, 72.70942372801900433 ) ) ;
#147140 = CARTESIAN_POINT ( 'NONE',  ( -16.51473224551069308, -9.474510206698971260, 91.66557627198103830 ) ) ;
#147141 = CARTESIAN_POINT ( 'NONE',  ( -19.03943276465977164, -0.05219959533935918106, 93.75109039468566152 ) ) ;
#147142 = CARTESIAN_POINT ( 'NONE',  ( 12.06949235617739724, 12.14591786802326823, 36.87609039468568994 ) ) ;
#147143 = CARTESIAN_POINT ( 'NONE',  ( -16.52544592524342804, 4.483927247898546575, 96.04057627198102409 ) ) ;
#147144 = CARTESIAN_POINT ( 'NONE',  ( -0.05219959533909027116, -19.03943276465977164, 72.49890960531435269 ) ) ;
#147145 = CARTESIAN_POINT ( 'NONE',  ( 0.05219959533907565091, 21.53943276465977519, 64.99890960531435269 ) ) ;
#147146 = CARTESIAN_POINT ( 'NONE',  ( 16.53943276465976808, 0.05219959533934440121, 31.25109039468568639 ) ) ;
#147147 = CARTESIAN_POINT ( 'NONE',  ( 5.823673210054444382, -21.52544592524334988, 35.20942372801901854 ) ) ;
#147148 = CARTESIAN_POINT ( 'NONE',  ( -5.823673210054431948, 21.52544592524334988, 87.70942372801901854 ) ) ;
#147149 = CARTESIAN_POINT ( 'NONE',  ( -8.224510206698735004, -14.34966873604973081, 84.58442372801903275 ) ) ;
#147150 = CARTESIAN_POINT ( 'NONE',  ( 19.02544592524343514, -5.153800228976328945, 68.54057627198103830 ) ) ;
#147151 = CARTESIAN_POINT ( 'NONE',  ( 4.483927247898545687, 16.52544592524342804, 79.79057627198102409 ) ) ;
#147152 = CARTESIAN_POINT ( 'NONE',  ( -8.314922557961024197, 14.29746914071037800, 97.91775706135236135 ) ) ;
#147153 = CARTESIAN_POINT ( 'NONE',  ( -9.474510206698720793, -16.51473224551083518, 49.58442372801899722 ) ) ;
#147154 = CARTESIAN_POINT ( 'NONE',  ( 18.67979575497194134, -10.72451020669871369, 25.83442372801901499 ) ) ;
#147155 = CARTESIAN_POINT ( 'NONE',  ( 16.53943276465976808, -0.05219959533910856209, 73.74890960531433848 ) ) ;
#147156 = CARTESIAN_POINT ( 'NONE',  ( 16.51473224551069308, 9.474510206698969483, 99.16557627198102409 ) ) ;
#147157 = CARTESIAN_POINT ( 'NONE',  ( -12.14591786802326823, 12.06949235617739902, 103.1260903946856757 ) ) ;
#147158 = CARTESIAN_POINT ( 'NONE',  ( 15.72974639402176855, 15.80617190586768217, 76.87609039468567573 ) ) ;
#147159 = CARTESIAN_POINT ( 'NONE',  ( -12.14591786802326823, 12.06949235617739902, 48.12609039468568284 ) ) ;
#147160 = CARTESIAN_POINT ( 'NONE',  ( -0.05219959533937732626, 21.53943276465977519, 47.50109039468568994 ) ) ;
#147161 = CARTESIAN_POINT ( 'NONE',  ( -14.29746914071049879, 8.314922557960819915, 75.83224293864769550 ) ) ;
#147162 = EDGE_LOOP ( 'NONE', ( #98232, #150406, #79847, #78611 ) ) ;
#147163 = CARTESIAN_POINT ( 'NONE',  ( -18.62759615963270932, 10.81492255796079327, 115.8322429386477097 ) ) ;
#147164 = CARTESIAN_POINT ( 'NONE',  ( -19.34837522270365895, -5.499999999999739764, 50.86337684832579953 ) ) ;
#147165 = CARTESIAN_POINT ( 'NONE',  ( 16.52544592524342804, -4.483927247898539470, 48.54057627198103120 ) ) ;
#147166 = CARTESIAN_POINT ( 'NONE',  ( 16.46253265017160672, -9.564922557960803928, 28.33224293864769550 ) ) ;
#147167 = CARTESIAN_POINT ( 'NONE',  ( 21.53943276465977519, -0.05219959533907433946, 38.74890960531435979 ) ) ;
#147168 = CARTESIAN_POINT ( 'NONE',  ( 8.314922557960818139, 14.29746914071049879, 79.58224293864769550 ) ) ;
#147169 = CARTESIAN_POINT ( 'NONE',  ( 10.72451020669898902, -18.67979575497178502, 77.91557627198102409 ) ) ;
#147170 = CARTESIAN_POINT ( 'NONE',  ( -5.153800228976328057, -19.02544592524343514, 77.29057627198099567 ) ) ;
#147172 = CARTESIAN_POINT ( 'NONE',  ( -19.05341960407617563, 5.049401038297882671, 73.54275706135233293 ) ) ;
#147171 = CARTESIAN_POINT ( 'NONE',  ( 13.97604488694527802, 13.89961937509977652, 34.37390960531436690 ) ) ;
#147174 = CARTESIAN_POINT ( 'NONE',  ( -10.72451020669898014, 18.67979575497178502, 60.41557627198102409 ) ) ;
#147173 = CARTESIAN_POINT ( 'NONE',  ( -15.72974639402176322, -15.80617190586768395, 54.37609039468568994 ) ) ;
#147175 = CARTESIAN_POINT ( 'NONE',  ( 5.153800228976335163, 19.02544592524342804, 44.79057627198103830 ) ) ;
#147176 = CARTESIAN_POINT ( 'NONE',  ( 16.46253265017160672, -9.564922557960803928, 68.33224293864770971 ) ) ;
#147177 = EDGE_LOOP ( 'NONE', ( #101161, #149118, #68925, #165354 ) ) ;
#147178 = CARTESIAN_POINT ( 'NONE',  ( -8.314922557961024197, 14.29746914071037800, 52.91775706135235424 ) ) ;
#147179 = CARTESIAN_POINT ( 'NONE',  ( 21.52544592524334988, 5.823673210054432836, 26.45942372801901854 ) ) ;
#147180 = CARTESIAN_POINT ( 'NONE',  ( -21.52544592524334988, -5.823673210054445271, 58.95942372801902565 ) ) ;
#147181 = CARTESIAN_POINT ( 'NONE',  ( -19.05341960407611168, -5.049401038298163336, 106.4572429386476955 ) ) ;
#147182 = CARTESIAN_POINT ( 'NONE',  ( -18.62759615963270932, 10.81492255796079327, 90.83224293864769550 ) ) ;
#147184 = CARTESIAN_POINT ( 'NONE',  ( 14.34966873604972726, -8.224510206698740333, 45.83442372801901854 ) ) ;
#147183 = CARTESIAN_POINT ( 'NONE',  ( -0.05219959533937732626, 21.53943276465977519, 27.50109039468567929 ) ) ;
#147185 = CARTESIAN_POINT ( 'NONE',  ( -21.55341960407610458, -5.719274019375992779, 51.45724293864770260 ) ) ;
#147186 = CARTESIAN_POINT ( 'NONE',  ( 13.89961937509957401, 13.97604488694547697, 26.87609039468566507 ) ) ;
#147187 = CARTESIAN_POINT ( 'NONE',  ( 5.049401038298161559, -19.05341960407611168, 52.70724293864767418 ) ) ;
#147188 = CARTESIAN_POINT ( 'NONE',  ( -9.564922557960796823, -16.46253265017161027, 112.0822429386476955 ) ) ;
#147189 = CARTESIAN_POINT ( 'NONE',  ( -9.564922557960796823, -16.46253265017161027, 87.08224293864769550 ) ) ;
#147190 = ORIENTED_EDGE ( 'NONE', *, *, #68244, .T. ) ;
#147191 = CARTESIAN_POINT ( 'NONE',  ( 21.71449870906583257, 22.98327899303666300, -46.07764953322298140 ) ) ;
#147192 = CARTESIAN_POINT ( 'NONE',  ( -9.564922557961040184, 16.46253265017147172, 72.91775706135233293 ) ) ;
#147193 = CARTESIAN_POINT ( 'NONE',  ( 21.55341960407610458, 5.719274019375980345, 48.95724293864770971 ) ) ;
#147194 = CARTESIAN_POINT ( 'NONE',  ( -16.52544592524342804, 4.483927247898546575, 26.04057627198103475 ) ) ;
#147195 = CARTESIAN_POINT ( 'NONE',  ( -19.03943276465977164, -0.05219959533935918106, 98.75109039468567573 ) ) ;
#147196 = CYLINDRICAL_SURFACE ( 'NONE', #188682, 5.000000000000000888 ) ;
#147197 = CARTESIAN_POINT ( 'NONE',  ( 15.72974639402176855, 15.80617190586768217, 111.8760903946856615 ) ) ;
#147198 = CARTESIAN_POINT ( 'NONE',  ( -0.05219959533936034679, 19.03943276465977164, 92.50109039468566152 ) ) ;
#147199 = CARTESIAN_POINT ( 'NONE',  ( 16.46253265017146816, 9.564922557961045513, 41.66775706135234003 ) ) ;
#147200 = CARTESIAN_POINT ( 'NONE',  ( 16.36317988757056341, 7.306389748694959607, 108.4021039163677358 ) ) ;
#147201 = CARTESIAN_POINT ( 'NONE',  ( 13.89961937509977652, -13.97604488694527269, 58.12390960531436690 ) ) ;
#147202 = CARTESIAN_POINT ( 'NONE',  ( 16.53943276465976808, -0.05219959533910856209, 58.74890960531436690 ) ) ;
#147203 = CARTESIAN_POINT ( 'NONE',  ( -19.05341960407611168, -5.049401038298163336, 36.45724293864766707 ) ) ;
#147204 = CARTESIAN_POINT ( 'NONE',  ( 0.05219959533910956823, 16.53943276465976808, 34.99890960531435979 ) ) ;
#147205 = CARTESIAN_POINT ( 'NONE',  ( -29.23421922662623373, -26.92455035691573073, -20.45761606001068245 ) ) ;
#147206 = CARTESIAN_POINT ( 'NONE',  ( -14.29746914071037622, -8.314922557961029526, 104.1677570613523471 ) ) ;
#147207 = CARTESIAN_POINT ( 'NONE',  ( 13.97604488694527802, 13.89961937509977652, 59.37390960531434558 ) ) ;
#147208 = CARTESIAN_POINT ( 'NONE',  ( 19.02544592524334988, 5.153800228976608722, 26.45942372801899722 ) ) ;
#147209 = CARTESIAN_POINT ( 'NONE',  ( -12.14591786802326823, 12.06949235617739902, 28.12609039468568284 ) ) ;
#147210 = CARTESIAN_POINT ( 'NONE',  ( 10.81492255796078972, 18.62759615963270932, 54.58224293864769550 ) ) ;
#147212 = VERTEX_POINT ( 'NONE', #44920 ) ;
#147211 = CARTESIAN_POINT ( 'NONE',  ( 5.823673210054444382, -21.52544592524334988, 105.2094237280190328 ) ) ;
#147213 = CARTESIAN_POINT ( 'NONE',  ( -5.153800228976328057, -19.02544592524343514, 67.29057627198102409 ) ) ;
#147214 = CARTESIAN_POINT ( 'NONE',  ( -16.51473224551069308, -9.474510206698971260, 106.6655762719810383 ) ) ;
#147215 = CARTESIAN_POINT ( 'NONE',  ( 5.049401038298161559, -19.05341960407611168, 97.70724293864766707 ) ) ;
#147216 = CARTESIAN_POINT ( 'NONE',  ( -11.40812507854754720, -35.11059874428192273, -4.224999997268813701 ) ) ;
#147217 = CARTESIAN_POINT ( 'NONE',  ( 18.67979575497194134, -10.72451020669871369, 20.83442372801901143 ) ) ;
#147218 = AXIS2_PLACEMENT_3D ( 'NONE', #26619, #40775, #133780 ) ;
#147219 = CARTESIAN_POINT ( 'NONE',  ( 0.05219959533910956823, 16.53943276465976808, 89.99890960531438111 ) ) ;
#147221 = CARTESIAN_POINT ( 'NONE',  ( -5.049401038298153566, 19.05341960407611168, 65.20724293864765286 ) ) ;
#147220 = CARTESIAN_POINT ( 'NONE',  ( -18.62759615963270932, 10.81492255796079327, 85.83224293864768129 ) ) ;
#147222 = CARTESIAN_POINT ( 'NONE',  ( -5.049401038298153566, 19.05341960407611168, 75.20724293864769550 ) ) ;
#147223 = CARTESIAN_POINT ( 'NONE',  ( 18.67979575497178502, 10.72451020669898547, 109.1655762719810383 ) ) ;
#147224 = ORIENTED_EDGE ( 'NONE', *, *, #123873, .F. ) ;
#147225 = CARTESIAN_POINT ( 'NONE',  ( 9.564922557960805705, 16.46253265017160317, 69.58224293864770971 ) ) ;
#147226 = CARTESIAN_POINT ( 'NONE',  ( -30.98568851139534530, -22.00224967906137863, -21.15899255711320492 ) ) ;
#147228 = CARTESIAN_POINT ( 'NONE',  ( -18.22780087662122028, 5.500000000000031086, 53.51540105326106556 ) ) ;
#147227 = CARTESIAN_POINT ( 'NONE',  ( 14.34966873604960469, 8.224510206698951720, 109.1655762719810383 ) ) ;
#147229 = CARTESIAN_POINT ( 'NONE',  ( -19.05341960407617563, 5.049401038297882671, 88.54275706135230450 ) ) ;
#147230 = CARTESIAN_POINT ( 'NONE',  ( 16.52544592524342804, -4.483927247898539470, 103.5405762719810383 ) ) ;
#147231 = CARTESIAN_POINT ( 'NONE',  ( 5.823673210054444382, -21.52544592524334988, 75.20942372801901854 ) ) ;
#147233 = CARTESIAN_POINT ( 'NONE',  ( -10.72451020669870658, -18.67979575497194134, 34.58442372801900433 ) ) ;
#147232 = CARTESIAN_POINT ( 'NONE',  ( -19.02544592524342804, 5.153800228976336051, 51.04057627198103120 ) ) ;
#147234 = CARTESIAN_POINT ( 'NONE',  ( -21.53943276465977519, -0.05219959533937600094, 18.75109039468568639 ) ) ;
#147235 = CARTESIAN_POINT ( 'NONE',  ( -5.429308488886486681E-15, 30.30510711980690175, 143.4999999999999432 ) ) ;
#147236 = CARTESIAN_POINT ( 'NONE',  ( -13.97604488694527625, -13.89961937509977652, 66.87390960531436690 ) ) ;
#147237 = CARTESIAN_POINT ( 'NONE',  ( -8.906447517083060816, 27.41122689804195645, 143.8500000054623911 ) ) ;
#147239 = CARTESIAN_POINT ( 'NONE',  ( -15.80617190586745835, -15.72974639402198527, 31.87390960531435979 ) ) ;
#147238 = CARTESIAN_POINT ( 'NONE',  ( 19.03943276465977164, 0.05219959533936151252, 106.2510903946856615 ) ) ;
#147240 = CARTESIAN_POINT ( 'NONE',  ( 10.72451020669871369, 18.67979575497193778, 67.08442372801901854 ) ) ;
#147241 = CARTESIAN_POINT ( 'NONE',  ( -16.51473224551069308, -9.474510206698971260, 91.66557627198103830 ) ) ;
#147242 = CARTESIAN_POINT ( 'NONE',  ( -19.05341960407617563, 5.049401038297882671, 78.54275706135233293 ) ) ;
#147243 = CARTESIAN_POINT ( 'NONE',  ( 13.89961937509977652, -13.97604488694527269, 48.12390960531435979 ) ) ;
#147244 = CARTESIAN_POINT ( 'NONE',  ( -0.05219959533909027116, -19.03943276465977164, 67.49890960531436690 ) ) ;
#147245 = EDGE_CURVE ( 'NONE', #11758, #82858, #168253, .T. ) ;
#147246 = CARTESIAN_POINT ( 'NONE',  ( 16.55341960407611168, 4.379528057220329451, 88.95724293864769550 ) ) ;
#147247 = CARTESIAN_POINT ( 'NONE',  ( 0.05219959533909260263, 19.03943276465977164, 104.9989096053143669 ) ) ;
#147248 = CARTESIAN_POINT ( 'NONE',  ( 16.52544592524342804, -4.483927247898539470, 93.54057627198103830 ) ) ;
#147249 = CARTESIAN_POINT ( 'NONE',  ( 5.049401038298161559, -19.05341960407611168, 102.7072429386476955 ) ) ;
#147251 = CARTESIAN_POINT ( 'NONE',  ( 19.03943276465977164, -0.05219959533909143690, 23.74890960531435269 ) ) ;
#147250 = CARTESIAN_POINT ( 'NONE',  ( 12.06949235617757843, -12.14591786802309237, 38.12390960531436690 ) ) ;
#147252 = ORIENTED_EDGE ( 'NONE', *, *, #45518, .T. ) ;
#147253 = CARTESIAN_POINT ( 'NONE',  ( -18.62759615963255300, -10.81492255796106328, 59.16775706135234714 ) ) ;
#147254 = CARTESIAN_POINT ( 'NONE',  ( -5.049401038297874678, -19.05341960407617918, 74.79275706135231871 ) ) ;
#147255 = CARTESIAN_POINT ( 'NONE',  ( -4.483927247898539470, -16.52544592524342804, 52.29057627198102409 ) ) ;
#147256 = CARTESIAN_POINT ( 'NONE',  ( -18.62759615963270932, 10.81492255796079327, 100.8322429386477097 ) ) ;
#147257 = CARTESIAN_POINT ( 'NONE',  ( 18.62759615963271287, -10.81492255796078972, 28.33224293864769550 ) ) ;
#147259 = CARTESIAN_POINT ( 'NONE',  ( -12.14591786802309592, -12.06949235617757132, 76.87390960531439532 ) ) ;
#147258 = AXIS2_PLACEMENT_3D ( 'NONE', #91772, #26170, #181837 ) ;
#147260 = CARTESIAN_POINT ( 'NONE',  ( -19.03943276465977164, 0.05219959533909376836, 56.24890960531435979 ) ) ;
#147261 = CARTESIAN_POINT ( 'NONE',  ( 12.14591786802309770, 12.06949235617756955, 24.37390960531435979 ) ) ;
#147262 = CARTESIAN_POINT ( 'NONE',  ( 16.55341960407618274, -4.379528057220086978, 106.0427570613523471 ) ) ;
#147263 = CARTESIAN_POINT ( 'NONE',  ( 14.34966873604972726, -8.224510206698740333, 70.83442372801901854 ) ) ;
#147264 = CARTESIAN_POINT ( 'NONE',  ( 9.564922557961047289, -16.46253265017146816, 20.41775706135233293 ) ) ;
#147265 = CARTESIAN_POINT ( 'NONE',  ( 16.46253265017160672, -9.564922557960803928, 103.3322429386476955 ) ) ;
#147266 = CARTESIAN_POINT ( 'NONE',  ( 19.05341960407611168, 5.049401038298154454, 73.95724293864768129 ) ) ;
#147267 = CARTESIAN_POINT ( 'NONE',  ( 9.564922557960805705, 16.46253265017160317, 34.58224293864770260 ) ) ;
#147268 = CARTESIAN_POINT ( 'NONE',  ( 4.483927247898545687, 16.52544592524342804, 49.79057627198102409 ) ) ;
#147270 = CARTESIAN_POINT ( 'NONE',  ( -0.05219959533909027116, -19.03943276465977164, 102.4989096053143669 ) ) ;
#147269 = CARTESIAN_POINT ( 'NONE',  ( -28.82186960331499037, 2.428612866367529932E-14, 138.2500000054623683 ) ) ;
#147271 = CARTESIAN_POINT ( 'NONE',  ( 21.53943276465977519, -0.05219959533907433946, 43.74890960531435979 ) ) ;
#147272 = CARTESIAN_POINT ( 'NONE',  ( -12.06949235617756955, 12.14591786802309770, 80.62390960531438111 ) ) ;
#147273 = CARTESIAN_POINT ( 'NONE',  ( 16.55341960407618274, -4.379528057220086978, 21.04275706135234714 ) ) ;
#147274 = ORIENTED_EDGE ( 'NONE', *, *, #95409, .T. ) ;
#147275 = CARTESIAN_POINT ( 'NONE',  ( -8.224510206698948167, 14.34966873604960824, 70.41557627198102409 ) ) ;
#147276 = CARTESIAN_POINT ( 'NONE',  ( 17.50000000000000000, -5.500000000000000888, 33.29690382534174375 ) ) ;
#147277 = CARTESIAN_POINT ( 'NONE',  ( 9.474510206698729675, 16.51473224551082808, 62.08442372801899722 ) ) ;
#147278 = CARTESIAN_POINT ( 'NONE',  ( -19.05341960407611168, -5.049401038298163336, 106.4572429386476955 ) ) ;
#147279 = CARTESIAN_POINT ( 'NONE',  ( -19.03943276465977164, -0.05219959533935918106, 83.75109039468567573 ) ) ;
#147280 = CARTESIAN_POINT ( 'NONE',  ( -18.22780087662126647, -5.499999999999827693, 38.98236817873107185 ) ) ;
#147282 = CARTESIAN_POINT ( 'NONE',  ( 8.224510206698742110, 14.34966873604972548, 107.0844237280190043 ) ) ;
#147281 = CARTESIAN_POINT ( 'NONE',  ( 12.14591786802327356, -12.06949235617739191, 20.62609039468568639 ) ) ;
#147283 = CARTESIAN_POINT ( 'NONE',  ( -9.474510206698964154, 16.51473224551069663, 40.41557627198103120 ) ) ;
#147284 = CARTESIAN_POINT ( 'NONE',  ( 10.81492255796078972, 18.62759615963270932, 39.58224293864769550 ) ) ;
#147285 = CARTESIAN_POINT ( 'NONE',  ( 18.62759615963255655, 10.81492255796105972, 61.66775706135235424 ) ) ;
#147286 = CARTESIAN_POINT ( 'NONE',  ( -23.84827716990831803, -9.022217638662285211, 168.8513102586128412 ) ) ;
#147287 = CARTESIAN_POINT ( 'NONE',  ( 16.55341960407618274, -4.379528057220086978, 21.04275706135234714 ) ) ;
#147289 = CARTESIAN_POINT ( 'NONE',  ( -9.474510206698964154, 16.51473224551069663, 70.41557627198102409 ) ) ;
#147288 = CARTESIAN_POINT ( 'NONE',  ( 17.49999999999984368, 3.200006130778718205, 22.58407523517191962 ) ) ;
#147290 = CARTESIAN_POINT ( 'NONE',  ( 19.02544592524343514, -5.153800228976328945, 23.54057627198102054 ) ) ;
#147292 = CARTESIAN_POINT ( 'NONE',  ( 16.46253265017160672, -9.564922557960803928, 78.33224293864769550 ) ) ;
#147291 = CARTESIAN_POINT ( 'NONE',  ( 4.379528057220339221, -16.55341960407611168, 92.70724293864770971 ) ) ;
#147293 = ITEM_DEFINED_TRANSFORMATION ( 'NONE', 'NONE', #62886,  #82054 ) ;
#147294 = CARTESIAN_POINT ( 'NONE',  ( 16.51473224551069308, 9.474510206698969483, 94.16557627198103830 ) ) ;
#147295 = ORIENTED_EDGE ( 'NONE', *, *, #97920, .T. ) ;
#147296 = CARTESIAN_POINT ( 'NONE',  ( 16.46253265017146816, 9.564922557961045513, 91.66775706135234714 ) ) ;
#147297 = CARTESIAN_POINT ( 'NONE',  ( 18.67979575497178502, 10.72451020669898547, 84.16557627198103830 ) ) ;
#147298 = CARTESIAN_POINT ( 'NONE',  ( -19.02544592524342804, 5.153800228976336051, 36.04057627198100988 ) ) ;
#147299 = CARTESIAN_POINT ( 'NONE',  ( -13.97604488694547697, 13.89961937509957934, 58.12609039468566863 ) ) ;
#147300 = CARTESIAN_POINT ( 'NONE',  ( 16.46253265017160672, -9.564922557960803928, 53.33224293864768839 ) ) ;
#147301 = CARTESIAN_POINT ( 'NONE',  ( -19.02544592524342804, 5.153800228976336051, 96.04057627198103830 ) ) ;
#147302 = ORIENTED_EDGE ( 'NONE', *, *, #186961, .F. ) ;
#147303 = CARTESIAN_POINT ( 'NONE',  ( 0.05219959533907565091, 21.53943276465977519, 99.99890960531436690 ) ) ;
#147306 = CARTESIAN_POINT ( 'NONE',  ( -19.03943276465977164, -0.05219959533935918106, 58.75109039468566863 ) ) ;
#147305 = CARTESIAN_POINT ( 'NONE',  ( -9.474510206698964154, 16.51473224551069663, 85.41557627198102409 ) ) ;
#147304 = CARTESIAN_POINT ( 'NONE',  ( 14.34966873604960469, 8.224510206698951720, 99.16557627198100988 ) ) ;
#147307 = CARTESIAN_POINT ( 'NONE',  ( -10.81492255796078084, -18.62759615963271287, 92.08224293864769550 ) ) ;
#147308 = CARTESIAN_POINT ( 'NONE',  ( 21.52544592524344225, -5.823673210054117533, 68.54057627198103830 ) ) ;
#147309 = CARTESIAN_POINT ( 'NONE',  ( -14.29746914071049879, 8.314922557960819915, 30.83224293864770260 ) ) ;
#147310 = CARTESIAN_POINT ( 'NONE',  ( -21.55341960407619339, 5.719274019375674811, 98.54275706135234714 ) ) ;
#147311 = CARTESIAN_POINT ( 'NONE',  ( -8.224510206698735004, -14.34966873604973081, 59.58442372801901854 ) ) ;
#147312 = CARTESIAN_POINT ( 'NONE',  ( -16.51473224551069308, -9.474510206698971260, 76.66557627198103830 ) ) ;
#147313 = CARTESIAN_POINT ( 'NONE',  ( -9.474510206698964154, 16.51473224551069663, 30.41557627198102054 ) ) ;
#147314 = CARTESIAN_POINT ( 'NONE',  ( -15.72974639402176322, -15.80617190586768395, 34.37609039468568284 ) ) ;
#147315 = CARTESIAN_POINT ( 'NONE',  ( -0.05219959533937732626, 21.53943276465977519, 57.50109039468568994 ) ) ;
#147316 = CARTESIAN_POINT ( 'NONE',  ( 5.049401038298161559, -19.05341960407611168, 52.70724293864767418 ) ) ;
#147317 = CARTESIAN_POINT ( 'NONE',  ( -5.719274019375665041, -21.55341960407619695, 19.79275706135235069 ) ) ;
#147318 = EDGE_CURVE ( 'NONE', #194492, #130499, #181464, .T. ) ;
#147319 = CARTESIAN_POINT ( 'NONE',  ( 19.03943276465977164, 0.05219959533936151252, 76.25109039468566152 ) ) ;
#147321 = CARTESIAN_POINT ( 'NONE',  ( -5.153800228976607833, 19.02544592524334988, 77.70942372801900433 ) ) ;
#147320 = B_SPLINE_CURVE_WITH_KNOTS ( 'NONE', 3,
 ( #42498, #133494, #27340, #69826, #9166, #178016, #120311, #88986, #182004, #116327, #43487, #132501, #71826, #105154, #8149, #117327, #131493, #179023, #102163, #163849, #195186, #56667, #180033, #30292 ),
 .UNSPECIFIED., .F., .F.,
 ( 4, 2, 2, 2, 2, 2, 2, 2, 2, 2, 2, 4 ),
 ( 0.01933719746734626627, 0.02187858767233087642, 0.02441997787731549352, 0.02696136808230011062, 0.02823206318479242263, 0.02950275828728473812, 0.03013810583853089586, 0.03077345338977705361, 0.03204414849226937256, 0.03458553869725403129, 0.03712692890223869002, 0.03966831910722334875 ),
 .UNSPECIFIED. ) ;
#147322 = CARTESIAN_POINT ( 'NONE',  ( 16.46253265017160672, -9.564922557960803928, 23.33224293864769194 ) ) ;
#147323 = CARTESIAN_POINT ( 'NONE',  ( 8.224510206698742110, 14.34966873604972548, 72.08442372801899012 ) ) ;
#147324 = CARTESIAN_POINT ( 'NONE',  ( -0.05219959533909027116, -19.03943276465977164, 57.49890960531435979 ) ) ;
#147325 = FACE_OUTER_BOUND ( 'NONE', #79645, .T. ) ;
#147326 = CARTESIAN_POINT ( 'NONE',  ( 9.564922557960805705, 16.46253265017160317, 99.58224293864770971 ) ) ;
#147327 = CARTESIAN_POINT ( 'NONE',  ( -19.03943276465977164, 0.05219959533909376836, 41.24890960531435269 ) ) ;
#147328 = CARTESIAN_POINT ( 'NONE',  ( -5.823673210054116645, -21.52544592524344225, 67.29057627198103830 ) ) ;
#147329 = CARTESIAN_POINT ( 'NONE',  ( 14.29746914071037800, 8.314922557961029526, 66.66775706135234714 ) ) ;
#147330 = CARTESIAN_POINT ( 'NONE',  ( -5.719274019375665041, -21.55341960407619695, 109.7927570613523613 ) ) ;
#147331 = CARTESIAN_POINT ( 'NONE',  ( 13.97604488694527802, 13.89961937509977652, 49.37390960531434558 ) ) ;
#147332 = CARTESIAN_POINT ( 'NONE',  ( 16.53943276465976808, -0.05219959533910856209, 43.74890960531435979 ) ) ;
#147334 = CARTESIAN_POINT ( 'NONE',  ( 12.14591786802309770, 12.06949235617756955, 64.37390960531435269 ) ) ;
#147333 = B_SPLINE_CURVE_WITH_KNOTS ( 'NONE', 3,
 ( #189575, #97517, #50062, #191549, #20698, #187599, #67204, #81356, #49068, #176400, #66211, #114707, #69203, #82354, #145037, #4518, #113693, #126875, #188581, #175389, #36857, #142051, #157238, #35871, #53026, #127871, #98524, #18731, #110724, #99533, #172405, #37875 ),
 .UNSPECIFIED., .F., .F.,
 ( 4, 2, 2, 2, 2, 2, 2, 2, 2, 2, 2, 2, 2, 2, 2, 4 ),
 ( 2.625112965618923682E-17, 0.0003712461730036965900, 0.0007424923460073669422, 0.001113738519011037240, 0.001484984692014707647, 0.002227477038022048460, 0.002598723211025719300, 0.002969969384029389706, 0.003341215557033060547, 0.003712461730036731820, 0.004083707903040401793, 0.004454954076044073501, 0.004826200249047744341, 0.005197446422051415181, 0.005568692595055086021, 0.005939938768058756861 ),
 .UNSPECIFIED. ) ;
#147335 = CARTESIAN_POINT ( 'NONE',  ( -19.02544592524342804, 5.153800228976336051, 81.04057627198103830 ) ) ;
#147336 = CARTESIAN_POINT ( 'NONE',  ( 15.72974639402176855, 15.80617190586768217, 41.87609039468568284 ) ) ;
#147337 = CARTESIAN_POINT ( 'NONE',  ( -5.049401038298153566, 19.05341960407611168, 90.20724293864766707 ) ) ;
#147338 = CARTESIAN_POINT ( 'NONE',  ( 10.72451020669871369, 18.67979575497193778, 97.08442372801904696 ) ) ;
#147339 = CARTESIAN_POINT ( 'NONE',  ( 16.52544592524335698, 4.483927247898782831, 71.45942372801901854 ) ) ;
#147340 = CARTESIAN_POINT ( 'NONE',  ( 0.05219959533909260263, 19.03943276465977164, 109.9989096053143669 ) ) ;
#147341 = CARTESIAN_POINT ( 'NONE',  ( -5.719274019375978568, 21.55341960407610458, 85.20724293864770971 ) ) ;
#147342 = CARTESIAN_POINT ( 'NONE',  ( 16.55341960407611168, 4.379528057220329451, 43.95724293864769550 ) ) ;
#147343 = CARTESIAN_POINT ( 'NONE',  ( -5.049401038298153566, 19.05341960407611168, 45.20724293864769550 ) ) ;
#147344 = CARTESIAN_POINT ( 'NONE',  ( 4.483927247898790824, -16.52544592524335698, 50.20942372801901854 ) ) ;
#147345 = CARTESIAN_POINT ( 'NONE',  ( -8.224510206698948167, 14.34966873604960824, 65.41557627198102409 ) ) ;
#147346 = CARTESIAN_POINT ( 'NONE',  ( 5.153800228976335163, 19.02544592524342804, 114.7905762719810241 ) ) ;
#147347 = CARTESIAN_POINT ( 'NONE',  ( -10.72451020669898014, 18.67979575497178502, 25.41557627198103120 ) ) ;
#147348 = CARTESIAN_POINT ( 'NONE',  ( -13.89961937509957401, -13.97604488694547875, 29.37609039468565797 ) ) ;
#147349 = CARTESIAN_POINT ( 'NONE',  ( -8.224510206698948167, 14.34966873604960824, 95.41557627198102409 ) ) ;
#147350 = CARTESIAN_POINT ( 'NONE',  ( 5.049401038298161559, -19.05341960407611168, 112.7072429386476813 ) ) ;
#147351 = ORIENTED_EDGE ( 'NONE', *, *, #163221, .T. ) ;
#147352 = CARTESIAN_POINT ( 'NONE',  ( 16.55341960407618274, -4.379528057220086978, 56.04275706135235424 ) ) ;
#147353 = CARTESIAN_POINT ( 'NONE',  ( 13.97604488694527802, 13.89961937509977652, 59.37390960531434558 ) ) ;
#147354 = CARTESIAN_POINT ( 'NONE',  ( -8.571926809382601320, -26.38167802310801591, 139.2750000027311899 ) ) ;
#147355 = CARTESIAN_POINT ( 'NONE',  ( -9.564922557961040184, 16.46253265017147172, 52.91775706135233293 ) ) ;
#147356 = CARTESIAN_POINT ( 'NONE',  ( -0.05219959533934338120, 16.53943276465976808, 92.50109039468567573 ) ) ;
#147357 = CARTESIAN_POINT ( 'NONE',  ( -9.474510206698720793, -16.51473224551083518, 89.58442372801900433 ) ) ;
#147358 = CARTESIAN_POINT ( 'NONE',  ( 10.72451020669871369, 18.67979575497193778, 62.08442372801901143 ) ) ;
#147359 = CARTESIAN_POINT ( 'NONE',  ( -19.02544592524342804, 5.153800228976336051, 81.04057627198103830 ) ) ;
#147360 = CARTESIAN_POINT ( 'NONE',  ( 21.55341960407610458, 5.719274019375980345, 88.95724293864769550 ) ) ;
#147361 = CARTESIAN_POINT ( 'NONE',  ( -0.05219959533910754901, -16.53943276465976808, 112.4989096053143669 ) ) ;
#147362 = CARTESIAN_POINT ( 'NONE',  ( -13.89961937509957401, -13.97604488694547875, 84.37609039468567573 ) ) ;
#147363 = CARTESIAN_POINT ( 'NONE',  ( 21.55341960407610458, 5.719274019375980345, 78.95724293864769550 ) ) ;
#147364 = CARTESIAN_POINT ( 'NONE',  ( 5.153800228976615827, -19.02544592524334988, 40.20942372801898301 ) ) ;
#147365 = FACE_OUTER_BOUND ( 'NONE', #145671, .T. ) ;
#147366 = CARTESIAN_POINT ( 'NONE',  ( -21.53943276465977519, 0.05219959533907696930, 96.24890960531435269 ) ) ;
#147367 = CARTESIAN_POINT ( 'NONE',  ( 18.22780087662123805, -5.499999999999976019, 83.51763182126894947 ) ) ;
#147368 = CARTESIAN_POINT ( 'NONE',  ( -9.564922557960796823, -16.46253265017161027, 62.08224293864769550 ) ) ;
#147369 = CARTESIAN_POINT ( 'NONE',  ( -18.09867054820431775, -5.499999999999928058, 88.98393025253589883 ) ) ;
#147370 = CARTESIAN_POINT ( 'NONE',  ( -16.46253265017146816, -9.564922557961047289, 109.1677570613523471 ) ) ;
#147371 = CARTESIAN_POINT ( 'NONE',  ( 12.86046501205820825, -37.87763584681607654, -12.00524328043752575 ) ) ;
#147372 = CARTESIAN_POINT ( 'NONE',  ( 19.03943276465977164, -0.05219959533909143690, 48.74890960531435979 ) ) ;
#147373 = CARTESIAN_POINT ( 'NONE',  ( -21.55341960407610458, -5.719274019375992779, 21.45724293864769550 ) ) ;
#147375 = CARTESIAN_POINT ( 'NONE',  ( -16.55341960407611168, -4.379528057220339221, 46.45724293864769550 ) ) ;
#147374 = CARTESIAN_POINT ( 'NONE',  ( -10.81492255796078084, -18.62759615963271287, 107.0822429386476955 ) ) ;
#147376 = CARTESIAN_POINT ( 'NONE',  ( 5.719274019375673035, 21.55341960407619339, 77.29275706135234714 ) ) ;
#147378 = CARTESIAN_POINT ( 'NONE',  ( -19.02544592524334988, -5.153800228976617603, 28.95942372801900433 ) ) ;
#147377 = CARTESIAN_POINT ( 'NONE',  ( -8.314922557961024197, 14.29746914071037800, 22.91775706135235069 ) ) ;
#147379 = CARTESIAN_POINT ( 'NONE',  ( 16.53943276465976808, -0.05219959533910856209, 23.74890960531435269 ) ) ;
#147380 = CARTESIAN_POINT ( 'NONE',  ( -0.05219959533937732626, 21.53943276465977519, 42.50109039468567573 ) ) ;
#147381 = CARTESIAN_POINT ( 'NONE',  ( 10.81492255796078972, 18.62759615963270932, 114.5822429386477097 ) ) ;
#147382 = CARTESIAN_POINT ( 'NONE',  ( 12.14591786802309770, 12.06949235617756955, 49.37390960531436690 ) ) ;
#147384 = CARTESIAN_POINT ( 'NONE',  ( -9.564922557961040184, 16.46253265017147172, 92.91775706135233293 ) ) ;
#147383 = B_SPLINE_CURVE_WITH_KNOTS ( 'NONE', 3,
 ( #164651, #59439, #178826, #40296, #25153, #165647, #28149, #148482, #120123, #26146 ),
 .UNSPECIFIED., .F., .F.,
 ( 4, 2, 2, 2, 4 ),
 ( 0.000000000000000000, 0.0009193652485010883092, 0.001838730497002176618, 0.002758095745503264928, 0.003677460994004353237 ),
 .UNSPECIFIED. ) ;
#147385 = CARTESIAN_POINT ( 'NONE',  ( -16.46253265017146816, -9.564922557961047289, 74.16775706135234714 ) ) ;
#147386 = CARTESIAN_POINT ( 'NONE',  ( -10.72451020669870658, -18.67979575497194134, 69.58442372801900433 ) ) ;
#147387 = CARTESIAN_POINT ( 'NONE',  ( -19.02544592524334988, -5.153800228976617603, 58.95942372801900433 ) ) ;
#147388 = CARTESIAN_POINT ( 'NONE',  ( 0.05219959533910956823, 16.53943276465976808, 114.9989096053143669 ) ) ;
#147389 = CARTESIAN_POINT ( 'NONE',  ( -21.53943276465977519, 0.05219959533907696930, 41.24890960531435269 ) ) ;
#147390 = CARTESIAN_POINT ( 'NONE',  ( -16.55341960407611168, -4.379528057220339221, 56.45724293864768839 ) ) ;
#147391 = CARTESIAN_POINT ( 'NONE',  ( -19.53037848336979110, 5.499999999999998224, 94.85532783611444074 ) ) ;
#147392 = CARTESIAN_POINT ( 'NONE',  ( -15.80617190586768217, 15.72974639402176855, 113.1260903946856899 ) ) ;
#147393 = CARTESIAN_POINT ( 'NONE',  ( 16.53943276465976808, 0.05219959533934440121, 86.25109039468568994 ) ) ;
#147394 = CARTESIAN_POINT ( 'NONE',  ( -8.314922557960811034, -14.29746914071050412, 37.08224293864768129 ) ) ;
#147395 = CARTESIAN_POINT ( 'NONE',  ( -5.719274019375665041, -21.55341960407619695, 69.79275706135234714 ) ) ;
#147396 = CARTESIAN_POINT ( 'NONE',  ( -15.80617190586768217, 15.72974639402176855, 83.12609039468568994 ) ) ;
#147397 = CARTESIAN_POINT ( 'NONE',  ( 18.62759615963271287, -10.81492255796078972, 83.33224293864769550 ) ) ;
#147398 = CARTESIAN_POINT ( 'NONE',  ( -19.02544592524342804, 5.153800228976336051, 36.04057627198100988 ) ) ;
#147399 = CARTESIAN_POINT ( 'NONE',  ( -0.05219959533937732626, 21.53943276465977519, 57.50109039468568994 ) ) ;
#147400 = CARTESIAN_POINT ( 'NONE',  ( -9.564922557960796823, -16.46253265017161027, 42.08224293864769550 ) ) ;
#147401 = CARTESIAN_POINT ( 'NONE',  ( -9.474510206698964154, 16.51473224551069663, 55.41557627198103120 ) ) ;
#147402 = CARTESIAN_POINT ( 'NONE',  ( 14.34966873604960469, 8.224510206698951720, 94.16557627198103830 ) ) ;
#147403 = CARTESIAN_POINT ( 'NONE',  ( -13.89961937509977652, 13.97604488694528158, 100.6239096053143669 ) ) ;
#147404 = CARTESIAN_POINT ( 'NONE',  ( -8.314922557960811034, -14.29746914071050412, 47.08224293864770260 ) ) ;
#147405 = CARTESIAN_POINT ( 'NONE',  ( 5.049401038298161559, -19.05341960407611168, 22.70724293864769194 ) ) ;
#147406 = CARTESIAN_POINT ( 'NONE',  ( -15.80617190586745835, -15.72974639402198527, 76.87390960531439532 ) ) ;
#147407 = AXIS2_PLACEMENT_3D ( 'NONE', #47780, #185289, #46781 ) ;
#147408 = CARTESIAN_POINT ( 'NONE',  ( -21.53943276465977519, 0.05219959533907696930, 116.2489096053143669 ) ) ;
#147409 = CARTESIAN_POINT ( 'NONE',  ( -15.14060719587552128, 14.98214168267144508, -56.46919128290399215 ) ) ;
#147410 = CARTESIAN_POINT ( 'NONE',  ( 14.34966873604972726, -8.224510206698740333, 25.83442372801901499 ) ) ;
#147411 = CARTESIAN_POINT ( 'NONE',  ( -21.52544592524343514, 5.823673210054127303, 76.04057627198102409 ) ) ;
#147412 = CARTESIAN_POINT ( 'NONE',  ( 15.72974639402176855, 15.80617190586768217, 91.87609039468568994 ) ) ;
#147413 = CARTESIAN_POINT ( 'NONE',  ( -0.05219959533909027116, -19.03943276465977164, 77.49890960531435269 ) ) ;
#147414 = CARTESIAN_POINT ( 'NONE',  ( -21.55341960407619339, 5.719274019375674811, 28.54275706135234358 ) ) ;
#147415 = ADVANCED_FACE ( 'NONE', ( #91384 ), #77229, .F. ) ;
#147416 = CARTESIAN_POINT ( 'NONE',  ( -9.474510206698964154, 16.51473224551069663, 110.4155762719810383 ) ) ;
#147417 = CARTESIAN_POINT ( 'NONE',  ( -4.379528057220086978, -16.55341960407618274, 84.79275706135234714 ) ) ;
#147418 = CARTESIAN_POINT ( 'NONE',  ( 15.80617190586769283, -15.72974639402175789, 75.62609039468567573 ) ) ;
#147419 = CARTESIAN_POINT ( 'NONE',  ( -10.72451020669870658, -18.67979575497194134, 109.5844237280190328 ) ) ;
#147420 = CARTESIAN_POINT ( 'NONE',  ( 14.29746914071037800, 8.314922557961029526, 71.66775706135234714 ) ) ;
#147421 = CARTESIAN_POINT ( 'NONE',  ( -0.05219959533937732626, 21.53943276465977519, 32.50109039468568284 ) ) ;
#147422 = CARTESIAN_POINT ( 'NONE',  ( 13.89961937509977652, -13.97604488694527269, 23.12390960531436335 ) ) ;
#147423 = CARTESIAN_POINT ( 'NONE',  ( -5.719274019375665041, -21.55341960407619695, 89.79275706135236135 ) ) ;
#147424 = CARTESIAN_POINT ( 'NONE',  ( 9.474510206698971260, -16.51473224551069308, 87.91557627198102409 ) ) ;
#147425 = CARTESIAN_POINT ( 'NONE',  ( -10.72451020669898014, 18.67979575497178502, 95.41557627198102409 ) ) ;
#147426 = CARTESIAN_POINT ( 'NONE',  ( -13.89961937509957401, -13.97604488694547875, 64.37609039468567573 ) ) ;
#147428 = CARTESIAN_POINT ( 'NONE',  ( -10.72451020669898014, 18.67979575497178502, 50.41557627198103120 ) ) ;
#147427 = DIRECTION ( 'NONE',  ( -0.000000000000000000, -0.000000000000000000, -1.000000000000000000 ) ) ;
#147430 = CARTESIAN_POINT ( 'NONE',  ( -16.55341960407611168, -4.379528057220339221, 51.45724293864770260 ) ) ;
#147429 = CARTESIAN_POINT ( 'NONE',  ( -5.049401038298153566, 19.05341960407611168, 90.20724293864766707 ) ) ;
#147431 = DIRECTION ( 'NONE',  ( -0.7071067811865466846, 2.468850131082262583E-15, 0.7071067811865484609 ) ) ;
#147432 = CARTESIAN_POINT ( 'NONE',  ( 9.474510206698729675, 16.51473224551082808, 77.08442372801900433 ) ) ;
#147433 = CARTESIAN_POINT ( 'NONE',  ( -0.5018587474792274294, -16.61713888009426299, -61.38171595447353468 ) ) ;
#147434 = CARTESIAN_POINT ( 'NONE',  ( -0.05219959533936034679, 19.03943276465977164, 102.5010903946856757 ) ) ;
#147435 = CARTESIAN_POINT ( 'NONE',  ( 18.67979575497178502, 10.72451020669898547, 79.16557627198103830 ) ) ;
#147436 = CARTESIAN_POINT ( 'NONE',  ( 8.314922557960818139, 14.29746914071049879, 64.58224293864769550 ) ) ;
#147437 = CARTESIAN_POINT ( 'NONE',  ( 19.03943276465977164, -0.05219959533909143690, 103.7489096053143669 ) ) ;
#147438 = CARTESIAN_POINT ( 'NONE',  ( 12.14591786802327356, -12.06949235617739191, 50.62609039468568994 ) ) ;
#147439 = CARTESIAN_POINT ( 'NONE',  ( -19.02544592524342804, 5.153800228976336051, 56.04057627198100988 ) ) ;
#147441 = CARTESIAN_POINT ( 'NONE',  ( -5.049401038297874678, -19.05341960407617918, 99.79275706135234714 ) ) ;
#147440 = CARTESIAN_POINT ( 'NONE',  ( -10.72451020669898014, 18.67979575497178502, 110.4155762719810383 ) ) ;
#147442 = CARTESIAN_POINT ( 'NONE',  ( -19.05341960407611168, -5.049401038298163336, 101.4572429386476955 ) ) ;
#147443 = CARTESIAN_POINT ( 'NONE',  ( -13.97604488694527625, -13.89961937509977652, 76.87390960531433848 ) ) ;
#147444 = CARTESIAN_POINT ( 'NONE',  ( -10.72451020669898014, 18.67979575497178502, 75.41557627198102409 ) ) ;
#147445 = CARTESIAN_POINT ( 'NONE',  ( -9.474510206698964154, 16.51473224551069663, 45.41557627198103120 ) ) ;
#147446 = CARTESIAN_POINT ( 'NONE',  ( -12.36037464099328176, 35.70181166999180533, -7.999999999999996447 ) ) ;
#147447 = CARTESIAN_POINT ( 'NONE',  ( -16.55341960407611168, -4.379528057220339221, 61.45724293864770260 ) ) ;
#147448 = CARTESIAN_POINT ( 'NONE',  ( 16.51473224551069308, 9.474510206698969483, 99.16557627198102409 ) ) ;
#147449 = DIRECTION ( 'NONE',  ( 4.336808689942018352E-17, -1.000000000000000000, 0.000000000000000000 ) ) ;
#147450 = CARTESIAN_POINT ( 'NONE',  ( -16.46253265017146816, -9.564922557961047289, 59.16775706135233293 ) ) ;
#147451 = CARTESIAN_POINT ( 'NONE',  ( -18.67979575497178146, -10.72451020669898902, 96.66557627198102409 ) ) ;
#147452 = CARTESIAN_POINT ( 'NONE',  ( 9.564922557961047289, -16.46253265017146816, 55.41775706135234003 ) ) ;
#147453 = CARTESIAN_POINT ( 'NONE',  ( -5.049401038298153566, 19.05341960407611168, 95.20724293864770971 ) ) ;
#147454 = CARTESIAN_POINT ( 'NONE',  ( 19.25918095147778786, 5.499999999999573674, 66.95284276293935477 ) ) ;
#147455 = CARTESIAN_POINT ( 'NONE',  ( -21.55341960407610458, -5.719274019375992779, 46.45724293864769550 ) ) ;
#147456 = CARTESIAN_POINT ( 'NONE',  ( -9.474510206698964154, 16.51473224551069663, 70.41557627198102409 ) ) ;
#147457 = CARTESIAN_POINT ( 'NONE',  ( -0.05219959533937732626, 21.53943276465977519, 62.50109039468568284 ) ) ;
#147458 = CARTESIAN_POINT ( 'NONE',  ( 19.03943276465977164, -0.05219959533909143690, 38.74890960531436690 ) ) ;
#147460 = ORIENTED_EDGE ( 'NONE', *, *, #64457, .T. ) ;
#147459 = CARTESIAN_POINT ( 'NONE',  ( 14.34966873604960469, 8.224510206698951720, 79.16557627198103830 ) ) ;
#147461 = CARTESIAN_POINT ( 'NONE',  ( -14.34966873604972548, 8.224510206698743886, 23.33442372801901499 ) ) ;
#147462 = CARTESIAN_POINT ( 'NONE',  ( -21.55341960407619339, 5.719274019375674811, 53.54275706135234714 ) ) ;
#147463 = ORIENTED_EDGE ( 'NONE', *, *, #121212, .T. ) ;
#147464 = CARTESIAN_POINT ( 'NONE',  ( 0.05219959533909260263, 19.03943276465977164, 109.9989096053143669 ) ) ;
#147465 = CARTESIAN_POINT ( 'NONE',  ( 9.564922557961047289, -16.46253265017146816, 70.41775706135233293 ) ) ;
#147466 = CARTESIAN_POINT ( 'NONE',  ( -17.50000000000001066, -5.500000000000021316, 46.28230962303566542 ) ) ;
#147467 = CARTESIAN_POINT ( 'NONE',  ( 10.81492255796106328, -18.62759615963255655, 20.41775706135234714 ) ) ;
#147468 = CARTESIAN_POINT ( 'NONE',  ( -0.05219959533909027116, -19.03943276465977164, 57.49890960531435979 ) ) ;
#147469 = CARTESIAN_POINT ( 'NONE',  ( 23.48529157249600630, -32.32473071737749137, -5.049999994537627046 ) ) ;
#147470 = CARTESIAN_POINT ( 'NONE',  ( -5.719274019375665041, -21.55341960407619695, 109.7927570613523613 ) ) ;
#147471 = CARTESIAN_POINT ( 'NONE',  ( -16.51473224551069308, -9.474510206698971260, 46.66557627198102409 ) ) ;
#147472 = CARTESIAN_POINT ( 'NONE',  ( -16.46253265017146816, -9.564922557961047289, 19.16775706135233293 ) ) ;
#147473 = CARTESIAN_POINT ( 'NONE',  ( 8.314922557961029526, -14.29746914071037800, 95.41775706135234714 ) ) ;
#147475 = CARTESIAN_POINT ( 'NONE',  ( 10.72451020669871369, 18.67979575497193778, 72.08442372801899012 ) ) ;
#147474 = CARTESIAN_POINT ( 'NONE',  ( 13.97604488694527802, 13.89961937509977652, 99.37390960531436690 ) ) ;
#147476 = CARTESIAN_POINT ( 'NONE',  ( 6.767139177214389179, -4.798834252846686077, -62.08368047933343803 ) ) ;
#147477 = CARTESIAN_POINT ( 'NONE',  ( -13.97604488694527625, -13.89961937509977652, 106.8739096053143669 ) ) ;
#147478 = PLANE ( 'NONE',  #163096 ) ;
#147480 = CARTESIAN_POINT ( 'NONE',  ( 5.719274019375673035, 21.55341960407619339, 67.29275706135234714 ) ) ;
#147479 = CARTESIAN_POINT ( 'NONE',  ( 12.06949235617739724, 12.14591786802326823, 66.87609039468568994 ) ) ;
#147481 = CARTESIAN_POINT ( 'NONE',  ( -10.81492255796105439, 18.62759615963255655, 107.9177570613523471 ) ) ;
#147482 = DIRECTION ( 'NONE',  ( 0.000000000000000000, 0.000000000000000000, 1.000000000000000000 ) ) ;
#147483 = CARTESIAN_POINT ( 'NONE',  ( -8.314922557961024197, 14.29746914071037800, 42.91775706135235424 ) ) ;
#147484 = CARTESIAN_POINT ( 'NONE',  ( -13.97604488694527625, -13.89961937509977652, 91.87390960531432427 ) ) ;
#147485 = CARTESIAN_POINT ( 'NONE',  ( 19.02544592524343514, -5.153800228976328945, 113.5405762719810241 ) ) ;
#147486 = ORIENTED_EDGE ( 'NONE', *, *, #9309, .F. ) ;
#147487 = CARTESIAN_POINT ( 'NONE',  ( 17.40805194822029378, 6.112264579159354838, 41.66628727489390371 ) ) ;
#147488 = CARTESIAN_POINT ( 'NONE',  ( -16.46253265017160317, 9.564922557960807481, 35.83224293864768839 ) ) ;
#147489 = CARTESIAN_POINT ( 'NONE',  ( -15.80617190586745835, -15.72974639402198527, 36.87390960531435979 ) ) ;
#147490 = CARTESIAN_POINT ( 'NONE',  ( 8.224510206698742110, 14.34966873604972548, 102.0844237280190185 ) ) ;
#147492 = CARTESIAN_POINT ( 'NONE',  ( 13.97604488694527802, 13.89961937509977652, 79.37390960531435269 ) ) ;
#147491 = CARTESIAN_POINT ( 'NONE',  ( -16.52544592524342804, 4.483927247898546575, 86.04057627198102409 ) ) ;
#147493 = CARTESIAN_POINT ( 'NONE',  ( 21.52544592524334988, 5.823673210054432836, 101.4594237280190185 ) ) ;
#147494 = CARTESIAN_POINT ( 'NONE',  ( -14.29746914071037622, -8.314922557961029526, 29.16775706135234003 ) ) ;
#147495 = CARTESIAN_POINT ( 'NONE',  ( -8.314922557960811034, -14.29746914071050412, 87.08224293864769550 ) ) ;
#147496 = CARTESIAN_POINT ( 'NONE',  ( 21.52544592524334988, 5.823673210054432836, 36.45942372801901143 ) ) ;
#147497 = CARTESIAN_POINT ( 'NONE',  ( -21.55341960407610458, -5.719274019375992779, 91.45724293864769550 ) ) ;
#147498 = CARTESIAN_POINT ( 'NONE',  ( 16.51473224551083163, -9.474510206698727899, 50.83442372801899722 ) ) ;
#147499 = CARTESIAN_POINT ( 'NONE',  ( 13.97604488694527802, 13.89961937509977830, 44.37390960531435979 ) ) ;
#147500 = CARTESIAN_POINT ( 'NONE',  ( -19.02544592524342804, 5.153800228976336051, 101.0405762719810241 ) ) ;
#147501 = CARTESIAN_POINT ( 'NONE',  ( 4.483927247898545687, 16.52544592524342804, 64.79057627198103830 ) ) ;
#147502 = VECTOR ( 'NONE', #133704, 1000.000000000000000 ) ;
#147503 = CARTESIAN_POINT ( 'NONE',  ( -12.06949235617756955, 12.14591786802309770, 45.62390960531436690 ) ) ;
#147504 = CARTESIAN_POINT ( 'NONE',  ( -14.29746914071037622, -8.314922557961029526, 104.1677570613523471 ) ) ;
#147505 = CARTESIAN_POINT ( 'NONE',  ( 13.89961937509957401, 13.97604488694547697, 66.87609039468567573 ) ) ;
#147506 = FACE_OUTER_BOUND ( 'NONE', #10269, .T. ) ;
#147507 = CARTESIAN_POINT ( 'NONE',  ( 5.719274019375991003, -21.55341960407610458, 27.70724293864769905 ) ) ;
#147508 = EDGE_CURVE ( 'NONE', #185456, #180340, #163296, .T. ) ;
#147509 = CARTESIAN_POINT ( 'NONE',  ( -8.314922557960811034, -14.29746914071050412, 92.08224293864769550 ) ) ;
#147510 = DIRECTION ( 'NONE',  ( 0.000000000000000000, 0.000000000000000000, -1.000000000000000000 ) ) ;
#147512 = CARTESIAN_POINT ( 'NONE',  ( -15.72974639402197994, 15.80617190586746368, 45.62390960531436690 ) ) ;
#147511 = CARTESIAN_POINT ( 'NONE',  ( 0.05219959533909260263, 19.03943276465977164, 44.99890960531435979 ) ) ;
#147513 = CARTESIAN_POINT ( 'NONE',  ( -0.05219959533909027116, -19.03943276465977164, 27.49890960531435624 ) ) ;
#147515 = CARTESIAN_POINT ( 'NONE',  ( 13.97604488694527802, 13.89961937509977652, 64.37390960531436690 ) ) ;
#147514 = CARTESIAN_POINT ( 'NONE',  ( 16.53943276465976808, 0.05219959533934440121, 81.25109039468568994 ) ) ;
#147516 = CARTESIAN_POINT ( 'NONE',  ( -19.03943276465977164, -0.05219959533935918106, 38.75109039468566152 ) ) ;
#147517 = CARTESIAN_POINT ( 'NONE',  ( -5.719274019375665041, -21.55341960407619695, 49.79275706135234714 ) ) ;
#147518 = EDGE_LOOP ( 'NONE', ( #40103, #8410, #51452, #36328 ) ) ;
#147519 = CARTESIAN_POINT ( 'NONE',  ( 5.719274019375991003, -21.55341960407610458, 37.70724293864769550 ) ) ;
#147520 = AXIS2_PLACEMENT_3D ( 'NONE', #197183, #184971, #46456 ) ;
#147521 = CARTESIAN_POINT ( 'NONE',  ( -4.483927247898539470, -16.52544592524342804, 102.2905762719810383 ) ) ;
#147522 = CARTESIAN_POINT ( 'NONE',  ( 13.89961937509957401, 13.97604488694547697, 86.87609039468567573 ) ) ;
#147523 = CARTESIAN_POINT ( 'NONE',  ( -36.91746825000000598, 11.99521256947798520, -5.224999997268812812 ) ) ;
#147525 = CARTESIAN_POINT ( 'NONE',  ( 18.62759615963271287, -10.81492255796078972, 48.33224293864770260 ) ) ;
#147524 = CARTESIAN_POINT ( 'NONE',  ( -17.50000000001354294, 5.500000000000027534, 95.79690382535056870 ) ) ;
#147526 = CARTESIAN_POINT ( 'NONE',  ( 19.02544592524343514, -5.153800228976328945, 23.54057627198102054 ) ) ;
#147527 = CARTESIAN_POINT ( 'NONE',  ( -5.823673210054431948, 21.52544592524334988, 87.70942372801901854 ) ) ;
#147528 = CARTESIAN_POINT ( 'NONE',  ( 4.483927247898545687, 16.52544592524342804, 49.79057627198102409 ) ) ;
#147530 = CARTESIAN_POINT ( 'NONE',  ( -8.314922557960811034, -14.29746914071050412, 57.08224293864769550 ) ) ;
#147529 = CARTESIAN_POINT ( 'NONE',  ( -16.53943276465976808, -0.05219959533934237506, 53.75109039468568994 ) ) ;
#147531 = CARTESIAN_POINT ( 'NONE',  ( -15.80617190586745835, -15.72974639402198527, 86.87390960531438111 ) ) ;
#147532 = CARTESIAN_POINT ( 'NONE',  ( -21.52544592524343514, 5.823673210054127303, 71.04057627198103830 ) ) ;
#147533 = CARTESIAN_POINT ( 'NONE',  ( -27.83212366386707615, -25.89052209088941225, -16.12745387078197012 ) ) ;
#147534 = CARTESIAN_POINT ( 'NONE',  ( -13.89961937509977652, 13.97604488694528158, 115.6239096053143669 ) ) ;
#147535 = CARTESIAN_POINT ( 'NONE',  ( -9.474510206698964154, 16.51473224551069663, 65.41557627198102409 ) ) ;
#147536 = CARTESIAN_POINT ( 'NONE',  ( -19.05341960407611168, -5.049401038298163336, 31.45724293864769550 ) ) ;
#147537 = DIRECTION ( 'NONE',  ( -0.000000000000000000, -0.000000000000000000, 1.000000000000000000 ) ) ;
#147538 = CARTESIAN_POINT ( 'NONE',  ( -12.06949235617739369, -12.14591786802326823, 84.37609039468570415 ) ) ;
#147539 = CARTESIAN_POINT ( 'NONE',  ( -15.72974639402176322, -15.80617190586768395, 24.37609039468567573 ) ) ;
#147540 = CARTESIAN_POINT ( 'NONE',  ( 13.89961937509977652, -13.97604488694527269, 68.12390960531436690 ) ) ;
#147541 = CARTESIAN_POINT ( 'NONE',  ( 21.52544592524334988, 5.823673210054432836, 56.45942372801902565 ) ) ;
#147542 = CARTESIAN_POINT ( 'NONE',  ( -19.03943276465977164, 0.05219959533909376836, 91.24890960531436690 ) ) ;
#147543 = CARTESIAN_POINT ( 'NONE',  ( -25.01910340989286752, -31.27285607037816462, -17.23782325462181220 ) ) ;
#147544 = ORIENTED_EDGE ( 'NONE', *, *, #79191, .F. ) ;
#147545 = CARTESIAN_POINT ( 'NONE',  ( -15.72974639402176322, -15.80617190586768395, 44.37609039468567573 ) ) ;
#147547 = CARTESIAN_POINT ( 'NONE',  ( 19.03943276465977164, -0.05219959533909143690, 103.7489096053143669 ) ) ;
#147546 = CARTESIAN_POINT ( 'NONE',  ( -9.474510206698964154, 16.51473224551069663, 30.41557627198102054 ) ) ;
#147548 = CARTESIAN_POINT ( 'NONE',  ( 9.474510206698729675, 16.51473224551082808, 57.08442372801900433 ) ) ;
#147549 = CARTESIAN_POINT ( 'NONE',  ( -10.81492255796078084, -18.62759615963271287, 107.0822429386476955 ) ) ;
#147550 = CARTESIAN_POINT ( 'NONE',  ( -13.89961937509957401, -13.97604488694547875, 49.37609039468567573 ) ) ;
#147551 = CARTESIAN_POINT ( 'NONE',  ( -9.564922557961040184, 16.46253265017147172, 47.91775706135233293 ) ) ;
#147553 = ORIENTED_EDGE ( 'NONE', *, *, #111017, .F. ) ;
#147552 = CARTESIAN_POINT ( 'NONE',  ( -8.314922557961024197, 14.29746914071037800, 107.9177570613523471 ) ) ;
#147555 = ORIENTED_EDGE ( 'NONE', *, *, #168309, .T. ) ;
#147554 = CARTESIAN_POINT ( 'NONE',  ( 11.80868324581537543, 11.80868324581533990, -61.34707691135562868 ) ) ;
#147556 = CARTESIAN_POINT ( 'NONE',  ( -13.97604488694527625, -13.89961937509977652, 76.87390960531433848 ) ) ;
#147557 = AXIS2_PLACEMENT_3D ( 'NONE', #110701, #2531, #31887 ) ;
#147558 = CARTESIAN_POINT ( 'NONE',  ( 18.67979575497194134, -10.72451020669871369, 85.83442372801901854 ) ) ;
#147559 = CARTESIAN_POINT ( 'NONE',  ( 18.67979575497194134, -10.72451020669871369, 95.83442372801903275 ) ) ;
#147560 = CARTESIAN_POINT ( 'NONE',  ( -2.577820198429831642E-15, -9.100000000000001421, -63.95112321872120731 ) ) ;
#147561 = CARTESIAN_POINT ( 'NONE',  ( -9.564922557960796823, -16.46253265017161027, 97.08224293864769550 ) ) ;
#147562 = CARTESIAN_POINT ( 'NONE',  ( -18.62759615963255300, -10.81492255796106328, 74.16775706135231871 ) ) ;
#147563 = CARTESIAN_POINT ( 'NONE',  ( 16.52544592524335698, 4.483927247898782831, 21.45942372801901499 ) ) ;
#147564 = CARTESIAN_POINT ( 'NONE',  ( 5.153800228976335163, 19.02544592524342804, 79.79057627198102409 ) ) ;
#147565 = CARTESIAN_POINT ( 'NONE',  ( -21.53943276465977519, 0.05219959533907696930, 21.24890960531436690 ) ) ;
#147566 = CARTESIAN_POINT ( 'NONE',  ( 19.05341960407611168, 5.049401038298154454, 93.95724293864769550 ) ) ;
#147567 = CARTESIAN_POINT ( 'NONE',  ( 27.16368555717295763, -26.59078835260041629, -15.56371235017464727 ) ) ;
#147568 = CARTESIAN_POINT ( 'NONE',  ( 16.51473224551069308, 9.474510206698969483, 79.16557627198103830 ) ) ;
#147569 = CARTESIAN_POINT ( 'NONE',  ( 9.474510206698971260, -16.51473224551069308, 67.91557627198102409 ) ) ;
#147570 = CARTESIAN_POINT ( 'NONE',  ( -0.05219959533907301413, -21.53943276465977519, 107.4989096053143669 ) ) ;
#147571 = CARTESIAN_POINT ( 'NONE',  ( 0.05219959533934541429, -16.53943276465976808, 100.0010903946857042 ) ) ;
#147572 = DIRECTION ( 'NONE',  ( -0.000000000000000000, -0.000000000000000000, 1.000000000000000000 ) ) ;
#147573 = CARTESIAN_POINT ( 'NONE',  ( 16.46253265017146816, 9.564922557961045513, 51.66775706135233293 ) ) ;
#147574 = CARTESIAN_POINT ( 'NONE',  ( -19.05341960407611168, -5.049401038298163336, 96.45724293864769550 ) ) ;
#147575 = CARTESIAN_POINT ( 'NONE',  ( 4.379528057220339221, -16.55341960407611168, 82.70724293864770971 ) ) ;
#147576 = CARTESIAN_POINT ( 'NONE',  ( 19.02544592524343514, -5.153800228976328945, 28.54057627198102409 ) ) ;
#147577 = CARTESIAN_POINT ( 'NONE',  ( -21.55341960407610458, -5.719274019375992779, 36.45724293864768839 ) ) ;
#147578 = CARTESIAN_POINT ( 'NONE',  ( -21.55341960407610458, -5.719274019375992779, 26.45724293864768839 ) ) ;
#147579 = CARTESIAN_POINT ( 'NONE',  ( -8.314922557960811034, -14.29746914071050412, 87.08224293864769550 ) ) ;
#147580 = DIRECTION ( 'NONE',  ( 1.000000000000000000, 0.000000000000000000, 0.000000000000000000 ) ) ;
#147581 = CARTESIAN_POINT ( 'NONE',  ( 13.97604488694548053, -13.89961937509957401, 40.62609039468564731 ) ) ;
#147582 = CARTESIAN_POINT ( 'NONE',  ( 4.483927247898790824, -16.52544592524335698, 105.2094237280190328 ) ) ;
#147583 = CARTESIAN_POINT ( 'NONE',  ( 16.46253265017160672, -9.564922557960803928, 93.33224293864769550 ) ) ;
#147584 = CARTESIAN_POINT ( 'NONE',  ( 15.80617190586769283, -15.72974639402175789, 65.62609039468568994 ) ) ;
#147585 = CARTESIAN_POINT ( 'NONE',  ( -5.719274019375978568, 21.55341960407610458, 45.20724293864769550 ) ) ;
#147587 = EDGE_LOOP ( 'NONE', ( #186664, #5177, #38837, #160908 ) ) ;
#147586 = CARTESIAN_POINT ( 'NONE',  ( 21.53943276465977519, 0.05219959533937863772, 26.25109039468567573 ) ) ;
#147588 = CARTESIAN_POINT ( 'NONE',  ( -21.55341960407610458, -5.719274019375992779, 86.45724293864770971 ) ) ;
#147589 = CARTESIAN_POINT ( 'NONE',  ( -14.29746914071049879, 8.314922557960819915, 110.8322429386476955 ) ) ;
#147590 = CARTESIAN_POINT ( 'NONE',  ( -13.97604488694547697, 13.89961937509957934, 68.12609039468563310 ) ) ;
#147591 = CARTESIAN_POINT ( 'NONE',  ( 9.474510206698971260, -16.51473224551069308, 42.91557627198103120 ) ) ;
#147592 = CARTESIAN_POINT ( 'NONE',  ( -19.02544592524342804, 5.153800228976336051, 91.04057627198100988 ) ) ;
#147593 = CARTESIAN_POINT ( 'NONE',  ( -9.474510206698964154, 16.51473224551069663, 95.41557627198102409 ) ) ;
#147594 = CARTESIAN_POINT ( 'NONE',  ( 4.379528057220339221, -16.55341960407611168, 112.7072429386476955 ) ) ;
#147595 = CARTESIAN_POINT ( 'NONE',  ( 14.29746914071049879, -8.314922557960816363, 43.33224293864769550 ) ) ;
#147596 = CARTESIAN_POINT ( 'NONE',  ( -12.14591786802326823, 12.06949235617739902, 38.12609039468567573 ) ) ;
#147597 = CARTESIAN_POINT ( 'NONE',  ( 21.52544592524334988, 5.823673210054432836, 106.4594237280190328 ) ) ;
#147599 = CARTESIAN_POINT ( 'NONE',  ( -16.52544592524342804, 4.483927247898546575, 26.04057627198103475 ) ) ;
#147598 = FACE_OUTER_BOUND ( 'NONE', #87792, .T. ) ;
#147600 = CARTESIAN_POINT ( 'NONE',  ( 15.72974639402176855, 15.80617190586768217, 26.87609039468567218 ) ) ;
#147601 = CARTESIAN_POINT ( 'NONE',  ( 19.05341960407611168, 5.049401038298154454, 108.9572429386477097 ) ) ;
#147602 = CARTESIAN_POINT ( 'NONE',  ( 8.224510206698742110, 14.34966873604972548, 112.0844237280190185 ) ) ;
#147603 = CARTESIAN_POINT ( 'NONE',  ( -12.14591786802326823, 12.06949235617739902, 93.12609039468568994 ) ) ;
#147604 = CARTESIAN_POINT ( 'NONE',  ( -16.52544592524335698, -4.483927247898792601, 28.95942372801902209 ) ) ;
#147605 = CARTESIAN_POINT ( 'NONE',  ( -19.02544592524342804, 5.153800228976336051, 51.04057627198103120 ) ) ;
#147606 = CARTESIAN_POINT ( 'NONE',  ( -16.52544592524342804, 4.483927247898546575, 106.0405762719810525 ) ) ;
#147607 = CARTESIAN_POINT ( 'NONE',  ( 21.53943276465977519, 0.05219959533937863772, 21.25109039468567218 ) ) ;
#147608 = CARTESIAN_POINT ( 'NONE',  ( 16.46253265017160672, -9.564922557960803928, 28.33224293864769550 ) ) ;
#147609 = CARTESIAN_POINT ( 'NONE',  ( -19.03943276465977164, 0.05219959533909376836, 106.2489096053143669 ) ) ;
#147610 = CARTESIAN_POINT ( 'NONE',  ( 21.52544592524334988, 5.823673210054432836, 26.45942372801901854 ) ) ;
#147611 = CARTESIAN_POINT ( 'NONE',  ( 16.51473224551069308, 9.474510206698969483, 29.16557627198103475 ) ) ;
#147612 = EDGE_CURVE ( 'NONE', #122157, #27947, #61062, .T. ) ;
#147613 = CARTESIAN_POINT ( 'NONE',  ( -13.89961937509977652, 13.97604488694528158, 110.6239096053143243 ) ) ;
#147614 = CARTESIAN_POINT ( 'NONE',  ( -16.29526858892874586, -7.335722546920246501, 35.79670597800209464 ) ) ;
#147615 = CARTESIAN_POINT ( 'NONE',  ( -0.05219959533909027116, -19.03943276465977164, 102.4989096053143669 ) ) ;
#147617 = CARTESIAN_POINT ( 'NONE',  ( -16.52544592524342804, 4.483927247898546575, 96.04057627198102409 ) ) ;
#147616 = CARTESIAN_POINT ( 'NONE',  ( 5.823673210054444382, -21.52544592524334988, 40.20942372801901854 ) ) ;
#147618 = CARTESIAN_POINT ( 'NONE',  ( 13.97604488694527802, 13.89961937509977652, 94.37390960531436690 ) ) ;
#147619 = CARTESIAN_POINT ( 'NONE',  ( -26.58496454516998853, -7.626754437231455519, 167.9682100371138915 ) ) ;
#147620 = CARTESIAN_POINT ( 'NONE',  ( -8.314922557961024197, 14.29746914071037800, 67.91775706135234714 ) ) ;
#147621 = CARTESIAN_POINT ( 'NONE',  ( 10.81492255796106328, -18.62759615963255655, 85.41775706135236135 ) ) ;
#147622 = CARTESIAN_POINT ( 'NONE',  ( -8.314922557961024197, 14.29746914071037800, 42.91775706135235424 ) ) ;
#147623 = CARTESIAN_POINT ( 'NONE',  ( 9.474510206698971260, -16.51473224551069308, 87.91557627198102409 ) ) ;
#147624 = CARTESIAN_POINT ( 'NONE',  ( 9.474510206698729675, 16.51473224551082808, 107.0844237280190043 ) ) ;
#147625 = CARTESIAN_POINT ( 'NONE',  ( -8.224510206698735004, -14.34966873604973081, 64.58442372801900433 ) ) ;
#147626 = CARTESIAN_POINT ( 'NONE',  ( 9.474510206698729675, 16.51473224551082808, 97.08442372801900433 ) ) ;
#147627 = CARTESIAN_POINT ( 'NONE',  ( 5.049401038298161559, -19.05341960407611168, 67.70724293864769550 ) ) ;
#147628 = CARTESIAN_POINT ( 'NONE',  ( 0.05219959533907565091, 21.53943276465977519, 89.99890960531438111 ) ) ;
#147630 = CARTESIAN_POINT ( 'NONE',  ( 5.049401038297881783, 19.05341960407617563, 97.29275706135233293 ) ) ;
#147629 = CARTESIAN_POINT ( 'NONE',  ( 14.34966873604960469, 8.224510206698951720, 84.16557627198103830 ) ) ;
#147631 = CARTESIAN_POINT ( 'NONE',  ( -14.29746914071037622, -8.314922557961029526, 54.16775706135235424 ) ) ;
#147632 = CARTESIAN_POINT ( 'NONE',  ( 24.14511064691323838, 7.743397529683260672, 169.7652520481095735 ) ) ;
#147633 = CARTESIAN_POINT ( 'NONE',  ( -9.474510206698720793, -16.51473224551083518, 54.58442372801899722 ) ) ;
#147634 = CARTESIAN_POINT ( 'NONE',  ( 16.53943276465976808, -0.05219959533910856209, 28.74890960531435624 ) ) ;
#147635 = CARTESIAN_POINT ( 'NONE',  ( -12.06949235617756955, 12.14591786802309770, 75.62390960531439532 ) ) ;
#147637 = CARTESIAN_POINT ( 'NONE',  ( -17.31728774477213406, 6.344390552233685199, 40.81906651689308063 ) ) ;
#147636 = CARTESIAN_POINT ( 'NONE',  ( 5.049401038297881783, 19.05341960407617563, 22.29275706135233648 ) ) ;
#147638 = CARTESIAN_POINT ( 'NONE',  ( -10.72451020669870658, -18.67979575497194134, 24.58442372801901499 ) ) ;
#147639 = CARTESIAN_POINT ( 'NONE',  ( 16.46253265017160672, -9.564922557960803928, 108.3322429386476955 ) ) ;
#147640 = CARTESIAN_POINT ( 'NONE',  ( 5.049401038298161559, -19.05341960407611168, 77.70724293864765286 ) ) ;
#147641 = CARTESIAN_POINT ( 'NONE',  ( 21.52544592524334988, 5.823673210054432836, 101.4594237280190185 ) ) ;
#147642 = CARTESIAN_POINT ( 'NONE',  ( 0.05219959533909260263, 19.03943276465977164, 74.99890960531435269 ) ) ;
#147643 = CARTESIAN_POINT ( 'NONE',  ( 5.823673210054125526, 21.52544592524343514, 49.79057627198102409 ) ) ;
#147644 = CARTESIAN_POINT ( 'NONE',  ( -12.14591786802309592, -12.06949235617757132, 76.87390960531439532 ) ) ;
#147645 = CARTESIAN_POINT ( 'NONE',  ( 19.05341960407611168, 5.049401038298154454, 53.95724293864770260 ) ) ;
#147646 = CARTESIAN_POINT ( 'NONE',  ( -8.224510206698948167, 14.34966873604960824, 110.4155762719810383 ) ) ;
#147647 = CONICAL_SURFACE ( 'NONE', #102468, 30.82560697742735556, 0.1745329251994333364 ) ;
#147648 = CARTESIAN_POINT ( 'NONE',  ( 5.719274019375673035, 21.55341960407619339, 22.29275706135235069 ) ) ;
#147649 = CARTESIAN_POINT ( 'NONE',  ( -21.53943276465977519, -0.05219959533937600094, 63.75109039468568284 ) ) ;
#147650 = CARTESIAN_POINT ( 'NONE',  ( -13.97604488694527625, -13.89961937509977652, 41.87390960531435979 ) ) ;
#147651 = CARTESIAN_POINT ( 'NONE',  ( -4.483927247898782831, 16.52544592524335698, 57.70942372801901143 ) ) ;
#147652 = CARTESIAN_POINT ( 'NONE',  ( -21.53943276465977519, 0.05219959533907696930, 111.2489096053143669 ) ) ;
#147653 = CARTESIAN_POINT ( 'NONE',  ( 0.05219959533907565091, 21.53943276465977519, 109.9989096053143527 ) ) ;
#147655 = CARTESIAN_POINT ( 'NONE',  ( -9.564922557960796823, -16.46253265017161027, 67.08224293864769550 ) ) ;
#147654 = CARTESIAN_POINT ( 'NONE',  ( 19.02544592524334988, 5.153800228976608722, 41.45942372801900433 ) ) ;
#147656 = CARTESIAN_POINT ( 'NONE',  ( 0.000000000000000000, 0.000000000000000000, -65.00100000000003320 ) ) ;
#147657 = CARTESIAN_POINT ( 'NONE',  ( 21.53943276465977519, 0.05219959533937863772, 66.25109039468567573 ) ) ;
#147658 = EDGE_CURVE ( 'NONE', #3830, #142224, #27790, .T. ) ;
#147659 = CARTESIAN_POINT ( 'NONE',  ( -5.719274019375978568, 21.55341960407610458, 55.20724293864770260 ) ) ;
#147660 = CARTESIAN_POINT ( 'NONE',  ( 8.224510206698953496, -14.34966873604960469, 37.91557627198102409 ) ) ;
#147662 = CARTESIAN_POINT ( 'NONE',  ( 19.02544592524334988, 5.153800228976608722, 21.45942372801899012 ) ) ;
#147661 = CARTESIAN_POINT ( 'NONE',  ( 5.823673210054444382, -21.52544592524334988, 80.20942372801901854 ) ) ;
#147663 = CARTESIAN_POINT ( 'NONE',  ( 16.55341960407611168, 4.379528057220329451, 53.95724293864770260 ) ) ;
#147664 = CARTESIAN_POINT ( 'NONE',  ( 16.53943276465976808, -0.05219959533910856209, 108.7489096053143669 ) ) ;
#147665 = CARTESIAN_POINT ( 'NONE',  ( -9.474510206698720793, -16.51473224551083518, 59.58442372801900433 ) ) ;
#147666 = CARTESIAN_POINT ( 'NONE',  ( -12.14591786802309592, -12.06949235617757132, 21.87390960531436690 ) ) ;
#147667 = CARTESIAN_POINT ( 'NONE',  ( 10.72451020669871369, 18.67979575497193778, 62.08442372801901143 ) ) ;
#147668 = CARTESIAN_POINT ( 'NONE',  ( 19.03943276465977164, -0.05219959533909143690, 78.74890960531436690 ) ) ;
#147669 = CARTESIAN_POINT ( 'NONE',  ( 13.89961937509957401, 13.97604488694547697, 36.87609039468565442 ) ) ;
#147670 = CARTESIAN_POINT ( 'NONE',  ( -5.823673210054116645, -21.52544592524344225, 32.29057627198102409 ) ) ;
#147671 = CARTESIAN_POINT ( 'NONE',  ( -10.81492255796105439, 18.62759615963255655, 32.91775706135234714 ) ) ;
#147672 = CARTESIAN_POINT ( 'NONE',  ( 5.719274019375991003, -21.55341960407610458, 107.7072429386476955 ) ) ;
#147673 = CARTESIAN_POINT ( 'NONE',  ( -13.89961937509957401, -13.97604488694547875, 94.37609039468566152 ) ) ;
#147674 = CARTESIAN_POINT ( 'NONE',  ( 8.224510206698742110, 14.34966873604972548, 52.08442372801901854 ) ) ;
#147676 = CARTESIAN_POINT ( 'NONE',  ( -5.823673210054116645, -21.52544592524344225, 97.29057627198105251 ) ) ;
#147675 = DIRECTION ( 'NONE',  ( 1.000000000000000000, -0.000000000000000000, -0.000000000000000000 ) ) ;
#147677 = CARTESIAN_POINT ( 'NONE',  ( -0.05219959533910754901, -16.53943276465976808, 87.49890960531436690 ) ) ;
#147678 = CARTESIAN_POINT ( 'NONE',  ( 2.400000000000000799, 2.694222958124176020E-16, -2.199999999999999289 ) ) ;
#147679 = CARTESIAN_POINT ( 'NONE',  ( 14.29746914071037800, 8.314922557961029526, 26.66775706135235424 ) ) ;
#147680 = CARTESIAN_POINT ( 'NONE',  ( 21.55341960407610458, 5.719274019375980345, 53.95724293864770260 ) ) ;
#147682 = CARTESIAN_POINT ( 'NONE',  ( 0.05219959533934541429, -16.53943276465976808, 95.00109039468568994 ) ) ;
#147681 = COLOUR_RGB ( '', 0.08235294, 0.09019608, 0.10196078) ;
#147683 = CARTESIAN_POINT ( 'NONE',  ( -18.22780087662123094, -5.499999999999984901, 76.48459894673894155 ) ) ;
#147684 = CARTESIAN_POINT ( 'NONE',  ( -4.483927247898782831, 16.52544592524335698, 47.70942372801902565 ) ) ;
#147685 = CARTESIAN_POINT ( 'NONE',  ( -5.823673210054431948, 21.52544592524334988, 27.70942372801901854 ) ) ;
#147686 = CARTESIAN_POINT ( 'NONE',  ( 21.52544592524344225, -5.823673210054117533, 43.54057627198103830 ) ) ;
#147687 = CARTESIAN_POINT ( 'NONE',  ( 4.483927247898790824, -16.52544592524335698, 90.20942372801903275 ) ) ;
#147688 = CARTESIAN_POINT ( 'NONE',  ( 13.89961937509977652, -13.97604488694527269, 103.1239096053143527 ) ) ;
#147689 = CARTESIAN_POINT ( 'NONE',  ( 18.62759615963255655, 10.81492255796105972, 71.66775706135234714 ) ) ;
#147690 = CARTESIAN_POINT ( 'NONE',  ( 21.52544592524344225, -5.823673210054117533, 33.54057627198102409 ) ) ;
#147691 = CARTESIAN_POINT ( 'NONE',  ( -21.55341960407610458, -5.719274019375992779, 21.45724293864769550 ) ) ;
#147692 = ORIENTED_EDGE ( 'NONE', *, *, #70540, .T. ) ;
#147693 = CARTESIAN_POINT ( 'NONE',  ( 9.564922557961047289, -16.46253265017146816, 55.41775706135234003 ) ) ;
#147694 = CARTESIAN_POINT ( 'NONE',  ( 4.483927247898790824, -16.52544592524335698, 65.20942372801901854 ) ) ;
#147695 = CARTESIAN_POINT ( 'NONE',  ( 21.55341960407610458, 5.719274019375980345, 33.95724293864769550 ) ) ;
#147696 = VERTEX_POINT ( 'NONE', #182448 ) ;
#147697 = CARTESIAN_POINT ( 'NONE',  ( -5.049401038298153566, 19.05341960407611168, 80.20724293864769550 ) ) ;
#147698 = CARTESIAN_POINT ( 'NONE',  ( -16.55341960407617563, 4.379528057220093196, 93.54275706135234714 ) ) ;
#147699 = CARTESIAN_POINT ( 'NONE',  ( 11.02000550219334407, -37.94488912280207416, -31.28304700362889079 ) ) ;
#147700 = CARTESIAN_POINT ( 'NONE',  ( -16.53943276465976808, 0.05219959533911058130, 111.2489096053143669 ) ) ;
#147701 = CARTESIAN_POINT ( 'NONE',  ( -10.81492255796078084, -18.62759615963271287, 47.08224293864770260 ) ) ;
#147702 = CARTESIAN_POINT ( 'NONE',  ( 19.02544592524343514, -5.153800228976328945, 38.54057627198103120 ) ) ;
#147703 = CARTESIAN_POINT ( 'NONE',  ( -14.34966873604972548, 8.224510206698743886, 73.33442372801901854 ) ) ;
#147704 = CARTESIAN_POINT ( 'NONE',  ( -10.81492255796105439, 18.62759615963255655, 32.91775706135234714 ) ) ;
#147705 = CARTESIAN_POINT ( 'NONE',  ( 13.97604488694548053, -13.89961937509957401, 90.62609039468567573 ) ) ;
#147706 = CARTESIAN_POINT ( 'NONE',  ( 4.483927247898545687, 16.52544592524342804, 94.79057627198105251 ) ) ;
#147707 = CARTESIAN_POINT ( 'NONE',  ( 5.153800228976335163, 19.02544592524342804, 49.79057627198100988 ) ) ;
#147708 = AXIS2_PLACEMENT_3D ( 'NONE', #129254, #158610, #161606 ) ;
#147709 = CARTESIAN_POINT ( 'NONE',  ( -16.51473224551069308, -9.474510206698971260, 26.66557627198103120 ) ) ;
#147710 = CARTESIAN_POINT ( 'NONE',  ( -18.67979575497193778, 10.72451020669871902, 108.3344237280190185 ) ) ;
#147711 = CARTESIAN_POINT ( 'NONE',  ( 19.02544592524343514, -5.153800228976328945, 78.54057627198099567 ) ) ;
#147712 = CARTESIAN_POINT ( 'NONE',  ( 16.53943276465976808, 0.05219959533934440121, 61.25109039468567573 ) ) ;
#147713 = CARTESIAN_POINT ( 'NONE',  ( 21.55341960407619695, -5.719274019375665929, 96.04275706135236135 ) ) ;
#147714 = CARTESIAN_POINT ( 'NONE',  ( -0.05219959533934338120, 16.53943276465976808, 77.50109039468567573 ) ) ;
#147715 = CARTESIAN_POINT ( 'NONE',  ( 19.05341960407617918, -5.049401038297876454, 56.04275706135234714 ) ) ;
#147716 = CARTESIAN_POINT ( 'NONE',  ( -16.46253265017146816, -9.564922557961047289, 69.16775706135233293 ) ) ;
#147717 = CARTESIAN_POINT ( 'NONE',  ( -10.81492255796105439, 18.62759615963255655, 62.91775706135236135 ) ) ;
#147718 = CARTESIAN_POINT ( 'NONE',  ( -9.474510206698964154, 16.51473224551069663, 70.41557627198102409 ) ) ;
#147719 = CARTESIAN_POINT ( 'NONE',  ( -30.00000000000000000, -1.163414459189985801E-14, 95.00000000000000000 ) ) ;
#147720 = CARTESIAN_POINT ( 'NONE',  ( 5.153800228976615827, -19.02544592524334988, 65.20942372801900433 ) ) ;
#147721 = CARTESIAN_POINT ( 'NONE',  ( -0.05219959533909027116, -19.03943276465977164, 112.4989096053143669 ) ) ;
#147722 = CARTESIAN_POINT ( 'NONE',  ( -13.89961937509977652, 13.97604488694528158, 80.62390960531436690 ) ) ;
#147723 = CARTESIAN_POINT ( 'NONE',  ( 12.06949235617757843, -12.14591786802309237, 33.12390960531435979 ) ) ;
#147724 = CARTESIAN_POINT ( 'NONE',  ( -21.52544592524343514, 5.823673210054127303, 51.04057627198103120 ) ) ;
#147725 = CARTESIAN_POINT ( 'NONE',  ( 22.00000000000000000, -5.510910596163089556E-15, 45.00000000000000000 ) ) ;
#147726 = CARTESIAN_POINT ( 'NONE',  ( -9.474510206698720793, -16.51473224551083518, 19.58442372801899722 ) ) ;
#147727 = CARTESIAN_POINT ( 'NONE',  ( -16.81555441253555117, -7.025013491695478507, 79.36314554665743515 ) ) ;
#147728 = CARTESIAN_POINT ( 'NONE',  ( 19.05341960407611168, 5.049401038298154454, 33.95724293864769550 ) ) ;
#147729 = CARTESIAN_POINT ( 'NONE',  ( 13.97604488694527802, 13.89961937509977652, 29.37390960531435979 ) ) ;
#147730 = CARTESIAN_POINT ( 'NONE',  ( 37.99999999999999289, 2.893978650043524126E-14, -5.000000000000000000 ) ) ;
#147731 = CARTESIAN_POINT ( 'NONE',  ( 5.719274019375673035, 21.55341960407619339, 67.29275706135234714 ) ) ;
#147732 = FACE_OUTER_BOUND ( 'NONE', #62943, .T. ) ;
#147733 = CARTESIAN_POINT ( 'NONE',  ( 8.224510206698742110, 14.34966873604972548, 57.08442372801901854 ) ) ;
#147734 = CARTESIAN_POINT ( 'NONE',  ( -18.62759615963270932, 10.81492255796079327, 85.83224293864768129 ) ) ;
#147735 = CARTESIAN_POINT ( 'NONE',  ( 16.53943276465976808, -0.05219959533910856209, 53.74890960531437401 ) ) ;
#147737 = CARTESIAN_POINT ( 'NONE',  ( -11.74264578624799782, -36.14014761921581709, -5.349999994537626868 ) ) ;
#147736 = CARTESIAN_POINT ( 'NONE',  ( 9.564922557960805705, 16.46253265017160317, 24.58224293864769194 ) ) ;
#147738 = CARTESIAN_POINT ( 'NONE',  ( 21.55341960407619695, -5.719274019375665929, 41.04275706135236135 ) ) ;
#147739 = CARTESIAN_POINT ( 'NONE',  ( 13.89961937509957401, 13.97604488694547697, 46.87609039468565442 ) ) ;
#147740 = CARTESIAN_POINT ( 'NONE',  ( 19.03943276465977164, -0.05219959533909143690, 28.74890960531435624 ) ) ;
#147741 = CARTESIAN_POINT ( 'NONE',  ( -15.80617190586768217, 15.72974639402176855, 88.12609039468570415 ) ) ;
#147742 = CARTESIAN_POINT ( 'NONE',  ( -16.51473224551069308, -9.474510206698971260, 21.66557627198102765 ) ) ;
#147743 = CARTESIAN_POINT ( 'NONE',  ( 8.314922557960818139, 14.29746914071049879, 44.58224293864769550 ) ) ;
#147744 = CARTESIAN_POINT ( 'NONE',  ( -11.40812507854755609, 35.11059874428196537, -1.524999997268813301 ) ) ;
#147745 = CARTESIAN_POINT ( 'NONE',  ( -21.55341960407610458, -5.719274019375992779, 46.45724293864769550 ) ) ;
#147746 = CARTESIAN_POINT ( 'NONE',  ( -17.14385361876520264, -23.59649016807271238, 143.1750000027311671 ) ) ;
#147747 = CARTESIAN_POINT ( 'NONE',  ( -9.564922557960796823, -16.46253265017161027, 87.08224293864769550 ) ) ;
#147748 = CARTESIAN_POINT ( 'NONE',  ( -8.314922557960811034, -14.29746914071050412, 92.08224293864769550 ) ) ;
#147749 = CARTESIAN_POINT ( 'NONE',  ( 8.224510206698742110, 14.34966873604972548, 22.08442372801901143 ) ) ;
#147750 = CARTESIAN_POINT ( 'NONE',  ( -21.53943276465977519, 0.05219959533907696930, 61.24890960531435979 ) ) ;
#147751 = EDGE_LOOP ( 'NONE', ( #161993, #1179, #137715, #29388 ) ) ;
#147752 = EDGE_CURVE ( 'NONE', #75168, #36560, #185946, .T. ) ;
#147753 = CARTESIAN_POINT ( 'NONE',  ( 13.89961937509977652, -13.97604488694527269, 33.12390960531434558 ) ) ;
#147755 = CARTESIAN_POINT ( 'NONE',  ( -18.62759615963270932, 10.81492255796079327, 90.83224293864769550 ) ) ;
#147754 = CARTESIAN_POINT ( 'NONE',  ( 0.05219959533909260263, 19.03943276465977164, 79.99890960531436690 ) ) ;
#147757 = CARTESIAN_POINT ( 'NONE',  ( -0.05219959533909027116, -19.03943276465977164, 97.49890960531436690 ) ) ;
#147756 = CARTESIAN_POINT ( 'NONE',  ( 14.34966873604960469, 8.224510206698951720, 29.16557627198103120 ) ) ;
#147758 = CARTESIAN_POINT ( 'NONE',  ( -16.46253265017146816, -9.564922557961047289, 74.16775706135234714 ) ) ;
#147759 = CARTESIAN_POINT ( 'NONE',  ( 5.719274019375673035, 21.55341960407619339, 112.2927570613523471 ) ) ;
#147760 = CARTESIAN_POINT ( 'NONE',  ( -5.719274019375978568, 21.55341960407610458, 70.20724293864769550 ) ) ;
#147761 = CARTESIAN_POINT ( 'NONE',  ( 5.719274019375991003, -21.55341960407610458, 37.70724293864769550 ) ) ;
#147762 = CARTESIAN_POINT ( 'NONE',  ( -9.564922557960796823, -16.46253265017161027, 52.08224293864768839 ) ) ;
#147763 = CARTESIAN_POINT ( 'NONE',  ( 8.314922557960818139, 14.29746914071049879, 24.58224293864768839 ) ) ;
#147764 = CARTESIAN_POINT ( 'NONE',  ( -5.049401038298153566, 19.05341960407611168, 75.20724293864769550 ) ) ;
#147765 = VERTEX_POINT ( 'NONE', #167276 ) ;
#147766 = CARTESIAN_POINT ( 'NONE',  ( 17.49999999999999645, -5.500000000000031086, 83.29690382534172954 ) ) ;
#147767 = CARTESIAN_POINT ( 'NONE',  ( 0.05219959533936267826, -19.03943276465977164, 30.00109039468566863 ) ) ;
#147768 = CARTESIAN_POINT ( 'NONE',  ( -12.06949235617756955, 12.14591786802309770, 85.62390960531436690 ) ) ;
#147769 = CARTESIAN_POINT ( 'NONE',  ( 5.823673210054444382, -21.52544592524334988, 20.20942372801900788 ) ) ;
#147770 = CARTESIAN_POINT ( 'NONE',  ( -8.571926809382608425, 26.38167802310805854, 142.9750000027312069 ) ) ;
#147771 = CARTESIAN_POINT ( 'NONE',  ( -21.55341960407610458, -5.719274019375992779, 61.45724293864770260 ) ) ;
#147772 = CARTESIAN_POINT ( 'NONE',  ( -8.314922557961024197, 14.29746914071037800, 87.91775706135234714 ) ) ;
#147773 = CARTESIAN_POINT ( 'NONE',  ( -12.14591786802309592, -12.06949235617757132, 111.8739096053143669 ) ) ;
#147774 = CARTESIAN_POINT ( 'NONE',  ( 9.474510206698971260, -16.51473224551069308, 72.91557627198102409 ) ) ;
#147775 = FACE_OUTER_BOUND ( 'NONE', #20155, .T. ) ;
#147776 = CARTESIAN_POINT ( 'NONE',  ( 14.34966873604960469, 8.224510206698951720, 24.16557627198103120 ) ) ;
#147777 = EDGE_CURVE ( 'NONE', #88586, #4577, #64462, .T. ) ;
#147778 = CARTESIAN_POINT ( 'NONE',  ( 21.55341960407619695, -5.719274019375665929, 56.04275706135235424 ) ) ;
#147779 = CARTESIAN_POINT ( 'NONE',  ( -19.03943276465977164, 0.05219959533909376836, 116.2489096053143669 ) ) ;
#147780 = CARTESIAN_POINT ( 'NONE',  ( -15.72974639402176322, -15.80617190586768395, 99.37609039468568994 ) ) ;
#147781 = CARTESIAN_POINT ( 'NONE',  ( 13.89961937509977652, -13.97604488694527269, 48.12390960531435979 ) ) ;
#147782 = CARTESIAN_POINT ( 'NONE',  ( -13.89961937509977652, 13.97604488694528158, 50.62390960531435979 ) ) ;
#147783 = VERTEX_POINT ( 'NONE', #139881 ) ;
#147784 = CARTESIAN_POINT ( 'NONE',  ( -15.72974639402176322, -15.80617190586768395, 99.37609039468568994 ) ) ;
#147785 = CARTESIAN_POINT ( 'NONE',  ( -16.55341960407617563, 4.379528057220093196, 63.54275706135234003 ) ) ;
#147786 = CARTESIAN_POINT ( 'NONE',  ( -21.53943276465977519, -0.05219959533937600094, 88.75109039468567573 ) ) ;
#147787 = CARTESIAN_POINT ( 'NONE',  ( -5.719274019375978568, 21.55341960407610458, 25.20724293864769550 ) ) ;
#147788 = CARTESIAN_POINT ( 'NONE',  ( -5.153800228976607833, 19.02544592524334988, 92.70942372801901854 ) ) ;
#147789 = CARTESIAN_POINT ( 'NONE',  ( -5.719274019375665041, -21.55341960407619695, 49.79275706135234714 ) ) ;
#147790 = CARTESIAN_POINT ( 'NONE',  ( -4.483927247898782831, 16.52544592524335698, 42.70942372801901854 ) ) ;
#147791 = CARTESIAN_POINT ( 'NONE',  ( 21.55341960407610458, 5.719274019375980345, 83.95724293864770971 ) ) ;
#147792 = CARTESIAN_POINT ( 'NONE',  ( -19.03943276465977164, -0.05219959533935918106, 83.75109039468567573 ) ) ;
#147793 = CARTESIAN_POINT ( 'NONE',  ( 5.153800228976335163, 19.02544592524342804, 64.79057627198100988 ) ) ;
#147794 = CARTESIAN_POINT ( 'NONE',  ( 13.97604488694548053, -13.89961937509957401, 100.6260903946856615 ) ) ;
#147795 = AXIS2_PLACEMENT_3D ( 'NONE', #11524, #195541, #26688 ) ;
#147796 = CARTESIAN_POINT ( 'NONE',  ( 16.46253265017146816, 9.564922557961045513, 91.66775706135234714 ) ) ;
#147797 = CARTESIAN_POINT ( 'NONE',  ( 16.53943276465976808, -0.05219959533910856209, 48.74890960531435979 ) ) ;
#147798 = CARTESIAN_POINT ( 'NONE',  ( 19.02544592524334988, 5.153800228976608722, 76.45942372801897591 ) ) ;
#147799 = CARTESIAN_POINT ( 'NONE',  ( 8.224510206698742110, 14.34966873604972548, 62.08442372801901143 ) ) ;
#147800 = CARTESIAN_POINT ( 'NONE',  ( 5.153800228976615827, -19.02544592524334988, 25.20942372801900433 ) ) ;
#147801 = CARTESIAN_POINT ( 'NONE',  ( 13.97604488694527802, 13.89961937509977652, 44.37390960531435269 ) ) ;
#147802 = CARTESIAN_POINT ( 'NONE',  ( -16.51473224551069308, -9.474510206698971260, 46.66557627198102409 ) ) ;
#147803 = CARTESIAN_POINT ( 'NONE',  ( 12.06949235617739724, 12.14591786802326823, 61.87609039468568284 ) ) ;
#147804 = DIRECTION ( 'NONE',  ( 0.000000000000000000, -0.8164965809277221487, 0.5773502691896313932 ) ) ;
#147805 = CARTESIAN_POINT ( 'NONE',  ( -8.571926809382608425, 26.38167802310805854, 148.4750000027311785 ) ) ;
#147806 = CARTESIAN_POINT ( 'NONE',  ( 13.97604488694527802, 13.89961937509977652, 104.3739096053143385 ) ) ;
#147807 = DIRECTION ( 'NONE',  ( -0.000000000000000000, 0.000000000000000000, 1.000000000000000000 ) ) ;
#147808 = VERTEX_POINT ( 'NONE', #143866 ) ;
#147809 = CARTESIAN_POINT ( 'NONE',  ( -16.46253265017146816, -9.564922557961047289, 94.16775706135233293 ) ) ;
#147810 = CARTESIAN_POINT ( 'NONE',  ( 0.05219959533907565091, 21.53943276465977519, 39.99890960531436690 ) ) ;
#147812 = CARTESIAN_POINT ( 'NONE',  ( 16.51473224551083163, -9.474510206698727899, 105.8344237280190043 ) ) ;
#147811 = CARTESIAN_POINT ( 'NONE',  ( 5.049401038297881783, 19.05341960407617563, 32.29275706135233293 ) ) ;
#147813 = CARTESIAN_POINT ( 'NONE',  ( -13.97604488694527625, -13.89961937509977652, 31.87390960531435979 ) ) ;
#147814 = CARTESIAN_POINT ( 'NONE',  ( 16.51473224551069308, 9.474510206698969483, 44.16557627198103120 ) ) ;
#147815 = CARTESIAN_POINT ( 'NONE',  ( -21.53943276465977519, 0.05219959533907696930, 66.24890960531436690 ) ) ;
#147816 = CARTESIAN_POINT ( 'NONE',  ( -0.05219959533909027116, -19.03943276465977164, 97.49890960531436690 ) ) ;
#147817 = CARTESIAN_POINT ( 'NONE',  ( 16.46253265017160672, -9.564922557960803928, 38.33224293864768839 ) ) ;
#147818 = CARTESIAN_POINT ( 'NONE',  ( 22.44159573604009594, -16.30477369853687364, 144.1750000027311671 ) ) ;
#147819 = CARTESIAN_POINT ( 'NONE',  ( -9.474510206698720793, -16.51473224551083518, 84.58442372801900433 ) ) ;
#147821 = VECTOR ( 'NONE', #198093, 1000.000000000000000 ) ;
#147820 = CARTESIAN_POINT ( 'NONE',  ( 16.53943276465976808, -0.05219959533910856209, 48.74890960531435979 ) ) ;
#147822 = CARTESIAN_POINT ( 'NONE',  ( 18.67979575497178502, 10.72451020669898547, 29.16557627198103120 ) ) ;
#147823 = CARTESIAN_POINT ( 'NONE',  ( -21.55341960407619339, 5.719274019375674811, 103.5427570613523613 ) ) ;
#147824 = CARTESIAN_POINT ( 'NONE',  ( -0.05219959533907301413, -21.53943276465977519, 102.4989096053143811 ) ) ;
#147825 = CARTESIAN_POINT ( 'NONE',  ( -5.719274019375665041, -21.55341960407619695, 74.79275706135234714 ) ) ;
#147826 = CARTESIAN_POINT ( 'NONE',  ( 15.72974639402176855, 15.80617190586768217, 76.87609039468567573 ) ) ;
#147827 = CARTESIAN_POINT ( 'NONE',  ( -16.46253265017160317, 9.564922557960807481, 115.8322429386477097 ) ) ;
#147829 = CARTESIAN_POINT ( 'NONE',  ( 5.719274019375673035, 21.55341960407619339, 57.29275706135234714 ) ) ;
#147828 = CARTESIAN_POINT ( 'NONE',  ( -14.34966873604972548, 8.224510206698743886, 108.3344237280190185 ) ) ;
#147830 = CARTESIAN_POINT ( 'NONE',  ( -9.564922557960796823, -16.46253265017161027, 72.08224293864770971 ) ) ;
#147831 = CARTESIAN_POINT ( 'NONE',  ( -19.05341960407617563, 5.049401038297882671, 38.54275706135233293 ) ) ;
#147832 = CARTESIAN_POINT ( 'NONE',  ( -0.05219959533937732626, 21.53943276465977519, 27.50109039468567929 ) ) ;
#147833 = CARTESIAN_POINT ( 'NONE',  ( -0.05219959533909027116, -19.03943276465977164, 62.49890960531435979 ) ) ;
#147834 = CARTESIAN_POINT ( 'NONE',  ( 14.34966873604960469, 8.224510206698951720, 84.16557627198103830 ) ) ;
#147835 = CARTESIAN_POINT ( 'NONE',  ( -16.52544592524342804, 4.483927247898546575, 41.04057627198103120 ) ) ;
#147836 = CARTESIAN_POINT ( 'NONE',  ( -21.55341960407610458, -5.719274019375992779, 51.45724293864770260 ) ) ;
#147837 = CARTESIAN_POINT ( 'NONE',  ( 5.153800228976335163, 19.02544592524342804, 64.79057627198100988 ) ) ;
#147838 = CARTESIAN_POINT ( 'NONE',  ( 18.62759615963271287, -10.81492255796078972, 78.33224293864770971 ) ) ;
#147839 = CARTESIAN_POINT ( 'NONE',  ( -19.02544592524334988, -5.153800228976617603, 53.95942372801898301 ) ) ;
#147841 = CARTESIAN_POINT ( 'NONE',  ( -14.34966873604960291, -8.224510206698953496, 56.66557627198103830 ) ) ;
#147840 = CARTESIAN_POINT ( 'NONE',  ( 13.89961937509957579, 13.97604488694547520, 21.87609039468566152 ) ) ;
#147842 = CARTESIAN_POINT ( 'NONE',  ( 10.72451020669898902, -18.67979575497178502, 42.91557627198103120 ) ) ;
#147843 = ORIENTED_EDGE ( 'NONE', *, *, #61909, .F. ) ;
#147844 = DIRECTION ( 'NONE',  ( 0.000000000000000000, -1.000000000000000000, 0.000000000000000000 ) ) ;
#147846 = CARTESIAN_POINT ( 'NONE',  ( 27.73933785331498925, -9.013057229001034898, 147.7750000027311899 ) ) ;
#147845 = CARTESIAN_POINT ( 'NONE',  ( 14.34966873604972726, -8.224510206698740333, 85.83442372801901854 ) ) ;
#147847 = CARTESIAN_POINT ( 'NONE',  ( 5.153800228976615827, -19.02544592524334988, 90.20942372801900433 ) ) ;
#147848 = CARTESIAN_POINT ( 'NONE',  ( 16.53943276465976808, -0.05219959533910856209, 58.74890960531436690 ) ) ;
#147849 = CARTESIAN_POINT ( 'NONE',  ( -3.573655867282028392E-15, 2.428612866367529932E-14, -25.00000000000000000 ) ) ;
#147850 = CARTESIAN_POINT ( 'NONE',  ( 13.97604488694527802, 13.89961937509977652, 44.37390960531435269 ) ) ;
#147851 = CARTESIAN_POINT ( 'NONE',  ( -12.14591786802309592, -12.06949235617757132, 41.87390960531435979 ) ) ;
#147852 = CARTESIAN_POINT ( 'NONE',  ( 9.474510206698971260, -16.51473224551069308, 87.91557627198102409 ) ) ;
#147853 = CARTESIAN_POINT ( 'NONE',  ( -13.97604488694527625, -13.89961937509977652, 51.87390960531436690 ) ) ;
#147854 = CARTESIAN_POINT ( 'NONE',  ( -5.823673210054431948, 21.52544592524334988, 57.70942372801901143 ) ) ;
#147855 = CARTESIAN_POINT ( 'NONE',  ( 19.02544592524343514, -5.153800228976328945, 78.54057627198099567 ) ) ;
#147856 = CARTESIAN_POINT ( 'NONE',  ( -19.03943276465977164, 0.05219959533909376836, 26.24890960531435624 ) ) ;
#147857 = CARTESIAN_POINT ( 'NONE',  ( 19.03943276465977164, -0.05219959533909143690, 73.74890960531435269 ) ) ;
#147858 = ADVANCED_FACE ( 'NONE', ( #66031 ), #1370, .F. ) ;
#147859 = CARTESIAN_POINT ( 'NONE',  ( -18.67979575497178146, -10.72451020669898902, 46.66557627198102409 ) ) ;
#147860 = CARTESIAN_POINT ( 'NONE',  ( 9.474510206698971260, -16.51473224551069308, 32.91557627198102409 ) ) ;
#147861 = CARTESIAN_POINT ( 'NONE',  ( -10.81492255796078084, -18.62759615963271287, 47.08224293864770260 ) ) ;
#147862 = CARTESIAN_POINT ( 'NONE',  ( 16.55341960407618274, -4.379528057220086978, 101.0427570613523756 ) ) ;
#147863 = CARTESIAN_POINT ( 'NONE',  ( 9.564922557961047289, -16.46253265017146816, 25.41775706135234003 ) ) ;
#147865 = CARTESIAN_POINT ( 'NONE',  ( -16.52544592524335698, -4.483927247898792601, 73.95942372801901854 ) ) ;
#147864 = CARTESIAN_POINT ( 'NONE',  ( 14.34966873604972726, -8.224510206698740333, 45.83442372801901854 ) ) ;
#147866 = FACE_OUTER_BOUND ( 'NONE', #180160, .T. ) ;
#147867 = CARTESIAN_POINT ( 'NONE',  ( 16.53943276465976808, 0.05219959533934440121, 71.25109039468568994 ) ) ;
#147868 = CARTESIAN_POINT ( 'NONE',  ( 10.81492255796078972, 18.62759615963270932, 24.58224293864768839 ) ) ;
#147869 = CARTESIAN_POINT ( 'NONE',  ( -5.153800228976328057, -19.02544592524343514, 37.29057627198102409 ) ) ;
#147870 = CARTESIAN_POINT ( 'NONE',  ( 8.314922557961029526, -14.29746914071037800, 35.41775706135234003 ) ) ;
#147871 = CARTESIAN_POINT ( 'NONE',  ( 19.02544592524343514, -5.153800228976328945, 48.54057627198103120 ) ) ;
#147872 = CARTESIAN_POINT ( 'NONE',  ( 21.53943276465977519, 0.05219959533937863772, 46.25109039468567573 ) ) ;
#147873 = CARTESIAN_POINT ( 'NONE',  ( -14.29746914071037622, -8.314922557961029526, 34.16775706135234714 ) ) ;
#147874 = CARTESIAN_POINT ( 'NONE',  ( -16.55341960407617563, 4.379528057220093196, 103.5427570613523613 ) ) ;
#147875 = CARTESIAN_POINT ( 'NONE',  ( -4.999999999999999112, -140.0000000000000000, 0.0009999999999992653654 ) ) ;
#147876 = CARTESIAN_POINT ( 'NONE',  ( 15.80617190586769283, -15.72974639402175789, 95.62609039468568994 ) ) ;
#147877 = CARTESIAN_POINT ( 'NONE',  ( 13.89961937509957401, 13.97604488694547697, 101.8760903946856331 ) ) ;
#147878 = CARTESIAN_POINT ( 'NONE',  ( -5.049401038297874678, -19.05341960407617918, 49.79275706135231871 ) ) ;
#147879 = CARTESIAN_POINT ( 'NONE',  ( -12.06949235617756955, 12.14591786802309770, 75.62390960531439532 ) ) ;
#147880 = CARTESIAN_POINT ( 'NONE',  ( 0.05219959533909260263, 19.03943276465977164, 29.99890960531435979 ) ) ;
#147882 = CARTESIAN_POINT ( 'NONE',  ( -27.29906736325805383, 2.072701884453516521E-14, 169.9999999999999716 ) ) ;
#147881 = CARTESIAN_POINT ( 'NONE',  ( 19.02544592524334988, 5.153800228976608722, 56.45942372801898301 ) ) ;
#147883 = CARTESIAN_POINT ( 'NONE',  ( -5.823673210054431948, 21.52544592524334988, 57.70942372801901143 ) ) ;
#147884 = CARTESIAN_POINT ( 'NONE',  ( -16.52544592524335698, -4.483927247898792601, 23.95942372801901143 ) ) ;
#147885 = DIRECTION ( 'NONE',  ( 0.000000000000000000, 1.224646799147330774E-16, 1.000000000000000000 ) ) ;
#147886 = CARTESIAN_POINT ( 'NONE',  ( 10.81492255796078972, 18.62759615963270932, 24.58224293864768839 ) ) ;
#147887 = CARTESIAN_POINT ( 'NONE',  ( -19.02544592524334988, -5.153800228976617603, 103.9594237280190043 ) ) ;
#147888 = CARTESIAN_POINT ( 'NONE',  ( -13.89961937509977652, 13.97604488694528158, 115.6239096053143669 ) ) ;
#147889 = DIRECTION ( 'NONE',  ( -0.1178549842436478201, -0.9930308165857339997, -0.000000000000000000 ) ) ;
#147890 = CARTESIAN_POINT ( 'NONE',  ( -14.29746914071049879, 8.314922557960819915, 115.8322429386477097 ) ) ;
#147891 = CARTESIAN_POINT ( 'NONE',  ( -19.02544592524334988, -5.153800228976617603, 18.95942372801899722 ) ) ;
#147892 = CARTESIAN_POINT ( 'NONE',  ( -9.564922557960796823, -16.46253265017161027, 57.08224293864769550 ) ) ;
#147893 = CARTESIAN_POINT ( 'NONE',  ( 21.53943276465977519, 0.05219959533937863772, 66.25109039468567573 ) ) ;
#147894 = CARTESIAN_POINT ( 'NONE',  ( -21.53943276465977519, -0.05219959533937600094, 108.7510903946857042 ) ) ;
#147895 = CARTESIAN_POINT ( 'NONE',  ( -12.06949235617756955, 12.14591786802309770, 25.62390960531435624 ) ) ;
#147896 = CARTESIAN_POINT ( 'NONE',  ( -5.049401038298153566, 19.05341960407611168, 80.20724293864769550 ) ) ;
#147897 = CARTESIAN_POINT ( 'NONE',  ( 0.05219959533937995610, -21.53943276465977519, 55.00109039468568284 ) ) ;
#147898 = CARTESIAN_POINT ( 'NONE',  ( 5.823673210054444382, -21.52544592524334988, 50.20942372801901854 ) ) ;
#147900 = CARTESIAN_POINT ( 'NONE',  ( -16.46253265017160317, 9.564922557960807481, 110.8322429386476955 ) ) ;
#147899 = CARTESIAN_POINT ( 'NONE',  ( 19.05341960407617918, -5.049401038297876454, 76.04275706135230450 ) ) ;
#147901 = CARTESIAN_POINT ( 'NONE',  ( 0.05219959533910956823, 16.53943276465976808, 114.9989096053143669 ) ) ;
#147902 = CARTESIAN_POINT ( 'NONE',  ( 21.53943276465977519, -0.05219959533907433946, 98.74890960531438111 ) ) ;
#147903 = CARTESIAN_POINT ( 'NONE',  ( -13.97604488694547697, 13.89961937509957934, 23.12609039468565442 ) ) ;
#147904 = CARTESIAN_POINT ( 'NONE',  ( -16.52544592524342804, 4.483927247898546575, 101.0405762719810383 ) ) ;
#147905 = CARTESIAN_POINT ( 'NONE',  ( -19.03943276465977164, 0.05219959533909376836, 46.24890960531435979 ) ) ;
#147906 = CARTESIAN_POINT ( 'NONE',  ( 5.049401038297881783, 19.05341960407617563, 97.29275706135233293 ) ) ;
#147907 = CARTESIAN_POINT ( 'NONE',  ( -16.53943276465976808, 0.05219959533911058130, 66.24890960531436690 ) ) ;
#147908 = CARTESIAN_POINT ( 'NONE',  ( 18.62759615963255655, 10.81492255796105972, 106.6677570613523756 ) ) ;
#147909 = CARTESIAN_POINT ( 'NONE',  ( 19.05341960407611168, 5.049401038298154454, 98.95724293864766707 ) ) ;
#147910 = CARTESIAN_POINT ( 'NONE',  ( -5.049401038297874678, -19.05341960407617918, 74.79275706135231871 ) ) ;
#147911 = CARTESIAN_POINT ( 'NONE',  ( -18.67979575497178146, -10.72451020669898902, 91.66557627198103830 ) ) ;
#147912 = CARTESIAN_POINT ( 'NONE',  ( -18.67979575497193778, 10.72451020669871902, 48.33442372801902565 ) ) ;
#147913 = CARTESIAN_POINT ( 'NONE',  ( -4.483927247898782831, 16.52544592524335698, 47.70942372801902565 ) ) ;
#147914 = CARTESIAN_POINT ( 'NONE',  ( -0.05219959533934338120, 16.53943276465976808, 87.50109039468568994 ) ) ;
#147916 = CARTESIAN_POINT ( 'NONE',  ( 10.72451020669871369, 18.67979575497193778, 32.08442372801901854 ) ) ;
#147915 = CARTESIAN_POINT ( 'NONE',  ( 16.53943276465976808, 0.05219959533934440121, 46.25109039468567573 ) ) ;
#147917 = CARTESIAN_POINT ( 'NONE',  ( 10.72451020669898902, -18.67979575497178502, 47.91557627198102409 ) ) ;
#147918 = CARTESIAN_POINT ( 'NONE',  ( -5.153800228976328057, -19.02544592524343514, 32.29057627198102409 ) ) ;
#147919 = CARTESIAN_POINT ( 'NONE',  ( -38.00000000000001421, -12.34694845685042708, -9.649999994537626691 ) ) ;
#147920 = CARTESIAN_POINT ( 'NONE',  ( -14.34966873604972548, 8.224510206698743886, 58.33442372801901143 ) ) ;
#147921 = CARTESIAN_POINT ( 'NONE',  ( -5.719274019375978568, 21.55341960407610458, 85.20724293864770971 ) ) ;
#147922 = CARTESIAN_POINT ( 'NONE',  ( 16.53943276465976808, -0.05219959533910856209, 43.74890960531435979 ) ) ;
#147923 = CARTESIAN_POINT ( 'NONE',  ( 8.314922557961029526, -14.29746914071037800, 60.41775706135235424 ) ) ;
#147924 = CARTESIAN_POINT ( 'NONE',  ( -13.97604488694527625, -13.89961937509977652, 61.87390960531435979 ) ) ;
#147925 = CARTESIAN_POINT ( 'NONE',  ( -9.564922557961040184, 16.46253265017147172, 92.91775706135233293 ) ) ;
#147926 = CARTESIAN_POINT ( 'NONE',  ( 21.55341960407610458, 5.719274019375980345, 78.95724293864769550 ) ) ;
#147927 = CARTESIAN_POINT ( 'NONE',  ( -16.55341960407611168, -4.379528057220339221, 36.45724293864768839 ) ) ;
#147928 = ORIENTED_EDGE ( 'NONE', *, *, #62085, .F. ) ;
#147929 = DIRECTION ( 'NONE',  ( -0.000000000000000000, -1.000000000000000000, 0.000000000000000000 ) ) ;
#147930 = CARTESIAN_POINT ( 'NONE',  ( 18.62759615963271287, -10.81492255796078972, 63.33224293864770260 ) ) ;
#147931 = ORIENTED_EDGE ( 'NONE', *, *, #59992, .T. ) ;
#147932 = CARTESIAN_POINT ( 'NONE',  ( 14.34966873604972726, -8.224510206698740333, 110.8344237280190043 ) ) ;
#147933 = ORIENTED_EDGE ( 'NONE', *, *, #7594, .F. ) ;
#147934 = CARTESIAN_POINT ( 'NONE',  ( 19.34837522270367671, 5.499999999999739764, 88.36337684832572847 ) ) ;
#147935 = CARTESIAN_POINT ( 'NONE',  ( -21.53943276465977519, 0.05219959533907696930, 86.24890960531436690 ) ) ;
#147936 = CARTESIAN_POINT ( 'NONE',  ( 8.314922557960818139, 14.29746914071049879, 24.58224293864768839 ) ) ;
#147937 = CARTESIAN_POINT ( 'NONE',  ( 16.55341960407618274, -4.379528057220086978, 36.04275706135234714 ) ) ;
#147938 = CARTESIAN_POINT ( 'NONE',  ( 16.46253265017160672, -9.564922557960803928, 38.33224293864768839 ) ) ;
#147939 = CARTESIAN_POINT ( 'NONE',  ( 5.153800228976335163, 19.02544592524342804, 64.79057627198100988 ) ) ;
#147940 = CARTESIAN_POINT ( 'NONE',  ( -17.81289503416611808, 24.51734667627700404, 145.6999999999999886 ) ) ;
#147941 = CARTESIAN_POINT ( 'NONE',  ( -9.564922557960796823, -16.46253265017161027, 112.0822429386476955 ) ) ;
#147942 = CARTESIAN_POINT ( 'NONE',  ( 0.7923078531248324285, 29.12150355453722028, -52.41032305705210348 ) ) ;
#147943 = CARTESIAN_POINT ( 'NONE',  ( -16.53943276465976808, -0.05219959533934237506, 98.75109039468568994 ) ) ;
#147944 = CARTESIAN_POINT ( 'NONE',  ( 16.51473224551083163, -9.474510206698727899, 105.8344237280190043 ) ) ;
#147945 = CARTESIAN_POINT ( 'NONE',  ( -13.97604488694547697, 13.89961937509957934, 38.12609039468566152 ) ) ;
#147946 = CARTESIAN_POINT ( 'NONE',  ( 21.52544592524344225, -5.823673210054117533, 83.54057627198102409 ) ) ;
#147947 = CARTESIAN_POINT ( 'NONE',  ( 8.224510206698742110, 14.34966873604972548, 112.0844237280190185 ) ) ;
#147948 = CARTESIAN_POINT ( 'NONE',  ( 0.05219959533907565091, 21.53943276465977519, 44.99890960531435979 ) ) ;
#147950 = CARTESIAN_POINT ( 'NONE',  ( -5.153800228976607833, 19.02544592524334988, 112.7094237280190043 ) ) ;
#147949 = CARTESIAN_POINT ( 'NONE',  ( -21.52544592524343514, 5.823673210054127303, 81.04057627198102409 ) ) ;
#147951 = CARTESIAN_POINT ( 'NONE',  ( -16.51473224551069308, -9.474510206698971260, 101.6655762719810241 ) ) ;
#147952 = CARTESIAN_POINT ( 'NONE',  ( 10.72451020669871369, 18.67979575497193778, 82.08442372801901854 ) ) ;
#147953 = CARTESIAN_POINT ( 'NONE',  ( -9.474510206698964154, 16.51473224551069663, 55.41557627198103120 ) ) ;
#147954 = CARTESIAN_POINT ( 'NONE',  ( 16.53943276465976808, -0.05219959533910856209, 103.7489096053143669 ) ) ;
#147955 = CARTESIAN_POINT ( 'NONE',  ( 31.65987002919143478, 2.420393710425480904, 102.1029948765363713 ) ) ;
#147956 = CARTESIAN_POINT ( 'NONE',  ( -13.97604488694527625, -13.89961937509977652, 71.87390960531433848 ) ) ;
#147957 = CARTESIAN_POINT ( 'NONE',  ( -14.29746914071049879, 8.314922557960819915, 95.83224293864770971 ) ) ;
#147958 = VERTEX_POINT ( 'NONE', #2374 ) ;
#147959 = CARTESIAN_POINT ( 'NONE',  ( 16.51473224551083163, -9.474510206698727899, 90.83442372801900433 ) ) ;
#147960 = DIRECTION ( 'NONE',  ( 0.000000000000000000, 0.000000000000000000, 1.000000000000000000 ) ) ;
#147961 = CARTESIAN_POINT ( 'NONE',  ( 9.474510206698971260, -16.51473224551069308, 62.91557627198102409 ) ) ;
#147962 = CIRCLE ( 'NONE', #54418, 24.30000000000003268 ) ;
#147964 = CARTESIAN_POINT ( 'NONE',  ( 16.46253265017160672, -9.564922557960803928, 98.33224293864769550 ) ) ;
#147963 = CARTESIAN_POINT ( 'NONE',  ( -10.81492255796105439, 18.62759615963255655, 82.91775706135234714 ) ) ;
#147965 = CARTESIAN_POINT ( 'NONE',  ( 14.34966873604972726, -8.224510206698740333, 75.83442372801900433 ) ) ;
#147966 = CARTESIAN_POINT ( 'NONE',  ( -16.31925111598457789, -7.325300261831486637, 49.83575461032751264 ) ) ;
#147967 = CARTESIAN_POINT ( 'NONE',  ( -16.51473224551082808, 9.474510206698731452, 48.33442372801900433 ) ) ;
#147968 = CARTESIAN_POINT ( 'NONE',  ( -21.52544592524334988, -5.823673210054445271, 103.9594237280190185 ) ) ;
#147969 = CARTESIAN_POINT ( 'NONE',  ( 17.23854840241255815, -15.08343195521229774, -57.79379418917771005 ) ) ;
#147970 = CARTESIAN_POINT ( 'NONE',  ( -23.48529157249599919, -32.32473071737749848, -7.449999994537625625 ) ) ;
#147971 = CARTESIAN_POINT ( 'NONE',  ( -12.14591786802326823, 12.06949235617739902, 98.12609039468570415 ) ) ;
#147972 = CARTESIAN_POINT ( 'NONE',  ( 16.08916976210840843, -1.211883243535162524, -59.40465844715060229 ) ) ;
#147973 = CARTESIAN_POINT ( 'NONE',  ( 8.224510206698742110, 14.34966873604972548, 87.08442372801901854 ) ) ;
#147974 = CARTESIAN_POINT ( 'NONE',  ( 32.86279873472853552, -22.80822080465439328, -22.12545596063183240 ) ) ;
#147975 = CARTESIAN_POINT ( 'NONE',  ( -0.05219959533934338120, 16.53943276465976808, 67.50109039468568994 ) ) ;
#147976 = ORIENTED_EDGE ( 'NONE', *, *, #58944, .F. ) ;
#147977 = CARTESIAN_POINT ( 'NONE',  ( -10.72451020669870658, -18.67979575497194134, 74.58442372801901854 ) ) ;
#147978 = CARTESIAN_POINT ( 'NONE',  ( -5.049401038297874678, -19.05341960407617918, 84.79275706135233293 ) ) ;
#147979 = CARTESIAN_POINT ( 'NONE',  ( -13.97604488694547697, 13.89961937509957934, 28.12609039468565797 ) ) ;
#147980 = CARTESIAN_POINT ( 'NONE',  ( -9.564922557960796823, -16.46253265017161027, 72.08224293864770971 ) ) ;
#147981 = CARTESIAN_POINT ( 'NONE',  ( 19.03943276465977164, -0.05219959533909143690, 58.74890960531435979 ) ) ;
#147982 = CARTESIAN_POINT ( 'NONE',  ( 17.23220907382109957, -6.508304012115882387, 23.29902788568567473 ) ) ;
#147983 = CARTESIAN_POINT ( 'NONE',  ( 5.823673210054125526, 21.52544592524343514, 74.79057627198105251 ) ) ;
#147984 = CARTESIAN_POINT ( 'NONE',  ( -5.823673210054116645, -21.52544592524344225, 32.29057627198102409 ) ) ;
#147985 = CARTESIAN_POINT ( 'NONE',  ( -5.153800228976328057, -19.02544592524343514, 32.29057627198102409 ) ) ;
#147986 = CARTESIAN_POINT ( 'NONE',  ( 8.314922557961029526, -14.29746914071037800, 70.41775706135236135 ) ) ;
#147987 = ORIENTED_EDGE ( 'NONE', *, *, #175772, .F. ) ;
#147988 = CARTESIAN_POINT ( 'NONE',  ( -15.72974639402176322, -15.80617190586768395, 29.37609039468568284 ) ) ;
#147990 = CARTESIAN_POINT ( 'NONE',  ( -5.950531402560715689E-15, 38.81732327939063509, -9.124999997268815832 ) ) ;
#147989 = CARTESIAN_POINT ( 'NONE',  ( 8.314922557960818139, 14.29746914071049879, 69.58224293864769550 ) ) ;
#147991 = CARTESIAN_POINT ( 'NONE',  ( 14.34966873604972726, -8.224510206698740333, 20.83442372801901143 ) ) ;
#147992 = CARTESIAN_POINT ( 'NONE',  ( -19.03943276465977164, -0.05219959533935918106, 58.75109039468566863 ) ) ;
#147993 = CARTESIAN_POINT ( 'NONE',  ( -12.06949235617756955, 12.14591786802309770, 55.62390960531436690 ) ) ;
#147994 = CARTESIAN_POINT ( 'NONE',  ( -18.67979575497193778, 10.72451020669871902, 28.33442372801902209 ) ) ;
#147996 = CARTESIAN_POINT ( 'NONE',  ( -10.81492255796078084, -18.62759615963271287, 77.08224293864769550 ) ) ;
#147995 = CARTESIAN_POINT ( 'NONE',  ( -18.96320343559654731, -23.46320343559632704, 8.889087296526001936 ) ) ;
#147997 = CARTESIAN_POINT ( 'NONE',  ( 5.153800228976335163, 19.02544592524342804, 104.7905762719809957 ) ) ;
#147998 = CARTESIAN_POINT ( 'NONE',  ( 14.34966873604960469, 8.224510206698951720, 59.16557627198103120 ) ) ;
#147999 = CARTESIAN_POINT ( 'NONE',  ( 37.91032098691110264, -19.19859865632790630, -20.09511994390771150 ) ) ;
#148000 = LINE ( 'NONE', #24662, #37553 ) ;
#148001 = CARTESIAN_POINT ( 'NONE',  ( -0.05219959533936034679, 19.03943276465977164, 62.50109039468566863 ) ) ;
#148002 = CARTESIAN_POINT ( 'NONE',  ( 10.81492255796078972, 18.62759615963270932, 104.5822429386477097 ) ) ;
#148003 = CARTESIAN_POINT ( 'NONE',  ( -19.02544592524342804, 5.153800228976336051, 61.04057627198103120 ) ) ;
#148004 = CARTESIAN_POINT ( 'NONE',  ( 0.05219959533936267826, -19.03943276465977164, 40.00109039468566152 ) ) ;
#148005 = CARTESIAN_POINT ( 'NONE',  ( -0.05219959533909027116, -19.03943276465977164, 27.49890960531435624 ) ) ;
#148006 = CARTESIAN_POINT ( 'NONE',  ( -15.72974639402176322, -15.80617190586768395, 69.37609039468567573 ) ) ;
#148007 = CARTESIAN_POINT ( 'NONE',  ( -17.05587630539786659, -6.762274262135686165, 69.25819690962687503 ) ) ;
#148008 = CARTESIAN_POINT ( 'NONE',  ( -14.34966873604960291, -8.224510206698953496, 41.66557627198103120 ) ) ;
#148009 = CARTESIAN_POINT ( 'NONE',  ( 19.02544592524343514, -5.153800228976328945, 58.54057627198102409 ) ) ;
#148010 = CARTESIAN_POINT ( 'NONE',  ( 15.72974639402199770, -15.80617190586745480, 78.12390960531436690 ) ) ;
#148011 = CARTESIAN_POINT ( 'NONE',  ( 19.02544592524343514, -5.153800228976328945, 63.54057627198103830 ) ) ;
#148012 = CARTESIAN_POINT ( 'NONE',  ( -18.67979575497178146, -10.72451020669898902, 71.66557627198100988 ) ) ;
#148013 = EDGE_CURVE ( 'NONE', #146762, #37464, #169766, .T. ) ;
#148014 = CARTESIAN_POINT ( 'NONE',  ( -15.72974639402176322, -15.80617190586768395, 104.3760903946856899 ) ) ;
#148017 = CARTESIAN_POINT ( 'NONE',  ( -4.483927247898539470, -16.52544592524342804, 87.29057627198103830 ) ) ;
#148016 = CARTESIAN_POINT ( 'NONE',  ( 16.52544592524335698, 4.483927247898782831, 91.45942372801901854 ) ) ;
#148015 = CARTESIAN_POINT ( 'NONE',  ( 4.347827484049394897, -37.01609572857267239, -32.59999999895043743 ) ) ;
#148018 = CARTESIAN_POINT ( 'NONE',  ( 16.51473224551083163, -9.474510206698727899, 95.83442372801900433 ) ) ;
#148019 = ORIENTED_EDGE ( 'NONE', *, *, #200190, .T. ) ;
#148020 = CARTESIAN_POINT ( 'NONE',  ( -19.05341960407617563, 5.049401038297882671, 33.54275706135231871 ) ) ;
#148021 = CARTESIAN_POINT ( 'NONE',  ( 12.06949235617739724, 12.14591786802326823, 101.8760903946857042 ) ) ;
#148022 = CARTESIAN_POINT ( 'NONE',  ( -19.03943276465977164, -0.05219959533935918106, 28.75109039468566507 ) ) ;
#148023 = CARTESIAN_POINT ( 'NONE',  ( -5.049401038298153566, 19.05341960407611168, 90.20724293864766707 ) ) ;
#148024 = CARTESIAN_POINT ( 'NONE',  ( 5.823673210054125526, 21.52544592524343514, 64.79057627198103830 ) ) ;
#148025 = CARTESIAN_POINT ( 'NONE',  ( 27.60098488412532447, -5.861468761074972278, 164.8187539380760143 ) ) ;
#148026 = CARTESIAN_POINT ( 'NONE',  ( -14.34966873604960291, -8.224510206698953496, 111.6655762719810525 ) ) ;
#148027 = CARTESIAN_POINT ( 'NONE',  ( -10.81492255796105439, 18.62759615963255655, 92.91775706135236135 ) ) ;
#148028 = CARTESIAN_POINT ( 'NONE',  ( 16.53943276465976808, 0.05219959533934440121, 71.25109039468568994 ) ) ;
#148029 = CARTESIAN_POINT ( 'NONE',  ( -21.52544592524334988, -5.823673210054445271, 28.95942372801902209 ) ) ;
#148030 = CARTESIAN_POINT ( 'NONE',  ( 0.05219959533934541429, -16.53943276465976808, 25.00109039468567218 ) ) ;
#148031 = CARTESIAN_POINT ( 'NONE',  ( -5.049401038298153566, 19.05341960407611168, 110.2072429386476671 ) ) ;
#148032 = CARTESIAN_POINT ( 'NONE',  ( 9.474510206698971260, -16.51473224551069308, 37.91557627198102409 ) ) ;
#148033 = CARTESIAN_POINT ( 'NONE',  ( -13.89961937509977652, 13.97604488694528158, 55.62390960531434558 ) ) ;
#148034 = CARTESIAN_POINT ( 'NONE',  ( -14.34966873604972548, 8.224510206698743886, 53.33442372801901854 ) ) ;
#148035 = CARTESIAN_POINT ( 'NONE',  ( 16.52544592524342804, -4.483927247898539470, 88.54057627198103830 ) ) ;
#148036 = CARTESIAN_POINT ( 'NONE',  ( 8.314922557961029526, -14.29746914071037800, 100.4177570613523471 ) ) ;
#148039 = CARTESIAN_POINT ( 'NONE',  ( 9.474510206698971260, -16.51473224551069308, 67.91557627198102409 ) ) ;
#148038 = CARTESIAN_POINT ( 'NONE',  ( 9.564922557960805705, 16.46253265017160317, 79.58224293864769550 ) ) ;
#148037 = CARTESIAN_POINT ( 'NONE',  ( -15.72974639402176322, -15.80617190586768395, 49.37609039468569705 ) ) ;
#148040 = CARTESIAN_POINT ( 'NONE',  ( 9.564922557960805705, 16.46253265017160317, 84.58224293864769550 ) ) ;
#148041 = CARTESIAN_POINT ( 'NONE',  ( 16.53943276465976808, -0.05219959533910856209, 33.74890960531436690 ) ) ;
#148042 = CARTESIAN_POINT ( 'NONE',  ( 16.53943276465976808, 0.05219959533934440121, 96.25109039468568994 ) ) ;
#148043 = CARTESIAN_POINT ( 'NONE',  ( -5.049401038297874678, -19.05341960407617918, 39.79275706135232582 ) ) ;
#148044 = CARTESIAN_POINT ( 'NONE',  ( 5.049401038298161559, -19.05341960407611168, 107.7072429386476955 ) ) ;
#148045 = CARTESIAN_POINT ( 'NONE',  ( 9.564922557960805705, 16.46253265017160317, 59.58224293864769550 ) ) ;
#148046 = CARTESIAN_POINT ( 'NONE',  ( 9.564922557961047289, -16.46253265017146816, 40.41775706135234003 ) ) ;
#148047 = CARTESIAN_POINT ( 'NONE',  ( -36.91746825000001309, 11.99521256947798342, -6.724999997268813701 ) ) ;
#148048 = CARTESIAN_POINT ( 'NONE',  ( 4.379528057220092307, 16.55341960407617563, 47.29275706135234003 ) ) ;
#148050 = CARTESIAN_POINT ( 'NONE',  ( 12.06949235617739724, 12.14591786802326823, 51.87609039468568284 ) ) ;
#148049 = CARTESIAN_POINT ( 'NONE',  ( -19.02544592524334988, -5.153800228976617603, 73.95942372801900433 ) ) ;
#148051 = CARTESIAN_POINT ( 'NONE',  ( -7.500000000000000888, -1.380023386739105851, 5.672916605552547509 ) ) ;
#148052 = CARTESIAN_POINT ( 'NONE',  ( -16.46253265017160317, 9.564922557960807481, 90.83224293864769550 ) ) ;
#148053 = CARTESIAN_POINT ( 'NONE',  ( -21.52544592524343514, 5.823673210054127303, 111.0405762719810525 ) ) ;
#148054 = CARTESIAN_POINT ( 'NONE',  ( 5.153800228976615827, -19.02544592524334988, 80.20942372801901854 ) ) ;
#148056 = CARTESIAN_POINT ( 'NONE',  ( -19.02544592524342804, 5.153800228976336051, 41.04057627198103120 ) ) ;
#148055 = CARTESIAN_POINT ( 'NONE',  ( 9.564922557960805705, 16.46253265017160317, 104.5822429386476955 ) ) ;
#148057 = CARTESIAN_POINT ( 'NONE',  ( 16.46253265017160672, -9.564922557960803928, 73.33224293864769550 ) ) ;
#148059 = CARTESIAN_POINT ( 'NONE',  ( -19.05341960407611168, -5.049401038298163336, 31.45724293864769550 ) ) ;
#148058 = CARTESIAN_POINT ( 'NONE',  ( 16.55341960407611168, 4.379528057220329451, 33.95724293864769550 ) ) ;
#148060 = CARTESIAN_POINT ( 'NONE',  ( 0.05219959533936267826, -19.03943276465977164, 55.00109039468566863 ) ) ;
#148061 = CARTESIAN_POINT ( 'NONE',  ( -4.379528057220328563, 16.55341960407611168, 90.20724293864770971 ) ) ;
#148062 = CARTESIAN_POINT ( 'NONE',  ( -18.62759615963255300, -10.81492255796106328, 109.1677570613523613 ) ) ;
#148063 = CARTESIAN_POINT ( 'NONE',  ( 13.97604488694527802, 13.89961937509977652, 59.37390960531434558 ) ) ;
#148064 = CARTESIAN_POINT ( 'NONE',  ( 21.52544592524344225, -5.823673210054117533, 48.54057627198103120 ) ) ;
#148066 = CARTESIAN_POINT ( 'NONE',  ( 5.719274019375673035, 21.55341960407619339, 97.29275706135234714 ) ) ;
#148065 = CARTESIAN_POINT ( 'NONE',  ( -16.52544592524342804, 4.483927247898546575, 56.04057627198102409 ) ) ;
#148067 = CARTESIAN_POINT ( 'NONE',  ( -19.02544592524342804, 5.153800228976336051, 106.0405762719810241 ) ) ;
#148068 = CARTESIAN_POINT ( 'NONE',  ( 16.46253265017160672, -9.564922557960803928, 113.3322429386476955 ) ) ;
#148069 = CARTESIAN_POINT ( 'NONE',  ( -9.564922557960796823, -16.46253265017161027, 37.08224293864768839 ) ) ;
#148070 = CARTESIAN_POINT ( 'NONE',  ( -19.05341960407611168, -5.049401038298163336, 21.45724293864768839 ) ) ;
#148071 = CARTESIAN_POINT ( 'NONE',  ( -16.53943276465976808, 0.05219959533911058130, 86.24890960531436690 ) ) ;
#148072 = CARTESIAN_POINT ( 'NONE',  ( -5.719274019375978568, 21.55341960407610458, 95.20724293864769550 ) ) ;
#148073 = CARTESIAN_POINT ( 'NONE',  ( 19.02544592524343514, -5.153800228976328945, 103.5405762719809957 ) ) ;
#148074 = CARTESIAN_POINT ( 'NONE',  ( -21.52544592524334988, -5.823673210054445271, 18.95942372801901143 ) ) ;
#148075 = CARTESIAN_POINT ( 'NONE',  ( -9.474510206698964154, 16.51473224551069663, 110.4155762719810383 ) ) ;
#148077 = CARTESIAN_POINT ( 'NONE',  ( 16.52544592524342804, -4.483927247898539470, 98.54057627198105251 ) ) ;
#148076 = DIRECTION ( 'NONE',  ( 0.000000000000000000, 0.000000000000000000, 1.000000000000000000 ) ) ;
#148078 = CARTESIAN_POINT ( 'NONE',  ( -13.97604488694527625, -13.89961937509977652, 76.87390960531433848 ) ) ;
#148079 = CARTESIAN_POINT ( 'NONE',  ( 10.81492255796078972, 18.62759615963270932, 79.58224293864769550 ) ) ;
#148080 = DIRECTION ( 'NONE',  ( 0.000000000000000000, 0.000000000000000000, -1.000000000000000000 ) ) ;
#148081 = FACE_OUTER_BOUND ( 'NONE', #185131, .T. ) ;
#148083 = CARTESIAN_POINT ( 'NONE',  ( -17.49999999999999645, 5.499999999999992895, 73.71769037696435589 ) ) ;
#148082 = CARTESIAN_POINT ( 'NONE',  ( 15.72974639402199770, -15.80617190586745480, 33.12390960531435979 ) ) ;
#148084 = CARTESIAN_POINT ( 'NONE',  ( 12.06949235617739724, 12.14591786802326823, 31.87609039468567929 ) ) ;
#148085 = CARTESIAN_POINT ( 'NONE',  ( -16.55341960407611168, -4.379528057220339221, 91.45724293864769550 ) ) ;
#148086 = CARTESIAN_POINT ( 'NONE',  ( 19.52217212775660471, -5.499999999999920064, 52.43993709005258808 ) ) ;
#148087 = CARTESIAN_POINT ( 'NONE',  ( -13.89961937509977652, 13.97604488694528158, 85.62390960531433848 ) ) ;
#148088 = CARTESIAN_POINT ( 'NONE',  ( 0.05219959533909260263, 19.03943276465977164, 54.99890960531435979 ) ) ;
#148089 = CARTESIAN_POINT ( 'NONE',  ( -12.14591786802309592, -12.06949235617757132, 76.87390960531439532 ) ) ;
#148090 = CARTESIAN_POINT ( 'NONE',  ( -15.80617190586745835, -15.72974639402198527, 31.87390960531435979 ) ) ;
#148091 = CARTESIAN_POINT ( 'NONE',  ( -12.14591786802309592, -12.06949235617757132, 51.87390960531437401 ) ) ;
#148092 = CARTESIAN_POINT ( 'NONE',  ( 16.55341960407618274, -4.379528057220086978, 26.04275706135235779 ) ) ;
#148093 = CARTESIAN_POINT ( 'NONE',  ( 21.55341960407619695, -5.719274019375665929, 76.04275706135237556 ) ) ;
#148094 = CARTESIAN_POINT ( 'NONE',  ( 8.571926809382603096, -26.38167802310801235, 145.4750000027311785 ) ) ;
#148095 = CARTESIAN_POINT ( 'NONE',  ( 21.55341960407610458, 5.719274019375980345, 23.95724293864769550 ) ) ;
#148096 = CARTESIAN_POINT ( 'NONE',  ( 4.379528057220092307, 16.55341960407617563, 87.29275706135236135 ) ) ;
#148097 = CARTESIAN_POINT ( 'NONE',  ( -9.474510206698964154, 16.51473224551069663, 30.41557627198102054 ) ) ;
#148098 = CARTESIAN_POINT ( 'NONE',  ( -19.03943276465977164, 0.05219959533909376836, 71.24890960531435269 ) ) ;
#148099 = CARTESIAN_POINT ( 'NONE',  ( -5.719274019375978568, 21.55341960407610458, 100.2072429386476955 ) ) ;
#148100 = CARTESIAN_POINT ( 'NONE',  ( 4.379528057220092307, 16.55341960407617563, 27.29275706135234358 ) ) ;
#148102 = CARTESIAN_POINT ( 'NONE',  ( 5.823673210054444382, -21.52544592524334988, 75.20942372801901854 ) ) ;
#148101 = CARTESIAN_POINT ( 'NONE',  ( 12.14591786802309770, 12.06949235617756955, 49.37390960531436690 ) ) ;
#148103 = CIRCLE ( 'NONE', #164280, 5.000000000000000888 ) ;
#148105 = CARTESIAN_POINT ( 'NONE',  ( 0.05219959533909260263, 19.03943276465977164, 114.9989096053143669 ) ) ;
#148104 = CARTESIAN_POINT ( 'NONE',  ( -12.14591786802326823, 12.06949235617739902, 88.12609039468570415 ) ) ;
#148106 = CARTESIAN_POINT ( 'NONE',  ( 17.12812012977025233, 6.668231424566067211, 28.85948759323144941 ) ) ;
#148107 = CARTESIAN_POINT ( 'NONE',  ( -38.00000000000000711, 2.428612866367529932E-14, -7.749999994537626336 ) ) ;
#148108 = CARTESIAN_POINT ( 'NONE',  ( -16.55341960407617563, 4.379528057220093196, 103.5427570613523613 ) ) ;
#148109 = CARTESIAN_POINT ( 'NONE',  ( -12.06949235617739369, -12.14591786802326823, 59.37609039468568284 ) ) ;
#148110 = CARTESIAN_POINT ( 'NONE',  ( 5.049401038298161559, -19.05341960407611168, 72.70724293864768129 ) ) ;
#148111 = CARTESIAN_POINT ( 'NONE',  ( -13.89961937509977652, 13.97604488694528158, 85.62390960531433848 ) ) ;
#148112 = CARTESIAN_POINT ( 'NONE',  ( 21.55341960407619695, -5.719274019375665929, 66.04275706135236135 ) ) ;
#148113 = CARTESIAN_POINT ( 'NONE',  ( 4.483927247898790824, -16.52544592524335698, 70.20942372801904696 ) ) ;
#148114 = CARTESIAN_POINT ( 'NONE',  ( 0.05219959533910956823, 16.53943276465976808, 44.99890960531435979 ) ) ;
#148115 = CARTESIAN_POINT ( 'NONE',  ( 5.049401038298161559, -19.05341960407611168, 57.70724293864769550 ) ) ;
#148116 = CARTESIAN_POINT ( 'NONE',  ( 19.03943276465977164, -0.05219959533909143690, 53.74890960531436690 ) ) ;
#148117 = ORIENTED_EDGE ( 'NONE', *, *, #114637, .F. ) ;
#148118 = CARTESIAN_POINT ( 'NONE',  ( -19.02544592524334988, -5.153800228976617603, 108.9594237280189759 ) ) ;
#148119 = CARTESIAN_POINT ( 'NONE',  ( -8.314922557960811034, -14.29746914071050412, 107.0822429386476955 ) ) ;
#148120 = CARTESIAN_POINT ( 'NONE',  ( -13.97604488694527625, -13.89961937509977652, 66.87390960531436690 ) ) ;
#148122 = CARTESIAN_POINT ( 'NONE',  ( 30.74264578624800137, -22.33583958711395212, -7.200000000000001066 ) ) ;
#148121 = CARTESIAN_POINT ( 'NONE',  ( 9.564922557961047289, -16.46253265017146816, 95.41775706135233293 ) ) ;
#148123 = CARTESIAN_POINT ( 'NONE',  ( -0.05219959533937732626, 21.53943276465977519, 102.5010903946856899 ) ) ;
#148124 = CARTESIAN_POINT ( 'NONE',  ( -4.379528057220086978, -16.55341960407618274, 64.79275706135234714 ) ) ;
#148125 = CARTESIAN_POINT ( 'NONE',  ( -16.51473224551082808, 9.474510206698731452, 93.33442372801900433 ) ) ;
#148126 = CARTESIAN_POINT ( 'NONE',  ( -21.55341960407610458, -5.719274019375992779, 61.45724293864770260 ) ) ;
#148127 = CARTESIAN_POINT ( 'NONE',  ( 12.14591786802327356, -12.06949235617739191, 50.62609039468568994 ) ) ;
#148128 = CARTESIAN_POINT ( 'NONE',  ( -18.22780087662122028, 5.500000000000031086, 68.51540105326107266 ) ) ;
#148129 = CARTESIAN_POINT ( 'NONE',  ( 9.474510206698729675, 16.51473224551082808, 62.08442372801899722 ) ) ;
#148130 = CARTESIAN_POINT ( 'NONE',  ( -21.55341960407619339, 5.719274019375674811, 93.54275706135234714 ) ) ;
#148131 = CARTESIAN_POINT ( 'NONE',  ( 14.29746914071049879, -8.314922557960816363, 113.3322429386476955 ) ) ;
#148132 = CARTESIAN_POINT ( 'NONE',  ( -19.05341960407611168, -5.049401038298163336, 66.45724293864769550 ) ) ;
#148133 = CARTESIAN_POINT ( 'NONE',  ( -16.55341960407611168, -4.379528057220339221, 61.45724293864770260 ) ) ;
#148134 = CARTESIAN_POINT ( 'NONE',  ( -21.55341960407619339, 5.719274019375674811, 83.54275706135234714 ) ) ;
#148135 = CARTESIAN_POINT ( 'NONE',  ( -19.02544592524334988, -5.153800228976617603, 43.95942372801899012 ) ) ;
#148136 = CARTESIAN_POINT ( 'NONE',  ( -19.03943276465977164, -0.05219959533935918106, 33.75109039468566863 ) ) ;
#148137 = CARTESIAN_POINT ( 'NONE',  ( -18.62759615963270932, 10.81492255796079327, 25.83224293864769194 ) ) ;
#148138 = CARTESIAN_POINT ( 'NONE',  ( 18.67979575497194134, -10.72451020669871369, 90.83442372801901854 ) ) ;
#148139 = CARTESIAN_POINT ( 'NONE',  ( -13.97604488694527625, -13.89961937509977652, 76.87390960531433848 ) ) ;
#148140 = CARTESIAN_POINT ( 'NONE',  ( -10.81492255796105439, 18.62759615963255655, 92.91775706135236135 ) ) ;
#148141 = CARTESIAN_POINT ( 'NONE',  ( -21.55341960407610458, -5.719274019375992779, 51.45724293864770260 ) ) ;
#148142 = CARTESIAN_POINT ( 'NONE',  ( -13.89961937509977652, 13.97604488694528158, 85.62390960531433848 ) ) ;
#148143 = CARTESIAN_POINT ( 'NONE',  ( -19.03943276465977164, -0.05219959533935918106, 68.75109039468566152 ) ) ;
#148144 = CARTESIAN_POINT ( 'NONE',  ( -5.049401038298153566, 19.05341960407611168, 40.20724293864768839 ) ) ;
#148145 = CARTESIAN_POINT ( 'NONE',  ( -16.46253265017160317, 9.564922557960807481, 95.83224293864769550 ) ) ;
#148146 = CARTESIAN_POINT ( 'NONE',  ( 9.564922557961047289, -16.46253265017146816, 85.41775706135233293 ) ) ;
#148147 = CARTESIAN_POINT ( 'NONE',  ( 8.314922557961029526, -14.29746914071037800, 45.41775706135234003 ) ) ;
#148148 = CARTESIAN_POINT ( 'NONE',  ( -14.34966873604960291, -8.224510206698953496, 106.6655762719810383 ) ) ;
#148149 = CARTESIAN_POINT ( 'NONE',  ( 9.564922557960805705, 16.46253265017160317, 74.58224293864769550 ) ) ;
#148150 = CARTESIAN_POINT ( 'NONE',  ( -10.81492255796078084, -18.62759615963271287, 52.08224293864768839 ) ) ;
#148151 = CARTESIAN_POINT ( 'NONE',  ( 16.52544592524335698, 4.483927247898782831, 31.45942372801901854 ) ) ;
#148152 = CARTESIAN_POINT ( 'NONE',  ( -21.53943276465977519, -0.05219959533937600094, 38.75109039468567573 ) ) ;
#148153 = CARTESIAN_POINT ( 'NONE',  ( 5.823673210054444382, -21.52544592524334988, 90.20942372801903275 ) ) ;
#148154 = CARTESIAN_POINT ( 'NONE',  ( -16.52544592524335698, -4.483927247898792601, 83.95942372801900433 ) ) ;
#148155 = CARTESIAN_POINT ( 'NONE',  ( -5.153800228976328057, -19.02544592524343514, 77.29057627198099567 ) ) ;
#148156 = CARTESIAN_POINT ( 'NONE',  ( -16.52544592524335698, -4.483927247898792601, 108.9594237280190185 ) ) ;
#148157 = CARTESIAN_POINT ( 'NONE',  ( -16.51473224551082808, 9.474510206698731452, 53.33442372801900433 ) ) ;
#148158 = EDGE_CURVE ( 'NONE', #60981, #95658, #63049, .T. ) ;
#148159 = CARTESIAN_POINT ( 'NONE',  ( 10.72451020669871369, 18.67979575497193778, 37.08442372801901143 ) ) ;
#148160 = CARTESIAN_POINT ( 'NONE',  ( 14.29746914071049879, -8.314922557960816363, 83.33224293864769550 ) ) ;
#148161 = CARTESIAN_POINT ( 'NONE',  ( 5.153800228976335163, 19.02544592524342804, 99.79057627198102409 ) ) ;
#148162 = CARTESIAN_POINT ( 'NONE',  ( 16.52544592524335698, 4.483927247898782831, 106.4594237280190328 ) ) ;
#148163 = CARTESIAN_POINT ( 'NONE',  ( -15.80617190586768217, 15.72974639402176855, 78.12609039468570415 ) ) ;
#148164 = CARTESIAN_POINT ( 'NONE',  ( -16.53943276465976808, -0.05219959533934237506, 38.75109039468567573 ) ) ;
#148165 = CARTESIAN_POINT ( 'NONE',  ( 10.72451020669871369, 18.67979575497193778, 27.08442372801901854 ) ) ;
#148166 = CARTESIAN_POINT ( 'NONE',  ( 0.05219959533910956823, 16.53943276465976808, 74.99890960531435269 ) ) ;
#148167 = ORIENTED_EDGE ( 'NONE', *, *, #154166, .T. ) ;
#148168 = CARTESIAN_POINT ( 'NONE',  ( -15.72974639402197994, 15.80617190586746368, 115.6239096053143669 ) ) ;
#148169 = CARTESIAN_POINT ( 'NONE',  ( 12.06949235617757843, -12.14591786802309237, 53.12390960531436690 ) ) ;
#148170 = CARTESIAN_POINT ( 'NONE',  ( 20.96320343559639454, -21.46320343559646560, 5.353553390593270400 ) ) ;
#148171 = CARTESIAN_POINT ( 'NONE',  ( 21.53943276465977519, -0.05219959533907433946, 28.74890960531435624 ) ) ;
#148172 = CARTESIAN_POINT ( 'NONE',  ( -18.67979575497193778, 10.72451020669871902, 48.33442372801902565 ) ) ;
#148173 = CARTESIAN_POINT ( 'NONE',  ( -16.52544592524342804, 4.483927247898546575, 66.04057627198103830 ) ) ;
#148174 = CARTESIAN_POINT ( 'NONE',  ( 21.55341960407610458, 5.719274019375980345, 78.95724293864769550 ) ) ;
#148175 = CARTESIAN_POINT ( 'NONE',  ( 13.97604488694527802, 13.89961937509977652, 79.37390960531435269 ) ) ;
#148177 = CARTESIAN_POINT ( 'NONE',  ( -19.02544592524334988, -5.153800228976617603, 73.95942372801900433 ) ) ;
#148176 = CARTESIAN_POINT ( 'NONE',  ( -0.05219959533909027116, -19.03943276465977164, 32.49890960531435979 ) ) ;
#148179 = CARTESIAN_POINT ( 'NONE',  ( -15.80617190586745835, -15.72974639402198527, 66.87390960531436690 ) ) ;
#148178 = CARTESIAN_POINT ( 'NONE',  ( -5.823673210054431948, 21.52544592524334988, 52.70942372801902565 ) ) ;
#148180 = CARTESIAN_POINT ( 'NONE',  ( -16.51473224551069308, -9.474510206698971260, 41.66557627198103120 ) ) ;
#148181 = CARTESIAN_POINT ( 'NONE',  ( -19.05341960407611168, -5.049401038298163336, 66.45724293864769550 ) ) ;
#148182 = CARTESIAN_POINT ( 'NONE',  ( 12.06949235617739724, 12.14591786802326823, 46.87609039468568994 ) ) ;
#148183 = CARTESIAN_POINT ( 'NONE',  ( 18.67979575497194134, -10.72451020669871369, 35.83442372801901143 ) ) ;
#148184 = CARTESIAN_POINT ( 'NONE',  ( 5.823673210054444382, -21.52544592524334988, 55.20942372801902565 ) ) ;
#148185 = CARTESIAN_POINT ( 'NONE',  ( -5.049401038298153566, 19.05341960407611168, 100.2072429386476955 ) ) ;
#148186 = CARTESIAN_POINT ( 'NONE',  ( -5.719274019375978568, 21.55341960407610458, 80.20724293864769550 ) ) ;
#148188 = CARTESIAN_POINT ( 'NONE',  ( 8.224510206698742110, 14.34966873604972548, 52.08442372801901854 ) ) ;
#148187 = CARTESIAN_POINT ( 'NONE',  ( 5.719274019375673035, 21.55341960407619339, 22.29275706135235069 ) ) ;
#148189 = CARTESIAN_POINT ( 'NONE',  ( 18.62759615963271287, -10.81492255796078972, 53.33224293864769550 ) ) ;
#148190 = CARTESIAN_POINT ( 'NONE',  ( -16.46253265017146816, -9.564922557961047289, 24.16775706135233648 ) ) ;
#148191 = AXIS2_PLACEMENT_3D ( 'NONE', #144702, #49719, #51703 ) ;
#148192 = CARTESIAN_POINT ( 'NONE',  ( 5.153800228976335163, 19.02544592524342804, 59.79057627198100988 ) ) ;
#148193 = CARTESIAN_POINT ( 'NONE',  ( 9.564922557960805705, 16.46253265017160317, 114.5822429386476955 ) ) ;
#148194 = CARTESIAN_POINT ( 'NONE',  ( -16.46253265017160317, 9.564922557960807481, 90.83224293864769550 ) ) ;
#148195 = CARTESIAN_POINT ( 'NONE',  ( 20.57406348593929479, 22.68986043004503372, -47.49330165217067901 ) ) ;
#148196 = CARTESIAN_POINT ( 'NONE',  ( 16.51473224551083163, -9.474510206698727899, 70.83442372801900433 ) ) ;
#148197 = CARTESIAN_POINT ( 'NONE',  ( -18.67979575497178146, -10.72451020669898902, 41.66557627198103120 ) ) ;
#148198 = CARTESIAN_POINT ( 'NONE',  ( 12.14591786802309770, 12.06949235617756955, 29.37390960531435269 ) ) ;
#148199 = CARTESIAN_POINT ( 'NONE',  ( -19.02544592524334988, -5.153800228976617603, 88.95942372801897591 ) ) ;
#148200 = FACE_OUTER_BOUND ( 'NONE', #162870, .T. ) ;
#148201 = CARTESIAN_POINT ( 'NONE',  ( -16.51473224551082808, 9.474510206698731452, 23.33442372801900078 ) ) ;
#148202 = CARTESIAN_POINT ( 'NONE',  ( -5.153800228976607833, 19.02544592524334988, 77.70942372801900433 ) ) ;
#148203 = CARTESIAN_POINT ( 'NONE',  ( 19.02544592524334988, 5.153800228976608722, 41.45942372801900433 ) ) ;
#148204 = CARTESIAN_POINT ( 'NONE',  ( 24.84743926645689172, -12.91388972341063202, 166.0204189386424787 ) ) ;
#148205 = CARTESIAN_POINT ( 'NONE',  ( 5.153800228976335163, 19.02544592524342804, 49.79057627198100988 ) ) ;
#148206 = CARTESIAN_POINT ( 'NONE',  ( -16.55341960407611168, -4.379528057220339221, 56.45724293864768839 ) ) ;
#148207 = CARTESIAN_POINT ( 'NONE',  ( 16.46253265017160672, -9.564922557960803928, 28.33224293864769550 ) ) ;
#148208 = CARTESIAN_POINT ( 'NONE',  ( 4.379528057220339221, -16.55341960407611168, 42.70724293864770260 ) ) ;
#148209 = DIRECTION ( 'NONE',  ( 0.000000000000000000, 0.04175967627138096189, 0.9991276842514722478 ) ) ;
#148210 = CARTESIAN_POINT ( 'NONE',  ( -0.05219959533934338120, 16.53943276465976808, 112.5010903946857042 ) ) ;
#148211 = CARTESIAN_POINT ( 'NONE',  ( 16.46253265017160672, -9.564922557960803928, 68.33224293864770971 ) ) ;
#148212 = CARTESIAN_POINT ( 'NONE',  ( 9.474510206698729675, 16.51473224551082808, 22.08442372801899722 ) ) ;
#148213 = CARTESIAN_POINT ( 'NONE',  ( 16.52544592524335698, 4.483927247898782831, 36.45942372801901143 ) ) ;
#148214 = CARTESIAN_POINT ( 'NONE',  ( 21.52544592524344225, -5.823673210054117533, 33.54057627198102409 ) ) ;
#148216 = ORIENTED_EDGE ( 'NONE', *, *, #95661, .F. ) ;
#148215 = CARTESIAN_POINT ( 'NONE',  ( 15.80617190586769283, -15.72974639402175789, 85.62609039468568994 ) ) ;
#148217 = CARTESIAN_POINT ( 'NONE',  ( -9.564922557960796823, -16.46253265017161027, 62.08224293864769550 ) ) ;
#148218 = CARTESIAN_POINT ( 'NONE',  ( -16.46253265017160317, 9.564922557960807481, 100.8322429386477097 ) ) ;
#148219 = CARTESIAN_POINT ( 'NONE',  ( 13.89961937509977652, -13.97604488694527269, 98.12390960531433848 ) ) ;
#148220 = CARTESIAN_POINT ( 'NONE',  ( 3.556970738554034288E-15, -38.81732327939057114, -4.124999997268813168 ) ) ;
#148221 = CARTESIAN_POINT ( 'NONE',  ( -0.05219959533937732626, 21.53943276465977519, 22.50109039468567573 ) ) ;
#148222 = CARTESIAN_POINT ( 'NONE',  ( -16.55341960407611168, -4.379528057220339221, 76.45724293864769550 ) ) ;
#148224 = CARTESIAN_POINT ( 'NONE',  ( 13.97604488694527802, 13.89961937509977652, 74.37390960531436690 ) ) ;
#148223 = CARTESIAN_POINT ( 'NONE',  ( -21.55341960407610458, -5.719274019375992779, 76.45724293864769550 ) ) ;
#148225 = CARTESIAN_POINT ( 'NONE',  ( -0.05219959533909027116, -19.03943276465977164, 72.49890960531435269 ) ) ;
#148226 = CARTESIAN_POINT ( 'NONE',  ( -21.53943276465977519, 0.05219959533907696930, 106.2489096053143811 ) ) ;
#148227 = ORIENTED_EDGE ( 'NONE', *, *, #120476, .F. ) ;
#148228 = CARTESIAN_POINT ( 'NONE',  ( 19.02544592524343514, -5.153800228976328945, 73.54057627198103830 ) ) ;
#148230 = CARTESIAN_POINT ( 'NONE',  ( -13.97604488694527625, -13.89961937509977652, 21.87390960531435979 ) ) ;
#148229 = CARTESIAN_POINT ( 'NONE',  ( -16.53943276465976808, 0.05219959533911058130, 111.2489096053143669 ) ) ;
#148231 = CARTESIAN_POINT ( 'NONE',  ( -19.02544592524342804, 5.153800228976336051, 61.04057627198103120 ) ) ;
#148232 = CARTESIAN_POINT ( 'NONE',  ( -19.02544592524334988, -5.153800228976617603, 93.95942372801900433 ) ) ;
#148233 = CARTESIAN_POINT ( 'NONE',  ( 14.34966873604960469, 8.224510206698951720, 104.1655762719810241 ) ) ;
#148234 = CARTESIAN_POINT ( 'NONE',  ( 15.80617190586769283, -15.72974639402175789, 70.62609039468567573 ) ) ;
#148236 = CARTESIAN_POINT ( 'NONE',  ( -18.67979575497178146, -10.72451020669898902, 111.6655762719810525 ) ) ;
#148235 = CARTESIAN_POINT ( 'NONE',  ( -9.474510206698964154, 16.51473224551069663, 50.41557627198102409 ) ) ;
#148237 = CARTESIAN_POINT ( 'NONE',  ( -15.72974639402176322, -15.80617190586768395, 19.37609039468568639 ) ) ;
#148238 = CARTESIAN_POINT ( 'NONE',  ( 1.993301997531345292E-15, -30.30510711980685912, 144.4999999999999432 ) ) ;
#148239 = CARTESIAN_POINT ( 'NONE',  ( -19.02544592524342804, 5.153800228976336051, 76.04057627198102409 ) ) ;
#148240 = DIRECTION ( 'NONE',  ( 1.000000000000000000, 0.000000000000000000, 0.000000000000000000 ) ) ;
#148242 = CARTESIAN_POINT ( 'NONE',  ( 18.62759615963271287, -10.81492255796078972, 33.33224293864769550 ) ) ;
#148241 = CARTESIAN_POINT ( 'NONE',  ( 13.89961937509957401, 13.97604488694547697, 101.8760903946856331 ) ) ;
#148243 = CARTESIAN_POINT ( 'NONE',  ( 15.72974639402176855, 15.80617190586768217, 51.87609039468568284 ) ) ;
#148244 = CARTESIAN_POINT ( 'NONE',  ( -13.89961937509977652, 13.97604488694528158, 90.62390960531432427 ) ) ;
#148245 = CARTESIAN_POINT ( 'NONE',  ( -9.564922557961040184, 16.46253265017147172, 77.91775706135234714 ) ) ;
#148246 = CARTESIAN_POINT ( 'NONE',  ( 13.97604488694527802, 13.89961937509977652, 69.37390960531436690 ) ) ;
#148247 = CARTESIAN_POINT ( 'NONE',  ( 4.483927247898545687, 16.52544592524342804, 84.79057627198102409 ) ) ;
#148248 = CARTESIAN_POINT ( 'NONE',  ( -9.474510206698964154, 16.51473224551069663, 105.4155762719810383 ) ) ;
#148249 = CARTESIAN_POINT ( 'NONE',  ( 12.14591786802309770, 12.06949235617756955, 89.37390960531435269 ) ) ;
#148250 = CARTESIAN_POINT ( 'NONE',  ( 16.46253265017160672, -9.564922557960803928, 103.3322429386476955 ) ) ;
#148251 = ADVANCED_FACE ( 'NONE', ( #158050 ), #127698, .T. ) ;
#148253 = CARTESIAN_POINT ( 'NONE',  ( -19.02544592524342804, 5.153800228976336051, 31.04057627198102409 ) ) ;
#148252 = CARTESIAN_POINT ( 'NONE',  ( 14.34966873604960469, 8.224510206698951720, 44.16557627198103120 ) ) ;
#148254 = EDGE_LOOP ( 'NONE', ( #137772, #139801, #186471, #164184, #169281 ) ) ;
#148255 = CARTESIAN_POINT ( 'NONE',  ( -18.67979575497193778, 10.72451020669871902, 53.33442372801901854 ) ) ;
#148256 = CARTESIAN_POINT ( 'NONE',  ( 9.564922557961047289, -16.46253265017146816, 75.41775706135234714 ) ) ;
#148257 = CARTESIAN_POINT ( 'NONE',  ( -14.34966873604960291, -8.224510206698953496, 46.66557627198102409 ) ) ;
#148258 = CARTESIAN_POINT ( 'NONE',  ( 5.823673210054125526, 21.52544592524343514, 104.7905762719810241 ) ) ;
#148259 = CARTESIAN_POINT ( 'NONE',  ( 5.823673210054125526, 21.52544592524343514, 39.79057627198103830 ) ) ;
#148260 = CARTESIAN_POINT ( 'NONE',  ( 8.314922557960818139, 14.29746914071049879, 84.58224293864769550 ) ) ;
#148261 = CARTESIAN_POINT ( 'NONE',  ( -9.564922557960796823, -16.46253265017161027, 57.08224293864769550 ) ) ;
#148262 = CARTESIAN_POINT ( 'NONE',  ( 16.52544592524342804, -4.483927247898539470, 28.54057627198103120 ) ) ;
#148263 = CARTESIAN_POINT ( 'NONE',  ( 4.483927247898790824, -16.52544592524335698, 90.20942372801903275 ) ) ;
#148264 = CARTESIAN_POINT ( 'NONE',  ( 8.224510206698742110, 14.34966873604972548, 67.08442372801901854 ) ) ;
#148265 = CARTESIAN_POINT ( 'NONE',  ( -19.03943276465977164, -0.05219959533935918106, 28.75109039468566507 ) ) ;
#148266 = B_SPLINE_CURVE_WITH_KNOTS ( 'NONE', 3,
 ( #173811, #50460, #5921, #95951, #130248, #6914, #3931, #160612, #192956, #37262, #161609, #67598, #23103, #36257 ),
 .UNSPECIFIED., .F., .F.,
 ( 4, 2, 2, 2, 2, 2, 4 ),
 ( 2.784207231363245562E-07, 0.0005083736299775801996, 0.001016468839232024125, 0.002032659257740903301, 0.003048849676249782478, 0.003556944885504227487, 0.004065040094758672930 ),
 .UNSPECIFIED. ) ;
#148267 = CARTESIAN_POINT ( 'NONE',  ( -9.474510206698964154, 16.51473224551069663, 95.41557627198102409 ) ) ;
#148268 = CARTESIAN_POINT ( 'NONE',  ( -19.02544592524342804, 5.153800228976336051, 76.04057627198102409 ) ) ;
#148269 = CARTESIAN_POINT ( 'NONE',  ( -0.05219959533934338120, 16.53943276465976808, 82.50109039468568994 ) ) ;
#148270 = CARTESIAN_POINT ( 'NONE',  ( -5.153800228976328057, -19.02544592524343514, 37.29057627198102409 ) ) ;
#148271 = CARTESIAN_POINT ( 'NONE',  ( -0.05219959533910754901, -16.53943276465976808, 52.49890960531435979 ) ) ;
#148273 = CARTESIAN_POINT ( 'NONE',  ( -0.05219959533909027116, -19.03943276465977164, 107.4989096053143527 ) ) ;
#148272 = CARTESIAN_POINT ( 'NONE',  ( -13.89961937509977652, 13.97604488694528158, 115.6239096053143669 ) ) ;
#148274 = CARTESIAN_POINT ( 'NONE',  ( -21.53943276465977519, 0.05219959533907696930, 46.24890960531435979 ) ) ;
#148275 = CARTESIAN_POINT ( 'NONE',  ( -16.52544592524342804, 4.483927247898546575, 66.04057627198103830 ) ) ;
#148276 = CARTESIAN_POINT ( 'NONE',  ( -4.379528057220086978, -16.55341960407618274, 29.79275706135234358 ) ) ;
#148277 = CARTESIAN_POINT ( 'NONE',  ( -8.314922557960811034, -14.29746914071050412, 62.08224293864769550 ) ) ;
#148278 = CARTESIAN_POINT ( 'NONE',  ( 29.56482114129866900, -1.249513161672083372, -48.84067647644820198 ) ) ;
#148279 = CARTESIAN_POINT ( 'NONE',  ( -19.05341960407617563, 5.049401038297882671, 58.54275706135234003 ) ) ;
#148280 = CARTESIAN_POINT ( 'NONE',  ( 16.51473224551069308, 9.474510206698969483, 99.16557627198102409 ) ) ;
#148281 = CARTESIAN_POINT ( 'NONE',  ( 16.46253265017146816, 9.564922557961045513, 81.66775706135233293 ) ) ;
#148282 = CARTESIAN_POINT ( 'NONE',  ( 17.14385361876520264, 23.59649016807275856, 148.6750000027311387 ) ) ;
#148284 = CARTESIAN_POINT ( 'NONE',  ( 0.05219959533934541429, -16.53943276465976808, 90.00109039468567573 ) ) ;
#148283 = CARTESIAN_POINT ( 'NONE',  ( 9.474510206698729675, 16.51473224551082808, 112.0844237280190043 ) ) ;
#148285 = CARTESIAN_POINT ( 'NONE',  ( -19.02544592524342804, 5.153800228976336051, 36.04057627198100988 ) ) ;
#148286 = CARTESIAN_POINT ( 'NONE',  ( 10.81492255796078972, 18.62759615963270932, 34.58224293864770260 ) ) ;
#148287 = CARTESIAN_POINT ( 'NONE',  ( 5.823673210054444382, -21.52544592524334988, 55.20942372801902565 ) ) ;
#148288 = CARTESIAN_POINT ( 'NONE',  ( -16.52544592524335698, -4.483927247898792601, 18.95942372801901143 ) ) ;
#148290 = CARTESIAN_POINT ( 'NONE',  ( -16.46253265017160317, 9.564922557960807481, 70.83224293864770971 ) ) ;
#148289 = CARTESIAN_POINT ( 'NONE',  ( 17.50000000000122213, 3.338341100222780966, 22.91083448979819082 ) ) ;
#148291 = CARTESIAN_POINT ( 'NONE',  ( -12.73749492396214578, -155.7167183371837496, -4.999999999999999112 ) ) ;
#148293 = CARTESIAN_POINT ( 'NONE',  ( 13.97604488694527802, 13.89961937509977652, 79.37390960531435269 ) ) ;
#148292 = CARTESIAN_POINT ( 'NONE',  ( -16.53943276465976808, 0.05219959533911058130, 91.24890960531436690 ) ) ;
#148294 = CARTESIAN_POINT ( 'NONE',  ( 19.05341960407611168, 5.049401038298154454, 93.95724293864769550 ) ) ;
#148295 = ORIENTED_EDGE ( 'NONE', *, *, #39724, .T. ) ;
#148296 = CARTESIAN_POINT ( 'NONE',  ( 5.153800228976615827, -19.02544592524334988, 95.20942372801897591 ) ) ;
#148297 = CARTESIAN_POINT ( 'NONE',  ( 5.823673210054125526, 21.52544592524343514, 59.79057627198103120 ) ) ;
#148298 = CARTESIAN_POINT ( 'NONE',  ( -19.05341960407611168, -5.049401038298163336, 31.45724293864769550 ) ) ;
#148299 = CARTESIAN_POINT ( 'NONE',  ( -9.564922557961040184, 16.46253265017147172, 52.91775706135233293 ) ) ;
#148300 = CARTESIAN_POINT ( 'NONE',  ( -13.97604488694527625, -13.89961937509977652, 61.87390960531435979 ) ) ;
#148301 = CARTESIAN_POINT ( 'NONE',  ( -9.564922557960796823, -16.46253265017161027, 87.08224293864769550 ) ) ;
#148302 = ORIENTED_EDGE ( 'NONE', *, *, #56349, .F. ) ;
#148303 = CARTESIAN_POINT ( 'NONE',  ( 18.67979575497178502, 10.72451020669898547, 89.16557627198102409 ) ) ;
#148305 = CARTESIAN_POINT ( 'NONE',  ( -16.46253265017146816, -9.564922557961047289, 64.16775706135233293 ) ) ;
#148304 = CARTESIAN_POINT ( 'NONE',  ( 14.34966873604960469, 8.224510206698951720, 89.16557627198102409 ) ) ;
#148306 = CARTESIAN_POINT ( 'NONE',  ( 10.81492255796078972, 18.62759615963270932, 89.58224293864768129 ) ) ;
#148307 = CARTESIAN_POINT ( 'NONE',  ( -21.55341960407610458, -5.719274019375992779, 76.45724293864769550 ) ) ;
#148308 = CARTESIAN_POINT ( 'NONE',  ( -8.224510206698948167, 14.34966873604960824, 30.41557627198101699 ) ) ;
#148309 = CARTESIAN_POINT ( 'NONE',  ( 10.72451020669871369, 18.67979575497193778, 102.0844237280190185 ) ) ;
#148310 = CARTESIAN_POINT ( 'NONE',  ( 14.29746914071037800, 8.314922557961029526, 51.66775706135234714 ) ) ;
#148311 = CARTESIAN_POINT ( 'NONE',  ( -9.564922557960796823, -16.46253265017161027, 82.08224293864768129 ) ) ;
#148312 = CARTESIAN_POINT ( 'NONE',  ( -9.564922557960796823, -16.46253265017161027, 27.08224293864769550 ) ) ;
#148313 = CARTESIAN_POINT ( 'NONE',  ( 21.52544592524334988, 5.823673210054432836, 41.45942372801901143 ) ) ;
#148314 = CARTESIAN_POINT ( 'NONE',  ( -5.719274019375665041, -21.55341960407619695, 54.79275706135235424 ) ) ;
#148315 = CARTESIAN_POINT ( 'NONE',  ( -5.153800228976328057, -19.02544592524343514, 42.29057627198101699 ) ) ;
#148316 = CARTESIAN_POINT ( 'NONE',  ( 21.53943276465977519, 0.05219959533937863772, 21.25109039468567218 ) ) ;
#148317 = CARTESIAN_POINT ( 'NONE',  ( 0.05219959533936267826, -19.03943276465977164, 55.00109039468566863 ) ) ;
#148318 = CARTESIAN_POINT ( 'NONE',  ( -16.51473224551082808, 9.474510206698731452, 73.33442372801900433 ) ) ;
#148319 = CARTESIAN_POINT ( 'NONE',  ( -14.29746914071037622, -8.314922557961029526, 29.16775706135234003 ) ) ;
#148320 = FACE_OUTER_BOUND ( 'NONE', #155233, .T. ) ;
#148321 = CARTESIAN_POINT ( 'NONE',  ( 4.379528057220092307, 16.55341960407617563, 67.29275706135234714 ) ) ;
#148322 = CARTESIAN_POINT ( 'NONE',  ( -16.51473224551069308, -9.474510206698971260, 36.66557627198102409 ) ) ;
#148323 = CARTESIAN_POINT ( 'NONE',  ( 24.50238749460113397, -2.981321037229046400, 173.3223451563237916 ) ) ;
#148324 = CARTESIAN_POINT ( 'NONE',  ( 0.05219959533909260263, 19.03943276465977164, 104.9989096053143669 ) ) ;
#148325 = CARTESIAN_POINT ( 'NONE',  ( 4.483927247898545687, 16.52544592524342804, 114.7905762719810383 ) ) ;
#148326 = CARTESIAN_POINT ( 'NONE',  ( 5.823673210054125526, 21.52544592524343514, 74.79057627198105251 ) ) ;
#148327 = CARTESIAN_POINT ( 'NONE',  ( 16.52544592524335698, 4.483927247898782831, 66.45942372801903275 ) ) ;
#148328 = CARTESIAN_POINT ( 'NONE',  ( -15.72974639402176322, -15.80617190586768395, 109.3760903946857042 ) ) ;
#148329 = CARTESIAN_POINT ( 'NONE',  ( -16.46253265017160317, 9.564922557960807481, 45.83224293864769550 ) ) ;
#148330 = CARTESIAN_POINT ( 'NONE',  ( -12.14591786802309592, -12.06949235617757132, 26.87390960531435979 ) ) ;
#148331 = CARTESIAN_POINT ( 'NONE',  ( -16.55341960407611168, -4.379528057220339221, 66.45724293864768129 ) ) ;
#148332 = AXIS2_PLACEMENT_3D ( 'NONE', #115748, #161245, #71243 ) ;
#148333 = CARTESIAN_POINT ( 'NONE',  ( 13.89961937509977652, -13.97604488694527269, 63.12390960531435979 ) ) ;
#148334 = CARTESIAN_POINT ( 'NONE',  ( 15.80617190586769283, -15.72974639402175789, 40.62609039468567573 ) ) ;
#148335 = CARTESIAN_POINT ( 'NONE',  ( 19.05341960407611168, 5.049401038298154454, 83.95724293864766707 ) ) ;
#148336 = CARTESIAN_POINT ( 'NONE',  ( -15.72974639402176322, -15.80617190586768395, 89.37609039468568994 ) ) ;
#148337 = CARTESIAN_POINT ( 'NONE',  ( 8.224510206698742110, 14.34966873604972548, 72.08442372801899012 ) ) ;
#148338 = CARTESIAN_POINT ( 'NONE',  ( -19.02544592524342804, 5.153800228976336051, 106.0405762719810241 ) ) ;
#148339 = CARTESIAN_POINT ( 'NONE',  ( 14.34966873604960469, 8.224510206698951720, 49.16557627198102409 ) ) ;
#148340 = CARTESIAN_POINT ( 'NONE',  ( 19.03943276465977164, -0.05219959533909143690, 33.74890960531435979 ) ) ;
#148341 = CARTESIAN_POINT ( 'NONE',  ( -14.34966873604972548, 8.224510206698743886, 53.33442372801901854 ) ) ;
#148342 = CARTESIAN_POINT ( 'NONE',  ( -12.06949235617756955, 12.14591786802309770, 50.62390960531435979 ) ) ;
#148343 = CARTESIAN_POINT ( 'NONE',  ( -16.51473224551069308, -9.474510206698971260, 106.6655762719810383 ) ) ;
#148344 = CARTESIAN_POINT ( 'NONE',  ( 21.52544592524344225, -5.823673210054117533, 38.54057627198103120 ) ) ;
#148345 = CARTESIAN_POINT ( 'NONE',  ( -16.51473224551082808, 9.474510206698731452, 23.33442372801900078 ) ) ;
#148346 = CARTESIAN_POINT ( 'NONE',  ( 4.379528057220339221, -16.55341960407611168, 87.70724293864769550 ) ) ;
#148347 = CARTESIAN_POINT ( 'NONE',  ( -19.03943276465977164, 0.05219959533909376836, 91.24890960531436690 ) ) ;
#148348 = ORIENTED_EDGE ( 'NONE', *, *, #25449, .T. ) ;
#148349 = CARTESIAN_POINT ( 'NONE',  ( 4.379528057220092307, 16.55341960407617563, 47.29275706135234003 ) ) ;
#148350 = CARTESIAN_POINT ( 'NONE',  ( -16.51473224551069308, -9.474510206698971260, 51.66557627198102409 ) ) ;
#148351 = CARTESIAN_POINT ( 'NONE',  ( 17.50000000000000000, 5.499999999999992895, 101.7030961746583131 ) ) ;
#148352 = CARTESIAN_POINT ( 'NONE',  ( -9.564922557961040184, 16.46253265017147172, 42.91775706135234003 ) ) ;
#148353 = CARTESIAN_POINT ( 'NONE',  ( 16.52544592524335698, 4.483927247898782831, 86.45942372801901854 ) ) ;
#148354 = CARTESIAN_POINT ( 'NONE',  ( -9.474510206698720793, -16.51473224551083518, 99.58442372801900433 ) ) ;
#148355 = CARTESIAN_POINT ( 'NONE',  ( 5.719274019375673035, 21.55341960407619339, 72.29275706135236135 ) ) ;
#148356 = CARTESIAN_POINT ( 'NONE',  ( -19.05341960407611168, -5.049401038298163336, 76.45724293864769550 ) ) ;
#148357 = CARTESIAN_POINT ( 'NONE',  ( -21.53943276465977519, 0.05219959533907696930, 96.24890960531435269 ) ) ;
#148358 = CARTESIAN_POINT ( 'NONE',  ( -14.29746914071049879, 8.314922557960819915, 100.8322429386477097 ) ) ;
#148359 = CIRCLE ( 'NONE', #151690, 61.99999999999998579 ) ;
#148360 = CARTESIAN_POINT ( 'NONE',  ( 9.474510206698729675, 16.51473224551082808, 62.08442372801899722 ) ) ;
#148361 = CARTESIAN_POINT ( 'NONE',  ( -10.81492255796078084, -18.62759615963271287, 82.08224293864768129 ) ) ;
#148362 = CARTESIAN_POINT ( 'NONE',  ( 19.02544592524334988, 5.153800228976608722, 41.45942372801900433 ) ) ;
#148363 = CARTESIAN_POINT ( 'NONE',  ( 18.22780087662122384, 5.500000000000018652, 98.98459894673892734 ) ) ;
#148364 = CARTESIAN_POINT ( 'NONE',  ( -21.55341960407610458, -5.719274019375992779, 86.45724293864770971 ) ) ;
#148365 = CARTESIAN_POINT ( 'NONE',  ( 17.50000000000000000, 5.499999999999997335, 120.0000000000000142 ) ) ;
#148366 = CARTESIAN_POINT ( 'NONE',  ( 9.474510206698971260, -16.51473224551069308, 62.91557627198102409 ) ) ;
#148367 = CARTESIAN_POINT ( 'NONE',  ( -13.97604488694527625, -13.89961937509977830, 91.87390960531433848 ) ) ;
#148368 = CARTESIAN_POINT ( 'NONE',  ( 0.05219959533934541429, -16.53943276465976808, 20.00109039468568639 ) ) ;
#148369 = CARTESIAN_POINT ( 'NONE',  ( -19.48894818550242292, 5.500000000000115463, 60.10307310435243267 ) ) ;
#148370 = CARTESIAN_POINT ( 'NONE',  ( -13.97604488694527625, -13.89961937509977652, 51.87390960531436690 ) ) ;
#148371 = CARTESIAN_POINT ( 'NONE',  ( -19.02544592524342804, 5.153800228976336051, 111.0405762719810099 ) ) ;
#148373 = CARTESIAN_POINT ( 'NONE',  ( 4.483927247898545687, 16.52544592524342804, 54.79057627198104541 ) ) ;
#148372 = CARTESIAN_POINT ( 'NONE',  ( -21.55341960407610458, -5.719274019375992779, 91.45724293864769550 ) ) ;
#148374 = CARTESIAN_POINT ( 'NONE',  ( 15.80617190586769283, -15.72974639402175789, 70.62609039468567573 ) ) ;
#148376 = CARTESIAN_POINT ( 'NONE',  ( 19.03943276465977164, 0.05219959533936151252, 31.25109039468566863 ) ) ;
#148375 = CARTESIAN_POINT ( 'NONE',  ( -8.314922557961024197, 14.29746914071037800, 27.91775706135234358 ) ) ;
#148377 = CARTESIAN_POINT ( 'NONE',  ( 4.483927247898545687, 16.52544592524342804, 29.79057627198102409 ) ) ;
#148378 = CARTESIAN_POINT ( 'NONE',  ( -5.719274019375978568, 21.55341960407610458, 110.2072429386477239 ) ) ;
#148379 = CARTESIAN_POINT ( 'NONE',  ( 8.224510206698953496, -14.34966873604960469, 47.91557627198102409 ) ) ;
#148380 = CARTESIAN_POINT ( 'NONE',  ( 19.03943276465977164, 0.05219959533936151252, 96.25109039468567573 ) ) ;
#148381 = EDGE_CURVE ( 'NONE', #109664, #68126, #100627, .T. ) ;
#148382 = CARTESIAN_POINT ( 'NONE',  ( 19.03943276465977164, 0.05219959533936151252, 71.25109039468566152 ) ) ;
#148383 = CARTESIAN_POINT ( 'NONE',  ( 5.823673210054444382, -21.52544592524334988, 70.20942372801904696 ) ) ;
#148384 = CARTESIAN_POINT ( 'NONE',  ( 0.05219959533936267826, -19.03943276465977164, 55.00109039468566863 ) ) ;
#148385 = CARTESIAN_POINT ( 'NONE',  ( 8.224510206698953496, -14.34966873604960469, 112.9155762719810383 ) ) ;
#148386 = CARTESIAN_POINT ( 'NONE',  ( 21.55341960407610458, 5.719274019375980345, 38.95724293864768839 ) ) ;
#148387 = CARTESIAN_POINT ( 'NONE',  ( 16.55341960407611168, 4.379528057220329451, 43.95724293864769550 ) ) ;
#148388 = CARTESIAN_POINT ( 'NONE',  ( -17.40861289039006010, -6.110651285853202275, 26.37232470827433062 ) ) ;
#148389 = CARTESIAN_POINT ( 'NONE',  ( -18.67979575497193778, 10.72451020669871902, 113.3344237280190328 ) ) ;
#148390 = CARTESIAN_POINT ( 'NONE',  ( -16.55341960407617563, 4.379528057220093196, 78.54275706135236135 ) ) ;
#148391 = CARTESIAN_POINT ( 'NONE',  ( -12.06949235617756955, 12.14591786802309770, 40.62390960531435269 ) ) ;
#148392 = CARTESIAN_POINT ( 'NONE',  ( 21.55341960407619695, -5.719274019375665929, 76.04275706135237556 ) ) ;
#148393 = CARTESIAN_POINT ( 'NONE',  ( 21.55341960407619695, -5.719274019375665929, 71.04275706135234714 ) ) ;
#148394 = CARTESIAN_POINT ( 'NONE',  ( 18.62759615963271287, -10.81492255796078972, 78.33224293864770971 ) ) ;
#148395 = CARTESIAN_POINT ( 'NONE',  ( -9.564922557960796823, -16.46253265017161027, 37.08224293864768839 ) ) ;
#148396 = CARTESIAN_POINT ( 'NONE',  ( -21.55341960407619339, 5.719274019375674811, 53.54275706135234714 ) ) ;
#148397 = CARTESIAN_POINT ( 'NONE',  ( 16.51473224551069308, 9.474510206698969483, 39.16557627198103120 ) ) ;
#148398 = CARTESIAN_POINT ( 'NONE',  ( -5.049401038298153566, 19.05341960407611168, 55.20724293864769550 ) ) ;
#148399 = CARTESIAN_POINT ( 'NONE',  ( 0.05219959533910956823, 16.53943276465976808, 94.99890960531436690 ) ) ;
#148400 = CARTESIAN_POINT ( 'NONE',  ( 13.97604488694527802, 13.89961937509977652, 79.37390960531435269 ) ) ;
#148401 = CARTESIAN_POINT ( 'NONE',  ( 14.34966873604960469, 8.224510206698951720, 44.16557627198103120 ) ) ;
#148402 = CARTESIAN_POINT ( 'NONE',  ( 4.483927247898545687, 16.52544592524342804, 99.79057627198103830 ) ) ;
#148403 = CARTESIAN_POINT ( 'NONE',  ( -10.81492255796078084, -18.62759615963271287, 67.08224293864770971 ) ) ;
#148404 = CARTESIAN_POINT ( 'NONE',  ( -10.81492255796105439, 18.62759615963255655, 27.91775706135234358 ) ) ;
#148405 = CARTESIAN_POINT ( 'NONE',  ( -16.01221511231805650, 14.62261807015716997, -56.20577350945247019 ) ) ;
#148407 = CARTESIAN_POINT ( 'NONE',  ( -16.55341960407617563, 4.379528057220093196, 23.54275706135235424 ) ) ;
#148406 = CARTESIAN_POINT ( 'NONE',  ( 5.153800228976335163, 19.02544592524342804, 79.79057627198102409 ) ) ;
#148408 = CARTESIAN_POINT ( 'NONE',  ( 10.81492255796078972, 18.62759615963270932, 64.58224293864769550 ) ) ;
#148409 = CARTESIAN_POINT ( 'NONE',  ( 21.53943276465977519, 0.05219959533937863772, 101.2510903946856757 ) ) ;
#148410 = CARTESIAN_POINT ( 'NONE',  ( 9.564922557960805705, 16.46253265017160317, 74.58224293864769550 ) ) ;
#148411 = CARTESIAN_POINT ( 'NONE',  ( -15.72974639402176322, -15.80617190586768395, 19.37609039468568639 ) ) ;
#148412 = CARTESIAN_POINT ( 'NONE',  ( -0.05219959533909027116, -19.03943276465977164, 107.4989096053143527 ) ) ;
#148413 = CARTESIAN_POINT ( 'NONE',  ( -16.53943276465976808, -0.05219959533934237506, 83.75109039468568994 ) ) ;
#148414 = CARTESIAN_POINT ( 'NONE',  ( 18.67979575497194134, -10.72451020669871369, 75.83442372801900433 ) ) ;
#148415 = CARTESIAN_POINT ( 'NONE',  ( -18.62759615963255300, -10.81492255796106328, 94.16775706135237556 ) ) ;
#148416 = CARTESIAN_POINT ( 'NONE',  ( 12.06949235617739724, 12.14591786802326823, 56.87609039468568994 ) ) ;
#148417 = CARTESIAN_POINT ( 'NONE',  ( 10.72451020669871369, 18.67979575497193778, 32.08442372801901854 ) ) ;
#148418 = CARTESIAN_POINT ( 'NONE',  ( 5.153800228976335163, 19.02544592524342804, 114.7905762719810241 ) ) ;
#148419 = CARTESIAN_POINT ( 'NONE',  ( 21.52544592524334988, 5.823673210054432836, 96.45942372801901854 ) ) ;
#148420 = CARTESIAN_POINT ( 'NONE',  ( 0.05219959533909260263, 19.03943276465977164, 99.99890960531436690 ) ) ;
#148421 = CARTESIAN_POINT ( 'NONE',  ( 21.52544592524344225, -5.823673210054117533, 88.54057627198103830 ) ) ;
#148422 = CARTESIAN_POINT ( 'NONE',  ( 19.03943276465977164, 0.05219959533936151252, 61.25109039468566863 ) ) ;
#148424 = CARTESIAN_POINT ( 'NONE',  ( 10.81492255796078972, 18.62759615963270932, 54.58224293864769550 ) ) ;
#148423 = CARTESIAN_POINT ( 'NONE',  ( -14.77336750280015387, -39.52550427972444425, -19.86057791183451116 ) ) ;
#148426 = CARTESIAN_POINT ( 'NONE',  ( -0.05219959533910754901, -16.53943276465976808, 42.49890960531435979 ) ) ;
#148425 = CARTESIAN_POINT ( 'NONE',  ( 19.05341960407611168, 5.049401038298154454, 88.95724293864769550 ) ) ;
#148427 = CARTESIAN_POINT ( 'NONE',  ( 21.44939319537015265, 9.428468639168977816, 168.6471776813584711 ) ) ;
#148428 = CARTESIAN_POINT ( 'NONE',  ( -5.049401038297874678, -19.05341960407617918, 79.79275706135233293 ) ) ;
#148429 = CARTESIAN_POINT ( 'NONE',  ( -1.455575599910876816, -15.57446157010955012, -61.81477736546833057 ) ) ;
#148430 = CARTESIAN_POINT ( 'NONE',  ( 9.474510206698729675, 16.51473224551082808, 112.0844237280190043 ) ) ;
#148431 = CARTESIAN_POINT ( 'NONE',  ( 10.81492255796078972, 18.62759615963270932, 84.58224293864769550 ) ) ;
#148432 = CARTESIAN_POINT ( 'NONE',  ( 12.14591786802309770, 12.06949235617756955, 59.37390960531436690 ) ) ;
#148433 = CARTESIAN_POINT ( 'NONE',  ( -0.05219959533909027116, -19.03943276465977164, 97.49890960531436690 ) ) ;
#148434 = CARTESIAN_POINT ( 'NONE',  ( 14.29746914071037800, 8.314922557961029526, 31.66775706135234358 ) ) ;
#148435 = CARTESIAN_POINT ( 'NONE',  ( -13.97604488694527625, -13.89961937509977652, 56.87390960531434558 ) ) ;
#148437 = CARTESIAN_POINT ( 'NONE',  ( -19.03943276465977164, -0.05219959533935918106, 88.75109039468567573 ) ) ;
#148436 = CARTESIAN_POINT ( 'NONE',  ( 10.72451020669871369, 18.67979575497193778, 22.08442372801901143 ) ) ;
#148438 = CARTESIAN_POINT ( 'NONE',  ( -13.97604488694527625, -13.89961937509977652, 91.87390960531432427 ) ) ;
#148439 = CARTESIAN_POINT ( 'NONE',  ( 19.02544592524343514, -5.153800228976328945, 73.54057627198103830 ) ) ;
#148440 = CARTESIAN_POINT ( 'NONE',  ( -18.62759615963270932, 10.81492255796079327, 75.83224293864769550 ) ) ;
#148441 = CARTESIAN_POINT ( 'NONE',  ( 5.049401038298161559, -19.05341960407611168, 52.70724293864767418 ) ) ;
#148442 = DIRECTION ( 'NONE',  ( 1.000000000000000000, 0.000000000000000000, -0.000000000000000000 ) ) ;
#148443 = CARTESIAN_POINT ( 'NONE',  ( -8.224510206698948167, 14.34966873604960824, 50.41557627198103120 ) ) ;
#148444 = CARTESIAN_POINT ( 'NONE',  ( -5.049401038298153566, 19.05341960407611168, 110.2072429386476671 ) ) ;
#148445 = DIRECTION ( 'NONE',  ( 0.000000000000000000, 0.6427876096865403621, 0.7660444431189770143 ) ) ;
#148446 = CARTESIAN_POINT ( 'NONE',  ( 13.89961937509957401, 13.97604488694547697, 66.87609039468567573 ) ) ;
#148447 = CARTESIAN_POINT ( 'NONE',  ( 10.72451020669898902, -18.67979575497178502, 77.91557627198102409 ) ) ;
#148448 = CARTESIAN_POINT ( 'NONE',  ( 16.46253265017146816, 9.564922557961045513, 56.66775706135233293 ) ) ;
#148449 = CARTESIAN_POINT ( 'NONE',  ( 9.474510206698971260, -16.51473224551069308, 102.9155762719810241 ) ) ;
#148450 = CARTESIAN_POINT ( 'NONE',  ( -17.49999999999999289, 3.512728167236932375, 115.2280999518112310 ) ) ;
#148451 = CARTESIAN_POINT ( 'NONE',  ( -15.72974639402197994, 15.80617190586746368, 45.62390960531436690 ) ) ;
#148452 = CARTESIAN_POINT ( 'NONE',  ( 9.474510206698971260, -16.51473224551069308, 67.91557627198102409 ) ) ;
#148453 = CARTESIAN_POINT ( 'NONE',  ( -21.53943276465977519, -0.05219959533937600094, 63.75109039468568284 ) ) ;
#148454 = CARTESIAN_POINT ( 'NONE',  ( -0.05219959533909027116, -19.03943276465977164, 32.49890960531435979 ) ) ;
#148455 = EDGE_CURVE ( 'NONE', #147958, #150223, #17946, .T. ) ;
#148457 = ORIENTED_EDGE ( 'NONE', *, *, #91512, .T. ) ;
#148456 = CARTESIAN_POINT ( 'NONE',  ( 10.81492255796078972, 18.62759615963270932, 109.5822429386476955 ) ) ;
#148458 = CARTESIAN_POINT ( 'NONE',  ( -21.52544592524334988, -5.823673210054445271, 53.95942372801900433 ) ) ;
#148460 = ORIENTED_EDGE ( 'NONE', *, *, #84216, .F. ) ;
#148459 = B_SPLINE_CURVE_WITH_KNOTS ( 'NONE', 3,
 ( #121700, #124685, #186381, #199550, #15529, #137871, #61020, #171194, #125679, #122692, #172182, #64010, #187377, #33667, #47859, #123670, #109512, #184381, #32683, #183395, #94336, #2329, #152055, #75206, #44877, #106533, #91339, #153030, #107515, #30698, #92349, #154035 ),
 .UNSPECIFIED., .F., .F.,
 ( 4, 2, 2, 2, 2, 2, 2, 2, 2, 2, 2, 2, 2, 2, 2, 4 ),
 ( 7.806255641895631925E-18, 0.0003712461730036849890, 0.0007424923460073621717, 0.001113738519011039192, 0.001484984692014716537, 0.002227477038022070577, 0.002598723211025750959, 0.002969969384029430906, 0.003341215557033111287, 0.003712461730036792102, 0.004083707903040472049, 0.004454954076044152431, 0.004826200249047833679, 0.005197446422051514060, 0.005568692595055194441, 0.005939938768058873955 ),
 .UNSPECIFIED. ) ;
#148461 = CARTESIAN_POINT ( 'NONE',  ( 13.89961937509977652, -13.97604488694527269, 108.1239096053143669 ) ) ;
#148462 = CARTESIAN_POINT ( 'NONE',  ( -16.46253265017146816, -9.564922557961047289, 69.16775706135233293 ) ) ;
#148463 = LINE ( 'NONE', #23120, #79370 ) ;
#148464 = CARTESIAN_POINT ( 'NONE',  ( 0.05219959533937995610, -21.53943276465977519, 25.00109039468567218 ) ) ;
#148465 = CARTESIAN_POINT ( 'NONE',  ( -16.51473224551069308, -9.474510206698971260, 61.66557627198103120 ) ) ;
#148466 = CARTESIAN_POINT ( 'NONE',  ( 14.34966873604972726, -8.224510206698740333, 35.83442372801901143 ) ) ;
#148467 = CARTESIAN_POINT ( 'NONE',  ( 11.74264578624800315, -36.14014761921581709, -5.149999994537626691 ) ) ;
#148468 = CARTESIAN_POINT ( 'NONE',  ( 0.05219959533937995610, -21.53943276465977519, 110.0010903946856757 ) ) ;
#148469 = CARTESIAN_POINT ( 'NONE',  ( 16.51473224551069308, 9.474510206698969483, 39.16557627198103120 ) ) ;
#148470 = CARTESIAN_POINT ( 'NONE',  ( -15.72974639402176322, -15.80617190586768395, 109.3760903946857042 ) ) ;
#148471 = CARTESIAN_POINT ( 'NONE',  ( -12.14591786802326823, 12.06949235617739902, 93.12609039468568994 ) ) ;
#148472 = ADVANCED_FACE ( 'NONE', ( #190385 ), #21525, .F. ) ;
#148474 = CARTESIAN_POINT ( 'NONE',  ( -18.67979575497193778, 10.72451020669871902, 58.33442372801901143 ) ) ;
#148473 = CARTESIAN_POINT ( 'NONE',  ( -19.05341960407611168, -5.049401038298163336, 91.45724293864766707 ) ) ;
#148475 = AXIS2_PLACEMENT_3D ( 'NONE', #146829, #51820, #68989 ) ;
#148476 = CARTESIAN_POINT ( 'NONE',  ( -27.73933785331498925, 9.013057229001089965, 149.2750000027311330 ) ) ;
#148477 = DIRECTION ( 'NONE',  ( 0.000000000000000000, 0.000000000000000000, 1.000000000000000000 ) ) ;
#148478 = CARTESIAN_POINT ( 'NONE',  ( -17.49999999999999645, 3.305555262949589235, 29.62517152156600986 ) ) ;
#148480 = CARTESIAN_POINT ( 'NONE',  ( 21.52544592524334988, 5.823673210054432836, 76.45942372801901854 ) ) ;
#148479 = CARTESIAN_POINT ( 'NONE',  ( -14.29746914071037622, -8.314922557961029526, 59.16775706135234714 ) ) ;
#148481 = CARTESIAN_POINT ( 'NONE',  ( 5.823673210054444382, -21.52544592524334988, 105.2094237280190328 ) ) ;
#148482 = CARTESIAN_POINT ( 'NONE',  ( 25.31021317688468031, -7.802057701675677137, 170.7256852586635318 ) ) ;
#148483 = CARTESIAN_POINT ( 'NONE',  ( 4.483927247898790824, -16.52544592524335698, 30.20942372801902565 ) ) ;
#148484 = CARTESIAN_POINT ( 'NONE',  ( -19.05341960407611168, -5.049401038298163336, 91.45724293864766707 ) ) ;
#148485 = CARTESIAN_POINT ( 'NONE',  ( 9.564922557960805705, 16.46253265017160317, 109.5822429386476955 ) ) ;
#148486 = ORIENTED_EDGE ( 'NONE', *, *, #7273, .F. ) ;
#148487 = CARTESIAN_POINT ( 'NONE',  ( 16.62475595723695676, 7.163666690055255692, 41.97286648189537317 ) ) ;
#148488 = CARTESIAN_POINT ( 'NONE',  ( -16.51473224551069308, -9.474510206698971260, 21.66557627198102765 ) ) ;
#148489 = CARTESIAN_POINT ( 'NONE',  ( -5.823673210054116645, -21.52544592524344225, 42.29057627198103120 ) ) ;
#148490 = CARTESIAN_POINT ( 'NONE',  ( 4.379528057220092307, 16.55341960407617563, 112.2927570613523471 ) ) ;
#148492 = CARTESIAN_POINT ( 'NONE',  ( 13.89961937509977652, -13.97604488694527269, 73.12390960531436690 ) ) ;
#148491 = CARTESIAN_POINT ( 'NONE',  ( 0.05219959533910956823, 16.53943276465976808, 89.99890960531438111 ) ) ;
#148493 = CARTESIAN_POINT ( 'NONE',  ( -5.719274019375665041, -21.55341960407619695, 89.79275706135236135 ) ) ;
#148494 = CARTESIAN_POINT ( 'NONE',  ( -8.224510206698735004, -14.34966873604973081, 19.58442372801901143 ) ) ;
#148495 = CARTESIAN_POINT ( 'NONE',  ( -4.379528057220328563, 16.55341960407611168, 95.20724293864769550 ) ) ;
#148496 = CARTESIAN_POINT ( 'NONE',  ( 18.62759615963255655, 10.81492255796105972, 41.66775706135235424 ) ) ;
#148497 = CARTESIAN_POINT ( 'NONE',  ( 21.55341960407610458, 5.719274019375980345, 73.95724293864769550 ) ) ;
#148498 = CARTESIAN_POINT ( 'NONE',  ( -5.049401038297874678, -19.05341960407617918, 39.79275706135232582 ) ) ;
#148499 = CARTESIAN_POINT ( 'NONE',  ( -34.78522506798723413, -4.592425496937305498E-15, 52.50000000000000000 ) ) ;
#148500 = CARTESIAN_POINT ( 'NONE',  ( 19.02544592524343514, -5.153800228976328945, 93.54057627198102409 ) ) ;
#148501 = CARTESIAN_POINT ( 'NONE',  ( -14.29746914071049879, 8.314922557960819915, 65.83224293864769550 ) ) ;
#148502 = CIRCLE ( 'NONE', #48483, 38.00000000000000000 ) ;
#148503 = CARTESIAN_POINT ( 'NONE',  ( 12.14591786802309770, 12.06949235617756955, 49.37390960531436690 ) ) ;
#148504 = CARTESIAN_POINT ( 'NONE',  ( -4.483927247898539470, -16.52544592524342804, 22.29057627198102765 ) ) ;
#148505 = CARTESIAN_POINT ( 'NONE',  ( 5.049401038297881783, 19.05341960407617563, 62.29275706135234003 ) ) ;
#148506 = CARTESIAN_POINT ( 'NONE',  ( 5.153800228976617603, -19.02544592524335343, 90.20942372801900433 ) ) ;
#148507 = CARTESIAN_POINT ( 'NONE',  ( 15.80617190586746368, 15.72974639402197994, 24.37390960531435979 ) ) ;
#148508 = CARTESIAN_POINT ( 'NONE',  ( -14.34966873604960291, -8.224510206698953496, 91.66557627198103830 ) ) ;
#148509 = CARTESIAN_POINT ( 'NONE',  ( 24.95432927374997334, 3.806786798636384805, 190.0000000000000000 ) ) ;
#148511 = CARTESIAN_POINT ( 'NONE',  ( 15.72974639402199770, -15.80617190586745480, 53.12390960531436690 ) ) ;
#148510 = CARTESIAN_POINT ( 'NONE',  ( 13.89961937509977652, -13.97604488694527269, 48.12390960531435979 ) ) ;
#148512 = CARTESIAN_POINT ( 'NONE',  ( 10.72451020669898902, -18.67979575497178502, 82.91557627198103830 ) ) ;
#148513 = CARTESIAN_POINT ( 'NONE',  ( -9.564922557960796823, -16.46253265017161027, 22.08224293864768839 ) ) ;
#148515 = CARTESIAN_POINT ( 'NONE',  ( -19.05341960407611168, -5.049401038298163336, 51.45724293864770260 ) ) ;
#148514 = CARTESIAN_POINT ( 'NONE',  ( -12.06949235617739369, -12.14591786802326823, 69.37609039468567573 ) ) ;
#148516 = CARTESIAN_POINT ( 'NONE',  ( -19.02544592524334988, -5.153800228976617603, 43.95942372801899012 ) ) ;
#148517 = CARTESIAN_POINT ( 'NONE',  ( 18.62759615963255655, 10.81492255796105972, 56.66775706135235424 ) ) ;
#148518 = CARTESIAN_POINT ( 'NONE',  ( -12.14591786802309592, -12.06949235617757132, 111.8739096053143669 ) ) ;
#148519 = CARTESIAN_POINT ( 'NONE',  ( 13.97604488694548053, -13.89961937509957401, 85.62609039468568994 ) ) ;
#148520 = CARTESIAN_POINT ( 'NONE',  ( -22.81625015709509441, -31.40387420917324590, -4.824999997268813345 ) ) ;
#148522 = CARTESIAN_POINT ( 'NONE',  ( -18.67979575497178146, -10.72451020669898902, 51.66557627198102409 ) ) ;
#148521 = CARTESIAN_POINT ( 'NONE',  ( -1.227931366032057224E-14, -24.30000000000003268, -56.77278709839600879 ) ) ;
#148523 = CARTESIAN_POINT ( 'NONE',  ( -16.51473224551069308, -9.474510206698971260, 26.66557627198103120 ) ) ;
#148524 = CARTESIAN_POINT ( 'NONE',  ( 0.05219959533937995610, -21.53943276465977519, 80.00109039468568994 ) ) ;
#148525 = CARTESIAN_POINT ( 'NONE',  ( -12.14591786802309592, -12.06949235617757132, 26.87390960531435979 ) ) ;
#148527 = CARTESIAN_POINT ( 'NONE',  ( 16.55341960407611168, 4.379528057220329451, 48.95724293864770971 ) ) ;
#148526 = CARTESIAN_POINT ( 'NONE',  ( -0.05219959533934338120, 16.53943276465976808, 52.50109039468567573 ) ) ;
#148528 = CARTESIAN_POINT ( 'NONE',  ( -18.67979575497178146, -10.72451020669898902, 86.66557627198102409 ) ) ;
#148529 = CARTESIAN_POINT ( 'NONE',  ( 5.719274019375991003, -21.55341960407610458, 77.70724293864770971 ) ) ;
#148530 = CARTESIAN_POINT ( 'NONE',  ( -3.573655867282028392E-15, 2.428612866367529932E-14, 139.9999999999999716 ) ) ;
#148532 = CARTESIAN_POINT ( 'NONE',  ( 19.05341960407611168, 5.049401038298154454, 113.9572429386477097 ) ) ;
#148531 = CARTESIAN_POINT ( 'NONE',  ( 5.049401038297881783, 19.05341960407617563, 77.29275706135231871 ) ) ;
#148533 = CARTESIAN_POINT ( 'NONE',  ( -13.97604488694527625, -13.89961937509977652, 46.87390960531435979 ) ) ;
#148534 = CARTESIAN_POINT ( 'NONE',  ( 13.97604488694527802, 13.89961937509977652, 39.37390960531435269 ) ) ;
#148535 = LINE ( 'NONE', #10026, #44451 ) ;
#148536 = ORIENTED_EDGE ( 'NONE', *, *, #24130, .T. ) ;
#148537 = CARTESIAN_POINT ( 'NONE',  ( -12.06949235617739369, -12.14591786802326823, 89.37609039468568994 ) ) ;
#148538 = CARTESIAN_POINT ( 'NONE',  ( 21.53943276465977519, -0.05219959533907433946, 98.74890960531438111 ) ) ;
#148539 = CARTESIAN_POINT ( 'NONE',  ( 19.03943276465977164, -0.05219959533909143690, 68.74890960531436690 ) ) ;
#148540 = CARTESIAN_POINT ( 'NONE',  ( -21.55341960407619339, 5.719274019375674811, 38.54275706135234714 ) ) ;
#148541 = CARTESIAN_POINT ( 'NONE',  ( 0.05219959533909260263, 19.03943276465977164, 99.99890960531436690 ) ) ;
#148542 = CARTESIAN_POINT ( 'NONE',  ( -27.28412861566019743, -28.99984389462718681, -16.93987563810431851 ) ) ;
#148543 = VERTEX_POINT ( 'NONE', #83186 ) ;
#148544 = CARTESIAN_POINT ( 'NONE',  ( -10.81492255796105439, 18.62759615963255655, 32.91775706135234714 ) ) ;
#148546 = CARTESIAN_POINT ( 'NONE',  ( 16.51473224551069308, 9.474510206698969483, 109.1655762719810383 ) ) ;
#148545 = CARTESIAN_POINT ( 'NONE',  ( -13.89961937509977652, 13.97604488694528158, 115.6239096053143669 ) ) ;
#148547 = CARTESIAN_POINT ( 'NONE',  ( -5.153800228976607833, 19.02544592524334988, 37.70942372801899722 ) ) ;
#148548 = CARTESIAN_POINT ( 'NONE',  ( 18.67979575497178502, 10.72451020669898547, 109.1655762719810383 ) ) ;
#148549 = CARTESIAN_POINT ( 'NONE',  ( 9.474510206698729675, 16.51473224551082808, 42.08442372801900433 ) ) ;
#148550 = CARTESIAN_POINT ( 'NONE',  ( -19.03943276465977164, -0.05219959533935918106, 43.75109039468566863 ) ) ;
#148551 = CARTESIAN_POINT ( 'NONE',  ( -8.314922557961024197, 14.29746914071037800, 92.91775706135236135 ) ) ;
#148552 = CARTESIAN_POINT ( 'NONE',  ( -13.89961937509977652, 13.97604488694528158, 115.6239096053143669 ) ) ;
#148553 = CARTESIAN_POINT ( 'NONE',  ( 9.564922557960805705, 16.46253265017160317, 74.58224293864769550 ) ) ;
#148554 = CARTESIAN_POINT ( 'NONE',  ( -15.72974639402176322, -15.80617190586768395, 84.37609039468570415 ) ) ;
#148555 = CARTESIAN_POINT ( 'NONE',  ( 15.72974639402176855, 15.80617190586768217, 96.87609039468568994 ) ) ;
#148556 = CARTESIAN_POINT ( 'NONE',  ( -1.499903966022400947, -7.794767548047344619, -64.20498622968422353 ) ) ;
#148557 = CARTESIAN_POINT ( 'NONE',  ( 19.03943276465977164, -0.05219959533909143690, 88.74890960531436690 ) ) ;
#148558 = CARTESIAN_POINT ( 'NONE',  ( -15.80617190586768217, 15.72974639402176855, 63.12609039468568994 ) ) ;
#148559 = CARTESIAN_POINT ( 'NONE',  ( -19.03943276465977164, -0.05219959533935918106, 98.75109039468567573 ) ) ;
#148560 = CARTESIAN_POINT ( 'NONE',  ( 13.89961937509977652, -13.97604488694527269, 68.12390960531436690 ) ) ;
#148562 = EDGE_CURVE ( 'NONE', #66839, #90870, #168326, .T. ) ;
#148561 = CARTESIAN_POINT ( 'NONE',  ( -0.05219959533909027116, -19.03943276465977164, 107.4989096053143527 ) ) ;
#148563 = CARTESIAN_POINT ( 'NONE',  ( 16.51473224551069308, 9.474510206698969483, 99.16557627198102409 ) ) ;
#148564 = DIRECTION ( 'NONE',  ( 0.000000000000000000, -1.000000000000000000, 0.000000000000000000 ) ) ;
#148565 = CARTESIAN_POINT ( 'NONE',  ( 9.564922557960805705, 16.46253265017160317, 59.58224293864769550 ) ) ;
#148566 = CARTESIAN_POINT ( 'NONE',  ( -16.51473224551069308, -9.474510206698971260, 51.66557627198102409 ) ) ;
#148567 = CARTESIAN_POINT ( 'NONE',  ( 18.62759615963255655, 10.81492255796105972, 21.66775706135235069 ) ) ;
#148568 = CARTESIAN_POINT ( 'NONE',  ( -16.55341960407617563, 4.379528057220093196, 103.5427570613523613 ) ) ;
#148569 = CARTESIAN_POINT ( 'NONE',  ( 7.052343178074640839, -2.552343178074650609, 8.889087296526001936 ) ) ;
#148570 = CARTESIAN_POINT ( 'NONE',  ( 19.05341960407617918, -5.049401038297876454, 56.04275706135234714 ) ) ;
#148571 = CARTESIAN_POINT ( 'NONE',  ( -9.474510206698964154, 16.51473224551069663, 90.41557627198103830 ) ) ;
#148572 = CARTESIAN_POINT ( 'NONE',  ( 16.52544592524342804, -4.483927247898539470, 68.54057627198103830 ) ) ;
#148573 = CARTESIAN_POINT ( 'NONE',  ( 14.34966873604960469, 8.224510206698951720, 109.1655762719810383 ) ) ;
#148574 = CARTESIAN_POINT ( 'NONE',  ( -18.67979575497178146, -10.72451020669898902, 31.66557627198102054 ) ) ;
#148575 = CARTESIAN_POINT ( 'NONE',  ( 16.51473224551069308, 9.474510206698969483, 114.1655762719810241 ) ) ;
#148576 = CARTESIAN_POINT ( 'NONE',  ( -8.224510206698948167, 14.34966873604960824, 95.41557627198102409 ) ) ;
#148577 = CARTESIAN_POINT ( 'NONE',  ( -17.26172910966779028, 6.454744622555849354, 55.80646908649224969 ) ) ;
#148578 = CARTESIAN_POINT ( 'NONE',  ( -5.153800228976607833, 19.02544592524334988, 32.70942372801899722 ) ) ;
#148579 = CARTESIAN_POINT ( 'NONE',  ( 4.483927247898790824, -16.52544592524335698, 110.2094237280190185 ) ) ;
#148580 = CARTESIAN_POINT ( 'NONE',  ( -19.03943276465977164, 0.05219959533909376836, 86.24890960531436690 ) ) ;
#148581 = CARTESIAN_POINT ( 'NONE',  ( -21.53943276465977519, -0.05219959533937600094, 48.75109039468568284 ) ) ;
#148582 = CARTESIAN_POINT ( 'NONE',  ( 5.823673210054125526, 21.52544592524343514, 44.79057627198103120 ) ) ;
#148583 = CARTESIAN_POINT ( 'NONE',  ( -5.823673210054431948, 21.52544592524334988, 37.70942372801900433 ) ) ;
#148584 = CARTESIAN_POINT ( 'NONE',  ( 15.80617190586746368, 15.72974639402197994, 79.37390960531436690 ) ) ;
#148585 = CARTESIAN_POINT ( 'NONE',  ( -12.14591786802309592, -12.06949235617757132, 101.8739096053143811 ) ) ;
#148586 = CARTESIAN_POINT ( 'NONE',  ( -5.153800228976607833, 19.02544592524334988, 57.70942372801899012 ) ) ;
#148587 = CARTESIAN_POINT ( 'NONE',  ( -9.564922557960796823, -16.46253265017161027, 42.08224293864769550 ) ) ;
#148588 = CARTESIAN_POINT ( 'NONE',  ( 16.51473224551069308, 9.474510206698969483, 94.16557627198103830 ) ) ;
#148589 = CARTESIAN_POINT ( 'NONE',  ( 16.46253265017160672, -9.564922557960803928, 93.33224293864769550 ) ) ;
#148590 = CARTESIAN_POINT ( 'NONE',  ( 16.55341960407611168, 4.379528057220329451, 113.9572429386477239 ) ) ;
#148591 = CARTESIAN_POINT ( 'NONE',  ( 12.06949235617757843, -12.14591786802309237, 38.12390960531436690 ) ) ;
#148592 = CARTESIAN_POINT ( 'NONE',  ( -0.05219959533934338120, 16.53943276465976808, 42.50109039468567573 ) ) ;
#148593 = CARTESIAN_POINT ( 'NONE',  ( -15.72974639402176322, -15.80617190586768395, 109.3760903946857042 ) ) ;
#148595 = CARTESIAN_POINT ( 'NONE',  ( -16.55341960407617563, 4.379528057220093196, 113.5427570613523756 ) ) ;
#148594 = CARTESIAN_POINT ( 'NONE',  ( 9.474510206698971260, -16.51473224551069308, 112.9155762719810383 ) ) ;
#148596 = CARTESIAN_POINT ( 'NONE',  ( 10.81492255796106328, -18.62759615963255655, 35.41775706135234003 ) ) ;
#148597 = CARTESIAN_POINT ( 'NONE',  ( 9.564922557960805705, 16.46253265017160317, 104.5822429386476955 ) ) ;
#148598 = CARTESIAN_POINT ( 'NONE',  ( 4.379528057220092307, 16.55341960407617563, 52.29275706135236135 ) ) ;
#148599 = CARTESIAN_POINT ( 'NONE',  ( 0.05219959533934541429, -16.53943276465976808, 110.0010903946856757 ) ) ;
#148600 = CARTESIAN_POINT ( 'NONE',  ( 14.34966873604972726, -8.224510206698740333, 90.83442372801901854 ) ) ;
#148601 = CARTESIAN_POINT ( 'NONE',  ( 12.06949235617739724, 12.14591786802326823, 21.87609039468567573 ) ) ;
#148602 = CARTESIAN_POINT ( 'NONE',  ( 0.05219959533909260263, 19.03943276465977164, 44.99890960531435979 ) ) ;
#148603 = CARTESIAN_POINT ( 'NONE',  ( -16.55341960407611168, -4.379528057220339221, 101.4572429386476955 ) ) ;
#148604 = CARTESIAN_POINT ( 'NONE',  ( 15.72974639402199770, -15.80617190586745480, 113.1239096053143953 ) ) ;
#148605 = CARTESIAN_POINT ( 'NONE',  ( -13.89961937509977652, 13.97604488694528158, 35.62390960531435269 ) ) ;
#148606 = CARTESIAN_POINT ( 'NONE',  ( -16.46253265017160317, 9.564922557960807481, 105.8322429386476955 ) ) ;
#148607 = CARTESIAN_POINT ( 'NONE',  ( -15.80617190586768217, 15.72974639402176855, 28.12609039468568284 ) ) ;
#148608 = CARTESIAN_POINT ( 'NONE',  ( 30.73962218707677607, 22.33364281372847060, -2.802157773949823127 ) ) ;
#148609 = CARTESIAN_POINT ( 'NONE',  ( 19.03943276465977164, -0.05219959533909143690, 108.7489096053143527 ) ) ;
#148610 = CARTESIAN_POINT ( 'NONE',  ( 28.79475375365586132, 2.781246896534039337E-14, 142.9843446568999639 ) ) ;
#148611 = CIRCLE ( 'NONE', #71105, 6.100000000000006750 ) ;
#148612 = CARTESIAN_POINT ( 'NONE',  ( 5.153800228976335163, 19.02544592524342804, 94.79057627198103830 ) ) ;
#148614 = CARTESIAN_POINT ( 'NONE',  ( -14.29746914071049879, 8.314922557960819915, 95.83224293864770971 ) ) ;
#148613 = CARTESIAN_POINT ( 'NONE',  ( -15.80617190586768217, 15.72974639402176855, 48.12609039468568284 ) ) ;
#148615 = CARTESIAN_POINT ( 'NONE',  ( 13.89961937509977652, -13.97604488694527269, 98.12390960531433848 ) ) ;
#148616 = CARTESIAN_POINT ( 'NONE',  ( -27.95742675678272704, -7.330130391662396327, 160.9071069586228191 ) ) ;
#148617 = CARTESIAN_POINT ( 'NONE',  ( 16.53943276465976808, 0.05219959533934440121, 66.25109039468567573 ) ) ;
#148618 = CARTESIAN_POINT ( 'NONE',  ( 15.72974639402176855, 15.80617190586768217, 81.87609039468568994 ) ) ;
#148619 = CARTESIAN_POINT ( 'NONE',  ( -12.14591786802326823, 12.06949235617739902, 43.12609039468568284 ) ) ;
#148621 = EDGE_CURVE ( 'NONE', #192521, #11672, #122469, .T. ) ;
#148620 = CARTESIAN_POINT ( 'NONE',  ( 9.564922557960805705, 16.46253265017160317, 84.58224293864769550 ) ) ;
#148622 = CARTESIAN_POINT ( 'NONE',  ( -19.03943276465977164, -0.05219959533935918106, 103.7510903946856757 ) ) ;
#148623 = CARTESIAN_POINT ( 'NONE',  ( 0.05219959533934541429, -16.53943276465976808, 70.00109039468568994 ) ) ;
#148624 = CARTESIAN_POINT ( 'NONE',  ( 15.80617190586769283, -15.72974639402175789, 105.6260903946856899 ) ) ;
#148625 = CARTESIAN_POINT ( 'NONE',  ( 9.474510206698729675, 16.51473224551082808, 92.08442372801900433 ) ) ;
#148626 = CARTESIAN_POINT ( 'NONE',  ( 13.89961937509977652, -13.97604488694527269, 58.12390960531436690 ) ) ;
#148627 = CARTESIAN_POINT ( 'NONE',  ( -21.53943276465977519, 0.05219959533907696930, 81.24890960531436690 ) ) ;
#148629 = CARTESIAN_POINT ( 'NONE',  ( -5.153800228976607833, 19.02544592524334988, 97.70942372801900433 ) ) ;
#148628 = CARTESIAN_POINT ( 'NONE',  ( -4.379528057220328563, 16.55341960407611168, 90.20724293864770971 ) ) ;
#148630 = CARTESIAN_POINT ( 'NONE',  ( -0.05219959533934338120, 16.53943276465976808, 62.50109039468568284 ) ) ;
#148631 = CARTESIAN_POINT ( 'NONE',  ( 24.73536985823908196, 3.645104810706905507, 171.5180696409492782 ) ) ;
#148632 = CARTESIAN_POINT ( 'NONE',  ( 16.46253265017146816, 9.564922557961045513, 56.66775706135233293 ) ) ;
#148633 = CARTESIAN_POINT ( 'NONE',  ( 16.52544592524342804, -4.483927247898539470, 38.54057627198103120 ) ) ;
#148634 = CARTESIAN_POINT ( 'NONE',  ( -12.06949235617756955, 12.14591786802309770, 85.62390960531436690 ) ) ;
#148636 = CARTESIAN_POINT ( 'NONE',  ( -17.40861289039010629, 6.110651285853060166, 38.62767529172569425 ) ) ;
#148635 = CARTESIAN_POINT ( 'NONE',  ( -5.049401038297874678, -19.05341960407617918, 24.79275706135233648 ) ) ;
#148637 = CARTESIAN_POINT ( 'NONE',  ( -15.80617190586768217, 15.72974639402176855, 23.12609039468567573 ) ) ;
#148638 = CARTESIAN_POINT ( 'NONE',  ( -13.89961937509977652, 13.97604488694528158, 105.6239096053143527 ) ) ;
#148639 = CARTESIAN_POINT ( 'NONE',  ( 19.05341960407611168, 5.049401038298154454, 83.95724293864766707 ) ) ;
#148640 = CARTESIAN_POINT ( 'NONE',  ( 15.72974639402176855, 15.80617190586768217, 101.8760903946857042 ) ) ;
#148641 = CARTESIAN_POINT ( 'NONE',  ( 13.89961937509977652, -13.97604488694527269, 78.12390960531433848 ) ) ;
#148642 = VERTEX_POINT ( 'NONE', #145858 ) ;
#148643 = CARTESIAN_POINT ( 'NONE',  ( 18.62759615963271287, -10.81492255796078972, 48.33224293864770260 ) ) ;
#148644 = CARTESIAN_POINT ( 'NONE',  ( 12.14591786802309770, 12.06949235617756955, 79.37390960531436690 ) ) ;
#148645 = CARTESIAN_POINT ( 'NONE',  ( -19.03943276465977164, 0.05219959533909376836, 61.24890960531436690 ) ) ;
#148646 = CARTESIAN_POINT ( 'NONE',  ( 4.379528057220339221, -16.55341960407611168, 92.70724293864770971 ) ) ;
#148647 = CARTESIAN_POINT ( 'NONE',  ( -10.81492255796105439, 18.62759615963255655, 27.91775706135234358 ) ) ;
#148648 = CIRCLE ( 'NONE', #42144, 5.000000000000000000 ) ;
#148649 = CARTESIAN_POINT ( 'NONE',  ( -21.55341960407619339, 5.719274019375674811, 63.54275706135234003 ) ) ;
#148650 = CARTESIAN_POINT ( 'NONE',  ( 13.97604488694527802, 13.89961937509977652, 34.37390960531436690 ) ) ;
#148651 = CARTESIAN_POINT ( 'NONE',  ( 4.379528057220092307, 16.55341960407617563, 57.29275706135234714 ) ) ;
#148652 = EDGE_CURVE ( 'NONE', #199732, #89527, #40606, .T. ) ;
#148653 = CARTESIAN_POINT ( 'NONE',  ( 10.72451020669871369, 18.67979575497193778, 22.08442372801901143 ) ) ;
#148654 = CARTESIAN_POINT ( 'NONE',  ( 10.81492255796078972, 18.62759615963270932, 114.5822429386477097 ) ) ;
#148656 = CARTESIAN_POINT ( 'NONE',  ( 13.97604488694527802, 13.89961937509977652, 49.37390960531434558 ) ) ;
#148655 = CARTESIAN_POINT ( 'NONE',  ( -19.05341960407617563, 5.049401038297882671, 38.54275706135233293 ) ) ;
#148657 = DIRECTION ( 'NONE',  ( -0.000000000000000000, 0.7071067811865467956, 0.7071067811865483499 ) ) ;
#148658 = CARTESIAN_POINT ( 'NONE',  ( 18.67979575497194134, -10.72451020669871369, 70.83442372801901854 ) ) ;
#148659 = CARTESIAN_POINT ( 'NONE',  ( 0.05219959533907565091, 21.53943276465977519, 59.99890960531436690 ) ) ;
#148660 = CARTESIAN_POINT ( 'NONE',  ( 12.14591786802309770, 12.06949235617756955, 34.37390960531435979 ) ) ;
#148662 = CARTESIAN_POINT ( 'NONE',  ( -19.02544592524334988, -5.153800228976617603, 18.95942372801899722 ) ) ;
#148661 = CARTESIAN_POINT ( 'NONE',  ( 0.05219959533937995610, -21.53943276465977519, 75.00109039468568994 ) ) ;
#148663 = CARTESIAN_POINT ( 'NONE',  ( -8.224510206698948167, 14.34966873604960824, 55.41557627198102409 ) ) ;
#148664 = CARTESIAN_POINT ( 'NONE',  ( -16.53943276465976808, 0.05219959533911058130, 111.2489096053143669 ) ) ;
#148665 = CARTESIAN_POINT ( 'NONE',  ( -13.97604488694547697, 13.89961937509957934, 48.12609039468566863 ) ) ;
#148666 = CARTESIAN_POINT ( 'NONE',  ( 0.05219959533934541429, -16.53943276465976808, 110.0010903946856757 ) ) ;
#148667 = CARTESIAN_POINT ( 'NONE',  ( 10.81492255796106328, -18.62759615963255655, 70.41775706135236135 ) ) ;
#148668 = CARTESIAN_POINT ( 'NONE',  ( 0.05219959533909260263, 19.03943276465977164, 59.99890960531436690 ) ) ;
#148669 = CARTESIAN_POINT ( 'NONE',  ( -16.51473224551082808, 9.474510206698731452, 33.33442372801899722 ) ) ;
#148670 = CARTESIAN_POINT ( 'NONE',  ( -21.52544592524343514, 5.823673210054127303, 41.04057627198103120 ) ) ;
#148671 = CARTESIAN_POINT ( 'NONE',  ( -21.55341960407619339, 5.719274019375674811, 33.54275706135234714 ) ) ;
#148672 = CARTESIAN_POINT ( 'NONE',  ( 18.67979575497178502, 10.72451020669898547, 84.16557627198103830 ) ) ;
#148673 = CARTESIAN_POINT ( 'NONE',  ( 13.97604488694548053, -13.89961937509957401, 80.62609039468567573 ) ) ;
#148674 = CARTESIAN_POINT ( 'NONE',  ( -4.379528057220086978, -16.55341960407618274, 49.79275706135234714 ) ) ;
#148676 = CARTESIAN_POINT ( 'NONE',  ( 10.72451020669898902, -18.67979575497178502, 92.91557627198103830 ) ) ;
#148675 = CARTESIAN_POINT ( 'NONE',  ( -21.38418241377624085, 7.427326039334300134, 174.4773576836617224 ) ) ;
#148677 = CARTESIAN_POINT ( 'NONE',  ( 16.55341960407611168, 4.379528057220329451, 93.95724293864770971 ) ) ;
#148678 = CARTESIAN_POINT ( 'NONE',  ( 1.474428118389591535, 30.72100710653361233, -47.31857186563917850 ) ) ;
#148679 = CARTESIAN_POINT ( 'NONE',  ( 0.05219959533934541429, -16.53943276465976808, 20.00109039468568639 ) ) ;
#148680 = CARTESIAN_POINT ( 'NONE',  ( -21.55341960407610458, -5.719274019375992779, 46.45724293864769550 ) ) ;
#148681 = CARTESIAN_POINT ( 'NONE',  ( 4.379528057220092307, 16.55341960407617563, 82.29275706135234714 ) ) ;
#148682 = LINE ( 'NONE', #118344, #122078 ) ;
#148683 = CARTESIAN_POINT ( 'NONE',  ( -16.52544592524335698, -4.483927247898792601, 53.95942372801900433 ) ) ;
#148684 = CARTESIAN_POINT ( 'NONE',  ( -21.53943276465977519, -0.05219959533937600094, 33.75109039468568284 ) ) ;
#148685 = CARTESIAN_POINT ( 'NONE',  ( -21.55341960407610458, -5.719274019375992779, 46.45724293864769550 ) ) ;
#148686 = CARTESIAN_POINT ( 'NONE',  ( 8.314922557961029526, -14.29746914071037800, 75.41775706135233293 ) ) ;
#148687 = CARTESIAN_POINT ( 'NONE',  ( 9.564922557960805705, 16.46253265017160317, 94.58224293864769550 ) ) ;
#148689 = CARTESIAN_POINT ( 'NONE',  ( 16.46253265017160672, -9.564922557960803928, 23.33224293864769194 ) ) ;
#148688 = CARTESIAN_POINT ( 'NONE',  ( 21.52544592524334988, 5.823673210054432836, 56.45942372801902565 ) ) ;
#148690 = CARTESIAN_POINT ( 'NONE',  ( 5.719274019375991003, -21.55341960407610458, 37.70724293864769550 ) ) ;
#148691 = CARTESIAN_POINT ( 'NONE',  ( 0.05219959533907565091, 21.53943276465977519, 24.99890960531435624 ) ) ;
#148692 = ORIENTED_EDGE ( 'NONE', *, *, #108955, .F. ) ;
#148693 = CARTESIAN_POINT ( 'NONE',  ( 19.02544592524334988, 5.153800228976608722, 41.45942372801900433 ) ) ;
#148694 = CARTESIAN_POINT ( 'NONE',  ( 14.34966873604972726, -8.224510206698740333, 45.83442372801901854 ) ) ;
#148695 = CARTESIAN_POINT ( 'NONE',  ( -13.97604488694527625, -13.89961937509977652, 111.8739096053143243 ) ) ;
#148696 = ORIENTED_EDGE ( 'NONE', *, *, #81756, .T. ) ;
#148697 = CARTESIAN_POINT ( 'NONE',  ( 0.05219959533909260263, 19.03943276465977164, 84.99890960531436690 ) ) ;
#148698 = CARTESIAN_POINT ( 'NONE',  ( 14.29746914071037800, 8.314922557961029526, 96.66775706135234714 ) ) ;
#148699 = DIRECTION ( 'NONE',  ( -1.000000000000000000, 0.000000000000000000, 0.000000000000000000 ) ) ;
#148700 = CARTESIAN_POINT ( 'NONE',  ( 14.29746914071049879, -8.314922557960816363, 98.33224293864769550 ) ) ;
#148701 = CARTESIAN_POINT ( 'NONE',  ( 21.52544592524344225, -5.823673210054117533, 43.54057627198103830 ) ) ;
#148702 = CARTESIAN_POINT ( 'NONE',  ( -0.05219959533909027116, -19.03943276465977164, 27.49890960531435624 ) ) ;
#148703 = CARTESIAN_POINT ( 'NONE',  ( -12.06949235617739369, -12.14591786802326823, 74.37609039468568994 ) ) ;
#148704 = CARTESIAN_POINT ( 'NONE',  ( -18.62759615963255300, -10.81492255796106328, 34.16775706135234714 ) ) ;
#148705 = CARTESIAN_POINT ( 'NONE',  ( -19.03943276465977164, -0.05219959533935918106, 88.75109039468567573 ) ) ;
#148706 = CARTESIAN_POINT ( 'NONE',  ( -9.474510206698964154, 16.51473224551069663, 40.41557627198103120 ) ) ;
#148707 = CARTESIAN_POINT ( 'NONE',  ( -20.96320343559653665, -21.46320343559631638, 4.646446609406719830 ) ) ;
#148708 = CARTESIAN_POINT ( 'NONE',  ( 5.823673210054444382, -21.52544592524334988, 110.2094237280190185 ) ) ;
#148709 = CARTESIAN_POINT ( 'NONE',  ( -13.97604488694527625, -13.89961937509977652, 81.87390960531436690 ) ) ;
#148710 = CARTESIAN_POINT ( 'NONE',  ( 4.379528057220092307, 16.55341960407617563, 57.29275706135234714 ) ) ;
#148711 = CARTESIAN_POINT ( 'NONE',  ( 10.72451020669871369, 18.67979575497193778, 97.08442372801904696 ) ) ;
#148712 = CARTESIAN_POINT ( 'NONE',  ( -19.02544592524334988, -5.153800228976617603, 58.95942372801900433 ) ) ;
#148713 = CARTESIAN_POINT ( 'NONE',  ( -16.51473224551082808, 9.474510206698731452, 73.33442372801900433 ) ) ;
#148714 = ORIENTED_EDGE ( 'NONE', *, *, #92523, .T. ) ;
#148715 = CARTESIAN_POINT ( 'NONE',  ( -18.62759615963255300, -10.81492255796106328, 64.16775706135234714 ) ) ;
#148716 = CARTESIAN_POINT ( 'NONE',  ( 19.03943276465977164, -0.05219959533909143690, 63.74890960531435979 ) ) ;
#148717 = CARTESIAN_POINT ( 'NONE',  ( -13.97604488694527625, -13.89961937509977652, 21.87390960531435979 ) ) ;
#148718 = CARTESIAN_POINT ( 'NONE',  ( 19.03943276465977164, 0.05219959533936151252, 61.25109039468566863 ) ) ;
#148719 = DIRECTION ( 'NONE',  ( 0.000000000000000000, 0.000000000000000000, 1.000000000000000000 ) ) ;
#148720 = CARTESIAN_POINT ( 'NONE',  ( -5.049401038298153566, 19.05341960407611168, 85.20724293864766707 ) ) ;
#148721 = CARTESIAN_POINT ( 'NONE',  ( -14.29746914071049879, 8.314922557960819915, 35.83224293864768839 ) ) ;
#148722 = CARTESIAN_POINT ( 'NONE',  ( -15.80617190586745835, -15.72974639402198527, 36.87390960531435979 ) ) ;
#148723 = DIRECTION ( 'NONE',  ( 0.000000000000000000, 0.000000000000000000, 1.000000000000000000 ) ) ;
#148724 = CARTESIAN_POINT ( 'NONE',  ( 10.81492255796106328, -18.62759615963255655, 105.4177570613523613 ) ) ;
#148725 = CARTESIAN_POINT ( 'NONE',  ( -27.96619922901617628, 7.272069078173023726, 160.9422763814154962 ) ) ;
#148726 = CARTESIAN_POINT ( 'NONE',  ( -13.89961937509977652, 13.97604488694528158, 35.62390960531435269 ) ) ;
#148727 = CARTESIAN_POINT ( 'NONE',  ( -15.49999999999999822, 7.499999999999998224, 22.00000000000000711 ) ) ;
#148728 = CARTESIAN_POINT ( 'NONE',  ( -34.35275354914907098, -2.907972467998146016, 90.32821402270536737 ) ) ;
#148729 = CARTESIAN_POINT ( 'NONE',  ( 15.72974639402176855, 15.80617190586768217, 66.87609039468568994 ) ) ;
#148730 = CARTESIAN_POINT ( 'NONE',  ( -14.13632694027962167, -34.57669575970837883, -7.999999999999994671 ) ) ;
#148731 = CARTESIAN_POINT ( 'NONE',  ( 4.483927247898790824, -16.52544592524335698, 60.20942372801902565 ) ) ;
#148732 = CARTESIAN_POINT ( 'NONE',  ( -15.80617190586745835, -15.72974639402198527, 86.87390960531438111 ) ) ;
#148733 = CARTESIAN_POINT ( 'NONE',  ( -8.224510206698948167, 14.34966873604960824, 50.41557627198103120 ) ) ;
#148735 = CARTESIAN_POINT ( 'NONE',  ( -16.51473224551069308, -9.474510206698971260, 106.6655762719810383 ) ) ;
#148734 = CARTESIAN_POINT ( 'NONE',  ( 19.02544592524343514, -5.153800228976328945, 23.54057627198102054 ) ) ;
#148736 = CARTESIAN_POINT ( 'NONE',  ( 5.719274019375673035, 21.55341960407619339, 32.29275706135235424 ) ) ;
#148737 = CARTESIAN_POINT ( 'NONE',  ( -9.564922557961040184, 16.46253265017147172, 47.91775706135233293 ) ) ;
#148738 = CARTESIAN_POINT ( 'NONE',  ( -5.049401038298153566, 19.05341960407611168, 40.20724293864768839 ) ) ;
#148739 = CARTESIAN_POINT ( 'NONE',  ( 21.52544592524334988, 5.823673210054432836, 81.45942372801900433 ) ) ;
#148740 = CARTESIAN_POINT ( 'NONE',  ( 17.50000000000002132, 5.622605283950869115, 98.81207310596117566 ) ) ;
#148741 = CARTESIAN_POINT ( 'NONE',  ( 8.224510206698953496, -14.34966873604960469, 27.91557627198103830 ) ) ;
#148742 = CARTESIAN_POINT ( 'NONE',  ( -36.91746825000000598, 2.428612866367529932E-14, -3.124999997268813168 ) ) ;
#148743 = CARTESIAN_POINT ( 'NONE',  ( -21.52544592524343514, 5.823673210054127303, 41.04057627198103120 ) ) ;
#148744 = CARTESIAN_POINT ( 'NONE',  ( 9.021937450273815884, -0.4877194249720462338, -63.96635223026898842 ) ) ;
#148745 = CARTESIAN_POINT ( 'NONE',  ( 16.46253265017160672, -9.564922557960803928, 88.33224293864769550 ) ) ;
#148746 = CARTESIAN_POINT ( 'NONE',  ( 14.34966873604960469, 8.224510206698951720, 89.16557627198102409 ) ) ;
#148747 = CARTESIAN_POINT ( 'NONE',  ( 19.03943276465977164, 0.05219959533936151252, 111.2510903946856757 ) ) ;
#148748 = CARTESIAN_POINT ( 'NONE',  ( -0.05219959533907301413, -21.53943276465977519, 62.49890960531436690 ) ) ;
#148749 = ORIENTED_EDGE ( 'NONE', *, *, #174036, .F. ) ;
#148750 = CARTESIAN_POINT ( 'NONE',  ( -5.049401038298153566, 19.05341960407611168, 30.20724293864768839 ) ) ;
#148752 = CARTESIAN_POINT ( 'NONE',  ( 5.719274019375991003, -21.55341960407610458, 82.70724293864770971 ) ) ;
#148751 = CARTESIAN_POINT ( 'NONE',  ( 9.474510206698971260, -16.51473224551069308, 82.91557627198103830 ) ) ;
#148754 = CARTESIAN_POINT ( 'NONE',  ( 5.153800228976335163, 19.02544592524342804, 99.79057627198102409 ) ) ;
#148753 = CARTESIAN_POINT ( 'NONE',  ( 8.314922557961029526, -14.29746914071037800, 105.4177570613523613 ) ) ;
#148755 = CARTESIAN_POINT ( 'NONE',  ( -9.564922557961040184, 16.46253265017147172, 77.91775706135234714 ) ) ;
#148756 = CARTESIAN_POINT ( 'NONE',  ( -21.55341960407619339, 5.719274019375674811, 93.54275706135234714 ) ) ;
#148757 = CARTESIAN_POINT ( 'NONE',  ( -21.53943276465977519, 0.05219959533907696930, 81.24890960531436690 ) ) ;
#148758 = CARTESIAN_POINT ( 'NONE',  ( 10.72451020669898902, -18.67979575497178502, 42.91557627198103120 ) ) ;
#148759 = CARTESIAN_POINT ( 'NONE',  ( -19.03943276465977164, 0.05219959533909376836, 51.24890960531436690 ) ) ;
#148760 = CARTESIAN_POINT ( 'NONE',  ( -0.05219959533910754901, -16.53943276465976808, 22.49890960531436335 ) ) ;
#148761 = CARTESIAN_POINT ( 'NONE',  ( -19.05341960407611168, -5.049401038298163336, 61.45724293864769550 ) ) ;
#148762 = VERTEX_POINT ( 'NONE', #8360 ) ;
#148763 = CARTESIAN_POINT ( 'NONE',  ( -32.64453336272028849, -0.4913453444576352802, 87.50000000000004263 ) ) ;
#148764 = CARTESIAN_POINT ( 'NONE',  ( 16.46253265017146816, 9.564922557961045513, 26.66775706135234003 ) ) ;
#148765 = CARTESIAN_POINT ( 'NONE',  ( -12.06949235617756955, 12.14591786802309770, 70.62390960531436690 ) ) ;
#148766 = CARTESIAN_POINT ( 'NONE',  ( -5.823673210054431948, 21.52544592524334988, 22.70942372801901499 ) ) ;
#148767 = CARTESIAN_POINT ( 'NONE',  ( -17.14385361876520264, -23.59649016807271593, 141.6750000027311103 ) ) ;
#148768 = CARTESIAN_POINT ( 'NONE',  ( -21.53943276465977519, 0.05219959533907696930, 61.24890960531435979 ) ) ;
#148769 = CARTESIAN_POINT ( 'NONE',  ( 12.14591786802327356, -12.06949235617739191, 95.62609039468568994 ) ) ;
#148770 = CARTESIAN_POINT ( 'NONE',  ( -16.53943276465976808, 0.05219959533911058130, 106.2489096053143811 ) ) ;
#148771 = CARTESIAN_POINT ( 'NONE',  ( -5.049401038298153566, 19.05341960407611168, 75.20724293864769550 ) ) ;
#148772 = PRESENTATION_STYLE_ASSIGNMENT (( #104255 ) ) ;
#148773 = CARTESIAN_POINT ( 'NONE',  ( 23.48298174826590667, -32.32155151706770368, -7.047842220587802409 ) ) ;
#148774 = CARTESIAN_POINT ( 'NONE',  ( 12.06949235617757843, -12.14591786802309237, 33.12390960531435979 ) ) ;
#148775 = CARTESIAN_POINT ( 'NONE',  ( 5.719274019375673035, 21.55341960407619339, 57.29275706135234714 ) ) ;
#148776 = CARTESIAN_POINT ( 'NONE',  ( 13.97604488694527802, 13.89961937509977652, 109.3739096053143669 ) ) ;
#148777 = CARTESIAN_POINT ( 'NONE',  ( -5.719274019375665041, -21.55341960407619695, 84.79275706135234714 ) ) ;
#148778 = CARTESIAN_POINT ( 'NONE',  ( -9.474510206698964154, 16.51473224551069663, 35.41557627198102409 ) ) ;
#148779 = CARTESIAN_POINT ( 'NONE',  ( 9.564922557960805705, 16.46253265017160317, 44.58224293864769550 ) ) ;
#148780 = ORIENTED_EDGE ( 'NONE', *, *, #2128, .T. ) ;
#148781 = CARTESIAN_POINT ( 'NONE',  ( -15.80617190586768217, 15.72974639402176855, 93.12609039468568994 ) ) ;
#148782 = CARTESIAN_POINT ( 'NONE',  ( 14.29746914071037800, 8.314922557961029526, 46.66775706135234714 ) ) ;
#148783 = CARTESIAN_POINT ( 'NONE',  ( 21.53943276465977519, 0.05219959533937863772, 91.25109039468568994 ) ) ;
#148784 = CARTESIAN_POINT ( 'NONE',  ( 19.05341960407611168, 5.049401038298154454, 108.9572429386477097 ) ) ;
#148785 = CARTESIAN_POINT ( 'NONE',  ( 9.564922557961047289, -16.46253265017146816, 95.41775706135233293 ) ) ;
#148786 = CARTESIAN_POINT ( 'NONE',  ( -5.719274019375665041, -21.55341960407619695, 59.79275706135234714 ) ) ;
#148787 = CARTESIAN_POINT ( 'NONE',  ( 16.52544592524335698, 4.483927247898782831, 26.45942372801901854 ) ) ;
#148788 = CARTESIAN_POINT ( 'NONE',  ( 13.89961937509957401, 13.97604488694547697, 81.87609039468564731 ) ) ;
#148789 = CARTESIAN_POINT ( 'NONE',  ( -0.05219959533909027116, -19.03943276465977164, 52.49890960531436690 ) ) ;
#148790 = CARTESIAN_POINT ( 'NONE',  ( 9.564922557961047289, -16.46253265017146816, 95.41775706135233293 ) ) ;
#148791 = CARTESIAN_POINT ( 'NONE',  ( -14.29746914071049879, 8.314922557960819915, 25.83224293864769194 ) ) ;
#148792 = CARTESIAN_POINT ( 'NONE',  ( -5.049401038297874678, -19.05341960407617918, 94.79275706135230450 ) ) ;
#148793 = CARTESIAN_POINT ( 'NONE',  ( 12.06949235617757843, -12.14591786802309237, 48.12390960531436690 ) ) ;
#148794 = CARTESIAN_POINT ( 'NONE',  ( -16.51473224551082808, 9.474510206698731452, 68.33442372801900433 ) ) ;
#148795 = CARTESIAN_POINT ( 'NONE',  ( -0.05219959533934338120, 16.53943276465976808, 57.50109039468568994 ) ) ;
#148796 = CARTESIAN_POINT ( 'NONE',  ( -5.153800228976607833, 19.02544592524334988, 22.70942372801899012 ) ) ;
#148797 = CARTESIAN_POINT ( 'NONE',  ( -16.51473224551069308, -9.474510206698971260, 21.66557627198102765 ) ) ;
#148798 = CARTESIAN_POINT ( 'NONE',  ( -19.02544592524342804, 5.153800228976336051, 41.04057627198103120 ) ) ;
#148799 = CARTESIAN_POINT ( 'NONE',  ( -0.05219959533934338120, 16.53943276465976808, 57.50109039468568994 ) ) ;
#148800 = CARTESIAN_POINT ( 'NONE',  ( -3.573655867282028392E-15, 2.428612866367529932E-14, 150.0000000000000000 ) ) ;
#148801 = EDGE_CURVE ( 'NONE', #119464, #89770, #86315, .T. ) ;
#148802 = CARTESIAN_POINT ( 'NONE',  ( 27.73933785331498214, 9.013057229001095294, 147.9750000027311501 ) ) ;
#148803 = CARTESIAN_POINT ( 'NONE',  ( -16.51473224551069308, -9.474510206698971260, 101.6655762719810241 ) ) ;
#148804 = CARTESIAN_POINT ( 'NONE',  ( 17.78921395495471103, 1.086248361264983142, 102.5000000000000142 ) ) ;
#148805 = ORIENTED_EDGE ( 'NONE', *, *, #101326, .F. ) ;
#148806 = CARTESIAN_POINT ( 'NONE',  ( 0.05219959533936267826, -19.03943276465977164, 100.0010903946856757 ) ) ;
#148807 = CARTESIAN_POINT ( 'NONE',  ( 21.53943276465977519, -0.05219959533907433946, 38.74890960531435979 ) ) ;
#148809 = CARTESIAN_POINT ( 'NONE',  ( -0.05219959533936034679, 19.03943276465977164, 112.5010903946856757 ) ) ;
#148808 = CARTESIAN_POINT ( 'NONE',  ( 13.89961937509957401, 13.97604488694547697, 26.87609039468566507 ) ) ;
#148810 = CARTESIAN_POINT ( 'NONE',  ( -19.02544592524342804, 5.153800228976336051, 31.04057627198102409 ) ) ;
#148811 = CARTESIAN_POINT ( 'NONE',  ( -13.97604488694527625, -13.89961937509977652, 41.87390960531435979 ) ) ;
#148812 = CARTESIAN_POINT ( 'NONE',  ( 15.72974639402199770, -15.80617190586745480, 73.12390960531436690 ) ) ;
#148813 = CARTESIAN_POINT ( 'NONE',  ( 0.05219959533909260263, 19.03943276465977164, 34.99890960531435979 ) ) ;
#148814 = CARTESIAN_POINT ( 'NONE',  ( 27.73933785331498569, 2.768321779492822058E-14, 142.3750000027311842 ) ) ;
#148815 = CARTESIAN_POINT ( 'NONE',  ( -0.05219959533936034679, 19.03943276465977164, 82.50109039468567573 ) ) ;
#148816 = CARTESIAN_POINT ( 'NONE',  ( -14.34966873604960291, -8.224510206698953496, 51.66557627198102409 ) ) ;
#148817 = CARTESIAN_POINT ( 'NONE',  ( 10.81492255796078972, 18.62759615963270932, 29.58224293864769905 ) ) ;
#148818 = CARTESIAN_POINT ( 'NONE',  ( -10.72451020669870658, -18.67979575497194134, 109.5844237280190328 ) ) ;
#148819 = CARTESIAN_POINT ( 'NONE',  ( 10.72451020669898902, -18.67979575497178502, 87.91557627198103830 ) ) ;
#148820 = CARTESIAN_POINT ( 'NONE',  ( -15.80617190586768217, 15.72974639402176855, 73.12609039468567573 ) ) ;
#148821 = CARTESIAN_POINT ( 'NONE',  ( -15.72974639402176322, -15.80617190586768395, 69.37609039468567573 ) ) ;
#148822 = CARTESIAN_POINT ( 'NONE',  ( 5.153800228976335163, 19.02544592524342804, 109.7905762719810099 ) ) ;
#148824 = CARTESIAN_POINT ( 'NONE',  ( -18.62759615963255300, -10.81492255796106328, 64.16775706135234714 ) ) ;
#148823 = CARTESIAN_POINT ( 'NONE',  ( 12.14591786802327356, -12.06949235617739191, 100.6260903946857184 ) ) ;
#148825 = CARTESIAN_POINT ( 'NONE',  ( -19.05341960407611168, -5.049401038298163336, 56.45724293864768129 ) ) ;
#148826 = CARTESIAN_POINT ( 'NONE',  ( 16.51473224551083163, -9.474510206698727899, 35.83442372801899722 ) ) ;
#148827 = CARTESIAN_POINT ( 'NONE',  ( 15.80617190586769283, -15.72974639402175789, 35.62609039468568994 ) ) ;
#148828 = CARTESIAN_POINT ( 'NONE',  ( 5.049401038298161559, -19.05341960407611168, 67.70724293864769550 ) ) ;
#148829 = CARTESIAN_POINT ( 'NONE',  ( -14.29746914071049879, 8.314922557960819915, 80.83224293864769550 ) ) ;
#148830 = CARTESIAN_POINT ( 'NONE',  ( -12.14591786802309592, -12.06949235617757132, 46.87390960531435979 ) ) ;
#148831 = CARTESIAN_POINT ( 'NONE',  ( 15.80617190586746368, 15.72974639402197994, 59.37390960531436690 ) ) ;
#148832 = CARTESIAN_POINT ( 'NONE',  ( 13.97604488694527802, 13.89961937509977652, 54.37390960531435979 ) ) ;
#148833 = CARTESIAN_POINT ( 'NONE',  ( -21.55341960407610458, -5.719274019375992779, 66.45724293864768129 ) ) ;
#148834 = CARTESIAN_POINT ( 'NONE',  ( -19.03943276465977164, -0.05219959533935918106, 48.75109039468566863 ) ) ;
#148836 = CARTESIAN_POINT ( 'NONE',  ( 12.14591786802309770, 12.06949235617756955, 69.37390960531436690 ) ) ;
#148835 = CARTESIAN_POINT ( 'NONE',  ( 19.05341960407618274, -5.049401038297876454, 21.04275706135233293 ) ) ;
#148837 = CARTESIAN_POINT ( 'NONE',  ( -5.823673210054116645, -21.52544592524344225, 42.29057627198103120 ) ) ;
#148838 = ORIENTED_EDGE ( 'NONE', *, *, #72845, .T. ) ;
#148839 = LINE ( 'NONE', #166005, #117405 ) ;
#148841 = CARTESIAN_POINT ( 'NONE',  ( 1.304474898271996253, 6.853129728370680240, -64.38708764409373941 ) ) ;
#148840 = CARTESIAN_POINT ( 'NONE',  ( 12.14591786802327356, -12.06949235617739191, 80.62609039468567573 ) ) ;
#148842 = CARTESIAN_POINT ( 'NONE',  ( -16.51473224551082808, 9.474510206698731452, 88.33442372801900433 ) ) ;
#148843 = CARTESIAN_POINT ( 'NONE',  ( -12.06949235617756955, 12.14591786802309770, 50.62390960531435979 ) ) ;
#148844 = FACE_OUTER_BOUND ( 'NONE', #131582, .T. ) ;
#148845 = CARTESIAN_POINT ( 'NONE',  ( 16.51473224551069308, 9.474510206698969483, 49.16557627198102409 ) ) ;
#148846 = CARTESIAN_POINT ( 'NONE',  ( -12.06949235617756955, 12.14591786802309770, 40.62390960531435269 ) ) ;
#148847 = CARTESIAN_POINT ( 'NONE',  ( 19.03943276465977164, -0.05219959533909143690, 93.74890960531435269 ) ) ;
#148848 = CARTESIAN_POINT ( 'NONE',  ( 9.564922557960805705, 16.46253265017160317, 49.58224293864770260 ) ) ;
#148849 = CARTESIAN_POINT ( 'NONE',  ( -21.52544592524334988, -5.823673210054445271, 58.95942372801902565 ) ) ;
#148850 = CARTESIAN_POINT ( 'NONE',  ( -9.474510206698964154, 16.51473224551069663, 75.41557627198103830 ) ) ;
#148851 = CARTESIAN_POINT ( 'NONE',  ( 5.049401038298161559, -19.05341960407611168, 27.70724293864769550 ) ) ;
#148852 = CARTESIAN_POINT ( 'NONE',  ( -13.89961937509977652, 13.97604488694528158, 55.62390960531434558 ) ) ;
#148853 = CARTESIAN_POINT ( 'NONE',  ( 21.52544592524344225, -5.823673210054117533, 43.54057627198103830 ) ) ;
#148854 = CARTESIAN_POINT ( 'NONE',  ( -9.474510206698964154, 16.51473224551069663, 30.41557627198102054 ) ) ;
#148855 = CARTESIAN_POINT ( 'NONE',  ( -21.55341960407610458, -5.719274019375992779, 41.45724293864769550 ) ) ;
#148856 = CARTESIAN_POINT ( 'NONE',  ( 16.55341960407618274, -4.379528057220086978, 106.0427570613523471 ) ) ;
#148857 = CARTESIAN_POINT ( 'NONE',  ( 9.564922557961047289, -16.46253265017146816, 30.41775706135232937 ) ) ;
#148859 = CARTESIAN_POINT ( 'NONE',  ( -4.379528057220086978, -16.55341960407618274, 79.79275706135236135 ) ) ;
#148858 = CARTESIAN_POINT ( 'NONE',  ( -8.314922557961024197, 14.29746914071037800, 52.91775706135235424 ) ) ;
#148860 = DIRECTION ( 'NONE',  ( 0.000000000000000000, 0.000000000000000000, -1.000000000000000000 ) ) ;
#148861 = CARTESIAN_POINT ( 'NONE',  ( 8.224510206698742110, 14.34966873604972548, 67.08442372801901854 ) ) ;
#148862 = CARTESIAN_POINT ( 'NONE',  ( 12.06949235617739724, 12.14591786802326823, 51.87609039468568284 ) ) ;
#148863 = CARTESIAN_POINT ( 'NONE',  ( -0.05219959533909027116, -19.03943276465977164, 107.4989096053143527 ) ) ;
#148864 = CARTESIAN_POINT ( 'NONE',  ( 16.46253265017160672, -9.564922557960803928, 33.33224293864770260 ) ) ;
#148865 = CARTESIAN_POINT ( 'NONE',  ( 0.05219959533934541429, -16.53943276465976808, 35.00109039468568284 ) ) ;
#148866 = CARTESIAN_POINT ( 'NONE',  ( -19.03943276465977164, 0.05219959533909376836, 46.24890960531435979 ) ) ;
#148867 = CARTESIAN_POINT ( 'NONE',  ( -0.05219959533937732626, 21.53943276465977519, 22.50109039468567573 ) ) ;
#148868 = CARTESIAN_POINT ( 'NONE',  ( 16.53943276465976808, 0.05219959533934440121, 31.25109039468568639 ) ) ;
#148869 = CARTESIAN_POINT ( 'NONE',  ( -4.379528057220086978, -16.55341960407618274, 99.79275706135234714 ) ) ;
#148870 = CARTESIAN_POINT ( 'NONE',  ( -19.05341960407611168, -5.049401038298163336, 21.45724293864768839 ) ) ;
#148871 = CARTESIAN_POINT ( 'NONE',  ( -18.62759615963255300, -10.81492255796106328, 94.16775706135237556 ) ) ;
#148872 = CARTESIAN_POINT ( 'NONE',  ( 16.51473224551083163, -9.474510206698727899, 100.8344237280190043 ) ) ;
#148873 = CARTESIAN_POINT ( 'NONE',  ( -9.474510206698720793, -16.51473224551083518, 49.58442372801899722 ) ) ;
#148874 = CARTESIAN_POINT ( 'NONE',  ( -14.34966873604960291, -8.224510206698953496, 51.66557627198102409 ) ) ;
#148875 = CARTESIAN_POINT ( 'NONE',  ( -5.153800228976328057, -19.02544592524343514, 22.29057627198102765 ) ) ;
#148877 = CARTESIAN_POINT ( 'NONE',  ( 17.13100169013227259, -6.664070546374125215, 58.26789835699826625 ) ) ;
#148876 = CARTESIAN_POINT ( 'NONE',  ( -16.46253265017146816, -9.564922557961047289, 54.16775706135234003 ) ) ;
#148878 = CARTESIAN_POINT ( 'NONE',  ( -10.81492255796105439, 18.62759615963255655, 62.91775706135236135 ) ) ;
#148879 = CARTESIAN_POINT ( 'NONE',  ( 14.34966873604972726, -8.224510206698740333, 20.83442372801901143 ) ) ;
#148880 = CARTESIAN_POINT ( 'NONE',  ( 16.62475595723701716, 7.163666690055268127, 81.97286648189530922 ) ) ;
#148881 = CARTESIAN_POINT ( 'NONE',  ( -5.719274019375978568, 21.55341960407610458, 25.20724293864769550 ) ) ;
#148882 = CARTESIAN_POINT ( 'NONE',  ( 13.89961937509957401, 13.97604488694547697, 101.8760903946856331 ) ) ;
#148883 = CARTESIAN_POINT ( 'NONE',  ( 0.05219959533909260263, 19.03943276465977164, 114.9989096053143669 ) ) ;
#148884 = CARTESIAN_POINT ( 'NONE',  ( -26.70292545465260758, 6.820347898102890660, 168.5277281069536741 ) ) ;
#148885 = CARTESIAN_POINT ( 'NONE',  ( 13.89961937509977652, -13.97604488694527269, 28.12390960531435624 ) ) ;
#148886 = CARTESIAN_POINT ( 'NONE',  ( 15.80617190586769283, -15.72974639402175789, 110.6260903946857042 ) ) ;
#148887 = CARTESIAN_POINT ( 'NONE',  ( -5.153800228976328057, -19.02544592524343514, 37.29057627198102409 ) ) ;
#148888 = CARTESIAN_POINT ( 'NONE',  ( 15.72974639402176855, 15.80617190586768217, 66.87609039468568994 ) ) ;
#148889 = CARTESIAN_POINT ( 'NONE',  ( -0.05219959533937732626, 21.53943276465977519, 107.5010903946856899 ) ) ;
#148890 = CARTESIAN_POINT ( 'NONE',  ( -16.52544592524335698, -4.483927247898792601, 103.9594237280190185 ) ) ;
#148891 = ADVANCED_FACE ( 'NONE', ( #117533 ), #67029, .T. ) ;
#148892 = CARTESIAN_POINT ( 'NONE',  ( 19.02544592524343514, -5.153800228976328945, 78.54057627198099567 ) ) ;
#148893 = CARTESIAN_POINT ( 'NONE',  ( -0.05219959533937732626, 21.53943276465977519, 57.50109039468568994 ) ) ;
#148894 = CARTESIAN_POINT ( 'NONE',  ( 18.62759615963255655, 10.81492255796105972, 46.66775706135234714 ) ) ;
#148896 = CARTESIAN_POINT ( 'NONE',  ( -0.05219959533909027116, -19.03943276465977164, 102.4989096053143669 ) ) ;
#148895 = CARTESIAN_POINT ( 'NONE',  ( -16.51473224551082808, 9.474510206698731452, 78.33442372801900433 ) ) ;
#148897 = CARTESIAN_POINT ( 'NONE',  ( 5.153800228976335163, 19.02544592524342804, 24.79057627198102765 ) ) ;
#148898 = CARTESIAN_POINT ( 'NONE',  ( -21.53943276465977519, 0.05219959533907696930, 91.24890960531436690 ) ) ;
#148899 = CARTESIAN_POINT ( 'NONE',  ( -19.03943276465977164, -0.05219959533935918106, 18.75109039468567218 ) ) ;
#148900 = CARTESIAN_POINT ( 'NONE',  ( -16.55341960407611168, -4.379528057220339221, 101.4572429386476955 ) ) ;
#148901 = CARTESIAN_POINT ( 'NONE',  ( -5.049401038298153566, 19.05341960407611168, 55.20724293864769550 ) ) ;
#148902 = CARTESIAN_POINT ( 'NONE',  ( -16.46253265017146816, -9.564922557961047289, 99.16775706135233293 ) ) ;
#148903 = CARTESIAN_POINT ( 'NONE',  ( -14.34966873604960291, -8.224510206698953496, 61.66557627198103120 ) ) ;
#148904 = CARTESIAN_POINT ( 'NONE',  ( -21.53943276465977519, -0.05219959533937600094, 108.7510903946857042 ) ) ;
#148905 = CARTESIAN_POINT ( 'NONE',  ( -5.153800228976328057, -19.02544592524343514, 102.2905762719810383 ) ) ;
#148906 = CARTESIAN_POINT ( 'NONE',  ( 13.89961937509957401, 13.97604488694547697, 71.87609039468567573 ) ) ;
#148907 = CARTESIAN_POINT ( 'NONE',  ( -18.67979575497178146, -10.72451020669898902, 76.66557627198103830 ) ) ;
#148908 = CARTESIAN_POINT ( 'NONE',  ( -5.719274019375665041, -21.55341960407619695, 29.79275706135234358 ) ) ;
#148909 = CARTESIAN_POINT ( 'NONE',  ( 12.14591786802327356, -12.06949235617739191, 35.62609039468568994 ) ) ;
#148910 = CARTESIAN_POINT ( 'NONE',  ( 4.483927247898790824, -16.52544592524335698, 90.20942372801903275 ) ) ;
#148912 = CARTESIAN_POINT ( 'NONE',  ( 0.05219959533937995610, -21.53943276465977519, 40.00109039468567573 ) ) ;
#148911 = CARTESIAN_POINT ( 'NONE',  ( -0.05219959533934338120, 16.53943276465976808, 47.50109039468568994 ) ) ;
#148913 = CARTESIAN_POINT ( 'NONE',  ( -21.55341960407610458, -5.719274019375992779, 46.45724293864769550 ) ) ;
#148914 =( BOUNDED_CURVE ( )  B_SPLINE_CURVE ( 3, ( #51619, #128448, #70794, #176988 ),
 .UNSPECIFIED., .F., .F. ) 
 B_SPLINE_CURVE_WITH_KNOTS ( ( 4, 4 ),
 ( 1.025647941782810602, 2.008945357379067431 ),
 .UNSPECIFIED. ) 
 CURVE ( )  GEOMETRIC_REPRESENTATION_ITEM ( )  RATIONAL_B_SPLINE_CURVE ( ( 1.000000000000000000, 0.9210371567966662010, 0.9210371567966662010, 1.000000000000000000 ) ) 
 REPRESENTATION_ITEM ( '' )  );
#148915 = CARTESIAN_POINT ( 'NONE',  ( -5.049401038298153566, 19.05341960407611168, 40.20724293864768839 ) ) ;
#148916 = CARTESIAN_POINT ( 'NONE',  ( 36.91746824999999887, 11.99521256947799053, -2.024999997268813523 ) ) ;
#148917 = CARTESIAN_POINT ( 'NONE',  ( -8.314922557961024197, 14.29746914071037800, 62.91775706135236135 ) ) ;
#148918 = CARTESIAN_POINT ( 'NONE',  ( 18.62759615963271287, -10.81492255796078972, 83.33224293864769550 ) ) ;
#148919 = CARTESIAN_POINT ( 'NONE',  ( 16.53943276465976808, -0.05219959533910856209, 38.74890960531435979 ) ) ;
#148920 = CARTESIAN_POINT ( 'NONE',  ( -4.483927247898782831, 16.52544592524335698, 47.70942372801902565 ) ) ;
#148921 = CARTESIAN_POINT ( 'NONE',  ( -9.564922557960796823, -16.46253265017161027, 57.08224293864769550 ) ) ;
#148922 = CARTESIAN_POINT ( 'NONE',  ( -4.483927247898782831, 16.52544592524335698, 92.70942372801901854 ) ) ;
#148923 = CARTESIAN_POINT ( 'NONE',  ( 19.05341960407617918, -5.049401038297876454, 91.04275706135234714 ) ) ;
#148924 = CARTESIAN_POINT ( 'NONE',  ( -21.53943276465977519, 0.05219959533907696930, 91.24890960531436690 ) ) ;
#148925 = CARTESIAN_POINT ( 'NONE',  ( 4.379528057220339221, -16.55341960407611168, 27.70724293864769905 ) ) ;
#148926 = VERTEX_POINT ( 'NONE', #175214 ) ;
#148927 = CARTESIAN_POINT ( 'NONE',  ( 26.45763050569054542, 3.219288925403916313, 173.6696415116524861 ) ) ;
#148928 = CARTESIAN_POINT ( 'NONE',  ( -15.80617190586745835, -15.72974639402198527, 56.87390960531436690 ) ) ;
#148929 = CARTESIAN_POINT ( 'NONE',  ( -4.379528057220086978, -16.55341960407618274, 99.79275706135234714 ) ) ;
#148930 = EDGE_LOOP ( 'NONE', ( #71374, #20942, #134131 ) ) ;
#148931 = CARTESIAN_POINT ( 'NONE',  ( -10.72451020669898014, 18.67979575497178502, 25.41557627198103120 ) ) ;
#148932 = CARTESIAN_POINT ( 'NONE',  ( 17.50000000000001421, -3.307050604923627457, 102.5791036533545793 ) ) ;
#148933 = CARTESIAN_POINT ( 'NONE',  ( 18.62759615963271287, -10.81492255796078972, 83.33224293864769550 ) ) ;
#148934 = CARTESIAN_POINT ( 'NONE',  ( 4.379528057220092307, 16.55341960407617563, 112.2927570613523471 ) ) ;
#148935 = CARTESIAN_POINT ( 'NONE',  ( -16.53943276465976808, -0.05219959533934237506, 33.75109039468568284 ) ) ;
#148936 = CARTESIAN_POINT ( 'NONE',  ( 5.153800228976335163, 19.02544592524342804, 39.79057627198100988 ) ) ;
#148937 = CARTESIAN_POINT ( 'NONE',  ( -0.05219959533934338120, 16.53943276465976808, 27.50109039468567929 ) ) ;
#148938 = CARTESIAN_POINT ( 'NONE',  ( 19.02544592524343514, -5.153800228976328945, 48.54057627198103120 ) ) ;
#148939 = CARTESIAN_POINT ( 'NONE',  ( -22.44159573604010305, 16.30477369853692338, 141.1750000027311671 ) ) ;
#148940 = CARTESIAN_POINT ( 'NONE',  ( 16.51473224551069308, 9.474510206698969483, 114.1655762719810241 ) ) ;
#148941 = CARTESIAN_POINT ( 'NONE',  ( 9.564922557960805705, 16.46253265017160317, 114.5822429386476955 ) ) ;
#148942 = CARTESIAN_POINT ( 'NONE',  ( 4.379528057220092307, 16.55341960407617563, 97.29275706135234714 ) ) ;
#148943 = CARTESIAN_POINT ( 'NONE',  ( 13.89961937509957401, 13.97604488694547697, 91.87609039468567573 ) ) ;
#148944 = CARTESIAN_POINT ( 'NONE',  ( -9.564922557961040184, 16.46253265017147172, 37.91775706135233293 ) ) ;
#148945 = CARTESIAN_POINT ( 'NONE',  ( 15.80617190586746368, 15.72974639402197994, 94.37390960531436690 ) ) ;
#148946 = CARTESIAN_POINT ( 'NONE',  ( 0.05219959533934541429, -16.53943276465976808, 110.0010903946856757 ) ) ;
#148947 = CARTESIAN_POINT ( 'NONE',  ( -15.72974639402197994, 15.80617190586746368, 30.62390960531436335 ) ) ;
#148948 = CARTESIAN_POINT ( 'NONE',  ( -9.474510206698720793, -16.51473224551083518, 109.5844237280190043 ) ) ;
#148949 = CARTESIAN_POINT ( 'NONE',  ( -19.05341960407611168, -5.049401038298163336, 111.4572429386476671 ) ) ;
#148950 = CARTESIAN_POINT ( 'NONE',  ( 18.67979575497194134, -10.72451020669871369, 60.83442372801901854 ) ) ;
#148951 = CARTESIAN_POINT ( 'NONE',  ( 9.474510206698971260, -16.51473224551069308, 57.91557627198103120 ) ) ;
#148952 = CARTESIAN_POINT ( 'NONE',  ( 8.314922557960818139, 14.29746914071049879, 104.5822429386477097 ) ) ;
#148953 = CARTESIAN_POINT ( 'NONE',  ( 32.23033374730683676, 4.573250637950146746, 89.03582022910541127 ) ) ;
#148954 = CARTESIAN_POINT ( 'NONE',  ( -9.564922557960796823, -16.46253265017161027, 67.08224293864769550 ) ) ;
#148955 = CARTESIAN_POINT ( 'NONE',  ( 12.06949235617757843, -12.14591786802309237, 73.12390960531436690 ) ) ;
#148956 = ORIENTED_EDGE ( 'NONE', *, *, #82699, .F. ) ;
#148957 = CARTESIAN_POINT ( 'NONE',  ( -0.05219959533936034679, 19.03943276465977164, 92.50109039468566152 ) ) ;
#148958 = DIRECTION ( 'NONE',  ( -7.855351589328939542E-15, 0.000000000000000000, 1.000000000000000000 ) ) ;
#148959 = CARTESIAN_POINT ( 'NONE',  ( 13.89961937509977652, -13.97604488694527269, 63.12390960531435979 ) ) ;
#148960 = CARTESIAN_POINT ( 'NONE',  ( 0.3921787546847190220, 9.051185887784736650, -61.90436275749404160 ) ) ;
#148962 = CARTESIAN_POINT ( 'NONE',  ( -13.97604488694527625, -13.89961937509977652, 106.8739096053143669 ) ) ;
#148961 = CARTESIAN_POINT ( 'NONE',  ( -19.02544592524342804, 5.153800228976336051, 81.04057627198103830 ) ) ;
#148963 = CARTESIAN_POINT ( 'NONE',  ( -16.52544592524335698, -4.483927247898792601, 58.95942372801902565 ) ) ;
#148964 = CARTESIAN_POINT ( 'NONE',  ( -17.31747979337947996, -6.344076630961017926, 51.37944868065184778 ) ) ;
#148965 = CARTESIAN_POINT ( 'NONE',  ( 19.05341960407617918, -5.049401038297876454, 41.04275706135233293 ) ) ;
#148966 = CARTESIAN_POINT ( 'NONE',  ( 5.823673210054444382, -21.52544592524334988, 105.2094237280190328 ) ) ;
#148967 = DIRECTION ( 'NONE',  ( 0.000000000000000000, -0.7071067811865483499, -0.7071067811865465735 ) ) ;
#148968 = CARTESIAN_POINT ( 'NONE',  ( -0.05219959533909027116, -19.03943276465977164, 112.4989096053143669 ) ) ;
#148969 = CARTESIAN_POINT ( 'NONE',  ( 16.52544592524335698, 4.483927247898782831, 96.45942372801901854 ) ) ;
#148970 = CARTESIAN_POINT ( 'NONE',  ( -34.45224964297660364, -5.970420695714335757, 49.56603145559585499 ) ) ;
#148971 = CARTESIAN_POINT ( 'NONE',  ( -16.53943276465976808, -0.05219959533934237506, 93.75109039468567573 ) ) ;
#148972 = CARTESIAN_POINT ( 'NONE',  ( -17.49999999999999289, 5.624438216177594541, 30.81670344914645199 ) ) ;
#148973 = CARTESIAN_POINT ( 'NONE',  ( 16.55341960407618274, -4.379528057220086978, 71.04275706135234714 ) ) ;
#148974 = ORIENTED_EDGE ( 'NONE', *, *, #192660, .F. ) ;
#148975 = CARTESIAN_POINT ( 'NONE',  ( -21.53943276465977519, -0.05219959533937600094, 83.75109039468568994 ) ) ;
#148976 = CARTESIAN_POINT ( 'NONE',  ( -0.05219959533936034679, 19.03943276465977164, 87.50109039468567573 ) ) ;
#148977 = CARTESIAN_POINT ( 'NONE',  ( -13.97604488694547697, 13.89961937509957934, 23.12609039468565442 ) ) ;
#148978 = CARTESIAN_POINT ( 'NONE',  ( 19.03943276465977164, -0.05219959533909143690, 68.74890960531436690 ) ) ;
#148979 = CARTESIAN_POINT ( 'NONE',  ( 16.46253265017160672, -9.564922557960803928, 43.33224293864769550 ) ) ;
#148980 = FACE_OUTER_BOUND ( 'NONE', #153973, .T. ) ;
#148981 = CARTESIAN_POINT ( 'NONE',  ( -10.81492255796078084, -18.62759615963271287, 87.08224293864769550 ) ) ;
#148982 = CARTESIAN_POINT ( 'NONE',  ( 21.55341960407610458, 5.719274019375980345, 28.95724293864769905 ) ) ;
#148983 = CARTESIAN_POINT ( 'NONE',  ( 19.05341960407611168, 5.049401038298154454, 38.95724293864767418 ) ) ;
#148984 = CARTESIAN_POINT ( 'NONE',  ( 16.53943276465976808, 0.05219959533934440121, 46.25109039468567573 ) ) ;
#148985 = EDGE_LOOP ( 'NONE', ( #122324, #76659, #142684, #36987 ) ) ;
#148986 = CARTESIAN_POINT ( 'NONE',  ( 5.823673210054444382, -21.52544592524334988, 25.20942372801901854 ) ) ;
#148988 = CARTESIAN_POINT ( 'NONE',  ( -22.81625015709509441, -31.40387420917324590, -8.324999997268815122 ) ) ;
#148987 = CARTESIAN_POINT ( 'NONE',  ( -8.314922557960811034, -14.29746914071050412, 72.08224293864769550 ) ) ;
#148989 = CARTESIAN_POINT ( 'NONE',  ( -14.29746914071037622, -8.314922557961029526, 19.16775706135234714 ) ) ;
#148990 = CARTESIAN_POINT ( 'NONE',  ( 5.049401038297881783, 19.05341960407617563, 42.29275706135234003 ) ) ;
#148991 = CARTESIAN_POINT ( 'NONE',  ( -4.483927247898539470, -16.52544592524342804, 52.29057627198102409 ) ) ;
#148993 = EDGE_CURVE ( 'NONE', #112403, #197846, #66956, .T. ) ;
#148992 = CARTESIAN_POINT ( 'NONE',  ( 18.67979575497178502, 10.72451020669898547, 114.1655762719810383 ) ) ;
#148995 = CARTESIAN_POINT ( 'NONE',  ( -18.67979575497178146, -10.72451020669898902, 81.66557627198103830 ) ) ;
#148994 = CARTESIAN_POINT ( 'NONE',  ( 1.022580077288041090E-15, 16.70000000000002061, -59.13370768023891344 ) ) ;
#148996 = CARTESIAN_POINT ( 'NONE',  ( 19.05341960407611168, 5.049401038298154454, 83.95724293864766707 ) ) ;
#148997 = CARTESIAN_POINT ( 'NONE',  ( -14.29746914071049879, 8.314922557960819915, 55.83224293864770260 ) ) ;
#148998 = CARTESIAN_POINT ( 'NONE',  ( -19.02544592524342804, 5.153800228976336051, 116.0405762719810383 ) ) ;
#148999 = CARTESIAN_POINT ( 'NONE',  ( 36.91746824999999177, 2.880721459617395097E-14, -7.624999997268813168 ) ) ;
#149000 = CARTESIAN_POINT ( 'NONE',  ( 13.89961937509957401, 13.97604488694547697, 66.87609039468567573 ) ) ;
#149001 = CARTESIAN_POINT ( 'NONE',  ( -15.80617190586745835, -15.72974639402198527, 101.8739096053143811 ) ) ;
#149002 = CARTESIAN_POINT ( 'NONE',  ( 16.46253265017160672, -9.564922557960803928, 53.33224293864768839 ) ) ;
#149003 = CARTESIAN_POINT ( 'NONE',  ( -13.89961937509957401, -13.97604488694547875, 44.37609039468566863 ) ) ;
#149004 = CARTESIAN_POINT ( 'NONE',  ( 9.474510206698971260, -16.51473224551069308, 37.91557627198102409 ) ) ;
#149005 = CARTESIAN_POINT ( 'NONE',  ( -15.72974639402176322, -15.80617190586768395, 64.37609039468568994 ) ) ;
#149006 = CARTESIAN_POINT ( 'NONE',  ( -16.20579543436678449, -7.371946100355100562, 70.56520834171880097 ) ) ;
#149007 = ADVANCED_FACE ( 'NONE', ( #39687 ), #184183, .T. ) ;
#149008 = CARTESIAN_POINT ( 'NONE',  ( -12.14591786802309592, -12.06949235617757132, 41.87390960531435979 ) ) ;
#149009 = CARTESIAN_POINT ( 'NONE',  ( 13.89961937509977652, -13.97604488694527269, 63.12390960531435979 ) ) ;
#149010 = CARTESIAN_POINT ( 'NONE',  ( -21.55341960407610458, -5.719274019375992779, 71.45724293864769550 ) ) ;
#149011 = CARTESIAN_POINT ( 'NONE',  ( 19.05341960407611168, 5.049401038298154454, 53.95724293864770260 ) ) ;
#149012 = ORIENTED_EDGE ( 'NONE', *, *, #177696, .F. ) ;
#149013 = CARTESIAN_POINT ( 'NONE',  ( -21.53943276465977519, 0.05219959533907696930, 71.24890960531435269 ) ) ;
#149014 = ORIENTED_EDGE ( 'NONE', *, *, #93499, .F. ) ;
#149015 = CARTESIAN_POINT ( 'NONE',  ( 15.80617190586769283, -15.72974639402175789, 105.6260903946856899 ) ) ;
#149018 = CARTESIAN_POINT ( 'NONE',  ( -0.05219959533910754901, -16.53943276465976808, 87.49890960531436690 ) ) ;
#149017 = CARTESIAN_POINT ( 'NONE',  ( 16.52544592524335698, 4.483927247898782831, 101.4594237280190185 ) ) ;
#149016 = CARTESIAN_POINT ( 'NONE',  ( 7.005188342142080415, -46.65430082754588170, -22.59844067006618573 ) ) ;
#149019 = CARTESIAN_POINT ( 'NONE',  ( -19.02544592524342804, 5.153800228976336051, 66.04057627198103830 ) ) ;
#149020 = ORIENTED_EDGE ( 'NONE', *, *, #49003, .F. ) ;
#149021 = CARTESIAN_POINT ( 'NONE',  ( 9.564922557961047289, -16.46253265017146816, 35.41775706135233293 ) ) ;
#149022 = CARTESIAN_POINT ( 'NONE',  ( -12.14591786802326823, 12.06949235617739902, 83.12609039468568994 ) ) ;
#149023 = CARTESIAN_POINT ( 'NONE',  ( -19.05341960407617563, 5.049401038297882671, 33.54275706135231871 ) ) ;
#149024 = CARTESIAN_POINT ( 'NONE',  ( 13.89961937509977652, -13.97604488694527269, 83.12390960531436690 ) ) ;
#149025 = CARTESIAN_POINT ( 'NONE',  ( -21.55341960407610458, -5.719274019375992779, 56.45724293864768839 ) ) ;
#149026 = LINE ( 'NONE', #41850, #170435 ) ;
#149027 = CARTESIAN_POINT ( 'NONE',  ( -16.52544592524342804, 4.483927247898546575, 116.0405762719810383 ) ) ;
#149028 = CARTESIAN_POINT ( 'NONE',  ( -10.72451020669870658, -18.67979575497194134, 94.58442372801901854 ) ) ;
#149029 = CARTESIAN_POINT ( 'NONE',  ( 16.55341960407618274, -4.379528057220086978, 66.04275706135236135 ) ) ;
#149030 = CARTESIAN_POINT ( 'NONE',  ( 10.81492255796106328, -18.62759615963255655, 30.41775706135234358 ) ) ;
#149031 = CARTESIAN_POINT ( 'NONE',  ( 8.314922557961029526, -14.29746914071037800, 35.41775706135234003 ) ) ;
#149032 = CARTESIAN_POINT ( 'NONE',  ( -16.51473224551069308, -9.474510206698971260, 86.66557627198102409 ) ) ;
#149033 = CARTESIAN_POINT ( 'NONE',  ( -19.03943276465977164, 0.05219959533909376836, 46.24890960531435979 ) ) ;
#149034 = CARTESIAN_POINT ( 'NONE',  ( -19.02544592524342804, 5.153800228976336051, 56.04057627198100988 ) ) ;
#149035 = CARTESIAN_POINT ( 'NONE',  ( 12.14591786802327356, -12.06949235617739191, 35.62609039468568994 ) ) ;
#149036 = CARTESIAN_POINT ( 'NONE',  ( -12.06949235617756955, 12.14591786802309770, 95.62390960531436690 ) ) ;
#149037 = CARTESIAN_POINT ( 'NONE',  ( -12.14591786802326823, 12.06949235617739902, 98.12609039468570415 ) ) ;
#149040 = CARTESIAN_POINT ( 'NONE',  ( 13.89961937509977652, -13.97604488694527269, 53.12390960531434558 ) ) ;
#149039 = CARTESIAN_POINT ( 'NONE',  ( -16.46253265017160317, 9.564922557960807481, 75.83224293864769550 ) ) ;
#149038 = CARTESIAN_POINT ( 'NONE',  ( 5.823673210054444382, -21.52544592524334988, 45.20942372801901854 ) ) ;
#149041 = CARTESIAN_POINT ( 'NONE',  ( -9.474510206698964154, 16.51473224551069663, 85.41557627198102409 ) ) ;
#149042 = CARTESIAN_POINT ( 'NONE',  ( -14.34966873604960291, -8.224510206698953496, 36.66557627198103120 ) ) ;
#149043 = CARTESIAN_POINT ( 'NONE',  ( 14.34966873604972726, -8.224510206698740333, 105.8344237280190328 ) ) ;
#149044 = EDGE_CURVE ( 'NONE', #1850, #40791, #4276, .T. ) ;
#149045 = CARTESIAN_POINT ( 'NONE',  ( 5.153800228976615827, -19.02544592524334988, 50.20942372801897591 ) ) ;
#149046 = FACE_OUTER_BOUND ( 'NONE', #156875, .T. ) ;
#149047 = CARTESIAN_POINT ( 'NONE',  ( 16.51473224551069308, 9.474510206698969483, 44.16557627198103120 ) ) ;
#149048 = CARTESIAN_POINT ( 'NONE',  ( -9.564922557961040184, 16.46253265017147172, 22.91775706135233648 ) ) ;
#149049 = CARTESIAN_POINT ( 'NONE',  ( -22.81625015709510507, 31.40387420917330275, -6.924999997268812990 ) ) ;
#149050 = CARTESIAN_POINT ( 'NONE',  ( -8.314922557961024197, 14.29746914071037800, 37.91775706135235424 ) ) ;
#149052 = CARTESIAN_POINT ( 'NONE',  ( 14.29746914071037800, 8.314922557961029526, 61.66775706135235424 ) ) ;
#149051 = CARTESIAN_POINT ( 'NONE',  ( -0.05219959533936034679, 19.03943276465977164, 72.50109039468566152 ) ) ;
#149053 = CARTESIAN_POINT ( 'NONE',  ( 4.313351365237961588, -4.313351365237934942, -64.53213882399992940 ) ) ;
#149054 = CARTESIAN_POINT ( 'NONE',  ( -13.89961937509977652, 13.97604488694528158, 75.62390960531438111 ) ) ;
#149055 = CARTESIAN_POINT ( 'NONE',  ( -21.53943276465977519, 0.05219959533907696930, 111.2489096053143669 ) ) ;
#149056 = CARTESIAN_POINT ( 'NONE',  ( 5.049401038297881783, 19.05341960407617563, 72.29275706135234714 ) ) ;
#149058 = CARTESIAN_POINT ( 'NONE',  ( 9.474510206698971260, -16.51473224551069308, 37.91557627198102409 ) ) ;
#149057 = CARTESIAN_POINT ( 'NONE',  ( -0.05219959533909027116, -19.03943276465977164, 107.4989096053143527 ) ) ;
#149059 = CARTESIAN_POINT ( 'NONE',  ( -5.049401038298153566, 19.05341960407611168, 75.20724293864769550 ) ) ;
#149061 = CARTESIAN_POINT ( 'NONE',  ( 5.153800228976335163, 19.02544592524342804, 39.79057627198100988 ) ) ;
#149060 = CARTESIAN_POINT ( 'NONE',  ( 16.55341960407611168, 4.379528057220329451, 28.95724293864769905 ) ) ;
#149062 = CARTESIAN_POINT ( 'NONE',  ( -13.97604488694547697, 13.89961937509957934, 48.12609039468566863 ) ) ;
#149063 = CARTESIAN_POINT ( 'NONE',  ( -12.14591786802309592, -12.06949235617757132, 71.87390960531438111 ) ) ;
#149064 = CARTESIAN_POINT ( 'NONE',  ( 19.03943276465977164, 0.05219959533936151252, 21.25109039468565797 ) ) ;
#149065 = CARTESIAN_POINT ( 'NONE',  ( -9.474510206698964154, 16.51473224551069663, 55.41557627198103120 ) ) ;
#149066 = CARTESIAN_POINT ( 'NONE',  ( -18.62759615963270932, 10.81492255796079327, 55.83224293864770260 ) ) ;
#149068 = CARTESIAN_POINT ( 'NONE',  ( 18.62759615963255655, 10.81492255796105972, 101.6677570613523613 ) ) ;
#149067 = CARTESIAN_POINT ( 'NONE',  ( -16.55341960407611168, -4.379528057220339221, 51.45724293864770260 ) ) ;
#149069 = CARTESIAN_POINT ( 'NONE',  ( 9.474510206698971260, -16.51473224551069308, 92.91557627198103830 ) ) ;
#149070 = CARTESIAN_POINT ( 'NONE',  ( 16.51473224551069308, 9.474510206698969483, 109.1655762719810383 ) ) ;
#149071 = CARTESIAN_POINT ( 'NONE',  ( 19.05341960407611168, 5.049401038298154454, 38.95724293864767418 ) ) ;
#149072 = CARTESIAN_POINT ( 'NONE',  ( 9.474510206698971260, -16.51473224551069308, 27.91557627198103120 ) ) ;
#149073 = CARTESIAN_POINT ( 'NONE',  ( 16.52544592524342804, -4.483927247898539470, 88.54057627198103830 ) ) ;
#149074 = CARTESIAN_POINT ( 'NONE',  ( -21.52544592524343514, 5.823673210054127303, 101.0405762719810383 ) ) ;
#149075 = CARTESIAN_POINT ( 'NONE',  ( -19.05341960407611168, -5.049401038298163336, 101.4572429386476955 ) ) ;
#149076 = CARTESIAN_POINT ( 'NONE',  ( -15.72974639402176322, -15.80617190586768395, 19.37609039468568639 ) ) ;
#149077 = CARTESIAN_POINT ( 'NONE',  ( -5.153800228976328057, -19.02544592524343514, 97.29057627198099567 ) ) ;
#149079 = CARTESIAN_POINT ( 'NONE',  ( 16.53943276465976808, -0.05219959533910856209, 98.74890960531438111 ) ) ;
#149078 = FACE_OUTER_BOUND ( 'NONE', #132751, .T. ) ;
#149080 = CARTESIAN_POINT ( 'NONE',  ( 19.05341960407611168, 5.049401038298154454, 68.95724293864769550 ) ) ;
#149081 = CARTESIAN_POINT ( 'NONE',  ( 21.55341960407610458, 5.719274019375980345, 73.95724293864769550 ) ) ;
#149082 = CARTESIAN_POINT ( 'NONE',  ( -31.56642711641982757, 3.769985069464013350, 101.5021612967808409 ) ) ;
#149083 = CARTESIAN_POINT ( 'NONE',  ( 28.82186960331491221, -9.364793116373624215, 146.8999999999999773 ) ) ;
#149085 = CARTESIAN_POINT ( 'NONE',  ( 19.01533133064924996, -5.499999999999441336, 66.26586590595739779 ) ) ;
#149084 = CARTESIAN_POINT ( 'NONE',  ( 10.81492255796078972, 18.62759615963270932, 34.58224293864770260 ) ) ;
#149086 = CARTESIAN_POINT ( 'NONE',  ( 0.05219959533934541429, -16.53943276465976808, 35.00109039468568284 ) ) ;
#149087 = CARTESIAN_POINT ( 'NONE',  ( -14.29746914071049879, 8.314922557960819915, 90.83224293864769550 ) ) ;
#149088 = FACE_OUTER_BOUND ( 'NONE', #108797, .T. ) ;
#149089 = CARTESIAN_POINT ( 'NONE',  ( 19.03943276465977164, -0.05219959533909143690, 83.74890960531436690 ) ) ;
#149090 = CARTESIAN_POINT ( 'NONE',  ( 16.51473224551069308, 9.474510206698969483, 49.16557627198102409 ) ) ;
#149091 = CARTESIAN_POINT ( 'NONE',  ( 12.14591786802309770, 12.06949235617756955, 74.37390960531436690 ) ) ;
#149092 = CARTESIAN_POINT ( 'NONE',  ( -10.72451020669898014, 18.67979575497178502, 35.41557627198102409 ) ) ;
#149093 = CARTESIAN_POINT ( 'NONE',  ( -16.55341960407611168, -4.379528057220339221, 56.45724293864768839 ) ) ;
#149094 = CARTESIAN_POINT ( 'NONE',  ( 19.02544592524334988, 5.153800228976608722, 101.4594237280189759 ) ) ;
#149095 = CARTESIAN_POINT ( 'NONE',  ( 0.05219959533937995610, -21.53943276465977519, 75.00109039468568994 ) ) ;
#149096 = DIRECTION ( 'NONE',  ( -1.000000000000000000, 0.000000000000000000, 0.000000000000000000 ) ) ;
#149097 = CARTESIAN_POINT ( 'NONE',  ( -16.46253265017160317, 9.564922557960807481, 115.8322429386477097 ) ) ;
#149098 = CARTESIAN_POINT ( 'NONE',  ( -4.483927247898782831, 16.52544592524335698, 82.70942372801900433 ) ) ;
#149099 = CARTESIAN_POINT ( 'NONE',  ( -17.49999999999999645, 5.624438216177559902, 95.81670344914641646 ) ) ;
#149100 = CARTESIAN_POINT ( 'NONE',  ( -5.049401038298153566, 19.05341960407611168, 75.20724293864769550 ) ) ;
#149101 = CARTESIAN_POINT ( 'NONE',  ( -15.72974639402197994, 15.80617190586746368, 85.62390960531436690 ) ) ;
#149102 = CARTESIAN_POINT ( 'NONE',  ( -14.34966873604972548, 8.224510206698743886, 23.33442372801901499 ) ) ;
#149104 = CARTESIAN_POINT ( 'NONE',  ( -21.52544592524334988, -5.823673210054445271, 73.95942372801901854 ) ) ;
#149103 = CARTESIAN_POINT ( 'NONE',  ( 14.34966873604960469, 8.224510206698951720, 54.16557627198103120 ) ) ;
#149106 = CARTESIAN_POINT ( 'NONE',  ( 5.823673210054125526, 21.52544592524343514, 24.79057627198103120 ) ) ;
#149105 = CARTESIAN_POINT ( 'NONE',  ( 16.55341960407618274, -4.379528057220086978, 86.04275706135236135 ) ) ;
#149107 = LINE ( 'NONE', #57099, #143667 ) ;
#149108 = CARTESIAN_POINT ( 'NONE',  ( -24.13306144861384794, -5.795830589372931385, 190.0000000000000000 ) ) ;
#149109 = CARTESIAN_POINT ( 'NONE',  ( 14.34966873604972726, -8.224510206698740333, 105.8344237280190328 ) ) ;
#149110 = CARTESIAN_POINT ( 'NONE',  ( 16.52544592524335698, 4.483927247898782831, 56.45942372801902565 ) ) ;
#149111 = CARTESIAN_POINT ( 'NONE',  ( -19.05341960407611168, -5.049401038298163336, 66.45724293864769550 ) ) ;
#149112 = CARTESIAN_POINT ( 'NONE',  ( 9.474510206698971260, -16.51473224551069308, 87.91557627198102409 ) ) ;
#149113 = CARTESIAN_POINT ( 'NONE',  ( -10.81492255796105439, 18.62759615963255655, 72.91775706135234714 ) ) ;
#149114 = CARTESIAN_POINT ( 'NONE',  ( 4.379528057220092307, 16.55341960407617563, 82.29275706135234714 ) ) ;
#149115 = CARTESIAN_POINT ( 'NONE',  ( -14.34966873604960291, -8.224510206698953496, 41.66557627198103120 ) ) ;
#149116 = CARTESIAN_POINT ( 'NONE',  ( -16.51473224551069308, -9.474510206698971260, 61.66557627198103120 ) ) ;
#149117 = CARTESIAN_POINT ( 'NONE',  ( -5.153800228976328057, -19.02544592524343514, 42.29057627198101699 ) ) ;
#149118 = ORIENTED_EDGE ( 'NONE', *, *, #34170, .T. ) ;
#149119 = CARTESIAN_POINT ( 'NONE',  ( 13.97604488694548053, -13.89961937509957401, 100.6260903946856615 ) ) ;
#149120 = CARTESIAN_POINT ( 'NONE',  ( -8.224510206698948167, 14.34966873604960824, 95.41557627198102409 ) ) ;
#149121 = CARTESIAN_POINT ( 'NONE',  ( 0.05219959533909260263, 19.03943276465977164, 59.99890960531436690 ) ) ;
#149123 = CARTESIAN_POINT ( 'NONE',  ( 3.766062262543149401E-15, -39.95556452105413570, -5.500000000000000000 ) ) ;
#149122 = CARTESIAN_POINT ( 'NONE',  ( 16.51473224551083163, -9.474510206698727899, 105.8344237280190043 ) ) ;
#149124 = CARTESIAN_POINT ( 'NONE',  ( -21.55341960407619339, 5.719274019375674811, 103.5427570613523613 ) ) ;
#149125 = CARTESIAN_POINT ( 'NONE',  ( -0.05219959533934338120, 16.53943276465976808, 67.50109039468568994 ) ) ;
#149126 = CARTESIAN_POINT ( 'NONE',  ( -9.564922557961040184, 16.46253265017147172, 87.91775706135233293 ) ) ;
#149127 = CARTESIAN_POINT ( 'NONE',  ( 5.823673210054125526, 21.52544592524343514, 64.79057627198103830 ) ) ;
#149128 = CARTESIAN_POINT ( 'NONE',  ( -0.05219959533934338120, 16.53943276465976808, 57.50109039468568994 ) ) ;
#149129 = CARTESIAN_POINT ( 'NONE',  ( 17.47980958864297918, 5.499999999999998224, 21.71653220162190934 ) ) ;
#149130 = CARTESIAN_POINT ( 'NONE',  ( -19.03943276465977164, -0.05219959533935918106, 53.75109039468566863 ) ) ;
#149131 = CARTESIAN_POINT ( 'NONE',  ( -21.53943276465977519, -0.05219959533937600094, 93.75109039468567573 ) ) ;
#149132 = CARTESIAN_POINT ( 'NONE',  ( -14.34966873604960291, -8.224510206698953496, 111.6655762719810525 ) ) ;
#149133 = CARTESIAN_POINT ( 'NONE',  ( -13.89961937509977652, 13.97604488694528158, 60.62390960531436690 ) ) ;
#149134 = CARTESIAN_POINT ( 'NONE',  ( 16.53943276465976808, -0.05219959533910856209, 53.74890960531437401 ) ) ;
#149135 = EDGE_CURVE ( 'NONE', #64689, #175496, #168989, .T. ) ;
#149136 = CARTESIAN_POINT ( 'NONE',  ( 15.72974639402176855, 15.80617190586768217, 91.87609039468568994 ) ) ;
#149137 = CARTESIAN_POINT ( 'NONE',  ( 9.564922557961047289, -16.46253265017146816, 45.41775706135232582 ) ) ;
#149138 = CARTESIAN_POINT ( 'NONE',  ( -13.97604488694547697, 13.89961937509957934, 33.12609039468566863 ) ) ;
#149139 = CARTESIAN_POINT ( 'NONE',  ( -19.03943276465977164, 0.05219959533909376836, 116.2489096053143669 ) ) ;
#149140 = CARTESIAN_POINT ( 'NONE',  ( -5.823673210054431948, 21.52544592524334988, 92.70942372801901854 ) ) ;
#149141 = CARTESIAN_POINT ( 'NONE',  ( 0.05219959533909260263, 19.03943276465977164, 79.99890960531436690 ) ) ;
#149142 = CARTESIAN_POINT ( 'NONE',  ( 15.72974639402176855, 15.80617190586768217, 91.87609039468568994 ) ) ;
#149143 = CARTESIAN_POINT ( 'NONE',  ( -5.823673210054116645, -21.52544592524344225, 47.29057627198103120 ) ) ;
#149144 = AXIS2_PLACEMENT_3D ( 'NONE', #47587, #18248, #95065 ) ;
#149145 = CARTESIAN_POINT ( 'NONE',  ( 9.474510206698971260, -16.51473224551069308, 87.91557627198102409 ) ) ;
#149146 = CARTESIAN_POINT ( 'NONE',  ( -5.049401038297874678, -19.05341960407617918, 64.79275706135233293 ) ) ;
#149147 = CARTESIAN_POINT ( 'NONE',  ( 19.03943276465977164, -0.05219959533909143690, 43.74890960531435979 ) ) ;
#149148 = CARTESIAN_POINT ( 'NONE',  ( 13.89961937509977652, -13.97604488694527269, 83.12390960531436690 ) ) ;
#149149 = CARTESIAN_POINT ( 'NONE',  ( -13.89961937509957401, -13.97604488694547875, 89.37609039468563310 ) ) ;
#149150 = CARTESIAN_POINT ( 'NONE',  ( 4.379528057220092307, 16.55341960407617563, 42.29275706135235424 ) ) ;
#149151 = CARTESIAN_POINT ( 'NONE',  ( 4.483927247898545687, 16.52544592524342804, 99.79057627198103830 ) ) ;
#149152 = CARTESIAN_POINT ( 'NONE',  ( -5.049401038298153566, 19.05341960407611168, 75.20724293864769550 ) ) ;
#149153 = CARTESIAN_POINT ( 'NONE',  ( 21.53943276465977519, -0.05219959533907433946, 43.74890960531435979 ) ) ;
#149154 = CARTESIAN_POINT ( 'NONE',  ( 19.03943276465977164, 0.05219959533936151252, 111.2510903946856757 ) ) ;
#149155 = CARTESIAN_POINT ( 'NONE',  ( 0.05219959533937995610, -21.53943276465977519, 25.00109039468567218 ) ) ;
#149156 = CARTESIAN_POINT ( 'NONE',  ( -18.67979575497193778, 10.72451020669871902, 73.33442372801901854 ) ) ;
#149157 = CARTESIAN_POINT ( 'NONE',  ( -16.55341960407617563, 4.379528057220093196, 83.54275706135234714 ) ) ;
#149158 = CARTESIAN_POINT ( 'NONE',  ( 16.51473224551069308, 9.474510206698969483, 74.16557627198103830 ) ) ;
#149159 = CARTESIAN_POINT ( 'NONE',  ( -4.379528057220086978, -16.55341960407618274, 104.7927570613523898 ) ) ;
#149160 = CARTESIAN_POINT ( 'NONE',  ( -13.97604488694547697, 13.89961937509957934, 58.12609039468566863 ) ) ;
#149161 = CARTESIAN_POINT ( 'NONE',  ( 21.53943276465977519, 0.05219959533937863772, 31.25109039468568639 ) ) ;
#149162 = CARTESIAN_POINT ( 'NONE',  ( 16.55341960407611168, 4.379528057220329451, 73.95724293864769550 ) ) ;
#149163 = CARTESIAN_POINT ( 'NONE',  ( -5.153800228976328057, -19.02544592524343514, 97.29057627198099567 ) ) ;
#149164 = CARTESIAN_POINT ( 'NONE',  ( -16.52544592524335698, -4.483927247898792601, 83.95942372801900433 ) ) ;
#149165 = CARTESIAN_POINT ( 'NONE',  ( 18.67979575497194134, -10.72451020669871369, 70.83442372801901854 ) ) ;
#149166 = CARTESIAN_POINT ( 'NONE',  ( 0.05219959533934541429, -16.53943276465976808, 30.00109039468568284 ) ) ;
#149167 = CARTESIAN_POINT ( 'NONE',  ( -10.81492255796105439, 18.62759615963255655, 22.91775706135235069 ) ) ;
#149168 = CARTESIAN_POINT ( 'NONE',  ( -4.483927247898539470, -16.52544592524342804, 77.29057627198102409 ) ) ;
#149169 = EDGE_CURVE ( 'NONE', #22576, #190052, #194844, .T. ) ;
#149170 = ORIENTED_EDGE ( 'NONE', *, *, #28639, .T. ) ;
#149171 = CARTESIAN_POINT ( 'NONE',  ( 18.67979575497178502, 10.72451020669898547, 104.1655762719810241 ) ) ;
#149172 = CARTESIAN_POINT ( 'NONE',  ( 4.483927247898545687, 16.52544592524342804, 49.79057627198102409 ) ) ;
#149173 = VERTEX_POINT ( 'NONE', #183194 ) ;
#149174 = CARTESIAN_POINT ( 'NONE',  ( 19.03943276465977164, -0.05219959533909143690, 23.74890960531435269 ) ) ;
#149175 = CARTESIAN_POINT ( 'NONE',  ( 15.72974639402199770, -15.80617190586745480, 23.12390960531436335 ) ) ;
#149176 = CARTESIAN_POINT ( 'NONE',  ( 0.05219959533937995610, -21.53943276465977519, 55.00109039468568284 ) ) ;
#149177 = CARTESIAN_POINT ( 'NONE',  ( 4.483927247898545687, 16.52544592524342804, 64.79057627198103830 ) ) ;
#149178 = EDGE_CURVE ( 'NONE', #14250, #15991, #63242, .T. ) ;
#149179 = CARTESIAN_POINT ( 'NONE',  ( -0.05219959533907301413, -21.53943276465977519, 72.49890960531435269 ) ) ;
#149180 = CARTESIAN_POINT ( 'NONE',  ( 0.05219959533909260263, 19.03943276465977164, 79.99890960531436690 ) ) ;
#149182 = CARTESIAN_POINT ( 'NONE',  ( 16.46253265017146816, 9.564922557961045513, 76.66775706135234714 ) ) ;
#149181 = CARTESIAN_POINT ( 'NONE',  ( 13.89961937509977652, -13.97604488694527269, 28.12390960531435624 ) ) ;
#149183 = CARTESIAN_POINT ( 'NONE',  ( -10.72451020669898014, 18.67979575497178502, 65.41557627198102409 ) ) ;
#149184 = CARTESIAN_POINT ( 'NONE',  ( 13.89961937509977652, -13.97604488694527269, 38.12390960531436690 ) ) ;
#149185 = CARTESIAN_POINT ( 'NONE',  ( -13.89961937509977652, 13.97604488694528158, 65.62390960531436690 ) ) ;
#149186 = CARTESIAN_POINT ( 'NONE',  ( 4.483927247898790824, -16.52544592524335698, 50.20942372801901854 ) ) ;
#149187 = CARTESIAN_POINT ( 'NONE',  ( -0.05219959533937732626, 21.53943276465977519, 27.50109039468567929 ) ) ;
#149188 = CARTESIAN_POINT ( 'NONE',  ( -18.62759615963255300, -10.81492255796106328, 54.16775706135235424 ) ) ;
#149189 = CARTESIAN_POINT ( 'NONE',  ( -9.474510206698964154, 16.51473224551069663, 100.4155762719810241 ) ) ;
#149190 = CARTESIAN_POINT ( 'NONE',  ( -15.80617190586745835, -15.72974639402198527, 71.87390960531438111 ) ) ;
#149192 = CARTESIAN_POINT ( 'NONE',  ( 12.06949235617739724, 12.14591786802326823, 51.87609039468568284 ) ) ;
#149191 = CARTESIAN_POINT ( 'NONE',  ( -10.81492255796078084, -18.62759615963271287, 107.0822429386476955 ) ) ;
#149193 = CARTESIAN_POINT ( 'NONE',  ( 21.52544592524344225, -5.823673210054117533, 48.54057627198103120 ) ) ;
#149194 = CARTESIAN_POINT ( 'NONE',  ( -10.72451020669870658, -18.67979575497194134, 104.5844237280190185 ) ) ;
#149195 = CARTESIAN_POINT ( 'NONE',  ( 0.05219959533909260263, 19.03943276465977164, 54.99890960531435979 ) ) ;
#149196 = CARTESIAN_POINT ( 'NONE',  ( 19.02544592524343514, -5.153800228976328945, 113.5405762719810241 ) ) ;
#149197 = CARTESIAN_POINT ( 'NONE',  ( 19.05341960407611168, 5.049401038298154454, 78.95724293864769550 ) ) ;
#149198 = DIRECTION ( 'NONE',  ( -1.000000000000000000, 0.000000000000000000, -0.000000000000000000 ) ) ;
#149199 = CARTESIAN_POINT ( 'NONE',  ( -16.51473224551082808, 9.474510206698731452, 73.33442372801900433 ) ) ;
#149201 = CARTESIAN_POINT ( 'NONE',  ( 21.55341960407610458, 5.719274019375980345, 43.95724293864769550 ) ) ;
#149200 = CARTESIAN_POINT ( 'NONE',  ( 19.05341960407617918, -5.049401038297876454, 21.04275706135232582 ) ) ;
#149202 = CARTESIAN_POINT ( 'NONE',  ( 12.06949235617739724, 12.14591786802326823, 106.8760903946856899 ) ) ;
#149203 = CARTESIAN_POINT ( 'NONE',  ( 16.51473224551083163, -9.474510206698727899, 90.83442372801900433 ) ) ;
#149204 = DIRECTION ( 'NONE',  ( 0.000000000000000000, 0.000000000000000000, 1.000000000000000000 ) ) ;
#149205 = CARTESIAN_POINT ( 'NONE',  ( -13.89961937509957401, -13.97604488694547875, 19.37609039468566507 ) ) ;
#149206 = CARTESIAN_POINT ( 'NONE',  ( -5.049401038297874678, -19.05341960407617918, 89.79275706135230450 ) ) ;
#149207 = CARTESIAN_POINT ( 'NONE',  ( -5.153800228976607833, 19.02544592524334988, 42.70942372801901143 ) ) ;
#149208 = CARTESIAN_POINT ( 'NONE',  ( 17.31747979337948351, 6.344076630961065888, 108.8794486806518762 ) ) ;
#149209 = CARTESIAN_POINT ( 'NONE',  ( 9.474510206698971260, -16.51473224551069308, 42.91557627198103120 ) ) ;
#149210 = CARTESIAN_POINT ( 'NONE',  ( 14.29746914071049879, -8.314922557960816363, 43.33224293864769550 ) ) ;
#149211 = CARTESIAN_POINT ( 'NONE',  ( 13.97604488694527802, 13.89961937509977652, 34.37390960531436690 ) ) ;
#149212 = CARTESIAN_POINT ( 'NONE',  ( 0.05219959533910956823, 16.53943276465976808, 39.99890960531436690 ) ) ;
#149213 = CARTESIAN_POINT ( 'NONE',  ( -26.05560406886080216, -30.01072603040635300, -20.45417971608944185 ) ) ;
#149214 = CARTESIAN_POINT ( 'NONE',  ( -16.53943276465976808, -0.05219959533934237506, 108.7510903946857042 ) ) ;
#149215 = CARTESIAN_POINT ( 'NONE',  ( 19.03943276465977164, -0.05219959533909143690, 48.74890960531435979 ) ) ;
#149216 = CARTESIAN_POINT ( 'NONE',  ( -19.02544592524334988, -5.153800228976617603, 18.95942372801899722 ) ) ;
#149217 = CARTESIAN_POINT ( 'NONE',  ( 4.379528057220092307, 16.55341960407617563, 37.29275706135235424 ) ) ;
#149218 = CARTESIAN_POINT ( 'NONE',  ( -15.80617190586745835, -15.72974639402198527, 41.87390960531435979 ) ) ;
#149220 = ORIENTED_EDGE ( 'NONE', *, *, #172537, .T. ) ;
#149219 = CARTESIAN_POINT ( 'NONE',  ( -15.80617190586768217, 15.72974639402176855, 98.12609039468570415 ) ) ;
#149221 = CARTESIAN_POINT ( 'NONE',  ( 19.05341960407611168, 5.049401038298154454, 108.9572429386477097 ) ) ;
#149222 = CARTESIAN_POINT ( 'NONE',  ( -0.05219959533909027116, -19.03943276465977164, 92.49890960531436690 ) ) ;
#149223 = CARTESIAN_POINT ( 'NONE',  ( 29.86685920354754842, -21.69954338932559068, -7.824999997268813345 ) ) ;
#149224 = CARTESIAN_POINT ( 'NONE',  ( -15.72974639402176322, -15.80617190586768395, 19.37609039468568639 ) ) ;
#149225 = CARTESIAN_POINT ( 'NONE',  ( -8.314922557960811034, -14.29746914071050412, 77.08224293864769550 ) ) ;
#149227 = CARTESIAN_POINT ( 'NONE',  ( -16.51473224551069308, -9.474510206698971260, 71.66557627198102409 ) ) ;
#149226 = CARTESIAN_POINT ( 'NONE',  ( 15.80617190586746368, 15.72974639402197994, 69.37390960531436690 ) ) ;
#149228 = CARTESIAN_POINT ( 'NONE',  ( 5.153800228976335163, 19.02544592524342804, 79.79057627198102409 ) ) ;
#149229 = CARTESIAN_POINT ( 'NONE',  ( 21.52544592524344225, -5.823673210054117533, 108.5405762719810241 ) ) ;
#149230 = ORIENTED_EDGE ( 'NONE', *, *, #185592, .T. ) ;
#149231 = CARTESIAN_POINT ( 'NONE',  ( -13.97604488694527625, -13.89961937509977652, 61.87390960531435979 ) ) ;
#149233 = FACE_BOUND ( 'NONE', #90014, .T. ) ;
#149232 = CARTESIAN_POINT ( 'NONE',  ( -12.14591786802309592, -12.06949235617757132, 111.8739096053143669 ) ) ;
#149234 = CARTESIAN_POINT ( 'NONE',  ( -0.05219959533909027116, -19.03943276465977164, 62.49890960531435979 ) ) ;
#149235 = CARTESIAN_POINT ( 'NONE',  ( 13.89961937509957401, 13.97604488694547697, 86.87609039468567573 ) ) ;
#149236 = CARTESIAN_POINT ( 'NONE',  ( -8.314922557960811034, -14.29746914071050412, 97.08224293864770971 ) ) ;
#149237 = CARTESIAN_POINT ( 'NONE',  ( -21.52544592524334988, -5.823673210054445271, 53.95942372801900433 ) ) ;
#149239 = CARTESIAN_POINT ( 'NONE',  ( -21.53943276465977519, 0.05219959533907696930, 111.2489096053143669 ) ) ;
#149238 = CARTESIAN_POINT ( 'NONE',  ( 13.89961937509977652, -13.97604488694527269, 53.12390960531434558 ) ) ;
#149240 = CARTESIAN_POINT ( 'NONE',  ( -16.55341960407611168, -4.379528057220339221, 101.4572429386476955 ) ) ;
#149241 = CARTESIAN_POINT ( 'NONE',  ( 23.31738231874054890, -16.94106989632523508, 140.7999999999999829 ) ) ;
#149242 = CARTESIAN_POINT ( 'NONE',  ( 13.89961937509977652, -13.97604488694527269, 78.12390960531433848 ) ) ;
#149243 = CARTESIAN_POINT ( 'NONE',  ( -28.82186960331489445, 9.364793116373697046, 144.1500000054623456 ) ) ;
#149245 = CARTESIAN_POINT ( 'NONE',  ( -0.05219959533907301413, -21.53943276465977519, 27.49890960531435269 ) ) ;
#149244 = CARTESIAN_POINT ( 'NONE',  ( -0.05219959533936034679, 19.03943276465977164, 112.5010903946856757 ) ) ;
#149246 = CARTESIAN_POINT ( 'NONE',  ( 10.81492255796106328, -18.62759615963255655, 45.41775706135234003 ) ) ;
#149247 = CARTESIAN_POINT ( 'NONE',  ( 16.51473224551069308, 9.474510206698969483, 94.16557627198103830 ) ) ;
#149248 = CARTESIAN_POINT ( 'NONE',  ( -19.05341960407617563, 5.049401038297882671, 88.54275706135230450 ) ) ;
#149249 = CARTESIAN_POINT ( 'NONE',  ( -19.05341960407611168, -5.049401038298163336, 66.45724293864769550 ) ) ;
#149250 = CARTESIAN_POINT ( 'NONE',  ( -14.34966873604960291, -8.224510206698953496, 86.66557627198102409 ) ) ;
#149251 = CARTESIAN_POINT ( 'NONE',  ( -16.51473224551069308, -9.474510206698971260, 96.66557627198102409 ) ) ;
#149252 = CARTESIAN_POINT ( 'NONE',  ( -16.55341960407611168, -4.379528057220339221, 76.45724293864769550 ) ) ;
#149253 = CARTESIAN_POINT ( 'NONE',  ( 19.03943276465977164, -0.05219959533909143690, 98.74890960531436690 ) ) ;
#149256 = CARTESIAN_POINT ( 'NONE',  ( -0.05219959533909027116, -19.03943276465977164, 32.49890960531435979 ) ) ;
#149255 = CARTESIAN_POINT ( 'NONE',  ( -12.06949235617756955, 12.14591786802309770, 40.62390960531435269 ) ) ;
#149254 = CARTESIAN_POINT ( 'NONE',  ( -9.564922557960796823, -16.46253265017161027, 47.08224293864769550 ) ) ;
#149257 = ORIENTED_EDGE ( 'NONE', *, *, #24149, .T. ) ;
#149258 = CARTESIAN_POINT ( 'NONE',  ( 18.67979575497194134, -10.72451020669871369, 40.83442372801901854 ) ) ;
#149259 = CARTESIAN_POINT ( 'NONE',  ( 13.89961937509957401, 13.97604488694547697, 76.87609039468566152 ) ) ;
#149260 = CARTESIAN_POINT ( 'NONE',  ( -12.14591786802309592, -12.06949235617757132, 51.87390960531437401 ) ) ;
#149261 = CARTESIAN_POINT ( 'NONE',  ( 10.72451020669898902, -18.67979575497178502, 102.9155762719810383 ) ) ;
#149262 = CARTESIAN_POINT ( 'NONE',  ( 21.55341960407610458, 5.719274019375980345, 38.95724293864768839 ) ) ;
#149263 = CARTESIAN_POINT ( 'NONE',  ( -4.483927247898539470, -16.52544592524342804, 87.29057627198103830 ) ) ;
#149264 = CARTESIAN_POINT ( 'NONE',  ( -5.153800228976328057, -19.02544592524343514, 47.29057627198102409 ) ) ;
#149265 = CARTESIAN_POINT ( 'NONE',  ( 12.06949235617757843, -12.14591786802309237, 23.12390960531436335 ) ) ;
#149266 = CARTESIAN_POINT ( 'NONE',  ( 16.52544592524335698, 4.483927247898782831, 86.45942372801901854 ) ) ;
#149267 = CARTESIAN_POINT ( 'NONE',  ( -0.05219959533934338120, 16.53943276465976808, 72.50109039468568994 ) ) ;
#149268 = CARTESIAN_POINT ( 'NONE',  ( 9.474510206698729675, 16.51473224551082808, 32.08442372801900433 ) ) ;
#149269 = CARTESIAN_POINT ( 'NONE',  ( 13.89961937509977652, -13.97604488694527269, 98.12390960531433848 ) ) ;
#149270 = CARTESIAN_POINT ( 'NONE',  ( 9.564922557960805705, 16.46253265017160317, 74.58224293864769550 ) ) ;
#149271 = CARTESIAN_POINT ( 'NONE',  ( -14.29746914071037622, -8.314922557961029526, 74.16775706135231871 ) ) ;
#149272 = CARTESIAN_POINT ( 'NONE',  ( 19.03943276465977164, -0.05219959533909143690, 38.74890960531436690 ) ) ;
#149273 = CARTESIAN_POINT ( 'NONE',  ( 16.53943276465976808, -0.05219959533910856209, 53.74890960531437401 ) ) ;
#149274 = CARTESIAN_POINT ( 'NONE',  ( 19.03943276465977164, -0.05219959533909143690, 98.74890960531436690 ) ) ;
#149275 = CARTESIAN_POINT ( 'NONE',  ( 21.55341960407610458, 5.719274019375980345, 33.95724293864769550 ) ) ;
#149276 = CARTESIAN_POINT ( 'NONE',  ( -14.29746914071049879, 8.314922557960819915, 65.83224293864769550 ) ) ;
#149277 = CARTESIAN_POINT ( 'NONE',  ( 14.34966873604960469, 8.224510206698951720, 64.16557627198102409 ) ) ;
#149278 = CARTESIAN_POINT ( 'NONE',  ( 29.41559601785650102, -1.135674102528286156, -49.03020479230155360 ) ) ;
#149279 = CARTESIAN_POINT ( 'NONE',  ( -19.03943276465977164, -0.05219959533935918106, 68.75109039468566152 ) ) ;
#149280 = CARTESIAN_POINT ( 'NONE',  ( -9.474510206698964154, 16.51473224551069663, 95.41557627198102409 ) ) ;
#149281 = CARTESIAN_POINT ( 'NONE',  ( -0.05219959533936034679, 19.03943276465977164, 82.50109039468567573 ) ) ;
#149282 = CARTESIAN_POINT ( 'NONE',  ( 18.22780087662122384, -5.500000000000022204, 96.01540105326108687 ) ) ;
#149284 = CARTESIAN_POINT ( 'NONE',  ( 14.34966873604972726, -8.224510206698740333, 100.8344237280190185 ) ) ;
#149283 = CARTESIAN_POINT ( 'NONE',  ( 0.05219959533936267826, -19.03943276465977164, 105.0010903946856615 ) ) ;
#149285 = CARTESIAN_POINT ( 'NONE',  ( 9.474510206698971260, -16.51473224551069308, 32.91557627198102409 ) ) ;
#149286 = CARTESIAN_POINT ( 'NONE',  ( -10.81492255796078084, -18.62759615963271287, 37.08224293864768129 ) ) ;
#149287 = CARTESIAN_POINT ( 'NONE',  ( 5.719274019375673035, 21.55341960407619339, 52.29275706135236135 ) ) ;
#149288 = CARTESIAN_POINT ( 'NONE',  ( -14.34966873604972548, 8.224510206698743886, 28.33442372801902209 ) ) ;
#149290 = CARTESIAN_POINT ( 'NONE',  ( 19.02544592524343514, -5.153800228976328945, 78.54057627198099567 ) ) ;
#149289 = CARTESIAN_POINT ( 'NONE',  ( 17.50000000000000355, 3.656949067071755710, 22.19957421800376451 ) ) ;
#149291 = CARTESIAN_POINT ( 'NONE',  ( -0.05219959533909027116, -19.03943276465977164, 112.4989096053143669 ) ) ;
#149293 = CARTESIAN_POINT ( 'NONE',  ( -19.02544592524342804, 5.153800228976336051, 76.04057627198102409 ) ) ;
#149292 = CARTESIAN_POINT ( 'NONE',  ( 14.29746914071049879, -8.314922557960816363, 78.33224293864770971 ) ) ;
#149294 = CARTESIAN_POINT ( 'NONE',  ( 13.89961937509977652, -13.97604488694527269, 78.12390960531433848 ) ) ;
#149295 = ORIENTED_EDGE ( 'NONE', *, *, #25866, .F. ) ;
#149296 = CARTESIAN_POINT ( 'NONE',  ( 5.153800228976615827, -19.02544592524334988, 90.20942372801900433 ) ) ;
#149297 = CARTESIAN_POINT ( 'NONE',  ( -5.823673210054116645, -21.52544592524344225, 67.29057627198103830 ) ) ;
#149298 = CARTESIAN_POINT ( 'NONE',  ( 5.049401038298161559, -19.05341960407611168, 32.70724293864768129 ) ) ;
#149299 = CARTESIAN_POINT ( 'NONE',  ( -5.153800228976607833, 19.02544592524334988, 57.70942372801899012 ) ) ;
#149300 = CARTESIAN_POINT ( 'NONE',  ( 19.03943276465977164, -0.05219959533909143690, 58.74890960531435979 ) ) ;
#149301 = CARTESIAN_POINT ( 'NONE',  ( 5.049401038298161559, -19.05341960407611168, 97.70724293864766707 ) ) ;
#149302 = ORIENTED_EDGE ( 'NONE', *, *, #87955, .T. ) ;
#149303 = CARTESIAN_POINT ( 'NONE',  ( 0.05219959533907565091, 21.53943276465977519, 84.99890960531436690 ) ) ;
#149305 = CARTESIAN_POINT ( 'NONE',  ( -9.474510206698720793, -16.51473224551083518, 49.58442372801899722 ) ) ;
#149304 = CARTESIAN_POINT ( 'NONE',  ( 0.05219959533910956823, 16.53943276465976808, 99.99890960531436690 ) ) ;
#149306 = CARTESIAN_POINT ( 'NONE',  ( -0.05219959533907301413, -21.53943276465977519, 87.49890960531436690 ) ) ;
#149307 = CARTESIAN_POINT ( 'NONE',  ( 21.53943276465977519, -0.05219959533907433946, 73.74890960531433848 ) ) ;
#149308 = CARTESIAN_POINT ( 'NONE',  ( 8.314922557960818139, 14.29746914071049879, 34.58224293864770260 ) ) ;
#149309 = CARTESIAN_POINT ( 'NONE',  ( -10.72451020669870658, -18.67979575497194134, 99.58442372801900433 ) ) ;
#149310 = CARTESIAN_POINT ( 'NONE',  ( -9.474510206698964154, 16.51473224551069663, 85.41557627198102409 ) ) ;
#149311 = CARTESIAN_POINT ( 'NONE',  ( 19.02544592524343514, -5.153800228976328945, 38.54057627198103120 ) ) ;
#149312 = CARTESIAN_POINT ( 'NONE',  ( -10.72451020669870658, -18.67979575497194134, 39.58442372801901143 ) ) ;
#149313 = CARTESIAN_POINT ( 'NONE',  ( 21.53943276465977519, 0.05219959533937863772, 51.25109039468568994 ) ) ;
#149314 = CARTESIAN_POINT ( 'NONE',  ( 9.564922557960805705, 16.46253265017160317, 54.58224293864769550 ) ) ;
#149315 = CARTESIAN_POINT ( 'NONE',  ( 21.53943276465977519, -0.05219959533907433946, 113.7489096053143527 ) ) ;
#149316 = CARTESIAN_POINT ( 'NONE',  ( -9.474510206698720793, -16.51473224551083518, 59.58442372801900433 ) ) ;
#149317 = CARTESIAN_POINT ( 'NONE',  ( -19.05341960407611168, -5.049401038298163336, 36.45724293864766707 ) ) ;
#149318 = CARTESIAN_POINT ( 'NONE',  ( -16.52544592524335698, -4.483927247898792601, 23.95942372801901143 ) ) ;
#149319 = CARTESIAN_POINT ( 'NONE',  ( 9.474510206698971260, -16.51473224551069308, 22.91557627198102765 ) ) ;
#149320 = CARTESIAN_POINT ( 'NONE',  ( -4.379528057220086978, -16.55341960407618274, 74.79275706135234714 ) ) ;
#149321 = CARTESIAN_POINT ( 'NONE',  ( -13.97604488694527625, -13.89961937509977652, 41.87390960531435979 ) ) ;
#149322 = CARTESIAN_POINT ( 'NONE',  ( 24.83221077041874736, -4.296110748028930892, 170.3917201292316292 ) ) ;
#149323 = CARTESIAN_POINT ( 'NONE',  ( -0.05219959533909027116, -19.03943276465977164, 82.49890960531436690 ) ) ;
#149324 = CARTESIAN_POINT ( 'NONE',  ( 19.03943276465977164, -0.05219959533909143690, 28.74890960531435624 ) ) ;
#149325 = CARTESIAN_POINT ( 'NONE',  ( 18.67979575497178502, 10.72451020669898547, 74.16557627198102409 ) ) ;
#149326 = CARTESIAN_POINT ( 'NONE',  ( 14.29746914071037800, 8.314922557961029526, 41.66775706135235424 ) ) ;
#149327 = CARTESIAN_POINT ( 'NONE',  ( 15.80617190586769283, -15.72974639402175789, 110.6260903946857042 ) ) ;
#149328 = CARTESIAN_POINT ( 'NONE',  ( 19.05341960407611168, 5.049401038298154454, 33.95724293864769550 ) ) ;
#149329 = CARTESIAN_POINT ( 'NONE',  ( 14.34966873604960469, 8.224510206698951720, 34.16557627198102409 ) ) ;
#149330 = CARTESIAN_POINT ( 'NONE',  ( -16.55341960407611168, -4.379528057220339221, 61.45724293864770260 ) ) ;
#149331 = CARTESIAN_POINT ( 'NONE',  ( -16.46253265017160317, 9.564922557960807481, 60.83224293864769550 ) ) ;
#149332 = CARTESIAN_POINT ( 'NONE',  ( 0.05219959533937995610, -21.53943276465977519, 110.0010903946856757 ) ) ;
#149333 = CARTESIAN_POINT ( 'NONE',  ( -18.62759615963270932, 10.81492255796079327, 115.8322429386477097 ) ) ;
#149334 = CARTESIAN_POINT ( 'NONE',  ( 9.564922557960805705, 16.46253265017160317, 84.58224293864769550 ) ) ;
#149335 = CARTESIAN_POINT ( 'NONE',  ( 18.67979575497194134, -10.72451020669871369, 90.83442372801901854 ) ) ;
#149336 = CARTESIAN_POINT ( 'NONE',  ( -12.06949235617739369, -12.14591786802326823, 69.37609039468567573 ) ) ;
#149337 = CARTESIAN_POINT ( 'NONE',  ( 13.89961937509977652, -13.97604488694527269, 113.1239096053143527 ) ) ;
#149338 = CARTESIAN_POINT ( 'NONE',  ( 12.06949235617757843, -12.14591786802309237, 28.12390960531435979 ) ) ;
#149339 = CARTESIAN_POINT ( 'NONE',  ( -13.97604488694527625, -13.89961937509977652, 26.87390960531434558 ) ) ;
#149340 = CARTESIAN_POINT ( 'NONE',  ( -12.06949235617739369, -12.14591786802326823, 49.37609039468569705 ) ) ;
#149341 = CARTESIAN_POINT ( 'NONE',  ( 14.29746914071049879, -8.314922557960816363, 58.33224293864768839 ) ) ;
#149342 = CARTESIAN_POINT ( 'NONE',  ( 12.06949235617739724, 12.14591786802326823, 101.8760903946857042 ) ) ;
#149343 = CARTESIAN_POINT ( 'NONE',  ( -13.97604488694527625, -13.89961937509977652, 111.8739096053143243 ) ) ;
#149344 = CARTESIAN_POINT ( 'NONE',  ( -18.62759615963270932, 10.81492255796079327, 30.83224293864770260 ) ) ;
#149345 = CARTESIAN_POINT ( 'NONE',  ( 21.52544592524334988, 5.823673210054432836, 106.4594237280190328 ) ) ;
#149346 = CARTESIAN_POINT ( 'NONE',  ( 0.05219959533910956823, 16.53943276465976808, 84.99890960531436690 ) ) ;
#149347 = CARTESIAN_POINT ( 'NONE',  ( -5.049401038298153566, 19.05341960407611168, 90.20724293864766707 ) ) ;
#149348 = ORIENTED_EDGE ( 'NONE', *, *, #131670, .F. ) ;
#149349 = CARTESIAN_POINT ( 'NONE',  ( -8.314922557961024197, 14.29746914071037800, 42.91775706135235424 ) ) ;
#149350 = CARTESIAN_POINT ( 'NONE',  ( -13.97604488694527625, -13.89961937509977652, 56.87390960531434558 ) ) ;
#149351 = CARTESIAN_POINT ( 'NONE',  ( 17.50000000000000000, -5.500000000000000888, 120.0000000000000142 ) ) ;
#149352 = CARTESIAN_POINT ( 'NONE',  ( -19.03943276465977164, -0.05219959533935918106, 53.75109039468566863 ) ) ;
#149353 = CARTESIAN_POINT ( 'NONE',  ( 5.049401038298161559, -19.05341960407611168, 47.70724293864770260 ) ) ;
#149354 = CARTESIAN_POINT ( 'NONE',  ( -4.379528057220086978, -16.55341960407618274, 74.79275706135234714 ) ) ;
#149355 = CARTESIAN_POINT ( 'NONE',  ( -19.03943276465977164, -0.05219959533935918106, 93.75109039468566152 ) ) ;
#149356 = CARTESIAN_POINT ( 'NONE',  ( 19.05341960407611168, 5.049401038298154454, 58.95724293864768129 ) ) ;
#149357 = CARTESIAN_POINT ( 'NONE',  ( -21.52544592524343514, 5.823673210054127303, 91.04057627198103830 ) ) ;
#149358 = CARTESIAN_POINT ( 'NONE',  ( 12.06949235617757843, -12.14591786802309237, 98.12390960531436690 ) ) ;
#149359 = EDGE_CURVE ( 'NONE', #113576, #53672, #88185, .T. ) ;
#149360 = CARTESIAN_POINT ( 'NONE',  ( -0.05219959533936034679, 19.03943276465977164, 67.50109039468566152 ) ) ;
#149361 = CARTESIAN_POINT ( 'NONE',  ( -21.52544592524343514, 5.823673210054127303, 66.04057627198103830 ) ) ;
#149362 = CARTESIAN_POINT ( 'NONE',  ( 13.97604488694548053, -13.89961937509957401, 35.62609039468567573 ) ) ;
#149363 = CARTESIAN_POINT ( 'NONE',  ( 18.39639308325437739, 5.500000000000011546, 98.98252246182197212 ) ) ;
#149364 = CARTESIAN_POINT ( 'NONE',  ( -10.81492255796078084, -18.62759615963271287, 97.08224293864770971 ) ) ;
#149365 = LINE ( 'NONE', #148365, #1505 ) ;
#149366 = CARTESIAN_POINT ( 'NONE',  ( -13.97604488694547697, 13.89961937509957934, 98.12609039468566152 ) ) ;
#149367 = DIRECTION ( 'NONE',  ( -0.000000000000000000, -0.000000000000000000, 1.000000000000000000 ) ) ;
#149368 = CARTESIAN_POINT ( 'NONE',  ( 4.483927247898790824, -16.52544592524335698, 25.20942372801901854 ) ) ;
#149369 = CARTESIAN_POINT ( 'NONE',  ( 9.474510206698971260, -16.51473224551069308, 47.91557627198102409 ) ) ;
#149370 = CARTESIAN_POINT ( 'NONE',  ( -10.81492255796078084, -18.62759615963271287, 22.08224293864769194 ) ) ;
#149371 = CARTESIAN_POINT ( 'NONE',  ( -0.05219959533907301413, -21.53943276465977519, 92.49890960531436690 ) ) ;
#149372 = CARTESIAN_POINT ( 'NONE',  ( -0.05219959533937732626, 21.53943276465977519, 57.50109039468568994 ) ) ;
#149374 = CARTESIAN_POINT ( 'NONE',  ( -9.564922557961040184, 16.46253265017147172, 27.91775706135232582 ) ) ;
#149373 = CARTESIAN_POINT ( 'NONE',  ( -4.379528057220086978, -16.55341960407618274, 24.79275706135235779 ) ) ;
#149375 = CARTESIAN_POINT ( 'NONE',  ( -8.314922557960811034, -14.29746914071050412, 27.08224293864769550 ) ) ;
#149376 = CARTESIAN_POINT ( 'NONE',  ( 21.53943276465977519, 0.05219959533937863772, 21.25109039468567218 ) ) ;
#149377 = CARTESIAN_POINT ( 'NONE',  ( 14.34966873604960469, 8.224510206698951720, 49.16557627198102409 ) ) ;
#149378 = CARTESIAN_POINT ( 'NONE',  ( -5.153800228976607833, 19.02544592524334988, 92.70942372801901854 ) ) ;
#149379 = CARTESIAN_POINT ( 'NONE',  ( 9.474510206698729675, 16.51473224551082808, 52.08442372801900433 ) ) ;
#149380 = CARTESIAN_POINT ( 'NONE',  ( -10.81492255796105439, 18.62759615963255655, 67.91775706135234714 ) ) ;
#149381 = CARTESIAN_POINT ( 'NONE',  ( -19.03943276465977164, -0.05219959533935918106, 43.75109039468566863 ) ) ;
#149382 = CARTESIAN_POINT ( 'NONE',  ( 9.474510206698971260, -16.51473224551069308, 22.91557627198102765 ) ) ;
#149383 = CARTESIAN_POINT ( 'NONE',  ( 5.823673210054125526, 21.52544592524343514, 49.79057627198102409 ) ) ;
#149384 = CARTESIAN_POINT ( 'NONE',  ( -16.55341960407611168, -4.379528057220339221, 31.45724293864769550 ) ) ;
#149385 = CARTESIAN_POINT ( 'NONE',  ( -19.03943276465977164, -0.05219959533935918106, 18.75109039468567218 ) ) ;
#149386 = CARTESIAN_POINT ( 'NONE',  ( 12.06949235617739724, 12.14591786802326823, 71.87609039468568994 ) ) ;
#149387 = CARTESIAN_POINT ( 'NONE',  ( -12.14591786802309592, -12.06949235617757132, 36.87390960531435979 ) ) ;
#149388 = CARTESIAN_POINT ( 'NONE',  ( -21.53943276465977519, -0.05219959533937600094, 78.75109039468568994 ) ) ;
#149389 = CARTESIAN_POINT ( 'NONE',  ( -0.05219959533937732626, 21.53943276465977519, 62.50109039468568284 ) ) ;
#149390 = CARTESIAN_POINT ( 'NONE',  ( -10.81492255796078084, -18.62759615963271287, 62.08224293864769550 ) ) ;
#149391 = EDGE_CURVE ( 'NONE', #16157, #87857, #150877, .T. ) ;
#149392 = CARTESIAN_POINT ( 'NONE',  ( -13.89961937509977652, 13.97604488694528158, 35.62390960531435269 ) ) ;
#149393 = CARTESIAN_POINT ( 'NONE',  ( -5.719274019375665041, -21.55341960407619695, 44.79275706135234714 ) ) ;
#149394 = CARTESIAN_POINT ( 'NONE',  ( 13.89961937509977652, -13.97604488694527269, 28.12390960531435624 ) ) ;
#149395 = CARTESIAN_POINT ( 'NONE',  ( 19.03943276465977164, -0.05219959533909143690, 33.74890960531435979 ) ) ;
#149396 = CARTESIAN_POINT ( 'NONE',  ( -16.52544592524342804, 4.483927247898546575, 96.04057627198102409 ) ) ;
#149397 = CARTESIAN_POINT ( 'NONE',  ( -5.153800228976328057, -19.02544592524343514, 82.29057627198103830 ) ) ;
#149398 = CARTESIAN_POINT ( 'NONE',  ( -4.379528057220328563, 16.55341960407611168, 35.20724293864768839 ) ) ;
#149399 = CARTESIAN_POINT ( 'NONE',  ( -8.224510206698948167, 14.34966873604960824, 95.41557627198102409 ) ) ;
#149400 = CARTESIAN_POINT ( 'NONE',  ( 15.80617190586746368, 15.72974639402197994, 64.37390960531435269 ) ) ;
#149401 = CARTESIAN_POINT ( 'NONE',  ( -21.53943276465977519, 0.05219959533907696930, 106.2489096053143811 ) ) ;
#149402 = CARTESIAN_POINT ( 'NONE',  ( 5.153800228976335163, 19.02544592524342804, 109.7905762719810099 ) ) ;
#149404 = CARTESIAN_POINT ( 'NONE',  ( -12.14591786802326823, 12.06949235617739902, 28.12609039468568284 ) ) ;
#149403 = CARTESIAN_POINT ( 'NONE',  ( -16.51473224551069308, -9.474510206698971260, 66.66557627198102409 ) ) ;
#149405 = CARTESIAN_POINT ( 'NONE',  ( 21.55341960407610458, 5.719274019375980345, 53.95724293864770260 ) ) ;
#149406 = CARTESIAN_POINT ( 'NONE',  ( -18.67979575497193778, 10.72451020669871902, 98.33442372801901854 ) ) ;
#149407 = CARTESIAN_POINT ( 'NONE',  ( -19.05341960407611168, -5.049401038298163336, 81.45724293864769550 ) ) ;
#149408 = CARTESIAN_POINT ( 'NONE',  ( -18.67979575497193778, 10.72451020669871902, 23.33442372801901499 ) ) ;
#149409 = CARTESIAN_POINT ( 'NONE',  ( -10.81492255796078084, -18.62759615963271287, 22.08224293864769194 ) ) ;
#149410 = CARTESIAN_POINT ( 'NONE',  ( 16.52544592524335698, 4.483927247898782831, 91.45942372801901854 ) ) ;
#149411 = CARTESIAN_POINT ( 'NONE',  ( -21.52544592524334988, -5.823673210054445271, 68.95942372801901854 ) ) ;
#149412 = CARTESIAN_POINT ( 'NONE',  ( 21.53943276465977519, 0.05219959533937863772, 101.2510903946856757 ) ) ;
#149413 = CARTESIAN_POINT ( 'NONE',  ( -8.314922557961024197, 14.29746914071037800, 67.91775706135234714 ) ) ;
#149414 = CARTESIAN_POINT ( 'NONE',  ( -10.81492255796105439, 18.62759615963255655, 32.91775706135234714 ) ) ;
#149415 = CARTESIAN_POINT ( 'NONE',  ( -16.51473224551069308, -9.474510206698971260, 111.6655762719810383 ) ) ;
#149416 = CARTESIAN_POINT ( 'NONE',  ( -10.81492255796105439, 18.62759615963255655, 87.91775706135234714 ) ) ;
#149417 = CARTESIAN_POINT ( 'NONE',  ( 9.564922557960805705, 16.46253265017160317, 94.58224293864769550 ) ) ;
#149418 = CARTESIAN_POINT ( 'NONE',  ( -10.81492255796078084, -18.62759615963271287, 92.08224293864769550 ) ) ;
#149419 = CARTESIAN_POINT ( 'NONE',  ( 19.03943276465977164, 0.05219959533936151252, 66.25109039468567573 ) ) ;
#149420 = CARTESIAN_POINT ( 'NONE',  ( 10.81492255796078972, 18.62759615963270932, 59.58224293864770260 ) ) ;
#149422 = CARTESIAN_POINT ( 'NONE',  ( 12.06949235617757843, -12.14591786802309237, 33.12390960531435979 ) ) ;
#149421 = CARTESIAN_POINT ( 'NONE',  ( 16.46253265017160672, -9.564922557960803928, 98.33224293864769550 ) ) ;
#149423 = CARTESIAN_POINT ( 'NONE',  ( -3.889087296526137383, -34.99999999999999289, 1.818019484660534424 ) ) ;
#149424 = CARTESIAN_POINT ( 'NONE',  ( 5.153800228976615827, -19.02544592524334988, 80.20942372801901854 ) ) ;
#149425 = DIRECTION ( 'NONE',  ( 1.000000000000000000, 0.000000000000000000, 0.000000000000000000 ) ) ;
#149426 = CARTESIAN_POINT ( 'NONE',  ( 16.46253265017146816, 9.564922557961045513, 106.6677570613523471 ) ) ;
#149427 = CARTESIAN_POINT ( 'NONE',  ( 21.53943276465977519, -0.05219959533907433946, 78.74890960531436690 ) ) ;
#149428 = CARTESIAN_POINT ( 'NONE',  ( 4.483927247898545687, 16.52544592524342804, 69.79057627198102409 ) ) ;
#149429 = CARTESIAN_POINT ( 'NONE',  ( -4.483927247898782831, 16.52544592524335698, 27.70942372801901854 ) ) ;
#149430 = CARTESIAN_POINT ( 'NONE',  ( -16.51473224551069308, -9.474510206698971260, 41.66557627198103120 ) ) ;
#149432 = CARTESIAN_POINT ( 'NONE',  ( 19.02544592524334988, 5.153800228976608722, 81.45942372801897591 ) ) ;
#149431 = CARTESIAN_POINT ( 'NONE',  ( 21.55341960407610458, 5.719274019375980345, 113.9572429386477239 ) ) ;
#149433 = CARTESIAN_POINT ( 'NONE',  ( 19.05341960407611168, 5.049401038298154454, 88.95724293864769550 ) ) ;
#149434 = CARTESIAN_POINT ( 'NONE',  ( 19.02544592524343514, -5.153800228976328945, 78.54057627198099567 ) ) ;
#149435 = CARTESIAN_POINT ( 'NONE',  ( 0.05219959533907565091, 21.53943276465977519, 69.99890960531435269 ) ) ;
#149436 = CARTESIAN_POINT ( 'NONE',  ( -13.89961937509977652, 13.97604488694528158, 50.62390960531435979 ) ) ;
#149437 = FACE_BOUND ( 'NONE', #167555, .T. ) ;
#149438 = CARTESIAN_POINT ( 'NONE',  ( -4.483927247898539470, -16.52544592524342804, 52.29057627198102409 ) ) ;
#149439 = CARTESIAN_POINT ( 'NONE',  ( -9.474510206698964154, 16.51473224551069663, 85.41557627198102409 ) ) ;
#149440 = CARTESIAN_POINT ( 'NONE',  ( 18.22780087662119897, -5.500000000000096811, 43.51763182126894236 ) ) ;
#149441 = CARTESIAN_POINT ( 'NONE',  ( 0.05219959533936267826, -19.03943276465977164, 70.00109039468566152 ) ) ;
#149442 = CARTESIAN_POINT ( 'NONE',  ( -21.52544592524343514, 5.823673210054127303, 81.04057627198102409 ) ) ;
#149443 = CARTESIAN_POINT ( 'NONE',  ( 19.05341960407617918, -5.049401038297876454, 36.04275706135234003 ) ) ;
#149444 = CARTESIAN_POINT ( 'NONE',  ( -9.564922557960796823, -16.46253265017161027, 102.0822429386477097 ) ) ;
#149445 = CARTESIAN_POINT ( 'NONE',  ( -69.65682714487590488, -71.74905178543390605, -13.00000000000000000 ) ) ;
#149446 = CARTESIAN_POINT ( 'NONE',  ( -21.52544592524343514, 5.823673210054127303, 46.04057627198103830 ) ) ;
#149447 = CARTESIAN_POINT ( 'NONE',  ( 19.03943276465977164, -0.05219959533909143690, 68.74890960531436690 ) ) ;
#149448 = CARTESIAN_POINT ( 'NONE',  ( 21.53943276465977519, 0.05219959533937863772, 61.25109039468567573 ) ) ;
#149449 = CARTESIAN_POINT ( 'NONE',  ( 13.97604488694527802, 13.89961937509977652, 24.37390960531435624 ) ) ;
#149451 = VERTEX_POINT ( 'NONE', #134716 ) ;
#149450 = CARTESIAN_POINT ( 'NONE',  ( -21.53943276465977519, 0.05219959533907696930, 111.2489096053143669 ) ) ;
#149452 = CARTESIAN_POINT ( 'NONE',  ( -10.81492255796105439, 18.62759615963255655, 52.91775706135235424 ) ) ;
#149453 = ORIENTED_EDGE ( 'NONE', *, *, #163221, .F. ) ;
#149454 = CARTESIAN_POINT ( 'NONE',  ( -19.02544592524342804, 5.153800228976336051, 116.0405762719810383 ) ) ;
#149455 = CARTESIAN_POINT ( 'NONE',  ( -19.05341960407617563, 5.049401038297882671, 68.54275706135230450 ) ) ;
#149456 = AXIS2_PLACEMENT_3D ( 'NONE', #171946, #80914, #173949 ) ;
#149457 = FACE_OUTER_BOUND ( 'NONE', #21407, .T. ) ;
#149458 = CARTESIAN_POINT ( 'NONE',  ( -15.72974639402197994, 15.80617190586746368, 105.6239096053143669 ) ) ;
#149459 = CARTESIAN_POINT ( 'NONE',  ( -19.02544592524342804, 5.153800228976336051, 61.04057627198103120 ) ) ;
#149460 = CARTESIAN_POINT ( 'NONE',  ( 4.379528057220092307, 16.55341960407617563, 32.29275706135235424 ) ) ;
#149461 = CARTESIAN_POINT ( 'NONE',  ( -23.48529157249600985, 32.32473071737754111, -10.04999999453762705 ) ) ;
#149462 = CARTESIAN_POINT ( 'NONE',  ( -5.823673210054431948, 21.52544592524334988, 97.70942372801904696 ) ) ;
#149463 = CARTESIAN_POINT ( 'NONE',  ( 5.153800228976335163, 19.02544592524342804, 39.79057627198100988 ) ) ;
#149464 = CARTESIAN_POINT ( 'NONE',  ( 21.55341960407619695, -5.719274019375665929, 96.04275706135236135 ) ) ;
#149466 = CARTESIAN_POINT ( 'NONE',  ( -21.52544592524334988, -5.823673210054445271, 58.95942372801902565 ) ) ;
#149465 = CARTESIAN_POINT ( 'NONE',  ( -19.05341960407611168, -5.049401038298163336, 86.45724293864769550 ) ) ;
#149467 = CARTESIAN_POINT ( 'NONE',  ( 29.86685920354754487, 21.69954338932564752, -9.424999997268814766 ) ) ;
#149468 = DIRECTION ( 'NONE',  ( 0.4999999999999933387, -0.5000000000000055511, 0.7071067811865483499 ) ) ;
#149469 = CARTESIAN_POINT ( 'NONE',  ( 2.577820198429831642E-15, 9.100000000000001421, -63.95112321872120731 ) ) ;
#149471 = CARTESIAN_POINT ( 'NONE',  ( 10.81492255796106328, -18.62759615963255655, 70.41775706135236135 ) ) ;
#149470 = CARTESIAN_POINT ( 'NONE',  ( -16.53943276465976808, -0.05219959533934237506, 53.75109039468568994 ) ) ;
#149472 = CARTESIAN_POINT ( 'NONE',  ( 15.80617190586769283, -15.72974639402175789, 85.62609039468568994 ) ) ;
#149473 = CYLINDRICAL_SURFACE ( 'NONE', #138138, 7.500000000000007105 ) ;
#149474 = CARTESIAN_POINT ( 'NONE',  ( 8.224510206698742110, 14.34966873604972548, 22.08442372801901143 ) ) ;
#149475 = CARTESIAN_POINT ( 'NONE',  ( 9.474510206698971260, -16.51473224551069308, 82.91557627198103830 ) ) ;
#149476 = CARTESIAN_POINT ( 'NONE',  ( -9.564922557960796823, -16.46253265017161027, 107.0822429386476955 ) ) ;
#149477 = VERTEX_POINT ( 'NONE', #196399 ) ;
#149478 = LINE ( 'NONE', #86800, #111514 ) ;
#149479 = CARTESIAN_POINT ( 'NONE',  ( 19.03943276465977164, -0.05219959533909143690, 23.74890960531435269 ) ) ;
#149480 = CARTESIAN_POINT ( 'NONE',  ( -18.62759615963270932, 10.81492255796079327, 45.83224293864769550 ) ) ;
#149481 = CARTESIAN_POINT ( 'NONE',  ( 14.34966873604972726, -8.224510206698740333, 95.83442372801903275 ) ) ;
#149483 = CARTESIAN_POINT ( 'NONE',  ( -19.05341960407611168, -5.049401038298163336, 66.45724293864769550 ) ) ;
#149482 = CARTESIAN_POINT ( 'NONE',  ( 8.224510206698953496, -14.34966873604960469, 87.91557627198103830 ) ) ;
#149484 = CARTESIAN_POINT ( 'NONE',  ( -0.05219959533937732626, 21.53943276465977519, 87.50109039468568994 ) ) ;
#149485 = DIRECTION ( 'NONE',  ( -1.000000000000000000, -0.000000000000000000, -0.000000000000000000 ) ) ;
#149486 = CARTESIAN_POINT ( 'NONE',  ( -16.53943276465976808, -0.05219959533934237506, 18.75109039468568639 ) ) ;
#149487 = CARTESIAN_POINT ( 'NONE',  ( -16.53943276465976808, 0.05219959533911058130, 86.24890960531436690 ) ) ;
#149488 = CARTESIAN_POINT ( 'NONE',  ( -15.80617190586768217, 15.72974639402176855, 43.12609039468568284 ) ) ;
#149489 = CARTESIAN_POINT ( 'NONE',  ( -10.81492255796078084, -18.62759615963271287, 77.08224293864769550 ) ) ;
#149490 = CARTESIAN_POINT ( 'NONE',  ( 19.03943276465977164, 0.05219959533936151252, 36.25109039468567573 ) ) ;
#149491 = CARTESIAN_POINT ( 'NONE',  ( -17.58332526062525858, 7.635886036038558977, 45.92334959558467489 ) ) ;
#149492 = CARTESIAN_POINT ( 'NONE',  ( 16.46253265017160672, -9.564922557960803928, 78.33224293864769550 ) ) ;
#149493 = CARTESIAN_POINT ( 'NONE',  ( 16.53943276465976808, -0.05219959533910856209, 58.74890960531436690 ) ) ;
#149494 = CARTESIAN_POINT ( 'NONE',  ( 16.52544592524342804, -4.483927247898539470, 33.54057627198102409 ) ) ;
#149495 = CARTESIAN_POINT ( 'NONE',  ( 0.05219959533934541429, -16.53943276465976808, 110.0010903946856757 ) ) ;
#149496 = CARTESIAN_POINT ( 'NONE',  ( -9.474510206698720793, -16.51473224551083518, 59.58442372801900433 ) ) ;
#149497 = CARTESIAN_POINT ( 'NONE',  ( 17.44279575226823553, 5.990770900252484488, 46.66442432485681024 ) ) ;
#149498 = CARTESIAN_POINT ( 'NONE',  ( 18.62759615963271287, -10.81492255796078972, 28.33224293864769550 ) ) ;
#149499 = CARTESIAN_POINT ( 'NONE',  ( 12.14591786802309770, 12.06949235617756955, 89.37390960531435269 ) ) ;
#149500 = CARTESIAN_POINT ( 'NONE',  ( 20.73749492396215288, -155.7167183371838064, -15.00000000000000178 ) ) ;
#149502 = CARTESIAN_POINT ( 'NONE',  ( -21.52544592524343514, 5.823673210054127303, 46.04057627198103830 ) ) ;
#149501 = CARTESIAN_POINT ( 'NONE',  ( -19.05341960407611168, -5.049401038298163336, 41.45724293864769550 ) ) ;
#149503 = CARTESIAN_POINT ( 'NONE',  ( 5.719274019375991003, -21.55341960407610458, 67.70724293864769550 ) ) ;
#149504 = CARTESIAN_POINT ( 'NONE',  ( 16.46253265017160672, -9.564922557960803928, 23.33224293864769194 ) ) ;
#149506 = CARTESIAN_POINT ( 'NONE',  ( -19.02544592524342804, 5.153800228976336051, 41.04057627198103120 ) ) ;
#149505 = CARTESIAN_POINT ( 'NONE',  ( 4.483927247898790824, -16.52544592524335698, 65.20942372801901854 ) ) ;
#149507 = CARTESIAN_POINT ( 'NONE',  ( -10.81492255796105439, 18.62759615963255655, 57.91775706135234714 ) ) ;
#149508 = CARTESIAN_POINT ( 'NONE',  ( -16.55341960407611168, -4.379528057220339221, 111.4572429386476813 ) ) ;
#149509 = CARTESIAN_POINT ( 'NONE',  ( -0.05219959533936034679, 19.03943276465977164, 92.50109039468566152 ) ) ;
#149510 = CARTESIAN_POINT ( 'NONE',  ( 36.91746824999999177, 11.99521256947799230, -2.024999997268813523 ) ) ;
#149512 = CARTESIAN_POINT ( 'NONE',  ( 21.52544592524344225, -5.823673210054117533, 53.54057627198103120 ) ) ;
#149511 = LINE ( 'NONE', #103005, #163727 ) ;
#149513 = CARTESIAN_POINT ( 'NONE',  ( -19.03943276465977164, 0.05219959533909376836, 26.24890960531435624 ) ) ;
#149514 = CARTESIAN_POINT ( 'NONE',  ( -18.67979575497193778, 10.72451020669871902, 88.33442372801901854 ) ) ;
#149515 = CARTESIAN_POINT ( 'NONE',  ( -4.483927247898539470, -16.52544592524342804, 32.29057627198102409 ) ) ;
#149517 = CARTESIAN_POINT ( 'NONE',  ( -4.483927247898539470, -16.52544592524342804, 37.29057627198102409 ) ) ;
#149516 = CARTESIAN_POINT ( 'NONE',  ( -16.53943276465976808, -0.05219959533934237506, 58.75109039468568994 ) ) ;
#149518 = CARTESIAN_POINT ( 'NONE',  ( -10.81492255796078084, -18.62759615963271287, 72.08224293864769550 ) ) ;
#149519 = CARTESIAN_POINT ( 'NONE',  ( -0.05219959533907301413, -21.53943276465977519, 77.49890960531433848 ) ) ;
#149520 = CARTESIAN_POINT ( 'NONE',  ( -21.59136165864583390, -7.527668378163608232, 173.8290135686407893 ) ) ;
#149523 = EDGE_CURVE ( 'NONE', #168659, #137596, #57868, .T. ) ;
#149522 = CARTESIAN_POINT ( 'NONE',  ( 16.46253265017160672, -9.564922557960803928, 113.3322429386476955 ) ) ;
#149521 = CARTESIAN_POINT ( 'NONE',  ( 9.474510206698729675, 16.51473224551082808, 87.08442372801900433 ) ) ;
#149524 = CARTESIAN_POINT ( 'NONE',  ( 5.153800228976335163, 19.02544592524342804, 49.79057627198100988 ) ) ;
#149525 = CARTESIAN_POINT ( 'NONE',  ( -16.52544592524342804, 4.483927247898546575, 116.0405762719810383 ) ) ;
#149526 = FILL_AREA_STYLE ('',( #166698 ) ) ;
#149527 = CARTESIAN_POINT ( 'NONE',  ( 17.97214573761829470, 5.500000000000074607, 48.96970049038657180 ) ) ;
#149528 = ORIENTED_EDGE ( 'NONE', *, *, #195188, .F. ) ;
#149529 = CARTESIAN_POINT ( 'NONE',  ( -8.224510206698735004, -14.34966873604973081, 79.58442372801903275 ) ) ;
#149530 = CARTESIAN_POINT ( 'NONE',  ( -0.05219959533907301413, -21.53943276465977519, 107.4989096053143669 ) ) ;
#149531 = CARTESIAN_POINT ( 'NONE',  ( -5.153800228976328057, -19.02544592524343514, 72.29057627198102409 ) ) ;
#149532 = CARTESIAN_POINT ( 'NONE',  ( 18.62759615963255655, 10.81492255796105972, 46.66775706135234714 ) ) ;
#149533 = CARTESIAN_POINT ( 'NONE',  ( -5.153800228976328057, -19.02544592524343514, 92.29057627198099567 ) ) ;
#149534 = CARTESIAN_POINT ( 'NONE',  ( -29.21837264310262228, -26.94013878454652300, -20.44914777674790685 ) ) ;
#149535 = EDGE_LOOP ( 'NONE', ( #109364, #115350, #92809, #174650, #189502 ) ) ;
#149536 = CARTESIAN_POINT ( 'NONE',  ( 21.52544592524334988, 5.823673210054432836, 26.45942372801901854 ) ) ;
#149538 = CARTESIAN_POINT ( 'NONE',  ( 16.51473224551083163, -9.474510206698727899, 90.83442372801900433 ) ) ;
#149537 = CARTESIAN_POINT ( 'NONE',  ( 16.51473224551069308, 9.474510206698969483, 24.16557627198102765 ) ) ;
#149539 = CARTESIAN_POINT ( 'NONE',  ( 19.03943276465977164, 0.05219959533936151252, 36.25109039468567573 ) ) ;
#149540 = CARTESIAN_POINT ( 'NONE',  ( 18.62759615963255655, 10.81492255796105972, 21.66775706135235069 ) ) ;
#149541 = CARTESIAN_POINT ( 'NONE',  ( -9.474510206698720793, -16.51473224551083518, 29.58442372801900433 ) ) ;
#149542 = CARTESIAN_POINT ( 'NONE',  ( -9.564922557961040184, 16.46253265017147172, 52.91775706135233293 ) ) ;
#149543 = CARTESIAN_POINT ( 'NONE',  ( 16.53943276465976808, 0.05219959533934440121, 91.25109039468568994 ) ) ;
#149545 = VERTEX_POINT ( 'NONE', #181223 ) ;
#149544 = CARTESIAN_POINT ( 'NONE',  ( 0.000000000000000000, 1.178949249685217193, 2.041999999999998483 ) ) ;
#149546 = CARTESIAN_POINT ( 'NONE',  ( 5.153800228976335163, 19.02544592524342804, 74.79057627198103830 ) ) ;
#149547 = CARTESIAN_POINT ( 'NONE',  ( 15.72974639402176855, 15.80617190586768217, 81.87609039468568994 ) ) ;
#149548 = CARTESIAN_POINT ( 'NONE',  ( 10.72451020669871369, 18.67979575497193778, 92.08442372801901854 ) ) ;
#149549 = CARTESIAN_POINT ( 'NONE',  ( -21.23184647844206552, -181.1785498424364675, -4.999999999999999112 ) ) ;
#149550 = CARTESIAN_POINT ( 'NONE',  ( -13.89961937509977652, 13.97604488694528158, 85.62390960531433848 ) ) ;
#149551 = CARTESIAN_POINT ( 'NONE',  ( 15.72974639402176855, 15.80617190586768217, 61.87609039468568284 ) ) ;
#149552 = CARTESIAN_POINT ( 'NONE',  ( 9.564922557961047289, -16.46253265017146816, 95.41775706135233293 ) ) ;
#149553 = CARTESIAN_POINT ( 'NONE',  ( 16.46253265017160672, -9.564922557960803928, 68.33224293864770971 ) ) ;
#149554 = CARTESIAN_POINT ( 'NONE',  ( -21.55341960407610458, -5.719274019375992779, 21.45724293864769550 ) ) ;
#149555 = CARTESIAN_POINT ( 'NONE',  ( -5.049401038298153566, 19.05341960407611168, 75.20724293864769550 ) ) ;
#149556 = CARTESIAN_POINT ( 'NONE',  ( -17.05587630539787725, -6.762274262135687053, 89.25819690962691766 ) ) ;
#149557 = CARTESIAN_POINT ( 'NONE',  ( 19.05341960407611168, 5.049401038298154454, 58.95724293864768129 ) ) ;
#149558 = CARTESIAN_POINT ( 'NONE',  ( -5.153800228976328057, -19.02544592524343514, 47.29057627198102409 ) ) ;
#149559 = CARTESIAN_POINT ( 'NONE',  ( 18.67979575497194134, -10.72451020669871369, 20.83442372801901143 ) ) ;
#149560 = CARTESIAN_POINT ( 'NONE',  ( -14.29746914071037622, -8.314922557961029526, 104.1677570613523471 ) ) ;
#149561 = DIRECTION ( 'NONE',  ( 0.8164965809277262565, 0.000000000000000000, 0.5773502691896253980 ) ) ;
#149562 = LINE ( 'NONE', #12070, #20684 ) ;
#149563 = CARTESIAN_POINT ( 'NONE',  ( -16.46253265017146816, -9.564922557961047289, 54.16775706135234003 ) ) ;
#149564 = CARTESIAN_POINT ( 'NONE',  ( 13.89961937509977652, -13.97604488694527269, 83.12390960531436690 ) ) ;
#149565 = CARTESIAN_POINT ( 'NONE',  ( -8.314922557960811034, -14.29746914071050412, 72.08224293864769550 ) ) ;
#149566 = CARTESIAN_POINT ( 'NONE',  ( -16.55341960407611168, -4.379528057220339221, 106.4572429386477097 ) ) ;
#149567 = CARTESIAN_POINT ( 'NONE',  ( -21.53943276465977519, 0.05219959533907696930, 36.24890960531435979 ) ) ;
#149568 = CARTESIAN_POINT ( 'NONE',  ( -19.03943276465977164, 0.05219959533909376836, 106.2489096053143669 ) ) ;
#149569 = CARTESIAN_POINT ( 'NONE',  ( 4.379528057220339221, -16.55341960407611168, 87.70724293864769550 ) ) ;
#149570 = CARTESIAN_POINT ( 'NONE',  ( 30.73962218707677962, -22.33364281372841376, -3.202157773949823039 ) ) ;
#149571 = CARTESIAN_POINT ( 'NONE',  ( -13.89961937509957401, -13.97604488694547875, 34.37609039468566863 ) ) ;
#149572 = CARTESIAN_POINT ( 'NONE',  ( 0.05219959533934541429, -16.53943276465976808, 105.0010903946856757 ) ) ;
#149573 = CARTESIAN_POINT ( 'NONE',  ( 9.564922557960805705, 16.46253265017160317, 89.58224293864769550 ) ) ;
#149574 = CARTESIAN_POINT ( 'NONE',  ( 15.72974639402176855, 15.80617190586768217, 46.87609039468568994 ) ) ;
#149575 = CARTESIAN_POINT ( 'NONE',  ( 10.72451020669898902, -18.67979575497178502, 37.91557627198102409 ) ) ;
#149576 = CARTESIAN_POINT ( 'NONE',  ( 15.80617190586769283, -15.72974639402175789, 25.62609039468567929 ) ) ;
#149577 = CARTESIAN_POINT ( 'NONE',  ( 0.05219959533907565091, 21.53943276465977519, 74.99890960531435269 ) ) ;
#149578 = CARTESIAN_POINT ( 'NONE',  ( 0.05219959533910956823, 16.53943276465976808, 94.99890960531436690 ) ) ;
#149579 = CARTESIAN_POINT ( 'NONE',  ( -9.564922557961040184, 16.46253265017147172, 52.91775706135233293 ) ) ;
#149580 = CARTESIAN_POINT ( 'NONE',  ( 9.564922557960805705, 16.46253265017160317, 34.58224293864770260 ) ) ;
#149581 = CARTESIAN_POINT ( 'NONE',  ( -0.05219959533909027116, -19.03943276465977164, 97.49890960531436690 ) ) ;
#149582 = CARTESIAN_POINT ( 'NONE',  ( 19.05341960407611168, 5.049401038298154454, 93.95724293864769550 ) ) ;
#149583 = CARTESIAN_POINT ( 'NONE',  ( 14.34966873604960469, 8.224510206698951720, 114.1655762719810383 ) ) ;
#149584 = CARTESIAN_POINT ( 'NONE',  ( 12.06949235617757843, -12.14591786802309237, 28.12390960531435979 ) ) ;
#149585 = CARTESIAN_POINT ( 'NONE',  ( -14.29746914071037622, -8.314922557961029526, 39.16775706135235424 ) ) ;
#149586 = CARTESIAN_POINT ( 'NONE',  ( 18.62759615963255655, 10.81492255796105972, 106.6677570613523756 ) ) ;
#149588 = CARTESIAN_POINT ( 'NONE',  ( -8.224510206698948167, 14.34966873604960824, 25.41557627198103120 ) ) ;
#149587 = CARTESIAN_POINT ( 'NONE',  ( -16.46253265017160317, 9.564922557960807481, 105.8322429386476955 ) ) ;
#149589 = CARTESIAN_POINT ( 'NONE',  ( -5.719274019375665041, -21.55341960407619695, 29.79275706135234358 ) ) ;
#149590 = CARTESIAN_POINT ( 'NONE',  ( 5.049401038298161559, -19.05341960407611168, 47.70724293864770260 ) ) ;
#149591 = EDGE_CURVE ( 'NONE', #97477, #77271, #108419, .T. ) ;
#149592 = CARTESIAN_POINT ( 'NONE',  ( -12.14591786802326823, 12.06949235617739902, 48.12609039468568284 ) ) ;
#149593 = CARTESIAN_POINT ( 'NONE',  ( 14.29746914071037800, 8.314922557961029526, 111.6677570613523613 ) ) ;
#149594 = CARTESIAN_POINT ( 'NONE',  ( 4.483927247898790824, -16.52544592524335698, 90.20942372801903275 ) ) ;
#149595 = CARTESIAN_POINT ( 'NONE',  ( 19.03943276465977164, 0.05219959533936151252, 106.2510903946856615 ) ) ;
#149596 = CARTESIAN_POINT ( 'NONE',  ( 19.05341960407611168, 5.049401038298154454, 38.95724293864767418 ) ) ;
#149597 = VECTOR ( 'NONE', #5301, 1000.000000000000000 ) ;
#149598 = CARTESIAN_POINT ( 'NONE',  ( 8.314922557960818139, 14.29746914071049879, 99.58224293864770971 ) ) ;
#149599 = CARTESIAN_POINT ( 'NONE',  ( 21.52544592524344225, -5.823673210054117533, 108.5405762719810241 ) ) ;
#149600 = CARTESIAN_POINT ( 'NONE',  ( 9.474510206698971260, -16.51473224551069308, 32.91557627198102409 ) ) ;
#149601 = CARTESIAN_POINT ( 'NONE',  ( 16.51473224551069308, 9.474510206698969483, 104.1655762719810241 ) ) ;
#149602 = CARTESIAN_POINT ( 'NONE',  ( -18.67979575497193778, 10.72451020669871902, 28.33442372801902209 ) ) ;
#149603 = LINE ( 'NONE', #72776, #72558 ) ;
#149604 = CARTESIAN_POINT ( 'NONE',  ( -19.02544592524342804, 5.153800228976336051, 101.0405762719810241 ) ) ;
#149605 = CARTESIAN_POINT ( 'NONE',  ( 17.48853670773245028, -5.747243402303102044, 111.1667129974999000 ) ) ;
#149606 = CARTESIAN_POINT ( 'NONE',  ( -13.89961937509977652, 13.97604488694528158, 80.62390960531436690 ) ) ;
#149608 = CARTESIAN_POINT ( 'NONE',  ( 14.34966873604960469, 8.224510206698951720, 94.16557627198103830 ) ) ;
#149607 = CARTESIAN_POINT ( 'NONE',  ( -0.05219959533937732626, 21.53943276465977519, 27.50109039468567929 ) ) ;
#149609 = CARTESIAN_POINT ( 'NONE',  ( -19.05341960407611168, -5.049401038298163336, 101.4572429386476955 ) ) ;
#149610 = CARTESIAN_POINT ( 'NONE',  ( -16.46253265017146816, -9.564922557961047289, 29.16775706135232937 ) ) ;
#149611 = CARTESIAN_POINT ( 'NONE',  ( 4.483927247898790824, -16.52544592524335698, 65.20942372801901854 ) ) ;
#149612 = CARTESIAN_POINT ( 'NONE',  ( 15.80617190586769283, -15.72974639402175789, 80.62609039468567573 ) ) ;
#149613 = CARTESIAN_POINT ( 'NONE',  ( -14.29746914071037622, -8.314922557961029526, 34.16775706135234714 ) ) ;
#149614 = CARTESIAN_POINT ( 'NONE',  ( -0.05219959533909027116, -19.03943276465977164, 77.49890960531435269 ) ) ;
#149615 = CARTESIAN_POINT ( 'NONE',  ( 19.03943276465977164, 0.05219959533936151252, 91.25109039468566152 ) ) ;
#149616 = CARTESIAN_POINT ( 'NONE',  ( -14.34966873604972548, 8.224510206698743886, 63.33442372801900433 ) ) ;
#149617 = CARTESIAN_POINT ( 'NONE',  ( -10.72451020669870658, -18.67979575497194134, 109.5844237280190328 ) ) ;
#149618 = CARTESIAN_POINT ( 'NONE',  ( 13.89961937509957401, 13.97604488694547697, 86.87609039468567573 ) ) ;
#149619 = CARTESIAN_POINT ( 'NONE',  ( 19.03943276465977164, -0.05219959533909143690, 68.74890960531436690 ) ) ;
#149620 = CARTESIAN_POINT ( 'NONE',  ( -5.719274019375978568, 21.55341960407610458, 80.20724293864769550 ) ) ;
#149622 = CARTESIAN_POINT ( 'NONE',  ( 19.03943276465977164, 0.05219959533936151252, 86.25109039468567573 ) ) ;
#149621 = CARTESIAN_POINT ( 'NONE',  ( -0.05219959533910754901, -16.53943276465976808, 87.49890960531436690 ) ) ;
#149623 = CARTESIAN_POINT ( 'NONE',  ( 12.06949235617739724, 12.14591786802326823, 56.87609039468568994 ) ) ;
#149624 = CARTESIAN_POINT ( 'NONE',  ( 24.85901545656365386, 5.346793810781362843, 169.1018111888376723 ) ) ;
#149625 = CARTESIAN_POINT ( 'NONE',  ( 13.97604488694548053, -13.89961937509957401, 60.62609039468564731 ) ) ;
#149626 = CARTESIAN_POINT ( 'NONE',  ( 14.34966873604960469, 8.224510206698951720, 24.16557627198103120 ) ) ;
#149627 = CARTESIAN_POINT ( 'NONE',  ( 4.379528057220339221, -16.55341960407611168, 77.70724293864770971 ) ) ;
#149629 = CARTESIAN_POINT ( 'NONE',  ( -18.87580814761075487, 5.500000000000055067, 90.87172394265756736 ) ) ;
#149628 = CARTESIAN_POINT ( 'NONE',  ( -5.823673210054431948, 21.52544592524334988, 112.7094237280190328 ) ) ;
#149630 = CARTESIAN_POINT ( 'NONE',  ( -5.823673210054431948, 21.52544592524334988, 22.70942372801901499 ) ) ;
#149631 = CARTESIAN_POINT ( 'NONE',  ( -19.02544592524342804, 5.153800228976336051, 101.0405762719810241 ) ) ;
#149632 = CARTESIAN_POINT ( 'NONE',  ( 19.05341960407611168, 5.049401038298154454, 78.95724293864769550 ) ) ;
#149633 = CARTESIAN_POINT ( 'NONE',  ( 10.81492255796106328, -18.62759615963255655, 90.41775706135236135 ) ) ;
#149634 = CARTESIAN_POINT ( 'NONE',  ( 19.02544592524343514, -5.153800228976328945, 68.54057627198103830 ) ) ;
#149635 = ORIENTED_EDGE ( 'NONE', *, *, #199141, .F. ) ;
#149636 = CARTESIAN_POINT ( 'NONE',  ( 5.823673210054125526, 21.52544592524343514, 29.79057627198102409 ) ) ;
#149637 = CARTESIAN_POINT ( 'NONE',  ( -8.224510206698948167, 14.34966873604960824, 80.41557627198103830 ) ) ;
#149638 = ORIENTED_EDGE ( 'NONE', *, *, #179710, .F. ) ;
#149639 = CARTESIAN_POINT ( 'NONE',  ( 9.474510206698971260, -16.51473224551069308, 47.91557627198102409 ) ) ;
#149640 = CARTESIAN_POINT ( 'NONE',  ( 8.224510206698953496, -14.34966873604960469, 102.9155762719810383 ) ) ;
#149641 = CARTESIAN_POINT ( 'NONE',  ( -21.53943276465977519, 0.05219959533907696930, 116.2489096053143669 ) ) ;
#149642 = CARTESIAN_POINT ( 'NONE',  ( -15.80617190586768217, 15.72974639402176855, 63.12609039468568994 ) ) ;
#149643 = CARTESIAN_POINT ( 'NONE',  ( -19.05341960407611168, -5.049401038298163336, 31.45724293864769550 ) ) ;
#149644 = CARTESIAN_POINT ( 'NONE',  ( -4.379528057220086978, -16.55341960407618274, 59.79275706135234714 ) ) ;
#149645 = CARTESIAN_POINT ( 'NONE',  ( 18.67979575497178502, 10.72451020669898547, 104.1655762719810241 ) ) ;
#149646 = CARTESIAN_POINT ( 'NONE',  ( 21.55341960407610458, 5.719274019375980345, 108.9572429386476955 ) ) ;
#149648 = CARTESIAN_POINT ( 'NONE',  ( 5.153800228976335163, 19.02544592524342804, 54.79057627198103120 ) ) ;
#149647 = CARTESIAN_POINT ( 'NONE',  ( 5.153800228976615827, -19.02544592524334988, 40.20942372801898301 ) ) ;
#149649 = CARTESIAN_POINT ( 'NONE',  ( -38.00000000000000711, 2.428612866367529932E-14, -0.8749999972688132788 ) ) ;
#149650 = CARTESIAN_POINT ( 'NONE',  ( 15.80617190586769283, -15.72974639402175789, 55.62609039468568284 ) ) ;
#149651 = CARTESIAN_POINT ( 'NONE',  ( -10.72451020669898014, 18.67979575497178502, 55.41557627198102409 ) ) ;
#149652 = CARTESIAN_POINT ( 'NONE',  ( 12.06949235617757843, -12.14591786802309237, 33.12390960531435979 ) ) ;
#149654 = CARTESIAN_POINT ( 'NONE',  ( -19.03943276465977164, -0.05219959533935918106, 18.75109039468567218 ) ) ;
#149653 = CARTESIAN_POINT ( 'NONE',  ( 15.80617190586769283, -15.72974639402175789, 80.62609039468567573 ) ) ;
#149655 = CARTESIAN_POINT ( 'NONE',  ( -8.314922557960811034, -14.29746914071050412, 57.08224293864769550 ) ) ;
#149656 = CARTESIAN_POINT ( 'NONE',  ( -14.29746914071049879, 8.314922557960819915, 110.8322429386476955 ) ) ;
#149657 = CARTESIAN_POINT ( 'NONE',  ( -5.049401038297874678, -19.05341960407617918, 39.79275706135232582 ) ) ;
#149658 = CARTESIAN_POINT ( 'NONE',  ( 12.14591786802327356, -12.06949235617739191, 100.6260903946857184 ) ) ;
#149659 = CARTESIAN_POINT ( 'NONE',  ( -10.72451020669870658, -18.67979575497194134, 69.58442372801900433 ) ) ;
#149660 = CARTESIAN_POINT ( 'NONE',  ( 19.03943276465977164, -0.05219959533909143690, 63.74890960531435979 ) ) ;
#149661 = CARTESIAN_POINT ( 'NONE',  ( 19.03943276465977164, 0.05219959533936151252, 41.25109039468566152 ) ) ;
#149662 = CARTESIAN_POINT ( 'NONE',  ( -18.67979575497178146, -10.72451020669898902, 36.66557627198103120 ) ) ;
#149663 = CARTESIAN_POINT ( 'NONE',  ( -21.55341960407619339, 5.719274019375674811, 38.54275706135234714 ) ) ;
#149664 = CARTESIAN_POINT ( 'NONE',  ( 15.72974639402199770, -15.80617190586745480, 83.12390960531436690 ) ) ;
#149665 = CARTESIAN_POINT ( 'NONE',  ( -16.46253265017146816, -9.564922557961047289, 84.16775706135233293 ) ) ;
#149666 = CARTESIAN_POINT ( 'NONE',  ( -14.34966873604972548, 8.224510206698743886, 58.33442372801901143 ) ) ;
#149668 = CARTESIAN_POINT ( 'NONE',  ( -18.62759615963270932, 10.81492255796079327, 90.83224293864769550 ) ) ;
#149667 = CARTESIAN_POINT ( 'NONE',  ( 17.50000000000001776, -3.210308386893660604, 37.45106242668933305 ) ) ;
#149669 = CARTESIAN_POINT ( 'NONE',  ( 14.34966873604960469, 8.224510206698951720, 79.16557627198103830 ) ) ;
#149670 = CARTESIAN_POINT ( 'NONE',  ( 1.290379407950561275, 31.18582982555689753, -46.67606730179129215 ) ) ;
#149671 = CARTESIAN_POINT ( 'NONE',  ( -13.97604488694547697, 13.89961937509957934, 113.1260903946856757 ) ) ;
#149672 = CARTESIAN_POINT ( 'NONE',  ( 0.05219959533907565091, 21.53943276465977519, 39.99890960531436690 ) ) ;
#149673 = CARTESIAN_POINT ( 'NONE',  ( 16.52544592524335698, 4.483927247898782831, 76.45942372801901854 ) ) ;
#149674 = FACE_OUTER_BOUND ( 'NONE', #10721, .T. ) ;
#149675 = CARTESIAN_POINT ( 'NONE',  ( -8.314922557961024197, 14.29746914071037800, 52.91775706135235424 ) ) ;
#149676 = CARTESIAN_POINT ( 'NONE',  ( 15.72974639402176855, 15.80617190586768217, 31.87609039468567929 ) ) ;
#149677 = CARTESIAN_POINT ( 'NONE',  ( -21.55341960407610458, -5.719274019375992779, 51.45724293864770260 ) ) ;
#149678 = CARTESIAN_POINT ( 'NONE',  ( -14.34966873604972548, 8.224510206698743886, 73.33442372801901854 ) ) ;
#149679 = CARTESIAN_POINT ( 'NONE',  ( -0.05219959533909027116, -19.03943276465977164, 82.49890960531436690 ) ) ;
#149681 = CARTESIAN_POINT ( 'NONE',  ( -9.564922557960796823, -16.46253265017161027, 22.08224293864768839 ) ) ;
#149680 = CARTESIAN_POINT ( 'NONE',  ( 21.55341960407619695, -5.719274019375665929, 51.04275706135234714 ) ) ;
#149682 = CARTESIAN_POINT ( 'NONE',  ( -10.81492255796078084, -18.62759615963271287, 37.08224293864768129 ) ) ;
#149683 = CARTESIAN_POINT ( 'NONE',  ( -19.05341960407611168, -5.049401038298163336, 111.4572429386476671 ) ) ;
#149684 = VERTEX_POINT ( 'NONE', #157819 ) ;
#149685 = CARTESIAN_POINT ( 'NONE',  ( -19.05341960407617563, 5.049401038297882671, 38.54275706135233293 ) ) ;
#149686 = CARTESIAN_POINT ( 'NONE',  ( 8.224510206698742110, 14.34966873604972548, 52.08442372801901854 ) ) ;
#149687 = CARTESIAN_POINT ( 'NONE',  ( 0.05219959533907565091, 21.53943276465977519, 24.99890960531435624 ) ) ;
#149688 = ORIENTED_EDGE ( 'NONE', *, *, #134338, .T. ) ;
#149689 = CARTESIAN_POINT ( 'NONE',  ( 5.049401038298161559, -19.05341960407611168, 87.70724293864769550 ) ) ;
#149690 = CARTESIAN_POINT ( 'NONE',  ( 16.53943276465976808, 0.05219959533934440121, 96.25109039468568994 ) ) ;
#149691 = CARTESIAN_POINT ( 'NONE',  ( 25.63014143074630269, 6.600872056147826683, 163.2069976173305292 ) ) ;
#149692 = CARTESIAN_POINT ( 'NONE',  ( 0.05219959533910956823, 16.53943276465976808, 89.99890960531438111 ) ) ;
#149693 = CARTESIAN_POINT ( 'NONE',  ( 15.72974639402199770, -15.80617190586745480, 48.12390960531436690 ) ) ;
#149694 = CARTESIAN_POINT ( 'NONE',  ( 13.97604488694527802, 13.89961937509977652, 29.37390960531435979 ) ) ;
#149695 = CARTESIAN_POINT ( 'NONE',  ( 8.224510206698742110, 14.34966873604972548, 82.08442372801901854 ) ) ;
#149696 = CARTESIAN_POINT ( 'NONE',  ( 21.55341960407610458, 5.719274019375980345, 113.9572429386477239 ) ) ;
#149697 = CARTESIAN_POINT ( 'NONE',  ( 16.51473224551083163, -9.474510206698727899, 75.83442372801900433 ) ) ;
#149698 = CARTESIAN_POINT ( 'NONE',  ( -16.46253265017160317, 9.564922557960807481, 35.83224293864768839 ) ) ;
#149699 = CARTESIAN_POINT ( 'NONE',  ( 9.474510206698971260, -16.51473224551069308, 112.9155762719810383 ) ) ;
#149700 = CARTESIAN_POINT ( 'NONE',  ( -18.62759615963255300, -10.81492255796106328, 99.16775706135234714 ) ) ;
#149701 = CARTESIAN_POINT ( 'NONE',  ( 13.89961937509977652, -13.97604488694527269, 68.12390960531436690 ) ) ;
#149702 = CARTESIAN_POINT ( 'NONE',  ( -8.314922557961024197, 14.29746914071037800, 42.91775706135235424 ) ) ;
#149703 = CARTESIAN_POINT ( 'NONE',  ( -5.823673210054431948, 21.52544592524334988, 87.70942372801901854 ) ) ;
#149704 = CARTESIAN_POINT ( 'NONE',  ( 9.474510206698729675, 16.51473224551082808, 52.08442372801900433 ) ) ;
#149705 = CARTESIAN_POINT ( 'NONE',  ( 13.89961937509957401, 13.97604488694547697, 51.87609039468566863 ) ) ;
#149706 = ORIENTED_EDGE ( 'NONE', *, *, #151158, .T. ) ;
#149707 = CARTESIAN_POINT ( 'NONE',  ( -10.72451020669870658, -18.67979575497194134, 49.58442372801901143 ) ) ;
#149708 = CARTESIAN_POINT ( 'NONE',  ( 13.89961937509977652, -13.97604488694527269, 23.12390960531436335 ) ) ;
#149709 = CARTESIAN_POINT ( 'NONE',  ( -16.51473224551082808, 9.474510206698731452, 43.33442372801900433 ) ) ;
#149710 = CARTESIAN_POINT ( 'NONE',  ( 19.05341960407611168, 5.049401038298154454, 98.95724293864766707 ) ) ;
#149711 = CARTESIAN_POINT ( 'NONE',  ( -19.05341960407611168, -5.049401038298163336, 86.45724293864769550 ) ) ;
#149712 = CARTESIAN_POINT ( 'NONE',  ( 16.52544592524342804, -4.483927247898539470, 38.54057627198103120 ) ) ;
#149713 = CARTESIAN_POINT ( 'NONE',  ( -5.719274019375978568, 21.55341960407610458, 30.20724293864769550 ) ) ;
#149714 = CARTESIAN_POINT ( 'NONE',  ( 36.91746825000000598, -11.99521256947793546, -2.224999997268813701 ) ) ;
#149715 = CARTESIAN_POINT ( 'NONE',  ( 23.29544513554940011, 16.92513159979228021, 141.1843446569000093 ) ) ;
#149716 = CARTESIAN_POINT ( 'NONE',  ( 13.97604488694548053, -13.89961937509957401, 20.62609039468567573 ) ) ;
#149717 = CARTESIAN_POINT ( 'NONE',  ( 1.300000000000000044, 0.7216878364870328300, 1.249999999999999778 ) ) ;
#149718 = CARTESIAN_POINT ( 'NONE',  ( -19.05341960407611168, -5.049401038298163336, 31.45724293864769550 ) ) ;
#149719 = CARTESIAN_POINT ( 'NONE',  ( 0.05219959533909260263, 19.03943276465977164, 84.99890960531436690 ) ) ;
#149720 = CARTESIAN_POINT ( 'NONE',  ( -9.248023074035634394, -11.04474067092430190, -60.16509628334827653 ) ) ;
#149721 = CARTESIAN_POINT ( 'NONE',  ( -26.85942494856799101, -26.31850930613038742, -8.000000000000003553 ) ) ;
#149722 = CARTESIAN_POINT ( 'NONE',  ( 8.314922557961029526, -14.29746914071037800, 65.41775706135234714 ) ) ;
#149723 = CARTESIAN_POINT ( 'NONE',  ( 10.81492255796078972, 18.62759615963270932, 84.58224293864769550 ) ) ;
#149724 = CARTESIAN_POINT ( 'NONE',  ( 16.52544592524342804, -4.483927247898539470, 58.54057627198103120 ) ) ;
#149726 = CARTESIAN_POINT ( 'NONE',  ( -16.51473224551069308, -9.474510206698971260, 101.6655762719810241 ) ) ;
#149725 = CARTESIAN_POINT ( 'NONE',  ( 16.46253265017160672, -9.564922557960803928, 33.33224293864770260 ) ) ;
#149727 = CARTESIAN_POINT ( 'NONE',  ( -21.52544592524334988, -5.823673210054445271, 33.95942372801901143 ) ) ;
#149728 = CARTESIAN_POINT ( 'NONE',  ( 19.03943276465977164, 0.05219959533936151252, 41.25109039468566152 ) ) ;
#149729 = CARTESIAN_POINT ( 'NONE',  ( 19.02544592524343514, -5.153800228976328945, 33.54057627198102409 ) ) ;
#149730 = CARTESIAN_POINT ( 'NONE',  ( -21.55341960407619339, 5.719274019375674811, 78.54275706135236135 ) ) ;
#149731 = CARTESIAN_POINT ( 'NONE',  ( 17.13100169013300089, -6.664070546373146442, 33.26789835699850073 ) ) ;
#149732 = CARTESIAN_POINT ( 'NONE',  ( 16.52544592524342804, -4.483927247898539470, 28.54057627198103120 ) ) ;
#149733 = CARTESIAN_POINT ( 'NONE',  ( 17.50000000000014566, 3.417042746626842931, 112.3261960376753024 ) ) ;
#149734 = CARTESIAN_POINT ( 'NONE',  ( 5.719274019375991003, -21.55341960407610458, 42.70724293864770260 ) ) ;
#149735 = CARTESIAN_POINT ( 'NONE',  ( 16.53943276465976808, -0.05219959533910856209, 108.7489096053143669 ) ) ;
#149736 = CARTESIAN_POINT ( 'NONE',  ( 14.53388260107743868, -39.78846373132473957, -19.96647037889509946 ) ) ;
#149737 = CARTESIAN_POINT ( 'NONE',  ( -5.049401038298153566, 19.05341960407611168, 85.20724293864766707 ) ) ;
#149738 = CARTESIAN_POINT ( 'NONE',  ( -4.379528057220328563, 16.55341960407611168, 75.20724293864769550 ) ) ;
#149739 = CARTESIAN_POINT ( 'NONE',  ( 5.153800228976615827, -19.02544592524334988, 105.2094237280190185 ) ) ;
#149740 = CARTESIAN_POINT ( 'NONE',  ( 10.81492255796078972, 18.62759615963270932, 69.58224293864769550 ) ) ;
#149741 = ORIENTED_EDGE ( 'NONE', *, *, #175002, .F. ) ;
#149742 = CARTESIAN_POINT ( 'NONE',  ( -16.51473224551069308, -9.474510206698971260, 31.66557627198102054 ) ) ;
#149744 = CARTESIAN_POINT ( 'NONE',  ( 18.62759615963271287, -10.81492255796078972, 88.33224293864769550 ) ) ;
#149743 = CARTESIAN_POINT ( 'NONE',  ( 13.89961937509977652, -13.97604488694527269, 88.12390960531438111 ) ) ;
#149746 = CARTESIAN_POINT ( 'NONE',  ( 0.05219959533909260263, 19.03943276465977164, 89.99890960531436690 ) ) ;
#149745 = CARTESIAN_POINT ( 'NONE',  ( 8.224510206698742110, 14.34966873604972548, 102.0844237280190185 ) ) ;
#149747 = CARTESIAN_POINT ( 'NONE',  ( -19.03943276465977164, -0.05219959533935918106, 78.75109039468567573 ) ) ;
#149748 = CARTESIAN_POINT ( 'NONE',  ( -5.719274019375665041, -21.55341960407619695, 94.79275706135234714 ) ) ;
#149749 = CARTESIAN_POINT ( 'NONE',  ( -21.55341960407610458, -5.719274019375992779, 71.45724293864769550 ) ) ;
#149750 = CARTESIAN_POINT ( 'NONE',  ( -5.719274019375978568, 21.55341960407610458, 40.20724293864769550 ) ) ;
#149751 = CARTESIAN_POINT ( 'NONE',  ( 19.05341960407611168, 5.049401038298154454, 53.95724293864770260 ) ) ;
#149752 = CARTESIAN_POINT ( 'NONE',  ( -12.14591786802326823, 12.06949235617739902, 113.1260903946856899 ) ) ;
#149753 = CARTESIAN_POINT ( 'NONE',  ( -5.153800228976328057, -19.02544592524343514, 62.29057627198100988 ) ) ;
#149754 = CARTESIAN_POINT ( 'NONE',  ( 17.97394159160245408, 5.500000000000056843, 38.98772563323827001 ) ) ;
#149755 = CARTESIAN_POINT ( 'NONE',  ( -16.51473224551082808, 9.474510206698731452, 33.33442372801899722 ) ) ;
#149756 = CARTESIAN_POINT ( 'NONE',  ( 4.379528057220339221, -16.55341960407611168, 72.70724293864769550 ) ) ;
#149757 = CARTESIAN_POINT ( 'NONE',  ( -15.80617190586745835, -15.72974639402198527, 106.8739096053143811 ) ) ;
#149758 = CARTESIAN_POINT ( 'NONE',  ( -5.359611314223446995E-15, 29.16686587814335496, 140.8750000027311842 ) ) ;
#149760 = ADVANCED_FACE ( 'NONE', ( #140646 ), #188168, .F. ) ;
#149759 = CARTESIAN_POINT ( 'NONE',  ( 21.52544592524344225, -5.823673210054117533, 63.54057627198103830 ) ) ;
#149761 = CARTESIAN_POINT ( 'NONE',  ( -4.483927247898782831, 16.52544592524335698, 97.70942372801904696 ) ) ;
#149762 = CARTESIAN_POINT ( 'NONE',  ( -16.53943276465976808, 0.05219959533911058130, 101.2489096053143669 ) ) ;
#149763 = CARTESIAN_POINT ( 'NONE',  ( -13.97604488694527625, -13.89961937509977652, 76.87390960531433848 ) ) ;
#149764 =( NAMED_UNIT ( * ) SI_UNIT ( $, .STERADIAN. ) SOLID_ANGLE_UNIT ( ) );
#149765 = CARTESIAN_POINT ( 'NONE',  ( -4.379528057220328563, 16.55341960407611168, 30.20724293864769550 ) ) ;
#149766 = CARTESIAN_POINT ( 'NONE',  ( -5.719274019375665041, -21.55341960407619695, 44.79275706135234714 ) ) ;
#149767 = CARTESIAN_POINT ( 'NONE',  ( 19.05341960407611168, 5.049401038298154454, 113.9572429386477097 ) ) ;
#149768 = CARTESIAN_POINT ( 'NONE',  ( -10.72451020669870658, -18.67979575497194134, 74.58442372801901854 ) ) ;
#149769 = CARTESIAN_POINT ( 'NONE',  ( 9.564922557960805705, 16.46253265017160317, 29.58224293864769550 ) ) ;
#149770 = CARTESIAN_POINT ( 'NONE',  ( 16.51473224551069308, 9.474510206698969483, 39.16557627198103120 ) ) ;
#149771 = ORIENTED_EDGE ( 'NONE', *, *, #11536, .F. ) ;
#149772 = CARTESIAN_POINT ( 'NONE',  ( -18.67979575497193778, 10.72451020669871902, 93.33442372801901854 ) ) ;
#149773 = CARTESIAN_POINT ( 'NONE',  ( 16.52544592524335698, 4.483927247898782831, 46.45942372801901854 ) ) ;
#149774 = CARTESIAN_POINT ( 'NONE',  ( 21.53943276465977519, 0.05219959533937863772, 76.25109039468568994 ) ) ;
#149775 = CARTESIAN_POINT ( 'NONE',  ( -5.153800228976328057, -19.02544592524343514, 97.29057627198099567 ) ) ;
#149776 = CARTESIAN_POINT ( 'NONE',  ( -9.564922557961040184, 16.46253265017147172, 77.91775706135234714 ) ) ;
#149777 = CARTESIAN_POINT ( 'NONE',  ( -18.67979575497193778, 10.72451020669871902, 53.33442372801901854 ) ) ;
#149778 = CARTESIAN_POINT ( 'NONE',  ( 4.379528057220092307, 16.55341960407617563, 27.29275706135234358 ) ) ;
#149779 = CARTESIAN_POINT ( 'NONE',  ( 19.02544592524334988, 5.153800228976608722, 86.45942372801900433 ) ) ;
#149780 = CARTESIAN_POINT ( 'NONE',  ( -5.049401038298153566, 19.05341960407611168, 45.20724293864769550 ) ) ;
#149781 = CARTESIAN_POINT ( 'NONE',  ( -13.97604488694547697, 13.89961937509957934, 88.12609039468563310 ) ) ;
#149782 = CARTESIAN_POINT ( 'NONE',  ( -4.379528057220328563, 16.55341960407611168, 30.20724293864769550 ) ) ;
#149783 = CARTESIAN_POINT ( 'NONE',  ( -5.153800228976607833, 19.02544592524334988, 82.70942372801897591 ) ) ;
#149784 = CARTESIAN_POINT ( 'NONE',  ( -12.14591786802309592, -12.06949235617757132, 36.87390960531435979 ) ) ;
#149785 = CARTESIAN_POINT ( 'NONE',  ( -13.97604488694547697, 13.89961937509957934, 68.12609039468563310 ) ) ;
#149786 = CARTESIAN_POINT ( 'NONE',  ( 12.06949235617739724, 12.14591786802326823, 51.87609039468568284 ) ) ;
#149787 = CARTESIAN_POINT ( 'NONE',  ( -16.51473224551082808, 9.474510206698731452, 28.33442372801900433 ) ) ;
#149788 = CARTESIAN_POINT ( 'NONE',  ( 16.51473224551069308, 9.474510206698969483, 24.16557627198102765 ) ) ;
#149789 = CARTESIAN_POINT ( 'NONE',  ( 9.564922557960805705, 16.46253265017160317, 44.58224293864769550 ) ) ;
#149790 = CARTESIAN_POINT ( 'NONE',  ( -8.314922557961024197, 14.29746914071037800, 47.91775706135234714 ) ) ;
#149791 = DIRECTION ( 'NONE',  ( -1.000000000000000000, 0.000000000000000000, 4.336808689942017736E-16 ) ) ;
#149792 = CARTESIAN_POINT ( 'NONE',  ( 17.81289503416611453, -24.51734667627695785, 142.9500000054623854 ) ) ;
#149793 = CARTESIAN_POINT ( 'NONE',  ( 16.51473224551069308, 9.474510206698969483, 89.16557627198103830 ) ) ;
#149794 = CARTESIAN_POINT ( 'NONE',  ( -5.049401038297874678, -19.05341960407618274, 84.79275706135233293 ) ) ;
#149795 = ORIENTED_EDGE ( 'NONE', *, *, #41507, .F. ) ;
#149796 = CARTESIAN_POINT ( 'NONE',  ( -13.89961937509957401, -13.97604488694547875, 104.3760903946856757 ) ) ;
#149797 = CARTESIAN_POINT ( 'NONE',  ( -10.81492255796078084, -18.62759615963271287, 27.08224293864769550 ) ) ;
#149799 = CARTESIAN_POINT ( 'NONE',  ( 0.05219959533936267826, -19.03943276465977164, 105.0010903946856615 ) ) ;
#149798 = CARTESIAN_POINT ( 'NONE',  ( 9.564922557961047289, -16.46253265017146816, 30.41775706135232937 ) ) ;
#149800 = CARTESIAN_POINT ( 'NONE',  ( -4.379528057220328563, 16.55341960407611168, 115.2072429386476955 ) ) ;
#149801 = CARTESIAN_POINT ( 'NONE',  ( 16.51473224551069308, 9.474510206698969483, 39.16557627198103120 ) ) ;
#149802 = CARTESIAN_POINT ( 'NONE',  ( 10.81492255796078972, 18.62759615963270932, 69.58224293864769550 ) ) ;
#149803 = AXIS2_PLACEMENT_3D ( 'NONE', #126704, #51867, #175221 ) ;
#149804 = CARTESIAN_POINT ( 'NONE',  ( -16.51473224551069308, -9.474510206698971260, 41.66557627198103120 ) ) ;
#149805 = CARTESIAN_POINT ( 'NONE',  ( -9.474510206698720793, -16.51473224551083518, 74.58442372801900433 ) ) ;
#149806 = CARTESIAN_POINT ( 'NONE',  ( 14.34966873604960469, 8.224510206698951720, 54.16557627198103120 ) ) ;
#149807 = CARTESIAN_POINT ( 'NONE',  ( -21.52544592524343514, 5.823673210054127303, 36.04057627198102409 ) ) ;
#149808 = CARTESIAN_POINT ( 'NONE',  ( 10.72451020669871369, 18.67979575497193778, 97.08442372801904696 ) ) ;
#149809 = CARTESIAN_POINT ( 'NONE',  ( -15.72974639402197994, 15.80617190586746368, 85.62390960531436690 ) ) ;
#149810 = CARTESIAN_POINT ( 'NONE',  ( -21.52544592524334988, -5.823673210054445271, 68.95942372801901854 ) ) ;
#149811 = CARTESIAN_POINT ( 'NONE',  ( -15.80617190586768217, 15.72974639402176855, 63.12609039468568994 ) ) ;
#149812 = CARTESIAN_POINT ( 'NONE',  ( -16.46253265017160317, 9.564922557960807481, 95.83224293864769550 ) ) ;
#149814 = CARTESIAN_POINT ( 'NONE',  ( -10.72451020669870658, -18.67979575497194134, 59.58442372801901854 ) ) ;
#149813 = CARTESIAN_POINT ( 'NONE',  ( 8.314922557961029526, -14.29746914071037800, 95.41775706135234714 ) ) ;
#149815 = CARTESIAN_POINT ( 'NONE',  ( 5.153800228976335163, 19.02544592524342804, 59.79057627198100988 ) ) ;
#149816 = CARTESIAN_POINT ( 'NONE',  ( 21.52544592524334988, 5.823673210054432836, 26.45942372801901854 ) ) ;
#149817 = CARTESIAN_POINT ( 'NONE',  ( 9.564922557960805705, 16.46253265017160317, 74.58224293864769550 ) ) ;
#149818 = CARTESIAN_POINT ( 'NONE',  ( -16.55341960407611168, -4.379528057220339221, 71.45724293864769550 ) ) ;
#149819 = CARTESIAN_POINT ( 'NONE',  ( 14.29746914071049879, -8.314922557960816363, 48.33224293864770260 ) ) ;
#149820 = CARTESIAN_POINT ( 'NONE',  ( 0.05219959533907565091, 21.53943276465977519, 54.99890960531435269 ) ) ;
#149821 = CARTESIAN_POINT ( 'NONE',  ( 16.51473224551069308, 9.474510206698969483, 44.16557627198103120 ) ) ;
#149822 = CARTESIAN_POINT ( 'NONE',  ( -15.80617190586745835, -15.72974639402198527, 61.87390960531436690 ) ) ;
#149824 = AXIS2_PLACEMENT_3D ( 'NONE', #136930, #44930, #8858 ) ;
#149823 = CARTESIAN_POINT ( 'NONE',  ( 19.03943276465977164, 0.05219959533936151252, 56.25109039468566863 ) ) ;
#149826 = CARTESIAN_POINT ( 'NONE',  ( 16.53943276465976808, -0.05219959533910856209, 58.74890960531436690 ) ) ;
#149825 = CARTESIAN_POINT ( 'NONE',  ( 19.02544592524335343, 5.153800228976608722, 21.45942372801899367 ) ) ;
#149827 = CARTESIAN_POINT ( 'NONE',  ( -5.719274019375978568, 21.55341960407610458, 45.20724293864769550 ) ) ;
#149828 = ORIENTED_EDGE ( 'NONE', *, *, #134802, .T. ) ;
#149829 = DIRECTION ( 'NONE',  ( -0.000000000000000000, -0.000000000000000000, 1.000000000000000000 ) ) ;
#149830 = CARTESIAN_POINT ( 'NONE',  ( 14.29746914071037800, 8.314922557961029526, 86.66775706135234714 ) ) ;
#149831 = ADVANCED_FACE ( 'NONE', ( #63816 ), #96130, .T. ) ;
#149832 = CARTESIAN_POINT ( 'NONE',  ( 13.89961937509957401, 13.97604488694547697, 86.87609039468567573 ) ) ;
#149833 = CARTESIAN_POINT ( 'NONE',  ( -0.05219959533910754901, -16.53943276465976808, 52.49890960531435979 ) ) ;
#149834 = LINE ( 'NONE', #199320, #57986 ) ;
#149835 = CARTESIAN_POINT ( 'NONE',  ( 13.97604488694527802, 13.89961937509977652, 54.37390960531435979 ) ) ;
#149836 = CARTESIAN_POINT ( 'NONE',  ( 12.06949235617757843, -12.14591786802309237, 38.12390960531436690 ) ) ;
#149837 = CARTESIAN_POINT ( 'NONE',  ( -0.05219959533909027116, -19.03943276465977164, 52.49890960531436690 ) ) ;
#149838 = CARTESIAN_POINT ( 'NONE',  ( -16.51473224551069308, -9.474510206698971260, 71.66557627198102409 ) ) ;
#149839 = CARTESIAN_POINT ( 'NONE',  ( -16.46253265017160317, 9.564922557960807481, 55.83224293864769550 ) ) ;
#149840 = CARTESIAN_POINT ( 'NONE',  ( -15.72974639402176322, -15.80617190586768395, 44.37609039468567573 ) ) ;
#149841 = CARTESIAN_POINT ( 'NONE',  ( -9.474510206698964154, 16.51473224551069663, 70.41557627198102409 ) ) ;
#149842 = CARTESIAN_POINT ( 'NONE',  ( 19.03943276465977164, -0.05219959533909143690, 28.74890960531435624 ) ) ;
#149843 = CARTESIAN_POINT ( 'NONE',  ( -16.46253265017160317, 9.564922557960807481, 55.83224293864769550 ) ) ;
#149844 = CARTESIAN_POINT ( 'NONE',  ( -15.72974639402197994, 15.80617190586746368, 50.62390960531435979 ) ) ;
#149845 = CARTESIAN_POINT ( 'NONE',  ( 13.89961937509977652, -13.97604488694527269, 38.12390960531436690 ) ) ;
#149846 = CARTESIAN_POINT ( 'NONE',  ( -15.80617190586745835, -15.72974639402198527, 41.87390960531435979 ) ) ;
#149847 = CARTESIAN_POINT ( 'NONE',  ( 16.55341960407618274, -4.379528057220086978, 111.0427570613523613 ) ) ;
#149848 = CARTESIAN_POINT ( 'NONE',  ( -5.153800228976607833, 19.02544592524334988, 22.70942372801899012 ) ) ;
#149850 = CARTESIAN_POINT ( 'NONE',  ( 4.483927247898790824, -16.52544592524335698, 75.20942372801901854 ) ) ;
#149849 = CARTESIAN_POINT ( 'NONE',  ( 0.05219959533934541429, -16.53943276465976808, 45.00109039468568284 ) ) ;
#149851 = CARTESIAN_POINT ( 'NONE',  ( -17.60691670004652565, -5.500000000000036415, 94.13333313366442212 ) ) ;
#149852 = CARTESIAN_POINT ( 'NONE',  ( 12.06949235617739724, 12.14591786802326823, 71.87609039468568994 ) ) ;
#149853 = CARTESIAN_POINT ( 'NONE',  ( 14.34966873604972726, -8.224510206698740333, 55.83442372801901854 ) ) ;
#149854 = CARTESIAN_POINT ( 'NONE',  ( -9.564922557960796823, -16.46253265017161027, 112.0822429386476955 ) ) ;
#149855 = CARTESIAN_POINT ( 'NONE',  ( 4.379528057220092307, 16.55341960407617563, 37.29275706135235424 ) ) ;
#149856 = CARTESIAN_POINT ( 'NONE',  ( -19.05341960407611168, -5.049401038298163336, 36.45724293864766707 ) ) ;
#149857 = CARTESIAN_POINT ( 'NONE',  ( -5.823673210054431948, 21.52544592524334988, 27.70942372801901854 ) ) ;
#149858 = CARTESIAN_POINT ( 'NONE',  ( 16.52544592524335698, 4.483927247898782831, 31.45942372801901854 ) ) ;
#149859 = CARTESIAN_POINT ( 'NONE',  ( 0.05219959533934541429, -16.53943276465976808, 95.00109039468568994 ) ) ;
#149860 = CARTESIAN_POINT ( 'NONE',  ( 0.000000000000000000, 0.000000000000000000, -65.00100000000003320 ) ) ;
#149861 = CARTESIAN_POINT ( 'NONE',  ( -18.62759615963255300, -10.81492255796106328, 104.1677570613523471 ) ) ;
#149862 = CARTESIAN_POINT ( 'NONE',  ( 5.049401038297881783, 19.05341960407617563, 97.29275706135233293 ) ) ;
#149863 = CARTESIAN_POINT ( 'NONE',  ( 16.52544592524342804, -4.483927247898539470, 63.54057627198103830 ) ) ;
#149864 = CARTESIAN_POINT ( 'NONE',  ( 0.05219959533909260263, 19.03943276465977164, 24.99890960531435269 ) ) ;
#149866 = DIRECTION ( 'NONE',  ( -0.5000000000000002220, -0.4999999999999985567, 0.7071067811865484609 ) ) ;
#149865 = CARTESIAN_POINT ( 'NONE',  ( -5.153800228976607833, 19.02544592524334988, 57.70942372801899012 ) ) ;
#149867 = CARTESIAN_POINT ( 'NONE',  ( 10.81492255796106328, -18.62759615963255655, 65.41775706135234714 ) ) ;
#149868 = CARTESIAN_POINT ( 'NONE',  ( -14.34966873604972548, 8.224510206698743886, 33.33442372801900433 ) ) ;
#149869 = CARTESIAN_POINT ( 'NONE',  ( 17.49999999999999289, 5.500000000000007994, 83.78230962303564411 ) ) ;
#149870 = CARTESIAN_POINT ( 'NONE',  ( 16.51473224551069308, 9.474510206698969483, 114.1655762719810241 ) ) ;
#149871 = CARTESIAN_POINT ( 'NONE',  ( -19.02544592524334988, -5.153800228976617603, 108.9594237280189759 ) ) ;
#149872 = CARTESIAN_POINT ( 'NONE',  ( 1.300000000000000044, -0.7216878364870318308, -1.250000000000000000 ) ) ;
#149873 = CARTESIAN_POINT ( 'NONE',  ( -13.89961937509957401, -13.97604488694547697, 49.37609039468566863 ) ) ;
#149874 = CARTESIAN_POINT ( 'NONE',  ( -16.51473224551069308, -9.474510206698971260, 26.66557627198103120 ) ) ;
#149875 = CARTESIAN_POINT ( 'NONE',  ( 21.55341960407619695, -5.719274019375665929, 101.0427570613523756 ) ) ;
#149876 = CARTESIAN_POINT ( 'NONE',  ( 9.564922557960805705, 16.46253265017160317, 44.58224293864769550 ) ) ;
#149877 = CARTESIAN_POINT ( 'NONE',  ( 18.62759615963255655, 10.81492255796105972, 46.66775706135234714 ) ) ;
#149878 = CARTESIAN_POINT ( 'NONE',  ( -18.67979575497193778, 10.72451020669871902, 103.3344237280190043 ) ) ;
#149879 = CARTESIAN_POINT ( 'NONE',  ( 8.224510206698742110, 14.34966873604972548, 102.0844237280190185 ) ) ;
#149880 = CARTESIAN_POINT ( 'NONE',  ( 13.97604488694527802, 13.89961937509977652, 79.37390960531435269 ) ) ;
#149881 = CARTESIAN_POINT ( 'NONE',  ( 15.72974639402176855, 15.80617190586768217, 46.87609039468568994 ) ) ;
#149882 = CARTESIAN_POINT ( 'NONE',  ( 18.67979575497194134, -10.72451020669871369, 50.83442372801901143 ) ) ;
#149884 = CARTESIAN_POINT ( 'NONE',  ( 0.05219959533909260263, 19.03943276465977164, 94.99890960531436690 ) ) ;
#149883 = CARTESIAN_POINT ( 'NONE',  ( 5.153800228976615827, -19.02544592524334988, 80.20942372801901854 ) ) ;
#149885 = CARTESIAN_POINT ( 'NONE',  ( 16.55341960407611168, 4.379528057220329451, 103.9572429386476813 ) ) ;
#149886 = CARTESIAN_POINT ( 'NONE',  ( 15.80617190586746368, 15.72974639402197994, 99.37390960531436690 ) ) ;
#149887 = CARTESIAN_POINT ( 'NONE',  ( -16.51473224551082808, 9.474510206698731452, 28.33442372801900433 ) ) ;
#149888 = CARTESIAN_POINT ( 'NONE',  ( -0.05219959533910754901, -16.53943276465976808, 102.4989096053143811 ) ) ;
#149889 = CARTESIAN_POINT ( 'NONE',  ( 13.97604488694527802, 13.89961937509977652, 54.37390960531435979 ) ) ;
#149890 = CARTESIAN_POINT ( 'NONE',  ( -5.049401038297874678, -19.05341960407617918, 89.79275706135230450 ) ) ;
#149891 = CARTESIAN_POINT ( 'NONE',  ( 14.34966873604960469, 8.224510206698951720, 44.16557627198103120 ) ) ;
#149892 = CARTESIAN_POINT ( 'NONE',  ( -0.05219959533937732626, 21.53943276465977519, 102.5010903946856899 ) ) ;
#149893 = CARTESIAN_POINT ( 'NONE',  ( -16.46253265017160317, 9.564922557960807481, 110.8322429386476955 ) ) ;
#149894 = CARTESIAN_POINT ( 'NONE',  ( -16.46253265017146816, -9.564922557961047289, 74.16775706135234714 ) ) ;
#149895 = CARTESIAN_POINT ( 'NONE',  ( 21.55341960407610458, 5.719274019375980345, 73.95724293864769550 ) ) ;
#149896 = CARTESIAN_POINT ( 'NONE',  ( 15.72974639402176855, 15.80617190586768217, 31.87609039468567929 ) ) ;
#149897 = CARTESIAN_POINT ( 'NONE',  ( 16.55341960407618274, -4.379528057220086978, 31.04275706135234714 ) ) ;
#149898 = CARTESIAN_POINT ( 'NONE',  ( -16.52544592524335698, -4.483927247898792601, 98.95942372801903275 ) ) ;
#149900 = CARTESIAN_POINT ( 'NONE',  ( -5.719274019375665041, -21.55341960407619695, 34.79275706135235424 ) ) ;
#149899 = CARTESIAN_POINT ( 'NONE',  ( -9.474510206698964154, 16.51473224551069663, 30.41557627198102054 ) ) ;
#149901 = CARTESIAN_POINT ( 'NONE',  ( -18.67979575497178146, -10.72451020669898902, 46.66557627198102409 ) ) ;
#149902 = CARTESIAN_POINT ( 'NONE',  ( 0.05219959533910956823, 16.53943276465976808, 114.9989096053143669 ) ) ;
#149903 = CARTESIAN_POINT ( 'NONE',  ( 22.81625015709510151, -31.40387420917324590, -2.424999997268812546 ) ) ;
#149904 = CARTESIAN_POINT ( 'NONE',  ( -12.06949235617739369, -12.14591786802326823, 59.37609039468568284 ) ) ;
#149905 = CARTESIAN_POINT ( 'NONE',  ( 12.14591786802309770, 12.06949235617756955, 94.37390960531436690 ) ) ;
#149906 = CARTESIAN_POINT ( 'NONE',  ( 5.719274019375991003, -21.55341960407610458, 82.70724293864770971 ) ) ;
#149907 = CARTESIAN_POINT ( 'NONE',  ( -12.06949235617756955, 12.14591786802309770, 30.62390960531436335 ) ) ;
#149908 = CARTESIAN_POINT ( 'NONE',  ( 14.29746914071037800, 8.314922557961029526, 46.66775706135234714 ) ) ;
#149909 = CARTESIAN_POINT ( 'NONE',  ( 16.46253265017160672, -9.564922557960803928, 58.33224293864769550 ) ) ;
#149910 = CARTESIAN_POINT ( 'NONE',  ( -4.379528057220086978, -16.55341960407618274, 89.79275706135236135 ) ) ;
#149911 = CARTESIAN_POINT ( 'NONE',  ( 0.05219959533936267826, -19.03943276465977164, 85.00109039468567573 ) ) ;
#149912 = CARTESIAN_POINT ( 'NONE',  ( -0.05219959533907301413, -21.53943276465977519, 82.49890960531436690 ) ) ;
#149913 = CARTESIAN_POINT ( 'NONE',  ( -12.06949235617739369, -12.14591786802326823, 109.3760903946857042 ) ) ;
#149914 = ORIENTED_EDGE ( 'NONE', *, *, #139157, .F. ) ;
#149915 = CARTESIAN_POINT ( 'NONE',  ( 0.05219959533909260263, 19.03943276465977164, 114.9989096053143669 ) ) ;
#149916 = AXIS2_PLACEMENT_3D ( 'NONE', #157616, #112101, #80757 ) ;
#149917 = CARTESIAN_POINT ( 'NONE',  ( -18.62759615963270932, 10.81492255796079327, 60.83224293864769550 ) ) ;
#149918 = CARTESIAN_POINT ( 'NONE',  ( 16.55341960407618274, -4.379528057220086978, 91.04275706135236135 ) ) ;
#149919 = ORIENTED_EDGE ( 'NONE', *, *, #133810, .F. ) ;
#149920 = CARTESIAN_POINT ( 'NONE',  ( 15.72974639402199770, -15.80617190586745480, 28.12390960531435979 ) ) ;
#149921 = CARTESIAN_POINT ( 'NONE',  ( -19.49149378614660932, 5.499999999999579892, 74.43757513605362419 ) ) ;
#149922 = CARTESIAN_POINT ( 'NONE',  ( -21.53943276465977519, 0.05219959533907696930, 91.24890960531436690 ) ) ;
#149923 = CARTESIAN_POINT ( 'NONE',  ( 16.55341960407618274, -4.379528057220086978, 111.0427570613523613 ) ) ;
#149924 = CARTESIAN_POINT ( 'NONE',  ( 14.34966873604972726, -8.224510206698740333, 40.83442372801901854 ) ) ;
#149925 = CARTESIAN_POINT ( 'NONE',  ( 5.153800228976335163, 19.02544592524342804, 34.79057627198102409 ) ) ;
#149926 = CARTESIAN_POINT ( 'NONE',  ( 14.29746914071037800, 8.314922557961029526, 26.66775706135235424 ) ) ;
#149927 = CARTESIAN_POINT ( 'NONE',  ( 16.46253265017160672, -9.564922557960803928, 58.33224293864769550 ) ) ;
#149928 = CARTESIAN_POINT ( 'NONE',  ( -23.31738231874055245, -16.94106989632524574, 148.1999999999999886 ) ) ;
#149929 = CARTESIAN_POINT ( 'NONE',  ( 13.89961937509977652, -13.97604488694527269, 108.1239096053143669 ) ) ;
#149930 = CARTESIAN_POINT ( 'NONE',  ( 5.049401038298161559, -19.05341960407611168, 112.7072429386476813 ) ) ;
#149931 = CARTESIAN_POINT ( 'NONE',  ( 8.224510206698742110, 14.34966873604972548, 97.08442372801904696 ) ) ;
#149932 = CARTESIAN_POINT ( 'NONE',  ( 5.049401038297881783, 19.05341960407617563, 92.29275706135234714 ) ) ;
#149933 = CARTESIAN_POINT ( 'NONE',  ( -19.03943276465977164, -0.05219959533935918106, 33.75109039468566863 ) ) ;
#149934 = CARTESIAN_POINT ( 'NONE',  ( -21.53943276465977519, 0.05219959533907696930, 81.24890960531436690 ) ) ;
#149935 = EDGE_CURVE ( 'NONE', #112132, #171824, #111304, .T. ) ;
#149936 = CARTESIAN_POINT ( 'NONE',  ( -16.55341960407617563, 4.379528057220093196, 103.5427570613523613 ) ) ;
#149937 = CARTESIAN_POINT ( 'NONE',  ( -21.53943276465977519, 0.05219959533907696930, 31.24890960531435979 ) ) ;
#149938 = CARTESIAN_POINT ( 'NONE',  ( 5.049401038297881783, 19.05341960407617563, 97.29275706135233293 ) ) ;
#149940 = AXIS2_PLACEMENT_3D ( 'NONE', #171088, #187277, #126558 ) ;
#149939 = CARTESIAN_POINT ( 'NONE',  ( 19.02544592524343514, -5.153800228976328945, 103.5405762719809957 ) ) ;
#149941 = CARTESIAN_POINT ( 'NONE',  ( -5.719274019375665041, -21.55341960407619695, 64.79275706135234714 ) ) ;
#149942 = CARTESIAN_POINT ( 'NONE',  ( -13.97604488694527625, -13.89961937509977652, 61.87390960531435979 ) ) ;
#149943 = CARTESIAN_POINT ( 'NONE',  ( 12.14591786802309770, 12.06949235617756955, 94.37390960531436690 ) ) ;
#149944 = CARTESIAN_POINT ( 'NONE',  ( -16.19135201231366850, -7.376712067591933319, 85.18680854052034590 ) ) ;
#149945 = CARTESIAN_POINT ( 'NONE',  ( -0.05219959533910754901, -16.53943276465976808, 77.49890960531433848 ) ) ;
#149946 = CARTESIAN_POINT ( 'NONE',  ( -0.05219959533907301413, -21.53943276465977519, 72.49890960531435269 ) ) ;
#149947 = EDGE_LOOP ( 'NONE', ( #75479, #102202, #87064, #53917, #133531, #4478, #112880, #99486 ) ) ;
#149948 = CARTESIAN_POINT ( 'NONE',  ( -5.049401038297874678, -19.05341960407617918, 94.79275706135230450 ) ) ;
#149949 = STYLED_ITEM ( 'NONE', ( #94036 ), #146166 ) ;
#149950 = CARTESIAN_POINT ( 'NONE',  ( 19.25176906914650843, 5.499999999999797495, 93.49927264242278113 ) ) ;
#149951 = CARTESIAN_POINT ( 'NONE',  ( -16.46253265017160317, 9.564922557960807481, 60.83224293864769550 ) ) ;
#149952 = CARTESIAN_POINT ( 'NONE',  ( 17.44270441346517231, -5.991230190322924365, 71.13664920735772057 ) ) ;
#149954 = CARTESIAN_POINT ( 'NONE',  ( -9.564922557960796823, -16.46253265017161027, 92.08224293864769550 ) ) ;
#149953 = CARTESIAN_POINT ( 'NONE',  ( -19.02544592524342804, 5.153800228976336051, 76.04057627198102409 ) ) ;
#149955 = CARTESIAN_POINT ( 'NONE',  ( -16.55341960407617563, 4.379528057220093196, 58.54275706135235424 ) ) ;
#149956 = DIRECTION ( 'NONE',  ( -0.3041824702427711191, -0.9526137857479313187, 0.000000000000000000 ) ) ;
#149957 = CARTESIAN_POINT ( 'NONE',  ( -9.564922557961040184, 16.46253265017147172, 42.91775706135234003 ) ) ;
#149958 = CARTESIAN_POINT ( 'NONE',  ( 17.02936912484732801, -14.89509079785907275, -57.98861440449752536 ) ) ;
#149959 = CARTESIAN_POINT ( 'NONE',  ( 13.89961937509977652, -13.97604488694527269, 113.1239096053143527 ) ) ;
#149960 = CARTESIAN_POINT ( 'NONE',  ( 16.55341960407618274, -4.379528057220086978, 101.0427570613523756 ) ) ;
#149961 = CARTESIAN_POINT ( 'NONE',  ( -13.89961937509957401, -13.97604488694547697, 74.37609039468564731 ) ) ;
#149962 = CARTESIAN_POINT ( 'NONE',  ( -12.06949235617739369, -12.14591786802326823, 99.37609039468568994 ) ) ;
#149963 = CARTESIAN_POINT ( 'NONE',  ( -17.31747979337949417, 6.344076630960995722, 28.62055131934817354 ) ) ;
#149964 = CARTESIAN_POINT ( 'NONE',  ( -16.55341960407617563, 4.379528057220093196, 68.54275706135234714 ) ) ;
#149965 = DIRECTION ( 'NONE',  ( -0.000000000000000000, -0.9396926207859095381, 0.3420201433256656043 ) ) ;
#149966 = CARTESIAN_POINT ( 'NONE',  ( -21.55341960407619339, 5.719274019375674811, 68.54275706135234714 ) ) ;
#149967 = CARTESIAN_POINT ( 'NONE',  ( 16.46253265017146816, 9.564922557961045513, 71.66775706135233293 ) ) ;
#149968 = CARTESIAN_POINT ( 'NONE',  ( -0.05219959533936034679, 19.03943276465977164, 27.50109039468566507 ) ) ;
#149969 = CARTESIAN_POINT ( 'NONE',  ( 5.153800228976335163, 19.02544592524342804, 64.79057627198100988 ) ) ;
#149970 = CARTESIAN_POINT ( 'NONE',  ( -19.02544592524342804, 5.153800228976336051, 41.04057627198103120 ) ) ;
#149971 = CARTESIAN_POINT ( 'NONE',  ( -19.52983155694575501, -34.90836132267833847, -6.822515721995922711 ) ) ;
#149972 = CARTESIAN_POINT ( 'NONE',  ( 5.719274019375991003, -21.55341960407610458, 77.70724293864770971 ) ) ;
#149973 = CIRCLE ( 'NONE', #146774, 216.0437394197456911 ) ;
#149974 = CARTESIAN_POINT ( 'NONE',  ( 18.67979575497178502, 10.72451020669898547, 39.16557627198102409 ) ) ;
#149975 = CARTESIAN_POINT ( 'NONE',  ( -13.97604488694527625, -13.89961937509977652, 31.87390960531435979 ) ) ;
#149976 = CARTESIAN_POINT ( 'NONE',  ( 12.14591786802327356, -12.06949235617739191, 55.62609039468568284 ) ) ;
#149977 = ORIENTED_EDGE ( 'NONE', *, *, #97418, .F. ) ;
#149978 = CARTESIAN_POINT ( 'NONE',  ( -18.62759615963255300, -10.81492255796106328, 34.16775706135234714 ) ) ;
#149980 = CARTESIAN_POINT ( 'NONE',  ( -38.00000000000000711, 2.428612866367529932E-14, -8.000000000000000000 ) ) ;
#149979 = CARTESIAN_POINT ( 'NONE',  ( 14.29746914071049879, -8.314922557960816363, 58.33224293864768839 ) ) ;
#149981 = CARTESIAN_POINT ( 'NONE',  ( 12.06949235617739724, 12.14591786802326823, 31.87609039468567929 ) ) ;
#149982 = CARTESIAN_POINT ( 'NONE',  ( 19.05341960407617918, -5.049401038297876454, 41.04275706135233293 ) ) ;
#149983 = CARTESIAN_POINT ( 'NONE',  ( 4.379528057220339221, -16.55341960407611168, 62.70724293864769550 ) ) ;
#149984 = CARTESIAN_POINT ( 'NONE',  ( -21.53943276465977519, 0.05219959533907696930, 111.2489096053143669 ) ) ;
#149986 = CARTESIAN_POINT ( 'NONE',  ( 10.72451020669898902, -18.67979575497178502, 77.91557627198102409 ) ) ;
#149985 = DIRECTION ( 'NONE',  ( -1.000000000000000000, -0.000000000000000000, -3.709348145883536076E-20 ) ) ;
#149987 = CARTESIAN_POINT ( 'NONE',  ( -16.46253265017160317, 9.564922557960807481, 95.83224293864769550 ) ) ;
#149988 = CARTESIAN_POINT ( 'NONE',  ( -0.05219959533910754901, -16.53943276465976808, 62.49890960531436690 ) ) ;
#149989 = CARTESIAN_POINT ( 'NONE',  ( 5.153800228976335163, 19.02544592524342804, 104.7905762719809957 ) ) ;
#149990 = CARTESIAN_POINT ( 'NONE',  ( -37.19778934971984796, 4.370295695334256436, 41.64163531972152299 ) ) ;
#149991 = CARTESIAN_POINT ( 'NONE',  ( 19.05341960407617918, -5.049401038297876454, 71.04275706135234714 ) ) ;
#149992 = CARTESIAN_POINT ( 'NONE',  ( 21.53943276465977519, -0.05219959533907433946, 113.7489096053143527 ) ) ;
#149993 = CARTESIAN_POINT ( 'NONE',  ( -5.049401038298153566, 19.05341960407611168, 50.20724293864770260 ) ) ;
#149994 = CARTESIAN_POINT ( 'NONE',  ( 9.474510206698729675, 16.51473224551082808, 47.08442372801900433 ) ) ;
#149995 = CARTESIAN_POINT ( 'NONE',  ( -0.05219959533910754901, -16.53943276465976808, 107.4989096053143669 ) ) ;
#149996 = CARTESIAN_POINT ( 'NONE',  ( -21.53943276465977519, -0.05219959533937600094, 58.75109039468568994 ) ) ;
#149997 = CARTESIAN_POINT ( 'NONE',  ( -3.573655867282028392E-15, 2.428612866367529932E-14, -25.00000000000000000 ) ) ;
#149998 = CARTESIAN_POINT ( 'NONE',  ( 14.29746914071049879, -8.314922557960816363, 43.33224293864769550 ) ) ;
#149999 = CARTESIAN_POINT ( 'NONE',  ( 0.05219959533909260263, 19.03943276465977164, 49.99890960531435979 ) ) ;
#150000 = CARTESIAN_POINT ( 'NONE',  ( -19.02544592524342804, 5.153800228976336051, 111.0405762719810099 ) ) ;
#150001 = CARTESIAN_POINT ( 'NONE',  ( 5.719274019375991003, -21.55341960407610458, 77.70724293864770971 ) ) ;
#150002 = CARTESIAN_POINT ( 'NONE',  ( -17.14385361876520264, -23.59649016807271593, 147.1750000027311671 ) ) ;
#150003 = CARTESIAN_POINT ( 'NONE',  ( -5.153800228976328057, -19.02544592524343514, 42.29057627198101699 ) ) ;
#150004 = ORIENTED_EDGE ( 'NONE', *, *, #161905, .F. ) ;
#150005 = CARTESIAN_POINT ( 'NONE',  ( 15.72974639402199770, -15.80617190586745480, 68.12390960531436690 ) ) ;
#150006 = ORIENTED_EDGE ( 'NONE', *, *, #33328, .T. ) ;
#150007 = CARTESIAN_POINT ( 'NONE',  ( -0.05219959533937732626, 21.53943276465977519, 82.50109039468568994 ) ) ;
#150010 = CARTESIAN_POINT ( 'NONE',  ( -12.06949235617756955, 12.14591786802309770, 80.62390960531438111 ) ) ;
#150009 = CARTESIAN_POINT ( 'NONE',  ( 4.379528057220092307, 16.55341960407617563, 102.2927570613523613 ) ) ;
#150008 = DIRECTION ( 'NONE',  ( 0.000000000000000000, -0.8164965809277252573, 0.5773502691896267303 ) ) ;
#150011 = CARTESIAN_POINT ( 'NONE',  ( 19.05341960407611168, 5.049401038298154454, 63.95724293864769550 ) ) ;
#150012 = ORIENTED_EDGE ( 'NONE', *, *, #79855, .F. ) ;
#150013 = CARTESIAN_POINT ( 'NONE',  ( -19.03943276465977164, -0.05219959533935918106, 43.75109039468566863 ) ) ;
#150014 = CARTESIAN_POINT ( 'NONE',  ( 4.379528057220092307, 16.55341960407617563, 82.29275706135234714 ) ) ;
#150015 = EDGE_CURVE ( 'NONE', #176035, #71451, #46659, .T. ) ;
#150016 = CARTESIAN_POINT ( 'NONE',  ( -9.474510206698720793, -16.51473224551083518, 19.58442372801899722 ) ) ;
#150017 = CARTESIAN_POINT ( 'NONE',  ( 13.97604488694527802, 13.89961937509977652, 84.37390960531433848 ) ) ;
#150018 = CARTESIAN_POINT ( 'NONE',  ( 15.80617190586746368, 15.72974639402197994, 44.37390960531435979 ) ) ;
#150019 = DIRECTION ( 'NONE',  ( 1.000000000000000000, 0.000000000000000000, 0.000000000000000000 ) ) ;
#150020 = CARTESIAN_POINT ( 'NONE',  ( 18.62759615963255655, 10.81492255796105972, 101.6677570613523613 ) ) ;
#150021 = CARTESIAN_POINT ( 'NONE',  ( -16.53943276465976808, -0.05219959533934237506, 58.75109039468568994 ) ) ;
#150022 = CARTESIAN_POINT ( 'NONE',  ( -5.719274019375978568, 21.55341960407610458, 110.2072429386477239 ) ) ;
#150023 = CARTESIAN_POINT ( 'NONE',  ( -8.314922557961024197, 14.29746914071037800, 32.91775706135234714 ) ) ;
#150024 = CARTESIAN_POINT ( 'NONE',  ( -5.153800228976328057, -19.02544592524343514, 92.29057627198099567 ) ) ;
#150025 = CARTESIAN_POINT ( 'NONE',  ( 13.97604488694527802, 13.89961937509977652, 44.37390960531435269 ) ) ;
#150026 = CARTESIAN_POINT ( 'NONE',  ( -9.564922557960796823, -16.46253265017161027, 57.08224293864769550 ) ) ;
#150027 = CARTESIAN_POINT ( 'NONE',  ( -16.52544592524335698, -4.483927247898792601, 28.95942372801902209 ) ) ;
#150028 = CARTESIAN_POINT ( 'NONE',  ( 12.06949235617757843, -12.14591786802309237, 83.12390960531436690 ) ) ;
#150029 = CARTESIAN_POINT ( 'NONE',  ( 16.55341960407618274, -4.379528057220086978, 81.04275706135236135 ) ) ;
#150032 = CARTESIAN_POINT ( 'NONE',  ( 16.51473224551069308, 9.474510206698969483, 49.16557627198102409 ) ) ;
#150031 = CARTESIAN_POINT ( 'NONE',  ( -13.89961937509977652, 13.97604488694528158, 70.62390960531432427 ) ) ;
#150030 = CARTESIAN_POINT ( 'NONE',  ( -15.80617190586768217, 15.72974639402176855, 43.12609039468568284 ) ) ;
#150034 = EDGE_CURVE ( 'NONE', #129810, #20570, #135922, .T. ) ;
#150033 = CARTESIAN_POINT ( 'NONE',  ( 19.05341960407611168, 5.049401038298154454, 83.95724293864766707 ) ) ;
#150035 = CARTESIAN_POINT ( 'NONE',  ( -12.14591786802309592, -12.06949235617757132, 31.87390960531435979 ) ) ;
#150036 = CARTESIAN_POINT ( 'NONE',  ( -14.34966873604972548, 8.224510206698743886, 83.33442372801903275 ) ) ;
#150037 = AXIS2_PLACEMENT_3D ( 'NONE', #82881, #160734, #55558 ) ;
#150038 = VERTEX_POINT ( 'NONE', #171991 ) ;
#150039 = CARTESIAN_POINT ( 'NONE',  ( 16.51473224551083163, -9.474510206698727899, 25.83442372801900078 ) ) ;
#150040 = CARTESIAN_POINT ( 'NONE',  ( 0.05219959533909260263, 19.03943276465977164, 94.99890960531436690 ) ) ;
#150041 = CARTESIAN_POINT ( 'NONE',  ( 13.97604488694527802, 13.89961937509977652, 49.37390960531434558 ) ) ;
#150042 = CARTESIAN_POINT ( 'NONE',  ( 16.51473224551083163, -9.474510206698727899, 20.83442372801899722 ) ) ;
#150043 = CARTESIAN_POINT ( 'NONE',  ( -29.86685920354755552, 21.69954338932564397, -6.824999997268814234 ) ) ;
#150044 = CARTESIAN_POINT ( 'NONE',  ( 14.29746914071037800, 8.314922557961029526, 41.66775706135235424 ) ) ;
#150046 = CARTESIAN_POINT ( 'NONE',  ( 16.53943276465976808, 0.05219959533934440121, 51.25109039468568994 ) ) ;
#150045 = CARTESIAN_POINT ( 'NONE',  ( 19.03943276465977164, 0.05219959533936151252, 66.25109039468567573 ) ) ;
#150047 = CARTESIAN_POINT ( 'NONE',  ( 4.943711336861328576, -3.929442668020362017, -64.49862517692662323 ) ) ;
#150048 = CARTESIAN_POINT ( 'NONE',  ( -9.564922557960796823, -16.46253265017161027, 82.08224293864768129 ) ) ;
#150049 = CARTESIAN_POINT ( 'NONE',  ( 0.05219959533907565091, 21.53943276465977519, 109.9989096053143527 ) ) ;
#150050 = CARTESIAN_POINT ( 'NONE',  ( -19.05341960407617563, 5.049401038297882671, 68.54275706135230450 ) ) ;
#150052 = CARTESIAN_POINT ( 'NONE',  ( -9.564922557960796823, -16.46253265017161027, 32.08224293864769550 ) ) ;
#150051 = CARTESIAN_POINT ( 'NONE',  ( -13.97604488694527625, -13.89961937509977652, 101.8739096053143811 ) ) ;
#150053 = CARTESIAN_POINT ( 'NONE',  ( 13.89961937509977652, -13.97604488694527269, 83.12390960531436690 ) ) ;
#150055 = CARTESIAN_POINT ( 'NONE',  ( -13.97604488694527625, -13.89961937509977652, 21.87390960531435979 ) ) ;
#150054 = CARTESIAN_POINT ( 'NONE',  ( 12.14591786802309770, 12.06949235617756955, 39.37390960531436690 ) ) ;
#150056 = CARTESIAN_POINT ( 'NONE',  ( -9.564922557961040184, 16.46253265017147172, 32.91775706135233293 ) ) ;
#150057 = CARTESIAN_POINT ( 'NONE',  ( 8.224510206698953496, -14.34966873604960469, 77.91557627198102409 ) ) ;
#150058 = CARTESIAN_POINT ( 'NONE',  ( 19.05341960407617918, -5.049401038297876454, 21.04275706135232582 ) ) ;
#150059 = CARTESIAN_POINT ( 'NONE',  ( -19.03943276465977164, 0.05219959533909376836, 51.24890960531436690 ) ) ;
#150060 = VECTOR ( 'NONE', #172726, 1000.000000000000000 ) ;
#150062 = CARTESIAN_POINT ( 'NONE',  ( -18.67979575497193778, 10.72451020669871902, 108.3344237280190185 ) ) ;
#150061 = CARTESIAN_POINT ( 'NONE',  ( 4.483927247898545687, 16.52544592524342804, 59.79057627198103120 ) ) ;
#150063 = CARTESIAN_POINT ( 'NONE',  ( 13.89961937509977652, -13.97604488694527269, 98.12390960531433848 ) ) ;
#150064 = CARTESIAN_POINT ( 'NONE',  ( -0.05219959533909027116, -19.03943276465977164, 102.4989096053143669 ) ) ;
#150065 = CARTESIAN_POINT ( 'NONE',  ( 9.474510206698971260, -16.51473224551069308, 42.91557627198103120 ) ) ;
#150066 = CARTESIAN_POINT ( 'NONE',  ( -4.379528057220328563, 16.55341960407611168, 115.2072429386476955 ) ) ;
#150067 = CARTESIAN_POINT ( 'NONE',  ( 16.55341960407611168, 4.379528057220329451, 83.95724293864770971 ) ) ;
#150068 = CARTESIAN_POINT ( 'NONE',  ( 21.53943276465977519, -0.05219959533907433946, 93.74890960531436690 ) ) ;
#150069 = CARTESIAN_POINT ( 'NONE',  ( -13.89961937509977652, 13.97604488694528158, 90.62390960531432427 ) ) ;
#150070 = CARTESIAN_POINT ( 'NONE',  ( 18.62759615963271287, -10.81492255796078972, 98.33224293864769550 ) ) ;
#150071 = CARTESIAN_POINT ( 'NONE',  ( -5.049401038298153566, 19.05341960407611168, 90.20724293864766707 ) ) ;
#150073 = CARTESIAN_POINT ( 'NONE',  ( 8.224510206698953496, -14.34966873604960469, 107.9155762719810241 ) ) ;
#150072 = CARTESIAN_POINT ( 'NONE',  ( 28.82186960331498327, 2.428612866367529932E-14, 139.9999999999999716 ) ) ;
#150074 = CARTESIAN_POINT ( 'NONE',  ( -0.05219959533909027116, -19.03943276465977164, 67.49890960531436690 ) ) ;
#150075 = CARTESIAN_POINT ( 'NONE',  ( -18.62759615963270932, 10.81492255796079327, 80.83224293864769550 ) ) ;
#150076 = LINE ( 'NONE', #72234, #136742 ) ;
#150078 = CARTESIAN_POINT ( 'NONE',  ( 19.36337904590691750, -5.499999999999941380, 67.91494137495620009 ) ) ;
#150077 = CARTESIAN_POINT ( 'NONE',  ( 5.823673210054125526, 21.52544592524343514, 24.79057627198103120 ) ) ;
#150079 = CARTESIAN_POINT ( 'NONE',  ( 16.55341960407618274, -4.379528057220086978, 31.04275706135234714 ) ) ;
#150081 = TOROIDAL_SURFACE ( 'NONE', #175900, 206.0437394197456911, 10.00000000000000000 ) ;
#150080 = CARTESIAN_POINT ( 'NONE',  ( -8.224510206698948167, 14.34966873604960824, 95.41557627198102409 ) ) ;
#150082 = DIRECTION ( 'NONE',  ( 0.000000000000000000, 0.000000000000000000, -1.000000000000000000 ) ) ;
#150083 = CARTESIAN_POINT ( 'NONE',  ( 5.049401038298161559, -19.05341960407611168, 87.70724293864769550 ) ) ;
#150084 = CARTESIAN_POINT ( 'NONE',  ( -0.05219959533909027116, -19.03943276465977164, 47.49890960531435979 ) ) ;
#150085 = CARTESIAN_POINT ( 'NONE',  ( -4.379528057220328563, 16.55341960407611168, 85.20724293864770971 ) ) ;
#150086 = CARTESIAN_POINT ( 'NONE',  ( -5.719274019375978568, 21.55341960407610458, 30.20724293864769550 ) ) ;
#150087 = CARTESIAN_POINT ( 'NONE',  ( -12.14591786802309592, -12.06949235617757132, 56.87390960531436690 ) ) ;
#150088 = CARTESIAN_POINT ( 'NONE',  ( 13.89961937509957401, 13.97604488694547697, 96.87609039468566152 ) ) ;
#150089 = CARTESIAN_POINT ( 'NONE',  ( -0.05219959533937732626, 21.53943276465977519, 62.50109039468568284 ) ) ;
#150090 = CIRCLE ( 'NONE', #172586, 206.0437394197456911 ) ;
#150091 = CARTESIAN_POINT ( 'NONE',  ( -193.3062444957834884, -155.7167183371838064, -4.999999999999999112 ) ) ;
#150092 = CARTESIAN_POINT ( 'NONE',  ( -0.05219959533909027116, -19.03943276465977164, 102.4989096053143669 ) ) ;
#150093 = CARTESIAN_POINT ( 'NONE',  ( -14.34966873604972548, 8.224510206698743886, 83.33442372801903275 ) ) ;
#150094 = CARTESIAN_POINT ( 'NONE',  ( 16.46253265017160672, -9.564922557960803928, 23.33224293864769194 ) ) ;
#150095 = CARTESIAN_POINT ( 'NONE',  ( -19.03943276465977164, 0.05219959533909376836, 81.24890960531436690 ) ) ;
#150096 = CARTESIAN_POINT ( 'NONE',  ( 10.72451020669898902, -18.67979575497178502, 82.91557627198103830 ) ) ;
#150097 =( GEOMETRIC_REPRESENTATION_CONTEXT ( 3 ) GLOBAL_UNCERTAINTY_ASSIGNED_CONTEXT ( ( #175748 ) ) GLOBAL_UNIT_ASSIGNED_CONTEXT ( ( #795, #155487, #29181 ) ) REPRESENTATION_CONTEXT ( 'NONE', 'WORKASPACE' ) );
#150098 =( BOUNDED_CURVE ( )  B_SPLINE_CURVE ( 2, ( #17739, #13753, #62224, #63228, #122909, #170417, #45095, #106752, #31909, #93562, #78386 ),
 .UNSPECIFIED., .F., .T. ) 
 B_SPLINE_CURVE_WITH_KNOTS ( ( 3, 2, 2, 2, 2, 3 ),
 ( 0.2000000000000000111, 0.2200000000000000011, 0.2400000000000000189, 0.2600000000000000644, 0.2800000000000000822, 0.3000000000000000444 ),
 .UNSPECIFIED. ) 
 CURVE ( )  GEOMETRIC_REPRESENTATION_ITEM ( )  RATIONAL_B_SPLINE_CURVE ( ( 1.000000000000000000, 0.9510565162951535312, 1.000000000000000000, 0.9510565162951535312, 1.000000000000000000, 0.9510565162951535312, 1.000000000000000000, 0.9510565162951535312, 1.000000000000000000, 0.9510565162951534202, 1.000000000000000222 ) ) 
 REPRESENTATION_ITEM ( '' )  );
#150099 = CARTESIAN_POINT ( 'NONE',  ( 19.03943276465977164, 0.05219959533936151252, 106.2510903946856615 ) ) ;
#150101 = CARTESIAN_POINT ( 'NONE',  ( 18.67979575497194134, -10.72451020669871369, 60.83442372801901854 ) ) ;
#150100 = CARTESIAN_POINT ( 'NONE',  ( 0.05219959533910956823, 16.53943276465976808, 49.99890960531437401 ) ) ;
#150103 = CARTESIAN_POINT ( 'NONE',  ( -16.46253265017160317, 9.564922557960807481, 115.8322429386477097 ) ) ;
#150102 = CARTESIAN_POINT ( 'NONE',  ( 16.55341960407618274, -4.379528057220086978, 81.04275706135236135 ) ) ;
#150104 = CARTESIAN_POINT ( 'NONE',  ( 16.51473224551069308, 9.474510206698969483, 114.1655762719810241 ) ) ;
#150105 = CARTESIAN_POINT ( 'NONE',  ( 17.50000000000000000, -5.500000000000000888, 43.29690382534172244 ) ) ;
#150106 = CARTESIAN_POINT ( 'NONE',  ( 4.483927247898790824, -16.52544592524335698, 105.2094237280190328 ) ) ;
#150107 = CARTESIAN_POINT ( 'NONE',  ( 14.29746914071037800, 8.314922557961029526, 66.66775706135234714 ) ) ;
#150108 = CARTESIAN_POINT ( 'NONE',  ( -13.89961937509977652, 13.97604488694528158, 70.62390960531432427 ) ) ;
#150109 = CARTESIAN_POINT ( 'NONE',  ( 16.46253265017160672, -9.564922557960803928, 93.33224293864769550 ) ) ;
#150110 = CARTESIAN_POINT ( 'NONE',  ( -0.05219959533937732626, 21.53943276465977519, 72.50109039468568994 ) ) ;
#150111 = CARTESIAN_POINT ( 'NONE',  ( 16.55341960407618274, -4.379528057220086978, 76.04275706135237556 ) ) ;
#150112 = CARTESIAN_POINT ( 'NONE',  ( -16.52544592524342804, 4.483927247898546575, 46.04057627198103830 ) ) ;
#150113 = CARTESIAN_POINT ( 'NONE',  ( 13.89961937509977652, -13.97604488694527269, 53.12390960531434558 ) ) ;
#150114 = CARTESIAN_POINT ( 'NONE',  ( -16.46253265017160317, 9.564922557960807481, 50.83224293864770260 ) ) ;
#150116 = EDGE_LOOP ( 'NONE', ( #63532, #187837, #169641, #148838, #35799 ) ) ;
#150115 = CARTESIAN_POINT ( 'NONE',  ( -8.314922557961024197, 14.29746914071037800, 37.91775706135235424 ) ) ;
#150117 = CARTESIAN_POINT ( 'NONE',  ( -0.05219959533936034679, 19.03943276465977164, 92.50109039468566152 ) ) ;
#150118 = CARTESIAN_POINT ( 'NONE',  ( -14.29746914071049879, 8.314922557960819915, 100.8322429386477097 ) ) ;
#150119 = CARTESIAN_POINT ( 'NONE',  ( -16.51473224551069308, -9.474510206698971260, 61.66557627198103120 ) ) ;
#150121 = CARTESIAN_POINT ( 'NONE',  ( 37.99999999999999289, 2.893978650043524126E-14, -5.000000000000000000 ) ) ;
#150120 = CARTESIAN_POINT ( 'NONE',  ( 19.02544592524334988, 5.153800228976608722, 96.45942372801897591 ) ) ;
#150122 = CARTESIAN_POINT ( 'NONE',  ( -18.62759615963255300, -10.81492255796106328, 104.1677570613523471 ) ) ;
#150123 = CARTESIAN_POINT ( 'NONE',  ( -8.314922557961024197, 14.29746914071037800, 67.91775706135234714 ) ) ;
#150124 = DIRECTION ( 'NONE',  ( 1.000000000000000000, 0.000000000000000000, 0.000000000000000000 ) ) ;
#150125 = CARTESIAN_POINT ( 'NONE',  ( -18.62759615963270932, 10.81492255796079327, 65.83224293864769550 ) ) ;
#150126 = CARTESIAN_POINT ( 'NONE',  ( -16.53943276465976808, -0.05219959533934237506, 58.75109039468568994 ) ) ;
#150127 = DIRECTION ( 'NONE',  ( 0.000000000000000000, 0.000000000000000000, 1.000000000000000000 ) ) ;
#150128 = CARTESIAN_POINT ( 'NONE',  ( -19.03943276465977164, -0.05219959533935918106, 48.75109039468566863 ) ) ;
#150129 = CARTESIAN_POINT ( 'NONE',  ( -19.03943276465977164, 0.05219959533909376836, 91.24890960531436690 ) ) ;
#150130 = CARTESIAN_POINT ( 'NONE',  ( -19.03943276465977164, 0.05219959533909376836, 21.24890960531436335 ) ) ;
#150131 = CARTESIAN_POINT ( 'NONE',  ( -19.02544592524342804, 5.153800228976336051, 61.04057627198103120 ) ) ;
#150132 = CARTESIAN_POINT ( 'NONE',  ( 0.05219959533910956823, 16.53943276465976808, 64.99890960531435269 ) ) ;
#150133 = VECTOR ( 'NONE', #23131, 1000.000000000000114 ) ;
#150134 = CARTESIAN_POINT ( 'NONE',  ( -21.52544592524334988, -5.823673210054445271, 73.95942372801901854 ) ) ;
#150135 = CARTESIAN_POINT ( 'NONE',  ( 19.03943276465977164, 0.05219959533936151252, 51.25109039468567573 ) ) ;
#150136 = CARTESIAN_POINT ( 'NONE',  ( -13.89961937509957401, -13.97604488694547875, 34.37609039468566863 ) ) ;
#150137 = CARTESIAN_POINT ( 'NONE',  ( -16.51473224551069308, -9.474510206698971260, 51.66557627198102409 ) ) ;
#150138 = CARTESIAN_POINT ( 'NONE',  ( 15.72974639402199770, -15.80617190586745480, 28.12390960531435979 ) ) ;
#150139 = CARTESIAN_POINT ( 'NONE',  ( 0.05219959533937995610, -21.53943276465977519, 90.00109039468567573 ) ) ;
#150140 = CARTESIAN_POINT ( 'NONE',  ( 9.474510206698971260, -16.51473224551069308, 62.91557627198102409 ) ) ;
#150141 = CARTESIAN_POINT ( 'NONE',  ( -21.52544592524334988, -5.823673210054445271, 98.95942372801903275 ) ) ;
#150142 = CARTESIAN_POINT ( 'NONE',  ( 15.80617190586746368, 15.72974639402197994, 39.37390960531436690 ) ) ;
#150143 = CARTESIAN_POINT ( 'NONE',  ( 19.03943276465977164, -0.05219959533909143690, 88.74890960531436690 ) ) ;
#150144 = CARTESIAN_POINT ( 'NONE',  ( 19.05341960407617918, -5.049401038297876454, 56.04275706135234714 ) ) ;
#150145 = CARTESIAN_POINT ( 'NONE',  ( 9.564922557960805705, 16.46253265017160317, 44.58224293864769550 ) ) ;
#150146 = CARTESIAN_POINT ( 'NONE',  ( 5.049401038298161559, -19.05341960407611168, 87.70724293864769550 ) ) ;
#150147 = EDGE_CURVE ( 'NONE', #167327, #117002, #59929, .T. ) ;
#150148 = CARTESIAN_POINT ( 'NONE',  ( 8.224510206698742110, 14.34966873604972548, 32.08442372801901854 ) ) ;
#150149 = CARTESIAN_POINT ( 'NONE',  ( -16.52544592524342804, 4.483927247898546575, 101.0405762719810383 ) ) ;
#150150 = CARTESIAN_POINT ( 'NONE',  ( 16.46253265017160672, -9.564922557960803928, 73.33224293864769550 ) ) ;
#150151 = CARTESIAN_POINT ( 'NONE',  ( 21.52544592524344225, -5.823673210054117533, 43.54057627198103830 ) ) ;
#150152 = CARTESIAN_POINT ( 'NONE',  ( -12.06949235617739369, -12.14591786802326823, 24.37609039468567573 ) ) ;
#150153 = CARTESIAN_POINT ( 'NONE',  ( -21.53943276465977519, -0.05219959533937600094, 18.75109039468568639 ) ) ;
#150154 = CARTESIAN_POINT ( 'NONE',  ( -21.53943276465977519, -0.05219959533937600094, 68.75109039468568994 ) ) ;
#150155 = CARTESIAN_POINT ( 'NONE',  ( -14.34966873604972548, 8.224510206698743886, 73.33442372801901854 ) ) ;
#150156 = CARTESIAN_POINT ( 'NONE',  ( 16.52544592524335698, 4.483927247898782831, 66.45942372801903275 ) ) ;
#150157 = CARTESIAN_POINT ( 'NONE',  ( -19.02544592524342804, 5.153800228976336051, 81.04057627198103830 ) ) ;
#150158 = CARTESIAN_POINT ( 'NONE',  ( -8.224510206698735004, -14.34966873604973081, 104.5844237280190185 ) ) ;
#150159 = CARTESIAN_POINT ( 'NONE',  ( -5.153800228976607833, 19.02544592524334988, 37.70942372801899722 ) ) ;
#150160 = CARTESIAN_POINT ( 'NONE',  ( -5.719274019375665041, -21.55341960407619695, 34.79275706135235424 ) ) ;
#150161 = EDGE_CURVE ( 'NONE', #71928, #1233, #47638, .T. ) ;
#150162 = CARTESIAN_POINT ( 'NONE',  ( -0.05219959533910754901, -16.53943276465976808, 62.49890960531436690 ) ) ;
#150163 = CARTESIAN_POINT ( 'NONE',  ( 19.03943276465977164, -0.05219959533909143690, 98.74890960531436690 ) ) ;
#150164 = CARTESIAN_POINT ( 'NONE',  ( -14.34966873604972548, 8.224510206698743886, 83.33442372801903275 ) ) ;
#150165 = CARTESIAN_POINT ( 'NONE',  ( 21.53943276465977519, 0.05219959533937863772, 66.25109039468567573 ) ) ;
#150166 = CARTESIAN_POINT ( 'NONE',  ( 14.29746914071037800, 8.314922557961029526, 26.66775706135235424 ) ) ;
#150167 = CARTESIAN_POINT ( 'NONE',  ( -18.62759615963255300, -10.81492255796106328, 24.16775706135235424 ) ) ;
#150168 = CARTESIAN_POINT ( 'NONE',  ( -16.55341960407611168, -4.379528057220339221, 56.45724293864768839 ) ) ;
#150169 = ORIENTED_EDGE ( 'NONE', *, *, #198323, .T. ) ;
#150170 = CARTESIAN_POINT ( 'NONE',  ( -18.62759615963270932, 10.81492255796079327, 105.8322429386476955 ) ) ;
#150171 = CARTESIAN_POINT ( 'NONE',  ( 12.14591786802309770, 12.06949235617756955, 44.37390960531435979 ) ) ;
#150172 = ORIENTED_EDGE ( 'NONE', *, *, #120340, .T. ) ;
#150173 = CARTESIAN_POINT ( 'NONE',  ( -19.03943276465977164, 0.05219959533909376836, 31.24890960531435979 ) ) ;
#150174 = CARTESIAN_POINT ( 'NONE',  ( -15.72974639402197994, 15.80617190586746368, 25.62390960531435624 ) ) ;
#150175 = CARTESIAN_POINT ( 'NONE',  ( -18.67979575497193778, 10.72451020669871902, 33.33442372801900433 ) ) ;
#150176 = CARTESIAN_POINT ( 'NONE',  ( -8.224510206698948167, 14.34966873604960824, 65.41557627198102409 ) ) ;
#150177 = CARTESIAN_POINT ( 'NONE',  ( -21.52544592524343514, 5.823673210054127303, 61.04057627198103120 ) ) ;
#150178 = CARTESIAN_POINT ( 'NONE',  ( 19.05341960407611168, 5.049401038298154454, 73.95724293864768129 ) ) ;
#150180 = CARTESIAN_POINT ( 'NONE',  ( -19.02544592524334988, -5.153800228976617603, 83.95942372801901854 ) ) ;
#150179 = CARTESIAN_POINT ( 'NONE',  ( -9.474510206698964154, 16.51473224551069663, 25.41557627198103120 ) ) ;
#150181 = CARTESIAN_POINT ( 'NONE',  ( -0.05219959533907301413, -21.53943276465977519, 47.49890960531435979 ) ) ;
#150182 = CARTESIAN_POINT ( 'NONE',  ( -9.474510206698964154, 16.51473224551069663, 40.41557627198103120 ) ) ;
#150183 = CARTESIAN_POINT ( 'NONE',  ( 19.02544592524343514, -5.153800228976328945, 78.54057627198099567 ) ) ;
#150184 = ORIENTED_EDGE ( 'NONE', *, *, #199827, .F. ) ;
#150185 = CARTESIAN_POINT ( 'NONE',  ( -12.14591786802326823, 12.06949235617739902, 38.12609039468567573 ) ) ;
#150186 = CARTESIAN_POINT ( 'NONE',  ( 15.72974639402199770, -15.80617190586745480, 113.1239096053143953 ) ) ;
#150187 = EDGE_CURVE ( 'NONE', #70273, #106917, #15326, .T. ) ;
#150188 = CARTESIAN_POINT ( 'NONE',  ( 16.53943276465976808, -0.05219959533910856209, 53.74890960531437401 ) ) ;
#150189 = CIRCLE ( 'NONE', #62964, 2.500000000000000000 ) ;
#150190 = CARTESIAN_POINT ( 'NONE',  ( 21.55341960407619695, -5.719274019375665929, 56.04275706135235424 ) ) ;
#150191 = CARTESIAN_POINT ( 'NONE',  ( 9.474510206698971260, -16.51473224551069308, 107.9155762719810383 ) ) ;
#150192 = CARTESIAN_POINT ( 'NONE',  ( -0.05219959533907301413, -21.53943276465977519, 67.49890960531436690 ) ) ;
#150194 = CARTESIAN_POINT ( 'NONE',  ( 4.379528057220092307, 16.55341960407617563, 47.29275706135234003 ) ) ;
#150193 = CARTESIAN_POINT ( 'NONE',  ( -10.72451020669898014, 18.67979575497178502, 105.4155762719810383 ) ) ;
#150195 = CARTESIAN_POINT ( 'NONE',  ( 5.719274019375991003, -21.55341960407610458, 47.70724293864770260 ) ) ;
#150196 = CARTESIAN_POINT ( 'NONE',  ( -18.62759615963255300, -10.81492255796106328, 99.16775706135234714 ) ) ;
#150197 = CARTESIAN_POINT ( 'NONE',  ( -5.049401038298153566, 19.05341960407611168, 60.20724293864768129 ) ) ;
#150198 = CARTESIAN_POINT ( 'NONE',  ( -16.46253265017160317, 9.564922557960807481, 90.83224293864769550 ) ) ;
#150199 = CARTESIAN_POINT ( 'NONE',  ( -9.474510206698964154, 16.51473224551069663, 70.41557627198102409 ) ) ;
#150200 = CARTESIAN_POINT ( 'NONE',  ( -26.33511944008826688, -27.18111610334197081, -16.53814760372663173 ) ) ;
#150201 = CARTESIAN_POINT ( 'NONE',  ( 13.97604488694548053, -13.89961937509957401, 55.62609039468566863 ) ) ;
#150203 = CARTESIAN_POINT ( 'NONE',  ( -18.67979575497178146, -10.72451020669898902, 31.66557627198102054 ) ) ;
#150202 = CARTESIAN_POINT ( 'NONE',  ( 13.97604488694548053, -13.89961937509957401, 20.62609039468567573 ) ) ;
#150204 = CARTESIAN_POINT ( 'NONE',  ( -12.06949235617739369, -12.14591786802326823, 104.3760903946856899 ) ) ;
#150205 = CARTESIAN_POINT ( 'NONE',  ( -13.97604488694547697, 13.89961937509957934, 88.12609039468563310 ) ) ;
#150206 = CARTESIAN_POINT ( 'NONE',  ( 9.564922557960805705, 16.46253265017160317, 39.58224293864768839 ) ) ;
#150207 = AXIS2_PLACEMENT_3D ( 'NONE', #125266, #186964, #2908 ) ;
#150208 = CARTESIAN_POINT ( 'NONE',  ( -5.049401038297874678, -19.05341960407617918, 19.79275706135233293 ) ) ;
#150209 = CARTESIAN_POINT ( 'NONE',  ( 5.153800228976615827, -19.02544592524334988, 85.20942372801900433 ) ) ;
#150210 = CARTESIAN_POINT ( 'NONE',  ( 13.97604488694548053, -13.89961937509957401, 40.62609039468564731 ) ) ;
#150211 = CARTESIAN_POINT ( 'NONE',  ( -32.00000000000000000, -1.163414459189985801E-14, 95.00000000000000000 ) ) ;
#150212 = CARTESIAN_POINT ( 'NONE',  ( 16.51473224551069308, 9.474510206698969483, 39.16557627198103120 ) ) ;
#150213 = CARTESIAN_POINT ( 'NONE',  ( -8.224510206698948167, 14.34966873604960824, 45.41557627198103830 ) ) ;
#150214 = CARTESIAN_POINT ( 'NONE',  ( 5.049401038298161559, -19.05341960407611168, 32.70724293864768129 ) ) ;
#150215 = CARTESIAN_POINT ( 'NONE',  ( -14.34966873604960291, -8.224510206698953496, 36.66557627198103120 ) ) ;
#150216 = DIRECTION ( 'NONE',  ( -1.000000000000000000, -0.000000000000000000, -0.000000000000000000 ) ) ;
#150217 = CARTESIAN_POINT ( 'NONE',  ( 16.55341960407618274, -4.379528057220086978, 106.0427570613523471 ) ) ;
#150218 = CARTESIAN_POINT ( 'NONE',  ( 9.564922557960805705, 16.46253265017160317, 49.58224293864770260 ) ) ;
#150219 = CARTESIAN_POINT ( 'NONE',  ( -18.67979575497193778, 10.72451020669871902, 108.3344237280190185 ) ) ;
#150220 = CARTESIAN_POINT ( 'NONE',  ( -12.06949235617739369, -12.14591786802326823, 29.37609039468568284 ) ) ;
#150221 = CARTESIAN_POINT ( 'NONE',  ( -21.53943276465977519, 0.05219959533907696930, 36.24890960531435979 ) ) ;
#150223 = VERTEX_POINT ( 'NONE', #79976 ) ;
#150222 = CARTESIAN_POINT ( 'NONE',  ( 18.67979575497194134, -10.72451020669871369, 95.83442372801903275 ) ) ;
#150224 = CARTESIAN_POINT ( 'NONE',  ( 19.05341960407611168, 5.049401038298154454, 103.9572429386476671 ) ) ;
#150225 = CARTESIAN_POINT ( 'NONE',  ( -13.97604488694527625, -13.89961937509977652, 81.87390960531436690 ) ) ;
#150226 = CARTESIAN_POINT ( 'NONE',  ( 11.40812507854754365, 35.11059874428196537, -7.224999997268813701 ) ) ;
#150227 = CARTESIAN_POINT ( 'NONE',  ( 21.55341960407610458, 5.719274019375980345, 108.9572429386476955 ) ) ;
#150228 = CIRCLE ( 'NONE', #153367, 28.82186960331498682 ) ;
#150229 = CARTESIAN_POINT ( 'NONE',  ( 14.34966873604960469, 8.224510206698951720, 84.16557627198103830 ) ) ;
#150231 = CARTESIAN_POINT ( 'NONE',  ( -16.51473224551069308, -9.474510206698971260, 66.66557627198102409 ) ) ;
#150230 = CARTESIAN_POINT ( 'NONE',  ( 15.72974639402199770, -15.80617190586745480, 78.12390960531436690 ) ) ;
#150232 = CARTESIAN_POINT ( 'NONE',  ( 0.05219959533909260263, 19.03943276465977164, 69.99890960531435269 ) ) ;
#150233 = CARTESIAN_POINT ( 'NONE',  ( -5.719274019375978568, 21.55341960407610458, 95.20724293864769550 ) ) ;
#150234 = ORIENTED_EDGE ( 'NONE', *, *, #28043, .T. ) ;
#150235 = CARTESIAN_POINT ( 'NONE',  ( 19.05341960407611168, 5.049401038298154454, 53.95724293864770260 ) ) ;
#150237 = CARTESIAN_POINT ( 'NONE',  ( -19.03943276465977164, 0.05219959533909376836, 21.24890960531436335 ) ) ;
#150236 = CARTESIAN_POINT ( 'NONE',  ( 14.29746914071049879, -8.314922557960816363, 98.33224293864769550 ) ) ;
#150238 = CARTESIAN_POINT ( 'NONE',  ( -5.049401038298153566, 19.05341960407611168, 70.20724293864769550 ) ) ;
#150239 = CARTESIAN_POINT ( 'NONE',  ( 0.05219959533936267826, -19.03943276465977164, 80.00109039468567573 ) ) ;
#150240 = AXIS2_PLACEMENT_3D ( 'NONE', #139839, #169193, #155027 ) ;
#150241 = CARTESIAN_POINT ( 'NONE',  ( 16.52544592524342804, -4.483927247898539470, 98.54057627198105251 ) ) ;
#150242 = CARTESIAN_POINT ( 'NONE',  ( -0.05219959533937732626, 21.53943276465977519, 52.50109039468567573 ) ) ;
#150244 = CARTESIAN_POINT ( 'NONE',  ( -15.72974639402197994, 15.80617190586746368, 115.6239096053143669 ) ) ;
#150243 = CARTESIAN_POINT ( 'NONE',  ( -5.153800228976328057, -19.02544592524343514, 47.29057627198102409 ) ) ;
#150245 = CARTESIAN_POINT ( 'NONE',  ( -16.55341960407611168, -4.379528057220339221, 106.4572429386477097 ) ) ;
#150246 = CARTESIAN_POINT ( 'NONE',  ( 23.31738231874054534, 16.94106989632529192, 147.4500000054623854 ) ) ;
#150247 = CARTESIAN_POINT ( 'NONE',  ( -9.474510206698964154, 16.51473224551069663, 55.41557627198103120 ) ) ;
#150248 = VECTOR ( 'NONE', #71878, 1000.000000000000000 ) ;
#150249 = CARTESIAN_POINT ( 'NONE',  ( 4.500000000000000888, -116.8122400552013431, 54.87277500418469600 ) ) ;
#150251 = CARTESIAN_POINT ( 'NONE',  ( 5.049401038298161559, -19.05341960407611168, 112.7072429386476813 ) ) ;
#150250 = CARTESIAN_POINT ( 'NONE',  ( 9.564922557961047289, -16.46253265017146816, 105.4177570613523471 ) ) ;
#150252 = CARTESIAN_POINT ( 'NONE',  ( -15.72974639402176322, -15.80617190586768395, 44.37609039468567573 ) ) ;
#150253 = CARTESIAN_POINT ( 'NONE',  ( -19.05341960407611168, -5.049401038298163336, 101.4572429386476955 ) ) ;
#150254 = CARTESIAN_POINT ( 'NONE',  ( 19.05341960407617918, -5.049401038297876454, 86.04275706135233293 ) ) ;
#150255 = CARTESIAN_POINT ( 'NONE',  ( 16.46253265017160672, -9.564922557960803928, 53.33224293864768839 ) ) ;
#150256 = CARTESIAN_POINT ( 'NONE',  ( 12.06949235617757843, -12.14591786802309237, 83.12390960531436690 ) ) ;
#150257 = CARTESIAN_POINT ( 'NONE',  ( 13.89961937509977652, -13.97604488694527269, 83.12390960531436690 ) ) ;
#150258 = CARTESIAN_POINT ( 'NONE',  ( 16.55341960407611168, 4.379528057220329451, 73.95724293864769550 ) ) ;
#150259 = CARTESIAN_POINT ( 'NONE',  ( -0.05219959533909027116, -19.03943276465977164, 82.49890960531436690 ) ) ;
#150260 = CARTESIAN_POINT ( 'NONE',  ( -5.153800228976607833, 19.02544592524334988, 37.70942372801899722 ) ) ;
#150263 = CARTESIAN_POINT ( 'NONE',  ( 16.51473224551069308, 9.474510206698969483, 24.16557627198102765 ) ) ;
#150262 = CARTESIAN_POINT ( 'NONE',  ( -4.379528057220328563, 16.55341960407611168, 50.20724293864769550 ) ) ;
#150261 = CARTESIAN_POINT ( 'NONE',  ( 16.51473224551069308, 9.474510206698969483, 44.16557627198103120 ) ) ;
#150264 = ORIENTED_EDGE ( 'NONE', *, *, #118593, .T. ) ;
#150265 = CARTESIAN_POINT ( 'NONE',  ( 10.81492255796106328, -18.62759615963255655, 50.41775706135235424 ) ) ;
#150266 = CARTESIAN_POINT ( 'NONE',  ( 19.02544592524334988, 5.153800228976608722, 81.45942372801897591 ) ) ;
#150267 = CARTESIAN_POINT ( 'NONE',  ( -4.483927247898539470, -16.52544592524342804, 37.29057627198102409 ) ) ;
#150268 = CARTESIAN_POINT ( 'NONE',  ( 0.05219959533907565091, 21.53943276465977519, 99.99890960531436690 ) ) ;
#150269 = CARTESIAN_POINT ( 'NONE',  ( -0.05219959533907301413, -21.53943276465977519, 37.49890960531436690 ) ) ;
#150270 = CARTESIAN_POINT ( 'NONE',  ( -14.29746914071049879, 8.314922557960819915, 75.83224293864769550 ) ) ;
#150271 = CARTESIAN_POINT ( 'NONE',  ( 19.02544592524343514, -5.153800228976328945, 38.54057627198103120 ) ) ;
#150272 = CARTESIAN_POINT ( 'NONE',  ( -14.34966873604972548, 8.224510206698743886, 108.3344237280190185 ) ) ;
#150273 = CARTESIAN_POINT ( 'NONE',  ( 8.314922557961029526, -14.29746914071037800, 75.41775706135233293 ) ) ;
#150274 = CARTESIAN_POINT ( 'NONE',  ( -16.51473224551082808, 9.474510206698731452, 23.33442372801900078 ) ) ;
#150275 = CARTESIAN_POINT ( 'NONE',  ( -0.05219959533909027116, -19.03943276465977164, 92.49890960531436690 ) ) ;
#150276 = CARTESIAN_POINT ( 'NONE',  ( 13.89961937509977652, -13.97604488694527269, 78.12390960531433848 ) ) ;
#150277 = CARTESIAN_POINT ( 'NONE',  ( -14.34966873604972548, 8.224510206698743886, 73.33442372801901854 ) ) ;
#150278 = CARTESIAN_POINT ( 'NONE',  ( -19.02544592524342804, 5.153800228976336051, 31.04057627198102409 ) ) ;
#150279 = CARTESIAN_POINT ( 'NONE',  ( -14.34966873604960291, -8.224510206698953496, 51.66557627198102409 ) ) ;
#150281 = CARTESIAN_POINT ( 'NONE',  ( 19.05341960407611168, 5.049401038298154454, 88.95724293864769550 ) ) ;
#150280 = CARTESIAN_POINT ( 'NONE',  ( -19.05341960407611168, -5.049401038298163336, 101.4572429386476955 ) ) ;
#150283 = ADVANCED_FACE ( 'NONE', ( #186181 ), #189119, .F. ) ;
#150282 = CARTESIAN_POINT ( 'NONE',  ( 15.72974639402199770, -15.80617190586745480, 23.12390960531436335 ) ) ;
#150284 = CARTESIAN_POINT ( 'NONE',  ( 14.34966873604960469, 8.224510206698951720, 69.16557627198102409 ) ) ;
#150285 = VERTEX_POINT ( 'NONE', #108318 ) ;
#150286 = CARTESIAN_POINT ( 'NONE',  ( 12.06949235617757843, -12.14591786802309237, 63.12390960531435979 ) ) ;
#150288 = CARTESIAN_POINT ( 'NONE',  ( 17.49999999999999289, -3.305555262949580797, 32.12517152156607381 ) ) ;
#150287 = CARTESIAN_POINT ( 'NONE',  ( -4.379528057220086978, -16.55341960407618274, 49.79275706135234714 ) ) ;
#150289 = CARTESIAN_POINT ( 'NONE',  ( -16.51473224551082808, 9.474510206698731452, 63.33442372801900433 ) ) ;
#150290 = CARTESIAN_POINT ( 'NONE',  ( 16.51473224551069308, 9.474510206698969483, 84.16557627198102409 ) ) ;
#150291 = CARTESIAN_POINT ( 'NONE',  ( 19.05341960407617918, -5.049401038297876454, 61.04275706135232582 ) ) ;
#150293 = CARTESIAN_POINT ( 'NONE',  ( -4.379528057220086978, -16.55341960407618274, 99.79275706135234714 ) ) ;
#150292 = CARTESIAN_POINT ( 'NONE',  ( -5.153800228976607833, 19.02544592524334988, 112.7094237280190043 ) ) ;
#150294 = CARTESIAN_POINT ( 'NONE',  ( 13.89961937509977652, -13.97604488694527269, 38.12390960531436690 ) ) ;
#150295 = CARTESIAN_POINT ( 'NONE',  ( 0.05219959533907565091, 21.53943276465977519, 24.99890960531435624 ) ) ;
#150296 = CARTESIAN_POINT ( 'NONE',  ( 21.52544592524334988, 5.823673210054432836, 56.45942372801902565 ) ) ;
#150297 = CARTESIAN_POINT ( 'NONE',  ( -0.05219959533936034679, 19.03943276465977164, 107.5010903946856615 ) ) ;
#150299 = CARTESIAN_POINT ( 'NONE',  ( -19.02544592524342804, 5.153800228976336051, 76.04057627198102409 ) ) ;
#150298 = LINE ( 'NONE', #104775, #63772 ) ;
#150300 = CARTESIAN_POINT ( 'NONE',  ( -16.46253265017160317, 9.564922557960807481, 115.8322429386477097 ) ) ;
#150302 = CARTESIAN_POINT ( 'NONE',  ( -19.03943276465977164, 0.05219959533909376836, 76.24890960531435269 ) ) ;
#150301 = CARTESIAN_POINT ( 'NONE',  ( -16.53943276465976808, 0.05219959533911058130, 81.24890960531436690 ) ) ;
#150303 = CARTESIAN_POINT ( 'NONE',  ( 13.97604488694527802, 13.89961937509977652, 79.37390960531435269 ) ) ;
#150304 = CARTESIAN_POINT ( 'NONE',  ( -13.97604488694547697, 13.89961937509957934, 83.12609039468564731 ) ) ;
#150305 = CARTESIAN_POINT ( 'NONE',  ( -21.53943276465977519, 0.05219959533907696930, 66.24890960531436690 ) ) ;
#150306 = CARTESIAN_POINT ( 'NONE',  ( -0.05219959533909027116, -19.03943276465977164, 27.49890960531435624 ) ) ;
#150307 = CARTESIAN_POINT ( 'NONE',  ( 0.05219959533936267826, -19.03943276465977164, 55.00109039468566863 ) ) ;
#150308 = CARTESIAN_POINT ( 'NONE',  ( -16.51473224551069308, -9.474510206698971260, 56.66557627198103120 ) ) ;
#150310 = EDGE_CURVE ( 'NONE', #21338, #190522, #138656, .T. ) ;
#150309 = CARTESIAN_POINT ( 'NONE',  ( 9.564922557960805705, 16.46253265017160317, 94.58224293864769550 ) ) ;
#150311 = EDGE_LOOP ( 'NONE', ( #61198, #5983, #12043, #7479 ) ) ;
#150312 = CARTESIAN_POINT ( 'NONE',  ( 5.719274019375991003, -21.55341960407610458, 87.70724293864769550 ) ) ;
#150314 = CARTESIAN_POINT ( 'NONE',  ( -16.51473224551082808, 9.474510206698731452, 43.33442372801900433 ) ) ;
#150313 = CARTESIAN_POINT ( 'NONE',  ( -12.06949235617756955, 12.14591786802309770, 90.62390960531436690 ) ) ;
#150315 = CARTESIAN_POINT ( 'NONE',  ( -21.53943276465977519, 0.05219959533907696930, 81.24890960531436690 ) ) ;
#150316 = CARTESIAN_POINT ( 'NONE',  ( 15.80617190586746368, 15.72974639402197994, 54.37390960531435979 ) ) ;
#150317 = AXIS2_PLACEMENT_3D ( 'NONE', #49693, #1181, #155871 ) ;
#150318 = CARTESIAN_POINT ( 'NONE',  ( 0.05219959533910956823, 16.53943276465976808, 29.99890960531435979 ) ) ;
#150319 = CARTESIAN_POINT ( 'NONE',  ( -0.05219959533937732626, 21.53943276465977519, 107.5010903946856899 ) ) ;
#150320 = CARTESIAN_POINT ( 'NONE',  ( 19.05341960407611168, 5.049401038298154454, 78.95724293864769550 ) ) ;
#150321 = CARTESIAN_POINT ( 'NONE',  ( 13.89961937509977652, -13.97604488694527269, 33.12390960531434558 ) ) ;
#150322 = CARTESIAN_POINT ( 'NONE',  ( -21.52544592524334988, -5.823673210054445271, 33.95942372801901143 ) ) ;
#150323 = CARTESIAN_POINT ( 'NONE',  ( 18.67979575497194134, -10.72451020669871369, 60.83442372801901854 ) ) ;
#150324 = CARTESIAN_POINT ( 'NONE',  ( 19.03943276465977164, -0.05219959533909143690, 48.74890960531435979 ) ) ;
#150325 = CARTESIAN_POINT ( 'NONE',  ( 18.62759615963255655, 10.81492255796105972, 26.66775706135235424 ) ) ;
#150326 = CARTESIAN_POINT ( 'NONE',  ( 19.05341960407617918, -5.049401038297876454, 56.04275706135234714 ) ) ;
#150327 = CARTESIAN_POINT ( 'NONE',  ( -19.05341960407611168, -5.049401038298163336, 31.45724293864769550 ) ) ;
#150328 = CARTESIAN_POINT ( 'NONE',  ( -0.05219959533934338120, 16.53943276465976808, 22.50109039468567573 ) ) ;
#150329 = CARTESIAN_POINT ( 'NONE',  ( 5.153800228976335163, 19.02544592524342804, 29.79057627198102409 ) ) ;
#150330 = CARTESIAN_POINT ( 'NONE',  ( -12.14591786802326823, 12.06949235617739902, 78.12609039468570415 ) ) ;
#150331 = CARTESIAN_POINT ( 'NONE',  ( 16.51473224551069308, 9.474510206698969483, 44.16557627198103120 ) ) ;
#150332 = CARTESIAN_POINT ( 'NONE',  ( -24.05407591190816063, -13.01182159662975302, 169.7785964492051960 ) ) ;
#150333 = CARTESIAN_POINT ( 'NONE',  ( -9.564922557960796823, -16.46253265017161027, 82.08224293864768129 ) ) ;
#150334 = CARTESIAN_POINT ( 'NONE',  ( 5.049401038298161559, -19.05341960407611168, 22.70724293864769194 ) ) ;
#150335 = CARTESIAN_POINT ( 'NONE',  ( -15.72974639402197994, 15.80617190586746368, 70.62390960531436690 ) ) ;
#150336 = CARTESIAN_POINT ( 'NONE',  ( 16.53943276465976808, 0.05219959533934440121, 51.25109039468568994 ) ) ;
#150337 = CARTESIAN_POINT ( 'NONE',  ( -21.52544592524334988, -5.823673210054445271, 98.95942372801903275 ) ) ;
#150338 = CARTESIAN_POINT ( 'NONE',  ( -19.05341960407611168, -5.049401038298163336, 41.45724293864769550 ) ) ;
#150339 = CARTESIAN_POINT ( 'NONE',  ( 4.379528057220339221, -16.55341960407611168, 27.70724293864769905 ) ) ;
#150340 = CARTESIAN_POINT ( 'NONE',  ( -14.29746914071049879, 8.314922557960819915, 65.83224293864769550 ) ) ;
#150341 = CARTESIAN_POINT ( 'NONE',  ( -13.89961937509977652, 13.97604488694528158, 60.62390960531436690 ) ) ;
#150342 = CARTESIAN_POINT ( 'NONE',  ( 16.51473224551083163, -9.474510206698727899, 20.83442372801899722 ) ) ;
#150343 = CARTESIAN_POINT ( 'NONE',  ( -5.719274019375665041, -21.55341960407619695, 29.79275706135234358 ) ) ;
#150344 = CARTESIAN_POINT ( 'NONE',  ( 0.05219959533909260263, 19.03943276465977164, 79.99890960531436690 ) ) ;
#150345 = CARTESIAN_POINT ( 'NONE',  ( 15.72974639402176855, 15.80617190586768217, 81.87609039468568994 ) ) ;
#150346 = CARTESIAN_POINT ( 'NONE',  ( 16.55341960407618274, -4.379528057220086978, 71.04275706135234714 ) ) ;
#150347 = CARTESIAN_POINT ( 'NONE',  ( -12.06949235617739369, -12.14591786802326823, 24.37609039468567573 ) ) ;
#150349 = CARTESIAN_POINT ( 'NONE',  ( -18.67979575497193778, 10.72451020669871902, 103.3344237280190043 ) ) ;
#150348 = CARTESIAN_POINT ( 'NONE',  ( 12.06949235617757843, -12.14591786802309237, 93.12390960531436690 ) ) ;
#150350 = CARTESIAN_POINT ( 'NONE',  ( 16.52544592524342804, -4.483927247898539470, 38.54057627198103120 ) ) ;
#150351 = CARTESIAN_POINT ( 'NONE',  ( -19.02544592524342804, 5.153800228976336051, 26.04057627198103120 ) ) ;
#150352 = CARTESIAN_POINT ( 'NONE',  ( 14.29746914071037800, 8.314922557961029526, 46.66775706135234714 ) ) ;
#150353 = CARTESIAN_POINT ( 'NONE',  ( 16.55341960407611168, 4.379528057220329451, 53.95724293864770260 ) ) ;
#150354 = CARTESIAN_POINT ( 'NONE',  ( 4.483927247898790824, -16.52544592524335698, 100.2094237280190043 ) ) ;
#150355 = CARTESIAN_POINT ( 'NONE',  ( 19.03943276465977164, -0.05219959533909143690, 113.7489096053143669 ) ) ;
#150356 = CARTESIAN_POINT ( 'NONE',  ( -21.53943276465977519, 0.05219959533907696930, 36.24890960531435979 ) ) ;
#150357 = CARTESIAN_POINT ( 'NONE',  ( -9.474510206698720793, -16.51473224551083518, 19.58442372801899722 ) ) ;
#150358 = CARTESIAN_POINT ( 'NONE',  ( -0.05219959533910754901, -16.53943276465976808, 82.49890960531436690 ) ) ;
#150359 = CARTESIAN_POINT ( 'NONE',  ( -19.05341960407611168, -5.049401038298163336, 101.4572429386476955 ) ) ;
#150360 = VERTEX_POINT ( 'NONE', #61806 ) ;
#150361 = ORIENTED_EDGE ( 'NONE', *, *, #4389, .F. ) ;
#150362 = CARTESIAN_POINT ( 'NONE',  ( -16.55341960407617563, 4.379528057220093196, 43.54275706135235424 ) ) ;
#150363 = CARTESIAN_POINT ( 'NONE',  ( 9.564922557960805705, 16.46253265017160317, 44.58224293864769550 ) ) ;
#150365 = DIRECTION ( 'NONE',  ( -1.000000000000000000, 0.000000000000000000, 0.000000000000000000 ) ) ;
#150364 = CARTESIAN_POINT ( 'NONE',  ( 16.53943276465976808, 0.05219959533934440121, 46.25109039468567573 ) ) ;
#150366 = CARTESIAN_POINT ( 'NONE',  ( 16.46253265017146816, 9.564922557961045513, 51.66775706135233293 ) ) ;
#150367 = CARTESIAN_POINT ( 'NONE',  ( -19.03943276465977164, 0.05219959533909376836, 46.24890960531435979 ) ) ;
#150368 = CARTESIAN_POINT ( 'NONE',  ( 8.314922557961029526, -14.29746914071037800, 80.41775706135234714 ) ) ;
#150369 = CARTESIAN_POINT ( 'NONE',  ( 19.05341960407617918, -5.049401038297876454, 101.0427570613523045 ) ) ;
#150370 = CARTESIAN_POINT ( 'NONE',  ( 13.97604488694548053, -13.89961937509957401, 30.62609039468566863 ) ) ;
#150371 = CARTESIAN_POINT ( 'NONE',  ( -13.89961937509977652, 13.97604488694528158, 60.62390960531436690 ) ) ;
#150373 = CARTESIAN_POINT ( 'NONE',  ( 4.379528057220339221, -16.55341960407611168, 97.70724293864772392 ) ) ;
#150372 = VECTOR ( 'NONE', #73898, 1000.000000000000000 ) ;
#150374 = CARTESIAN_POINT ( 'NONE',  ( 19.02544592524334988, 5.153800228976608722, 71.45942372801900433 ) ) ;
#150375 = CARTESIAN_POINT ( 'NONE',  ( -10.81492255796078084, -18.62759615963271287, 67.08224293864770971 ) ) ;
#150376 = CARTESIAN_POINT ( 'NONE',  ( 19.05341960407617918, -5.049401038297876454, 41.04275706135233293 ) ) ;
#150377 = CARTESIAN_POINT ( 'NONE',  ( 19.02544592524343514, -5.153800228976328945, 108.5405762719810383 ) ) ;
#150378 = CARTESIAN_POINT ( 'NONE',  ( 5.823673210054125526, 21.52544592524343514, 84.79057627198102409 ) ) ;
#150379 = LINE ( 'NONE', #11876, #53183 ) ;
#150380 = CARTESIAN_POINT ( 'NONE',  ( 13.89961937509957401, 13.97604488694547697, 106.8760903946856757 ) ) ;
#150381 = CARTESIAN_POINT ( 'NONE',  ( 5.049401038297881783, 19.05341960407617918, 97.29275706135233293 ) ) ;
#150382 = ADVANCED_FACE ( 'NONE', ( #123476 ), #169998, .F. ) ;
#150383 = CARTESIAN_POINT ( 'NONE',  ( 12.06949235617739724, 12.14591786802326823, 26.87609039468567218 ) ) ;
#150384 = CARTESIAN_POINT ( 'NONE',  ( 0.05219959533909260263, 19.03943276465977164, 44.99890960531435979 ) ) ;
#150385 = CARTESIAN_POINT ( 'NONE',  ( -9.474510206698964154, 16.51473224551069663, 115.4155762719810241 ) ) ;
#150386 = CARTESIAN_POINT ( 'NONE',  ( 15.80617190586746368, 15.72974639402197994, 89.37390960531435269 ) ) ;
#150387 = CARTESIAN_POINT ( 'NONE',  ( 18.62759615963255655, 10.81492255796105972, 56.66775706135235424 ) ) ;
#150389 = CARTESIAN_POINT ( 'NONE',  ( 5.823673210054444382, -21.52544592524334988, 105.2094237280190328 ) ) ;
#150388 = CARTESIAN_POINT ( 'NONE',  ( 19.02544592524334988, 5.153800228976608722, 106.4594237280190185 ) ) ;
#150390 = CARTESIAN_POINT ( 'NONE',  ( -8.314922557961024197, 14.29746914071037800, 112.9177570613523329 ) ) ;
#150391 = CARTESIAN_POINT ( 'NONE',  ( -10.81492255796078084, -18.62759615963271287, 97.08224293864770971 ) ) ;
#150392 = CARTESIAN_POINT ( 'NONE',  ( 12.14591786802309770, 12.06949235617756955, 54.37390960531435979 ) ) ;
#150393 = CARTESIAN_POINT ( 'NONE',  ( 9.564922557961047289, -16.46253265017146816, 85.41775706135233293 ) ) ;
#150394 = CARTESIAN_POINT ( 'NONE',  ( 19.02544592524334988, 5.153800228976608722, 51.45942372801900433 ) ) ;
#150395 = CARTESIAN_POINT ( 'NONE',  ( 21.52544592524334988, 5.823673210054432836, 66.45942372801903275 ) ) ;
#150396 = CARTESIAN_POINT ( 'NONE',  ( 0.05219959533936267826, -19.03943276465977164, 35.00109039468566863 ) ) ;
#150397 = CARTESIAN_POINT ( 'NONE',  ( -5.049401038298153566, 19.05341960407611168, 30.20724293864768839 ) ) ;
#150398 = CARTESIAN_POINT ( 'NONE',  ( 15.80617190586746368, 15.72974639402197994, 44.37390960531435979 ) ) ;
#150399 = CARTESIAN_POINT ( 'NONE',  ( -8.314922557960811034, -14.29746914071050412, 32.08224293864769550 ) ) ;
#150400 = CARTESIAN_POINT ( 'NONE',  ( 15.72974639402176855, 15.80617190586768217, 106.8760903946856899 ) ) ;
#150401 = CARTESIAN_POINT ( 'NONE',  ( 14.29746914071037800, 8.314922557961029526, 66.66775706135234714 ) ) ;
#150402 = CARTESIAN_POINT ( 'NONE',  ( -4.379528057220328563, 16.55341960407611168, 45.20724293864769550 ) ) ;
#150403 = CARTESIAN_POINT ( 'NONE',  ( 21.53943276465977519, 0.05219959533937863772, 66.25109039468567573 ) ) ;
#150404 = CARTESIAN_POINT ( 'NONE',  ( -5.719274019375665041, -21.55341960407619695, 64.79275706135234714 ) ) ;
#150405 = CARTESIAN_POINT ( 'NONE',  ( -21.52544592524343514, 5.823673210054127303, 71.04057627198103830 ) ) ;
#150406 = ORIENTED_EDGE ( 'NONE', *, *, #142150, .T. ) ;
#150407 = CARTESIAN_POINT ( 'NONE',  ( 19.05341960407611168, 5.049401038298154454, 28.95724293864769550 ) ) ;
#150408 = CARTESIAN_POINT ( 'NONE',  ( 10.72451020669871369, 18.67979575497193778, 37.08442372801901143 ) ) ;
#150409 = CARTESIAN_POINT ( 'NONE',  ( 13.97604488694527802, 13.89961937509977652, 24.37390960531435624 ) ) ;
#150410 = CARTESIAN_POINT ( 'NONE',  ( 9.474510206698971260, -16.51473224551069308, 32.91557627198102409 ) ) ;
#150411 = CARTESIAN_POINT ( 'NONE',  ( 8.224510206698953496, -14.34966873604960469, 92.91557627198103830 ) ) ;
#150412 = CARTESIAN_POINT ( 'NONE',  ( 9.564922557960805705, 16.46253265017160317, 89.58224293864769550 ) ) ;
#150413 = CARTESIAN_POINT ( 'NONE',  ( -12.06949235617756955, 12.14591786802309770, 30.62390960531436335 ) ) ;
#150414 = CARTESIAN_POINT ( 'NONE',  ( 12.14591786802309770, 12.06949235617756955, 104.3739096053143669 ) ) ;
#150415 = CARTESIAN_POINT ( 'NONE',  ( -5.719274019375978568, 21.55341960407610458, 75.20724293864769550 ) ) ;
#150416 = VECTOR ( 'NONE', #4904, 1000.000000000000000 ) ;
#150417 = CARTESIAN_POINT ( 'NONE',  ( 15.72974639402199770, -15.80617190586745480, 113.1239096053143953 ) ) ;
#150418 = CARTESIAN_POINT ( 'NONE',  ( 9.564922557960805705, 16.46253265017160317, 114.5822429386476955 ) ) ;
#150420 = CARTESIAN_POINT ( 'NONE',  ( -8.314922557961024197, 14.29746914071037800, 22.91775706135235069 ) ) ;
#150419 = CARTESIAN_POINT ( 'NONE',  ( 19.05341960407611168, 5.049401038298154454, 58.95724293864768129 ) ) ;
#150421 = CARTESIAN_POINT ( 'NONE',  ( -21.55341960407610458, -5.719274019375992779, 61.45724293864770260 ) ) ;
#150422 = CARTESIAN_POINT ( 'NONE',  ( 0.05219959533937995610, -21.53943276465977519, 85.00109039468568994 ) ) ;
#150423 = CARTESIAN_POINT ( 'NONE',  ( 5.049401038298161559, -19.05341960407611168, 82.70724293864770971 ) ) ;
#150424 = CARTESIAN_POINT ( 'NONE',  ( -19.02544592524342804, 5.153800228976336051, 106.0405762719810241 ) ) ;
#150425 = CARTESIAN_POINT ( 'NONE',  ( -16.53943276465976808, -0.05219959533934237506, 73.75109039468567573 ) ) ;
#150426 = CARTESIAN_POINT ( 'NONE',  ( 10.72451020669871369, 18.67979575497193778, 72.08442372801899012 ) ) ;
#150427 = CARTESIAN_POINT ( 'NONE',  ( 10.72451020669871369, 18.67979575497193778, 102.0844237280190185 ) ) ;
#150428 = CARTESIAN_POINT ( 'NONE',  ( 14.34966873604972726, -8.224510206698740333, 60.83442372801901854 ) ) ;
#150429 = CARTESIAN_POINT ( 'NONE',  ( -21.53943276465977519, 0.05219959533907696930, 111.2489096053143669 ) ) ;
#150430 = CARTESIAN_POINT ( 'NONE',  ( -5.049401038298153566, 19.05341960407611168, 115.2072429386477097 ) ) ;
#150431 = CARTESIAN_POINT ( 'NONE',  ( 10.81492255796078972, 18.62759615963270932, 94.58224293864769550 ) ) ;
#150432 = CARTESIAN_POINT ( 'NONE',  ( -9.474510206698720793, -16.51473224551083518, 44.58442372801900433 ) ) ;
#150433 = CARTESIAN_POINT ( 'NONE',  ( 10.72451020669898902, -18.67979575497178502, 47.91557627198102409 ) ) ;
#150435 = CARTESIAN_POINT ( 'NONE',  ( 14.34966873604960469, 8.224510206698951720, 34.16557627198102409 ) ) ;
#150434 = CARTESIAN_POINT ( 'NONE',  ( 13.97604488694527802, 13.89961937509977652, 99.37390960531436690 ) ) ;
#150436 = CARTESIAN_POINT ( 'NONE',  ( -23.31738231874055600, 16.94106989632528837, 145.7999999999999829 ) ) ;
#150437 = DIRECTION ( 'NONE',  ( -0.000000000000000000, -0.000000000000000000, 1.000000000000000000 ) ) ;
#150438 = CARTESIAN_POINT ( 'NONE',  ( -16.52544592524335698, -4.483927247898792601, 18.95942372801901143 ) ) ;
#150439 = CARTESIAN_POINT ( 'NONE',  ( 0.05219959533907565091, 21.53943276465977519, 84.99890960531436690 ) ) ;
#150440 = CARTESIAN_POINT ( 'NONE',  ( 8.224510206698953496, -14.34966873604960469, 57.91557627198103120 ) ) ;
#150441 = CARTESIAN_POINT ( 'NONE',  ( 16.52544592524335698, 4.483927247898782831, 31.45942372801901854 ) ) ;
#150442 = CARTESIAN_POINT ( 'NONE',  ( 16.46253265017160672, -9.564922557960803928, 38.33224293864768839 ) ) ;
#150444 = CARTESIAN_POINT ( 'NONE',  ( -5.049401038297874678, -19.05341960407617918, 84.79275706135233293 ) ) ;
#150443 = CARTESIAN_POINT ( 'NONE',  ( 18.62759615963271287, -10.81492255796078972, 113.3322429386476955 ) ) ;
#150445 = CARTESIAN_POINT ( 'NONE',  ( 19.02544592524343514, -5.153800228976328945, 83.54057627198100988 ) ) ;
#150446 = CARTESIAN_POINT ( 'NONE',  ( 16.51473224551069308, 9.474510206698969483, 74.16557627198103830 ) ) ;
#150447 = CARTESIAN_POINT ( 'NONE',  ( 21.55341960407610458, 5.719274019375980345, 78.95724293864769550 ) ) ;
#150448 = CARTESIAN_POINT ( 'NONE',  ( -5.049401038298153566, 19.05341960407611168, 35.20724293864768839 ) ) ;
#150449 = CARTESIAN_POINT ( 'NONE',  ( 14.47172084996136121, 34.43943601750907391, -7.999999999999994671 ) ) ;
#150450 = CARTESIAN_POINT ( 'NONE',  ( -12.06949235617756955, 12.14591786802309770, 55.62390960531436690 ) ) ;
#150451 = CARTESIAN_POINT ( 'NONE',  ( 19.05341960407611168, 5.049401038298154454, 83.95724293864766707 ) ) ;
#150452 = LINE ( 'NONE', #11948, #170341 ) ;
#150453 = CARTESIAN_POINT ( 'NONE',  ( 16.51473224551083163, -9.474510206698727899, 65.83442372801900433 ) ) ;
#150454 = AXIS2_PLACEMENT_3D ( 'NONE', #6343, #99354, #147885 ) ;
#150455 = CARTESIAN_POINT ( 'NONE',  ( 0.05219959533907565091, 21.53943276465977519, 79.99890960531435269 ) ) ;
#150456 = CARTESIAN_POINT ( 'NONE',  ( 5.049401038297881783, 19.05341960407617563, 42.29275706135234003 ) ) ;
#150457 = CARTESIAN_POINT ( 'NONE',  ( -5.049401038298153566, 19.05341960407611168, 105.2072429386476671 ) ) ;
#150458 = CARTESIAN_POINT ( 'NONE',  ( -17.49999999999999645, 4.013004640162621151, 115.4460572099441293 ) ) ;
#150459 = CARTESIAN_POINT ( 'NONE',  ( -5.719274019375978568, 21.55341960407610458, 25.20724293864769550 ) ) ;
#150460 = CARTESIAN_POINT ( 'NONE',  ( -9.474510206698964154, 16.51473224551069663, 75.41557627198103830 ) ) ;
#150461 = CARTESIAN_POINT ( 'NONE',  ( 10.72451020669871369, 18.67979575497193778, 57.08442372801901854 ) ) ;
#150462 = CARTESIAN_POINT ( 'NONE',  ( 9.564922557960805705, 16.46253265017160317, 29.58224293864769550 ) ) ;
#150464 = ORIENTED_EDGE ( 'NONE', *, *, #19233, .F. ) ;
#150463 = CARTESIAN_POINT ( 'NONE',  ( 15.80617190586746368, 15.72974639402197994, 114.3739096053143527 ) ) ;
#150465 = CARTESIAN_POINT ( 'NONE',  ( -5.823673210054431948, 21.52544592524334988, 37.70942372801900433 ) ) ;
#150466 = ORIENTED_EDGE ( 'NONE', *, *, #12228, .F. ) ;
#150467 = CARTESIAN_POINT ( 'NONE',  ( -13.89961937509977652, 13.97604488694528158, 95.62390960531436690 ) ) ;
#150468 = CARTESIAN_POINT ( 'NONE',  ( -21.48948823426666976, 5.485118590273159178, 173.8226827327241608 ) ) ;
#150469 = CARTESIAN_POINT ( 'NONE',  ( -18.67979575497178146, -10.72451020669898902, 101.6655762719810383 ) ) ;
#150470 = CARTESIAN_POINT ( 'NONE',  ( 16.51473224551069308, 9.474510206698969483, 64.16557627198102409 ) ) ;
#150471 = CARTESIAN_POINT ( 'NONE',  ( 14.29746914071037800, 8.314922557961029526, 26.66775706135235424 ) ) ;
#150472 = CARTESIAN_POINT ( 'NONE',  ( 38.00000000000000000, 12.34694845685046616, -4.649999994537627579 ) ) ;
#150473 = CARTESIAN_POINT ( 'NONE',  ( 21.52544592524334988, 5.823673210054432836, 101.4594237280190185 ) ) ;
#150474 = CARTESIAN_POINT ( 'NONE',  ( 13.89961937509977652, -13.97604488694527269, 48.12390960531435979 ) ) ;
#150475 = CARTESIAN_POINT ( 'NONE',  ( 5.823673210054444382, -21.52544592524334988, 100.2094237280190043 ) ) ;
#150477 = CARTESIAN_POINT ( 'NONE',  ( -18.67979575497193778, 10.72451020669871902, 53.33442372801901854 ) ) ;
#150476 = CARTESIAN_POINT ( 'NONE',  ( -19.02544592524342804, 5.153800228976336051, 86.04057627198103830 ) ) ;
#150478 = CARTESIAN_POINT ( 'NONE',  ( 6.442991741790385696, -4.311730449243174945, -62.20106008945930398 ) ) ;
#150479 = CARTESIAN_POINT ( 'NONE',  ( -9.564922557960796823, -16.46253265017161027, 112.0822429386476955 ) ) ;
#150480 = DIRECTION ( 'NONE',  ( -1.000000000000000000, 0.000000000000000000, -0.000000000000000000 ) ) ;
#150483 = CARTESIAN_POINT ( 'NONE',  ( -21.55341960407619339, 5.719274019375674811, 63.54275706135234003 ) ) ;
#150482 = CARTESIAN_POINT ( 'NONE',  ( -8.224510206698735004, -14.34966873604973081, 69.58442372801900433 ) ) ;
#150481 = CARTESIAN_POINT ( 'NONE',  ( -4.483927247898782831, 16.52544592524335698, 57.70942372801901143 ) ) ;
#150484 = CARTESIAN_POINT ( 'NONE',  ( -15.72974639402176322, -15.80617190586768395, 84.37609039468570415 ) ) ;
#150485 = CARTESIAN_POINT ( 'NONE',  ( -12.25194888441104091, 10.91206588261560562, -59.27621954310795616 ) ) ;
#150486 = CARTESIAN_POINT ( 'NONE',  ( -12.14591786802326823, 12.06949235617739902, 28.12609039468568284 ) ) ;
#150487 = CARTESIAN_POINT ( 'NONE',  ( -9.474510206698964154, 16.51473224551069663, 75.41557627198103830 ) ) ;
#150488 = CARTESIAN_POINT ( 'NONE',  ( -19.02544592524342804, 5.153800228976336051, 106.0405762719810241 ) ) ;
#150489 = CARTESIAN_POINT ( 'NONE',  ( 17.05116617787827238, 6.768360034955703597, 43.84324446740802017 ) ) ;
#150490 = CARTESIAN_POINT ( 'NONE',  ( -13.97604488694527625, -13.89961937509977652, 21.87390960531435979 ) ) ;
#150491 = CARTESIAN_POINT ( 'NONE',  ( 18.62759615963271287, -10.81492255796078972, 38.33224293864768839 ) ) ;
#150492 = CARTESIAN_POINT ( 'NONE',  ( -4.379528057220086978, -16.55341960407618274, 89.79275706135236135 ) ) ;
#150494 = CARTESIAN_POINT ( 'NONE',  ( -13.97604488694527625, -13.89961937509977652, 61.87390960531435979 ) ) ;
#150493 = CARTESIAN_POINT ( 'NONE',  ( 16.53943276465976808, -0.05219959533910856209, 88.74890960531436690 ) ) ;
#150495 = CARTESIAN_POINT ( 'NONE',  ( -18.62759615963255300, -10.81492255796106328, 84.16775706135234714 ) ) ;
#150496 = CARTESIAN_POINT ( 'NONE',  ( 28.79475375365498380, -9.355982642740388044, 145.1656553485623817 ) ) ;
#150497 = CARTESIAN_POINT ( 'NONE',  ( -4.483927247898782831, 16.52544592524335698, 27.70942372801901854 ) ) ;
#150498 = CARTESIAN_POINT ( 'NONE',  ( -4.379528057220328563, 16.55341960407611168, 70.20724293864769550 ) ) ;
#150499 = CARTESIAN_POINT ( 'NONE',  ( -5.719274019375665041, -21.55341960407619695, 44.79275706135234714 ) ) ;
#150500 = CARTESIAN_POINT ( 'NONE',  ( 18.67979575497178502, 10.72451020669898547, 69.16557627198102409 ) ) ;
#150501 = CARTESIAN_POINT ( 'NONE',  ( 19.03943276465977164, 0.05219959533936151252, 41.25109039468566152 ) ) ;
#150502 = CARTESIAN_POINT ( 'NONE',  ( -9.474510206698964154, 16.51473224551069663, 45.41557627198103120 ) ) ;
#150503 = CARTESIAN_POINT ( 'NONE',  ( -16.51473224551069308, -9.474510206698971260, 86.66557627198102409 ) ) ;
#150504 = CARTESIAN_POINT ( 'NONE',  ( 16.52544592524342804, -4.483927247898539470, 48.54057627198103120 ) ) ;
#150505 = VECTOR ( 'NONE', #16273, 1000.000000000000000 ) ;
#150506 = CARTESIAN_POINT ( 'NONE',  ( 0.05219959533910956823, 16.53943276465976808, 29.99890960531435979 ) ) ;
#150507 = CARTESIAN_POINT ( 'NONE',  ( -14.34966873604972548, 8.224510206698743886, 113.3344237280190328 ) ) ;
#150508 = CARTESIAN_POINT ( 'NONE',  ( 0.05219959533936267826, -19.03943276465977164, 65.00109039468567573 ) ) ;
#150509 = CARTESIAN_POINT ( 'NONE',  ( 16.62475595723695321, 7.163666690055254804, 46.97286648189537317 ) ) ;
#150510 = CARTESIAN_POINT ( 'NONE',  ( -15.72974639402197994, 15.80617190586746368, 25.62390960531435624 ) ) ;
#150511 = CARTESIAN_POINT ( 'NONE',  ( -8.314922557960811034, -14.29746914071050412, 87.08224293864769550 ) ) ;
#150512 = DIRECTION ( 'NONE',  ( 4.336808689942017120E-17, 1.000000000000000000, 0.000000000000000000 ) ) ;
#150514 = CARTESIAN_POINT ( 'NONE',  ( -5.823673210054116645, -21.52544592524344225, 32.29057627198102409 ) ) ;
#150513 = CARTESIAN_POINT ( 'NONE',  ( 19.02544592524343514, -5.153800228976328945, 43.54057627198103120 ) ) ;
#150515 = CARTESIAN_POINT ( 'NONE',  ( 18.62759615963271287, -10.81492255796078972, 63.33224293864770260 ) ) ;
#150516 = CARTESIAN_POINT ( 'NONE',  ( -16.52544592524342804, 4.483927247898546575, 106.0405762719810525 ) ) ;
#150518 = CARTESIAN_POINT ( 'NONE',  ( 16.46253265017160672, -9.564922557960803928, 53.33224293864768839 ) ) ;
#150517 = CARTESIAN_POINT ( 'NONE',  ( 14.34966873604972726, -8.224510206698740333, 70.83442372801901854 ) ) ;
#150519 = CARTESIAN_POINT ( 'NONE',  ( -5.719274019375665041, -21.55341960407619695, 59.79275706135234714 ) ) ;
#150520 = CARTESIAN_POINT ( 'NONE',  ( 8.224510206698953496, -14.34966873604960469, 102.9155762719810383 ) ) ;
#150521 = CARTESIAN_POINT ( 'NONE',  ( 13.97604488694548053, -13.89961937509957401, 90.62609039468567573 ) ) ;
#150522 = CARTESIAN_POINT ( 'NONE',  ( 36.91746824999999887, -11.99521256947793546, -2.224999997268813701 ) ) ;
#150524 = CARTESIAN_POINT ( 'NONE',  ( 5.719274019375991003, -21.55341960407610458, 37.70724293864769550 ) ) ;
#150523 = CARTESIAN_POINT ( 'NONE',  ( -1.304248841091933035E-15, -21.30000000000002913, -58.85720012050612837 ) ) ;
#150525 = CARTESIAN_POINT ( 'NONE',  ( -19.03943276465977164, 0.05219959533909376836, 116.2489096053143669 ) ) ;
#150526 = CARTESIAN_POINT ( 'NONE',  ( -10.81492255796105439, 18.62759615963255655, 72.91775706135234714 ) ) ;
#150528 = CARTESIAN_POINT ( 'NONE',  ( 12.06949235617757843, -12.14591786802309237, 48.12390960531436690 ) ) ;
#150527 = CARTESIAN_POINT ( 'NONE',  ( 8.224510206698742110, 14.34966873604972548, 52.08442372801901854 ) ) ;
#150529 = CARTESIAN_POINT ( 'NONE',  ( -0.05219959533907301413, -21.53943276465977519, 62.49890960531436690 ) ) ;
#150530 = CARTESIAN_POINT ( 'NONE',  ( 21.53943276465977519, -0.05219959533907433946, 63.74890960531435979 ) ) ;
#150532 = CARTESIAN_POINT ( 'NONE',  ( 19.02544592524343514, -5.153800228976328945, 108.5405762719810383 ) ) ;
#150531 = CARTESIAN_POINT ( 'NONE',  ( -16.46253265017146816, -9.564922557961047289, 89.16775706135234714 ) ) ;
#150533 = CARTESIAN_POINT ( 'NONE',  ( -9.474510206698964154, 16.51473224551069663, 55.41557627198103120 ) ) ;
#150534 = CARTESIAN_POINT ( 'NONE',  ( -5.153800228976328057, -19.02544592524343514, 22.29057627198102765 ) ) ;
#150535 = CARTESIAN_POINT ( 'NONE',  ( -16.51473224551069308, -9.474510206698971260, 111.6655762719810383 ) ) ;
#150536 = VERTEX_POINT ( 'NONE', #16324 ) ;
#150537 = CARTESIAN_POINT ( 'NONE',  ( 16.55341960407618274, -4.379528057220086978, 71.04275706135234714 ) ) ;
#150538 = CARTESIAN_POINT ( 'NONE',  ( -10.81492255796078084, -18.62759615963271287, 107.0822429386476955 ) ) ;
#150539 = CARTESIAN_POINT ( 'NONE',  ( -5.049401038298153566, 19.05341960407611168, 70.20724293864769550 ) ) ;
#150540 = CARTESIAN_POINT ( 'NONE',  ( 21.53943276465977519, 0.05219959533937863772, 46.25109039468567573 ) ) ;
#150541 = CARTESIAN_POINT ( 'NONE',  ( -13.89961937509977652, 13.97604488694528158, 95.62390960531436690 ) ) ;
#150543 = ADVANCED_FACE ( 'NONE', ( #77974 ), #66415, .F. ) ;
#150542 = CARTESIAN_POINT ( 'NONE',  ( -23.38344545171685240, -32.96869167543736978, -17.70766473210117198 ) ) ;
#150544 = EDGE_LOOP ( 'NONE', ( #165945, #27356, #63978, #29419, #156296, #47566, #24620, #187074 ) ) ;
#150545 = CARTESIAN_POINT ( 'NONE',  ( -18.67979575497193778, 10.72451020669871902, 38.33442372801900433 ) ) ;
#150547 = CARTESIAN_POINT ( 'NONE',  ( -16.51473224551082808, 9.474510206698731452, 83.33442372801899012 ) ) ;
#150546 = CARTESIAN_POINT ( 'NONE',  ( 9.564922557960805705, 16.46253265017160317, 29.58224293864769550 ) ) ;
#150548 = CARTESIAN_POINT ( 'NONE',  ( -0.05219959533936034679, 19.03943276465977164, 42.50109039468566152 ) ) ;
#150549 = CARTESIAN_POINT ( 'NONE',  ( 5.719274019375673035, 21.55341960407619339, 22.29275706135235069 ) ) ;
#150550 = CARTESIAN_POINT ( 'NONE',  ( -9.564922557961040184, 16.46253265017147172, 37.91775706135233293 ) ) ;
#150551 = CARTESIAN_POINT ( 'NONE',  ( -5.153800228976607833, 19.02544592524334988, 47.70942372801900433 ) ) ;
#150552 = CARTESIAN_POINT ( 'NONE',  ( 16.52544592524335698, 4.483927247898782831, 91.45942372801901854 ) ) ;
#150554 = ORIENTED_EDGE ( 'NONE', *, *, #11846, .T. ) ;
#150553 = DIRECTION ( 'NONE',  ( -1.000000000000000000, 0.000000000000000000, 0.000000000000000000 ) ) ;
#150555 = CARTESIAN_POINT ( 'NONE',  ( -13.97604488694527625, -13.89961937509977652, 66.87390960531436690 ) ) ;
#150556 = AXIS2_PLACEMENT_3D ( 'NONE', #116612, #146951, #67105 ) ;
#150557 = CARTESIAN_POINT ( 'NONE',  ( 15.80617190586769283, -15.72974639402175789, 85.62609039468568994 ) ) ;
#150558 = CARTESIAN_POINT ( 'NONE',  ( -10.81492255796105439, 18.62759615963255655, 97.91775706135236135 ) ) ;
#150559 = CARTESIAN_POINT ( 'NONE',  ( 5.000000000000000000, -139.2199041982123617, 21.73825240834792538 ) ) ;
#150560 = CARTESIAN_POINT ( 'NONE',  ( 19.02544592524343514, -5.153800228976328945, 88.54057627198102409 ) ) ;
#150561 = CARTESIAN_POINT ( 'NONE',  ( 21.52544592524334988, 5.823673210054432836, 61.45942372801901854 ) ) ;
#150562 = CARTESIAN_POINT ( 'NONE',  ( -5.153800228976607833, 19.02544592524334988, 102.7094237280189759 ) ) ;
#150563 = CARTESIAN_POINT ( 'NONE',  ( 9.474510206698971260, -16.51473224551069308, 67.91557627198102409 ) ) ;
#150564 = CARTESIAN_POINT ( 'NONE',  ( 18.62759615963271287, -10.81492255796078972, 23.33224293864769194 ) ) ;
#150565 = CARTESIAN_POINT ( 'NONE',  ( 16.46253265017160672, -9.564922557960803928, 78.33224293864769550 ) ) ;
#150566 = CARTESIAN_POINT ( 'NONE',  ( 13.89961937509978007, -13.97604488694527269, 78.12390960531435269 ) ) ;
#150567 = CARTESIAN_POINT ( 'NONE',  ( 16.46253265017160672, -9.564922557960803928, 68.33224293864770971 ) ) ;
#150568 = CARTESIAN_POINT ( 'NONE',  ( -16.46253265017160317, 9.564922557960807481, 50.83224293864770260 ) ) ;
#150569 = CARTESIAN_POINT ( 'NONE',  ( -18.62759615963270932, 10.81492255796079327, 110.8322429386476955 ) ) ;
#150570 = CARTESIAN_POINT ( 'NONE',  ( 8.314922557961029526, -14.29746914071037800, 85.41775706135236135 ) ) ;
#150571 = CARTESIAN_POINT ( 'NONE',  ( 4.999999999999997335, 0.000000000000000000, 0.000000000000000000 ) ) ;
#150572 = CARTESIAN_POINT ( 'NONE',  ( -5.049401038297874678, -19.05341960407617918, 59.79275706135231871 ) ) ;
#150573 = CARTESIAN_POINT ( 'NONE',  ( 0.05219959533909260263, 19.03943276465977164, 79.99890960531436690 ) ) ;
#150574 = CARTESIAN_POINT ( 'NONE',  ( 14.29746914071049879, -8.314922557960816363, 78.33224293864770971 ) ) ;
#150575 = CARTESIAN_POINT ( 'NONE',  ( 4.379528057220339221, -16.55341960407611168, 112.7072429386476955 ) ) ;
#150576 = CARTESIAN_POINT ( 'NONE',  ( 16.46253265017160672, -9.564922557960803928, 113.3322429386476955 ) ) ;
#150577 = CARTESIAN_POINT ( 'NONE',  ( -16.46253265017160317, 9.564922557960807481, 110.8322429386476955 ) ) ;
#150578 = CARTESIAN_POINT ( 'NONE',  ( -8.224510206698948167, 14.34966873604960824, 75.41557627198102409 ) ) ;
#150579 = CARTESIAN_POINT ( 'NONE',  ( 13.97604488694527802, 13.89961937509977652, 114.3739096053143669 ) ) ;
#150580 = CARTESIAN_POINT ( 'NONE',  ( -5.049401038297874678, -19.05341960407617918, 29.79275706135232227 ) ) ;
#150581 = CARTESIAN_POINT ( 'NONE',  ( 14.34966873604972726, -8.224510206698740333, 105.8344237280190328 ) ) ;
#150582 = CARTESIAN_POINT ( 'NONE',  ( 9.474510206698971260, -16.51473224551069308, 87.91557627198102409 ) ) ;
#150583 = CARTESIAN_POINT ( 'NONE',  ( -21.55341960407619339, 5.719274019375674811, 53.54275706135234714 ) ) ;
#150584 = CARTESIAN_POINT ( 'NONE',  ( 5.719274019375991003, -21.55341960407610458, 42.70724293864770260 ) ) ;
#150585 = CARTESIAN_POINT ( 'NONE',  ( 18.62759615963255655, 10.81492255796105972, 21.66775706135235069 ) ) ;
#150586 = CARTESIAN_POINT ( 'NONE',  ( 21.55341960407610458, 5.719274019375980345, 63.95724293864770260 ) ) ;
#150587 = CARTESIAN_POINT ( 'NONE',  ( 16.52544592524342804, -4.483927247898539470, 88.54057627198103830 ) ) ;
#150588 = CARTESIAN_POINT ( 'NONE',  ( -0.05219959533936034679, 19.03943276465977164, 52.50109039468566863 ) ) ;
#150589 = CARTESIAN_POINT ( 'NONE',  ( -19.02544592524342804, 5.153800228976336051, 26.04057627198103120 ) ) ;
#150590 = CARTESIAN_POINT ( 'NONE',  ( 19.02544592524343514, -5.153800228976328945, 83.54057627198100988 ) ) ;
#150591 = CARTESIAN_POINT ( 'NONE',  ( 9.564922557960805705, 16.46253265017160317, 79.58224293864769550 ) ) ;
#150592 = CARTESIAN_POINT ( 'NONE',  ( -16.52544592524342804, 4.483927247898546575, 106.0405762719810525 ) ) ;
#150593 = VERTEX_POINT ( 'NONE', #170993 ) ;
#150594 = VECTOR ( 'NONE', #168124, 1000.000000000000000 ) ;
#150595 = CARTESIAN_POINT ( 'NONE',  ( -4.379528057220328563, 16.55341960407611168, 30.20724293864769550 ) ) ;
#150596 = CARTESIAN_POINT ( 'NONE',  ( 8.224510206698742110, 14.34966873604972548, 42.08442372801901854 ) ) ;
#150597 = CARTESIAN_POINT ( 'NONE',  ( 10.72451020669871369, 18.67979575497193778, 112.0844237280190185 ) ) ;
#150598 = CARTESIAN_POINT ( 'NONE',  ( -19.05341960407611168, -5.049401038298163336, 96.45724293864769550 ) ) ;
#150599 = CARTESIAN_POINT ( 'NONE',  ( -18.62759615963255300, -10.81492255796106328, 39.16775706135235424 ) ) ;
#150600 = CARTESIAN_POINT ( 'NONE',  ( 13.89961937509977652, -13.97604488694527269, 43.12390960531434558 ) ) ;
#150601 = AXIS2_PLACEMENT_3D ( 'NONE', #124605, #182326, #120629 ) ;
#150602 = CARTESIAN_POINT ( 'NONE',  ( -16.55341960407617563, 4.379528057220093196, 48.54275706135234714 ) ) ;
#150603 = CARTESIAN_POINT ( 'NONE',  ( -16.52544592524335698, -4.483927247898792601, 78.95942372801901854 ) ) ;
#150604 = CARTESIAN_POINT ( 'NONE',  ( -0.05219959533936034679, 19.03943276465977164, 112.5010903946856757 ) ) ;
#150605 = CARTESIAN_POINT ( 'NONE',  ( -9.564922557960796823, -16.46253265017161027, 37.08224293864768839 ) ) ;
#150606 = CARTESIAN_POINT ( 'NONE',  ( -8.314922557960811034, -14.29746914071050412, 92.08224293864769550 ) ) ;
#150607 = CARTESIAN_POINT ( 'NONE',  ( 5.823673210054125526, 21.52544592524343514, 109.7905762719810383 ) ) ;
#150608 = CARTESIAN_POINT ( 'NONE',  ( 19.02544592524334988, 5.153800228976608722, 86.45942372801900433 ) ) ;
#150609 = CARTESIAN_POINT ( 'NONE',  ( 16.51473224551069308, 9.474510206698969483, 34.16557627198102409 ) ) ;
#150610 = CARTESIAN_POINT ( 'NONE',  ( 19.03943276465977164, -0.05219959533909143690, 93.74890960531435269 ) ) ;
#150611 = CARTESIAN_POINT ( 'NONE',  ( 15.72974639402176855, 15.80617190586768217, 26.87609039468567218 ) ) ;
#150612 = CARTESIAN_POINT ( 'NONE',  ( -23.48298174826590667, 32.32155151706776053, -4.047842220587802409 ) ) ;
#150613 = CARTESIAN_POINT ( 'NONE',  ( 13.89961937509977652, -13.97604488694527269, 98.12390960531433848 ) ) ;
#150614 = CARTESIAN_POINT ( 'NONE',  ( 16.29526858892874941, -7.335722546920136367, 111.7032940219980048 ) ) ;
#150615 = CARTESIAN_POINT ( 'NONE',  ( 16.46253265017160672, -9.564922557960803928, 88.33224293864769550 ) ) ;
#150617 = CARTESIAN_POINT ( 'NONE',  ( -12.06949235617756955, 12.14591786802309770, 85.62390960531436690 ) ) ;
#150616 = CARTESIAN_POINT ( 'NONE',  ( -21.52544592524334988, -5.823673210054445271, 38.95942372801901854 ) ) ;
#150618 = CARTESIAN_POINT ( 'NONE',  ( -19.02544592524342804, 5.153800228976336051, 96.04057627198103830 ) ) ;
#150619 = CARTESIAN_POINT ( 'NONE',  ( -19.03943276465977164, -0.05219959533935918106, 18.75109039468567218 ) ) ;
#150620 = CARTESIAN_POINT ( 'NONE',  ( 0.05219959533934541429, -16.53943276465976808, 55.00109039468568284 ) ) ;
#150621 = CARTESIAN_POINT ( 'NONE',  ( 10.81492255796106328, -18.62759615963255655, 80.41775706135234714 ) ) ;
#150622 = CARTESIAN_POINT ( 'NONE',  ( 14.29746914071037800, 8.314922557961029526, 41.66775706135235424 ) ) ;
#150623 = CARTESIAN_POINT ( 'NONE',  ( 9.474510206698971260, -16.51473224551069308, 67.91557627198102409 ) ) ;
#150624 = CARTESIAN_POINT ( 'NONE',  ( 19.05341960407617918, -5.049401038297876454, 91.04275706135234714 ) ) ;
#150625 = CARTESIAN_POINT ( 'NONE',  ( -12.14591786802326823, 12.06949235617739902, 68.12609039468567573 ) ) ;
#150626 = CARTESIAN_POINT ( 'NONE',  ( -15.80617190586768217, 15.72974639402176855, 108.1260903946856757 ) ) ;
#150627 = CARTESIAN_POINT ( 'NONE',  ( 16.46253265017146816, 9.564922557961045513, 81.66775706135233293 ) ) ;
#150628 = CARTESIAN_POINT ( 'NONE',  ( -9.474510206698964154, 16.51473224551069663, 60.41557627198102409 ) ) ;
#150629 = CARTESIAN_POINT ( 'NONE',  ( 10.81492255796078972, 18.62759615963270932, 79.58224293864769550 ) ) ;
#150631 = CARTESIAN_POINT ( 'NONE',  ( -19.05341960407617563, 5.049401038297882671, 83.54275706135233293 ) ) ;
#150630 = CARTESIAN_POINT ( 'NONE',  ( -16.55341960407611168, -4.379528057220339221, 81.45724293864769550 ) ) ;
#150632 = CARTESIAN_POINT ( 'NONE',  ( -18.87580814761074777, 5.500000000000053291, 80.87172394265761000 ) ) ;
#150633 = CARTESIAN_POINT ( 'NONE',  ( -0.05219959533936034679, 19.03943276465977164, 62.50109039468566863 ) ) ;
#150634 = CARTESIAN_POINT ( 'NONE',  ( 16.53943276465976808, 0.05219959533934440121, 111.2510903946856899 ) ) ;
#150635 = CARTESIAN_POINT ( 'NONE',  ( 8.224510206698953496, -14.34966873604960469, 82.91557627198103830 ) ) ;
#150637 = CARTESIAN_POINT ( 'NONE',  ( -27.73933785331498925, 2.428612866367529932E-14, 148.8750000027311842 ) ) ;
#150636 = CARTESIAN_POINT ( 'NONE',  ( 9.474510206698729675, 16.51473224551082808, 27.08442372801900433 ) ) ;
#150638 = CARTESIAN_POINT ( 'NONE',  ( 21.52544592524344225, -5.823673210054117533, 113.5405762719810383 ) ) ;
#150639 = CARTESIAN_POINT ( 'NONE',  ( 19.02544592524343514, -5.153800228976328945, 98.54057627198100988 ) ) ;
#150640 = CARTESIAN_POINT ( 'NONE',  ( 19.05341960407611168, 5.049401038298154454, 73.95724293864768129 ) ) ;
#150641 = CARTESIAN_POINT ( 'NONE',  ( 21.55341960407619695, -5.719274019375665929, 81.04275706135236135 ) ) ;
#150642 = CARTESIAN_POINT ( 'NONE',  ( 5.049401038298161559, -19.05341960407611168, 57.70724293864769550 ) ) ;
#150643 = CARTESIAN_POINT ( 'NONE',  ( 16.46253265017160672, -9.564922557960803928, 38.33224293864768839 ) ) ;
#150644 = CARTESIAN_POINT ( 'NONE',  ( 21.53943276465977519, -0.05219959533907433946, 33.74890960531436690 ) ) ;
#150645 = CARTESIAN_POINT ( 'NONE',  ( -8.224510206698948167, 14.34966873604960824, 75.41557627198102409 ) ) ;
#150646 = CARTESIAN_POINT ( 'NONE',  ( -13.97604488694527625, -13.89961937509977652, 41.87390960531435979 ) ) ;
#150647 = CARTESIAN_POINT ( 'NONE',  ( -12.06949235617756955, 12.14591786802309770, 95.62390960531436690 ) ) ;
#150648 = CARTESIAN_POINT ( 'NONE',  ( 5.823673210054125526, 21.52544592524343514, 109.7905762719810383 ) ) ;
#150649 = CARTESIAN_POINT ( 'NONE',  ( -21.55341960407619339, 5.719274019375674811, 53.54275706135234714 ) ) ;
#150650 = CARTESIAN_POINT ( 'NONE',  ( 13.97604488694527802, 13.89961937509977652, 24.37390960531435624 ) ) ;
#150651 = CARTESIAN_POINT ( 'NONE',  ( 14.34966873604972726, -8.224510206698740333, 65.83442372801900433 ) ) ;
#150652 = CARTESIAN_POINT ( 'NONE',  ( 18.62759615963271287, -10.81492255796078972, 98.33224293864769550 ) ) ;
#150653 = CARTESIAN_POINT ( 'NONE',  ( -21.53943276465977519, 0.05219959533907696930, 101.2489096053143669 ) ) ;
#150655 = CARTESIAN_POINT ( 'NONE',  ( -5.153800228976328057, -19.02544592524343514, 47.29057627198102409 ) ) ;
#150654 = CARTESIAN_POINT ( 'NONE',  ( 19.05341960407617918, -5.049401038297876454, 41.04275706135233293 ) ) ;
#150656 = CARTESIAN_POINT ( 'NONE',  ( 19.03943276465977164, -0.05219959533909143690, 113.7489096053143669 ) ) ;
#150657 = CARTESIAN_POINT ( 'NONE',  ( 0.05219959533937995610, -21.53943276465977519, 60.00109039468568284 ) ) ;
#150658 = CARTESIAN_POINT ( 'NONE',  ( 5.719274019375991003, -21.55341960407610458, 52.70724293864769550 ) ) ;
#150659 = CARTESIAN_POINT ( 'NONE',  ( 14.29746914071049879, -8.314922557960816363, 43.33224293864769550 ) ) ;
#150661 = CARTESIAN_POINT ( 'NONE',  ( -5.719274019375665041, -21.55341960407619695, 109.7927570613523613 ) ) ;
#150660 = CARTESIAN_POINT ( 'NONE',  ( 21.53943276465977519, 0.05219959533937863772, 81.25109039468568994 ) ) ;
#150662 = CARTESIAN_POINT ( 'NONE',  ( -16.51473224551082808, 9.474510206698731452, 43.33442372801900433 ) ) ;
#150663 = CARTESIAN_POINT ( 'NONE',  ( -4.483927247898782831, 16.52544592524335698, 102.7094237280190185 ) ) ;
#150664 = CARTESIAN_POINT ( 'NONE',  ( 0.05219959533937995610, -21.53943276465977519, 60.00109039468568284 ) ) ;
#150665 = CARTESIAN_POINT ( 'NONE',  ( -0.05219959533909027116, -19.03943276465977164, 57.49890960531435979 ) ) ;
#150666 = CARTESIAN_POINT ( 'NONE',  ( -19.03943276465977164, -0.05219959533935918106, 28.75109039468566507 ) ) ;
#150667 = CARTESIAN_POINT ( 'NONE',  ( -10.81492255796078084, -18.62759615963271287, 37.08224293864768129 ) ) ;
#150668 = CARTESIAN_POINT ( 'NONE',  ( -15.72974639402176322, -15.80617190586768395, 29.37609039468568284 ) ) ;
#150669 = CARTESIAN_POINT ( 'NONE',  ( 10.81492255796078972, 18.62759615963270932, 89.58224293864768129 ) ) ;
#150670 = CARTESIAN_POINT ( 'NONE',  ( 13.97604488694548053, -13.89961937509957401, 90.62609039468567573 ) ) ;
#150671 = CARTESIAN_POINT ( 'NONE',  ( -12.06949235617739369, -12.14591786802326823, 59.37609039468568284 ) ) ;
#150673 = CARTESIAN_POINT ( 'NONE',  ( 0.05219959533907565091, 21.53943276465977519, 99.99890960531436690 ) ) ;
#150672 = CARTESIAN_POINT ( 'NONE',  ( -19.03943276465977164, -0.05219959533935946555, 18.75109039468567218 ) ) ;
#150675 = CARTESIAN_POINT ( 'NONE',  ( 16.52544592524342804, -4.483927247898539470, 73.54057627198102409 ) ) ;
#150674 = CARTESIAN_POINT ( 'NONE',  ( 16.55341960407618274, -4.379528057220086978, 81.04275706135236135 ) ) ;
#150676 = CARTESIAN_POINT ( 'NONE',  ( -16.20579543436678449, -7.371946100355109444, 100.5652083417188152 ) ) ;
#150677 = CARTESIAN_POINT ( 'NONE',  ( 5.153800228976615827, -19.02544592524334988, 110.2094237280189901 ) ) ;
#150678 = EDGE_CURVE ( 'NONE', #118125, #22637, #118257, .T. ) ;
#150679 = CARTESIAN_POINT ( 'NONE',  ( 0.05219959533907565091, 21.53943276465977519, 29.99890960531435979 ) ) ;
#150680 = CARTESIAN_POINT ( 'NONE',  ( -11.30153831258471442, -180.0000000000000000, -25.00000000000000000 ) ) ;
#150681 = CARTESIAN_POINT ( 'NONE',  ( 8.224510206698742110, 14.34966873604972548, 52.08442372801901854 ) ) ;
#150682 = CARTESIAN_POINT ( 'NONE',  ( 5.719274019375673035, 21.55341960407619339, 32.29275706135235424 ) ) ;
#150683 = CARTESIAN_POINT ( 'NONE',  ( -15.80617190586745835, -15.72974639402198527, 51.87390960531437401 ) ) ;
#150684 = CARTESIAN_POINT ( 'NONE',  ( 8.224510206698742110, 14.34966873604972548, 67.08442372801901854 ) ) ;
#150685 = CARTESIAN_POINT ( 'NONE',  ( 13.89961937509977652, -13.97604488694527269, 83.12390960531436690 ) ) ;
#150687 = CARTESIAN_POINT ( 'NONE',  ( -5.049401038298153566, 19.05341960407611168, 30.20724293864768839 ) ) ;
#150686 = CARTESIAN_POINT ( 'NONE',  ( -5.823673210054431948, 21.52544592524334988, 52.70942372801902565 ) ) ;
#150688 = CARTESIAN_POINT ( 'NONE',  ( 0.05219959533907565091, 21.53943276465977519, 29.99890960531435979 ) ) ;
#150689 = EDGE_LOOP ( 'NONE', ( #5992, #91522, #172861, #115437 ) ) ;
#150690 = CARTESIAN_POINT ( 'NONE',  ( -9.474510206698720793, -16.51473224551083518, 39.58442372801899722 ) ) ;
#150691 = CARTESIAN_POINT ( 'NONE',  ( -0.05219959533934338120, 16.53943276465976808, 47.50109039468568994 ) ) ;
#150692 = CARTESIAN_POINT ( 'NONE',  ( 21.52544592524344225, -5.823673210054117533, 23.54057627198102765 ) ) ;
#150693 = ORIENTED_EDGE ( 'NONE', *, *, #65800, .F. ) ;
#150694 = CARTESIAN_POINT ( 'NONE',  ( -9.564922557960796823, -16.46253265017161027, 87.08224293864769550 ) ) ;
#150695 = CARTESIAN_POINT ( 'NONE',  ( 16.52544592524335698, 4.483927247898782831, 96.45942372801901854 ) ) ;
#150696 = CARTESIAN_POINT ( 'NONE',  ( 8.898068258721465895, 27.38543819252877398, 141.6656553485623817 ) ) ;
#150697 = CARTESIAN_POINT ( 'NONE',  ( 0.05219959533910956823, 16.53943276465976808, 99.99890960531436690 ) ) ;
#150698 = CARTESIAN_POINT ( 'NONE',  ( -21.55341960407610458, -5.719274019375992779, 31.45724293864769550 ) ) ;
#150699 = CARTESIAN_POINT ( 'NONE',  ( -0.05219959533909027116, -19.03943276465977164, 37.49890960531436690 ) ) ;
#150700 = CARTESIAN_POINT ( 'NONE',  ( 16.53943276465976808, 0.05219959533934440121, 76.25109039468568994 ) ) ;
#150701 = CARTESIAN_POINT ( 'NONE',  ( 10.72451020669871369, 18.67979575497193778, 22.08442372801901143 ) ) ;
#150702 = CARTESIAN_POINT ( 'NONE',  ( -13.97604488694547697, 13.89961937509957934, 83.12609039468564731 ) ) ;
#150703 = CARTESIAN_POINT ( 'NONE',  ( -13.97604488694527625, -13.89961937509977652, 46.87390960531435979 ) ) ;
#150704 = AXIS2_PLACEMENT_3D ( 'NONE', #147875, #71026, #179221 ) ;
#150705 = CARTESIAN_POINT ( 'NONE',  ( 16.46253265017160672, -9.564922557960803928, 113.3322429386476955 ) ) ;
#150706 = CARTESIAN_POINT ( 'NONE',  ( 15.72974639402176855, 15.80617190586768217, 111.8760903946856615 ) ) ;
#150707 = CARTESIAN_POINT ( 'NONE',  ( 16.51473224551069308, 9.474510206698969483, 59.16557627198102409 ) ) ;
#150708 = CARTESIAN_POINT ( 'NONE',  ( 4.483927247898790824, -16.52544592524335698, 45.20942372801901854 ) ) ;
#150709 = CARTESIAN_POINT ( 'NONE',  ( -21.53943276465977519, -0.05219959533937600094, 93.75109039468567573 ) ) ;
#150710 = CARTESIAN_POINT ( 'NONE',  ( 19.02544592524334988, 5.153800228976608722, 41.45942372801900433 ) ) ;
#150711 = CARTESIAN_POINT ( 'NONE',  ( -5.153800228976607833, 19.02544592524334988, 57.70942372801899012 ) ) ;
#150712 = ORIENTED_EDGE ( 'NONE', *, *, #89344, .F. ) ;
#150713 = CARTESIAN_POINT ( 'NONE',  ( -15.72974639402176322, -15.80617190586768395, 44.37609039468567573 ) ) ;
#150714 = CARTESIAN_POINT ( 'NONE',  ( -17.58332526062525858, 7.635886036038558977, 55.92334959558466068 ) ) ;
#150715 = CARTESIAN_POINT ( 'NONE',  ( -19.02544592524334988, -5.153800228976617603, 43.95942372801899012 ) ) ;
#150716 = CARTESIAN_POINT ( 'NONE',  ( 9.564922557960805705, 16.46253265017160317, 99.58224293864770971 ) ) ;
#150717 = CARTESIAN_POINT ( 'NONE',  ( 16.46253265017160672, -9.564922557960803928, 78.33224293864769550 ) ) ;
#150718 = CARTESIAN_POINT ( 'NONE',  ( -16.55341960407611168, -4.379528057220339221, 31.45724293864769550 ) ) ;
#150719 = CARTESIAN_POINT ( 'NONE',  ( -10.72451020669898014, 18.67979575497178502, 35.41557627198102409 ) ) ;
#150720 = CARTESIAN_POINT ( 'NONE',  ( -29.86685920354755552, 21.69954338932564397, -1.324999997268813345 ) ) ;
#150721 = CARTESIAN_POINT ( 'NONE',  ( 0.000000000000000000, 0.000000000000000000, 10.00000000000000000 ) ) ;
#150722 = CARTESIAN_POINT ( 'NONE',  ( -15.80617190586768217, 15.72974639402176855, 93.12609039468568994 ) ) ;
#150723 = CARTESIAN_POINT ( 'NONE',  ( -27.95720134624904318, 7.331398113985295062, 160.9065205403411767 ) ) ;
#150724 = CARTESIAN_POINT ( 'NONE',  ( 16.51473224551069308, 9.474510206698969483, 34.16557627198102409 ) ) ;
#150725 = CARTESIAN_POINT ( 'NONE',  ( 13.97604488694527802, 13.89961937509977652, 109.3739096053143669 ) ) ;
#150726 = CARTESIAN_POINT ( 'NONE',  ( -37.99626262588765968, -12.34573411038913626, -1.902157773949822772 ) ) ;
#150727 = CARTESIAN_POINT ( 'NONE',  ( 16.55341960407618274, -4.379528057220086978, 61.04275706135234714 ) ) ;
#150728 = CARTESIAN_POINT ( 'NONE',  ( -5.719274019375978568, 21.55341960407610458, 85.20724293864770971 ) ) ;
#150729 = CARTESIAN_POINT ( 'NONE',  ( 14.34966873604960469, 8.224510206698951720, 44.16557627198103120 ) ) ;
#150731 = CARTESIAN_POINT ( 'NONE',  ( 19.03943276465977164, -0.05219959533909143690, 108.7489096053143527 ) ) ;
#150730 = CARTESIAN_POINT ( 'NONE',  ( 5.049401038298161559, -19.05341960407611168, 32.70724293864768129 ) ) ;
#150732 = CARTESIAN_POINT ( 'NONE',  ( -18.67979575497193778, 10.72451020669871902, 23.33442372801901499 ) ) ;
#150733 = CARTESIAN_POINT ( 'NONE',  ( -5.049401038297874678, -19.05341960407617918, 39.79275706135232582 ) ) ;
#150734 = CARTESIAN_POINT ( 'NONE',  ( 9.564922557960805705, 16.46253265017160317, 39.58224293864768839 ) ) ;
#150735 = CARTESIAN_POINT ( 'NONE',  ( 21.52544592524334988, 5.823673210054432836, 86.45942372801901854 ) ) ;
#150736 = DIRECTION ( 'NONE',  ( -0.000000000000000000, -0.000000000000000000, 1.000000000000000000 ) ) ;
#150737 = CARTESIAN_POINT ( 'NONE',  ( -8.314922557960811034, -14.29746914071050412, 22.08224293864769194 ) ) ;
#150738 = CARTESIAN_POINT ( 'NONE',  ( -3.573655867282028392E-15, 2.428612866367529932E-14, 169.9999999999999716 ) ) ;
#150739 = CARTESIAN_POINT ( 'NONE',  ( 15.72974639402199770, -15.80617190586745480, 33.12390960531435979 ) ) ;
#150740 = CARTESIAN_POINT ( 'NONE',  ( 12.06949235617757843, -12.14591786802309237, 108.1239096053143811 ) ) ;
#150741 = CARTESIAN_POINT ( 'NONE',  ( -3.981139134329680029, -5.949693216777165006, -64.35446363059463692 ) ) ;
#150742 = CONICAL_SURFACE ( 'NONE', #176569, 38.00373040315628259, 0.06108652381980166773 ) ;
#150743 = CARTESIAN_POINT ( 'NONE',  ( -5.153800228976328057, -19.02544592524343514, 87.29057627198103830 ) ) ;
#150744 = CARTESIAN_POINT ( 'NONE',  ( -16.53943276465976808, 0.05219959533911058130, 76.24890960531435269 ) ) ;
#150745 = CARTESIAN_POINT ( 'NONE',  ( -5.153800228976607833, 19.02544592524334988, 107.7094237280189759 ) ) ;
#150746 = ADVANCED_FACE ( 'NONE', ( #115295 ), #194153, .T. ) ;
#150747 = CARTESIAN_POINT ( 'NONE',  ( 18.67979575497178502, 10.72451020669898547, 64.16557627198102409 ) ) ;
#150748 = ORIENTED_EDGE ( 'NONE', *, *, #25084, .T. ) ;
#150749 = CARTESIAN_POINT ( 'NONE',  ( 16.51473224551069308, 9.474510206698969483, 29.16557627198103475 ) ) ;
#150751 = CARTESIAN_POINT ( 'NONE',  ( -21.52544592524343514, 5.823673210054127303, 91.04057627198103830 ) ) ;
#150750 = CARTESIAN_POINT ( 'NONE',  ( 13.97604488694527802, 13.89961937509977652, 84.37390960531433848 ) ) ;
#150753 = CARTESIAN_POINT ( 'NONE',  ( -0.05219959533909027116, -19.03943276465977164, 92.49890960531436690 ) ) ;
#150752 = CARTESIAN_POINT ( 'NONE',  ( -12.06949235617739369, -12.14591786802326823, 99.37609039468568994 ) ) ;
#150754 = CARTESIAN_POINT ( 'NONE',  ( 5.049401038297881783, 19.05341960407617563, 82.29275706135229029 ) ) ;
#150755 = CARTESIAN_POINT ( 'NONE',  ( 21.55341960407619695, -5.719274019375665929, 101.0427570613523756 ) ) ;
#150756 = CARTESIAN_POINT ( 'NONE',  ( 5.823673210054125526, 21.52544592524343514, 79.79057627198102409 ) ) ;
#150757 = CARTESIAN_POINT ( 'NONE',  ( -15.80617190586745835, -15.72974639402198527, 36.87390960531435979 ) ) ;
#150758 = CARTESIAN_POINT ( 'NONE',  ( -5.153800228976328057, -19.02544592524343514, 47.29057627198102409 ) ) ;
#150759 = CARTESIAN_POINT ( 'NONE',  ( 8.224510206698742110, 14.34966873604972548, 112.0844237280190185 ) ) ;
#150760 = CARTESIAN_POINT ( 'NONE',  ( 16.51473224551069308, 9.474510206698969483, 69.16557627198102409 ) ) ;
#150761 = CARTESIAN_POINT ( 'NONE',  ( 17.58332526062524437, 7.635886036038643354, 81.57665040441534643 ) ) ;
#150762 = CARTESIAN_POINT ( 'NONE',  ( 15.72974639402176855, 15.80617190586768217, 106.8760903946856899 ) ) ;
#150763 = CARTESIAN_POINT ( 'NONE',  ( -14.34966873604960291, -8.224510206698953496, 76.66557627198103830 ) ) ;
#150764 = CARTESIAN_POINT ( 'NONE',  ( 18.62759615963271287, -10.81492255796078972, 108.3322429386477097 ) ) ;
#150765 = CARTESIAN_POINT ( 'NONE',  ( -21.52544592524343514, 5.823673210054127303, 111.0405762719810525 ) ) ;
#150766 = CARTESIAN_POINT ( 'NONE',  ( -17.49999999999999645, 5.499999999999997335, 120.0000000000000142 ) ) ;
#150767 = CARTESIAN_POINT ( 'NONE',  ( -5.823673210054116645, -21.52544592524344225, 57.29057627198103120 ) ) ;
#150768 = CARTESIAN_POINT ( 'NONE',  ( 14.29746914071037800, 8.314922557961029526, 96.66775706135234714 ) ) ;
#150769 = CARTESIAN_POINT ( 'NONE',  ( -16.52544592524342804, 4.483927247898546575, 111.0405762719810525 ) ) ;
#150770 = CARTESIAN_POINT ( 'NONE',  ( -9.474510206698964154, 16.51473224551069663, 55.41557627198103120 ) ) ;
#150771 =( LENGTH_UNIT ( ) NAMED_UNIT ( * ) SI_UNIT ( .MILLI., .METRE. ) );
#150772 = CARTESIAN_POINT ( 'NONE',  ( 16.53943276465976808, 0.05219959533934440121, 106.2510903946856757 ) ) ;
#150773 = ORIENTED_EDGE ( 'NONE', *, *, #133407, .T. ) ;
#150774 = CARTESIAN_POINT ( 'NONE',  ( 5.823673210054444382, -21.52544592524334988, 50.20942372801901854 ) ) ;
#150775 = CARTESIAN_POINT ( 'NONE',  ( 19.02544592524343514, -5.153800228976328945, 108.5405762719810383 ) ) ;
#150776 = CARTESIAN_POINT ( 'NONE',  ( -0.05219959533937732626, 21.53943276465977519, 82.50109039468568994 ) ) ;
#150777 = CARTESIAN_POINT ( 'NONE',  ( 13.97604488694527802, 13.89961937509977652, 29.37390960531435979 ) ) ;
#150778 = CARTESIAN_POINT ( 'NONE',  ( 19.03943276465977164, -0.05219959533909143690, 43.74890960531435979 ) ) ;
#150779 = VERTEX_POINT ( 'NONE', #53619 ) ;
#150780 = CARTESIAN_POINT ( 'NONE',  ( 5.719274019375673035, 21.55341960407619339, 77.29275706135234714 ) ) ;
#150781 = CARTESIAN_POINT ( 'NONE',  ( -5.823673210054431948, 21.52544592524334988, 67.70942372801901854 ) ) ;
#150782 = CARTESIAN_POINT ( 'NONE',  ( -9.474510206698964154, 16.51473224551069663, 105.4155762719810383 ) ) ;
#150783 = CARTESIAN_POINT ( 'NONE',  ( -5.049401038297874678, -19.05341960407617918, 74.79275706135231871 ) ) ;
#150784 = CARTESIAN_POINT ( 'NONE',  ( -15.72974639402176322, -15.80617190586768395, 54.37609039468568994 ) ) ;
#150785 = CARTESIAN_POINT ( 'NONE',  ( -0.05219959533934338120, 16.53943276465976808, 27.50109039468567929 ) ) ;
#150786 = CARTESIAN_POINT ( 'NONE',  ( -9.564922557961040184, 16.46253265017147172, 72.91775706135233293 ) ) ;
#150787 = CARTESIAN_POINT ( 'NONE',  ( -16.51473224551069308, -9.474510206698971260, 51.66557627198102409 ) ) ;
#150788 = CARTESIAN_POINT ( 'NONE',  ( -13.97604488694547697, 13.89961937509957934, 78.12609039468567573 ) ) ;
#150789 = CARTESIAN_POINT ( 'NONE',  ( 8.224510206698742110, 14.34966873604972548, 112.0844237280190185 ) ) ;
#150790 = CARTESIAN_POINT ( 'NONE',  ( -16.46253265017146816, -9.564922557961047289, 94.16775706135233293 ) ) ;
#150791 = CARTESIAN_POINT ( 'NONE',  ( 14.29746914071049879, -8.314922557960816363, 33.33224293864769550 ) ) ;
#150792 = CARTESIAN_POINT ( 'NONE',  ( -5.049401038297874678, -19.05341960407617918, 59.79275706135231871 ) ) ;
#150793 = CARTESIAN_POINT ( 'NONE',  ( 16.55341960407618274, -4.379528057220086978, 46.04275706135234714 ) ) ;
#150794 = CARTESIAN_POINT ( 'NONE',  ( 0.05219959533936267826, -19.03943276465977164, 25.00109039468566152 ) ) ;
#150795 = CARTESIAN_POINT ( 'NONE',  ( -13.89961937509977652, 13.97604488694528158, 40.62390960531435979 ) ) ;
#150796 = CARTESIAN_POINT ( 'NONE',  ( 18.39635199886970440, -5.499999999999976019, 73.51967076360001840 ) ) ;
#150797 = CARTESIAN_POINT ( 'NONE',  ( -12.14591786802326823, 12.06949235617739902, 48.12609039468568284 ) ) ;
#150798 = DIRECTION ( 'NONE',  ( 0.000000000000000000, 0.000000000000000000, -1.000000000000000000 ) ) ;
#150799 = CARTESIAN_POINT ( 'NONE',  ( 22.44159573604009594, -16.30477369853687364, 143.6750000027311671 ) ) ;
#150800 = CARTESIAN_POINT ( 'NONE',  ( -16.51473224551069308, -9.474510206698971260, 96.66557627198102409 ) ) ;
#150801 = LINE ( 'NONE', #70958, #174947 ) ;
#150802 = CARTESIAN_POINT ( 'NONE',  ( -13.89961937509957401, -13.97604488694547875, 99.37609039468567573 ) ) ;
#150803 = CARTESIAN_POINT ( 'NONE',  ( -5.823673210054116645, -21.52544592524344225, 27.29057627198103120 ) ) ;
#150805 = CARTESIAN_POINT ( 'NONE',  ( 4.483927247898790824, -16.52544592524335698, 20.20942372801900788 ) ) ;
#150804 = CARTESIAN_POINT ( 'NONE',  ( -19.03943276465977164, -0.05219959533935918106, 18.75109039468567218 ) ) ;
#150806 = CARTESIAN_POINT ( 'NONE',  ( -12.06949235617756955, 12.14591786802309770, 110.6239096053143669 ) ) ;
#150807 = CARTESIAN_POINT ( 'NONE',  ( -5.153800228976328057, -19.02544592524343514, 32.29057627198102409 ) ) ;
#150808 = CARTESIAN_POINT ( 'NONE',  ( 21.55341960407610458, 5.719274019375980345, 63.95724293864770260 ) ) ;
#150809 = CARTESIAN_POINT ( 'NONE',  ( -9.564922557960796823, -16.46253265017161027, 42.08224293864769550 ) ) ;
#150810 = DIRECTION ( 'NONE',  ( 0.000000000000000000, 0.000000000000000000, -1.000000000000000000 ) ) ;
#150811 = CARTESIAN_POINT ( 'NONE',  ( -13.89961937509957401, -13.97604488694547875, 64.37609039468567573 ) ) ;
#150812 = CARTESIAN_POINT ( 'NONE',  ( -4.483927247898539470, -16.52544592524342804, 47.29057627198103120 ) ) ;
#150813 = CARTESIAN_POINT ( 'NONE',  ( -18.62759615963270932, 10.81492255796079327, 35.83224293864768839 ) ) ;
#150814 = CARTESIAN_POINT ( 'NONE',  ( -5.823673210054431948, 21.52544592524334988, 97.70942372801904696 ) ) ;
#150815 = CARTESIAN_POINT ( 'NONE',  ( 15.80617190586746368, 15.72974639402197994, 89.37390960531435269 ) ) ;
#150816 = CARTESIAN_POINT ( 'NONE',  ( -5.719274019375665041, -21.55341960407619695, 64.79275706135234714 ) ) ;
#150817 = CARTESIAN_POINT ( 'NONE',  ( -10.72451020669870658, -18.67979575497194134, 64.58442372801900433 ) ) ;
#150818 = CARTESIAN_POINT ( 'NONE',  ( -9.564922557960796823, -16.46253265017161027, 92.08224293864769550 ) ) ;
#150820 = CARTESIAN_POINT ( 'NONE',  ( 10.72451020669871369, 18.67979575497193778, 67.08442372801901854 ) ) ;
#150819 = CARTESIAN_POINT ( 'NONE',  ( 8.224510206698742110, 14.34966873604972548, 87.08442372801901854 ) ) ;
#150821 = CARTESIAN_POINT ( 'NONE',  ( 13.97604488694527802, 13.89961937509977652, 54.37390960531435979 ) ) ;
#150822 = CARTESIAN_POINT ( 'NONE',  ( 13.97604488694527802, 13.89961937509977652, 29.37390960531435979 ) ) ;
#150823 = CARTESIAN_POINT ( 'NONE',  ( -19.05341960407611168, -5.049401038298163336, 51.45724293864770260 ) ) ;
#150824 = CARTESIAN_POINT ( 'NONE',  ( 8.224510206698953496, -14.34966873604960469, 62.91557627198102409 ) ) ;
#150825 = CARTESIAN_POINT ( 'NONE',  ( 16.55341960407611168, 4.379528057220329451, 33.95724293864769550 ) ) ;
#150826 = CARTESIAN_POINT ( 'NONE',  ( -15.80617190586745835, -15.72974639402198527, 41.87390960531435979 ) ) ;
#150827 = CARTESIAN_POINT ( 'NONE',  ( -9.474510206698964154, 16.51473224551069663, 50.41557627198102409 ) ) ;
#150828 = CARTESIAN_POINT ( 'NONE',  ( 15.72974639402199770, -15.80617190586745480, 53.12390960531436690 ) ) ;
#150829 = CARTESIAN_POINT ( 'NONE',  ( -19.03943276465977164, -0.05219959533935918106, 53.75109039468566863 ) ) ;
#150832 = CARTESIAN_POINT ( 'NONE',  ( 8.224510206698953496, -14.34966873604960469, 52.91557627198103830 ) ) ;
#150831 = CARTESIAN_POINT ( 'NONE',  ( -17.40805194822030799, -6.112264579159367273, 39.16628727489390371 ) ) ;
#150830 = VECTOR ( 'NONE', #101123, 1000.000000000000000 ) ;
#150833 = CARTESIAN_POINT ( 'NONE',  ( -15.80617190586745835, -15.72974639402198527, 26.87390960531435979 ) ) ;
#150834 = ORIENTED_EDGE ( 'NONE', *, *, #7150, .F. ) ;
#150835 = ORIENTED_EDGE ( 'NONE', *, *, #57463, .T. ) ;
#150836 = CARTESIAN_POINT ( 'NONE',  ( -3.573655867282028392E-15, 2.428612866367529932E-14, 139.9999999999999716 ) ) ;
#150837 = CARTESIAN_POINT ( 'NONE',  ( -16.52544592524335698, -4.483927247898792601, 88.95942372801901854 ) ) ;
#150838 = CARTESIAN_POINT ( 'NONE',  ( -16.46253265017146816, -9.564922557961047289, 69.16775706135233293 ) ) ;
#150839 = CARTESIAN_POINT ( 'NONE',  ( 4.483927247898545687, 16.52544592524342804, 59.79057627198103120 ) ) ;
#150840 = CARTESIAN_POINT ( 'NONE',  ( -19.25918095147781983, -5.499999999999586109, 59.45284276293935477 ) ) ;
#150841 = CARTESIAN_POINT ( 'NONE',  ( 16.55341960407611168, 4.379528057220329451, 33.95724293864769550 ) ) ;
#150842 = CARTESIAN_POINT ( 'NONE',  ( 9.474510206698971260, -16.51473224551069308, 47.91557627198102409 ) ) ;
#150843 = CARTESIAN_POINT ( 'NONE',  ( 19.02544592524343514, -5.153800228976328945, 68.54057627198103830 ) ) ;
#150844 = CARTESIAN_POINT ( 'NONE',  ( 19.05341960407611168, 5.049401038298154454, 38.95724293864767418 ) ) ;
#150845 = CARTESIAN_POINT ( 'NONE',  ( 5.823673210054444382, -21.52544592524334988, 45.20942372801901854 ) ) ;
#150846 = CARTESIAN_POINT ( 'NONE',  ( 5.153800228976335163, 19.02544592524342804, 74.79057627198103830 ) ) ;
#150847 = CARTESIAN_POINT ( 'NONE',  ( -5.153800228976328057, -19.02544592524343514, 22.29057627198102765 ) ) ;
#150848 = VECTOR ( 'NONE', #34781, 1000.000000000000000 ) ;
#150849 = CARTESIAN_POINT ( 'NONE',  ( -13.89961937509977652, 13.97604488694528158, 60.62390960531436690 ) ) ;
#150850 = CARTESIAN_POINT ( 'NONE',  ( -21.52544592524343514, 5.823673210054127303, 56.04057627198102409 ) ) ;
#150851 = B_SPLINE_CURVE_WITH_KNOTS ( 'NONE', 3,
 ( #148499, #196019, #10987, #119164, #25171, #179852, #197007, #162656, #195006, #178844, #9990, #70658, #86813, #41323, #193006, #131316, #71650, #180847, #103985, #181831, #133317, #166665, #8990, #54483, #56484, #118162, #132324, #43310, #102983, #100971, #165664, #26164, #28166, #194016, #55479, #117149, #33110, #46284, #108946, #168624, #77612, #169627, #45299, #182824, #14957, #75619, #44306, #61441 ),
 .UNSPECIFIED., .F., .F.,
 ( 4, 2, 2, 2, 2, 2, 2, 2, 2, 2, 2, 2, 2, 2, 2, 2, 2, 2, 2, 2, 2, 2, 2, 4 ),
 ( 0.01768515071410573999, 0.01915622216236231162, 0.01989175788649060264, 0.02062729361061889019, 0.02209836505887546876, 0.02283390078300375631, 0.02356943650713204733, 0.02504050795538863977, 0.02651157940364523569, 0.02724711512777353017, 0.02798265085190182813, 0.02945372230015839976, 0.03092479374841497486, 0.03239586519667154996, 0.03313140092079983057, 0.03386693664492811118, 0.03460247236905639873, 0.03533800809318467934, 0.03680907954144126137, 0.03754461526556955586, 0.03828015098969785035, 0.03975122243795443933, 0.04048675816208274075, 0.04122229388621103524 ),
 .UNSPECIFIED. ) ;
#150852 = CARTESIAN_POINT ( 'NONE',  ( -13.97604488694527625, -13.89961937509977652, 41.87390960531435979 ) ) ;
#150853 = CARTESIAN_POINT ( 'NONE',  ( -18.67979575497178146, -10.72451020669898902, 46.66557627198102409 ) ) ;
#150854 = CARTESIAN_POINT ( 'NONE',  ( 8.224510206698742110, 14.34966873604972548, 102.0844237280190185 ) ) ;
#150855 = CARTESIAN_POINT ( 'NONE',  ( -19.02544592524334988, -5.153800228976617603, 18.95942372801899722 ) ) ;
#150856 = EDGE_CURVE ( 'NONE', #49688, #189055, #99110, .T. ) ;
#150858 = CARTESIAN_POINT ( 'NONE',  ( -12.14591786802326823, 12.06949235617739902, 83.12609039468568994 ) ) ;
#150857 = CARTESIAN_POINT ( 'NONE',  ( 4.483927247898790824, -16.52544592524335698, 45.20942372801901854 ) ) ;
#150859 = PLANE ( 'NONE',  #14510 ) ;
#150860 = CARTESIAN_POINT ( 'NONE',  ( -0.05219959533934338120, 16.53943276465976808, 62.50109039468568284 ) ) ;
#150861 = CARTESIAN_POINT ( 'NONE',  ( 0.05219959533934541429, -16.53943276465976808, 45.00109039468568284 ) ) ;
#150862 = CARTESIAN_POINT ( 'NONE',  ( 16.46253265017160672, -9.564922557960803928, 113.3322429386476955 ) ) ;
#150863 = CARTESIAN_POINT ( 'NONE',  ( 16.52544592524335698, 4.483927247898782831, 26.45942372801901854 ) ) ;
#150864 = CARTESIAN_POINT ( 'NONE',  ( 16.46253265017160672, -9.564922557960803928, 38.33224293864768839 ) ) ;
#150865 = CARTESIAN_POINT ( 'NONE',  ( 18.62759615963255655, 10.81492255796105972, 21.66775706135235069 ) ) ;
#150866 = CARTESIAN_POINT ( 'NONE',  ( 0.05219959533934541429, -16.53943276465976808, 40.00109039468567573 ) ) ;
#150867 = CARTESIAN_POINT ( 'NONE',  ( -12.06949235617739369, -12.14591786802326823, 94.37609039468568994 ) ) ;
#150868 = FACE_OUTER_BOUND ( 'NONE', #154550, .T. ) ;
#150869 = CARTESIAN_POINT ( 'NONE',  ( 15.80617190586769283, -15.72974639402175789, 100.6260903946857184 ) ) ;
#150870 = CARTESIAN_POINT ( 'NONE',  ( -13.89961937509957401, -13.97604488694547875, 99.37609039468567573 ) ) ;
#150871 = CARTESIAN_POINT ( 'NONE',  ( -12.14591786802309592, -12.06949235617757132, 56.87390960531436690 ) ) ;
#150872 = CARTESIAN_POINT ( 'NONE',  ( 16.46253265017160672, -9.564922557960803928, 23.33224293864769194 ) ) ;
#150874 = DIRECTION ( 'NONE',  ( 0.8164965809277262565, 0.000000000000000000, 0.5773502691896253980 ) ) ;
#150873 = CARTESIAN_POINT ( 'NONE',  ( -16.51473224551082808, 9.474510206698731452, 58.33442372801900433 ) ) ;
#150875 = CARTESIAN_POINT ( 'NONE',  ( 15.80617190586769283, -15.72974639402175789, 55.62609039468568284 ) ) ;
#150876 = CARTESIAN_POINT ( 'NONE',  ( 0.05219959533934541429, -16.53943276465976808, 25.00109039468567218 ) ) ;
#150877 = LINE ( 'NONE', #58841, #1906 ) ;
#150878 = CARTESIAN_POINT ( 'NONE',  ( -18.67979575497178146, -10.72451020669898902, 21.66557627198102409 ) ) ;
#150879 = CARTESIAN_POINT ( 'NONE',  ( -21.52544592524343514, 5.823673210054127303, 76.04057627198102409 ) ) ;
#150880 = CARTESIAN_POINT ( 'NONE',  ( 19.03943276465977164, 0.05219959533936151252, 111.2510903946856757 ) ) ;
#150881 = CARTESIAN_POINT ( 'NONE',  ( 5.049401038298161559, -19.05341960407611168, 97.70724293864766707 ) ) ;
#150882 = CARTESIAN_POINT ( 'NONE',  ( 8.004588480676682494, -26.62287193706184496, 139.9999999999999716 ) ) ;
#150883 = CARTESIAN_POINT ( 'NONE',  ( -9.564922557960796823, -16.46253265017161027, 22.08224293864768839 ) ) ;
#150884 = CARTESIAN_POINT ( 'NONE',  ( 10.72451020669871369, 18.67979575497193778, 112.0844237280190185 ) ) ;
#150885 = CARTESIAN_POINT ( 'NONE',  ( 5.049401038298161559, -19.05341960407611168, 37.70724293864768839 ) ) ;
#150887 = CARTESIAN_POINT ( 'NONE',  ( -15.72974639402176322, -15.80617190586768395, 54.37609039468568994 ) ) ;
#150886 = CONICAL_SURFACE ( 'NONE', #176712, 2.055000000000000160, 0.7853981633974712606 ) ;
#150888 = CARTESIAN_POINT ( 'NONE',  ( -15.72974639402176322, -15.80617190586768395, 94.37609039468568994 ) ) ;
#150889 = CARTESIAN_POINT ( 'NONE',  ( -4.483927247898782831, 16.52544592524335698, 102.7094237280190185 ) ) ;
#150890 = CARTESIAN_POINT ( 'NONE',  ( 5.153800228976335163, 19.02544592524342804, 84.79057627198099567 ) ) ;
#150891 = CARTESIAN_POINT ( 'NONE',  ( 21.55341960407619695, -5.719274019375665929, 46.04275706135234714 ) ) ;
#150892 = CARTESIAN_POINT ( 'NONE',  ( 21.55341960407619695, -5.719274019375665929, 36.04275706135234714 ) ) ;
#150894 = CARTESIAN_POINT ( 'NONE',  ( -9.564922557960796823, -16.46253265017161027, 97.08224293864769550 ) ) ;
#150893 = CARTESIAN_POINT ( 'NONE',  ( 19.03943276465977164, 0.05219959533936151252, 81.25109039468567573 ) ) ;
#150895 = CARTESIAN_POINT ( 'NONE',  ( 8.314922557960818139, 14.29746914071049879, 104.5822429386477097 ) ) ;
#150896 = CARTESIAN_POINT ( 'NONE',  ( -21.52544592524343514, 5.823673210054127303, 101.0405762719810383 ) ) ;
#150897 = CARTESIAN_POINT ( 'NONE',  ( 16.55341960407611168, 4.379528057220329451, 83.95724293864770971 ) ) ;
#150898 = CARTESIAN_POINT ( 'NONE',  ( 13.97604488694548053, -13.89961937509957401, 25.62609039468566507 ) ) ;
#150899 = CARTESIAN_POINT ( 'NONE',  ( 14.29746914071049879, -8.314922557960816363, 98.33224293864769550 ) ) ;
#150900 = CARTESIAN_POINT ( 'NONE',  ( -19.05341960407611168, -5.049401038298163336, 46.45724293864768129 ) ) ;
#150901 = CARTESIAN_POINT ( 'NONE',  ( -19.03943276465977164, -0.05219959533935918106, 88.75109039468567573 ) ) ;
#150902 = CARTESIAN_POINT ( 'NONE',  ( 8.224510206698953496, -14.34966873604960469, 52.91557627198103830 ) ) ;
#150903 = CARTESIAN_POINT ( 'NONE',  ( -15.80617190586768217, 15.72974639402176855, 103.1260903946856757 ) ) ;
#150904 = CARTESIAN_POINT ( 'NONE',  ( -9.474510206698964154, 16.51473224551069663, 110.4155762719810383 ) ) ;
#150905 = CARTESIAN_POINT ( 'NONE',  ( -13.89961937509957401, -13.97604488694547875, 79.37609039468567573 ) ) ;
#150906 = CARTESIAN_POINT ( 'NONE',  ( 0.05219959533907565091, 21.53943276465977519, 79.99890960531435269 ) ) ;
#150907 = CARTESIAN_POINT ( 'NONE',  ( -15.72974639402176322, -15.80617190586768395, 34.37609039468568284 ) ) ;
#150908 = CARTESIAN_POINT ( 'NONE',  ( -14.29746914071037622, -8.314922557961029526, 24.16775706135235424 ) ) ;
#150909 = CARTESIAN_POINT ( 'NONE',  ( 8.314922557961029526, -14.29746914071037800, 95.41775706135234714 ) ) ;
#150911 = CARTESIAN_POINT ( 'NONE',  ( -10.72451020669870658, -18.67979575497194134, 29.58442372801901854 ) ) ;
#150910 = CARTESIAN_POINT ( 'NONE',  ( 9.474510206698971260, -16.51473224551069308, 27.91557627198103120 ) ) ;
#150912 = CARTESIAN_POINT ( 'NONE',  ( 9.564922557960805705, 16.46253265017160317, 24.58224293864769194 ) ) ;
#150913 = CARTESIAN_POINT ( 'NONE',  ( -5.950531402560715689E-15, 38.81732327939063509, -1.624999997268813612 ) ) ;
#150914 = CARTESIAN_POINT ( 'NONE',  ( -16.52544592524335698, -4.483927247898792601, 53.95942372801900433 ) ) ;
#150915 = EDGE_CURVE ( 'NONE', #50238, #196966, #148914, .T. ) ;
#150916 = CARTESIAN_POINT ( 'NONE',  ( 16.52544592524342804, -4.483927247898539470, 83.54057627198102409 ) ) ;
#150917 = CARTESIAN_POINT ( 'NONE',  ( -10.81492255796078084, -18.62759615963271287, 77.08224293864769550 ) ) ;
#150918 = CARTESIAN_POINT ( 'NONE',  ( -12.14591786802309592, -12.06949235617757132, 21.87390960531436690 ) ) ;
#150919 = CARTESIAN_POINT ( 'NONE',  ( 16.55341960407618274, -4.379528057220086978, 46.04275706135234714 ) ) ;
#150920 = CARTESIAN_POINT ( 'NONE',  ( 9.564922557960805705, 16.46253265017160317, 49.58224293864770260 ) ) ;
#150921 = CARTESIAN_POINT ( 'NONE',  ( 16.52544592524335698, 4.483927247898782831, 96.45942372801901854 ) ) ;
#150922 = CARTESIAN_POINT ( 'NONE',  ( -5.153800228976607833, 19.02544592524334988, 87.70942372801897591 ) ) ;
#150923 = CARTESIAN_POINT ( 'NONE',  ( 21.53943276465977519, -0.05219959533907433946, 83.74890960531435269 ) ) ;
#150924 = CARTESIAN_POINT ( 'NONE',  ( -4.379528057220086978, -16.55341960407618274, 104.7927570613523898 ) ) ;
#150925 = DIRECTION ( 'NONE',  ( -1.000000000000000000, 0.000000000000000000, 0.000000000000000000 ) ) ;
#150926 =( BOUNDED_SURFACE ( )  B_SPLINE_SURFACE ( 1, 2, ( 
 ( #130274, #148476, #164645, #7945, #26140, #87782, #10962, #57470, #192983, #84774, #177820, #191969, #88785, #68618, #69628, #131294, #54461, #24138, #39290, #100947, #166640, #62407, #45275, #106928, #46261, #90760, #198957, #123089, #107916, #168601, #44282, #30101, #91741, #735, #74620, #76594, #29122, #77588, #31099, #154435, #93749, #152443, #181807, #92747, #60424, #13929, #153436, #138270, #105940, #89782, #14934, #199953, #108922, #61418, #15929, #75596, #137275, #135309, #184775, #196982, #122097, #120116, #183788, #169601, #151467, #43285, #139259, #58448, #124077, #185778, #47265, #170602, #104954, #32092, #11973, #73638, #28142, #12956, #136286, #197962, #59432, #121105, #182799, #167625, #20886, #37050, #127059, #66395, #34078, #172592, #188766, #96718, #49248, #82544, #52219, #18916, #189759, #111906, #173594, #187778, #155430 ),
 ( #1739, #80561, #5710, #63417, #143223, #190745, #110906, #95736, #171598, #158406, #94742, #2736, #128057, #67387, #48261, #141247, #142236, #129044, #79578, #144226, #3721, #113876, #78573, #175573, #51231, #16920, #112892, #65398, #157422, #174586, #50250, #109914, #35063, #140247, #19895, #81536, #36051, #125092, #186790, #4705, #33086, #97700, #156422, #159391, #17923, #64413, #126082, #21892, #57236, #115898, #71396, #163411, #191732, #38060, #24907, #148238, #6703, #101721, #86554, #176586, #68381, #133060, #9732, #41065, #164417, #147235, #130033, #194750, #116890, #56222, #53214, #117904, #114892, #69386, #162393, #118910, #179593, #98709, #180594, #131055, #40047, #146215, #23896, #161400, #102728, #70396, #25910, #87554, #99716, #72396, #22892, #160403, #149241, #132064, #10732, #84538, #134072, #83542, #195762, #55221, #7703 ) ),
 .UNSPECIFIED., .F., .F., .T. ) 
 B_SPLINE_SURFACE_WITH_KNOTS ( ( 2, 2 ),
 ( 3, 2, 2, 2, 2, 2, 2, 2, 2, 2, 2, 2, 2, 2, 2, 2, 2, 2, 2, 2, 2, 2, 2, 2, 2, 2, 2, 2, 2, 2, 2, 2, 2, 2, 2, 2, 2, 2, 2, 2, 2, 2, 2, 2, 2, 2, 2, 2, 2, 2, 3 ),
 ( 0.000000000000000000, 1.000000000000000000 ),
 ( 0.000000000000000000, 0.02000000000000000042, 0.04000000000000000083, 0.05999999999999999778, 0.08000000000000000167, 0.1000000000000000056, 0.1199999999999999956, 0.1400000000000000133, 0.1600000000000000033, 0.1799999999999999933, 0.2000000000000000111, 0.2200000000000000011, 0.2399999999999999911, 0.2600000000000000089, 0.2800000000000000266, 0.2999999999999999889, 0.3200000000000000067, 0.3400000000000000244, 0.3599999999999999867, 0.3800000000000000044, 0.4000000000000000222, 0.4199999999999999845, 0.4400000000000000022, 0.4600000000000000200, 0.4799999999999999822, 0.5000000000000000000, 0.5200000000000000178, 0.5400000000000000355, 0.5600000000000000533, 0.5799999999999999600, 0.5999999999999999778, 0.6199999999999999956, 0.6400000000000000133, 0.6600000000000000311, 0.6800000000000000488, 0.6999999999999999556, 0.7199999999999999734, 0.7399999999999999911, 0.7600000000000000089, 0.7800000000000000266, 0.8000000000000000444, 0.8199999999999999512, 0.8399999999999999689, 0.8599999999999999867, 0.8800000000000000044, 0.9000000000000000222, 0.9200000000000000400, 0.9399999999999999467, 0.9599999999999999645, 0.9799999999999999822, 1.000000000000000000 ),
 .UNSPECIFIED. ) 
 GEOMETRIC_REPRESENTATION_ITEM ( )  RATIONAL_B_SPLINE_SURFACE ( (
 ( 1.000000000000000000, 0.9510565162951535312, 1.000000000000000000, 0.9510565162951535312, 1.000000000000000000, 0.9510565162951535312, 1.000000000000000000, 0.9510565162951535312, 1.000000000000000000, 0.9510565162951535312, 1.000000000000000000, 0.9510565162951535312, 1.000000000000000000, 0.9510565162951535312, 1.000000000000000000, 0.9510565162951535312, 1.000000000000000000, 0.9510565162951535312, 1.000000000000000000, 0.9510565162951535312, 1.000000000000000000, 0.9510565162951535312, 1.000000000000000000, 0.9510565162951535312, 1.000000000000000000, 0.9510565162951535312, 1.000000000000000000, 0.9510565162951535312, 1.000000000000000000, 0.9510565162951535312, 1.000000000000000000, 0.9510565162951535312, 1.000000000000000000, 0.9510565162951535312, 1.000000000000000000, 0.9510565162951535312, 1.000000000000000000, 0.9510565162951535312, 1.000000000000000000, 0.9510565162951535312, 1.000000000000000000, 0.9510565162951535312, 1.000000000000000000, 0.9510565162951535312, 1.000000000000000000, 0.9510565162951535312, 1.000000000000000000, 0.9510565162951535312, 1.000000000000000000, 0.9510565162951535312, 1.000000000000000000, 0.9510565162951535312, 1.000000000000000000, 0.9510565162951535312, 1.000000000000000000, 0.9510565162951535312, 1.000000000000000000, 0.9510565162951535312, 1.000000000000000000, 0.9510565162951535312, 1.000000000000000000, 0.9510565162951535312, 1.000000000000000000, 0.9510565162951535312, 1.000000000000000000, 0.9510565162951535312, 1.000000000000000000, 0.9510565162951535312, 1.000000000000000000, 0.9510565162951535312, 1.000000000000000000, 0.9510565162951535312, 1.000000000000000000, 0.9510565162951535312, 1.000000000000000000, 0.9510565162951535312, 1.000000000000000000, 0.9510565162951535312, 1.000000000000000000, 0.9510565162951535312, 1.000000000000000000, 0.9510565162951535312, 1.000000000000000000, 0.9510565162951535312, 1.000000000000000000, 0.9510565162951535312, 1.000000000000000000, 0.9510565162951535312, 1.000000000000000000, 0.9510565162951535312, 1.000000000000000000, 0.9510565162951535312, 1.000000000000000000, 0.9510565162951535312, 1.000000000000000000, 0.9510565162951535312, 1.000000000000000000, 0.9510565162951535312, 1.000000000000000000, 0.9510565162951535312, 1.000000000000000000),
 ( 1.000000000000000000, 0.9510565162951535312, 1.000000000000000000, 0.9510565162951535312, 1.000000000000000000, 0.9510565162951535312, 1.000000000000000000, 0.9510565162951535312, 1.000000000000000000, 0.9510565162951535312, 1.000000000000000000, 0.9510565162951535312, 1.000000000000000000, 0.9510565162951535312, 1.000000000000000000, 0.9510565162951535312, 1.000000000000000000, 0.9510565162951535312, 1.000000000000000000, 0.9510565162951535312, 1.000000000000000000, 0.9510565162951535312, 1.000000000000000000, 0.9510565162951535312, 1.000000000000000000, 0.9510565162951535312, 1.000000000000000000, 0.9510565162951535312, 1.000000000000000000, 0.9510565162951535312, 1.000000000000000000, 0.9510565162951535312, 1.000000000000000000, 0.9510565162951535312, 1.000000000000000000, 0.9510565162951535312, 1.000000000000000000, 0.9510565162951535312, 1.000000000000000000, 0.9510565162951535312, 1.000000000000000000, 0.9510565162951535312, 1.000000000000000000, 0.9510565162951535312, 1.000000000000000000, 0.9510565162951535312, 1.000000000000000000, 0.9510565162951535312, 1.000000000000000000, 0.9510565162951535312, 1.000000000000000000, 0.9510565162951535312, 1.000000000000000000, 0.9510565162951535312, 1.000000000000000000, 0.9510565162951535312, 1.000000000000000000, 0.9510565162951535312, 1.000000000000000000, 0.9510565162951535312, 1.000000000000000000, 0.9510565162951535312, 1.000000000000000000, 0.9510565162951535312, 1.000000000000000000, 0.9510565162951535312, 1.000000000000000000, 0.9510565162951535312, 1.000000000000000000, 0.9510565162951535312, 1.000000000000000000, 0.9510565162951535312, 1.000000000000000000, 0.9510565162951535312, 1.000000000000000000, 0.9510565162951535312, 1.000000000000000000, 0.9510565162951535312, 1.000000000000000000, 0.9510565162951535312, 1.000000000000000000, 0.9510565162951535312, 1.000000000000000000, 0.9510565162951535312, 1.000000000000000000, 0.9510565162951535312, 1.000000000000000000, 0.9510565162951535312, 1.000000000000000000, 0.9510565162951535312, 1.000000000000000000, 0.9510565162951535312, 1.000000000000000000, 0.9510565162951535312, 1.000000000000000000, 0.9510565162951535312, 1.000000000000000000, 0.9510565162951535312, 1.000000000000000000, 0.9510565162951535312, 1.000000000000000000) ) ) 
 REPRESENTATION_ITEM ( '' )  SURFACE ( )  );
#150927 = CARTESIAN_POINT ( 'NONE',  ( -10.81492255796078084, -18.62759615963271287, 62.08224293864769550 ) ) ;
#150928 = VERTEX_POINT ( 'NONE', #38458 ) ;
#150929 = CARTESIAN_POINT ( 'NONE',  ( -8.314922557961024197, 14.29746914071037800, 87.91775706135234714 ) ) ;
#150930 = ORIENTED_EDGE ( 'NONE', *, *, #12591, .T. ) ;
#150931 = CARTESIAN_POINT ( 'NONE',  ( 21.52544592524344225, -5.823673210054117533, 33.54057627198102409 ) ) ;
#150932 = CARTESIAN_POINT ( 'NONE',  ( -19.52837319214027545, 5.499999999999899636, 74.60471352585540217 ) ) ;
#150933 = CARTESIAN_POINT ( 'NONE',  ( -5.823673210054116645, -21.52544592524344225, 77.29057627198102409 ) ) ;
#150934 = CARTESIAN_POINT ( 'NONE',  ( 16.52544592524342804, -4.483927247898539470, 23.54057627198102765 ) ) ;
#150935 = CARTESIAN_POINT ( 'NONE',  ( -16.52544592524335698, -4.483927247898792601, 18.95942372801901143 ) ) ;
#150936 = CARTESIAN_POINT ( 'NONE',  ( -13.89961937509977652, 13.97604488694528158, 35.62390960531435269 ) ) ;
#150937 = CARTESIAN_POINT ( 'NONE',  ( -12.14591786802326823, 12.06949235617739902, 33.12609039468569705 ) ) ;
#150938 = CARTESIAN_POINT ( 'NONE',  ( -5.153800228976328057, -19.02544592524343514, 47.29057627198102409 ) ) ;
#150939 = CARTESIAN_POINT ( 'NONE',  ( -17.81289503416611097, -24.51734667627696496, 146.2999999999999829 ) ) ;
#150940 = CARTESIAN_POINT ( 'NONE',  ( 19.02544592524343514, -5.153800228976328945, 108.5405762719810383 ) ) ;
#150941 = CARTESIAN_POINT ( 'NONE',  ( -16.51473224551069308, -9.474510206698971260, 106.6655762719810383 ) ) ;
#150942 = CARTESIAN_POINT ( 'NONE',  ( 8.314922557961029526, -14.29746914071037800, 95.41775706135234714 ) ) ;
#150943 = CARTESIAN_POINT ( 'NONE',  ( -19.05341960407617563, 5.049401038297882671, 88.54275706135230450 ) ) ;
#150944 = CARTESIAN_POINT ( 'NONE',  ( 16.51473224551083163, -9.474510206698727899, 35.83442372801899722 ) ) ;
#150945 = CARTESIAN_POINT ( 'NONE',  ( 18.67979575497178502, 10.72451020669898547, 79.16557627198103830 ) ) ;
#150946 = CARTESIAN_POINT ( 'NONE',  ( 16.52544592524335698, 4.483927247898782831, 96.45942372801901854 ) ) ;
#150947 = CARTESIAN_POINT ( 'NONE',  ( -15.80617190586745835, -15.72974639402198527, 36.87390960531435979 ) ) ;
#150948 = CARTESIAN_POINT ( 'NONE',  ( -16.46253265017146816, -9.564922557961047289, 89.16775706135234714 ) ) ;
#150949 = CARTESIAN_POINT ( 'NONE',  ( -16.46253265017160317, 9.564922557960807481, 45.83224293864769550 ) ) ;
#150950 = CARTESIAN_POINT ( 'NONE',  ( -13.89961937509977652, 13.97604488694528158, 95.62390960531436690 ) ) ;
#150951 = CARTESIAN_POINT ( 'NONE',  ( 5.719274019375673035, 21.55341960407619339, 67.29275706135234714 ) ) ;
#150952 = CARTESIAN_POINT ( 'NONE',  ( -19.02544592524342804, 5.153800228976336051, 56.04057627198100988 ) ) ;
#150953 = CARTESIAN_POINT ( 'NONE',  ( 4.379528057220339221, -16.55341960407611168, 97.70724293864772392 ) ) ;
#150954 = CARTESIAN_POINT ( 'NONE',  ( 19.83801684532465615, -12.12952959760455585, 169.9999999999999716 ) ) ;
#150955 = CARTESIAN_POINT ( 'NONE',  ( -12.14591786802309592, -12.06949235617757132, 76.87390960531439532 ) ) ;
#150956 = CARTESIAN_POINT ( 'NONE',  ( 15.72974639402199770, -15.80617190586745480, 73.12390960531436690 ) ) ;
#150957 = CARTESIAN_POINT ( 'NONE',  ( -9.564922557961040184, 16.46253265017147172, 92.91775706135233293 ) ) ;
#150958 = CARTESIAN_POINT ( 'NONE',  ( 19.52851543214744368, 5.499999999999982236, 92.89357721762581832 ) ) ;
#150959 = CARTESIAN_POINT ( 'NONE',  ( 5.153800228976335163, 19.02544592524342804, 59.79057627198100988 ) ) ;
#150960 = CARTESIAN_POINT ( 'NONE',  ( 16.81555441253470562, -7.025013491696157075, 73.13685445334213853 ) ) ;
#150962 = CARTESIAN_POINT ( 'NONE',  ( -9.564922557960796823, -16.46253265017161027, 82.08224293864768129 ) ) ;
#150961 = CARTESIAN_POINT ( 'NONE',  ( 5.153800228976335163, 19.02544592524342804, 79.79057627198102409 ) ) ;
#150963 = CARTESIAN_POINT ( 'NONE',  ( 16.55341960407618274, -4.379528057220086978, 66.04275706135236135 ) ) ;
#150964 = CARTESIAN_POINT ( 'NONE',  ( -17.31728774477271671, -6.344390552232404445, 49.18093348310683410 ) ) ;
#150965 = CARTESIAN_POINT ( 'NONE',  ( -9.474510206698720793, -16.51473224551083518, 39.58442372801899722 ) ) ;
#150966 = CARTESIAN_POINT ( 'NONE',  ( 0.000000000000000000, 0.000000000000000000, -45.64921306006598201 ) ) ;
#150967 = CARTESIAN_POINT ( 'NONE',  ( -16.46253265017160317, 9.564922557960807481, 110.8322429386476955 ) ) ;
#150968 = CARTESIAN_POINT ( 'NONE',  ( -12.06949235617739369, -12.14591786802326823, 104.3760903946856899 ) ) ;
#150969 = CARTESIAN_POINT ( 'NONE',  ( -1.498759781556145754, -23.15940025311443407, -55.09305739490149989 ) ) ;
#150970 = CARTESIAN_POINT ( 'NONE',  ( -16.53943276465976808, -0.05219959533934237506, 83.75109039468568994 ) ) ;
#150971 = CARTESIAN_POINT ( 'NONE',  ( -25.25560589046783733, 4.310829775027161581, 167.9999999999999716 ) ) ;
#150972 = CARTESIAN_POINT ( 'NONE',  ( -8.224510206698735004, -14.34966873604973081, 49.58442372801901143 ) ) ;
#150973 = DIRECTION ( 'NONE',  ( -1.000000000000000000, 0.000000000000000000, 4.336808689942017736E-16 ) ) ;
#150974 = CARTESIAN_POINT ( 'NONE',  ( 5.719274019375673035, 21.55341960407619339, 62.29275706135236845 ) ) ;
#150975 = CARTESIAN_POINT ( 'NONE',  ( 13.97604488694548053, -13.89961937509957401, 75.62609039468564731 ) ) ;
#150976 = CARTESIAN_POINT ( 'NONE',  ( -19.02544592524334988, -5.153800228976617603, 23.95942372801900078 ) ) ;
#150977 = CARTESIAN_POINT ( 'NONE',  ( 16.46253265017160672, -9.564922557960803928, 68.33224293864770971 ) ) ;
#150978 = CARTESIAN_POINT ( 'NONE',  ( -19.03943276465977164, 0.05219959533909376836, 41.24890960531435269 ) ) ;
#150979 = DIRECTION ( 'NONE',  ( 1.000000000000000000, 0.000000000000000000, 0.000000000000000000 ) ) ;
#150980 = CARTESIAN_POINT ( 'NONE',  ( 5.823673210054125526, 21.52544592524343514, 64.79057627198103830 ) ) ;
#150981 = AXIS2_PLACEMENT_3D ( 'NONE', #102779, #42121, #163462 ) ;
#150982 = CARTESIAN_POINT ( 'NONE',  ( -21.53943276465977519, 0.05219959533907696930, 36.24890960531435979 ) ) ;
#150983 = CARTESIAN_POINT ( 'NONE',  ( -13.89961937509977652, 13.97604488694528158, 25.62390960531434558 ) ) ;
#150984 = CARTESIAN_POINT ( 'NONE',  ( 16.55341960407618274, -4.379528057220086978, 46.04275706135234714 ) ) ;
#150985 = ADVANCED_FACE ( 'NONE', ( #158792 ), #171923, .T. ) ;
#150986 = ORIENTED_EDGE ( 'NONE', *, *, #73257, .T. ) ;
#150987 = CARTESIAN_POINT ( 'NONE',  ( 5.719274019375673035, 21.55341960407619339, 32.29275706135235424 ) ) ;
#150989 = CARTESIAN_POINT ( 'NONE',  ( 23.48529157249599919, 32.32473071737754111, -2.700000000000000622 ) ) ;
#150988 = CARTESIAN_POINT ( 'NONE',  ( 16.52544592524342804, -4.483927247898539470, 48.54057627198103120 ) ) ;
#150990 = CARTESIAN_POINT ( 'NONE',  ( -0.05219959533934338120, 16.53943276465976808, 27.50109039468567929 ) ) ;
#150991 = CARTESIAN_POINT ( 'NONE',  ( 13.97604488694548053, -13.89961937509957401, 40.62609039468564731 ) ) ;
#150992 = CARTESIAN_POINT ( 'NONE',  ( 16.53943276465976808, -0.05219959533910856209, 48.74890960531435979 ) ) ;
#150993 = CARTESIAN_POINT ( 'NONE',  ( 10.72451020669871369, 18.67979575497193778, 22.08442372801901143 ) ) ;
#150995 = CARTESIAN_POINT ( 'NONE',  ( -18.62759615963270932, 10.81492255796079327, 75.83224293864769550 ) ) ;
#150994 = DIRECTION ( 'NONE',  ( 0.000000000000000000, 0.000000000000000000, -1.000000000000000000 ) ) ;
#150996 = CARTESIAN_POINT ( 'NONE',  ( -13.89961937509977652, 13.97604488694528158, 90.62390960531432427 ) ) ;
#150997 = CARTESIAN_POINT ( 'NONE',  ( 8.314922557960818139, 14.29746914071049879, 59.58224293864770260 ) ) ;
#150998 = CARTESIAN_POINT ( 'NONE',  ( 5.153800228976335163, 19.02544592524342804, 109.7905762719810099 ) ) ;
#150999 = EDGE_CURVE ( 'NONE', #45569, #101009, #40751, .T. ) ;
#151000 = FACE_OUTER_BOUND ( 'NONE', #115887, .T. ) ;
#151001 = CARTESIAN_POINT ( 'NONE',  ( 5.049401038297881783, 19.05341960407617563, 67.29275706135234714 ) ) ;
#151002 = CARTESIAN_POINT ( 'NONE',  ( 21.53943276465977519, -0.05219959533907433946, 108.7489096053143669 ) ) ;
#151003 = CARTESIAN_POINT ( 'NONE',  ( 19.05341960407611168, 5.049401038298154454, 53.95724293864770260 ) ) ;
#151004 = CARTESIAN_POINT ( 'NONE',  ( -16.53943276465976808, 0.05219959533911058130, 116.2489096053143669 ) ) ;
#151005 = CARTESIAN_POINT ( 'NONE',  ( 5.823673210054444382, -21.52544592524334988, 50.20942372801901854 ) ) ;
#151006 = CARTESIAN_POINT ( 'NONE',  ( -17.14385361876520264, -23.59649016807271593, 147.1750000027311671 ) ) ;
#151007 = CARTESIAN_POINT ( 'NONE',  ( 14.34966873604960469, 8.224510206698951720, 39.16557627198102409 ) ) ;
#151008 = CARTESIAN_POINT ( 'NONE',  ( 19.05341960407611168, 5.049401038298154454, 43.95724293864769550 ) ) ;
#151009 = CARTESIAN_POINT ( 'NONE',  ( -13.97604488694527625, -13.89961937509977652, 96.87390960531433848 ) ) ;
#151010 = CARTESIAN_POINT ( 'NONE',  ( 21.53943276465977519, -0.05219959533907433946, 73.74890960531433848 ) ) ;
#151011 = CARTESIAN_POINT ( 'NONE',  ( -22.44159573604009950, -16.30477369853688430, 143.0750000027311728 ) ) ;
#151012 = CARTESIAN_POINT ( 'NONE',  ( -5.153800228976328057, -19.02544592524343514, 47.29057627198102409 ) ) ;
#151013 = CARTESIAN_POINT ( 'NONE',  ( 21.55341960407610458, 5.719274019375980345, 68.95724293864769550 ) ) ;
#151014 = CARTESIAN_POINT ( 'NONE',  ( 5.823673210054444382, -21.52544592524334988, 80.20942372801901854 ) ) ;
#151017 = CARTESIAN_POINT ( 'NONE',  ( 16.53943276465976808, -0.05219959533910856209, 83.74890960531435269 ) ) ;
#151016 = CARTESIAN_POINT ( 'NONE',  ( -8.314922557961024197, 14.29746914071037800, 82.91775706135234714 ) ) ;
#151015 = DIRECTION ( 'NONE',  ( 0.000000000000000000, 0.000000000000000000, -1.000000000000000000 ) ) ;
#151018 = CARTESIAN_POINT ( 'NONE',  ( 9.564922557960805705, 16.46253265017160317, 64.58224293864769550 ) ) ;
#151019 = ORIENTED_EDGE ( 'NONE', *, *, #121441, .F. ) ;
#151020 = CARTESIAN_POINT ( 'NONE',  ( -13.89961937509957401, -13.97604488694547875, 24.37609039468565442 ) ) ;
#151021 = CARTESIAN_POINT ( 'NONE',  ( -12.06949235617739369, -12.14591786802326823, 89.37609039468568994 ) ) ;
#151022 = CARTESIAN_POINT ( 'NONE',  ( 13.97604488694548053, -13.89961937509957401, 20.62609039468567573 ) ) ;
#151023 = CARTESIAN_POINT ( 'NONE',  ( 16.51473224551069308, 9.474510206698969483, 89.16557627198103830 ) ) ;
#151024 = CARTESIAN_POINT ( 'NONE',  ( -0.05219959533907301413, -21.53943276465977519, 47.49890960531435979 ) ) ;
#151025 = CARTESIAN_POINT ( 'NONE',  ( -0.05219959533937732626, 21.53943276465977519, 97.50109039468567573 ) ) ;
#151026 = CARTESIAN_POINT ( 'NONE',  ( 0.05219959533934541429, -16.53943276465976808, 60.00109039468568284 ) ) ;
#151027 = CARTESIAN_POINT ( 'NONE',  ( -21.53943276465977519, 0.05219959533907696930, 111.2489096053143669 ) ) ;
#151028 = CARTESIAN_POINT ( 'NONE',  ( 12.06949235617739724, 12.14591786802326823, 21.87609039468567573 ) ) ;
#151029 = CARTESIAN_POINT ( 'NONE',  ( -19.03943276465977164, 0.05219959533909376836, 86.24890960531436690 ) ) ;
#151030 = CARTESIAN_POINT ( 'NONE',  ( 12.06949235617739724, 12.14591786802326823, 31.87609039468567929 ) ) ;
#151031 = CARTESIAN_POINT ( 'NONE',  ( -5.153800228976328057, -19.02544592524343514, 57.29057627198103120 ) ) ;
#151032 = CIRCLE ( 'NONE', #28369, 69.99999999999998579 ) ;
#151033 = CARTESIAN_POINT ( 'NONE',  ( -16.55341960407617563, 4.379528057220093196, 38.54275706135234714 ) ) ;
#151034 = CARTESIAN_POINT ( 'NONE',  ( -12.14591786802309592, -12.06949235617757132, 76.87390960531439532 ) ) ;
#151035 = CARTESIAN_POINT ( 'NONE',  ( 0.05219959533934541429, -16.53943276465976808, 85.00109039468568994 ) ) ;
#151037 = CARTESIAN_POINT ( 'NONE',  ( -13.89961937509977652, 13.97604488694528158, 65.62390960531436690 ) ) ;
#151036 = CARTESIAN_POINT ( 'NONE',  ( -21.55341960407619339, 5.719274019375674811, 48.54275706135234714 ) ) ;
#151038 = CARTESIAN_POINT ( 'NONE',  ( 16.51473224551069308, 9.474510206698969483, 84.16557627198102409 ) ) ;
#151039 = CARTESIAN_POINT ( 'NONE',  ( 16.52544592524335698, 4.483927247898782831, 86.45942372801901854 ) ) ;
#151040 = CARTESIAN_POINT ( 'NONE',  ( 69.65682714487590488, -71.74905178543389184, 0.000000000000000000 ) ) ;
#151041 = ORIENTED_EDGE ( 'NONE', *, *, #122840, .T. ) ;
#151042 = CARTESIAN_POINT ( 'NONE',  ( -13.89961937509957401, -13.97604488694547875, 24.37609039468565442 ) ) ;
#151043 = CARTESIAN_POINT ( 'NONE',  ( 16.51473224551069308, 9.474510206698969483, 94.16557627198103830 ) ) ;
#151044 = CARTESIAN_POINT ( 'NONE',  ( -9.474510206698964154, 16.51473224551069663, 50.41557627198102409 ) ) ;
#151045 = CARTESIAN_POINT ( 'NONE',  ( 19.05341960407611168, 5.049401038298154454, 113.9572429386477097 ) ) ;
#151046 = CARTESIAN_POINT ( 'NONE',  ( -4.379528057220086978, -16.55341960407618274, 39.79275706135235424 ) ) ;
#151048 = CARTESIAN_POINT ( 'NONE',  ( 4.379528057220092307, 16.55341960407617563, 62.29275706135236845 ) ) ;
#151047 = CARTESIAN_POINT ( 'NONE',  ( -0.05219959533936034679, 19.03943276465977164, 62.50109039468566863 ) ) ;
#151049 = CARTESIAN_POINT ( 'NONE',  ( -0.05219959533909027116, -19.03943276465977164, 82.49890960531436690 ) ) ;
#151050 = CARTESIAN_POINT ( 'NONE',  ( 21.53943276465977519, -0.05219959533907433946, 108.7489096053143669 ) ) ;
#151051 = CARTESIAN_POINT ( 'NONE',  ( -19.05341960407617563, 5.049401038297882671, 63.54275706135234003 ) ) ;
#151053 = SPHERICAL_SURFACE ( 'NONE', #127883, 8.000000000000000000 ) ;
#151052 = CARTESIAN_POINT ( 'NONE',  ( -5.049401038298153566, 19.05341960407611168, 100.2072429386476955 ) ) ;
#151054 = CARTESIAN_POINT ( 'NONE',  ( -19.03943276465977164, 0.05219959533909376836, 71.24890960531435269 ) ) ;
#151056 = DIRECTION ( 'NONE',  ( 1.000000000000000000, -0.000000000000000000, -0.000000000000000000 ) ) ;
#151055 = CARTESIAN_POINT ( 'NONE',  ( -16.53943276465976808, 0.05219959533911058130, 31.24890960531435979 ) ) ;
#151057 = CARTESIAN_POINT ( 'NONE',  ( 19.05341960407617918, -5.049401038297876454, 41.04275706135233293 ) ) ;
#151058 = CARTESIAN_POINT ( 'NONE',  ( 0.05219959533910956823, 16.53943276465976808, 69.99890960531435269 ) ) ;
#151059 = CARTESIAN_POINT ( 'NONE',  ( -5.719274019375665041, -21.55341960407619695, 99.79275706135234714 ) ) ;
#151060 = CARTESIAN_POINT ( 'NONE',  ( 5.049401038298161559, -19.05341960407611168, 37.70724293864768839 ) ) ;
#151062 = CARTESIAN_POINT ( 'NONE',  ( -5.719274019375665041, -21.55341960407619695, 109.7927570613523613 ) ) ;
#151061 = CARTESIAN_POINT ( 'NONE',  ( 16.53943276465976808, -0.05219959533910856209, 43.74890960531435979 ) ) ;
#151063 = CARTESIAN_POINT ( 'NONE',  ( -0.05219959533909027116, -19.03943276465977164, 87.49890960531436690 ) ) ;
#151064 = CARTESIAN_POINT ( 'NONE',  ( 5.153800228976335163, 19.02544592524342804, 109.7905762719810099 ) ) ;
#151065 = CARTESIAN_POINT ( 'NONE',  ( 9.564922557960805705, 16.46253265017160317, 44.58224293864769550 ) ) ;
#151066 = CARTESIAN_POINT ( 'NONE',  ( 12.14591786802309770, 12.06949235617756955, 109.3739096053143811 ) ) ;
#151067 = CARTESIAN_POINT ( 'NONE',  ( -14.29746914071049879, 8.314922557960819915, 80.83224293864769550 ) ) ;
#151068 = CARTESIAN_POINT ( 'NONE',  ( 21.53943276465977519, -0.05219959533907433946, 88.74890960531436690 ) ) ;
#151069 = CARTESIAN_POINT ( 'NONE',  ( 13.97604488694527802, 13.89961937509977652, 89.37390960531436690 ) ) ;
#151070 = CARTESIAN_POINT ( 'NONE',  ( -0.05219959533907301413, -21.53943276465977519, 92.49890960531436690 ) ) ;
#151071 = CARTESIAN_POINT ( 'NONE',  ( 19.03943276465977164, -0.05219959533909143690, 93.74890960531435269 ) ) ;
#151073 = CARTESIAN_POINT ( 'NONE',  ( -16.55341960407611168, -4.379528057220339221, 106.4572429386477097 ) ) ;
#151072 = CARTESIAN_POINT ( 'NONE',  ( 19.36337904590692105, -5.499999999999937828, 47.91494137495620720 ) ) ;
#151074 = CARTESIAN_POINT ( 'NONE',  ( -19.03943276465977164, 0.05219959533909376836, 66.24890960531436690 ) ) ;
#151075 = CARTESIAN_POINT ( 'NONE',  ( -5.719274019375978568, 21.55341960407610458, 80.20724293864769550 ) ) ;
#151076 = DIRECTION ( 'NONE',  ( 0.8164965809277259234, 0.000000000000000000, 0.5773502691896259531 ) ) ;
#151078 = DIRECTION ( 'NONE',  ( -0.000000000000000000, -0.000000000000000000, -1.000000000000000000 ) ) ;
#151077 = CARTESIAN_POINT ( 'NONE',  ( -21.55341960407610458, -5.719274019375992779, 26.45724293864768839 ) ) ;
#151079 = CARTESIAN_POINT ( 'NONE',  ( -8.224510206698735004, -14.34966873604973081, 19.58442372801901143 ) ) ;
#151080 = CARTESIAN_POINT ( 'NONE',  ( -8.224510206698948167, 14.34966873604960824, 100.4155762719810241 ) ) ;
#151081 = CARTESIAN_POINT ( 'NONE',  ( -18.22780087662122028, 5.500000000000031086, 43.51540105326107977 ) ) ;
#151082 = CARTESIAN_POINT ( 'NONE',  ( 19.05341960407611168, 5.049401038298154454, 93.95724293864769550 ) ) ;
#151083 = CARTESIAN_POINT ( 'NONE',  ( -13.97604488694527625, -13.89961937509977652, 46.87390960531435979 ) ) ;
#151085 = ADVANCED_FACE ( 'NONE', ( #89364 ), #151053, .F. ) ;
#151084 = CARTESIAN_POINT ( 'NONE',  ( -0.05219959533910754901, -16.53943276465976808, 82.49890960531436690 ) ) ;
#151086 = CARTESIAN_POINT ( 'NONE',  ( 9.564922557960805705, 16.46253265017160317, 114.5822429386476955 ) ) ;
#151087 = CARTESIAN_POINT ( 'NONE',  ( 8.224510206698953496, -14.34966873604960469, 47.91557627198102409 ) ) ;
#151088 = CARTESIAN_POINT ( 'NONE',  ( -16.46253265017146816, -9.564922557961047289, 109.1677570613523471 ) ) ;
#151089 = CARTESIAN_POINT ( 'NONE',  ( -21.52544592524334988, -5.823673210054445271, 63.95942372801901854 ) ) ;
#151090 = CARTESIAN_POINT ( 'NONE',  ( 22.44159573604009594, -16.30477369853687364, 147.6750000027311671 ) ) ;
#151091 = CARTESIAN_POINT ( 'NONE',  ( -16.46253265017160317, 9.564922557960807481, 105.8322429386476955 ) ) ;
#151092 = CARTESIAN_POINT ( 'NONE',  ( 10.81492255796078972, 18.62759615963270932, 94.58224293864769550 ) ) ;
#151093 = CARTESIAN_POINT ( 'NONE',  ( -8.314922557961024197, 14.29746914071037800, 82.91775706135234714 ) ) ;
#151094 = CARTESIAN_POINT ( 'NONE',  ( 19.02544592524343514, -5.153800228976328945, 23.54057627198102054 ) ) ;
#151095 = CARTESIAN_POINT ( 'NONE',  ( -9.564922557960796823, -16.46253265017161027, 82.08224293864768129 ) ) ;
#151096 = CARTESIAN_POINT ( 'NONE',  ( -18.67979575497178146, -10.72451020669898902, 86.66557627198102409 ) ) ;
#151097 = CARTESIAN_POINT ( 'NONE',  ( -13.89961937509957401, -13.97604488694547875, 104.3760903946856757 ) ) ;
#151099 = CARTESIAN_POINT ( 'NONE',  ( -5.719274019375665041, -21.55341960407619695, 54.79275706135235424 ) ) ;
#151098 = CARTESIAN_POINT ( 'NONE',  ( -14.29746914071049879, 8.314922557960819915, 55.83224293864770260 ) ) ;
#151101 = CARTESIAN_POINT ( 'NONE',  ( 10.72451020669898902, -18.67979575497178502, 27.91557627198103830 ) ) ;
#151100 = CARTESIAN_POINT ( 'NONE',  ( 8.314922557961029526, -14.29746914071037800, 85.41775706135236135 ) ) ;
#151102 = CARTESIAN_POINT ( 'NONE',  ( 0.05219959533909260263, 19.03943276465977164, 109.9989096053143669 ) ) ;
#151103 = DIRECTION ( 'NONE',  ( -1.000000000000000000, 0.000000000000000000, -6.982962677686266711E-15 ) ) ;
#151104 = CARTESIAN_POINT ( 'NONE',  ( 12.14591786802327356, -12.06949235617739191, 105.6260903946856899 ) ) ;
#151105 = CARTESIAN_POINT ( 'NONE',  ( 12.14591786802327356, -12.06949235617739191, 65.62609039468568994 ) ) ;
#151106 = CARTESIAN_POINT ( 'NONE',  ( -13.97604488694527625, -13.89961937509977652, 76.87390960531433848 ) ) ;
#151107 = CARTESIAN_POINT ( 'NONE',  ( -16.46253265017160317, 9.564922557960807481, 70.83224293864770971 ) ) ;
#151108 = CARTESIAN_POINT ( 'NONE',  ( -14.29746914071037622, -8.314922557961029526, 74.16775706135231871 ) ) ;
#151109 = CARTESIAN_POINT ( 'NONE',  ( -4.379528057220328563, 16.55341960407611168, 45.20724293864769550 ) ) ;
#151110 = CARTESIAN_POINT ( 'NONE',  ( 16.46253265017160672, -9.564922557960803928, 53.33224293864768839 ) ) ;
#151111 = CARTESIAN_POINT ( 'NONE',  ( 19.05341960407611168, 5.049401038298154454, 43.95724293864769550 ) ) ;
#151113 = ORIENTED_EDGE ( 'NONE', *, *, #51286, .F. ) ;
#151112 = CARTESIAN_POINT ( 'NONE',  ( -16.55341960407617563, 4.379528057220093196, 43.54275706135235424 ) ) ;
#151114 = CARTESIAN_POINT ( 'NONE',  ( 9.474510206698729675, 16.51473224551082808, 97.08442372801900433 ) ) ;
#151115 = CARTESIAN_POINT ( 'NONE',  ( -12.14591786802309592, -12.06949235617757132, 101.8739096053143811 ) ) ;
#151116 = CARTESIAN_POINT ( 'NONE',  ( 13.89961937509977652, -13.97604488694527269, 63.12390960531435979 ) ) ;
#151118 = CARTESIAN_POINT ( 'NONE',  ( 23.48529157249600630, -32.32473071737749137, -1.299999999999999822 ) ) ;
#151117 = CARTESIAN_POINT ( 'NONE',  ( 9.564922557961047289, -16.46253265017146816, 105.4177570613523471 ) ) ;
#151119 = CARTESIAN_POINT ( 'NONE',  ( -21.53943276465977519, -0.05219959533937600094, 108.7510903946857042 ) ) ;
#151120 = CARTESIAN_POINT ( 'NONE',  ( -14.34966873604972548, 8.224510206698743886, 63.33442372801900433 ) ) ;
#151121 = CARTESIAN_POINT ( 'NONE',  ( 18.67979575497178502, 10.72451020669898547, 69.16557627198102409 ) ) ;
#151122 = CARTESIAN_POINT ( 'NONE',  ( -4.483927247898782831, 16.52544592524335698, 57.70942372801901143 ) ) ;
#151123 = CARTESIAN_POINT ( 'NONE',  ( -19.03943276465977164, 0.05219959533909376836, 36.24890960531436690 ) ) ;
#151124 = CARTESIAN_POINT ( 'NONE',  ( -16.46253265017146816, -9.564922557961047289, 39.16775706135234003 ) ) ;
#151125 = CARTESIAN_POINT ( 'NONE',  ( -19.05341960407611168, -5.049401038298163336, 91.45724293864766707 ) ) ;
#151126 = CARTESIAN_POINT ( 'NONE',  ( -5.153800228976328057, -19.02544592524343514, 27.29057627198103120 ) ) ;
#151127 = CARTESIAN_POINT ( 'NONE',  ( -0.05219959533909027116, -19.03943276465977164, 62.49890960531435979 ) ) ;
#151128 = CIRCLE ( 'NONE', #63916, 37.99626262588765968 ) ;
#151129 = CARTESIAN_POINT ( 'NONE',  ( -5.823673210054431948, 21.52544592524334988, 77.70942372801900433 ) ) ;
#151130 = CARTESIAN_POINT ( 'NONE',  ( -16.51473224551082808, 9.474510206698731452, 53.33442372801900433 ) ) ;
#151131 = ORIENTED_EDGE ( 'NONE', *, *, #49707, .F. ) ;
#151132 = CARTESIAN_POINT ( 'NONE',  ( -16.46253265017146816, -9.564922557961047289, 29.16775706135232937 ) ) ;
#151133 = CARTESIAN_POINT ( 'NONE',  ( -16.46253265017160317, 9.564922557960807481, 60.83224293864769550 ) ) ;
#151134 = CARTESIAN_POINT ( 'NONE',  ( 19.02544592524343514, -5.153800228976328945, 113.5405762719810241 ) ) ;
#151135 = CARTESIAN_POINT ( 'NONE',  ( -5.719274019375665041, -21.55341960407619695, 89.79275706135236135 ) ) ;
#151136 = CARTESIAN_POINT ( 'NONE',  ( -0.05219959533909027116, -19.03943276465977164, 62.49890960531435979 ) ) ;
#151137 = CARTESIAN_POINT ( 'NONE',  ( 5.719274019375673035, 21.55341960407619339, 92.29275706135236135 ) ) ;
#151138 = CARTESIAN_POINT ( 'NONE',  ( -0.05219959533907301413, -21.53943276465977519, 32.49890960531435979 ) ) ;
#151139 = CARTESIAN_POINT ( 'NONE',  ( -0.05219959533909027116, -19.03943276465977164, 77.49890960531435269 ) ) ;
#151140 = CARTESIAN_POINT ( 'NONE',  ( -21.55341960407619339, 5.719274019375674811, 43.54275706135235424 ) ) ;
#151141 = CARTESIAN_POINT ( 'NONE',  ( -16.46253265017146816, -9.564922557961047289, 59.16775706135233293 ) ) ;
#151142 = CARTESIAN_POINT ( 'NONE',  ( 9.564922557960805705, 16.46253265017160317, 39.58224293864768839 ) ) ;
#151143 = CARTESIAN_POINT ( 'NONE',  ( 13.89961937509977652, -13.97604488694527269, 93.12390960531436690 ) ) ;
#151144 = CARTESIAN_POINT ( 'NONE',  ( -8.224510206698735004, -14.34966873604973081, 34.58442372801900433 ) ) ;
#151145 = CARTESIAN_POINT ( 'NONE',  ( 16.52544592524342804, -4.483927247898539470, 83.54057627198102409 ) ) ;
#151146 = CARTESIAN_POINT ( 'NONE',  ( -19.03943276465977164, 0.05219959533909376836, 66.24890960531436690 ) ) ;
#151147 = CARTESIAN_POINT ( 'NONE',  ( 18.62759615963271287, -10.81492255796078972, 53.33224293864769550 ) ) ;
#151148 = CARTESIAN_POINT ( 'NONE',  ( 9.564922557961047289, -16.46253265017146816, 110.4177570613523471 ) ) ;
#151149 = CARTESIAN_POINT ( 'NONE',  ( -15.80617190586745835, -15.72974639402198527, 111.8739096053143669 ) ) ;
#151150 = CARTESIAN_POINT ( 'NONE',  ( -21.52544592524334988, -5.823673210054445271, 68.95942372801901854 ) ) ;
#151152 = CARTESIAN_POINT ( 'NONE',  ( -16.52544592524335698, -4.483927247898792601, 63.95942372801901854 ) ) ;
#151151 = B_SPLINE_CURVE_WITH_KNOTS ( 'NONE', 3,
 ( #5972, #36308, #162662, #100978 ),
 .UNSPECIFIED., .F., .F.,
 ( 4, 4 ),
 ( 0.001482540648255906276, 0.002244533994399153676 ),
 .UNSPECIFIED. ) ;
#151153 = CARTESIAN_POINT ( 'NONE',  ( -4.483927247898782831, 16.52544592524335698, 62.70942372801902565 ) ) ;
#151154 = CARTESIAN_POINT ( 'NONE',  ( 19.02544592524343514, -5.153800228976328945, 63.54057627198103830 ) ) ;
#151155 = CARTESIAN_POINT ( 'NONE',  ( 8.224510206698742110, 14.34966873604972548, 102.0844237280190185 ) ) ;
#151156 = CARTESIAN_POINT ( 'NONE',  ( 5.153800228976615827, -19.02544592524334988, 45.20942372801901143 ) ) ;
#151157 = VECTOR ( 'NONE', #159517, 1000.000000000000000 ) ;
#151158 = EDGE_CURVE ( 'NONE', #166090, #128112, #168186, .T. ) ;
#151159 = CARTESIAN_POINT ( 'NONE',  ( -5.719274019375978568, 21.55341960407610458, 110.2072429386477239 ) ) ;
#151160 = CARTESIAN_POINT ( 'NONE',  ( -0.05219959533910754901, -16.53943276465976808, 67.49890960531436690 ) ) ;
#151161 = CARTESIAN_POINT ( 'NONE',  ( -13.97604488694527625, -13.89961937509977652, 91.87390960531432427 ) ) ;
#151162 = CARTESIAN_POINT ( 'NONE',  ( -4.483927247898782831, 16.52544592524335698, 82.70942372801900433 ) ) ;
#151163 = CARTESIAN_POINT ( 'NONE',  ( -15.72974639402176322, -15.80617190586768395, 59.37609039468568284 ) ) ;
#151164 = CARTESIAN_POINT ( 'NONE',  ( 14.29746914071037800, 8.314922557961029526, 36.66775706135234714 ) ) ;
#151165 = CARTESIAN_POINT ( 'NONE',  ( -18.67979575497193778, 10.72451020669871902, 33.33442372801900433 ) ) ;
#151166 = CARTESIAN_POINT ( 'NONE',  ( -4.379528057220328563, 16.55341960407611168, 55.20724293864770260 ) ) ;
#151167 = VERTEX_POINT ( 'NONE', #90345 ) ;
#151168 = CARTESIAN_POINT ( 'NONE',  ( -21.55341960407610458, -5.719274019375992779, 106.4572429386477097 ) ) ;
#151169 = CARTESIAN_POINT ( 'NONE',  ( 14.29746914071049879, -8.314922557960816363, 33.33224293864769550 ) ) ;
#151170 = ORIENTED_EDGE ( 'NONE', *, *, #103145, .T. ) ;
#151171 = CARTESIAN_POINT ( 'NONE',  ( 34.40392893854398437, 6.519971432731299643, 48.73974290947561627 ) ) ;
#151172 = CARTESIAN_POINT ( 'NONE',  ( -21.52544592524343514, 5.823673210054127303, 26.04057627198103475 ) ) ;
#151173 = CARTESIAN_POINT ( 'NONE',  ( -21.55341960407619339, 5.719274019375674811, 43.54275706135235424 ) ) ;
#151174 = CARTESIAN_POINT ( 'NONE',  ( -14.34966873604960291, -8.224510206698953496, 66.66557627198102409 ) ) ;
#151175 = CARTESIAN_POINT ( 'NONE',  ( 15.72974639402199770, -15.80617190586745480, 68.12390960531436690 ) ) ;
#151176 = CARTESIAN_POINT ( 'NONE',  ( 0.05219959533909260263, 19.03943276465977164, 74.99890960531435269 ) ) ;
#151178 = CARTESIAN_POINT ( 'NONE',  ( 13.89961937509957401, 13.97604488694547697, 61.87609039468566863 ) ) ;
#151177 = CARTESIAN_POINT ( 'NONE',  ( -5.049401038298153566, 19.05341960407611168, 25.20724293864768484 ) ) ;
#151179 = ADVANCED_FACE ( 'NONE', ( #75181 ), #76167, .F. ) ;
#151180 = CARTESIAN_POINT ( 'NONE',  ( 15.72974639402199770, -15.80617190586745480, 48.12390960531436690 ) ) ;
#151181 = CARTESIAN_POINT ( 'NONE',  ( 16.46253265017160672, -9.564922557960803928, 63.33224293864769550 ) ) ;
#151182 = CARTESIAN_POINT ( 'NONE',  ( -0.05219959533934338120, 16.53943276465976808, 42.50109039468567573 ) ) ;
#151183 = CARTESIAN_POINT ( 'NONE',  ( 0.05219959533907565091, 21.53943276465977519, 109.9989096053143527 ) ) ;
#151184 = CARTESIAN_POINT ( 'NONE',  ( 8.224510206698953496, -14.34966873604960469, 52.91557627198103830 ) ) ;
#151185 = CARTESIAN_POINT ( 'NONE',  ( -0.05219959533909027116, -19.03943276465977164, 97.49890960531436690 ) ) ;
#151186 = CARTESIAN_POINT ( 'NONE',  ( 10.72451020669898902, -18.67979575497178502, 77.91557627198102409 ) ) ;
#151188 = CARTESIAN_POINT ( 'NONE',  ( -12.06949235617739369, -12.14591786802326823, 34.37609039468568284 ) ) ;
#151187 = CARTESIAN_POINT ( 'NONE',  ( -10.72451020669898014, 18.67979575497178502, 110.4155762719810383 ) ) ;
#151189 = CARTESIAN_POINT ( 'NONE',  ( 0.05219959533907565091, 21.53943276465977519, 34.99890960531435979 ) ) ;
#151190 = CARTESIAN_POINT ( 'NONE',  ( 21.52544592524334988, 5.823673210054432836, 96.45942372801901854 ) ) ;
#151191 = CARTESIAN_POINT ( 'NONE',  ( -19.05341960407611168, -5.049401038298163336, 36.45724293864766707 ) ) ;
#151192 = CARTESIAN_POINT ( 'NONE',  ( -13.89961937509977652, 13.97604488694528158, 95.62390960531436690 ) ) ;
#151193 = CARTESIAN_POINT ( 'NONE',  ( -0.05219959533909027116, -19.03943276465977164, 82.49890960531436690 ) ) ;
#151194 = PRODUCT_RELATED_PRODUCT_CATEGORY ( 'part', '', ( #155079 ) ) ;
#151195 = PLANE ( 'NONE',  #37804 ) ;
#151196 = CARTESIAN_POINT ( 'NONE',  ( 16.51473224551083163, -9.474510206698727899, 55.83442372801899722 ) ) ;
#151198 = CARTESIAN_POINT ( 'NONE',  ( -15.80617190586745835, -15.72974639402198527, 36.87390960531435979 ) ) ;
#151197 = CARTESIAN_POINT ( 'NONE',  ( 5.153800228976615827, -19.02544592524334988, 20.20942372801899722 ) ) ;
#151199 = CARTESIAN_POINT ( 'NONE',  ( 8.224510206698742110, 14.34966873604972548, 107.0844237280190043 ) ) ;
#151200 = CARTESIAN_POINT ( 'NONE',  ( 16.46253265017146816, 9.564922557961045513, 91.66775706135234714 ) ) ;
#151201 = DIRECTION ( 'NONE',  ( 0.000000000000000000, -0.000000000000000000, 1.000000000000000000 ) ) ;
#151202 = CARTESIAN_POINT ( 'NONE',  ( -9.474510206698720793, -16.51473224551083518, 89.58442372801900433 ) ) ;
#151203 = CARTESIAN_POINT ( 'NONE',  ( 0.05219959533936267826, -19.03943276465977164, 40.00109039468566152 ) ) ;
#151204 = CARTESIAN_POINT ( 'NONE',  ( -10.59477242850411649, -90.60836494048552936, -4.999999999999999112 ) ) ;
#151205 = CARTESIAN_POINT ( 'NONE',  ( 0.05219959533909260263, 19.03943276465977164, 44.99890960531435979 ) ) ;
#151206 = CARTESIAN_POINT ( 'NONE',  ( -16.52544592524342804, 4.483927247898546575, 56.04057627198102409 ) ) ;
#151207 = CARTESIAN_POINT ( 'NONE',  ( 9.474510206698971260, -16.51473224551069308, 37.91557627198102409 ) ) ;
#151208 = CARTESIAN_POINT ( 'NONE',  ( -12.14591786802309592, -12.06949235617757132, 26.87390960531435979 ) ) ;
#151209 = CARTESIAN_POINT ( 'NONE',  ( 17.60769864724391454, -5.499999999999980460, 46.15024842019165163 ) ) ;
#151210 = CARTESIAN_POINT ( 'NONE',  ( -16.53943276465976808, -0.05219959533934237506, 113.7510903946856757 ) ) ;
#151211 = CARTESIAN_POINT ( 'NONE',  ( 9.474510206698971260, -16.51473224551069308, 47.91557627198102409 ) ) ;
#151212 = CARTESIAN_POINT ( 'NONE',  ( -18.62759615963255300, -10.81492255796106328, 104.1677570613523471 ) ) ;
#151213 = CARTESIAN_POINT ( 'NONE',  ( -4.379528057220086978, -16.55341960407618274, 24.79275706135235779 ) ) ;
#151214 = CARTESIAN_POINT ( 'NONE',  ( 10.81492255796078972, 18.62759615963270932, 34.58224293864770260 ) ) ;
#151215 = CARTESIAN_POINT ( 'NONE',  ( 15.72974639402176855, 15.80617190586768217, 91.87609039468568994 ) ) ;
#151216 = CARTESIAN_POINT ( 'NONE',  ( 13.97604488694527802, 13.89961937509977652, 99.37390960531436690 ) ) ;
#151217 = CARTESIAN_POINT ( 'NONE',  ( 13.89961937509977652, -13.97604488694527269, 88.12390960531438111 ) ) ;
#151218 = CARTESIAN_POINT ( 'NONE',  ( -30.20036327792369235, -26.22857331006468229, -17.18026671435357500 ) ) ;
#151219 = CARTESIAN_POINT ( 'NONE',  ( 15.80617190586746368, 15.72974639402197994, 104.3739096053143669 ) ) ;
#151220 = CARTESIAN_POINT ( 'NONE',  ( 4.379528057220339221, -16.55341960407611168, 82.70724293864770971 ) ) ;
#151221 = CARTESIAN_POINT ( 'NONE',  ( -18.67979575497178146, -10.72451020669898902, 71.66557627198100988 ) ) ;
#151222 = CARTESIAN_POINT ( 'NONE',  ( 0.05219959533909260263, 19.03943276465977164, 54.99890960531435979 ) ) ;
#151223 = CARTESIAN_POINT ( 'NONE',  ( 21.53943276465977519, -0.05219959533907433946, 98.74890960531438111 ) ) ;
#151224 = ORIENTED_EDGE ( 'NONE', *, *, #26654, .F. ) ;
#151225 = CARTESIAN_POINT ( 'NONE',  ( -13.89961937509977652, 13.97604488694528158, 60.62390960531436690 ) ) ;
#151227 = CARTESIAN_POINT ( 'NONE',  ( 35.99626262588764547, 2.869439944428138037E-14, -8.000000000000000000 ) ) ;
#151226 = CARTESIAN_POINT ( 'NONE',  ( -4.483927247898539470, -16.52544592524342804, 92.29057627198103830 ) ) ;
#151228 = CARTESIAN_POINT ( 'NONE',  ( -19.02544592524342804, 5.153800228976336051, 66.04057627198103830 ) ) ;
#151229 = CARTESIAN_POINT ( 'NONE',  ( -19.02544592524334988, -5.153800228976617603, 73.95942372801900433 ) ) ;
#151230 = CARTESIAN_POINT ( 'NONE',  ( -16.52544592524342804, 4.483927247898546575, 86.04057627198102409 ) ) ;
#151231 = CARTESIAN_POINT ( 'NONE',  ( 5.719274019375673035, 21.55341960407619339, 52.29275706135236135 ) ) ;
#151233 = CARTESIAN_POINT ( 'NONE',  ( -10.81492255796105439, 18.62759615963255655, 22.91775706135235069 ) ) ;
#151232 = CARTESIAN_POINT ( 'NONE',  ( -5.049401038298153566, 19.05341960407611168, 45.20724293864769550 ) ) ;
#151234 = CARTESIAN_POINT ( 'NONE',  ( 16.55341960407611168, 4.379528057220329451, 103.9572429386476813 ) ) ;
#151235 = CARTESIAN_POINT ( 'NONE',  ( 13.56018889279821771, -37.30201529093263701, -30.04439950253996017 ) ) ;
#151236 = CARTESIAN_POINT ( 'NONE',  ( -13.89961937509977652, 13.97604488694528158, 65.62390960531436690 ) ) ;
#151237 = CARTESIAN_POINT ( 'NONE',  ( 16.62475595723701005, 7.163666690055288555, 111.9728664818952950 ) ) ;
#151239 = CARTESIAN_POINT ( 'NONE',  ( 16.51473224551069308, 9.474510206698969483, 109.1655762719810383 ) ) ;
#151238 = CARTESIAN_POINT ( 'NONE',  ( -13.97604488694547697, 13.89961937509957934, 113.1260903946856757 ) ) ;
#151240 = CARTESIAN_POINT ( 'NONE',  ( 0.05219959533937995610, -21.53943276465977519, 50.00109039468568994 ) ) ;
#151241 = CARTESIAN_POINT ( 'NONE',  ( 19.05341960407611168, 5.049401038298154454, 93.95724293864769550 ) ) ;
#151242 = CARTESIAN_POINT ( 'NONE',  ( 16.46253265017146816, 9.564922557961045513, 86.66775706135233293 ) ) ;
#151243 = CARTESIAN_POINT ( 'NONE',  ( -13.89961937509977652, 13.97604488694528158, 55.62390960531434558 ) ) ;
#151244 = CARTESIAN_POINT ( 'NONE',  ( 16.55341960407611168, 4.379528057220329451, 78.95724293864769550 ) ) ;
#151245 = CARTESIAN_POINT ( 'NONE',  ( -8.314922557960811034, -14.29746914071050412, 82.08224293864768129 ) ) ;
#151246 = CARTESIAN_POINT ( 'NONE',  ( -9.564922557960796823, -16.46253265017161027, 92.08224293864769550 ) ) ;
#151247 = CARTESIAN_POINT ( 'NONE',  ( 0.05219959533910956823, 16.53943276465976808, 84.99890960531436690 ) ) ;
#151248 = CARTESIAN_POINT ( 'NONE',  ( -0.05219959533909027116, -19.03943276465977164, 87.49890960531436690 ) ) ;
#151249 = CARTESIAN_POINT ( 'NONE',  ( -5.049401038297874678, -19.05341960407617918, 34.79275706135233293 ) ) ;
#151252 = CARTESIAN_POINT ( 'NONE',  ( -19.02544592524342804, 5.153800228976336051, 26.04057627198103120 ) ) ;
#151251 = CARTESIAN_POINT ( 'NONE',  ( -4.379528057220328563, 16.55341960407611168, 25.20724293864769550 ) ) ;
#151250 = CARTESIAN_POINT ( 'NONE',  ( 9.474510206698971260, -16.51473224551069308, 47.91557627198102409 ) ) ;
#151253 = ORIENTED_EDGE ( 'NONE', *, *, #12591, .F. ) ;
#151254 = CARTESIAN_POINT ( 'NONE',  ( 15.72974639402176855, 15.80617190586768217, 46.87609039468568994 ) ) ;
#151255 = CARTESIAN_POINT ( 'NONE',  ( -0.05219959533936034679, 19.03943276465977164, 77.50109039468566152 ) ) ;
#151256 = CARTESIAN_POINT ( 'NONE',  ( -8.224510206698948167, 14.34966873604960824, 35.41557627198102409 ) ) ;
#151257 = CARTESIAN_POINT ( 'NONE',  ( 18.67979575497178502, 10.72451020669898547, 89.16557627198102409 ) ) ;
#151258 = CARTESIAN_POINT ( 'NONE',  ( 5.823673210054125526, 21.52544592524343514, 29.79057627198102409 ) ) ;
#151259 = CARTESIAN_POINT ( 'NONE',  ( -16.55341960407611168, -4.379528057220339221, 66.45724293864768129 ) ) ;
#151260 = CARTESIAN_POINT ( 'NONE',  ( -16.46253265017160317, 9.564922557960807481, 40.83224293864769550 ) ) ;
#151261 = CARTESIAN_POINT ( 'NONE',  ( -16.53943276465976808, -0.05219959533934237506, 98.75109039468568994 ) ) ;
#151262 = CARTESIAN_POINT ( 'NONE',  ( 12.14591786802327356, -12.06949235617739191, 75.62609039468567573 ) ) ;
#151263 = CARTESIAN_POINT ( 'NONE',  ( -18.62759615963270932, 10.81492255796079327, 40.83224293864769550 ) ) ;
#151264 = CARTESIAN_POINT ( 'NONE',  ( 5.153800228976615827, -19.02544592524334988, 25.20942372801900433 ) ) ;
#151265 = CARTESIAN_POINT ( 'NONE',  ( -13.89961937509977652, 13.97604488694528158, 90.62390960531432427 ) ) ;
#151266 = CARTESIAN_POINT ( 'NONE',  ( 12.14591786802327356, -12.06949235617739191, 70.62609039468567573 ) ) ;
#151267 = CARTESIAN_POINT ( 'NONE',  ( 16.51473224551069308, 9.474510206698969483, 29.16557627198103475 ) ) ;
#151268 = CARTESIAN_POINT ( 'NONE',  ( 0.05219959533910956823, 16.53943276465976808, 39.99890960531436690 ) ) ;
#151270 = CARTESIAN_POINT ( 'NONE',  ( -5.049401038298153566, 19.05341960407611168, 90.20724293864766707 ) ) ;
#151269 = CARTESIAN_POINT ( 'NONE',  ( -16.46253265017160317, 9.564922557960807481, 100.8322429386477097 ) ) ;
#151271 = CARTESIAN_POINT ( 'NONE',  ( -21.55341960407610458, -5.719274019375992779, 21.45724293864769550 ) ) ;
#151272 = CARTESIAN_POINT ( 'NONE',  ( -14.29746914071049879, 8.314922557960819915, 75.83224293864769550 ) ) ;
#151273 = VERTEX_POINT ( 'NONE', #45839 ) ;
#151274 = CARTESIAN_POINT ( 'NONE',  ( -12.06949235617756955, 12.14591786802309770, 50.62390960531435979 ) ) ;
#151275 = ORIENTED_EDGE ( 'NONE', *, *, #142962, .T. ) ;
#151277 = CARTESIAN_POINT ( 'NONE',  ( 18.22780087662122384, -5.500000000000022204, 81.01540105326105845 ) ) ;
#151276 = CARTESIAN_POINT ( 'NONE',  ( 0.05219959533934541429, -16.53943276465976808, 60.00109039468568284 ) ) ;
#151278 = CARTESIAN_POINT ( 'NONE',  ( -9.564922557961040184, 16.46253265017147172, 52.91775706135233293 ) ) ;
#151279 = CARTESIAN_POINT ( 'NONE',  ( 16.51473224551069308, 9.474510206698969483, 94.16557627198103830 ) ) ;
#151280 = CARTESIAN_POINT ( 'NONE',  ( 5.153800228976615827, -19.02544592524334988, 70.20942372801899012 ) ) ;
#151281 = CARTESIAN_POINT ( 'NONE',  ( -22.44159573604009950, -16.30477369853688430, 143.5750000027311728 ) ) ;
#151283 = CARTESIAN_POINT ( 'NONE',  ( 12.14591786802327356, -12.06949235617739191, 90.62609039468567573 ) ) ;
#151282 = CARTESIAN_POINT ( 'NONE',  ( 5.153800228976615827, -19.02544592524334988, 110.2094237280189901 ) ) ;
#151284 = CARTESIAN_POINT ( 'NONE',  ( 16.46253265017160672, -9.564922557960803928, 33.33224293864770260 ) ) ;
#151285 =( BOUNDED_CURVE ( )  B_SPLINE_CURVE ( 2, ( #109634, #110620, #31810, #79295, #92467, #154155, #140964, #2451, #187500, #93461, #78287, #139961, #45980 ),
 .UNSPECIFIED., .F., .T. ) 
 B_SPLINE_CURVE_WITH_KNOTS ( ( 3, 2, 2, 2, 2, 2, 3 ),
 ( 0.7393182215122932055, 0.7412280701754385692, 0.7456140350877192846, 0.7500000000000000000, 0.7543859649122807154, 0.7587719298245614308, 0.7607274583097971554 ),
 .UNSPECIFIED. ) 
 CURVE ( )  GEOMETRIC_REPRESENTATION_ITEM ( )  RATIONAL_B_SPLINE_CURVE ( ( 0.9832469066685285419, 0.9851625545550100060, 1.000000000000000000, 0.9659258262890683122, 1.000000000000000000, 0.9659258262890683122, 1.000000000000000000, 0.9659258262890683122, 1.000000000000000000, 0.9659258262890683122, 1.000000000000000000, 0.9848076720550078544, 0.9831626618144001517 ) ) 
 REPRESENTATION_ITEM ( '' )  );
#151286 = CARTESIAN_POINT ( 'NONE',  ( 16.46253265017160672, -9.564922557960803928, 113.3322429386476955 ) ) ;
#151287 = CARTESIAN_POINT ( 'NONE',  ( -21.53943276465977519, -0.05219959533937600094, 48.75109039468568284 ) ) ;
#151288 = CARTESIAN_POINT ( 'NONE',  ( -16.51473224551082808, 9.474510206698731452, 98.33442372801900433 ) ) ;
#151290 = CARTESIAN_POINT ( 'NONE',  ( -5.049401038298153566, 19.05341960407611168, 55.20724293864769550 ) ) ;
#151289 = CARTESIAN_POINT ( 'NONE',  ( 17.50000000000000000, 3.880681150310165251, 22.10217894668021188 ) ) ;
#151291 = AXIS2_PLACEMENT_3D ( 'NONE', #159929, #194285, #55751 ) ;
#151292 = DIRECTION ( 'NONE',  ( 0.000000000000000000, 0.000000000000000000, -1.000000000000000000 ) ) ;
#151294 = CARTESIAN_POINT ( 'NONE',  ( 16.51473224551069308, 9.474510206698969483, 64.16557627198102409 ) ) ;
#151293 = CARTESIAN_POINT ( 'NONE',  ( -4.483927247898539470, -16.52544592524342804, 72.29057627198102409 ) ) ;
#151295 = CARTESIAN_POINT ( 'NONE',  ( 0.05219959533909260263, 19.03943276465977164, 74.99890960531435269 ) ) ;
#151296 = CARTESIAN_POINT ( 'NONE',  ( -0.05219959533936034679, 19.03943276465977164, 72.50109039468566152 ) ) ;
#151297 = CARTESIAN_POINT ( 'NONE',  ( 5.823673210054125526, 21.52544592524343514, 64.79057627198103830 ) ) ;
#151298 = CARTESIAN_POINT ( 'NONE',  ( 12.06949235617757843, -12.14591786802309237, 113.1239096053143953 ) ) ;
#151299 = CARTESIAN_POINT ( 'NONE',  ( -5.153800228976607833, 19.02544592524334988, 52.70942372801900433 ) ) ;
#151300 = CARTESIAN_POINT ( 'NONE',  ( -0.05219959533909027116, -19.03943276465977164, 57.49890960531435979 ) ) ;
#151301 = CARTESIAN_POINT ( 'NONE',  ( 19.05341960407611168, 5.049401038298154454, 98.95724293864766707 ) ) ;
#151302 = CARTESIAN_POINT ( 'NONE',  ( 21.53943276465977519, -0.05219959533907433946, 93.74890960531436690 ) ) ;
#151304 = CARTESIAN_POINT ( 'NONE',  ( 0.05219959533936267826, -19.03943276465977164, 55.00109039468566863 ) ) ;
#151303 = CARTESIAN_POINT ( 'NONE',  ( 12.14591786802309770, 12.06949235617756955, 84.37390960531438111 ) ) ;
#151305 = CARTESIAN_POINT ( 'NONE',  ( -18.62759615963270932, 10.81492255796079327, 75.83224293864769550 ) ) ;
#151306 = CARTESIAN_POINT ( 'NONE',  ( -5.719274019375978568, 21.55341960407610458, 60.20724293864768839 ) ) ;
#151307 = CARTESIAN_POINT ( 'NONE',  ( -0.05219959533910754901, -16.53943276465976808, 27.49890960531435269 ) ) ;
#151308 = CARTESIAN_POINT ( 'NONE',  ( 0.05219959533937995610, -21.53943276465977519, 95.00109039468568994 ) ) ;
#151309 = CARTESIAN_POINT ( 'NONE',  ( 19.02544592524343514, -5.153800228976328945, 78.54057627198099567 ) ) ;
#151310 = CARTESIAN_POINT ( 'NONE',  ( -13.97604488694527625, -13.89961937509977652, 31.87390960531435979 ) ) ;
#151311 = CARTESIAN_POINT ( 'NONE',  ( -18.62759615963255300, -10.81492255796106328, 24.16775706135235424 ) ) ;
#151312 = CARTESIAN_POINT ( 'NONE',  ( -21.53943276465977519, -0.05219959533937600094, 43.75109039468568284 ) ) ;
#151313 = CARTESIAN_POINT ( 'NONE',  ( -16.46253265017160317, 9.564922557960807481, 50.83224293864770260 ) ) ;
#151314 = CARTESIAN_POINT ( 'NONE',  ( -21.52544592524334988, -5.823673210054445271, 18.95942372801901143 ) ) ;
#151315 = CARTESIAN_POINT ( 'NONE',  ( 9.564922557961047289, -16.46253265017146816, 65.41775706135233293 ) ) ;
#151316 = CARTESIAN_POINT ( 'NONE',  ( -5.049401038298153566, 19.05341960407611168, 40.20724293864768839 ) ) ;
#151317 = CARTESIAN_POINT ( 'NONE',  ( -12.06949235617739369, -12.14591786802326823, 34.37609039468568284 ) ) ;
#151318 = DIRECTION ( 'NONE',  ( 1.000000000000000000, -0.000000000000000000, -0.000000000000000000 ) ) ;
#151319 = CARTESIAN_POINT ( 'NONE',  ( -12.14591786802326823, 12.06949235617739902, 73.12609039468567573 ) ) ;
#151320 = CARTESIAN_POINT ( 'NONE',  ( -0.05219959533909027116, -19.03943276465977164, 37.49890960531436690 ) ) ;
#151321 = CARTESIAN_POINT ( 'NONE',  ( -25.66129429279898844, -9.008087060823562808, 171.3163768196905323 ) ) ;
#151322 = CARTESIAN_POINT ( 'NONE',  ( -19.02544592524342804, 5.153800228976336051, 86.04057627198103830 ) ) ;
#151324 = EDGE_CURVE ( 'NONE', #38283, #135811, #175095, .T. ) ;
#151323 = CARTESIAN_POINT ( 'NONE',  ( -19.02544592524342804, 5.153800228976336051, 26.04057627198103120 ) ) ;
#151325 = CARTESIAN_POINT ( 'NONE',  ( 10.72451020669898902, -18.67979575497178502, 62.91557627198102409 ) ) ;
#151326 = CARTESIAN_POINT ( 'NONE',  ( 0.05219959533934541429, -16.53943276465976808, 45.00109039468568284 ) ) ;
#151327 = CARTESIAN_POINT ( 'NONE',  ( -18.62759615963255300, -10.81492255796106328, 94.16775706135237556 ) ) ;
#151328 = CARTESIAN_POINT ( 'NONE',  ( -19.05341960407611168, -5.049401038298163336, 36.45724293864766707 ) ) ;
#151329 = CARTESIAN_POINT ( 'NONE',  ( -14.29746914071049879, 8.314922557960819915, 35.83224293864768839 ) ) ;
#151330 = CARTESIAN_POINT ( 'NONE',  ( 16.52544592524342804, -4.483927247898539470, 68.54057627198103830 ) ) ;
#151331 = CARTESIAN_POINT ( 'NONE',  ( -16.46253265017160317, 9.564922557960807481, 65.83224293864769550 ) ) ;
#151332 = CARTESIAN_POINT ( 'NONE',  ( -21.52544592524334988, -5.823673210054445271, 108.9594237280190185 ) ) ;
#151333 = CARTESIAN_POINT ( 'NONE',  ( 15.72974639402176855, 15.80617190586768217, 26.87609039468567218 ) ) ;
#151334 = CARTESIAN_POINT ( 'NONE',  ( -0.05219959533909027116, -19.03943276465977164, 82.49890960531436690 ) ) ;
#151335 = CARTESIAN_POINT ( 'NONE',  ( -21.52544592524334988, -5.823673210054445271, 83.95942372801900433 ) ) ;
#151336 = CARTESIAN_POINT ( 'NONE',  ( 16.53943276465976808, 0.05219959533934440121, 51.25109039468568994 ) ) ;
#151337 = CARTESIAN_POINT ( 'NONE',  ( 14.29746914071037800, 8.314922557961029526, 31.66775706135234358 ) ) ;
#151339 = CARTESIAN_POINT ( 'NONE',  ( 21.52544592524334988, 5.823673210054432836, 96.45942372801901854 ) ) ;
#151338 = CARTESIAN_POINT ( 'NONE',  ( 0.05219959533910956823, 16.53943276465976808, 94.99890960531436690 ) ) ;
#151340 = CARTESIAN_POINT ( 'NONE',  ( 8.224510206698953496, -14.34966873604960469, 32.91557627198102409 ) ) ;
#151341 = CARTESIAN_POINT ( 'NONE',  ( 5.049401038298161559, -19.05341960407611168, 22.70724293864769194 ) ) ;
#151342 = CARTESIAN_POINT ( 'NONE',  ( -8.224510206698735004, -14.34966873604973081, 59.58442372801901854 ) ) ;
#151343 = CARTESIAN_POINT ( 'NONE',  ( -16.53943276465976808, 0.05219959533911058130, 56.24890960531436690 ) ) ;
#151344 = CARTESIAN_POINT ( 'NONE',  ( -14.34966873604972548, 8.224510206698743886, 103.3344237280190043 ) ) ;
#151345 = CARTESIAN_POINT ( 'NONE',  ( -19.02544592524342804, 5.153800228976336051, 116.0405762719810383 ) ) ;
#151346 = CARTESIAN_POINT ( 'NONE',  ( -18.67979575497178146, -10.72451020669898902, 21.66557627198102409 ) ) ;
#151347 = CARTESIAN_POINT ( 'NONE',  ( -10.81492255796105439, 18.62759615963255655, 112.9177570613523329 ) ) ;
#151348 = CARTESIAN_POINT ( 'NONE',  ( -0.05219959533910754901, -16.53943276465976808, 87.49890960531436690 ) ) ;
#151349 = CARTESIAN_POINT ( 'NONE',  ( -5.153800228976328057, -19.02544592524343514, 97.29057627198099567 ) ) ;
#151350 = ORIENTED_EDGE ( 'NONE', *, *, #78467, .F. ) ;
#151351 = CARTESIAN_POINT ( 'NONE',  ( 0.05219959533934541429, -16.53943276465976808, 40.00109039468567573 ) ) ;
#151352 = CARTESIAN_POINT ( 'NONE',  ( -19.03943276465977164, 0.05219959533909376836, 36.24890960531436690 ) ) ;
#151354 = LINE ( 'NONE', #25024, #198575 ) ;
#151353 = CARTESIAN_POINT ( 'NONE',  ( 4.483927247898790824, -16.52544592524335698, 45.20942372801901854 ) ) ;
#151355 = CARTESIAN_POINT ( 'NONE',  ( -19.02544592524334988, -5.153800228976617603, 43.95942372801899012 ) ) ;
#151356 = CARTESIAN_POINT ( 'NONE',  ( 5.153800228976335163, 19.02544592524342804, 44.79057627198103830 ) ) ;
#151357 = CARTESIAN_POINT ( 'NONE',  ( 16.53943276465976808, 0.05219959533934440121, 81.25109039468568994 ) ) ;
#151358 = CARTESIAN_POINT ( 'NONE',  ( -19.02544592524334988, -5.153800228976617603, 88.95942372801897591 ) ) ;
#151359 = CARTESIAN_POINT ( 'NONE',  ( -19.03943276465977164, -0.05219959533935918106, 23.75109039468566152 ) ) ;
#151360 = CARTESIAN_POINT ( 'NONE',  ( -9.564922557960796823, -16.46253265017161027, 57.08224293864769550 ) ) ;
#151361 = CARTESIAN_POINT ( 'NONE',  ( -8.224510206698948167, 14.34966873604960824, 95.41557627198102409 ) ) ;
#151362 = CARTESIAN_POINT ( 'NONE',  ( -16.46253265017146816, -9.564922557961047289, 69.16775706135233293 ) ) ;
#151363 = CARTESIAN_POINT ( 'NONE',  ( 0.05219959533907565091, 21.53943276465977519, 64.99890960531435269 ) ) ;
#151364 = CARTESIAN_POINT ( 'NONE',  ( 5.049401038297881783, 19.05341960407617563, 32.29275706135233293 ) ) ;
#151365 = CARTESIAN_POINT ( 'NONE',  ( -13.89961937509977652, 13.97604488694528158, 105.6239096053143527 ) ) ;
#151366 = CARTESIAN_POINT ( 'NONE',  ( 18.62759615963271287, -10.81492255796078972, 78.33224293864770971 ) ) ;
#151367 = DIRECTION ( 'NONE',  ( -1.000000000000000000, -0.000000000000000000, -0.000000000000000000 ) ) ;
#151368 = CARTESIAN_POINT ( 'NONE',  ( 5.153800228976615827, -19.02544592524334988, 100.2094237280190043 ) ) ;
#151369 = CARTESIAN_POINT ( 'NONE',  ( -18.87075004821572222, 5.499999999999904077, 58.67408112101050222 ) ) ;
#151370 = CARTESIAN_POINT ( 'NONE',  ( -12.06949235617739369, -12.14591786802326823, 24.37609039468567573 ) ) ;
#151371 = CARTESIAN_POINT ( 'NONE',  ( 9.474510206698971260, -16.51473224551069308, 37.91557627198102409 ) ) ;
#151372 = CARTESIAN_POINT ( 'NONE',  ( 9.474510206698971260, -16.51473224551069308, 112.9155762719810383 ) ) ;
#151373 = CARTESIAN_POINT ( 'NONE',  ( 21.53943276465977519, -0.05219959533907433946, 88.74890960531436690 ) ) ;
#151374 = CARTESIAN_POINT ( 'NONE',  ( -10.72451020669870658, -18.67979575497194134, 54.58442372801901143 ) ) ;
#151376 = CARTESIAN_POINT ( 'NONE',  ( 10.72451020669871369, 18.67979575497193778, 107.0844237280190043 ) ) ;
#151375 = CARTESIAN_POINT ( 'NONE',  ( 0.05219959533936267826, -19.03943276465977164, 110.0010903946856757 ) ) ;
#151377 = CARTESIAN_POINT ( 'NONE',  ( -4.379528057220086978, -16.55341960407618274, 109.7927570613523613 ) ) ;
#151378 = APPLICATION_CONTEXT ( 'automotive_design' ) ;
#151379 = CARTESIAN_POINT ( 'NONE',  ( -10.72451020669898014, 18.67979575497178502, 105.4155762719810383 ) ) ;
#151380 = CARTESIAN_POINT ( 'NONE',  ( 16.53943276465976808, -0.05219959533910856209, 43.74890960531435979 ) ) ;
#151381 = CARTESIAN_POINT ( 'NONE',  ( 16.51473224551083163, -9.474510206698727899, 75.83442372801900433 ) ) ;
#151382 = CARTESIAN_POINT ( 'NONE',  ( -9.564922557961040184, 16.46253265017147172, 57.91775706135233293 ) ) ;
#151383 = CARTESIAN_POINT ( 'NONE',  ( -5.823673210054431948, 21.52544592524334988, 67.70942372801901854 ) ) ;
#151384 = CARTESIAN_POINT ( 'NONE',  ( -13.97604488694547697, 13.89961937509957934, 43.12609039468566152 ) ) ;
#151385 = CARTESIAN_POINT ( 'NONE',  ( -12.14591786802309592, -12.06949235617757132, 111.8739096053143669 ) ) ;
#151386 = CARTESIAN_POINT ( 'NONE',  ( 5.823673210054125526, 21.52544592524343514, 39.79057627198103830 ) ) ;
#151387 = CARTESIAN_POINT ( 'NONE',  ( -14.29746914071049879, 8.314922557960819915, 35.83224293864768839 ) ) ;
#151388 = CARTESIAN_POINT ( 'NONE',  ( -21.52544592524334988, -5.823673210054445271, 103.9594237280190185 ) ) ;
#151389 = CARTESIAN_POINT ( 'NONE',  ( 4.379528057220092307, 16.55341960407617563, 67.29275706135234714 ) ) ;
#151390 = CARTESIAN_POINT ( 'NONE',  ( 8.224510206698953496, -14.34966873604960469, 32.91557627198102409 ) ) ;
#151391 = CARTESIAN_POINT ( 'NONE',  ( 5.719274019375673035, 21.55341960407619339, 57.29275706135234714 ) ) ;
#151392 = CARTESIAN_POINT ( 'NONE',  ( 18.62759615963255655, 10.81492255796105972, 66.66775706135234714 ) ) ;
#151393 = CARTESIAN_POINT ( 'NONE',  ( -21.55341960407610458, -5.719274019375992779, 66.45724293864768129 ) ) ;
#151394 = ORIENTED_EDGE ( 'NONE', *, *, #51079, .F. ) ;
#151395 = CARTESIAN_POINT ( 'NONE',  ( -5.153800228976328057, -19.02544592524343514, 27.29057627198103120 ) ) ;
#151396 = CARTESIAN_POINT ( 'NONE',  ( 5.719274019375673035, 21.55341960407619339, 42.29275706135235424 ) ) ;
#151397 = CARTESIAN_POINT ( 'NONE',  ( 16.51473224551069308, 9.474510206698969483, 29.16557627198103475 ) ) ;
#151398 = CARTESIAN_POINT ( 'NONE',  ( 5.153800228976335163, 19.02544592524342804, 44.79057627198103830 ) ) ;
#151399 = CARTESIAN_POINT ( 'NONE',  ( 14.29746914071049879, -8.314922557960816363, 73.33224293864769550 ) ) ;
#151400 = CARTESIAN_POINT ( 'NONE',  ( 13.97604488694527802, 13.89961937509977652, 84.37390960531433848 ) ) ;
#151401 = CARTESIAN_POINT ( 'NONE',  ( -16.53943276465976808, 0.05219959533911058130, 21.24890960531436690 ) ) ;
#151402 = CARTESIAN_POINT ( 'NONE',  ( 14.29746914071049879, -8.314922557960816363, 98.33224293864769550 ) ) ;
#151403 = CARTESIAN_POINT ( 'NONE',  ( 15.72974639402199770, -15.80617190586745480, 73.12390960531436690 ) ) ;
#151404 = CARTESIAN_POINT ( 'NONE',  ( -10.72451020669898014, 18.67979575497178502, 100.4155762719810241 ) ) ;
#151405 = CARTESIAN_POINT ( 'NONE',  ( 16.51473224551069308, 9.474510206698969483, 114.1655762719810241 ) ) ;
#151407 = CARTESIAN_POINT ( 'NONE',  ( 8.224510206698742110, 14.34966873604972548, 22.08442372801901143 ) ) ;
#151406 = CARTESIAN_POINT ( 'NONE',  ( 9.474510206698971260, -16.51473224551069308, 67.91557627198102409 ) ) ;
#151408 = ADVANCED_FACE ( 'NONE', ( #138833 ), #46835, .F. ) ;
#151409 = CARTESIAN_POINT ( 'NONE',  ( -21.55341960407610458, -5.719274019375992779, 51.45724293864770260 ) ) ;
#151410 = CARTESIAN_POINT ( 'NONE',  ( 10.72451020669871369, 18.67979575497193778, 77.08442372801901854 ) ) ;
#151411 = CARTESIAN_POINT ( 'NONE',  ( 19.03943276465977164, -0.05219959533909143690, 68.74890960531436690 ) ) ;
#151412 = CARTESIAN_POINT ( 'NONE',  ( -16.46253265017160317, 9.564922557960807481, 100.8322429386477097 ) ) ;
#151413 = CARTESIAN_POINT ( 'NONE',  ( 14.34966873604972726, -8.224510206698740333, 75.83442372801900433 ) ) ;
#151414 = CARTESIAN_POINT ( 'NONE',  ( -21.53943276465977519, -0.05219959533937600094, 58.75109039468568994 ) ) ;
#151415 = CARTESIAN_POINT ( 'NONE',  ( 21.55341960407619695, -5.719274019375665929, 96.04275706135236135 ) ) ;
#151416 = CARTESIAN_POINT ( 'NONE',  ( 21.53943276465977519, -0.05219959533907433946, 113.7489096053143527 ) ) ;
#151417 = CARTESIAN_POINT ( 'NONE',  ( -19.05341960407611168, -5.049401038298163336, 21.45724293864768839 ) ) ;
#151418 = CARTESIAN_POINT ( 'NONE',  ( 21.53943276465977519, -0.05219959533907433946, 88.74890960531436690 ) ) ;
#151419 = CARTESIAN_POINT ( 'NONE',  ( 0.05219959533936267826, -19.03943276465977164, 45.00109039468566863 ) ) ;
#151420 = CARTESIAN_POINT ( 'NONE',  ( 15.72974639402199770, -15.80617190586745480, 38.12390960531436690 ) ) ;
#151422 = CARTESIAN_POINT ( 'NONE',  ( -16.55341960407611168, -4.379528057220339221, 31.45724293864769550 ) ) ;
#151421 = CARTESIAN_POINT ( 'NONE',  ( -9.564922557960796823, -16.46253265017161027, 77.08224293864769550 ) ) ;
#151423 = CARTESIAN_POINT ( 'NONE',  ( -17.40805194822031154, 6.112264579159341515, 65.83371272510615313 ) ) ;
#151424 = CARTESIAN_POINT ( 'NONE',  ( -19.01529144963334872, -5.500000000000081712, 81.23431955728439391 ) ) ;
#151425 = CARTESIAN_POINT ( 'NONE',  ( 9.564922557961047289, -16.46253265017146816, 100.4177570613523329 ) ) ;
#151426 = CARTESIAN_POINT ( 'NONE',  ( -15.80617190586745835, -15.72974639402198527, 66.87390960531436690 ) ) ;
#151427 = CARTESIAN_POINT ( 'NONE',  ( 4.379528057220339221, -16.55341960407611168, 57.70724293864770260 ) ) ;
#151428 = CARTESIAN_POINT ( 'NONE',  ( -12.14591786802326823, 12.06949235617739902, 28.12609039468568284 ) ) ;
#151429 = CARTESIAN_POINT ( 'NONE',  ( -19.02544592524342804, 5.153800228976336051, 41.04057627198103120 ) ) ;
#151431 = CARTESIAN_POINT ( 'NONE',  ( -13.89961937509957401, -13.97604488694547875, 89.37609039468563310 ) ) ;
#151430 = CARTESIAN_POINT ( 'NONE',  ( 18.62759615963271287, -10.81492255796078972, 108.3322429386477097 ) ) ;
#151432 = CARTESIAN_POINT ( 'NONE',  ( -19.02544592524342804, 5.153800228976336051, 76.04057627198102409 ) ) ;
#151433 = CARTESIAN_POINT ( 'NONE',  ( 8.314922557960818139, 14.29746914071049879, 94.58224293864769550 ) ) ;
#151434 = CARTESIAN_POINT ( 'NONE',  ( 16.46253265017160672, -9.564922557960803928, 68.33224293864770971 ) ) ;
#151435 = CARTESIAN_POINT ( 'NONE',  ( 10.81492255796078972, 18.62759615963270932, 74.58224293864768129 ) ) ;
#151436 = CARTESIAN_POINT ( 'NONE',  ( -16.51473224551069308, -9.474510206698971260, 31.66557627198102054 ) ) ;
#151437 = LINE ( 'NONE', #186759, #89675 ) ;
#151438 = CARTESIAN_POINT ( 'NONE',  ( 14.29746914071049879, -8.314922557960816363, 58.33224293864768839 ) ) ;
#151439 = CARTESIAN_POINT ( 'NONE',  ( 0.05219959533909260263, 19.03943276465977164, 89.99890960531436690 ) ) ;
#151440 = CARTESIAN_POINT ( 'NONE',  ( -4.999999999999999112, -140.0000000000000000, -13.00000000000000000 ) ) ;
#151441 = CARTESIAN_POINT ( 'NONE',  ( 0.05219959533936267826, -19.03943276465977164, 55.00109039468566863 ) ) ;
#151442 = CARTESIAN_POINT ( 'NONE',  ( 0.05219959533934541429, -16.53943276465976808, 55.00109039468568284 ) ) ;
#151443 = CARTESIAN_POINT ( 'NONE',  ( -18.67979575497178146, -10.72451020669898902, 71.66557627198100988 ) ) ;
#151444 = CARTESIAN_POINT ( 'NONE',  ( 13.89961937509957401, 13.97604488694547697, 41.87609039468566152 ) ) ;
#151445 = CARTESIAN_POINT ( 'NONE',  ( 9.564922557960805705, 16.46253265017160317, 94.58224293864769550 ) ) ;
#151446 = CARTESIAN_POINT ( 'NONE',  ( -17.49999999999999645, 5.499999999999997335, 115.7969038253417438 ) ) ;
#151447 = CARTESIAN_POINT ( 'NONE',  ( 21.52544592524344225, -5.823673210054117533, 28.54057627198103120 ) ) ;
#151448 = CARTESIAN_POINT ( 'NONE',  ( -5.049401038298153566, 19.05341960407611168, 75.20724293864769550 ) ) ;
#151449 = CARTESIAN_POINT ( 'NONE',  ( -5.823673210054431948, 21.52544592524334988, 57.70942372801901143 ) ) ;
#151450 = CARTESIAN_POINT ( 'NONE',  ( -13.89961937509977652, 13.97604488694528158, 25.62390960531434558 ) ) ;
#151453 = ORIENTED_EDGE ( 'NONE', *, *, #21485, .T. ) ;
#151452 = CARTESIAN_POINT ( 'NONE',  ( -5.153800228976328057, -19.02544592524343514, 92.29057627198099567 ) ) ;
#151451 = CARTESIAN_POINT ( 'NONE',  ( 18.67979575497194134, -10.72451020669871369, 20.83442372801901143 ) ) ;
#151454 = CARTESIAN_POINT ( 'NONE',  ( -21.53943276465977519, -0.05219959533937600094, 33.75109039468568284 ) ) ;
#151455 = ORIENTED_EDGE ( 'NONE', *, *, #64457, .F. ) ;
#151456 = CARTESIAN_POINT ( 'NONE',  ( 16.51473224551069308, 9.474510206698969483, 104.1655762719810241 ) ) ;
#151457 = CARTESIAN_POINT ( 'NONE',  ( -21.93187539022925847, 6.436421874423674083, 171.3066408880984852 ) ) ;
#151458 = CARTESIAN_POINT ( 'NONE',  ( 21.53943276465977519, -0.05219959533907433946, 113.7489096053143527 ) ) ;
#151459 = CARTESIAN_POINT ( 'NONE',  ( -19.03943276465977164, 0.05219959533909376836, 46.24890960531435979 ) ) ;
#151460 = CARTESIAN_POINT ( 'NONE',  ( -14.29746914071037622, -8.314922557961029526, 29.16775706135234003 ) ) ;
#151461 = CARTESIAN_POINT ( 'NONE',  ( -5.950531402560715689E-15, 38.81732327939063509, -3.624999997268813168 ) ) ;
#151462 = CARTESIAN_POINT ( 'NONE',  ( -5.719274019375665041, -21.55341960407619695, 99.79275706135234714 ) ) ;
#151463 = CARTESIAN_POINT ( 'NONE',  ( -0.05219959533909027116, -19.03943276465977164, 37.49890960531436690 ) ) ;
#151464 = CARTESIAN_POINT ( 'NONE',  ( -18.67979575497193778, 10.72451020669871902, 93.33442372801901854 ) ) ;
#151466 = CARTESIAN_POINT ( 'NONE',  ( 10.81492255796106328, -18.62759615963255655, 65.41775706135234714 ) ) ;
#151465 = CARTESIAN_POINT ( 'NONE',  ( 16.51473224551069308, 9.474510206698969483, 94.16557627198103830 ) ) ;
#151467 = CARTESIAN_POINT ( 'NONE',  ( -8.571926809382608425, 26.38167802310805854, 142.9750000027312069 ) ) ;
#151468 = CARTESIAN_POINT ( 'NONE',  ( 5.049401038298161559, -19.05341960407611168, 102.7072429386476955 ) ) ;
#151469 = CARTESIAN_POINT ( 'NONE',  ( 18.09867054820434262, 5.499999999999818812, 46.48393025253587041 ) ) ;
#151472 = CARTESIAN_POINT ( 'NONE',  ( -10.81492255796105439, 18.62759615963255655, 57.91775706135234714 ) ) ;
#151471 = CARTESIAN_POINT ( 'NONE',  ( -12.14591786802326823, 12.06949235617739902, 63.12609039468568994 ) ) ;
#151470 = CARTESIAN_POINT ( 'NONE',  ( 0.05219959533934541429, -16.53943276465976808, 55.00109039468568284 ) ) ;
#151473 = CARTESIAN_POINT ( 'NONE',  ( -18.62759615963255300, -10.81492255796106328, 84.16775706135234714 ) ) ;
#151474 = CARTESIAN_POINT ( 'NONE',  ( 8.314922557961029526, -14.29746914071037800, 30.41775706135234358 ) ) ;
#151475 = CARTESIAN_POINT ( 'NONE',  ( -5.153800228976328057, -19.02544592524343514, 77.29057627198099567 ) ) ;
#151476 = CARTESIAN_POINT ( 'NONE',  ( 19.03943276465977164, -0.05219959533909143690, 103.7489096053143669 ) ) ;
#151477 = CARTESIAN_POINT ( 'NONE',  ( -19.05341960407611168, -5.049401038298163336, 111.4572429386476671 ) ) ;
#151478 = CARTESIAN_POINT ( 'NONE',  ( -5.049401038298153566, 19.05341960407611168, 30.20724293864768839 ) ) ;
#151479 = CARTESIAN_POINT ( 'NONE',  ( 10.81492255796078972, 18.62759615963270932, 24.58224293864768839 ) ) ;
#151480 = CARTESIAN_POINT ( 'NONE',  ( 4.483927247898790824, -16.52544592524335698, 90.20942372801903275 ) ) ;
#151482 = CARTESIAN_POINT ( 'NONE',  ( 19.03943276465977164, -0.05219959533909143690, 68.74890960531436690 ) ) ;
#151481 = CARTESIAN_POINT ( 'NONE',  ( -4.379528057220328563, 16.55341960407611168, 90.20724293864770971 ) ) ;
#151483 = CARTESIAN_POINT ( 'NONE',  ( -10.81492255796105439, 18.62759615963255655, 87.91775706135234714 ) ) ;
#151484 = CARTESIAN_POINT ( 'NONE',  ( -22.62413958104530209, 1.500431131851542643, -57.95367621771161026 ) ) ;
#151485 = CARTESIAN_POINT ( 'NONE',  ( -8.314922557961024197, 14.29746914071037800, 27.91775706135234358 ) ) ;
#151486 = CARTESIAN_POINT ( 'NONE',  ( 8.314922557960818139, 14.29746914071049879, 69.58224293864769550 ) ) ;
#151487 = CARTESIAN_POINT ( 'NONE',  ( -21.52544592524334988, -5.823673210054445271, 28.95942372801902209 ) ) ;
#151488 = CARTESIAN_POINT ( 'NONE',  ( -5.823673210054116645, -21.52544592524344225, 67.29057627198103830 ) ) ;
#151489 = CARTESIAN_POINT ( 'NONE',  ( 19.05341960407617918, -5.049401038297876454, 36.04275706135234003 ) ) ;
#151490 = CARTESIAN_POINT ( 'NONE',  ( -23.31738231874055600, 16.94106989632528837, 146.0500000054623797 ) ) ;
#151491 = CARTESIAN_POINT ( 'NONE',  ( -13.89961937509977652, 13.97604488694528158, 85.62390960531433848 ) ) ;
#151492 = CARTESIAN_POINT ( 'NONE',  ( 14.34966873604960469, 8.224510206698951720, 44.16557627198103120 ) ) ;
#151493 = CARTESIAN_POINT ( 'NONE',  ( 16.53943276465976808, -0.05219959533910856209, 38.74890960531435979 ) ) ;
#151494 = CARTESIAN_POINT ( 'NONE',  ( -14.29746914071037622, -8.314922557961029526, 109.1677570613523613 ) ) ;
#151495 = CARTESIAN_POINT ( 'NONE',  ( -13.89961937509957401, -13.97604488694547875, 69.37609039468564731 ) ) ;
#151496 = CARTESIAN_POINT ( 'NONE',  ( 17.40805194822030799, 6.112264579159357503, 46.66628727489389661 ) ) ;
#151497 = CARTESIAN_POINT ( 'NONE',  ( 18.62759615963271287, -10.81492255796078972, 23.33224293864769194 ) ) ;
#151498 = CARTESIAN_POINT ( 'NONE',  ( 8.314922557960818139, 14.29746914071049879, 69.58224293864769550 ) ) ;
#151499 = DIRECTION ( 'NONE',  ( -0.000000000000000000, -0.000000000000000000, 1.000000000000000000 ) ) ;
#151501 = CARTESIAN_POINT ( 'NONE',  ( 21.55341960407610458, 5.719274019375980345, 33.95724293864769550 ) ) ;
#151500 = CARTESIAN_POINT ( 'NONE',  ( -13.97604488694527625, -13.89961937509977652, 31.87390960531435979 ) ) ;
#151502 = CARTESIAN_POINT ( 'NONE',  ( 5.719274019375991003, -21.55341960407610458, 72.70724293864769550 ) ) ;
#151503 = CARTESIAN_POINT ( 'NONE',  ( -8.224510206698948167, 14.34966873604960824, 110.4155762719810383 ) ) ;
#151505 = CARTESIAN_POINT ( 'NONE',  ( 9.564922557960805705, 16.46253265017160317, 44.58224293864769550 ) ) ;
#151504 = CARTESIAN_POINT ( 'NONE',  ( -8.314922557961024197, 14.29746914071037800, 67.91775706135234714 ) ) ;
#151506 = CARTESIAN_POINT ( 'NONE',  ( -18.62759615963255300, -10.81492255796106328, 54.16775706135235424 ) ) ;
#151507 = CARTESIAN_POINT ( 'NONE',  ( -12.14591786802309592, -12.06949235617757132, 106.8739096053143811 ) ) ;
#151508 = EDGE_CURVE ( 'NONE', #37352, #162114, #82102, .T. ) ;
#151509 = CARTESIAN_POINT ( 'NONE',  ( 16.19135201231362942, -7.376712067592066546, 37.31319145947968252 ) ) ;
#151510 = CARTESIAN_POINT ( 'NONE',  ( -29.86685920354755197, -21.69954338932560134, -8.924999997268812990 ) ) ;
#151511 = CARTESIAN_POINT ( 'NONE',  ( -21.53943276465977519, 0.05219959533907696930, 36.24890960531435979 ) ) ;
#151512 = FACE_OUTER_BOUND ( 'NONE', #168359, .T. ) ;
#151513 = CARTESIAN_POINT ( 'NONE',  ( -0.05219959533937732626, 21.53943276465977519, 67.50109039468568994 ) ) ;
#151514 = CIRCLE ( 'NONE', #125649, 9.100000000000001421 ) ;
#151516 = CARTESIAN_POINT ( 'NONE',  ( 12.14591786802309770, 12.06949235617756955, 39.37390960531436690 ) ) ;
#151515 = CARTESIAN_POINT ( 'NONE',  ( -4.483927247898782831, 16.52544592524335698, 62.70942372801902565 ) ) ;
#151517 = CARTESIAN_POINT ( 'NONE',  ( -15.80617190586745835, -15.72974639402198527, 61.87390960531436690 ) ) ;
#151518 = CARTESIAN_POINT ( 'NONE',  ( 5.823673210054125526, 21.52544592524343514, 59.79057627198103120 ) ) ;
#151519 = CARTESIAN_POINT ( 'NONE',  ( 0.000000000000000000, 0.000000000000000000, 0.000000000000000000 ) ) ;
#151521 = CARTESIAN_POINT ( 'NONE',  ( 13.89961937509977652, -13.97604488694527269, 113.1239096053143527 ) ) ;
#151520 = CARTESIAN_POINT ( 'NONE',  ( 9.564922557961047289, -16.46253265017146816, 80.41775706135234714 ) ) ;
#151522 = CARTESIAN_POINT ( 'NONE',  ( -9.564922557960796823, -16.46253265017161027, 47.08224293864769550 ) ) ;
#151524 = EDGE_CURVE ( 'NONE', #140935, #93860, #95565, .T. ) ;
#151523 = CARTESIAN_POINT ( 'NONE',  ( 14.34966873604960469, 8.224510206698951720, 109.1655762719810383 ) ) ;
#151525 =( LENGTH_UNIT ( ) NAMED_UNIT ( * ) SI_UNIT ( .MILLI., .METRE. ) );
#151526 = CARTESIAN_POINT ( 'NONE',  ( 13.89961937509977652, -13.97604488694527269, 108.1239096053143669 ) ) ;
#151527 = ORIENTED_EDGE ( 'NONE', *, *, #141950, .T. ) ;
#151528 = CARTESIAN_POINT ( 'NONE',  ( -8.314922557961024197, 14.29746914071037800, 72.91775706135234714 ) ) ;
#151529 = CARTESIAN_POINT ( 'NONE',  ( 18.67979575497178502, 10.72451020669898547, 109.1655762719810383 ) ) ;
#151530 = CARTESIAN_POINT ( 'NONE',  ( -0.05219959533909027116, -19.03943276465977164, 52.49890960531436690 ) ) ;
#151531 = CARTESIAN_POINT ( 'NONE',  ( 18.67979575497194134, -10.72451020669871369, 40.83442372801901854 ) ) ;
#151532 = CARTESIAN_POINT ( 'NONE',  ( 19.03943276465977164, -0.05219959533909143690, 93.74890960531435269 ) ) ;
#151533 = CARTESIAN_POINT ( 'NONE',  ( -22.96436041963305286, -32.42578188300798558, -19.82561655441343973 ) ) ;
#151534 = ORIENTED_EDGE ( 'NONE', *, *, #67877, .T. ) ;
#151535 = CARTESIAN_POINT ( 'NONE',  ( -15.80617190586768217, 15.72974639402176855, 33.12609039468569705 ) ) ;
#151537 = CARTESIAN_POINT ( 'NONE',  ( -13.89961937509957401, -13.97604488694547875, 89.37609039468563310 ) ) ;
#151536 = CARTESIAN_POINT ( 'NONE',  ( 0.05219959533909260263, 19.03943276465977164, 109.9989096053143669 ) ) ;
#151538 = CARTESIAN_POINT ( 'NONE',  ( 16.46253265017146816, 9.564922557961045513, 46.66775706135233293 ) ) ;
#151539 = CARTESIAN_POINT ( 'NONE',  ( -10.81492255796078084, -18.62759615963271287, 102.0822429386476955 ) ) ;
#151540 = CARTESIAN_POINT ( 'NONE',  ( -0.05219959533936034679, 19.03943276465977164, 37.50109039468567573 ) ) ;
#151541 = CARTESIAN_POINT ( 'NONE',  ( -13.97604488694547697, 13.89961937509957934, 43.12609039468566152 ) ) ;
#151542 = CARTESIAN_POINT ( 'NONE',  ( 8.314922557961029526, -14.29746914071037800, 95.41775706135234714 ) ) ;
#151543 = CARTESIAN_POINT ( 'NONE',  ( -69.65682714487590488, -71.74905178543390605, 8.936314941956774358E-29 ) ) ;
#151544 = CARTESIAN_POINT ( 'NONE',  ( 19.02544592524343514, -5.153800228976328945, 68.54057627198103830 ) ) ;
#151545 = CARTESIAN_POINT ( 'NONE',  ( 10.81492255796106328, -18.62759615963255655, 75.41775706135233293 ) ) ;
#151546 = CARTESIAN_POINT ( 'NONE',  ( -5.719274019375665041, -21.55341960407619695, 79.79275706135236135 ) ) ;
#151547 = DIRECTION ( 'NONE',  ( 0.000000000000000000, -0.9945218953682734009, 0.1045284632676537068 ) ) ;
#151548 = CARTESIAN_POINT ( 'NONE',  ( 16.51473224551069308, 9.474510206698969483, 94.16557627198103830 ) ) ;
#151549 = CARTESIAN_POINT ( 'NONE',  ( 21.55341960407619695, -5.719274019375665929, 56.04275706135235424 ) ) ;
#151550 = CARTESIAN_POINT ( 'NONE',  ( 5.049401038297881783, 19.05341960407617563, 107.2927570613523187 ) ) ;
#151551 = CARTESIAN_POINT ( 'NONE',  ( -19.02544592524342804, 5.153800228976336051, 71.04057627198099567 ) ) ;
#151552 = CARTESIAN_POINT ( 'NONE',  ( 5.049401038298161559, -19.05341960407611168, 107.7072429386476955 ) ) ;
#151553 = CARTESIAN_POINT ( 'NONE',  ( 9.474510206698971260, -16.51473224551069308, 77.91557627198103830 ) ) ;
#151554 = DIRECTION ( 'NONE',  ( -1.000000000000000000, 0.000000000000000000, -5.204170427930421283E-16 ) ) ;
#151556 = ADVANCED_FACE ( 'NONE', ( #109488 ), #39062, .T. ) ;
#151555 = CARTESIAN_POINT ( 'NONE',  ( -19.03943276465977164, 0.05219959533909376836, 61.24890960531436690 ) ) ;
#151557 = CARTESIAN_POINT ( 'NONE',  ( -13.89961937509977652, 13.97604488694528158, 50.62390960531435979 ) ) ;
#151558 = CARTESIAN_POINT ( 'NONE',  ( 18.67979575497178502, 10.72451020669898547, 109.1655762719810383 ) ) ;
#151559 = CARTESIAN_POINT ( 'NONE',  ( 8.224510206698742110, 14.34966873604972548, 87.08442372801901854 ) ) ;
#151560 = CARTESIAN_POINT ( 'NONE',  ( 7.503727747132447057, -1.500047742438187059, -64.26135111332261829 ) ) ;
#151561 = CARTESIAN_POINT ( 'NONE',  ( 5.153800228976615827, -19.02544592524334988, 45.20942372801901143 ) ) ;
#151562 = CARTESIAN_POINT ( 'NONE',  ( 13.97604488694527802, 13.89961937509977652, 84.37390960531433848 ) ) ;
#151563 = CARTESIAN_POINT ( 'NONE',  ( 4.483927247898545687, 16.52544592524342804, 69.79057627198102409 ) ) ;
#151564 = CARTESIAN_POINT ( 'NONE',  ( -16.55341960407611168, -4.379528057220339221, 101.4572429386476955 ) ) ;
#151565 = CARTESIAN_POINT ( 'NONE',  ( 21.53943276465977519, -0.05219959533907433946, 23.74890960531435269 ) ) ;
#151566 = CARTESIAN_POINT ( 'NONE',  ( -13.89961937509977652, 13.97604488694528158, 105.6239096053143527 ) ) ;
#151567 = CARTESIAN_POINT ( 'NONE',  ( 0.05219959533910956823, 16.53943276465976808, 79.99890960531435269 ) ) ;
#151568 = DIRECTION ( 'NONE',  ( -3.491481338843133355E-15, 0.000000000000000000, 1.000000000000000000 ) ) ;
#151569 = CARTESIAN_POINT ( 'NONE',  ( 19.03943276465977164, 0.05219959533936151252, 26.25109039468566507 ) ) ;
#151570 = CARTESIAN_POINT ( 'NONE',  ( -8.224510206698735004, -14.34966873604973081, 94.58442372801901854 ) ) ;
#151571 = CARTESIAN_POINT ( 'NONE',  ( 19.02544592524343514, -5.153800228976328945, 73.54057627198103830 ) ) ;
#151572 = CARTESIAN_POINT ( 'NONE',  ( 21.52544592524334988, 5.823673210054432836, 51.45942372801901854 ) ) ;
#151573 = CARTESIAN_POINT ( 'NONE',  ( 10.81492255796078972, 18.62759615963270932, 39.58224293864769550 ) ) ;
#151574 = CARTESIAN_POINT ( 'NONE',  ( -5.719274019375978568, 21.55341960407610458, 110.2072429386477239 ) ) ;
#151575 = CARTESIAN_POINT ( 'NONE',  ( -21.55341960407610458, -5.719274019375992779, 71.45724293864769550 ) ) ;
#151576 = CARTESIAN_POINT ( 'NONE',  ( -12.06949235617756955, 12.14591786802309770, 95.62390960531436690 ) ) ;
#151577 = CARTESIAN_POINT ( 'NONE',  ( -19.05341960407617563, 5.049401038297882671, 53.54275706135231871 ) ) ;
#151578 = CARTESIAN_POINT ( 'NONE',  ( 9.474510206698971260, -16.51473224551069308, 37.91557627198102409 ) ) ;
#151579 = CARTESIAN_POINT ( 'NONE',  ( 0.05219959533909260263, 19.03943276465977164, 79.99890960531436690 ) ) ;
#151580 = CARTESIAN_POINT ( 'NONE',  ( -0.05219959533909027116, -19.03943276465977164, 87.49890960531436690 ) ) ;
#151581 = CARTESIAN_POINT ( 'NONE',  ( -8.314922557960811034, -14.29746914071050412, 97.08224293864770971 ) ) ;
#151582 = CARTESIAN_POINT ( 'NONE',  ( -16.55341960407611168, -4.379528057220339221, 31.45724293864769550 ) ) ;
#151583 = CARTESIAN_POINT ( 'NONE',  ( 4.483927247898790824, -16.52544592524335698, 30.20942372801902565 ) ) ;
#151584 = CARTESIAN_POINT ( 'NONE',  ( -21.55341960407619339, 5.719274019375674811, 108.5427570613523756 ) ) ;
#151585 = CARTESIAN_POINT ( 'NONE',  ( -5.049401038298153566, 19.05341960407611168, 105.2072429386476671 ) ) ;
#151586 = CARTESIAN_POINT ( 'NONE',  ( 21.52544592524334988, 5.823673210054432836, 26.45942372801901854 ) ) ;
#151587 = CARTESIAN_POINT ( 'NONE',  ( -5.049401038298153566, 19.05341960407611168, 50.20724293864770260 ) ) ;
#151588 = CARTESIAN_POINT ( 'NONE',  ( 4.379528057220092307, 16.55341960407617563, 47.29275706135234003 ) ) ;
#151589 = CARTESIAN_POINT ( 'NONE',  ( 13.89961937509957401, 13.97604488694547697, 111.8760903946856757 ) ) ;
#151590 = CARTESIAN_POINT ( 'NONE',  ( 13.89961937509977652, -13.97604488694527269, 38.12390960531436690 ) ) ;
#151591 = CARTESIAN_POINT ( 'NONE',  ( 4.483927247898545687, 16.52544592524342804, 94.79057627198105251 ) ) ;
#151592 = CARTESIAN_POINT ( 'NONE',  ( 10.81492255796078972, 18.62759615963270932, 104.5822429386477097 ) ) ;
#151593 = CARTESIAN_POINT ( 'NONE',  ( 13.97604488694548053, -13.89961937509957401, 80.62609039468567573 ) ) ;
#151594 = DIRECTION ( 'NONE',  ( -0.000000000000000000, -0.000000000000000000, -1.000000000000000000 ) ) ;
#151595 = CARTESIAN_POINT ( 'NONE',  ( -13.89961937509977652, 13.97604488694528158, 85.62390960531433848 ) ) ;
#151596 = CARTESIAN_POINT ( 'NONE',  ( 21.52544592524344225, -5.823673210054117533, 113.5405762719810383 ) ) ;
#151597 = CARTESIAN_POINT ( 'NONE',  ( 37.99626262588765258, 2.893932880411085066E-14, -3.002157773949822861 ) ) ;
#151598 = CARTESIAN_POINT ( 'NONE',  ( -9.564922557960796823, -16.46253265017161027, 87.08224293864769550 ) ) ;
#151599 = CARTESIAN_POINT ( 'NONE',  ( 16.81555441253555827, -7.025013491695464296, 113.1368544533426359 ) ) ;
#151600 = CARTESIAN_POINT ( 'NONE',  ( 9.564922557960805705, 16.46253265017160317, 84.58224293864769550 ) ) ;
#151602 = CARTESIAN_POINT ( 'NONE',  ( -14.34966873604960291, -8.224510206698953496, 76.66557627198103830 ) ) ;
#151601 = CARTESIAN_POINT ( 'NONE',  ( -18.67979575497193778, 10.72451020669871902, 28.33442372801902209 ) ) ;
#151603 = CARTESIAN_POINT ( 'NONE',  ( -19.03943276465977164, 0.05219959533909376836, 96.24890960531436690 ) ) ;
#151604 = CARTESIAN_POINT ( 'NONE',  ( -19.05341960407617563, 5.049401038297882671, 28.54275706135232937 ) ) ;
#151605 = CARTESIAN_POINT ( 'NONE',  ( 16.52544592524335698, 4.483927247898782831, 46.45942372801901854 ) ) ;
#151606 = CARTESIAN_POINT ( 'NONE',  ( 0.05219959533937995610, -21.53943276465977519, 65.00109039468568994 ) ) ;
#151607 = CARTESIAN_POINT ( 'NONE',  ( -4.379528057220086978, -16.55341960407618274, 29.79275706135234358 ) ) ;
#151608 = CARTESIAN_POINT ( 'NONE',  ( 0.05219959533909260263, 19.03943276465977164, 64.99890960531436690 ) ) ;
#151609 = CARTESIAN_POINT ( 'NONE',  ( 16.51473224551083163, -9.474510206698727899, 90.83442372801900433 ) ) ;
#151610 = CARTESIAN_POINT ( 'NONE',  ( 4.379528057220092307, 16.55341960407617563, 72.29275706135236135 ) ) ;
#151611 = CARTESIAN_POINT ( 'NONE',  ( -0.05219959533937732626, 21.53943276465977519, 107.5010903946856899 ) ) ;
#151612 = CARTESIAN_POINT ( 'NONE',  ( -5.153800228976607833, 19.02544592524334988, 82.70942372801897591 ) ) ;
#151613 = CARTESIAN_POINT ( 'NONE',  ( 19.03943276465977164, -0.05219959533909143690, 53.74890960531436690 ) ) ;
#151614 = CARTESIAN_POINT ( 'NONE',  ( -15.80617190586745835, -15.72974639402198527, 86.87390960531438111 ) ) ;
#151616 = CARTESIAN_POINT ( 'NONE',  ( -5.153800228976607833, 19.02544592524334988, 77.70942372801900433 ) ) ;
#151615 = CARTESIAN_POINT ( 'NONE',  ( -12.14591786802309592, -12.06949235617757132, 76.87390960531439532 ) ) ;
#151617 = CARTESIAN_POINT ( 'NONE',  ( 33.85315667487628133, 2.428612866512670557E-14, 100.5000000000010232 ) ) ;
#151618 = CARTESIAN_POINT ( 'NONE',  ( -19.05341960407617563, 5.049401038297882671, 58.54275706135234003 ) ) ;
#151619 = CARTESIAN_POINT ( 'NONE',  ( -4.379528057220086978, -16.55341960407618274, 109.7927570613523613 ) ) ;
#151620 = CARTESIAN_POINT ( 'NONE',  ( 4.379528057220339221, -16.55341960407611168, 72.70724293864769550 ) ) ;
#151622 = CARTESIAN_POINT ( 'NONE',  ( 27.73933785331498925, -9.013057229001033122, 147.7750000027311899 ) ) ;
#151621 = CARTESIAN_POINT ( 'NONE',  ( -10.72451020669870658, -18.67979575497194134, 99.58442372801900433 ) ) ;
#151623 = CARTESIAN_POINT ( 'NONE',  ( -5.823673210054116645, -21.52544592524344225, 112.2905762719810241 ) ) ;
#151624 = CARTESIAN_POINT ( 'NONE',  ( -0.05219959533909027116, -19.03943276465977164, 62.49890960531435979 ) ) ;
#151625 = CARTESIAN_POINT ( 'NONE',  ( -18.67979575497193778, 10.72451020669871902, 78.33442372801901854 ) ) ;
#151626 = CARTESIAN_POINT ( 'NONE',  ( -13.89961937509977652, 13.97604488694528158, 65.62390960531436690 ) ) ;
#151627 = CARTESIAN_POINT ( 'NONE',  ( -9.564922557960796823, -16.46253265017161027, 22.08224293864768839 ) ) ;
#151628 = CARTESIAN_POINT ( 'NONE',  ( 21.55341960407610458, 5.719274019375980345, 28.95724293864769905 ) ) ;
#151629 = CARTESIAN_POINT ( 'NONE',  ( 12.06949235617757843, -12.14591786802309237, 73.12390960531436690 ) ) ;
#151630 = CARTESIAN_POINT ( 'NONE',  ( 16.46253265017160672, -9.564922557960803928, 48.33224293864769550 ) ) ;
#151631 = CARTESIAN_POINT ( 'NONE',  ( 8.314922557960818139, 14.29746914071049879, 104.5822429386477097 ) ) ;
#151632 = CARTESIAN_POINT ( 'NONE',  ( -5.719274019375978568, 21.55341960407610458, 110.2072429386477239 ) ) ;
#151633 = CARTESIAN_POINT ( 'NONE',  ( -10.72451020669870658, -18.67979575497194134, 49.58442372801901143 ) ) ;
#151634 = CARTESIAN_POINT ( 'NONE',  ( -13.97604488694527625, -13.89961937509977652, 31.87390960531435979 ) ) ;
#151635 = CARTESIAN_POINT ( 'NONE',  ( 16.55341960407618274, -4.379528057220086978, 61.04275706135234714 ) ) ;
#151636 = CARTESIAN_POINT ( 'NONE',  ( -15.72974639402197994, 15.80617190586746368, 100.6239096053143811 ) ) ;
#151637 = CARTESIAN_POINT ( 'NONE',  ( -10.81492255796078084, -18.62759615963271287, 92.08224293864769550 ) ) ;
#151639 = CARTESIAN_POINT ( 'NONE',  ( 9.474510206698971260, -16.51473224551069308, 52.91557627198102409 ) ) ;
#151638 = CARTESIAN_POINT ( 'NONE',  ( -19.05341960407617563, 5.049401038297882671, 23.54275706135233648 ) ) ;
#151640 = CARTESIAN_POINT ( 'NONE',  ( -17.50000000001356781, 5.500000000000039968, 40.79690382535057580 ) ) ;
#151641 = CARTESIAN_POINT ( 'NONE',  ( 15.72974639402176855, 15.80617190586768217, 56.87609039468568994 ) ) ;
#151642 = CARTESIAN_POINT ( 'NONE',  ( 0.05219959533907565091, 21.53943276465977519, 54.99890960531435269 ) ) ;
#151643 = CARTESIAN_POINT ( 'NONE',  ( -14.34966873604960291, -8.224510206698953496, 26.66557627198103475 ) ) ;
#151645 = CARTESIAN_POINT ( 'NONE',  ( -10.72451020669870658, -18.67979575497194134, 99.58442372801900433 ) ) ;
#151644 = CARTESIAN_POINT ( 'NONE',  ( -10.72451020669870658, -18.67979575497194134, 74.58442372801901854 ) ) ;
#151646 = CARTESIAN_POINT ( 'NONE',  ( -13.89961937509957401, -13.97604488694547875, 39.37609039468566152 ) ) ;
#151647 = CARTESIAN_POINT ( 'NONE',  ( -4.483927247898782831, 16.52544592524335698, 107.7094237280190328 ) ) ;
#151648 = CARTESIAN_POINT ( 'NONE',  ( 15.80617190586769283, -15.72974639402175789, 50.62609039468568994 ) ) ;
#151649 = CARTESIAN_POINT ( 'NONE',  ( -13.97604488694527625, -13.89961937509977652, 56.87390960531434558 ) ) ;
#151650 = CARTESIAN_POINT ( 'NONE',  ( 9.474510206698729675, 16.51473224551082808, 32.08442372801900433 ) ) ;
#151651 = CARTESIAN_POINT ( 'NONE',  ( 15.80617190586746368, 15.72974639402197994, 39.37390960531436690 ) ) ;
#151652 = CARTESIAN_POINT ( 'NONE',  ( 10.72451020669871369, 18.67979575497193778, 27.08442372801901854 ) ) ;
#151653 = VECTOR ( 'NONE', #116739, 1000.000000000000000 ) ;
#151654 = CARTESIAN_POINT ( 'NONE',  ( -5.719274019375978568, 21.55341960407610458, 85.20724293864770971 ) ) ;
#151655 = CARTESIAN_POINT ( 'NONE',  ( 19.03943276465977164, 0.05219959533936151252, 86.25109039468567573 ) ) ;
#151656 = CARTESIAN_POINT ( 'NONE',  ( 8.224510206698742110, 14.34966873604972548, 57.08442372801901854 ) ) ;
#151658 = CARTESIAN_POINT ( 'NONE',  ( -21.53943276465977519, 0.05219959533907696930, 86.24890960531436690 ) ) ;
#151657 = CARTESIAN_POINT ( 'NONE',  ( -6.297279900606389980, 4.176031345420732954, -62.24169944404286525 ) ) ;
#151660 = CARTESIAN_POINT ( 'NONE',  ( -4.483927247898539470, -16.52544592524342804, 77.29057627198102409 ) ) ;
#151659 = CARTESIAN_POINT ( 'NONE',  ( 8.314922557961029526, -14.29746914071037800, 75.41775706135233293 ) ) ;
#151661 = FACE_OUTER_BOUND ( 'NONE', #10508, .T. ) ;
#151662 = CARTESIAN_POINT ( 'NONE',  ( -19.05341960407617563, 5.049401038297882671, 108.5427570613523187 ) ) ;
#151663 = CARTESIAN_POINT ( 'NONE',  ( 21.53943276465977519, -0.05219959533907433946, 33.74890960531436690 ) ) ;
#151664 = DIRECTION ( 'NONE',  ( -0.000000000000000000, -1.000000000000000000, 0.000000000000000000 ) ) ;
#151665 = CARTESIAN_POINT ( 'NONE',  ( -4.483927247898782831, 16.52544592524335698, 37.70942372801900433 ) ) ;
#151666 = CARTESIAN_POINT ( 'NONE',  ( 21.53943276465977519, -0.05219959533907433946, 108.7489096053143669 ) ) ;
#151667 = CARTESIAN_POINT ( 'NONE',  ( 5.823673210054125526, 21.52544592524343514, 29.79057627198102409 ) ) ;
#151668 = CARTESIAN_POINT ( 'NONE',  ( 16.52544592524335698, 4.483927247898782831, 71.45942372801901854 ) ) ;
#151669 = CARTESIAN_POINT ( 'NONE',  ( 0.05219959533909260263, 19.03943276465977164, 89.99890960531436690 ) ) ;
#151671 = CARTESIAN_POINT ( 'NONE',  ( -5.153800228976328057, -19.02544592524343514, 27.29057627198103120 ) ) ;
#151670 = CARTESIAN_POINT ( 'NONE',  ( 10.81492255796106328, -18.62759615963255655, 60.41775706135235424 ) ) ;
#151672 = EDGE_CURVE ( 'NONE', #76856, #171158, #68135, .T. ) ;
#151673 = CARTESIAN_POINT ( 'NONE',  ( -5.823673210054116645, -21.52544592524344225, 22.29057627198102765 ) ) ;
#151674 = ORIENTED_EDGE ( 'NONE', *, *, #84216, .T. ) ;
#151675 = CARTESIAN_POINT ( 'NONE',  ( -9.474510206698720793, -16.51473224551083518, 34.58442372801899722 ) ) ;
#151676 = CARTESIAN_POINT ( 'NONE',  ( -4.379528057220086978, -16.55341960407618274, 49.79275706135234714 ) ) ;
#151677 = CARTESIAN_POINT ( 'NONE',  ( -16.46253265017160317, 9.564922557960807481, 115.8322429386477097 ) ) ;
#151678 = CARTESIAN_POINT ( 'NONE',  ( -19.05341960407611168, -5.049401038298163336, 71.45724293864766707 ) ) ;
#151679 = CARTESIAN_POINT ( 'NONE',  ( -16.53943276465976808, -0.05219959533934237506, 98.75109039468568994 ) ) ;
#151680 = CARTESIAN_POINT ( 'NONE',  ( -2.260530480648137177E-15, -78.64506293871966136, -22.99999966871703094 ) ) ;
#151681 = CARTESIAN_POINT ( 'NONE',  ( -4.379528057220328563, 16.55341960407611168, 95.20724293864769550 ) ) ;
#151682 = CARTESIAN_POINT ( 'NONE',  ( -5.719274019375978568, 21.55341960407610458, 35.20724293864768839 ) ) ;
#151683 = CARTESIAN_POINT ( 'NONE',  ( -13.97604488694527625, -13.89961937509977652, 26.87390960531434558 ) ) ;
#151684 = CARTESIAN_POINT ( 'NONE',  ( 16.52544592524335698, 4.483927247898782831, 66.45942372801903275 ) ) ;
#151685 = CARTESIAN_POINT ( 'NONE',  ( -0.05219959533937732626, 21.53943276465977519, 22.50109039468567573 ) ) ;
#151686 = CARTESIAN_POINT ( 'NONE',  ( -19.02544592524334988, -5.153800228976617603, 78.95942372801900433 ) ) ;
#151687 = EDGE_CURVE ( 'NONE', #197216, #185765, #92395, .T. ) ;
#151688 = CARTESIAN_POINT ( 'NONE',  ( 19.05341960407611168, 5.049401038298154454, 43.95724293864769550 ) ) ;
#151689 = CARTESIAN_POINT ( 'NONE',  ( -0.05219959533907301413, -21.53943276465977519, 72.49890960531435269 ) ) ;
#151690 = AXIS2_PLACEMENT_3D ( 'NONE', #69579, #147427, #189942 ) ;
#151691 = CARTESIAN_POINT ( 'NONE',  ( -9.474510206698964154, 16.51473224551069663, 110.4155762719810383 ) ) ;
#151692 = CARTESIAN_POINT ( 'NONE',  ( -5.823673210054431948, 21.52544592524334988, 97.70942372801904696 ) ) ;
#151693 = CARTESIAN_POINT ( 'NONE',  ( -13.97604488694527625, -13.89961937509977652, 66.87390960531436690 ) ) ;
#151694 = CARTESIAN_POINT ( 'NONE',  ( -4.483927247898782831, 16.52544592524335698, 47.70942372801902565 ) ) ;
#151695 = CARTESIAN_POINT ( 'NONE',  ( -15.72974639402176322, -15.80617190586768395, 84.37609039468570415 ) ) ;
#151696 = CARTESIAN_POINT ( 'NONE',  ( 9.474510206698729675, 16.51473224551082808, 37.08442372801899722 ) ) ;
#151697 = CARTESIAN_POINT ( 'NONE',  ( -0.05219959533936034679, 19.03943276465977164, 57.50109039468566863 ) ) ;
#151698 = ORIENTED_EDGE ( 'NONE', *, *, #148158, .F. ) ;
#151699 = CARTESIAN_POINT ( 'NONE',  ( -21.55341960407619339, 5.719274019375674811, 43.54275706135235424 ) ) ;
#151700 = CARTESIAN_POINT ( 'NONE',  ( 5.049401038297881783, 19.05341960407617563, 52.29275706135234003 ) ) ;
#151701 = CARTESIAN_POINT ( 'NONE',  ( 19.02544592524343514, -5.153800228976328945, 93.54057627198102409 ) ) ;
#151702 = CARTESIAN_POINT ( 'NONE',  ( -19.05341960407611168, -5.049401038298163336, 76.45724293864769550 ) ) ;
#151703 = CARTESIAN_POINT ( 'NONE',  ( 4.379528057220339221, -16.55341960407611168, 37.70724293864769550 ) ) ;
#151704 = CARTESIAN_POINT ( 'NONE',  ( -18.67979575497178146, -10.72451020669898902, 36.66557627198103120 ) ) ;
#151705 = CARTESIAN_POINT ( 'NONE',  ( 36.91746824999999887, 11.99521256947799053, -10.02499999726881086 ) ) ;
#151706 = CARTESIAN_POINT ( 'NONE',  ( 17.05587630539786304, 6.762274262135712810, 56.75819690962690345 ) ) ;
#151707 = CARTESIAN_POINT ( 'NONE',  ( 5.719274019375673035, 21.55341960407619339, 102.2927570613523613 ) ) ;
#151708 = CYLINDRICAL_SURFACE ( 'NONE', #50812, 1.499999999999996225 ) ;
#151709 = CARTESIAN_POINT ( 'NONE',  ( 0.05219959533909260263, 19.03943276465977164, 34.99890960531435979 ) ) ;
#151710 = CARTESIAN_POINT ( 'NONE',  ( 19.03943276465977164, -0.05219959533909143690, 113.7489096053143669 ) ) ;
#151711 = CARTESIAN_POINT ( 'NONE',  ( 23.48298174826590667, -32.32155151706770368, -1.302157773949822683 ) ) ;
#151712 = CARTESIAN_POINT ( 'NONE',  ( -16.55341960407617563, 4.379528057220093196, 53.54275706135234714 ) ) ;
#151713 = CARTESIAN_POINT ( 'NONE',  ( 21.52544592524344225, -5.823673210054117533, 68.54057627198103830 ) ) ;
#151714 = CARTESIAN_POINT ( 'NONE',  ( 16.55341960407611168, 4.379528057220329451, 33.95724293864769550 ) ) ;
#151716 = CARTESIAN_POINT ( 'NONE',  ( 19.05341960407611168, 5.049401038298154454, 103.9572429386476671 ) ) ;
#151715 = CARTESIAN_POINT ( 'NONE',  ( -19.05341960407611168, -5.049401038298163336, 26.45724293864769550 ) ) ;
#151717 = CARTESIAN_POINT ( 'NONE',  ( -10.81492255796105439, 18.62759615963255655, 32.91775706135234714 ) ) ;
#151718 = CARTESIAN_POINT ( 'NONE',  ( -13.97604488694547697, 13.89961937509957934, 38.12609039468566152 ) ) ;
#151719 = CARTESIAN_POINT ( 'NONE',  ( -19.05341960407611168, -5.049401038298163336, 26.45724293864769550 ) ) ;
#151720 = CARTESIAN_POINT ( 'NONE',  ( 21.55341960407619695, -5.719274019375665929, 81.04275706135236135 ) ) ;
#151721 = CARTESIAN_POINT ( 'NONE',  ( 17.05587630539787369, -6.762274262135690606, 33.24180309037313918 ) ) ;
#151722 = CARTESIAN_POINT ( 'NONE',  ( -4.379528057220328563, 16.55341960407611168, 30.20724293864769550 ) ) ;
#151723 = CARTESIAN_POINT ( 'NONE',  ( 17.50000000000000000, 5.068104630630361207, 111.7718159465997445 ) ) ;
#151724 = CARTESIAN_POINT ( 'NONE',  ( -21.55341960407610458, -5.719274019375992779, 31.45724293864769550 ) ) ;
#151725 = CARTESIAN_POINT ( 'NONE',  ( -4.379528057220328563, 16.55341960407611168, 90.20724293864770971 ) ) ;
#151726 = CARTESIAN_POINT ( 'NONE',  ( -17.49999999999999645, 5.499999999999997335, 120.0000000000000142 ) ) ;
#151727 = CARTESIAN_POINT ( 'NONE',  ( 13.89961937509977652, -13.97604488694527269, 78.12390960531433848 ) ) ;
#151728 = CARTESIAN_POINT ( 'NONE',  ( 12.06949235617757843, -12.14591786802309237, 73.12390960531436690 ) ) ;
#151729 = CARTESIAN_POINT ( 'NONE',  ( -0.05219959533936034679, 19.03943276465977164, 112.5010903946856757 ) ) ;
#151730 = CARTESIAN_POINT ( 'NONE',  ( -18.62759615963270932, 10.81492255796079327, 60.83224293864769550 ) ) ;
#151731 = EDGE_LOOP ( 'NONE', ( #153734, #94823, #46950, #181327 ) ) ;
#151732 = CARTESIAN_POINT ( 'NONE',  ( -16.46253265017160317, 9.564922557960807481, 35.83224293864768839 ) ) ;
#151734 = CARTESIAN_POINT ( 'NONE',  ( 10.72451020669898902, -18.67979575497178502, 77.91557627198102409 ) ) ;
#151733 = CARTESIAN_POINT ( 'NONE',  ( 19.05341960407611168, 5.049401038298154454, 78.95724293864769550 ) ) ;
#151736 = CARTESIAN_POINT ( 'NONE',  ( 13.89961937509977652, -13.97604488694527269, 93.12390960531436690 ) ) ;
#151735 = CARTESIAN_POINT ( 'NONE',  ( 8.224510206698742110, 14.34966873604972548, 107.0844237280190043 ) ) ;
#151737 = CARTESIAN_POINT ( 'NONE',  ( 16.51473224551083163, -9.474510206698727899, 65.83442372801900433 ) ) ;
#151738 = CARTESIAN_POINT ( 'NONE',  ( -5.719274019375665041, -21.55341960407619695, 99.79275706135234714 ) ) ;
#151739 = CARTESIAN_POINT ( 'NONE',  ( -0.05219959533907301413, -21.53943276465977519, 77.49890960531433848 ) ) ;
#151740 = CARTESIAN_POINT ( 'NONE',  ( 18.62759615963271287, -10.81492255796078972, 23.33224293864769194 ) ) ;
#151741 = CARTESIAN_POINT ( 'NONE',  ( -19.02544592524342804, 5.153800228976336051, 56.04057627198100988 ) ) ;
#151742 = CARTESIAN_POINT ( 'NONE',  ( -0.05219959533910754901, -16.53943276465976808, 27.49890960531435269 ) ) ;
#151743 = CARTESIAN_POINT ( 'NONE',  ( 5.049401038298161559, -19.05341960407611168, 67.70724293864769550 ) ) ;
#151744 = CYLINDRICAL_SURFACE ( 'NONE', #121559, 2.500000000000002220 ) ;
#151745 = CARTESIAN_POINT ( 'NONE',  ( -21.52544592524334988, -5.823673210054445271, 103.9594237280190185 ) ) ;
#151746 = CARTESIAN_POINT ( 'NONE',  ( -8.314922557960811034, -14.29746914071050412, 67.08224293864770971 ) ) ;
#151747 = CARTESIAN_POINT ( 'NONE',  ( 21.53943276465977519, -0.05219959533907433946, 108.7489096053143669 ) ) ;
#151748 = CARTESIAN_POINT ( 'NONE',  ( 18.67979575497178502, 10.72451020669898547, 99.16557627198100988 ) ) ;
#151749 = LINE ( 'NONE', #182093, #182155 ) ;
#151750 = CARTESIAN_POINT ( 'NONE',  ( -15.72974639402197994, 15.80617190586746368, 55.62390960531436690 ) ) ;
#151751 = CARTESIAN_POINT ( 'NONE',  ( 12.06949235617739724, 12.14591786802326823, 81.87609039468568994 ) ) ;
#151752 = CARTESIAN_POINT ( 'NONE',  ( 4.379528057220339221, -16.55341960407611168, 102.7072429386476955 ) ) ;
#151753 = CARTESIAN_POINT ( 'NONE',  ( -9.564922557960796823, -16.46253265017161027, 62.08224293864769550 ) ) ;
#151754 =( LENGTH_UNIT ( ) NAMED_UNIT ( * ) SI_UNIT ( .MILLI., .METRE. ) );
#151755 = CARTESIAN_POINT ( 'NONE',  ( 16.53943276465976808, 0.05219959533934440121, 111.2510903946856899 ) ) ;
#151756 = CARTESIAN_POINT ( 'NONE',  ( 18.62759615963255655, 10.81492255796105972, 51.66775706135234714 ) ) ;
#151757 = CARTESIAN_POINT ( 'NONE',  ( 13.89961937509977652, -13.97604488694527269, 108.1239096053143669 ) ) ;
#151758 = CARTESIAN_POINT ( 'NONE',  ( 15.80617190586769283, -15.72974639402175789, 85.62609039468568994 ) ) ;
#151759 = CARTESIAN_POINT ( 'NONE',  ( -16.51473224551069308, -9.474510206698971260, 31.66557627198102054 ) ) ;
#151760 = CARTESIAN_POINT ( 'NONE',  ( 0.05219959533909260263, 19.03943276465977164, 34.99890960531435979 ) ) ;
#151761 = ORIENTED_EDGE ( 'NONE', *, *, #142268, .T. ) ;
#151762 = CARTESIAN_POINT ( 'NONE',  ( 18.67979575497194134, -10.72451020669871369, 65.83442372801900433 ) ) ;
#151763 = CARTESIAN_POINT ( 'NONE',  ( -19.05341960407611168, -5.049401038298163336, 101.4572429386476955 ) ) ;
#151764 = CARTESIAN_POINT ( 'NONE',  ( -0.05219959533936034679, 19.03943276465977164, 77.50109039468566152 ) ) ;
#151765 = CARTESIAN_POINT ( 'NONE',  ( -15.80617190586768217, 15.72974639402176855, 48.12609039468568284 ) ) ;
#151766 = CARTESIAN_POINT ( 'NONE',  ( -12.06949235617739369, -12.14591786802326823, 19.37609039468568639 ) ) ;
#151767 = CARTESIAN_POINT ( 'NONE',  ( 5.153800228976615827, -19.02544592524334988, 70.20942372801899012 ) ) ;
#151768 = CARTESIAN_POINT ( 'NONE',  ( 13.97604488694527802, 13.89961937509977652, 54.37390960531435979 ) ) ;
#151769 = CARTESIAN_POINT ( 'NONE',  ( -19.02544592524334988, -5.153800228976617603, 88.95942372801897591 ) ) ;
#151770 = CARTESIAN_POINT ( 'NONE',  ( 16.55341960407611168, 4.379528057220329451, 28.95724293864769905 ) ) ;
#151771 = CARTESIAN_POINT ( 'NONE',  ( -0.05219959533936034679, 19.03943276465977164, 92.50109039468566152 ) ) ;
#151772 = CARTESIAN_POINT ( 'NONE',  ( 14.34966873604960469, 8.224510206698951720, 44.16557627198103120 ) ) ;
#151773 = CARTESIAN_POINT ( 'NONE',  ( -19.02544592524334988, -5.153800228976617603, 58.95942372801900433 ) ) ;
#151774 = CARTESIAN_POINT ( 'NONE',  ( 8.224510206698742110, 14.34966873604972548, 52.08442372801901854 ) ) ;
#151775 = CARTESIAN_POINT ( 'NONE',  ( -9.474510206698720793, -16.51473224551083518, 24.58442372801900078 ) ) ;
#151776 = CARTESIAN_POINT ( 'NONE',  ( 19.05341960407611168, 5.049401038298154454, 38.95724293864767418 ) ) ;
#151777 = CARTESIAN_POINT ( 'NONE',  ( -17.05116617787826172, -6.768360034955708038, 66.34324446740804149 ) ) ;
#151778 = CARTESIAN_POINT ( 'NONE',  ( 14.29746914071037800, 8.314922557961029526, 46.66775706135234714 ) ) ;
#151779 = CYLINDRICAL_SURFACE ( 'NONE', #182265, 216.0437394197456342 ) ;
#151780 = CARTESIAN_POINT ( 'NONE',  ( 8.571926809382603096, -26.38167802310801235, 145.4750000027311785 ) ) ;
#151781 = CARTESIAN_POINT ( 'NONE',  ( -9.564922557960796823, -16.46253265017161027, 92.08224293864769550 ) ) ;
#151782 = DIRECTION ( 'NONE',  ( -1.000000000000000000, 0.000000000000000000, 0.000000000000000000 ) ) ;
#151783 = EDGE_LOOP ( 'NONE', ( #162646, #159454, #84481, #91300 ) ) ;
#151784 = CARTESIAN_POINT ( 'NONE',  ( 13.97604488694548053, -13.89961937509957401, 85.62609039468568994 ) ) ;
#151786 = CARTESIAN_POINT ( 'NONE',  ( 15.80617190586746368, 15.72974639402197994, 29.37390960531435269 ) ) ;
#151785 = AXIS2_PLACEMENT_3D ( 'NONE', #86525, #177559, #148209 ) ;
#151788 = CARTESIAN_POINT ( 'NONE',  ( -13.97604488694547697, 13.89961937509957934, 98.12609039468566152 ) ) ;
#151787 = CARTESIAN_POINT ( 'NONE',  ( -5.049401038297874678, -19.05341960407617918, 24.79275706135233648 ) ) ;
#151789 = CARTESIAN_POINT ( 'NONE',  ( -14.29746914071049879, 8.314922557960819915, 115.8322429386477097 ) ) ;
#151790 = CARTESIAN_POINT ( 'NONE',  ( 13.89961937509977652, -13.97604488694527269, 33.12390960531434558 ) ) ;
#151791 = CARTESIAN_POINT ( 'NONE',  ( -0.05219959533907301413, -21.53943276465977519, 57.49890960531435979 ) ) ;
#151792 = CARTESIAN_POINT ( 'NONE',  ( 9.564922557960805705, 16.46253265017160317, 29.58224293864769550 ) ) ;
#151793 = CARTESIAN_POINT ( 'NONE',  ( 2.500000000000000000, -1.178949249685214307, 2.042000000000002036 ) ) ;
#151794 = CARTESIAN_POINT ( 'NONE',  ( 19.05341960407617918, -5.049401038297876454, 71.04275706135234714 ) ) ;
#151795 = CARTESIAN_POINT ( 'NONE',  ( -16.52544592524342804, 4.483927247898546575, 56.04057627198102409 ) ) ;
#151796 = CARTESIAN_POINT ( 'NONE',  ( -21.53943276465977519, 0.05219959533907696930, 31.24890960531435979 ) ) ;
#151797 = CARTESIAN_POINT ( 'NONE',  ( 15.80617190586769283, -15.72974639402175789, 95.62609039468568994 ) ) ;
#151798 = CARTESIAN_POINT ( 'NONE',  ( 18.67979575497178502, 10.72451020669898547, 89.16557627198102409 ) ) ;
#151799 = CARTESIAN_POINT ( 'NONE',  ( 15.80617190586769283, -15.72974639402175789, 60.62609039468567573 ) ) ;
#151800 = CARTESIAN_POINT ( 'NONE',  ( 21.53943276465977519, 0.05219959533937863772, 66.25109039468567573 ) ) ;
#151801 = CARTESIAN_POINT ( 'NONE',  ( -16.51473224551069308, -9.474510206698971260, 96.66557627198102409 ) ) ;
#151803 = CARTESIAN_POINT ( 'NONE',  ( 15.80617190586769283, -15.72974639402175789, 60.62609039468567573 ) ) ;
#151802 = CARTESIAN_POINT ( 'NONE',  ( 16.55341960407618274, -4.379528057220086978, 91.04275706135236135 ) ) ;
#151804 = CARTESIAN_POINT ( 'NONE',  ( 0.05219959533910956823, 16.53943276465976808, 114.9989096053143669 ) ) ;
#151805 = CARTESIAN_POINT ( 'NONE',  ( -14.34966873604960291, -8.224510206698953496, 61.66557627198103120 ) ) ;
#151806 = CARTESIAN_POINT ( 'NONE',  ( -14.29746914071049879, 8.314922557960819915, 35.83224293864768839 ) ) ;
#151807 = CARTESIAN_POINT ( 'NONE',  ( 18.67979575497178502, 10.72451020669898547, 39.16557627198102409 ) ) ;
#151808 = CARTESIAN_POINT ( 'NONE',  ( 9.474510206698971260, -16.51473224551069308, 52.91557627198102409 ) ) ;
#151809 = CARTESIAN_POINT ( 'NONE',  ( 21.53943276465977519, -0.05219959533907433946, 58.74890960531436690 ) ) ;
#151810 = CARTESIAN_POINT ( 'NONE',  ( -5.049401038297874678, -19.05341960407617918, 49.79275706135231871 ) ) ;
#151812 = CARTESIAN_POINT ( 'NONE',  ( 14.29746914071049879, -8.314922557960816363, 43.33224293864769550 ) ) ;
#151811 = CARTESIAN_POINT ( 'NONE',  ( -16.20579543436681291, -7.371946100354977105, 40.56520834171877254 ) ) ;
#151814 = AXIS2_PLACEMENT_3D ( 'NONE', #78941, #5076, #114244 ) ;
#151813 = CARTESIAN_POINT ( 'NONE',  ( 18.67979575497178502, 10.72451020669898547, 24.16557627198103120 ) ) ;
#151815 = ORIENTED_EDGE ( 'NONE', *, *, #10475, .F. ) ;
#151816 = ORIENTED_EDGE ( 'NONE', *, *, #31673, .T. ) ;
#151817 = CARTESIAN_POINT ( 'NONE',  ( -17.49999999999999645, 5.499999999999992895, 83.71769037696435589 ) ) ;
#151818 = CARTESIAN_POINT ( 'NONE',  ( -12.14591786802326823, 12.06949235617739902, 73.12609039468567573 ) ) ;
#151819 = CARTESIAN_POINT ( 'NONE',  ( 13.89961937509957401, 13.97604488694547697, 76.87609039468566152 ) ) ;
#151820 = CARTESIAN_POINT ( 'NONE',  ( -0.05219959533910754901, -16.53943276465976808, 37.49890960531436690 ) ) ;
#151821 = DIRECTION ( 'NONE',  ( 1.000000000000000000, 0.000000000000000000, 0.000000000000000000 ) ) ;
#151822 = CARTESIAN_POINT ( 'NONE',  ( -0.05219959533910754901, -16.53943276465976808, 27.49890960531435269 ) ) ;
#151823 = CARTESIAN_POINT ( 'NONE',  ( -19.03943276465977164, 0.05219959533909376836, 51.24890960531436690 ) ) ;
#151824 = CARTESIAN_POINT ( 'NONE',  ( -16.51473224551069308, -9.474510206698971260, 76.66557627198103830 ) ) ;
#151825 = CARTESIAN_POINT ( 'NONE',  ( 5.153800228976335163, 19.02544592524342804, 34.79057627198102409 ) ) ;
#151826 = CARTESIAN_POINT ( 'NONE',  ( 21.53943276465977519, 0.05219959533937863772, 51.25109039468568994 ) ) ;
#151827 = CARTESIAN_POINT ( 'NONE',  ( 19.02544592524343514, -5.153800228976328945, 58.54057627198102409 ) ) ;
#151828 = DIRECTION ( 'NONE',  ( -1.000000000000000000, 0.000000000000000000, 0.000000000000000000 ) ) ;
#151829 = CARTESIAN_POINT ( 'NONE',  ( -16.46253265017160317, 9.564922557960807481, 65.83224293864769550 ) ) ;
#151830 = CARTESIAN_POINT ( 'NONE',  ( 5.823673210054125526, 21.52544592524343514, 39.79057627198103830 ) ) ;
#151831 = CARTESIAN_POINT ( 'NONE',  ( -16.46253265017160317, 9.564922557960807481, 35.83224293864768839 ) ) ;
#151832 = CARTESIAN_POINT ( 'NONE',  ( -15.80617190586745835, -15.72974639402198527, 36.87390960531435979 ) ) ;
#151833 = CARTESIAN_POINT ( 'NONE',  ( -4.483927247898782831, 16.52544592524335698, 87.70942372801901854 ) ) ;
#151834 = CARTESIAN_POINT ( 'NONE',  ( 13.97604488694548053, -13.89961937509957401, 20.62609039468567573 ) ) ;
#151835 = CARTESIAN_POINT ( 'NONE',  ( -12.14591786802326823, 12.06949235617739902, 68.12609039468567573 ) ) ;
#151836 = CARTESIAN_POINT ( 'NONE',  ( -0.05219959533909027116, -19.03943276465977164, 107.4989096053143527 ) ) ;
#151837 = CARTESIAN_POINT ( 'NONE',  ( -16.53943276465976808, -0.05219959533934237506, 58.75109039468568994 ) ) ;
#151838 = CARTESIAN_POINT ( 'NONE',  ( 14.34966873604972726, -8.224510206698740333, 40.83442372801901854 ) ) ;
#151839 = CARTESIAN_POINT ( 'NONE',  ( -13.89961937509977652, 13.97604488694528158, 110.6239096053143243 ) ) ;
#151840 = CARTESIAN_POINT ( 'NONE',  ( 8.314922557961029526, -14.29746914071037800, 20.41775706135234714 ) ) ;
#151841 = CARTESIAN_POINT ( 'NONE',  ( -0.05219959533909027116, -19.03943276465977164, 32.49890960531435979 ) ) ;
#151842 = CARTESIAN_POINT ( 'NONE',  ( -18.62759615963255300, -10.81492255796106328, 29.16775706135234003 ) ) ;
#151843 = CARTESIAN_POINT ( 'NONE',  ( -14.34966873604972548, 8.224510206698743886, 23.33442372801901499 ) ) ;
#151844 = CARTESIAN_POINT ( 'NONE',  ( -4.483927247898782831, 16.52544592524335698, 92.70942372801901854 ) ) ;
#151845 = CARTESIAN_POINT ( 'NONE',  ( 38.00000000000001421, 12.34694845685043951, -4.649999994537627579 ) ) ;
#151846 = CARTESIAN_POINT ( 'NONE',  ( 18.62759615963255655, 10.81492255796105972, 101.6677570613523613 ) ) ;
#151847 = CARTESIAN_POINT ( 'NONE',  ( 19.03943276465977164, 0.05219959533936151252, 91.25109039468566152 ) ) ;
#151848 = CARTESIAN_POINT ( 'NONE',  ( 16.55341960407611168, 4.379528057220329451, 58.95724293864770971 ) ) ;
#151849 = CARTESIAN_POINT ( 'NONE',  ( 9.474510206698971260, -16.51473224551069308, 27.91557627198103120 ) ) ;
#151851 = CARTESIAN_POINT ( 'NONE',  ( -5.000000000000000000, -116.8122400552013431, 54.87277500418469600 ) ) ;
#151850 = CARTESIAN_POINT ( 'NONE',  ( 19.03943276465977164, 0.05219959533936151252, 51.25109039468567573 ) ) ;
#151852 = CARTESIAN_POINT ( 'NONE',  ( 10.72451020669871369, 18.67979575497193778, 52.08442372801901854 ) ) ;
#151853 = CARTESIAN_POINT ( 'NONE',  ( 16.53943276465976808, 0.05219959533934440121, 26.25109039468567573 ) ) ;
#151854 = CARTESIAN_POINT ( 'NONE',  ( 17.31747979337948706, 6.344076630961015262, 83.87944868065183357 ) ) ;
#151855 = CARTESIAN_POINT ( 'NONE',  ( 0.05219959533909260263, 19.03943276465977164, 104.9989096053143669 ) ) ;
#151856 = CARTESIAN_POINT ( 'NONE',  ( 21.55341960407610458, 5.719274019375980345, 78.95724293864769550 ) ) ;
#151857 = CARTESIAN_POINT ( 'NONE',  ( -5.153800228976607833, 19.02544592524334988, 97.70942372801900433 ) ) ;
#151858 = CARTESIAN_POINT ( 'NONE',  ( 19.05341960407611168, 5.049401038298154454, 98.95724293864766707 ) ) ;
#151859 = CARTESIAN_POINT ( 'NONE',  ( -21.37649426270061426, -18.77044942199658806, 140.0000000000000568 ) ) ;
#151860 = CARTESIAN_POINT ( 'NONE',  ( -8.314922557960811034, -14.29746914071050412, 107.0822429386476955 ) ) ;
#151861 = CARTESIAN_POINT ( 'NONE',  ( 0.05219959533937995610, -21.53943276465977519, 100.0010903946857042 ) ) ;
#151862 = CARTESIAN_POINT ( 'NONE',  ( 16.46253265017160672, -9.564922557960803928, 48.33224293864769550 ) ) ;
#151863 = CARTESIAN_POINT ( 'NONE',  ( -15.80617190586768217, 15.72974639402176855, 58.12609039468568994 ) ) ;
#151864 = EDGE_CURVE ( 'NONE', #147958, #178033, #7454, .T. ) ;
#151865 = CARTESIAN_POINT ( 'NONE',  ( 5.823673210054444382, -21.52544592524334988, 90.20942372801903275 ) ) ;
#151866 = CARTESIAN_POINT ( 'NONE',  ( -8.224510206698735004, -14.34966873604973081, 104.5844237280190185 ) ) ;
#151867 = CARTESIAN_POINT ( 'NONE',  ( 19.03943276465977164, -0.05219959533909143690, 83.74890960531436690 ) ) ;
#151868 = CARTESIAN_POINT ( 'NONE',  ( -18.67979575497193778, 10.72451020669871902, 38.33442372801900433 ) ) ;
#151869 = CARTESIAN_POINT ( 'NONE',  ( -21.53943276465977519, -0.05219959533937600094, 43.75109039468568284 ) ) ;
#151871 = CARTESIAN_POINT ( 'NONE',  ( 0.05219959533909260263, 19.03943276465977164, 89.99890960531436690 ) ) ;
#151870 = CARTESIAN_POINT ( 'NONE',  ( -9.474510206698720793, -16.51473224551083518, 69.58442372801901854 ) ) ;
#151872 = CARTESIAN_POINT ( 'NONE',  ( 12.14591786802309770, 12.06949235617756955, 99.37390960531436690 ) ) ;
#151873 = CARTESIAN_POINT ( 'NONE',  ( -10.72451020669898014, 18.67979575497178502, 100.4155762719810241 ) ) ;
#151874 = CARTESIAN_POINT ( 'NONE',  ( 16.55341960407611168, 4.379528057220329451, 68.95724293864769550 ) ) ;
#151875 = CARTESIAN_POINT ( 'NONE',  ( -5.153800228976607833, 19.02544592524334988, 22.70942372801899012 ) ) ;
#151876 = CARTESIAN_POINT ( 'NONE',  ( -14.34966873604960291, -8.224510206698953496, 81.66557627198103830 ) ) ;
#151877 = CARTESIAN_POINT ( 'NONE',  ( -5.049401038298153566, 19.05341960407611168, 35.20724293864768839 ) ) ;
#151878 = CARTESIAN_POINT ( 'NONE',  ( -0.05219959533936034679, 19.03943276465977164, 87.50109039468567573 ) ) ;
#151879 = CARTESIAN_POINT ( 'NONE',  ( -14.34966873604960291, -8.224510206698953496, 51.66557627198102409 ) ) ;
#151880 = CARTESIAN_POINT ( 'NONE',  ( 18.62759615963255655, 10.81492255796105972, 96.66775706135234714 ) ) ;
#151881 = CARTESIAN_POINT ( 'NONE',  ( 13.89961937509977652, -13.97604488694527269, 98.12390960531433848 ) ) ;
#151882 = CARTESIAN_POINT ( 'NONE',  ( 19.03943276465977164, 0.05219959533936151252, 71.25109039468566152 ) ) ;
#151883 = CARTESIAN_POINT ( 'NONE',  ( 5.823673210054125526, 21.52544592524343514, 79.79057627198102409 ) ) ;
#151884 = CARTESIAN_POINT ( 'NONE',  ( 5.719274019375673035, 21.55341960407619339, 32.29275706135235424 ) ) ;
#151885 = CARTESIAN_POINT ( 'NONE',  ( 16.52544592524335698, 4.483927247898782831, 26.45942372801901854 ) ) ;
#151886 = CARTESIAN_POINT ( 'NONE',  ( 4.483927247898790824, -16.52544592524335698, 95.20942372801903275 ) ) ;
#151888 = CARTESIAN_POINT ( 'NONE',  ( 10.81492255796106328, -18.62759615963255655, 35.41775706135234003 ) ) ;
#151887 = CARTESIAN_POINT ( 'NONE',  ( -5.049401038298153566, 19.05341960407611168, 30.20724293864768839 ) ) ;
#151889 = CARTESIAN_POINT ( 'NONE',  ( -13.97604488694527625, -13.89961937509977652, 26.87390960531434558 ) ) ;
#151890 = CARTESIAN_POINT ( 'NONE',  ( -11.40812507854755609, 35.11059874428196537, -1.524999997268813301 ) ) ;
#151891 = CARTESIAN_POINT ( 'NONE',  ( 16.52544592524335698, 4.483927247898782831, 46.45942372801901854 ) ) ;
#151892 = CARTESIAN_POINT ( 'NONE',  ( -16.52544592524342804, 4.483927247898546575, 76.04057627198102409 ) ) ;
#151893 = CARTESIAN_POINT ( 'NONE',  ( 10.81492255796078972, 18.62759615963270932, 69.58224293864769550 ) ) ;
#151894 = CARTESIAN_POINT ( 'NONE',  ( 14.34966873604960469, 8.224510206698951720, 24.16557627198103120 ) ) ;
#151895 = CARTESIAN_POINT ( 'NONE',  ( -12.06949235617739369, -12.14591786802326823, 49.37609039468569705 ) ) ;
#151896 = CARTESIAN_POINT ( 'NONE',  ( -16.46253265017160317, 9.564922557960807481, 40.83224293864769550 ) ) ;
#151897 = CARTESIAN_POINT ( 'NONE',  ( -8.224510206698735004, -14.34966873604973081, 94.58442372801901854 ) ) ;
#151898 = CARTESIAN_POINT ( 'NONE',  ( 13.89961937509957401, 13.97604488694547697, 81.87609039468564731 ) ) ;
#151899 = CARTESIAN_POINT ( 'NONE',  ( 15.72974639402199770, -15.80617190586745480, 78.12390960531436690 ) ) ;
#151900 = CARTESIAN_POINT ( 'NONE',  ( -4.483927247898539470, -16.52544592524342804, 22.29057627198102765 ) ) ;
#151901 = ORIENTED_EDGE ( 'NONE', *, *, #4039, .F. ) ;
#151902 = CARTESIAN_POINT ( 'NONE',  ( 5.049401038298161559, -19.05341960407611168, 112.7072429386476813 ) ) ;
#151903 = EDGE_CURVE ( 'NONE', #118975, #31542, #158160, .T. ) ;
#151904 = CARTESIAN_POINT ( 'NONE',  ( -10.72451020669898014, 18.67979575497178502, 65.41557627198102409 ) ) ;
#151905 = VERTEX_POINT ( 'NONE', #112645 ) ;
#151906 = CARTESIAN_POINT ( 'NONE',  ( 4.483927247898790824, -16.52544592524335698, 90.20942372801903275 ) ) ;
#151907 = ORIENTED_EDGE ( 'NONE', *, *, #95241, .T. ) ;
#151908 = CARTESIAN_POINT ( 'NONE',  ( 13.89961937509977652, -13.97604488694527269, 108.1239096053143669 ) ) ;
#151909 = CARTESIAN_POINT ( 'NONE',  ( -18.22780087662123805, 5.499999999999981348, 76.01763182126894947 ) ) ;
#151910 = CARTESIAN_POINT ( 'NONE',  ( -18.62759615963270932, 10.81492255796079327, 75.83224293864769550 ) ) ;
#151911 = CARTESIAN_POINT ( 'NONE',  ( 14.29746914071037800, 8.314922557961029526, 106.6677570613523756 ) ) ;
#151912 = CARTESIAN_POINT ( 'NONE',  ( -12.06949235617739369, -12.14591786802326823, 19.37609039468568639 ) ) ;
#151913 = CARTESIAN_POINT ( 'NONE',  ( -19.03943276465977164, 0.05219959533909376836, 26.24890960531435624 ) ) ;
#151914 = CARTESIAN_POINT ( 'NONE',  ( -16.55341960407617563, 4.379528057220093196, 33.54275706135234714 ) ) ;
#151915 = CARTESIAN_POINT ( 'NONE',  ( 5.049401038298161559, -19.05341960407611168, 52.70724293864767418 ) ) ;
#151916 = CARTESIAN_POINT ( 'NONE',  ( 17.81289503416611453, -24.51734667627695785, 142.6999999999999886 ) ) ;
#151917 = CARTESIAN_POINT ( 'NONE',  ( 0.05219959533909260263, 19.03943276465977164, 99.99890960531436690 ) ) ;
#151918 = CARTESIAN_POINT ( 'NONE',  ( -0.05219959533934338120, 16.53943276465976808, 87.50109039468568994 ) ) ;
#151919 = CARTESIAN_POINT ( 'NONE',  ( -16.51473224551082808, 9.474510206698731452, 93.33442372801900433 ) ) ;
#151920 = CARTESIAN_POINT ( 'NONE',  ( 16.51473224551083163, -9.474510206698727899, 20.83442372801899722 ) ) ;
#151921 = CARTESIAN_POINT ( 'NONE',  ( -5.719274019375978568, 21.55341960407610458, 70.20724293864769550 ) ) ;
#151922 = CARTESIAN_POINT ( 'NONE',  ( 16.52544592524335698, 4.483927247898782831, 101.4594237280190185 ) ) ;
#151923 = CARTESIAN_POINT ( 'NONE',  ( 13.89961937509957401, 13.97604488694547697, 91.87609039468567573 ) ) ;
#151924 = CARTESIAN_POINT ( 'NONE',  ( -13.89961937509977652, 13.97604488694528158, 50.62390960531435979 ) ) ;
#151925 = CARTESIAN_POINT ( 'NONE',  ( -5.153800228976328057, -19.02544592524343514, 87.29057627198103830 ) ) ;
#151926 = CARTESIAN_POINT ( 'NONE',  ( 5.719274019375673035, 21.55341960407619339, 62.29275706135236845 ) ) ;
#151927 = CARTESIAN_POINT ( 'NONE',  ( -19.02544592524342804, 5.153800228976336051, 61.04057627198103120 ) ) ;
#151928 = CARTESIAN_POINT ( 'NONE',  ( -12.06949235617756955, 12.14591786802309770, 90.62390960531436690 ) ) ;
#151929 = CARTESIAN_POINT ( 'NONE',  ( 20.96320343559639099, -21.46320343559646915, 5.353553390593268624 ) ) ;
#151930 = CARTESIAN_POINT ( 'NONE',  ( -16.52544592524342804, 4.483927247898546575, 76.04057627198102409 ) ) ;
#151931 = CARTESIAN_POINT ( 'NONE',  ( 10.81492255796078972, 18.62759615963270932, 69.58224293864769550 ) ) ;
#151932 = CARTESIAN_POINT ( 'NONE',  ( 9.474510206698729675, 16.51473224551082808, 92.08442372801900433 ) ) ;
#151933 = CARTESIAN_POINT ( 'NONE',  ( 19.49671883438227482, 5.500000000000019540, 92.39279849105682274 ) ) ;
#151934 = CARTESIAN_POINT ( 'NONE',  ( -19.03943276465977164, -0.05219959533935918106, 43.75109039468566863 ) ) ;
#151935 = CARTESIAN_POINT ( 'NONE',  ( -22.55670631985108443, -22.55670631985069008, -45.64921306006598201 ) ) ;
#151937 = CARTESIAN_POINT ( 'NONE',  ( 5.049401038298161559, -19.05341960407611168, 92.70724293864769550 ) ) ;
#151936 = CARTESIAN_POINT ( 'NONE',  ( 5.049401038298161559, -19.05341960407611168, 77.70724293864765286 ) ) ;
#151938 = CARTESIAN_POINT ( 'NONE',  ( 16.55341960407618274, -4.379528057220086978, 71.04275706135234714 ) ) ;
#151939 = CARTESIAN_POINT ( 'NONE',  ( -16.79531203550649465, -7.028104445595491079, 51.25244988220442366 ) ) ;
#151940 = CARTESIAN_POINT ( 'NONE',  ( 16.51473224551083163, -9.474510206698727899, 45.83442372801900433 ) ) ;
#151941 = CARTESIAN_POINT ( 'NONE',  ( 36.90816834587730710, 0.7173862878750157934, 50.46507289210756397 ) ) ;
#151942 = CARTESIAN_POINT ( 'NONE',  ( -5.049401038298153566, 19.05341960407611168, 105.2072429386476671 ) ) ;
#151943 = CARTESIAN_POINT ( 'NONE',  ( 16.55341960407618274, -4.379528057220086978, 106.0427570613523471 ) ) ;
#151944 = CARTESIAN_POINT ( 'NONE',  ( 17.49999999999998579, -5.500000000000023981, 68.29690382534171533 ) ) ;
#151945 = CARTESIAN_POINT ( 'NONE',  ( -0.05219959533934338120, 16.53943276465976808, 77.50109039468567573 ) ) ;
#151946 = FACE_OUTER_BOUND ( 'NONE', #89567, .T. ) ;
#151947 = CARTESIAN_POINT ( 'NONE',  ( -14.34966873604972548, 8.224510206698743886, 48.33442372801902565 ) ) ;
#151948 = DIRECTION ( 'NONE',  ( 0.000000000000000000, 0.000000000000000000, 1.000000000000000000 ) ) ;
#151949 = CARTESIAN_POINT ( 'NONE',  ( 0.05219959533937995610, -21.53943276465977519, 65.00109039468568994 ) ) ;
#151950 = CARTESIAN_POINT ( 'NONE',  ( -19.02544592524334988, -5.153800228976617603, 68.95942372801896170 ) ) ;
#151951 = CARTESIAN_POINT ( 'NONE',  ( 16.51473224551083163, -9.474510206698727899, 20.83442372801899722 ) ) ;
#151952 = CARTESIAN_POINT ( 'NONE',  ( 13.89961937509977652, -13.97604488694527269, 53.12390960531434558 ) ) ;
#151953 = CARTESIAN_POINT ( 'NONE',  ( -19.05341960407611168, -5.049401038298163336, 41.45724293864769550 ) ) ;
#151954 = CARTESIAN_POINT ( 'NONE',  ( 17.39620827691126692, -6.149463919001277645, 23.33264299213259108 ) ) ;
#151955 = CARTESIAN_POINT ( 'NONE',  ( 18.67979575497178502, 10.72451020669898547, 64.16557627198102409 ) ) ;
#151956 = AXIS2_PLACEMENT_3D ( 'NONE', #196621, #179460, #100581 ) ;
#151957 = CARTESIAN_POINT ( 'NONE',  ( 5.719274019375991003, -21.55341960407610458, 27.70724293864769905 ) ) ;
#151958 = CARTESIAN_POINT ( 'NONE',  ( 16.55341960407611168, 4.379528057220329451, 113.9572429386477239 ) ) ;
#151959 = CARTESIAN_POINT ( 'NONE',  ( 14.34966873604972726, -8.224510206698740333, 45.83442372801901854 ) ) ;
#151960 = ORIENTED_EDGE ( 'NONE', *, *, #155303, .F. ) ;
#151961 = CARTESIAN_POINT ( 'NONE',  ( 0.05219959533907565091, 21.53943276465977519, 109.9989096053143527 ) ) ;
#151963 = CARTESIAN_POINT ( 'NONE',  ( -38.00000000000001421, 12.34694845685046438, -8.099999999999997868 ) ) ;
#151962 = CARTESIAN_POINT ( 'NONE',  ( -4.483927247898539470, -16.52544592524342804, 52.29057627198102409 ) ) ;
#151964 = CARTESIAN_POINT ( 'NONE',  ( 5.049401038297881783, 19.05341960407617563, 112.2927570613523471 ) ) ;
#151965 = CARTESIAN_POINT ( 'NONE',  ( 16.51473224551083163, -9.474510206698727899, 40.83442372801900433 ) ) ;
#151966 = CARTESIAN_POINT ( 'NONE',  ( -14.29746914071049879, 8.314922557960819915, 40.83224293864769550 ) ) ;
#151967 = CARTESIAN_POINT ( 'NONE',  ( 15.72974639402199770, -15.80617190586745480, 113.1239096053143953 ) ) ;
#151969 = CARTESIAN_POINT ( 'NONE',  ( -18.62759615963270932, 10.81492255796079327, 60.83224293864769550 ) ) ;
#151968 = DIRECTION ( 'NONE',  ( 1.000000000000000000, 0.000000000000000000, 0.000000000000000000 ) ) ;
#151970 = CARTESIAN_POINT ( 'NONE',  ( 13.89961937509977652, -13.97604488694527269, 88.12390960531438111 ) ) ;
#151971 = CARTESIAN_POINT ( 'NONE',  ( -8.314922557960811034, -14.29746914071050412, 62.08224293864769550 ) ) ;
#151972 = CARTESIAN_POINT ( 'NONE',  ( 16.46253265017160672, -9.564922557960803928, 108.3322429386476955 ) ) ;
#151973 = CARTESIAN_POINT ( 'NONE',  ( -13.89961937509977830, 13.97604488694528158, 80.62390960531436690 ) ) ;
#151974 = CARTESIAN_POINT ( 'NONE',  ( -13.89961937509957401, -13.97604488694547875, 59.37609039468566863 ) ) ;
#151975 = CARTESIAN_POINT ( 'NONE',  ( 21.53943276465977519, -0.05219959533907433946, 103.7489096053143669 ) ) ;
#151976 = CARTESIAN_POINT ( 'NONE',  ( -19.03943276465977164, 0.05219959533909376836, 46.24890960531435979 ) ) ;
#151977 = CARTESIAN_POINT ( 'NONE',  ( 8.314922557960818139, 14.29746914071049879, 114.5822429386477097 ) ) ;
#151978 = CARTESIAN_POINT ( 'NONE',  ( 10.72451020669871369, 18.67979575497193778, 47.08442372801901854 ) ) ;
#151979 = CARTESIAN_POINT ( 'NONE',  ( -17.14385361876520619, 23.59649016807275856, 148.5750000027311444 ) ) ;
#151980 = CARTESIAN_POINT ( 'NONE',  ( -8.224510206698948167, 14.34966873604960824, 30.41557627198101699 ) ) ;
#151981 = CARTESIAN_POINT ( 'NONE',  ( -16.51473224551069308, -9.474510206698971260, 51.66557627198102409 ) ) ;
#151982 = B_SPLINE_CURVE_WITH_KNOTS ( 'NONE', 3,
 ( #178542, #69346, #160362, #22852, #192704, #53175 ),
 .UNSPECIFIED., .F., .F.,
 ( 4, 2, 4 ),
 ( 0.003239945802372246487, 0.003620412082092121231, 0.004000878361811995541 ),
 .UNSPECIFIED. ) ;
#151983 = CARTESIAN_POINT ( 'NONE',  ( 16.51473224551069308, 9.474510206698969483, 94.16557627198103830 ) ) ;
#151984 = CARTESIAN_POINT ( 'NONE',  ( -10.81492255796078084, -18.62759615963271287, 77.08224293864769550 ) ) ;
#151985 = CARTESIAN_POINT ( 'NONE',  ( 27.73933785331498925, -9.013057229001033122, 141.7750000027311899 ) ) ;
#151986 = CARTESIAN_POINT ( 'NONE',  ( -13.97604488694527625, -13.89961937509977652, 41.87390960531435979 ) ) ;
#151987 = VERTEX_POINT ( 'NONE', #99469 ) ;
#151988 = CARTESIAN_POINT ( 'NONE',  ( -0.05219959533907301413, -21.53943276465977519, 47.49890960531435979 ) ) ;
#151989 = CARTESIAN_POINT ( 'NONE',  ( 10.72451020669871369, 18.67979575497193778, 92.08442372801901854 ) ) ;
#151992 = CARTESIAN_POINT ( 'NONE',  ( 16.55341960407611168, 4.379528057220329451, 63.95724293864770260 ) ) ;
#151991 = CARTESIAN_POINT ( 'NONE',  ( 16.52544592524335698, 4.483927247898782831, 81.45942372801900433 ) ) ;
#151990 = FACE_OUTER_BOUND ( 'NONE', #42989, .T. ) ;
#151993 = CARTESIAN_POINT ( 'NONE',  ( -19.02544592524342804, 5.153800228976336051, 71.04057627198099567 ) ) ;
#151994 = ORIENTED_EDGE ( 'NONE', *, *, #78055, .T. ) ;
#151995 = CARTESIAN_POINT ( 'NONE',  ( 9.474510206698729675, 16.51473224551082808, 27.08442372801900433 ) ) ;
#151996 = CARTESIAN_POINT ( 'NONE',  ( 0.05219959533934541429, -16.53943276465976808, 95.00109039468568994 ) ) ;
#151997 = CARTESIAN_POINT ( 'NONE',  ( 0.05219959533936267826, -19.03943276465977164, 20.00109039468567218 ) ) ;
#151998 = CARTESIAN_POINT ( 'NONE',  ( 0.05219959533909260263, 19.03943276465977164, 69.99890960531435269 ) ) ;
#151999 = CARTESIAN_POINT ( 'NONE',  ( -10.72451020669898014, 18.67979575497178502, 45.41557627198103830 ) ) ;
#152000 = CARTESIAN_POINT ( 'NONE',  ( 4.483927247898790824, -16.52544592524335698, 30.20942372801902565 ) ) ;
#152001 = CARTESIAN_POINT ( 'NONE',  ( 5.719274019375673035, 21.55341960407619339, 92.29275706135236135 ) ) ;
#152002 = CARTESIAN_POINT ( 'NONE',  ( -0.05219959533934338120, 16.53943276465976808, 67.50109039468568994 ) ) ;
#152003 = CARTESIAN_POINT ( 'NONE',  ( 21.55341960407610458, 5.719274019375980345, 108.9572429386476955 ) ) ;
#152004 = CARTESIAN_POINT ( 'NONE',  ( -12.06949235617739369, -12.14591786802326823, 19.37609039468568639 ) ) ;
#152005 = CARTESIAN_POINT ( 'NONE',  ( -19.02544592524342804, 5.153800228976336051, 96.04057627198103830 ) ) ;
#152006 = CARTESIAN_POINT ( 'NONE',  ( -16.55341960407617563, 4.379528057220093196, 33.54275706135234714 ) ) ;
#152007 = CARTESIAN_POINT ( 'NONE',  ( -16.51473224551069308, -9.474510206698971260, 51.66557627198102409 ) ) ;
#152008 = CARTESIAN_POINT ( 'NONE',  ( 12.14591786802327356, -12.06949235617739191, 40.62609039468567573 ) ) ;
#152009 = CARTESIAN_POINT ( 'NONE',  ( -14.29746914071049879, 8.314922557960819915, 80.83224293864769550 ) ) ;
#152010 = CARTESIAN_POINT ( 'NONE',  ( -16.52544592524335698, -4.483927247898792601, 93.95942372801903275 ) ) ;
#152012 = CARTESIAN_POINT ( 'NONE',  ( 19.03943276465977164, -0.05219959533909143690, 68.74890960531436690 ) ) ;
#152011 = CARTESIAN_POINT ( 'NONE',  ( 15.80617190586769283, -15.72974639402175789, 30.62609039468567929 ) ) ;
#152013 = CARTESIAN_POINT ( 'NONE',  ( 5.049401038298161559, -19.05341960407611168, 77.70724293864765286 ) ) ;
#152014 = CARTESIAN_POINT ( 'NONE',  ( 16.53943276465976808, 0.05219959533934440121, 81.25109039468568994 ) ) ;
#152016 = ORIENTED_EDGE ( 'NONE', *, *, #47644, .F. ) ;
#152015 = CARTESIAN_POINT ( 'NONE',  ( -24.86035471869060842, -4.680034064337221800, 169.8578160361097105 ) ) ;
#152017 = VERTEX_POINT ( 'NONE', #53980 ) ;
#152018 = CARTESIAN_POINT ( 'NONE',  ( -13.97604488694547697, 13.89961937509957934, 33.12609039468566863 ) ) ;
#152019 = CARTESIAN_POINT ( 'NONE',  ( 9.474510206698971260, -16.51473224551069308, 92.91557627198103830 ) ) ;
#152020 = CARTESIAN_POINT ( 'NONE',  ( -0.05219959533909027116, -19.03943276465977164, 47.49890960531435979 ) ) ;
#152021 = CARTESIAN_POINT ( 'NONE',  ( -19.03943276465977164, 0.05219959533909376836, 111.2489096053143669 ) ) ;
#152022 = CARTESIAN_POINT ( 'NONE',  ( -8.224510206698735004, -14.34966873604973081, 44.58442372801901854 ) ) ;
#152024 = CARTESIAN_POINT ( 'NONE',  ( 14.29746914071037800, 8.314922557961029526, 46.66775706135234714 ) ) ;
#152023 = CARTESIAN_POINT ( 'NONE',  ( 19.02544592524334988, 5.153800228976608722, 56.45942372801898301 ) ) ;
#152025 = CARTESIAN_POINT ( 'NONE',  ( 13.97604488694527802, 13.89961937509977652, 104.3739096053143385 ) ) ;
#152026 = CARTESIAN_POINT ( 'NONE',  ( 19.03943276465977164, -0.05219959533909143690, 73.74890960531435269 ) ) ;
#152027 = CARTESIAN_POINT ( 'NONE',  ( -10.72451020669898014, 18.67979575497178502, 105.4155762719810383 ) ) ;
#152028 = CARTESIAN_POINT ( 'NONE',  ( -9.474510206698720793, -16.51473224551083518, 64.58442372801900433 ) ) ;
#152030 = CARTESIAN_POINT ( 'NONE',  ( 17.46738742707146841, -4.282736719227863809, 21.63625758046896763 ) ) ;
#152029 = CARTESIAN_POINT ( 'NONE',  ( -13.97604488694527625, -13.89961937509977652, 86.87390960531436690 ) ) ;
#152031 = ADVANCED_FACE ( 'NONE', ( #115653 ), #4455, .T. ) ;
#152032 = CARTESIAN_POINT ( 'NONE',  ( 9.474510206698971260, -16.51473224551069308, 62.91557627198102409 ) ) ;
#152034 = CARTESIAN_POINT ( 'NONE',  ( 13.89961937509977652, -13.97604488694527269, 28.12390960531435624 ) ) ;
#152033 = CARTESIAN_POINT ( 'NONE',  ( 16.55341960407611168, 4.379528057220329451, 38.95724293864768839 ) ) ;
#152035 = CARTESIAN_POINT ( 'NONE',  ( -16.51473224551082808, 9.474510206698731452, 38.33442372801899722 ) ) ;
#152036 = CARTESIAN_POINT ( 'NONE',  ( -8.224510206698948167, 14.34966873604960824, 80.41557627198103830 ) ) ;
#152037 = CARTESIAN_POINT ( 'NONE',  ( 10.72451020669871369, 18.67979575497193778, 97.08442372801904696 ) ) ;
#152038 = CARTESIAN_POINT ( 'NONE',  ( 5.153800228976335163, 19.02544592524342804, 44.79057627198103830 ) ) ;
#152039 = CARTESIAN_POINT ( 'NONE',  ( 14.34966873604972726, -8.224510206698740333, 50.83442372801901143 ) ) ;
#152041 = CARTESIAN_POINT ( 'NONE',  ( 0.05219959533937995610, -21.53943276465977519, 100.0010903946857042 ) ) ;
#152040 = CARTESIAN_POINT ( 'NONE',  ( 12.14591786802309770, 12.06949235617756955, 44.37390960531435979 ) ) ;
#152042 = CARTESIAN_POINT ( 'NONE',  ( 16.46253265017160672, -9.564922557960803928, 93.33224293864769550 ) ) ;
#152043 = CARTESIAN_POINT ( 'NONE',  ( 9.474510206698971260, -16.51473224551069308, 92.91557627198103830 ) ) ;
#152044 = CARTESIAN_POINT ( 'NONE',  ( -8.224510206698948167, 14.34966873604960824, 115.4155762719810241 ) ) ;
#152045 = CARTESIAN_POINT ( 'NONE',  ( -16.53943276465976808, 0.05219959533911058130, 106.2489096053143811 ) ) ;
#152046 = CARTESIAN_POINT ( 'NONE',  ( 14.34966873604960469, 8.224510206698951720, 69.16557627198102409 ) ) ;
#152047 = CARTESIAN_POINT ( 'NONE',  ( -21.52544592524343514, 5.823673210054127303, 86.04057627198102409 ) ) ;
#152048 = CARTESIAN_POINT ( 'NONE',  ( 0.05219959533909260263, 19.03943276465977164, 89.99890960531436690 ) ) ;
#152049 = CARTESIAN_POINT ( 'NONE',  ( 15.80617190586746368, 15.72974639402197994, 94.37390960531436690 ) ) ;
#152050 = CARTESIAN_POINT ( 'NONE',  ( 16.51473224551069308, 9.474510206698969483, 84.16557627198102409 ) ) ;
#152052 = CARTESIAN_POINT ( 'NONE',  ( 14.29746914071049879, -8.314922557960816363, 88.33224293864769550 ) ) ;
#152051 = CARTESIAN_POINT ( 'NONE',  ( 18.87580814761071935, -5.500000000000033751, 48.37172394265761000 ) ) ;
#152053 = CARTESIAN_POINT ( 'NONE',  ( 9.564922557960805705, 16.46253265017160317, 59.58224293864769550 ) ) ;
#152054 = CARTESIAN_POINT ( 'NONE',  ( -21.52544592524343514, 5.823673210054127303, 66.04057627198103830 ) ) ;
#152055 = CARTESIAN_POINT ( 'NONE',  ( 16.88567814943165857, -6.947325034625571050, 26.20998877347415856 ) ) ;
#152057 = DIRECTION ( 'NONE',  ( -1.000000000000000000, 0.000000000000000000, 0.000000000000000000 ) ) ;
#152056 = CARTESIAN_POINT ( 'NONE',  ( 12.06949235617739724, 12.14591786802326823, 106.8760903946856899 ) ) ;
#152058 = CARTESIAN_POINT ( 'NONE',  ( 0.05219959533934541429, -16.53943276465976808, 20.00109039468568639 ) ) ;
#152059 = CARTESIAN_POINT ( 'NONE',  ( 0.05219959533910956823, 16.53943276465976808, 89.99890960531438111 ) ) ;
#152060 = DIRECTION ( 'NONE',  ( 0.000000000000000000, 0.000000000000000000, -1.000000000000000000 ) ) ;
#152061 = CARTESIAN_POINT ( 'NONE',  ( 5.049401038298161559, -19.05341960407611168, 77.70724293864765286 ) ) ;
#152062 = CARTESIAN_POINT ( 'NONE',  ( -5.153800228976328057, -19.02544592524343514, 47.29057627198102409 ) ) ;
#152063 = CARTESIAN_POINT ( 'NONE',  ( 4.483927247898545687, 16.52544592524342804, 69.79057627198102409 ) ) ;
#152064 = CARTESIAN_POINT ( 'NONE',  ( 15.72974639402199770, -15.80617190586745480, 23.12390960531436335 ) ) ;
#152065 = CARTESIAN_POINT ( 'NONE',  ( 13.97604488694548053, -13.89961937509957401, 100.6260903946856615 ) ) ;
#152066 = CARTESIAN_POINT ( 'NONE',  ( -18.67979575497193778, 10.72451020669871902, 58.33442372801901143 ) ) ;
#152067 = CARTESIAN_POINT ( 'NONE',  ( -13.97604488694527625, -13.89961937509977652, 101.8739096053143811 ) ) ;
#152068 = CARTESIAN_POINT ( 'NONE',  ( -21.52544592524343514, 5.823673210054127303, 76.04057627198102409 ) ) ;
#152069 = CARTESIAN_POINT ( 'NONE',  ( -4.379528057220086978, -16.55341960407618274, 69.79275706135234714 ) ) ;
#152070 = CARTESIAN_POINT ( 'NONE',  ( -19.05341960407611168, -5.049401038298163336, 31.45724293864769550 ) ) ;
#152071 = CARTESIAN_POINT ( 'NONE',  ( -13.97604488694527625, -13.89961937509977652, 76.87390960531433848 ) ) ;
#152072 = CARTESIAN_POINT ( 'NONE',  ( -18.62759615963270932, 10.81492255796079327, 75.83224293864769550 ) ) ;
#152073 = CARTESIAN_POINT ( 'NONE',  ( -13.97604488694547697, 13.89961937509957934, 103.1260903946856473 ) ) ;
#152075 = CARTESIAN_POINT ( 'NONE',  ( -15.80617190586768217, 15.72974639402176855, 63.12609039468568994 ) ) ;
#152074 = CARTESIAN_POINT ( 'NONE',  ( -16.55341960407611168, -4.379528057220339221, 36.45724293864768839 ) ) ;
#152077 = CARTESIAN_POINT ( 'NONE',  ( 13.89961937509977652, -13.97604488694527269, 103.1239096053143527 ) ) ;
#152076 = CARTESIAN_POINT ( 'NONE',  ( 4.483927247898790824, -16.52544592524335698, 85.20942372801901854 ) ) ;
#152078 = CARTESIAN_POINT ( 'NONE',  ( -9.564922557960796823, -16.46253265017161027, 102.0822429386477097 ) ) ;
#152079 = DIRECTION ( 'NONE',  ( 0.000000000000000000, 0.000000000000000000, 1.000000000000000000 ) ) ;
#152080 = CARTESIAN_POINT ( 'NONE',  ( 8.314922557961029526, -14.29746914071037800, 110.4177570613523756 ) ) ;
#152081 = CARTESIAN_POINT ( 'NONE',  ( 0.05219959533934541429, -16.53943276465976808, 45.00109039468568284 ) ) ;
#152082 = CARTESIAN_POINT ( 'NONE',  ( 19.03943276465977164, -0.05219959533909143690, 58.74890960531435979 ) ) ;
#152083 = CARTESIAN_POINT ( 'NONE',  ( -16.51473224551069308, -9.474510206698971260, 76.66557627198103830 ) ) ;
#152084 = CARTESIAN_POINT ( 'NONE',  ( -21.52544592524334988, -5.823673210054445271, 63.95942372801901854 ) ) ;
#152085 = CARTESIAN_POINT ( 'NONE',  ( 16.53943276465976808, 0.05219959533934440121, 61.25109039468567573 ) ) ;
#152086 = CARTESIAN_POINT ( 'NONE',  ( -4.483927247898539470, -16.52544592524342804, 42.29057627198103120 ) ) ;
#152087 = CARTESIAN_POINT ( 'NONE',  ( -13.97604488694527625, -13.89961937509977652, 51.87390960531436690 ) ) ;
#152088 = CARTESIAN_POINT ( 'NONE',  ( -5.049401038298153566, 19.05341960407611168, 45.20724293864769550 ) ) ;
#152089 = CARTESIAN_POINT ( 'NONE',  ( 4.483927247898790824, -16.52544592524335698, 40.20942372801901854 ) ) ;
#152091 = CARTESIAN_POINT ( 'NONE',  ( -19.02544592524334988, -5.153800228976617603, 93.95942372801900433 ) ) ;
#152090 =( BOUNDED_CURVE ( )  B_SPLINE_CURVE ( 2, ( #169245, #168263, #9862, #25040, #43939, #15580, #31744, #71521, #105600, #148367, #386, #117020, #178715 ),
 .UNSPECIFIED., .F., .F. ) 
 B_SPLINE_CURVE_WITH_KNOTS ( ( 3, 2, 2, 2, 2, 2, 3 ),
 ( 0.2392725416902030389, 0.2412280701754385970, 0.2456140350877192846, 0.2500000000000000000, 0.2543859649122807154, 0.2587719298245614308, 0.2606817784877069055 ),
 .UNSPECIFIED. ) 
 CURVE ( )  GEOMETRIC_REPRESENTATION_ITEM ( )  RATIONAL_B_SPLINE_CURVE ( ( 0.9831626618144004848, 0.9848076720550091867, 1.000000000000000000, 0.9659258262890683122, 1.000000000000000000, 0.9659258262890683122, 1.000000000000000000, 0.9659258262890683122, 1.000000000000000000, 0.9659258262890683122, 1.000000000000000000, 0.9851625545550088958, 0.9832469066685279868 ) ) 
 REPRESENTATION_ITEM ( '' )  );
#152092 = CARTESIAN_POINT ( 'NONE',  ( -16.55341960407611168, -4.379528057220339221, 91.45724293864769550 ) ) ;
#152093 = CARTESIAN_POINT ( 'NONE',  ( 19.05341960407611168, 5.049401038298154454, 68.95724293864769550 ) ) ;
#152095 = CARTESIAN_POINT ( 'NONE',  ( -23.48529157249600985, 32.32473071737754111, -8.300000000000000711 ) ) ;
#152094 = CARTESIAN_POINT ( 'NONE',  ( 19.05341960407617918, -5.049401038297876454, 106.0427570613523471 ) ) ;
#152096 = CARTESIAN_POINT ( 'NONE',  ( 15.80617190586769283, -15.72974639402175789, 95.62609039468568994 ) ) ;
#152097 = CARTESIAN_POINT ( 'NONE',  ( 16.52544592524335698, 4.483927247898782831, 61.45942372801901854 ) ) ;
#152098 = CARTESIAN_POINT ( 'NONE',  ( 17.50000000000000711, -5.499999999999992895, 31.21769037696435589 ) ) ;
#152099 = CARTESIAN_POINT ( 'NONE',  ( 18.62759615963271287, -10.81492255796078972, 58.33224293864768839 ) ) ;
#152100 = CARTESIAN_POINT ( 'NONE',  ( -4.379528057220086978, -16.55341960407618274, 54.79275706135235424 ) ) ;
#152101 = CARTESIAN_POINT ( 'NONE',  ( -19.26498983726237668, 5.499999999999803713, 70.55319577422000066 ) ) ;
#152102 = CARTESIAN_POINT ( 'NONE',  ( 9.474510206698729675, 16.51473224551082808, 37.08442372801899722 ) ) ;
#152103 = CARTESIAN_POINT ( 'NONE',  ( -16.51473224551069308, -9.474510206698971260, 86.66557627198102409 ) ) ;
#152104 = CARTESIAN_POINT ( 'NONE',  ( -0.05219959533909027116, -19.03943276465977164, 27.49890960531435624 ) ) ;
#152105 = CARTESIAN_POINT ( 'NONE',  ( -19.03943276465977164, 0.05219959533909376836, 71.24890960531435269 ) ) ;
#152106 = CARTESIAN_POINT ( 'NONE',  ( 14.64731493820428021, 16.60031353666870402, -55.88827192845551650 ) ) ;
#152107 = CARTESIAN_POINT ( 'NONE',  ( -15.80617190586768217, 15.72974639402176855, 73.12609039468567573 ) ) ;
#152108 = CARTESIAN_POINT ( 'NONE',  ( -18.22780087662126647, -5.499999999999827693, 53.98236817873107185 ) ) ;
#152109 = EDGE_CURVE ( 'NONE', #64290, #174040, #169910, .T. ) ;
#152110 = CARTESIAN_POINT ( 'NONE',  ( -0.05219959533936034679, 19.03943276465977164, 32.50109039468566863 ) ) ;
#152111 = CARTESIAN_POINT ( 'NONE',  ( 16.51473224551083163, -9.474510206698727899, 30.83442372801900433 ) ) ;
#152112 = CARTESIAN_POINT ( 'NONE',  ( -12.06949235617756955, 12.14591786802309770, 50.62390960531435979 ) ) ;
#152113 = CARTESIAN_POINT ( 'NONE',  ( -5.049401038298153566, 19.05341960407611168, 55.20724293864769550 ) ) ;
#152114 = CARTESIAN_POINT ( 'NONE',  ( -5.719274019375978568, 21.55341960407610458, 25.20724293864769550 ) ) ;
#152115 = CARTESIAN_POINT ( 'NONE',  ( -10.72451020669870658, -18.67979575497194134, 79.58442372801903275 ) ) ;
#152116 = CARTESIAN_POINT ( 'NONE',  ( -5.049401038298153566, 19.05341960407611168, 70.20724293864769550 ) ) ;
#152117 = CARTESIAN_POINT ( 'NONE',  ( -15.72974639402176322, -15.80617190586768395, 79.37609039468567573 ) ) ;
#152118 = CARTESIAN_POINT ( 'NONE',  ( -21.53943276465977519, 0.05219959533907696930, 31.24890960531435979 ) ) ;
#152119 = CARTESIAN_POINT ( 'NONE',  ( 9.474510206698971260, -16.51473224551069308, 67.91557627198102409 ) ) ;
#152120 = CARTESIAN_POINT ( 'NONE',  ( 10.81492255796106328, -18.62759615963255655, 45.41775706135234003 ) ) ;
#152121 = CARTESIAN_POINT ( 'NONE',  ( 13.97604488694548053, -13.89961937509957401, 55.62609039468566863 ) ) ;
#152122 = CARTESIAN_POINT ( 'NONE',  ( 9.474510206698971260, -16.51473224551069308, 47.91557627198102409 ) ) ;
#152123 = CARTESIAN_POINT ( 'NONE',  ( -5.049401038298153566, 19.05341960407611168, 80.20724293864769550 ) ) ;
#152124 = CARTESIAN_POINT ( 'NONE',  ( 8.314922557961029526, -14.29746914071037800, 25.41775706135235779 ) ) ;
#152125 = CARTESIAN_POINT ( 'NONE',  ( -0.05219959533910754901, -16.53943276465976808, 82.49890960531436690 ) ) ;
#152126 = CARTESIAN_POINT ( 'NONE',  ( 19.03943276465977164, -0.05219959533909143690, 63.74890960531435979 ) ) ;
#152127 = CARTESIAN_POINT ( 'NONE',  ( -18.62759615963270932, 10.81492255796079327, 45.83224293864769550 ) ) ;
#152128 = CARTESIAN_POINT ( 'NONE',  ( 5.049401038297881783, 19.05341960407617563, 112.2927570613523471 ) ) ;
#152129 = CARTESIAN_POINT ( 'NONE',  ( 21.55341960407619695, -5.719274019375665929, 26.04275706135235779 ) ) ;
#152130 = CARTESIAN_POINT ( 'NONE',  ( 10.81492255796106328, -18.62759615963255655, 75.41775706135233293 ) ) ;
#152131 = CARTESIAN_POINT ( 'NONE',  ( -12.14591786802326823, 12.06949235617739902, 68.12609039468567573 ) ) ;
#152132 = CARTESIAN_POINT ( 'NONE',  ( -4.379528057220086978, -16.55341960407618274, 64.79275706135234714 ) ) ;
#152133 = CARTESIAN_POINT ( 'NONE',  ( -5.049401038298153566, 19.05341960407611168, 55.20724293864769550 ) ) ;
#152134 = CARTESIAN_POINT ( 'NONE',  ( -12.14591786802326823, 12.06949235617739902, 93.12609039468568994 ) ) ;
#152135 = CARTESIAN_POINT ( 'NONE',  ( -19.03943276465977164, -0.05219959533935918106, 38.75109039468566152 ) ) ;
#152136 = CARTESIAN_POINT ( 'NONE',  ( 18.67979575497178502, 10.72451020669898547, 109.1655762719810383 ) ) ;
#152137 = CARTESIAN_POINT ( 'NONE',  ( -14.29746914071049879, 8.314922557960819915, 65.83224293864769550 ) ) ;
#152138 = CARTESIAN_POINT ( 'NONE',  ( 13.89961937509977652, -13.97604488694527269, 83.12390960531436690 ) ) ;
#152139 = CARTESIAN_POINT ( 'NONE',  ( -0.05219959533934338120, 16.53943276465976808, 92.50109039468567573 ) ) ;
#152140 = CARTESIAN_POINT ( 'NONE',  ( 21.52544592524334988, 5.823673210054432836, 61.45942372801901854 ) ) ;
#152141 = CARTESIAN_POINT ( 'NONE',  ( -4.483927247898782831, 16.52544592524335698, 32.70942372801900433 ) ) ;
#152142 = CARTESIAN_POINT ( 'NONE',  ( -10.72451020669870658, -18.67979575497194134, 29.58442372801901854 ) ) ;
#152143 = CARTESIAN_POINT ( 'NONE',  ( 16.53943276465976808, -0.05219959533910856209, 58.74890960531436690 ) ) ;
#152144 = ORIENTED_EDGE ( 'NONE', *, *, #172898, .T. ) ;
#152145 = CARTESIAN_POINT ( 'NONE',  ( 10.72451020669898902, -18.67979575497178502, 102.9155762719810383 ) ) ;
#152146 = CARTESIAN_POINT ( 'NONE',  ( 8.224510206698953496, -14.34966873604960469, 32.91557627198102409 ) ) ;
#152147 = ORIENTED_EDGE ( 'NONE', *, *, #94811, .T. ) ;
#152148 = DIRECTION ( 'NONE',  ( -0.000000000000000000, 0.000000000000000000, 1.000000000000000000 ) ) ;
#152149 = CARTESIAN_POINT ( 'NONE',  ( -5.719274019375978568, 21.55341960407610458, 25.20724293864769550 ) ) ;
#152150 = CARTESIAN_POINT ( 'NONE',  ( -15.80617190586768217, 15.72974639402176855, 43.12609039468568284 ) ) ;
#152151 = CARTESIAN_POINT ( 'NONE',  ( 12.06949235617757843, -12.14591786802309237, 63.12390960531435979 ) ) ;
#152152 = CARTESIAN_POINT ( 'NONE',  ( -13.89961937509977652, 13.97604488694528158, 65.62390960531436690 ) ) ;
#152154 = CARTESIAN_POINT ( 'NONE',  ( -13.97604488694547697, 13.89961937509957934, 63.12609039468566152 ) ) ;
#152153 = CARTESIAN_POINT ( 'NONE',  ( -0.05219959533909027116, -19.03943276465977164, 22.49890960531436690 ) ) ;
#152155 = CARTESIAN_POINT ( 'NONE',  ( 15.72974639402199770, -15.80617190586745480, 43.12390960531435269 ) ) ;
#152156 = CARTESIAN_POINT ( 'NONE',  ( -9.524678007112646227, -44.64363251549263367, -21.91146642400208577 ) ) ;
#152157 = CARTESIAN_POINT ( 'NONE',  ( -13.97604488694527625, -13.89961937509977652, 61.87390960531435979 ) ) ;
#152158 = CARTESIAN_POINT ( 'NONE',  ( 0.05219959533934541429, -16.53943276465976808, 40.00109039468567573 ) ) ;
#152159 = CARTESIAN_POINT ( 'NONE',  ( -21.52544592524334988, -5.823673210054445271, 23.95942372801901143 ) ) ;
#152160 = CARTESIAN_POINT ( 'NONE',  ( -12.06949235617756955, 12.14591786802309770, 45.62390960531436690 ) ) ;
#152161 = VERTEX_POINT ( 'NONE', #127807 ) ;
#152162 = CARTESIAN_POINT ( 'NONE',  ( 5.049401038298161559, -19.05341960407611168, 92.70724293864769550 ) ) ;
#152163 = CARTESIAN_POINT ( 'NONE',  ( -0.05219959533907301413, -21.53943276465977519, 72.49890960531435269 ) ) ;
#152165 = CARTESIAN_POINT ( 'NONE',  ( -12.06949235617739369, -12.14591786802326823, 44.37609039468567573 ) ) ;
#152164 = CARTESIAN_POINT ( 'NONE',  ( 0.05219959533907565091, 21.53943276465977519, 114.9989096053143669 ) ) ;
#152166 = CARTESIAN_POINT ( 'NONE',  ( -18.62759615963270932, 10.81492255796079327, 40.83224293864769550 ) ) ;
#152167 = CARTESIAN_POINT ( 'NONE',  ( 5.823673210054444382, -21.52544592524334988, 105.2094237280190328 ) ) ;
#152168 = CARTESIAN_POINT ( 'NONE',  ( 19.05341960407611168, 5.049401038298154454, 93.95724293864769550 ) ) ;
#152169 = CARTESIAN_POINT ( 'NONE',  ( 16.51473224551069308, 9.474510206698969483, 44.16557627198103120 ) ) ;
#152170 = CARTESIAN_POINT ( 'NONE',  ( -5.049401038298153566, 19.05341960407611168, 95.20724293864770971 ) ) ;
#152171 = CARTESIAN_POINT ( 'NONE',  ( -9.474510206698964154, 16.51473224551069663, 80.41557627198103830 ) ) ;
#152172 = CARTESIAN_POINT ( 'NONE',  ( 16.62475595723613608, -7.163666690055876529, 88.02713351810406550 ) ) ;
#152173 = CARTESIAN_POINT ( 'NONE',  ( 19.05341960407617918, -5.049401038297876454, 56.04275706135234714 ) ) ;
#152175 = CARTESIAN_POINT ( 'NONE',  ( 5.719274019375991003, -21.55341960407610458, 27.70724293864769905 ) ) ;
#152174 = CARTESIAN_POINT ( 'NONE',  ( 15.80617190586769283, -15.72974639402175789, 105.6260903946856899 ) ) ;
#152176 = CARTESIAN_POINT ( 'NONE',  ( 12.14591786802327356, -12.06949235617739191, 105.6260903946856899 ) ) ;
#152177 = CARTESIAN_POINT ( 'NONE',  ( 9.474510206698729675, 16.51473224551082808, 77.08442372801900433 ) ) ;
#152178 = CARTESIAN_POINT ( 'NONE',  ( -16.61371651742604172, 7.165104196376024248, 58.85415069992998838 ) ) ;
#152179 = CARTESIAN_POINT ( 'NONE',  ( -16.46253265017146816, -9.564922557961047289, 89.16775706135234714 ) ) ;
#152180 = CARTESIAN_POINT ( 'NONE',  ( 9.564922557961047289, -16.46253265017146816, 30.41775706135232937 ) ) ;
#152181 = CARTESIAN_POINT ( 'NONE',  ( -16.19135201231368981, -7.376712067591810751, 45.18680854052031037 ) ) ;
#152182 = CARTESIAN_POINT ( 'NONE',  ( 16.51473224551069308, 9.474510206698969483, 44.16557627198103120 ) ) ;
#152183 = CARTESIAN_POINT ( 'NONE',  ( -4.379528057220328563, 16.55341960407611168, 45.20724293864769550 ) ) ;
#152184 = CARTESIAN_POINT ( 'NONE',  ( 19.05341960407611168, 5.049401038298154454, 23.95724293864769194 ) ) ;
#152185 = CARTESIAN_POINT ( 'NONE',  ( 12.14591786802309770, 12.06949235617756955, 24.37390960531435979 ) ) ;
#152186 = CARTESIAN_POINT ( 'NONE',  ( 20.43538597629128262, -20.43538597629122222, -52.65483682830183199 ) ) ;
#152187 = CARTESIAN_POINT ( 'NONE',  ( -16.53943276465976808, -0.05219959533934237506, 88.75109039468567573 ) ) ;
#152188 = CARTESIAN_POINT ( 'NONE',  ( 16.51473224551069308, 9.474510206698969483, 44.16557627198103120 ) ) ;
#152189 = CARTESIAN_POINT ( 'NONE',  ( 10.72451020669871369, 18.67979575497193778, 112.0844237280190185 ) ) ;
#152190 = CARTESIAN_POINT ( 'NONE',  ( 9.564922557961047289, -16.46253265017146816, 110.4177570613523471 ) ) ;
#152192 = ORIENTED_EDGE ( 'NONE', *, *, #102808, .F. ) ;
#152191 = CARTESIAN_POINT ( 'NONE',  ( 15.72974639402176855, 15.80617190586768217, 96.87609039468568994 ) ) ;
#152193 = CARTESIAN_POINT ( 'NONE',  ( -13.97604488694527625, -13.89961937509977652, 91.87390960531432427 ) ) ;
#152194 = CARTESIAN_POINT ( 'NONE',  ( -19.03943276465977164, 0.05219959533909376836, 86.24890960531436690 ) ) ;
#152195 = CARTESIAN_POINT ( 'NONE',  ( 36.91746824999999887, -11.99521256947793546, -9.724999997268813701 ) ) ;
#152196 = CARTESIAN_POINT ( 'NONE',  ( -15.72974639402197994, 15.80617190586746368, 115.6239096053143669 ) ) ;
#152197 = CARTESIAN_POINT ( 'NONE',  ( -0.05219959533910754901, -16.53943276465976808, 82.49890960531436690 ) ) ;
#152198 = CARTESIAN_POINT ( 'NONE',  ( 21.55341960407610458, 5.719274019375980345, 78.95724293864769550 ) ) ;
#152199 = CARTESIAN_POINT ( 'NONE',  ( 19.02544592524343514, -5.153800228976328945, 53.54057627198102409 ) ) ;
#152201 = CARTESIAN_POINT ( 'NONE',  ( 12.14591786802327356, -12.06949235617739191, 90.62609039468567573 ) ) ;
#152200 = CARTESIAN_POINT ( 'NONE',  ( 0.05219959533907565091, 21.53943276465977519, 94.99890960531436690 ) ) ;
#152202 = VERTEX_POINT ( 'NONE', #189511 ) ;
#152203 = CARTESIAN_POINT ( 'NONE',  ( 9.474510206698971260, -16.51473224551069308, 62.91557627198102409 ) ) ;
#152205 = CARTESIAN_POINT ( 'NONE',  ( 26.56065628307859683, -7.402157598701552210, 155.5832749335749270 ) ) ;
#152204 = CARTESIAN_POINT ( 'NONE',  ( -0.05219959533910754901, -16.53943276465976808, 97.49890960531436690 ) ) ;
#152206 = CARTESIAN_POINT ( 'NONE',  ( 0.05219959533909260263, 19.03943276465977164, 49.99890960531435979 ) ) ;
#152207 = CARTESIAN_POINT ( 'NONE',  ( -19.03943276465977164, -0.05219959533935918106, 83.75109039468567573 ) ) ;
#152208 = CARTESIAN_POINT ( 'NONE',  ( 4.483927247898545687, 16.52544592524342804, 79.79057627198102409 ) ) ;
#152209 = CARTESIAN_POINT ( 'NONE',  ( -18.62759615963255300, -10.81492255796106328, 64.16775706135234714 ) ) ;
#152211 = CARTESIAN_POINT ( 'NONE',  ( 10.81492255796078972, 18.62759615963270932, 114.5822429386477097 ) ) ;
#152210 = CARTESIAN_POINT ( 'NONE',  ( -16.46253265017160317, 9.564922557960807481, 35.83224293864768839 ) ) ;
#152212 = CARTESIAN_POINT ( 'NONE',  ( 8.314922557960818139, 14.29746914071049879, 104.5822429386477097 ) ) ;
#152213 = CARTESIAN_POINT ( 'NONE',  ( 7.905529020989565225, -46.70198807554292841, -24.42054064165401428 ) ) ;
#152214 = CARTESIAN_POINT ( 'NONE',  ( 13.89961937509977652, -13.97604488694527269, 53.12390960531434558 ) ) ;
#152215 = CARTESIAN_POINT ( 'NONE',  ( -9.338259190353433326, -11.33508666705209933, -62.20763404149727194 ) ) ;
#152217 = CARTESIAN_POINT ( 'NONE',  ( 9.474510206698971260, -16.51473224551069308, 107.9155762719810383 ) ) ;
#152216 = CARTESIAN_POINT ( 'NONE',  ( 13.89961937509957401, 13.97604488694547697, 91.87609039468567573 ) ) ;
#152218 = CARTESIAN_POINT ( 'NONE',  ( -10.72451020669870658, -18.67979575497194134, 44.58442372801901854 ) ) ;
#152219 = CARTESIAN_POINT ( 'NONE',  ( 5.049401038298161559, -19.05341960407611168, 82.70724293864770971 ) ) ;
#152220 = CARTESIAN_POINT ( 'NONE',  ( 9.564922557961047289, -16.46253265017146816, 70.41775706135233293 ) ) ;
#152221 = CARTESIAN_POINT ( 'NONE',  ( 16.46253265017160672, -9.564922557960803928, 58.33224293864769550 ) ) ;
#152222 = CARTESIAN_POINT ( 'NONE',  ( 14.34966873604960469, 8.224510206698951720, 74.16557627198102409 ) ) ;
#152223 = CARTESIAN_POINT ( 'NONE',  ( 12.14591786802309770, 12.06949235617756955, 74.37390960531436690 ) ) ;
#152224 = CARTESIAN_POINT ( 'NONE',  ( 16.46253265017160672, -9.564922557960803928, 88.33224293864769550 ) ) ;
#152225 = CARTESIAN_POINT ( 'NONE',  ( 16.53943276465976808, -0.05219959533910856209, 78.74890960531436690 ) ) ;
#152226 = CARTESIAN_POINT ( 'NONE',  ( -9.474510206698964154, 16.51473224551069663, 85.41557627198102409 ) ) ;
#152227 = CARTESIAN_POINT ( 'NONE',  ( -0.05219959533936034679, 19.03943276465977164, 32.50109039468566863 ) ) ;
#152230 = CARTESIAN_POINT ( 'NONE',  ( 4.379528057220339221, -16.55341960407611168, 107.7072429386476955 ) ) ;
#152229 = CARTESIAN_POINT ( 'NONE',  ( 16.55341960407611168, 4.379528057220329451, 23.95724293864769550 ) ) ;
#152228 = CARTESIAN_POINT ( 'NONE',  ( -19.02544592524342804, 5.153800228976336051, 56.04057627198100988 ) ) ;
#152231 = ORIENTED_EDGE ( 'NONE', *, *, #20577, .T. ) ;
#152232 = CARTESIAN_POINT ( 'NONE',  ( 5.719274019375673035, 21.55341960407619339, 42.29275706135235424 ) ) ;
#152233 = CARTESIAN_POINT ( 'NONE',  ( -9.564922557961040184, 16.46253265017147172, 72.91775706135233293 ) ) ;
#152234 = CARTESIAN_POINT ( 'NONE',  ( 12.06949235617757843, -12.14591786802309237, 33.12390960531435979 ) ) ;
#152235 = CARTESIAN_POINT ( 'NONE',  ( -15.72974639402197994, 15.80617190586746368, 80.62390960531438111 ) ) ;
#152236 = CARTESIAN_POINT ( 'NONE',  ( 16.51473224551069308, 9.474510206698969483, 109.1655762719810383 ) ) ;
#152237 = CARTESIAN_POINT ( 'NONE',  ( -8.314922557960811034, -14.29746914071050412, 72.08224293864769550 ) ) ;
#152238 = CARTESIAN_POINT ( 'NONE',  ( -16.46253265017160317, 9.564922557960807481, 45.83224293864769550 ) ) ;
#152239 = CARTESIAN_POINT ( 'NONE',  ( -5.153800228976607833, 19.02544592524334988, 37.70942372801899722 ) ) ;
#152240 = CARTESIAN_POINT ( 'NONE',  ( 14.34966873604972726, -8.224510206698740333, 105.8344237280190328 ) ) ;
#152241 = CARTESIAN_POINT ( 'NONE',  ( -8.314922557961024197, 14.29746914071037800, 52.91775706135235424 ) ) ;
#152242 = CARTESIAN_POINT ( 'NONE',  ( -0.05219959533907301413, -21.53943276465977519, 32.49890960531435979 ) ) ;
#152243 = CARTESIAN_POINT ( 'NONE',  ( -5.823673210054431948, 21.52544592524334988, 102.7094237280190185 ) ) ;
#152244 = CARTESIAN_POINT ( 'NONE',  ( -5.153800228976328057, -19.02544592524343514, 97.29057627198099567 ) ) ;
#152245 = CARTESIAN_POINT ( 'NONE',  ( 8.314922557961029526, -14.29746914071037800, 80.41775706135234714 ) ) ;
#152246 = CARTESIAN_POINT ( 'NONE',  ( -9.474510206698964154, 16.51473224551069663, 30.41557627198102054 ) ) ;
#152247 = CARTESIAN_POINT ( 'NONE',  ( 8.314922557960818139, 14.29746914071049879, 29.58224293864769905 ) ) ;
#152249 = CARTESIAN_POINT ( 'NONE',  ( 5.049401038298161559, -19.05341960407611168, 87.70724293864769550 ) ) ;
#152248 = CARTESIAN_POINT ( 'NONE',  ( -9.474510206698964154, 16.51473224551069663, 105.4155762719810383 ) ) ;
#152250 = CARTESIAN_POINT ( 'NONE',  ( 10.72451020669898902, -18.67979575497178502, 27.91557627198103830 ) ) ;
#152251 = CARTESIAN_POINT ( 'NONE',  ( -0.05219959533910754901, -16.53943276465976808, 67.49890960531436690 ) ) ;
#152252 = CARTESIAN_POINT ( 'NONE',  ( 4.483927247898545687, 16.52544592524342804, 49.79057627198102409 ) ) ;
#152253 = ORIENTED_EDGE ( 'NONE', *, *, #186961, .T. ) ;
#152255 = CARTESIAN_POINT ( 'NONE',  ( 17.50000000000001776, -4.658240926743138388, 31.44470417816803831 ) ) ;
#152254 = CARTESIAN_POINT ( 'NONE',  ( -14.34966873604972548, 8.224510206698743886, 53.33442372801901854 ) ) ;
#152256 = CARTESIAN_POINT ( 'NONE',  ( 13.89961937509957401, 13.97604488694547697, 51.87609039468566863 ) ) ;
#152257 = CARTESIAN_POINT ( 'NONE',  ( -5.049401038298153566, 19.05341960407611168, 90.20724293864766707 ) ) ;
#152258 = CARTESIAN_POINT ( 'NONE',  ( -9.564922557961040184, 16.46253265017147172, 62.91775706135233293 ) ) ;
#152259 = CARTESIAN_POINT ( 'NONE',  ( -22.44159573604010305, 16.30477369853692338, 145.1750000027311671 ) ) ;
#152260 = CARTESIAN_POINT ( 'NONE',  ( 19.03943276465977164, 0.05219959533936151252, 51.25109039468567573 ) ) ;
#152262 = CARTESIAN_POINT ( 'NONE',  ( 4.483927247898790824, -16.52544592524335698, 100.2094237280190043 ) ) ;
#152261 = CARTESIAN_POINT ( 'NONE',  ( -13.97604488694547697, 13.89961937509957934, 98.12609039468566152 ) ) ;
#152263 = CARTESIAN_POINT ( 'NONE',  ( 22.44159573604009594, -16.30477369853687364, 144.1750000027311671 ) ) ;
#152264 = CARTESIAN_POINT ( 'NONE',  ( -16.46253265017160317, 9.564922557960807481, 25.83224293864769194 ) ) ;
#152265 = CARTESIAN_POINT ( 'NONE',  ( 19.03943276465977164, -0.05219959533909143690, 113.7489096053143669 ) ) ;
#152266 = CARTESIAN_POINT ( 'NONE',  ( 15.72974639402176855, 15.80617190586768217, 41.87609039468568284 ) ) ;
#152267 = CARTESIAN_POINT ( 'NONE',  ( 9.474510206698729675, 16.51473224551082808, 107.0844237280190043 ) ) ;
#152269 = CARTESIAN_POINT ( 'NONE',  ( -5.153800228976328057, -19.02544592524343514, 67.29057627198102409 ) ) ;
#152268 = DIRECTION ( 'NONE',  ( 1.000000000000000000, 6.391086490440868450E-16, 0.000000000000000000 ) ) ;
#152270 = EDGE_CURVE ( 'NONE', #6817, #154699, #108568, .T. ) ;
#152271 = CARTESIAN_POINT ( 'NONE',  ( -3.573655867282028392E-15, 2.428612866367529932E-14, -15.00000000000000000 ) ) ;
#152273 = CARTESIAN_POINT ( 'NONE',  ( -0.05219959533909027116, -19.03943276465977164, 62.49890960531435979 ) ) ;
#152272 = CARTESIAN_POINT ( 'NONE',  ( 4.379528057220339221, -16.55341960407611168, 77.70724293864770971 ) ) ;
#152274 = CARTESIAN_POINT ( 'NONE',  ( 13.97604488694527802, 13.89961937509977652, 74.37390960531436690 ) ) ;
#152275 = CARTESIAN_POINT ( 'NONE',  ( 13.97604488694548053, -13.89961937509957401, 80.62609039468567573 ) ) ;
#152276 = CARTESIAN_POINT ( 'NONE',  ( -21.53943276465977519, 0.05219959533907696930, 61.24890960531435979 ) ) ;
#152277 = CARTESIAN_POINT ( 'NONE',  ( 4.483927247898545687, 16.52544592524342804, 109.7905762719810383 ) ) ;
#152278 = CARTESIAN_POINT ( 'NONE',  ( 13.97604488694548053, -13.89961937509957401, 40.62609039468564731 ) ) ;
#152279 = CARTESIAN_POINT ( 'NONE',  ( -5.049401038298153566, 19.05341960407611168, 75.20724293864769550 ) ) ;
#152280 = CARTESIAN_POINT ( 'NONE',  ( -18.62759615963270932, 10.81492255796079327, 95.83224293864770971 ) ) ;
#152282 = CARTESIAN_POINT ( 'NONE',  ( 19.05341960407617918, -5.049401038297876454, 51.04275706135231871 ) ) ;
#152281 = CARTESIAN_POINT ( 'NONE',  ( 4.483927247898545687, 16.52544592524342804, 79.79057627198102409 ) ) ;
#152283 = CARTESIAN_POINT ( 'NONE',  ( 21.53943276465977519, -0.05219959533907433946, 73.74890960531433848 ) ) ;
#152284 = CARTESIAN_POINT ( 'NONE',  ( -5.719274019375978568, 21.55341960407610458, 65.20724293864768129 ) ) ;
#152285 = CARTESIAN_POINT ( 'NONE',  ( 5.823673210054125526, 21.52544592524343514, 44.79057627198103120 ) ) ;
#152286 = CARTESIAN_POINT ( 'NONE',  ( 10.72451020669871369, 18.67979575497193778, 92.08442372801901854 ) ) ;
#152287 = CARTESIAN_POINT ( 'NONE',  ( 9.474510206698971260, -16.51473224551069308, 67.91557627198102409 ) ) ;
#152288 = CARTESIAN_POINT ( 'NONE',  ( -14.29746914071049879, 8.314922557960819915, 110.8322429386476955 ) ) ;
#152289 = CARTESIAN_POINT ( 'NONE',  ( -5.823673210054431948, 21.52544592524334988, 22.70942372801901499 ) ) ;
#152290 = CARTESIAN_POINT ( 'NONE',  ( -10.72451020669870658, -18.67979575497194134, 34.58442372801900433 ) ) ;
#152291 = CARTESIAN_POINT ( 'NONE',  ( 13.97604488694527802, 13.89961937509977652, 34.37390960531436690 ) ) ;
#152292 = CARTESIAN_POINT ( 'NONE',  ( 10.72451020669898902, -18.67979575497178502, 107.9155762719810241 ) ) ;
#152293 = CARTESIAN_POINT ( 'NONE',  ( 16.46253265017146816, 9.564922557961045513, 56.66775706135233293 ) ) ;
#152294 = EDGE_CURVE ( 'NONE', #6681, #96881, #70148, .T. ) ;
#152295 = CARTESIAN_POINT ( 'NONE',  ( 5.049401038298161559, -19.05341960407611168, 42.70724293864767418 ) ) ;
#152296 = CARTESIAN_POINT ( 'NONE',  ( 14.29746914071037800, 8.314922557961029526, 31.66775706135234358 ) ) ;
#152297 = CARTESIAN_POINT ( 'NONE',  ( 16.37381404539904750, -7.261601738933634032, 21.61892339308662159 ) ) ;
#152298 = CARTESIAN_POINT ( 'NONE',  ( 16.55341960407618274, -4.379528057220086978, 66.04275706135236135 ) ) ;
#152299 = CARTESIAN_POINT ( 'NONE',  ( 5.049401038298161559, -19.05341960407611168, 37.70724293864768839 ) ) ;
#152300 = CARTESIAN_POINT ( 'NONE',  ( -26.68407921138531336, -3.932373394476914807, 171.8653659962664619 ) ) ;
#152301 = CARTESIAN_POINT ( 'NONE',  ( 13.97604488694527802, 13.89961937509977652, 84.37390960531433848 ) ) ;
#152302 = CARTESIAN_POINT ( 'NONE',  ( -0.05219959533909027116, -19.03943276465977164, 27.49890960531435624 ) ) ;
#152303 = CARTESIAN_POINT ( 'NONE',  ( 18.67979575497178502, 10.72451020669898547, 64.16557627198102409 ) ) ;
#152304 = CARTESIAN_POINT ( 'NONE',  ( -14.29746914071037622, -8.314922557961029526, 49.16775706135234003 ) ) ;
#152305 = CARTESIAN_POINT ( 'NONE',  ( 15.72974639402176855, 15.80617190586768217, 101.8760903946857042 ) ) ;
#152306 = CARTESIAN_POINT ( 'NONE',  ( -13.97604488694527625, -13.89961937509977652, 36.87390960531436690 ) ) ;
#152307 = CARTESIAN_POINT ( 'NONE',  ( -8.224510206698948167, 14.34966873604960824, 30.41557627198101699 ) ) ;
#152308 = CARTESIAN_POINT ( 'NONE',  ( 4.483927247898545687, 16.52544592524342804, 59.79057627198103120 ) ) ;
#152309 = CARTESIAN_POINT ( 'NONE',  ( 16.46253265017160672, -9.564922557960803928, 68.33224293864770971 ) ) ;
#152310 = CARTESIAN_POINT ( 'NONE',  ( -5.823673210054431948, 21.52544592524334988, 107.7094237280190328 ) ) ;
#152311 = CARTESIAN_POINT ( 'NONE',  ( -5.719274019375665041, -21.55341960407619695, 24.79275706135235779 ) ) ;
#152312 = CARTESIAN_POINT ( 'NONE',  ( 0.05219959533937995610, -21.53943276465977519, 90.00109039468567573 ) ) ;
#152313 = CARTESIAN_POINT ( 'NONE',  ( -12.14591786802326823, 12.06949235617739902, 53.12609039468568284 ) ) ;
#152314 = CARTESIAN_POINT ( 'NONE',  ( 16.55341960407618274, -4.379528057220086978, 31.04275706135234714 ) ) ;
#152316 = CARTESIAN_POINT ( 'NONE',  ( -18.67979575497193778, 10.72451020669871902, 98.33442372801901854 ) ) ;
#152315 = CARTESIAN_POINT ( 'NONE',  ( 4.483927247898545687, 16.52544592524342804, 74.79057627198105251 ) ) ;
#152317 = CARTESIAN_POINT ( 'NONE',  ( 8.224510206698953496, -14.34966873604960469, 37.91557627198102409 ) ) ;
#152318 = CARTESIAN_POINT ( 'NONE',  ( 13.89961937509977652, -13.97604488694527269, 33.12390960531434558 ) ) ;
#152319 = CARTESIAN_POINT ( 'NONE',  ( -16.52544592524335698, -4.483927247898792601, 43.95942372801902565 ) ) ;
#152320 = CARTESIAN_POINT ( 'NONE',  ( 16.53943276465976808, -0.05219959533910856209, 53.74890960531437401 ) ) ;
#152321 = CARTESIAN_POINT ( 'NONE',  ( 16.55341960407618274, -4.379528057220086978, 86.04275706135236135 ) ) ;
#152322 = CARTESIAN_POINT ( 'NONE',  ( 13.97604488694527802, 13.89961937509977652, 94.37390960531436690 ) ) ;
#152323 = CARTESIAN_POINT ( 'NONE',  ( 0.05219959533909260263, 19.03943276465977164, 109.9989096053143669 ) ) ;
#152324 = CARTESIAN_POINT ( 'NONE',  ( 19.05341960407617918, -5.049401038297876454, 21.04275706135232582 ) ) ;
#152325 = CARTESIAN_POINT ( 'NONE',  ( 16.52544592524342804, -4.483927247898539470, 88.54057627198103830 ) ) ;
#152326 = CARTESIAN_POINT ( 'NONE',  ( 9.564922557960805705, 16.46253265017160317, 99.58224293864770971 ) ) ;
#152327 = VERTEX_POINT ( 'NONE', #147995 ) ;
#152328 = CARTESIAN_POINT ( 'NONE',  ( -12.06949235617739369, -12.14591786802326823, 39.37609039468567573 ) ) ;
#152329 = CARTESIAN_POINT ( 'NONE',  ( -13.97604488694527625, -13.89961937509977652, 46.87390960531435979 ) ) ;
#152330 = CARTESIAN_POINT ( 'NONE',  ( -16.51473224551069308, -9.474510206698971260, 111.6655762719810383 ) ) ;
#152332 = CARTESIAN_POINT ( 'NONE',  ( -31.80000000000000782, -1.163414459189985801E-14, 95.00000000000000000 ) ) ;
#152331 = CARTESIAN_POINT ( 'NONE',  ( 16.52544592524335698, 4.483927247898782831, 41.45942372801901143 ) ) ;
#152333 = CARTESIAN_POINT ( 'NONE',  ( -9.474510206698720793, -16.51473224551083518, 39.58442372801899722 ) ) ;
#152334 = CARTESIAN_POINT ( 'NONE',  ( -19.05341960407611168, -5.049401038298163336, 41.45724293864769550 ) ) ;
#152335 = CARTESIAN_POINT ( 'NONE',  ( -12.06949235617739369, -12.14591786802326823, 84.37609039468570415 ) ) ;
#152336 = CARTESIAN_POINT ( 'NONE',  ( 5.153800228976615827, -19.02544592524334988, 85.20942372801900433 ) ) ;
#152337 = CARTESIAN_POINT ( 'NONE',  ( -19.02544592524334988, -5.153800228976617603, 23.95942372801900078 ) ) ;
#152338 = CARTESIAN_POINT ( 'NONE',  ( 9.564922557960805705, 16.46253265017160317, 64.58224293864769550 ) ) ;
#152339 = CARTESIAN_POINT ( 'NONE',  ( 12.06949235617757843, -12.14591786802309237, 103.1239096053143811 ) ) ;
#152340 = EDGE_CURVE ( 'NONE', #115964, #81412, #18090, .T. ) ;
#152341 = CARTESIAN_POINT ( 'NONE',  ( 19.05341960407617918, -5.049401038297876454, 66.04275706135233293 ) ) ;
#152342 = CARTESIAN_POINT ( 'NONE',  ( 21.55341960407610458, 5.719274019375980345, 58.95724293864770971 ) ) ;
#152343 = CARTESIAN_POINT ( 'NONE',  ( -9.564922557961040184, 16.46253265017147172, 22.91775706135233648 ) ) ;
#152344 = CARTESIAN_POINT ( 'NONE',  ( 19.03943276465977164, -0.05219959533909143690, 108.7489096053143527 ) ) ;
#152345 = CARTESIAN_POINT ( 'NONE',  ( -0.05219959533907301413, -21.53943276465977519, 72.49890960531435269 ) ) ;
#152346 = CARTESIAN_POINT ( 'NONE',  ( -16.46253265017160317, 9.564922557960807481, 110.8322429386476955 ) ) ;
#152347 = CARTESIAN_POINT ( 'NONE',  ( -13.97604488694547697, 13.89961937509957934, 103.1260903946856473 ) ) ;
#152348 = CARTESIAN_POINT ( 'NONE',  ( -19.52217212775657629, 5.500000000000115463, 59.93993709005261650 ) ) ;
#152349 = CARTESIAN_POINT ( 'NONE',  ( -0.05219959533934338120, 16.53943276465976808, 22.50109039468567573 ) ) ;
#152350 = CARTESIAN_POINT ( 'NONE',  ( -5.049401038298153566, 19.05341960407611168, 30.20724293864768839 ) ) ;
#152351 = CARTESIAN_POINT ( 'NONE',  ( 5.049401038298161559, -19.05341960407611168, 97.70724293864766707 ) ) ;
#152352 = CARTESIAN_POINT ( 'NONE',  ( 21.52544592524344225, -5.823673210054117533, 88.54057627198103830 ) ) ;
#152353 = CARTESIAN_POINT ( 'NONE',  ( -21.55341960407619339, 5.719274019375674811, 63.54275706135234003 ) ) ;
#152355 = CARTESIAN_POINT ( 'NONE',  ( -18.62759615963255300, -10.81492255796106328, 104.1677570613523471 ) ) ;
#152354 = CARTESIAN_POINT ( 'NONE',  ( 16.51473224551083163, -9.474510206698727899, 110.8344237280190043 ) ) ;
#152356 = CARTESIAN_POINT ( 'NONE',  ( -8.314922557961024197, 14.29746914071037800, 107.9177570613523471 ) ) ;
#152357 = CARTESIAN_POINT ( 'NONE',  ( -21.55341960407610458, -5.719274019375992779, 96.45724293864770971 ) ) ;
#152358 = CARTESIAN_POINT ( 'NONE',  ( -16.53943276465976808, 0.05219959533911058130, 41.24890960531435269 ) ) ;
#152359 = CARTESIAN_POINT ( 'NONE',  ( 13.89961937509957401, 13.97604488694547697, 81.87609039468564731 ) ) ;
#152360 = CARTESIAN_POINT ( 'NONE',  ( -19.05341960407617563, 5.049401038297882671, 58.54275706135234003 ) ) ;
#152361 = CARTESIAN_POINT ( 'NONE',  ( 5.719274019375673035, 21.55341960407619339, 57.29275706135234714 ) ) ;
#152362 = CARTESIAN_POINT ( 'NONE',  ( -5.049401038297874678, -19.05341960407617918, 39.79275706135232582 ) ) ;
#152363 = CARTESIAN_POINT ( 'NONE',  ( 14.29746914071049879, -8.314922557960816363, 108.3322429386477097 ) ) ;
#152364 = CARTESIAN_POINT ( 'NONE',  ( 10.72451020669898902, -18.67979575497178502, 32.91557627198102409 ) ) ;
#152365 = CARTESIAN_POINT ( 'NONE',  ( 4.483927247898545687, 16.52544592524342804, 39.79057627198103830 ) ) ;
#152366 = CARTESIAN_POINT ( 'NONE',  ( 18.67979575497194134, -10.72451020669871369, 100.8344237280190185 ) ) ;
#152367 = CARTESIAN_POINT ( 'NONE',  ( 16.53943276465976808, 0.05219959533934440121, 71.25109039468568994 ) ) ;
#152368 = CARTESIAN_POINT ( 'NONE',  ( -16.53943276465976808, -0.05219959533934237506, 113.7510903946856757 ) ) ;
#152369 = CARTESIAN_POINT ( 'NONE',  ( 21.55341960407619695, -5.719274019375665929, 56.04275706135235424 ) ) ;
#152370 = CARTESIAN_POINT ( 'NONE',  ( -21.52544592524334988, -5.823673210054445271, 73.95942372801901854 ) ) ;
#152371 = CARTESIAN_POINT ( 'NONE',  ( 21.53943276465977519, -0.05219959533907433946, 68.74890960531435269 ) ) ;
#152372 = ORIENTED_EDGE ( 'NONE', *, *, #28811, .F. ) ;
#152373 = CARTESIAN_POINT ( 'NONE',  ( -19.02544592524342804, 5.153800228976336051, 31.04057627198102409 ) ) ;
#152374 = CARTESIAN_POINT ( 'NONE',  ( 18.62759615963255655, 10.81492255796105972, 46.66775706135234714 ) ) ;
#152375 = CARTESIAN_POINT ( 'NONE',  ( 19.02544592524343514, -5.153800228976328945, 28.54057627198102409 ) ) ;
#152376 = CARTESIAN_POINT ( 'NONE',  ( 13.97604488694527802, 13.89961937509977652, 34.37390960531436690 ) ) ;
#152377 = CARTESIAN_POINT ( 'NONE',  ( 8.314922557960818139, 14.29746914071049879, 84.58224293864769550 ) ) ;
#152378 = CARTESIAN_POINT ( 'NONE',  ( -0.05219959533909027116, -19.03943276465977164, 82.49890960531436690 ) ) ;
#152379 = CARTESIAN_POINT ( 'NONE',  ( -14.29746914071049879, 8.314922557960819915, 30.83224293864770260 ) ) ;
#152380 = CARTESIAN_POINT ( 'NONE',  ( 18.67979575497178502, 10.72451020669898547, 74.16557627198102409 ) ) ;
#152381 = CARTESIAN_POINT ( 'NONE',  ( 21.53943276465977519, -0.05219959533907433946, 108.7489096053143669 ) ) ;
#152382 = CARTESIAN_POINT ( 'NONE',  ( 0.05219959533909260263, 19.03943276465977164, 114.9989096053143669 ) ) ;
#152384 = CARTESIAN_POINT ( 'NONE',  ( 9.564922557961047289, -16.46253265017146816, 105.4177570613523471 ) ) ;
#152383 = CARTESIAN_POINT ( 'NONE',  ( 5.049401038298161559, -19.05341960407611168, 67.70724293864769550 ) ) ;
#152385 = CARTESIAN_POINT ( 'NONE',  ( 15.72974639402199770, -15.80617190586745480, 53.12390960531436690 ) ) ;
#152386 = CARTESIAN_POINT ( 'NONE',  ( 5.719274019375673035, 21.55341960407619339, 82.29275706135234714 ) ) ;
#152387 = CARTESIAN_POINT ( 'NONE',  ( -19.03943276465977164, 0.05219959533909376836, 71.24890960531435269 ) ) ;
#152388 = CARTESIAN_POINT ( 'NONE',  ( 16.46253265017160672, -9.564922557960803928, 93.33224293864769550 ) ) ;
#152389 = CARTESIAN_POINT ( 'NONE',  ( -8.314922557961024197, 14.29746914071037800, 77.91775706135231871 ) ) ;
#152390 = CARTESIAN_POINT ( 'NONE',  ( 5.823673210054444382, -21.52544592524334988, 55.20942372801902565 ) ) ;
#152391 = CARTESIAN_POINT ( 'NONE',  ( -15.80617190586768217, 15.72974639402176855, 103.1260903946856757 ) ) ;
#152392 = CARTESIAN_POINT ( 'NONE',  ( 18.67979575497178502, 10.72451020669898547, 114.1655762719810383 ) ) ;
#152393 = CARTESIAN_POINT ( 'NONE',  ( -0.05219959533907301413, -21.53943276465977519, 82.49890960531436690 ) ) ;
#152394 = CARTESIAN_POINT ( 'NONE',  ( -0.05219959533936034679, 19.03943276465977164, 47.50109039468566863 ) ) ;
#152395 = CARTESIAN_POINT ( 'NONE',  ( -21.53943276465977519, 0.05219959533907696930, 36.24890960531435979 ) ) ;
#152397 = CARTESIAN_POINT ( 'NONE',  ( -14.29746914071049879, 8.314922557960819915, 30.83224293864770260 ) ) ;
#152396 = CARTESIAN_POINT ( 'NONE',  ( 13.97604488694527802, 13.89961937509977652, 84.37390960531433848 ) ) ;
#152398 = DIRECTION ( 'NONE',  ( -1.000000000000000000, 0.000000000000000000, -0.000000000000000000 ) ) ;
#152399 = CARTESIAN_POINT ( 'NONE',  ( 6.874011537017776341, -5.374011537017756801, -64.92279855667830191 ) ) ;
#152400 = CARTESIAN_POINT ( 'NONE',  ( -5.153800228976607833, 19.02544592524334988, 97.70942372801900433 ) ) ;
#152401 = CARTESIAN_POINT ( 'NONE',  ( -21.53943276465977519, 0.05219959533907696930, 66.24890960531436690 ) ) ;
#152402 = CARTESIAN_POINT ( 'NONE',  ( 14.29746914071049879, -8.314922557960816363, 58.33224293864768839 ) ) ;
#152403 = CARTESIAN_POINT ( 'NONE',  ( 0.05219959533934541429, -16.53943276465976808, 30.00109039468568284 ) ) ;
#152404 = CARTESIAN_POINT ( 'NONE',  ( 19.02544592524343514, -5.153800228976328945, 43.54057627198103120 ) ) ;
#152406 = CARTESIAN_POINT ( 'NONE',  ( 19.03943276465977164, 0.05219959533936151252, 91.25109039468566152 ) ) ;
#152405 = CARTESIAN_POINT ( 'NONE',  ( -21.52544592524343514, 5.823673210054127303, 106.0405762719810525 ) ) ;
#152407 = CARTESIAN_POINT ( 'NONE',  ( -13.97604488694527625, -13.89961937509977652, 86.87390960531436690 ) ) ;
#152408 = CARTESIAN_POINT ( 'NONE',  ( 16.53943276465976808, -0.05219959533910856209, 83.74890960531435269 ) ) ;
#152409 = CARTESIAN_POINT ( 'NONE',  ( 0.05219959533909260263, 19.03943276465977164, 64.99890960531436690 ) ) ;
#152410 = CARTESIAN_POINT ( 'NONE',  ( -14.34966873604960291, -8.224510206698953496, 71.66557627198100988 ) ) ;
#152411 = CARTESIAN_POINT ( 'NONE',  ( 9.564922557960805705, 16.46253265017160317, 29.58224293864769550 ) ) ;
#152412 = CARTESIAN_POINT ( 'NONE',  ( -36.89607807516672722, -1.430951785632631701, 50.32279621992264396 ) ) ;
#152413 = CARTESIAN_POINT ( 'NONE',  ( 16.52544592524342804, -4.483927247898539470, 48.54057627198103120 ) ) ;
#152414 = CARTESIAN_POINT ( 'NONE',  ( 19.03943276465977164, -0.05219959533909143690, 88.74890960531436690 ) ) ;
#152415 = CARTESIAN_POINT ( 'NONE',  ( -0.9487569900773351605, -16.37811251030164073, -59.27680374464308244 ) ) ;
#152416 = CARTESIAN_POINT ( 'NONE',  ( -16.46253265017146816, -9.564922557961047289, 54.16775706135234003 ) ) ;
#152417 = CARTESIAN_POINT ( 'NONE',  ( -4.379528057220086978, -16.55341960407618274, 64.79275706135234714 ) ) ;
#152418 = CARTESIAN_POINT ( 'NONE',  ( 15.72974639402199770, -15.80617190586745480, 83.12390960531436690 ) ) ;
#152419 = CARTESIAN_POINT ( 'NONE',  ( 0.05219959533936267826, -19.03943276465977164, 35.00109039468566863 ) ) ;
#152420 = CARTESIAN_POINT ( 'NONE',  ( 19.02544592524343514, -5.153800228976328945, 93.54057627198102409 ) ) ;
#152421 = CARTESIAN_POINT ( 'NONE',  ( 0.000000000000000000, 0.000000000000000000, -64.92279855667830191 ) ) ;
#152422 = CARTESIAN_POINT ( 'NONE',  ( -21.55341960407610458, -5.719274019375992779, 31.45724293864769550 ) ) ;
#152423 = CARTESIAN_POINT ( 'NONE',  ( 0.05219959533909260263, 19.03943276465977164, 54.99890960531435979 ) ) ;
#152424 = CARTESIAN_POINT ( 'NONE',  ( 18.67979575497194134, -10.72451020669871369, 55.83442372801901854 ) ) ;
#152425 = CARTESIAN_POINT ( 'NONE',  ( -19.03943276465977164, 0.05219959533909376836, 26.24890960531435624 ) ) ;
#152428 = ORIENTED_EDGE ( 'NONE', *, *, #111893, .T. ) ;
#152427 = CARTESIAN_POINT ( 'NONE',  ( 5.153800228976335163, 19.02544592524342804, 89.79057627198102409 ) ) ;
#152426 = CARTESIAN_POINT ( 'NONE',  ( 5.719274019375991003, -21.55341960407610458, 112.7072429386476955 ) ) ;
#152429 = CARTESIAN_POINT ( 'NONE',  ( 5.823673210054444382, -21.52544592524334988, 45.20942372801901854 ) ) ;
#152430 = VERTEX_POINT ( 'NONE', #56983 ) ;
#152431 = CARTESIAN_POINT ( 'NONE',  ( 13.89961937509977652, -13.97604488694527269, 103.1239096053143527 ) ) ;
#152432 = ADVANCED_FACE ( 'NONE', ( #133819 ), #103484, .T. ) ;
#152433 = CARTESIAN_POINT ( 'NONE',  ( -17.58332526062529411, 7.635886036038502134, 90.92334959558465357 ) ) ;
#152434 = CARTESIAN_POINT ( 'NONE',  ( 5.719274019375991003, -21.55341960407610458, 112.7072429386476955 ) ) ;
#152435 = CARTESIAN_POINT ( 'NONE',  ( -19.05341960407611168, -5.049401038298163336, 46.45724293864768129 ) ) ;
#152436 = CARTESIAN_POINT ( 'NONE',  ( 12.06949235617739724, 12.14591786802326823, 26.87609039468567218 ) ) ;
#152437 = CARTESIAN_POINT ( 'NONE',  ( -23.48529157249599919, -32.32473071737750558, -11.44999999453762385 ) ) ;
#152438 = CARTESIAN_POINT ( 'NONE',  ( -10.81492255796105439, 18.62759615963255655, 97.91775706135236135 ) ) ;
#152439 = CARTESIAN_POINT ( 'NONE',  ( -9.564922557960796823, -16.46253265017161027, 27.08224293864769550 ) ) ;
#152440 = CARTESIAN_POINT ( 'NONE',  ( 0.05219959533937995610, -21.53943276465977519, 105.0010903946856757 ) ) ;
#152442 = CARTESIAN_POINT ( 'NONE',  ( 21.53943276465977519, 0.05219959533937863772, 56.25109039468568284 ) ) ;
#152441 = CARTESIAN_POINT ( 'NONE',  ( -9.474510206698964154, 16.51473224551069663, 95.41557627198102409 ) ) ;
#152443 = CARTESIAN_POINT ( 'NONE',  ( -27.73933785331498925, 9.013057229001089965, 145.2750000027311899 ) ) ;
#152444 = CARTESIAN_POINT ( 'NONE',  ( -19.03943276465977164, 0.05219959533909376836, 96.24890960531436690 ) ) ;
#152445 = CARTESIAN_POINT ( 'NONE',  ( 17.97058386085788229, 5.500000000000048850, 46.50390968646216550 ) ) ;
#152448 = CARTESIAN_POINT ( 'NONE',  ( 10.81492255796106328, -18.62759615963255655, 55.41775706135234714 ) ) ;
#152447 = CARTESIAN_POINT ( 'NONE',  ( -0.05219959533934338120, 16.53943276465976808, 62.50109039468568284 ) ) ;
#152446 = CARTESIAN_POINT ( 'NONE',  ( -4.483927247898782831, 16.52544592524335698, 52.70942372801902565 ) ) ;
#152449 = CARTESIAN_POINT ( 'NONE',  ( 21.55341960407619695, -5.719274019375665929, 91.04275706135236135 ) ) ;
#152450 = CARTESIAN_POINT ( 'NONE',  ( 0.000000000000000000, -1.443375672974063884, -3.691112476943992763E-18 ) ) ;
#152451 =( BOUNDED_CURVE ( )  B_SPLINE_CURVE ( 2, ( #114744, #34916, #113731, #158260, #50099, #159241, #96572, #147093, #176438, #98561, #68234, #54081, #175428 ),
 .UNSPECIFIED., .F., .F. ) 
 B_SPLINE_CURVE_WITH_KNOTS ( ( 3, 2, 2, 2, 2, 2, 3 ),
 ( 0.5287919057228195330, 0.5307017543859648967, 0.5350877192982456121, 0.5394736842105263275, 0.5438596491228070429, 0.5482456140350877583, 0.5502011425203234829 ),
 .UNSPECIFIED. ) 
 CURVE ( )  GEOMETRIC_REPRESENTATION_ITEM ( )  RATIONAL_B_SPLINE_CURVE ( ( 0.9832469066685285419, 0.9851625545550100060, 1.000000000000000000, 0.9659258262890683122, 1.000000000000000000, 0.9659258262890683122, 1.000000000000000000, 0.9659258262890683122, 1.000000000000000000, 0.9659258262890683122, 1.000000000000000000, 0.9848076720550078544, 0.9831626618144001517 ) ) 
 REPRESENTATION_ITEM ( '' )  );
#152452 = CARTESIAN_POINT ( 'NONE',  ( -4.483927247898782831, 16.52544592524335698, 22.70942372801901499 ) ) ;
#152453 = CARTESIAN_POINT ( 'NONE',  ( 5.153800228976335163, 19.02544592524342804, 74.79057627198103830 ) ) ;
#152454 = CARTESIAN_POINT ( 'NONE',  ( 19.02544592524343514, -5.153800228976328945, 93.54057627198102409 ) ) ;
#152455 = CARTESIAN_POINT ( 'NONE',  ( -16.53943276465976808, 0.05219959533911058130, 116.2489096053143669 ) ) ;
#152456 = CARTESIAN_POINT ( 'NONE',  ( 21.53943276465977519, -0.05219959533907433946, 23.74890960531435269 ) ) ;
#152457 = CARTESIAN_POINT ( 'NONE',  ( 16.53943276465976808, 0.05219959533934440121, 96.25109039468568994 ) ) ;
#152459 = CARTESIAN_POINT ( 'NONE',  ( -19.03943276465977164, 0.05219959533909376836, 66.24890960531436690 ) ) ;
#152458 = CARTESIAN_POINT ( 'NONE',  ( -16.53943276465976808, 0.05219959533911058130, 66.24890960531436690 ) ) ;
#152460 = CARTESIAN_POINT ( 'NONE',  ( 0.05219959533937995610, -21.53943276465977519, 90.00109039468567573 ) ) ;
#152461 = CARTESIAN_POINT ( 'NONE',  ( -17.79613651744293890, -24.49428055684528260, 144.5656553485623874 ) ) ;
#152462 = CARTESIAN_POINT ( 'NONE',  ( 13.97604488694548053, -13.89961937509957401, 105.6260903946856757 ) ) ;
#152463 = CARTESIAN_POINT ( 'NONE',  ( -16.55341960407611168, -4.379528057220339221, 81.45724293864769550 ) ) ;
#152464 = CARTESIAN_POINT ( 'NONE',  ( -10.81492255796105439, 18.62759615963255655, 22.91775706135235069 ) ) ;
#152465 = CARTESIAN_POINT ( 'NONE',  ( 21.53943276465977519, -0.05219959533907433946, 73.74890960531433848 ) ) ;
#152466 = CARTESIAN_POINT ( 'NONE',  ( 13.89961937509957401, 13.97604488694547697, 41.87609039468566152 ) ) ;
#152467 = CARTESIAN_POINT ( 'NONE',  ( 17.81289503416610742, 24.51734667627700404, 145.5500000054623513 ) ) ;
#152468 = CARTESIAN_POINT ( 'NONE',  ( -5.049401038298153566, 19.05341960407611168, 80.20724293864769550 ) ) ;
#152469 = CARTESIAN_POINT ( 'NONE',  ( 16.53943276465976808, -0.05219959533910856209, 53.74890960531437401 ) ) ;
#152470 = CARTESIAN_POINT ( 'NONE',  ( 8.314922557960818139, 14.29746914071049879, 29.58224293864769905 ) ) ;
#152471 = CARTESIAN_POINT ( 'NONE',  ( 4.379528057220092307, 16.55341960407617563, 102.2927570613523613 ) ) ;
#152472 = CARTESIAN_POINT ( 'NONE',  ( -9.564922557961040184, 16.46253265017147172, 52.91775706135233293 ) ) ;
#152473 = CARTESIAN_POINT ( 'NONE',  ( 19.25176906914649422, 5.499999999999731770, 53.49927264242280245 ) ) ;
#152474 = CARTESIAN_POINT ( 'NONE',  ( -9.474510206698964154, 16.51473224551069663, 110.4155762719810383 ) ) ;
#152475 = CARTESIAN_POINT ( 'NONE',  ( 8.224510206698953496, -14.34966873604960469, 77.91557627198102409 ) ) ;
#152476 = CARTESIAN_POINT ( 'NONE',  ( -19.05341960407617563, 5.049401038297882671, 38.54275706135233293 ) ) ;
#152478 = CARTESIAN_POINT ( 'NONE',  ( 15.80617190586746368, 15.72974639402197994, 29.37390960531435269 ) ) ;
#152477 = CARTESIAN_POINT ( 'NONE',  ( 9.474510206698971260, -16.51473224551069308, 32.91557627198102409 ) ) ;
#152479 = CARTESIAN_POINT ( 'NONE',  ( 10.72451020669898902, -18.67979575497178502, 72.91557627198103830 ) ) ;
#152480 = CARTESIAN_POINT ( 'NONE',  ( -12.14591786802309592, -12.06949235617757132, 106.8739096053143811 ) ) ;
#152482 = CARTESIAN_POINT ( 'NONE',  ( -19.03943276465977164, 0.05219959533909376836, 46.24890960531435979 ) ) ;
#152481 = CARTESIAN_POINT ( 'NONE',  ( 8.314922557961029526, -14.29746914071037800, 70.41775706135236135 ) ) ;
#152483 = CARTESIAN_POINT ( 'NONE',  ( -15.72974639402176322, -15.80617190586768395, 39.37609039468567573 ) ) ;
#152484 = CARTESIAN_POINT ( 'NONE',  ( -14.34966873604960291, -8.224510206698953496, 86.66557627198102409 ) ) ;
#152485 = CARTESIAN_POINT ( 'NONE',  ( -18.22780087662123805, -5.499999999999968026, 93.98236817873105053 ) ) ;
#152486 = CARTESIAN_POINT ( 'NONE',  ( -17.44270441346514389, 5.991230190323086013, 48.63664920735773478 ) ) ;
#152487 = CARTESIAN_POINT ( 'NONE',  ( 15.80617190586746368, 15.72974639402197994, 29.37390960531435269 ) ) ;
#152488 = CARTESIAN_POINT ( 'NONE',  ( -36.91746825000000598, 2.428612866367529932E-14, -1.124999997268813390 ) ) ;
#152489 = CARTESIAN_POINT ( 'NONE',  ( 0.2184195620311772945, 24.28793279613386957, -56.78144967823585887 ) ) ;
#152491 = CARTESIAN_POINT ( 'NONE',  ( 8.224510206698953496, -14.34966873604960469, 47.91557627198102409 ) ) ;
#152490 = CARTESIAN_POINT ( 'NONE',  ( -16.53943276465976808, -0.05219959533934237506, 38.75109039468567573 ) ) ;
#152492 = CARTESIAN_POINT ( 'NONE',  ( -18.67979575497178146, -10.72451020669898902, 71.66557627198100988 ) ) ;
#152493 = CARTESIAN_POINT ( 'NONE',  ( -21.53943276465977519, 0.05219959533907696930, 56.24890960531436690 ) ) ;
#152494 = CARTESIAN_POINT ( 'NONE',  ( -31.80000000000000782, -1.163414459189985801E-14, 95.00000000000000000 ) ) ;
#152496 = CARTESIAN_POINT ( 'NONE',  ( 5.153800228976335163, 19.02544592524342804, 104.7905762719809957 ) ) ;
#152495 = CARTESIAN_POINT ( 'NONE',  ( 19.05341960407617918, -5.049401038297876454, 86.04275706135233293 ) ) ;
#152497 = CARTESIAN_POINT ( 'NONE',  ( 19.05341960407611168, 5.049401038298154454, 53.95724293864770260 ) ) ;
#152498 = CARTESIAN_POINT ( 'NONE',  ( 0.05219959533909260263, 19.03943276465977164, 24.99890960531435269 ) ) ;
#152499 = FACE_BOUND ( 'NONE', #58157, .T. ) ;
#152500 = ORIENTED_EDGE ( 'NONE', *, *, #24668, .T. ) ;
#152501 = CARTESIAN_POINT ( 'NONE',  ( -16.52544592524335698, -4.483927247898792601, 73.95942372801901854 ) ) ;
#152502 = CARTESIAN_POINT ( 'NONE',  ( 10.81492255796078972, 18.62759615963270932, 99.58224293864770971 ) ) ;
#152503 = CARTESIAN_POINT ( 'NONE',  ( -19.02544592524342804, 5.153800228976336051, 56.04057627198100988 ) ) ;
#152504 = CARTESIAN_POINT ( 'NONE',  ( -21.52544592524334988, -5.823673210054445271, 43.95942372801902565 ) ) ;
#152505 = CARTESIAN_POINT ( 'NONE',  ( 16.51473224551069308, 9.474510206698969483, 84.16557627198102409 ) ) ;
#152506 = CARTESIAN_POINT ( 'NONE',  ( 16.51473224551069308, 9.474510206698969483, 114.1655762719810241 ) ) ;
#152507 = ORIENTED_EDGE ( 'NONE', *, *, #108640, .F. ) ;
#152508 = CARTESIAN_POINT ( 'NONE',  ( -21.52544592524334988, -5.823673210054445271, 28.95942372801902209 ) ) ;
#152510 = CARTESIAN_POINT ( 'NONE',  ( -16.51473224551082808, 9.474510206698731452, 88.33442372801900433 ) ) ;
#152509 = CARTESIAN_POINT ( 'NONE',  ( -0.05219959533909027116, -19.03943276465977164, 112.4989096053143669 ) ) ;
#152511 = ADVANCED_FACE ( 'NONE', ( #118657 ), #11491, .T. ) ;
#152512 = CARTESIAN_POINT ( 'NONE',  ( -9.474510206698720793, -16.51473224551083518, 44.58442372801900433 ) ) ;
#152513 = CARTESIAN_POINT ( 'NONE',  ( -5.719274019375978568, 21.55341960407610458, 100.2072429386476955 ) ) ;
#152514 = CARTESIAN_POINT ( 'NONE',  ( 5.049401038297881783, 19.05341960407617563, 32.29275706135233293 ) ) ;
#152515 = CARTESIAN_POINT ( 'NONE',  ( -19.05341960407617563, 5.049401038297882671, 33.54275706135231871 ) ) ;
#152516 = CARTESIAN_POINT ( 'NONE',  ( -8.224510206698735004, -14.34966873604973081, 94.58442372801901854 ) ) ;
#152517 = CARTESIAN_POINT ( 'NONE',  ( 24.75981654686065170, -6.635759577896797268, 167.9384007923203512 ) ) ;
#152518 = CARTESIAN_POINT ( 'NONE',  ( -16.46253265017160317, 9.564922557960807481, 60.83224293864769550 ) ) ;
#152519 = CARTESIAN_POINT ( 'NONE',  ( 5.719274019375673035, 21.55341960407619339, 67.29275706135234714 ) ) ;
#152520 = CARTESIAN_POINT ( 'NONE',  ( -5.823673210054431948, 21.52544592524334988, 82.70942372801900433 ) ) ;
#152521 = CARTESIAN_POINT ( 'NONE',  ( -31.80000000000000782, -5.510910596163089556E-15, 45.00000000000000000 ) ) ;
#152522 = CARTESIAN_POINT ( 'NONE',  ( 5.049401038298161559, -19.05341960407611168, 82.70724293864770971 ) ) ;
#152523 = CARTESIAN_POINT ( 'NONE',  ( -21.55341960407619339, 5.719274019375674811, 68.54275706135234714 ) ) ;
#152524 = CARTESIAN_POINT ( 'NONE',  ( -19.03943276465977164, -0.05219959533935918106, 103.7510903946856757 ) ) ;
#152525 = ADVANCED_FACE ( 'NONE', ( #38813 ), #166161, .F. ) ;
#152526 = CARTESIAN_POINT ( 'NONE',  ( -19.03943276465977164, 0.05219959533909376836, 61.24890960531436690 ) ) ;
#152527 = CARTESIAN_POINT ( 'NONE',  ( -16.51473224551069308, -9.474510206698971260, 96.66557627198102409 ) ) ;
#152528 = CARTESIAN_POINT ( 'NONE',  ( 19.03943276465977164, -0.05219959533909143690, 73.74890960531435269 ) ) ;
#152529 = CARTESIAN_POINT ( 'NONE',  ( -0.05219959533909027116, -19.03943276465977164, 77.49890960531435269 ) ) ;
#152530 = CARTESIAN_POINT ( 'NONE',  ( -13.89961937509977652, 13.97604488694528158, 60.62390960531436690 ) ) ;
#152531 = CARTESIAN_POINT ( 'NONE',  ( -18.62759615963270932, 10.81492255796079327, 100.8322429386477097 ) ) ;
#152532 = CARTESIAN_POINT ( 'NONE',  ( -16.53943276465976808, -0.05219959533934237506, 93.75109039468567573 ) ) ;
#152533 = DIRECTION ( 'NONE',  ( 0.000000000000000000, 0.000000000000000000, 1.000000000000000000 ) ) ;
#152534 = CARTESIAN_POINT ( 'NONE',  ( -19.02544592524334988, -5.153800228976617603, 38.95942372801900433 ) ) ;
#152535 = CARTESIAN_POINT ( 'NONE',  ( 13.89961937509977652, -13.97604488694527269, 78.12390960531433848 ) ) ;
#152536 = CARTESIAN_POINT ( 'NONE',  ( 14.34966873604960469, 8.224510206698951720, 74.16557627198102409 ) ) ;
#152537 = CARTESIAN_POINT ( 'NONE',  ( -0.05219959533910754901, -16.53943276465976808, 107.4989096053143669 ) ) ;
#152538 = CARTESIAN_POINT ( 'NONE',  ( 13.89961937509977652, -13.97604488694527269, 108.1239096053143669 ) ) ;
#152539 = CARTESIAN_POINT ( 'NONE',  ( 16.51473224551069308, 9.474510206698969483, 109.1655762719810383 ) ) ;
#152540 = LINE ( 'NONE', #135413, #104851 ) ;
#152541 = CARTESIAN_POINT ( 'NONE',  ( -9.564922557961040184, 16.46253265017147172, 32.91775706135233293 ) ) ;
#152542 = CARTESIAN_POINT ( 'NONE',  ( -4.483927247898782831, 16.52544592524335698, 92.70942372801901854 ) ) ;
#152543 = CARTESIAN_POINT ( 'NONE',  ( -16.46253265017160317, 9.564922557960807481, 70.83224293864770971 ) ) ;
#152544 = CARTESIAN_POINT ( 'NONE',  ( -0.05219959533937732626, 21.53943276465977519, 57.50109039468568994 ) ) ;
#152545 = CARTESIAN_POINT ( 'NONE',  ( 10.72451020669898902, -18.67979575497178502, 27.91557627198103830 ) ) ;
#152546 = CARTESIAN_POINT ( 'NONE',  ( -15.72974639402176322, -15.80617190586768395, 24.37609039468567573 ) ) ;
#152547 = CARTESIAN_POINT ( 'NONE',  ( -21.55341960407610458, -5.719274019375992779, 66.45724293864768129 ) ) ;
#152548 = CARTESIAN_POINT ( 'NONE',  ( -16.55341960407611168, -4.379528057220339221, 96.45724293864770971 ) ) ;
#152549 = CARTESIAN_POINT ( 'NONE',  ( -5.049401038297874678, -19.05341960407617918, 59.79275706135231871 ) ) ;
#152550 = CARTESIAN_POINT ( 'NONE',  ( 19.02544592524343514, -5.153800228976328945, 28.54057627198102409 ) ) ;
#152551 = CARTESIAN_POINT ( 'NONE',  ( 19.03943276465977164, -0.05219959533909143690, 78.74890960531436690 ) ) ;
#152552 = CARTESIAN_POINT ( 'NONE',  ( -16.46253265017160317, 9.564922557960807481, 80.83224293864769550 ) ) ;
#152553 = CARTESIAN_POINT ( 'NONE',  ( 1.784210473542230573E-15, -29.16686587814331588, 141.8750000027311842 ) ) ;
#152554 = CARTESIAN_POINT ( 'NONE',  ( -4.483927247898539470, -16.52544592524342804, 107.2905762719810525 ) ) ;
#152555 = CARTESIAN_POINT ( 'NONE',  ( 14.29746914071049879, -8.314922557960816363, 28.33224293864769550 ) ) ;
#152556 = CARTESIAN_POINT ( 'NONE',  ( -14.29746914071037622, -8.314922557961029526, 29.16775706135234003 ) ) ;
#152557 = CARTESIAN_POINT ( 'NONE',  ( -10.72451020669870658, -18.67979575497194134, 89.58442372801901854 ) ) ;
#152558 = CARTESIAN_POINT ( 'NONE',  ( 9.474510206698971260, -16.51473224551069308, 107.9155762719810383 ) ) ;
#152559 = CARTESIAN_POINT ( 'NONE',  ( 5.823673210054444382, -21.52544592524334988, 20.20942372801900788 ) ) ;
#152560 = CARTESIAN_POINT ( 'NONE',  ( 13.89961937509977652, -13.97604488694527269, 38.12390960531436690 ) ) ;
#152561 = CARTESIAN_POINT ( 'NONE',  ( -16.55341960407617563, 4.379528057220093196, 43.54275706135235424 ) ) ;
#152562 = CARTESIAN_POINT ( 'NONE',  ( 13.89961937509957401, 13.97604488694547697, 106.8760903946856757 ) ) ;
#152564 = B_SPLINE_CURVE_WITH_KNOTS ( 'NONE', 3,
 ( #93648, #123974, #185671, #168508, #15826, #187682, #110810, #47162, #49152, #2640, #16821, #153333, #125984, #108821, #48160, #77487, #634, #171501, #1638, #92646, #30006, #198861 ),
 .UNSPECIFIED., .F., .F.,
 ( 4, 2, 2, 2, 2, 2, 2, 2, 2, 2, 4 ),
 ( 2.602085213965210642E-18, 0.001309639967555231059, 0.001964459951332838024, 0.002291869943221640747, 0.002455574939166055553, 0.002619279935110470359, 0.002782984931054886032, 0.002946689926999300404, 0.003274099918888157337, 0.003928919902665849520, 0.005238559870221237355 ),
 .UNSPECIFIED. ) ;
#152563 = CARTESIAN_POINT ( 'NONE',  ( 19.03943276465977164, -0.05219959533909143690, 33.74890960531435979 ) ) ;
#152565 = CARTESIAN_POINT ( 'NONE',  ( -14.29746914071049879, 8.314922557960819915, 90.83224293864769550 ) ) ;
#152566 = CARTESIAN_POINT ( 'NONE',  ( 15.72974639402199770, -15.80617190586745480, 108.1239096053143811 ) ) ;
#152567 = CARTESIAN_POINT ( 'NONE',  ( -9.474510206698720793, -16.51473224551083518, 69.58442372801901854 ) ) ;
#152568 = CARTESIAN_POINT ( 'NONE',  ( 19.03943276465977164, -0.05219959533909143690, 23.74890960531435269 ) ) ;
#152569 = CARTESIAN_POINT ( 'NONE',  ( -5.823673210054116645, -21.52544592524344225, 112.2905762719810241 ) ) ;
#152570 = DIRECTION ( 'NONE',  ( -0.000000000000000000, -0.000000000000000000, 1.000000000000000000 ) ) ;
#152571 = CARTESIAN_POINT ( 'NONE',  ( 9.474510206698971260, -16.51473224551069308, 87.91557627198102409 ) ) ;
#152572 = CARTESIAN_POINT ( 'NONE',  ( 17.44279575226825330, -5.990770900252416986, 113.3355756751431755 ) ) ;
#152573 = CARTESIAN_POINT ( 'NONE',  ( -19.03943276465977164, 0.05219959533909376836, 81.24890960531436690 ) ) ;
#152575 = CARTESIAN_POINT ( 'NONE',  ( -0.05219959533910754901, -16.53943276465976808, 82.49890960531436690 ) ) ;
#152574 = CARTESIAN_POINT ( 'NONE',  ( -18.62759615963255300, -10.81492255796106328, 29.16775706135234003 ) ) ;
#152576 = CARTESIAN_POINT ( 'NONE',  ( -13.97604488694527625, -13.89961937509977652, 76.87390960531433848 ) ) ;
#152578 = CARTESIAN_POINT ( 'NONE',  ( -16.46253265017146816, -9.564922557961047289, 49.16775706135233293 ) ) ;
#152577 = CARTESIAN_POINT ( 'NONE',  ( -14.34966873604972548, 8.224510206698743886, 48.33442372801902565 ) ) ;
#152579 = CARTESIAN_POINT ( 'NONE',  ( 0.05219959533937995610, -21.53943276465977519, 60.00109039468568284 ) ) ;
#152580 = CARTESIAN_POINT ( 'NONE',  ( -8.314922557961024197, 14.29746914071037800, 32.91775706135234714 ) ) ;
#152581 = CARTESIAN_POINT ( 'NONE',  ( 13.97604488694527802, 13.89961937509977652, 69.37390960531436690 ) ) ;
#152582 = CARTESIAN_POINT ( 'NONE',  ( -5.049401038297874678, -19.05341960407617918, 99.79275706135234714 ) ) ;
#152583 = CARTESIAN_POINT ( 'NONE',  ( -4.483927247898782831, 16.52544592524335698, 62.70942372801902565 ) ) ;
#152584 = CARTESIAN_POINT ( 'NONE',  ( 15.80617190586769283, -15.72974639402175789, 100.6260903946857184 ) ) ;
#152585 = CARTESIAN_POINT ( 'NONE',  ( -9.474510206698720793, -16.51473224551083518, 84.58442372801900433 ) ) ;
#152586 = CARTESIAN_POINT ( 'NONE',  ( -13.97604488694527625, -13.89961937509977652, 51.87390960531436690 ) ) ;
#152587 = CARTESIAN_POINT ( 'NONE',  ( 10.81492255796078972, 18.62759615963270932, 64.58224293864769550 ) ) ;
#152589 = CARTESIAN_POINT ( 'NONE',  ( 13.97604488694548053, -13.89961937509957401, 80.62609039468567573 ) ) ;
#152588 = CARTESIAN_POINT ( 'NONE',  ( -16.52544592524342804, 4.483927247898546575, 76.04057627198102409 ) ) ;
#152590 = CARTESIAN_POINT ( 'NONE',  ( 17.12812012977027720, -6.668231424565975729, 61.14051240676858612 ) ) ;
#152591 = CARTESIAN_POINT ( 'NONE',  ( -19.03943276465977164, -0.05219959533935918106, 43.75109039468566863 ) ) ;
#152592 = CARTESIAN_POINT ( 'NONE',  ( 4.379528057220092307, 16.55341960407617563, 112.2927570613523471 ) ) ;
#152593 = CARTESIAN_POINT ( 'NONE',  ( -4.483927247898539470, -16.52544592524342804, 62.29057627198102409 ) ) ;
#152595 = CARTESIAN_POINT ( 'NONE',  ( 22.44159573604009239, 16.30477369853692693, 144.0750000027311728 ) ) ;
#152594 = CARTESIAN_POINT ( 'NONE',  ( 5.719274019375673035, 21.55341960407619339, 107.2927570613523471 ) ) ;
#152596 = CARTESIAN_POINT ( 'NONE',  ( 15.72974639402199770, -15.80617190586745480, 113.1239096053143953 ) ) ;
#152597 = CARTESIAN_POINT ( 'NONE',  ( 16.46253265017160672, -9.564922557960803928, 68.33224293864770971 ) ) ;
#152598 = CARTESIAN_POINT ( 'NONE',  ( -18.62759615963255300, -10.81492255796106328, 89.16775706135236135 ) ) ;
#152599 = CARTESIAN_POINT ( 'NONE',  ( -5.049401038298153566, 19.05341960407611168, 65.20724293864765286 ) ) ;
#152600 = ORIENTED_EDGE ( 'NONE', *, *, #188509, .T. ) ;
#152601 = CARTESIAN_POINT ( 'NONE',  ( 14.29746914071049879, -8.314922557960816363, 113.3322429386476955 ) ) ;
#152602 = CARTESIAN_POINT ( 'NONE',  ( 18.67979575497178502, 10.72451020669898547, 29.16557627198103120 ) ) ;
#152603 = CARTESIAN_POINT ( 'NONE',  ( -16.55341960407611168, -4.379528057220339221, 61.45724293864770260 ) ) ;
#152604 = CARTESIAN_POINT ( 'NONE',  ( 13.97604488694527802, 13.89961937509977652, 44.37390960531435269 ) ) ;
#152605 = CARTESIAN_POINT ( 'NONE',  ( 4.483927247898545687, 16.52544592524342804, 94.79057627198105251 ) ) ;
#152606 = CARTESIAN_POINT ( 'NONE',  ( -21.55341960407610458, -5.719274019375992779, 106.4572429386477097 ) ) ;
#152607 = CARTESIAN_POINT ( 'NONE',  ( 15.80617190586769283, -15.72974639402175789, 45.62609039468567573 ) ) ;
#152608 = CARTESIAN_POINT ( 'NONE',  ( 9.564922557960805705, 16.46253265017160317, 24.58224293864769194 ) ) ;
#152609 = CARTESIAN_POINT ( 'NONE',  ( 16.55341960407618274, -4.379528057220086978, 46.04275706135234714 ) ) ;
#152610 = CARTESIAN_POINT ( 'NONE',  ( 5.823673210054125526, 21.52544592524343514, 104.7905762719810241 ) ) ;
#152611 = CARTESIAN_POINT ( 'NONE',  ( 10.81492255796078972, 18.62759615963270932, 99.58224293864770971 ) ) ;
#152613 = CARTESIAN_POINT ( 'NONE',  ( -13.89961937509977652, 13.97604488694528158, 50.62390960531435979 ) ) ;
#152612 = CARTESIAN_POINT ( 'NONE',  ( -0.05219959533936034679, 19.03943276465977164, 27.50109039468566507 ) ) ;
#152614 = CARTESIAN_POINT ( 'NONE',  ( -13.97604488694527625, -13.89961937509977652, 111.8739096053143243 ) ) ;
#152615 = CARTESIAN_POINT ( 'NONE',  ( 21.52544592524334988, 5.823673210054432836, 56.45942372801902565 ) ) ;
#152616 = CARTESIAN_POINT ( 'NONE',  ( -15.80617190586745835, -15.72974639402198527, 41.87390960531435979 ) ) ;
#152617 = CARTESIAN_POINT ( 'NONE',  ( 12.06949235617739724, 12.14591786802326823, 111.8760903946856615 ) ) ;
#152619 = CARTESIAN_POINT ( 'NONE',  ( -21.53943276465977519, -0.05219959533937600094, 93.75109039468567573 ) ) ;
#152618 = CARTESIAN_POINT ( 'NONE',  ( 5.719274019375673035, 21.55341960407619339, 67.29275706135234714 ) ) ;
#152620 = CARTESIAN_POINT ( 'NONE',  ( 9.474510206698729675, 16.51473224551082808, 42.08442372801900433 ) ) ;
#152621 = CARTESIAN_POINT ( 'NONE',  ( 8.314922557961029526, -14.29746914071037800, 100.4177570613523471 ) ) ;
#152623 = EDGE_CURVE ( 'NONE', #85226, #114628, #13613, .T. ) ;
#152622 = CARTESIAN_POINT ( 'NONE',  ( -21.55341960407619339, 5.719274019375674811, 48.54275706135234714 ) ) ;
#152624 = CARTESIAN_POINT ( 'NONE',  ( 19.02544592524343514, -5.153800228976328945, 63.54057627198103830 ) ) ;
#152625 = CARTESIAN_POINT ( 'NONE',  ( 10.81492255796106328, -18.62759615963255655, 110.4177570613523756 ) ) ;
#152626 = CARTESIAN_POINT ( 'NONE',  ( -16.46253265017160317, 9.564922557960807481, 115.8322429386477097 ) ) ;
#152627 = CARTESIAN_POINT ( 'NONE',  ( -21.55341960407610458, -5.719274019375992779, 111.4572429386476813 ) ) ;
#152628 = CARTESIAN_POINT ( 'NONE',  ( -15.72974639402197994, 15.80617190586746368, 75.62390960531439532 ) ) ;
#152629 = CARTESIAN_POINT ( 'NONE',  ( 4.483927247898790824, -16.52544592524335698, 45.20942372801901854 ) ) ;
#152631 = CARTESIAN_POINT ( 'NONE',  ( 0.05219959533907565091, 21.53943276465977519, 74.99890960531435269 ) ) ;
#152630 = CARTESIAN_POINT ( 'NONE',  ( -5.577594645134348994, 3.875073520655145654, -62.38867879588715937 ) ) ;
#152633 = CARTESIAN_POINT ( 'NONE',  ( 16.52544592524342804, -4.483927247898539470, 78.54057627198103830 ) ) ;
#152632 = CARTESIAN_POINT ( 'NONE',  ( 16.55341960407618274, -4.379528057220086978, 61.04275706135234714 ) ) ;
#152634 = CARTESIAN_POINT ( 'NONE',  ( -22.98327899303673405, 21.71449870906575796, -46.07764953322298140 ) ) ;
#152635 = CARTESIAN_POINT ( 'NONE',  ( 9.564922557961047289, -16.46253265017146816, 105.4177570613523471 ) ) ;
#152636 = CARTESIAN_POINT ( 'NONE',  ( -21.55341960407610458, -5.719274019375992779, 31.45724293864769550 ) ) ;
#152637 = EDGE_CURVE ( 'NONE', #36339, #35831, #67394, .T. ) ;
#152638 = CARTESIAN_POINT ( 'NONE',  ( 16.55341960407618274, -4.379528057220086978, 36.04275706135234714 ) ) ;
#152639 = CARTESIAN_POINT ( 'NONE',  ( -10.81492255796078084, -18.62759615963271287, 112.0822429386477097 ) ) ;
#152640 = CARTESIAN_POINT ( 'NONE',  ( -5.823673210054116645, -21.52544592524344225, 27.29057627198103120 ) ) ;
#152641 = CARTESIAN_POINT ( 'NONE',  ( -16.53943276465976808, -0.05219959533934237506, 68.75109039468568994 ) ) ;
#152642 = CARTESIAN_POINT ( 'NONE',  ( 19.03943276465977164, -0.05219959533909143690, 88.74890960531436690 ) ) ;
#152644 = CARTESIAN_POINT ( 'NONE',  ( 13.89961937509977652, -13.97604488694527269, 23.12390960531436335 ) ) ;
#152643 = CARTESIAN_POINT ( 'NONE',  ( -10.72451020669870658, -18.67979575497194134, 59.58442372801901854 ) ) ;
#152645 = CARTESIAN_POINT ( 'NONE',  ( -19.03943276465977164, 0.05219959533909376836, 116.2489096053143669 ) ) ;
#152646 = ORIENTED_EDGE ( 'NONE', *, *, #131087, .F. ) ;
#152647 = CARTESIAN_POINT ( 'NONE',  ( -16.46253265017146816, -9.564922557961047289, 34.16775706135233293 ) ) ;
#152648 = CARTESIAN_POINT ( 'NONE',  ( -12.06949235617739369, -12.14591786802326823, 54.37609039468568994 ) ) ;
#152649 = CARTESIAN_POINT ( 'NONE',  ( -9.564922557960796823, -16.46253265017161027, 102.0822429386477097 ) ) ;
#152650 = CARTESIAN_POINT ( 'NONE',  ( 5.719274019375991003, -21.55341960407610458, 97.70724293864772392 ) ) ;
#152651 = CARTESIAN_POINT ( 'NONE',  ( 5.153800228976335163, 19.02544592524342804, 69.79057627198103830 ) ) ;
#152652 = CARTESIAN_POINT ( 'NONE',  ( -16.29526858892879204, 7.335722546919972942, 24.20329402199794444 ) ) ;
#152653 = CARTESIAN_POINT ( 'NONE',  ( -8.898068258721474777, 27.38543819252877398, 141.8656553485623704 ) ) ;
#152654 = CARTESIAN_POINT ( 'NONE',  ( 0.05219959533910956823, 16.53943276465976808, 79.99890960531435269 ) ) ;
#152655 = CARTESIAN_POINT ( 'NONE',  ( -18.67979575497178146, -10.72451020669898902, 41.66557627198103120 ) ) ;
#152656 = CARTESIAN_POINT ( 'NONE',  ( -16.88567814943165502, 6.947325034625571938, 33.70998877347415146 ) ) ;
#152657 = CARTESIAN_POINT ( 'NONE',  ( 16.52544592524335698, 4.483927247898782831, 61.45942372801901854 ) ) ;
#152658 = CARTESIAN_POINT ( 'NONE',  ( -10.72451020669870658, -18.67979575497194134, 24.58442372801901499 ) ) ;
#152659 = CARTESIAN_POINT ( 'NONE',  ( -5.049401038297874678, -19.05341960407617918, 74.79275706135231871 ) ) ;
#152660 = CARTESIAN_POINT ( 'NONE',  ( -5.153800228976328057, -19.02544592524343514, 37.29057627198102409 ) ) ;
#152661 = CARTESIAN_POINT ( 'NONE',  ( 15.80617190586746368, 15.72974639402197994, 64.37390960531435269 ) ) ;
#152662 = FACE_OUTER_BOUND ( 'NONE', #159848, .T. ) ;
#152663 = CARTESIAN_POINT ( 'NONE',  ( -21.52544592524334988, -5.823673210054445271, 93.95942372801903275 ) ) ;
#152664 = CARTESIAN_POINT ( 'NONE',  ( -13.89961937509977652, 13.97604488694528158, 60.62390960531436690 ) ) ;
#152665 = CARTESIAN_POINT ( 'NONE',  ( -8.314922557961024197, 14.29746914071037800, 47.91775706135234714 ) ) ;
#152666 = CARTESIAN_POINT ( 'NONE',  ( -9.564922557960796823, -16.46253265017161027, 57.08224293864769550 ) ) ;
#152667 = CARTESIAN_POINT ( 'NONE',  ( 15.80617190586769283, -15.72974639402175789, 80.62609039468567573 ) ) ;
#152668 = CARTESIAN_POINT ( 'NONE',  ( -5.049401038297874678, -19.05341960407617918, 39.79275706135232582 ) ) ;
#152669 = EDGE_CURVE ( 'NONE', #135262, #9294, #192604, .T. ) ;
#152670 = CARTESIAN_POINT ( 'NONE',  ( -5.153800228976607833, 19.02544592524334988, 47.70942372801900433 ) ) ;
#152671 = CARTESIAN_POINT ( 'NONE',  ( -0.05219959533937732626, 21.53943276465977519, 52.50109039468567573 ) ) ;
#152672 = DIRECTION ( 'NONE',  ( -0.000000000000000000, -0.000000000000000000, 1.000000000000000000 ) ) ;
#152673 = CARTESIAN_POINT ( 'NONE',  ( 19.02544592524334988, 5.153800228976608722, 41.45942372801900433 ) ) ;
#152674 = CARTESIAN_POINT ( 'NONE',  ( -16.46253265017160317, 9.564922557960807481, 100.8322429386477097 ) ) ;
#152675 = CARTESIAN_POINT ( 'NONE',  ( 13.97604488694527802, 13.89961937509977652, 74.37390960531436690 ) ) ;
#152676 = CARTESIAN_POINT ( 'NONE',  ( 16.53943276465976808, -0.05219959533910856209, 28.74890960531435624 ) ) ;
#152678 = CARTESIAN_POINT ( 'NONE',  ( 5.719274019375673035, 21.55341960407619339, 102.2927570613523613 ) ) ;
#152677 = CARTESIAN_POINT ( 'NONE',  ( 18.67979575497178502, 10.72451020669898547, 29.16557627198103120 ) ) ;
#152679 = CARTESIAN_POINT ( 'NONE',  ( -29.86685920354755197, -21.69954338932560134, -2.424999997268813434 ) ) ;
#152680 = DIRECTION ( 'NONE',  ( -0.000000000000000000, -0.000000000000000000, 1.000000000000000000 ) ) ;
#152681 = CARTESIAN_POINT ( 'NONE',  ( -5.823673210054431948, 21.52544592524334988, 102.7094237280190185 ) ) ;
#152682 = CARTESIAN_POINT ( 'NONE',  ( -27.96122637818069023, 7.045120623242314473, 161.2893955982185048 ) ) ;
#152683 = CARTESIAN_POINT ( 'NONE',  ( 4.483927247898545687, 16.52544592524342804, 114.7905762719810383 ) ) ;
#152684 = CARTESIAN_POINT ( 'NONE',  ( -16.51473224551069308, -9.474510206698971260, 111.6655762719810383 ) ) ;
#152685 = CARTESIAN_POINT ( 'NONE',  ( -22.00000000000000000, -1.132798289211302014E-14, 92.50000000000000000 ) ) ;
#152686 = CARTESIAN_POINT ( 'NONE',  ( -0.05219959533934338120, 16.53943276465976808, 52.50109039468567573 ) ) ;
#152687 = CARTESIAN_POINT ( 'NONE',  ( 10.81492255796078972, 18.62759615963270932, 74.58224293864768129 ) ) ;
#152688 = CARTESIAN_POINT ( 'NONE',  ( -8.224510206698948167, 14.34966873604960824, 45.41557627198103830 ) ) ;
#152690 = CARTESIAN_POINT ( 'NONE',  ( -16.51473224551069308, -9.474510206698971260, 111.6655762719810383 ) ) ;
#152689 = CARTESIAN_POINT ( 'NONE',  ( -14.34966873604960291, -8.224510206698953496, 106.6655762719810383 ) ) ;
#152691 = CARTESIAN_POINT ( 'NONE',  ( 5.823673210054444382, -21.52544592524334988, 30.20942372801902565 ) ) ;
#152692 = CARTESIAN_POINT ( 'NONE',  ( -9.564922557961040184, 16.46253265017147172, 37.91775706135233293 ) ) ;
#152693 = CARTESIAN_POINT ( 'NONE',  ( -16.51473224551069308, -9.474510206698971260, 21.66557627198102765 ) ) ;
#152694 = CARTESIAN_POINT ( 'NONE',  ( -18.67979575497193778, 10.72451020669871902, 68.33442372801900433 ) ) ;
#152695 = CARTESIAN_POINT ( 'NONE',  ( 16.38665767535053774, -7.295008042176018392, 32.76400864214546260 ) ) ;
#152696 = CARTESIAN_POINT ( 'NONE',  ( -8.314922557960811034, -14.29746914071050412, 32.08224293864769550 ) ) ;
#152697 = CARTESIAN_POINT ( 'NONE',  ( -22.81625015709509441, -31.40387420917324590, -4.824999997268813345 ) ) ;
#152698 = CARTESIAN_POINT ( 'NONE',  ( 18.62759615963271287, -10.81492255796078972, 33.33224293864769550 ) ) ;
#152699 = CARTESIAN_POINT ( 'NONE',  ( 12.14591786802309770, 12.06949235617756955, 84.37390960531438111 ) ) ;
#152700 = CARTESIAN_POINT ( 'NONE',  ( 12.56216403881617083, -41.81473846791988080, -20.79002063418672464 ) ) ;
#152701 = CARTESIAN_POINT ( 'NONE',  ( -13.89961937509977652, 13.97604488694528158, 80.62390960531436690 ) ) ;
#152702 = CARTESIAN_POINT ( 'NONE',  ( 8.314922557960818139, 14.29746914071049879, 69.58224293864769550 ) ) ;
#152703 = CARTESIAN_POINT ( 'NONE',  ( 9.474510206698729675, 16.51473224551082808, 107.0844237280190043 ) ) ;
#152704 = CARTESIAN_POINT ( 'NONE',  ( -15.72974639402197994, 15.80617190586746368, 45.62390960531436690 ) ) ;
#152705 = ORIENTED_EDGE ( 'NONE', *, *, #169362, .F. ) ;
#152706 = CARTESIAN_POINT ( 'NONE',  ( -12.06949235617756955, 12.14591786802309770, 110.6239096053143669 ) ) ;
#152708 = CARTESIAN_POINT ( 'NONE',  ( -5.823673210054116645, -21.52544592524344225, 77.29057627198102409 ) ) ;
#152707 = CARTESIAN_POINT ( 'NONE',  ( 13.89961937509977652, -13.97604488694527269, 68.12390960531436690 ) ) ;
#152710 = CARTESIAN_POINT ( 'NONE',  ( 13.97604488694527802, 13.89961937509977652, 84.37390960531433848 ) ) ;
#152709 = CARTESIAN_POINT ( 'NONE',  ( 12.14591786802327356, -12.06949235617739191, 100.6260903946857184 ) ) ;
#152711 = CARTESIAN_POINT ( 'NONE',  ( 5.049401038297881783, 19.05341960407617563, 67.29275706135234714 ) ) ;
#152712 = CARTESIAN_POINT ( 'NONE',  ( 21.53943276465977519, 0.05219959533937863772, 91.25109039468568994 ) ) ;
#152713 = CARTESIAN_POINT ( 'NONE',  ( -10.72451020669898014, 18.67979575497178502, 65.41557627198102409 ) ) ;
#152714 = CARTESIAN_POINT ( 'NONE',  ( -21.53943276465977519, 0.05219959533907696930, 26.24890960531435624 ) ) ;
#152715 = CARTESIAN_POINT ( 'NONE',  ( -13.89961937509977652, 13.97604488694528158, 30.62390960531435269 ) ) ;
#152716 = CARTESIAN_POINT ( 'NONE',  ( -16.55341960407617563, 4.379528057220093196, 103.5427570613523613 ) ) ;
#152717 = CARTESIAN_POINT ( 'NONE',  ( -16.46253265017160317, 9.564922557960807481, 60.83224293864769550 ) ) ;
#152718 = CARTESIAN_POINT ( 'NONE',  ( 16.55341960407618274, -4.379528057220086978, 26.04275706135235779 ) ) ;
#152719 = CARTESIAN_POINT ( 'NONE',  ( -31.69386653422660061, -1.706804019390318006, 102.3073255780427075 ) ) ;
#152720 = CARTESIAN_POINT ( 'NONE',  ( -5.719274019375665041, -21.55341960407619695, 109.7927570613523613 ) ) ;
#152721 = CARTESIAN_POINT ( 'NONE',  ( 16.55341960407611168, 4.379528057220329451, 78.95724293864769550 ) ) ;
#152722 = VECTOR ( 'NONE', #31842, 1000.000000000000000 ) ;
#152723 = CARTESIAN_POINT ( 'NONE',  ( -15.80617190586745835, -15.72974639402198527, 111.8739096053143669 ) ) ;
#152724 = CARTESIAN_POINT ( 'NONE',  ( 18.62759615963271287, -10.81492255796078972, 103.3322429386476955 ) ) ;
#152725 = CARTESIAN_POINT ( 'NONE',  ( -22.44159573604009950, -16.30477369853688430, 139.5750000027311728 ) ) ;
#152726 = CARTESIAN_POINT ( 'NONE',  ( 10.81492255796078972, 18.62759615963270932, 44.58224293864769550 ) ) ;
#152727 = CARTESIAN_POINT ( 'NONE',  ( -16.53943276465976808, -0.05219959533934237506, 83.75109039468568994 ) ) ;
#152728 = CARTESIAN_POINT ( 'NONE',  ( -14.29746914071049879, 8.314922557960819915, 100.8322429386477097 ) ) ;
#152729 = CARTESIAN_POINT ( 'NONE',  ( 0.05219959533909260263, 19.03943276465977164, 59.99890960531436690 ) ) ;
#152730 = PRESENTATION_STYLE_ASSIGNMENT (( #103262 ) ) ;
#152731 = CARTESIAN_POINT ( 'NONE',  ( 14.34966873604972726, -8.224510206698740333, 105.8344237280190328 ) ) ;
#152732 = CARTESIAN_POINT ( 'NONE',  ( -15.80617190586768217, 15.72974639402176855, 43.12609039468568284 ) ) ;
#152733 = CARTESIAN_POINT ( 'NONE',  ( -9.564922557960796823, -16.46253265017161027, 102.0822429386477097 ) ) ;
#152734 = CARTESIAN_POINT ( 'NONE',  ( -15.80617190586768217, 15.72974639402176855, 78.12609039468570415 ) ) ;
#152735 = CARTESIAN_POINT ( 'NONE',  ( -19.02544592524342804, 5.153800228976336051, 31.04057627198102409 ) ) ;
#152736 = CARTESIAN_POINT ( 'NONE',  ( -16.46253265017160317, 9.564922557960807481, 35.83224293864768839 ) ) ;
#152737 = EDGE_LOOP ( 'NONE', ( #108845, #164934 ) ) ;
#152738 = CARTESIAN_POINT ( 'NONE',  ( 21.55341960407619695, -5.719274019375665929, 71.04275706135234714 ) ) ;
#152739 = CARTESIAN_POINT ( 'NONE',  ( 13.89961937509977652, -13.97604488694527269, 103.1239096053143527 ) ) ;
#152740 = CARTESIAN_POINT ( 'NONE',  ( -13.89961937509957401, -13.97604488694547875, 84.37609039468567573 ) ) ;
#152741 = CARTESIAN_POINT ( 'NONE',  ( 5.719274019375673035, 21.55341960407619339, 37.29275706135235424 ) ) ;
#152742 = CARTESIAN_POINT ( 'NONE',  ( 4.379528057220092307, 16.55341960407617563, 22.29275706135235069 ) ) ;
#152743 = CARTESIAN_POINT ( 'NONE',  ( 0.05219959533936267826, -19.03943276465977164, 75.00109039468566152 ) ) ;
#152744 = CARTESIAN_POINT ( 'NONE',  ( 5.153800228976335163, 19.02544592524342804, 54.79057627198103120 ) ) ;
#152745 = CARTESIAN_POINT ( 'NONE',  ( -16.51473224551082808, 9.474510206698731452, 78.33442372801900433 ) ) ;
#152746 = CARTESIAN_POINT ( 'NONE',  ( -12.06949235617756955, 12.14591786802309770, 30.62390960531436335 ) ) ;
#152747 = CARTESIAN_POINT ( 'NONE',  ( -5.153800228976607833, 19.02544592524334988, 72.70942372801900433 ) ) ;
#152748 = CARTESIAN_POINT ( 'NONE',  ( 16.53943276465976808, -0.05219959533910856209, 43.74890960531435979 ) ) ;
#152749 = CARTESIAN_POINT ( 'NONE',  ( 5.049401038297881783, 19.05341960407617563, 67.29275706135234714 ) ) ;
#152750 = CARTESIAN_POINT ( 'NONE',  ( -12.14591786802326823, 12.06949235617739902, 43.12609039468568284 ) ) ;
#152751 = CARTESIAN_POINT ( 'NONE',  ( -5.823673210054431948, 21.52544592524334988, 112.7094237280190328 ) ) ;
#152752 = CARTESIAN_POINT ( 'NONE',  ( 16.51473224551069308, 9.474510206698969483, 34.16557627198102409 ) ) ;
#152753 = CARTESIAN_POINT ( 'NONE',  ( -16.20579543436680936, -7.371946100354975329, 65.56520834171874412 ) ) ;
#152754 = CARTESIAN_POINT ( 'NONE',  ( 4.483927247898790824, -16.52544592524335698, 50.20942372801901854 ) ) ;
#152755 = CARTESIAN_POINT ( 'NONE',  ( -3.573655867282028392E-15, 2.428612866367529932E-14, 167.9999999999999716 ) ) ;
#152756 = CIRCLE ( 'NONE', #139747, 0.5000000000000004441 ) ;
#152757 = CARTESIAN_POINT ( 'NONE',  ( 22.44159573604009239, 16.30477369853692693, 144.0750000027311728 ) ) ;
#152758 = CARTESIAN_POINT ( 'NONE',  ( 19.02544592524343514, -5.153800228976328945, 88.54057627198102409 ) ) ;
#152759 = CARTESIAN_POINT ( 'NONE',  ( 0.000000000000000000, 0.000000000000000000, -59.13370768023891344 ) ) ;
#152760 = ORIENTED_EDGE ( 'NONE', *, *, #133785, .T. ) ;
#152761 = CARTESIAN_POINT ( 'NONE',  ( -5.049401038297874678, -19.05341960407617918, 79.79275706135233293 ) ) ;
#152762 = CARTESIAN_POINT ( 'NONE',  ( 0.05219959533907565091, 21.53943276465977519, 24.99890960531435624 ) ) ;
#152764 = CARTESIAN_POINT ( 'NONE',  ( 19.05341960407617918, -5.049401038297876454, 96.04275706135231871 ) ) ;
#152763 = CARTESIAN_POINT ( 'NONE',  ( 10.72451020669871369, 18.67979575497193778, 112.0844237280190185 ) ) ;
#152765 = CARTESIAN_POINT ( 'NONE',  ( 0.05219959533910956823, 16.53943276465976808, 114.9989096053143669 ) ) ;
#152766 = CARTESIAN_POINT ( 'NONE',  ( 19.03943276465977164, -0.05219959533909143690, 43.74890960531435979 ) ) ;
#152767 = CARTESIAN_POINT ( 'NONE',  ( 5.823673210054125526, 21.52544592524343514, 54.79057627198104541 ) ) ;
#152768 = CARTESIAN_POINT ( 'NONE',  ( 5.823673210054125526, 21.52544592524343514, 49.79057627198102409 ) ) ;
#152769 = CARTESIAN_POINT ( 'NONE',  ( -19.02544592524342804, 5.153800228976336051, 26.04057627198103120 ) ) ;
#152770 = CARTESIAN_POINT ( 'NONE',  ( 0.000000000000000000, 0.000000000000000000, -49.13275782002545355 ) ) ;
#152771 = CARTESIAN_POINT ( 'NONE',  ( 13.97604488694548053, -13.89961937509957401, 70.62609039468567573 ) ) ;
#152772 = CARTESIAN_POINT ( 'NONE',  ( 16.55341960407611168, 4.379528057220329451, 38.95724293864768839 ) ) ;
#152773 = CARTESIAN_POINT ( 'NONE',  ( -5.719274019375978568, 21.55341960407610458, 25.20724293864769550 ) ) ;
#152774 = CARTESIAN_POINT ( 'NONE',  ( 21.53943276465977519, 0.05219959533937863772, 96.25109039468568994 ) ) ;
#152775 = CARTESIAN_POINT ( 'NONE',  ( -5.719274019375978568, 21.55341960407610458, 80.20724293864769550 ) ) ;
#152776 = CARTESIAN_POINT ( 'NONE',  ( -15.72974639402176322, -15.80617190586768395, 64.37609039468568994 ) ) ;
#152777 = CARTESIAN_POINT ( 'NONE',  ( 5.719274019375673035, 21.55341960407619339, 62.29275706135236845 ) ) ;
#152778 = EDGE_CURVE ( 'NONE', #99125, #118785, #53570, .T. ) ;
#152779 = CARTESIAN_POINT ( 'NONE',  ( -19.02544592524342804, 5.153800228976336051, 101.0405762719810241 ) ) ;
#152781 = CARTESIAN_POINT ( 'NONE',  ( 21.53943276465977519, 0.05219959533937863772, 46.25109039468567573 ) ) ;
#152780 = CARTESIAN_POINT ( 'NONE',  ( 12.14591786802327356, -12.06949235617739191, 95.62609039468568994 ) ) ;
#152782 = CARTESIAN_POINT ( 'NONE',  ( 9.564922557960805705, 16.46253265017160317, 24.58224293864769194 ) ) ;
#152783 = CARTESIAN_POINT ( 'NONE',  ( -31.72709406046301339, 2.040068635034919209E-14, 102.5000000000000142 ) ) ;
#152784 = CARTESIAN_POINT ( 'NONE',  ( 12.14591786802309770, 12.06949235617756955, 64.37390960531435269 ) ) ;
#152785 = CARTESIAN_POINT ( 'NONE',  ( 0.05219959533910956823, 16.53943276465976808, 39.99890960531436690 ) ) ;
#152786 = CARTESIAN_POINT ( 'NONE',  ( -21.52544592524343514, 5.823673210054127303, 41.04057627198103120 ) ) ;
#152787 = CARTESIAN_POINT ( 'NONE',  ( -9.564922557960796823, -16.46253265017161027, 72.08224293864770971 ) ) ;
#152788 = CARTESIAN_POINT ( 'NONE',  ( 13.97604488694527802, 13.89961937509977652, 49.37390960531434558 ) ) ;
#152789 = CARTESIAN_POINT ( 'NONE',  ( -10.72451020669898014, 18.67979575497178502, 55.41557627198102409 ) ) ;
#152790 = CARTESIAN_POINT ( 'NONE',  ( -9.564922557961040184, 16.46253265017147172, 37.91775706135233293 ) ) ;
#152792 = CARTESIAN_POINT ( 'NONE',  ( -0.05219959533910754901, -16.53943276465976808, 52.49890960531435979 ) ) ;
#152791 = DIRECTION ( 'NONE',  ( 1.000000000000000000, -0.000000000000000000, 0.000000000000000000 ) ) ;
#152793 = CARTESIAN_POINT ( 'NONE',  ( -21.53943276465977519, 0.05219959533907696930, 21.24890960531436690 ) ) ;
#152794 = ORIENTED_EDGE ( 'NONE', *, *, #113718, .F. ) ;
#152795 = CARTESIAN_POINT ( 'NONE',  ( -21.96747269023789428, 18.79906110326631463, 140.0254762022684645 ) ) ;
#152796 = CARTESIAN_POINT ( 'NONE',  ( -0.05219959533934338120, 16.53943276465976808, 67.50109039468568994 ) ) ;
#152797 = CARTESIAN_POINT ( 'NONE',  ( -16.46253265017146816, -9.564922557961047289, 79.16775706135234714 ) ) ;
#152798 = CARTESIAN_POINT ( 'NONE',  ( -8.314922557960811034, -14.29746914071050412, 37.08224293864768129 ) ) ;
#152799 = ORIENTED_EDGE ( 'NONE', *, *, #143157, .T. ) ;
#152800 = CARTESIAN_POINT ( 'NONE',  ( 11.30153831258470731, -188.0000000000000000, 0.000000000000000000 ) ) ;
#152801 = CARTESIAN_POINT ( 'NONE',  ( -16.53943276465976808, 0.05219959533911058130, 21.24890960531436690 ) ) ;
#152802 = CARTESIAN_POINT ( 'NONE',  ( -19.05341960407611168, -5.049401038298163336, 56.45724293864768129 ) ) ;
#152803 = CARTESIAN_POINT ( 'NONE',  ( -5.049401038298153566, 19.05341960407611168, 80.20724293864769550 ) ) ;
#152804 = CARTESIAN_POINT ( 'NONE',  ( 19.02544592524343514, -5.153800228976328945, 38.54057627198103120 ) ) ;
#152805 = CARTESIAN_POINT ( 'NONE',  ( 10.72451020669871369, 18.67979575497193778, 52.08442372801901854 ) ) ;
#152806 = CARTESIAN_POINT ( 'NONE',  ( -16.51473224551069308, -9.474510206698971260, 56.66557627198103120 ) ) ;
#152807 = CARTESIAN_POINT ( 'NONE',  ( -24.13306144861384084, 5.795830589372935826, 189.9999999999999716 ) ) ;
#152808 = CARTESIAN_POINT ( 'NONE',  ( 19.03943276465977164, -0.05219959533909143690, 53.74890960531436690 ) ) ;
#152809 = CARTESIAN_POINT ( 'NONE',  ( -18.67979575497178146, -10.72451020669898902, 41.66557627198103120 ) ) ;
#152810 = CARTESIAN_POINT ( 'NONE',  ( 9.564922557960805705, 16.46253265017160317, 24.58224293864769194 ) ) ;
#152811 = CARTESIAN_POINT ( 'NONE',  ( 10.81492255796078972, 18.62759615963270932, 29.58224293864769905 ) ) ;
#152812 = CIRCLE ( 'NONE', #165845, 10.00000000000000355 ) ;
#152813 = CARTESIAN_POINT ( 'NONE',  ( 8.314922557961029526, -14.29746914071037800, 85.41775706135236135 ) ) ;
#152814 = CARTESIAN_POINT ( 'NONE',  ( 0.05219959533937995610, -21.53943276465977519, 105.0010903946856757 ) ) ;
#152815 = CARTESIAN_POINT ( 'NONE',  ( -14.34966873604972548, 8.224510206698743886, 63.33442372801900433 ) ) ;
#152816 = CARTESIAN_POINT ( 'NONE',  ( 19.02544592524343514, -5.153800228976328945, 108.5405762719810383 ) ) ;
#152817 = CARTESIAN_POINT ( 'NONE',  ( 4.379528057220092307, 16.55341960407617563, 57.29275706135234714 ) ) ;
#152818 = CARTESIAN_POINT ( 'NONE',  ( -16.53943276465976808, -0.05219959533934237506, 33.75109039468568284 ) ) ;
#152819 = CARTESIAN_POINT ( 'NONE',  ( 9.474510206698971260, -16.51473224551069308, 112.9155762719810383 ) ) ;
#152820 = CARTESIAN_POINT ( 'NONE',  ( 12.14591786802327356, -12.06949235617739191, 25.62609039468567929 ) ) ;
#152821 = CARTESIAN_POINT ( 'NONE',  ( -19.03943276465977164, 0.05219959533909376836, 31.24890960531435979 ) ) ;
#152822 = CARTESIAN_POINT ( 'NONE',  ( 15.80617190586769283, -15.72974639402175789, 20.62609039468568639 ) ) ;
#152823 = CARTESIAN_POINT ( 'NONE',  ( 14.29746914071037800, 8.314922557961029526, 21.66775706135235069 ) ) ;
#152824 = CARTESIAN_POINT ( 'NONE',  ( -4.379528057220086978, -16.55341960407618274, 79.79275706135236135 ) ) ;
#152825 = CARTESIAN_POINT ( 'NONE',  ( -23.48529157249600985, 32.32473071737754111, -4.049999994537626158 ) ) ;
#152826 = CARTESIAN_POINT ( 'NONE',  ( -10.81492255796105439, 18.62759615963255655, 92.91775706135236135 ) ) ;
#152827 = CARTESIAN_POINT ( 'NONE',  ( 16.51473224551083163, -9.474510206698727899, 85.83442372801900433 ) ) ;
#152828 = CARTESIAN_POINT ( 'NONE',  ( -4.483927247898539470, -16.52544592524342804, 62.29057627198102409 ) ) ;
#152829 = CARTESIAN_POINT ( 'NONE',  ( -4.483927247898539470, -16.52544592524342804, 107.2905762719810525 ) ) ;
#152831 = CARTESIAN_POINT ( 'NONE',  ( -7.405238625847228917, 1.490470117976274045, -64.28041130758167299 ) ) ;
#152830 = CARTESIAN_POINT ( 'NONE',  ( -9.564922557961040184, 16.46253265017147172, 52.91775706135233293 ) ) ;
#152832 = CARTESIAN_POINT ( 'NONE',  ( 21.52544592524334988, 5.823673210054432836, 56.45942372801902565 ) ) ;
#152833 = CARTESIAN_POINT ( 'NONE',  ( -5.049401038297874678, -19.05341960407617918, 109.7927570613523187 ) ) ;
#152834 = CARTESIAN_POINT ( 'NONE',  ( -18.22780087662122028, 5.500000000000031086, 63.51540105326107266 ) ) ;
#152835 = CARTESIAN_POINT ( 'NONE',  ( 13.89961937509977652, -13.97604488694527269, 103.1239096053143527 ) ) ;
#152836 = CARTESIAN_POINT ( 'NONE',  ( 10.72451020669898902, -18.67979575497178502, 72.91557627198103830 ) ) ;
#152837 = CARTESIAN_POINT ( 'NONE',  ( 16.46253265017146816, 9.564922557961045513, 96.66775706135233293 ) ) ;
#152838 = CARTESIAN_POINT ( 'NONE',  ( -5.153800228976328057, -19.02544592524343514, 102.2905762719810383 ) ) ;
#152839 = CARTESIAN_POINT ( 'NONE',  ( 18.22780087662125226, -5.499999999999864997, 51.01540105326108687 ) ) ;
#152840 = CARTESIAN_POINT ( 'NONE',  ( 12.14591786802309770, 12.06949235617756955, 109.3739096053143811 ) ) ;
#152841 = CARTESIAN_POINT ( 'NONE',  ( 10.72451020669871369, 18.67979575497193778, 97.08442372801904696 ) ) ;
#152842 = CARTESIAN_POINT ( 'NONE',  ( 13.97604488694527802, 13.89961937509977652, 49.37390960531434558 ) ) ;
#152843 = CARTESIAN_POINT ( 'NONE',  ( -21.52544592524334988, -5.823673210054445271, 53.95942372801900433 ) ) ;
#152844 = CARTESIAN_POINT ( 'NONE',  ( -10.81492255796105439, 18.62759615963255655, 92.91775706135236135 ) ) ;
#152845 = CARTESIAN_POINT ( 'NONE',  ( -16.52544592524335698, -4.483927247898792601, 98.95942372801903275 ) ) ;
#152846 = CARTESIAN_POINT ( 'NONE',  ( -10.72451020669870658, -18.67979575497194134, 49.58442372801901143 ) ) ;
#152847 = CARTESIAN_POINT ( 'NONE',  ( -21.53943276465977519, -0.05219959533937600094, 33.75109039468568284 ) ) ;
#152849 = CARTESIAN_POINT ( 'NONE',  ( 5.049401038298161559, -19.05341960407611168, 97.70724293864766707 ) ) ;
#152848 = CARTESIAN_POINT ( 'NONE',  ( -9.564922557961040184, 16.46253265017147172, 62.91775706135233293 ) ) ;
#152850 = CARTESIAN_POINT ( 'NONE',  ( 12.14591786802309770, 12.06949235617756955, 109.3739096053143811 ) ) ;
#152851 = CARTESIAN_POINT ( 'NONE',  ( 0.05219959533907565091, 21.53943276465977519, 84.99890960531436690 ) ) ;
#152852 = CARTESIAN_POINT ( 'NONE',  ( 16.53943276465976808, -0.05219959533910856209, 58.74890960531436690 ) ) ;
#152853 = CARTESIAN_POINT ( 'NONE',  ( -15.72974639402176322, -15.80617190586768395, 99.37609039468568994 ) ) ;
#152854 = CARTESIAN_POINT ( 'NONE',  ( 16.55341960407611168, 4.379528057220329451, 78.95724293864769550 ) ) ;
#152855 = CARTESIAN_POINT ( 'NONE',  ( -13.89961937509977652, 13.97604488694528158, 35.62390960531435269 ) ) ;
#152856 = CARTESIAN_POINT ( 'NONE',  ( 16.51473224551083163, -9.474510206698727899, 80.83442372801899012 ) ) ;
#152857 = CARTESIAN_POINT ( 'NONE',  ( -14.29746914071049879, 8.314922557960819915, 50.83224293864770971 ) ) ;
#152858 = CARTESIAN_POINT ( 'NONE',  ( -21.53943276465977519, -0.05219959533937600094, 98.75109039468568994 ) ) ;
#152859 = CARTESIAN_POINT ( 'NONE',  ( 19.03943276465977164, -0.05219959533909143690, 88.74890960531436690 ) ) ;
#152860 = CARTESIAN_POINT ( 'NONE',  ( 16.51473224551083163, -9.474510206698727899, 60.83442372801900433 ) ) ;
#152861 = CARTESIAN_POINT ( 'NONE',  ( 21.55341960407610458, 5.719274019375980345, 63.95724293864770260 ) ) ;
#152862 = CARTESIAN_POINT ( 'NONE',  ( -10.72451020669870658, -18.67979575497194134, 24.58442372801901499 ) ) ;
#152863 = CARTESIAN_POINT ( 'NONE',  ( -12.06949235617739369, -12.14591786802326823, 29.37609039468568284 ) ) ;
#152864 = CARTESIAN_POINT ( 'NONE',  ( 12.06949235617739724, 12.14591786802326823, 76.87609039468567573 ) ) ;
#152866 = CARTESIAN_POINT ( 'NONE',  ( 10.81492255796078972, 18.62759615963270932, 114.5822429386477097 ) ) ;
#152865 = CARTESIAN_POINT ( 'NONE',  ( 16.46253265017160672, -9.564922557960803928, 28.33224293864769550 ) ) ;
#152867 = CARTESIAN_POINT ( 'NONE',  ( 4.379528057220339221, -16.55341960407611168, 112.7072429386476955 ) ) ;
#152868 = CARTESIAN_POINT ( 'NONE',  ( 36.91746825000000598, -11.99521256947793546, -4.224999997268812812 ) ) ;
#152869 = CARTESIAN_POINT ( 'NONE',  ( 8.224510206698742110, 14.34966873604972548, 47.08442372801901854 ) ) ;
#152870 = CARTESIAN_POINT ( 'NONE',  ( 16.55341960407611168, 4.379528057220329451, 73.95724293864769550 ) ) ;
#152871 = CARTESIAN_POINT ( 'NONE',  ( -21.53943276465977519, 0.05219959533907696930, 81.24890960531436690 ) ) ;
#152872 = CARTESIAN_POINT ( 'NONE',  ( 12.14591786802309770, 12.06949235617756955, 29.37390960531435269 ) ) ;
#152873 = CARTESIAN_POINT ( 'NONE',  ( 8.224510206698742110, 14.34966873604972548, 37.08442372801901143 ) ) ;
#152874 = CARTESIAN_POINT ( 'NONE',  ( 9.474510206698971260, -16.51473224551069308, 47.91557627198102409 ) ) ;
#152875 = CARTESIAN_POINT ( 'NONE',  ( 8.224510206698742110, 14.34966873604972548, 82.08442372801901854 ) ) ;
#152876 = CARTESIAN_POINT ( 'NONE',  ( 19.03943276465977164, 0.05219959533936151252, 76.25109039468566152 ) ) ;
#152877 = CARTESIAN_POINT ( 'NONE',  ( -0.05219959533907301413, -21.53943276465977519, 72.49890960531435269 ) ) ;
#152878 = CARTESIAN_POINT ( 'NONE',  ( -16.55341960407617563, 4.379528057220093196, 108.5427570613523756 ) ) ;
#152879 = ORIENTED_EDGE ( 'NONE', *, *, #198827, .F. ) ;
#152880 = CARTESIAN_POINT ( 'NONE',  ( 25.73063820182081685, 8.702599028576305074, 171.6270364942766946 ) ) ;
#152881 = CARTESIAN_POINT ( 'NONE',  ( -18.62759615963270932, 10.81492255796079327, 45.83224293864769550 ) ) ;
#152882 = EDGE_LOOP ( 'NONE', ( #24973, #106993, #58888, #152799 ) ) ;
#152883 = CARTESIAN_POINT ( 'NONE',  ( -16.52544592524335698, -4.483927247898792601, 93.95942372801903275 ) ) ;
#152884 = ORIENTED_EDGE ( 'NONE', *, *, #92125, .F. ) ;
#152885 = CARTESIAN_POINT ( 'NONE',  ( -18.67979575497178146, -10.72451020669898902, 21.66557627198102409 ) ) ;
#152886 = CARTESIAN_POINT ( 'NONE',  ( 0.000000000000000000, 0.7216878364870328300, 1.249999999999999778 ) ) ;
#152887 = CARTESIAN_POINT ( 'NONE',  ( -21.55341960407610458, -5.719274019375992779, 81.45724293864769550 ) ) ;
#152888 = CARTESIAN_POINT ( 'NONE',  ( 12.14591786802327356, -12.06949235617739191, 110.6260903946857042 ) ) ;
#152889 = CARTESIAN_POINT ( 'NONE',  ( 19.05341960407617918, -5.049401038297876454, 111.0427570613523329 ) ) ;
#152890 = CARTESIAN_POINT ( 'NONE',  ( -14.29746914071049879, 8.314922557960819915, 110.8322429386476955 ) ) ;
#152891 = CARTESIAN_POINT ( 'NONE',  ( -14.34966873604972548, 8.224510206698743886, 28.33442372801902209 ) ) ;
#152892 = CARTESIAN_POINT ( 'NONE',  ( 19.05341960407611168, 5.049401038298154454, 58.95724293864768129 ) ) ;
#152893 = CARTESIAN_POINT ( 'NONE',  ( 17.81289503416611453, -24.51734667627695785, 140.6999999999999602 ) ) ;
#152894 = CARTESIAN_POINT ( 'NONE',  ( -16.46253265017160317, 9.564922557960807481, 110.8322429386476955 ) ) ;
#152895 = CARTESIAN_POINT ( 'NONE',  ( -12.14591786802326823, 12.06949235617739902, 93.12609039468568994 ) ) ;
#152896 = CARTESIAN_POINT ( 'NONE',  ( -19.02544592524334988, -5.153800228976617603, 93.95942372801900433 ) ) ;
#152897 = CARTESIAN_POINT ( 'NONE',  ( 9.564922557961047289, -16.46253265017146816, 25.41775706135234003 ) ) ;
#152898 = CARTESIAN_POINT ( 'NONE',  ( -10.81492255796078084, -18.62759615963271287, 72.08224293864769550 ) ) ;
#152899 = CARTESIAN_POINT ( 'NONE',  ( -16.53943276465976808, -0.05219959533934237506, 98.75109039468568994 ) ) ;
#152900 = VECTOR ( 'NONE', #90370, 1000.000000000000000 ) ;
#152901 = CARTESIAN_POINT ( 'NONE',  ( -5.153800228976607833, 19.02544592524334988, 92.70942372801901854 ) ) ;
#152902 = CARTESIAN_POINT ( 'NONE',  ( 9.474510206698971260, -16.51473224551069308, 47.91557627198102409 ) ) ;
#152903 = CARTESIAN_POINT ( 'NONE',  ( -19.03943276465977164, 0.05219959533909376836, 96.24890960531436690 ) ) ;
#152904 = CARTESIAN_POINT ( 'NONE',  ( -15.72974639402176322, -15.80617190586768395, 64.37609039468568994 ) ) ;
#152905 = CARTESIAN_POINT ( 'NONE',  ( 19.02544592524343514, -5.153800228976328945, 43.54057627198103120 ) ) ;
#152906 = CARTESIAN_POINT ( 'NONE',  ( -16.88567814943165502, -6.947325034625698059, 86.29001122652586275 ) ) ;
#152907 = CARTESIAN_POINT ( 'NONE',  ( 14.29746914071049879, -8.314922557960816363, 78.33224293864770971 ) ) ;
#152908 = CARTESIAN_POINT ( 'NONE',  ( -15.80617190586745835, -15.72974639402198527, 71.87390960531438111 ) ) ;
#152909 = CARTESIAN_POINT ( 'NONE',  ( -3.424326230466362198, -6.677994727576205491, 1.353258418600858493 ) ) ;
#152910 = CARTESIAN_POINT ( 'NONE',  ( -1.227931366032057224E-14, -24.30000000000003268, -64.92279855667830191 ) ) ;
#152911 = CARTESIAN_POINT ( 'NONE',  ( -0.05219959533936034679, 19.03943276465977164, 37.50109039468567573 ) ) ;
#152912 = CYLINDRICAL_SURFACE ( 'NONE', #73511, 5.000000000000000888 ) ;
#152914 = CARTESIAN_POINT ( 'NONE',  ( -0.05219959533909027116, -19.03943276465977164, 82.49890960531436690 ) ) ;
#152913 = CARTESIAN_POINT ( 'NONE',  ( 19.03943276465977164, -0.05219959533909143690, 73.74890960531435269 ) ) ;
#152915 = CARTESIAN_POINT ( 'NONE',  ( 16.55341960407618274, -4.379528057220086978, 61.04275706135234714 ) ) ;
#152916 = CARTESIAN_POINT ( 'NONE',  ( -16.46253265017146816, -9.564922557961047289, 79.16775706135234714 ) ) ;
#152917 = CARTESIAN_POINT ( 'NONE',  ( -16.46253265017146816, -9.564922557961047289, 29.16775706135232937 ) ) ;
#152918 = CARTESIAN_POINT ( 'NONE',  ( 18.09805431107249873, -5.499999999999973355, 93.51606229291884631 ) ) ;
#152919 = CARTESIAN_POINT ( 'NONE',  ( -12.14591786802326823, 12.06949235617739902, 88.12609039468570415 ) ) ;
#152920 = CARTESIAN_POINT ( 'NONE',  ( -0.2213677808126943147, -24.28759355007370857, -54.22458008397515528 ) ) ;
#152921 = CARTESIAN_POINT ( 'NONE',  ( -12.14591786802326823, 12.06949235617739902, 73.12609039468567573 ) ) ;
#152922 = CARTESIAN_POINT ( 'NONE',  ( -14.29746914071037622, -8.314922557961029526, 59.16775706135234714 ) ) ;
#152923 = DIRECTION ( 'NONE',  ( -1.000000000000000000, -0.000000000000000000, -0.000000000000000000 ) ) ;
#152924 = CARTESIAN_POINT ( 'NONE',  ( -5.719274019375665041, -21.55341960407619695, 69.79275706135234714 ) ) ;
#152925 = CARTESIAN_POINT ( 'NONE',  ( 19.02544592524334988, 5.153800228976608722, 76.45942372801897591 ) ) ;
#152926 = CARTESIAN_POINT ( 'NONE',  ( 21.55341960407619695, -5.719274019375665929, 106.0427570613523471 ) ) ;
#152927 = CARTESIAN_POINT ( 'NONE',  ( -19.03943276465977164, 0.05219959533909376836, 51.24890960531436690 ) ) ;
#152928 = CARTESIAN_POINT ( 'NONE',  ( 9.474510206698971260, -16.51473224551069308, 37.91557627198102409 ) ) ;
#152929 = CARTESIAN_POINT ( 'NONE',  ( -15.06137443927351249, 15.06137443927345210, -58.85720012050612837 ) ) ;
#152930 = CARTESIAN_POINT ( 'NONE',  ( 21.55341960407610458, 5.719274019375980345, 73.95724293864769550 ) ) ;
#152931 = CARTESIAN_POINT ( 'NONE',  ( -19.03943276465977164, 0.05219959533909376836, 116.2489096053143669 ) ) ;
#152932 = CARTESIAN_POINT ( 'NONE',  ( -16.51473224551069308, -9.474510206698971260, 21.66557627198102765 ) ) ;
#152933 = CARTESIAN_POINT ( 'NONE',  ( -0.05219959533934338120, 16.53943276465976808, 47.50109039468568994 ) ) ;
#152934 = CARTESIAN_POINT ( 'NONE',  ( -4.379528057220328563, 16.55341960407611168, 25.20724293864769550 ) ) ;
#152935 = ORIENTED_EDGE ( 'NONE', *, *, #96176, .T. ) ;
#152936 = CARTESIAN_POINT ( 'NONE',  ( -21.52544592524343514, 5.823673210054127303, 116.0405762719810383 ) ) ;
#152938 = CARTESIAN_POINT ( 'NONE',  ( 38.00000000000000711, -12.34694845685040754, -5.099999999999999645 ) ) ;
#152937 = CARTESIAN_POINT ( 'NONE',  ( -4.483927247898539470, -16.52544592524342804, 47.29057627198103120 ) ) ;
#152939 = CARTESIAN_POINT ( 'NONE',  ( -13.97604488694547697, 13.89961937509957934, 108.1260903946856331 ) ) ;
#152940 = CARTESIAN_POINT ( 'NONE',  ( 19.05341960407617918, -5.049401038297876454, 36.04275706135234003 ) ) ;
#152941 = CARTESIAN_POINT ( 'NONE',  ( 14.29746914071049879, -8.314922557960816363, 38.33224293864768839 ) ) ;
#152942 = CARTESIAN_POINT ( 'NONE',  ( 21.53943276465977519, -0.05219959533907433946, 98.74890960531438111 ) ) ;
#152944 = CARTESIAN_POINT ( 'NONE',  ( -21.53943276465977519, 0.05219959533907696930, 61.24890960531435979 ) ) ;
#152943 = DIRECTION ( 'NONE',  ( 1.000000000000000000, -0.000000000000000000, -0.000000000000000000 ) ) ;
#152945 = CARTESIAN_POINT ( 'NONE',  ( -13.97604488694527625, -13.89961937509977652, 96.87390960531433848 ) ) ;
#152946 = CARTESIAN_POINT ( 'NONE',  ( -0.05219959533910754901, -16.53943276465976808, 52.49890960531435979 ) ) ;
#152947 = CARTESIAN_POINT ( 'NONE',  ( -19.02544592524342804, 5.153800228976336051, 106.0405762719810241 ) ) ;
#152948 = CARTESIAN_POINT ( 'NONE',  ( -36.86581981986046230, 2.436233122106819415, 49.93429970834160514 ) ) ;
#152949 = CARTESIAN_POINT ( 'NONE',  ( 13.97604488694548053, -13.89961937509957401, 60.62609039468564731 ) ) ;
#152950 = CARTESIAN_POINT ( 'NONE',  ( -5.823673210054116645, -21.52544592524344225, 97.29057627198105251 ) ) ;
#152951 = CARTESIAN_POINT ( 'NONE',  ( -0.05219959533909027116, -19.03943276465977164, 42.49890960531435269 ) ) ;
#152952 = CARTESIAN_POINT ( 'NONE',  ( -16.51473224551069308, -9.474510206698971260, 21.66557627198102765 ) ) ;
#152953 = CIRCLE ( 'NONE', #23810, 31.90000000000003411 ) ;
#152954 = CARTESIAN_POINT ( 'NONE',  ( 21.55341960407619695, -5.719274019375665929, 56.04275706135235424 ) ) ;
#152955 = CARTESIAN_POINT ( 'NONE',  ( 1.784210473542230573E-15, -29.16686587814331588, 147.3750000027311842 ) ) ;
#152956 = CARTESIAN_POINT ( 'NONE',  ( -12.14591786802309592, -12.06949235617757132, 21.87390960531436690 ) ) ;
#152957 = CARTESIAN_POINT ( 'NONE',  ( 19.05341960407611168, 5.049401038298154454, 53.95724293864770260 ) ) ;
#152958 = CARTESIAN_POINT ( 'NONE',  ( 9.474510206698971260, -16.51473224551069308, 92.91557627198103830 ) ) ;
#152959 = CARTESIAN_POINT ( 'NONE',  ( -10.81492255796078084, -18.62759615963271287, 62.08224293864769550 ) ) ;
#152960 = CARTESIAN_POINT ( 'NONE',  ( 1.784210473542230573E-15, -29.16686587814331588, 143.3750000027311557 ) ) ;
#152961 = CARTESIAN_POINT ( 'NONE',  ( 13.89961937509977652, -13.97604488694527269, 48.12390960531435979 ) ) ;
#152962 = CARTESIAN_POINT ( 'NONE',  ( -10.72451020669898014, 18.67979575497178502, 55.41557627198102409 ) ) ;
#152963 = CARTESIAN_POINT ( 'NONE',  ( -21.53943276465977519, -0.05219959533937600094, 83.75109039468568994 ) ) ;
#152966 = CARTESIAN_POINT ( 'NONE',  ( 4.483927247898545687, 16.52544592524342804, 69.79057627198102409 ) ) ;
#152965 = CARTESIAN_POINT ( 'NONE',  ( 4.483927247898790824, -16.52544592524335698, 85.20942372801901854 ) ) ;
#152964 = CARTESIAN_POINT ( 'NONE',  ( 12.11826072627459183, -36.49684537641077497, -23.43927118307718160 ) ) ;
#152967 = CARTESIAN_POINT ( 'NONE',  ( -16.55341960407617563, 4.379528057220093196, 88.54275706135236135 ) ) ;
#152968 = CARTESIAN_POINT ( 'NONE',  ( 19.03943276465977164, -0.05219959533909143690, 68.74890960531436690 ) ) ;
#152969 = EDGE_LOOP ( 'NONE', ( #122545, #151901, #104232 ) ) ;
#152970 = CARTESIAN_POINT ( 'NONE',  ( 0.05219959533936267826, -19.03943276465977164, 20.00109039468567218 ) ) ;
#152971 = CARTESIAN_POINT ( 'NONE',  ( -4.483927247898782831, 16.52544592524335698, 92.70942372801901854 ) ) ;
#152972 = CARTESIAN_POINT ( 'NONE',  ( -5.719274019375665041, -21.55341960407619695, 109.7927570613523613 ) ) ;
#152973 = CARTESIAN_POINT ( 'NONE',  ( -19.05341960407611168, -5.049401038298163336, 81.45724293864769550 ) ) ;
#152974 = CARTESIAN_POINT ( 'NONE',  ( 15.80617190586746368, 15.72974639402197994, 49.37390960531436690 ) ) ;
#152975 = CARTESIAN_POINT ( 'NONE',  ( 12.06949235617739724, 12.14591786802326823, 31.87609039468567929 ) ) ;
#152976 = CARTESIAN_POINT ( 'NONE',  ( -21.53943276465977519, -0.05219959533937600094, 83.75109039468568994 ) ) ;
#152977 = CARTESIAN_POINT ( 'NONE',  ( -12.14591786802326823, 12.06949235617739902, 63.12609039468568994 ) ) ;
#152978 = CARTESIAN_POINT ( 'NONE',  ( -10.72451020669870658, -18.67979575497194134, 19.58442372801901143 ) ) ;
#152979 = CARTESIAN_POINT ( 'NONE',  ( 8.314922557961029526, -14.29746914071037800, 20.41775706135234714 ) ) ;
#152980 = CARTESIAN_POINT ( 'NONE',  ( -19.02544592524342804, 5.153800228976336051, 86.04057627198103830 ) ) ;
#152981 = CARTESIAN_POINT ( 'NONE',  ( -8.224510206698735004, -14.34966873604973081, 29.58442372801901854 ) ) ;
#152982 = CARTESIAN_POINT ( 'NONE',  ( 5.153800228976335163, 19.02544592524342804, 39.79057627198100988 ) ) ;
#152983 = CARTESIAN_POINT ( 'NONE',  ( -8.314922557961024197, 14.29746914071037800, 37.91775706135235424 ) ) ;
#152984 = CARTESIAN_POINT ( 'NONE',  ( -16.53943276465976808, 0.05219959533911058130, 81.24890960531436690 ) ) ;
#152985 = CARTESIAN_POINT ( 'NONE',  ( -12.14591786802326823, 12.06949235617739902, 93.12609039468568994 ) ) ;
#152987 = CARTESIAN_POINT ( 'NONE',  ( -13.97604488694527625, -13.89961937509977652, 61.87390960531435979 ) ) ;
#152986 = CARTESIAN_POINT ( 'NONE',  ( 21.53943276465977519, 0.05219959533937863772, 26.25109039468567573 ) ) ;
#152988 = CARTESIAN_POINT ( 'NONE',  ( 19.05341960407611168, 5.049401038298154454, 63.95724293864769550 ) ) ;
#152989 = CARTESIAN_POINT ( 'NONE',  ( -16.53943276465976808, -0.05219959533934237506, 83.75109039468568994 ) ) ;
#152991 = EDGE_LOOP ( 'NONE', ( #129837, #36863, #170379, #158953 ) ) ;
#152990 = CARTESIAN_POINT ( 'NONE',  ( 17.50000000000002132, -5.499999999999878320, 63.29690382534172954 ) ) ;
#152992 = ORIENTED_EDGE ( 'NONE', *, *, #42515, .F. ) ;
#152993 = CARTESIAN_POINT ( 'NONE',  ( -19.05341960407617563, 5.049401038297882671, 28.54275706135232937 ) ) ;
#152995 = EDGE_CURVE ( 'NONE', #95725, #24895, #49760, .T. ) ;
#152994 = CARTESIAN_POINT ( 'NONE',  ( 16.51473224551069308, 9.474510206698969483, 54.16557627198103120 ) ) ;
#152997 = ORIENTED_EDGE ( 'NONE', *, *, #76080, .T. ) ;
#152996 = CARTESIAN_POINT ( 'NONE',  ( 1.500000000000166533, 15.01069668396672618, -62.04687407567888613 ) ) ;
#152998 = CARTESIAN_POINT ( 'NONE',  ( -16.55341960407617563, 4.379528057220093196, 23.54275706135235424 ) ) ;
#153000 = CARTESIAN_POINT ( 'NONE',  ( -12.06949235617739369, -12.14591786802326823, 39.37609039468567573 ) ) ;
#152999 = CARTESIAN_POINT ( 'NONE',  ( -5.153800228976607833, 19.02544592524334988, 52.70942372801900433 ) ) ;
#153001 = CARTESIAN_POINT ( 'NONE',  ( -16.51473224551069308, -9.474510206698971260, 101.6655762719810241 ) ) ;
#153002 = CARTESIAN_POINT ( 'NONE',  ( -16.51473224551069308, -9.474510206698971260, 81.66557627198103830 ) ) ;
#153003 = CARTESIAN_POINT ( 'NONE',  ( 15.72974639402199770, -15.80617190586745480, 93.12390960531436690 ) ) ;
#153004 = CARTESIAN_POINT ( 'NONE',  ( -13.97604488694547697, 13.89961937509957934, 63.12609039468566152 ) ) ;
#153006 = CARTESIAN_POINT ( 'NONE',  ( 19.05341960407611168, 5.049401038298154454, 23.95724293864769194 ) ) ;
#153005 = CARTESIAN_POINT ( 'NONE',  ( -13.89961937509977652, 13.97604488694528158, 85.62390960531433848 ) ) ;
#153007 = CARTESIAN_POINT ( 'NONE',  ( -5.153800228976328057, -19.02544592524343514, 57.29057627198103120 ) ) ;
#153009 = CARTESIAN_POINT ( 'NONE',  ( 19.02544592524343514, -5.153800228976328945, 28.54057627198102409 ) ) ;
#153008 = CARTESIAN_POINT ( 'NONE',  ( 8.224510206698953496, -14.34966873604960469, 27.91557627198103830 ) ) ;
#153010 = CARTESIAN_POINT ( 'NONE',  ( 19.05341960407617918, -5.049401038297876454, 36.04275706135234003 ) ) ;
#153011 = CARTESIAN_POINT ( 'NONE',  ( -16.52544592524342804, 4.483927247898546575, 76.04057627198102409 ) ) ;
#153012 = CARTESIAN_POINT ( 'NONE',  ( -15.80617190586768217, 15.72974639402176855, 93.12609039468568994 ) ) ;
#153013 = CARTESIAN_POINT ( 'NONE',  ( 19.03943276465977164, -0.05219959533909143690, 43.74890960531435979 ) ) ;
#153014 = CARTESIAN_POINT ( 'NONE',  ( -8.224510206698735004, -14.34966873604973081, 49.58442372801901143 ) ) ;
#153015 = ADVANCED_FACE ( 'NONE', ( #81798 ), #31605, .F. ) ;
#153017 = CARTESIAN_POINT ( 'NONE',  ( -10.72451020669870658, -18.67979575497194134, 89.58442372801901854 ) ) ;
#153016 = CARTESIAN_POINT ( 'NONE',  ( 12.06949235617757843, -12.14591786802309237, 38.12390960531436690 ) ) ;
#153018 = CARTESIAN_POINT ( 'NONE',  ( 16.51473224551069308, 9.474510206698969483, 99.16557627198102409 ) ) ;
#153019 = CARTESIAN_POINT ( 'NONE',  ( 13.89961937509977652, -13.97604488694527269, 93.12390960531436690 ) ) ;
#153020 = CARTESIAN_POINT ( 'NONE',  ( -8.314922557960811034, -14.29746914071050412, 112.0822429386477097 ) ) ;
#153021 = CARTESIAN_POINT ( 'NONE',  ( 16.52544592524342804, -4.483927247898539470, 68.54057627198103830 ) ) ;
#153022 = CARTESIAN_POINT ( 'NONE',  ( 21.52544592524344225, -5.823673210054117533, 83.54057627198102409 ) ) ;
#153023 = CARTESIAN_POINT ( 'NONE',  ( -9.564922557960796823, -16.46253265017161027, 92.08224293864769550 ) ) ;
#153024 = CARTESIAN_POINT ( 'NONE',  ( 21.52544592524344225, -5.823673210054117533, 98.54057627198105251 ) ) ;
#153025 = CARTESIAN_POINT ( 'NONE',  ( -19.05341960407617563, 5.049401038297882671, 73.54275706135233293 ) ) ;
#153027 = CARTESIAN_POINT ( 'NONE',  ( 4.379528057220339221, -16.55341960407611168, 87.70724293864769550 ) ) ;
#153026 = CARTESIAN_POINT ( 'NONE',  ( 5.000000000000000000, -130.0000000000000000, 13.99999999999999822 ) ) ;
#153028 = CARTESIAN_POINT ( 'NONE',  ( 19.03943276465977164, -0.05219959533909143690, 53.74890960531436690 ) ) ;
#153029 = CARTESIAN_POINT ( 'NONE',  ( -21.53943276465977519, 0.05219959533907696930, 71.24890960531435269 ) ) ;
#153030 = CARTESIAN_POINT ( 'NONE',  ( 17.40861289039004234, -6.110651285853252901, 26.12767529172568715 ) ) ;
#153032 = DIRECTION ( 'NONE',  ( 0.000000000000000000, 1.000000000000000000, 0.000000000000000000 ) ) ;
#153031 = CARTESIAN_POINT ( 'NONE',  ( -12.14591786802326823, 12.06949235617739902, 113.1260903946856899 ) ) ;
#153033 = CARTESIAN_POINT ( 'NONE',  ( 14.29746914071037800, 8.314922557961029526, 26.66775706135235424 ) ) ;
#153034 = CARTESIAN_POINT ( 'NONE',  ( -12.14591786802309592, -12.06949235617757132, 86.87390960531438111 ) ) ;
#153035 = CARTESIAN_POINT ( 'NONE',  ( -19.99999999999998224, -190.0000000000000000, -4.999999999999999112 ) ) ;
#153036 = CARTESIAN_POINT ( 'NONE',  ( -13.89961937509977652, 13.97604488694528158, 75.62390960531438111 ) ) ;
#153037 = CARTESIAN_POINT ( 'NONE',  ( -9.564922557960796823, -16.46253265017161027, 52.08224293864768839 ) ) ;
#153038 = CARTESIAN_POINT ( 'NONE',  ( -8.224510206698948167, 14.34966873604960824, 70.41557627198102409 ) ) ;
#153039 = AXIS2_PLACEMENT_3D ( 'NONE', #9541, #118717, #24717 ) ;
#153040 = CARTESIAN_POINT ( 'NONE',  ( -19.05341960407611168, -5.049401038298163336, 111.4572429386476671 ) ) ;
#153041 = CARTESIAN_POINT ( 'NONE',  ( 5.049401038297881783, 19.05341960407617563, 97.29275706135233293 ) ) ;
#153042 = CARTESIAN_POINT ( 'NONE',  ( 13.97604488694527802, 13.89961937509977652, 104.3739096053143385 ) ) ;
#153043 = CARTESIAN_POINT ( 'NONE',  ( 15.72974639402199770, -15.80617190586745480, 73.12390960531436690 ) ) ;
#153044 = CARTESIAN_POINT ( 'NONE',  ( -8.224510206698735004, -14.34966873604973081, 74.58442372801901854 ) ) ;
#153045 = CARTESIAN_POINT ( 'NONE',  ( -17.12812012977046550, 6.668231424565701282, 93.64051240676855059 ) ) ;
#153046 = CARTESIAN_POINT ( 'NONE',  ( 19.02544592524343514, -5.153800228976328945, 68.54057627198103830 ) ) ;
#153047 = CARTESIAN_POINT ( 'NONE',  ( -18.62759615963270932, 10.81492255796079327, 85.83224293864768129 ) ) ;
#153048 = CARTESIAN_POINT ( 'NONE',  ( -16.53943276465976808, -0.05219959533934237506, 18.75109039468568639 ) ) ;
#153050 = CARTESIAN_POINT ( 'NONE',  ( -10.81492255796105439, 18.62759615963255655, 57.91775706135234714 ) ) ;
#153049 = CARTESIAN_POINT ( 'NONE',  ( 16.55341960407611168, 4.379528057220329451, 33.95724293864769550 ) ) ;
#153051 = DIRECTION ( 'NONE',  ( 0.000000000000000000, 0.000000000000000000, 1.000000000000000000 ) ) ;
#153053 = CARTESIAN_POINT ( 'NONE',  ( 0.05219959533909260263, 19.03943276465977164, 109.9989096053143669 ) ) ;
#153052 = CARTESIAN_POINT ( 'NONE',  ( -12.14591786802326823, 12.06949235617739902, 73.12609039468567573 ) ) ;
#153054 = CARTESIAN_POINT ( 'NONE',  ( 1.300000000000000044, 1.443375672974065216, 7.017607234860990640E-28 ) ) ;
#153055 = CARTESIAN_POINT ( 'NONE',  ( 0.2597368657414628190, 31.90000000000004121, -49.13275782002544645 ) ) ;
#153056 = CARTESIAN_POINT ( 'NONE',  ( -14.34966873604972548, 8.224510206698743886, 93.33442372801901854 ) ) ;
#153057 = CARTESIAN_POINT ( 'NONE',  ( 16.52544592524335698, 4.483927247898782831, 46.45942372801901854 ) ) ;
#153058 = CARTESIAN_POINT ( 'NONE',  ( -9.474510206698964154, 16.51473224551069663, 55.41557627198103120 ) ) ;
#153059 = CARTESIAN_POINT ( 'NONE',  ( 16.51473224551069308, 9.474510206698969483, 74.16557627198103830 ) ) ;
#153060 = CARTESIAN_POINT ( 'NONE',  ( 15.72974639402176855, 15.80617190586768217, 71.87609039468568994 ) ) ;
#153061 = CARTESIAN_POINT ( 'NONE',  ( -16.52544592524335698, -4.483927247898792601, 63.95942372801901854 ) ) ;
#153062 = CARTESIAN_POINT ( 'NONE',  ( 16.52544592524342804, -4.483927247898539470, 38.54057627198103120 ) ) ;
#153063 = CARTESIAN_POINT ( 'NONE',  ( -13.89961937509977652, 13.97604488694528158, 40.62390960531435979 ) ) ;
#153064 = CARTESIAN_POINT ( 'NONE',  ( 5.049401038298161559, -19.05341960407611168, 37.70724293864768839 ) ) ;
#153065 = CARTESIAN_POINT ( 'NONE',  ( -16.52544592524335698, -4.483927247898792601, 43.95942372801902565 ) ) ;
#153066 = CARTESIAN_POINT ( 'NONE',  ( 9.474510206698729675, 16.51473224551082808, 102.0844237280190043 ) ) ;
#153067 = CARTESIAN_POINT ( 'NONE',  ( 16.52544592524342804, -4.483927247898539470, 98.54057627198105251 ) ) ;
#153068 = CARTESIAN_POINT ( 'NONE',  ( -19.03943276465977164, 0.05219959533909376836, 51.24890960531436690 ) ) ;
#153070 = CARTESIAN_POINT ( 'NONE',  ( -30.74264578624800492, -22.33583958711396278, -7.800000000000000711 ) ) ;
#153069 = CARTESIAN_POINT ( 'NONE',  ( -16.46253265017146816, -9.564922557961047289, 84.16775706135233293 ) ) ;
#153071 = CARTESIAN_POINT ( 'NONE',  ( -10.72451020669870658, -18.67979575497194134, 94.58442372801901854 ) ) ;
#153072 = CARTESIAN_POINT ( 'NONE',  ( -16.53943276465976808, -0.05219959533934237506, 53.75109039468568994 ) ) ;
#153073 = DIRECTION ( 'NONE',  ( -1.000000000000000000, 1.154084784954514691E-14, 0.000000000000000000 ) ) ;
#153074 = CARTESIAN_POINT ( 'NONE',  ( -15.80617190586745835, -15.72974639402198527, 46.87390960531435979 ) ) ;
#153075 = CARTESIAN_POINT ( 'NONE',  ( -12.14591786802326823, 12.06949235617739902, 38.12609039468567573 ) ) ;
#153076 = CARTESIAN_POINT ( 'NONE',  ( -19.01533133064923931, 5.499999999999444000, 68.76586590595741200 ) ) ;
#153077 = CARTESIAN_POINT ( 'NONE',  ( 19.03943276465977164, 0.05219959533936151252, 41.25109039468566152 ) ) ;
#153078 = CARTESIAN_POINT ( 'NONE',  ( 9.474510206698971260, -16.51473224551069308, 87.91557627198102409 ) ) ;
#153079 = CARTESIAN_POINT ( 'NONE',  ( 16.55341960407611168, 4.379528057220329451, 98.95724293864770971 ) ) ;
#153080 = CARTESIAN_POINT ( 'NONE',  ( -9.564922557960796823, -16.46253265017161027, 52.08224293864768839 ) ) ;
#153081 = CARTESIAN_POINT ( 'NONE',  ( -20.43538597629143538, -20.43538597629106945, -52.65483682830182488 ) ) ;
#153082 = CARTESIAN_POINT ( 'NONE',  ( 18.67979575497194134, -10.72451020669871369, 75.83442372801900433 ) ) ;
#153083 = FACE_OUTER_BOUND ( 'NONE', #119822, .T. ) ;
#153084 = CARTESIAN_POINT ( 'NONE',  ( -5.153800228976607833, 19.02544592524334988, 27.70942372801899722 ) ) ;
#153085 = CARTESIAN_POINT ( 'NONE',  ( 18.62759615963255655, 10.81492255796105972, 111.6677570613523613 ) ) ;
#153086 = CARTESIAN_POINT ( 'NONE',  ( 14.29746914071049879, -8.314922557960816363, 53.33224293864769550 ) ) ;
#153087 = CARTESIAN_POINT ( 'NONE',  ( -5.153800228976328057, -19.02544592524343514, 57.29057627198103120 ) ) ;
#153088 = CARTESIAN_POINT ( 'NONE',  ( -19.03943276465977164, 0.05219959533909376836, 111.2489096053143669 ) ) ;
#153089 = CARTESIAN_POINT ( 'NONE',  ( 18.67979575497194134, -10.72451020669871369, 85.83442372801901854 ) ) ;
#153090 = CARTESIAN_POINT ( 'NONE',  ( 9.564922557960805705, 16.46253265017160317, 59.58224293864769550 ) ) ;
#153091 = CARTESIAN_POINT ( 'NONE',  ( 18.62759615963255655, 10.81492255796105972, 81.66775706135236135 ) ) ;
#153092 = CARTESIAN_POINT ( 'NONE',  ( 5.823673210054125526, 21.52544592524343514, 34.79057627198103120 ) ) ;
#153093 = CARTESIAN_POINT ( 'NONE',  ( 10.81492255796106328, -18.62759615963255655, 35.41775706135234003 ) ) ;
#153094 = CARTESIAN_POINT ( 'NONE',  ( 19.03943276465977164, 0.05219959533936151252, 66.25109039468567573 ) ) ;
#153095 = CARTESIAN_POINT ( 'NONE',  ( 5.153800228976335163, 19.02544592524342804, 24.79057627198102765 ) ) ;
#153096 = CARTESIAN_POINT ( 'NONE',  ( -19.03943276465977164, 0.05219959533909376836, 71.24890960531435269 ) ) ;
#153097 = CARTESIAN_POINT ( 'NONE',  ( 4.483927247898790824, -16.52544592524335698, 25.20942372801901854 ) ) ;
#153098 = CARTESIAN_POINT ( 'NONE',  ( 4.379528057220339221, -16.55341960407611168, 87.70724293864769550 ) ) ;
#153099 = CARTESIAN_POINT ( 'NONE',  ( -9.564922557960796823, -16.46253265017161027, 62.08224293864769550 ) ) ;
#153100 = CARTESIAN_POINT ( 'NONE',  ( -18.62759615963270932, 10.81492255796079327, 40.83224293864769550 ) ) ;
#153101 = CARTESIAN_POINT ( 'NONE',  ( 14.29746914071037800, 8.314922557961029526, 21.66775706135235069 ) ) ;
#153102 = CARTESIAN_POINT ( 'NONE',  ( 18.62759615963255655, 10.81492255796105972, 21.66775706135235069 ) ) ;
#153103 = CARTESIAN_POINT ( 'NONE',  ( -10.72451020669870658, -18.67979575497194134, 69.58442372801900433 ) ) ;
#153104 = CARTESIAN_POINT ( 'NONE',  ( -4.483927247898782831, 16.52544592524335698, 72.70942372801901854 ) ) ;
#153105 = CARTESIAN_POINT ( 'NONE',  ( -8.224510206698735004, -14.34966873604973081, 69.58442372801900433 ) ) ;
#153106 = CARTESIAN_POINT ( 'NONE',  ( -9.474510206698964154, 16.51473224551069663, 60.41557627198102409 ) ) ;
#153107 = CARTESIAN_POINT ( 'NONE',  ( 4.379528057220092307, 16.55341960407617563, 87.29275706135236135 ) ) ;
#153108 = CARTESIAN_POINT ( 'NONE',  ( -16.46253265017146816, -9.564922557961047289, 39.16775706135234003 ) ) ;
#153109 = CARTESIAN_POINT ( 'NONE',  ( -18.67979575497178146, -10.72451020669898902, 111.6655762719810525 ) ) ;
#153110 = CARTESIAN_POINT ( 'NONE',  ( -16.55341960407611168, -4.379528057220339221, 61.45724293864770260 ) ) ;
#153111 = CARTESIAN_POINT ( 'NONE',  ( -9.564922557960796823, -16.46253265017161027, 82.08224293864768129 ) ) ;
#153112 = CARTESIAN_POINT ( 'NONE',  ( 14.29746914071037800, 8.314922557961029526, 91.66775706135234714 ) ) ;
#153113 = CARTESIAN_POINT ( 'NONE',  ( -5.719274019375665041, -21.55341960407619695, 64.79275706135234714 ) ) ;
#153114 = CARTESIAN_POINT ( 'NONE',  ( 16.52544592524335698, 4.483927247898782831, 21.45942372801901499 ) ) ;
#153115 = CARTESIAN_POINT ( 'NONE',  ( 5.719274019375991003, -21.55341960407610458, 107.7072429386476955 ) ) ;
#153116 = CARTESIAN_POINT ( 'NONE',  ( 8.314922557960818139, 14.29746914071049879, 59.58224293864770260 ) ) ;
#153117 = ORIENTED_EDGE ( 'NONE', *, *, #23834, .F. ) ;
#153118 = CARTESIAN_POINT ( 'NONE',  ( -18.67979575497178146, -10.72451020669898902, 106.6655762719810383 ) ) ;
#153119 = CARTESIAN_POINT ( 'NONE',  ( 14.29746914071049879, -8.314922557960816363, 43.33224293864769550 ) ) ;
#153120 = ORIENTED_EDGE ( 'NONE', *, *, #142268, .F. ) ;
#153121 = DIRECTION ( 'NONE',  ( 0.000000000000000000, 0.000000000000000000, -1.000000000000000000 ) ) ;
#153122 = CARTESIAN_POINT ( 'NONE',  ( -5.719274019375978568, 21.55341960407610458, 110.2072429386477239 ) ) ;
#153123 = CARTESIAN_POINT ( 'NONE',  ( -16.46253265017160317, 9.564922557960807481, 115.8322429386477097 ) ) ;
#153124 = CARTESIAN_POINT ( 'NONE',  ( -21.55341960407619339, 5.719274019375674811, 38.54275706135234714 ) ) ;
#153125 = CARTESIAN_POINT ( 'NONE',  ( -16.55341960407611168, -4.379528057220339221, 46.45724293864769550 ) ) ;
#153126 = CIRCLE ( 'NONE', #156314, 1.500000000000001332 ) ;
#153127 = CARTESIAN_POINT ( 'NONE',  ( 5.049401038298161559, -19.05341960407611168, 57.70724293864769550 ) ) ;
#153128 = CARTESIAN_POINT ( 'NONE',  ( -19.03943276465977164, -0.05219959533935918106, 68.75109039468566152 ) ) ;
#153129 = CARTESIAN_POINT ( 'NONE',  ( -19.03943276465977164, 0.05219959533909376836, 91.24890960531436690 ) ) ;
#153130 = CARTESIAN_POINT ( 'NONE',  ( -15.72974639402197994, 15.80617190586746368, 45.62390960531436690 ) ) ;
#153131 = CARTESIAN_POINT ( 'NONE',  ( -21.54936698787217253, -30.95672727791941625, -19.59590204859394191 ) ) ;
#153132 = CARTESIAN_POINT ( 'NONE',  ( 5.049401038298161559, -19.05341960407611168, 52.70724293864767418 ) ) ;
#153133 = CARTESIAN_POINT ( 'NONE',  ( -8.224510206698735004, -14.34966873604973081, 34.58442372801900433 ) ) ;
#153134 = CARTESIAN_POINT ( 'NONE',  ( -13.89961937509957401, -13.97604488694547875, 69.37609039468564731 ) ) ;
#153135 = CARTESIAN_POINT ( 'NONE',  ( 5.719274019375991003, -21.55341960407610458, 112.7072429386476955 ) ) ;
#153136 = CARTESIAN_POINT ( 'NONE',  ( 14.34966873604960469, 8.224510206698951720, 44.16557627198103120 ) ) ;
#153137 = VERTEX_POINT ( 'NONE', #138770 ) ;
#153138 = CARTESIAN_POINT ( 'NONE',  ( -9.474510206698964154, 16.51473224551069663, 85.41557627198102409 ) ) ;
#153139 = CARTESIAN_POINT ( 'NONE',  ( 5.719274019375991003, -21.55341960407610458, 77.70724293864770971 ) ) ;
#153141 = CARTESIAN_POINT ( 'NONE',  ( 16.53943276465976808, 0.05219959533934440121, 36.25109039468567573 ) ) ;
#153140 = CARTESIAN_POINT ( 'NONE',  ( 0.05219959533907565091, 21.53943276465977519, 109.9989096053143527 ) ) ;
#153142 = CARTESIAN_POINT ( 'NONE',  ( -18.62759615963270932, 10.81492255796079327, 35.83224293864768839 ) ) ;
#153143 = CARTESIAN_POINT ( 'NONE',  ( -18.67979575497193778, 10.72451020669871902, 103.3344237280190043 ) ) ;
#153144 = CARTESIAN_POINT ( 'NONE',  ( -5.049401038298153566, 19.05341960407611168, 85.20724293864766707 ) ) ;
#153145 = CARTESIAN_POINT ( 'NONE',  ( 13.97604488694527802, 13.89961937509977652, 44.37390960531435269 ) ) ;
#153146 = CARTESIAN_POINT ( 'NONE',  ( -16.51473224551069308, -9.474510206698971260, 91.66557627198103830 ) ) ;
#153147 = CARTESIAN_POINT ( 'NONE',  ( -5.153800228976328057, -19.02544592524343514, 72.29057627198102409 ) ) ;
#153148 = CARTESIAN_POINT ( 'NONE',  ( 12.06949235617739724, 12.14591786802326823, 21.87609039468567573 ) ) ;
#153149 = EDGE_CURVE ( 'NONE', #163522, #134824, #8415, .T. ) ;
#153150 = CARTESIAN_POINT ( 'NONE',  ( -16.46253265017146816, -9.564922557961047289, 54.16775706135234003 ) ) ;
#153152 = CARTESIAN_POINT ( 'NONE',  ( -15.80617190586745835, -15.72974639402198527, 31.87390960531435979 ) ) ;
#153151 = CARTESIAN_POINT ( 'NONE',  ( 0.05219959533937995610, -21.53943276465977519, 105.0010903946856757 ) ) ;
#153153 = CARTESIAN_POINT ( 'NONE',  ( 0.05219959533934541429, -16.53943276465976808, 100.0010903946857042 ) ) ;
#153154 = VECTOR ( 'NONE', #24631, 1000.000000000000000 ) ;
#153155 = CARTESIAN_POINT ( 'NONE',  ( 21.28441087011643162, -20.00855284718919336, -49.30314046027508113 ) ) ;
#153156 = CARTESIAN_POINT ( 'NONE',  ( -9.474510206698720793, -16.51473224551083518, 64.58442372801900433 ) ) ;
#153157 = CARTESIAN_POINT ( 'NONE',  ( -9.564922557961040184, 16.46253265017147172, 37.91775706135233293 ) ) ;
#153158 = CARTESIAN_POINT ( 'NONE',  ( 25.64061671795035124, 10.58440545630783269, 139.9999999999999716 ) ) ;
#153159 = CARTESIAN_POINT ( 'NONE',  ( -13.89961937509977652, 13.97604488694528158, 35.62390960531435269 ) ) ;
#153160 = CARTESIAN_POINT ( 'NONE',  ( -8.314922557960811034, -14.29746914071050412, 42.08224293864769550 ) ) ;
#153161 = CARTESIAN_POINT ( 'NONE',  ( 9.564922557960805705, 16.46253265017160317, 24.58224293864769194 ) ) ;
#153162 = CARTESIAN_POINT ( 'NONE',  ( 8.224510206698953496, -14.34966873604960469, 22.91557627198102765 ) ) ;
#153163 = CARTESIAN_POINT ( 'NONE',  ( -30.00000000000000000, -1.163414459189985801E-14, 97.50000000000000000 ) ) ;
#153164 = CARTESIAN_POINT ( 'NONE',  ( -14.29746914071037622, -8.314922557961029526, 94.16775706135237556 ) ) ;
#153165 = CARTESIAN_POINT ( 'NONE',  ( -16.46253265017160317, 9.564922557960807481, 45.83224293864769550 ) ) ;
#153166 = CARTESIAN_POINT ( 'NONE',  ( 18.67979575497194134, -10.72451020669871369, 110.8344237280190043 ) ) ;
#153167 = CARTESIAN_POINT ( 'NONE',  ( 4.483927247898790824, -16.52544592524335698, 20.20942372801900788 ) ) ;
#153168 = CARTESIAN_POINT ( 'NONE',  ( -21.55341960407619339, 5.719274019375674811, 73.54275706135234714 ) ) ;
#153169 = CARTESIAN_POINT ( 'NONE',  ( 13.97604488694548053, -13.89961937509957401, 60.62609039468564731 ) ) ;
#153170 = CARTESIAN_POINT ( 'NONE',  ( -5.153800228976328057, -19.02544592524343514, 87.29057627198103830 ) ) ;
#153171 = CARTESIAN_POINT ( 'NONE',  ( 0.05219959533909260263, 19.03943276465977164, 89.99890960531436690 ) ) ;
#153172 = CARTESIAN_POINT ( 'NONE',  ( 22.81625015709510151, -31.40387420917324590, -5.924999997268812990 ) ) ;
#153173 = CARTESIAN_POINT ( 'NONE',  ( -10.72451020669898014, 18.67979575497178502, 110.4155762719810383 ) ) ;
#153174 = CARTESIAN_POINT ( 'NONE',  ( -16.55341960407611168, -4.379528057220339221, 66.45724293864768129 ) ) ;
#153175 = CARTESIAN_POINT ( 'NONE',  ( -15.80617190586745835, -15.72974639402198527, 61.87390960531436690 ) ) ;
#153176 = CARTESIAN_POINT ( 'NONE',  ( 9.474510206698971260, -16.51473224551069308, 62.91557627198102409 ) ) ;
#153178 = CARTESIAN_POINT ( 'NONE',  ( -12.06949235617739369, -12.14591786802326823, 89.37609039468568994 ) ) ;
#153177 = CARTESIAN_POINT ( 'NONE',  ( 0.05219959533907565091, 21.53943276465977519, 99.99890960531436690 ) ) ;
#153179 = ORIENTED_EDGE ( 'NONE', *, *, #110272, .T. ) ;
#153180 = CARTESIAN_POINT ( 'NONE',  ( 13.97604488694527802, 13.89961937509977652, 59.37390960531434558 ) ) ;
#153182 = LINE ( 'NONE', #166402, #30056 ) ;
#153181 = CARTESIAN_POINT ( 'NONE',  ( -16.53943276465976808, 0.05219959533911058130, 96.24890960531435269 ) ) ;
#153183 = CARTESIAN_POINT ( 'NONE',  ( -16.46253265017160317, 9.564922557960807481, 45.83224293864769550 ) ) ;
#153184 = CARTESIAN_POINT ( 'NONE',  ( 9.474510206698729675, 16.51473224551082808, 77.08442372801900433 ) ) ;
#153185 = CARTESIAN_POINT ( 'NONE',  ( 16.55341960407611168, 4.379528057220329451, 78.95724293864769550 ) ) ;
#153186 = CARTESIAN_POINT ( 'NONE',  ( -18.67979575497193778, 10.72451020669871902, 63.33442372801900433 ) ) ;
#153188 = CARTESIAN_POINT ( 'NONE',  ( -21.53943276465977519, 0.05219959533907696930, 101.2489096053143669 ) ) ;
#153187 = CARTESIAN_POINT ( 'NONE',  ( -19.03943276465977164, 0.05219959533909376836, 31.24890960531435979 ) ) ;
#153189 = CARTESIAN_POINT ( 'NONE',  ( -14.29746914071049879, 8.314922557960819915, 90.83224293864769550 ) ) ;
#153190 = DIRECTION ( 'NONE',  ( -0.000000000000000000, -0.000000000000000000, 1.000000000000000000 ) ) ;
#153191 = CARTESIAN_POINT ( 'NONE',  ( -9.564922557960796823, -16.46253265017161027, 57.08224293864769550 ) ) ;
#153192 = CARTESIAN_POINT ( 'NONE',  ( 18.22780087662121673, 5.500000000000056843, 48.98459894673892734 ) ) ;
#153194 = CARTESIAN_POINT ( 'NONE',  ( -5.153800228976328057, -19.02544592524343514, 107.2905762719810383 ) ) ;
#153193 = CARTESIAN_POINT ( 'NONE',  ( 16.51473224551083163, -9.474510206698727899, 100.8344237280190043 ) ) ;
#153195 = CARTESIAN_POINT ( 'NONE',  ( 21.52544592524334988, 5.823673210054432836, 31.45942372801901854 ) ) ;
#153196 = CARTESIAN_POINT ( 'NONE',  ( -19.03943276465977164, 0.05219959533909376836, 86.24890960531436690 ) ) ;
#153197 = CARTESIAN_POINT ( 'NONE',  ( 16.51473224551083163, -9.474510206698727899, 65.83442372801900433 ) ) ;
#153198 = CARTESIAN_POINT ( 'NONE',  ( -19.02544592524342804, 5.153800228976336051, 56.04057627198100988 ) ) ;
#153199 = CARTESIAN_POINT ( 'NONE',  ( -0.05219959533910754901, -16.53943276465976808, 77.49890960531433848 ) ) ;
#153200 = CARTESIAN_POINT ( 'NONE',  ( -4.483927247898539470, -16.52544592524342804, 72.29057627198102409 ) ) ;
#153201 = CARTESIAN_POINT ( 'NONE',  ( 19.02544592524343514, -5.153800228976328945, 93.54057627198102409 ) ) ;
#153202 = CARTESIAN_POINT ( 'NONE',  ( 4.483927247898545687, 16.52544592524342804, 74.79057627198105251 ) ) ;
#153203 = CARTESIAN_POINT ( 'NONE',  ( 16.51473224551069308, 9.474510206698969483, 89.16557627198103830 ) ) ;
#153204 = AXIS2_PLACEMENT_3D ( 'NONE', #149423, #147431, #192938 ) ;
#153205 = CARTESIAN_POINT ( 'NONE',  ( 5.049401038297881783, 19.05341960407617563, 37.29275706135232582 ) ) ;
#153208 = CARTESIAN_POINT ( 'NONE',  ( -8.224510206698948167, 14.34966873604960824, 105.4155762719810383 ) ) ;
#153207 = CARTESIAN_POINT ( 'NONE',  ( -4.379528057220328563, 16.55341960407611168, 35.20724293864768839 ) ) ;
#153206 = CARTESIAN_POINT ( 'NONE',  ( 5.153800228976335163, 19.02544592524342804, 34.79057627198102409 ) ) ;
#153209 = ORIENTED_EDGE ( 'NONE', *, *, #134802, .F. ) ;
#153210 = CARTESIAN_POINT ( 'NONE',  ( -21.53943276465977519, -0.05219959533937600094, 43.75109039468568284 ) ) ;
#153211 = CARTESIAN_POINT ( 'NONE',  ( 19.03943276465977164, 0.05219959533936151252, 61.25109039468566863 ) ) ;
#153212 = CARTESIAN_POINT ( 'NONE',  ( 0.05219959533910956823, 16.53943276465976808, 34.99890960531435979 ) ) ;
#153213 = CARTESIAN_POINT ( 'NONE',  ( -18.62759615963270932, 10.81492255796079327, 80.83224293864769550 ) ) ;
#153214 = CARTESIAN_POINT ( 'NONE',  ( -19.03943276465977164, 0.05219959533909376836, 116.2489096053143669 ) ) ;
#153215 = CARTESIAN_POINT ( 'NONE',  ( -16.53943276465976808, 0.05219959533911058130, 76.24890960531435269 ) ) ;
#153216 = CARTESIAN_POINT ( 'NONE',  ( -19.03943276465977164, 0.05219959533909376836, 46.24890960531435979 ) ) ;
#153217 = CARTESIAN_POINT ( 'NONE',  ( 13.89961937509957401, 13.97604488694547697, 26.87609039468566507 ) ) ;
#153218 = CARTESIAN_POINT ( 'NONE',  ( -0.05219959533934338120, 16.53943276465976808, 97.50109039468567573 ) ) ;
#153219 = CARTESIAN_POINT ( 'NONE',  ( -14.29746914071037622, -8.314922557961029526, 54.16775706135235424 ) ) ;
#153220 = CARTESIAN_POINT ( 'NONE',  ( -5.823673210054116645, -21.52544592524344225, 37.29057627198102409 ) ) ;
#153221 = CARTESIAN_POINT ( 'NONE',  ( -21.55341960407619339, 5.719274019375674811, 103.5427570613523613 ) ) ;
#153222 = CARTESIAN_POINT ( 'NONE',  ( 19.05341960407611168, 5.049401038298154454, 83.95724293864766707 ) ) ;
#153223 = CARTESIAN_POINT ( 'NONE',  ( -8.314922557961024197, 14.29746914071037800, 67.91775706135234714 ) ) ;
#153224 = CARTESIAN_POINT ( 'NONE',  ( 13.97604488694527802, 13.89961937509977652, 29.37390960531435979 ) ) ;
#153225 = ADVANCED_FACE ( 'NONE', ( #46776 ), #96981, .F. ) ;
#153226 = CARTESIAN_POINT ( 'NONE',  ( -14.29746914071049879, 8.314922557960819915, 40.83224293864769550 ) ) ;
#153228 = CARTESIAN_POINT ( 'NONE',  ( 16.51473224551069308, 9.474510206698969483, 94.16557627198103830 ) ) ;
#153227 = CARTESIAN_POINT ( 'NONE',  ( -16.51473224551069308, -9.474510206698971260, 111.6655762719810383 ) ) ;
#153229 = CARTESIAN_POINT ( 'NONE',  ( -18.62759615963270932, 10.81492255796079327, 25.83224293864769194 ) ) ;
#153230 = AXIS2_PLACEMENT_3D ( 'NONE', #87114, #58761, #45588 ) ;
#153231 = CARTESIAN_POINT ( 'NONE',  ( -16.53943276465976808, 0.05219959533911058130, 61.24890960531435979 ) ) ;
#153232 = CARTESIAN_POINT ( 'NONE',  ( -0.05219959533910754901, -16.53943276465976808, 32.49890960531435979 ) ) ;
#153233 = ORIENTED_EDGE ( 'NONE', *, *, #190360, .T. ) ;
#153234 = CARTESIAN_POINT ( 'NONE',  ( -16.52544592524342804, 4.483927247898546575, 56.04057627198102409 ) ) ;
#153236 = LINE ( 'NONE', #122895, #109252 ) ;
#153235 = CARTESIAN_POINT ( 'NONE',  ( -16.55341960407617563, 4.379528057220093196, 43.54275706135235424 ) ) ;
#153237 = CARTESIAN_POINT ( 'NONE',  ( 5.049401038297881783, 19.05341960407617563, 47.29275706135231161 ) ) ;
#153238 = CARTESIAN_POINT ( 'NONE',  ( -13.97604488694527625, -13.89961937509977652, 91.87390960531432427 ) ) ;
#153239 = CARTESIAN_POINT ( 'NONE',  ( 19.02544592524334988, 5.153800228976608722, 66.45942372801899012 ) ) ;
#153240 = CARTESIAN_POINT ( 'NONE',  ( 27.73933785331498925, -9.013057229001033122, 142.2750000027311899 ) ) ;
#153241 = CARTESIAN_POINT ( 'NONE',  ( -19.03943276465977164, -0.05219959533935918106, 58.75109039468566863 ) ) ;
#153243 = CARTESIAN_POINT ( 'NONE',  ( 14.29746914071037800, 8.314922557961029526, 76.66775706135234714 ) ) ;
#153242 = CARTESIAN_POINT ( 'NONE',  ( 0.05219959533936267826, -19.03943276465977164, 95.00109039468567573 ) ) ;
#153244 = CARTESIAN_POINT ( 'NONE',  ( 22.44159573604009594, -16.30477369853687364, 146.1750000027311671 ) ) ;
#153246 = CARTESIAN_POINT ( 'NONE',  ( -0.05219959533909027116, -19.03943276465977164, 27.49890960531435624 ) ) ;
#153245 = AXIS2_PLACEMENT_3D ( 'NONE', #76651, #2794, #137331 ) ;
#153247 = CARTESIAN_POINT ( 'NONE',  ( 15.80617190586746368, 15.72974639402197994, 24.37390960531435979 ) ) ;
#153248 = CARTESIAN_POINT ( 'NONE',  ( -21.55341960407619339, 5.719274019375674811, 38.54275706135234714 ) ) ;
#153249 = CARTESIAN_POINT ( 'NONE',  ( -19.05341960407617563, 5.049401038297882671, 108.5427570613523187 ) ) ;
#153251 = CARTESIAN_POINT ( 'NONE',  ( 9.474510206698971260, -16.51473224551069308, 67.91557627198102409 ) ) ;
#153250 = CARTESIAN_POINT ( 'NONE',  ( 17.49999999999999645, -4.640572885337595821, 108.1378816454884060 ) ) ;
#153252 = CARTESIAN_POINT ( 'NONE',  ( 19.03943276465977164, -0.05219959533909143690, 103.7489096053143669 ) ) ;
#153254 = CARTESIAN_POINT ( 'NONE',  ( -5.153800228976328057, -19.02544592524343514, 62.29057627198100988 ) ) ;
#153253 = CARTESIAN_POINT ( 'NONE',  ( 16.55341960407611168, 4.379528057220329451, 68.95724293864769550 ) ) ;
#153255 = CARTESIAN_POINT ( 'NONE',  ( 16.46253265017160672, -9.564922557960803928, 68.33224293864770971 ) ) ;
#153256 = CARTESIAN_POINT ( 'NONE',  ( 16.46253265017146816, 9.564922557961045513, 76.66775706135234714 ) ) ;
#153257 = CARTESIAN_POINT ( 'NONE',  ( 15.80617190586746368, 15.72974639402197994, 49.37390960531436690 ) ) ;
#153258 = CARTESIAN_POINT ( 'NONE',  ( -12.06949235617756955, 12.14591786802309770, 110.6239096053143669 ) ) ;
#153259 = CARTESIAN_POINT ( 'NONE',  ( 19.03943276465977164, 0.05219959533936151252, 46.25109039468566863 ) ) ;
#153260 = CARTESIAN_POINT ( 'NONE',  ( 9.474510206698971260, -16.51473224551069308, 82.91557627198103830 ) ) ;
#153261 =( BOUNDED_CURVE ( )  B_SPLINE_CURVE ( 3, ( #45082, #168414, #14739, #76400 ),
 .UNSPECIFIED., .F., .T. ) 
 B_SPLINE_CURVE_WITH_KNOTS ( ( 4, 4 ),
 ( 2.008945357379068319, 2.115944711806983847 ),
 .UNSPECIFIED. ) 
 CURVE ( )  GEOMETRIC_REPRESENTATION_ITEM ( )  RATIONAL_B_SPLINE_CURVE ( ( 1.000000000000000000, 0.9990461557208837329, 0.9990461557208837329, 1.000000000000000000 ) ) 
 REPRESENTATION_ITEM ( '' )  );
#153262 = CARTESIAN_POINT ( 'NONE',  ( -5.823673210054116645, -21.52544592524344225, 82.29057627198103830 ) ) ;
#153264 = CARTESIAN_POINT ( 'NONE',  ( 9.474510206698729675, 16.51473224551082808, 32.08442372801900433 ) ) ;
#153263 = CARTESIAN_POINT ( 'NONE',  ( -4.379528057220328563, 16.55341960407611168, 75.20724293864769550 ) ) ;
#153265 = CARTESIAN_POINT ( 'NONE',  ( -10.81492255796078084, -18.62759615963271287, 72.08224293864769550 ) ) ;
#153266 = CARTESIAN_POINT ( 'NONE',  ( -5.823673210054116645, -21.52544592524344225, 62.29057627198102409 ) ) ;
#153267 = CARTESIAN_POINT ( 'NONE',  ( -21.53943276465977519, 0.05219959533907696930, 46.24890960531435979 ) ) ;
#153268 = CARTESIAN_POINT ( 'NONE',  ( -21.52544592524334988, -5.823673210054445271, 88.95942372801901854 ) ) ;
#153269 = CARTESIAN_POINT ( 'NONE',  ( 9.474510206698971260, -16.51473224551069308, 72.91557627198102409 ) ) ;
#153270 = CARTESIAN_POINT ( 'NONE',  ( -9.564922557960796823, -16.46253265017161027, 22.08224293864768839 ) ) ;
#153271 = CIRCLE ( 'NONE', #24115, 0.5000000000000004441 ) ;
#153272 = CARTESIAN_POINT ( 'NONE',  ( 18.62759615963255655, 10.81492255796105972, 21.66775706135235069 ) ) ;
#153273 = DIRECTION ( 'NONE',  ( -0.000000000000000000, 0.000000000000000000, 1.000000000000000000 ) ) ;
#153274 = CARTESIAN_POINT ( 'NONE',  ( -10.81492255796105439, 18.62759615963255655, 42.91775706135235424 ) ) ;
#153275 = CARTESIAN_POINT ( 'NONE',  ( 9.474510206698971260, -16.51473224551069308, 32.91557627198102409 ) ) ;
#153276 = CARTESIAN_POINT ( 'NONE',  ( -10.72451020669898014, 18.67979575497178502, 110.4155762719810383 ) ) ;
#153277 = CARTESIAN_POINT ( 'NONE',  ( 5.153800228976615827, -19.02544592524334988, 50.20942372801897591 ) ) ;
#153278 = CARTESIAN_POINT ( 'NONE',  ( -13.97604488694527625, -13.89961937509977652, 31.87390960531435979 ) ) ;
#153279 = DIRECTION ( 'NONE',  ( 0.000000000000000000, -0.8164965809277251463, 0.5773502691896268413 ) ) ;
#153280 = DIRECTION ( 'NONE',  ( 1.000000000000000000, 0.000000000000000000, 0.000000000000000000 ) ) ;
#153281 = CARTESIAN_POINT ( 'NONE',  ( -8.224510206698735004, -14.34966873604973081, 59.58442372801901854 ) ) ;
#153282 = CARTESIAN_POINT ( 'NONE',  ( -5.153800228976328057, -19.02544592524343514, 32.29057627198102409 ) ) ;
#153283 = CARTESIAN_POINT ( 'NONE',  ( -25.41223161463591040, -11.66315983254872712, 166.2610598689585117 ) ) ;
#153284 = CARTESIAN_POINT ( 'NONE',  ( 9.564922557960805705, 16.46253265017160317, 79.58224293864769550 ) ) ;
#153285 = CARTESIAN_POINT ( 'NONE',  ( 0.05219959533910956823, 16.53943276465976808, 109.9989096053143527 ) ) ;
#153286 = CARTESIAN_POINT ( 'NONE',  ( 18.62759615963271287, -10.81492255796078972, 53.33224293864769550 ) ) ;
#153287 = CARTESIAN_POINT ( 'NONE',  ( -12.06949235617739369, -12.14591786802326823, 49.37609039468569705 ) ) ;
#153288 = CARTESIAN_POINT ( 'NONE',  ( 5.823673210054444382, -21.52544592524334988, 95.20942372801903275 ) ) ;
#153289 = CARTESIAN_POINT ( 'NONE',  ( -9.474510206698964154, 16.51473224551069663, 30.41557627198102054 ) ) ;
#153290 = CARTESIAN_POINT ( 'NONE',  ( 8.224510206698953496, -14.34966873604960469, 22.91557627198102765 ) ) ;
#153291 = CARTESIAN_POINT ( 'NONE',  ( -16.55341960407611168, -4.379528057220339221, 51.45724293864770260 ) ) ;
#153292 = CARTESIAN_POINT ( 'NONE',  ( -9.564922557960796823, -16.46253265017161027, 57.08224293864769550 ) ) ;
#153293 = CARTESIAN_POINT ( 'NONE',  ( 15.80617190586769283, -15.72974639402175789, 110.6260903946857042 ) ) ;
#153294 = CARTESIAN_POINT ( 'NONE',  ( 5.823673210054444382, -21.52544592524334988, 25.20942372801901854 ) ) ;
#153295 = CARTESIAN_POINT ( 'NONE',  ( -15.80617190586768217, 15.72974639402176855, 78.12609039468570415 ) ) ;
#153296 = CARTESIAN_POINT ( 'NONE',  ( 12.14591786802327356, -12.06949235617739191, 55.62609039468568284 ) ) ;
#153297 = CARTESIAN_POINT ( 'NONE',  ( -14.34966873604972548, 8.224510206698743886, 33.33442372801900433 ) ) ;
#153299 = CARTESIAN_POINT ( 'NONE',  ( -15.72974639402176322, -15.80617190586768395, 104.3760903946856899 ) ) ;
#153298 = CARTESIAN_POINT ( 'NONE',  ( 16.52544592524342804, -4.483927247898539470, 73.54057627198102409 ) ) ;
#153300 = CARTESIAN_POINT ( 'NONE',  ( 14.29746914071049879, -8.314922557960816363, 38.33224293864768839 ) ) ;
#153301 = DIRECTION ( 'NONE',  ( 0.000000000000000000, 1.000000000000000000, -1.224646799147353207E-16 ) ) ;
#153302 = CARTESIAN_POINT ( 'NONE',  ( -4.379528057220086978, -16.55341960407618274, 34.79275706135235424 ) ) ;
#153303 = CARTESIAN_POINT ( 'NONE',  ( -16.53943276465976808, 0.05219959533911058130, 41.24890960531435269 ) ) ;
#153304 = CARTESIAN_POINT ( 'NONE',  ( -14.34966873604972548, 8.224510206698743886, 88.33442372801901854 ) ) ;
#153305 = CARTESIAN_POINT ( 'NONE',  ( 19.03943276465977164, -0.05219959533909143690, 98.74890960531436690 ) ) ;
#153306 = CARTESIAN_POINT ( 'NONE',  ( -13.89961937509977652, 13.97604488694528158, 115.6239096053143669 ) ) ;
#153307 = CARTESIAN_POINT ( 'NONE',  ( 21.55341960407619695, -5.719274019375665929, 96.04275706135236135 ) ) ;
#153308 = CARTESIAN_POINT ( 'NONE',  ( 0.05219959533934541429, -16.53943276465976808, 100.0010903946857042 ) ) ;
#153309 = CARTESIAN_POINT ( 'NONE',  ( 4.379528057220339221, -16.55341960407611168, 72.70724293864769550 ) ) ;
#153310 = CARTESIAN_POINT ( 'NONE',  ( -19.05341960407611168, -5.049401038298163336, 86.45724293864769550 ) ) ;
#153311 = ORIENTED_EDGE ( 'NONE', *, *, #117840, .T. ) ;
#153312 = CARTESIAN_POINT ( 'NONE',  ( 12.06949235617739724, 12.14591786802326823, 41.87609039468568284 ) ) ;
#153313 = CARTESIAN_POINT ( 'NONE',  ( 9.474510206698971260, -16.51473224551069308, 37.91557627198102409 ) ) ;
#153314 = CARTESIAN_POINT ( 'NONE',  ( -9.474510206698964154, 16.51473224551069663, 100.4155762719810241 ) ) ;
#153316 = CARTESIAN_POINT ( 'NONE',  ( -36.91746825000001309, 11.99521256947798342, -0.7249999972688133676 ) ) ;
#153315 = CARTESIAN_POINT ( 'NONE',  ( 12.06949235617739724, 12.14591786802326823, 36.87609039468568994 ) ) ;
#153317 = CARTESIAN_POINT ( 'NONE',  ( -19.02544592524334988, -5.153800228976617603, 28.95942372801900433 ) ) ;
#153318 = CARTESIAN_POINT ( 'NONE',  ( -4.483927247898782831, 16.52544592524335698, 102.7094237280190185 ) ) ;
#153319 = CARTESIAN_POINT ( 'NONE',  ( -13.89961937509977652, 13.97604488694528158, 35.62390960531435269 ) ) ;
#153320 = CARTESIAN_POINT ( 'NONE',  ( -0.05219959533934338120, 16.53943276465976808, 72.50109039468568994 ) ) ;
#153321 = CARTESIAN_POINT ( 'NONE',  ( -0.05219959533936034679, 19.03943276465977164, 87.50109039468567573 ) ) ;
#153322 = CARTESIAN_POINT ( 'NONE',  ( -13.97604488694547697, 13.89961937509957934, 33.12609039468566863 ) ) ;
#153323 = CARTESIAN_POINT ( 'NONE',  ( 0.05219959533909260263, 19.03943276465977164, 59.99890960531436690 ) ) ;
#153324 = CARTESIAN_POINT ( 'NONE',  ( -4.483927247898539470, -16.52544592524342804, 92.29057627198103830 ) ) ;
#153325 = CARTESIAN_POINT ( 'NONE',  ( 13.89961937509957401, 13.97604488694547697, 56.87609039468564731 ) ) ;
#153326 = CARTESIAN_POINT ( 'NONE',  ( -5.719274019375978568, 21.55341960407610458, 55.20724293864770260 ) ) ;
#153327 = CARTESIAN_POINT ( 'NONE',  ( -5.153800228976607833, 19.02544592524334988, 22.70942372801899012 ) ) ;
#153328 = CARTESIAN_POINT ( 'NONE',  ( -13.89961937509977652, 13.97604488694528158, 110.6239096053143243 ) ) ;
#153329 = VECTOR ( 'NONE', #79146, 1000.000000000000000 ) ;
#153330 = CARTESIAN_POINT ( 'NONE',  ( -15.72974639402197994, 15.80617190586746368, 70.62390960531436690 ) ) ;
#153331 = CARTESIAN_POINT ( 'NONE',  ( 16.46253265017160672, -9.564922557960803928, 113.3322429386476955 ) ) ;
#153332 = CARTESIAN_POINT ( 'NONE',  ( 16.46253265017146816, 9.564922557961045513, 96.66775706135233293 ) ) ;
#153333 = CARTESIAN_POINT ( 'NONE',  ( -17.49999999999998934, 3.209263204892635724, 109.7619682560626870 ) ) ;
#153334 = CARTESIAN_POINT ( 'NONE',  ( 16.55341960407618274, -4.379528057220086978, 26.04275706135235779 ) ) ;
#153335 = CARTESIAN_POINT ( 'NONE',  ( 19.05341960407611168, 5.049401038298154454, 38.95724293864767418 ) ) ;
#153336 = CARTESIAN_POINT ( 'NONE',  ( -13.97604488694527625, -13.89961937509977652, 101.8739096053143811 ) ) ;
#153337 = CARTESIAN_POINT ( 'NONE',  ( -15.72974639402197994, 15.80617190586746368, 75.62390960531439532 ) ) ;
#153338 = CARTESIAN_POINT ( 'NONE',  ( 12.14591786802327356, -12.06949235617739191, 55.62609039468568284 ) ) ;
#153339 = CARTESIAN_POINT ( 'NONE',  ( 18.62759615963255655, 10.81492255796105972, 61.66775706135235424 ) ) ;
#153341 = CARTESIAN_POINT ( 'NONE',  ( 5.823673210054444382, -21.52544592524334988, 110.2094237280190185 ) ) ;
#153340 = CARTESIAN_POINT ( 'NONE',  ( 5.153800228976615827, -19.02544592524334988, 100.2094237280190043 ) ) ;
#153342 = CARTESIAN_POINT ( 'NONE',  ( 14.29746914071049879, -8.314922557960816363, 23.33224293864769194 ) ) ;
#153343 = CARTESIAN_POINT ( 'NONE',  ( 15.80617190586746368, 15.72974639402197994, 94.37390960531436690 ) ) ;
#153344 = CARTESIAN_POINT ( 'NONE',  ( 16.53943276465976808, -0.05219959533910856209, 38.74890960531435979 ) ) ;
#153345 = CARTESIAN_POINT ( 'NONE',  ( 19.05341960407617918, -5.049401038297876454, 86.04275706135233293 ) ) ;
#153346 = CARTESIAN_POINT ( 'NONE',  ( -0.05219959533937732626, 21.53943276465977519, 52.50109039468567573 ) ) ;
#153347 = CARTESIAN_POINT ( 'NONE',  ( -19.03943276465977164, -0.05219959533935918106, 38.75109039468566152 ) ) ;
#153348 = CARTESIAN_POINT ( 'NONE',  ( -8.314922557960811034, -14.29746914071050412, 107.0822429386476955 ) ) ;
#153349 = CARTESIAN_POINT ( 'NONE',  ( -5.719274019375978568, 21.55341960407610458, 30.20724293864769550 ) ) ;
#153350 = CARTESIAN_POINT ( 'NONE',  ( 4.483927247898545687, 16.52544592524342804, 34.79057627198103120 ) ) ;
#153351 = VECTOR ( 'NONE', #47436, 1000.000000000000000 ) ;
#153352 = CARTESIAN_POINT ( 'NONE',  ( 10.72451020669871369, 18.67979575497193778, 102.0844237280190185 ) ) ;
#153353 = CARTESIAN_POINT ( 'NONE',  ( 16.52544592524335698, 4.483927247898782831, 66.45942372801903275 ) ) ;
#153354 = CARTESIAN_POINT ( 'NONE',  ( 16.53943276465976808, -0.05219959533910856209, 23.74890960531435269 ) ) ;
#153355 = CARTESIAN_POINT ( 'NONE',  ( 21.55341960407619695, -5.719274019375665929, 61.04275706135234714 ) ) ;
#153356 = CARTESIAN_POINT ( 'NONE',  ( -18.67979575497193778, 10.72451020669871902, 58.33442372801901143 ) ) ;
#153357 = ORIENTED_EDGE ( 'NONE', *, *, #147777, .F. ) ;
#153358 = CARTESIAN_POINT ( 'NONE',  ( -5.049401038298153566, 19.05341960407611168, 25.20724293864768484 ) ) ;
#153359 = CARTESIAN_POINT ( 'NONE',  ( -18.62759615963255300, -10.81492255796106328, 39.16775706135235424 ) ) ;
#153360 = CARTESIAN_POINT ( 'NONE',  ( 9.474510206698971260, -16.51473224551069308, 27.91557627198103120 ) ) ;
#153361 = CARTESIAN_POINT ( 'NONE',  ( 16.51473224551069308, 9.474510206698969483, 44.16557627198103120 ) ) ;
#153362 = CARTESIAN_POINT ( 'NONE',  ( -16.52544592524342804, 4.483927247898546575, 76.04057627198102409 ) ) ;
#153363 = CARTESIAN_POINT ( 'NONE',  ( -16.51473224551069308, -9.474510206698971260, 76.66557627198103830 ) ) ;
#153364 = CARTESIAN_POINT ( 'NONE',  ( 4.379528057220339221, -16.55341960407611168, 32.70724293864770260 ) ) ;
#153365 = CARTESIAN_POINT ( 'NONE',  ( -5.719274019375978568, 21.55341960407610458, 55.20724293864770260 ) ) ;
#153366 = CARTESIAN_POINT ( 'NONE',  ( -4.483927247898539470, -16.52544592524342804, 92.29057627198103830 ) ) ;
#153367 = AXIS2_PLACEMENT_3D ( 'NONE', #47243, #139238, #122076 ) ;
#153368 = CARTESIAN_POINT ( 'NONE',  ( 21.55341960407610458, 5.719274019375980345, 103.9572429386476813 ) ) ;
#153369 = CARTESIAN_POINT ( 'NONE',  ( -0.05219959533909027116, -19.03943276465977164, 97.49890960531436690 ) ) ;
#153371 = CARTESIAN_POINT ( 'NONE',  ( -19.05341960407617563, 5.049401038297882671, 103.5427570613523329 ) ) ;
#153370 = CARTESIAN_POINT ( 'NONE',  ( -16.51473224551069308, -9.474510206698971260, 61.66557627198103120 ) ) ;
#153372 = CARTESIAN_POINT ( 'NONE',  ( -21.52544592524343514, 5.823673210054127303, 56.04057627198102409 ) ) ;
#153373 = CARTESIAN_POINT ( 'NONE',  ( -5.719274019375665041, -21.55341960407619695, 79.79275706135236135 ) ) ;
#153374 = CARTESIAN_POINT ( 'NONE',  ( -13.97604488694527625, -13.89961937509977652, 66.87390960531436690 ) ) ;
#153375 = CARTESIAN_POINT ( 'NONE',  ( -5.153800228976328057, -19.02544592524343514, 97.29057627198099567 ) ) ;
#153376 = CARTESIAN_POINT ( 'NONE',  ( 16.53943276465976808, 0.05219959533934440121, 81.25109039468568994 ) ) ;
#153377 = CARTESIAN_POINT ( 'NONE',  ( 18.67979575497194134, -10.72451020669871369, 60.83442372801901854 ) ) ;
#153378 = CARTESIAN_POINT ( 'NONE',  ( -0.05219959533937732626, 21.53943276465977519, 92.50109039468567573 ) ) ;
#153379 = CARTESIAN_POINT ( 'NONE',  ( -18.62759615963270932, 10.81492255796079327, 110.8322429386476955 ) ) ;
#153380 = AXIS2_PLACEMENT_3D ( 'NONE', #1367, #63046, #183432 ) ;
#153381 = CARTESIAN_POINT ( 'NONE',  ( 12.14591786802327356, -12.06949235617739191, 80.62609039468567573 ) ) ;
#153382 = CARTESIAN_POINT ( 'NONE',  ( -10.81492255796078084, -18.62759615963271287, 72.08224293864769550 ) ) ;
#153383 = CARTESIAN_POINT ( 'NONE',  ( 19.05341960407617918, -5.049401038297876454, 46.04275706135233293 ) ) ;
#153384 = CARTESIAN_POINT ( 'NONE',  ( 15.72974639402199770, -15.80617190586745480, 43.12390960531435269 ) ) ;
#153385 = CIRCLE ( 'NONE', #108206, 5.000000000000000000 ) ;
#153387 = CARTESIAN_POINT ( 'NONE',  ( 8.224510206698953496, -14.34966873604960469, 22.91557627198102765 ) ) ;
#153386 = CARTESIAN_POINT ( 'NONE',  ( -13.89961937509977652, 13.97604488694528158, 75.62390960531438111 ) ) ;
#153388 = DIRECTION ( 'NONE',  ( 0.000000000000000000, 1.000000000000000000, -0.000000000000000000 ) ) ;
#153389 = CARTESIAN_POINT ( 'NONE',  ( 14.29746914071049879, -8.314922557960816363, 38.33224293864768839 ) ) ;
#153390 = CARTESIAN_POINT ( 'NONE',  ( 10.72451020669898902, -18.67979575497178502, 22.91557627198102765 ) ) ;
#153391 = CARTESIAN_POINT ( 'NONE',  ( -4.999999999999996447, 5.000000000000003553, -15.00000000000000000 ) ) ;
#153392 = ADVANCED_FACE ( 'NONE', ( #4970 ), #30610, .T. ) ;
#153393 = CARTESIAN_POINT ( 'NONE',  ( -5.049401038297874678, -19.05341960407617918, 94.79275706135230450 ) ) ;
#153394 = CARTESIAN_POINT ( 'NONE',  ( 18.67979575497178502, 10.72451020669898547, 69.16557627198102409 ) ) ;
#153395 = CARTESIAN_POINT ( 'NONE',  ( -8.224510206698948167, 14.34966873604960824, 55.41557627198102409 ) ) ;
#153396 = CARTESIAN_POINT ( 'NONE',  ( 16.53943276465976808, 0.05219959533934440121, 21.25109039468567218 ) ) ;
#153397 = CARTESIAN_POINT ( 'NONE',  ( 13.97604488694527802, 13.89961937509977652, 49.37390960531434558 ) ) ;
#153399 = CARTESIAN_POINT ( 'NONE',  ( -5.049401038297874678, -19.05341960407617918, 74.79275706135231871 ) ) ;
#153398 = CARTESIAN_POINT ( 'NONE',  ( 21.53943276465977519, -0.05219959533907433946, 98.74890960531438111 ) ) ;
#153400 = CARTESIAN_POINT ( 'NONE',  ( 13.89961937509977652, -13.97604488694527269, 88.12390960531438111 ) ) ;
#153401 = CARTESIAN_POINT ( 'NONE',  ( -12.06949235617756955, 12.14591786802309770, 80.62390960531438111 ) ) ;
#153402 = CARTESIAN_POINT ( 'NONE',  ( 16.46253265017160672, -9.564922557960803928, 63.33224293864769550 ) ) ;
#153403 = CARTESIAN_POINT ( 'NONE',  ( -0.05219959533910754901, -16.53943276465976808, 72.49890960531435269 ) ) ;
#153404 = CARTESIAN_POINT ( 'NONE',  ( -13.89961937509977652, 13.97604488694528158, 30.62390960531435269 ) ) ;
#153405 = CARTESIAN_POINT ( 'NONE',  ( -36.90807327575559071, -0.7244114042849736368, 50.46397389534120492 ) ) ;
#153406 = CARTESIAN_POINT ( 'NONE',  ( -8.314922557960811034, -14.29746914071050412, 47.08224293864770260 ) ) ;
#153407 = CARTESIAN_POINT ( 'NONE',  ( 16.51473224551069308, 9.474510206698969483, 94.16557627198103830 ) ) ;
#153408 = FACE_BOUND ( 'NONE', #162272, .T. ) ;
#153409 = CARTESIAN_POINT ( 'NONE',  ( -13.97604488694547697, 13.89961937509957934, 53.12609039468565442 ) ) ;
#153410 = CARTESIAN_POINT ( 'NONE',  ( 16.52544592524335698, 4.483927247898782831, 61.45942372801901854 ) ) ;
#153411 = CARTESIAN_POINT ( 'NONE',  ( -21.53943276465977519, 0.05219959533907696930, 61.24890960531435979 ) ) ;
#153412 = CARTESIAN_POINT ( 'NONE',  ( -13.97604488694547697, 13.89961937509957934, 43.12609039468566152 ) ) ;
#153413 = CARTESIAN_POINT ( 'NONE',  ( 13.89961937509977652, -13.97604488694527269, 93.12390960531436690 ) ) ;
#153414 = CYLINDRICAL_SURFACE ( 'NONE', #43693, 216.0437394197456911 ) ;
#153415 = CARTESIAN_POINT ( 'NONE',  ( 21.55341960407610458, 5.719274019375980345, 28.95724293864769905 ) ) ;
#153416 = AXIS2_PLACEMENT_3D ( 'NONE', #5434, #37781, #187511 ) ;
#153417 = CARTESIAN_POINT ( 'NONE',  ( -19.03943276465977164, 0.05219959533909376836, 56.24890960531435979 ) ) ;
#153418 = CARTESIAN_POINT ( 'NONE',  ( -21.55341960407619339, 5.719274019375674811, 58.54275706135235424 ) ) ;
#153420 = CARTESIAN_POINT ( 'NONE',  ( -4.379528057220328563, 16.55341960407611168, 115.2072429386476955 ) ) ;
#153419 = PRODUCT_DEFINITION_SHAPE ( 'NONE', 'NONE',  #200201 ) ;
#153423 = EDGE_LOOP ( 'NONE', ( #187319, #70935, #42011, #171046 ) ) ;
#153422 = CARTESIAN_POINT ( 'NONE',  ( 19.03943276465977164, -0.05219959533909143690, 88.74890960531436690 ) ) ;
#153421 = CARTESIAN_POINT ( 'NONE',  ( 21.55341960407610458, 5.719274019375980345, 98.95724293864770971 ) ) ;
#153424 = CARTESIAN_POINT ( 'NONE',  ( 21.55341960407619695, -5.719274019375665929, 36.04275706135234714 ) ) ;
#153425 = ORIENTED_EDGE ( 'NONE', *, *, #169539, .T. ) ;
#153426 = CARTESIAN_POINT ( 'NONE',  ( -9.564922557960796823, -16.46253265017161027, 102.0822429386477097 ) ) ;
#153427 = PLANE ( 'NONE',  #62457 ) ;
#153428 = CARTESIAN_POINT ( 'NONE',  ( -0.05219959533907301413, -21.53943276465977519, 107.4989096053143669 ) ) ;
#153429 = CARTESIAN_POINT ( 'NONE',  ( -16.51473224551069308, -9.474510206698971260, 51.66557627198102409 ) ) ;
#153430 = CARTESIAN_POINT ( 'NONE',  ( -16.55341960407617563, 4.379528057220093196, 23.54275706135235424 ) ) ;
#153431 = CARTESIAN_POINT ( 'NONE',  ( 23.48529157249600630, -32.32473071737749137, -11.04999999453762527 ) ) ;
#153432 = CARTESIAN_POINT ( 'NONE',  ( 19.03943276465977164, -0.05219959533909143690, 23.74890960531435269 ) ) ;
#153433 = CARTESIAN_POINT ( 'NONE',  ( -10.72451020669870658, -18.67979575497194134, 94.58442372801901854 ) ) ;
#153435 = CARTESIAN_POINT ( 'NONE',  ( -21.55341960407619339, 5.719274019375674811, 48.54275706135234714 ) ) ;
#153434 = CARTESIAN_POINT ( 'NONE',  ( 5.049401038298161559, -19.05341960407611168, 77.70724293864765286 ) ) ;
#153436 = CARTESIAN_POINT ( 'NONE',  ( 8.571926809382597767, 26.38167802310806209, 144.7750000027311899 ) ) ;
#153437 = CARTESIAN_POINT ( 'NONE',  ( -9.564922557960796823, -16.46253265017161027, 102.0822429386477097 ) ) ;
#153438 = FACE_OUTER_BOUND ( 'NONE', #153876, .T. ) ;
#153441 = CARTESIAN_POINT ( 'NONE',  ( -18.62759615963255300, -10.81492255796106328, 54.16775706135235424 ) ) ;
#153440 = CARTESIAN_POINT ( 'NONE',  ( -4.379528057220086978, -16.55341960407618274, 74.79275706135234714 ) ) ;
#153439 = CARTESIAN_POINT ( 'NONE',  ( -4.483927247898782831, 16.52544592524335698, 37.70942372801900433 ) ) ;
#153442 = CARTESIAN_POINT ( 'NONE',  ( -5.719274019375665041, -21.55341960407619695, 84.79275706135234714 ) ) ;
#153443 = DIRECTION ( 'NONE',  ( -0.000000000000000000, -0.4999999999999999445, -0.8660254037844387076 ) ) ;
#153444 = CARTESIAN_POINT ( 'NONE',  ( 4.483927247898790824, -16.52544592524335698, 20.20942372801900788 ) ) ;
#153445 = CARTESIAN_POINT ( 'NONE',  ( -13.89961937509977652, 13.97604488694528158, 70.62390960531432427 ) ) ;
#153446 = CARTESIAN_POINT ( 'NONE',  ( -19.03943276465977164, 0.05219959533909376836, 96.24890960531436690 ) ) ;
#153447 = CARTESIAN_POINT ( 'NONE',  ( -16.52544592524342804, 4.483927247898546575, 106.0405762719810525 ) ) ;
#153448 = CARTESIAN_POINT ( 'NONE',  ( -15.80617190586745835, -15.72974639402198527, 26.87390960531435979 ) ) ;
#153449 = CARTESIAN_POINT ( 'NONE',  ( 16.55341960407618274, -4.379528057220086978, 91.04275706135236135 ) ) ;
#153451 = CARTESIAN_POINT ( 'NONE',  ( 19.02544592524343514, -5.153800228976328945, 53.54057627198102409 ) ) ;
#153450 = CARTESIAN_POINT ( 'NONE',  ( -16.53943276465976808, 0.05219959533911058130, 76.24890960531435269 ) ) ;
#153452 = CARTESIAN_POINT ( 'NONE',  ( -5.719274019375665041, -21.55341960407619695, 74.79275706135234714 ) ) ;
#153453 = CARTESIAN_POINT ( 'NONE',  ( 23.29544513554940366, -16.92513159979222337, 145.0656553485623590 ) ) ;
#153454 = CARTESIAN_POINT ( 'NONE',  ( 19.03943276465977164, 0.05219959533936151252, 101.2510903946856757 ) ) ;
#153455 = CARTESIAN_POINT ( 'NONE',  ( -4.379528057220328563, 16.55341960407611168, 75.20724293864769550 ) ) ;
#153456 = CARTESIAN_POINT ( 'NONE',  ( 0.05219959533937995610, -21.53943276465977519, 35.00109039468568284 ) ) ;
#153457 = CARTESIAN_POINT ( 'NONE',  ( -21.53943276465977519, 0.05219959533907696930, 56.24890960531436690 ) ) ;
#153459 = CARTESIAN_POINT ( 'NONE',  ( -16.61371651742599553, -7.165104196376157475, 106.1458493000700685 ) ) ;
#153458 = AXIS2_PLACEMENT_3D ( 'NONE', #83572, #69417, #96745 ) ;
#153460 = CARTESIAN_POINT ( 'NONE',  ( -8.906447517083053711, -27.41122689804191026, 144.6500000054623740 ) ) ;
#153461 = CARTESIAN_POINT ( 'NONE',  ( -13.97604488694527625, -13.89961937509977652, 86.87390960531436690 ) ) ;
#153462 = CARTESIAN_POINT ( 'NONE',  ( 0.05219959533910956823, 16.53943276465976808, 54.99890960531435269 ) ) ;
#153463 = CARTESIAN_POINT ( 'NONE',  ( 4.379528057220339221, -16.55341960407611168, 32.70724293864770260 ) ) ;
#153464 = CARTESIAN_POINT ( 'NONE',  ( -16.53943276465976808, -0.05219959533934237506, 93.75109039468567573 ) ) ;
#153465 = CARTESIAN_POINT ( 'NONE',  ( -5.049401038297874678, -19.05341960407617918, 54.79275706135234003 ) ) ;
#153466 = LINE ( 'NONE', #2766, #166758 ) ;
#153467 = CARTESIAN_POINT ( 'NONE',  ( -13.89961937509977652, 13.97604488694528158, 100.6239096053143669 ) ) ;
#153468 = ADVANCED_FACE ( 'NONE', ( #182321 ), #92263, .F. ) ;
#153469 = CARTESIAN_POINT ( 'NONE',  ( 16.52544592524342804, -4.483927247898539470, 78.54057627198103830 ) ) ;
#153470 = CARTESIAN_POINT ( 'NONE',  ( -13.97604488694547697, 13.89961937509957934, 38.12609039468566152 ) ) ;
#153472 = CARTESIAN_POINT ( 'NONE',  ( -15.80617190586745835, -15.72974639402198527, 36.87390960531435979 ) ) ;
#153471 = CARTESIAN_POINT ( 'NONE',  ( 5.049401038298161559, -19.05341960407611168, 37.70724293864768839 ) ) ;
#153473 = CARTESIAN_POINT ( 'NONE',  ( -21.55341960407610458, -5.719274019375992779, 61.45724293864770260 ) ) ;
#153474 = CARTESIAN_POINT ( 'NONE',  ( -14.34966873604960291, -8.224510206698953496, 96.66557627198102409 ) ) ;
#153475 = CARTESIAN_POINT ( 'NONE',  ( 4.379528057220092307, 16.55341960407617563, 57.29275706135234714 ) ) ;
#153476 = CARTESIAN_POINT ( 'NONE',  ( -10.72451020669870658, -18.67979575497194134, 39.58442372801901143 ) ) ;
#153477 = CARTESIAN_POINT ( 'NONE',  ( 8.224510206698953496, -14.34966873604960469, 97.91557627198103830 ) ) ;
#153478 = CARTESIAN_POINT ( 'NONE',  ( 16.61371651742597777, -7.165104196376268497, 36.35415069992995996 ) ) ;
#153479 = CARTESIAN_POINT ( 'NONE',  ( -16.52216118717209170, 7.221426719304505859, 48.92400978953009627 ) ) ;
#153480 = CARTESIAN_POINT ( 'NONE',  ( 0.05219959533907565091, 21.53943276465977519, 39.99890960531436690 ) ) ;
#153481 = CARTESIAN_POINT ( 'NONE',  ( -3.573655867282028392E-15, 2.428612866367529932E-14, 149.6527036446661327 ) ) ;
#153482 = CARTESIAN_POINT ( 'NONE',  ( 0.7217796442344650565, 24.11907168720511407, -56.90237149053705679 ) ) ;
#153484 = CARTESIAN_POINT ( 'NONE',  ( 4.483927247898545687, 16.52544592524342804, 34.79057627198103120 ) ) ;
#153483 = CARTESIAN_POINT ( 'NONE',  ( -12.14591786802326823, 12.06949235617739902, 38.12609039468567573 ) ) ;
#153485 = CARTESIAN_POINT ( 'NONE',  ( -5.719274019375978568, 21.55341960407610458, 65.20724293864768129 ) ) ;
#153486 = CARTESIAN_POINT ( 'NONE',  ( -13.97604488694547697, 13.89961937509957934, 88.12609039468563310 ) ) ;
#153487 = CARTESIAN_POINT ( 'NONE',  ( -10.81492255796078084, -18.62759615963271287, 67.08224293864770971 ) ) ;
#153488 = CARTESIAN_POINT ( 'NONE',  ( -19.76513836702804738, 12.18681594171306060, 170.0000000000000000 ) ) ;
#153489 = CARTESIAN_POINT ( 'NONE',  ( -4.483927247898782831, 16.52544592524335698, 52.70942372801902565 ) ) ;
#153491 = CARTESIAN_POINT ( 'NONE',  ( 5.153800228976335163, 19.02544592524342804, 99.79057627198102409 ) ) ;
#153490 = CARTESIAN_POINT ( 'NONE',  ( 13.97604488694527802, 13.89961937509977652, 34.37390960531436690 ) ) ;
#153492 = CARTESIAN_POINT ( 'NONE',  ( 5.153800228976335163, 19.02544592524342804, 39.79057627198100988 ) ) ;
#153493 = CARTESIAN_POINT ( 'NONE',  ( -13.89961937509977652, 13.97604488694528158, 25.62390960531434558 ) ) ;
#153494 = SHAPE_DEFINITION_REPRESENTATION ( #146780, #71529 ) ;
#153495 = DIRECTION ( 'NONE',  ( 0.000000000000000000, 0.000000000000000000, -1.000000000000000000 ) ) ;
#153496 = CARTESIAN_POINT ( 'NONE',  ( -0.05219959533934338120, 16.53943276465976808, 72.50109039468568994 ) ) ;
#153497 = CARTESIAN_POINT ( 'NONE',  ( 0.05219959533907565091, 21.53943276465977519, 94.99890960531436690 ) ) ;
#153498 = CARTESIAN_POINT ( 'NONE',  ( 9.564922557960805705, 16.46253265017160317, 59.58224293864769550 ) ) ;
#153499 = CARTESIAN_POINT ( 'NONE',  ( -15.80617190586768217, 15.72974639402176855, 23.12609039468567573 ) ) ;
#153500 = CARTESIAN_POINT ( 'NONE',  ( 9.564922557960805705, 16.46253265017160317, 79.58224293864769550 ) ) ;
#153501 = CARTESIAN_POINT ( 'NONE',  ( 19.03943276465977164, -0.05219959533909143690, 113.7489096053143669 ) ) ;
#153502 = ORIENTED_EDGE ( 'NONE', *, *, #182203, .T. ) ;
#153503 = CARTESIAN_POINT ( 'NONE',  ( -18.67979575497193778, 10.72451020669871902, 23.33442372801901499 ) ) ;
#153506 = CARTESIAN_POINT ( 'NONE',  ( -16.46253265017146816, -9.564922557961047289, 89.16775706135234714 ) ) ;
#153505 = CARTESIAN_POINT ( 'NONE',  ( -19.02544592524342804, 5.153800228976336051, 111.0405762719810099 ) ) ;
#153504 = CARTESIAN_POINT ( 'NONE',  ( 19.05341960407611168, 5.049401038298154454, 28.95724293864769550 ) ) ;
#153507 = CARTESIAN_POINT ( 'NONE',  ( -9.564922557961040184, 16.46253265017147172, 27.91775706135232582 ) ) ;
#153508 = CARTESIAN_POINT ( 'NONE',  ( 0.05219959533907565091, 21.53943276465977519, 104.9989096053143669 ) ) ;
#153509 = CARTESIAN_POINT ( 'NONE',  ( -9.474510206698720793, -16.51473224551083518, 29.58442372801900433 ) ) ;
#153510 = CARTESIAN_POINT ( 'NONE',  ( 0.05219959533934541429, -16.53943276465976808, 75.00109039468568994 ) ) ;
#153511 = CARTESIAN_POINT ( 'NONE',  ( 19.03943276465977164, -0.05219959533909143690, 108.7489096053143527 ) ) ;
#153512 = CARTESIAN_POINT ( 'NONE',  ( -16.51473224551069308, -9.474510206698971260, 61.66557627198103120 ) ) ;
#153513 = AXIS2_PLACEMENT_3D ( 'NONE', #161896, #23392, #51718 ) ;
#153514 = CARTESIAN_POINT ( 'NONE',  ( 18.67979575497194134, -10.72451020669871369, 65.83442372801900433 ) ) ;
#153515 = CARTESIAN_POINT ( 'NONE',  ( 5.823673210054444382, -21.52544592524334988, 85.20942372801901854 ) ) ;
#153516 = CARTESIAN_POINT ( 'NONE',  ( 16.51473224551069308, 9.474510206698969483, 114.1655762719810241 ) ) ;
#153517 = CARTESIAN_POINT ( 'NONE',  ( -13.89961937509977652, 13.97604488694528158, 80.62390960531436690 ) ) ;
#153518 = CARTESIAN_POINT ( 'NONE',  ( 18.62759615963255655, 10.81492255796105972, 51.66775706135234714 ) ) ;
#153519 = CARTESIAN_POINT ( 'NONE',  ( -19.02544592524334988, -5.153800228976617603, 88.95942372801897591 ) ) ;
#153520 = CARTESIAN_POINT ( 'NONE',  ( -16.51473224551069308, -9.474510206698971260, 46.66557627198102409 ) ) ;
#153521 = CARTESIAN_POINT ( 'NONE',  ( -19.05341960407611168, -5.049401038298163336, 96.45724293864769550 ) ) ;
#153522 = CARTESIAN_POINT ( 'NONE',  ( -19.03943276465977164, 0.05219959533909376836, 66.24890960531436690 ) ) ;
#153523 = CARTESIAN_POINT ( 'NONE',  ( 17.50000000000000355, -3.786494350217929572, 22.85920472064934117 ) ) ;
#153524 = CARTESIAN_POINT ( 'NONE',  ( 13.89961937509977652, -13.97604488694527269, 48.12390960531435979 ) ) ;
#153525 = CARTESIAN_POINT ( 'NONE',  ( 15.72974639402199770, -15.80617190586745480, 93.12390960531436690 ) ) ;
#153526 = CARTESIAN_POINT ( 'NONE',  ( -0.05219959533934338120, 16.53943276465976808, 87.50109039468568994 ) ) ;
#153527 = CARTESIAN_POINT ( 'NONE',  ( 7.121805330552581914, -1.425084765988108071, -64.33521149768084513 ) ) ;
#153528 = CARTESIAN_POINT ( 'NONE',  ( 19.05341960407617918, -5.049401038297876454, 41.04275706135233293 ) ) ;
#153529 = CARTESIAN_POINT ( 'NONE',  ( 19.05341960407611168, 5.049401038298154454, 78.95724293864769550 ) ) ;
#153530 = CARTESIAN_POINT ( 'NONE',  ( -0.05219959533910754901, -16.53943276465976808, 62.49890960531436690 ) ) ;
#153531 = CARTESIAN_POINT ( 'NONE',  ( 8.224510206698953496, -14.34966873604960469, 97.91557627198103830 ) ) ;
#153532 = VECTOR ( 'NONE', #95038, 1000.000000000000000 ) ;
#153533 = CARTESIAN_POINT ( 'NONE',  ( 9.474510206698971260, -16.51473224551069308, 112.9155762719810383 ) ) ;
#153534 = CARTESIAN_POINT ( 'NONE',  ( 5.153800228976335163, 19.02544592524342804, 99.79057627198102409 ) ) ;
#153535 = CARTESIAN_POINT ( 'NONE',  ( -13.97604488694527625, -13.89961937509977652, 111.8739096053143243 ) ) ;
#153536 = CARTESIAN_POINT ( 'NONE',  ( 18.62759615963255655, 10.81492255796105972, 111.6677570613523613 ) ) ;
#153537 = CARTESIAN_POINT ( 'NONE',  ( -16.52544592524335698, -4.483927247898792601, 88.95942372801901854 ) ) ;
#153538 = CARTESIAN_POINT ( 'NONE',  ( 13.89961937509977652, -13.97604488694527269, 78.12390960531433848 ) ) ;
#153539 = CARTESIAN_POINT ( 'NONE',  ( 21.55341960407619695, -5.719274019375665929, 41.04275706135236135 ) ) ;
#153540 = CARTESIAN_POINT ( 'NONE',  ( -21.52544592524343514, 5.823673210054127303, 36.04057627198102409 ) ) ;
#153541 = CARTESIAN_POINT ( 'NONE',  ( -18.67979575497178146, -10.72451020669898902, 111.6655762719810525 ) ) ;
#153542 = CARTESIAN_POINT ( 'NONE',  ( -5.719274019375978568, 21.55341960407610458, 65.20724293864768129 ) ) ;
#153543 = CARTESIAN_POINT ( 'NONE',  ( -12.06949235617756955, 12.14591786802309770, 75.62390960531439532 ) ) ;
#153544 = CARTESIAN_POINT ( 'NONE',  ( -16.46253265017146816, -9.564922557961047289, 44.16775706135232582 ) ) ;
#153545 = CARTESIAN_POINT ( 'NONE',  ( -16.51473224551069308, -9.474510206698971260, 36.66557627198102409 ) ) ;
#153546 = CARTESIAN_POINT ( 'NONE',  ( 9.564922557960805705, 16.46253265017160317, 79.58224293864769550 ) ) ;
#153547 = CARTESIAN_POINT ( 'NONE',  ( 5.049401038298161559, -19.05341960407611168, 77.70724293864765286 ) ) ;
#153548 = CARTESIAN_POINT ( 'NONE',  ( 1.784210473542230573E-15, -29.16686587814331588, 143.3750000027311557 ) ) ;
#153549 = CARTESIAN_POINT ( 'NONE',  ( -0.05219959533910754901, -16.53943276465976808, 97.49890960531436690 ) ) ;
#153550 = ORIENTED_EDGE ( 'NONE', *, *, #132031, .T. ) ;
#153551 = CARTESIAN_POINT ( 'NONE',  ( -8.314922557960811034, -14.29746914071050412, 22.08224293864769194 ) ) ;
#153552 = CARTESIAN_POINT ( 'NONE',  ( 12.14591786802327356, -12.06949235617739191, 30.62609039468567929 ) ) ;
#153553 = CARTESIAN_POINT ( 'NONE',  ( 15.80617190586769283, -15.72974639402175789, 95.62609039468568994 ) ) ;
#153554 = CARTESIAN_POINT ( 'NONE',  ( 16.46253265017160672, -9.564922557960803928, 103.3322429386476955 ) ) ;
#153555 = CARTESIAN_POINT ( 'NONE',  ( 0.05219959533937995610, -21.53943276465977519, 25.00109039468567218 ) ) ;
#153556 = CARTESIAN_POINT ( 'NONE',  ( -0.05219959533909027116, -19.03943276465977164, 37.49890960531436690 ) ) ;
#153557 = CARTESIAN_POINT ( 'NONE',  ( -8.314922557961024197, 14.29746914071037800, 47.91775706135234714 ) ) ;
#153558 = CARTESIAN_POINT ( 'NONE',  ( 5.153800228976615827, -19.02544592524334988, 105.2094237280190185 ) ) ;
#153559 = EDGE_CURVE ( 'NONE', #99775, #76130, #198474, .T. ) ;
#153560 = CARTESIAN_POINT ( 'NONE',  ( 21.53943276465977519, -0.05219959533907433946, 98.74890960531438111 ) ) ;
#153561 = CARTESIAN_POINT ( 'NONE',  ( -16.51473224551082808, 9.474510206698731452, 63.33442372801900433 ) ) ;
#153562 = DIRECTION ( 'NONE',  ( 0.000000000000000000, 0.000000000000000000, -1.000000000000000000 ) ) ;
#153563 = CARTESIAN_POINT ( 'NONE',  ( -10.72451020669898014, 18.67979575497178502, 115.4155762719810241 ) ) ;
#153564 = CARTESIAN_POINT ( 'NONE',  ( -17.81289503416611808, 24.51734667627700404, 141.9500000054623570 ) ) ;
#153565 = CARTESIAN_POINT ( 'NONE',  ( -16.51473224551069308, -9.474510206698971260, 96.66557627198102409 ) ) ;
#153566 = CARTESIAN_POINT ( 'NONE',  ( 38.00373040315627549, 2.428612866367529932E-14, -0.1220970790697140096 ) ) ;
#153567 = CARTESIAN_POINT ( 'NONE',  ( 19.03943276465977164, -0.05219959533909143690, 78.74890960531436690 ) ) ;
#153569 = CARTESIAN_POINT ( 'NONE',  ( 12.06949235617757843, -12.14591786802309237, 83.12390960531436690 ) ) ;
#153568 = CARTESIAN_POINT ( 'NONE',  ( 0.05219959533937995610, -21.53943276465977519, 30.00109039468568284 ) ) ;
#153570 = CARTESIAN_POINT ( 'NONE',  ( -5.153800228976328057, -19.02544592524343514, 87.29057627198103830 ) ) ;
#153572 = CARTESIAN_POINT ( 'NONE',  ( -9.474510206698720793, -16.51473224551083518, 54.58442372801899722 ) ) ;
#153571 = CARTESIAN_POINT ( 'NONE',  ( -12.06949235617739369, -12.14591786802326823, 54.37609039468568994 ) ) ;
#153573 = CARTESIAN_POINT ( 'NONE',  ( 21.53943276465977519, 0.05219959533937863772, 66.25109039468567573 ) ) ;
#153574 = CARTESIAN_POINT ( 'NONE',  ( -12.14591786802326823, 12.06949235617739902, 23.12609039468567573 ) ) ;
#153575 = CARTESIAN_POINT ( 'NONE',  ( -9.564922557960796823, -16.46253265017161027, 67.08224293864769550 ) ) ;
#153576 = CARTESIAN_POINT ( 'NONE',  ( 19.02544592524334988, 5.153800228976608722, 101.4594237280189759 ) ) ;
#153577 = CARTESIAN_POINT ( 'NONE',  ( 16.52544592524335698, 4.483927247898782831, 51.45942372801901854 ) ) ;
#153578 = CARTESIAN_POINT ( 'NONE',  ( -15.80617190586768217, 15.72974639402176855, 98.12609039468570415 ) ) ;
#153579 = CARTESIAN_POINT ( 'NONE',  ( 13.97604488694548053, -13.89961937509957401, 85.62609039468568994 ) ) ;
#153580 = CARTESIAN_POINT ( 'NONE',  ( -19.02544592524342804, 5.153800228976336051, 46.04057627198101699 ) ) ;
#153581 = CARTESIAN_POINT ( 'NONE',  ( -21.53943276465977519, 0.05219959533907696930, 76.24890960531435269 ) ) ;
#153583 = CARTESIAN_POINT ( 'NONE',  ( -0.05219959533936034679, 19.03943276465977164, 82.50109039468567573 ) ) ;
#153582 = CARTESIAN_POINT ( 'NONE',  ( 4.379528057220339221, -16.55341960407611168, 77.70724293864770971 ) ) ;
#153584 = CARTESIAN_POINT ( 'NONE',  ( -19.39056639909675539, -5.499999999999970690, 70.78948781074340957 ) ) ;
#153585 = CARTESIAN_POINT ( 'NONE',  ( 19.03943276465977164, 0.05219959533936151252, 41.25109039468566152 ) ) ;
#153586 = CARTESIAN_POINT ( 'NONE',  ( -16.53943276465976808, -0.05219959533934237506, 113.7510903946856757 ) ) ;
#153587 = CARTESIAN_POINT ( 'NONE',  ( 0.05219959533910956823, 16.53943276465976808, 64.99890960531435269 ) ) ;
#153589 = CARTESIAN_POINT ( 'NONE',  ( 1.784210473542230573E-15, -29.16686587814331588, 145.3750000027311842 ) ) ;
#153588 = CARTESIAN_POINT ( 'NONE',  ( 21.53943276465977519, 0.05219959533937863772, 101.2510903946856757 ) ) ;
#153590 = CARTESIAN_POINT ( 'NONE',  ( 18.67979575497178502, 10.72451020669898547, 114.1655762719810383 ) ) ;
#153591 = CARTESIAN_POINT ( 'NONE',  ( -19.02544592524342804, 5.153800228976336051, 71.04057627198099567 ) ) ;
#153592 = B_SPLINE_CURVE_WITH_KNOTS ( 'NONE', 3,
 ( #82341, #67193, #160206, #97505, #19702, #49056 ),
 .UNSPECIFIED., .F., .F.,
 ( 4, 2, 4 ),
 ( 0.003989672132298028098, 0.004372778065220449609, 0.004755883998142871986 ),
 .UNSPECIFIED. ) ;
#153593 = CARTESIAN_POINT ( 'NONE',  ( 5.823673210054444382, -21.52544592524334988, 85.20942372801901854 ) ) ;
#153594 = CARTESIAN_POINT ( 'NONE',  ( -19.02544592524342804, 5.153800228976336051, 61.04057627198103120 ) ) ;
#153595 = EDGE_LOOP ( 'NONE', ( #1786, #61973, #175262, #192969, #137152 ) ) ;
#153596 = CARTESIAN_POINT ( 'NONE',  ( 9.474510206698971260, -16.51473224551069308, 22.91557627198102765 ) ) ;
#153597 = CARTESIAN_POINT ( 'NONE',  ( 15.80617190586746368, 15.72974639402197994, 34.37390960531435979 ) ) ;
#153598 = AXIS2_PLACEMENT_3D ( 'NONE', #179231, #51860, #193385 ) ;
#153599 = CARTESIAN_POINT ( 'NONE',  ( -14.29746914071049879, 8.314922557960819915, 60.83224293864769550 ) ) ;
#153600 = CARTESIAN_POINT ( 'NONE',  ( 9.564922557960805705, 16.46253265017160317, 39.58224293864768839 ) ) ;
#153601 = CARTESIAN_POINT ( 'NONE',  ( 16.53943276465976808, -0.05219959533910856209, 88.74890960531436690 ) ) ;
#153602 = ADVANCED_FACE ( 'NONE', ( #122607 ), #61920, .F. ) ;
#153603 = CARTESIAN_POINT ( 'NONE',  ( 5.823673210054125526, 21.52544592524343514, 99.79057627198103830 ) ) ;
#153604 = CARTESIAN_POINT ( 'NONE',  ( 0.05219959533937995610, -21.53943276465977519, 55.00109039468568284 ) ) ;
#153605 = CARTESIAN_POINT ( 'NONE',  ( 0.2002308779610947886, 6.100000000000010303, -62.50719930893269805 ) ) ;
#153606 = CARTESIAN_POINT ( 'NONE',  ( -14.29746914071037622, -8.314922557961029526, 54.16775706135235424 ) ) ;
#153607 = CARTESIAN_POINT ( 'NONE',  ( 10.72451020669898902, -18.67979575497178502, 102.9155762719810383 ) ) ;
#153609 = CARTESIAN_POINT ( 'NONE',  ( -13.97604488694527625, -13.89961937509977652, 41.87390960531435979 ) ) ;
#153608 = CARTESIAN_POINT ( 'NONE',  ( 9.564922557961047289, -16.46253265017146816, 25.41775706135234003 ) ) ;
#153610 = CARTESIAN_POINT ( 'NONE',  ( -5.153800228976328057, -19.02544592524343514, 102.2905762719810383 ) ) ;
#153611 = CARTESIAN_POINT ( 'NONE',  ( -15.80617190586768217, 15.72974639402176855, 53.12609039468568284 ) ) ;
#153612 = CARTESIAN_POINT ( 'NONE',  ( 21.52544592524344225, -5.823673210054117533, 48.54057627198103120 ) ) ;
#153613 = CARTESIAN_POINT ( 'NONE',  ( 16.55341960407611168, 4.379528057220329451, 23.95724293864769550 ) ) ;
#153615 = CARTESIAN_POINT ( 'NONE',  ( 5.719274019375673035, 21.55341960407619339, 92.29275706135236135 ) ) ;
#153614 = CARTESIAN_POINT ( 'NONE',  ( 18.62759615963255655, 10.81492255796105972, 66.66775706135234714 ) ) ;
#153616 = CARTESIAN_POINT ( 'NONE',  ( 19.03943276465977164, 0.05219959533936151252, 36.25109039468567573 ) ) ;
#153617 = CARTESIAN_POINT ( 'NONE',  ( 8.314922557961029526, -14.29746914071037800, 95.41775706135234714 ) ) ;
#153618 = CARTESIAN_POINT ( 'NONE',  ( 10.81492255796106328, -18.62759615963255655, 55.41775706135234714 ) ) ;
#153619 = CARTESIAN_POINT ( 'NONE',  ( 16.46253265017160672, -9.564922557960803928, 43.33224293864769550 ) ) ;
#153620 = CARTESIAN_POINT ( 'NONE',  ( 0.05219959533936267826, -19.03943276465977164, 20.00109039468567218 ) ) ;
#153621 = CARTESIAN_POINT ( 'NONE',  ( 10.81492255796078972, 18.62759615963270932, 29.58224293864769905 ) ) ;
#153622 = CARTESIAN_POINT ( 'NONE',  ( 5.823673210054444382, -21.52544592524334988, 20.20942372801900788 ) ) ;
#153623 = CARTESIAN_POINT ( 'NONE',  ( 0.05219959533907565091, 21.53943276465977519, 69.99890960531435269 ) ) ;
#153624 = CARTESIAN_POINT ( 'NONE',  ( 12.06949235617739724, 12.14591786802326823, 41.87609039468568284 ) ) ;
#153626 = CARTESIAN_POINT ( 'NONE',  ( -21.52544592524343514, 5.823673210054127303, 81.04057627198102409 ) ) ;
#153625 = FACE_OUTER_BOUND ( 'NONE', #103203, .T. ) ;
#153629 = CARTESIAN_POINT ( 'NONE',  ( -0.05219959533910754901, -16.53943276465976808, 77.49890960531433848 ) ) ;
#153628 = B_SPLINE_CURVE_WITH_KNOTS ( 'NONE', 3,
 ( #90789, #43317, #164675, #149497, #151496, #72666, #119170, #42330, #88816, #12007, #150509, #126113, #185810, #33116, #1770, #109947, #138301, #107947, #46290, #188796, #171628, #18946, #35093, #32122, #63448, #199982, #169633, #47296, #108953, #17954, #31129, #94773 ),
 .UNSPECIFIED., .F., .F.,
 ( 4, 2, 2, 2, 2, 2, 2, 2, 2, 2, 2, 2, 2, 2, 2, 4 ),
 ( 2.625112965618923374E-17, 0.0003712461730036948552, 0.0007424923460073634728, 0.001113738519011032253, 0.001484984692014700708, 0.002227477038022038485, 0.002598723211025717565, 0.002969969384029396645, 0.003341215557033075725, 0.003712461730036755239, 0.004083707903040433886, 0.004454954076044113399, 0.004826200249047792046, 0.005197446422051471560, 0.005568692595055150206, 0.005939938768058829720 ),
 .UNSPECIFIED. ) ;
#153627 = CARTESIAN_POINT ( 'NONE',  ( 0.05219959533934541429, -16.53943276465976808, 70.00109039468568994 ) ) ;
#153630 = CARTESIAN_POINT ( 'NONE',  ( -27.88129983271673851, -6.733757357603135318, 162.1517353552107750 ) ) ;
#153631 = CARTESIAN_POINT ( 'NONE',  ( 9.564922557961047289, -16.46253265017146816, 110.4177570613523471 ) ) ;
#153632 = CARTESIAN_POINT ( 'NONE',  ( 21.53943276465977519, -0.05219959533907433946, 38.74890960531435979 ) ) ;
#153633 = DIRECTION ( 'NONE',  ( 1.000000000000000000, 0.000000000000000000, 0.000000000000000000 ) ) ;
#153634 = CARTESIAN_POINT ( 'NONE',  ( 16.53943276465976808, 0.05219959533934440121, 41.25109039468568284 ) ) ;
#153635 = CARTESIAN_POINT ( 'NONE',  ( -15.72974639402197994, 15.80617190586746368, 115.6239096053143669 ) ) ;
#153636 = CARTESIAN_POINT ( 'NONE',  ( 15.72974639402199770, -15.80617190586745480, 28.12390960531435979 ) ) ;
#153637 = CARTESIAN_POINT ( 'NONE',  ( -16.55341960407617563, 4.379528057220093196, 58.54275706135235424 ) ) ;
#153638 = CARTESIAN_POINT ( 'NONE',  ( 0.05219959533909260263, 19.03943276465977164, 84.99890960531436690 ) ) ;
#153640 = CARTESIAN_POINT ( 'NONE',  ( 13.97604488694548053, -13.89961937509957401, 105.6260903946856757 ) ) ;
#153639 = CARTESIAN_POINT ( 'NONE',  ( -10.72451020669870658, -18.67979575497194134, 44.58442372801901854 ) ) ;
#153641 = CARTESIAN_POINT ( 'NONE',  ( 21.55341960407610458, 5.719274019375980345, 28.95724293864769905 ) ) ;
#153642 = ORIENTED_EDGE ( 'NONE', *, *, #158809, .F. ) ;
#153643 = CARTESIAN_POINT ( 'NONE',  ( -5.049401038297874678, -19.05341960407617918, 29.79275706135232227 ) ) ;
#153644 = CARTESIAN_POINT ( 'NONE',  ( 8.224510206698742110, 14.34966873604972548, 37.08442372801901143 ) ) ;
#153645 = CARTESIAN_POINT ( 'NONE',  ( 0.05219959533909260263, 19.03943276465977164, 99.99890960531436690 ) ) ;
#153646 = CARTESIAN_POINT ( 'NONE',  ( 10.81492255796078972, 18.62759615963270932, 99.58224293864770971 ) ) ;
#153647 = CARTESIAN_POINT ( 'NONE',  ( -16.51473224551069308, -9.474510206698971260, 66.66557627198102409 ) ) ;
#153648 = CARTESIAN_POINT ( 'NONE',  ( -17.31747979337950838, 6.344076630961000163, 23.62055131934818064 ) ) ;
#153649 = CARTESIAN_POINT ( 'NONE',  ( -16.55341960407611168, -4.379528057220339221, 81.45724293864769550 ) ) ;
#153650 = CARTESIAN_POINT ( 'NONE',  ( 18.62759615963271287, -10.81492255796078972, 38.33224293864768839 ) ) ;
#153651 = CARTESIAN_POINT ( 'NONE',  ( -16.62475595723696742, 7.163666690055234376, 35.52713351810466946 ) ) ;
#153652 = CARTESIAN_POINT ( 'NONE',  ( -0.05219959533934338120, 16.53943276465976808, 62.50109039468568284 ) ) ;
#153653 = CARTESIAN_POINT ( 'NONE',  ( -15.80617190586745835, -15.72974639402198527, 111.8739096053143669 ) ) ;
#153654 = CARTESIAN_POINT ( 'NONE',  ( -16.46253265017146816, -9.564922557961047289, 79.16775706135234714 ) ) ;
#153655 = CARTESIAN_POINT ( 'NONE',  ( -5.049401038298153566, 19.05341960407611168, 30.20724293864768839 ) ) ;
#153656 = CARTESIAN_POINT ( 'NONE',  ( 10.81492255796078972, 18.62759615963270932, 69.58224293864769550 ) ) ;
#153657 = CARTESIAN_POINT ( 'NONE',  ( 19.02544592524343514, -5.153800228976328945, 98.54057627198100988 ) ) ;
#153658 = CARTESIAN_POINT ( 'NONE',  ( -10.81492255796105439, 18.62759615963255655, 92.91775706135236135 ) ) ;
#153659 = CARTESIAN_POINT ( 'NONE',  ( -5.049401038298153566, 19.05341960407611168, 70.20724293864769550 ) ) ;
#153660 = EDGE_CURVE ( 'NONE', #101588, #167413, #98973, .T. ) ;
#153661 = CARTESIAN_POINT ( 'NONE',  ( -16.55341960407617563, 4.379528057220093196, 43.54275706135235424 ) ) ;
#153662 = CARTESIAN_POINT ( 'NONE',  ( 9.474510206698971260, -16.51473224551069308, 62.91557627198102409 ) ) ;
#153663 = CARTESIAN_POINT ( 'NONE',  ( -18.67979575497193778, 10.72451020669871902, 83.33442372801903275 ) ) ;
#153664 = ORIENTED_EDGE ( 'NONE', *, *, #53439, .T. ) ;
#153665 = CARTESIAN_POINT ( 'NONE',  ( -19.05341960407617563, 5.049401038297882671, 33.54275706135231871 ) ) ;
#153666 = CARTESIAN_POINT ( 'NONE',  ( -9.564922557961040184, 16.46253265017147172, 57.91775706135233293 ) ) ;
#153667 = CARTESIAN_POINT ( 'NONE',  ( 18.62759615963255655, 10.81492255796105972, 56.66775706135235424 ) ) ;
#153668 = CARTESIAN_POINT ( 'NONE',  ( -6.100000000000006750, 6.426762577456935076E-14, -62.50719930893269805 ) ) ;
#153669 = CARTESIAN_POINT ( 'NONE',  ( 19.03943276465977164, 0.05219959533936151252, 46.25109039468566863 ) ) ;
#153670 = CARTESIAN_POINT ( 'NONE',  ( -9.564922557960796823, -16.46253265017161027, 102.0822429386477097 ) ) ;
#153671 = CARTESIAN_POINT ( 'NONE',  ( 13.89961937509977652, -13.97604488694527269, 73.12390960531436690 ) ) ;
#153672 = CARTESIAN_POINT ( 'NONE',  ( -16.53943276465976808, 0.05219959533911058130, 26.24890960531435624 ) ) ;
#153674 = CARTESIAN_POINT ( 'NONE',  ( 21.52544592524334988, 5.823673210054432836, 101.4594237280190185 ) ) ;
#153673 = CARTESIAN_POINT ( 'NONE',  ( -9.474510206698964154, 16.51473224551069663, 115.4155762719810241 ) ) ;
#153675 = CARTESIAN_POINT ( 'NONE',  ( 36.91746824999999177, 2.880721459617395097E-14, -8.124999997268814056 ) ) ;
#153676 = CARTESIAN_POINT ( 'NONE',  ( -33.98302989258739615, 4.936846515367097510, 92.54907045995909698 ) ) ;
#153677 = CARTESIAN_POINT ( 'NONE',  ( 21.53943276465977519, 0.05219959533937863772, 96.25109039468568994 ) ) ;
#153678 = CARTESIAN_POINT ( 'NONE',  ( 23.50300173439386242, -1.337618122189738967, -57.33987540012255835 ) ) ;
#153680 = CARTESIAN_POINT ( 'NONE',  ( 8.314922557960818139, 14.29746914071049879, 114.5822429386477097 ) ) ;
#153679 = PRODUCT_RELATED_PRODUCT_CATEGORY ( 'part', '', ( #98692 ) ) ;
#153681 = DIRECTION ( 'NONE',  ( -0.000000000000000000, -0.000000000000000000, 1.000000000000000000 ) ) ;
#153682 = CARTESIAN_POINT ( 'NONE',  ( -25.41627434887079673, -11.65185368830121604, 166.2643564577822985 ) ) ;
#153683 = CARTESIAN_POINT ( 'NONE',  ( -14.29746914071037622, -8.314922557961029526, 54.16775706135235424 ) ) ;
#153684 = CARTESIAN_POINT ( 'NONE',  ( -18.67979575497178146, -10.72451020669898902, 66.66557627198102409 ) ) ;
#153685 = CARTESIAN_POINT ( 'NONE',  ( 12.14591786802309770, 12.06949235617756955, 39.37390960531436690 ) ) ;
#153687 = CARTESIAN_POINT ( 'NONE',  ( 5.049401038298161559, -19.05341960407611168, 92.70724293864769550 ) ) ;
#153686 = CARTESIAN_POINT ( 'NONE',  ( 8.224510206698953496, -14.34966873604960469, 112.9155762719810383 ) ) ;
#153688 = CARTESIAN_POINT ( 'NONE',  ( 19.02544592524334988, 5.153800228976608722, 41.45942372801900433 ) ) ;
#153689 = CARTESIAN_POINT ( 'NONE',  ( -14.34966873604960291, -8.224510206698953496, 111.6655762719810525 ) ) ;
#153690 = CARTESIAN_POINT ( 'NONE',  ( 18.62759615963255655, 10.81492255796105972, 71.66775706135234714 ) ) ;
#153691 = CARTESIAN_POINT ( 'NONE',  ( 1.499999999999999556, 15.20000000000001883, -65.00100000000003320 ) ) ;
#153692 = CARTESIAN_POINT ( 'NONE',  ( -16.53943276465976808, -0.05219959533934237506, 103.7510903946857042 ) ) ;
#153693 = CARTESIAN_POINT ( 'NONE',  ( 3.556970738554034288E-15, -38.81732327939057114, -4.624999997268814056 ) ) ;
#153694 = CARTESIAN_POINT ( 'NONE',  ( 21.55341960407610458, 5.719274019375980345, 33.95724293864769550 ) ) ;
#153695 = CARTESIAN_POINT ( 'NONE',  ( -0.05219959533910754901, -16.53943276465976808, 92.49890960531436690 ) ) ;
#153697 = CARTESIAN_POINT ( 'NONE',  ( -13.89961937509957401, -13.97604488694547875, 54.37609039468565442 ) ) ;
#153696 = TOROIDAL_SURFACE ( 'NONE', #40705, 206.0437394197456911, 10.00000000000000000 ) ;
#153698 = CARTESIAN_POINT ( 'NONE',  ( -9.474510206698964154, 16.51473224551069663, 80.41557627198103830 ) ) ;
#153699 = CARTESIAN_POINT ( 'NONE',  ( 12.14591786802309770, 12.06949235617756955, 79.37390960531436690 ) ) ;
#153700 = CARTESIAN_POINT ( 'NONE',  ( -19.02544592524334988, -5.153800228976617603, 98.95942372801900433 ) ) ;
#153701 = CARTESIAN_POINT ( 'NONE',  ( -21.52544592524343514, 5.823673210054127303, 46.04057627198103830 ) ) ;
#153702 = ORIENTED_EDGE ( 'NONE', *, *, #1430, .F. ) ;
#153703 = CARTESIAN_POINT ( 'NONE',  ( -8.224510206698948167, 14.34966873604960824, 110.4155762719810383 ) ) ;
#153704 = CARTESIAN_POINT ( 'NONE',  ( -16.79531203550650176, -7.028104445595493743, 31.25244988220443076 ) ) ;
#153706 = CARTESIAN_POINT ( 'NONE',  ( 5.823673210054125526, 21.52544592524343514, 79.79057627198102409 ) ) ;
#153705 = CARTESIAN_POINT ( 'NONE',  ( 9.564922557960805705, 16.46253265017160317, 69.58224293864770971 ) ) ;
#153708 = CARTESIAN_POINT ( 'NONE',  ( -16.46253265017160317, 9.564922557960807481, 85.83224293864769550 ) ) ;
#153707 = CARTESIAN_POINT ( 'NONE',  ( -4.379528057220086978, -16.55341960407618274, 94.79275706135234714 ) ) ;
#153709 = CARTESIAN_POINT ( 'NONE',  ( -13.97604488694547697, 13.89961937509957934, 68.12609039468563310 ) ) ;
#153710 = CARTESIAN_POINT ( 'NONE',  ( 21.52544592524334988, 5.823673210054432836, 76.45942372801901854 ) ) ;
#153711 = CARTESIAN_POINT ( 'NONE',  ( -0.05219959533907301413, -21.53943276465977519, 57.49890960531435979 ) ) ;
#153712 = CARTESIAN_POINT ( 'NONE',  ( -0.05219959533907301413, -21.53943276465977519, 27.49890960531435269 ) ) ;
#153713 = CARTESIAN_POINT ( 'NONE',  ( -16.46253265017160317, 9.564922557960807481, 40.83224293864769550 ) ) ;
#153714 = CARTESIAN_POINT ( 'NONE',  ( -12.06949235617739369, -12.14591786802326823, 99.37609039468568994 ) ) ;
#153715 = CARTESIAN_POINT ( 'NONE',  ( 13.89961937509977652, -13.97604488694527269, 48.12390960531435979 ) ) ;
#153716 = CARTESIAN_POINT ( 'NONE',  ( -12.06949235617739369, -12.14591786802326823, 19.37609039468568639 ) ) ;
#153717 = CARTESIAN_POINT ( 'NONE',  ( -31.49170352461663214, -4.578070284816035951, 100.9457761758980325 ) ) ;
#153718 = CARTESIAN_POINT ( 'NONE',  ( 5.719274019375673035, 21.55341960407619339, 107.2927570613523471 ) ) ;
#153719 = CARTESIAN_POINT ( 'NONE',  ( 0.05219959533910956823, 16.53943276465976808, 59.99890960531436690 ) ) ;
#153720 = CARTESIAN_POINT ( 'NONE',  ( 18.67979575497178502, 10.72451020669898547, 114.1655762719810383 ) ) ;
#153721 = CARTESIAN_POINT ( 'NONE',  ( 15.80617190586746368, 15.72974639402197994, 99.37390960531436690 ) ) ;
#153722 = CARTESIAN_POINT ( 'NONE',  ( 27.73933785331498214, 9.013057229001095294, 140.4750000027311785 ) ) ;
#153723 = CARTESIAN_POINT ( 'NONE',  ( -10.72451020669898014, 18.67979575497178502, 45.41557627198103830 ) ) ;
#153724 = CARTESIAN_POINT ( 'NONE',  ( 4.483927247898790824, -16.52544592524335698, 80.20942372801901854 ) ) ;
#153725 = CARTESIAN_POINT ( 'NONE',  ( -12.14591786802309592, -12.06949235617757132, 86.87390960531438111 ) ) ;
#153726 = CARTESIAN_POINT ( 'NONE',  ( -19.02544592524342804, 5.153800228976336051, 56.04057627198100988 ) ) ;
#153727 = CARTESIAN_POINT ( 'NONE',  ( 27.74069374691376311, -6.311165852667638632, 163.4895129000218503 ) ) ;
#153728 = CARTESIAN_POINT ( 'NONE',  ( -12.14591786802326823, 12.06949235617739902, 113.1260903946856899 ) ) ;
#153729 = CARTESIAN_POINT ( 'NONE',  ( 5.823673210054444382, -21.52544592524334988, 35.20942372801901854 ) ) ;
#153730 = CARTESIAN_POINT ( 'NONE',  ( 5.049401038298161559, -19.05341960407611168, 102.7072429386476955 ) ) ;
#153731 = CARTESIAN_POINT ( 'NONE',  ( 5.719274019375673035, 21.55341960407619339, 67.29275706135234714 ) ) ;
#153732 = LINE ( 'NONE', #187089, #56712 ) ;
#153733 = CARTESIAN_POINT ( 'NONE',  ( -16.51473224551069308, -9.474510206698971260, 21.66557627198102765 ) ) ;
#153734 = ORIENTED_EDGE ( 'NONE', *, *, #34928, .F. ) ;
#153735 = CARTESIAN_POINT ( 'NONE',  ( -0.05219959533937732626, 21.53943276465977519, 77.50109039468567573 ) ) ;
#153736 = CARTESIAN_POINT ( 'NONE',  ( -19.05341960407611168, -5.049401038298163336, 46.45724293864768129 ) ) ;
#153737 = CARTESIAN_POINT ( 'NONE',  ( 5.153800228976335163, 19.02544592524342804, 84.79057627198099567 ) ) ;
#153738 = CARTESIAN_POINT ( 'NONE',  ( 16.46253265017146816, 9.564922557961045513, 76.66775706135234714 ) ) ;
#153739 = CARTESIAN_POINT ( 'NONE',  ( 21.52544592524334988, 5.823673210054432836, 36.45942372801901143 ) ) ;
#153740 = CARTESIAN_POINT ( 'NONE',  ( -13.97604488694547697, 13.89961937509957934, 108.1260903946856331 ) ) ;
#153741 = AXIS2_PLACEMENT_3D ( 'NONE', #111475, #171171, #66959 ) ;
#153742 = CARTESIAN_POINT ( 'NONE',  ( 5.049401038297881783, 19.05341960407617563, 77.29275706135231871 ) ) ;
#153743 = CARTESIAN_POINT ( 'NONE',  ( -9.564922557960796823, -16.46253265017161027, 37.08224293864768839 ) ) ;
#153744 = CARTESIAN_POINT ( 'NONE',  ( 19.02544592524334988, 5.153800228976608722, 81.45942372801897591 ) ) ;
#153745 = CARTESIAN_POINT ( 'NONE',  ( 14.34966873604972726, -8.224510206698740333, 105.8344237280190328 ) ) ;
#153746 = CARTESIAN_POINT ( 'NONE',  ( 13.89961937509957401, 13.97604488694547697, 76.87609039468566152 ) ) ;
#153747 = CARTESIAN_POINT ( 'NONE',  ( 16.55341960407611168, 4.379528057220329451, 38.95724293864768839 ) ) ;
#153748 = CARTESIAN_POINT ( 'NONE',  ( 9.474510206698729675, 16.51473224551082808, 47.08442372801900433 ) ) ;
#153749 = CARTESIAN_POINT ( 'NONE',  ( -18.67979575497193778, 10.72451020669871902, 103.3344237280190043 ) ) ;
#153750 = CARTESIAN_POINT ( 'NONE',  ( 13.89961937509957401, 13.97604488694547697, 21.87609039468566152 ) ) ;
#153751 = CARTESIAN_POINT ( 'NONE',  ( -9.474510206698964154, 16.51473224551069663, 35.41557627198102409 ) ) ;
#153752 = CARTESIAN_POINT ( 'NONE',  ( 5.823673210054444382, -21.52544592524334988, 85.20942372801901854 ) ) ;
#153753 = CARTESIAN_POINT ( 'NONE',  ( 16.52544592524335698, 4.483927247898782831, 41.45942372801901143 ) ) ;
#153754 = CARTESIAN_POINT ( 'NONE',  ( 0.05219959533909260263, 19.03943276465977164, 89.99890960531436690 ) ) ;
#153755 = CARTESIAN_POINT ( 'NONE',  ( 1.784210473542230573E-15, -29.16686587814331588, 143.3750000027311557 ) ) ;
#153756 = CARTESIAN_POINT ( 'NONE',  ( 19.05341960407611168, 5.049401038298154454, 93.95724293864769550 ) ) ;
#153757 = EDGE_CURVE ( 'NONE', #198282, #62281, #151151, .T. ) ;
#153758 = CARTESIAN_POINT ( 'NONE',  ( 2.500000000000000000, -1.768423874527823569, 1.021000000000002794 ) ) ;
#153759 = ORIENTED_EDGE ( 'NONE', *, *, #14345, .T. ) ;
#153760 = CARTESIAN_POINT ( 'NONE',  ( -13.89961937509957401, -13.97604488694547875, 79.37609039468567573 ) ) ;
#153761 = CARTESIAN_POINT ( 'NONE',  ( -21.52544592524343514, 5.823673210054127303, 31.04057627198102409 ) ) ;
#153763 = CARTESIAN_POINT ( 'NONE',  ( 5.049401038297881783, 19.05341960407617563, 102.2927570613523045 ) ) ;
#153762 = CARTESIAN_POINT ( 'NONE',  ( -13.89961937509957401, -13.97604488694547875, 19.37609039468566507 ) ) ;
#153764 = CARTESIAN_POINT ( 'NONE',  ( 16.55341960407611168, 4.379528057220329451, 98.95724293864770971 ) ) ;
#153765 = CARTESIAN_POINT ( 'NONE',  ( 13.89961937509977652, -13.97604488694527269, 23.12390960531436335 ) ) ;
#153766 = CARTESIAN_POINT ( 'NONE',  ( -5.719274019375978568, 21.55341960407610458, 65.20724293864768129 ) ) ;
#153767 = CARTESIAN_POINT ( 'NONE',  ( 10.81492255796078972, 18.62759615963270932, 54.58224293864769550 ) ) ;
#153768 = CARTESIAN_POINT ( 'NONE',  ( 5.153800228976335163, 19.02544592524342804, 24.79057627198102765 ) ) ;
#153769 = CARTESIAN_POINT ( 'NONE',  ( -3.573655867282028392E-15, 2.428612866367529932E-14, 155.0000000000000000 ) ) ;
#153770 = CARTESIAN_POINT ( 'NONE',  ( 5.153800228976615827, -19.02544592524334988, 65.20942372801900433 ) ) ;
#153771 = CARTESIAN_POINT ( 'NONE',  ( -14.29746914071049879, 8.314922557960819915, 45.83224293864769550 ) ) ;
#153772 = CARTESIAN_POINT ( 'NONE',  ( -19.02544592524342804, 5.153800228976336051, 116.0405762719810383 ) ) ;
#153773 = CARTESIAN_POINT ( 'NONE',  ( -21.52544592524334988, -5.823673210054445271, 78.95942372801901854 ) ) ;
#153774 = CARTESIAN_POINT ( 'NONE',  ( -5.719274019375978568, 21.55341960407610458, 70.20724293864769550 ) ) ;
#153775 = CARTESIAN_POINT ( 'NONE',  ( 0.05219959533937995610, -21.53943276465977519, 65.00109039468568994 ) ) ;
#153776 = CARTESIAN_POINT ( 'NONE',  ( -21.53943276465977519, -0.05219959533937600094, 48.75109039468568284 ) ) ;
#153777 = CARTESIAN_POINT ( 'NONE',  ( -9.474510206698964154, 16.51473224551069663, 95.41557627198102409 ) ) ;
#153778 = CARTESIAN_POINT ( 'NONE',  ( 12.14591786802327356, -12.06949235617739191, 90.62609039468567573 ) ) ;
#153779 = CARTESIAN_POINT ( 'NONE',  ( -8.314922557960811034, -14.29746914071050412, 112.0822429386477097 ) ) ;
#153780 = CARTESIAN_POINT ( 'NONE',  ( -31.30058771566195830, 6.382914491190407880, 98.94581565101640308 ) ) ;
#153781 = CARTESIAN_POINT ( 'NONE',  ( 14.29746914071049879, -8.314922557960816363, 73.33224293864769550 ) ) ;
#153782 = CARTESIAN_POINT ( 'NONE',  ( -8.224510206698948167, 14.34966873604960824, 40.41557627198103120 ) ) ;
#153783 = CARTESIAN_POINT ( 'NONE',  ( -19.03943276465977164, 0.05219959533909376836, 61.24890960531436690 ) ) ;
#153784 = CARTESIAN_POINT ( 'NONE',  ( 16.46253265017160672, -9.564922557960803928, 38.33224293864768839 ) ) ;
#153785 = CARTESIAN_POINT ( 'NONE',  ( 10.81492255796078972, 18.62759615963270932, 54.58224293864769550 ) ) ;
#153786 = CARTESIAN_POINT ( 'NONE',  ( -13.89961937509957401, -13.97604488694547875, 39.37609039468566152 ) ) ;
#153788 = CARTESIAN_POINT ( 'NONE',  ( -16.52544592524342804, 4.483927247898546575, 51.04057627198103120 ) ) ;
#153787 = DIRECTION ( 'NONE',  ( -1.000000000000000000, 0.000000000000000000, 0.000000000000000000 ) ) ;
#153789 = CARTESIAN_POINT ( 'NONE',  ( 0.05219959533907565091, 21.53943276465977519, 29.99890960531435979 ) ) ;
#153790 = EDGE_LOOP ( 'NONE', ( #45028, #24590, #84223, #42569 ) ) ;
#153791 = CARTESIAN_POINT ( 'NONE',  ( 17.50000000000000000, -5.500000000000000888, 120.0000000000000142 ) ) ;
#153792 = CARTESIAN_POINT ( 'NONE',  ( 4.483927247898790824, -16.52544592524335698, 75.20942372801901854 ) ) ;
#153793 = CARTESIAN_POINT ( 'NONE',  ( 16.46253265017146816, 9.564922557961045513, 81.66775706135233293 ) ) ;
#153794 = CARTESIAN_POINT ( 'NONE',  ( -12.06949235617756955, 12.14591786802309770, 35.62390960531437401 ) ) ;
#153795 = CARTESIAN_POINT ( 'NONE',  ( 16.88567814943160172, -6.947325034625743356, 51.20998877347416567 ) ) ;
#153796 = CARTESIAN_POINT ( 'NONE',  ( 8.314922557960818139, 14.29746914071049879, 29.58224293864769905 ) ) ;
#153797 = CARTESIAN_POINT ( 'NONE',  ( 16.46253265017160672, -9.564922557960803928, 53.33224293864768839 ) ) ;
#153798 = ADVANCED_FACE ( 'NONE', ( #70664 ), #84802, .F. ) ;
#153799 = CARTESIAN_POINT ( 'NONE',  ( 19.05341960407611168, 5.049401038298154454, 78.95724293864769550 ) ) ;
#153800 = CARTESIAN_POINT ( 'NONE',  ( 16.46253265017160672, -9.564922557960803928, 33.33224293864770260 ) ) ;
#153801 = CARTESIAN_POINT ( 'NONE',  ( 15.72974639402176855, 15.80617190586768217, 46.87609039468568994 ) ) ;
#153802 = CARTESIAN_POINT ( 'NONE',  ( -19.02544592524342804, 5.153800228976336051, 56.04057627198100988 ) ) ;
#153803 = DIRECTION ( 'NONE',  ( 0.000000000000000000, 0.000000000000000000, -1.000000000000000000 ) ) ;
#153804 = CARTESIAN_POINT ( 'NONE',  ( -19.03943276465977164, 0.05219959533909376836, 51.24890960531436690 ) ) ;
#153805 = CARTESIAN_POINT ( 'NONE',  ( 0.05219959533907565091, 21.53943276465977519, 34.99890960531435979 ) ) ;
#153807 = CARTESIAN_POINT ( 'NONE',  ( 9.474510206698971260, -16.51473224551069308, 22.91557627198102765 ) ) ;
#153806 = CARTESIAN_POINT ( 'NONE',  ( -18.67979575497193778, 10.72451020669871902, 68.33442372801900433 ) ) ;
#153808 = CARTESIAN_POINT ( 'NONE',  ( 10.72451020669898902, -18.67979575497178502, 27.91557627198103830 ) ) ;
#153809 = CARTESIAN_POINT ( 'NONE',  ( 8.314922557961029526, -14.29746914071037800, 90.41775706135236135 ) ) ;
#153810 = CARTESIAN_POINT ( 'NONE',  ( 21.53943276465977519, 0.05219959533937863772, 101.2510903946856757 ) ) ;
#153811 = CARTESIAN_POINT ( 'NONE',  ( -12.06949235617739369, -12.14591786802326823, 69.37609039468567573 ) ) ;
#153812 = CARTESIAN_POINT ( 'NONE',  ( -19.05341960407611168, -5.049401038298163336, 111.4572429386476671 ) ) ;
#153813 = CARTESIAN_POINT ( 'NONE',  ( -0.05219959533934338120, 16.53943276465976808, 57.50109039468568994 ) ) ;
#153814 = CARTESIAN_POINT ( 'NONE',  ( 16.52544592524335698, 4.483927247898782831, 41.45942372801901143 ) ) ;
#153815 = CARTESIAN_POINT ( 'NONE',  ( 16.53943276465976808, 0.05219959533934440121, 101.2510903946856757 ) ) ;
#153816 = CARTESIAN_POINT ( 'NONE',  ( 21.53943276465977519, 0.05219959533937863772, 51.25109039468568994 ) ) ;
#153817 = CARTESIAN_POINT ( 'NONE',  ( 0.05219959533934541429, -16.53943276465976808, 25.00109039468567218 ) ) ;
#153818 = CARTESIAN_POINT ( 'NONE',  ( -18.67979575497178146, -10.72451020669898902, 111.6655762719810525 ) ) ;
#153819 = CARTESIAN_POINT ( 'NONE',  ( 19.02544592524334988, 5.153800228976608722, 111.4594237280190043 ) ) ;
#153820 = CARTESIAN_POINT ( 'NONE',  ( -8.314922557961024197, 14.29746914071037800, 87.91775706135234714 ) ) ;
#153821 = CARTESIAN_POINT ( 'NONE',  ( 4.999999999999999112, 5.000000000000000888, -15.00000000000000000 ) ) ;
#153822 = CARTESIAN_POINT ( 'NONE',  ( 15.72974639402176855, 15.80617190586768217, 81.87609039468568994 ) ) ;
#153823 = CARTESIAN_POINT ( 'NONE',  ( -19.03943276465977164, -0.05219959533935918106, 78.75109039468567573 ) ) ;
#153824 = CARTESIAN_POINT ( 'NONE',  ( -12.06949235617756955, 12.14591786802309770, 60.62390960531437401 ) ) ;
#153825 = CARTESIAN_POINT ( 'NONE',  ( 8.314922557960818139, 14.29746914071049879, 39.58224293864769550 ) ) ;
#153826 = CARTESIAN_POINT ( 'NONE',  ( -12.06949235617756955, 12.14591786802309770, 100.6239096053143811 ) ) ;
#153828 = CARTESIAN_POINT ( 'NONE',  ( -6.100000000000006750, 6.426762577456935076E-14, -64.53213882399991519 ) ) ;
#153827 = CARTESIAN_POINT ( 'NONE',  ( 16.46253265017146816, 9.564922557961045513, 46.66775706135233293 ) ) ;
#153829 = CARTESIAN_POINT ( 'NONE',  ( -10.81492255796105439, 18.62759615963255655, 47.91775706135234714 ) ) ;
#153830 = CARTESIAN_POINT ( 'NONE',  ( -9.474510206698720793, -16.51473224551083518, 109.5844237280190043 ) ) ;
#153831 = CARTESIAN_POINT ( 'NONE',  ( -16.51473224551069308, -9.474510206698971260, 101.6655762719810241 ) ) ;
#153832 = CARTESIAN_POINT ( 'NONE',  ( 0.05219959533907565091, 21.53943276465977519, 74.99890960531435269 ) ) ;
#153833 = CARTESIAN_POINT ( 'NONE',  ( -16.46253265017146816, -9.564922557961047289, 99.16775706135233293 ) ) ;
#153834 = CARTESIAN_POINT ( 'NONE',  ( -5.049401038298153566, 19.05341960407611168, 105.2072429386476671 ) ) ;
#153835 = CARTESIAN_POINT ( 'NONE',  ( -0.2989490121399997480, -27.96601393914107803, 140.0000000000000853 ) ) ;
#153836 = CARTESIAN_POINT ( 'NONE',  ( -12.06949235617756955, 12.14591786802309770, 105.6239096053143669 ) ) ;
#153837 = CARTESIAN_POINT ( 'NONE',  ( -10.72451020669870658, -18.67979575497194134, 94.58442372801901854 ) ) ;
#153838 = CARTESIAN_POINT ( 'NONE',  ( -9.474510206698964154, 16.51473224551069663, 25.41557627198103120 ) ) ;
#153839 = AXIS2_PLACEMENT_3D ( 'NONE', #58662, #28360, #198178 ) ;
#153840 = CARTESIAN_POINT ( 'NONE',  ( -0.05219959533937732626, 21.53943276465977519, 47.50109039468568994 ) ) ;
#153841 = CARTESIAN_POINT ( 'NONE',  ( -15.72974639402176322, -15.80617190586768395, 84.37609039468570415 ) ) ;
#153842 = CARTESIAN_POINT ( 'NONE',  ( -8.224510206698735004, -14.34966873604973081, 89.58442372801901854 ) ) ;
#153843 = CARTESIAN_POINT ( 'NONE',  ( -21.53943276465977519, -0.05219959533937600094, 48.75109039468568284 ) ) ;
#153844 = CARTESIAN_POINT ( 'NONE',  ( -21.53943276465977519, -0.05219959533937600094, 38.75109039468567573 ) ) ;
#153846 = CARTESIAN_POINT ( 'NONE',  ( -5.049401038298153566, 19.05341960407611168, 95.20724293864770971 ) ) ;
#153845 = CARTESIAN_POINT ( 'NONE',  ( 16.51473224551083163, -9.474510206698727899, 65.83442372801900433 ) ) ;
#153847 = CARTESIAN_POINT ( 'NONE',  ( 0.05219959533910956823, 16.53943276465976808, 99.99890960531436690 ) ) ;
#153848 = CARTESIAN_POINT ( 'NONE',  ( -15.80617190586745835, -15.72974639402198527, 86.87390960531438111 ) ) ;
#153849 = CARTESIAN_POINT ( 'NONE',  ( -16.55341960407611168, -4.379528057220339221, 61.45724293864770260 ) ) ;
#153850 = CARTESIAN_POINT ( 'NONE',  ( -18.67979575497193778, 10.72451020669871902, 98.33442372801901854 ) ) ;
#153851 = CARTESIAN_POINT ( 'NONE',  ( 14.34966873604960469, 8.224510206698951720, 89.16557627198102409 ) ) ;
#153852 = CARTESIAN_POINT ( 'NONE',  ( 16.46253265017160672, -9.564922557960803928, 33.33224293864770260 ) ) ;
#153853 = CARTESIAN_POINT ( 'NONE',  ( 9.564922557961047289, -16.46253265017146816, 75.41775706135234714 ) ) ;
#153854 = CARTESIAN_POINT ( 'NONE',  ( 4.483927247898545687, 16.52544592524342804, 44.79057627198103120 ) ) ;
#153855 = CARTESIAN_POINT ( 'NONE',  ( -15.72974639402176322, -15.80617190586768395, 99.37609039468568994 ) ) ;
#153856 = CARTESIAN_POINT ( 'NONE',  ( -9.564922557960796823, -16.46253265017161027, 92.08224293864769550 ) ) ;
#153857 = CARTESIAN_POINT ( 'NONE',  ( 19.05341960407617918, -5.049401038297876454, 56.04275706135234714 ) ) ;
#153858 = CARTESIAN_POINT ( 'NONE',  ( 21.53943276465977519, -0.05219959533907433946, 58.74890960531436690 ) ) ;
#153859 = CARTESIAN_POINT ( 'NONE',  ( -15.80617190586745835, -15.72974639402198527, 111.8739096053143669 ) ) ;
#153860 = CARTESIAN_POINT ( 'NONE',  ( -4.379528057220086978, -16.55341960407618274, 19.79275706135235069 ) ) ;
#153861 = CARTESIAN_POINT ( 'NONE',  ( -4.483927247898782831, 16.52544592524335698, 77.70942372801900433 ) ) ;
#153863 = CARTESIAN_POINT ( 'NONE',  ( 18.67979575497194134, -10.72451020669871369, 20.83442372801901143 ) ) ;
#153862 = CARTESIAN_POINT ( 'NONE',  ( 5.049401038298161559, -19.05341960407611168, 27.70724293864769550 ) ) ;
#153864 = CARTESIAN_POINT ( 'NONE',  ( -12.14591786802309592, -12.06949235617757132, 111.8739096053143669 ) ) ;
#153865 = CARTESIAN_POINT ( 'NONE',  ( -29.86685920354755197, -21.69954338932560134, -6.924999997268813878 ) ) ;
#153866 = CARTESIAN_POINT ( 'NONE',  ( -4.379528057220086978, -16.55341960407618274, 49.79275706135234714 ) ) ;
#153867 = CARTESIAN_POINT ( 'NONE',  ( -0.05219959533910754901, -16.53943276465976808, 82.49890960531436690 ) ) ;
#153868 = CARTESIAN_POINT ( 'NONE',  ( -21.53943276465977519, 0.05219959533907696930, 76.24890960531435269 ) ) ;
#153869 = CARTESIAN_POINT ( 'NONE',  ( -8.314922557960811034, -14.29746914071050412, 22.08224293864769194 ) ) ;
#153870 = CARTESIAN_POINT ( 'NONE',  ( -16.53943276465976808, -0.05219959533934237506, 33.75109039468568284 ) ) ;
#153871 = CARTESIAN_POINT ( 'NONE',  ( 13.97604488694527802, 13.89961937509977652, 39.37390960531435269 ) ) ;
#153872 = CARTESIAN_POINT ( 'NONE',  ( -12.06949235617739369, -12.14591786802326823, 74.37609039468568994 ) ) ;
#153873 = CARTESIAN_POINT ( 'NONE',  ( 9.474510206698729675, 16.51473224551082808, 72.08442372801900433 ) ) ;
#153874 = CARTESIAN_POINT ( 'NONE',  ( -15.80617190586745835, -15.72974639402198527, 66.87390960531436690 ) ) ;
#153875 = CARTESIAN_POINT ( 'NONE',  ( 14.29746914071037800, 8.314922557961029526, 106.6677570613523756 ) ) ;
#153876 = EDGE_LOOP ( 'NONE', ( #23664, #108606, #65893 ) ) ;
#153877 = CARTESIAN_POINT ( 'NONE',  ( 21.52544592524334988, 5.823673210054432836, 76.45942372801901854 ) ) ;
#153878 = CARTESIAN_POINT ( 'NONE',  ( -10.81492255796078084, -18.62759615963271287, 42.08224293864769550 ) ) ;
#153879 = ORIENTED_EDGE ( 'NONE', *, *, #116955, .F. ) ;
#153880 = ORIENTED_EDGE ( 'NONE', *, *, #172144, .T. ) ;
#153881 = CARTESIAN_POINT ( 'NONE',  ( -8.314922557961024197, 14.29746914071037800, 92.91775706135236135 ) ) ;
#153882 = CARTESIAN_POINT ( 'NONE',  ( 10.81492255796078972, 18.62759615963270932, 39.58224293864769550 ) ) ;
#153883 = ORIENTED_EDGE ( 'NONE', *, *, #43390, .T. ) ;
#153884 = CARTESIAN_POINT ( 'NONE',  ( 19.02544592524343514, -5.153800228976328945, 108.5405762719810383 ) ) ;
#153885 = CARTESIAN_POINT ( 'NONE',  ( 17.50000000000000355, 3.345213924137354411, 107.9123137690565670 ) ) ;
#153886 = CARTESIAN_POINT ( 'NONE',  ( -13.97604488694527625, -13.89961937509977652, 26.87390960531434558 ) ) ;
#153887 = CARTESIAN_POINT ( 'NONE',  ( -21.53943276465977519, 0.05219959533907696930, 81.24890960531436690 ) ) ;
#153888 = CARTESIAN_POINT ( 'NONE',  ( -8.314922557961024197, 14.29746914071037800, 102.9177570613523756 ) ) ;
#153889 = CARTESIAN_POINT ( 'NONE',  ( -10.72451020669870658, -18.67979575497194134, 54.58442372801901143 ) ) ;
#153890 = CARTESIAN_POINT ( 'NONE',  ( -14.34966873604972548, 8.224510206698743886, 23.33442372801901499 ) ) ;
#153891 = CARTESIAN_POINT ( 'NONE',  ( -12.14591786802309592, -12.06949235617757132, 111.8739096053143669 ) ) ;
#153892 = CARTESIAN_POINT ( 'NONE',  ( 13.97604488694548053, -13.89961937509957401, 110.6260903946856615 ) ) ;
#153893 = TOROIDAL_SURFACE ( 'NONE', #111887, 69.99999999999998579, 8.000000000000000000 ) ;
#153894 = CARTESIAN_POINT ( 'NONE',  ( -19.03943276465977164, 0.05219959533909376836, 36.24890960531436690 ) ) ;
#153895 = CARTESIAN_POINT ( 'NONE',  ( 17.81289503416610742, 24.51734667627700404, 145.2999999999999829 ) ) ;
#153896 = CARTESIAN_POINT ( 'NONE',  ( 0.05219959533909260263, 19.03943276465977164, 104.9989096053143669 ) ) ;
#153897 = ADVANCED_FACE ( 'NONE', ( #147506 ), #146481, .F. ) ;
#153898 = CARTESIAN_POINT ( 'NONE',  ( -16.52544592524335698, -4.483927247898792601, 83.95942372801900433 ) ) ;
#153899 = CARTESIAN_POINT ( 'NONE',  ( 13.97604488694548053, -13.89961937509957401, 80.62609039468567573 ) ) ;
#153900 = CARTESIAN_POINT ( 'NONE',  ( -19.02544592524334988, -5.153800228976617603, 28.95942372801900433 ) ) ;
#153901 = CARTESIAN_POINT ( 'NONE',  ( 15.80617190586746368, 15.72974639402197994, 74.37390960531436690 ) ) ;
#153902 = CARTESIAN_POINT ( 'NONE',  ( -16.53943276465976808, -0.05219959533934237506, 93.75109039468567573 ) ) ;
#153903 = CARTESIAN_POINT ( 'NONE',  ( -9.474510206698720793, -16.51473224551083518, 89.58442372801900433 ) ) ;
#153904 = CARTESIAN_POINT ( 'NONE',  ( -19.02544592524342804, 5.153800228976336051, 56.04057627198100988 ) ) ;
#153905 = CARTESIAN_POINT ( 'NONE',  ( -0.05219959533909027116, -19.03943276465977164, 87.49890960531436690 ) ) ;
#153906 = CARTESIAN_POINT ( 'NONE',  ( 0.05219959533937995610, -21.53943276465977519, 50.00109039468568994 ) ) ;
#153907 = CARTESIAN_POINT ( 'NONE',  ( 19.02544592524343514, -5.153800228976328945, 48.54057627198103120 ) ) ;
#153908 = CARTESIAN_POINT ( 'NONE',  ( -16.18388926212238133, -7.379444403734527924, 85.43953151366152099 ) ) ;
#153909 = CARTESIAN_POINT ( 'NONE',  ( -16.51473224551069308, -9.474510206698971260, 106.6655762719810383 ) ) ;
#153910 = CARTESIAN_POINT ( 'NONE',  ( 14.29746914071049879, -8.314922557960816363, 63.33224293864770260 ) ) ;
#153911 = CARTESIAN_POINT ( 'NONE',  ( 5.719274019375991003, -21.55341960407610458, 77.70724293864770971 ) ) ;
#153912 = DIRECTION ( 'NONE',  ( 1.000000000000000000, 0.000000000000000000, 0.000000000000000000 ) ) ;
#153913 = CARTESIAN_POINT ( 'NONE',  ( -13.97604488694547697, 13.89961937509957934, 48.12609039468566863 ) ) ;
#153914 = DIRECTION ( 'NONE',  ( -1.000000000000000000, -0.000000000000000000, -0.000000000000000000 ) ) ;
#153916 = CARTESIAN_POINT ( 'NONE',  ( -16.46253265017160317, 9.564922557960807481, 85.83224293864769550 ) ) ;
#153915 = CARTESIAN_POINT ( 'NONE',  ( -0.05219959533909027116, -19.03943276465977164, 67.49890960531436690 ) ) ;
#153917 = CARTESIAN_POINT ( 'NONE',  ( 4.379528057220092307, 16.55341960407617563, 52.29275706135236135 ) ) ;
#153918 = CARTESIAN_POINT ( 'NONE',  ( 6.259396865588135128, -47.62116666102460272, -24.77619460540839214 ) ) ;
#153919 = CARTESIAN_POINT ( 'NONE',  ( -5.153800228976607833, 19.02544592524334988, 32.70942372801899722 ) ) ;
#153920 = CARTESIAN_POINT ( 'NONE',  ( 17.72517630440434289, -5.499999999999968026, 93.42175719257213018 ) ) ;
#153921 = CARTESIAN_POINT ( 'NONE',  ( 12.06949235617739724, 12.14591786802326823, 86.87609039468568994 ) ) ;
#153922 = EDGE_CURVE ( 'NONE', #199703, #25133, #122099, .T. ) ;
#153923 = CARTESIAN_POINT ( 'NONE',  ( -4.180869859159739299, -4.459673755041124288, -64.53025741665265969 ) ) ;
#153924 = CARTESIAN_POINT ( 'NONE',  ( -4.379528057220086978, -16.55341960407618274, 84.79275706135234714 ) ) ;
#153925 = CARTESIAN_POINT ( 'NONE',  ( -8.224510206698735004, -14.34966873604973081, 59.58442372801901854 ) ) ;
#153926 = CARTESIAN_POINT ( 'NONE',  ( -15.80617190586768217, 15.72974639402176855, 113.1260903946856899 ) ) ;
#153928 = CARTESIAN_POINT ( 'NONE',  ( 9.564922557960805705, 16.46253265017160317, 74.58224293864769550 ) ) ;
#153927 = CARTESIAN_POINT ( 'NONE',  ( 16.46253265017160672, -9.564922557960803928, 53.33224293864768839 ) ) ;
#153929 = CARTESIAN_POINT ( 'NONE',  ( 5.823673210054444382, -21.52544592524334988, 65.20942372801901854 ) ) ;
#153930 = CARTESIAN_POINT ( 'NONE',  ( 16.46253265017146816, 9.564922557961045513, 76.66775706135234714 ) ) ;
#153931 = CARTESIAN_POINT ( 'NONE',  ( -21.52544592524334988, -5.823673210054445271, 103.9594237280190185 ) ) ;
#153932 = CARTESIAN_POINT ( 'NONE',  ( 19.03943276465977164, -0.05219959533909143690, 28.74890960531435624 ) ) ;
#153933 = CARTESIAN_POINT ( 'NONE',  ( -27.86273085795037474, -28.69962071417356242, -4.999999999999999112 ) ) ;
#153934 = CARTESIAN_POINT ( 'NONE',  ( 10.81492255796078972, 18.62759615963270932, 64.58224293864769550 ) ) ;
#153935 = CARTESIAN_POINT ( 'NONE',  ( -5.719274019375978568, 21.55341960407610458, 25.20724293864769550 ) ) ;
#153936 = CARTESIAN_POINT ( 'NONE',  ( -8.224510206698948167, 14.34966873604960824, 110.4155762719810383 ) ) ;
#153937 = CARTESIAN_POINT ( 'NONE',  ( -16.55341960407617563, 4.379528057220093196, 38.54275706135234714 ) ) ;
#153938 = CARTESIAN_POINT ( 'NONE',  ( 14.34966873604960469, 8.224510206698951720, 29.16557627198103120 ) ) ;
#153939 = VERTEX_POINT ( 'NONE', #39319 ) ;
#153940 = CARTESIAN_POINT ( 'NONE',  ( -10.72451020669898014, 18.67979575497178502, 110.4155762719810383 ) ) ;
#153942 = CARTESIAN_POINT ( 'NONE',  ( 23.48529157249600630, -32.32473071737749137, -7.299999999999998934 ) ) ;
#153941 = CARTESIAN_POINT ( 'NONE',  ( 16.53943276465976808, -0.05219959533910856209, 38.74890960531435979 ) ) ;
#153943 = CARTESIAN_POINT ( 'NONE',  ( -19.05341960407617563, 5.049401038297882671, 108.5427570613523187 ) ) ;
#153944 = CARTESIAN_POINT ( 'NONE',  ( -0.05219959533936034679, 19.03943276465977164, 27.50109039468566507 ) ) ;
#153945 = CARTESIAN_POINT ( 'NONE',  ( -4.379528057220328563, 16.55341960407611168, 50.20724293864769550 ) ) ;
#153946 = CARTESIAN_POINT ( 'NONE',  ( 18.62759615963271287, -10.81492255796078972, 108.3322429386477097 ) ) ;
#153948 = CARTESIAN_POINT ( 'NONE',  ( -21.55341960407610458, -5.719274019375992779, 61.45724293864770260 ) ) ;
#153947 = CARTESIAN_POINT ( 'NONE',  ( 16.19135201231369336, 7.376712067591808974, 32.68680854052032458 ) ) ;
#153949 = CARTESIAN_POINT ( 'NONE',  ( 9.474510206698971260, -16.51473224551069308, 82.91557627198103830 ) ) ;
#153950 = CARTESIAN_POINT ( 'NONE',  ( 14.34966873604960469, 8.224510206698951720, 44.16557627198103120 ) ) ;
#153951 = CARTESIAN_POINT ( 'NONE',  ( -16.51473224551069308, -9.474510206698971260, 106.6655762719810383 ) ) ;
#153952 = CARTESIAN_POINT ( 'NONE',  ( 1.300000000000000044, -0.7216878364870318308, -1.250000000000000000 ) ) ;
#153953 = CARTESIAN_POINT ( 'NONE',  ( 5.153800228976615827, -19.02544592524334988, 60.20942372801899012 ) ) ;
#153954 = CARTESIAN_POINT ( 'NONE',  ( 15.80617190586746368, 15.72974639402197994, 94.37390960531436690 ) ) ;
#153955 = CARTESIAN_POINT ( 'NONE',  ( -19.05341960407611168, -5.049401038298163336, 41.45724293864769550 ) ) ;
#153956 = CARTESIAN_POINT ( 'NONE',  ( 4.483927247898545687, 16.52544592524342804, 109.7905762719810383 ) ) ;
#153957 = CARTESIAN_POINT ( 'NONE',  ( 15.72974639402176855, 15.80617190586768217, 46.87609039468568994 ) ) ;
#153958 = CARTESIAN_POINT ( 'NONE',  ( -22.44159573604010305, 16.30477369853692338, 146.6750000027311671 ) ) ;
#153959 = CARTESIAN_POINT ( 'NONE',  ( 8.224510206698953496, -14.34966873604960469, 32.91557627198102409 ) ) ;
#153960 = CARTESIAN_POINT ( 'NONE',  ( -13.89961937509977652, 13.97604488694528158, 50.62390960531435979 ) ) ;
#153961 = CARTESIAN_POINT ( 'NONE',  ( 19.03943276465977164, -0.05219959533909143690, 98.74890960531436690 ) ) ;
#153962 = CARTESIAN_POINT ( 'NONE',  ( -5.823673210054116645, -21.52544592524344225, 62.29057627198102409 ) ) ;
#153963 = CARTESIAN_POINT ( 'NONE',  ( -19.36337904590690329, 5.499999999999949374, 45.41494137495620720 ) ) ;
#153964 = CARTESIAN_POINT ( 'NONE',  ( -0.05219959533909027116, -19.03943276465977164, 47.49890960531435979 ) ) ;
#153965 = CARTESIAN_POINT ( 'NONE',  ( -5.719274019375978568, 21.55341960407610458, 55.20724293864770260 ) ) ;
#153966 = ORIENTED_EDGE ( 'NONE', *, *, #97744, .T. ) ;
#153967 = CARTESIAN_POINT ( 'NONE',  ( -10.81492255796105439, 18.62759615963255655, 92.91775706135236135 ) ) ;
#153969 = CARTESIAN_POINT ( 'NONE',  ( -12.06949235617739369, -12.14591786802326823, 89.37609039468568994 ) ) ;
#153968 = CARTESIAN_POINT ( 'NONE',  ( 12.81081878836725707, -36.21111560917147898, -23.25335493478531745 ) ) ;
#153970 = CARTESIAN_POINT ( 'NONE',  ( 4.379528057220092307, 16.55341960407617563, 92.29275706135236135 ) ) ;
#153971 = CARTESIAN_POINT ( 'NONE',  ( 9.474510206698971260, -16.51473224551069308, 57.91557627198103120 ) ) ;
#153972 = CARTESIAN_POINT ( 'NONE',  ( -13.89961937509977652, 13.97604488694528158, 60.62390960531436690 ) ) ;
#153973 = EDGE_LOOP ( 'NONE', ( #122841, #114332, #184837, #198023 ) ) ;
#153974 = CARTESIAN_POINT ( 'NONE',  ( 19.05341960407617918, -5.049401038297876454, 26.04275706135233293 ) ) ;
#153975 = CARTESIAN_POINT ( 'NONE',  ( 8.224510206698742110, 14.34966873604972548, 72.08442372801899012 ) ) ;
#153976 = CARTESIAN_POINT ( 'NONE',  ( -18.67979575497193778, 10.72451020669871902, 108.3344237280190185 ) ) ;
#153977 = CARTESIAN_POINT ( 'NONE',  ( 5.049401038298161559, -19.05341960407611168, 72.70724293864768129 ) ) ;
#153978 = CARTESIAN_POINT ( 'NONE',  ( -0.05219959533907301413, -21.53943276465977519, 52.49890960531435979 ) ) ;
#153979 = CARTESIAN_POINT ( 'NONE',  ( -12.06949235617739369, -12.14591786802326823, 29.37609039468568284 ) ) ;
#153980 = CARTESIAN_POINT ( 'NONE',  ( 18.67979575497194134, -10.72451020669871369, 75.83442372801900433 ) ) ;
#153981 = CARTESIAN_POINT ( 'NONE',  ( 8.224510206698742110, 14.34966873604972548, 47.08442372801901854 ) ) ;
#153982 = CARTESIAN_POINT ( 'NONE',  ( -5.823673210054116645, -21.52544592524344225, 107.2905762719810525 ) ) ;
#153983 = CARTESIAN_POINT ( 'NONE',  ( -16.53943276465976808, -0.05219959533934237506, 23.75109039468567929 ) ) ;
#153984 = CARTESIAN_POINT ( 'NONE',  ( -19.02544592524342804, 5.153800228976336051, 76.04057627198102409 ) ) ;
#153985 = CARTESIAN_POINT ( 'NONE',  ( -4.379528057220086978, -16.55341960407618274, 29.79275706135234358 ) ) ;
#153986 = CARTESIAN_POINT ( 'NONE',  ( -13.89961937509977652, 13.97604488694528158, 45.62390960531433848 ) ) ;
#153987 = CARTESIAN_POINT ( 'NONE',  ( 12.14591786802327356, -12.06949235617739191, 25.62609039468567929 ) ) ;
#153988 = CARTESIAN_POINT ( 'NONE',  ( 0.05219959533910956823, 16.53943276465976808, 74.99890960531435269 ) ) ;
#153989 = CARTESIAN_POINT ( 'NONE',  ( 14.29746914071037800, 8.314922557961029526, 91.66775706135234714 ) ) ;
#153991 = CARTESIAN_POINT ( 'NONE',  ( 16.51473224551069308, 9.474510206698969483, 64.16557627198102409 ) ) ;
#153990 = CARTESIAN_POINT ( 'NONE',  ( -21.55341960407619339, 5.719274019375674811, 28.54275706135234358 ) ) ;
#153992 = CARTESIAN_POINT ( 'NONE',  ( -5.049401038298153566, 19.05341960407611168, 70.20724293864769550 ) ) ;
#153993 = CARTESIAN_POINT ( 'NONE',  ( 4.483927247898790824, -16.52544592524335698, 85.20942372801901854 ) ) ;
#153995 = ORIENTED_EDGE ( 'NONE', *, *, #16822, .T. ) ;
#153994 = CARTESIAN_POINT ( 'NONE',  ( 17.50000000000000000, 5.499999999999992895, 51.70309617465830598 ) ) ;
#153996 = VERTEX_POINT ( 'NONE', #174843 ) ;
#153997 = CARTESIAN_POINT ( 'NONE',  ( -0.05219959533936034679, 19.03943276465977164, 32.50109039468566863 ) ) ;
#153998 = TOROIDAL_SURFACE ( 'NONE', #37365, 69.99999999999998579, 8.000000000000000000 ) ;
#153999 = EDGE_CURVE ( 'NONE', #96409, #118975, #53723, .T. ) ;
#154000 = CARTESIAN_POINT ( 'NONE',  ( -9.564922557960796823, -16.46253265017161027, 32.08224293864769550 ) ) ;
#154002 = ORIENTED_EDGE ( 'NONE', *, *, #116795, .F. ) ;
#154001 = CARTESIAN_POINT ( 'NONE',  ( 9.474510206698971260, -16.51473224551069308, 112.9155762719810383 ) ) ;
#154003 = CARTESIAN_POINT ( 'NONE',  ( -8.314922557961024197, 14.29746914071037800, 22.91775706135235069 ) ) ;
#154005 = CARTESIAN_POINT ( 'NONE',  ( -16.53943276465976808, -0.05219959533934237506, 38.75109039468567573 ) ) ;
#154004 = CARTESIAN_POINT ( 'NONE',  ( -9.564922557961040184, 16.46253265017147172, 52.91775706135233293 ) ) ;
#154006 = CARTESIAN_POINT ( 'NONE',  ( 13.89961937509977652, -13.97604488694527269, 108.1239096053143669 ) ) ;
#154007 = CARTESIAN_POINT ( 'NONE',  ( -5.049401038298153566, 19.05341960407611168, 65.20724293864765286 ) ) ;
#154008 = CARTESIAN_POINT ( 'NONE',  ( 15.72974639402199770, -15.80617190586745480, 98.12390960531436690 ) ) ;
#154010 = CARTESIAN_POINT ( 'NONE',  ( 17.37577197770832527, -5.499999999999936939, 21.30611277022550354 ) ) ;
#154009 = CARTESIAN_POINT ( 'NONE',  ( 13.89961937509977652, -13.97604488694527269, 98.12390960531433848 ) ) ;
#154011 =( REPRESENTATION_RELATIONSHIP ('NONE','NONE', #154205, #8335 ) REPRESENTATION_RELATIONSHIP_WITH_TRANSFORMATION ( #66449 )SHAPE_REPRESENTATION_RELATIONSHIP( ) );
#154012 = CARTESIAN_POINT ( 'NONE',  ( -5.049401038298153566, 19.05341960407611168, 65.20724293864765286 ) ) ;
#154014 = CARTESIAN_POINT ( 'NONE',  ( -13.89961937509977652, 13.97604488694528158, 25.62390960531434558 ) ) ;
#154013 = CARTESIAN_POINT ( 'NONE',  ( -12.06949235617756955, 12.14591786802309770, 25.62390960531435624 ) ) ;
#154015 = CARTESIAN_POINT ( 'NONE',  ( -9.474510206698720793, -16.51473224551083518, 39.58442372801899722 ) ) ;
#154016 = CARTESIAN_POINT ( 'NONE',  ( -12.14591786802309592, -12.06949235617757132, 61.87390960531436690 ) ) ;
#154017 = CARTESIAN_POINT ( 'NONE',  ( -21.55341960407619339, 5.719274019375674811, 103.5427570613523613 ) ) ;
#154018 = CARTESIAN_POINT ( 'NONE',  ( -5.049401038298153566, 19.05341960407611168, 35.20724293864768839 ) ) ;
#154019 = CARTESIAN_POINT ( 'NONE',  ( -8.314922557961024197, 14.29746914071037800, 57.91775706135234714 ) ) ;
#154021 = CARTESIAN_POINT ( 'NONE',  ( 21.55341960407619695, -5.719274019375665929, 86.04275706135236135 ) ) ;
#154020 = CARTESIAN_POINT ( 'NONE',  ( -16.55341960407611168, -4.379528057220339221, 36.45724293864768839 ) ) ;
#154022 = CARTESIAN_POINT ( 'NONE',  ( 19.03943276465977164, -0.05219959533909143690, 78.74890960531436690 ) ) ;
#154023 = CARTESIAN_POINT ( 'NONE',  ( 9.564922557960805705, 16.46253265017160317, 99.58224293864770971 ) ) ;
#154024 = CARTESIAN_POINT ( 'NONE',  ( 14.34966873604960469, 8.224510206698951720, 114.1655762719810383 ) ) ;
#154025 = CARTESIAN_POINT ( 'NONE',  ( 4.379528057220339221, -16.55341960407611168, 72.70724293864769550 ) ) ;
#154026 = CARTESIAN_POINT ( 'NONE',  ( -5.823673210054116645, -21.52544592524344225, 87.29057627198103830 ) ) ;
#154027 = CARTESIAN_POINT ( 'NONE',  ( -9.564922557960796823, -16.46253265017161027, 72.08224293864770971 ) ) ;
#154028 = CARTESIAN_POINT ( 'NONE',  ( -0.05219959533907301413, -21.53943276465977519, 102.4989096053143811 ) ) ;
#154029 = CARTESIAN_POINT ( 'NONE',  ( 19.02544592524334988, 5.153800228976608722, 76.45942372801897591 ) ) ;
#154031 = CARTESIAN_POINT ( 'NONE',  ( 12.06949235617757843, -12.14591786802309237, 93.12390960531436690 ) ) ;
#154030 = CARTESIAN_POINT ( 'NONE',  ( 19.48894818550242292, -5.500000000000105693, 47.60307310435243267 ) ) ;
#154033 = CARTESIAN_POINT ( 'NONE',  ( -9.474510206698964154, 16.51473224551069663, 60.41557627198102409 ) ) ;
#154032 = AXIS2_PLACEMENT_3D ( 'NONE', #185566, #15724, #166686 ) ;
#154034 = CARTESIAN_POINT ( 'NONE',  ( 5.719274019375991003, -21.55341960407610458, 72.70724293864769550 ) ) ;
#154035 = CARTESIAN_POINT ( 'NONE',  ( 17.50000000000000355, -5.499999999999992006, 26.21769037696436300 ) ) ;
#154036 = CARTESIAN_POINT ( 'NONE',  ( 0.05219959533934541429, -16.53943276465976808, 110.0010903946856757 ) ) ;
#154037 = CARTESIAN_POINT ( 'NONE',  ( 14.29746914071037800, 8.314922557961029526, 21.66775706135235069 ) ) ;
#154038 = CARTESIAN_POINT ( 'NONE',  ( -16.52544592524342804, 4.483927247898546575, 81.04057627198102409 ) ) ;
#154039 = CARTESIAN_POINT ( 'NONE',  ( -17.50000000000001066, -5.500000000000021316, 46.28230962303566542 ) ) ;
#154040 = CARTESIAN_POINT ( 'NONE',  ( 13.89961937509977652, -13.97604488694527269, 68.12390960531436690 ) ) ;
#154041 = CARTESIAN_POINT ( 'NONE',  ( -5.153800228976328057, -19.02544592524343514, 37.29057627198102409 ) ) ;
#154042 = CARTESIAN_POINT ( 'NONE',  ( 16.53943276465976808, -0.05219959533910856209, 63.74890960531435979 ) ) ;
#154043 = CARTESIAN_POINT ( 'NONE',  ( 0.05219959533909260263, 19.03943276465977164, 109.9989096053143669 ) ) ;
#154044 = CARTESIAN_POINT ( 'NONE',  ( -5.153800228976607833, 19.02544592524334988, 92.70942372801901854 ) ) ;
#154045 = CARTESIAN_POINT ( 'NONE',  ( -19.02544592524342804, 5.153800228976336051, 106.0405762719810241 ) ) ;
#154046 = CARTESIAN_POINT ( 'NONE',  ( -18.62759615963270932, 10.81492255796079327, 70.83224293864770971 ) ) ;
#154047 = CARTESIAN_POINT ( 'NONE',  ( 12.06949235617739724, 12.14591786802326823, 66.87609039468568994 ) ) ;
#154048 = CARTESIAN_POINT ( 'NONE',  ( -16.88567814943195344, 6.947325034625343676, 93.70998877347403777 ) ) ;
#154049 = CARTESIAN_POINT ( 'NONE',  ( 9.474510206698971260, -16.51473224551069308, 57.91557627198103120 ) ) ;
#154050 = CARTESIAN_POINT ( 'NONE',  ( -0.05219959533907301413, -21.53943276465977519, 72.49890960531435269 ) ) ;
#154051 = CARTESIAN_POINT ( 'NONE',  ( 16.46253265017146816, 9.564922557961045513, 101.6677570613523329 ) ) ;
#154053 = CARTESIAN_POINT ( 'NONE',  ( 15.80617190586769283, -15.72974639402175789, 60.62609039468567573 ) ) ;
#154052 = CARTESIAN_POINT ( 'NONE',  ( -16.55341960407611168, -4.379528057220339221, 41.45724293864769550 ) ) ;
#154054 = CARTESIAN_POINT ( 'NONE',  ( -26.58496454516998853, -7.626754437231455519, 167.9682100371138915 ) ) ;
#154056 = CARTESIAN_POINT ( 'NONE',  ( -13.89961937509977652, 13.97604488694528158, 105.6239096053143527 ) ) ;
#154055 = CARTESIAN_POINT ( 'NONE',  ( -16.53943276465976808, -0.05219959533934237506, 68.75109039468568994 ) ) ;
#154057 = DIRECTION ( 'NONE',  ( -0.000000000000000000, -0.000000000000000000, -1.000000000000000000 ) ) ;
#154058 = LINE ( 'NONE', #15553, #29290 ) ;
#154059 = CARTESIAN_POINT ( 'NONE',  ( 12.06949235617739724, 12.14591786802326823, 91.87609039468568994 ) ) ;
#154060 = CARTESIAN_POINT ( 'NONE',  ( 4.379528057220092307, 16.55341960407617563, 47.29275706135234003 ) ) ;
#154061 = CARTESIAN_POINT ( 'NONE',  ( -5.049401038298153566, 19.05341960407611168, 65.20724293864765286 ) ) ;
#154062 = CARTESIAN_POINT ( 'NONE',  ( -9.564922557960796823, -16.46253265017161027, 72.08224293864770971 ) ) ;
#154063 = CARTESIAN_POINT ( 'NONE',  ( 10.72451020669871369, 18.67979575497193778, 52.08442372801901854 ) ) ;
#154064 = CARTESIAN_POINT ( 'NONE',  ( -0.05219959533934338120, 16.53943276465976808, 57.50109039468568994 ) ) ;
#154065 = CARTESIAN_POINT ( 'NONE',  ( 8.224510206698953496, -14.34966873604960469, 27.91557627198103830 ) ) ;
#154066 = CARTESIAN_POINT ( 'NONE',  ( -19.05341960407611168, -5.049401038298163336, 36.45724293864766707 ) ) ;
#154067 = CARTESIAN_POINT ( 'NONE',  ( -16.51473224551069308, -9.474510206698971260, 31.66557627198102054 ) ) ;
#154069 = VERTEX_POINT ( 'NONE', #8996 ) ;
#154068 = CARTESIAN_POINT ( 'NONE',  ( -8.224510206698735004, -14.34966873604973081, 29.58442372801901854 ) ) ;
#154070 = CARTESIAN_POINT ( 'NONE',  ( 13.89961937509957401, 13.97604488694547697, 81.87609039468564731 ) ) ;
#154071 = CARTESIAN_POINT ( 'NONE',  ( 12.06949235617757843, -12.14591786802309237, 78.12390960531436690 ) ) ;
#154072 = CARTESIAN_POINT ( 'NONE',  ( -9.564922557960796823, -16.46253265017161027, 47.08224293864769550 ) ) ;
#154074 = CARTESIAN_POINT ( 'NONE',  ( 3.766062262543149401E-15, -39.95556452105413570, -7.500000000000000888 ) ) ;
#154073 = CARTESIAN_POINT ( 'NONE',  ( 16.46253265017146816, 9.564922557961045513, 86.66775706135233293 ) ) ;
#154075 = CARTESIAN_POINT ( 'NONE',  ( -21.52544592524334988, -5.823673210054445271, 83.95942372801900433 ) ) ;
#154076 = CARTESIAN_POINT ( 'NONE',  ( 16.55341960407618274, -4.379528057220086978, 56.04275706135235424 ) ) ;
#154077 = CARTESIAN_POINT ( 'NONE',  ( -15.49999999999999822, 7.499999999999998224, 120.0000000000000142 ) ) ;
#154078 = CARTESIAN_POINT ( 'NONE',  ( -21.52544592524343514, 5.823673210054127303, 46.04057627198103830 ) ) ;
#154079 = CARTESIAN_POINT ( 'NONE',  ( 0.05219959533934541429, -16.53943276465976808, 35.00109039468568284 ) ) ;
#154080 = CARTESIAN_POINT ( 'NONE',  ( -0.05219959533909027116, -19.03943276465977164, 37.49890960531436690 ) ) ;
#154081 = CARTESIAN_POINT ( 'NONE',  ( 19.03943276465977164, 0.05219959533936151252, 36.25109039468567573 ) ) ;
#154082 = CARTESIAN_POINT ( 'NONE',  ( -19.02544592524342804, 5.153800228976336051, 91.04057627198100988 ) ) ;
#154083 = CARTESIAN_POINT ( 'NONE',  ( 0.05219959533909260263, 19.03943276465977164, 49.99890960531435979 ) ) ;
#154084 = CARTESIAN_POINT ( 'NONE',  ( 15.84704938773726823, 17.60909914540862431, -54.71262039249373998 ) ) ;
#154085 = CARTESIAN_POINT ( 'NONE',  ( 10.72451020669871369, 18.67979575497193778, 77.08442372801901854 ) ) ;
#154086 = CARTESIAN_POINT ( 'NONE',  ( 28.85599147140293752, 2.428612866367529932E-14, 149.6527036446661327 ) ) ;
#154087 = CARTESIAN_POINT ( 'NONE',  ( -5.049401038297874678, -19.05341960407617918, 34.79275706135233293 ) ) ;
#154088 = CARTESIAN_POINT ( 'NONE',  ( -21.52544592524334988, -5.823673210054445271, 108.9594237280190185 ) ) ;
#154089 = CARTESIAN_POINT ( 'NONE',  ( 14.29746914071049879, -8.314922557960816363, 43.33224293864769550 ) ) ;
#154090 = CARTESIAN_POINT ( 'NONE',  ( 16.51473224551069308, 9.474510206698969483, 49.16557627198102409 ) ) ;
#154091 = CARTESIAN_POINT ( 'NONE',  ( 19.03943276465977164, -0.05219959533909143690, 108.7489096053143527 ) ) ;
#154092 = CARTESIAN_POINT ( 'NONE',  ( 21.55341960407619695, -5.719274019375665929, 81.04275706135236135 ) ) ;
#154093 = CARTESIAN_POINT ( 'NONE',  ( 0.05219959533909260263, 19.03943276465977164, 59.99890960531436690 ) ) ;
#154094 = CARTESIAN_POINT ( 'NONE',  ( 5.823673210054444382, -21.52544592524334988, 80.20942372801901854 ) ) ;
#154095 = CARTESIAN_POINT ( 'NONE',  ( -15.72974639402197994, 15.80617190586746368, 40.62390960531435269 ) ) ;
#154096 = CARTESIAN_POINT ( 'NONE',  ( 15.72974639402176855, 15.80617190586768217, 31.87609039468567929 ) ) ;
#154097 = CARTESIAN_POINT ( 'NONE',  ( -13.89961937509957401, -13.97604488694547875, 49.37609039468567573 ) ) ;
#154098 = CARTESIAN_POINT ( 'NONE',  ( 16.46253265017160672, -9.564922557960803928, 23.33224293864769194 ) ) ;
#154099 = CARTESIAN_POINT ( 'NONE',  ( -19.03943276465977164, 0.05219959533909376836, 81.24890960531436690 ) ) ;
#154100 = CARTESIAN_POINT ( 'NONE',  ( 0.05219959533934541429, -16.53943276465976808, 30.00109039468568284 ) ) ;
#154101 = CARTESIAN_POINT ( 'NONE',  ( -4.379528057220328563, 16.55341960407611168, 90.20724293864770971 ) ) ;
#154102 = CARTESIAN_POINT ( 'NONE',  ( -5.153800228976328057, -19.02544592524343514, 52.29057627198100988 ) ) ;
#154103 = CARTESIAN_POINT ( 'NONE',  ( 10.72451020669898902, -18.67979575497178502, 37.91557627198102409 ) ) ;
#154104 = CARTESIAN_POINT ( 'NONE',  ( -5.049401038297874678, -19.05341960407617918, 104.7927570613523471 ) ) ;
#154105 = CARTESIAN_POINT ( 'NONE',  ( -18.62759615963270932, 10.81492255796079327, 110.8322429386476955 ) ) ;
#154106 = CARTESIAN_POINT ( 'NONE',  ( 10.81492255796106328, -18.62759615963255655, 55.41775706135234714 ) ) ;
#154107 = CARTESIAN_POINT ( 'NONE',  ( -16.55341960407617563, 4.379528057220093196, 68.54275706135234714 ) ) ;
#154108 = CARTESIAN_POINT ( 'NONE',  ( -12.14591786802326823, 12.06949235617739902, 63.12609039468568994 ) ) ;
#154109 = ORIENTED_EDGE ( 'NONE', *, *, #196054, .F. ) ;
#154110 = CARTESIAN_POINT ( 'NONE',  ( -19.02544592524342804, 5.153800228976336051, 66.04057627198103830 ) ) ;
#154111 = CARTESIAN_POINT ( 'NONE',  ( 8.314922557961029526, -14.29746914071037800, 85.41775706135236135 ) ) ;
#154112 = CARTESIAN_POINT ( 'NONE',  ( -18.62759615963270932, 10.81492255796079327, 115.8322429386477097 ) ) ;
#154113 = CARTESIAN_POINT ( 'NONE',  ( 12.06949235617757843, -12.14591786802309237, 68.12390960531436690 ) ) ;
#154114 = CARTESIAN_POINT ( 'NONE',  ( -19.05341960407611168, -5.049401038298163336, 81.45724293864769550 ) ) ;
#154115 = CARTESIAN_POINT ( 'NONE',  ( 14.34966873604972726, -8.224510206698740333, 75.83442372801900433 ) ) ;
#154116 = B_SPLINE_CURVE_WITH_KNOTS ( 'NONE', 3,
 ( #29133, #59443, #156176, #155188, #16678, #3477 ),
 .UNSPECIFIED., .F., .F.,
 ( 4, 2, 4 ),
 ( 0.003989672132298151264, 0.004372778065220565835, 0.004755883998142980407 ),
 .UNSPECIFIED. ) ;
#154117 = CARTESIAN_POINT ( 'NONE',  ( -10.72451020669870658, -18.67979575497194134, 59.58442372801901854 ) ) ;
#154118 = CARTESIAN_POINT ( 'NONE',  ( 16.51473224551083163, -9.474510206698727899, 110.8344237280190043 ) ) ;
#154119 = CARTESIAN_POINT ( 'NONE',  ( 18.62759615963271287, -10.81492255796078972, 113.3322429386476955 ) ) ;
#154120 = CARTESIAN_POINT ( 'NONE',  ( 4.483927247898545687, 16.52544592524342804, 54.79057627198104541 ) ) ;
#154121 = ORIENTED_EDGE ( 'NONE', *, *, #50509, .F. ) ;
#154122 = CARTESIAN_POINT ( 'NONE',  ( -21.53943276465977519, 0.05219959533907696930, 86.24890960531436690 ) ) ;
#154123 = CARTESIAN_POINT ( 'NONE',  ( -4.379528057220328563, 16.55341960407611168, 35.20724293864768839 ) ) ;
#154124 = EDGE_LOOP ( 'NONE', ( #112765, #98483, #147928, #172580 ) ) ;
#154125 = CARTESIAN_POINT ( 'NONE',  ( 35.59978325014670730, 2.421353778481764252, 37.88472941744216627 ) ) ;
#154126 = CARTESIAN_POINT ( 'NONE',  ( -5.719274019375978568, 21.55341960407610458, 115.2072429386476955 ) ) ;
#154127 = CARTESIAN_POINT ( 'NONE',  ( -21.53943276465977519, 0.05219959533907696930, 21.24890960531436690 ) ) ;
#154128 = CARTESIAN_POINT ( 'NONE',  ( 18.67979575497194134, -10.72451020669871369, 25.83442372801901499 ) ) ;
#154129 = CARTESIAN_POINT ( 'NONE',  ( 16.53943276465976808, -0.05219959533910856209, 48.74890960531435979 ) ) ;
#154130 = CARTESIAN_POINT ( 'NONE',  ( -16.55341960407617563, 4.379528057220093196, 63.54275706135234003 ) ) ;
#154131 = AXIS2_PLACEMENT_3D ( 'NONE', #161215, #80379, #68198 ) ;
#154133 = EDGE_CURVE ( 'NONE', #114656, #86241, #11932, .T. ) ;
#154132 = CARTESIAN_POINT ( 'NONE',  ( 13.89961937509977652, -13.97604488694527269, 58.12390960531436690 ) ) ;
#154134 = CARTESIAN_POINT ( 'NONE',  ( 5.153800228976615827, -19.02544592524334988, 60.20942372801899012 ) ) ;
#154135 = CARTESIAN_POINT ( 'NONE',  ( 9.564922557960805705, 16.46253265017160317, 99.58224293864770971 ) ) ;
#154136 = CARTESIAN_POINT ( 'NONE',  ( 10.81492255796078972, 18.62759615963270932, 49.58224293864769550 ) ) ;
#154137 = CARTESIAN_POINT ( 'NONE',  ( -18.67464278970884806, -33.09908666442120051, -25.63618526509586815 ) ) ;
#154138 = CARTESIAN_POINT ( 'NONE',  ( -9.564922557960796823, -16.46253265017161027, 52.08224293864768839 ) ) ;
#154139 = CARTESIAN_POINT ( 'NONE',  ( 16.53943276465976808, 0.05219959533934440121, 36.25109039468567573 ) ) ;
#154140 = CARTESIAN_POINT ( 'NONE',  ( 5.153800228976615827, -19.02544592524334988, 60.20942372801899012 ) ) ;
#154141 = CARTESIAN_POINT ( 'NONE',  ( 0.05219959533907565091, 21.53943276465977519, 114.9989096053143669 ) ) ;
#154142 = CARTESIAN_POINT ( 'NONE',  ( 0.05219959533910956823, 16.53943276465976808, 44.99890960531435979 ) ) ;
#154143 = CARTESIAN_POINT ( 'NONE',  ( 16.51473224551069308, 9.474510206698969483, 84.16557627198102409 ) ) ;
#154144 = CARTESIAN_POINT ( 'NONE',  ( 21.53943276465977519, -0.05219959533907433946, 63.74890960531435979 ) ) ;
#154146 = CARTESIAN_POINT ( 'NONE',  ( 4.483927247898790824, -16.52544592524335698, 35.20942372801901854 ) ) ;
#154145 = CARTESIAN_POINT ( 'NONE',  ( -15.80617190586745835, -15.72974639402198527, 101.8739096053143811 ) ) ;
#154147 = CARTESIAN_POINT ( 'NONE',  ( -10.81492255796078084, -18.62759615963271287, 42.08224293864769550 ) ) ;
#154148 = CARTESIAN_POINT ( 'NONE',  ( 10.81492255796106328, -18.62759615963255655, 95.41775706135234714 ) ) ;
#154149 = CARTESIAN_POINT ( 'NONE',  ( 16.51473224551069308, 9.474510206698969483, 84.16557627198102409 ) ) ;
#154150 = CARTESIAN_POINT ( 'NONE',  ( 16.46253265017160672, -9.564922557960803928, 38.33224293864768839 ) ) ;
#154151 = CARTESIAN_POINT ( 'NONE',  ( 5.049401038298161559, -19.05341960407611168, 102.7072429386476955 ) ) ;
#154152 = CARTESIAN_POINT ( 'NONE',  ( 4.483927247898545687, 16.52544592524342804, 104.7905762719810241 ) ) ;
#154153 = CARTESIAN_POINT ( 'NONE',  ( -9.564922557960796823, -16.46253265017161027, 67.08224293864769550 ) ) ;
#154154 = CARTESIAN_POINT ( 'NONE',  ( 12.06949235617739724, 12.14591786802326823, 26.87609039468567218 ) ) ;
#154155 = CARTESIAN_POINT ( 'NONE',  ( -5.153800228976607833, 19.02544592524335343, 42.70942372801900433 ) ) ;
#154156 = CARTESIAN_POINT ( 'NONE',  ( 5.049401038297881783, 19.05341960407617563, 57.29275706135231871 ) ) ;
#154157 = CIRCLE ( 'NONE', #66964, 38.00000000000000711 ) ;
#154159 = CARTESIAN_POINT ( 'NONE',  ( 10.72451020669898902, -18.67979575497178502, 27.91557627198103830 ) ) ;
#154158 = CARTESIAN_POINT ( 'NONE',  ( -21.55341960407619339, 5.719274019375674811, 93.54275706135234714 ) ) ;
#154160 = CARTESIAN_POINT ( 'NONE',  ( -12.06949235617739369, -12.14591786802326823, 89.37609039468568994 ) ) ;
#154161 = CARTESIAN_POINT ( 'NONE',  ( -13.97604488694547697, 13.89961937509957934, 68.12609039468563310 ) ) ;
#154162 = CARTESIAN_POINT ( 'NONE',  ( -0.05219959533936034679, 19.03943276465977164, 32.50109039468566863 ) ) ;
#154163 = CARTESIAN_POINT ( 'NONE',  ( -15.49999999999999822, 5.499999999999998224, 118.0000000000000142 ) ) ;
#154164 = CARTESIAN_POINT ( 'NONE',  ( -9.564922557960796823, -16.46253265017161027, 27.08224293864769550 ) ) ;
#154165 = CARTESIAN_POINT ( 'NONE',  ( -14.29746914071049879, 8.314922557960819915, 40.83224293864769550 ) ) ;
#154166 = EDGE_CURVE ( 'NONE', #182496, #132514, #5380, .T. ) ;
#154167 = CARTESIAN_POINT ( 'NONE',  ( 9.474510206698971260, -16.51473224551069308, 22.91557627198102765 ) ) ;
#154168 = CARTESIAN_POINT ( 'NONE',  ( -0.05219959533910754901, -16.53943276465976808, 22.49890960531436335 ) ) ;
#154169 = CARTESIAN_POINT ( 'NONE',  ( 18.22780087662123805, -5.499999999999976019, 88.51763182126893525 ) ) ;
#154170 = CARTESIAN_POINT ( 'NONE',  ( 12.14591786802327356, -12.06949235617739191, 100.6260903946857184 ) ) ;
#154171 = CARTESIAN_POINT ( 'NONE',  ( 13.89961937509977652, -13.97604488694527269, 38.12390960531436690 ) ) ;
#154172 = CARTESIAN_POINT ( 'NONE',  ( 18.67979575497194134, -10.72451020669871369, 100.8344237280190185 ) ) ;
#154173 = CARTESIAN_POINT ( 'NONE',  ( -8.224510206698735004, -14.34966873604973081, 19.58442372801901143 ) ) ;
#154174 = CARTESIAN_POINT ( 'NONE',  ( 15.80617190586769283, -15.72974639402175789, 80.62609039468567573 ) ) ;
#154175 = CARTESIAN_POINT ( 'NONE',  ( -16.51473224551082808, 9.474510206698731452, 58.33442372801900433 ) ) ;
#154176 = CARTESIAN_POINT ( 'NONE',  ( 9.474510206698971260, -16.51473224551069308, 92.91557627198103830 ) ) ;
#154177 = CARTESIAN_POINT ( 'NONE',  ( 16.46253265017160672, -9.564922557960803928, 83.33224293864768129 ) ) ;
#154178 = DIRECTION ( 'NONE',  ( -0.000000000000000000, -0.000000000000000000, -1.000000000000000000 ) ) ;
#154179 = CARTESIAN_POINT ( 'NONE',  ( -5.823673210054116645, -21.52544592524344225, 112.2905762719810241 ) ) ;
#154180 = AXIS2_PLACEMENT_3D ( 'NONE', #43259, #87755, #88759 ) ;
#154181 = CARTESIAN_POINT ( 'NONE',  ( -16.55341960407611168, -4.379528057220339221, 61.45724293864770260 ) ) ;
#154182 = CARTESIAN_POINT ( 'NONE',  ( 21.55341960407610458, 5.719274019375980345, 58.95724293864770971 ) ) ;
#154183 = CARTESIAN_POINT ( 'NONE',  ( -9.564922557960796823, -16.46253265017161027, 57.08224293864769550 ) ) ;
#154185 = CARTESIAN_POINT ( 'NONE',  ( 14.29746914071037800, 8.314922557961029526, 96.66775706135234714 ) ) ;
#154184 = CARTESIAN_POINT ( 'NONE',  ( 5.823673210054125526, 21.52544592524343514, 99.79057627198103830 ) ) ;
#154186 = ORIENTED_EDGE ( 'NONE', *, *, #156407, .F. ) ;
#154187 = CARTESIAN_POINT ( 'NONE',  ( 13.97604488694527802, 13.89961937509977652, 44.37390960531435269 ) ) ;
#154189 = FACE_OUTER_BOUND ( 'NONE', #33349, .T. ) ;
#154188 = CARTESIAN_POINT ( 'NONE',  ( 12.06949235617757843, -12.14591786802309237, 88.12390960531436690 ) ) ;
#154190 = CARTESIAN_POINT ( 'NONE',  ( 13.97604488694527802, 13.89961937509977652, 49.37390960531434558 ) ) ;
#154191 = CARTESIAN_POINT ( 'NONE',  ( -13.97604488694527625, -13.89961937509977652, 26.87390960531434558 ) ) ;
#154192 = CARTESIAN_POINT ( 'NONE',  ( -13.89961937509957401, -13.97604488694547875, 79.37609039468567573 ) ) ;
#154193 = CARTESIAN_POINT ( 'NONE',  ( 12.14591786802309770, 12.06949235617756955, 89.37390960531435269 ) ) ;
#154194 = CARTESIAN_POINT ( 'NONE',  ( -10.81492255796105439, 18.62759615963255655, 47.91775706135234714 ) ) ;
#154196 = CARTESIAN_POINT ( 'NONE',  ( -21.52544592524343514, 5.823673210054127303, 106.0405762719810525 ) ) ;
#154195 = CARTESIAN_POINT ( 'NONE',  ( 13.97604488694527802, 13.89961937509977652, 34.37390960531436690 ) ) ;
#154197 = CARTESIAN_POINT ( 'NONE',  ( 16.52544592524342804, -4.483927247898539470, 88.54057627198103830 ) ) ;
#154198 = CARTESIAN_POINT ( 'NONE',  ( 7.765519415021292282, -39.80263117873665379, -25.57543461820742436 ) ) ;
#154199 = CARTESIAN_POINT ( 'NONE',  ( 5.153800228976335163, 19.02544592524342804, 59.79057627198100988 ) ) ;
#154200 = CARTESIAN_POINT ( 'NONE',  ( 17.31747979337948706, 6.344076630961062335, 113.8794486806519046 ) ) ;
#154202 = CARTESIAN_POINT ( 'NONE',  ( -0.05219959533907301413, -21.53943276465977519, 22.49890960531436335 ) ) ;
#154201 = CARTESIAN_POINT ( 'NONE',  ( 19.02544592524334988, 5.153800228976608722, 96.45942372801897591 ) ) ;
#154203 = CARTESIAN_POINT ( 'NONE',  ( -10.72451020669870658, -18.67979575497194134, 39.58442372801901143 ) ) ;
#154204 = CARTESIAN_POINT ( 'NONE',  ( -16.51473224551069308, -9.474510206698971260, 86.66557627198102409 ) ) ;
#154205 = SHAPE_REPRESENTATION ( 'BR-835', ( #1548, #156568, #137228, #124223, #127393, #4711, #49912, #40243, #162921, #188772, #62886, #101576, #14406, #153245 ), #150097 ) ;
#154206 = CARTESIAN_POINT ( 'NONE',  ( -19.05341960407617563, 5.049401038297882671, 63.54275706135234003 ) ) ;
#154207 = CARTESIAN_POINT ( 'NONE',  ( -9.564922557960796823, -16.46253265017161027, 52.08224293864768839 ) ) ;
#154208 = CARTESIAN_POINT ( 'NONE',  ( 8.224510206698953496, -14.34966873604960469, 72.91557627198103830 ) ) ;
#154209 = CARTESIAN_POINT ( 'NONE',  ( -12.06949235617756955, 12.14591786802309770, 70.62390960531436690 ) ) ;
#154210 = CARTESIAN_POINT ( 'NONE',  ( -9.474510206698964154, 16.51473224551069663, 85.41557627198102409 ) ) ;
#154211 = CARTESIAN_POINT ( 'NONE',  ( -10.72451020669898014, 18.67979575497178502, 95.41557627198102409 ) ) ;
#154212 = CARTESIAN_POINT ( 'NONE',  ( -5.153800228976328057, -19.02544592524343514, 82.29057627198103830 ) ) ;
#154213 = CARTESIAN_POINT ( 'NONE',  ( -9.474510206698720793, -16.51473224551083518, 34.58442372801899722 ) ) ;
#154216 = CARTESIAN_POINT ( 'NONE',  ( 14.34966873604960469, 8.224510206698951720, 104.1655762719810241 ) ) ;
#154215 = CARTESIAN_POINT ( 'NONE',  ( -14.34966873604960291, -8.224510206698953496, 36.66557627198103120 ) ) ;
#154214 = CARTESIAN_POINT ( 'NONE',  ( -9.474510206698964154, 16.51473224551069663, 35.41557627198102409 ) ) ;
#154217 = VERTEX_POINT ( 'NONE', #161663 ) ;
#154218 = CARTESIAN_POINT ( 'NONE',  ( 10.81492255796106328, -18.62759615963255655, 30.41775706135234358 ) ) ;
#154219 = CARTESIAN_POINT ( 'NONE',  ( -5.153800228976607833, 19.02544592524334988, 62.70942372801899722 ) ) ;
#154220 = CARTESIAN_POINT ( 'NONE',  ( 12.14591786802309770, 12.06949235617756955, 39.37390960531436690 ) ) ;
#154221 = CARTESIAN_POINT ( 'NONE',  ( 5.823673210054125526, 21.52544592524343514, 89.79057627198103830 ) ) ;
#154222 = CARTESIAN_POINT ( 'NONE',  ( -5.153800228976328057, -19.02544592524343514, 112.2905762719810099 ) ) ;
#154223 = CARTESIAN_POINT ( 'NONE',  ( -16.55341960407611168, -4.379528057220339221, 71.45724293864769550 ) ) ;
#154224 = CARTESIAN_POINT ( 'NONE',  ( 19.05341960407611168, 5.049401038298154454, 33.95724293864769550 ) ) ;
#154225 = CARTESIAN_POINT ( 'NONE',  ( 16.46253265017146816, 9.564922557961045513, 21.66775706135233648 ) ) ;
#154226 = CARTESIAN_POINT ( 'NONE',  ( 8.314922557961029526, -14.29746914071037800, 105.4177570613523613 ) ) ;
#154227 = CARTESIAN_POINT ( 'NONE',  ( -0.05219959533934338120, 16.53943276465976808, 62.50109039468568284 ) ) ;
#154228 = CARTESIAN_POINT ( 'NONE',  ( -21.52544592524343514, 5.823673210054127303, 36.04057627198102409 ) ) ;
#154229 = CARTESIAN_POINT ( 'NONE',  ( -10.72451020669870658, -18.67979575497194134, 104.5844237280190185 ) ) ;
#154230 = CARTESIAN_POINT ( 'NONE',  ( 16.46253265017160672, -9.564922557960803928, 73.33224293864769550 ) ) ;
#154231 = CARTESIAN_POINT ( 'NONE',  ( -4.379528057220086978, -16.55341960407618274, 54.79275706135235424 ) ) ;
#154232 = CARTESIAN_POINT ( 'NONE',  ( 14.34966873604960469, 8.224510206698951720, 114.1655762719810383 ) ) ;
#154233 = CARTESIAN_POINT ( 'NONE',  ( -4.379528057220328563, 16.55341960407611168, 40.20724293864769550 ) ) ;
#154234 = DIRECTION ( 'NONE',  ( 0.000000000000000000, 0.000000000000000000, 1.000000000000000000 ) ) ;
#154236 = CARTESIAN_POINT ( 'NONE',  ( -19.02544592524342804, 5.153800228976336051, 96.04057627198103830 ) ) ;
#154235 = CARTESIAN_POINT ( 'NONE',  ( -13.97604488694527625, -13.89961937509977652, 106.8739096053143669 ) ) ;
#154237 = CARTESIAN_POINT ( 'NONE',  ( 19.02544592524343514, -5.153800228976328945, 103.5405762719809957 ) ) ;
#154238 = CARTESIAN_POINT ( 'NONE',  ( 16.55341960407611168, 4.379528057220329451, 58.95724293864770971 ) ) ;
#154239 = CARTESIAN_POINT ( 'NONE',  ( 4.483927247898545687, 16.52544592524342804, 34.79057627198103120 ) ) ;
#154240 = CARTESIAN_POINT ( 'NONE',  ( 4.379528057220339221, -16.55341960407611168, 47.70724293864770260 ) ) ;
#154242 = CARTESIAN_POINT ( 'NONE',  ( 17.50000000000000711, -5.076555817581199115, 31.32048507950228355 ) ) ;
#154241 = CARTESIAN_POINT ( 'NONE',  ( -4.483927247898782831, 16.52544592524335698, 37.70942372801900433 ) ) ;
#154243 = CARTESIAN_POINT ( 'NONE',  ( -9.564922557961040184, 16.46253265017147172, 47.91775706135233293 ) ) ;
#154244 = CARTESIAN_POINT ( 'NONE',  ( -16.46253265017160317, 9.564922557960807481, 75.83224293864769550 ) ) ;
#154245 = CARTESIAN_POINT ( 'NONE',  ( -5.153800228976607833, 19.02544592524334988, 67.70942372801900433 ) ) ;
#154246 = CARTESIAN_POINT ( 'NONE',  ( 1.784210473542230573E-15, -29.16686587814331588, 143.8750000027311557 ) ) ;
#154247 = CARTESIAN_POINT ( 'NONE',  ( 9.564922557961047289, -16.46253265017146816, 60.41775706135233293 ) ) ;
#154249 = CARTESIAN_POINT ( 'NONE',  ( 14.34966873604972726, -8.224510206698740333, 85.83442372801901854 ) ) ;
#154248 = CARTESIAN_POINT ( 'NONE',  ( -19.05341960407617563, 5.049401038297882671, 103.5427570613523329 ) ) ;
#154250 = CARTESIAN_POINT ( 'NONE',  ( 1.784210473542230573E-15, -29.16686587814331588, 143.8750000027311557 ) ) ;
#154251 = CARTESIAN_POINT ( 'NONE',  ( 13.97604488694527802, 13.89961937509977652, 29.37390960531435979 ) ) ;
#154252 = CARTESIAN_POINT ( 'NONE',  ( -10.81492255796078084, -18.62759615963271287, 27.08224293864769550 ) ) ;
#154253 = CARTESIAN_POINT ( 'NONE',  ( 18.62759615963255655, 10.81492255796105972, 41.66775706135235424 ) ) ;
#154254 = CARTESIAN_POINT ( 'NONE',  ( 19.03943276465977164, 0.05219959533936151252, 106.2510903946856615 ) ) ;
#154256 = CARTESIAN_POINT ( 'NONE',  ( 9.564922557960805705, 16.46253265017160317, 59.58224293864769550 ) ) ;
#154255 = LINE ( 'NONE', #21707, #15282 ) ;
#154257 = CARTESIAN_POINT ( 'NONE',  ( -5.153800228976328057, -19.02544592524343514, 107.2905762719810383 ) ) ;
#154259 = CARTESIAN_POINT ( 'NONE',  ( -5.153800228976328057, -19.02544592524343514, 57.29057627198103120 ) ) ;
#154258 = CARTESIAN_POINT ( 'NONE',  ( 4.483927247898545687, 16.52544592524342804, 59.79057627198103120 ) ) ;
#154260 = CARTESIAN_POINT ( 'NONE',  ( -5.153800228976328057, -19.02544592524343514, 57.29057627198103120 ) ) ;
#154261 = CARTESIAN_POINT ( 'NONE',  ( -16.46253265017146816, -9.564922557961047289, 74.16775706135234714 ) ) ;
#154262 = CARTESIAN_POINT ( 'NONE',  ( -21.53943276465977519, 0.05219959533907696930, 46.24890960531435979 ) ) ;
#154263 = CARTESIAN_POINT ( 'NONE',  ( -16.52544592524342804, 4.483927247898546575, 111.0405762719810525 ) ) ;
#154264 = CARTESIAN_POINT ( 'NONE',  ( -13.97604488694547697, 13.89961937509957934, 48.12609039468566863 ) ) ;
#154265 = CARTESIAN_POINT ( 'NONE',  ( 13.89961937509977652, -13.97604488694527269, 83.12390960531436690 ) ) ;
#154266 = CARTESIAN_POINT ( 'NONE',  ( 18.67979575497178502, 10.72451020669898547, 74.16557627198102409 ) ) ;
#154268 = CARTESIAN_POINT ( 'NONE',  ( -16.46253265017146816, -9.564922557961047289, 34.16775706135233293 ) ) ;
#154267 = CARTESIAN_POINT ( 'NONE',  ( -14.29746914071049879, 8.314922557960819915, 85.83224293864768129 ) ) ;
#154269 = CARTESIAN_POINT ( 'NONE',  ( 15.80617190586746368, 15.72974639402197994, 64.37390960531435269 ) ) ;
#154270 = CARTESIAN_POINT ( 'NONE',  ( -21.52544592524343514, 5.823673210054127303, 41.04057627198103120 ) ) ;
#154271 = CARTESIAN_POINT ( 'NONE',  ( -21.55341960407619339, 5.719274019375674811, 88.54275706135236135 ) ) ;
#154272 = CARTESIAN_POINT ( 'NONE',  ( -9.474510206698964154, 16.51473224551069663, 65.41557627198102409 ) ) ;
#154273 = CARTESIAN_POINT ( 'NONE',  ( 4.483927247898545687, 16.52544592524342804, 114.7905762719810383 ) ) ;
#154274 = CIRCLE ( 'NONE', #160755, 2.000000000000000000 ) ;
#154275 = CARTESIAN_POINT ( 'NONE',  ( -15.72974639402176322, -15.80617190586768395, 24.37609039468567573 ) ) ;
#154276 = DIRECTION ( 'NONE',  ( -0.8571673007021135549, 1.049727191138620175E-16, 0.5150380749100520461 ) ) ;
#154277 = CARTESIAN_POINT ( 'NONE',  ( -15.80617190586768217, 15.72974639402176855, 43.12609039468568284 ) ) ;
#154278 = CARTESIAN_POINT ( 'NONE',  ( -9.474510206698964154, 16.51473224551069663, 30.41557627198102054 ) ) ;
#154279 = CARTESIAN_POINT ( 'NONE',  ( -15.72974639402197994, 15.80617190586746368, 105.6239096053143669 ) ) ;
#154280 = CARTESIAN_POINT ( 'NONE',  ( 0.05219959533936267826, -19.03943276465977164, 50.00109039468566863 ) ) ;
#154281 = CARTESIAN_POINT ( 'NONE',  ( 17.37577197770832527, -5.499999999999936939, 21.30611277022550354 ) ) ;
#154282 = CARTESIAN_POINT ( 'NONE',  ( -9.564922557960796823, -16.46253265017161027, 22.08224293864768839 ) ) ;
#154283 = CARTESIAN_POINT ( 'NONE',  ( -5.000000000000000888, -130.0000000000000000, -13.99999999999999822 ) ) ;
#154284 = CARTESIAN_POINT ( 'NONE',  ( -14.29746914071037622, -8.314922557961029526, 59.16775706135234714 ) ) ;
#154285 = CARTESIAN_POINT ( 'NONE',  ( -16.46253265017160317, 9.564922557960807481, 30.83224293864769550 ) ) ;
#154286 = CARTESIAN_POINT ( 'NONE',  ( -25.93326183087831893, -10.28624940747432959, 166.6531433017871962 ) ) ;
#154287 = CARTESIAN_POINT ( 'NONE',  ( -19.02544592524342804, 5.153800228976336051, 71.04057627198099567 ) ) ;
#154288 = CARTESIAN_POINT ( 'NONE',  ( -0.05219959533910754901, -16.53943276465976808, 107.4989096053143669 ) ) ;
#154289 = CARTESIAN_POINT ( 'NONE',  ( -18.62759615963270932, 10.81492255796079327, 65.83224293864769550 ) ) ;
#154290 = CARTESIAN_POINT ( 'NONE',  ( 14.29746914071037800, 8.314922557961029526, 36.66775706135234714 ) ) ;
#154291 = CARTESIAN_POINT ( 'NONE',  ( 18.67979575497194134, -10.72451020669871369, 105.8344237280190328 ) ) ;
#154292 = LINE ( 'NONE', #15782, #156223 ) ;
#154293 = CARTESIAN_POINT ( 'NONE',  ( 12.06949235617739724, 12.14591786802326823, 106.8760903946856899 ) ) ;
#154294 = CARTESIAN_POINT ( 'NONE',  ( 12.14591786802309770, 12.06949235617756955, 49.37390960531436690 ) ) ;
#154295 = CARTESIAN_POINT ( 'NONE',  ( -16.46253265017160317, 9.564922557960807481, 45.83224293864769550 ) ) ;
#154296 = CARTESIAN_POINT ( 'NONE',  ( -18.62759615963255300, -10.81492255796106328, 99.16775706135234714 ) ) ;
#154297 = CARTESIAN_POINT ( 'NONE',  ( -10.72451020669898014, 18.67979575497178502, 105.4155762719810383 ) ) ;
#154298 = CARTESIAN_POINT ( 'NONE',  ( -15.72974639402176322, -15.80617190586768395, 69.37609039468567573 ) ) ;
#154299 = CARTESIAN_POINT ( 'NONE',  ( -8.224510206698735004, -14.34966873604973081, 54.58442372801901143 ) ) ;
#154300 = EDGE_CURVE ( 'NONE', #22413, #12839, #122129, .T. ) ;
#154302 = CARTESIAN_POINT ( 'NONE',  ( 15.72974639402176855, 15.80617190586768217, 101.8760903946857042 ) ) ;
#154301 = CARTESIAN_POINT ( 'NONE',  ( 12.14591786802309770, 12.06949235617756955, 74.37390960531436690 ) ) ;
#154303 = CARTESIAN_POINT ( 'NONE',  ( -14.34966873604960291, -8.224510206698953496, 21.66557627198102409 ) ) ;
#154304 = CARTESIAN_POINT ( 'NONE',  ( 17.50000000000000000, -5.499999999999992895, 61.21769037696436300 ) ) ;
#154305 = CARTESIAN_POINT ( 'NONE',  ( -8.224510206698735004, -14.34966873604973081, 34.58442372801900433 ) ) ;
#154306 = CARTESIAN_POINT ( 'NONE',  ( 16.55341960407611168, 4.379528057220329451, 43.95724293864769550 ) ) ;
#154307 = CARTESIAN_POINT ( 'NONE',  ( -14.34966873604972548, 8.224510206698743886, 93.33442372801901854 ) ) ;
#154308 = CARTESIAN_POINT ( 'NONE',  ( -16.46253265017160317, 9.564922557960807481, 100.8322429386477097 ) ) ;
#154309 = CARTESIAN_POINT ( 'NONE',  ( 18.67979575497178502, 10.72451020669898547, 24.16557627198103120 ) ) ;
#154310 = CARTESIAN_POINT ( 'NONE',  ( -5.823673210054431948, 21.52544592524334988, 97.70942372801904696 ) ) ;
#154311 = CARTESIAN_POINT ( 'NONE',  ( -14.29746914071037622, -8.314922557961029526, 109.1677570613523613 ) ) ;
#154312 = CARTESIAN_POINT ( 'NONE',  ( -16.55341960407611168, -4.379528057220339221, 71.45724293864769550 ) ) ;
#154313 = CARTESIAN_POINT ( 'NONE',  ( 9.474510206698971260, -16.51473224551069308, 77.91557627198103830 ) ) ;
#154314 = EDGE_LOOP ( 'NONE', ( #194274, #144214, #117578, #179283, #81227, #122892 ) ) ;
#154315 = CARTESIAN_POINT ( 'NONE',  ( 4.483927247898790824, -16.52544592524335698, 30.20942372801902565 ) ) ;
#154316 = CARTESIAN_POINT ( 'NONE',  ( 19.05341960407611168, 5.049401038298154454, 43.95724293864769550 ) ) ;
#154317 = CARTESIAN_POINT ( 'NONE',  ( 16.51473224551069308, 9.474510206698969483, 89.16557627198103830 ) ) ;
#154319 = CARTESIAN_POINT ( 'NONE',  ( 17.50000000000000000, 5.500000000000011546, 68.78230962303564411 ) ) ;
#154318 = CARTESIAN_POINT ( 'NONE',  ( 12.14591786802327356, -12.06949235617739191, 30.62609039468567929 ) ) ;
#154320 = CARTESIAN_POINT ( 'NONE',  ( 19.05341960407617918, -5.049401038297876454, 41.04275706135233293 ) ) ;
#154321 = CARTESIAN_POINT ( 'NONE',  ( 14.34966873604972726, -8.224510206698740333, 90.83442372801901854 ) ) ;
#154322 = CARTESIAN_POINT ( 'NONE',  ( 19.02544592524343514, -5.153800228976328945, 28.54057627198102409 ) ) ;
#154323 = CARTESIAN_POINT ( 'NONE',  ( 8.314922557961029526, -14.29746914071037800, 75.41775706135233293 ) ) ;
#154324 = CARTESIAN_POINT ( 'NONE',  ( 16.55341960407618274, -4.379528057220086978, 61.04275706135234714 ) ) ;
#154325 = CARTESIAN_POINT ( 'NONE',  ( -5.049401038297874678, -19.05341960407617918, 84.79275706135233293 ) ) ;
#154326 = CARTESIAN_POINT ( 'NONE',  ( -0.05219959533936034679, 19.03943276465977164, 32.50109039468566863 ) ) ;
#154327 = CARTESIAN_POINT ( 'NONE',  ( 13.89961937509977652, -13.97604488694527269, 48.12390960531435979 ) ) ;
#154328 = CARTESIAN_POINT ( 'NONE',  ( 12.14591786802309770, 12.06949235617756955, 89.37390960531435269 ) ) ;
#154329 = CARTESIAN_POINT ( 'NONE',  ( 16.51473224551083163, -9.474510206698727899, 50.83442372801899722 ) ) ;
#154330 = CARTESIAN_POINT ( 'NONE',  ( 5.719274019375991003, -21.55341960407610458, 52.70724293864769550 ) ) ;
#154331 = CARTESIAN_POINT ( 'NONE',  ( -16.46253265017146816, -9.564922557961047289, 29.16775706135232937 ) ) ;
#154332 = CARTESIAN_POINT ( 'NONE',  ( -5.049401038298153566, 19.05341960407611168, 100.2072429386476955 ) ) ;
#154333 = CARTESIAN_POINT ( 'NONE',  ( 0.05219959533907565091, 21.53943276465977519, 79.99890960531435269 ) ) ;
#154334 = CARTESIAN_POINT ( 'NONE',  ( 16.51473224551083163, -9.474510206698727899, 85.83442372801900433 ) ) ;
#154335 = CARTESIAN_POINT ( 'NONE',  ( -29.17999648465609397, -8.032454009542489004, 149.7954620931811291 ) ) ;
#154336 = CARTESIAN_POINT ( 'NONE',  ( 12.14591786802327356, -12.06949235617739191, 20.62609039468568639 ) ) ;
#154337 = CARTESIAN_POINT ( 'NONE',  ( -13.97604488694527625, -13.89961937509977652, 31.87390960531435979 ) ) ;
#154338 = CARTESIAN_POINT ( 'NONE',  ( 16.46253265017160672, -9.564922557960803928, 103.3322429386476955 ) ) ;
#154339 = CARTESIAN_POINT ( 'NONE',  ( 5.719274019375991003, -21.55341960407610458, 72.70724293864769550 ) ) ;
#154340 = CARTESIAN_POINT ( 'NONE',  ( -8.224510206698735004, -14.34966873604973081, 44.58442372801901854 ) ) ;
#154341 = CARTESIAN_POINT ( 'NONE',  ( -18.62759615963255300, -10.81492255796106328, 44.16775706135234714 ) ) ;
#154343 = CARTESIAN_POINT ( 'NONE',  ( -10.81492255796105439, 18.62759615963255655, 107.9177570613523471 ) ) ;
#154342 = CARTESIAN_POINT ( 'NONE',  ( -9.474510206698720793, -16.51473224551083518, 109.5844237280190043 ) ) ;
#154344 = CARTESIAN_POINT ( 'NONE',  ( 14.29746914071037800, 8.314922557961029526, 111.6677570613523613 ) ) ;
#154345 = CARTESIAN_POINT ( 'NONE',  ( -13.97604488694527625, -13.89961937509977652, 96.87390960531433848 ) ) ;
#154346 = CARTESIAN_POINT ( 'NONE',  ( 10.81492255796078972, 18.62759615963270932, 104.5822429386477097 ) ) ;
#154347 = CARTESIAN_POINT ( 'NONE',  ( 4.483927247898545687, 16.52544592524342804, 29.79057627198102409 ) ) ;
#154348 = CARTESIAN_POINT ( 'NONE',  ( -5.049401038297874678, -19.05341960407617918, 79.79275706135233293 ) ) ;
#154349 = CARTESIAN_POINT ( 'NONE',  ( -15.72974639402176322, -15.80617190586768395, 59.37609039468568284 ) ) ;
#154350 = CARTESIAN_POINT ( 'NONE',  ( -13.97604488694547697, 13.89961937509957934, 28.12609039468565797 ) ) ;
#154351 = CARTESIAN_POINT ( 'NONE',  ( -14.34966873604960291, -8.224510206698953496, 101.6655762719810383 ) ) ;
#154352 = CARTESIAN_POINT ( 'NONE',  ( -21.52544592524343514, 5.823673210054127303, 36.04057627198102409 ) ) ;
#154353 = CARTESIAN_POINT ( 'NONE',  ( 4.379528057220339221, -16.55341960407611168, 22.70724293864769194 ) ) ;
#154354 = CARTESIAN_POINT ( 'NONE',  ( 5.823673210054444382, -21.52544592524334988, 100.2094237280190043 ) ) ;
#154355 = CARTESIAN_POINT ( 'NONE',  ( 14.34966873604972726, -8.224510206698740333, 55.83442372801901854 ) ) ;
#154356 = CARTESIAN_POINT ( 'NONE',  ( 16.53943276465976808, -0.05219959533910856209, 28.74890960531435624 ) ) ;
#154357 = CARTESIAN_POINT ( 'NONE',  ( -10.81492255796105439, 18.62759615963255655, 62.91775706135236135 ) ) ;
#154358 = CARTESIAN_POINT ( 'NONE',  ( -21.52544592524334988, -5.823673210054445271, 53.95942372801900433 ) ) ;
#154359 = ORIENTED_EDGE ( 'NONE', *, *, #87117, .F. ) ;
#154360 = CARTESIAN_POINT ( 'NONE',  ( 9.474510206698971260, -16.51473224551069308, 27.91557627198103120 ) ) ;
#154361 = CARTESIAN_POINT ( 'NONE',  ( 10.81492255796106328, -18.62759615963255655, 35.41775706135234003 ) ) ;
#154362 = CARTESIAN_POINT ( 'NONE',  ( 16.55341960407611168, 4.379528057220329451, 108.9572429386476955 ) ) ;
#154363 = CARTESIAN_POINT ( 'NONE',  ( 19.50973618000807619, -5.499999999999992895, 37.50000000000000000 ) ) ;
#154364 = CARTESIAN_POINT ( 'NONE',  ( 12.06949235617757843, -12.14591786802309237, 78.12390960531436690 ) ) ;
#154365 = CARTESIAN_POINT ( 'NONE',  ( 19.05341960407611168, 5.049401038298154454, 68.95724293864769550 ) ) ;
#154366 = CARTESIAN_POINT ( 'NONE',  ( 4.483927247898545687, 16.52544592524342804, 24.79057627198103120 ) ) ;
#154367 = CARTESIAN_POINT ( 'NONE',  ( -18.67979575497178146, -10.72451020669898902, 56.66557627198103830 ) ) ;
#154368 = CARTESIAN_POINT ( 'NONE',  ( 12.06949235617757843, -12.14591786802309237, 93.12390960531436690 ) ) ;
#154369 = CARTESIAN_POINT ( 'NONE',  ( 18.62759615963271287, -10.81492255796078972, 93.33224293864769550 ) ) ;
#154370 = CARTESIAN_POINT ( 'NONE',  ( -13.89961937509977652, 13.97604488694528158, 95.62390960531436690 ) ) ;
#154372 = CARTESIAN_POINT ( 'NONE',  ( -16.46253265017146816, -9.564922557961047289, 104.1677570613523329 ) ) ;
#154371 = CARTESIAN_POINT ( 'NONE',  ( 5.153800228976335163, 19.02544592524342804, 49.79057627198100988 ) ) ;
#154373 = CARTESIAN_POINT ( 'NONE',  ( 5.823673210054125526, 21.52544592524343514, 44.79057627198103120 ) ) ;
#154374 = CARTESIAN_POINT ( 'NONE',  ( 5.823673210054444382, -21.52544592524334988, 85.20942372801901854 ) ) ;
#154375 = CARTESIAN_POINT ( 'NONE',  ( -13.89961937509977652, 13.97604488694528158, 65.62390960531436690 ) ) ;
#154376 = CARTESIAN_POINT ( 'NONE',  ( -9.564922557960796823, -16.46253265017161027, 97.08224293864769550 ) ) ;
#154377 = CARTESIAN_POINT ( 'NONE',  ( 0.05219959533934541429, -16.53943276465976808, 80.00109039468568994 ) ) ;
#154378 = CARTESIAN_POINT ( 'NONE',  ( -10.81492255796105439, 18.62759615963255655, 62.91775706135236135 ) ) ;
#154379 = CARTESIAN_POINT ( 'NONE',  ( -18.62759615963255300, -10.81492255796106328, 84.16775706135234714 ) ) ;
#154380 = CARTESIAN_POINT ( 'NONE',  ( -21.55341960407610458, -5.719274019375992779, 106.4572429386477097 ) ) ;
#154381 = CARTESIAN_POINT ( 'NONE',  ( -16.52544592524335698, -4.483927247898792601, 78.95942372801901854 ) ) ;
#154382 = CARTESIAN_POINT ( 'NONE',  ( 10.81492255796078972, 18.62759615963270932, 74.58224293864768129 ) ) ;
#154383 = CARTESIAN_POINT ( 'NONE',  ( -19.03943276465977164, -0.05219959533935918106, 48.75109039468566863 ) ) ;
#154384 = CARTESIAN_POINT ( 'NONE',  ( -21.53943276465977519, 0.05219959533907696930, 41.24890960531435269 ) ) ;
#154386 = CARTESIAN_POINT ( 'NONE',  ( 12.14591786802309770, 12.06949235617756955, 24.37390960531435979 ) ) ;
#154385 = CARTESIAN_POINT ( 'NONE',  ( -0.05219959533909027116, -19.03943276465977164, 77.49890960531435269 ) ) ;
#154387 = CARTESIAN_POINT ( 'NONE',  ( -16.31925111598458500, 7.325300261831455551, 65.16424538967254421 ) ) ;
#154388 = CARTESIAN_POINT ( 'NONE',  ( 5.153800228976335163, 19.02544592524342804, 114.7905762719810241 ) ) ;
#154389 = CARTESIAN_POINT ( 'NONE',  ( 0.000000000000000000, 0.000000000000000000, -58.85720012050612837 ) ) ;
#154390 = CARTESIAN_POINT ( 'NONE',  ( 19.02544592524334988, 5.153800228976608722, 101.4594237280189759 ) ) ;
#154391 = CARTESIAN_POINT ( 'NONE',  ( 10.72451020669898902, -18.67979575497178502, 77.91557627198102409 ) ) ;
#154392 = CARTESIAN_POINT ( 'NONE',  ( 8.314922557960818139, 14.29746914071049879, 44.58224293864769550 ) ) ;
#154393 = CARTESIAN_POINT ( 'NONE',  ( -12.06949235617739369, -12.14591786802326823, 19.37609039468568639 ) ) ;
#154394 = CARTESIAN_POINT ( 'NONE',  ( -9.564922557960796823, -16.46253265017161027, 37.08224293864768839 ) ) ;
#154395 = CARTESIAN_POINT ( 'NONE',  ( 19.02544592524334988, 5.153800228976608722, 106.4594237280190185 ) ) ;
#154397 = CARTESIAN_POINT ( 'NONE',  ( -5.049401038297874678, -19.05341960407617918, 69.79275706135233293 ) ) ;
#154396 = CARTESIAN_POINT ( 'NONE',  ( 18.67979575497178502, 10.72451020669898547, 104.1655762719810241 ) ) ;
#154398 = CARTESIAN_POINT ( 'NONE',  ( -12.06949235617739369, -12.14591786802326823, 84.37609039468570415 ) ) ;
#154399 = CARTESIAN_POINT ( 'NONE',  ( 9.474510206698971260, -16.51473224551069308, 87.91557627198102409 ) ) ;
#154400 = CARTESIAN_POINT ( 'NONE',  ( -12.06949235617756955, 12.14591786802309770, 70.62390960531436690 ) ) ;
#154401 = EDGE_CURVE ( 'NONE', #149477, #84987, #34243, .T. ) ;
#154402 = CARTESIAN_POINT ( 'NONE',  ( 19.02544592524343514, -5.153800228976328945, 63.54057627198103830 ) ) ;
#154403 = CARTESIAN_POINT ( 'NONE',  ( 4.379528057220339221, -16.55341960407611168, 72.70724293864769550 ) ) ;
#154404 = CARTESIAN_POINT ( 'NONE',  ( -19.03943276465977164, 0.05219959533909376836, 31.24890960531435979 ) ) ;
#154405 = CARTESIAN_POINT ( 'NONE',  ( -36.82872320124401710, -3.359544971329626595, 49.36946820683673565 ) ) ;
#154406 = CARTESIAN_POINT ( 'NONE',  ( -12.14591786802309592, -12.06949235617757132, 36.87390960531435979 ) ) ;
#154407 = CARTESIAN_POINT ( 'NONE',  ( 19.02544592524343514, -5.153800228976328945, 73.54057627198103830 ) ) ;
#154408 = CARTESIAN_POINT ( 'NONE',  ( -0.4100021152176883121, -13.74275686049845291, -60.42614020214177373 ) ) ;
#154409 = CARTESIAN_POINT ( 'NONE',  ( -19.05341960407617563, 5.049401038297882671, 48.54275706135233293 ) ) ;
#154410 = CARTESIAN_POINT ( 'NONE',  ( 4.379528057220092307, 16.55341960407617563, 57.29275706135234714 ) ) ;
#154411 = CARTESIAN_POINT ( 'NONE',  ( 15.72974639402199770, -15.80617190586745480, 58.12390960531435979 ) ) ;
#154412 = CARTESIAN_POINT ( 'NONE',  ( 13.89961937509957401, 13.97604488694547697, 26.87609039468566507 ) ) ;
#154413 = CARTESIAN_POINT ( 'NONE',  ( 19.02544592524343514, -5.153800228976328945, 83.54057627198100988 ) ) ;
#154414 = CARTESIAN_POINT ( 'NONE',  ( -20.66645964050063000, -22.75219995122948546, -47.34454927323474038 ) ) ;
#154415 = CARTESIAN_POINT ( 'NONE',  ( -5.823673210054116645, -21.52544592524344225, 27.29057627198103120 ) ) ;
#154416 = CARTESIAN_POINT ( 'NONE',  ( 16.46253265017160672, -9.564922557960803928, 63.33224293864769550 ) ) ;
#154417 = CARTESIAN_POINT ( 'NONE',  ( 5.719274019375673035, 21.55341960407619339, 47.29275706135234003 ) ) ;
#154418 = CARTESIAN_POINT ( 'NONE',  ( -14.34966873604960291, -8.224510206698953496, 106.6655762719810383 ) ) ;
#154421 = ORIENTED_EDGE ( 'NONE', *, *, #182367, .T. ) ;
#154420 = CARTESIAN_POINT ( 'NONE',  ( 13.97604488694527802, 13.89961937509977652, 94.37390960531436690 ) ) ;
#154419 = CARTESIAN_POINT ( 'NONE',  ( 5.719274019375991003, -21.55341960407610458, 97.70724293864772392 ) ) ;
#154422 = CARTESIAN_POINT ( 'NONE',  ( 5.823673210054444382, -21.52544592524334988, 40.20942372801901854 ) ) ;
#154423 = EDGE_LOOP ( 'NONE', ( #83765, #185647, #7472, #87327 ) ) ;
#154424 = CARTESIAN_POINT ( 'NONE',  ( -13.97604488694527625, -13.89961937509977652, 96.87390960531433848 ) ) ;
#154425 = CARTESIAN_POINT ( 'NONE',  ( -9.474510206698964154, 16.51473224551069663, 90.41557627198103830 ) ) ;
#154426 = CARTESIAN_POINT ( 'NONE',  ( -18.67979575497178146, -10.72451020669898902, 91.66557627198103830 ) ) ;
#154427 = CARTESIAN_POINT ( 'NONE',  ( -19.02544592524342804, 5.153800228976336051, 41.04057627198103120 ) ) ;
#154428 = CARTESIAN_POINT ( 'NONE',  ( 4.379528057220092307, 16.55341960407617563, 22.29275706135235069 ) ) ;
#154429 = CARTESIAN_POINT ( 'NONE',  ( -22.81625015709510507, 31.40387420917330275, -3.424999997268813434 ) ) ;
#154430 = CARTESIAN_POINT ( 'NONE',  ( 9.564922557960805705, 16.46253265017160317, 24.58224293864769194 ) ) ;
#154431 = CARTESIAN_POINT ( 'NONE',  ( 0.05219959533937995610, -21.53943276465977519, 80.00109039468568994 ) ) ;
#154433 = CARTESIAN_POINT ( 'NONE',  ( -5.823673210054431948, 21.52544592524334988, 52.70942372801902565 ) ) ;
#154432 = CARTESIAN_POINT ( 'NONE',  ( -19.05341960407611168, -5.049401038298163336, 81.45724293864769550 ) ) ;
#154434 = CARTESIAN_POINT ( 'NONE',  ( -5.719274019375665041, -21.55341960407619695, 24.79275706135235779 ) ) ;
#154435 = CARTESIAN_POINT ( 'NONE',  ( -27.73933785331498925, -9.013057229001049109, 145.4750000027311501 ) ) ;
#154436 = CARTESIAN_POINT ( 'NONE',  ( 19.02544592524343514, -5.153800228976328945, 98.54057627198100988 ) ) ;
#154437 = CARTESIAN_POINT ( 'NONE',  ( 1.300000000000000044, -0.7216878364870318308, -1.250000000000000000 ) ) ;
#154440 = CARTESIAN_POINT ( 'NONE',  ( 21.52544592524334988, 5.823673210054432836, 61.45942372801901854 ) ) ;
#154439 = CARTESIAN_POINT ( 'NONE',  ( -12.14591786802326823, 12.06949235617739902, 73.12609039468567573 ) ) ;
#154438 = CARTESIAN_POINT ( 'NONE',  ( 4.483927247898790824, -16.52544592524335698, 35.20942372801901854 ) ) ;
#154441 = CARTESIAN_POINT ( 'NONE',  ( -18.62759615963255300, -10.81492255796106328, 79.16775706135234714 ) ) ;
#154442 = DIRECTION ( 'NONE',  ( -1.000000000000000000, 0.000000000000000000, 0.000000000000000000 ) ) ;
#154443 = CARTESIAN_POINT ( 'NONE',  ( 9.474510206698729675, 16.51473224551082808, 112.0844237280190043 ) ) ;
#154444 = CARTESIAN_POINT ( 'NONE',  ( -5.049401038298153566, 19.05341960407611168, 75.20724293864769550 ) ) ;
#154445 = CARTESIAN_POINT ( 'NONE',  ( 0.05219959533909260263, 19.03943276465977164, 99.99890960531436690 ) ) ;
#154446 = CONICAL_SURFACE ( 'NONE', #122236, 2.500000000000002220, 1.029744258676656754 ) ;
#154447 = CARTESIAN_POINT ( 'NONE',  ( 16.52544592524342804, -4.483927247898539470, 103.5405762719810383 ) ) ;
#154448 = CARTESIAN_POINT ( 'NONE',  ( -14.29746914071049879, 8.314922557960819915, 110.8322429386476955 ) ) ;
#154449 = CARTESIAN_POINT ( 'NONE',  ( 0.05219959533907565091, 21.53943276465977519, 29.99890960531435979 ) ) ;
#154450 = CARTESIAN_POINT ( 'NONE',  ( 16.55341960407618274, -4.379528057220086978, 86.04275706135236135 ) ) ;
#154453 = CARTESIAN_POINT ( 'NONE',  ( 19.02544592524343514, -5.153800228976328945, 58.54057627198102409 ) ) ;
#154452 =( BOUNDED_CURVE ( )  B_SPLINE_CURVE ( 2, ( #11371, #133698, #9368, #89182, #177226, #55856, #72025, #132700, #197373, #195390, #100355 ),
 .UNSPECIFIED., .F., .T. ) 
 B_SPLINE_CURVE_WITH_KNOTS ( ( 3, 2, 2, 2, 2, 3 ),
 ( 0.1000000000000000056, 0.1199999999999999956, 0.1400000000000000133, 0.1600000000000000033, 0.1799999999999999933, 0.2000000000000000111 ),
 .UNSPECIFIED. ) 
 CURVE ( )  GEOMETRIC_REPRESENTATION_ITEM ( )  RATIONAL_B_SPLINE_CURVE ( ( 1.000000000000000000, 0.9510565162951535312, 1.000000000000000000, 0.9510565162951535312, 1.000000000000000000, 0.9510565162951535312, 1.000000000000000000, 0.9510565162951535312, 1.000000000000000000, 0.9510565162951535312, 1.000000000000000000 ) ) 
 REPRESENTATION_ITEM ( '' )  );
#154451 = CARTESIAN_POINT ( 'NONE',  ( -14.29746914071049879, 8.314922557960819915, 70.83224293864770971 ) ) ;
#154454 = CARTESIAN_POINT ( 'NONE',  ( -0.05219959533937732626, 21.53943276465977519, 72.50109039468568994 ) ) ;
#154455 = CARTESIAN_POINT ( 'NONE',  ( 21.52544592524334988, 5.823673210054432836, 71.45942372801901854 ) ) ;
#154456 = CARTESIAN_POINT ( 'NONE',  ( -5.153800228976607833, 19.02544592524334988, 112.7094237280190043 ) ) ;
#154457 = CARTESIAN_POINT ( 'NONE',  ( -14.29746914071049879, 8.314922557960819915, 75.83224293864769550 ) ) ;
#154458 = CARTESIAN_POINT ( 'NONE',  ( -15.72974639402176322, -15.80617190586768395, 24.37609039468567573 ) ) ;
#154459 = CARTESIAN_POINT ( 'NONE',  ( 18.67979575497178502, 10.72451020669898547, 59.16557627198103120 ) ) ;
#154460 = CARTESIAN_POINT ( 'NONE',  ( -17.12812012977025589, -6.668231424565998822, 106.3594875932314636 ) ) ;
#154461 = CARTESIAN_POINT ( 'NONE',  ( -17.81289503416611808, 24.51734667627700404, 145.9500000054623854 ) ) ;
#154462 = CARTESIAN_POINT ( 'NONE',  ( 13.97604488694527802, 13.89961937509977652, 74.37390960531436690 ) ) ;
#154463 = CARTESIAN_POINT ( 'NONE',  ( -14.29746914071049879, 8.314922557960819915, 55.83224293864770260 ) ) ;
#154464 = CARTESIAN_POINT ( 'NONE',  ( -16.53943276465976808, -0.05219959533934237506, 113.7510903946856757 ) ) ;
#154465 = CARTESIAN_POINT ( 'NONE',  ( 16.53943276465976808, 0.05219959533934440121, 91.25109039468568994 ) ) ;
#154466 = CARTESIAN_POINT ( 'NONE',  ( -5.153800228976607833, 19.02544592524334988, 57.70942372801899012 ) ) ;
#154467 = CARTESIAN_POINT ( 'NONE',  ( -23.27014042476074707, -11.64952740454485003, 165.7333935355015626 ) ) ;
#154468 = CARTESIAN_POINT ( 'NONE',  ( 0.05219959533909260263, 19.03943276465977164, 109.9989096053143669 ) ) ;
#154469 = CARTESIAN_POINT ( 'NONE',  ( -14.34966873604960291, -8.224510206698953496, 76.66557627198103830 ) ) ;
#154470 = CARTESIAN_POINT ( 'NONE',  ( 19.03943276465977164, 0.05219959533936151252, 41.25109039468566152 ) ) ;
#154472 = CARTESIAN_POINT ( 'NONE',  ( -15.72974639402197994, 15.80617190586746368, 35.62390960531437401 ) ) ;
#154471 = CARTESIAN_POINT ( 'NONE',  ( -16.51473224551069308, -9.474510206698971260, 36.66557627198102409 ) ) ;
#154473 = CARTESIAN_POINT ( 'NONE',  ( 18.67979575497178502, 10.72451020669898547, 59.16557627198103120 ) ) ;
#154474 = CARTESIAN_POINT ( 'NONE',  ( -8.314922557960811034, -14.29746914071050412, 102.0822429386476955 ) ) ;
#154475 = CARTESIAN_POINT ( 'NONE',  ( 16.53943276465976808, 0.05219959533934440121, 56.25109039468568284 ) ) ;
#154476 = CARTESIAN_POINT ( 'NONE',  ( 12.14591786802309770, 12.06949235617756955, 89.37390960531435269 ) ) ;
#154477 = CARTESIAN_POINT ( 'NONE',  ( 17.05587630539787369, -6.762274262135693270, 38.24180309037314629 ) ) ;
#154478 = CARTESIAN_POINT ( 'NONE',  ( -17.49999999999999645, 5.500000000000037303, 50.79690382534172244 ) ) ;
#154479 = CARTESIAN_POINT ( 'NONE',  ( -10.72451020669898014, 18.67979575497178502, 35.41557627198102409 ) ) ;
#154480 = CYLINDRICAL_SURFACE ( 'NONE', #178590, 13.70000000000001528 ) ;
#154481 = CARTESIAN_POINT ( 'NONE',  ( -17.72696623605163779, 5.499999999999873879, 43.59811031808418136 ) ) ;
#154483 = CARTESIAN_POINT ( 'NONE',  ( 0.05219959533910956823, 16.53943276465976808, 24.99890960531435624 ) ) ;
#154482 = CARTESIAN_POINT ( 'NONE',  ( -16.52544592524335698, -4.483927247898792601, 48.95942372801902565 ) ) ;
#154484 = CARTESIAN_POINT ( 'NONE',  ( 5.719274019375991003, -21.55341960407610458, 57.70724293864770260 ) ) ;
#154485 = CARTESIAN_POINT ( 'NONE',  ( 19.05341960407617918, -5.049401038297876454, 86.04275706135233293 ) ) ;
#154486 = CARTESIAN_POINT ( 'NONE',  ( 21.52544592524344225, -5.823673210054117533, 58.54057627198103120 ) ) ;
#154487 = CARTESIAN_POINT ( 'NONE',  ( 15.72974639402176855, 15.80617190586768217, 86.87609039468568994 ) ) ;
#154488 = CARTESIAN_POINT ( 'NONE',  ( -10.10090423873405285, 9.391041506135623607, -62.54717694538948791 ) ) ;
#154489 = CARTESIAN_POINT ( 'NONE',  ( -0.05219959533934338120, 16.53943276465976808, 42.50109039468567573 ) ) ;
#154491 = CARTESIAN_POINT ( 'NONE',  ( 0.05219959533909260263, 19.03943276465977164, 94.99890960531436690 ) ) ;
#154490 = CARTESIAN_POINT ( 'NONE',  ( -19.03943276465977164, 0.05219959533909376836, 36.24890960531436690 ) ) ;
#154492 = CARTESIAN_POINT ( 'NONE',  ( 13.97604488694527802, 13.89961937509977652, 34.37390960531436690 ) ) ;
#154493 = CARTESIAN_POINT ( 'NONE',  ( -16.52544592524342804, 4.483927247898546575, 96.04057627198102409 ) ) ;
#154494 = DIRECTION ( 'NONE',  ( 0.000000000000000000, 0.000000000000000000, 1.000000000000000000 ) ) ;
#154495 = CARTESIAN_POINT ( 'NONE',  ( -9.474510206698964154, 16.51473224551069663, 115.4155762719810241 ) ) ;
#154496 = ORIENTED_EDGE ( 'NONE', *, *, #169612, .F. ) ;
#154497 = CARTESIAN_POINT ( 'NONE',  ( 8.314922557961029526, -14.29746914071037800, 65.41775706135234714 ) ) ;
#154498 = CARTESIAN_POINT ( 'NONE',  ( -10.72451020669898014, 18.67979575497178502, 85.41557627198102409 ) ) ;
#154499 = CARTESIAN_POINT ( 'NONE',  ( 0.05219959533909260263, 19.03943276465977164, 54.99890960531435979 ) ) ;
#154500 = CARTESIAN_POINT ( 'NONE',  ( -15.72974639402176322, -15.80617190586768395, 29.37609039468568284 ) ) ;
#154501 = CARTESIAN_POINT ( 'NONE',  ( -0.05219959533909027116, -19.03943276465977164, 77.49890960531435269 ) ) ;
#154502 = ORIENTED_EDGE ( 'NONE', *, *, #85978, .F. ) ;
#154503 = CARTESIAN_POINT ( 'NONE',  ( -21.52544592524343514, 5.823673210054127303, 116.0405762719810383 ) ) ;
#154506 = CARTESIAN_POINT ( 'NONE',  ( 16.51473224551083163, -9.474510206698727899, 75.83442372801900433 ) ) ;
#154505 = CARTESIAN_POINT ( 'NONE',  ( 9.474510206698971260, -16.51473224551069308, 112.9155762719810383 ) ) ;
#154504 = CARTESIAN_POINT ( 'NONE',  ( 13.89961937509977652, -13.97604488694527269, 23.12390960531436335 ) ) ;
#154507 = CARTESIAN_POINT ( 'NONE',  ( -13.89961937509957401, -13.97604488694547875, 24.37609039468565442 ) ) ;
#154508 = CARTESIAN_POINT ( 'NONE',  ( -15.72974639402197994, 15.80617190586746368, 105.6239096053143669 ) ) ;
#154509 = CARTESIAN_POINT ( 'NONE',  ( 9.564922557961047289, -16.46253265017146816, 40.41775706135234003 ) ) ;
#154510 = CARTESIAN_POINT ( 'NONE',  ( 14.29746914071037800, 8.314922557961029526, 76.66775706135234714 ) ) ;
#154511 = CARTESIAN_POINT ( 'NONE',  ( 5.049401038298161559, -19.05341960407611168, 112.7072429386476813 ) ) ;
#154512 = CARTESIAN_POINT ( 'NONE',  ( 19.05341960407611168, 5.049401038298154454, 63.95724293864769550 ) ) ;
#154513 = CARTESIAN_POINT ( 'NONE',  ( 18.62759615963255655, 10.81492255796105972, 61.66775706135235424 ) ) ;
#154514 = CARTESIAN_POINT ( 'NONE',  ( -15.80617190586768217, 15.72974639402176855, 83.12609039468568994 ) ) ;
#154515 = CARTESIAN_POINT ( 'NONE',  ( 13.97604488694527802, 13.89961937509977652, 79.37390960531435269 ) ) ;
#154516 = CARTESIAN_POINT ( 'NONE',  ( -5.719274019375665041, -21.55341960407619695, 49.79275706135234714 ) ) ;
#154517 = CARTESIAN_POINT ( 'NONE',  ( -5.049401038297874678, -19.05341960407617918, 89.79275706135230450 ) ) ;
#154518 = CARTESIAN_POINT ( 'NONE',  ( 19.02544592524343514, -5.153800228976328945, 53.54057627198102409 ) ) ;
#154519 = CARTESIAN_POINT ( 'NONE',  ( 5.049401038298161559, -19.05341960407611168, 97.70724293864766707 ) ) ;
#154520 = CARTESIAN_POINT ( 'NONE',  ( -16.51473224551069308, -9.474510206698971260, 71.66557627198102409 ) ) ;
#154521 = CARTESIAN_POINT ( 'NONE',  ( -13.97604488694527625, -13.89961937509977652, 111.8739096053143243 ) ) ;
#154522 = CARTESIAN_POINT ( 'NONE',  ( -19.03943276465977164, 0.05219959533909376836, 46.24890960531435979 ) ) ;
#154523 = CARTESIAN_POINT ( 'NONE',  ( -18.62759615963270932, 10.81492255796079327, 105.8322429386476955 ) ) ;
#154524 = CARTESIAN_POINT ( 'NONE',  ( 16.55341960407618274, -4.379528057220086978, 86.04275706135236135 ) ) ;
#154525 = CARTESIAN_POINT ( 'NONE',  ( -22.78714015945951132, 11.73760554535606104, 167.9671921004704132 ) ) ;
#154526 = CARTESIAN_POINT ( 'NONE',  ( 0.05219959533936267826, -19.03943276465977164, 40.00109039468566152 ) ) ;
#154527 = CARTESIAN_POINT ( 'NONE',  ( -19.03943276465977164, 0.05219959533909376836, 71.24890960531435269 ) ) ;
#154528 = CARTESIAN_POINT ( 'NONE',  ( -8.314922557960811034, -14.29746914071050412, 62.08224293864769550 ) ) ;
#154529 = CARTESIAN_POINT ( 'NONE',  ( -4.379528057220328563, 16.55341960407611168, 90.20724293864770971 ) ) ;
#154530 = CARTESIAN_POINT ( 'NONE',  ( 21.55341960407610458, 5.719274019375980345, 23.95724293864769550 ) ) ;
#154531 = CARTESIAN_POINT ( 'NONE',  ( 9.474510206698971260, -16.51473224551069308, 92.91557627198103830 ) ) ;
#154532 = CARTESIAN_POINT ( 'NONE',  ( 0.05219959533909260263, 19.03943276465977164, 99.99890960531436690 ) ) ;
#154533 = CARTESIAN_POINT ( 'NONE',  ( -10.81492255796105439, 18.62759615963255655, 107.9177570613523471 ) ) ;
#154534 = CARTESIAN_POINT ( 'NONE',  ( 12.14591786802327356, -12.06949235617739191, 90.62609039468567573 ) ) ;
#154536 = ADVANCED_FACE ( 'NONE', ( #75626 ), #182830, .T. ) ;
#154535 = CARTESIAN_POINT ( 'NONE',  ( -16.46253265017160317, 9.564922557960807481, 80.83224293864769550 ) ) ;
#154537 = CARTESIAN_POINT ( 'NONE',  ( 21.53943276465977519, 0.05219959533937863772, 36.25109039468567573 ) ) ;
#154538 = CARTESIAN_POINT ( 'NONE',  ( 0.05219959533907565091, 21.53943276465977519, 24.99890960531435624 ) ) ;
#154539 = CARTESIAN_POINT ( 'NONE',  ( 10.72451020669898902, -18.67979575497178502, 97.91557627198103830 ) ) ;
#154540 = ADVANCED_FACE ( 'NONE', ( #134343 ), #198933, .F. ) ;
#154541 = CARTESIAN_POINT ( 'NONE',  ( 14.34966873604960469, 8.224510206698951720, 64.16557627198102409 ) ) ;
#154542 = CARTESIAN_POINT ( 'NONE',  ( 19.03943276465977164, -0.05219959533909143690, 58.74890960531435979 ) ) ;
#154543 = CARTESIAN_POINT ( 'NONE',  ( -16.55341960407611168, -4.379528057220339221, 76.45724293864769550 ) ) ;
#154544 = CARTESIAN_POINT ( 'NONE',  ( -19.02544592524334988, -5.153800228976617603, 43.95942372801899012 ) ) ;
#154545 = CARTESIAN_POINT ( 'NONE',  ( -14.29746914071049879, 8.314922557960819915, 110.8322429386476955 ) ) ;
#154546 = CARTESIAN_POINT ( 'NONE',  ( 13.89961937509977652, -13.97604488694527269, 88.12390960531438111 ) ) ;
#154547 = CARTESIAN_POINT ( 'NONE',  ( 16.51473224551069308, 9.474510206698969483, 84.16557627198102409 ) ) ;
#154548 = CARTESIAN_POINT ( 'NONE',  ( -22.44159573604009950, -16.30477369853688430, 147.0750000027312012 ) ) ;
#154549 = CARTESIAN_POINT ( 'NONE',  ( -14.29746914071049879, 8.314922557960819915, 95.83224293864770971 ) ) ;
#154550 = EDGE_LOOP ( 'NONE', ( #151994, #196475, #63974, #102717 ) ) ;
#154551 = CARTESIAN_POINT ( 'NONE',  ( 16.53943276465976808, 0.05219959533934440121, 111.2510903946856899 ) ) ;
#154552 = CARTESIAN_POINT ( 'NONE',  ( -14.34966873604972548, 8.224510206698743886, 28.33442372801902209 ) ) ;
#154553 = CARTESIAN_POINT ( 'NONE',  ( 5.823673210054444382, -21.52544592524334988, 90.20942372801903275 ) ) ;
#154554 = CARTESIAN_POINT ( 'NONE',  ( 9.564922557960805705, 16.46253265017160317, 94.58224293864769550 ) ) ;
#154555 = CARTESIAN_POINT ( 'NONE',  ( -15.72974639402176322, -15.80617190586768395, 19.37609039468568639 ) ) ;
#154556 = CARTESIAN_POINT ( 'NONE',  ( 9.474510206698971260, -16.51473224551069308, 32.91557627198102409 ) ) ;
#154557 = CARTESIAN_POINT ( 'NONE',  ( -4.483927247898782831, 16.52544592524335698, 27.70942372801901854 ) ) ;
#154558 = CARTESIAN_POINT ( 'NONE',  ( -19.03943276465977164, -0.05219959533935918106, 93.75109039468566152 ) ) ;
#154559 = CARTESIAN_POINT ( 'NONE',  ( -5.719274019375978568, 21.55341960407610458, 95.20724293864769550 ) ) ;
#154560 = CARTESIAN_POINT ( 'NONE',  ( 0.05219959533936267826, -19.03943276465977164, 70.00109039468566152 ) ) ;
#154561 = LINE ( 'NONE', #76719, #183473 ) ;
#154562 = CARTESIAN_POINT ( 'NONE',  ( -15.72974639402176322, -15.80617190586768395, 24.37609039468567573 ) ) ;
#154563 = CARTESIAN_POINT ( 'NONE',  ( 28.82186960331498327, 2.781578969918950771E-14, 141.2500000054623683 ) ) ;
#154564 = CARTESIAN_POINT ( 'NONE',  ( -0.05219959533909027116, -19.03943276465977164, 97.49890960531436690 ) ) ;
#154565 = CARTESIAN_POINT ( 'NONE',  ( 8.314922557961029526, -14.29746914071037800, 50.41775706135235424 ) ) ;
#154566 = CARTESIAN_POINT ( 'NONE',  ( -3.573655867282028392E-15, 2.428612866367529932E-14, -15.00000000000000000 ) ) ;
#154567 = CARTESIAN_POINT ( 'NONE',  ( -16.46253265017146816, -9.564922557961047289, 54.16775706135234003 ) ) ;
#154569 = CARTESIAN_POINT ( 'NONE',  ( 14.34966873604960469, 8.224510206698951720, 74.16557627198102409 ) ) ;
#154568 = CARTESIAN_POINT ( 'NONE',  ( -5.719274019375665041, -21.55341960407619695, 24.79275706135235779 ) ) ;
#154570 = CARTESIAN_POINT ( 'NONE',  ( 9.474510206698971260, -16.51473224551069308, 82.91557627198103830 ) ) ;
#154572 = CARTESIAN_POINT ( 'NONE',  ( 0.05219959533936267826, -19.03943276465977164, 55.00109039468566863 ) ) ;
#154571 = CARTESIAN_POINT ( 'NONE',  ( -16.55341960407617563, 4.379528057220093196, 53.54275706135234714 ) ) ;
#154573 = CARTESIAN_POINT ( 'NONE',  ( 10.81492255796106328, -18.62759615963255655, 65.41775706135234714 ) ) ;
#154574 = CARTESIAN_POINT ( 'NONE',  ( -4.483927247898782831, 16.52544592524335698, 27.70942372801901854 ) ) ;
#154575 = CARTESIAN_POINT ( 'NONE',  ( 19.02544592524343514, -5.153800228976328945, 73.54057627198103830 ) ) ;
#154576 = CARTESIAN_POINT ( 'NONE',  ( 9.474510206698729675, 16.51473224551082808, 82.08442372801899012 ) ) ;
#154577 = CARTESIAN_POINT ( 'NONE',  ( 16.53943276465976808, 0.05219959533934440121, 56.25109039468568284 ) ) ;
#154578 = CARTESIAN_POINT ( 'NONE',  ( 15.80617190586769283, -15.72974639402175789, 95.62609039468568994 ) ) ;
#154579 = CARTESIAN_POINT ( 'NONE',  ( 0.05219959533936267826, -19.03943276465977164, 80.00109039468567573 ) ) ;
#154580 = CARTESIAN_POINT ( 'NONE',  ( -13.97604488694527625, -13.89961937509977652, 56.87390960531434558 ) ) ;
#154581 = CARTESIAN_POINT ( 'NONE',  ( 0.05219959533907565091, 21.53943276465977519, 64.99890960531435269 ) ) ;
#154583 = CARTESIAN_POINT ( 'NONE',  ( -9.474510206698720793, -16.51473224551083518, 74.58442372801900433 ) ) ;
#154582 = CARTESIAN_POINT ( 'NONE',  ( -16.52544592524342804, 4.483927247898546575, 71.04057627198103830 ) ) ;
#154584 = CARTESIAN_POINT ( 'NONE',  ( 16.31925111598454947, -7.325300261831691806, 62.66424538967256552 ) ) ;
#154585 = CARTESIAN_POINT ( 'NONE',  ( 13.89961937509957401, 13.97604488694547697, 46.87609039468565442 ) ) ;
#154586 = CARTESIAN_POINT ( 'NONE',  ( 8.314922557961029526, -14.29746914071037800, 100.4177570613523471 ) ) ;
#154587 = CARTESIAN_POINT ( 'NONE',  ( -4.483927247898539470, -16.52544592524342804, 72.29057627198102409 ) ) ;
#154589 = CARTESIAN_POINT ( 'NONE',  ( 17.14385361876520264, 23.59649016807275856, 148.1750000027311955 ) ) ;
#154588 = CARTESIAN_POINT ( 'NONE',  ( 5.823673210054444382, -21.52544592524334988, 100.2094237280190043 ) ) ;
#154590 = CARTESIAN_POINT ( 'NONE',  ( 18.62759615963271287, -10.81492255796078972, 103.3322429386476955 ) ) ;
#154591 = CARTESIAN_POINT ( 'NONE',  ( -13.97604488694527625, -13.89961937509977652, 66.87390960531436690 ) ) ;
#154592 = CARTESIAN_POINT ( 'NONE',  ( -18.62759615963255300, -10.81492255796106328, 69.16775706135234714 ) ) ;
#154593 = CARTESIAN_POINT ( 'NONE',  ( -9.474510206698964154, 16.51473224551069663, 50.41557627198102409 ) ) ;
#154594 = ORIENTED_EDGE ( 'NONE', *, *, #93672, .F. ) ;
#154595 = CARTESIAN_POINT ( 'NONE',  ( 5.049401038298161559, -19.05341960407611168, 22.70724293864769194 ) ) ;
#154596 = CARTESIAN_POINT ( 'NONE',  ( 0.05219959533909260263, 19.03943276465977164, 109.9989096053143669 ) ) ;
#154597 = CARTESIAN_POINT ( 'NONE',  ( 0.05219959533910956823, 16.53943276465976808, 69.99890960531435269 ) ) ;
#154598 = CARTESIAN_POINT ( 'NONE',  ( -19.02544592524342804, 5.153800228976336051, 36.04057627198100988 ) ) ;
#154599 = CARTESIAN_POINT ( 'NONE',  ( 4.379528057220339221, -16.55341960407611168, 82.70724293864770971 ) ) ;
#154600 = CARTESIAN_POINT ( 'NONE',  ( -21.52544592524343514, 5.823673210054127303, 91.04057627198103830 ) ) ;
#154601 = CARTESIAN_POINT ( 'NONE',  ( -0.05219959533937732626, 21.53943276465977519, 42.50109039468567573 ) ) ;
#154602 = CARTESIAN_POINT ( 'NONE',  ( 20.73749492396215288, -155.7167183371838064, 0.000000000000000000 ) ) ;
#154603 = EDGE_CURVE ( 'NONE', #107085, #14621, #93075, .T. ) ;
#154604 = CARTESIAN_POINT ( 'NONE',  ( 16.52544592524335698, 4.483927247898782831, 56.45942372801902565 ) ) ;
#154605 = CARTESIAN_POINT ( 'NONE',  ( 15.72974639402199770, -15.80617190586745480, 103.1239096053143811 ) ) ;
#154606 = CARTESIAN_POINT ( 'NONE',  ( 13.89961937509957401, 13.97604488694547697, 31.87609039468566863 ) ) ;
#154607 = CARTESIAN_POINT ( 'NONE',  ( 13.97604488694527802, 13.89961937509977652, 109.3739096053143669 ) ) ;
#154608 = CARTESIAN_POINT ( 'NONE',  ( 15.80617190586769283, -15.72974639402175789, 50.62609039468568994 ) ) ;
#154609 = CARTESIAN_POINT ( 'NONE',  ( 10.81492255796078972, 18.62759615963270932, 49.58224293864769550 ) ) ;
#154610 = CARTESIAN_POINT ( 'NONE',  ( 4.379528057220339221, -16.55341960407611168, 27.70724293864769905 ) ) ;
#154612 = CARTESIAN_POINT ( 'NONE',  ( -21.52544592524334988, -5.823673210054445271, 103.9594237280190185 ) ) ;
#154611 = CARTESIAN_POINT ( 'NONE',  ( -21.53943276465977519, -0.05219959533937600094, 63.75109039468568284 ) ) ;
#154613 = CARTESIAN_POINT ( 'NONE',  ( -16.51473224551082808, 9.474510206698731452, 33.33442372801899722 ) ) ;
#154614 = CARTESIAN_POINT ( 'NONE',  ( -4.483927247898782831, 16.52544592524335698, 92.70942372801901854 ) ) ;
#154615 = CARTESIAN_POINT ( 'NONE',  ( -0.05219959533937732626, 21.53943276465977519, 52.50109039468567573 ) ) ;
#154616 = EDGE_CURVE ( 'NONE', #135352, #61770, #40244, .T. ) ;
#154617 = CARTESIAN_POINT ( 'NONE',  ( -13.89961937509977652, 13.97604488694528158, 40.62390960531435979 ) ) ;
#154618 = CARTESIAN_POINT ( 'NONE',  ( -5.823673210054431948, 21.52544592524334988, 112.7094237280190328 ) ) ;
#154619 = CARTESIAN_POINT ( 'NONE',  ( -21.55341960407610458, -5.719274019375992779, 26.45724293864768839 ) ) ;
#154620 = EDGE_CURVE ( 'NONE', #36346, #41468, #85907, .T. ) ;
#154621 = CARTESIAN_POINT ( 'NONE',  ( -5.823673210054116645, -21.52544592524344225, 112.2905762719810241 ) ) ;
#154622 = CARTESIAN_POINT ( 'NONE',  ( 21.52544592524344225, -5.823673210054117533, 78.54057627198103830 ) ) ;
#154623 = CARTESIAN_POINT ( 'NONE',  ( -4.483927247898782831, 16.52544592524335698, 42.70942372801901854 ) ) ;
#154625 = CARTESIAN_POINT ( 'NONE',  ( 10.72451020669898902, -18.67979575497178502, 82.91557627198103830 ) ) ;
#154624 = CARTESIAN_POINT ( 'NONE',  ( 30.00000000000000000, -5.510910596163089556E-15, 42.35000000000000142 ) ) ;
#154627 = CARTESIAN_POINT ( 'NONE',  ( 4.483927247898545687, 16.52544592524342804, 64.79057627198103830 ) ) ;
#154626 = CARTESIAN_POINT ( 'NONE',  ( 14.34966873604972726, -8.224510206698740333, 70.83442372801901854 ) ) ;
#154628 = CARTESIAN_POINT ( 'NONE',  ( -20.43538597629128262, 20.43538597629122222, -49.67367017693150189 ) ) ;
#154629 = CARTESIAN_POINT ( 'NONE',  ( -19.02544592524334988, -5.153800228976617603, 98.95942372801900433 ) ) ;
#154630 = CARTESIAN_POINT ( 'NONE',  ( -22.45286902209802449, 1.470710558936617840, -55.62279185774873724 ) ) ;
#154631 = CARTESIAN_POINT ( 'NONE',  ( 4.483927247898790824, -16.52544592524335698, 40.20942372801901854 ) ) ;
#154632 = CARTESIAN_POINT ( 'NONE',  ( -10.81492255796078084, -18.62759615963271287, 107.0822429386476955 ) ) ;
#154633 = CARTESIAN_POINT ( 'NONE',  ( -0.05219959533907301413, -21.53943276465977519, 32.49890960531435979 ) ) ;
#154634 = CARTESIAN_POINT ( 'NONE',  ( -8.224510206698735004, -14.34966873604973081, 59.58442372801901854 ) ) ;
#154635 = CARTESIAN_POINT ( 'NONE',  ( -13.97604488694527625, -13.89961937509977652, 71.87390960531433848 ) ) ;
#154637 = CARTESIAN_POINT ( 'NONE',  ( -16.51473224551082808, 9.474510206698731452, 108.3344237280190043 ) ) ;
#154636 = CARTESIAN_POINT ( 'NONE',  ( 15.72974639402176855, 15.80617190586768217, 41.87609039468568284 ) ) ;
#154638 = CARTESIAN_POINT ( 'NONE',  ( -18.67979575497178146, -10.72451020669898902, 26.66557627198103475 ) ) ;
#154639 = EDGE_LOOP ( 'NONE', ( #57794, #74662 ) ) ;
#154640 = CARTESIAN_POINT ( 'NONE',  ( 19.03943276465977164, 0.05219959533936151252, 31.25109039468566863 ) ) ;
#154641 = CARTESIAN_POINT ( 'NONE',  ( 8.224510206698742110, 14.34966873604972548, 42.08442372801901854 ) ) ;
#154642 = CARTESIAN_POINT ( 'NONE',  ( -5.049401038298153566, 19.05341960407611168, 95.20724293864770971 ) ) ;
#154643 = CARTESIAN_POINT ( 'NONE',  ( 0.05219959533907565091, 21.53943276465977519, 99.99890960531436690 ) ) ;
#154644 = CARTESIAN_POINT ( 'NONE',  ( -19.05341960407611168, -5.049401038298163336, 66.45724293864769550 ) ) ;
#154645 = CARTESIAN_POINT ( 'NONE',  ( -2.802625768539467543, -39.09149893265183806, -33.00000000000000000 ) ) ;
#154646 = CARTESIAN_POINT ( 'NONE',  ( -14.29746914071049879, 8.314922557960819915, 85.83224293864768129 ) ) ;
#154647 = CARTESIAN_POINT ( 'NONE',  ( 18.67979575497178502, 10.72451020669898547, 24.16557627198103120 ) ) ;
#154648 = CARTESIAN_POINT ( 'NONE',  ( -16.36317988757058828, 7.306389748694926745, 34.09789608363226421 ) ) ;
#154649 = CARTESIAN_POINT ( 'NONE',  ( -4.483927247898782831, 16.52544592524335698, 62.70942372801902565 ) ) ;
#154650 = CARTESIAN_POINT ( 'NONE',  ( -21.53943276465977519, 0.05219959533907696930, 101.2489096053143669 ) ) ;
#154651 = CARTESIAN_POINT ( 'NONE',  ( 16.46253265017146816, 9.564922557961045513, 66.66775706135233293 ) ) ;
#154652 = CARTESIAN_POINT ( 'NONE',  ( -10.72451020669898014, 18.67979575497178502, 35.41557627198102409 ) ) ;
#154653 = CARTESIAN_POINT ( 'NONE',  ( -16.51473224551069308, -9.474510206698971260, 31.66557627198102054 ) ) ;
#154654 = CARTESIAN_POINT ( 'NONE',  ( 5.719274019375991003, -21.55341960407610458, 67.70724293864769550 ) ) ;
#154655 = CARTESIAN_POINT ( 'NONE',  ( 19.02544592524343514, -5.153800228976328945, 93.54057627198102409 ) ) ;
#154656 = CARTESIAN_POINT ( 'NONE',  ( 5.719274019375673035, 21.55341960407619339, 92.29275706135236135 ) ) ;
#154657 = CARTESIAN_POINT ( 'NONE',  ( -16.51473224551069308, -9.474510206698971260, 51.66557627198102409 ) ) ;
#154658 = CARTESIAN_POINT ( 'NONE',  ( 12.06949235617739724, 12.14591786802326823, 36.87609039468568994 ) ) ;
#154659 = CARTESIAN_POINT ( 'NONE',  ( 16.46253265017160672, -9.564922557960803928, 53.33224293864768839 ) ) ;
#154660 = CARTESIAN_POINT ( 'NONE',  ( 5.719274019375673035, 21.55341960407619339, 82.29275706135234714 ) ) ;
#154661 = ORIENTED_EDGE ( 'NONE', *, *, #2143, .T. ) ;
#154662 = CARTESIAN_POINT ( 'NONE',  ( -9.474510206698720793, -16.51473224551083518, 39.58442372801899722 ) ) ;
#154663 = CARTESIAN_POINT ( 'NONE',  ( 16.46253265017146816, 9.564922557961045513, 46.66775706135233293 ) ) ;
#154664 = CARTESIAN_POINT ( 'NONE',  ( -10.81492255796105439, 18.62759615963255655, 42.91775706135235424 ) ) ;
#154665 = CARTESIAN_POINT ( 'NONE',  ( 28.79475375365586132, 2.781246896534039337E-14, 142.9843446568999639 ) ) ;
#154666 = CARTESIAN_POINT ( 'NONE',  ( 19.03943276465977164, 0.05219959533936151252, 36.25109039468567573 ) ) ;
#154667 = CARTESIAN_POINT ( 'NONE',  ( -0.05219959533909027116, -19.03943276465977164, 82.49890960531436690 ) ) ;
#154668 = CARTESIAN_POINT ( 'NONE',  ( -5.153800228976328057, -19.02544592524343514, 67.29057627198102409 ) ) ;
#154669 = CARTESIAN_POINT ( 'NONE',  ( -14.29746914071049879, 8.314922557960819915, 30.83224293864770260 ) ) ;
#154671 = CARTESIAN_POINT ( 'NONE',  ( -15.72974639402176322, -15.80617190586768395, 89.37609039468568994 ) ) ;
#154670 = CARTESIAN_POINT ( 'NONE',  ( 19.03943276465977164, -0.05219959533909143690, 113.7489096053143669 ) ) ;
#154672 = CIRCLE ( 'NONE', #6136, 7.500000000000000000 ) ;
#154673 = CARTESIAN_POINT ( 'NONE',  ( -29.86685920354755197, -21.69954338932560134, -10.92499999726881299 ) ) ;
#154674 = CARTESIAN_POINT ( 'NONE',  ( 16.62475595723696031, 7.163666690055254804, 56.97286648189535896 ) ) ;
#154675 = CARTESIAN_POINT ( 'NONE',  ( -5.823673210054431948, 21.52544592524334988, 97.70942372801904696 ) ) ;
#154676 = CARTESIAN_POINT ( 'NONE',  ( 17.49999999999999645, -5.624438216177595429, 43.31670344914645199 ) ) ;
#154677 = CARTESIAN_POINT ( 'NONE',  ( 19.03943276465977164, -0.05219959533909143690, 28.74890960531435624 ) ) ;
#154678 = CARTESIAN_POINT ( 'NONE',  ( -25.25560589046783733, 2.428612866367529932E-14, 167.9999999999999716 ) ) ;
#154679 = CARTESIAN_POINT ( 'NONE',  ( 33.84955102792976334, 0.7177882281432049760, 100.4649514046631680 ) ) ;
#154680 = CARTESIAN_POINT ( 'NONE',  ( 16.55341960407618274, -4.379528057220086978, 46.04275706135234714 ) ) ;
#154681 = CARTESIAN_POINT ( 'NONE',  ( 10.72451020669898902, -18.67979575497178502, 67.91557627198102409 ) ) ;
#154682 = CARTESIAN_POINT ( 'NONE',  ( -4.379528057220328563, 16.55341960407611168, 45.20724293864769550 ) ) ;
#154684 = CARTESIAN_POINT ( 'NONE',  ( -13.97604488694527625, -13.89961937509977652, 91.87390960531432427 ) ) ;
#154683 = CARTESIAN_POINT ( 'NONE',  ( 16.55341960407611168, 4.379528057220329451, 113.9572429386477239 ) ) ;
#154685 = CARTESIAN_POINT ( 'NONE',  ( 16.51473224551083163, -9.474510206698727899, 25.83442372801900078 ) ) ;
#154686 = CARTESIAN_POINT ( 'NONE',  ( -16.51473224551069308, -9.474510206698971260, 26.66557627198103120 ) ) ;
#154687 = CARTESIAN_POINT ( 'NONE',  ( 21.55341960407619695, -5.719274019375665929, 66.04275706135236135 ) ) ;
#154688 = CARTESIAN_POINT ( 'NONE',  ( 22.96528548301342809, -5.795830589372932273, 190.0000000000000000 ) ) ;
#154689 = CARTESIAN_POINT ( 'NONE',  ( -0.05219959533934338120, 16.53943276465976808, 112.5010903946857042 ) ) ;
#154690 = CARTESIAN_POINT ( 'NONE',  ( -19.05341960407617563, 5.049401038297882671, 68.54275706135230450 ) ) ;
#154691 = CARTESIAN_POINT ( 'NONE',  ( -36.91746825000000598, -11.99521256947794789, -7.024999997268812635 ) ) ;
#154692 = CARTESIAN_POINT ( 'NONE',  ( -0.05219959533907301413, -21.53943276465977519, 27.49890960531435269 ) ) ;
#154693 = CARTESIAN_POINT ( 'NONE',  ( -16.52544592524342804, 4.483927247898546575, 86.04057627198102409 ) ) ;
#154694 = CARTESIAN_POINT ( 'NONE',  ( 0.05219959533936267826, -19.03943276465977164, 60.00109039468566863 ) ) ;
#154695 = CARTESIAN_POINT ( 'NONE',  ( -9.474510206698964154, 16.51473224551069663, 70.41557627198102409 ) ) ;
#154696 = CARTESIAN_POINT ( 'NONE',  ( -12.06949235617756955, 12.14591786802309770, 60.62390960531437401 ) ) ;
#154697 = CARTESIAN_POINT ( 'NONE',  ( 16.46253265017146816, 9.564922557961045513, 96.66775706135233293 ) ) ;
#154698 = CARTESIAN_POINT ( 'NONE',  ( -21.53943276465977519, 0.05219959533907696930, 46.24890960531435979 ) ) ;
#154699 = VERTEX_POINT ( 'NONE', #27169 ) ;
#154700 = CARTESIAN_POINT ( 'NONE',  ( 13.97604488694527802, 13.89961937509977652, 24.37390960531435624 ) ) ;
#154701 = CARTESIAN_POINT ( 'NONE',  ( 16.51473224551083163, -9.474510206698727899, 100.8344237280190043 ) ) ;
#154702 = EDGE_CURVE ( 'NONE', #188324, #30166, #153628, .T. ) ;
#154705 = CARTESIAN_POINT ( 'NONE',  ( 5.823673210054125526, 21.52544592524343514, 74.79057627198105251 ) ) ;
#154704 = B_SPLINE_CURVE_WITH_KNOTS ( 'NONE', 3,
 ( #48629, #6077, #80928, #36409, #158764, #110281, #81900, #67755, #142605, #171962, #111274, #96102, #33450, #143593 ),
 .UNSPECIFIED., .F., .F.,
 ( 4, 2, 2, 2, 2, 2, 4 ),
 ( 0.001176765026004452036, 0.002067183656864254610, 0.002957602287724056967, 0.003402811603153957712, 0.003848020918583858023, 0.004293230234013758334, 0.004738439549443658645 ),
 .UNSPECIFIED. ) ;
#154703 = CARTESIAN_POINT ( 'NONE',  ( 9.474510206698971260, -16.51473224551069308, 77.91557627198103830 ) ) ;
#154707 = CARTESIAN_POINT ( 'NONE',  ( 19.03943276465977164, -0.05219959533909143690, 68.74890960531436690 ) ) ;
#154706 = CARTESIAN_POINT ( 'NONE',  ( 8.224510206698742110, 14.34966873604972548, 87.08442372801901854 ) ) ;
#154708 = CARTESIAN_POINT ( 'NONE',  ( 5.049401038297881783, 19.05341960407617563, 72.29275706135234714 ) ) ;
#154709 = CARTESIAN_POINT ( 'NONE',  ( 15.80617190586769283, -15.72974639402175789, 75.62609039468567573 ) ) ;
#154710 = CARTESIAN_POINT ( 'NONE',  ( -21.55341960407610458, -5.719274019375992779, 61.45724293864770260 ) ) ;
#154711 = CARTESIAN_POINT ( 'NONE',  ( -18.62759615963270932, 10.81492255796079327, 30.83224293864770260 ) ) ;
#154712 = CARTESIAN_POINT ( 'NONE',  ( -19.03943276465977164, 0.05219959533909376836, 31.24890960531435979 ) ) ;
#154713 = CARTESIAN_POINT ( 'NONE',  ( -14.29746914071037622, -8.314922557961029526, 99.16775706135234714 ) ) ;
#154714 = CARTESIAN_POINT ( 'NONE',  ( -0.05219959533909027116, -19.03943276465977164, 47.49890960531435979 ) ) ;
#154715 = CARTESIAN_POINT ( 'NONE',  ( -8.224510206698735004, -14.34966873604973081, 24.58442372801901499 ) ) ;
#154716 = CARTESIAN_POINT ( 'NONE',  ( -31.64627301717024821, -2.653341670344202097, 102.0192792579183276 ) ) ;
#154717 = CARTESIAN_POINT ( 'NONE',  ( 9.564922557961047289, -16.46253265017146816, 20.41775706135233293 ) ) ;
#154718 = CARTESIAN_POINT ( 'NONE',  ( -16.53943276465976808, 0.05219959533911058130, 61.24890960531435979 ) ) ;
#154719 = CARTESIAN_POINT ( 'NONE',  ( -21.55341960407610458, -5.719274019375992779, 91.45724293864769550 ) ) ;
#154720 = CARTESIAN_POINT ( 'NONE',  ( -18.62759615963270932, 10.81492255796079327, 95.83224293864770971 ) ) ;
#154721 = CARTESIAN_POINT ( 'NONE',  ( 17.26172910966780094, -6.454744622555848466, 98.30646908649228521 ) ) ;
#154722 = CARTESIAN_POINT ( 'NONE',  ( -5.823673210054116645, -21.52544592524344225, 42.29057627198103120 ) ) ;
#154723 = CARTESIAN_POINT ( 'NONE',  ( -14.29746914071037622, -8.314922557961029526, 79.16775706135234714 ) ) ;
#154724 = CARTESIAN_POINT ( 'NONE',  ( 0.05219959533910956823, 16.53943276465976808, 94.99890960531436690 ) ) ;
#154725 = CARTESIAN_POINT ( 'NONE',  ( 5.049401038298161559, -19.05341960407611168, 47.70724293864770260 ) ) ;
#154726 = LINE ( 'NONE', #72177, #115597 ) ;
#154727 = CARTESIAN_POINT ( 'NONE',  ( -16.53943276465976808, 0.05219959533911058130, 21.24890960531436690 ) ) ;
#154728 = CARTESIAN_POINT ( 'NONE',  ( -21.52544592524334988, -5.823673210054445271, 38.95942372801901854 ) ) ;
#154729 = CARTESIAN_POINT ( 'NONE',  ( -9.474510206698964154, 16.51473224551069663, 90.41557627198103830 ) ) ;
#154730 = CARTESIAN_POINT ( 'NONE',  ( -18.62759615963255300, -10.81492255796106328, 69.16775706135234714 ) ) ;
#154731 = DIRECTION ( 'NONE',  ( 0.000000000000000000, 0.000000000000000000, 1.000000000000000000 ) ) ;
#154732 = DIRECTION ( 'NONE',  ( 1.000000000000000000, 0.000000000000000000, 0.000000000000000000 ) ) ;
#154733 = EDGE_LOOP ( 'NONE', ( #195705, #181456, #167373, #98148 ) ) ;
#154734 = CARTESIAN_POINT ( 'NONE',  ( 15.72974639402176855, 15.80617190586768217, 61.87609039468568284 ) ) ;
#154736 = CARTESIAN_POINT ( 'NONE',  ( -13.89961937509977652, 13.97604488694528158, 110.6239096053143243 ) ) ;
#154735 = CARTESIAN_POINT ( 'NONE',  ( -9.564922557960796823, -16.46253265017161027, 57.08224293864769550 ) ) ;
#154737 = CARTESIAN_POINT ( 'NONE',  ( -16.51473224551069308, -9.474510206698971260, 91.66557627198103830 ) ) ;
#154738 = CARTESIAN_POINT ( 'NONE',  ( 19.03943276465977164, 0.05219959533936151252, 66.25109039468567573 ) ) ;
#154739 = CARTESIAN_POINT ( 'NONE',  ( -5.823673210054431948, 21.52544592524334988, 42.70942372801901854 ) ) ;
#154740 = CARTESIAN_POINT ( 'NONE',  ( -9.564922557961040184, 16.46253265017147172, 102.9177570613523329 ) ) ;
#154741 = CARTESIAN_POINT ( 'NONE',  ( -19.02544592524334988, -5.153800228976617603, 73.95942372801900433 ) ) ;
#154742 = CARTESIAN_POINT ( 'NONE',  ( 19.02544592524343514, -5.153800228976328945, 33.54057627198102409 ) ) ;
#154743 = CARTESIAN_POINT ( 'NONE',  ( -8.224510206698735004, -14.34966873604973081, 104.5844237280190185 ) ) ;
#154744 = CARTESIAN_POINT ( 'NONE',  ( 16.46253265017146816, 9.564922557961045513, 71.66775706135233293 ) ) ;
#154745 = CARTESIAN_POINT ( 'NONE',  ( 16.52544592524342804, -4.483927247898539470, 28.54057627198103120 ) ) ;
#154746 = CARTESIAN_POINT ( 'NONE',  ( -5.049401038297874678, -19.05341960407617918, 54.79275706135234003 ) ) ;
#154747 = CARTESIAN_POINT ( 'NONE',  ( 21.55341960407619695, -5.719274019375665929, 101.0427570613523756 ) ) ;
#154748 = CARTESIAN_POINT ( 'NONE',  ( 5.049401038297881783, 19.05341960407617563, 27.29275706135232937 ) ) ;
#154749 = CARTESIAN_POINT ( 'NONE',  ( 9.474510206698971260, -16.51473224551069308, 22.91557627198102765 ) ) ;
#154750 = CARTESIAN_POINT ( 'NONE',  ( -10.81492255796105439, 18.62759615963255655, 82.91775706135234714 ) ) ;
#154751 = CARTESIAN_POINT ( 'NONE',  ( -0.05219959533934338120, 16.53943276465976808, 27.50109039468567929 ) ) ;
#154752 = CARTESIAN_POINT ( 'NONE',  ( -13.97604488694527625, -13.89961937509977652, 96.87390960531433848 ) ) ;
#154753 = CARTESIAN_POINT ( 'NONE',  ( -5.359611314223446995E-15, 29.16686587814335496, 142.3750000027311557 ) ) ;
#154754 = CARTESIAN_POINT ( 'NONE',  ( -19.05341960407611168, -5.049401038298163336, 81.45724293864769550 ) ) ;
#154755 = CARTESIAN_POINT ( 'NONE',  ( -17.50000000001358202, 5.499999999999951150, 100.7969038253505687 ) ) ;
#154756 = CARTESIAN_POINT ( 'NONE',  ( -5.153800228976607833, 19.02544592524334988, 82.70942372801897591 ) ) ;
#154757 = CARTESIAN_POINT ( 'NONE',  ( 0.05219959533909260263, 19.03943276465977164, 104.9989096053143669 ) ) ;
#154758 = CARTESIAN_POINT ( 'NONE',  ( -21.53943276465977519, -0.05219959533937600094, 108.7510903946857042 ) ) ;
#154759 = CARTESIAN_POINT ( 'NONE',  ( 12.14591786802309770, 12.06949235617756955, 94.37390960531436690 ) ) ;
#154760 = CARTESIAN_POINT ( 'NONE',  ( -0.05219959533909027116, -19.03943276465977164, 27.49890960531435624 ) ) ;
#154761 = CARTESIAN_POINT ( 'NONE',  ( 18.62759615963271287, -10.81492255796078972, 53.33224293864769550 ) ) ;
#154762 = CARTESIAN_POINT ( 'NONE',  ( 21.52544592524344225, -5.823673210054117533, 33.54057627198102409 ) ) ;
#154763 = CARTESIAN_POINT ( 'NONE',  ( 16.52544592524342804, -4.483927247898539470, 113.5405762719810383 ) ) ;
#154764 = CARTESIAN_POINT ( 'NONE',  ( -16.49741402511618560, 0.7792920370543191533, -61.43171317168472001 ) ) ;
#154765 = CARTESIAN_POINT ( 'NONE',  ( -5.153800228976607833, 19.02544592524334988, 57.70942372801899012 ) ) ;
#154766 = CARTESIAN_POINT ( 'NONE',  ( -14.34966873604960291, -8.224510206698953496, 41.66557627198103120 ) ) ;
#154768 = EDGE_CURVE ( 'NONE', #23117, #65708, #69890, .T. ) ;
#154767 = CARTESIAN_POINT ( 'NONE',  ( -21.55341960407610458, -5.719274019375992779, 21.45724293864769550 ) ) ;
#154769 = CARTESIAN_POINT ( 'NONE',  ( 21.53943276465977519, 0.05219959533937863772, 81.25109039468568994 ) ) ;
#154770 = CARTESIAN_POINT ( 'NONE',  ( -21.53943276465977519, 0.05219959533907696930, 76.24890960531435269 ) ) ;
#154771 = CARTESIAN_POINT ( 'NONE',  ( -21.55341960407619339, 5.719274019375674811, 63.54275706135234003 ) ) ;
#154772 = CARTESIAN_POINT ( 'NONE',  ( 5.823673210054444382, -21.52544592524334988, 50.20942372801901854 ) ) ;
#154773 = CARTESIAN_POINT ( 'NONE',  ( 13.97604488694527802, 13.89961937509977652, 89.37390960531436690 ) ) ;
#154774 = CARTESIAN_POINT ( 'NONE',  ( 16.53943276465976808, 0.05219959533934440121, 81.25109039468568994 ) ) ;
#154775 = CARTESIAN_POINT ( 'NONE',  ( 16.46253265017160672, -9.564922557960803928, 23.33224293864769194 ) ) ;
#154776 = CARTESIAN_POINT ( 'NONE',  ( -32.64453336272028139, 2.028832619897439204E-14, 87.50000000000000000 ) ) ;
#154777 = CARTESIAN_POINT ( 'NONE',  ( 16.53943276465976808, -0.05219959533910856209, 53.74890960531437401 ) ) ;
#154778 = CARTESIAN_POINT ( 'NONE',  ( 12.06949235617757843, -12.14591786802309237, 28.12390960531435979 ) ) ;
#154779 = CARTESIAN_POINT ( 'NONE',  ( 13.97604488694527802, 13.89961937509977652, 64.37390960531436690 ) ) ;
#154780 = CARTESIAN_POINT ( 'NONE',  ( -13.89961937509977652, 13.97604488694528158, 40.62390960531435979 ) ) ;
#154781 = CARTESIAN_POINT ( 'NONE',  ( 21.53943276465977519, -0.05219959533907433946, 38.74890960531435979 ) ) ;
#154782 = CARTESIAN_POINT ( 'NONE',  ( -9.474510206698720793, -16.51473224551083518, 44.58442372801900433 ) ) ;
#154784 = CARTESIAN_POINT ( 'NONE',  ( -12.06949235617756955, 12.14591786802309770, 50.62390960531435979 ) ) ;
#154783 = CARTESIAN_POINT ( 'NONE',  ( -17.49999999999999645, -5.500000000000000888, 39.20309617465829177 ) ) ;
#154785 = CARTESIAN_POINT ( 'NONE',  ( 15.72974639402199770, -15.80617190586745480, 23.12390960531436335 ) ) ;
#154786 = CARTESIAN_POINT ( 'NONE',  ( 17.69326672847925508, -2.167987141922157690, 37.50000000000000000 ) ) ;
#154787 = CARTESIAN_POINT ( 'NONE',  ( -14.34966873604972548, 8.224510206698743886, 68.33442372801900433 ) ) ;
#154788 = CARTESIAN_POINT ( 'NONE',  ( 13.97604488694548053, -13.89961937509957401, 75.62609039468564731 ) ) ;
#154789 = EDGE_CURVE ( 'NONE', #64219, #70273, #75085, .T. ) ;
#154790 = CARTESIAN_POINT ( 'NONE',  ( 8.314922557960818139, 14.29746914071049879, 39.58224293864769550 ) ) ;
#154791 = FACE_OUTER_BOUND ( 'NONE', #154423, .T. ) ;
#154792 = CARTESIAN_POINT ( 'NONE',  ( 0.05219959533910956823, 16.53943276465976808, 29.99890960531435979 ) ) ;
#154793 = CARTESIAN_POINT ( 'NONE',  ( 13.97604488694527802, 13.89961937509977652, 44.37390960531435269 ) ) ;
#154794 = CARTESIAN_POINT ( 'NONE',  ( -13.97604488694527625, -13.89961937509977652, 56.87390960531434558 ) ) ;
#154795 = CARTESIAN_POINT ( 'NONE',  ( -5.153800228976328057, -19.02544592524343514, 42.29057627198101699 ) ) ;
#154796 = CARTESIAN_POINT ( 'NONE',  ( -18.62759615963255300, -10.81492255796106328, 29.16775706135234003 ) ) ;
#154797 = CARTESIAN_POINT ( 'NONE',  ( -9.564922557960796823, -16.46253265017161027, 57.08224293864769550 ) ) ;
#154798 = DIRECTION ( 'NONE',  ( 1.000000000000000000, -0.000000000000000000, -0.000000000000000000 ) ) ;
#154799 = CARTESIAN_POINT ( 'NONE',  ( 9.564922557960805705, 16.46253265017160317, 44.58224293864769550 ) ) ;
#154800 = CARTESIAN_POINT ( 'NONE',  ( 21.52544592524344225, -5.823673210054117533, 33.54057627198102409 ) ) ;
#154802 = CARTESIAN_POINT ( 'NONE',  ( -13.97604488694527625, -13.89961937509977652, 26.87390960531434558 ) ) ;
#154801 = CARTESIAN_POINT ( 'NONE',  ( -18.67979575497193778, 10.72451020669871902, 58.33442372801901143 ) ) ;
#154803 = CARTESIAN_POINT ( 'NONE',  ( -15.80617190586745835, -15.72974639402198527, 21.87390960531436690 ) ) ;
#154804 = CARTESIAN_POINT ( 'NONE',  ( 16.55341960407618274, -4.379528057220086978, 91.04275706135236135 ) ) ;
#154805 = CARTESIAN_POINT ( 'NONE',  ( -21.52544592524334988, -5.823673210054445271, 103.9594237280190185 ) ) ;
#154806 = CARTESIAN_POINT ( 'NONE',  ( 12.06949235617739724, 12.14591786802326823, 66.87609039468568994 ) ) ;
#154807 = CARTESIAN_POINT ( 'NONE',  ( 0.05219959533909260263, 19.03943276465977164, 104.9989096053143669 ) ) ;
#154808 = CARTESIAN_POINT ( 'NONE',  ( -12.06949235617739369, -12.14591786802326823, 49.37609039468569705 ) ) ;
#154809 = CARTESIAN_POINT ( 'NONE',  ( 0.05219959533934541429, -16.53943276465976808, 40.00109039468567573 ) ) ;
#154810 = CARTESIAN_POINT ( 'NONE',  ( -16.55341960407617563, 4.379528057220093196, 93.54275706135234714 ) ) ;
#154811 = CARTESIAN_POINT ( 'NONE',  ( 0.05219959533937995610, -21.53943276465977519, 60.00109039468568284 ) ) ;
#154812 = CARTESIAN_POINT ( 'NONE',  ( 8.314922557961029526, -14.29746914071037800, 25.41775706135235779 ) ) ;
#154813 = CARTESIAN_POINT ( 'NONE',  ( -15.80617190586745835, -15.72974639402198527, 106.8739096053143811 ) ) ;
#154814 = CARTESIAN_POINT ( 'NONE',  ( 16.52544592524335698, 4.483927247898782831, 26.45942372801901854 ) ) ;
#154815 = CARTESIAN_POINT ( 'NONE',  ( 16.52544592524335698, 4.483927247898782831, 91.45942372801901854 ) ) ;
#154816 = CARTESIAN_POINT ( 'NONE',  ( -11.74264578624800670, 36.14014761921585972, -4.149999994537627579 ) ) ;
#154817 = CARTESIAN_POINT ( 'NONE',  ( 10.81492255796106328, -18.62759615963255655, 90.41775706135236135 ) ) ;
#154818 = CARTESIAN_POINT ( 'NONE',  ( -5.049401038297874678, -19.05341960407617918, 89.79275706135230450 ) ) ;
#154819 = CARTESIAN_POINT ( 'NONE',  ( -4.379528057220328563, 16.55341960407611168, 65.20724293864768129 ) ) ;
#154820 = CARTESIAN_POINT ( 'NONE',  ( -12.06949235617756955, 12.14591786802309770, 40.62390960531435269 ) ) ;
#154821 = CARTESIAN_POINT ( 'NONE',  ( -8.314922557960811034, -14.29746914071050412, 107.0822429386476955 ) ) ;
#154823 = CARTESIAN_POINT ( 'NONE',  ( -8.898962301217514081, 0.7565710328821524389, -63.99033069988504963 ) ) ;
#154822 = CARTESIAN_POINT ( 'NONE',  ( 19.02544592524334988, 5.153800228976608722, 46.45942372801899012 ) ) ;
#154824 = CARTESIAN_POINT ( 'NONE',  ( 21.53943276465977519, 0.05219959533937863772, 51.25109039468568994 ) ) ;
#154825 = CARTESIAN_POINT ( 'NONE',  ( -9.564922557961040184, 16.46253265017147172, 112.9177570613523329 ) ) ;
#154826 = DIRECTION ( 'NONE',  ( 0.000000000000000000, -1.000000000000000000, 0.000000000000000000 ) ) ;
#154827 = CARTESIAN_POINT ( 'NONE',  ( -13.89961937509977652, 13.97604488694528158, 100.6239096053143669 ) ) ;
#154828 = CARTESIAN_POINT ( 'NONE',  ( -18.67979575497178146, -10.72451020669898902, 66.66557627198102409 ) ) ;
#154829 = CARTESIAN_POINT ( 'NONE',  ( -19.03943276465977164, -0.05219959533935918106, 93.75109039468566152 ) ) ;
#154830 = CARTESIAN_POINT ( 'NONE',  ( 13.89961937509977652, -13.97604488694527269, 98.12390960531433848 ) ) ;
#154831 = CARTESIAN_POINT ( 'NONE',  ( 15.72974639402199770, -15.80617190586745480, 53.12390960531436690 ) ) ;
#154832 = CARTESIAN_POINT ( 'NONE',  ( 16.52544592524342804, -4.483927247898539470, 108.5405762719810241 ) ) ;
#154833 = CARTESIAN_POINT ( 'NONE',  ( -5.719274019375665041, -21.55341960407619695, 89.79275706135236135 ) ) ;
#154834 = CARTESIAN_POINT ( 'NONE',  ( 9.564922557960805705, 16.46253265017160317, 34.58224293864770260 ) ) ;
#154835 = CARTESIAN_POINT ( 'NONE',  ( -5.823673210054431948, 21.52544592524334988, 37.70942372801900433 ) ) ;
#154836 = CIRCLE ( 'NONE', #187194, 0.2000000000000000944 ) ;
#154837 = CARTESIAN_POINT ( 'NONE',  ( -5.719274019375665041, -21.55341960407619695, 94.79275706135234714 ) ) ;
#154838 = ADVANCED_FACE ( 'NONE', ( #142266 ), #44072, .F. ) ;
#154839 = CARTESIAN_POINT ( 'NONE',  ( 4.483927247898790824, -16.52544592524335698, 90.20942372801903275 ) ) ;
#154840 = CARTESIAN_POINT ( 'NONE',  ( 21.55341960407619695, -5.719274019375665929, 31.04275706135234714 ) ) ;
#154841 = CARTESIAN_POINT ( 'NONE',  ( -15.72974639402176322, -15.80617190586768395, 39.37609039468567573 ) ) ;
#154843 = CARTESIAN_POINT ( 'NONE',  ( 13.89961937509977652, -13.97604488694527269, 83.12390960531436690 ) ) ;
#154842 = CARTESIAN_POINT ( 'NONE',  ( -19.02544592524334988, -5.153800228976617603, 68.95942372801896170 ) ) ;
#154844 = CARTESIAN_POINT ( 'NONE',  ( 10.72451020669871369, 18.67979575497193778, 82.08442372801901854 ) ) ;
#154845 = CARTESIAN_POINT ( 'NONE',  ( -5.719274019375978568, 21.55341960407610458, 85.20724293864770971 ) ) ;
#154846 = CARTESIAN_POINT ( 'NONE',  ( 12.06949235617757843, -12.14591786802309237, 58.12390960531435979 ) ) ;
#154847 = CARTESIAN_POINT ( 'NONE',  ( 18.62759615963255655, 10.81492255796105972, 106.6677570613523756 ) ) ;
#154848 = CARTESIAN_POINT ( 'NONE',  ( 14.29746914071049879, -8.314922557960816363, 88.33224293864769550 ) ) ;
#154849 = CARTESIAN_POINT ( 'NONE',  ( 13.89961937509977652, -13.97604488694527269, 38.12390960531436690 ) ) ;
#154850 = CARTESIAN_POINT ( 'NONE',  ( 19.03943276465977164, 0.05219959533936151252, 71.25109039468566152 ) ) ;
#154851 = CARTESIAN_POINT ( 'NONE',  ( -8.224510206698948167, 14.34966873604960824, 40.41557627198103120 ) ) ;
#154852 = CARTESIAN_POINT ( 'NONE',  ( -0.05219959533937732626, 21.53943276465977519, 97.50109039468567573 ) ) ;
#154853 = CARTESIAN_POINT ( 'NONE',  ( -9.474510206698964154, 16.51473224551069663, 95.41557627198102409 ) ) ;
#154854 = CARTESIAN_POINT ( 'NONE',  ( -19.02544592524334988, -5.153800228976617603, 63.95942372801899012 ) ) ;
#154855 = CARTESIAN_POINT ( 'NONE',  ( 18.62759615963271287, -10.81492255796078972, 68.33224293864769550 ) ) ;
#154856 = CARTESIAN_POINT ( 'NONE',  ( 21.55341960407619695, -5.719274019375665929, 21.04275706135234714 ) ) ;
#154857 = CARTESIAN_POINT ( 'NONE',  ( -0.05219959533936034679, 19.03943276465977164, 107.5010903946856615 ) ) ;
#154858 = CARTESIAN_POINT ( 'NONE',  ( -8.314922557961024197, 14.29746914071037800, 77.91775706135231871 ) ) ;
#154860 = CARTESIAN_POINT ( 'NONE',  ( 15.80617190586769283, -15.72974639402175789, 25.62609039468567929 ) ) ;
#154859 = CARTESIAN_POINT ( 'NONE',  ( 16.52216118717207749, 7.221426719304521846, 63.57599021046996057 ) ) ;
#154861 = CARTESIAN_POINT ( 'NONE',  ( -16.52544592524342804, 4.483927247898546575, 106.0405762719810525 ) ) ;
#154862 = CARTESIAN_POINT ( 'NONE',  ( -11.40812507854755609, 35.11059874428196537, -5.524999997268813523 ) ) ;
#154863 = CARTESIAN_POINT ( 'NONE',  ( -16.55341960407617563, 4.379528057220093196, 48.54275706135234714 ) ) ;
#154864 = CARTESIAN_POINT ( 'NONE',  ( -8.224510206698948167, 14.34966873604960824, 80.41557627198103830 ) ) ;
#154865 = CARTESIAN_POINT ( 'NONE',  ( 15.72974639402199770, -15.80617190586745480, 73.12390960531436690 ) ) ;
#154866 = CARTESIAN_POINT ( 'NONE',  ( 16.52544592524335698, 4.483927247898782831, 106.4594237280190328 ) ) ;
#154867 = CARTESIAN_POINT ( 'NONE',  ( 12.06949235617739724, 12.14591786802326823, 36.87609039468568994 ) ) ;
#154868 = CARTESIAN_POINT ( 'NONE',  ( -19.05341960407611168, -5.049401038298163336, 51.45724293864770260 ) ) ;
#154869 = CARTESIAN_POINT ( 'NONE',  ( -16.53943276465976808, -0.05219959533934237506, 73.75109039468567573 ) ) ;
#154870 = CARTESIAN_POINT ( 'NONE',  ( 16.46253265017146816, 9.564922557961045513, 76.66775706135234714 ) ) ;
#154871 = CARTESIAN_POINT ( 'NONE',  ( -18.62759615963270932, 10.81492255796079327, 70.83224293864770971 ) ) ;
#154872 = CARTESIAN_POINT ( 'NONE',  ( 12.06949235617739724, 12.14591786802326823, 91.87609039468568994 ) ) ;
#154873 = CARTESIAN_POINT ( 'NONE',  ( 18.67979575497194134, -10.72451020669871369, 80.83442372801901854 ) ) ;
#154874 = CARTESIAN_POINT ( 'NONE',  ( -21.55341960407610458, -5.719274019375992779, 66.45724293864768129 ) ) ;
#154875 = CARTESIAN_POINT ( 'NONE',  ( -15.80617190586745835, -15.72974639402198527, 51.87390960531437401 ) ) ;
#154876 = EDGE_LOOP ( 'NONE', ( #151960, #164655, #152147, #83657 ) ) ;
#154877 = CARTESIAN_POINT ( 'NONE',  ( 16.55341960407618274, -4.379528057220086978, 81.04275706135236135 ) ) ;
#154878 = CARTESIAN_POINT ( 'NONE',  ( 10.81492255796078972, 18.62759615963270932, 44.58224293864769550 ) ) ;
#154879 = ORIENTED_EDGE ( 'NONE', *, *, #32834, .F. ) ;
#154880 = CARTESIAN_POINT ( 'NONE',  ( 18.67979575497178502, 10.72451020669898547, 24.16557627198103120 ) ) ;
#154881 = CARTESIAN_POINT ( 'NONE',  ( -21.54612633733209748, -7.439814990120659388, 174.3585332542294566 ) ) ;
#154882 = CARTESIAN_POINT ( 'NONE',  ( -13.89961937509977652, 13.97604488694528158, 25.62390960531434558 ) ) ;
#154883 = CARTESIAN_POINT ( 'NONE',  ( -18.67979575497178146, -10.72451020669898902, 76.66557627198103830 ) ) ;
#154884 = CARTESIAN_POINT ( 'NONE',  ( 14.34966873604972726, -8.224510206698740333, 110.8344237280190043 ) ) ;
#154885 = CARTESIAN_POINT ( 'NONE',  ( -21.53943276465977519, -0.05219959533937600094, 43.75109039468568284 ) ) ;
#154886 = CARTESIAN_POINT ( 'NONE',  ( -5.153800228976607833, 19.02544592524334988, 112.7094237280190043 ) ) ;
#154887 = CARTESIAN_POINT ( 'NONE',  ( -8.224510206698948167, 14.34966873604960824, 115.4155762719810241 ) ) ;
#154888 = CARTESIAN_POINT ( 'NONE',  ( 19.02544592524334988, 5.153800228976608722, 106.4594237280190185 ) ) ;
#154889 = CARTESIAN_POINT ( 'NONE',  ( 19.03943276465977164, -0.05219959533909143690, 33.74890960531435979 ) ) ;
#154890 = CARTESIAN_POINT ( 'NONE',  ( -23.31738231874055600, 16.94106989632528837, 143.7999999999999829 ) ) ;
#154891 = CARTESIAN_POINT ( 'NONE',  ( 9.474510206698971260, -16.51473224551069308, 107.9155762719810383 ) ) ;
#154892 = CARTESIAN_POINT ( 'NONE',  ( -0.05219959533934338120, 16.53943276465976808, 92.50109039468567573 ) ) ;
#154893 = CARTESIAN_POINT ( 'NONE',  ( -13.97604488694547697, 13.89961937509957934, 83.12609039468564731 ) ) ;
#154894 = CARTESIAN_POINT ( 'NONE',  ( 19.05341960407617918, -5.049401038297876454, 21.04275706135232582 ) ) ;
#154895 = CARTESIAN_POINT ( 'NONE',  ( -15.72974639402197994, 15.80617190586746368, 55.62390960531436690 ) ) ;
#154896 = CARTESIAN_POINT ( 'NONE',  ( -4.483927247898782831, 16.52544592524335698, 82.70942372801900433 ) ) ;
#154897 = CARTESIAN_POINT ( 'NONE',  ( 5.049401038297881783, 19.05341960407617563, 82.29275706135229029 ) ) ;
#154898 = CARTESIAN_POINT ( 'NONE',  ( 16.51473224551069308, 9.474510206698969483, 39.16557627198103120 ) ) ;
#154899 = CARTESIAN_POINT ( 'NONE',  ( -5.153800228976328057, -19.02544592524343514, 92.29057627198099567 ) ) ;
#154900 = CARTESIAN_POINT ( 'NONE',  ( -10.72451020669870658, -18.67979575497194134, 49.58442372801901143 ) ) ;
#154901 = CARTESIAN_POINT ( 'NONE',  ( 5.049401038298161559, -19.05341960407611168, 47.70724293864770260 ) ) ;
#154902 = CARTESIAN_POINT ( 'NONE',  ( 25.80209238092669466, -7.370998251474716767, 174.5109820657625050 ) ) ;
#154903 = CARTESIAN_POINT ( 'NONE',  ( -16.46253265017160317, 9.564922557960807481, 115.8322429386477097 ) ) ;
#154904 = CARTESIAN_POINT ( 'NONE',  ( -8.224510206698948167, 14.34966873604960824, 65.41557627198102409 ) ) ;
#154905 = CARTESIAN_POINT ( 'NONE',  ( -15.72974639402197994, 15.80617190586746368, 60.62390960531437401 ) ) ;
#154906 = CARTESIAN_POINT ( 'NONE',  ( -3.889087296526037463, -6.412877669190318208, 1.818019484660534424 ) ) ;
#154907 = CARTESIAN_POINT ( 'NONE',  ( 19.02544592524334988, 5.153800228976608722, 41.45942372801900433 ) ) ;
#154908 =( NAMED_UNIT ( * ) PLANE_ANGLE_UNIT ( ) SI_UNIT ( $, .RADIAN. ) );
#154910 = CARTESIAN_POINT ( 'NONE',  ( -0.05219959533909027116, -19.03943276465977164, 72.49890960531435269 ) ) ;
#154909 = CARTESIAN_POINT ( 'NONE',  ( -5.049401038298153566, 19.05341960407611168, 60.20724293864768129 ) ) ;
#154911 = CARTESIAN_POINT ( 'NONE',  ( -16.53943276465976808, -0.05219959533934237506, 48.75109039468568284 ) ) ;
#154912 = CARTESIAN_POINT ( 'NONE',  ( -28.82186960331499037, 2.428612866367530248E-14, 144.0000000000000000 ) ) ;
#154913 = DIRECTION ( 'NONE',  ( 0.000000000000000000, 0.000000000000000000, -1.000000000000000000 ) ) ;
#154914 = CARTESIAN_POINT ( 'NONE',  ( 4.483927247898790824, -16.52544592524335698, 95.20942372801903275 ) ) ;
#154915 = CARTESIAN_POINT ( 'NONE',  ( -1.304248841091933035E-15, -21.30000000000002913, -56.46919128290398504 ) ) ;
#154916 = CARTESIAN_POINT ( 'NONE',  ( 8.314922557961029526, -14.29746914071037800, 80.41775706135234714 ) ) ;
#154917 = CARTESIAN_POINT ( 'NONE',  ( 16.52544592524335698, 4.483927247898782831, 56.45942372801902565 ) ) ;
#154918 = CARTESIAN_POINT ( 'NONE',  ( 5.719274019375673035, 21.55341960407619339, 112.2927570613523471 ) ) ;
#154920 = FACE_BOUND ( 'NONE', #56916, .T. ) ;
#154919 = CARTESIAN_POINT ( 'NONE',  ( -16.46253265017160317, 9.564922557960807481, 60.83224293864769550 ) ) ;
#154921 = CARTESIAN_POINT ( 'NONE',  ( -15.80617190586768217, 15.72974639402176855, 48.12609039468568284 ) ) ;
#154922 = CARTESIAN_POINT ( 'NONE',  ( 9.474510206698729675, 16.51473224551082808, 67.08442372801900433 ) ) ;
#154923 = CARTESIAN_POINT ( 'NONE',  ( -0.05219959533937732626, 21.53943276465977519, 107.5010903946856899 ) ) ;
#154924 = CARTESIAN_POINT ( 'NONE',  ( -16.51473224551069308, -9.474510206698971260, 26.66557627198103120 ) ) ;
#154925 = CARTESIAN_POINT ( 'NONE',  ( -17.31426855362218831, 15.19424636789215910, -57.70166256124682747 ) ) ;
#154926 = CARTESIAN_POINT ( 'NONE',  ( -15.80617190586745835, -15.72974639402198527, 71.87390960531438111 ) ) ;
#154927 = CARTESIAN_POINT ( 'NONE',  ( 13.89961937509977652, -13.97604488694527269, 113.1239096053143527 ) ) ;
#154928 = CARTESIAN_POINT ( 'NONE',  ( -9.474510206698964154, 16.51473224551069663, 25.41557627198103120 ) ) ;
#154929 = CARTESIAN_POINT ( 'NONE',  ( -12.14591786802326823, 12.06949235617739902, 38.12609039468567573 ) ) ;
#154930 = CARTESIAN_POINT ( 'NONE',  ( -4.379528057220328563, 16.55341960407611168, 35.20724293864768839 ) ) ;
#154931 = ORIENTED_EDGE ( 'NONE', *, *, #137048, .T. ) ;
#154932 = EDGE_CURVE ( 'NONE', #65515, #122026, #155460, .T. ) ;
#154933 = CARTESIAN_POINT ( 'NONE',  ( 18.67979575497194134, -10.72451020669871369, 20.83442372801901143 ) ) ;
#154935 = CARTESIAN_POINT ( 'NONE',  ( -5.049401038298153566, 19.05341960407611168, 110.2072429386476671 ) ) ;
#154934 = CARTESIAN_POINT ( 'NONE',  ( 16.52544592524342804, -4.483927247898539470, 43.54057627198103830 ) ) ;
#154936 = CARTESIAN_POINT ( 'NONE',  ( -16.51473224551082808, 9.474510206698731452, 113.3344237280190043 ) ) ;
#154937 = CARTESIAN_POINT ( 'NONE',  ( 9.474510206698729675, 16.51473224551082808, 27.08442372801900433 ) ) ;
#154938 = CARTESIAN_POINT ( 'NONE',  ( 0.05219959533910956823, 16.53943276465976808, 39.99890960531436690 ) ) ;
#154939 = CARTESIAN_POINT ( 'NONE',  ( -21.52544592524343514, 5.823673210054127303, 106.0405762719810525 ) ) ;
#154941 = CARTESIAN_POINT ( 'NONE',  ( 21.52544592524344225, -5.823673210054117533, 63.54057627198103830 ) ) ;
#154940 = DIRECTION ( 'NONE',  ( 0.8164965809277259234, 0.000000000000000000, 0.5773502691896259531 ) ) ;
#154942 = CARTESIAN_POINT ( 'NONE',  ( -19.02544592524342804, 5.153800228976336051, 71.04057627198099567 ) ) ;
#154943 = CARTESIAN_POINT ( 'NONE',  ( 8.224510206698953496, -14.34966873604960469, 52.91557627198103830 ) ) ;
#154944 = CARTESIAN_POINT ( 'NONE',  ( -16.46253265017160317, 9.564922557960807481, 85.83224293864769550 ) ) ;
#154945 = CIRCLE ( 'NONE', #16115, 40.00000000000002132 ) ;
#154946 = LINE ( 'NONE', #167154, #31219 ) ;
#154947 = CARTESIAN_POINT ( 'NONE',  ( 19.02544592524334988, 5.153800228976608722, 51.45942372801900433 ) ) ;
#154948 = CARTESIAN_POINT ( 'NONE',  ( 5.719274019375991003, -21.55341960407610458, 97.70724293864772392 ) ) ;
#154949 = CARTESIAN_POINT ( 'NONE',  ( 8.314922557960818139, 14.29746914071049879, 104.5822429386477097 ) ) ;
#154950 = CARTESIAN_POINT ( 'NONE',  ( 10.81492255796106328, -18.62759615963255655, 45.41775706135234003 ) ) ;
#154951 = CARTESIAN_POINT ( 'NONE',  ( 22.44159573604009594, -16.30477369853687364, 143.6750000027311671 ) ) ;
#154952 = CARTESIAN_POINT ( 'NONE',  ( -16.55341960407611168, -4.379528057220339221, 31.45724293864769550 ) ) ;
#154953 = CARTESIAN_POINT ( 'NONE',  ( -13.89961937509977652, 13.97604488694528158, 40.62390960531435979 ) ) ;
#154954 = CARTESIAN_POINT ( 'NONE',  ( 13.89961937509977652, -13.97604488694527269, 103.1239096053143527 ) ) ;
#154955 = CARTESIAN_POINT ( 'NONE',  ( -5.823673210054116645, -21.52544592524344225, 67.29057627198103830 ) ) ;
#154956 = CARTESIAN_POINT ( 'NONE',  ( -25.22509938781154304, 6.326560822155829378, 165.8168946714179128 ) ) ;
#154957 = CARTESIAN_POINT ( 'NONE',  ( -13.97604488694527625, -13.89961937509977652, 36.87390960531436690 ) ) ;
#154958 = CARTESIAN_POINT ( 'NONE',  ( 21.53943276465977519, -0.05219959533907433946, 48.74890960531435979 ) ) ;
#154959 = CARTESIAN_POINT ( 'NONE',  ( -15.80617190586768217, 15.72974639402176855, 73.12609039468567573 ) ) ;
#154961 = CARTESIAN_POINT ( 'NONE',  ( 14.29746914071037800, 8.314922557961029526, 81.66775706135236135 ) ) ;
#154960 = CARTESIAN_POINT ( 'NONE',  ( 10.08838716500822130, -37.25234734385448832, -23.84483522324828542 ) ) ;
#154962 = CARTESIAN_POINT ( 'NONE',  ( 19.05341960407611168, 5.049401038298154454, 58.95724293864768129 ) ) ;
#154963 = CARTESIAN_POINT ( 'NONE',  ( -9.564922557960796823, -16.46253265017161027, 67.08224293864769550 ) ) ;
#154964 = VERTEX_POINT ( 'NONE', #125124 ) ;
#154965 = CARTESIAN_POINT ( 'NONE',  ( 19.03943276465977164, 0.05219959533936151252, 26.25109039468566507 ) ) ;
#154966 = CARTESIAN_POINT ( 'NONE',  ( 14.34966873604972726, -8.224510206698740333, 80.83442372801901854 ) ) ;
#154967 = CARTESIAN_POINT ( 'NONE',  ( -10.81492255796105439, 18.62759615963255655, 97.91775706135236135 ) ) ;
#154968 = CARTESIAN_POINT ( 'NONE',  ( 5.153800228976335163, 19.02544592524342804, 69.79057627198103830 ) ) ;
#154969 = CARTESIAN_POINT ( 'NONE',  ( -21.55341960407610458, -5.719274019375992779, 31.45724293864769550 ) ) ;
#154970 = CARTESIAN_POINT ( 'NONE',  ( -9.564922557961040184, 16.46253265017147172, 112.9177570613523329 ) ) ;
#154971 = CARTESIAN_POINT ( 'NONE',  ( -15.80617190586768217, 15.72974639402176855, 88.12609039468570415 ) ) ;
#154972 = CARTESIAN_POINT ( 'NONE',  ( -16.53943276465976808, -0.05219959533934237506, 43.75109039468568284 ) ) ;
#154973 = CARTESIAN_POINT ( 'NONE',  ( 18.62759615963271287, -10.81492255796078972, 103.3322429386476955 ) ) ;
#154974 = CARTESIAN_POINT ( 'NONE',  ( 16.52544592524335698, 4.483927247898782831, 21.45942372801901499 ) ) ;
#154975 = CARTESIAN_POINT ( 'NONE',  ( -19.03943276465977164, 0.05219959533909376836, 81.24890960531436690 ) ) ;
#154976 = CARTESIAN_POINT ( 'NONE',  ( 16.55341960407618274, -4.379528057220086978, 26.04275706135235779 ) ) ;
#154977 = CARTESIAN_POINT ( 'NONE',  ( -16.51473224551069308, -9.474510206698971260, 41.66557627198103120 ) ) ;
#154978 = CIRCLE ( 'NONE', #9665, 28.82186960331498682 ) ;
#154979 = CARTESIAN_POINT ( 'NONE',  ( 13.89961937509957401, 13.97604488694547697, 111.8760903946856757 ) ) ;
#154980 = CARTESIAN_POINT ( 'NONE',  ( -12.06949235617756955, 12.14591786802309770, 70.62390960531436690 ) ) ;
#154981 = CARTESIAN_POINT ( 'NONE',  ( 8.224510206698742110, 14.34966873604972548, 72.08442372801899012 ) ) ;
#154983 = CARTESIAN_POINT ( 'NONE',  ( 5.049401038298161559, -19.05341960407611168, 47.70724293864770260 ) ) ;
#154982 = CARTESIAN_POINT ( 'NONE',  ( -15.80617190586768217, 15.72974639402176855, 28.12609039468568284 ) ) ;
#154984 = CARTESIAN_POINT ( 'NONE',  ( 16.46253265017160672, -9.564922557960803928, 73.33224293864769550 ) ) ;
#154985 = CARTESIAN_POINT ( 'NONE',  ( 14.34966873604972726, -8.224510206698740333, 75.83442372801900433 ) ) ;
#154987 = EDGE_LOOP ( 'NONE', ( #38353, #23666, #12330, #187844, #192434 ) ) ;
#154986 = CARTESIAN_POINT ( 'NONE',  ( -24.06756124613667680, -8.142616467496756272, 169.4332804344566057 ) ) ;
#154988 = ORIENTED_EDGE ( 'NONE', *, *, #102901, .F. ) ;
#154989 = CARTESIAN_POINT ( 'NONE',  ( 16.46253265017146816, 9.564922557961045513, 21.66775706135233648 ) ) ;
#154990 = CARTESIAN_POINT ( 'NONE',  ( 16.46253265017160672, -9.564922557960803928, 38.33224293864768839 ) ) ;
#154992 = ORIENTED_EDGE ( 'NONE', *, *, #64542, .F. ) ;
#154991 = CARTESIAN_POINT ( 'NONE',  ( -16.46253265017160317, 9.564922557960807481, 110.8322429386476955 ) ) ;
#154993 = CARTESIAN_POINT ( 'NONE',  ( -4.483927247898782831, 16.52544592524335698, 32.70942372801900433 ) ) ;
#154995 = CARTESIAN_POINT ( 'NONE',  ( -14.29746914071037622, -8.314922557961029526, 44.16775706135234714 ) ) ;
#154994 = CARTESIAN_POINT ( 'NONE',  ( -0.05219959533936034679, 19.03943276465977164, 57.50109039468566863 ) ) ;
#154996 = CARTESIAN_POINT ( 'NONE',  ( 19.05341960407611168, 5.049401038298154454, 38.95724293864767418 ) ) ;
#154997 = CARTESIAN_POINT ( 'NONE',  ( 16.51473224551069308, 9.474510206698969483, 104.1655762719810241 ) ) ;
#154998 = CARTESIAN_POINT ( 'NONE',  ( -19.03943276465977164, 0.05219959533909376836, 61.24890960531436690 ) ) ;
#154999 = CARTESIAN_POINT ( 'NONE',  ( -15.80617190586745835, -15.72974639402198527, 101.8739096053143811 ) ) ;
#155001 = CARTESIAN_POINT ( 'NONE',  ( -16.51473224551069308, -9.474510206698971260, 21.66557627198102765 ) ) ;
#155000 = CARTESIAN_POINT ( 'NONE',  ( -9.474510206698964154, 16.51473224551069663, 90.41557627198103830 ) ) ;
#155002 = CARTESIAN_POINT ( 'NONE',  ( 13.97604488694527802, 13.89961937509977652, 59.37390960531434558 ) ) ;
#155004 = DIRECTION ( 'NONE',  ( 1.000000000000000000, -0.000000000000000000, -0.000000000000000000 ) ) ;
#155003 = CARTESIAN_POINT ( 'NONE',  ( -0.05219959533910754901, -16.53943276465976808, 22.49890960531436335 ) ) ;
#155005 = CARTESIAN_POINT ( 'NONE',  ( 16.51473224551083163, -9.474510206698727899, 100.8344237280190043 ) ) ;
#155006 = CARTESIAN_POINT ( 'NONE',  ( 13.97604488694548053, -13.89961937509957401, 25.62609039468566507 ) ) ;
#155007 = CARTESIAN_POINT ( 'NONE',  ( 16.53943276465976808, -0.05219959533910856209, 58.74890960531436690 ) ) ;
#155008 = CARTESIAN_POINT ( 'NONE',  ( -10.81492255796105439, 18.62759615963255655, 97.91775706135236135 ) ) ;
#155010 = B_SPLINE_CURVE_WITH_KNOTS ( 'NONE', 3,
 ( #180226, #8350, #100348, #134707, #42690, #9361 ),
 .UNSPECIFIED., .F., .F.,
 ( 4, 2, 4 ),
 ( 0.007228050697041582193, 0.007608510107495067287, 0.007988969517948552382 ),
 .UNSPECIFIED. ) ;
#155009 = CARTESIAN_POINT ( 'NONE',  ( 0.05219959533909260263, 19.03943276465977164, 44.99890960531435979 ) ) ;
#155012 = CARTESIAN_POINT ( 'NONE',  ( 18.62759615963255655, 10.81492255796105972, 91.66775706135234714 ) ) ;
#155011 = CARTESIAN_POINT ( 'NONE',  ( -12.06949235617756955, 12.14591786802309770, 25.62390960531435624 ) ) ;
#155013 = CARTESIAN_POINT ( 'NONE',  ( -9.564922557960796823, -16.46253265017161027, 77.08224293864769550 ) ) ;
#155014 = CARTESIAN_POINT ( 'NONE',  ( -0.05219959533909027116, -19.03943276465977164, 97.49890960531436690 ) ) ;
#155015 = CARTESIAN_POINT ( 'NONE',  ( 4.483927247898545687, 16.52544592524342804, 104.7905762719810241 ) ) ;
#155016 = CARTESIAN_POINT ( 'NONE',  ( -12.06949235617756955, 12.14591786802309770, 75.62390960531439532 ) ) ;
#155017 = CARTESIAN_POINT ( 'NONE',  ( -18.67979575497178146, -10.72451020669898902, 81.66557627198103830 ) ) ;
#155018 = CARTESIAN_POINT ( 'NONE',  ( -13.97604488694527625, -13.89961937509977652, 76.87390960531433848 ) ) ;
#155019 = CARTESIAN_POINT ( 'NONE',  ( 15.72974639402199770, -15.80617190586745480, 83.12390960531436690 ) ) ;
#155020 = CARTESIAN_POINT ( 'NONE',  ( 9.564922557961047289, -16.46253265017146816, 80.41775706135234714 ) ) ;
#155022 = CARTESIAN_POINT ( 'NONE',  ( 4.379528057220339221, -16.55341960407611168, 92.70724293864770971 ) ) ;
#155021 = CARTESIAN_POINT ( 'NONE',  ( 19.02130022317637525, -5.499999999999588773, 48.28188669246576836 ) ) ;
#155023 = CARTESIAN_POINT ( 'NONE',  ( 13.97604488694527802, 13.89961937509977652, 59.37390960531434558 ) ) ;
#155024 = CARTESIAN_POINT ( 'NONE',  ( 10.72451020669898902, -18.67979575497178502, 62.91557627198102409 ) ) ;
#155025 = CARTESIAN_POINT ( 'NONE',  ( -24.93942350307309752, -7.769968609432603479, 171.2173313942149662 ) ) ;
#155027 = DIRECTION ( 'NONE',  ( -1.000000000000000000, 0.000000000000000000, 0.000000000000000000 ) ) ;
#155026 = CARTESIAN_POINT ( 'NONE',  ( 16.55341960407618274, -4.379528057220086978, 111.0427570613523613 ) ) ;
#155028 = CARTESIAN_POINT ( 'NONE',  ( 16.55341960407618274, -4.379528057220086978, 26.04275706135235779 ) ) ;
#155029 = EDGE_CURVE ( 'NONE', #177280, #50694, #186821, .T. ) ;
#155030 = CARTESIAN_POINT ( 'NONE',  ( 16.55341960407611168, 4.379528057220329451, 78.95724293864769550 ) ) ;
#155031 = CARTESIAN_POINT ( 'NONE',  ( 8.945340038113744896, -0.6707077324887430470, -61.92615459704094150 ) ) ;
#155032 = CARTESIAN_POINT ( 'NONE',  ( 16.46253265017160672, -9.564922557960803928, 73.33224293864769550 ) ) ;
#155033 = CARTESIAN_POINT ( 'NONE',  ( -0.05219959533909027116, -19.03943276465977164, 27.49890960531435624 ) ) ;
#155034 = CARTESIAN_POINT ( 'NONE',  ( -0.05219959533910754901, -16.53943276465976808, 72.49890960531435269 ) ) ;
#155035 = CARTESIAN_POINT ( 'NONE',  ( 16.46253265017160672, -9.564922557960803928, 113.3322429386476955 ) ) ;
#155037 = CARTESIAN_POINT ( 'NONE',  ( 9.474510206698971260, -16.51473224551069308, 72.91557627198102409 ) ) ;
#155036 = CARTESIAN_POINT ( 'NONE',  ( 0.05219959533936267826, -19.03943276465977164, 95.00109039468567573 ) ) ;
#155038 = CARTESIAN_POINT ( 'NONE',  ( -5.049401038298153566, 19.05341960407611168, 85.20724293864766707 ) ) ;
#155039 = CARTESIAN_POINT ( 'NONE',  ( 15.72974639402199770, -15.80617190586745480, 78.12390960531436690 ) ) ;
#155040 = CARTESIAN_POINT ( 'NONE',  ( -12.06949235617739369, -12.14591786802326823, 74.37609039468568994 ) ) ;
#155041 = CARTESIAN_POINT ( 'NONE',  ( 9.474510206698729675, 16.51473224551082808, 112.0844237280190043 ) ) ;
#155042 = CARTESIAN_POINT ( 'NONE',  ( -19.02544592524342804, 5.153800228976336051, 56.04057627198100988 ) ) ;
#155043 = CARTESIAN_POINT ( 'NONE',  ( -10.72451020669898014, 18.67979575497178502, 70.41557627198102409 ) ) ;
#155044 = CARTESIAN_POINT ( 'NONE',  ( -5.049401038297874678, -19.05341960407617918, 99.79275706135234714 ) ) ;
#155046 = CARTESIAN_POINT ( 'NONE',  ( 5.719274019375673035, 21.55341960407619339, 52.29275706135236135 ) ) ;
#155045 = CARTESIAN_POINT ( 'NONE',  ( 14.29746914071049879, -8.314922557960816363, 33.33224293864769550 ) ) ;
#155047 = FACE_OUTER_BOUND ( 'NONE', #81459, .T. ) ;
#155049 = CARTESIAN_POINT ( 'NONE',  ( 9.564922557960805705, 16.46253265017160317, 109.5822429386476955 ) ) ;
#155048 = CARTESIAN_POINT ( 'NONE',  ( -12.06949235617739369, -12.14591786802326823, 74.37609039468568994 ) ) ;
#155050 = DIRECTION ( 'NONE',  ( 1.000000000000000000, 0.000000000000000000, 0.000000000000000000 ) ) ;
#155051 = CARTESIAN_POINT ( 'NONE',  ( 30.00000000000000000, 5.499999999999992895, 102.5000000000000142 ) ) ;
#155052 = CARTESIAN_POINT ( 'NONE',  ( 16.52544592524335698, 4.483927247898782831, 96.45942372801901854 ) ) ;
#155053 = CARTESIAN_POINT ( 'NONE',  ( -12.06949235617739369, -12.14591786802326823, 44.37609039468567573 ) ) ;
#155054 = CARTESIAN_POINT ( 'NONE',  ( -13.89961937509977652, 13.97604488694528158, 65.62390960531436690 ) ) ;
#155055 = CARTESIAN_POINT ( 'NONE',  ( -16.51473224551069308, -9.474510206698971260, 71.66557627198102409 ) ) ;
#155056 = CARTESIAN_POINT ( 'NONE',  ( 21.53943276465977519, 0.05219959533937863772, 56.25109039468568284 ) ) ;
#155057 = CARTESIAN_POINT ( 'NONE',  ( 14.34966873604972726, -8.224510206698740333, 60.83442372801901854 ) ) ;
#155058 = CARTESIAN_POINT ( 'NONE',  ( -4.483927247898539470, -16.52544592524342804, 32.29057627198102409 ) ) ;
#155059 = CARTESIAN_POINT ( 'NONE',  ( 13.97604488694527802, 13.89961937509977652, 39.37390960531435269 ) ) ;
#155060 = CARTESIAN_POINT ( 'NONE',  ( 19.05341960407611168, 5.049401038298154454, 33.95724293864769550 ) ) ;
#155061 = CARTESIAN_POINT ( 'NONE',  ( 4.379528057220092307, 16.55341960407617563, 22.29275706135235069 ) ) ;
#155062 = CARTESIAN_POINT ( 'NONE',  ( 5.153800228976615827, -19.02544592524334988, 80.20942372801901854 ) ) ;
#155063 = CARTESIAN_POINT ( 'NONE',  ( -12.06949235617756955, 12.14591786802309770, 85.62390960531436690 ) ) ;
#155064 = CARTESIAN_POINT ( 'NONE',  ( -19.02544592524342804, 5.153800228976336051, 46.04057627198101699 ) ) ;
#155066 = LINE ( 'NONE', #16561, #159872 ) ;
#155065 = CARTESIAN_POINT ( 'NONE',  ( 19.02544592524334988, 5.153800228976608722, 91.45942372801900433 ) ) ;
#155067 = CARTESIAN_POINT ( 'NONE',  ( 10.81492255796106328, -18.62759615963255655, 85.41775706135236135 ) ) ;
#155068 = CARTESIAN_POINT ( 'NONE',  ( -14.29746914071037622, -8.314922557961029526, 54.16775706135235424 ) ) ;
#155069 = CARTESIAN_POINT ( 'NONE',  ( -17.49999999999999645, 3.209263204892513599, 24.76196825606288598 ) ) ;
#155070 = CARTESIAN_POINT ( 'NONE',  ( 18.67979575497178502, 10.72451020669898547, 54.16557627198103120 ) ) ;
#155071 = CARTESIAN_POINT ( 'NONE',  ( -14.29746914071037622, -8.314922557961029526, 39.16775706135235424 ) ) ;
#155072 = LINE ( 'NONE', #47905, #18326 ) ;
#155073 = CARTESIAN_POINT ( 'NONE',  ( 19.05341960407617918, -5.049401038297876454, 26.04275706135233293 ) ) ;
#155074 = CARTESIAN_POINT ( 'NONE',  ( 13.97604488694527802, 13.89961937509977652, 79.37390960531435269 ) ) ;
#155075 = CARTESIAN_POINT ( 'NONE',  ( 5.049401038298161559, -19.05341960407611168, 47.70724293864770260 ) ) ;
#155076 = CARTESIAN_POINT ( 'NONE',  ( 30.00000000000000000, -5.204748896376250896E-15, 47.50000000000000000 ) ) ;
#155077 = CARTESIAN_POINT ( 'NONE',  ( 13.89961937509977652, -13.97604488694527269, 63.12390960531435979 ) ) ;
#155078 = CARTESIAN_POINT ( 'NONE',  ( 37.99626262588765258, 2.893932880411085066E-14, -3.002157773949822861 ) ) ;
#155079 = PRODUCT ( 'Switch', 'Switch', '', ( #146275 ) ) ;
#155080 = CARTESIAN_POINT ( 'NONE',  ( -9.474510206698720793, -16.51473224551083518, 29.58442372801900433 ) ) ;
#155081 = CARTESIAN_POINT ( 'NONE',  ( 21.55341960407619695, -5.719274019375665929, 106.0427570613523471 ) ) ;
#155082 = CARTESIAN_POINT ( 'NONE',  ( 14.34966873604960469, 8.224510206698951720, 34.16557627198102409 ) ) ;
#155083 = CARTESIAN_POINT ( 'NONE',  ( 19.03943276465977164, -0.05219959533909143690, 43.74890960531435979 ) ) ;
#155084 = CARTESIAN_POINT ( 'NONE',  ( -19.03943276465977164, 0.05219959533909376836, 106.2489096053143669 ) ) ;
#155085 = CARTESIAN_POINT ( 'NONE',  ( -15.80617190586768217, 15.72974639402176855, 78.12609039468570415 ) ) ;
#155086 = CARTESIAN_POINT ( 'NONE',  ( 9.474510206698971260, -16.51473224551069308, 52.91557627198102409 ) ) ;
#155087 = CARTESIAN_POINT ( 'NONE',  ( -10.72451020669870658, -18.67979575497194134, 79.58442372801903275 ) ) ;
#155088 = CARTESIAN_POINT ( 'NONE',  ( 9.564922557960805705, 16.46253265017160317, 114.5822429386476955 ) ) ;
#155089 = CARTESIAN_POINT ( 'NONE',  ( -21.53943276465977519, -0.05219959533937600094, 23.75109039468567929 ) ) ;
#155090 = CARTESIAN_POINT ( 'NONE',  ( -13.97604488694547697, 13.89961937509957934, 53.12609039468565442 ) ) ;
#155091 = CARTESIAN_POINT ( 'NONE',  ( -19.05341960407611168, -5.049401038298163336, 31.45724293864769550 ) ) ;
#155092 = CARTESIAN_POINT ( 'NONE',  ( -13.97604488694527625, -13.89961937509977652, 81.87390960531436690 ) ) ;
#155093 = CARTESIAN_POINT ( 'NONE',  ( -12.06949235617739369, -12.14591786802326823, 19.37609039468568639 ) ) ;
#155094 = CARTESIAN_POINT ( 'NONE',  ( -12.06949235617756955, 12.14591786802309770, 70.62390960531436690 ) ) ;
#155095 = CARTESIAN_POINT ( 'NONE',  ( -15.80617190586745835, -15.72974639402198527, 36.87390960531435979 ) ) ;
#155096 = CARTESIAN_POINT ( 'NONE',  ( 9.564922557961047289, -16.46253265017146816, 95.41775706135233293 ) ) ;
#155097 = CARTESIAN_POINT ( 'NONE',  ( 10.81492255796078972, 18.62759615963270932, 99.58224293864770971 ) ) ;
#155098 = CARTESIAN_POINT ( 'NONE',  ( 21.55341960407619695, -5.719274019375665929, 51.04275706135234714 ) ) ;
#155099 = CARTESIAN_POINT ( 'NONE',  ( -12.06949235617739369, -12.14591786802326823, 54.37609039468568994 ) ) ;
#155100 = CARTESIAN_POINT ( 'NONE',  ( 16.55341960407618274, -4.379528057220086978, 61.04275706135234714 ) ) ;
#155101 = ORIENTED_EDGE ( 'NONE', *, *, #153757, .F. ) ;
#155102 = CARTESIAN_POINT ( 'NONE',  ( -5.153800228976328057, -19.02544592524343514, 52.29057627198100988 ) ) ;
#155103 = CARTESIAN_POINT ( 'NONE',  ( 16.52544592524335698, 4.483927247898782831, 86.45942372801901854 ) ) ;
#155104 = CARTESIAN_POINT ( 'NONE',  ( 18.62759615963271287, -10.81492255796078972, 113.3322429386476955 ) ) ;
#155105 = CARTESIAN_POINT ( 'NONE',  ( 12.06949235617757843, -12.14591786802309237, 58.12390960531435979 ) ) ;
#155106 = CARTESIAN_POINT ( 'NONE',  ( 19.03943276465977164, -0.05219959533909143690, 88.74890960531436690 ) ) ;
#155107 = CARTESIAN_POINT ( 'NONE',  ( 14.29746914071037800, 8.314922557961029526, 71.66775706135234714 ) ) ;
#155108 = CARTESIAN_POINT ( 'NONE',  ( -5.823673210054431948, 21.52544592524334988, 57.70942372801901143 ) ) ;
#155109 = CARTESIAN_POINT ( 'NONE',  ( -9.564922557961040184, 16.46253265017147172, 107.9177570613523471 ) ) ;
#155110 = CARTESIAN_POINT ( 'NONE',  ( -5.823673210054116645, -21.52544592524344225, 112.2905762719810241 ) ) ;
#155111 = CARTESIAN_POINT ( 'NONE',  ( 16.52544592524342804, -4.483927247898539470, 43.54057627198103830 ) ) ;
#155112 = EDGE_LOOP ( 'NONE', ( #96287, #156731, #190441, #74605, #34302, #13167, #101455, #135608, #74322, #105397, #122782, #22345 ) ) ;
#155113 = CARTESIAN_POINT ( 'NONE',  ( -17.40805194822031154, 6.112264579159341515, 75.83371272510613892 ) ) ;
#155114 = CARTESIAN_POINT ( 'NONE',  ( -21.55341960407610458, -5.719274019375992779, 81.45724293864769550 ) ) ;
#155115 = CARTESIAN_POINT ( 'NONE',  ( -14.29746914071049879, 8.314922557960819915, 25.83224293864769194 ) ) ;
#155116 = ORIENTED_EDGE ( 'NONE', *, *, #45144, .F. ) ;
#155117 = CARTESIAN_POINT ( 'NONE',  ( 17.50000000000000000, -5.500000000000000888, 120.0000000000000142 ) ) ;
#155118 = CARTESIAN_POINT ( 'NONE',  ( -0.05219959533937732626, 21.53943276465977519, 22.50109039468567573 ) ) ;
#155119 = CARTESIAN_POINT ( 'NONE',  ( 0.05219959533909260263, 19.03943276465977164, 109.9989096053143669 ) ) ;
#155120 = CARTESIAN_POINT ( 'NONE',  ( 15.72974639402176855, 15.80617190586768217, 26.87609039468567218 ) ) ;
#155121 = CARTESIAN_POINT ( 'NONE',  ( 16.55341960407611168, 4.379528057220329451, 53.95724293864770260 ) ) ;
#155122 = CARTESIAN_POINT ( 'NONE',  ( -4.379528057220086978, -16.55341960407618274, 64.79275706135234714 ) ) ;
#155123 = AXIS2_PLACEMENT_3D ( 'NONE', #142101, #111771, #96584 ) ;
#155124 = CARTESIAN_POINT ( 'NONE',  ( 13.97604488694527802, 13.89961937509977652, 59.37390960531434558 ) ) ;
#155125 = CARTESIAN_POINT ( 'NONE',  ( -19.03943276465977164, -0.05219959533935918106, 63.75109039468566863 ) ) ;
#155126 = CARTESIAN_POINT ( 'NONE',  ( -16.51473224551069308, -9.474510206698971260, 86.66557627198102409 ) ) ;
#155127 = CARTESIAN_POINT ( 'NONE',  ( 5.719274019375991003, -21.55341960407610458, 32.70724293864770260 ) ) ;
#155128 = CARTESIAN_POINT ( 'NONE',  ( -20.74701606029278267, -32.99105665081369665, -17.50853973932211005 ) ) ;
#155129 = CARTESIAN_POINT ( 'NONE',  ( 5.049401038298161559, -19.05341960407611168, 57.70724293864769550 ) ) ;
#155130 = CARTESIAN_POINT ( 'NONE',  ( 16.55341960407618274, -4.379528057220086978, 26.04275706135235779 ) ) ;
#155131 = CARTESIAN_POINT ( 'NONE',  ( 0.05219959533936267826, -19.03943276465977164, 70.00109039468566152 ) ) ;
#155132 = CARTESIAN_POINT ( 'NONE',  ( 15.80617190586746368, 15.72974639402197994, 99.37390960531436690 ) ) ;
#155133 = CARTESIAN_POINT ( 'NONE',  ( 14.29746914071049879, -8.314922557960816363, 28.33224293864769550 ) ) ;
#155134 = CARTESIAN_POINT ( 'NONE',  ( 13.89961937509977652, -13.97604488694527269, 88.12390960531438111 ) ) ;
#155135 = CARTESIAN_POINT ( 'NONE',  ( 15.80617190586746368, 15.72974639402197994, 54.37390960531435979 ) ) ;
#155137 = CARTESIAN_POINT ( 'NONE',  ( -14.29746914071037622, -8.314922557961029526, 44.16775706135234714 ) ) ;
#155136 = CARTESIAN_POINT ( 'NONE',  ( 15.72974639402199770, -15.80617190586745480, 98.12390960531436690 ) ) ;
#155138 = EDGE_CURVE ( 'NONE', #176035, #17478, #8550, .T. ) ;
#155139 = CARTESIAN_POINT ( 'NONE',  ( 5.719274019375991003, -21.55341960407610458, 37.70724293864769550 ) ) ;
#155140 = CARTESIAN_POINT ( 'NONE',  ( 21.55341960407619695, -5.719274019375665929, 86.04275706135236135 ) ) ;
#155141 = CARTESIAN_POINT ( 'NONE',  ( -9.564922557960796823, -16.46253265017161027, 92.08224293864769550 ) ) ;
#155142 = CARTESIAN_POINT ( 'NONE',  ( 9.474510206698971260, -16.51473224551069308, 42.91557627198103120 ) ) ;
#155143 = CARTESIAN_POINT ( 'NONE',  ( -0.05219959533909027116, -19.03943276465977164, 82.49890960531436690 ) ) ;
#155144 = CARTESIAN_POINT ( 'NONE',  ( 12.14591786802309770, 12.06949235617756955, 109.3739096053143811 ) ) ;
#155145 = CARTESIAN_POINT ( 'NONE',  ( 19.03943276465977164, -0.05219959533909143690, 63.74890960531435979 ) ) ;
#155146 = CARTESIAN_POINT ( 'NONE',  ( 16.46253265017146816, 9.564922557961045513, 111.6677570613523329 ) ) ;
#155147 = CARTESIAN_POINT ( 'NONE',  ( 17.48853670773245028, -5.747243402303063853, 86.16671299749992841 ) ) ;
#155149 = CARTESIAN_POINT ( 'NONE',  ( 19.02544592524343514, -5.153800228976328945, 108.5405762719810383 ) ) ;
#155148 = CARTESIAN_POINT ( 'NONE',  ( 15.80617190586769283, -15.72974639402175789, 95.62609039468568994 ) ) ;
#155151 = EDGE_CURVE ( 'NONE', #18983, #167324, #153466, .T. ) ;
#155150 = CARTESIAN_POINT ( 'NONE',  ( 14.29746914071037800, 8.314922557961029526, 96.66775706135234714 ) ) ;
#155152 = CARTESIAN_POINT ( 'NONE',  ( -38.00000000000000711, -12.34694845685042708, -9.899999999999998579 ) ) ;
#155153 = CARTESIAN_POINT ( 'NONE',  ( -5.049401038297874678, -19.05341960407617918, 74.79275706135231871 ) ) ;
#155154 = CARTESIAN_POINT ( 'NONE',  ( -9.564922557961040184, 16.46253265017147172, 27.91775706135232582 ) ) ;
#155155 = CARTESIAN_POINT ( 'NONE',  ( -17.48853670773242897, -5.747243402303181981, 46.33328700250010712 ) ) ;
#155156 = CARTESIAN_POINT ( 'NONE',  ( -0.05219959533909027116, -19.03943276465977164, 32.49890960531435979 ) ) ;
#155157 = CARTESIAN_POINT ( 'NONE',  ( -4.483927247898539470, -16.52544592524342804, 42.29057627198103120 ) ) ;
#155158 = CARTESIAN_POINT ( 'NONE',  ( -17.26058549869091507, -6.457015423128543929, 111.3774583747606925 ) ) ;
#155159 = CARTESIAN_POINT ( 'NONE',  ( 14.29746914071049879, -8.314922557960816363, 33.33224293864769550 ) ) ;
#155160 = CARTESIAN_POINT ( 'NONE',  ( -19.52851543214744368, -5.499999999999943157, 85.39357721762581832 ) ) ;
#155161 = CARTESIAN_POINT ( 'NONE',  ( 12.14591786802327356, -12.06949235617739191, 90.62609039468567573 ) ) ;
#155162 = CARTESIAN_POINT ( 'NONE',  ( 16.46253265017160672, -9.564922557960803928, 43.33224293864769550 ) ) ;
#155163 = CARTESIAN_POINT ( 'NONE',  ( -10.72451020669870658, -18.67979575497194134, 94.58442372801901854 ) ) ;
#155164 = CARTESIAN_POINT ( 'NONE',  ( 16.46253265017146816, 9.564922557961045513, 111.6677570613523329 ) ) ;
#155165 = CARTESIAN_POINT ( 'NONE',  ( 21.55341960407619695, -5.719274019375665929, 81.04275706135236135 ) ) ;
#155166 = CARTESIAN_POINT ( 'NONE',  ( -16.46253265017146816, -9.564922557961047289, 59.16775706135233293 ) ) ;
#155167 = CARTESIAN_POINT ( 'NONE',  ( 9.474510206698971260, -16.51473224551069308, 87.91557627198102409 ) ) ;
#155168 = CARTESIAN_POINT ( 'NONE',  ( 16.51473224551069308, 9.474510206698969483, 69.16557627198102409 ) ) ;
#155169 = CARTESIAN_POINT ( 'NONE',  ( 16.52216118717204196, 7.221426719304506747, 73.57599021046989662 ) ) ;
#155170 = CARTESIAN_POINT ( 'NONE',  ( -18.62759615963270932, 10.81492255796079327, 90.83224293864769550 ) ) ;
#155171 = CARTESIAN_POINT ( 'NONE',  ( -12.14591786802309592, -12.06949235617757132, 71.87390960531438111 ) ) ;
#155172 = CARTESIAN_POINT ( 'NONE',  ( -10.81492255796078084, -18.62759615963271287, 67.08224293864770971 ) ) ;
#155173 = CARTESIAN_POINT ( 'NONE',  ( 13.89961937509977652, -13.97604488694527269, 58.12390960531436690 ) ) ;
#155175 = CARTESIAN_POINT ( 'NONE',  ( -16.53943276465976808, -0.05219959533934237506, 78.75109039468568994 ) ) ;
#155174 = CARTESIAN_POINT ( 'NONE',  ( 5.823673210054125526, 21.52544592524343514, 79.79057627198102409 ) ) ;
#155176 = VERTEX_POINT ( 'NONE', #111936 ) ;
#155177 = CARTESIAN_POINT ( 'NONE',  ( -13.89961937509977652, 13.97604488694528158, 40.62390960531435979 ) ) ;
#155178 = EDGE_CURVE ( 'NONE', #79565, #75891, #66583, .T. ) ;
#155180 = DIRECTION ( 'NONE',  ( -0.000000000000000000, -0.000000000000000000, 1.000000000000000000 ) ) ;
#155179 = CARTESIAN_POINT ( 'NONE',  ( -0.05219959533910754901, -16.53943276465976808, 77.49890960531433848 ) ) ;
#155181 = CARTESIAN_POINT ( 'NONE',  ( -0.05219959533909027116, -19.03943276465977164, 52.49890960531436690 ) ) ;
#155182 = CARTESIAN_POINT ( 'NONE',  ( 19.05341960407611168, 5.049401038298154454, 23.95724293864769194 ) ) ;
#155183 = CARTESIAN_POINT ( 'NONE',  ( 0.05219959533936267826, -19.03943276465977164, 60.00109039468566863 ) ) ;
#155184 = CARTESIAN_POINT ( 'NONE',  ( 14.34966873604960469, 8.224510206698951720, 89.16557627198102409 ) ) ;
#155185 = CARTESIAN_POINT ( 'NONE',  ( 21.52544592524334988, 5.823673210054432836, 51.45942372801901854 ) ) ;
#155187 = CARTESIAN_POINT ( 'NONE',  ( -18.62759615963270932, 10.81492255796079327, 110.8322429386476955 ) ) ;
#155186 = CARTESIAN_POINT ( 'NONE',  ( -13.89961937509977652, 13.97604488694528158, 35.62390960531435269 ) ) ;
#155188 = CARTESIAN_POINT ( 'NONE',  ( 17.72560187377285601, 5.500000000000007105, 91.57814504131319211 ) ) ;
#155189 = CARTESIAN_POINT ( 'NONE',  ( -16.55341960407611168, -4.379528057220339221, 91.45724293864769550 ) ) ;
#155190 = CARTESIAN_POINT ( 'NONE',  ( 14.09403216840226669, -37.74807521950865663, -24.22002746648481875 ) ) ;
#155191 = CARTESIAN_POINT ( 'NONE',  ( -16.51473224551069308, -9.474510206698971260, 46.66557627198102409 ) ) ;
#155192 = DIRECTION ( 'NONE',  ( -0.5367108174878557625, 0.8437662581494461689, 1.463701136248949969E-16 ) ) ;
#155194 = CARTESIAN_POINT ( 'NONE',  ( -13.89961937509977652, 13.97604488694528158, 105.6239096053143527 ) ) ;
#155193 = CARTESIAN_POINT ( 'NONE',  ( 13.89961937509957401, 13.97604488694547697, 96.87609039468566152 ) ) ;
#155195 = CARTESIAN_POINT ( 'NONE',  ( 0.05219959533937995610, -21.53943276465977519, 40.00109039468567573 ) ) ;
#155196 = CARTESIAN_POINT ( 'NONE',  ( 5.153800228976335163, 19.02544592524342804, 89.79057627198102409 ) ) ;
#155197 = CARTESIAN_POINT ( 'NONE',  ( -19.02544592524334988, -5.153800228976617603, 63.95942372801899012 ) ) ;
#155198 = CARTESIAN_POINT ( 'NONE',  ( -0.05219959533909027116, -19.03943276465977164, 42.49890960531435269 ) ) ;
#155199 = CARTESIAN_POINT ( 'NONE',  ( -16.53943276465976808, 0.05219959533911058130, 71.24890960531435269 ) ) ;
#155200 = CARTESIAN_POINT ( 'NONE',  ( -8.224510206698948167, 14.34966873604960824, 70.41557627198102409 ) ) ;
#155201 = CARTESIAN_POINT ( 'NONE',  ( -19.03943276465977164, 0.05219959533909376836, 81.24890960531436690 ) ) ;
#155202 = CARTESIAN_POINT ( 'NONE',  ( 10.81492255796078972, 18.62759615963270932, 94.58224293864769550 ) ) ;
#155203 = CARTESIAN_POINT ( 'NONE',  ( -16.51473224551069308, -9.474510206698971260, 66.66557627198102409 ) ) ;
#155204 = CARTESIAN_POINT ( 'NONE',  ( -21.55341960407619339, 5.719274019375674811, 108.5427570613523756 ) ) ;
#155207 = CARTESIAN_POINT ( 'NONE',  ( 4.483927247898545687, 16.52544592524342804, 109.7905762719810383 ) ) ;
#155206 = CARTESIAN_POINT ( 'NONE',  ( 4.483927247898545687, 16.52544592524342804, 29.79057627198102409 ) ) ;
#155205 = CARTESIAN_POINT ( 'NONE',  ( -5.153800228976328057, -19.02544592524343514, 37.29057627198102409 ) ) ;
#155208 = CARTESIAN_POINT ( 'NONE',  ( -5.049401038297874678, -19.05341960407617918, 109.7927570613523187 ) ) ;
#155209 = ORIENTED_EDGE ( 'NONE', *, *, #199317, .F. ) ;
#155210 = CARTESIAN_POINT ( 'NONE',  ( 10.72451020669871369, 18.67979575497193778, 27.08442372801901854 ) ) ;
#155211 = CARTESIAN_POINT ( 'NONE',  ( -0.05219959533936034679, 19.03943276465977164, 67.50109039468566152 ) ) ;
#155212 = CARTESIAN_POINT ( 'NONE',  ( 12.06949235617757843, -12.14591786802309237, 23.12390960531436335 ) ) ;
#155213 = CARTESIAN_POINT ( 'NONE',  ( -10.81492255796078084, -18.62759615963271287, 82.08224293864768129 ) ) ;
#155214 = CARTESIAN_POINT ( 'NONE',  ( 5.153800228976335163, 19.02544592524342804, 109.7905762719810099 ) ) ;
#155215 = CARTESIAN_POINT ( 'NONE',  ( 14.29746914071049879, -8.314922557960816363, 58.33224293864768839 ) ) ;
#155216 = CARTESIAN_POINT ( 'NONE',  ( -5.153800228976328057, -19.02544592524343514, 32.29057627198102409 ) ) ;
#155217 = CARTESIAN_POINT ( 'NONE',  ( 19.02544592524334988, 5.153800228976608722, 21.45942372801899012 ) ) ;
#155218 = CARTESIAN_POINT ( 'NONE',  ( -4.379528057220086978, -16.55341960407618274, 84.79275706135234714 ) ) ;
#155219 = CARTESIAN_POINT ( 'NONE',  ( -4.483927247898782831, 16.52544592524335698, 52.70942372801902565 ) ) ;
#155220 = CARTESIAN_POINT ( 'NONE',  ( -21.53943276465977519, 0.05219959533907696930, 26.24890960531435624 ) ) ;
#155221 = CARTESIAN_POINT ( 'NONE',  ( 18.67979575497194134, -10.72451020669871369, 105.8344237280190328 ) ) ;
#155222 = CARTESIAN_POINT ( 'NONE',  ( -16.46253265017160317, 9.564922557960807481, 75.83224293864769550 ) ) ;
#155223 = CARTESIAN_POINT ( 'NONE',  ( -14.29746914071037622, -8.314922557961029526, 54.16775706135235424 ) ) ;
#155224 = CARTESIAN_POINT ( 'NONE',  ( -5.153800228976328057, -19.02544592524343514, 22.29057627198102765 ) ) ;
#155225 = CARTESIAN_POINT ( 'NONE',  ( -8.314922557960811034, -14.29746914071050412, 37.08224293864768129 ) ) ;
#155226 = CARTESIAN_POINT ( 'NONE',  ( -17.49999999999999645, 5.499999999999985789, 38.71769037696434879 ) ) ;
#155229 = CARTESIAN_POINT ( 'NONE',  ( 16.46253265017160672, -9.564922557960803928, 73.33224293864769550 ) ) ;
#155228 = CARTESIAN_POINT ( 'NONE',  ( 5.049401038298161559, -19.05341960407611168, 87.70724293864769550 ) ) ;
#155227 = CARTESIAN_POINT ( 'NONE',  ( 10.72451020669871369, 18.67979575497193778, 72.08442372801899012 ) ) ;
#155230 = CARTESIAN_POINT ( 'NONE',  ( 5.049401038298161559, -19.05341960407611168, 107.7072429386476955 ) ) ;
#155231 = CARTESIAN_POINT ( 'NONE',  ( 16.52544592524342804, -4.483927247898539470, 58.54057627198103120 ) ) ;
#155232 = CARTESIAN_POINT ( 'NONE',  ( 4.483927247898545687, 16.52544592524342804, 29.79057627198102409 ) ) ;
#155233 = EDGE_LOOP ( 'NONE', ( #168588, #19644, #190280, #171586 ) ) ;
#155234 = CARTESIAN_POINT ( 'NONE',  ( 8.314922557960818139, 14.29746914071049879, 54.58224293864769550 ) ) ;
#155236 = DIRECTION ( 'NONE',  ( 0.000000000000000000, 0.000000000000000000, 1.000000000000000000 ) ) ;
#155235 = CARTESIAN_POINT ( 'NONE',  ( 16.52544592524335698, 4.483927247898782831, 36.45942372801901143 ) ) ;
#155237 = CARTESIAN_POINT ( 'NONE',  ( 0.05219959533936267826, -19.03943276465977164, 45.00109039468566863 ) ) ;
#155238 = CARTESIAN_POINT ( 'NONE',  ( 5.153800228976335163, 19.02544592524342804, 69.79057627198103830 ) ) ;
#155239 = CARTESIAN_POINT ( 'NONE',  ( -16.51473224551082808, 9.474510206698731452, 58.33442372801900433 ) ) ;
#155240 = CARTESIAN_POINT ( 'NONE',  ( -9.564922557961040184, 16.46253265017147172, 62.91775706135233293 ) ) ;
#155242 = CARTESIAN_POINT ( 'NONE',  ( 0.05219959533934541429, -16.53943276465976808, 85.00109039468568994 ) ) ;
#155241 = CARTESIAN_POINT ( 'NONE',  ( -16.46253265017146816, -9.564922557961047289, 94.16775706135233293 ) ) ;
#155243 = CARTESIAN_POINT ( 'NONE',  ( -8.571926809382608425, 26.38167802310805854, 144.9750000027312069 ) ) ;
#155244 = CARTESIAN_POINT ( 'NONE',  ( 0.05219959533909260263, 19.03943276465977164, 29.99890960531435979 ) ) ;
#155245 = CARTESIAN_POINT ( 'NONE',  ( 16.46253265017160672, -9.564922557960803928, 103.3322429386476955 ) ) ;
#155246 = CARTESIAN_POINT ( 'NONE',  ( 10.72451020669871369, 18.67979575497193778, 37.08442372801901143 ) ) ;
#155247 = CARTESIAN_POINT ( 'NONE',  ( -19.02544592524334988, -5.153800228976617603, 93.95942372801900433 ) ) ;
#155249 = CARTESIAN_POINT ( 'NONE',  ( 16.51473224551069308, 9.474510206698969483, 64.16557627198102409 ) ) ;
#155248 = CARTESIAN_POINT ( 'NONE',  ( 15.50000000000000178, 0.000000000000000000, 118.0000000000000142 ) ) ;
#155250 = CARTESIAN_POINT ( 'NONE',  ( 5.153800228976335163, 19.02544592524342804, 104.7905762719809957 ) ) ;
#155252 = CARTESIAN_POINT ( 'NONE',  ( 16.46253265017160672, -9.564922557960803928, 68.33224293864770971 ) ) ;
#155251 = CARTESIAN_POINT ( 'NONE',  ( -14.34966873604960291, -8.224510206698953496, 56.66557627198103830 ) ) ;
#155253 = CARTESIAN_POINT ( 'NONE',  ( 19.02544592524343514, -5.153800228976328945, 63.54057627198103830 ) ) ;
#155254 = CARTESIAN_POINT ( 'NONE',  ( -16.51473224551082808, 9.474510206698731452, 63.33442372801900433 ) ) ;
#155255 = CARTESIAN_POINT ( 'NONE',  ( 5.719274019375991003, -21.55341960407610458, 57.70724293864770260 ) ) ;
#155256 = CARTESIAN_POINT ( 'NONE',  ( 5.153800228976615827, -19.02544592524334988, 40.20942372801898301 ) ) ;
#155257 = CARTESIAN_POINT ( 'NONE',  ( -19.05341960407611168, -5.049401038298163336, 76.45724293864769550 ) ) ;
#155258 = CARTESIAN_POINT ( 'NONE',  ( -18.62759615963270932, 10.81492255796079327, 75.83224293864769550 ) ) ;
#155260 = CARTESIAN_POINT ( 'NONE',  ( 19.02544592524334988, 5.153800228976608722, 31.45942372801900433 ) ) ;
#155259 = CARTESIAN_POINT ( 'NONE',  ( -12.06949235617756955, 12.14591786802309770, 85.62390960531436690 ) ) ;
#155261 = CARTESIAN_POINT ( 'NONE',  ( -21.52544592524343514, 5.823673210054127303, 41.04057627198103120 ) ) ;
#155262 = CARTESIAN_POINT ( 'NONE',  ( -21.53943276465977519, 0.05219959533907696930, 41.24890960531435269 ) ) ;
#155263 = CARTESIAN_POINT ( 'NONE',  ( -16.51473224551069308, -9.474510206698971260, 66.66557627198102409 ) ) ;
#155264 = CARTESIAN_POINT ( 'NONE',  ( -5.153800228976328057, -19.02544592524343514, 52.29057627198100988 ) ) ;
#155265 = CARTESIAN_POINT ( 'NONE',  ( -4.379528057220328563, 16.55341960407611168, 115.2072429386476955 ) ) ;
#155266 = CARTESIAN_POINT ( 'NONE',  ( 0.05219959533937995610, -21.53943276465977519, 25.00109039468567218 ) ) ;
#155268 = EDGE_CURVE ( 'NONE', #99233, #24708, #161429, .T. ) ;
#155267 = CARTESIAN_POINT ( 'NONE',  ( -3.573655867282028392E-15, 2.428612866367529932E-14, 0.000000000000000000 ) ) ;
#155269 = CARTESIAN_POINT ( 'NONE',  ( -18.62759615963255300, -10.81492255796106328, 24.16775706135235424 ) ) ;
#155270 = CARTESIAN_POINT ( 'NONE',  ( -19.05341960407611168, -5.049401038298163336, 31.45724293864769550 ) ) ;
#155271 = CARTESIAN_POINT ( 'NONE',  ( -5.719274019375978568, 21.55341960407610458, 110.2072429386477239 ) ) ;
#155272 = CARTESIAN_POINT ( 'NONE',  ( -19.02544592524334988, -5.153800228976617603, 43.95942372801899012 ) ) ;
#155273 = CARTESIAN_POINT ( 'NONE',  ( 19.02544592524343514, -5.153800228976328945, 28.54057627198102409 ) ) ;
#155274 = CARTESIAN_POINT ( 'NONE',  ( 13.97604488694527802, 13.89961937509977652, 24.37390960531435624 ) ) ;
#155275 = CARTESIAN_POINT ( 'NONE',  ( 17.37577197770832527, -5.499999999999936939, 21.30611277022550354 ) ) ;
#155276 = CARTESIAN_POINT ( 'NONE',  ( -16.53943276465976808, -0.05219959533934237506, 53.75109039468568994 ) ) ;
#155277 = CARTESIAN_POINT ( 'NONE',  ( 16.46253265017160672, -9.564922557960803928, 28.33224293864769550 ) ) ;
#155278 = CARTESIAN_POINT ( 'NONE',  ( 33.78625674316657523, -2.758724085166796236, 99.76151011743465347 ) ) ;
#155279 = CARTESIAN_POINT ( 'NONE',  ( -13.97604488694527625, -13.89961937509977652, 66.87390960531436690 ) ) ;
#155280 = CARTESIAN_POINT ( 'NONE',  ( 14.34966873604960469, 8.224510206698951720, 109.1655762719810383 ) ) ;
#155281 = CARTESIAN_POINT ( 'NONE',  ( 5.719274019375991003, -21.55341960407610458, 62.70724293864769550 ) ) ;
#155282 = CARTESIAN_POINT ( 'NONE',  ( 14.34966873604960469, 8.224510206698951720, 74.16557627198102409 ) ) ;
#155283 = CARTESIAN_POINT ( 'NONE',  ( 16.55341960407618274, -4.379528057220086978, 31.04275706135234714 ) ) ;
#155284 = CARTESIAN_POINT ( 'NONE',  ( 10.72451020669871369, 18.67979575497193778, 92.08442372801901854 ) ) ;
#155285 = CARTESIAN_POINT ( 'NONE',  ( -5.153800228976328057, -19.02544592524343514, 32.29057627198102409 ) ) ;
#155286 = CARTESIAN_POINT ( 'NONE',  ( -4.483927247898539470, -16.52544592524342804, 22.29057627198102765 ) ) ;
#155287 = CARTESIAN_POINT ( 'NONE',  ( -8.314922557960811034, -14.29746914071050412, 52.08224293864768839 ) ) ;
#155288 = CARTESIAN_POINT ( 'NONE',  ( 19.02544592524343514, -5.153800228976328945, 53.54057627198102409 ) ) ;
#155289 = CARTESIAN_POINT ( 'NONE',  ( 5.719274019375673035, 21.55341960407619339, 92.29275706135236135 ) ) ;
#155290 = CARTESIAN_POINT ( 'NONE',  ( -0.05219959533907301413, -21.53943276465977519, 102.4989096053143811 ) ) ;
#155291 = CARTESIAN_POINT ( 'NONE',  ( 15.72974639402176855, 15.80617190586768217, 66.87609039468568994 ) ) ;
#155292 = CARTESIAN_POINT ( 'NONE',  ( 12.14591786802327356, -12.06949235617739191, 50.62609039468568994 ) ) ;
#155294 = CARTESIAN_POINT ( 'NONE',  ( 21.53943276465977519, 0.05219959533937863772, 91.25109039468568994 ) ) ;
#155293 = CARTESIAN_POINT ( 'NONE',  ( 12.14591786802309770, 12.06949235617756955, 84.37390960531438111 ) ) ;
#155295 = CARTESIAN_POINT ( 'NONE',  ( -16.55341960407617563, 4.379528057220093196, 113.5427570613523756 ) ) ;
#155296 = DIRECTION ( 'NONE',  ( 0.000000000000000000, 1.224646799147373422E-16, 1.000000000000000000 ) ) ;
#155297 = CARTESIAN_POINT ( 'NONE',  ( -4.379528057220086978, -16.55341960407618274, 44.79275706135234714 ) ) ;
#155298 = CARTESIAN_POINT ( 'NONE',  ( -16.55341960407611168, -4.379528057220339221, 36.45724293864768839 ) ) ;
#155299 = CARTESIAN_POINT ( 'NONE',  ( -16.53943276465976808, -0.05219959533934237506, 88.75109039468567573 ) ) ;
#155300 = CARTESIAN_POINT ( 'NONE',  ( -19.05341960407611168, -5.049401038298163336, 101.4572429386476955 ) ) ;
#155301 = CARTESIAN_POINT ( 'NONE',  ( 16.46253265017160672, -9.564922557960803928, 113.3322429386476955 ) ) ;
#155302 = CARTESIAN_POINT ( 'NONE',  ( 15.80617190586769283, -15.72974639402175789, 95.62609039468568994 ) ) ;
#155303 = EDGE_CURVE ( 'NONE', #27205, #63497, #7731, .T. ) ;
#155304 = CARTESIAN_POINT ( 'NONE',  ( 14.34966873604972726, -8.224510206698740333, 105.8344237280190328 ) ) ;
#155305 = CARTESIAN_POINT ( 'NONE',  ( 4.379528057220339221, -16.55341960407611168, 77.70724293864770971 ) ) ;
#155306 = CARTESIAN_POINT ( 'NONE',  ( -5.049401038298153566, 19.05341960407611168, 75.20724293864769550 ) ) ;
#155307 = EDGE_LOOP ( 'NONE', ( #83600, #130587, #58800, #193769 ) ) ;
#155308 = CARTESIAN_POINT ( 'NONE',  ( -12.06949235617739369, -12.14591786802326823, 29.37609039468568284 ) ) ;
#155309 = CARTESIAN_POINT ( 'NONE',  ( -9.564922557960796823, -16.46253265017161027, 27.08224293864769550 ) ) ;
#155310 = CARTESIAN_POINT ( 'NONE',  ( 9.564922557960805705, 16.46253265017160317, 89.58224293864769550 ) ) ;
#155312 = CARTESIAN_POINT ( 'NONE',  ( 18.22780087662121673, 5.500000000000056843, 68.98459894673892734 ) ) ;
#155311 = CARTESIAN_POINT ( 'NONE',  ( 8.314922557961029526, -14.29746914071037800, 35.41775706135234003 ) ) ;
#155313 = CARTESIAN_POINT ( 'NONE',  ( 0.05219959533936267826, -19.03943276465977164, 40.00109039468566152 ) ) ;
#155314 = CARTESIAN_POINT ( 'NONE',  ( -4.483927247898782831, 16.52544592524335698, 87.70942372801901854 ) ) ;
#155315 = CARTESIAN_POINT ( 'NONE',  ( 5.049401038297881783, 19.05341960407617563, 102.2927570613523045 ) ) ;
#155316 = CARTESIAN_POINT ( 'NONE',  ( 9.474510206698971260, -16.51473224551069308, 37.91557627198102409 ) ) ;
#155317 = CARTESIAN_POINT ( 'NONE',  ( -16.53943276465976808, -0.05219959533934237506, 73.75109039468567573 ) ) ;
#155318 = CARTESIAN_POINT ( 'NONE',  ( -16.55341960407617563, 4.379528057220093196, 63.54275706135234003 ) ) ;
#155319 = CARTESIAN_POINT ( 'NONE',  ( 5.049401038297881783, 19.05341960407617563, 82.29275706135229029 ) ) ;
#155320 = CARTESIAN_POINT ( 'NONE',  ( 0.05219959533937995610, -21.53943276465977519, 110.0010903946856757 ) ) ;
#155321 = CARTESIAN_POINT ( 'NONE',  ( -9.564922557960796823, -16.46253265017161027, 42.08224293864769550 ) ) ;
#155322 = EDGE_CURVE ( 'NONE', #125536, #56096, #162422, .T. ) ;
#155323 = CARTESIAN_POINT ( 'NONE',  ( -9.474510206698964154, 16.51473224551069663, 95.41557627198102409 ) ) ;
#155324 = CARTESIAN_POINT ( 'NONE',  ( -8.224510206698948167, 14.34966873604960824, 90.41557627198103830 ) ) ;
#155325 = CARTESIAN_POINT ( 'NONE',  ( 13.97604488694548053, -13.89961937509957401, 55.62609039468566863 ) ) ;
#155326 = CARTESIAN_POINT ( 'NONE',  ( -5.823673210054116645, -21.52544592524344225, 52.29057627198102409 ) ) ;
#155327 = CARTESIAN_POINT ( 'NONE',  ( 5.153800228976615827, -19.02544592524334988, 25.20942372801900433 ) ) ;
#155328 = CARTESIAN_POINT ( 'NONE',  ( 19.02544592524343514, -5.153800228976328945, 88.54057627198102409 ) ) ;
#155329 = CARTESIAN_POINT ( 'NONE',  ( 5.049401038297881783, 19.05341960407617563, 27.29275706135232937 ) ) ;
#155330 = CARTESIAN_POINT ( 'NONE',  ( -18.62759615963270932, 10.81492255796079327, 80.83224293864769550 ) ) ;
#155331 = CARTESIAN_POINT ( 'NONE',  ( 19.03943276465977164, -0.05219959533909143690, 108.7489096053143527 ) ) ;
#155332 = CARTESIAN_POINT ( 'NONE',  ( 5.049401038297881783, 19.05341960407617563, 82.29275706135229029 ) ) ;
#155333 = CARTESIAN_POINT ( 'NONE',  ( -19.05341960407611168, -5.049401038298163336, 111.4572429386476671 ) ) ;
#155334 = CARTESIAN_POINT ( 'NONE',  ( 0.05219959533934541429, -16.53943276465976808, 20.00109039468568639 ) ) ;
#155335 = CARTESIAN_POINT ( 'NONE',  ( -9.474510206698964154, 16.51473224551069663, 30.41557627198102054 ) ) ;
#155336 = CARTESIAN_POINT ( 'NONE',  ( 19.02544592524343514, -5.153800228976328945, 93.54057627198102409 ) ) ;
#155337 = CARTESIAN_POINT ( 'NONE',  ( -18.67979575497178146, -10.72451020669898902, 71.66557627198100988 ) ) ;
#155338 = CARTESIAN_POINT ( 'NONE',  ( -4.483927247898782831, 16.52544592524335698, 52.70942372801902565 ) ) ;
#155339 = CARTESIAN_POINT ( 'NONE',  ( -0.05219959533937732626, 21.53943276465977519, 47.50109039468568994 ) ) ;
#155341 = CARTESIAN_POINT ( 'NONE',  ( 10.72451020669871369, 18.67979575497193778, 102.0844237280190185 ) ) ;
#155340 = CARTESIAN_POINT ( 'NONE',  ( 16.46253265017146816, 9.564922557961045513, 91.66775706135234714 ) ) ;
#155342 = CARTESIAN_POINT ( 'NONE',  ( 16.52544592524335698, 4.483927247898782831, 96.45942372801901854 ) ) ;
#155343 = CARTESIAN_POINT ( 'NONE',  ( -19.05341960407611168, -5.049401038298163336, 106.4572429386476955 ) ) ;
#155344 = CARTESIAN_POINT ( 'NONE',  ( 14.34966873604960469, 8.224510206698951720, 94.16557627198103830 ) ) ;
#155345 = CARTESIAN_POINT ( 'NONE',  ( 12.06949235617757843, -12.14591786802309237, 33.12390960531435979 ) ) ;
#155346 = CARTESIAN_POINT ( 'NONE',  ( -9.474510206698720793, -16.51473224551083518, 74.58442372801900433 ) ) ;
#155347 = CARTESIAN_POINT ( 'NONE',  ( -21.55341960407619339, 5.719274019375674811, 63.54275706135234003 ) ) ;
#155348 = CARTESIAN_POINT ( 'NONE',  ( 13.97604488694548053, -13.89961937509957401, 30.62609039468566863 ) ) ;
#155349 = CARTESIAN_POINT ( 'NONE',  ( -12.14591786802309592, -12.06949235617757132, 101.8739096053143811 ) ) ;
#155350 = CARTESIAN_POINT ( 'NONE',  ( -0.05219959533907301413, -21.53943276465977519, 32.49890960531435979 ) ) ;
#155351 = CARTESIAN_POINT ( 'NONE',  ( -12.14591786802326823, 12.06949235617739902, 113.1260903946856899 ) ) ;
#155352 = CARTESIAN_POINT ( 'NONE',  ( -21.55341960407619339, 5.719274019375674811, 98.54275706135234714 ) ) ;
#155353 = CARTESIAN_POINT ( 'NONE',  ( -16.55341960407617563, 4.379528057220093196, 58.54275706135235424 ) ) ;
#155354 = CARTESIAN_POINT ( 'NONE',  ( 14.34966873604960469, 8.224510206698951720, 24.16557627198103120 ) ) ;
#155355 = CARTESIAN_POINT ( 'NONE',  ( 21.53943276465977519, 0.05219959533937863772, 46.25109039468567573 ) ) ;
#155356 = CARTESIAN_POINT ( 'NONE',  ( 18.62759615963255655, 10.81492255796105972, 56.66775706135235424 ) ) ;
#155357 = ORIENTED_EDGE ( 'NONE', *, *, #162596, .T. ) ;
#155358 = CARTESIAN_POINT ( 'NONE',  ( -5.719274019375665041, -21.55341960407619695, 34.79275706135235424 ) ) ;
#155359 = CARTESIAN_POINT ( 'NONE',  ( 4.483927247898545687, 16.52544592524342804, 99.79057627198103830 ) ) ;
#155360 = CARTESIAN_POINT ( 'NONE',  ( -5.049401038298153566, 19.05341960407611168, 25.20724293864768484 ) ) ;
#155361 = CARTESIAN_POINT ( 'NONE',  ( 8.314922557960818139, 14.29746914071049879, 74.58224293864768129 ) ) ;
#155362 = CARTESIAN_POINT ( 'NONE',  ( 9.564922557960805705, 16.46253265017160317, 74.58224293864769550 ) ) ;
#155363 = CARTESIAN_POINT ( 'NONE',  ( 16.53943276465976808, 0.05219959533934440121, 111.2510903946856899 ) ) ;
#155364 = CARTESIAN_POINT ( 'NONE',  ( -10.72451020669898014, 18.67979575497178502, 60.41557627198102409 ) ) ;
#155365 = CARTESIAN_POINT ( 'NONE',  ( 14.34966873604960469, 8.224510206698951720, 94.16557627198103830 ) ) ;
#155366 = CARTESIAN_POINT ( 'NONE',  ( 10.72451020669898902, -18.67979575497178502, 87.91557627198103830 ) ) ;
#155367 = CARTESIAN_POINT ( 'NONE',  ( -9.564922557960796823, -16.46253265017161027, 97.08224293864769550 ) ) ;
#155369 = CARTESIAN_POINT ( 'NONE',  ( 19.05341960407617918, -5.049401038297876454, 106.0427570613523471 ) ) ;
#155368 = CARTESIAN_POINT ( 'NONE',  ( -19.02544592524342804, 5.153800228976336051, 51.04057627198103120 ) ) ;
#155370 = CARTESIAN_POINT ( 'NONE',  ( 21.55341960407610458, 5.719274019375980345, 48.95724293864770971 ) ) ;
#155371 = CARTESIAN_POINT ( 'NONE',  ( -18.62759615963255300, -10.81492255796106328, 69.16775706135234714 ) ) ;
#155372 = CARTESIAN_POINT ( 'NONE',  ( -9.564922557960796823, -16.46253265017161027, 62.08224293864769550 ) ) ;
#155373 = CARTESIAN_POINT ( 'NONE',  ( 9.474510206698971260, -16.51473224551069308, 102.9155762719810241 ) ) ;
#155374 = CARTESIAN_POINT ( 'NONE',  ( 12.14591786802327356, -12.06949235617739191, 60.62609039468567573 ) ) ;
#155375 = CARTESIAN_POINT ( 'NONE',  ( -15.72974639402176322, -15.80617190586768395, 59.37609039468568284 ) ) ;
#155376 = CARTESIAN_POINT ( 'NONE',  ( 10.72451020669871369, 18.67979575497193778, 92.08442372801901854 ) ) ;
#155377 = CARTESIAN_POINT ( 'NONE',  ( 21.52544592524344225, -5.823673210054117533, 93.54057627198103830 ) ) ;
#155379 = CARTESIAN_POINT ( 'NONE',  ( -8.314922557961024197, 14.29746914071037800, 72.91775706135234714 ) ) ;
#155378 = CARTESIAN_POINT ( 'NONE',  ( 15.80617190586769283, -15.72974639402175789, 35.62609039468568994 ) ) ;
#155380 = CARTESIAN_POINT ( 'NONE',  ( 15.72974639402199770, -15.80617190586745480, 83.12390960531436690 ) ) ;
#155381 = CARTESIAN_POINT ( 'NONE',  ( -19.02544592524334988, -5.153800228976617603, 38.95942372801900433 ) ) ;
#155383 = CARTESIAN_POINT ( 'NONE',  ( -14.34966873604960291, -8.224510206698953496, 26.66557627198103475 ) ) ;
#155382 = CARTESIAN_POINT ( 'NONE',  ( -9.474510206698964154, 16.51473224551069663, 85.41557627198102409 ) ) ;
#155384 = CARTESIAN_POINT ( 'NONE',  ( -3.573655867282028392E-15, 2.428612866367529932E-14, -25.00000000000000000 ) ) ;
#155385 = CARTESIAN_POINT ( 'NONE',  ( 13.97604488694527802, 13.89961937509977652, 104.3739096053143385 ) ) ;
#155386 = CARTESIAN_POINT ( 'NONE',  ( -9.474510206698720793, -16.51473224551083518, 99.58442372801900433 ) ) ;
#155387 = CARTESIAN_POINT ( 'NONE',  ( -10.81492255796078084, -18.62759615963271287, 77.08224293864769550 ) ) ;
#155388 = CARTESIAN_POINT ( 'NONE',  ( -16.55341960407611168, -4.379528057220339221, 36.45724293864768839 ) ) ;
#155389 = CARTESIAN_POINT ( 'NONE',  ( -8.224510206698735004, -14.34966873604973081, 19.58442372801901143 ) ) ;
#155390 = CARTESIAN_POINT ( 'NONE',  ( 13.97604488694527802, 13.89961937509977652, 29.37390960531435979 ) ) ;
#155391 = CARTESIAN_POINT ( 'NONE',  ( 16.51473224551083163, -9.474510206698727899, 110.8344237280190043 ) ) ;
#155393 = CARTESIAN_POINT ( 'NONE',  ( 13.97604488694548053, -13.89961937509957401, 70.62609039468567573 ) ) ;
#155392 = CARTESIAN_POINT ( 'NONE',  ( 15.80617190586746368, 15.72974639402197994, 99.37390960531436690 ) ) ;
#155394 = CARTESIAN_POINT ( 'NONE',  ( 12.06949235617739724, 12.14591786802326823, 86.87609039468568994 ) ) ;
#155395 = CARTESIAN_POINT ( 'NONE',  ( 13.89961937509977652, -13.97604488694527269, 68.12390960531436690 ) ) ;
#155396 = CARTESIAN_POINT ( 'NONE',  ( -14.29746914071049879, 8.314922557960819915, 75.83224293864769550 ) ) ;
#155397 = CARTESIAN_POINT ( 'NONE',  ( -5.049401038298153566, 19.05341960407611168, 65.20724293864765286 ) ) ;
#155398 = CARTESIAN_POINT ( 'NONE',  ( -16.55341960407611168, -4.379528057220339221, 66.45724293864768129 ) ) ;
#155399 = CARTESIAN_POINT ( 'NONE',  ( -13.89961937509977652, 13.97604488694528158, 25.62390960531434558 ) ) ;
#155400 = CARTESIAN_POINT ( 'NONE',  ( 17.33018265901952759, -17.03520690664669957, -54.21489346206826809 ) ) ;
#155401 = CARTESIAN_POINT ( 'NONE',  ( 14.29746914071049879, -8.314922557960816363, 48.33224293864770260 ) ) ;
#155402 = CARTESIAN_POINT ( 'NONE',  ( -5.049401038298153566, 19.05341960407611168, 80.20724293864769550 ) ) ;
#155403 = CARTESIAN_POINT ( 'NONE',  ( -0.4052355915353688109, -16.64782025964801448, -59.15693706287432008 ) ) ;
#155404 = CARTESIAN_POINT ( 'NONE',  ( -19.05341960407617563, 5.049401038297882671, 53.54275706135231871 ) ) ;
#155405 = CARTESIAN_POINT ( 'NONE',  ( 4.483927247898790824, -16.52544592524335698, 55.20942372801902565 ) ) ;
#155406 = CARTESIAN_POINT ( 'NONE',  ( 18.67979575497178502, 10.72451020669898547, 69.16557627198102409 ) ) ;
#155407 = CARTESIAN_POINT ( 'NONE',  ( -19.05341960407617563, 5.049401038297882671, 28.54275706135232937 ) ) ;
#155408 = CARTESIAN_POINT ( 'NONE',  ( -13.89961937509977652, 13.97604488694528158, 75.62390960531438111 ) ) ;
#155409 = CARTESIAN_POINT ( 'NONE',  ( 1.304248841091933035E-15, 21.30000000000002913, -58.85720012050612837 ) ) ;
#155410 = CARTESIAN_POINT ( 'NONE',  ( 9.564922557960805705, 16.46253265017160317, 109.5822429386476955 ) ) ;
#155411 = CARTESIAN_POINT ( 'NONE',  ( -16.51473224551069308, -9.474510206698971260, 56.66557627198103120 ) ) ;
#155412 = CARTESIAN_POINT ( 'NONE',  ( -15.80617190586768217, 15.72974639402176855, 33.12609039468569705 ) ) ;
#155413 = CARTESIAN_POINT ( 'NONE',  ( -14.29746914071049879, 8.314922557960819915, 110.8322429386476955 ) ) ;
#155416 = VERTEX_POINT ( 'NONE', #112919 ) ;
#155415 = CARTESIAN_POINT ( 'NONE',  ( -19.05341960407611168, -5.049401038298163336, 96.45724293864769550 ) ) ;
#155414 = CARTESIAN_POINT ( 'NONE',  ( -15.72974639402197994, 15.80617190586746368, 105.6239096053143669 ) ) ;
#155417 = CARTESIAN_POINT ( 'NONE',  ( 5.823673210054444382, -21.52544592524334988, 20.20942372801900788 ) ) ;
#155418 = ORIENTED_EDGE ( 'NONE', *, *, #150147, .T. ) ;
#155419 = CARTESIAN_POINT ( 'NONE',  ( 19.02544592524343514, -5.153800228976328945, 93.54057627198102409 ) ) ;
#155420 = CARTESIAN_POINT ( 'NONE',  ( 0.000000000000000000, 5.499999999999998224, 118.0000000000000142 ) ) ;
#155421 = CARTESIAN_POINT ( 'NONE',  ( 18.67979575497178502, 10.72451020669898547, 99.16557627198100988 ) ) ;
#155422 = CARTESIAN_POINT ( 'NONE',  ( -5.049401038298153566, 19.05341960407611168, 50.20724293864770260 ) ) ;
#155423 = CARTESIAN_POINT ( 'NONE',  ( -0.05219959533936034679, 19.03943276465977164, 102.5010903946856757 ) ) ;
#155424 = CARTESIAN_POINT ( 'NONE',  ( -36.91746825000000598, 2.428612866367529932E-14, -1.124999997268813390 ) ) ;
#155425 = CARTESIAN_POINT ( 'NONE',  ( 16.51473224551069308, 9.474510206698969483, 29.16557627198103475 ) ) ;
#155426 = CARTESIAN_POINT ( 'NONE',  ( -21.53943276465977519, -0.05219959533937600094, 88.75109039468567573 ) ) ;
#155428 = CARTESIAN_POINT ( 'NONE',  ( -18.67979575497193778, 10.72451020669871902, 43.33442372801901143 ) ) ;
#155427 = CARTESIAN_POINT ( 'NONE',  ( 16.51473224551069308, 9.474510206698969483, 79.16557627198103830 ) ) ;
#155429 = CARTESIAN_POINT ( 'NONE',  ( -0.05219959533937732626, 21.53943276465977519, 22.50109039468567573 ) ) ;
#155430 = CARTESIAN_POINT ( 'NONE',  ( -27.73933785331498925, 2.428612866367529932E-14, 139.3750000027311842 ) ) ;
#155431 = CARTESIAN_POINT ( 'NONE',  ( 19.05341960407611168, 5.049401038298154454, 103.9572429386476671 ) ) ;
#155432 = CARTESIAN_POINT ( 'NONE',  ( -12.72656435003161235, 25.68303923411528800, 139.9999999999999432 ) ) ;
#155435 = CARTESIAN_POINT ( 'NONE',  ( 10.81492255796106328, -18.62759615963255655, 40.41775706135234714 ) ) ;
#155434 = CARTESIAN_POINT ( 'NONE',  ( -15.80617190586745835, -15.72974639402198527, 46.87390960531435979 ) ) ;
#155433 = CARTESIAN_POINT ( 'NONE',  ( -4.379528057220086978, -16.55341960407618274, 44.79275706135234714 ) ) ;
#155436 = CARTESIAN_POINT ( 'NONE',  ( -21.53943276465977519, -0.05219959533937600094, 73.75109039468567573 ) ) ;
#155437 = CARTESIAN_POINT ( 'NONE',  ( 5.758699013978453074, 6.837351365824950733, -61.93409818843134929 ) ) ;
#155438 = CARTESIAN_POINT ( 'NONE',  ( -9.564922557961040184, 16.46253265017147172, 112.9177570613523329 ) ) ;
#155439 = CARTESIAN_POINT ( 'NONE',  ( -19.03943276465977164, 0.05219959533909376836, 66.24890960531436690 ) ) ;
#155440 = CARTESIAN_POINT ( 'NONE',  ( 9.474510206698971260, -16.51473224551069308, 92.91557627198103830 ) ) ;
#155441 = CARTESIAN_POINT ( 'NONE',  ( -8.314922557960811034, -14.29746914071050412, 107.0822429386476955 ) ) ;
#155442 = CARTESIAN_POINT ( 'NONE',  ( 14.29746914071049879, -8.314922557960816363, 108.3322429386477097 ) ) ;
#155443 = CARTESIAN_POINT ( 'NONE',  ( -5.719274019375978568, 21.55341960407610458, 30.20724293864769550 ) ) ;
#155444 = CARTESIAN_POINT ( 'NONE',  ( 14.29746914071037800, 8.314922557961029526, 81.66775706135236135 ) ) ;
#155446 = CARTESIAN_POINT ( 'NONE',  ( 16.51473224551069308, 9.474510206698969483, 49.16557627198102409 ) ) ;
#155445 = CARTESIAN_POINT ( 'NONE',  ( -4.379528057220328563, 16.55341960407611168, 65.20724293864768129 ) ) ;
#155447 = CARTESIAN_POINT ( 'NONE',  ( 18.67979575497194134, -10.72451020669871369, 70.83442372801901854 ) ) ;
#155448 = CARTESIAN_POINT ( 'NONE',  ( 10.72451020669871369, 18.67979575497193778, 77.08442372801901854 ) ) ;
#155449 = CARTESIAN_POINT ( 'NONE',  ( 13.89961937509957401, 13.97604488694547697, 101.8760903946856331 ) ) ;
#155450 = CARTESIAN_POINT ( 'NONE',  ( 0.05219959533910956823, 16.53943276465976808, 59.99890960531436690 ) ) ;
#155451 = CARTESIAN_POINT ( 'NONE',  ( 21.53943276465977519, 0.05219959533937863772, 26.25109039468567573 ) ) ;
#155452 = CARTESIAN_POINT ( 'NONE',  ( 18.67979575497178502, 10.72451020669898547, 54.16557627198103120 ) ) ;
#155453 = CARTESIAN_POINT ( 'NONE',  ( 18.39639308325437383, 5.500000000000037303, 73.98252246182197212 ) ) ;
#155454 = CARTESIAN_POINT ( 'NONE',  ( -23.31738231874055600, 16.94106989632528837, 148.0500000054623797 ) ) ;
#155455 = CARTESIAN_POINT ( 'NONE',  ( 19.05341960407611168, 5.049401038298154454, 63.95724293864769550 ) ) ;
#155456 = CARTESIAN_POINT ( 'NONE',  ( -16.53943276465976808, 0.05219959533911058130, 31.24890960531435979 ) ) ;
#155457 = CARTESIAN_POINT ( 'NONE',  ( -12.14591786802309592, -12.06949235617757132, 21.87390960531436690 ) ) ;
#155458 = CARTESIAN_POINT ( 'NONE',  ( -8.224510206698735004, -14.34966873604973081, 94.58442372801901854 ) ) ;
#155459 = CARTESIAN_POINT ( 'NONE',  ( 19.05341960407617918, -5.049401038297876454, 51.04275706135231871 ) ) ;
#155460 = LINE ( 'NONE', #80591, #95712 ) ;
#155461 = CARTESIAN_POINT ( 'NONE',  ( -9.564922557960796823, -16.46253265017161027, 102.0822429386477097 ) ) ;
#155462 = CARTESIAN_POINT ( 'NONE',  ( 8.224510206698953496, -14.34966873604960469, 72.91557627198103830 ) ) ;
#155463 = CARTESIAN_POINT ( 'NONE',  ( -5.049401038297874678, -19.05341960407617918, 39.79275706135232582 ) ) ;
#155465 = CARTESIAN_POINT ( 'NONE',  ( -5.823673210054116645, -21.52544592524344225, 27.29057627198103120 ) ) ;
#155464 = CARTESIAN_POINT ( 'NONE',  ( -9.564922557960796823, -16.46253265017161027, 32.08224293864769550 ) ) ;
#155466 = CARTESIAN_POINT ( 'NONE',  ( -10.81492255796078084, -18.62759615963271287, 52.08224293864768839 ) ) ;
#155467 = CARTESIAN_POINT ( 'NONE',  ( -14.29746914071049879, 8.314922557960819915, 100.8322429386477097 ) ) ;
#155468 = CARTESIAN_POINT ( 'NONE',  ( -12.14591786802326823, 12.06949235617739902, 48.12609039468568284 ) ) ;
#155469 = CARTESIAN_POINT ( 'NONE',  ( -4.483927247898539470, -16.52544592524342804, 87.29057627198103830 ) ) ;
#155470 = CARTESIAN_POINT ( 'NONE',  ( -38.00000000000000711, -12.34694845685042708, -11.64999999453762669 ) ) ;
#155471 = CARTESIAN_POINT ( 'NONE',  ( -16.81555441253551919, 7.025013491695482948, 50.63685445334259327 ) ) ;
#155472 = CARTESIAN_POINT ( 'NONE',  ( -16.51473224551069308, -9.474510206698971260, 111.6655762719810383 ) ) ;
#155473 = CARTESIAN_POINT ( 'NONE',  ( 29.86685920354754842, -21.69954338932559068, -2.324999997268813345 ) ) ;
#155474 = CARTESIAN_POINT ( 'NONE',  ( 0.8113027391198349703, 24.06567881303553236, -56.94052085246004680 ) ) ;
#155476 = CARTESIAN_POINT ( 'NONE',  ( -8.224510206698948167, 14.34966873604960824, 25.41557627198103120 ) ) ;
#155475 = CARTESIAN_POINT ( 'NONE',  ( 16.52544592524335698, 4.483927247898782831, 46.45942372801901854 ) ) ;
#155477 = CARTESIAN_POINT ( 'NONE',  ( -21.52544592524343514, 5.823673210054127303, 51.04057627198103120 ) ) ;
#155478 = CARTESIAN_POINT ( 'NONE',  ( 19.02544592524334988, 5.153800228976608722, 86.45942372801900433 ) ) ;
#155479 = CARTESIAN_POINT ( 'NONE',  ( -18.67979575497178146, -10.72451020669898902, 46.66557627198102409 ) ) ;
#155480 = CARTESIAN_POINT ( 'NONE',  ( -18.67979575497193778, 10.72451020669871902, 88.33442372801901854 ) ) ;
#155481 = CARTESIAN_POINT ( 'NONE',  ( -21.97181142354054018, 8.379174292515184419, 172.0076905927031419 ) ) ;
#155482 = CARTESIAN_POINT ( 'NONE',  ( 12.06949235617739724, 12.14591786802326823, 51.87609039468568284 ) ) ;
#155484 = CARTESIAN_POINT ( 'NONE',  ( -0.05219959533909027116, -19.03943276465977164, 107.4989096053143527 ) ) ;
#155483 = CARTESIAN_POINT ( 'NONE',  ( -19.05341960407611168, -5.049401038298163336, 41.45724293864769550 ) ) ;
#155485 = CARTESIAN_POINT ( 'NONE',  ( 13.89961937509977652, -13.97604488694527269, 33.12390960531434558 ) ) ;
#155486 = CARTESIAN_POINT ( 'NONE',  ( -16.52544592524342804, 4.483927247898546575, 106.0405762719810525 ) ) ;
#155487 =( NAMED_UNIT ( * ) PLANE_ANGLE_UNIT ( ) SI_UNIT ( $, .RADIAN. ) );
#155488 = CARTESIAN_POINT ( 'NONE',  ( -9.474510206698964154, 16.51473224551069663, 95.41557627198102409 ) ) ;
#155489 = VERTEX_POINT ( 'NONE', #84567 ) ;
#155490 = CARTESIAN_POINT ( 'NONE',  ( 16.53943276465976808, 0.05219959533934440121, 56.25109039468568284 ) ) ;
#155491 = CARTESIAN_POINT ( 'NONE',  ( -10.72451020669898014, 18.67979575497178502, 95.41557627198102409 ) ) ;
#155492 = CARTESIAN_POINT ( 'NONE',  ( 9.474510206698971260, -16.51473224551069308, 52.91557627198102409 ) ) ;
#155493 = CARTESIAN_POINT ( 'NONE',  ( 15.80617190586769283, -15.72974639402175789, 30.62609039468567929 ) ) ;
#155494 = CARTESIAN_POINT ( 'NONE',  ( 9.564922557960805705, 16.46253265017160317, 89.58224293864769550 ) ) ;
#155495 = DIRECTION ( 'NONE',  ( 1.000000000000000000, 0.000000000000000000, -0.000000000000000000 ) ) ;
#155496 = ORIENTED_EDGE ( 'NONE', *, *, #146462, .F. ) ;
#155497 = CARTESIAN_POINT ( 'NONE',  ( 10.72451020669898902, -18.67979575497178502, 112.9155762719810383 ) ) ;
#155500 = CARTESIAN_POINT ( 'NONE',  ( 9.474510206698729675, 16.51473224551082808, 77.08442372801900433 ) ) ;
#155499 = CARTESIAN_POINT ( 'NONE',  ( 19.02544592524343514, -5.153800228976328945, 103.5405762719809957 ) ) ;
#155498 = CARTESIAN_POINT ( 'NONE',  ( -16.52544592524342804, 4.483927247898546575, 116.0405762719810383 ) ) ;
#155501 = CARTESIAN_POINT ( 'NONE',  ( -9.474510206698720793, -16.51473224551083518, 29.58442372801900433 ) ) ;
#155502 = CARTESIAN_POINT ( 'NONE',  ( 18.67979575497178502, 10.72451020669898547, 99.16557627198100988 ) ) ;
#155503 = CARTESIAN_POINT ( 'NONE',  ( -16.51473224551082808, 9.474510206698731452, 33.33442372801899722 ) ) ;
#155504 = CARTESIAN_POINT ( 'NONE',  ( 12.06949235617739724, 12.14591786802326823, 76.87609039468567573 ) ) ;
#155505 = CARTESIAN_POINT ( 'NONE',  ( -16.46253265017160317, 9.564922557960807481, 100.8322429386477097 ) ) ;
#155506 = CARTESIAN_POINT ( 'NONE',  ( 19.03943276465977164, -0.05219959533909143690, 63.74890960531435979 ) ) ;
#155507 = CARTESIAN_POINT ( 'NONE',  ( 18.62759615963255655, 10.81492255796105972, 71.66775706135234714 ) ) ;
#155508 = CARTESIAN_POINT ( 'NONE',  ( -21.52544592524334988, -5.823673210054445271, 83.95942372801900433 ) ) ;
#155509 = CARTESIAN_POINT ( 'NONE',  ( 16.51473224551069308, 9.474510206698969483, 74.16557627198103830 ) ) ;
#155510 = CARTESIAN_POINT ( 'NONE',  ( 0.05219959533937995610, -21.53943276465977519, 55.00109039468568284 ) ) ;
#155511 = CARTESIAN_POINT ( 'NONE',  ( 16.51473224551083163, -9.474510206698727899, 90.83442372801900433 ) ) ;
#155512 = CARTESIAN_POINT ( 'NONE',  ( -0.05219959533909027116, -19.03943276465977164, 57.49890960531435979 ) ) ;
#155513 = CARTESIAN_POINT ( 'NONE',  ( 19.03943276465977164, -0.05219959533909143690, 98.74890960531436690 ) ) ;
#155514 = CARTESIAN_POINT ( 'NONE',  ( 9.564922557960805705, 16.46253265017160317, 59.58224293864769550 ) ) ;
#155515 = CARTESIAN_POINT ( 'NONE',  ( -19.03943276465977164, 0.05219959533909376836, 116.2489096053143669 ) ) ;
#155516 = CARTESIAN_POINT ( 'NONE',  ( 19.02544592524343514, -5.153800228976328945, 53.54057627198102409 ) ) ;
#155517 = CARTESIAN_POINT ( 'NONE',  ( 5.719274019375991003, -21.55341960407610458, 97.70724293864772392 ) ) ;
#155518 = CARTESIAN_POINT ( 'NONE',  ( -16.55341960407617563, 4.379528057220093196, 73.54275706135234714 ) ) ;
#155519 = CARTESIAN_POINT ( 'NONE',  ( -21.04946095171203169, 10.24435024061036437, 168.3368280404225459 ) ) ;
#155520 = CARTESIAN_POINT ( 'NONE',  ( 0.05219959533936267826, -19.03943276465977164, 50.00109039468566863 ) ) ;
#155521 = CARTESIAN_POINT ( 'NONE',  ( -16.51473224551069308, -9.474510206698971260, 66.66557627198102409 ) ) ;
#155522 = CARTESIAN_POINT ( 'NONE',  ( 8.224510206698953496, -14.34966873604960469, 52.91557627198103830 ) ) ;
#155523 = CARTESIAN_POINT ( 'NONE',  ( -8.314922557960811034, -14.29746914071050412, 97.08224293864770971 ) ) ;
#155524 = CARTESIAN_POINT ( 'NONE',  ( -19.02544592524342804, 5.153800228976336051, 106.0405762719810241 ) ) ;
#155525 = CARTESIAN_POINT ( 'NONE',  ( 13.97604488694527802, 13.89961937509977652, 94.37390960531436690 ) ) ;
#155526 = CARTESIAN_POINT ( 'NONE',  ( 19.05341960407611168, 5.049401038298154454, 108.9572429386477097 ) ) ;
#155527 = CARTESIAN_POINT ( 'NONE',  ( -21.55341960407619339, 5.719274019375674811, 113.5427570613523756 ) ) ;
#155528 = CARTESIAN_POINT ( 'NONE',  ( 12.14591786802327356, -12.06949235617739191, 95.62609039468568994 ) ) ;
#155529 = CARTESIAN_POINT ( 'NONE',  ( 18.62759615963255655, 10.81492255796105972, 41.66775706135235424 ) ) ;
#155530 = CARTESIAN_POINT ( 'NONE',  ( 5.719274019375991003, -21.55341960407610458, 32.70724293864770260 ) ) ;
#155531 = CARTESIAN_POINT ( 'NONE',  ( -21.55341960407610458, -5.719274019375992779, 101.4572429386476955 ) ) ;
#155532 = CARTESIAN_POINT ( 'NONE',  ( -16.52544592524342804, 4.483927247898546575, 56.04057627198102409 ) ) ;
#155533 = CARTESIAN_POINT ( 'NONE',  ( 19.03943276465977164, -0.05219959533909143690, 53.74890960531436690 ) ) ;
#155534 = CARTESIAN_POINT ( 'NONE',  ( -4.483927247898539470, -16.52544592524342804, 77.29057627198102409 ) ) ;
#155535 = CARTESIAN_POINT ( 'NONE',  ( -9.564922557961040184, 16.46253265017147172, 42.91775706135234003 ) ) ;
#155536 = ADVANCED_FACE ( 'NONE', ( #177617 ), #158435, .T. ) ;
#155537 = CARTESIAN_POINT ( 'NONE',  ( 19.03943276465977164, -0.05219959533909143690, 23.74890960531435269 ) ) ;
#155538 = EDGE_LOOP ( 'NONE', ( #85257, #156713 ) ) ;
#155539 = CARTESIAN_POINT ( 'NONE',  ( 8.314922557961029526, -14.29746914071037800, 65.41775706135234714 ) ) ;
#155540 = CARTESIAN_POINT ( 'NONE',  ( -16.46253265017160317, 9.564922557960807481, 70.83224293864770971 ) ) ;
#155541 = CARTESIAN_POINT ( 'NONE',  ( -22.44159573604009950, -16.30477369853688430, 145.0750000027311728 ) ) ;
#155542 = CARTESIAN_POINT ( 'NONE',  ( 14.34966873604960469, 8.224510206698951720, 89.16557627198102409 ) ) ;
#155543 = CARTESIAN_POINT ( 'NONE',  ( 15.72974639402199770, -15.80617190586745480, 43.12390960531435269 ) ) ;
#155544 = ORIENTED_EDGE ( 'NONE', *, *, #109403, .F. ) ;
#155545 = CARTESIAN_POINT ( 'NONE',  ( -0.05219959533934338120, 16.53943276465976808, 112.5010903946857042 ) ) ;
#155546 = CARTESIAN_POINT ( 'NONE',  ( 16.53943276465976808, 0.05219959533934440121, 26.25109039468567573 ) ) ;
#155547 = CARTESIAN_POINT ( 'NONE',  ( 21.55341960407619695, -5.719274019375665929, 91.04275706135236135 ) ) ;
#155548 = CARTESIAN_POINT ( 'NONE',  ( 0.05219959533909260263, 19.03943276465977164, 89.99890960531436690 ) ) ;
#155549 = CARTESIAN_POINT ( 'NONE',  ( 0.05219959533907565091, 21.53943276465977519, 114.9989096053143669 ) ) ;
#155550 = CARTESIAN_POINT ( 'NONE',  ( -16.46253265017160317, 9.564922557960807481, 30.83224293864769550 ) ) ;
#155551 = CARTESIAN_POINT ( 'NONE',  ( 12.14591786802327356, -12.06949235617739191, 35.62609039468568994 ) ) ;
#155552 = CARTESIAN_POINT ( 'NONE',  ( -5.049401038297874678, -19.05341960407617918, 89.79275706135230450 ) ) ;
#155553 = CARTESIAN_POINT ( 'NONE',  ( 18.62759615963271287, -10.81492255796078972, 88.33224293864769550 ) ) ;
#155554 = CARTESIAN_POINT ( 'NONE',  ( -13.97604488694547697, 13.89961937509957934, 68.12609039468563310 ) ) ;
#155555 = CARTESIAN_POINT ( 'NONE',  ( 16.51473224551069308, 9.474510206698969483, 24.16557627198102765 ) ) ;
#155556 = CARTESIAN_POINT ( 'NONE',  ( -21.52544592524343514, 5.823673210054127303, 116.0405762719810383 ) ) ;
#155557 = CARTESIAN_POINT ( 'NONE',  ( -19.99999999999998224, -190.0000000000000000, 0.000000000000000000 ) ) ;
#155558 = CARTESIAN_POINT ( 'NONE',  ( 9.564922557960805705, 16.46253265017160317, 79.58224293864769550 ) ) ;
#155559 = CARTESIAN_POINT ( 'NONE',  ( 14.34966873604972726, -8.224510206698740333, 30.83442372801902209 ) ) ;
#155560 = CARTESIAN_POINT ( 'NONE',  ( 19.73275029929832414, -34.79402272588036737, -6.352102039474952555 ) ) ;
#155561 = CARTESIAN_POINT ( 'NONE',  ( 9.564922557961047289, -16.46253265017146816, 60.41775706135233293 ) ) ;
#155563 = CARTESIAN_POINT ( 'NONE',  ( 12.14591786802309770, 12.06949235617756955, 79.37390960531436690 ) ) ;
#155562 = CARTESIAN_POINT ( 'NONE',  ( 21.52544592524344225, -5.823673210054117533, 113.5405762719810383 ) ) ;
#155564 = CARTESIAN_POINT ( 'NONE',  ( -19.03943276465977164, 0.05219959533909376836, 81.24890960531436690 ) ) ;
#155566 = CARTESIAN_POINT ( 'NONE',  ( 9.474510206698729675, 16.51473224551082808, 42.08442372801900433 ) ) ;
#155565 = CARTESIAN_POINT ( 'NONE',  ( 16.55341960407618274, -4.379528057220086978, 36.04275706135234714 ) ) ;
#155567 = CARTESIAN_POINT ( 'NONE',  ( -0.05219959533937732626, 21.53943276465977519, 67.50109039468568994 ) ) ;
#155568 = CARTESIAN_POINT ( 'NONE',  ( -8.224510206698735004, -14.34966873604973081, 19.58442372801901143 ) ) ;
#155569 = CARTESIAN_POINT ( 'NONE',  ( -13.97604488694527625, -13.89961937509977652, 61.87390960531435979 ) ) ;
#155570 = CARTESIAN_POINT ( 'NONE',  ( 9.474510206698729675, 16.51473224551082808, 77.08442372801900433 ) ) ;
#155571 = CARTESIAN_POINT ( 'NONE',  ( 14.34966873604972726, -8.224510206698740333, 50.83442372801901143 ) ) ;
#155572 = CARTESIAN_POINT ( 'NONE',  ( -15.72974639402176322, -15.80617190586768395, 99.37609039468568994 ) ) ;
#155573 = CARTESIAN_POINT ( 'NONE',  ( 9.474510206698729675, 16.51473224551082808, 72.08442372801900433 ) ) ;
#155574 = CARTESIAN_POINT ( 'NONE',  ( -0.05219959533909027116, -19.03943276465977164, 52.49890960531436690 ) ) ;
#155575 = CARTESIAN_POINT ( 'NONE',  ( 5.719274019375991003, -21.55341960407610458, 67.70724293864769550 ) ) ;
#155577 = CARTESIAN_POINT ( 'NONE',  ( -19.02544592524334988, -5.153800228976617603, 63.95942372801899012 ) ) ;
#155576 = CARTESIAN_POINT ( 'NONE',  ( -8.314922557960811034, -14.29746914071050412, 62.08224293864769550 ) ) ;
#155578 = CARTESIAN_POINT ( 'NONE',  ( -19.39720447994790575, -5.500000000000073719, 69.66317477297171479 ) ) ;
#155579 = CARTESIAN_POINT ( 'NONE',  ( -19.05341960407617563, 5.049401038297882671, 43.54275706135232582 ) ) ;
#155580 = CARTESIAN_POINT ( 'NONE',  ( -4.483927247898782831, 16.52544592524335698, 97.70942372801904696 ) ) ;
#155581 = CARTESIAN_POINT ( 'NONE',  ( 8.314922557960818139, 14.29746914071049879, 64.58224293864769550 ) ) ;
#155583 = CARTESIAN_POINT ( 'NONE',  ( 1.784210473542230573E-15, -29.16686587814331588, 141.3750000027311557 ) ) ;
#155582 = CARTESIAN_POINT ( 'NONE',  ( -5.719274019375665041, -21.55341960407619695, 99.79275706135234714 ) ) ;
#155584 = CARTESIAN_POINT ( 'NONE',  ( 18.67979575497178502, 10.72451020669898547, 94.16557627198103830 ) ) ;
#155585 = CARTESIAN_POINT ( 'NONE',  ( -9.474510206698964154, 16.51473224551069663, 70.41557627198102409 ) ) ;
#155586 = CARTESIAN_POINT ( 'NONE',  ( 18.67979575497194134, -10.72451020669871369, 75.83442372801900433 ) ) ;
#155587 = CARTESIAN_POINT ( 'NONE',  ( 9.564922557960805705, 16.46253265017160317, 44.58224293864769550 ) ) ;
#155588 = ORIENTED_EDGE ( 'NONE', *, *, #101839, .T. ) ;
#155589 = CARTESIAN_POINT ( 'NONE',  ( 13.97604488694527802, 13.89961937509977652, 69.37390960531436690 ) ) ;
#155590 = CARTESIAN_POINT ( 'NONE',  ( 19.02544592524343514, -5.153800228976328945, 28.54057627198102409 ) ) ;
#155591 = CARTESIAN_POINT ( 'NONE',  ( -5.153800228976328057, -19.02544592524343514, 107.2905762719810383 ) ) ;
#155592 = CARTESIAN_POINT ( 'NONE',  ( 8.314922557960818139, 14.29746914071049879, 69.58224293864769550 ) ) ;
#155593 = CARTESIAN_POINT ( 'NONE',  ( -16.46253265017160317, 9.564922557960807481, 35.83224293864768839 ) ) ;
#155594 = CARTESIAN_POINT ( 'NONE',  ( 12.14591786802309770, 12.06949235617756955, 84.37390960531438111 ) ) ;
#155595 = CARTESIAN_POINT ( 'NONE',  ( 0.05219959533907565091, 21.53943276465977519, 94.99890960531436690 ) ) ;
#155596 = CARTESIAN_POINT ( 'NONE',  ( 21.55341960407619695, -5.719274019375665929, 41.04275706135236135 ) ) ;
#155597 = CARTESIAN_POINT ( 'NONE',  ( 4.999999999999996447, 37.66961640367475184, -18.00000000000000355 ) ) ;
#155598 = CARTESIAN_POINT ( 'NONE',  ( 12.06949235617739724, 12.14591786802326823, 46.87609039468568994 ) ) ;
#155599 = CARTESIAN_POINT ( 'NONE',  ( -21.55341960407610458, -5.719274019375992779, 86.45724293864770971 ) ) ;
#155600 = CARTESIAN_POINT ( 'NONE',  ( -5.153800228976607833, 19.02544592524334988, 27.70942372801899722 ) ) ;
#155601 = CARTESIAN_POINT ( 'NONE',  ( -5.049401038298153566, 19.05341960407611168, 100.2072429386476955 ) ) ;
#155602 = CARTESIAN_POINT ( 'NONE',  ( -18.67979575497193778, 10.72451020669871902, 38.33442372801900433 ) ) ;
#155603 = CARTESIAN_POINT ( 'NONE',  ( -10.81492255796078084, -18.62759615963271287, 42.08224293864769550 ) ) ;
#155604 = CARTESIAN_POINT ( 'NONE',  ( 14.34966873604960469, 8.224510206698951720, 24.16557627198103120 ) ) ;
#155605 = AXIS2_PLACEMENT_3D ( 'NONE', #103293, #44603, #10294 ) ;
#155607 = CARTESIAN_POINT ( 'NONE',  ( 5.823673210054444382, -21.52544592524334988, 100.2094237280190043 ) ) ;
#155606 = CARTESIAN_POINT ( 'NONE',  ( 15.72974639402176855, 15.80617190586768217, 66.87609039468568994 ) ) ;
#155608 = CARTESIAN_POINT ( 'NONE',  ( 5.153800228976615827, -19.02544592524334988, 30.20942372801900433 ) ) ;
#155609 = CARTESIAN_POINT ( 'NONE',  ( 12.14591786802327356, -12.06949235617739191, 85.62609039468568994 ) ) ;
#155610 = CARTESIAN_POINT ( 'NONE',  ( -5.823673210054431948, 21.52544592524334988, 47.70942372801902565 ) ) ;
#155611 = CARTESIAN_POINT ( 'NONE',  ( 13.97604488694527802, 13.89961937509977652, 49.37390960531434558 ) ) ;
#155612 = CARTESIAN_POINT ( 'NONE',  ( -5.049401038297874678, -19.05341960407617918, 24.79275706135233648 ) ) ;
#155613 = CARTESIAN_POINT ( 'NONE',  ( 15.80617190586746368, 15.72974639402197994, 24.37390960531435979 ) ) ;
#155614 = CARTESIAN_POINT ( 'NONE',  ( -21.52544592524343514, 5.823673210054127303, 116.0405762719810383 ) ) ;
#155615 = CARTESIAN_POINT ( 'NONE',  ( 21.53943276465977519, -0.05219959533907433946, 73.74890960531433848 ) ) ;
#155616 = CARTESIAN_POINT ( 'NONE',  ( -16.52544592524335698, -4.483927247898792601, 38.95942372801901854 ) ) ;
#155618 = CARTESIAN_POINT ( 'NONE',  ( -18.62759615963270932, 10.81492255796079327, 80.83224293864769550 ) ) ;
#155617 = CARTESIAN_POINT ( 'NONE',  ( -6.551653823223136719, -3.660253528765625486, 8.410814283099844246 ) ) ;
#155620 = CARTESIAN_POINT ( 'NONE',  ( 14.34966873604960469, 8.224510206698951720, 69.16557627198102409 ) ) ;
#155619 = CARTESIAN_POINT ( 'NONE',  ( 16.52544592524335698, 4.483927247898782831, 61.45942372801901854 ) ) ;
#155621 = CARTESIAN_POINT ( 'NONE',  ( 24.93942350307308686, 7.769968609432599926, 171.2173313942149946 ) ) ;
#155622 = CARTESIAN_POINT ( 'NONE',  ( 19.05341960407617918, -5.049401038297876454, 86.04275706135233293 ) ) ;
#155623 = CARTESIAN_POINT ( 'NONE',  ( 6.434671708797603529, -6.434671708797564449, -61.89430850415821794 ) ) ;
#155624 = CARTESIAN_POINT ( 'NONE',  ( 16.53943276465976808, 0.05219959533934440121, 46.25109039468567573 ) ) ;
#155625 = CARTESIAN_POINT ( 'NONE',  ( -21.55341960407610458, -5.719274019375992779, 111.4572429386476813 ) ) ;
#155626 = CARTESIAN_POINT ( 'NONE',  ( -5.823673210054116645, -21.52544592524344225, 72.29057627198102409 ) ) ;
#155627 = CARTESIAN_POINT ( 'NONE',  ( -18.67979575497178146, -10.72451020669898902, 31.66557627198102054 ) ) ;
#155628 = CARTESIAN_POINT ( 'NONE',  ( -4.483927247898782831, 16.52544592524335698, 57.70942372801901143 ) ) ;
#155629 = CARTESIAN_POINT ( 'NONE',  ( -0.05219959533909027116, -19.03943276465977164, 67.49890960531436690 ) ) ;
#155631 = CARTESIAN_POINT ( 'NONE',  ( 8.314922557961029526, -14.29746914071037800, 20.41775706135234714 ) ) ;
#155630 = CARTESIAN_POINT ( 'NONE',  ( 15.72974639402176855, 15.80617190586768217, 46.87609039468568994 ) ) ;
#155632 = CARTESIAN_POINT ( 'NONE',  ( -19.03943276465977164, 0.05219959533909376836, 106.2489096053143669 ) ) ;
#155633 = CARTESIAN_POINT ( 'NONE',  ( 5.153800228976615827, -19.02544592524334988, 25.20942372801900433 ) ) ;
#155634 =( BOUNDED_CURVE ( )  B_SPLINE_CURVE ( 3, ( #148569, #30940, #177915, #56557 ),
 .UNSPECIFIED., .F., .T. ) 
 B_SPLINE_CURVE_WITH_KNOTS ( ( 4, 4 ),
 ( 5.150538010968860547, 5.257537365396776075 ),
 .UNSPECIFIED. ) 
 CURVE ( )  GEOMETRIC_REPRESENTATION_ITEM ( )  RATIONAL_B_SPLINE_CURVE ( ( 1.000000000000000000, 0.9990461557208837329, 0.9990461557208837329, 1.000000000000000000 ) ) 
 REPRESENTATION_ITEM ( '' )  );
#155635 = CARTESIAN_POINT ( 'NONE',  ( -8.224510206698735004, -14.34966873604973081, 39.58442372801901143 ) ) ;
#155636 = CARTESIAN_POINT ( 'NONE',  ( 13.97604488694527802, 13.89961937509977652, 99.37390960531436690 ) ) ;
#155637 = CARTESIAN_POINT ( 'NONE',  ( 21.55341960407610458, 5.719274019375980345, 108.9572429386476955 ) ) ;
#155638 = CARTESIAN_POINT ( 'NONE',  ( -5.049401038298153566, 19.05341960407611168, 60.20724293864768129 ) ) ;
#155639 = CARTESIAN_POINT ( 'NONE',  ( -4.500000000000001776, -139.5000000000000000, 21.82407087589996308 ) ) ;
#155640 = CARTESIAN_POINT ( 'NONE',  ( 16.55341960407611168, 4.379528057220329451, 78.95724293864769550 ) ) ;
#155641 = CARTESIAN_POINT ( 'NONE',  ( -15.80617190586745835, -15.72974639402198527, 21.87390960531436690 ) ) ;
#155642 = CARTESIAN_POINT ( 'NONE',  ( -16.51473224551069308, -9.474510206698971260, 21.66557627198102765 ) ) ;
#155643 = CARTESIAN_POINT ( 'NONE',  ( -15.72974639402197994, 15.80617190586746368, 100.6239096053143811 ) ) ;
#155644 = CARTESIAN_POINT ( 'NONE',  ( -13.89961937509957401, -13.97604488694547875, 59.37609039468566863 ) ) ;
#155645 = CARTESIAN_POINT ( 'NONE',  ( 21.52544592524344225, -5.823673210054117533, 28.54057627198103120 ) ) ;
#155646 = CARTESIAN_POINT ( 'NONE',  ( 5.049401038298161559, -19.05341960407611168, 27.70724293864769550 ) ) ;
#155647 = CARTESIAN_POINT ( 'NONE',  ( -21.52544592524343514, 5.823673210054127303, 66.04057627198103830 ) ) ;
#155648 = CARTESIAN_POINT ( 'NONE',  ( -9.474510206698964154, 16.51473224551069663, 100.4155762719810241 ) ) ;
#155649 = CARTESIAN_POINT ( 'NONE',  ( 21.52544592524334988, 5.823673210054432836, 86.45942372801901854 ) ) ;
#155650 = CARTESIAN_POINT ( 'NONE',  ( 19.03943276465977164, -0.05219959533909143690, 48.74890960531435979 ) ) ;
#155651 = CARTESIAN_POINT ( 'NONE',  ( 14.29746914071049879, -8.314922557960816363, 88.33224293864769550 ) ) ;
#155652 = CARTESIAN_POINT ( 'NONE',  ( 12.14591786802327356, -12.06949235617739191, 30.62609039468567929 ) ) ;
#155653 = CARTESIAN_POINT ( 'NONE',  ( -13.89961937509977652, 13.97604488694528158, 55.62390960531434558 ) ) ;
#155654 = CARTESIAN_POINT ( 'NONE',  ( -10.81492255796105439, 18.62759615963255655, 72.91775706135234714 ) ) ;
#155655 = EDGE_LOOP ( 'NONE', ( #3467, #87009, #61679, #44341 ) ) ;
#155656 = CARTESIAN_POINT ( 'NONE',  ( 13.97604488694548053, -13.89961937509957401, 25.62609039468566507 ) ) ;
#155657 = CARTESIAN_POINT ( 'NONE',  ( 5.153800228976615827, -19.02544592524334988, 45.20942372801901143 ) ) ;
#155658 = CARTESIAN_POINT ( 'NONE',  ( 18.67979575497194134, -10.72451020669871369, 30.83442372801902209 ) ) ;
#155659 = CARTESIAN_POINT ( 'NONE',  ( -7.794582437828422528, 1.499905742985387480, -62.16226466885328961 ) ) ;
#155660 = CARTESIAN_POINT ( 'NONE',  ( 19.02544592524334988, 5.153800228976608722, 36.45942372801900433 ) ) ;
#155661 = CARTESIAN_POINT ( 'NONE',  ( 13.89961937509977652, -13.97604488694527269, 88.12390960531438111 ) ) ;
#155662 = CARTESIAN_POINT ( 'NONE',  ( 19.05341960407611168, 5.049401038298154454, 73.95724293864768129 ) ) ;
#155663 = CARTESIAN_POINT ( 'NONE',  ( 12.14591786802309770, 12.06949235617756955, 29.37390960531435269 ) ) ;
#155665 = CARTESIAN_POINT ( 'NONE',  ( 18.62759615963255655, 10.81492255796105972, 81.66775706135236135 ) ) ;
#155664 = CARTESIAN_POINT ( 'NONE',  ( 15.80617190586746368, 15.72974639402197994, 24.37390960531435979 ) ) ;
#155666 = CARTESIAN_POINT ( 'NONE',  ( -22.81625015709510507, 31.40387420917330275, -7.424999997268812990 ) ) ;
#155667 = CARTESIAN_POINT ( 'NONE',  ( 17.50000000000000000, 5.622605283950888655, 58.81207310596111881 ) ) ;
#155668 = CARTESIAN_POINT ( 'NONE',  ( -21.55341960407619339, 5.719274019375674811, 78.54275706135236135 ) ) ;
#155669 = CARTESIAN_POINT ( 'NONE',  ( 16.19135201231362586, -7.376712067592065658, 42.31319145947967542 ) ) ;
#155670 = CARTESIAN_POINT ( 'NONE',  ( -19.02544592524342804, 5.153800228976336051, 96.04057627198103830 ) ) ;
#155671 = ADVANCED_FACE ( 'NONE', ( #115927 ), #192143, .F. ) ;
#155672 = CARTESIAN_POINT ( 'NONE',  ( 33.76801240946110028, 5.498839508946048227, 94.61983786177952993 ) ) ;
#155673 = CARTESIAN_POINT ( 'NONE',  ( -21.52544592524343514, 5.823673210054127303, 66.04057627198103830 ) ) ;
#155674 = CARTESIAN_POINT ( 'NONE',  ( -14.34966873604960291, -8.224510206698953496, 31.66557627198102054 ) ) ;
#155676 = CARTESIAN_POINT ( 'NONE',  ( 9.474510206698971260, -16.51473224551069308, 92.91557627198103830 ) ) ;
#155675 = CARTESIAN_POINT ( 'NONE',  ( -12.06949235617756955, 12.14591786802309770, 115.6239096053143669 ) ) ;
#155677 = CARTESIAN_POINT ( 'NONE',  ( -0.05219959533937732626, 21.53943276465977519, 112.5010903946857042 ) ) ;
#155678 = CARTESIAN_POINT ( 'NONE',  ( 9.474510206698971260, -16.51473224551069308, 22.91557627198102765 ) ) ;
#155679 = CARTESIAN_POINT ( 'NONE',  ( -10.81492255796105439, 18.62759615963255655, 62.91775706135236135 ) ) ;
#155680 = CARTESIAN_POINT ( 'NONE',  ( -9.564922557960796823, -16.46253265017161027, 97.08224293864769550 ) ) ;
#155681 = CARTESIAN_POINT ( 'NONE',  ( -12.06949235617739369, -12.14591786802326823, 109.3760903946857042 ) ) ;
#155682 = CARTESIAN_POINT ( 'NONE',  ( -19.02544592524334988, -5.153800228976617603, 68.95942372801896170 ) ) ;
#155683 = CARTESIAN_POINT ( 'NONE',  ( -29.86685920354755197, -21.69954338932560134, -4.924999997268813878 ) ) ;
#155684 = CARTESIAN_POINT ( 'NONE',  ( 0.05219959533909260263, 19.03943276465977164, 114.9989096053143669 ) ) ;
#155685 = CARTESIAN_POINT ( 'NONE',  ( -8.314922557960811034, -14.29746914071050412, 87.08224293864769550 ) ) ;
#155686 = CARTESIAN_POINT ( 'NONE',  ( -5.049401038297874678, -19.05341960407617918, 64.79275706135233293 ) ) ;
#155687 = CARTESIAN_POINT ( 'NONE',  ( -19.05341960407611168, -5.049401038298163336, 81.45724293864769550 ) ) ;
#155688 = CARTESIAN_POINT ( 'NONE',  ( 14.29746914071049879, -8.314922557960816363, 63.33224293864770260 ) ) ;
#155689 = CARTESIAN_POINT ( 'NONE',  ( -16.46253265017146816, -9.564922557961047289, 94.16775706135233293 ) ) ;
#155690 = CARTESIAN_POINT ( 'NONE',  ( -10.72451020669898014, 18.67979575497178502, 55.41557627198102409 ) ) ;
#155691 = ORIENTED_EDGE ( 'NONE', *, *, #30090, .F. ) ;
#155692 = CARTESIAN_POINT ( 'NONE',  ( -16.51473224551069308, -9.474510206698971260, 21.66557627198102765 ) ) ;
#155693 = CARTESIAN_POINT ( 'NONE',  ( -17.49999999999999645, -5.624438216177606975, 29.18329655085356578 ) ) ;
#155695 = CARTESIAN_POINT ( 'NONE',  ( 18.67979575497178502, 10.72451020669898547, 79.16557627198103830 ) ) ;
#155694 = CARTESIAN_POINT ( 'NONE',  ( 13.89961937509977652, -13.97604488694527269, 73.12390960531436690 ) ) ;
#155697 = CARTESIAN_POINT ( 'NONE',  ( -5.049401038298153566, 19.05341960407611168, 80.20724293864769550 ) ) ;
#155696 = CARTESIAN_POINT ( 'NONE',  ( -4.483927247898782831, 16.52544592524335698, 87.70942372801901854 ) ) ;
#155698 = CARTESIAN_POINT ( 'NONE',  ( 5.049401038297881783, 19.05341960407617563, 52.29275706135234003 ) ) ;
#155699 = CARTESIAN_POINT ( 'NONE',  ( -18.67979575497193778, 10.72451020669871902, 88.33442372801901854 ) ) ;
#155700 = CARTESIAN_POINT ( 'NONE',  ( -0.05219959533907301413, -21.53943276465977519, 62.49890960531436690 ) ) ;
#155701 = CARTESIAN_POINT ( 'NONE',  ( 18.67979575497178502, 10.72451020669898547, 24.16557627198103120 ) ) ;
#155702 = CARTESIAN_POINT ( 'NONE',  ( -9.564922557960796823, -16.46253265017161027, 37.08224293864768839 ) ) ;
#155703 = CARTESIAN_POINT ( 'NONE',  ( 8.314922557961029526, -14.29746914071037800, 100.4177570613523471 ) ) ;
#155704 = CARTESIAN_POINT ( 'NONE',  ( -14.34966873604972548, 8.224510206698743886, 28.33442372801902209 ) ) ;
#155705 = DIRECTION ( 'NONE',  ( -1.000000000000000000, 0.000000000000000000, 0.000000000000000000 ) ) ;
#155706 = CARTESIAN_POINT ( 'NONE',  ( 18.67979575497194134, -10.72451020669871369, 90.83442372801901854 ) ) ;
#155707 = CARTESIAN_POINT ( 'NONE',  ( -0.05219959533910754901, -16.53943276465976808, 62.49890960531436690 ) ) ;
#155708 = CARTESIAN_POINT ( 'NONE',  ( -10.72451020669898014, 18.67979575497178502, 90.41557627198103830 ) ) ;
#155709 = CARTESIAN_POINT ( 'NONE',  ( 0.05219959533907565091, 21.53943276465977519, 89.99890960531438111 ) ) ;
#155710 = DIRECTION ( 'NONE',  ( -1.000000000000000000, -1.071875439572228152E-15, -5.204170427930421283E-16 ) ) ;
#155711 = CARTESIAN_POINT ( 'NONE',  ( -5.823673210054116645, -21.52544592524344225, 52.29057627198102409 ) ) ;
#155712 = CARTESIAN_POINT ( 'NONE',  ( -16.53943276465976808, -0.05219959533934237506, 73.75109039468567573 ) ) ;
#155713 = CARTESIAN_POINT ( 'NONE',  ( 16.53943276465976808, -0.05219959533910856209, 93.74890960531436690 ) ) ;
#155714 = CARTESIAN_POINT ( 'NONE',  ( -5.153800228976328057, -19.02544592524343514, 52.29057627198100988 ) ) ;
#155715 = CARTESIAN_POINT ( 'NONE',  ( 34.78522506798721992, 2.428612866353961525E-14, 52.50000000000000000 ) ) ;
#155716 = CARTESIAN_POINT ( 'NONE',  ( 16.53943276465976808, 0.05219959533934440121, 96.25109039468568994 ) ) ;
#155717 = CARTESIAN_POINT ( 'NONE',  ( 18.62759615963255655, 10.81492255796105972, 36.66775706135234714 ) ) ;
#155718 = CARTESIAN_POINT ( 'NONE',  ( -19.03943276465977164, 0.05219959533909376836, 101.2489096053143669 ) ) ;
#155719 = CARTESIAN_POINT ( 'NONE',  ( -5.719274019375665041, -21.55341960407619695, 64.79275706135234714 ) ) ;
#155720 = CARTESIAN_POINT ( 'NONE',  ( 3.503282210674365071, -48.86437366581479580, -35.00000000000000000 ) ) ;
#155721 = CARTESIAN_POINT ( 'NONE',  ( 0.05219959533909260263, 19.03943276465977164, 24.99890960531435269 ) ) ;
#155722 = VERTEX_POINT ( 'NONE', #176615 ) ;
#155723 = CARTESIAN_POINT ( 'NONE',  ( -15.80617190586768217, 15.72974639402176855, 58.12609039468568994 ) ) ;
#155725 = CARTESIAN_POINT ( 'NONE',  ( 17.72517630441460312, -5.499999999999974243, 58.42175719257605238 ) ) ;
#155724 = CARTESIAN_POINT ( 'NONE',  ( 0.05219959533909260263, 19.03943276465977164, 49.99890960531435979 ) ) ;
#155726 = CARTESIAN_POINT ( 'NONE',  ( -13.97604488694527625, -13.89961937509977652, 86.87390960531436690 ) ) ;
#155727 = CARTESIAN_POINT ( 'NONE',  ( -5.153800228976607833, 19.02544592524334988, 67.70942372801900433 ) ) ;
#155728 = CARTESIAN_POINT ( 'NONE',  ( 18.62759615963255655, 10.81492255796105972, 41.66775706135235424 ) ) ;
#155729 = CARTESIAN_POINT ( 'NONE',  ( -19.02544592524334988, -5.153800228976617603, 63.95942372801899012 ) ) ;
#155730 = CARTESIAN_POINT ( 'NONE',  ( 16.51473224551069308, 9.474510206698969483, 34.16557627198102409 ) ) ;
#155731 = CARTESIAN_POINT ( 'NONE',  ( 16.53943276465976808, 0.05219959533934440121, 101.2510903946856757 ) ) ;
#155732 = CARTESIAN_POINT ( 'NONE',  ( -16.46253265017146816, -9.564922557961047289, 74.16775706135234714 ) ) ;
#155733 = CARTESIAN_POINT ( 'NONE',  ( -14.34966873604960291, -8.224510206698953496, 21.66557627198102409 ) ) ;
#155734 = CARTESIAN_POINT ( 'NONE',  ( -5.153800228976607833, 19.02544592524334988, 52.70942372801900433 ) ) ;
#155735 = CARTESIAN_POINT ( 'NONE',  ( 0.05219959533909260263, 19.03943276465977164, 99.99890960531436690 ) ) ;
#155736 = CARTESIAN_POINT ( 'NONE',  ( 15.80617190586769283, -15.72974639402175789, 110.6260903946857042 ) ) ;
#155738 = EDGE_CURVE ( 'NONE', #144934, #146461, #163323, .T. ) ;
#155737 = CARTESIAN_POINT ( 'NONE',  ( 9.564922557961047289, -16.46253265017146816, 25.41775706135234003 ) ) ;
#155739 = CARTESIAN_POINT ( 'NONE',  ( 13.97604488694527802, 13.89961937509977652, 29.37390960531435979 ) ) ;
#155740 = CARTESIAN_POINT ( 'NONE',  ( -5.823673210054431948, 21.52544592524334988, 82.70942372801900433 ) ) ;
#155741 = CARTESIAN_POINT ( 'NONE',  ( 16.52544592524335698, 4.483927247898782831, 31.45942372801901854 ) ) ;
#155742 = CARTESIAN_POINT ( 'NONE',  ( -9.474510206698964154, 16.51473224551069663, 95.41557627198102409 ) ) ;
#155743 = CARTESIAN_POINT ( 'NONE',  ( 32.00000000000000000, -5.510910596163089556E-15, 45.00000000000000000 ) ) ;
#155744 = CARTESIAN_POINT ( 'NONE',  ( -9.564922557960796823, -16.46253265017161027, 82.08224293864768129 ) ) ;
#155745 = DIRECTION ( 'NONE',  ( -1.000000000000000000, 0.000000000000000000, -3.652049423109065657E-15 ) ) ;
#155746 = CARTESIAN_POINT ( 'NONE',  ( -19.03943276465977164, -0.05219959533935918106, 83.75109039468567573 ) ) ;
#155747 = CARTESIAN_POINT ( 'NONE',  ( 16.51473224551069308, 9.474510206698969483, 109.1655762719810383 ) ) ;
#155748 = CARTESIAN_POINT ( 'NONE',  ( 21.55341960407619695, -5.719274019375665929, 101.0427570613523756 ) ) ;
#155749 = CARTESIAN_POINT ( 'NONE',  ( -8.314922557960811034, -14.29746914071050412, 97.08224293864770971 ) ) ;
#155750 = CARTESIAN_POINT ( 'NONE',  ( 13.97604488694527802, 13.89961937509977652, 24.37390960531435624 ) ) ;
#155751 = CARTESIAN_POINT ( 'NONE',  ( 5.823673210054125526, 21.52544592524343514, 39.79057627198103830 ) ) ;
#155752 = CARTESIAN_POINT ( 'NONE',  ( 15.72974639402199770, -15.80617190586745480, 38.12390960531436690 ) ) ;
#155753 = CARTESIAN_POINT ( 'NONE',  ( 14.34966873604960469, 8.224510206698951720, 114.1655762719810383 ) ) ;
#155754 = CARTESIAN_POINT ( 'NONE',  ( -16.64831001466044214, 0.4033639900676664891, -61.36868776158049599 ) ) ;
#155755 = CARTESIAN_POINT ( 'NONE',  ( 5.049401038297881783, 19.05341960407617563, 57.29275706135231871 ) ) ;
#155756 = CARTESIAN_POINT ( 'NONE',  ( 0.05219959533910956823, 16.53943276465976808, 39.99890960531436690 ) ) ;
#155757 = CARTESIAN_POINT ( 'NONE',  ( 9.564922557960805705, 16.46253265017160317, 114.5822429386476955 ) ) ;
#155758 = CARTESIAN_POINT ( 'NONE',  ( 15.80617190586769283, -15.72974639402175789, 85.62609039468568994 ) ) ;
#155759 = CARTESIAN_POINT ( 'NONE',  ( 15.80617190586746368, 15.72974639402197994, 74.37390960531436690 ) ) ;
#155760 = CARTESIAN_POINT ( 'NONE',  ( -15.80617190586768217, 15.72974639402176855, 48.12609039468568284 ) ) ;
#155761 = CARTESIAN_POINT ( 'NONE',  ( -5.719274019375978568, 21.55341960407610458, 100.2072429386476955 ) ) ;
#155762 = CARTESIAN_POINT ( 'NONE',  ( 5.823673210054444382, -21.52544592524334988, 55.20942372801902565 ) ) ;
#155763 = CARTESIAN_POINT ( 'NONE',  ( -19.02544592524342804, 5.153800228976336051, 26.04057627198103120 ) ) ;
#155764 = CARTESIAN_POINT ( 'NONE',  ( 19.02544592524343514, -5.153800228976328945, 78.54057627198099567 ) ) ;
#155765 = CARTESIAN_POINT ( 'NONE',  ( 8.314922557961029526, -14.29746914071037800, 75.41775706135233293 ) ) ;
#155766 = CARTESIAN_POINT ( 'NONE',  ( -16.55341960407611168, -4.379528057220339221, 111.4572429386476813 ) ) ;
#155767 = CARTESIAN_POINT ( 'NONE',  ( -31.24420449012919931, 7.031618440654747282, 97.62038805904604999 ) ) ;
#155768 = CARTESIAN_POINT ( 'NONE',  ( 4.379528057220339221, -16.55341960407611168, 47.70724293864770260 ) ) ;
#155769 = CARTESIAN_POINT ( 'NONE',  ( -12.06949235617756955, 12.14591786802309770, 25.62390960531435624 ) ) ;
#155770 = CARTESIAN_POINT ( 'NONE',  ( 0.05219959533909260263, 19.03943276465977164, 64.99890960531436690 ) ) ;
#155771 = CARTESIAN_POINT ( 'NONE',  ( -0.05219959533909027116, -19.03943276465977164, 32.49890960531435979 ) ) ;
#155772 = CARTESIAN_POINT ( 'NONE',  ( -15.80617190586745835, -15.72974639402198527, 46.87390960531435979 ) ) ;
#155773 = CARTESIAN_POINT ( 'NONE',  ( -16.51473224551082808, 9.474510206698731452, 43.33442372801900433 ) ) ;
#155775 = CARTESIAN_POINT ( 'NONE',  ( -12.06949235617756955, 12.14591786802309770, 35.62390960531437401 ) ) ;
#155774 = CARTESIAN_POINT ( 'NONE',  ( 17.50000000000000000, 5.499999999999992895, 51.70309617465830598 ) ) ;
#155776 = CARTESIAN_POINT ( 'NONE',  ( 16.46253265017160672, -9.564922557960803928, 108.3322429386476955 ) ) ;
#155777 = CARTESIAN_POINT ( 'NONE',  ( 21.55341960407619695, -5.719274019375665929, 56.04275706135235424 ) ) ;
#155778 = B_SPLINE_CURVE_WITH_KNOTS ( 'NONE', 3,
 ( #25437, #193267, #149754, #87078 ),
 .UNSPECIFIED., .F., .F.,
 ( 4, 4 ),
 ( 0.001482540648255936417, 0.002244533994399181866 ),
 .UNSPECIFIED. ) ;
#155779 = CARTESIAN_POINT ( 'NONE',  ( -23.31738231874055600, 16.94106989632528837, 140.0500000054623513 ) ) ;
#155780 = CARTESIAN_POINT ( 'NONE',  ( -0.05219959533934338120, 16.53943276465976808, 77.50109039468567573 ) ) ;
#155781 = CARTESIAN_POINT ( 'NONE',  ( 19.02544592524334988, 5.153800228976608722, 61.45942372801900433 ) ) ;
#155782 = CARTESIAN_POINT ( 'NONE',  ( 16.55341960407611168, 4.379528057220329451, 38.95724293864768839 ) ) ;
#155783 = LINE ( 'NONE', #15290, #12819 ) ;
#155784 = CARTESIAN_POINT ( 'NONE',  ( 12.14591786802309770, 12.06949235617756955, 24.37390960531435979 ) ) ;
#155785 = CARTESIAN_POINT ( 'NONE',  ( 16.46253265017160672, -9.564922557960803928, 43.33224293864769550 ) ) ;
#155786 = CARTESIAN_POINT ( 'NONE',  ( -16.51473224551069308, -9.474510206698971260, 61.66557627198103120 ) ) ;
#155787 = CARTESIAN_POINT ( 'NONE',  ( -19.03943276465977164, 0.05219959533909376836, 26.24890960531435624 ) ) ;
#155788 = CARTESIAN_POINT ( 'NONE',  ( 18.62759615963255655, 10.81492255796105972, 26.66775706135235424 ) ) ;
#155789 = CARTESIAN_POINT ( 'NONE',  ( 16.51473224551069308, 9.474510206698969483, 54.16557627198103120 ) ) ;
#155790 = CARTESIAN_POINT ( 'NONE',  ( -22.73749492396214933, -155.7167183371837496, -4.999999999999999112 ) ) ;
#155791 = CARTESIAN_POINT ( 'NONE',  ( 5.049401038298161559, -19.05341960407611168, 52.70724293864767418 ) ) ;
#155792 = CARTESIAN_POINT ( 'NONE',  ( -10.81492255796078084, -18.62759615963271287, 32.08224293864769550 ) ) ;
#155794 = CARTESIAN_POINT ( 'NONE',  ( 0.05219959533909260263, 19.03943276465977164, 24.99890960531435269 ) ) ;
#155793 = CARTESIAN_POINT ( 'NONE',  ( -15.72974639402176322, -15.80617190586768395, 54.37609039468568994 ) ) ;
#155795 = CARTESIAN_POINT ( 'NONE',  ( 5.719274019375991003, -21.55341960407610458, 32.70724293864770260 ) ) ;
#155796 = CARTESIAN_POINT ( 'NONE',  ( 8.224510206698742110, 14.34966873604972548, 77.08442372801901854 ) ) ;
#155797 = CARTESIAN_POINT ( 'NONE',  ( 21.53943276465977519, 0.05219959533937863772, 111.2510903946856899 ) ) ;
#155798 = CARTESIAN_POINT ( 'NONE',  ( 12.14591786802327356, -12.06949235617739191, 70.62609039468567573 ) ) ;
#155799 = CARTESIAN_POINT ( 'NONE',  ( -9.564922557960796823, -16.46253265017161027, 107.0822429386476955 ) ) ;
#155800 = CARTESIAN_POINT ( 'NONE',  ( 14.29746914071037800, 8.314922557961029526, 51.66775706135234714 ) ) ;
#155801 = CARTESIAN_POINT ( 'NONE',  ( 16.53943276465976808, 0.05219959533934440121, 26.25109039468567573 ) ) ;
#155802 = CARTESIAN_POINT ( 'NONE',  ( -16.53943276465976808, -0.05219959533934237506, 98.75109039468568994 ) ) ;
#155803 = CARTESIAN_POINT ( 'NONE',  ( 10.81492255796106328, -18.62759615963255655, 50.41775706135235424 ) ) ;
#155804 = CARTESIAN_POINT ( 'NONE',  ( 19.05341960407617918, -5.049401038297876454, 106.0427570613523471 ) ) ;
#155805 = CARTESIAN_POINT ( 'NONE',  ( 21.55341960407610458, 5.719274019375980345, 108.9572429386476955 ) ) ;
#155806 = CARTESIAN_POINT ( 'NONE',  ( 0.05219959533934541429, -16.53943276465976808, 20.00109039468568639 ) ) ;
#155807 = CARTESIAN_POINT ( 'NONE',  ( -4.483927247898782831, 16.52544592524335698, 87.70942372801901854 ) ) ;
#155808 = CARTESIAN_POINT ( 'NONE',  ( 21.46320343559639454, -20.96320343559646915, 4.646446609406721606 ) ) ;
#155809 = CARTESIAN_POINT ( 'NONE',  ( -10.81492255796105439, 18.62759615963255655, 82.91775706135234714 ) ) ;
#155810 = CARTESIAN_POINT ( 'NONE',  ( 9.564922557961047289, -16.46253265017146816, 80.41775706135234714 ) ) ;
#155811 = CARTESIAN_POINT ( 'NONE',  ( -14.29746914071049879, 8.314922557960819915, 45.83224293864769550 ) ) ;
#155812 = CARTESIAN_POINT ( 'NONE',  ( 4.483927247898545687, 16.52544592524342804, 44.79057627198103120 ) ) ;
#155813 = CARTESIAN_POINT ( 'NONE',  ( 14.34966873604960469, 8.224510206698951720, 104.1655762719810241 ) ) ;
#155815 = CARTESIAN_POINT ( 'NONE',  ( -8.788868155854840936, 0.9199430937699365485, -64.01178436185547582 ) ) ;
#155814 = CARTESIAN_POINT ( 'NONE',  ( -19.03943276465977164, -0.05219959533935918106, 43.75109039468566863 ) ) ;
#155816 = CARTESIAN_POINT ( 'NONE',  ( -0.05219959533937732626, 21.53943276465977519, 37.50109039468568284 ) ) ;
#155817 = CARTESIAN_POINT ( 'NONE',  ( -12.06949235617739369, -12.14591786802326823, 19.37609039468568639 ) ) ;
#155818 = DIRECTION ( 'NONE',  ( 0.000000000000000000, -0.000000000000000000, -1.000000000000000000 ) ) ;
#155819 = CARTESIAN_POINT ( 'NONE',  ( 19.02544592524343514, -5.153800228976328945, 98.54057627198100988 ) ) ;
#155820 = CARTESIAN_POINT ( 'NONE',  ( 15.72974639402199770, -15.80617190586745480, 53.12390960531436690 ) ) ;
#155821 = CARTESIAN_POINT ( 'NONE',  ( 13.89961937509957401, 13.97604488694547697, 91.87609039468567573 ) ) ;
#155822 = CARTESIAN_POINT ( 'NONE',  ( -16.51473224551069308, -9.474510206698971260, 86.66557627198102409 ) ) ;
#155823 = CARTESIAN_POINT ( 'NONE',  ( 21.53943276465977519, -0.05219959533907433946, 53.74890960531437401 ) ) ;
#155824 = CARTESIAN_POINT ( 'NONE',  ( 8.224510206698953496, -14.34966873604960469, 102.9155762719810383 ) ) ;
#155825 = CARTESIAN_POINT ( 'NONE',  ( -16.46253265017160317, 9.564922557960807481, 75.83224293864769550 ) ) ;
#155826 = CARTESIAN_POINT ( 'NONE',  ( -9.564922557960796823, -16.46253265017161027, 32.08224293864769550 ) ) ;
#155827 = CARTESIAN_POINT ( 'NONE',  ( -10.81492255796105439, 18.62759615963255655, 32.91775706135234714 ) ) ;
#155828 = CARTESIAN_POINT ( 'NONE',  ( -21.53943276465977519, -0.05219959533937600094, 78.75109039468568994 ) ) ;
#155829 = CARTESIAN_POINT ( 'NONE',  ( -0.05219959533934338120, 16.53943276465976808, 92.50109039468567573 ) ) ;
#155830 = CARTESIAN_POINT ( 'NONE',  ( -21.53943276465977519, -0.05219959533937600094, 33.75109039468568284 ) ) ;
#155831 = CARTESIAN_POINT ( 'NONE',  ( -18.67979575497193778, 10.72451020669871902, 23.33442372801901499 ) ) ;
#155833 = CARTESIAN_POINT ( 'NONE',  ( 0.05219959533909260263, 19.03943276465977164, 79.99890960531436690 ) ) ;
#155832 = CARTESIAN_POINT ( 'NONE',  ( 9.564922557961047289, -16.46253265017146816, 60.41775706135233293 ) ) ;
#155834 = CARTESIAN_POINT ( 'NONE',  ( -21.53943276465977519, -0.05219959533937600094, 78.75109039468568994 ) ) ;
#155835 = CARTESIAN_POINT ( 'NONE',  ( 0.05219959533907565091, 21.53943276465977519, 89.99890960531438111 ) ) ;
#155836 = CARTESIAN_POINT ( 'NONE',  ( -4.379528057220328563, 16.55341960407611168, 70.20724293864769550 ) ) ;
#155837 = CARTESIAN_POINT ( 'NONE',  ( 18.67979575497194134, -10.72451020669871369, 100.8344237280190185 ) ) ;
#155838 = CARTESIAN_POINT ( 'NONE',  ( 8.224510206698953496, -14.34966873604960469, 87.91557627198103830 ) ) ;
#155839 = CARTESIAN_POINT ( 'NONE',  ( -0.05219959533909027116, -19.03943276465977164, 42.49890960531435269 ) ) ;
#155840 = CARTESIAN_POINT ( 'NONE',  ( 5.153800228976615827, -19.02544592524334988, 70.20942372801899012 ) ) ;
#155841 = CARTESIAN_POINT ( 'NONE',  ( -16.53943276465976808, 0.05219959533911058130, 36.24890960531435979 ) ) ;
#155842 = CARTESIAN_POINT ( 'NONE',  ( -10.72451020669870658, -18.67979575497194134, 94.58442372801901854 ) ) ;
#155843 = CARTESIAN_POINT ( 'NONE',  ( -19.02544592524342804, 5.153800228976336051, 91.04057627198100988 ) ) ;
#155844 = CARTESIAN_POINT ( 'NONE',  ( 19.02544592524334988, 5.153800228976608722, 66.45942372801899012 ) ) ;
#155845 = CARTESIAN_POINT ( 'NONE',  ( -15.72974639402197994, 15.80617190586746368, 65.62390960531436690 ) ) ;
#155846 = CARTESIAN_POINT ( 'NONE',  ( -0.05219959533937732626, 21.53943276465977519, 22.50109039468567573 ) ) ;
#155847 = CARTESIAN_POINT ( 'NONE',  ( 16.53943276465976808, 0.05219959533934440121, 21.25109039468567218 ) ) ;
#155848 = CARTESIAN_POINT ( 'NONE',  ( 8.224510206698742110, 14.34966873604972548, 82.08442372801901854 ) ) ;
#155850 = CARTESIAN_POINT ( 'NONE',  ( 5.823673210054444382, -21.52544592524334988, 25.20942372801901854 ) ) ;
#155849 = CARTESIAN_POINT ( 'NONE',  ( -2.260530480648141910E-15, -78.64506293871966136, -12.99999966871702917 ) ) ;
#155851 = CARTESIAN_POINT ( 'NONE',  ( 4.379528057220339221, -16.55341960407611168, 102.7072429386476955 ) ) ;
#155852 = CARTESIAN_POINT ( 'NONE',  ( 3.556970738554033499E-15, -38.81732327939057825, -6.624999997268814056 ) ) ;
#155853 = CARTESIAN_POINT ( 'NONE',  ( -14.29746914071037622, -8.314922557961029526, 34.16775706135234714 ) ) ;
#155854 = CARTESIAN_POINT ( 'NONE',  ( 21.55341960407610458, 5.719274019375980345, 63.95724293864770260 ) ) ;
#155855 = CARTESIAN_POINT ( 'NONE',  ( 0.05219959533934541429, -16.53943276465976808, 110.0010903946856757 ) ) ;
#155856 = CARTESIAN_POINT ( 'NONE',  ( 14.29746914071037800, 8.314922557961029526, 31.66775706135234358 ) ) ;
#155857 = CARTESIAN_POINT ( 'NONE',  ( 13.89961937509977652, -13.97604488694527269, 38.12390960531436690 ) ) ;
#155858 = CARTESIAN_POINT ( 'NONE',  ( 8.314922557961029526, -14.29746914071037800, 80.41775706135234714 ) ) ;
#155859 = CARTESIAN_POINT ( 'NONE',  ( 19.05341960407617918, -5.049401038297876454, 71.04275706135234714 ) ) ;
#155860 = CARTESIAN_POINT ( 'NONE',  ( -15.72974639402197994, 15.80617190586746368, 75.62390960531439532 ) ) ;
#155861 = CARTESIAN_POINT ( 'NONE',  ( 14.34966873604972726, -8.224510206698740333, 100.8344237280190185 ) ) ;
#155862 = CARTESIAN_POINT ( 'NONE',  ( -15.80617190586768217, 15.72974639402176855, 88.12609039468570415 ) ) ;
#155863 = CARTESIAN_POINT ( 'NONE',  ( 21.55341960407610458, 5.719274019375980345, 63.95724293864770260 ) ) ;
#155864 = CARTESIAN_POINT ( 'NONE',  ( 10.72451020669898902, -18.67979575497178502, 52.91557627198103830 ) ) ;
#155865 = ORIENTED_EDGE ( 'NONE', *, *, #65094, .F. ) ;
#155866 = VERTEX_POINT ( 'NONE', #66423 ) ;
#155867 = CARTESIAN_POINT ( 'NONE',  ( 0.05219959533934541429, -16.53943276465976808, 80.00109039468568994 ) ) ;
#155868 = CARTESIAN_POINT ( 'NONE',  ( -18.67979575497178146, -10.72451020669898902, 51.66557627198102409 ) ) ;
#155869 = VERTEX_POINT ( 'NONE', #189788 ) ;
#155870 = CARTESIAN_POINT ( 'NONE',  ( 13.97604488694527802, 13.89961937509977652, 109.3739096053143669 ) ) ;
#155871 = DIRECTION ( 'NONE',  ( 1.000000000000000000, 0.000000000000000000, 0.000000000000000000 ) ) ;
#155872 = CARTESIAN_POINT ( 'NONE',  ( -5.049401038298153566, 19.05341960407611168, 25.20724293864768484 ) ) ;
#155873 = CARTESIAN_POINT ( 'NONE',  ( 10.72451020669898902, -18.67979575497178502, 62.91557627198102409 ) ) ;
#155874 = CARTESIAN_POINT ( 'NONE',  ( -16.53943276465976808, -0.05219959533934237506, 98.75109039468568994 ) ) ;
#155875 = CARTESIAN_POINT ( 'NONE',  ( -15.80617190586768217, 15.72974639402176855, 43.12609039468568284 ) ) ;
#155876 = CARTESIAN_POINT ( 'NONE',  ( -16.51473224551082808, 9.474510206698731452, 98.33442372801900433 ) ) ;
#155877 = CARTESIAN_POINT ( 'NONE',  ( 19.03943276465977164, -0.05219959533909143690, 23.74890960531435269 ) ) ;
#155878 = CARTESIAN_POINT ( 'NONE',  ( -4.379528057220086978, -16.55341960407618274, 19.79275706135235069 ) ) ;
#155879 = CARTESIAN_POINT ( 'NONE',  ( -13.97604488694527625, -13.89961937509977652, 41.87390960531435979 ) ) ;
#155880 = CARTESIAN_POINT ( 'NONE',  ( -28.82186960331499392, -9.364793116373526516, 140.0999999999999943 ) ) ;
#155881 = CARTESIAN_POINT ( 'NONE',  ( 19.02544592524343514, -5.153800228976328945, 88.54057627198102409 ) ) ;
#155882 = CARTESIAN_POINT ( 'NONE',  ( 8.314922557961029526, -14.29746914071037800, 75.41775706135233293 ) ) ;
#155883 = CARTESIAN_POINT ( 'NONE',  ( -19.03943276465977164, -0.05219959533935918106, 73.75109039468566152 ) ) ;
#155884 = CARTESIAN_POINT ( 'NONE',  ( 16.46253265017146816, 9.564922557961045513, 26.66775706135234003 ) ) ;
#155885 = CARTESIAN_POINT ( 'NONE',  ( -21.53943276465977519, 0.05219959533907696930, 61.24890960531435979 ) ) ;
#155886 = CARTESIAN_POINT ( 'NONE',  ( 14.34966873604972726, -8.224510206698740333, 80.83442372801901854 ) ) ;
#155887 = CARTESIAN_POINT ( 'NONE',  ( 9.564922557961047289, -16.46253265017146816, 80.41775706135234714 ) ) ;
#155888 = CARTESIAN_POINT ( 'NONE',  ( 19.02544592524343514, -5.153800228976328945, 38.54057627198103120 ) ) ;
#155889 = CARTESIAN_POINT ( 'NONE',  ( 5.153800228976335163, 19.02544592524342804, 84.79057627198099567 ) ) ;
#155890 = CARTESIAN_POINT ( 'NONE',  ( -5.823673210054431948, 21.52544592524334988, 47.70942372801902565 ) ) ;
#155891 = CARTESIAN_POINT ( 'NONE',  ( -9.564922557960796823, -16.46253265017161027, 52.08224293864768839 ) ) ;
#155892 = CARTESIAN_POINT ( 'NONE',  ( -5.049401038297874678, -19.05341960407617918, 69.79275706135233293 ) ) ;
#155893 = CARTESIAN_POINT ( 'NONE',  ( 25.66129429279841290, -9.008087060820539449, 171.3163768196949945 ) ) ;
#155894 = CARTESIAN_POINT ( 'NONE',  ( 13.97604488694527802, 13.89961937509977652, 104.3739096053143385 ) ) ;
#155895 = CARTESIAN_POINT ( 'NONE',  ( -8.224510206698948167, 14.34966873604960824, 70.41557627198102409 ) ) ;
#155896 = CARTESIAN_POINT ( 'NONE',  ( 0.05219959533907565091, 21.53943276465977519, 64.99890960531435269 ) ) ;
#155897 = DIRECTION ( 'NONE',  ( 0.000000000000000000, 0.000000000000000000, -1.000000000000000000 ) ) ;
#155898 = CIRCLE ( 'NONE', #52697, 0.5000000000000004441 ) ;
#155899 = CARTESIAN_POINT ( 'NONE',  ( 9.564922557961047289, -16.46253265017146816, 40.41775706135234003 ) ) ;
#155900 = CARTESIAN_POINT ( 'NONE',  ( 21.49230329115315286, -7.461674882483882776, 174.1505502713556837 ) ) ;
#155902 = CARTESIAN_POINT ( 'NONE',  ( -9.564922557960796823, -16.46253265017161027, 67.08224293864769550 ) ) ;
#155901 = CARTESIAN_POINT ( 'NONE',  ( 9.564922557960805705, 16.46253265017160317, 59.58224293864769550 ) ) ;
#155903 = EDGE_CURVE ( 'NONE', #115616, #129907, #81256, .T. ) ;
#155904 = CARTESIAN_POINT ( 'NONE',  ( 12.14591786802327356, -12.06949235617739191, 45.62609039468567573 ) ) ;
#155905 = CARTESIAN_POINT ( 'NONE',  ( 28.82186960331498327, 2.781578969918950771E-14, 143.0000000000000000 ) ) ;
#155906 = FACE_OUTER_BOUND ( 'NONE', #60982, .T. ) ;
#155907 = CARTESIAN_POINT ( 'NONE',  ( -4.483927247898782831, 16.52544592524335698, 92.70942372801901854 ) ) ;
#155908 = DIRECTION ( 'NONE',  ( -1.000000000000000000, 0.000000000000000000, 0.000000000000000000 ) ) ;
#155909 = CARTESIAN_POINT ( 'NONE',  ( 12.14591786802327356, -12.06949235617739191, 70.62609039468567573 ) ) ;
#155910 = CARTESIAN_POINT ( 'NONE',  ( -4.379528057220086978, -16.55341960407618274, 44.79275706135234714 ) ) ;
#155911 = CARTESIAN_POINT ( 'NONE',  ( 13.89961937509957401, 13.97604488694547697, 21.87609039468566152 ) ) ;
#155913 = FACE_BOUND ( 'NONE', #37038, .T. ) ;
#155912 = CARTESIAN_POINT ( 'NONE',  ( 0.05219959533909260263, 19.03943276465977164, 59.99890960531436690 ) ) ;
#155914 = CARTESIAN_POINT ( 'NONE',  ( -0.05219959533937732626, 21.53943276465977519, 47.50109039468568994 ) ) ;
#155915 = CARTESIAN_POINT ( 'NONE',  ( 19.05341960407617918, -5.049401038297876454, 66.04275706135233293 ) ) ;
#155916 = CARTESIAN_POINT ( 'NONE',  ( -21.55341960407619339, 5.719274019375674811, 113.5427570613523756 ) ) ;
#155917 = CARTESIAN_POINT ( 'NONE',  ( 19.02544592524343514, -5.153800228976328945, 28.54057627198102409 ) ) ;
#155918 = CARTESIAN_POINT ( 'NONE',  ( 17.47993547923482893, 5.827241545460860372, 23.84623249736978323 ) ) ;
#155919 = CARTESIAN_POINT ( 'NONE',  ( -21.53943276465977519, 0.05219959533907696930, 56.24890960531436690 ) ) ;
#155920 = CARTESIAN_POINT ( 'NONE',  ( -21.55341960407610458, -5.719274019375992779, 26.45724293864768839 ) ) ;
#155921 = CARTESIAN_POINT ( 'NONE',  ( -16.55341960407611168, -4.379528057220339221, 96.45724293864770971 ) ) ;
#155922 = CARTESIAN_POINT ( 'NONE',  ( -16.55341960407617563, 4.379528057220093196, 43.54275706135235424 ) ) ;
#155923 = CARTESIAN_POINT ( 'NONE',  ( -4.483927247898539470, -16.52544592524342804, 27.29057627198103120 ) ) ;
#155924 = ORIENTED_EDGE ( 'NONE', *, *, #106368, .T. ) ;
#155925 = CARTESIAN_POINT ( 'NONE',  ( 5.823673210054125526, 21.52544592524343514, 109.7905762719810383 ) ) ;
#155926 = AXIS2_PLACEMENT_3D ( 'NONE', #89142, #123431, #108276 ) ;
#155928 = CARTESIAN_POINT ( 'NONE',  ( 16.46253265017160672, -9.564922557960803928, 108.3322429386476955 ) ) ;
#155927 = CARTESIAN_POINT ( 'NONE',  ( 14.29746914071049879, -8.314922557960816363, 33.33224293864769550 ) ) ;
#155929 = CARTESIAN_POINT ( 'NONE',  ( 13.89961937509957401, 13.97604488694547697, 101.8760903946856331 ) ) ;
#155930 = CARTESIAN_POINT ( 'NONE',  ( -13.89961937509957401, -13.97604488694547875, 24.37609039468565442 ) ) ;
#155931 = CARTESIAN_POINT ( 'NONE',  ( -14.34966873604960291, -8.224510206698953496, 36.66557627198103120 ) ) ;
#155932 = CARTESIAN_POINT ( 'NONE',  ( -10.81492255796078084, -18.62759615963271287, 107.0822429386476955 ) ) ;
#155933 = CARTESIAN_POINT ( 'NONE',  ( -18.67979575497178146, -10.72451020669898902, 66.66557627198102409 ) ) ;
#155934 = CARTESIAN_POINT ( 'NONE',  ( 5.153800228976335163, 19.02544592524342804, 74.79057627198103830 ) ) ;
#155935 = CARTESIAN_POINT ( 'NONE',  ( 12.14591786802309770, 12.06949235617756955, 44.37390960531435979 ) ) ;
#155936 = CARTESIAN_POINT ( 'NONE',  ( -9.474510206698964154, 16.51473224551069663, 90.41557627198103830 ) ) ;
#155937 = CARTESIAN_POINT ( 'NONE',  ( -18.22780087662126647, -5.499999999999827693, 38.98236817873107185 ) ) ;
#155938 = CARTESIAN_POINT ( 'NONE',  ( 19.02544592524334988, 5.153800228976608722, 56.45942372801898301 ) ) ;
#155939 = CARTESIAN_POINT ( 'NONE',  ( 0.05219959533907565091, 21.53943276465977519, 89.99890960531438111 ) ) ;
#155940 = CARTESIAN_POINT ( 'NONE',  ( -16.55341960407611168, -4.379528057220339221, 96.45724293864770971 ) ) ;
#155941 = CARTESIAN_POINT ( 'NONE',  ( -21.52544592524334988, -5.823673210054445271, 43.95942372801902565 ) ) ;
#155942 = CARTESIAN_POINT ( 'NONE',  ( 8.571926809382603096, -26.38167802310801235, 147.9750000027311785 ) ) ;
#155943 = CARTESIAN_POINT ( 'NONE',  ( -16.53943276465976808, 0.05219959533911058130, 26.24890960531435624 ) ) ;
#155944 = CARTESIAN_POINT ( 'NONE',  ( -9.474510206698964154, 16.51473224551069663, 30.41557627198102054 ) ) ;
#155945 = CARTESIAN_POINT ( 'NONE',  ( -19.02544592524342804, 5.153800228976336051, 91.04057627198100988 ) ) ;
#155946 = CARTESIAN_POINT ( 'NONE',  ( 15.80617190586746368, 15.72974639402197994, 59.37390960531436690 ) ) ;
#155947 = CARTESIAN_POINT ( 'NONE',  ( 0.05219959533909260263, 19.03943276465977164, 29.99890960531435979 ) ) ;
#155948 = CARTESIAN_POINT ( 'NONE',  ( -18.67979575497178146, -10.72451020669898902, 46.66557627198102409 ) ) ;
#155949 = CARTESIAN_POINT ( 'NONE',  ( 10.81492255796106328, -18.62759615963255655, 70.41775706135236135 ) ) ;
#155951 = CARTESIAN_POINT ( 'NONE',  ( -14.29746914071037622, -8.314922557961029526, 64.16775706135234714 ) ) ;
#155950 = CARTESIAN_POINT ( 'NONE',  ( 22.30909568230050155, -31.30078617543998476, -17.06157116626960502 ) ) ;
#155952 = CARTESIAN_POINT ( 'NONE',  ( -19.02544592524342804, 5.153800228976336051, 61.04057627198103120 ) ) ;
#155953 = CARTESIAN_POINT ( 'NONE',  ( 19.02544592524343514, -5.153800228976328945, 63.54057627198103830 ) ) ;
#155954 = ORIENTED_EDGE ( 'NONE', *, *, #152995, .T. ) ;
#155955 = CARTESIAN_POINT ( 'NONE',  ( -5.719274019375665041, -21.55341960407619695, 109.7927570613523613 ) ) ;
#155956 = CARTESIAN_POINT ( 'NONE',  ( -8.224510206698735004, -14.34966873604973081, 74.58442372801901854 ) ) ;
#155957 = CARTESIAN_POINT ( 'NONE',  ( 15.80617190586769283, -15.72974639402175789, 105.6260903946856899 ) ) ;
#155958 = CARTESIAN_POINT ( 'NONE',  ( -19.02544592524342804, 5.153800228976336051, 76.04057627198102409 ) ) ;
#155959 = CARTESIAN_POINT ( 'NONE',  ( 18.62759615963271287, -10.81492255796078972, 38.33224293864768839 ) ) ;
#155960 = CARTESIAN_POINT ( 'NONE',  ( -19.02544592524334988, -5.153800228976617603, 103.9594237280190043 ) ) ;
#155961 = CARTESIAN_POINT ( 'NONE',  ( -18.67979575497193778, 10.72451020669871902, 83.33442372801903275 ) ) ;
#155962 = CARTESIAN_POINT ( 'NONE',  ( -12.14591786802326823, 12.06949235617739902, 53.12609039468568284 ) ) ;
#155963 = CARTESIAN_POINT ( 'NONE',  ( 21.52544592524344225, -5.823673210054117533, 93.54057627198103830 ) ) ;
#155964 = CARTESIAN_POINT ( 'NONE',  ( -5.153800228976607833, 19.02544592524334988, 97.70942372801900433 ) ) ;
#155965 = CARTESIAN_POINT ( 'NONE',  ( -9.564922557960796823, -16.46253265017161027, 72.08224293864770971 ) ) ;
#155966 = CARTESIAN_POINT ( 'NONE',  ( 9.564922557961047289, -16.46253265017146816, 110.4177570613523471 ) ) ;
#155967 = CARTESIAN_POINT ( 'NONE',  ( -16.46253265017160317, 9.564922557960807481, 35.83224293864768839 ) ) ;
#155968 = CARTESIAN_POINT ( 'NONE',  ( 4.483927247898790824, -16.52544592524335698, 25.20942372801901854 ) ) ;
#155969 = CARTESIAN_POINT ( 'NONE',  ( -4.379528057220328563, 16.55341960407611168, 65.20724293864768129 ) ) ;
#155970 = CARTESIAN_POINT ( 'NONE',  ( -8.224510206698735004, -14.34966873604973081, 69.58442372801900433 ) ) ;
#155971 = EDGE_CURVE ( 'NONE', #27411, #6927, #180166, .T. ) ;
#155973 = CARTESIAN_POINT ( 'NONE',  ( -9.474510206698964154, 16.51473224551069663, 45.41557627198103120 ) ) ;
#155972 = CARTESIAN_POINT ( 'NONE',  ( 10.81492255796106328, -18.62759615963255655, 30.41775706135234358 ) ) ;
#155974 = CARTESIAN_POINT ( 'NONE',  ( 9.564922557960805705, 16.46253265017160317, 69.58224293864770971 ) ) ;
#155975 = CARTESIAN_POINT ( 'NONE',  ( -16.52544592524335698, -4.483927247898792601, 73.95942372801901854 ) ) ;
#155976 = CARTESIAN_POINT ( 'NONE',  ( -28.82186960331499037, 2.428612866367529932E-14, 146.2500000054623683 ) ) ;
#155977 = ORIENTED_EDGE ( 'NONE', *, *, #44393, .T. ) ;
#155978 = CARTESIAN_POINT ( 'NONE',  ( 5.153800228976615827, -19.02544592524334988, 20.20942372801899722 ) ) ;
#155979 = CARTESIAN_POINT ( 'NONE',  ( -13.89961937509977652, 13.97604488694528158, 30.62390960531435269 ) ) ;
#155981 = ORIENTED_EDGE ( 'NONE', *, *, #194548, .T. ) ;
#155980 = CARTESIAN_POINT ( 'NONE',  ( 0.05219959533909260263, 19.03943276465977164, 104.9989096053143669 ) ) ;
#155982 = CARTESIAN_POINT ( 'NONE',  ( 8.314922557961029526, -14.29746914071037800, 30.41775706135234358 ) ) ;
#155984 = CARTESIAN_POINT ( 'NONE',  ( -16.53943276465976808, -0.05219959533934237506, 48.75109039468568284 ) ) ;
#155983 = CARTESIAN_POINT ( 'NONE',  ( 13.89961937509957401, 13.97604488694547697, 41.87609039468566152 ) ) ;
#155985 = CARTESIAN_POINT ( 'NONE',  ( -5.049401038298153566, 19.05341960407611168, 45.20724293864769550 ) ) ;
#155986 = CARTESIAN_POINT ( 'NONE',  ( 5.153800228976335163, 19.02544592524342804, 104.7905762719809957 ) ) ;
#155987 = CARTESIAN_POINT ( 'NONE',  ( 9.474510206698971260, -16.51473224551069308, 57.91557627198103120 ) ) ;
#155988 = CARTESIAN_POINT ( 'NONE',  ( 10.72451020669898902, -18.67979575497178502, 102.9155762719810383 ) ) ;
#155990 = CARTESIAN_POINT ( 'NONE',  ( -5.153800228976328057, -19.02544592524343514, 112.2905762719810099 ) ) ;
#155989 = CARTESIAN_POINT ( 'NONE',  ( 0.05219959533909260263, 19.03943276465977164, 89.99890960531436690 ) ) ;
#155991 = CARTESIAN_POINT ( 'NONE',  ( 19.05341960407611168, 5.049401038298154454, 63.95724293864769550 ) ) ;
#155993 = CARTESIAN_POINT ( 'NONE',  ( -27.73933785331498925, 9.013057229001088189, 147.2750000027311614 ) ) ;
#155992 = CARTESIAN_POINT ( 'NONE',  ( 8.314922557960818139, 14.29746914071049879, 24.58224293864768839 ) ) ;
#155994 = CARTESIAN_POINT ( 'NONE',  ( 9.564922557961047289, -16.46253265017146816, 95.41775706135233293 ) ) ;
#155995 = CARTESIAN_POINT ( 'NONE',  ( 5.153800228976615827, -19.02544592524334988, 30.20942372801900433 ) ) ;
#155996 = CARTESIAN_POINT ( 'NONE',  ( 0.05219959533910956823, 16.53943276465976808, 59.99890960531436690 ) ) ;
#155997 = CARTESIAN_POINT ( 'NONE',  ( 0.05219959533937995610, -21.53943276465977519, 85.00109039468568994 ) ) ;
#155998 = CARTESIAN_POINT ( 'NONE',  ( -0.05219959533909027116, -19.03943276465977164, 22.49890960531436690 ) ) ;
#156000 = CARTESIAN_POINT ( 'NONE',  ( 18.67979575497194134, -10.72451020669871369, 95.83442372801903275 ) ) ;
#155999 = CARTESIAN_POINT ( 'NONE',  ( -16.53943276465976808, -0.05219959533934237506, 113.7510903946856757 ) ) ;
#156001 = CARTESIAN_POINT ( 'NONE',  ( -5.049401038298153566, 19.05341960407611168, 85.20724293864766707 ) ) ;
#156002 = CARTESIAN_POINT ( 'NONE',  ( -18.62759615963255300, -10.81492255796106328, 44.16775706135234714 ) ) ;
#156003 = CARTESIAN_POINT ( 'NONE',  ( -16.51473224551069308, -9.474510206698971260, 86.66557627198102409 ) ) ;
#156004 = CARTESIAN_POINT ( 'NONE',  ( -14.29746914071049879, 8.314922557960819915, 90.83224293864769550 ) ) ;
#156005 = CARTESIAN_POINT ( 'NONE',  ( -4.379528057220328563, 16.55341960407611168, 65.20724293864768129 ) ) ;
#156006 = CARTESIAN_POINT ( 'NONE',  ( -21.53943276465977519, 0.05219959533907696930, 76.24890960531435269 ) ) ;
#156007 = CARTESIAN_POINT ( 'NONE',  ( 16.46253265017160672, -9.564922557960803928, 78.33224293864769550 ) ) ;
#156008 = CARTESIAN_POINT ( 'NONE',  ( -18.67979575497178146, -10.72451020669898902, 91.66557627198103830 ) ) ;
#156009 = CARTESIAN_POINT ( 'NONE',  ( -5.153800228976607833, 19.02544592524334988, 77.70942372801900433 ) ) ;
#156011 = CARTESIAN_POINT ( 'NONE',  ( 8.314922557960818139, 14.29746914071049879, 84.58224293864769550 ) ) ;
#156010 = CARTESIAN_POINT ( 'NONE',  ( -19.25918095147782338, -5.499999999999492850, 89.45284276293935477 ) ) ;
#156012 = CARTESIAN_POINT ( 'NONE',  ( -9.474510206698964154, 16.51473224551069663, 55.41557627198103120 ) ) ;
#156013 = CARTESIAN_POINT ( 'NONE',  ( 15.80617190586746368, 15.72974639402197994, 69.37390960531436690 ) ) ;
#156014 = CARTESIAN_POINT ( 'NONE',  ( 26.58496454516998142, -7.626754437231455519, 167.9682100371138915 ) ) ;
#156016 = DIRECTION ( 'NONE',  ( -1.387778780781444413E-14, 0.000000000000000000, 1.000000000000000000 ) ) ;
#156015 = CARTESIAN_POINT ( 'NONE',  ( -4.483927247898539470, -16.52544592524342804, 22.29057627198102765 ) ) ;
#156017 = CARTESIAN_POINT ( 'NONE',  ( 0.05219959533936267826, -19.03943276465977164, 100.0010903946856757 ) ) ;
#156018 = CARTESIAN_POINT ( 'NONE',  ( -8.224510206698948167, 14.34966873604960824, 85.41557627198102409 ) ) ;
#156019 = CARTESIAN_POINT ( 'NONE',  ( -17.50000000000000355, -5.499999999999980460, 96.28230962303564411 ) ) ;
#156020 = CARTESIAN_POINT ( 'NONE',  ( -0.05219959533909027116, -19.03943276465977164, 72.49890960531435269 ) ) ;
#156021 = CARTESIAN_POINT ( 'NONE',  ( 19.05341960407611168, 5.049401038298154454, 38.95724293864767418 ) ) ;
#156022 = CARTESIAN_POINT ( 'NONE',  ( -14.29746914071049879, 8.314922557960819915, 65.83224293864769550 ) ) ;
#156023 = CARTESIAN_POINT ( 'NONE',  ( -9.564922557960796823, -16.46253265017161027, 97.08224293864769550 ) ) ;
#156025 = CARTESIAN_POINT ( 'NONE',  ( 9.564922557960805705, 16.46253265017160317, 64.58224293864769550 ) ) ;
#156024 = CARTESIAN_POINT ( 'NONE',  ( -13.89961937509957401, -13.97604488694547875, 89.37609039468563310 ) ) ;
#156026 = CARTESIAN_POINT ( 'NONE',  ( -19.03943276465977164, 0.05219959533909376836, 91.24890960531436690 ) ) ;
#156027 = CARTESIAN_POINT ( 'NONE',  ( 5.719274019375991003, -21.55341960407610458, 72.70724293864769550 ) ) ;
#156028 = CARTESIAN_POINT ( 'NONE',  ( -12.14591786802326823, 12.06949235617739902, 68.12609039468567573 ) ) ;
#156029 = CARTESIAN_POINT ( 'NONE',  ( 16.51473224551083163, -9.474510206698727899, 110.8344237280190043 ) ) ;
#156030 = CARTESIAN_POINT ( 'NONE',  ( -19.02544592524342804, 5.153800228976336051, 66.04057627198103830 ) ) ;
#156031 = CARTESIAN_POINT ( 'NONE',  ( 5.823673210054125526, 21.52544592524343514, 64.79057627198103830 ) ) ;
#156032 = CARTESIAN_POINT ( 'NONE',  ( -16.46253265017146816, -9.564922557961047289, 89.16775706135234714 ) ) ;
#156034 = CARTESIAN_POINT ( 'NONE',  ( 15.80617190586769283, -15.72974639402175789, 50.62609039468568994 ) ) ;
#156033 = CARTESIAN_POINT ( 'NONE',  ( 8.224510206698953496, -14.34966873604960469, 37.91557627198102409 ) ) ;
#156035 = CARTESIAN_POINT ( 'NONE',  ( 11.45643923738959735, 5.000000000000007105, -15.00000000000000000 ) ) ;
#156037 = CARTESIAN_POINT ( 'NONE',  ( -16.46253265017160317, 9.564922557960807481, 110.8322429386476955 ) ) ;
#156036 = CARTESIAN_POINT ( 'NONE',  ( 16.53943276465976808, 0.05219959533934440121, 71.25109039468568994 ) ) ;
#156038 = CARTESIAN_POINT ( 'NONE',  ( 5.049401038298163336, -19.05341960407611168, 102.7072429386476955 ) ) ;
#156039 = CARTESIAN_POINT ( 'NONE',  ( -17.49999999999999645, 5.499999999999992895, 78.71769037696437010 ) ) ;
#156040 = CARTESIAN_POINT ( 'NONE',  ( -4.483927247898782831, 16.52544592524335698, 92.70942372801901854 ) ) ;
#156041 = CARTESIAN_POINT ( 'NONE',  ( 12.14591786802327356, -12.06949235617739191, 50.62609039468568994 ) ) ;
#156042 = CARTESIAN_POINT ( 'NONE',  ( 16.51473224551069308, 9.474510206698969483, 54.16557627198103120 ) ) ;
#156043 = CARTESIAN_POINT ( 'NONE',  ( -5.049401038298153566, 19.05341960407611168, 55.20724293864769550 ) ) ;
#156044 = CARTESIAN_POINT ( 'NONE',  ( 10.72451020669871369, 18.67979575497193778, 47.08442372801901854 ) ) ;
#156045 = CARTESIAN_POINT ( 'NONE',  ( -12.06949235617739369, -12.14591786802326823, 59.37609039468568284 ) ) ;
#156046 = CARTESIAN_POINT ( 'NONE',  ( -12.06949235617756955, 12.14591786802309770, 35.62390960531437401 ) ) ;
#156047 = CARTESIAN_POINT ( 'NONE',  ( 16.46253265017160672, -9.564922557960803928, 43.33224293864769550 ) ) ;
#156048 = CARTESIAN_POINT ( 'NONE',  ( -5.153800228976328057, -19.02544592524343514, 37.29057627198102409 ) ) ;
#156050 = EDGE_LOOP ( 'NONE', ( #155357, #24008, #67610, #145393, #42287, #173879 ) ) ;
#156049 = CARTESIAN_POINT ( 'NONE',  ( 8.314922557961029526, -14.29746914071037800, 30.41775706135234358 ) ) ;
#156051 = CARTESIAN_POINT ( 'NONE',  ( 13.97604488694548053, -13.89961937509957401, 80.62609039468567573 ) ) ;
#156052 = CARTESIAN_POINT ( 'NONE',  ( -4.483927247898539470, -16.52544592524342804, 82.29057627198103830 ) ) ;
#156053 = CARTESIAN_POINT ( 'NONE',  ( 16.46253265017160672, -9.564922557960803928, 48.33224293864769550 ) ) ;
#156055 = CARTESIAN_POINT ( 'NONE',  ( -30.74264578624800492, 22.33583958711400186, -8.200000000000001066 ) ) ;
#156054 = CARTESIAN_POINT ( 'NONE',  ( -19.05341960407617563, 5.049401038297882671, 93.54275706135234714 ) ) ;
#156056 = CARTESIAN_POINT ( 'NONE',  ( 10.81492255796106328, -18.62759615963255655, 95.41775706135234714 ) ) ;
#156057 = CARTESIAN_POINT ( 'NONE',  ( 4.483927247898790824, -16.52544592524335698, 50.20942372801901854 ) ) ;
#156058 = CARTESIAN_POINT ( 'NONE',  ( 16.21995358207305671, 7.366697692864114799, 37.56448998487844193 ) ) ;
#156059 = CARTESIAN_POINT ( 'NONE',  ( 10.81492255796078972, 18.62759615963270932, 44.58224293864769550 ) ) ;
#156060 = CARTESIAN_POINT ( 'NONE',  ( -8.314922557961024197, 14.29746914071037800, 37.91775706135235424 ) ) ;
#156061 = CARTESIAN_POINT ( 'NONE',  ( -9.474510206698720793, -16.51473224551083518, 24.58442372801900078 ) ) ;
#156062 = CARTESIAN_POINT ( 'NONE',  ( 5.153800228976335163, 19.02544592524342804, 74.79057627198103830 ) ) ;
#156063 = CARTESIAN_POINT ( 'NONE',  ( 9.549542882988127701, 9.840250911107702336, -60.43989527633940639 ) ) ;
#156064 = CARTESIAN_POINT ( 'NONE',  ( 5.153800228976335163, 19.02544592524342804, 49.79057627198100988 ) ) ;
#156065 = CARTESIAN_POINT ( 'NONE',  ( -20.56965321856878148, -22.68274384282698009, -50.73755258313430971 ) ) ;
#156066 = CARTESIAN_POINT ( 'NONE',  ( -19.03943276465977164, 0.05219959533909376836, 71.24890960531435269 ) ) ;
#156067 = CARTESIAN_POINT ( 'NONE',  ( -19.25918095147781628, -5.499999999999586109, 54.45284276293936188 ) ) ;
#156068 = CARTESIAN_POINT ( 'NONE',  ( -19.05341960407617563, 5.049401038297882671, 38.54275706135233293 ) ) ;
#156069 = CARTESIAN_POINT ( 'NONE',  ( 19.02544592524334988, 5.153800228976608722, 21.45942372801899012 ) ) ;
#156070 = CARTESIAN_POINT ( 'NONE',  ( 12.14591786802309770, 12.06949235617756955, 39.37390960531436690 ) ) ;
#156071 = CARTESIAN_POINT ( 'NONE',  ( -5.049401038298153566, 19.05341960407611168, 45.20724293864769550 ) ) ;
#156072 = CARTESIAN_POINT ( 'NONE',  ( -13.89961937509977652, 13.97604488694528158, 100.6239096053143669 ) ) ;
#156073 = CARTESIAN_POINT ( 'NONE',  ( 21.53943276465977519, 0.05219959533937863772, 71.25109039468568994 ) ) ;
#156074 = CARTESIAN_POINT ( 'NONE',  ( -16.46253265017160317, 9.564922557960807481, 50.83224293864770260 ) ) ;
#156075 = EDGE_CURVE ( 'NONE', #182496, #15494, #16121, .T. ) ;
#156076 = AXIS2_PLACEMENT_3D ( 'NONE', #179189, #169957, #32446 ) ;
#156077 = CARTESIAN_POINT ( 'NONE',  ( 15.80617190586769283, -15.72974639402175789, 85.62609039468568994 ) ) ;
#156078 = CARTESIAN_POINT ( 'NONE',  ( 0.05219959533909260263, 19.03943276465977164, 114.9989096053143669 ) ) ;
#156079 = CARTESIAN_POINT ( 'NONE',  ( -16.51473224551069308, -9.474510206698971260, 41.66557627198103120 ) ) ;
#156080 = CARTESIAN_POINT ( 'NONE',  ( -5.719274019375665041, -21.55341960407619695, 24.79275706135235779 ) ) ;
#156081 = CARTESIAN_POINT ( 'NONE',  ( 13.89961937509957401, 13.97604488694547697, 51.87609039468566863 ) ) ;
#156082 = CARTESIAN_POINT ( 'NONE',  ( 16.51473224551069308, 9.474510206698969483, 29.16557627198103475 ) ) ;
#156083 = CARTESIAN_POINT ( 'NONE',  ( 9.474510206698971260, -16.51473224551069308, 72.91557627198102409 ) ) ;
#156084 = CARTESIAN_POINT ( 'NONE',  ( 16.46253265017146816, 9.564922557961045513, 106.6677570613523471 ) ) ;
#156085 = CARTESIAN_POINT ( 'NONE',  ( -8.224510206698948167, 14.34966873604960824, 70.41557627198102409 ) ) ;
#156086 = CARTESIAN_POINT ( 'NONE',  ( 10.72451020669898902, -18.67979575497178502, 32.91557627198102409 ) ) ;
#156087 = CARTESIAN_POINT ( 'NONE',  ( 19.02544592524334988, 5.153800228976608722, 106.4594237280190185 ) ) ;
#156088 = CARTESIAN_POINT ( 'NONE',  ( -10.72451020669898014, 18.67979575497178502, 105.4155762719810383 ) ) ;
#156089 = CARTESIAN_POINT ( 'NONE',  ( -10.72451020669870658, -18.67979575497194134, 59.58442372801901854 ) ) ;
#156090 = CARTESIAN_POINT ( 'NONE',  ( 8.314922557961029526, -14.29746914071037800, 50.41775706135235424 ) ) ;
#156091 = CARTESIAN_POINT ( 'NONE',  ( 12.14591786802327356, -12.06949235617739191, 50.62609039468568994 ) ) ;
#156092 = CARTESIAN_POINT ( 'NONE',  ( 15.72974639402199770, -15.80617190586745480, 68.12390960531436690 ) ) ;
#156093 = CARTESIAN_POINT ( 'NONE',  ( 9.474510206698971260, -16.51473224551069308, 52.91557627198102409 ) ) ;
#156094 = CARTESIAN_POINT ( 'NONE',  ( -0.05219959533934338120, 16.53943276465976808, 82.50109039468568994 ) ) ;
#156095 = CARTESIAN_POINT ( 'NONE',  ( 5.719274019375991003, -21.55341960407610458, 107.7072429386476955 ) ) ;
#156096 = CARTESIAN_POINT ( 'NONE',  ( 4.379528057220339221, -16.55341960407611168, 52.70724293864769550 ) ) ;
#156097 = CARTESIAN_POINT ( 'NONE',  ( 19.03943276465977164, -0.05219959533909143690, 73.74890960531435269 ) ) ;
#156098 = CARTESIAN_POINT ( 'NONE',  ( -16.52544592524335698, -4.483927247898792601, 73.95942372801901854 ) ) ;
#156099 = CARTESIAN_POINT ( 'NONE',  ( -19.05341960407617563, 5.049401038297882671, 113.5427570613523471 ) ) ;
#156100 = CARTESIAN_POINT ( 'NONE',  ( -21.53943276465977519, 0.05219959533907696930, 111.2489096053143669 ) ) ;
#156101 = CARTESIAN_POINT ( 'NONE',  ( -16.53943276465976808, 0.05219959533911058130, 41.24890960531435269 ) ) ;
#156102 = ORIENTED_EDGE ( 'NONE', *, *, #119343, .F. ) ;
#156103 = CARTESIAN_POINT ( 'NONE',  ( -17.49999999999999645, 5.624438216177592764, 75.81670344914645909 ) ) ;
#156104 = CARTESIAN_POINT ( 'NONE',  ( 5.719274019375991003, -21.55341960407610458, 92.70724293864770971 ) ) ;
#156105 = B_SPLINE_CURVE_WITH_KNOTS ( 'NONE', 3,
 ( #63463, #90806, #152489, #125139, #93794, #153482, #155474, #61464, #30145, #137321, #16966, #76638, #74669, #13976 ),
 .UNSPECIFIED., .F., .F.,
 ( 4, 2, 2, 2, 2, 2, 4 ),
 ( 1.968491853561852430E-07, 0.0003266071820641947465, 0.0006530175149430332950, 0.0009794278478218718977, 0.001305838180700710392, 0.001958658846458394536, 0.002611479512216078464 ),
 .UNSPECIFIED. ) ;
#156106 = CARTESIAN_POINT ( 'NONE',  ( 14.29746914071049879, -8.314922557960816363, 28.33224293864769550 ) ) ;
#156107 = ORIENTED_EDGE ( 'NONE', *, *, #170373, .F. ) ;
#156108 = DIRECTION ( 'NONE',  ( 1.000000000000000000, 9.445700745138859830E-17, -0.000000000000000000 ) ) ;
#156109 = CARTESIAN_POINT ( 'NONE',  ( -18.67979575497178146, -10.72451020669898902, 101.6655762719810383 ) ) ;
#156110 = CARTESIAN_POINT ( 'NONE',  ( -13.97604488694527625, -13.89961937509977652, 106.8739096053143669 ) ) ;
#156111 = CARTESIAN_POINT ( 'NONE',  ( -21.53943276465977519, -0.05219959533937600094, 18.75109039468568639 ) ) ;
#156112 = CARTESIAN_POINT ( 'NONE',  ( 4.379528057220339221, -16.55341960407611168, 57.70724293864770260 ) ) ;
#156113 = CARTESIAN_POINT ( 'NONE',  ( 14.29746914071037800, 8.314922557961029526, 51.66775706135234714 ) ) ;
#156114 = CARTESIAN_POINT ( 'NONE',  ( 13.97604488694527802, 13.89961937509977652, 64.37390960531436690 ) ) ;
#156115 = CARTESIAN_POINT ( 'NONE',  ( 13.89961937509957401, 13.97604488694547697, 46.87609039468565442 ) ) ;
#156116 = CARTESIAN_POINT ( 'NONE',  ( -16.51473224551069308, -9.474510206698971260, 81.66557627198103830 ) ) ;
#156117 = CARTESIAN_POINT ( 'NONE',  ( -10.72451020669898014, 18.67979575497178502, 40.41557627198103120 ) ) ;
#156118 = CARTESIAN_POINT ( 'NONE',  ( -31.84446081652459526, -20.74826690461117806, -24.63985244029139565 ) ) ;
#156119 = CARTESIAN_POINT ( 'NONE',  ( 19.02544592524343514, -5.153800228976328945, 43.54057627198103120 ) ) ;
#156120 = CARTESIAN_POINT ( 'NONE',  ( 4.483927247898790824, -16.52544592524335698, 20.20942372801900788 ) ) ;
#156121 = CARTESIAN_POINT ( 'NONE',  ( -5.153800228976607833, 19.02544592524334988, 57.70942372801899012 ) ) ;
#156122 = CARTESIAN_POINT ( 'NONE',  ( -5.823673210054116645, -21.52544592524344225, 97.29057627198105251 ) ) ;
#156123 = CARTESIAN_POINT ( 'NONE',  ( -8.224510206698948167, 14.34966873604960824, 30.41557627198101699 ) ) ;
#156124 = CARTESIAN_POINT ( 'NONE',  ( -0.05219959533909027116, -19.03943276465977164, 87.49890960531436690 ) ) ;
#156125 = CARTESIAN_POINT ( 'NONE',  ( 10.72451020669898902, -18.67979575497178502, 52.91557627198103830 ) ) ;
#156127 = CARTESIAN_POINT ( 'NONE',  ( -12.06949235617739369, -12.14591786802326823, 29.37609039468568284 ) ) ;
#156126 = CARTESIAN_POINT ( 'NONE',  ( -15.72974639402197994, 15.80617190586746368, 90.62390960531436690 ) ) ;
#156128 = CARTESIAN_POINT ( 'NONE',  ( -21.52544592524343514, 5.823673210054127303, 26.04057627198103475 ) ) ;
#156129 = CARTESIAN_POINT ( 'NONE',  ( 0.05219959533937995610, -21.53943276465977519, 90.00109039468567573 ) ) ;
#156130 = CARTESIAN_POINT ( 'NONE',  ( -13.97604488694527625, -13.89961937509977652, 86.87390960531436690 ) ) ;
#156131 = CARTESIAN_POINT ( 'NONE',  ( -0.05219959533909027116, -19.03943276465977164, 27.49890960531435624 ) ) ;
#156132 = CARTESIAN_POINT ( 'NONE',  ( 9.474510206698971260, -16.51473224551069308, 82.91557627198103830 ) ) ;
#156133 = CARTESIAN_POINT ( 'NONE',  ( -4.379528057220328563, 16.55341960407611168, 100.2072429386476955 ) ) ;
#156134 = CARTESIAN_POINT ( 'NONE',  ( 9.474510206698971260, -16.51473224551069308, 62.91557627198102409 ) ) ;
#156135 = CARTESIAN_POINT ( 'NONE',  ( -8.314922557961024197, 14.29746914071037800, 27.91775706135234358 ) ) ;
#156136 = CIRCLE ( 'NONE', #182006, 2.649999999999999467 ) ;
#156137 = CARTESIAN_POINT ( 'NONE',  ( 3.181980515339834614, 34.99999999999997158, 1.110912703473986074 ) ) ;
#156139 = CARTESIAN_POINT ( 'NONE',  ( 5.049401038298161559, -19.05341960407611168, 112.7072429386476813 ) ) ;
#156138 = CARTESIAN_POINT ( 'NONE',  ( 10.72451020669871369, 18.67979575497193778, 92.08442372801901854 ) ) ;
#156140 = CARTESIAN_POINT ( 'NONE',  ( -16.55341960407617563, 4.379528057220093196, 88.54275706135236135 ) ) ;
#156141 = CARTESIAN_POINT ( 'NONE',  ( -1.227931366032057224E-14, -24.30000000000003268, -56.77278709839600879 ) ) ;
#156142 = CARTESIAN_POINT ( 'NONE',  ( 19.03943276465977164, 0.05219959533936151252, 71.25109039468566152 ) ) ;
#156143 = CARTESIAN_POINT ( 'NONE',  ( -9.474510206698720793, -16.51473224551083518, 34.58442372801899722 ) ) ;
#156144 = CARTESIAN_POINT ( 'NONE',  ( -17.50000000000001066, -5.500000000000021316, 46.28230962303566542 ) ) ;
#156145 = CARTESIAN_POINT ( 'NONE',  ( -13.97604488694527625, -13.89961937509977652, 21.87390960531435979 ) ) ;
#156146 = CARTESIAN_POINT ( 'NONE',  ( -4.483927247898539470, -16.52544592524342804, 37.29057627198102409 ) ) ;
#156147 = FACE_OUTER_BOUND ( 'NONE', #92434, .T. ) ;
#156148 = CARTESIAN_POINT ( 'NONE',  ( 16.55341960407618274, -4.379528057220086978, 111.0427570613523613 ) ) ;
#156149 = CARTESIAN_POINT ( 'NONE',  ( 17.44279575226823553, 5.990770900252482711, 66.66442432485683867 ) ) ;
#156150 = CARTESIAN_POINT ( 'NONE',  ( -8.314922557961024197, 14.29746914071037800, 77.91775706135231871 ) ) ;
#156151 = CARTESIAN_POINT ( 'NONE',  ( -13.97604488694527625, -13.89961937509977652, 41.87390960531435979 ) ) ;
#156152 = CARTESIAN_POINT ( 'NONE',  ( -10.81492255796105439, 18.62759615963255655, 87.91775706135234714 ) ) ;
#156153 = CARTESIAN_POINT ( 'NONE',  ( -9.564922557961040184, 16.46253265017147172, 97.91775706135233293 ) ) ;
#156154 = CARTESIAN_POINT ( 'NONE',  ( -10.81492255796105439, 18.62759615963255655, 77.91775706135231871 ) ) ;
#156155 = CARTESIAN_POINT ( 'NONE',  ( 16.46253265017146816, 9.564922557961045513, 56.66775706135233293 ) ) ;
#156156 = CARTESIAN_POINT ( 'NONE',  ( 5.049401038298161559, -19.05341960407611168, 92.70724293864769550 ) ) ;
#156157 = CARTESIAN_POINT ( 'NONE',  ( -16.46253265017160317, 9.564922557960807481, 65.83224293864769550 ) ) ;
#156158 = CARTESIAN_POINT ( 'NONE',  ( 16.18388926212237067, 7.379444403734554569, 72.93953151366149257 ) ) ;
#156159 = CARTESIAN_POINT ( 'NONE',  ( -14.34966873604960291, -8.224510206698953496, 66.66557627198102409 ) ) ;
#156160 = CARTESIAN_POINT ( 'NONE',  ( -5.823673210054116645, -21.52544592524344225, 67.29057627198103830 ) ) ;
#156161 = CARTESIAN_POINT ( 'NONE',  ( -5.153800228976328057, -19.02544592524343514, 42.29057627198101699 ) ) ;
#156163 = CARTESIAN_POINT ( 'NONE',  ( 12.06949235617739724, 12.14591786802326823, 71.87609039468568994 ) ) ;
#156162 = CARTESIAN_POINT ( 'NONE',  ( -21.55341960407610458, -5.719274019375992779, 86.45724293864770971 ) ) ;
#156164 = EDGE_CURVE ( 'NONE', #108481, #186418, #185801, .T. ) ;
#156165 = ORIENTED_EDGE ( 'NONE', *, *, #11642, .F. ) ;
#156166 = CARTESIAN_POINT ( 'NONE',  ( -13.89961937509977652, 13.97604488694528158, 45.62390960531433848 ) ) ;
#156168 = CARTESIAN_POINT ( 'NONE',  ( 22.81625015709510151, -31.40387420917324590, -5.924999997268812990 ) ) ;
#156167 = CARTESIAN_POINT ( 'NONE',  ( 16.55341960407611168, 4.379528057220329451, 83.95724293864770971 ) ) ;
#156169 = CARTESIAN_POINT ( 'NONE',  ( 5.153800228976335163, 19.02544592524342804, 54.79057627198103120 ) ) ;
#156170 = CARTESIAN_POINT ( 'NONE',  ( -9.564922557960796823, -16.46253265017161027, 27.08224293864769550 ) ) ;
#156171 = CARTESIAN_POINT ( 'NONE',  ( 13.97604488694548053, -13.89961937509957401, 65.62609039468567573 ) ) ;
#156172 = CARTESIAN_POINT ( 'NONE',  ( 4.379528057220339221, -16.55341960407611168, 72.70724293864769550 ) ) ;
#156173 = CARTESIAN_POINT ( 'NONE',  ( -21.52544592524334988, -5.823673210054445271, 48.95942372801902565 ) ) ;
#156175 = CARTESIAN_POINT ( 'NONE',  ( -5.823673210054116645, -21.52544592524344225, 107.2905762719810525 ) ) ;
#156174 = CARTESIAN_POINT ( 'NONE',  ( -13.97604488694527625, -13.89961937509977652, 41.87390960531435979 ) ) ;
#156176 = CARTESIAN_POINT ( 'NONE',  ( 17.97058386085786807, 5.500000000000006217, 91.50390968646219392 ) ) ;
#156177 = CARTESIAN_POINT ( 'NONE',  ( -12.14591786802309592, -12.06949235617757132, 91.87390960531436690 ) ) ;
#156178 = CARTESIAN_POINT ( 'NONE',  ( 16.14548778791511907, -40.33029071462300408, -21.07572238977685686 ) ) ;
#156179 = CARTESIAN_POINT ( 'NONE',  ( -13.97604488694527625, -13.89961937509977652, 41.87390960531435979 ) ) ;
#156180 = CARTESIAN_POINT ( 'NONE',  ( 19.01529144963331674, 5.500000000000154543, 48.73431955728439391 ) ) ;
#156182 = CARTESIAN_POINT ( 'NONE',  ( 19.05341960407611168, 5.049401038298154454, 93.95724293864769550 ) ) ;
#156181 = CARTESIAN_POINT ( 'NONE',  ( -16.46253265017146816, -9.564922557961047289, 99.16775706135233293 ) ) ;
#156183 = CARTESIAN_POINT ( 'NONE',  ( 18.62759615963255655, 10.81492255796105972, 41.66775706135235424 ) ) ;
#156184 = CARTESIAN_POINT ( 'NONE',  ( 9.474510206698971260, -16.51473224551069308, 82.91557627198103830 ) ) ;
#156185 = CARTESIAN_POINT ( 'NONE',  ( -13.89961937509957401, -13.97604488694547875, 69.37609039468564731 ) ) ;
#156186 = CARTESIAN_POINT ( 'NONE',  ( 13.97604488694527802, 13.89961937509977652, 49.37390960531434558 ) ) ;
#156187 = CARTESIAN_POINT ( 'NONE',  ( 14.29746914071049879, -8.314922557960816363, 63.33224293864770260 ) ) ;
#156188 = CARTESIAN_POINT ( 'NONE',  ( 14.34966873604960469, 8.224510206698951720, 74.16557627198102409 ) ) ;
#156189 = CARTESIAN_POINT ( 'NONE',  ( 16.51473224551069308, 9.474510206698969483, 74.16557627198103830 ) ) ;
#156190 = CARTESIAN_POINT ( 'NONE',  ( 15.80617190586746368, 15.72974639402197994, 99.37390960531436690 ) ) ;
#156191 = CARTESIAN_POINT ( 'NONE',  ( -19.05341960407611168, -5.049401038298163336, 76.45724293864769550 ) ) ;
#156192 = CARTESIAN_POINT ( 'NONE',  ( 10.81492255796106328, -18.62759615963255655, 110.4177570613523756 ) ) ;
#156195 = CARTESIAN_POINT ( 'NONE',  ( 8.314922557960818139, 14.29746914071049879, 109.5822429386476955 ) ) ;
#156194 = CARTESIAN_POINT ( 'NONE',  ( 4.483927247898790824, -16.52544592524335698, 105.2094237280190328 ) ) ;
#156193 = CARTESIAN_POINT ( 'NONE',  ( 19.03943276465977164, -0.05219959533909143690, 33.74890960531435979 ) ) ;
#156196 = CARTESIAN_POINT ( 'NONE',  ( 0.05219959533936267826, -19.03943276465977164, 110.0010903946856757 ) ) ;
#156197 = ORIENTED_EDGE ( 'NONE', *, *, #78228, .F. ) ;
#156198 = CARTESIAN_POINT ( 'NONE',  ( -18.67979575497193778, 10.72451020669871902, 33.33442372801900433 ) ) ;
#156199 = CARTESIAN_POINT ( 'NONE',  ( -9.474510206698720793, -16.51473224551083518, 69.58442372801901854 ) ) ;
#156200 = CARTESIAN_POINT ( 'NONE',  ( 4.483927247898790824, -16.52544592524335698, 110.2094237280190185 ) ) ;
#156201 = CARTESIAN_POINT ( 'NONE',  ( -18.67979575497178146, -10.72451020669898902, 76.66557627198103830 ) ) ;
#156202 = CARTESIAN_POINT ( 'NONE',  ( 21.52544592524344225, -5.823673210054117533, 23.54057627198102765 ) ) ;
#156203 = CARTESIAN_POINT ( 'NONE',  ( 8.224510206698953496, -14.34966873604960469, 57.91557627198103120 ) ) ;
#156204 = CARTESIAN_POINT ( 'NONE',  ( 16.51473224551069308, 9.474510206698969483, 34.16557627198102409 ) ) ;
#156205 = CARTESIAN_POINT ( 'NONE',  ( -9.564922557960796823, -16.46253265017161027, 32.08224293864769550 ) ) ;
#156206 = CARTESIAN_POINT ( 'NONE',  ( -5.049401038297874678, -19.05341960407617918, 29.79275706135232227 ) ) ;
#156207 = CARTESIAN_POINT ( 'NONE',  ( -16.55341960407617563, 4.379528057220093196, 88.54275706135236135 ) ) ;
#156208 = CARTESIAN_POINT ( 'NONE',  ( 14.29746914071037800, 8.314922557961029526, 51.66775706135234714 ) ) ;
#156209 = CARTESIAN_POINT ( 'NONE',  ( -21.53943276465977519, 0.05219959533907696930, 21.24890960531436690 ) ) ;
#156211 = CARTESIAN_POINT ( 'NONE',  ( -18.67979575497193778, 10.72451020669871902, 103.3344237280190043 ) ) ;
#156210 = CARTESIAN_POINT ( 'NONE',  ( 19.02544592524343514, -5.153800228976328945, 53.54057627198102409 ) ) ;
#156212 = CARTESIAN_POINT ( 'NONE',  ( -13.97604488694527625, -13.89961937509977652, 76.87390960531433848 ) ) ;
#156213 = CARTESIAN_POINT ( 'NONE',  ( 16.55341960407618274, -4.379528057220086978, 61.04275706135234714 ) ) ;
#156214 = CARTESIAN_POINT ( 'NONE',  ( 12.14591786802309770, 12.06949235617756955, 104.3739096053143669 ) ) ;
#156215 = CARTESIAN_POINT ( 'NONE',  ( -4.379528057220328563, 16.55341960407611168, 25.20724293864769550 ) ) ;
#156216 = CARTESIAN_POINT ( 'NONE',  ( -17.72696623605164135, 5.499999999999875655, 38.59811031808416004 ) ) ;
#156219 = CARTESIAN_POINT ( 'NONE',  ( -9.564922557960796823, -16.46253265017161027, 72.08224293864770971 ) ) ;
#156218 = CARTESIAN_POINT ( 'NONE',  ( -9.564922557960796823, -16.46253265017161027, 87.08224293864769550 ) ) ;
#156217 = CARTESIAN_POINT ( 'NONE',  ( -5.823673210054431948, 21.52544592524334988, 67.70942372801901854 ) ) ;
#156220 = CARTESIAN_POINT ( 'NONE',  ( 19.05341960407611168, 5.049401038298154454, 108.9572429386477097 ) ) ;
#156221 = CARTESIAN_POINT ( 'NONE',  ( 4.483927247898545687, 16.52544592524342804, 54.79057627198104541 ) ) ;
#156222 = CARTESIAN_POINT ( 'NONE',  ( 8.314922557961029526, -14.29746914071037800, 110.4177570613523756 ) ) ;
#156223 = VECTOR ( 'NONE', #77441, 1000.000000000000000 ) ;
#156224 = CARTESIAN_POINT ( 'NONE',  ( 16.52544592524342804, -4.483927247898539470, 33.54057627198102409 ) ) ;
#156226 = CARTESIAN_POINT ( 'NONE',  ( -6.674792076160493082, 4.273745901508186229, 5.990689250852173409 ) ) ;
#156225 = CARTESIAN_POINT ( 'NONE',  ( -16.52544592524335698, -4.483927247898792601, 38.95942372801901854 ) ) ;
#156227 = CARTESIAN_POINT ( 'NONE',  ( -5.049401038297874678, -19.05341960407617918, 34.79275706135233293 ) ) ;
#156228 = CARTESIAN_POINT ( 'NONE',  ( 19.05341960407611168, 5.049401038298154454, 78.95724293864769550 ) ) ;
#156229 = CARTESIAN_POINT ( 'NONE',  ( -16.51473224551082808, 9.474510206698731452, 53.33442372801900433 ) ) ;
#156230 = CARTESIAN_POINT ( 'NONE',  ( -36.91746825000000598, 2.428612866367529932E-14, -2.624999997268813168 ) ) ;
#156232 = CARTESIAN_POINT ( 'NONE',  ( -16.52544592524335698, -4.483927247898792601, 78.95942372801901854 ) ) ;
#156231 = CARTESIAN_POINT ( 'NONE',  ( -9.474510206698720793, -16.51473224551083518, 94.58442372801900433 ) ) ;
#156233 = CARTESIAN_POINT ( 'NONE',  ( -19.05341960407611168, -5.049401038298163336, 31.45724293864769550 ) ) ;
#156234 = CARTESIAN_POINT ( 'NONE',  ( 19.02544592524343514, -5.153800228976328945, 103.5405762719809957 ) ) ;
#156235 = CARTESIAN_POINT ( 'NONE',  ( -0.05219959533937732626, 21.53943276465977519, 42.50109039468567573 ) ) ;
#156236 = CARTESIAN_POINT ( 'NONE',  ( -0.05219959533936034679, 19.03943276465977164, 87.50109039468567573 ) ) ;
#156238 = CARTESIAN_POINT ( 'NONE',  ( 13.89961937509977652, -13.97604488694527269, 48.12390960531435979 ) ) ;
#156237 = DIRECTION ( 'NONE',  ( 0.000000000000000000, 1.000000000000000000, 0.000000000000000000 ) ) ;
#156239 = CARTESIAN_POINT ( 'NONE',  ( 19.03943276465977164, -0.05219959533909143690, 108.7489096053143527 ) ) ;
#156241 = CARTESIAN_POINT ( 'NONE',  ( -13.89961937509977652, 13.97604488694528158, 45.62390960531433848 ) ) ;
#156240 = CARTESIAN_POINT ( 'NONE',  ( -16.55341960407611168, -4.379528057220339221, 56.45724293864768839 ) ) ;
#156242 = CARTESIAN_POINT ( 'NONE',  ( -16.51473224551069308, -9.474510206698971260, 66.66557627198102409 ) ) ;
#156243 = CARTESIAN_POINT ( 'NONE',  ( 16.51473224551083163, -9.474510206698727899, 65.83442372801900433 ) ) ;
#156244 = CARTESIAN_POINT ( 'NONE',  ( 16.51473224551083163, -9.474510206698727899, 30.83442372801900433 ) ) ;
#156245 = CARTESIAN_POINT ( 'NONE',  ( 9.564922557961047289, -16.46253265017146816, 45.41775706135232582 ) ) ;
#156246 = CARTESIAN_POINT ( 'NONE',  ( -16.51473224551069308, -9.474510206698971260, 81.66557627198103830 ) ) ;
#156247 = CARTESIAN_POINT ( 'NONE',  ( 21.53943276465977519, -0.05219959533907433946, 73.74890960531433848 ) ) ;
#156249 = CARTESIAN_POINT ( 'NONE',  ( -9.474510206698720793, -16.51473224551083518, 34.58442372801899722 ) ) ;
#156248 = CARTESIAN_POINT ( 'NONE',  ( -8.314922557960811034, -14.29746914071050412, 67.08224293864770971 ) ) ;
#156250 = CARTESIAN_POINT ( 'NONE',  ( 0.05219959533907565091, 21.53943276465977519, 49.99890960531437401 ) ) ;
#156251 = CARTESIAN_POINT ( 'NONE',  ( 21.52544592524344225, -5.823673210054117533, 38.54057627198103120 ) ) ;
#156252 = CARTESIAN_POINT ( 'NONE',  ( 0.05219959533909260263, 19.03943276465977164, 69.99890960531435269 ) ) ;
#156253 = CARTESIAN_POINT ( 'NONE',  ( -13.89961937509977652, 13.97604488694528158, 35.62390960531435269 ) ) ;
#156254 = CARTESIAN_POINT ( 'NONE',  ( 4.483927247898545687, 16.52544592524342804, 94.79057627198105251 ) ) ;
#156255 = CARTESIAN_POINT ( 'NONE',  ( 21.53943276465977519, -0.05219959533907433946, 113.7489096053143527 ) ) ;
#156256 = CARTESIAN_POINT ( 'NONE',  ( 19.03943276465977164, -0.05219959533909143690, 108.7489096053143527 ) ) ;
#156257 = CARTESIAN_POINT ( 'NONE',  ( -5.719274019375665041, -21.55341960407619695, 29.79275706135234358 ) ) ;
#156258 = CARTESIAN_POINT ( 'NONE',  ( -16.46253265017160317, 9.564922557960807481, 40.83224293864769550 ) ) ;
#156259 = CARTESIAN_POINT ( 'NONE',  ( 21.55341960407610458, 5.719274019375980345, 108.9572429386476955 ) ) ;
#156260 = CARTESIAN_POINT ( 'NONE',  ( -0.05219959533936034679, 19.03943276465977164, 52.50109039468566863 ) ) ;
#156261 = CARTESIAN_POINT ( 'NONE',  ( 19.05341960407611168, 5.049401038298154454, 28.95724293864769550 ) ) ;
#156262 = B_SPLINE_CURVE_WITH_KNOTS ( 'NONE', 3,
 ( #117266, #131430, #177954, #98067, #39422, #79196, #67758, #140865, #9101, #64035, #115269, #161772, #159766, #48872, #85925, #2354, #52588, #147614, #132436, #194128, #125705, #21261, #110527, #55591, #178959, #82916, #144594, #130412, #6080, #129416, #114248, #175954 ),
 .UNSPECIFIED., .F., .F.,
 ( 4, 2, 2, 2, 2, 2, 2, 2, 2, 2, 2, 2, 2, 2, 2, 4 ),
 ( 2.883244014823444873E-17, 0.0003712461730037102509, 0.0007424923460073916620, 0.001113738519011073019, 0.001484984692014754484, 0.002227477038022119150, 0.002598723211025801699, 0.002969969384029484249, 0.003341215557033166798, 0.003712461730036849782, 0.004083707903040531897, 0.004454954076044214881, 0.004826200249047897864, 0.005197446422051580847, 0.005568692595055262963, 0.005939938768058946814 ),
 .UNSPECIFIED. ) ;
#156263 = CARTESIAN_POINT ( 'NONE',  ( -16.51473224551069308, -9.474510206698971260, 21.66557627198102765 ) ) ;
#156264 = FILL_AREA_STYLE ('',( #15773 ) ) ;
#156265 = CARTESIAN_POINT ( 'NONE',  ( 12.06949235617739724, 12.14591786802326823, 56.87609039468568994 ) ) ;
#156266 = CARTESIAN_POINT ( 'NONE',  ( -9.564922557960796823, -16.46253265017161027, 32.08224293864769550 ) ) ;
#156267 = CARTESIAN_POINT ( 'NONE',  ( -25.76143648877098968, -7.343476467573589517, 174.8772314887148696 ) ) ;
#156268 = CARTESIAN_POINT ( 'NONE',  ( -16.51473224551069308, -9.474510206698971260, 76.66557627198103830 ) ) ;
#156269 = CARTESIAN_POINT ( 'NONE',  ( -4.379528057220328563, 16.55341960407611168, 105.2072429386477097 ) ) ;
#156270 = CARTESIAN_POINT ( 'NONE',  ( -21.53943276465977519, 0.05219959533907696930, 41.24890960531435269 ) ) ;
#156271 = CARTESIAN_POINT ( 'NONE',  ( -8.224510206698948167, 14.34966873604960824, 80.41557627198103830 ) ) ;
#156272 = CARTESIAN_POINT ( 'NONE',  ( 8.224510206698742110, 14.34966873604972548, 37.08442372801901143 ) ) ;
#156273 = CARTESIAN_POINT ( 'NONE',  ( 21.55341960407619695, -5.719274019375665929, 81.04275706135236135 ) ) ;
#156274 = ADVANCED_FACE ( 'NONE', ( #114570, #38747 ), #82219, .F. ) ;
#156275 = CARTESIAN_POINT ( 'NONE',  ( -13.97604488694527625, -13.89961937509977652, 21.87390960531435979 ) ) ;
#156276 = CARTESIAN_POINT ( 'NONE',  ( 16.55341960407611168, 4.379528057220329451, 23.95724293864769550 ) ) ;
#156277 = CARTESIAN_POINT ( 'NONE',  ( -16.53943276465976808, 0.05219959533911058130, 51.24890960531436690 ) ) ;
#156278 = CARTESIAN_POINT ( 'NONE',  ( 19.05341960407611168, 5.049401038298154454, 48.95724293864768129 ) ) ;
#156279 = CARTESIAN_POINT ( 'NONE',  ( 5.719274019375673035, 21.55341960407619339, 97.29275706135234714 ) ) ;
#156280 = CARTESIAN_POINT ( 'NONE',  ( 21.52544592524344225, -5.823673210054117533, 108.5405762719810241 ) ) ;
#156281 = CARTESIAN_POINT ( 'NONE',  ( -21.53943276465977519, -0.05219959533937600094, 78.75109039468568994 ) ) ;
#156282 = CARTESIAN_POINT ( 'NONE',  ( 14.34966873604972726, -8.224510206698740333, 40.83442372801901854 ) ) ;
#156284 = CARTESIAN_POINT ( 'NONE',  ( -10.81492255796105439, 18.62759615963255655, 82.91775706135234714 ) ) ;
#156283 = CARTESIAN_POINT ( 'NONE',  ( 14.34966873604960469, 8.224510206698951720, 84.16557627198103830 ) ) ;
#156285 = ADVANCED_FACE ( 'NONE', ( #98387 ), #68575, .T. ) ;
#156286 = CARTESIAN_POINT ( 'NONE',  ( -14.29746914071037622, -8.314922557961029526, 109.1677570613523613 ) ) ;
#156287 = CARTESIAN_POINT ( 'NONE',  ( 4.379528057220092307, 16.55341960407617563, 37.29275706135235424 ) ) ;
#156288 = CARTESIAN_POINT ( 'NONE',  ( -8.314922557960811034, -14.29746914071050412, 42.08224293864769550 ) ) ;
#156289 = CARTESIAN_POINT ( 'NONE',  ( -14.34966873604972548, 8.224510206698743886, 83.33442372801903275 ) ) ;
#156290 = CARTESIAN_POINT ( 'NONE',  ( -19.05341960407611168, -5.049401038298163336, 96.45724293864769550 ) ) ;
#156291 = CARTESIAN_POINT ( 'NONE',  ( -16.51473224551069308, -9.474510206698971260, 96.66557627198102409 ) ) ;
#156292 = CARTESIAN_POINT ( 'NONE',  ( 15.80617190586769283, -15.72974639402175789, 105.6260903946856899 ) ) ;
#156293 = CARTESIAN_POINT ( 'NONE',  ( 8.314922557961029526, -14.29746914071037800, 100.4177570613523471 ) ) ;
#156294 = CARTESIAN_POINT ( 'NONE',  ( -4.483927247898539470, -16.52544592524342804, 72.29057627198102409 ) ) ;
#156295 = CARTESIAN_POINT ( 'NONE',  ( -13.97604488694527625, -13.89961937509977652, 81.87390960531436690 ) ) ;
#156296 = ORIENTED_EDGE ( 'NONE', *, *, #193877, .T. ) ;
#156297 = CARTESIAN_POINT ( 'NONE',  ( 8.224510206698742110, 14.34966873604972548, 32.08442372801901854 ) ) ;
#156298 = CARTESIAN_POINT ( 'NONE',  ( 19.03943276465977164, -0.05219959533909143690, 28.74890960531435624 ) ) ;
#156299 = CARTESIAN_POINT ( 'NONE',  ( -0.05219959533909027116, -19.03943276465977164, 92.49890960531436690 ) ) ;
#156301 = CARTESIAN_POINT ( 'NONE',  ( -22.55670631985108443, -22.55670631985069008, -64.92279855667830191 ) ) ;
#156300 = CARTESIAN_POINT ( 'NONE',  ( -4.379528057220086978, -16.55341960407618274, 29.79275706135234358 ) ) ;
#156302 = CARTESIAN_POINT ( 'NONE',  ( 5.049401038297881783, 19.05341960407617563, 32.29275706135233293 ) ) ;
#156303 = CARTESIAN_POINT ( 'NONE',  ( -16.55341960407617563, 4.379528057220093196, 98.54275706135234714 ) ) ;
#156304 = CARTESIAN_POINT ( 'NONE',  ( -19.03943276465977164, -0.05219959533935918106, 108.7510903946856615 ) ) ;
#156305 = CARTESIAN_POINT ( 'NONE',  ( -9.474510206698964154, 16.51473224551069663, 35.41557627198102409 ) ) ;
#156306 = CARTESIAN_POINT ( 'NONE',  ( -14.34966873604972548, 8.224510206698743886, 78.33442372801901854 ) ) ;
#156307 = CARTESIAN_POINT ( 'NONE',  ( -4.483927247898782831, 16.52544592524335698, 62.70942372801902565 ) ) ;
#156308 = CARTESIAN_POINT ( 'NONE',  ( -5.049401038298153566, 19.05341960407611168, 30.20724293864768839 ) ) ;
#156309 = CARTESIAN_POINT ( 'NONE',  ( -9.474510206698720793, -16.51473224551083518, 69.58442372801901854 ) ) ;
#156310 = CARTESIAN_POINT ( 'NONE',  ( -21.55341960407619339, 5.719274019375674811, 108.5427570613523756 ) ) ;
#156311 = CARTESIAN_POINT ( 'NONE',  ( 19.03943276465977164, -0.05219959533909143690, 53.74890960531436690 ) ) ;
#156312 = CARTESIAN_POINT ( 'NONE',  ( -9.474510206698964154, 16.51473224551069663, 90.41557627198103830 ) ) ;
#156313 = CARTESIAN_POINT ( 'NONE',  ( 8.224510206698953496, -14.34966873604960469, 82.91557627198103830 ) ) ;
#156314 = AXIS2_PLACEMENT_3D ( 'NONE', #89075, #166929, #120400 ) ;
#156315 = CARTESIAN_POINT ( 'NONE',  ( 9.564922557961047289, -16.46253265017146816, 60.41775706135233293 ) ) ;
#156316 = CARTESIAN_POINT ( 'NONE',  ( -0.05219959533907301413, -21.53943276465977519, 47.49890960531435979 ) ) ;
#156317 = CARTESIAN_POINT ( 'NONE',  ( 10.81492255796106328, -18.62759615963255655, 110.4177570613523756 ) ) ;
#156318 = CARTESIAN_POINT ( 'NONE',  ( 19.03943276465977164, -0.05219959533909143690, 93.74890960531435269 ) ) ;
#156319 = EDGE_CURVE ( 'NONE', #42366, #186567, #169625, .T. ) ;
#156320 = CARTESIAN_POINT ( 'NONE',  ( 16.46253265017146816, 9.564922557961045513, 26.66775706135234003 ) ) ;
#156321 = CARTESIAN_POINT ( 'NONE',  ( 10.72451020669898902, -18.67979575497178502, 62.91557627198102409 ) ) ;
#156322 = CARTESIAN_POINT ( 'NONE',  ( -5.049401038298153566, 19.05341960407611168, 105.2072429386476671 ) ) ;
#156323 = CARTESIAN_POINT ( 'NONE',  ( -0.05219959533936034679, 19.03943276465977164, 87.50109039468567573 ) ) ;
#156324 = CARTESIAN_POINT ( 'NONE',  ( -1.784589286804288299, -7.284589286804248331, 8.181980515339454030 ) ) ;
#156325 = CARTESIAN_POINT ( 'NONE',  ( -0.05219959533936034679, 19.03943276465977164, 112.5010903946856757 ) ) ;
#156326 = CARTESIAN_POINT ( 'NONE',  ( -8.314922557960811034, -14.29746914071050412, 112.0822429386477097 ) ) ;
#156327 = CARTESIAN_POINT ( 'NONE',  ( -5.049401038298153566, 19.05341960407611168, 95.20724293864770971 ) ) ;
#156328 = CARTESIAN_POINT ( 'NONE',  ( 5.719274019375991003, -21.55341960407610458, 77.70724293864770971 ) ) ;
#156329 = CARTESIAN_POINT ( 'NONE',  ( -4.379528057220086978, -16.55341960407618274, 49.79275706135234714 ) ) ;
#156330 = CARTESIAN_POINT ( 'NONE',  ( -21.55341960407619339, 5.719274019375674811, 48.54275706135234714 ) ) ;
#156331 = CARTESIAN_POINT ( 'NONE',  ( 10.72451020669871369, 18.67979575497193778, 97.08442372801904696 ) ) ;
#156332 = CARTESIAN_POINT ( 'NONE',  ( 14.34966873604972726, -8.224510206698740333, 95.83442372801903275 ) ) ;
#156333 = CARTESIAN_POINT ( 'NONE',  ( 16.51473224551069308, 9.474510206698969483, 84.16557627198102409 ) ) ;
#156334 = CARTESIAN_POINT ( 'NONE',  ( -4.483927247898539470, -16.52544592524342804, 97.29057627198105251 ) ) ;
#156335 = CARTESIAN_POINT ( 'NONE',  ( -16.52544592524342804, 4.483927247898546575, 31.04057627198102409 ) ) ;
#156336 = CARTESIAN_POINT ( 'NONE',  ( 13.89961937509957401, 13.97604488694547697, 71.87609039468567573 ) ) ;
#156337 = CARTESIAN_POINT ( 'NONE',  ( 21.53943276465977519, 0.05219959533937863772, 46.25109039468567573 ) ) ;
#156338 = CARTESIAN_POINT ( 'NONE',  ( 9.564922557961047289, -16.46253265017146816, 25.41775706135234003 ) ) ;
#156339 = CARTESIAN_POINT ( 'NONE',  ( -8.314922557960811034, -14.29746914071050412, 92.08224293864769550 ) ) ;
#156340 = CARTESIAN_POINT ( 'NONE',  ( 5.823673210054125526, 21.52544592524343514, 34.79057627198103120 ) ) ;
#156341 = CARTESIAN_POINT ( 'NONE',  ( 12.14591786802309770, 12.06949235617756955, 29.37390960531435269 ) ) ;
#156342 = CARTESIAN_POINT ( 'NONE',  ( 21.55341960407619695, -5.719274019375665929, 81.04275706135236135 ) ) ;
#156343 = CARTESIAN_POINT ( 'NONE',  ( -8.224510206698735004, -14.34966873604973081, 64.58442372801900433 ) ) ;
#156344 = CARTESIAN_POINT ( 'NONE',  ( 0.05219959533934541429, -16.53943276465976808, 105.0010903946856757 ) ) ;
#156345 = CARTESIAN_POINT ( 'NONE',  ( -21.53943276465977519, -0.05219959533937600094, 48.75109039468568284 ) ) ;
#156346 = EDGE_LOOP ( 'NONE', ( #39646, #54740, #43738 ) ) ;
#156347 = CARTESIAN_POINT ( 'NONE',  ( 21.55341960407619695, -5.719274019375665929, 36.04275706135234714 ) ) ;
#156348 = CARTESIAN_POINT ( 'NONE',  ( 12.06949235617757843, -12.14591786802309237, 108.1239096053143811 ) ) ;
#156349 = CARTESIAN_POINT ( 'NONE',  ( -19.03943276465977164, 0.05219959533909376836, 26.24890960531435624 ) ) ;
#156350 = CARTESIAN_POINT ( 'NONE',  ( -4.379528057220328563, 16.55341960407611168, 60.20724293864768839 ) ) ;
#156351 = CARTESIAN_POINT ( 'NONE',  ( -19.02544592524342804, 5.153800228976336051, 76.04057627198102409 ) ) ;
#156352 = CARTESIAN_POINT ( 'NONE',  ( 16.55341960407618274, -4.379528057220086978, 106.0427570613523471 ) ) ;
#156353 = CARTESIAN_POINT ( 'NONE',  ( -21.53943276465977519, 0.05219959533907696930, 56.24890960531436690 ) ) ;
#156354 = CARTESIAN_POINT ( 'NONE',  ( 12.06949235617757843, -12.14591786802309237, 98.12390960531436690 ) ) ;
#156355 = CARTESIAN_POINT ( 'NONE',  ( -18.67979575497178146, -10.72451020669898902, 91.66557627198103830 ) ) ;
#156356 = CARTESIAN_POINT ( 'NONE',  ( -5.049401038298153566, 19.05341960407611168, 95.20724293864770971 ) ) ;
#156358 = CARTESIAN_POINT ( 'NONE',  ( 16.51473224551083163, -9.474510206698727899, 100.8344237280190043 ) ) ;
#156357 = CARTESIAN_POINT ( 'NONE',  ( -16.46253265017160317, 9.564922557960807481, 55.83224293864769550 ) ) ;
#156359 = CARTESIAN_POINT ( 'NONE',  ( 15.72974639402199770, -15.80617190586745480, 43.12390960531435269 ) ) ;
#156360 = CARTESIAN_POINT ( 'NONE',  ( 5.719274019375673035, 21.55341960407619339, 62.29275706135236845 ) ) ;
#156361 = CARTESIAN_POINT ( 'NONE',  ( 19.05341960407611168, 5.049401038298154454, 53.95724293864770260 ) ) ;
#156362 = CARTESIAN_POINT ( 'NONE',  ( 13.97604488694527802, 13.89961937509977652, 84.37390960531433848 ) ) ;
#156363 = CARTESIAN_POINT ( 'NONE',  ( 4.379528057220092307, 16.55341960407617563, 57.29275706135234714 ) ) ;
#156364 = CARTESIAN_POINT ( 'NONE',  ( -10.72451020669870658, -18.67979575497194134, 39.58442372801901143 ) ) ;
#156365 = CARTESIAN_POINT ( 'NONE',  ( 15.80617190586769283, -15.72974639402175789, 85.62609039468568994 ) ) ;
#156366 = CARTESIAN_POINT ( 'NONE',  ( -10.81492255796078084, -18.62759615963271287, 102.0822429386476955 ) ) ;
#156368 = CARTESIAN_POINT ( 'NONE',  ( -4.379528057220086978, -16.55341960407618274, 69.79275706135234714 ) ) ;
#156367 = CARTESIAN_POINT ( 'NONE',  ( -18.67979575497193778, 10.72451020669871902, 33.33442372801900433 ) ) ;
#156369 = CARTESIAN_POINT ( 'NONE',  ( 21.52544592524344225, -5.823673210054117533, 73.54057627198102409 ) ) ;
#156370 = CARTESIAN_POINT ( 'NONE',  ( -5.049401038297874678, -19.05341960407617918, 39.79275706135232582 ) ) ;
#156372 = CARTESIAN_POINT ( 'NONE',  ( -0.05219959533910754901, -16.53943276465976808, 27.49890960531435269 ) ) ;
#156371 = CARTESIAN_POINT ( 'NONE',  ( 16.51473224551069308, 9.474510206698969483, 64.16557627198102409 ) ) ;
#156373 = CARTESIAN_POINT ( 'NONE',  ( 4.313351365237949153, 4.313351365237946489, -64.53213882399992940 ) ) ;
#156374 = CARTESIAN_POINT ( 'NONE',  ( -13.97604488694527625, -13.89961937509977652, 96.87390960531433848 ) ) ;
#156375 = CARTESIAN_POINT ( 'NONE',  ( -9.474510206698720793, -16.51473224551083518, 84.58442372801900433 ) ) ;
#156376 = CARTESIAN_POINT ( 'NONE',  ( -10.72451020669898014, 18.67979575497178502, 60.41557627198102409 ) ) ;
#156377 = CARTESIAN_POINT ( 'NONE',  ( 8.314922557960818139, 14.29746914071049879, 34.58224293864770260 ) ) ;
#156378 = CARTESIAN_POINT ( 'NONE',  ( -16.52544592524335698, -4.483927247898792601, 18.95942372801901143 ) ) ;
#156379 = CARTESIAN_POINT ( 'NONE',  ( 5.153800228976335163, 19.02544592524342804, 29.79057627198102409 ) ) ;
#156380 = CARTESIAN_POINT ( 'NONE',  ( 19.02544592524334988, 5.153800228976608722, 111.4594237280190043 ) ) ;
#156382 = CARTESIAN_POINT ( 'NONE',  ( -0.05219959533936034679, 19.03943276465977164, 72.50109039468566152 ) ) ;
#156381 = CARTESIAN_POINT ( 'NONE',  ( 15.72974639402199770, -15.80617190586745480, 98.12390960531436690 ) ) ;
#156383 = CARTESIAN_POINT ( 'NONE',  ( 16.52544592524335698, 4.483927247898782831, 76.45942372801901854 ) ) ;
#156384 = CARTESIAN_POINT ( 'NONE',  ( -13.89961937509977652, 13.97604488694528158, 70.62390960531432427 ) ) ;
#156385 = CARTESIAN_POINT ( 'NONE',  ( 4.379528057220339221, -16.55341960407611168, 77.70724293864770971 ) ) ;
#156386 = VECTOR ( 'NONE', #17051, 1000.000000000000000 ) ;
#156387 = CARTESIAN_POINT ( 'NONE',  ( 5.153800228976335163, 19.02544592524342804, 54.79057627198103120 ) ) ;
#156388 = CARTESIAN_POINT ( 'NONE',  ( 16.52544592524342804, -4.483927247898539470, 63.54057627198103830 ) ) ;
#156389 = CARTESIAN_POINT ( 'NONE',  ( 9.474510206698971260, -16.51473224551069308, 22.91557627198102765 ) ) ;
#156390 = CARTESIAN_POINT ( 'NONE',  ( -17.29957754486504129, -5.500000000000000888, 21.12734848878977445 ) ) ;
#156391 = CARTESIAN_POINT ( 'NONE',  ( 16.53943276465976808, -0.05219959533910856209, 38.74890960531435979 ) ) ;
#156392 = CARTESIAN_POINT ( 'NONE',  ( 19.02544592524343514, -5.153800228976328945, 83.54057627198100988 ) ) ;
#156393 = CARTESIAN_POINT ( 'NONE',  ( -23.31738231874055245, -16.94106989632524574, 144.1999999999999886 ) ) ;
#156394 = CARTESIAN_POINT ( 'NONE',  ( 9.564922557961047289, -16.46253265017146816, 40.41775706135234003 ) ) ;
#156395 = CARTESIAN_POINT ( 'NONE',  ( -8.224510206698735004, -14.34966873604973081, 44.58442372801901854 ) ) ;
#156396 = CARTESIAN_POINT ( 'NONE',  ( -10.72451020669898014, 18.67979575497178502, 65.41557627198102409 ) ) ;
#156397 = CARTESIAN_POINT ( 'NONE',  ( -9.564922557961040184, 16.46253265017147172, 22.91775706135233648 ) ) ;
#156398 = CARTESIAN_POINT ( 'NONE',  ( 5.049401038298161559, -19.05341960407611168, 77.70724293864765286 ) ) ;
#156399 = CARTESIAN_POINT ( 'NONE',  ( 193.3062444957835453, -155.7167183371837496, -15.00000000000000000 ) ) ;
#156400 = CARTESIAN_POINT ( 'NONE',  ( -19.02544592524342804, 5.153800228976336051, 106.0405762719810241 ) ) ;
#156401 = CARTESIAN_POINT ( 'NONE',  ( 10.72451020669871369, 18.67979575497193778, 32.08442372801901854 ) ) ;
#156402 = CARTESIAN_POINT ( 'NONE',  ( -4.379528057220328563, 16.55341960407611168, 110.2072429386477239 ) ) ;
#156405 = VERTEX_POINT ( 'NONE', #45711 ) ;
#156404 = CARTESIAN_POINT ( 'NONE',  ( 5.153800228976335163, 19.02544592524342804, 84.79057627198099567 ) ) ;
#156403 = CARTESIAN_POINT ( 'NONE',  ( -15.72974639402197994, 15.80617190586746368, 100.6239096053143811 ) ) ;
#156406 = CARTESIAN_POINT ( 'NONE',  ( -5.823673210054431948, 21.52544592524334988, 22.70942372801901499 ) ) ;
#156407 = EDGE_CURVE ( 'NONE', #9769, #193343, #82426, .T. ) ;
#156408 = CIRCLE ( 'NONE', #159711, 4.500000000000000000 ) ;
#156409 = EDGE_LOOP ( 'NONE', ( #72623, #25657, #86298, #85776, #35330, #179652, #175746, #119127 ) ) ;
#156410 = CARTESIAN_POINT ( 'NONE',  ( -13.89961937509977652, 13.97604488694528158, 85.62390960531433848 ) ) ;
#156411 = CYLINDRICAL_SURFACE ( 'NONE', #136651, 2.500000000000000444 ) ;
#156412 = CARTESIAN_POINT ( 'NONE',  ( 10.81492255796078972, 18.62759615963270932, 94.58224293864769550 ) ) ;
#156413 = CARTESIAN_POINT ( 'NONE',  ( 5.049401038298161559, -19.05341960407611168, 32.70724293864768129 ) ) ;
#156414 = CARTESIAN_POINT ( 'NONE',  ( -19.05341960407617563, 5.049401038297882671, 103.5427570613523329 ) ) ;
#156415 = CARTESIAN_POINT ( 'NONE',  ( 22.81625015709509441, 31.40387420917330275, -9.824999997268811569 ) ) ;
#156416 = VECTOR ( 'NONE', #20191, 1000.000000000000114 ) ;
#156417 = CARTESIAN_POINT ( 'NONE',  ( 0.05219959533909260263, 19.03943276465977164, 29.99890960531435979 ) ) ;
#156418 = CARTESIAN_POINT ( 'NONE',  ( 5.719274019375673035, 21.55341960407619339, 87.29275706135236135 ) ) ;
#156420 = CARTESIAN_POINT ( 'NONE',  ( -21.53943276465977519, -0.05219959533937600094, 43.75109039468568284 ) ) ;
#156419 = CARTESIAN_POINT ( 'NONE',  ( -9.564922557960796823, -16.46253265017161027, 77.08224293864769550 ) ) ;
#156421 = CARTESIAN_POINT ( 'NONE',  ( -5.823673210054431948, 21.52544592524334988, 32.70942372801900433 ) ) ;
#156422 = CARTESIAN_POINT ( 'NONE',  ( -23.31738231874055600, 16.94106989632528837, 145.7999999999999829 ) ) ;
#156423 = CARTESIAN_POINT ( 'NONE',  ( -19.02544592524342804, 5.153800228976336051, 86.04057627198103830 ) ) ;
#156424 = CARTESIAN_POINT ( 'NONE',  ( 19.34837522270365895, 5.499999999999733546, 63.36337684832578532 ) ) ;
#156427 = CARTESIAN_POINT ( 'NONE',  ( 21.55341960407619695, -5.719274019375665929, 46.04275706135234714 ) ) ;
#156426 = CARTESIAN_POINT ( 'NONE',  ( -10.81492255796078084, -18.62759615963271287, 42.08224293864769550 ) ) ;
#156425 = CARTESIAN_POINT ( 'NONE',  ( 16.53943276465976808, 0.05219959533934440121, 36.25109039468567573 ) ) ;
#156428 = CARTESIAN_POINT ( 'NONE',  ( 15.80617190586769283, -15.72974639402175789, 75.62609039468567573 ) ) ;
#156429 = MECHANICAL_DESIGN_GEOMETRIC_PRESENTATION_REPRESENTATION (  '', ( #117611 ), #49762 ) ;
#156430 = DIRECTION ( 'NONE',  ( 0.000000000000000000, -0.7071067811865483499, 0.7071067811865467956 ) ) ;
#156431 = CARTESIAN_POINT ( 'NONE',  ( 19.02544592524334988, 5.153800228976608722, 106.4594237280190185 ) ) ;
#156432 = CARTESIAN_POINT ( 'NONE',  ( -16.51473224551069308, -9.474510206698971260, 61.66557627198103120 ) ) ;
#156433 = CARTESIAN_POINT ( 'NONE',  ( 13.97604488694527802, 13.89961937509977652, 89.37390960531436690 ) ) ;
#156434 = CARTESIAN_POINT ( 'NONE',  ( 16.52544592524342804, -4.483927247898539470, 113.5405762719810383 ) ) ;
#156435 = CARTESIAN_POINT ( 'NONE',  ( -16.52544592524342804, 4.483927247898546575, 111.0405762719810525 ) ) ;
#156437 = ADVANCED_FACE ( 'NONE', ( #121547 ), #195493, .F. ) ;
#156436 = CARTESIAN_POINT ( 'NONE',  ( 19.03943276465977164, -0.05219959533909143690, 108.7489096053143527 ) ) ;
#156438 = CARTESIAN_POINT ( 'NONE',  ( -16.52544592524335698, -4.483927247898792601, 83.95942372801900433 ) ) ;
#156440 = CARTESIAN_POINT ( 'NONE',  ( 16.46253265017160672, -9.564922557960803928, 48.33224293864769550 ) ) ;
#156439 = CARTESIAN_POINT ( 'NONE',  ( -16.52544592524342804, 4.483927247898546575, 71.04057627198103830 ) ) ;
#156441 = CARTESIAN_POINT ( 'NONE',  ( -21.53943276465977519, -0.05219959533937600094, 83.75109039468568994 ) ) ;
#156442 = CARTESIAN_POINT ( 'NONE',  ( 10.81492255796106328, -18.62759615963255655, 65.41775706135234714 ) ) ;
#156443 = CARTESIAN_POINT ( 'NONE',  ( 9.564922557961047289, -16.46253265017146816, 110.4177570613523471 ) ) ;
#156444 = CARTESIAN_POINT ( 'NONE',  ( 16.53943276465976808, -0.05219959533910856209, 58.74890960531436690 ) ) ;
#156445 = CARTESIAN_POINT ( 'NONE',  ( -10.81492255796078084, -18.62759615963271287, 112.0822429386477097 ) ) ;
#156446 = CARTESIAN_POINT ( 'NONE',  ( 10.72451020669898902, -18.67979575497178502, 57.91557627198103120 ) ) ;
#156447 = CARTESIAN_POINT ( 'NONE',  ( -16.52216118717204552, -7.221426719304545827, 106.0759902104699250 ) ) ;
#156448 = CARTESIAN_POINT ( 'NONE',  ( -8.906447517083053711, -27.41122689804191026, 140.6500000054623740 ) ) ;
#156449 = CARTESIAN_POINT ( 'NONE',  ( 19.05341960407611168, 5.049401038298154454, 68.95724293864769550 ) ) ;
#156450 = CARTESIAN_POINT ( 'NONE',  ( 8.224510206698953496, -14.34966873604960469, 42.91557627198103120 ) ) ;
#156451 = AXIS2_PLACEMENT_3D ( 'NONE', #195038, #10021, #160686 ) ;
#156452 = CARTESIAN_POINT ( 'NONE',  ( -4.483927247898782831, 16.52544592524335698, 112.7094237280190328 ) ) ;
#156453 = CARTESIAN_POINT ( 'NONE',  ( 16.55341960407618274, -4.379528057220086978, 101.0427570613523756 ) ) ;
#156454 = CARTESIAN_POINT ( 'NONE',  ( 13.89961937509957401, 13.97604488694547697, 51.87609039468566863 ) ) ;
#156455 = CARTESIAN_POINT ( 'NONE',  ( -23.48529157249600985, 32.32473071737754111, -8.300000000000000711 ) ) ;
#156456 = CARTESIAN_POINT ( 'NONE',  ( 19.03943276465977164, -0.05219959533909143690, 93.74890960531435269 ) ) ;
#156457 = CARTESIAN_POINT ( 'NONE',  ( 4.379528057220339221, -16.55341960407611168, 62.70724293864769550 ) ) ;
#156459 = CARTESIAN_POINT ( 'NONE',  ( -0.05219959533909027116, -19.03943276465977164, 112.4989096053143669 ) ) ;
#156458 = CARTESIAN_POINT ( 'NONE',  ( 16.36317988757058473, -7.306389748694911646, 101.5978960836322642 ) ) ;
#156460 = CARTESIAN_POINT ( 'NONE',  ( 21.55341960407610458, 5.719274019375980345, 53.95724293864770260 ) ) ;
#156461 = CARTESIAN_POINT ( 'NONE',  ( 4.379528057220339221, -16.55341960407611168, 97.70724293864772392 ) ) ;
#156462 = CARTESIAN_POINT ( 'NONE',  ( 12.14591786802327356, -12.06949235617739191, 45.62609039468567573 ) ) ;
#156463 = CARTESIAN_POINT ( 'NONE',  ( 4.379528057220339221, -16.55341960407611168, 97.70724293864772392 ) ) ;
#156464 = CARTESIAN_POINT ( 'NONE',  ( 26.11842041226233846, 7.699311778675188123, 169.4341694154020956 ) ) ;
#156465 = CARTESIAN_POINT ( 'NONE',  ( -13.89961937509957401, -13.97604488694547875, 79.37609039468567573 ) ) ;
#156466 = CARTESIAN_POINT ( 'NONE',  ( 10.72451020669898902, -18.67979575497178502, 22.91557627198102765 ) ) ;
#156467 = CARTESIAN_POINT ( 'NONE',  ( 36.91746824999999887, 11.99521256947799053, -2.024999997268813523 ) ) ;
#156468 = DIRECTION ( 'NONE',  ( -1.000000000000000000, -0.000000000000000000, -0.000000000000000000 ) ) ;
#156470 = CARTESIAN_POINT ( 'NONE',  ( 16.53943276465976808, -0.05219959533910856209, 33.74890960531436690 ) ) ;
#156469 = CARTESIAN_POINT ( 'NONE',  ( 8.224510206698742110, 14.34966873604972548, 47.08442372801901854 ) ) ;
#156471 = CARTESIAN_POINT ( 'NONE',  ( 21.55341960407610458, 5.719274019375980345, 53.95724293864770260 ) ) ;
#156472 = CARTESIAN_POINT ( 'NONE',  ( -9.474510206698720793, -16.51473224551083518, 84.58442372801900433 ) ) ;
#156473 = CARTESIAN_POINT ( 'NONE',  ( 15.80617190586746368, 15.72974639402197994, 44.37390960531435979 ) ) ;
#156474 = CARTESIAN_POINT ( 'NONE',  ( 15.80617190586769283, -15.72974639402175789, 80.62609039468567573 ) ) ;
#156475 = CARTESIAN_POINT ( 'NONE',  ( -10.38198520235570221, 9.279464826303270186, -62.49863477660405664 ) ) ;
#156476 = CARTESIAN_POINT ( 'NONE',  ( -4.483927247898782831, 16.52544592524335698, 32.70942372801900433 ) ) ;
#156478 = CARTESIAN_POINT ( 'NONE',  ( 16.46253265017160672, -9.564922557960803928, 98.33224293864769550 ) ) ;
#156477 = CARTESIAN_POINT ( 'NONE',  ( 5.153800228976335163, 19.02544592524342804, 39.79057627198100988 ) ) ;
#156479 = CARTESIAN_POINT ( 'NONE',  ( -19.05341960407611168, -5.049401038298163336, 36.45724293864766707 ) ) ;
#156480 = CARTESIAN_POINT ( 'NONE',  ( 4.483927247898545687, 16.52544592524342804, 94.79057627198105251 ) ) ;
#156481 = DIRECTION ( 'NONE',  ( 6.982962677686266711E-15, 0.000000000000000000, -1.000000000000000000 ) ) ;
#156482 = CARTESIAN_POINT ( 'NONE',  ( 16.46253265017160672, -9.564922557960803928, 103.3322429386476955 ) ) ;
#156483 = ORIENTED_EDGE ( 'NONE', *, *, #177098, .T. ) ;
#156484 = CARTESIAN_POINT ( 'NONE',  ( -8.224510206698735004, -14.34966873604973081, 54.58442372801901143 ) ) ;
#156485 = CARTESIAN_POINT ( 'NONE',  ( -15.72974639402197994, 15.80617190586746368, 95.62390960531436690 ) ) ;
#156486 = CARTESIAN_POINT ( 'NONE',  ( 9.474510206698971260, -16.51473224551069308, 42.91557627198103120 ) ) ;
#156487 = CARTESIAN_POINT ( 'NONE',  ( -0.05219959533937732626, 21.53943276465977519, 27.50109039468567929 ) ) ;
#156488 = CARTESIAN_POINT ( 'NONE',  ( -5.049401038298153566, 19.05341960407611168, 80.20724293864769550 ) ) ;
#156489 = CARTESIAN_POINT ( 'NONE',  ( 5.153800228976335163, 19.02544592524342804, 114.7905762719810241 ) ) ;
#156490 = ORIENTED_EDGE ( 'NONE', *, *, #58712, .T. ) ;
#156491 = CARTESIAN_POINT ( 'NONE',  ( -12.14591786802326823, 12.06949235617739902, 53.12609039468568284 ) ) ;
#156492 = CARTESIAN_POINT ( 'NONE',  ( 21.52544592524334988, 5.823673210054432836, 21.45942372801901499 ) ) ;
#156495 = CARTESIAN_POINT ( 'NONE',  ( -0.05219959533936034679, 19.03943276465977164, 77.50109039468566152 ) ) ;
#156494 = CARTESIAN_POINT ( 'NONE',  ( 9.564922557960805705, 16.46253265017160317, 99.58224293864770971 ) ) ;
#156493 = CARTESIAN_POINT ( 'NONE',  ( 8.314922557960818139, 14.29746914071049879, 104.5822429386477097 ) ) ;
#156496 = CARTESIAN_POINT ( 'NONE',  ( 13.89961937509957401, 13.97604488694547697, 26.87609039468566507 ) ) ;
#156497 = CARTESIAN_POINT ( 'NONE',  ( 5.719274019375991003, -21.55341960407610458, 82.70724293864770971 ) ) ;
#156498 = CARTESIAN_POINT ( 'NONE',  ( 16.46253265017146816, 9.564922557961045513, 41.66775706135234003 ) ) ;
#156499 = CARTESIAN_POINT ( 'NONE',  ( 12.06949235617739724, 12.14591786802326823, 81.87609039468568994 ) ) ;
#156500 = CARTESIAN_POINT ( 'NONE',  ( -13.89961937509977652, 13.97604488694528158, 100.6239096053143669 ) ) ;
#156501 = CARTESIAN_POINT ( 'NONE',  ( 9.474510206698971260, -16.51473224551069308, 62.91557627198102409 ) ) ;
#156502 = CARTESIAN_POINT ( 'NONE',  ( 21.52544592524334988, 5.823673210054432836, 66.45942372801903275 ) ) ;
#156503 = CARTESIAN_POINT ( 'NONE',  ( -18.62759615963255300, -10.81492255796106328, 69.16775706135234714 ) ) ;
#156504 = CARTESIAN_POINT ( 'NONE',  ( 19.05341960407611168, 5.049401038298154454, 73.95724293864768129 ) ) ;
#156505 = CARTESIAN_POINT ( 'NONE',  ( 15.72974639402176855, 15.80617190586768217, 51.87609039468568284 ) ) ;
#156506 = VERTEX_POINT ( 'NONE', #133747 ) ;
#156507 = CARTESIAN_POINT ( 'NONE',  ( -19.05341960407617563, 5.049401038297882671, 88.54275706135230450 ) ) ;
#156508 = CARTESIAN_POINT ( 'NONE',  ( 5.153800228976335163, 19.02544592524342804, 49.79057627198100988 ) ) ;
#156509 = CARTESIAN_POINT ( 'NONE',  ( 19.02544592524343514, -5.153800228976328945, 98.54057627198100988 ) ) ;
#156510 = CARTESIAN_POINT ( 'NONE',  ( 19.02544592524343514, -5.153800228976328945, 63.54057627198103830 ) ) ;
#156511 = CARTESIAN_POINT ( 'NONE',  ( 19.02544592524343514, -5.153800228976328945, 108.5405762719810383 ) ) ;
#156512 = CARTESIAN_POINT ( 'NONE',  ( -19.02544592524342804, 5.153800228976336051, 46.04057627198101699 ) ) ;
#156513 = VECTOR ( 'NONE', #75693, 1000.000000000000227 ) ;
#156514 = CARTESIAN_POINT ( 'NONE',  ( 5.719274019375991003, -21.55341960407610458, 92.70724293864770971 ) ) ;
#156515 = CARTESIAN_POINT ( 'NONE',  ( 8.314922557961029526, -14.29746914071037800, 70.41775706135236135 ) ) ;
#156516 = CARTESIAN_POINT ( 'NONE',  ( -24.02130208663010791, 8.352503713166791854, 169.2769999910313174 ) ) ;
#156517 = CARTESIAN_POINT ( 'NONE',  ( 9.564922557961047289, -16.46253265017146816, 35.41775706135233293 ) ) ;
#156518 = EDGE_CURVE ( 'NONE', #139003, #26356, #105395, .T. ) ;
#156519 = CARTESIAN_POINT ( 'NONE',  ( 9.564922557960805705, 16.46253265017160317, 69.58224293864770971 ) ) ;
#156520 = CARTESIAN_POINT ( 'NONE',  ( 8.224510206698953496, -14.34966873604960469, 62.91557627198102409 ) ) ;
#156521 = CARTESIAN_POINT ( 'NONE',  ( 4.483927247898545687, 16.52544592524342804, 99.79057627198103830 ) ) ;
#156522 = CARTESIAN_POINT ( 'NONE',  ( -5.153800228976328057, -19.02544592524343514, 102.2905762719810383 ) ) ;
#156523 = B_SPLINE_CURVE_WITH_KNOTS ( 'NONE', 3,
 ( #63452, #143254, #109951, #171631, #160435, #65429, #82576, #4738, #186826, #188799, #64446, #110938, #126116, #18949, #95769, #36083, #3752, #127090, #156458, #5744, #48295, #128088, #113908, #174618, #175607, #144257, #189792, #51263, #141280, #21925, #187811, #112923 ),
 .UNSPECIFIED., .F., .F.,
 ( 4, 2, 2, 2, 2, 2, 2, 2, 2, 2, 2, 2, 2, 2, 2, 4 ),
 ( 7.806255641895631925E-18, 0.0003712461730036603234, 0.0007424923460073128405, 0.001113738519010965249, 0.001484984692014617875, 0.002227477038021939172, 0.002598723211025618252, 0.002969969384029296899, 0.003341215557032975545, 0.003712461730036654625, 0.004083707903040333272, 0.004454954076044012785, 0.004826200249047691432, 0.005197446422051370078, 0.005568692595055048725, 0.005939938768058727371 ),
 .UNSPECIFIED. ) ;
#156524 = CARTESIAN_POINT ( 'NONE',  ( -16.51473224551069308, -9.474510206698971260, 91.66557627198103830 ) ) ;
#156525 = CARTESIAN_POINT ( 'NONE',  ( -5.719274019375665041, -21.55341960407619695, 49.79275706135234714 ) ) ;
#156526 = CARTESIAN_POINT ( 'NONE',  ( 13.97604488694527802, 13.89961937509977652, 109.3739096053143669 ) ) ;
#156527 = CARTESIAN_POINT ( 'NONE',  ( -16.51473224551082808, 9.474510206698731452, 23.33442372801900078 ) ) ;
#156528 = CARTESIAN_POINT ( 'NONE',  ( 16.52544592524335698, 4.483927247898782831, 81.45942372801900433 ) ) ;
#156529 = CARTESIAN_POINT ( 'NONE',  ( 18.67979575497194134, -10.72451020669871369, 40.83442372801901854 ) ) ;
#156530 = CARTESIAN_POINT ( 'NONE',  ( -21.52544592524343514, 5.823673210054127303, 31.04057627198102409 ) ) ;
#156531 = CARTESIAN_POINT ( 'NONE',  ( 18.67979575497178502, 10.72451020669898547, 99.16557627198100988 ) ) ;
#156532 = CARTESIAN_POINT ( 'NONE',  ( -16.52544592524342804, 4.483927247898546575, 66.04057627198103830 ) ) ;
#156533 = CARTESIAN_POINT ( 'NONE',  ( 9.564922557960805705, 16.46253265017160317, 49.58224293864770260 ) ) ;
#156534 = CARTESIAN_POINT ( 'NONE',  ( 8.224510206698953496, -14.34966873604960469, 77.91557627198102409 ) ) ;
#156535 = CARTESIAN_POINT ( 'NONE',  ( 10.72451020669898902, -18.67979575497178502, 47.91557627198102409 ) ) ;
#156536 = CARTESIAN_POINT ( 'NONE',  ( -16.51473224551082808, 9.474510206698731452, 48.33442372801900433 ) ) ;
#156537 = CARTESIAN_POINT ( 'NONE',  ( -19.03943276465977164, 0.05219959533909376836, 21.24890960531436335 ) ) ;
#156538 = ORIENTED_EDGE ( 'NONE', *, *, #122945, .F. ) ;
#156539 = CARTESIAN_POINT ( 'NONE',  ( -8.224510206698735004, -14.34966873604973081, 69.58442372801900433 ) ) ;
#156540 = CARTESIAN_POINT ( 'NONE',  ( 9.474510206698971260, -16.51473224551069308, 62.91557627198102409 ) ) ;
#156541 = CARTESIAN_POINT ( 'NONE',  ( -5.359611314223446995E-15, 29.16686587814335851, 142.3750000027311557 ) ) ;
#156542 = CARTESIAN_POINT ( 'NONE',  ( 16.53943276465976808, -0.05219959533910856209, 83.74890960531435269 ) ) ;
#156543 = CARTESIAN_POINT ( 'NONE',  ( -0.05219959533907301413, -21.53943276465977519, 32.49890960531435979 ) ) ;
#156544 = EDGE_LOOP ( 'NONE', ( #23582, #183356, #39762 ) ) ;
#156545 = CARTESIAN_POINT ( 'NONE',  ( 8.314922557961029526, -14.29746914071037800, 110.4177570613523756 ) ) ;
#156546 = CARTESIAN_POINT ( 'NONE',  ( 13.97604488694548053, -13.89961937509957401, 105.6260903946856757 ) ) ;
#156547 = CARTESIAN_POINT ( 'NONE',  ( -21.52544592524334988, -5.823673210054445271, 73.95942372801901854 ) ) ;
#156548 = CARTESIAN_POINT ( 'NONE',  ( 19.03943276465977164, -0.05219959533909143690, 93.74890960531435269 ) ) ;
#156549 = CARTESIAN_POINT ( 'NONE',  ( -21.53943276465977519, 0.05219959533907696930, 101.2489096053143669 ) ) ;
#156550 = CARTESIAN_POINT ( 'NONE',  ( 4.379528057220092307, 16.55341960407617563, 57.29275706135234714 ) ) ;
#156551 = CARTESIAN_POINT ( 'NONE',  ( -9.564922557960796823, -16.46253265017161027, 27.08224293864769550 ) ) ;
#156552 = CARTESIAN_POINT ( 'NONE',  ( -14.29746914071037622, -8.314922557961029526, 29.16775706135234003 ) ) ;
#156553 = CARTESIAN_POINT ( 'NONE',  ( -19.05341960407617563, 5.049401038297882671, 88.54275706135230450 ) ) ;
#156554 = CARTESIAN_POINT ( 'NONE',  ( 18.67979575497178502, 10.72451020669898547, 94.16557627198103830 ) ) ;
#156555 = CARTESIAN_POINT ( 'NONE',  ( 19.05341960407617918, -5.049401038297876454, 71.04275706135234714 ) ) ;
#156556 = CYLINDRICAL_SURFACE ( 'NONE', #105951, 0.5000000000000037748 ) ;
#156557 = CARTESIAN_POINT ( 'NONE',  ( -21.52544592524343514, 5.823673210054127303, 101.0405762719810383 ) ) ;
#156558 = DIRECTION ( 'NONE',  ( 0.000000000000000000, 0.000000000000000000, -1.000000000000000000 ) ) ;
#156559 = CARTESIAN_POINT ( 'NONE',  ( 9.474510206698971260, -16.51473224551069308, 77.91557627198103830 ) ) ;
#156560 = AXIS2_PLACEMENT_3D ( 'NONE', #152332, #27024, #88669 ) ;
#156561 = CARTESIAN_POINT ( 'NONE',  ( 8.314922557961029526, -14.29746914071037800, 30.41775706135234358 ) ) ;
#156562 = CARTESIAN_POINT ( 'NONE',  ( 37.99626262588763126, 12.34573411038920732, -6.902157773949824104 ) ) ;
#156563 = CARTESIAN_POINT ( 'NONE',  ( 19.02544592524334988, 5.153800228976608722, 56.45942372801898301 ) ) ;
#156565 = CARTESIAN_POINT ( 'NONE',  ( -4.483927247898539470, -16.52544592524342804, 62.29057627198102409 ) ) ;
#156564 = CARTESIAN_POINT ( 'NONE',  ( 21.55341960407619695, -5.719274019375665929, 21.04275706135234714 ) ) ;
#156566 = CARTESIAN_POINT ( 'NONE',  ( 9.474510206698971260, -16.51473224551069308, 87.91557627198102409 ) ) ;
#156567 = AXIS2_PLACEMENT_3D ( 'NONE', #117622, #102453, #148967 ) ;
#156568 = AXIS2_PLACEMENT_3D ( 'NONE', #186851, #124140, #61476 ) ;
#156571 = CARTESIAN_POINT ( 'NONE',  ( -5.049401038297874678, -19.05341960407617918, 44.79275706135232582 ) ) ;
#156570 =( BOUNDED_CURVE ( )  B_SPLINE_CURVE ( 2, ( #36178, #21015, #6834, #68513, #50381, #82671, #23024, #189886, #20025, #100841, #67518 ),
 .UNSPECIFIED., .F., .T. ) 
 B_SPLINE_CURVE_WITH_KNOTS ( ( 3, 2, 2, 2, 2, 3 ),
 ( 0.1000000000000000888, 0.1200000000000000927, 0.1400000000000001243, 0.1600000000000001421, 0.1800000000000001321, 0.2000000000000001776 ),
 .UNSPECIFIED. ) 
 CURVE ( )  GEOMETRIC_REPRESENTATION_ITEM ( )  RATIONAL_B_SPLINE_CURVE ( ( 0.9999999999999997780, 0.9510565162951537532, 1.000000000000000000, 0.9510565162951535312, 1.000000000000000000, 0.9510565162951535312, 1.000000000000000000, 0.9510565162951535312, 1.000000000000000000, 0.9510565162951530871, 1.000000000000000444 ) ) 
 REPRESENTATION_ITEM ( '' )  );
#156569 = CARTESIAN_POINT ( 'NONE',  ( 8.224510206698742110, 14.34966873604972548, 42.08442372801901854 ) ) ;
#156572 = CARTESIAN_POINT ( 'NONE',  ( -10.81492255796105439, 18.62759615963255655, 52.91775706135235424 ) ) ;
#156573 = CARTESIAN_POINT ( 'NONE',  ( 19.03943276465977164, 0.05219959533936151252, 111.2510903946856757 ) ) ;
#156574 = CARTESIAN_POINT ( 'NONE',  ( 5.153800228976335163, 19.02544592524342804, 54.79057627198103120 ) ) ;
#156575 = CARTESIAN_POINT ( 'NONE',  ( 19.02544592524334988, 5.153800228976608722, 76.45942372801897591 ) ) ;
#156576 = CARTESIAN_POINT ( 'NONE',  ( -5.719274019375665041, -21.55341960407619695, 94.79275706135234714 ) ) ;
#156577 = CARTESIAN_POINT ( 'NONE',  ( 19.02544592524334988, 5.153800228976608722, 61.45942372801900433 ) ) ;
#156578 = CARTESIAN_POINT ( 'NONE',  ( 19.03943276465977164, -0.05219959533909143690, 38.74890960531436690 ) ) ;
#156579 = CARTESIAN_POINT ( 'NONE',  ( -0.05219959533907301413, -21.53943276465977519, 67.49890960531436690 ) ) ;
#156581 = CARTESIAN_POINT ( 'NONE',  ( 9.564922557961047289, -16.46253265017146816, 70.41775706135233293 ) ) ;
#156580 = CARTESIAN_POINT ( 'NONE',  ( -14.29746914071049879, 8.314922557960819915, 65.83224293864769550 ) ) ;
#156582 = CARTESIAN_POINT ( 'NONE',  ( -17.40805194822032220, -6.112264579159275790, 24.16628727489389306 ) ) ;
#156583 = CARTESIAN_POINT ( 'NONE',  ( -5.153800228976607833, 19.02544592524334988, 37.70942372801899722 ) ) ;
#156584 = CARTESIAN_POINT ( 'NONE',  ( 4.379528057220092307, 16.55341960407617563, 97.29275706135234714 ) ) ;
#156585 = CARTESIAN_POINT ( 'NONE',  ( 16.53943276465976808, -0.05219959533910856209, 58.74890960531436690 ) ) ;
#156587 = CARTESIAN_POINT ( 'NONE',  ( -5.359611314223446995E-15, 29.16686587814335496, 142.3750000027311557 ) ) ;
#156586 = CARTESIAN_POINT ( 'NONE',  ( -18.62759615963255300, -10.81492255796106328, 94.16775706135237556 ) ) ;
#156588 = CARTESIAN_POINT ( 'NONE',  ( -21.53943276465977519, 0.05219959533907696930, 101.2489096053143669 ) ) ;
#156589 = CARTESIAN_POINT ( 'NONE',  ( 13.97604488694527802, 13.89961937509977652, 49.37390960531434558 ) ) ;
#156590 = CARTESIAN_POINT ( 'NONE',  ( 10.72451020669871369, 18.67979575497193778, 72.08442372801899012 ) ) ;
#156591 = CARTESIAN_POINT ( 'NONE',  ( 19.02544592524343514, -5.153800228976328945, 43.54057627198103120 ) ) ;
#156592 = ORIENTED_EDGE ( 'NONE', *, *, #117399, .F. ) ;
#156593 = CARTESIAN_POINT ( 'NONE',  ( 16.51473224551069308, 9.474510206698969483, 59.16557627198102409 ) ) ;
#156594 = CARTESIAN_POINT ( 'NONE',  ( -0.05219959533910754901, -16.53943276465976808, 107.4989096053143669 ) ) ;
#156595 = CARTESIAN_POINT ( 'NONE',  ( -0.05219959533909027116, -19.03943276465977164, 112.4989096053143669 ) ) ;
#156596 = CARTESIAN_POINT ( 'NONE',  ( 16.53943276465976808, -0.05219959533910856209, 53.74890960531437401 ) ) ;
#156597 = CARTESIAN_POINT ( 'NONE',  ( 19.03943276465977164, -0.05219959533909143690, 33.74890960531435979 ) ) ;
#156598 = CARTESIAN_POINT ( 'NONE',  ( 16.52544592524342804, -4.483927247898539470, 78.54057627198103830 ) ) ;
#156599 = AXIS2_PLACEMENT_3D ( 'NONE', #227, #61895, #185260 ) ;
#156600 = CARTESIAN_POINT ( 'NONE',  ( 21.52544592524344225, -5.823673210054117533, 98.54057627198105251 ) ) ;
#156601 = CARTESIAN_POINT ( 'NONE',  ( -15.72974639402176322, -15.80617190586768395, 29.37609039468568284 ) ) ;
#156602 = CARTESIAN_POINT ( 'NONE',  ( -26.03370437638690049, -6.875205692009850544, 160.5968874236872637 ) ) ;
#156603 = CARTESIAN_POINT ( 'NONE',  ( -14.29746914071037622, -8.314922557961029526, 44.16775706135234714 ) ) ;
#156604 = CARTESIAN_POINT ( 'NONE',  ( 5.719274019375991003, -21.55341960407610458, 87.70724293864769550 ) ) ;
#156605 = CARTESIAN_POINT ( 'NONE',  ( 0.05219959533937995610, -21.53943276465977519, 105.0010903946856757 ) ) ;
#156606 = CARTESIAN_POINT ( 'NONE',  ( -16.51473224551069308, -9.474510206698971260, 111.6655762719810383 ) ) ;
#156607 = CARTESIAN_POINT ( 'NONE',  ( 21.53943276465977519, 0.05219959533937863772, 41.25109039468568284 ) ) ;
#156608 = CARTESIAN_POINT ( 'NONE',  ( -0.05219959533907301413, -21.53943276465977519, 37.49890960531436690 ) ) ;
#156609 = CARTESIAN_POINT ( 'NONE',  ( 14.29746914071037800, 8.314922557961029526, 106.6677570613523756 ) ) ;
#156611 = CARTESIAN_POINT ( 'NONE',  ( 21.55341960407619695, -5.719274019375665929, 81.04275706135236135 ) ) ;
#156610 = CARTESIAN_POINT ( 'NONE',  ( -5.719274019375665041, -21.55341960407619695, 59.79275706135234714 ) ) ;
#156612 = CARTESIAN_POINT ( 'NONE',  ( 19.05341960407617918, -5.049401038297876454, 31.04275706135232227 ) ) ;
#156613 = CARTESIAN_POINT ( 'NONE',  ( 8.224510206698742110, 14.34966873604972548, 92.08442372801901854 ) ) ;
#156614 = CARTESIAN_POINT ( 'NONE',  ( 21.52544592524334988, 5.823673210054432836, 41.45942372801901143 ) ) ;
#156615 = CARTESIAN_POINT ( 'NONE',  ( -5.153800228976328057, -19.02544592524343514, 52.29057627198100988 ) ) ;
#156616 = CARTESIAN_POINT ( 'NONE',  ( 19.02544592524334988, 5.153800228976608722, 21.45942372801899012 ) ) ;
#156617 = CARTESIAN_POINT ( 'NONE',  ( -5.719274019375978568, 21.55341960407610458, 25.20724293864769550 ) ) ;
#156618 = CARTESIAN_POINT ( 'NONE',  ( -21.53943276465977519, 0.05219959533907696930, 116.2489096053143669 ) ) ;
#156619 = CARTESIAN_POINT ( 'NONE',  ( 21.55341960407610458, 5.719274019375980345, 73.95724293864769550 ) ) ;
#156621 = CARTESIAN_POINT ( 'NONE',  ( -5.823673210054116645, -21.52544592524344225, 67.29057627198103830 ) ) ;
#156620 = DIRECTION ( 'NONE',  ( -1.000000000000000000, 0.000000000000000000, 0.000000000000000000 ) ) ;
#156623 = CARTESIAN_POINT ( 'NONE',  ( 16.53943276465976808, -0.05219959533910856209, 63.74890960531435979 ) ) ;
#156622 = CARTESIAN_POINT ( 'NONE',  ( -8.224510206698735004, -14.34966873604973081, 69.58442372801900433 ) ) ;
#156624 = CARTESIAN_POINT ( 'NONE',  ( 23.58953014017657779, 7.613468834709956390, 172.7063272879298950 ) ) ;
#156625 = CARTESIAN_POINT ( 'NONE',  ( 13.97604488694548053, -13.89961937509957401, 90.62609039468567573 ) ) ;
#156626 = CARTESIAN_POINT ( 'NONE',  ( -23.15940025311441630, 1.498759781556387560, -55.09305739490149989 ) ) ;
#156627 = CARTESIAN_POINT ( 'NONE',  ( 16.52544592524335698, 4.483927247898782831, 31.45942372801901854 ) ) ;
#156628 = CARTESIAN_POINT ( 'NONE',  ( -5.823673210054116645, -21.52544592524344225, 102.2905762719810383 ) ) ;
#156629 = CARTESIAN_POINT ( 'NONE',  ( 18.67979575497178502, 10.72451020669898547, 74.16557627198102409 ) ) ;
#156630 = CARTESIAN_POINT ( 'NONE',  ( 0.05219959533909260263, 19.03943276465977164, 114.9989096053143669 ) ) ;
#156631 = CARTESIAN_POINT ( 'NONE',  ( 14.34966873604972726, -8.224510206698740333, 55.83442372801901854 ) ) ;
#156632 = CARTESIAN_POINT ( 'NONE',  ( -19.03943276465977164, 0.05219959533909376836, 66.24890960531436690 ) ) ;
#156634 = CARTESIAN_POINT ( 'NONE',  ( 12.14591786802327356, -12.06949235617739191, 20.62609039468568639 ) ) ;
#156633 = CARTESIAN_POINT ( 'NONE',  ( 21.52544592524334988, 5.823673210054432836, 41.45942372801901143 ) ) ;
#156635 = CARTESIAN_POINT ( 'NONE',  ( 9.474510206698971260, -16.51473224551069308, 112.9155762719810383 ) ) ;
#156636 = CARTESIAN_POINT ( 'NONE',  ( 16.46253265017146816, 9.564922557961045513, 31.66775706135232937 ) ) ;
#156637 = CARTESIAN_POINT ( 'NONE',  ( -16.51473224551069308, -9.474510206698971260, 96.66557627198102409 ) ) ;
#156638 = CARTESIAN_POINT ( 'NONE',  ( -18.62759615963270932, 10.81492255796079327, 105.8322429386476955 ) ) ;
#156639 = CARTESIAN_POINT ( 'NONE',  ( 0.05219959533909260263, 19.03943276465977164, 54.99890960531435979 ) ) ;
#156640 = CARTESIAN_POINT ( 'NONE',  ( -17.48853670773244673, 5.747243402303159776, 23.66671299749991775 ) ) ;
#156641 = CARTESIAN_POINT ( 'NONE',  ( -8.224510206698948167, 14.34966873604960824, 80.41557627198103830 ) ) ;
#156642 = CARTESIAN_POINT ( 'NONE',  ( -19.05341960407611168, -5.049401038298163336, 111.4572429386476671 ) ) ;
#156643 = CARTESIAN_POINT ( 'NONE',  ( -16.81555441253551209, 7.025013491695475842, 35.63685445334257196 ) ) ;
#156644 = VECTOR ( 'NONE', #169043, 1000.000000000000000 ) ;
#156645 = CARTESIAN_POINT ( 'NONE',  ( -18.62759615963270932, 10.81492255796079327, 100.8322429386477097 ) ) ;
#156646 = CARTESIAN_POINT ( 'NONE',  ( -5.049401038297874678, -19.05341960407617918, 59.79275706135231871 ) ) ;
#156647 = CARTESIAN_POINT ( 'NONE',  ( 19.05341960407611168, 5.049401038298154454, 113.9572429386477097 ) ) ;
#156648 = CARTESIAN_POINT ( 'NONE',  ( -16.46253265017160317, 9.564922557960807481, 25.83224293864769194 ) ) ;
#156649 = CARTESIAN_POINT ( 'NONE',  ( 21.53943276465977519, -0.05219959533907433946, 53.74890960531437401 ) ) ;
#156650 = CARTESIAN_POINT ( 'NONE',  ( 13.89961937509977652, -13.97604488694527269, 98.12390960531433848 ) ) ;
#156651 = CARTESIAN_POINT ( 'NONE',  ( -5.823673210054431948, 21.52544592524334988, 82.70942372801900433 ) ) ;
#156652 = CARTESIAN_POINT ( 'NONE',  ( -5.153800228976328057, -19.02544592524343514, 52.29057627198100988 ) ) ;
#156653 = CARTESIAN_POINT ( 'NONE',  ( -0.05219959533910754901, -16.53943276465976808, 82.49890960531436690 ) ) ;
#156654 = CARTESIAN_POINT ( 'NONE',  ( 4.379528057220092307, 16.55341960407617563, 42.29275706135235424 ) ) ;
#156655 = CARTESIAN_POINT ( 'NONE',  ( 10.72451020669871369, 18.67979575497193778, 67.08442372801901854 ) ) ;
#156656 = ORIENTED_EDGE ( 'NONE', *, *, #176185, .F. ) ;
#156657 = CARTESIAN_POINT ( 'NONE',  ( 9.564922557961047289, -16.46253265017146816, 20.41775706135233293 ) ) ;
#156658 = CARTESIAN_POINT ( 'NONE',  ( -5.049401038297874678, -19.05341960407617918, 74.79275706135231871 ) ) ;
#156659 = CIRCLE ( 'NONE', #140483, 40.00000000000000000 ) ;
#156660 = CARTESIAN_POINT ( 'NONE',  ( -13.89961937509957401, -13.97604488694547875, 44.37609039468566863 ) ) ;
#156661 = CARTESIAN_POINT ( 'NONE',  ( 32.99455490591380880, -22.60464286593626326, -23.90693389968299698 ) ) ;
#156662 = CARTESIAN_POINT ( 'NONE',  ( 18.62759615963255655, 10.81492255796105972, 36.66775706135234714 ) ) ;
#156663 = CARTESIAN_POINT ( 'NONE',  ( -18.56399227203345603, -5.499999999999827693, 43.97830131249903474 ) ) ;
#156664 = CARTESIAN_POINT ( 'NONE',  ( 5.153800228976615827, -19.02544592524334988, 35.20942372801899722 ) ) ;
#156665 = CARTESIAN_POINT ( 'NONE',  ( -19.02544592524342804, 5.153800228976336051, 71.04057627198099567 ) ) ;
#156666 = CARTESIAN_POINT ( 'NONE',  ( -14.34966873604960291, -8.224510206698953496, 21.66557627198102409 ) ) ;
#156668 = CARTESIAN_POINT ( 'NONE',  ( -21.52544592524334988, -5.823673210054445271, 83.95942372801900433 ) ) ;
#156667 = CARTESIAN_POINT ( 'NONE',  ( -5.049401038298153566, 19.05341960407611168, 115.2072429386477097 ) ) ;
#156669 = CARTESIAN_POINT ( 'NONE',  ( 22.81625015709509441, 31.40387420917330275, -3.324999997268812901 ) ) ;
#156670 = CARTESIAN_POINT ( 'NONE',  ( -17.50000000000002487, -4.658240926743203225, 36.05529582183199722 ) ) ;
#156671 = CARTESIAN_POINT ( 'NONE',  ( 10.81492255796106328, -18.62759615963255655, 90.41775706135236135 ) ) ;
#156672 = CARTESIAN_POINT ( 'NONE',  ( 16.36317988757059538, -7.306389748694922304, 41.59789608363227842 ) ) ;
#156673 = CARTESIAN_POINT ( 'NONE',  ( -13.89961937509977652, 13.97604488694528158, 95.62390960531436690 ) ) ;
#156674 = CYLINDRICAL_SURFACE ( 'NONE', #72888, 5.000000000000000888 ) ;
#156675 = CARTESIAN_POINT ( 'NONE',  ( 13.97604488694527802, 13.89961937509977652, 49.37390960531434558 ) ) ;
#156677 = ADVANCED_FACE ( 'NONE', ( #118592 ), #33748, .T. ) ;
#156676 = CARTESIAN_POINT ( 'NONE',  ( 15.80617190586746368, 15.72974639402197994, 54.37390960531435979 ) ) ;
#156678 = CARTESIAN_POINT ( 'NONE',  ( -8.314922557960811034, -14.29746914071050412, 27.08224293864769550 ) ) ;
#156680 = CARTESIAN_POINT ( 'NONE',  ( -19.05341960407611168, -5.049401038298163336, 91.45724293864766707 ) ) ;
#156679 = CARTESIAN_POINT ( 'NONE',  ( -19.03943276465977164, 0.05219959533909376836, 21.24890960531436335 ) ) ;
#156681 = CARTESIAN_POINT ( 'NONE',  ( -0.05219959533936034679, 19.03943276465977164, 27.50109039468566507 ) ) ;
#156682 = CARTESIAN_POINT ( 'NONE',  ( 14.34966873604960469, 8.224510206698951720, 99.16557627198100988 ) ) ;
#156683 = CARTESIAN_POINT ( 'NONE',  ( 15.80617190586769283, -15.72974639402175789, 65.62609039468568994 ) ) ;
#156684 = CARTESIAN_POINT ( 'NONE',  ( 9.564922557960805705, 16.46253265017160317, 114.5822429386476955 ) ) ;
#156685 = CARTESIAN_POINT ( 'NONE',  ( -0.05219959533934338120, 16.53943276465976808, 102.5010903946856899 ) ) ;
#156686 = CARTESIAN_POINT ( 'NONE',  ( -9.474510206698720793, -16.51473224551083518, 69.58442372801901854 ) ) ;
#156687 = CARTESIAN_POINT ( 'NONE',  ( 11.40812507854754365, 35.11059874428196537, -7.724999997268813701 ) ) ;
#156688 = CARTESIAN_POINT ( 'NONE',  ( -9.564922557960796823, -16.46253265017161027, 107.0822429386476955 ) ) ;
#156689 = CARTESIAN_POINT ( 'NONE',  ( 12.06949235617757843, -12.14591786802309237, 78.12390960531436690 ) ) ;
#156690 = CIRCLE ( 'NONE', #24218, 28.90000000000004476 ) ;
#156691 = CARTESIAN_POINT ( 'NONE',  ( 9.474510206698729675, 16.51473224551082808, 52.08442372801900433 ) ) ;
#156692 = CARTESIAN_POINT ( 'NONE',  ( 9.564922557960805705, 16.46253265017160317, 69.58224293864770971 ) ) ;
#156693 = CARTESIAN_POINT ( 'NONE',  ( 16.52544592524342804, -4.483927247898539470, 63.54057627198103830 ) ) ;
#156694 = CARTESIAN_POINT ( 'NONE',  ( -9.564922557961040184, 16.46253265017147172, 92.91775706135233293 ) ) ;
#156695 = CARTESIAN_POINT ( 'NONE',  ( -0.05219959533907301413, -21.53943276465977519, 47.49890960531435979 ) ) ;
#156696 = ORIENTED_EDGE ( 'NONE', *, *, #93154, .T. ) ;
#156697 = CARTESIAN_POINT ( 'NONE',  ( 16.46253265017160672, -9.564922557960803928, 23.33224293864769194 ) ) ;
#156698 = CARTESIAN_POINT ( 'NONE',  ( -16.19135201231369336, -7.376712067591812527, 30.18680854052031748 ) ) ;
#156700 = CARTESIAN_POINT ( 'NONE',  ( 10.81492255796078972, 18.62759615963270932, 59.58224293864770260 ) ) ;
#156699 = CARTESIAN_POINT ( 'NONE',  ( 9.564922557960805705, 16.46253265017160317, 64.58224293864769550 ) ) ;
#156702 = CARTESIAN_POINT ( 'NONE',  ( 5.049401038298161559, -19.05341960407611168, 77.70724293864765286 ) ) ;
#156701 = CARTESIAN_POINT ( 'NONE',  ( 16.53943276465976808, 0.05219959533934440121, 91.25109039468568994 ) ) ;
#156703 = CARTESIAN_POINT ( 'NONE',  ( -19.02544592524334988, -5.153800228976617603, 48.95942372801900433 ) ) ;
#156704 = CARTESIAN_POINT ( 'NONE',  ( -5.823673210054431948, 21.52544592524334988, 77.70942372801900433 ) ) ;
#156705 = CARTESIAN_POINT ( 'NONE',  ( 21.55341960407610458, 5.719274019375980345, 58.95724293864770971 ) ) ;
#156706 = CARTESIAN_POINT ( 'NONE',  ( -9.564922557960796823, -16.46253265017161027, 107.0822429386476955 ) ) ;
#156707 = AXIS2_PLACEMENT_3D ( 'NONE', #164053, #131701, #85176 ) ;
#156708 = CARTESIAN_POINT ( 'NONE',  ( 5.049401038298161559, -19.05341960407611168, 37.70724293864768839 ) ) ;
#156709 = CARTESIAN_POINT ( 'NONE',  ( -8.314922557961024197, 14.29746914071037800, 87.91775706135234714 ) ) ;
#156710 = CARTESIAN_POINT ( 'NONE',  ( 5.049401038297881783, 19.05341960407617563, 112.2927570613523471 ) ) ;
#156711 = CARTESIAN_POINT ( 'NONE',  ( 18.22780087662121673, 5.500000000000056843, 78.98459894673892734 ) ) ;
#156712 = CARTESIAN_POINT ( 'NONE',  ( 5.719274019375673035, 21.55341960407619339, 102.2927570613523613 ) ) ;
#156713 = ORIENTED_EDGE ( 'NONE', *, *, #145916, .F. ) ;
#156714 = CARTESIAN_POINT ( 'NONE',  ( 8.314922557960818139, 14.29746914071049879, 59.58224293864770260 ) ) ;
#156715 = CARTESIAN_POINT ( 'NONE',  ( 0.05219959533910956823, 16.53943276465976808, 74.99890960531435269 ) ) ;
#156716 = CARTESIAN_POINT ( 'NONE',  ( 21.52544592524344225, -5.823673210054117533, 88.54057627198103830 ) ) ;
#156717 = CARTESIAN_POINT ( 'NONE',  ( 18.67979575497178502, 10.72451020669898547, 84.16557627198103830 ) ) ;
#156718 = CARTESIAN_POINT ( 'NONE',  ( 17.44279575226823553, -5.990770900252461395, 98.33557567514324660 ) ) ;
#156719 = CARTESIAN_POINT ( 'NONE',  ( -0.05219959533907301413, -21.53943276465977519, 52.49890960531435979 ) ) ;
#156720 = CARTESIAN_POINT ( 'NONE',  ( -16.52544592524335698, -4.483927247898792601, 63.95942372801901854 ) ) ;
#156721 = CARTESIAN_POINT ( 'NONE',  ( 8.224510206698953496, -14.34966873604960469, 92.91557627198103830 ) ) ;
#156722 = CARTESIAN_POINT ( 'NONE',  ( -19.03943276465977164, 0.05219959533909376836, 46.24890960531435979 ) ) ;
#156723 = FILL_AREA_STYLE_COLOUR ( '', #143416 ) ;
#156724 = CARTESIAN_POINT ( 'NONE',  ( 26.03370437638690049, -6.875205692009868308, 160.5968874236871784 ) ) ;
#156725 = CARTESIAN_POINT ( 'NONE',  ( -16.52544592524335698, -4.483927247898792601, 93.95942372801903275 ) ) ;
#156726 = CARTESIAN_POINT ( 'NONE',  ( -5.823673210054431948, 21.52544592524334988, 37.70942372801900433 ) ) ;
#156727 = CARTESIAN_POINT ( 'NONE',  ( -19.05341960407611168, -5.049401038298163336, 81.45724293864769550 ) ) ;
#156728 = CARTESIAN_POINT ( 'NONE',  ( -21.53943276465977519, -0.05219959533937600094, 73.75109039468567573 ) ) ;
#156729 = CARTESIAN_POINT ( 'NONE',  ( 4.500000000000000888, -130.0000000000000000, 13.99999999999999822 ) ) ;
#156730 = CARTESIAN_POINT ( 'NONE',  ( 16.46253265017160672, -9.564922557960803928, 23.33224293864769194 ) ) ;
#156731 = ORIENTED_EDGE ( 'NONE', *, *, #118198, .T. ) ;
#156732 = CARTESIAN_POINT ( 'NONE',  ( -21.52544592524334988, -5.823673210054445271, 63.95942372801901854 ) ) ;
#156734 = CARTESIAN_POINT ( 'NONE',  ( 17.97161686094259991, -5.499999999999976019, 58.49637206859247840 ) ) ;
#156733 = CARTESIAN_POINT ( 'NONE',  ( 5.049401038298161559, -19.05341960407611168, 42.70724293864767418 ) ) ;
#156735 = CARTESIAN_POINT ( 'NONE',  ( 9.564922557960805705, 16.46253265017160317, 89.58224293864769550 ) ) ;
#156736 = CARTESIAN_POINT ( 'NONE',  ( -5.049401038297874678, -19.05341960407617918, 69.79275706135233293 ) ) ;
#156737 = CARTESIAN_POINT ( 'NONE',  ( -10.81492255796105439, 18.62759615963255655, 32.91775706135234714 ) ) ;
#156738 = CARTESIAN_POINT ( 'NONE',  ( 9.564922557961047289, -16.46253265017146816, 55.41775706135234003 ) ) ;
#156739 = CARTESIAN_POINT ( 'NONE',  ( 16.46253265017160672, -9.564922557960803928, 38.33224293864768839 ) ) ;
#156740 = CARTESIAN_POINT ( 'NONE',  ( -12.06949235617739369, -12.14591786802326823, 99.37609039468568994 ) ) ;
#156741 = CARTESIAN_POINT ( 'NONE',  ( 16.51473224551083163, -9.474510206698727899, 70.83442372801900433 ) ) ;
#156742 = CARTESIAN_POINT ( 'NONE',  ( -0.05219959533910754901, -16.53943276465976808, 22.49890960531436335 ) ) ;
#156743 = CARTESIAN_POINT ( 'NONE',  ( 13.97604488694548053, -13.89961937509957401, 55.62609039468566863 ) ) ;
#156744 = CARTESIAN_POINT ( 'NONE',  ( -13.89961937509977652, 13.97604488694528158, 105.6239096053143527 ) ) ;
#156745 = CARTESIAN_POINT ( 'NONE',  ( -18.62759615963255300, -10.81492255796106328, 104.1677570613523471 ) ) ;
#156746 = PRODUCT_DEFINITION_SHAPE ( 'NONE', 'NONE',  #52321 ) ;
#156747 = CARTESIAN_POINT ( 'NONE',  ( -21.52544592524334988, -5.823673210054445271, 103.9594237280190185 ) ) ;
#156748 = CARTESIAN_POINT ( 'NONE',  ( -13.89961937509977652, 13.97604488694528158, 25.62390960531434558 ) ) ;
#156749 = CARTESIAN_POINT ( 'NONE',  ( -18.62759615963255300, -10.81492255796106328, 94.16775706135237556 ) ) ;
#156750 = CARTESIAN_POINT ( 'NONE',  ( 16.55341960407618274, -4.379528057220086978, 31.04275706135234714 ) ) ;
#156751 = CARTESIAN_POINT ( 'NONE',  ( 19.05341960407611168, 5.049401038298154454, 98.95724293864766707 ) ) ;
#156752 = DIRECTION ( 'NONE',  ( 1.000000000000000000, -0.000000000000000000, -0.000000000000000000 ) ) ;
#156753 = CARTESIAN_POINT ( 'NONE',  ( -13.89961937509977652, 13.97604488694528158, 85.62390960531433848 ) ) ;
#156754 = DIRECTION ( 'NONE',  ( 3.613946018757868503E-15, 0.000000000000000000, -1.000000000000000000 ) ) ;
#156755 = CARTESIAN_POINT ( 'NONE',  ( 13.97604488694548053, -13.89961937509957401, 65.62609039468567573 ) ) ;
#156756 = CARTESIAN_POINT ( 'NONE',  ( -19.05341960407611168, -5.049401038298163336, 111.4572429386476671 ) ) ;
#156757 = CARTESIAN_POINT ( 'NONE',  ( -5.823673210054431948, 21.52544592524334988, 97.70942372801904696 ) ) ;
#156758 = CARTESIAN_POINT ( 'NONE',  ( -16.52544592524342804, 4.483927247898546575, 101.0405762719810383 ) ) ;
#156759 = CARTESIAN_POINT ( 'NONE',  ( -21.52544592524343514, 5.823673210054127303, 46.04057627198103830 ) ) ;
#156760 = CARTESIAN_POINT ( 'NONE',  ( -21.55341960407610458, -5.719274019375992779, 36.45724293864768839 ) ) ;
#156761 = CARTESIAN_POINT ( 'NONE',  ( 14.34966873604960469, 8.224510206698951720, 104.1655762719810241 ) ) ;
#156762 = CARTESIAN_POINT ( 'NONE',  ( -0.1985533113405554273, -9.090072183657236238, -61.89635373339110913 ) ) ;
#156763 = CARTESIAN_POINT ( 'NONE',  ( 0.05219959533936267826, -19.03943276465977164, 55.00109039468566863 ) ) ;
#156764 = CARTESIAN_POINT ( 'NONE',  ( -16.53943276465976808, -0.05219959533934237506, 113.7510903946856757 ) ) ;
#156765 = CARTESIAN_POINT ( 'NONE',  ( 10.72451020669898902, -18.67979575497178502, 22.91557627198102765 ) ) ;
#156766 = CARTESIAN_POINT ( 'NONE',  ( 5.719274019375673035, 21.55341960407619339, 77.29275706135234714 ) ) ;
#156767 = CARTESIAN_POINT ( 'NONE',  ( 10.81492255796078972, 18.62759615963270932, 69.58224293864769550 ) ) ;
#156768 = CARTESIAN_POINT ( 'NONE',  ( 10.81492255796106328, -18.62759615963255655, 45.41775706135234003 ) ) ;
#156769 = CARTESIAN_POINT ( 'NONE',  ( 10.72451020669898902, -18.67979575497178502, 92.91557627198103830 ) ) ;
#156770 = CARTESIAN_POINT ( 'NONE',  ( 15.72974639402176855, 15.80617190586768217, 51.87609039468568284 ) ) ;
#156771 = CARTESIAN_POINT ( 'NONE',  ( -16.53943276465976808, 0.05219959533911058130, 116.2489096053143669 ) ) ;
#156772 = CARTESIAN_POINT ( 'NONE',  ( 19.05341960407611168, 5.049401038298154454, 88.95724293864769550 ) ) ;
#156773 = CARTESIAN_POINT ( 'NONE',  ( -12.14591786802326823, 12.06949235617739902, 83.12609039468568994 ) ) ;
#156774 = CARTESIAN_POINT ( 'NONE',  ( 14.29746914071049879, -8.314922557960816363, 108.3322429386477097 ) ) ;
#156775 = CARTESIAN_POINT ( 'NONE',  ( -13.89961937509977652, 13.97604488694528158, 105.6239096053143527 ) ) ;
#156776 = VECTOR ( 'NONE', #49641, 1000.000000000000000 ) ;
#156777 = CARTESIAN_POINT ( 'NONE',  ( 4.483927247898545687, 16.52544592524342804, 49.79057627198102409 ) ) ;
#156778 = CARTESIAN_POINT ( 'NONE',  ( 4.379528057220092307, 16.55341960407617563, 112.2927570613523471 ) ) ;
#156779 = CARTESIAN_POINT ( 'NONE',  ( -19.03943276465977164, 0.05219959533909376836, 66.24890960531436690 ) ) ;
#156780 = CARTESIAN_POINT ( 'NONE',  ( 13.97604488694527802, 13.89961937509977652, 39.37390960531435269 ) ) ;
#156781 = CARTESIAN_POINT ( 'NONE',  ( -21.55341960407610458, -5.719274019375992779, 41.45724293864769550 ) ) ;
#156782 = CARTESIAN_POINT ( 'NONE',  ( 9.564922557961047289, -16.46253265017146816, 40.41775706135234003 ) ) ;
#156784 = CARTESIAN_POINT ( 'NONE',  ( -16.55341960407611168, -4.379528057220339221, 36.45724293864768839 ) ) ;
#156783 = CARTESIAN_POINT ( 'NONE',  ( -2.973862142520652174, -93.04182470242764680, -15.00000000000000178 ) ) ;
#156785 = CARTESIAN_POINT ( 'NONE',  ( -16.46253265017160317, 9.564922557960807481, 110.8322429386476955 ) ) ;
#156786 = CARTESIAN_POINT ( 'NONE',  ( 5.719274019375673035, 21.55341960407619339, 62.29275706135236845 ) ) ;
#156787 = CARTESIAN_POINT ( 'NONE',  ( 9.474510206698971260, -16.51473224551069308, 112.9155762719810383 ) ) ;
#156788 = CARTESIAN_POINT ( 'NONE',  ( 4.483927247898790824, -16.52544592524335698, 60.20942372801902565 ) ) ;
#156789 = CARTESIAN_POINT ( 'NONE',  ( 9.474510206698729675, 16.51473224551082808, 67.08442372801900433 ) ) ;
#156790 = CARTESIAN_POINT ( 'NONE',  ( 8.314922557960818139, 14.29746914071049879, 34.58224293864770260 ) ) ;
#156791 = DIRECTION ( 'NONE',  ( 1.000000000000000000, -0.000000000000000000, -0.000000000000000000 ) ) ;
#156792 = CARTESIAN_POINT ( 'NONE',  ( 16.53943276465976808, 0.05219959533934440121, 106.2510903946856757 ) ) ;
#156793 = CARTESIAN_POINT ( 'NONE',  ( -16.46253265017160317, 9.564922557960807481, 35.83224293864768839 ) ) ;
#156794 = CARTESIAN_POINT ( 'NONE',  ( -19.05341960407611168, -5.049401038298163336, 66.45724293864769550 ) ) ;
#156795 = CARTESIAN_POINT ( 'NONE',  ( -13.97604488694527625, -13.89961937509977652, 21.87390960531435979 ) ) ;
#156796 = CARTESIAN_POINT ( 'NONE',  ( -10.72451020669870658, -18.67979575497194134, 34.58442372801900433 ) ) ;
#156797 = CARTESIAN_POINT ( 'NONE',  ( -5.153800228976328057, -19.02544592524343514, 42.29057627198101699 ) ) ;
#156798 = CARTESIAN_POINT ( 'NONE',  ( 5.153800228976335163, 19.02544592524342804, 114.7905762719810241 ) ) ;
#156799 = CARTESIAN_POINT ( 'NONE',  ( 13.97604488694527802, 13.89961937509977652, 49.37390960531434558 ) ) ;
#156800 = CARTESIAN_POINT ( 'NONE',  ( -13.89961937509977652, 13.97604488694528158, 115.6239096053143669 ) ) ;
#156802 = CARTESIAN_POINT ( 'NONE',  ( -9.564922557960796823, -16.46253265017161027, 22.08224293864768839 ) ) ;
#156801 = CARTESIAN_POINT ( 'NONE',  ( -5.823673210054431948, 21.52544592524334988, 52.70942372801902565 ) ) ;
#156803 = CARTESIAN_POINT ( 'NONE',  ( 15.72974639402199770, -15.80617190586745480, 33.12390960531435979 ) ) ;
#156804 = CARTESIAN_POINT ( 'NONE',  ( -4.379528057220086978, -16.55341960407618274, 74.79275706135234714 ) ) ;
#156805 = ADVANCED_FACE ( 'NONE', ( #178512 ), #102662, .F. ) ;
#156806 = CARTESIAN_POINT ( 'NONE',  ( 10.81492255796106328, -18.62759615963255655, 100.4177570613523471 ) ) ;
#156807 = CARTESIAN_POINT ( 'NONE',  ( 14.34966873604972726, -8.224510206698740333, 55.83442372801901854 ) ) ;
#156808 = CARTESIAN_POINT ( 'NONE',  ( -13.89961937509977652, 13.97604488694528158, 100.6239096053143669 ) ) ;
#156809 = CARTESIAN_POINT ( 'NONE',  ( 16.53943276465976808, 0.05219959533934440121, 36.25109039468567573 ) ) ;
#156810 = CARTESIAN_POINT ( 'NONE',  ( 12.06949235617739724, 12.14591786802326823, 31.87609039468567929 ) ) ;
#156811 = CARTESIAN_POINT ( 'NONE',  ( -8.224510206698735004, -14.34966873604973081, 89.58442372801901854 ) ) ;
#156812 = CARTESIAN_POINT ( 'NONE',  ( 10.81492255796106328, -18.62759615963255655, 60.41775706135235424 ) ) ;
#156813 = CARTESIAN_POINT ( 'NONE',  ( -9.564922557961040184, 16.46253265017147172, 112.9177570613523329 ) ) ;
#156814 = CARTESIAN_POINT ( 'NONE',  ( 10.72451020669898902, -18.67979575497178502, 112.9155762719810383 ) ) ;
#156816 = CARTESIAN_POINT ( 'NONE',  ( -16.46253265017146816, -9.564922557961047289, 109.1677570613523471 ) ) ;
#156815 = CARTESIAN_POINT ( 'NONE',  ( 12.06949235617757843, -12.14591786802309237, 98.12390960531436690 ) ) ;
#156817 = CARTESIAN_POINT ( 'NONE',  ( -12.14591786802326823, 12.06949235617739902, 78.12609039468570415 ) ) ;
#156818 = CARTESIAN_POINT ( 'NONE',  ( 22.78714015945950422, 11.73760554535660638, 167.9671921004704416 ) ) ;
#156819 = CARTESIAN_POINT ( 'NONE',  ( -5.153800228976607833, 19.02544592524334988, 87.70942372801897591 ) ) ;
#156820 = CARTESIAN_POINT ( 'NONE',  ( -8.314922557960811034, -14.29746914071050412, 47.08224293864770260 ) ) ;
#156821 = CARTESIAN_POINT ( 'NONE',  ( -8.224510206698948167, 14.34966873604960824, 45.41557627198103830 ) ) ;
#156822 = CARTESIAN_POINT ( 'NONE',  ( 8.224510206698953496, -14.34966873604960469, 107.9155762719810241 ) ) ;
#156823 = CARTESIAN_POINT ( 'NONE',  ( -16.46253265017146816, -9.564922557961047289, 34.16775706135233293 ) ) ;
#156824 = CARTESIAN_POINT ( 'NONE',  ( 15.80617190586769283, -15.72974639402175789, 30.62609039468567929 ) ) ;
#156825 = CARTESIAN_POINT ( 'NONE',  ( -16.51473224551082808, 9.474510206698731452, 113.3344237280190043 ) ) ;
#156826 = CARTESIAN_POINT ( 'NONE',  ( -20.41037832431298682, -34.40082058117823749, -25.00000000000009592 ) ) ;
#156827 = CARTESIAN_POINT ( 'NONE',  ( -9.474510206698964154, 16.51473224551069663, 95.41557627198102409 ) ) ;
#156828 = CARTESIAN_POINT ( 'NONE',  ( 5.049401038298161559, -19.05341960407611168, 92.70724293864769550 ) ) ;
#156829 = CARTESIAN_POINT ( 'NONE',  ( 5.823673210054125526, 21.52544592524343514, 54.79057627198104541 ) ) ;
#156830 = CARTESIAN_POINT ( 'NONE',  ( 0.05219959533910956823, 16.53943276465976808, 94.99890960531436690 ) ) ;
#156831 = CARTESIAN_POINT ( 'NONE',  ( 0.05219959533909260263, 19.03943276465977164, 64.99890960531436690 ) ) ;
#156832 = CARTESIAN_POINT ( 'NONE',  ( 19.02544592524343514, -5.153800228976328945, 28.54057627198102409 ) ) ;
#156833 = CARTESIAN_POINT ( 'NONE',  ( -0.05219959533937732626, 21.53943276465977519, 37.50109039468568284 ) ) ;
#156834 = CARTESIAN_POINT ( 'NONE',  ( 15.80617190586769283, -15.72974639402175789, 70.62609039468567573 ) ) ;
#156835 = CARTESIAN_POINT ( 'NONE',  ( 8.314922557961029526, -14.29746914071037800, 95.41775706135234714 ) ) ;
#156836 = CARTESIAN_POINT ( 'NONE',  ( -21.53943276465977519, -0.05219959533937600094, 23.75109039468567929 ) ) ;
#156837 = CARTESIAN_POINT ( 'NONE',  ( 21.52544592524334988, 5.823673210054432836, 21.45942372801901499 ) ) ;
#156839 = CARTESIAN_POINT ( 'NONE',  ( 9.474510206698971260, -16.51473224551069308, 72.91557627198102409 ) ) ;
#156838 = CARTESIAN_POINT ( 'NONE',  ( -5.153800228976607833, 19.02544592524334988, 57.70942372801899012 ) ) ;
#156840 = CARTESIAN_POINT ( 'NONE',  ( 18.62759615963255655, 10.81492255796105972, 81.66775706135236135 ) ) ;
#156841 = CARTESIAN_POINT ( 'NONE',  ( -10.72451020669898014, 18.67979575497178502, 80.41557627198103830 ) ) ;
#156842 = CARTESIAN_POINT ( 'NONE',  ( -16.52544592524342804, 4.483927247898546575, 46.04057627198103830 ) ) ;
#156844 = CARTESIAN_POINT ( 'NONE',  ( 0.05219959533936267826, -19.03943276465977164, 45.00109039468566863 ) ) ;
#156843 = CARTESIAN_POINT ( 'NONE',  ( -21.55341960407619339, 5.719274019375674811, 108.5427570613523756 ) ) ;
#156845 = CARTESIAN_POINT ( 'NONE',  ( -14.29746914071049879, 8.314922557960819915, 75.83224293864769550 ) ) ;
#156846 = CARTESIAN_POINT ( 'NONE',  ( -9.564922557960796823, -16.46253265017161027, 22.08224293864768839 ) ) ;
#156847 = CARTESIAN_POINT ( 'NONE',  ( -19.02544592524334988, -5.153800228976617603, 68.95942372801896170 ) ) ;
#156848 = CARTESIAN_POINT ( 'NONE',  ( -4.483927247898539470, -16.52544592524342804, 37.29057627198102409 ) ) ;
#156849 = CARTESIAN_POINT ( 'NONE',  ( -15.80617190586768217, 15.72974639402176855, 88.12609039468570415 ) ) ;
#156850 = CARTESIAN_POINT ( 'NONE',  ( 13.89961937509977652, -13.97604488694527269, 83.12390960531436690 ) ) ;
#156851 = CARTESIAN_POINT ( 'NONE',  ( -0.05219959533936034679, 19.03943276465977164, 67.50109039468566152 ) ) ;
#156852 = CARTESIAN_POINT ( 'NONE',  ( -21.52544592524343514, 5.823673210054127303, 71.04057627198103830 ) ) ;
#156853 = CARTESIAN_POINT ( 'NONE',  ( -5.719274019375978568, 21.55341960407610458, 110.2072429386477239 ) ) ;
#156854 = CARTESIAN_POINT ( 'NONE',  ( 4.483927247898790824, -16.52544592524335698, 20.20942372801900788 ) ) ;
#156855 = CARTESIAN_POINT ( 'NONE',  ( 4.379528057220092307, 16.55341960407617563, 82.29275706135234714 ) ) ;
#156857 = CARTESIAN_POINT ( 'NONE',  ( 21.52544592524334988, 5.823673210054432836, 21.45942372801901499 ) ) ;
#156856 = CARTESIAN_POINT ( 'NONE',  ( 17.44270441346512257, 5.991230190323099336, 63.86335079264228654 ) ) ;
#156858 = CARTESIAN_POINT ( 'NONE',  ( 4.379528057220339221, -16.55341960407611168, 97.70724293864772392 ) ) ;
#156859 = CARTESIAN_POINT ( 'NONE',  ( 3.556970738554033499E-15, -38.81732327939057825, -4.624999997268814056 ) ) ;
#156860 = CARTESIAN_POINT ( 'NONE',  ( 14.29746914071037800, 8.314922557961029526, 36.66775706135234714 ) ) ;
#156861 = CARTESIAN_POINT ( 'NONE',  ( 21.55341960407610458, 5.719274019375980345, 58.95724293864770971 ) ) ;
#156862 = CARTESIAN_POINT ( 'NONE',  ( 14.29746914071037800, 8.314922557961029526, 101.6677570613523613 ) ) ;
#156863 = CARTESIAN_POINT ( 'NONE',  ( -0.05219959533934338120, 16.53943276465976808, 37.50109039468568284 ) ) ;
#156864 = CARTESIAN_POINT ( 'NONE',  ( -9.474510206698964154, 16.51473224551069663, 35.41557627198102409 ) ) ;
#156865 = CARTESIAN_POINT ( 'NONE',  ( 12.14591786802327356, -12.06949235617739191, 85.62609039468568994 ) ) ;
#156866 = CARTESIAN_POINT ( 'NONE',  ( 16.51473224551083163, -9.474510206698727899, 70.83442372801900433 ) ) ;
#156867 = CARTESIAN_POINT ( 'NONE',  ( -18.62759615963255300, -10.81492255796106328, 34.16775706135234714 ) ) ;
#156868 = CARTESIAN_POINT ( 'NONE',  ( -21.55341960407610458, -5.719274019375992779, 56.45724293864768839 ) ) ;
#156869 = CARTESIAN_POINT ( 'NONE',  ( -4.379528057220086978, -16.55341960407618274, 94.79275706135234714 ) ) ;
#156870 = CARTESIAN_POINT ( 'NONE',  ( 10.72451020669871369, 18.67979575497193778, 77.08442372801901854 ) ) ;
#156871 = CARTESIAN_POINT ( 'NONE',  ( -10.72451020669898014, 18.67979575497178502, 55.41557627198102409 ) ) ;
#156872 = CARTESIAN_POINT ( 'NONE',  ( 18.67979575497178502, 10.72451020669898547, 44.16557627198103120 ) ) ;
#156873 = CARTESIAN_POINT ( 'NONE',  ( -14.29746914071037622, -8.314922557961029526, 74.16775706135231871 ) ) ;
#156874 = CARTESIAN_POINT ( 'NONE',  ( -5.719274019375978568, 21.55341960407610458, 50.20724293864769550 ) ) ;
#156875 = EDGE_LOOP ( 'NONE', ( #174145, #95610, #116399, #130822, #123438, #7772, #70339, #112352 ) ) ;
#156876 = CARTESIAN_POINT ( 'NONE',  ( 9.564922557960805705, 16.46253265017160317, 94.58224293864769550 ) ) ;
#156877 = CARTESIAN_POINT ( 'NONE',  ( -26.45595770381631340, 7.620359626981985990, 168.5711898564603359 ) ) ;
#156878 = CARTESIAN_POINT ( 'NONE',  ( 0.05219959533909260263, 19.03943276465977164, 29.99890960531435979 ) ) ;
#156879 = CARTESIAN_POINT ( 'NONE',  ( -10.72451020669898014, 18.67979575497178502, 55.41557627198102409 ) ) ;
#156880 = CARTESIAN_POINT ( 'NONE',  ( -16.52544592524335698, -4.483927247898792601, 93.95942372801903275 ) ) ;
#156881 = CARTESIAN_POINT ( 'NONE',  ( -15.80617190586768217, 15.72974639402176855, 48.12609039468568284 ) ) ;
#156882 = CARTESIAN_POINT ( 'NONE',  ( 9.474510206698729675, 16.51473224551082808, 97.08442372801900433 ) ) ;
#156883 = CARTESIAN_POINT ( 'NONE',  ( 12.14591786802309770, 12.06949235617756955, 104.3739096053143669 ) ) ;
#156884 = CARTESIAN_POINT ( 'NONE',  ( 12.06949235617739724, 12.14591786802326823, 21.87609039468567573 ) ) ;
#156885 = VECTOR ( 'NONE', #41289, 1000.000000000000114 ) ;
#156886 = CARTESIAN_POINT ( 'NONE',  ( 19.02544592524343514, -5.153800228976328945, 38.54057627198103120 ) ) ;
#156887 = EDGE_CURVE ( 'NONE', #24124, #46712, #163340, .T. ) ;
#156888 = CARTESIAN_POINT ( 'NONE',  ( 15.66706267174406264, -1.428615351859153559, -61.77652290643386834 ) ) ;
#156889 = CARTESIAN_POINT ( 'NONE',  ( -5.049401038298153566, 19.05341960407611168, 85.20724293864766707 ) ) ;
#156890 = CARTESIAN_POINT ( 'NONE',  ( 14.34966873604972726, -8.224510206698740333, 80.83442372801901854 ) ) ;
#156891 = CARTESIAN_POINT ( 'NONE',  ( 10.72451020669871369, 18.67979575497193778, 102.0844237280190185 ) ) ;
#156892 = CARTESIAN_POINT ( 'NONE',  ( -5.719274019375978568, 21.55341960407610458, 65.20724293864768129 ) ) ;
#156893 = CARTESIAN_POINT ( 'NONE',  ( 12.14591786802327356, -12.06949235617739191, 90.62609039468567573 ) ) ;
#156894 = CARTESIAN_POINT ( 'NONE',  ( -13.89961937509957401, -13.97604488694547875, 74.37609039468566152 ) ) ;
#156895 = CARTESIAN_POINT ( 'NONE',  ( -0.05219959533909027116, -19.03943276465977164, 42.49890960531435269 ) ) ;
#156896 = CARTESIAN_POINT ( 'NONE',  ( 13.89961937509977652, -13.97604488694527269, 78.12390960531433848 ) ) ;
#156897 = CARTESIAN_POINT ( 'NONE',  ( -10.72451020669870658, -18.67979575497194134, 44.58442372801901854 ) ) ;
#156898 = CARTESIAN_POINT ( 'NONE',  ( 16.46253265017160672, -9.564922557960803928, 53.33224293864768839 ) ) ;
#156899 = CARTESIAN_POINT ( 'NONE',  ( -16.51473224551082808, 9.474510206698731452, 73.33442372801900433 ) ) ;
#156900 = CARTESIAN_POINT ( 'NONE',  ( 20.93662873023657411, -11.00447265502299388, 170.1964094900432372 ) ) ;
#156901 = CARTESIAN_POINT ( 'NONE',  ( 19.02544592524343514, -5.153800228976328945, 103.5405762719809957 ) ) ;
#156902 = CARTESIAN_POINT ( 'NONE',  ( 12.06949235617757843, -12.14591786802309237, 63.12390960531435979 ) ) ;
#156903 = CARTESIAN_POINT ( 'NONE',  ( -21.52544592524343514, 5.823673210054127303, 66.04057627198103830 ) ) ;
#156904 = CARTESIAN_POINT ( 'NONE',  ( 0.000000000000000000, 0.000000000000000000, -35.00000000000000000 ) ) ;
#156905 = CARTESIAN_POINT ( 'NONE',  ( -13.97604488694547697, 13.89961937509957934, 23.12609039468565442 ) ) ;
#156906 = CARTESIAN_POINT ( 'NONE',  ( 21.16427095311446038, -10.71512246325695550, 170.2843762835011319 ) ) ;
#156908 = CARTESIAN_POINT ( 'NONE',  ( 9.474510206698971260, -16.51473224551069308, 72.91557627198102409 ) ) ;
#156907 = CARTESIAN_POINT ( 'NONE',  ( 0.05219959533909260263, 19.03943276465977164, 64.99890960531436690 ) ) ;
#156909 = CARTESIAN_POINT ( 'NONE',  ( -8.314922557961024197, 14.29746914071037800, 57.91775706135234714 ) ) ;
#156910 = CARTESIAN_POINT ( 'NONE',  ( 12.39597446193840469, -43.61540881465730735, -22.87833536075120122 ) ) ;
#156911 = CARTESIAN_POINT ( 'NONE',  ( -16.38665767535055906, 7.295008042176100105, 110.2640086421455123 ) ) ;
#156912 = CARTESIAN_POINT ( 'NONE',  ( -0.05219959533934338120, 16.53943276465976808, 77.50109039468567573 ) ) ;
#156913 = CARTESIAN_POINT ( 'NONE',  ( 17.60691670004652565, 5.500000000000026645, 96.63333313366440791 ) ) ;
#156914 = CARTESIAN_POINT ( 'NONE',  ( 16.53943276465976808, 0.05219959533934440121, 71.25109039468568994 ) ) ;
#156915 = CARTESIAN_POINT ( 'NONE',  ( -16.55341960407617563, 4.379528057220093196, 38.54275706135234714 ) ) ;
#156917 = DIRECTION ( 'NONE',  ( -0.5367108174878556515, 0.8437662581494462799, -7.967771471296434353E-17 ) ) ;
#156916 = CARTESIAN_POINT ( 'NONE',  ( 19.03943276465977164, -0.05219959533909143690, 53.74890960531436690 ) ) ;
#156918 = CARTESIAN_POINT ( 'NONE',  ( -5.719274019375665041, -21.55341960407619695, 59.79275706135234714 ) ) ;
#156919 = CARTESIAN_POINT ( 'NONE',  ( 13.89961937509957401, 13.97604488694547697, 56.87609039468564731 ) ) ;
#156920 = CARTESIAN_POINT ( 'NONE',  ( -21.53943276465977519, -0.05219959533937600094, 108.7510903946857042 ) ) ;
#156921 = CARTESIAN_POINT ( 'NONE',  ( 16.51473224551069308, 9.474510206698969483, 34.16557627198102409 ) ) ;
#156922 = CARTESIAN_POINT ( 'NONE',  ( -16.57870055856065861, 14.68143632974463664, -58.31140971112358073 ) ) ;
#156923 = CARTESIAN_POINT ( 'NONE',  ( 5.823673210054125526, 21.52544592524343514, 59.79057627198103120 ) ) ;
#156924 = CARTESIAN_POINT ( 'NONE',  ( 19.05341960407611168, 5.049401038298154454, 103.9572429386476671 ) ) ;
#156925 = CARTESIAN_POINT ( 'NONE',  ( 16.52544592524342804, -4.483927247898539470, 103.5405762719810383 ) ) ;
#156926 = CARTESIAN_POINT ( 'NONE',  ( -12.06949235617739369, -12.14591786802326823, 34.37609039468568284 ) ) ;
#156927 = CARTESIAN_POINT ( 'NONE',  ( -16.52544592524342804, 4.483927247898546575, 31.04057627198102409 ) ) ;
#156928 = VERTEX_POINT ( 'NONE', #86485 ) ;
#156929 = CARTESIAN_POINT ( 'NONE',  ( -15.80617190586745835, -15.72974639402198527, 96.87390960531436690 ) ) ;
#156931 = CARTESIAN_POINT ( 'NONE',  ( -0.05219959533909027116, -19.03943276465977164, 112.4989096053143669 ) ) ;
#156930 = CARTESIAN_POINT ( 'NONE',  ( 16.52544592524342804, -4.483927247898539470, 38.54057627198103120 ) ) ;
#156932 = CARTESIAN_POINT ( 'NONE',  ( 0.05219959533936267826, -19.03943276465977164, 95.00109039468567573 ) ) ;
#156933 = CARTESIAN_POINT ( 'NONE',  ( -13.89961937509957401, -13.97604488694547875, 29.37609039468565797 ) ) ;
#156934 = CARTESIAN_POINT ( 'NONE',  ( -4.483927247898539470, -16.52544592524342804, 32.29057627198102409 ) ) ;
#156935 = CARTESIAN_POINT ( 'NONE',  ( 15.72974639402199770, -15.80617190586745480, 108.1239096053143811 ) ) ;
#156936 = CARTESIAN_POINT ( 'NONE',  ( 21.52544592524344225, -5.823673210054117533, 53.54057627198103120 ) ) ;
#156937 = CARTESIAN_POINT ( 'NONE',  ( 5.153800228976335163, 19.02544592524342804, 79.79057627198102409 ) ) ;
#156938 = CARTESIAN_POINT ( 'NONE',  ( -14.34966873604960291, -8.224510206698953496, 46.66557627198102409 ) ) ;
#156939 = CARTESIAN_POINT ( 'NONE',  ( -19.02544592524342804, 5.153800228976336051, 96.04057627198103830 ) ) ;
#156940 = CARTESIAN_POINT ( 'NONE',  ( 19.26498983726237313, -5.499999999999806377, 63.05319577422002908 ) ) ;
#156941 = CARTESIAN_POINT ( 'NONE',  ( 19.05341960407617918, -5.049401038297876454, 46.04275706135233293 ) ) ;
#156942 = CARTESIAN_POINT ( 'NONE',  ( 10.81492255796078972, 18.62759615963270932, 89.58224293864768129 ) ) ;
#156943 = CARTESIAN_POINT ( 'NONE',  ( -0.05219959533910754901, -16.53943276465976808, 97.49890960531436690 ) ) ;
#156944 = CARTESIAN_POINT ( 'NONE',  ( 21.52544592524334988, 5.823673210054432836, 36.45942372801901143 ) ) ;
#156945 = CARTESIAN_POINT ( 'NONE',  ( 22.44159573604009594, -16.30477369853687364, 139.6750000027311955 ) ) ;
#156946 = CARTESIAN_POINT ( 'NONE',  ( -12.14591786802326823, 12.06949235617739902, 113.1260903946856899 ) ) ;
#156947 = CARTESIAN_POINT ( 'NONE',  ( -5.153800228976328057, -19.02544592524343514, 32.29057627198102409 ) ) ;
#156948 = CARTESIAN_POINT ( 'NONE',  ( 16.46253265017160672, -9.564922557960803928, 83.33224293864768129 ) ) ;
#156949 = CARTESIAN_POINT ( 'NONE',  ( -18.22780087662122028, 5.500000000000031086, 93.51540105326107266 ) ) ;
#156950 = CARTESIAN_POINT ( 'NONE',  ( 13.89961937509977652, -13.97604488694527269, 38.12390960531436690 ) ) ;
#156951 = CARTESIAN_POINT ( 'NONE',  ( 4.379528057220339221, -16.55341960407611168, 42.70724293864770260 ) ) ;
#156952 = CARTESIAN_POINT ( 'NONE',  ( -0.05219959533937732626, 21.53943276465977519, 77.50109039468567573 ) ) ;
#156954 = CARTESIAN_POINT ( 'NONE',  ( -16.53943276465976808, -0.05219959533934237506, 73.75109039468567573 ) ) ;
#156953 = CARTESIAN_POINT ( 'NONE',  ( 22.27567441219162703, -30.36413145305563788, -19.29304740692434805 ) ) ;
#156955 = CARTESIAN_POINT ( 'NONE',  ( -16.46253265017160317, 9.564922557960807481, 60.83224293864769550 ) ) ;
#156956 = CARTESIAN_POINT ( 'NONE',  ( 0.05219959533909260263, 19.03943276465977164, 69.99890960531435269 ) ) ;
#156957 = ORIENTED_EDGE ( 'NONE', *, *, #115666, .F. ) ;
#156958 = CARTESIAN_POINT ( 'NONE',  ( -10.81492255796105439, 18.62759615963255655, 102.9177570613523756 ) ) ;
#156959 = CARTESIAN_POINT ( 'NONE',  ( 8.314922557961029526, -14.29746914071037800, 70.41775706135236135 ) ) ;
#156960 = CARTESIAN_POINT ( 'NONE',  ( 18.62759615963255655, 10.81492255796105972, 101.6677570613523613 ) ) ;
#156961 = CARTESIAN_POINT ( 'NONE',  ( -16.46253265017160317, 9.564922557960807481, 60.83224293864769550 ) ) ;
#156962 = CARTESIAN_POINT ( 'NONE',  ( 21.52544592524344225, -5.823673210054117533, 38.54057627198103120 ) ) ;
#156963 = CARTESIAN_POINT ( 'NONE',  ( 19.03943276465977164, 0.05219959533936151252, 101.2510903946856757 ) ) ;
#156964 = CARTESIAN_POINT ( 'NONE',  ( -18.62759615963255300, -10.81492255796106328, 84.16775706135234714 ) ) ;
#156965 = CARTESIAN_POINT ( 'NONE',  ( 16.55341960407618274, -4.379528057220086978, 51.04275706135234714 ) ) ;
#156966 = CARTESIAN_POINT ( 'NONE',  ( 21.52544592524344225, -5.823673210054117533, 98.54057627198105251 ) ) ;
#156968 = CIRCLE ( 'NONE', #105299, 2.500000000000000000 ) ;
#156967 = CARTESIAN_POINT ( 'NONE',  ( 13.97604488694548053, -13.89961937509957401, 95.62609039468563310 ) ) ;
#156969 = CARTESIAN_POINT ( 'NONE',  ( -13.97604488694527625, -13.89961937509977652, 81.87390960531436690 ) ) ;
#156970 = CARTESIAN_POINT ( 'NONE',  ( 5.153800228976615827, -19.02544592524334988, 105.2094237280190185 ) ) ;
#156971 = CARTESIAN_POINT ( 'NONE',  ( 8.224510206698742110, 14.34966873604972548, 27.08442372801901854 ) ) ;
#156972 = CARTESIAN_POINT ( 'NONE',  ( 14.34966873604960469, 8.224510206698951720, 64.16557627198102409 ) ) ;
#156973 = CARTESIAN_POINT ( 'NONE',  ( -12.14591786802326823, 12.06949235617739902, 68.12609039468567573 ) ) ;
#156975 = CARTESIAN_POINT ( 'NONE',  ( 16.46253265017160672, -9.564922557960803928, 58.33224293864769550 ) ) ;
#156974 = CARTESIAN_POINT ( 'NONE',  ( 21.52544592524344225, -5.823673210054117533, 113.5405762719810383 ) ) ;
#156976 = CARTESIAN_POINT ( 'NONE',  ( 9.474510206698971260, -16.51473224551069308, 67.91557627198102409 ) ) ;
#156977 = CARTESIAN_POINT ( 'NONE',  ( -16.52544592524335698, -4.483927247898792601, 78.95942372801901854 ) ) ;
#156978 = CARTESIAN_POINT ( 'NONE',  ( -5.429308488886486681E-15, 30.30510711980690175, 145.7500000054623115 ) ) ;
#156979 = ORIENTED_EDGE ( 'NONE', *, *, #132574, .T. ) ;
#156980 = CARTESIAN_POINT ( 'NONE',  ( 21.53943276465977519, 0.05219959533937863772, 106.2510903946856757 ) ) ;
#156981 = CARTESIAN_POINT ( 'NONE',  ( -5.049401038298153566, 19.05341960407611168, 40.20724293864768839 ) ) ;
#156982 = ORIENTED_EDGE ( 'NONE', *, *, #20248, .F. ) ;
#156983 = CARTESIAN_POINT ( 'NONE',  ( 0.05219959533934541429, -16.53943276465976808, 20.00109039468568639 ) ) ;
#156985 = CARTESIAN_POINT ( 'NONE',  ( -8.224510206698735004, -14.34966873604973081, 24.58442372801901499 ) ) ;
#156984 = CARTESIAN_POINT ( 'NONE',  ( 9.564922557961047289, -16.46253265017146816, 40.41775706135234003 ) ) ;
#156986 = CARTESIAN_POINT ( 'NONE',  ( -19.03943276465977164, 0.05219959533909376836, 41.24890960531435269 ) ) ;
#156987 = CARTESIAN_POINT ( 'NONE',  ( 19.02544592524343514, -5.153800228976328945, 68.54057627198103830 ) ) ;
#156988 = CARTESIAN_POINT ( 'NONE',  ( 0.05219959533907565091, 21.53943276465977519, 79.99890960531435269 ) ) ;
#156989 = CARTESIAN_POINT ( 'NONE',  ( -19.03943276465977164, 0.05219959533909376836, 116.2489096053143669 ) ) ;
#156990 = CARTESIAN_POINT ( 'NONE',  ( 16.51473224551069308, 9.474510206698969483, 44.16557627198103120 ) ) ;
#156991 = CARTESIAN_POINT ( 'NONE',  ( -5.359611314223446995E-15, 29.16686587814335851, 146.8750000027311557 ) ) ;
#156992 = CARTESIAN_POINT ( 'NONE',  ( -19.03943276465977164, -0.05219959533935918106, 103.7510903946856757 ) ) ;
#156993 = CARTESIAN_POINT ( 'NONE',  ( -21.55341960407610458, -5.719274019375992779, 71.45724293864769550 ) ) ;
#156994 = EDGE_CURVE ( 'NONE', #195827, #132628, #198659, .T. ) ;
#156995 = CARTESIAN_POINT ( 'NONE',  ( 0.05219959533936267826, -19.03943276465977164, 30.00109039468566863 ) ) ;
#156996 = CARTESIAN_POINT ( 'NONE',  ( -12.14591786802309592, -12.06949235617757132, 66.87390960531436690 ) ) ;
#156997 = CARTESIAN_POINT ( 'NONE',  ( 10.81492255796106328, -18.62759615963255655, 85.41775706135236135 ) ) ;
#156998 = CARTESIAN_POINT ( 'NONE',  ( 4.483927247898545687, 16.52544592524342804, 114.7905762719810383 ) ) ;
#157000 = CARTESIAN_POINT ( 'NONE',  ( -15.72974639402176322, -15.80617190586768395, 89.37609039468568994 ) ) ;
#156999 = CARTESIAN_POINT ( 'NONE',  ( -8.314922557960811034, -14.29746914071050412, 32.08224293864769550 ) ) ;
#157001 = CARTESIAN_POINT ( 'NONE',  ( -19.03943276465977164, 0.05219959533909376836, 81.24890960531436690 ) ) ;
#157002 = CARTESIAN_POINT ( 'NONE',  ( 18.62759615963255655, 10.81492255796105972, 41.66775706135235424 ) ) ;
#157003 = CARTESIAN_POINT ( 'NONE',  ( 19.05341960407611168, 5.049401038298154454, 78.95724293864769550 ) ) ;
#157004 = CARTESIAN_POINT ( 'NONE',  ( 16.55341960407611168, 4.379528057220329451, 88.95724293864769550 ) ) ;
#157005 = CARTESIAN_POINT ( 'NONE',  ( -4.483927247898539470, -16.52544592524342804, 62.29057627198102409 ) ) ;
#157006 = CARTESIAN_POINT ( 'NONE',  ( 5.823673210054125526, 21.52544592524343514, 69.79057627198102409 ) ) ;
#157007 = CARTESIAN_POINT ( 'NONE',  ( 5.049401038298161559, -19.05341960407611168, 77.70724293864765286 ) ) ;
#157008 = CARTESIAN_POINT ( 'NONE',  ( 21.52544592524344225, -5.823673210054117533, 88.54057627198103830 ) ) ;
#157009 = CARTESIAN_POINT ( 'NONE',  ( 19.03943276465977164, 0.05219959533936151252, 76.25109039468566152 ) ) ;
#157012 = CARTESIAN_POINT ( 'NONE',  ( 0.05219959533910956823, 16.53943276465976808, 69.99890960531435269 ) ) ;
#157011 = CARTESIAN_POINT ( 'NONE',  ( -16.51473224551082808, 9.474510206698731452, 28.33442372801900433 ) ) ;
#157010 = VECTOR ( 'NONE', #41696, 1000.000000000000114 ) ;
#157013 = CARTESIAN_POINT ( 'NONE',  ( 5.719274019375991003, -21.55341960407610458, 52.70724293864769550 ) ) ;
#157014 = DIRECTION ( 'NONE',  ( -1.000000000000000000, -0.000000000000000000, -0.000000000000000000 ) ) ;
#157016 = CARTESIAN_POINT ( 'NONE',  ( 22.44159573604009239, 16.30477369853692693, 144.5750000027311728 ) ) ;
#157015 = CARTESIAN_POINT ( 'NONE',  ( -16.53943276465976808, -0.05219959533934237506, 98.75109039468568994 ) ) ;
#157017 = CARTESIAN_POINT ( 'NONE',  ( -19.05341960407617563, 5.049401038297882671, 98.54275706135233293 ) ) ;
#157018 = CARTESIAN_POINT ( 'NONE',  ( 16.53943276465976808, -0.05219959533910856209, 68.74890960531435269 ) ) ;
#157019 = CARTESIAN_POINT ( 'NONE',  ( -17.49999999999999645, 5.499999999999997335, 35.79690382534171533 ) ) ;
#157020 = CARTESIAN_POINT ( 'NONE',  ( -16.46253265017160317, 9.564922557960807481, 55.83224293864769550 ) ) ;
#157021 = CARTESIAN_POINT ( 'NONE',  ( 16.46253265017160672, -9.564922557960803928, 28.33224293864769550 ) ) ;
#157022 = CARTESIAN_POINT ( 'NONE',  ( 16.52544592524342804, -4.483927247898539470, 48.54057627198103120 ) ) ;
#157023 = CARTESIAN_POINT ( 'NONE',  ( 13.97604488694527802, 13.89961937509977652, 104.3739096053143385 ) ) ;
#157025 = CARTESIAN_POINT ( 'NONE',  ( -0.05219959533909027116, -19.03943276465977164, 67.49890960531436690 ) ) ;
#157024 = CARTESIAN_POINT ( 'NONE',  ( 13.97604488694548053, -13.89961937509957401, 85.62609039468568994 ) ) ;
#157026 = CARTESIAN_POINT ( 'NONE',  ( -12.14591786802326823, 12.06949235617739902, 23.12609039468567573 ) ) ;
#157027 = CARTESIAN_POINT ( 'NONE',  ( -19.03943276465977164, 0.05219959533909376836, 81.24890960531436690 ) ) ;
#157028 = CARTESIAN_POINT ( 'NONE',  ( -21.55341960407610458, -5.719274019375992779, 66.45724293864768129 ) ) ;
#157029 = CARTESIAN_POINT ( 'NONE',  ( 14.34966873604972726, -8.224510206698740333, 55.83442372801901854 ) ) ;
#157030 = CARTESIAN_POINT ( 'NONE',  ( -9.564922557961040184, 16.46253265017147172, 107.9177570613523471 ) ) ;
#157031 = CARTESIAN_POINT ( 'NONE',  ( 9.474510206698971260, -16.51473224551069308, 62.91557627198102409 ) ) ;
#157032 = CARTESIAN_POINT ( 'NONE',  ( -15.80617190586745835, -15.72974639402198527, 61.87390960531436690 ) ) ;
#157033 = CARTESIAN_POINT ( 'NONE',  ( -16.51473224551082808, 9.474510206698731452, 88.33442372801900433 ) ) ;
#157035 = CARTESIAN_POINT ( 'NONE',  ( 5.823673210054444382, -21.52544592524334988, 50.20942372801901854 ) ) ;
#157034 = CARTESIAN_POINT ( 'NONE',  ( 16.52544592524335698, 4.483927247898782831, 111.4594237280190328 ) ) ;
#157036 = EDGE_CURVE ( 'NONE', #40357, #57973, #31782, .T. ) ;
#157037 = CARTESIAN_POINT ( 'NONE',  ( -4.243022077861292374, -4.383680652614605933, -62.50719930893269805 ) ) ;
#157039 = CARTESIAN_POINT ( 'NONE',  ( -16.52544592524335698, -4.483927247898792601, 98.95942372801903275 ) ) ;
#157038 = CARTESIAN_POINT ( 'NONE',  ( -8.314922557961024197, 14.29746914071037800, 67.91775706135234714 ) ) ;
#157040 = CARTESIAN_POINT ( 'NONE',  ( 19.53037848336981241, -5.499999999999889866, 42.35532783611441943 ) ) ;
#157041 = CARTESIAN_POINT ( 'NONE',  ( -8.314922557961024197, 14.29746914071037800, 77.91775706135231871 ) ) ;
#157042 = CARTESIAN_POINT ( 'NONE',  ( 16.53943276465976808, 0.05219959533934440121, 31.25109039468568639 ) ) ;
#157043 = CARTESIAN_POINT ( 'NONE',  ( -16.51473224551069308, -9.474510206698971260, 46.66557627198102409 ) ) ;
#157044 = CARTESIAN_POINT ( 'NONE',  ( -19.03943276465977164, 0.05219959533909376836, 56.24890960531435979 ) ) ;
#157045 = CARTESIAN_POINT ( 'NONE',  ( -19.02544592524342804, 5.153800228976336051, 66.04057627198103830 ) ) ;
#157046 = CARTESIAN_POINT ( 'NONE',  ( -0.05219959533937732626, 21.53943276465977519, 57.50109039468568994 ) ) ;
#157047 = CARTESIAN_POINT ( 'NONE',  ( -16.55341960407617563, 4.379528057220093196, 48.54275706135234714 ) ) ;
#157048 = CARTESIAN_POINT ( 'NONE',  ( 4.483927247898545687, 16.52544592524342804, 39.79057627198103830 ) ) ;
#157049 = CARTESIAN_POINT ( 'NONE',  ( 13.97604488694527802, 13.89961937509977652, 24.37390960531435624 ) ) ;
#157050 = CARTESIAN_POINT ( 'NONE',  ( 13.89961937509977652, -13.97604488694527269, 33.12390960531434558 ) ) ;
#157051 = CARTESIAN_POINT ( 'NONE',  ( -8.314922557961024197, 14.29746914071037800, 27.91775706135234358 ) ) ;
#157052 = CARTESIAN_POINT ( 'NONE',  ( -9.564922557961040184, 16.46253265017147172, 82.91775706135233293 ) ) ;
#157053 = CARTESIAN_POINT ( 'NONE',  ( 16.53943276465976808, -0.05219959533910856209, 78.74890960531436690 ) ) ;
#157054 = CARTESIAN_POINT ( 'NONE',  ( -5.049401038298153566, 19.05341960407611168, 55.20724293864769550 ) ) ;
#157056 = DIRECTION ( 'NONE',  ( 0.000000000000000000, -0.7071067811865485719, 0.7071067811865465735 ) ) ;
#157055 = CARTESIAN_POINT ( 'NONE',  ( -19.02544592524334988, -5.153800228976617603, 93.95942372801900433 ) ) ;
#157057 = CARTESIAN_POINT ( 'NONE',  ( 5.823673210054444382, -21.52544592524334988, 80.20942372801901854 ) ) ;
#157058 = CARTESIAN_POINT ( 'NONE',  ( -16.53943276465976808, -0.05219959533934237506, 58.75109039468568994 ) ) ;
#157059 = CARTESIAN_POINT ( 'NONE',  ( 17.40805194822031510, 6.112264579159359279, 36.66628727489388950 ) ) ;
#157060 = CARTESIAN_POINT ( 'NONE',  ( -21.52544592524343514, 5.823673210054127303, 56.04057627198102409 ) ) ;
#157061 = CARTESIAN_POINT ( 'NONE',  ( 4.483927247898790824, -16.52544592524335698, 40.20942372801901854 ) ) ;
#157062 = CARTESIAN_POINT ( 'NONE',  ( -8.906447517083060816, 27.41122689804195645, 147.5999999999999943 ) ) ;
#157063 = CARTESIAN_POINT ( 'NONE',  ( 9.564922557961047289, -16.46253265017146816, 35.41775706135233293 ) ) ;
#157064 = AXIS2_PLACEMENT_3D ( 'NONE', #3749, #65426, #141277 ) ;
#157065 = CARTESIAN_POINT ( 'NONE',  ( 9.409695640424901697, 11.43209428340594158, -59.99679127084682051 ) ) ;
#157066 = CARTESIAN_POINT ( 'NONE',  ( 16.51473224551069308, 9.474510206698969483, 49.16557627198102409 ) ) ;
#157067 = DIRECTION ( 'NONE',  ( -9.445700745138859830E-17, 1.000000000000000000, 0.000000000000000000 ) ) ;
#157068 = CARTESIAN_POINT ( 'NONE',  ( -16.46253265017160317, 9.564922557960807481, 75.83224293864769550 ) ) ;
#157070 = CARTESIAN_POINT ( 'NONE',  ( -19.52837319214026479, 5.499999999999998224, 99.60471352585541638 ) ) ;
#157069 = CIRCLE ( 'NONE', #73104, 3.000000000000001332 ) ;
#157071 = CARTESIAN_POINT ( 'NONE',  ( 13.89961937509957401, 13.97604488694547697, 26.87609039468566507 ) ) ;
#157072 = CARTESIAN_POINT ( 'NONE',  ( 8.224510206698953496, -14.34966873604960469, 42.91557627198103120 ) ) ;
#157073 = CARTESIAN_POINT ( 'NONE',  ( 19.03943276465977164, -0.05219959533909143690, 48.74890960531435979 ) ) ;
#157074 = CARTESIAN_POINT ( 'NONE',  ( -9.564922557960796823, -16.46253265017161027, 112.0822429386476955 ) ) ;
#157075 = CARTESIAN_POINT ( 'NONE',  ( -18.67979575497193778, 10.72451020669871902, 73.33442372801901854 ) ) ;
#157076 = CARTESIAN_POINT ( 'NONE',  ( 9.474510206698971260, -16.51473224551069308, 47.91557627198102409 ) ) ;
#157077 = CARTESIAN_POINT ( 'NONE',  ( -18.67979575497193778, 10.72451020669871902, 63.33442372801900433 ) ) ;
#157078 = CARTESIAN_POINT ( 'NONE',  ( -16.46253265017160317, 9.564922557960807481, 115.8322429386477097 ) ) ;
#157079 = CARTESIAN_POINT ( 'NONE',  ( -16.51473224551069308, -9.474510206698971260, 31.66557627198102054 ) ) ;
#157080 = CARTESIAN_POINT ( 'NONE',  ( 0.05219959533937995610, -21.53943276465977519, 25.00109039468567218 ) ) ;
#157081 = CARTESIAN_POINT ( 'NONE',  ( -9.474510206698720793, -16.51473224551083518, 44.58442372801900433 ) ) ;
#157082 = CARTESIAN_POINT ( 'NONE',  ( -19.03943276465977164, 0.05219959533909376836, 31.24890960531435979 ) ) ;
#157083 = CARTESIAN_POINT ( 'NONE',  ( 16.51473224551069308, 9.474510206698969483, 64.16557627198102409 ) ) ;
#157084 = CARTESIAN_POINT ( 'NONE',  ( 4.483927247898790824, -16.52544592524335698, 20.20942372801900788 ) ) ;
#157085 = CARTESIAN_POINT ( 'NONE',  ( 12.14591786802309770, 12.06949235617756955, 79.37390960531436690 ) ) ;
#157086 = CARTESIAN_POINT ( 'NONE',  ( -21.53943276465977519, 0.05219959533907696930, 31.24890960531435979 ) ) ;
#157087 = CARTESIAN_POINT ( 'NONE',  ( 5.049401038297881783, 19.05341960407617563, 97.29275706135233293 ) ) ;
#157088 = CARTESIAN_POINT ( 'NONE',  ( 10.72451020669898902, -18.67979575497178502, 107.9155762719810241 ) ) ;
#157089 = CARTESIAN_POINT ( 'NONE',  ( -21.55341960407619339, 5.719274019375674811, 53.54275706135234714 ) ) ;
#157090 = CARTESIAN_POINT ( 'NONE',  ( 16.55341960407618274, -4.379528057220086978, 61.04275706135234714 ) ) ;
#157091 = CARTESIAN_POINT ( 'NONE',  ( 14.34966873604972726, -8.224510206698740333, 50.83442372801901143 ) ) ;
#157092 = CARTESIAN_POINT ( 'NONE',  ( -18.67979575497178146, -10.72451020669898902, 56.66557627198103830 ) ) ;
#157093 = CARTESIAN_POINT ( 'NONE',  ( -9.474510206698964154, 16.51473224551069663, 45.41557627198103120 ) ) ;
#157094 = CARTESIAN_POINT ( 'NONE',  ( 16.52544592524335698, 4.483927247898782831, 71.45942372801901854 ) ) ;
#157095 = CARTESIAN_POINT ( 'NONE',  ( 18.67979575497178502, 10.72451020669898547, 99.16557627198100988 ) ) ;
#157096 = CARTESIAN_POINT ( 'NONE',  ( 14.34966873604960469, 8.224510206698951720, 54.16557627198103120 ) ) ;
#157097 = CARTESIAN_POINT ( 'NONE',  ( 5.049401038298161559, -19.05341960407611168, 77.70724293864765286 ) ) ;
#157098 = CARTESIAN_POINT ( 'NONE',  ( -8.224510206698735004, -14.34966873604973081, 79.58442372801903275 ) ) ;
#157099 = CARTESIAN_POINT ( 'NONE',  ( 19.03943276465977164, 0.05219959533936151252, 111.2510903946856757 ) ) ;
#157100 = CARTESIAN_POINT ( 'NONE',  ( -0.05219959533907301413, -21.53943276465977519, 107.4989096053143669 ) ) ;
#157101 = CARTESIAN_POINT ( 'NONE',  ( 14.29746914071049879, -8.314922557960816363, 38.33224293864768839 ) ) ;
#157102 = ORIENTED_EDGE ( 'NONE', *, *, #32959, .F. ) ;
#157103 = CARTESIAN_POINT ( 'NONE',  ( -16.81555441253553695, 7.025013491695482060, 75.63685445334260748 ) ) ;
#157104 = CARTESIAN_POINT ( 'NONE',  ( -0.05219959533907301413, -21.53943276465977519, 92.49890960531436690 ) ) ;
#157105 = CARTESIAN_POINT ( 'NONE',  ( -8.224510206698948167, 14.34966873604960824, 30.41557627198101699 ) ) ;
#157106 = ORIENTED_EDGE ( 'NONE', *, *, #192484, .T. ) ;
#157107 = CYLINDRICAL_SURFACE ( 'NONE', #1624, 5.000000000000000888 ) ;
#157108 = CARTESIAN_POINT ( 'NONE',  ( -21.52544592524343514, 5.823673210054127303, 101.0405762719810383 ) ) ;
#157109 = CARTESIAN_POINT ( 'NONE',  ( 5.153800228976335163, 19.02544592524342804, 104.7905762719809957 ) ) ;
#157110 = CARTESIAN_POINT ( 'NONE',  ( 18.67979575497194134, -10.72451020669871369, 20.83442372801901143 ) ) ;
#157111 = CARTESIAN_POINT ( 'NONE',  ( 8.224510206698953496, -14.34966873604960469, 47.91557627198102409 ) ) ;
#157112 = CARTESIAN_POINT ( 'NONE',  ( 12.14591786802327356, -12.06949235617739191, 45.62609039468567573 ) ) ;
#157113 = CARTESIAN_POINT ( 'NONE',  ( -5.049401038298153566, 19.05341960407611168, 50.20724293864770260 ) ) ;
#157114 = CARTESIAN_POINT ( 'NONE',  ( 19.02544592524334988, 5.153800228976608722, 56.45942372801898301 ) ) ;
#157115 = CARTESIAN_POINT ( 'NONE',  ( 13.97604488694527802, 13.89961937509977652, 84.37390960531433848 ) ) ;
#157116 = EDGE_CURVE ( 'NONE', #188457, #89992, #15619, .T. ) ;
#157117 = CARTESIAN_POINT ( 'NONE',  ( -18.67979575497178146, -10.72451020669898902, 41.66557627198103120 ) ) ;
#157118 = CARTESIAN_POINT ( 'NONE',  ( -18.22780087662119897, 5.500000000000102141, 66.01763182126894947 ) ) ;
#157119 = CARTESIAN_POINT ( 'NONE',  ( -14.34966873604972548, 8.224510206698743886, 23.33442372801901499 ) ) ;
#157120 = CARTESIAN_POINT ( 'NONE',  ( -13.97604488694547697, 13.89961937509957934, 48.12609039468566863 ) ) ;
#157121 = CARTESIAN_POINT ( 'NONE',  ( 18.67979575497178502, 10.72451020669898547, 99.16557627198100988 ) ) ;
#157122 = CARTESIAN_POINT ( 'NONE',  ( 4.483927247898545687, 16.52544592524342804, 39.79057627198103830 ) ) ;
#157123 = CARTESIAN_POINT ( 'NONE',  ( -16.46253265017160317, 9.564922557960807481, 75.83224293864769550 ) ) ;
#157124 = CARTESIAN_POINT ( 'NONE',  ( -5.719274019375978568, 21.55341960407610458, 60.20724293864768839 ) ) ;
#157126 = CARTESIAN_POINT ( 'NONE',  ( 16.53943276465976808, 0.05219959533934440121, 26.25109039468567573 ) ) ;
#157125 = CARTESIAN_POINT ( 'NONE',  ( 5.823673210054125526, 21.52544592524343514, 94.79057627198105251 ) ) ;
#157127 = CARTESIAN_POINT ( 'NONE',  ( 19.05341960407611168, 5.049401038298154454, 113.9572429386477097 ) ) ;
#157128 = CARTESIAN_POINT ( 'NONE',  ( -21.53943276465977519, -0.05219959533937600094, 93.75109039468567573 ) ) ;
#157130 = EDGE_CURVE ( 'NONE', #77704, #121632, #14625, .T. ) ;
#157129 = CARTESIAN_POINT ( 'NONE',  ( 19.03943276465977164, -0.05219959533909143690, 83.74890960531436690 ) ) ;
#157131 = CARTESIAN_POINT ( 'NONE',  ( 19.03943276465977164, -0.05219959533909143690, 28.74890960531435624 ) ) ;
#157132 = CARTESIAN_POINT ( 'NONE',  ( 5.049401038298161559, -19.05341960407611168, 82.70724293864770971 ) ) ;
#157133 = CARTESIAN_POINT ( 'NONE',  ( 16.52544592524342804, -4.483927247898539470, 108.5405762719810241 ) ) ;
#157134 = CARTESIAN_POINT ( 'NONE',  ( 5.153800228976335163, 19.02544592524342804, 59.79057627198100988 ) ) ;
#157135 = CARTESIAN_POINT ( 'NONE',  ( -8.314922557961024197, 14.29746914071037800, 22.91775706135235069 ) ) ;
#157136 = DIRECTION ( 'NONE',  ( 0.000000000000000000, 0.000000000000000000, 1.000000000000000000 ) ) ;
#157137 = CARTESIAN_POINT ( 'NONE',  ( 19.02544592524343514, -5.153800228976328945, 73.54057627198103830 ) ) ;
#157139 = CARTESIAN_POINT ( 'NONE',  ( -13.89961937509977652, 13.97604488694528158, 115.6239096053143669 ) ) ;
#157138 = CARTESIAN_POINT ( 'NONE',  ( -18.62759615963255300, -10.81492255796106328, 104.1677570613523471 ) ) ;
#157140 = CARTESIAN_POINT ( 'NONE',  ( -4.379528057220086978, -16.55341960407618274, 89.79275706135236135 ) ) ;
#157141 = LINE ( 'NONE', #185494, #77679 ) ;
#157142 = CARTESIAN_POINT ( 'NONE',  ( 19.05341960407617918, -5.049401038297876454, 71.04275706135234714 ) ) ;
#157143 = CARTESIAN_POINT ( 'NONE',  ( 10.72451020669871369, 18.67979575497193778, 112.0844237280190185 ) ) ;
#157144 = B_SPLINE_CURVE_WITH_KNOTS ( 'NONE', 3,
 ( #132480, #166820, #135489, #198140, #120291, #151640 ),
 .UNSPECIFIED., .F., .F.,
 ( 4, 2, 4 ),
 ( 0.000000000000000000, 0.0003837532665554082493, 0.0007675065331108164987 ),
 .UNSPECIFIED. ) ;
#157145 = CARTESIAN_POINT ( 'NONE',  ( -19.30190589895974185, 21.36759865781276346, 139.9999999999999716 ) ) ;
#157146 = CARTESIAN_POINT ( 'NONE',  ( 9.474510206698971260, -16.51473224551069308, 32.91557627198102409 ) ) ;
#157147 = CARTESIAN_POINT ( 'NONE',  ( 12.06949235617757843, -12.14591786802309237, 38.12390960531436690 ) ) ;
#157148 = CARTESIAN_POINT ( 'NONE',  ( 0.000000000000000000, 0.000000000000000000, -64.92279855667830191 ) ) ;
#157149 = CARTESIAN_POINT ( 'NONE',  ( -14.34966873604972548, 8.224510206698743886, 103.3344237280190043 ) ) ;
#157150 = DIRECTION ( 'NONE',  ( 0.000000000000000000, 0.000000000000000000, -1.000000000000000000 ) ) ;
#157151 = CARTESIAN_POINT ( 'NONE',  ( 4.379528057220092307, 16.55341960407617563, 77.29275706135234714 ) ) ;
#157152 = CARTESIAN_POINT ( 'NONE',  ( -9.474510206698964154, 16.51473224551069663, 40.41557627198103120 ) ) ;
#157153 = CARTESIAN_POINT ( 'NONE',  ( -21.53943276465977519, -0.05219959533937600094, 93.75109039468567573 ) ) ;
#157154 = CARTESIAN_POINT ( 'NONE',  ( 19.03943276465977164, 0.05219959533936151252, 96.25109039468567573 ) ) ;
#157155 = CARTESIAN_POINT ( 'NONE',  ( 21.55341960407619695, -5.719274019375665929, 76.04275706135237556 ) ) ;
#157156 = CARTESIAN_POINT ( 'NONE',  ( 13.97604488694548053, -13.89961937509957401, 55.62609039468566863 ) ) ;
#157157 = CARTESIAN_POINT ( 'NONE',  ( 5.153800228976335163, 19.02544592524342804, 79.79057627198102409 ) ) ;
#157158 = CARTESIAN_POINT ( 'NONE',  ( -13.89961937509977652, 13.97604488694528158, 75.62390960531438111 ) ) ;
#157159 = CARTESIAN_POINT ( 'NONE',  ( 67.00000000000000000, -5.510910596163089556E-15, 45.00000000000000000 ) ) ;
#157160 = AXIS2_PLACEMENT_3D ( 'NONE', #119783, #40947, #146103 ) ;
#157161 = CARTESIAN_POINT ( 'NONE',  ( 16.52544592524342804, -4.483927247898539470, 63.54057627198103830 ) ) ;
#157162 = CARTESIAN_POINT ( 'NONE',  ( -15.80617190586745835, -15.72974639402198527, 66.87390960531436690 ) ) ;
#157163 = CARTESIAN_POINT ( 'NONE',  ( 16.46253265017160672, -9.564922557960803928, 53.33224293864768839 ) ) ;
#157165 = CARTESIAN_POINT ( 'NONE',  ( 0.05219959533934541429, -16.53943276465976808, 75.00109039468568994 ) ) ;
#157164 = CARTESIAN_POINT ( 'NONE',  ( 21.53943276465977519, -0.05219959533907433946, 83.74890960531435269 ) ) ;
#157166 = ORIENTED_EDGE ( 'NONE', *, *, #118105, .T. ) ;
#157168 = CARTESIAN_POINT ( 'NONE',  ( -36.91746825000000598, 2.428612866367529932E-14, -6.624999997268814056 ) ) ;
#157167 = CARTESIAN_POINT ( 'NONE',  ( -16.55341960407611168, -4.379528057220339221, 81.45724293864769550 ) ) ;
#157169 = CARTESIAN_POINT ( 'NONE',  ( 8.314922557961029526, -14.29746914071037800, 35.41775706135234003 ) ) ;
#157170 = CARTESIAN_POINT ( 'NONE',  ( -16.52544592524342804, 4.483927247898546575, 111.0405762719810525 ) ) ;
#157171 = CARTESIAN_POINT ( 'NONE',  ( -16.46253265017146816, -9.564922557961047289, 69.16775706135233293 ) ) ;
#157172 = CARTESIAN_POINT ( 'NONE',  ( -12.14591786802309592, -12.06949235617757132, 71.87390960531438111 ) ) ;
#157173 = CARTESIAN_POINT ( 'NONE',  ( 18.62759615963255655, 10.81492255796105972, 46.66775706135234714 ) ) ;
#157175 = CARTESIAN_POINT ( 'NONE',  ( -21.55341960407610458, -5.719274019375992779, 106.4572429386477097 ) ) ;
#157174 = DIRECTION ( 'NONE',  ( -0.06104853953485701173, -7.476289853398329258E-18, -0.9981347984218670311 ) ) ;
#157176 = DIRECTION ( 'NONE',  ( -0.000000000000000000, -0.000000000000000000, 1.000000000000000000 ) ) ;
#157177 = CARTESIAN_POINT ( 'NONE',  ( -12.14591786802309592, -12.06949235617757132, 81.87390960531435269 ) ) ;
#157178 = CARTESIAN_POINT ( 'NONE',  ( 19.41322597532352745, -37.10879518268426125, -19.41738833682490650 ) ) ;
#157179 = CARTESIAN_POINT ( 'NONE',  ( -5.049401038298153566, 19.05341960407611168, 40.20724293864768839 ) ) ;
#157180 = CARTESIAN_POINT ( 'NONE',  ( -36.91746825000000598, 11.99521256947798520, -6.724999997268813701 ) ) ;
#157181 = CARTESIAN_POINT ( 'NONE',  ( 5.049401038297881783, 19.05341960407617563, 77.29275706135231871 ) ) ;
#157182 = CARTESIAN_POINT ( 'NONE',  ( 5.823673210054444382, -21.52544592524334988, 40.20942372801901854 ) ) ;
#157183 = CARTESIAN_POINT ( 'NONE',  ( 9.564922557960805705, 16.46253265017160317, 69.58224293864770971 ) ) ;
#157184 = CARTESIAN_POINT ( 'NONE',  ( 19.03943276465977164, 0.05219959533936151252, 51.25109039468567573 ) ) ;
#157185 = CARTESIAN_POINT ( 'NONE',  ( -19.02544592524342804, 5.153800228976336051, 51.04057627198103120 ) ) ;
#157186 = CARTESIAN_POINT ( 'NONE',  ( 4.379528057220339221, -16.55341960407611168, 67.70724293864769550 ) ) ;
#157187 = CARTESIAN_POINT ( 'NONE',  ( 16.55341960407611168, 4.379528057220329451, 68.95724293864769550 ) ) ;
#157188 = CARTESIAN_POINT ( 'NONE',  ( -16.46253265017160317, 9.564922557960807481, 75.83224293864769550 ) ) ;
#157189 = CARTESIAN_POINT ( 'NONE',  ( 21.52544592524344225, -5.823673210054117533, 98.54057627198105251 ) ) ;
#157190 = CARTESIAN_POINT ( 'NONE',  ( -13.97604488694527625, -13.89961937509977652, 71.87390960531433848 ) ) ;
#157191 = CARTESIAN_POINT ( 'NONE',  ( 18.67979575497178502, 10.72451020669898547, 84.16557627198103830 ) ) ;
#157192 = CARTESIAN_POINT ( 'NONE',  ( -16.46253265017146816, -9.564922557961047289, 24.16775706135233648 ) ) ;
#157195 = CARTESIAN_POINT ( 'NONE',  ( 12.06949235617757843, -12.14591786802309237, 103.1239096053143811 ) ) ;
#157194 = CARTESIAN_POINT ( 'NONE',  ( -8.314922557961024197, 14.29746914071037800, 112.9177570613523329 ) ) ;
#157193 = CARTESIAN_POINT ( 'NONE',  ( -5.049401038298153566, 19.05341960407611168, 40.20724293864768839 ) ) ;
#157196 = CARTESIAN_POINT ( 'NONE',  ( 9.564922557961047289, -16.46253265017146816, 110.4177570613523471 ) ) ;
#157197 = ORIENTED_EDGE ( 'NONE', *, *, #111391, .T. ) ;
#157198 = CARTESIAN_POINT ( 'NONE',  ( -10.72451020669870658, -18.67979575497194134, 34.58442372801900433 ) ) ;
#157199 = CARTESIAN_POINT ( 'NONE',  ( 9.474510206698729675, 16.51473224551082808, 52.08442372801900433 ) ) ;
#157200 = CARTESIAN_POINT ( 'NONE',  ( -14.34966873604960291, -8.224510206698953496, 21.66557627198102409 ) ) ;
#157201 = CARTESIAN_POINT ( 'NONE',  ( -18.67979575497178146, -10.72451020669898902, 66.66557627198102409 ) ) ;
#157202 = CARTESIAN_POINT ( 'NONE',  ( -19.05341960407611168, -5.049401038298163336, 96.45724293864769550 ) ) ;
#157203 = CARTESIAN_POINT ( 'NONE',  ( 14.29746914071049879, -8.314922557960816363, 63.33224293864770260 ) ) ;
#157204 = CARTESIAN_POINT ( 'NONE',  ( 5.153800228976335163, 19.02544592524342804, 34.79057627198102409 ) ) ;
#157205 = CARTESIAN_POINT ( 'NONE',  ( 5.153800228976335163, 19.02544592524342804, 34.79057627198102409 ) ) ;
#157206 = CARTESIAN_POINT ( 'NONE',  ( -19.03943276465977164, -0.05219959533935918106, 23.75109039468566152 ) ) ;
#157207 = CARTESIAN_POINT ( 'NONE',  ( 12.14591786802327356, -12.06949235617739191, 95.62609039468568994 ) ) ;
#157208 = CARTESIAN_POINT ( 'NONE',  ( -5.719274019375665041, -21.55341960407619695, 44.79275706135234714 ) ) ;
#157209 = CARTESIAN_POINT ( 'NONE',  ( -4.483927247898782831, 16.52544592524335698, 47.70942372801902565 ) ) ;
#157210 = CARTESIAN_POINT ( 'NONE',  ( 18.62759615963271287, -10.81492255796078972, 28.33224293864769550 ) ) ;
#157212 = CARTESIAN_POINT ( 'NONE',  ( -21.55341960407619339, 5.719274019375674811, 98.54275706135234714 ) ) ;
#157211 = CARTESIAN_POINT ( 'NONE',  ( -16.46253265017160317, 9.564922557960807481, 55.83224293864769550 ) ) ;
#157213 = CARTESIAN_POINT ( 'NONE',  ( -19.05341960407611168, -5.049401038298163336, 81.45724293864769550 ) ) ;
#157214 = AXIS2_PLACEMENT_3D ( 'NONE', #18711, #104999, #104007 ) ;
#157215 = CARTESIAN_POINT ( 'NONE',  ( -14.34966873604972548, 8.224510206698743886, 63.33442372801900433 ) ) ;
#157216 = CARTESIAN_POINT ( 'NONE',  ( -14.34966873604960291, -8.224510206698953496, 101.6655762719810383 ) ) ;
#157217 = CARTESIAN_POINT ( 'NONE',  ( 12.06949235617739724, 12.14591786802326823, 111.8760903946856615 ) ) ;
#157218 = CARTESIAN_POINT ( 'NONE',  ( -11.45643923738960268, -4.999999999999992006, -18.00000000000000000 ) ) ;
#157221 = CARTESIAN_POINT ( 'NONE',  ( 16.51473224551069308, 9.474510206698969483, 79.16557627198103830 ) ) ;
#157220 = CARTESIAN_POINT ( 'NONE',  ( -5.153800228976328057, -19.02544592524343514, 92.29057627198099567 ) ) ;
#157219 = CARTESIAN_POINT ( 'NONE',  ( 18.62759615963255655, 10.81492255796105972, 66.66775706135234714 ) ) ;
#157222 = CARTESIAN_POINT ( 'NONE',  ( 13.97604488694527802, 13.89961937509977652, 104.3739096053143385 ) ) ;
#157223 = CARTESIAN_POINT ( 'NONE',  ( -16.55341960407611168, -4.379528057220339221, 56.45724293864768839 ) ) ;
#157224 = ADVANCED_FACE ( 'NONE', ( #139931, #16611 ), #137961, .F. ) ;
#157225 = CARTESIAN_POINT ( 'NONE',  ( -0.05219959533910754901, -16.53943276465976808, 22.49890960531436335 ) ) ;
#157226 = CARTESIAN_POINT ( 'NONE',  ( 16.53943276465976808, -0.05219959533910856209, 43.74890960531435979 ) ) ;
#157227 = CARTESIAN_POINT ( 'NONE',  ( -17.06066397988011829, -17.30472558578613729, -54.21489346206830362 ) ) ;
#157228 = CARTESIAN_POINT ( 'NONE',  ( 16.51473224551083163, -9.474510206698727899, 40.83442372801900433 ) ) ;
#157229 = CARTESIAN_POINT ( 'NONE',  ( 9.474510206698971260, -16.51473224551069308, 72.91557627198102409 ) ) ;
#157230 = CARTESIAN_POINT ( 'NONE',  ( 5.153800228976615827, -19.02544592524334988, 50.20942372801897591 ) ) ;
#157231 = CARTESIAN_POINT ( 'NONE',  ( 22.81625015709510151, -31.40387420917324590, -10.42499999726881477 ) ) ;
#157232 = CARTESIAN_POINT ( 'NONE',  ( 17.50000000000000000, 5.499999999999997335, 120.0000000000000142 ) ) ;
#157234 = CARTESIAN_POINT ( 'NONE',  ( 16.55341960407618274, -4.379528057220086978, 81.04275706135236135 ) ) ;
#157233 = CARTESIAN_POINT ( 'NONE',  ( -13.89961937509957401, -13.97604488694547875, 89.37609039468563310 ) ) ;
#157235 = CARTESIAN_POINT ( 'NONE',  ( 19.02544592524343514, -5.153800228976328945, 98.54057627198100988 ) ) ;
#157236 = CARTESIAN_POINT ( 'NONE',  ( -18.62759615963255300, -10.81492255796106328, 34.16775706135234714 ) ) ;
#157237 = CARTESIAN_POINT ( 'NONE',  ( 19.02544592524334988, 5.153800228976608722, 91.45942372801900433 ) ) ;
#157239 = CARTESIAN_POINT ( 'NONE',  ( 5.153800228976335163, 19.02544592524342804, 49.79057627198100988 ) ) ;
#157238 = CARTESIAN_POINT ( 'NONE',  ( 16.88567814943163725, 6.947325034625719375, 88.79001122652589117 ) ) ;
#157240 = CARTESIAN_POINT ( 'NONE',  ( 19.05341960407611168, 5.049401038298154454, 103.9572429386476671 ) ) ;
#157242 = CARTESIAN_POINT ( 'NONE',  ( 19.05341960407611168, 5.049401038298154454, 43.95724293864769550 ) ) ;
#157241 = CARTESIAN_POINT ( 'NONE',  ( -16.52544592524342804, 4.483927247898546575, 56.04057627198102409 ) ) ;
#157243 = CARTESIAN_POINT ( 'NONE',  ( -19.02544592524342804, 5.153800228976336051, 61.04057627198103120 ) ) ;
#157244 = CARTESIAN_POINT ( 'NONE',  ( -16.51473224551082808, 9.474510206698731452, 68.33442372801900433 ) ) ;
#157245 = CARTESIAN_POINT ( 'NONE',  ( 19.02544592524334988, 5.153800228976608722, 26.45942372801899722 ) ) ;
#157246 = CARTESIAN_POINT ( 'NONE',  ( 13.97604488694527802, 13.89961937509977652, 64.37390960531436690 ) ) ;
#157247 = CARTESIAN_POINT ( 'NONE',  ( -0.05219959533907301413, -21.53943276465977519, 72.49890960531435269 ) ) ;
#157249 = CARTESIAN_POINT ( 'NONE',  ( -13.89961937509957401, -13.97604488694547875, 34.37609039468566863 ) ) ;
#157248 = CARTESIAN_POINT ( 'NONE',  ( -16.52544592524342804, 4.483927247898546575, 71.04057627198103830 ) ) ;
#157250 = CARTESIAN_POINT ( 'NONE',  ( -19.02544592524342804, 5.153800228976336051, 116.0405762719810383 ) ) ;
#157251 = CARTESIAN_POINT ( 'NONE',  ( -10.72451020669898014, 18.67979575497178502, 40.41557627198103120 ) ) ;
#157252 = CARTESIAN_POINT ( 'NONE',  ( 18.67979575497178502, 10.72451020669898547, 24.16557627198103120 ) ) ;
#157253 = CARTESIAN_POINT ( 'NONE',  ( 16.46253265017160672, -9.564922557960803928, 53.33224293864768839 ) ) ;
#157254 = CARTESIAN_POINT ( 'NONE',  ( 5.153800228976335163, 19.02544592524342804, 34.79057627198102409 ) ) ;
#157255 = CARTESIAN_POINT ( 'NONE',  ( 8.314922557960818139, 14.29746914071049879, 104.5822429386477097 ) ) ;
#157256 = CARTESIAN_POINT ( 'NONE',  ( -21.53943276465977519, 0.05219959533907696930, 111.2489096053143669 ) ) ;
#157257 = CARTESIAN_POINT ( 'NONE',  ( 13.89961937509977652, -13.97604488694527269, 113.1239096053143527 ) ) ;
#157258 = CARTESIAN_POINT ( 'NONE',  ( 15.72974639402176855, 15.80617190586768217, 21.87609039468567573 ) ) ;
#157259 = CARTESIAN_POINT ( 'NONE',  ( -16.52544592524342804, 4.483927247898546575, 116.0405762719810383 ) ) ;
#157260 = CARTESIAN_POINT ( 'NONE',  ( -18.62759615963270932, 10.81492255796079327, 90.83224293864769550 ) ) ;
#157261 = CARTESIAN_POINT ( 'NONE',  ( 16.46253265017146816, 9.564922557961045513, 41.66775706135234003 ) ) ;
#157262 = CARTESIAN_POINT ( 'NONE',  ( -19.05341960407611168, -5.049401038298163336, 26.45724293864769550 ) ) ;
#157263 = CARTESIAN_POINT ( 'NONE',  ( -13.97604488694527625, -13.89961937509977652, 26.87390960531434558 ) ) ;
#157264 = CARTESIAN_POINT ( 'NONE',  ( -8.224510206698735004, -14.34966873604973081, 44.58442372801901854 ) ) ;
#157265 = CARTESIAN_POINT ( 'NONE',  ( -0.05219959533909027116, -19.03943276465977164, 27.49890960531435624 ) ) ;
#157266 = DIRECTION ( 'NONE',  ( 1.000000000000000000, -0.000000000000000000, -0.000000000000000000 ) ) ;
#157267 = CARTESIAN_POINT ( 'NONE',  ( -13.97604488694527625, -13.89961937509977652, 76.87390960531433848 ) ) ;
#157268 = CARTESIAN_POINT ( 'NONE',  ( -8.314922557960811034, -14.29746914071050412, 107.0822429386476955 ) ) ;
#157269 = CARTESIAN_POINT ( 'NONE',  ( 0.05219959533907565091, 21.53943276465977519, 44.99890960531435979 ) ) ;
#157270 = CARTESIAN_POINT ( 'NONE',  ( -8.314922557960811034, -14.29746914071050412, 82.08224293864768129 ) ) ;
#157271 = CARTESIAN_POINT ( 'NONE',  ( 14.34966873604972726, -8.224510206698740333, 35.83442372801901143 ) ) ;
#157272 = CARTESIAN_POINT ( 'NONE',  ( -18.62759615963255300, -10.81492255796106328, 84.16775706135234714 ) ) ;
#157273 = CARTESIAN_POINT ( 'NONE',  ( 0.05219959533909260263, 19.03943276465977164, 29.99890960531435979 ) ) ;
#157274 = CARTESIAN_POINT ( 'NONE',  ( -16.52544592524335698, -4.483927247898792601, 93.95942372801903275 ) ) ;
#157275 = CARTESIAN_POINT ( 'NONE',  ( 16.55341960407611168, 4.379528057220329451, 43.95724293864769550 ) ) ;
#157276 = CARTESIAN_POINT ( 'NONE',  ( 9.564922557960805705, 16.46253265017160317, 49.58224293864770260 ) ) ;
#157277 = CARTESIAN_POINT ( 'NONE',  ( 5.823673210054444382, -21.52544592524334988, 95.20942372801903275 ) ) ;
#157278 = CARTESIAN_POINT ( 'NONE',  ( 18.62759615963271287, -10.81492255796078972, 108.3322429386477097 ) ) ;
#157279 = CARTESIAN_POINT ( 'NONE',  ( -0.05219959533937732626, 21.53943276465977519, 67.50109039468568994 ) ) ;
#157280 = CARTESIAN_POINT ( 'NONE',  ( 12.06949235617739724, 12.14591786802326823, 41.87609039468568284 ) ) ;
#157282 = CARTESIAN_POINT ( 'NONE',  ( -21.55341960407619339, 5.719274019375674811, 88.54275706135236135 ) ) ;
#157281 = CARTESIAN_POINT ( 'NONE',  ( 14.29746914071049879, -8.314922557960816363, 68.33224293864769550 ) ) ;
#157283 = EDGE_CURVE ( 'NONE', #60925, #168659, #39351, .T. ) ;
#157284 = CARTESIAN_POINT ( 'NONE',  ( 4.379528057220092307, 16.55341960407617563, 107.2927570613523471 ) ) ;
#157285 = CARTESIAN_POINT ( 'NONE',  ( -17.12812012977025589, 6.668231424565989052, 113.6405124067685790 ) ) ;
#157286 = DIRECTION ( 'NONE',  ( -0.000000000000000000, -0.4999999999999999445, -0.8660254037844387076 ) ) ;
#157287 = CARTESIAN_POINT ( 'NONE',  ( -4.379528057220328563, 16.55341960407611168, 35.20724293864768839 ) ) ;
#157288 = CARTESIAN_POINT ( 'NONE',  ( -16.55341960407617563, 4.379528057220093196, 68.54275706135234714 ) ) ;
#157289 = CARTESIAN_POINT ( 'NONE',  ( -16.51473224551069308, -9.474510206698971260, 81.66557627198103830 ) ) ;
#157290 = CARTESIAN_POINT ( 'NONE',  ( 5.049401038298161559, -19.05341960407611168, 102.7072429386476955 ) ) ;
#157291 = CARTESIAN_POINT ( 'NONE',  ( 5.823673210054444382, -21.52544592524334988, 100.2094237280190043 ) ) ;
#157292 = CARTESIAN_POINT ( 'NONE',  ( -8.224510206698735004, -14.34966873604973081, 99.58442372801900433 ) ) ;
#157293 = CARTESIAN_POINT ( 'NONE',  ( 12.14591786802309770, 12.06949235617756955, 79.37390960531436690 ) ) ;
#157294 = CARTESIAN_POINT ( 'NONE',  ( 16.51473224551069308, 9.474510206698969483, 84.16557627198102409 ) ) ;
#157295 = ORIENTED_EDGE ( 'NONE', *, *, #57355, .F. ) ;
#157296 = CARTESIAN_POINT ( 'NONE',  ( 8.314922557961029526, -14.29746914071037800, 25.41775706135235779 ) ) ;
#157297 = CARTESIAN_POINT ( 'NONE',  ( 19.03943276465977164, -0.05219959533909143690, 33.74890960531435979 ) ) ;
#157298 = CARTESIAN_POINT ( 'NONE',  ( -19.02544592524342804, 5.153800228976336051, 86.04057627198103830 ) ) ;
#157300 = CARTESIAN_POINT ( 'NONE',  ( 17.97214573761831247, 5.500000000000079048, 68.96970049038654338 ) ) ;
#157299 = CARTESIAN_POINT ( 'NONE',  ( 4.379528057220092307, 16.55341960407617563, 37.29275706135235424 ) ) ;
#157301 = CARTESIAN_POINT ( 'NONE',  ( -10.81492255796105439, 18.62759615963255655, 112.9177570613523329 ) ) ;
#157302 = CARTESIAN_POINT ( 'NONE',  ( 8.314922557961029526, -14.29746914071037800, 90.41775706135236135 ) ) ;
#157303 = CARTESIAN_POINT ( 'NONE',  ( 5.153800228976615827, -19.02544592524334988, 100.2094237280190043 ) ) ;
#157304 = CARTESIAN_POINT ( 'NONE',  ( -13.97604488694527625, -13.89961937509977652, 26.87390960531434558 ) ) ;
#157305 = CARTESIAN_POINT ( 'NONE',  ( -16.55341960407617563, 4.379528057220093196, 78.54275706135236135 ) ) ;
#157306 = CARTESIAN_POINT ( 'NONE',  ( 4.483927247898790824, -16.52544592524335698, 65.20942372801901854 ) ) ;
#157307 = CARTESIAN_POINT ( 'NONE',  ( 27.70335742114823319, -28.85434677204553111, -5.143381789178917529 ) ) ;
#157308 = CARTESIAN_POINT ( 'NONE',  ( 5.153800228976615827, -19.02544592524334988, 75.20942372801896170 ) ) ;
#157309 = CARTESIAN_POINT ( 'NONE',  ( 0.05219959533937995610, -21.53943276465977519, 105.0010903946856757 ) ) ;
#157310 = CARTESIAN_POINT ( 'NONE',  ( -19.03943276465977164, 0.05219959533909376836, 51.24890960531436690 ) ) ;
#157311 = CARTESIAN_POINT ( 'NONE',  ( 19.02544592524343514, -5.153800228976328945, 98.54057627198100988 ) ) ;
#157312 = CARTESIAN_POINT ( 'NONE',  ( 12.14591786802309770, 12.06949235617756955, 84.37390960531438111 ) ) ;
#157313 = AXIS2_PLACEMENT_3D ( 'NONE', #78641, #31165, #155495 ) ;
#157314 = EDGE_CURVE ( 'NONE', #49756, #40748, #159077, .T. ) ;
#157315 = CARTESIAN_POINT ( 'NONE',  ( -5.153800228976607833, 19.02544592524334988, 57.70942372801899012 ) ) ;
#157316 = CARTESIAN_POINT ( 'NONE',  ( -10.81492255796078084, -18.62759615963271287, 47.08224293864770260 ) ) ;
#157317 = CARTESIAN_POINT ( 'NONE',  ( 0.05219959533936267826, -19.03943276465977164, 20.00109039468567218 ) ) ;
#157318 = CARTESIAN_POINT ( 'NONE',  ( 9.474510206698971260, -16.51473224551069308, 87.91557627198102409 ) ) ;
#157319 = CARTESIAN_POINT ( 'NONE',  ( 10.72451020669871369, 18.67979575497193778, 112.0844237280190185 ) ) ;
#157320 = CARTESIAN_POINT ( 'NONE',  ( -18.67979575497178146, -10.72451020669898902, 61.66557627198103120 ) ) ;
#157321 = CARTESIAN_POINT ( 'NONE',  ( 19.05341960407611168, 5.049401038298154454, 98.95724293864766707 ) ) ;
#157322 = CIRCLE ( 'NONE', #105658, 2.649999999999999467 ) ;
#157323 = CARTESIAN_POINT ( 'NONE',  ( 13.89961937509957401, 13.97604488694547697, 91.87609039468567573 ) ) ;
#157324 = CARTESIAN_POINT ( 'NONE',  ( -16.51473224551069308, -9.474510206698971260, 111.6655762719810383 ) ) ;
#157325 = CARTESIAN_POINT ( 'NONE',  ( 16.46253265017146816, 9.564922557961045513, 106.6677570613523471 ) ) ;
#157326 = CARTESIAN_POINT ( 'NONE',  ( -4.379528057220328563, 16.55341960407611168, 110.2072429386477239 ) ) ;
#157327 = CARTESIAN_POINT ( 'NONE',  ( -0.05219959533909027116, -19.03943276465977164, 87.49890960531436690 ) ) ;
#157328 = CARTESIAN_POINT ( 'NONE',  ( 0.05219959533907565091, 21.53943276465977519, 74.99890960531435269 ) ) ;
#157329 = CARTESIAN_POINT ( 'NONE',  ( 0.05219959533934541429, -16.53943276465976808, 50.00109039468568994 ) ) ;
#157330 = CARTESIAN_POINT ( 'NONE',  ( 15.72974639402176855, 15.80617190586768217, 51.87609039468568284 ) ) ;
#157331 = CARTESIAN_POINT ( 'NONE',  ( -21.52544592524334988, -5.823673210054445271, 93.95942372801903275 ) ) ;
#157332 = CARTESIAN_POINT ( 'NONE',  ( 12.06949235617739724, 12.14591786802326823, 96.87609039468568994 ) ) ;
#157333 = CARTESIAN_POINT ( 'NONE',  ( -9.564922557960796823, -16.46253265017161027, 82.08224293864768129 ) ) ;
#157334 = CARTESIAN_POINT ( 'NONE',  ( -0.05219959533910754901, -16.53943276465976808, 87.49890960531436690 ) ) ;
#157335 = CARTESIAN_POINT ( 'NONE',  ( 14.29746914071049879, -8.314922557960816363, 28.33224293864769550 ) ) ;
#157336 = CARTESIAN_POINT ( 'NONE',  ( -5.153800228976607833, 19.02544592524334988, 72.70942372801900433 ) ) ;
#157337 = CARTESIAN_POINT ( 'NONE',  ( -21.53943276465977519, -0.05219959533937600094, 43.75109039468568284 ) ) ;
#157338 = CARTESIAN_POINT ( 'NONE',  ( -16.51473224551082808, 9.474510206698731452, 23.33442372801900078 ) ) ;
#157339 = CARTESIAN_POINT ( 'NONE',  ( 4.483927247898545687, 16.52544592524342804, 94.79057627198105251 ) ) ;
#157340 = CARTESIAN_POINT ( 'NONE',  ( -19.03943276465977164, 0.05219959533909376836, 111.2489096053143669 ) ) ;
#157341 = CARTESIAN_POINT ( 'NONE',  ( 12.14591786802309770, 12.06949235617756955, 24.37390960531435979 ) ) ;
#157342 = CARTESIAN_POINT ( 'NONE',  ( -15.72974639402176322, -15.80617190586768395, 79.37609039468567573 ) ) ;
#157343 = CARTESIAN_POINT ( 'NONE',  ( -14.29746914071037622, -8.314922557961029526, 59.16775706135234714 ) ) ;
#157344 = CARTESIAN_POINT ( 'NONE',  ( 4.483927247898790824, -16.52544592524335698, 100.2094237280190043 ) ) ;
#157345 = CARTESIAN_POINT ( 'NONE',  ( 15.80617190586769283, -15.72974639402175789, 55.62609039468568284 ) ) ;
#157346 = ORIENTED_EDGE ( 'NONE', *, *, #42622, .T. ) ;
#157347 = CARTESIAN_POINT ( 'NONE',  ( 18.67979575497194134, -10.72451020669871369, 30.83442372801902209 ) ) ;
#157348 = CARTESIAN_POINT ( 'NONE',  ( -14.29746914071049879, 8.314922557960819915, 110.8322429386476955 ) ) ;
#157349 = CARTESIAN_POINT ( 'NONE',  ( -0.05219959533909027116, -19.03943276465977164, 22.49890960531436690 ) ) ;
#157350 = CARTESIAN_POINT ( 'NONE',  ( 4.379528057220339221, -16.55341960407611168, 62.70724293864769550 ) ) ;
#157351 = CARTESIAN_POINT ( 'NONE',  ( 16.51473224551069308, 9.474510206698969483, 69.16557627198102409 ) ) ;
#157352 = CARTESIAN_POINT ( 'NONE',  ( -0.05219959533934338120, 16.53943276465976808, 102.5010903946856899 ) ) ;
#157353 = CARTESIAN_POINT ( 'NONE',  ( 13.89961937509977652, -13.97604488694527269, 33.12390960531434558 ) ) ;
#157354 = CARTESIAN_POINT ( 'NONE',  ( -10.81492255796078084, -18.62759615963271287, 52.08224293864768839 ) ) ;
#157355 = CARTESIAN_POINT ( 'NONE',  ( -0.05219959533910754901, -16.53943276465976808, 92.49890960531436690 ) ) ;
#157356 = TOROIDAL_SURFACE ( 'NONE', #183203, 2.199999999999999289, 0.2000000000000000111 ) ;
#157357 = CARTESIAN_POINT ( 'NONE',  ( -5.719274019375978568, 21.55341960407610458, 90.20724293864770971 ) ) ;
#157358 = CARTESIAN_POINT ( 'NONE',  ( -0.05219959533909027116, -19.03943276465977164, 107.4989096053143527 ) ) ;
#157360 = CARTESIAN_POINT ( 'NONE',  ( -13.89961937509957401, -13.97604488694547875, 94.37609039468566152 ) ) ;
#157359 = CARTESIAN_POINT ( 'NONE',  ( -13.97604488694527625, -13.89961937509977652, 46.87390960531435979 ) ) ;
#157361 = CARTESIAN_POINT ( 'NONE',  ( 21.55341960407610458, 5.719274019375980345, 43.95724293864769550 ) ) ;
#157362 = CARTESIAN_POINT ( 'NONE',  ( 15.80617190586769283, -15.72974639402175789, 65.62609039468568994 ) ) ;
#157363 = CARTESIAN_POINT ( 'NONE',  ( -9.564922557960796823, -16.46253265017161027, 52.08224293864768839 ) ) ;
#157364 = CARTESIAN_POINT ( 'NONE',  ( -9.474510206698964154, 16.51473224551069663, 85.41557627198102409 ) ) ;
#157365 = CARTESIAN_POINT ( 'NONE',  ( 8.224510206698742110, 14.34966873604972548, 62.08442372801901143 ) ) ;
#157366 = CARTESIAN_POINT ( 'NONE',  ( -21.55341960407619339, 5.719274019375674811, 43.54275706135235424 ) ) ;
#157367 = CARTESIAN_POINT ( 'NONE',  ( 5.719274019375673035, 21.55341960407619339, 77.29275706135234714 ) ) ;
#157368 = CARTESIAN_POINT ( 'NONE',  ( -13.97604488694527625, -13.89961937509977652, 111.8739096053143243 ) ) ;
#157369 = CARTESIAN_POINT ( 'NONE',  ( 0.05219959533907565091, 21.53943276465977519, 94.99890960531436690 ) ) ;
#157371 = CARTESIAN_POINT ( 'NONE',  ( 8.314922557961029526, -14.29746914071037800, 60.41775706135235424 ) ) ;
#157370 = CARTESIAN_POINT ( 'NONE',  ( 21.53943276465977519, 0.05219959533937863772, 36.25109039468567573 ) ) ;
#157372 = CARTESIAN_POINT ( 'NONE',  ( -21.52544592524343514, 5.823673210054127303, 61.04057627198103120 ) ) ;
#157373 = CARTESIAN_POINT ( 'NONE',  ( -9.564922557961040184, 16.46253265017147172, 27.91775706135232582 ) ) ;
#157374 = B_SPLINE_CURVE_WITH_KNOTS ( 'NONE', 3,
 ( #148128, #164305, #106579, #183438, #153076, #92393, #381, #168256, #44923, #136923, #121746, #29752, #14578, #107561, #152101, #93386, #198610, #169239, #76236, #182451 ),
 .UNSPECIFIED., .F., .F.,
 ( 4, 2, 2, 2, 2, 2, 2, 2, 2, 4 ),
 ( 0.004000878361812006817, 0.004499404418916007169, 0.004997930476020007520, 0.005496456533124007005, 0.005994982590228007356, 0.006244245618780007098, 0.006493508647332007708, 0.006992034704436007192, 0.007490560761540007544, 0.007989086818644007895 ),
 .UNSPECIFIED. ) ;
#157376 = CARTESIAN_POINT ( 'NONE',  ( 0.05219959533934541429, -16.53943276465976808, 110.0010903946856757 ) ) ;
#157375 = CARTESIAN_POINT ( 'NONE',  ( -16.51473224551069308, -9.474510206698971260, 61.66557627198103120 ) ) ;
#157377 = CARTESIAN_POINT ( 'NONE',  ( -17.49999999999999645, -3.305555262949684270, 105.3748284784340967 ) ) ;
#157378 = CARTESIAN_POINT ( 'NONE',  ( 13.97604488694527802, 13.89961937509977652, 109.3739096053143669 ) ) ;
#157379 = DIRECTION ( 'NONE',  ( -1.000000000000000000, 0.000000000000000000, 0.000000000000000000 ) ) ;
#157380 = CARTESIAN_POINT ( 'NONE',  ( 19.03943276465977164, 0.05219959533936151252, 86.25109039468567573 ) ) ;
#157381 = CARTESIAN_POINT ( 'NONE',  ( -21.55341960407610458, -5.719274019375992779, 56.45724293864768839 ) ) ;
#157382 = CARTESIAN_POINT ( 'NONE',  ( 8.224510206698953496, -14.34966873604960469, 37.91557627198102409 ) ) ;
#157383 = CARTESIAN_POINT ( 'NONE',  ( 0.05219959533936267826, -19.03943276465977164, 110.0010903946856757 ) ) ;
#157384 = CARTESIAN_POINT ( 'NONE',  ( -19.03943276465977164, 0.05219959533909376836, 31.24890960531435979 ) ) ;
#157385 = CARTESIAN_POINT ( 'NONE',  ( 13.89961937509957401, 13.97604488694547697, 111.8760903946856757 ) ) ;
#157387 = CARTESIAN_POINT ( 'NONE',  ( 16.46253265017146816, 9.564922557961045513, 56.66775706135233293 ) ) ;
#157386 = CARTESIAN_POINT ( 'NONE',  ( -21.53943276465977519, 0.05219959533907696930, 91.24890960531436690 ) ) ;
#157388 = CARTESIAN_POINT ( 'NONE',  ( 14.29746914071037800, 8.314922557961029526, 81.66775706135236135 ) ) ;
#157389 = CARTESIAN_POINT ( 'NONE',  ( -19.03943276465977164, 0.05219959533909376836, 71.24890960531435269 ) ) ;
#157390 = CARTESIAN_POINT ( 'NONE',  ( -12.14591786802309592, -12.06949235617757132, 81.87390960531435269 ) ) ;
#157391 = CARTESIAN_POINT ( 'NONE',  ( 5.153800228976335163, 19.02544592524342804, 44.79057627198103830 ) ) ;
#157392 = CARTESIAN_POINT ( 'NONE',  ( 12.06949235617757843, -12.14591786802309237, 53.12390960531436690 ) ) ;
#157393 = DIRECTION ( 'NONE',  ( -1.000000000000000000, 0.000000000000000000, 0.000000000000000000 ) ) ;
#157394 = CARTESIAN_POINT ( 'NONE',  ( 32.22964258392465808, -4.577260022299252107, 89.03854312871816035 ) ) ;
#157395 = CARTESIAN_POINT ( 'NONE',  ( 14.29746914071049879, -8.314922557960816363, 28.33224293864769550 ) ) ;
#157396 = CARTESIAN_POINT ( 'NONE',  ( 19.02544592524343514, -5.153800228976328945, 78.54057627198099567 ) ) ;
#157397 = CARTESIAN_POINT ( 'NONE',  ( -30.00000000000000000, -5.510910596163089556E-15, 47.50000000000000000 ) ) ;
#157398 = CARTESIAN_POINT ( 'NONE',  ( -16.51473224551082808, 9.474510206698731452, 43.33442372801900433 ) ) ;
#157399 = CARTESIAN_POINT ( 'NONE',  ( 12.14591786802327356, -12.06949235617739191, 40.62609039468567573 ) ) ;
#157400 = CARTESIAN_POINT ( 'NONE',  ( 5.823673210054125526, 21.52544592524343514, 69.79057627198102409 ) ) ;
#157401 = CARTESIAN_POINT ( 'NONE',  ( -9.474510206698720793, -16.51473224551083518, 24.58442372801900078 ) ) ;
#157402 = CARTESIAN_POINT ( 'NONE',  ( 19.02544592524343514, -5.153800228976328945, 68.54057627198103830 ) ) ;
#157403 = DIRECTION ( 'NONE',  ( 1.000000000000000000, 0.000000000000000000, -0.000000000000000000 ) ) ;
#157404 = CARTESIAN_POINT ( 'NONE',  ( 9.564922557960805705, 16.46253265017160317, 104.5822429386476955 ) ) ;
#157405 = CARTESIAN_POINT ( 'NONE',  ( 15.80617190586769283, -15.72974639402175789, 40.62609039468567573 ) ) ;
#157406 = CARTESIAN_POINT ( 'NONE',  ( -12.06949235617756955, 12.14591786802309770, 110.6239096053143669 ) ) ;
#157409 = ORIENTED_EDGE ( 'NONE', *, *, #100701, .T. ) ;
#157408 = CARTESIAN_POINT ( 'NONE',  ( -9.564922557960796823, -16.46253265017161027, 82.08224293864768129 ) ) ;
#157407 = CARTESIAN_POINT ( 'NONE',  ( 5.823673210054125526, 21.52544592524343514, 99.79057627198103830 ) ) ;
#157410 = CARTESIAN_POINT ( 'NONE',  ( -15.80617190586768217, 15.72974639402176855, 23.12609039468567573 ) ) ;
#157411 = ORIENTED_EDGE ( 'NONE', *, *, #147245, .T. ) ;
#157412 = CARTESIAN_POINT ( 'NONE',  ( -5.049401038298153566, 19.05341960407611168, 85.20724293864766707 ) ) ;
#157413 = CARTESIAN_POINT ( 'NONE',  ( -31.74999999999995737, 0.000000000000000000, 4.250000000000000000 ) ) ;
#157414 = CARTESIAN_POINT ( 'NONE',  ( 13.97604488694527802, 13.89961937509977652, 39.37390960531435269 ) ) ;
#157415 = CARTESIAN_POINT ( 'NONE',  ( -5.049401038297874678, -19.05341960407617918, 109.7927570613523187 ) ) ;
#157416 = CARTESIAN_POINT ( 'NONE',  ( 36.91746825000000598, -11.99521256947793546, -8.224999997268810148 ) ) ;
#157417 = CARTESIAN_POINT ( 'NONE',  ( -12.06949235617756955, 12.14591786802309770, 110.6239096053143669 ) ) ;
#157418 = CARTESIAN_POINT ( 'NONE',  ( 15.72974639402176855, 15.80617190586768217, 86.87609039468568994 ) ) ;
#157420 = CARTESIAN_POINT ( 'NONE',  ( 21.52544592524334988, 5.823673210054432836, 41.45942372801901143 ) ) ;
#157419 = CARTESIAN_POINT ( 'NONE',  ( -19.05341960407611168, -5.049401038298163336, 71.45724293864766707 ) ) ;
#157421 = CARTESIAN_POINT ( 'NONE',  ( 5.719274019375673035, 21.55341960407619339, 27.29275706135234358 ) ) ;
#157422 = CARTESIAN_POINT ( 'NONE',  ( 23.31738231874054534, 16.94106989632529192, 147.1999999999999886 ) ) ;
#157423 = CARTESIAN_POINT ( 'NONE',  ( -13.97604488694527625, -13.89961937509977652, 81.87390960531436690 ) ) ;
#157424 = DIRECTION ( 'NONE',  ( -0.000000000000000000, -0.000000000000000000, 1.000000000000000000 ) ) ;
#157426 = CARTESIAN_POINT ( 'NONE',  ( 21.53943276465977519, -0.05219959533907433946, 38.74890960531435979 ) ) ;
#157425 = CARTESIAN_POINT ( 'NONE',  ( -4.483927247898782831, 16.52544592524335698, 22.70942372801901499 ) ) ;
#157427 = CARTESIAN_POINT ( 'NONE',  ( 5.719274019375673035, 21.55341960407619339, 72.29275706135236135 ) ) ;
#157428 = CARTESIAN_POINT ( 'NONE',  ( 19.05341960407611168, 5.049401038298154454, 103.9572429386476671 ) ) ;
#157429 = CARTESIAN_POINT ( 'NONE',  ( 16.46253265017146816, 9.564922557961045513, 111.6677570613523329 ) ) ;
#157430 = CARTESIAN_POINT ( 'NONE',  ( 0.05219959533909260263, 19.03943276465977164, 64.99890960531436690 ) ) ;
#157431 = CARTESIAN_POINT ( 'NONE',  ( 16.51473224551069308, 9.474510206698969483, 84.16557627198102409 ) ) ;
#157432 = CARTESIAN_POINT ( 'NONE',  ( -14.34966873604960291, -8.224510206698953496, 101.6655762719810383 ) ) ;
#157433 = CARTESIAN_POINT ( 'NONE',  ( -16.55341960407611168, -4.379528057220339221, 111.4572429386476813 ) ) ;
#157434 = CARTESIAN_POINT ( 'NONE',  ( -16.51473224551069308, -9.474510206698971260, 106.6655762719810383 ) ) ;
#157435 = CARTESIAN_POINT ( 'NONE',  ( -16.52544592524335698, -4.483927247898792601, 78.95942372801901854 ) ) ;
#157437 = CARTESIAN_POINT ( 'NONE',  ( -19.02544592524342804, 5.153800228976336051, 56.04057627198100988 ) ) ;
#157436 = CARTESIAN_POINT ( 'NONE',  ( 8.314922557960818139, 14.29746914071049879, 59.58224293864770260 ) ) ;
#157438 = CARTESIAN_POINT ( 'NONE',  ( -15.80617190586768217, 15.72974639402176855, 78.12609039468570415 ) ) ;
#157439 = CARTESIAN_POINT ( 'NONE',  ( 21.55341960407619695, -5.719274019375665929, 71.04275706135234714 ) ) ;
#157440 = CARTESIAN_POINT ( 'NONE',  ( 0.05219959533936267826, -19.03943276465977164, 90.00109039468567573 ) ) ;
#157441 = CARTESIAN_POINT ( 'NONE',  ( -12.14591786802309592, -12.06949235617757132, 61.87390960531436690 ) ) ;
#157442 = CARTESIAN_POINT ( 'NONE',  ( 21.55341960407610458, 5.719274019375980345, 108.9572429386476955 ) ) ;
#157443 = CARTESIAN_POINT ( 'NONE',  ( 0.05219959533907565091, 21.53943276465977519, 44.99890960531435979 ) ) ;
#157444 = CARTESIAN_POINT ( 'NONE',  ( -16.19135201231367560, -7.376712067591916444, 105.1868085405203175 ) ) ;
#157445 = CARTESIAN_POINT ( 'NONE',  ( 17.81289503416611453, -24.51734667627695785, 138.9500000054623570 ) ) ;
#157446 = CARTESIAN_POINT ( 'NONE',  ( 5.153800228976335163, 19.02544592524342804, 64.79057627198100988 ) ) ;
#157447 = CARTESIAN_POINT ( 'NONE',  ( -14.29746914071049879, 8.314922557960819915, 30.83224293864770260 ) ) ;
#157448 = CIRCLE ( 'NONE', #141418, 7.500000000000000000 ) ;
#157449 = CARTESIAN_POINT ( 'NONE',  ( -12.06949235617739369, -12.14591786802326823, 109.3760903946857042 ) ) ;
#157450 = CARTESIAN_POINT ( 'NONE',  ( -4.483927247898782831, 16.52544592524335698, 87.70942372801901854 ) ) ;
#157451 = CARTESIAN_POINT ( 'NONE',  ( -19.03943276465977164, -0.05219959533935918106, 33.75109039468566863 ) ) ;
#157452 = DIRECTION ( 'NONE',  ( 0.000000000000000000, 0.000000000000000000, -1.000000000000000000 ) ) ;
#157453 = CARTESIAN_POINT ( 'NONE',  ( -19.02544592524342804, 5.153800228976336051, 96.04057627198103830 ) ) ;
#157454 = CARTESIAN_POINT ( 'NONE',  ( 8.224510206698953496, -14.34966873604960469, 57.91557627198103120 ) ) ;
#157456 = CARTESIAN_POINT ( 'NONE',  ( 21.52544592524344225, -5.823673210054117533, 28.54057627198103120 ) ) ;
#157455 = CARTESIAN_POINT ( 'NONE',  ( 13.97604488694527802, 13.89961937509977652, 24.37390960531435624 ) ) ;
#157458 = ORIENTED_EDGE ( 'NONE', *, *, #38420, .T. ) ;
#157457 = CARTESIAN_POINT ( 'NONE',  ( 10.81492255796078972, 18.62759615963270932, 59.58224293864770260 ) ) ;
#157459 = CARTESIAN_POINT ( 'NONE',  ( -16.55341960407611168, -4.379528057220339221, 101.4572429386476955 ) ) ;
#157460 = CARTESIAN_POINT ( 'NONE',  ( 0.05219959533934541429, -16.53943276465976808, 35.00109039468568284 ) ) ;
#157461 = EDGE_CURVE ( 'NONE', #172390, #26894, #111592, .T. ) ;
#157462 = CARTESIAN_POINT ( 'NONE',  ( -14.34966873604960291, -8.224510206698953496, 76.66557627198103830 ) ) ;
#157463 = CARTESIAN_POINT ( 'NONE',  ( 25.66012929990208136, 7.783344152590474962, 170.2244316400881701 ) ) ;
#157464 = CARTESIAN_POINT ( 'NONE',  ( 19.05341960407617918, -5.049401038297876454, 81.04275706135231871 ) ) ;
#157465 = CARTESIAN_POINT ( 'NONE',  ( -16.46253265017160317, 9.564922557960807481, 115.8322429386477097 ) ) ;
#157466 = CARTESIAN_POINT ( 'NONE',  ( 11.40812507854754365, 35.11059874428196537, -3.724999997268813701 ) ) ;
#157467 = CARTESIAN_POINT ( 'NONE',  ( 17.50000000000000000, 5.499999999999997335, 120.0000000000000142 ) ) ;
#157469 = CARTESIAN_POINT ( 'NONE',  ( 8.224510206698953496, -14.34966873604960469, 32.91557627198102409 ) ) ;
#157468 = CARTESIAN_POINT ( 'NONE',  ( -0.05219959533934338120, 16.53943276465976808, 27.50109039468567929 ) ) ;
#157470 = CARTESIAN_POINT ( 'NONE',  ( -5.719274019375978568, 21.55341960407610458, 60.20724293864768839 ) ) ;
#157471 = CARTESIAN_POINT ( 'NONE',  ( -19.03943276465977164, -0.05219959533935918106, 88.75109039468567573 ) ) ;
#157472 = CARTESIAN_POINT ( 'NONE',  ( 21.52544592524344225, -5.823673210054117533, 43.54057627198103830 ) ) ;
#157473 = CARTESIAN_POINT ( 'NONE',  ( 21.53943276465977519, 0.05219959533937863772, 86.25109039468568994 ) ) ;
#157474 = CARTESIAN_POINT ( 'NONE',  ( 8.969129508634463122, -36.34711360786827328, -31.52745775292089547 ) ) ;
#157475 = CARTESIAN_POINT ( 'NONE',  ( -16.55341960407617563, 4.379528057220093196, 33.54275706135234714 ) ) ;
#157477 = CARTESIAN_POINT ( 'NONE',  ( -19.02544592524342804, 5.153800228976336051, 91.04057627198100988 ) ) ;
#157476 = CARTESIAN_POINT ( 'NONE',  ( -13.97604488694527625, -13.89961937509977652, 21.87390960531435979 ) ) ;
#157478 = VECTOR ( 'NONE', #181303, 1000.000000000000000 ) ;
#157479 = CARTESIAN_POINT ( 'NONE',  ( 9.474510206698971260, -16.51473224551069308, 32.91557627198102409 ) ) ;
#157480 = CARTESIAN_POINT ( 'NONE',  ( -0.05219959533910754901, -16.53943276465976808, 107.4989096053143669 ) ) ;
#157481 = CARTESIAN_POINT ( 'NONE',  ( -19.05341960407611168, -5.049401038298163336, 101.4572429386476955 ) ) ;
#157482 = ORIENTED_EDGE ( 'NONE', *, *, #138326, .T. ) ;
#157483 = CARTESIAN_POINT ( 'NONE',  ( -8.224510206698735004, -14.34966873604973081, 59.58442372801901854 ) ) ;
#157484 = CARTESIAN_POINT ( 'NONE',  ( 18.67979575497178502, 10.72451020669898547, 94.16557627198103830 ) ) ;
#157485 = CARTESIAN_POINT ( 'NONE',  ( 5.049401038298161559, -19.05341960407611168, 37.70724293864768839 ) ) ;
#157487 = CARTESIAN_POINT ( 'NONE',  ( -18.62759615963255300, -10.81492255796106328, 34.16775706135234714 ) ) ;
#157486 = CARTESIAN_POINT ( 'NONE',  ( -5.153800228976607833, 19.02544592524334988, 72.70942372801900433 ) ) ;
#157488 = CARTESIAN_POINT ( 'NONE',  ( -5.049401038298153566, 19.05341960407611168, 65.20724293864765286 ) ) ;
#157489 = CARTESIAN_POINT ( 'NONE',  ( -19.03943276465977164, 0.05219959533909376836, 101.2489096053143669 ) ) ;
#157490 = EDGE_LOOP ( 'NONE', ( #41588, #179188, #22881, #183846 ) ) ;
#157491 = CARTESIAN_POINT ( 'NONE',  ( 4.483927247898790824, -16.52544592524335698, 40.20942372801901854 ) ) ;
#157492 = CARTESIAN_POINT ( 'NONE',  ( -15.72974639402197994, 15.80617190586746368, 115.6239096053143669 ) ) ;
#157495 = CARTESIAN_POINT ( 'NONE',  ( 19.02544592524334988, 5.153800228976608722, 76.45942372801897591 ) ) ;
#157494 = CARTESIAN_POINT ( 'NONE',  ( -9.564922557960796823, -16.46253265017161027, 92.08224293864769550 ) ) ;
#157493 = CARTESIAN_POINT ( 'NONE',  ( -16.52544592524342804, 4.483927247898546575, 101.0405762719810383 ) ) ;
#157496 = CARTESIAN_POINT ( 'NONE',  ( 15.80617190586746368, 15.72974639402197994, 89.37390960531435269 ) ) ;
#157497 = CARTESIAN_POINT ( 'NONE',  ( -4.483927247898539470, -16.52544592524342804, 47.29057627198103120 ) ) ;
#157498 = CARTESIAN_POINT ( 'NONE',  ( -9.564922557961040184, 16.46253265017147172, 22.91775706135233648 ) ) ;
#157499 = CARTESIAN_POINT ( 'NONE',  ( -16.53943276465976808, -0.05219959533934237506, 83.75109039468568994 ) ) ;
#157500 = CARTESIAN_POINT ( 'NONE',  ( -13.97604488694527625, -13.89961937509977652, 111.8739096053143243 ) ) ;
#157501 = CARTESIAN_POINT ( 'NONE',  ( 16.46253265017160672, -9.564922557960803928, 48.33224293864769550 ) ) ;
#157502 = CARTESIAN_POINT ( 'NONE',  ( 10.81492255796106328, -18.62759615963255655, 55.41775706135234714 ) ) ;
#157503 = CARTESIAN_POINT ( 'NONE',  ( 18.62759615963255655, 10.81492255796105972, 71.66775706135234714 ) ) ;
#157504 = CARTESIAN_POINT ( 'NONE',  ( 13.89961937509977652, -13.97604488694527269, 68.12390960531436690 ) ) ;
#157505 = CARTESIAN_POINT ( 'NONE',  ( -10.72451020669870658, -18.67979575497194134, 54.58442372801901143 ) ) ;
#157506 = CARTESIAN_POINT ( 'NONE',  ( -16.46253265017146816, -9.564922557961047289, 89.16775706135234714 ) ) ;
#157507 = CARTESIAN_POINT ( 'NONE',  ( 5.049401038298161559, -19.05341960407611168, 57.70724293864769550 ) ) ;
#157508 = CARTESIAN_POINT ( 'NONE',  ( -8.314922557961024197, 14.29746914071037800, 87.91775706135234714 ) ) ;
#157509 = CARTESIAN_POINT ( 'NONE',  ( 16.51473224551069308, 9.474510206698969483, 64.16557627198102409 ) ) ;
#157510 = CARTESIAN_POINT ( 'NONE',  ( 37.99626262588765258, 2.893932880411085066E-14, -2.747842220587803475 ) ) ;
#157511 = CARTESIAN_POINT ( 'NONE',  ( -9.564922557960796823, -16.46253265017161027, 47.08224293864769550 ) ) ;
#157512 = CARTESIAN_POINT ( 'NONE',  ( 10.72451020669898902, -18.67979575497178502, 87.91557627198103830 ) ) ;
#157513 = CARTESIAN_POINT ( 'NONE',  ( -14.29746914071037622, -8.314922557961029526, 69.16775706135234714 ) ) ;
#157514 = CARTESIAN_POINT ( 'NONE',  ( -23.62199046085639864, 10.84149981712537603, 165.9137635136253266 ) ) ;
#157515 = CARTESIAN_POINT ( 'NONE',  ( 16.51473224551083163, -9.474510206698727899, 25.83442372801900078 ) ) ;
#157516 = CARTESIAN_POINT ( 'NONE',  ( 13.97604488694527802, 13.89961937509977652, 69.37390960531436690 ) ) ;
#157517 = CARTESIAN_POINT ( 'NONE',  ( 16.55341960407611168, 4.379528057220329451, 53.95724293864770260 ) ) ;
#157518 = CARTESIAN_POINT ( 'NONE',  ( -16.52544592524342804, 4.483927247898546575, 101.0405762719810383 ) ) ;
#157519 = CARTESIAN_POINT ( 'NONE',  ( 9.564922557960805705, 16.46253265017160317, 104.5822429386476955 ) ) ;
#157520 = CARTESIAN_POINT ( 'NONE',  ( 16.51473224551069308, 9.474510206698969483, 89.16557627198103830 ) ) ;
#157521 = CARTESIAN_POINT ( 'NONE',  ( 18.62759615963255655, 10.81492255796105972, 56.66775706135235424 ) ) ;
#157522 = CARTESIAN_POINT ( 'NONE',  ( -19.05341960407611168, -5.049401038298163336, 106.4572429386476955 ) ) ;
#157523 = CARTESIAN_POINT ( 'NONE',  ( -19.02544592524334988, -5.153800228976617603, 18.95942372801899722 ) ) ;
#157524 = CARTESIAN_POINT ( 'NONE',  ( 12.14591786802327356, -12.06949235617739191, 85.62609039468568994 ) ) ;
#157525 = CARTESIAN_POINT ( 'NONE',  ( 5.823673210054444382, -21.52544592524334988, 35.20942372801901854 ) ) ;
#157526 = CARTESIAN_POINT ( 'NONE',  ( 9.564922557960805705, 16.46253265017160317, 109.5822429386476955 ) ) ;
#157527 = CARTESIAN_POINT ( 'NONE',  ( -15.80617190586745835, -15.72974639402198527, 96.87390960531436690 ) ) ;
#157528 = CARTESIAN_POINT ( 'NONE',  ( 4.379528057220339221, -16.55341960407611168, 62.70724293864769550 ) ) ;
#157529 = CARTESIAN_POINT ( 'NONE',  ( -5.049401038298153566, 19.05341960407611168, 60.20724293864768129 ) ) ;
#157530 = CARTESIAN_POINT ( 'NONE',  ( -12.14591786802309592, -12.06949235617757132, 81.87390960531435269 ) ) ;
#157531 = CARTESIAN_POINT ( 'NONE',  ( -10.72451020669898014, 18.67979575497178502, 30.41557627198101699 ) ) ;
#157532 = CARTESIAN_POINT ( 'NONE',  ( 13.89961937509957401, 13.97604488694547697, 41.87609039468566152 ) ) ;
#157533 = CARTESIAN_POINT ( 'NONE',  ( -8.224510206698948167, 14.34966873604960824, 110.4155762719810383 ) ) ;
#157534 = ORIENTED_EDGE ( 'NONE', *, *, #11291, .F. ) ;
#157535 = CARTESIAN_POINT ( 'NONE',  ( 14.34966873604972726, -8.224510206698740333, 65.83442372801900433 ) ) ;
#157536 = CARTESIAN_POINT ( 'NONE',  ( -13.89961937509977652, 13.97604488694528158, 65.62390960531436690 ) ) ;
#157537 = CARTESIAN_POINT ( 'NONE',  ( -27.73933785331498925, 2.428612866367529932E-14, 146.8750000027311842 ) ) ;
#157538 = CARTESIAN_POINT ( 'NONE',  ( -4.379528057220328563, 16.55341960407611168, 90.20724293864770971 ) ) ;
#157539 = CARTESIAN_POINT ( 'NONE',  ( 18.67979575497178502, 10.72451020669898547, 34.16557627198102409 ) ) ;
#157540 = CARTESIAN_POINT ( 'NONE',  ( -12.14591786802326823, 12.06949235617739902, 103.1260903946856757 ) ) ;
#157541 = CARTESIAN_POINT ( 'NONE',  ( -16.53943276465976808, -0.05219959533934237506, 18.75109039468568639 ) ) ;
#157542 = CARTESIAN_POINT ( 'NONE',  ( -18.62759615963255300, -10.81492255796106328, 79.16775706135234714 ) ) ;
#157543 = CARTESIAN_POINT ( 'NONE',  ( 19.05341960407611168, 5.049401038298154454, 88.95724293864769550 ) ) ;
#157544 = CARTESIAN_POINT ( 'NONE',  ( 18.67979575497178502, 10.72451020669898547, 99.16557627198100988 ) ) ;
#157545 = CARTESIAN_POINT ( 'NONE',  ( -12.06949235617739369, -12.14591786802326823, 49.37609039468569705 ) ) ;
#157546 = CARTESIAN_POINT ( 'NONE',  ( -9.564922557960796823, -16.46253265017161027, 37.08224293864768839 ) ) ;
#157547 = CARTESIAN_POINT ( 'NONE',  ( -16.52544592524335698, -4.483927247898792601, 28.95942372801902209 ) ) ;
#157548 = EDGE_CURVE ( 'NONE', #17604, #146728, #140467, .T. ) ;
#157549 = CARTESIAN_POINT ( 'NONE',  ( -19.02544592524334988, -5.153800228976617603, 98.95942372801900433 ) ) ;
#157550 = CARTESIAN_POINT ( 'NONE',  ( -18.67979575497178146, -10.72451020669898902, 86.66557627198102409 ) ) ;
#157551 = CARTESIAN_POINT ( 'NONE',  ( -19.03943276465977164, -0.05219959533935918106, 58.75109039468566863 ) ) ;
#157552 = CARTESIAN_POINT ( 'NONE',  ( 18.87580814761075132, -5.500000000000047073, 88.37172394265761000 ) ) ;
#157553 = CARTESIAN_POINT ( 'NONE',  ( 10.72451020669898902, -18.67979575497178502, 97.91557627198103830 ) ) ;
#157554 = CARTESIAN_POINT ( 'NONE',  ( -0.05219959533909027116, -19.03943276465977164, 72.49890960531435269 ) ) ;
#157555 = CARTESIAN_POINT ( 'NONE',  ( -5.049401038298153566, 19.05341960407611168, 80.20724293864769550 ) ) ;
#157556 = CARTESIAN_POINT ( 'NONE',  ( -14.29746914071037622, -8.314922557961029526, 34.16775706135234714 ) ) ;
#157557 = DIRECTION ( 'NONE',  ( 0.000000000000000000, 0.000000000000000000, 1.000000000000000000 ) ) ;
#157558 = CARTESIAN_POINT ( 'NONE',  ( -0.05219959533936034679, 19.03943276465977164, 57.50109039468566863 ) ) ;
#157560 = CARTESIAN_POINT ( 'NONE',  ( 12.14591786802309770, 12.06949235617756955, 59.37390960531436690 ) ) ;
#157559 = CARTESIAN_POINT ( 'NONE',  ( 15.80617190586746368, 15.72974639402197994, 114.3739096053143527 ) ) ;
#157561 = CARTESIAN_POINT ( 'NONE',  ( -5.153800228976328057, -19.02544592524343514, 67.29057627198102409 ) ) ;
#157563 = CARTESIAN_POINT ( 'NONE',  ( 19.05341960407617918, -5.049401038297876454, 36.04275706135234003 ) ) ;
#157562 = CARTESIAN_POINT ( 'NONE',  ( 8.224510206698742110, 14.34966873604972548, 32.08442372801901854 ) ) ;
#157564 = CARTESIAN_POINT ( 'NONE',  ( 15.72974639402176855, 15.80617190586768217, 51.87609039468568284 ) ) ;
#157565 = CARTESIAN_POINT ( 'NONE',  ( -19.03943276465977164, -0.05219959533935918106, 108.7510903946856615 ) ) ;
#157566 = CARTESIAN_POINT ( 'NONE',  ( -19.03943276465977164, 0.05219959533909376836, 61.24890960531436690 ) ) ;
#157567 = CARTESIAN_POINT ( 'NONE',  ( -13.89961937509957401, -13.97604488694547875, 84.37609039468567573 ) ) ;
#157568 = CARTESIAN_POINT ( 'NONE',  ( 21.55341960407619695, -5.719274019375665929, 91.04275706135236135 ) ) ;
#157569 = CARTESIAN_POINT ( 'NONE',  ( 19.03943276465977164, 0.05219959533936151252, 61.25109039468566863 ) ) ;
#157570 = CARTESIAN_POINT ( 'NONE',  ( -13.89961937509977652, 13.97604488694528158, 30.62390960531435269 ) ) ;
#157571 = CARTESIAN_POINT ( 'NONE',  ( 5.719274019375991003, -21.55341960407610458, 62.70724293864769550 ) ) ;
#157573 = CARTESIAN_POINT ( 'NONE',  ( -9.474510206698720793, -16.51473224551083518, 69.58442372801901854 ) ) ;
#157572 = CARTESIAN_POINT ( 'NONE',  ( 16.53943276465976808, -0.05219959533910856209, 63.74890960531435979 ) ) ;
#157574 = CARTESIAN_POINT ( 'NONE',  ( -17.13100169013301155, -6.664070546373100257, 24.23210164300151703 ) ) ;
#157575 = CARTESIAN_POINT ( 'NONE',  ( -9.474510206698720793, -16.51473224551083518, 34.58442372801899722 ) ) ;
#157576 = CARTESIAN_POINT ( 'NONE',  ( -14.29746914071037622, -8.314922557961029526, 94.16775706135237556 ) ) ;
#157577 = CARTESIAN_POINT ( 'NONE',  ( 12.06949235617757843, -12.14591786802309237, 48.12390960531436690 ) ) ;
#157579 = CARTESIAN_POINT ( 'NONE',  ( 8.571926809382597767, 26.38167802310806209, 140.2750000027311899 ) ) ;
#157578 = CARTESIAN_POINT ( 'NONE',  ( 18.67979575497194134, -10.72451020669871369, 90.83442372801901854 ) ) ;
#157580 = CARTESIAN_POINT ( 'NONE',  ( -5.719274019375978568, 21.55341960407610458, 90.20724293864770971 ) ) ;
#157581 = CARTESIAN_POINT ( 'NONE',  ( -13.89961937509977652, 13.97604488694528158, 50.62390960531435979 ) ) ;
#157582 = CARTESIAN_POINT ( 'NONE',  ( 10.81492255796106328, -18.62759615963255655, 70.41775706135236135 ) ) ;
#157583 = CARTESIAN_POINT ( 'NONE',  ( -16.46253265017160317, 9.564922557960807481, 55.83224293864769550 ) ) ;
#157584 = ORIENTED_EDGE ( 'NONE', *, *, #136149, .F. ) ;
#157585 = CARTESIAN_POINT ( 'NONE',  ( 13.97604488694527802, 13.89961937509977652, 64.37390960531436690 ) ) ;
#157586 = CARTESIAN_POINT ( 'NONE',  ( -4.379528057220328563, 16.55341960407611168, 105.2072429386477097 ) ) ;
#157587 = CARTESIAN_POINT ( 'NONE',  ( 15.72974639402199770, -15.80617190586745480, 23.12390960531436335 ) ) ;
#157588 = CARTESIAN_POINT ( 'NONE',  ( -16.55341960407611168, -4.379528057220339221, 56.45724293864768839 ) ) ;
#157589 = CARTESIAN_POINT ( 'NONE',  ( 19.02544592524343514, -5.153800228976328945, 28.54057627198102409 ) ) ;
#157590 = CARTESIAN_POINT ( 'NONE',  ( -16.55341960407611168, -4.379528057220339221, 91.45724293864769550 ) ) ;
#157591 = AXIS2_PLACEMENT_3D ( 'NONE', #165847, #104165, #60619 ) ;
#157592 = CARTESIAN_POINT ( 'NONE',  ( -21.52544592524343514, 5.823673210054127303, 101.0405762719810383 ) ) ;
#157593 = CARTESIAN_POINT ( 'NONE',  ( 18.62759615963255655, 10.81492255796105972, 41.66775706135235424 ) ) ;
#157594 = CARTESIAN_POINT ( 'NONE',  ( -8.224510206698735004, -14.34966873604973081, 34.58442372801900433 ) ) ;
#157595 = CARTESIAN_POINT ( 'NONE',  ( -15.80617190586745835, -15.72974639402198527, 81.87390960531435269 ) ) ;
#157596 = CARTESIAN_POINT ( 'NONE',  ( -21.53943276465977519, -0.05219959533937600094, 113.7510903946856757 ) ) ;
#157597 = CARTESIAN_POINT ( 'NONE',  ( -0.05219959533909027116, -19.03943276465977164, 97.49890960531436690 ) ) ;
#157598 = CARTESIAN_POINT ( 'NONE',  ( 5.823673210054444382, -21.52544592524334988, 40.20942372801901854 ) ) ;
#157599 = B_SPLINE_CURVE_WITH_KNOTS ( 'NONE', 3,
 ( #34676, #142839, #84151, #190354, #114491, #4318, #160009 ),
 .UNSPECIFIED., .F., .F.,
 ( 4, 3, 4 ),
 ( -4.032110379226884939E-05, 0.000000000000000000, 0.006882574723720362095 ),
 .UNSPECIFIED. ) ;
#157600 = CARTESIAN_POINT ( 'NONE',  ( 21.52544592524344225, -5.823673210054117533, 28.54057627198103120 ) ) ;
#157601 = CARTESIAN_POINT ( 'NONE',  ( 16.52544592524335698, 4.483927247898782831, 101.4594237280190185 ) ) ;
#157603 = CARTESIAN_POINT ( 'NONE',  ( -5.823673210054431948, 21.52544592524334988, 77.70942372801900433 ) ) ;
#157602 = CARTESIAN_POINT ( 'NONE',  ( 15.72974639402176855, 15.80617190586768217, 51.87609039468568284 ) ) ;
#157604 = CARTESIAN_POINT ( 'NONE',  ( -16.46253265017146816, -9.564922557961047289, 29.16775706135232937 ) ) ;
#157605 = CARTESIAN_POINT ( 'NONE',  ( -16.53943276465976808, -0.05219959533934237506, 93.75109039468567573 ) ) ;
#157606 = CARTESIAN_POINT ( 'NONE',  ( -18.67979575497193778, 10.72451020669871902, 48.33442372801902565 ) ) ;
#157607 = CARTESIAN_POINT ( 'NONE',  ( 16.46253265017160672, -9.564922557960803928, 48.33224293864769550 ) ) ;
#157608 = CARTESIAN_POINT ( 'NONE',  ( -21.53943276465977519, -0.05219959533937600094, 98.75109039468568994 ) ) ;
#157609 = CARTESIAN_POINT ( 'NONE',  ( 16.46253265017160672, -9.564922557960803928, 108.3322429386476955 ) ) ;
#157610 = CARTESIAN_POINT ( 'NONE',  ( -15.80617190586745835, -15.72974639402198527, 101.8739096053143811 ) ) ;
#157611 = CARTESIAN_POINT ( 'NONE',  ( -5.719274019375978568, 21.55341960407610458, 55.20724293864770260 ) ) ;
#157613 = CARTESIAN_POINT ( 'NONE',  ( 18.62759615963271287, -10.81492255796078972, 63.33224293864770260 ) ) ;
#157612 = FACE_OUTER_BOUND ( 'NONE', #163117, .T. ) ;
#157615 = CARTESIAN_POINT ( 'NONE',  ( 4.483927247898545687, 16.52544592524342804, 69.79057627198102409 ) ) ;
#157614 = CARTESIAN_POINT ( 'NONE',  ( -16.55341960407617563, 4.379528057220093196, 48.54275706135234714 ) ) ;
#157616 = CARTESIAN_POINT ( 'NONE',  ( 5.374011537017776341, 5.374011537017758577, -64.92279855667830191 ) ) ;
#157617 = CARTESIAN_POINT ( 'NONE',  ( 5.153800228976615827, -19.02544592524334988, 90.20942372801900433 ) ) ;
#157618 = CIRCLE ( 'NONE', #96249, 2.500000000000000000 ) ;
#157619 = CARTESIAN_POINT ( 'NONE',  ( -9.285066906530433428, -10.36274924941840681, -60.36157103788103484 ) ) ;
#157620 = CARTESIAN_POINT ( 'NONE',  ( 14.34966873604972726, -8.224510206698740333, 20.83442372801901143 ) ) ;
#157621 = CARTESIAN_POINT ( 'NONE',  ( 18.62759615963271287, -10.81492255796078972, 103.3322429386476955 ) ) ;
#157622 = CARTESIAN_POINT ( 'NONE',  ( 15.80617190586746368, 15.72974639402197994, 79.37390960531436690 ) ) ;
#157623 = CARTESIAN_POINT ( 'NONE',  ( -9.474510206698964154, 16.51473224551069663, 115.4155762719810241 ) ) ;
#157624 = CARTESIAN_POINT ( 'NONE',  ( -12.06949235617739369, -12.14591786802326823, 54.37609039468568994 ) ) ;
#157625 = CARTESIAN_POINT ( 'NONE',  ( 0.05219959533909260263, 19.03943276465977164, 64.99890960531436690 ) ) ;
#157627 = CARTESIAN_POINT ( 'NONE',  ( -13.97604488694547697, 13.89961937509957934, 113.1260903946856757 ) ) ;
#157626 = CARTESIAN_POINT ( 'NONE',  ( -5.823673210054431948, 21.52544592524334988, 37.70942372801900433 ) ) ;
#157628 = CARTESIAN_POINT ( 'NONE',  ( 9.564922557960805705, 16.46253265017160317, 114.5822429386476955 ) ) ;
#157629 = ORIENTED_EDGE ( 'NONE', *, *, #145916, .T. ) ;
#157630 = CARTESIAN_POINT ( 'NONE',  ( 13.97604488694527802, 13.89961937509977652, 94.37390960531436690 ) ) ;
#157631 = CARTESIAN_POINT ( 'NONE',  ( 10.72451020669898902, -18.67979575497178502, 87.91557627198103830 ) ) ;
#157632 = CARTESIAN_POINT ( 'NONE',  ( -19.02544592524342804, 5.153800228976336051, 61.04057627198103120 ) ) ;
#157633 = FACE_OUTER_BOUND ( 'NONE', #67790, .T. ) ;
#157634 = CARTESIAN_POINT ( 'NONE',  ( 4.379528057220339221, -16.55341960407611168, 72.70724293864769550 ) ) ;
#157635 = CARTESIAN_POINT ( 'NONE',  ( 16.51473224551069308, 9.474510206698969483, 114.1655762719810241 ) ) ;
#157636 = CARTESIAN_POINT ( 'NONE',  ( -29.77433414031400716, 1.366177905283920024, -51.67655205196553680 ) ) ;
#157637 = CARTESIAN_POINT ( 'NONE',  ( 10.72451020669898902, -18.67979575497178502, 102.9155762719810383 ) ) ;
#157638 = CARTESIAN_POINT ( 'NONE',  ( 9.474510206698729675, 16.51473224551082808, 67.08442372801900433 ) ) ;
#157639 = CARTESIAN_POINT ( 'NONE',  ( 19.03943276465977164, -0.05219959533909143690, 108.7489096053143527 ) ) ;
#157640 = CARTESIAN_POINT ( 'NONE',  ( -16.46253265017160317, 9.564922557960807481, 30.83224293864769550 ) ) ;
#157641 = CARTESIAN_POINT ( 'NONE',  ( 18.67979575497178502, 10.72451020669898547, 59.16557627198103120 ) ) ;
#157642 = CARTESIAN_POINT ( 'NONE',  ( 9.474510206698971260, -16.51473224551069308, 97.91557627198102409 ) ) ;
#157643 = CARTESIAN_POINT ( 'NONE',  ( -0.05219959533937732626, 21.53943276465977519, 77.50109039468567573 ) ) ;
#157644 = CARTESIAN_POINT ( 'NONE',  ( 13.97604488694527802, 13.89961937509977652, 54.37390960531435979 ) ) ;
#157645 = CARTESIAN_POINT ( 'NONE',  ( 12.06949235617757843, -12.14591786802309237, 93.12390960531436690 ) ) ;
#157646 = CARTESIAN_POINT ( 'NONE',  ( 12.06949235617739724, 12.14591786802326823, 41.87609039468568284 ) ) ;
#157647 = CARTESIAN_POINT ( 'NONE',  ( -5.719274019375665041, -21.55341960407619695, 59.79275706135234714 ) ) ;
#157648 = VERTEX_POINT ( 'NONE', #144910 ) ;
#157649 = CARTESIAN_POINT ( 'NONE',  ( -9.474510206698720793, -16.51473224551083518, 24.58442372801900078 ) ) ;
#157650 = CARTESIAN_POINT ( 'NONE',  ( -13.89961937509957401, -13.97604488694547875, 79.37609039468567573 ) ) ;
#157651 = CARTESIAN_POINT ( 'NONE',  ( -5.049401038297874678, -19.05341960407617918, 39.79275706135232582 ) ) ;
#157652 = CARTESIAN_POINT ( 'NONE',  ( -11.74264578624800670, 36.14014761921585972, -6.149999994537627579 ) ) ;
#157653 = CARTESIAN_POINT ( 'NONE',  ( 21.55341960407619695, -5.719274019375665929, 36.04275706135234714 ) ) ;
#157654 = ADVANCED_FACE ( 'NONE', ( #141921 ), #3412, .F. ) ;
#157655 = CARTESIAN_POINT ( 'NONE',  ( 23.48529157249600630, -32.32473071737749137, -3.049999994537627490 ) ) ;
#157656 = CARTESIAN_POINT ( 'NONE',  ( -19.02544592524334988, -5.153800228976617603, 38.95942372801900433 ) ) ;
#157657 = CARTESIAN_POINT ( 'NONE',  ( -16.46253265017160317, 9.564922557960807481, 60.83224293864769550 ) ) ;
#157658 = CARTESIAN_POINT ( 'NONE',  ( 13.97604488694548053, -13.89961937509957401, 30.62609039468566863 ) ) ;
#157659 = CARTESIAN_POINT ( 'NONE',  ( -8.224510206698735004, -14.34966873604973081, 99.58442372801900433 ) ) ;
#157661 = CARTESIAN_POINT ( 'NONE',  ( 21.52544592524334988, 5.823673210054432836, 86.45942372801901854 ) ) ;
#157660 = CARTESIAN_POINT ( 'NONE',  ( -5.049401038298153566, 19.05341960407611168, 110.2072429386476671 ) ) ;
#157662 = CARTESIAN_POINT ( 'NONE',  ( 3.556970738554033499E-15, -38.81732327939057825, -8.124999997268814056 ) ) ;
#157663 = CARTESIAN_POINT ( 'NONE',  ( -33.78659134798514430, 2.758747016945830133, 99.77194732211482631 ) ) ;
#157664 = CARTESIAN_POINT ( 'NONE',  ( -18.62759615963255300, -10.81492255796106328, 89.16775706135236135 ) ) ;
#157665 = CARTESIAN_POINT ( 'NONE',  ( -37.99626262588766679, 2.428612866367529932E-14, -3.747842220587803475 ) ) ;
#157666 = CARTESIAN_POINT ( 'NONE',  ( 19.03943276465977164, -0.05219959533909143690, 93.74890960531435269 ) ) ;
#157667 = EDGE_CURVE ( 'NONE', #2854, #144758, #4921, .T. ) ;
#157668 = CARTESIAN_POINT ( 'NONE',  ( 32.09281931051394565, -20.34824190692416934, -24.99999999999997868 ) ) ;
#157669 = CARTESIAN_POINT ( 'NONE',  ( -16.46253265017160317, 9.564922557960807481, 55.83224293864769550 ) ) ;
#157670 = CARTESIAN_POINT ( 'NONE',  ( -15.80617190586745835, -15.72974639402198527, 61.87390960531436690 ) ) ;
#157671 = CARTESIAN_POINT ( 'NONE',  ( 8.224510206698953496, -14.34966873604960469, 32.91557627198102409 ) ) ;
#157673 = CARTESIAN_POINT ( 'NONE',  ( -9.474510206698964154, 16.51473224551069663, 95.41557627198102409 ) ) ;
#157672 = CARTESIAN_POINT ( 'NONE',  ( -16.55341960407611168, -4.379528057220339221, 101.4572429386476955 ) ) ;
#157674 = CARTESIAN_POINT ( 'NONE',  ( 13.97604488694548053, -13.89961937509957401, 20.62609039468567573 ) ) ;
#157675 = CARTESIAN_POINT ( 'NONE',  ( -16.53943276465976808, 0.05219959533911058130, 101.2489096053143669 ) ) ;
#157676 = CARTESIAN_POINT ( 'NONE',  ( 21.53943276465977519, 0.05219959533937863772, 61.25109039468567573 ) ) ;
#157677 = CARTESIAN_POINT ( 'NONE',  ( -16.53943276465976808, -0.05219959533934237506, 113.7510903946856757 ) ) ;
#157678 = CARTESIAN_POINT ( 'NONE',  ( -13.89961937509957401, -13.97604488694547875, 69.37609039468564731 ) ) ;
#157679 = CARTESIAN_POINT ( 'NONE',  ( -4.500000000000001776, -126.1226662136678272, 8.481152457036383652 ) ) ;
#157680 = CARTESIAN_POINT ( 'NONE',  ( -9.474510206698964154, 16.51473224551069663, 110.4155762719810383 ) ) ;
#157681 = CARTESIAN_POINT ( 'NONE',  ( -14.29746914071049879, 8.314922557960819915, 75.83224293864769550 ) ) ;
#157682 = CARTESIAN_POINT ( 'NONE',  ( -16.46253265017146816, -9.564922557961047289, 59.16775706135233293 ) ) ;
#157683 = CARTESIAN_POINT ( 'NONE',  ( 5.153800228976335163, 19.02544592524342804, 64.79057627198100988 ) ) ;
#157684 = CARTESIAN_POINT ( 'NONE',  ( 12.14591786802309770, 12.06949235617756955, 59.37390960531436690 ) ) ;
#157685 = CARTESIAN_POINT ( 'NONE',  ( 13.97604488694548053, -13.89961937509957401, 95.62609039468563310 ) ) ;
#157686 = CARTESIAN_POINT ( 'NONE',  ( -5.823673210054116645, -21.52544592524344225, 42.29057627198103120 ) ) ;
#157687 = ORIENTED_EDGE ( 'NONE', *, *, #87024, .T. ) ;
#157688 = CARTESIAN_POINT ( 'NONE',  ( -0.05219959533910754901, -16.53943276465976808, 102.4989096053143811 ) ) ;
#157689 = CARTESIAN_POINT ( 'NONE',  ( 18.22780087662122384, -5.500000000000022204, 76.01540105326107266 ) ) ;
#157691 = CARTESIAN_POINT ( 'NONE',  ( -18.67979575497178146, -10.72451020669898902, 66.66557627198102409 ) ) ;
#157690 = CARTESIAN_POINT ( 'NONE',  ( -9.474510206698964154, 16.51473224551069663, 65.41557627198102409 ) ) ;
#157692 = CARTESIAN_POINT ( 'NONE',  ( -16.46253265017160317, 9.564922557960807481, 40.83224293864769550 ) ) ;
#157694 = CARTESIAN_POINT ( 'NONE',  ( -9.474510206698964154, 16.51473224551069663, 80.41557627198103830 ) ) ;
#157693 = CARTESIAN_POINT ( 'NONE',  ( 12.06949235617739724, 12.14591786802326823, 86.87609039468568994 ) ) ;
#157696 = EDGE_CURVE ( 'NONE', #106494, #160325, #17605, .T. ) ;
#157695 = CARTESIAN_POINT ( 'NONE',  ( 5.049401038297881783, 19.05341960407617563, 47.29275706135231161 ) ) ;
#157697 = CARTESIAN_POINT ( 'NONE',  ( 10.72451020669871369, 18.67979575497193778, 82.08442372801901854 ) ) ;
#157698 = CARTESIAN_POINT ( 'NONE',  ( 10.72451020669898902, -18.67979575497178502, 52.91557627198103830 ) ) ;
#157699 = CARTESIAN_POINT ( 'NONE',  ( -5.153800228976328057, -19.02544592524343514, 102.2905762719810383 ) ) ;
#157700 = CARTESIAN_POINT ( 'NONE',  ( -9.474510206698964154, 16.51473224551069663, 25.41557627198103120 ) ) ;
#157701 = CARTESIAN_POINT ( 'NONE',  ( -16.52544592524335698, -4.483927247898792601, 83.95942372801900433 ) ) ;
#157702 = CARTESIAN_POINT ( 'NONE',  ( -9.474510206698720793, -16.51473224551083518, 104.5844237280190043 ) ) ;
#157703 = CARTESIAN_POINT ( 'NONE',  ( -9.564922557960796823, -16.46253265017161027, 22.08224293864768839 ) ) ;
#157704 = CARTESIAN_POINT ( 'NONE',  ( 19.01529144963336648, 5.499999999999969802, 78.73431955728439391 ) ) ;
#157705 = CARTESIAN_POINT ( 'NONE',  ( 21.55341960407619695, -5.719274019375665929, 101.0427570613523756 ) ) ;
#157706 = ORIENTED_EDGE ( 'NONE', *, *, #63840, .T. ) ;
#157707 = CARTESIAN_POINT ( 'NONE',  ( -16.53943276465976808, 0.05219959533911058130, 56.24890960531436690 ) ) ;
#157708 = CARTESIAN_POINT ( 'NONE',  ( -16.53943276465976808, 0.05219959533911058130, 66.24890960531436690 ) ) ;
#157709 = CARTESIAN_POINT ( 'NONE',  ( -5.719274019375978568, 21.55341960407610458, 100.2072429386476955 ) ) ;
#157710 = CARTESIAN_POINT ( 'NONE',  ( -18.67979575497178146, -10.72451020669898902, 86.66557627198102409 ) ) ;
#157711 = CARTESIAN_POINT ( 'NONE',  ( 17.26058549869091507, -6.457015423128540377, 96.12254162523933587 ) ) ;
#157712 = CARTESIAN_POINT ( 'NONE',  ( 10.81492255796078972, 18.62759615963270932, 34.58224293864770260 ) ) ;
#157713 = CARTESIAN_POINT ( 'NONE',  ( 4.379528057220092307, 16.55341960407617563, 62.29275706135236845 ) ) ;
#157714 = CARTESIAN_POINT ( 'NONE',  ( -4.379528057220328563, 16.55341960407611168, 95.20724293864769550 ) ) ;
#157715 = CARTESIAN_POINT ( 'NONE',  ( -5.153800228976328057, -19.02544592524343514, 42.29057627198101699 ) ) ;
#157716 =( NAMED_UNIT ( * ) PLANE_ANGLE_UNIT ( ) SI_UNIT ( $, .RADIAN. ) );
#157717 = CARTESIAN_POINT ( 'NONE',  ( 35.59965464630456466, -2.422542088861788567, 37.88523239209962412 ) ) ;
#157718 = CARTESIAN_POINT ( 'NONE',  ( 14.34966873604972726, -8.224510206698740333, 90.83442372801901854 ) ) ;
#157719 = CARTESIAN_POINT ( 'NONE',  ( -21.53943276465977519, -0.05219959533937600094, 38.75109039468567573 ) ) ;
#157720 = CARTESIAN_POINT ( 'NONE',  ( -9.564922557960796823, -16.46253265017161027, 82.08224293864768129 ) ) ;
#157721 = CARTESIAN_POINT ( 'NONE',  ( 18.67979575497194134, -10.72451020669871369, 65.83442372801900433 ) ) ;
#157722 = DIRECTION ( 'NONE',  ( -1.000000000000000000, -8.921435019309295657E-15, 0.000000000000000000 ) ) ;
#157723 = CARTESIAN_POINT ( 'NONE',  ( 5.153800228976335163, 19.02544592524342804, 24.79057627198102765 ) ) ;
#157724 = ORIENTED_EDGE ( 'NONE', *, *, #52038, .T. ) ;
#157725 = CARTESIAN_POINT ( 'NONE',  ( -15.72974639402176322, -15.80617190586768395, 54.37609039468568994 ) ) ;
#157727 = LINE ( 'NONE', #80866, #117754 ) ;
#157726 = CARTESIAN_POINT ( 'NONE',  ( -19.05341960407611168, -5.049401038298163336, 41.45724293864769550 ) ) ;
#157728 = CARTESIAN_POINT ( 'NONE',  ( -5.153800228976328057, -19.02544592524343514, 87.29057627198103830 ) ) ;
#157729 = CARTESIAN_POINT ( 'NONE',  ( -13.97604488694547697, 13.89961937509957934, 63.12609039468566152 ) ) ;
#157730 = CARTESIAN_POINT ( 'NONE',  ( -10.72451020669870658, -18.67979575497194134, 24.58442372801901499 ) ) ;
#157731 = CARTESIAN_POINT ( 'NONE',  ( -5.049401038297874678, -19.05341960407617918, 64.79275706135233293 ) ) ;
#157732 = CARTESIAN_POINT ( 'NONE',  ( -5.049401038298153566, 19.05341960407611168, 40.20724293864768839 ) ) ;
#157733 = CARTESIAN_POINT ( 'NONE',  ( 8.314922557961029526, -14.29746914071037800, 110.4177570613523756 ) ) ;
#157734 = CARTESIAN_POINT ( 'NONE',  ( -16.51473224551082808, 9.474510206698731452, 68.33442372801900433 ) ) ;
#157735 = CARTESIAN_POINT ( 'NONE',  ( -12.06949235617756955, 12.14591786802309770, 30.62390960531436335 ) ) ;
#157737 = EDGE_LOOP ( 'NONE', ( #174573, #116118, #42806, #86029 ) ) ;
#157736 = CARTESIAN_POINT ( 'NONE',  ( 19.02544592524334988, 5.153800228976608722, 56.45942372801898301 ) ) ;
#157738 = CARTESIAN_POINT ( 'NONE',  ( 19.03943276465977164, -0.05219959533909143690, 83.74890960531436690 ) ) ;
#157739 = CARTESIAN_POINT ( 'NONE',  ( -21.55341960407619339, 5.719274019375674811, 98.54275706135234714 ) ) ;
#157740 = CARTESIAN_POINT ( 'NONE',  ( -0.05219959533937732626, 21.53943276465977519, 112.5010903946857042 ) ) ;
#157741 = DIRECTION ( 'NONE',  ( 0.000000000000000000, 0.000000000000000000, 1.000000000000000000 ) ) ;
#157742 = CARTESIAN_POINT ( 'NONE',  ( 5.823673210054444382, -21.52544592524334988, 95.20942372801903275 ) ) ;
#157743 = CARTESIAN_POINT ( 'NONE',  ( -12.06949235617739369, -12.14591786802326823, 34.37609039468568284 ) ) ;
#157744 = CARTESIAN_POINT ( 'NONE',  ( 13.89961937509977652, -13.97604488694527269, 98.12390960531433848 ) ) ;
#157745 = CARTESIAN_POINT ( 'NONE',  ( -22.44159573604010305, 16.30477369853692338, 140.6750000027311671 ) ) ;
#157746 = CARTESIAN_POINT ( 'NONE',  ( 16.51473224551069308, 9.474510206698969483, 84.16557627198102409 ) ) ;
#157747 = CARTESIAN_POINT ( 'NONE',  ( -15.06137443927361019, -15.06137443927335440, -56.46919128290398504 ) ) ;
#157748 = CARTESIAN_POINT ( 'NONE',  ( -13.89961937509957401, -13.97604488694547875, 69.37609039468564731 ) ) ;
#157749 = CARTESIAN_POINT ( 'NONE',  ( -19.02544592524342804, 5.153800228976336051, 101.0405762719810241 ) ) ;
#157750 = CARTESIAN_POINT ( 'NONE',  ( 21.53943276465977519, 0.05219959533937863772, 106.2510903946856757 ) ) ;
#157751 = CARTESIAN_POINT ( 'NONE',  ( -16.53943276465976808, 0.05219959533911058130, 101.2489096053143669 ) ) ;
#157752 = CARTESIAN_POINT ( 'NONE',  ( 21.53943276465977519, -0.05219959533907433946, 48.74890960531435979 ) ) ;
#157753 =( BOUNDED_SURFACE ( )  B_SPLINE_SURFACE ( 3, 2, ( 
 ( #199012, #135371, #14991, #13988, #154495, #75654, #169663, #60481, #200011, #138330, #137332, #122156, #45333, #27197, #76652, #119198, #88843, #197041, #15990, #106985, #168658, #123148, #150535, #57529, #73699, #198022, #31158, #42358, #105015, #104021, #30158, #61477, #184836, #44340, #58509, #121165, #91801, #120175, #181865, #151526, #13015, #2795, #81592, #64473, #126140, #18974, #141306, #94803, #110964, #173654, #20941, #96773, #47327, #109976, #170663, #49305, #35121, #187836, #50306, #127117, #4762, #172648, #156482, #51287, #159446, #19950, #80620, #158462, #142297, #16980, #108983, #157481, #97758, #34136, #171656, #95795, #63477, #17984, #3777, #185840, #124141, #62469, #78634, #143277, #33145, #79637, #32151, #93808, #65454, #66450, #188823, #111962, #128111, #189815, #112948, #174641, #82598, #36106, #796, #140309, #155488, #1799, #125153, #186852, #48321, #85607, #147294, #148294, #69446, #53272, #7763, #101780, #116947, #100769, #130094, #54284, #133115, #99774, #8783, #179651, #194804, #98765, #70453, #176644, #177645, #191791, #131113, #25965, #114951, #52274, #67443, #9788, #163468, #56278, #39113, #102785, #132118, #162451, #144279, #84597, #117960, #37105, #83599, #193811, #38120, #175631, #86611, #115956, #160458, #71450, #5768, #161459, #41121, #23952, #22949, #129101, #146276, #55276, #145278, #164471, #178639, #190800, #21950, #113932, #6761, #192801, #68440, #40102, #24965, #44110, #13758, #57291, #46083, #103788, #134130, #89606, #197791, #150303, #91567, #120926, #87608, #167455, #181632, #149294, #76418, #166468, #14757, #169419, #182625, #45100, #104780, #75426, #26964, #88607, #137100, #198786, #121923, #27966, #151295, #11800, #183617, #152274, #118968, #28951, #73464, #138094, #199775, #72456, #43112, #135137, #12784, #105768, #74449, #90592, #59257, #196811, #136115, #42126, #107738, #195819, #29928, #60252, #58278, #180651, #106757, #168432, #61242, #122914, #119947, #10788, #153255, #184602, #165468, #109739, #34885, #63234, #32909, #111728, #156242, #185596, #124913, #186611, #18737, #48083, #171423, #79401, #94563, #140067, #17744, #172410, #96540, #95556, #15751, #155253, #139080, #141072, #33899, #2557, #49073, #187604, #142056, #64239, #1558, #126880, #173414, #157243, #125905, #80384, #110729, #123897, #77410, #3542, #30924, #65220, #78391, #188586, #31914, #50067, #92572, #558, #62229, #47085, #108746, #154260, #170422, #93567, #16742, #57938, #14398, #153904, #91211, #28603, #136744, #105419, #76064, #92218, #170071, #46732, #122564, #208, #11445, #30567, #169061, #134786, #199423, #108394, #137739, #29580, #167102, #45736, #75077, #166115, #119609, #59902, #77056, #151924, #184254, #42770, #73117, #123547, #93213, #12443, #183265, #61877, #181292, #15399, #31562, #196468, #152902, #89257, #107388, #106401, #104432, #168083, #185241, #60888, #138728, #27618, #150949, #74105, #44745, #135775, #197446, #58912, #120580, #182273, #43755, #90241, #13413, #198428, #121570, #51695, #47732, #95208, #156895, #143695, #109385, #94209, #19378, #63887, #186254, #97179, #126537, #171065, #158865, #16397, #2206, #66859, #188236, #187255, #154898, #48724, #65861, #155888, #113358, #157889, #20354, #32555, #1200, #82002, #18391, #5178, #33547, #173064, #111375, #81027, #124557, #175050, #17386, #62876, #80042, #64876, #79041, #128522, #49711, #78043, #34541, #110377, #139712, #190216, #141711, #36514, #140716, #96200, #112371, #172060, #142703, #125558, #3202, #4182, #127532, #189235, #50713, #174063, #35531, #30444, #104308, #150822, #119487, #31437, #1077, #120456, #91094, #169946, #27491, #138603, #77924, #181169, #60768, #197324, #15274, #14273, #16272, #75942, #93091, #122440, #61755, #85, #199301, #184132, #152782, #89134, #123423, #42646, #12319, #58788, #154775, #45614, #107266, #185116, #73984, #139591, #135653, #59780, #165991, #108267, #105295 ),
 ( #182148, #28486, #43632, #166983, #46606, #90120, #151804, #137617, #13295, #168937, #74960, #136622, #198303, #121449, #183141, #44626, #92090, #106278, #167963, #29462, #153779, #76934, #51572, #155766, #2084, #127408, #171938, #94087, #5053, #34421, #17264, #66739, #124432, #110257, #174927, #96080, #95086, #62752, #156774, #173941, #63764, #21238, #65740, #128400, #78917, #109262, #190097, #3081, #113236, #141594, #80906, #19260, #189117, #32433, #82893, #140594, #170941, #64757, #172942, #125437, #36390, #157769, #186129, #142583, #18268, #47608, #98044, #126419, #159742, #144571, #4062, #20231, #79921, #50590, #187133, #48605, #112249, #35408, #97060, #188117, #49588, #111251, #33427, #158742, #81879, #143571, #192084, #136159, #120969, #191089, #100063, #145570, #23243, #27008, #161748, #88652, #119012, #7047, #57336, #160746, #28993, #114223, #151338, #180695, #53566, #175928, #42171, #104823, #197834, #68729, #103831, #150348, #44151, #182667, #135181, #11844, #73509, #12827, #134176, #115244, #72502, #166512, #181675, #165512, #176936, #196855, #59300, #84887, #58321, #105810, #167497, #22238, #119989, #38406, #43156, #146566, #195864, #90633, #10832, #37399, #28010, #89650, #99058, #74493, #6057, #67735, #130387, #129393, #52563, #83887, #64277, #78432, #93608, #155293, #156283, #77450, #61285, #15790, #109778, #124954, #108784, #138136, #62268, #141110, #107777, #16783, #187642, #2598, #106799, #140107, #184642, #185634, #199817, #139121, #33939, #122954, #60292, #75467, #17784, #171461, #125944, #47126, #121965, #49113, #110770, #46123, #92610, #172452, #45142, #91610, #1598, #169462, #183658, #94604, #123936, #168473, #79439, #13801, #30963, #152315, #170462, #154301, #137140, #597, #63274, #153298, #198828, #186650, #29971, #14799, #76460, #31953, #48121, #32949, #174445, #113738, #52082, #21752, #65260, #54088, #111767, #142097, #97560, #5568, #158269, #99577, #128906, #95597, #175435, #189618, #157281, #84402, #35914, #22753, #177450, #190606, #53073, #112751, #83403, #34925, #96580, #145081, #6564, #129894, #159248, #20744, #82399, #188627, #50107, #173456, #36905, #81399, #146078, #7563, #80424, #51091, #19758, #144087, #98568, #67247, #160262, #68241, #143085, #191594, #4564, #115762, #3582, #37918, #69249, #114751, #130915, #18777, #176445, #161259, #192606, #126920, #66256, #127916, #165270, #26764, #73269, #179454, #117762, #25772, #131927, #193611, #116753, #180457, #24769, #166268, #151098, #23758, #132922, #178444, #56081, #57094, #194609, #118768, #149103, #39911, #87418, #55083, #59060, #147100, #181439, #10593, #86416, #8585, #72254, #134938, #27766, #101578, #133932, #41929, #74254, #12589, #88404, #103595, #150100, #42918, #164278, #148101, #102593, #196616, #11601, #195622, #9593, #58086, #89409, #40920, #119756, #135924, #197594, #163267, #104583, #71258, #120727, #38920, #100577, #162259, #85408, #70259, #105568, #186401, #1345, #32703, #77205, #90389, #17530, #140859, #76209, #122710, #171213, #75226, #121720, #46878, #91358, #13559, #124704, #154052, #136897, #47878, #43905, #29725, #94354, #15547, #14551, #182427, #137888, #93359, #183412, #2348, #185387, #109531, #198584, #28753, #156033, #184400, #79189, #61038, #354, #138874, #108538, #152074, #64029, #60052, #44895, #45880, #92366, #106552, #167254, #62024, #168228, #123688, #199569, #153049, #170217, #31710, #155045, #107534, #169210, #30719, #16540, #78187, #139857, #63026, #129652, #159004, #125699, #5320, #19516, #187398, #114495, #4322, #52826, #7316, #20497, #83162, #142843, #51835, #65017, #126673, #113494, #175189, #160013, #66006, #127674, #112508, #18532, #80179, #3342, #67004, #111519, #176197, #37666, #110521, #81161, #188377, #189374, #143841, #50851, #128663, #35670, #49854, #174202, #141851, #145834, #33687, #67999, #97318, #173205, #95350, #82145, #21501, #99331, #34680, #190358 ),
 ( #84155, #36655, #144836, #191348, #98313, #48866, #6320, #161014, #22508, #172202, #96338, #157034, #158025, #149847, #71013, #194369, #87175, #9348, #163014, #179206, #146843, #117509, #165025, #166022, #178200, #38679, #40674, #41682, #55836, #118523, #195368, #73022, #132681, #24521, #119518, #27522, #88163, #148856, #26518, #10347, #85157, #177206, #25531, #89163, #102344, #39664, #164033, #131681, #86172, #72004, #53844, #192361, #130667, #8337, #100335, #133677, #150854, #56847, #101325, #180212, #193362, #147862, #103346, #115518, #162013, #23509, #70012, #11351, #134693, #196377, #54838, #116513, #57846, #181200, #42677, #104338, #69001, #106308, #76963, #93119, #170971, #47639, #123453, #1106, #12348, #31467, #169975, #135682, #115, #109292, #138634, #30471, #167993, #46636, #75972, #167013, #120486, #137645, #197354, #185146, #58818, #43663, #74012, #124462, #94117, #13323, #184161, #62781, #182177, #154804, #32464, #105325, #153809, #90149, #108296, #107294, #28514, #168966, #186159, #15303, #16302, #77952, #92121, #61784, #45642, #151833, #139619, #74988, #136652, #198333, #59809, #121479, #183172, #44655, #29490, #91123, #152813, #14305, #199332, #60797, #122470, #114255, #5083, #113262, #159771, #142611, #175960, #172971, #65769, #52594, #50617, #33457, #157797, #19288, #36417, #80935, #4090, #173968, #96108, #49619, #127438, #95115, #189144, #51598, #37429, #64787, #125467, #112276, #128426, #35436, #66765, #81906, #21266, #97088, #111281, #6086, #155796, #174954, #158771, #98072, #20260, #143599, #190122, #63794, #82923, #17294, #187164, #156804, #191120, #144600, #67765, #129422, #48635, #78947, #110287, #171969, #140623, #2113, #34449, #18297, #79952, #141622, #3111, #126448, #188146, #116270, #9107, #196139, #194134, #176968, #101088, #162774, #179974, #24282, #85931, #117272, #39428, #193122, #70774, #38438, #147620, #195128, #57610, #8090, #68761, #132443, #71768, #55597, #148617, #25291, #103107, #178966, #54596, #149611, #119279, #118283, #40433, #56609, #102105, #115275, #7080, #163790, #180962, #86934, #69767, #10108, #161778, #177960, #133438, #83919, #22269, #160780, #100094, #41440, #131436, #164788, #130419, #145601, #26282, #87924, #11109, #72784, #134454, #99089, #192117, #53599, #23273, #84917, #146597, #31235, #42439, #61553, #200085, #165785, #30237, #139391, #168733, #60558, #136424, #76729, #106075, #197121, #150620, #167762, #27281, #153571, #88928, #73779, #104102, #154571, #124224, #43428, #14067, #92884, #12116, #123222, #873, #135452, #183924, #120254, #138404, #137410, #62548, #199090, #16067, #45409, #184912, #46397, #122233, #181945, #44422, #29260, #108056, #90891, #152577, #107062, #182939, #198104, #75734, #105097, #91880, #169740, #58588, #151605, #166783, #15068, #77725, #28284, #89923, #13096, #74762, #59570, #121245, #36186, #144364, #4850, #65537, #143358, #3858, #1878, #93887, #142379, #82680, #172736, #156569, #187916, #48401, #2877, #19055, #170739, #109061, #47405, #63559, #20033, #18065, #64556, #17059, #32229, #188911, #128197, #127197, #126220, #111048, #79720, #50389, #66534, #5851, #21027, #96859, #174723, #185920, #189895, #51370, #155565, #173737, #67527, #112049, #35206, #141389, #81675, #49385, #140390, #78714, #34216, #125233, #158543, #186931, #110058, #171738, #97840, #33226, #94886, #157562, #159528, #95879, #113031, #80702, #10869, #70533, #6844, #25048, #24036, #26043, #85691, #41204, #132202, #71530, #9870, #8866, #193893, #162532, #37191, #148375, #190882, #98848, #68523, #164550, #55358, #117028, #194887, #22032, #87688, #83684, #160543, #133196, #175712, #84679, #149373, #178723, #86691, #56361, #116036, #129184, #146358, #39194, #52358, #147377, #130177, #177725, #118044, #114015, #38201, #145362, #100850, #101865, #54364, #40185, #163548, #179734, #69532, #23034, #102865, #191874, #53358, #115035, #176728, #99857 ),
 ( #7845, #161541, #131196, #192886, #42208, #31004, #88692, #119050, #74531, #182706, #135220, #76504, #105850, #72539, #152354, #166550, #134216, #61327, #151375, #199862, #154342, #167537, #30013, #89690, #198867, #11884, #73547, #60334, #122008, #106840, #12866, #136196, #59338, #165549, #27046, #150388, #13839, #58359, #122998, #184684, #57377, #28049, #196892, #197871, #90672, #121008, #75506, #44191, #120026, #29032, #181711, #92653, #180732, #14841, #137179, #43193, #103868, #183699, #168515, #46167, #104861, #45186, #91651, #107821, #169505, #153340, #138180, #195902, #22548, #143882, #127715, #82189, #99370, #190402, #145874, #185679, #128705, #7357, #174245, #160056, #53883, #69042, #170507, #21543, #50892, #51878, #1645, #5363, #100375, #189417, #123981, #139164, #84194, #37708, #130707, #113537, #93655, #20540, #67047, #161053, #175231, #36696, #98357, #159046, #112550, #83203, #155340, #144878, #114537, #115558, #35713, #47169, #6360, #191389, #68040, #129692, #52866, #192401, #176237, #97360, #177245, #38717, #15835, #77494, #641, #62311, #31998, #108828, #16829, #78480, #140153, #63323, #164070, #24560, #179247, #195408, #146885, #85197, #23549, #178240, #196413, #132717, #40713, #193402, #8377, #165062, #104376, #41720, #102382, #87213, #55875, #26556, #42714, #120523, #197391, #73059, #150893, #162053, #181238, #119555, #70052, #149883, #58856, #88199, #180250, #117548, #57883, #25569, #116551, #131720, #148895, #54877, #134731, #39701, #101364, #163053, #74049, #43700, #86209, #133716, #12387, #147899, #166059, #182216, #9385, #103384, #71051, #27560, #56886, #194405, #118560, #135720, #11389, #89200, #10385, #72042, #170013, #138671, #13360, #124501, #167049, #75024, #183210, #140659, #185183, #31504, #171010, #198371, #2151, #59848, #136689, #109328, #151870, #60832, #63829, #154842, #62817, #32501, #92158, #125501, #122507, #15343, #187199, #151, #186196, #123490, #121515, #44691, #61820, #105362, #153845, #76008, #107330, #168029, #184197, #46673, #90187, #28550, #106345, #29526, #139655, #137683, #45679, #91159, #152848, #108333, #47677, #93157, #169003, #30507, #199368, #16339, #94153, #14342, #76999, #77988, #155832, #1143, #17329, #78984, #172003, #36453, #145636, #174989, #66799, #142646, #82960, #112312, #3147, #156838, #174002, #33491, #159808, #95149, #79988, #48670, #160817, #130457, #49653, #20294, #99127, #18333, #67803, #7116, #110322, #190158, #126483, #144637, #143633, #68798, #5117, #22305, #51634, #191157, #129458, #128462, #113298, #81942, #141656, #52630, #64821, #188181, #111317, #83956, #98111, #21303, #114294, #173006, #34485, #96143, #157832, #175996, #19323, #4125, #80970, #6120, #37466, #65804, #35473, #127472, #189178, #158805, #50651, #97122, #69802, #194167, #55631, #72819, #117304, #179000, #10143, #132478, #85965, #102140, #131470, #40468, #87959, #88964, #101121, #161811, #163825, #164823, #25326, #41477, #118317, #196175, #86968, #147654, #42475, #150654, #11145, #71803, #134488, #149647, #115312, #180010, #12152, #103141, #133472, #9142, #26319, #148655, #146632, #100130, #195163, #177004, #57647, #38473, #23306, #192154, #104138, #73817, #193157, #56644, #165820, #84950, #119313, #53635, #8124, #180999, #54629, #27317, #116304, #177993, #39460, #162807, #24316, #70809, #16101, #15104, #200119, #168767, #43464, #154606, #197157, #105132, #13133, #170775, #76765, #61588, #907, #28319, #32265, #89958, #166818, #139425, #181982, #90926, #93922, #184947, #92920, #62582, #122269, #155600, #152612, #45444, #17095, #30270, #74795, #137448, #199127, #77759, #60594, #183957, #153608, #75770, #29296, #107097, #136457, #91915, #31269, #135487, #44458, #151638, #138438, #108091, #123256, #46432, #169775, #124260, #185955, #14102, #47439, #58622, #109096, #120289, #198138, #59608, #121281, #182974, #106112, #167796, #65573, #49420, #80736, #141425, #95912 ),
 ( #157596, #3894, #172772, #143395, #159564, #37226, #114050, #189928, #67561, #78748, #171772, #18099, #4884, #187951, #110094, #21062, #50424, #33261, #82717, #140425, #126254, #190916, #112083, #111082, #1915, #34253, #51403, #79754, #98883, #81709, #144399, #94920, #125269, #5885, #19088, #129219, #142415, #96893, #35239, #66566, #48437, #160577, #156605, #186967, #127233, #188947, #2911, #52393, #173773, #63594, #158576, #20066, #64590, #175749, #128231, #113063, #174755, #36220, #97872, #39227, #148409, #161574, #23067, #9904, #71564, #56396, #162566, #100883, #8900, #115070, #176762, #99889, #163581, #7880, #149406, #134249, #6878, #116070, #84713, #24070, #40222, #177758, #101899, #132236, #146391, #70568, #38234, #42240, #130212, #164583, #193928, #69565, #191907, #55391, #118078, #10901, #131231, #117061, #25081, #57410, #195936, #133229, #86724, #194920, #26077, #147412, #192920, #85725, #102898, #178756, #72575, #53392, #179768, #119082, #41237, #87721, #180764, #103901, #54398, #22066, #83717, #145395, #68556, #90703, #47201, #74562, #73581, #88727, #169537, #184715, #15868, #60368, #135253, #673, #124013, #59373, #105883, #154374, #150422, #11917, #27080, #181746, #199894, #136229, #182741, #196925, #58392, #168544, #107852, #45216, #44225, #152386, #121045, #30042, #46199, #185711, #62344, #76536, #77526, #165582, #31037, #123029, #120059, #153373, #43228, #91681, #183730, #167570, #61358, #29064, #104895, #166584, #13871, #28084, #138212, #89724, #151410, #12898, #139198, #197904, #75538, #137213, #198900, #122040, #92686, #106871, #14875, #50186, #186728, #4641, #3659, #5646, #65337, #20820, #111843, #51169, #189696, #188704, #173533, #142175, #16860, #127993, #170540, #78511, #48199, #144161, #35002, #96657, #174521, #1677, #67323, #63355, #140185, #112829, #155371, #64354, #128985, #158344, #66332, #35988, #95676, #190683, #126023, #18856, #108861, #126997, #109853, #110848, #172532, #97635, #34018, #157362, #19833, #49190, #2677, #80502, #171538, #81474, #159324, #32030, #17863, #125032, #143161, #82476, #93688, #33026, #94681, #156360, #79518, #187719, #141188, #194689, #178519, #162334, #39986, #100652, #145159, #98646, #38996, #132998, #192682, #37999, #7640, #191671, #22830, #115838, #69324, #53150, #84477, #177527, #175510, #113815, #36984, #6643, #55158, #99654, #146154, #21829, #160340, #23835, #101657, #85484, #130990, #54165, #161338, #147173, #163348, #56159, #71336, #132002, #86493, #52158, #9671, #148178, #68321, #24844, #83481, #117841, #129971, #8662, #114829, #193690, #70335, #116828, #176523, #17499, #143808, #79156, #63998, #32671, #144806, #114462, #33656, #4292, #83130, #140827, #51804, #191317, #94324, #174171, #110489, #128633, #127643, #129622, #189343, #6289, #35641, #175157, #113463, #112478, #97287, #65974, #2316, #36624, #156002, #125668, #172171, #67968, #158974, #20466, #98281, #187366, #52794, #48835, #95317, #159982, #157002, #188346, #18500, #82116, #190327, #21469, #19486, #80148, #49824, #142812, #141819, #50821, #3312, #34649, #96308, #64985, #157994, #81131, #5290, #173173, #126643, #66973, #111488, #24490, #71973, #72992, #85127, #145804, #86141, #148827, #101296, #25500, #102314, #180183, #116481, #69982, #26490, #134661, #195338, #55807, #133647, #194339, #192330, #84125, #132651, #196347, #162985, #146811, #57815, #8305, #7287, #99298, #41652, #56818, #88132, #70983, #68971, #11322, #176164, #131650, #178170, #164996, #130635, #115486, #40645, #193332, #53811, #118492, #147832, #177174, #103316, #37634, #23478, #149816, #9318, #54806, #160983, #39635, #87144, #38647, #22477, #179177, #100304, #161982, #117479, #164004, #10317, #41282, #44266, #42286, #10946, #103945, #118124, #133275, #89766, #29105, #166624, #165624, #11958, #180807, #151451, #167609, #45259, #122082, #197945, #75580, #86772, #105924, #90743, #9950, #74603 ),
 ( #28126, #72620, #13914, #198942, #71609, #27123, #26123, #88770, #104938, #150463, #12938, #196965, #87765, #135293, #102944, #106913, #194966, #152426, #58433, #134295, #56445, #120100, #182783, #137259, #149450, #181789, #136270, #183773, #60409, #59415, #121089, #168586, #148456, #73623, #195981, #43269, #179812, #164628, #57454, #119126, #140230, #18900, #185761, #171582, #65382, #80546, #184759, #33070, #62390, #63399, #15913, #155414, #188749, #124060, #170586, #142220, #123073, #169585, #94725, #139243, #61402, #172576, #1723, #46244, #34062, #91725, #77571, #3704, #125076, #47249, #30084, #108906, #141230, #31083, #50234, #156403, #95721, #107898, #76579, #157407, #32076, #127042, #111889, #153421, #14919, #79563, #199938, #138255, #92731, #154419, #93733, #186773, #718, #16904, #48244, #78555, #109898, #17907, #2721, #64398, #126067, #187763, #49233, #110891, #131040, #190730, #99701, #112875, #174568, #161385, #22876, #7686, #113861, #52203, #160388, #66379, #128040, #51214, #114877, #159373, #100697, #85532, #158390, #67370, #36034, #175557, #191716, #129029, #53200, #83527, #97683, #21877, #189741, #193737, #81520, #115883, #145205, #20869, #143206, #6688, #69370, #162378, #82527, #68366, #176571, #8711, #147220, #84523, #38045, #146200, #177573, #98694, #144209, #37033, #54212, #130017, #23880, #4687, #192730, #70380, #39040, #132048, #55205, #173578, #5694, #35047, #96701, #19879, #102713, #42053, #198709, #25894, #24891, #40030, #120850, #136041, #167379, #11726, #86539, #152198, #118894, #179578, #134055, #150230, #101704, #163394, #71381, #74376, #72380, #41049, #195747, #148223, #9717, #119877, #59181, #196741, #57221, #103717, #10717, #181562, #197716, #75349, #13682, #27892, #105693, #116874, #182550, #44032, #133045, #104706, #137019, #43040, #135065, #180579, #151221, #165397, #194735, #56205, #26890, #117888, #89534, #164402, #87539, #178565, #28876, #149226, #88533, #73394, #90516, #58208, #166396, #12710, #141975, #1473, #138016, #156160, #155172, #157162, #16663, #30846, #187525, #91488, #29851, #108665, #17658, #48990, #199699, #93486, #63152, #95475, #172326, #186531, #124831, #48004, #64157, #185514, #169337, #123816, #140988, #31835, #110645, #153175, #170343, #33815, #15672, #109660, #18656, #80302, #14678, #171340, #92493, #78311, #46005, #47006, #60176, #154182, #168355, #183538, #125822, #79318, #121845, #139984, #76340, #45023, #106682, #77332, #478, #61165, #122836, #184525, #32828, #138999, #107660, #2476, #94479, #62152, #7441, #65140, #50973, #115641, #36781, #35795, #3463, #97442, #114624, #4443, #162138, #34805, #69126, #49982, #159127, #23634, #52949, #161136, #130792, #190489, #85283, #20625, #113620, #100458, #98446, #81281, #5447, #67130, #84279, #128788, #51960, #21629, #143967, #82274, #175314, #142964, #160140, #99456, #126797, #112633, #173332, #83285, #176324, #144959, #37793, #129774, #192485, #6441, #68122, #53967, #188503, #22633, #191470, #145960, #177330, #19639, #111646, #38802, #96460, #158148, #174326, #66131, #127796, #189497, #180337, #131807, #70136, #101452, #104465, #102469, #71137, #164156, #178324, #193486, #149974, #89290, #26642, #25654, #72132, #40799, #11479, #27651, #105452, #182309, #57970, #135808, #146974, #166149, #150982, #54964, #134821, #43788, #73150, #165151, #87299, #181324, #10471, #163143, #116635, #133807, #39787, #119642, #24646, #86295, #8462, #58945, #28636, #147984, #118646, #197478, #9473, #12475, #167137, #132802, #88285, #194489, #42803, #41805, #55961, #74136, #120613, #117638, #179336, #148982, #196500, #195498, #103473, #56972, #109416, #151957, #59934, #168113, #125586, #170099, #16425, #155920, #183297, #187283, #44778, #92251, #171095, #153935, #15430, #108423, #30598, #184284, #239, #29609, #138757, #186283, #48754, #199453, #121601, #61906, #62908, #77088, #139740, #78072, #94240, #123577, #45766 ),
 ( #152931, #107418, #185272, #75109, #13445, #106431, #47763, #169091, #14430, #46764, #91241, #136777, #93242, #32587, #31593, #154927, #1229, #124588, #17415, #79073, #110407, #172089, #140746, #2234, #90273, #63917, #198463, #76093, #137768, #60921, #122595, #51723, #127564, #67889, #97208, #188264, #141740, #158894, #18421, #144723, #80071, #64904, #33576, #145726, #115405, #34571, #5207, #84047, #3230, #52716, #192248, #95238, #175076, #111408, #129542, #128549, #130551, #37554, #176084, #156924, #173093, #114380, #113386, #98198, #66888, #126565, #99216, #49739, #96228, #157916, #68891, #36542, #159902, #160904, #19406, #53730, #81055, #142732, #22397, #4211, #189265, #65889, #83049, #191242, #7207, #20384, #50740, #112399, #143728, #174091, #190246, #35560, #82031, #21390, #6209, #179095, #87060, #39553, #181090, #10233, #177093, #56739, #70901, #38565, #165909, #55724, #104228, #58707, #71893, #134582, #194257, #103234, #116395, #178084, #164916, #26410, #11238, #117396, #40564, #163922, #69898, #131565, #54722, #118410, #162900, #27407, #89053, #161902, #132568, #101211, #102234, #195254, #25418, #180103, #148745, #24409, #133564, #193249, #197246, #150743, #147747, #12242, #8221, #146724, #41571, #72912, #73904, #86058, #88049, #149737, #135574, #100221, #196268, #57737, #119407, #42565, #23396, #9234, #85043, #995, #92004, #47528, #90045, #30361, #109183, #75860, #61675, #155687, #170862, #74883, #123344, #152701, #153698, #106201, #45531, #2004, #29384, #28406, #43553, #124350, #139512, #32353, #15193, #151727, #17182, #78836, #14190, #60684, #94006, #13220, #59698, #185037, #91015, #136545, #62669, #76852, #198226, #186045, #182070, #167885, #140514, #138523, #137536, #120377, #199218, #31359, #121370, #105219, #46524, #166907, #183063, #44546, #122359, #184048, #107185, #168856, #1, #108184, #169865, #93009, #154695, #16190, #77845, #160661, #156692, #95004, #67648, #110178, #19173, #22152, #113150, #21149, #129306, #50506, #83802, #80822, #173858, #145483, #158659, #141512, #65658, #127320, #144486, #189032, #112170, #81795, #3978, #157683, #35324, #2997, #96978, #159652, #63683, #172857, #33345, #20150, #36305, #143482, #174840, #190015, #191002, #4967, #142500, #114137, #125357, #82804, #66653, #5969, #128315, #79843, #171857, #51488, #187054, #97960, #34338, #52478, #126337, #175838, #37312, #48524, #18186, #64675, #98970, #188034, #49504, #111167, #95999, #56236, #12739, #152228, #89564, #26920, #135093, #103747, #74405, #90546, #168386, #45054, #120881, #198741, #6963, #28906, #167410, #130299, #197745, #106712, #136071, #27921, #165426, #44063, #73422, #164430, #117917, #196769, #191993, #182580, #179606, #41078, #68643, #121876, #91519, #10746, #181591, #60206, #102742, #13713, #29881, #25924, #151250, #87567, #105723, #104735, #149254, #75379, #137051, #72410, #134087, #183569, #59212, #195777, #43068, #57250, #118924, #180609, #42082, #88563, #150261, #11755, #58237, #119905, #166426, #186563, #61195, #172357, #14711, #122867, #30878, #188536, #32861, #79350, #18687, #46036, #50014, #107691, #184555, #157193, #199729, #108696, #111679, #2508, #110677, #80334, #140018, #173366, #170375, #63184, #34836, #48036, #92525, #155205, #16694, #33847, #78344, #1507, #171374, #93520, #47039, #124864, #154214, #109692, #49022, #153206, #62183, #169370, #94511, #125855, #156193, #64188, #141021, #142006, #17693, #31866, #3495, #76371, #95507, #187555, #65171, #126830, #15704, #77364, #138048, #139032, #511, #123847, #185545, #159159, #113651, #129806, #81313, #19671, #51004, #54000, #51992, #20654, #175345, #127826, #142996, #99489, #38833, #176356, #36813, #21662, #190518, #161169, #177362, #54996, #131838, #7475, #85316, #96491, #115674, #100491, #4474, #84313, #193521, #22666, #114660, #98479, #130826, #160172, #112665, #66164, #83316, #189532, #69159, #174357, #35827 ) ),
 .UNSPECIFIED., .T., .F., .T. ) 
 B_SPLINE_SURFACE_WITH_KNOTS ( ( 4, 3, 4 ),
 ( 3, 2, 2, 2, 2, 2, 2, 2, 2, 2, 2, 2, 2, 2, 2, 2, 2, 2, 2, 2, 2, 2, 2, 2, 2, 2, 2, 2, 2, 2, 2, 2, 2, 2, 2, 2, 2, 2, 2, 2, 2, 2, 2, 2, 2, 2, 2, 2, 2, 2, 2, 2, 2, 2, 2, 2, 2, 2, 2, 2, 2, 2, 2, 2, 2, 2, 2, 2, 2, 2, 2, 2, 2, 2, 2, 2, 2, 2, 2, 2, 2, 2, 2, 2, 2, 2, 2, 2, 2, 2, 2, 2, 2, 2, 2, 2, 2, 2, 2, 2, 2, 2, 2, 2, 2, 2, 2, 2, 2, 2, 2, 2, 2, 2, 2, 2, 2, 2, 2, 2, 2, 2, 2, 2, 2, 2, 2, 2, 2, 2, 2, 2, 2, 2, 2, 2, 2, 2, 2, 2, 2, 2, 2, 2, 2, 2, 2, 2, 2, 2, 2, 2, 2, 2, 2, 2, 2, 2, 2, 2, 2, 2, 2, 2, 2, 2, 2, 2, 2, 2, 2, 2, 2, 2, 2, 2, 2, 2, 2, 2, 2, 2, 2, 2, 2, 2, 2, 2, 2, 2, 2, 2, 2, 2, 2, 2, 2, 2, 2, 2, 2, 2, 2, 2, 2, 2, 2, 2, 2, 2, 2, 2, 2, 2, 2, 2, 2, 2, 2, 2, 2, 2, 2, 2, 2, 2, 2, 2, 3 ),
 ( 0.000000000000000000, 0.5000000000000000000, 1.000000000000000000 ),
 ( 0.000000000000000000, 0.004385964912280701511, 0.008771929824561403022, 0.01315789473684210453, 0.01754385964912280604, 0.02192982456140350755, 0.02631578947368420907, 0.03070175438596491058, 0.03508771929824561209, 0.03947368421052631360, 0.04385964912280701511, 0.04824561403508771662, 0.05263157894736841813, 0.05701754385964911964, 0.06140350877192982115, 0.06578947368421052266, 0.07017543859649122417, 0.07456140350877192569, 0.07894736842105262720, 0.08333333333333332871, 0.08771929824561403022, 0.09210526315789473173, 0.09649122807017543324, 0.1008771929824561348, 0.1052631578947368363, 0.1096491228070175378, 0.1140350877192982393, 0.1184210526315789408, 0.1228070175438596423, 0.1271929824561403577, 0.1315789473684210453, 0.1359649122807017607, 0.1403508771929824483, 0.1447368421052631637, 0.1491228070175438514, 0.1535087719298245668, 0.1578947368421052544, 0.1622807017543859698, 0.1666666666666666574, 0.1710526315789473728, 0.1754385964912280604, 0.1798245614035087758, 0.1842105263157894635, 0.1885964912280701788, 0.1929824561403508665, 0.1973684210526315819, 0.2017543859649122695, 0.2061403508771929849, 0.2105263157894736725, 0.2149122807017543879, 0.2192982456140350755, 0.2236842105263157909, 0.2280701754385964786, 0.2324561403508771940, 0.2368421052631578816, 0.2412280701754385970, 0.2456140350877192846, 0.2500000000000000000, 0.2543859649122807154, 0.2587719298245614308, 0.2631578947368420907, 0.2675438596491228060, 0.2719298245614035214, 0.2763157894736842368, 0.2807017543859648967, 0.2850877192982456121, 0.2894736842105263275, 0.2938596491228070429, 0.2982456140350877027, 0.3026315789473684181, 0.3070175438596491335, 0.3114035087719298489, 0.3157894736842105088, 0.3201754385964912242, 0.3245614035087719396, 0.3289473684210526550, 0.3333333333333333148, 0.3377192982456140302, 0.3421052631578947456, 0.3464912280701754610, 0.3508771929824561209, 0.3552631578947368363, 0.3596491228070175517, 0.3640350877192982670, 0.3684210526315789269, 0.3728070175438596423, 0.3771929824561403577, 0.3815789473684210731, 0.3859649122807017330, 0.3903508771929824483, 0.3947368421052631637, 0.3991228070175438791, 0.4035087719298245390, 0.4078947368421052544, 0.4122807017543859698, 0.4166666666666666852, 0.4210526315789473450, 0.4254385964912280604, 0.4298245614035087758, 0.4342105263157894912, 0.4385964912280701511, 0.4429824561403508665, 0.4473684210526315819, 0.4517543859649122973, 0.4561403508771929571, 0.4605263157894736725, 0.4649122807017543879, 0.4692982456140351033, 0.4736842105263157632, 0.4780701754385964786, 0.4824561403508771940, 0.4868421052631579093, 0.4912280701754385692, 0.4956140350877192846, 0.5000000000000000000, 0.5043859649122807154, 0.5087719298245614308, 0.5131578947368421462, 0.5175438596491228616, 0.5219298245614034659, 0.5263157894736841813, 0.5307017543859648967, 0.5350877192982456121, 0.5394736842105263275, 0.5438596491228070429, 0.5482456140350877583, 0.5526315789473684736, 0.5570175438596490780, 0.5614035087719297934, 0.5657894736842105088, 0.5701754385964912242, 0.5745614035087719396, 0.5789473684210526550, 0.5833333333333333703, 0.5877192982456140857, 0.5921052631578946901, 0.5964912280701754055, 0.6008771929824561209, 0.6052631578947368363, 0.6096491228070175517, 0.6140350877192982670, 0.6184210526315789824, 0.6228070175438596978, 0.6271929824561403022, 0.6315789473684210176, 0.6359649122807017330, 0.6403508771929824483, 0.6447368421052631637, 0.6491228070175438791, 0.6535087719298245945, 0.6578947368421053099, 0.6622807017543859143, 0.6666666666666666297, 0.6710526315789473450, 0.6754385964912280604, 0.6798245614035087758, 0.6842105263157894912, 0.6885964912280702066, 0.6929824561403509220, 0.6973684210526315264, 0.7017543859649122417, 0.7061403508771929571, 0.7105263157894736725, 0.7149122807017543879, 0.7192982456140351033, 0.7236842105263158187, 0.7280701754385965341, 0.7324561403508771384, 0.7368421052631578538, 0.7412280701754385692, 0.7456140350877192846, 0.7500000000000000000, 0.7543859649122807154, 0.7587719298245614308, 0.7631578947368421462, 0.7675438596491228616, 0.7719298245614034659, 0.7763157894736841813, 0.7807017543859648967, 0.7850877192982456121, 0.7894736842105263275, 0.7938596491228070429, 0.7982456140350877583, 0.8026315789473684736, 0.8070175438596490780, 0.8114035087719297934, 0.8157894736842105088, 0.8201754385964912242, 0.8245614035087719396, 0.8289473684210526550, 0.8333333333333333703, 0.8377192982456140857, 0.8421052631578946901, 0.8464912280701754055, 0.8508771929824561209, 0.8552631578947368363, 0.8596491228070175517, 0.8640350877192982670, 0.8684210526315789824, 0.8728070175438596978, 0.8771929824561403022, 0.8815789473684210176, 0.8859649122807017330, 0.8903508771929824483, 0.8947368421052631637, 0.8991228070175438791, 0.9035087719298245945, 0.9078947368421053099, 0.9122807017543859143, 0.9166666666666666297, 0.9210526315789473450, 0.9254385964912280604, 0.9298245614035087758, 0.9342105263157894912, 0.9385964912280702066, 0.9429824561403509220, 0.9473684210526315264, 0.9517543859649122417, 0.9561403508771929571, 0.9605263157894736725, 0.9649122807017543879, 0.9692982456140351033, 0.9736842105263158187, 0.9780701754385965341, 0.9824561403508771384, 0.9868421052631578538, 0.9912280701754385692, 0.9956140350877192846, 1.000000000000000000 ),
 .UNSPECIFIED. ) 
 GEOMETRIC_REPRESENTATION_ITEM ( )  RATIONAL_B_SPLINE_SURFACE ( (
 ( 1.000000000000000000, 0.9659258262890683122, 1.000000000000000000, 0.9659258262890683122, 1.000000000000000000, 0.9659258262890683122, 1.000000000000000000, 0.9659258262890683122, 1.000000000000000000, 0.9659258262890683122, 1.000000000000000000, 0.9659258262890683122, 1.000000000000000000, 0.9659258262890683122, 1.000000000000000000, 0.9659258262890683122, 1.000000000000000000, 0.9659258262890683122, 1.000000000000000000, 0.9659258262890683122, 1.000000000000000000, 0.9659258262890683122, 1.000000000000000000, 0.9659258262890683122, 1.000000000000000000, 0.9659258262890683122, 1.000000000000000000, 0.9659258262890683122, 1.000000000000000000, 0.9659258262890683122, 1.000000000000000000, 0.9659258262890683122, 1.000000000000000000, 0.9659258262890683122, 1.000000000000000000, 0.9659258262890683122, 1.000000000000000000, 0.9659258262890683122, 1.000000000000000000, 0.9659258262890683122, 1.000000000000000000, 0.9659258262890683122, 1.000000000000000000, 0.9659258262890683122, 1.000000000000000000, 0.9659258262890683122, 1.000000000000000000, 0.9659258262890683122, 1.000000000000000000, 0.9659258262890683122, 1.000000000000000000, 0.9659258262890683122, 1.000000000000000000, 0.9659258262890683122, 1.000000000000000000, 0.9659258262890683122, 1.000000000000000000, 0.9659258262890683122, 1.000000000000000000, 0.9659258262890683122, 1.000000000000000000, 0.9659258262890683122, 1.000000000000000000, 0.9659258262890683122, 1.000000000000000000, 0.9659258262890683122, 1.000000000000000000, 0.9659258262890683122, 1.000000000000000000, 0.9659258262890683122, 1.000000000000000000, 0.9659258262890683122, 1.000000000000000000, 0.9659258262890683122, 1.000000000000000000, 0.9659258262890683122, 1.000000000000000000, 0.9659258262890683122, 1.000000000000000000, 0.9659258262890683122, 1.000000000000000000, 0.9659258262890683122, 1.000000000000000000, 0.9659258262890683122, 1.000000000000000000, 0.9659258262890683122, 1.000000000000000000, 0.9659258262890683122, 1.000000000000000000, 0.9659258262890683122, 1.000000000000000000, 0.9659258262890683122, 1.000000000000000000, 0.9659258262890683122, 1.000000000000000000, 0.9659258262890683122, 1.000000000000000000, 0.9659258262890683122, 1.000000000000000000, 0.9659258262890683122, 1.000000000000000000, 0.9659258262890683122, 1.000000000000000000, 0.9659258262890683122, 1.000000000000000000, 0.9659258262890683122, 1.000000000000000000, 0.9659258262890683122, 1.000000000000000000, 0.9659258262890683122, 1.000000000000000000, 0.9659258262890683122, 1.000000000000000000, 0.9659258262890683122, 1.000000000000000000, 0.9659258262890683122, 1.000000000000000000, 0.9659258262890683122, 1.000000000000000000, 0.9659258262890683122, 1.000000000000000000, 0.9659258262890683122, 1.000000000000000000, 0.9659258262890683122, 1.000000000000000000, 0.9659258262890683122, 1.000000000000000000, 0.9659258262890683122, 1.000000000000000000, 0.9659258262890683122, 1.000000000000000000, 0.9659258262890683122, 1.000000000000000000, 0.9659258262890683122, 1.000000000000000000, 0.9659258262890683122, 1.000000000000000000, 0.9659258262890683122, 1.000000000000000000, 0.9659258262890683122, 1.000000000000000000, 0.9659258262890683122, 1.000000000000000000, 0.9659258262890683122, 1.000000000000000000, 0.9659258262890683122, 1.000000000000000000, 0.9659258262890683122, 1.000000000000000000, 0.9659258262890683122, 1.000000000000000000, 0.9659258262890683122, 1.000000000000000000, 0.9659258262890683122, 1.000000000000000000, 0.9659258262890683122, 1.000000000000000000, 0.9659258262890683122, 1.000000000000000000, 0.9659258262890683122, 1.000000000000000000, 0.9659258262890683122, 1.000000000000000000, 0.9659258262890683122, 1.000000000000000000, 0.9659258262890683122, 1.000000000000000000, 0.9659258262890683122, 1.000000000000000000, 0.9659258262890683122, 1.000000000000000000, 0.9659258262890683122, 1.000000000000000000, 0.9659258262890683122, 1.000000000000000000, 0.9659258262890683122, 1.000000000000000000, 0.9659258262890683122, 1.000000000000000000, 0.9659258262890683122, 1.000000000000000000, 0.9659258262890683122, 1.000000000000000000, 0.9659258262890683122, 1.000000000000000000, 0.9659258262890683122, 1.000000000000000000, 0.9659258262890683122, 1.000000000000000000, 0.9659258262890683122, 1.000000000000000000, 0.9659258262890683122, 1.000000000000000000, 0.9659258262890683122, 1.000000000000000000, 0.9659258262890683122, 1.000000000000000000, 0.9659258262890683122, 1.000000000000000000, 0.9659258262890683122, 1.000000000000000000, 0.9659258262890683122, 1.000000000000000000, 0.9659258262890683122, 1.000000000000000000, 0.9659258262890683122, 1.000000000000000000, 0.9659258262890683122, 1.000000000000000000, 0.9659258262890683122, 1.000000000000000000, 0.9659258262890683122, 1.000000000000000000, 0.9659258262890683122, 1.000000000000000000, 0.9659258262890683122, 1.000000000000000000, 0.9659258262890683122, 1.000000000000000000, 0.9659258262890683122, 1.000000000000000000, 0.9659258262890683122, 1.000000000000000000, 0.9659258262890683122, 1.000000000000000000, 0.9659258262890683122, 1.000000000000000000, 0.9659258262890683122, 1.000000000000000000, 0.9659258262890683122, 1.000000000000000000, 0.9659258262890683122, 1.000000000000000000, 0.9659258262890683122, 1.000000000000000000, 0.9659258262890683122, 1.000000000000000000, 0.9659258262890683122, 1.000000000000000000, 0.9659258262890683122, 1.000000000000000000, 0.9659258262890683122, 1.000000000000000000, 0.9659258262890683122, 1.000000000000000000, 0.9659258262890683122, 1.000000000000000000, 0.9659258262890683122, 1.000000000000000000, 0.9659258262890683122, 1.000000000000000000, 0.9659258262890683122, 1.000000000000000000, 0.9659258262890683122, 1.000000000000000000, 0.9659258262890683122, 1.000000000000000000, 0.9659258262890683122, 1.000000000000000000, 0.9659258262890683122, 1.000000000000000000, 0.9659258262890683122, 1.000000000000000000, 0.9659258262890683122, 1.000000000000000000, 0.9659258262890683122, 1.000000000000000000, 0.9659258262890683122, 1.000000000000000000, 0.9659258262890683122, 1.000000000000000000, 0.9659258262890683122, 1.000000000000000000, 0.9659258262890683122, 1.000000000000000000, 0.9659258262890683122, 1.000000000000000000, 0.9659258262890683122, 1.000000000000000000, 0.9659258262890683122, 1.000000000000000000, 0.9659258262890683122, 1.000000000000000000, 0.9659258262890683122, 1.000000000000000000, 0.9659258262890683122, 1.000000000000000000, 0.9659258262890683122, 1.000000000000000000, 0.9659258262890683122, 1.000000000000000000, 0.9659258262890683122, 1.000000000000000000, 0.9659258262890683122, 1.000000000000000000, 0.9659258262890683122, 1.000000000000000000, 0.9659258262890683122, 1.000000000000000000, 0.9659258262890683122, 1.000000000000000000, 0.9659258262890683122, 1.000000000000000000, 0.9659258262890683122, 1.000000000000000000, 0.9659258262890683122, 1.000000000000000000, 0.9659258262890683122, 1.000000000000000000, 0.9659258262890683122, 1.000000000000000000, 0.9659258262890683122, 1.000000000000000000, 0.9659258262890683122, 1.000000000000000000, 0.9659258262890683122, 1.000000000000000000, 0.9659258262890683122, 1.000000000000000000, 0.9659258262890683122, 1.000000000000000000, 0.9659258262890683122, 1.000000000000000000, 0.9659258262890683122, 1.000000000000000000, 0.9659258262890683122, 1.000000000000000000, 0.9659258262890683122, 1.000000000000000000, 0.9659258262890683122, 1.000000000000000000, 0.9659258262890683122, 1.000000000000000000, 0.9659258262890683122, 1.000000000000000000, 0.9659258262890683122, 1.000000000000000000, 0.9659258262890683122, 1.000000000000000000, 0.9659258262890683122, 1.000000000000000000, 0.9659258262890683122, 1.000000000000000000, 0.9659258262890683122, 1.000000000000000000, 0.9659258262890683122, 1.000000000000000000, 0.9659258262890683122, 1.000000000000000000, 0.9659258262890683122, 1.000000000000000000, 0.9659258262890683122, 1.000000000000000000, 0.9659258262890683122, 1.000000000000000000, 0.9659258262890683122, 1.000000000000000000, 0.9659258262890683122, 1.000000000000000000, 0.9659258262890683122, 1.000000000000000000, 0.9659258262890683122, 1.000000000000000000, 0.9659258262890683122, 1.000000000000000000, 0.9659258262890683122, 1.000000000000000000, 0.9659258262890683122, 1.000000000000000000, 0.9659258262890683122, 1.000000000000000000, 0.9659258262890683122, 1.000000000000000000, 0.9659258262890683122, 1.000000000000000000, 0.9659258262890683122, 1.000000000000000000, 0.9659258262890683122, 1.000000000000000000, 0.9659258262890683122, 1.000000000000000000, 0.9659258262890683122, 1.000000000000000000, 0.9659258262890683122, 1.000000000000000000, 0.9659258262890683122, 1.000000000000000000, 0.9659258262890683122, 1.000000000000000000, 0.9659258262890683122, 1.000000000000000000, 0.9659258262890683122, 1.000000000000000000, 0.9659258262890683122, 1.000000000000000000, 0.9659258262890683122, 1.000000000000000000, 0.9659258262890683122, 1.000000000000000000, 0.9659258262890683122, 1.000000000000000000, 0.9659258262890683122, 1.000000000000000000, 0.9659258262890683122, 1.000000000000000000, 0.9659258262890683122, 1.000000000000000000, 0.9659258262890683122, 1.000000000000000000, 0.9659258262890683122, 1.000000000000000000, 0.9659258262890683122, 1.000000000000000000, 0.9659258262890683122, 1.000000000000000000, 0.9659258262890683122, 1.000000000000000000, 0.9659258262890683122, 1.000000000000000000, 0.9659258262890683122, 1.000000000000000000, 0.9659258262890683122, 1.000000000000000000, 0.9659258262890683122, 1.000000000000000000, 0.9659258262890683122, 1.000000000000000000, 0.9659258262890683122, 1.000000000000000000, 0.9659258262890683122, 1.000000000000000000, 0.9659258262890683122, 1.000000000000000000, 0.9659258262890683122, 1.000000000000000000, 0.9659258262890683122, 1.000000000000000000, 0.9659258262890683122, 1.000000000000000000, 0.9659258262890683122, 1.000000000000000000, 0.9659258262890683122, 1.000000000000000000, 0.9659258262890683122, 1.000000000000000000, 0.9659258262890683122, 1.000000000000000000, 0.9659258262890683122, 1.000000000000000000, 0.9659258262890683122, 1.000000000000000000, 0.9659258262890683122, 1.000000000000000000, 0.9659258262890683122, 1.000000000000000000, 0.9659258262890683122, 1.000000000000000000),
 ( 0.3333333333333333703, 0.3219752754296894559, 0.3333333333333333703, 0.3219752754296894559, 0.3333333333333333703, 0.3219752754296894559, 0.3333333333333333703, 0.3219752754296894559, 0.3333333333333333703, 0.3219752754296894559, 0.3333333333333333703, 0.3219752754296894559, 0.3333333333333333703, 0.3219752754296894559, 0.3333333333333333703, 0.3219752754296894559, 0.3333333333333333703, 0.3219752754296894559, 0.3333333333333333703, 0.3219752754296894559, 0.3333333333333333703, 0.3219752754296894559, 0.3333333333333333703, 0.3219752754296894559, 0.3333333333333333703, 0.3219752754296894559, 0.3333333333333333703, 0.3219752754296894559, 0.3333333333333333703, 0.3219752754296894559, 0.3333333333333333703, 0.3219752754296894559, 0.3333333333333333703, 0.3219752754296894559, 0.3333333333333333703, 0.3219752754296894559, 0.3333333333333333703, 0.3219752754296894559, 0.3333333333333333703, 0.3219752754296894559, 0.3333333333333333703, 0.3219752754296894559, 0.3333333333333333703, 0.3219752754296894559, 0.3333333333333333703, 0.3219752754296894559, 0.3333333333333333703, 0.3219752754296894559, 0.3333333333333333703, 0.3219752754296894559, 0.3333333333333333703, 0.3219752754296894559, 0.3333333333333333703, 0.3219752754296894559, 0.3333333333333333703, 0.3219752754296894559, 0.3333333333333333703, 0.3219752754296894559, 0.3333333333333333703, 0.3219752754296894559, 0.3333333333333333703, 0.3219752754296894559, 0.3333333333333333703, 0.3219752754296894559, 0.3333333333333333703, 0.3219752754296894559, 0.3333333333333333703, 0.3219752754296894559, 0.3333333333333333703, 0.3219752754296894559, 0.3333333333333333703, 0.3219752754296894559, 0.3333333333333333703, 0.3219752754296894559, 0.3333333333333333703, 0.3219752754296894559, 0.3333333333333333703, 0.3219752754296894559, 0.3333333333333333703, 0.3219752754296894559, 0.3333333333333333703, 0.3219752754296894559, 0.3333333333333333703, 0.3219752754296894559, 0.3333333333333333703, 0.3219752754296894559, 0.3333333333333333703, 0.3219752754296894559, 0.3333333333333333703, 0.3219752754296894559, 0.3333333333333333703, 0.3219752754296894559, 0.3333333333333333703, 0.3219752754296894559, 0.3333333333333333703, 0.3219752754296894559, 0.3333333333333333703, 0.3219752754296894559, 0.3333333333333333703, 0.3219752754296894559, 0.3333333333333333703, 0.3219752754296894559, 0.3333333333333333703, 0.3219752754296894559, 0.3333333333333333703, 0.3219752754296894559, 0.3333333333333333703, 0.3219752754296894559, 0.3333333333333333703, 0.3219752754296894559, 0.3333333333333333703, 0.3219752754296894559, 0.3333333333333333703, 0.3219752754296894559, 0.3333333333333333703, 0.3219752754296894559, 0.3333333333333333703, 0.3219752754296894559, 0.3333333333333333703, 0.3219752754296894559, 0.3333333333333333703, 0.3219752754296894559, 0.3333333333333333703, 0.3219752754296894559, 0.3333333333333333703, 0.3219752754296894559, 0.3333333333333333703, 0.3219752754296894559, 0.3333333333333333703, 0.3219752754296894559, 0.3333333333333333703, 0.3219752754296894559, 0.3333333333333333703, 0.3219752754296894559, 0.3333333333333333703, 0.3219752754296894559, 0.3333333333333333703, 0.3219752754296894559, 0.3333333333333333703, 0.3219752754296894559, 0.3333333333333333703, 0.3219752754296894559, 0.3333333333333333703, 0.3219752754296894559, 0.3333333333333333703, 0.3219752754296894559, 0.3333333333333333703, 0.3219752754296894559, 0.3333333333333333703, 0.3219752754296894559, 0.3333333333333333703, 0.3219752754296894559, 0.3333333333333333703, 0.3219752754296894559, 0.3333333333333333703, 0.3219752754296894559, 0.3333333333333333703, 0.3219752754296894559, 0.3333333333333333703, 0.3219752754296894559, 0.3333333333333333703, 0.3219752754296894559, 0.3333333333333333703, 0.3219752754296894559, 0.3333333333333333703, 0.3219752754296894559, 0.3333333333333333703, 0.3219752754296894559, 0.3333333333333333703, 0.3219752754296894559, 0.3333333333333333703, 0.3219752754296894559, 0.3333333333333333703, 0.3219752754296894559, 0.3333333333333333703, 0.3219752754296894559, 0.3333333333333333703, 0.3219752754296894559, 0.3333333333333333703, 0.3219752754296894559, 0.3333333333333333703, 0.3219752754296894559, 0.3333333333333333703, 0.3219752754296894559, 0.3333333333333333703, 0.3219752754296894559, 0.3333333333333333703, 0.3219752754296894559, 0.3333333333333333703, 0.3219752754296894559, 0.3333333333333333703, 0.3219752754296894559, 0.3333333333333333703, 0.3219752754296894559, 0.3333333333333333703, 0.3219752754296894559, 0.3333333333333333703, 0.3219752754296894559, 0.3333333333333333703, 0.3219752754296894559, 0.3333333333333333703, 0.3219752754296894559, 0.3333333333333333703, 0.3219752754296894559, 0.3333333333333333703, 0.3219752754296894559, 0.3333333333333333703, 0.3219752754296894559, 0.3333333333333333703, 0.3219752754296894559, 0.3333333333333333703, 0.3219752754296894559, 0.3333333333333333703, 0.3219752754296894559, 0.3333333333333333703, 0.3219752754296894559, 0.3333333333333333703, 0.3219752754296894559, 0.3333333333333333703, 0.3219752754296894559, 0.3333333333333333703, 0.3219752754296894559, 0.3333333333333333703, 0.3219752754296894559, 0.3333333333333333703, 0.3219752754296894559, 0.3333333333333333703, 0.3219752754296894559, 0.3333333333333333703, 0.3219752754296894559, 0.3333333333333333703, 0.3219752754296894559, 0.3333333333333333703, 0.3219752754296894559, 0.3333333333333333703, 0.3219752754296894559, 0.3333333333333333703, 0.3219752754296894559, 0.3333333333333333703, 0.3219752754296894559, 0.3333333333333333703, 0.3219752754296894559, 0.3333333333333333703, 0.3219752754296894559, 0.3333333333333333703, 0.3219752754296894559, 0.3333333333333333703, 0.3219752754296894559, 0.3333333333333333703, 0.3219752754296894559, 0.3333333333333333703, 0.3219752754296894559, 0.3333333333333333703, 0.3219752754296894559, 0.3333333333333333703, 0.3219752754296894559, 0.3333333333333333703, 0.3219752754296894559, 0.3333333333333333703, 0.3219752754296894559, 0.3333333333333333703, 0.3219752754296894559, 0.3333333333333333703, 0.3219752754296894559, 0.3333333333333333703, 0.3219752754296894559, 0.3333333333333333703, 0.3219752754296894559, 0.3333333333333333703, 0.3219752754296894559, 0.3333333333333333703, 0.3219752754296894559, 0.3333333333333333703, 0.3219752754296894559, 0.3333333333333333703, 0.3219752754296894559, 0.3333333333333333703, 0.3219752754296894559, 0.3333333333333333703, 0.3219752754296894559, 0.3333333333333333703, 0.3219752754296894559, 0.3333333333333333703, 0.3219752754296894559, 0.3333333333333333703, 0.3219752754296894559, 0.3333333333333333703, 0.3219752754296894559, 0.3333333333333333703, 0.3219752754296894559, 0.3333333333333333703, 0.3219752754296894559, 0.3333333333333333703, 0.3219752754296894559, 0.3333333333333333703, 0.3219752754296894559, 0.3333333333333333703, 0.3219752754296894559, 0.3333333333333333703, 0.3219752754296894559, 0.3333333333333333703, 0.3219752754296894559, 0.3333333333333333703, 0.3219752754296894559, 0.3333333333333333703, 0.3219752754296894559, 0.3333333333333333703, 0.3219752754296894559, 0.3333333333333333703, 0.3219752754296894559, 0.3333333333333333703, 0.3219752754296894559, 0.3333333333333333703, 0.3219752754296894559, 0.3333333333333333703, 0.3219752754296894559, 0.3333333333333333703, 0.3219752754296894559, 0.3333333333333333703, 0.3219752754296894559, 0.3333333333333333703, 0.3219752754296894559, 0.3333333333333333703, 0.3219752754296894559, 0.3333333333333333703, 0.3219752754296894559, 0.3333333333333333703, 0.3219752754296894559, 0.3333333333333333703, 0.3219752754296894559, 0.3333333333333333703, 0.3219752754296894559, 0.3333333333333333703, 0.3219752754296894559, 0.3333333333333333703, 0.3219752754296894559, 0.3333333333333333703, 0.3219752754296894559, 0.3333333333333333703, 0.3219752754296894559, 0.3333333333333333703, 0.3219752754296894559, 0.3333333333333333703, 0.3219752754296894559, 0.3333333333333333703, 0.3219752754296894559, 0.3333333333333333703, 0.3219752754296894559, 0.3333333333333333703, 0.3219752754296894559, 0.3333333333333333703, 0.3219752754296894559, 0.3333333333333333703, 0.3219752754296894559, 0.3333333333333333703, 0.3219752754296894559, 0.3333333333333333703, 0.3219752754296894559, 0.3333333333333333703, 0.3219752754296894559, 0.3333333333333333703, 0.3219752754296894559, 0.3333333333333333703, 0.3219752754296894559, 0.3333333333333333703, 0.3219752754296894559, 0.3333333333333333703, 0.3219752754296894559, 0.3333333333333333703, 0.3219752754296894559, 0.3333333333333333703, 0.3219752754296894559, 0.3333333333333333703, 0.3219752754296894559, 0.3333333333333333703, 0.3219752754296894559, 0.3333333333333333703, 0.3219752754296894559, 0.3333333333333333703, 0.3219752754296894559, 0.3333333333333333703, 0.3219752754296894559, 0.3333333333333333703, 0.3219752754296894559, 0.3333333333333333703, 0.3219752754296894559, 0.3333333333333333703, 0.3219752754296894559, 0.3333333333333333703, 0.3219752754296894559, 0.3333333333333333703, 0.3219752754296894559, 0.3333333333333333703, 0.3219752754296894559, 0.3333333333333333703, 0.3219752754296894559, 0.3333333333333333703, 0.3219752754296894559, 0.3333333333333333703, 0.3219752754296894559, 0.3333333333333333703, 0.3219752754296894559, 0.3333333333333333703, 0.3219752754296894559, 0.3333333333333333703, 0.3219752754296894559, 0.3333333333333333703, 0.3219752754296894559, 0.3333333333333333703, 0.3219752754296894559, 0.3333333333333333703, 0.3219752754296894559, 0.3333333333333333703, 0.3219752754296894559, 0.3333333333333333703, 0.3219752754296894559, 0.3333333333333333703, 0.3219752754296894559, 0.3333333333333333703, 0.3219752754296894559, 0.3333333333333333703, 0.3219752754296894559, 0.3333333333333333703, 0.3219752754296894559, 0.3333333333333333703, 0.3219752754296894559, 0.3333333333333333703, 0.3219752754296894559, 0.3333333333333333703, 0.3219752754296894559, 0.3333333333333333703, 0.3219752754296894559, 0.3333333333333333703, 0.3219752754296894559, 0.3333333333333333703, 0.3219752754296894559, 0.3333333333333333703, 0.3219752754296894559, 0.3333333333333333703, 0.3219752754296894559, 0.3333333333333333703, 0.3219752754296894559, 0.3333333333333333703, 0.3219752754296894559, 0.3333333333333333703, 0.3219752754296894559, 0.3333333333333333703, 0.3219752754296894559, 0.3333333333333333703, 0.3219752754296894559, 0.3333333333333333703, 0.3219752754296894559, 0.3333333333333333703, 0.3219752754296894559, 0.3333333333333333703, 0.3219752754296894559, 0.3333333333333333703),
 ( 0.3333333333333333703, 0.3219752754296894559, 0.3333333333333333703, 0.3219752754296894559, 0.3333333333333333703, 0.3219752754296894559, 0.3333333333333333703, 0.3219752754296894559, 0.3333333333333333703, 0.3219752754296894559, 0.3333333333333333703, 0.3219752754296894559, 0.3333333333333333703, 0.3219752754296894559, 0.3333333333333333703, 0.3219752754296894559, 0.3333333333333333703, 0.3219752754296894559, 0.3333333333333333703, 0.3219752754296894559, 0.3333333333333333703, 0.3219752754296894559, 0.3333333333333333703, 0.3219752754296894559, 0.3333333333333333703, 0.3219752754296894559, 0.3333333333333333703, 0.3219752754296894559, 0.3333333333333333703, 0.3219752754296894559, 0.3333333333333333703, 0.3219752754296894559, 0.3333333333333333703, 0.3219752754296894559, 0.3333333333333333703, 0.3219752754296894559, 0.3333333333333333703, 0.3219752754296894559, 0.3333333333333333703, 0.3219752754296894559, 0.3333333333333333703, 0.3219752754296894559, 0.3333333333333333703, 0.3219752754296894559, 0.3333333333333333703, 0.3219752754296894559, 0.3333333333333333703, 0.3219752754296894559, 0.3333333333333333703, 0.3219752754296894559, 0.3333333333333333703, 0.3219752754296894559, 0.3333333333333333703, 0.3219752754296894559, 0.3333333333333333703, 0.3219752754296894559, 0.3333333333333333703, 0.3219752754296894559, 0.3333333333333333703, 0.3219752754296894559, 0.3333333333333333703, 0.3219752754296894559, 0.3333333333333333703, 0.3219752754296894559, 0.3333333333333333703, 0.3219752754296894559, 0.3333333333333333703, 0.3219752754296894559, 0.3333333333333333703, 0.3219752754296894559, 0.3333333333333333703, 0.3219752754296894559, 0.3333333333333333703, 0.3219752754296894559, 0.3333333333333333703, 0.3219752754296894559, 0.3333333333333333703, 0.3219752754296894559, 0.3333333333333333703, 0.3219752754296894559, 0.3333333333333333703, 0.3219752754296894559, 0.3333333333333333703, 0.3219752754296894559, 0.3333333333333333703, 0.3219752754296894559, 0.3333333333333333703, 0.3219752754296894559, 0.3333333333333333703, 0.3219752754296894559, 0.3333333333333333703, 0.3219752754296894559, 0.3333333333333333703, 0.3219752754296894559, 0.3333333333333333703, 0.3219752754296894559, 0.3333333333333333703, 0.3219752754296894559, 0.3333333333333333703, 0.3219752754296894559, 0.3333333333333333703, 0.3219752754296894559, 0.3333333333333333703, 0.3219752754296894559, 0.3333333333333333703, 0.3219752754296894559, 0.3333333333333333703, 0.3219752754296894559, 0.3333333333333333703, 0.3219752754296894559, 0.3333333333333333703, 0.3219752754296894559, 0.3333333333333333703, 0.3219752754296894559, 0.3333333333333333703, 0.3219752754296894559, 0.3333333333333333703, 0.3219752754296894559, 0.3333333333333333703, 0.3219752754296894559, 0.3333333333333333703, 0.3219752754296894559, 0.3333333333333333703, 0.3219752754296894559, 0.3333333333333333703, 0.3219752754296894559, 0.3333333333333333703, 0.3219752754296894559, 0.3333333333333333703, 0.3219752754296894559, 0.3333333333333333703, 0.3219752754296894559, 0.3333333333333333703, 0.3219752754296894559, 0.3333333333333333703, 0.3219752754296894559, 0.3333333333333333703, 0.3219752754296894559, 0.3333333333333333703, 0.3219752754296894559, 0.3333333333333333703, 0.3219752754296894559, 0.3333333333333333703, 0.3219752754296894559, 0.3333333333333333703, 0.3219752754296894559, 0.3333333333333333703, 0.3219752754296894559, 0.3333333333333333703, 0.3219752754296894559, 0.3333333333333333703, 0.3219752754296894559, 0.3333333333333333703, 0.3219752754296894559, 0.3333333333333333703, 0.3219752754296894559, 0.3333333333333333703, 0.3219752754296894559, 0.3333333333333333703, 0.3219752754296894559, 0.3333333333333333703, 0.3219752754296894559, 0.3333333333333333703, 0.3219752754296894559, 0.3333333333333333703, 0.3219752754296894559, 0.3333333333333333703, 0.3219752754296894559, 0.3333333333333333703, 0.3219752754296894559, 0.3333333333333333703, 0.3219752754296894559, 0.3333333333333333703, 0.3219752754296894559, 0.3333333333333333703, 0.3219752754296894559, 0.3333333333333333703, 0.3219752754296894559, 0.3333333333333333703, 0.3219752754296894559, 0.3333333333333333703, 0.3219752754296894559, 0.3333333333333333703, 0.3219752754296894559, 0.3333333333333333703, 0.3219752754296894559, 0.3333333333333333703, 0.3219752754296894559, 0.3333333333333333703, 0.3219752754296894559, 0.3333333333333333703, 0.3219752754296894559, 0.3333333333333333703, 0.3219752754296894559, 0.3333333333333333703, 0.3219752754296894559, 0.3333333333333333703, 0.3219752754296894559, 0.3333333333333333703, 0.3219752754296894559, 0.3333333333333333703, 0.3219752754296894559, 0.3333333333333333703, 0.3219752754296894559, 0.3333333333333333703, 0.3219752754296894559, 0.3333333333333333703, 0.3219752754296894559, 0.3333333333333333703, 0.3219752754296894559, 0.3333333333333333703, 0.3219752754296894559, 0.3333333333333333703, 0.3219752754296894559, 0.3333333333333333703, 0.3219752754296894559, 0.3333333333333333703, 0.3219752754296894559, 0.3333333333333333703, 0.3219752754296894559, 0.3333333333333333703, 0.3219752754296894559, 0.3333333333333333703, 0.3219752754296894559, 0.3333333333333333703, 0.3219752754296894559, 0.3333333333333333703, 0.3219752754296894559, 0.3333333333333333703, 0.3219752754296894559, 0.3333333333333333703, 0.3219752754296894559, 0.3333333333333333703, 0.3219752754296894559, 0.3333333333333333703, 0.3219752754296894559, 0.3333333333333333703, 0.3219752754296894559, 0.3333333333333333703, 0.3219752754296894559, 0.3333333333333333703, 0.3219752754296894559, 0.3333333333333333703, 0.3219752754296894559, 0.3333333333333333703, 0.3219752754296894559, 0.3333333333333333703, 0.3219752754296894559, 0.3333333333333333703, 0.3219752754296894559, 0.3333333333333333703, 0.3219752754296894559, 0.3333333333333333703, 0.3219752754296894559, 0.3333333333333333703, 0.3219752754296894559, 0.3333333333333333703, 0.3219752754296894559, 0.3333333333333333703, 0.3219752754296894559, 0.3333333333333333703, 0.3219752754296894559, 0.3333333333333333703, 0.3219752754296894559, 0.3333333333333333703, 0.3219752754296894559, 0.3333333333333333703, 0.3219752754296894559, 0.3333333333333333703, 0.3219752754296894559, 0.3333333333333333703, 0.3219752754296894559, 0.3333333333333333703, 0.3219752754296894559, 0.3333333333333333703, 0.3219752754296894559, 0.3333333333333333703, 0.3219752754296894559, 0.3333333333333333703, 0.3219752754296894559, 0.3333333333333333703, 0.3219752754296894559, 0.3333333333333333703, 0.3219752754296894559, 0.3333333333333333703, 0.3219752754296894559, 0.3333333333333333703, 0.3219752754296894559, 0.3333333333333333703, 0.3219752754296894559, 0.3333333333333333703, 0.3219752754296894559, 0.3333333333333333703, 0.3219752754296894559, 0.3333333333333333703, 0.3219752754296894559, 0.3333333333333333703, 0.3219752754296894559, 0.3333333333333333703, 0.3219752754296894559, 0.3333333333333333703, 0.3219752754296894559, 0.3333333333333333703, 0.3219752754296894559, 0.3333333333333333703, 0.3219752754296894559, 0.3333333333333333703, 0.3219752754296894559, 0.3333333333333333703, 0.3219752754296894559, 0.3333333333333333703, 0.3219752754296894559, 0.3333333333333333703, 0.3219752754296894559, 0.3333333333333333703, 0.3219752754296894559, 0.3333333333333333703, 0.3219752754296894559, 0.3333333333333333703, 0.3219752754296894559, 0.3333333333333333703, 0.3219752754296894559, 0.3333333333333333703, 0.3219752754296894559, 0.3333333333333333703, 0.3219752754296894559, 0.3333333333333333703, 0.3219752754296894559, 0.3333333333333333703, 0.3219752754296894559, 0.3333333333333333703, 0.3219752754296894559, 0.3333333333333333703, 0.3219752754296894559, 0.3333333333333333703, 0.3219752754296894559, 0.3333333333333333703, 0.3219752754296894559, 0.3333333333333333703, 0.3219752754296894559, 0.3333333333333333703, 0.3219752754296894559, 0.3333333333333333703, 0.3219752754296894559, 0.3333333333333333703, 0.3219752754296894559, 0.3333333333333333703, 0.3219752754296894559, 0.3333333333333333703, 0.3219752754296894559, 0.3333333333333333703, 0.3219752754296894559, 0.3333333333333333703, 0.3219752754296894559, 0.3333333333333333703, 0.3219752754296894559, 0.3333333333333333703, 0.3219752754296894559, 0.3333333333333333703, 0.3219752754296894559, 0.3333333333333333703, 0.3219752754296894559, 0.3333333333333333703, 0.3219752754296894559, 0.3333333333333333703, 0.3219752754296894559, 0.3333333333333333703, 0.3219752754296894559, 0.3333333333333333703, 0.3219752754296894559, 0.3333333333333333703, 0.3219752754296894559, 0.3333333333333333703, 0.3219752754296894559, 0.3333333333333333703, 0.3219752754296894559, 0.3333333333333333703, 0.3219752754296894559, 0.3333333333333333703, 0.3219752754296894559, 0.3333333333333333703, 0.3219752754296894559, 0.3333333333333333703, 0.3219752754296894559, 0.3333333333333333703, 0.3219752754296894559, 0.3333333333333333703, 0.3219752754296894559, 0.3333333333333333703, 0.3219752754296894559, 0.3333333333333333703, 0.3219752754296894559, 0.3333333333333333703, 0.3219752754296894559, 0.3333333333333333703, 0.3219752754296894559, 0.3333333333333333703, 0.3219752754296894559, 0.3333333333333333703, 0.3219752754296894559, 0.3333333333333333703, 0.3219752754296894559, 0.3333333333333333703, 0.3219752754296894559, 0.3333333333333333703, 0.3219752754296894559, 0.3333333333333333703, 0.3219752754296894559, 0.3333333333333333703, 0.3219752754296894559, 0.3333333333333333703, 0.3219752754296894559, 0.3333333333333333703, 0.3219752754296894559, 0.3333333333333333703, 0.3219752754296894559, 0.3333333333333333703, 0.3219752754296894559, 0.3333333333333333703, 0.3219752754296894559, 0.3333333333333333703, 0.3219752754296894559, 0.3333333333333333703, 0.3219752754296894559, 0.3333333333333333703, 0.3219752754296894559, 0.3333333333333333703, 0.3219752754296894559, 0.3333333333333333703, 0.3219752754296894559, 0.3333333333333333703, 0.3219752754296894559, 0.3333333333333333703, 0.3219752754296894559, 0.3333333333333333703, 0.3219752754296894559, 0.3333333333333333703, 0.3219752754296894559, 0.3333333333333333703, 0.3219752754296894559, 0.3333333333333333703, 0.3219752754296894559, 0.3333333333333333703, 0.3219752754296894559, 0.3333333333333333703, 0.3219752754296894559, 0.3333333333333333703, 0.3219752754296894559, 0.3333333333333333703, 0.3219752754296894559, 0.3333333333333333703, 0.3219752754296894559, 0.3333333333333333703, 0.3219752754296894559, 0.3333333333333333703, 0.3219752754296894559, 0.3333333333333333703),
 ( 1.000000000000000000, 0.9659258262890683122, 1.000000000000000000, 0.9659258262890683122, 1.000000000000000000, 0.9659258262890683122, 1.000000000000000000, 0.9659258262890683122, 1.000000000000000000, 0.9659258262890683122, 1.000000000000000000, 0.9659258262890683122, 1.000000000000000000, 0.9659258262890683122, 1.000000000000000000, 0.9659258262890683122, 1.000000000000000000, 0.9659258262890683122, 1.000000000000000000, 0.9659258262890683122, 1.000000000000000000, 0.9659258262890683122, 1.000000000000000000, 0.9659258262890683122, 1.000000000000000000, 0.9659258262890683122, 1.000000000000000000, 0.9659258262890683122, 1.000000000000000000, 0.9659258262890683122, 1.000000000000000000, 0.9659258262890683122, 1.000000000000000000, 0.9659258262890683122, 1.000000000000000000, 0.9659258262890683122, 1.000000000000000000, 0.9659258262890683122, 1.000000000000000000, 0.9659258262890683122, 1.000000000000000000, 0.9659258262890683122, 1.000000000000000000, 0.9659258262890683122, 1.000000000000000000, 0.9659258262890683122, 1.000000000000000000, 0.9659258262890683122, 1.000000000000000000, 0.9659258262890683122, 1.000000000000000000, 0.9659258262890683122, 1.000000000000000000, 0.9659258262890683122, 1.000000000000000000, 0.9659258262890683122, 1.000000000000000000, 0.9659258262890683122, 1.000000000000000000, 0.9659258262890683122, 1.000000000000000000, 0.9659258262890683122, 1.000000000000000000, 0.9659258262890683122, 1.000000000000000000, 0.9659258262890683122, 1.000000000000000000, 0.9659258262890683122, 1.000000000000000000, 0.9659258262890683122, 1.000000000000000000, 0.9659258262890683122, 1.000000000000000000, 0.9659258262890683122, 1.000000000000000000, 0.9659258262890683122, 1.000000000000000000, 0.9659258262890683122, 1.000000000000000000, 0.9659258262890683122, 1.000000000000000000, 0.9659258262890683122, 1.000000000000000000, 0.9659258262890683122, 1.000000000000000000, 0.9659258262890683122, 1.000000000000000000, 0.9659258262890683122, 1.000000000000000000, 0.9659258262890683122, 1.000000000000000000, 0.9659258262890683122, 1.000000000000000000, 0.9659258262890683122, 1.000000000000000000, 0.9659258262890683122, 1.000000000000000000, 0.9659258262890683122, 1.000000000000000000, 0.9659258262890683122, 1.000000000000000000, 0.9659258262890683122, 1.000000000000000000, 0.9659258262890683122, 1.000000000000000000, 0.9659258262890683122, 1.000000000000000000, 0.9659258262890683122, 1.000000000000000000, 0.9659258262890683122, 1.000000000000000000, 0.9659258262890683122, 1.000000000000000000, 0.9659258262890683122, 1.000000000000000000, 0.9659258262890683122, 1.000000000000000000, 0.9659258262890683122, 1.000000000000000000, 0.9659258262890683122, 1.000000000000000000, 0.9659258262890683122, 1.000000000000000000, 0.9659258262890683122, 1.000000000000000000, 0.9659258262890683122, 1.000000000000000000, 0.9659258262890683122, 1.000000000000000000, 0.9659258262890683122, 1.000000000000000000, 0.9659258262890683122, 1.000000000000000000, 0.9659258262890683122, 1.000000000000000000, 0.9659258262890683122, 1.000000000000000000, 0.9659258262890683122, 1.000000000000000000, 0.9659258262890683122, 1.000000000000000000, 0.9659258262890683122, 1.000000000000000000, 0.9659258262890683122, 1.000000000000000000, 0.9659258262890683122, 1.000000000000000000, 0.9659258262890683122, 1.000000000000000000, 0.9659258262890683122, 1.000000000000000000, 0.9659258262890683122, 1.000000000000000000, 0.9659258262890683122, 1.000000000000000000, 0.9659258262890683122, 1.000000000000000000, 0.9659258262890683122, 1.000000000000000000, 0.9659258262890683122, 1.000000000000000000, 0.9659258262890683122, 1.000000000000000000, 0.9659258262890683122, 1.000000000000000000, 0.9659258262890683122, 1.000000000000000000, 0.9659258262890683122, 1.000000000000000000, 0.9659258262890683122, 1.000000000000000000, 0.9659258262890683122, 1.000000000000000000, 0.9659258262890683122, 1.000000000000000000, 0.9659258262890683122, 1.000000000000000000, 0.9659258262890683122, 1.000000000000000000, 0.9659258262890683122, 1.000000000000000000, 0.9659258262890683122, 1.000000000000000000, 0.9659258262890683122, 1.000000000000000000, 0.9659258262890683122, 1.000000000000000000, 0.9659258262890683122, 1.000000000000000000, 0.9659258262890683122, 1.000000000000000000, 0.9659258262890683122, 1.000000000000000000, 0.9659258262890683122, 1.000000000000000000, 0.9659258262890683122, 1.000000000000000000, 0.9659258262890683122, 1.000000000000000000, 0.9659258262890683122, 1.000000000000000000, 0.9659258262890683122, 1.000000000000000000, 0.9659258262890683122, 1.000000000000000000, 0.9659258262890683122, 1.000000000000000000, 0.9659258262890683122, 1.000000000000000000, 0.9659258262890683122, 1.000000000000000000, 0.9659258262890683122, 1.000000000000000000, 0.9659258262890683122, 1.000000000000000000, 0.9659258262890683122, 1.000000000000000000, 0.9659258262890683122, 1.000000000000000000, 0.9659258262890683122, 1.000000000000000000, 0.9659258262890683122, 1.000000000000000000, 0.9659258262890683122, 1.000000000000000000, 0.9659258262890683122, 1.000000000000000000, 0.9659258262890683122, 1.000000000000000000, 0.9659258262890683122, 1.000000000000000000, 0.9659258262890683122, 1.000000000000000000, 0.9659258262890683122, 1.000000000000000000, 0.9659258262890683122, 1.000000000000000000, 0.9659258262890683122, 1.000000000000000000, 0.9659258262890683122, 1.000000000000000000, 0.9659258262890683122, 1.000000000000000000, 0.9659258262890683122, 1.000000000000000000, 0.9659258262890683122, 1.000000000000000000, 0.9659258262890683122, 1.000000000000000000, 0.9659258262890683122, 1.000000000000000000, 0.9659258262890683122, 1.000000000000000000, 0.9659258262890683122, 1.000000000000000000, 0.9659258262890683122, 1.000000000000000000, 0.9659258262890683122, 1.000000000000000000, 0.9659258262890683122, 1.000000000000000000, 0.9659258262890683122, 1.000000000000000000, 0.9659258262890683122, 1.000000000000000000, 0.9659258262890683122, 1.000000000000000000, 0.9659258262890683122, 1.000000000000000000, 0.9659258262890683122, 1.000000000000000000, 0.9659258262890683122, 1.000000000000000000, 0.9659258262890683122, 1.000000000000000000, 0.9659258262890683122, 1.000000000000000000, 0.9659258262890683122, 1.000000000000000000, 0.9659258262890683122, 1.000000000000000000, 0.9659258262890683122, 1.000000000000000000, 0.9659258262890683122, 1.000000000000000000, 0.9659258262890683122, 1.000000000000000000, 0.9659258262890683122, 1.000000000000000000, 0.9659258262890683122, 1.000000000000000000, 0.9659258262890683122, 1.000000000000000000, 0.9659258262890683122, 1.000000000000000000, 0.9659258262890683122, 1.000000000000000000, 0.9659258262890683122, 1.000000000000000000, 0.9659258262890683122, 1.000000000000000000, 0.9659258262890683122, 1.000000000000000000, 0.9659258262890683122, 1.000000000000000000, 0.9659258262890683122, 1.000000000000000000, 0.9659258262890683122, 1.000000000000000000, 0.9659258262890683122, 1.000000000000000000, 0.9659258262890683122, 1.000000000000000000, 0.9659258262890683122, 1.000000000000000000, 0.9659258262890683122, 1.000000000000000000, 0.9659258262890683122, 1.000000000000000000, 0.9659258262890683122, 1.000000000000000000, 0.9659258262890683122, 1.000000000000000000, 0.9659258262890683122, 1.000000000000000000, 0.9659258262890683122, 1.000000000000000000, 0.9659258262890683122, 1.000000000000000000, 0.9659258262890683122, 1.000000000000000000, 0.9659258262890683122, 1.000000000000000000, 0.9659258262890683122, 1.000000000000000000, 0.9659258262890683122, 1.000000000000000000, 0.9659258262890683122, 1.000000000000000000, 0.9659258262890683122, 1.000000000000000000, 0.9659258262890683122, 1.000000000000000000, 0.9659258262890683122, 1.000000000000000000, 0.9659258262890683122, 1.000000000000000000, 0.9659258262890683122, 1.000000000000000000, 0.9659258262890683122, 1.000000000000000000, 0.9659258262890683122, 1.000000000000000000, 0.9659258262890683122, 1.000000000000000000, 0.9659258262890683122, 1.000000000000000000, 0.9659258262890683122, 1.000000000000000000, 0.9659258262890683122, 1.000000000000000000, 0.9659258262890683122, 1.000000000000000000, 0.9659258262890683122, 1.000000000000000000, 0.9659258262890683122, 1.000000000000000000, 0.9659258262890683122, 1.000000000000000000, 0.9659258262890683122, 1.000000000000000000, 0.9659258262890683122, 1.000000000000000000, 0.9659258262890683122, 1.000000000000000000, 0.9659258262890683122, 1.000000000000000000, 0.9659258262890683122, 1.000000000000000000, 0.9659258262890683122, 1.000000000000000000, 0.9659258262890683122, 1.000000000000000000, 0.9659258262890683122, 1.000000000000000000, 0.9659258262890683122, 1.000000000000000000, 0.9659258262890683122, 1.000000000000000000, 0.9659258262890683122, 1.000000000000000000, 0.9659258262890683122, 1.000000000000000000, 0.9659258262890683122, 1.000000000000000000, 0.9659258262890683122, 1.000000000000000000, 0.9659258262890683122, 1.000000000000000000, 0.9659258262890683122, 1.000000000000000000, 0.9659258262890683122, 1.000000000000000000, 0.9659258262890683122, 1.000000000000000000, 0.9659258262890683122, 1.000000000000000000, 0.9659258262890683122, 1.000000000000000000, 0.9659258262890683122, 1.000000000000000000, 0.9659258262890683122, 1.000000000000000000, 0.9659258262890683122, 1.000000000000000000, 0.9659258262890683122, 1.000000000000000000, 0.9659258262890683122, 1.000000000000000000, 0.9659258262890683122, 1.000000000000000000, 0.9659258262890683122, 1.000000000000000000, 0.9659258262890683122, 1.000000000000000000, 0.9659258262890683122, 1.000000000000000000, 0.9659258262890683122, 1.000000000000000000, 0.9659258262890683122, 1.000000000000000000, 0.9659258262890683122, 1.000000000000000000, 0.9659258262890683122, 1.000000000000000000, 0.9659258262890683122, 1.000000000000000000, 0.9659258262890683122, 1.000000000000000000, 0.9659258262890683122, 1.000000000000000000, 0.9659258262890683122, 1.000000000000000000, 0.9659258262890683122, 1.000000000000000000, 0.9659258262890683122, 1.000000000000000000, 0.9659258262890683122, 1.000000000000000000, 0.9659258262890683122, 1.000000000000000000, 0.9659258262890683122, 1.000000000000000000, 0.9659258262890683122, 1.000000000000000000, 0.9659258262890683122, 1.000000000000000000),
 ( 0.3333333333333333703, 0.3219752754296894559, 0.3333333333333333703, 0.3219752754296894559, 0.3333333333333333703, 0.3219752754296894559, 0.3333333333333333703, 0.3219752754296894559, 0.3333333333333333703, 0.3219752754296894559, 0.3333333333333333703, 0.3219752754296894559, 0.3333333333333333703, 0.3219752754296894559, 0.3333333333333333703, 0.3219752754296894559, 0.3333333333333333703, 0.3219752754296894559, 0.3333333333333333703, 0.3219752754296894559, 0.3333333333333333703, 0.3219752754296894559, 0.3333333333333333703, 0.3219752754296894559, 0.3333333333333333703, 0.3219752754296894559, 0.3333333333333333703, 0.3219752754296894559, 0.3333333333333333703, 0.3219752754296894559, 0.3333333333333333703, 0.3219752754296894559, 0.3333333333333333703, 0.3219752754296894559, 0.3333333333333333703, 0.3219752754296894559, 0.3333333333333333703, 0.3219752754296894559, 0.3333333333333333703, 0.3219752754296894559, 0.3333333333333333703, 0.3219752754296894559, 0.3333333333333333703, 0.3219752754296894559, 0.3333333333333333703, 0.3219752754296894559, 0.3333333333333333703, 0.3219752754296894559, 0.3333333333333333703, 0.3219752754296894559, 0.3333333333333333703, 0.3219752754296894559, 0.3333333333333333703, 0.3219752754296894559, 0.3333333333333333703, 0.3219752754296894559, 0.3333333333333333703, 0.3219752754296894559, 0.3333333333333333703, 0.3219752754296894559, 0.3333333333333333703, 0.3219752754296894559, 0.3333333333333333703, 0.3219752754296894559, 0.3333333333333333703, 0.3219752754296894559, 0.3333333333333333703, 0.3219752754296894559, 0.3333333333333333703, 0.3219752754296894559, 0.3333333333333333703, 0.3219752754296894559, 0.3333333333333333703, 0.3219752754296894559, 0.3333333333333333703, 0.3219752754296894559, 0.3333333333333333703, 0.3219752754296894559, 0.3333333333333333703, 0.3219752754296894559, 0.3333333333333333703, 0.3219752754296894559, 0.3333333333333333703, 0.3219752754296894559, 0.3333333333333333703, 0.3219752754296894559, 0.3333333333333333703, 0.3219752754296894559, 0.3333333333333333703, 0.3219752754296894559, 0.3333333333333333703, 0.3219752754296894559, 0.3333333333333333703, 0.3219752754296894559, 0.3333333333333333703, 0.3219752754296894559, 0.3333333333333333703, 0.3219752754296894559, 0.3333333333333333703, 0.3219752754296894559, 0.3333333333333333703, 0.3219752754296894559, 0.3333333333333333703, 0.3219752754296894559, 0.3333333333333333703, 0.3219752754296894559, 0.3333333333333333703, 0.3219752754296894559, 0.3333333333333333703, 0.3219752754296894559, 0.3333333333333333703, 0.3219752754296894559, 0.3333333333333333703, 0.3219752754296894559, 0.3333333333333333703, 0.3219752754296894559, 0.3333333333333333703, 0.3219752754296894559, 0.3333333333333333703, 0.3219752754296894559, 0.3333333333333333703, 0.3219752754296894559, 0.3333333333333333703, 0.3219752754296894559, 0.3333333333333333703, 0.3219752754296894559, 0.3333333333333333703, 0.3219752754296894559, 0.3333333333333333703, 0.3219752754296894559, 0.3333333333333333703, 0.3219752754296894559, 0.3333333333333333703, 0.3219752754296894559, 0.3333333333333333703, 0.3219752754296894559, 0.3333333333333333703, 0.3219752754296894559, 0.3333333333333333703, 0.3219752754296894559, 0.3333333333333333703, 0.3219752754296894559, 0.3333333333333333703, 0.3219752754296894559, 0.3333333333333333703, 0.3219752754296894559, 0.3333333333333333703, 0.3219752754296894559, 0.3333333333333333703, 0.3219752754296894559, 0.3333333333333333703, 0.3219752754296894559, 0.3333333333333333703, 0.3219752754296894559, 0.3333333333333333703, 0.3219752754296894559, 0.3333333333333333703, 0.3219752754296894559, 0.3333333333333333703, 0.3219752754296894559, 0.3333333333333333703, 0.3219752754296894559, 0.3333333333333333703, 0.3219752754296894559, 0.3333333333333333703, 0.3219752754296894559, 0.3333333333333333703, 0.3219752754296894559, 0.3333333333333333703, 0.3219752754296894559, 0.3333333333333333703, 0.3219752754296894559, 0.3333333333333333703, 0.3219752754296894559, 0.3333333333333333703, 0.3219752754296894559, 0.3333333333333333703, 0.3219752754296894559, 0.3333333333333333703, 0.3219752754296894559, 0.3333333333333333703, 0.3219752754296894559, 0.3333333333333333703, 0.3219752754296894559, 0.3333333333333333703, 0.3219752754296894559, 0.3333333333333333703, 0.3219752754296894559, 0.3333333333333333703, 0.3219752754296894559, 0.3333333333333333703, 0.3219752754296894559, 0.3333333333333333703, 0.3219752754296894559, 0.3333333333333333703, 0.3219752754296894559, 0.3333333333333333703, 0.3219752754296894559, 0.3333333333333333703, 0.3219752754296894559, 0.3333333333333333703, 0.3219752754296894559, 0.3333333333333333703, 0.3219752754296894559, 0.3333333333333333703, 0.3219752754296894559, 0.3333333333333333703, 0.3219752754296894559, 0.3333333333333333703, 0.3219752754296894559, 0.3333333333333333703, 0.3219752754296894559, 0.3333333333333333703, 0.3219752754296894559, 0.3333333333333333703, 0.3219752754296894559, 0.3333333333333333703, 0.3219752754296894559, 0.3333333333333333703, 0.3219752754296894559, 0.3333333333333333703, 0.3219752754296894559, 0.3333333333333333703, 0.3219752754296894559, 0.3333333333333333703, 0.3219752754296894559, 0.3333333333333333703, 0.3219752754296894559, 0.3333333333333333703, 0.3219752754296894559, 0.3333333333333333703, 0.3219752754296894559, 0.3333333333333333703, 0.3219752754296894559, 0.3333333333333333703, 0.3219752754296894559, 0.3333333333333333703, 0.3219752754296894559, 0.3333333333333333703, 0.3219752754296894559, 0.3333333333333333703, 0.3219752754296894559, 0.3333333333333333703, 0.3219752754296894559, 0.3333333333333333703, 0.3219752754296894559, 0.3333333333333333703, 0.3219752754296894559, 0.3333333333333333703, 0.3219752754296894559, 0.3333333333333333703, 0.3219752754296894559, 0.3333333333333333703, 0.3219752754296894559, 0.3333333333333333703, 0.3219752754296894559, 0.3333333333333333703, 0.3219752754296894559, 0.3333333333333333703, 0.3219752754296894559, 0.3333333333333333703, 0.3219752754296894559, 0.3333333333333333703, 0.3219752754296894559, 0.3333333333333333703, 0.3219752754296894559, 0.3333333333333333703, 0.3219752754296894559, 0.3333333333333333703, 0.3219752754296894559, 0.3333333333333333703, 0.3219752754296894559, 0.3333333333333333703, 0.3219752754296894559, 0.3333333333333333703, 0.3219752754296894559, 0.3333333333333333703, 0.3219752754296894559, 0.3333333333333333703, 0.3219752754296894559, 0.3333333333333333703, 0.3219752754296894559, 0.3333333333333333703, 0.3219752754296894559, 0.3333333333333333703, 0.3219752754296894559, 0.3333333333333333703, 0.3219752754296894559, 0.3333333333333333703, 0.3219752754296894559, 0.3333333333333333703, 0.3219752754296894559, 0.3333333333333333703, 0.3219752754296894559, 0.3333333333333333703, 0.3219752754296894559, 0.3333333333333333703, 0.3219752754296894559, 0.3333333333333333703, 0.3219752754296894559, 0.3333333333333333703, 0.3219752754296894559, 0.3333333333333333703, 0.3219752754296894559, 0.3333333333333333703, 0.3219752754296894559, 0.3333333333333333703, 0.3219752754296894559, 0.3333333333333333703, 0.3219752754296894559, 0.3333333333333333703, 0.3219752754296894559, 0.3333333333333333703, 0.3219752754296894559, 0.3333333333333333703, 0.3219752754296894559, 0.3333333333333333703, 0.3219752754296894559, 0.3333333333333333703, 0.3219752754296894559, 0.3333333333333333703, 0.3219752754296894559, 0.3333333333333333703, 0.3219752754296894559, 0.3333333333333333703, 0.3219752754296894559, 0.3333333333333333703, 0.3219752754296894559, 0.3333333333333333703, 0.3219752754296894559, 0.3333333333333333703, 0.3219752754296894559, 0.3333333333333333703, 0.3219752754296894559, 0.3333333333333333703, 0.3219752754296894559, 0.3333333333333333703, 0.3219752754296894559, 0.3333333333333333703, 0.3219752754296894559, 0.3333333333333333703, 0.3219752754296894559, 0.3333333333333333703, 0.3219752754296894559, 0.3333333333333333703, 0.3219752754296894559, 0.3333333333333333703, 0.3219752754296894559, 0.3333333333333333703, 0.3219752754296894559, 0.3333333333333333703, 0.3219752754296894559, 0.3333333333333333703, 0.3219752754296894559, 0.3333333333333333703, 0.3219752754296894559, 0.3333333333333333703, 0.3219752754296894559, 0.3333333333333333703, 0.3219752754296894559, 0.3333333333333333703, 0.3219752754296894559, 0.3333333333333333703, 0.3219752754296894559, 0.3333333333333333703, 0.3219752754296894559, 0.3333333333333333703, 0.3219752754296894559, 0.3333333333333333703, 0.3219752754296894559, 0.3333333333333333703, 0.3219752754296894559, 0.3333333333333333703, 0.3219752754296894559, 0.3333333333333333703, 0.3219752754296894559, 0.3333333333333333703, 0.3219752754296894559, 0.3333333333333333703, 0.3219752754296894559, 0.3333333333333333703, 0.3219752754296894559, 0.3333333333333333703, 0.3219752754296894559, 0.3333333333333333703, 0.3219752754296894559, 0.3333333333333333703, 0.3219752754296894559, 0.3333333333333333703, 0.3219752754296894559, 0.3333333333333333703, 0.3219752754296894559, 0.3333333333333333703, 0.3219752754296894559, 0.3333333333333333703, 0.3219752754296894559, 0.3333333333333333703, 0.3219752754296894559, 0.3333333333333333703, 0.3219752754296894559, 0.3333333333333333703, 0.3219752754296894559, 0.3333333333333333703, 0.3219752754296894559, 0.3333333333333333703, 0.3219752754296894559, 0.3333333333333333703, 0.3219752754296894559, 0.3333333333333333703, 0.3219752754296894559, 0.3333333333333333703, 0.3219752754296894559, 0.3333333333333333703, 0.3219752754296894559, 0.3333333333333333703, 0.3219752754296894559, 0.3333333333333333703, 0.3219752754296894559, 0.3333333333333333703, 0.3219752754296894559, 0.3333333333333333703, 0.3219752754296894559, 0.3333333333333333703, 0.3219752754296894559, 0.3333333333333333703, 0.3219752754296894559, 0.3333333333333333703, 0.3219752754296894559, 0.3333333333333333703, 0.3219752754296894559, 0.3333333333333333703, 0.3219752754296894559, 0.3333333333333333703, 0.3219752754296894559, 0.3333333333333333703, 0.3219752754296894559, 0.3333333333333333703, 0.3219752754296894559, 0.3333333333333333703, 0.3219752754296894559, 0.3333333333333333703, 0.3219752754296894559, 0.3333333333333333703, 0.3219752754296894559, 0.3333333333333333703, 0.3219752754296894559, 0.3333333333333333703, 0.3219752754296894559, 0.3333333333333333703, 0.3219752754296894559, 0.3333333333333333703, 0.3219752754296894559, 0.3333333333333333703, 0.3219752754296894559, 0.3333333333333333703, 0.3219752754296894559, 0.3333333333333333703),
 ( 0.3333333333333333703, 0.3219752754296894559, 0.3333333333333333703, 0.3219752754296894559, 0.3333333333333333703, 0.3219752754296894559, 0.3333333333333333703, 0.3219752754296894559, 0.3333333333333333703, 0.3219752754296894559, 0.3333333333333333703, 0.3219752754296894559, 0.3333333333333333703, 0.3219752754296894559, 0.3333333333333333703, 0.3219752754296894559, 0.3333333333333333703, 0.3219752754296894559, 0.3333333333333333703, 0.3219752754296894559, 0.3333333333333333703, 0.3219752754296894559, 0.3333333333333333703, 0.3219752754296894559, 0.3333333333333333703, 0.3219752754296894559, 0.3333333333333333703, 0.3219752754296894559, 0.3333333333333333703, 0.3219752754296894559, 0.3333333333333333703, 0.3219752754296894559, 0.3333333333333333703, 0.3219752754296894559, 0.3333333333333333703, 0.3219752754296894559, 0.3333333333333333703, 0.3219752754296894559, 0.3333333333333333703, 0.3219752754296894559, 0.3333333333333333703, 0.3219752754296894559, 0.3333333333333333703, 0.3219752754296894559, 0.3333333333333333703, 0.3219752754296894559, 0.3333333333333333703, 0.3219752754296894559, 0.3333333333333333703, 0.3219752754296894559, 0.3333333333333333703, 0.3219752754296894559, 0.3333333333333333703, 0.3219752754296894559, 0.3333333333333333703, 0.3219752754296894559, 0.3333333333333333703, 0.3219752754296894559, 0.3333333333333333703, 0.3219752754296894559, 0.3333333333333333703, 0.3219752754296894559, 0.3333333333333333703, 0.3219752754296894559, 0.3333333333333333703, 0.3219752754296894559, 0.3333333333333333703, 0.3219752754296894559, 0.3333333333333333703, 0.3219752754296894559, 0.3333333333333333703, 0.3219752754296894559, 0.3333333333333333703, 0.3219752754296894559, 0.3333333333333333703, 0.3219752754296894559, 0.3333333333333333703, 0.3219752754296894559, 0.3333333333333333703, 0.3219752754296894559, 0.3333333333333333703, 0.3219752754296894559, 0.3333333333333333703, 0.3219752754296894559, 0.3333333333333333703, 0.3219752754296894559, 0.3333333333333333703, 0.3219752754296894559, 0.3333333333333333703, 0.3219752754296894559, 0.3333333333333333703, 0.3219752754296894559, 0.3333333333333333703, 0.3219752754296894559, 0.3333333333333333703, 0.3219752754296894559, 0.3333333333333333703, 0.3219752754296894559, 0.3333333333333333703, 0.3219752754296894559, 0.3333333333333333703, 0.3219752754296894559, 0.3333333333333333703, 0.3219752754296894559, 0.3333333333333333703, 0.3219752754296894559, 0.3333333333333333703, 0.3219752754296894559, 0.3333333333333333703, 0.3219752754296894559, 0.3333333333333333703, 0.3219752754296894559, 0.3333333333333333703, 0.3219752754296894559, 0.3333333333333333703, 0.3219752754296894559, 0.3333333333333333703, 0.3219752754296894559, 0.3333333333333333703, 0.3219752754296894559, 0.3333333333333333703, 0.3219752754296894559, 0.3333333333333333703, 0.3219752754296894559, 0.3333333333333333703, 0.3219752754296894559, 0.3333333333333333703, 0.3219752754296894559, 0.3333333333333333703, 0.3219752754296894559, 0.3333333333333333703, 0.3219752754296894559, 0.3333333333333333703, 0.3219752754296894559, 0.3333333333333333703, 0.3219752754296894559, 0.3333333333333333703, 0.3219752754296894559, 0.3333333333333333703, 0.3219752754296894559, 0.3333333333333333703, 0.3219752754296894559, 0.3333333333333333703, 0.3219752754296894559, 0.3333333333333333703, 0.3219752754296894559, 0.3333333333333333703, 0.3219752754296894559, 0.3333333333333333703, 0.3219752754296894559, 0.3333333333333333703, 0.3219752754296894559, 0.3333333333333333703, 0.3219752754296894559, 0.3333333333333333703, 0.3219752754296894559, 0.3333333333333333703, 0.3219752754296894559, 0.3333333333333333703, 0.3219752754296894559, 0.3333333333333333703, 0.3219752754296894559, 0.3333333333333333703, 0.3219752754296894559, 0.3333333333333333703, 0.3219752754296894559, 0.3333333333333333703, 0.3219752754296894559, 0.3333333333333333703, 0.3219752754296894559, 0.3333333333333333703, 0.3219752754296894559, 0.3333333333333333703, 0.3219752754296894559, 0.3333333333333333703, 0.3219752754296894559, 0.3333333333333333703, 0.3219752754296894559, 0.3333333333333333703, 0.3219752754296894559, 0.3333333333333333703, 0.3219752754296894559, 0.3333333333333333703, 0.3219752754296894559, 0.3333333333333333703, 0.3219752754296894559, 0.3333333333333333703, 0.3219752754296894559, 0.3333333333333333703, 0.3219752754296894559, 0.3333333333333333703, 0.3219752754296894559, 0.3333333333333333703, 0.3219752754296894559, 0.3333333333333333703, 0.3219752754296894559, 0.3333333333333333703, 0.3219752754296894559, 0.3333333333333333703, 0.3219752754296894559, 0.3333333333333333703, 0.3219752754296894559, 0.3333333333333333703, 0.3219752754296894559, 0.3333333333333333703, 0.3219752754296894559, 0.3333333333333333703, 0.3219752754296894559, 0.3333333333333333703, 0.3219752754296894559, 0.3333333333333333703, 0.3219752754296894559, 0.3333333333333333703, 0.3219752754296894559, 0.3333333333333333703, 0.3219752754296894559, 0.3333333333333333703, 0.3219752754296894559, 0.3333333333333333703, 0.3219752754296894559, 0.3333333333333333703, 0.3219752754296894559, 0.3333333333333333703, 0.3219752754296894559, 0.3333333333333333703, 0.3219752754296894559, 0.3333333333333333703, 0.3219752754296894559, 0.3333333333333333703, 0.3219752754296894559, 0.3333333333333333703, 0.3219752754296894559, 0.3333333333333333703, 0.3219752754296894559, 0.3333333333333333703, 0.3219752754296894559, 0.3333333333333333703, 0.3219752754296894559, 0.3333333333333333703, 0.3219752754296894559, 0.3333333333333333703, 0.3219752754296894559, 0.3333333333333333703, 0.3219752754296894559, 0.3333333333333333703, 0.3219752754296894559, 0.3333333333333333703, 0.3219752754296894559, 0.3333333333333333703, 0.3219752754296894559, 0.3333333333333333703, 0.3219752754296894559, 0.3333333333333333703, 0.3219752754296894559, 0.3333333333333333703, 0.3219752754296894559, 0.3333333333333333703, 0.3219752754296894559, 0.3333333333333333703, 0.3219752754296894559, 0.3333333333333333703, 0.3219752754296894559, 0.3333333333333333703, 0.3219752754296894559, 0.3333333333333333703, 0.3219752754296894559, 0.3333333333333333703, 0.3219752754296894559, 0.3333333333333333703, 0.3219752754296894559, 0.3333333333333333703, 0.3219752754296894559, 0.3333333333333333703, 0.3219752754296894559, 0.3333333333333333703, 0.3219752754296894559, 0.3333333333333333703, 0.3219752754296894559, 0.3333333333333333703, 0.3219752754296894559, 0.3333333333333333703, 0.3219752754296894559, 0.3333333333333333703, 0.3219752754296894559, 0.3333333333333333703, 0.3219752754296894559, 0.3333333333333333703, 0.3219752754296894559, 0.3333333333333333703, 0.3219752754296894559, 0.3333333333333333703, 0.3219752754296894559, 0.3333333333333333703, 0.3219752754296894559, 0.3333333333333333703, 0.3219752754296894559, 0.3333333333333333703, 0.3219752754296894559, 0.3333333333333333703, 0.3219752754296894559, 0.3333333333333333703, 0.3219752754296894559, 0.3333333333333333703, 0.3219752754296894559, 0.3333333333333333703, 0.3219752754296894559, 0.3333333333333333703, 0.3219752754296894559, 0.3333333333333333703, 0.3219752754296894559, 0.3333333333333333703, 0.3219752754296894559, 0.3333333333333333703, 0.3219752754296894559, 0.3333333333333333703, 0.3219752754296894559, 0.3333333333333333703, 0.3219752754296894559, 0.3333333333333333703, 0.3219752754296894559, 0.3333333333333333703, 0.3219752754296894559, 0.3333333333333333703, 0.3219752754296894559, 0.3333333333333333703, 0.3219752754296894559, 0.3333333333333333703, 0.3219752754296894559, 0.3333333333333333703, 0.3219752754296894559, 0.3333333333333333703, 0.3219752754296894559, 0.3333333333333333703, 0.3219752754296894559, 0.3333333333333333703, 0.3219752754296894559, 0.3333333333333333703, 0.3219752754296894559, 0.3333333333333333703, 0.3219752754296894559, 0.3333333333333333703, 0.3219752754296894559, 0.3333333333333333703, 0.3219752754296894559, 0.3333333333333333703, 0.3219752754296894559, 0.3333333333333333703, 0.3219752754296894559, 0.3333333333333333703, 0.3219752754296894559, 0.3333333333333333703, 0.3219752754296894559, 0.3333333333333333703, 0.3219752754296894559, 0.3333333333333333703, 0.3219752754296894559, 0.3333333333333333703, 0.3219752754296894559, 0.3333333333333333703, 0.3219752754296894559, 0.3333333333333333703, 0.3219752754296894559, 0.3333333333333333703, 0.3219752754296894559, 0.3333333333333333703, 0.3219752754296894559, 0.3333333333333333703, 0.3219752754296894559, 0.3333333333333333703, 0.3219752754296894559, 0.3333333333333333703, 0.3219752754296894559, 0.3333333333333333703, 0.3219752754296894559, 0.3333333333333333703, 0.3219752754296894559, 0.3333333333333333703, 0.3219752754296894559, 0.3333333333333333703, 0.3219752754296894559, 0.3333333333333333703, 0.3219752754296894559, 0.3333333333333333703, 0.3219752754296894559, 0.3333333333333333703, 0.3219752754296894559, 0.3333333333333333703, 0.3219752754296894559, 0.3333333333333333703, 0.3219752754296894559, 0.3333333333333333703, 0.3219752754296894559, 0.3333333333333333703, 0.3219752754296894559, 0.3333333333333333703, 0.3219752754296894559, 0.3333333333333333703, 0.3219752754296894559, 0.3333333333333333703, 0.3219752754296894559, 0.3333333333333333703, 0.3219752754296894559, 0.3333333333333333703, 0.3219752754296894559, 0.3333333333333333703, 0.3219752754296894559, 0.3333333333333333703, 0.3219752754296894559, 0.3333333333333333703, 0.3219752754296894559, 0.3333333333333333703, 0.3219752754296894559, 0.3333333333333333703, 0.3219752754296894559, 0.3333333333333333703, 0.3219752754296894559, 0.3333333333333333703, 0.3219752754296894559, 0.3333333333333333703, 0.3219752754296894559, 0.3333333333333333703, 0.3219752754296894559, 0.3333333333333333703, 0.3219752754296894559, 0.3333333333333333703, 0.3219752754296894559, 0.3333333333333333703, 0.3219752754296894559, 0.3333333333333333703, 0.3219752754296894559, 0.3333333333333333703, 0.3219752754296894559, 0.3333333333333333703, 0.3219752754296894559, 0.3333333333333333703, 0.3219752754296894559, 0.3333333333333333703, 0.3219752754296894559, 0.3333333333333333703, 0.3219752754296894559, 0.3333333333333333703, 0.3219752754296894559, 0.3333333333333333703, 0.3219752754296894559, 0.3333333333333333703, 0.3219752754296894559, 0.3333333333333333703, 0.3219752754296894559, 0.3333333333333333703, 0.3219752754296894559, 0.3333333333333333703, 0.3219752754296894559, 0.3333333333333333703, 0.3219752754296894559, 0.3333333333333333703, 0.3219752754296894559, 0.3333333333333333703),
 ( 1.000000000000000000, 0.9659258262890683122, 1.000000000000000000, 0.9659258262890683122, 1.000000000000000000, 0.9659258262890683122, 1.000000000000000000, 0.9659258262890683122, 1.000000000000000000, 0.9659258262890683122, 1.000000000000000000, 0.9659258262890683122, 1.000000000000000000, 0.9659258262890683122, 1.000000000000000000, 0.9659258262890683122, 1.000000000000000000, 0.9659258262890683122, 1.000000000000000000, 0.9659258262890683122, 1.000000000000000000, 0.9659258262890683122, 1.000000000000000000, 0.9659258262890683122, 1.000000000000000000, 0.9659258262890683122, 1.000000000000000000, 0.9659258262890683122, 1.000000000000000000, 0.9659258262890683122, 1.000000000000000000, 0.9659258262890683122, 1.000000000000000000, 0.9659258262890683122, 1.000000000000000000, 0.9659258262890683122, 1.000000000000000000, 0.9659258262890683122, 1.000000000000000000, 0.9659258262890683122, 1.000000000000000000, 0.9659258262890683122, 1.000000000000000000, 0.9659258262890683122, 1.000000000000000000, 0.9659258262890683122, 1.000000000000000000, 0.9659258262890683122, 1.000000000000000000, 0.9659258262890683122, 1.000000000000000000, 0.9659258262890683122, 1.000000000000000000, 0.9659258262890683122, 1.000000000000000000, 0.9659258262890683122, 1.000000000000000000, 0.9659258262890683122, 1.000000000000000000, 0.9659258262890683122, 1.000000000000000000, 0.9659258262890683122, 1.000000000000000000, 0.9659258262890683122, 1.000000000000000000, 0.9659258262890683122, 1.000000000000000000, 0.9659258262890683122, 1.000000000000000000, 0.9659258262890683122, 1.000000000000000000, 0.9659258262890683122, 1.000000000000000000, 0.9659258262890683122, 1.000000000000000000, 0.9659258262890683122, 1.000000000000000000, 0.9659258262890683122, 1.000000000000000000, 0.9659258262890683122, 1.000000000000000000, 0.9659258262890683122, 1.000000000000000000, 0.9659258262890683122, 1.000000000000000000, 0.9659258262890683122, 1.000000000000000000, 0.9659258262890683122, 1.000000000000000000, 0.9659258262890683122, 1.000000000000000000, 0.9659258262890683122, 1.000000000000000000, 0.9659258262890683122, 1.000000000000000000, 0.9659258262890683122, 1.000000000000000000, 0.9659258262890683122, 1.000000000000000000, 0.9659258262890683122, 1.000000000000000000, 0.9659258262890683122, 1.000000000000000000, 0.9659258262890683122, 1.000000000000000000, 0.9659258262890683122, 1.000000000000000000, 0.9659258262890683122, 1.000000000000000000, 0.9659258262890683122, 1.000000000000000000, 0.9659258262890683122, 1.000000000000000000, 0.9659258262890683122, 1.000000000000000000, 0.9659258262890683122, 1.000000000000000000, 0.9659258262890683122, 1.000000000000000000, 0.9659258262890683122, 1.000000000000000000, 0.9659258262890683122, 1.000000000000000000, 0.9659258262890683122, 1.000000000000000000, 0.9659258262890683122, 1.000000000000000000, 0.9659258262890683122, 1.000000000000000000, 0.9659258262890683122, 1.000000000000000000, 0.9659258262890683122, 1.000000000000000000, 0.9659258262890683122, 1.000000000000000000, 0.9659258262890683122, 1.000000000000000000, 0.9659258262890683122, 1.000000000000000000, 0.9659258262890683122, 1.000000000000000000, 0.9659258262890683122, 1.000000000000000000, 0.9659258262890683122, 1.000000000000000000, 0.9659258262890683122, 1.000000000000000000, 0.9659258262890683122, 1.000000000000000000, 0.9659258262890683122, 1.000000000000000000, 0.9659258262890683122, 1.000000000000000000, 0.9659258262890683122, 1.000000000000000000, 0.9659258262890683122, 1.000000000000000000, 0.9659258262890683122, 1.000000000000000000, 0.9659258262890683122, 1.000000000000000000, 0.9659258262890683122, 1.000000000000000000, 0.9659258262890683122, 1.000000000000000000, 0.9659258262890683122, 1.000000000000000000, 0.9659258262890683122, 1.000000000000000000, 0.9659258262890683122, 1.000000000000000000, 0.9659258262890683122, 1.000000000000000000, 0.9659258262890683122, 1.000000000000000000, 0.9659258262890683122, 1.000000000000000000, 0.9659258262890683122, 1.000000000000000000, 0.9659258262890683122, 1.000000000000000000, 0.9659258262890683122, 1.000000000000000000, 0.9659258262890683122, 1.000000000000000000, 0.9659258262890683122, 1.000000000000000000, 0.9659258262890683122, 1.000000000000000000, 0.9659258262890683122, 1.000000000000000000, 0.9659258262890683122, 1.000000000000000000, 0.9659258262890683122, 1.000000000000000000, 0.9659258262890683122, 1.000000000000000000, 0.9659258262890683122, 1.000000000000000000, 0.9659258262890683122, 1.000000000000000000, 0.9659258262890683122, 1.000000000000000000, 0.9659258262890683122, 1.000000000000000000, 0.9659258262890683122, 1.000000000000000000, 0.9659258262890683122, 1.000000000000000000, 0.9659258262890683122, 1.000000000000000000, 0.9659258262890683122, 1.000000000000000000, 0.9659258262890683122, 1.000000000000000000, 0.9659258262890683122, 1.000000000000000000, 0.9659258262890683122, 1.000000000000000000, 0.9659258262890683122, 1.000000000000000000, 0.9659258262890683122, 1.000000000000000000, 0.9659258262890683122, 1.000000000000000000, 0.9659258262890683122, 1.000000000000000000, 0.9659258262890683122, 1.000000000000000000, 0.9659258262890683122, 1.000000000000000000, 0.9659258262890683122, 1.000000000000000000, 0.9659258262890683122, 1.000000000000000000, 0.9659258262890683122, 1.000000000000000000, 0.9659258262890683122, 1.000000000000000000, 0.9659258262890683122, 1.000000000000000000, 0.9659258262890683122, 1.000000000000000000, 0.9659258262890683122, 1.000000000000000000, 0.9659258262890683122, 1.000000000000000000, 0.9659258262890683122, 1.000000000000000000, 0.9659258262890683122, 1.000000000000000000, 0.9659258262890683122, 1.000000000000000000, 0.9659258262890683122, 1.000000000000000000, 0.9659258262890683122, 1.000000000000000000, 0.9659258262890683122, 1.000000000000000000, 0.9659258262890683122, 1.000000000000000000, 0.9659258262890683122, 1.000000000000000000, 0.9659258262890683122, 1.000000000000000000, 0.9659258262890683122, 1.000000000000000000, 0.9659258262890683122, 1.000000000000000000, 0.9659258262890683122, 1.000000000000000000, 0.9659258262890683122, 1.000000000000000000, 0.9659258262890683122, 1.000000000000000000, 0.9659258262890683122, 1.000000000000000000, 0.9659258262890683122, 1.000000000000000000, 0.9659258262890683122, 1.000000000000000000, 0.9659258262890683122, 1.000000000000000000, 0.9659258262890683122, 1.000000000000000000, 0.9659258262890683122, 1.000000000000000000, 0.9659258262890683122, 1.000000000000000000, 0.9659258262890683122, 1.000000000000000000, 0.9659258262890683122, 1.000000000000000000, 0.9659258262890683122, 1.000000000000000000, 0.9659258262890683122, 1.000000000000000000, 0.9659258262890683122, 1.000000000000000000, 0.9659258262890683122, 1.000000000000000000, 0.9659258262890683122, 1.000000000000000000, 0.9659258262890683122, 1.000000000000000000, 0.9659258262890683122, 1.000000000000000000, 0.9659258262890683122, 1.000000000000000000, 0.9659258262890683122, 1.000000000000000000, 0.9659258262890683122, 1.000000000000000000, 0.9659258262890683122, 1.000000000000000000, 0.9659258262890683122, 1.000000000000000000, 0.9659258262890683122, 1.000000000000000000, 0.9659258262890683122, 1.000000000000000000, 0.9659258262890683122, 1.000000000000000000, 0.9659258262890683122, 1.000000000000000000, 0.9659258262890683122, 1.000000000000000000, 0.9659258262890683122, 1.000000000000000000, 0.9659258262890683122, 1.000000000000000000, 0.9659258262890683122, 1.000000000000000000, 0.9659258262890683122, 1.000000000000000000, 0.9659258262890683122, 1.000000000000000000, 0.9659258262890683122, 1.000000000000000000, 0.9659258262890683122, 1.000000000000000000, 0.9659258262890683122, 1.000000000000000000, 0.9659258262890683122, 1.000000000000000000, 0.9659258262890683122, 1.000000000000000000, 0.9659258262890683122, 1.000000000000000000, 0.9659258262890683122, 1.000000000000000000, 0.9659258262890683122, 1.000000000000000000, 0.9659258262890683122, 1.000000000000000000, 0.9659258262890683122, 1.000000000000000000, 0.9659258262890683122, 1.000000000000000000, 0.9659258262890683122, 1.000000000000000000, 0.9659258262890683122, 1.000000000000000000, 0.9659258262890683122, 1.000000000000000000, 0.9659258262890683122, 1.000000000000000000, 0.9659258262890683122, 1.000000000000000000, 0.9659258262890683122, 1.000000000000000000, 0.9659258262890683122, 1.000000000000000000, 0.9659258262890683122, 1.000000000000000000, 0.9659258262890683122, 1.000000000000000000, 0.9659258262890683122, 1.000000000000000000, 0.9659258262890683122, 1.000000000000000000, 0.9659258262890683122, 1.000000000000000000, 0.9659258262890683122, 1.000000000000000000, 0.9659258262890683122, 1.000000000000000000, 0.9659258262890683122, 1.000000000000000000, 0.9659258262890683122, 1.000000000000000000, 0.9659258262890683122, 1.000000000000000000, 0.9659258262890683122, 1.000000000000000000, 0.9659258262890683122, 1.000000000000000000, 0.9659258262890683122, 1.000000000000000000, 0.9659258262890683122, 1.000000000000000000, 0.9659258262890683122, 1.000000000000000000, 0.9659258262890683122, 1.000000000000000000, 0.9659258262890683122, 1.000000000000000000, 0.9659258262890683122, 1.000000000000000000, 0.9659258262890683122, 1.000000000000000000, 0.9659258262890683122, 1.000000000000000000, 0.9659258262890683122, 1.000000000000000000, 0.9659258262890683122, 1.000000000000000000, 0.9659258262890683122, 1.000000000000000000, 0.9659258262890683122, 1.000000000000000000, 0.9659258262890683122, 1.000000000000000000, 0.9659258262890683122, 1.000000000000000000, 0.9659258262890683122, 1.000000000000000000, 0.9659258262890683122, 1.000000000000000000, 0.9659258262890683122, 1.000000000000000000, 0.9659258262890683122, 1.000000000000000000, 0.9659258262890683122, 1.000000000000000000, 0.9659258262890683122, 1.000000000000000000, 0.9659258262890683122, 1.000000000000000000, 0.9659258262890683122, 1.000000000000000000, 0.9659258262890683122, 1.000000000000000000, 0.9659258262890683122, 1.000000000000000000, 0.9659258262890683122, 1.000000000000000000, 0.9659258262890683122, 1.000000000000000000, 0.9659258262890683122, 1.000000000000000000, 0.9659258262890683122, 1.000000000000000000, 0.9659258262890683122, 1.000000000000000000, 0.9659258262890683122, 1.000000000000000000) ) ) 
 REPRESENTATION_ITEM ( '' )  SURFACE ( )  );
#157754 = CARTESIAN_POINT ( 'NONE',  ( 10.81492255796078972, 18.62759615963270932, 39.58224293864769550 ) ) ;
#157755 = CARTESIAN_POINT ( 'NONE',  ( -14.29746914071049879, 8.314922557960819915, 100.8322429386477097 ) ) ;
#157756 = CARTESIAN_POINT ( 'NONE',  ( -16.70000000000002416, 0.1032682159775897418, -61.34707691135562868 ) ) ;
#157757 = CARTESIAN_POINT ( 'NONE',  ( -0.05219959533936034679, 19.03943276465977164, 57.50109039468566863 ) ) ;
#157759 = AXIS2_PLACEMENT_3D ( 'NONE', #31897, #182607, #28933 ) ;
#157758 = CARTESIAN_POINT ( 'NONE',  ( 14.34966873604960469, 8.224510206698951720, 24.16557627198103120 ) ) ;
#157760 = CARTESIAN_POINT ( 'NONE',  ( -9.564922557960796823, -16.46253265017161027, 97.08224293864769550 ) ) ;
#157761 = CARTESIAN_POINT ( 'NONE',  ( 21.52544592524334988, 5.823673210054432836, 81.45942372801900433 ) ) ;
#157762 = CARTESIAN_POINT ( 'NONE',  ( -5.823673210054116645, -21.52544592524344225, 67.29057627198103830 ) ) ;
#157763 = CARTESIAN_POINT ( 'NONE',  ( -0.05219959533937732626, 21.53943276465977519, 42.50109039468567573 ) ) ;
#157764 = CARTESIAN_POINT ( 'NONE',  ( 5.823673210054125526, 21.52544592524343514, 94.79057627198105251 ) ) ;
#157765 = CARTESIAN_POINT ( 'NONE',  ( 10.72451020669871369, 18.67979575497193778, 57.08442372801901854 ) ) ;
#157766 = CARTESIAN_POINT ( 'NONE',  ( 16.46253265017160672, -9.564922557960803928, 23.33224293864769194 ) ) ;
#157767 = CARTESIAN_POINT ( 'NONE',  ( 16.51473224551069308, 9.474510206698969483, 84.16557627198102409 ) ) ;
#157768 = CARTESIAN_POINT ( 'NONE',  ( -4.483927247898782831, 16.52544592524335698, 77.70942372801900433 ) ) ;
#157769 = CARTESIAN_POINT ( 'NONE',  ( 16.52544592524342804, -4.483927247898539470, 103.5405762719810383 ) ) ;
#157770 = CARTESIAN_POINT ( 'NONE',  ( -5.153800228976328057, -19.02544592524343514, 102.2905762719810383 ) ) ;
#157771 = CARTESIAN_POINT ( 'NONE',  ( 8.314922557960818139, 14.29746914071049879, 49.58224293864769550 ) ) ;
#157772 = CARTESIAN_POINT ( 'NONE',  ( -4.483927247898782831, 16.52544592524335698, 107.7094237280190328 ) ) ;
#157773 = CARTESIAN_POINT ( 'NONE',  ( -16.51473224551069308, -9.474510206698971260, 56.66557627198103120 ) ) ;
#157774 = CARTESIAN_POINT ( 'NONE',  ( 5.153800228976335163, 19.02544592524342804, 29.79057627198102409 ) ) ;
#157775 = CARTESIAN_POINT ( 'NONE',  ( -15.80617190586745835, -15.72974639402198527, 51.87390960531437401 ) ) ;
#157776 = CARTESIAN_POINT ( 'NONE',  ( -13.97604488694547697, 13.89961937509957934, 23.12609039468565442 ) ) ;
#157778 = CARTESIAN_POINT ( 'NONE',  ( 14.34966873604960469, 8.224510206698951720, 39.16557627198102409 ) ) ;
#157777 = CARTESIAN_POINT ( 'NONE',  ( 17.97058386085788229, 5.500000000000048850, 51.50390968646216550 ) ) ;
#157779 = CARTESIAN_POINT ( 'NONE',  ( 21.52544592524334988, 5.823673210054432836, 41.45942372801901143 ) ) ;
#157780 = EDGE_CURVE ( 'NONE', #10418, #166568, #174353, .T. ) ;
#157781 = CARTESIAN_POINT ( 'NONE',  ( -13.29753078558959878, -35.33598341332324821, -29.59763579011278978 ) ) ;
#157782 = CARTESIAN_POINT ( 'NONE',  ( -8.224510206698735004, -14.34966873604973081, 59.58442372801901854 ) ) ;
#157783 = CARTESIAN_POINT ( 'NONE',  ( 16.51473224551083163, -9.474510206698727899, 60.83442372801900433 ) ) ;
#157784 = CARTESIAN_POINT ( 'NONE',  ( -16.55341960407611168, -4.379528057220339221, 26.45724293864768839 ) ) ;
#157785 = CARTESIAN_POINT ( 'NONE',  ( 16.52544592524335698, 4.483927247898782831, 101.4594237280190185 ) ) ;
#157786 = CARTESIAN_POINT ( 'NONE',  ( 16.46253265017160672, -9.564922557960803928, 33.33224293864770260 ) ) ;
#157787 = CARTESIAN_POINT ( 'NONE',  ( 5.049401038298161559, -19.05341960407611168, 67.70724293864769550 ) ) ;
#157788 = CARTESIAN_POINT ( 'NONE',  ( 13.89961937509977652, -13.97604488694527269, 28.12390960531435624 ) ) ;
#157789 = CARTESIAN_POINT ( 'NONE',  ( 5.823673210054444382, -21.52544592524334988, 35.20942372801901854 ) ) ;
#157790 = CARTESIAN_POINT ( 'NONE',  ( -13.89961937509977652, 13.97604488694528158, 40.62390960531435979 ) ) ;
#157791 = CARTESIAN_POINT ( 'NONE',  ( 21.23184647844206197, -181.1785498424364675, 0.000000000000000000 ) ) ;
#157792 = CARTESIAN_POINT ( 'NONE',  ( 19.02544592524343514, -5.153800228976328945, 43.54057627198103120 ) ) ;
#157793 = CARTESIAN_POINT ( 'NONE',  ( 9.564922557960805705, 16.46253265017160317, 114.5822429386476955 ) ) ;
#157795 = CARTESIAN_POINT ( 'NONE',  ( 16.52544592524342804, -4.483927247898539470, 108.5405762719810241 ) ) ;
#157794 = CARTESIAN_POINT ( 'NONE',  ( -15.80617190586768217, 15.72974639402176855, 63.12609039468568994 ) ) ;
#157796 = CARTESIAN_POINT ( 'NONE',  ( 16.51473224551069308, 9.474510206698969483, 109.1655762719810383 ) ) ;
#157797 = CARTESIAN_POINT ( 'NONE',  ( 8.224510206698742110, 14.34966873604972548, 82.08442372801901854 ) ) ;
#157798 = CARTESIAN_POINT ( 'NONE',  ( 10.81492255796106328, -18.62759615963255655, 95.41775706135234714 ) ) ;
#157799 = CARTESIAN_POINT ( 'NONE',  ( 8.224510206698742110, 14.34966873604972548, 57.08442372801901854 ) ) ;
#157800 = CARTESIAN_POINT ( 'NONE',  ( 5.153800228976335163, 19.02544592524342804, 89.79057627198102409 ) ) ;
#157801 = CARTESIAN_POINT ( 'NONE',  ( 8.314922557961029526, -14.29746914071037800, 35.41775706135234003 ) ) ;
#157802 = CARTESIAN_POINT ( 'NONE',  ( -8.314922557961024197, 14.29746914071037800, 27.91775706135234358 ) ) ;
#157803 = CARTESIAN_POINT ( 'NONE',  ( 16.55341960407618274, -4.379528057220086978, 101.0427570613523756 ) ) ;
#157804 = CARTESIAN_POINT ( 'NONE',  ( -5.049401038297874678, -19.05341960407617918, 109.7927570613523187 ) ) ;
#157805 = CARTESIAN_POINT ( 'NONE',  ( 10.81492255796078972, 18.62759615963270932, 114.5822429386477097 ) ) ;
#157807 = CARTESIAN_POINT ( 'NONE',  ( 13.97604488694548053, -13.89961937509957401, 100.6260903946856615 ) ) ;
#157806 = CARTESIAN_POINT ( 'NONE',  ( -12.06949235617756955, 12.14591786802309770, 105.6239096053143669 ) ) ;
#157808 = CARTESIAN_POINT ( 'NONE',  ( 4.379528057220092307, 16.55341960407617563, 72.29275706135236135 ) ) ;
#157809 = CARTESIAN_POINT ( 'NONE',  ( 24.02130208662955013, 8.352503713167605426, 169.2769999910313174 ) ) ;
#157811 = ADVANCED_FACE ( 'NONE', ( #33763 ), #157107, .T. ) ;
#157810 = CARTESIAN_POINT ( 'NONE',  ( 13.89961937509957401, 13.97604488694547697, 71.87609039468567573 ) ) ;
#157812 = CARTESIAN_POINT ( 'NONE',  ( 14.34966873604960469, 8.224510206698951720, 39.16557627198102409 ) ) ;
#157813 = CARTESIAN_POINT ( 'NONE',  ( -14.34966873604960291, -8.224510206698953496, 41.66557627198103120 ) ) ;
#157814 = CARTESIAN_POINT ( 'NONE',  ( -12.14591786802309592, -12.06949235617757132, 91.87390960531436690 ) ) ;
#157816 =( NAMED_UNIT ( * ) SI_UNIT ( $, .STERADIAN. ) SOLID_ANGLE_UNIT ( ) );
#157815 = CARTESIAN_POINT ( 'NONE',  ( -19.05341960407617563, 5.049401038297882671, 28.54275706135232937 ) ) ;
#157817 = CARTESIAN_POINT ( 'NONE',  ( -15.80617190586768217, 15.72974639402176855, 38.12609039468567573 ) ) ;
#157818 = CARTESIAN_POINT ( 'NONE',  ( 0.05219959533936267826, -19.03943276465977164, 95.00109039468567573 ) ) ;
#157819 = CARTESIAN_POINT ( 'NONE',  ( 1.500000000000020872, 22.80000000000002913, -55.36297086913598520 ) ) ;
#157820 = CARTESIAN_POINT ( 'NONE',  ( -13.89961937509977652, 13.97604488694528158, 85.62390960531433848 ) ) ;
#157821 = CARTESIAN_POINT ( 'NONE',  ( 9.474510206698971260, -16.51473224551069308, 92.91557627198103830 ) ) ;
#157822 = CARTESIAN_POINT ( 'NONE',  ( -18.62759615963270932, 10.81492255796079327, 55.83224293864770260 ) ) ;
#157823 = CARTESIAN_POINT ( 'NONE',  ( 16.55341960407611168, 4.379528057220329451, 88.95724293864769550 ) ) ;
#157824 = CARTESIAN_POINT ( 'NONE',  ( 5.153800228976335163, 19.02544592524342804, 69.79057627198103830 ) ) ;
#157825 = CARTESIAN_POINT ( 'NONE',  ( 16.51473224551069308, 9.474510206698969483, 34.16557627198102409 ) ) ;
#157826 = CARTESIAN_POINT ( 'NONE',  ( 5.719274019375673035, 21.55341960407619339, 42.29275706135235424 ) ) ;
#157827 = CARTESIAN_POINT ( 'NONE',  ( 21.55341960407619695, -5.719274019375665929, 76.04275706135237556 ) ) ;
#157828 = CARTESIAN_POINT ( 'NONE',  ( -16.51473224551069308, -9.474510206698971260, 56.66557627198103120 ) ) ;
#157829 = CARTESIAN_POINT ( 'NONE',  ( 14.34966873604972726, -8.224510206698740333, 80.83442372801901854 ) ) ;
#157830 = CARTESIAN_POINT ( 'NONE',  ( -15.80617190586768217, 15.72974639402176855, 33.12609039468569705 ) ) ;
#157831 = CARTESIAN_POINT ( 'NONE',  ( 15.80617190586769283, -15.72974639402175789, 20.62609039468568639 ) ) ;
#157833 = CARTESIAN_POINT ( 'NONE',  ( -16.46253265017160317, 9.564922557960807481, 80.83224293864769550 ) ) ;
#157832 = CARTESIAN_POINT ( 'NONE',  ( -16.46253265017146816, -9.564922557961047289, 49.16775706135233293 ) ) ;
#157834 = CARTESIAN_POINT ( 'NONE',  ( 13.89961937509957401, 13.97604488694547697, 31.87609039468566863 ) ) ;
#157835 = CARTESIAN_POINT ( 'NONE',  ( -21.55341960407619339, 5.719274019375674811, 88.54275706135236135 ) ) ;
#157836 = CARTESIAN_POINT ( 'NONE',  ( -5.823673210054116645, -21.52544592524344225, 72.29057627198102409 ) ) ;
#157837 = CARTESIAN_POINT ( 'NONE',  ( 8.314922557960818139, 14.29746914071049879, 44.58224293864769550 ) ) ;
#157839 = CARTESIAN_POINT ( 'NONE',  ( 16.46253265017146816, 9.564922557961045513, 31.66775706135232937 ) ) ;
#157838 = CARTESIAN_POINT ( 'NONE',  ( 10.81492255796106328, -18.62759615963255655, 95.41775706135234714 ) ) ;
#157840 = CARTESIAN_POINT ( 'NONE',  ( 8.314922557960818139, 14.29746914071049879, 69.58224293864769550 ) ) ;
#157841 = CARTESIAN_POINT ( 'NONE',  ( 16.55341960407611168, 4.379528057220329451, 113.9572429386477239 ) ) ;
#157842 = CARTESIAN_POINT ( 'NONE',  ( 13.89961937509957401, 13.97604488694547697, 66.87609039468567573 ) ) ;
#157843 = CARTESIAN_POINT ( 'NONE',  ( -8.314922557960811034, -14.29746914071050412, 37.08224293864768129 ) ) ;
#157844 = CARTESIAN_POINT ( 'NONE',  ( -18.62759615963255300, -10.81492255796106328, 84.16775706135234714 ) ) ;
#157845 = CARTESIAN_POINT ( 'NONE',  ( 13.97604488694527802, 13.89961937509977652, 74.37390960531436690 ) ) ;
#157846 = CARTESIAN_POINT ( 'NONE',  ( -19.02544592524334988, -5.153800228976617603, 43.95942372801899012 ) ) ;
#157847 = CARTESIAN_POINT ( 'NONE',  ( 10.72451020669898902, -18.67979575497178502, 47.91557627198102409 ) ) ;
#157848 = CARTESIAN_POINT ( 'NONE',  ( -15.72974639402197994, 15.80617190586746368, 110.6239096053143669 ) ) ;
#157849 = CARTESIAN_POINT ( 'NONE',  ( -19.03943276465977164, -0.05219959533935918106, 108.7510903946856615 ) ) ;
#157850 = CARTESIAN_POINT ( 'NONE',  ( -8.224510206698735004, -14.34966873604973081, 69.58442372801900433 ) ) ;
#157852 = CARTESIAN_POINT ( 'NONE',  ( 18.62759615963271287, -10.81492255796078972, 103.3322429386476955 ) ) ;
#157851 = CARTESIAN_POINT ( 'NONE',  ( 16.19135201231370047, 7.376712067591811639, 62.68680854052030327 ) ) ;
#157853 = CARTESIAN_POINT ( 'NONE',  ( -4.379528057220328563, 16.55341960407611168, 105.2072429386477097 ) ) ;
#157854 = CARTESIAN_POINT ( 'NONE',  ( -3.573655867282028392E-15, 2.428612866367529932E-14, 139.9999999999999716 ) ) ;
#157855 = CARTESIAN_POINT ( 'NONE',  ( -8.314922557961024197, 14.29746914071037800, 32.91775706135234714 ) ) ;
#157856 =( REPRESENTATION_RELATIONSHIP ('NONE','NONE', #154205, #71529 ) REPRESENTATION_RELATIONSHIP_WITH_TRANSFORMATION ( #12783 )SHAPE_REPRESENTATION_RELATIONSHIP( ) );
#157857 = CARTESIAN_POINT ( 'NONE',  ( -21.52544592524343514, 5.823673210054127303, 66.04057627198103830 ) ) ;
#157858 = CARTESIAN_POINT ( 'NONE',  ( -4.483927247898782831, 16.52544592524335698, 102.7094237280190185 ) ) ;
#157859 = CARTESIAN_POINT ( 'NONE',  ( 16.46253265017160672, -9.564922557960803928, 33.33224293864770260 ) ) ;
#157860 = CARTESIAN_POINT ( 'NONE',  ( -4.379528057220086978, -16.55341960407618274, 69.79275706135234714 ) ) ;
#157861 = CARTESIAN_POINT ( 'NONE',  ( -5.153800228976607833, 19.02544592524334988, 62.70942372801899722 ) ) ;
#157862 = CARTESIAN_POINT ( 'NONE',  ( 21.53943276465977519, 0.05219959533937863772, 41.25109039468568284 ) ) ;
#157863 = CARTESIAN_POINT ( 'NONE',  ( 18.67979575497178502, 10.72451020669898547, 54.16557627198103120 ) ) ;
#157864 = CARTESIAN_POINT ( 'NONE',  ( 4.379528057220092307, 16.55341960407617563, 92.29275706135236135 ) ) ;
#157865 = CARTESIAN_POINT ( 'NONE',  ( -21.55341960407619339, 5.719274019375674811, 88.54275706135236135 ) ) ;
#157866 = CARTESIAN_POINT ( 'NONE',  ( -21.55341960407610458, -5.719274019375992779, 51.45724293864770260 ) ) ;
#157867 = CARTESIAN_POINT ( 'NONE',  ( 0.05219959533907565091, 21.53943276465977519, 29.99890960531435979 ) ) ;
#157868 = EDGE_LOOP ( 'NONE', ( #2417, #157106, #128732, #100225, #44637 ) ) ;
#157869 = CARTESIAN_POINT ( 'NONE',  ( 16.55341960407618274, -4.379528057220086978, 76.04275706135237556 ) ) ;
#157870 = CARTESIAN_POINT ( 'NONE',  ( 18.67979575497178502, 10.72451020669898547, 44.16557627198103120 ) ) ;
#157871 = ORIENTED_EDGE ( 'NONE', *, *, #26840, .F. ) ;
#157872 = CARTESIAN_POINT ( 'NONE',  ( 19.05341960407611168, 5.049401038298154454, 103.9572429386476671 ) ) ;
#157873 = FACE_OUTER_BOUND ( 'NONE', #148985, .T. ) ;
#157874 = CARTESIAN_POINT ( 'NONE',  ( -5.153800228976328057, -19.02544592524343514, 32.29057627198102409 ) ) ;
#157875 = CARTESIAN_POINT ( 'NONE',  ( -21.52544592524343514, 5.823673210054127303, 66.04057627198103830 ) ) ;
#157876 = CARTESIAN_POINT ( 'NONE',  ( -8.314922557961024197, 14.29746914071037800, 87.91775706135234714 ) ) ;
#157877 = CARTESIAN_POINT ( 'NONE',  ( -0.05219959533937732626, 21.53943276465977519, 47.50109039468568994 ) ) ;
#157878 = CARTESIAN_POINT ( 'NONE',  ( -13.89961937509957401, -13.97604488694547875, 109.3760903946856331 ) ) ;
#157879 = CARTESIAN_POINT ( 'NONE',  ( 16.55341960407611168, 4.379528057220329451, 103.9572429386476813 ) ) ;
#157880 = CARTESIAN_POINT ( 'NONE',  ( 19.03943276465977164, 0.05219959533936151252, 111.2510903946856757 ) ) ;
#157881 = CARTESIAN_POINT ( 'NONE',  ( -13.97604488694527625, -13.89961937509977652, 46.87390960531435979 ) ) ;
#157882 = CARTESIAN_POINT ( 'NONE',  ( -30.00000000000000000, 0.000000000000000000, 0.000000000000000000 ) ) ;
#157883 = CARTESIAN_POINT ( 'NONE',  ( 13.89961937509977652, -13.97604488694527269, 93.12390960531436690 ) ) ;
#157884 = CARTESIAN_POINT ( 'NONE',  ( -8.224510206698735004, -14.34966873604973081, 79.58442372801903275 ) ) ;
#157885 = CARTESIAN_POINT ( 'NONE',  ( 18.62759615963255655, 10.81492255796105972, 101.6677570613523613 ) ) ;
#157886 = CARTESIAN_POINT ( 'NONE',  ( 10.72451020669898902, -18.67979575497178502, 57.91557627198103120 ) ) ;
#157887 = CARTESIAN_POINT ( 'NONE',  ( 16.55341960407618274, -4.379528057220086978, 86.04275706135236135 ) ) ;
#157888 = CARTESIAN_POINT ( 'NONE',  ( 5.153800228976615827, -19.02544592524334988, 80.20942372801901854 ) ) ;
#157889 = CARTESIAN_POINT ( 'NONE',  ( 13.89961937509977652, -13.97604488694527269, 38.12390960531436690 ) ) ;
#157890 = CARTESIAN_POINT ( 'NONE',  ( 19.03943276465977164, -0.05219959533909143690, 73.74890960531435269 ) ) ;
#157891 = CARTESIAN_POINT ( 'NONE',  ( 16.46253265017160672, -9.564922557960803928, 28.33224293864769550 ) ) ;
#157892 = CARTESIAN_POINT ( 'NONE',  ( -0.05219959533936034679, 19.03943276465977164, 72.50109039468566152 ) ) ;
#157893 = CARTESIAN_POINT ( 'NONE',  ( 26.68407921138530625, -3.932373394476913919, 171.8653659962664619 ) ) ;
#157894 = CARTESIAN_POINT ( 'NONE',  ( -5.153800228976328057, -19.02544592524343514, 107.2905762719810383 ) ) ;
#157895 = CARTESIAN_POINT ( 'NONE',  ( 14.29746914071049879, -8.314922557960816363, 58.33224293864768839 ) ) ;
#157896 = CARTESIAN_POINT ( 'NONE',  ( 15.72974639402199770, -15.80617190586745480, 63.12390960531435979 ) ) ;
#157897 = CARTESIAN_POINT ( 'NONE',  ( -17.49999999999999289, 4.013004640162588288, 105.4460572099440725 ) ) ;
#157898 = CARTESIAN_POINT ( 'NONE',  ( -5.049401038297874678, -19.05341960407617918, 24.79275706135233648 ) ) ;
#157899 = LINE ( 'NONE', #19388, #8828 ) ;
#157901 = CARTESIAN_POINT ( 'NONE',  ( -19.02544592524342804, 5.153800228976336051, 76.04057627198102409 ) ) ;
#157900 = CARTESIAN_POINT ( 'NONE',  ( 9.474510206698971260, -16.51473224551069308, 62.91557627198102409 ) ) ;
#157902 = CARTESIAN_POINT ( 'NONE',  ( -16.53943276465976808, -0.05219959533934237506, 33.75109039468568284 ) ) ;
#157903 = DIRECTION ( 'NONE',  ( -1.000000000000000000, 0.000000000000000000, 0.000000000000000000 ) ) ;
#157904 = CARTESIAN_POINT ( 'NONE',  ( 4.645199820668773683, -36.77942965383466145, -8.000000000000001776 ) ) ;
#157905 = CARTESIAN_POINT ( 'NONE',  ( 14.34966873604972726, -8.224510206698740333, 80.83442372801901854 ) ) ;
#157906 = CARTESIAN_POINT ( 'NONE',  ( 0.05219959533934541429, -16.53943276465976808, 60.00109039468568284 ) ) ;
#157907 = CARTESIAN_POINT ( 'NONE',  ( -4.379528057220086978, -16.55341960407618274, 34.79275706135235424 ) ) ;
#157909 = CARTESIAN_POINT ( 'NONE',  ( 0.000000000000000000, 0.000000000000000000, -25.00000000000000000 ) ) ;
#157908 = CARTESIAN_POINT ( 'NONE',  ( -16.46253265017160317, 9.564922557960807481, 45.83224293864769550 ) ) ;
#157910 = CARTESIAN_POINT ( 'NONE',  ( -5.719274019375665041, -21.55341960407619695, 49.79275706135234714 ) ) ;
#157911 = CARTESIAN_POINT ( 'NONE',  ( -9.474510206698720793, -16.51473224551083518, 64.58442372801900433 ) ) ;
#157912 = CARTESIAN_POINT ( 'NONE',  ( 18.62759615963255655, 10.81492255796105972, 96.66775706135234714 ) ) ;
#157913 = CARTESIAN_POINT ( 'NONE',  ( -0.05219959533909027116, -19.03943276465977164, 27.49890960531435624 ) ) ;
#157914 = CARTESIAN_POINT ( 'NONE',  ( 4.647474457565486646E-15, -28.90000000000004476, -49.67367017693150189 ) ) ;
#157915 = CARTESIAN_POINT ( 'NONE',  ( -18.62759615963270932, 10.81492255796079327, 60.83224293864769550 ) ) ;
#157916 = CARTESIAN_POINT ( 'NONE',  ( -13.97604488694527625, -13.89961937509977652, 101.8739096053143811 ) ) ;
#157917 = CARTESIAN_POINT ( 'NONE',  ( 12.14591786802309770, 12.06949235617756955, 99.37390960531436690 ) ) ;
#157918 = CARTESIAN_POINT ( 'NONE',  ( 8.224510206698742110, 14.34966873604972548, 42.08442372801901854 ) ) ;
#157919 = CARTESIAN_POINT ( 'NONE',  ( 16.55341960407618274, -4.379528057220086978, 111.0427570613523613 ) ) ;
#157920 = VERTEX_POINT ( 'NONE', #189447 ) ;
#157921 = CARTESIAN_POINT ( 'NONE',  ( 10.72451020669898902, -18.67979575497178502, 97.91557627198103830 ) ) ;
#157923 = CARTESIAN_POINT ( 'NONE',  ( 13.89961937509977652, -13.97604488694527269, 113.1239096053143527 ) ) ;
#157922 = CARTESIAN_POINT ( 'NONE',  ( 4.379528057220339221, -16.55341960407611168, 37.70724293864769550 ) ) ;
#157924 = CARTESIAN_POINT ( 'NONE',  ( -19.02544592524334988, -5.153800228976617603, 93.95942372801900433 ) ) ;
#157925 = CARTESIAN_POINT ( 'NONE',  ( 19.03943276465977164, 0.05219959533936151252, 31.25109039468566863 ) ) ;
#157926 = CARTESIAN_POINT ( 'NONE',  ( 8.224510206698953496, -14.34966873604960469, 32.91557627198102409 ) ) ;
#157927 = CARTESIAN_POINT ( 'NONE',  ( 15.72974639402199770, -15.80617190586745480, 88.12390960531436690 ) ) ;
#157928 = CARTESIAN_POINT ( 'NONE',  ( 5.823673210054125526, 21.52544592524343514, 54.79057627198104541 ) ) ;
#157929 = CARTESIAN_POINT ( 'NONE',  ( 16.51473224551069308, 9.474510206698969483, 74.16557627198103830 ) ) ;
#157930 = CARTESIAN_POINT ( 'NONE',  ( 16.55341960407611168, 4.379528057220329451, 38.95724293864768839 ) ) ;
#157931 = CARTESIAN_POINT ( 'NONE',  ( -19.02544592524342804, 5.153800228976336051, 86.04057627198103830 ) ) ;
#157932 = CARTESIAN_POINT ( 'NONE',  ( 18.22780087662121673, 5.500000000000056843, 58.98459894673892023 ) ) ;
#157933 = CARTESIAN_POINT ( 'NONE',  ( 13.89961937509957401, 13.97604488694547697, 46.87609039468565442 ) ) ;
#157934 = CARTESIAN_POINT ( 'NONE',  ( -21.52544592524343514, 5.823673210054127303, 76.04057627198102409 ) ) ;
#157935 = CARTESIAN_POINT ( 'NONE',  ( -14.34966873604960291, -8.224510206698953496, 101.6655762719810383 ) ) ;
#157936 = CARTESIAN_POINT ( 'NONE',  ( -10.81492255796105439, 18.62759615963255655, 37.91775706135235424 ) ) ;
#157937 = CARTESIAN_POINT ( 'NONE',  ( 17.14385361876520264, 23.59649016807275856, 140.1750000027311955 ) ) ;
#157938 = CARTESIAN_POINT ( 'NONE',  ( 4.379528057220092307, 16.55341960407617563, 102.2927570613523613 ) ) ;
#157939 = CARTESIAN_POINT ( 'NONE',  ( -19.05341960407611168, -5.049401038298163336, 36.45724293864766707 ) ) ;
#157940 = CARTESIAN_POINT ( 'NONE',  ( 5.153800228976335163, 19.02544592524342804, 89.79057627198102409 ) ) ;
#157941 = CARTESIAN_POINT ( 'NONE',  ( -19.48894818550241936, 5.500000000000114575, 45.10307310435242556 ) ) ;
#157942 = CARTESIAN_POINT ( 'NONE',  ( -13.89961937509977652, 13.97604488694528158, 35.62390960531435269 ) ) ;
#157943 = CARTESIAN_POINT ( 'NONE',  ( -4.379528057220328563, 16.55341960407611168, 45.20724293864769550 ) ) ;
#157944 = CARTESIAN_POINT ( 'NONE',  ( -5.823673210054431948, 21.52544592524334988, 72.70942372801901854 ) ) ;
#157946 = CARTESIAN_POINT ( 'NONE',  ( 16.55341960407618274, -4.379528057220086978, 76.04275706135237556 ) ) ;
#157945 = CARTESIAN_POINT ( 'NONE',  ( 27.86627820654178223, -25.72419401237037562, -16.61045157393441940 ) ) ;
#157947 = CARTESIAN_POINT ( 'NONE',  ( 13.89961937509977652, -13.97604488694527269, 58.12390960531436690 ) ) ;
#157948 = CARTESIAN_POINT ( 'NONE',  ( -0.05219959533909027116, -19.03943276465977164, 62.49890960531435979 ) ) ;
#157949 = VERTEX_POINT ( 'NONE', #65087 ) ;
#157950 = CARTESIAN_POINT ( 'NONE',  ( -10.72451020669870658, -18.67979575497194134, 104.5844237280190185 ) ) ;
#157951 = CARTESIAN_POINT ( 'NONE',  ( -4.483927247898782831, 16.52544592524335698, 77.70942372801900433 ) ) ;
#157952 = CARTESIAN_POINT ( 'NONE',  ( 21.52544592524334988, 5.823673210054432836, 101.4594237280190185 ) ) ;
#157953 = CARTESIAN_POINT ( 'NONE',  ( 13.89961937509977652, -13.97604488694527269, 63.12390960531435979 ) ) ;
#157954 = CARTESIAN_POINT ( 'NONE',  ( -21.53943276465977519, 0.05219959533907696930, 36.24890960531435979 ) ) ;
#157955 = CARTESIAN_POINT ( 'NONE',  ( -5.049401038297874678, -19.05341960407617918, 109.7927570613523187 ) ) ;
#157956 = CARTESIAN_POINT ( 'NONE',  ( 18.67979575497194134, -10.72451020669871369, 65.83442372801900433 ) ) ;
#157957 = CARTESIAN_POINT ( 'NONE',  ( 8.224510206698742110, 14.34966873604972548, 52.08442372801901854 ) ) ;
#157958 = CARTESIAN_POINT ( 'NONE',  ( 15.72974639402199770, -15.80617190586745480, 98.12390960531436690 ) ) ;
#157959 = CARTESIAN_POINT ( 'NONE',  ( -16.51473224551082808, 9.474510206698731452, 93.33442372801900433 ) ) ;
#157960 = CARTESIAN_POINT ( 'NONE',  ( -19.02544592524342804, 5.153800228976336051, 81.04057627198103830 ) ) ;
#157961 = CARTESIAN_POINT ( 'NONE',  ( -19.02544592524334988, -5.153800228976617603, 103.9594237280190043 ) ) ;
#157962 = CARTESIAN_POINT ( 'NONE',  ( -14.29746914071037622, -8.314922557961029526, 24.16775706135235424 ) ) ;
#157963 = CARTESIAN_POINT ( 'NONE',  ( -14.29746914071049879, 8.314922557960819915, 70.83224293864770971 ) ) ;
#157964 = CARTESIAN_POINT ( 'NONE',  ( 4.379528057220092307, 16.55341960407617563, 77.29275706135234714 ) ) ;
#157966 = CARTESIAN_POINT ( 'NONE',  ( -5.153800228976328057, -19.02544592524343514, 57.29057627198103120 ) ) ;
#157965 = CARTESIAN_POINT ( 'NONE',  ( -18.62759615963270932, 10.81492255796079327, 110.8322429386476955 ) ) ;
#157967 = CARTESIAN_POINT ( 'NONE',  ( -9.474510206698964154, 16.51473224551069663, 55.41557627198103120 ) ) ;
#157968 = CARTESIAN_POINT ( 'NONE',  ( -4.379528057220086978, -16.55341960407618274, 69.79275706135234714 ) ) ;
#157969 = CARTESIAN_POINT ( 'NONE',  ( -8.906447517083060816, 27.41122689804195645, 147.8500000054623627 ) ) ;
#157970 = ORIENTED_EDGE ( 'NONE', *, *, #181979, .F. ) ;
#157971 = CARTESIAN_POINT ( 'NONE',  ( -21.52544592524334988, -5.823673210054445271, 108.9594237280190185 ) ) ;
#157972 = CARTESIAN_POINT ( 'NONE',  ( 19.02544592524343514, -5.153800228976328945, 33.54057627198102409 ) ) ;
#157973 = VERTEX_POINT ( 'NONE', #126746 ) ;
#157974 = CARTESIAN_POINT ( 'NONE',  ( 8.314922557961029526, -14.29746914071037800, 20.41775706135234714 ) ) ;
#157975 = VECTOR ( 'NONE', #63663, 1000.000000000000000 ) ;
#157977 = CARTESIAN_POINT ( 'NONE',  ( 0.05219959533934541429, -16.53943276465976808, 30.00109039468568284 ) ) ;
#157976 = CARTESIAN_POINT ( 'NONE',  ( 16.51473224551083163, -9.474510206698727899, 40.83442372801900433 ) ) ;
#157978 = CARTESIAN_POINT ( 'NONE',  ( 16.46253265017160672, -9.564922557960803928, 48.33224293864769550 ) ) ;
#157979 = CARTESIAN_POINT ( 'NONE',  ( -13.89961937509977652, 13.97604488694528158, 60.62390960531436690 ) ) ;
#157980 = CARTESIAN_POINT ( 'NONE',  ( -10.72451020669898014, 18.67979575497178502, 90.41557627198103830 ) ) ;
#157981 = CARTESIAN_POINT ( 'NONE',  ( 9.564922557960805705, 16.46253265017160317, 114.5822429386476955 ) ) ;
#157982 = CARTESIAN_POINT ( 'NONE',  ( 19.03943276465977164, -0.05219959533909143690, 53.74890960531436690 ) ) ;
#157983 = DIRECTION ( 'NONE',  ( 0.000000000000000000, 0.000000000000000000, 1.000000000000000000 ) ) ;
#157984 = CARTESIAN_POINT ( 'NONE',  ( -13.89961937509957401, -13.97604488694547875, 99.37609039468567573 ) ) ;
#157985 = CARTESIAN_POINT ( 'NONE',  ( -12.14591786802309592, -12.06949235617757132, 66.87390960531436690 ) ) ;
#157986 = CARTESIAN_POINT ( 'NONE',  ( 19.03943276465977164, 0.05219959533936151252, 21.25109039468565797 ) ) ;
#157987 = CARTESIAN_POINT ( 'NONE',  ( -14.34966873604960291, -8.224510206698953496, 66.66557627198102409 ) ) ;
#157988 = CARTESIAN_POINT ( 'NONE',  ( -10.81492255796105439, 18.62759615963255655, 87.91775706135234714 ) ) ;
#157989 = CARTESIAN_POINT ( 'NONE',  ( -9.474510206698964154, 16.51473224551069663, 30.41557627198102054 ) ) ;
#157990 = CARTESIAN_POINT ( 'NONE',  ( 0.05219959533937995610, -21.53943276465977519, 85.00109039468568994 ) ) ;
#157992 = CARTESIAN_POINT ( 'NONE',  ( 21.55341960407619695, -5.719274019375665929, 71.04275706135234714 ) ) ;
#157991 = CARTESIAN_POINT ( 'NONE',  ( -0.05219959533910754901, -16.53943276465976808, 32.49890960531435979 ) ) ;
#157993 = CARTESIAN_POINT ( 'NONE',  ( 19.05341960407611168, 5.049401038298154454, 73.95724293864768129 ) ) ;
#157994 = CARTESIAN_POINT ( 'NONE',  ( -18.67979575497193778, 10.72451020669871902, 38.33442372801900433 ) ) ;
#157995 = CARTESIAN_POINT ( 'NONE',  ( 0.05219959533909260263, 19.03943276465977164, 74.99890960531435269 ) ) ;
#157996 = CARTESIAN_POINT ( 'NONE',  ( 14.29746914071049879, -8.314922557960816363, 88.33224293864769550 ) ) ;
#157997 = CARTESIAN_POINT ( 'NONE',  ( -14.34966873604960291, -8.224510206698953496, 61.66557627198103120 ) ) ;
#157998 = CARTESIAN_POINT ( 'NONE',  ( -0.05219959533907301413, -21.53943276465977519, 67.49890960531436690 ) ) ;
#157999 = CARTESIAN_POINT ( 'NONE',  ( 13.97604488694527802, 13.89961937509977652, 74.37390960531436690 ) ) ;
#158000 = CARTESIAN_POINT ( 'NONE',  ( -21.55341960407610458, -5.719274019375992779, 86.45724293864770971 ) ) ;
#158001 = CARTESIAN_POINT ( 'NONE',  ( 16.51473224551083163, -9.474510206698727899, 65.83442372801900433 ) ) ;
#158003 = CARTESIAN_POINT ( 'NONE',  ( 8.224510206698953496, -14.34966873604960469, 72.91557627198103830 ) ) ;
#158002 = CARTESIAN_POINT ( 'NONE',  ( 19.02544592524335343, 5.153800228976608722, 36.45942372801900433 ) ) ;
#158005 = AXIS2_PLACEMENT_3D ( 'NONE', #48453, #126269, #80753 ) ;
#158004 = CARTESIAN_POINT ( 'NONE',  ( 10.72451020669898902, -18.67979575497178502, 57.91557627198103120 ) ) ;
#158006 = LINE ( 'NONE', #144817, #149597 ) ;
#158008 = CARTESIAN_POINT ( 'NONE',  ( 8.571926809382603096, -26.38167802310801235, 147.9750000027311785 ) ) ;
#158007 = CARTESIAN_POINT ( 'NONE',  ( 0.05219959533934541429, -16.53943276465976808, 100.0010903946857042 ) ) ;
#158009 = CARTESIAN_POINT ( 'NONE',  ( 5.049401038297881783, 19.05341960407617563, 107.2927570613523187 ) ) ;
#158010 = CARTESIAN_POINT ( 'NONE',  ( 12.14591786802309770, 12.06949235617756955, 64.37390960531435269 ) ) ;
#158011 = CARTESIAN_POINT ( 'NONE',  ( -17.49999999999995381, 3.512728167237034516, 35.22809995181123810 ) ) ;
#158012 = CARTESIAN_POINT ( 'NONE',  ( -19.05341960407611168, -5.049401038298163336, 66.45724293864769550 ) ) ;
#158013 = CARTESIAN_POINT ( 'NONE',  ( 4.483927247898545687, 16.52544592524342804, 59.79057627198103120 ) ) ;
#158014 = CARTESIAN_POINT ( 'NONE',  ( 13.89961937509977652, -13.97604488694527269, 108.1239096053143669 ) ) ;
#158016 = CARTESIAN_POINT ( 'NONE',  ( -13.97604488694527625, -13.89961937509977652, 66.87390960531436690 ) ) ;
#158015 = CARTESIAN_POINT ( 'NONE',  ( -16.46253265017146816, -9.564922557961047289, 84.16775706135233293 ) ) ;
#158017 = CARTESIAN_POINT ( 'NONE',  ( 19.03943276465977164, -0.05219959533909143690, 88.74890960531436690 ) ) ;
#158018 = CARTESIAN_POINT ( 'NONE',  ( -16.46253265017160317, 9.564922557960807481, 85.83224293864769550 ) ) ;
#158019 = CARTESIAN_POINT ( 'NONE',  ( 5.719274019375991003, -21.55341960407610458, 57.70724293864770260 ) ) ;
#158020 = CARTESIAN_POINT ( 'NONE',  ( 16.55341960407618274, -4.379528057220086978, 61.04275706135234714 ) ) ;
#158021 = CARTESIAN_POINT ( 'NONE',  ( 17.50000000000002132, 5.499999999999984013, 98.78230962303568674 ) ) ;
#158022 = CARTESIAN_POINT ( 'NONE',  ( 16.51473224551069308, 9.474510206698969483, 49.16557627198102409 ) ) ;
#158023 = CARTESIAN_POINT ( 'NONE',  ( 10.72451020669898902, -18.67979575497178502, 67.91557627198102409 ) ) ;
#158024 = CARTESIAN_POINT ( 'NONE',  ( 0.05219959533936267826, -19.03943276465977164, 95.00109039468567573 ) ) ;
#158026 = CARTESIAN_POINT ( 'NONE',  ( 5.719274019375673035, 21.55341960407619339, 42.29275706135235424 ) ) ;
#158025 = CARTESIAN_POINT ( 'NONE',  ( 16.53943276465976808, 0.05219959533934440121, 111.2510903946856899 ) ) ;
#158027 = CARTESIAN_POINT ( 'NONE',  ( -9.564922557961040184, 16.46253265017147172, 37.91775706135233293 ) ) ;
#158029 = CARTESIAN_POINT ( 'NONE',  ( -8.314922557961024197, 14.29746914071037800, 92.91775706135236135 ) ) ;
#158028 = CARTESIAN_POINT ( 'NONE',  ( -14.29746914071037622, -8.314922557961029526, 54.16775706135235424 ) ) ;
#158030 = DIRECTION ( 'NONE',  ( 0.000000000000000000, 0.000000000000000000, 1.000000000000000000 ) ) ;
#158031 = CARTESIAN_POINT ( 'NONE',  ( 16.55341960407618274, -4.379528057220086978, 76.04275706135237556 ) ) ;
#158032 = CARTESIAN_POINT ( 'NONE',  ( -12.06949235617739369, -12.14591786802326823, 39.37609039468567573 ) ) ;
#158033 = CARTESIAN_POINT ( 'NONE',  ( -5.153800228976328057, -19.02544592524343514, 42.29057627198101699 ) ) ;
#158034 = CARTESIAN_POINT ( 'NONE',  ( -19.02544592524342804, 5.153800228976336051, 46.04057627198101699 ) ) ;
#158035 = CARTESIAN_POINT ( 'NONE',  ( -9.474510206698964154, 16.51473224551069663, 60.41557627198102409 ) ) ;
#158036 = CARTESIAN_POINT ( 'NONE',  ( -15.80617190586768217, 15.72974639402176855, 58.12609039468568994 ) ) ;
#158037 = CARTESIAN_POINT ( 'NONE',  ( -8.224510206698735004, -14.34966873604973081, 44.58442372801901854 ) ) ;
#158038 = CARTESIAN_POINT ( 'NONE',  ( 12.06949235617739724, 12.14591786802326823, 111.8760903946856615 ) ) ;
#158039 = CARTESIAN_POINT ( 'NONE',  ( -19.03943276465977164, 0.05219959533909376836, 31.24890960531435979 ) ) ;
#158040 = CARTESIAN_POINT ( 'NONE',  ( 5.719274019375673035, 21.55341960407619339, 112.2927570613523471 ) ) ;
#158042 = EDGE_CURVE ( 'NONE', #152327, #17363, #50924, .T. ) ;
#158041 = CARTESIAN_POINT ( 'NONE',  ( 0.05219959533934541429, -16.53943276465976808, 35.00109039468568284 ) ) ;
#158043 = CARTESIAN_POINT ( 'NONE',  ( -16.51473224551082808, 9.474510206698731452, 88.33442372801900433 ) ) ;
#158044 = CARTESIAN_POINT ( 'NONE',  ( -8.314922557960811034, -14.29746914071050412, 82.08224293864768129 ) ) ;
#158045 = CARTESIAN_POINT ( 'NONE',  ( -19.03943276465977164, 0.05219959533909376836, 36.24890960531436690 ) ) ;
#158047 = CARTESIAN_POINT ( 'NONE',  ( 17.13100169013299734, 6.664070546373172199, 76.73210164300155611 ) ) ;
#158046 = CARTESIAN_POINT ( 'NONE',  ( 19.02544592524334988, 5.153800228976608722, 76.45942372801897591 ) ) ;
#158048 = CARTESIAN_POINT ( 'NONE',  ( 15.80617190586769283, -15.72974639402175789, 70.62609039468567573 ) ) ;
#158049 = CARTESIAN_POINT ( 'NONE',  ( -16.52544592524335698, -4.483927247898792601, 43.95942372801902565 ) ) ;
#158050 = FACE_OUTER_BOUND ( 'NONE', #81231, .T. ) ;
#158051 = CARTESIAN_POINT ( 'NONE',  ( -21.53943276465977519, 0.05219959533907696930, 31.24890960531435979 ) ) ;
#158052 = CARTESIAN_POINT ( 'NONE',  ( 16.53943276465976808, 0.05219959533934440121, 31.25109039468568639 ) ) ;
#158053 = CARTESIAN_POINT ( 'NONE',  ( -13.97604488694527625, -13.89961937509977830, 26.87390960531435269 ) ) ;
#158054 = CARTESIAN_POINT ( 'NONE',  ( 9.474510206698729675, 16.51473224551082808, 27.08442372801900433 ) ) ;
#158055 = CARTESIAN_POINT ( 'NONE',  ( 30.00000000000000000, -40.00099999999999767, 37.49999999999999289 ) ) ;
#158056 = CARTESIAN_POINT ( 'NONE',  ( 13.89961937509977652, -13.97604488694527269, 43.12390960531434558 ) ) ;
#158057 = CARTESIAN_POINT ( 'NONE',  ( 28.79475375365494116, -9.355982642740455546, 143.1656553485623533 ) ) ;
#158058 = CARTESIAN_POINT ( 'NONE',  ( -13.89961937509977652, 13.97604488694528158, 65.62390960531436690 ) ) ;
#158059 = CARTESIAN_POINT ( 'NONE',  ( -18.22780087662119541, 5.500000000000102141, 66.01763182126894947 ) ) ;
#158060 = CARTESIAN_POINT ( 'NONE',  ( 5.153800228976615827, -19.02544592524334988, 25.20942372801900433 ) ) ;
#158061 = CARTESIAN_POINT ( 'NONE',  ( 14.34966873604960469, 8.224510206698951720, 39.16557627198102409 ) ) ;
#158062 = CARTESIAN_POINT ( 'NONE',  ( 19.03943276465977164, -0.05219959533909143690, 38.74890960531436690 ) ) ;
#158063 = CARTESIAN_POINT ( 'NONE',  ( -19.02544592524342804, 5.153800228976336051, 96.04057627198103830 ) ) ;
#158064 = CARTESIAN_POINT ( 'NONE',  ( -5.719274019375665041, -21.55341960407619695, 69.79275706135234714 ) ) ;
#158065 = CARTESIAN_POINT ( 'NONE',  ( 9.564922557960805705, 16.46253265017160317, 44.58224293864769550 ) ) ;
#158066 = CARTESIAN_POINT ( 'NONE',  ( 10.81492255796106328, -18.62759615963255655, 60.41775706135235424 ) ) ;
#158067 = CARTESIAN_POINT ( 'NONE',  ( 21.53943276465977519, -0.05219959533907433946, 28.74890960531435624 ) ) ;
#158068 = CARTESIAN_POINT ( 'NONE',  ( 19.05341960407611168, 5.049401038298154454, 33.95724293864769550 ) ) ;
#158069 = CARTESIAN_POINT ( 'NONE',  ( 18.62759615963255655, 10.81492255796105972, 26.66775706135235424 ) ) ;
#158070 = CARTESIAN_POINT ( 'NONE',  ( -13.97604488694547697, 13.89961937509957934, 43.12609039468566152 ) ) ;
#158071 = CARTESIAN_POINT ( 'NONE',  ( -4.379528057220328563, 16.55341960407611168, 110.2072429386477239 ) ) ;
#158072 = CARTESIAN_POINT ( 'NONE',  ( -16.51473224551069308, -9.474510206698971260, 56.66557627198103120 ) ) ;
#158073 = CARTESIAN_POINT ( 'NONE',  ( 19.03943276465977164, 0.05219959533936151252, 106.2510903946856615 ) ) ;
#158074 = CARTESIAN_POINT ( 'NONE',  ( -16.52544592524342804, 4.483927247898546575, 81.04057627198102409 ) ) ;
#158075 = CARTESIAN_POINT ( 'NONE',  ( -18.67979575497178146, -10.72451020669898902, 21.66557627198102409 ) ) ;
#158076 = CARTESIAN_POINT ( 'NONE',  ( -0.05219959533936034679, 19.03943276465977164, 87.50109039468567573 ) ) ;
#158077 = CARTESIAN_POINT ( 'NONE',  ( -10.81492255796078084, -18.62759615963271287, 102.0822429386476955 ) ) ;
#158078 = CARTESIAN_POINT ( 'NONE',  ( 5.719274019375673035, 21.55341960407619339, 57.29275706135234714 ) ) ;
#158079 = CARTESIAN_POINT ( 'NONE',  ( 8.314922557961029526, -14.29746914071037800, 60.41775706135235424 ) ) ;
#158080 = CARTESIAN_POINT ( 'NONE',  ( -16.53943276465976808, -0.05219959533934237506, 53.75109039468568994 ) ) ;
#158081 = CARTESIAN_POINT ( 'NONE',  ( 18.67979575497178502, 10.72451020669898547, 49.16557627198102409 ) ) ;
#158082 = CARTESIAN_POINT ( 'NONE',  ( 9.474510206698971260, -16.51473224551069308, 42.91557627198103120 ) ) ;
#158083 = CARTESIAN_POINT ( 'NONE',  ( 11.74264578624800315, -36.14014761921581709, -3.149999994537626247 ) ) ;
#158084 = CARTESIAN_POINT ( 'NONE',  ( 8.314922557961029526, -14.29746914071037800, 80.41775706135234714 ) ) ;
#158085 = CARTESIAN_POINT ( 'NONE',  ( 5.823673210054125526, 21.52544592524343514, 99.79057627198103830 ) ) ;
#158086 = CARTESIAN_POINT ( 'NONE',  ( 4.379528057220339221, -16.55341960407611168, 57.70724293864770260 ) ) ;
#158087 = CARTESIAN_POINT ( 'NONE',  ( -16.51473224551069308, -9.474510206698971260, 66.66557627198102409 ) ) ;
#158088 = CARTESIAN_POINT ( 'NONE',  ( 8.314922557961029526, -14.29746914071037800, 75.41775706135233293 ) ) ;
#158089 = CARTESIAN_POINT ( 'NONE',  ( -19.02544592524334988, -5.153800228976617603, 93.95942372801900433 ) ) ;
#158090 = CARTESIAN_POINT ( 'NONE',  ( 5.719274019375991003, -21.55341960407610458, 102.7072429386476955 ) ) ;
#158091 = CARTESIAN_POINT ( 'NONE',  ( -16.53943276465976808, 0.05219959533911058130, 51.24890960531436690 ) ) ;
#158092 = EDGE_LOOP ( 'NONE', ( #84052, #37345, #152992, #118469 ) ) ;
#158093 = CARTESIAN_POINT ( 'NONE',  ( 19.01533133064925352, -5.499999999999442224, 91.26586590595742621 ) ) ;
#158094 = CARTESIAN_POINT ( 'NONE',  ( 10.72451020669898902, -18.67979575497178502, 67.91557627198102409 ) ) ;
#158095 = CARTESIAN_POINT ( 'NONE',  ( -12.06949235617756955, 12.14591786802309770, 25.62390960531435624 ) ) ;
#158096 = VERTEX_POINT ( 'NONE', #115592 ) ;
#158097 = CARTESIAN_POINT ( 'NONE',  ( -17.40805194822029733, -6.112264579159361944, 54.16628727489391792 ) ) ;
#158098 = CARTESIAN_POINT ( 'NONE',  ( -5.719274019375978568, 21.55341960407610458, 105.2072429386477097 ) ) ;
#158099 = CARTESIAN_POINT ( 'NONE',  ( -15.72974639402176322, -15.80617190586768395, 29.37609039468568284 ) ) ;
#158100 = CARTESIAN_POINT ( 'NONE',  ( -12.06949235617756955, 12.14591786802309770, 40.62390960531435269 ) ) ;
#158101 = CARTESIAN_POINT ( 'NONE',  ( -8.224510206698735004, -14.34966873604973081, 49.58442372801901143 ) ) ;
#158102 = CARTESIAN_POINT ( 'NONE',  ( 16.51473224551069308, 9.474510206698969483, 44.16557627198103120 ) ) ;
#158103 = CARTESIAN_POINT ( 'NONE',  ( -0.05219959533936034679, 19.03943276465977164, 57.50109039468566863 ) ) ;
#158104 = CARTESIAN_POINT ( 'NONE',  ( -16.51473224551069308, -9.474510206698971260, 76.66557627198103830 ) ) ;
#158105 = ORIENTED_EDGE ( 'NONE', *, *, #84631, .F. ) ;
#158106 = CARTESIAN_POINT ( 'NONE',  ( 21.52544592524344225, -5.823673210054117533, 33.54057627198102409 ) ) ;
#158107 = CARTESIAN_POINT ( 'NONE',  ( -31.73299246115864136, -20.69072564976222850, -20.42656251076715535 ) ) ;
#158108 = CARTESIAN_POINT ( 'NONE',  ( 8.224510206698742110, 14.34966873604972548, 27.08442372801901854 ) ) ;
#158109 = CARTESIAN_POINT ( 'NONE',  ( -5.049401038297874678, -19.05341960407617918, 54.79275706135234003 ) ) ;
#158110 = CARTESIAN_POINT ( 'NONE',  ( -21.53943276465977519, 0.05219959533907696930, 106.2489096053143811 ) ) ;
#158111 = CARTESIAN_POINT ( 'NONE',  ( 4.379528057220339221, -16.55341960407611168, 37.70724293864769550 ) ) ;
#158112 = CARTESIAN_POINT ( 'NONE',  ( 13.97604488694527802, 13.89961937509977652, 74.37390960531436690 ) ) ;
#158113 = CARTESIAN_POINT ( 'NONE',  ( 21.55341960407610458, 5.719274019375980345, 53.95724293864770260 ) ) ;
#158115 = CARTESIAN_POINT ( 'NONE',  ( 12.14591786802327356, -12.06949235617739191, 25.62609039468567929 ) ) ;
#158114 = CARTESIAN_POINT ( 'NONE',  ( 21.53943276465977519, -0.05219959533907433946, 88.74890960531436690 ) ) ;
#158116 = CARTESIAN_POINT ( 'NONE',  ( -16.46253265017160317, 9.564922557960807481, 115.8322429386477097 ) ) ;
#158117 = CARTESIAN_POINT ( 'NONE',  ( 0.05219959533937995610, -21.53943276465977519, 85.00109039468568994 ) ) ;
#158118 = CARTESIAN_POINT ( 'NONE',  ( -9.564922557960796823, -16.46253265017161027, 77.08224293864769550 ) ) ;
#158119 = TOROIDAL_SURFACE ( 'NONE', #54784, 69.99999999999998579, 8.000000000000000000 ) ;
#158120 = CARTESIAN_POINT ( 'NONE',  ( 16.46253265017160672, -9.564922557960803928, 28.33224293864769550 ) ) ;
#158121 = CARTESIAN_POINT ( 'NONE',  ( 13.89961937509977652, -13.97604488694527269, 83.12390960531436690 ) ) ;
#158122 = CARTESIAN_POINT ( 'NONE',  ( -4.483927247898539470, -16.52544592524342804, 102.2905762719810383 ) ) ;
#158123 = CARTESIAN_POINT ( 'NONE',  ( 13.89961937509957401, 13.97604488694547697, 101.8760903946856331 ) ) ;
#158124 = CARTESIAN_POINT ( 'NONE',  ( 21.38418241377623019, -5.438282248597753110, 174.2683007571264113 ) ) ;
#158125 = CARTESIAN_POINT ( 'NONE',  ( 13.89961937509977652, -13.97604488694527269, 78.12390960531433848 ) ) ;
#158127 = CARTESIAN_POINT ( 'NONE',  ( -16.51473224551069308, -9.474510206698971260, 111.6655762719810383 ) ) ;
#158126 = CARTESIAN_POINT ( 'NONE',  ( 5.823673210054444382, -21.52544592524334988, 95.20942372801903275 ) ) ;
#158128 = CARTESIAN_POINT ( 'NONE',  ( 16.52544592524335698, 4.483927247898782831, 91.45942372801901854 ) ) ;
#158129 = CARTESIAN_POINT ( 'NONE',  ( -31.48176515315801538, 1.054302444750109702, -46.25693415911323569 ) ) ;
#158130 = CARTESIAN_POINT ( 'NONE',  ( 13.97604488694548053, -13.89961937509957401, 60.62609039468564731 ) ) ;
#158131 = CARTESIAN_POINT ( 'NONE',  ( -5.823673210054431948, 21.52544592524334988, 112.7094237280190328 ) ) ;
#158132 = CARTESIAN_POINT ( 'NONE',  ( -30.00000000000000000, -4.592425496802575156E-15, 52.50000000000000000 ) ) ;
#158133 = CARTESIAN_POINT ( 'NONE',  ( 19.05341960407611168, 5.049401038298154454, 28.95724293864769550 ) ) ;
#158134 = CARTESIAN_POINT ( 'NONE',  ( 16.53943276465976808, -0.05219959533910856209, 28.74890960531435624 ) ) ;
#158135 = CARTESIAN_POINT ( 'NONE',  ( 15.50000000000000178, -5.500000000000000888, 120.0000000000000142 ) ) ;
#158136 = CARTESIAN_POINT ( 'NONE',  ( 4.483927247898790824, -16.52544592524335698, 100.2094237280190043 ) ) ;
#158137 = CARTESIAN_POINT ( 'NONE',  ( 6.575215748390261794, -6.294127669204910625, -63.95112321872122152 ) ) ;
#158138 = CARTESIAN_POINT ( 'NONE',  ( -4.379528057220086978, -16.55341960407618274, 74.79275706135234714 ) ) ;
#158139 = CARTESIAN_POINT ( 'NONE',  ( 9.564922557960805705, 16.46253265017160317, 84.58224293864769550 ) ) ;
#158140 = CARTESIAN_POINT ( 'NONE',  ( 18.67979575497194134, -10.72451020669871369, 95.83442372801903275 ) ) ;
#158141 = CARTESIAN_POINT ( 'NONE',  ( 13.97604488694548053, -13.89961937509957401, 105.6260903946856757 ) ) ;
#158142 = CARTESIAN_POINT ( 'NONE',  ( 15.80617190586769283, -15.72974639402175789, 65.62609039468568994 ) ) ;
#158143 = CARTESIAN_POINT ( 'NONE',  ( -0.05219959533936034679, 19.03943276465977164, 47.50109039468566863 ) ) ;
#158144 = CARTESIAN_POINT ( 'NONE',  ( -9.474510206698964154, 16.51473224551069663, 75.41557627198103830 ) ) ;
#158145 = CARTESIAN_POINT ( 'NONE',  ( -13.89961937509977652, 13.97604488694528158, 70.62390960531432427 ) ) ;
#158146 = CARTESIAN_POINT ( 'NONE',  ( 16.29526858892873165, 7.335722546920136367, 73.29670597800203780 ) ) ;
#158147 = AXIS2_PLACEMENT_3D ( 'NONE', #50513, #54491, #66660 ) ;
#158148 = CARTESIAN_POINT ( 'NONE',  ( -5.823673210054116645, -21.52544592524344225, 42.29057627198103120 ) ) ;
#158149 = CARTESIAN_POINT ( 'NONE',  ( -9.474510206698964154, 16.51473224551069663, 40.41557627198103120 ) ) ;
#158151 = CARTESIAN_POINT ( 'NONE',  ( -4.379528057220086978, -16.55341960407618274, 74.79275706135234714 ) ) ;
#158150 = CARTESIAN_POINT ( 'NONE',  ( -10.72451020669898014, 18.67979575497178502, 80.41557627198103830 ) ) ;
#158152 = ORIENTED_EDGE ( 'NONE', *, *, #151158, .F. ) ;
#158154 = CARTESIAN_POINT ( 'NONE',  ( -11.40812507854754720, -35.11059874428192273, -2.224999997268813701 ) ) ;
#158153 = CARTESIAN_POINT ( 'NONE',  ( 14.34966873604960469, 8.224510206698951720, 79.16557627198103830 ) ) ;
#158155 = CARTESIAN_POINT ( 'NONE',  ( 4.379528057220092307, 16.55341960407617563, 32.29275706135235424 ) ) ;
#158156 = CARTESIAN_POINT ( 'NONE',  ( -9.474510206698964154, 16.51473224551069663, 25.41557627198103120 ) ) ;
#158157 = CARTESIAN_POINT ( 'NONE',  ( -9.564922557961040184, 16.46253265017147172, 62.91775706135233293 ) ) ;
#158158 = CARTESIAN_POINT ( 'NONE',  ( -4.483927247898539470, -16.52544592524342804, 72.29057627198102409 ) ) ;
#158159 = CARTESIAN_POINT ( 'NONE',  ( 5.823673210054444382, -21.52544592524334988, 50.20942372801901854 ) ) ;
#158161 = CARTESIAN_POINT ( 'NONE',  ( -5.719274019375978568, 21.55341960407610458, 95.20724293864769550 ) ) ;
#158160 = LINE ( 'NONE', #37808, #182774 ) ;
#158162 = CYLINDRICAL_SURFACE ( 'NONE', #185879, 4.250000000000000000 ) ;
#158163 = CARTESIAN_POINT ( 'NONE',  ( 16.55341960407611168, 4.379528057220329451, 78.95724293864769550 ) ) ;
#158164 = CARTESIAN_POINT ( 'NONE',  ( 16.41350681615404739, -36.34403388527339729, -28.23867313180933536 ) ) ;
#158165 = CARTESIAN_POINT ( 'NONE',  ( 19.03943276465977164, -0.05219959533909143690, 43.74890960531435979 ) ) ;
#158166 = CARTESIAN_POINT ( 'NONE',  ( -29.86685920354755552, 21.69954338932564397, -0.8249999972688133454 ) ) ;
#158167 = CARTESIAN_POINT ( 'NONE',  ( 16.51473224551083163, -9.474510206698727899, 75.83442372801900433 ) ) ;
#158168 = CARTESIAN_POINT ( 'NONE',  ( -5.719274019375665041, -21.55341960407619695, 24.79275706135235779 ) ) ;
#158169 = CARTESIAN_POINT ( 'NONE',  ( -5.153800228976328057, -19.02544592524343514, 72.29057627198102409 ) ) ;
#158170 = CARTESIAN_POINT ( 'NONE',  ( -5.049401038297874678, -19.05341960407617918, 59.79275706135231871 ) ) ;
#158171 = CARTESIAN_POINT ( 'NONE',  ( -9.474510206698964154, 16.51473224551069663, 50.41557627198102409 ) ) ;
#158172 = EDGE_CURVE ( 'NONE', #153137, #176832, #146923, .T. ) ;
#158173 = CARTESIAN_POINT ( 'NONE',  ( -12.14591786802309592, -12.06949235617757132, 66.87390960531436690 ) ) ;
#158174 = CARTESIAN_POINT ( 'NONE',  ( 14.34966873604960469, 8.224510206698951720, 59.16557627198103120 ) ) ;
#158175 = CARTESIAN_POINT ( 'NONE',  ( 0.05219959533909260263, 19.03943276465977164, 74.99890960531435269 ) ) ;
#158176 = EDGE_CURVE ( 'NONE', #167693, #117777, #191407, .T. ) ;
#158177 = CARTESIAN_POINT ( 'NONE',  ( -18.67979575497178146, -10.72451020669898902, 101.6655762719810383 ) ) ;
#158178 = CARTESIAN_POINT ( 'NONE',  ( 19.03943276465977164, -0.05219959533909143690, 68.74890960531436690 ) ) ;
#158179 = CARTESIAN_POINT ( 'NONE',  ( 15.80617190586746368, 15.72974639402197994, 74.37390960531436690 ) ) ;
#158180 = CARTESIAN_POINT ( 'NONE',  ( -16.46253265017146816, -9.564922557961047289, 19.16775706135233293 ) ) ;
#158183 = CARTESIAN_POINT ( 'NONE',  ( -4.379528057220328563, 16.55341960407611168, 95.20724293864769550 ) ) ;
#158182 = CARTESIAN_POINT ( 'NONE',  ( 8.224510206698742110, 14.34966873604972548, 112.0844237280190185 ) ) ;
#158181 = CARTESIAN_POINT ( 'NONE',  ( -69.65682714487590488, -71.74905178543390605, 8.936314941956774358E-29 ) ) ;
#158184 = CARTESIAN_POINT ( 'NONE',  ( -16.46253265017146816, -9.564922557961047289, 109.1677570613523471 ) ) ;
#158185 = ORIENTED_EDGE ( 'NONE', *, *, #53802, .F. ) ;
#158186 = CARTESIAN_POINT ( 'NONE',  ( 5.719274019375673035, 21.55341960407619339, 32.29275706135235424 ) ) ;
#158187 = CARTESIAN_POINT ( 'NONE',  ( -19.05341960407617563, 5.049401038297882671, 53.54275706135231871 ) ) ;
#158188 = CARTESIAN_POINT ( 'NONE',  ( -16.53943276465976808, 0.05219959533911058130, 26.24890960531435624 ) ) ;
#158189 = CARTESIAN_POINT ( 'NONE',  ( 5.719274019375991003, -21.55341960407610458, 72.70724293864769550 ) ) ;
#158190 = CARTESIAN_POINT ( 'NONE',  ( 13.89961937509977652, -13.97604488694527269, 103.1239096053143527 ) ) ;
#158191 = CARTESIAN_POINT ( 'NONE',  ( 14.34966873604960469, 8.224510206698951720, 54.16557627198103120 ) ) ;
#158192 = CARTESIAN_POINT ( 'NONE',  ( 16.46253265017160672, -9.564922557960803928, 28.33224293864769550 ) ) ;
#158193 = CARTESIAN_POINT ( 'NONE',  ( -0.05219959533909027116, -19.03943276465977164, 27.49890960531435624 ) ) ;
#158194 = CARTESIAN_POINT ( 'NONE',  ( -0.05219959533937732626, 21.53943276465977519, 107.5010903946856899 ) ) ;
#158195 = CARTESIAN_POINT ( 'NONE',  ( 14.34966873604972726, -8.224510206698740333, 90.83442372801901854 ) ) ;
#158196 = CARTESIAN_POINT ( 'NONE',  ( 21.52544592524334988, 5.823673210054432836, 36.45942372801901143 ) ) ;
#158197 = CARTESIAN_POINT ( 'NONE',  ( 0.05219959533934541429, -16.53943276465976808, 40.00109039468567573 ) ) ;
#158198 = CARTESIAN_POINT ( 'NONE',  ( -5.153800228976328057, -19.02544592524343514, 112.2905762719810099 ) ) ;
#158199 = CARTESIAN_POINT ( 'NONE',  ( -5.153800228976328057, -19.02544592524343514, 52.29057627198100988 ) ) ;
#158200 = CARTESIAN_POINT ( 'NONE',  ( 9.564922557960805705, 16.46253265017160317, 64.58224293864769550 ) ) ;
#158201 = CARTESIAN_POINT ( 'NONE',  ( -0.05219959533934338120, 16.53943276465976808, 62.50109039468568284 ) ) ;
#158202 = CARTESIAN_POINT ( 'NONE',  ( 4.483927247898545687, 16.52544592524342804, 99.79057627198103830 ) ) ;
#158203 = CARTESIAN_POINT ( 'NONE',  ( 14.34966873604960469, 8.224510206698951720, 24.16557627198103120 ) ) ;
#158204 = CARTESIAN_POINT ( 'NONE',  ( -4.999999999999999112, -140.0000000000000000, -13.00000000000000000 ) ) ;
#158207 = CARTESIAN_POINT ( 'NONE',  ( -0.05219959533909027116, -19.03943276465977164, 82.49890960531436690 ) ) ;
#158206 = CARTESIAN_POINT ( 'NONE',  ( -19.03943276465977164, 0.05219959533909376836, 91.24890960531436690 ) ) ;
#158205 = CARTESIAN_POINT ( 'NONE',  ( -18.67979575497193778, 10.72451020669871902, 58.33442372801901143 ) ) ;
#158208 = CARTESIAN_POINT ( 'NONE',  ( -13.97604488694527625, -13.89961937509977652, 106.8739096053143669 ) ) ;
#158209 = CARTESIAN_POINT ( 'NONE',  ( -16.55341960407611168, -4.379528057220339221, 51.45724293864770260 ) ) ;
#158210 = CARTESIAN_POINT ( 'NONE',  ( -16.52544592524342804, 4.483927247898546575, 26.04057627198103475 ) ) ;
#158211 = CARTESIAN_POINT ( 'NONE',  ( 12.06949235617757843, -12.14591786802309237, 33.12390960531435979 ) ) ;
#158212 = CARTESIAN_POINT ( 'NONE',  ( 37.99999999999999289, 2.428612866367529932E-14, -25.00000000000000000 ) ) ;
#158213 = CARTESIAN_POINT ( 'NONE',  ( 19.02544592524334988, 5.153800228976608722, 31.45942372801900433 ) ) ;
#158214 = CARTESIAN_POINT ( 'NONE',  ( 13.89961937509977652, -13.97604488694527269, 73.12390960531436690 ) ) ;
#158215 = CARTESIAN_POINT ( 'NONE',  ( -13.97604488694547697, 13.89961937509957934, 48.12609039468566863 ) ) ;
#158216 = CARTESIAN_POINT ( 'NONE',  ( 36.91746825000000598, -11.99521256947793546, -1.724999997268813479 ) ) ;
#158217 = DIRECTION ( 'NONE',  ( -0.000000000000000000, -0.000000000000000000, -1.000000000000000000 ) ) ;
#158219 = CARTESIAN_POINT ( 'NONE',  ( -4.379528057220086978, -16.55341960407618274, 74.79275706135234714 ) ) ;
#158218 = CARTESIAN_POINT ( 'NONE',  ( 9.474510206698729675, 16.51473224551082808, 82.08442372801899012 ) ) ;
#158220 = CARTESIAN_POINT ( 'NONE',  ( -21.46320343559653665, -20.96320343559631638, 5.353553390593268624 ) ) ;
#158221 = CARTESIAN_POINT ( 'NONE',  ( 13.97604488694527802, 13.89961937509977652, 99.37390960531436690 ) ) ;
#158222 = CARTESIAN_POINT ( 'NONE',  ( -18.67979575497193778, 10.72451020669871902, 28.33442372801902209 ) ) ;
#158223 = CARTESIAN_POINT ( 'NONE',  ( 5.049401038297881783, 19.05341960407617563, 92.29275706135234714 ) ) ;
#158225 = CARTESIAN_POINT ( 'NONE',  ( -5.153800228976328057, -19.02544592524343514, 47.29057627198102409 ) ) ;
#158224 = CARTESIAN_POINT ( 'NONE',  ( 13.89961937509977652, -13.97604488694527269, 113.1239096053143527 ) ) ;
#158226 = CARTESIAN_POINT ( 'NONE',  ( -9.564922557960796823, -16.46253265017161027, 87.08224293864769550 ) ) ;
#158228 = CARTESIAN_POINT ( 'NONE',  ( -9.474510206698964154, 16.51473224551069663, 45.41557627198103120 ) ) ;
#158227 = CARTESIAN_POINT ( 'NONE',  ( -8.224510206698948167, 14.34966873604960824, 45.41557627198103830 ) ) ;
#158229 = CARTESIAN_POINT ( 'NONE',  ( 13.97604488694548053, -13.89961937509957401, 65.62609039468567573 ) ) ;
#158230 = CARTESIAN_POINT ( 'NONE',  ( 19.03943276465977164, 0.05219959533936151252, 36.25109039468567573 ) ) ;
#158231 = CARTESIAN_POINT ( 'NONE',  ( -13.89961937509977652, 13.97604488694528158, 65.62390960531436690 ) ) ;
#158232 = CARTESIAN_POINT ( 'NONE',  ( -18.67979575497178146, -10.72451020669898902, 61.66557627198103120 ) ) ;
#158234 = CARTESIAN_POINT ( 'NONE',  ( 19.05341960407617918, -5.049401038297876454, 26.04275706135233293 ) ) ;
#158233 = CARTESIAN_POINT ( 'NONE',  ( 12.14591786802309770, 12.06949235617756955, 69.37390960531436690 ) ) ;
#158235 = CARTESIAN_POINT ( 'NONE',  ( -17.97058386085787163, -5.500000000000058620, 54.00390968646216550 ) ) ;
#158236 = CARTESIAN_POINT ( 'NONE',  ( -21.55341960407610458, -5.719274019375992779, 21.45724293864769550 ) ) ;
#158237 = CARTESIAN_POINT ( 'NONE',  ( -16.51473224551069308, -9.474510206698971260, 56.66557627198103120 ) ) ;
#158238 = CARTESIAN_POINT ( 'NONE',  ( -0.05219959533909027116, -19.03943276465977164, 37.49890960531436690 ) ) ;
#158239 = CARTESIAN_POINT ( 'NONE',  ( -0.05219959533910754901, -16.53943276465976808, 102.4989096053143811 ) ) ;
#158240 = CARTESIAN_POINT ( 'NONE',  ( -21.53943276465977519, -0.05219959533937600094, 18.75109039468568639 ) ) ;
#158241 = CARTESIAN_POINT ( 'NONE',  ( -13.89961937509977652, 13.97604488694528158, 115.6239096053143669 ) ) ;
#158242 = CARTESIAN_POINT ( 'NONE',  ( 15.72974639402176855, 15.80617190586768217, 26.87609039468567218 ) ) ;
#158243 = CARTESIAN_POINT ( 'NONE',  ( -12.06949235617756955, 12.14591786802309770, 110.6239096053143669 ) ) ;
#158244 = CARTESIAN_POINT ( 'NONE',  ( 10.81492255796106328, -18.62759615963255655, 75.41775706135233293 ) ) ;
#158245 = CARTESIAN_POINT ( 'NONE',  ( -15.80617190586745835, -15.72974639402198527, 86.87390960531438111 ) ) ;
#158246 = EDGE_CURVE ( 'NONE', #64113, #77120, #124434, .T. ) ;
#158247 = CARTESIAN_POINT ( 'NONE',  ( 13.97604488694548053, -13.89961937509957401, 35.62609039468567573 ) ) ;
#158248 = CARTESIAN_POINT ( 'NONE',  ( -5.153800228976328057, -19.02544592524343514, 22.29057627198102765 ) ) ;
#158249 = FACE_OUTER_BOUND ( 'NONE', #35620, .T. ) ;
#158250 = CARTESIAN_POINT ( 'NONE',  ( -16.46253265017160317, 9.564922557960807481, 60.83224293864769550 ) ) ;
#158251 = CARTESIAN_POINT ( 'NONE',  ( -14.34966873604972548, 8.224510206698743886, 48.33442372801902565 ) ) ;
#158252 = CARTESIAN_POINT ( 'NONE',  ( 8.224510206698953496, -14.34966873604960469, 102.9155762719810383 ) ) ;
#158253 = CARTESIAN_POINT ( 'NONE',  ( 34.46475727851696291, -1.773375775694352674, 89.78131888620558243 ) ) ;
#158254 = CARTESIAN_POINT ( 'NONE',  ( -16.46253265017160317, 9.564922557960807481, 65.83224293864769550 ) ) ;
#158255 = CARTESIAN_POINT ( 'NONE',  ( -4.483927247898539470, -16.52544592524342804, 87.29057627198103830 ) ) ;
#158256 = CARTESIAN_POINT ( 'NONE',  ( -10.72451020669898014, 18.67979575497178502, 45.41557627198103830 ) ) ;
#158257 = CARTESIAN_POINT ( 'NONE',  ( -12.06949235617756955, 12.14591786802309770, 60.62390960531437401 ) ) ;
#158258 = CARTESIAN_POINT ( 'NONE',  ( 12.14591786802327356, -12.06949235617739191, 40.62609039468567573 ) ) ;
#158259 = CARTESIAN_POINT ( 'NONE',  ( 21.53943276465977519, 0.05219959533937863772, 91.25109039468568994 ) ) ;
#158260 = CARTESIAN_POINT ( 'NONE',  ( -13.97604488694547520, 13.89961937509957934, 63.12609039468566863 ) ) ;
#158261 = CARTESIAN_POINT ( 'NONE',  ( -14.29746914071037622, -8.314922557961029526, 104.1677570613523471 ) ) ;
#158262 = CARTESIAN_POINT ( 'NONE',  ( -12.14591786802309592, -12.06949235617757132, 41.87390960531435979 ) ) ;
#158263 = CONICAL_SURFACE ( 'NONE', #80751, 2.500000000000002220, 1.029744258676656754 ) ;
#158264 = CARTESIAN_POINT ( 'NONE',  ( 16.46253265017160672, -9.564922557960803928, 38.33224293864768839 ) ) ;
#158265 = CARTESIAN_POINT ( 'NONE',  ( 15.72974639402176855, 15.80617190586768217, 96.87609039468568994 ) ) ;
#158266 = CARTESIAN_POINT ( 'NONE',  ( 21.53943276465977519, -0.05219959533907433946, 113.7489096053143527 ) ) ;
#158267 = CARTESIAN_POINT ( 'NONE',  ( 0.05219959533937995610, -21.53943276465977519, 60.00109039468568284 ) ) ;
#158268 = CARTESIAN_POINT ( 'NONE',  ( 0.05219959533934541429, -16.53943276465976808, 40.00109039468567573 ) ) ;
#158270 = CARTESIAN_POINT ( 'NONE',  ( 15.80617190586769283, -15.72974639402175789, 80.62609039468567573 ) ) ;
#158269 = CARTESIAN_POINT ( 'NONE',  ( 8.314922557960818139, 14.29746914071049879, 69.58224293864769550 ) ) ;
#158271 = CARTESIAN_POINT ( 'NONE',  ( -16.55341960407611168, -4.379528057220339221, 26.45724293864768839 ) ) ;
#158272 = CARTESIAN_POINT ( 'NONE',  ( 16.29526858892879204, 7.335722546919999587, 28.29670597800209464 ) ) ;
#158273 = LINE ( 'NONE', #19762, #106632 ) ;
#158274 = CARTESIAN_POINT ( 'NONE',  ( 16.52544592524342804, -4.483927247898539470, 23.54057627198102765 ) ) ;
#158275 = CARTESIAN_POINT ( 'NONE',  ( 12.14591786802327356, -12.06949235617739191, 75.62609039468567573 ) ) ;
#158276 = CARTESIAN_POINT ( 'NONE',  ( 9.564922557960805705, 16.46253265017160317, 79.58224293864769550 ) ) ;
#158277 = CARTESIAN_POINT ( 'NONE',  ( 19.03943276465977164, -0.05219959533909143690, 103.7489096053143669 ) ) ;
#158278 = CARTESIAN_POINT ( 'NONE',  ( 15.72974639402176855, 15.80617190586768217, 81.87609039468568994 ) ) ;
#158279 = CARTESIAN_POINT ( 'NONE',  ( -8.314922557961024197, 14.29746914071037800, 82.91775706135234714 ) ) ;
#158280 = CARTESIAN_POINT ( 'NONE',  ( -16.55341960407611168, -4.379528057220339221, 61.45724293864770260 ) ) ;
#158281 = CARTESIAN_POINT ( 'NONE',  ( -19.02544592524342804, 5.153800228976336051, 71.04057627198099567 ) ) ;
#158282 = VERTEX_POINT ( 'NONE', #129726 ) ;
#158283 = CARTESIAN_POINT ( 'NONE',  ( 16.55341960407618274, -4.379528057220086978, 21.04275706135234714 ) ) ;
#158284 = CARTESIAN_POINT ( 'NONE',  ( 9.564922557960805705, 16.46253265017160317, 34.58224293864770260 ) ) ;
#158285 = CARTESIAN_POINT ( 'NONE',  ( 19.03943276465977164, -0.05219959533909143690, 73.74890960531435269 ) ) ;
#158287 = CARTESIAN_POINT ( 'NONE',  ( 3.556970738554033499E-15, -38.81732327939057825, -6.124999997268812280 ) ) ;
#158286 = CARTESIAN_POINT ( 'NONE',  ( 16.53943276465976808, 0.05219959533934440121, 21.25109039468567218 ) ) ;
#158288 = CARTESIAN_POINT ( 'NONE',  ( -13.97604488694547697, 13.89961937509957934, 23.12609039468565442 ) ) ;
#158289 = CARTESIAN_POINT ( 'NONE',  ( -16.53943276465976808, -0.05219959533934237506, 98.75109039468568994 ) ) ;
#158290 = CARTESIAN_POINT ( 'NONE',  ( 0.05219959533936267826, -19.03943276465977164, 105.0010903946856615 ) ) ;
#158291 = CARTESIAN_POINT ( 'NONE',  ( -5.049401038298153566, 19.05341960407611168, 25.20724293864768484 ) ) ;
#158292 = CARTESIAN_POINT ( 'NONE',  ( 16.55341960407618274, -4.379528057220086978, 66.04275706135236135 ) ) ;
#158293 = CARTESIAN_POINT ( 'NONE',  ( -12.06949235617739369, -12.14591786802326823, 54.37609039468568994 ) ) ;
#158294 = CARTESIAN_POINT ( 'NONE',  ( 14.65784320516234018, -37.23156113918972210, -13.64775320819145144 ) ) ;
#158295 = CARTESIAN_POINT ( 'NONE',  ( 19.02544592524334988, 5.153800228976608722, 66.45942372801899012 ) ) ;
#158296 = CARTESIAN_POINT ( 'NONE',  ( 5.823673210054444382, -21.52544592524334988, 110.2094237280190185 ) ) ;
#158297 = CARTESIAN_POINT ( 'NONE',  ( 16.46253265017160672, -9.564922557960803928, 48.33224293864769550 ) ) ;
#158298 = CARTESIAN_POINT ( 'NONE',  ( -0.05219959533909027116, -19.03943276465977164, 82.49890960531436690 ) ) ;
#158299 = CARTESIAN_POINT ( 'NONE',  ( -8.314922557960811034, -14.29746914071050412, 77.08224293864769550 ) ) ;
#158300 = AXIS2_PLACEMENT_3D ( 'NONE', #95601, #18782, #80428 ) ;
#158301 = CARTESIAN_POINT ( 'NONE',  ( -19.02544592524334988, -5.153800228976617603, 43.95942372801899012 ) ) ;
#158302 = CARTESIAN_POINT ( 'NONE',  ( -21.52544592524343514, 5.823673210054127303, 31.04057627198102409 ) ) ;
#158303 = CARTESIAN_POINT ( 'NONE',  ( 9.564922557961047289, -16.46253265017146816, 20.41775706135233293 ) ) ;
#158304 = CARTESIAN_POINT ( 'NONE',  ( -5.153800228976328057, -19.02544592524343514, 97.29057627198099567 ) ) ;
#158305 = CARTESIAN_POINT ( 'NONE',  ( -21.52544592524334988, -5.823673210054445271, 108.9594237280190185 ) ) ;
#158306 = CARTESIAN_POINT ( 'NONE',  ( -21.53943276465977519, 0.05219959533907696930, 66.24890960531436690 ) ) ;
#158307 = CARTESIAN_POINT ( 'NONE',  ( -19.03943276465977164, 0.05219959533909376836, 91.24890960531436690 ) ) ;
#158308 = CARTESIAN_POINT ( 'NONE',  ( 13.97604488694548053, -13.89961937509957401, 90.62609039468567573 ) ) ;
#158309 = CARTESIAN_POINT ( 'NONE',  ( -13.97604488694527625, -13.89961937509977652, 106.8739096053143669 ) ) ;
#158310 = CARTESIAN_POINT ( 'NONE',  ( -13.97604488694547697, 13.89961937509957934, 103.1260903946856473 ) ) ;
#158311 = CARTESIAN_POINT ( 'NONE',  ( 9.474510206698971260, -16.51473224551069308, 22.91557627198102765 ) ) ;
#158312 = CARTESIAN_POINT ( 'NONE',  ( 9.564922557960805705, 16.46253265017160317, 89.58224293864769550 ) ) ;
#158313 = CARTESIAN_POINT ( 'NONE',  ( 18.62759615963271287, -10.81492255796078972, 58.33224293864768839 ) ) ;
#158314 = CARTESIAN_POINT ( 'NONE',  ( 14.34966873604972726, -8.224510206698740333, 40.83442372801901854 ) ) ;
#158315 = CARTESIAN_POINT ( 'NONE',  ( 21.55341960407619695, -5.719274019375665929, 41.04275706135236135 ) ) ;
#158316 = CARTESIAN_POINT ( 'NONE',  ( 15.72974639402176855, 15.80617190586768217, 91.87609039468568994 ) ) ;
#158317 = CARTESIAN_POINT ( 'NONE',  ( 12.14591786802327356, -12.06949235617739191, 100.6260903946857184 ) ) ;
#158318 = CARTESIAN_POINT ( 'NONE',  ( -13.89961937509977652, 13.97604488694528158, 90.62390960531432427 ) ) ;
#158319 = CARTESIAN_POINT ( 'NONE',  ( -8.314922557960811034, -14.29746914071050412, 92.08224293864769550 ) ) ;
#158320 = CARTESIAN_POINT ( 'NONE',  ( -14.34966873604972548, 8.224510206698743886, 113.3344237280190328 ) ) ;
#158321 = CARTESIAN_POINT ( 'NONE',  ( 13.97604488694548053, -13.89961937509957401, 65.62609039468567573 ) ) ;
#158322 = CARTESIAN_POINT ( 'NONE',  ( 15.80617190586769283, -15.72974639402175789, 45.62609039468567573 ) ) ;
#158323 = CARTESIAN_POINT ( 'NONE',  ( -12.06949235617756955, 12.14591786802309770, 85.62390960531436690 ) ) ;
#158324 = CARTESIAN_POINT ( 'NONE',  ( -9.564922557960796823, -16.46253265017161027, 107.0822429386476955 ) ) ;
#158325 = CARTESIAN_POINT ( 'NONE',  ( -8.224510206698735004, -14.34966873604973081, 109.5844237280190328 ) ) ;
#158326 = CARTESIAN_POINT ( 'NONE',  ( 0.05219959533937995610, -21.53943276465977519, 85.00109039468568994 ) ) ;
#158327 = CARTESIAN_POINT ( 'NONE',  ( -0.05219959533934338120, 16.53943276465976808, 62.50109039468568284 ) ) ;
#158328 = CARTESIAN_POINT ( 'NONE',  ( -5.719274019375665041, -21.55341960407619695, 44.79275706135234714 ) ) ;
#158329 = ORIENTED_EDGE ( 'NONE', *, *, #34682, .F. ) ;
#158330 = CARTESIAN_POINT ( 'NONE',  ( -0.05219959533937732626, 21.53943276465977519, 32.50109039468568284 ) ) ;
#158331 = CARTESIAN_POINT ( 'NONE',  ( -14.29746914071049879, 8.314922557960819915, 105.8322429386476955 ) ) ;
#158332 = CARTESIAN_POINT ( 'NONE',  ( -13.97604488694527625, -13.89961937509977652, 21.87390960531435979 ) ) ;
#158333 = CARTESIAN_POINT ( 'NONE',  ( 0.05219959533910956823, 16.53943276465976808, 69.99890960531435269 ) ) ;
#158334 = CARTESIAN_POINT ( 'NONE',  ( 16.46253265017160672, -9.564922557960803928, 63.33224293864769550 ) ) ;
#158335 = CARTESIAN_POINT ( 'NONE',  ( 12.14591786802327356, -12.06949235617739191, 100.6260903946857184 ) ) ;
#158336 = CARTESIAN_POINT ( 'NONE',  ( 19.03943276465977164, -0.05219959533909143690, 33.74890960531435979 ) ) ;
#158337 = CARTESIAN_POINT ( 'NONE',  ( 5.719274019375991003, -21.55341960407610458, 37.70724293864769550 ) ) ;
#158338 = CARTESIAN_POINT ( 'NONE',  ( -16.52544592524342804, 4.483927247898546575, 81.04057627198102409 ) ) ;
#158339 = CARTESIAN_POINT ( 'NONE',  ( -15.80617190586745835, -15.72974639402198527, 86.87390960531438111 ) ) ;
#158340 = CARTESIAN_POINT ( 'NONE',  ( -19.05341960407611168, -5.049401038298163336, 91.45724293864766707 ) ) ;
#158342 = CARTESIAN_POINT ( 'NONE',  ( -19.02544592524334988, -5.153800228976617603, 88.95942372801897591 ) ) ;
#158341 = CARTESIAN_POINT ( 'NONE',  ( -9.474510206698964154, 16.51473224551069663, 55.41557627198103120 ) ) ;
#158343 = CARTESIAN_POINT ( 'NONE',  ( 21.55341960407610458, 5.719274019375980345, 38.95724293864768839 ) ) ;
#158344 = CARTESIAN_POINT ( 'NONE',  ( -21.55341960407619339, 5.719274019375674811, 68.54275706135234714 ) ) ;
#158345 = CARTESIAN_POINT ( 'NONE',  ( 5.049401038298161559, -19.05341960407611168, 57.70724293864769550 ) ) ;
#158346 = CARTESIAN_POINT ( 'NONE',  ( -5.153800228976328057, -19.02544592524343514, 82.29057627198103830 ) ) ;
#158347 = ORIENTED_EDGE ( 'NONE', *, *, #158649, .T. ) ;
#158348 = CARTESIAN_POINT ( 'NONE',  ( -12.06949235617739369, -12.14591786802326823, 69.37609039468567573 ) ) ;
#158349 = CARTESIAN_POINT ( 'NONE',  ( 21.52544592524334988, 5.823673210054432836, 41.45942372801901143 ) ) ;
#158350 = CARTESIAN_POINT ( 'NONE',  ( 0.05219959533937995610, -21.53943276465977519, 75.00109039468568994 ) ) ;
#158351 = CARTESIAN_POINT ( 'NONE',  ( -19.02544592524342804, 5.153800228976336051, 111.0405762719810099 ) ) ;
#158352 = CARTESIAN_POINT ( 'NONE',  ( -18.67979575497178146, -10.72451020669898902, 101.6655762719810383 ) ) ;
#158354 = CARTESIAN_POINT ( 'NONE',  ( -14.34966873604972548, 8.224510206698743886, 63.33442372801900433 ) ) ;
#158353 = CARTESIAN_POINT ( 'NONE',  ( -21.55341960407619339, 5.719274019375674811, 43.54275706135235424 ) ) ;
#158356 = CARTESIAN_POINT ( 'NONE',  ( -10.81492255796078084, -18.62759615963271287, 62.08224293864769550 ) ) ;
#158355 = B_SPLINE_CURVE_WITH_KNOTS ( 'NONE', 3,
 ( #4442, #127795, #20623, #112632, #5444, #128786, #190486, #113618, #175312, #87296, #41803, #12473, #167134, #164154, #55959, #28634, #9471, #117635, #11477, #132800, #134818, #149971, #179334, #181322, #90271, #121599, #29607, #183294, #73148, #198460 ),
 .UNSPECIFIED., .F., .F.,
 ( 4, 2, 2, 2, 2, 2, 2, 2, 2, 2, 2, 2, 2, 2, 4 ),
 ( 0.008686738875643574415, 0.01074815216733882375, 0.01280956545903407309, 0.01384027210488169776, 0.01487097875072932243, 0.01693239204242456830, 0.01899380533411981417, 0.02002451197996743537, 0.02105521862581505310, 0.02208592527166267083, 0.02311663191751028856, 0.02363198524043409743, 0.02414733856335790629, 0.02466269188628171516, 0.02517804520920552402 ),
 .UNSPECIFIED. ) ;
#158357 = CARTESIAN_POINT ( 'NONE',  ( -13.97604488694547697, 13.89961937509957934, 28.12609039468565797 ) ) ;
#158359 = CARTESIAN_POINT ( 'NONE',  ( -14.34966873604972548, 8.224510206698743886, 108.3344237280190185 ) ) ;
#158358 = CARTESIAN_POINT ( 'NONE',  ( 19.03943276465977164, -0.05219959533909143690, 73.74890960531435269 ) ) ;
#158360 = CARTESIAN_POINT ( 'NONE',  ( -17.49999999999999645, -5.068104630630367424, 104.2718159465997161 ) ) ;
#158361 = CARTESIAN_POINT ( 'NONE',  ( -13.89961937509977652, 13.97604488694528158, 105.6239096053143527 ) ) ;
#158362 = CARTESIAN_POINT ( 'NONE',  ( -3.573655867282028392E-15, 2.428612866367529932E-14, 155.0000000000000000 ) ) ;
#158363 = CARTESIAN_POINT ( 'NONE',  ( 13.89961937509957401, 13.97604488694547697, 76.87609039468566152 ) ) ;
#158364 = CARTESIAN_POINT ( 'NONE',  ( 15.72974639402199770, -15.80617190586745480, 53.12390960531436690 ) ) ;
#158365 = CARTESIAN_POINT ( 'NONE',  ( -14.34966873604960291, -8.224510206698953496, 41.66557627198103120 ) ) ;
#158366 = CARTESIAN_POINT ( 'NONE',  ( 16.51473224551083163, -9.474510206698727899, 95.83442372801900433 ) ) ;
#158367 = CARTESIAN_POINT ( 'NONE',  ( -0.05219959533909027116, -19.03943276465977164, 37.49890960531436690 ) ) ;
#158368 = CARTESIAN_POINT ( 'NONE',  ( -16.52544592524335698, -4.483927247898792601, 18.95942372801901143 ) ) ;
#158370 = CARTESIAN_POINT ( 'NONE',  ( -9.564922557961040184, 16.46253265017147172, 52.91775706135233293 ) ) ;
#158369 = CARTESIAN_POINT ( 'NONE',  ( 18.62759615963271287, -10.81492255796078972, 83.33224293864769550 ) ) ;
#158371 = CARTESIAN_POINT ( 'NONE',  ( -16.52544592524335698, -4.483927247898792601, 73.95942372801901854 ) ) ;
#158372 = CARTESIAN_POINT ( 'NONE',  ( 13.97604488694527802, 13.89961937509977652, 69.37390960531436690 ) ) ;
#158373 = CARTESIAN_POINT ( 'NONE',  ( 16.53943276465976808, -0.05219959533910856209, 63.74890960531435979 ) ) ;
#158374 = CARTESIAN_POINT ( 'NONE',  ( 19.02544592524343514, -5.153800228976328945, 43.54057627198103120 ) ) ;
#158375 = CARTESIAN_POINT ( 'NONE',  ( 16.53943276465976808, -0.05219959533910856209, 58.74890960531436690 ) ) ;
#158376 = CARTESIAN_POINT ( 'NONE',  ( 5.153800228976335163, 19.02544592524342804, 24.79057627198102765 ) ) ;
#158377 = CARTESIAN_POINT ( 'NONE',  ( 31.23717829866982498, -7.254840157072012907, 96.91794063280339344 ) ) ;
#158378 = CARTESIAN_POINT ( 'NONE',  ( -8.314922557960811034, -14.29746914071050412, 22.08224293864769194 ) ) ;
#158379 = CARTESIAN_POINT ( 'NONE',  ( -19.05341960407611168, -5.049401038298163336, 81.45724293864769550 ) ) ;
#158380 = CARTESIAN_POINT ( 'NONE',  ( -31.80000000000000782, -1.163414459189985801E-14, 92.30000000000001137 ) ) ;
#158381 = CARTESIAN_POINT ( 'NONE',  ( -19.05341960407617563, 5.049401038297882671, 33.54275706135231871 ) ) ;
#158382 = CARTESIAN_POINT ( 'NONE',  ( -16.55341960407617563, 4.379528057220093196, 48.54275706135234714 ) ) ;
#158383 = CARTESIAN_POINT ( 'NONE',  ( -21.52544592524343514, 5.823673210054127303, 46.04057627198103830 ) ) ;
#158384 = CARTESIAN_POINT ( 'NONE',  ( -21.53943276465977519, -0.05219959533937600094, 113.7510903946856757 ) ) ;
#158385 = CARTESIAN_POINT ( 'NONE',  ( 16.46253265017160672, -9.564922557960803928, 78.33224293864769550 ) ) ;
#158386 = DIRECTION ( 'NONE',  ( -1.000000000000000000, -0.000000000000000000, -0.000000000000000000 ) ) ;
#158387 = CARTESIAN_POINT ( 'NONE',  ( 9.474510206698971260, -16.51473224551069308, 107.9155762719810383 ) ) ;
#158388 = CARTESIAN_POINT ( 'NONE',  ( 5.719274019375673035, 21.55341960407619339, 42.29275706135235424 ) ) ;
#158389 = CARTESIAN_POINT ( 'NONE',  ( -12.14591786802309592, -12.06949235617757132, 111.8739096053143669 ) ) ;
#158392 = ORIENTED_EDGE ( 'NONE', *, *, #77698, .T. ) ;
#158391 = CARTESIAN_POINT ( 'NONE',  ( -16.46253265017160317, 9.564922557960807481, 85.83224293864769550 ) ) ;
#158390 = CARTESIAN_POINT ( 'NONE',  ( -18.62759615963270932, 10.81492255796079327, 90.83224293864769550 ) ) ;
#158393 = CARTESIAN_POINT ( 'NONE',  ( 10.72451020669871369, 18.67979575497193778, 32.08442372801901854 ) ) ;
#158394 = ORIENTED_EDGE ( 'NONE', *, *, #118900, .T. ) ;
#158395 = CARTESIAN_POINT ( 'NONE',  ( -19.05341960407611168, -5.049401038298163336, 86.45724293864769550 ) ) ;
#158396 = PLANE ( 'NONE',  #194848 ) ;
#158398 = CARTESIAN_POINT ( 'NONE',  ( -13.97604488694527625, -13.89961937509977652, 36.87390960531436690 ) ) ;
#158397 = CARTESIAN_POINT ( 'NONE',  ( 9.474510206698971260, -16.51473224551069308, 27.91557627198103120 ) ) ;
#158399 = CARTESIAN_POINT ( 'NONE',  ( 5.049401038297881783, 19.05341960407617563, 112.2927570613523471 ) ) ;
#158400 = CARTESIAN_POINT ( 'NONE',  ( 3.556970738554033499E-15, -38.81732327939057825, -6.624999997268814056 ) ) ;
#158401 = CARTESIAN_POINT ( 'NONE',  ( -8.314922557960811034, -14.29746914071050412, 107.0822429386476955 ) ) ;
#158402 = CARTESIAN_POINT ( 'NONE',  ( -5.823673210054431948, 21.52544592524334988, 87.70942372801901854 ) ) ;
#158404 = CARTESIAN_POINT ( 'NONE',  ( -15.80617190586768217, 15.72974639402176855, 38.12609039468567573 ) ) ;
#158403 = CARTESIAN_POINT ( 'NONE',  ( 19.02544592524343514, -5.153800228976328945, 63.54057627198103830 ) ) ;
#158405 = CARTESIAN_POINT ( 'NONE',  ( 15.80617190586769283, -15.72974639402175789, 30.62609039468567929 ) ) ;
#158406 = CARTESIAN_POINT ( 'NONE',  ( 28.82186960331498327, 9.364793116373570925, 149.0999999999999943 ) ) ;
#158407 = CARTESIAN_POINT ( 'NONE',  ( -16.46253265017160317, 9.564922557960807481, 80.83224293864769550 ) ) ;
#158408 = CARTESIAN_POINT ( 'NONE',  ( 3.885274725274726393, -8.673617379884035472E-16, 0.000000000000000000 ) ) ;
#158410 = CARTESIAN_POINT ( 'NONE',  ( -18.67979575497178146, -10.72451020669898902, 46.66557627198102409 ) ) ;
#158409 = CARTESIAN_POINT ( 'NONE',  ( 12.06949235617739724, 12.14591786802326823, 21.87609039468567573 ) ) ;
#158411 = CARTESIAN_POINT ( 'NONE',  ( -0.05219959533937732626, 21.53943276465977519, 77.50109039468567573 ) ) ;
#158412 = CARTESIAN_POINT ( 'NONE',  ( -13.89961937509977652, 13.97604488694528158, 105.6239096053143527 ) ) ;
#158413 = CARTESIAN_POINT ( 'NONE',  ( -9.474510206698720793, -16.51473224551083518, 94.58442372801900433 ) ) ;
#158414 = CARTESIAN_POINT ( 'NONE',  ( -13.97604488694527625, -13.89961937509977652, 56.87390960531434558 ) ) ;
#158415 = CARTESIAN_POINT ( 'NONE',  ( 19.02544592524343514, -5.153800228976328945, 83.54057627198100988 ) ) ;
#158416 = EDGE_CURVE ( 'NONE', #35769, #165759, #180288, .T. ) ;
#158417 = CARTESIAN_POINT ( 'NONE',  ( -12.14591786802309592, -12.06949235617757132, 96.87390960531436690 ) ) ;
#158418 = CARTESIAN_POINT ( 'NONE',  ( 14.29746914071049879, -8.314922557960816363, 103.3322429386476955 ) ) ;
#158419 = CARTESIAN_POINT ( 'NONE',  ( 19.05341960407611168, 5.049401038298154454, 113.9572429386477097 ) ) ;
#158421 = CARTESIAN_POINT ( 'NONE',  ( 16.51473224551069308, 9.474510206698969483, 44.16557627198103120 ) ) ;
#158420 = CARTESIAN_POINT ( 'NONE',  ( -12.14591786802309592, -12.06949235617757132, 51.87390960531437401 ) ) ;
#158422 = CARTESIAN_POINT ( 'NONE',  ( -21.55341960407619339, 5.719274019375674811, 68.54275706135234714 ) ) ;
#158423 = CARTESIAN_POINT ( 'NONE',  ( -9.564922557961040184, 16.46253265017147172, 87.91775706135233293 ) ) ;
#158424 = CARTESIAN_POINT ( 'NONE',  ( -16.53943276465976808, 0.05219959533911058130, 66.24890960531436690 ) ) ;
#158425 = CARTESIAN_POINT ( 'NONE',  ( -5.719274019375978568, 21.55341960407610458, 110.2072429386477239 ) ) ;
#158426 = CARTESIAN_POINT ( 'NONE',  ( 5.719274019375991003, -21.55341960407610458, 42.70724293864770260 ) ) ;
#158427 = CARTESIAN_POINT ( 'NONE',  ( 19.05341960407611168, 5.049401038298154454, 108.9572429386477097 ) ) ;
#158428 = CARTESIAN_POINT ( 'NONE',  ( -23.31738231874055245, -16.94106989632524574, 138.4500000054623570 ) ) ;
#158429 = CARTESIAN_POINT ( 'NONE',  ( -13.97604488694527625, -13.89961937509977652, 66.87390960531436690 ) ) ;
#158430 = CARTESIAN_POINT ( 'NONE',  ( 12.14591786802309770, 12.06949235617756955, 34.37390960531435979 ) ) ;
#158431 = CIRCLE ( 'NONE', #184283, 39.99999999999999289 ) ;
#158432 = CARTESIAN_POINT ( 'NONE',  ( -16.53943276465976808, -0.05219959533934237506, 108.7510903946857042 ) ) ;
#158433 = CARTESIAN_POINT ( 'NONE',  ( 12.14591786802327356, -12.06949235617739191, 80.62609039468567573 ) ) ;
#158434 = CARTESIAN_POINT ( 'NONE',  ( 13.97604488694548053, -13.89961937509957401, 45.62609039468566863 ) ) ;
#158435 = CYLINDRICAL_SURFACE ( 'NONE', #56634, 61.99999999999998579 ) ;
#158436 = CARTESIAN_POINT ( 'NONE',  ( -19.05341960407611168, -5.049401038298163336, 96.45724293864769550 ) ) ;
#158437 = CARTESIAN_POINT ( 'NONE',  ( -5.153800228976328057, -19.02544592524343514, 52.29057627198100988 ) ) ;
#158438 = CARTESIAN_POINT ( 'NONE',  ( 4.379528057220339221, -16.55341960407611168, 67.70724293864769550 ) ) ;
#158440 = CARTESIAN_POINT ( 'NONE',  ( 10.72451020669898902, -18.67979575497178502, 27.91557627198103830 ) ) ;
#158439 = CARTESIAN_POINT ( 'NONE',  ( -9.564922557960796823, -16.46253265017161027, 22.08224293864768839 ) ) ;
#158441 = CARTESIAN_POINT ( 'NONE',  ( 10.72451020669898902, -18.67979575497178502, 52.91557627198103830 ) ) ;
#158442 = CARTESIAN_POINT ( 'NONE',  ( 8.314922557960818139, 14.29746914071049879, 84.58224293864769550 ) ) ;
#158443 = CARTESIAN_POINT ( 'NONE',  ( -16.53943276465976808, -0.05219959533934237506, 38.75109039468567573 ) ) ;
#158444 = CARTESIAN_POINT ( 'NONE',  ( 14.34966873604960469, 8.224510206698951720, 79.16557627198103830 ) ) ;
#158445 = CARTESIAN_POINT ( 'NONE',  ( 18.46320343559638388, -23.96320343559646915, 1.818019484660534424 ) ) ;
#158446 = CARTESIAN_POINT ( 'NONE',  ( 0.05219959533936267826, -19.03943276465977164, 75.00109039468566152 ) ) ;
#158447 = CARTESIAN_POINT ( 'NONE',  ( -21.53943276465977519, 0.05219959533907696930, 21.24890960531436690 ) ) ;
#158448 = CARTESIAN_POINT ( 'NONE',  ( 36.91746824999999887, 11.99521256947799053, -4.024999997268814411 ) ) ;
#158449 = LINE ( 'NONE', #157467, #9256 ) ;
#158451 = CARTESIAN_POINT ( 'NONE',  ( -4.483927247898782831, 16.52544592524335698, 107.7094237280190328 ) ) ;
#158450 = CARTESIAN_POINT ( 'NONE',  ( 12.14591786802327356, -12.06949235617739191, 25.62609039468567929 ) ) ;
#158452 = CARTESIAN_POINT ( 'NONE',  ( 13.97604488694548053, -13.89961937509957401, 65.62609039468567573 ) ) ;
#158453 = CARTESIAN_POINT ( 'NONE',  ( -10.81492255796078084, -18.62759615963271287, 47.08224293864770260 ) ) ;
#158454 = CARTESIAN_POINT ( 'NONE',  ( 15.80617190586769283, -15.72974639402175789, 65.62609039468568994 ) ) ;
#158455 = DIRECTION ( 'NONE',  ( -0.000000000000000000, -0.000000000000000000, 1.000000000000000000 ) ) ;
#158456 = CARTESIAN_POINT ( 'NONE',  ( 8.314922557961029526, -14.29746914071037800, 30.41775706135234358 ) ) ;
#158458 = CARTESIAN_POINT ( 'NONE',  ( -9.564922557960796823, -16.46253265017161027, 87.08224293864769550 ) ) ;
#158457 = CARTESIAN_POINT ( 'NONE',  ( -9.474510206698964154, 16.51473224551069663, 25.41557627198103120 ) ) ;
#158459 = CARTESIAN_POINT ( 'NONE',  ( 15.06137443927350361, 15.06137443927346098, -58.85720012050613548 ) ) ;
#158460 = CARTESIAN_POINT ( 'NONE',  ( 14.29746914071049879, -8.314922557960816363, 98.33224293864769550 ) ) ;
#158461 = APPLICATION_PROTOCOL_DEFINITION ( 'draft international standard', 'automotive_design', 1998, #36479 ) ;
#158462 = CARTESIAN_POINT ( 'NONE',  ( -5.153800228976328057, -19.02544592524343514, 102.2905762719810383 ) ) ;
#158463 = ORIENTED_EDGE ( 'NONE', *, *, #83102, .F. ) ;
#158464 = CARTESIAN_POINT ( 'NONE',  ( 14.34966873604972726, -8.224510206698740333, 60.83442372801901854 ) ) ;
#158465 = CARTESIAN_POINT ( 'NONE',  ( -16.46253265017146816, -9.564922557961047289, 109.1677570613523471 ) ) ;
#158466 = CARTESIAN_POINT ( 'NONE',  ( -10.81492255796078084, -18.62759615963271287, 82.08224293864768129 ) ) ;
#158467 = CARTESIAN_POINT ( 'NONE',  ( -16.51473224551069308, -9.474510206698971260, 41.66557627198103120 ) ) ;
#158469 = CARTESIAN_POINT ( 'NONE',  ( -15.80617190586745835, -15.72974639402198527, 111.8739096053143669 ) ) ;
#158468 = CARTESIAN_POINT ( 'NONE',  ( -19.05341960407617563, 5.049401038297882671, 68.54275706135230450 ) ) ;
#158470 = CARTESIAN_POINT ( 'NONE',  ( -9.564922557960796823, -16.46253265017161027, 72.08224293864770971 ) ) ;
#158471 = CARTESIAN_POINT ( 'NONE',  ( 9.564922557960805705, 16.46253265017160317, 99.58224293864770971 ) ) ;
#158472 = ORIENTED_EDGE ( 'NONE', *, *, #146153, .F. ) ;
#158473 = CARTESIAN_POINT ( 'NONE',  ( 8.224510206698742110, 14.34966873604972548, 32.08442372801901854 ) ) ;
#158474 = CARTESIAN_POINT ( 'NONE',  ( 10.72451020669898902, -18.67979575497178502, 107.9155762719810241 ) ) ;
#158477 = CARTESIAN_POINT ( 'NONE',  ( 19.03943276465977164, 0.05219959533936151252, 76.25109039468566152 ) ) ;
#158476 = CARTESIAN_POINT ( 'NONE',  ( 13.89961937509977652, -13.97604488694527269, 98.12390960531433848 ) ) ;
#158475 = CARTESIAN_POINT ( 'NONE',  ( -8.224510206698948167, 14.34966873604960824, 105.4155762719810383 ) ) ;
#158478 = CARTESIAN_POINT ( 'NONE',  ( 18.62759615963271287, -10.81492255796078972, 88.33224293864769550 ) ) ;
#158479 = CARTESIAN_POINT ( 'NONE',  ( 12.14591786802309770, 12.06949235617756955, 44.37390960531435979 ) ) ;
#158480 = CARTESIAN_POINT ( 'NONE',  ( 9.564922557961047289, -16.46253265017146816, 25.41775706135234003 ) ) ;
#158481 = CARTESIAN_POINT ( 'NONE',  ( 8.314922557961029526, -14.29746914071037800, 70.41775706135236135 ) ) ;
#158482 = CARTESIAN_POINT ( 'NONE',  ( 5.049401038298161559, -19.05341960407611168, 92.70724293864769550 ) ) ;
#158483 = CARTESIAN_POINT ( 'NONE',  ( 13.97604488694527802, 13.89961937509977652, 44.37390960531435269 ) ) ;
#158484 = CARTESIAN_POINT ( 'NONE',  ( -15.72974639402176322, -15.80617190586768395, 54.37609039468568994 ) ) ;
#158485 = CARTESIAN_POINT ( 'NONE',  ( -15.80617190586768217, 15.72974639402176855, 63.12609039468568994 ) ) ;
#158486 = CARTESIAN_POINT ( 'NONE',  ( 13.89961937509977652, -13.97604488694527269, 63.12390960531435979 ) ) ;
#158487 = CARTESIAN_POINT ( 'NONE',  ( -10.81492255796105439, 18.62759615963255655, 32.91775706135234714 ) ) ;
#158488 = ADVANCED_FACE ( 'NONE', ( #163092 ), #24596, .F. ) ;
#158489 = CARTESIAN_POINT ( 'NONE',  ( -5.153800228976607833, 19.02544592524334988, 77.70942372801900433 ) ) ;
#158490 = CARTESIAN_POINT ( 'NONE',  ( 5.153800228976335163, 19.02544592524342804, 44.79057627198103830 ) ) ;
#158491 = CARTESIAN_POINT ( 'NONE',  ( -4.483927247898782831, 16.52544592524335698, 87.70942372801901854 ) ) ;
#158492 = CARTESIAN_POINT ( 'NONE',  ( -19.02544592524342804, 5.153800228976336051, 56.04057627198100988 ) ) ;
#158493 = CARTESIAN_POINT ( 'NONE',  ( -9.564922557960796823, -16.46253265017161027, 107.0822429386476955 ) ) ;
#158494 = CARTESIAN_POINT ( 'NONE',  ( 16.46253265017160672, -9.564922557960803928, 43.33224293864769550 ) ) ;
#158495 = CARTESIAN_POINT ( 'NONE',  ( -15.72974639402197994, 15.80617190586746368, 90.62390960531436690 ) ) ;
#158496 = CARTESIAN_POINT ( 'NONE',  ( -14.34966873604972548, 8.224510206698743886, 73.33442372801901854 ) ) ;
#158497 = CARTESIAN_POINT ( 'NONE',  ( -24.20757866959954541, 5.698759791480812353, 172.9004493943157570 ) ) ;
#158498 = CARTESIAN_POINT ( 'NONE',  ( -5.049401038297874678, -19.05341960407617918, 34.79275706135233293 ) ) ;
#158499 = CARTESIAN_POINT ( 'NONE',  ( -9.564922557960796823, -16.46253265017161027, 72.08224293864770971 ) ) ;
#158500 = CARTESIAN_POINT ( 'NONE',  ( 8.314922557960818139, 14.29746914071049879, 44.58224293864769550 ) ) ;
#158501 = CARTESIAN_POINT ( 'NONE',  ( 8.224510206698953496, -14.34966873604960469, 77.91557627198102409 ) ) ;
#158502 = CARTESIAN_POINT ( 'NONE',  ( -9.564922557960796823, -16.46253265017161027, 102.0822429386477097 ) ) ;
#158503 = CARTESIAN_POINT ( 'NONE',  ( 13.89961937509977652, -13.97604488694527269, 88.12390960531438111 ) ) ;
#158504 = CARTESIAN_POINT ( 'NONE',  ( -5.823673210054431948, 21.52544592524334988, 52.70942372801902565 ) ) ;
#158505 = CARTESIAN_POINT ( 'NONE',  ( 9.474510206698971260, -16.51473224551069308, 97.91557627198102409 ) ) ;
#158506 = CARTESIAN_POINT ( 'NONE',  ( 10.81492255796106328, -18.62759615963255655, 100.4177570613523471 ) ) ;
#158507 = CARTESIAN_POINT ( 'NONE',  ( 4.483927247898790824, -16.52544592524335698, 85.20942372801901854 ) ) ;
#158508 = CARTESIAN_POINT ( 'NONE',  ( 21.55341960407619695, -5.719274019375665929, 26.04275706135235779 ) ) ;
#158509 = CARTESIAN_POINT ( 'NONE',  ( 21.53943276465977519, -0.05219959533907433946, 103.7489096053143669 ) ) ;
#158510 = CARTESIAN_POINT ( 'NONE',  ( 4.483927247898545687, 16.52544592524342804, 59.79057627198103120 ) ) ;
#158511 = CARTESIAN_POINT ( 'NONE',  ( 19.02544592524343514, -5.153800228976328945, 43.54057627198103120 ) ) ;
#158512 = CARTESIAN_POINT ( 'NONE',  ( 16.53943276465976808, -0.05219959533910856209, 68.74890960531435269 ) ) ;
#158513 = CARTESIAN_POINT ( 'NONE',  ( -18.62759615963270932, 10.81492255796079327, 25.83224293864769194 ) ) ;
#158514 = CARTESIAN_POINT ( 'NONE',  ( 5.153800228976615827, -19.02544592524334988, 35.20942372801899722 ) ) ;
#158515 = CARTESIAN_POINT ( 'NONE',  ( 16.52544592524342804, -4.483927247898539470, 108.5405762719810241 ) ) ;
#158516 = ORIENTED_EDGE ( 'NONE', *, *, #69017, .T. ) ;
#158517 = CARTESIAN_POINT ( 'NONE',  ( 8.314922557961029526, -14.29746914071037800, 60.41775706135235424 ) ) ;
#158518 = CARTESIAN_POINT ( 'NONE',  ( -13.97604488694527625, -13.89961937509977652, 71.87390960531433848 ) ) ;
#158519 = LINE ( 'NONE', #113991, #24234 ) ;
#158520 = CARTESIAN_POINT ( 'NONE',  ( 16.52544592524342804, -4.483927247898539470, 93.54057627198103830 ) ) ;
#158521 = CARTESIAN_POINT ( 'NONE',  ( 5.823673210054125526, 21.52544592524343514, 34.79057627198103120 ) ) ;
#158522 = VERTEX_POINT ( 'NONE', #176272 ) ;
#158523 = CARTESIAN_POINT ( 'NONE',  ( -8.314922557961024197, 14.29746914071037800, 112.9177570613523329 ) ) ;
#158524 = CARTESIAN_POINT ( 'NONE',  ( 16.51473224551083163, -9.474510206698727899, 105.8344237280190043 ) ) ;
#158525 = CARTESIAN_POINT ( 'NONE',  ( 18.67979575497194134, -10.72451020669871369, 75.83442372801900433 ) ) ;
#158526 = CARTESIAN_POINT ( 'NONE',  ( 16.51473224551069308, 9.474510206698969483, 89.16557627198103830 ) ) ;
#158527 = CARTESIAN_POINT ( 'NONE',  ( 10.81492255796078972, 18.62759615963270932, 99.58224293864770971 ) ) ;
#158528 = CARTESIAN_POINT ( 'NONE',  ( -16.55341960407617563, 4.379528057220093196, 48.54275706135234714 ) ) ;
#158529 = CARTESIAN_POINT ( 'NONE',  ( -19.03943276465977164, 0.05219959533909376836, 31.24890960531435979 ) ) ;
#158530 = CARTESIAN_POINT ( 'NONE',  ( 12.06949235617739724, 12.14591786802326823, 31.87609039468567929 ) ) ;
#158531 = CARTESIAN_POINT ( 'NONE',  ( 19.05341960407617918, -5.049401038297876454, 91.04275706135234714 ) ) ;
#158532 = CARTESIAN_POINT ( 'NONE',  ( 10.72451020669898902, -18.67979575497178502, 87.91557627198103830 ) ) ;
#158533 = CARTESIAN_POINT ( 'NONE',  ( 16.46253265017146816, 9.564922557961045513, 56.66775706135233293 ) ) ;
#158534 = CARTESIAN_POINT ( 'NONE',  ( -3.573655867282028392E-15, 2.428612866367529932E-14, 150.0000000000000000 ) ) ;
#158535 = CARTESIAN_POINT ( 'NONE',  ( 21.53943276465977519, -0.05219959533907433946, 98.74890960531438111 ) ) ;
#158536 = CARTESIAN_POINT ( 'NONE',  ( -5.153800228976328057, -19.02544592524343514, 82.29057627198103830 ) ) ;
#158537 = DIRECTION ( 'NONE',  ( 0.000000000000000000, 0.000000000000000000, 1.000000000000000000 ) ) ;
#158538 = CARTESIAN_POINT ( 'NONE',  ( 16.52544592524335698, 4.483927247898782831, 31.45942372801901854 ) ) ;
#158539 = CARTESIAN_POINT ( 'NONE',  ( 36.95458794302616212, -5.320992724678918151, 43.56214547691708816 ) ) ;
#158541 = CARTESIAN_POINT ( 'NONE',  ( 4.379528057220339221, -16.55341960407611168, 62.70724293864769550 ) ) ;
#158540 = CARTESIAN_POINT ( 'NONE',  ( -0.05219959533937732626, 21.53943276465977519, 22.50109039468567573 ) ) ;
#158542 = CARTESIAN_POINT ( 'NONE',  ( -9.474510206698964154, 16.51473224551069663, 65.41557627198102409 ) ) ;
#158544 = CARTESIAN_POINT ( 'NONE',  ( -19.02544592524334988, -5.153800228976617603, 43.95942372801899012 ) ) ;
#158543 = CARTESIAN_POINT ( 'NONE',  ( -16.55341960407617563, 4.379528057220093196, 33.54275706135234714 ) ) ;
#158545 = CARTESIAN_POINT ( 'NONE',  ( 18.62759615963255655, 10.81492255796105972, 51.66775706135234714 ) ) ;
#158546 = CARTESIAN_POINT ( 'NONE',  ( 8.314922557961029526, -14.29746914071037800, 20.41775706135234714 ) ) ;
#158547 = CARTESIAN_POINT ( 'NONE',  ( 9.474510206698971260, -16.51473224551069308, 57.91557627198103120 ) ) ;
#158548 = CARTESIAN_POINT ( 'NONE',  ( -9.564922557961040184, 16.46253265017147172, 82.91775706135233293 ) ) ;
#158549 = CARTESIAN_POINT ( 'NONE',  ( -21.55341960407619339, 5.719274019375674811, 88.54275706135236135 ) ) ;
#158550 = CARTESIAN_POINT ( 'NONE',  ( -19.02544592524334988, -5.153800228976617603, 63.95942372801899012 ) ) ;
#158551 = CARTESIAN_POINT ( 'NONE',  ( -16.46253265017160317, 9.564922557960807481, 40.83224293864769550 ) ) ;
#158552 = CARTESIAN_POINT ( 'NONE',  ( 15.72974639402199770, -15.80617190586745480, 63.12390960531435979 ) ) ;
#158553 = CARTESIAN_POINT ( 'NONE',  ( 12.06949235617757843, -12.14591786802309237, 58.12390960531435979 ) ) ;
#158554 = CARTESIAN_POINT ( 'NONE',  ( 0.000000000000000000, 0.000000000000000000, -18.00000000000000000 ) ) ;
#158555 = CARTESIAN_POINT ( 'NONE',  ( 19.03943276465977164, 0.05219959533936151252, 36.25109039468567573 ) ) ;
#158556 = CARTESIAN_POINT ( 'NONE',  ( -4.483927247898782831, 16.52544592524335698, 102.7094237280190185 ) ) ;
#158557 = CARTESIAN_POINT ( 'NONE',  ( -14.34966873604960291, -8.224510206698953496, 51.66557627198102409 ) ) ;
#158558 = CARTESIAN_POINT ( 'NONE',  ( 15.80617190586769283, -15.72974639402175789, 85.62609039468568994 ) ) ;
#158559 = CARTESIAN_POINT ( 'NONE',  ( 18.67979575497194134, -10.72451020669871369, 80.83442372801901854 ) ) ;
#158560 = CARTESIAN_POINT ( 'NONE',  ( 18.62759615963271287, -10.81492255796078972, 88.33224293864769550 ) ) ;
#158561 =( BOUNDED_SURFACE ( )  B_SPLINE_SURFACE ( 3, 2, ( 
 ( #42400, #104063, #165744, #122196, #30200, #27238, #183888, #45373, #107026, #150579, #73741, #168698, #91841, #118243, #164748, #179934, #41401, #138368, #125195, #35165, #112008, #153535, #94845, #15032, #76692, #140350, #108016, #61518, #95838, #127158, #124180, #186891, #139355, #156526, #50349, #155526, #3818, #79678, #48362, #18025, #17021, #141349, #173697, #47367, #171697, #49344, #78674, #157522, #16029, #34177, #1838, #65496, #200049, #33186, #185882, #836, #77687, #62509, #109022, #123187, #111006, #19016, #2836, #169702, #80662, #184876, #142338, #110016, #170701, #64514, #63520, #126181, #46358, #188866, #187876, #32190, #31196, #92847, #154532, #172692, #93848, #96820, #51331, #37148, #4805, #38162, #7806, #68482, #158505, #99817, #146317, #192844, #132160, #67487, #85650, #19992, #175674, #22992, #143318, #162492, #130137, #128157, #189857, #113976, #66494, #129145, #174684, #69490, #191834, #190842, #112991, #116988, #23993, #81635, #36149, #145321, #131155, #100809, #161502, #178681, #83644, #53315, #54324, #97801, #52318, #147337, #115996, #6804, #114993, #159490, #176687, #177685, #20983, #84640, #82640, #39153, #8824, #70493, #193852, #144323, #5812, #55317, #98807, #160501, #21991, #101821, #87648, #181671, #196851, #195860, #139848, #102827, #149334, #89646, #163509, #148335, #78179, #135177, #27003, #197830, #40144, #88648, #151334, #74489, #1337, #133156, #58317, #119985, #43150, #73505, #123680, #46869, #16532, #165507, #150344, #63017, #104819, #25007, #166508, #124696, #86651, #136155, #9830, #10828, #26006, #71490, #11840, #185379, #194847, #72498, #62016, #108530, #12823, #170209, #42167, #179692, #56320, #134172, #28006, #31702, #57332, #118003, #164513, #119008, #93351, #41164, #180691, #103827, #155037, #173195, #143831, #186393, #34671, #97309, #20488, #21492, #79180, #81152, #142834, #4313, #19507, #66995, #190349, #160004, #111509, #96329, #83153, #127665, #47870, #112499, #144827, #109523, #82137, #171205, #157025, #172193, #17522, #158016, #128654, #32695, #18523, #5311, #51825, #35661, #113485, #188368, #65996, #6311, #156025, #189365, #80170, #50842, #175179, #174193, #158995, #95340, #36645, #141842, #3333, #98304, #94346, #140851, #126664, #2340, #67989, #64021, #125690, #187389, #48857, #110512, #33678, #65007, #49845, #118514, #129643, #8327, #55828, #176188, #195360, #101317, #161006, #22500, #146834, #37657, #100325, #7309, #40666, #163006, #162004, #84147, #149839, #56839, #114485, #99322, #178191, #164025, #133669, #71005, #11343, #116503, #24513, #87167, #145826, #23500, #180204, #179198, #39656, #86163, #191339, #147853, #102335, #53835, #9340, #68994, #132673, #194361, #117501, #25521, #130659, #192352, #148848, #10339, #115509, #88154, #71995, #52817, #177197, #38670, #41673, #85148, #103337, #54829, #70002, #131672, #193353, #165017, #26510, #31458, #75964, #137637, #57837, #28506, #61775, #123443, #60789, #29483, #76954, #15294, #199324, #43655, #13314, #91114, #45634, #44647, #136642, #154795, #93110, #185136, #198325, #122460, #167985, #135674, #89155, #167004, #138624, #73014, #197346, #46627, #108287, #168957, #105317, #150844, #134683, #152804, #184153, #166014, #107286, #90140, #119510, #106299, #196369, #181191, #42669, #14296, #104330, #27514, #59801, #12340, #74004, #105, #169965, #151825, #30463, #58809, #92111, #120478, #74980, #182169, #153800, #121471, #183163, #18288, #80925, #113253, #110278, #34440, #112267, #79943, #20251, #78938, #97079, #3100, #128417, #98061, #96099, #187154, #2104, #140614, #63785, #125457, #174944, #173959, #81897, #157788, #32455, #143590, #36406, #5073, #64778, #62772, #141613, #48626, #155787, #19278, #126439, #142602, #4081, #17284, #95106, #16293, #188137, #171959, #65759, #49608, #127428, #139610, #66756, #111271, #33447, #158760, #190113, #189136, #172962, #156795, #77943, #1096, #35426 ),
 ( #50608, #51588, #124453, #186149, #47628, #109283, #170961, #94108, #10095, #84905, #24269, #54584, #22257, #175948, #53587, #163777, #179960, #83906, #71755, #195113, #55584, #192104, #37417, #118270, #116257, #85918, #52582, #9094, #130406, #144588, #131424, #41427, #159760, #21255, #101075, #82910, #6074, #146584, #114241, #67752, #102092, #133425, #115263, #193110, #145589, #162760, #56596, #161766, #129410, #147606, #177948, #70761, #23261, #132429, #191107, #176956, #39416, #117259, #8078, #25278, #7067, #40421, #69754, #99077, #160767, #194121, #38425, #68749, #100081, #178951, #86921, #148603, #167749, #14054, #13082, #196126, #75721, #45397, #137397, #43413, #149598, #58575, #165771, #119266, #136410, #105083, #74747, #198090, #180949, #135438, #103093, #28270, #73765, #121233, #166769, #59555, #87911, #199078, #89909, #88914, #60546, #122221, #107050, #151591, #26269, #164775, #11095, #106063, #27265, #72771, #182926, #29247, #42426, #168723, #44409, #104088, #150606, #90881, #12102, #120241, #197108, #183912, #152565, #181932, #134441, #57597, #10755, #68403, #130055, #132086, #117926, #87576, #24931, #103756, #70419, #116912, #41088, #176608, #54249, #149263, #133081, #193775, #55244, #145244, #101745, #194771, #7725, #178605, #191755, #86576, #163434, #40068, #148260, #22914, #99738, #9753, #164439, #69411, #84560, #6725, #131077, #71417, #56245, #39079, #180618, #146238, #192766, #179616, #53238, #114915, #118933, #102751, #25933, #72419, #83565, #134096, #195787, #57259, #42091, #38082, #165435, #161422, #115921, #177611, #100735, #162416, #23918, #8749, #85572, #147259, #168395, #88572, #153215, #62193, #150270, #61204, #11765, #197754, #12749, #58246, #137060, #169379, #73431, #59221, #122876, #107700, #76380, #92534, #28915, #121885, #185555, #196778, #152237, #120890, #106721, #154223, #29890, #183578, #136080, #15713, #182589, #44073, #138057, #26930, #181600, #167419, #135102, #91528, #199738, #198750, #119914, #14720, #184564, #46045, #123857, #105732, #77373, #13722, #30887, #151259, #166435, #43077, #74414, #139041, #45063, #90555, #47049, #89573, #75388, #521, #104744, #27930, #108706, #60215, #157203, #127836, #170385, #18697, #81323, #4484, #5489, #63194, #65181, #126840, #188546, #3505, #51014, #174367, #144008, #95517, #80344, #67172, #111689, #31876, #96501, #128829, #93530, #66174, #155215, #141031, #156203, #1517, #142016, #112675, #16704, #2518, #189542, #35837, #19681, #97483, #172367, #50024, #190528, #140028, #173376, #64198, #34846, #159169, #158191, #143006, #79360, #20664, #125865, #187565, #82318, #78354, #124874, #110687, #186573, #52002, #48046, #109702, #171384, #32871, #94521, #17703, #49032, #33857, #188294, #112428, #52742, #114409, #51751, #20412, #67917, #6238, #66917, #34598, #4240, #82062, #36571, #35589, #127593, #145752, #84073, #176111, #189292, #128581, #158922, #126592, #80099, #157943, #129570, #63946, #49771, #37581, #99244, #159930, #96256, #141767, #22423, #143755, #190275, #156951, #113412, #19434, #48784, #97235, #125614, #187313, #110438, #5236, #172119, #33605, #175103, #65920, #98227, #160932, #81081, #21417, #83077, #50769, #191267, #111436, #144753, #174118, #95268, #18448, #3259, #142760, #173123, #64933, #69928, #131593, #165938, #164944, #72940, #87088, #23425, #134609, #104256, #196294, #55752, #53757, #9263, #54752, #146755, #10263, #117426, #148774, #71921, #8249, #86086, #7234, #179124, #162930, #133592, #40592, #195284, #130581, #57764, #194286, #116426, #149765, #119434, #27438, #102263, #68919, #192275, #89081, #56765, #85072, #118437, #132596, #193278, #115431, #177122, #26437, #180130, #38593, #11267, #181118, #178114, #163951, #42592, #100249, #41599, #25448, #161930, #39582, #103263, #101241, #147776, #88079, #24437, #70929, #14221, #32383, #170891, #1027, #75890, #15224, #45562, #13248, #166934, #44574, #154727 ),
 ( #74911, #199249, #197273, #153728, #168886, #60716, #122390, #90072, #28436, #137565, #31390, #136574, #151755, #12268, #198254, #92039, #107216, #106230, #47559, #59730, #121399, #32, #73933, #109212, #120405, #184078, #183093, #30392, #77875, #76883, #138554, #167913, #16223, #29413, #91044, #61705, #150772, #105248, #152731, #58735, #123375, #185067, #46555, #135602, #108217, #169897, #93040, #186077, #182098, #139542, #62699, #124382, #43582, #140545, #159686, #65690, #125388, #187085, #111200, #2033, #64708, #171889, #5004, #127355, #126370, #48555, #114171, #21184, #78865, #63713, #142533, #128349, #97993, #35360, #175874, #80857, #189068, #51522, #110208, #188067, #82840, #143515, #4012, #50540, #155716, #112201, #66687, #18217, #173891, #33376, #97012, #158693, #20182, #81828, #95034, #156725, #190047, #174874, #79874, #141543, #17213, #3032, #113185, #36340, #49538, #191037, #172892, #34371, #144519, #96031, #157718, #129342, #6004, #67684, #52510, #94038, #19207, #148537, #71688, #72699, #130333, #132363, #194056, #55517, #70695, #118202, #41359, #11024, #162694, #24200, #134372, #178883, #99004, #163708, #196058, #160695, #133355, #22186, #8004, #23192, #68678, #147538, #179893, #83834, #69687, #195045, #103024, #86853, #164707, #39350, #117190, #40351, #9026, #102025, #25211, #176883, #116193, #37346, #10028, #193043, #56524, #26202, #87841, #145516, #149529, #85849, #146514, #57531, #119200, #6996, #192031, #53513, #115191, #38354, #100009, #161695, #84835, #131354, #54520, #177882, #101010, #138332, #91804, #139318, #106000, #46323, #199014, #169665, #106987, #27199, #107977, #152501, #12037, #73701, #198024, #88845, #151528, #58511, #153496, #13990, #13017, #135373, #798, #31160, #165702, #150537, #29184, #14993, #184838, #122158, #62471, #167687, #75657, #200012, #197043, #74682, #92810, #30160, #90818, #137334, #42360, #60483, #76653, #105017, #183847, #120177, #45335, #168660, #61479, #123150, #181867, #43346, #154497, #15992, #166701, #28204, #104023, #89845, #77650, #180885, #136348, #59492, #121167, #182861, #44342, #47329, #32153, #162206, #18976, #110966, #81594, #124143, #172650, #35123, #158464, #23704, #16982, #80622, #142299, #3779, #157483, #4764, #130863, #100527, #49307, #34138, #85352, #65456, #185842, #50308, #147045, #108984, #19952, #170665, #94805, #109978, #155490, #95797, #192554, #126142, #127119, #8529, #93810, #188825, #156484, #111964, #54037, #173656, #96775, #33147, #115711, #17986, #79639, #143278, #78636, #140311, #64475, #1801, #69196, #177399, #38871, #63479, #125155, #186854, #48323, #171658, #141308, #2797, #187838, #59009, #196563, #116701, #135870, #41875, #101521, #163211, #87365, #178391, #40865, #148048, #181387, #103542, #102539, #24714, #90337, #197541, #55031, #39855, #118713, #104531, #74201, #11549, #152022, #57040, #165217, #27713, #86363, #164222, #120676, #119704, #180403, #26712, #131874, #88351, #42866, #194557, #150044, #9538, #73216, #134887, #58034, #166212, #71205, #132868, #89356, #151046, #56027, #117705, #193559, #179401, #12536, #182375, #25719, #167203, #149050, #10538, #43852, #72202, #133876, #105518, #28701, #70207, #195566, #13508, #61974, #124652, #47828, #48816, #106501, #108487, #170166, #31659, #46827, #94304, #17479, #187346, #138826, #306, #110469, #154993, #75173, #139806, #172151, #136845, #109479, #198530, #184350, #199520, #44845, #123640, #155982, #60001, #45832, #171163, #79136, #62972, #33637, #15499, #63979, #1294, #93308, #16489, #77155, #78138, #95299, #107483, #186348, #32650, #185337, #140807, #76159, #2297, #125648, #121668, #183363, #168178, #169161, #60987, #137839, #122662, #30665, #29674, #91306, #152998, #14497, #92318, #154003, #53788, #22455, #5269, #3293, #158954, #4272, #96288, #159961, #66951, #98259, #21448, #157974, #35621, #156983, #128613, #112458, #83109, #190305, #144785, #80130 ),
 ( #82095, #19467, #115463, #18481, #114442, #67947, #177152, #38624, #51782, #84104, #143787, #145783, #7264, #6268, #113442, #160962, #99275, #129601, #127623, #97266, #175135, #191297, #36602, #20444, #141799, #64965, #68949, #52773, #176143, #37613, #81112, #173154, #50800, #130612, #126624, #142792, #192308, #188325, #49804, #189323, #34629, #111469, #65952, #174149, #193310, #149796, #70960, #85103, #71953, #182128, #58767, #100281, #41631, #161960, #23456, #87120, #54783, #8282, #42624, #73964, #132629, #133625, #86118, #103295, #146789, #27471, #148806, #9295, #104288, #150802, #120435, #195317, #69960, #131626, #116459, #164975, #178147, #180161, #25479, #39613, #101272, #162962, #57795, #11301, #24468, #197303, #10296, #89113, #56798, #12298, #135632, #88112, #118470, #165969, #147809, #26470, #194317, #40623, #72972, #134641, #196327, #163982, #55784, #117456, #179155, #119465, #181149, #102293, #106260, #59761, #137597, #47588, #63743, #167943, #94066, #78896, #139572, #75922, #121429, #2064, #138584, #108247, #136603, #93071, #14251, #28466, #15255, #125417, #43612, #105276, #185097, #166963, #90101, #30424, #198283, #151784, #186107, #17244, #199280, #76913, #29442, #46586, #140574, #45593, #155746, #169927, #64, #31419, #107247, #154756, #13276, #60747, #61736, #1057, #168918, #109241, #91074, #124413, #92071, #74940, #183122, #123404, #122420, #152761, #184111, #153760, #16253, #44605, #62731, #170920, #77905, #32412, #52544, #83869, #114205, #35390, #33408, #189098, #34402, #126400, #190078, #97041, #128382, #51554, #188096, #65720, #187113, #158722, #142564, #113218, #20213, #174908, #36372, #145551, #50571, #37381, #98026, #81861, #159722, #112231, #21218, #7029, #80887, #5035, #82875, #173921, #191071, #49569, #67717, #143550, #99038, #68711, #66721, #157748, #172923, #111232, #96060, #19239, #48585, #144553, #175910, #6038, #3061, #160728, #110237, #22220, #129374, #95067, #171918, #4043, #127388, #156755, #18249, #79902, #141573, #64738, #9058, #130368, #102059, #85885, #56560, #40386, #71720, #53547, #57564, #117224, #39384, #72735, #180918, #88880, #163744, #192065, #115225, #12071, #195080, #8040, #10060, #55551, #69721, #150572, #176917, #87875, #41394, #38388, #27231, #25244, #119234, #178918, #42393, #104056, #118236, #86885, #134407, #196094, #133389, #101043, #70729, #148570, #103059, #179927, #194089, #100044, #161730, #165736, #164741, #26236, #149563, #193077, #146546, #24235, #23225, #84868, #54552, #131388, #116225, #11059, #162729, #177916, #147573, #132396, #138362, #166734, #123181, #44376, #58544, #45367, #155520, #32184, #73733, #15025, #135406, #197077, #60515, #28238, #181900, #16023, #47361, #106032, #107020, #59523, #184870, #167718, #120210, #168692, #43378, #93841, #105050, #76686, #89878, #151561, #122190, #13050, #74717, #77681, #109016, #29216, #30193, #121200, #200043, #170695, #75687, #124174, #61512, #91835, #46352, #137366, #108010, #136380, #90849, #153528, #169695, #199045, #139349, #198057, #154526, #183882, #185875, #182892, #31189, #152534, #14021, #92841, #828, #62503, #175667, #174677, #82633, #96812, #33179, #144316, #113968, #5805, #65489, #63514, #19009, #64507, #156517, #19985, #127151, #158498, #81628, #18018, #95831, #17015, #188859, #172685, #143311, #50342, #4798, #140344, #67478, #3811, #126174, #159482, #129138, #37142, #112000, #78667, #1832, #98801, #66487, #94838, #128150, #142331, #79671, #125189, #186885, #36142, #189849, #48355, #110009, #173690, #190835, #35156, #52311, #171690, #51323, #112984, #20976, #141342, #97794, #187869, #157515, #2829, #49337, #110999, #80655, #34169, #180684, #10821, #85644, #25001, #55310, #22984, #176681, #54318, #164505, #42160, #84634, #72491, #195853, #56313, #192838, #38156, #119001, #116982, #86645, #53309, #21985, #7800, #101815, #178674, #115990, #57325, #146311, #69484, #9823 ),
 ( #134164, #160495, #40138, #131149, #177679, #39147, #100802, #162486, #83637, #117996, #25999, #163503, #99810, #87641, #145314, #149327, #8818, #6798, #23987, #147330, #161496, #148328, #70487, #71484, #133149, #132153, #193846, #68476, #194840, #179685, #41157, #102820, #130131, #191828, #114987, #90623, #12815, #46114, #154291, #62259, #75456, #165500, #26996, #185625, #168463, #181664, #183648, #28982, #43143, #123927, #103820, #61274, #14789, #88641, #587, #13790, #30954, #152305, #92601, #15781, #91598, #60282, #107767, #169452, #106789, #74482, #44141, #121955, #76449, #137130, #167486, #150337, #11832, #77440, #198817, #29961, #45130, #166501, #119978, #197823, #139112, #73498, #27999, #135170, #196843, #199807, #136147, #104812, #58310, #153288, #138126, #89638, #122944, #59289, #151327, #184633, #120958, #182657, #105800, #188617, #47116, #108775, #33930, #1589, #155284, #189609, #20734, #50098, #158259, #18768, #170453, #111758, #96571, #143076, #82391, #172442, #112743, #65251, #35906, #173447, #93598, #174436, #80415, #78422, #140098, #64268, #16774, #17775, #124944, #19749, #142087, #79430, #63264, #67239, #97552, #31944, #186641, #95588, #81390, #51083, #34915, #128898, #157272, #3573, #4554, #48112, #141101, #159240, #66247, #126911, #127907, #109768, #144079, #5560, #171452, #32940, #94595, #156273, #2588, #125934, #187633, #49103, #110761, #177442, #71250, #114743, #129886, #52074, #37911, #131919, #147092, #146070, #87410, #53064, #99570, #39903, #113730, #98560, #25764, #85399, #38912, #148093, #190597, #100569, #101568, #24761, #149095, #83396, #8576, #70251, #193603, #23750, #132914, #194601, #164269, #115754, #162251, #10585, #55075, #175427, #116745, #72246, #36895, #86408, #160254, #161251, #176437, #21744, #178435, #56073, #145073, #22745, #9584, #117753, #163259, #179446, #192597, #40912, #6555, #68233, #102585, #84394, #191586, #7555, #69241, #130907, #54080, #2095, #42909, #27757, #47619, #133923, #88396, #74245, #41921, #63776, #105560, #165262, #26756, #151089, #180449, #104575, #11593, #109273, #167246, #166257, #150089, #156786, #125448, #118760, #103587, #182417, #170952, #140605, #75217, #18279, #120719, #28745, #94098, #73261, #89400, #187144, #186140, #43897, #90381, #195614, #152066, #32445, #58078, #13551, #134930, #136889, #198574, #60044, #124444, #196607, #119748, #155777, #17275, #181431, #12580, #57086, #135914, #78929, #48617, #197585, #33438, #59052, #110268, #171949, #95097, #81889, #144581, #176948, #173951, #98053, #175940, #143582, #83898, #142593, #160758, #66749, #192096, #161759, #159753, #50600, #65750, #4073, #127419, #189128, #38417, #37411, #145581, #21248, #96091, #7059, #100074, #68740, #128410, #126430, #5064, #112259, #19270, #82902, #190106, #6067, #67745, #80917, #158752, #79933, #51581, #35418, #129403, #113245, #191099, #3091, #130398, #174936, #97071, #22249, #53578, #141604, #36399, #64768, #188127, #49598, #52574, #157779, #114234, #99069, #20241, #111262, #172953, #115255, #34431, #181926, #120235, #133417, #150599, #10088, #12097, #73760, #9087, #54578, #195106, #165764, #84897, #194114, #57589, #104082, #72764, #88908, #25271, #118263, #43407, #193104, #148596, #55578, #103086, #135432, #26262, #179953, #132423, #197103, #117252, #178944, #134434, #23254, #177942, #163770, #131416, #164767, #196119, #56589, #146576, #87903, #119259, #180943, #58570, #71746, #105077, #41420, #8071, #149589, #69747, #116250, #11087, #39409, #101069, #40415, #162754, #102086, #24263, #42419, #27258, #86913, #85912, #147600, #70755, #151586, #13075, #15052, #857, #170722, #108038, #186913, #153555, #200070, #124204, #59550, #137392, #32214, #16050, #76713, #138388, #28265, #184897, #77709, #90875, #61538, #74742, #169724, #46379, #123207, #31217, #106058, #182919, #92868, #47389, #152559, #167744, #89903, #14048, #154555, #139375, #125217, #29242 ),
 ( #1861, #121228, #62531, #185904, #109044, #93870, #155549, #17043, #140374, #91862, #78697, #63543, #48384, #136405, #166763, #198083, #44404, #75714, #199072, #60541, #122217, #183908, #45393, #107046, #168718, #30220, #49366, #68503, #110041, #67509, #21006, #130158, #6825, #20015, #37169, #96842, #98828, #160522, #97821, #66516, #113996, #52340, #113012, #80685, #50371, #128178, #82661, #81658, #173720, #191855, #171720, #22013, #35188, #174705, #4828, #172716, #126203, #3841, #175694, #33209, #34199, #83665, #145343, #5833, #142361, #187899, #94868, #189877, #36169, #2859, #159510, #65520, #156549, #143341, #18048, #79701, #141372, #51352, #64537, #111030, #158527, #95861, #157544, #19038, #127180, #188890, #144345, #112031, #129166, #190863, #41187, #85673, #9853, #178706, #25030, #8848, #148357, #195886, #100833, #101844, #56343, #70516, #164535, #192868, #102850, #193875, #10854, #119034, #163530, #39175, #54347, #116018, #177708, #162516, #57360, #118025, #26028, #86674, #146339, #87673, #53336, #149357, #55341, #161523, #132184, #24018, #131178, #71512, #117011, #133180, #194870, #147360, #40168, #115015, #179715, #72523, #134198, #176709, #38183, #23015, #99839, #84661, #7827, #69512, #84311, #192514, #5477, #95505, #33845, #67160, #189530, #160170, #143996, #175343, #157191, #161167, #20652, #142994, #176354, #145990, #53998, #128817, #18685, #80332, #115672, #98477, #111677, #113649, #159156, #173364, #142004, #3492, #191503, #144991, #65169, #130823, #190516, #22664, #82306, #7473, #69157, #21660, #51990, #37827, #99487, #36810, #4472, #174355, #83314, #6472, #68152, #97471, #126828, #188534, #50012, #129804, #52979, #114657, #96489, #34834, #127824, #158179, #19669, #81310, #66162, #51002, #112663, #35825, #54994, #135838, #72163, #41836, #70167, #26676, #148012, #162168, #149013, #58974, #197507, #177360, #118676, #38831, #100489, #164185, #131836, #85314, #119671, #151013, #9502, #10501, #163172, #150005, #132832, #58001, #55991, #103504, #133838, #180368, #179365, #165181, #74167, #71167, #195528, #73181, #40828, #181353, #39817, #42833, #25682, #89321, #23665, #57002, #194518, #24676, #101483, #86326, #117669, #147005, #134852, #104498, #88316, #193518, #166179, #8491, #27680, #87328, #116663, #102500, #11511, #178354, #196531, #12504, #61938, #185302, #59965, #199485, #13475, #170128, #91271, #105482, #92281, #2263, #79101, #120642, #123607, #182340, #43818, #107449, #75139, #28667, #62937, #94270, #152962, #153965, #106463, #93273, #76123, #1260, #60951, #46793, #15463, #108452, #122626, #31623, #17445, #14460, #138789, #16454, #184316, #124617, #183327, #186312, #169123, #32616, #167168, #270, #137801, #168142, #44808, #29638, #45797, #140774, #78103, #47793, #154958, #136808, #109444, #90302, #171127, #30628, #151988, #77119, #139772, #121631, #155948, #198493, #153267, #137111, #17753, #48091, #184612, #77420, #141080, #152285, #107748, #14769, #62238, #109747, #185605, #139092, #91578, #171431, #76429, #138105, #93577, #182638, #198798, #122924, #90603, #123906, #155262, #154270, #44121, #47095, #31923, #78400, #79410, #169430, #32918, #567, #94573, #108755, #28962, #156251, #15761, #13769, #75437, #199786, #60263, #61254, #121934, #16752, #170431, #46093, #183629, #2565, #64247, #167467, #45111, #30935, #140076, #186619, #1567, #105780, #92582, #63243, #124922, #106768, #168443, #29939, #175404, #112721, #174414, #187612, #110739, #172420, #35883, #160231, #129864, #67217, #146048, #97530, #159217, #83374, #18746, #96549, #191562, #36872, #20712, #82368, #49082, #144057, #98537, #50076, #5538, #33908, #128875, #190575, #52051, #113707, #65229, #142065, #21721, #6532, #111737, #126889, #95566, #173424, #145051, #68212, #84371, #188595, #157252, #53041, #114721, #80393, #3551, #161229, #176414, #37889, #99547, #125914, #22723, #7532, #34893, #158236, #19727 ),
 ( #81368, #143052, #4531, #66223, #127884, #189587, #51059, #116722, #8551, #72222, #58053, #100547, #88370, #119724, #148068, #69217, #40886, #24734, #195588, #179421, #10558, #192575, #196583, #56047, #178411, #11569, #181407, #27732, #102559, #130885, #54058, #151064, #133897, #147067, #149070, #194577, #70227, #89375, #115732, #26731, #180423, #177419, #166232, #164244, #42885, #117726, #104550, #38890, #57060, #25739, #73235, #134906, #118735, #39875, #9559, #87385, #41896, #103562, #132888, #162226, #23725, #85374, #131895, #165237, #193579, #55051, #150064, #101542, #163234, #86384, #71225, #183384, #184370, #198551, #185356, #168199, #93329, #91327, #138845, #45851, #154023, #14518, #77175, #109501, #106522, #30686, #108507, #76179, #16510, #75194, #155014, #199539, #124672, #94325, #92337, #44866, #60021, #136865, #121688, #29696, #171183, #170186, #78158, #15518, #28721, #139826, #32672, #1315, #61009, #59028, #137859, #153019, #152043, #325, #62994, #43872, #31680, #186369, #122681, #12555, #107504, #169180, #61993, #123659, #46847, #135889, #47848, #74221, #197561, #120695, #182394, #105537, #167223, #90358, #13528, #37635, #20467, #33657, #35642, #81132, #95318, #114463, #156003, #113464, #66974, #176165, #52795, #65975, #83131, #142813, #144807, #6290, #143809, #112479, #159983, #98282, #158975, #126644, #96309, #174172, #128634, #127644, #19487, #17500, #79157, #67969, #4293, #82117, #50822, #18501, #172172, #49825, #21470, #140828, #80149, #129623, #191318, #51805, #188347, #157003, #2317, #97288, #5291, #48836, #190328, #111489, #63999, #189344, #125669, #187367, #110490, #141820, #175158, #36625, #3313, #64986, #173174, #34650, #157995, #88133, #149817, #87145, #55808, #103317, #41653, #102315, #69983, #39636, #117480, #71974, #70984, #162986, #181170, #119488, #11323, #24491, #164005, #194340, #161983, #115487, #193333, #164997, #99299, #23479, #72993, #134662, #195339, #131651, #177175, #57816, #179178, #25501, #192331, #148828, #54807, #84126, #132652, #160984, #22478, #145805, #40646, #7288, #68972, #86142, #53812, #130636, #26491, #196348, #116482, #10318, #85128, #133648, #178171, #180184, #101297, #56819, #118493, #38648, #147833, #100305, #146812, #9319, #8306, #141356, #47375, #49351, #108024, #126188, #32199, #157529, #127165, #125202, #16037, #31204, #169711, #92855, #154542, #3825, #2843, #111013, #186898, #58789, #172700, #142345, #34184, #93856, #89135, #109030, #77695, #184884, #48369, #95845, #73985, #64521, #19023, #124189, #42647, #17028, #844, #171704, #155533, #110026, #165992, #80669, #78681, #139363, #187884, #65504, #104309, #140357, #27492, #150823, #12320, #33193, #120457, #94852, #170709, #46366, #1845, #63527, #156533, #18032, #135654, #197325, #62517, #79686, #185890, #24000, #130144, #50356, #115001, #85656, #112015, #23001, #173704, #159496, #174691, #19998, #98814, #131162, #35172, #147343, #20992, #143326, #8831, #54331, #190848, #83651, #70499, #158511, #113982, #82646, #68489, #116002, #191841, #145329, #97807, #177691, #144329, #5818, #99824, #188874, #4813, #129151, #96827, #53322, #161509, #160508, #81642, #176695, #38169, #84647, #66500, #175680, #39159, #6811, #100816, #146324, #128163, #162499, #21998, #189863, #51337, #67494, #112997, #52325, #36155, #7813, #69497, #37155, #192852, #104826, #57340, #196858, #27011, #194853, #148340, #26011, #136162, #152318, #56326, #182670, #167501, #28013, #164518, #9836, #90636, #88655, #58324, #25013, #181678, #102832, #116994, #103834, #13804, #132167, #193858, #73513, #55323, #178689, #119015, #86656, #40151, #74496, #105814, #87654, #165515, #118008, #166515, #149339, #12830, #10835, #119992, #150351, #135184, #134180, #43159, #28996, #72505, #11848, #89655, #195867, #197837, #179697, #59303, #180698, #42174, #44154, #101827, #151341, #120972, #41169, #163514, #71495, #133161, #33942, #32952 ) ),
 .UNSPECIFIED., .T., .F., .F. ) 
 B_SPLINE_SURFACE_WITH_KNOTS ( ( 4, 3, 4 ),
 ( 3, 2, 2, 2, 2, 2, 2, 2, 2, 2, 2, 2, 2, 2, 2, 2, 2, 2, 2, 2, 2, 2, 2, 2, 2, 2, 2, 2, 2, 2, 2, 2, 2, 2, 2, 2, 2, 2, 2, 2, 2, 2, 2, 2, 2, 2, 2, 2, 2, 2, 2, 2, 2, 2, 2, 2, 2, 2, 2, 2, 2, 2, 2, 2, 2, 2, 2, 2, 2, 2, 2, 2, 2, 2, 2, 2, 2, 2, 2, 2, 2, 2, 2, 2, 2, 2, 2, 2, 2, 2, 2, 2, 2, 2, 2, 2, 2, 2, 2, 2, 2, 2, 2, 2, 2, 2, 2, 2, 2, 2, 2, 2, 2, 2, 2, 2, 2, 2, 2, 2, 2, 2, 2, 2, 2, 2, 2, 2, 2, 2, 2, 2, 2, 2, 2, 2, 2, 2, 2, 2, 2, 2, 2, 2, 2, 2, 2, 2, 2, 2, 2, 2, 2, 2, 2, 2, 2, 2, 2, 2, 2, 2, 2, 2, 2, 2, 2, 2, 2, 2, 2, 2, 2, 2, 2, 2, 2, 2, 2, 2, 2, 2, 2, 2, 2, 2, 2, 2, 2, 2, 2, 2, 2, 2, 2, 2, 2, 2, 2, 2, 2, 2, 2, 2, 2, 2, 2, 2, 2, 2, 2, 2, 2, 2, 2, 2, 2, 2, 2, 2, 2, 2, 2, 2, 2, 2, 2, 2, 3 ),
 ( 0.000000000000000000, 0.5000000000000000000, 1.000000000000000000 ),
 ( 0.000000000000000000, 0.004385964912280701511, 0.008771929824561403022, 0.01315789473684210453, 0.01754385964912280604, 0.02192982456140350755, 0.02631578947368420907, 0.03070175438596491058, 0.03508771929824561209, 0.03947368421052631360, 0.04385964912280701511, 0.04824561403508771662, 0.05263157894736841813, 0.05701754385964911964, 0.06140350877192982115, 0.06578947368421052266, 0.07017543859649122417, 0.07456140350877192569, 0.07894736842105262720, 0.08333333333333332871, 0.08771929824561403022, 0.09210526315789473173, 0.09649122807017543324, 0.1008771929824561348, 0.1052631578947368363, 0.1096491228070175378, 0.1140350877192982393, 0.1184210526315789408, 0.1228070175438596423, 0.1271929824561403577, 0.1315789473684210453, 0.1359649122807017607, 0.1403508771929824483, 0.1447368421052631637, 0.1491228070175438514, 0.1535087719298245668, 0.1578947368421052544, 0.1622807017543859698, 0.1666666666666666574, 0.1710526315789473728, 0.1754385964912280604, 0.1798245614035087758, 0.1842105263157894635, 0.1885964912280701788, 0.1929824561403508665, 0.1973684210526315819, 0.2017543859649122695, 0.2061403508771929849, 0.2105263157894736725, 0.2149122807017543879, 0.2192982456140350755, 0.2236842105263157909, 0.2280701754385964786, 0.2324561403508771940, 0.2368421052631578816, 0.2412280701754385970, 0.2456140350877192846, 0.2500000000000000000, 0.2543859649122807154, 0.2587719298245614308, 0.2631578947368420907, 0.2675438596491228060, 0.2719298245614035214, 0.2763157894736842368, 0.2807017543859648967, 0.2850877192982456121, 0.2894736842105263275, 0.2938596491228070429, 0.2982456140350877027, 0.3026315789473684181, 0.3070175438596491335, 0.3114035087719298489, 0.3157894736842105088, 0.3201754385964912242, 0.3245614035087719396, 0.3289473684210526550, 0.3333333333333333148, 0.3377192982456140302, 0.3421052631578947456, 0.3464912280701754610, 0.3508771929824561209, 0.3552631578947368363, 0.3596491228070175517, 0.3640350877192982670, 0.3684210526315789269, 0.3728070175438596423, 0.3771929824561403577, 0.3815789473684210731, 0.3859649122807017330, 0.3903508771929824483, 0.3947368421052631637, 0.3991228070175438791, 0.4035087719298245390, 0.4078947368421052544, 0.4122807017543859698, 0.4166666666666666852, 0.4210526315789473450, 0.4254385964912280604, 0.4298245614035087758, 0.4342105263157894912, 0.4385964912280701511, 0.4429824561403508665, 0.4473684210526315819, 0.4517543859649122973, 0.4561403508771929571, 0.4605263157894736725, 0.4649122807017543879, 0.4692982456140351033, 0.4736842105263157632, 0.4780701754385964786, 0.4824561403508771940, 0.4868421052631579093, 0.4912280701754385692, 0.4956140350877192846, 0.5000000000000000000, 0.5043859649122807154, 0.5087719298245614308, 0.5131578947368421462, 0.5175438596491228616, 0.5219298245614034659, 0.5263157894736841813, 0.5307017543859648967, 0.5350877192982456121, 0.5394736842105263275, 0.5438596491228070429, 0.5482456140350877583, 0.5526315789473684736, 0.5570175438596490780, 0.5614035087719297934, 0.5657894736842105088, 0.5701754385964912242, 0.5745614035087719396, 0.5789473684210526550, 0.5833333333333333703, 0.5877192982456140857, 0.5921052631578946901, 0.5964912280701754055, 0.6008771929824561209, 0.6052631578947368363, 0.6096491228070175517, 0.6140350877192982670, 0.6184210526315789824, 0.6228070175438596978, 0.6271929824561403022, 0.6315789473684210176, 0.6359649122807017330, 0.6403508771929824483, 0.6447368421052631637, 0.6491228070175438791, 0.6535087719298245945, 0.6578947368421053099, 0.6622807017543859143, 0.6666666666666666297, 0.6710526315789473450, 0.6754385964912280604, 0.6798245614035087758, 0.6842105263157894912, 0.6885964912280702066, 0.6929824561403509220, 0.6973684210526315264, 0.7017543859649122417, 0.7061403508771929571, 0.7105263157894736725, 0.7149122807017543879, 0.7192982456140351033, 0.7236842105263158187, 0.7280701754385965341, 0.7324561403508771384, 0.7368421052631578538, 0.7412280701754385692, 0.7456140350877192846, 0.7500000000000000000, 0.7543859649122807154, 0.7587719298245614308, 0.7631578947368421462, 0.7675438596491228616, 0.7719298245614034659, 0.7763157894736841813, 0.7807017543859648967, 0.7850877192982456121, 0.7894736842105263275, 0.7938596491228070429, 0.7982456140350877583, 0.8026315789473684736, 0.8070175438596490780, 0.8114035087719297934, 0.8157894736842105088, 0.8201754385964912242, 0.8245614035087719396, 0.8289473684210526550, 0.8333333333333333703, 0.8377192982456140857, 0.8421052631578946901, 0.8464912280701754055, 0.8508771929824561209, 0.8552631578947368363, 0.8596491228070175517, 0.8640350877192982670, 0.8684210526315789824, 0.8728070175438596978, 0.8771929824561403022, 0.8815789473684210176, 0.8859649122807017330, 0.8903508771929824483, 0.8947368421052631637, 0.8991228070175438791, 0.9035087719298245945, 0.9078947368421053099, 0.9122807017543859143, 0.9166666666666666297, 0.9210526315789473450, 0.9254385964912280604, 0.9298245614035087758, 0.9342105263157894912, 0.9385964912280702066, 0.9429824561403509220, 0.9473684210526315264, 0.9517543859649122417, 0.9561403508771929571, 0.9605263157894736725, 0.9649122807017543879, 0.9692982456140351033, 0.9736842105263158187, 0.9780701754385965341, 0.9824561403508771384, 0.9868421052631578538, 0.9912280701754385692, 0.9956140350877192846, 1.000000000000000000 ),
 .UNSPECIFIED. ) 
 GEOMETRIC_REPRESENTATION_ITEM ( )  RATIONAL_B_SPLINE_SURFACE ( (
 ( 1.000000000000000000, 0.9659258262890683122, 1.000000000000000000, 0.9659258262890683122, 1.000000000000000000, 0.9659258262890683122, 1.000000000000000000, 0.9659258262890683122, 1.000000000000000000, 0.9659258262890683122, 1.000000000000000000, 0.9659258262890683122, 1.000000000000000000, 0.9659258262890683122, 1.000000000000000000, 0.9659258262890683122, 1.000000000000000000, 0.9659258262890683122, 1.000000000000000000, 0.9659258262890683122, 1.000000000000000000, 0.9659258262890683122, 1.000000000000000000, 0.9659258262890683122, 1.000000000000000000, 0.9659258262890683122, 1.000000000000000000, 0.9659258262890683122, 1.000000000000000000, 0.9659258262890683122, 1.000000000000000000, 0.9659258262890683122, 1.000000000000000000, 0.9659258262890683122, 1.000000000000000000, 0.9659258262890683122, 1.000000000000000000, 0.9659258262890683122, 1.000000000000000000, 0.9659258262890683122, 1.000000000000000000, 0.9659258262890683122, 1.000000000000000000, 0.9659258262890683122, 1.000000000000000000, 0.9659258262890683122, 1.000000000000000000, 0.9659258262890683122, 1.000000000000000000, 0.9659258262890683122, 1.000000000000000000, 0.9659258262890683122, 1.000000000000000000, 0.9659258262890683122, 1.000000000000000000, 0.9659258262890683122, 1.000000000000000000, 0.9659258262890683122, 1.000000000000000000, 0.9659258262890683122, 1.000000000000000000, 0.9659258262890683122, 1.000000000000000000, 0.9659258262890683122, 1.000000000000000000, 0.9659258262890683122, 1.000000000000000000, 0.9659258262890683122, 1.000000000000000000, 0.9659258262890683122, 1.000000000000000000, 0.9659258262890683122, 1.000000000000000000, 0.9659258262890683122, 1.000000000000000000, 0.9659258262890683122, 1.000000000000000000, 0.9659258262890683122, 1.000000000000000000, 0.9659258262890683122, 1.000000000000000000, 0.9659258262890683122, 1.000000000000000000, 0.9659258262890683122, 1.000000000000000000, 0.9659258262890683122, 1.000000000000000000, 0.9659258262890683122, 1.000000000000000000, 0.9659258262890683122, 1.000000000000000000, 0.9659258262890683122, 1.000000000000000000, 0.9659258262890683122, 1.000000000000000000, 0.9659258262890683122, 1.000000000000000000, 0.9659258262890683122, 1.000000000000000000, 0.9659258262890683122, 1.000000000000000000, 0.9659258262890683122, 1.000000000000000000, 0.9659258262890683122, 1.000000000000000000, 0.9659258262890683122, 1.000000000000000000, 0.9659258262890683122, 1.000000000000000000, 0.9659258262890683122, 1.000000000000000000, 0.9659258262890683122, 1.000000000000000000, 0.9659258262890683122, 1.000000000000000000, 0.9659258262890683122, 1.000000000000000000, 0.9659258262890683122, 1.000000000000000000, 0.9659258262890683122, 1.000000000000000000, 0.9659258262890683122, 1.000000000000000000, 0.9659258262890683122, 1.000000000000000000, 0.9659258262890683122, 1.000000000000000000, 0.9659258262890683122, 1.000000000000000000, 0.9659258262890683122, 1.000000000000000000, 0.9659258262890683122, 1.000000000000000000, 0.9659258262890683122, 1.000000000000000000, 0.9659258262890683122, 1.000000000000000000, 0.9659258262890683122, 1.000000000000000000, 0.9659258262890683122, 1.000000000000000000, 0.9659258262890683122, 1.000000000000000000, 0.9659258262890683122, 1.000000000000000000, 0.9659258262890683122, 1.000000000000000000, 0.9659258262890683122, 1.000000000000000000, 0.9659258262890683122, 1.000000000000000000, 0.9659258262890683122, 1.000000000000000000, 0.9659258262890683122, 1.000000000000000000, 0.9659258262890683122, 1.000000000000000000, 0.9659258262890683122, 1.000000000000000000, 0.9659258262890683122, 1.000000000000000000, 0.9659258262890683122, 1.000000000000000000, 0.9659258262890683122, 1.000000000000000000, 0.9659258262890683122, 1.000000000000000000, 0.9659258262890683122, 1.000000000000000000, 0.9659258262890683122, 1.000000000000000000, 0.9659258262890683122, 1.000000000000000000, 0.9659258262890683122, 1.000000000000000000, 0.9659258262890683122, 1.000000000000000000, 0.9659258262890683122, 1.000000000000000000, 0.9659258262890683122, 1.000000000000000000, 0.9659258262890683122, 1.000000000000000000, 0.9659258262890683122, 1.000000000000000000, 0.9659258262890683122, 1.000000000000000000, 0.9659258262890683122, 1.000000000000000000, 0.9659258262890683122, 1.000000000000000000, 0.9659258262890683122, 1.000000000000000000, 0.9659258262890683122, 1.000000000000000000, 0.9659258262890683122, 1.000000000000000000, 0.9659258262890683122, 1.000000000000000000, 0.9659258262890683122, 1.000000000000000000, 0.9659258262890683122, 1.000000000000000000, 0.9659258262890683122, 1.000000000000000000, 0.9659258262890683122, 1.000000000000000000, 0.9659258262890683122, 1.000000000000000000, 0.9659258262890683122, 1.000000000000000000, 0.9659258262890683122, 1.000000000000000000, 0.9659258262890683122, 1.000000000000000000, 0.9659258262890683122, 1.000000000000000000, 0.9659258262890683122, 1.000000000000000000, 0.9659258262890683122, 1.000000000000000000, 0.9659258262890683122, 1.000000000000000000, 0.9659258262890683122, 1.000000000000000000, 0.9659258262890683122, 1.000000000000000000, 0.9659258262890683122, 1.000000000000000000, 0.9659258262890683122, 1.000000000000000000, 0.9659258262890683122, 1.000000000000000000, 0.9659258262890683122, 1.000000000000000000, 0.9659258262890683122, 1.000000000000000000, 0.9659258262890683122, 1.000000000000000000, 0.9659258262890683122, 1.000000000000000000, 0.9659258262890683122, 1.000000000000000000, 0.9659258262890683122, 1.000000000000000000, 0.9659258262890683122, 1.000000000000000000, 0.9659258262890683122, 1.000000000000000000, 0.9659258262890683122, 1.000000000000000000, 0.9659258262890683122, 1.000000000000000000, 0.9659258262890683122, 1.000000000000000000, 0.9659258262890683122, 1.000000000000000000, 0.9659258262890683122, 1.000000000000000000, 0.9659258262890683122, 1.000000000000000000, 0.9659258262890683122, 1.000000000000000000, 0.9659258262890683122, 1.000000000000000000, 0.9659258262890683122, 1.000000000000000000, 0.9659258262890683122, 1.000000000000000000, 0.9659258262890683122, 1.000000000000000000, 0.9659258262890683122, 1.000000000000000000, 0.9659258262890683122, 1.000000000000000000, 0.9659258262890683122, 1.000000000000000000, 0.9659258262890683122, 1.000000000000000000, 0.9659258262890683122, 1.000000000000000000, 0.9659258262890683122, 1.000000000000000000, 0.9659258262890683122, 1.000000000000000000, 0.9659258262890683122, 1.000000000000000000, 0.9659258262890683122, 1.000000000000000000, 0.9659258262890683122, 1.000000000000000000, 0.9659258262890683122, 1.000000000000000000, 0.9659258262890683122, 1.000000000000000000, 0.9659258262890683122, 1.000000000000000000, 0.9659258262890683122, 1.000000000000000000, 0.9659258262890683122, 1.000000000000000000, 0.9659258262890683122, 1.000000000000000000, 0.9659258262890683122, 1.000000000000000000, 0.9659258262890683122, 1.000000000000000000, 0.9659258262890683122, 1.000000000000000000, 0.9659258262890683122, 1.000000000000000000, 0.9659258262890683122, 1.000000000000000000, 0.9659258262890683122, 1.000000000000000000, 0.9659258262890683122, 1.000000000000000000, 0.9659258262890683122, 1.000000000000000000, 0.9659258262890683122, 1.000000000000000000, 0.9659258262890683122, 1.000000000000000000, 0.9659258262890683122, 1.000000000000000000, 0.9659258262890683122, 1.000000000000000000, 0.9659258262890683122, 1.000000000000000000, 0.9659258262890683122, 1.000000000000000000, 0.9659258262890683122, 1.000000000000000000, 0.9659258262890683122, 1.000000000000000000, 0.9659258262890683122, 1.000000000000000000, 0.9659258262890683122, 1.000000000000000000, 0.9659258262890683122, 1.000000000000000000, 0.9659258262890683122, 1.000000000000000000, 0.9659258262890683122, 1.000000000000000000, 0.9659258262890683122, 1.000000000000000000, 0.9659258262890683122, 1.000000000000000000, 0.9659258262890683122, 1.000000000000000000, 0.9659258262890683122, 1.000000000000000000, 0.9659258262890683122, 1.000000000000000000, 0.9659258262890683122, 1.000000000000000000, 0.9659258262890683122, 1.000000000000000000, 0.9659258262890683122, 1.000000000000000000, 0.9659258262890683122, 1.000000000000000000, 0.9659258262890683122, 1.000000000000000000, 0.9659258262890683122, 1.000000000000000000, 0.9659258262890683122, 1.000000000000000000, 0.9659258262890683122, 1.000000000000000000, 0.9659258262890683122, 1.000000000000000000, 0.9659258262890683122, 1.000000000000000000, 0.9659258262890683122, 1.000000000000000000, 0.9659258262890683122, 1.000000000000000000, 0.9659258262890683122, 1.000000000000000000, 0.9659258262890683122, 1.000000000000000000, 0.9659258262890683122, 1.000000000000000000, 0.9659258262890683122, 1.000000000000000000, 0.9659258262890683122, 1.000000000000000000, 0.9659258262890683122, 1.000000000000000000, 0.9659258262890683122, 1.000000000000000000, 0.9659258262890683122, 1.000000000000000000, 0.9659258262890683122, 1.000000000000000000, 0.9659258262890683122, 1.000000000000000000, 0.9659258262890683122, 1.000000000000000000, 0.9659258262890683122, 1.000000000000000000, 0.9659258262890683122, 1.000000000000000000, 0.9659258262890683122, 1.000000000000000000, 0.9659258262890683122, 1.000000000000000000, 0.9659258262890683122, 1.000000000000000000, 0.9659258262890683122, 1.000000000000000000, 0.9659258262890683122, 1.000000000000000000, 0.9659258262890683122, 1.000000000000000000, 0.9659258262890683122, 1.000000000000000000, 0.9659258262890683122, 1.000000000000000000, 0.9659258262890683122, 1.000000000000000000, 0.9659258262890683122, 1.000000000000000000, 0.9659258262890683122, 1.000000000000000000, 0.9659258262890683122, 1.000000000000000000, 0.9659258262890683122, 1.000000000000000000, 0.9659258262890683122, 1.000000000000000000, 0.9659258262890683122, 1.000000000000000000, 0.9659258262890683122, 1.000000000000000000, 0.9659258262890683122, 1.000000000000000000, 0.9659258262890683122, 1.000000000000000000, 0.9659258262890683122, 1.000000000000000000, 0.9659258262890683122, 1.000000000000000000, 0.9659258262890683122, 1.000000000000000000, 0.9659258262890683122, 1.000000000000000000, 0.9659258262890683122, 1.000000000000000000, 0.9659258262890683122, 1.000000000000000000, 0.9659258262890683122, 1.000000000000000000, 0.9659258262890683122, 1.000000000000000000),
 ( 0.3333333333333333703, 0.3219752754296894559, 0.3333333333333333703, 0.3219752754296894559, 0.3333333333333333703, 0.3219752754296894559, 0.3333333333333333703, 0.3219752754296894559, 0.3333333333333333703, 0.3219752754296894559, 0.3333333333333333703, 0.3219752754296894559, 0.3333333333333333703, 0.3219752754296894559, 0.3333333333333333703, 0.3219752754296894559, 0.3333333333333333703, 0.3219752754296894559, 0.3333333333333333703, 0.3219752754296894559, 0.3333333333333333703, 0.3219752754296894559, 0.3333333333333333703, 0.3219752754296894559, 0.3333333333333333703, 0.3219752754296894559, 0.3333333333333333703, 0.3219752754296894559, 0.3333333333333333703, 0.3219752754296894559, 0.3333333333333333703, 0.3219752754296894559, 0.3333333333333333703, 0.3219752754296894559, 0.3333333333333333703, 0.3219752754296894559, 0.3333333333333333703, 0.3219752754296894559, 0.3333333333333333703, 0.3219752754296894559, 0.3333333333333333703, 0.3219752754296894559, 0.3333333333333333703, 0.3219752754296894559, 0.3333333333333333703, 0.3219752754296894559, 0.3333333333333333703, 0.3219752754296894559, 0.3333333333333333703, 0.3219752754296894559, 0.3333333333333333703, 0.3219752754296894559, 0.3333333333333333703, 0.3219752754296894559, 0.3333333333333333703, 0.3219752754296894559, 0.3333333333333333703, 0.3219752754296894559, 0.3333333333333333703, 0.3219752754296894559, 0.3333333333333333703, 0.3219752754296894559, 0.3333333333333333703, 0.3219752754296894559, 0.3333333333333333703, 0.3219752754296894559, 0.3333333333333333703, 0.3219752754296894559, 0.3333333333333333703, 0.3219752754296894559, 0.3333333333333333703, 0.3219752754296894559, 0.3333333333333333703, 0.3219752754296894559, 0.3333333333333333703, 0.3219752754296894559, 0.3333333333333333703, 0.3219752754296894559, 0.3333333333333333703, 0.3219752754296894559, 0.3333333333333333703, 0.3219752754296894559, 0.3333333333333333703, 0.3219752754296894559, 0.3333333333333333703, 0.3219752754296894559, 0.3333333333333333703, 0.3219752754296894559, 0.3333333333333333703, 0.3219752754296894559, 0.3333333333333333703, 0.3219752754296894559, 0.3333333333333333703, 0.3219752754296894559, 0.3333333333333333703, 0.3219752754296894559, 0.3333333333333333703, 0.3219752754296894559, 0.3333333333333333703, 0.3219752754296894559, 0.3333333333333333703, 0.3219752754296894559, 0.3333333333333333703, 0.3219752754296894559, 0.3333333333333333703, 0.3219752754296894559, 0.3333333333333333703, 0.3219752754296894559, 0.3333333333333333703, 0.3219752754296894559, 0.3333333333333333703, 0.3219752754296894559, 0.3333333333333333703, 0.3219752754296894559, 0.3333333333333333703, 0.3219752754296894559, 0.3333333333333333703, 0.3219752754296894559, 0.3333333333333333703, 0.3219752754296894559, 0.3333333333333333703, 0.3219752754296894559, 0.3333333333333333703, 0.3219752754296894559, 0.3333333333333333703, 0.3219752754296894559, 0.3333333333333333703, 0.3219752754296894559, 0.3333333333333333703, 0.3219752754296894559, 0.3333333333333333703, 0.3219752754296894559, 0.3333333333333333703, 0.3219752754296894559, 0.3333333333333333703, 0.3219752754296894559, 0.3333333333333333703, 0.3219752754296894559, 0.3333333333333333703, 0.3219752754296894559, 0.3333333333333333703, 0.3219752754296894559, 0.3333333333333333703, 0.3219752754296894559, 0.3333333333333333703, 0.3219752754296894559, 0.3333333333333333703, 0.3219752754296894559, 0.3333333333333333703, 0.3219752754296894559, 0.3333333333333333703, 0.3219752754296894559, 0.3333333333333333703, 0.3219752754296894559, 0.3333333333333333703, 0.3219752754296894559, 0.3333333333333333703, 0.3219752754296894559, 0.3333333333333333703, 0.3219752754296894559, 0.3333333333333333703, 0.3219752754296894559, 0.3333333333333333703, 0.3219752754296894559, 0.3333333333333333703, 0.3219752754296894559, 0.3333333333333333703, 0.3219752754296894559, 0.3333333333333333703, 0.3219752754296894559, 0.3333333333333333703, 0.3219752754296894559, 0.3333333333333333703, 0.3219752754296894559, 0.3333333333333333703, 0.3219752754296894559, 0.3333333333333333703, 0.3219752754296894559, 0.3333333333333333703, 0.3219752754296894559, 0.3333333333333333703, 0.3219752754296894559, 0.3333333333333333703, 0.3219752754296894559, 0.3333333333333333703, 0.3219752754296894559, 0.3333333333333333703, 0.3219752754296894559, 0.3333333333333333703, 0.3219752754296894559, 0.3333333333333333703, 0.3219752754296894559, 0.3333333333333333703, 0.3219752754296894559, 0.3333333333333333703, 0.3219752754296894559, 0.3333333333333333703, 0.3219752754296894559, 0.3333333333333333703, 0.3219752754296894559, 0.3333333333333333703, 0.3219752754296894559, 0.3333333333333333703, 0.3219752754296894559, 0.3333333333333333703, 0.3219752754296894559, 0.3333333333333333703, 0.3219752754296894559, 0.3333333333333333703, 0.3219752754296894559, 0.3333333333333333703, 0.3219752754296894559, 0.3333333333333333703, 0.3219752754296894559, 0.3333333333333333703, 0.3219752754296894559, 0.3333333333333333703, 0.3219752754296894559, 0.3333333333333333703, 0.3219752754296894559, 0.3333333333333333703, 0.3219752754296894559, 0.3333333333333333703, 0.3219752754296894559, 0.3333333333333333703, 0.3219752754296894559, 0.3333333333333333703, 0.3219752754296894559, 0.3333333333333333703, 0.3219752754296894559, 0.3333333333333333703, 0.3219752754296894559, 0.3333333333333333703, 0.3219752754296894559, 0.3333333333333333703, 0.3219752754296894559, 0.3333333333333333703, 0.3219752754296894559, 0.3333333333333333703, 0.3219752754296894559, 0.3333333333333333703, 0.3219752754296894559, 0.3333333333333333703, 0.3219752754296894559, 0.3333333333333333703, 0.3219752754296894559, 0.3333333333333333703, 0.3219752754296894559, 0.3333333333333333703, 0.3219752754296894559, 0.3333333333333333703, 0.3219752754296894559, 0.3333333333333333703, 0.3219752754296894559, 0.3333333333333333703, 0.3219752754296894559, 0.3333333333333333703, 0.3219752754296894559, 0.3333333333333333703, 0.3219752754296894559, 0.3333333333333333703, 0.3219752754296894559, 0.3333333333333333703, 0.3219752754296894559, 0.3333333333333333703, 0.3219752754296894559, 0.3333333333333333703, 0.3219752754296894559, 0.3333333333333333703, 0.3219752754296894559, 0.3333333333333333703, 0.3219752754296894559, 0.3333333333333333703, 0.3219752754296894559, 0.3333333333333333703, 0.3219752754296894559, 0.3333333333333333703, 0.3219752754296894559, 0.3333333333333333703, 0.3219752754296894559, 0.3333333333333333703, 0.3219752754296894559, 0.3333333333333333703, 0.3219752754296894559, 0.3333333333333333703, 0.3219752754296894559, 0.3333333333333333703, 0.3219752754296894559, 0.3333333333333333703, 0.3219752754296894559, 0.3333333333333333703, 0.3219752754296894559, 0.3333333333333333703, 0.3219752754296894559, 0.3333333333333333703, 0.3219752754296894559, 0.3333333333333333703, 0.3219752754296894559, 0.3333333333333333703, 0.3219752754296894559, 0.3333333333333333703, 0.3219752754296894559, 0.3333333333333333703, 0.3219752754296894559, 0.3333333333333333703, 0.3219752754296894559, 0.3333333333333333703, 0.3219752754296894559, 0.3333333333333333703, 0.3219752754296894559, 0.3333333333333333703, 0.3219752754296894559, 0.3333333333333333703, 0.3219752754296894559, 0.3333333333333333703, 0.3219752754296894559, 0.3333333333333333703, 0.3219752754296894559, 0.3333333333333333703, 0.3219752754296894559, 0.3333333333333333703, 0.3219752754296894559, 0.3333333333333333703, 0.3219752754296894559, 0.3333333333333333703, 0.3219752754296894559, 0.3333333333333333703, 0.3219752754296894559, 0.3333333333333333703, 0.3219752754296894559, 0.3333333333333333703, 0.3219752754296894559, 0.3333333333333333703, 0.3219752754296894559, 0.3333333333333333703, 0.3219752754296894559, 0.3333333333333333703, 0.3219752754296894559, 0.3333333333333333703, 0.3219752754296894559, 0.3333333333333333703, 0.3219752754296894559, 0.3333333333333333703, 0.3219752754296894559, 0.3333333333333333703, 0.3219752754296894559, 0.3333333333333333703, 0.3219752754296894559, 0.3333333333333333703, 0.3219752754296894559, 0.3333333333333333703, 0.3219752754296894559, 0.3333333333333333703, 0.3219752754296894559, 0.3333333333333333703, 0.3219752754296894559, 0.3333333333333333703, 0.3219752754296894559, 0.3333333333333333703, 0.3219752754296894559, 0.3333333333333333703, 0.3219752754296894559, 0.3333333333333333703, 0.3219752754296894559, 0.3333333333333333703, 0.3219752754296894559, 0.3333333333333333703, 0.3219752754296894559, 0.3333333333333333703, 0.3219752754296894559, 0.3333333333333333703, 0.3219752754296894559, 0.3333333333333333703, 0.3219752754296894559, 0.3333333333333333703, 0.3219752754296894559, 0.3333333333333333703, 0.3219752754296894559, 0.3333333333333333703, 0.3219752754296894559, 0.3333333333333333703, 0.3219752754296894559, 0.3333333333333333703, 0.3219752754296894559, 0.3333333333333333703, 0.3219752754296894559, 0.3333333333333333703, 0.3219752754296894559, 0.3333333333333333703, 0.3219752754296894559, 0.3333333333333333703, 0.3219752754296894559, 0.3333333333333333703, 0.3219752754296894559, 0.3333333333333333703, 0.3219752754296894559, 0.3333333333333333703, 0.3219752754296894559, 0.3333333333333333703, 0.3219752754296894559, 0.3333333333333333703, 0.3219752754296894559, 0.3333333333333333703, 0.3219752754296894559, 0.3333333333333333703, 0.3219752754296894559, 0.3333333333333333703, 0.3219752754296894559, 0.3333333333333333703, 0.3219752754296894559, 0.3333333333333333703, 0.3219752754296894559, 0.3333333333333333703, 0.3219752754296894559, 0.3333333333333333703, 0.3219752754296894559, 0.3333333333333333703, 0.3219752754296894559, 0.3333333333333333703, 0.3219752754296894559, 0.3333333333333333703, 0.3219752754296894559, 0.3333333333333333703, 0.3219752754296894559, 0.3333333333333333703, 0.3219752754296894559, 0.3333333333333333703, 0.3219752754296894559, 0.3333333333333333703, 0.3219752754296894559, 0.3333333333333333703, 0.3219752754296894559, 0.3333333333333333703, 0.3219752754296894559, 0.3333333333333333703, 0.3219752754296894559, 0.3333333333333333703, 0.3219752754296894559, 0.3333333333333333703, 0.3219752754296894559, 0.3333333333333333703, 0.3219752754296894559, 0.3333333333333333703, 0.3219752754296894559, 0.3333333333333333703, 0.3219752754296894559, 0.3333333333333333703, 0.3219752754296894559, 0.3333333333333333703, 0.3219752754296894559, 0.3333333333333333703, 0.3219752754296894559, 0.3333333333333333703, 0.3219752754296894559, 0.3333333333333333703, 0.3219752754296894559, 0.3333333333333333703),
 ( 0.3333333333333333703, 0.3219752754296894559, 0.3333333333333333703, 0.3219752754296894559, 0.3333333333333333703, 0.3219752754296894559, 0.3333333333333333703, 0.3219752754296894559, 0.3333333333333333703, 0.3219752754296894559, 0.3333333333333333703, 0.3219752754296894559, 0.3333333333333333703, 0.3219752754296894559, 0.3333333333333333703, 0.3219752754296894559, 0.3333333333333333703, 0.3219752754296894559, 0.3333333333333333703, 0.3219752754296894559, 0.3333333333333333703, 0.3219752754296894559, 0.3333333333333333703, 0.3219752754296894559, 0.3333333333333333703, 0.3219752754296894559, 0.3333333333333333703, 0.3219752754296894559, 0.3333333333333333703, 0.3219752754296894559, 0.3333333333333333703, 0.3219752754296894559, 0.3333333333333333703, 0.3219752754296894559, 0.3333333333333333703, 0.3219752754296894559, 0.3333333333333333703, 0.3219752754296894559, 0.3333333333333333703, 0.3219752754296894559, 0.3333333333333333703, 0.3219752754296894559, 0.3333333333333333703, 0.3219752754296894559, 0.3333333333333333703, 0.3219752754296894559, 0.3333333333333333703, 0.3219752754296894559, 0.3333333333333333703, 0.3219752754296894559, 0.3333333333333333703, 0.3219752754296894559, 0.3333333333333333703, 0.3219752754296894559, 0.3333333333333333703, 0.3219752754296894559, 0.3333333333333333703, 0.3219752754296894559, 0.3333333333333333703, 0.3219752754296894559, 0.3333333333333333703, 0.3219752754296894559, 0.3333333333333333703, 0.3219752754296894559, 0.3333333333333333703, 0.3219752754296894559, 0.3333333333333333703, 0.3219752754296894559, 0.3333333333333333703, 0.3219752754296894559, 0.3333333333333333703, 0.3219752754296894559, 0.3333333333333333703, 0.3219752754296894559, 0.3333333333333333703, 0.3219752754296894559, 0.3333333333333333703, 0.3219752754296894559, 0.3333333333333333703, 0.3219752754296894559, 0.3333333333333333703, 0.3219752754296894559, 0.3333333333333333703, 0.3219752754296894559, 0.3333333333333333703, 0.3219752754296894559, 0.3333333333333333703, 0.3219752754296894559, 0.3333333333333333703, 0.3219752754296894559, 0.3333333333333333703, 0.3219752754296894559, 0.3333333333333333703, 0.3219752754296894559, 0.3333333333333333703, 0.3219752754296894559, 0.3333333333333333703, 0.3219752754296894559, 0.3333333333333333703, 0.3219752754296894559, 0.3333333333333333703, 0.3219752754296894559, 0.3333333333333333703, 0.3219752754296894559, 0.3333333333333333703, 0.3219752754296894559, 0.3333333333333333703, 0.3219752754296894559, 0.3333333333333333703, 0.3219752754296894559, 0.3333333333333333703, 0.3219752754296894559, 0.3333333333333333703, 0.3219752754296894559, 0.3333333333333333703, 0.3219752754296894559, 0.3333333333333333703, 0.3219752754296894559, 0.3333333333333333703, 0.3219752754296894559, 0.3333333333333333703, 0.3219752754296894559, 0.3333333333333333703, 0.3219752754296894559, 0.3333333333333333703, 0.3219752754296894559, 0.3333333333333333703, 0.3219752754296894559, 0.3333333333333333703, 0.3219752754296894559, 0.3333333333333333703, 0.3219752754296894559, 0.3333333333333333703, 0.3219752754296894559, 0.3333333333333333703, 0.3219752754296894559, 0.3333333333333333703, 0.3219752754296894559, 0.3333333333333333703, 0.3219752754296894559, 0.3333333333333333703, 0.3219752754296894559, 0.3333333333333333703, 0.3219752754296894559, 0.3333333333333333703, 0.3219752754296894559, 0.3333333333333333703, 0.3219752754296894559, 0.3333333333333333703, 0.3219752754296894559, 0.3333333333333333703, 0.3219752754296894559, 0.3333333333333333703, 0.3219752754296894559, 0.3333333333333333703, 0.3219752754296894559, 0.3333333333333333703, 0.3219752754296894559, 0.3333333333333333703, 0.3219752754296894559, 0.3333333333333333703, 0.3219752754296894559, 0.3333333333333333703, 0.3219752754296894559, 0.3333333333333333703, 0.3219752754296894559, 0.3333333333333333703, 0.3219752754296894559, 0.3333333333333333703, 0.3219752754296894559, 0.3333333333333333703, 0.3219752754296894559, 0.3333333333333333703, 0.3219752754296894559, 0.3333333333333333703, 0.3219752754296894559, 0.3333333333333333703, 0.3219752754296894559, 0.3333333333333333703, 0.3219752754296894559, 0.3333333333333333703, 0.3219752754296894559, 0.3333333333333333703, 0.3219752754296894559, 0.3333333333333333703, 0.3219752754296894559, 0.3333333333333333703, 0.3219752754296894559, 0.3333333333333333703, 0.3219752754296894559, 0.3333333333333333703, 0.3219752754296894559, 0.3333333333333333703, 0.3219752754296894559, 0.3333333333333333703, 0.3219752754296894559, 0.3333333333333333703, 0.3219752754296894559, 0.3333333333333333703, 0.3219752754296894559, 0.3333333333333333703, 0.3219752754296894559, 0.3333333333333333703, 0.3219752754296894559, 0.3333333333333333703, 0.3219752754296894559, 0.3333333333333333703, 0.3219752754296894559, 0.3333333333333333703, 0.3219752754296894559, 0.3333333333333333703, 0.3219752754296894559, 0.3333333333333333703, 0.3219752754296894559, 0.3333333333333333703, 0.3219752754296894559, 0.3333333333333333703, 0.3219752754296894559, 0.3333333333333333703, 0.3219752754296894559, 0.3333333333333333703, 0.3219752754296894559, 0.3333333333333333703, 0.3219752754296894559, 0.3333333333333333703, 0.3219752754296894559, 0.3333333333333333703, 0.3219752754296894559, 0.3333333333333333703, 0.3219752754296894559, 0.3333333333333333703, 0.3219752754296894559, 0.3333333333333333703, 0.3219752754296894559, 0.3333333333333333703, 0.3219752754296894559, 0.3333333333333333703, 0.3219752754296894559, 0.3333333333333333703, 0.3219752754296894559, 0.3333333333333333703, 0.3219752754296894559, 0.3333333333333333703, 0.3219752754296894559, 0.3333333333333333703, 0.3219752754296894559, 0.3333333333333333703, 0.3219752754296894559, 0.3333333333333333703, 0.3219752754296894559, 0.3333333333333333703, 0.3219752754296894559, 0.3333333333333333703, 0.3219752754296894559, 0.3333333333333333703, 0.3219752754296894559, 0.3333333333333333703, 0.3219752754296894559, 0.3333333333333333703, 0.3219752754296894559, 0.3333333333333333703, 0.3219752754296894559, 0.3333333333333333703, 0.3219752754296894559, 0.3333333333333333703, 0.3219752754296894559, 0.3333333333333333703, 0.3219752754296894559, 0.3333333333333333703, 0.3219752754296894559, 0.3333333333333333703, 0.3219752754296894559, 0.3333333333333333703, 0.3219752754296894559, 0.3333333333333333703, 0.3219752754296894559, 0.3333333333333333703, 0.3219752754296894559, 0.3333333333333333703, 0.3219752754296894559, 0.3333333333333333703, 0.3219752754296894559, 0.3333333333333333703, 0.3219752754296894559, 0.3333333333333333703, 0.3219752754296894559, 0.3333333333333333703, 0.3219752754296894559, 0.3333333333333333703, 0.3219752754296894559, 0.3333333333333333703, 0.3219752754296894559, 0.3333333333333333703, 0.3219752754296894559, 0.3333333333333333703, 0.3219752754296894559, 0.3333333333333333703, 0.3219752754296894559, 0.3333333333333333703, 0.3219752754296894559, 0.3333333333333333703, 0.3219752754296894559, 0.3333333333333333703, 0.3219752754296894559, 0.3333333333333333703, 0.3219752754296894559, 0.3333333333333333703, 0.3219752754296894559, 0.3333333333333333703, 0.3219752754296894559, 0.3333333333333333703, 0.3219752754296894559, 0.3333333333333333703, 0.3219752754296894559, 0.3333333333333333703, 0.3219752754296894559, 0.3333333333333333703, 0.3219752754296894559, 0.3333333333333333703, 0.3219752754296894559, 0.3333333333333333703, 0.3219752754296894559, 0.3333333333333333703, 0.3219752754296894559, 0.3333333333333333703, 0.3219752754296894559, 0.3333333333333333703, 0.3219752754296894559, 0.3333333333333333703, 0.3219752754296894559, 0.3333333333333333703, 0.3219752754296894559, 0.3333333333333333703, 0.3219752754296894559, 0.3333333333333333703, 0.3219752754296894559, 0.3333333333333333703, 0.3219752754296894559, 0.3333333333333333703, 0.3219752754296894559, 0.3333333333333333703, 0.3219752754296894559, 0.3333333333333333703, 0.3219752754296894559, 0.3333333333333333703, 0.3219752754296894559, 0.3333333333333333703, 0.3219752754296894559, 0.3333333333333333703, 0.3219752754296894559, 0.3333333333333333703, 0.3219752754296894559, 0.3333333333333333703, 0.3219752754296894559, 0.3333333333333333703, 0.3219752754296894559, 0.3333333333333333703, 0.3219752754296894559, 0.3333333333333333703, 0.3219752754296894559, 0.3333333333333333703, 0.3219752754296894559, 0.3333333333333333703, 0.3219752754296894559, 0.3333333333333333703, 0.3219752754296894559, 0.3333333333333333703, 0.3219752754296894559, 0.3333333333333333703, 0.3219752754296894559, 0.3333333333333333703, 0.3219752754296894559, 0.3333333333333333703, 0.3219752754296894559, 0.3333333333333333703, 0.3219752754296894559, 0.3333333333333333703, 0.3219752754296894559, 0.3333333333333333703, 0.3219752754296894559, 0.3333333333333333703, 0.3219752754296894559, 0.3333333333333333703, 0.3219752754296894559, 0.3333333333333333703, 0.3219752754296894559, 0.3333333333333333703, 0.3219752754296894559, 0.3333333333333333703, 0.3219752754296894559, 0.3333333333333333703, 0.3219752754296894559, 0.3333333333333333703, 0.3219752754296894559, 0.3333333333333333703, 0.3219752754296894559, 0.3333333333333333703, 0.3219752754296894559, 0.3333333333333333703, 0.3219752754296894559, 0.3333333333333333703, 0.3219752754296894559, 0.3333333333333333703, 0.3219752754296894559, 0.3333333333333333703, 0.3219752754296894559, 0.3333333333333333703, 0.3219752754296894559, 0.3333333333333333703, 0.3219752754296894559, 0.3333333333333333703, 0.3219752754296894559, 0.3333333333333333703, 0.3219752754296894559, 0.3333333333333333703, 0.3219752754296894559, 0.3333333333333333703, 0.3219752754296894559, 0.3333333333333333703, 0.3219752754296894559, 0.3333333333333333703, 0.3219752754296894559, 0.3333333333333333703, 0.3219752754296894559, 0.3333333333333333703, 0.3219752754296894559, 0.3333333333333333703, 0.3219752754296894559, 0.3333333333333333703, 0.3219752754296894559, 0.3333333333333333703, 0.3219752754296894559, 0.3333333333333333703, 0.3219752754296894559, 0.3333333333333333703, 0.3219752754296894559, 0.3333333333333333703, 0.3219752754296894559, 0.3333333333333333703, 0.3219752754296894559, 0.3333333333333333703, 0.3219752754296894559, 0.3333333333333333703, 0.3219752754296894559, 0.3333333333333333703, 0.3219752754296894559, 0.3333333333333333703, 0.3219752754296894559, 0.3333333333333333703, 0.3219752754296894559, 0.3333333333333333703, 0.3219752754296894559, 0.3333333333333333703, 0.3219752754296894559, 0.3333333333333333703, 0.3219752754296894559, 0.3333333333333333703),
 ( 1.000000000000000000, 0.9659258262890683122, 1.000000000000000000, 0.9659258262890683122, 1.000000000000000000, 0.9659258262890683122, 1.000000000000000000, 0.9659258262890683122, 1.000000000000000000, 0.9659258262890683122, 1.000000000000000000, 0.9659258262890683122, 1.000000000000000000, 0.9659258262890683122, 1.000000000000000000, 0.9659258262890683122, 1.000000000000000000, 0.9659258262890683122, 1.000000000000000000, 0.9659258262890683122, 1.000000000000000000, 0.9659258262890683122, 1.000000000000000000, 0.9659258262890683122, 1.000000000000000000, 0.9659258262890683122, 1.000000000000000000, 0.9659258262890683122, 1.000000000000000000, 0.9659258262890683122, 1.000000000000000000, 0.9659258262890683122, 1.000000000000000000, 0.9659258262890683122, 1.000000000000000000, 0.9659258262890683122, 1.000000000000000000, 0.9659258262890683122, 1.000000000000000000, 0.9659258262890683122, 1.000000000000000000, 0.9659258262890683122, 1.000000000000000000, 0.9659258262890683122, 1.000000000000000000, 0.9659258262890683122, 1.000000000000000000, 0.9659258262890683122, 1.000000000000000000, 0.9659258262890683122, 1.000000000000000000, 0.9659258262890683122, 1.000000000000000000, 0.9659258262890683122, 1.000000000000000000, 0.9659258262890683122, 1.000000000000000000, 0.9659258262890683122, 1.000000000000000000, 0.9659258262890683122, 1.000000000000000000, 0.9659258262890683122, 1.000000000000000000, 0.9659258262890683122, 1.000000000000000000, 0.9659258262890683122, 1.000000000000000000, 0.9659258262890683122, 1.000000000000000000, 0.9659258262890683122, 1.000000000000000000, 0.9659258262890683122, 1.000000000000000000, 0.9659258262890683122, 1.000000000000000000, 0.9659258262890683122, 1.000000000000000000, 0.9659258262890683122, 1.000000000000000000, 0.9659258262890683122, 1.000000000000000000, 0.9659258262890683122, 1.000000000000000000, 0.9659258262890683122, 1.000000000000000000, 0.9659258262890683122, 1.000000000000000000, 0.9659258262890683122, 1.000000000000000000, 0.9659258262890683122, 1.000000000000000000, 0.9659258262890683122, 1.000000000000000000, 0.9659258262890683122, 1.000000000000000000, 0.9659258262890683122, 1.000000000000000000, 0.9659258262890683122, 1.000000000000000000, 0.9659258262890683122, 1.000000000000000000, 0.9659258262890683122, 1.000000000000000000, 0.9659258262890683122, 1.000000000000000000, 0.9659258262890683122, 1.000000000000000000, 0.9659258262890683122, 1.000000000000000000, 0.9659258262890683122, 1.000000000000000000, 0.9659258262890683122, 1.000000000000000000, 0.9659258262890683122, 1.000000000000000000, 0.9659258262890683122, 1.000000000000000000, 0.9659258262890683122, 1.000000000000000000, 0.9659258262890683122, 1.000000000000000000, 0.9659258262890683122, 1.000000000000000000, 0.9659258262890683122, 1.000000000000000000, 0.9659258262890683122, 1.000000000000000000, 0.9659258262890683122, 1.000000000000000000, 0.9659258262890683122, 1.000000000000000000, 0.9659258262890683122, 1.000000000000000000, 0.9659258262890683122, 1.000000000000000000, 0.9659258262890683122, 1.000000000000000000, 0.9659258262890683122, 1.000000000000000000, 0.9659258262890683122, 1.000000000000000000, 0.9659258262890683122, 1.000000000000000000, 0.9659258262890683122, 1.000000000000000000, 0.9659258262890683122, 1.000000000000000000, 0.9659258262890683122, 1.000000000000000000, 0.9659258262890683122, 1.000000000000000000, 0.9659258262890683122, 1.000000000000000000, 0.9659258262890683122, 1.000000000000000000, 0.9659258262890683122, 1.000000000000000000, 0.9659258262890683122, 1.000000000000000000, 0.9659258262890683122, 1.000000000000000000, 0.9659258262890683122, 1.000000000000000000, 0.9659258262890683122, 1.000000000000000000, 0.9659258262890683122, 1.000000000000000000, 0.9659258262890683122, 1.000000000000000000, 0.9659258262890683122, 1.000000000000000000, 0.9659258262890683122, 1.000000000000000000, 0.9659258262890683122, 1.000000000000000000, 0.9659258262890683122, 1.000000000000000000, 0.9659258262890683122, 1.000000000000000000, 0.9659258262890683122, 1.000000000000000000, 0.9659258262890683122, 1.000000000000000000, 0.9659258262890683122, 1.000000000000000000, 0.9659258262890683122, 1.000000000000000000, 0.9659258262890683122, 1.000000000000000000, 0.9659258262890683122, 1.000000000000000000, 0.9659258262890683122, 1.000000000000000000, 0.9659258262890683122, 1.000000000000000000, 0.9659258262890683122, 1.000000000000000000, 0.9659258262890683122, 1.000000000000000000, 0.9659258262890683122, 1.000000000000000000, 0.9659258262890683122, 1.000000000000000000, 0.9659258262890683122, 1.000000000000000000, 0.9659258262890683122, 1.000000000000000000, 0.9659258262890683122, 1.000000000000000000, 0.9659258262890683122, 1.000000000000000000, 0.9659258262890683122, 1.000000000000000000, 0.9659258262890683122, 1.000000000000000000, 0.9659258262890683122, 1.000000000000000000, 0.9659258262890683122, 1.000000000000000000, 0.9659258262890683122, 1.000000000000000000, 0.9659258262890683122, 1.000000000000000000, 0.9659258262890683122, 1.000000000000000000, 0.9659258262890683122, 1.000000000000000000, 0.9659258262890683122, 1.000000000000000000, 0.9659258262890683122, 1.000000000000000000, 0.9659258262890683122, 1.000000000000000000, 0.9659258262890683122, 1.000000000000000000, 0.9659258262890683122, 1.000000000000000000, 0.9659258262890683122, 1.000000000000000000, 0.9659258262890683122, 1.000000000000000000, 0.9659258262890683122, 1.000000000000000000, 0.9659258262890683122, 1.000000000000000000, 0.9659258262890683122, 1.000000000000000000, 0.9659258262890683122, 1.000000000000000000, 0.9659258262890683122, 1.000000000000000000, 0.9659258262890683122, 1.000000000000000000, 0.9659258262890683122, 1.000000000000000000, 0.9659258262890683122, 1.000000000000000000, 0.9659258262890683122, 1.000000000000000000, 0.9659258262890683122, 1.000000000000000000, 0.9659258262890683122, 1.000000000000000000, 0.9659258262890683122, 1.000000000000000000, 0.9659258262890683122, 1.000000000000000000, 0.9659258262890683122, 1.000000000000000000, 0.9659258262890683122, 1.000000000000000000, 0.9659258262890683122, 1.000000000000000000, 0.9659258262890683122, 1.000000000000000000, 0.9659258262890683122, 1.000000000000000000, 0.9659258262890683122, 1.000000000000000000, 0.9659258262890683122, 1.000000000000000000, 0.9659258262890683122, 1.000000000000000000, 0.9659258262890683122, 1.000000000000000000, 0.9659258262890683122, 1.000000000000000000, 0.9659258262890683122, 1.000000000000000000, 0.9659258262890683122, 1.000000000000000000, 0.9659258262890683122, 1.000000000000000000, 0.9659258262890683122, 1.000000000000000000, 0.9659258262890683122, 1.000000000000000000, 0.9659258262890683122, 1.000000000000000000, 0.9659258262890683122, 1.000000000000000000, 0.9659258262890683122, 1.000000000000000000, 0.9659258262890683122, 1.000000000000000000, 0.9659258262890683122, 1.000000000000000000, 0.9659258262890683122, 1.000000000000000000, 0.9659258262890683122, 1.000000000000000000, 0.9659258262890683122, 1.000000000000000000, 0.9659258262890683122, 1.000000000000000000, 0.9659258262890683122, 1.000000000000000000, 0.9659258262890683122, 1.000000000000000000, 0.9659258262890683122, 1.000000000000000000, 0.9659258262890683122, 1.000000000000000000, 0.9659258262890683122, 1.000000000000000000, 0.9659258262890683122, 1.000000000000000000, 0.9659258262890683122, 1.000000000000000000, 0.9659258262890683122, 1.000000000000000000, 0.9659258262890683122, 1.000000000000000000, 0.9659258262890683122, 1.000000000000000000, 0.9659258262890683122, 1.000000000000000000, 0.9659258262890683122, 1.000000000000000000, 0.9659258262890683122, 1.000000000000000000, 0.9659258262890683122, 1.000000000000000000, 0.9659258262890683122, 1.000000000000000000, 0.9659258262890683122, 1.000000000000000000, 0.9659258262890683122, 1.000000000000000000, 0.9659258262890683122, 1.000000000000000000, 0.9659258262890683122, 1.000000000000000000, 0.9659258262890683122, 1.000000000000000000, 0.9659258262890683122, 1.000000000000000000, 0.9659258262890683122, 1.000000000000000000, 0.9659258262890683122, 1.000000000000000000, 0.9659258262890683122, 1.000000000000000000, 0.9659258262890683122, 1.000000000000000000, 0.9659258262890683122, 1.000000000000000000, 0.9659258262890683122, 1.000000000000000000, 0.9659258262890683122, 1.000000000000000000, 0.9659258262890683122, 1.000000000000000000, 0.9659258262890683122, 1.000000000000000000, 0.9659258262890683122, 1.000000000000000000, 0.9659258262890683122, 1.000000000000000000, 0.9659258262890683122, 1.000000000000000000, 0.9659258262890683122, 1.000000000000000000, 0.9659258262890683122, 1.000000000000000000, 0.9659258262890683122, 1.000000000000000000, 0.9659258262890683122, 1.000000000000000000, 0.9659258262890683122, 1.000000000000000000, 0.9659258262890683122, 1.000000000000000000, 0.9659258262890683122, 1.000000000000000000, 0.9659258262890683122, 1.000000000000000000, 0.9659258262890683122, 1.000000000000000000, 0.9659258262890683122, 1.000000000000000000, 0.9659258262890683122, 1.000000000000000000, 0.9659258262890683122, 1.000000000000000000, 0.9659258262890683122, 1.000000000000000000, 0.9659258262890683122, 1.000000000000000000, 0.9659258262890683122, 1.000000000000000000, 0.9659258262890683122, 1.000000000000000000, 0.9659258262890683122, 1.000000000000000000, 0.9659258262890683122, 1.000000000000000000, 0.9659258262890683122, 1.000000000000000000, 0.9659258262890683122, 1.000000000000000000, 0.9659258262890683122, 1.000000000000000000, 0.9659258262890683122, 1.000000000000000000, 0.9659258262890683122, 1.000000000000000000, 0.9659258262890683122, 1.000000000000000000, 0.9659258262890683122, 1.000000000000000000, 0.9659258262890683122, 1.000000000000000000, 0.9659258262890683122, 1.000000000000000000, 0.9659258262890683122, 1.000000000000000000, 0.9659258262890683122, 1.000000000000000000, 0.9659258262890683122, 1.000000000000000000, 0.9659258262890683122, 1.000000000000000000, 0.9659258262890683122, 1.000000000000000000, 0.9659258262890683122, 1.000000000000000000, 0.9659258262890683122, 1.000000000000000000, 0.9659258262890683122, 1.000000000000000000, 0.9659258262890683122, 1.000000000000000000, 0.9659258262890683122, 1.000000000000000000, 0.9659258262890683122, 1.000000000000000000),
 ( 0.3333333333333333703, 0.3219752754296894559, 0.3333333333333333703, 0.3219752754296894559, 0.3333333333333333703, 0.3219752754296894559, 0.3333333333333333703, 0.3219752754296894559, 0.3333333333333333703, 0.3219752754296894559, 0.3333333333333333703, 0.3219752754296894559, 0.3333333333333333703, 0.3219752754296894559, 0.3333333333333333703, 0.3219752754296894559, 0.3333333333333333703, 0.3219752754296894559, 0.3333333333333333703, 0.3219752754296894559, 0.3333333333333333703, 0.3219752754296894559, 0.3333333333333333703, 0.3219752754296894559, 0.3333333333333333703, 0.3219752754296894559, 0.3333333333333333703, 0.3219752754296894559, 0.3333333333333333703, 0.3219752754296894559, 0.3333333333333333703, 0.3219752754296894559, 0.3333333333333333703, 0.3219752754296894559, 0.3333333333333333703, 0.3219752754296894559, 0.3333333333333333703, 0.3219752754296894559, 0.3333333333333333703, 0.3219752754296894559, 0.3333333333333333703, 0.3219752754296894559, 0.3333333333333333703, 0.3219752754296894559, 0.3333333333333333703, 0.3219752754296894559, 0.3333333333333333703, 0.3219752754296894559, 0.3333333333333333703, 0.3219752754296894559, 0.3333333333333333703, 0.3219752754296894559, 0.3333333333333333703, 0.3219752754296894559, 0.3333333333333333703, 0.3219752754296894559, 0.3333333333333333703, 0.3219752754296894559, 0.3333333333333333703, 0.3219752754296894559, 0.3333333333333333703, 0.3219752754296894559, 0.3333333333333333703, 0.3219752754296894559, 0.3333333333333333703, 0.3219752754296894559, 0.3333333333333333703, 0.3219752754296894559, 0.3333333333333333703, 0.3219752754296894559, 0.3333333333333333703, 0.3219752754296894559, 0.3333333333333333703, 0.3219752754296894559, 0.3333333333333333703, 0.3219752754296894559, 0.3333333333333333703, 0.3219752754296894559, 0.3333333333333333703, 0.3219752754296894559, 0.3333333333333333703, 0.3219752754296894559, 0.3333333333333333703, 0.3219752754296894559, 0.3333333333333333703, 0.3219752754296894559, 0.3333333333333333703, 0.3219752754296894559, 0.3333333333333333703, 0.3219752754296894559, 0.3333333333333333703, 0.3219752754296894559, 0.3333333333333333703, 0.3219752754296894559, 0.3333333333333333703, 0.3219752754296894559, 0.3333333333333333703, 0.3219752754296894559, 0.3333333333333333703, 0.3219752754296894559, 0.3333333333333333703, 0.3219752754296894559, 0.3333333333333333703, 0.3219752754296894559, 0.3333333333333333703, 0.3219752754296894559, 0.3333333333333333703, 0.3219752754296894559, 0.3333333333333333703, 0.3219752754296894559, 0.3333333333333333703, 0.3219752754296894559, 0.3333333333333333703, 0.3219752754296894559, 0.3333333333333333703, 0.3219752754296894559, 0.3333333333333333703, 0.3219752754296894559, 0.3333333333333333703, 0.3219752754296894559, 0.3333333333333333703, 0.3219752754296894559, 0.3333333333333333703, 0.3219752754296894559, 0.3333333333333333703, 0.3219752754296894559, 0.3333333333333333703, 0.3219752754296894559, 0.3333333333333333703, 0.3219752754296894559, 0.3333333333333333703, 0.3219752754296894559, 0.3333333333333333703, 0.3219752754296894559, 0.3333333333333333703, 0.3219752754296894559, 0.3333333333333333703, 0.3219752754296894559, 0.3333333333333333703, 0.3219752754296894559, 0.3333333333333333703, 0.3219752754296894559, 0.3333333333333333703, 0.3219752754296894559, 0.3333333333333333703, 0.3219752754296894559, 0.3333333333333333703, 0.3219752754296894559, 0.3333333333333333703, 0.3219752754296894559, 0.3333333333333333703, 0.3219752754296894559, 0.3333333333333333703, 0.3219752754296894559, 0.3333333333333333703, 0.3219752754296894559, 0.3333333333333333703, 0.3219752754296894559, 0.3333333333333333703, 0.3219752754296894559, 0.3333333333333333703, 0.3219752754296894559, 0.3333333333333333703, 0.3219752754296894559, 0.3333333333333333703, 0.3219752754296894559, 0.3333333333333333703, 0.3219752754296894559, 0.3333333333333333703, 0.3219752754296894559, 0.3333333333333333703, 0.3219752754296894559, 0.3333333333333333703, 0.3219752754296894559, 0.3333333333333333703, 0.3219752754296894559, 0.3333333333333333703, 0.3219752754296894559, 0.3333333333333333703, 0.3219752754296894559, 0.3333333333333333703, 0.3219752754296894559, 0.3333333333333333703, 0.3219752754296894559, 0.3333333333333333703, 0.3219752754296894559, 0.3333333333333333703, 0.3219752754296894559, 0.3333333333333333703, 0.3219752754296894559, 0.3333333333333333703, 0.3219752754296894559, 0.3333333333333333703, 0.3219752754296894559, 0.3333333333333333703, 0.3219752754296894559, 0.3333333333333333703, 0.3219752754296894559, 0.3333333333333333703, 0.3219752754296894559, 0.3333333333333333703, 0.3219752754296894559, 0.3333333333333333703, 0.3219752754296894559, 0.3333333333333333703, 0.3219752754296894559, 0.3333333333333333703, 0.3219752754296894559, 0.3333333333333333703, 0.3219752754296894559, 0.3333333333333333703, 0.3219752754296894559, 0.3333333333333333703, 0.3219752754296894559, 0.3333333333333333703, 0.3219752754296894559, 0.3333333333333333703, 0.3219752754296894559, 0.3333333333333333703, 0.3219752754296894559, 0.3333333333333333703, 0.3219752754296894559, 0.3333333333333333703, 0.3219752754296894559, 0.3333333333333333703, 0.3219752754296894559, 0.3333333333333333703, 0.3219752754296894559, 0.3333333333333333703, 0.3219752754296894559, 0.3333333333333333703, 0.3219752754296894559, 0.3333333333333333703, 0.3219752754296894559, 0.3333333333333333703, 0.3219752754296894559, 0.3333333333333333703, 0.3219752754296894559, 0.3333333333333333703, 0.3219752754296894559, 0.3333333333333333703, 0.3219752754296894559, 0.3333333333333333703, 0.3219752754296894559, 0.3333333333333333703, 0.3219752754296894559, 0.3333333333333333703, 0.3219752754296894559, 0.3333333333333333703, 0.3219752754296894559, 0.3333333333333333703, 0.3219752754296894559, 0.3333333333333333703, 0.3219752754296894559, 0.3333333333333333703, 0.3219752754296894559, 0.3333333333333333703, 0.3219752754296894559, 0.3333333333333333703, 0.3219752754296894559, 0.3333333333333333703, 0.3219752754296894559, 0.3333333333333333703, 0.3219752754296894559, 0.3333333333333333703, 0.3219752754296894559, 0.3333333333333333703, 0.3219752754296894559, 0.3333333333333333703, 0.3219752754296894559, 0.3333333333333333703, 0.3219752754296894559, 0.3333333333333333703, 0.3219752754296894559, 0.3333333333333333703, 0.3219752754296894559, 0.3333333333333333703, 0.3219752754296894559, 0.3333333333333333703, 0.3219752754296894559, 0.3333333333333333703, 0.3219752754296894559, 0.3333333333333333703, 0.3219752754296894559, 0.3333333333333333703, 0.3219752754296894559, 0.3333333333333333703, 0.3219752754296894559, 0.3333333333333333703, 0.3219752754296894559, 0.3333333333333333703, 0.3219752754296894559, 0.3333333333333333703, 0.3219752754296894559, 0.3333333333333333703, 0.3219752754296894559, 0.3333333333333333703, 0.3219752754296894559, 0.3333333333333333703, 0.3219752754296894559, 0.3333333333333333703, 0.3219752754296894559, 0.3333333333333333703, 0.3219752754296894559, 0.3333333333333333703, 0.3219752754296894559, 0.3333333333333333703, 0.3219752754296894559, 0.3333333333333333703, 0.3219752754296894559, 0.3333333333333333703, 0.3219752754296894559, 0.3333333333333333703, 0.3219752754296894559, 0.3333333333333333703, 0.3219752754296894559, 0.3333333333333333703, 0.3219752754296894559, 0.3333333333333333703, 0.3219752754296894559, 0.3333333333333333703, 0.3219752754296894559, 0.3333333333333333703, 0.3219752754296894559, 0.3333333333333333703, 0.3219752754296894559, 0.3333333333333333703, 0.3219752754296894559, 0.3333333333333333703, 0.3219752754296894559, 0.3333333333333333703, 0.3219752754296894559, 0.3333333333333333703, 0.3219752754296894559, 0.3333333333333333703, 0.3219752754296894559, 0.3333333333333333703, 0.3219752754296894559, 0.3333333333333333703, 0.3219752754296894559, 0.3333333333333333703, 0.3219752754296894559, 0.3333333333333333703, 0.3219752754296894559, 0.3333333333333333703, 0.3219752754296894559, 0.3333333333333333703, 0.3219752754296894559, 0.3333333333333333703, 0.3219752754296894559, 0.3333333333333333703, 0.3219752754296894559, 0.3333333333333333703, 0.3219752754296894559, 0.3333333333333333703, 0.3219752754296894559, 0.3333333333333333703, 0.3219752754296894559, 0.3333333333333333703, 0.3219752754296894559, 0.3333333333333333703, 0.3219752754296894559, 0.3333333333333333703, 0.3219752754296894559, 0.3333333333333333703, 0.3219752754296894559, 0.3333333333333333703, 0.3219752754296894559, 0.3333333333333333703, 0.3219752754296894559, 0.3333333333333333703, 0.3219752754296894559, 0.3333333333333333703, 0.3219752754296894559, 0.3333333333333333703, 0.3219752754296894559, 0.3333333333333333703, 0.3219752754296894559, 0.3333333333333333703, 0.3219752754296894559, 0.3333333333333333703, 0.3219752754296894559, 0.3333333333333333703, 0.3219752754296894559, 0.3333333333333333703, 0.3219752754296894559, 0.3333333333333333703, 0.3219752754296894559, 0.3333333333333333703, 0.3219752754296894559, 0.3333333333333333703, 0.3219752754296894559, 0.3333333333333333703, 0.3219752754296894559, 0.3333333333333333703, 0.3219752754296894559, 0.3333333333333333703, 0.3219752754296894559, 0.3333333333333333703, 0.3219752754296894559, 0.3333333333333333703, 0.3219752754296894559, 0.3333333333333333703, 0.3219752754296894559, 0.3333333333333333703, 0.3219752754296894559, 0.3333333333333333703, 0.3219752754296894559, 0.3333333333333333703, 0.3219752754296894559, 0.3333333333333333703, 0.3219752754296894559, 0.3333333333333333703, 0.3219752754296894559, 0.3333333333333333703, 0.3219752754296894559, 0.3333333333333333703, 0.3219752754296894559, 0.3333333333333333703, 0.3219752754296894559, 0.3333333333333333703, 0.3219752754296894559, 0.3333333333333333703, 0.3219752754296894559, 0.3333333333333333703, 0.3219752754296894559, 0.3333333333333333703, 0.3219752754296894559, 0.3333333333333333703, 0.3219752754296894559, 0.3333333333333333703, 0.3219752754296894559, 0.3333333333333333703, 0.3219752754296894559, 0.3333333333333333703, 0.3219752754296894559, 0.3333333333333333703, 0.3219752754296894559, 0.3333333333333333703, 0.3219752754296894559, 0.3333333333333333703, 0.3219752754296894559, 0.3333333333333333703, 0.3219752754296894559, 0.3333333333333333703, 0.3219752754296894559, 0.3333333333333333703, 0.3219752754296894559, 0.3333333333333333703, 0.3219752754296894559, 0.3333333333333333703, 0.3219752754296894559, 0.3333333333333333703, 0.3219752754296894559, 0.3333333333333333703, 0.3219752754296894559, 0.3333333333333333703),
 ( 0.3333333333333333703, 0.3219752754296894559, 0.3333333333333333703, 0.3219752754296894559, 0.3333333333333333703, 0.3219752754296894559, 0.3333333333333333703, 0.3219752754296894559, 0.3333333333333333703, 0.3219752754296894559, 0.3333333333333333703, 0.3219752754296894559, 0.3333333333333333703, 0.3219752754296894559, 0.3333333333333333703, 0.3219752754296894559, 0.3333333333333333703, 0.3219752754296894559, 0.3333333333333333703, 0.3219752754296894559, 0.3333333333333333703, 0.3219752754296894559, 0.3333333333333333703, 0.3219752754296894559, 0.3333333333333333703, 0.3219752754296894559, 0.3333333333333333703, 0.3219752754296894559, 0.3333333333333333703, 0.3219752754296894559, 0.3333333333333333703, 0.3219752754296894559, 0.3333333333333333703, 0.3219752754296894559, 0.3333333333333333703, 0.3219752754296894559, 0.3333333333333333703, 0.3219752754296894559, 0.3333333333333333703, 0.3219752754296894559, 0.3333333333333333703, 0.3219752754296894559, 0.3333333333333333703, 0.3219752754296894559, 0.3333333333333333703, 0.3219752754296894559, 0.3333333333333333703, 0.3219752754296894559, 0.3333333333333333703, 0.3219752754296894559, 0.3333333333333333703, 0.3219752754296894559, 0.3333333333333333703, 0.3219752754296894559, 0.3333333333333333703, 0.3219752754296894559, 0.3333333333333333703, 0.3219752754296894559, 0.3333333333333333703, 0.3219752754296894559, 0.3333333333333333703, 0.3219752754296894559, 0.3333333333333333703, 0.3219752754296894559, 0.3333333333333333703, 0.3219752754296894559, 0.3333333333333333703, 0.3219752754296894559, 0.3333333333333333703, 0.3219752754296894559, 0.3333333333333333703, 0.3219752754296894559, 0.3333333333333333703, 0.3219752754296894559, 0.3333333333333333703, 0.3219752754296894559, 0.3333333333333333703, 0.3219752754296894559, 0.3333333333333333703, 0.3219752754296894559, 0.3333333333333333703, 0.3219752754296894559, 0.3333333333333333703, 0.3219752754296894559, 0.3333333333333333703, 0.3219752754296894559, 0.3333333333333333703, 0.3219752754296894559, 0.3333333333333333703, 0.3219752754296894559, 0.3333333333333333703, 0.3219752754296894559, 0.3333333333333333703, 0.3219752754296894559, 0.3333333333333333703, 0.3219752754296894559, 0.3333333333333333703, 0.3219752754296894559, 0.3333333333333333703, 0.3219752754296894559, 0.3333333333333333703, 0.3219752754296894559, 0.3333333333333333703, 0.3219752754296894559, 0.3333333333333333703, 0.3219752754296894559, 0.3333333333333333703, 0.3219752754296894559, 0.3333333333333333703, 0.3219752754296894559, 0.3333333333333333703, 0.3219752754296894559, 0.3333333333333333703, 0.3219752754296894559, 0.3333333333333333703, 0.3219752754296894559, 0.3333333333333333703, 0.3219752754296894559, 0.3333333333333333703, 0.3219752754296894559, 0.3333333333333333703, 0.3219752754296894559, 0.3333333333333333703, 0.3219752754296894559, 0.3333333333333333703, 0.3219752754296894559, 0.3333333333333333703, 0.3219752754296894559, 0.3333333333333333703, 0.3219752754296894559, 0.3333333333333333703, 0.3219752754296894559, 0.3333333333333333703, 0.3219752754296894559, 0.3333333333333333703, 0.3219752754296894559, 0.3333333333333333703, 0.3219752754296894559, 0.3333333333333333703, 0.3219752754296894559, 0.3333333333333333703, 0.3219752754296894559, 0.3333333333333333703, 0.3219752754296894559, 0.3333333333333333703, 0.3219752754296894559, 0.3333333333333333703, 0.3219752754296894559, 0.3333333333333333703, 0.3219752754296894559, 0.3333333333333333703, 0.3219752754296894559, 0.3333333333333333703, 0.3219752754296894559, 0.3333333333333333703, 0.3219752754296894559, 0.3333333333333333703, 0.3219752754296894559, 0.3333333333333333703, 0.3219752754296894559, 0.3333333333333333703, 0.3219752754296894559, 0.3333333333333333703, 0.3219752754296894559, 0.3333333333333333703, 0.3219752754296894559, 0.3333333333333333703, 0.3219752754296894559, 0.3333333333333333703, 0.3219752754296894559, 0.3333333333333333703, 0.3219752754296894559, 0.3333333333333333703, 0.3219752754296894559, 0.3333333333333333703, 0.3219752754296894559, 0.3333333333333333703, 0.3219752754296894559, 0.3333333333333333703, 0.3219752754296894559, 0.3333333333333333703, 0.3219752754296894559, 0.3333333333333333703, 0.3219752754296894559, 0.3333333333333333703, 0.3219752754296894559, 0.3333333333333333703, 0.3219752754296894559, 0.3333333333333333703, 0.3219752754296894559, 0.3333333333333333703, 0.3219752754296894559, 0.3333333333333333703, 0.3219752754296894559, 0.3333333333333333703, 0.3219752754296894559, 0.3333333333333333703, 0.3219752754296894559, 0.3333333333333333703, 0.3219752754296894559, 0.3333333333333333703, 0.3219752754296894559, 0.3333333333333333703, 0.3219752754296894559, 0.3333333333333333703, 0.3219752754296894559, 0.3333333333333333703, 0.3219752754296894559, 0.3333333333333333703, 0.3219752754296894559, 0.3333333333333333703, 0.3219752754296894559, 0.3333333333333333703, 0.3219752754296894559, 0.3333333333333333703, 0.3219752754296894559, 0.3333333333333333703, 0.3219752754296894559, 0.3333333333333333703, 0.3219752754296894559, 0.3333333333333333703, 0.3219752754296894559, 0.3333333333333333703, 0.3219752754296894559, 0.3333333333333333703, 0.3219752754296894559, 0.3333333333333333703, 0.3219752754296894559, 0.3333333333333333703, 0.3219752754296894559, 0.3333333333333333703, 0.3219752754296894559, 0.3333333333333333703, 0.3219752754296894559, 0.3333333333333333703, 0.3219752754296894559, 0.3333333333333333703, 0.3219752754296894559, 0.3333333333333333703, 0.3219752754296894559, 0.3333333333333333703, 0.3219752754296894559, 0.3333333333333333703, 0.3219752754296894559, 0.3333333333333333703, 0.3219752754296894559, 0.3333333333333333703, 0.3219752754296894559, 0.3333333333333333703, 0.3219752754296894559, 0.3333333333333333703, 0.3219752754296894559, 0.3333333333333333703, 0.3219752754296894559, 0.3333333333333333703, 0.3219752754296894559, 0.3333333333333333703, 0.3219752754296894559, 0.3333333333333333703, 0.3219752754296894559, 0.3333333333333333703, 0.3219752754296894559, 0.3333333333333333703, 0.3219752754296894559, 0.3333333333333333703, 0.3219752754296894559, 0.3333333333333333703, 0.3219752754296894559, 0.3333333333333333703, 0.3219752754296894559, 0.3333333333333333703, 0.3219752754296894559, 0.3333333333333333703, 0.3219752754296894559, 0.3333333333333333703, 0.3219752754296894559, 0.3333333333333333703, 0.3219752754296894559, 0.3333333333333333703, 0.3219752754296894559, 0.3333333333333333703, 0.3219752754296894559, 0.3333333333333333703, 0.3219752754296894559, 0.3333333333333333703, 0.3219752754296894559, 0.3333333333333333703, 0.3219752754296894559, 0.3333333333333333703, 0.3219752754296894559, 0.3333333333333333703, 0.3219752754296894559, 0.3333333333333333703, 0.3219752754296894559, 0.3333333333333333703, 0.3219752754296894559, 0.3333333333333333703, 0.3219752754296894559, 0.3333333333333333703, 0.3219752754296894559, 0.3333333333333333703, 0.3219752754296894559, 0.3333333333333333703, 0.3219752754296894559, 0.3333333333333333703, 0.3219752754296894559, 0.3333333333333333703, 0.3219752754296894559, 0.3333333333333333703, 0.3219752754296894559, 0.3333333333333333703, 0.3219752754296894559, 0.3333333333333333703, 0.3219752754296894559, 0.3333333333333333703, 0.3219752754296894559, 0.3333333333333333703, 0.3219752754296894559, 0.3333333333333333703, 0.3219752754296894559, 0.3333333333333333703, 0.3219752754296894559, 0.3333333333333333703, 0.3219752754296894559, 0.3333333333333333703, 0.3219752754296894559, 0.3333333333333333703, 0.3219752754296894559, 0.3333333333333333703, 0.3219752754296894559, 0.3333333333333333703, 0.3219752754296894559, 0.3333333333333333703, 0.3219752754296894559, 0.3333333333333333703, 0.3219752754296894559, 0.3333333333333333703, 0.3219752754296894559, 0.3333333333333333703, 0.3219752754296894559, 0.3333333333333333703, 0.3219752754296894559, 0.3333333333333333703, 0.3219752754296894559, 0.3333333333333333703, 0.3219752754296894559, 0.3333333333333333703, 0.3219752754296894559, 0.3333333333333333703, 0.3219752754296894559, 0.3333333333333333703, 0.3219752754296894559, 0.3333333333333333703, 0.3219752754296894559, 0.3333333333333333703, 0.3219752754296894559, 0.3333333333333333703, 0.3219752754296894559, 0.3333333333333333703, 0.3219752754296894559, 0.3333333333333333703, 0.3219752754296894559, 0.3333333333333333703, 0.3219752754296894559, 0.3333333333333333703, 0.3219752754296894559, 0.3333333333333333703, 0.3219752754296894559, 0.3333333333333333703, 0.3219752754296894559, 0.3333333333333333703, 0.3219752754296894559, 0.3333333333333333703, 0.3219752754296894559, 0.3333333333333333703, 0.3219752754296894559, 0.3333333333333333703, 0.3219752754296894559, 0.3333333333333333703, 0.3219752754296894559, 0.3333333333333333703, 0.3219752754296894559, 0.3333333333333333703, 0.3219752754296894559, 0.3333333333333333703, 0.3219752754296894559, 0.3333333333333333703, 0.3219752754296894559, 0.3333333333333333703, 0.3219752754296894559, 0.3333333333333333703, 0.3219752754296894559, 0.3333333333333333703, 0.3219752754296894559, 0.3333333333333333703, 0.3219752754296894559, 0.3333333333333333703, 0.3219752754296894559, 0.3333333333333333703, 0.3219752754296894559, 0.3333333333333333703, 0.3219752754296894559, 0.3333333333333333703, 0.3219752754296894559, 0.3333333333333333703, 0.3219752754296894559, 0.3333333333333333703, 0.3219752754296894559, 0.3333333333333333703, 0.3219752754296894559, 0.3333333333333333703, 0.3219752754296894559, 0.3333333333333333703, 0.3219752754296894559, 0.3333333333333333703, 0.3219752754296894559, 0.3333333333333333703, 0.3219752754296894559, 0.3333333333333333703, 0.3219752754296894559, 0.3333333333333333703, 0.3219752754296894559, 0.3333333333333333703, 0.3219752754296894559, 0.3333333333333333703, 0.3219752754296894559, 0.3333333333333333703, 0.3219752754296894559, 0.3333333333333333703, 0.3219752754296894559, 0.3333333333333333703, 0.3219752754296894559, 0.3333333333333333703, 0.3219752754296894559, 0.3333333333333333703, 0.3219752754296894559, 0.3333333333333333703, 0.3219752754296894559, 0.3333333333333333703, 0.3219752754296894559, 0.3333333333333333703, 0.3219752754296894559, 0.3333333333333333703, 0.3219752754296894559, 0.3333333333333333703, 0.3219752754296894559, 0.3333333333333333703, 0.3219752754296894559, 0.3333333333333333703, 0.3219752754296894559, 0.3333333333333333703, 0.3219752754296894559, 0.3333333333333333703, 0.3219752754296894559, 0.3333333333333333703, 0.3219752754296894559, 0.3333333333333333703),
 ( 1.000000000000000000, 0.9659258262890683122, 1.000000000000000000, 0.9659258262890683122, 1.000000000000000000, 0.9659258262890683122, 1.000000000000000000, 0.9659258262890683122, 1.000000000000000000, 0.9659258262890683122, 1.000000000000000000, 0.9659258262890683122, 1.000000000000000000, 0.9659258262890683122, 1.000000000000000000, 0.9659258262890683122, 1.000000000000000000, 0.9659258262890683122, 1.000000000000000000, 0.9659258262890683122, 1.000000000000000000, 0.9659258262890683122, 1.000000000000000000, 0.9659258262890683122, 1.000000000000000000, 0.9659258262890683122, 1.000000000000000000, 0.9659258262890683122, 1.000000000000000000, 0.9659258262890683122, 1.000000000000000000, 0.9659258262890683122, 1.000000000000000000, 0.9659258262890683122, 1.000000000000000000, 0.9659258262890683122, 1.000000000000000000, 0.9659258262890683122, 1.000000000000000000, 0.9659258262890683122, 1.000000000000000000, 0.9659258262890683122, 1.000000000000000000, 0.9659258262890683122, 1.000000000000000000, 0.9659258262890683122, 1.000000000000000000, 0.9659258262890683122, 1.000000000000000000, 0.9659258262890683122, 1.000000000000000000, 0.9659258262890683122, 1.000000000000000000, 0.9659258262890683122, 1.000000000000000000, 0.9659258262890683122, 1.000000000000000000, 0.9659258262890683122, 1.000000000000000000, 0.9659258262890683122, 1.000000000000000000, 0.9659258262890683122, 1.000000000000000000, 0.9659258262890683122, 1.000000000000000000, 0.9659258262890683122, 1.000000000000000000, 0.9659258262890683122, 1.000000000000000000, 0.9659258262890683122, 1.000000000000000000, 0.9659258262890683122, 1.000000000000000000, 0.9659258262890683122, 1.000000000000000000, 0.9659258262890683122, 1.000000000000000000, 0.9659258262890683122, 1.000000000000000000, 0.9659258262890683122, 1.000000000000000000, 0.9659258262890683122, 1.000000000000000000, 0.9659258262890683122, 1.000000000000000000, 0.9659258262890683122, 1.000000000000000000, 0.9659258262890683122, 1.000000000000000000, 0.9659258262890683122, 1.000000000000000000, 0.9659258262890683122, 1.000000000000000000, 0.9659258262890683122, 1.000000000000000000, 0.9659258262890683122, 1.000000000000000000, 0.9659258262890683122, 1.000000000000000000, 0.9659258262890683122, 1.000000000000000000, 0.9659258262890683122, 1.000000000000000000, 0.9659258262890683122, 1.000000000000000000, 0.9659258262890683122, 1.000000000000000000, 0.9659258262890683122, 1.000000000000000000, 0.9659258262890683122, 1.000000000000000000, 0.9659258262890683122, 1.000000000000000000, 0.9659258262890683122, 1.000000000000000000, 0.9659258262890683122, 1.000000000000000000, 0.9659258262890683122, 1.000000000000000000, 0.9659258262890683122, 1.000000000000000000, 0.9659258262890683122, 1.000000000000000000, 0.9659258262890683122, 1.000000000000000000, 0.9659258262890683122, 1.000000000000000000, 0.9659258262890683122, 1.000000000000000000, 0.9659258262890683122, 1.000000000000000000, 0.9659258262890683122, 1.000000000000000000, 0.9659258262890683122, 1.000000000000000000, 0.9659258262890683122, 1.000000000000000000, 0.9659258262890683122, 1.000000000000000000, 0.9659258262890683122, 1.000000000000000000, 0.9659258262890683122, 1.000000000000000000, 0.9659258262890683122, 1.000000000000000000, 0.9659258262890683122, 1.000000000000000000, 0.9659258262890683122, 1.000000000000000000, 0.9659258262890683122, 1.000000000000000000, 0.9659258262890683122, 1.000000000000000000, 0.9659258262890683122, 1.000000000000000000, 0.9659258262890683122, 1.000000000000000000, 0.9659258262890683122, 1.000000000000000000, 0.9659258262890683122, 1.000000000000000000, 0.9659258262890683122, 1.000000000000000000, 0.9659258262890683122, 1.000000000000000000, 0.9659258262890683122, 1.000000000000000000, 0.9659258262890683122, 1.000000000000000000, 0.9659258262890683122, 1.000000000000000000, 0.9659258262890683122, 1.000000000000000000, 0.9659258262890683122, 1.000000000000000000, 0.9659258262890683122, 1.000000000000000000, 0.9659258262890683122, 1.000000000000000000, 0.9659258262890683122, 1.000000000000000000, 0.9659258262890683122, 1.000000000000000000, 0.9659258262890683122, 1.000000000000000000, 0.9659258262890683122, 1.000000000000000000, 0.9659258262890683122, 1.000000000000000000, 0.9659258262890683122, 1.000000000000000000, 0.9659258262890683122, 1.000000000000000000, 0.9659258262890683122, 1.000000000000000000, 0.9659258262890683122, 1.000000000000000000, 0.9659258262890683122, 1.000000000000000000, 0.9659258262890683122, 1.000000000000000000, 0.9659258262890683122, 1.000000000000000000, 0.9659258262890683122, 1.000000000000000000, 0.9659258262890683122, 1.000000000000000000, 0.9659258262890683122, 1.000000000000000000, 0.9659258262890683122, 1.000000000000000000, 0.9659258262890683122, 1.000000000000000000, 0.9659258262890683122, 1.000000000000000000, 0.9659258262890683122, 1.000000000000000000, 0.9659258262890683122, 1.000000000000000000, 0.9659258262890683122, 1.000000000000000000, 0.9659258262890683122, 1.000000000000000000, 0.9659258262890683122, 1.000000000000000000, 0.9659258262890683122, 1.000000000000000000, 0.9659258262890683122, 1.000000000000000000, 0.9659258262890683122, 1.000000000000000000, 0.9659258262890683122, 1.000000000000000000, 0.9659258262890683122, 1.000000000000000000, 0.9659258262890683122, 1.000000000000000000, 0.9659258262890683122, 1.000000000000000000, 0.9659258262890683122, 1.000000000000000000, 0.9659258262890683122, 1.000000000000000000, 0.9659258262890683122, 1.000000000000000000, 0.9659258262890683122, 1.000000000000000000, 0.9659258262890683122, 1.000000000000000000, 0.9659258262890683122, 1.000000000000000000, 0.9659258262890683122, 1.000000000000000000, 0.9659258262890683122, 1.000000000000000000, 0.9659258262890683122, 1.000000000000000000, 0.9659258262890683122, 1.000000000000000000, 0.9659258262890683122, 1.000000000000000000, 0.9659258262890683122, 1.000000000000000000, 0.9659258262890683122, 1.000000000000000000, 0.9659258262890683122, 1.000000000000000000, 0.9659258262890683122, 1.000000000000000000, 0.9659258262890683122, 1.000000000000000000, 0.9659258262890683122, 1.000000000000000000, 0.9659258262890683122, 1.000000000000000000, 0.9659258262890683122, 1.000000000000000000, 0.9659258262890683122, 1.000000000000000000, 0.9659258262890683122, 1.000000000000000000, 0.9659258262890683122, 1.000000000000000000, 0.9659258262890683122, 1.000000000000000000, 0.9659258262890683122, 1.000000000000000000, 0.9659258262890683122, 1.000000000000000000, 0.9659258262890683122, 1.000000000000000000, 0.9659258262890683122, 1.000000000000000000, 0.9659258262890683122, 1.000000000000000000, 0.9659258262890683122, 1.000000000000000000, 0.9659258262890683122, 1.000000000000000000, 0.9659258262890683122, 1.000000000000000000, 0.9659258262890683122, 1.000000000000000000, 0.9659258262890683122, 1.000000000000000000, 0.9659258262890683122, 1.000000000000000000, 0.9659258262890683122, 1.000000000000000000, 0.9659258262890683122, 1.000000000000000000, 0.9659258262890683122, 1.000000000000000000, 0.9659258262890683122, 1.000000000000000000, 0.9659258262890683122, 1.000000000000000000, 0.9659258262890683122, 1.000000000000000000, 0.9659258262890683122, 1.000000000000000000, 0.9659258262890683122, 1.000000000000000000, 0.9659258262890683122, 1.000000000000000000, 0.9659258262890683122, 1.000000000000000000, 0.9659258262890683122, 1.000000000000000000, 0.9659258262890683122, 1.000000000000000000, 0.9659258262890683122, 1.000000000000000000, 0.9659258262890683122, 1.000000000000000000, 0.9659258262890683122, 1.000000000000000000, 0.9659258262890683122, 1.000000000000000000, 0.9659258262890683122, 1.000000000000000000, 0.9659258262890683122, 1.000000000000000000, 0.9659258262890683122, 1.000000000000000000, 0.9659258262890683122, 1.000000000000000000, 0.9659258262890683122, 1.000000000000000000, 0.9659258262890683122, 1.000000000000000000, 0.9659258262890683122, 1.000000000000000000, 0.9659258262890683122, 1.000000000000000000, 0.9659258262890683122, 1.000000000000000000, 0.9659258262890683122, 1.000000000000000000, 0.9659258262890683122, 1.000000000000000000, 0.9659258262890683122, 1.000000000000000000, 0.9659258262890683122, 1.000000000000000000, 0.9659258262890683122, 1.000000000000000000, 0.9659258262890683122, 1.000000000000000000, 0.9659258262890683122, 1.000000000000000000, 0.9659258262890683122, 1.000000000000000000, 0.9659258262890683122, 1.000000000000000000, 0.9659258262890683122, 1.000000000000000000, 0.9659258262890683122, 1.000000000000000000, 0.9659258262890683122, 1.000000000000000000, 0.9659258262890683122, 1.000000000000000000, 0.9659258262890683122, 1.000000000000000000, 0.9659258262890683122, 1.000000000000000000, 0.9659258262890683122, 1.000000000000000000, 0.9659258262890683122, 1.000000000000000000, 0.9659258262890683122, 1.000000000000000000, 0.9659258262890683122, 1.000000000000000000, 0.9659258262890683122, 1.000000000000000000, 0.9659258262890683122, 1.000000000000000000, 0.9659258262890683122, 1.000000000000000000, 0.9659258262890683122, 1.000000000000000000, 0.9659258262890683122, 1.000000000000000000, 0.9659258262890683122, 1.000000000000000000, 0.9659258262890683122, 1.000000000000000000, 0.9659258262890683122, 1.000000000000000000, 0.9659258262890683122, 1.000000000000000000, 0.9659258262890683122, 1.000000000000000000, 0.9659258262890683122, 1.000000000000000000, 0.9659258262890683122, 1.000000000000000000, 0.9659258262890683122, 1.000000000000000000, 0.9659258262890683122, 1.000000000000000000, 0.9659258262890683122, 1.000000000000000000, 0.9659258262890683122, 1.000000000000000000, 0.9659258262890683122, 1.000000000000000000, 0.9659258262890683122, 1.000000000000000000, 0.9659258262890683122, 1.000000000000000000, 0.9659258262890683122, 1.000000000000000000, 0.9659258262890683122, 1.000000000000000000, 0.9659258262890683122, 1.000000000000000000, 0.9659258262890683122, 1.000000000000000000, 0.9659258262890683122, 1.000000000000000000, 0.9659258262890683122, 1.000000000000000000, 0.9659258262890683122, 1.000000000000000000, 0.9659258262890683122, 1.000000000000000000, 0.9659258262890683122, 1.000000000000000000, 0.9659258262890683122, 1.000000000000000000, 0.9659258262890683122, 1.000000000000000000, 0.9659258262890683122, 1.000000000000000000) ) ) 
 REPRESENTATION_ITEM ( '' )  SURFACE ( )  );
#158562 = CARTESIAN_POINT ( 'NONE',  ( -9.564922557960796823, -16.46253265017161027, 57.08224293864769550 ) ) ;
#158563 = CARTESIAN_POINT ( 'NONE',  ( -5.823673210054431948, 21.52544592524334988, 67.70942372801901854 ) ) ;
#158564 = CARTESIAN_POINT ( 'NONE',  ( -19.02544592524342804, 5.153800228976336051, 46.04057627198101699 ) ) ;
#158565 = CARTESIAN_POINT ( 'NONE',  ( -13.97604488694527625, -13.89961937509977652, 71.87390960531433848 ) ) ;
#158566 = CARTESIAN_POINT ( 'NONE',  ( -12.06949235617756955, 12.14591786802309770, 105.6239096053143669 ) ) ;
#158567 = CARTESIAN_POINT ( 'NONE',  ( 19.02544592524343514, -5.153800228976328945, 113.5405762719810241 ) ) ;
#158568 = CARTESIAN_POINT ( 'NONE',  ( 14.29746914071049879, -8.314922557960816363, 48.33224293864770260 ) ) ;
#158569 = CARTESIAN_POINT ( 'NONE',  ( -4.483927247898539470, -16.52544592524342804, 112.2905762719810241 ) ) ;
#158570 = CARTESIAN_POINT ( 'NONE',  ( 8.314922557960818139, 14.29746914071049879, 74.58224293864768129 ) ) ;
#158571 = CARTESIAN_POINT ( 'NONE',  ( -5.719274019375978568, 21.55341960407610458, 85.20724293864770971 ) ) ;
#158572 = CARTESIAN_POINT ( 'NONE',  ( -0.05219959533937732626, 21.53943276465977519, 32.50109039468568284 ) ) ;
#158573 = CARTESIAN_POINT ( 'NONE',  ( 27.79722099587822370, -7.618187661584347126, 161.3616444162216226 ) ) ;
#158574 = CARTESIAN_POINT ( 'NONE',  ( 16.55341960407618274, -4.379528057220086978, 31.04275706135234714 ) ) ;
#158575 = CARTESIAN_POINT ( 'NONE',  ( 18.62759615963271287, -10.81492255796078972, 83.33224293864769550 ) ) ;
#158576 = CARTESIAN_POINT ( 'NONE',  ( -18.67979575497193778, 10.72451020669871902, 103.3344237280190043 ) ) ;
#158577 = CARTESIAN_POINT ( 'NONE',  ( -9.564922557960796823, -16.46253265017161027, 92.08224293864769550 ) ) ;
#158578 = CARTESIAN_POINT ( 'NONE',  ( 15.72974639402176855, 15.80617190586768217, 46.87609039468568994 ) ) ;
#158579 = EDGE_CURVE ( 'NONE', #187465, #81647, #17495, .T. ) ;
#158580 = CARTESIAN_POINT ( 'NONE',  ( 21.52544592524344225, -5.823673210054117533, 23.54057627198102765 ) ) ;
#158581 = CARTESIAN_POINT ( 'NONE',  ( 16.55341960407618274, -4.379528057220086978, 101.0427570613523756 ) ) ;
#158583 = CARTESIAN_POINT ( 'NONE',  ( -15.80617190586768217, 15.72974639402176855, 83.12609039468568994 ) ) ;
#158582 = CARTESIAN_POINT ( 'NONE',  ( 5.719274019375673035, 21.55341960407619339, 47.29275706135234003 ) ) ;
#158584 = CARTESIAN_POINT ( 'NONE',  ( 10.72451020669871369, 18.67979575497193778, 112.0844237280190185 ) ) ;
#158585 = CARTESIAN_POINT ( 'NONE',  ( -4.483927247898782831, 16.52544592524335698, 72.70942372801901854 ) ) ;
#158586 = CARTESIAN_POINT ( 'NONE',  ( -18.67979575497193778, 10.72451020669871902, 43.33442372801901143 ) ) ;
#158587 = CARTESIAN_POINT ( 'NONE',  ( 13.97604488694527802, 13.89961937509977652, 39.37390960531435269 ) ) ;
#158588 = CARTESIAN_POINT ( 'NONE',  ( 5.719274019375673035, 21.55341960407619339, 97.29275706135234714 ) ) ;
#158589 = CARTESIAN_POINT ( 'NONE',  ( -19.05341960407611168, -5.049401038298163336, 106.4572429386476955 ) ) ;
#158590 = CARTESIAN_POINT ( 'NONE',  ( 21.55341960407610458, 5.719274019375980345, 98.95724293864770971 ) ) ;
#158592 = CARTESIAN_POINT ( 'NONE',  ( -10.81492255796078084, -18.62759615963271287, 62.08224293864769550 ) ) ;
#158591 = CARTESIAN_POINT ( 'NONE',  ( 18.56101223717332616, 5.499999999999948486, 83.94978406935679516 ) ) ;
#158594 = CARTESIAN_POINT ( 'NONE',  ( -12.14591786802309592, -12.06949235617757132, 46.87390960531435979 ) ) ;
#158593 = CARTESIAN_POINT ( 'NONE',  ( 16.52544592524335698, 4.483927247898782831, 51.45942372801901854 ) ) ;
#158595 = CARTESIAN_POINT ( 'NONE',  ( 19.54388014595539858, -5.500000000000015099, 102.3151885665635774 ) ) ;
#158596 = CARTESIAN_POINT ( 'NONE',  ( 13.89961937509957401, 13.97604488694547697, 96.87609039468566152 ) ) ;
#158597 = CARTESIAN_POINT ( 'NONE',  ( 0.000000000000000000, 0.000000000000000000, 0.000000000000000000 ) ) ;
#158598 = CARTESIAN_POINT ( 'NONE',  ( 8.314922557961029526, -14.29746914071037800, 25.41775706135235779 ) ) ;
#158599 = CARTESIAN_POINT ( 'NONE',  ( -0.05219959533907301413, -21.53943276465977519, 102.4989096053143811 ) ) ;
#158600 = CARTESIAN_POINT ( 'NONE',  ( -10.72451020669898014, 18.67979575497178502, 80.41557627198103830 ) ) ;
#158601 = CARTESIAN_POINT ( 'NONE',  ( -5.823673210054116645, -21.52544592524344225, 22.29057627198102765 ) ) ;
#158602 = CARTESIAN_POINT ( 'NONE',  ( 4.483927247898790824, -16.52544592524335698, 45.20942372801901854 ) ) ;
#158603 = CARTESIAN_POINT ( 'NONE',  ( 9.474510206698971260, -16.51473224551069308, 77.91557627198103830 ) ) ;
#158605 = CARTESIAN_POINT ( 'NONE',  ( 13.89961937509957401, 13.97604488694547697, 96.87609039468566152 ) ) ;
#158604 = CARTESIAN_POINT ( 'NONE',  ( -18.67979575497193778, 10.72451020669871902, 33.33442372801900433 ) ) ;
#158606 = CARTESIAN_POINT ( 'NONE',  ( -19.03943276465977164, 0.05219959533909376836, 111.2489096053143669 ) ) ;
#158607 = CARTESIAN_POINT ( 'NONE',  ( 13.89961937509977652, -13.97604488694527269, 88.12390960531438111 ) ) ;
#158608 = CARTESIAN_POINT ( 'NONE',  ( 15.72974639402199770, -15.80617190586745480, 88.12390960531436690 ) ) ;
#158609 = CARTESIAN_POINT ( 'NONE',  ( -5.049401038298153566, 19.05341960407611168, 65.20724293864765286 ) ) ;
#158610 = DIRECTION ( 'NONE',  ( -0.5000000000000049960, -0.4999999999999962252, 0.7071067811865466846 ) ) ;
#158611 = CARTESIAN_POINT ( 'NONE',  ( -4.379528057220328563, 16.55341960407611168, 75.20724293864769550 ) ) ;
#158612 = CARTESIAN_POINT ( 'NONE',  ( -21.55341960407610458, -5.719274019375992779, 26.45724293864768839 ) ) ;
#158613 = CARTESIAN_POINT ( 'NONE',  ( 4.999999999999997335, 0.000000000000000000, 4.250000000000000000 ) ) ;
#158614 = CARTESIAN_POINT ( 'NONE',  ( 5.823673210054125526, 21.52544592524343514, 104.7905762719810241 ) ) ;
#158615 = CARTESIAN_POINT ( 'NONE',  ( -5.153800228976607833, 19.02544592524334988, 62.70942372801899722 ) ) ;
#158616 = CARTESIAN_POINT ( 'NONE',  ( 16.51473224551069308, 9.474510206698969483, 109.1655762719810383 ) ) ;
#158617 = DIRECTION ( 'NONE',  ( 0.000000000000000000, 0.000000000000000000, 1.000000000000000000 ) ) ;
#158618 = CARTESIAN_POINT ( 'NONE',  ( -10.72451020669898014, 18.67979575497178502, 55.41557627198102409 ) ) ;
#158619 = CARTESIAN_POINT ( 'NONE',  ( 13.97604488694527802, 13.89961937509977652, 84.37390960531433848 ) ) ;
#158620 = CARTESIAN_POINT ( 'NONE',  ( 18.62759615963255655, 10.81492255796105972, 76.66775706135234714 ) ) ;
#158621 = CARTESIAN_POINT ( 'NONE',  ( -19.03943276465977164, 0.05219959533909376836, 46.24890960531435979 ) ) ;
#158622 = CARTESIAN_POINT ( 'NONE',  ( 12.14591786802309770, 12.06949235617756955, 84.37390960531438111 ) ) ;
#158623 = CARTESIAN_POINT ( 'NONE',  ( -14.34966873604972548, 8.224510206698743886, 33.33442372801900433 ) ) ;
#158624 = CARTESIAN_POINT ( 'NONE',  ( -5.823673210054431948, 21.52544592524334988, 67.70942372801901854 ) ) ;
#158625 = EDGE_LOOP ( 'NONE', ( #72457, #144917, #53915 ) ) ;
#158626 = CARTESIAN_POINT ( 'NONE',  ( 13.97604488694548053, -13.89961937509957401, 20.62609039468567573 ) ) ;
#158627 = CARTESIAN_POINT ( 'NONE',  ( 9.564922557961047289, -16.46253265017146816, 80.41775706135234714 ) ) ;
#158628 = CARTESIAN_POINT ( 'NONE',  ( -17.72662750342728444, -5.500000000000021316, 91.40179492283749596 ) ) ;
#158629 = CARTESIAN_POINT ( 'NONE',  ( 18.67979575497194134, -10.72451020669871369, 40.83442372801901854 ) ) ;
#158630 = CARTESIAN_POINT ( 'NONE',  ( -5.000000000000000888, -130.0000000000000000, -15.00000000000000000 ) ) ;
#158631 = CARTESIAN_POINT ( 'NONE',  ( -16.46253265017146816, -9.564922557961047289, 29.16775706135232937 ) ) ;
#158632 = CARTESIAN_POINT ( 'NONE',  ( 19.05341960407611168, 5.049401038298154454, 53.95724293864770260 ) ) ;
#158633 = CARTESIAN_POINT ( 'NONE',  ( -16.46253265017146816, -9.564922557961047289, 24.16775706135233648 ) ) ;
#158634 = CARTESIAN_POINT ( 'NONE',  ( -12.06949235617739369, -12.14591786802326823, 109.3760903946857042 ) ) ;
#158636 = CARTESIAN_POINT ( 'NONE',  ( 18.67979575497194134, -10.72451020669871369, 90.83442372801901854 ) ) ;
#158635 = CARTESIAN_POINT ( 'NONE',  ( 9.564922557960805705, 16.46253265017160317, 104.5822429386476955 ) ) ;
#158637 = CARTESIAN_POINT ( 'NONE',  ( 11.40812507854755253, -35.11059874428192273, -4.024999997268814411 ) ) ;
#158638 = CARTESIAN_POINT ( 'NONE',  ( -17.50000000000149925, -3.254303733634381857, 34.97604106928617540 ) ) ;
#158639 = CARTESIAN_POINT ( 'NONE',  ( 18.62759615963255655, 10.81492255796105972, 86.66775706135234714 ) ) ;
#158640 = DIRECTION ( 'NONE',  ( -0.000000000000000000, -0.000000000000000000, 1.000000000000000000 ) ) ;
#158641 = CARTESIAN_POINT ( 'NONE',  ( -13.89961937509977652, 13.97604488694528158, 105.6239096053143527 ) ) ;
#158642 = CARTESIAN_POINT ( 'NONE',  ( 19.38985940809749309, -32.68077955211924035, -24.99999999999992895 ) ) ;
#158643 = CARTESIAN_POINT ( 'NONE',  ( -5.153800228976328057, -19.02544592524343514, 37.29057627198102409 ) ) ;
#158644 = CARTESIAN_POINT ( 'NONE',  ( -15.72974639402197994, 15.80617190586746368, 60.62390960531437401 ) ) ;
#158645 = CARTESIAN_POINT ( 'NONE',  ( -4.483927247898539470, -16.52544592524342804, 27.29057627198103120 ) ) ;
#158647 = CARTESIAN_POINT ( 'NONE',  ( 9.564922557960805705, 16.46253265017160317, 79.58224293864769550 ) ) ;
#158646 = CARTESIAN_POINT ( 'NONE',  ( -0.05219959533910754901, -16.53943276465976808, 92.49890960531436690 ) ) ;
#158648 = CARTESIAN_POINT ( 'NONE',  ( -16.46253265017146816, -9.564922557961047289, 19.16775706135233293 ) ) ;
#158649 = EDGE_CURVE ( 'NONE', #199255, #15160, #53918, .T. ) ;
#158650 = CARTESIAN_POINT ( 'NONE',  ( 9.564922557960805705, 16.46253265017160317, 39.58224293864768839 ) ) ;
#158651 = CARTESIAN_POINT ( 'NONE',  ( 12.06949235617757843, -12.14591786802309237, 108.1239096053143811 ) ) ;
#158652 = CARTESIAN_POINT ( 'NONE',  ( -18.67979575497193778, 10.72451020669871902, 53.33442372801901854 ) ) ;
#158653 = CARTESIAN_POINT ( 'NONE',  ( -21.52544592524343514, 5.823673210054127303, 81.04057627198102409 ) ) ;
#158654 = CARTESIAN_POINT ( 'NONE',  ( -19.05341960407617563, 5.049401038297882671, 63.54275706135234003 ) ) ;
#158655 = CARTESIAN_POINT ( 'NONE',  ( -24.48769569731326357, -31.64124327689851768, -7.859335325863215260 ) ) ;
#158656 = CARTESIAN_POINT ( 'NONE',  ( 13.97604488694527802, 13.89961937509977652, 114.3739096053143669 ) ) ;
#158657 = CARTESIAN_POINT ( 'NONE',  ( -12.14591786802309592, -12.06949235617757132, 76.87390960531439532 ) ) ;
#158658 = CARTESIAN_POINT ( 'NONE',  ( -13.89961937509957401, -13.97604488694547875, 39.37609039468566152 ) ) ;
#158659 = CARTESIAN_POINT ( 'NONE',  ( -16.51473224551069308, -9.474510206698971260, 66.66557627198102409 ) ) ;
#158660 = CARTESIAN_POINT ( 'NONE',  ( -4.379528057220328563, 16.55341960407611168, 60.20724293864768839 ) ) ;
#158661 = CARTESIAN_POINT ( 'NONE',  ( -9.474510206698720793, -16.51473224551083518, 74.58442372801900433 ) ) ;
#158662 = CARTESIAN_POINT ( 'NONE',  ( 17.05116617787826172, 6.768360034955700044, 33.84324446740802728 ) ) ;
#158663 = CARTESIAN_POINT ( 'NONE',  ( -10.72451020669898014, 18.67979575497178502, 40.41557627198103120 ) ) ;
#158664 = ORIENTED_EDGE ( 'NONE', *, *, #153149, .F. ) ;
#158665 = EDGE_CURVE ( 'NONE', #12092, #112608, #32201, .T. ) ;
#158666 = CARTESIAN_POINT ( 'NONE',  ( -8.224510206698948167, 14.34966873604960824, 95.41557627198102409 ) ) ;
#158667 = FACE_OUTER_BOUND ( 'NONE', #82001, .T. ) ;
#158669 = CARTESIAN_POINT ( 'NONE',  ( -21.55341960407610458, -5.719274019375992779, 56.45724293864768839 ) ) ;
#158668 = CARTESIAN_POINT ( 'NONE',  ( 19.05341960407611168, 5.049401038298154454, 53.95724293864770260 ) ) ;
#158670 = CARTESIAN_POINT ( 'NONE',  ( -5.153800228976328057, -19.02544592524343514, 37.29057627198102409 ) ) ;
#158672 = CARTESIAN_POINT ( 'NONE',  ( -13.89961937509977652, 13.97604488694528158, 80.62390960531436690 ) ) ;
#158671 = CARTESIAN_POINT ( 'NONE',  ( 16.55341960407618274, -4.379528057220086978, 81.04275706135236135 ) ) ;
#158673 = CARTESIAN_POINT ( 'NONE',  ( -9.474510206698720793, -16.51473224551083518, 54.58442372801899722 ) ) ;
#158674 = CARTESIAN_POINT ( 'NONE',  ( -21.55341960407619339, 5.719274019375674811, 63.54275706135234003 ) ) ;
#158675 = ORIENTED_EDGE ( 'NONE', *, *, #11833, .T. ) ;
#158676 = CARTESIAN_POINT ( 'NONE',  ( 21.53943276465977519, -0.05219959533907433946, 48.74890960531435979 ) ) ;
#158677 = CARTESIAN_POINT ( 'NONE',  ( -5.153800228976328057, -19.02544592524343514, 27.29057627198103120 ) ) ;
#158678 = CARTESIAN_POINT ( 'NONE',  ( -12.14591786802326823, 12.06949235617739902, 93.12609039468568994 ) ) ;
#158679 = CARTESIAN_POINT ( 'NONE',  ( -0.05219959533936034679, 19.03943276465977164, 102.5010903946856757 ) ) ;
#158680 = CARTESIAN_POINT ( 'NONE',  ( 2.400000000000000799, 0.000000000000000000, 0.000000000000000000 ) ) ;
#158681 = CARTESIAN_POINT ( 'NONE',  ( 18.89770734986044687, 5.500000000000083489, 76.60214472496639360 ) ) ;
#158682 = CARTESIAN_POINT ( 'NONE',  ( -15.80617190586768217, 15.72974639402176855, 93.12609039468568994 ) ) ;
#158683 = CARTESIAN_POINT ( 'NONE',  ( -12.06949235617756955, 12.14591786802309770, 40.62390960531435269 ) ) ;
#158684 = CARTESIAN_POINT ( 'NONE',  ( -8.314922557960811034, -14.29746914071050412, 72.08224293864769550 ) ) ;
#158685 = CARTESIAN_POINT ( 'NONE',  ( -18.67979575497178146, -10.72451020669898902, 96.66557627198102409 ) ) ;
#158686 = CARTESIAN_POINT ( 'NONE',  ( -18.62759615963270932, 10.81492255796079327, 90.83224293864769550 ) ) ;
#158687 = CARTESIAN_POINT ( 'NONE',  ( 17.12812012977027720, -6.668231424565983723, 96.14051240676860743 ) ) ;
#158688 = CARTESIAN_POINT ( 'NONE',  ( 15.72974639402199770, -15.80617190586745480, 28.12390960531435979 ) ) ;
#158689 = CARTESIAN_POINT ( 'NONE',  ( -14.34966873604972548, 8.224510206698743886, 68.33442372801900433 ) ) ;
#158690 = CARTESIAN_POINT ( 'NONE',  ( -12.06949235617756955, 12.14591786802309770, 80.62390960531438111 ) ) ;
#158691 = CARTESIAN_POINT ( 'NONE',  ( 9.564922557960805705, 16.46253265017160317, 39.58224293864768839 ) ) ;
#158692 = CARTESIAN_POINT ( 'NONE',  ( 34.74703293042576746, -1.945922946419409216, 52.24735972161444408 ) ) ;
#158693 = CARTESIAN_POINT ( 'NONE',  ( -4.379528057220086978, -16.55341960407618274, 94.79275706135234714 ) ) ;
#158694 = CARTESIAN_POINT ( 'NONE',  ( -5.823673210054116645, -21.52544592524344225, 112.2905762719810241 ) ) ;
#158695 = CARTESIAN_POINT ( 'NONE',  ( 19.02544592524343514, -5.153800228976328945, 78.54057627198099567 ) ) ;
#158696 = CARTESIAN_POINT ( 'NONE',  ( -18.62759615963255300, -10.81492255796106328, 59.16775706135234714 ) ) ;
#158697 = CARTESIAN_POINT ( 'NONE',  ( -16.46253265017160317, 9.564922557960807481, 105.8322429386476955 ) ) ;
#158698 = CARTESIAN_POINT ( 'NONE',  ( -15.50653001719018143, -40.92458772716549475, -21.39878705119700797 ) ) ;
#158699 = ORIENTED_EDGE ( 'NONE', *, *, #184816, .T. ) ;
#158700 = CARTESIAN_POINT ( 'NONE',  ( -10.81492255796105439, 18.62759615963255655, 47.91775706135234714 ) ) ;
#158702 = CARTESIAN_POINT ( 'NONE',  ( 13.89961937509977652, -13.97604488694527269, 23.12390960531436335 ) ) ;
#158701 = CARTESIAN_POINT ( 'NONE',  ( -9.564922557960796823, -16.46253265017161027, 37.08224293864768839 ) ) ;
#158703 = CARTESIAN_POINT ( 'NONE',  ( -13.89961937509957401, -13.97604488694547875, 69.37609039468564731 ) ) ;
#158704 = CARTESIAN_POINT ( 'NONE',  ( -15.80617190586768217, 15.72974639402176855, 28.12609039468568284 ) ) ;
#158705 = CARTESIAN_POINT ( 'NONE',  ( -13.97604488694547697, 13.89961937509957934, 58.12609039468566863 ) ) ;
#158706 = CARTESIAN_POINT ( 'NONE',  ( 19.02544592524343514, -5.153800228976328945, 23.54057627198102054 ) ) ;
#158707 = CARTESIAN_POINT ( 'NONE',  ( -4.483927247898782831, 16.52544592524335698, 97.70942372801904696 ) ) ;
#158708 = CARTESIAN_POINT ( 'NONE',  ( 19.02544592524334988, 5.153800228976608722, 66.45942372801899012 ) ) ;
#158709 = CARTESIAN_POINT ( 'NONE',  ( 8.224510206698953496, -14.34966873604960469, 27.91557627198103830 ) ) ;
#158710 = CARTESIAN_POINT ( 'NONE',  ( -19.24578484527059175, -180.9428398739492252, -4.999999999999999112 ) ) ;
#158711 = CARTESIAN_POINT ( 'NONE',  ( 0.05219959533909260263, 19.03943276465977164, 79.99890960531436690 ) ) ;
#158712 = CARTESIAN_POINT ( 'NONE',  ( -21.53943276465977519, -0.05219959533937600094, 88.75109039468567573 ) ) ;
#158713 = CARTESIAN_POINT ( 'NONE',  ( 21.53943276465977519, 0.05219959533937863772, 106.2510903946856757 ) ) ;
#158714 = CARTESIAN_POINT ( 'NONE',  ( -37.99626262588766679, 2.428612866367529932E-14, -4.002157773949823749 ) ) ;
#158715 = CARTESIAN_POINT ( 'NONE',  ( -10.81492255796105439, 18.62759615963255655, 72.91775706135234714 ) ) ;
#158716 = CARTESIAN_POINT ( 'NONE',  ( -8.224510206698735004, -14.34966873604973081, 34.58442372801900433 ) ) ;
#158717 = CARTESIAN_POINT ( 'NONE',  ( 16.51473224551069308, 9.474510206698969483, 74.16557627198103830 ) ) ;
#158718 = CARTESIAN_POINT ( 'NONE',  ( -21.52544592524343514, 5.823673210054127303, 31.04057627198102409 ) ) ;
#158719 = CARTESIAN_POINT ( 'NONE',  ( 27.73933785331498569, 2.768321779492822058E-14, 139.8750000027311842 ) ) ;
#158720 = CARTESIAN_POINT ( 'NONE',  ( 13.89961937509977652, -13.97604488694527269, 63.12390960531435979 ) ) ;
#158721 = CARTESIAN_POINT ( 'NONE',  ( -17.26058549869106429, 6.457015423128241949, 98.62254162523932166 ) ) ;
#158722 = CARTESIAN_POINT ( 'NONE',  ( -5.049401038297874678, -19.05341960407617918, 74.79275706135231871 ) ) ;
#158723 = B_SPLINE_CURVE_WITH_KNOTS ( 'NONE', 3,
 ( #134720, #198361, #196403, #121505, #150882, #44681, #181228, #42704, #142, #58846, #153835, #104365, #122497, #106334, #12377, #74039, #135710, #168020, #29516, #120513, #182205, #199358, #43689, #105351, #167038, #168994, #28540, #151859, #164632, #54449, #179816, #39278, #118128, #84763, #70622, #26127, #41286, #83766, #132288, #161624 ),
 .UNSPECIFIED., .F., .F.,
 ( 4, 2, 2, 2, 2, 2, 2, 2, 2, 2, 2, 2, 2, 2, 2, 2, 2, 2, 2, 4 ),
 ( 0.000000000000000000, 0.001704564650157686578, 0.003409129300315373156, 0.006818258600630746312, 0.01022738790094612077, 0.01193195255110380756, 0.01363651720126149262, 0.02045477580189224154, 0.02215934045204992833, 0.02386390510220762207, 0.02727303440252299219, 0.03068216370283836578, 0.03238672835299604563, 0.03409129300315372202, 0.03750042230346907479, 0.04090955160378442756, 0.04772781020441514005, 0.04943237485457282337, 0.05113693950473050670, 0.05454606880504585253 ),
 .UNSPECIFIED. ) ;
#158724 = CARTESIAN_POINT ( 'NONE',  ( -0.05219959533909027116, -19.03943276465977164, 102.4989096053143669 ) ) ;
#158725 = CARTESIAN_POINT ( 'NONE',  ( 5.719274019375673035, 21.55341960407619339, 102.2927570613523613 ) ) ;
#158726 = CARTESIAN_POINT ( 'NONE',  ( -4.379528057220328563, 16.55341960407611168, 80.20724293864769550 ) ) ;
#158727 = CARTESIAN_POINT ( 'NONE',  ( -21.53943276465977519, 0.05219959533907696930, 46.24890960531435979 ) ) ;
#158728 = CARTESIAN_POINT ( 'NONE',  ( 18.62759615963271287, -10.81492255796078972, 43.33224293864769550 ) ) ;
#158729 = CARTESIAN_POINT ( 'NONE',  ( 14.34966873604960469, 8.224510206698951720, 99.16557627198100988 ) ) ;
#158730 = CARTESIAN_POINT ( 'NONE',  ( -1.461410587780170633, -7.989781499195990122, -62.12232043736380405 ) ) ;
#158731 = CARTESIAN_POINT ( 'NONE',  ( 13.97604488694548053, -13.89961937509957401, 60.62609039468564731 ) ) ;
#158732 = CARTESIAN_POINT ( 'NONE',  ( 4.379528057220339221, -16.55341960407611168, 22.70724293864769194 ) ) ;
#158733 = CARTESIAN_POINT ( 'NONE',  ( -13.97604488694527625, -13.89961937509977652, 101.8739096053143811 ) ) ;
#158734 = CARTESIAN_POINT ( 'NONE',  ( -5.719274019375665041, -21.55341960407619695, 69.79275706135234714 ) ) ;
#158735 = CARTESIAN_POINT ( 'NONE',  ( -5.823673210054116645, -21.52544592524344225, 57.29057627198103120 ) ) ;
#158736 = B_SPLINE_CURVE_WITH_KNOTS ( 'NONE', 3,
 ( #26151, #196007, #69638, #55467, #147487, #56471, #118150, #27149, #120127, #73649, #148487, #88796, #165651, #132312, #9978, #71638, #100958, #119152, #180834, #131304, #8978, #135321, #70646, #150489, #85801, #41311, #117137, #194004, #179840, #196993, #133305, #194994 ),
 .UNSPECIFIED., .F., .F.,
 ( 4, 2, 2, 2, 2, 2, 2, 2, 2, 2, 2, 2, 2, 2, 2, 4 ),
 ( 4.563344992840995729E-17, 0.0003712461730037242913, 0.0007424923460074029377, 0.001113738519011081476, 0.001484984692014760122, 0.002227477038022111343, 0.002598723211025783918, 0.002969969384029456493, 0.003341215557033128634, 0.003712461730036799908, 0.004083707903040472917, 0.004454954076044144624, 0.004826200249047817199, 0.005197446422051488907, 0.005568692595055160614, 0.005939938768058833189 ),
 .UNSPECIFIED. ) ;
#158737 = CARTESIAN_POINT ( 'NONE',  ( -18.62759615963255300, -10.81492255796106328, 49.16775706135234003 ) ) ;
#158738 = CARTESIAN_POINT ( 'NONE',  ( 10.81492255796078972, 18.62759615963270932, 99.58224293864770971 ) ) ;
#158739 = CARTESIAN_POINT ( 'NONE',  ( -15.80617190586768217, 15.72974639402176855, 38.12609039468567573 ) ) ;
#158740 = CARTESIAN_POINT ( 'NONE',  ( 0.05219959533910956823, 16.53943276465976808, 114.9989096053143669 ) ) ;
#158741 = CARTESIAN_POINT ( 'NONE',  ( -5.049401038298153566, 19.05341960407611168, 85.20724293864766707 ) ) ;
#158742 = CARTESIAN_POINT ( 'NONE',  ( 16.55341960407611168, 4.379528057220329451, 98.95724293864770971 ) ) ;
#158743 = CARTESIAN_POINT ( 'NONE',  ( 5.153800228976335163, 19.02544592524342804, 109.7905762719810099 ) ) ;
#158744 = CARTESIAN_POINT ( 'NONE',  ( 4.379528057220339221, -16.55341960407611168, 57.70724293864770260 ) ) ;
#158745 = CARTESIAN_POINT ( 'NONE',  ( 16.55341960407618274, -4.379528057220086978, 111.0427570613523613 ) ) ;
#158746 = CARTESIAN_POINT ( 'NONE',  ( -16.51473224551069308, -9.474510206698971260, 46.66557627198102409 ) ) ;
#158747 = CARTESIAN_POINT ( 'NONE',  ( -19.03943276465977164, 0.05219959533909376836, 21.24890960531436335 ) ) ;
#158748 = CARTESIAN_POINT ( 'NONE',  ( -18.62759615963270932, 10.81492255796079327, 35.83224293864768839 ) ) ;
#158749 = CARTESIAN_POINT ( 'NONE',  ( -5.049401038297874678, -19.05341960407617918, 19.79275706135233293 ) ) ;
#158751 = CARTESIAN_POINT ( 'NONE',  ( 16.53943276465976808, -0.05219959533910856209, 38.74890960531435979 ) ) ;
#158750 = CARTESIAN_POINT ( 'NONE',  ( -16.61371651742603461, -7.165104196376044676, 41.14584930007004004 ) ) ;
#158752 = CARTESIAN_POINT ( 'NONE',  ( 10.81492255796106328, -18.62759615963255655, 45.41775706135234003 ) ) ;
#158753 = CARTESIAN_POINT ( 'NONE',  ( 19.02544592524343514, -5.153800228976328945, 113.5405762719810241 ) ) ;
#158754 = CARTESIAN_POINT ( 'NONE',  ( 14.34966873604972726, -8.224510206698740333, 55.83442372801901854 ) ) ;
#158755 = CARTESIAN_POINT ( 'NONE',  ( -13.89961937509957401, -13.97604488694547875, 64.37609039468567573 ) ) ;
#158756 = CARTESIAN_POINT ( 'NONE',  ( -4.483927247898539470, -16.52544592524342804, 32.29057627198102409 ) ) ;
#158757 = CARTESIAN_POINT ( 'NONE',  ( 4.483927247898790824, -16.52544592524335698, 105.2094237280190328 ) ) ;
#158758 = CARTESIAN_POINT ( 'NONE',  ( 9.564922557960805705, 16.46253265017160317, 44.58224293864769550 ) ) ;
#158759 = CARTESIAN_POINT ( 'NONE',  ( 13.89961937509977652, -13.97604488694527269, 68.12390960531436690 ) ) ;
#158760 = CARTESIAN_POINT ( 'NONE',  ( 5.049401038298161559, -19.05341960407611168, 22.70724293864769194 ) ) ;
#158761 = CARTESIAN_POINT ( 'NONE',  ( 10.81492255796106328, -18.62759615963255655, 35.41775706135234003 ) ) ;
#158762 = CARTESIAN_POINT ( 'NONE',  ( -13.97604488694527625, -13.89961937509977652, 41.87390960531435979 ) ) ;
#158763 = AXIS2_PLACEMENT_3D ( 'NONE', #17243, #156754, #155745 ) ;
#158764 = CARTESIAN_POINT ( 'NONE',  ( -4.520441824858469460, -6.641858834016538538, -62.14216519528071103 ) ) ;
#158765 = CARTESIAN_POINT ( 'NONE',  ( 9.474510206698971260, -16.51473224551069308, 32.91557627198102409 ) ) ;
#158766 = EDGE_CURVE ( 'NONE', #175318, #175994, #170053, .T. ) ;
#158767 = CARTESIAN_POINT ( 'NONE',  ( 9.474510206698971260, -16.51473224551069308, 112.9155762719810383 ) ) ;
#158769 = CARTESIAN_POINT ( 'NONE',  ( 14.34966873604960469, 8.224510206698951720, 109.1655762719810383 ) ) ;
#158768 = CARTESIAN_POINT ( 'NONE',  ( -18.62759615963255300, -10.81492255796106328, 64.16775706135234714 ) ) ;
#158770 = CARTESIAN_POINT ( 'NONE',  ( -19.02544592524342804, 5.153800228976336051, 111.0405762719810099 ) ) ;
#158771 = CARTESIAN_POINT ( 'NONE',  ( 14.29746914071037800, 8.314922557961029526, 76.66775706135234714 ) ) ;
#158772 = CARTESIAN_POINT ( 'NONE',  ( 5.719274019375673035, 21.55341960407619339, 87.29275706135236135 ) ) ;
#158773 = CARTESIAN_POINT ( 'NONE',  ( -0.05219959533934338120, 16.53943276465976808, 57.50109039468568994 ) ) ;
#158774 = CARTESIAN_POINT ( 'NONE',  ( -9.474510206698964154, 16.51473224551069663, 100.4155762719810241 ) ) ;
#158775 = EDGE_CURVE ( 'NONE', #28211, #193677, #119592, .T. ) ;
#158776 = CARTESIAN_POINT ( 'NONE',  ( 4.483927247898790824, -16.52544592524335698, 40.20942372801901854 ) ) ;
#158777 = CARTESIAN_POINT ( 'NONE',  ( -14.29746914071037622, -8.314922557961029526, 29.16775706135234003 ) ) ;
#158778 = CARTESIAN_POINT ( 'NONE',  ( -14.34966873604972548, 8.224510206698743886, 88.33442372801901854 ) ) ;
#158779 = CARTESIAN_POINT ( 'NONE',  ( -13.97604488694547697, 13.89961937509957934, 103.1260903946856473 ) ) ;
#158780 = CARTESIAN_POINT ( 'NONE',  ( 10.72451020669898902, -18.67979575497178502, 97.91557627198103830 ) ) ;
#158782 = CARTESIAN_POINT ( 'NONE',  ( 16.51473224551083163, -9.474510206698727899, 100.8344237280190043 ) ) ;
#158781 = CARTESIAN_POINT ( 'NONE',  ( -4.379528057220328563, 16.55341960407611168, 100.2072429386476955 ) ) ;
#158783 = CARTESIAN_POINT ( 'NONE',  ( 16.52544592524335698, 4.483927247898782831, 66.45942372801903275 ) ) ;
#158784 = CARTESIAN_POINT ( 'NONE',  ( 23.19706360625337993, 11.80427776162510156, 165.7059442611694067 ) ) ;
#158785 = CARTESIAN_POINT ( 'NONE',  ( -16.46253265017146816, -9.564922557961047289, 64.16775706135233293 ) ) ;
#158786 = CARTESIAN_POINT ( 'NONE',  ( -12.14591786802309592, -12.06949235617757132, 46.87390960531435979 ) ) ;
#158787 = CARTESIAN_POINT ( 'NONE',  ( -14.34966873604960291, -8.224510206698953496, 26.66557627198103475 ) ) ;
#158788 = CARTESIAN_POINT ( 'NONE',  ( 4.379528057220339221, -16.55341960407611168, 87.70724293864769550 ) ) ;
#158789 = CARTESIAN_POINT ( 'NONE',  ( -5.049401038297874678, -19.05341960407617918, 34.79275706135233293 ) ) ;
#158790 = CARTESIAN_POINT ( 'NONE',  ( -15.72974639402176322, -15.80617190586768395, 39.37609039468567573 ) ) ;
#158791 = CARTESIAN_POINT ( 'NONE',  ( -19.05341960407617563, 5.049401038297882671, 98.54275706135233293 ) ) ;
#158792 = FACE_OUTER_BOUND ( 'NONE', #165625, .T. ) ;
#158793 = CARTESIAN_POINT ( 'NONE',  ( -5.049401038298153566, 19.05341960407611168, 85.20724293864766707 ) ) ;
#158794 = CARTESIAN_POINT ( 'NONE',  ( 9.564922557960805705, 16.46253265017160317, 89.58224293864769550 ) ) ;
#158795 = CARTESIAN_POINT ( 'NONE',  ( 18.67979575497178502, 10.72451020669898547, 59.16557627198103120 ) ) ;
#158796 = CARTESIAN_POINT ( 'NONE',  ( 14.34966873604960469, 8.224510206698951720, 99.16557627198100988 ) ) ;
#158797 = CARTESIAN_POINT ( 'NONE',  ( 9.564922557960805705, 16.46253265017160317, 69.58224293864770971 ) ) ;
#158798 = CARTESIAN_POINT ( 'NONE',  ( -16.55341960407611168, -4.379528057220339221, 111.4572429386476813 ) ) ;
#158799 = CARTESIAN_POINT ( 'NONE',  ( -15.72974639402176322, -15.80617190586768395, 44.37609039468567573 ) ) ;
#158800 = CARTESIAN_POINT ( 'NONE',  ( -5.719274019375665041, -21.55341960407619695, 74.79275706135234714 ) ) ;
#158801 = CARTESIAN_POINT ( 'NONE',  ( -13.97604488694527625, -13.89961937509977652, 56.87390960531434558 ) ) ;
#158802 = CARTESIAN_POINT ( 'NONE',  ( 4.483927247898790824, -16.52544592524335698, 75.20942372801901854 ) ) ;
#158803 = CARTESIAN_POINT ( 'NONE',  ( -5.719274019375665041, -21.55341960407619695, 29.79275706135234358 ) ) ;
#158804 = CARTESIAN_POINT ( 'NONE',  ( -15.80617190586768217, 15.72974639402176855, 23.12609039468567573 ) ) ;
#158806 = CARTESIAN_POINT ( 'NONE',  ( -16.51473224551069308, -9.474510206698971260, 76.66557627198103830 ) ) ;
#158805 = CARTESIAN_POINT ( 'NONE',  ( 13.89961937509957401, 13.97604488694547697, 46.87609039468565442 ) ) ;
#158807 = CARTESIAN_POINT ( 'NONE',  ( 5.049401038297881783, 19.05341960407617563, 27.29275706135232937 ) ) ;
#158808 = CARTESIAN_POINT ( 'NONE',  ( -10.81492255796105439, 18.62759615963255655, 77.91775706135231871 ) ) ;
#158809 = EDGE_CURVE ( 'NONE', #183245, #47139, #102026, .T. ) ;
#158810 = CARTESIAN_POINT ( 'NONE',  ( -21.52544592524343514, 5.823673210054127303, 66.04057627198103830 ) ) ;
#158811 = CARTESIAN_POINT ( 'NONE',  ( -12.06949235617756955, 12.14591786802309770, 50.62390960531435979 ) ) ;
#158813 = CARTESIAN_POINT ( 'NONE',  ( -5.049401038297874678, -19.05341960407617918, 29.79275706135232227 ) ) ;
#158812 = CARTESIAN_POINT ( 'NONE',  ( -21.55341960407619339, 5.719274019375674811, 88.54275706135236135 ) ) ;
#158814 = CARTESIAN_POINT ( 'NONE',  ( 12.14591786802309770, 12.06949235617756955, 74.37390960531436690 ) ) ;
#158815 = CARTESIAN_POINT ( 'NONE',  ( -19.02544592524342804, 5.153800228976336051, 26.04057627198103120 ) ) ;
#158816 = CARTESIAN_POINT ( 'NONE',  ( 19.03943276465977164, 0.05219959533936151252, 56.25109039468566863 ) ) ;
#158817 = CARTESIAN_POINT ( 'NONE',  ( 12.14591786802309770, 12.06949235617756955, 39.37390960531436690 ) ) ;
#158818 = CARTESIAN_POINT ( 'NONE',  ( 0.05219959533937995610, -21.53943276465977519, 80.00109039468568994 ) ) ;
#158819 = CARTESIAN_POINT ( 'NONE',  ( 5.049401038298161559, -19.05341960407611168, 72.70724293864768129 ) ) ;
#158820 = CARTESIAN_POINT ( 'NONE',  ( 5.049401038297881783, 19.05341960407617563, 52.29275706135234003 ) ) ;
#158821 = CARTESIAN_POINT ( 'NONE',  ( -10.81492255796078084, -18.62759615963271287, 47.08224293864770260 ) ) ;
#158822 = CARTESIAN_POINT ( 'NONE',  ( 18.62759615963255655, 10.81492255796105972, 46.66775706135234714 ) ) ;
#158823 = CARTESIAN_POINT ( 'NONE',  ( 0.05219959533907565091, 21.53943276465977519, 99.99890960531436690 ) ) ;
#158824 = CARTESIAN_POINT ( 'NONE',  ( -0.05219959533936034679, 19.03943276465977164, 97.50109039468567573 ) ) ;
#158825 = CARTESIAN_POINT ( 'NONE',  ( -16.52544592524335698, -4.483927247898792601, 63.95942372801901854 ) ) ;
#158827 = CARTESIAN_POINT ( 'NONE',  ( -10.72451020669898014, 18.67979575497178502, 105.4155762719810383 ) ) ;
#158826 = CARTESIAN_POINT ( 'NONE',  ( 69.65682714487590488, -71.74905178543389184, -23.00000000000000000 ) ) ;
#158828 = CARTESIAN_POINT ( 'NONE',  ( -0.05219959533910754901, -16.53943276465976808, 97.49890960531436690 ) ) ;
#158829 = CARTESIAN_POINT ( 'NONE',  ( -17.49999999999999645, -4.640572885337608255, 29.36211835451158692 ) ) ;
#158830 = CARTESIAN_POINT ( 'NONE',  ( -14.34966873604972548, 8.224510206698743886, 38.33442372801900433 ) ) ;
#158831 = CARTESIAN_POINT ( 'NONE',  ( -5.719274019375978568, 21.55341960407610458, 65.20724293864768129 ) ) ;
#158832 = CARTESIAN_POINT ( 'NONE',  ( -14.29746914071037622, -8.314922557961029526, 109.1677570613523613 ) ) ;
#158833 = CARTESIAN_POINT ( 'NONE',  ( 9.564922557960805705, 16.46253265017160317, 34.58224293864770260 ) ) ;
#158834 = CARTESIAN_POINT ( 'NONE',  ( 14.29746914071037800, 8.314922557961029526, 61.66775706135235424 ) ) ;
#158835 = CARTESIAN_POINT ( 'NONE',  ( 13.89961937509957401, 13.97604488694547697, 56.87609039468564731 ) ) ;
#158836 = CARTESIAN_POINT ( 'NONE',  ( 15.72974639402176855, 15.80617190586768217, 36.87609039468568994 ) ) ;
#158837 = CARTESIAN_POINT ( 'NONE',  ( 18.67979575497178502, 10.72451020669898547, 64.16557627198102409 ) ) ;
#158838 = CARTESIAN_POINT ( 'NONE',  ( 14.34966873604972726, -8.224510206698740333, 95.83442372801903275 ) ) ;
#158839 = CARTESIAN_POINT ( 'NONE',  ( 5.823673210054444382, -21.52544592524334988, 75.20942372801901854 ) ) ;
#158840 = CARTESIAN_POINT ( 'NONE',  ( -0.05219959533907301413, -21.53943276465977519, 57.49890960531435979 ) ) ;
#158841 = CARTESIAN_POINT ( 'NONE',  ( 10.72451020669898902, -18.67979575497178502, 27.91557627198103830 ) ) ;
#158842 = ORIENTED_EDGE ( 'NONE', *, *, #8681, .T. ) ;
#158843 = CARTESIAN_POINT ( 'NONE',  ( 14.34966873604972726, -8.224510206698740333, 80.83442372801901854 ) ) ;
#158844 = CARTESIAN_POINT ( 'NONE',  ( 18.67979575497178502, 10.72451020669898547, 29.16557627198103120 ) ) ;
#158845 = ORIENTED_EDGE ( 'NONE', *, *, #20984, .T. ) ;
#158846 = CARTESIAN_POINT ( 'NONE',  ( -16.46253265017160317, 9.564922557960807481, 105.8322429386476955 ) ) ;
#158847 = CARTESIAN_POINT ( 'NONE',  ( -14.34966873604972548, 8.224510206698743886, 108.3344237280190185 ) ) ;
#158848 = SPHERICAL_SURFACE ( 'NONE', #75944, 10.00000000000000000 ) ;
#158849 = CARTESIAN_POINT ( 'NONE',  ( 12.14591786802309770, 12.06949235617756955, 109.3739096053143811 ) ) ;
#158850 = CARTESIAN_POINT ( 'NONE',  ( 0.05219959533907565091, 21.53943276465977519, 59.99890960531436690 ) ) ;
#158851 = CARTESIAN_POINT ( 'NONE',  ( 0.05219959533934541429, -16.53943276465976808, 85.00109039468568994 ) ) ;
#158852 = CARTESIAN_POINT ( 'NONE',  ( -21.55341960407619339, 5.719274019375674811, 48.54275706135234714 ) ) ;
#158853 = CARTESIAN_POINT ( 'NONE',  ( 9.564922557961047289, -16.46253265017146816, 100.4177570613523329 ) ) ;
#158854 = CARTESIAN_POINT ( 'NONE',  ( -16.55341960407611168, -4.379528057220339221, 106.4572429386477097 ) ) ;
#158855 = CARTESIAN_POINT ( 'NONE',  ( -19.05341960407611168, -5.049401038298163336, 56.45724293864768129 ) ) ;
#158856 = CARTESIAN_POINT ( 'NONE',  ( 9.564922557960805705, 16.46253265017160317, 24.58224293864769194 ) ) ;
#158857 = CARTESIAN_POINT ( 'NONE',  ( 0.5391882481685079664, 24.20369912164904491, -54.28997303946584196 ) ) ;
#158858 = CARTESIAN_POINT ( 'NONE',  ( 9.474510206698971260, -16.51473224551069308, 92.91557627198103830 ) ) ;
#158859 = CARTESIAN_POINT ( 'NONE',  ( 12.14591786802327356, -12.06949235617739191, 75.62609039468567573 ) ) ;
#158860 = CARTESIAN_POINT ( 'NONE',  ( -0.05219959533937732626, 21.53943276465977519, 102.5010903946856899 ) ) ;
#158861 = CARTESIAN_POINT ( 'NONE',  ( -10.72451020669898014, 18.67979575497178502, 65.41557627198102409 ) ) ;
#158862 = CARTESIAN_POINT ( 'NONE',  ( 8.224510206698742110, 14.34966873604972548, 92.08442372801901854 ) ) ;
#158863 = CARTESIAN_POINT ( 'NONE',  ( 16.46253265017146816, 9.564922557961045513, 86.66775706135233293 ) ) ;
#158864 = EDGE_LOOP ( 'NONE', ( #75803, #128280, #10474, #6267, #14043, #36969 ) ) ;
#158865 = CARTESIAN_POINT ( 'NONE',  ( -9.474510206698964154, 16.51473224551069663, 40.41557627198103120 ) ) ;
#158866 = CARTESIAN_POINT ( 'NONE',  ( 13.89961937509977652, -13.97604488694527269, 83.12390960531436690 ) ) ;
#158867 = CARTESIAN_POINT ( 'NONE',  ( 13.97604488694527802, 13.89961937509977652, 39.37390960531435269 ) ) ;
#158868 = CARTESIAN_POINT ( 'NONE',  ( -19.05341960407617563, 5.049401038297882671, 78.54275706135233293 ) ) ;
#158869 = CARTESIAN_POINT ( 'NONE',  ( 21.84611564451294541, -9.363109600221314111, 171.0247306346274172 ) ) ;
#158870 = CARTESIAN_POINT ( 'NONE',  ( 19.05341960407611168, 5.049401038298154454, 93.95724293864769550 ) ) ;
#158871 = CARTESIAN_POINT ( 'NONE',  ( -8.224510206698948167, 14.34966873604960824, 55.41557627198102409 ) ) ;
#158872 = CARTESIAN_POINT ( 'NONE',  ( -15.72974639402197994, 15.80617190586746368, 55.62390960531436690 ) ) ;
#158873 = DIRECTION ( 'NONE',  ( 1.000000000000000000, 0.000000000000000000, 0.000000000000000000 ) ) ;
#158874 = CARTESIAN_POINT ( 'NONE',  ( 9.474510206698729675, 16.51473224551082808, 32.08442372801900433 ) ) ;
#158875 = DIRECTION ( 'NONE',  ( -0.000000000000000000, -0.000000000000000000, 1.000000000000000000 ) ) ;
#158877 = CARTESIAN_POINT ( 'NONE',  ( -5.153800228976328057, -19.02544592524343514, 77.29057627198099567 ) ) ;
#158876 = CARTESIAN_POINT ( 'NONE',  ( -9.564922557960796823, -16.46253265017161027, 57.08224293864769550 ) ) ;
#158878 = CARTESIAN_POINT ( 'NONE',  ( 14.29746914071037800, 8.314922557961029526, 31.66775706135234358 ) ) ;
#158879 = CARTESIAN_POINT ( 'NONE',  ( -33.82551795724113930, -1.774401534882018350, 100.2184796937738724 ) ) ;
#158880 = DIRECTION ( 'NONE',  ( 0.000000000000000000, 0.000000000000000000, 1.000000000000000000 ) ) ;
#158881 = CARTESIAN_POINT ( 'NONE',  ( 8.314922557961029526, -14.29746914071037800, 70.41775706135236135 ) ) ;
#158882 = CARTESIAN_POINT ( 'NONE',  ( -5.719274019375978568, 21.55341960407610458, 100.2072429386476955 ) ) ;
#158883 = CARTESIAN_POINT ( 'NONE',  ( -12.06949235617739369, -12.14591786802326823, 44.37609039468567573 ) ) ;
#158885 = CARTESIAN_POINT ( 'NONE',  ( -23.48529157249599919, -32.32473071737749848, -5.449999994537626513 ) ) ;
#158884 = CARTESIAN_POINT ( 'NONE',  ( -9.474510206698964154, 16.51473224551069663, 40.41557627198103120 ) ) ;
#158886 = CARTESIAN_POINT ( 'NONE',  ( 5.823673210054444382, -21.52544592524334988, 60.20942372801902565 ) ) ;
#158887 = CARTESIAN_POINT ( 'NONE',  ( -13.89961937509957401, -13.97604488694547875, 64.37609039468567573 ) ) ;
#158888 = CARTESIAN_POINT ( 'NONE',  ( -21.55341960407619339, 5.719274019375674811, 88.54275706135236135 ) ) ;
#158889 = CARTESIAN_POINT ( 'NONE',  ( -17.49999999999999645, 5.499999999999992895, 48.71769037696437010 ) ) ;
#158890 = CARTESIAN_POINT ( 'NONE',  ( 14.34966873604960469, 8.224510206698951720, 39.16557627198102409 ) ) ;
#158891 = CARTESIAN_POINT ( 'NONE',  ( 19.39056639909672342, 5.500000000000043521, 43.28948781074344510 ) ) ;
#158892 = CARTESIAN_POINT ( 'NONE',  ( -10.72451020669898014, 18.67979575497178502, 50.41557627198103120 ) ) ;
#158893 = CARTESIAN_POINT ( 'NONE',  ( -8.571926809382601320, -26.38167802310801591, 141.2750000027311899 ) ) ;
#158894 = CARTESIAN_POINT ( 'NONE',  ( 19.02544592524343514, -5.153800228976328945, 108.5405762719810383 ) ) ;
#158895 = CARTESIAN_POINT ( 'NONE',  ( -16.52544592524342804, 4.483927247898546575, 106.0405762719810525 ) ) ;
#158896 = CARTESIAN_POINT ( 'NONE',  ( -16.53943276465976808, -0.05219959533934237506, 28.75109039468567929 ) ) ;
#158897 = CARTESIAN_POINT ( 'NONE',  ( 14.34966873604972726, -8.224510206698740333, 105.8344237280190328 ) ) ;
#158898 = VERTEX_POINT ( 'NONE', #106386 ) ;
#158899 = CARTESIAN_POINT ( 'NONE',  ( -0.05219959533907301413, -21.53943276465977519, 107.4989096053143669 ) ) ;
#158901 = CARTESIAN_POINT ( 'NONE',  ( -19.02544592524342804, 5.153800228976336051, 116.0405762719810383 ) ) ;
#158900 = CARTESIAN_POINT ( 'NONE',  ( -16.52544592524342804, 4.483927247898546575, 26.04057627198103475 ) ) ;
#158902 = CARTESIAN_POINT ( 'NONE',  ( 5.153800228976615827, -19.02544592524334988, 90.20942372801900433 ) ) ;
#158903 = CARTESIAN_POINT ( 'NONE',  ( -10.81492255796105439, 18.62759615963255655, 102.9177570613523756 ) ) ;
#158904 = CARTESIAN_POINT ( 'NONE',  ( 14.34966873604960469, 8.224510206698951720, 29.16557627198103120 ) ) ;
#158905 = CARTESIAN_POINT ( 'NONE',  ( 21.52544592524344225, -5.823673210054117533, 88.54057627198103830 ) ) ;
#158906 = CARTESIAN_POINT ( 'NONE',  ( -21.52544592524343514, 5.823673210054127303, 56.04057627198102409 ) ) ;
#158907 = CARTESIAN_POINT ( 'NONE',  ( 13.97604488694527802, 13.89961937509977652, 59.37390960531434558 ) ) ;
#158908 = CARTESIAN_POINT ( 'NONE',  ( -14.34966873604960291, -8.224510206698953496, 36.66557627198103120 ) ) ;
#158909 = CARTESIAN_POINT ( 'NONE',  ( 19.03943276465977164, -0.05219959533909143690, 73.74890960531435269 ) ) ;
#158910 = ORIENTED_EDGE ( 'NONE', *, *, #124931, .F. ) ;
#158911 = CARTESIAN_POINT ( 'NONE',  ( 19.19724070472091171, 5.500000000000159872, 58.56193348274382515 ) ) ;
#158912 = CARTESIAN_POINT ( 'NONE',  ( -13.89961937509957401, -13.97604488694547875, 44.37609039468566863 ) ) ;
#158913 = CARTESIAN_POINT ( 'NONE',  ( 18.62759615963271287, -10.81492255796078972, 78.33224293864770971 ) ) ;
#158914 = CARTESIAN_POINT ( 'NONE',  ( -16.52544592524342804, 4.483927247898546575, 106.0405762719810525 ) ) ;
#158915 =( BOUNDED_CURVE ( )  B_SPLINE_CURVE ( 3, ( #167988, #152807, #90143, #138627 ),
 .UNSPECIFIED., .F., .F. ) 
 B_SPLINE_CURVE_WITH_KNOTS ( ( 4, 4 ),
 ( 5.503250352303675541, 7.063120262055497811 ),
 .UNSPECIFIED. ) 
 CURVE ( )  GEOMETRIC_REPRESENTATION_ITEM ( )  RATIONAL_B_SPLINE_CURVE ( ( 1.000000000000000000, 0.8073061876036302653, 0.8073061876036302653, 1.000000000000000000 ) ) 
 REPRESENTATION_ITEM ( '' )  );
#158916 = CARTESIAN_POINT ( 'NONE',  ( -15.72974639402176322, -15.80617190586768395, 39.37609039468567573 ) ) ;
#158917 = CARTESIAN_POINT ( 'NONE',  ( -22.44159573604009950, -16.30477369853688430, 141.0750000027311728 ) ) ;
#158918 = CARTESIAN_POINT ( 'NONE',  ( -0.05219959533934338120, 16.53943276465976808, 102.5010903946856899 ) ) ;
#158919 = CARTESIAN_POINT ( 'NONE',  ( 9.474510206698971260, -16.51473224551069308, 32.91557627198102409 ) ) ;
#158920 = CARTESIAN_POINT ( 'NONE',  ( 0.05219959533909260263, 19.03943276465977164, 84.99890960531436690 ) ) ;
#158921 = CARTESIAN_POINT ( 'NONE',  ( 9.474510206698971260, -16.51473224551069308, 37.91557627198102409 ) ) ;
#158922 = CARTESIAN_POINT ( 'NONE',  ( -14.29746914071049879, 8.314922557960819915, 45.83224293864769550 ) ) ;
#158923 = EDGE_CURVE ( 'NONE', #9532, #107482, #20000, .T. ) ;
#158924 = CARTESIAN_POINT ( 'NONE',  ( -21.53943276465977519, -0.05219959533937600094, 78.75109039468568994 ) ) ;
#158926 = CARTESIAN_POINT ( 'NONE',  ( 16.53943276465976808, 0.05219959533934440121, 66.25109039468567573 ) ) ;
#158925 = CARTESIAN_POINT ( 'NONE',  ( 28.40128899757106495, -24.57310642927003741, -18.78835905295402853 ) ) ;
#158927 = CARTESIAN_POINT ( 'NONE',  ( -19.05341960407611168, -5.049401038298163336, 46.45724293864768129 ) ) ;
#158928 = CARTESIAN_POINT ( 'NONE',  ( -13.97604488694527625, -13.89961937509977652, 51.87390960531436690 ) ) ;
#158929 = ORIENTED_EDGE ( 'NONE', *, *, #60319, .T. ) ;
#158930 = CARTESIAN_POINT ( 'NONE',  ( -18.67979575497193778, 10.72451020669871902, 103.3344237280190043 ) ) ;
#158931 = CARTESIAN_POINT ( 'NONE',  ( -16.52544592524335698, -4.483927247898792601, 58.95942372801902565 ) ) ;
#158932 = CARTESIAN_POINT ( 'NONE',  ( 10.81492255796106328, -18.62759615963255655, 105.4177570613523613 ) ) ;
#158933 = CARTESIAN_POINT ( 'NONE',  ( -21.52544592524343514, 5.823673210054127303, 41.04057627198103120 ) ) ;
#158934 = CARTESIAN_POINT ( 'NONE',  ( 19.03943276465977164, 0.05219959533936151252, 111.2510903946856757 ) ) ;
#158935 = CARTESIAN_POINT ( 'NONE',  ( -5.719274019375665041, -21.55341960407619695, 69.79275706135234714 ) ) ;
#158936 = CARTESIAN_POINT ( 'NONE',  ( -12.14591786802326823, 12.06949235617739902, 33.12609039468569705 ) ) ;
#158937 = CARTESIAN_POINT ( 'NONE',  ( 10.81492255796078972, 18.62759615963270932, 104.5822429386477097 ) ) ;
#158938 = CARTESIAN_POINT ( 'NONE',  ( -9.564922557961040184, 16.46253265017147172, 97.91775706135233293 ) ) ;
#158939 = CARTESIAN_POINT ( 'NONE',  ( -9.474510206698964154, 16.51473224551069663, 70.41557627198102409 ) ) ;
#158940 = CARTESIAN_POINT ( 'NONE',  ( 4.483927247898790824, -16.52544592524335698, 20.20942372801900788 ) ) ;
#158941 = CARTESIAN_POINT ( 'NONE',  ( 9.564922557961047289, -16.46253265017146816, 105.4177570613523471 ) ) ;
#158942 = CARTESIAN_POINT ( 'NONE',  ( -12.14591786802309592, -12.06949235617757132, 66.87390960531436690 ) ) ;
#158943 = CARTESIAN_POINT ( 'NONE',  ( -16.55341960407617563, 4.379528057220093196, 73.54275706135234714 ) ) ;
#158945 = CARTESIAN_POINT ( 'NONE',  ( -16.51473224551069308, -9.474510206698971260, 46.66557627198102409 ) ) ;
#158944 = CARTESIAN_POINT ( 'NONE',  ( -15.80617190586768217, 15.72974639402176855, 23.12609039468567573 ) ) ;
#158946 = CARTESIAN_POINT ( 'NONE',  ( 19.02544592524343514, -5.153800228976328945, 53.54057627198102409 ) ) ;
#158947 = CARTESIAN_POINT ( 'NONE',  ( -16.55341960407617563, 4.379528057220093196, 68.54275706135234714 ) ) ;
#158948 = CARTESIAN_POINT ( 'NONE',  ( -27.73933785331498925, -9.013057229001049109, 147.4750000027311785 ) ) ;
#158949 = CARTESIAN_POINT ( 'NONE',  ( 28.82186960331499392, -9.364793116373510529, 147.1500000054623456 ) ) ;
#158950 = ORIENTED_EDGE ( 'NONE', *, *, #72173, .T. ) ;
#158951 = CARTESIAN_POINT ( 'NONE',  ( -13.97604488694547697, 13.89961937509957934, 23.12609039468565442 ) ) ;
#158952 = CARTESIAN_POINT ( 'NONE',  ( 9.564922557960805705, 16.46253265017160317, 24.58224293864769194 ) ) ;
#158953 = ORIENTED_EDGE ( 'NONE', *, *, #1893, .F. ) ;
#158954 = CARTESIAN_POINT ( 'NONE',  ( 12.06949235617739724, 12.14591786802326823, 21.87609039468567573 ) ) ;
#158955 = CARTESIAN_POINT ( 'NONE',  ( 21.55341960407610458, 5.719274019375980345, 53.95724293864770260 ) ) ;
#158957 = CARTESIAN_POINT ( 'NONE',  ( 8.224510206698742110, 14.34966873604972548, 32.08442372801901854 ) ) ;
#158956 = CARTESIAN_POINT ( 'NONE',  ( 19.02544592524334988, 5.153800228976608722, 51.45942372801900433 ) ) ;
#158958 = CARTESIAN_POINT ( 'NONE',  ( 9.474510206698971260, -16.51473224551069308, 42.91557627198103120 ) ) ;
#158959 = CARTESIAN_POINT ( 'NONE',  ( -0.05219959533909027116, -19.03943276465977164, 47.49890960531435979 ) ) ;
#158960 = CARTESIAN_POINT ( 'NONE',  ( 10.72451020669898902, -18.67979575497178502, 87.91557627198103830 ) ) ;
#158961 = CARTESIAN_POINT ( 'NONE',  ( -9.474510206698964154, 16.51473224551069663, 110.4155762719810383 ) ) ;
#158962 = CARTESIAN_POINT ( 'NONE',  ( -5.153800228976328057, -19.02544592524343514, 52.29057627198100988 ) ) ;
#158963 = CARTESIAN_POINT ( 'NONE',  ( 17.49999999999999289, 5.500000000000006217, 48.78230962303565121 ) ) ;
#158964 = CARTESIAN_POINT ( 'NONE',  ( -13.97604488694547697, 13.89961937509957934, 98.12609039468566152 ) ) ;
#158965 = CARTESIAN_POINT ( 'NONE',  ( -12.14591786802309592, -12.06949235617757132, 61.87390960531436690 ) ) ;
#158966 = CARTESIAN_POINT ( 'NONE',  ( 19.05341960407617918, -5.049401038297876454, 31.04275706135232227 ) ) ;
#158967 = CARTESIAN_POINT ( 'NONE',  ( -10.81492255796078084, -18.62759615963271287, 102.0822429386476955 ) ) ;
#158968 = CARTESIAN_POINT ( 'NONE',  ( 5.823673210054444382, -21.52544592524334988, 90.20942372801903275 ) ) ;
#158969 = CARTESIAN_POINT ( 'NONE',  ( 19.03943276465977164, -0.05219959533909143690, 23.74890960531435269 ) ) ;
#158970 = CARTESIAN_POINT ( 'NONE',  ( -15.72974639402176322, -15.80617190586768395, 74.37609039468568994 ) ) ;
#158972 = CARTESIAN_POINT ( 'NONE',  ( 5.719274019375673035, 21.55341960407619339, 77.29275706135234714 ) ) ;
#158971 = CARTESIAN_POINT ( 'NONE',  ( -8.314922557960811034, -14.29746914071050412, 22.08224293864769194 ) ) ;
#158973 = CARTESIAN_POINT ( 'NONE',  ( -16.46253265017160317, 9.564922557960807481, 70.83224293864770971 ) ) ;
#158974 = CARTESIAN_POINT ( 'NONE',  ( -18.67979575497193778, 10.72451020669871902, 43.33442372801901143 ) ) ;
#158975 = CARTESIAN_POINT ( 'NONE',  ( 19.03943276465977164, -0.05219959533909143690, 83.74890960531436690 ) ) ;
#158976 = CARTESIAN_POINT ( 'NONE',  ( 4.379528057220339221, -16.55341960407611168, 87.70724293864769550 ) ) ;
#158977 = CARTESIAN_POINT ( 'NONE',  ( 8.224510206698953496, -14.34966873604960469, 57.91557627198103120 ) ) ;
#158978 = CARTESIAN_POINT ( 'NONE',  ( -15.80617190586745835, -15.72974639402198527, 76.87390960531439532 ) ) ;
#158979 = CARTESIAN_POINT ( 'NONE',  ( 5.153800228976335163, 19.02544592524342804, 59.79057627198100988 ) ) ;
#158980 = CARTESIAN_POINT ( 'NONE',  ( -5.823673210054116645, -21.52544592524344225, 87.29057627198103830 ) ) ;
#158981 = CARTESIAN_POINT ( 'NONE',  ( 16.46253265017146816, 9.564922557961045513, 61.66775706135234003 ) ) ;
#158983 = CARTESIAN_POINT ( 'NONE',  ( -16.53943276465976808, 0.05219959533911058130, 81.24890960531436690 ) ) ;
#158982 = CARTESIAN_POINT ( 'NONE',  ( -9.564922557961040184, 16.46253265017147172, 27.91775706135232582 ) ) ;
#158984 = CARTESIAN_POINT ( 'NONE',  ( 5.719274019375991003, -21.55341960407610458, 47.70724293864770260 ) ) ;
#158985 = FACE_OUTER_BOUND ( 'NONE', #127093, .T. ) ;
#158987 = CARTESIAN_POINT ( 'NONE',  ( 17.14385361876520264, -23.59649016807270883, 144.0750000027311444 ) ) ;
#158986 = CARTESIAN_POINT ( 'NONE',  ( -14.29746914071037622, -8.314922557961029526, 104.1677570613523471 ) ) ;
#158988 = CARTESIAN_POINT ( 'NONE',  ( -16.46253265017146816, -9.564922557961047289, 104.1677570613523329 ) ) ;
#158989 = CARTESIAN_POINT ( 'NONE',  ( -16.55341960407611168, -4.379528057220339221, 61.45724293864770260 ) ) ;
#158990 = CARTESIAN_POINT ( 'NONE',  ( -17.50000000000001776, 3.565345528327884317, 34.42494486806472054 ) ) ;
#158991 = CARTESIAN_POINT ( 'NONE',  ( -13.97604488694527625, -13.89961937509977652, 61.87390960531435979 ) ) ;
#158992 = CARTESIAN_POINT ( 'NONE',  ( -0.05219959533910754901, -16.53943276465976808, 47.49890960531435979 ) ) ;
#158993 = CARTESIAN_POINT ( 'NONE',  ( -5.049401038298153566, 19.05341960407611168, 100.2072429386476955 ) ) ;
#158995 = CARTESIAN_POINT ( 'NONE',  ( 16.46253265017160672, -9.564922557960803928, 63.33224293864769550 ) ) ;
#158994 = CARTESIAN_POINT ( 'NONE',  ( -13.89961937509957401, -13.97604488694547875, 74.37609039468566152 ) ) ;
#158996 = CARTESIAN_POINT ( 'NONE',  ( -16.51473224551069308, -9.474510206698971260, 81.66557627198103830 ) ) ;
#158997 = CARTESIAN_POINT ( 'NONE',  ( 5.153800228976335163, 19.02544592524342804, 79.79057627198102409 ) ) ;
#158998 = CARTESIAN_POINT ( 'NONE',  ( 21.53943276465977519, -0.05219959533907433946, 58.74890960531436690 ) ) ;
#158999 = CARTESIAN_POINT ( 'NONE',  ( -16.52544592524335698, -4.483927247898792601, 53.95942372801900433 ) ) ;
#159000 = CARTESIAN_POINT ( 'NONE',  ( 0.05219959533936267826, -19.03943276465977164, 105.0010903946856615 ) ) ;
#159001 = CARTESIAN_POINT ( 'NONE',  ( 0.05219959533909260263, 19.03943276465977164, 49.99890960531435979 ) ) ;
#159002 = CARTESIAN_POINT ( 'NONE',  ( -15.80617190586745835, -15.72974639402198527, 51.87390960531437401 ) ) ;
#159003 = CARTESIAN_POINT ( 'NONE',  ( -16.46253265017146816, -9.564922557961047289, 94.16775706135233293 ) ) ;
#159005 = CARTESIAN_POINT ( 'NONE',  ( 21.55341960407619695, -5.719274019375665929, 41.04275706135236135 ) ) ;
#159004 = CARTESIAN_POINT ( 'NONE',  ( -16.55341960407611168, -4.379528057220339221, 31.45724293864769550 ) ) ;
#159006 = CARTESIAN_POINT ( 'NONE',  ( -19.05341960407617563, 5.049401038297882671, 33.54275706135231871 ) ) ;
#159008 = CARTESIAN_POINT ( 'NONE',  ( -16.53943276465976808, -0.05219959533934237506, 88.75109039468567573 ) ) ;
#159007 = CARTESIAN_POINT ( 'NONE',  ( -14.34966873604972548, 8.224510206698743886, 53.33442372801901854 ) ) ;
#159009 = LINE ( 'NONE', #81166, #198543 ) ;
#159010 = CARTESIAN_POINT ( 'NONE',  ( -12.06949235617739369, -12.14591786802326823, 74.37609039468568994 ) ) ;
#159012 = CARTESIAN_POINT ( 'NONE',  ( -8.314922557961024197, 14.29746914071037800, 37.91775706135235424 ) ) ;
#159011 = CARTESIAN_POINT ( 'NONE',  ( -5.823673210054116645, -21.52544592524344225, 32.29057627198102409 ) ) ;
#159013 = CARTESIAN_POINT ( 'NONE',  ( -16.51473224551069308, -9.474510206698971260, 41.66557627198103120 ) ) ;
#159014 = CARTESIAN_POINT ( 'NONE',  ( 19.02544592524343514, -5.153800228976328945, 43.54057627198103120 ) ) ;
#159015 = CARTESIAN_POINT ( 'NONE',  ( 19.03943276465977164, -0.05219959533909143690, 58.74890960531435979 ) ) ;
#159016 = CARTESIAN_POINT ( 'NONE',  ( 0.05219959533937995610, -21.53943276465977519, 35.00109039468568284 ) ) ;
#159017 = CARTESIAN_POINT ( 'NONE',  ( -16.52544592524335698, -4.483927247898792601, 53.95942372801900433 ) ) ;
#159018 = CARTESIAN_POINT ( 'NONE',  ( 12.06949235617739724, 12.14591786802326823, 106.8760903946856899 ) ) ;
#159019 = CARTESIAN_POINT ( 'NONE',  ( -9.564922557960796823, -16.46253265017161027, 22.08224293864768839 ) ) ;
#159020 = CARTESIAN_POINT ( 'NONE',  ( -21.53943276465977519, -0.05219959533937600094, 108.7510903946857042 ) ) ;
#159021 = CARTESIAN_POINT ( 'NONE',  ( -8.224510206698735004, -14.34966873604973081, 19.58442372801901143 ) ) ;
#159022 = CARTESIAN_POINT ( 'NONE',  ( 19.03943276465977164, 0.05219959533936151252, 66.25109039468567573 ) ) ;
#159023 = CARTESIAN_POINT ( 'NONE',  ( 8.314922557960818139, 14.29746914071049879, 64.58224293864769550 ) ) ;
#159024 = CARTESIAN_POINT ( 'NONE',  ( -16.51473224551069308, -9.474510206698971260, 41.66557627198103120 ) ) ;
#159026 = CARTESIAN_POINT ( 'NONE',  ( 17.05587630539786304, 6.762274262135719027, 76.75819690962691766 ) ) ;
#159025 = CARTESIAN_POINT ( 'NONE',  ( 9.564922557961047289, -16.46253265017146816, 70.41775706135233293 ) ) ;
#159027 = CARTESIAN_POINT ( 'NONE',  ( 10.81492255796106328, -18.62759615963255655, 80.41775706135234714 ) ) ;
#159028 = CARTESIAN_POINT ( 'NONE',  ( 16.55341960407618274, -4.379528057220086978, 41.04275706135236135 ) ) ;
#159029 = DIRECTION ( 'NONE',  ( -1.000000000000000000, -0.000000000000000000, 0.000000000000000000 ) ) ;
#159030 = CARTESIAN_POINT ( 'NONE',  ( -5.823673210054116645, -21.52544592524344225, 37.29057627198102409 ) ) ;
#159031 = CARTESIAN_POINT ( 'NONE',  ( 8.224510206698742110, 14.34966873604972548, 27.08442372801901854 ) ) ;
#159032 = CARTESIAN_POINT ( 'NONE',  ( 17.72662750342729510, 5.499999999999909406, 88.90179492283745333 ) ) ;
#159033 = CARTESIAN_POINT ( 'NONE',  ( 0.05219959533936267826, -19.03943276465977164, 30.00109039468566863 ) ) ;
#159034 = CARTESIAN_POINT ( 'NONE',  ( -30.14078780231637467, -23.14917332716833087, -18.99124320735420568 ) ) ;
#159035 = CARTESIAN_POINT ( 'NONE',  ( 0.05219959533909260263, 19.03943276465977164, 44.99890960531435979 ) ) ;
#159036 = CARTESIAN_POINT ( 'NONE',  ( -16.51473224551082808, 9.474510206698731452, 58.33442372801900433 ) ) ;
#159037 = CARTESIAN_POINT ( 'NONE',  ( 16.51473224551069308, 9.474510206698969483, 64.16557627198102409 ) ) ;
#159038 = CARTESIAN_POINT ( 'NONE',  ( -19.02130022317636815, 5.499999999999802824, 100.7818866924657897 ) ) ;
#159039 = CARTESIAN_POINT ( 'NONE',  ( 13.89961937509957401, 13.97604488694547697, 21.87609039468566152 ) ) ;
#159040 = CARTESIAN_POINT ( 'NONE',  ( 0.05219959533910956823, 16.53943276465976808, 24.99890960531435624 ) ) ;
#159041 = CARTESIAN_POINT ( 'NONE',  ( -9.474510206698964154, 16.51473224551069663, 30.41557627198102054 ) ) ;
#159042 = CARTESIAN_POINT ( 'NONE',  ( -5.049401038298153566, 19.05341960407611168, 95.20724293864770971 ) ) ;
#159043 = CARTESIAN_POINT ( 'NONE',  ( 15.80617190586769283, -15.72974639402175789, 75.62609039468567573 ) ) ;
#159044 = CARTESIAN_POINT ( 'NONE',  ( 19.05341960407611168, 5.049401038298154454, 53.95724293864770260 ) ) ;
#159045 = CARTESIAN_POINT ( 'NONE',  ( -21.52544592524334988, -5.823673210054445271, 68.95942372801901854 ) ) ;
#159047 = CARTESIAN_POINT ( 'NONE',  ( 21.55341960407610458, 5.719274019375980345, 23.95724293864769550 ) ) ;
#159046 = CARTESIAN_POINT ( 'NONE',  ( 5.049401038297881783, 19.05341960407617563, 92.29275706135234714 ) ) ;
#159048 = CARTESIAN_POINT ( 'NONE',  ( -16.51473224551069308, -9.474510206698971260, 36.66557627198102409 ) ) ;
#159049 = CARTESIAN_POINT ( 'NONE',  ( -21.53943276465977519, 0.05219959533907696930, 116.2489096053143669 ) ) ;
#159050 = CARTESIAN_POINT ( 'NONE',  ( -16.46253265017146816, -9.564922557961047289, 39.16775706135234003 ) ) ;
#159051 = CARTESIAN_POINT ( 'NONE',  ( -8.314922557960811034, -14.29746914071050412, 112.0822429386477097 ) ) ;
#159052 = CARTESIAN_POINT ( 'NONE',  ( -16.51473224551069308, -9.474510206698971260, 66.66557627198102409 ) ) ;
#159053 = CARTESIAN_POINT ( 'NONE',  ( -13.97604488694547697, 13.89961937509957934, 113.1260903946856757 ) ) ;
#159054 = CARTESIAN_POINT ( 'NONE',  ( -16.55341960407611168, -4.379528057220339221, 81.45724293864769550 ) ) ;
#159055 = CARTESIAN_POINT ( 'NONE',  ( 15.80617190586746368, 15.72974639402197994, 29.37390960531435269 ) ) ;
#159056 = CARTESIAN_POINT ( 'NONE',  ( -19.03943276465977164, -0.05219959533935918106, 83.75109039468567573 ) ) ;
#159057 = CARTESIAN_POINT ( 'NONE',  ( 21.53943276465977519, -0.05219959533907433946, 93.74890960531436690 ) ) ;
#159058 = CARTESIAN_POINT ( 'NONE',  ( -10.81492255796105439, 18.62759615963255655, 42.91775706135235424 ) ) ;
#159059 = CARTESIAN_POINT ( 'NONE',  ( 12.06949235617739724, 12.14591786802326823, 61.87609039468568284 ) ) ;
#159061 = CARTESIAN_POINT ( 'NONE',  ( 5.823673210054444382, -21.52544592524334988, 50.20942372801901854 ) ) ;
#159060 = CARTESIAN_POINT ( 'NONE',  ( 16.53943276465976808, 0.05219959533934440121, 51.25109039468568994 ) ) ;
#159062 = CARTESIAN_POINT ( 'NONE',  ( -15.80617190586745835, -15.72974639402198527, 51.87390960531437401 ) ) ;
#159063 = CARTESIAN_POINT ( 'NONE',  ( 0.05219959533909260263, 19.03943276465977164, 49.99890960531435979 ) ) ;
#159064 = CARTESIAN_POINT ( 'NONE',  ( -6.020228577223754586E-15, 39.95556452105416412, -6.249999994537626336 ) ) ;
#159065 = CARTESIAN_POINT ( 'NONE',  ( 16.52544592524335698, 4.483927247898782831, 76.45942372801901854 ) ) ;
#159066 = CARTESIAN_POINT ( 'NONE',  ( -21.55341960407610458, -5.719274019375992779, 101.4572429386476955 ) ) ;
#159067 = CARTESIAN_POINT ( 'NONE',  ( -16.55341960407611168, -4.379528057220339221, 46.45724293864769550 ) ) ;
#159068 = CARTESIAN_POINT ( 'NONE',  ( 0.05219959533934541429, -16.53943276465976808, 60.00109039468568284 ) ) ;
#159069 = CARTESIAN_POINT ( 'NONE',  ( 16.46253265017146816, 9.564922557961045513, 96.66775706135233293 ) ) ;
#159070 = CARTESIAN_POINT ( 'NONE',  ( 5.823673210054125526, 21.52544592524343514, 94.79057627198105251 ) ) ;
#159071 = CARTESIAN_POINT ( 'NONE',  ( -4.483927247898539470, -16.52544592524342804, 42.29057627198103120 ) ) ;
#159072 = EDGE_LOOP ( 'NONE', ( #23697, #188753, #170671, #158347 ) ) ;
#159073 = CARTESIAN_POINT ( 'NONE',  ( -17.49999999999999289, 5.500000000000036415, 75.79690382534175797 ) ) ;
#159074 = CARTESIAN_POINT ( 'NONE',  ( -0.05219959533907301413, -21.53943276465977519, 77.49890960531433848 ) ) ;
#159075 = CARTESIAN_POINT ( 'NONE',  ( -16.52544592524342804, 4.483927247898546575, 31.04057627198102409 ) ) ;
#159076 = ORIENTED_EDGE ( 'NONE', *, *, #57173, .T. ) ;
#159077 = LINE ( 'NONE', #34751, #134144 ) ;
#159078 = CARTESIAN_POINT ( 'NONE',  ( -10.81492255796078084, -18.62759615963271287, 107.0822429386476955 ) ) ;
#159079 = CARTESIAN_POINT ( 'NONE',  ( -10.72451020669898014, 18.67979575497178502, 110.4155762719810383 ) ) ;
#159080 = CARTESIAN_POINT ( 'NONE',  ( -4.483927247898539470, -16.52544592524342804, 32.29057627198102409 ) ) ;
#159081 = CARTESIAN_POINT ( 'NONE',  ( -12.14591786802326823, 12.06949235617739902, 53.12609039468568284 ) ) ;
#159082 = CARTESIAN_POINT ( 'NONE',  ( 9.474510206698971260, -16.51473224551069308, 47.91557627198102409 ) ) ;
#159083 = CARTESIAN_POINT ( 'NONE',  ( 9.474510206698971260, -16.51473224551069308, 62.91557627198102409 ) ) ;
#159084 = VERTEX_POINT ( 'NONE', #152886 ) ;
#159085 = CARTESIAN_POINT ( 'NONE',  ( -15.72974639402197994, 15.80617190586746368, 40.62390960531435269 ) ) ;
#159086 = CARTESIAN_POINT ( 'NONE',  ( -32.72233185157555369, -19.32382731393326125, -21.08582493607484665 ) ) ;
#159087 = CARTESIAN_POINT ( 'NONE',  ( -16.55341960407617563, 4.379528057220093196, 23.54275706135235424 ) ) ;
#159088 = CARTESIAN_POINT ( 'NONE',  ( -9.474510206698720793, -16.51473224551083518, 44.58442372801900433 ) ) ;
#159089 = CARTESIAN_POINT ( 'NONE',  ( 10.72451020669898902, -18.67979575497178502, 107.9155762719810241 ) ) ;
#159090 = CARTESIAN_POINT ( 'NONE',  ( 12.14591786802309770, 12.06949235617756955, 34.37390960531435979 ) ) ;
#159091 = AXIS2_PLACEMENT_3D ( 'NONE', #138611, #27500, #15283 ) ;
#159092 = CARTESIAN_POINT ( 'NONE',  ( 19.03943276465977164, -0.05219959533909143690, 83.74890960531436690 ) ) ;
#159093 = CARTESIAN_POINT ( 'NONE',  ( -10.72451020669898014, 18.67979575497178502, 45.41557627198103830 ) ) ;
#159095 = CARTESIAN_POINT ( 'NONE',  ( -16.53943276465976808, -0.05219959533934237506, 23.75109039468567929 ) ) ;
#159094 = CARTESIAN_POINT ( 'NONE',  ( -10.72451020669898014, 18.67979575497178502, 80.41557627198103830 ) ) ;
#159096 = CARTESIAN_POINT ( 'NONE',  ( -0.05219959533907301413, -21.53943276465977519, 22.49890960531436335 ) ) ;
#159097 = CARTESIAN_POINT ( 'NONE',  ( -15.72974639402176322, -15.80617190586768395, 74.37609039468568994 ) ) ;
#159098 = CARTESIAN_POINT ( 'NONE',  ( 13.89961937509977652, -13.97604488694527269, 78.12390960531433848 ) ) ;
#159099 = CARTESIAN_POINT ( 'NONE',  ( -19.02544592524342804, 5.153800228976336051, 31.04057627198102409 ) ) ;
#159100 = CARTESIAN_POINT ( 'NONE',  ( -5.153800228976328057, -19.02544592524343514, 82.29057627198103830 ) ) ;
#159101 = CARTESIAN_POINT ( 'NONE',  ( -16.55341960407611168, -4.379528057220339221, 86.45724293864770971 ) ) ;
#159102 = ORIENTED_EDGE ( 'NONE', *, *, #127759, .F. ) ;
#159103 = CARTESIAN_POINT ( 'NONE',  ( -5.049401038297874678, -19.05341960407617918, 109.7927570613523187 ) ) ;
#159104 = DIRECTION ( 'NONE',  ( 0.000000000000000000, 0.000000000000000000, 1.000000000000000000 ) ) ;
#159105 = CARTESIAN_POINT ( 'NONE',  ( 13.89961937509977652, -13.97604488694527269, 68.12390960531436690 ) ) ;
#159107 = CARTESIAN_POINT ( 'NONE',  ( 5.153800228976335163, 19.02544592524342804, 114.7905762719810241 ) ) ;
#159106 = CARTESIAN_POINT ( 'NONE',  ( -15.72974639402176322, -15.80617190586768395, 89.37609039468568994 ) ) ;
#159108 = CARTESIAN_POINT ( 'NONE',  ( -8.224510206698735004, -14.34966873604973081, 79.58442372801903275 ) ) ;
#159109 = CARTESIAN_POINT ( 'NONE',  ( -17.05587630539786659, -6.762274262135682612, 74.25819690962691766 ) ) ;
#159110 = CARTESIAN_POINT ( 'NONE',  ( 0.05219959533936267826, -19.03943276465977164, 55.00109039468566863 ) ) ;
#159111 = CARTESIAN_POINT ( 'NONE',  ( 13.97604488694548053, -13.89961937509957401, 20.62609039468567573 ) ) ;
#159112 = CARTESIAN_POINT ( 'NONE',  ( 4.979424220691216263, 6.824450432131265565, -64.09785073354592555 ) ) ;
#159113 = CARTESIAN_POINT ( 'NONE',  ( -31.80000000000000782, -5.510910596163089556E-15, 45.00000000000000000 ) ) ;
#159114 = CARTESIAN_POINT ( 'NONE',  ( -36.91746825000001309, 11.99521256947798342, -5.224999997268811924 ) ) ;
#159115 = CARTESIAN_POINT ( 'NONE',  ( 0.05219959533910956823, 16.53943276465976808, 24.99890960531435624 ) ) ;
#159116 = CARTESIAN_POINT ( 'NONE',  ( -35.70266437024448436, -0.4905633046376467465, 37.50000000000000000 ) ) ;
#159117 = CARTESIAN_POINT ( 'NONE',  ( -4.483927247898782831, 16.52544592524335698, 107.7094237280190328 ) ) ;
#159118 = CARTESIAN_POINT ( 'NONE',  ( 32.05902467079202012, -23.92572825132751291, -20.04789607283224839 ) ) ;
#159119 = CARTESIAN_POINT ( 'NONE',  ( -16.53943276465976808, -0.05219959533934237506, 83.75109039468568994 ) ) ;
#159120 = CARTESIAN_POINT ( 'NONE',  ( -5.719274019375665041, -21.55341960407619695, 89.79275706135236135 ) ) ;
#159121 = CARTESIAN_POINT ( 'NONE',  ( 19.02544592524334988, 5.153800228976608722, 101.4594237280189759 ) ) ;
#159122 = CARTESIAN_POINT ( 'NONE',  ( 15.72974639402176855, 15.80617190586768217, 61.87609039468568284 ) ) ;
#159123 = CARTESIAN_POINT ( 'NONE',  ( 13.97604488694548053, -13.89961937509957401, 40.62609039468564731 ) ) ;
#159124 = CARTESIAN_POINT ( 'NONE',  ( -13.89961937509977652, 13.97604488694528158, 85.62390960531433848 ) ) ;
#159125 = CARTESIAN_POINT ( 'NONE',  ( 5.049401038298161559, -19.05341960407611168, 72.70724293864768129 ) ) ;
#159126 = CARTESIAN_POINT ( 'NONE',  ( -17.49999999999999645, 5.499999999999997335, 120.0000000000000142 ) ) ;
#159127 = CARTESIAN_POINT ( 'NONE',  ( -18.67979575497178146, -10.72451020669898902, 51.66557627198102409 ) ) ;
#159128 = CARTESIAN_POINT ( 'NONE',  ( -0.05219959533909027116, -19.03943276465977164, 47.49890960531435979 ) ) ;
#159129 = CARTESIAN_POINT ( 'NONE',  ( -14.34966873604972548, 8.224510206698743886, 83.33442372801903275 ) ) ;
#159130 = UNCERTAINTY_MEASURE_WITH_UNIT (LENGTH_MEASURE( 1.000000000000000082E-05 ), #82837, 'distance_accuracy_value', 'NONE');
#159131 = VERTEX_POINT ( 'NONE', #137723 ) ;
#159133 = CARTESIAN_POINT ( 'NONE',  ( 29.86685920354754487, 21.69954338932564752, -5.424999997268813878 ) ) ;
#159132 = CARTESIAN_POINT ( 'NONE',  ( 12.14591786802309770, 12.06949235617756955, 79.37390960531436690 ) ) ;
#159134 = CARTESIAN_POINT ( 'NONE',  ( -16.53943276465976808, -0.05219959533934237506, 43.75109039468568284 ) ) ;
#159135 = CARTESIAN_POINT ( 'NONE',  ( -8.314922557960811034, -14.29746914071050412, 102.0822429386476955 ) ) ;
#159136 = CARTESIAN_POINT ( 'NONE',  ( -9.474510206698720793, -16.51473224551083518, 69.58442372801901854 ) ) ;
#159137 = CARTESIAN_POINT ( 'NONE',  ( 16.55341960407611168, 4.379528057220329451, 73.95724293864769550 ) ) ;
#159138 = CARTESIAN_POINT ( 'NONE',  ( -5.719274019375665041, -21.55341960407619695, 29.79275706135234358 ) ) ;
#159140 = CARTESIAN_POINT ( 'NONE',  ( -10.81492255796078084, -18.62759615963271287, 87.08224293864769550 ) ) ;
#159139 = CARTESIAN_POINT ( 'NONE',  ( 16.46253265017160672, -9.564922557960803928, 23.33224293864769194 ) ) ;
#159141 = CARTESIAN_POINT ( 'NONE',  ( -16.51473224551069308, -9.474510206698971260, 101.6655762719810241 ) ) ;
#159142 = CARTESIAN_POINT ( 'NONE',  ( -12.14591786802309592, -12.06949235617757132, 71.87390960531438111 ) ) ;
#159143 = CARTESIAN_POINT ( 'NONE',  ( 20.09009762001922894, -36.41118502145469904, -19.08443133123336111 ) ) ;
#159144 = CARTESIAN_POINT ( 'NONE',  ( -16.51473224551069308, -9.474510206698971260, 51.66557627198102409 ) ) ;
#159145 = CARTESIAN_POINT ( 'NONE',  ( -5.950531402560715689E-15, 38.81732327939063509, -5.124999997268813168 ) ) ;
#159146 = CARTESIAN_POINT ( 'NONE',  ( 16.51473224551083163, -9.474510206698727899, 80.83442372801899012 ) ) ;
#159147 = CARTESIAN_POINT ( 'NONE',  ( -10.72451020669898014, 18.67979575497178502, 115.4155762719810241 ) ) ;
#159148 = CARTESIAN_POINT ( 'NONE',  ( 19.02544592524343514, -5.153800228976328945, 73.54057627198103830 ) ) ;
#159149 = CARTESIAN_POINT ( 'NONE',  ( 16.51473224551083163, -9.474510206698727899, 60.83442372801900433 ) ) ;
#159150 = CARTESIAN_POINT ( 'NONE',  ( 13.97604488694527802, 13.89961937509977652, 39.37390960531435269 ) ) ;
#159151 = CARTESIAN_POINT ( 'NONE',  ( 16.53943276465976808, -0.05219959533910856209, 68.74890960531435269 ) ) ;
#159152 = CARTESIAN_POINT ( 'NONE',  ( 12.14591786802309770, 12.06949235617756955, 49.37390960531436690 ) ) ;
#159153 = CARTESIAN_POINT ( 'NONE',  ( -9.474510206698964154, 16.51473224551069663, 75.41557627198103830 ) ) ;
#159154 = CARTESIAN_POINT ( 'NONE',  ( -21.55341960407610458, -5.719274019375992779, 81.45724293864769550 ) ) ;
#159155 = CARTESIAN_POINT ( 'NONE',  ( -16.46253265017160317, 9.564922557960807481, 70.83224293864770971 ) ) ;
#159156 = CARTESIAN_POINT ( 'NONE',  ( -21.53943276465977519, 0.05219959533907696930, 81.24890960531436690 ) ) ;
#159157 = EDGE_CURVE ( 'NONE', #89664, #106917, #81543, .T. ) ;
#159158 = CARTESIAN_POINT ( 'NONE',  ( -9.474510206698720793, -16.51473224551083518, 24.58442372801900078 ) ) ;
#159161 = CARTESIAN_POINT ( 'NONE',  ( -14.29746914071049879, 8.314922557960819915, 95.83224293864770971 ) ) ;
#159160 = CARTESIAN_POINT ( 'NONE',  ( 12.14591786802327356, -12.06949235617739191, 110.6260903946857042 ) ) ;
#159159 = CARTESIAN_POINT ( 'NONE',  ( 5.153800228976335163, 19.02544592524342804, 29.79057627198102409 ) ) ;
#159162 = CARTESIAN_POINT ( 'NONE',  ( 5.153800228976615827, -19.02544592524334988, 100.2094237280190043 ) ) ;
#159163 = ORIENTED_EDGE ( 'NONE', *, *, #173288, .F. ) ;
#159164 = CARTESIAN_POINT ( 'NONE',  ( 15.72974639402199770, -15.80617190586745480, 113.1239096053143953 ) ) ;
#159165 = CARTESIAN_POINT ( 'NONE',  ( 19.05341960407617918, -5.049401038297876454, 56.04275706135234714 ) ) ;
#159166 = CARTESIAN_POINT ( 'NONE',  ( -16.52544592524342804, 4.483927247898546575, 26.04057627198103475 ) ) ;
#159167 = CARTESIAN_POINT ( 'NONE',  ( 13.89961937509957401, 13.97604488694547697, 41.87609039468566152 ) ) ;
#159168 = CARTESIAN_POINT ( 'NONE',  ( -19.03943276465977164, 0.05219959533909376836, 106.2489096053143669 ) ) ;
#159169 = CARTESIAN_POINT ( 'NONE',  ( 12.14591786802309770, 12.06949235617756955, 54.37390960531435979 ) ) ;
#159170 = CARTESIAN_POINT ( 'NONE',  ( -19.05341960407611168, -5.049401038298163336, 21.45724293864768839 ) ) ;
#159171 = CARTESIAN_POINT ( 'NONE',  ( 19.02544592524343514, -5.153800228976328945, 33.54057627198102409 ) ) ;
#159172 = CARTESIAN_POINT ( 'NONE',  ( 0.05219959533936267826, -19.03943276465977164, 20.00109039468567218 ) ) ;
#159173 = CARTESIAN_POINT ( 'NONE',  ( 4.379528057220092307, 16.55341960407617563, 87.29275706135236135 ) ) ;
#159174 = CARTESIAN_POINT ( 'NONE',  ( -18.67979575497193778, 10.72451020669871902, 43.33442372801901143 ) ) ;
#159175 = CARTESIAN_POINT ( 'NONE',  ( -12.14591786802326823, 12.06949235617739902, 38.12609039468567573 ) ) ;
#159176 = CARTESIAN_POINT ( 'NONE',  ( 5.049401038298161559, -19.05341960407611168, 102.7072429386476955 ) ) ;
#159177 = CARTESIAN_POINT ( 'NONE',  ( -9.474510206698964154, 16.51473224551069663, 50.41557627198102409 ) ) ;
#159178 = CARTESIAN_POINT ( 'NONE',  ( -13.89961937509977652, 13.97604488694528158, 70.62390960531432427 ) ) ;
#159179 = CARTESIAN_POINT ( 'NONE',  ( -16.53943276465976808, -0.05219959533934237506, 53.75109039468568994 ) ) ;
#159180 = CARTESIAN_POINT ( 'NONE',  ( -14.29746914071049879, 8.314922557960819915, 105.8322429386476955 ) ) ;
#159181 = CARTESIAN_POINT ( 'NONE',  ( 0.05219959533934541429, -16.53943276465976808, 110.0010903946856757 ) ) ;
#159182 = CARTESIAN_POINT ( 'NONE',  ( 30.82560697742735201, 2.428612866367529932E-14, 150.0000000000000000 ) ) ;
#159185 = CARTESIAN_POINT ( 'NONE',  ( -13.89961937509977652, 13.97604488694528158, 80.62390960531436690 ) ) ;
#159184 = CARTESIAN_POINT ( 'NONE',  ( -13.89961937509977652, 13.97604488694528158, 95.62390960531436690 ) ) ;
#159183 = CARTESIAN_POINT ( 'NONE',  ( -10.72451020669870658, -18.67979575497194134, 59.58442372801901854 ) ) ;
#159186 = CARTESIAN_POINT ( 'NONE',  ( -16.46253265017160317, 9.564922557960807481, 95.83224293864769550 ) ) ;
#159187 = CARTESIAN_POINT ( 'NONE',  ( -12.14591786802309592, -12.06949235617757132, 46.87390960531435979 ) ) ;
#159188 = CARTESIAN_POINT ( 'NONE',  ( 8.224510206698742110, 14.34966873604972548, 107.0844237280190043 ) ) ;
#159189 = CARTESIAN_POINT ( 'NONE',  ( 16.53943276465976808, -0.05219959533910856209, 38.74890960531435979 ) ) ;
#159190 = VERTEX_POINT ( 'NONE', #139695 ) ;
#159191 = CARTESIAN_POINT ( 'NONE',  ( -14.71331571979865949, -16.70575312364977094, -55.79855980662914305 ) ) ;
#159192 = CARTESIAN_POINT ( 'NONE',  ( -13.97604488694547697, 13.89961937509957934, 43.12609039468566152 ) ) ;
#159193 = CARTESIAN_POINT ( 'NONE',  ( 5.153800228976335163, 19.02544592524342804, 64.79057627198100988 ) ) ;
#159194 = CARTESIAN_POINT ( 'NONE',  ( -16.46253265017146816, -9.564922557961047289, 54.16775706135234003 ) ) ;
#159195 = CARTESIAN_POINT ( 'NONE',  ( -29.86685920354755552, 21.69954338932564397, -0.8249999972688133454 ) ) ;
#159196 = LINE ( 'NONE', #157232, #105502 ) ;
#159198 = CARTESIAN_POINT ( 'NONE',  ( 16.55341960407618274, -4.379528057220086978, 66.04275706135236135 ) ) ;
#159197 = CARTESIAN_POINT ( 'NONE',  ( 0.05219959533936267826, -19.03943276465977164, 85.00109039468567573 ) ) ;
#159199 = CARTESIAN_POINT ( 'NONE',  ( 193.3062444957835453, -155.7167183371837496, -15.00000000000000178 ) ) ;
#159200 = CARTESIAN_POINT ( 'NONE',  ( -19.02544592524342804, 5.153800228976336051, 86.04057627198103830 ) ) ;
#159201 = CARTESIAN_POINT ( 'NONE',  ( -21.55341960407619339, 5.719274019375674811, 28.54275706135234358 ) ) ;
#159202 = VECTOR ( 'NONE', #138024, 1000.000000000000000 ) ;
#159203 = CARTESIAN_POINT ( 'NONE',  ( -9.474510206698720793, -16.51473224551083518, 84.58442372801900433 ) ) ;
#159205 = CARTESIAN_POINT ( 'NONE',  ( -19.05341960407611168, -5.049401038298163336, 46.45724293864768129 ) ) ;
#159204 = CARTESIAN_POINT ( 'NONE',  ( -5.153800228976328057, -19.02544592524343514, 112.2905762719810099 ) ) ;
#159206 = CARTESIAN_POINT ( 'NONE',  ( -13.89961937509977652, 13.97604488694528158, 95.62390960531436690 ) ) ;
#159208 = CARTESIAN_POINT ( 'NONE',  ( -13.97604488694527625, -13.89961937509977652, 46.87390960531435979 ) ) ;
#159207 = CARTESIAN_POINT ( 'NONE',  ( 14.29746914071049879, -8.314922557960816363, 43.33224293864769550 ) ) ;
#159209 = CARTESIAN_POINT ( 'NONE',  ( 9.564922557961047289, -16.46253265017146816, 60.41775706135233293 ) ) ;
#159210 = VERTEX_POINT ( 'NONE', #125541 ) ;
#159211 = CARTESIAN_POINT ( 'NONE',  ( -5.049401038297874678, -19.05341960407617918, 24.79275706135233648 ) ) ;
#159212 = CARTESIAN_POINT ( 'NONE',  ( -9.474510206698964154, 16.51473224551069663, 65.41557627198102409 ) ) ;
#159213 = CARTESIAN_POINT ( 'NONE',  ( 10.72451020669898902, -18.67979575497178502, 67.91557627198102409 ) ) ;
#159215 = CARTESIAN_POINT ( 'NONE',  ( -5.049401038297874678, -19.05341960407617918, 24.79275706135233648 ) ) ;
#159214 = CARTESIAN_POINT ( 'NONE',  ( 16.55341960407611168, 4.379528057220329451, 63.95724293864770260 ) ) ;
#159216 = CARTESIAN_POINT ( 'NONE',  ( 5.153800228976335163, 19.02544592524342804, 104.7905762719809957 ) ) ;
#159217 = CARTESIAN_POINT ( 'NONE',  ( -10.72451020669898014, 18.67979575497178502, 30.41557627198101699 ) ) ;
#159218 = CARTESIAN_POINT ( 'NONE',  ( 9.564922557960805705, 16.46253265017160317, 49.58224293864770260 ) ) ;
#159219 = CARTESIAN_POINT ( 'NONE',  ( 9.474510206698971260, -16.51473224551069308, 37.91557627198102409 ) ) ;
#159220 = CARTESIAN_POINT ( 'NONE',  ( -12.14591786802309592, -12.06949235617757132, 106.8739096053143811 ) ) ;
#159221 = CARTESIAN_POINT ( 'NONE',  ( -15.80617190586745835, -15.72974639402198527, 106.8739096053143811 ) ) ;
#159222 = CARTESIAN_POINT ( 'NONE',  ( -5.153800228976328057, -19.02544592524343514, 112.2905762719810099 ) ) ;
#159223 = CARTESIAN_POINT ( 'NONE',  ( -15.72974639402176322, -15.80617190586768395, 24.37609039468567573 ) ) ;
#159224 = CARTESIAN_POINT ( 'NONE',  ( 16.46253265017160672, -9.564922557960803928, 108.3322429386476955 ) ) ;
#159225 = CARTESIAN_POINT ( 'NONE',  ( 14.29746914071049879, -8.314922557960816363, 113.3322429386476955 ) ) ;
#159226 = CARTESIAN_POINT ( 'NONE',  ( -0.05219959533937732626, 21.53943276465977519, 72.50109039468568994 ) ) ;
#159227 = CARTESIAN_POINT ( 'NONE',  ( 21.52544592524344225, -5.823673210054117533, 93.54057627198103830 ) ) ;
#159228 = CARTESIAN_POINT ( 'NONE',  ( 17.31747979337947285, -6.344076630961067664, 106.1205513193481664 ) ) ;
#159229 = CARTESIAN_POINT ( 'NONE',  ( 19.53037848336980886, -5.499999999999890754, 77.35532783611445495 ) ) ;
#159230 = CARTESIAN_POINT ( 'NONE',  ( -9.474510206698964154, 16.51473224551069663, 60.41557627198102409 ) ) ;
#159231 = CARTESIAN_POINT ( 'NONE',  ( -4.483927247898782831, 16.52544592524335698, 47.70942372801902565 ) ) ;
#159232 = CARTESIAN_POINT ( 'NONE',  ( 12.06949235617757843, -12.14591786802309237, 108.1239096053143811 ) ) ;
#159233 = CARTESIAN_POINT ( 'NONE',  ( 33.80025371042794546, -2.440809870420986183, 99.93203653199846315 ) ) ;
#159234 = CARTESIAN_POINT ( 'NONE',  ( 19.03943276465977164, -0.05219959533909143690, 53.74890960531436690 ) ) ;
#159235 = CARTESIAN_POINT ( 'NONE',  ( 16.55341960407611168, 4.379528057220329451, 98.95724293864770971 ) ) ;
#159236 = CIRCLE ( 'NONE', #1053, 2.000000000000001776 ) ;
#159237 = CARTESIAN_POINT ( 'NONE',  ( 15.80617190586746368, 15.72974639402197994, 44.37390960531435979 ) ) ;
#159238 = CARTESIAN_POINT ( 'NONE',  ( 12.14591786802309770, 12.06949235617756955, 59.37390960531436690 ) ) ;
#159239 = CARTESIAN_POINT ( 'NONE',  ( -9.474510206698720793, -16.51473224551083518, 109.5844237280190043 ) ) ;
#159240 = CARTESIAN_POINT ( 'NONE',  ( -15.80617190586768217, 15.72974639402176855, 83.12609039468568994 ) ) ;
#159241 = CARTESIAN_POINT ( 'NONE',  ( -5.153800228976607833, 19.02544592524335343, 62.70942372801899012 ) ) ;
#159242 = CARTESIAN_POINT ( 'NONE',  ( 8.314922557961029526, -14.29746914071037800, 95.41775706135234714 ) ) ;
#159243 = CARTESIAN_POINT ( 'NONE',  ( 8.224510206698953496, -14.34966873604960469, 37.91557627198102409 ) ) ;
#159244 = CARTESIAN_POINT ( 'NONE',  ( 19.02544592524343514, -5.153800228976328945, 43.54057627198103120 ) ) ;
#159245 = CARTESIAN_POINT ( 'NONE',  ( 0.05219959533909260263, 19.03943276465977164, 89.99890960531436690 ) ) ;
#159246 = CARTESIAN_POINT ( 'NONE',  ( -10.72451020669898014, 18.67979575497178502, 90.41557627198103830 ) ) ;
#159247 = CARTESIAN_POINT ( 'NONE',  ( -14.29746914071037622, -8.314922557961029526, 39.16775706135235424 ) ) ;
#159249 = CARTESIAN_POINT ( 'NONE',  ( 5.823673210054444382, -21.52544592524334988, 90.20942372801903275 ) ) ;
#159248 = CARTESIAN_POINT ( 'NONE',  ( -8.224510206698948167, 14.34966873604960824, 65.41557627198102409 ) ) ;
#159250 = CARTESIAN_POINT ( 'NONE',  ( 8.314922557961029526, -14.29746914071037800, 95.41775706135234714 ) ) ;
#159251 = CARTESIAN_POINT ( 'NONE',  ( 17.40805194822030089, 6.112264579159360167, 26.66628727489388950 ) ) ;
#159252 = DIRECTION ( 'NONE',  ( -0.000000000000000000, 0.000000000000000000, 1.000000000000000000 ) ) ;
#159253 = CARTESIAN_POINT ( 'NONE',  ( -8.224510206698948167, 14.34966873604960824, 25.41557627198103120 ) ) ;
#159254 = CARTESIAN_POINT ( 'NONE',  ( -14.29746914071037622, -8.314922557961029526, 74.16775706135231871 ) ) ;
#159255 = CARTESIAN_POINT ( 'NONE',  ( -19.02544592524342804, 5.153800228976336051, 81.04057627198103830 ) ) ;
#159256 = CARTESIAN_POINT ( 'NONE',  ( 19.03943276465977164, -0.05219959533909143690, 98.74890960531436690 ) ) ;
#159257 = CARTESIAN_POINT ( 'NONE',  ( 5.719274019375673035, 21.55341960407619339, 87.29275706135236135 ) ) ;
#159258 = CARTESIAN_POINT ( 'NONE',  ( 4.379528057220092307, 16.55341960407617563, 92.29275706135236135 ) ) ;
#159259 = CARTESIAN_POINT ( 'NONE',  ( 12.14591786802309770, 12.06949235617756955, 64.37390960531435269 ) ) ;
#159260 = CARTESIAN_POINT ( 'NONE',  ( 5.153800228976335163, 19.02544592524342804, 69.79057627198103830 ) ) ;
#159261 = EDGE_LOOP ( 'NONE', ( #116818, #43071, #3499, #184892 ) ) ;
#159262 = CARTESIAN_POINT ( 'NONE',  ( 0.05219959533936267826, -19.03943276465977164, 110.0010903946856757 ) ) ;
#159263 = CARTESIAN_POINT ( 'NONE',  ( 19.05341960407611168, 5.049401038298154454, 33.95724293864769550 ) ) ;
#159264 = CARTESIAN_POINT ( 'NONE',  ( 19.03943276465977164, -0.05219959533909143690, 78.74890960531436690 ) ) ;
#159266 = CARTESIAN_POINT ( 'NONE',  ( -5.950531402560715689E-15, 38.81732327939063509, -7.124999997268814944 ) ) ;
#159265 = CARTESIAN_POINT ( 'NONE',  ( 0.05219959533936267826, -19.03943276465977164, 110.0010903946856757 ) ) ;
#159267 = CARTESIAN_POINT ( 'NONE',  ( -9.564922557961040184, 16.46253265017147172, 27.91775706135232582 ) ) ;
#159268 = CARTESIAN_POINT ( 'NONE',  ( -0.05219959533934338120, 16.53943276465976808, 82.50109039468568994 ) ) ;
#159269 = CARTESIAN_POINT ( 'NONE',  ( 9.474510206698729675, 16.51473224551082808, 107.0844237280190043 ) ) ;
#159270 = CARTESIAN_POINT ( 'NONE',  ( 4.483927247898545687, 16.52544592524342804, 114.7905762719810383 ) ) ;
#159271 = CARTESIAN_POINT ( 'NONE',  ( -14.29746914071037622, -8.314922557961029526, 69.16775706135234714 ) ) ;
#159272 = CARTESIAN_POINT ( 'NONE',  ( -14.34966873604972548, 8.224510206698743886, 48.33442372801902565 ) ) ;
#159273 = CARTESIAN_POINT ( 'NONE',  ( -19.05341960407611168, -5.049401038298163336, 26.45724293864769550 ) ) ;
#159274 = CARTESIAN_POINT ( 'NONE',  ( 5.153800228976615827, -19.02544592524334988, 65.20942372801900433 ) ) ;
#159275 = CARTESIAN_POINT ( 'NONE',  ( 10.72451020669871369, 18.67979575497193778, 112.0844237280190185 ) ) ;
#159276 = CARTESIAN_POINT ( 'NONE',  ( 5.049401038298161559, -19.05341960407611168, 37.70724293864768839 ) ) ;
#159277 = CARTESIAN_POINT ( 'NONE',  ( 16.46253265017160672, -9.564922557960803928, 73.33224293864769550 ) ) ;
#159278 = CARTESIAN_POINT ( 'NONE',  ( -16.52544592524342804, 4.483927247898546575, 66.04057627198103830 ) ) ;
#159279 = CARTESIAN_POINT ( 'NONE',  ( 13.97604488694548053, -13.89961937509957401, 45.62609039468566863 ) ) ;
#159280 = CARTESIAN_POINT ( 'NONE',  ( 10.81492255796078972, 18.62759615963270932, 34.58224293864770260 ) ) ;
#159281 = CARTESIAN_POINT ( 'NONE',  ( -5.823673210054431948, 21.52544592524334988, 112.7094237280190328 ) ) ;
#159282 = CARTESIAN_POINT ( 'NONE',  ( -19.03943276465977164, 0.05219959533909376836, 91.24890960531436690 ) ) ;
#159283 = CARTESIAN_POINT ( 'NONE',  ( 5.823673210054444382, -21.52544592524334988, 105.2094237280190328 ) ) ;
#159284 = CARTESIAN_POINT ( 'NONE',  ( 18.62759615963271287, -10.81492255796078972, 68.33224293864769550 ) ) ;
#159285 = CARTESIAN_POINT ( 'NONE',  ( -19.03943276465977164, 0.05219959533909376836, 101.2489096053143669 ) ) ;
#159286 = CARTESIAN_POINT ( 'NONE',  ( 5.153800228976615827, -19.02544592524334988, 80.20942372801901854 ) ) ;
#159287 = CARTESIAN_POINT ( 'NONE',  ( 16.51473224551069308, 9.474510206698969483, 99.16557627198102409 ) ) ;
#159288 = CARTESIAN_POINT ( 'NONE',  ( -19.02544592524334988, -5.153800228976617603, 98.95942372801900433 ) ) ;
#159289 = CARTESIAN_POINT ( 'NONE',  ( 16.52544592524335698, 4.483927247898782831, 61.45942372801901854 ) ) ;
#159290 = CARTESIAN_POINT ( 'NONE',  ( 0.05219959533909260263, 19.03943276465977164, 24.99890960531435269 ) ) ;
#159291 = CARTESIAN_POINT ( 'NONE',  ( 5.049401038298161559, -19.05341960407611168, 87.70724293864769550 ) ) ;
#159292 = CARTESIAN_POINT ( 'NONE',  ( 15.72974639402199770, -15.80617190586745480, 68.12390960531436690 ) ) ;
#159293 = CARTESIAN_POINT ( 'NONE',  ( -12.06949235617739369, -12.14591786802326823, 29.37609039468568284 ) ) ;
#159294 = CARTESIAN_POINT ( 'NONE',  ( -10.72451020669870658, -18.67979575497194134, 34.58442372801900433 ) ) ;
#159295 = CARTESIAN_POINT ( 'NONE',  ( -10.81492255796105439, 18.62759615963255655, 97.91775706135236135 ) ) ;
#159296 = CARTESIAN_POINT ( 'NONE',  ( -8.224510206698735004, -14.34966873604973081, 94.58442372801901854 ) ) ;
#159297 = VECTOR ( 'NONE', #54218, 1000.000000000000000 ) ;
#159298 = CARTESIAN_POINT ( 'NONE',  ( -5.049401038298153566, 19.05341960407611168, 85.20724293864766707 ) ) ;
#159299 = CARTESIAN_POINT ( 'NONE',  ( -8.224510206698948167, 14.34966873604960824, 75.41557627198102409 ) ) ;
#159300 = CARTESIAN_POINT ( 'NONE',  ( -14.29746914071049879, 8.314922557960819915, 25.83224293864769194 ) ) ;
#159301 = CARTESIAN_POINT ( 'NONE',  ( 5.049401038297881783, 19.05341960407617563, 72.29275706135234714 ) ) ;
#159302 = EDGE_CURVE ( 'NONE', #8238, #138761, #98595, .T. ) ;
#159303 = CARTESIAN_POINT ( 'NONE',  ( 5.719274019375673035, 21.55341960407619339, 42.29275706135235424 ) ) ;
#159304 = CARTESIAN_POINT ( 'NONE',  ( 4.379528057220339221, -16.55341960407611168, 87.70724293864769550 ) ) ;
#159305 = CARTESIAN_POINT ( 'NONE',  ( 5.049401038298161559, -19.05341960407611168, 112.7072429386476813 ) ) ;
#159306 = CARTESIAN_POINT ( 'NONE',  ( -4.379528057220086978, -16.55341960407618274, 99.79275706135234714 ) ) ;
#159307 = CARTESIAN_POINT ( 'NONE',  ( 18.62759615963255655, 10.81492255796105972, 86.66775706135234714 ) ) ;
#159308 = CARTESIAN_POINT ( 'NONE',  ( -4.483927247898782831, 16.52544592524335698, 47.70942372801902565 ) ) ;
#159309 = CARTESIAN_POINT ( 'NONE',  ( 18.62759615963255655, 10.81492255796105972, 41.66775706135235424 ) ) ;
#159310 = ORIENTED_EDGE ( 'NONE', *, *, #179291, .T. ) ;
#159311 = CARTESIAN_POINT ( 'NONE',  ( 10.81492255796106328, -18.62759615963255655, 20.41775706135234714 ) ) ;
#159312 = CARTESIAN_POINT ( 'NONE',  ( 16.52544592524342804, -4.483927247898539470, 88.54057627198103830 ) ) ;
#159313 = CARTESIAN_POINT ( 'NONE',  ( 0.000000000000000000, 0.000000000000000000, -61.89430850415821794 ) ) ;
#159314 = CARTESIAN_POINT ( 'NONE',  ( -4.379528057220328563, 16.55341960407611168, 65.20724293864768129 ) ) ;
#159315 = CARTESIAN_POINT ( 'NONE',  ( 8.224510206698742110, 14.34966873604972548, 112.0844237280190185 ) ) ;
#159316 = CARTESIAN_POINT ( 'NONE',  ( -16.46253265017160317, 9.564922557960807481, 35.83224293864768839 ) ) ;
#159317 = CARTESIAN_POINT ( 'NONE',  ( -5.823673210054116645, -21.52544592524344225, 37.29057627198102409 ) ) ;
#159318 = CARTESIAN_POINT ( 'NONE',  ( 4.483927247898545687, 16.52544592524342804, 84.79057627198102409 ) ) ;
#159319 = CARTESIAN_POINT ( 'NONE',  ( 21.52544592524344225, -5.823673210054117533, 83.54057627198102409 ) ) ;
#159320 = CARTESIAN_POINT ( 'NONE',  ( -9.564922557960796823, -16.46253265017161027, 92.08224293864769550 ) ) ;
#159322 = CARTESIAN_POINT ( 'NONE',  ( 5.049401038297881783, 19.05341960407617563, 92.29275706135234714 ) ) ;
#159321 = CARTESIAN_POINT ( 'NONE',  ( 19.05341960407611168, 5.049401038298154454, 43.95724293864769550 ) ) ;
#159323 = CARTESIAN_POINT ( 'NONE',  ( 10.72451020669898902, -18.67979575497178502, 27.91557627198103830 ) ) ;
#159324 = CARTESIAN_POINT ( 'NONE',  ( -18.62759615963255300, -10.81492255796106328, 64.16775706135234714 ) ) ;
#159325 = CARTESIAN_POINT ( 'NONE',  ( -16.46253265017160317, 9.564922557960807481, 50.83224293864770260 ) ) ;
#159326 = CARTESIAN_POINT ( 'NONE',  ( -19.05341960407611168, -5.049401038298163336, 91.45724293864766707 ) ) ;
#159327 = ORIENTED_EDGE ( 'NONE', *, *, #96802, .F. ) ;
#159328 = CARTESIAN_POINT ( 'NONE',  ( -16.53943276465976808, -0.05219959533934237506, 63.75109039468568284 ) ) ;
#159329 = CARTESIAN_POINT ( 'NONE',  ( 5.823673210054444382, -21.52544592524334988, 45.20942372801901854 ) ) ;
#159330 = CARTESIAN_POINT ( 'NONE',  ( -5.719274019375665041, -21.55341960407619695, 74.79275706135234714 ) ) ;
#159331 = CARTESIAN_POINT ( 'NONE',  ( 19.05341960407611168, 5.049401038298154454, 113.9572429386477097 ) ) ;
#159332 = CARTESIAN_POINT ( 'NONE',  ( -5.823673210054116645, -21.52544592524344225, 102.2905762719810383 ) ) ;
#159334 = CARTESIAN_POINT ( 'NONE',  ( -16.53943276465976808, -0.05219959533934237506, 63.75109039468568284 ) ) ;
#159333 = CARTESIAN_POINT ( 'NONE',  ( -5.719274019375665041, -21.55341960407619695, 29.79275706135234358 ) ) ;
#159335 = CARTESIAN_POINT ( 'NONE',  ( -21.52544592524343514, 5.823673210054127303, 66.04057627198103830 ) ) ;
#159336 = CARTESIAN_POINT ( 'NONE',  ( 21.53943276465977519, 0.05219959533937863772, 111.2510903946856899 ) ) ;
#159338 = CARTESIAN_POINT ( 'NONE',  ( 0.05219959533934541429, -16.53943276465976808, 105.0010903946856757 ) ) ;
#159337 = CARTESIAN_POINT ( 'NONE',  ( -9.564922557960796823, -16.46253265017161027, 67.08224293864769550 ) ) ;
#159339 = CARTESIAN_POINT ( 'NONE',  ( -17.50000000000015277, -3.417042746626872685, 104.8261960376753450 ) ) ;
#159340 = CARTESIAN_POINT ( 'NONE',  ( -13.89961937509977652, 13.97604488694528158, 100.6239096053143669 ) ) ;
#159341 = EDGE_CURVE ( 'NONE', #181921, #146141, #56185, .T. ) ;
#159342 = CARTESIAN_POINT ( 'NONE',  ( -14.34966873604972548, 8.224510206698743886, 43.33442372801901143 ) ) ;
#159343 = CARTESIAN_POINT ( 'NONE',  ( 22.02608267474400350, 22.90350128981412325, -45.83983912514963066 ) ) ;
#159344 = CARTESIAN_POINT ( 'NONE',  ( 19.02544592524334988, 5.153800228976608722, 81.45942372801897591 ) ) ;
#159345 = CARTESIAN_POINT ( 'NONE',  ( -21.52544592524343514, 5.823673210054127303, 61.04057627198103120 ) ) ;
#159346 = CARTESIAN_POINT ( 'NONE',  ( -12.14591786802309592, -12.06949235617757132, 26.87390960531435979 ) ) ;
#159347 = CARTESIAN_POINT ( 'NONE',  ( -19.05341960407617563, 5.049401038297882671, 98.54275706135233293 ) ) ;
#159348 = LINE ( 'NONE', #20844, #162836 ) ;
#159349 = CARTESIAN_POINT ( 'NONE',  ( 13.97604488694548053, -13.89961937509957401, 95.62609039468563310 ) ) ;
#159351 = CARTESIAN_POINT ( 'NONE',  ( -5.153800228976607833, 19.02544592524334988, 57.70942372801899012 ) ) ;
#159350 = CARTESIAN_POINT ( 'NONE',  ( 21.53943276465977519, -0.05219959533907433946, 93.74890960531436690 ) ) ;
#159352 = CARTESIAN_POINT ( 'NONE',  ( 25.41560487745633168, -11.65347601360406848, 166.2639678467665760 ) ) ;
#159353 = CARTESIAN_POINT ( 'NONE',  ( 9.564922557960805705, 16.46253265017160317, 74.58224293864769550 ) ) ;
#159354 = CARTESIAN_POINT ( 'NONE',  ( 12.14591786802309770, 12.06949235617756955, 59.37390960531436690 ) ) ;
#159355 = CARTESIAN_POINT ( 'NONE',  ( -19.05341960407611168, -5.049401038298163336, 51.45724293864770260 ) ) ;
#159356 = CARTESIAN_POINT ( 'NONE',  ( -8.224510206698948167, 14.34966873604960824, 50.41557627198103120 ) ) ;
#159357 = CARTESIAN_POINT ( 'NONE',  ( -29.43349580481984162, 2.016473703290251599E-14, 139.9999999999999716 ) ) ;
#159358 = CARTESIAN_POINT ( 'NONE',  ( 31.49170352461661793, -4.578070284816052826, 100.9457761758980325 ) ) ;
#159359 = CARTESIAN_POINT ( 'NONE',  ( 8.314922557960818139, 14.29746914071049879, 29.58224293864769905 ) ) ;
#159360 = CARTESIAN_POINT ( 'NONE',  ( 19.03943276465977164, -0.05219959533909143690, 68.74890960531436690 ) ) ;
#159361 = CARTESIAN_POINT ( 'NONE',  ( -17.49999999999999645, 5.500000000000037303, 50.79690382534172244 ) ) ;
#159362 = CARTESIAN_POINT ( 'NONE',  ( 16.46253265017146816, 9.564922557961045513, 36.66775706135233293 ) ) ;
#159363 = CARTESIAN_POINT ( 'NONE',  ( 4.483927247898790824, -16.52544592524335698, 50.20942372801901854 ) ) ;
#159364 = CARTESIAN_POINT ( 'NONE',  ( -18.67979575497178146, -10.72451020669898902, 56.66557627198103830 ) ) ;
#159365 = CARTESIAN_POINT ( 'NONE',  ( -5.719274019375665041, -21.55341960407619695, 99.79275706135234714 ) ) ;
#159366 = CARTESIAN_POINT ( 'NONE',  ( 16.46253265017160672, -9.564922557960803928, 73.33224293864769550 ) ) ;
#159367 = CARTESIAN_POINT ( 'NONE',  ( 1.531793102469823607E-14, -74.04165629597446241, -24.99410988461188055 ) ) ;
#159368 = CARTESIAN_POINT ( 'NONE',  ( -5.049401038298153566, 19.05341960407611168, 115.2072429386477097 ) ) ;
#159369 = CARTESIAN_POINT ( 'NONE',  ( 22.81625015709509441, 31.40387420917330275, -1.324999997268813123 ) ) ;
#159370 = CARTESIAN_POINT ( 'NONE',  ( 5.823673210054444382, -21.52544592524334988, 35.20942372801901854 ) ) ;
#159371 = CARTESIAN_POINT ( 'NONE',  ( 16.55341960407611168, 4.379528057220329451, 93.95724293864770971 ) ) ;
#159372 = ADVANCED_FACE ( 'NONE', ( #112355 ), #97163, .T. ) ;
#159375 = CARTESIAN_POINT ( 'NONE',  ( 5.000000000000000000, 0.000000000000000000, -15.00000000000000000 ) ) ;
#159374 = CARTESIAN_POINT ( 'NONE',  ( -16.51473224551069308, -9.474510206698971260, 76.66557627198103830 ) ) ;
#159373 = CARTESIAN_POINT ( 'NONE',  ( -21.55341960407610458, -5.719274019375992779, 91.45724293864769550 ) ) ;
#159376 = CARTESIAN_POINT ( 'NONE',  ( -19.02544592524342804, 5.153800228976336051, 86.04057627198103830 ) ) ;
#159377 = CARTESIAN_POINT ( 'NONE',  ( 18.67979575497194134, -10.72451020669871369, 30.83442372801902209 ) ) ;
#159378 = ORIENTED_EDGE ( 'NONE', *, *, #92161, .T. ) ;
#159379 = CARTESIAN_POINT ( 'NONE',  ( 19.02544592524343514, -5.153800228976328945, 78.54057627198099567 ) ) ;
#159380 = AXIS2_PLACEMENT_3D ( 'NONE', #115131, #178820, #27138 ) ;
#159381 = LINE ( 'NONE', #23887, #159297 ) ;
#159383 = CARTESIAN_POINT ( 'NONE',  ( 13.97604488694527802, 13.89961937509977652, 34.37390960531436690 ) ) ;
#159382 = CARTESIAN_POINT ( 'NONE',  ( -9.474510206698964154, 16.51473224551069663, 30.41557627198102054 ) ) ;
#159384 = CARTESIAN_POINT ( 'NONE',  ( -19.03943276465977164, -0.05219959533935918106, 108.7510903946856615 ) ) ;
#159385 = CARTESIAN_POINT ( 'NONE',  ( 29.86685920354754842, -21.69954338932559068, -10.32499999726881335 ) ) ;
#159386 = CARTESIAN_POINT ( 'NONE',  ( -0.05219959533910754901, -16.53943276465976808, 112.4989096053143669 ) ) ;
#159387 = CARTESIAN_POINT ( 'NONE',  ( -21.53943276465977519, -0.05219959533937600094, 68.75109039468568994 ) ) ;
#159389 = CARTESIAN_POINT ( 'NONE',  ( -21.52544592524334988, -5.823673210054445271, 38.95942372801901854 ) ) ;
#159388 = CARTESIAN_POINT ( 'NONE',  ( 9.474510206698971260, -16.51473224551069308, 67.91557627198102409 ) ) ;
#159390 = CARTESIAN_POINT ( 'NONE',  ( -21.53943276465977519, 0.05219959533907696930, 116.2489096053143669 ) ) ;
#159391 = CARTESIAN_POINT ( 'NONE',  ( -17.81289503416611808, 24.51734667627700404, 145.6999999999999886 ) ) ;
#159392 = CARTESIAN_POINT ( 'NONE',  ( 5.049401038298161559, -19.05341960407611168, 82.70724293864770971 ) ) ;
#159393 = CARTESIAN_POINT ( 'NONE',  ( 27.91252812236343317, 7.473505457733358170, 160.9450913315119180 ) ) ;
#159395 = CARTESIAN_POINT ( 'NONE',  ( -15.72974639402197994, 15.80617190586746368, 45.62390960531436690 ) ) ;
#159394 = CARTESIAN_POINT ( 'NONE',  ( -4.379528057220086978, -16.55341960407618274, 19.79275706135235069 ) ) ;
#159396 = CARTESIAN_POINT ( 'NONE',  ( -5.823673210054431948, 21.52544592524334988, 67.70942372801901854 ) ) ;
#159397 = FACE_OUTER_BOUND ( 'NONE', #62526, .T. ) ;
#159398 = CARTESIAN_POINT ( 'NONE',  ( 0.05219959533936267826, -19.03943276465977164, 95.00109039468567573 ) ) ;
#159399 = CARTESIAN_POINT ( 'NONE',  ( 13.89961937509977652, -13.97604488694527269, 63.12390960531435979 ) ) ;
#159400 = CARTESIAN_POINT ( 'NONE',  ( 5.153800228976335163, 19.02544592524342804, 84.79057627198099567 ) ) ;
#159401 = CARTESIAN_POINT ( 'NONE',  ( 12.06949235617757843, -12.14591786802309237, 98.12390960531436690 ) ) ;
#159402 = CARTESIAN_POINT ( 'NONE',  ( 8.314922557960818139, 14.29746914071049879, 89.58224293864768129 ) ) ;
#159403 = CARTESIAN_POINT ( 'NONE',  ( 10.72451020669898902, -18.67979575497178502, 22.91557627198102765 ) ) ;
#159405 = CARTESIAN_POINT ( 'NONE',  ( 5.049401038298161559, -19.05341960407611168, 37.70724293864768839 ) ) ;
#159404 = CARTESIAN_POINT ( 'NONE',  ( 4.379528057220339221, -16.55341960407611168, 62.70724293864769550 ) ) ;
#159406 = CARTESIAN_POINT ( 'NONE',  ( 5.823673210054444382, -21.52544592524334988, 60.20942372801902565 ) ) ;
#159407 = CARTESIAN_POINT ( 'NONE',  ( 13.89961937509957401, 13.97604488694547697, 86.87609039468567573 ) ) ;
#159408 = CARTESIAN_POINT ( 'NONE',  ( 16.52544592524342804, -4.483927247898539470, 68.54057627198103830 ) ) ;
#159409 = CARTESIAN_POINT ( 'NONE',  ( -15.72974639402176322, -15.80617190586768395, 19.37609039468568639 ) ) ;
#159410 = CARTESIAN_POINT ( 'NONE',  ( -21.52544592524343514, 5.823673210054127303, 41.04057627198103120 ) ) ;
#159411 = CARTESIAN_POINT ( 'NONE',  ( -16.46253265017160317, 9.564922557960807481, 110.8322429386476955 ) ) ;
#159412 = CARTESIAN_POINT ( 'NONE',  ( 1.993301997531345292E-15, -30.30510711980685912, 140.7500000054623683 ) ) ;
#159413 = CARTESIAN_POINT ( 'NONE',  ( -0.05219959533909027116, -19.03943276465977164, 57.49890960531435979 ) ) ;
#159414 = CARTESIAN_POINT ( 'NONE',  ( -8.314922557960811034, -14.29746914071050412, 32.08224293864769550 ) ) ;
#159415 = CARTESIAN_POINT ( 'NONE',  ( 16.52544592524335698, 4.483927247898782831, 101.4594237280190185 ) ) ;
#159416 = CARTESIAN_POINT ( 'NONE',  ( -0.05219959533934338120, 16.53943276465976808, 82.50109039468568994 ) ) ;
#159417 = CARTESIAN_POINT ( 'NONE',  ( -16.46253265017146816, -9.564922557961047289, 39.16775706135234003 ) ) ;
#159418 = DIRECTION ( 'NONE',  ( -1.000000000000000000, -0.000000000000000000, -0.000000000000000000 ) ) ;
#159419 = CARTESIAN_POINT ( 'NONE',  ( -9.474510206698964154, 16.51473224551069663, 90.41557627198103830 ) ) ;
#159420 = CARTESIAN_POINT ( 'NONE',  ( 9.474510206698971260, -16.51473224551069308, 52.91557627198102409 ) ) ;
#159421 = CARTESIAN_POINT ( 'NONE',  ( 16.53943276465976808, -0.05219959533910856209, 63.74890960531435979 ) ) ;
#159423 = CARTESIAN_POINT ( 'NONE',  ( -10.81492255796078084, -18.62759615963271287, 27.08224293864769550 ) ) ;
#159422 = CARTESIAN_POINT ( 'NONE',  ( -0.05219959533909027116, -19.03943276465977164, 22.49890960531436690 ) ) ;
#159424 = CARTESIAN_POINT ( 'NONE',  ( -5.719274019375978568, 21.55341960407610458, 45.20724293864769550 ) ) ;
#159425 = CARTESIAN_POINT ( 'NONE',  ( 16.52544592524342804, -4.483927247898539470, 83.54057627198102409 ) ) ;
#159426 = CARTESIAN_POINT ( 'NONE',  ( -8.314922557961024197, 14.29746914071037800, 32.91775706135234714 ) ) ;
#159427 = CARTESIAN_POINT ( 'NONE',  ( 8.224510206698953496, -14.34966873604960469, 82.91557627198103830 ) ) ;
#159428 = CARTESIAN_POINT ( 'NONE',  ( -18.56453257813359770, 5.500000000000041744, 65.99000423690688422 ) ) ;
#159429 = CARTESIAN_POINT ( 'NONE',  ( -13.97604488694547697, 13.89961937509957934, 73.12609039468568994 ) ) ;
#159430 = CARTESIAN_POINT ( 'NONE',  ( 21.53943276465977519, -0.05219959533907433946, 23.74890960531435269 ) ) ;
#159431 = CARTESIAN_POINT ( 'NONE',  ( -22.81625015709509441, -31.40387420917324590, -2.824999997268812901 ) ) ;
#159432 = CARTESIAN_POINT ( 'NONE',  ( -22.32700255269489276, 20.23564678862942401, -51.30755147637197666 ) ) ;
#159434 = CARTESIAN_POINT ( 'NONE',  ( -14.29746914071037622, -8.314922557961029526, 104.1677570613523471 ) ) ;
#159433 = CARTESIAN_POINT ( 'NONE',  ( -14.34966873604972548, 8.224510206698743886, 23.33442372801901499 ) ) ;
#159436 = CARTESIAN_POINT ( 'NONE',  ( -13.97604488694547697, 13.89961937509957934, 73.12609039468568994 ) ) ;
#159435 = CIRCLE ( 'NONE', #85259, 31.90000000000003411 ) ;
#159437 = CARTESIAN_POINT ( 'NONE',  ( 10.81492255796078972, 18.62759615963270932, 44.58224293864769550 ) ) ;
#159438 = CARTESIAN_POINT ( 'NONE',  ( -21.55341960407619339, 5.719274019375674811, 73.54275706135234714 ) ) ;
#159439 = CARTESIAN_POINT ( 'NONE',  ( -22.24685556490157623, -12.75834802357607600, 167.9013491530738520 ) ) ;
#159440 = CARTESIAN_POINT ( 'NONE',  ( -4.379528057220086978, -16.55341960407618274, 34.79275706135235424 ) ) ;
#159442 = CARTESIAN_POINT ( 'NONE',  ( -0.05219959533909027116, -19.03943276465977164, 92.49890960531436690 ) ) ;
#159441 = CARTESIAN_POINT ( 'NONE',  ( 9.564922557960805705, 16.46253265017160317, 24.58224293864769194 ) ) ;
#159443 = CARTESIAN_POINT ( 'NONE',  ( 16.46253265017160672, -9.564922557960803928, 23.33224293864769194 ) ) ;
#159444 = CARTESIAN_POINT ( 'NONE',  ( -12.06949235617756955, 12.14591786802309770, 90.62390960531436690 ) ) ;
#159445 = ITEM_DEFINED_TRANSFORMATION ( 'NONE', 'NONE', #156568,  #82054 ) ;
#159446 = CARTESIAN_POINT ( 'NONE',  ( 9.474510206698971260, -16.51473224551069308, 102.9155762719810241 ) ) ;
#159447 = CARTESIAN_POINT ( 'NONE',  ( -19.05341960407617563, 5.049401038297882671, 108.5427570613523187 ) ) ;
#159448 = CARTESIAN_POINT ( 'NONE',  ( 21.55341960407610458, 5.719274019375980345, 83.95724293864770971 ) ) ;
#159449 = CARTESIAN_POINT ( 'NONE',  ( 13.89961937509977652, -13.97604488694527269, 43.12390960531434558 ) ) ;
#159451 = CARTESIAN_POINT ( 'NONE',  ( -10.72451020669870658, -18.67979575497194134, 19.58442372801901143 ) ) ;
#159450 = CARTESIAN_POINT ( 'NONE',  ( 9.474510206698729675, 16.51473224551082808, 67.08442372801900433 ) ) ;
#159452 = CARTESIAN_POINT ( 'NONE',  ( -9.474510206698964154, 16.51473224551069663, 70.41557627198102409 ) ) ;
#159453 = CARTESIAN_POINT ( 'NONE',  ( 0.05219959533909260263, 19.03943276465977164, 109.9989096053143669 ) ) ;
#159454 = ORIENTED_EDGE ( 'NONE', *, *, #13191, .T. ) ;
#159455 = CARTESIAN_POINT ( 'NONE',  ( -8.314922557961024197, 14.29746914071037800, 37.91775706135235424 ) ) ;
#159456 = CARTESIAN_POINT ( 'NONE',  ( -0.05219959533907301413, -21.53943276465977519, 107.4989096053143669 ) ) ;
#159459 = CARTESIAN_POINT ( 'NONE',  ( 16.51473224551083163, -9.474510206698727899, 55.83442372801899722 ) ) ;
#159458 = CARTESIAN_POINT ( 'NONE',  ( -19.05341960407611168, -5.049401038298163336, 96.45724293864769550 ) ) ;
#159457 = CARTESIAN_POINT ( 'NONE',  ( -12.14591786802309592, -12.06949235617757132, 111.8739096053143669 ) ) ;
#159460 = CARTESIAN_POINT ( 'NONE',  ( -15.72974639402197994, 15.80617190586746368, 90.62390960531436690 ) ) ;
#159461 = CARTESIAN_POINT ( 'NONE',  ( -12.14591786802309592, -12.06949235617757132, 41.87390960531435979 ) ) ;
#159462 = CARTESIAN_POINT ( 'NONE',  ( -0.05219959533936034679, 19.03943276465977164, 22.50109039468566152 ) ) ;
#159463 = CARTESIAN_POINT ( 'NONE',  ( -14.29746914071037622, -8.314922557961029526, 59.16775706135234714 ) ) ;
#159464 = CARTESIAN_POINT ( 'NONE',  ( 16.46253265017160672, -9.564922557960803928, 88.33224293864769550 ) ) ;
#159465 = CARTESIAN_POINT ( 'NONE',  ( -0.05219959533909027116, -19.03943276465977164, 42.49890960531435269 ) ) ;
#159466 = AXIS2_PLACEMENT_3D ( 'NONE', #149997, #176348, #71160 ) ;
#159467 = CARTESIAN_POINT ( 'NONE',  ( -10.81492255796105439, 18.62759615963255655, 47.91775706135234714 ) ) ;
#159468 = CARTESIAN_POINT ( 'NONE',  ( 21.52544592524334988, 5.823673210054432836, 66.45942372801903275 ) ) ;
#159469 = CARTESIAN_POINT ( 'NONE',  ( 0.05219959533909260263, 19.03943276465977164, 54.99890960531435979 ) ) ;
#159470 = CARTESIAN_POINT ( 'NONE',  ( 18.67979575497194134, -10.72451020669871369, 30.83442372801902209 ) ) ;
#159471 = CARTESIAN_POINT ( 'NONE',  ( -5.049401038297874678, -19.05341960407617918, 74.79275706135231871 ) ) ;
#159473 = CARTESIAN_POINT ( 'NONE',  ( 5.153800228976615827, -19.02544592524334988, 80.20942372801901854 ) ) ;
#159472 = B_SPLINE_CURVE_WITH_KNOTS ( 'NONE', 3,
 ( #139842, #108524, #172187, #142828, #33672, #155031, #127660, #31696, #34666, #63011, #3328, #79174, #16526, #78173, #124690, #109517, #126659, #171199, #65991, #188363, #189360, #93345, #32689, #96324, #17516, #140845 ),
 .UNSPECIFIED., .F., .F.,
 ( 4, 2, 2, 2, 2, 2, 2, 2, 2, 2, 2, 2, 4 ),
 ( 1.971390913921884457E-07, 0.0002963316798228788642, 0.0005924662205543656125, 0.0008886007612858520897, 0.001184735302017338784, 0.001777004383480311955, 0.002369273464943285126, 0.002665408005674770736, 0.002961542546406256346, 0.003257677087137742390, 0.003553811627869227566, 0.004146080709332196183, 0.004738349790795163934 ),
 .UNSPECIFIED. ) ;
#159474 = CARTESIAN_POINT ( 'NONE',  ( -19.03943276465977164, 0.05219959533909376836, 36.24890960531436690 ) ) ;
#159475 = CARTESIAN_POINT ( 'NONE',  ( -4.483927247898782831, 16.52544592524335698, 92.70942372801901854 ) ) ;
#159476 = CARTESIAN_POINT ( 'NONE',  ( 0.05219959533909260263, 19.03943276465977164, 54.99890960531435979 ) ) ;
#159477 = CARTESIAN_POINT ( 'NONE',  ( -19.03943276465977164, 0.05219959533909376836, 21.24890960531436335 ) ) ;
#159478 = CARTESIAN_POINT ( 'NONE',  ( -19.03943276465977164, 0.05219959533909376836, 101.2489096053143669 ) ) ;
#159479 = CARTESIAN_POINT ( 'NONE',  ( 5.049401038298161559, -19.05341960407611168, 32.70724293864768129 ) ) ;
#159480 = CARTESIAN_POINT ( 'NONE',  ( -21.53943276465977519, 0.05219959533907696930, 86.24890960531436690 ) ) ;
#159481 = CARTESIAN_POINT ( 'NONE',  ( 0.05219959533934541429, -16.53943276465976808, 75.00109039468568994 ) ) ;
#159482 = CARTESIAN_POINT ( 'NONE',  ( 13.89961937509957401, 13.97604488694547697, 31.87609039468566863 ) ) ;
#159483 = CARTESIAN_POINT ( 'NONE',  ( 16.51473224551069308, 9.474510206698969483, 49.16557627198102409 ) ) ;
#159484 = CARTESIAN_POINT ( 'NONE',  ( 14.29746914071049879, -8.314922557960816363, 48.33224293864770260 ) ) ;
#159486 = B_SPLINE_CURVE_WITH_KNOTS ( 'NONE', 3,
 ( #83189, #32729, #159032, #6346, #129677, #94381 ),
 .UNSPECIFIED., .F., .F.,
 ( 4, 2, 4 ),
 ( 0.007228050697041539692, 0.007608510107495016980, 0.007988969517948495136 ),
 .UNSPECIFIED. ) ;
#159485 = CARTESIAN_POINT ( 'NONE',  ( -8.314922557960811034, -14.29746914071050412, 87.08224293864769550 ) ) ;
#159487 = CARTESIAN_POINT ( 'NONE',  ( -19.05341960407611168, -5.049401038298163336, 96.45724293864769550 ) ) ;
#159488 = CARTESIAN_POINT ( 'NONE',  ( -9.564922557960796823, -16.46253265017161027, 82.08224293864768129 ) ) ;
#159489 = CARTESIAN_POINT ( 'NONE',  ( 10.81492255796106328, -18.62759615963255655, 40.41775706135234714 ) ) ;
#159490 = CARTESIAN_POINT ( 'NONE',  ( 13.97604488694527802, 13.89961937509977652, 89.37390960531436690 ) ) ;
#159491 = CARTESIAN_POINT ( 'NONE',  ( -21.55341960407619339, 5.719274019375674811, 93.54275706135234714 ) ) ;
#159492 = CARTESIAN_POINT ( 'NONE',  ( 4.483927247898790824, -16.52544592524335698, 75.20942372801901854 ) ) ;
#159493 = CARTESIAN_POINT ( 'NONE',  ( -18.62759615963255300, -10.81492255796106328, 24.16775706135235424 ) ) ;
#159494 = CARTESIAN_POINT ( 'NONE',  ( 21.52544592524344225, -5.823673210054117533, 93.54057627198103830 ) ) ;
#159495 = CARTESIAN_POINT ( 'NONE',  ( 4.379528057220339221, -16.55341960407611168, 47.70724293864770260 ) ) ;
#159496 = CARTESIAN_POINT ( 'NONE',  ( -19.05341960407611168, -5.049401038298163336, 46.45724293864768129 ) ) ;
#159497 = CARTESIAN_POINT ( 'NONE',  ( 16.52544592524342804, -4.483927247898539470, 68.54057627198103830 ) ) ;
#159498 = CARTESIAN_POINT ( 'NONE',  ( -0.05219959533907301413, -21.53943276465977519, 27.49890960531435269 ) ) ;
#159499 = CARTESIAN_POINT ( 'NONE',  ( -9.474510206698720793, -16.51473224551083518, 34.58442372801899722 ) ) ;
#159500 = CARTESIAN_POINT ( 'NONE',  ( 4.483927247898545687, 16.52544592524342804, 94.79057627198105251 ) ) ;
#159501 = EDGE_LOOP ( 'NONE', ( #127126, #109977, #109954, #96263 ) ) ;
#159502 = CARTESIAN_POINT ( 'NONE',  ( -14.29746914071037622, -8.314922557961029526, 69.16775706135234714 ) ) ;
#159503 = CARTESIAN_POINT ( 'NONE',  ( 19.03943276465977164, -0.05219959533909143690, 63.74890960531435979 ) ) ;
#159504 = CARTESIAN_POINT ( 'NONE',  ( -27.73933785331498925, -9.013057229001049109, 138.9750000027311785 ) ) ;
#159505 = CARTESIAN_POINT ( 'NONE',  ( -21.53943276465977519, 0.05219959533907696930, 36.24890960531435979 ) ) ;
#159506 = CARTESIAN_POINT ( 'NONE',  ( -14.29746914071037622, -8.314922557961029526, 94.16775706135237556 ) ) ;
#159507 = CARTESIAN_POINT ( 'NONE',  ( 5.153800228976615827, -19.02544592524334988, 110.2094237280189901 ) ) ;
#159508 = CARTESIAN_POINT ( 'NONE',  ( -5.823673210054431948, 21.52544592524334988, 77.70942372801900433 ) ) ;
#159509 = CARTESIAN_POINT ( 'NONE',  ( 19.05341960407611168, 5.049401038298154454, 73.95724293864768129 ) ) ;
#159510 = CARTESIAN_POINT ( 'NONE',  ( -18.67979575497178146, -10.72451020669898902, 101.6655762719810383 ) ) ;
#159511 = CARTESIAN_POINT ( 'NONE',  ( -16.53943276465976808, -0.05219959533934237506, 58.75109039468568994 ) ) ;
#159512 = CARTESIAN_POINT ( 'NONE',  ( -4.483927247898539470, -16.52544592524342804, 112.2905762719810241 ) ) ;
#159513 = CARTESIAN_POINT ( 'NONE',  ( -0.05219959533934338120, 16.53943276465976808, 22.50109039468567573 ) ) ;
#159514 = CARTESIAN_POINT ( 'NONE',  ( 9.474510206698729675, 16.51473224551082808, 82.08442372801899012 ) ) ;
#159515 = CARTESIAN_POINT ( 'NONE',  ( 21.52544592524344225, -5.823673210054117533, 78.54057627198103830 ) ) ;
#159516 = CARTESIAN_POINT ( 'NONE',  ( -5.049401038297874678, -19.05341960407617918, 49.79275706135231871 ) ) ;
#159517 = DIRECTION ( 'NONE',  ( -9.445700745138859830E-17, 1.000000000000000000, 0.000000000000000000 ) ) ;
#159518 = CARTESIAN_POINT ( 'NONE',  ( -0.05219959533907301413, -21.53943276465977519, 97.49890960531436690 ) ) ;
#159519 = CARTESIAN_POINT ( 'NONE',  ( 7.500000000000001776, -1.104226503365433709, 3.188666715448014610 ) ) ;
#159520 = CARTESIAN_POINT ( 'NONE',  ( -9.474510206698964154, 16.51473224551069663, 75.41557627198103830 ) ) ;
#159521 = CARTESIAN_POINT ( 'NONE',  ( 20.13687146691633245, -33.41269836094259205, -11.07851503421889561 ) ) ;
#159522 = CARTESIAN_POINT ( 'NONE',  ( -4.379528057220086978, -16.55341960407618274, 34.79275706135235424 ) ) ;
#159523 = CARTESIAN_POINT ( 'NONE',  ( 36.78376627615639194, -4.378768456387976293, 48.34741972342520455 ) ) ;
#159525 = CARTESIAN_POINT ( 'NONE',  ( 14.34966873604960469, 8.224510206698951720, 64.16557627198102409 ) ) ;
#159524 = CARTESIAN_POINT ( 'NONE',  ( -0.05219959533907301413, -21.53943276465977519, 97.49890960531436690 ) ) ;
#159526 = CARTESIAN_POINT ( 'NONE',  ( 19.02544592524343514, -5.153800228976328945, 63.54057627198103830 ) ) ;
#159527 = CARTESIAN_POINT ( 'NONE',  ( -5.823673210054431948, 21.52544592524334988, 92.70942372801901854 ) ) ;
#159529 = CARTESIAN_POINT ( 'NONE',  ( -19.05341960407617563, 5.049401038297882671, 38.54275706135233293 ) ) ;
#159528 = CARTESIAN_POINT ( 'NONE',  ( 12.06949235617739724, 12.14591786802326823, 31.87609039468567929 ) ) ;
#159530 = CARTESIAN_POINT ( 'NONE',  ( 21.52544592524334988, 5.823673210054432836, 46.45942372801901854 ) ) ;
#159531 = CARTESIAN_POINT ( 'NONE',  ( 5.719274019375991003, -21.55341960407610458, 62.70724293864769550 ) ) ;
#159532 = CARTESIAN_POINT ( 'NONE',  ( -9.564922557961040184, 16.46253265017147172, 102.9177570613523329 ) ) ;
#159534 = ADVANCED_FACE ( 'NONE', ( #16379 ), #158848, .T. ) ;
#159533 = CARTESIAN_POINT ( 'NONE',  ( -19.03943276465977164, 0.05219959533909376836, 51.24890960531436690 ) ) ;
#159535 = CARTESIAN_POINT ( 'NONE',  ( 5.153800228976615827, -19.02544592524334988, 65.20942372801900433 ) ) ;
#159536 = CARTESIAN_POINT ( 'NONE',  ( 21.55341960407619695, -5.719274019375665929, 81.04275706135236135 ) ) ;
#159537 = CARTESIAN_POINT ( 'NONE',  ( -9.474510206698720793, -16.51473224551083518, 69.58442372801901854 ) ) ;
#159538 = CARTESIAN_POINT ( 'NONE',  ( -13.97604488694527625, -13.89961937509977652, 31.87390960531435979 ) ) ;
#159539 = CARTESIAN_POINT ( 'NONE',  ( -15.80617190586745835, -15.72974639402198527, 51.87390960531437401 ) ) ;
#159540 = CARTESIAN_POINT ( 'NONE',  ( -8.314922557960811034, -14.29746914071050412, 57.08224293864769550 ) ) ;
#159541 = FACE_OUTER_BOUND ( 'NONE', #99250, .T. ) ;
#159542 = CARTESIAN_POINT ( 'NONE',  ( 0.05219959533936267826, -19.03943276465977164, 35.00109039468566863 ) ) ;
#159543 = CARTESIAN_POINT ( 'NONE',  ( -8.224510206698735004, -14.34966873604973081, 84.58442372801903275 ) ) ;
#159544 = CARTESIAN_POINT ( 'NONE',  ( -4.379528057220328563, 16.55341960407611168, 55.20724293864770260 ) ) ;
#159545 = CARTESIAN_POINT ( 'NONE',  ( 18.62759615963255655, 10.81492255796105972, 91.66775706135234714 ) ) ;
#159546 = CARTESIAN_POINT ( 'NONE',  ( -5.719274019375665041, -21.55341960407619695, 79.79275706135236135 ) ) ;
#159547 = CARTESIAN_POINT ( 'NONE',  ( -18.62759615963270932, 10.81492255796079327, 95.83224293864770971 ) ) ;
#159548 = CIRCLE ( 'NONE', #63150, 2.500000000000002220 ) ;
#159549 = CARTESIAN_POINT ( 'NONE',  ( -9.564922557960796823, -16.46253265017161027, 52.08224293864768839 ) ) ;
#159550 = CARTESIAN_POINT ( 'NONE',  ( 18.62759615963255655, 10.81492255796105972, 61.66775706135235424 ) ) ;
#159551 = CARTESIAN_POINT ( 'NONE',  ( -5.049401038298153566, 19.05341960407611168, 35.20724293864768839 ) ) ;
#159552 = CARTESIAN_POINT ( 'NONE',  ( 5.153800228976335163, 19.02544592524342804, 54.79057627198103120 ) ) ;
#159553 = CARTESIAN_POINT ( 'NONE',  ( -16.52544592524342804, 4.483927247898546575, 111.0405762719810525 ) ) ;
#159554 = CARTESIAN_POINT ( 'NONE',  ( -19.03943276465977164, 0.05219959533909376836, 96.24890960531436690 ) ) ;
#159555 = CARTESIAN_POINT ( 'NONE',  ( 12.06949235617757843, -12.14591786802309237, 53.12390960531436690 ) ) ;
#159556 = CARTESIAN_POINT ( 'NONE',  ( -12.14591786802309592, -12.06949235617757132, 111.8739096053143669 ) ) ;
#159557 = CARTESIAN_POINT ( 'NONE',  ( 18.67979575497178502, 10.72451020669898547, 79.16557627198103830 ) ) ;
#159558 = CARTESIAN_POINT ( 'NONE',  ( -18.67979575497193778, 10.72451020669871902, 33.33442372801900433 ) ) ;
#159559 = CARTESIAN_POINT ( 'NONE',  ( 10.20000000000000107, 0.000000000000000000, 0.000000000000000000 ) ) ;
#159560 = CARTESIAN_POINT ( 'NONE',  ( -14.34966873604972548, 8.224510206698743886, 43.33442372801901143 ) ) ;
#159561 = VERTEX_POINT ( 'NONE', #34524 ) ;
#159562 = CARTESIAN_POINT ( 'NONE',  ( 21.55341960407610458, 5.719274019375980345, 78.95724293864769550 ) ) ;
#159564 = CARTESIAN_POINT ( 'NONE',  ( -10.81492255796105439, 18.62759615963255655, 112.9177570613523329 ) ) ;
#159563 = PRODUCT_DEFINITION_CONTEXT ( 'detailed design', #60997, 'design' ) ;
#159565 = CARTESIAN_POINT ( 'NONE',  ( 16.51473224551069308, 9.474510206698969483, 99.16557627198102409 ) ) ;
#159566 = CARTESIAN_POINT ( 'NONE',  ( 0.05219959533937995610, -21.53943276465977519, 30.00109039468568284 ) ) ;
#159567 = CARTESIAN_POINT ( 'NONE',  ( 21.53943276465977519, -0.05219959533907433946, 33.74890960531436690 ) ) ;
#159568 = CARTESIAN_POINT ( 'NONE',  ( -16.52544592524335698, -4.483927247898792601, 98.95942372801903275 ) ) ;
#159570 = CARTESIAN_POINT ( 'NONE',  ( -21.53943276465977519, -0.05219959533937600094, 78.75109039468568994 ) ) ;
#159569 = CARTESIAN_POINT ( 'NONE',  ( -5.823673210054431948, 21.52544592524334988, 52.70942372801902565 ) ) ;
#159571 = CARTESIAN_POINT ( 'NONE',  ( -0.05219959533936034679, 19.03943276465977164, 22.50109039468566152 ) ) ;
#159572 = CARTESIAN_POINT ( 'NONE',  ( -14.29746914071037622, -8.314922557961029526, 69.16775706135234714 ) ) ;
#159573 = CARTESIAN_POINT ( 'NONE',  ( -10.81492255796105439, 18.62759615963255655, 42.91775706135235424 ) ) ;
#159574 = TOROIDAL_SURFACE ( 'NONE', #149940, 2.700000000000000622, 0.2000000000000000111 ) ;
#159575 = CARTESIAN_POINT ( 'NONE',  ( -16.51473224551069308, -9.474510206698971260, 36.66557627198102409 ) ) ;
#159576 = CARTESIAN_POINT ( 'NONE',  ( 18.67979575497194134, -10.72451020669871369, 105.8344237280190328 ) ) ;
#159577 = CARTESIAN_POINT ( 'NONE',  ( -16.51473224551069308, -9.474510206698971260, 106.6655762719810383 ) ) ;
#159578 = CARTESIAN_POINT ( 'NONE',  ( -21.55341960407610458, -5.719274019375992779, 101.4572429386476955 ) ) ;
#159580 = CARTESIAN_POINT ( 'NONE',  ( -5.719274019375978568, 21.55341960407610458, 65.20724293864768129 ) ) ;
#159579 = CARTESIAN_POINT ( 'NONE',  ( -4.562484170633083203, -48.30423733477558557, -22.99999999999999645 ) ) ;
#159582 = CARTESIAN_POINT ( 'NONE',  ( 16.53943276465976808, -0.05219959533910856209, 48.74890960531435979 ) ) ;
#159581 = CARTESIAN_POINT ( 'NONE',  ( 16.53943276465976808, 0.05219959533934440121, 51.25109039468568994 ) ) ;
#159583 = LINE ( 'NONE', #18119, #4670 ) ;
#159584 = CARTESIAN_POINT ( 'NONE',  ( -16.51473224551082808, 9.474510206698731452, 88.33442372801900433 ) ) ;
#159585 = CARTESIAN_POINT ( 'NONE',  ( -16.29526858892876007, 7.335722546920112386, 104.2032940219980048 ) ) ;
#159586 = CARTESIAN_POINT ( 'NONE',  ( 12.14591786802327356, -12.06949235617739191, 25.62609039468567929 ) ) ;
#159587 = CARTESIAN_POINT ( 'NONE',  ( 5.719274019375991003, -21.55341960407610458, 102.7072429386476955 ) ) ;
#159588 = CARTESIAN_POINT ( 'NONE',  ( 10.81492255796078972, 18.62759615963270932, 69.58224293864769550 ) ) ;
#159589 = CARTESIAN_POINT ( 'NONE',  ( -13.89961937509977652, 13.97604488694528158, 110.6239096053143243 ) ) ;
#159590 = CARTESIAN_POINT ( 'NONE',  ( 0.05219959533934541429, -16.53943276465976808, 40.00109039468567573 ) ) ;
#159591 = CARTESIAN_POINT ( 'NONE',  ( 13.97604488694527802, 13.89961937509977652, 59.37390960531434558 ) ) ;
#159593 = CARTESIAN_POINT ( 'NONE',  ( -5.153800228976607833, 19.02544592524334988, 97.70942372801900433 ) ) ;
#159592 = CARTESIAN_POINT ( 'NONE',  ( 0.05219959533937995610, -21.53943276465977519, 30.00109039468568284 ) ) ;
#159594 = CARTESIAN_POINT ( 'NONE',  ( 13.97604488694527802, 13.89961937509977652, 104.3739096053143385 ) ) ;
#159595 = CARTESIAN_POINT ( 'NONE',  ( 19.03943276465977164, -0.05219959533909143690, 83.74890960531436690 ) ) ;
#159596 = CARTESIAN_POINT ( 'NONE',  ( -15.80617190586745835, -15.72974639402198527, 91.87390960531436690 ) ) ;
#159597 = CARTESIAN_POINT ( 'NONE',  ( -19.05341960407611168, -5.049401038298163336, 61.45724293864769550 ) ) ;
#159598 = FACE_OUTER_BOUND ( 'NONE', #101482, .T. ) ;
#159599 = CARTESIAN_POINT ( 'NONE',  ( -12.06949235617756955, 12.14591786802309770, 70.62390960531436690 ) ) ;
#159600 = CARTESIAN_POINT ( 'NONE',  ( 9.564922557960805705, 16.46253265017160317, 99.58224293864770971 ) ) ;
#159601 = CARTESIAN_POINT ( 'NONE',  ( -28.90000000000004476, 2.980639576201346218E-13, -52.65483682830183199 ) ) ;
#159602 = CARTESIAN_POINT ( 'NONE',  ( -19.03943276465977164, -0.05219959533935918106, 83.75109039468567573 ) ) ;
#159603 = CARTESIAN_POINT ( 'NONE',  ( -0.05219959533907301413, -21.53943276465977519, 87.49890960531436690 ) ) ;
#159604 = CARTESIAN_POINT ( 'NONE',  ( 13.97604488694548053, -13.89961937509957401, 50.62609039468566152 ) ) ;
#159605 = CARTESIAN_POINT ( 'NONE',  ( -19.03943276465977164, 0.05219959533909376836, 111.2489096053143669 ) ) ;
#159606 = CARTESIAN_POINT ( 'NONE',  ( 18.39639308325437383, 5.500000000000037303, 68.98252246182197212 ) ) ;
#159607 = CARTESIAN_POINT ( 'NONE',  ( -15.72974639402197994, 15.80617190586746368, 60.62390960531437401 ) ) ;
#159608 = CIRCLE ( 'NONE', #185466, 5.000000000000000000 ) ;
#159609 = CARTESIAN_POINT ( 'NONE',  ( -9.474510206698964154, 16.51473224551069663, 80.41557627198103830 ) ) ;
#159610 = CARTESIAN_POINT ( 'NONE',  ( -10.72451020669870658, -18.67979575497194134, 79.58442372801903275 ) ) ;
#159612 = CARTESIAN_POINT ( 'NONE',  ( -5.049401038298153566, 19.05341960407611168, 40.20724293864768839 ) ) ;
#159611 = PRODUCT ( 'BR-835', 'BR-835', '', ( #92807 ) ) ;
#159613 = ADVANCED_FACE ( 'NONE', ( #157873 ), #96184, .T. ) ;
#159614 = CARTESIAN_POINT ( 'NONE',  ( 12.06949235617757843, -12.14591786802309237, 68.12390960531436690 ) ) ;
#159615 = CARTESIAN_POINT ( 'NONE',  ( -0.05219959533934338120, 16.53943276465976808, 27.50109039468567929 ) ) ;
#159616 = CARTESIAN_POINT ( 'NONE',  ( -21.55341960407619339, 5.719274019375674811, 68.54275706135234714 ) ) ;
#159617 = ORIENTED_EDGE ( 'NONE', *, *, #19140, .F. ) ;
#159618 = CARTESIAN_POINT ( 'NONE',  ( -9.564922557961040184, 16.46253265017147172, 22.91775706135233648 ) ) ;
#159619 = CARTESIAN_POINT ( 'NONE',  ( -13.89961937509957401, -13.97604488694547875, 74.37609039468566152 ) ) ;
#159620 = DIRECTION ( 'NONE',  ( -0.000000000000000000, -0.000000000000000000, 1.000000000000000000 ) ) ;
#159621 = CARTESIAN_POINT ( 'NONE',  ( -18.67979575497193778, 10.72451020669871902, 28.33442372801902209 ) ) ;
#159622 = CARTESIAN_POINT ( 'NONE',  ( -19.19724070472091526, -5.500000000000168754, 46.06193348274383936 ) ) ;
#159623 = CARTESIAN_POINT ( 'NONE',  ( -10.81492255796105439, 18.62759615963255655, 112.9177570613523329 ) ) ;
#159624 = CARTESIAN_POINT ( 'NONE',  ( -19.03943276465977164, 0.05219959533909376836, 51.24890960531436690 ) ) ;
#159625 = CARTESIAN_POINT ( 'NONE',  ( 13.89961937509957401, 13.97604488694547697, 36.87609039468565442 ) ) ;
#159626 = CARTESIAN_POINT ( 'NONE',  ( 8.314922557961029526, -14.29746914071037800, 110.4177570613523756 ) ) ;
#159628 = CARTESIAN_POINT ( 'NONE',  ( 5.719274019375673035, 21.55341960407619339, 67.29275706135234714 ) ) ;
#159627 = CARTESIAN_POINT ( 'NONE',  ( -9.564922557960796823, -16.46253265017161027, 97.08224293864769550 ) ) ;
#159629 = CARTESIAN_POINT ( 'NONE',  ( 22.81625015709509441, 31.40387420917330275, -5.324999997268812457 ) ) ;
#159630 = CARTESIAN_POINT ( 'NONE',  ( -33.71430530369729439, 4.147805181855619416, 98.62971388258593208 ) ) ;
#159631 = CARTESIAN_POINT ( 'NONE',  ( 10.72451020669871369, 18.67979575497193778, 87.08442372801901854 ) ) ;
#159632 = CARTESIAN_POINT ( 'NONE',  ( -15.80617190586768217, 15.72974639402176855, 108.1260903946856757 ) ) ;
#159633 = CARTESIAN_POINT ( 'NONE',  ( 11.45643923738960446, -4.999999999999992895, -18.00000000000000000 ) ) ;
#159634 = CARTESIAN_POINT ( 'NONE',  ( -16.46253265017160317, 9.564922557960807481, 100.8322429386477097 ) ) ;
#159635 = CARTESIAN_POINT ( 'NONE',  ( -19.02544592524334988, -5.153800228976617603, 18.95942372801899722 ) ) ;
#159636 = CARTESIAN_POINT ( 'NONE',  ( 31.34482716061813434, -21.47441072263943695, -23.96158720469882653 ) ) ;
#159637 = CARTESIAN_POINT ( 'NONE',  ( 9.474510206698971260, -16.51473224551069308, 42.91557627198103120 ) ) ;
#159638 = CARTESIAN_POINT ( 'NONE',  ( -0.05219959533907301413, -21.53943276465977519, 52.49890960531435979 ) ) ;
#159639 = CARTESIAN_POINT ( 'NONE',  ( -0.05219959533910754901, -16.53943276465976808, 22.49890960531436335 ) ) ;
#159641 = CARTESIAN_POINT ( 'NONE',  ( -16.46253265017160317, 9.564922557960807481, 80.83224293864769550 ) ) ;
#159640 = CARTESIAN_POINT ( 'NONE',  ( -8.224510206698948167, 14.34966873604960824, 90.41557627198103830 ) ) ;
#159642 = CARTESIAN_POINT ( 'NONE',  ( 10.81492255796106328, -18.62759615963255655, 110.4177570613523756 ) ) ;
#159643 = CARTESIAN_POINT ( 'NONE',  ( 19.02544592524343514, -5.153800228976328945, 38.54057627198103120 ) ) ;
#159644 = CARTESIAN_POINT ( 'NONE',  ( -8.314922557960811034, -14.29746914071050412, 107.0822429386476955 ) ) ;
#159645 = CARTESIAN_POINT ( 'NONE',  ( -21.52544592524334988, -5.823673210054445271, 58.95942372801902565 ) ) ;
#159646 = CARTESIAN_POINT ( 'NONE',  ( 5.719274019375991003, -21.55341960407610458, 87.70724293864769550 ) ) ;
#159647 = CARTESIAN_POINT ( 'NONE',  ( 19.03943276465977164, 0.05219959533936151252, 56.25109039468566863 ) ) ;
#159648 = CARTESIAN_POINT ( 'NONE',  ( -20.05760019694261587, -21.05943304104360791, -49.45823509044233646 ) ) ;
#159649 = CARTESIAN_POINT ( 'NONE',  ( 5.049401038298161559, -19.05341960407611168, 112.7072429386476813 ) ) ;
#159650 = CARTESIAN_POINT ( 'NONE',  ( -0.05219959533910754901, -16.53943276465976808, 72.49890960531435269 ) ) ;
#159651 = CARTESIAN_POINT ( 'NONE',  ( -16.46253265017146816, -9.564922557961047289, 49.16775706135233293 ) ) ;
#159652 = CARTESIAN_POINT ( 'NONE',  ( 19.05341960407611168, 5.049401038298154454, 63.95724293864769550 ) ) ;
#159653 = CARTESIAN_POINT ( 'NONE',  ( 4.379528057220339221, -16.55341960407611168, 47.70724293864770260 ) ) ;
#159654 = CARTESIAN_POINT ( 'NONE',  ( 13.89961937509957401, 13.97604488694547697, 81.87609039468564731 ) ) ;
#159655 = CARTESIAN_POINT ( 'NONE',  ( -19.46398650005391318, 5.499999999999953815, 85.18269651486372140 ) ) ;
#159656 = CARTESIAN_POINT ( 'NONE',  ( -15.72974639402197994, 15.80617190586746368, 40.62390960531435269 ) ) ;
#159657 = CARTESIAN_POINT ( 'NONE',  ( 16.55341960407611168, 4.379528057220329451, 103.9572429386476813 ) ) ;
#159658 = CARTESIAN_POINT ( 'NONE',  ( -17.50000000000015632, -3.292511757969812436, 24.93479729789453003 ) ) ;
#159660 = CARTESIAN_POINT ( 'NONE',  ( 0.05219959533907565091, 21.53943276465977519, 64.99890960531435269 ) ) ;
#159659 = CARTESIAN_POINT ( 'NONE',  ( 19.05341960407611168, 5.049401038298154454, 63.95724293864769550 ) ) ;
#159661 = CARTESIAN_POINT ( 'NONE',  ( -16.51473224551069308, -9.474510206698971260, 36.66557627198102409 ) ) ;
#159663 = CARTESIAN_POINT ( 'NONE',  ( -19.02544592524342804, 5.153800228976336051, 61.04057627198103120 ) ) ;
#159662 = CARTESIAN_POINT ( 'NONE',  ( -16.53943276465976808, -0.05219959533934237506, 73.75109039468567573 ) ) ;
#159664 = CARTESIAN_POINT ( 'NONE',  ( 13.89961937509957401, 13.97604488694547697, 56.87609039468564731 ) ) ;
#159665 = VECTOR ( 'NONE', #4050, 1000.000000000000000 ) ;
#159666 = CARTESIAN_POINT ( 'NONE',  ( 10.72451020669871369, 18.67979575497193778, 62.08442372801901143 ) ) ;
#159667 = CARTESIAN_POINT ( 'NONE',  ( -0.05219959533907301413, -21.53943276465977519, 52.49890960531435979 ) ) ;
#159668 = CARTESIAN_POINT ( 'NONE',  ( 0.05219959533909260263, 19.03943276465977164, 29.99890960531435979 ) ) ;
#159669 = CARTESIAN_POINT ( 'NONE',  ( -16.52544592524335698, -4.483927247898792601, 93.95942372801903275 ) ) ;
#159670 = CARTESIAN_POINT ( 'NONE',  ( 0.05219959533936267826, -19.03943276465977164, 100.0010903946856757 ) ) ;
#159671 = CARTESIAN_POINT ( 'NONE',  ( -29.86685920354755552, 21.69954338932564397, -1.324999997268813345 ) ) ;
#159673 = CARTESIAN_POINT ( 'NONE',  ( -5.823673210054116645, -21.52544592524344225, 57.29057627198103120 ) ) ;
#159672 = CARTESIAN_POINT ( 'NONE',  ( 19.35543954521080678, 5.499999999999573674, 77.08901960356448058 ) ) ;
#159674 = CARTESIAN_POINT ( 'NONE',  ( 5.719274019375673035, 21.55341960407619339, 97.29275706135234714 ) ) ;
#159675 = ORIENTED_EDGE ( 'NONE', *, *, #48406, .T. ) ;
#159676 = CARTESIAN_POINT ( 'NONE',  ( -16.52544592524342804, 4.483927247898546575, 41.04057627198103120 ) ) ;
#159677 = CARTESIAN_POINT ( 'NONE',  ( 4.379528057220339221, -16.55341960407611168, 57.70724293864770260 ) ) ;
#159678 = CARTESIAN_POINT ( 'NONE',  ( 10.81492255796078972, 18.62759615963270932, 84.58224293864769550 ) ) ;
#159679 = CARTESIAN_POINT ( 'NONE',  ( -10.81492255796078084, -18.62759615963271287, 87.08224293864769550 ) ) ;
#159680 = DIRECTION ( 'NONE',  ( 1.000000000000000000, 0.000000000000000000, 0.000000000000000000 ) ) ;
#159681 = CARTESIAN_POINT ( 'NONE',  ( 21.55341960407610458, 5.719274019375980345, 28.95724293864769905 ) ) ;
#159682 = CARTESIAN_POINT ( 'NONE',  ( 16.53943276465976808, 0.05219959533934440121, 71.25109039468568994 ) ) ;
#159683 = CARTESIAN_POINT ( 'NONE',  ( 16.53943276465976808, -0.05219959533910856209, 73.74890960531433848 ) ) ;
#159684 = CARTESIAN_POINT ( 'NONE',  ( 5.153800228976335163, 19.02544592524342804, 34.79057627198102409 ) ) ;
#159685 = CARTESIAN_POINT ( 'NONE',  ( 34.36947210329395119, -7.112397586384675563, 47.39260519897412394 ) ) ;
#159686 = CARTESIAN_POINT ( 'NONE',  ( -0.05219959533934338120, 16.53943276465976808, 102.5010903946856899 ) ) ;
#159687 = CARTESIAN_POINT ( 'NONE',  ( -5.719274019375665041, -21.55341960407619695, 24.79275706135235779 ) ) ;
#159688 = CARTESIAN_POINT ( 'NONE',  ( -0.05219959533909027116, -19.03943276465977164, 87.49890960531436690 ) ) ;
#159689 = CARTESIAN_POINT ( 'NONE',  ( 0.05219959533937995610, -21.53943276465977519, 60.00109039468568284 ) ) ;
#159690 = CARTESIAN_POINT ( 'NONE',  ( -13.89961937509977652, 13.97604488694528158, 115.6239096053143669 ) ) ;
#159691 = CARTESIAN_POINT ( 'NONE',  ( -7.095528360789167266, -39.96100899395969464, -25.59277598900286321 ) ) ;
#159692 = VECTOR ( 'NONE', #59561, 1000.000000000000000 ) ;
#159693 = ORIENTED_EDGE ( 'NONE', *, *, #158042, .F. ) ;
#159694 = CARTESIAN_POINT ( 'NONE',  ( -18.67979575497193778, 10.72451020669871902, 43.33442372801901143 ) ) ;
#159696 = CARTESIAN_POINT ( 'NONE',  ( -16.46253265017160317, 9.564922557960807481, 105.8322429386476955 ) ) ;
#159695 = CARTESIAN_POINT ( 'NONE',  ( -19.03943276465977164, 0.05219959533909376836, 36.24890960531436690 ) ) ;
#159697 = CARTESIAN_POINT ( 'NONE',  ( 16.46253265017146816, 9.564922557961045513, 51.66775706135233293 ) ) ;
#159698 = CARTESIAN_POINT ( 'NONE',  ( 21.52544592524334988, 5.823673210054432836, 31.45942372801901854 ) ) ;
#159699 = CARTESIAN_POINT ( 'NONE',  ( -13.89961937509957401, -13.97604488694547875, 59.37609039468566863 ) ) ;
#159700 = CARTESIAN_POINT ( 'NONE',  ( 28.82186960331498327, 2.781578969918950771E-14, 141.0000000000000000 ) ) ;
#159701 = CARTESIAN_POINT ( 'NONE',  ( 4.483927247898790824, -16.52544592524335698, 95.20942372801903275 ) ) ;
#159702 = CARTESIAN_POINT ( 'NONE',  ( 5.153800228976615827, -19.02544592524334988, 60.20942372801899012 ) ) ;
#159703 = CARTESIAN_POINT ( 'NONE',  ( 8.314922557961029526, -14.29746914071037800, 105.4177570613523613 ) ) ;
#159704 = DIRECTION ( 'NONE',  ( 0.000000000000000000, 0.000000000000000000, -1.000000000000000000 ) ) ;
#159705 = CARTESIAN_POINT ( 'NONE',  ( -0.05219959533909027116, -19.03943276465977164, 82.49890960531436690 ) ) ;
#159706 = CARTESIAN_POINT ( 'NONE',  ( 21.53943276465977519, 0.05219959533937863772, 86.25109039468568994 ) ) ;
#159707 = CARTESIAN_POINT ( 'NONE',  ( 21.53943276465977519, 0.05219959533937863772, 111.2510903946856899 ) ) ;
#159708 = CARTESIAN_POINT ( 'NONE',  ( -13.89961937509977652, 13.97604488694528158, 95.62390960531436690 ) ) ;
#159709 = CARTESIAN_POINT ( 'NONE',  ( -0.05219959533937732626, 21.53943276465977519, 77.50109039468567573 ) ) ;
#159710 = CARTESIAN_POINT ( 'NONE',  ( 8.314922557961029526, -14.29746914071037800, 25.41775706135235779 ) ) ;
#159711 = AXIS2_PLACEMENT_3D ( 'NONE', #25474, #29437, #60742 ) ;
#159712 = CARTESIAN_POINT ( 'NONE',  ( -13.89961937509977652, 13.97604488694528158, 80.62390960531436690 ) ) ;
#159714 = ADVANCED_FACE ( 'NONE', ( #113340 ), #19362, .T. ) ;
#159713 = CARTESIAN_POINT ( 'NONE',  ( 21.53943276465977519, -0.05219959533907433946, 33.74890960531436690 ) ) ;
#159715 = CARTESIAN_POINT ( 'NONE',  ( -9.564922557960796823, -16.46253265017161027, 97.08224293864769550 ) ) ;
#159716 = CARTESIAN_POINT ( 'NONE',  ( -11.74264578624799782, -36.14014761921581709, -9.349999994537627757 ) ) ;
#159717 = CARTESIAN_POINT ( 'NONE',  ( 0.05219959533909260263, 19.03943276465977164, 74.99890960531435269 ) ) ;
#159718 = CARTESIAN_POINT ( 'NONE',  ( -0.05219959533909027116, -19.03943276465977164, 62.49890960531435979 ) ) ;
#159719 = CARTESIAN_POINT ( 'NONE',  ( -4.379528057220328563, 16.55341960407611168, 25.20724293864769550 ) ) ;
#159720 = DIRECTION ( 'NONE',  ( 1.000000000000000000, 0.000000000000000000, 0.000000000000000000 ) ) ;
#159721 = VECTOR ( 'NONE', #86041, 1000.000000000000114 ) ;
#159722 = CARTESIAN_POINT ( 'NONE',  ( -0.05219959533936034679, 19.03943276465977164, 72.50109039468566152 ) ) ;
#159723 = CARTESIAN_POINT ( 'NONE',  ( 16.46253265017160672, -9.564922557960803928, 93.33224293864769550 ) ) ;
#159724 = CARTESIAN_POINT ( 'NONE',  ( -16.55341960407611168, -4.379528057220339221, 91.45724293864769550 ) ) ;
#159725 = CARTESIAN_POINT ( 'NONE',  ( 10.72451020669898902, -18.67979575497178502, 42.91557627198103120 ) ) ;
#159726 = COLOUR_RGB ( '', 0.66274510, 0.83137255, 0.94901961) ;
#159727 = CARTESIAN_POINT ( 'NONE',  ( 21.53943276465977519, -0.05219959533907433946, 28.74890960531435624 ) ) ;
#159728 = CARTESIAN_POINT ( 'NONE',  ( 8.224510206698953496, -14.34966873604960469, 102.9155762719810383 ) ) ;
#159729 = CARTESIAN_POINT ( 'NONE',  ( -16.62475595723696387, 7.163666690055236153, 55.52713351810467657 ) ) ;
#159730 = CARTESIAN_POINT ( 'NONE',  ( 19.03943276465977164, 0.05219959533936151252, 46.25109039468566863 ) ) ;
#159731 = CARTESIAN_POINT ( 'NONE',  ( -16.53943276465976808, 0.05219959533911058130, 31.24890960531435979 ) ) ;
#159732 = CARTESIAN_POINT ( 'NONE',  ( 5.153800228976335163, 19.02544592524342804, 99.79057627198102409 ) ) ;
#159733 = CARTESIAN_POINT ( 'NONE',  ( 18.62759615963255655, 10.81492255796105972, 61.66775706135235424 ) ) ;
#159734 = CARTESIAN_POINT ( 'NONE',  ( 5.719274019375991003, -21.55341960407610458, 52.70724293864769550 ) ) ;
#159735 = CARTESIAN_POINT ( 'NONE',  ( 5.719274019375673035, 21.55341960407619339, 47.29275706135234003 ) ) ;
#159736 = CARTESIAN_POINT ( 'NONE',  ( 18.67979575497178502, 10.72451020669898547, 99.16557627198100988 ) ) ;
#159737 = CARTESIAN_POINT ( 'NONE',  ( 15.80617190586769283, -15.72974639402175789, 35.62609039468568994 ) ) ;
#159738 = CARTESIAN_POINT ( 'NONE',  ( -8.224510206698948167, 14.34966873604960824, 110.4155762719810383 ) ) ;
#159739 = CARTESIAN_POINT ( 'NONE',  ( -0.05219959533936034679, 19.03943276465977164, 72.50109039468566152 ) ) ;
#159740 = CARTESIAN_POINT ( 'NONE',  ( -19.03943276465977164, 0.05219959533909376836, 46.24890960531435979 ) ) ;
#159741 =( BOUNDED_CURVE ( )  B_SPLINE_CURVE ( 2, ( #61507, #32179, #34164, #79666, #93835, #112979, #189844, #17010, #51317, #823, #157510 ),
 .UNSPECIFIED., .F., .F. ) 
 B_SPLINE_CURVE_WITH_KNOTS ( ( 3, 2, 2, 2, 2, 3 ),
 ( 0.000000000000000000, 0.01999999999999999348, 0.03999999999999998695, 0.05999999999999998390, 0.07999999999999997391, 0.09999999999999997780 ),
 .UNSPECIFIED. ) 
 CURVE ( )  GEOMETRIC_REPRESENTATION_ITEM ( )  RATIONAL_B_SPLINE_CURVE ( ( 1.000000000000000000, 0.9510565162951535312, 1.000000000000000000, 0.9510565162951535312, 1.000000000000000000, 0.9510565162951535312, 1.000000000000000000, 0.9510565162951535312, 1.000000000000000000, 0.9510565162951536422, 0.9999999999999998890 ) ) 
 REPRESENTATION_ITEM ( '' )  );
#159742 = CARTESIAN_POINT ( 'NONE',  ( -8.314922557960811034, -14.29746914071050412, 102.0822429386476955 ) ) ;
#159743 = CARTESIAN_POINT ( 'NONE',  ( -0.05219959533909027116, -19.03943276465977164, 107.4989096053143527 ) ) ;
#159744 = CARTESIAN_POINT ( 'NONE',  ( 8.224510206698953496, -14.34966873604960469, 37.91557627198102409 ) ) ;
#159745 = CARTESIAN_POINT ( 'NONE',  ( 16.52544592524335698, 4.483927247898782831, 101.4594237280190185 ) ) ;
#159746 = CARTESIAN_POINT ( 'NONE',  ( -16.46253265017160317, 9.564922557960807481, 50.83224293864770260 ) ) ;
#159747 = CARTESIAN_POINT ( 'NONE',  ( 8.224510206698953496, -14.34966873604960469, 112.9155762719810383 ) ) ;
#159748 = ADVANCED_FACE ( 'NONE', ( #79023 ), #140698, .T. ) ;
#159750 = CONICAL_SURFACE ( 'NONE', #37075, 2.500000000000002220, 1.029744260000000189 ) ;
#159749 = CARTESIAN_POINT ( 'NONE',  ( 13.89961937509957401, 13.97604488694547697, 21.87609039468566152 ) ) ;
#159752 = CARTESIAN_POINT ( 'NONE',  ( 16.55341960407611168, 4.379528057220329451, 38.95724293864768839 ) ) ;
#159751 = PLANE ( 'NONE',  #149456 ) ;
#159753 = CARTESIAN_POINT ( 'NONE',  ( 10.81492255796106328, -18.62759615963255655, 50.41775706135235424 ) ) ;
#159754 = PLANE ( 'NONE',  #32280 ) ;
#159755 = CARTESIAN_POINT ( 'NONE',  ( -14.29746914071037622, -8.314922557961029526, 54.16775706135235424 ) ) ;
#159756 = CARTESIAN_POINT ( 'NONE',  ( 16.53943276465976808, -0.05219959533910856209, 28.74890960531435624 ) ) ;
#159757 = CARTESIAN_POINT ( 'NONE',  ( -8.224510206698735004, -14.34966873604973081, 109.5844237280190328 ) ) ;
#159758 = CARTESIAN_POINT ( 'NONE',  ( 0.05219959533934541429, -16.53943276465976808, 30.00109039468568284 ) ) ;
#159759 = CARTESIAN_POINT ( 'NONE',  ( -19.03943276465977164, 0.05219959533909376836, 46.24890960531435979 ) ) ;
#159760 = CARTESIAN_POINT ( 'NONE',  ( 8.314922557960818139, 14.29746914071049879, 109.5822429386476955 ) ) ;
#159761 = CARTESIAN_POINT ( 'NONE',  ( 18.62759615963271287, -10.81492255796078972, 113.3322429386476955 ) ) ;
#159762 = CARTESIAN_POINT ( 'NONE',  ( -19.02544592524342804, 5.153800228976336051, 41.04057627198103120 ) ) ;
#159763 = CARTESIAN_POINT ( 'NONE',  ( 16.46253265017160672, -9.564922557960803928, 113.3322429386476955 ) ) ;
#159764 = CARTESIAN_POINT ( 'NONE',  ( -19.05341960407611168, -5.049401038298163336, 31.45724293864769550 ) ) ;
#159765 = CARTESIAN_POINT ( 'NONE',  ( -21.53943276465977519, 0.05219959533907696930, 21.24890960531436690 ) ) ;
#159766 = CARTESIAN_POINT ( 'NONE',  ( -16.31925111598458855, -7.325300261831428905, 34.83575461032747711 ) ) ;
#159767 = CARTESIAN_POINT ( 'NONE',  ( 13.97604488694527802, 13.89961937509977652, 104.3739096053143385 ) ) ;
#159769 = CARTESIAN_POINT ( 'NONE',  ( -4.483927247898539470, -16.52544592524342804, 102.2905762719810383 ) ) ;
#159768 = CARTESIAN_POINT ( 'NONE',  ( 18.62759615963255655, 10.81492255796105972, 51.66775706135234714 ) ) ;
#159770 = CARTESIAN_POINT ( 'NONE',  ( 16.51473224551069308, 9.474510206698969483, 104.1655762719810241 ) ) ;
#159771 = CARTESIAN_POINT ( 'NONE',  ( -16.53943276465976808, -0.05219959533934237506, 83.75109039468568994 ) ) ;
#159772 = CARTESIAN_POINT ( 'NONE',  ( -15.72974639402176322, -15.80617190586768395, 94.37609039468568994 ) ) ;
#159773 = CARTESIAN_POINT ( 'NONE',  ( 16.52544592524335698, 4.483927247898782831, 56.45942372801902565 ) ) ;
#159774 = CARTESIAN_POINT ( 'NONE',  ( -9.474510206698964154, 16.51473224551069663, 95.41557627198102409 ) ) ;
#159775 = CARTESIAN_POINT ( 'NONE',  ( 16.52544592524335698, 4.483927247898782831, 46.45942372801901854 ) ) ;
#159776 = CARTESIAN_POINT ( 'NONE',  ( 14.34966873604972726, -8.224510206698740333, 20.83442372801901143 ) ) ;
#159777 = CARTESIAN_POINT ( 'NONE',  ( 16.55341960407618274, -4.379528057220086978, 86.04275706135236135 ) ) ;
#159778 = CARTESIAN_POINT ( 'NONE',  ( -5.153800228976607833, 19.02544592524334988, 102.7094237280189759 ) ) ;
#159779 = CARTESIAN_POINT ( 'NONE',  ( 13.89961937509977652, -13.97604488694527269, 78.12390960531433848 ) ) ;
#159780 = CARTESIAN_POINT ( 'NONE',  ( -21.55341960407610458, -5.719274019375992779, 101.4572429386476955 ) ) ;
#159782 = CARTESIAN_POINT ( 'NONE',  ( -13.97604488694547697, 13.89961937509957934, 98.12609039468566152 ) ) ;
#159781 = CARTESIAN_POINT ( 'NONE',  ( 16.53943276465976808, -0.05219959533910856209, 108.7489096053143669 ) ) ;
#159783 = CARTESIAN_POINT ( 'NONE',  ( -8.314922557961024197, 14.29746914071037800, 67.91775706135234714 ) ) ;
#159784 = CARTESIAN_POINT ( 'NONE',  ( 23.62199046085638088, 10.84149981712535471, 165.9137635136254119 ) ) ;
#159785 = CARTESIAN_POINT ( 'NONE',  ( -5.153800228976607833, 19.02544592524334988, 67.70942372801900433 ) ) ;
#159786 = CARTESIAN_POINT ( 'NONE',  ( -16.53943276465976808, 0.05219959533911058130, 41.24890960531435269 ) ) ;
#159787 = CARTESIAN_POINT ( 'NONE',  ( 16.55341960407611168, 4.379528057220329451, 98.95724293864770971 ) ) ;
#159789 = CARTESIAN_POINT ( 'NONE',  ( -16.18388926212237777, 7.379444403734526148, 89.56046848633847901 ) ) ;
#159788 = CARTESIAN_POINT ( 'NONE',  ( 9.474510206698729675, 16.51473224551082808, 32.08442372801900433 ) ) ;
#159790 = CARTESIAN_POINT ( 'NONE',  ( 18.62759615963255655, 10.81492255796105972, 41.66775706135235424 ) ) ;
#159791 = CARTESIAN_POINT ( 'NONE',  ( -13.89961937509957401, -13.97604488694547875, 99.37609039468567573 ) ) ;
#159792 = CARTESIAN_POINT ( 'NONE',  ( 19.02544592524343514, -5.153800228976328945, 113.5405762719810241 ) ) ;
#159793 = CARTESIAN_POINT ( 'NONE',  ( 5.153800228976335163, 19.02544592524342804, 94.79057627198103830 ) ) ;
#159794 = CARTESIAN_POINT ( 'NONE',  ( 18.67979575497194134, -10.72451020669871369, 110.8344237280190043 ) ) ;
#159795 = CARTESIAN_POINT ( 'NONE',  ( 5.049401038298161559, -19.05341960407611168, 87.70724293864769550 ) ) ;
#159796 = CARTESIAN_POINT ( 'NONE',  ( 15.80617190586746368, 15.72974639402197994, 49.37390960531436690 ) ) ;
#159797 = CARTESIAN_POINT ( 'NONE',  ( 4.379528057220339221, -16.55341960407611168, 92.70724293864770971 ) ) ;
#159798 = CARTESIAN_POINT ( 'NONE',  ( 16.46253265017160672, -9.564922557960803928, 63.33224293864769550 ) ) ;
#159799 = CARTESIAN_POINT ( 'NONE',  ( -16.53943276465976808, 0.05219959533911058130, 106.2489096053143811 ) ) ;
#159800 = CARTESIAN_POINT ( 'NONE',  ( 15.72974639402176855, 15.80617190586768217, 21.87609039468567573 ) ) ;
#159801 = CARTESIAN_POINT ( 'NONE',  ( 18.62759615963255655, 10.81492255796105972, 71.66775706135234714 ) ) ;
#159802 = CARTESIAN_POINT ( 'NONE',  ( -5.153800228976328057, -19.02544592524343514, 42.29057627198101699 ) ) ;
#159803 = CARTESIAN_POINT ( 'NONE',  ( -0.05219959533934338120, 16.53943276465976808, 77.50109039468567573 ) ) ;
#159804 = ADVANCED_FACE ( 'NONE', ( #187237 ), #189218, .F. ) ;
#159805 = CARTESIAN_POINT ( 'NONE',  ( 18.62759615963255655, 10.81492255796105972, 21.66775706135235069 ) ) ;
#159806 = ORIENTED_EDGE ( 'NONE', *, *, #77897, .F. ) ;
#159807 = CARTESIAN_POINT ( 'NONE',  ( -10.81492255796105439, 18.62759615963255655, 22.91775706135235069 ) ) ;
#159809 = CARTESIAN_POINT ( 'NONE',  ( -13.89961937509977652, 13.97604488694528158, 65.62390960531436690 ) ) ;
#159808 = CARTESIAN_POINT ( 'NONE',  ( 9.474510206698729675, 16.51473224551082808, 57.08442372801900433 ) ) ;
#159810 = CARTESIAN_POINT ( 'NONE',  ( -5.153800228976607833, 19.02544592524334988, 37.70942372801899722 ) ) ;
#159811 = CARTESIAN_POINT ( 'NONE',  ( 5.719274019375673035, 21.55341960407619339, 67.29275706135234714 ) ) ;
#159812 = CARTESIAN_POINT ( 'NONE',  ( 0.05219959533907565091, 21.53943276465977519, 64.99890960531435269 ) ) ;
#159813 = CARTESIAN_POINT ( 'NONE',  ( 12.14591786802309770, 12.06949235617756955, 49.37390960531436690 ) ) ;
#159815 = CARTESIAN_POINT ( 'NONE',  ( 13.97604488694548053, -13.89961937509957401, 35.62609039468567573 ) ) ;
#159814 = CARTESIAN_POINT ( 'NONE',  ( -15.72974639402176322, -15.80617190586768395, 89.37609039468568994 ) ) ;
#159816 = CARTESIAN_POINT ( 'NONE',  ( 16.53943276465976808, -0.05219959533910856209, 68.74890960531435269 ) ) ;
#159817 = CARTESIAN_POINT ( 'NONE',  ( -19.03943276465977164, 0.05219959533909376836, 21.24890960531436335 ) ) ;
#159818 = CARTESIAN_POINT ( 'NONE',  ( -9.564922557961040184, 16.46253265017147172, 52.91775706135233293 ) ) ;
#159819 = CARTESIAN_POINT ( 'NONE',  ( 12.06949235617757843, -12.14591786802309237, 23.12390960531436335 ) ) ;
#159820 = CARTESIAN_POINT ( 'NONE',  ( -5.719274019375665041, -21.55341960407619695, 79.79275706135236135 ) ) ;
#159821 = CARTESIAN_POINT ( 'NONE',  ( -0.05219959533909027116, -19.03943276465977164, 82.49890960531436690 ) ) ;
#159822 = CARTESIAN_POINT ( 'NONE',  ( -9.564922557961040184, 16.46253265017147172, 52.91775706135233293 ) ) ;
#159823 = CARTESIAN_POINT ( 'NONE',  ( 10.81492255796078972, 18.62759615963270932, 54.58224293864769550 ) ) ;
#159824 = CARTESIAN_POINT ( 'NONE',  ( -18.67979575497193778, 10.72451020669871902, 48.33442372801902565 ) ) ;
#159825 = CARTESIAN_POINT ( 'NONE',  ( 15.80617190586746368, 15.72974639402197994, 104.3739096053143669 ) ) ;
#159826 = CARTESIAN_POINT ( 'NONE',  ( -19.05341960407617563, 5.049401038297882671, 98.54275706135233293 ) ) ;
#159827 = CARTESIAN_POINT ( 'NONE',  ( 0.05219959533934541429, -16.53943276465976808, 70.00109039468568994 ) ) ;
#159829 = CARTESIAN_POINT ( 'NONE',  ( -21.55341960407610458, -5.719274019375992779, 106.4572429386477097 ) ) ;
#159828 = CARTESIAN_POINT ( 'NONE',  ( -3.573655867282028392E-15, 2.428612866367529932E-14, -18.00000000000000000 ) ) ;
#159830 = CARTESIAN_POINT ( 'NONE',  ( 0.05219959533910956823, 16.53943276465976808, 89.99890960531438111 ) ) ;
#159831 = CARTESIAN_POINT ( 'NONE',  ( -17.50000000000002132, -4.658240926743158816, 31.05529582183199011 ) ) ;
#159832 = CARTESIAN_POINT ( 'NONE',  ( 16.55341960407618274, -4.379528057220086978, 36.04275706135234714 ) ) ;
#159833 = PRODUCT_RELATED_PRODUCT_CATEGORY ( 'part', '', ( #113205 ) ) ;
#159834 = CARTESIAN_POINT ( 'NONE',  ( 0.05219959533907565091, 21.53943276465977519, 49.99890960531437401 ) ) ;
#159835 = CARTESIAN_POINT ( 'NONE',  ( 16.53943276465976808, 0.05219959533934440121, 91.25109039468568994 ) ) ;
#159836 = CARTESIAN_POINT ( 'NONE',  ( 13.97604488694527802, 13.89961937509977652, 34.37390960531436690 ) ) ;
#159837 = CARTESIAN_POINT ( 'NONE',  ( 4.483927247898790824, -16.52544592524335698, 70.20942372801904696 ) ) ;
#159838 = CARTESIAN_POINT ( 'NONE',  ( -18.62759615963255300, -10.81492255796106328, 39.16775706135235424 ) ) ;
#159839 = VECTOR ( 'NONE', #114046, 1000.000000000000000 ) ;
#159840 = CARTESIAN_POINT ( 'NONE',  ( -18.62759615963270932, 10.81492255796079327, 55.83224293864770260 ) ) ;
#159841 = CARTESIAN_POINT ( 'NONE',  ( -4.379528057220086978, -16.55341960407618274, 89.79275706135236135 ) ) ;
#159842 = CARTESIAN_POINT ( 'NONE',  ( 10.81492255796106328, -18.62759615963255655, 65.41775706135234714 ) ) ;
#159843 = CARTESIAN_POINT ( 'NONE',  ( -15.80617190586745835, -15.72974639402198527, 56.87390960531436690 ) ) ;
#159844 = CARTESIAN_POINT ( 'NONE',  ( -15.72974639402197994, 15.80617190586746368, 40.62390960531435269 ) ) ;
#159845 = ORIENTED_EDGE ( 'NONE', *, *, #40503, .F. ) ;
#159846 = CARTESIAN_POINT ( 'NONE',  ( 14.29746914071037800, 8.314922557961029526, 61.66775706135235424 ) ) ;
#159847 = CARTESIAN_POINT ( 'NONE',  ( -21.52544592524343514, 5.823673210054127303, 26.04057627198103475 ) ) ;
#159848 = EDGE_LOOP ( 'NONE', ( #49938, #86775, #62912, #35341 ) ) ;
#159849 = CARTESIAN_POINT ( 'NONE',  ( -19.03943276465977164, 0.05219959533909376836, 96.24890960531436690 ) ) ;
#159850 = CARTESIAN_POINT ( 'NONE',  ( -4.483927247898782831, 16.52544592524335698, 112.7094237280190328 ) ) ;
#159851 = CARTESIAN_POINT ( 'NONE',  ( 20.41037832431316090, -34.40082058117813801, -24.99999999999991829 ) ) ;
#159852 = CARTESIAN_POINT ( 'NONE',  ( 4.379528057220339221, -16.55341960407611168, 107.7072429386476955 ) ) ;
#159853 = CARTESIAN_POINT ( 'NONE',  ( 18.62759615963271287, -10.81492255796078972, 58.33224293864768839 ) ) ;
#159854 = CARTESIAN_POINT ( 'NONE',  ( 5.153800228976335163, 19.02544592524342804, 39.79057627198100988 ) ) ;
#159855 = CARTESIAN_POINT ( 'NONE',  ( 14.34966873604972726, -8.224510206698740333, 90.83442372801901854 ) ) ;
#159856 = CARTESIAN_POINT ( 'NONE',  ( -15.80617190586768217, 15.72974639402176855, 38.12609039468567573 ) ) ;
#159857 = CARTESIAN_POINT ( 'NONE',  ( -19.05341960407617563, 5.049401038297882671, 103.5427570613523329 ) ) ;
#159858 = CARTESIAN_POINT ( 'NONE',  ( -16.55341960407611168, -4.379528057220339221, 101.4572429386476955 ) ) ;
#159859 = CARTESIAN_POINT ( 'NONE',  ( 16.46253265017160672, -9.564922557960803928, 48.33224293864769550 ) ) ;
#159860 = CIRCLE ( 'NONE', #134053, 1.000000000000000888 ) ;
#159861 = CARTESIAN_POINT ( 'NONE',  ( -16.51473224551069308, -9.474510206698971260, 21.66557627198102765 ) ) ;
#159862 = CARTESIAN_POINT ( 'NONE',  ( 14.30340603398756016, -1.218621689577097822, -62.33590500446656790 ) ) ;
#159863 = CARTESIAN_POINT ( 'NONE',  ( -5.153800228976328057, -19.02544592524343514, 77.29057627198099567 ) ) ;
#159864 = CARTESIAN_POINT ( 'NONE',  ( -14.34966873604972548, 8.224510206698743886, 73.33442372801901854 ) ) ;
#159865 = CARTESIAN_POINT ( 'NONE',  ( 21.52544592524334988, 5.823673210054432836, 106.4594237280190328 ) ) ;
#159866 = CARTESIAN_POINT ( 'NONE',  ( 10.81492255796078972, 18.62759615963270932, 54.58224293864769550 ) ) ;
#159867 = CARTESIAN_POINT ( 'NONE',  ( -4.483927247898782831, 16.52544592524335698, 77.70942372801900433 ) ) ;
#159868 = CARTESIAN_POINT ( 'NONE',  ( 9.474510206698729675, 16.51473224551082808, 67.08442372801900433 ) ) ;
#159869 = ORIENTED_EDGE ( 'NONE', *, *, #147612, .F. ) ;
#159870 = CARTESIAN_POINT ( 'NONE',  ( -10.72451020669870658, -18.67979575497194134, 59.58442372801901854 ) ) ;
#159872 = VECTOR ( 'NONE', #139878, 1000.000000000000000 ) ;
#159871 = CARTESIAN_POINT ( 'NONE',  ( 5.049401038298161559, -19.05341960407611168, 77.70724293864765286 ) ) ;
#159873 = CARTESIAN_POINT ( 'NONE',  ( -5.153800228976328057, -19.02544592524343514, 37.29057627198102409 ) ) ;
#159874 = CARTESIAN_POINT ( 'NONE',  ( -5.153800228976607833, 19.02544592524334988, 57.70942372801899012 ) ) ;
#159875 = CARTESIAN_POINT ( 'NONE',  ( -19.02544592524342804, 5.153800228976336051, 111.0405762719810099 ) ) ;
#159876 = CARTESIAN_POINT ( 'NONE',  ( 13.89961937509977652, -13.97604488694527269, 93.12390960531436690 ) ) ;
#159877 = CARTESIAN_POINT ( 'NONE',  ( 0.05219959533910956823, 16.53943276465976808, 44.99890960531435979 ) ) ;
#159878 = CARTESIAN_POINT ( 'NONE',  ( -18.62759615963270932, 10.81492255796079327, 50.83224293864770971 ) ) ;
#159879 = VECTOR ( 'NONE', #104212, 1000.000000000000000 ) ;
#159880 = LINE ( 'NONE', #3210, #57843 ) ;
#159881 = CARTESIAN_POINT ( 'NONE',  ( 15.80617190586746368, 15.72974639402197994, 69.37390960531436690 ) ) ;
#159882 = CARTESIAN_POINT ( 'NONE',  ( -19.03943276465977164, -0.05219959533935918106, 28.75109039468566507 ) ) ;
#159883 = CARTESIAN_POINT ( 'NONE',  ( -17.40861289039004944, -6.110651285853239578, 81.37232470827431996 ) ) ;
#159884 = CARTESIAN_POINT ( 'NONE',  ( -5.049401038298153566, 19.05341960407611168, 45.20724293864769550 ) ) ;
#159885 = CARTESIAN_POINT ( 'NONE',  ( -16.55341960407617563, 4.379528057220093196, 33.54275706135234714 ) ) ;
#159886 = CARTESIAN_POINT ( 'NONE',  ( -33.68492599513093211, -4.777136547582186310, 97.74919260172214308 ) ) ;
#159887 = DIRECTION ( 'NONE',  ( 0.8660254037844392627, 0.000000000000000000, 0.4999999999999988898 ) ) ;
#159888 = CARTESIAN_POINT ( 'NONE',  ( 16.55341960407618274, -4.379528057220086978, 76.04275706135237556 ) ) ;
#159889 = CARTESIAN_POINT ( 'NONE',  ( 18.67979575497178502, 10.72451020669898547, 99.16557627198100988 ) ) ;
#159891 = CARTESIAN_POINT ( 'NONE',  ( 6.412877669190335972, -3.889087296526014814, 1.818019484660534424 ) ) ;
#159890 = CARTESIAN_POINT ( 'NONE',  ( -19.03943276465977164, 0.05219959533909376836, 36.24890960531436690 ) ) ;
#159892 = CARTESIAN_POINT ( 'NONE',  ( 10.72451020669871369, 18.67979575497193778, 42.08442372801901854 ) ) ;
#159893 = CARTESIAN_POINT ( 'NONE',  ( 16.51473224551083163, -9.474510206698727899, 50.83442372801899722 ) ) ;
#159894 = CARTESIAN_POINT ( 'NONE',  ( 19.03943276465977164, -0.05219959533909143690, 48.74890960531435979 ) ) ;
#159895 = CARTESIAN_POINT ( 'NONE',  ( 21.53943276465977519, 0.05219959533937863772, 91.25109039468568994 ) ) ;
#159896 = CARTESIAN_POINT ( 'NONE',  ( 16.36317988757059894, 7.306389748694943620, 98.40210391636779264 ) ) ;
#159897 = CARTESIAN_POINT ( 'NONE',  ( 0.05219959533910956823, 16.53943276465976808, 44.99890960531435979 ) ) ;
#159898 = CARTESIAN_POINT ( 'NONE',  ( 4.313351365237961588, -4.313351365237934942, -64.53213882399992940 ) ) ;
#159899 = CARTESIAN_POINT ( 'NONE',  ( 10.81492255796078972, 18.62759615963270932, 49.58224293864769550 ) ) ;
#159900 = CIRCLE ( 'NONE', #195451, 1.000000000000000888 ) ;
#159901 = CARTESIAN_POINT ( 'NONE',  ( 1.784210473542230573E-15, -29.16686587814331588, 143.3750000027311557 ) ) ;
#159902 = CARTESIAN_POINT ( 'NONE',  ( -19.03943276465977164, 0.05219959533909376836, 101.2489096053143669 ) ) ;
#159903 = CARTESIAN_POINT ( 'NONE',  ( -4.483927247898539470, -16.52544592524342804, 102.2905762719810383 ) ) ;
#159904 = CARTESIAN_POINT ( 'NONE',  ( 14.29746914071037800, 8.314922557961029526, 26.66775706135235424 ) ) ;
#159905 = CARTESIAN_POINT ( 'NONE',  ( -16.52544592524335698, -4.483927247898792601, 108.9594237280190185 ) ) ;
#159906 = ORIENTED_EDGE ( 'NONE', *, *, #147658, .T. ) ;
#159908 = CARTESIAN_POINT ( 'NONE',  ( -5.719274019375978568, 21.55341960407610458, 100.2072429386476955 ) ) ;
#159907 = CARTESIAN_POINT ( 'NONE',  ( 16.46253265017160672, -9.564922557960803928, 103.3322429386476955 ) ) ;
#159910 = CARTESIAN_POINT ( 'NONE',  ( -9.474510206698964154, 16.51473224551069663, 105.4155762719810383 ) ) ;
#159909 = CARTESIAN_POINT ( 'NONE',  ( -12.06949235617756955, 12.14591786802309770, 25.62390960531435624 ) ) ;
#159911 = CARTESIAN_POINT ( 'NONE',  ( 16.46253265017146816, 9.564922557961045513, 96.66775706135233293 ) ) ;
#159912 = CARTESIAN_POINT ( 'NONE',  ( -18.62759615963255300, -10.81492255796106328, 109.1677570613523613 ) ) ;
#159913 = CARTESIAN_POINT ( 'NONE',  ( -10.72451020669898014, 18.67979575497178502, 95.41557627198102409 ) ) ;
#159914 = CARTESIAN_POINT ( 'NONE',  ( -18.62759615963270932, 10.81492255796079327, 45.83224293864769550 ) ) ;
#159915 = CARTESIAN_POINT ( 'NONE',  ( 16.46253265017160672, -9.564922557960803928, 58.33224293864769550 ) ) ;
#159916 = CARTESIAN_POINT ( 'NONE',  ( -12.06949235617756955, 12.14591786802309770, 30.62390960531436335 ) ) ;
#159917 = CARTESIAN_POINT ( 'NONE',  ( 19.02544592524343514, -5.153800228976328945, 83.54057627198100988 ) ) ;
#159918 = ORIENTED_EDGE ( 'NONE', *, *, #62342, .F. ) ;
#159919 = CARTESIAN_POINT ( 'NONE',  ( 19.46398650005386699, -5.500000000000144773, 62.68269651486372851 ) ) ;
#159920 = CARTESIAN_POINT ( 'NONE',  ( -0.05219959533936034679, 19.03943276465977164, 37.50109039468567573 ) ) ;
#159921 = CARTESIAN_POINT ( 'NONE',  ( 5.823673210054125526, 21.52544592524343514, 79.79057627198102409 ) ) ;
#159922 = CARTESIAN_POINT ( 'NONE',  ( -8.314922557960811034, -14.29746914071050412, 82.08224293864768129 ) ) ;
#159923 = CARTESIAN_POINT ( 'NONE',  ( -10.72451020669870658, -18.67979575497194134, 34.58442372801900433 ) ) ;
#159924 = CARTESIAN_POINT ( 'NONE',  ( -27.73933785331498925, -9.013057229001049109, 147.4750000027311785 ) ) ;
#159925 = CARTESIAN_POINT ( 'NONE',  ( -4.483927247898782831, 16.52544592524335698, 107.7094237280190328 ) ) ;
#159926 = CARTESIAN_POINT ( 'NONE',  ( 16.52544592524342804, -4.483927247898539470, 113.5405762719810383 ) ) ;
#159927 = CARTESIAN_POINT ( 'NONE',  ( 5.049401038298161559, -19.05341960407611168, 87.70724293864769550 ) ) ;
#159928 = CARTESIAN_POINT ( 'NONE',  ( 18.10062525802553779, -5.500000000000023093, 71.01383468041922242 ) ) ;
#159929 = CARTESIAN_POINT ( 'NONE',  ( 0.000000000000000000, 0.000000000000000000, -25.00000000000000000 ) ) ;
#159930 = CARTESIAN_POINT ( 'NONE',  ( 16.55341960407611168, 4.379528057220329451, 43.95724293864769550 ) ) ;
#159931 = CARTESIAN_POINT ( 'NONE',  ( 21.52544592524334988, 5.823673210054432836, 56.45942372801902565 ) ) ;
#159932 = CARTESIAN_POINT ( 'NONE',  ( 25.66183622254818175, -27.84411637527792749, -16.56099493762766883 ) ) ;
#159933 = CARTESIAN_POINT ( 'NONE',  ( -0.05219959533909027116, -19.03943276465977164, 47.49890960531435979 ) ) ;
#159934 = CARTESIAN_POINT ( 'NONE',  ( -5.153800228976328057, -19.02544592524343514, 47.29057627198102409 ) ) ;
#159935 = ORIENTED_EDGE ( 'NONE', *, *, #117511, .T. ) ;
#159936 = CARTESIAN_POINT ( 'NONE',  ( 15.72974639402176855, 15.80617190586768217, 111.8760903946856615 ) ) ;
#159937 = CARTESIAN_POINT ( 'NONE',  ( 8.314922557961029526, -14.29746914071037800, 65.41775706135234714 ) ) ;
#159938 = CARTESIAN_POINT ( 'NONE',  ( 5.823673210054444382, -21.52544592524334988, 90.20942372801903275 ) ) ;
#159939 = CARTESIAN_POINT ( 'NONE',  ( -19.02544592524342804, 5.153800228976336051, 111.0405762719810099 ) ) ;
#159940 = CARTESIAN_POINT ( 'NONE',  ( 9.474510206698729675, 16.51473224551082808, 92.08442372801900433 ) ) ;
#159941 = CARTESIAN_POINT ( 'NONE',  ( 21.53943276465977519, 0.05219959533937863772, 71.25109039468568994 ) ) ;
#159942 = CARTESIAN_POINT ( 'NONE',  ( 12.06949235617739724, 12.14591786802326823, 36.87609039468568994 ) ) ;
#159943 = CARTESIAN_POINT ( 'NONE',  ( -18.67979575497178146, -10.72451020669898902, 86.66557627198102409 ) ) ;
#159944 = CARTESIAN_POINT ( 'NONE',  ( -19.03943276465977164, -0.05219959533935918106, 93.75109039468566152 ) ) ;
#159945 = CARTESIAN_POINT ( 'NONE',  ( -9.474510206698964154, 16.51473224551069663, 65.41557627198102409 ) ) ;
#159946 = CARTESIAN_POINT ( 'NONE',  ( -4.379528057220086978, -16.55341960407618274, 19.79275706135235069 ) ) ;
#159947 = CARTESIAN_POINT ( 'NONE',  ( 16.46253265017146816, 9.564922557961045513, 106.6677570613523471 ) ) ;
#159948 = CARTESIAN_POINT ( 'NONE',  ( -14.29746914071049879, 8.314922557960819915, 55.83224293864770260 ) ) ;
#159949 = CARTESIAN_POINT ( 'NONE',  ( -9.474510206698720793, -16.51473224551083518, 79.58442372801899012 ) ) ;
#159950 = CARTESIAN_POINT ( 'NONE',  ( -4.483927247898782831, 16.52544592524335698, 62.70942372801902565 ) ) ;
#159952 = CARTESIAN_POINT ( 'NONE',  ( -19.02544592524342804, 5.153800228976336051, 41.04057627198103120 ) ) ;
#159951 = CARTESIAN_POINT ( 'NONE',  ( -5.719274019375665041, -21.55341960407619695, 19.79275706135235069 ) ) ;
#159953 = CARTESIAN_POINT ( 'NONE',  ( -9.474510206698964154, 16.51473224551069663, 50.41557627198102409 ) ) ;
#159954 = CARTESIAN_POINT ( 'NONE',  ( 4.483927247898790824, -16.52544592524335698, 65.20942372801901854 ) ) ;
#159955 = CARTESIAN_POINT ( 'NONE',  ( -27.73933785331498925, -9.013057229001049109, 141.4750000027311785 ) ) ;
#159956 = EDGE_CURVE ( 'NONE', #2773, #135939, #193717, .T. ) ;
#159957 = CARTESIAN_POINT ( 'NONE',  ( 28.82186960331498327, 9.364793116373570925, 145.3500000054623627 ) ) ;
#159958 = CARTESIAN_POINT ( 'NONE',  ( 5.153800228976335163, 19.02544592524342804, 104.7905762719809957 ) ) ;
#159959 = CARTESIAN_POINT ( 'NONE',  ( -27.05641397906351742, 3.631740835637567333, 169.9999999999999716 ) ) ;
#159960 = ORIENTED_EDGE ( 'NONE', *, *, #76322, .F. ) ;
#159961 = CARTESIAN_POINT ( 'NONE',  ( 16.53943276465976808, 0.05219959533934440121, 21.25109039468567218 ) ) ;
#159962 = CARTESIAN_POINT ( 'NONE',  ( 10.72451020669898902, -18.67979575497178502, 42.91557627198103120 ) ) ;
#159964 = CARTESIAN_POINT ( 'NONE',  ( -4.483927247898782831, 16.52544592524335698, 32.70942372801900433 ) ) ;
#159963 = CARTESIAN_POINT ( 'NONE',  ( -5.153800228976607833, 19.02544592524334988, 42.70942372801901143 ) ) ;
#159965 = CARTESIAN_POINT ( 'NONE',  ( -13.89961937509977652, 13.97604488694528158, 25.62390960531434558 ) ) ;
#159966 = CARTESIAN_POINT ( 'NONE',  ( -9.564922557960796823, -16.46253265017161027, 57.08224293864769550 ) ) ;
#159967 = CARTESIAN_POINT ( 'NONE',  ( -21.55341960407610458, -5.719274019375992779, 91.45724293864769550 ) ) ;
#159968 = CARTESIAN_POINT ( 'NONE',  ( -9.474510206698964154, 16.51473224551069663, 115.4155762719810241 ) ) ;
#159969 = CARTESIAN_POINT ( 'NONE',  ( -16.46253265017160317, 9.564922557960807481, 50.83224293864770260 ) ) ;
#159970 = CARTESIAN_POINT ( 'NONE',  ( 8.571926809382597767, 26.38167802310806209, 140.7750000027311899 ) ) ;
#159971 = CARTESIAN_POINT ( 'NONE',  ( -13.97604488694547697, 13.89961937509957934, 78.12609039468567573 ) ) ;
#159972 = CARTESIAN_POINT ( 'NONE',  ( 16.52544592524342804, -4.483927247898539470, 68.54057627198103830 ) ) ;
#159973 = CARTESIAN_POINT ( 'NONE',  ( -10.81492255796105439, 18.62759615963255655, 107.9177570613523471 ) ) ;
#159974 = CARTESIAN_POINT ( 'NONE',  ( -21.53943276465977519, 0.05219959533907696930, 101.2489096053143669 ) ) ;
#159975 = CARTESIAN_POINT ( 'NONE',  ( 0.05219959533937995610, -21.53943276465977519, 80.00109039468568994 ) ) ;
#159976 = CARTESIAN_POINT ( 'NONE',  ( -19.02544592524342804, 5.153800228976336051, 31.04057627198102409 ) ) ;
#159977 = CARTESIAN_POINT ( 'NONE',  ( 18.62759615963255655, 10.81492255796105972, 71.66775706135234714 ) ) ;
#159978 = CARTESIAN_POINT ( 'NONE',  ( 19.03943276465977164, -0.05219959533909143690, 108.7489096053143527 ) ) ;
#159980 = CARTESIAN_POINT ( 'NONE',  ( -18.67979575497193778, 10.72451020669871902, 78.33442372801901854 ) ) ;
#159979 = CARTESIAN_POINT ( 'NONE',  ( 0.05219959533934541429, -16.53943276465976808, 100.0010903946857042 ) ) ;
#159981 = CARTESIAN_POINT ( 'NONE',  ( 16.46253265017160672, -9.564922557960803928, 63.33224293864769550 ) ) ;
#159982 = CARTESIAN_POINT ( 'NONE',  ( 15.72974639402176855, 15.80617190586768217, 41.87609039468568284 ) ) ;
#159983 = CARTESIAN_POINT ( 'NONE',  ( 16.51473224551069308, 9.474510206698969483, 84.16557627198102409 ) ) ;
#159984 = CARTESIAN_POINT ( 'NONE',  ( -16.55341960407611168, -4.379528057220339221, 91.45724293864769550 ) ) ;
#159985 = CARTESIAN_POINT ( 'NONE',  ( -4.379528057220328563, 16.55341960407611168, 55.20724293864770260 ) ) ;
#159986 = CARTESIAN_POINT ( 'NONE',  ( 0.05219959533907565091, 21.53943276465977519, 64.99890960531435269 ) ) ;
#159987 = CARTESIAN_POINT ( 'NONE',  ( -19.02544592524342804, 5.153800228976336051, 66.04057627198103830 ) ) ;
#159988 = CARTESIAN_POINT ( 'NONE',  ( 21.52544592524344225, -5.823673210054117533, 73.54057627198102409 ) ) ;
#159989 = AXIS2_PLACEMENT_3D ( 'NONE', #188089, #157741, #80879 ) ;
#159990 = CARTESIAN_POINT ( 'NONE',  ( 0.05219959533936267826, -19.03943276465977164, 65.00109039468567573 ) ) ;
#159992 = CARTESIAN_POINT ( 'NONE',  ( 0.05219959533910956823, 16.53943276465976808, 79.99890960531435269 ) ) ;
#159991 = CARTESIAN_POINT ( 'NONE',  ( -18.56399227203342761, -5.499999999999929834, 88.97830131249907026 ) ) ;
#159993 = CARTESIAN_POINT ( 'NONE',  ( 21.52544592524344225, -5.823673210054117533, 58.54057627198103120 ) ) ;
#159994 = CARTESIAN_POINT ( 'NONE',  ( 69.65682714487590488, -71.74905178543389184, 0.000000000000000000 ) ) ;
#159996 = CARTESIAN_POINT ( 'NONE',  ( -27.73933785331498925, 9.013057229001088189, 143.2750000027311899 ) ) ;
#159995 = CARTESIAN_POINT ( 'NONE',  ( -8.224510206698735004, -14.34966873604973081, 99.58442372801900433 ) ) ;
#159997 = CARTESIAN_POINT ( 'NONE',  ( -16.51473224551082808, 9.474510206698731452, 103.3344237280190043 ) ) ;
#159998 = CARTESIAN_POINT ( 'NONE',  ( 16.52544592524342804, -4.483927247898539470, 68.54057627198103830 ) ) ;
#159999 = CARTESIAN_POINT ( 'NONE',  ( -17.50000000000004263, 4.049696124445827827, 34.18039670665945806 ) ) ;
#160000 = CARTESIAN_POINT ( 'NONE',  ( -19.03943276465977164, 0.05219959533909376836, 66.24890960531436690 ) ) ;
#160001 = CARTESIAN_POINT ( 'NONE',  ( -16.53943276465976808, 0.05219959533911058130, 51.24890960531436690 ) ) ;
#160002 = CARTESIAN_POINT ( 'NONE',  ( 19.02544592524343514, -5.153800228976328945, 88.54057627198102409 ) ) ;
#160004 = CARTESIAN_POINT ( 'NONE',  ( 5.153800228976335163, 19.02544592524342804, 69.79057627198103830 ) ) ;
#160003 = CARTESIAN_POINT ( 'NONE',  ( 19.02544592524334988, 5.153800228976608722, 71.45942372801900433 ) ) ;
#160005 = CARTESIAN_POINT ( 'NONE',  ( 5.049401038298161559, -19.05341960407611168, 87.70724293864769550 ) ) ;
#160006 = CARTESIAN_POINT ( 'NONE',  ( 16.46253265017160672, -9.564922557960803928, 73.33224293864769550 ) ) ;
#160007 = CARTESIAN_POINT ( 'NONE',  ( 21.53943276465977519, -0.05219959533907433946, 63.74890960531435979 ) ) ;
#160008 = CARTESIAN_POINT ( 'NONE',  ( 12.14591786802327356, -12.06949235617739191, 60.62609039468567573 ) ) ;
#160009 = CARTESIAN_POINT ( 'NONE',  ( -6.856101608890801443E-16, -71.74905178543389184, -22.99263613531268291 ) ) ;
#160010 = CARTESIAN_POINT ( 'NONE',  ( 5.049401038298161559, -19.05341960407611168, 42.70724293864767418 ) ) ;
#160011 = CARTESIAN_POINT ( 'NONE',  ( -18.62759615963270932, 10.81492255796079327, 55.83224293864770260 ) ) ;
#160012 = CARTESIAN_POINT ( 'NONE',  ( -9.564922557961040184, 16.46253265017147172, 87.91775706135233293 ) ) ;
#160014 = CARTESIAN_POINT ( 'NONE',  ( -15.72974639402176322, -15.80617190586768395, 29.37609039468568284 ) ) ;
#160013 = CARTESIAN_POINT ( 'NONE',  ( 8.224510206698953496, -14.34966873604960469, 27.91557627198103830 ) ) ;
#160015 = CARTESIAN_POINT ( 'NONE',  ( 9.474510206698729675, 16.51473224551082808, 37.08442372801899722 ) ) ;
#160017 = CARTESIAN_POINT ( 'NONE',  ( 8.314922557961029526, -14.29746914071037800, 95.41775706135234714 ) ) ;
#160016 = CARTESIAN_POINT ( 'NONE',  ( -12.14591786802326823, 12.06949235617739902, 63.12609039468568994 ) ) ;
#160018 = LINE ( 'NONE', #173210, #121020 ) ;
#160019 = CARTESIAN_POINT ( 'NONE',  ( -0.05219959533934338120, 16.53943276465976808, 87.50109039468568994 ) ) ;
#160021 = CARTESIAN_POINT ( 'NONE',  ( -12.14591786802326823, 12.06949235617739902, 33.12609039468569705 ) ) ;
#160020 = CARTESIAN_POINT ( 'NONE',  ( 0.05219959533907565091, 21.53943276465977519, 29.99890960531435979 ) ) ;
#160022 = CARTESIAN_POINT ( 'NONE',  ( -19.03943276465977164, 0.05219959533909376836, 51.24890960531436690 ) ) ;
#160023 = CARTESIAN_POINT ( 'NONE',  ( 16.51473224551069308, 9.474510206698969483, 54.16557627198103120 ) ) ;
#160024 = CARTESIAN_POINT ( 'NONE',  ( -13.89961937509977652, 13.97604488694528158, 65.62390960531436690 ) ) ;
#160025 = CARTESIAN_POINT ( 'NONE',  ( 10.72451020669871369, 18.67979575497193778, 42.08442372801901854 ) ) ;
#160026 = CARTESIAN_POINT ( 'NONE',  ( -12.06949235617739369, -12.14591786802326823, 44.37609039468567573 ) ) ;
#160027 = CARTESIAN_POINT ( 'NONE',  ( -14.34966873604960291, -8.224510206698953496, 21.66557627198102409 ) ) ;
#160028 = CARTESIAN_POINT ( 'NONE',  ( -5.049401038298153566, 19.05341960407611168, 25.20724293864768484 ) ) ;
#160029 = CARTESIAN_POINT ( 'NONE',  ( 18.67979575497194134, -10.72451020669871369, 110.8344237280190043 ) ) ;
#160030 = CARTESIAN_POINT ( 'NONE',  ( 12.14591786802327356, -12.06949235617739191, 20.62609039468568639 ) ) ;
#160031 = CARTESIAN_POINT ( 'NONE',  ( 19.02544592524334988, 5.153800228976608722, 71.45942372801900433 ) ) ;
#160032 = CARTESIAN_POINT ( 'NONE',  ( 14.29746914071049879, -8.314922557960816363, 68.33224293864769550 ) ) ;
#160033 = CARTESIAN_POINT ( 'NONE',  ( 19.03943276465977164, -0.05219959533909143690, 43.74890960531435979 ) ) ;
#160035 = CARTESIAN_POINT ( 'NONE',  ( 17.12812012977027010, -6.668231424565981058, 91.14051240676852217 ) ) ;
#160034 = CARTESIAN_POINT ( 'NONE',  ( -19.03943276465977164, -0.05219959533935918106, 78.75109039468567573 ) ) ;
#160036 = CARTESIAN_POINT ( 'NONE',  ( 15.80617190586769283, -15.72974639402175789, 80.62609039468567573 ) ) ;
#160037 = CARTESIAN_POINT ( 'NONE',  ( -14.34966873604972548, 8.224510206698743886, 38.33442372801900433 ) ) ;
#160038 = CARTESIAN_POINT ( 'NONE',  ( 17.40861289039003879, 6.110651285853278658, 38.87232470827432707 ) ) ;
#160039 = CARTESIAN_POINT ( 'NONE',  ( -21.53943276465977519, 0.05219959533907696930, 36.24890960531435979 ) ) ;
#160040 = CARTESIAN_POINT ( 'NONE',  ( 8.314922557961029526, -14.29746914071037800, 30.41775706135234358 ) ) ;
#160041 = CARTESIAN_POINT ( 'NONE',  ( -16.51473224551069308, -9.474510206698971260, 21.66557627198102765 ) ) ;
#160042 = CARTESIAN_POINT ( 'NONE',  ( 15.72974639402176855, 15.80617190586768217, 106.8760903946856899 ) ) ;
#160043 = CARTESIAN_POINT ( 'NONE',  ( 1.227931366032057224E-14, 24.30000000000003268, -56.77278709839600879 ) ) ;
#160044 = CARTESIAN_POINT ( 'NONE',  ( 16.46253265017160672, -9.564922557960803928, 38.33224293864768839 ) ) ;
#160045 = CARTESIAN_POINT ( 'NONE',  ( 8.898068258721473001, -27.38543819252872069, 142.8656553485623704 ) ) ;
#160046 = CARTESIAN_POINT ( 'NONE',  ( -9.474510206698964154, 16.51473224551069663, 55.41557627198103120 ) ) ;
#160047 = CARTESIAN_POINT ( 'NONE',  ( -15.80617190586768217, 15.72974639402176855, 68.12609039468567573 ) ) ;
#160048 = CARTESIAN_POINT ( 'NONE',  ( 9.564922557961047289, -16.46253265017146816, 25.41775706135234003 ) ) ;
#160049 = CARTESIAN_POINT ( 'NONE',  ( -0.05219959533910754901, -16.53943276465976808, 27.49890960531435269 ) ) ;
#160050 = CARTESIAN_POINT ( 'NONE',  ( 19.03943276465977164, -0.05219959533909143690, 33.74890960531435979 ) ) ;
#160051 = EDGE_CURVE ( 'NONE', #193517, #40598, #141695, .T. ) ;
#160052 = CARTESIAN_POINT ( 'NONE',  ( 16.46253265017160672, -9.564922557960803928, 98.33224293864769550 ) ) ;
#160053 = CARTESIAN_POINT ( 'NONE',  ( 21.53943276465977519, 0.05219959533937863772, 66.25109039468567573 ) ) ;
#160054 = CARTESIAN_POINT ( 'NONE',  ( 9.474510206698971260, -16.51473224551069308, 42.91557627198103120 ) ) ;
#160055 = CARTESIAN_POINT ( 'NONE',  ( 21.52544592524334988, 5.823673210054432836, 66.45942372801903275 ) ) ;
#160057 = CARTESIAN_POINT ( 'NONE',  ( -13.89961937509977652, 13.97604488694528158, 100.6239096053143669 ) ) ;
#160056 = CARTESIAN_POINT ( 'NONE',  ( 5.049401038297881783, 19.05341960407617563, 97.29275706135233293 ) ) ;
#160058 = CARTESIAN_POINT ( 'NONE',  ( 5.153800228976335163, 19.02544592524342804, 39.79057627198100988 ) ) ;
#160059 = CARTESIAN_POINT ( 'NONE',  ( -0.05219959533907301413, -21.53943276465977519, 112.4989096053143669 ) ) ;
#160060 = CARTESIAN_POINT ( 'NONE',  ( 0.05219959533936267826, -19.03943276465977164, 40.00109039468566152 ) ) ;
#160061 = CARTESIAN_POINT ( 'NONE',  ( 16.53943276465976808, -0.05219959533910856209, 113.7489096053143527 ) ) ;
#160062 = CARTESIAN_POINT ( 'NONE',  ( 19.02544592524343514, -5.153800228976328945, 63.54057627198103830 ) ) ;
#160063 = CARTESIAN_POINT ( 'NONE',  ( 9.564922557961047289, -16.46253265017146816, 100.4177570613523329 ) ) ;
#160064 = CARTESIAN_POINT ( 'NONE',  ( 4.379528057220339221, -16.55341960407611168, 57.70724293864770260 ) ) ;
#160065 = CARTESIAN_POINT ( 'NONE',  ( 18.62759615963271287, -10.81492255796078972, 23.33224293864769194 ) ) ;
#160066 = CARTESIAN_POINT ( 'NONE',  ( -13.89961937509957401, -13.97604488694547875, 84.37609039468567573 ) ) ;
#160067 = CARTESIAN_POINT ( 'NONE',  ( -15.80617190586745835, -15.72974639402198527, 96.87390960531436690 ) ) ;
#160068 = CARTESIAN_POINT ( 'NONE',  ( -21.52544592524334988, -5.823673210054445271, 43.95942372801902565 ) ) ;
#160069 = CARTESIAN_POINT ( 'NONE',  ( 14.29746914071037800, 8.314922557961029526, 41.66775706135235424 ) ) ;
#160071 = CARTESIAN_POINT ( 'NONE',  ( 15.72974639402176855, 15.80617190586768217, 51.87609039468568284 ) ) ;
#160070 = CARTESIAN_POINT ( 'NONE',  ( 4.483927247898790824, -16.52544592524335698, 40.20942372801901854 ) ) ;
#160072 = CARTESIAN_POINT ( 'NONE',  ( -21.52544592524343514, 5.823673210054127303, 56.04057627198102409 ) ) ;
#160073 = CARTESIAN_POINT ( 'NONE',  ( 0.05219959533909260263, 19.03943276465977164, 39.99890960531436690 ) ) ;
#160074 = CARTESIAN_POINT ( 'NONE',  ( -11.74264578624800670, 36.14014761921585972, -2.149999994537626691 ) ) ;
#160075 = CARTESIAN_POINT ( 'NONE',  ( -16.53943276465976808, -0.05219959533934237506, 78.75109039468568994 ) ) ;
#160076 = CARTESIAN_POINT ( 'NONE',  ( -21.53943276465977519, 0.05219959533907696930, 106.2489096053143811 ) ) ;
#160077 = CARTESIAN_POINT ( 'NONE',  ( 14.29746914071049879, -8.314922557960816363, 38.33224293864768839 ) ) ;
#160078 = CARTESIAN_POINT ( 'NONE',  ( -12.14591786802326823, 12.06949235617739902, 68.12609039468567573 ) ) ;
#160079 = CARTESIAN_POINT ( 'NONE',  ( -16.46253265017146816, -9.564922557961047289, 94.16775706135233293 ) ) ;
#160080 = CARTESIAN_POINT ( 'NONE',  ( 15.80617190586746368, 15.72974639402197994, 104.3739096053143669 ) ) ;
#160081 = CARTESIAN_POINT ( 'NONE',  ( -16.55341960407611168, -4.379528057220339221, 26.45724293864768839 ) ) ;
#160082 = ADVANCED_FACE ( 'NONE', ( #65844 ), #182498, .T. ) ;
#160083 = ORIENTED_EDGE ( 'NONE', *, *, #134292, .T. ) ;
#160084 = CARTESIAN_POINT ( 'NONE',  ( -14.34966873604972548, 8.224510206698743886, 78.33442372801901854 ) ) ;
#160085 = CARTESIAN_POINT ( 'NONE',  ( 19.26498983726236602, -5.499999999999790390, 93.05319577422004329 ) ) ;
#160086 = CARTESIAN_POINT ( 'NONE',  ( 21.53943276465977519, -0.05219959533907433946, 73.74890960531433848 ) ) ;
#160087 = CARTESIAN_POINT ( 'NONE',  ( 8.224510206698742110, 14.34966873604972548, 107.0844237280190043 ) ) ;
#160088 = ORIENTED_EDGE ( 'NONE', *, *, #130640, .T. ) ;
#160089 = CARTESIAN_POINT ( 'NONE',  ( -17.26172910966778318, -6.454744622555873335, 54.19353091350776452 ) ) ;
#160090 = CARTESIAN_POINT ( 'NONE',  ( 18.62759615963271287, -10.81492255796078972, 98.33224293864769550 ) ) ;
#160091 = AXIS2_PLACEMENT_3D ( 'NONE', #166294, #74277, #120749 ) ;
#160092 = CARTESIAN_POINT ( 'NONE',  ( -5.823673210054116645, -21.52544592524344225, 107.2905762719810525 ) ) ;
#160093 = CARTESIAN_POINT ( 'NONE',  ( -12.06949235617756955, 12.14591786802309770, 35.62390960531437401 ) ) ;
#160094 = CARTESIAN_POINT ( 'NONE',  ( -0.05219959533934338120, 16.53943276465976808, 42.50109039468567573 ) ) ;
#160095 = CARTESIAN_POINT ( 'NONE',  ( 16.46253265017160672, -9.564922557960803928, 43.33224293864769550 ) ) ;
#160096 = CARTESIAN_POINT ( 'NONE',  ( 16.46253265017160672, -9.564922557960803928, 63.33224293864769550 ) ) ;
#160097 = CARTESIAN_POINT ( 'NONE',  ( -16.51473224551069308, -9.474510206698971260, 111.6655762719810383 ) ) ;
#160098 = CARTESIAN_POINT ( 'NONE',  ( -26.12775673971868784, -26.86876869530775380, -18.42961048235722288 ) ) ;
#160099 = CARTESIAN_POINT ( 'NONE',  ( 0.05219959533936267826, -19.03943276465977164, 100.0010903946856757 ) ) ;
#160100 = CARTESIAN_POINT ( 'NONE',  ( 16.51473224551083163, -9.474510206698727899, 50.83442372801899722 ) ) ;
#160101 = CARTESIAN_POINT ( 'NONE',  ( 15.72974639402199770, -15.80617190586745480, 93.12390960531436690 ) ) ;
#160102 = CARTESIAN_POINT ( 'NONE',  ( 12.14591786802309770, 12.06949235617756955, 24.37390960531435979 ) ) ;
#160103 = CARTESIAN_POINT ( 'NONE',  ( 16.51473224551069308, 9.474510206698969483, 79.16557627198103830 ) ) ;
#160104 = CARTESIAN_POINT ( 'NONE',  ( -5.823673210054116645, -21.52544592524344225, 52.29057627198102409 ) ) ;
#160106 = CARTESIAN_POINT ( 'NONE',  ( -4.379528057220086978, -16.55341960407618274, 24.79275706135235779 ) ) ;
#160105 = CARTESIAN_POINT ( 'NONE',  ( 18.62759615963271287, -10.81492255796078972, 88.33224293864769550 ) ) ;
#160107 = CARTESIAN_POINT ( 'NONE',  ( 18.62759615963271287, -10.81492255796078972, 23.33224293864769194 ) ) ;
#160108 = CARTESIAN_POINT ( 'NONE',  ( -5.719274019375665041, -21.55341960407619695, 69.79275706135234714 ) ) ;
#160109 = CARTESIAN_POINT ( 'NONE',  ( 19.05341960407611168, 5.049401038298154454, 78.95724293864769550 ) ) ;
#160110 = CARTESIAN_POINT ( 'NONE',  ( 9.474510206698971260, -16.51473224551069308, 32.91557627198102409 ) ) ;
#160111 = CARTESIAN_POINT ( 'NONE',  ( -13.89961937509977652, 13.97604488694528158, 75.62390960531438111 ) ) ;
#160112 = CARTESIAN_POINT ( 'NONE',  ( -14.34966873604960291, -8.224510206698953496, 96.66557627198102409 ) ) ;
#160113 = ORIENTED_EDGE ( 'NONE', *, *, #178569, .F. ) ;
#160114 = CARTESIAN_POINT ( 'NONE',  ( -19.03943276465977164, -0.05219959533935918106, 98.75109039468567573 ) ) ;
#160115 =( BOUNDED_CURVE ( )  B_SPLINE_CURVE ( 3, ( #142206, #125061, #36019, #93717 ),
 .UNSPECIFIED., .F., .F. ) 
 B_SPLINE_CURVE_WITH_KNOTS ( ( 4, 4 ),
 ( 1.025647941782810824, 2.008945357379067875 ),
 .UNSPECIFIED. ) 
 CURVE ( )  GEOMETRIC_REPRESENTATION_ITEM ( )  RATIONAL_B_SPLINE_CURVE ( ( 1.000000000000000000, 0.9210371567966660900, 0.9210371567966660900, 1.000000000000000000 ) ) 
 REPRESENTATION_ITEM ( '' )  );
#160116 = CARTESIAN_POINT ( 'NONE',  ( -1.221313414957698099E-14, 31.90000000000003411, -45.64921306006598201 ) ) ;
#160117 = CARTESIAN_POINT ( 'NONE',  ( -5.153800228976328057, -19.02544592524343514, 77.29057627198099567 ) ) ;
#160119 = CARTESIAN_POINT ( 'NONE',  ( 13.89961937509977652, -13.97604488694527269, 103.1239096053143527 ) ) ;
#160118 = CARTESIAN_POINT ( 'NONE',  ( 10.81492255796106328, -18.62759615963255655, 80.41775706135234714 ) ) ;
#160120 = CARTESIAN_POINT ( 'NONE',  ( -16.53943276465976808, -0.05219959533934237506, 78.75109039468568994 ) ) ;
#160121 = CARTESIAN_POINT ( 'NONE',  ( -29.56482114129869743, 1.249513161672317851, -48.84067647644815224 ) ) ;
#160122 = CARTESIAN_POINT ( 'NONE',  ( 9.474510206698729675, 16.51473224551082808, 57.08442372801900433 ) ) ;
#160123 = CARTESIAN_POINT ( 'NONE',  ( 0.05219959533937995610, -21.53943276465977519, 110.0010903946856757 ) ) ;
#160124 = CARTESIAN_POINT ( 'NONE',  ( 0.000000000000000000, -105.0000000000000000, 12.00000000000000355 ) ) ;
#160125 = CARTESIAN_POINT ( 'NONE',  ( 16.62544781628812274, 7.153289815129877383, 22.00000000000000000 ) ) ;
#160126 = CARTESIAN_POINT ( 'NONE',  ( -29.86685920354755197, -21.69954338932560134, -2.924999997268813878 ) ) ;
#160127 = CARTESIAN_POINT ( 'NONE',  ( -8.314922557960811034, -14.29746914071050412, 27.08224293864769550 ) ) ;
#160128 = CYLINDRICAL_SURFACE ( 'NONE', #59745, 2.649999999999999467 ) ;
#160129 = CARTESIAN_POINT ( 'NONE',  ( -4.379528057220086978, -16.55341960407618274, 109.7927570613523613 ) ) ;
#160130 = CARTESIAN_POINT ( 'NONE',  ( 17.31747979337950127, 6.344076630961018815, 68.87944868065181936 ) ) ;
#160131 = CARTESIAN_POINT ( 'NONE',  ( 12.06949235617739724, 12.14591786802326823, 81.87609039468568994 ) ) ;
#160132 = CARTESIAN_POINT ( 'NONE',  ( 5.719274019375673035, 21.55341960407619339, 77.29275706135234714 ) ) ;
#160133 = CARTESIAN_POINT ( 'NONE',  ( -9.474510206698720793, -16.51473224551083518, 99.58442372801900433 ) ) ;
#160134 = CARTESIAN_POINT ( 'NONE',  ( -21.52544592524334988, -5.823673210054445271, 63.95942372801901854 ) ) ;
#160135 = CARTESIAN_POINT ( 'NONE',  ( -19.03943276465977164, -0.05219959533935918106, 38.75109039468566152 ) ) ;
#160136 = CARTESIAN_POINT ( 'NONE',  ( -5.049401038298153566, 19.05341960407611168, 75.20724293864769550 ) ) ;
#160137 = CARTESIAN_POINT ( 'NONE',  ( -9.474510206698964154, 16.51473224551069663, 60.41557627198102409 ) ) ;
#160138 = CARTESIAN_POINT ( 'NONE',  ( 18.10062525802546674, -5.499999999999985789, 41.01383468041921532 ) ) ;
#160139 = CARTESIAN_POINT ( 'NONE',  ( -21.55341960407610458, -5.719274019375992779, 91.45724293864769550 ) ) ;
#160140 = CARTESIAN_POINT ( 'NONE',  ( -10.81492255796078084, -18.62759615963271287, 47.08224293864770260 ) ) ;
#160141 = CARTESIAN_POINT ( 'NONE',  ( -13.89961937509977652, 13.97604488694528158, 50.62390960531435979 ) ) ;
#160142 = CARTESIAN_POINT ( 'NONE',  ( -16.53943276465976808, -0.05219959533934237506, 58.75109039468568994 ) ) ;
#160143 = ORIENTED_EDGE ( 'NONE', *, *, #142697, .F. ) ;
#160144 = CARTESIAN_POINT ( 'NONE',  ( -21.55341960407619339, 5.719274019375674811, 38.54275706135234714 ) ) ;
#160146 = CARTESIAN_POINT ( 'NONE',  ( -22.81625015709509441, -31.40387420917324590, -4.324999997268812457 ) ) ;
#160145 = CARTESIAN_POINT ( 'NONE',  ( -12.14591786802309592, -12.06949235617757132, 71.87390960531438111 ) ) ;
#160147 = CARTESIAN_POINT ( 'NONE',  ( 12.06949235617739724, 12.14591786802326823, 36.87609039468568994 ) ) ;
#160148 = CARTESIAN_POINT ( 'NONE',  ( -16.55341960407611168, -4.379528057220339221, 106.4572429386477097 ) ) ;
#160149 = CARTESIAN_POINT ( 'NONE',  ( -5.153800228976607833, 19.02544592524334988, 57.70942372801899012 ) ) ;
#160150 = CARTESIAN_POINT ( 'NONE',  ( -0.05219959533910754901, -16.53943276465976808, 72.49890960531435269 ) ) ;
#160152 = EDGE_CURVE ( 'NONE', #88773, #193461, #63335, .T. ) ;
#160151 = CARTESIAN_POINT ( 'NONE',  ( -18.67979575497193778, 10.72451020669871902, 33.33442372801900433 ) ) ;
#160154 = CARTESIAN_POINT ( 'NONE',  ( 15.72974639402199770, -15.80617190586745480, 88.12390960531436690 ) ) ;
#160153 = CARTESIAN_POINT ( 'NONE',  ( -16.51473224551069308, -9.474510206698971260, 21.66557627198102765 ) ) ;
#160155 = CARTESIAN_POINT ( 'NONE',  ( -5.153800228976328057, -19.02544592524343514, 102.2905762719810383 ) ) ;
#160156 = CARTESIAN_POINT ( 'NONE',  ( -16.53943276465976808, 0.05219959533911058130, 81.24890960531436690 ) ) ;
#160157 = CARTESIAN_POINT ( 'NONE',  ( 29.18329815487453160, -27.17471096552231202, -17.01306446742700018 ) ) ;
#160158 = CARTESIAN_POINT ( 'NONE',  ( 29.86685920354754487, 21.69954338932564752, -5.424999997268813878 ) ) ;
#160159 = CARTESIAN_POINT ( 'NONE',  ( 9.474510206698729675, 16.51473224551082808, 87.08442372801900433 ) ) ;
#160160 = CARTESIAN_POINT ( 'NONE',  ( 5.719274019375673035, 21.55341960407619339, 22.29275706135235069 ) ) ;
#160161 = CARTESIAN_POINT ( 'NONE',  ( -9.474510206698964154, 16.51473224551069663, 65.41557627198102409 ) ) ;
#160162 = CARTESIAN_POINT ( 'NONE',  ( -9.564922557961040184, 16.46253265017147172, 52.91775706135233293 ) ) ;
#160163 = CARTESIAN_POINT ( 'NONE',  ( -5.153800228976328057, -19.02544592524343514, 27.29057627198103120 ) ) ;
#160164 = CARTESIAN_POINT ( 'NONE',  ( -8.314922557960811034, -14.29746914071050412, 57.08224293864769550 ) ) ;
#160165 = EDGE_CURVE ( 'NONE', #106382, #197536, #101794, .T. ) ;
#160166 = CARTESIAN_POINT ( 'NONE',  ( 16.55341960407611168, 4.379528057220329451, 53.95724293864770260 ) ) ;
#160167 = CARTESIAN_POINT ( 'NONE',  ( 19.05341960407611168, 5.049401038298154454, 68.95724293864769550 ) ) ;
#160168 = CARTESIAN_POINT ( 'NONE',  ( -21.52544592524343514, 5.823673210054127303, 81.04057627198102409 ) ) ;
#160169 = CARTESIAN_POINT ( 'NONE',  ( 16.51473224551069308, 9.474510206698969483, 59.16557627198102409 ) ) ;
#160170 = CARTESIAN_POINT ( 'NONE',  ( 5.823673210054125526, 21.52544592524343514, 84.79057627198102409 ) ) ;
#160171 = CARTESIAN_POINT ( 'NONE',  ( -18.67979575497193778, 10.72451020669871902, 98.33442372801901854 ) ) ;
#160174 = CARTESIAN_POINT ( 'NONE',  ( -12.06949235617756955, 12.14591786802309770, 100.6239096053143811 ) ) ;
#160173 = CARTESIAN_POINT ( 'NONE',  ( -14.29746914071037622, -8.314922557961029526, 109.1677570613523613 ) ) ;
#160172 = CARTESIAN_POINT ( 'NONE',  ( 5.049401038298161559, -19.05341960407611168, 22.70724293864769194 ) ) ;
#160175 = CARTESIAN_POINT ( 'NONE',  ( 19.05341960407617918, -5.049401038297876454, 86.04275706135233293 ) ) ;
#160176 = VERTEX_POINT ( 'NONE', #163872 ) ;
#160177 = CARTESIAN_POINT ( 'NONE',  ( 5.823673210054125526, 21.52544592524343514, 114.7905762719810383 ) ) ;
#160178 = CARTESIAN_POINT ( 'NONE',  ( -19.02544592524334988, -5.153800228976617603, 48.95942372801900433 ) ) ;
#160179 = CARTESIAN_POINT ( 'NONE',  ( -12.06949235617739369, -12.14591786802326823, 99.37609039468568994 ) ) ;
#160180 = CARTESIAN_POINT ( 'NONE',  ( 19.05341960407617918, -5.049401038297876454, 26.04275706135233293 ) ) ;
#160181 = CARTESIAN_POINT ( 'NONE',  ( 9.474510206698971260, -16.51473224551069308, 102.9155762719810241 ) ) ;
#160182 = CARTESIAN_POINT ( 'NONE',  ( -5.823673210054116645, -21.52544592524344225, 67.29057627198103830 ) ) ;
#160183 = CARTESIAN_POINT ( 'NONE',  ( -19.46398650005391318, 5.499999999999952927, 50.18269651486372851 ) ) ;
#160184 = CARTESIAN_POINT ( 'NONE',  ( 16.46253265017160672, -9.564922557960803928, 33.33224293864770260 ) ) ;
#160185 = CARTESIAN_POINT ( 'NONE',  ( -21.53943276465977519, -0.05219959533937600094, 108.7510903946857042 ) ) ;
#160186 = CARTESIAN_POINT ( 'NONE',  ( 8.224510206698742110, 14.34966873604972548, 77.08442372801901854 ) ) ;
#160187 = CARTESIAN_POINT ( 'NONE',  ( 0.05219959533937995610, -21.53943276465977519, 35.00109039468568284 ) ) ;
#160188 = CARTESIAN_POINT ( 'NONE',  ( -14.29746914071037622, -8.314922557961029526, 49.16775706135234003 ) ) ;
#160189 = CARTESIAN_POINT ( 'NONE',  ( -13.89961937509977652, 13.97604488694528158, 100.6239096053143669 ) ) ;
#160190 = CARTESIAN_POINT ( 'NONE',  ( 16.46253265017160672, -9.564922557960803928, 58.33224293864769550 ) ) ;
#160191 = CARTESIAN_POINT ( 'NONE',  ( 9.474510206698971260, -16.51473224551069308, 67.91557627198102409 ) ) ;
#160192 = VECTOR ( 'NONE', #126308, 1000.000000000000000 ) ;
#160193 = CARTESIAN_POINT ( 'NONE',  ( -14.29746914071037622, -8.314922557961029526, 44.16775706135234714 ) ) ;
#160194 = CARTESIAN_POINT ( 'NONE',  ( -0.05219959533910754901, -16.53943276465976808, 102.4989096053143811 ) ) ;
#160195 = CARTESIAN_POINT ( 'NONE',  ( 14.29746914071037800, 8.314922557961029526, 111.6677570613523613 ) ) ;
#160196 = CARTESIAN_POINT ( 'NONE',  ( -18.22780087662119897, 5.500000000000102141, 51.01763182126894947 ) ) ;
#160199 = CARTESIAN_POINT ( 'NONE',  ( 19.05341960407611168, 5.049401038298154454, 68.95724293864769550 ) ) ;
#160198 = CARTESIAN_POINT ( 'NONE',  ( 0.05219959533909260263, 19.03943276465977164, 84.99890960531436690 ) ) ;
#160197 = CARTESIAN_POINT ( 'NONE',  ( 15.72974639402176855, 15.80617190586768217, 61.87609039468568284 ) ) ;
#160200 = CARTESIAN_POINT ( 'NONE',  ( -13.89961937509977652, 13.97604488694528158, 90.62390960531432427 ) ) ;
#160201 = CARTESIAN_POINT ( 'NONE',  ( -14.34966873604960291, -8.224510206698953496, 46.66557627198102409 ) ) ;
#160202 = CARTESIAN_POINT ( 'NONE',  ( -4.483927247898539470, -16.52544592524342804, 22.29057627198102765 ) ) ;
#160203 = CARTESIAN_POINT ( 'NONE',  ( 14.34966873604960469, 8.224510206698951720, 39.16557627198102409 ) ) ;
#160204 = ORIENTED_EDGE ( 'NONE', *, *, #115041, .T. ) ;
#160205 = CARTESIAN_POINT ( 'NONE',  ( 0.05219959533936267826, -19.03943276465977164, 45.00109039468566863 ) ) ;
#160206 = CARTESIAN_POINT ( 'NONE',  ( 17.97058386085787873, 5.500000000000048850, 56.50390968646217260 ) ) ;
#160207 = CARTESIAN_POINT ( 'NONE',  ( 0.05219959533909260263, 19.03943276465977164, 64.99890960531436690 ) ) ;
#160208 = CARTESIAN_POINT ( 'NONE',  ( -5.153800228976607833, 19.02544592524334988, 32.70942372801899722 ) ) ;
#160209 = CARTESIAN_POINT ( 'NONE',  ( 36.91746824999999177, 2.880721459617395097E-14, -8.124999997268814056 ) ) ;
#160210 = DIRECTION ( 'NONE',  ( -1.000000000000000000, 0.000000000000000000, 0.000000000000000000 ) ) ;
#160212 = CARTESIAN_POINT ( 'NONE',  ( 4.483927247898790824, -16.52544592524335698, 65.20942372801901854 ) ) ;
#160211 = CARTESIAN_POINT ( 'NONE',  ( 13.97604488694548053, -13.89961937509957401, 90.62609039468567573 ) ) ;
#160213 = CARTESIAN_POINT ( 'NONE',  ( 16.36317988757057762, 7.306389748694928521, 93.40210391636776421 ) ) ;
#160214 = CARTESIAN_POINT ( 'NONE',  ( 0.05219959533909260263, 19.03943276465977164, 89.99890960531436690 ) ) ;
#160215 = CARTESIAN_POINT ( 'NONE',  ( -5.823673210054431948, 21.52544592524334988, 32.70942372801900433 ) ) ;
#160216 = CARTESIAN_POINT ( 'NONE',  ( 9.564922557961047289, -16.46253265017146816, 75.41775706135234714 ) ) ;
#160218 = CARTESIAN_POINT ( 'NONE',  ( 19.03943276465977164, -0.05219959533909143690, 48.74890960531435979 ) ) ;
#160217 = CYLINDRICAL_SURFACE ( 'NONE', #154131, 38.00000000000000000 ) ;
#160219 = CARTESIAN_POINT ( 'NONE',  ( 19.05341960407611168, 5.049401038298154454, 83.95724293864766707 ) ) ;
#160221 = CARTESIAN_POINT ( 'NONE',  ( -5.049401038298153566, 19.05341960407611168, 55.20724293864769550 ) ) ;
#160220 = CARTESIAN_POINT ( 'NONE',  ( 12.14591786802309770, 12.06949235617756955, 49.37390960531436690 ) ) ;
#160222 = CARTESIAN_POINT ( 'NONE',  ( -13.89961937509957401, -13.97604488694547875, 54.37609039468565442 ) ) ;
#160223 = CARTESIAN_POINT ( 'NONE',  ( 16.52544592524342804, -4.483927247898539470, 88.54057627198103830 ) ) ;
#160224 = CARTESIAN_POINT ( 'NONE',  ( -16.51473224551082808, 9.474510206698731452, 28.33442372801900433 ) ) ;
#160225 = CARTESIAN_POINT ( 'NONE',  ( 9.474510206698971260, -16.51473224551069308, 67.91557627198102409 ) ) ;
#160226 = CARTESIAN_POINT ( 'NONE',  ( 15.80617190586746368, 15.72974639402197994, 69.37390960531436690 ) ) ;
#160228 = CARTESIAN_POINT ( 'NONE',  ( -19.05341960407617563, 5.049401038297882671, 23.54275706135233648 ) ) ;
#160227 = CARTESIAN_POINT ( 'NONE',  ( 8.224510206698953496, -14.34966873604960469, 67.91557627198102409 ) ) ;
#160229 = CARTESIAN_POINT ( 'NONE',  ( -9.564922557960796823, -16.46253265017161027, 107.0822429386476955 ) ) ;
#160230 = AXIS2_PLACEMENT_3D ( 'NONE', #170111, #199466, #93255 ) ;
#160231 = CARTESIAN_POINT ( 'NONE',  ( -21.55341960407610458, -5.719274019375992779, 31.45724293864769550 ) ) ;
#160232 = CARTESIAN_POINT ( 'NONE',  ( 16.51473224551069308, 9.474510206698969483, 59.16557627198102409 ) ) ;
#160233 = CARTESIAN_POINT ( 'NONE',  ( -5.049401038298153566, 19.05341960407611168, 40.20724293864768839 ) ) ;
#160234 = CARTESIAN_POINT ( 'NONE',  ( -16.52544592524342804, 4.483927247898546575, 101.0405762719810383 ) ) ;
#160235 = CARTESIAN_POINT ( 'NONE',  ( 21.53943276465977519, -0.05219959533907433946, 108.7489096053143669 ) ) ;
#160236 = CARTESIAN_POINT ( 'NONE',  ( -0.05219959533909027116, -19.03943276465977164, 102.4989096053143669 ) ) ;
#160237 = CARTESIAN_POINT ( 'NONE',  ( 5.719274019375991003, -21.55341960407610458, 112.7072429386476955 ) ) ;
#160238 = CARTESIAN_POINT ( 'NONE',  ( -9.474510206698964154, 16.51473224551069663, 100.4155762719810241 ) ) ;
#160239 = CARTESIAN_POINT ( 'NONE',  ( -9.474510206698964154, 16.51473224551069663, 25.41557627198103120 ) ) ;
#160241 = CARTESIAN_POINT ( 'NONE',  ( -5.823673210054431948, 21.52544592524334988, 77.70942372801900433 ) ) ;
#160240 = AXIS2_PLACEMENT_3D ( 'NONE', #73410, #134074, #148240 ) ;
#160242 = CARTESIAN_POINT ( 'NONE',  ( 18.67979575497178502, 10.72451020669898547, 99.16557627198100988 ) ) ;
#160243 = DIRECTION ( 'NONE',  ( 0.000000000000000000, 0.7071067811865467956, -0.7071067811865483499 ) ) ;
#160244 = CARTESIAN_POINT ( 'NONE',  ( 19.02130022317637881, -5.499999999999793054, 78.28188669246573284 ) ) ;
#160245 = CARTESIAN_POINT ( 'NONE',  ( 30.58708291193884676, -1.497147075633630919, -50.73425184351845729 ) ) ;
#160246 = CARTESIAN_POINT ( 'NONE',  ( 0.05219959533934541429, -16.53943276465976808, 50.00109039468568994 ) ) ;
#160247 = CARTESIAN_POINT ( 'NONE',  ( -16.52544592524342804, 4.483927247898546575, 111.0405762719810525 ) ) ;
#160248 = DIRECTION ( 'NONE',  ( 0.000000000000000000, 0.000000000000000000, 1.000000000000000000 ) ) ;
#160249 = CARTESIAN_POINT ( 'NONE',  ( 5.049401038298161559, -19.05341960407611168, 57.70724293864769550 ) ) ;
#160250 = CARTESIAN_POINT ( 'NONE',  ( -14.29746914071049879, 8.314922557960819915, 95.83224293864770971 ) ) ;
#160251 = CARTESIAN_POINT ( 'NONE',  ( 5.823673210054125526, 21.52544592524343514, 49.79057627198102409 ) ) ;
#160252 = CARTESIAN_POINT ( 'NONE',  ( -16.52544592524342804, 4.483927247898546575, 71.04057627198103830 ) ) ;
#160253 = CARTESIAN_POINT ( 'NONE',  ( 8.314922557961029526, -14.29746914071037800, 20.41775706135234714 ) ) ;
#160254 = CARTESIAN_POINT ( 'NONE',  ( 21.53943276465977519, 0.05219959533937863772, 71.25109039468568994 ) ) ;
#160255 = CARTESIAN_POINT ( 'NONE',  ( 17.13100169013300800, -6.664070546373153547, 78.26789835699852915 ) ) ;
#160256 = CARTESIAN_POINT ( 'NONE',  ( -16.55341960407617563, 4.379528057220093196, 98.54275706135234714 ) ) ;
#160257 = CARTESIAN_POINT ( 'NONE',  ( -0.05219959533910754901, -16.53943276465976808, 42.49890960531435979 ) ) ;
#160258 = CARTESIAN_POINT ( 'NONE',  ( -9.474510206698964154, 16.51473224551069663, 35.41557627198102409 ) ) ;
#160259 = CARTESIAN_POINT ( 'NONE',  ( -13.97604488694527625, -13.89961937509977652, 86.87390960531436690 ) ) ;
#160260 = CARTESIAN_POINT ( 'NONE',  ( -21.53943276465977519, 0.05219959533907696930, 96.24890960531435269 ) ) ;
#160261 = CARTESIAN_POINT ( 'NONE',  ( 14.34966873604972726, -8.224510206698740333, 20.83442372801901143 ) ) ;
#160263 = CARTESIAN_POINT ( 'NONE',  ( -10.81492255796105439, 18.62759615963255655, 77.91775706135231871 ) ) ;
#160262 = CARTESIAN_POINT ( 'NONE',  ( -8.314922557960811034, -14.29746914071050412, 62.08224293864769550 ) ) ;
#160264 = CARTESIAN_POINT ( 'NONE',  ( -4.483927247898782831, 16.52544592524335698, 97.70942372801904696 ) ) ;
#160265 = CARTESIAN_POINT ( 'NONE',  ( 17.13100169013228324, -6.664070546374126103, 48.26789835699824494 ) ) ;
#160266 = FACE_OUTER_BOUND ( 'NONE', #7445, .T. ) ;
#160267 = CARTESIAN_POINT ( 'NONE',  ( 8.224510206698953496, -14.34966873604960469, 27.91557627198103830 ) ) ;
#160268 = CARTESIAN_POINT ( 'NONE',  ( -12.14591786802326823, 12.06949235617739902, 68.12609039468567573 ) ) ;
#160269 = CARTESIAN_POINT ( 'NONE',  ( -19.03943276465977164, 0.05219959533909376836, 86.24890960531436690 ) ) ;
#160270 = CARTESIAN_POINT ( 'NONE',  ( 5.153800228976335163, 19.02544592524342804, 104.7905762719809957 ) ) ;
#160271 = CARTESIAN_POINT ( 'NONE',  ( 21.53943276465977519, 0.05219959533937863772, 91.25109039468568994 ) ) ;
#160272 = CARTESIAN_POINT ( 'NONE',  ( -8.314922557961024197, 14.29746914071037800, 92.91775706135236135 ) ) ;
#160273 = CARTESIAN_POINT ( 'NONE',  ( -16.52544592524342804, 4.483927247898546575, 66.04057627198103830 ) ) ;
#160274 = CARTESIAN_POINT ( 'NONE',  ( 9.564922557960805705, 16.46253265017160317, 64.58224293864769550 ) ) ;
#160275 = ORIENTED_EDGE ( 'NONE', *, *, #9184, .F. ) ;
#160276 = CARTESIAN_POINT ( 'NONE',  ( -13.97604488694547697, 13.89961937509957934, 113.1260903946856757 ) ) ;
#160277 = CARTESIAN_POINT ( 'NONE',  ( 8.314922557960818139, 14.29746914071049879, 104.5822429386477097 ) ) ;
#160278 = CARTESIAN_POINT ( 'NONE',  ( -19.05341960407611168, -5.049401038298163336, 76.45724293864769550 ) ) ;
#160280 = CARTESIAN_POINT ( 'NONE',  ( -38.00000000000000711, 2.428612866367529932E-14, 1.084202172485504434E-16 ) ) ;
#160279 = CARTESIAN_POINT ( 'NONE',  ( -14.29746914071037622, -8.314922557961029526, 19.16775706135234714 ) ) ;
#160281 = CARTESIAN_POINT ( 'NONE',  ( -0.05219959533937732626, 21.53943276465977519, 112.5010903946857042 ) ) ;
#160282 = CARTESIAN_POINT ( 'NONE',  ( -8.314922557961024197, 14.29746914071037800, 82.91775706135234714 ) ) ;
#160283 = CARTESIAN_POINT ( 'NONE',  ( -5.049401038297874678, -19.05341960407617918, 99.79275706135234714 ) ) ;
#160284 = CARTESIAN_POINT ( 'NONE',  ( 13.89961937509977652, -13.97604488694527269, 23.12390960531436335 ) ) ;
#160285 = CARTESIAN_POINT ( 'NONE',  ( -12.14591786802326823, 12.06949235617739902, 68.12609039468567573 ) ) ;
#160286 = CARTESIAN_POINT ( 'NONE',  ( 12.06949235617739724, 12.14591786802326823, 56.87609039468568994 ) ) ;
#160287 = CARTESIAN_POINT ( 'NONE',  ( 24.48796087919907905, -31.64103850882386126, -7.859127186814490074 ) ) ;
#160288 = CARTESIAN_POINT ( 'NONE',  ( -13.89961937509957401, -13.97604488694547875, 74.37609039468566152 ) ) ;
#160289 = CARTESIAN_POINT ( 'NONE',  ( 10.72451020669871369, 18.67979575497193778, 97.08442372801904696 ) ) ;
#160290 = CARTESIAN_POINT ( 'NONE',  ( 9.564922557960805705, 16.46253265017160317, 34.58224293864770260 ) ) ;
#160291 = CARTESIAN_POINT ( 'NONE',  ( 9.474510206698971260, -16.51473224551069308, 72.91557627198102409 ) ) ;
#160292 = CARTESIAN_POINT ( 'NONE',  ( -16.52544592524342804, 4.483927247898546575, 76.04057627198102409 ) ) ;
#160293 = EDGE_CURVE ( 'NONE', #97685, #123075, #45553, .T. ) ;
#160294 = CARTESIAN_POINT ( 'NONE',  ( 18.67979575497194134, -10.72451020669871369, 95.83442372801903275 ) ) ;
#160295 = CARTESIAN_POINT ( 'NONE',  ( 0.05219959533936267826, -19.03943276465977164, 35.00109039468566863 ) ) ;
#160296 = CARTESIAN_POINT ( 'NONE',  ( -10.72451020669898014, 18.67979575497178502, 40.41557627198103120 ) ) ;
#160297 = CARTESIAN_POINT ( 'NONE',  ( -9.474510206698720793, -16.51473224551083518, 19.58442372801899722 ) ) ;
#160298 = CARTESIAN_POINT ( 'NONE',  ( 5.049401038298161559, -19.05341960407611168, 82.70724293864770971 ) ) ;
#160299 = CARTESIAN_POINT ( 'NONE',  ( -5.823673210054431948, 21.52544592524334988, 112.7094237280190328 ) ) ;
#160300 = CARTESIAN_POINT ( 'NONE',  ( -5.719274019375978568, 21.55341960407610458, 60.20724293864768839 ) ) ;
#160301 = CARTESIAN_POINT ( 'NONE',  ( -19.05341960407611168, -5.049401038298163336, 101.4572429386476955 ) ) ;
#160302 = CARTESIAN_POINT ( 'NONE',  ( 16.51473224551083163, -9.474510206698727899, 70.83442372801900433 ) ) ;
#160303 = CARTESIAN_POINT ( 'NONE',  ( 19.02544592524343514, -5.153800228976328945, 98.54057627198100988 ) ) ;
#160304 = CARTESIAN_POINT ( 'NONE',  ( 16.51473224551083163, -9.474510206698727899, 90.83442372801900433 ) ) ;
#160305 = CARTESIAN_POINT ( 'NONE',  ( 0.05219959533934541429, -16.53943276465976808, 45.00109039468568284 ) ) ;
#160306 = CARTESIAN_POINT ( 'NONE',  ( -14.29746914071049879, 8.314922557960819915, 115.8322429386477097 ) ) ;
#160307 = CARTESIAN_POINT ( 'NONE',  ( -19.05341960407611168, -5.049401038298163336, 81.45724293864769550 ) ) ;
#160308 = CARTESIAN_POINT ( 'NONE',  ( -5.823673210054116645, -21.52544592524344225, 57.29057627198103120 ) ) ;
#160309 = CARTESIAN_POINT ( 'NONE',  ( 8.224510206698742110, 14.34966873604972548, 27.08442372801901854 ) ) ;
#160310 = CARTESIAN_POINT ( 'NONE',  ( -10.81492255796105439, 18.62759615963255655, 27.91775706135234358 ) ) ;
#160311 = CARTESIAN_POINT ( 'NONE',  ( 21.52544592524334988, 5.823673210054432836, 81.45942372801900433 ) ) ;
#160312 = CARTESIAN_POINT ( 'NONE',  ( -16.53943276465976808, -0.05219959533934237506, 88.75109039468567573 ) ) ;
#160313 = CARTESIAN_POINT ( 'NONE',  ( -13.97604488694527625, -13.89961937509977652, 91.87390960531432427 ) ) ;
#160314 = CARTESIAN_POINT ( 'NONE',  ( 8.224510206698953496, -14.34966873604960469, 82.91557627198103830 ) ) ;
#160315 = CARTESIAN_POINT ( 'NONE',  ( 16.55341960407611168, 4.379528057220329451, 23.95724293864769550 ) ) ;
#160316 = CARTESIAN_POINT ( 'NONE',  ( -19.02544592524334988, -5.153800228976617603, 58.95942372801900433 ) ) ;
#160317 = CARTESIAN_POINT ( 'NONE',  ( 15.72974639402176855, 15.80617190586768217, 41.87609039468568284 ) ) ;
#160318 = CARTESIAN_POINT ( 'NONE',  ( -14.34966873604960291, -8.224510206698953496, 96.66557627198102409 ) ) ;
#160319 = CARTESIAN_POINT ( 'NONE',  ( -9.474510206698964154, 16.51473224551069663, 110.4155762719810383 ) ) ;
#160320 = CARTESIAN_POINT ( 'NONE',  ( -14.34966873604972548, 8.224510206698743886, 98.33442372801901854 ) ) ;
#160321 = CARTESIAN_POINT ( 'NONE',  ( -5.719274019375665041, -21.55341960407619695, 84.79275706135234714 ) ) ;
#160322 = CARTESIAN_POINT ( 'NONE',  ( -16.53943276465976808, -0.05219959533934237506, 48.75109039468568284 ) ) ;
#160323 = CARTESIAN_POINT ( 'NONE',  ( 15.72974639402176855, 15.80617190586768217, 36.87609039468568994 ) ) ;
#160324 = ADVANCED_FACE ( 'NONE', ( #24359 ), #86010, .T. ) ;
#160325 = VERTEX_POINT ( 'NONE', #21344 ) ;
#160326 = CARTESIAN_POINT ( 'NONE',  ( 10.72451020669871369, 18.67979575497193778, 22.08442372801901143 ) ) ;
#160327 = CARTESIAN_POINT ( 'NONE',  ( 12.06949235617757843, -12.14591786802309237, 98.12390960531436690 ) ) ;
#160328 = CARTESIAN_POINT ( 'NONE',  ( -18.56399227203345959, -5.499999999999828582, 48.97830131249904895 ) ) ;
#160329 = CARTESIAN_POINT ( 'NONE',  ( 12.14591786802309770, 12.06949235617756955, 69.37390960531436690 ) ) ;
#160330 = CARTESIAN_POINT ( 'NONE',  ( -12.06949235617739369, -12.14591786802326823, 94.37609039468568994 ) ) ;
#160331 = CARTESIAN_POINT ( 'NONE',  ( 16.46253265017160672, -9.564922557960803928, 33.33224293864770260 ) ) ;
#160332 = CARTESIAN_POINT ( 'NONE',  ( -15.80617190586745835, -15.72974639402198527, 41.87390960531435979 ) ) ;
#160333 = CARTESIAN_POINT ( 'NONE',  ( -16.53943276465976808, 0.05219959533911058130, 81.24890960531436690 ) ) ;
#160334 = AXIS2_PLACEMENT_3D ( 'NONE', #105109, #168746, #28296 ) ;
#160335 = CARTESIAN_POINT ( 'NONE',  ( 10.81492255796078972, 18.62759615963270932, 74.58224293864768129 ) ) ;
#160336 = CARTESIAN_POINT ( 'NONE',  ( 9.474510206698971260, -16.51473224551069308, 87.91557627198102409 ) ) ;
#160338 = CARTESIAN_POINT ( 'NONE',  ( 13.89961937509957401, 13.97604488694547697, 96.87609039468566152 ) ) ;
#160337 = CARTESIAN_POINT ( 'NONE',  ( -19.02544592524342804, 5.153800228976336051, 41.04057627198103120 ) ) ;
#160339 = CARTESIAN_POINT ( 'NONE',  ( -15.80617190586745835, -15.72974639402198527, 26.87390960531435979 ) ) ;
#160340 = CARTESIAN_POINT ( 'NONE',  ( 18.67979575497194134, -10.72451020669871369, 55.83442372801901854 ) ) ;
#160341 = CARTESIAN_POINT ( 'NONE',  ( 5.153800228976335163, 19.02544592524342804, 49.79057627198100988 ) ) ;
#160342 = CARTESIAN_POINT ( 'NONE',  ( 13.89961937509977652, -13.97604488694527269, 83.12390960531436690 ) ) ;
#160343 = EDGE_LOOP ( 'NONE', ( #116662, #73963, #78560, #120103 ) ) ;
#160344 = CARTESIAN_POINT ( 'NONE',  ( -4.379528057220086978, -16.55341960407618274, 44.79275706135234714 ) ) ;
#160345 = CARTESIAN_POINT ( 'NONE',  ( -18.62759615963255300, -10.81492255796106328, 39.16775706135235424 ) ) ;
#160346 = CARTESIAN_POINT ( 'NONE',  ( 18.62759615963255655, 10.81492255796105972, 71.66775706135234714 ) ) ;
#160347 = CARTESIAN_POINT ( 'NONE',  ( -19.02544592524342804, 5.153800228976336051, 116.0405762719810383 ) ) ;
#160348 = CARTESIAN_POINT ( 'NONE',  ( -0.05219959533907301413, -21.53943276465977519, 92.49890960531436690 ) ) ;
#160350 = CARTESIAN_POINT ( 'NONE',  ( 0.05219959533934541429, -16.53943276465976808, 65.00109039468568994 ) ) ;
#160349 = CARTESIAN_POINT ( 'NONE',  ( -21.52544592524334988, -5.823673210054445271, 23.95942372801901143 ) ) ;
#160351 = CARTESIAN_POINT ( 'NONE',  ( 10.72451020669898902, -18.67979575497178502, 67.91557627198102409 ) ) ;
#160352 = CARTESIAN_POINT ( 'NONE',  ( -5.823673210054431948, 21.52544592524334988, 112.7094237280190328 ) ) ;
#160354 = CARTESIAN_POINT ( 'NONE',  ( 4.379528057220092307, 16.55341960407617563, 107.2927570613523471 ) ) ;
#160353 = CARTESIAN_POINT ( 'NONE',  ( 5.049401038298161559, -19.05341960407611168, 67.70724293864769550 ) ) ;
#160355 = DIRECTION ( 'NONE',  ( -1.000000000000000000, -0.000000000000000000, -0.000000000000000000 ) ) ;
#160356 = CARTESIAN_POINT ( 'NONE',  ( -5.153800228976328057, -19.02544592524343514, 87.29057627198103830 ) ) ;
#160357 = CARTESIAN_POINT ( 'NONE',  ( -5.153800228976607833, 19.02544592524335343, 52.70942372801900433 ) ) ;
#160358 = CARTESIAN_POINT ( 'NONE',  ( 5.049401038297881783, 19.05341960407617563, 82.29275706135229029 ) ) ;
#160359 = CARTESIAN_POINT ( 'NONE',  ( 0.05219959533907565091, 21.53943276465977519, 44.99890960531435979 ) ) ;
#160360 = CARTESIAN_POINT ( 'NONE',  ( 4.379528057220092307, 16.55341960407617563, 112.2927570613523471 ) ) ;
#160361 = CARTESIAN_POINT ( 'NONE',  ( -13.89961937509957401, -13.97604488694547875, 99.37609039468567573 ) ) ;
#160362 = CARTESIAN_POINT ( 'NONE',  ( 17.72696623605160227, -5.500000000000076383, 51.09811031808416004 ) ) ;
#160363 = CARTESIAN_POINT ( 'NONE',  ( 19.02544592524334988, 5.153800228976608722, 91.45942372801900433 ) ) ;
#160365 = CARTESIAN_POINT ( 'NONE',  ( 5.153800228976615827, -19.02544592524334988, 55.20942372801899722 ) ) ;
#160364 = CARTESIAN_POINT ( 'NONE',  ( -5.823673210054116645, -21.52544592524344225, 92.29057627198103830 ) ) ;
#160366 = CARTESIAN_POINT ( 'NONE',  ( 17.13100169013301155, 6.664070546373133119, 106.7321016430015561 ) ) ;
#160367 = CARTESIAN_POINT ( 'NONE',  ( 19.02544592524343514, -5.153800228976328945, 48.54057627198103120 ) ) ;
#160368 = CARTESIAN_POINT ( 'NONE',  ( -14.34966873604960291, -8.224510206698953496, 56.66557627198103830 ) ) ;
#160369 = CARTESIAN_POINT ( 'NONE',  ( -9.474510206698964154, 16.51473224551069663, 45.41557627198103120 ) ) ;
#160370 = CARTESIAN_POINT ( 'NONE',  ( -4.483927247898539470, -16.52544592524342804, 52.29057627198102409 ) ) ;
#160371 = CARTESIAN_POINT ( 'NONE',  ( 11.30153831258469843, -180.0000000000000000, -25.00000000000000000 ) ) ;
#160372 = CARTESIAN_POINT ( 'NONE',  ( 0.5380129132520025115, 21.39578437401996425, -56.39973404422107706 ) ) ;
#160373 = CARTESIAN_POINT ( 'NONE',  ( 8.314922557960818139, 14.29746914071049879, 34.58224293864770260 ) ) ;
#160374 = CARTESIAN_POINT ( 'NONE',  ( -13.97604488694527625, -13.89961937509977652, 66.87390960531436690 ) ) ;
#160375 = CARTESIAN_POINT ( 'NONE',  ( -3.889087296525950421, 6.412877669190374164, 8.181980515339454030 ) ) ;
#160376 = CARTESIAN_POINT ( 'NONE',  ( -0.05219959533936034679, 19.03943276465977164, 42.50109039468566152 ) ) ;
#160377 = CARTESIAN_POINT ( 'NONE',  ( -14.34966873604972548, 8.224510206698743886, 48.33442372801902565 ) ) ;
#160378 = CARTESIAN_POINT ( 'NONE',  ( 0.05219959533907565091, 21.53943276465977519, 44.99890960531435979 ) ) ;
#160380 = ORIENTED_EDGE ( 'NONE', *, *, #171523, .T. ) ;
#160379 = CARTESIAN_POINT ( 'NONE',  ( -5.719274019375665041, -21.55341960407619695, 104.7927570613523898 ) ) ;
#160381 = CARTESIAN_POINT ( 'NONE',  ( -9.474510206698964154, 16.51473224551069663, 65.41557627198102409 ) ) ;
#160382 = CARTESIAN_POINT ( 'NONE',  ( 2.500000000000000000, 0.000000000000000000, 0.000000000000000000 ) ) ;
#160383 = CARTESIAN_POINT ( 'NONE',  ( -16.51473224551069308, -9.474510206698971260, 101.6655762719810241 ) ) ;
#160384 = CARTESIAN_POINT ( 'NONE',  ( -29.86685920354755552, 21.69954338932564397, -4.824999997268814234 ) ) ;
#160385 = CARTESIAN_POINT ( 'NONE',  ( 15.80617190586769283, -15.72974639402175789, 20.62609039468568639 ) ) ;
#160386 = VECTOR ( 'NONE', #197494, 1000.000000000000000 ) ;
#160387 = CARTESIAN_POINT ( 'NONE',  ( 16.53943276465976808, -0.05219959533910856209, 88.74890960531436690 ) ) ;
#160389 = CARTESIAN_POINT ( 'NONE',  ( -5.049401038298153566, 19.05341960407611168, 80.20724293864769550 ) ) ;
#160388 = CARTESIAN_POINT ( 'NONE',  ( -0.05219959533907301413, -21.53943276465977519, 92.49890960531436690 ) ) ;
#160390 = CARTESIAN_POINT ( 'NONE',  ( -0.05219959533909027116, -19.03943276465977164, 92.49890960531436690 ) ) ;
#160391 = CARTESIAN_POINT ( 'NONE',  ( -18.62759615963270932, 10.81492255796079327, 105.8322429386476955 ) ) ;
#160392 = EDGE_LOOP ( 'NONE', ( #107222, #79135, #197098, #71411 ) ) ;
#160393 = CARTESIAN_POINT ( 'NONE',  ( -5.153800228976328057, -19.02544592524343514, 72.29057627198102409 ) ) ;
#160394 = CARTESIAN_POINT ( 'NONE',  ( -31.98945468063500641, -20.51126642791109944, -24.61382517110271806 ) ) ;
#160396 = CARTESIAN_POINT ( 'NONE',  ( 5.153800228976335163, 19.02544592524342804, 34.79057627198102409 ) ) ;
#160395 = CARTESIAN_POINT ( 'NONE',  ( -16.53943276465976808, 0.05219959533911058130, 101.2489096053143669 ) ) ;
#160397 = CARTESIAN_POINT ( 'NONE',  ( -5.153800228976607833, 19.02544592524334988, 97.70942372801900433 ) ) ;
#160398 = CARTESIAN_POINT ( 'NONE',  ( -4.379528057220328563, 16.55341960407611168, 105.2072429386477097 ) ) ;
#160399 = CARTESIAN_POINT ( 'NONE',  ( -5.823673210054431948, 21.52544592524334988, 67.70942372801901854 ) ) ;
#160401 = CARTESIAN_POINT ( 'NONE',  ( -21.53943276465977519, -0.05219959533937600094, 38.75109039468567573 ) ) ;
#160400 = CARTESIAN_POINT ( 'NONE',  ( 9.564922557960805705, 16.46253265017160317, 59.58224293864769550 ) ) ;
#160402 = CARTESIAN_POINT ( 'NONE',  ( 5.823673210054125526, 21.52544592524343514, 114.7905762719810383 ) ) ;
#160403 = CARTESIAN_POINT ( 'NONE',  ( 28.82186960331499392, -9.364793116373510529, 140.9000000000000057 ) ) ;
#160404 = CARTESIAN_POINT ( 'NONE',  ( 9.474510206698971260, -16.51473224551069308, 87.91557627198102409 ) ) ;
#160405 = DIRECTION ( 'NONE',  ( 0.000000000000000000, 1.000000000000000000, 1.224646799147353207E-16 ) ) ;
#160407 = CARTESIAN_POINT ( 'NONE',  ( -10.81492255796078084, -18.62759615963271287, 37.08224293864768129 ) ) ;
#160406 = CARTESIAN_POINT ( 'NONE',  ( 16.55341960407618274, -4.379528057220086978, 26.04275706135235779 ) ) ;
#160408 = CARTESIAN_POINT ( 'NONE',  ( -21.55341960407619339, 5.719274019375674811, 68.54275706135234714 ) ) ;
#160409 = CARTESIAN_POINT ( 'NONE',  ( 5.153800228976335163, 19.02544592524342804, 104.7905762719809957 ) ) ;
#160410 = CARTESIAN_POINT ( 'NONE',  ( -9.564922557961040184, 16.46253265017147172, 102.9177570613523329 ) ) ;
#160411 = CARTESIAN_POINT ( 'NONE',  ( -19.03943276465977164, 0.05219959533909376836, 46.24890960531435979 ) ) ;
#160412 = CARTESIAN_POINT ( 'NONE',  ( 0.05219959533909260263, 19.03943276465977164, 64.99890960531436690 ) ) ;
#160413 = CARTESIAN_POINT ( 'NONE',  ( 8.224510206698953496, -14.34966873604960469, 92.91557627198103830 ) ) ;
#160414 = CARTESIAN_POINT ( 'NONE',  ( -9.564922557960796823, -16.46253265017161027, 112.0822429386476955 ) ) ;
#160415 = CARTESIAN_POINT ( 'NONE',  ( -12.06949235617756955, 12.14591786802309770, 85.62390960531436690 ) ) ;
#160416 = CARTESIAN_POINT ( 'NONE',  ( -9.474510206698964154, 16.51473224551069663, 110.4155762719810383 ) ) ;
#160418 = CARTESIAN_POINT ( 'NONE',  ( -0.05219959533909027116, -19.03943276465977164, 37.49890960531436690 ) ) ;
#160417 = CARTESIAN_POINT ( 'NONE',  ( 8.224510206698953496, -14.34966873604960469, 57.91557627198103120 ) ) ;
#160419 = CARTESIAN_POINT ( 'NONE',  ( 5.719274019375673035, 21.55341960407619339, 57.29275706135234714 ) ) ;
#160420 = CARTESIAN_POINT ( 'NONE',  ( -19.05341960407617563, 5.049401038297882671, 98.54275706135233293 ) ) ;
#160421 = CARTESIAN_POINT ( 'NONE',  ( 14.29746914071049879, -8.314922557960816363, 53.33224293864769550 ) ) ;
#160422 = CARTESIAN_POINT ( 'NONE',  ( 15.80617190586746368, 15.72974639402197994, 114.3739096053143527 ) ) ;
#160423 = CARTESIAN_POINT ( 'NONE',  ( 21.55341960407610458, 5.719274019375980345, 43.95724293864769550 ) ) ;
#160424 = CARTESIAN_POINT ( 'NONE',  ( -5.153800228976328057, -19.02544592524343514, 112.2905762719810099 ) ) ;
#160425 = CARTESIAN_POINT ( 'NONE',  ( 1.993301997531345292E-15, -30.30510711980685912, 138.7500000054623683 ) ) ;
#160426 = CARTESIAN_POINT ( 'NONE',  ( -9.474510206698964154, 16.51473224551069663, 50.41557627198102409 ) ) ;
#160427 = CARTESIAN_POINT ( 'NONE',  ( 16.52544592524335698, 4.483927247898782831, 111.4594237280190328 ) ) ;
#160428 = CARTESIAN_POINT ( 'NONE',  ( 8.224510206698742110, 14.34966873604972548, 102.0844237280190185 ) ) ;
#160429 = CARTESIAN_POINT ( 'NONE',  ( -12.14591786802326823, 12.06949235617739902, 88.12609039468570415 ) ) ;
#160430 = CARTESIAN_POINT ( 'NONE',  ( -5.153800228976607833, 19.02544592524334988, 32.70942372801899722 ) ) ;
#160431 = CARTESIAN_POINT ( 'NONE',  ( -24.79445957992282601, 6.337972767934357599, 168.1743082258863353 ) ) ;
#160432 = CARTESIAN_POINT ( 'NONE',  ( 5.049401038298161559, -19.05341960407611168, 87.70724293864769550 ) ) ;
#160433 = CARTESIAN_POINT ( 'NONE',  ( 19.02544592524343514, -5.153800228976328945, 53.54057627198102409 ) ) ;
#160434 = CARTESIAN_POINT ( 'NONE',  ( 16.52544592524342804, -4.483927247898539470, 63.54057627198103830 ) ) ;
#160436 = CARTESIAN_POINT ( 'NONE',  ( 9.564922557960805705, 16.46253265017160317, 104.5822429386476955 ) ) ;
#160435 = CARTESIAN_POINT ( 'NONE',  ( 17.40805194822030799, -6.112264579159331745, 103.3337127251061105 ) ) ;
#160437 = CARTESIAN_POINT ( 'NONE',  ( -5.823673210054116645, -21.52544592524344225, 47.29057627198103120 ) ) ;
#160438 = CARTESIAN_POINT ( 'NONE',  ( 14.29746914071049879, -8.314922557960816363, 83.33224293864769550 ) ) ;
#160439 = CARTESIAN_POINT ( 'NONE',  ( 8.314922557961029526, -14.29746914071037800, 35.41775706135234003 ) ) ;
#160440 = CARTESIAN_POINT ( 'NONE',  ( -14.29746914071049879, 8.314922557960819915, 80.83224293864769550 ) ) ;
#160441 = DIRECTION ( 'NONE',  ( -0.000000000000000000, -0.000000000000000000, -1.000000000000000000 ) ) ;
#160442 = CARTESIAN_POINT ( 'NONE',  ( -9.564922557961040184, 16.46253265017147172, 77.91775706135234714 ) ) ;
#160443 = CARTESIAN_POINT ( 'NONE',  ( 5.049401038298161559, -19.05341960407611168, 102.7072429386476955 ) ) ;
#160444 = CARTESIAN_POINT ( 'NONE',  ( 16.51473224551083163, -9.474510206698727899, 80.83442372801899012 ) ) ;
#160445 = CARTESIAN_POINT ( 'NONE',  ( -22.89469264416805316, 22.04895058596750701, -49.28358967601001694 ) ) ;
#160447 = CARTESIAN_POINT ( 'NONE',  ( -8.314922557961024197, 14.29746914071037800, 112.9177570613523329 ) ) ;
#160446 = CARTESIAN_POINT ( 'NONE',  ( 8.224510206698742110, 14.34966873604972548, 27.08442372801901854 ) ) ;
#160448 = CARTESIAN_POINT ( 'NONE',  ( 9.474510206698729675, 16.51473224551082808, 72.08442372801900433 ) ) ;
#160449 = CARTESIAN_POINT ( 'NONE',  ( -15.80617190586745835, -15.72974639402198527, 36.87390960531435979 ) ) ;
#160450 = CARTESIAN_POINT ( 'NONE',  ( 21.52544592524334988, 5.823673210054432836, 71.45942372801901854 ) ) ;
#160451 = CARTESIAN_POINT ( 'NONE',  ( -23.62199046085637733, -10.84149981712538136, 165.9137635136253266 ) ) ;
#160452 = CARTESIAN_POINT ( 'NONE',  ( -12.06949235617739369, -12.14591786802326823, 39.37609039468567573 ) ) ;
#160454 = CARTESIAN_POINT ( 'NONE',  ( 19.05341960407611168, 5.049401038298154454, 93.95724293864769550 ) ) ;
#160453 = CARTESIAN_POINT ( 'NONE',  ( -19.05341960407611168, -5.049401038298163336, 21.45724293864768839 ) ) ;
#160455 = CARTESIAN_POINT ( 'NONE',  ( -35.99626262588765968, 2.428612866367529932E-14, 2.000000000000000000 ) ) ;
#160456 = CARTESIAN_POINT ( 'NONE',  ( 8.224510206698953496, -14.34966873604960469, 82.91557627198103830 ) ) ;
#160457 = CONTEXT_DEPENDENT_SHAPE_REPRESENTATION ( #26193, #64729 ) ;
#160458 = CARTESIAN_POINT ( 'NONE',  ( -9.474510206698964154, 16.51473224551069663, 85.41557627198102409 ) ) ;
#160459 = ORIENTED_EDGE ( 'NONE', *, *, #196667, .T. ) ;
#160460 = CARTESIAN_POINT ( 'NONE',  ( 19.03943276465977164, 0.05219959533936151252, 111.2510903946856757 ) ) ;
#160461 = CARTESIAN_POINT ( 'NONE',  ( 15.80617190586746368, 15.72974639402197994, 79.37390960531436690 ) ) ;
#160462 = CARTESIAN_POINT ( 'NONE',  ( 19.02544592524343514, -5.153800228976328945, 38.54057627198103120 ) ) ;
#160464 = CARTESIAN_POINT ( 'NONE',  ( 0.05219959533937995610, -21.53943276465977519, 20.00109039468568639 ) ) ;
#160463 = CARTESIAN_POINT ( 'NONE',  ( -13.97604488694547697, 13.89961937509957934, 73.12609039468568994 ) ) ;
#160465 = CARTESIAN_POINT ( 'NONE',  ( -5.049401038298153566, 19.05341960407611168, 70.20724293864769550 ) ) ;
#160466 = CARTESIAN_POINT ( 'NONE',  ( -9.474510206698964154, 16.51473224551069663, 110.4155762719810383 ) ) ;
#160467 = ORIENTED_EDGE ( 'NONE', *, *, #164973, .F. ) ;
#160468 = CARTESIAN_POINT ( 'NONE',  ( -14.29746914071037622, -8.314922557961029526, 34.16775706135234714 ) ) ;
#160469 = CARTESIAN_POINT ( 'NONE',  ( 21.52544592524344225, -5.823673210054117533, 108.5405762719810241 ) ) ;
#160472 = CARTESIAN_POINT ( 'NONE',  ( -5.153800228976607833, 19.02544592524334988, 57.70942372801899012 ) ) ;
#160471 = CARTESIAN_POINT ( 'NONE',  ( -13.89961937509977652, 13.97604488694528158, 95.62390960531436690 ) ) ;
#160470 = CARTESIAN_POINT ( 'NONE',  ( 12.06949235617757843, -12.14591786802309237, 108.1239096053143811 ) ) ;
#160473 = CARTESIAN_POINT ( 'NONE',  ( 21.53943276465977519, -0.05219959533907433946, 83.74890960531435269 ) ) ;
#160474 = CARTESIAN_POINT ( 'NONE',  ( 5.719274019375991003, -21.55341960407610458, 92.70724293864770971 ) ) ;
#160475 = CARTESIAN_POINT ( 'NONE',  ( 4.483927247898545687, 16.52544592524342804, 44.79057627198103120 ) ) ;
#160476 = CARTESIAN_POINT ( 'NONE',  ( -13.97604488694547697, 13.89961937509957934, 23.12609039468565442 ) ) ;
#160477 = CARTESIAN_POINT ( 'NONE',  ( -16.53943276465976808, -0.05219959533934237506, 68.75109039468568994 ) ) ;
#160478 = CARTESIAN_POINT ( 'NONE',  ( 19.02544592524343514, -5.153800228976328945, 98.54057627198100988 ) ) ;
#160479 = CARTESIAN_POINT ( 'NONE',  ( 19.05341960407611168, 5.049401038298154454, 48.95724293864768129 ) ) ;
#160480 = VECTOR ( 'NONE', #126867, 1000.000000000000000 ) ;
#160481 = CARTESIAN_POINT ( 'NONE',  ( -21.53943276465977519, -0.05219959533937600094, 48.75109039468568284 ) ) ;
#160482 = CARTESIAN_POINT ( 'NONE',  ( -5.719274019375665041, -21.55341960407619695, 64.79275706135234714 ) ) ;
#160483 = CARTESIAN_POINT ( 'NONE',  ( -5.153800228976328057, -19.02544592524343514, 62.29057627198100988 ) ) ;
#160484 = CARTESIAN_POINT ( 'NONE',  ( -21.52544592524334988, -5.823673210054445271, 28.95942372801902209 ) ) ;
#160485 = CARTESIAN_POINT ( 'NONE',  ( -9.564922557961040184, 16.46253265017147172, 77.91775706135234714 ) ) ;
#160486 = CARTESIAN_POINT ( 'NONE',  ( -19.05341960407617563, 5.049401038297882671, 73.54275706135233293 ) ) ;
#160487 = CARTESIAN_POINT ( 'NONE',  ( 16.46253265017160672, -9.564922557960803928, 33.33224293864770260 ) ) ;
#160488 = CARTESIAN_POINT ( 'NONE',  ( -8.314922557961024197, 14.29746914071037800, 82.91775706135234714 ) ) ;
#160489 = CARTESIAN_POINT ( 'NONE',  ( -19.05341960407611168, -5.049401038298163336, 56.45724293864768129 ) ) ;
#160490 = CARTESIAN_POINT ( 'NONE',  ( 0.05219959533909260263, 19.03943276465977164, 29.99890960531435979 ) ) ;
#160491 = CARTESIAN_POINT ( 'NONE',  ( 9.564922557960805705, 16.46253265017160317, 94.58224293864769550 ) ) ;
#160492 = CARTESIAN_POINT ( 'NONE',  ( 19.02544592524343514, -5.153800228976328945, 38.54057627198103120 ) ) ;
#160493 = CARTESIAN_POINT ( 'NONE',  ( 5.719274019375991003, -21.55341960407610458, 82.70724293864770971 ) ) ;
#160494 = CARTESIAN_POINT ( 'NONE',  ( 4.483927247898790824, -16.52544592524335698, 65.20942372801901854 ) ) ;
#160495 = CARTESIAN_POINT ( 'NONE',  ( -21.55341960407619339, 5.719274019375674811, 113.5427570613523756 ) ) ;
#160496 = CARTESIAN_POINT ( 'NONE',  ( -13.89961937509977652, 13.97604488694528158, 50.62390960531435979 ) ) ;
#160497 = CARTESIAN_POINT ( 'NONE',  ( 4.379528057220339221, -16.55341960407611168, 42.70724293864770260 ) ) ;
#160498 = CARTESIAN_POINT ( 'NONE',  ( 0.05219959533910956823, 16.53943276465976808, 84.99890960531436690 ) ) ;
#160499 = CARTESIAN_POINT ( 'NONE',  ( 19.02544592524343514, -5.153800228976328945, 73.54057627198103830 ) ) ;
#160500 = CARTESIAN_POINT ( 'NONE',  ( -15.80617190586768217, 15.72974639402176855, 38.12609039468567573 ) ) ;
#160501 = CARTESIAN_POINT ( 'NONE',  ( -19.05341960407611168, -5.049401038298163336, 86.45724293864769550 ) ) ;
#160502 = CARTESIAN_POINT ( 'NONE',  ( -21.52544592524334988, -5.823673210054445271, 98.95942372801903275 ) ) ;
#160503 = CARTESIAN_POINT ( 'NONE',  ( -0.05219959533934338120, 16.53943276465976808, 77.50109039468567573 ) ) ;
#160504 = CARTESIAN_POINT ( 'NONE',  ( 15.72974639402176855, 15.80617190586768217, 31.87609039468567929 ) ) ;
#160505 = CARTESIAN_POINT ( 'NONE',  ( 13.97604488694527802, 13.89961937509977652, 114.3739096053143669 ) ) ;
#160506 = CARTESIAN_POINT ( 'NONE',  ( -21.52544592524343514, 5.823673210054127303, 86.04057627198102409 ) ) ;
#160507 = CARTESIAN_POINT ( 'NONE',  ( -8.314922557960811034, -14.29746914071050412, 42.08224293864769550 ) ) ;
#160508 = CARTESIAN_POINT ( 'NONE',  ( 5.153800228976335163, 19.02544592524342804, 39.79057627198100988 ) ) ;
#160509 = CARTESIAN_POINT ( 'NONE',  ( 8.224510206698953496, -14.34966873604960469, 72.91557627198103830 ) ) ;
#160510 = CARTESIAN_POINT ( 'NONE',  ( 21.53943276465977519, -0.05219959533907433946, 28.74890960531435624 ) ) ;
#160511 = CARTESIAN_POINT ( 'NONE',  ( -16.46253265017146816, -9.564922557961047289, 34.16775706135233293 ) ) ;
#160512 = CARTESIAN_POINT ( 'NONE',  ( -14.29746914071049879, 8.314922557960819915, 100.8322429386477097 ) ) ;
#160513 = CARTESIAN_POINT ( 'NONE',  ( -19.05341960407611168, -5.049401038298163336, 106.4572429386476955 ) ) ;
#160514 = ORIENTED_EDGE ( 'NONE', *, *, #40971, .F. ) ;
#160515 = CARTESIAN_POINT ( 'NONE',  ( -4.483927247898782831, 16.52544592524335698, 47.70942372801902565 ) ) ;
#160516 = CARTESIAN_POINT ( 'NONE',  ( 9.474510206698971260, -16.51473224551069308, 52.91557627198102409 ) ) ;
#160517 = CARTESIAN_POINT ( 'NONE',  ( 22.44159573604009594, -16.30477369853687364, 139.6750000027311955 ) ) ;
#160518 = CARTESIAN_POINT ( 'NONE',  ( -12.14591786802326823, 12.06949235617739902, 88.12609039468570415 ) ) ;
#160519 = CARTESIAN_POINT ( 'NONE',  ( 19.02544592524334988, 5.153800228976608722, 106.4594237280190185 ) ) ;
#160520 = CARTESIAN_POINT ( 'NONE',  ( 15.80617190586769283, -15.72974639402175789, 80.62609039468567573 ) ) ;
#160521 = CARTESIAN_POINT ( 'NONE',  ( 19.02544592524343514, -5.153800228976328945, 78.54057627198099567 ) ) ;
#160522 = CARTESIAN_POINT ( 'NONE',  ( 21.52544592524344225, -5.823673210054117533, 108.5405762719810241 ) ) ;
#160523 = CARTESIAN_POINT ( 'NONE',  ( -16.55341960407617563, 4.379528057220093196, 58.54275706135235424 ) ) ;
#160524 = CARTESIAN_POINT ( 'NONE',  ( 16.53943276465976808, -0.05219959533910856209, 113.7489096053143527 ) ) ;
#160525 = AXIS2_PLACEMENT_3D ( 'NONE', #130317, #192014, #114157 ) ;
#160526 = EDGE_CURVE ( 'NONE', #1176, #8743, #181543, .T. ) ;
#160527 = CARTESIAN_POINT ( 'NONE',  ( -16.52544592524335698, -4.483927247898792601, 18.95942372801901143 ) ) ;
#160528 = CARTESIAN_POINT ( 'NONE',  ( -19.02544592524334988, -5.153800228976617603, 78.95942372801900433 ) ) ;
#160529 = CARTESIAN_POINT ( 'NONE',  ( 18.67979575497178502, 10.72451020669898547, 79.16557627198103830 ) ) ;
#160530 = CARTESIAN_POINT ( 'NONE',  ( -19.02544592524334988, -5.153800228976617603, 48.95942372801900433 ) ) ;
#160531 = DIRECTION ( 'NONE',  ( -1.000000000000000000, 0.000000000000000000, 0.000000000000000000 ) ) ;
#160532 = CARTESIAN_POINT ( 'NONE',  ( 15.80617190586746368, 15.72974639402197994, 104.3739096053143669 ) ) ;
#160533 = CARTESIAN_POINT ( 'NONE',  ( 17.50000000000002132, 3.305555262949611439, 27.87482847843411804 ) ) ;
#160534 = CARTESIAN_POINT ( 'NONE',  ( -13.97604488694527625, -13.89961937509977652, 66.87390960531436690 ) ) ;
#160535 = CARTESIAN_POINT ( 'NONE',  ( 27.86273085795036408, -28.69962071417356242, -15.00000000000000000 ) ) ;
#160536 = CARTESIAN_POINT ( 'NONE',  ( 13.89961937509957401, 13.97604488694547697, 111.8760903946856757 ) ) ;
#160537 = LINE ( 'NONE', #7839, #112823 ) ;
#160538 = CARTESIAN_POINT ( 'NONE',  ( -18.62759615963255300, -10.81492255796106328, 54.16775706135235424 ) ) ;
#160540 = CARTESIAN_POINT ( 'NONE',  ( -14.29746914071049879, 8.314922557960819915, 65.83224293864769550 ) ) ;
#160539 = CARTESIAN_POINT ( 'NONE',  ( 21.52544592524344225, -5.823673210054117533, 98.54057627198105251 ) ) ;
#160541 = CARTESIAN_POINT ( 'NONE',  ( 16.46253265017160672, -9.564922557960803928, 68.33224293864770971 ) ) ;
#160542 = CARTESIAN_POINT ( 'NONE',  ( 21.53943276465977519, 0.05219959533937863772, 76.25109039468568994 ) ) ;
#160544 = CARTESIAN_POINT ( 'NONE',  ( -5.049401038297874678, -19.05341960407617918, 34.79275706135233293 ) ) ;
#160543 = CARTESIAN_POINT ( 'NONE',  ( 12.14591786802327356, -12.06949235617739191, 25.62609039468567929 ) ) ;
#160545 = CARTESIAN_POINT ( 'NONE',  ( -15.80617190586768217, 15.72974639402176855, 58.12609039468568994 ) ) ;
#160546 = CARTESIAN_POINT ( 'NONE',  ( 21.52544592524344225, -5.823673210054117533, 108.5405762719810241 ) ) ;
#160547 = CARTESIAN_POINT ( 'NONE',  ( -10.72451020669898014, 18.67979575497178502, 65.41557627198102409 ) ) ;
#160548 = CARTESIAN_POINT ( 'NONE',  ( 5.153800228976615827, -19.02544592524334988, 100.2094237280190043 ) ) ;
#160549 = CARTESIAN_POINT ( 'NONE',  ( -9.474510206698720793, -16.51473224551083518, 64.58442372801900433 ) ) ;
#160550 = CARTESIAN_POINT ( 'NONE',  ( -21.52544592524334988, -5.823673210054445271, 88.95942372801901854 ) ) ;
#160551 = CARTESIAN_POINT ( 'NONE',  ( 13.97604488694548053, -13.89961937509957401, 50.62609039468566152 ) ) ;
#160552 = CARTESIAN_POINT ( 'NONE',  ( 0.05219959533909260263, 19.03943276465977164, 39.99890960531436690 ) ) ;
#160553 = CARTESIAN_POINT ( 'NONE',  ( 18.67979575497178502, 10.72451020669898547, 64.16557627198102409 ) ) ;
#160554 = CARTESIAN_POINT ( 'NONE',  ( 4.379528057220339221, -16.55341960407611168, 47.70724293864770260 ) ) ;
#160555 = CARTESIAN_POINT ( 'NONE',  ( -16.61371651742599553, -7.165104196376250734, 26.14584930007006491 ) ) ;
#160556 = CARTESIAN_POINT ( 'NONE',  ( 19.05341960407617918, -5.049401038297876454, 31.04275706135232227 ) ) ;
#160557 = CARTESIAN_POINT ( 'NONE',  ( 8.314922557961029526, -14.29746914071037800, 80.41775706135234714 ) ) ;
#160558 = CARTESIAN_POINT ( 'NONE',  ( -4.379528057220328563, 16.55341960407611168, 60.20724293864768839 ) ) ;
#160559 = CARTESIAN_POINT ( 'NONE',  ( -15.80617190586768217, 15.72974639402176855, 93.12609039468568994 ) ) ;
#160560 = CARTESIAN_POINT ( 'NONE',  ( -10.81492255796105439, 18.62759615963255655, 77.91775706135231871 ) ) ;
#160561 = CARTESIAN_POINT ( 'NONE',  ( -0.05219959533907301413, -21.53943276465977519, 77.49890960531433848 ) ) ;
#160562 = ADVANCED_FACE ( 'NONE', ( #179045 ), #53680, .F. ) ;
#160563 = CARTESIAN_POINT ( 'NONE',  ( 13.97604488694527802, 13.89961937509977652, 54.37390960531435979 ) ) ;
#160564 = CARTESIAN_POINT ( 'NONE',  ( 10.72451020669871369, 18.67979575497193778, 52.08442372801901854 ) ) ;
#160565 = CARTESIAN_POINT ( 'NONE',  ( -9.564922557960796823, -16.46253265017161027, 32.08224293864769550 ) ) ;
#160566 = CARTESIAN_POINT ( 'NONE',  ( -5.049401038298153566, 19.05341960407611168, 50.20724293864770260 ) ) ;
#160567 = CARTESIAN_POINT ( 'NONE',  ( 0.05219959533910956823, 16.53943276465976808, 104.9989096053143669 ) ) ;
#160568 = CARTESIAN_POINT ( 'NONE',  ( -9.564922557960796823, -16.46253265017161027, 97.08224293864769550 ) ) ;
#160569 = CARTESIAN_POINT ( 'NONE',  ( -12.06949235617756955, 12.14591786802309770, 55.62390960531436690 ) ) ;
#160570 = CARTESIAN_POINT ( 'NONE',  ( -4.483927247898539470, -16.52544592524342804, 107.2905762719810525 ) ) ;
#160571 = CARTESIAN_POINT ( 'NONE',  ( -0.05219959533907301413, -21.53943276465977519, 77.49890960531433848 ) ) ;
#160572 = CARTESIAN_POINT ( 'NONE',  ( 10.81492255796106328, -18.62759615963255655, 25.41775706135235779 ) ) ;
#160573 = CARTESIAN_POINT ( 'NONE',  ( 26.70613957415102035, -7.662257527287521519, 167.2521143936660906 ) ) ;
#160574 = CARTESIAN_POINT ( 'NONE',  ( -16.55341960407617563, 4.379528057220093196, 38.54275706135234714 ) ) ;
#160575 = ORIENTED_EDGE ( 'NONE', *, *, #49370, .T. ) ;
#160576 = CARTESIAN_POINT ( 'NONE',  ( 21.52544592524344225, -5.823673210054117533, 68.54057627198103830 ) ) ;
#160577 = CARTESIAN_POINT ( 'NONE',  ( 5.823673210054444382, -21.52544592524334988, 105.2094237280190328 ) ) ;
#160578 = CARTESIAN_POINT ( 'NONE',  ( 13.97604488694527802, 13.89961937509977652, 94.37390960531436690 ) ) ;
#160579 = CARTESIAN_POINT ( 'NONE',  ( -15.72974639402176322, -15.80617190586768395, 29.37609039468568284 ) ) ;
#160580 = CARTESIAN_POINT ( 'NONE',  ( -5.823673210054116645, -21.52544592524344225, 27.29057627198103120 ) ) ;
#160581 = CARTESIAN_POINT ( 'NONE',  ( -14.29746914071037622, -8.314922557961029526, 104.1677570613523471 ) ) ;
#160582 = CARTESIAN_POINT ( 'NONE',  ( 21.52544592524334988, 5.823673210054432836, 86.45942372801901854 ) ) ;
#160583 = CARTESIAN_POINT ( 'NONE',  ( -19.03943276465977164, -0.05219959533935918106, 23.75109039468566152 ) ) ;
#160584 = CARTESIAN_POINT ( 'NONE',  ( 16.55341960407618274, -4.379528057220086978, 76.04275706135237556 ) ) ;
#160585 = CARTESIAN_POINT ( 'NONE',  ( 0.05219959533937995610, -21.53943276465977519, 35.00109039468568284 ) ) ;
#160586 = CARTESIAN_POINT ( 'NONE',  ( -16.51473224551069308, -9.474510206698971260, 31.66557627198102054 ) ) ;
#160587 = CARTESIAN_POINT ( 'NONE',  ( 5.823673210054444382, -21.52544592524334988, 100.2094237280190043 ) ) ;
#160588 = CARTESIAN_POINT ( 'NONE',  ( 16.46253265017160672, -9.564922557960803928, 103.3322429386476955 ) ) ;
#160589 = CARTESIAN_POINT ( 'NONE',  ( -5.719274019375978568, 21.55341960407610458, 100.2072429386476955 ) ) ;
#160591 = CARTESIAN_POINT ( 'NONE',  ( 5.719274019375991003, -21.55341960407610458, 72.70724293864769550 ) ) ;
#160590 = CARTESIAN_POINT ( 'NONE',  ( 19.19724070472096855, 5.499999999999978684, 83.56193348274379673 ) ) ;
#160593 = CARTESIAN_POINT ( 'NONE',  ( 12.14591786802309770, 12.06949235617756955, 54.37390960531435979 ) ) ;
#160592 = CARTESIAN_POINT ( 'NONE',  ( 12.06949235617739724, 12.14591786802326823, 56.87609039468568994 ) ) ;
#160594 = CARTESIAN_POINT ( 'NONE',  ( 21.70980307670622267, 7.452553642297959691, 174.2373330747591638 ) ) ;
#160595 = CARTESIAN_POINT ( 'NONE',  ( 9.564922557961047289, -16.46253265017146816, 80.41775706135234714 ) ) ;
#160596 = CARTESIAN_POINT ( 'NONE',  ( -0.9453496423218898936, -14.01879992551668153, -62.45159313300390380 ) ) ;
#160597 = CARTESIAN_POINT ( 'NONE',  ( -8.314922557961024197, 14.29746914071037800, 22.91775706135235069 ) ) ;
#160598 = CARTESIAN_POINT ( 'NONE',  ( 5.823673210054125526, 21.52544592524343514, 94.79057627198105251 ) ) ;
#160599 = CARTESIAN_POINT ( 'NONE',  ( -14.29746914071049879, 8.314922557960819915, 70.83224293864770971 ) ) ;
#160600 = CARTESIAN_POINT ( 'NONE',  ( -5.719274019375978568, 21.55341960407610458, 25.20724293864769550 ) ) ;
#160601 = CARTESIAN_POINT ( 'NONE',  ( -8.224510206698735004, -14.34966873604973081, 39.58442372801901143 ) ) ;
#160602 = CARTESIAN_POINT ( 'NONE',  ( -16.51473224551069308, -9.474510206698971260, 51.66557627198102409 ) ) ;
#160604 = CARTESIAN_POINT ( 'NONE',  ( 16.46253265017146816, 9.564922557961045513, 96.66775706135233293 ) ) ;
#160603 = CARTESIAN_POINT ( 'NONE',  ( 21.55341960407619695, -5.719274019375665929, 36.04275706135234714 ) ) ;
#160605 = CARTESIAN_POINT ( 'NONE',  ( 19.02544592524343514, -5.153800228976328945, 98.54057627198100988 ) ) ;
#160606 = CARTESIAN_POINT ( 'NONE',  ( 19.02544592524343514, -5.153800228976328945, 93.54057627198102409 ) ) ;
#160607 = CARTESIAN_POINT ( 'NONE',  ( -0.05219959533907301413, -21.53943276465977519, 92.49890960531436690 ) ) ;
#160608 = CARTESIAN_POINT ( 'NONE',  ( 5.049401038298161559, -19.05341960407611168, 42.70724293864767418 ) ) ;
#160609 = CARTESIAN_POINT ( 'NONE',  ( -16.31925111598457079, -7.325300261831483972, 59.83575461032751264 ) ) ;
#160610 = CARTESIAN_POINT ( 'NONE',  ( -12.14591786802309592, -12.06949235617757132, 66.87390960531436690 ) ) ;
#160611 = CARTESIAN_POINT ( 'NONE',  ( -13.97604488694527625, -13.89961937509977652, 106.8739096053143669 ) ) ;
#160612 = CARTESIAN_POINT ( 'NONE',  ( 17.03646098637157280, -14.90092349631553859, -55.52600481601552218 ) ) ;
#160613 = CARTESIAN_POINT ( 'NONE',  ( 13.89961937509957401, 13.97604488694547697, 81.87609039468564731 ) ) ;
#160614 = CARTESIAN_POINT ( 'NONE',  ( -18.62759615963270932, 10.81492255796079327, 95.83224293864770971 ) ) ;
#160615 = CARTESIAN_POINT ( 'NONE',  ( -13.89961937509957401, -13.97604488694547875, 49.37609039468567573 ) ) ;
#160616 = CARTESIAN_POINT ( 'NONE',  ( -16.46253265017160317, 9.564922557960807481, 110.8322429386476955 ) ) ;
#160617 = CARTESIAN_POINT ( 'NONE',  ( -18.67979575497178146, -10.72451020669898902, 56.66557627198103830 ) ) ;
#160618 = CARTESIAN_POINT ( 'NONE',  ( 0.05219959533909260263, 19.03943276465977164, 89.99890960531436690 ) ) ;
#160619 = CARTESIAN_POINT ( 'NONE',  ( 15.80617190586769283, -15.72974639402175789, 60.62609039468567573 ) ) ;
#160620 = CARTESIAN_POINT ( 'NONE',  ( -0.05219959533909027116, -19.03943276465977164, 37.49890960531436690 ) ) ;
#160621 = CARTESIAN_POINT ( 'NONE',  ( 8.224510206698953496, -14.34966873604960469, 72.91557627198103830 ) ) ;
#160622 = CARTESIAN_POINT ( 'NONE',  ( -16.53943276465976808, -0.05219959533934237506, 18.75109039468568639 ) ) ;
#160623 = CARTESIAN_POINT ( 'NONE',  ( -5.823673210054431948, 21.52544592524334988, 57.70942372801901143 ) ) ;
#160624 = VERTEX_POINT ( 'NONE', #100173 ) ;
#160625 = CARTESIAN_POINT ( 'NONE',  ( 16.51473224551069308, 9.474510206698969483, 114.1655762719810241 ) ) ;
#160626 = CARTESIAN_POINT ( 'NONE',  ( -19.05341960407617563, 5.049401038297882671, 73.54275706135233293 ) ) ;
#160627 = CARTESIAN_POINT ( 'NONE',  ( 21.02068080879936218, -34.03872152684782293, -24.45646120681608338 ) ) ;
#160628 = CARTESIAN_POINT ( 'NONE',  ( 0.05219959533907565091, 21.53943276465977519, 114.9989096053143669 ) ) ;
#160629 = CARTESIAN_POINT ( 'NONE',  ( -38.00000000000001421, 12.34694845685046438, -1.849999994537626424 ) ) ;
#160630 = CARTESIAN_POINT ( 'NONE',  ( -9.474510206698720793, -16.51473224551083518, 19.58442372801899722 ) ) ;
#160631 = CARTESIAN_POINT ( 'NONE',  ( -13.89961937509977652, 13.97604488694528158, 60.62390960531436690 ) ) ;
#160632 = CARTESIAN_POINT ( 'NONE',  ( 21.53943276465977519, 0.05219959533937863772, 106.2510903946856757 ) ) ;
#160633 = CARTESIAN_POINT ( 'NONE',  ( 16.55341960407618274, -4.379528057220086978, 106.0427570613523471 ) ) ;
#160635 = CARTESIAN_POINT ( 'NONE',  ( 0.05219959533937995610, -21.53943276465977519, 70.00109039468568994 ) ) ;
#160634 = CARTESIAN_POINT ( 'NONE',  ( 5.049401038298161559, -19.05341960407611168, 102.7072429386476955 ) ) ;
#160636 = CARTESIAN_POINT ( 'NONE',  ( 22.81625015709510151, -31.40387420917324590, -3.924999997268811658 ) ) ;
#160637 = CARTESIAN_POINT ( 'NONE',  ( -33.80093248007431583, 2.440252113607738416, 99.94207534358628209 ) ) ;
#160638 = CARTESIAN_POINT ( 'NONE',  ( 22.87925077421024511, 5.621762139875928099, 172.5226062014847059 ) ) ;
#160639 = CARTESIAN_POINT ( 'NONE',  ( 0.05219959533937995610, -21.53943276465977519, 75.00109039468568994 ) ) ;
#160640 = CARTESIAN_POINT ( 'NONE',  ( 21.55341960407619695, -5.719274019375665929, 106.0427570613523471 ) ) ;
#160641 = CARTESIAN_POINT ( 'NONE',  ( 0.000000000000000000, 0.000000000000000000, -60.44446360152740283 ) ) ;
#160642 = CARTESIAN_POINT ( 'NONE',  ( -9.474510206698964154, 16.51473224551069663, 90.41557627198103830 ) ) ;
#160643 = CARTESIAN_POINT ( 'NONE',  ( -5.153800228976607833, 19.02544592524334988, 22.70942372801899012 ) ) ;
#160644 = CARTESIAN_POINT ( 'NONE',  ( -0.2515199893712041779, -31.88380457335792428, -49.15318026754364666 ) ) ;
#160645 = CARTESIAN_POINT ( 'NONE',  ( 19.02544592524343514, -5.153800228976328945, 43.54057627198103120 ) ) ;
#160646 = CARTESIAN_POINT ( 'NONE',  ( 21.52544592524344225, -5.823673210054117533, 58.54057627198103120 ) ) ;
#160647 = CARTESIAN_POINT ( 'NONE',  ( -14.34966873604972548, 8.224510206698743886, 108.3344237280190185 ) ) ;
#160649 = CARTESIAN_POINT ( 'NONE',  ( -13.97604488694527625, -13.89961937509977652, 86.87390960531436690 ) ) ;
#160648 = CARTESIAN_POINT ( 'NONE',  ( -14.34966873604960291, -8.224510206698953496, 101.6655762719810383 ) ) ;
#160650 = CARTESIAN_POINT ( 'NONE',  ( -5.823673210054431948, 21.52544592524334988, 97.70942372801904696 ) ) ;
#160651 = CARTESIAN_POINT ( 'NONE',  ( 9.474510206698971260, -16.51473224551069308, 37.91557627198102409 ) ) ;
#160652 = CARTESIAN_POINT ( 'NONE',  ( -4.483927247898539470, -16.52544592524342804, 97.29057627198105251 ) ) ;
#160653 = CARTESIAN_POINT ( 'NONE',  ( 15.80617190586769283, -15.72974639402175789, 50.62609039468568994 ) ) ;
#160654 = CARTESIAN_POINT ( 'NONE',  ( -15.80617190586745835, -15.72974639402198527, 91.87390960531436690 ) ) ;
#160655 = CARTESIAN_POINT ( 'NONE',  ( 5.153800228976615827, -19.02544592524334988, 55.20942372801899722 ) ) ;
#160656 = CARTESIAN_POINT ( 'NONE',  ( -0.05219959533909027116, -19.03943276465977164, 47.49890960531435979 ) ) ;
#160657 = CARTESIAN_POINT ( 'NONE',  ( 9.474510206698971260, -16.51473224551069308, 92.91557627198103830 ) ) ;
#160658 = CARTESIAN_POINT ( 'NONE',  ( -8.314922557960811034, -14.29746914071050412, 72.08224293864769550 ) ) ;
#160659 = CARTESIAN_POINT ( 'NONE',  ( -5.049401038297874678, -19.05341960407617918, 49.79275706135231871 ) ) ;
#160660 = VECTOR ( 'NONE', #135283, 1000.000000000000000 ) ;
#160661 = CARTESIAN_POINT ( 'NONE',  ( 5.153800228976335163, 19.02544592524342804, 69.79057627198103830 ) ) ;
#160662 = CARTESIAN_POINT ( 'NONE',  ( 16.55341960407611168, 4.379528057220329451, 48.95724293864770971 ) ) ;
#160663 = CARTESIAN_POINT ( 'NONE',  ( 19.03943276465977164, 0.05219959533936151252, 81.25109039468567573 ) ) ;
#160664 = CARTESIAN_POINT ( 'NONE',  ( -15.80617190586745835, -15.72974639402198527, 31.87390960531435979 ) ) ;
#160665 = CARTESIAN_POINT ( 'NONE',  ( 8.314922557960818139, 14.29746914071049879, 99.58224293864770971 ) ) ;
#160666 = CARTESIAN_POINT ( 'NONE',  ( -17.50000000000000000, -3.471454075611492218, 25.51667418855629421 ) ) ;
#160668 = CARTESIAN_POINT ( 'NONE',  ( 10.81492255796078972, 18.62759615963270932, 64.58224293864769550 ) ) ;
#160667 = CARTESIAN_POINT ( 'NONE',  ( 19.03943276465977164, -0.05219959533909143690, 63.74890960531435979 ) ) ;
#160669 = CARTESIAN_POINT ( 'NONE',  ( 19.02544592524343514, -5.153800228976328945, 28.54057627198102409 ) ) ;
#160671 = CARTESIAN_POINT ( 'NONE',  ( 0.05219959533909260263, 19.03943276465977164, 54.99890960531435979 ) ) ;
#160670 = CARTESIAN_POINT ( 'NONE',  ( 0.05219959533934541429, -16.53943276465976808, 85.00109039468568994 ) ) ;
#160672 = CARTESIAN_POINT ( 'NONE',  ( 9.474510206698729675, 16.51473224551082808, 47.08442372801900433 ) ) ;
#160673 = CARTESIAN_POINT ( 'NONE',  ( -10.72451020669870658, -18.67979575497194134, 69.58442372801900433 ) ) ;
#160674 = CARTESIAN_POINT ( 'NONE',  ( -18.62759615963270932, 10.81492255796079327, 55.83224293864770260 ) ) ;
#160675 = CARTESIAN_POINT ( 'NONE',  ( 19.02544592524343514, -5.153800228976328945, 23.54057627198102054 ) ) ;
#160676 = CARTESIAN_POINT ( 'NONE',  ( -8.224510206698735004, -14.34966873604973081, 84.58442372801903275 ) ) ;
#160677 = CARTESIAN_POINT ( 'NONE',  ( -19.03943276465977164, -0.05219959533935918106, 98.75109039468567573 ) ) ;
#160678 = CARTESIAN_POINT ( 'NONE',  ( -19.03943276465977164, 0.05219959533909376836, 21.24890960531436335 ) ) ;
#160680 = CARTESIAN_POINT ( 'NONE',  ( 21.52544592524344225, -5.823673210054117533, 48.54057627198103120 ) ) ;
#160679 = CARTESIAN_POINT ( 'NONE',  ( -193.3062444957834884, -155.7167183371838064, -25.00000000000000000 ) ) ;
#160681 = CARTESIAN_POINT ( 'NONE',  ( 5.823673210054444382, -21.52544592524334988, 80.20942372801901854 ) ) ;
#160682 = CARTESIAN_POINT ( 'NONE',  ( 14.34966873604960469, 8.224510206698951720, 44.16557627198103120 ) ) ;
#160683 = CARTESIAN_POINT ( 'NONE',  ( -12.06949235617756955, 12.14591786802309770, 55.62390960531436690 ) ) ;
#160684 = CARTESIAN_POINT ( 'NONE',  ( 21.53943276465977519, -0.05219959533907433946, 83.74890960531435269 ) ) ;
#160685 = CARTESIAN_POINT ( 'NONE',  ( -21.52544592524343514, 5.823673210054127303, 81.04057627198102409 ) ) ;
#160686 = DIRECTION ( 'NONE',  ( 0.000000000000000000, 0.000000000000000000, 1.000000000000000000 ) ) ;
#160688 = EDGE_CURVE ( 'NONE', #165125, #178804, #46509, .T. ) ;
#160687 = CARTESIAN_POINT ( 'NONE',  ( -21.55341960407610458, -5.719274019375992779, 31.45724293864769550 ) ) ;
#160689 = CARTESIAN_POINT ( 'NONE',  ( -16.55341960407617563, 4.379528057220093196, 63.54275706135234003 ) ) ;
#160690 = CARTESIAN_POINT ( 'NONE',  ( 12.14591786802309770, 12.06949235617756955, 79.37390960531436690 ) ) ;
#160691 = CARTESIAN_POINT ( 'NONE',  ( 16.51473224551069308, 9.474510206698969483, 29.16557627198103475 ) ) ;
#160692 = FILL_AREA_STYLE ('',( #191034 ) ) ;
#160693 = DIRECTION ( 'NONE',  ( -1.000000000000000000, 0.000000000000000000, 0.000000000000000000 ) ) ;
#160694 = ORIENTED_EDGE ( 'NONE', *, *, #120448, .T. ) ;
#160695 = CARTESIAN_POINT ( 'NONE',  ( 12.14591786802327356, -12.06949235617739191, 85.62609039468568994 ) ) ;
#160696 = CARTESIAN_POINT ( 'NONE',  ( -21.52544592524334988, -5.823673210054445271, 18.95942372801901143 ) ) ;
#160697 = CARTESIAN_POINT ( 'NONE',  ( -13.89961937509977652, 13.97604488694528158, 85.62390960531433848 ) ) ;
#160698 = CARTESIAN_POINT ( 'NONE',  ( 18.62759615963255655, 10.81492255796105972, 56.66775706135235424 ) ) ;
#160699 = CARTESIAN_POINT ( 'NONE',  ( -5.153800228976328057, -19.02544592524343514, 107.2905762719810383 ) ) ;
#160700 = CARTESIAN_POINT ( 'NONE',  ( -14.29384609392722183, -37.08231061483268576, -29.62140346006266967 ) ) ;
#160701 = ORIENTED_EDGE ( 'NONE', *, *, #6641, .F. ) ;
#160702 = CARTESIAN_POINT ( 'NONE',  ( 5.823673210054444382, -21.52544592524334988, 40.20942372801901854 ) ) ;
#160704 = CARTESIAN_POINT ( 'NONE',  ( -9.474510206698964154, 16.51473224551069663, 105.4155762719810383 ) ) ;
#160703 = CARTESIAN_POINT ( 'NONE',  ( 13.89961937509977652, -13.97604488694527269, 38.12390960531436690 ) ) ;
#160705 = CARTESIAN_POINT ( 'NONE',  ( -16.51473224551082808, 9.474510206698731452, 48.33442372801900433 ) ) ;
#160706 = CARTESIAN_POINT ( 'NONE',  ( -15.72974639402176322, -15.80617190586768395, 34.37609039468568284 ) ) ;
#160707 = CARTESIAN_POINT ( 'NONE',  ( -5.153800228976607833, 19.02544592524334988, 42.70942372801901143 ) ) ;
#160708 = CARTESIAN_POINT ( 'NONE',  ( 16.51473224551069308, 9.474510206698969483, 29.16557627198103475 ) ) ;
#160709 = CARTESIAN_POINT ( 'NONE',  ( 8.224510206698742110, 14.34966873604972548, 92.08442372801901854 ) ) ;
#160710 = CARTESIAN_POINT ( 'NONE',  ( 9.474510206698729675, 16.51473224551082808, 57.08442372801900433 ) ) ;
#160711 = CARTESIAN_POINT ( 'NONE',  ( 16.55341960407618274, -4.379528057220086978, 106.0427570613523471 ) ) ;
#160712 = CARTESIAN_POINT ( 'NONE',  ( 9.822853212439058623, 11.94381442052172204, -61.89036147510174146 ) ) ;
#160713 = CARTESIAN_POINT ( 'NONE',  ( 19.02544592524343514, -5.153800228976328945, 88.54057627198102409 ) ) ;
#160714 = CARTESIAN_POINT ( 'NONE',  ( -5.823673210054431948, 21.52544592524334988, 92.70942372801901854 ) ) ;
#160715 = CARTESIAN_POINT ( 'NONE',  ( -15.80617190586768217, 15.72974639402176855, 108.1260903946856757 ) ) ;
#160716 = CARTESIAN_POINT ( 'NONE',  ( 37.99626262588764547, 12.34573411038917357, -4.902157773949822328 ) ) ;
#160717 = CARTESIAN_POINT ( 'NONE',  ( -19.02544592524342804, 5.153800228976336051, 106.0405762719810241 ) ) ;
#160718 = CARTESIAN_POINT ( 'NONE',  ( 0.05219959533937995610, -21.53943276465977519, 70.00109039468568994 ) ) ;
#160719 = CARTESIAN_POINT ( 'NONE',  ( -14.29746914071037622, -8.314922557961029526, 19.16775706135234714 ) ) ;
#160720 = CARTESIAN_POINT ( 'NONE',  ( 13.89961937509977652, -13.97604488694527269, 73.12390960531436690 ) ) ;
#160721 = CARTESIAN_POINT ( 'NONE',  ( 21.53943276465977519, -0.05219959533907433946, 28.74890960531435624 ) ) ;
#160722 = CARTESIAN_POINT ( 'NONE',  ( 16.46253265017160672, -9.564922557960803928, 93.33224293864769550 ) ) ;
#160723 = CARTESIAN_POINT ( 'NONE',  ( -16.38665767535051643, -7.295008042176172935, 89.73599135785457293 ) ) ;
#160724 = CARTESIAN_POINT ( 'NONE',  ( 16.46253265017160672, -9.564922557960803928, 78.33224293864769550 ) ) ;
#160725 = CARTESIAN_POINT ( 'NONE',  ( 5.049401038298161559, -19.05341960407611168, 62.70724293864769550 ) ) ;
#160726 = CARTESIAN_POINT ( 'NONE',  ( 12.14591786802327356, -12.06949235617739191, 95.62609039468568994 ) ) ;
#160727 = FACE_OUTER_BOUND ( 'NONE', #135379, .T. ) ;
#160728 = CARTESIAN_POINT ( 'NONE',  ( 5.049401038297881783, 19.05341960407617563, 67.29275706135234714 ) ) ;
#160729 = CARTESIAN_POINT ( 'NONE',  ( -13.97604488694527625, -13.89961937509977652, 86.87390960531436690 ) ) ;
#160730 = CARTESIAN_POINT ( 'NONE',  ( -0.05219959533910754901, -16.53943276465976808, 82.49890960531436690 ) ) ;
#160731 = CARTESIAN_POINT ( 'NONE',  ( 10.81492255796078972, 18.62759615963270932, 34.58224293864770260 ) ) ;
#160732 = CARTESIAN_POINT ( 'NONE',  ( -16.46253265017160317, 9.564922557960807481, 115.8322429386477097 ) ) ;
#160733 = CARTESIAN_POINT ( 'NONE',  ( 12.14591786802309770, 12.06949235617756955, 109.3739096053143811 ) ) ;
#160734 = DIRECTION ( 'NONE',  ( 1.000000000000000000, 0.000000000000000000, 0.000000000000000000 ) ) ;
#160735 = CARTESIAN_POINT ( 'NONE',  ( -13.97604488694547697, 13.89961937509957934, 43.12609039468566152 ) ) ;
#160736 = CARTESIAN_POINT ( 'NONE',  ( 16.55341960407611168, 4.379528057220329451, 23.95724293864769550 ) ) ;
#160737 = CARTESIAN_POINT ( 'NONE',  ( -19.03943276465977164, 0.05219959533909376836, 106.2489096053143669 ) ) ;
#160738 = CARTESIAN_POINT ( 'NONE',  ( 21.55341960407619695, -5.719274019375665929, 71.04275706135234714 ) ) ;
#160739 = CARTESIAN_POINT ( 'NONE',  ( 21.53943276465977519, -0.05219959533907433946, 63.74890960531435979 ) ) ;
#160740 = CARTESIAN_POINT ( 'NONE',  ( 21.53943276465977519, 0.05219959533937863772, 36.25109039468567573 ) ) ;
#160741 = CARTESIAN_POINT ( 'NONE',  ( -0.05219959533907301413, -21.53943276465977519, 77.49890960531433848 ) ) ;
#160742 = CARTESIAN_POINT ( 'NONE',  ( -21.55341960407619339, 5.719274019375674811, 43.54275706135235424 ) ) ;
#160743 = CARTESIAN_POINT ( 'NONE',  ( 8.224510206698953496, -14.34966873604960469, 107.9155762719810241 ) ) ;
#160744 = CARTESIAN_POINT ( 'NONE',  ( 9.564922557961047289, -16.46253265017146816, 75.41775706135234714 ) ) ;
#160745 = CARTESIAN_POINT ( 'NONE',  ( -9.474510206698964154, 16.51473224551069663, 50.41557627198102409 ) ) ;
#160747 = CARTESIAN_POINT ( 'NONE',  ( 5.153800228976335163, 19.02544592524342804, 94.79057627198103830 ) ) ;
#160746 = CARTESIAN_POINT ( 'NONE',  ( -12.06949235617756955, 12.14591786802309770, 95.62390960531436690 ) ) ;
#160748 = CARTESIAN_POINT ( 'NONE',  ( 5.153800228976335163, 19.02544592524342804, 94.79057627198103830 ) ) ;
#160749 = CARTESIAN_POINT ( 'NONE',  ( -5.153800228976328057, -19.02544592524343514, 22.29057627198102765 ) ) ;
#160750 = CARTESIAN_POINT ( 'NONE',  ( -4.483927247898539470, -16.52544592524342804, 47.29057627198103120 ) ) ;
#160751 = CARTESIAN_POINT ( 'NONE',  ( -16.52544592524335698, -4.483927247898792601, 98.95942372801903275 ) ) ;
#160752 = CARTESIAN_POINT ( 'NONE',  ( 5.049401038298161559, -19.05341960407611168, 52.70724293864767418 ) ) ;
#160753 = CARTESIAN_POINT ( 'NONE',  ( 9.474510206698971260, -16.51473224551069308, 27.91557627198103120 ) ) ;
#160754 = CARTESIAN_POINT ( 'NONE',  ( -19.05341960407617563, 5.049401038297882671, 23.54275706135233648 ) ) ;
#160757 = CARTESIAN_POINT ( 'NONE',  ( -12.14591786802309592, -12.06949235617757132, 26.87390960531435979 ) ) ;
#160756 = FACE_OUTER_BOUND ( 'NONE', #5483, .T. ) ;
#160755 = AXIS2_PLACEMENT_3D ( 'NONE', #89323, #166181, #43820 ) ;
#160758 = CARTESIAN_POINT ( 'NONE',  ( 21.53943276465977519, 0.05219959533937863772, 51.25109039468568994 ) ) ;
#160759 = CARTESIAN_POINT ( 'NONE',  ( -11.19179774862103116, -35.88147526272305043, -30.64906824478842751 ) ) ;
#160760 = CARTESIAN_POINT ( 'NONE',  ( 4.379528057220092307, 16.55341960407617563, 52.29275706135236135 ) ) ;
#160761 = EDGE_CURVE ( 'NONE', #25133, #50018, #82648, .T. ) ;
#160762 = CARTESIAN_POINT ( 'NONE',  ( 16.53943276465976808, -0.05219959533910856209, 33.74890960531436690 ) ) ;
#160763 = CARTESIAN_POINT ( 'NONE',  ( -9.474510206698964154, 16.51473224551069663, 40.41557627198103120 ) ) ;
#160764 = CARTESIAN_POINT ( 'NONE',  ( -16.52544592524335698, -4.483927247898792601, 103.9594237280190185 ) ) ;
#160765 = CARTESIAN_POINT ( 'NONE',  ( 14.34966873604972726, -8.224510206698740333, 20.83442372801901143 ) ) ;
#160766 = CARTESIAN_POINT ( 'NONE',  ( -16.51473224551069308, -9.474510206698971260, 46.66557627198102409 ) ) ;
#160767 = CARTESIAN_POINT ( 'NONE',  ( 8.224510206698953496, -14.34966873604960469, 102.9155762719810383 ) ) ;
#160768 = CARTESIAN_POINT ( 'NONE',  ( 15.80617190586746368, 15.72974639402197994, 114.3739096053143527 ) ) ;
#160769 = CARTESIAN_POINT ( 'NONE',  ( -9.564922557960796823, -16.46253265017161027, 52.08224293864768839 ) ) ;
#160770 = CARTESIAN_POINT ( 'NONE',  ( -13.89961937509977652, 13.97604488694528158, 100.6239096053143669 ) ) ;
#160771 = CARTESIAN_POINT ( 'NONE',  ( 13.89961937509977652, -13.97604488694527269, 33.12390960531434558 ) ) ;
#160772 = CARTESIAN_POINT ( 'NONE',  ( 0.05219959533909260263, 19.03943276465977164, 99.99890960531436690 ) ) ;
#160773 = CARTESIAN_POINT ( 'NONE',  ( -32.00000000000000000, -1.163414459189985801E-14, 95.00000000000000000 ) ) ;
#160774 = ADVANCED_FACE ( 'NONE', ( #98151 ), #102184, .F. ) ;
#160775 = CARTESIAN_POINT ( 'NONE',  ( 13.89961937509977652, -13.97604488694527269, 93.12390960531436690 ) ) ;
#160777 = CARTESIAN_POINT ( 'NONE',  ( -4.379528057220328563, 16.55341960407611168, 100.2072429386476955 ) ) ;
#160776 = CARTESIAN_POINT ( 'NONE',  ( 15.80617190586769283, -15.72974639402175789, 40.62609039468567573 ) ) ;
#160778 = CARTESIAN_POINT ( 'NONE',  ( -13.89961937509977652, 13.97604488694528158, 110.6239096053143243 ) ) ;
#160779 = CARTESIAN_POINT ( 'NONE',  ( 16.51473224551083163, -9.474510206698727899, 70.83442372801900433 ) ) ;
#160780 = CARTESIAN_POINT ( 'NONE',  ( 16.52544592524335698, 4.483927247898782831, 61.45942372801901854 ) ) ;
#160781 = CARTESIAN_POINT ( 'NONE',  ( 15.72974639402176855, 15.80617190586768217, 96.87609039468568994 ) ) ;
#160782 = COLOUR_RGB ( '', 0.09019608, 0.27058824, 0.51372549) ;
#160783 = CARTESIAN_POINT ( 'NONE',  ( 16.53943276465976808, 0.05219959533934440121, 56.25109039468568284 ) ) ;
#160784 = CARTESIAN_POINT ( 'NONE',  ( -19.02544592524342804, 5.153800228976336051, 101.0405762719810241 ) ) ;
#160785 = CARTESIAN_POINT ( 'NONE',  ( -16.53943276465976808, -0.05219959533934237506, 43.75109039468568284 ) ) ;
#160786 = CARTESIAN_POINT ( 'NONE',  ( 0.05219959533936267826, -19.03943276465977164, 110.0010903946856757 ) ) ;
#160787 = CARTESIAN_POINT ( 'NONE',  ( -0.05219959533934338120, 16.53943276465976808, 87.50109039468568994 ) ) ;
#160788 = CARTESIAN_POINT ( 'NONE',  ( -5.153800228976607833, 19.02544592524334988, 97.70942372801900433 ) ) ;
#160789 = CARTESIAN_POINT ( 'NONE',  ( -19.03943276465977164, 0.05219959533909376836, 81.24890960531436690 ) ) ;
#160790 = CARTESIAN_POINT ( 'NONE',  ( 0.05219959533907565091, 21.53943276465977519, 99.99890960531436690 ) ) ;
#160792 = CARTESIAN_POINT ( 'NONE',  ( 9.474510206698729675, 16.51473224551082808, 107.0844237280190043 ) ) ;
#160791 = CARTESIAN_POINT ( 'NONE',  ( 4.379528057220339221, -16.55341960407611168, 87.70724293864769550 ) ) ;
#160793 = CARTESIAN_POINT ( 'NONE',  ( -0.05219959533934338120, 16.53943276465976808, 67.50109039468568994 ) ) ;
#160794 = CARTESIAN_POINT ( 'NONE',  ( 21.70479006154310397, 8.695791278452436046, 169.0563666577073150 ) ) ;
#160795 = CARTESIAN_POINT ( 'NONE',  ( -5.049401038297874678, -19.05341960407617918, 74.79275706135231871 ) ) ;
#160796 = CARTESIAN_POINT ( 'NONE',  ( 12.06949235617757843, -12.14591786802309237, 38.12390960531436690 ) ) ;
#160797 = CARTESIAN_POINT ( 'NONE',  ( -12.06949235617756955, 12.14591786802309770, 95.62390960531436690 ) ) ;
#160799 = CARTESIAN_POINT ( 'NONE',  ( -16.31925111598456368, 7.325300261831606541, 90.16424538967254421 ) ) ;
#160798 = CARTESIAN_POINT ( 'NONE',  ( 19.05341960407617918, -5.049401038297876454, 36.04275706135234003 ) ) ;
#160800 = CARTESIAN_POINT ( 'NONE',  ( -21.53943276465977519, -0.05219959533937600094, 23.75109039468567929 ) ) ;
#160801 = CARTESIAN_POINT ( 'NONE',  ( 5.049401038297881783, 19.05341960407617563, 102.2927570613523045 ) ) ;
#160802 = CARTESIAN_POINT ( 'NONE',  ( 9.564922557960805705, 16.46253265017160317, 114.5822429386476955 ) ) ;
#160803 = CARTESIAN_POINT ( 'NONE',  ( -13.97604488694527625, -13.89961937509977652, 86.87390960531436690 ) ) ;
#160804 = CARTESIAN_POINT ( 'NONE',  ( -5.719274019375665041, -21.55341960407619695, 99.79275706135234714 ) ) ;
#160805 = CARTESIAN_POINT ( 'NONE',  ( -0.05219959533909027116, -19.03943276465977164, 72.49890960531435269 ) ) ;
#160806 = CARTESIAN_POINT ( 'NONE',  ( -15.80617190586745835, -15.72974639402198527, 36.87390960531435979 ) ) ;
#160807 = CARTESIAN_POINT ( 'NONE',  ( -12.14591786802309592, -12.06949235617757132, 96.87390960531436690 ) ) ;
#160808 = CARTESIAN_POINT ( 'NONE',  ( -19.02544592524342804, 5.153800228976336051, 51.04057627198103120 ) ) ;
#160809 = CARTESIAN_POINT ( 'NONE',  ( 4.483927247898545687, 16.52544592524342804, 114.7905762719810383 ) ) ;
#160810 = CARTESIAN_POINT ( 'NONE',  ( 10.81492255796106328, -18.62759615963255655, 20.41775706135234714 ) ) ;
#160811 = CARTESIAN_POINT ( 'NONE',  ( -18.62759615963255300, -10.81492255796106328, 59.16775706135234714 ) ) ;
#160812 = CARTESIAN_POINT ( 'NONE',  ( 16.51473224551069308, 9.474510206698969483, 39.16557627198103120 ) ) ;
#160813 = CARTESIAN_POINT ( 'NONE',  ( 16.55341960407618274, -4.379528057220086978, 71.04275706135234714 ) ) ;
#160814 = CARTESIAN_POINT ( 'NONE',  ( -5.719274019375665041, -21.55341960407619695, 19.79275706135235069 ) ) ;
#160815 = ORIENTED_EDGE ( 'NONE', *, *, #197168, .T. ) ;
#160816 = CARTESIAN_POINT ( 'NONE',  ( -5.719274019375978568, 21.55341960407610458, 115.2072429386476955 ) ) ;
#160818 = CARTESIAN_POINT ( 'NONE',  ( 19.03943276465977164, -0.05219959533909143690, 63.74890960531435979 ) ) ;
#160817 = CARTESIAN_POINT ( 'NONE',  ( 19.03943276465977164, 0.05219959533936151252, 56.25109039468566863 ) ) ;
#160819 = CARTESIAN_POINT ( 'NONE',  ( -16.51473224551082808, 9.474510206698731452, 33.33442372801899722 ) ) ;
#160820 = CARTESIAN_POINT ( 'NONE',  ( 5.823673210054444382, -21.52544592524334988, 65.20942372801901854 ) ) ;
#160821 = CARTESIAN_POINT ( 'NONE',  ( 5.719274019375991003, -21.55341960407610458, 72.70724293864769550 ) ) ;
#160822 = CARTESIAN_POINT ( 'NONE',  ( 4.483927247898545687, 16.52544592524342804, 54.79057627198104541 ) ) ;
#160824 = CARTESIAN_POINT ( 'NONE',  ( 0.05219959533936267826, -19.03943276465977164, 25.00109039468566152 ) ) ;
#160823 = CARTESIAN_POINT ( 'NONE',  ( 18.67979575497194134, -10.72451020669871369, 90.83442372801901854 ) ) ;
#160825 = CARTESIAN_POINT ( 'NONE',  ( -16.53943276465976808, 0.05219959533911058130, 76.24890960531435269 ) ) ;
#160826 = CARTESIAN_POINT ( 'NONE',  ( 14.34966873604960469, 8.224510206698951720, 114.1655762719810383 ) ) ;
#160827 = CARTESIAN_POINT ( 'NONE',  ( 16.46253265017146816, 9.564922557961045513, 61.66775706135234003 ) ) ;
#160828 = CARTESIAN_POINT ( 'NONE',  ( -0.05219959533910754901, -16.53943276465976808, 22.49890960531436335 ) ) ;
#160829 = CARTESIAN_POINT ( 'NONE',  ( 10.81492255796106328, -18.62759615963255655, 75.41775706135233293 ) ) ;
#160830 = CARTESIAN_POINT ( 'NONE',  ( -16.51473224551082808, 9.474510206698731452, 43.33442372801900433 ) ) ;
#160831 = CARTESIAN_POINT ( 'NONE',  ( 5.823673210054125526, 21.52544592524343514, 54.79057627198104541 ) ) ;
#160832 = CARTESIAN_POINT ( 'NONE',  ( 15.80617190586769283, -15.72974639402175789, 40.62609039468567573 ) ) ;
#160833 = CARTESIAN_POINT ( 'NONE',  ( -5.719274019375978568, 21.55341960407610458, 95.20724293864769550 ) ) ;
#160834 = CARTESIAN_POINT ( 'NONE',  ( -19.03943276465977164, -0.05219959533935918106, 103.7510903946856757 ) ) ;
#160835 = CARTESIAN_POINT ( 'NONE',  ( 8.224510206698742110, 14.34966873604972548, 67.08442372801901854 ) ) ;
#160837 = CARTESIAN_POINT ( 'NONE',  ( 18.67979575497178502, 10.72451020669898547, 104.1655762719810241 ) ) ;
#160836 = CARTESIAN_POINT ( 'NONE',  ( 11.74149087413295156, -36.13659316521243881, -5.402157773949823216 ) ) ;
#160838 = CARTESIAN_POINT ( 'NONE',  ( -8.314922557960811034, -14.29746914071050412, 87.08224293864769550 ) ) ;
#160839 = CARTESIAN_POINT ( 'NONE',  ( -17.05587630539786304, -6.762274262135706593, 99.25819690962688924 ) ) ;
#160840 = CARTESIAN_POINT ( 'NONE',  ( 12.06949235617739724, 12.14591786802326823, 21.87609039468567573 ) ) ;
#160841 = CARTESIAN_POINT ( 'NONE',  ( 5.719274019375991003, -21.55341960407610458, 47.70724293864770260 ) ) ;
#160842 = CARTESIAN_POINT ( 'NONE',  ( -4.483927247898782831, 16.52544592524335698, 87.70942372801901854 ) ) ;
#160843 = CARTESIAN_POINT ( 'NONE',  ( -9.564922557960796823, -16.46253265017161027, 22.08224293864768839 ) ) ;
#160844 = CARTESIAN_POINT ( 'NONE',  ( -8.314922557961024197, 14.29746914071037800, 62.91775706135236135 ) ) ;
#160845 = CARTESIAN_POINT ( 'NONE',  ( -10.72451020669870658, -18.67979575497194134, 44.58442372801901854 ) ) ;
#160846 = CARTESIAN_POINT ( 'NONE',  ( 21.53943276465977519, -0.05219959533907433946, 63.74890960531435979 ) ) ;
#160847 = CARTESIAN_POINT ( 'NONE',  ( -4.483927247898782831, 16.52544592524335698, 82.70942372801900433 ) ) ;
#160848 = CARTESIAN_POINT ( 'NONE',  ( 16.51473224551069308, 9.474510206698969483, 94.16557627198103830 ) ) ;
#160849 = CARTESIAN_POINT ( 'NONE',  ( 18.67979575497194134, -10.72451020669871369, 75.83442372801900433 ) ) ;
#160850 = CARTESIAN_POINT ( 'NONE',  ( 18.62759615963271287, -10.81492255796078972, 58.33224293864768839 ) ) ;
#160851 = CARTESIAN_POINT ( 'NONE',  ( -5.823673210054116645, -21.52544592524344225, 37.29057627198102409 ) ) ;
#160852 = ORIENTED_EDGE ( 'NONE', *, *, #128318, .F. ) ;
#160853 = CARTESIAN_POINT ( 'NONE',  ( -4.379528057220086978, -16.55341960407618274, 59.79275706135234714 ) ) ;
#160854 = CARTESIAN_POINT ( 'NONE',  ( -10.72451020669898014, 18.67979575497178502, 35.41557627198102409 ) ) ;
#160855 = ORIENTED_EDGE ( 'NONE', *, *, #24918, .F. ) ;
#160856 = CARTESIAN_POINT ( 'NONE',  ( 9.474510206698971260, -16.51473224551069308, 102.9155762719810241 ) ) ;
#160857 = CARTESIAN_POINT ( 'NONE',  ( -0.05219959533910754901, -16.53943276465976808, 22.49890960531436335 ) ) ;
#160858 = DIRECTION ( 'NONE',  ( -1.000000000000000000, 0.000000000000000000, 0.000000000000000000 ) ) ;
#160859 = CARTESIAN_POINT ( 'NONE',  ( 16.53943276465976808, -0.05219959533910856209, 108.7489096053143669 ) ) ;
#160860 = CARTESIAN_POINT ( 'NONE',  ( 10.81492255796078972, 18.62759615963270932, 49.58224293864769550 ) ) ;
#160861 = CARTESIAN_POINT ( 'NONE',  ( -19.02544592524342804, 5.153800228976336051, 41.04057627198103120 ) ) ;
#160862 = CARTESIAN_POINT ( 'NONE',  ( 16.55341960407618274, -4.379528057220086978, 96.04275706135236135 ) ) ;
#160863 = CARTESIAN_POINT ( 'NONE',  ( 18.62759615963255655, 10.81492255796105972, 36.66775706135234714 ) ) ;
#160864 = CARTESIAN_POINT ( 'NONE',  ( -16.46253265017146816, -9.564922557961047289, 94.16775706135233293 ) ) ;
#160865 = CARTESIAN_POINT ( 'NONE',  ( 4.379528057220339221, -16.55341960407611168, 107.7072429386476955 ) ) ;
#160866 = CARTESIAN_POINT ( 'NONE',  ( 16.46253265017160672, -9.564922557960803928, 53.33224293864768839 ) ) ;
#160867 = CARTESIAN_POINT ( 'NONE',  ( 13.89961937509977652, -13.97604488694527269, 33.12390960531434558 ) ) ;
#160868 = CARTESIAN_POINT ( 'NONE',  ( 31.99364916730969455, -1.130961319020620804E-14, 97.65000000000020464 ) ) ;
#160869 = CARTESIAN_POINT ( 'NONE',  ( 19.05341960407611168, 5.049401038298154454, 73.95724293864768129 ) ) ;
#160870 = CARTESIAN_POINT ( 'NONE',  ( -14.34966873604972548, 8.224510206698743886, 63.33442372801900433 ) ) ;
#160871 = CARTESIAN_POINT ( 'NONE',  ( 18.62759615963255655, 10.81492255796105972, 111.6677570613523613 ) ) ;
#160872 = CARTESIAN_POINT ( 'NONE',  ( -21.53943276465977519, 0.05219959533907696930, 46.24890960531435979 ) ) ;
#160873 = CARTESIAN_POINT ( 'NONE',  ( -16.52544592524335698, -4.483927247898792601, 78.95942372801901854 ) ) ;
#160874 = CARTESIAN_POINT ( 'NONE',  ( -16.46253265017146816, -9.564922557961047289, 49.16775706135233293 ) ) ;
#160875 = CARTESIAN_POINT ( 'NONE',  ( 13.89961937509957401, 13.97604488694547697, 61.87609039468566863 ) ) ;
#160876 = CARTESIAN_POINT ( 'NONE',  ( -0.05219959533937732626, 21.53943276465977519, 57.50109039468568994 ) ) ;
#160877 = CARTESIAN_POINT ( 'NONE',  ( 16.51473224551069308, 9.474510206698969483, 64.16557627198102409 ) ) ;
#160878 = CARTESIAN_POINT ( 'NONE',  ( -9.564922557960796823, -16.46253265017161027, 32.08224293864769550 ) ) ;
#160879 = CARTESIAN_POINT ( 'NONE',  ( -13.89961937509957401, -13.97604488694547875, 64.37609039468567573 ) ) ;
#160880 = CARTESIAN_POINT ( 'NONE',  ( 13.89961937509977652, -13.97604488694527269, 108.1239096053143669 ) ) ;
#160881 = CARTESIAN_POINT ( 'NONE',  ( -19.02544592524342804, 5.153800228976336051, 96.04057627198103830 ) ) ;
#160882 = CARTESIAN_POINT ( 'NONE',  ( 4.483927247898545687, 16.52544592524342804, 54.79057627198104541 ) ) ;
#160883 = CARTESIAN_POINT ( 'NONE',  ( 21.52544592524344225, -5.823673210054117533, 53.54057627198103120 ) ) ;
#160884 = CARTESIAN_POINT ( 'NONE',  ( 17.60769864724391809, -5.499999999999981348, 91.15024842019167295 ) ) ;
#160885 = CARTESIAN_POINT ( 'NONE',  ( -19.02544592524334988, -5.153800228976617603, 33.95942372801897591 ) ) ;
#160886 = CARTESIAN_POINT ( 'NONE',  ( -17.44279575226823198, -5.990770900252435638, 79.16442432485685288 ) ) ;
#160887 = CARTESIAN_POINT ( 'NONE',  ( 16.51473224551069308, 9.474510206698969483, 54.16557627198103120 ) ) ;
#160888 = CARTESIAN_POINT ( 'NONE',  ( -19.35543954521080678, -5.499999999999533706, 99.58901960356450900 ) ) ;
#160889 = CARTESIAN_POINT ( 'NONE',  ( -7.052343178074620411, 2.552343178074692354, 8.889087296526001936 ) ) ;
#160890 = CARTESIAN_POINT ( 'NONE',  ( 4.483927247898790824, -16.52544592524335698, 75.20942372801901854 ) ) ;
#160891 = CARTESIAN_POINT ( 'NONE',  ( 10.72451020669898902, -18.67979575497178502, 97.91557627198103830 ) ) ;
#160892 = CARTESIAN_POINT ( 'NONE',  ( -16.53943276465976808, 0.05219959533911058130, 56.24890960531436690 ) ) ;
#160894 = CARTESIAN_POINT ( 'NONE',  ( -13.89961937509977652, 13.97604488694528158, 115.6239096053143669 ) ) ;
#160893 = CARTESIAN_POINT ( 'NONE',  ( -5.049401038298153566, 19.05341960407611168, 40.20724293864768839 ) ) ;
#160895 = CARTESIAN_POINT ( 'NONE',  ( 5.719274019375673035, 21.55341960407619339, 42.29275706135235424 ) ) ;
#160896 = CARTESIAN_POINT ( 'NONE',  ( 0.05219959533936267826, -19.03943276465977164, 50.00109039468566863 ) ) ;
#160897 = CARTESIAN_POINT ( 'NONE',  ( 0.05219959533909260263, 19.03943276465977164, 44.99890960531435979 ) ) ;
#160898 = CARTESIAN_POINT ( 'NONE',  ( -10.81492255796105439, 18.62759615963255655, 92.91775706135236135 ) ) ;
#160899 = CARTESIAN_POINT ( 'NONE',  ( 17.26058549869091863, 6.457015423128549259, 98.87745837476064992 ) ) ;
#160900 = CARTESIAN_POINT ( 'NONE',  ( -16.53943276465976808, 0.05219959533911058130, 41.24890960531435269 ) ) ;
#160901 = CARTESIAN_POINT ( 'NONE',  ( -14.02111363790005250, 0.9482109960936973003, -60.30654223653039736 ) ) ;
#160902 = CARTESIAN_POINT ( 'NONE',  ( 18.67979575497178502, 10.72451020669898547, 44.16557627198103120 ) ) ;
#160903 = CARTESIAN_POINT ( 'NONE',  ( -22.44159573604010305, 16.30477369853692338, 142.6750000027311671 ) ) ;
#160904 = CARTESIAN_POINT ( 'NONE',  ( -19.02544592524342804, 5.153800228976336051, 101.0405762719810241 ) ) ;
#160905 = CARTESIAN_POINT ( 'NONE',  ( 12.06949235617757843, -12.14591786802309237, 93.12390960531436690 ) ) ;
#160906 = CARTESIAN_POINT ( 'NONE',  ( -16.52544592524335698, -4.483927247898792601, 28.95942372801902209 ) ) ;
#160907 = CARTESIAN_POINT ( 'NONE',  ( -8.314922557960811034, -14.29746914071050412, 22.08224293864769194 ) ) ;
#160908 = ORIENTED_EDGE ( 'NONE', *, *, #150187, .F. ) ;
#160910 = CARTESIAN_POINT ( 'NONE',  ( -0.05219959533907301413, -21.53943276465977519, 102.4989096053143811 ) ) ;
#160909 = CARTESIAN_POINT ( 'NONE',  ( 5.153800228976335163, 19.02544592524342804, 94.79057627198103830 ) ) ;
#160912 = CARTESIAN_POINT ( 'NONE',  ( -13.97604488694527625, -13.89961937509977652, 96.87390960531433848 ) ) ;
#160911 = CARTESIAN_POINT ( 'NONE',  ( -14.29746914071049879, 8.314922557960819915, 30.83224293864770260 ) ) ;
#160913 = CARTESIAN_POINT ( 'NONE',  ( -16.46253265017146816, -9.564922557961047289, 99.16775706135233293 ) ) ;
#160914 = CARTESIAN_POINT ( 'NONE',  ( 18.62759615963255655, 10.81492255796105972, 106.6677570613523756 ) ) ;
#160915 = CARTESIAN_POINT ( 'NONE',  ( 5.719274019375991003, -21.55341960407610458, 92.70724293864770971 ) ) ;
#160916 = CARTESIAN_POINT ( 'NONE',  ( 5.823673210054125526, 21.52544592524343514, 44.79057627198103120 ) ) ;
#160917 = CARTESIAN_POINT ( 'NONE',  ( -5.049401038298153566, 19.05341960407611168, 65.20724293864765286 ) ) ;
#160918 = CARTESIAN_POINT ( 'NONE',  ( 12.14591786802309770, 12.06949235617756955, 34.37390960531435979 ) ) ;
#160919 = CARTESIAN_POINT ( 'NONE',  ( 19.02544592524343514, -5.153800228976328945, 73.54057627198103830 ) ) ;
#160920 = ORIENTED_EDGE ( 'NONE', *, *, #57173, .F. ) ;
#160921 = CARTESIAN_POINT ( 'NONE',  ( 18.39635199886970796, -5.499999999999989342, 63.51967076360001840 ) ) ;
#160922 = CARTESIAN_POINT ( 'NONE',  ( -13.89961937509957401, -13.97604488694547875, 34.37609039468566863 ) ) ;
#160923 = CARTESIAN_POINT ( 'NONE',  ( 0.05219959533910956823, 16.53943276465976808, 79.99890960531435269 ) ) ;
#160924 = CARTESIAN_POINT ( 'NONE',  ( -10.72451020669870658, -18.67979575497194134, 24.58442372801901499 ) ) ;
#160925 = AXIS2_PLACEMENT_3D ( 'NONE', #59239, #120908, #104763 ) ;
#160926 = CARTESIAN_POINT ( 'NONE',  ( -27.73933785331498925, 9.013057229001089965, 143.2750000027311899 ) ) ;
#160927 = EDGE_CURVE ( 'NONE', #107606, #148762, #131019, .T. ) ;
#160928 = CARTESIAN_POINT ( 'NONE',  ( -0.05219959533934338120, 16.53943276465976808, 107.5010903946856899 ) ) ;
#160929 = CARTESIAN_POINT ( 'NONE',  ( -0.05219959533910754901, -16.53943276465976808, 112.4989096053143669 ) ) ;
#160930 = CARTESIAN_POINT ( 'NONE',  ( 5.153800228976335163, 19.02544592524342804, 74.79057627198103830 ) ) ;
#160931 = CARTESIAN_POINT ( 'NONE',  ( -13.97604488694527625, -13.89961937509977652, 21.87390960531435979 ) ) ;
#160932 = CARTESIAN_POINT ( 'NONE',  ( 4.483927247898545687, 16.52544592524342804, 39.79057627198103830 ) ) ;
#160933 = CARTESIAN_POINT ( 'NONE',  ( -15.72974639402176322, -15.80617190586768395, 54.37609039468568994 ) ) ;
#160934 = CARTESIAN_POINT ( 'NONE',  ( 21.53943276465977519, 0.05219959533937863772, 96.25109039468568994 ) ) ;
#160935 = CARTESIAN_POINT ( 'NONE',  ( 0.05219959533909260263, 19.03943276465977164, 49.99890960531435979 ) ) ;
#160936 = CARTESIAN_POINT ( 'NONE',  ( -5.049401038298153566, 19.05341960407611168, 45.20724293864769550 ) ) ;
#160937 = EDGE_LOOP ( 'NONE', ( #88614, #193976 ) ) ;
#160938 = CARTESIAN_POINT ( 'NONE',  ( 21.52544592524334988, 5.823673210054432836, 91.45942372801901854 ) ) ;
#160939 = CARTESIAN_POINT ( 'NONE',  ( 12.06949235617739724, 12.14591786802326823, 56.87609039468568994 ) ) ;
#160940 = CARTESIAN_POINT ( 'NONE',  ( 18.62759615963255655, 10.81492255796105972, 81.66775706135236135 ) ) ;
#160941 = CARTESIAN_POINT ( 'NONE',  ( -21.53943276465977519, 0.05219959533907696930, 21.24890960531436690 ) ) ;
#160942 = CARTESIAN_POINT ( 'NONE',  ( -16.51473224551082808, 9.474510206698731452, 98.33442372801900433 ) ) ;
#160943 = CARTESIAN_POINT ( 'NONE',  ( -18.67979575497193778, 10.72451020669871902, 73.33442372801901854 ) ) ;
#160944 = CARTESIAN_POINT ( 'NONE',  ( -16.52544592524335698, -4.483927247898792601, 38.95942372801901854 ) ) ;
#160945 = CARTESIAN_POINT ( 'NONE',  ( -18.62759615963270932, 10.81492255796079327, 90.83224293864769550 ) ) ;
#160946 = CARTESIAN_POINT ( 'NONE',  ( 0.05219959533936267826, -19.03943276465977164, 80.00109039468567573 ) ) ;
#160947 = CARTESIAN_POINT ( 'NONE',  ( 19.03943276465977164, -0.05219959533909143690, 58.74890960531435979 ) ) ;
#160948 = CARTESIAN_POINT ( 'NONE',  ( -13.89961937509957401, -13.97604488694547875, 99.37609039468567573 ) ) ;
#160949 = CARTESIAN_POINT ( 'NONE',  ( 19.03943276465977164, 0.05219959533936151252, 96.25109039468567573 ) ) ;
#160950 = CARTESIAN_POINT ( 'NONE',  ( -16.55341960407611168, -4.379528057220339221, 46.45724293864769550 ) ) ;
#160951 = CARTESIAN_POINT ( 'NONE',  ( 19.05341960407617918, -5.049401038297876454, 71.04275706135234714 ) ) ;
#160952 = CARTESIAN_POINT ( 'NONE',  ( 14.29746914071037800, 8.314922557961029526, 56.66775706135235424 ) ) ;
#160953 = CARTESIAN_POINT ( 'NONE',  ( 16.46253265017160672, -9.564922557960803928, 33.33224293864770260 ) ) ;
#160955 = ADVANCED_FACE ( 'NONE', ( #161855 ), #88003, .F. ) ;
#160954 = CARTESIAN_POINT ( 'NONE',  ( -19.02544592524342804, 5.153800228976336051, 61.04057627198103120 ) ) ;
#160956 = CARTESIAN_POINT ( 'NONE',  ( -16.55341960407617563, 4.379528057220093196, 63.54275706135234003 ) ) ;
#160957 = CARTESIAN_POINT ( 'NONE',  ( 22.44159573604009239, 16.30477369853692693, 140.5750000027311728 ) ) ;
#160958 = CARTESIAN_POINT ( 'NONE',  ( 28.82186960331498327, 9.364793116373570925, 139.3500000054623911 ) ) ;
#160959 = CARTESIAN_POINT ( 'NONE',  ( -13.89961937509977652, 13.97604488694528158, 105.6239096053143527 ) ) ;
#160960 = DIRECTION ( 'NONE',  ( 1.000000000000000000, 6.391086490440868450E-16, 0.000000000000000000 ) ) ;
#160961 = ORIENTED_EDGE ( 'NONE', *, *, #35450, .F. ) ;
#160962 = CARTESIAN_POINT ( 'NONE',  ( 13.97604488694548053, -13.89961937509957401, 110.6260903946856615 ) ) ;
#160963 = CARTESIAN_POINT ( 'NONE',  ( 5.719274019375991003, -21.55341960407610458, 37.70724293864769550 ) ) ;
#160965 = CARTESIAN_POINT ( 'NONE',  ( 8.224510206698742110, 14.34966873604972548, 27.08442372801901854 ) ) ;
#160964 = CARTESIAN_POINT ( 'NONE',  ( 5.049401038297881783, 19.05341960407617563, 27.29275706135232937 ) ) ;
#160966 = CARTESIAN_POINT ( 'NONE',  ( 0.05219959533909260263, 19.03943276465977164, 24.99890960531435269 ) ) ;
#160967 = CARTESIAN_POINT ( 'NONE',  ( -13.89961937509977652, 13.97604488694528158, 45.62390960531433848 ) ) ;
#160968 = CARTESIAN_POINT ( 'NONE',  ( -10.81492255796078084, -18.62759615963271287, 92.08224293864769550 ) ) ;
#160969 = CARTESIAN_POINT ( 'NONE',  ( -13.89961937509977652, 13.97604488694528158, 100.6239096053143669 ) ) ;
#160970 = CARTESIAN_POINT ( 'NONE',  ( 0.05219959533909260263, 19.03943276465977164, 54.99890960531435979 ) ) ;
#160971 = CARTESIAN_POINT ( 'NONE',  ( 27.73933785331498569, 9.013057229001093518, 140.4750000027312069 ) ) ;
#160972 = CARTESIAN_POINT ( 'NONE',  ( -16.51473224551082808, 9.474510206698731452, 78.33442372801900433 ) ) ;
#160973 = CARTESIAN_POINT ( 'NONE',  ( -14.29746914071049879, 8.314922557960819915, 70.83224293864770971 ) ) ;
#160974 = CARTESIAN_POINT ( 'NONE',  ( 15.72974639402199770, -15.80617190586745480, 43.12390960531435269 ) ) ;
#160975 = CARTESIAN_POINT ( 'NONE',  ( 5.823673210054444382, -21.52544592524334988, 100.2094237280190043 ) ) ;
#160976 = CARTESIAN_POINT ( 'NONE',  ( 5.823673210054125526, 21.52544592524343514, 94.79057627198105251 ) ) ;
#160977 = CARTESIAN_POINT ( 'NONE',  ( -0.05219959533937732626, 21.53943276465977519, 77.50109039468567573 ) ) ;
#160978 = CARTESIAN_POINT ( 'NONE',  ( 5.719274019375673035, 21.55341960407619339, 82.29275706135234714 ) ) ;
#160979 = CARTESIAN_POINT ( 'NONE',  ( 9.474510206698971260, -16.51473224551069308, 107.9155762719810383 ) ) ;
#160981 = CARTESIAN_POINT ( 'NONE',  ( 0.05219959533937995610, -21.53943276465977519, 80.00109039468568994 ) ) ;
#160980 = CARTESIAN_POINT ( 'NONE',  ( -8.224510206698735004, -14.34966873604973081, 104.5844237280190185 ) ) ;
#160982 = CARTESIAN_POINT ( 'NONE',  ( -5.049401038298153566, 19.05341960407611168, 60.20724293864768129 ) ) ;
#160983 = CARTESIAN_POINT ( 'NONE',  ( 18.67979575497194134, -10.72451020669871369, 25.83442372801901499 ) ) ;
#160984 = CARTESIAN_POINT ( 'NONE',  ( -13.97604488694527625, -13.89961937509977652, 66.87390960531436690 ) ) ;
#160985 = CARTESIAN_POINT ( 'NONE',  ( -4.379528057220328563, 16.55341960407611168, 75.20724293864769550 ) ) ;
#160986 = CARTESIAN_POINT ( 'NONE',  ( 16.55341960407611168, 4.379528057220329451, 48.95724293864770971 ) ) ;
#160987 = CARTESIAN_POINT ( 'NONE',  ( -10.81492255796078084, -18.62759615963271287, 57.08224293864769550 ) ) ;
#160988 = CARTESIAN_POINT ( 'NONE',  ( 5.049401038298161559, -19.05341960407611168, 57.70724293864769550 ) ) ;
#160989 = CARTESIAN_POINT ( 'NONE',  ( -15.80617190586745835, -15.72974639402198527, 66.87390960531436690 ) ) ;
#160990 = CARTESIAN_POINT ( 'NONE',  ( -5.049401038297874678, -19.05341960407617918, 69.79275706135233293 ) ) ;
#160992 = CARTESIAN_POINT ( 'NONE',  ( 0.05219959533910956823, 16.53943276465976808, 74.99890960531435269 ) ) ;
#160991 = CARTESIAN_POINT ( 'NONE',  ( 16.46253265017146816, 9.564922557961045513, 21.66775706135233648 ) ) ;
#160993 = CARTESIAN_POINT ( 'NONE',  ( -18.62759615963270932, 10.81492255796079327, 50.83224293864770971 ) ) ;
#160994 = ORIENTED_EDGE ( 'NONE', *, *, #126809, .F. ) ;
#160995 = CARTESIAN_POINT ( 'NONE',  ( -17.50000000000000711, -5.499999999999956479, 36.28230962303565121 ) ) ;
#160997 = CARTESIAN_POINT ( 'NONE',  ( 27.73933785331498925, -9.013057229001034898, 148.2750000027311614 ) ) ;
#160996 = CARTESIAN_POINT ( 'NONE',  ( -14.34966873604972548, 8.224510206698743886, 93.33442372801901854 ) ) ;
#160998 = EDGE_CURVE ( 'NONE', #37352, #31966, #66207, .T. ) ;
#160999 = CARTESIAN_POINT ( 'NONE',  ( 16.51473224551083163, -9.474510206698727899, 85.83442372801900433 ) ) ;
#161000 = CARTESIAN_POINT ( 'NONE',  ( -0.05219959533910754901, -16.53943276465976808, 62.49890960531436690 ) ) ;
#161001 = FACE_OUTER_BOUND ( 'NONE', #128168, .T. ) ;
#161002 = CARTESIAN_POINT ( 'NONE',  ( -16.46253265017160317, 9.564922557960807481, 65.83224293864769550 ) ) ;
#161003 = CARTESIAN_POINT ( 'NONE',  ( 16.52544592524342804, -4.483927247898539470, 58.54057627198103120 ) ) ;
#161004 = CARTESIAN_POINT ( 'NONE',  ( 16.51473224551069308, 9.474510206698969483, 84.16557627198102409 ) ) ;
#161006 = CARTESIAN_POINT ( 'NONE',  ( 9.474510206698971260, -16.51473224551069308, 57.91557627198103120 ) ) ;
#161005 = CARTESIAN_POINT ( 'NONE',  ( 9.564922557961047289, -16.46253265017146816, 75.41775706135234714 ) ) ;
#161007 = CARTESIAN_POINT ( 'NONE',  ( 5.049401038298161559, -19.05341960407611168, 82.70724293864770971 ) ) ;
#161008 = CARTESIAN_POINT ( 'NONE',  ( -13.97604488694527625, -13.89961937509977652, 71.87390960531433848 ) ) ;
#161009 = CARTESIAN_POINT ( 'NONE',  ( 10.81492255796078972, 18.62759615963270932, 59.58224293864770260 ) ) ;
#161010 = SPHERICAL_SURFACE ( 'NONE', #42003, 2.000000000000000000 ) ;
#161011 = CARTESIAN_POINT ( 'NONE',  ( 19.02544592524343514, -5.153800228976328945, 53.54057627198102409 ) ) ;
#161012 = CARTESIAN_POINT ( 'NONE',  ( -15.72974639402197994, 15.80617190586746368, 55.62390960531436690 ) ) ;
#161013 = CARTESIAN_POINT ( 'NONE',  ( 5.153800228976615827, -19.02544592524334988, 85.20942372801900433 ) ) ;
#161014 = CARTESIAN_POINT ( 'NONE',  ( 4.379528057220092307, 16.55341960407617563, 112.2927570613523471 ) ) ;
#161015 = CARTESIAN_POINT ( 'NONE',  ( 9.564922557961047289, -16.46253265017146816, 40.41775706135234003 ) ) ;
#161017 = CARTESIAN_POINT ( 'NONE',  ( -16.55341960407617563, 4.379528057220093196, 88.54275706135236135 ) ) ;
#161016 = CARTESIAN_POINT ( 'NONE',  ( 16.55341960407618274, -4.379528057220086978, 66.04275706135236135 ) ) ;
#161018 = CARTESIAN_POINT ( 'NONE',  ( 26.79475375365586132, 2.756753960551091991E-14, 155.0000000000000000 ) ) ;
#161019 = CARTESIAN_POINT ( 'NONE',  ( 16.55341960407618274, -4.379528057220086978, 81.04275706135236135 ) ) ;
#161020 = CARTESIAN_POINT ( 'NONE',  ( -0.05219959533907301413, -21.53943276465977519, 27.49890960531435269 ) ) ;
#161021 = CARTESIAN_POINT ( 'NONE',  ( 19.05341960407611168, 5.049401038298154454, 28.95724293864769550 ) ) ;
#161022 = CARTESIAN_POINT ( 'NONE',  ( 9.474510206698971260, -16.51473224551069308, 47.91557627198102409 ) ) ;
#161023 = CARTESIAN_POINT ( 'NONE',  ( -13.89961937509977652, 13.97604488694528158, 40.62390960531435979 ) ) ;
#161024 = CARTESIAN_POINT ( 'NONE',  ( -18.67979575497193778, 10.72451020669871902, 33.33442372801900433 ) ) ;
#161025 = CARTESIAN_POINT ( 'NONE',  ( -0.05219959533934338120, 16.53943276465976808, 52.50109039468567573 ) ) ;
#161026 = CARTESIAN_POINT ( 'NONE',  ( 4.379528057220339221, -16.55341960407611168, 22.70724293864769194 ) ) ;
#161027 = CARTESIAN_POINT ( 'NONE',  ( -16.51473224551069308, -9.474510206698971260, 31.66557627198102054 ) ) ;
#161028 = CARTESIAN_POINT ( 'NONE',  ( 5.049401038297881783, 19.05341960407617563, 22.29275706135233648 ) ) ;
#161029 = CARTESIAN_POINT ( 'NONE',  ( -13.97604488694547697, 13.89961937509957934, 108.1260903946856331 ) ) ;
#161030 = CARTESIAN_POINT ( 'NONE',  ( -16.46253265017146816, -9.564922557961047289, 69.16775706135233293 ) ) ;
#161031 = CARTESIAN_POINT ( 'NONE',  ( -8.224510206698948167, 14.34966873604960824, 75.41557627198102409 ) ) ;
#161032 = CARTESIAN_POINT ( 'NONE',  ( 13.89961937509977652, -13.97604488694527269, 43.12390960531434558 ) ) ;
#161034 = DIRECTION ( 'NONE',  ( -0.000000000000000000, -0.000000000000000000, 1.000000000000000000 ) ) ;
#161033 = CARTESIAN_POINT ( 'NONE',  ( -16.51473224551082808, 9.474510206698731452, 68.33442372801900433 ) ) ;
#161035 = CARTESIAN_POINT ( 'NONE',  ( 5.719274019375673035, 21.55341960407619339, 82.29275706135234714 ) ) ;
#161036 = CARTESIAN_POINT ( 'NONE',  ( -4.483927247898782831, 16.52544592524335698, 42.70942372801901854 ) ) ;
#161037 = CARTESIAN_POINT ( 'NONE',  ( 17.97161686094261768, -5.499999999999982236, 73.49637206859250682 ) ) ;
#161038 = CARTESIAN_POINT ( 'NONE',  ( 21.55341960407610458, 5.719274019375980345, 33.95724293864769550 ) ) ;
#161039 = CARTESIAN_POINT ( 'NONE',  ( 12.14591786802327356, -12.06949235617739191, 25.62609039468567929 ) ) ;
#161040 = CARTESIAN_POINT ( 'NONE',  ( -19.02544592524342804, 5.153800228976336051, 116.0405762719810383 ) ) ;
#161041 = CARTESIAN_POINT ( 'NONE',  ( -26.73207562759454703, 6.543912086049501475, 168.7462576975894422 ) ) ;
#161042 = CARTESIAN_POINT ( 'NONE',  ( -13.97604488694527625, -13.89961937509977652, 36.87390960531436690 ) ) ;
#161043 = CARTESIAN_POINT ( 'NONE',  ( -0.05219959533936034679, 19.03943276465977164, 57.50109039468566863 ) ) ;
#161044 = CARTESIAN_POINT ( 'NONE',  ( 16.46253265017160672, -9.564922557960803928, 53.33224293864768839 ) ) ;
#161045 = CARTESIAN_POINT ( 'NONE',  ( -18.67979575497193778, 10.72451020669871902, 63.33442372801900433 ) ) ;
#161046 = CARTESIAN_POINT ( 'NONE',  ( 9.564922557961047289, -16.46253265017146816, 20.41775706135233293 ) ) ;
#161047 = CARTESIAN_POINT ( 'NONE',  ( 16.55341960407611168, 4.379528057220329451, 23.95724293864769550 ) ) ;
#161048 = CARTESIAN_POINT ( 'NONE',  ( 13.97604488694527802, 13.89961937509977652, 34.37390960531436690 ) ) ;
#161049 = CARTESIAN_POINT ( 'NONE',  ( 13.97604488694527802, 13.89961937509977652, 94.37390960531436690 ) ) ;
#161050 = CARTESIAN_POINT ( 'NONE',  ( 5.719274019375673035, 21.55341960407619339, 52.29275706135236135 ) ) ;
#161051 = CARTESIAN_POINT ( 'NONE',  ( 9.474510206698971260, -16.51473224551069308, 32.91557627198102409 ) ) ;
#161052 = CARTESIAN_POINT ( 'NONE',  ( 10.81492255796106328, -18.62759615963255655, 70.41775706135236135 ) ) ;
#161054 = CARTESIAN_POINT ( 'NONE',  ( 19.03943276465977164, -0.05219959533909143690, 103.7489096053143669 ) ) ;
#161053 = CARTESIAN_POINT ( 'NONE',  ( -13.97604488694547697, 13.89961937509957934, 93.12609039468566152 ) ) ;
#161055 = CARTESIAN_POINT ( 'NONE',  ( -16.52544592524342804, 4.483927247898546575, 116.0405762719810383 ) ) ;
#161056 = CARTESIAN_POINT ( 'NONE',  ( -5.719274019375978568, 21.55341960407610458, 115.2072429386476955 ) ) ;
#161057 = CARTESIAN_POINT ( 'NONE',  ( -19.02544592524334988, -5.153800228976617603, 33.95942372801897591 ) ) ;
#161058 = CARTESIAN_POINT ( 'NONE',  ( 8.224510206698953496, -14.34966873604960469, 107.9155762719810241 ) ) ;
#161059 = CARTESIAN_POINT ( 'NONE',  ( 13.97604488694527802, 13.89961937509977652, 64.37390960531436690 ) ) ;
#161060 = CARTESIAN_POINT ( 'NONE',  ( -5.153800228976607833, 19.02544592524334988, 97.70942372801900433 ) ) ;
#161061 = CARTESIAN_POINT ( 'NONE',  ( 16.52544592524342804, -4.483927247898539470, 58.54057627198103120 ) ) ;
#161062 = CARTESIAN_POINT ( 'NONE',  ( 9.474510206698729675, 16.51473224551082808, 22.08442372801899722 ) ) ;
#161063 = CARTESIAN_POINT ( 'NONE',  ( 21.53943276465977519, -0.05219959533907433946, 23.74890960531435269 ) ) ;
#161064 = CARTESIAN_POINT ( 'NONE',  ( -13.97604488694547697, 13.89961937509957934, 88.12609039468563310 ) ) ;
#161065 = CARTESIAN_POINT ( 'NONE',  ( -10.72451020669898014, 18.67979575497178502, 90.41557627198103830 ) ) ;
#161066 = CARTESIAN_POINT ( 'NONE',  ( 21.55341960407619695, -5.719274019375665929, 46.04275706135234714 ) ) ;
#161067 = CARTESIAN_POINT ( 'NONE',  ( 8.314922557961029526, -14.29746914071037800, 40.41775706135234714 ) ) ;
#161068 = CARTESIAN_POINT ( 'NONE',  ( -0.05219959533934338120, 16.53943276465976808, 107.5010903946856899 ) ) ;
#161070 = CARTESIAN_POINT ( 'NONE',  ( -21.55341960407619339, 5.719274019375674811, 48.54275706135234714 ) ) ;
#161069 = CARTESIAN_POINT ( 'NONE',  ( -16.53943276465976808, -0.05219959533934237506, 38.75109039468567573 ) ) ;
#161071 = CARTESIAN_POINT ( 'NONE',  ( 5.719274019375991003, -21.55341960407610458, 52.70724293864769550 ) ) ;
#161072 = CARTESIAN_POINT ( 'NONE',  ( 5.153800228976335163, 19.02544592524342804, 29.79057627198102409 ) ) ;
#161073 = CARTESIAN_POINT ( 'NONE',  ( 30.74264578624799782, 22.33583958711400541, -4.549999994537627046 ) ) ;
#161074 = CARTESIAN_POINT ( 'NONE',  ( 12.14591786802327356, -12.06949235617739191, 80.62609039468567573 ) ) ;
#161075 = CARTESIAN_POINT ( 'NONE',  ( 18.67979575497178502, 10.72451020669898547, 94.16557627198103830 ) ) ;
#161076 = CARTESIAN_POINT ( 'NONE',  ( 12.14591786802309770, 12.06949235617756955, 34.37390960531435979 ) ) ;
#161077 = CARTESIAN_POINT ( 'NONE',  ( 16.52544592524335698, 4.483927247898782831, 61.45942372801901854 ) ) ;
#161078 = CARTESIAN_POINT ( 'NONE',  ( 13.89961937509957401, 13.97604488694547697, 106.8760903946856757 ) ) ;
#161079 = CARTESIAN_POINT ( 'NONE',  ( 15.72974639402199770, -15.80617190586745480, 103.1239096053143811 ) ) ;
#161080 = CARTESIAN_POINT ( 'NONE',  ( -8.224510206698948167, 14.34966873604960824, 25.41557627198103120 ) ) ;
#161081 = ORIENTED_EDGE ( 'NONE', *, *, #158766, .T. ) ;
#161082 = CARTESIAN_POINT ( 'NONE',  ( -8.314922557961024197, 14.29746914071037800, 82.91775706135234714 ) ) ;
#161083 = CARTESIAN_POINT ( 'NONE',  ( 26.45594755429568323, 8.318738267476192050, 167.5492909577866385 ) ) ;
#161084 = CARTESIAN_POINT ( 'NONE',  ( -21.55341960407610458, -5.719274019375992779, 71.45724293864769550 ) ) ;
#161085 = CARTESIAN_POINT ( 'NONE',  ( 0.05219959533934541429, -16.53943276465976808, 100.0010903946857042 ) ) ;
#161086 = ORIENTED_EDGE ( 'NONE', *, *, #167192, .F. ) ;
#161087 = CARTESIAN_POINT ( 'NONE',  ( 19.35543954521079968, 5.499999999999572786, 87.08901960356450900 ) ) ;
#161088 = CARTESIAN_POINT ( 'NONE',  ( 15.80617190586746368, 15.72974639402197994, 94.37390960531436690 ) ) ;
#161089 = CARTESIAN_POINT ( 'NONE',  ( -5.719274019375978568, 21.55341960407610458, 105.2072429386477097 ) ) ;
#161090 = CARTESIAN_POINT ( 'NONE',  ( -16.52544592524342804, 4.483927247898546575, 41.04057627198103120 ) ) ;
#161091 = CARTESIAN_POINT ( 'NONE',  ( -12.14591786802326823, 12.06949235617739902, 38.12609039468567573 ) ) ;
#161092 = CARTESIAN_POINT ( 'NONE',  ( -19.02544592524342804, 5.153800228976336051, 46.04057627198101699 ) ) ;
#161093 = CARTESIAN_POINT ( 'NONE',  ( -9.474510206698964154, 16.51473224551069663, 60.41557627198102409 ) ) ;
#161094 = ORIENTED_EDGE ( 'NONE', *, *, #99422, .F. ) ;
#161095 = CARTESIAN_POINT ( 'NONE',  ( -9.474510206698964154, 16.51473224551069663, 115.4155762719810241 ) ) ;
#161096 = CARTESIAN_POINT ( 'NONE',  ( 19.02544592524343514, -5.153800228976328945, 113.5405762719810241 ) ) ;
#161097 = CARTESIAN_POINT ( 'NONE',  ( -19.03943276465977164, -0.05219959533935918106, 108.7510903946856615 ) ) ;
#161098 = CARTESIAN_POINT ( 'NONE',  ( 5.049401038297881783, 19.05341960407617563, 57.29275706135231871 ) ) ;
#161099 = CARTESIAN_POINT ( 'NONE',  ( -10.81492255796078084, -18.62759615963271287, 82.08224293864768129 ) ) ;
#161100 = EDGE_CURVE ( 'NONE', #167327, #153996, #126003, .T. ) ;
#161101 = CARTESIAN_POINT ( 'NONE',  ( -8.224510206698948167, 14.34966873604960824, 25.41557627198103120 ) ) ;
#161102 = CARTESIAN_POINT ( 'NONE',  ( -21.53943276465977519, 0.05219959533907696930, 41.24890960531435269 ) ) ;
#161104 = CARTESIAN_POINT ( 'NONE',  ( -9.474510206698720793, -16.51473224551083518, 104.5844237280190043 ) ) ;
#161103 = CARTESIAN_POINT ( 'NONE',  ( -5.823673210054116645, -21.52544592524344225, 77.29057627198102409 ) ) ;
#161105 = CARTESIAN_POINT ( 'NONE',  ( -9.474510206698964154, 16.51473224551069663, 105.4155762719810383 ) ) ;
#161106 = CARTESIAN_POINT ( 'NONE',  ( -0.05219959533937732626, 21.53943276465977519, 72.50109039468568994 ) ) ;
#161107 = CARTESIAN_POINT ( 'NONE',  ( -9.474510206698964154, 16.51473224551069663, 70.41557627198102409 ) ) ;
#161108 = CARTESIAN_POINT ( 'NONE',  ( 31.25082632804103255, 7.456723613865053224, 95.94516017006306186 ) ) ;
#161109 = CARTESIAN_POINT ( 'NONE',  ( 19.05341960407611168, 5.049401038298154454, 73.95724293864768129 ) ) ;
#161110 = CARTESIAN_POINT ( 'NONE',  ( -16.53943276465976808, 0.05219959533911058130, 96.24890960531435269 ) ) ;
#161111 = ORIENTED_EDGE ( 'NONE', *, *, #195501, .T. ) ;
#161112 = CARTESIAN_POINT ( 'NONE',  ( 19.03943276465977164, 0.05219959533936151252, 111.2510903946856757 ) ) ;
#161113 = DIRECTION ( 'NONE',  ( -0.000000000000000000, -0.4999999999999999445, -0.8660254037844387076 ) ) ;
#161114 = CARTESIAN_POINT ( 'NONE',  ( -19.02544592524342804, 5.153800228976336051, 71.04057627198099567 ) ) ;
#161116 = CARTESIAN_POINT ( 'NONE',  ( -9.474510206698964154, 16.51473224551069663, 95.41557627198102409 ) ) ;
#161115 = CARTESIAN_POINT ( 'NONE',  ( -10.72451020669870658, -18.67979575497194134, 79.58442372801903275 ) ) ;
#161117 = CARTESIAN_POINT ( 'NONE',  ( -12.14591786802326823, 12.06949235617739902, 78.12609039468570415 ) ) ;
#161118 = CARTESIAN_POINT ( 'NONE',  ( -16.18388926212238488, -7.379444403734526148, 75.43953151366153520 ) ) ;
#161119 = CARTESIAN_POINT ( 'NONE',  ( 19.05341960407617918, -5.049401038297876454, 51.04275706135231871 ) ) ;
#161120 = CARTESIAN_POINT ( 'NONE',  ( -21.52544592524334988, -5.823673210054445271, 108.9594237280190185 ) ) ;
#161121 = FACE_OUTER_BOUND ( 'NONE', #189446, .T. ) ;
#161122 = FACE_OUTER_BOUND ( 'NONE', #97992, .T. ) ;
#161123 = CARTESIAN_POINT ( 'NONE',  ( -36.91746825000001309, -11.99521256947794789, -5.024999997268813523 ) ) ;
#161124 = CARTESIAN_POINT ( 'NONE',  ( 16.53943276465976808, 0.05219959533934440121, 111.2510903946856899 ) ) ;
#161125 = CARTESIAN_POINT ( 'NONE',  ( -34.91229673954799040, -6.363315211036966623, 41.02293916657588824 ) ) ;
#161126 = CARTESIAN_POINT ( 'NONE',  ( -14.34966873604972548, 8.224510206698743886, 93.33442372801901854 ) ) ;
#161127 = CARTESIAN_POINT ( 'NONE',  ( -31.99364916731038022, -1.130961319012580892E-14, 92.35000000000000853 ) ) ;
#161128 = CARTESIAN_POINT ( 'NONE',  ( 12.06949235617739724, 12.14591786802326823, 61.87609039468568284 ) ) ;
#161129 = CARTESIAN_POINT ( 'NONE',  ( -10.72451020669870658, -18.67979575497194134, 84.58442372801903275 ) ) ;
#161130 = CARTESIAN_POINT ( 'NONE',  ( 5.153800228976615827, -19.02544592524334988, 95.20942372801897591 ) ) ;
#161131 = CARTESIAN_POINT ( 'NONE',  ( -13.89961937509957401, -13.97604488694547875, 39.37609039468566152 ) ) ;
#161132 = CARTESIAN_POINT ( 'NONE',  ( 19.02544592524343514, -5.153800228976328945, 83.54057627198100988 ) ) ;
#161133 = CARTESIAN_POINT ( 'NONE',  ( 13.97604488694527802, 13.89961937509977652, 59.37390960531434558 ) ) ;
#161134 = CARTESIAN_POINT ( 'NONE',  ( 9.474510206698971260, -16.51473224551069308, 87.91557627198102409 ) ) ;
#161135 = CARTESIAN_POINT ( 'NONE',  ( 18.67979575497178502, 10.72451020669898547, 84.16557627198103830 ) ) ;
#161136 = CARTESIAN_POINT ( 'NONE',  ( -21.52544592524343514, 5.823673210054127303, 51.04057627198103120 ) ) ;
#161137 = CARTESIAN_POINT ( 'NONE',  ( 0.05219959533909260263, 19.03943276465977164, 34.99890960531435979 ) ) ;
#161138 = CARTESIAN_POINT ( 'NONE',  ( 14.29746914071037800, 8.314922557961029526, 61.66775706135235424 ) ) ;
#161139 = UNCERTAINTY_MEASURE_WITH_UNIT (LENGTH_MEASURE( 1.000000000000000082E-05 ), #150771, 'distance_accuracy_value', 'NONE');
#161140 = ORIENTED_EDGE ( 'NONE', *, *, #186365, .T. ) ;
#161141 = CARTESIAN_POINT ( 'NONE',  ( -10.81492255796105439, 18.62759615963255655, 42.91775706135235424 ) ) ;
#161143 = CARTESIAN_POINT ( 'NONE',  ( -38.00000000000001421, 12.34694845685046438, -0.09999999999999989453 ) ) ;
#161142 = CARTESIAN_POINT ( 'NONE',  ( -12.06949235617756955, 12.14591786802309770, 65.62390960531436690 ) ) ;
#161144 = CARTESIAN_POINT ( 'NONE',  ( 0.05219959533934541429, -16.53943276465976808, 40.00109039468567573 ) ) ;
#161145 = CARTESIAN_POINT ( 'NONE',  ( -0.05219959533910754901, -16.53943276465976808, 107.4989096053143669 ) ) ;
#161146 = CARTESIAN_POINT ( 'NONE',  ( 19.02544592524334988, 5.153800228976608722, 56.45942372801898301 ) ) ;
#161147 = CARTESIAN_POINT ( 'NONE',  ( 12.14591786802309770, 12.06949235617756955, 59.37390960531436690 ) ) ;
#161148 = CARTESIAN_POINT ( 'NONE',  ( 21.53943276465977519, 0.05219959533937863772, 31.25109039468568639 ) ) ;
#161150 = CARTESIAN_POINT ( 'NONE',  ( -5.823673210054116645, -21.52544592524344225, 92.29057627198103830 ) ) ;
#161149 = CARTESIAN_POINT ( 'NONE',  ( -5.153800228976328057, -19.02544592524343514, 27.29057627198103120 ) ) ;
#161151 = CARTESIAN_POINT ( 'NONE',  ( 16.51473224551069308, 9.474510206698969483, 99.16557627198102409 ) ) ;
#161152 = CARTESIAN_POINT ( 'NONE',  ( -8.314922557960811034, -14.29746914071050412, 77.08224293864769550 ) ) ;
#161153 = CARTESIAN_POINT ( 'NONE',  ( -13.97604488694527625, -13.89961937509977652, 111.8739096053143243 ) ) ;
#161154 = TOROIDAL_SURFACE ( 'NONE', #177347, 4.000000000000000000, 0.2500000000000000000 ) ;
#161155 = CARTESIAN_POINT ( 'NONE',  ( -22.81625015709509441, -31.40387420917324590, -6.324999997268814234 ) ) ;
#161156 = CARTESIAN_POINT ( 'NONE',  ( -16.46253265017146816, -9.564922557961047289, 79.16775706135234714 ) ) ;
#161157 = CARTESIAN_POINT ( 'NONE',  ( -18.62759615963255300, -10.81492255796106328, 24.16775706135235424 ) ) ;
#161158 = CARTESIAN_POINT ( 'NONE',  ( 0.05219959533909260263, 19.03943276465977164, 64.99890960531436690 ) ) ;
#161159 = CARTESIAN_POINT ( 'NONE',  ( -0.05219959533936034679, 19.03943276465977164, 57.50109039468566863 ) ) ;
#161160 = CARTESIAN_POINT ( 'NONE',  ( -19.05341960407611168, -5.049401038298163336, 31.45724293864769550 ) ) ;
#161161 = CARTESIAN_POINT ( 'NONE',  ( -21.52544592524334988, -5.823673210054445271, 68.95942372801901854 ) ) ;
#161162 = DIRECTION ( 'NONE',  ( 0.000000000000000000, 0.000000000000000000, 1.000000000000000000 ) ) ;
#161163 = CARTESIAN_POINT ( 'NONE',  ( 0.05219959533910956823, 16.53943276465976808, 54.99890960531435269 ) ) ;
#161164 = CARTESIAN_POINT ( 'NONE',  ( -16.46253265017160317, 9.564922557960807481, 60.83224293864769550 ) ) ;
#161165 = CARTESIAN_POINT ( 'NONE',  ( 5.719274019375991003, -21.55341960407610458, 82.70724293864770971 ) ) ;
#161166 = CARTESIAN_POINT ( 'NONE',  ( 19.05341960407611168, 5.049401038298154454, 58.95724293864768129 ) ) ;
#161167 = CARTESIAN_POINT ( 'NONE',  ( 21.55341960407610458, 5.719274019375980345, 83.95724293864770971 ) ) ;
#161168 = CARTESIAN_POINT ( 'NONE',  ( -15.72974639402176322, -15.80617190586768395, 94.37609039468568994 ) ) ;
#161171 = CARTESIAN_POINT ( 'NONE',  ( 16.53943276465976808, -0.05219959533910856209, 98.74890960531438111 ) ) ;
#161170 = CARTESIAN_POINT ( 'NONE',  ( -12.06949235617739369, -12.14591786802326823, 99.37609039468568994 ) ) ;
#161169 = CARTESIAN_POINT ( 'NONE',  ( -19.02544592524342804, 5.153800228976336051, 26.04057627198103120 ) ) ;
#161172 = CARTESIAN_POINT ( 'NONE',  ( -19.02544592524334988, -5.153800228976617603, 93.95942372801900433 ) ) ;
#161173 = ORIENTED_EDGE ( 'NONE', *, *, #1535, .F. ) ;
#161174 = CARTESIAN_POINT ( 'NONE',  ( -18.67979575497193778, 10.72451020669871902, 23.33442372801901499 ) ) ;
#161175 = CARTESIAN_POINT ( 'NONE',  ( 13.97604488694548053, -13.89961937509957401, 50.62609039468566152 ) ) ;
#161176 = CARTESIAN_POINT ( 'NONE',  ( -8.224510206698735004, -14.34966873604973081, 104.5844237280190185 ) ) ;
#161177 = ADVANCED_FACE ( 'NONE', ( #184000, #45483, #180055 ), #44498, .F. ) ;
#161178 = CARTESIAN_POINT ( 'NONE',  ( 13.97604488694548053, -13.89961937509957401, 25.62609039468566507 ) ) ;
#161179 = CARTESIAN_POINT ( 'NONE',  ( -13.97604488694527625, -13.89961937509977652, 106.8739096053143669 ) ) ;
#161180 = CARTESIAN_POINT ( 'NONE',  ( 5.719274019375991003, -21.55341960407610458, 62.70724293864769550 ) ) ;
#161181 = CARTESIAN_POINT ( 'NONE',  ( -24.84743926645693080, 12.91388972341062136, 166.0204189386425639 ) ) ;
#161182 = CARTESIAN_POINT ( 'NONE',  ( 14.34966873604960469, 8.224510206698951720, 114.1655762719810383 ) ) ;
#161183 = CARTESIAN_POINT ( 'NONE',  ( -21.55341960407619339, 5.719274019375674811, 108.5427570613523756 ) ) ;
#161184 = CARTESIAN_POINT ( 'NONE',  ( 12.14591786802327356, -12.06949235617739191, 75.62609039468567573 ) ) ;
#161185 = CARTESIAN_POINT ( 'NONE',  ( -0.05219959533937732626, 21.53943276465977519, 32.50109039468568284 ) ) ;
#161186 = CARTESIAN_POINT ( 'NONE',  ( -16.52544592524335698, -4.483927247898792601, 38.95942372801901854 ) ) ;
#161187 = CARTESIAN_POINT ( 'NONE',  ( 13.97604488694527802, 13.89961937509977652, 104.3739096053143385 ) ) ;
#161188 = CARTESIAN_POINT ( 'NONE',  ( -19.03943276465977164, 0.05219959533909376836, 41.24890960531435269 ) ) ;
#161189 = CARTESIAN_POINT ( 'NONE',  ( -13.97604488694527625, -13.89961937509977652, 61.87390960531435979 ) ) ;
#161190 = CARTESIAN_POINT ( 'NONE',  ( 14.34966873604972726, -8.224510206698740333, 40.83442372801901854 ) ) ;
#161191 = CARTESIAN_POINT ( 'NONE',  ( -4.483927247898539470, -16.52544592524342804, 92.29057627198103830 ) ) ;
#161192 = CARTESIAN_POINT ( 'NONE',  ( 4.379528057220092307, 16.55341960407617563, 102.2927570613523613 ) ) ;
#161193 = CARTESIAN_POINT ( 'NONE',  ( 5.153800228976335163, 19.02544592524342804, 49.79057627198101699 ) ) ;
#161196 = CARTESIAN_POINT ( 'NONE',  ( 16.51473224551069308, 9.474510206698969483, 69.16557627198102409 ) ) ;
#161195 = CARTESIAN_POINT ( 'NONE',  ( -19.05341960407611168, -5.049401038298163336, 76.45724293864769550 ) ) ;
#161194 = CARTESIAN_POINT ( 'NONE',  ( -0.05219959533937732626, 21.53943276465977519, 52.50109039468567573 ) ) ;
#161198 = ADVANCED_FACE ( 'NONE', ( #119359 ), #135528, .T. ) ;
#161197 = CARTESIAN_POINT ( 'NONE',  ( -13.89961937509977652, 13.97604488694528158, 100.6239096053143669 ) ) ;
#161199 = CARTESIAN_POINT ( 'NONE',  ( 14.34966873604960469, 8.224510206698951720, 49.16557627198102409 ) ) ;
#161200 = CARTESIAN_POINT ( 'NONE',  ( -16.53943276465976808, -0.05219959533934237506, 103.7510903946857042 ) ) ;
#161201 = CARTESIAN_POINT ( 'NONE',  ( -16.53943276465976808, -0.05219959533934237506, 113.7510903946856757 ) ) ;
#161202 = VERTEX_POINT ( 'NONE', #164868 ) ;
#161203 = CARTESIAN_POINT ( 'NONE',  ( -19.02544592524334988, -5.153800228976617603, 43.95942372801899012 ) ) ;
#161204 = CARTESIAN_POINT ( 'NONE',  ( -5.153800228976328057, -19.02544592524343514, 112.2905762719810099 ) ) ;
#161205 = CARTESIAN_POINT ( 'NONE',  ( 16.46253265017160672, -9.564922557960803928, 63.33224293864769550 ) ) ;
#161206 = CARTESIAN_POINT ( 'NONE',  ( -16.51473224551082808, 9.474510206698731452, 38.33442372801899722 ) ) ;
#161207 = CARTESIAN_POINT ( 'NONE',  ( 11.40812507854754365, 35.11059874428196537, -7.224999997268813701 ) ) ;
#161208 = CARTESIAN_POINT ( 'NONE',  ( -27.49873734152928151, -21.99873734152901861, 1.818019484660534424 ) ) ;
#161210 = CARTESIAN_POINT ( 'NONE',  ( 8.314922557961029526, -14.29746914071037800, 70.41775706135236135 ) ) ;
#161209 = CARTESIAN_POINT ( 'NONE',  ( 0.05219959533936267826, -19.03943276465977164, 90.00109039468567573 ) ) ;
#161211 = CARTESIAN_POINT ( 'NONE',  ( 17.05116617787825462, 6.768360034955822613, 93.84324446740806991 ) ) ;
#161212 = CARTESIAN_POINT ( 'NONE',  ( 0.05219959533909260263, 19.03943276465977164, 84.99890960531436690 ) ) ;
#161213 = CARTESIAN_POINT ( 'NONE',  ( -10.81492255796105439, 18.62759615963255655, 32.91775706135234714 ) ) ;
#161214 = CARTESIAN_POINT ( 'NONE',  ( 13.97604488694548053, -13.89961937509957401, 70.62609039468567573 ) ) ;
#161216 = CARTESIAN_POINT ( 'NONE',  ( 5.153800228976335163, 19.02544592524342804, 29.79057627198102409 ) ) ;
#161215 = CARTESIAN_POINT ( 'NONE',  ( -3.573655867282028392E-15, 2.428612866367529932E-14, -25.00000000000000000 ) ) ;
#161217 = CARTESIAN_POINT ( 'NONE',  ( 19.03943276465977164, -0.05219959533909143690, 88.74890960531436690 ) ) ;
#161219 = CARTESIAN_POINT ( 'NONE',  ( -13.97604488694527625, -13.89961937509977652, 36.87390960531436690 ) ) ;
#161218 = CARTESIAN_POINT ( 'NONE',  ( 16.52544592524342804, -4.483927247898539470, 53.54057627198103120 ) ) ;
#161220 = CARTESIAN_POINT ( 'NONE',  ( 16.51473224551083163, -9.474510206698727899, 45.83442372801900433 ) ) ;
#161221 = ORIENTED_EDGE ( 'NONE', *, *, #85188, .T. ) ;
#161222 = CARTESIAN_POINT ( 'NONE',  ( -16.55341960407611168, -4.379528057220339221, 86.45724293864770971 ) ) ;
#161223 = CARTESIAN_POINT ( 'NONE',  ( 19.02544592524334988, 5.153800228976608722, 36.45942372801900433 ) ) ;
#161224 = CARTESIAN_POINT ( 'NONE',  ( 5.153800228976335163, 19.02544592524342804, 69.79057627198103830 ) ) ;
#161225 = CARTESIAN_POINT ( 'NONE',  ( -5.719274019375978568, 21.55341960407610458, 65.20724293864768129 ) ) ;
#161227 = CARTESIAN_POINT ( 'NONE',  ( 10.72451020669871369, 18.67979575497193778, 112.0844237280190185 ) ) ;
#161226 = CARTESIAN_POINT ( 'NONE',  ( 12.06949235617757843, -12.14591786802309237, 58.12390960531435979 ) ) ;
#161228 = CARTESIAN_POINT ( 'NONE',  ( -5.049401038298153566, 19.05341960407611168, 110.2072429386476671 ) ) ;
#161229 = CARTESIAN_POINT ( 'NONE',  ( 15.72974639402199770, -15.80617190586745480, 23.12390960531436335 ) ) ;
#161230 = CARTESIAN_POINT ( 'NONE',  ( 9.564922557960805705, 16.46253265017160317, 54.58224293864769550 ) ) ;
#161231 = CARTESIAN_POINT ( 'NONE',  ( -16.53943276465976808, 0.05219959533911058130, 116.2489096053143669 ) ) ;
#161232 = CARTESIAN_POINT ( 'NONE',  ( -0.05219959533910754901, -16.53943276465976808, 92.49890960531436690 ) ) ;
#161233 = CARTESIAN_POINT ( 'NONE',  ( 5.719274019375991003, -21.55341960407610458, 102.7072429386476955 ) ) ;
#161234 = CARTESIAN_POINT ( 'NONE',  ( 0.05219959533909260263, 19.03943276465977164, 104.9989096053143669 ) ) ;
#161235 = CARTESIAN_POINT ( 'NONE',  ( -18.62759615963270932, 10.81492255796079327, 105.8322429386476955 ) ) ;
#161236 = CARTESIAN_POINT ( 'NONE',  ( -13.97604488694527625, -13.89961937509977652, 106.8739096053143669 ) ) ;
#161237 = CARTESIAN_POINT ( 'NONE',  ( -0.05219959533909027116, -19.03943276465977164, 27.49890960531435624 ) ) ;
#161238 = CARTESIAN_POINT ( 'NONE',  ( 5.823673210054444382, -21.52544592524334988, 75.20942372801901854 ) ) ;
#161239 = CARTESIAN_POINT ( 'NONE',  ( -18.62759615963270932, 10.81492255796079327, 95.83224293864770971 ) ) ;
#161240 = CARTESIAN_POINT ( 'NONE',  ( 17.44279575226824974, -5.990770900252421427, 108.3355756751431898 ) ) ;
#161241 = CARTESIAN_POINT ( 'NONE',  ( -17.49999999999999645, 5.500000000000001776, 103.7176903769643701 ) ) ;
#161242 = CARTESIAN_POINT ( 'NONE',  ( 31.90000000000003411, 0.000000000000000000, -49.13275782002545355 ) ) ;
#161243 = CARTESIAN_POINT ( 'NONE',  ( -8.314922557961024197, 14.29746914071037800, 52.91775706135235424 ) ) ;
#161244 = CARTESIAN_POINT ( 'NONE',  ( 16.53943276465976808, -0.05219959533910856209, 108.7489096053143669 ) ) ;
#161245 = DIRECTION ( 'NONE',  ( -0.000000000000000000, -0.000000000000000000, 1.000000000000000000 ) ) ;
#161246 = CARTESIAN_POINT ( 'NONE',  ( 5.049401038298161559, -19.05341960407611168, 52.70724293864767418 ) ) ;
#161247 = CARTESIAN_POINT ( 'NONE',  ( 8.314922557960818139, 14.29746914071049879, 89.58224293864768129 ) ) ;
#161248 = CARTESIAN_POINT ( 'NONE',  ( -15.72974639402197994, 15.80617190586746368, 30.62390960531436335 ) ) ;
#161249 = CARTESIAN_POINT ( 'NONE',  ( -8.314922557960811034, -14.29746914071050412, 72.08224293864769550 ) ) ;
#161250 = CARTESIAN_POINT ( 'NONE',  ( -12.14591786802326823, 12.06949235617739902, 23.12609039468567573 ) ) ;
#161251 = CARTESIAN_POINT ( 'NONE',  ( 21.55341960407619695, -5.719274019375665929, 71.04275706135234714 ) ) ;
#161252 = CARTESIAN_POINT ( 'NONE',  ( 17.48847506799967988, -5.747544572773781724, 78.32697437843279431 ) ) ;
#161253 = CARTESIAN_POINT ( 'NONE',  ( 21.53943276465977519, -0.05219959533907433946, 23.74890960531435269 ) ) ;
#161254 = CARTESIAN_POINT ( 'NONE',  ( -12.14591786802326823, 12.06949235617739902, 98.12609039468570415 ) ) ;
#161255 = CARTESIAN_POINT ( 'NONE',  ( 0.05219959533909260263, 19.03943276465977164, 34.99890960531435979 ) ) ;
#161256 = CARTESIAN_POINT ( 'NONE',  ( 9.474510206698971260, -16.51473224551069308, 87.91557627198102409 ) ) ;
#161257 = CARTESIAN_POINT ( 'NONE',  ( -10.72451020669898014, 18.67979575497178502, 100.4155762719810241 ) ) ;
#161258 = CARTESIAN_POINT ( 'NONE',  ( -16.52544592524335698, -4.483927247898792601, 23.95942372801901143 ) ) ;
#161260 = CARTESIAN_POINT ( 'NONE',  ( 21.52544592524334988, 5.823673210054432836, 76.45942372801901854 ) ) ;
#161259 = CARTESIAN_POINT ( 'NONE',  ( 12.14591786802309770, 12.06949235617756955, 59.37390960531436690 ) ) ;
#161261 = CARTESIAN_POINT ( 'NONE',  ( -14.34966873604972548, 8.224510206698743886, 93.33442372801901854 ) ) ;
#161262 = CARTESIAN_POINT ( 'NONE',  ( 16.36317988757094710, -7.306389748694845920, 46.59789608363175262 ) ) ;
#161263 = CARTESIAN_POINT ( 'NONE',  ( -19.25918095147780207, -5.499999999999585221, 64.45284276293934056 ) ) ;
#161264 = CARTESIAN_POINT ( 'NONE',  ( 16.55341960407611168, 4.379528057220329451, 28.95724293864769905 ) ) ;
#161265 = CARTESIAN_POINT ( 'NONE',  ( 4.379528057220092307, 16.55341960407617563, 72.29275706135236135 ) ) ;
#161266 = CARTESIAN_POINT ( 'NONE',  ( -9.474510206698964154, 16.51473224551069663, 80.41557627198103830 ) ) ;
#161267 = CARTESIAN_POINT ( 'NONE',  ( -13.89961937509977652, 13.97604488694528158, 90.62390960531432427 ) ) ;
#161268 = CARTESIAN_POINT ( 'NONE',  ( -21.55341960407619339, 5.719274019375674811, 88.54275706135236135 ) ) ;
#161269 = CARTESIAN_POINT ( 'NONE',  ( 0.05219959533934541429, -16.53943276465976808, 85.00109039468568994 ) ) ;
#161270 = CARTESIAN_POINT ( 'NONE',  ( -12.06949235617756955, 12.14591786802309770, 60.62390960531437401 ) ) ;
#161271 = CARTESIAN_POINT ( 'NONE',  ( -9.564922557960796823, -16.46253265017161027, 62.08224293864769550 ) ) ;
#161272 = EDGE_LOOP ( 'NONE', ( #33365, #55965, #71325, #31870 ) ) ;
#161273 = CARTESIAN_POINT ( 'NONE',  ( 19.05341960407617918, -5.049401038297876454, 111.0427570613523329 ) ) ;
#161274 = CARTESIAN_POINT ( 'NONE',  ( -19.03943276465977164, 0.05219959533909376836, 21.24890960531436335 ) ) ;
#161275 = CARTESIAN_POINT ( 'NONE',  ( -13.97604488694527625, -13.89961937509977652, 81.87390960531436690 ) ) ;
#161277 = CARTESIAN_POINT ( 'NONE',  ( 38.00000000000000000, 12.34694845685046616, -0.9000000000000000222 ) ) ;
#161276 = CARTESIAN_POINT ( 'NONE',  ( 16.46253265017146816, 9.564922557961045513, 111.6677570613523329 ) ) ;
#161278 = CARTESIAN_POINT ( 'NONE',  ( 5.049401038297881783, 19.05341960407617563, 27.29275706135232937 ) ) ;
#161279 = CARTESIAN_POINT ( 'NONE',  ( 14.34966873604972726, -8.224510206698740333, 80.83442372801901854 ) ) ;
#161280 = CARTESIAN_POINT ( 'NONE',  ( 13.89961937509957401, 13.97604488694547697, 91.87609039468567573 ) ) ;
#161281 = CARTESIAN_POINT ( 'NONE',  ( -19.05341960407611168, -5.049401038298163336, 21.45724293864768839 ) ) ;
#161282 = CARTESIAN_POINT ( 'NONE',  ( 12.14591786802327356, -12.06949235617739191, 60.62609039468567573 ) ) ;
#161283 = CARTESIAN_POINT ( 'NONE',  ( 8.314922557961029526, -14.29746914071037800, 55.41775706135234714 ) ) ;
#161284 = CARTESIAN_POINT ( 'NONE',  ( 4.500000000000000888, -126.1226662136678272, 8.481152457036383652 ) ) ;
#161285 = CARTESIAN_POINT ( 'NONE',  ( 9.564922557961047289, -16.46253265017146816, 50.41775706135233293 ) ) ;
#161286 = CARTESIAN_POINT ( 'NONE',  ( -10.81492255796105439, 18.62759615963255655, 102.9177570613523756 ) ) ;
#161287 = CARTESIAN_POINT ( 'NONE',  ( 16.46253265017160672, -9.564922557960803928, 38.33224293864768839 ) ) ;
#161288 = CARTESIAN_POINT ( 'NONE',  ( 13.89961937509977652, -13.97604488694527269, 83.12390960531436690 ) ) ;
#161289 = CARTESIAN_POINT ( 'NONE',  ( 14.29746914071049879, -8.314922557960816363, 78.33224293864770971 ) ) ;
#161290 = CARTESIAN_POINT ( 'NONE',  ( 10.81492255796106328, -18.62759615963255655, 85.41775706135236135 ) ) ;
#161291 = CARTESIAN_POINT ( 'NONE',  ( -16.46253265017146816, -9.564922557961047289, 64.16775706135233293 ) ) ;
#161292 = CARTESIAN_POINT ( 'NONE',  ( 19.02544592524334988, 5.153800228976608722, 46.45942372801899012 ) ) ;
#161293 = CARTESIAN_POINT ( 'NONE',  ( -21.52544592524343514, 5.823673210054127303, 41.04057627198103120 ) ) ;
#161294 = CARTESIAN_POINT ( 'NONE',  ( 21.53943276465977519, 0.05219959533937863772, 101.2510903946856757 ) ) ;
#161295 = CARTESIAN_POINT ( 'NONE',  ( 19.02544592524343514, -5.153800228976328945, 83.54057627198100988 ) ) ;
#161296 = CARTESIAN_POINT ( 'NONE',  ( 21.55341960407619695, -5.719274019375665929, 101.0427570613523756 ) ) ;
#161297 = CARTESIAN_POINT ( 'NONE',  ( 10.72451020669898902, -18.67979575497178502, 47.91557627198102409 ) ) ;
#161298 = CARTESIAN_POINT ( 'NONE',  ( 5.153800228976335163, 19.02544592524342804, 94.79057627198103830 ) ) ;
#161299 = CARTESIAN_POINT ( 'NONE',  ( 19.02544592524334988, 5.153800228976608722, 81.45942372801897591 ) ) ;
#161300 = CARTESIAN_POINT ( 'NONE',  ( -19.03943276465977164, 0.05219959533909376836, 101.2489096053143669 ) ) ;
#161301 = ADVANCED_FACE ( 'NONE', ( #26363 ), #43506, .F. ) ;
#161302 = CARTESIAN_POINT ( 'NONE',  ( -9.564922557961040184, 16.46253265017147172, 97.91775706135233293 ) ) ;
#161303 = CARTESIAN_POINT ( 'NONE',  ( -16.55341960407617563, 4.379528057220093196, 38.54275706135234714 ) ) ;
#161304 = CARTESIAN_POINT ( 'NONE',  ( -8.314922557960811034, -14.29746914071050412, 102.0822429386476955 ) ) ;
#161305 = CARTESIAN_POINT ( 'NONE',  ( -19.05341960407611168, -5.049401038298163336, 86.45724293864769550 ) ) ;
#161306 = CARTESIAN_POINT ( 'NONE',  ( -18.62759615963270932, 10.81492255796079327, 60.83224293864769550 ) ) ;
#161307 = CIRCLE ( 'NONE', #61133, 8.000000000000000000 ) ;
#161308 = CARTESIAN_POINT ( 'NONE',  ( -8.224510206698735004, -14.34966873604973081, 34.58442372801900433 ) ) ;
#161309 = CARTESIAN_POINT ( 'NONE',  ( 15.72974639402176855, 15.80617190586768217, 31.87609039468567929 ) ) ;
#161310 = CARTESIAN_POINT ( 'NONE',  ( 10.81492255796106328, -18.62759615963255655, 90.41775706135236135 ) ) ;
#161311 = CARTESIAN_POINT ( 'NONE',  ( 14.29746914071037800, 8.314922557961029526, 76.66775706135234714 ) ) ;
#161312 = CARTESIAN_POINT ( 'NONE',  ( 13.97604488694527802, 13.89961937509977652, 79.37390960531435269 ) ) ;
#161313 = CARTESIAN_POINT ( 'NONE',  ( 14.34966873604960469, 8.224510206698951720, 74.16557627198102409 ) ) ;
#161314 = CARTESIAN_POINT ( 'NONE',  ( 12.14591786802327356, -12.06949235617739191, 110.6260903946857042 ) ) ;
#161315 = CARTESIAN_POINT ( 'NONE',  ( 9.474510206698729675, 16.51473224551082808, 62.08442372801899722 ) ) ;
#161316 = CARTESIAN_POINT ( 'NONE',  ( -18.67979575497193778, 10.72451020669871902, 33.33442372801900433 ) ) ;
#161317 = ADVANCED_FACE ( 'NONE', ( #89998 ), #102255, .T. ) ;
#161318 = CARTESIAN_POINT ( 'NONE',  ( -4.483927247898539470, -16.52544592524342804, 72.29057627198102409 ) ) ;
#161319 = CARTESIAN_POINT ( 'NONE',  ( 18.62759615963271287, -10.81492255796078972, 23.33224293864769194 ) ) ;
#161320 = CARTESIAN_POINT ( 'NONE',  ( -14.29746914071037622, -8.314922557961029526, 99.16775706135234714 ) ) ;
#161321 = CARTESIAN_POINT ( 'NONE',  ( -5.719274019375665041, -21.55341960407619695, 69.79275706135234714 ) ) ;
#161322 = CARTESIAN_POINT ( 'NONE',  ( -14.29746914071037622, -8.314922557961029526, 39.16775706135235424 ) ) ;
#161323 = CARTESIAN_POINT ( 'NONE',  ( 10.81492255796106328, -18.62759615963255655, 35.41775706135234003 ) ) ;
#161324 = ORIENTED_EDGE ( 'NONE', *, *, #193913, .T. ) ;
#161325 = CARTESIAN_POINT ( 'NONE',  ( -18.62759615963270932, 10.81492255796079327, 110.8322429386476955 ) ) ;
#161326 = CARTESIAN_POINT ( 'NONE',  ( -12.06949235617756955, 12.14591786802309770, 85.62390960531436690 ) ) ;
#161327 = CARTESIAN_POINT ( 'NONE',  ( -18.87255363501903105, -5.499999999999950262, 51.32513748171828638 ) ) ;
#161328 = CARTESIAN_POINT ( 'NONE',  ( -8.314922557960811034, -14.29746914071050412, 52.08224293864768839 ) ) ;
#161329 = CARTESIAN_POINT ( 'NONE',  ( -16.46253265017160317, 9.564922557960807481, 25.83224293864769194 ) ) ;
#161330 = CARTESIAN_POINT ( 'NONE',  ( 21.52544592524344225, -5.823673210054117533, 48.54057627198103120 ) ) ;
#161331 = CARTESIAN_POINT ( 'NONE',  ( 12.06949235617757843, -12.14591786802309237, 83.12390960531436690 ) ) ;
#161332 = AXIS2_PLACEMENT_3D ( 'NONE', #13833, #105843, #101858 ) ;
#161333 = CARTESIAN_POINT ( 'NONE',  ( -21.55341960407610458, -5.719274019375992779, 81.45724293864769550 ) ) ;
#161334 = CARTESIAN_POINT ( 'NONE',  ( 0.05219959533909260263, 19.03943276465977164, 84.99890960531436690 ) ) ;
#161336 = CARTESIAN_POINT ( 'NONE',  ( -5.153800228976607833, 19.02544592524334988, 72.70942372801900433 ) ) ;
#161335 = CARTESIAN_POINT ( 'NONE',  ( 13.97604488694527802, 13.89961937509977652, 39.37390960531435269 ) ) ;
#161337 = CARTESIAN_POINT ( 'NONE',  ( -15.80617190586745835, -15.72974639402198527, 36.87390960531435979 ) ) ;
#161339 = CARTESIAN_POINT ( 'NONE',  ( -15.72974639402197994, 15.80617190586746368, 65.62390960531436690 ) ) ;
#161338 = CARTESIAN_POINT ( 'NONE',  ( -10.72451020669870658, -18.67979575497194134, 54.58442372801901143 ) ) ;
#161340 = CARTESIAN_POINT ( 'NONE',  ( -16.51473224551069308, -9.474510206698971260, 36.66557627198102409 ) ) ;
#161341 = CARTESIAN_POINT ( 'NONE',  ( -13.97604488694527625, -13.89961937509977652, 71.87390960531433848 ) ) ;
#161342 = ORIENTED_EDGE ( 'NONE', *, *, #38220, .F. ) ;
#161343 = CARTESIAN_POINT ( 'NONE',  ( 14.34966873604972726, -8.224510206698740333, 45.83442372801901854 ) ) ;
#161344 = CARTESIAN_POINT ( 'NONE',  ( 5.719274019375673035, 21.55341960407619339, 32.29275706135235424 ) ) ;
#161345 = ADVANCED_FACE ( 'NONE', ( #10361 ), #25545, .T. ) ;
#161346 = CARTESIAN_POINT ( 'NONE',  ( 15.80617190586769283, -15.72974639402175789, 70.62609039468567573 ) ) ;
#161347 = CARTESIAN_POINT ( 'NONE',  ( 13.89961937509977652, -13.97604488694527269, 113.1239096053143527 ) ) ;
#161348 = CARTESIAN_POINT ( 'NONE',  ( 18.67979575497178502, 10.72451020669898547, 84.16557627198103830 ) ) ;
#161350 = CARTESIAN_POINT ( 'NONE',  ( 12.14591786802327356, -12.06949235617739191, 55.62609039468568284 ) ) ;
#161349 = CARTESIAN_POINT ( 'NONE',  ( -18.62759615963270932, 10.81492255796079327, 115.8322429386477097 ) ) ;
#161351 = CARTESIAN_POINT ( 'NONE',  ( 21.55341960407610458, 5.719274019375980345, 63.95724293864770260 ) ) ;
#161352 = CARTESIAN_POINT ( 'NONE',  ( 9.564922557961047289, -16.46253265017146816, 20.41775706135233293 ) ) ;
#161353 = CARTESIAN_POINT ( 'NONE',  ( 19.05341960407611168, 5.049401038298154454, 48.95724293864768129 ) ) ;
#161354 = CARTESIAN_POINT ( 'NONE',  ( -16.51473224551069308, -9.474510206698971260, 111.6655762719810383 ) ) ;
#161355 = CARTESIAN_POINT ( 'NONE',  ( 9.474510206698971260, -16.51473224551069308, 92.91557627198103830 ) ) ;
#161356 = DIRECTION ( 'NONE',  ( 1.000000000000000000, 0.000000000000000000, 0.000000000000000000 ) ) ;
#161357 = CARTESIAN_POINT ( 'NONE',  ( 13.97604488694548053, -13.89961937509957401, 65.62609039468567573 ) ) ;
#161358 = CARTESIAN_POINT ( 'NONE',  ( -10.81492255796078084, -18.62759615963271287, 42.08224293864769550 ) ) ;
#161359 = CARTESIAN_POINT ( 'NONE',  ( -12.06949235617756955, 12.14591786802309770, 25.62390960531435624 ) ) ;
#161360 = CARTESIAN_POINT ( 'NONE',  ( 0.05219959533936267826, -19.03943276465977164, 105.0010903946856615 ) ) ;
#161361 = CARTESIAN_POINT ( 'NONE',  ( -0.05219959533909027116, -19.03943276465977164, 22.49890960531436690 ) ) ;
#161362 = CARTESIAN_POINT ( 'NONE',  ( -5.049401038297874678, -19.05341960407617918, 24.79275706135233648 ) ) ;
#161363 = CARTESIAN_POINT ( 'NONE',  ( 16.46253265017146816, 9.564922557961045513, 96.66775706135233293 ) ) ;
#161365 = CARTESIAN_POINT ( 'NONE',  ( -19.05341960407617563, 5.049401038297882671, 53.54275706135231871 ) ) ;
#161364 = CARTESIAN_POINT ( 'NONE',  ( -10.81492255796078084, -18.62759615963271287, 87.08224293864769550 ) ) ;
#161366 = DIRECTION ( 'NONE',  ( -0.000000000000000000, -1.000000000000000000, -0.000000000000000000 ) ) ;
#161367 = CARTESIAN_POINT ( 'NONE',  ( 13.97604488694527802, 13.89961937509977652, 54.37390960531435979 ) ) ;
#161368 = CARTESIAN_POINT ( 'NONE',  ( 16.55341960407611168, 4.379528057220329451, 63.95724293864770260 ) ) ;
#161369 = CARTESIAN_POINT ( 'NONE',  ( 5.049401038298161559, -19.05341960407611168, 47.70724293864770260 ) ) ;
#161370 = CARTESIAN_POINT ( 'NONE',  ( 14.29746914071049879, -8.314922557960816363, 53.33224293864769550 ) ) ;
#161371 = CARTESIAN_POINT ( 'NONE',  ( 1.300000000000000044, 0.000000000000000000, -1.250000000000000000 ) ) ;
#161372 = CARTESIAN_POINT ( 'NONE',  ( -8.224510206698948167, 14.34966873604960824, 25.41557627198103120 ) ) ;
#161373 = CARTESIAN_POINT ( 'NONE',  ( 5.049401038298161559, -19.05341960407611168, 62.70724293864769550 ) ) ;
#161374 = CARTESIAN_POINT ( 'NONE',  ( -16.46253265017146816, -9.564922557961047289, 29.16775706135232937 ) ) ;
#161375 = CARTESIAN_POINT ( 'NONE',  ( -4.483927247898782831, 16.52544592524335698, 32.70942372801900433 ) ) ;
#161376 = CARTESIAN_POINT ( 'NONE',  ( -10.72451020669898014, 18.67979575497178502, 45.41557627198103830 ) ) ;
#161378 = ORIENTED_EDGE ( 'NONE', *, *, #128983, .T. ) ;
#161377 = CARTESIAN_POINT ( 'NONE',  ( 21.53943276465977519, 0.05219959533937863772, 111.2510903946856899 ) ) ;
#161379 = CARTESIAN_POINT ( 'NONE',  ( 19.03943276465977164, -0.05219959533909143690, 58.74890960531435979 ) ) ;
#161380 = DIRECTION ( 'NONE',  ( 0.000000000000000000, 0.000000000000000000, 1.000000000000000000 ) ) ;
#161381 = CARTESIAN_POINT ( 'NONE',  ( -5.153800228976328057, -19.02544592524343514, 92.29057627198099567 ) ) ;
#161382 = PLANE ( 'NONE',  #146596 ) ;
#161383 = CARTESIAN_POINT ( 'NONE',  ( 21.52544592524334988, 5.823673210054432836, 26.45942372801901854 ) ) ;
#161384 = CARTESIAN_POINT ( 'NONE',  ( 14.34966873604960469, 8.224510206698951720, 99.16557627198100988 ) ) ;
#161386 = CARTESIAN_POINT ( 'NONE',  ( 5.049401038298161559, -19.05341960407611168, 72.70724293864768129 ) ) ;
#161385 = CARTESIAN_POINT ( 'NONE',  ( 21.52544592524344225, -5.823673210054117533, 93.54057627198103830 ) ) ;
#161387 = CARTESIAN_POINT ( 'NONE',  ( 16.46253265017160672, -9.564922557960803928, 88.33224293864769550 ) ) ;
#161388 = CARTESIAN_POINT ( 'NONE',  ( -21.55341960407610458, -5.719274019375992779, 111.4572429386476813 ) ) ;
#161389 = VERTEX_POINT ( 'NONE', #40687 ) ;
#161390 = CARTESIAN_POINT ( 'NONE',  ( -16.51473224551069308, -9.474510206698971260, 71.66557627198102409 ) ) ;
#161391 = CARTESIAN_POINT ( 'NONE',  ( 19.01533133064924286, -5.499999999999438671, 96.26586590595742621 ) ) ;
#161393 = CARTESIAN_POINT ( 'NONE',  ( 5.049401038298161559, -19.05341960407611168, 22.70724293864769194 ) ) ;
#161392 = CARTESIAN_POINT ( 'NONE',  ( 8.314922557960818139, 14.29746914071049879, 109.5822429386476955 ) ) ;
#161394 = CARTESIAN_POINT ( 'NONE',  ( -0.05219959533936034679, 19.03943276465977164, 97.50109039468567573 ) ) ;
#161395 = CARTESIAN_POINT ( 'NONE',  ( 14.29746914071049879, -8.314922557960816363, 113.3322429386476955 ) ) ;
#161396 = CARTESIAN_POINT ( 'NONE',  ( -5.823673210054431948, 21.52544592524334988, 72.70942372801901854 ) ) ;
#161398 = CARTESIAN_POINT ( 'NONE',  ( -21.55341960407619339, 5.719274019375674811, 28.54275706135234358 ) ) ;
#161397 = CARTESIAN_POINT ( 'NONE',  ( -19.05341960407611168, -5.049401038298163336, 61.45724293864769550 ) ) ;
#161399 = CARTESIAN_POINT ( 'NONE',  ( 0.05219959533907565091, 21.53943276465977519, 104.9989096053143669 ) ) ;
#161400 = CARTESIAN_POINT ( 'NONE',  ( -17.81289503416611808, 24.51734667627700404, 141.6999999999999602 ) ) ;
#161401 = CARTESIAN_POINT ( 'NONE',  ( 9.564922557960805705, 16.46253265017160317, 74.58224293864769550 ) ) ;
#161402 = LINE ( 'NONE', #145223, #37219 ) ;
#161404 = CARTESIAN_POINT ( 'NONE',  ( -5.719274019375978568, 21.55341960407610458, 25.20724293864769550 ) ) ;
#161403 = CARTESIAN_POINT ( 'NONE',  ( 4.379528057220092307, 16.55341960407617563, 32.29275706135235424 ) ) ;
#161405 = CARTESIAN_POINT ( 'NONE',  ( -0.05219959533937732626, 21.53943276465977519, 57.50109039468568994 ) ) ;
#161406 = CARTESIAN_POINT ( 'NONE',  ( -0.05219959533909027116, -19.03943276465977164, 107.4989096053143527 ) ) ;
#161407 = CARTESIAN_POINT ( 'NONE',  ( 5.153800228976615827, -19.02544592524334988, 100.2094237280190043 ) ) ;
#161408 = CARTESIAN_POINT ( 'NONE',  ( 9.564922557960805705, 16.46253265017160317, 49.58224293864770260 ) ) ;
#161409 = CARTESIAN_POINT ( 'NONE',  ( -13.89961937509977652, 13.97604488694528158, 70.62390960531432427 ) ) ;
#161410 = CARTESIAN_POINT ( 'NONE',  ( -16.55341960407611168, -4.379528057220339221, 96.45724293864770971 ) ) ;
#161411 = CARTESIAN_POINT ( 'NONE',  ( -5.049401038298153566, 19.05341960407611168, 100.2072429386476955 ) ) ;
#161412 = CARTESIAN_POINT ( 'NONE',  ( -12.14591786802309592, -12.06949235617757132, 86.87390960531438111 ) ) ;
#161413 = CARTESIAN_POINT ( 'NONE',  ( 9.564922557960805705, 16.46253265017160317, 94.58224293864769550 ) ) ;
#161415 = CARTESIAN_POINT ( 'NONE',  ( -9.564922557960796823, -16.46253265017161027, 42.08224293864769550 ) ) ;
#161414 = CARTESIAN_POINT ( 'NONE',  ( 16.52544592524342804, -4.483927247898539470, 48.54057627198103120 ) ) ;
#161416 = CARTESIAN_POINT ( 'NONE',  ( 10.81492255796106328, -18.62759615963255655, 60.41775706135235424 ) ) ;
#161417 = CARTESIAN_POINT ( 'NONE',  ( -13.97604488694547697, 13.89961937509957934, 93.12609039468566152 ) ) ;
#161418 = CARTESIAN_POINT ( 'NONE',  ( 16.52544592524342804, -4.483927247898539470, 53.54057627198103120 ) ) ;
#161419 = CARTESIAN_POINT ( 'NONE',  ( 21.55341960407610458, 5.719274019375980345, 93.95724293864770971 ) ) ;
#161420 = CARTESIAN_POINT ( 'NONE',  ( -5.823673210054116645, -21.52544592524344225, 47.29057627198103120 ) ) ;
#161422 = CARTESIAN_POINT ( 'NONE',  ( 16.52544592524342804, -4.483927247898539470, 78.54057627198103830 ) ) ;
#161421 = CARTESIAN_POINT ( 'NONE',  ( 19.53091890409951503, 5.500000000000032863, 72.56097431831418021 ) ) ;
#161423 = CARTESIAN_POINT ( 'NONE',  ( -27.73933785331498925, -9.013057229001049109, 146.9750000027311785 ) ) ;
#161424 = CARTESIAN_POINT ( 'NONE',  ( 5.153800228976335163, 19.02544592524342804, 49.79057627198100988 ) ) ;
#161425 = CARTESIAN_POINT ( 'NONE',  ( 8.224510206698742110, 14.34966873604972548, 112.0844237280190185 ) ) ;
#161426 = CARTESIAN_POINT ( 'NONE',  ( -4.379528057220086978, -16.55341960407618274, 94.79275706135234714 ) ) ;
#161427 = CARTESIAN_POINT ( 'NONE',  ( 16.52544592524335698, 4.483927247898782831, 81.45942372801900433 ) ) ;
#161428 = CARTESIAN_POINT ( 'NONE',  ( -19.05341960407617563, 5.049401038297882671, 38.54275706135233293 ) ) ;
#161430 = CARTESIAN_POINT ( 'NONE',  ( 5.049401038298161559, -19.05341960407611168, 107.7072429386476955 ) ) ;
#161429 = LINE ( 'NONE', #37079, #192574 ) ;
#161431 = CARTESIAN_POINT ( 'NONE',  ( 19.05341960407611168, 5.049401038298154454, 78.95724293864769550 ) ) ;
#161432 = CARTESIAN_POINT ( 'NONE',  ( 9.474510206698971260, -16.51473224551069308, 42.91557627198103120 ) ) ;
#161433 = CARTESIAN_POINT ( 'NONE',  ( -14.29746914071049879, 8.314922557960819915, 50.83224293864770971 ) ) ;
#161435 = CARTESIAN_POINT ( 'NONE',  ( -5.153800228976328057, -19.02544592524343514, 107.2905762719810383 ) ) ;
#161434 = SURFACE_STYLE_USAGE ( .BOTH. , #8760 ) ;
#161436 = CARTESIAN_POINT ( 'NONE',  ( 10.81492255796078972, 18.62759615963270932, 34.58224293864770260 ) ) ;
#161437 = CARTESIAN_POINT ( 'NONE',  ( 16.53943276465976808, -0.05219959533910856209, 83.74890960531435269 ) ) ;
#161438 = CARTESIAN_POINT ( 'NONE',  ( -16.52544592524335698, -4.483927247898792601, 38.95942372801901854 ) ) ;
#161439 = CARTESIAN_POINT ( 'NONE',  ( -8.224510206698948167, 14.34966873604960824, 75.41557627198102409 ) ) ;
#161440 = CARTESIAN_POINT ( 'NONE',  ( 17.50000000000002487, -4.013004640162650460, 32.94605720994412934 ) ) ;
#161441 = CARTESIAN_POINT ( 'NONE',  ( 16.51473224551083163, -9.474510206698727899, 60.83442372801900433 ) ) ;
#161442 = CARTESIAN_POINT ( 'NONE',  ( -19.05341960407611168, -5.049401038298163336, 96.45724293864769550 ) ) ;
#161443 = CARTESIAN_POINT ( 'NONE',  ( 13.89961937509957401, 13.97604488694547697, 81.87609039468564731 ) ) ;
#161444 = CARTESIAN_POINT ( 'NONE',  ( 17.50000000000000000, 5.499999999999992895, 76.70309617465829888 ) ) ;
#161445 = VECTOR ( 'NONE', #120838, 1000.000000000000000 ) ;
#161447 = CARTESIAN_POINT ( 'NONE',  ( -8.314922557961024197, 14.29746914071037800, 107.9177570613523471 ) ) ;
#161446 = CARTESIAN_POINT ( 'NONE',  ( -16.52544592524335698, -4.483927247898792601, 28.95942372801902209 ) ) ;
#161448 = CARTESIAN_POINT ( 'NONE',  ( 5.049401038297881783, 19.05341960407617563, 77.29275706135231871 ) ) ;
#161449 = CARTESIAN_POINT ( 'NONE',  ( -18.67979575497178146, -10.72451020669898902, 31.66557627198102054 ) ) ;
#161450 = CARTESIAN_POINT ( 'NONE',  ( 21.53943276465977519, 0.05219959533937863772, 66.25109039468567573 ) ) ;
#161451 = CARTESIAN_POINT ( 'NONE',  ( -20.93662873023658122, -10.44628751056252369, 168.2749732860604013 ) ) ;
#161452 = CARTESIAN_POINT ( 'NONE',  ( 12.06949235617739724, 12.14591786802326823, 26.87609039468567218 ) ) ;
#161454 = CARTESIAN_POINT ( 'NONE',  ( 13.97604488694527802, 13.89961937509977652, 89.37390960531436690 ) ) ;
#161453 = CARTESIAN_POINT ( 'NONE',  ( 5.049401038298161559, -19.05341960407611168, 27.70724293864769550 ) ) ;
#161455 = CARTESIAN_POINT ( 'NONE',  ( -16.51473224551069308, -9.474510206698971260, 26.66557627198103120 ) ) ;
#161457 = CARTESIAN_POINT ( 'NONE',  ( -9.474510206698964154, 16.51473224551069663, 75.41557627198103830 ) ) ;
#161456 = CARTESIAN_POINT ( 'NONE',  ( -4.379528057220328563, 16.55341960407611168, 90.20724293864770971 ) ) ;
#161458 = APPLICATION_PROTOCOL_DEFINITION ( 'draft international standard', 'automotive_design', 1998, #57191 ) ;
#161459 = CARTESIAN_POINT ( 'NONE',  ( 5.153800228976335163, 19.02544592524342804, 84.79057627198099567 ) ) ;
#161460 = VERTEX_POINT ( 'NONE', #118537 ) ;
#161461 = CARTESIAN_POINT ( 'NONE',  ( 9.564922557961047289, -16.46253265017146816, 95.41775706135233293 ) ) ;
#161462 = CARTESIAN_POINT ( 'NONE',  ( 21.52544592524344225, -5.823673210054117533, 83.54057627198102409 ) ) ;
#161463 = CARTESIAN_POINT ( 'NONE',  ( -16.46253265017160317, 9.564922557960807481, 35.83224293864768839 ) ) ;
#161465 = CARTESIAN_POINT ( 'NONE',  ( -18.62759615963270932, 10.81492255796079327, 110.8322429386476955 ) ) ;
#161464 = CARTESIAN_POINT ( 'NONE',  ( -9.564922557961040184, 16.46253265017147172, 67.91775706135233293 ) ) ;
#161466 = CARTESIAN_POINT ( 'NONE',  ( -0.05219959533909027116, -19.03943276465977164, 67.49890960531436690 ) ) ;
#161468 = EDGE_CURVE ( 'NONE', #110145, #93013, #178213, .T. ) ;
#161467 = CARTESIAN_POINT ( 'NONE',  ( 5.049401038298161559, -19.05341960407611168, 112.7072429386476813 ) ) ;
#161469 = ORIENTED_EDGE ( 'NONE', *, *, #189746, .T. ) ;
#161470 = CARTESIAN_POINT ( 'NONE',  ( 18.62759615963271287, -10.81492255796078972, 103.3322429386476955 ) ) ;
#161473 = CARTESIAN_POINT ( 'NONE',  ( 19.03943276465977164, 0.05219959533936151252, 61.25109039468566863 ) ) ;
#161472 = CARTESIAN_POINT ( 'NONE',  ( -19.03943276465977164, 0.05219959533909376836, 81.24890960531436690 ) ) ;
#161471 = CARTESIAN_POINT ( 'NONE',  ( -16.55341960407611168, -4.379528057220339221, 91.45724293864769550 ) ) ;
#161474 = CARTESIAN_POINT ( 'NONE',  ( -0.05219959533907301413, -21.53943276465977519, 92.49890960531436690 ) ) ;
#161475 = CARTESIAN_POINT ( 'NONE',  ( -21.53943276465977519, 0.05219959533907696930, 71.24890960531435269 ) ) ;
#161476 = CARTESIAN_POINT ( 'NONE',  ( 4.379528057220339221, -16.55341960407611168, 52.70724293864769550 ) ) ;
#161477 = CARTESIAN_POINT ( 'NONE',  ( -19.03943276465977164, -0.05219959533935918106, 28.75109039468566507 ) ) ;
#161478 = CARTESIAN_POINT ( 'NONE',  ( 12.14591786802327356, -12.06949235617739191, 70.62609039468567573 ) ) ;
#161479 = EDGE_CURVE ( 'NONE', #128045, #138940, #115156, .T. ) ;
#161480 = CARTESIAN_POINT ( 'NONE',  ( 19.03943276465977164, -0.05219959533909143690, 98.74890960531436690 ) ) ;
#161481 = CARTESIAN_POINT ( 'NONE',  ( 0.05219959533909260263, 19.03943276465977164, 39.99890960531436690 ) ) ;
#161482 = CARTESIAN_POINT ( 'NONE',  ( -18.62759615963255300, -10.81492255796106328, 49.16775706135234003 ) ) ;
#161483 = CARTESIAN_POINT ( 'NONE',  ( -18.67979575497193778, 10.72451020669871902, 48.33442372801902565 ) ) ;
#161484 = CARTESIAN_POINT ( 'NONE',  ( -0.05219959533909027116, -19.03943276465977164, 62.49890960531435979 ) ) ;
#161485 = CARTESIAN_POINT ( 'NONE',  ( 10.72451020669871369, 18.67979575497193778, 42.08442372801901854 ) ) ;
#161486 = CARTESIAN_POINT ( 'NONE',  ( -5.049401038297874678, -19.05341960407617918, 79.79275706135233293 ) ) ;
#161487 = CARTESIAN_POINT ( 'NONE',  ( -0.05219959533936034679, 19.03943276465977164, 67.50109039468566152 ) ) ;
#161488 = CARTESIAN_POINT ( 'NONE',  ( 5.049401038298161559, -19.05341960407611168, 37.70724293864768839 ) ) ;
#161489 = CARTESIAN_POINT ( 'NONE',  ( 4.483927247898790824, -16.52544592524335698, 80.20942372801901854 ) ) ;
#161490 = CARTESIAN_POINT ( 'NONE',  ( 16.51473224551069308, 9.474510206698969483, 54.16557627198103120 ) ) ;
#161491 = CARTESIAN_POINT ( 'NONE',  ( 24.27995301597375288, -6.552671593954494611, 171.1165850637241874 ) ) ;
#161492 = CARTESIAN_POINT ( 'NONE',  ( 19.03943276465977164, -0.05219959533909143690, 98.74890960531436690 ) ) ;
#161493 = CARTESIAN_POINT ( 'NONE',  ( -13.97604488694527625, -13.89961937509977652, 41.87390960531435979 ) ) ;
#161494 = CARTESIAN_POINT ( 'NONE',  ( -21.53943276465977519, 0.05219959533907696930, 71.24890960531435269 ) ) ;
#161495 = CARTESIAN_POINT ( 'NONE',  ( 4.379528057220092307, 16.55341960407617563, 62.29275706135236845 ) ) ;
#161496 = CARTESIAN_POINT ( 'NONE',  ( -10.72451020669870658, -18.67979575497194134, 109.5844237280190328 ) ) ;
#161497 = CARTESIAN_POINT ( 'NONE',  ( -19.05341960407611168, -5.049401038298163336, 51.45724293864770260 ) ) ;
#161498 = CARTESIAN_POINT ( 'NONE',  ( -16.55341960407611168, -4.379528057220339221, 51.45724293864770260 ) ) ;
#161499 = CARTESIAN_POINT ( 'NONE',  ( -14.29746914071049879, 8.314922557960819915, 85.83224293864768129 ) ) ;
#161500 = CARTESIAN_POINT ( 'NONE',  ( -9.564922557960796823, -16.46253265017161027, 72.08224293864770971 ) ) ;
#161501 = CARTESIAN_POINT ( 'NONE',  ( 21.53943276465977519, 0.05219959533937863772, 31.25109039468568639 ) ) ;
#161502 = CARTESIAN_POINT ( 'NONE',  ( -16.51473224551069308, -9.474510206698971260, 91.66557627198103830 ) ) ;
#161503 = CARTESIAN_POINT ( 'NONE',  ( -18.62759615963255300, -10.81492255796106328, 99.16775706135234714 ) ) ;
#161504 = CARTESIAN_POINT ( 'NONE',  ( 12.06949235617739724, 12.14591786802326823, 66.87609039468568994 ) ) ;
#161505 = CARTESIAN_POINT ( 'NONE',  ( 10.81492255796106328, -18.62759615963255655, 25.41775706135235779 ) ) ;
#161506 = CARTESIAN_POINT ( 'NONE',  ( 19.03943276465977164, -0.05219959533909143690, 108.7489096053143527 ) ) ;
#161507 = CARTESIAN_POINT ( 'NONE',  ( -10.81492255796078084, -18.62759615963271287, 87.08224293864769550 ) ) ;
#161508 = CARTESIAN_POINT ( 'NONE',  ( -14.29746914071049879, 8.314922557960819915, 40.83224293864769550 ) ) ;
#161509 = CARTESIAN_POINT ( 'NONE',  ( 0.05219959533909260263, 19.03943276465977164, 39.99890960531436690 ) ) ;
#161510 = CARTESIAN_POINT ( 'NONE',  ( -0.05219959533910754901, -16.53943276465976808, 67.49890960531436690 ) ) ;
#161511 = CARTESIAN_POINT ( 'NONE',  ( 18.67979575497178502, 10.72451020669898547, 24.16557627198103120 ) ) ;
#161512 = CARTESIAN_POINT ( 'NONE',  ( -19.03943276465977164, -0.05219959533935918106, 28.75109039468566507 ) ) ;
#161513 = CARTESIAN_POINT ( 'NONE',  ( 4.483927247898545687, 16.52544592524342804, 99.79057627198103830 ) ) ;
#161514 = CARTESIAN_POINT ( 'NONE',  ( -19.03943276465977164, 0.05219959533909376836, 111.2489096053143669 ) ) ;
#161515 = VERTEX_POINT ( 'NONE', #196390 ) ;
#161516 = CARTESIAN_POINT ( 'NONE',  ( 14.29746914071037800, 8.314922557961029526, 56.66775706135235424 ) ) ;
#161517 = CARTESIAN_POINT ( 'NONE',  ( 5.153800228976335163, 19.02544592524342804, 49.79057627198100988 ) ) ;
#161518 = CARTESIAN_POINT ( 'NONE',  ( -16.78782133324386905, -5.971338504361712651, 20.53800302010647982 ) ) ;
#161519 = CARTESIAN_POINT ( 'NONE',  ( -8.314922557961024197, 14.29746914071037800, 97.91775706135236135 ) ) ;
#161520 = CARTESIAN_POINT ( 'NONE',  ( 16.46253265017146816, 9.564922557961045513, 101.6677570613523329 ) ) ;
#161521 = CARTESIAN_POINT ( 'NONE',  ( -15.72974639402176322, -15.80617190586768395, 69.37609039468567573 ) ) ;
#161522 = CARTESIAN_POINT ( 'NONE',  ( -16.51473224551069308, -9.474510206698971260, 76.66557627198103830 ) ) ;
#161523 = CARTESIAN_POINT ( 'NONE',  ( -15.72974639402197994, 15.80617190586746368, 90.62390960531436690 ) ) ;
#161524 = CARTESIAN_POINT ( 'NONE',  ( 14.34966873604972726, -8.224510206698740333, 40.83442372801901854 ) ) ;
#161525 = CARTESIAN_POINT ( 'NONE',  ( 12.14591786802309770, 12.06949235617756955, 109.3739096053143811 ) ) ;
#161526 = CARTESIAN_POINT ( 'NONE',  ( 19.03943276465977164, 0.05219959533936151252, 81.25109039468567573 ) ) ;
#161527 = CARTESIAN_POINT ( 'NONE',  ( -15.72974639402197994, 15.80617190586746368, 75.62390960531439532 ) ) ;
#161528 = CARTESIAN_POINT ( 'NONE',  ( 0.05219959533936267826, -19.03943276465977164, 55.00109039468566863 ) ) ;
#161529 = CARTESIAN_POINT ( 'NONE',  ( 16.46253265017160672, -9.564922557960803928, 113.3322429386476955 ) ) ;
#161530 = CARTESIAN_POINT ( 'NONE',  ( 21.55341960407610458, 5.719274019375980345, 83.95724293864770971 ) ) ;
#161531 = CARTESIAN_POINT ( 'NONE',  ( 17.50000000000002487, 3.237210098469580632, 27.78763012620467521 ) ) ;
#161532 = CARTESIAN_POINT ( 'NONE',  ( -16.51473224551069308, -9.474510206698971260, 61.66557627198103120 ) ) ;
#161533 = CARTESIAN_POINT ( 'NONE',  ( -30.00000000000000000, -1.071565949253934124E-14, 102.5000000000000142 ) ) ;
#161534 = CARTESIAN_POINT ( 'NONE',  ( -9.564922557961040184, 16.46253265017147172, 112.9177570613523329 ) ) ;
#161535 = CARTESIAN_POINT ( 'NONE',  ( 23.84689744903973008, 10.26551614244696076, 166.0764362378396868 ) ) ;
#161536 = CARTESIAN_POINT ( 'NONE',  ( -19.03943276465977164, 0.05219959533909376836, 41.24890960531435269 ) ) ;
#161538 = CARTESIAN_POINT ( 'NONE',  ( 12.06949235617757843, -12.14591786802309237, 48.12390960531436690 ) ) ;
#161537 = CARTESIAN_POINT ( 'NONE',  ( -21.55341960407610458, -5.719274019375992779, 101.4572429386476955 ) ) ;
#161539 = CARTESIAN_POINT ( 'NONE',  ( -13.97604488694527625, -13.89961937509977652, 66.87390960531436690 ) ) ;
#161540 = CARTESIAN_POINT ( 'NONE',  ( 18.67979575497194134, -10.72451020669871369, 70.83442372801901854 ) ) ;
#161542 = CARTESIAN_POINT ( 'NONE',  ( 9.564922557961047289, -16.46253265017146816, 30.41775706135232937 ) ) ;
#161541 = CARTESIAN_POINT ( 'NONE',  ( -19.05341960407617563, 5.049401038297882671, 113.5427570613523471 ) ) ;
#161543 = CARTESIAN_POINT ( 'NONE',  ( -15.80617190586768217, 15.72974639402176855, 38.12609039468567573 ) ) ;
#161544 = CARTESIAN_POINT ( 'NONE',  ( -21.53943276465977519, 0.05219959533907696930, 111.2489096053143669 ) ) ;
#161545 = CARTESIAN_POINT ( 'NONE',  ( 5.823673210054125526, 21.52544592524343514, 54.79057627198104541 ) ) ;
#161546 = CARTESIAN_POINT ( 'NONE',  ( 9.564922557961047289, -16.46253265017146816, 90.41775706135234714 ) ) ;
#161547 = CARTESIAN_POINT ( 'NONE',  ( -9.564922557961040184, 16.46253265017147172, 62.91775706135233293 ) ) ;
#161548 = CARTESIAN_POINT ( 'NONE',  ( 15.72974639402176855, 15.80617190586768217, 81.87609039468568994 ) ) ;
#161549 = CARTESIAN_POINT ( 'NONE',  ( 19.02544592524334988, 5.153800228976608722, 51.45942372801900433 ) ) ;
#161550 = CARTESIAN_POINT ( 'NONE',  ( 16.46253265017160672, -9.564922557960803928, 23.33224293864769194 ) ) ;
#161551 = CARTESIAN_POINT ( 'NONE',  ( -0.05219959533907301413, -21.53943276465977519, 62.49890960531436690 ) ) ;
#161552 = CARTESIAN_POINT ( 'NONE',  ( 14.34966873604960469, 8.224510206698951720, 44.16557627198103120 ) ) ;
#161553 = CARTESIAN_POINT ( 'NONE',  ( -17.72662750342725602, -5.500000000000090594, 51.40179492283743201 ) ) ;
#161554 = CARTESIAN_POINT ( 'NONE',  ( -19.03943276465977164, -0.05219959533935918106, 28.75109039468566507 ) ) ;
#161555 = CARTESIAN_POINT ( 'NONE',  ( -8.224510206698735004, -14.34966873604973081, 89.58442372801901854 ) ) ;
#161556 = CARTESIAN_POINT ( 'NONE',  ( -16.53943276465976808, 0.05219959533911058130, 46.24890960531435979 ) ) ;
#161557 = CARTESIAN_POINT ( 'NONE',  ( 5.823673210054444382, -21.52544592524334988, 75.20942372801901854 ) ) ;
#161558 = CARTESIAN_POINT ( 'NONE',  ( 15.80617190586769283, -15.72974639402175789, 80.62609039468567573 ) ) ;
#161559 = CARTESIAN_POINT ( 'NONE',  ( 21.52544592524344225, -5.823673210054117533, 78.54057627198103830 ) ) ;
#161560 = CARTESIAN_POINT ( 'NONE',  ( -0.05219959533909027116, -19.03943276465977164, 37.49890960531436690 ) ) ;
#161561 = CARTESIAN_POINT ( 'NONE',  ( 21.53943276465977519, 0.05219959533937863772, 56.25109039468568284 ) ) ;
#161562 = CARTESIAN_POINT ( 'NONE',  ( -13.89961937509977652, 13.97604488694528158, 30.62390960531435269 ) ) ;
#161563 = ORIENTED_EDGE ( 'NONE', *, *, #73579, .T. ) ;
#161564 = CARTESIAN_POINT ( 'NONE',  ( -9.564922557960796823, -16.46253265017161027, 57.08224293864769550 ) ) ;
#161565 = CARTESIAN_POINT ( 'NONE',  ( -12.06949235617756955, 12.14591786802309770, 90.62390960531436690 ) ) ;
#161566 = CARTESIAN_POINT ( 'NONE',  ( 19.03943276465977164, -0.05219959533909143690, 103.7489096053143669 ) ) ;
#161567 = CARTESIAN_POINT ( 'NONE',  ( -12.14591786802309592, -12.06949235617757132, 41.87390960531435979 ) ) ;
#161568 = CARTESIAN_POINT ( 'NONE',  ( -8.314922557960811034, -14.29746914071050412, 112.0822429386477097 ) ) ;
#161569 = CARTESIAN_POINT ( 'NONE',  ( 5.823673210054125526, 21.52544592524343514, 84.79057627198102409 ) ) ;
#161570 = CARTESIAN_POINT ( 'NONE',  ( -5.719274019375665041, -21.55341960407619695, 24.79275706135235779 ) ) ;
#161571 = CARTESIAN_POINT ( 'NONE',  ( 27.20489923017583322, -7.754340368643432235, 164.3890803562161977 ) ) ;
#161572 = CARTESIAN_POINT ( 'NONE',  ( -12.14591786802326823, 12.06949235617739902, 43.12609039468568284 ) ) ;
#161573 = CARTESIAN_POINT ( 'NONE',  ( -15.80617190586745835, -15.72974639402198527, 76.87390960531439532 ) ) ;
#161574 = CARTESIAN_POINT ( 'NONE',  ( 21.55341960407619695, -5.719274019375665929, 101.0427570613523756 ) ) ;
#161575 = CARTESIAN_POINT ( 'NONE',  ( -13.89961937509977652, 13.97604488694528158, 90.62390960531432427 ) ) ;
#161576 = CARTESIAN_POINT ( 'NONE',  ( -21.52544592524334988, -5.823673210054445271, 28.95942372801902209 ) ) ;
#161577 = CARTESIAN_POINT ( 'NONE',  ( -5.719274019375978568, 21.55341960407610458, 30.20724293864769550 ) ) ;
#161578 = CARTESIAN_POINT ( 'NONE',  ( 16.53943276465976808, 0.05219959533934440121, 96.25109039468568994 ) ) ;
#161579 = CARTESIAN_POINT ( 'NONE',  ( 5.823673210054444382, -21.52544592524334988, 65.20942372801901854 ) ) ;
#161580 = CARTESIAN_POINT ( 'NONE',  ( 18.67979575497194134, -10.72451020669871369, 110.8344237280190043 ) ) ;
#161581 = CARTESIAN_POINT ( 'NONE',  ( 16.52544592524335698, 4.483927247898782831, 76.45942372801901854 ) ) ;
#161582 = CARTESIAN_POINT ( 'NONE',  ( 5.719274019375673035, 21.55341960407619339, 32.29275706135235424 ) ) ;
#161583 = CARTESIAN_POINT ( 'NONE',  ( 19.05341960407611168, 5.049401038298154454, 38.95724293864767418 ) ) ;
#161584 = CARTESIAN_POINT ( 'NONE',  ( -18.62759615963255300, -10.81492255796106328, 94.16775706135237556 ) ) ;
#161585 = CARTESIAN_POINT ( 'NONE',  ( -13.97604488694527625, -13.89961937509977652, 106.8739096053143669 ) ) ;
#161586 = CARTESIAN_POINT ( 'NONE',  ( 18.67979575497178502, 10.72451020669898547, 109.1655762719810383 ) ) ;
#161588 = CARTESIAN_POINT ( 'NONE',  ( -18.62759615963270932, 10.81492255796079327, 55.83224293864770260 ) ) ;
#161587 = CARTESIAN_POINT ( 'NONE',  ( 18.89770734986046463, 5.500000000000088818, 81.60214472496643623 ) ) ;
#161590 = CARTESIAN_POINT ( 'NONE',  ( -14.34966873604960291, -8.224510206698953496, 46.66557627198102409 ) ) ;
#161589 = CARTESIAN_POINT ( 'NONE',  ( 16.51473224551069308, 9.474510206698969483, 99.16557627198102409 ) ) ;
#161591 = CARTESIAN_POINT ( 'NONE',  ( 21.93208748025632104, 6.437649280788581230, 171.3046185016227696 ) ) ;
#161592 = CARTESIAN_POINT ( 'NONE',  ( -19.02544592524334988, -5.153800228976617603, 78.95942372801900433 ) ) ;
#161593 = DIRECTION ( 'NONE',  ( 0.000000000000000000, 1.224646799147353207E-16, 1.000000000000000000 ) ) ;
#161594 = CARTESIAN_POINT ( 'NONE',  ( -16.51473224551082808, 9.474510206698731452, 108.3344237280190043 ) ) ;
#161595 = CARTESIAN_POINT ( 'NONE',  ( 0.05219959533907565091, 21.53943276465977519, 79.99890960531435269 ) ) ;
#161596 = CARTESIAN_POINT ( 'NONE',  ( 4.483927247898545687, 16.52544592524342804, 64.79057627198103830 ) ) ;
#161597 = CARTESIAN_POINT ( 'NONE',  ( -16.51473224551069308, -9.474510206698971260, 106.6655762719810383 ) ) ;
#161598 = CARTESIAN_POINT ( 'NONE',  ( -4.379528057220086978, -16.55341960407618274, 44.79275706135234714 ) ) ;
#161599 = CARTESIAN_POINT ( 'NONE',  ( 16.51473224551069308, 9.474510206698969483, 54.16557627198103120 ) ) ;
#161601 = CARTESIAN_POINT ( 'NONE',  ( 13.89961937509957401, 13.97604488694547697, 91.87609039468567573 ) ) ;
#161600 = CARTESIAN_POINT ( 'NONE',  ( -15.72974639402176322, -15.80617190586768395, 29.37609039468568284 ) ) ;
#161602 = CARTESIAN_POINT ( 'NONE',  ( 9.564922557960805705, 16.46253265017160317, 94.58224293864769550 ) ) ;
#161603 = CARTESIAN_POINT ( 'NONE',  ( 9.474510206698971260, -16.51473224551069308, 87.91557627198102409 ) ) ;
#161604 = CARTESIAN_POINT ( 'NONE',  ( 15.80617190586746368, 15.72974639402197994, 94.37390960531436690 ) ) ;
#161605 = CARTESIAN_POINT ( 'NONE',  ( -16.51473224551069308, -9.474510206698971260, 46.66557627198102409 ) ) ;
#161606 = DIRECTION ( 'NONE',  ( 0.8164965809277229258, 0.000000000000000000, 0.5773502691896299499 ) ) ;
#161607 = CARTESIAN_POINT ( 'NONE',  ( 12.14591786802309770, 12.06949235617756955, 64.37390960531435269 ) ) ;
#161608 = CARTESIAN_POINT ( 'NONE',  ( 13.89961937509977652, -13.97604488694527269, 103.1239096053143527 ) ) ;
#161609 = CARTESIAN_POINT ( 'NONE',  ( 17.52032980918965066, -15.56136713261939875, -54.91505165737924443 ) ) ;
#161610 = CARTESIAN_POINT ( 'NONE',  ( 16.46253265017146816, 9.564922557961045513, 61.66775706135234003 ) ) ;
#161611 = CARTESIAN_POINT ( 'NONE',  ( -15.80617190586745835, -15.72974639402198527, 86.87390960531438111 ) ) ;
#161612 = CARTESIAN_POINT ( 'NONE',  ( -9.564922557961040184, 16.46253265017147172, 52.91775706135233293 ) ) ;
#161613 = CARTESIAN_POINT ( 'NONE',  ( 13.89961937509977652, -13.97604488694527269, 103.1239096053143527 ) ) ;
#161614 = CARTESIAN_POINT ( 'NONE',  ( 19.20446147854521968, 5.500000000000079936, 66.88999695167673565 ) ) ;
#161615 = CARTESIAN_POINT ( 'NONE',  ( -15.80617190586745835, -15.72974639402198527, 36.87390960531435979 ) ) ;
#161616 = AXIS2_PLACEMENT_3D ( 'NONE', #87360, #38866, #37863 ) ;
#161617 = CARTESIAN_POINT ( 'NONE',  ( 5.153800228976335163, 19.02544592524342804, 89.79057627198102409 ) ) ;
#161618 = CARTESIAN_POINT ( 'NONE',  ( -5.823673210054431948, 21.52544592524334988, 62.70942372801902565 ) ) ;
#161619 = CARTESIAN_POINT ( 'NONE',  ( 0.05219959533909260263, 19.03943276465977164, 34.99890960531435979 ) ) ;
#161620 = CARTESIAN_POINT ( 'NONE',  ( -14.29746914071049879, 8.314922557960819915, 70.83224293864770971 ) ) ;
#161621 = CARTESIAN_POINT ( 'NONE',  ( 16.53943276465976808, 0.05219959533934440121, 26.25109039468567573 ) ) ;
#161622 = CARTESIAN_POINT ( 'NONE',  ( -21.53943276465977519, -0.05219959533937600094, 53.75109039468568994 ) ) ;
#161623 = ORIENTED_EDGE ( 'NONE', *, *, #171883, .F. ) ;
#161624 = CARTESIAN_POINT ( 'NONE',  ( -28.75808110634262604, -1.452795517301058048, 139.9999999999999716 ) ) ;
#161625 = CARTESIAN_POINT ( 'NONE',  ( -13.97604488694547697, 13.89961937509957934, 73.12609039468568994 ) ) ;
#161626 = CYLINDRICAL_SURFACE ( 'NONE', #134390, 37.99626262588765968 ) ;
#161627 = CARTESIAN_POINT ( 'NONE',  ( 0.05219959533937995610, -21.53943276465977519, 30.00109039468568284 ) ) ;
#161628 = CARTESIAN_POINT ( 'NONE',  ( -38.00000000000001421, 12.34694845685046438, -7.849999994537626868 ) ) ;
#161629 = CARTESIAN_POINT ( 'NONE',  ( -13.89961937509957401, -13.97604488694547875, 24.37609039468565442 ) ) ;
#161630 = CARTESIAN_POINT ( 'NONE',  ( -16.51473224551069308, -9.474510206698971260, 56.66557627198103120 ) ) ;
#161631 = CARTESIAN_POINT ( 'NONE',  ( -0.05219959533937732626, 21.53943276465977519, 112.5010903946857042 ) ) ;
#161632 = CARTESIAN_POINT ( 'NONE',  ( 4.379528057220092307, 16.55341960407617563, 107.2927570613523471 ) ) ;
#161634 = CARTESIAN_POINT ( 'NONE',  ( 21.55341960407619695, -5.719274019375665929, 76.04275706135237556 ) ) ;
#161633 = CARTESIAN_POINT ( 'NONE',  ( -19.03943276465977164, 0.05219959533909376836, 101.2489096053143669 ) ) ;
#161635 = CARTESIAN_POINT ( 'NONE',  ( 5.687983883489459380, -3.878490454473807247, -62.37234731589995107 ) ) ;
#161636 = FACE_OUTER_BOUND ( 'NONE', #126141, .T. ) ;
#161637 = CARTESIAN_POINT ( 'NONE',  ( -18.22780087662122028, 5.500000000000031086, 78.51540105326107266 ) ) ;
#161639 = CARTESIAN_POINT ( 'NONE',  ( 15.80617190586769283, -15.72974639402175789, 65.62609039468568994 ) ) ;
#161638 = CARTESIAN_POINT ( 'NONE',  ( 4.379528057220092307, 16.55341960407617563, 72.29275706135236135 ) ) ;
#161640 = CARTESIAN_POINT ( 'NONE',  ( -15.80617190586768217, 15.72974639402176855, 98.12609039468570415 ) ) ;
#161641 = CARTESIAN_POINT ( 'NONE',  ( 17.31747979337951548, -6.344076630960995722, 41.12055131934816643 ) ) ;
#161642 = CARTESIAN_POINT ( 'NONE',  ( 19.05341960407611168, 5.049401038298154454, 88.95724293864769550 ) ) ;
#161643 = CARTESIAN_POINT ( 'NONE',  ( -13.89961937509977652, 13.97604488694528158, 105.6239096053143527 ) ) ;
#161644 = CARTESIAN_POINT ( 'NONE',  ( 15.50000000000000355, -7.500000000000000888, 120.0000000000000142 ) ) ;
#161645 = CARTESIAN_POINT ( 'NONE',  ( 13.89961937509977652, -13.97604488694527269, 33.12390960531434558 ) ) ;
#161646 = CARTESIAN_POINT ( 'NONE',  ( 10.72451020669898902, -18.67979575497178502, 37.91557627198102409 ) ) ;
#161647 = CARTESIAN_POINT ( 'NONE',  ( 8.314922557961029526, -14.29746914071037800, 100.4177570613523471 ) ) ;
#161649 = CARTESIAN_POINT ( 'NONE',  ( 19.05341960407611168, 5.049401038298154454, 78.95724293864769550 ) ) ;
#161648 = CARTESIAN_POINT ( 'NONE',  ( 14.34966873604960469, 8.224510206698951720, 99.16557627198100988 ) ) ;
#161650 = CARTESIAN_POINT ( 'NONE',  ( 10.81492255796106328, -18.62759615963255655, 105.4177570613523613 ) ) ;
#161651 = CARTESIAN_POINT ( 'NONE',  ( -13.89961937509977652, 13.97604488694528158, 30.62390960531435269 ) ) ;
#161652 = CARTESIAN_POINT ( 'NONE',  ( 16.55341960407611168, 4.379528057220329451, 88.95724293864769550 ) ) ;
#161653 = CARTESIAN_POINT ( 'NONE',  ( -18.67979575497193778, 10.72451020669871902, 58.33442372801901143 ) ) ;
#161654 = CARTESIAN_POINT ( 'NONE',  ( -18.67979575497178146, -10.72451020669898902, 86.66557627198102409 ) ) ;
#161655 = CARTESIAN_POINT ( 'NONE',  ( 19.02544592524334988, 5.153800228976608722, 51.45942372801900433 ) ) ;
#161656 = CARTESIAN_POINT ( 'NONE',  ( -20.16212008049412319, -20.78213278888862448, -49.60977668010092856 ) ) ;
#161657 = CARTESIAN_POINT ( 'NONE',  ( 16.51473224551069308, 9.474510206698969483, 99.16557627198102409 ) ) ;
#161658 = CARTESIAN_POINT ( 'NONE',  ( -16.55341960407611168, -4.379528057220339221, 61.45724293864770260 ) ) ;
#161659 = CARTESIAN_POINT ( 'NONE',  ( -16.46253265017146816, -9.564922557961047289, 44.16775706135232582 ) ) ;
#161660 = CARTESIAN_POINT ( 'NONE',  ( 8.224510206698953496, -14.34966873604960469, 47.91557627198102409 ) ) ;
#161662 = ADVANCED_FACE ( 'NONE', ( #146857 ), #194382, .F. ) ;
#161661 = CARTESIAN_POINT ( 'NONE',  ( 13.89961937509957401, 13.97604488694547697, 76.87609039468566152 ) ) ;
#161663 = CARTESIAN_POINT ( 'NONE',  ( 18.22780087662119897, -5.500000000000096811, 48.51763182126894236 ) ) ;
#161664 = CARTESIAN_POINT ( 'NONE',  ( -10.72451020669898014, 18.67979575497178502, 35.41557627198102409 ) ) ;
#161665 = CARTESIAN_POINT ( 'NONE',  ( 0.05219959533910956823, 16.53943276465976808, 99.99890960531436690 ) ) ;
#161666 = CARTESIAN_POINT ( 'NONE',  ( -17.50000000000147438, -3.202012800152302052, 25.07177583972721280 ) ) ;
#161668 = CARTESIAN_POINT ( 'NONE',  ( 21.52544592524344225, -5.823673210054117533, 43.54057627198103830 ) ) ;
#161667 = CARTESIAN_POINT ( 'NONE',  ( 5.153800228976335163, 19.02544592524342804, 49.79057627198100988 ) ) ;
#161669 = CARTESIAN_POINT ( 'NONE',  ( -13.89961937509977652, 13.97604488694528158, 35.62390960531435269 ) ) ;
#161671 = CARTESIAN_POINT ( 'NONE',  ( 5.153800228976335163, 19.02544592524342804, 64.79057627198100988 ) ) ;
#161670 = CARTESIAN_POINT ( 'NONE',  ( -4.483927247898782831, 16.52544592524335698, 82.70942372801900433 ) ) ;
#161672 = CARTESIAN_POINT ( 'NONE',  ( 16.51473224551083163, -9.474510206698727899, 35.83442372801899722 ) ) ;
#161673 = CARTESIAN_POINT ( 'NONE',  ( -15.80617190586768217, 15.72974639402176855, 63.12609039468568994 ) ) ;
#161674 = CARTESIAN_POINT ( 'NONE',  ( -10.72451020669898014, 18.67979575497178502, 55.41557627198102409 ) ) ;
#161675 = CARTESIAN_POINT ( 'NONE',  ( 16.51473224551069308, 9.474510206698969483, 29.16557627198103475 ) ) ;
#161676 = CARTESIAN_POINT ( 'NONE',  ( -16.46253265017146816, -9.564922557961047289, 109.1677570613523471 ) ) ;
#161677 = CARTESIAN_POINT ( 'NONE',  ( 5.049401038298161559, -19.05341960407611168, 22.70724293864769194 ) ) ;
#161679 = CARTESIAN_POINT ( 'NONE',  ( 21.55341960407610458, 5.719274019375980345, 53.95724293864770260 ) ) ;
#161678 = FACE_OUTER_BOUND ( 'NONE', #143783, .T. ) ;
#161680 = CARTESIAN_POINT ( 'NONE',  ( -9.474510206698964154, 16.51473224551069663, 25.41557627198103120 ) ) ;
#161681 = CARTESIAN_POINT ( 'NONE',  ( -5.823673210054431948, 21.52544592524334988, 77.70942372801900433 ) ) ;
#161682 = CARTESIAN_POINT ( 'NONE',  ( -16.53943276465976808, 0.05219959533911058130, 51.24890960531436690 ) ) ;
#161683 = CARTESIAN_POINT ( 'NONE',  ( -0.05219959533910754901, -16.53943276465976808, 52.49890960531435979 ) ) ;
#161684 = CARTESIAN_POINT ( 'NONE',  ( -18.67979575497178146, -10.72451020669898902, 76.66557627198103830 ) ) ;
#161685 = APPLICATION_CONTEXT ( 'automotive_design' ) ;
#161686 = CARTESIAN_POINT ( 'NONE',  ( 21.53943276465977519, -0.05219959533907433946, 78.74890960531436690 ) ) ;
#161687 = DIRECTION ( 'NONE',  ( -2.775557561562891351E-15, -0.8164965809277244801, -0.5773502691896280625 ) ) ;
#161688 = B_SPLINE_CURVE_WITH_KNOTS ( 'NONE', 3,
 ( #148363, #149363, #180722, #177713, #70521, #178711, #40173, #54352, #103858, #101852, #115023, #39181, #24024, #85678, #99845, #192874, #42197, #102855, #100838, #164541 ),
 .UNSPECIFIED., .F., .F.,
 ( 4, 2, 2, 2, 2, 2, 2, 2, 2, 4 ),
 ( 0.000000000000000000, 0.0004987090165372657638, 0.0009974180330745315275, 0.001246772541343167933, 0.001496127049611804555, 0.001994836066149077800, 0.002493545082686351045, 0.002742899590954987667, 0.002992254099223623856, 0.003989672132298142590 ),
 .UNSPECIFIED. ) ;
#161689 = CARTESIAN_POINT ( 'NONE',  ( 10.72451020669898902, -18.67979575497178502, 27.91557627198103830 ) ) ;
#161690 = CARTESIAN_POINT ( 'NONE',  ( 0.05219959533934541429, -16.53943276465976808, 50.00109039468568994 ) ) ;
#161691 = CARTESIAN_POINT ( 'NONE',  ( -4.379528057220328563, 16.55341960407611168, 80.20724293864769550 ) ) ;
#161692 = CARTESIAN_POINT ( 'NONE',  ( -5.049401038298153566, 19.05341960407611168, 60.20724293864768129 ) ) ;
#161693 = CARTESIAN_POINT ( 'NONE',  ( -5.049401038298153566, 19.05341960407611168, 35.20724293864768839 ) ) ;
#161694 = DIRECTION ( 'NONE',  ( 1.000000000000000000, 0.000000000000000000, 0.000000000000000000 ) ) ;
#161695 = CARTESIAN_POINT ( 'NONE',  ( 4.379528057220092307, 16.55341960407617563, 77.29275706135234714 ) ) ;
#161696 = CARTESIAN_POINT ( 'NONE',  ( -21.53943276465977519, -0.05219959533937600094, 18.75109039468568639 ) ) ;
#161697 = CARTESIAN_POINT ( 'NONE',  ( 5.153800228976335163, 19.02544592524342804, 74.79057627198103830 ) ) ;
#161698 = CARTESIAN_POINT ( 'NONE',  ( -5.719274019375665041, -21.55341960407619695, 59.79275706135234714 ) ) ;
#161699 = CARTESIAN_POINT ( 'NONE',  ( 5.153800228976335163, 19.02544592524342804, 104.7905762719809957 ) ) ;
#161701 = ADVANCED_FACE ( 'NONE', ( #119531 ), #37642, .T. ) ;
#161700 = LINE ( 'NONE', #146519, #192822 ) ;
#161702 = ORIENTED_EDGE ( 'NONE', *, *, #194670, .T. ) ;
#161703 = CARTESIAN_POINT ( 'NONE',  ( 10.72451020669871369, 18.67979575497193778, 52.08442372801901854 ) ) ;
#161705 = CARTESIAN_POINT ( 'NONE',  ( 13.97604488694527802, 13.89961937509977652, 99.37390960531436690 ) ) ;
#161704 = CARTESIAN_POINT ( 'NONE',  ( -13.97604488694527625, -13.89961937509977652, 21.87390960531435979 ) ) ;
#161706 = CARTESIAN_POINT ( 'NONE',  ( -5.153800228976607833, 19.02544592524334988, 47.70942372801900433 ) ) ;
#161707 = CARTESIAN_POINT ( 'NONE',  ( -10.72451020669870658, -18.67979575497194134, 19.58442372801901143 ) ) ;
#161708 = CARTESIAN_POINT ( 'NONE',  ( -13.97604488694547697, 13.89961937509957934, 48.12609039468566863 ) ) ;
#161709 = CARTESIAN_POINT ( 'NONE',  ( -19.03943276465977164, 0.05219959533909376836, 31.24890960531435979 ) ) ;
#161710 = CARTESIAN_POINT ( 'NONE',  ( -4.483927247898782831, 16.52544592524335698, 92.70942372801901854 ) ) ;
#161711 = CARTESIAN_POINT ( 'NONE',  ( -16.46253265017146816, -9.564922557961047289, 69.16775706135233293 ) ) ;
#161712 = CARTESIAN_POINT ( 'NONE',  ( -16.53943276465976808, -0.05219959533934237506, 103.7510903946857042 ) ) ;
#161714 = ORIENTED_EDGE ( 'NONE', *, *, #20610, .F. ) ;
#161713 = CARTESIAN_POINT ( 'NONE',  ( -37.99626262588766679, 2.428612866367529932E-14, 2.000000000000000000 ) ) ;
#161715 = CARTESIAN_POINT ( 'NONE',  ( -19.05341960407611168, -5.049401038298163336, 81.45724293864769550 ) ) ;
#161716 = CARTESIAN_POINT ( 'NONE',  ( -21.55341960407619339, 5.719274019375674811, 88.54275706135236135 ) ) ;
#161717 = CARTESIAN_POINT ( 'NONE',  ( 15.80617190586769283, -15.72974639402175789, 100.6260903946857184 ) ) ;
#161718 = CARTESIAN_POINT ( 'NONE',  ( 18.22780087662123805, -5.499999999999976019, 98.51763182126896368 ) ) ;
#161719 = CARTESIAN_POINT ( 'NONE',  ( 5.153800228976335163, 19.02544592524342804, 99.79057627198102409 ) ) ;
#161720 = CARTESIAN_POINT ( 'NONE',  ( -15.72974639402176322, -15.80617190586768395, 79.37609039468567573 ) ) ;
#161721 = CARTESIAN_POINT ( 'NONE',  ( -13.89961937509957401, -13.97604488694547875, 109.3760903946856331 ) ) ;
#161722 = CARTESIAN_POINT ( 'NONE',  ( 9.474510206698971260, -16.51473224551069308, 82.91557627198103830 ) ) ;
#161723 = CARTESIAN_POINT ( 'NONE',  ( -15.72974639402197994, 15.80617190586746368, 30.62390960531436335 ) ) ;
#161724 = CARTESIAN_POINT ( 'NONE',  ( 5.049401038298161559, -19.05341960407611168, 92.70724293864769550 ) ) ;
#161725 = DIRECTION ( 'NONE',  ( 0.8164965809277261455, 0.000000000000000000, 0.5773502691896257311 ) ) ;
#161726 = CARTESIAN_POINT ( 'NONE',  ( 19.02544592524343514, -5.153800228976328945, 83.54057627198100988 ) ) ;
#161727 = CARTESIAN_POINT ( 'NONE',  ( 13.97604488694527802, 13.89961937509977652, 69.37390960531436690 ) ) ;
#161728 = CARTESIAN_POINT ( 'NONE',  ( -12.06949235617739369, -12.14591786802326823, 104.3760903946856899 ) ) ;
#161729 = CARTESIAN_POINT ( 'NONE',  ( -16.61371651742644318, 7.165104196375866152, 98.85415069992970416 ) ) ;
#161730 = CARTESIAN_POINT ( 'NONE',  ( 0.05219959533936267826, -19.03943276465977164, 55.00109039468566863 ) ) ;
#161731 = CARTESIAN_POINT ( 'NONE',  ( 9.564922557960805705, 16.46253265017160317, 94.58224293864769550 ) ) ;
#161732 = CARTESIAN_POINT ( 'NONE',  ( -4.379528057220328563, 16.55341960407611168, 90.20724293864770971 ) ) ;
#161733 = CARTESIAN_POINT ( 'NONE',  ( -18.67979575497178146, -10.72451020669898902, 26.66557627198103475 ) ) ;
#161734 = CARTESIAN_POINT ( 'NONE',  ( 9.474510206698971260, -16.51473224551069308, 112.9155762719810383 ) ) ;
#161735 = CARTESIAN_POINT ( 'NONE',  ( -12.06949235617756955, 12.14591786802309770, 85.62390960531436690 ) ) ;
#161736 = CARTESIAN_POINT ( 'NONE',  ( -16.19135201231369692, 7.376712067591781441, 54.81319145947971094 ) ) ;
#161737 = CARTESIAN_POINT ( 'NONE',  ( -13.97604488694547697, 13.89961937509957934, 48.12609039468566863 ) ) ;
#161738 = CARTESIAN_POINT ( 'NONE',  ( 14.29746914071037800, 8.314922557961029526, 101.6677570613523613 ) ) ;
#161739 = CARTESIAN_POINT ( 'NONE',  ( 13.89961937509977652, -13.97604488694527269, 103.1239096053143527 ) ) ;
#161740 = CARTESIAN_POINT ( 'NONE',  ( 10.72451020669871369, 18.67979575497193778, 72.08442372801899012 ) ) ;
#161741 = CARTESIAN_POINT ( 'NONE',  ( 21.55341960407610458, 5.719274019375980345, 53.95724293864770260 ) ) ;
#161742 = CARTESIAN_POINT ( 'NONE',  ( -21.52544592524334988, -5.823673210054445271, 33.95942372801901143 ) ) ;
#161743 = CARTESIAN_POINT ( 'NONE',  ( 18.67979575497178502, 10.72451020669898547, 89.16557627198102409 ) ) ;
#161744 = CARTESIAN_POINT ( 'NONE',  ( 15.72974639402176855, 15.80617190586768217, 36.87609039468568994 ) ) ;
#161745 = CARTESIAN_POINT ( 'NONE',  ( -16.53943276465976808, 0.05219959533911058130, 111.2489096053143669 ) ) ;
#161746 = CARTESIAN_POINT ( 'NONE',  ( 13.89961937509957401, 13.97604488694547697, 66.87609039468567573 ) ) ;
#161747 = CARTESIAN_POINT ( 'NONE',  ( 5.153800228976335163, 19.02544592524342804, 44.79057627198103830 ) ) ;
#161749 = CARTESIAN_POINT ( 'NONE',  ( 19.02544592524343514, -5.153800228976328945, 103.5405762719809957 ) ) ;
#161748 = CARTESIAN_POINT ( 'NONE',  ( -14.34966873604960291, -8.224510206698953496, 96.66557627198102409 ) ) ;
#161750 = CARTESIAN_POINT ( 'NONE',  ( 13.97604488694527802, 13.89961937509977652, 89.37390960531436690 ) ) ;
#161751 = CARTESIAN_POINT ( 'NONE',  ( -14.29746914071049879, 8.314922557960819915, 115.8322429386477097 ) ) ;
#161752 = CARTESIAN_POINT ( 'NONE',  ( 4.483927247898545687, 16.52544592524342804, 34.79057627198103120 ) ) ;
#161753 = CARTESIAN_POINT ( 'NONE',  ( -8.224510206698735004, -14.34966873604973081, 104.5844237280190185 ) ) ;
#161754 = CARTESIAN_POINT ( 'NONE',  ( 9.474510206698971260, -16.51473224551069308, 52.91557627198102409 ) ) ;
#161755 = CARTESIAN_POINT ( 'NONE',  ( 19.03943276465977164, -0.05219959533909143690, 23.74890960531435269 ) ) ;
#161756 = CARTESIAN_POINT ( 'NONE',  ( -13.89961937509957401, -13.97604488694547875, 24.37609039468565442 ) ) ;
#161758 = CARTESIAN_POINT ( 'NONE',  ( 12.14591786802327356, -12.06949235617739191, 110.6260903946857042 ) ) ;
#161757 = CARTESIAN_POINT ( 'NONE',  ( -0.05219959533909027116, -19.03943276465977164, 112.4989096053143669 ) ) ;
#161759 = CARTESIAN_POINT ( 'NONE',  ( 15.80617190586769283, -15.72974639402175789, 50.62609039468568994 ) ) ;
#161760 = CARTESIAN_POINT ( 'NONE',  ( 16.46253265017160672, -9.564922557960803928, 108.3322429386476955 ) ) ;
#161761 = CARTESIAN_POINT ( 'NONE',  ( -8.314922557961024197, 14.29746914071037800, 42.91775706135235424 ) ) ;
#161762 = CARTESIAN_POINT ( 'NONE',  ( -16.52544592524335698, -4.483927247898792601, 103.9594237280190185 ) ) ;
#161763 = CARTESIAN_POINT ( 'NONE',  ( -4.483927247898782831, 16.52544592524335698, 87.70942372801901854 ) ) ;
#161764 = CARTESIAN_POINT ( 'NONE',  ( 16.55341960407618274, -4.379528057220086978, 31.04275706135234714 ) ) ;
#161765 = CARTESIAN_POINT ( 'NONE',  ( -5.153800228976328057, -19.02544592524343514, 42.29057627198101699 ) ) ;
#161766 = CARTESIAN_POINT ( 'NONE',  ( -16.55341960407611168, -4.379528057220339221, 106.4572429386477097 ) ) ;
#161767 = CARTESIAN_POINT ( 'NONE',  ( -5.719274019375978568, 21.55341960407610458, 115.2072429386476955 ) ) ;
#161768 = CARTESIAN_POINT ( 'NONE',  ( 19.05341960407611168, 5.049401038298154454, 28.95724293864769550 ) ) ;
#161769 = CARTESIAN_POINT ( 'NONE',  ( 0.05219959533909260263, 19.03943276465977164, 99.99890960531436690 ) ) ;
#161770 = CARTESIAN_POINT ( 'NONE',  ( -5.153800228976328057, -19.02544592524343514, 32.29057627198102409 ) ) ;
#161771 = CARTESIAN_POINT ( 'NONE',  ( 9.564922557960805705, 16.46253265017160317, 99.58224293864770971 ) ) ;
#161772 = CARTESIAN_POINT ( 'NONE',  ( -16.38665767535055906, -7.295008042175999741, 34.73599135785454450 ) ) ;
#161773 = CARTESIAN_POINT ( 'NONE',  ( 9.564922557960805705, 16.46253265017160317, 99.58224293864770971 ) ) ;
#161775 = CARTESIAN_POINT ( 'NONE',  ( 16.53943276465976808, -0.05219959533910856209, 108.7489096053143669 ) ) ;
#161774 = CARTESIAN_POINT ( 'NONE',  ( 10.81492255796106328, -18.62759615963255655, 40.41775706135234714 ) ) ;
#161776 = CARTESIAN_POINT ( 'NONE',  ( 9.564922557960805705, 16.46253265017160317, 114.5822429386476955 ) ) ;
#161777 = DIRECTION ( 'NONE',  ( 1.000000000000000000, 0.000000000000000000, 0.000000000000000000 ) ) ;
#161778 = CARTESIAN_POINT ( 'NONE',  ( -0.05219959533934338120, 16.53943276465976808, 62.50109039468568284 ) ) ;
#161779 = CARTESIAN_POINT ( 'NONE',  ( 0.05219959533937995610, -21.53943276465977519, 75.00109039468568994 ) ) ;
#161780 = CARTESIAN_POINT ( 'NONE',  ( 12.14591786802327356, -12.06949235617739191, 45.62609039468567573 ) ) ;
#161781 = CARTESIAN_POINT ( 'NONE',  ( -19.02544592524342804, 5.153800228976336051, 76.04057627198102409 ) ) ;
#161782 = CARTESIAN_POINT ( 'NONE',  ( -19.05341960407617563, 5.049401038297882671, 108.5427570613523187 ) ) ;
#161783 = CARTESIAN_POINT ( 'NONE',  ( 16.52544592524335698, 4.483927247898782831, 76.45942372801901854 ) ) ;
#161784 = CARTESIAN_POINT ( 'NONE',  ( -0.05219959533936034679, 19.03943276465977164, 87.50109039468567573 ) ) ;
#161785 = CARTESIAN_POINT ( 'NONE',  ( -16.46253265017160317, 9.564922557960807481, 80.83224293864769550 ) ) ;
#161786 = CARTESIAN_POINT ( 'NONE',  ( -5.823673210054116645, -21.52544592524344225, 97.29057627198105251 ) ) ;
#161788 = CARTESIAN_POINT ( 'NONE',  ( 0.05219959533936267826, -19.03943276465977164, 85.00109039468567573 ) ) ;
#161787 = CARTESIAN_POINT ( 'NONE',  ( 16.55341960407611168, 4.379528057220329451, 83.95724293864770971 ) ) ;
#161789 = CARTESIAN_POINT ( 'NONE',  ( -16.53943276465976808, -0.05219959533934237506, 63.75109039468568284 ) ) ;
#161790 = CARTESIAN_POINT ( 'NONE',  ( -19.01533133064924996, 5.499999999999451106, 78.76586590595742621 ) ) ;
#161791 = CARTESIAN_POINT ( 'NONE',  ( -13.89961937509957401, -13.97604488694547875, 69.37609039468564731 ) ) ;
#161792 = CARTESIAN_POINT ( 'NONE',  ( -0.05219959533910754901, -16.53943276465976808, 27.49890960531435269 ) ) ;
#161793 = CARTESIAN_POINT ( 'NONE',  ( 16.55341960407611168, 4.379528057220329451, 78.95724293864769550 ) ) ;
#161795 = CARTESIAN_POINT ( 'NONE',  ( -19.26498983726238379, 5.499999999999807265, 90.55319577422004329 ) ) ;
#161794 = CARTESIAN_POINT ( 'NONE',  ( 13.97604488694548053, -13.89961937509957401, 20.62609039468567573 ) ) ;
#161796 = CARTESIAN_POINT ( 'NONE',  ( -18.62759615963255300, -10.81492255796106328, 24.16775706135235424 ) ) ;
#161797 = CARTESIAN_POINT ( 'NONE',  ( 19.05341960407611168, 5.049401038298154454, 108.9572429386477097 ) ) ;
#161798 = CARTESIAN_POINT ( 'NONE',  ( -9.474510206698964154, 16.51473224551069663, 80.41557627198103830 ) ) ;
#161799 = CARTESIAN_POINT ( 'NONE',  ( -0.05219959533937732626, 21.53943276465977519, 97.50109039468567573 ) ) ;
#161800 = CARTESIAN_POINT ( 'NONE',  ( -5.153800228976328057, -19.02544592524343514, 72.29057627198102409 ) ) ;
#161801 = CARTESIAN_POINT ( 'NONE',  ( -18.62759615963270932, 10.81492255796079327, 45.83224293864769550 ) ) ;
#161802 = CARTESIAN_POINT ( 'NONE',  ( 8.224510206698953496, -14.34966873604960469, 82.91557627198103830 ) ) ;
#161803 = CARTESIAN_POINT ( 'NONE',  ( -9.564922557960796823, -16.46253265017161027, 62.08224293864769550 ) ) ;
#161804 = CARTESIAN_POINT ( 'NONE',  ( -16.53943276465976808, 0.05219959533911058130, 111.2489096053143669 ) ) ;
#161805 = CARTESIAN_POINT ( 'NONE',  ( -10.72451020669870658, -18.67979575497194134, 24.58442372801901499 ) ) ;
#161806 = CARTESIAN_POINT ( 'NONE',  ( 5.719274019375673035, 21.55341960407619339, 57.29275706135234714 ) ) ;
#161807 = CARTESIAN_POINT ( 'NONE',  ( 9.564922557960805705, 16.46253265017160317, 44.58224293864769550 ) ) ;
#161808 = CARTESIAN_POINT ( 'NONE',  ( -16.55341960407617563, 4.379528057220093196, 83.54275706135234714 ) ) ;
#161809 = CARTESIAN_POINT ( 'NONE',  ( 10.72451020669898902, -18.67979575497178502, 107.9155762719810241 ) ) ;
#161810 = CARTESIAN_POINT ( 'NONE',  ( 5.823673210054125526, 21.52544592524343514, 104.7905762719810241 ) ) ;
#161812 = CARTESIAN_POINT ( 'NONE',  ( 19.03943276465977164, -0.05219959533909143690, 68.74890960531436690 ) ) ;
#161811 = CARTESIAN_POINT ( 'NONE',  ( -13.97604488694547697, 13.89961937509957934, 43.12609039468566152 ) ) ;
#161813 = CARTESIAN_POINT ( 'NONE',  ( -19.03943276465977164, -0.05219959533935918106, 38.75109039468566152 ) ) ;
#161814 = CARTESIAN_POINT ( 'NONE',  ( 15.80617190586769283, -15.72974639402175789, 70.62609039468567573 ) ) ;
#161815 = CARTESIAN_POINT ( 'NONE',  ( 21.55341960407610458, 5.719274019375980345, 63.95724293864770260 ) ) ;
#161816 = CARTESIAN_POINT ( 'NONE',  ( 16.52544592524342804, -4.483927247898539470, 33.54057627198102409 ) ) ;
#161818 = CARTESIAN_POINT ( 'NONE',  ( 21.53943276465977519, 0.05219959533937863772, 106.2510903946856757 ) ) ;
#161817 = CARTESIAN_POINT ( 'NONE',  ( -21.55341960407619339, 5.719274019375674811, 93.54275706135234714 ) ) ;
#161819 = CARTESIAN_POINT ( 'NONE',  ( -4.379528057220328563, 16.55341960407611168, 60.20724293864768839 ) ) ;
#161820 = CARTESIAN_POINT ( 'NONE',  ( -4.483927247898539470, -16.52544592524342804, 102.2905762719810383 ) ) ;
#161821 = CARTESIAN_POINT ( 'NONE',  ( -9.564922557961040184, 16.46253265017147172, 57.91775706135233293 ) ) ;
#161822 = CARTESIAN_POINT ( 'NONE',  ( 16.52544592524342804, -4.483927247898539470, 28.54057627198103120 ) ) ;
#161823 = CARTESIAN_POINT ( 'NONE',  ( -21.52544592524334988, -5.823673210054445271, 63.95942372801901854 ) ) ;
#161824 = CARTESIAN_POINT ( 'NONE',  ( -13.89961937509977652, 13.97604488694528158, 75.62390960531438111 ) ) ;
#161825 = CARTESIAN_POINT ( 'NONE',  ( -13.97604488694547697, 13.89961937509957934, 43.12609039468566152 ) ) ;
#161826 = CARTESIAN_POINT ( 'NONE',  ( 15.80617190586746368, 15.72974639402197994, 49.37390960531436690 ) ) ;
#161827 = CARTESIAN_POINT ( 'NONE',  ( 21.52544592524334988, 5.823673210054432836, 46.45942372801901854 ) ) ;
#161828 = CARTESIAN_POINT ( 'NONE',  ( 15.72974639402199770, -15.80617190586745480, 103.1239096053143811 ) ) ;
#161829 = CARTESIAN_POINT ( 'NONE',  ( -13.97604488694547697, 13.89961937509957934, 103.1260903946856473 ) ) ;
#161830 = CARTESIAN_POINT ( 'NONE',  ( 16.53943276465976808, 0.05219959533934440121, 71.25109039468568994 ) ) ;
#161832 = CARTESIAN_POINT ( 'NONE',  ( -15.72974639402197994, 15.80617190586746368, 110.6239096053143669 ) ) ;
#161831 = DIRECTION ( 'NONE',  ( 1.000000000000000000, 0.000000000000000000, 0.000000000000000000 ) ) ;
#161833 = CARTESIAN_POINT ( 'NONE',  ( -4.483927247898539470, -16.52544592524342804, 92.29057627198103830 ) ) ;
#161834 = CARTESIAN_POINT ( 'NONE',  ( -22.81625015709509441, -31.40387420917324590, -10.82499999726881157 ) ) ;
#161835 = CARTESIAN_POINT ( 'NONE',  ( -8.314922557961024197, 14.29746914071037800, 27.91775706135234358 ) ) ;
#161836 = ADVANCED_FACE ( 'NONE', ( #150868 ), #2002, .T. ) ;
#161837 = CARTESIAN_POINT ( 'NONE',  ( -15.72974639402197994, 15.80617190586746368, 45.62390960531436690 ) ) ;
#161838 = CARTESIAN_POINT ( 'NONE',  ( 12.06949235617739724, 12.14591786802326823, 86.87609039468568994 ) ) ;
#161839 = DIRECTION ( 'NONE',  ( 0.5150380749100522682, 0.000000000000000000, -0.8571673007021134438 ) ) ;
#161840 = CARTESIAN_POINT ( 'NONE',  ( -8.314922557961024197, 14.29746914071037800, 67.91775706135234714 ) ) ;
#161841 = CARTESIAN_POINT ( 'NONE',  ( -5.719274019375665041, -21.55341960407619695, 29.79275706135234358 ) ) ;
#161842 = CARTESIAN_POINT ( 'NONE',  ( -18.67979575497178146, -10.72451020669898902, 46.66557627198102409 ) ) ;
#161843 = CARTESIAN_POINT ( 'NONE',  ( 8.314922557961029526, -14.29746914071037800, 85.41775706135236135 ) ) ;
#161844 = CARTESIAN_POINT ( 'NONE',  ( -5.049401038298153566, 19.05341960407611168, 100.2072429386476955 ) ) ;
#161845 = CARTESIAN_POINT ( 'NONE',  ( -5.823673210054431948, 21.52544592524334988, 72.70942372801901854 ) ) ;
#161846 = CARTESIAN_POINT ( 'NONE',  ( 18.62759615963271287, -10.81492255796078972, 43.33224293864769550 ) ) ;
#161847 = CARTESIAN_POINT ( 'NONE',  ( -0.05219959533907301413, -21.53943276465977519, 32.49890960531435979 ) ) ;
#161848 = ORIENTED_EDGE ( 'NONE', *, *, #103351, .F. ) ;
#161849 = CARTESIAN_POINT ( 'NONE',  ( 19.03943276465977164, 0.05219959533936151252, 46.25109039468566863 ) ) ;
#161850 = CARTESIAN_POINT ( 'NONE',  ( 16.53943276465976808, 0.05219959533934440121, 66.25109039468567573 ) ) ;
#161851 = CARTESIAN_POINT ( 'NONE',  ( 5.719274019375991003, -21.55341960407610458, 37.70724293864769550 ) ) ;
#161852 = ORIENTED_EDGE ( 'NONE', *, *, #36961, .F. ) ;
#161853 = CARTESIAN_POINT ( 'NONE',  ( 13.89961937509977652, -13.97604488694527269, 88.12390960531438111 ) ) ;
#161854 = CARTESIAN_POINT ( 'NONE',  ( 0.05219959533910956823, 16.53943276465976808, 24.99890960531435624 ) ) ;
#161855 = FACE_OUTER_BOUND ( 'NONE', #75145, .T. ) ;
#161856 = CARTESIAN_POINT ( 'NONE',  ( -4.379528057220328563, 16.55341960407611168, 110.2072429386477239 ) ) ;
#161857 = CARTESIAN_POINT ( 'NONE',  ( -0.05219959533907301413, -21.53943276465977519, 42.49890960531435979 ) ) ;
#161858 = CARTESIAN_POINT ( 'NONE',  ( 13.97604488694527802, 13.89961937509977652, 49.37390960531434558 ) ) ;
#161859 = CARTESIAN_POINT ( 'NONE',  ( -4.483927247898782831, 16.52544592524335698, 77.70942372801900433 ) ) ;
#161860 = CARTESIAN_POINT ( 'NONE',  ( 15.72974639402176855, 15.80617190586768217, 26.87609039468567218 ) ) ;
#161861 = CARTESIAN_POINT ( 'NONE',  ( -19.03943276465977164, -0.05219959533935918106, 83.75109039468567573 ) ) ;
#161862 = CARTESIAN_POINT ( 'NONE',  ( 16.52544592524342804, -4.483927247898539470, 93.54057627198103830 ) ) ;
#161863 = CARTESIAN_POINT ( 'NONE',  ( 13.97604488694527802, 13.89961937509977652, 49.37390960531434558 ) ) ;
#161864 = CARTESIAN_POINT ( 'NONE',  ( 19.05341960407611168, 5.049401038298154454, 28.95724293864769550 ) ) ;
#161865 = CARTESIAN_POINT ( 'NONE',  ( 21.53943276465977519, 0.05219959533937863772, 111.2510903946856899 ) ) ;
#161866 = CARTESIAN_POINT ( 'NONE',  ( 9.564922557960805705, 16.46253265017160317, 74.58224293864769550 ) ) ;
#161867 = CARTESIAN_POINT ( 'NONE',  ( -16.55341960407617563, 4.379528057220093196, 68.54275706135234714 ) ) ;
#161868 = CARTESIAN_POINT ( 'NONE',  ( -15.72974639402176322, -15.80617190586768395, 89.37609039468568994 ) ) ;
#161869 = CARTESIAN_POINT ( 'NONE',  ( -18.62759615963270932, 10.81492255796079327, 50.83224293864770971 ) ) ;
#161870 = CARTESIAN_POINT ( 'NONE',  ( -4.483927247898782831, 16.52544592524335698, 67.70942372801901854 ) ) ;
#161871 = CARTESIAN_POINT ( 'NONE',  ( -19.05341960407617563, 5.049401038297882671, 53.54275706135231871 ) ) ;
#161872 = CARTESIAN_POINT ( 'NONE',  ( 13.97604488694548053, -13.89961937509957401, 70.62609039468567573 ) ) ;
#161873 = EDGE_LOOP ( 'NONE', ( #180048, #26427, #49508, #88000 ) ) ;
#161874 = CARTESIAN_POINT ( 'NONE',  ( 10.81492255796106328, -18.62759615963255655, 65.41775706135234714 ) ) ;
#161875 = CARTESIAN_POINT ( 'NONE',  ( -9.474510206698964154, 16.51473224551069663, 65.41557627198102409 ) ) ;
#161876 = CARTESIAN_POINT ( 'NONE',  ( 9.564922557960805705, 16.46253265017160317, 39.58224293864768839 ) ) ;
#161877 = CARTESIAN_POINT ( 'NONE',  ( 19.02544592524334988, 5.153800228976608722, 56.45942372801898301 ) ) ;
#161878 = CARTESIAN_POINT ( 'NONE',  ( -5.153800228976328057, -19.02544592524343514, 107.2905762719810383 ) ) ;
#161879 = CARTESIAN_POINT ( 'NONE',  ( -19.02544592524342804, 5.153800228976336051, 91.04057627198100988 ) ) ;
#161880 = CARTESIAN_POINT ( 'NONE',  ( -16.55341960407611168, -4.379528057220339221, 56.45724293864768839 ) ) ;
#161881 = CARTESIAN_POINT ( 'NONE',  ( 15.80617190586746368, 15.72974639402197994, 49.37390960531436690 ) ) ;
#161882 = CARTESIAN_POINT ( 'NONE',  ( -18.46320343559654731, -23.96320343559633059, 8.181980515339454030 ) ) ;
#161883 = CARTESIAN_POINT ( 'NONE',  ( 0.05219959533937995610, -21.53943276465977519, 110.0010903946856757 ) ) ;
#161884 = CARTESIAN_POINT ( 'NONE',  ( 19.03943276465977164, -0.05219959533909143690, 48.74890960531435979 ) ) ;
#161885 = CARTESIAN_POINT ( 'NONE',  ( -33.77897430376540910, -2.912663603757514874, 99.66889340242285300 ) ) ;
#161886 = DIRECTION ( 'NONE',  ( -1.000000000000000000, -0.000000000000000000, 0.000000000000000000 ) ) ;
#161887 = CARTESIAN_POINT ( 'NONE',  ( 14.34966873604972726, -8.224510206698740333, 65.83442372801900433 ) ) ;
#161888 = CARTESIAN_POINT ( 'NONE',  ( -18.67979575497178146, -10.72451020669898902, 91.66557627198103830 ) ) ;
#161889 = CARTESIAN_POINT ( 'NONE',  ( 12.14591786802309770, 12.06949235617756955, 49.37390960531436690 ) ) ;
#161891 = DIRECTION ( 'NONE',  ( -0.000000000000000000, -0.000000000000000000, 1.000000000000000000 ) ) ;
#161890 = CARTESIAN_POINT ( 'NONE',  ( 13.89961937509977652, -13.97604488694527269, 43.12390960531434558 ) ) ;
#161892 = CARTESIAN_POINT ( 'NONE',  ( 15.72974639402176855, 15.80617190586768217, 41.87609039468568284 ) ) ;
#161893 = CARTESIAN_POINT ( 'NONE',  ( -13.97604488694547697, 13.89961937509957934, 48.12609039468566863 ) ) ;
#161894 = CARTESIAN_POINT ( 'NONE',  ( -16.46253265017160317, 9.564922557960807481, 35.83224293864768839 ) ) ;
#161895 = CARTESIAN_POINT ( 'NONE',  ( 15.80617190586769283, -15.72974639402175789, 100.6260903946857184 ) ) ;
#161896 = CARTESIAN_POINT ( 'NONE',  ( 4.500000000000000888, -139.5000000000000000, 21.32407087589996308 ) ) ;
#161897 = ORIENTED_EDGE ( 'NONE', *, *, #69568, .T. ) ;
#161898 = CARTESIAN_POINT ( 'NONE',  ( -0.05219959533910754901, -16.53943276465976808, 37.49890960531436690 ) ) ;
#161899 = CARTESIAN_POINT ( 'NONE',  ( 19.34837522270364829, 5.499999999999730882, 43.36337684832574979 ) ) ;
#161900 = CARTESIAN_POINT ( 'NONE',  ( -5.719274019375978568, 21.55341960407610458, 35.20724293864768839 ) ) ;
#161901 = CARTESIAN_POINT ( 'NONE',  ( -5.359611314223446995E-15, 29.16686587814335851, 142.3750000027311557 ) ) ;
#161902 = CARTESIAN_POINT ( 'NONE',  ( 5.153800228976335163, 19.02544592524342804, 89.79057627198102409 ) ) ;
#161903 = CARTESIAN_POINT ( 'NONE',  ( 4.483927247898545687, 16.52544592524342804, 84.79057627198102409 ) ) ;
#161904 = CARTESIAN_POINT ( 'NONE',  ( -16.55341960407617563, 4.379528057220093196, 23.54275706135235424 ) ) ;
#161905 = EDGE_CURVE ( 'NONE', #194969, #152017, #155010, .T. ) ;
#161906 = CARTESIAN_POINT ( 'NONE',  ( 8.224510206698742110, 14.34966873604972548, 112.0844237280190185 ) ) ;
#161907 = ORIENTED_EDGE ( 'NONE', *, *, #17982, .T. ) ;
#161909 = CARTESIAN_POINT ( 'NONE',  ( -5.719274019375978568, 21.55341960407610458, 85.20724293864770971 ) ) ;
#161908 = CARTESIAN_POINT ( 'NONE',  ( 5.049401038298161559, -19.05341960407611168, 102.7072429386476955 ) ) ;
#161911 = CARTESIAN_POINT ( 'NONE',  ( -13.89961937509977652, 13.97604488694528158, 105.6239096053143527 ) ) ;
#161910 = CARTESIAN_POINT ( 'NONE',  ( 16.52544592524342804, -4.483927247898539470, 23.54057627198102765 ) ) ;
#161912 = CARTESIAN_POINT ( 'NONE',  ( 19.02544592524334988, 5.153800228976608722, 76.45942372801897591 ) ) ;
#161913 = CARTESIAN_POINT ( 'NONE',  ( 15.80617190586769283, -15.72974639402175789, 105.6260903946856899 ) ) ;
#161914 = CARTESIAN_POINT ( 'NONE',  ( 5.719274019375991003, -21.55341960407610458, 87.70724293864769550 ) ) ;
#161915 = CARTESIAN_POINT ( 'NONE',  ( -21.53943276465977519, 0.05219959533907696930, 36.24890960531435979 ) ) ;
#161916 = CARTESIAN_POINT ( 'NONE',  ( -9.474510206698964154, 16.51473224551069663, 65.41557627198102409 ) ) ;
#161917 = CARTESIAN_POINT ( 'NONE',  ( -14.29746914071049879, 8.314922557960819915, 40.83224293864769550 ) ) ;
#161918 = CARTESIAN_POINT ( 'NONE',  ( -19.05341960407611168, -5.049401038298163336, 76.45724293864769550 ) ) ;
#161919 = EDGE_LOOP ( 'NONE', ( #182867, #116584, #155865, #86153, #49356, #168860 ) ) ;
#161920 = CARTESIAN_POINT ( 'NONE',  ( 2.200000000000000622, 0.000000000000000000, 0.000000000000000000 ) ) ;
#161921 = CARTESIAN_POINT ( 'NONE',  ( -16.51473224551082808, 9.474510206698731452, 23.33442372801900078 ) ) ;
#161922 = CARTESIAN_POINT ( 'NONE',  ( 4.483927247898545687, 16.52544592524342804, 84.79057627198102409 ) ) ;
#161923 = CARTESIAN_POINT ( 'NONE',  ( 18.62759615963255655, 10.81492255796105972, 26.66775706135235424 ) ) ;
#161924 = CARTESIAN_POINT ( 'NONE',  ( -8.571926809382608425, 26.38167802310805854, 140.9750000027312069 ) ) ;
#161925 = CARTESIAN_POINT ( 'NONE',  ( 10.81492255796078972, 18.62759615963270932, 74.58224293864768129 ) ) ;
#161926 = CARTESIAN_POINT ( 'NONE',  ( -8.314922557961024197, 14.29746914071037800, 92.91775706135236135 ) ) ;
#161927 = CARTESIAN_POINT ( 'NONE',  ( 19.03943276465977164, -0.05219959533909143690, 23.74890960531435269 ) ) ;
#161928 = CARTESIAN_POINT ( 'NONE',  ( 5.049401038298161559, -19.05341960407611168, 67.70724293864769550 ) ) ;
#161929 = CARTESIAN_POINT ( 'NONE',  ( 19.03943276465977164, -0.05219959533909143690, 23.74890960531435269 ) ) ;
#161930 = CARTESIAN_POINT ( 'NONE',  ( 0.05219959533910956823, 16.53943276465976808, 24.99890960531435624 ) ) ;
#161931 = CARTESIAN_POINT ( 'NONE',  ( -21.52544592524334988, -5.823673210054445271, 58.95942372801902565 ) ) ;
#161932 = CARTESIAN_POINT ( 'NONE',  ( 32.19332086309600527, -20.18834286810123047, -25.14458231473971850 ) ) ;
#161933 = CARTESIAN_POINT ( 'NONE',  ( 15.80617190586769283, -15.72974639402175789, 95.62609039468568994 ) ) ;
#161934 = CARTESIAN_POINT ( 'NONE',  ( -13.89961937509977652, 13.97604488694528158, 40.62390960531435979 ) ) ;
#161935 = CARTESIAN_POINT ( 'NONE',  ( -16.51473224551069308, -9.474510206698971260, 51.66557627198102409 ) ) ;
#161936 = ORIENTED_EDGE ( 'NONE', *, *, #123538, .T. ) ;
#161937 = CARTESIAN_POINT ( 'NONE',  ( -21.53943276465977519, -0.05219959533937600094, 88.75109039468567573 ) ) ;
#161938 = CARTESIAN_POINT ( 'NONE',  ( 16.53943276465976808, 0.05219959533934440121, 66.25109039468567573 ) ) ;
#161939 = CARTESIAN_POINT ( 'NONE',  ( 21.53943276465977519, 0.05219959533937863772, 81.25109039468568994 ) ) ;
#161940 = CARTESIAN_POINT ( 'NONE',  ( 0.05219959533909260263, 19.03943276465977164, 114.9989096053143669 ) ) ;
#161941 = CARTESIAN_POINT ( 'NONE',  ( 9.564922557961047289, -16.46253265017146816, 100.4177570613523329 ) ) ;
#161942 = CARTESIAN_POINT ( 'NONE',  ( 18.62759615963255655, 10.81492255796105972, 56.66775706135235424 ) ) ;
#161943 = CARTESIAN_POINT ( 'NONE',  ( 16.53943276465976808, 0.05219959533934440121, 36.25109039468567573 ) ) ;
#161944 = CARTESIAN_POINT ( 'NONE',  ( -21.53943276465977519, 0.05219959533907696930, 91.24890960531436690 ) ) ;
#161945 = CARTESIAN_POINT ( 'NONE',  ( -19.02544592524334988, -5.153800228976617603, 88.95942372801897591 ) ) ;
#161946 = CARTESIAN_POINT ( 'NONE',  ( -13.89961937509977652, 13.97604488694528158, 60.62390960531436690 ) ) ;
#161947 = CARTESIAN_POINT ( 'NONE',  ( -5.049401038297874678, -19.05341960407617918, 94.79275706135230450 ) ) ;
#161948 = CARTESIAN_POINT ( 'NONE',  ( -9.474510206698720793, -16.51473224551083518, 99.58442372801900433 ) ) ;
#161949 = CARTESIAN_POINT ( 'NONE',  ( 12.06949235617757843, -12.14591786802309237, 53.12390960531436690 ) ) ;
#161950 = CARTESIAN_POINT ( 'NONE',  ( -13.97604488694547697, 13.89961937509957934, 73.12609039468568994 ) ) ;
#161951 = CARTESIAN_POINT ( 'NONE',  ( 16.55341960407618274, -4.379528057220086978, 56.04275706135235424 ) ) ;
#161952 = CARTESIAN_POINT ( 'NONE',  ( 16.46253265017160672, -9.564922557960803928, 38.33224293864768839 ) ) ;
#161953 = CARTESIAN_POINT ( 'NONE',  ( 19.02544592524343514, -5.153800228976328945, 58.54057627198102409 ) ) ;
#161954 = CARTESIAN_POINT ( 'NONE',  ( 0.05219959533934541429, -16.53943276465976808, 60.00109039468568284 ) ) ;
#161955 = DIRECTION ( 'NONE',  ( -1.000000000000000000, -0.000000000000000000, -3.709348145883536076E-20 ) ) ;
#161956 = CARTESIAN_POINT ( 'NONE',  ( -28.82186960331499037, 2.428612866367529932E-14, 142.2500000054623683 ) ) ;
#161957 = CARTESIAN_POINT ( 'NONE',  ( -16.46253265017160317, 9.564922557960807481, 105.8322429386476955 ) ) ;
#161958 = DIRECTION ( 'NONE',  ( -0.000000000000000000, 0.000000000000000000, -1.000000000000000000 ) ) ;
#161959 = EDGE_LOOP ( 'NONE', ( #100729, #139414, #115354, #65509 ) ) ;
#161960 = CARTESIAN_POINT ( 'NONE',  ( -5.153800228976607833, 19.02544592524334988, 102.7094237280189759 ) ) ;
#161961 = CARTESIAN_POINT ( 'NONE',  ( -5.823673210054116645, -21.52544592524344225, 42.29057627198103120 ) ) ;
#161963 = CARTESIAN_POINT ( 'NONE',  ( -4.379528057220086978, -16.55341960407618274, 19.79275706135235069 ) ) ;
#161962 = CARTESIAN_POINT ( 'NONE',  ( -5.153800228976607833, 19.02544592524334988, 32.70942372801899722 ) ) ;
#161964 = CARTESIAN_POINT ( 'NONE',  ( 16.46253265017160672, -9.564922557960803928, 23.33224293864769194 ) ) ;
#161965 = CARTESIAN_POINT ( 'NONE',  ( 0.05219959533909260263, 19.03943276465977164, 49.99890960531435979 ) ) ;
#161966 = CARTESIAN_POINT ( 'NONE',  ( -21.52544592524343514, 5.823673210054127303, 71.04057627198103830 ) ) ;
#161967 = CARTESIAN_POINT ( 'NONE',  ( 19.05341960407611168, 5.049401038298154454, 103.9572429386476671 ) ) ;
#161968 = CARTESIAN_POINT ( 'NONE',  ( -16.46253265017160317, 9.564922557960807481, 35.83224293864768839 ) ) ;
#161969 = CARTESIAN_POINT ( 'NONE',  ( -22.44159573604010305, 16.30477369853692338, 145.1750000027311671 ) ) ;
#161970 = CARTESIAN_POINT ( 'NONE',  ( -5.153800228976607833, 19.02544592524334988, 87.70942372801897591 ) ) ;
#161971 = CARTESIAN_POINT ( 'NONE',  ( -0.05219959533910754901, -16.53943276465976808, 67.49890960531436690 ) ) ;
#161972 = CARTESIAN_POINT ( 'NONE',  ( -21.52544592524343514, 5.823673210054127303, 51.04057627198103120 ) ) ;
#161973 = CARTESIAN_POINT ( 'NONE',  ( -18.62759615963255300, -10.81492255796106328, 104.1677570613523471 ) ) ;
#161974 = CARTESIAN_POINT ( 'NONE',  ( 15.80617190586746368, 15.72974639402197994, 94.37390960531436690 ) ) ;
#161975 = CARTESIAN_POINT ( 'NONE',  ( -5.823673210054431948, 21.52544592524334988, 67.70942372801901854 ) ) ;
#161976 = CARTESIAN_POINT ( 'NONE',  ( -21.55341960407619339, 5.719274019375674811, 83.54275706135234714 ) ) ;
#161977 = CARTESIAN_POINT ( 'NONE',  ( 19.02544592524343514, -5.153800228976328945, 108.5405762719810383 ) ) ;
#161979 = CARTESIAN_POINT ( 'NONE',  ( -0.05219959533937732626, 21.53943276465977519, 82.50109039468568994 ) ) ;
#161978 = CARTESIAN_POINT ( 'NONE',  ( -4.379528057220086978, -16.55341960407618274, 109.7927570613523613 ) ) ;
#161980 = CARTESIAN_POINT ( 'NONE',  ( -16.51473224551069308, -9.474510206698971260, 66.66557627198102409 ) ) ;
#161981 = CARTESIAN_POINT ( 'NONE',  ( -19.02544592524334988, -5.153800228976617603, 33.95942372801897591 ) ) ;
#161982 = CARTESIAN_POINT ( 'NONE',  ( -15.72974639402176322, -15.80617190586768395, 24.37609039468567573 ) ) ;
#161983 = CARTESIAN_POINT ( 'NONE',  ( -16.46253265017160317, 9.564922557960807481, 70.83224293864770971 ) ) ;
#161984 = CARTESIAN_POINT ( 'NONE',  ( -12.14591786802309592, -12.06949235617757132, 86.87390960531438111 ) ) ;
#161985 = CARTESIAN_POINT ( 'NONE',  ( -4.379528057220328563, 16.55341960407611168, 45.20724293864769550 ) ) ;
#161986 = CARTESIAN_POINT ( 'NONE',  ( 21.52544592524344225, -5.823673210054117533, 53.54057627198103120 ) ) ;
#161987 = CARTESIAN_POINT ( 'NONE',  ( -19.05341960407611168, -5.049401038298163336, 66.45724293864769550 ) ) ;
#161988 = CARTESIAN_POINT ( 'NONE',  ( 18.62759615963271287, -10.81492255796078972, 73.33224293864769550 ) ) ;
#161989 = CARTESIAN_POINT ( 'NONE',  ( -13.97604488694547697, 13.89961937509957934, 68.12609039468563310 ) ) ;
#161991 = CARTESIAN_POINT ( 'NONE',  ( -16.52544592524342804, 4.483927247898546575, 66.04057627198103830 ) ) ;
#161990 = CARTESIAN_POINT ( 'NONE',  ( 5.153800228976617603, -19.02544592524335343, 25.20942372801900433 ) ) ;
#161992 = CARTESIAN_POINT ( 'NONE',  ( 15.80617190586746368, 15.72974639402197994, 44.37390960531435979 ) ) ;
#161993 = ORIENTED_EDGE ( 'NONE', *, *, #116496, .F. ) ;
#161994 = CARTESIAN_POINT ( 'NONE',  ( 16.62475595723698873, 7.163666690055318753, 101.9728664818952666 ) ) ;
#161996 = CARTESIAN_POINT ( 'NONE',  ( -21.46320343559624533, 20.96320343559661836, 4.646446609406719830 ) ) ;
#161995 = CARTESIAN_POINT ( 'NONE',  ( -8.314922557961024197, 14.29746914071037800, 87.91775706135234714 ) ) ;
#161997 = CARTESIAN_POINT ( 'NONE',  ( 9.564922557961047289, -16.46253265017146816, 90.41775706135234714 ) ) ;
#161998 = CARTESIAN_POINT ( 'NONE',  ( -16.53943276465976808, 0.05219959533911058130, 51.24890960531436690 ) ) ;
#161999 = CARTESIAN_POINT ( 'NONE',  ( -19.39056639909674118, -5.500000000000059508, 60.78948781074343088 ) ) ;
#162000 = CARTESIAN_POINT ( 'NONE',  ( -0.05219959533909027116, -19.03943276465977164, 47.49890960531435979 ) ) ;
#162001 = CARTESIAN_POINT ( 'NONE',  ( 0.05219959533910956823, 16.53943276465976808, 34.99890960531435979 ) ) ;
#162002 = CARTESIAN_POINT ( 'NONE',  ( -19.03943276465977164, 0.05219959533909376836, 86.24890960531436690 ) ) ;
#162004 = CARTESIAN_POINT ( 'NONE',  ( -19.03943276465977164, 0.05219959533909376836, 56.24890960531435979 ) ) ;
#162003 = CARTESIAN_POINT ( 'NONE',  ( -9.564922557961040184, 16.46253265017147172, 77.91775706135234714 ) ) ;
#162005 = CARTESIAN_POINT ( 'NONE',  ( -10.81492255796105439, 18.62759615963255655, 62.91775706135236135 ) ) ;
#162006 = CARTESIAN_POINT ( 'NONE',  ( -19.02544592524342804, 5.153800228976336051, 66.04057627198103830 ) ) ;
#162007 = CARTESIAN_POINT ( 'NONE',  ( -13.97604488694527625, -13.89961937509977652, 31.87390960531435979 ) ) ;
#162008 = CARTESIAN_POINT ( 'NONE',  ( 16.46253265017160672, -9.564922557960803928, 78.33224293864769550 ) ) ;
#162009 = CARTESIAN_POINT ( 'NONE',  ( 21.52544592524344225, -5.823673210054117533, 53.54057627198103120 ) ) ;
#162010 = CARTESIAN_POINT ( 'NONE',  ( 16.46253265017160672, -9.564922557960803928, 43.33224293864769550 ) ) ;
#162011 = CARTESIAN_POINT ( 'NONE',  ( -5.719274019375978568, 21.55341960407610458, 60.20724293864768839 ) ) ;
#162012 = CARTESIAN_POINT ( 'NONE',  ( -5.049401038297874678, -19.05341960407617918, 84.79275706135233293 ) ) ;
#162013 = CARTESIAN_POINT ( 'NONE',  ( 8.314922557961029526, -14.29746914071037800, 100.4177570613523471 ) ) ;
#162014 = CARTESIAN_POINT ( 'NONE',  ( 13.97604488694548053, -13.89961937509957401, 30.62609039468566863 ) ) ;
#162015 = EDGE_CURVE ( 'NONE', #65144, #61486, #39677, .T. ) ;
#162017 = CARTESIAN_POINT ( 'NONE',  ( 16.53943276465976808, 0.05219959533934440121, 86.25109039468568994 ) ) ;
#162016 = CARTESIAN_POINT ( 'NONE',  ( 4.483927247898790824, -16.52544592524335698, 55.20942372801902565 ) ) ;
#162018 = CARTESIAN_POINT ( 'NONE',  ( 0.000000000000000000, 0.000000000000000000, 20.00000000000000000 ) ) ;
#162019 = CARTESIAN_POINT ( 'NONE',  ( 14.29746914071037800, 8.314922557961029526, 71.66775706135234714 ) ) ;
#162020 = CARTESIAN_POINT ( 'NONE',  ( 21.55341960407610458, 5.719274019375980345, 23.95724293864769550 ) ) ;
#162021 = CARTESIAN_POINT ( 'NONE',  ( 19.05341960407611168, 5.049401038298154454, 38.95724293864767418 ) ) ;
#162022 = CARTESIAN_POINT ( 'NONE',  ( 4.483927247898790824, -16.52544592524335698, 35.20942372801901854 ) ) ;
#162023 = CARTESIAN_POINT ( 'NONE',  ( -19.02544592524342804, 5.153800228976336051, 51.04057627198103120 ) ) ;
#162024 = CARTESIAN_POINT ( 'NONE',  ( -18.62759615963255300, -10.81492255796106328, 44.16775706135234714 ) ) ;
#162025 = CARTESIAN_POINT ( 'NONE',  ( 0.05219959533934541429, -16.53943276465976808, 30.00109039468568284 ) ) ;
#162026 = CARTESIAN_POINT ( 'NONE',  ( 0.05219959533910956823, 16.53943276465976808, 24.99890960531435624 ) ) ;
#162027 = DIRECTION ( 'NONE',  ( 1.000000000000000000, 0.000000000000000000, 0.000000000000000000 ) ) ;
#162028 = CARTESIAN_POINT ( 'NONE',  ( -10.81492255796105439, 18.62759615963255655, 112.9177570613523329 ) ) ;
#162029 = CARTESIAN_POINT ( 'NONE',  ( 16.46253265017146816, 9.564922557961045513, 106.6677570613523471 ) ) ;
#162030 = CARTESIAN_POINT ( 'NONE',  ( 13.97604488694548053, -13.89961937509957401, 65.62609039468567573 ) ) ;
#162031 = CARTESIAN_POINT ( 'NONE',  ( -16.52544592524342804, 4.483927247898546575, 76.04057627198102409 ) ) ;
#162032 = CARTESIAN_POINT ( 'NONE',  ( 13.97604488694527802, 13.89961937509977652, 44.37390960531435269 ) ) ;
#162034 = CARTESIAN_POINT ( 'NONE',  ( 17.44279575226787671, -5.990770900253882481, 58.33557567514320397 ) ) ;
#162033 = CARTESIAN_POINT ( 'NONE',  ( 16.51473224551083163, -9.474510206698727899, 75.83442372801900433 ) ) ;
#162035 = CARTESIAN_POINT ( 'NONE',  ( 21.55341960407619695, -5.719274019375665929, 61.04275706135234714 ) ) ;
#162036 = CARTESIAN_POINT ( 'NONE',  ( 4.379528057220092307, 16.55341960407617563, 37.29275706135235424 ) ) ;
#162037 = CARTESIAN_POINT ( 'NONE',  ( 19.46398650005389896, -5.499999999999940492, 57.68269651486372851 ) ) ;
#162038 = CARTESIAN_POINT ( 'NONE',  ( -13.97604488694527625, -13.89961937509977652, 111.8739096053143243 ) ) ;
#162039 = CARTESIAN_POINT ( 'NONE',  ( 12.06949235617739724, 12.14591786802326823, 31.87609039468567929 ) ) ;
#162040 = FACE_OUTER_BOUND ( 'NONE', #173632, .T. ) ;
#162041 = CARTESIAN_POINT ( 'NONE',  ( -25.27727188472089637, 10.29814791481115321, 170.4127952078933390 ) ) ;
#162042 = CARTESIAN_POINT ( 'NONE',  ( -9.474510206698964154, 16.51473224551069663, 35.41557627198102409 ) ) ;
#162043 = CARTESIAN_POINT ( 'NONE',  ( -5.719274019375665041, -21.55341960407619695, 104.7927570613523898 ) ) ;
#162044 = CARTESIAN_POINT ( 'NONE',  ( 13.89961937509977652, -13.97604488694527269, 53.12390960531434558 ) ) ;
#162045 = CARTESIAN_POINT ( 'NONE',  ( 21.55341960407619695, -5.719274019375665929, 61.04275706135234714 ) ) ;
#162046 = CARTESIAN_POINT ( 'NONE',  ( -10.81492255796105439, 18.62759615963255655, 97.91775706135236135 ) ) ;
#162047 = CARTESIAN_POINT ( 'NONE',  ( 14.29746914071049879, -8.314922557960816363, 23.33224293864769194 ) ) ;
#162048 = CARTESIAN_POINT ( 'NONE',  ( -9.564922557960796823, -16.46253265017161027, 27.08224293864769550 ) ) ;
#162049 = CARTESIAN_POINT ( 'NONE',  ( -0.05219959533909027116, -19.03943276465977164, 87.49890960531436690 ) ) ;
#162050 = CARTESIAN_POINT ( 'NONE',  ( -10.72451020669870658, -18.67979575497194134, 59.58442372801901854 ) ) ;
#162051 = CARTESIAN_POINT ( 'NONE',  ( -13.97604488694527625, -13.89961937509977652, 31.87390960531435979 ) ) ;
#162052 = CARTESIAN_POINT ( 'NONE',  ( 21.53943276465977519, 0.05219959533937863772, 56.25109039468568284 ) ) ;
#162054 = CARTESIAN_POINT ( 'NONE',  ( -19.03943276465977164, 0.05219959533909376836, 111.2489096053143669 ) ) ;
#162053 = CARTESIAN_POINT ( 'NONE',  ( 19.05341960407617918, -5.049401038297876454, 81.04275706135231871 ) ) ;
#162055 = CARTESIAN_POINT ( 'NONE',  ( 9.474510206698971260, -16.51473224551069308, 22.91557627198102765 ) ) ;
#162056 = CARTESIAN_POINT ( 'NONE',  ( 18.67979575497178502, 10.72451020669898547, 114.1655762719810383 ) ) ;
#162057 = CARTESIAN_POINT ( 'NONE',  ( 16.51473224551083163, -9.474510206698727899, 30.83442372801900433 ) ) ;
#162058 = CARTESIAN_POINT ( 'NONE',  ( 16.53943276465976808, -0.05219959533910856209, 108.7489096053143669 ) ) ;
#162059 = CARTESIAN_POINT ( 'NONE',  ( 16.46253265017160672, -9.564922557960803928, 53.33224293864768839 ) ) ;
#162060 = CARTESIAN_POINT ( 'NONE',  ( 13.89961937509957401, 13.97604488694547697, 101.8760903946856331 ) ) ;
#162061 = CARTESIAN_POINT ( 'NONE',  ( -8.314922557960811034, -14.29746914071050412, 57.08224293864769550 ) ) ;
#162062 = CARTESIAN_POINT ( 'NONE',  ( 18.62759615963255655, 10.81492255796105972, 111.6677570613523613 ) ) ;
#162063 = CARTESIAN_POINT ( 'NONE',  ( 15.72974639402199770, -15.80617190586745480, 28.12390960531435979 ) ) ;
#162064 = CARTESIAN_POINT ( 'NONE',  ( 0.05219959533936267826, -19.03943276465977164, 85.00109039468567573 ) ) ;
#162065 = CARTESIAN_POINT ( 'NONE',  ( -21.52544592524343514, 5.823673210054127303, 96.04057627198102409 ) ) ;
#162066 = CARTESIAN_POINT ( 'NONE',  ( 21.52544592524334988, 5.823673210054432836, 46.45942372801901854 ) ) ;
#162067 = CARTESIAN_POINT ( 'NONE',  ( 4.379528057220092307, 16.55341960407617563, 42.29275706135235424 ) ) ;
#162068 = CARTESIAN_POINT ( 'NONE',  ( -8.224510206698735004, -14.34966873604973081, 104.5844237280190185 ) ) ;
#162070 = CARTESIAN_POINT ( 'NONE',  ( -21.52544592524334988, -5.823673210054445271, 43.95942372801902565 ) ) ;
#162069 = CARTESIAN_POINT ( 'NONE',  ( -16.52544592524335698, -4.483927247898792601, 38.95942372801901854 ) ) ;
#162071 = CARTESIAN_POINT ( 'NONE',  ( 10.72451020669898902, -18.67979575497178502, 42.91557627198103120 ) ) ;
#162072 = CARTESIAN_POINT ( 'NONE',  ( 19.02544592524343514, -5.153800228976328945, 38.54057627198103120 ) ) ;
#162073 = CARTESIAN_POINT ( 'NONE',  ( 23.48529157249600630, -32.32473071737749137, -5.049999994537627046 ) ) ;
#162074 = CARTESIAN_POINT ( 'NONE',  ( 14.34966873604972726, -8.224510206698740333, 65.83442372801900433 ) ) ;
#162075 = B_SPLINE_CURVE_WITH_KNOTS ( 'NONE', 3,
 ( #65369, #187750, #110878, #143194, #117615, #113847, #50221, #172563, #128026, #83513, #20855, #157394, #145190, #18887, #67356, #81506, #71114, #40777, #111875, #52189, #190716, #174553, #173565, #179313, #9449, #98679, #35034, #96689, #158377, #175543, #97669, #4674, #164133, #5680, #189728, #51201, #112862, #159358, #102446, #82512, #195475, #105430, #73129, #43766, #167113, #44755, #89269, #90252 ),
 .UNSPECIFIED., .F., .F.,
 ( 4, 2, 2, 2, 2, 2, 2, 2, 2, 2, 2, 2, 2, 2, 2, 2, 2, 2, 2, 2, 2, 2, 2, 4 ),
 ( 0.04104976116627322147, 0.04252145193039932880, 0.04325729731246238247, 0.04399314269452542919, 0.04472898807658848286, 0.04546483345865153652, 0.04693652422277766467, 0.04840821498690379282, 0.04914406036896685342, 0.04987990575102992097, 0.05135159651515604912, 0.05208744189721910972, 0.05282328727928217726, 0.05429497804340830541, 0.05503082342547139377, 0.05576666880753447519, 0.05723835957166064498, 0.05871005033578681476, 0.05944589571784988230, 0.06018174109991294984, 0.06165343186403906411, 0.06238927724610211778, 0.06312512262816517838, 0.06459681339229128572 ),
 .UNSPECIFIED. ) ;
#162076 = ADVANCED_FACE ( 'NONE', ( #89176 ), #134541, .F. ) ;
#162077 = CARTESIAN_POINT ( 'NONE',  ( -10.81492255796078084, -18.62759615963271287, 92.08224293864769550 ) ) ;
#162078 = CARTESIAN_POINT ( 'NONE',  ( 12.14591786802309770, 12.06949235617756955, 39.37390960531436690 ) ) ;
#162079 = CARTESIAN_POINT ( 'NONE',  ( 16.55341960407618274, -4.379528057220086978, 56.04275706135235424 ) ) ;
#162080 = CARTESIAN_POINT ( 'NONE',  ( 19.03943276465977164, -0.05219959533909143690, 53.74890960531436690 ) ) ;
#162081 = CARTESIAN_POINT ( 'NONE',  ( 5.049401038297881783, 19.05341960407617563, 102.2927570613523045 ) ) ;
#162082 = CARTESIAN_POINT ( 'NONE',  ( -10.72451020669898014, 18.67979575497178502, 85.41557627198102409 ) ) ;
#162083 = CARTESIAN_POINT ( 'NONE',  ( 4.483927247898545687, 16.52544592524342804, 34.79057627198103120 ) ) ;
#162084 = VERTEX_POINT ( 'NONE', #135695 ) ;
#162085 = CARTESIAN_POINT ( 'NONE',  ( -4.483927247898782831, 16.52544592524335698, 82.70942372801900433 ) ) ;
#162086 = CARTESIAN_POINT ( 'NONE',  ( 25.04733094907663116, 10.92720321514006621, 170.1247377027656853 ) ) ;
#162087 = CARTESIAN_POINT ( 'NONE',  ( -18.62759615963270932, 10.81492255796079327, 75.83224293864769550 ) ) ;
#162088 = CARTESIAN_POINT ( 'NONE',  ( -16.52544592524335698, -4.483927247898792601, 98.95942372801903275 ) ) ;
#162089 = ORIENTED_EDGE ( 'NONE', *, *, #133615, .F. ) ;
#162090 = CARTESIAN_POINT ( 'NONE',  ( -11.74264578624799782, -36.14014761921581709, -3.600000000000000533 ) ) ;
#162091 = CARTESIAN_POINT ( 'NONE',  ( 0.05219959533907565091, 21.53943276465977519, 84.99890960531436690 ) ) ;
#162092 = CARTESIAN_POINT ( 'NONE',  ( -5.823673210054116645, -21.52544592524344225, 112.2905762719810241 ) ) ;
#162093 = CARTESIAN_POINT ( 'NONE',  ( -8.314922557960811034, -14.29746914071050412, 37.08224293864768129 ) ) ;
#162094 = CARTESIAN_POINT ( 'NONE',  ( 4.483927247898790824, -16.52544592524335698, 35.20942372801901854 ) ) ;
#162095 = CARTESIAN_POINT ( 'NONE',  ( 5.049401038298161559, -19.05341960407611168, 37.70724293864768839 ) ) ;
#162096 = CARTESIAN_POINT ( 'NONE',  ( 13.89961937509977652, -13.97604488694527269, 68.12390960531436690 ) ) ;
#162097 = CARTESIAN_POINT ( 'NONE',  ( -17.14385361876520619, 23.59649016807275856, 141.0750000027311728 ) ) ;
#162098 = CARTESIAN_POINT ( 'NONE',  ( -21.53943276465977519, 0.05219959533907696930, 21.24890960531436690 ) ) ;
#162099 = CARTESIAN_POINT ( 'NONE',  ( 0.4854043096289403225, 28.97561840829192903, -52.57160608660437617 ) ) ;
#162100 = CARTESIAN_POINT ( 'NONE',  ( -19.05341960407617563, 5.049401038297882671, 103.5427570613523329 ) ) ;
#162101 = CARTESIAN_POINT ( 'NONE',  ( -16.46253265017146816, -9.564922557961047289, 44.16775706135232582 ) ) ;
#162102 = CARTESIAN_POINT ( 'NONE',  ( 18.62759615963271287, -10.81492255796078972, 88.33224293864769550 ) ) ;
#162103 = CARTESIAN_POINT ( 'NONE',  ( -12.14591786802326823, 12.06949235617739902, 113.1260903946856899 ) ) ;
#162104 = CARTESIAN_POINT ( 'NONE',  ( 5.823673210054125526, 21.52544592524343514, 44.79057627198103120 ) ) ;
#162106 = CARTESIAN_POINT ( 'NONE',  ( -19.02544592524334988, -5.153800228976617603, 108.9594237280189759 ) ) ;
#162105 = CARTESIAN_POINT ( 'NONE',  ( -18.62759615963270932, 10.81492255796079327, 80.83224293864769550 ) ) ;
#162107 = CARTESIAN_POINT ( 'NONE',  ( -19.03943276465977164, 0.05219959533909376836, 111.2489096053143669 ) ) ;
#162108 = CARTESIAN_POINT ( 'NONE',  ( 15.72974639402176855, 15.80617190586768217, 71.87609039468568994 ) ) ;
#162109 = CARTESIAN_POINT ( 'NONE',  ( 5.049401038298161559, -19.05341960407611168, 72.70724293864768129 ) ) ;
#162110 = CARTESIAN_POINT ( 'NONE',  ( -12.06949235617756955, 12.14591786802309770, 105.6239096053143669 ) ) ;
#162111 = CARTESIAN_POINT ( 'NONE',  ( 31.54545164052520434, 7.106679946642015189, 92.55365670706888181 ) ) ;
#162112 = CARTESIAN_POINT ( 'NONE',  ( 9.564922557960805705, 16.46253265017160317, 64.58224293864769550 ) ) ;
#162113 = CARTESIAN_POINT ( 'NONE',  ( 0.05219959533910956823, 16.53943276465976808, 84.99890960531436690 ) ) ;
#162114 = VERTEX_POINT ( 'NONE', #131694 ) ;
#162115 = CARTESIAN_POINT ( 'NONE',  ( 19.03943276465977164, 0.05219959533936151252, 101.2510903946856757 ) ) ;
#162116 = DIRECTION ( 'NONE',  ( 0.000000000000000000, 0.000000000000000000, 1.000000000000000000 ) ) ;
#162117 = CARTESIAN_POINT ( 'NONE',  ( 0.05219959533909260263, 19.03943276465977164, 54.99890960531435979 ) ) ;
#162119 = CARTESIAN_POINT ( 'NONE',  ( 9.564922557960805705, 16.46253265017160317, 104.5822429386476955 ) ) ;
#162118 = CARTESIAN_POINT ( 'NONE',  ( -0.05219959533937732626, 21.53943276465977519, 82.50109039468568994 ) ) ;
#162120 = CARTESIAN_POINT ( 'NONE',  ( 0.05219959533934541429, -16.53943276465976808, 80.00109039468568994 ) ) ;
#162121 = CARTESIAN_POINT ( 'NONE',  ( -17.48847506799967988, -5.747544572773758631, 74.17302562156723411 ) ) ;
#162122 = CARTESIAN_POINT ( 'NONE',  ( 13.89961937509957401, 13.97604488694547697, 61.87609039468566863 ) ) ;
#162123 = CARTESIAN_POINT ( 'NONE',  ( -5.823673210054431948, 21.52544592524334988, 97.70942372801904696 ) ) ;
#162124 = CARTESIAN_POINT ( 'NONE',  ( -19.49401214000077687, 12.39993551617566681, 164.9999999999999716 ) ) ;
#162125 = CARTESIAN_POINT ( 'NONE',  ( 0.000000000000000000, 0.000000000000000000, 10.00000000000000000 ) ) ;
#162126 = CARTESIAN_POINT ( 'NONE',  ( -12.06949235617739369, -12.14591786802326823, 109.3760903946857042 ) ) ;
#162127 = CARTESIAN_POINT ( 'NONE',  ( -193.3062444957834884, -155.7167183371838064, -25.00000000000000000 ) ) ;
#162128 = CARTESIAN_POINT ( 'NONE',  ( -14.29746914071037622, -8.314922557961029526, 89.16775706135236135 ) ) ;
#162129 = CARTESIAN_POINT ( 'NONE',  ( 33.21859846492400692, -22.28383573948690710, -23.19796227011728007 ) ) ;
#162130 = CARTESIAN_POINT ( 'NONE',  ( -14.29746914071037622, -8.314922557961029526, 64.16775706135234714 ) ) ;
#162131 = CARTESIAN_POINT ( 'NONE',  ( 10.72451020669871369, 18.67979575497193778, 82.08442372801901854 ) ) ;
#162132 = CARTESIAN_POINT ( 'NONE',  ( -13.97604488694547697, 13.89961937509957934, 93.12609039468566152 ) ) ;
#162133 = CARTESIAN_POINT ( 'NONE',  ( 19.03943276465977164, 0.05219959533936151252, 41.25109039468566152 ) ) ;
#162134 = CARTESIAN_POINT ( 'NONE',  ( 19.05341960407611168, 5.049401038298154454, 68.95724293864769550 ) ) ;
#162135 = CARTESIAN_POINT ( 'NONE',  ( 13.89961937509977652, -13.97604488694527269, 63.12390960531435979 ) ) ;
#162136 = CYLINDRICAL_SURFACE ( 'NONE', #133633, 1.500000000000001332 ) ;
#162137 = CARTESIAN_POINT ( 'NONE',  ( 21.52544592524344225, -5.823673210054117533, 83.54057627198102409 ) ) ;
#162138 = CARTESIAN_POINT ( 'NONE',  ( -0.05219959533907301413, -21.53943276465977519, 52.49890960531435979 ) ) ;
#162139 = CARTESIAN_POINT ( 'NONE',  ( 19.02544592524343514, -5.153800228976328945, 33.54057627198102409 ) ) ;
#162140 = CARTESIAN_POINT ( 'NONE',  ( -14.34966873604972548, 8.224510206698743886, 58.33442372801901143 ) ) ;
#162141 = EDGE_CURVE ( 'NONE', #35378, #131506, #197367, .T. ) ;
#162142 = ORIENTED_EDGE ( 'NONE', *, *, #61248, .T. ) ;
#162143 = CARTESIAN_POINT ( 'NONE',  ( 0.05219959533937995610, -21.53943276465977519, 50.00109039468568994 ) ) ;
#162145 = CARTESIAN_POINT ( 'NONE',  ( -11.40812507854754720, -35.11059874428192273, -10.22499999726881548 ) ) ;
#162144 = CARTESIAN_POINT ( 'NONE',  ( -4.483927247898539470, -16.52544592524342804, 67.29057627198103830 ) ) ;
#162146 = CARTESIAN_POINT ( 'NONE',  ( 14.34966873604972726, -8.224510206698740333, 30.83442372801902209 ) ) ;
#162147 = CARTESIAN_POINT ( 'NONE',  ( -5.049401038297874678, -19.05341960407617918, 59.79275706135231871 ) ) ;
#162148 = CARTESIAN_POINT ( 'NONE',  ( -14.29746914071049879, 8.314922557960819915, 55.83224293864770260 ) ) ;
#162149 = CARTESIAN_POINT ( 'NONE',  ( 10.72451020669871369, 18.67979575497193778, 27.08442372801901854 ) ) ;
#162151 = CARTESIAN_POINT ( 'NONE',  ( -18.67979575497178146, -10.72451020669898902, 96.66557627198102409 ) ) ;
#162150 = DIRECTION ( 'NONE',  ( -0.000000000000000000, -0.000000000000000000, 1.000000000000000000 ) ) ;
#162152 = CARTESIAN_POINT ( 'NONE',  ( 9.474510206698971260, -16.51473224551069308, 102.9155762719810241 ) ) ;
#162153 = CARTESIAN_POINT ( 'NONE',  ( 12.06949235617757843, -12.14591786802309237, 73.12390960531436690 ) ) ;
#162154 = CARTESIAN_POINT ( 'NONE',  ( 32.73422133880311691, -23.92350924394424183, -17.85299461212022365 ) ) ;
#162155 = CARTESIAN_POINT ( 'NONE',  ( -36.99206003604233217, 5.206627989871537743, 43.21856904651837539 ) ) ;
#162156 = CARTESIAN_POINT ( 'NONE',  ( 5.153800228976615827, -19.02544592524334988, 65.20942372801900433 ) ) ;
#162157 = CARTESIAN_POINT ( 'NONE',  ( 18.67979575497178502, 10.72451020669898547, 114.1655762719810383 ) ) ;
#162158 = CARTESIAN_POINT ( 'NONE',  ( 13.97604488694527802, 13.89961937509977652, 59.37390960531434558 ) ) ;
#162159 = CARTESIAN_POINT ( 'NONE',  ( -9.564922557961040184, 16.46253265017147172, 42.91775706135234003 ) ) ;
#162160 = CARTESIAN_POINT ( 'NONE',  ( 19.03943276465977164, -0.05219959533909143690, 33.74890960531435979 ) ) ;
#162161 = CARTESIAN_POINT ( 'NONE',  ( -5.719274019375665041, -21.55341960407619695, 69.79275706135234714 ) ) ;
#162162 = CARTESIAN_POINT ( 'NONE',  ( -17.50000000000001066, -5.622605283950844246, 71.31207310596111881 ) ) ;
#162163 = CARTESIAN_POINT ( 'NONE',  ( -0.05219959533910754901, -16.53943276465976808, 42.49890960531435979 ) ) ;
#162164 = CARTESIAN_POINT ( 'NONE',  ( -19.02544592524342804, 5.153800228976336051, 61.04057627198103120 ) ) ;
#162165 = CARTESIAN_POINT ( 'NONE',  ( 15.80617190586746368, 15.72974639402197994, 89.37390960531435269 ) ) ;
#162166 = CARTESIAN_POINT ( 'NONE',  ( -5.049401038298153566, 19.05341960407611168, 60.20724293864768129 ) ) ;
#162167 = ORIENTED_EDGE ( 'NONE', *, *, #183827, .T. ) ;
#162168 = CARTESIAN_POINT ( 'NONE',  ( -21.55341960407610458, -5.719274019375992779, 71.45724293864769550 ) ) ;
#162169 = CARTESIAN_POINT ( 'NONE',  ( 10.81492255796106328, -18.62759615963255655, 100.4177570613523471 ) ) ;
#162172 = CARTESIAN_POINT ( 'NONE',  ( -8.224510206698948167, 14.34966873604960824, 85.41557627198102409 ) ) ;
#162171 = CARTESIAN_POINT ( 'NONE',  ( -8.314922557961024197, 14.29746914071037800, 97.91775706135236135 ) ) ;
#162170 = CARTESIAN_POINT ( 'NONE',  ( -30.00000000000000355, 3.889087296526014814, 1.818019484660534424 ) ) ;
#162173 = CARTESIAN_POINT ( 'NONE',  ( -19.02544592524334988, -5.153800228976617603, 98.95942372801900433 ) ) ;
#162174 = ORIENTED_EDGE ( 'NONE', *, *, #35192, .F. ) ;
#162175 = CARTESIAN_POINT ( 'NONE',  ( -18.67979575497178146, -10.72451020669898902, 111.6655762719810525 ) ) ;
#162176 = CARTESIAN_POINT ( 'NONE',  ( -0.05219959533936034679, 19.03943276465977164, 42.50109039468566152 ) ) ;
#162177 = CARTESIAN_POINT ( 'NONE',  ( -12.14591786802326823, 12.06949235617739902, 98.12609039468570415 ) ) ;
#162178 = CARTESIAN_POINT ( 'NONE',  ( -16.46253265017146816, -9.564922557961047289, 24.16775706135233648 ) ) ;
#162179 = CARTESIAN_POINT ( 'NONE',  ( 0.05219959533909260263, 19.03943276465977164, 89.99890960531436690 ) ) ;
#162180 = CARTESIAN_POINT ( 'NONE',  ( 0.05219959533907565091, 21.53943276465977519, 64.99890960531435269 ) ) ;
#162181 = DIRECTION ( 'NONE',  ( -1.000000000000000000, 0.000000000000000000, 0.000000000000000000 ) ) ;
#162182 = CARTESIAN_POINT ( 'NONE',  ( -19.05341960407611168, -5.049401038298163336, 26.45724293864769550 ) ) ;
#162183 = CARTESIAN_POINT ( 'NONE',  ( -18.67979575497193778, 10.72451020669871902, 113.3344237280190328 ) ) ;
#162184 = CARTESIAN_POINT ( 'NONE',  ( -12.06949235617739369, -12.14591786802326823, 79.37609039468567573 ) ) ;
#162185 = CARTESIAN_POINT ( 'NONE',  ( 0.05219959533937995610, -21.53943276465977519, 30.00109039468568284 ) ) ;
#162186 = CARTESIAN_POINT ( 'NONE',  ( -14.34966873604972548, 8.224510206698743886, 28.33442372801902209 ) ) ;
#162187 = CARTESIAN_POINT ( 'NONE',  ( 19.02544592524343514, -5.153800228976328945, 108.5405762719810383 ) ) ;
#162188 = CARTESIAN_POINT ( 'NONE',  ( -19.05341960407611168, -5.049401038298163336, 36.45724293864766707 ) ) ;
#162189 = CARTESIAN_POINT ( 'NONE',  ( -5.049401038298153566, 19.05341960407611168, 65.20724293864765286 ) ) ;
#162190 = CARTESIAN_POINT ( 'NONE',  ( -16.53943276465976808, -0.05219959533934237506, 48.75109039468568284 ) ) ;
#162191 = CARTESIAN_POINT ( 'NONE',  ( -16.53943276465976808, 0.05219959533911058130, 96.24890960531435269 ) ) ;
#162192 = CARTESIAN_POINT ( 'NONE',  ( 12.14591786802327356, -12.06949235617739191, 95.62609039468568994 ) ) ;
#162195 = CARTESIAN_POINT ( 'NONE',  ( 9.564922557960805705, 16.46253265017160317, 69.58224293864770971 ) ) ;
#162194 = CARTESIAN_POINT ( 'NONE',  ( 19.02544592524343514, -5.153800228976328945, 73.54057627198103830 ) ) ;
#162193 = CARTESIAN_POINT ( 'NONE',  ( 10.81492255796106328, -18.62759615963255655, 55.41775706135234714 ) ) ;
#162196 = CARTESIAN_POINT ( 'NONE',  ( 0.05219959533909260263, 19.03943276465977164, 94.99890960531436690 ) ) ;
#162197 = CARTESIAN_POINT ( 'NONE',  ( 14.34966873604960469, 8.224510206698951720, 39.16557627198102409 ) ) ;
#162198 = CARTESIAN_POINT ( 'NONE',  ( -12.06949235617739369, -12.14591786802326823, 104.3760903946856899 ) ) ;
#162199 = ORIENTED_EDGE ( 'NONE', *, *, #84003, .T. ) ;
#162200 = CARTESIAN_POINT ( 'NONE',  ( 9.564922557961047289, -16.46253265017146816, 40.41775706135234003 ) ) ;
#162201 = CARTESIAN_POINT ( 'NONE',  ( 0.05219959533909260263, 19.03943276465977164, 109.9989096053143669 ) ) ;
#162202 = CARTESIAN_POINT ( 'NONE',  ( -0.05219959533909027116, -19.03943276465977164, 57.49890960531435979 ) ) ;
#162203 = CARTESIAN_POINT ( 'NONE',  ( 19.05341960407617918, -5.049401038297876454, 41.04275706135233293 ) ) ;
#162204 = CARTESIAN_POINT ( 'NONE',  ( 11.40812507854754365, 35.11059874428196537, -9.224999997268813701 ) ) ;
#162205 = CARTESIAN_POINT ( 'NONE',  ( 18.87075004821567248, -5.500000000000077272, 71.17408112101045958 ) ) ;
#162206 = CARTESIAN_POINT ( 'NONE',  ( 4.379528057220092307, 16.55341960407617563, 62.29275706135236845 ) ) ;
#162208 = CARTESIAN_POINT ( 'NONE',  ( 16.52544592524335698, 4.483927247898782831, 66.45942372801903275 ) ) ;
#162207 = CARTESIAN_POINT ( 'NONE',  ( -9.474510206698720793, -16.51473224551083518, 69.58442372801901854 ) ) ;
#162209 = CARTESIAN_POINT ( 'NONE',  ( -7.128481858827109718, -2.709097808555398945, 7.001991027368838161 ) ) ;
#162210 = CARTESIAN_POINT ( 'NONE',  ( -5.049401038298153566, 19.05341960407611168, 90.20724293864766707 ) ) ;
#162211 = CARTESIAN_POINT ( 'NONE',  ( 5.823673210054444382, -21.52544592524334988, 20.20942372801900788 ) ) ;
#162212 = CARTESIAN_POINT ( 'NONE',  ( 16.46253265017146816, 9.564922557961045513, 76.66775706135234714 ) ) ;
#162214 = CARTESIAN_POINT ( 'NONE',  ( -19.05341960407611168, -5.049401038298163336, 36.45724293864766707 ) ) ;
#162213 = CARTESIAN_POINT ( 'NONE',  ( -9.474510206698964154, 16.51473224551069663, 100.4155762719810241 ) ) ;
#162215 = CARTESIAN_POINT ( 'NONE',  ( -19.05341960407611168, -5.049401038298163336, 91.45724293864766707 ) ) ;
#162217 = CARTESIAN_POINT ( 'NONE',  ( 5.049401038298161559, -19.05341960407611168, 37.70724293864768839 ) ) ;
#162216 = CARTESIAN_POINT ( 'NONE',  ( 4.483927247898545687, 16.52544592524342804, 49.79057627198102409 ) ) ;
#162218 = CARTESIAN_POINT ( 'NONE',  ( 5.049401038297881783, 19.05341960407617563, 52.29275706135234003 ) ) ;
#162219 = CARTESIAN_POINT ( 'NONE',  ( 8.314922557960818139, 14.29746914071049879, 84.58224293864769550 ) ) ;
#162220 = CARTESIAN_POINT ( 'NONE',  ( -10.81492255796105439, 18.62759615963255655, 112.9177570613523329 ) ) ;
#162221 = CARTESIAN_POINT ( 'NONE',  ( -9.474510206698964154, 16.51473224551069663, 50.41557627198102409 ) ) ;
#162222 = CARTESIAN_POINT ( 'NONE',  ( -5.719274019375978568, 21.55341960407610458, 55.20724293864770260 ) ) ;
#162224 = CARTESIAN_POINT ( 'NONE',  ( -16.46253265017146816, -9.564922557961047289, 24.16775706135233648 ) ) ;
#162223 = CARTESIAN_POINT ( 'NONE',  ( 12.06949235617757843, -12.14591786802309237, 48.12390960531436690 ) ) ;
#162225 = CARTESIAN_POINT ( 'NONE',  ( -19.05341960407611168, -5.049401038298163336, 106.4572429386476955 ) ) ;
#162226 = CARTESIAN_POINT ( 'NONE',  ( 19.05341960407611168, 5.049401038298154454, 103.9572429386476671 ) ) ;
#162227 = CARTESIAN_POINT ( 'NONE',  ( 16.51473224551069308, 9.474510206698969483, 39.16557627198103120 ) ) ;
#162228 = CARTESIAN_POINT ( 'NONE',  ( -9.474510206698964154, 16.51473224551069663, 30.41557627198102054 ) ) ;
#162229 = CARTESIAN_POINT ( 'NONE',  ( -8.314922557960811034, -14.29746914071050412, 82.08224293864768129 ) ) ;
#162230 = CARTESIAN_POINT ( 'NONE',  ( -15.80617190586745835, -15.72974639402198527, 91.87390960531436690 ) ) ;
#162231 = CARTESIAN_POINT ( 'NONE',  ( -13.89961937509977652, 13.97604488694528158, 105.6239096053143527 ) ) ;
#162232 = CARTESIAN_POINT ( 'NONE',  ( 5.823673210054125526, 21.52544592524343514, 109.7905762719810383 ) ) ;
#162233 = CARTESIAN_POINT ( 'NONE',  ( -9.564922557960796823, -16.46253265017161027, 102.0822429386477097 ) ) ;
#162234 = CARTESIAN_POINT ( 'NONE',  ( 16.53943276465976808, -0.05219959533910856209, 103.7489096053143669 ) ) ;
#162235 = CARTESIAN_POINT ( 'NONE',  ( -15.72974639402176322, -15.80617190586768395, 74.37609039468568994 ) ) ;
#162236 = CARTESIAN_POINT ( 'NONE',  ( -21.55341960407610458, -5.719274019375992779, 86.45724293864770971 ) ) ;
#162237 = CARTESIAN_POINT ( 'NONE',  ( 17.40861289039002457, -6.110651285853328396, 106.1276752917256516 ) ) ;
#162238 = CYLINDRICAL_SURFACE ( 'NONE', #94731, 1.499999999999997780 ) ;
#162240 = DIRECTION ( 'NONE',  ( 0.000000000000000000, -0.5000000000000001110, -0.8660254037844385966 ) ) ;
#162239 = CARTESIAN_POINT ( 'NONE',  ( 0.05219959533907565091, 21.53943276465977519, 34.99890960531435979 ) ) ;
#162241 = CARTESIAN_POINT ( 'NONE',  ( -12.06949235617739369, -12.14591786802326823, 29.37609039468568284 ) ) ;
#162242 = CARTESIAN_POINT ( 'NONE',  ( -0.05219959533910754901, -16.53943276465976808, 112.4989096053143669 ) ) ;
#162243 = DIRECTION ( 'NONE',  ( 1.000000000000000000, 1.776356839400250465E-15, 0.000000000000000000 ) ) ;
#162244 = CARTESIAN_POINT ( 'NONE',  ( 19.03943276465977164, -0.05219959533909143690, 58.74890960531435979 ) ) ;
#162246 = EDGE_CURVE ( 'NONE', #135144, #158282, #140689, .T. ) ;
#162245 = CARTESIAN_POINT ( 'NONE',  ( 12.06949235617757843, -12.14591786802309237, 88.12390960531436690 ) ) ;
#162247 = B_SPLINE_CURVE_WITH_KNOTS ( 'NONE', 3,
 ( #102427, #194447, #191431, #87256, #52908, #88245, #131764, #164114 ),
 .UNSPECIFIED., .F., .F.,
 ( 4, 2, 2, 4 ),
 ( 2.787258272608875357E-07, 0.0002976023950119189546, 0.0005949260641965769441, 0.001189573402565897910 ),
 .UNSPECIFIED. ) ;
#162248 = CARTESIAN_POINT ( 'NONE',  ( 18.67979575497178502, 10.72451020669898547, 34.16557627198102409 ) ) ;
#162249 = CARTESIAN_POINT ( 'NONE',  ( -14.34966873604960291, -8.224510206698953496, 61.66557627198103120 ) ) ;
#162250 = CARTESIAN_POINT ( 'NONE',  ( 4.483927247898790824, -16.52544592524335698, 25.20942372801901854 ) ) ;
#162251 = CARTESIAN_POINT ( 'NONE',  ( -10.81492255796105439, 18.62759615963255655, 72.91775706135234714 ) ) ;
#162252 = CARTESIAN_POINT ( 'NONE',  ( 17.31728774477272736, -6.344390552232384017, 78.31906651689315879 ) ) ;
#162253 = CARTESIAN_POINT ( 'NONE',  ( 16.51473224551069308, 9.474510206698969483, 109.1655762719810383 ) ) ;
#162254 = CARTESIAN_POINT ( 'NONE',  ( 14.29746914071037800, 8.314922557961029526, 81.66775706135236135 ) ) ;
#162255 = CARTESIAN_POINT ( 'NONE',  ( 16.51473224551069308, 9.474510206698969483, 39.16557627198103120 ) ) ;
#162256 = CARTESIAN_POINT ( 'NONE',  ( 0.05219959533909260263, 19.03943276465977164, 84.99890960531436690 ) ) ;
#162257 = CARTESIAN_POINT ( 'NONE',  ( 15.80617190586746368, 15.72974639402197994, 89.37390960531435269 ) ) ;
#162258 = CARTESIAN_POINT ( 'NONE',  ( 8.224510206698742110, 14.34966873604972548, 22.08442372801901143 ) ) ;
#162260 = CARTESIAN_POINT ( 'NONE',  ( 21.52544592524334988, 5.823673210054432836, 66.45942372801903275 ) ) ;
#162259 = CARTESIAN_POINT ( 'NONE',  ( -12.06949235617756955, 12.14591786802309770, 45.62390960531436690 ) ) ;
#162261 = CARTESIAN_POINT ( 'NONE',  ( -14.34966873604972548, 8.224510206698743886, 103.3344237280190043 ) ) ;
#162262 = CARTESIAN_POINT ( 'NONE',  ( 19.05341960407611168, 5.049401038298154454, 113.9572429386476955 ) ) ;
#162263 = CARTESIAN_POINT ( 'NONE',  ( -32.00000000000000711, -1.130348995613007185E-14, 97.69999999999998863 ) ) ;
#162264 = CARTESIAN_POINT ( 'NONE',  ( 4.379528057220339221, -16.55341960407611168, 22.70724293864769194 ) ) ;
#162265 = CARTESIAN_POINT ( 'NONE',  ( 0.05219959533934541429, -16.53943276465976808, 55.00109039468568284 ) ) ;
#162266 = CARTESIAN_POINT ( 'NONE',  ( 9.474510206698971260, -16.51473224551069308, 72.91557627198102409 ) ) ;
#162267 = CARTESIAN_POINT ( 'NONE',  ( -19.05341960407611168, -5.049401038298163336, 86.45724293864769550 ) ) ;
#162268 = CARTESIAN_POINT ( 'NONE',  ( 5.823673210054444382, -21.52544592524334988, 80.20942372801901854 ) ) ;
#162269 = CARTESIAN_POINT ( 'NONE',  ( 8.224510206698742110, 14.34966873604972548, 92.08442372801901854 ) ) ;
#162270 = CARTESIAN_POINT ( 'NONE',  ( -4.483927247898539470, -16.52544592524342804, 57.29057627198103120 ) ) ;
#162271 = CARTESIAN_POINT ( 'NONE',  ( 13.97604488694527802, 13.89961937509977652, 74.37390960531436690 ) ) ;
#162272 = EDGE_LOOP ( 'NONE', ( #133097, #176327, #44782, #111468 ) ) ;
#162273 = CARTESIAN_POINT ( 'NONE',  ( 9.564922557961047289, -16.46253265017146816, 110.4177570613523471 ) ) ;
#162274 = CARTESIAN_POINT ( 'NONE',  ( 4.379528057220339221, -16.55341960407611168, 107.7072429386476955 ) ) ;
#162275 = CARTESIAN_POINT ( 'NONE',  ( 19.02544592524343514, -5.153800228976328945, 78.54057627198099567 ) ) ;
#162277 = CARTESIAN_POINT ( 'NONE',  ( 29.86685920354754842, -21.69954338932559068, -9.824999997268813345 ) ) ;
#162276 = CARTESIAN_POINT ( 'NONE',  ( -19.05341960407617563, 5.049401038297882671, 113.5427570613523471 ) ) ;
#162278 = CARTESIAN_POINT ( 'NONE',  ( 15.80617190586769283, -15.72974639402175789, 105.6260903946856899 ) ) ;
#162279 = CARTESIAN_POINT ( 'NONE',  ( -14.34966873604972548, 8.224510206698743886, 83.33442372801903275 ) ) ;
#162280 = CARTESIAN_POINT ( 'NONE',  ( 9.564922557961047289, -16.46253265017146816, 90.41775706135234714 ) ) ;
#162281 = CARTESIAN_POINT ( 'NONE',  ( 12.14591786802309770, 12.06949235617756955, 109.3739096053143811 ) ) ;
#162282 = CARTESIAN_POINT ( 'NONE',  ( -12.06949235617739369, -12.14591786802326823, 69.37609039468567573 ) ) ;
#162283 = CARTESIAN_POINT ( 'NONE',  ( 7.652493125987819944, -39.26116846142902261, -15.00000000000000000 ) ) ;
#162284 = CARTESIAN_POINT ( 'NONE',  ( 16.46253265017146816, 9.564922557961045513, 51.66775706135233293 ) ) ;
#162285 = CARTESIAN_POINT ( 'NONE',  ( -5.823673210054431948, 21.52544592524334988, 102.7094237280190185 ) ) ;
#162286 = CARTESIAN_POINT ( 'NONE',  ( 16.51473224551069308, 9.474510206698969483, 34.16557627198102409 ) ) ;
#162287 = CARTESIAN_POINT ( 'NONE',  ( 9.564922557960805705, 16.46253265017160317, 74.58224293864769550 ) ) ;
#162289 = ADVANCED_FACE ( 'NONE', ( #86185 ), #133691, .F. ) ;
#162288 = CARTESIAN_POINT ( 'NONE',  ( -14.29746914071049879, 8.314922557960819915, 75.83224293864769550 ) ) ;
#162290 = CARTESIAN_POINT ( 'NONE',  ( 0.05219959533937995610, -21.53943276465977519, 85.00109039468568994 ) ) ;
#162291 = CARTESIAN_POINT ( 'NONE',  ( 5.153800228976615827, -19.02544592524334988, 50.20942372801897591 ) ) ;
#162292 = CARTESIAN_POINT ( 'NONE',  ( -0.05219959533936034679, 19.03943276465977164, 37.50109039468567573 ) ) ;
#162293 = CARTESIAN_POINT ( 'NONE',  ( 21.55341960407610458, 5.719274019375980345, 38.95724293864768839 ) ) ;
#162294 = CARTESIAN_POINT ( 'NONE',  ( -15.72974639402176322, -15.80617190586768395, 99.37609039468568994 ) ) ;
#162295 = CARTESIAN_POINT ( 'NONE',  ( 16.46253265017160672, -9.564922557960803928, 83.33224293864768129 ) ) ;
#162296 = CARTESIAN_POINT ( 'NONE',  ( 5.823673210054444382, -21.52544592524334988, 90.20942372801903275 ) ) ;
#162297 = CARTESIAN_POINT ( 'NONE',  ( 21.52544592524344225, -5.823673210054117533, 48.54057627198103120 ) ) ;
#162298 = CARTESIAN_POINT ( 'NONE',  ( 13.89961937509977652, -13.97604488694527269, 83.12390960531436690 ) ) ;
#162299 = CARTESIAN_POINT ( 'NONE',  ( 0.05219959533936267826, -19.03943276465977164, 75.00109039468566152 ) ) ;
#162300 = CARTESIAN_POINT ( 'NONE',  ( 9.474510206698971260, -16.51473224551069308, 97.91557627198102409 ) ) ;
#162301 = CARTESIAN_POINT ( 'NONE',  ( 9.564922557961047289, -16.46253265017146816, 100.4177570613523329 ) ) ;
#162302 = CARTESIAN_POINT ( 'NONE',  ( -8.314922557961024197, 14.29746914071037800, 47.91775706135234714 ) ) ;
#162303 = CARTESIAN_POINT ( 'NONE',  ( 16.53943276465976808, -0.05219959533910856209, 98.74890960531438111 ) ) ;
#162304 = CARTESIAN_POINT ( 'NONE',  ( 13.97604488694527802, 13.89961937509977652, 69.37390960531436690 ) ) ;
#162305 = CARTESIAN_POINT ( 'NONE',  ( 0.05219959533907565091, 21.53943276465977519, 69.99890960531435269 ) ) ;
#162306 = CARTESIAN_POINT ( 'NONE',  ( -14.29746914071037622, -8.314922557961029526, 34.16775706135234714 ) ) ;
#162307 = CARTESIAN_POINT ( 'NONE',  ( 0.05219959533937995610, -21.53943276465977519, 35.00109039468568284 ) ) ;
#162308 = CARTESIAN_POINT ( 'NONE',  ( -21.53943276465977519, -0.05219959533937600094, 83.75109039468568994 ) ) ;
#162309 = CARTESIAN_POINT ( 'NONE',  ( -12.14591786802326823, 12.06949235617739902, 88.12609039468570415 ) ) ;
#162310 = CARTESIAN_POINT ( 'NONE',  ( 16.51473224551069308, 9.474510206698969483, 69.16557627198102409 ) ) ;
#162311 = CARTESIAN_POINT ( 'NONE',  ( 16.52544592524342804, -4.483927247898539470, 83.54057627198102409 ) ) ;
#162312 = CARTESIAN_POINT ( 'NONE',  ( 4.483927247898790824, -16.52544592524335698, 105.2094237280190328 ) ) ;
#162313 = CARTESIAN_POINT ( 'NONE',  ( 0.05219959533936267826, -19.03943276465977164, 50.00109039468566863 ) ) ;
#162314 = CARTESIAN_POINT ( 'NONE',  ( 5.719274019375673035, 21.55341960407619339, 32.29275706135235424 ) ) ;
#162315 = CARTESIAN_POINT ( 'NONE',  ( 4.483927247898545687, 16.52544592524342804, 84.79057627198102409 ) ) ;
#162316 = CARTESIAN_POINT ( 'NONE',  ( -5.049401038298153566, 19.05341960407611168, 105.2072429386476671 ) ) ;
#162317 = CARTESIAN_POINT ( 'NONE',  ( 12.06949235617739724, 12.14591786802326823, 96.87609039468568994 ) ) ;
#162318 = CARTESIAN_POINT ( 'NONE',  ( -10.81492255796105439, 18.62759615963255655, 72.91775706135234714 ) ) ;
#162319 = CARTESIAN_POINT ( 'NONE',  ( 16.55341960407618274, -4.379528057220086978, 41.04275706135236135 ) ) ;
#162320 = CARTESIAN_POINT ( 'NONE',  ( -10.81492255796105439, 18.62759615963255655, 37.91775706135235424 ) ) ;
#162321 = CARTESIAN_POINT ( 'NONE',  ( 16.53943276465976808, -0.05219959533910856209, 68.74890960531435269 ) ) ;
#162322 = ORIENTED_EDGE ( 'NONE', *, *, #65800, .T. ) ;
#162323 = CARTESIAN_POINT ( 'NONE',  ( 15.72974639402176855, 15.80617190586768217, 21.87609039468567573 ) ) ;
#162324 = DIRECTION ( 'NONE',  ( 1.000000000000000000, 0.000000000000000000, 0.000000000000000000 ) ) ;
#162325 = CARTESIAN_POINT ( 'NONE',  ( 14.29746914071049879, -8.314922557960816363, 48.33224293864770260 ) ) ;
#162326 = CARTESIAN_POINT ( 'NONE',  ( -19.03943276465977164, 0.05219959533909376836, 21.24890960531436335 ) ) ;
#162327 = CARTESIAN_POINT ( 'NONE',  ( 18.62759615963271287, -10.81492255796078972, 43.33224293864769550 ) ) ;
#162328 = CARTESIAN_POINT ( 'NONE',  ( -0.05219959533910754901, -16.53943276465976808, 77.49890960531433848 ) ) ;
#162329 = CARTESIAN_POINT ( 'NONE',  ( 15.80617190586746368, 15.72974639402197994, 79.37390960531436690 ) ) ;
#162330 = CARTESIAN_POINT ( 'NONE',  ( -5.049401038298153566, 19.05341960407611168, 90.20724293864766707 ) ) ;
#162332 = CARTESIAN_POINT ( 'NONE',  ( 5.049401038297881783, 19.05341960407617563, 82.29275706135229029 ) ) ;
#162331 = CARTESIAN_POINT ( 'NONE',  ( -13.89961937509977652, 13.97604488694528158, 35.62390960531435269 ) ) ;
#162333 = EDGE_CURVE ( 'NONE', #199879, #17363, #177264, .T. ) ;
#162335 = CARTESIAN_POINT ( 'NONE',  ( 18.62759615963271287, -10.81492255796078972, 68.33224293864769550 ) ) ;
#162334 = CARTESIAN_POINT ( 'NONE',  ( 21.55341960407619695, -5.719274019375665929, 61.04275706135234714 ) ) ;
#162336 = CARTESIAN_POINT ( 'NONE',  ( 19.03943276465977164, -0.05219959533909143690, 43.74890960531435979 ) ) ;
#162337 = CARTESIAN_POINT ( 'NONE',  ( -9.564922557960796823, -16.46253265017161027, 72.08224293864770971 ) ) ;
#162338 = ORIENTED_EDGE ( 'NONE', *, *, #24130, .F. ) ;
#162339 = CARTESIAN_POINT ( 'NONE',  ( 16.55341960407618274, -4.379528057220086978, 51.04275706135234714 ) ) ;
#162340 = CARTESIAN_POINT ( 'NONE',  ( -18.67979575497193778, 10.72451020669871902, 33.33442372801900433 ) ) ;
#162341 = CARTESIAN_POINT ( 'NONE',  ( 21.53943276465977519, 0.05219959533937863772, 66.25109039468567573 ) ) ;
#162342 = CARTESIAN_POINT ( 'NONE',  ( 16.46253265017160672, -9.564922557960803928, 108.3322429386476955 ) ) ;
#162343 = CARTESIAN_POINT ( 'NONE',  ( -21.52544592524343514, 5.823673210054127303, 81.04057627198102409 ) ) ;
#162345 = CARTESIAN_POINT ( 'NONE',  ( 12.06949235617739724, 12.14591786802326823, 46.87609039468568994 ) ) ;
#162344 = CARTESIAN_POINT ( 'NONE',  ( -15.80617190586768217, 15.72974639402176855, 28.12609039468568284 ) ) ;
#162346 = CARTESIAN_POINT ( 'NONE',  ( -21.52544592524343514, 5.823673210054127303, 56.04057627198102409 ) ) ;
#162347 = CARTESIAN_POINT ( 'NONE',  ( -0.05219959533936034679, 19.03943276465977164, 22.50109039468566152 ) ) ;
#162348 = CARTESIAN_POINT ( 'NONE',  ( 16.46253265017160672, -9.564922557960803928, 48.33224293864769550 ) ) ;
#162349 = CARTESIAN_POINT ( 'NONE',  ( 16.46253265017160672, -9.564922557960803928, 108.3322429386476955 ) ) ;
#162350 = CARTESIAN_POINT ( 'NONE',  ( -13.89961937509977652, 13.97604488694528158, 95.62390960531436690 ) ) ;
#162351 = DIRECTION ( 'NONE',  ( -0.5000000000000037748, -0.4999999999999949485, -0.7071067811865484609 ) ) ;
#162352 = CARTESIAN_POINT ( 'NONE',  ( 5.049401038297881783, 19.05341960407617563, 62.29275706135234003 ) ) ;
#162353 = CARTESIAN_POINT ( 'NONE',  ( 5.719274019375991003, -21.55341960407610458, 42.70724293864770260 ) ) ;
#162354 = CARTESIAN_POINT ( 'NONE',  ( 16.53943276465976808, -0.05219959533910856209, 23.74890960531435269 ) ) ;
#162355 = CARTESIAN_POINT ( 'NONE',  ( 9.564922557961047289, -16.46253265017146816, 100.4177570613523329 ) ) ;
#162356 = CARTESIAN_POINT ( 'NONE',  ( -3.874011537017815421, -5.374011537017722162, -62.41807096325323556 ) ) ;
#162357 = CARTESIAN_POINT ( 'NONE',  ( -5.153800228976607833, 19.02544592524334988, 27.70942372801899722 ) ) ;
#162358 = CARTESIAN_POINT ( 'NONE',  ( -13.97604488694547697, 13.89961937509957934, 103.1260903946856473 ) ) ;
#162359 = CARTESIAN_POINT ( 'NONE',  ( -0.05219959533936034679, 19.03943276465977164, 47.50109039468566863 ) ) ;
#162360 = CARTESIAN_POINT ( 'NONE',  ( 17.44279575226825330, 5.990770900252411657, 106.6644243248568102 ) ) ;
#162361 = CARTESIAN_POINT ( 'NONE',  ( -9.564922557960796823, -16.46253265017161027, 57.08224293864769550 ) ) ;
#162362 = CARTESIAN_POINT ( 'NONE',  ( -8.224510206698948167, 14.34966873604960824, 60.41557627198102409 ) ) ;
#162363 = CARTESIAN_POINT ( 'NONE',  ( 16.46253265017160672, -9.564922557960803928, 33.33224293864770260 ) ) ;
#162364 = CARTESIAN_POINT ( 'NONE',  ( -16.55341960407611168, -4.379528057220339221, 46.45724293864769550 ) ) ;
#162365 = CARTESIAN_POINT ( 'NONE',  ( -27.33089735363342498, -28.79505088701986537, -20.09366309423209174 ) ) ;
#162366 = CARTESIAN_POINT ( 'NONE',  ( 4.379528057220092307, 16.55341960407617563, 107.2927570613523471 ) ) ;
#162367 = CARTESIAN_POINT ( 'NONE',  ( 16.51473224551069308, 9.474510206698969483, 64.16557627198102409 ) ) ;
#162368 = CARTESIAN_POINT ( 'NONE',  ( -9.474510206698720793, -16.51473224551083518, 29.58442372801900433 ) ) ;
#162369 = CARTESIAN_POINT ( 'NONE',  ( -8.224510206698735004, -14.34966873604973081, 39.58442372801901143 ) ) ;
#162370 = CARTESIAN_POINT ( 'NONE',  ( -18.67979575497178146, -10.72451020669898902, 51.66557627198102409 ) ) ;
#162371 = CARTESIAN_POINT ( 'NONE',  ( -15.72974639402176322, -15.80617190586768395, 104.3760903946856899 ) ) ;
#162372 = CARTESIAN_POINT ( 'NONE',  ( 9.474510206698971260, -16.51473224551069308, 62.91557627198102409 ) ) ;
#162373 = CARTESIAN_POINT ( 'NONE',  ( -9.474510206698964154, 16.51473224551069663, 110.4155762719810383 ) ) ;
#162374 = CARTESIAN_POINT ( 'NONE',  ( -19.02544592524342804, 5.153800228976336051, 96.04057627198103830 ) ) ;
#162375 = CARTESIAN_POINT ( 'NONE',  ( -29.86685920354755552, 21.69954338932564397, -2.824999997268813345 ) ) ;
#162376 = CARTESIAN_POINT ( 'NONE',  ( 10.81492255796106328, -18.62759615963255655, 30.41775706135234358 ) ) ;
#162377 = CARTESIAN_POINT ( 'NONE',  ( 16.55341960407611168, 4.379528057220329451, 98.95724293864770971 ) ) ;
#162379 = CARTESIAN_POINT ( 'NONE',  ( 16.51473224551069308, 9.474510206698969483, 64.16557627198102409 ) ) ;
#162378 = CARTESIAN_POINT ( 'NONE',  ( -15.80617190586745835, -15.72974639402198527, 86.87390960531438111 ) ) ;
#162380 = CARTESIAN_POINT ( 'NONE',  ( -19.02544592524342804, 5.153800228976336051, 76.04057627198102409 ) ) ;
#162381 = CARTESIAN_POINT ( 'NONE',  ( 21.55341960407610458, 5.719274019375980345, 113.9572429386477239 ) ) ;
#162382 = ORIENTED_EDGE ( 'NONE', *, *, #981, .T. ) ;
#162383 = CARTESIAN_POINT ( 'NONE',  ( -13.89961937509977652, 13.97604488694528158, 70.62390960531432427 ) ) ;
#162384 = CARTESIAN_POINT ( 'NONE',  ( -31.22445544967866837, -21.66088859369465425, -21.91603554745442040 ) ) ;
#162386 = DIRECTION ( 'NONE',  ( -0.3041824702427711746, 0.9526137857479314297, 1.533086186985162281E-15 ) ) ;
#162385 = CARTESIAN_POINT ( 'NONE',  ( -4.379528057220328563, 16.55341960407611168, 110.2072429386477239 ) ) ;
#162387 = CARTESIAN_POINT ( 'NONE',  ( 0.05219959533936267826, -19.03943276465977164, 90.00109039468567573 ) ) ;
#162388 = CARTESIAN_POINT ( 'NONE',  ( 8.314922557960818139, 14.29746914071049879, 99.58224293864770971 ) ) ;
#162389 = CARTESIAN_POINT ( 'NONE',  ( -18.67979575497193778, 10.72451020669871902, 68.33442372801900433 ) ) ;
#162391 = CARTESIAN_POINT ( 'NONE',  ( -15.80617190586768217, 15.72974639402176855, 28.12609039468568284 ) ) ;
#162390 = CARTESIAN_POINT ( 'NONE',  ( -19.03943276465977164, 0.05219959533909376836, 56.24890960531435979 ) ) ;
#162392 = CARTESIAN_POINT ( 'NONE',  ( -18.62759615963270932, 10.81492255796079327, 110.8322429386476955 ) ) ;
#162393 = CARTESIAN_POINT ( 'NONE',  ( 8.906447517083057264, -27.41122689804191026, 142.5999999999999943 ) ) ;
#162394 = CARTESIAN_POINT ( 'NONE',  ( -16.51473224551069308, -9.474510206698971260, 71.66557627198102409 ) ) ;
#162395 = CARTESIAN_POINT ( 'NONE',  ( 23.31738231874054890, -16.94106989632523508, 139.0500000054623513 ) ) ;
#162397 = CARTESIAN_POINT ( 'NONE',  ( -18.67979575497178146, -10.72451020669898902, 31.66557627198102054 ) ) ;
#162396 = CARTESIAN_POINT ( 'NONE',  ( 13.89961937509957401, 13.97604488694547697, 111.8760903946856757 ) ) ;
#162398 = CARTESIAN_POINT ( 'NONE',  ( 0.05219959533937995610, -21.53943276465977519, 60.00109039468568284 ) ) ;
#162399 = CARTESIAN_POINT ( 'NONE',  ( -16.46253265017160317, 9.564922557960807481, 95.83224293864769550 ) ) ;
#162400 = CARTESIAN_POINT ( 'NONE',  ( -16.46253265017146816, -9.564922557961047289, 79.16775706135234714 ) ) ;
#162401 = VECTOR ( 'NONE', #124125, 1000.000000000000000 ) ;
#162402 = CARTESIAN_POINT ( 'NONE',  ( 13.89961937509977652, -13.97604488694527269, 43.12390960531434558 ) ) ;
#162403 = CARTESIAN_POINT ( 'NONE',  ( 0.05219959533909260263, 19.03943276465977164, 69.99890960531435269 ) ) ;
#162404 = CARTESIAN_POINT ( 'NONE',  ( -16.52544592524342804, 4.483927247898546575, 91.04057627198103830 ) ) ;
#162405 = CARTESIAN_POINT ( 'NONE',  ( 16.46253265017160672, -9.564922557960803928, 98.33224293864769550 ) ) ;
#162406 = CARTESIAN_POINT ( 'NONE',  ( 14.29746914071049879, -8.314922557960816363, 88.33224293864769550 ) ) ;
#162407 = CARTESIAN_POINT ( 'NONE',  ( 5.153800228976335163, 19.02544592524342804, 99.79057627198102409 ) ) ;
#162409 = CARTESIAN_POINT ( 'NONE',  ( 9.474510206698971260, -16.51473224551069308, 22.91557627198102765 ) ) ;
#162408 = CARTESIAN_POINT ( 'NONE',  ( 8.224510206698953496, -14.34966873604960469, 42.91557627198103120 ) ) ;
#162410 = EDGE_LOOP ( 'NONE', ( #50949, #47335, #166094, #121166, #58565, #154109, #91278, #149230 ) ) ;
#162411 = CARTESIAN_POINT ( 'NONE',  ( 10.72451020669871369, 18.67979575497193778, 57.08442372801901854 ) ) ;
#162412 = CARTESIAN_POINT ( 'NONE',  ( 13.97604488694548053, -13.89961937509957401, 80.62609039468567573 ) ) ;
#162413 = CARTESIAN_POINT ( 'NONE',  ( -4.483927247898539470, -16.52544592524342804, 47.29057627198103120 ) ) ;
#162414 = CARTESIAN_POINT ( 'NONE',  ( -18.67979575497178146, -10.72451020669898902, 96.66557627198102409 ) ) ;
#162415 = CARTESIAN_POINT ( 'NONE',  ( 10.72451020669898902, -18.67979575497178502, 37.91557627198102409 ) ) ;
#162416 = CARTESIAN_POINT ( 'NONE',  ( 4.379528057220339221, -16.55341960407611168, 77.70724293864770971 ) ) ;
#162417 = CARTESIAN_POINT ( 'NONE',  ( 19.02544592524343514, -5.153800228976328945, 58.54057627198102409 ) ) ;
#162418 = CARTESIAN_POINT ( 'NONE',  ( -4.483927247898539470, -16.52544592524342804, 27.29057627198103120 ) ) ;
#162419 = CARTESIAN_POINT ( 'NONE',  ( -14.34966873604972548, 8.224510206698743886, 103.3344237280190043 ) ) ;
#162420 = CARTESIAN_POINT ( 'NONE',  ( -16.55341960407617563, 4.379528057220093196, 73.54275706135234714 ) ) ;
#162421 = CARTESIAN_POINT ( 'NONE',  ( -13.89961937509957401, -13.97604488694547875, 29.37609039468565797 ) ) ;
#162423 = CARTESIAN_POINT ( 'NONE',  ( -19.02544592524342804, 5.153800228976336051, 106.0405762719810241 ) ) ;
#162422 = LINE ( 'NONE', #5740, #53288 ) ;
#162424 = CARTESIAN_POINT ( 'NONE',  ( -9.564922557960796823, -16.46253265017161027, 72.08224293864770971 ) ) ;
#162425 = CARTESIAN_POINT ( 'NONE',  ( 5.049401038298161559, -19.05341960407611168, 42.70724293864767418 ) ) ;
#162426 = CARTESIAN_POINT ( 'NONE',  ( -14.34966873604960291, -8.224510206698953496, 41.66557627198103120 ) ) ;
#162428 = CARTESIAN_POINT ( 'NONE',  ( -13.89961937509977652, 13.97604488694528158, 110.6239096053143243 ) ) ;
#162427 = CARTESIAN_POINT ( 'NONE',  ( 32.00000000000000000, -5.510910596163089556E-15, 42.35000000000000142 ) ) ;
#162429 = CARTESIAN_POINT ( 'NONE',  ( -10.72451020669898014, 18.67979575497178502, 40.41557627198103120 ) ) ;
#162430 = CARTESIAN_POINT ( 'NONE',  ( 0.05219959533910956823, 16.53943276465976808, 79.99890960531435269 ) ) ;
#162431 = CARTESIAN_POINT ( 'NONE',  ( 12.06949235617739724, 12.14591786802326823, 21.87609039468567573 ) ) ;
#162432 = CIRCLE ( 'NONE', #49423, 38.00000000000000000 ) ;
#162433 = CARTESIAN_POINT ( 'NONE',  ( 8.224510206698953496, -14.34966873604960469, 67.91557627198102409 ) ) ;
#162434 = CARTESIAN_POINT ( 'NONE',  ( 17.50000000000000000, -5.499999999999992895, 86.21769037696435589 ) ) ;
#162435 = CARTESIAN_POINT ( 'NONE',  ( 19.02544592524334988, 5.153800228976608722, 61.45942372801900433 ) ) ;
#162436 = CARTESIAN_POINT ( 'NONE',  ( 13.97604488694527802, 13.89961937509977652, 109.3739096053143669 ) ) ;
#162437 = CARTESIAN_POINT ( 'NONE',  ( -13.89961937509957401, -13.97604488694547875, 84.37609039468567573 ) ) ;
#162438 = CARTESIAN_POINT ( 'NONE',  ( 13.97604488694548053, -13.89961937509957401, 95.62609039468566152 ) ) ;
#162440 = CARTESIAN_POINT ( 'NONE',  ( 4.483927247898790824, -16.52544592524335698, 110.2094237280190185 ) ) ;
#162439 = CARTESIAN_POINT ( 'NONE',  ( -16.51473224551082808, 9.474510206698731452, 108.3344237280190043 ) ) ;
#162441 = CARTESIAN_POINT ( 'NONE',  ( -0.05219959533936034679, 19.03943276465977164, 67.50109039468566152 ) ) ;
#162442 = CARTESIAN_POINT ( 'NONE',  ( -18.62759615963270932, 10.81492255796079327, 40.83224293864769550 ) ) ;
#162443 = CARTESIAN_POINT ( 'NONE',  ( -18.62759615963255300, -10.81492255796106328, 64.16775706135234714 ) ) ;
#162444 = CARTESIAN_POINT ( 'NONE',  ( -21.51693143705271893, -9.260949364272990536, 168.7281092719938442 ) ) ;
#162445 = CARTESIAN_POINT ( 'NONE',  ( 8.224510206698742110, 14.34966873604972548, 22.08442372801901143 ) ) ;
#162447 = CARTESIAN_POINT ( 'NONE',  ( 13.89961937509977652, -13.97604488694527269, 78.12390960531433848 ) ) ;
#162446 = CARTESIAN_POINT ( 'NONE',  ( 17.50000000000000711, 3.442889716078282092, 22.31504430846741727 ) ) ;
#162448 = CARTESIAN_POINT ( 'NONE',  ( 14.65320595882614896, 15.80137536867085046, -58.69884337265980179 ) ) ;
#162450 = CARTESIAN_POINT ( 'NONE',  ( -13.89961937509977652, 13.97604488694528158, 70.62390960531432427 ) ) ;
#162449 = CARTESIAN_POINT ( 'NONE',  ( 16.52544592524342804, -4.483927247898539470, 93.54057627198103830 ) ) ;
#162451 = CARTESIAN_POINT ( 'NONE',  ( 5.049401038298161559, -19.05341960407611168, 87.70724293864769550 ) ) ;
#162452 = VERTEX_POINT ( 'NONE', #72018 ) ;
#162453 = CARTESIAN_POINT ( 'NONE',  ( -19.05341960407617563, 5.049401038297882671, 88.54275706135230450 ) ) ;
#162454 = CARTESIAN_POINT ( 'NONE',  ( 21.53943276465977519, -0.05219959533907433946, 73.74890960531433848 ) ) ;
#162455 = CARTESIAN_POINT ( 'NONE',  ( 13.97604488694527802, 13.89961937509977652, 24.37390960531435624 ) ) ;
#162456 = CARTESIAN_POINT ( 'NONE',  ( 9.564922557961047289, -16.46253265017146816, 60.41775706135233293 ) ) ;
#162457 = CARTESIAN_POINT ( 'NONE',  ( -19.05341960407611168, -5.049401038298163336, 56.45724293864768129 ) ) ;
#162458 = CARTESIAN_POINT ( 'NONE',  ( -16.46253265017160317, 9.564922557960807481, 90.83224293864769550 ) ) ;
#162459 = ORIENTED_EDGE ( 'NONE', *, *, #199317, .T. ) ;
#162460 = CARTESIAN_POINT ( 'NONE',  ( -5.823673210054116645, -21.52544592524344225, 107.2905762719810525 ) ) ;
#162463 = CARTESIAN_POINT ( 'NONE',  ( -13.89961937509957401, -13.97604488694547875, 64.37609039468567573 ) ) ;
#162462 = CARTESIAN_POINT ( 'NONE',  ( -5.049401038298153566, 19.05341960407611168, 85.20724293864766707 ) ) ;
#162461 = CARTESIAN_POINT ( 'NONE',  ( -0.05219959533910754901, -16.53943276465976808, 87.49890960531436690 ) ) ;
#162464 = CARTESIAN_POINT ( 'NONE',  ( 21.52544592524344225, -5.823673210054117533, 93.54057627198103830 ) ) ;
#162465 = CARTESIAN_POINT ( 'NONE',  ( -5.719274019375978568, 21.55341960407610458, 75.20724293864769550 ) ) ;
#162466 = CARTESIAN_POINT ( 'NONE',  ( -14.29746914071049879, 8.314922557960819915, 35.83224293864768839 ) ) ;
#162467 = CARTESIAN_POINT ( 'NONE',  ( 18.67979575497194134, -10.72451020669871369, 100.8344237280190185 ) ) ;
#162468 = CARTESIAN_POINT ( 'NONE',  ( 4.379528057220092307, 16.55341960407617563, 67.29275706135234714 ) ) ;
#162469 = CARTESIAN_POINT ( 'NONE',  ( 16.51473224551069308, 9.474510206698969483, 99.16557627198102409 ) ) ;
#162470 = CARTESIAN_POINT ( 'NONE',  ( 19.03943276465977164, -0.05219959533909143690, 28.74890960531435624 ) ) ;
#162471 = CARTESIAN_POINT ( 'NONE',  ( 5.823673210054444382, -21.52544592524334988, 35.20942372801901854 ) ) ;
#162472 = CARTESIAN_POINT ( 'NONE',  ( 21.52544592524334988, 5.823673210054432836, 51.45942372801901854 ) ) ;
#162473 = CARTESIAN_POINT ( 'NONE',  ( 5.049401038298161559, -19.05341960407611168, 47.70724293864770260 ) ) ;
#162474 = CARTESIAN_POINT ( 'NONE',  ( 21.55341960407619695, -5.719274019375665929, 36.04275706135234714 ) ) ;
#162475 = CARTESIAN_POINT ( 'NONE',  ( 13.89961937509957401, 13.97604488694547697, 71.87609039468567573 ) ) ;
#162476 = CARTESIAN_POINT ( 'NONE',  ( -5.049401038297874678, -19.05341960407617918, 79.79275706135233293 ) ) ;
#162477 = CARTESIAN_POINT ( 'NONE',  ( 9.564922557960805705, 16.46253265017160317, 39.58224293864768839 ) ) ;
#162478 = CARTESIAN_POINT ( 'NONE',  ( -16.55341960407617563, 4.379528057220093196, 68.54275706135234714 ) ) ;
#162479 = CARTESIAN_POINT ( 'NONE',  ( -9.564922557960796823, -16.46253265017161027, 52.08224293864768839 ) ) ;
#162480 = CARTESIAN_POINT ( 'NONE',  ( 24.24385185424179667, -7.025880200331696024, 170.5073520790474788 ) ) ;
#162481 = CARTESIAN_POINT ( 'NONE',  ( 0.05219959533909260263, 19.03943276465977164, 99.99890960531436690 ) ) ;
#162483 = ADVANCED_FACE ( 'NONE', ( #198347 ), #31479, .T. ) ;
#162482 = CARTESIAN_POINT ( 'NONE',  ( 5.153800228976335163, 19.02544592524342804, 44.79057627198103830 ) ) ;
#162484 = CARTESIAN_POINT ( 'NONE',  ( 15.72974639402199770, -15.80617190586745480, 68.12390960531436690 ) ) ;
#162485 = CARTESIAN_POINT ( 'NONE',  ( -14.29746914071037622, -8.314922557961029526, 59.16775706135234714 ) ) ;
#162486 = CARTESIAN_POINT ( 'NONE',  ( 5.719274019375673035, 21.55341960407619339, 112.2927570613523471 ) ) ;
#162487 = CARTESIAN_POINT ( 'NONE',  ( -13.89961937509977652, 13.97604488694528158, 55.62390960531434558 ) ) ;
#162488 = CARTESIAN_POINT ( 'NONE',  ( 4.483927247898545687, 16.52544592524342804, 39.79057627198103830 ) ) ;
#162489 = CARTESIAN_POINT ( 'NONE',  ( -4.483927247898539470, -16.52544592524342804, 87.29057627198103830 ) ) ;
#162490 = CARTESIAN_POINT ( 'NONE',  ( -0.05219959533909027116, -19.03943276465977164, 77.49890960531435269 ) ) ;
#162491 = CARTESIAN_POINT ( 'NONE',  ( -5.823673210054431948, 21.52544592524334988, 32.70942372801900433 ) ) ;
#162492 = CARTESIAN_POINT ( 'NONE',  ( -13.89961937509977652, 13.97604488694528158, 95.62390960531436690 ) ) ;
#162493 = CIRCLE ( 'NONE', #55984, 5.000000000000000888 ) ;
#162494 = CARTESIAN_POINT ( 'NONE',  ( -0.05219959533937732626, 21.53943276465977519, 97.50109039468567573 ) ) ;
#162495 = CARTESIAN_POINT ( 'NONE',  ( 12.14591786802327356, -12.06949235617739191, 60.62609039468567573 ) ) ;
#162496 = CARTESIAN_POINT ( 'NONE',  ( -9.564922557960796823, -16.46253265017161027, 102.0822429386477097 ) ) ;
#162497 = CARTESIAN_POINT ( 'NONE',  ( -18.67979575497178146, -10.72451020669898902, 86.66557627198102409 ) ) ;
#162498 = CARTESIAN_POINT ( 'NONE',  ( -12.06949235617756955, 12.14591786802309770, 50.62390960531435979 ) ) ;
#162499 = CARTESIAN_POINT ( 'NONE',  ( -5.153800228976328057, -19.02544592524343514, 37.29057627198102409 ) ) ;
#162500 = CARTESIAN_POINT ( 'NONE',  ( -16.55341960407617563, 4.379528057220093196, 58.54275706135235424 ) ) ;
#162501 = CARTESIAN_POINT ( 'NONE',  ( 4.379528057220339221, -16.55341960407611168, 67.70724293864769550 ) ) ;
#162502 = CARTESIAN_POINT ( 'NONE',  ( 19.02544592524343514, -5.153800228976328945, 108.5405762719810383 ) ) ;
#162503 = CARTESIAN_POINT ( 'NONE',  ( -21.53943276465977519, 0.05219959533907696930, 31.24890960531435979 ) ) ;
#162504 = CARTESIAN_POINT ( 'NONE',  ( -5.153800228976607833, 19.02544592524334988, 32.70942372801899722 ) ) ;
#162505 = CARTESIAN_POINT ( 'NONE',  ( 16.53943276465976808, -0.05219959533910856209, 103.7489096053143669 ) ) ;
#162506 = CARTESIAN_POINT ( 'NONE',  ( 13.97604488694527802, 13.89961937509977652, 109.3739096053143669 ) ) ;
#162507 = VERTEX_POINT ( 'NONE', #32476 ) ;
#162508 = CARTESIAN_POINT ( 'NONE',  ( -12.06949235617739369, -12.14591786802326823, 49.37609039468569705 ) ) ;
#162509 = CARTESIAN_POINT ( 'NONE',  ( -9.474510206698964154, 16.51473224551069663, 55.41557627198103120 ) ) ;
#162510 = CARTESIAN_POINT ( 'NONE',  ( 5.000000000000000888, -140.0000000000000000, -15.00000000000000000 ) ) ;
#162511 = CARTESIAN_POINT ( 'NONE',  ( -0.05219959533936034679, 19.03943276465977164, 67.50109039468566152 ) ) ;
#162512 = CARTESIAN_POINT ( 'NONE',  ( 8.224510206698742110, 14.34966873604972548, 87.08442372801901854 ) ) ;
#162513 = CARTESIAN_POINT ( 'NONE',  ( 19.05341960407617918, -5.049401038297876454, 91.04275706135234714 ) ) ;
#162514 = CARTESIAN_POINT ( 'NONE',  ( -10.81492255796105439, 18.62759615963255655, 72.91775706135234714 ) ) ;
#162515 = CARTESIAN_POINT ( 'NONE',  ( -9.474510206698964154, 16.51473224551069663, 70.41557627198102409 ) ) ;
#162516 = CARTESIAN_POINT ( 'NONE',  ( 5.719274019375991003, -21.55341960407610458, 92.70724293864770971 ) ) ;
#162517 = CARTESIAN_POINT ( 'NONE',  ( -4.379528057220328563, 16.55341960407611168, 115.2072429386476955 ) ) ;
#162518 = CARTESIAN_POINT ( 'NONE',  ( 13.97604488694548053, -13.89961937509957401, 80.62609039468567573 ) ) ;
#162519 = CARTESIAN_POINT ( 'NONE',  ( 21.53943276465977519, -0.05219959533907433946, 83.74890960531435269 ) ) ;
#162520 = CARTESIAN_POINT ( 'NONE',  ( -9.564922557961040184, 16.46253265017147172, 42.91775706135234003 ) ) ;
#162521 = FACE_BOUND ( 'NONE', #90079, .T. ) ;
#162522 = CARTESIAN_POINT ( 'NONE',  ( 0.05219959533907565091, 21.53943276465977519, 94.99890960531436690 ) ) ;
#162523 = CARTESIAN_POINT ( 'NONE',  ( -15.49999999999999822, 7.499999999999999112, 20.00000000000000000 ) ) ;
#162524 = CARTESIAN_POINT ( 'NONE',  ( -19.02544592524342804, 5.153800228976336051, 61.04057627198103120 ) ) ;
#162525 = CARTESIAN_POINT ( 'NONE',  ( -4.647474457565486646E-15, 28.90000000000004476, -49.67367017693150189 ) ) ;
#162526 = CARTESIAN_POINT ( 'NONE',  ( 8.314922557961029526, -14.29746914071037800, 25.41775706135235779 ) ) ;
#162527 = CARTESIAN_POINT ( 'NONE',  ( 36.84749596837620089, -2.912325675875791386, 49.66910675224615801 ) ) ;
#162528 = CARTESIAN_POINT ( 'NONE',  ( -5.153800228976328057, -19.02544592524343514, 52.29057627198100988 ) ) ;
#162530 = CARTESIAN_POINT ( 'NONE',  ( 16.52544592524342804, -4.483927247898539470, 48.54057627198103120 ) ) ;
#162529 = CARTESIAN_POINT ( 'NONE',  ( -15.80617190586745835, -15.72974639402198527, 101.8739096053143811 ) ) ;
#162531 = CARTESIAN_POINT ( 'NONE',  ( -10.81492255796105439, 18.62759615963255655, 77.91775706135231871 ) ) ;
#162533 = CARTESIAN_POINT ( 'NONE',  ( -19.03943276465977164, -0.05219959533935918106, 28.75109039468566507 ) ) ;
#162532 = CARTESIAN_POINT ( 'NONE',  ( -14.34966873604972548, 8.224510206698743886, 28.33442372801902209 ) ) ;
#162534 = CARTESIAN_POINT ( 'NONE',  ( -14.34966873604960291, -8.224510206698953496, 36.66557627198103120 ) ) ;
#162535 = CARTESIAN_POINT ( 'NONE',  ( 0.05219959533937995610, -21.53943276465977519, 45.00109039468568284 ) ) ;
#162536 = CARTESIAN_POINT ( 'NONE',  ( -10.72451020669898014, 18.67979575497178502, 115.4155762719810241 ) ) ;
#162537 = CARTESIAN_POINT ( 'NONE',  ( -21.55341960407610458, -5.719274019375992779, 61.45724293864770260 ) ) ;
#162538 = CARTESIAN_POINT ( 'NONE',  ( -9.474510206698720793, -16.51473224551083518, 89.58442372801900433 ) ) ;
#162539 = CARTESIAN_POINT ( 'NONE',  ( 0.05219959533936267826, -19.03943276465977164, 75.00109039468566152 ) ) ;
#162540 = CARTESIAN_POINT ( 'NONE',  ( 10.72451020669871369, 18.67979575497193778, 77.08442372801901854 ) ) ;
#162541 = CARTESIAN_POINT ( 'NONE',  ( 0.05219959533936267826, -19.03943276465977164, 50.00109039468566863 ) ) ;
#162542 = CARTESIAN_POINT ( 'NONE',  ( 19.05341960407611168, 5.049401038298154454, 23.95724293864769194 ) ) ;
#162543 = CARTESIAN_POINT ( 'NONE',  ( 5.823673210054125526, 21.52544592524343514, 44.79057627198103120 ) ) ;
#162544 = CARTESIAN_POINT ( 'NONE',  ( -14.29746914071049879, 8.314922557960819915, 45.83224293864769550 ) ) ;
#162545 = CARTESIAN_POINT ( 'NONE',  ( -17.97214573761829470, -5.500000000000090594, 51.46970049038655048 ) ) ;
#162546 = CARTESIAN_POINT ( 'NONE',  ( -5.153800228976607833, 19.02544592524334988, 22.70942372801899012 ) ) ;
#162547 = CARTESIAN_POINT ( 'NONE',  ( -8.314922557961024197, 14.29746914071037800, 82.91775706135234714 ) ) ;
#162548 = CARTESIAN_POINT ( 'NONE',  ( 4.483927247898545687, 16.52544592524342804, 39.79057627198103830 ) ) ;
#162549 = CARTESIAN_POINT ( 'NONE',  ( 15.72974639402176855, 15.80617190586768217, 71.87609039468568994 ) ) ;
#162550 = CARTESIAN_POINT ( 'NONE',  ( 0.05219959533937995610, -21.53943276465977519, 85.00109039468568994 ) ) ;
#162551 = CARTESIAN_POINT ( 'NONE',  ( -5.719274019375978568, 21.55341960407610458, 85.20724293864770971 ) ) ;
#162552 = CARTESIAN_POINT ( 'NONE',  ( -0.05219959533909027116, -19.03943276465977164, 32.49890960531435979 ) ) ;
#162553 = CARTESIAN_POINT ( 'NONE',  ( -15.80617190586768217, 15.72974639402176855, 58.12609039468568994 ) ) ;
#162554 = CARTESIAN_POINT ( 'NONE',  ( -5.153800228976328057, -19.02544592524343514, 32.29057627198102409 ) ) ;
#162555 = CARTESIAN_POINT ( 'NONE',  ( -13.89961937509977652, 13.97604488694528158, 50.62390960531435979 ) ) ;
#162556 = CARTESIAN_POINT ( 'NONE',  ( -12.14591786802309592, -12.06949235617757132, 86.87390960531438111 ) ) ;
#162557 = CARTESIAN_POINT ( 'NONE',  ( -19.02544592524342804, 5.153800228976336051, 96.04057627198103830 ) ) ;
#162558 = CARTESIAN_POINT ( 'NONE',  ( -4.483927247898539470, -16.52544592524342804, 37.29057627198102409 ) ) ;
#162559 = CARTESIAN_POINT ( 'NONE',  ( 4.483927247898545687, 16.52544592524342804, 114.7905762719810383 ) ) ;
#162560 = CARTESIAN_POINT ( 'NONE',  ( -5.823673210054116645, -21.52544592524344225, 77.29057627198102409 ) ) ;
#162561 = CARTESIAN_POINT ( 'NONE',  ( 10.81492255796106328, -18.62759615963255655, 20.41775706135234714 ) ) ;
#162562 = CARTESIAN_POINT ( 'NONE',  ( -3.573655867282028392E-15, 2.428612866367529932E-14, 2.000000000000000000 ) ) ;
#162563 = CARTESIAN_POINT ( 'NONE',  ( 0.05219959533934541429, -16.53943276465976808, 20.00109039468568639 ) ) ;
#162564 = EDGE_CURVE ( 'NONE', #83320, #100314, #60809, .T. ) ;
#162565 = CARTESIAN_POINT ( 'NONE',  ( 0.05219959533907565091, 21.53943276465977519, 64.99890960531435269 ) ) ;
#162566 = CARTESIAN_POINT ( 'NONE',  ( 0.05219959533937995610, -21.53943276465977519, 100.0010903946857042 ) ) ;
#162567 = CARTESIAN_POINT ( 'NONE',  ( -16.51473224551069308, -9.474510206698971260, 81.66557627198103830 ) ) ;
#162568 = CARTESIAN_POINT ( 'NONE',  ( -15.72974639402176322, -15.80617190586768395, 34.37609039468568284 ) ) ;
#162569 = TOROIDAL_SURFACE ( 'NONE', #75405, 23.10356920737165254, 5.000000000000000000 ) ;
#162570 = CARTESIAN_POINT ( 'NONE',  ( 19.02544592524343514, -5.153800228976328945, 113.5405762719810241 ) ) ;
#162571 = CARTESIAN_POINT ( 'NONE',  ( -14.29746914071037622, -8.314922557961029526, 89.16775706135236135 ) ) ;
#162572 = CARTESIAN_POINT ( 'NONE',  ( -5.823673210054431948, 21.52544592524334988, 67.70942372801901854 ) ) ;
#162573 = CARTESIAN_POINT ( 'NONE',  ( -16.51473224551082808, 9.474510206698731452, 23.33442372801900078 ) ) ;
#162574 = CARTESIAN_POINT ( 'NONE',  ( -16.53943276465976808, -0.05219959533934237506, 78.75109039468568994 ) ) ;
#162575 = CARTESIAN_POINT ( 'NONE',  ( -5.719274019375665041, -21.55341960407619695, 34.79275706135235424 ) ) ;
#162576 = CARTESIAN_POINT ( 'NONE',  ( 19.03943276465977164, -0.05219959533909143690, 28.74890960531435624 ) ) ;
#162577 = CARTESIAN_POINT ( 'NONE',  ( 10.81492255796106328, -18.62759615963255655, 90.41775706135236135 ) ) ;
#162578 = CARTESIAN_POINT ( 'NONE',  ( 13.89961937509977652, -13.97604488694527269, 93.12390960531436690 ) ) ;
#162579 = CARTESIAN_POINT ( 'NONE',  ( 21.53943276465977519, -0.05219959533907433946, 83.74890960531435269 ) ) ;
#162580 = CARTESIAN_POINT ( 'NONE',  ( 13.97604488694548053, -13.89961937509957401, 65.62609039468567573 ) ) ;
#162582 = CARTESIAN_POINT ( 'NONE',  ( 21.52544592524344225, -5.823673210054117533, 48.54057627198103120 ) ) ;
#162581 = FACE_OUTER_BOUND ( 'NONE', #195982, .T. ) ;
#162584 = CARTESIAN_POINT ( 'NONE',  ( 0.05219959533910956823, 16.53943276465976808, 44.99890960531435979 ) ) ;
#162583 = CARTESIAN_POINT ( 'NONE',  ( -16.51473224551069308, -9.474510206698971260, 91.66557627198103830 ) ) ;
#162585 = CARTESIAN_POINT ( 'NONE',  ( 20.09068217638368736, 11.70722341973408120, 168.0245402885401518 ) ) ;
#162586 = CARTESIAN_POINT ( 'NONE',  ( -13.97604488694547697, 13.89961937509957934, 73.12609039468568994 ) ) ;
#162587 = CARTESIAN_POINT ( 'NONE',  ( -17.12812012977026299, 6.668231424565975729, 103.6405124067685506 ) ) ;
#162588 = CARTESIAN_POINT ( 'NONE',  ( -16.51473224551082808, 9.474510206698731452, 103.3344237280190043 ) ) ;
#162589 = CARTESIAN_POINT ( 'NONE',  ( -0.05219959533907301413, -21.53943276465977519, 87.49890960531436690 ) ) ;
#162590 = CARTESIAN_POINT ( 'NONE',  ( -14.29746914071049879, 8.314922557960819915, 65.83224293864769550 ) ) ;
#162591 = CARTESIAN_POINT ( 'NONE',  ( 16.46253265017160672, -9.564922557960803928, 98.33224293864769550 ) ) ;
#162592 = CARTESIAN_POINT ( 'NONE',  ( -16.52544592524335698, -4.483927247898792601, 43.95942372801902565 ) ) ;
#162593 = CARTESIAN_POINT ( 'NONE',  ( 9.564922557960805705, 16.46253265017160317, 54.58224293864769550 ) ) ;
#162595 = CARTESIAN_POINT ( 'NONE',  ( -5.153800228976607833, 19.02544592524334988, 92.70942372801901854 ) ) ;
#162594 = CARTESIAN_POINT ( 'NONE',  ( 15.80617190586769283, -15.72974639402175789, 35.62609039468568994 ) ) ;
#162596 = EDGE_CURVE ( 'NONE', #28437, #153939, #170007, .T. ) ;
#162597 = CARTESIAN_POINT ( 'NONE',  ( -9.564922557960796823, -16.46253265017161027, 97.08224293864769550 ) ) ;
#162598 = CARTESIAN_POINT ( 'NONE',  ( 19.03943276465977164, -0.05219959533909143690, 73.74890960531435269 ) ) ;
#162599 = CARTESIAN_POINT ( 'NONE',  ( -18.62759615963270932, 10.81492255796079327, 80.83224293864769550 ) ) ;
#162600 = CARTESIAN_POINT ( 'NONE',  ( -16.46253265017160317, 9.564922557960807481, 40.83224293864769550 ) ) ;
#162601 = CARTESIAN_POINT ( 'NONE',  ( -4.945344302077486986, 37.34563040183822835, -8.000000000000000000 ) ) ;
#162602 = CARTESIAN_POINT ( 'NONE',  ( 0.05219959533910956823, 16.53943276465976808, 54.99890960531435269 ) ) ;
#162603 = CARTESIAN_POINT ( 'NONE',  ( 16.46253265017160672, -9.564922557960803928, 108.3322429386476955 ) ) ;
#162604 = CARTESIAN_POINT ( 'NONE',  ( 0.000000000000000000, 0.000000000000000000, -61.89430850415821794 ) ) ;
#162605 = CARTESIAN_POINT ( 'NONE',  ( 19.05341960407617918, -5.049401038297876454, 71.04275706135234714 ) ) ;
#162606 = CARTESIAN_POINT ( 'NONE',  ( -0.05219959533907301413, -21.53943276465977519, 92.49890960531436690 ) ) ;
#162607 = CARTESIAN_POINT ( 'NONE',  ( 9.564922557961047289, -16.46253265017146816, 45.41775706135232582 ) ) ;
#162608 = CARTESIAN_POINT ( 'NONE',  ( -5.153800228976328057, -19.02544592524343514, 107.2905762719810383 ) ) ;
#162609 = CARTESIAN_POINT ( 'NONE',  ( 17.50000000000000000, 5.499999999999992895, 76.70309617465829888 ) ) ;
#162610 = CARTESIAN_POINT ( 'NONE',  ( -5.823673210054116645, -21.52544592524344225, 37.29057627198102409 ) ) ;
#162611 = CARTESIAN_POINT ( 'NONE',  ( 5.153800228976335163, 19.02544592524342804, 69.79057627198103830 ) ) ;
#162612 = CARTESIAN_POINT ( 'NONE',  ( -5.719274019375665041, -21.55341960407619695, 59.79275706135234714 ) ) ;
#162613 = CARTESIAN_POINT ( 'NONE',  ( 13.97604488694527802, 13.89961937509977652, 44.37390960531435269 ) ) ;
#162615 = ORIENTED_EDGE ( 'NONE', *, *, #33729, .T. ) ;
#162614 = CARTESIAN_POINT ( 'NONE',  ( -4.483927247898539470, -16.52544592524342804, 77.29057627198102409 ) ) ;
#162616 = CARTESIAN_POINT ( 'NONE',  ( -4.379528057220086978, -16.55341960407618274, 24.79275706135235779 ) ) ;
#162617 = CARTESIAN_POINT ( 'NONE',  ( 21.52544592524334988, 5.823673210054432836, 46.45942372801901854 ) ) ;
#162618 = ORIENTED_EDGE ( 'NONE', *, *, #105416, .T. ) ;
#162619 = CARTESIAN_POINT ( 'NONE',  ( -0.05219959533909027116, -19.03943276465977164, 112.4989096053143669 ) ) ;
#162620 = CARTESIAN_POINT ( 'NONE',  ( -5.049401038297874678, -19.05341960407617918, 69.79275706135233293 ) ) ;
#162621 = CARTESIAN_POINT ( 'NONE',  ( -3.573655867282028392E-15, 2.428612866367529932E-14, 2.000000000000000000 ) ) ;
#162622 = CARTESIAN_POINT ( 'NONE',  ( -21.52544592524334988, -5.823673210054445271, 28.95942372801902209 ) ) ;
#162623 = CARTESIAN_POINT ( 'NONE',  ( -9.564922557960796823, -16.46253265017161027, 62.08224293864769550 ) ) ;
#162624 = CARTESIAN_POINT ( 'NONE',  ( 11.74264578624800315, -36.14014761921581709, -9.149999994537626691 ) ) ;
#162625 = CARTESIAN_POINT ( 'NONE',  ( 18.67979575497194134, -10.72451020669871369, 110.8344237280190043 ) ) ;
#162626 = CARTESIAN_POINT ( 'NONE',  ( 13.89961937509977652, -13.97604488694527269, 43.12390960531434558 ) ) ;
#162627 = CARTESIAN_POINT ( 'NONE',  ( 19.05341960407617918, -5.049401038297876454, 21.04275706135232582 ) ) ;
#162628 = CARTESIAN_POINT ( 'NONE',  ( 16.52544592524335698, 4.483927247898782831, 86.45942372801901854 ) ) ;
#162630 = CARTESIAN_POINT ( 'NONE',  ( 5.823673210054444382, -21.52544592524334988, 75.20942372801901854 ) ) ;
#162629 = CARTESIAN_POINT ( 'NONE',  ( -19.05341960407611168, -5.049401038298163336, 106.4572429386476955 ) ) ;
#162631 = CARTESIAN_POINT ( 'NONE',  ( 22.81625015709510151, -31.40387420917324590, -9.924999997268814766 ) ) ;
#162632 = CARTESIAN_POINT ( 'NONE',  ( 5.153800228976335163, 19.02544592524342804, 114.7905762719810241 ) ) ;
#162633 = CARTESIAN_POINT ( 'NONE',  ( 22.63886992172671597, -22.47454271797507985, -45.64921306006598201 ) ) ;
#162635 = CARTESIAN_POINT ( 'NONE',  ( 0.05219959533937995610, -21.53943276465977519, 65.00109039468568994 ) ) ;
#162634 = CARTESIAN_POINT ( 'NONE',  ( 8.224510206698742110, 14.34966873604972548, 62.08442372801901143 ) ) ;
#162636 = CARTESIAN_POINT ( 'NONE',  ( 21.53943276465977519, 0.05219959533937863772, 101.2510903946856757 ) ) ;
#162637 = AXIS2_PLACEMENT_3D ( 'NONE', #105215, #70898, #12238 ) ;
#162638 = LINE ( 'NONE', #159633, #37976 ) ;
#162639 = CARTESIAN_POINT ( 'NONE',  ( 16.52544592524335698, 4.483927247898782831, 41.45942372801901143 ) ) ;
#162640 = CARTESIAN_POINT ( 'NONE',  ( 16.51473224551069308, 9.474510206698969483, 89.16557627198103830 ) ) ;
#162641 = DIRECTION ( 'NONE',  ( -0.000000000000000000, -0.000000000000000000, 1.000000000000000000 ) ) ;
#162642 = ORIENTED_EDGE ( 'NONE', *, *, #191015, .F. ) ;
#162643 = DIRECTION ( 'NONE',  ( -0.000000000000000000, -0.000000000000000000, 1.000000000000000000 ) ) ;
#162644 = CARTESIAN_POINT ( 'NONE',  ( 13.97604488694527802, 13.89961937509977652, 44.37390960531435269 ) ) ;
#162645 = CARTESIAN_POINT ( 'NONE',  ( -18.67979575497178146, -10.72451020669898902, 36.66557627198103120 ) ) ;
#162646 = ORIENTED_EDGE ( 'NONE', *, *, #121993, .T. ) ;
#162647 = CARTESIAN_POINT ( 'NONE',  ( 12.14591786802327356, -12.06949235617739191, 110.6260903946857042 ) ) ;
#162649 = CARTESIAN_POINT ( 'NONE',  ( -5.049401038298153566, 19.05341960407611168, 85.20724293864766707 ) ) ;
#162648 = CARTESIAN_POINT ( 'NONE',  ( 8.314922557960818139, 14.29746914071049879, 84.58224293864769550 ) ) ;
#162650 = CARTESIAN_POINT ( 'NONE',  ( -5.719274019375665041, -21.55341960407619695, 109.7927570613523613 ) ) ;
#162651 = CARTESIAN_POINT ( 'NONE',  ( -12.14591786802326823, 12.06949235617739902, 23.12609039468567573 ) ) ;
#162652 = CARTESIAN_POINT ( 'NONE',  ( 14.29746914071049879, -8.314922557960816363, 83.33224293864769550 ) ) ;
#162653 = CARTESIAN_POINT ( 'NONE',  ( -18.62759615963255300, -10.81492255796106328, 39.16775706135235424 ) ) ;
#162654 = CARTESIAN_POINT ( 'NONE',  ( 18.67979575497178502, 10.72451020669898547, 84.16557627198103830 ) ) ;
#162655 = CARTESIAN_POINT ( 'NONE',  ( -19.03943276465977164, -0.05219959533935918106, 53.75109039468566863 ) ) ;
#162656 = CARTESIAN_POINT ( 'NONE',  ( -34.67490207739297148, 3.335485537672764345, 51.73549893453299120 ) ) ;
#162657 = CARTESIAN_POINT ( 'NONE',  ( -19.05341960407611168, -5.049401038298163336, 96.45724293864769550 ) ) ;
#162658 = CARTESIAN_POINT ( 'NONE',  ( -14.29746914071049879, 8.314922557960819915, 60.83224293864769550 ) ) ;
#162659 = CARTESIAN_POINT ( 'NONE',  ( 12.14591786802309770, 12.06949235617756955, 54.37390960531435979 ) ) ;
#162660 = CARTESIAN_POINT ( 'NONE',  ( -12.14591786802309592, -12.06949235617757132, 31.87390960531435979 ) ) ;
#162661 = CARTESIAN_POINT ( 'NONE',  ( -5.153800228976607833, 19.02544592524334988, 82.70942372801897591 ) ) ;
#162662 = CARTESIAN_POINT ( 'NONE',  ( 17.97394159160245408, -5.500000000000022204, 101.0122743667617442 ) ) ;
#162663 = CARTESIAN_POINT ( 'NONE',  ( 9.564922557960805705, 16.46253265017160317, 114.5822429386476955 ) ) ;
#162664 = CARTESIAN_POINT ( 'NONE',  ( -0.05219959533910754901, -16.53943276465976808, 87.49890960531436690 ) ) ;
#162665 = FACE_OUTER_BOUND ( 'NONE', #37826, .T. ) ;
#162667 = CARTESIAN_POINT ( 'NONE',  ( 15.72974639402199770, -15.80617190586745480, 43.12390960531435269 ) ) ;
#162666 = CARTESIAN_POINT ( 'NONE',  ( -9.474510206698964154, 16.51473224551069663, 50.41557627198102409 ) ) ;
#162668 = CARTESIAN_POINT ( 'NONE',  ( 0.05219959533909260263, 19.03943276465977164, 29.99890960531435979 ) ) ;
#162670 = CARTESIAN_POINT ( 'NONE',  ( 13.89961937509977652, -13.97604488694527269, 58.12390960531436690 ) ) ;
#162669 = CARTESIAN_POINT ( 'NONE',  ( -8.314922557961024197, 14.29746914071037800, 82.91775706135234714 ) ) ;
#162671 = CARTESIAN_POINT ( 'NONE',  ( 13.97604488694548053, -13.89961937509957401, 40.62609039468564731 ) ) ;
#162672 = CARTESIAN_POINT ( 'NONE',  ( 0.05219959533937995610, -21.53943276465977519, 65.00109039468568994 ) ) ;
#162673 = CARTESIAN_POINT ( 'NONE',  ( 21.55341960407610458, 5.719274019375980345, 33.95724293864769550 ) ) ;
#162674 = CARTESIAN_POINT ( 'NONE',  ( 16.53943276465976808, -0.05219959533910856209, 103.7489096053143669 ) ) ;
#162675 = EDGE_CURVE ( 'NONE', #188321, #8281, #17306, .T. ) ;
#162676 = CARTESIAN_POINT ( 'NONE',  ( 5.049401038297881783, 19.05341960407617563, 97.29275706135233293 ) ) ;
#162677 = CARTESIAN_POINT ( 'NONE',  ( 11.40812507854754365, 35.11059874428196537, -1.724999997268813479 ) ) ;
#162679 = CARTESIAN_POINT ( 'NONE',  ( 5.719274019375991003, -21.55341960407610458, 52.70724293864769550 ) ) ;
#162678 = CARTESIAN_POINT ( 'NONE',  ( 17.50000000000001066, 3.307050604927454618, 37.42089634664176856 ) ) ;
#162680 = CARTESIAN_POINT ( 'NONE',  ( -0.05219959533909027116, -19.03943276465977164, 22.49890960531436690 ) ) ;
#162681 = CARTESIAN_POINT ( 'NONE',  ( -21.53943276465977519, -0.05219959533937600094, 83.75109039468568994 ) ) ;
#162682 = CARTESIAN_POINT ( 'NONE',  ( -12.06949235617756955, 12.14591786802309770, 45.62390960531436690 ) ) ;
#162684 = CARTESIAN_POINT ( 'NONE',  ( 8.314922557960818139, 14.29746914071049879, 59.58224293864770260 ) ) ;
#162683 = CARTESIAN_POINT ( 'NONE',  ( -4.379528057220086978, -16.55341960407618274, 64.79275706135234714 ) ) ;
#162685 = CARTESIAN_POINT ( 'NONE',  ( -5.823673210054116645, -21.52544592524344225, 87.29057627198103830 ) ) ;
#162686 = CARTESIAN_POINT ( 'NONE',  ( -10.81492255796078084, -18.62759615963271287, 72.08224293864769550 ) ) ;
#162687 = LINE ( 'NONE', #115183, #107943 ) ;
#162688 = CARTESIAN_POINT ( 'NONE',  ( -16.46253265017160317, 9.564922557960807481, 110.8322429386476955 ) ) ;
#162689 = CARTESIAN_POINT ( 'NONE',  ( 9.474510206698971260, -16.51473224551069308, 57.91557627198103120 ) ) ;
#162690 = CARTESIAN_POINT ( 'NONE',  ( 0.05219959533909260263, 19.03943276465977164, 29.99890960531435979 ) ) ;
#162691 =( LENGTH_UNIT ( ) NAMED_UNIT ( * ) SI_UNIT ( .MILLI., .METRE. ) );
#162692 = CARTESIAN_POINT ( 'NONE',  ( -2.500000000000000000, -165.0000000000000000, 12.00000000000000355 ) ) ;
#162693 = EDGE_LOOP ( 'NONE', ( #197302, #167080, #48705, #110965 ) ) ;
#162694 = CARTESIAN_POINT ( 'NONE',  ( 8.224510206698742110, 14.34966873604972548, 87.08442372801901854 ) ) ;
#162695 = CARTESIAN_POINT ( 'NONE',  ( -21.52544592524334988, -5.823673210054445271, 23.95942372801901143 ) ) ;
#162696 = CARTESIAN_POINT ( 'NONE',  ( -19.02544592524342804, 5.153800228976336051, 76.04057627198102409 ) ) ;
#162697 = CARTESIAN_POINT ( 'NONE',  ( -21.52544592524334988, -5.823673210054445271, 58.95942372801902565 ) ) ;
#162698 = ADVANCED_FACE ( 'NONE', ( #127 ), #124474, .F. ) ;
#162699 = CARTESIAN_POINT ( 'NONE',  ( -19.05341960407611168, -5.049401038298163336, 106.4572429386476955 ) ) ;
#162700 = CARTESIAN_POINT ( 'NONE',  ( -22.60381889853074711, -32.71308136366489094, -20.00853410803858523 ) ) ;
#162701 = ORIENTED_EDGE ( 'NONE', *, *, #599, .T. ) ;
#162702 = CARTESIAN_POINT ( 'NONE',  ( 10.81492255796106328, -18.62759615963255655, 45.41775706135234003 ) ) ;
#162704 = CARTESIAN_POINT ( 'NONE',  ( 19.05341960407611168, 5.049401038298154454, 108.9572429386477097 ) ) ;
#162703 = CARTESIAN_POINT ( 'NONE',  ( -5.049401038298153566, 19.05341960407611168, 115.2072429386477097 ) ) ;
#162705 = CARTESIAN_POINT ( 'NONE',  ( -9.474510206698720793, -16.51473224551083518, 59.58442372801900433 ) ) ;
#162706 = CARTESIAN_POINT ( 'NONE',  ( 5.823673210054444382, -21.52544592524334988, 20.20942372801900788 ) ) ;
#162707 = CARTESIAN_POINT ( 'NONE',  ( 19.03943276465977164, 0.05219959533936151252, 46.25109039468566863 ) ) ;
#162708 = CARTESIAN_POINT ( 'NONE',  ( 9.564922557961047289, -16.46253265017146816, 55.41775706135234003 ) ) ;
#162710 = ORIENTED_EDGE ( 'NONE', *, *, #129082, .T. ) ;
#162709 = CARTESIAN_POINT ( 'NONE',  ( 0.05219959533934541429, -16.53943276465976808, 100.0010903946857042 ) ) ;
#162711 = CARTESIAN_POINT ( 'NONE',  ( 10.52174046232667060, 12.24387616833794468, -61.59812483265029925 ) ) ;
#162712 = CARTESIAN_POINT ( 'NONE',  ( -13.89961937509977652, 13.97604488694528158, 75.62390960531438111 ) ) ;
#162713 = CARTESIAN_POINT ( 'NONE',  ( -10.81492255796105439, 18.62759615963255655, 82.91775706135234714 ) ) ;
#162714 = CARTESIAN_POINT ( 'NONE',  ( -10.81492255796105439, 18.62759615963255655, 87.91775706135234714 ) ) ;
#162715 = CARTESIAN_POINT ( 'NONE',  ( 21.53159096656794347, -0.8285391498303859015, -56.30101842015765357 ) ) ;
#162716 = CARTESIAN_POINT ( 'NONE',  ( 5.049401038298161559, -19.05341960407611168, 97.70724293864766707 ) ) ;
#162717 = CARTESIAN_POINT ( 'NONE',  ( 21.52544592524334988, 5.823673210054432836, 81.45942372801900433 ) ) ;
#162718 = CARTESIAN_POINT ( 'NONE',  ( 9.564922557961047289, -16.46253265017146816, 110.4177570613523471 ) ) ;
#162719 = CARTESIAN_POINT ( 'NONE',  ( 9.564922557960805705, 16.46253265017160317, 74.58224293864769550 ) ) ;
#162720 = CARTESIAN_POINT ( 'NONE',  ( -19.05341960407611168, -5.049401038298163336, 106.4572429386476955 ) ) ;
#162721 = CIRCLE ( 'NONE', #130361, 30.82560697742735556 ) ;
#162722 = CARTESIAN_POINT ( 'NONE',  ( -16.51473224551069308, -9.474510206698971260, 91.66557627198103830 ) ) ;
#162723 = CARTESIAN_POINT ( 'NONE',  ( -18.22780087662122028, 5.500000000000031086, 88.51540105326107266 ) ) ;
#162724 = CARTESIAN_POINT ( 'NONE',  ( -13.97604488694527625, -13.89961937509977652, 81.87390960531436690 ) ) ;
#162725 = CARTESIAN_POINT ( 'NONE',  ( -5.153800228976328057, -19.02544592524343514, 62.29057627198100988 ) ) ;
#162726 = CARTESIAN_POINT ( 'NONE',  ( -5.719274019375665041, -21.55341960407619695, 19.79275706135235069 ) ) ;
#162727 = CARTESIAN_POINT ( 'NONE',  ( -14.29746914071037622, -8.314922557961029526, 94.16775706135237556 ) ) ;
#162728 = CARTESIAN_POINT ( 'NONE',  ( -3.181980515339492221, -6.791538853603052317, 1.110912703473986074 ) ) ;
#162729 = CARTESIAN_POINT ( 'NONE',  ( 9.474510206698729675, 16.51473224551082808, 52.08442372801900433 ) ) ;
#162730 = CARTESIAN_POINT ( 'NONE',  ( 19.02544592524343514, -5.153800228976328945, 98.54057627198100988 ) ) ;
#162731 = CARTESIAN_POINT ( 'NONE',  ( 8.224510206698953496, -14.34966873604960469, 87.91557627198103830 ) ) ;
#162732 = CARTESIAN_POINT ( 'NONE',  ( -15.72974639402197994, 15.80617190586746368, 35.62390960531437401 ) ) ;
#162733 = CARTESIAN_POINT ( 'NONE',  ( -0.05219959533907301413, -21.53943276465977519, 22.49890960531436335 ) ) ;
#162734 = CARTESIAN_POINT ( 'NONE',  ( 12.06949235617757843, -12.14591786802309237, 98.12390960531436690 ) ) ;
#162735 = CARTESIAN_POINT ( 'NONE',  ( -3.735172737399431091E-16, -6.100000000000006750, -62.50719930893269805 ) ) ;
#162736 = CARTESIAN_POINT ( 'NONE',  ( 13.97604488694548053, -13.89961937509957401, 50.62609039468566152 ) ) ;
#162737 = CARTESIAN_POINT ( 'NONE',  ( -16.55341960407617563, 4.379528057220093196, 103.5427570613523613 ) ) ;
#162738 = CARTESIAN_POINT ( 'NONE',  ( 5.153800228976335163, 19.02544592524342804, 94.79057627198103830 ) ) ;
#162739 = CARTESIAN_POINT ( 'NONE',  ( 18.62759615963255655, 10.81492255796105972, 66.66775706135234714 ) ) ;
#162740 = CARTESIAN_POINT ( 'NONE',  ( -18.62759615963270932, 10.81492255796079327, 60.83224293864769550 ) ) ;
#162741 = CARTESIAN_POINT ( 'NONE',  ( 5.823673210054444382, -21.52544592524334988, 30.20942372801902565 ) ) ;
#162742 = CARTESIAN_POINT ( 'NONE',  ( 5.823673210054125526, 21.52544592524343514, 84.79057627198102409 ) ) ;
#162743 = CARTESIAN_POINT ( 'NONE',  ( 4.379528057220339221, -16.55341960407611168, 112.7072429386476955 ) ) ;
#162744 = CARTESIAN_POINT ( 'NONE',  ( 16.46253265017146816, 9.564922557961045513, 66.66775706135233293 ) ) ;
#162745 = CARTESIAN_POINT ( 'NONE',  ( -16.51473224551069308, -9.474510206698971260, 41.66557627198103120 ) ) ;
#162746 = CARTESIAN_POINT ( 'NONE',  ( 13.97604488694527802, 13.89961937509977652, 94.37390960531436690 ) ) ;
#162747 = CARTESIAN_POINT ( 'NONE',  ( 0.05219959533909260263, 19.03943276465977164, 89.99890960531436690 ) ) ;
#162748 = CARTESIAN_POINT ( 'NONE',  ( 13.97604488694527802, 13.89961937509977652, 24.37390960531435624 ) ) ;
#162749 = CARTESIAN_POINT ( 'NONE',  ( 16.53943276465976808, -0.05219959533910856209, 38.74890960531435979 ) ) ;
#162750 = CARTESIAN_POINT ( 'NONE',  ( -12.06949235617739369, -12.14591786802326823, 44.37609039468567573 ) ) ;
#162751 = CARTESIAN_POINT ( 'NONE',  ( 18.62759615963255655, 10.81492255796105972, 111.6677570613523613 ) ) ;
#162753 = CARTESIAN_POINT ( 'NONE',  ( 14.29746914071037800, 8.314922557961029526, 111.6677570613523613 ) ) ;
#162752 = CARTESIAN_POINT ( 'NONE',  ( -9.474510206698964154, 16.51473224551069663, 115.4155762719810241 ) ) ;
#162754 = CARTESIAN_POINT ( 'NONE',  ( -18.67979575497193778, 10.72451020669871902, 28.33442372801902209 ) ) ;
#162755 = CARTESIAN_POINT ( 'NONE',  ( -13.89961937509977652, 13.97604488694528158, 110.6239096053143243 ) ) ;
#162756 = CARTESIAN_POINT ( 'NONE',  ( -14.34966873604972548, 8.224510206698743886, 113.3344237280190328 ) ) ;
#162757 = CARTESIAN_POINT ( 'NONE',  ( -16.55341960407617563, 4.379528057220093196, 98.54275706135234714 ) ) ;
#162758 = CARTESIAN_POINT ( 'NONE',  ( 14.34966873604972726, -8.224510206698740333, 25.83442372801901499 ) ) ;
#162759 = CARTESIAN_POINT ( 'NONE',  ( -19.02544592524342804, 5.153800228976336051, 46.04057627198101699 ) ) ;
#162760 = CARTESIAN_POINT ( 'NONE',  ( -12.14591786802309592, -12.06949235617757132, 106.8739096053143811 ) ) ;
#162761 = CARTESIAN_POINT ( 'NONE',  ( 15.80617190586769283, -15.72974639402175789, 25.62609039468567929 ) ) ;
#162762 = CARTESIAN_POINT ( 'NONE',  ( -16.51473224551069308, -9.474510206698971260, 36.66557627198102409 ) ) ;
#162763 = CARTESIAN_POINT ( 'NONE',  ( -19.02544592524342804, 5.153800228976336051, 106.0405762719810241 ) ) ;
#162764 = CARTESIAN_POINT ( 'NONE',  ( 5.049401038298161559, -19.05341960407611168, 32.70724293864768129 ) ) ;
#162765 = CARTESIAN_POINT ( 'NONE',  ( -9.474510206698964154, 16.51473224551069663, 110.4155762719810383 ) ) ;
#162766 = AXIS2_PLACEMENT_3D ( 'NONE', #65384, #112877, #66381 ) ;
#162767 = DIRECTION ( 'NONE',  ( 1.000000000000000000, 0.000000000000000000, 0.000000000000000000 ) ) ;
#162768 = CARTESIAN_POINT ( 'NONE',  ( 13.89961937509977652, -13.97604488694527269, 103.1239096053143527 ) ) ;
#162770 = CARTESIAN_POINT ( 'NONE',  ( -14.34966873604960291, -8.224510206698953496, 96.66557627198102409 ) ) ;
#162769 = CARTESIAN_POINT ( 'NONE',  ( -5.823673210054431948, 21.52544592524334988, 47.70942372801902565 ) ) ;
#162771 = CARTESIAN_POINT ( 'NONE',  ( 9.564922557960805705, 16.46253265017160317, 99.58224293864770971 ) ) ;
#162772 = CARTESIAN_POINT ( 'NONE',  ( -26.82869043059639225, -7.693057566823084947, 166.5358880480777941 ) ) ;
#162773 = PRESENTATION_LAYER_ASSIGNMENT (  '', '', ( #166125 ) ) ;
#162774 = CARTESIAN_POINT ( 'NONE',  ( -4.379528057220086978, -16.55341960407618274, 69.79275706135234714 ) ) ;
#162775 = CARTESIAN_POINT ( 'NONE',  ( 10.72451020669871369, 18.67979575497193778, 82.08442372801901854 ) ) ;
#162776 = CARTESIAN_POINT ( 'NONE',  ( -14.29746914071037622, -8.314922557961029526, 39.16775706135235424 ) ) ;
#162777 = CARTESIAN_POINT ( 'NONE',  ( 5.153800228976335163, 19.02544592524342804, 79.79057627198102409 ) ) ;
#162778 = CARTESIAN_POINT ( 'NONE',  ( -16.52544592524335698, -4.483927247898792601, 18.95942372801901143 ) ) ;
#162779 = CARTESIAN_POINT ( 'NONE',  ( 4.483927247898790824, -16.52544592524335698, 85.20942372801901854 ) ) ;
#162780 = CARTESIAN_POINT ( 'NONE',  ( -19.02544592524334988, -5.153800228976617603, 98.95942372801900433 ) ) ;
#162781 = CARTESIAN_POINT ( 'NONE',  ( -5.049401038298153566, 19.05341960407611168, 65.20724293864765286 ) ) ;
#162782 = CARTESIAN_POINT ( 'NONE',  ( 18.62759615963271287, -10.81492255796078972, 78.33224293864770971 ) ) ;
#162784 = CARTESIAN_POINT ( 'NONE',  ( -5.049401038297874678, -19.05341960407617918, 94.79275706135230450 ) ) ;
#162783 = CARTESIAN_POINT ( 'NONE',  ( 14.29746914071049879, -8.314922557960816363, 83.33224293864769550 ) ) ;
#162785 = CARTESIAN_POINT ( 'NONE',  ( -8.224510206698735004, -14.34966873604973081, 54.58442372801901143 ) ) ;
#162786 = CARTESIAN_POINT ( 'NONE',  ( -19.52837319214028611, 5.499999999999900524, 79.60471352585538796 ) ) ;
#162787 = CARTESIAN_POINT ( 'NONE',  ( -19.03943276465977164, -0.05219959533935918106, 58.75109039468566863 ) ) ;
#162788 = CARTESIAN_POINT ( 'NONE',  ( 14.34966873604960469, 8.224510206698951720, 29.16557627198103120 ) ) ;
#162789 = CARTESIAN_POINT ( 'NONE',  ( -16.52544592524342804, 4.483927247898546575, 86.04057627198102409 ) ) ;
#162791 = CARTESIAN_POINT ( 'NONE',  ( -17.49999999999999289, 5.624438216177559902, 40.81670344914644488 ) ) ;
#162790 = CARTESIAN_POINT ( 'NONE',  ( 10.72451020669871369, 18.67979575497193778, 112.0844237280190185 ) ) ;
#162792 = CARTESIAN_POINT ( 'NONE',  ( -21.52544592524334988, -5.823673210054445271, 23.95942372801901143 ) ) ;
#162793 = CARTESIAN_POINT ( 'NONE',  ( -5.153800228976328057, -19.02544592524343514, 112.2905762719810099 ) ) ;
#162794 = CARTESIAN_POINT ( 'NONE',  ( -19.05341960407611168, -5.049401038298163336, 81.45724293864769550 ) ) ;
#162795 = CARTESIAN_POINT ( 'NONE',  ( -15.80617190586768217, 15.72974639402176855, 93.12609039468568994 ) ) ;
#162796 = CARTESIAN_POINT ( 'NONE',  ( 19.03943276465977164, -0.05219959533909143690, 78.74890960531436690 ) ) ;
#162797 = CARTESIAN_POINT ( 'NONE',  ( 18.67979575497178502, 10.72451020669898547, 44.16557627198103120 ) ) ;
#162798 = CARTESIAN_POINT ( 'NONE',  ( 0.05219959533910956823, 16.53943276465976808, 79.99890960531435269 ) ) ;
#162799 = CARTESIAN_POINT ( 'NONE',  ( 16.51473224551069308, 9.474510206698969483, 54.16557627198103120 ) ) ;
#162800 = CARTESIAN_POINT ( 'NONE',  ( -9.564922557960796823, -16.46253265017161027, 22.08224293864768839 ) ) ;
#162801 = CARTESIAN_POINT ( 'NONE',  ( 18.62759615963255655, 10.81492255796105972, 21.66775706135235069 ) ) ;
#162802 = CARTESIAN_POINT ( 'NONE',  ( -21.55341960407619339, 5.719274019375674811, 68.54275706135234714 ) ) ;
#162803 = CARTESIAN_POINT ( 'NONE',  ( 13.97604488694527802, 13.89961937509977652, 39.37390960531435269 ) ) ;
#162804 = CARTESIAN_POINT ( 'NONE',  ( -8.314922557961024197, 14.29746914071037800, 67.91775706135234714 ) ) ;
#162805 = CARTESIAN_POINT ( 'NONE',  ( 18.62759615963271287, -10.81492255796078972, 113.3322429386476955 ) ) ;
#162806 = CARTESIAN_POINT ( 'NONE',  ( -21.52544592524343514, 5.823673210054127303, 111.0405762719810525 ) ) ;
#162808 = CARTESIAN_POINT ( 'NONE',  ( -19.02544592524342804, 5.153800228976336051, 71.04057627198099567 ) ) ;
#162807 = CARTESIAN_POINT ( 'NONE',  ( -19.05341960407617563, 5.049401038297882671, 33.54275706135231871 ) ) ;
#162809 = CYLINDRICAL_SURFACE ( 'NONE', #50644, 9.100000000000001421 ) ;
#162810 = CARTESIAN_POINT ( 'NONE',  ( -0.05219959533937732626, 21.53943276465977519, 67.50109039468568994 ) ) ;
#162811 = CARTESIAN_POINT ( 'NONE',  ( -15.80617190586745835, -15.72974639402198527, 61.87390960531436690 ) ) ;
#162812 = CARTESIAN_POINT ( 'NONE',  ( -14.29746914071049879, 8.314922557960819915, 40.83224293864769550 ) ) ;
#162814 = CARTESIAN_POINT ( 'NONE',  ( 10.81492255796106328, -18.62759615963255655, 105.4177570613523613 ) ) ;
#162813 = CARTESIAN_POINT ( 'NONE',  ( -18.67979575497193778, 10.72451020669871902, 73.33442372801901854 ) ) ;
#162815 = CARTESIAN_POINT ( 'NONE',  ( 4.483927247898545687, 16.52544592524342804, 59.79057627198103120 ) ) ;
#162816 = CARTESIAN_POINT ( 'NONE',  ( 14.34966873604960469, 8.224510206698951720, 104.1655762719810241 ) ) ;
#162817 = CARTESIAN_POINT ( 'NONE',  ( 0.05219959533936267826, -19.03943276465977164, 60.00109039468566863 ) ) ;
#162818 = CARTESIAN_POINT ( 'NONE',  ( -12.14591786802309592, -12.06949235617757132, 26.87390960531435979 ) ) ;
#162819 = CARTESIAN_POINT ( 'NONE',  ( -21.55341960407619339, 5.719274019375674811, 68.54275706135234714 ) ) ;
#162820 = CARTESIAN_POINT ( 'NONE',  ( 13.89961937509977652, -13.97604488694527269, 68.12390960531436690 ) ) ;
#162821 = CARTESIAN_POINT ( 'NONE',  ( 19.02544592524334988, 5.153800228976608722, 36.45942372801900433 ) ) ;
#162822 = CARTESIAN_POINT ( 'NONE',  ( 21.53943276465977519, -0.05219959533907433946, 38.74890960531435979 ) ) ;
#162823 = CARTESIAN_POINT ( 'NONE',  ( 0.05219959533937995610, -21.53943276465977519, 40.00109039468567573 ) ) ;
#162824 = CARTESIAN_POINT ( 'NONE',  ( 21.55341960407610458, 5.719274019375980345, 98.95724293864770971 ) ) ;
#162825 = CARTESIAN_POINT ( 'NONE',  ( -19.05341960407617563, 5.049401038297882671, 103.5427570613523329 ) ) ;
#162826 = CARTESIAN_POINT ( 'NONE',  ( -0.05219959533934338120, 16.53943276465976808, 57.50109039468568994 ) ) ;
#162828 = CARTESIAN_POINT ( 'NONE',  ( 21.52544592524344225, -5.823673210054117533, 93.54057627198103830 ) ) ;
#162827 = FACE_OUTER_BOUND ( 'NONE', #175640, .T. ) ;
#162829 = CARTESIAN_POINT ( 'NONE',  ( 14.29746914071049879, -8.314922557960816363, 88.33224293864769550 ) ) ;
#162830 = CARTESIAN_POINT ( 'NONE',  ( -20.96320343559624177, 21.46320343559661126, 5.353553390593267736 ) ) ;
#162831 = CARTESIAN_POINT ( 'NONE',  ( -0.05219959533936034679, 19.03943276465977164, 112.5010903946856757 ) ) ;
#162832 = CARTESIAN_POINT ( 'NONE',  ( 18.67979575497178502, 10.72451020669898547, 54.16557627198103120 ) ) ;
#162833 = CARTESIAN_POINT ( 'NONE',  ( 8.314922557961029526, -14.29746914071037800, 95.41775706135234714 ) ) ;
#162834 = CARTESIAN_POINT ( 'NONE',  ( 26.98314665059723083, -25.22428982341646275, -8.000000000000003553 ) ) ;
#162835 = CARTESIAN_POINT ( 'NONE',  ( -14.34966873604972548, 8.224510206698743886, 48.33442372801902565 ) ) ;
#162836 = VECTOR ( 'NONE', #82502, 1000.000000000000000 ) ;
#162837 = CARTESIAN_POINT ( 'NONE',  ( 21.52544592524334988, 5.823673210054432836, 21.45942372801901499 ) ) ;
#162838 = CARTESIAN_POINT ( 'NONE',  ( -0.05219959533907301413, -21.53943276465977519, 42.49890960531435979 ) ) ;
#162839 = CARTESIAN_POINT ( 'NONE',  ( 16.53943276465976808, 0.05219959533934440121, 81.25109039468568994 ) ) ;
#162840 = CARTESIAN_POINT ( 'NONE',  ( 19.03943276465977164, -0.05219959533909143690, 103.7489096053143669 ) ) ;
#162841 = CARTESIAN_POINT ( 'NONE',  ( 21.53943276465977519, 0.05219959533937863772, 71.25109039468568994 ) ) ;
#162842 = EDGE_CURVE ( 'NONE', #168486, #122419, #82802, .T. ) ;
#162843 = CARTESIAN_POINT ( 'NONE',  ( 21.55341960407610458, 5.719274019375980345, 33.95724293864769550 ) ) ;
#162844 = CARTESIAN_POINT ( 'NONE',  ( -15.80617190586745835, -15.72974639402198527, 26.87390960531435979 ) ) ;
#162845 = ORIENTED_EDGE ( 'NONE', *, *, #48174, .T. ) ;
#162846 = CARTESIAN_POINT ( 'NONE',  ( 16.51473224551083163, -9.474510206698727899, 45.83442372801900433 ) ) ;
#162847 = CARTESIAN_POINT ( 'NONE',  ( -0.05219959533934338120, 16.53943276465976808, 67.50109039468568994 ) ) ;
#162848 = CARTESIAN_POINT ( 'NONE',  ( -18.67979575497178146, -10.72451020669898902, 31.66557627198102054 ) ) ;
#162849 = ORIENTED_EDGE ( 'NONE', *, *, #41288, .T. ) ;
#162850 = CARTESIAN_POINT ( 'NONE',  ( -9.474510206698964154, 16.51473224551069663, 80.41557627198103830 ) ) ;
#162851 = CARTESIAN_POINT ( 'NONE',  ( 16.52544592524335698, 4.483927247898782831, 111.4594237280190328 ) ) ;
#162852 = CARTESIAN_POINT ( 'NONE',  ( 2.802625768539491968, -39.09149893265183806, -33.00000000000000000 ) ) ;
#162853 = CARTESIAN_POINT ( 'NONE',  ( 16.52544592524342804, -4.483927247898539470, 108.5405762719810241 ) ) ;
#162854 = CARTESIAN_POINT ( 'NONE',  ( -18.67979575497178146, -10.72451020669898902, 46.66557627198102409 ) ) ;
#162855 = CARTESIAN_POINT ( 'NONE',  ( 13.97604488694527802, 13.89961937509977652, 44.37390960531435269 ) ) ;
#162856 = CARTESIAN_POINT ( 'NONE',  ( 16.52544592524335698, 4.483927247898782831, 81.45942372801900433 ) ) ;
#162857 = CARTESIAN_POINT ( 'NONE',  ( 10.72451020669871369, 18.67979575497193778, 32.08442372801901854 ) ) ;
#162858 = CARTESIAN_POINT ( 'NONE',  ( 19.05341960407617918, -5.049401038297876454, 86.04275706135233293 ) ) ;
#162859 = CARTESIAN_POINT ( 'NONE',  ( -8.224510206698948167, 14.34966873604960824, 95.41557627198102409 ) ) ;
#162860 = CARTESIAN_POINT ( 'NONE',  ( 19.03943276465977164, -0.05219959533909143690, 53.74890960531436690 ) ) ;
#162861 = CARTESIAN_POINT ( 'NONE',  ( 16.51473224551069308, 9.474510206698969483, 24.16557627198102765 ) ) ;
#162862 = CARTESIAN_POINT ( 'NONE',  ( 0.05219959533937995610, -21.53943276465977519, 110.0010903946856757 ) ) ;
#162863 = CARTESIAN_POINT ( 'NONE',  ( -5.049401038298153566, 19.05341960407611168, 80.20724293864769550 ) ) ;
#162864 = CARTESIAN_POINT ( 'NONE',  ( 8.224510206698742110, 14.34966873604972548, 62.08442372801901143 ) ) ;
#162865 = CARTESIAN_POINT ( 'NONE',  ( -15.80617190586768217, 15.72974639402176855, 88.12609039468570415 ) ) ;
#162866 = CARTESIAN_POINT ( 'NONE',  ( 5.823673210054125526, 21.52544592524343514, 54.79057627198104541 ) ) ;
#162867 = CARTESIAN_POINT ( 'NONE',  ( -14.34966873604972548, 8.224510206698743886, 68.33442372801900433 ) ) ;
#162868 = CARTESIAN_POINT ( 'NONE',  ( 16.46253265017146816, 9.564922557961045513, 56.66775706135233293 ) ) ;
#162869 = CARTESIAN_POINT ( 'NONE',  ( -13.97604488694547697, 13.89961937509957934, 73.12609039468568994 ) ) ;
#162870 = EDGE_LOOP ( 'NONE', ( #142766, #160694, #8190, #105394 ) ) ;
#162871 = CARTESIAN_POINT ( 'NONE',  ( 21.53943276465977519, 0.05219959533937863772, 66.25109039468567573 ) ) ;
#162872 = CARTESIAN_POINT ( 'NONE',  ( 19.02544592524343514, -5.153800228976328945, 68.54057627198103830 ) ) ;
#162873 = CARTESIAN_POINT ( 'NONE',  ( -0.05219959533909027116, -19.03943276465977164, 57.49890960531435979 ) ) ;
#162874 = CARTESIAN_POINT ( 'NONE',  ( -19.02544592524334988, -5.153800228976617603, 63.95942372801899012 ) ) ;
#162875 = CARTESIAN_POINT ( 'NONE',  ( 16.51473224551069308, 9.474510206698969483, 114.1655762719810241 ) ) ;
#162876 = CARTESIAN_POINT ( 'NONE',  ( -9.564922557960796823, -16.46253265017161027, 82.08224293864768129 ) ) ;
#162877 = CARTESIAN_POINT ( 'NONE',  ( -12.14591786802309592, -12.06949235617757132, 36.87390960531435979 ) ) ;
#162878 = CARTESIAN_POINT ( 'NONE',  ( -18.67979575497178146, -10.72451020669898902, 46.66557627198102409 ) ) ;
#162879 = DIRECTION ( 'NONE',  ( 0.000000000000000000, 0.000000000000000000, -1.000000000000000000 ) ) ;
#162880 = CARTESIAN_POINT ( 'NONE',  ( -5.823673210054431948, 21.52544592524334988, 107.7094237280190328 ) ) ;
#162881 = CARTESIAN_POINT ( 'NONE',  ( -17.49999999999999645, -5.499999999999992895, 79.20309617465829888 ) ) ;
#162882 = CARTESIAN_POINT ( 'NONE',  ( 9.564922557960805705, 16.46253265017160317, 44.58224293864769550 ) ) ;
#162883 = CARTESIAN_POINT ( 'NONE',  ( -5.153800228976328057, -19.02544592524343514, 27.29057627198103120 ) ) ;
#162884 = CARTESIAN_POINT ( 'NONE',  ( -34.16298174666833631, -4.140866818352566092, 91.36220571553955949 ) ) ;
#162885 = CARTESIAN_POINT ( 'NONE',  ( -30.00000000000000355, -0.3535533905932755627, 4.646446609406720718 ) ) ;
#162886 = CARTESIAN_POINT ( 'NONE',  ( -12.14591786802326823, 12.06949235617739902, 58.12609039468568994 ) ) ;
#162887 = CARTESIAN_POINT ( 'NONE',  ( 15.72974639402199770, -15.80617190586745480, 78.12390960531436690 ) ) ;
#162888 = CARTESIAN_POINT ( 'NONE',  ( 0.05219959533910956823, 16.53943276465976808, 49.99890960531437401 ) ) ;
#162890 = CARTESIAN_POINT ( 'NONE',  ( -69.65682714487590488, -71.74905178543390605, -25.00000000000000000 ) ) ;
#162889 = CARTESIAN_POINT ( 'NONE',  ( 9.474510206698971260, -16.51473224551069308, 27.91557627198103120 ) ) ;
#162891 = CARTESIAN_POINT ( 'NONE',  ( 21.52544592524334988, 5.823673210054432836, 41.45942372801901143 ) ) ;
#162892 = CARTESIAN_POINT ( 'NONE',  ( 0.05219959533936267826, -19.03943276465977164, 45.00109039468566863 ) ) ;
#162893 = CARTESIAN_POINT ( 'NONE',  ( 13.97604488694527802, 13.89961937509977652, 29.37390960531435979 ) ) ;
#162894 = CARTESIAN_POINT ( 'NONE',  ( 5.823673210054444382, -21.52544592524334988, 75.20942372801901854 ) ) ;
#162895 = CARTESIAN_POINT ( 'NONE',  ( 16.38665767535053419, 7.295008042176124086, 97.23599135785455871 ) ) ;
#162896 = CARTESIAN_POINT ( 'NONE',  ( 14.34966873604960469, 8.224510206698951720, 44.16557627198103120 ) ) ;
#162897 = CARTESIAN_POINT ( 'NONE',  ( -36.91746825000000598, 2.428612866367529932E-14, -1.124999997268813390 ) ) ;
#162898 = CARTESIAN_POINT ( 'NONE',  ( 10.72451020669898902, -18.67979575497178502, 37.91557627198102409 ) ) ;
#162899 = CARTESIAN_POINT ( 'NONE',  ( 37.99999999999999289, 2.893978650043524126E-14, -8.749999994537628112 ) ) ;
#162900 = CARTESIAN_POINT ( 'NONE',  ( -9.474510206698964154, 16.51473224551069663, 90.41557627198103830 ) ) ;
#162901 = CARTESIAN_POINT ( 'NONE',  ( 14.34966873604960469, 8.224510206698951720, 84.16557627198103830 ) ) ;
#162902 = CARTESIAN_POINT ( 'NONE',  ( -12.06949235617739369, -12.14591786802326823, 24.37609039468567573 ) ) ;
#162903 = CARTESIAN_POINT ( 'NONE',  ( 21.53943276465977519, -0.05219959533907433946, 63.74890960531435979 ) ) ;
#162904 = ORIENTED_EDGE ( 'NONE', *, *, #80939, .T. ) ;
#162905 = CARTESIAN_POINT ( 'NONE',  ( 16.46253265017160672, -9.564922557960803928, 38.33224293864768839 ) ) ;
#162906 = AXIS2_PLACEMENT_3D ( 'NONE', #114274, #145619, #127456 ) ;
#162908 = CARTESIAN_POINT ( 'NONE',  ( 21.53943276465977519, -0.05219959533907433946, 83.74890960531435269 ) ) ;
#162907 = CARTESIAN_POINT ( 'NONE',  ( 13.97604488694527802, 13.89961937509977652, 89.37390960531436690 ) ) ;
#162910 = CARTESIAN_POINT ( 'NONE',  ( 16.51473224551069308, 9.474510206698969483, 99.16557627198102409 ) ) ;
#162909 = CARTESIAN_POINT ( 'NONE',  ( -4.483927247898782831, 16.52544592524335698, 112.7094237280190328 ) ) ;
#162911 = CARTESIAN_POINT ( 'NONE',  ( -9.564922557961040184, 16.46253265017147172, 82.91775706135233293 ) ) ;
#162912 = CARTESIAN_POINT ( 'NONE',  ( -21.55341960407619339, 5.719274019375674811, 103.5427570613523613 ) ) ;
#162913 = CARTESIAN_POINT ( 'NONE',  ( 5.823673210054125526, 21.52544592524343514, 74.79057627198105251 ) ) ;
#162914 = CARTESIAN_POINT ( 'NONE',  ( -21.52544592524343514, 5.823673210054127303, 36.04057627198102409 ) ) ;
#162915 = CARTESIAN_POINT ( 'NONE',  ( -16.46253265017160317, 9.564922557960807481, 55.83224293864769550 ) ) ;
#162916 = CARTESIAN_POINT ( 'NONE',  ( 16.53943276465976808, -0.05219959533910856209, 23.74890960531435269 ) ) ;
#162917 = CARTESIAN_POINT ( 'NONE',  ( 16.51473224551069308, 9.474510206698969483, 74.16557627198103830 ) ) ;
#162918 = CARTESIAN_POINT ( 'NONE',  ( -31.64921935833423561, -6.825000981063952921, 91.88079052344197351 ) ) ;
#162919 = CARTESIAN_POINT ( 'NONE',  ( 16.46253265017146816, 9.564922557961045513, 21.66775706135233648 ) ) ;
#162920 = CARTESIAN_POINT ( 'NONE',  ( 16.52544592524342804, -4.483927247898539470, 88.54057627198103830 ) ) ;
#162921 = AXIS2_PLACEMENT_3D ( 'NONE', #78633, #156481, #170662 ) ;
#162922 = CARTESIAN_POINT ( 'NONE',  ( 15.80617190586769283, -15.72974639402175789, 30.62609039468567929 ) ) ;
#162923 = CARTESIAN_POINT ( 'NONE',  ( 8.571926809382597767, 26.38167802310806209, 142.7750000027311899 ) ) ;
#162924 = CARTESIAN_POINT ( 'NONE',  ( -21.53943276465977519, 0.05219959533907696930, 71.24890960531435269 ) ) ;
#162925 = CARTESIAN_POINT ( 'NONE',  ( -14.34966873604972548, 8.224510206698743886, 88.33442372801901854 ) ) ;
#162926 = CARTESIAN_POINT ( 'NONE',  ( 12.06949235617757843, -12.14591786802309237, 113.1239096053143953 ) ) ;
#162927 = CARTESIAN_POINT ( 'NONE',  ( 9.564922557960805705, 16.46253265017160317, 74.58224293864769550 ) ) ;
#162928 = CARTESIAN_POINT ( 'NONE',  ( 18.22780087662123805, 5.499999999999960032, 91.48236817873106475 ) ) ;
#162929 = DIRECTION ( 'NONE',  ( 0.000000000000000000, 0.000000000000000000, -1.000000000000000000 ) ) ;
#162930 = CARTESIAN_POINT ( 'NONE',  ( -12.14591786802309592, -12.06949235617757132, 31.87390960531435979 ) ) ;
#162931 = CARTESIAN_POINT ( 'NONE',  ( 18.62759615963255655, 10.81492255796105972, 56.66775706135235424 ) ) ;
#162932 = CARTESIAN_POINT ( 'NONE',  ( 9.474510206698971260, -16.51473224551069308, 107.9155762719810383 ) ) ;
#162933 = CARTESIAN_POINT ( 'NONE',  ( -5.823673210054431948, 21.52544592524334988, 92.70942372801901854 ) ) ;
#162934 = CARTESIAN_POINT ( 'NONE',  ( 5.049401038298161559, -19.05341960407611168, 42.70724293864767418 ) ) ;
#162935 = CARTESIAN_POINT ( 'NONE',  ( 13.89961937509977652, -13.97604488694527269, 53.12390960531434558 ) ) ;
#162936 = ORIENTED_EDGE ( 'NONE', *, *, #50976, .T. ) ;
#162937 = CARTESIAN_POINT ( 'NONE',  ( 5.823673210054444382, -21.52544592524334988, 90.20942372801903275 ) ) ;
#162938 = CARTESIAN_POINT ( 'NONE',  ( -14.34966873604972548, 8.224510206698743886, 68.33442372801900433 ) ) ;
#162939 = CARTESIAN_POINT ( 'NONE',  ( 18.67979575497194134, -10.72451020669871369, 90.83442372801901854 ) ) ;
#162940 = CARTESIAN_POINT ( 'NONE',  ( -15.72974639402197994, 15.80617190586746368, 25.62390960531435624 ) ) ;
#162941 = CARTESIAN_POINT ( 'NONE',  ( -9.474510206698720793, -16.51473224551083518, 94.58442372801900433 ) ) ;
#162942 = CARTESIAN_POINT ( 'NONE',  ( 5.823673210054444382, -21.52544592524334988, 60.20942372801902565 ) ) ;
#162943 = CARTESIAN_POINT ( 'NONE',  ( 16.55341960407618274, -4.379528057220086978, 41.04275706135236135 ) ) ;
#162944 = CARTESIAN_POINT ( 'NONE',  ( -15.72974639402197994, 15.80617190586746368, 85.62390960531436690 ) ) ;
#162945 = CARTESIAN_POINT ( 'NONE',  ( -13.89961937509957401, -13.97604488694547875, 84.37609039468567573 ) ) ;
#162946 = CARTESIAN_POINT ( 'NONE',  ( -19.05341960407611168, -5.049401038298163336, 66.45724293864769550 ) ) ;
#162947 = CARTESIAN_POINT ( 'NONE',  ( 16.46253265017146816, 9.564922557961045513, 96.66775706135233293 ) ) ;
#162948 = VECTOR ( 'NONE', #116184, 1000.000000000000000 ) ;
#162949 = CARTESIAN_POINT ( 'NONE',  ( -13.89961937509957401, -13.97604488694547875, 94.37609039468566152 ) ) ;
#162950 = CARTESIAN_POINT ( 'NONE',  ( -8.224510206698948167, 14.34966873604960824, 55.41557627198102409 ) ) ;
#162951 = CARTESIAN_POINT ( 'NONE',  ( -16.51473224551082808, 9.474510206698731452, 78.33442372801900433 ) ) ;
#162952 = CARTESIAN_POINT ( 'NONE',  ( -16.52544592524335698, -4.483927247898792601, 63.95942372801901854 ) ) ;
#162953 = CARTESIAN_POINT ( 'NONE',  ( 13.89961937509957401, 13.97604488694547697, 41.87609039468566152 ) ) ;
#162954 = CARTESIAN_POINT ( 'NONE',  ( 0.05219959533909260263, 19.03943276465977164, 34.99890960531435979 ) ) ;
#162955 = CARTESIAN_POINT ( 'NONE',  ( 5.153800228976335163, 19.02544592524342804, 44.79057627198103830 ) ) ;
#162956 = CARTESIAN_POINT ( 'NONE',  ( 8.314922557961029526, -14.29746914071037800, 55.41775706135234714 ) ) ;
#162957 = CARTESIAN_POINT ( 'NONE',  ( 22.49873734152949112, 26.99873734152889782, 8.889087296526001936 ) ) ;
#162958 = CARTESIAN_POINT ( 'NONE',  ( 28.82186960331498327, 2.781578969918950771E-14, 139.2500000054623683 ) ) ;
#162959 = CARTESIAN_POINT ( 'NONE',  ( 13.89961937509977652, -13.97604488694527269, 103.1239096053143527 ) ) ;
#162960 = CARTESIAN_POINT ( 'NONE',  ( -0.05219959533909027116, -19.03943276465977164, 22.49890960531436690 ) ) ;
#162961 = ORIENTED_EDGE ( 'NONE', *, *, #184979, .T. ) ;
#162962 = CARTESIAN_POINT ( 'NONE',  ( 13.89961937509957401, 13.97604488694547697, 96.87609039468566152 ) ) ;
#162963 = CARTESIAN_POINT ( 'NONE',  ( 21.55341960407610458, 5.719274019375980345, 38.95724293864768839 ) ) ;
#162965 = CARTESIAN_POINT ( 'NONE',  ( -9.474510206698720793, -16.51473224551083518, 109.5844237280190043 ) ) ;
#162964 = CARTESIAN_POINT ( 'NONE',  ( 13.97604488694548053, -13.89961937509957401, 25.62609039468566507 ) ) ;
#162966 = CARTESIAN_POINT ( 'NONE',  ( -0.05219959533909027116, -19.03943276465977164, 32.49890960531435979 ) ) ;
#162967 = CARTESIAN_POINT ( 'NONE',  ( -9.474510206698964154, 16.51473224551069663, 50.41557627198102409 ) ) ;
#162968 = CARTESIAN_POINT ( 'NONE',  ( -18.67979575497178146, -10.72451020669898902, 66.66557627198102409 ) ) ;
#162969 = CARTESIAN_POINT ( 'NONE',  ( 13.97604488694527802, 13.89961937509977652, 104.3739096053143385 ) ) ;
#162970 = EDGE_CURVE ( 'NONE', #4163, #89587, #11869, .T. ) ;
#162971 = CARTESIAN_POINT ( 'NONE',  ( 13.97604488694527802, 13.89961937509977652, 34.37390960531436690 ) ) ;
#162972 = CARTESIAN_POINT ( 'NONE',  ( 8.571926809382597767, 26.38167802310806209, 144.7750000027311899 ) ) ;
#162973 = CARTESIAN_POINT ( 'NONE',  ( -13.89961937509957401, -13.97604488694547875, 89.37609039468563310 ) ) ;
#162974 = CARTESIAN_POINT ( 'NONE',  ( -14.34966873604960291, -8.224510206698953496, 56.66557627198103830 ) ) ;
#162975 = CARTESIAN_POINT ( 'NONE',  ( -10.81492255796078084, -18.62759615963271287, 37.08224293864768129 ) ) ;
#162976 = CARTESIAN_POINT ( 'NONE',  ( -21.55341960407619339, 5.719274019375674811, 108.5427570613523756 ) ) ;
#162977 = CARTESIAN_POINT ( 'NONE',  ( 18.67979575497178502, 10.72451020669898547, 94.16557627198103830 ) ) ;
#162978 = CARTESIAN_POINT ( 'NONE',  ( 18.67979575497194134, -10.72451020669871369, 65.83442372801900433 ) ) ;
#162979 = CARTESIAN_POINT ( 'NONE',  ( -5.719274019375665041, -21.55341960407619695, 79.79275706135236135 ) ) ;
#162980 = CARTESIAN_POINT ( 'NONE',  ( -16.51473224551069308, -9.474510206698971260, 106.6655762719810383 ) ) ;
#162982 = CARTESIAN_POINT ( 'NONE',  ( -15.80617190586768217, 15.72974639402176855, 58.12609039468568994 ) ) ;
#162981 = CARTESIAN_POINT ( 'NONE',  ( 14.29746914071037800, 8.314922557961029526, 106.6677570613523756 ) ) ;
#162983 = CARTESIAN_POINT ( 'NONE',  ( -5.153800228976328057, -19.02544592524343514, 62.29057627198100988 ) ) ;
#162984 = CARTESIAN_POINT ( 'NONE',  ( -9.564922557961040184, 16.46253265017147172, 37.91775706135233293 ) ) ;
#162985 = CARTESIAN_POINT ( 'NONE',  ( 10.72451020669871369, 18.67979575497193778, 32.08442372801901854 ) ) ;
#162986 = CARTESIAN_POINT ( 'NONE',  ( -5.153800228976328057, -19.02544592524343514, 72.29057627198102409 ) ) ;
#162987 = CARTESIAN_POINT ( 'NONE',  ( 12.14591786802309770, 12.06949235617756955, 84.37390960531438111 ) ) ;
#162988 = CARTESIAN_POINT ( 'NONE',  ( 16.52544592524342804, -4.483927247898539470, 43.54057627198103830 ) ) ;
#162989 = CARTESIAN_POINT ( 'NONE',  ( -21.52544592524343514, 5.823673210054127303, 51.04057627198103120 ) ) ;
#162990 = CARTESIAN_POINT ( 'NONE',  ( -5.153800228976328057, -19.02544592524343514, 62.29057627198100988 ) ) ;
#162991 = CARTESIAN_POINT ( 'NONE',  ( 5.823673210054125526, 21.52544592524343514, 74.79057627198105251 ) ) ;
#162992 = CARTESIAN_POINT ( 'NONE',  ( -0.05219959533936034679, 19.03943276465977164, 47.50109039468566863 ) ) ;
#162994 = CARTESIAN_POINT ( 'NONE',  ( -14.29746914071049879, 8.314922557960819915, 60.83224293864769550 ) ) ;
#162993 = CARTESIAN_POINT ( 'NONE',  ( -0.05219959533936034679, 19.03943276465977164, 22.50109039468566152 ) ) ;
#162995 = CARTESIAN_POINT ( 'NONE',  ( 0.05219959533907565091, 21.53943276465977519, 44.99890960531435979 ) ) ;
#162996 = ORIENTED_EDGE ( 'NONE', *, *, #72915, .F. ) ;
#162997 = FACE_OUTER_BOUND ( 'NONE', #127170, .T. ) ;
#162999 = CARTESIAN_POINT ( 'NONE',  ( -22.44159573604010305, 16.30477369853692338, 148.6750000027311671 ) ) ;
#162998 = CARTESIAN_POINT ( 'NONE',  ( 14.34966873604972726, -8.224510206698740333, 90.83442372801901854 ) ) ;
#163000 = CARTESIAN_POINT ( 'NONE',  ( -9.474510206698720793, -16.51473224551083518, 94.58442372801900433 ) ) ;
#163001 = CARTESIAN_POINT ( 'NONE',  ( -14.29746914071049879, 8.314922557960819915, 55.83224293864770260 ) ) ;
#163002 = CARTESIAN_POINT ( 'NONE',  ( 3.885274725274726393, -8.673617379884035472E-16, 0.000000000000000000 ) ) ;
#163003 = CARTESIAN_POINT ( 'NONE',  ( -9.474510206698964154, 16.51473224551069663, 45.41557627198103120 ) ) ;
#163004 = CARTESIAN_POINT ( 'NONE',  ( 4.483927247898545687, 16.52544592524342804, 34.79057627198103120 ) ) ;
#163005 = CARTESIAN_POINT ( 'NONE',  ( -5.153800228976328057, -19.02544592524343514, 92.29057627198099567 ) ) ;
#163006 = CARTESIAN_POINT ( 'NONE',  ( -19.05341960407611168, -5.049401038298163336, 56.45724293864768129 ) ) ;
#163007 = CARTESIAN_POINT ( 'NONE',  ( -21.52544592524334988, -5.823673210054445271, 63.95942372801901854 ) ) ;
#163008 = CARTESIAN_POINT ( 'NONE',  ( -13.89961937509977652, 13.97604488694528158, 75.62390960531438111 ) ) ;
#163009 = DIRECTION ( 'NONE',  ( 1.000000000000000000, -0.000000000000000000, -0.000000000000000000 ) ) ;
#163010 = CARTESIAN_POINT ( 'NONE',  ( -16.46253265017160317, 9.564922557960807481, 70.83224293864770971 ) ) ;
#163011 = CARTESIAN_POINT ( 'NONE',  ( -18.62759615963270932, 10.81492255796079327, 55.83224293864770260 ) ) ;
#163012 = CARTESIAN_POINT ( 'NONE',  ( -16.46253265017160317, 9.564922557960807481, 40.83224293864769550 ) ) ;
#163013 = CARTESIAN_POINT ( 'NONE',  ( 0.05219959533907565091, 21.53943276465977519, 39.99890960531436690 ) ) ;
#163014 = CARTESIAN_POINT ( 'NONE',  ( 0.05219959533934541429, -16.53943276465976808, 110.0010903946856757 ) ) ;
#163015 = CARTESIAN_POINT ( 'NONE',  ( -13.89961937509957401, -13.97604488694547875, 19.37609039468566507 ) ) ;
#163017 = CARTESIAN_POINT ( 'NONE',  ( 12.06949235617739724, 12.14591786802326823, 76.87609039468567573 ) ) ;
#163016 = CARTESIAN_POINT ( 'NONE',  ( -16.52544592524335698, -4.483927247898792601, 48.95942372801902565 ) ) ;
#163018 = FACE_OUTER_BOUND ( 'NONE', #21113, .T. ) ;
#163019 = CARTESIAN_POINT ( 'NONE',  ( -8.224510206698735004, -14.34966873604973081, 64.58442372801900433 ) ) ;
#163020 = CARTESIAN_POINT ( 'NONE',  ( -21.55341960407610458, -5.719274019375992779, 26.45724293864768839 ) ) ;
#163021 = VECTOR ( 'NONE', #133681, 1000.000000000000000 ) ;
#163022 = CARTESIAN_POINT ( 'NONE',  ( -5.153800228976328057, -19.02544592524343514, 32.29057627198102409 ) ) ;
#163023 = CARTESIAN_POINT ( 'NONE',  ( -8.314922557961024197, 14.29746914071037800, 37.91775706135235424 ) ) ;
#163024 = CARTESIAN_POINT ( 'NONE',  ( 0.05219959533909260263, 19.03943276465977164, 44.99890960531435979 ) ) ;
#163025 = CARTESIAN_POINT ( 'NONE',  ( 5.823673210054444382, -21.52544592524334988, 35.20942372801901854 ) ) ;
#163026 = CARTESIAN_POINT ( 'NONE',  ( 14.29746914071037800, 8.314922557961029526, 41.66775706135235424 ) ) ;
#163027 = CARTESIAN_POINT ( 'NONE',  ( 12.14591786802327356, -12.06949235617739191, 95.62609039468568994 ) ) ;
#163028 = CARTESIAN_POINT ( 'NONE',  ( -25.38276140623241162, -4.833717845876328134, 166.7901960806511852 ) ) ;
#163029 = CARTESIAN_POINT ( 'NONE',  ( 21.52544592524334988, 5.823673210054432836, 96.45942372801901854 ) ) ;
#163030 = CARTESIAN_POINT ( 'NONE',  ( 13.97604488694548053, -13.89961937509957401, 90.62609039468567573 ) ) ;
#163031 = CARTESIAN_POINT ( 'NONE',  ( 16.51473224551083163, -9.474510206698727899, 65.83442372801900433 ) ) ;
#163032 = CARTESIAN_POINT ( 'NONE',  ( 8.314922557960818139, 14.29746914071049879, 69.58224293864769550 ) ) ;
#163033 = CARTESIAN_POINT ( 'NONE',  ( -19.05341960407611168, -5.049401038298163336, 21.45724293864768839 ) ) ;
#163035 = CARTESIAN_POINT ( 'NONE',  ( 17.26058549869092928, 6.457015423128504850, 78.87745837476070676 ) ) ;
#163034 = CARTESIAN_POINT ( 'NONE',  ( 13.97604488694548053, -13.89961937509957401, 60.62609039468564731 ) ) ;
#163036 = CARTESIAN_POINT ( 'NONE',  ( -10.81492255796105439, 18.62759615963255655, 57.91775706135234714 ) ) ;
#163037 = CARTESIAN_POINT ( 'NONE',  ( 14.34966873604972726, -8.224510206698740333, 25.83442372801901499 ) ) ;
#163038 = CARTESIAN_POINT ( 'NONE',  ( -5.374011537017813644, -5.374011537017721274, -64.92279855667830191 ) ) ;
#163039 = CARTESIAN_POINT ( 'NONE',  ( -21.55341960407610458, -5.719274019375992779, 21.45724293864769550 ) ) ;
#163040 = CARTESIAN_POINT ( 'NONE',  ( -16.46253265017146816, -9.564922557961047289, 104.1677570613523329 ) ) ;
#163041 = CARTESIAN_POINT ( 'NONE',  ( 18.22780087662123805, -5.499999999999976019, 98.51763182126896368 ) ) ;
#163042 = CARTESIAN_POINT ( 'NONE',  ( -25.04733094907774316, 10.92720321514004489, 170.1247377027656569 ) ) ;
#163043 = CARTESIAN_POINT ( 'NONE',  ( -19.05341960407611168, -5.049401038298163336, 26.45724293864769550 ) ) ;
#163044 = CARTESIAN_POINT ( 'NONE',  ( -21.53943276465977519, -0.05219959533937600094, 103.7510903946857042 ) ) ;
#163045 = CARTESIAN_POINT ( 'NONE',  ( 5.153800228976335163, 19.02544592524342804, 49.79057627198100988 ) ) ;
#163046 = AXIS2_PLACEMENT_3D ( 'NONE', #130012, #38040, #21872 ) ;
#163047 = CARTESIAN_POINT ( 'NONE',  ( -5.719274019375665041, -21.55341960407619695, 69.79275706135234714 ) ) ;
#163048 = CARTESIAN_POINT ( 'NONE',  ( 18.62759615963255655, 10.81492255796105972, 106.6677570613523756 ) ) ;
#163049 = CARTESIAN_POINT ( 'NONE',  ( -16.53943276465976808, 0.05219959533911058130, 26.24890960531435624 ) ) ;
#163050 = CARTESIAN_POINT ( 'NONE',  ( -9.474510206698964154, 16.51473224551069663, 80.41557627198103830 ) ) ;
#163051 = CARTESIAN_POINT ( 'NONE',  ( 10.72451020669871369, 18.67979575497193778, 62.08442372801901143 ) ) ;
#163052 = CARTESIAN_POINT ( 'NONE',  ( -21.55341960407619339, 5.719274019375674811, 53.54275706135234714 ) ) ;
#163054 = CARTESIAN_POINT ( 'NONE',  ( 13.97604488694527802, 13.89961937509977652, 109.3739096053143669 ) ) ;
#163053 = CARTESIAN_POINT ( 'NONE',  ( 5.049401038297881783, 19.05341960407617563, 77.29275706135231871 ) ) ;
#163055 = CARTESIAN_POINT ( 'NONE',  ( -16.53943276465976808, 0.05219959533911058130, 116.2489096053143669 ) ) ;
#163056 = CARTESIAN_POINT ( 'NONE',  ( 0.05219959533907565091, 21.53943276465977519, 104.9989096053143669 ) ) ;
#163057 = CARTESIAN_POINT ( 'NONE',  ( 16.51473224551083163, -9.474510206698727899, 35.83442372801899722 ) ) ;
#163058 = CARTESIAN_POINT ( 'NONE',  ( -16.52544592524342804, 4.483927247898546575, 91.04057627198103830 ) ) ;
#163059 = CARTESIAN_POINT ( 'NONE',  ( 13.89961937509977652, -13.97604488694527269, 43.12390960531434558 ) ) ;
#163061 = CIRCLE ( 'NONE', #72733, 2.000000000000000000 ) ;
#163060 = CARTESIAN_POINT ( 'NONE',  ( -13.89961937509957401, -13.97604488694547875, 94.37609039468566152 ) ) ;
#163062 = CARTESIAN_POINT ( 'NONE',  ( -12.14591786802309592, -12.06949235617757132, 66.87390960531436690 ) ) ;
#163063 = CARTESIAN_POINT ( 'NONE',  ( 21.53943276465977519, 0.05219959533937863772, 111.2510903946856899 ) ) ;
#163064 = CARTESIAN_POINT ( 'NONE',  ( -9.474510206698964154, 16.51473224551069663, 100.4155762719810241 ) ) ;
#163065 = CARTESIAN_POINT ( 'NONE',  ( -5.049401038297874678, -19.05341960407617918, 79.79275706135233293 ) ) ;
#163066 = CARTESIAN_POINT ( 'NONE',  ( 18.62759615963271287, -10.81492255796078972, 88.33224293864769550 ) ) ;
#163067 = CIRCLE ( 'NONE', #127541, 5.500000000001017852 ) ;
#163068 = CARTESIAN_POINT ( 'NONE',  ( -21.53943276465977519, -0.05219959533937600094, 48.75109039468568284 ) ) ;
#163069 = CARTESIAN_POINT ( 'NONE',  ( -12.14591786802326823, 12.06949235617739902, 43.12609039468568284 ) ) ;
#163070 = CARTESIAN_POINT ( 'NONE',  ( -14.34966873604972548, 8.224510206698743886, 108.3344237280190185 ) ) ;
#163072 = CARTESIAN_POINT ( 'NONE',  ( -15.80617190586768217, 15.72974639402176855, 33.12609039468569705 ) ) ;
#163071 = CARTESIAN_POINT ( 'NONE',  ( 12.06949235617739724, 12.14591786802326823, 36.87609039468568994 ) ) ;
#163073 = CARTESIAN_POINT ( 'NONE',  ( -18.67979575497178146, -10.72451020669898902, 41.66557627198103120 ) ) ;
#163074 = PRODUCT_DEFINITION_FORMATION_WITH_SPECIFIED_SOURCE ( 'ANY', '', #177482, .NOT_KNOWN. ) ;
#163075 =( BOUNDED_CURVE ( )  B_SPLINE_CURVE ( 2, ( #55409, #132255, #150436, #194939, #102916, #54415, #117080, #24089, #40241, #133247, #176779 ),
 .UNSPECIFIED., .F., .T. ) 
 B_SPLINE_CURVE_WITH_KNOTS ( ( 3, 2, 2, 2, 2, 3 ),
 ( 0.4000000000000003553, 0.4200000000000003175, 0.4400000000000003908, 0.4600000000000004086, 0.4800000000000004263, 0.5000000000000004441 ),
 .UNSPECIFIED. ) 
 CURVE ( )  GEOMETRIC_REPRESENTATION_ITEM ( )  RATIONAL_B_SPLINE_CURVE ( ( 0.9999999999999992228, 0.9510565162951543083, 1.000000000000000000, 0.9510565162951535312, 1.000000000000000000, 0.9510565162951535312, 1.000000000000000000, 0.9510565162951535312, 1.000000000000000000, 0.9510565162951524210, 1.000000000000001110 ) ) 
 REPRESENTATION_ITEM ( '' )  );
#163076 = CARTESIAN_POINT ( 'NONE',  ( 5.153800228976335163, 19.02544592524342804, 39.79057627198100988 ) ) ;
#163077 = CARTESIAN_POINT ( 'NONE',  ( -23.48529157249600985, 32.32473071737754111, -8.049999994537627046 ) ) ;
#163078 = CARTESIAN_POINT ( 'NONE',  ( -4.379528057220086978, -16.55341960407618274, 64.79275706135234714 ) ) ;
#163079 = CARTESIAN_POINT ( 'NONE',  ( 15.80617190586746368, 15.72974639402197994, 94.37390960531436690 ) ) ;
#163080 = CARTESIAN_POINT ( 'NONE',  ( -0.05219959533910754901, -16.53943276465976808, 32.49890960531435979 ) ) ;
#163081 = CARTESIAN_POINT ( 'NONE',  ( -4.483927247898782831, 16.52544592524335698, 67.70942372801901854 ) ) ;
#163082 = CARTESIAN_POINT ( 'NONE',  ( 9.564922557960805705, 16.46253265017160317, 64.58224293864769550 ) ) ;
#163083 = CARTESIAN_POINT ( 'NONE',  ( 16.46253265017146816, 9.564922557961045513, 91.66775706135234714 ) ) ;
#163084 = CARTESIAN_POINT ( 'NONE',  ( 15.80617190586746368, 15.72974639402197994, 79.37390960531436690 ) ) ;
#163085 = CARTESIAN_POINT ( 'NONE',  ( 4.483927247898545687, 16.52544592524342804, 29.79057627198102409 ) ) ;
#163086 = ORIENTED_EDGE ( 'NONE', *, *, #199224, .T. ) ;
#163087 = CARTESIAN_POINT ( 'NONE',  ( 25.34721418589430186, 10.09305078451787629, 170.5222919391072764 ) ) ;
#163088 = EDGE_CURVE ( 'NONE', #70701, #167830, #32565, .T. ) ;
#163089 = CARTESIAN_POINT ( 'NONE',  ( -10.72451020669898014, 18.67979575497178502, 60.41557627198102409 ) ) ;
#163090 = CARTESIAN_POINT ( 'NONE',  ( -16.52544592524335698, -4.483927247898792601, 103.9594237280190185 ) ) ;
#163091 = VERTEX_POINT ( 'NONE', #184173 ) ;
#163092 = FACE_OUTER_BOUND ( 'NONE', #145907, .T. ) ;
#163093 = CARTESIAN_POINT ( 'NONE',  ( -5.823673210054116645, -21.52544592524344225, 87.29057627198103830 ) ) ;
#163094 = CARTESIAN_POINT ( 'NONE',  ( 10.72451020669898902, -18.67979575497178502, 107.9155762719810241 ) ) ;
#163095 = CARTESIAN_POINT ( 'NONE',  ( -14.29746914071049879, 8.314922557960819915, 30.83224293864770260 ) ) ;
#163097 = CARTESIAN_POINT ( 'NONE',  ( -14.34966873604972548, 8.224510206698743886, 33.33442372801900433 ) ) ;
#163096 = AXIS2_PLACEMENT_3D ( 'NONE', #8968, #18410, #141729 ) ;
#163098 = CARTESIAN_POINT ( 'NONE',  ( 0.05219959533909260263, 19.03943276465977164, 34.99890960531435979 ) ) ;
#163099 = CARTESIAN_POINT ( 'NONE',  ( 13.97604488694527802, 13.89961937509977652, 69.37390960531436690 ) ) ;
#163100 = CARTESIAN_POINT ( 'NONE',  ( -28.82186960331499037, 2.428612866367529932E-14, 146.0000000000000000 ) ) ;
#163101 = CARTESIAN_POINT ( 'NONE',  ( -5.719274019375978568, 21.55341960407610458, 25.20724293864769550 ) ) ;
#163102 = CARTESIAN_POINT ( 'NONE',  ( -5.049401038297874678, -19.05341960407617918, 109.7927570613523187 ) ) ;
#163103 = CARTESIAN_POINT ( 'NONE',  ( -16.46253265017146816, -9.564922557961047289, 34.16775706135233293 ) ) ;
#163104 = CARTESIAN_POINT ( 'NONE',  ( 21.53943276465977519, -0.05219959533907433946, 93.74890960531436690 ) ) ;
#163105 = CARTESIAN_POINT ( 'NONE',  ( -14.29746914071049879, 8.314922557960819915, 25.83224293864769194 ) ) ;
#163106 = B_SPLINE_CURVE_WITH_KNOTS ( 'NONE', 3,
 ( #170328, #105678, #183524, #137005, #198695, #74361, #46991, #60161, #77317, #30830, #197701, #121830, #31821, #93471, #14662, #122821, #138985, #45007, #28862, #199684, #59167, #76323, #123802, #185500, #120836, #155158, #63138, #182535, #124817, #44017, #167364, #114611 ),
 .UNSPECIFIED., .F., .F.,
 ( 4, 2, 2, 2, 2, 2, 2, 2, 2, 2, 2, 2, 2, 2, 2, 4 ),
 ( 8.673617379884035472E-19, 0.0003712461730036809775, 0.0007424923460073610875, 0.001113738519011041143, 0.001484984692014721308, 0.002227477038022088358, 0.002598723211025757464, 0.002969969384029427437, 0.003341215557033096542, 0.003712461730036766515, 0.004083707903040435620, 0.004454954076044105593, 0.004826200249047775566, 0.005197446422051444671, 0.005568692595055114644, 0.005939938768058783750 ),
 .UNSPECIFIED. ) ;
#163107 = CARTESIAN_POINT ( 'NONE',  ( 15.72974639402199770, -15.80617190586745480, 48.12390960531436690 ) ) ;
#163109 = CARTESIAN_POINT ( 'NONE',  ( 19.02544592524334988, 5.153800228976608722, 106.4594237280190185 ) ) ;
#163108 = CARTESIAN_POINT ( 'NONE',  ( 10.72451020669898902, -18.67979575497178502, 77.91557627198102409 ) ) ;
#163110 = CARTESIAN_POINT ( 'NONE',  ( -9.474510206698964154, 16.51473224551069663, 100.4155762719810241 ) ) ;
#163111 = CARTESIAN_POINT ( 'NONE',  ( -15.72974639402176322, -15.80617190586768395, 69.37609039468567573 ) ) ;
#163112 = CARTESIAN_POINT ( 'NONE',  ( -9.564922557960796823, -16.46253265017161027, 62.08224293864769550 ) ) ;
#163113 = CARTESIAN_POINT ( 'NONE',  ( -14.29746914071049879, 8.314922557960819915, 105.8322429386476955 ) ) ;
#163114 = CARTESIAN_POINT ( 'NONE',  ( 31.76179951907201371, 6.484602924383669809, 91.22381659560102207 ) ) ;
#163115 = CARTESIAN_POINT ( 'NONE',  ( 0.05219959533909260263, 19.03943276465977164, 69.99890960531435269 ) ) ;
#163116 = CARTESIAN_POINT ( 'NONE',  ( 16.55341960407611168, 4.379528057220329451, 93.95724293864770971 ) ) ;
#163117 = EDGE_LOOP ( 'NONE', ( #88851, #66078, #194434, #199279 ) ) ;
#163118 = CARTESIAN_POINT ( 'NONE',  ( 13.89961937509957401, 13.97604488694547697, 91.87609039468567573 ) ) ;
#163119 = DIRECTION ( 'NONE',  ( -1.000000000000000000, 0.000000000000000000, -6.982962677686266711E-15 ) ) ;
#163120 = CARTESIAN_POINT ( 'NONE',  ( 9.474510206698971260, -16.51473224551069308, 57.91557627198103120 ) ) ;
#163122 = CARTESIAN_POINT ( 'NONE',  ( 5.049401038298161559, -19.05341960407611168, 97.70724293864766707 ) ) ;
#163121 = CARTESIAN_POINT ( 'NONE',  ( 21.55341960407619695, -5.719274019375665929, 91.04275706135236135 ) ) ;
#163123 = CARTESIAN_POINT ( 'NONE',  ( 16.52544592524335698, 4.483927247898782831, 81.45942372801900433 ) ) ;
#163124 = CARTESIAN_POINT ( 'NONE',  ( -17.48853670773242541, -5.747243402303182869, 51.33328700250012133 ) ) ;
#163125 = CARTESIAN_POINT ( 'NONE',  ( -0.05219959533936034679, 19.03943276465977164, 37.50109039468567573 ) ) ;
#163126 = CARTESIAN_POINT ( 'NONE',  ( 21.55341960407619695, -5.719274019375665929, 106.0427570613523471 ) ) ;
#163127 = CARTESIAN_POINT ( 'NONE',  ( 36.81781682666242261, 5.501098665926424935, 45.34601664933739329 ) ) ;
#163128 = DIRECTION ( 'NONE',  ( 1.000000000000000000, 1.790682297782510931E-15, 0.000000000000000000 ) ) ;
#163129 = CARTESIAN_POINT ( 'NONE',  ( 8.314922557961029526, -14.29746914071037800, 100.4177570613523471 ) ) ;
#163130 = CARTESIAN_POINT ( 'NONE',  ( 16.49581645235994642, -0.7820921006973431400, -59.22453004090981210 ) ) ;
#163131 = CARTESIAN_POINT ( 'NONE',  ( 16.53943276465976808, 0.05219959533934440121, 96.25109039468568994 ) ) ;
#163132 = CARTESIAN_POINT ( 'NONE',  ( 17.40861289039003523, 6.110651285853279546, 68.87232470827430575 ) ) ;
#163133 = CARTESIAN_POINT ( 'NONE',  ( -8.224510206698735004, -14.34966873604973081, 64.58442372801900433 ) ) ;
#163134 = ORIENTED_EDGE ( 'NONE', *, *, #109494, .F. ) ;
#163135 = CARTESIAN_POINT ( 'NONE',  ( 15.72974639402176855, 15.80617190586768217, 81.87609039468568994 ) ) ;
#163136 = CARTESIAN_POINT ( 'NONE',  ( 9.564922557961047289, -16.46253265017146816, 85.41775706135233293 ) ) ;
#163137 = CARTESIAN_POINT ( 'NONE',  ( 9.564922557961047289, -16.46253265017146816, 35.41775706135233293 ) ) ;
#163138 = AXIS2_PLACEMENT_3D ( 'NONE', #174046, #5159, #188220 ) ;
#163139 = CARTESIAN_POINT ( 'NONE',  ( -16.51473224551069308, -9.474510206698971260, 66.66557627198102409 ) ) ;
#163140 = CARTESIAN_POINT ( 'NONE',  ( -13.97604488694527625, -13.89961937509977652, 56.87390960531434558 ) ) ;
#163141 = CARTESIAN_POINT ( 'NONE',  ( -18.56453257813359770, 5.500000000000040856, 40.99000423690688422 ) ) ;
#163142 = CARTESIAN_POINT ( 'NONE',  ( -15.80617190586745835, -15.72974639402198527, 76.87390960531439532 ) ) ;
#163143 = CARTESIAN_POINT ( 'NONE',  ( 15.80617190586746368, 15.72974639402197994, 34.37390960531435979 ) ) ;
#163144 = CARTESIAN_POINT ( 'NONE',  ( 19.03943276465977164, -0.05219959533909143690, 33.74890960531435979 ) ) ;
#163145 = CARTESIAN_POINT ( 'NONE',  ( -8.224510206698735004, -14.34966873604973081, 59.58442372801901854 ) ) ;
#163146 = ORIENTED_EDGE ( 'NONE', *, *, #144706, .F. ) ;
#163147 = CARTESIAN_POINT ( 'NONE',  ( 21.52544592524334988, 5.823673210054432836, 26.45942372801901854 ) ) ;
#163149 = CARTESIAN_POINT ( 'NONE',  ( 29.86685920354754842, -21.69954338932559068, -7.824999997268813345 ) ) ;
#163148 = CARTESIAN_POINT ( 'NONE',  ( -8.224510206698948167, 14.34966873604960824, 70.41557627198102409 ) ) ;
#163150 = CARTESIAN_POINT ( 'NONE',  ( 16.52544592524335698, 4.483927247898782831, 21.45942372801901499 ) ) ;
#163151 = CARTESIAN_POINT ( 'NONE',  ( -16.46253265017146816, -9.564922557961047289, 54.16775706135234003 ) ) ;
#163152 = CARTESIAN_POINT ( 'NONE',  ( -8.314922557960811034, -14.29746914071050412, 57.08224293864769550 ) ) ;
#163153 = CARTESIAN_POINT ( 'NONE',  ( -0.05219959533937732626, 21.53943276465977519, 37.50109039468568284 ) ) ;
#163155 = CARTESIAN_POINT ( 'NONE',  ( 10.81492255796078972, 18.62759615963270932, 79.58224293864769550 ) ) ;
#163154 = CARTESIAN_POINT ( 'NONE',  ( 24.13306144861383729, -5.795830589372934050, 189.9999999999999716 ) ) ;
#163156 = CARTESIAN_POINT ( 'NONE',  ( 16.46253265017160672, -9.564922557960803928, 103.3322429386476955 ) ) ;
#163157 = CARTESIAN_POINT ( 'NONE',  ( -4.379528057220328563, 16.55341960407611168, 65.20724293864768129 ) ) ;
#163158 = CARTESIAN_POINT ( 'NONE',  ( 28.32820575348571168, -27.54591730359781820, -18.54425385668479365 ) ) ;
#163159 = CARTESIAN_POINT ( 'NONE',  ( 17.72662750342724181, 5.500000000000073719, 43.90179492283744622 ) ) ;
#163160 = CARTESIAN_POINT ( 'NONE',  ( -5.049401038297874678, -19.05341960407617918, 69.79275706135233293 ) ) ;
#163161 = CARTESIAN_POINT ( 'NONE',  ( -5.719274019375978568, 21.55341960407610458, 110.2072429386477239 ) ) ;
#163162 = CARTESIAN_POINT ( 'NONE',  ( 9.474510206698971260, -16.51473224551069308, 52.91557627198102409 ) ) ;
#163163 = CARTESIAN_POINT ( 'NONE',  ( 16.51473224551083163, -9.474510206698727899, 40.83442372801900433 ) ) ;
#163164 = CARTESIAN_POINT ( 'NONE',  ( 0.05219959533909260263, 19.03943276465977164, 29.99890960531435979 ) ) ;
#163165 = CARTESIAN_POINT ( 'NONE',  ( 21.52544592524334988, 5.823673210054432836, 61.45942372801901854 ) ) ;
#163166 = DIRECTION ( 'NONE',  ( -1.000000000000000000, 0.000000000000000000, 0.000000000000000000 ) ) ;
#163167 = CARTESIAN_POINT ( 'NONE',  ( 14.29746914071049879, -8.314922557960816363, 38.33224293864768839 ) ) ;
#163168 = CARTESIAN_POINT ( 'NONE',  ( -5.049401038298153566, 19.05341960407611168, 65.20724293864765286 ) ) ;
#163169 = CARTESIAN_POINT ( 'NONE',  ( 15.80617190586746368, 15.72974639402197994, 84.37390960531438111 ) ) ;
#163170 = CARTESIAN_POINT ( 'NONE',  ( -19.02544592524342804, 5.153800228976336051, 56.04057627198100988 ) ) ;
#163171 = ORIENTED_EDGE ( 'NONE', *, *, #111459, .F. ) ;
#163172 = CARTESIAN_POINT ( 'NONE',  ( 18.62759615963271287, -10.81492255796078972, 68.33224293864769550 ) ) ;
#163173 = VERTEX_POINT ( 'NONE', #16314 ) ;
#163174 = CARTESIAN_POINT ( 'NONE',  ( -5.823673210054431948, 21.52544592524334988, 97.70942372801904696 ) ) ;
#163177 = CARTESIAN_POINT ( 'NONE',  ( -0.05219959533910754901, -16.53943276465976808, 77.49890960531433848 ) ) ;
#163176 = CARTESIAN_POINT ( 'NONE',  ( 0.05219959533934541429, -16.53943276465976808, 90.00109039468567573 ) ) ;
#163175 = DIRECTION ( 'NONE',  ( 0.000000000000000000, 0.000000000000000000, -1.000000000000000000 ) ) ;
#163178 = CARTESIAN_POINT ( 'NONE',  ( 9.564922557961047289, -16.46253265017146816, 90.41775706135234714 ) ) ;
#163179 = ORIENTED_EDGE ( 'NONE', *, *, #71161, .F. ) ;
#163180 = CARTESIAN_POINT ( 'NONE',  ( -0.05219959533936034679, 19.03943276465977164, 37.50109039468567573 ) ) ;
#163181 = CARTESIAN_POINT ( 'NONE',  ( 4.483927247898790824, -16.52544592524335698, 95.20942372801903275 ) ) ;
#163182 = CARTESIAN_POINT ( 'NONE',  ( -5.049401038297874678, -19.05341960407617918, 29.79275706135232227 ) ) ;
#163183 = CARTESIAN_POINT ( 'NONE',  ( 19.05341960407611168, 5.049401038298154454, 83.95724293864766707 ) ) ;
#163184 = CARTESIAN_POINT ( 'NONE',  ( -18.67979575497178146, -10.72451020669898902, 61.66557627198103120 ) ) ;
#163185 = CARTESIAN_POINT ( 'NONE',  ( -13.97604488694527625, -13.89961937509977652, 21.87390960531435979 ) ) ;
#163186 = CARTESIAN_POINT ( 'NONE',  ( 16.46253265017160672, -9.564922557960803928, 23.33224293864769194 ) ) ;
#163187 = CARTESIAN_POINT ( 'NONE',  ( -18.62759615963255300, -10.81492255796106328, 94.16775706135237556 ) ) ;
#163188 = CARTESIAN_POINT ( 'NONE',  ( 0.05219959533934541429, -16.53943276465976808, 80.00109039468568994 ) ) ;
#163189 = CARTESIAN_POINT ( 'NONE',  ( -21.53943276465977519, -0.05219959533937600094, 33.75109039468568284 ) ) ;
#163190 = CARTESIAN_POINT ( 'NONE',  ( 16.52544592524335698, 4.483927247898782831, 26.45942372801901854 ) ) ;
#163191 = CARTESIAN_POINT ( 'NONE',  ( 5.153800228976335163, 19.02544592524342804, 104.7905762719809957 ) ) ;
#163192 = CARTESIAN_POINT ( 'NONE',  ( -9.474510206698964154, 16.51473224551069663, 45.41557627198103120 ) ) ;
#163193 = CARTESIAN_POINT ( 'NONE',  ( -16.51473224551069308, -9.474510206698971260, 46.66557627198102409 ) ) ;
#163194 = TOROIDAL_SURFACE ( 'NONE', #76002, 206.0437394197456911, 8.000000000000000000 ) ;
#163195 = CARTESIAN_POINT ( 'NONE',  ( 8.224510206698742110, 14.34966873604972548, 52.08442372801901854 ) ) ;
#163196 = CARTESIAN_POINT ( 'NONE',  ( 14.34966873604960469, 8.224510206698951720, 94.16557627198103830 ) ) ;
#163197 = CARTESIAN_POINT ( 'NONE',  ( 8.224510206698742110, 14.34966873604972548, 107.0844237280190043 ) ) ;
#163200 = CARTESIAN_POINT ( 'NONE',  ( 16.46253265017160672, -9.564922557960803928, 68.33224293864770971 ) ) ;
#163199 = CARTESIAN_POINT ( 'NONE',  ( -19.03943276465977164, 0.05219959533909376836, 81.24890960531436690 ) ) ;
#163198 = CARTESIAN_POINT ( 'NONE',  ( 10.72451020669871369, 18.67979575497193778, 47.08442372801901854 ) ) ;
#163201 = CARTESIAN_POINT ( 'NONE',  ( -9.564922557960796823, -16.46253265017161027, 97.08224293864769550 ) ) ;
#163202 = CARTESIAN_POINT ( 'NONE',  ( -4.483927247898539470, -16.52544592524342804, 32.29057627198102409 ) ) ;
#163203 = CARTESIAN_POINT ( 'NONE',  ( -16.52544592524335698, -4.483927247898792601, 98.95942372801903275 ) ) ;
#163204 = ORIENTED_EDGE ( 'NONE', *, *, #84050, .F. ) ;
#163205 = CARTESIAN_POINT ( 'NONE',  ( -16.46253265017146816, -9.564922557961047289, 49.16775706135233293 ) ) ;
#163206 = CARTESIAN_POINT ( 'NONE',  ( -16.46253265017160317, 9.564922557960807481, 115.8322429386477097 ) ) ;
#163207 = CARTESIAN_POINT ( 'NONE',  ( 19.03943276465977164, -0.05219959533909143690, 68.74890960531436690 ) ) ;
#163208 = CARTESIAN_POINT ( 'NONE',  ( 19.03943276465977164, 0.05219959533936151252, 36.25109039468567573 ) ) ;
#163209 = CARTESIAN_POINT ( 'NONE',  ( -36.91746825000000598, 2.428612866367529932E-14, -8.624999997268814056 ) ) ;
#163210 = CARTESIAN_POINT ( 'NONE',  ( 19.02130022317636104, -5.499999999999790390, 73.28188669246573284 ) ) ;
#163211 = CARTESIAN_POINT ( 'NONE',  ( -12.14591786802326823, 12.06949235617739902, 48.12609039468568284 ) ) ;
#163212 = AXIS2_PLACEMENT_3D ( 'NONE', #99960, #116141, #177832 ) ;
#163214 = CARTESIAN_POINT ( 'NONE',  ( -0.05219959533934338120, 16.53943276465976808, 52.50109039468567573 ) ) ;
#163213 = CARTESIAN_POINT ( 'NONE',  ( 9.474510206698729675, 16.51473224551082808, 77.08442372801900433 ) ) ;
#163215 = CARTESIAN_POINT ( 'NONE',  ( 13.97604488694527802, 13.89961937509977652, 114.3739096053143669 ) ) ;
#163216 = CARTESIAN_POINT ( 'NONE',  ( 19.03943276465977164, -0.05219959533909143690, 88.74890960531436690 ) ) ;
#163217 = CARTESIAN_POINT ( 'NONE',  ( -15.72974639402197994, 15.80617190586746368, 115.6239096053143669 ) ) ;
#163218 = CARTESIAN_POINT ( 'NONE',  ( -19.05341960407617563, 5.049401038297882671, 73.54275706135233293 ) ) ;
#163220 = CARTESIAN_POINT ( 'NONE',  ( -19.03943276465977164, 0.05219959533909376836, 41.24890960531435269 ) ) ;
#163219 = CARTESIAN_POINT ( 'NONE',  ( -9.474510206698964154, 16.51473224551069663, 110.4155762719810383 ) ) ;
#163221 = EDGE_CURVE ( 'NONE', #74970, #189816, #183185, .T. ) ;
#163222 = CARTESIAN_POINT ( 'NONE',  ( -16.51473224551069308, -9.474510206698971260, 71.66557627198102409 ) ) ;
#163224 = CARTESIAN_POINT ( 'NONE',  ( -13.89961937509977652, 13.97604488694528158, 35.62390960531435269 ) ) ;
#163223 = CARTESIAN_POINT ( 'NONE',  ( 12.14591786802309770, 12.06949235617756955, 34.37390960531435979 ) ) ;
#163225 = VECTOR ( 'NONE', #110400, 1000.000000000000000 ) ;
#163226 = CARTESIAN_POINT ( 'NONE',  ( -19.03943276465977164, -0.05219959533935918106, 53.75109039468566863 ) ) ;
#163227 = CARTESIAN_POINT ( 'NONE',  ( 16.52544592524342804, -4.483927247898539470, 83.54057627198102409 ) ) ;
#163228 = CARTESIAN_POINT ( 'NONE',  ( 15.80617190586769283, -15.72974639402175789, 105.6260903946856899 ) ) ;
#163229 = CARTESIAN_POINT ( 'NONE',  ( 5.049401038298161559, -19.05341960407611168, 47.70724293864770260 ) ) ;
#163230 = CARTESIAN_POINT ( 'NONE',  ( 0.05219959533907565091, 21.53943276465977519, 49.99890960531437401 ) ) ;
#163232 = CARTESIAN_POINT ( 'NONE',  ( 21.52544592524334988, 5.823673210054432836, 106.4594237280190328 ) ) ;
#163231 = CARTESIAN_POINT ( 'NONE',  ( -4.379528057220328563, 16.55341960407611168, 50.20724293864769550 ) ) ;
#163233 = CARTESIAN_POINT ( 'NONE',  ( 19.05341960407611168, 5.049401038298154454, 103.9572429386476671 ) ) ;
#163234 = CARTESIAN_POINT ( 'NONE',  ( -9.564922557960796823, -16.46253265017161027, 102.0822429386477097 ) ) ;
#163235 = CARTESIAN_POINT ( 'NONE',  ( -5.049401038298153566, 19.05341960407611168, 40.20724293864768839 ) ) ;
#163236 = CARTESIAN_POINT ( 'NONE',  ( 9.564922557960805705, 16.46253265017160317, 24.58224293864769194 ) ) ;
#163237 = CARTESIAN_POINT ( 'NONE',  ( -16.53943276465976808, 0.05219959533911058130, 91.24890960531436690 ) ) ;
#163238 = CARTESIAN_POINT ( 'NONE',  ( -21.52544592524343514, 5.823673210054127303, 91.04057627198103830 ) ) ;
#163239 = CARTESIAN_POINT ( 'NONE',  ( 19.03943276465977164, -0.05219959533909143690, 103.7489096053143669 ) ) ;
#163240 = CARTESIAN_POINT ( 'NONE',  ( 15.80617190586746368, 15.72974639402197994, 114.3739096053143527 ) ) ;
#163241 = CARTESIAN_POINT ( 'NONE',  ( 5.049401038298161559, -19.05341960407611168, 97.70724293864766707 ) ) ;
#163243 = CARTESIAN_POINT ( 'NONE',  ( -16.53943276465976808, 0.05219959533911058130, 101.2489096053143669 ) ) ;
#163242 = CARTESIAN_POINT ( 'NONE',  ( 16.51473224551083163, -9.474510206698727899, 65.83442372801900433 ) ) ;
#163244 = CARTESIAN_POINT ( 'NONE',  ( 9.474510206698971260, -16.51473224551069308, 77.91557627198103830 ) ) ;
#163245 = CARTESIAN_POINT ( 'NONE',  ( -21.55341960407610458, -5.719274019375992779, 81.45724293864769550 ) ) ;
#163246 = CARTESIAN_POINT ( 'NONE',  ( 17.05587630539787369, -6.762274262135683500, 108.2418030903731818 ) ) ;
#163247 = CARTESIAN_POINT ( 'NONE',  ( -19.80313217313587160, -12.05975691044382359, 167.9999999999999716 ) ) ;
#163249 = CARTESIAN_POINT ( 'NONE',  ( 18.39635199886966177, -5.500000000000095923, 68.51967076359998998 ) ) ;
#163248 = CARTESIAN_POINT ( 'NONE',  ( 21.55341960407610458, 5.719274019375980345, 23.95724293864769550 ) ) ;
#163250 = CARTESIAN_POINT ( 'NONE',  ( -14.29746914071037622, -8.314922557961029526, 39.16775706135235424 ) ) ;
#163251 = CARTESIAN_POINT ( 'NONE',  ( 16.55341960407611168, 4.379528057220329451, 98.95724293864770971 ) ) ;
#163252 = LINE ( 'NONE', #114737, #151653 ) ;
#163253 = CARTESIAN_POINT ( 'NONE',  ( -9.564922557960796823, -16.46253265017161027, 92.08224293864769550 ) ) ;
#163254 = CARTESIAN_POINT ( 'NONE',  ( 16.51473224551069308, 9.474510206698969483, 59.16557627198102409 ) ) ;
#163255 = CARTESIAN_POINT ( 'NONE',  ( 16.55341960407611168, 4.379528057220329451, 83.95724293864770971 ) ) ;
#163256 = CARTESIAN_POINT ( 'NONE',  ( 21.55341960407610458, 5.719274019375980345, 38.95724293864768839 ) ) ;
#163257 = CARTESIAN_POINT ( 'NONE',  ( -12.06949235617756955, 12.14591786802309770, 55.62390960531436690 ) ) ;
#163258 = CARTESIAN_POINT ( 'NONE',  ( 14.34966873604972726, -8.224510206698740333, 25.83442372801901499 ) ) ;
#163259 = CARTESIAN_POINT ( 'NONE',  ( -18.62759615963255300, -10.81492255796106328, 69.16775706135234714 ) ) ;
#163260 = CARTESIAN_POINT ( 'NONE',  ( -27.73933785331498925, 9.013057229001088189, 146.7750000027311899 ) ) ;
#163261 = CARTESIAN_POINT ( 'NONE',  ( 15.72974639402199770, -15.80617190586745480, 23.12390960531436335 ) ) ;
#163262 = CARTESIAN_POINT ( 'NONE',  ( -8.314922557961024197, 14.29746914071037800, 77.91775706135231871 ) ) ;
#163263 = CARTESIAN_POINT ( 'NONE',  ( 16.51473224551069308, 9.474510206698969483, 24.16557627198102765 ) ) ;
#163264 = CARTESIAN_POINT ( 'NONE',  ( -9.474510206698964154, 16.51473224551069663, 85.41557627198102409 ) ) ;
#163265 = CARTESIAN_POINT ( 'NONE',  ( -21.52544592524343514, 5.823673210054127303, 101.0405762719810383 ) ) ;
#163266 = CARTESIAN_POINT ( 'NONE',  ( -16.55341960407617563, 4.379528057220093196, 28.54275706135234358 ) ) ;
#163268 = CARTESIAN_POINT ( 'NONE',  ( 18.62759615963255655, 10.81492255796105972, 71.66775706135234714 ) ) ;
#163267 = CARTESIAN_POINT ( 'NONE',  ( -12.14591786802309592, -12.06949235617757132, 46.87390960531435979 ) ) ;
#163270 = CARTESIAN_POINT ( 'NONE',  ( 18.62759615963271287, -10.81492255796078972, 28.33224293864769550 ) ) ;
#163269 = CARTESIAN_POINT ( 'NONE',  ( 0.05219959533934541429, -16.53943276465976808, 100.0010903946857042 ) ) ;
#163271 = CARTESIAN_POINT ( 'NONE',  ( 0.05219959533909260263, 19.03943276465977164, 114.9989096053143669 ) ) ;
#163272 = CARTESIAN_POINT ( 'NONE',  ( -16.21995358207303539, 7.366697692864245361, 79.93551001512159360 ) ) ;
#163273 = CARTESIAN_POINT ( 'NONE',  ( 16.55341960407618274, -4.379528057220086978, 106.0427570613523471 ) ) ;
#163274 = CARTESIAN_POINT ( 'NONE',  ( -16.53943276465976808, -0.05219959533934237506, 53.75109039468568994 ) ) ;
#163276 = EDGE_LOOP ( 'NONE', ( #100191, #17909, #71612, #179705, #90460, #140363 ) ) ;
#163275 = CARTESIAN_POINT ( 'NONE',  ( -9.564922557960796823, -16.46253265017161027, 67.08224293864769550 ) ) ;
#163277 = CARTESIAN_POINT ( 'NONE',  ( 19.03943276465977164, -0.05219959533909143690, 93.74890960531435269 ) ) ;
#163278 = CARTESIAN_POINT ( 'NONE',  ( 15.80617190586769283, -15.72974639402175789, 75.62609039468567573 ) ) ;
#163279 = CARTESIAN_POINT ( 'NONE',  ( 16.55341960407618274, -4.379528057220086978, 71.04275706135234714 ) ) ;
#163280 = CARTESIAN_POINT ( 'NONE',  ( -14.29746914071049879, 8.314922557960819915, 50.83224293864770971 ) ) ;
#163281 = CARTESIAN_POINT ( 'NONE',  ( 19.05341960407611168, 5.049401038298154454, 53.95724293864770260 ) ) ;
#163282 = ORIENTED_EDGE ( 'NONE', *, *, #69568, .F. ) ;
#163283 = CARTESIAN_POINT ( 'NONE',  ( 16.46253265017146816, 9.564922557961045513, 111.6677570613523329 ) ) ;
#163284 = CARTESIAN_POINT ( 'NONE',  ( 0.05219959533910956823, 16.53943276465976808, 104.9989096053143669 ) ) ;
#163285 = CARTESIAN_POINT ( 'NONE',  ( 19.03943276465977164, -0.05219959533909143690, 63.74890960531435979 ) ) ;
#163287 = CARTESIAN_POINT ( 'NONE',  ( -38.00000000000001421, 12.34694845685046438, -6.099999999999999645 ) ) ;
#163286 = CARTESIAN_POINT ( 'NONE',  ( 19.05341960407617918, -5.049401038297876454, 96.04275706135231871 ) ) ;
#163288 = CARTESIAN_POINT ( 'NONE',  ( -10.72451020669870658, -18.67979575497194134, 99.58442372801900433 ) ) ;
#163289 = CARTESIAN_POINT ( 'NONE',  ( -16.52544592524335698, -4.483927247898792601, 68.95942372801901854 ) ) ;
#163290 = CARTESIAN_POINT ( 'NONE',  ( -16.51473224551082808, 9.474510206698731452, 98.33442372801900433 ) ) ;
#163292 = B_SPLINE_CURVE_WITH_KNOTS ( 'NONE', 3,
 ( #113919, #4748, #37093, #66437, #174628, #3763, #98752, #159432, #145265, #33131, #20928, #82586, #64458, #144267, #190787, #52261, #17968, #160445, #21935, #130079, #79623, #38105 ),
 .UNSPECIFIED., .F., .F.,
 ( 4, 2, 2, 2, 2, 2, 2, 2, 2, 2, 4 ),
 ( 2.778238173776314926E-07, 0.0007557225233028439957, 0.001511167222788310479, 0.002266611922273776419, 0.003022056621759243011, 0.003777501321244709602, 0.004532946020730175760, 0.004910668370472912742, 0.005288390720215648856, 0.005666113069958384971, 0.006043835419701121953 ),
 .UNSPECIFIED. ) ;
#163291 = CARTESIAN_POINT ( 'NONE',  ( -15.80617190586745835, -15.72974639402198527, 61.87390960531436690 ) ) ;
#163293 = CARTESIAN_POINT ( 'NONE',  ( 8.314922557961029526, -14.29746914071037800, 50.41775706135235424 ) ) ;
#163294 = DIRECTION ( 'NONE',  ( -1.000000000000000000, -0.000000000000000000, -3.709348145883536076E-20 ) ) ;
#163295 = CARTESIAN_POINT ( 'NONE',  ( 5.153800228976615827, -19.02544592524334988, 55.20942372801899722 ) ) ;
#163296 = CIRCLE ( 'NONE', #160091, 7.500000000000000000 ) ;
#163297 = CARTESIAN_POINT ( 'NONE',  ( 21.55341960407619695, -5.719274019375665929, 91.04275706135236135 ) ) ;
#163298 = CARTESIAN_POINT ( 'NONE',  ( -19.03943276465977164, 0.05219959533909376836, 41.24890960531435269 ) ) ;
#163299 = CARTESIAN_POINT ( 'NONE',  ( -5.153800228976328057, -19.02544592524343514, 67.29057627198102409 ) ) ;
#163300 = CARTESIAN_POINT ( 'NONE',  ( 4.483927247898545687, 16.52544592524342804, 64.79057627198103830 ) ) ;
#163301 = CARTESIAN_POINT ( 'NONE',  ( 0.05219959533937995610, -21.53943276465977519, 95.00109039468568994 ) ) ;
#163302 = ADVANCED_FACE ( 'NONE', ( #2126 ), #91135, .T. ) ;
#163303 = CARTESIAN_POINT ( 'NONE',  ( -13.97604488694547697, 13.89961937509957934, 48.12609039468566863 ) ) ;
#163304 = CARTESIAN_POINT ( 'NONE',  ( 13.89961937509957401, 13.97604488694547697, 21.87609039468566152 ) ) ;
#163305 = CARTESIAN_POINT ( 'NONE',  ( 19.05341960407611168, 5.049401038298154454, 113.9572429386477097 ) ) ;
#163306 = CARTESIAN_POINT ( 'NONE',  ( 21.55341960407619695, -5.719274019375665929, 91.04275706135236135 ) ) ;
#163307 = CARTESIAN_POINT ( 'NONE',  ( 13.89961937509977652, -13.97604488694527269, 73.12390960531436690 ) ) ;
#163308 = CARTESIAN_POINT ( 'NONE',  ( 21.52544592524334988, 5.823673210054432836, 96.45942372801901854 ) ) ;
#163309 = CARTESIAN_POINT ( 'NONE',  ( -5.719274019375978568, 21.55341960407610458, 50.20724293864769550 ) ) ;
#163310 = CARTESIAN_POINT ( 'NONE',  ( 19.02544592524343514, -5.153800228976328945, 78.54057627198099567 ) ) ;
#163311 = CARTESIAN_POINT ( 'NONE',  ( 19.05341960407617918, -5.049401038297876454, 76.04275706135230450 ) ) ;
#163312 = CARTESIAN_POINT ( 'NONE',  ( -19.02544592524342804, 5.153800228976336051, 41.04057627198103120 ) ) ;
#163313 = CARTESIAN_POINT ( 'NONE',  ( -13.97604488694527625, -13.89961937509977652, 86.87390960531436690 ) ) ;
#163314 = CARTESIAN_POINT ( 'NONE',  ( -19.05341960407617563, 5.049401038297882671, 88.54275706135230450 ) ) ;
#163315 = CARTESIAN_POINT ( 'NONE',  ( -16.53943276465976808, -0.05219959533934237506, 43.75109039468568284 ) ) ;
#163316 = CARTESIAN_POINT ( 'NONE',  ( -12.06949235617756955, 12.14591786802309770, 105.6239096053143669 ) ) ;
#163317 = CARTESIAN_POINT ( 'NONE',  ( 0.05219959533909260263, 19.03943276465977164, 64.99890960531436690 ) ) ;
#163318 = EDGE_CURVE ( 'NONE', #155722, #53380, #75137, .T. ) ;
#163319 = CARTESIAN_POINT ( 'NONE',  ( 15.80617190586746368, 15.72974639402197994, 49.37390960531436690 ) ) ;
#163320 = CARTESIAN_POINT ( 'NONE',  ( 16.55341960407618274, -4.379528057220086978, 36.04275706135234714 ) ) ;
#163321 = CARTESIAN_POINT ( 'NONE',  ( -21.52544592524334988, -5.823673210054445271, 38.95942372801901854 ) ) ;
#163322 = CARTESIAN_POINT ( 'NONE',  ( -21.53943276465977519, -0.05219959533937600094, 78.75109039468568994 ) ) ;
#163324 = CARTESIAN_POINT ( 'NONE',  ( -14.29746914071037622, -8.314922557961029526, 84.16775706135234714 ) ) ;
#163323 = B_SPLINE_CURVE_WITH_KNOTS ( 'NONE', 3,
 ( #128084, #160431, #192772, #6732, #100741, #54256, #98738, #19922, #81564, #97728, #143250, #4734, #68410, #82572 ),
 .UNSPECIFIED., .F., .F.,
 ( 4, 2, 2, 2, 2, 2, 4 ),
 ( 0.1559601203333475239, 0.1570958510570476530, 0.1582315817807478098, 0.1605030432281480957, 0.1616387739518482247, 0.1627745046755483815, 0.1650459661229486397 ),
 .UNSPECIFIED. ) ;
#163325 = CARTESIAN_POINT ( 'NONE',  ( -19.05341960407611168, -5.049401038298163336, 71.45724293864766707 ) ) ;
#163326 = CARTESIAN_POINT ( 'NONE',  ( 8.224510206698742110, 14.34966873604972548, 107.0844237280190043 ) ) ;
#163327 = CARTESIAN_POINT ( 'NONE',  ( 5.153800228976615827, -19.02544592524334988, 60.20942372801899012 ) ) ;
#163328 = CARTESIAN_POINT ( 'NONE',  ( -21.53943276465977519, -0.05219959533937600094, 33.75109039468568284 ) ) ;
#163329 = CARTESIAN_POINT ( 'NONE',  ( 8.314922557960818139, 14.29746914071049879, 79.58224293864769550 ) ) ;
#163330 = CARTESIAN_POINT ( 'NONE',  ( 19.05341960407611168, 5.049401038298154454, 98.95724293864766707 ) ) ;
#163331 = CARTESIAN_POINT ( 'NONE',  ( 8.224510206698742110, 14.34966873604972548, 107.0844237280190043 ) ) ;
#163332 = CARTESIAN_POINT ( 'NONE',  ( 18.62759615963255655, 10.81492255796105972, 76.66775706135234714 ) ) ;
#163333 = CARTESIAN_POINT ( 'NONE',  ( -8.314922557961024197, 14.29746914071037800, 47.91775706135234714 ) ) ;
#163334 = CARTESIAN_POINT ( 'NONE',  ( 15.80617190586769283, -15.72974639402175789, 30.62609039468567929 ) ) ;
#163335 = CARTESIAN_POINT ( 'NONE',  ( 14.29746914071049879, -8.314922557960816363, 73.33224293864769550 ) ) ;
#163336 = ORIENTED_EDGE ( 'NONE', *, *, #185965, .T. ) ;
#163337 =( BOUNDED_SURFACE ( )  B_SPLINE_SURFACE ( 1, 2, ( 
 ( #152488, #170647, #88832, #66436, #97743, #142281, #35107, #5753, #50292, #156467, #17967, #4747, #155473, #2780, #33130, #16965, #96758, #159431, #187821, #174627, #3762, #128097, #79622, #52260, #112933, #144266, #157466, #1784, #113918, #158448, #65439, #173638, #78618, #20927, #18959, #141290, #36092, #19936, #67429, #172633, #64456, #81578, #49290, #82585, #80604, #129086, #143263, #32135, #190786, #93793, #110948, #189801, #140293, #51273, #63462, #125138, #34121, #126126, #188809, #111949, #186836, #48304, #109961, #95780, #171640, #94786, #127100, #67196, #189567, #49060, #160209, #6511, #68190, #141058, #2544, #4510, #190554, #33886, #173401, #113685, #191541, #35863, #52027, #127863, #66200, #64226, #51039, #96526, #125891, #17731, #174393, #5516, #80370, #157231, #82345, #143032, #112701, #188573, #97509, #98515, #128854 ),
 ( #129842, #126866, #159195, #142043, #20690, #34872, #144034, #53018, #50053, #175380, #36849, #158216, #19706, #176392, #21699, #83353, #37866, #18723, #145029, #114698, #156230, #79389, #187591, #110715, #172397, #95543, #3531, #65207, #111715, #81348, #70205, #100525, #22702, #102538, #165216, #55029, #41874, #71204, #195565, #147043, #119703, #180402, #11548, #24713, #69194, #181386, #25718, #9537, #40864, #84349, #26711, #86362, #8527, #103541, #164221, #73215, #39853, #131872, #87364, #116699, #88350, #148047, #150043, #149049, #99525, #134886, #161207, #178389, #133875, #146027, #10537, #72201, #7510, #101519, #193557, #56026, #117704, #196562, #130861, #58033, #163209, #192552, #132867, #179400, #57039, #194556, #162204, #118712, #54035, #115709, #177397, #38869, #23702, #85350, #60985, #139804, #124650, #59008, #169159, #27712, #105517 ) ),
 .UNSPECIFIED., .F., .F., .T. ) 
 B_SPLINE_SURFACE_WITH_KNOTS ( ( 2, 2 ),
 ( 3, 2, 2, 2, 2, 2, 2, 2, 2, 2, 2, 2, 2, 2, 2, 2, 2, 2, 2, 2, 2, 2, 2, 2, 2, 2, 2, 2, 2, 2, 2, 2, 2, 2, 2, 2, 2, 2, 2, 2, 2, 2, 2, 2, 2, 2, 2, 2, 2, 2, 3 ),
 ( 0.000000000000000000, 1.000000000000000000 ),
 ( 0.000000000000000000, 0.02000000000000000042, 0.04000000000000000083, 0.05999999999999999778, 0.08000000000000000167, 0.1000000000000000056, 0.1199999999999999956, 0.1400000000000000133, 0.1600000000000000033, 0.1799999999999999933, 0.2000000000000000111, 0.2200000000000000011, 0.2399999999999999911, 0.2600000000000000089, 0.2800000000000000266, 0.2999999999999999889, 0.3200000000000000067, 0.3400000000000000244, 0.3599999999999999867, 0.3800000000000000044, 0.4000000000000000222, 0.4199999999999999845, 0.4400000000000000022, 0.4600000000000000200, 0.4799999999999999822, 0.5000000000000000000, 0.5200000000000000178, 0.5400000000000000355, 0.5600000000000000533, 0.5799999999999999600, 0.5999999999999999778, 0.6199999999999999956, 0.6400000000000000133, 0.6600000000000000311, 0.6800000000000000488, 0.6999999999999999556, 0.7199999999999999734, 0.7399999999999999911, 0.7600000000000000089, 0.7800000000000000266, 0.8000000000000000444, 0.8199999999999999512, 0.8399999999999999689, 0.8599999999999999867, 0.8800000000000000044, 0.9000000000000000222, 0.9200000000000000400, 0.9399999999999999467, 0.9599999999999999645, 0.9799999999999999822, 1.000000000000000000 ),
 .UNSPECIFIED. ) 
 GEOMETRIC_REPRESENTATION_ITEM ( )  RATIONAL_B_SPLINE_SURFACE ( (
 ( 1.000000000000000000, 0.9510565162951535312, 1.000000000000000000, 0.9510565162951535312, 1.000000000000000000, 0.9510565162951535312, 1.000000000000000000, 0.9510565162951535312, 1.000000000000000000, 0.9510565162951535312, 1.000000000000000000, 0.9510565162951535312, 1.000000000000000000, 0.9510565162951535312, 1.000000000000000000, 0.9510565162951535312, 1.000000000000000000, 0.9510565162951535312, 1.000000000000000000, 0.9510565162951535312, 1.000000000000000000, 0.9510565162951535312, 1.000000000000000000, 0.9510565162951535312, 1.000000000000000000, 0.9510565162951535312, 1.000000000000000000, 0.9510565162951535312, 1.000000000000000000, 0.9510565162951535312, 1.000000000000000000, 0.9510565162951535312, 1.000000000000000000, 0.9510565162951535312, 1.000000000000000000, 0.9510565162951535312, 1.000000000000000000, 0.9510565162951535312, 1.000000000000000000, 0.9510565162951535312, 1.000000000000000000, 0.9510565162951535312, 1.000000000000000000, 0.9510565162951535312, 1.000000000000000000, 0.9510565162951535312, 1.000000000000000000, 0.9510565162951535312, 1.000000000000000000, 0.9510565162951535312, 1.000000000000000000, 0.9510565162951535312, 1.000000000000000000, 0.9510565162951535312, 1.000000000000000000, 0.9510565162951535312, 1.000000000000000000, 0.9510565162951535312, 1.000000000000000000, 0.9510565162951535312, 1.000000000000000000, 0.9510565162951535312, 1.000000000000000000, 0.9510565162951535312, 1.000000000000000000, 0.9510565162951535312, 1.000000000000000000, 0.9510565162951535312, 1.000000000000000000, 0.9510565162951535312, 1.000000000000000000, 0.9510565162951535312, 1.000000000000000000, 0.9510565162951535312, 1.000000000000000000, 0.9510565162951535312, 1.000000000000000000, 0.9510565162951535312, 1.000000000000000000, 0.9510565162951535312, 1.000000000000000000, 0.9510565162951535312, 1.000000000000000000, 0.9510565162951535312, 1.000000000000000000, 0.9510565162951535312, 1.000000000000000000, 0.9510565162951535312, 1.000000000000000000, 0.9510565162951535312, 1.000000000000000000, 0.9510565162951535312, 1.000000000000000000, 0.9510565162951535312, 1.000000000000000000, 0.9510565162951535312, 1.000000000000000000, 0.9510565162951535312, 1.000000000000000000, 0.9510565162951535312, 1.000000000000000000),
 ( 1.000000000000000000, 0.9510565162951535312, 1.000000000000000000, 0.9510565162951535312, 1.000000000000000000, 0.9510565162951535312, 1.000000000000000000, 0.9510565162951535312, 1.000000000000000000, 0.9510565162951535312, 1.000000000000000000, 0.9510565162951535312, 1.000000000000000000, 0.9510565162951535312, 1.000000000000000000, 0.9510565162951535312, 1.000000000000000000, 0.9510565162951535312, 1.000000000000000000, 0.9510565162951535312, 1.000000000000000000, 0.9510565162951535312, 1.000000000000000000, 0.9510565162951535312, 1.000000000000000000, 0.9510565162951535312, 1.000000000000000000, 0.9510565162951535312, 1.000000000000000000, 0.9510565162951535312, 1.000000000000000000, 0.9510565162951535312, 1.000000000000000000, 0.9510565162951535312, 1.000000000000000000, 0.9510565162951535312, 1.000000000000000000, 0.9510565162951535312, 1.000000000000000000, 0.9510565162951535312, 1.000000000000000000, 0.9510565162951535312, 1.000000000000000000, 0.9510565162951535312, 1.000000000000000000, 0.9510565162951535312, 1.000000000000000000, 0.9510565162951535312, 1.000000000000000000, 0.9510565162951535312, 1.000000000000000000, 0.9510565162951535312, 1.000000000000000000, 0.9510565162951535312, 1.000000000000000000, 0.9510565162951535312, 1.000000000000000000, 0.9510565162951535312, 1.000000000000000000, 0.9510565162951535312, 1.000000000000000000, 0.9510565162951535312, 1.000000000000000000, 0.9510565162951535312, 1.000000000000000000, 0.9510565162951535312, 1.000000000000000000, 0.9510565162951535312, 1.000000000000000000, 0.9510565162951535312, 1.000000000000000000, 0.9510565162951535312, 1.000000000000000000, 0.9510565162951535312, 1.000000000000000000, 0.9510565162951535312, 1.000000000000000000, 0.9510565162951535312, 1.000000000000000000, 0.9510565162951535312, 1.000000000000000000, 0.9510565162951535312, 1.000000000000000000, 0.9510565162951535312, 1.000000000000000000, 0.9510565162951535312, 1.000000000000000000, 0.9510565162951535312, 1.000000000000000000, 0.9510565162951535312, 1.000000000000000000, 0.9510565162951535312, 1.000000000000000000, 0.9510565162951535312, 1.000000000000000000, 0.9510565162951535312, 1.000000000000000000, 0.9510565162951535312, 1.000000000000000000, 0.9510565162951535312, 1.000000000000000000) ) ) 
 REPRESENTATION_ITEM ( '' )  SURFACE ( )  );
#163338 = CARTESIAN_POINT ( 'NONE',  ( -21.52544592524343514, 5.823673210054127303, 111.0405762719810525 ) ) ;
#163339 = CARTESIAN_POINT ( 'NONE',  ( 14.34966873604960469, 8.224510206698951720, 54.16557627198103120 ) ) ;
#163340 = LINE ( 'NONE', #164347, #146969 ) ;
#163341 = CARTESIAN_POINT ( 'NONE',  ( -5.719274019375978568, 21.55341960407610458, 30.20724293864769550 ) ) ;
#163342 = CARTESIAN_POINT ( 'NONE',  ( -10.81492255796105439, 18.62759615963255655, 52.91775706135235424 ) ) ;
#163343 = CARTESIAN_POINT ( 'NONE',  ( -8.224510206698948167, 14.34966873604960824, 70.41557627198102409 ) ) ;
#163344 = CARTESIAN_POINT ( 'NONE',  ( 15.72974639402199770, -15.80617190586745480, 78.12390960531436690 ) ) ;
#163345 = CARTESIAN_POINT ( 'NONE',  ( -19.03943276465977164, 0.05219959533909376836, 81.24890960531436690 ) ) ;
#163347 = CARTESIAN_POINT ( 'NONE',  ( 5.049401038297881783, 19.05341960407617563, 77.29275706135231871 ) ) ;
#163346 = CARTESIAN_POINT ( 'NONE',  ( 9.474510206698971260, -16.51473224551069308, 32.91557627198102409 ) ) ;
#163349 = CARTESIAN_POINT ( 'NONE',  ( -18.67979575497178146, -10.72451020669898902, 66.66557627198102409 ) ) ;
#163348 = CARTESIAN_POINT ( 'NONE',  ( -18.62759615963255300, -10.81492255796106328, 54.16775706135235424 ) ) ;
#163350 = CARTESIAN_POINT ( 'NONE',  ( -16.46253265017160317, 9.564922557960807481, 45.83224293864769550 ) ) ;
#163351 = CARTESIAN_POINT ( 'NONE',  ( -16.46253265017160317, 9.564922557960807481, 70.83224293864770971 ) ) ;
#163352 = ORIENTED_EDGE ( 'NONE', *, *, #12432, .T. ) ;
#163353 = CARTESIAN_POINT ( 'NONE',  ( -4.379528057220086978, -16.55341960407618274, 49.79275706135234714 ) ) ;
#163354 = CARTESIAN_POINT ( 'NONE',  ( 18.62759615963255655, 10.81492255796105972, 31.66775706135234358 ) ) ;
#163355 = CARTESIAN_POINT ( 'NONE',  ( 18.62759615963255655, 10.81492255796105972, 56.66775706135235424 ) ) ;
#163356 = CARTESIAN_POINT ( 'NONE',  ( -16.46253265017160317, 9.564922557960807481, 105.8322429386476955 ) ) ;
#163357 = CARTESIAN_POINT ( 'NONE',  ( 5.823673210054125526, 21.52544592524343514, 89.79057627198103830 ) ) ;
#163359 = CARTESIAN_POINT ( 'NONE',  ( 14.29746914071037800, 8.314922557961029526, 56.66775706135235424 ) ) ;
#163358 = CARTESIAN_POINT ( 'NONE',  ( -18.62759615963255300, -10.81492255796106328, 29.16775706135234003 ) ) ;
#163360 = CARTESIAN_POINT ( 'NONE',  ( 21.52544592524344225, -5.823673210054117533, 43.54057627198103830 ) ) ;
#163361 = CARTESIAN_POINT ( 'NONE',  ( 0.05219959533936267826, -19.03943276465977164, 20.00109039468567218 ) ) ;
#163362 = CARTESIAN_POINT ( 'NONE',  ( -16.51473224551069308, -9.474510206698971260, 51.66557627198102409 ) ) ;
#163363 = CARTESIAN_POINT ( 'NONE',  ( 9.564922557960805705, 16.46253265017160317, 109.5822429386476955 ) ) ;
#163364 = CARTESIAN_POINT ( 'NONE',  ( 0.05219959533909260263, 19.03943276465977164, 84.99890960531436690 ) ) ;
#163365 = CARTESIAN_POINT ( 'NONE',  ( 17.50000000000002132, 5.272787497354016750, 103.7271518416984435 ) ) ;
#163366 = CARTESIAN_POINT ( 'NONE',  ( 13.89961937509957401, 13.97604488694547697, 71.87609039468567573 ) ) ;
#163367 = CARTESIAN_POINT ( 'NONE',  ( -5.719274019375978568, 21.55341960407610458, 50.20724293864769550 ) ) ;
#163368 = CARTESIAN_POINT ( 'NONE',  ( 8.314922557960818139, 14.29746914071049879, 29.58224293864769905 ) ) ;
#163369 = CARTESIAN_POINT ( 'NONE',  ( 19.02544592524334988, 5.153800228976608722, 91.45942372801900433 ) ) ;
#163370 = CARTESIAN_POINT ( 'NONE',  ( -14.65663629173027793, -15.74606964832901390, -58.72366780613685222 ) ) ;
#163371 = CARTESIAN_POINT ( 'NONE',  ( -16.46253265017146816, -9.564922557961047289, 19.16775706135233293 ) ) ;
#163372 = CARTESIAN_POINT ( 'NONE',  ( -13.97604488694547697, 13.89961937509957934, 98.12609039468566152 ) ) ;
#163373 = CARTESIAN_POINT ( 'NONE',  ( -13.89961937509957401, -13.97604488694547875, 39.37609039468566152 ) ) ;
#163374 = CARTESIAN_POINT ( 'NONE',  ( 0.000000000000000000, 0.7216878364870328300, -1.250000000000000000 ) ) ;
#163375 = CARTESIAN_POINT ( 'NONE',  ( 19.02544592524343514, -5.153800228976328945, 58.54057627198102409 ) ) ;
#163376 = CARTESIAN_POINT ( 'NONE',  ( -8.314922557960811034, -14.29746914071050412, 47.08224293864770260 ) ) ;
#163377 = CARTESIAN_POINT ( 'NONE',  ( -16.51473224551069308, -9.474510206698971260, 36.66557627198102409 ) ) ;
#163378 = CARTESIAN_POINT ( 'NONE',  ( -12.06949235617756955, 12.14591786802309770, 40.62390960531435269 ) ) ;
#163379 = CARTESIAN_POINT ( 'NONE',  ( 37.99626262588765258, 2.893932880411085066E-14, -6.747842220587804363 ) ) ;
#163380 = CARTESIAN_POINT ( 'NONE',  ( 16.52544592524335698, 4.483927247898782831, 101.4594237280190185 ) ) ;
#163381 = CARTESIAN_POINT ( 'NONE',  ( -16.51473224551069308, -9.474510206698971260, 66.66557627198102409 ) ) ;
#163382 = CARTESIAN_POINT ( 'NONE',  ( -16.51473224551082808, 9.474510206698731452, 28.33442372801900433 ) ) ;
#163383 = CARTESIAN_POINT ( 'NONE',  ( 8.224510206698742110, 14.34966873604972548, 37.08442372801901143 ) ) ;
#163384 = CARTESIAN_POINT ( 'NONE',  ( 0.05219959533907565091, 21.53943276465977519, 34.99890960531435979 ) ) ;
#163386 = EDGE_LOOP ( 'NONE', ( #5211, #198946, #8412, #117668 ) ) ;
#163385 = CARTESIAN_POINT ( 'NONE',  ( 15.80617190586769283, -15.72974639402175789, 100.6260903946857184 ) ) ;
#163387 = CARTESIAN_POINT ( 'NONE',  ( 13.97604488694527802, 13.89961937509977652, 64.37390960531436690 ) ) ;
#163388 = CARTESIAN_POINT ( 'NONE',  ( -19.03943276465977164, 0.05219959533909376836, 101.2489096053143669 ) ) ;
#163389 = CARTESIAN_POINT ( 'NONE',  ( 16.51473224551069308, 9.474510206698969483, 99.16557627198102409 ) ) ;
#163390 = CARTESIAN_POINT ( 'NONE',  ( -18.09867054820434262, -5.499999999999827693, 43.98393025253587041 ) ) ;
#163391 = CARTESIAN_POINT ( 'NONE',  ( 0.05219959533937995610, -21.53943276465977519, 25.00109039468567218 ) ) ;
#163392 = VECTOR ( 'NONE', #52925, 1000.000000000000000 ) ;
#163393 = CARTESIAN_POINT ( 'NONE',  ( -12.06949235617756955, 12.14591786802309770, 80.62390960531438111 ) ) ;
#163395 = CARTESIAN_POINT ( 'NONE',  ( 13.97604488694527802, 13.89961937509977652, 69.37390960531436690 ) ) ;
#163394 = CARTESIAN_POINT ( 'NONE',  ( 5.719274019375991003, -21.55341960407610458, 77.70724293864770971 ) ) ;
#163396 = CARTESIAN_POINT ( 'NONE',  ( -5.153800228976328057, -19.02544592524343514, 77.29057627198099567 ) ) ;
#163397 = CARTESIAN_POINT ( 'NONE',  ( 21.53943276465977519, -0.05219959533907433946, 113.7489096053143527 ) ) ;
#163398 = EDGE_LOOP ( 'NONE', ( #162710, #103184, #40929, #54666 ) ) ;
#163399 = CARTESIAN_POINT ( 'NONE',  ( 19.05341960407611168, 5.049401038298154454, 78.95724293864769550 ) ) ;
#163400 = EDGE_CURVE ( 'NONE', #184349, #177366, #34462, .T. ) ;
#163401 = CARTESIAN_POINT ( 'NONE',  ( -5.427562675786936573E-15, 30.27659582821221207, 147.4843446568999923 ) ) ;
#163403 = CARTESIAN_POINT ( 'NONE',  ( 30.20036327792367814, -26.22857331006468584, -17.18026671435356434 ) ) ;
#163402 = CARTESIAN_POINT ( 'NONE',  ( 14.29746914071049879, -8.314922557960816363, 103.3322429386476955 ) ) ;
#163404 = CARTESIAN_POINT ( 'NONE',  ( 5.049401038298161559, -19.05341960407611168, 62.70724293864769550 ) ) ;
#163405 = CARTESIAN_POINT ( 'NONE',  ( -19.03943276465977164, -0.05219959533935918106, 98.75109039468567573 ) ) ;
#163406 = CARTESIAN_POINT ( 'NONE',  ( 0.05219959533910956823, 16.53943276465976808, 99.99890960531436690 ) ) ;
#163407 = CARTESIAN_POINT ( 'NONE',  ( 21.55341960407619695, -5.719274019375665929, 66.04275706135236135 ) ) ;
#163409 = CARTESIAN_POINT ( 'NONE',  ( -10.72451020669898014, 18.67979575497178502, 115.4155762719810241 ) ) ;
#163408 = CARTESIAN_POINT ( 'NONE',  ( 9.474510206698971260, -16.51473224551069308, 52.91557627198102409 ) ) ;
#163410 = CARTESIAN_POINT ( 'NONE',  ( -21.55341960407610458, -5.719274019375992779, 106.4572429386477097 ) ) ;
#163411 = CARTESIAN_POINT ( 'NONE',  ( 28.82186960331499392, -9.364793116373510529, 144.9000000000000057 ) ) ;
#163412 = CARTESIAN_POINT ( 'NONE',  ( 19.02544592524343514, -5.153800228976328945, 73.54057627198103830 ) ) ;
#163413 = CARTESIAN_POINT ( 'NONE',  ( 17.26172910966780094, 6.454744622555824485, 111.6935309135077290 ) ) ;
#163415 = CARTESIAN_POINT ( 'NONE',  ( 21.52544592524344225, -5.823673210054117533, 33.54057627198102409 ) ) ;
#163414 = CARTESIAN_POINT ( 'NONE',  ( 9.474510206698729675, 16.51473224551082808, 102.0844237280190043 ) ) ;
#163416 = CARTESIAN_POINT ( 'NONE',  ( 15.72974639402176855, 15.80617190586768217, 46.87609039468568994 ) ) ;
#163417 = CARTESIAN_POINT ( 'NONE',  ( -5.153800228976328057, -19.02544592524343514, 97.29057627198099567 ) ) ;
#163418 = CARTESIAN_POINT ( 'NONE',  ( -19.03943276465977164, -0.05219959533935918106, 88.75109039468567573 ) ) ;
#163419 = CARTESIAN_POINT ( 'NONE',  ( 13.97604488694527802, 13.89961937509977652, 44.37390960531435269 ) ) ;
#163420 = CARTESIAN_POINT ( 'NONE',  ( -5.153800228976328057, -19.02544592524343514, 72.29057627198102409 ) ) ;
#163421 = CARTESIAN_POINT ( 'NONE',  ( 12.14591786802309770, 12.06949235617756955, 84.37390960531438111 ) ) ;
#163422 = CARTESIAN_POINT ( 'NONE',  ( -16.51473224551069308, -9.474510206698971260, 106.6655762719810383 ) ) ;
#163423 = CARTESIAN_POINT ( 'NONE',  ( 4.379528057220339221, -16.55341960407611168, 92.70724293864770971 ) ) ;
#163424 = CARTESIAN_POINT ( 'NONE',  ( 19.02544592524343514, -5.153800228976328945, 98.54057627198100988 ) ) ;
#163426 = CARTESIAN_POINT ( 'NONE',  ( 19.05341960407611168, 5.049401038298154454, 23.95724293864769194 ) ) ;
#163425 = CARTESIAN_POINT ( 'NONE',  ( -4.483927247898539470, -16.52544592524342804, 37.29057627198102409 ) ) ;
#163427 = ORIENTED_EDGE ( 'NONE', *, *, #177539, .T. ) ;
#163428 = CARTESIAN_POINT ( 'NONE',  ( 21.53943276465977519, 0.05219959533937863772, 56.25109039468568284 ) ) ;
#163429 = CARTESIAN_POINT ( 'NONE',  ( -19.05341960407617563, 5.049401038297882671, 73.54275706135233293 ) ) ;
#163430 = CARTESIAN_POINT ( 'NONE',  ( 8.224510206698953496, -14.34966873604960469, 42.91557627198103120 ) ) ;
#163431 = CARTESIAN_POINT ( 'NONE',  ( -10.72451020669898014, 18.67979575497178502, 105.4155762719810383 ) ) ;
#163432 = CARTESIAN_POINT ( 'NONE',  ( 21.52544592524344225, -5.823673210054117533, 38.54057627198103120 ) ) ;
#163434 = CARTESIAN_POINT ( 'NONE',  ( 0.05219959533910956823, 16.53943276465976808, 84.99890960531436690 ) ) ;
#163433 = AXIS2_PLACEMENT_3D ( 'NONE', #132462, #54614, #85951 ) ;
#163435 = CARTESIAN_POINT ( 'NONE',  ( 16.51473224551069308, 9.474510206698969483, 54.16557627198103120 ) ) ;
#163436 = CARTESIAN_POINT ( 'NONE',  ( 14.34966873604960469, 8.224510206698951720, 24.16557627198103120 ) ) ;
#163437 = CARTESIAN_POINT ( 'NONE',  ( -8.224510206698735004, -14.34966873604973081, 104.5844237280190185 ) ) ;
#163438 = CARTESIAN_POINT ( 'NONE',  ( -12.14591786802326823, 12.06949235617739902, 68.12609039468567573 ) ) ;
#163439 = CARTESIAN_POINT ( 'NONE',  ( 13.89961937509957401, 13.97604488694547697, 26.87609039468566507 ) ) ;
#163440 = CARTESIAN_POINT ( 'NONE',  ( -9.564922557960796823, -16.46253265017161027, 102.0822429386477097 ) ) ;
#163441 = CARTESIAN_POINT ( 'NONE',  ( 5.049401038298161559, -19.05341960407611168, 82.70724293864770971 ) ) ;
#163442 = CARTESIAN_POINT ( 'NONE',  ( -5.049401038298153566, 19.05341960407611168, 40.20724293864768839 ) ) ;
#163443 = CARTESIAN_POINT ( 'NONE',  ( -4.483927247898539470, -16.52544592524342804, 42.29057627198103120 ) ) ;
#163445 = CARTESIAN_POINT ( 'NONE',  ( 9.564922557960805705, 16.46253265017160317, 99.58224293864770971 ) ) ;
#163444 = LINE ( 'NONE', #26940, #140361 ) ;
#163446 = CARTESIAN_POINT ( 'NONE',  ( -21.53943276465977519, 0.05219959533907696930, 41.24890960531435269 ) ) ;
#163447 = CARTESIAN_POINT ( 'NONE',  ( -4.483927247898539470, -16.52544592524342804, 67.29057627198103830 ) ) ;
#163448 = CARTESIAN_POINT ( 'NONE',  ( 8.314922557961029526, -14.29746914071037800, 20.41775706135234714 ) ) ;
#163449 = CARTESIAN_POINT ( 'NONE',  ( 0.05219959533910956823, 16.53943276465976808, 59.99890960531436690 ) ) ;
#163450 = CARTESIAN_POINT ( 'NONE',  ( 17.50000000000000355, -5.068104630630418050, 33.22818405340032655 ) ) ;
#163451 = CARTESIAN_POINT ( 'NONE',  ( -19.03943276465977164, -0.05219959533935918106, 63.75109039468566863 ) ) ;
#163452 = CARTESIAN_POINT ( 'NONE',  ( -13.89961937509977652, 13.97604488694528158, 100.6239096053143669 ) ) ;
#163453 = CARTESIAN_POINT ( 'NONE',  ( 9.564922557961047289, -16.46253265017146816, 85.41775706135233293 ) ) ;
#163454 = CARTESIAN_POINT ( 'NONE',  ( -17.14385361876520619, 23.59649016807275856, 147.0750000027311728 ) ) ;
#163456 = CARTESIAN_POINT ( 'NONE',  ( -16.52544592524335698, -4.483927247898792601, 98.95942372801903275 ) ) ;
#163455 = CARTESIAN_POINT ( 'NONE',  ( -0.05219959533934338120, 16.53943276465976808, 22.50109039468567573 ) ) ;
#163457 = CARTESIAN_POINT ( 'NONE',  ( -16.46253265017160317, 9.564922557960807481, 45.83224293864769550 ) ) ;
#163458 = CARTESIAN_POINT ( 'NONE',  ( 21.52544592524344225, -5.823673210054117533, 38.54057627198103120 ) ) ;
#163459 = CARTESIAN_POINT ( 'NONE',  ( 15.72974639402176855, 15.80617190586768217, 51.87609039468568284 ) ) ;
#163460 = CARTESIAN_POINT ( 'NONE',  ( 23.31738231874054890, -16.94106989632523508, 147.0500000054623797 ) ) ;
#163461 = CARTESIAN_POINT ( 'NONE',  ( 4.483927247898790824, -16.52544592524335698, 20.20942372801900788 ) ) ;
#163463 = CARTESIAN_POINT ( 'NONE',  ( 19.03943276465977164, -0.05219959533909143690, 68.74890960531436690 ) ) ;
#163462 = DIRECTION ( 'NONE',  ( -1.000000000000000000, 0.000000000000000000, 0.000000000000000000 ) ) ;
#163464 = ADVANCED_FACE ( 'NONE', ( #190136 ), #183744, .F. ) ;
#163465 = CARTESIAN_POINT ( 'NONE',  ( 0.05219959533909260263, 19.03943276465977164, 114.9989096053143669 ) ) ;
#163467 = CARTESIAN_POINT ( 'NONE',  ( 19.02544592524343514, -5.153800228976328945, 78.54057627198099567 ) ) ;
#163466 = CARTESIAN_POINT ( 'NONE',  ( 16.53943276465976808, -0.05219959533910856209, 93.74890960531436690 ) ) ;
#163468 = CARTESIAN_POINT ( 'NONE',  ( 19.03943276465977164, -0.05219959533909143690, 88.74890960531436690 ) ) ;
#163469 = ORIENTED_EDGE ( 'NONE', *, *, #23111, .F. ) ;
#163470 = CARTESIAN_POINT ( 'NONE',  ( -5.153800228976607833, 19.02544592524334988, 92.70942372801901854 ) ) ;
#163471 = CARTESIAN_POINT ( 'NONE',  ( -15.72974639402197994, 15.80617190586746368, 65.62390960531436690 ) ) ;
#163472 = CARTESIAN_POINT ( 'NONE',  ( 9.564922557960805705, 16.46253265017160317, 24.58224293864769194 ) ) ;
#163473 = CARTESIAN_POINT ( 'NONE',  ( 19.05341960407617918, -5.049401038297876454, 51.04275706135231871 ) ) ;
#163474 = CARTESIAN_POINT ( 'NONE',  ( 13.89961937509977652, -13.97604488694527269, 63.12390960531435979 ) ) ;
#163475 = CARTESIAN_POINT ( 'NONE',  ( -19.03943276465977164, 0.05219959533909376836, 91.24890960531436690 ) ) ;
#163476 = ORIENTED_EDGE ( 'NONE', *, *, #7692, .T. ) ;
#163477 = CARTESIAN_POINT ( 'NONE',  ( 10.72451020669898902, -18.67979575497178502, 92.91557627198103830 ) ) ;
#163479 = CARTESIAN_POINT ( 'NONE',  ( 9.564922557961047289, -16.46253265017146816, 60.41775706135233293 ) ) ;
#163478 = CARTESIAN_POINT ( 'NONE',  ( -14.34966873604960291, -8.224510206698953496, 91.66557627198103830 ) ) ;
#163480 = CARTESIAN_POINT ( 'NONE',  ( -21.52544592524343514, 5.823673210054127303, 96.04057627198102409 ) ) ;
#163481 = CARTESIAN_POINT ( 'NONE',  ( -18.67979575497178146, -10.72451020669898902, 76.66557627198103830 ) ) ;
#163482 = CARTESIAN_POINT ( 'NONE',  ( -8.314922557960811034, -14.29746914071050412, 27.08224293864769550 ) ) ;
#163483 = CARTESIAN_POINT ( 'NONE',  ( -5.823673210054431948, 21.52544592524334988, 102.7094237280190185 ) ) ;
#163484 = CARTESIAN_POINT ( 'NONE',  ( -16.55341960407617563, 4.379528057220093196, 58.54275706135235424 ) ) ;
#163485 = CARTESIAN_POINT ( 'NONE',  ( 5.049401038298161559, -19.05341960407611168, 82.70724293864770971 ) ) ;
#163486 = CARTESIAN_POINT ( 'NONE',  ( -13.89961937509977652, 13.97604488694528158, 30.62390960531435269 ) ) ;
#163487 = CARTESIAN_POINT ( 'NONE',  ( -21.55341960407619339, 5.719274019375674811, 38.54275706135234714 ) ) ;
#163488 = CARTESIAN_POINT ( 'NONE',  ( 21.55341960407619695, -5.719274019375665929, 56.04275706135235424 ) ) ;
#163489 = CARTESIAN_POINT ( 'NONE',  ( 5.153800228976335163, 19.02544592524342804, 49.79057627198100988 ) ) ;
#163490 = CARTESIAN_POINT ( 'NONE',  ( -21.53943276465977519, -0.05219959533937600094, 23.75109039468567929 ) ) ;
#163491 = CARTESIAN_POINT ( 'NONE',  ( 5.153800228976615827, -19.02544592524334988, 55.20942372801899722 ) ) ;
#163492 = EDGE_CURVE ( 'NONE', #135352, #194071, #111290, .T. ) ;
#163493 = CARTESIAN_POINT ( 'NONE',  ( 13.89961937509957401, 13.97604488694547697, 76.87609039468566152 ) ) ;
#163494 = CARTESIAN_POINT ( 'NONE',  ( 0.05219959533934541429, -16.53943276465976808, 35.00109039468568284 ) ) ;
#163495 = DIRECTION ( 'NONE',  ( 0.000000000000000000, 0.000000000000000000, -1.000000000000000000 ) ) ;
#163496 = CARTESIAN_POINT ( 'NONE',  ( -4.483927247898782831, 16.52544592524335698, 67.70942372801901854 ) ) ;
#163497 = CARTESIAN_POINT ( 'NONE',  ( -9.564922557960796823, -16.46253265017161027, 42.08224293864769550 ) ) ;
#163498 = CARTESIAN_POINT ( 'NONE',  ( 21.81230582904620618, -5.969922009378142214, 172.1979875755925775 ) ) ;
#163499 = CARTESIAN_POINT ( 'NONE',  ( 16.46253265017160672, -9.564922557960803928, 103.3322429386476955 ) ) ;
#163500 = CARTESIAN_POINT ( 'NONE',  ( -19.05341960407611168, -5.049401038298163336, 26.45724293864769550 ) ) ;
#163501 = CARTESIAN_POINT ( 'NONE',  ( -21.55341960407610458, -5.719274019375992779, 66.45724293864768129 ) ) ;
#163502 = CARTESIAN_POINT ( 'NONE',  ( -4.483927247898782831, 16.52544592524335698, 57.70942372801901143 ) ) ;
#163503 = CARTESIAN_POINT ( 'NONE',  ( 21.52544592524334988, 5.823673210054432836, 111.4594237280190328 ) ) ;
#163504 = CARTESIAN_POINT ( 'NONE',  ( -5.049401038298153566, 19.05341960407611168, 45.20724293864769550 ) ) ;
#163505 = CARTESIAN_POINT ( 'NONE',  ( -16.52544592524342804, 4.483927247898546575, 31.04057627198102409 ) ) ;
#163506 = CARTESIAN_POINT ( 'NONE',  ( 12.06949235617757843, -12.14591786802309237, 73.12390960531436690 ) ) ;
#163507 = CARTESIAN_POINT ( 'NONE',  ( 19.02544592524343514, -5.153800228976328945, 83.54057627198100988 ) ) ;
#163508 = CARTESIAN_POINT ( 'NONE',  ( -5.823673210054431948, 21.52544592524334988, 42.70942372801901854 ) ) ;
#163509 = CARTESIAN_POINT ( 'NONE',  ( 16.51473224551069308, 9.474510206698969483, 84.16557627198102409 ) ) ;
#163510 = CARTESIAN_POINT ( 'NONE',  ( -10.81492255796105439, 18.62759615963255655, 82.91775706135234714 ) ) ;
#163511 = CARTESIAN_POINT ( 'NONE',  ( -8.314922557961024197, 14.29746914071037800, 62.91775706135236135 ) ) ;
#163512 = CARTESIAN_POINT ( 'NONE',  ( -19.05341960407611168, -5.049401038298163336, 106.4572429386476955 ) ) ;
#163513 = CARTESIAN_POINT ( 'NONE',  ( -16.53943276465976808, 0.05219959533911058130, 46.24890960531435979 ) ) ;
#163514 = CARTESIAN_POINT ( 'NONE',  ( -9.564922557960796823, -16.46253265017161027, 22.08224293864768839 ) ) ;
#163515 = CARTESIAN_POINT ( 'NONE',  ( 8.224510206698742110, 14.34966873604972548, 52.08442372801901854 ) ) ;
#163516 = CARTESIAN_POINT ( 'NONE',  ( -16.55341960407611168, -4.379528057220339221, 51.45724293864770260 ) ) ;
#163517 = CARTESIAN_POINT ( 'NONE',  ( -0.05219959533909027116, -19.03943276465977164, 107.4989096053143527 ) ) ;
#163518 = CARTESIAN_POINT ( 'NONE',  ( -21.55341960407610458, -5.719274019375992779, 31.45724293864769550 ) ) ;
#163519 = CARTESIAN_POINT ( 'NONE',  ( -18.67979575497193778, 10.72451020669871902, 108.3344237280190185 ) ) ;
#163520 = CARTESIAN_POINT ( 'NONE',  ( -12.14591786802309592, -12.06949235617757132, 101.8739096053143811 ) ) ;
#163521 = CARTESIAN_POINT ( 'NONE',  ( -9.564922557960796823, -16.46253265017161027, 92.08224293864769550 ) ) ;
#163522 = VERTEX_POINT ( 'NONE', #192131 ) ;
#163523 = CARTESIAN_POINT ( 'NONE',  ( -16.55341960407617563, 4.379528057220093196, 48.54275706135234714 ) ) ;
#163524 = CARTESIAN_POINT ( 'NONE',  ( 5.049401038298161559, -19.05341960407611168, 52.70724293864767418 ) ) ;
#163525 = CARTESIAN_POINT ( 'NONE',  ( -9.564922557961040184, 16.46253265017147172, 47.91775706135233293 ) ) ;
#163526 = CARTESIAN_POINT ( 'NONE',  ( 16.55341960407618274, -4.379528057220086978, 91.04275706135236135 ) ) ;
#163527 = CARTESIAN_POINT ( 'NONE',  ( 16.51473224551083163, -9.474510206698727899, 100.8344237280190043 ) ) ;
#163528 = CARTESIAN_POINT ( 'NONE',  ( -18.62759615963255300, -10.81492255796106328, 64.16775706135234714 ) ) ;
#163529 = CARTESIAN_POINT ( 'NONE',  ( -19.03943276465977164, 0.05219959533909376836, 81.24890960531436690 ) ) ;
#163530 = CARTESIAN_POINT ( 'NONE',  ( 21.53943276465977519, -0.05219959533907433946, 93.74890960531436690 ) ) ;
#163531 = CARTESIAN_POINT ( 'NONE',  ( 4.379528057220339221, -16.55341960407611168, 107.7072429386476955 ) ) ;
#163532 = VECTOR ( 'NONE', #146371, 1000.000000000000000 ) ;
#163533 = CARTESIAN_POINT ( 'NONE',  ( 16.46253265017146816, 9.564922557961045513, 86.66775706135233293 ) ) ;
#163534 = CARTESIAN_POINT ( 'NONE',  ( 21.53943276465977519, -0.05219959533907433946, 78.74890960531436690 ) ) ;
#163535 = CARTESIAN_POINT ( 'NONE',  ( 16.46253265017146816, 9.564922557961045513, 36.66775706135233293 ) ) ;
#163536 = FACE_BOUND ( 'NONE', #105166, .T. ) ;
#163537 = CARTESIAN_POINT ( 'NONE',  ( -21.52544592524343514, 5.823673210054127303, 96.04057627198102409 ) ) ;
#163538 = CARTESIAN_POINT ( 'NONE',  ( -28.88419406831849301, 24.88742053112121511, -7.973410913627005492 ) ) ;
#163539 = CARTESIAN_POINT ( 'NONE',  ( 19.02544592524343514, -5.153800228976328945, 63.54057627198103830 ) ) ;
#163540 = CARTESIAN_POINT ( 'NONE',  ( 0.000000000000000000, 0.000000000000000000, -64.92279855667830191 ) ) ;
#163541 = CARTESIAN_POINT ( 'NONE',  ( 14.29746914071037800, 8.314922557961029526, 21.66775706135235069 ) ) ;
#163542 = CARTESIAN_POINT ( 'NONE',  ( -18.22780087662122028, 5.500000000000031086, 58.51540105326107977 ) ) ;
#163543 = CARTESIAN_POINT ( 'NONE',  ( 0.05219959533909260263, 19.03943276465977164, 49.99890960531435979 ) ) ;
#163544 = CARTESIAN_POINT ( 'NONE',  ( 9.564922557960805705, 16.46253265017160317, 114.5822429386476955 ) ) ;
#163546 = CARTESIAN_POINT ( 'NONE',  ( 0.05219959533910956823, 16.53943276465976808, 49.99890960531437401 ) ) ;
#163545 = CARTESIAN_POINT ( 'NONE',  ( -21.53943276465977519, 0.05219959533907696930, 101.2489096053143669 ) ) ;
#163547 = CARTESIAN_POINT ( 'NONE',  ( -18.62759615963255300, -10.81492255796106328, 79.16775706135234714 ) ) ;
#163549 = CARTESIAN_POINT ( 'NONE',  ( -9.564922557961040184, 16.46253265017147172, 32.91775706135233293 ) ) ;
#163548 = CARTESIAN_POINT ( 'NONE',  ( 12.14591786802327356, -12.06949235617739191, 20.62609039468568639 ) ) ;
#163550 = CARTESIAN_POINT ( 'NONE',  ( -12.14591786802309592, -12.06949235617757132, 36.87390960531435979 ) ) ;
#163551 = CARTESIAN_POINT ( 'NONE',  ( 5.823673210054125526, 21.52544592524343514, 114.7905762719810383 ) ) ;
#163552 = CARTESIAN_POINT ( 'NONE',  ( -16.52544592524342804, 4.483927247898546575, 46.04057627198103830 ) ) ;
#163553 = CARTESIAN_POINT ( 'NONE',  ( 13.89961937509957401, 13.97604488694547697, 96.87609039468566152 ) ) ;
#163554 = CARTESIAN_POINT ( 'NONE',  ( 19.05341960407617918, -5.049401038297876454, 66.04275706135233293 ) ) ;
#163555 = CARTESIAN_POINT ( 'NONE',  ( 0.05219959533937995610, -21.53943276465977519, 65.00109039468568994 ) ) ;
#163556 = CARTESIAN_POINT ( 'NONE',  ( 19.03943276465977164, 0.05219959533936151252, 51.25109039468567573 ) ) ;
#163557 = CARTESIAN_POINT ( 'NONE',  ( 14.29746914071049879, -8.314922557960816363, 113.3322429386476955 ) ) ;
#163558 = CARTESIAN_POINT ( 'NONE',  ( 15.80617190586746368, 15.72974639402197994, 39.37390960531436690 ) ) ;
#163559 = CARTESIAN_POINT ( 'NONE',  ( -12.06949235617756955, 12.14591786802309770, 50.62390960531435979 ) ) ;
#163560 = CARTESIAN_POINT ( 'NONE',  ( -18.56197773271729901, 5.499999999999997335, 93.55066217314454491 ) ) ;
#163561 = CARTESIAN_POINT ( 'NONE',  ( -0.05219959533936034679, 19.03943276465977164, 22.50109039468566152 ) ) ;
#163562 = CARTESIAN_POINT ( 'NONE',  ( -14.29746914071037622, -8.314922557961029526, 79.16775706135234714 ) ) ;
#163563 = CARTESIAN_POINT ( 'NONE',  ( -12.14591786802309592, -12.06949235617757132, 41.87390960531435979 ) ) ;
#163564 = CARTESIAN_POINT ( 'NONE',  ( 5.823673210054444382, -21.52544592524334988, 80.20942372801901854 ) ) ;
#163565 = CARTESIAN_POINT ( 'NONE',  ( -5.719274019375665041, -21.55341960407619695, 69.79275706135234714 ) ) ;
#163566 = CARTESIAN_POINT ( 'NONE',  ( -5.719274019375978568, 21.55341960407610458, 80.20724293864769550 ) ) ;
#163567 = CARTESIAN_POINT ( 'NONE',  ( 16.46253265017160672, -9.564922557960803928, 43.33224293864769550 ) ) ;
#163568 = CARTESIAN_POINT ( 'NONE',  ( -15.72974639402176322, -15.80617190586768395, 54.37609039468568994 ) ) ;
#163569 = CARTESIAN_POINT ( 'NONE',  ( 19.02544592524343514, -5.153800228976328945, 33.54057627198102409 ) ) ;
#163570 = CARTESIAN_POINT ( 'NONE',  ( 13.89961937509977652, -13.97604488694527269, 48.12390960531435979 ) ) ;
#163571 = CARTESIAN_POINT ( 'NONE',  ( -12.14591786802309592, -12.06949235617757132, 91.87390960531436690 ) ) ;
#163572 = CARTESIAN_POINT ( 'NONE',  ( 19.02544592524343514, -5.153800228976328945, 93.54057627198102409 ) ) ;
#163573 = CARTESIAN_POINT ( 'NONE',  ( -16.55341960407611168, -4.379528057220339221, 36.45724293864768839 ) ) ;
#163574 = CARTESIAN_POINT ( 'NONE',  ( -16.52544592524342804, 4.483927247898546575, 101.0405762719810383 ) ) ;
#163575 = CARTESIAN_POINT ( 'NONE',  ( 18.62759615963271287, -10.81492255796078972, 68.33224293864769550 ) ) ;
#163576 = CARTESIAN_POINT ( 'NONE',  ( -10.72451020669870658, -18.67979575497194134, 19.58442372801901143 ) ) ;
#163577 = CARTESIAN_POINT ( 'NONE',  ( -19.02544592524342804, 5.153800228976336051, 116.0405762719810383 ) ) ;
#163579 = CARTESIAN_POINT ( 'NONE',  ( -4.379528057220086978, -16.55341960407618274, 29.79275706135234358 ) ) ;
#163578 = CARTESIAN_POINT ( 'NONE',  ( -19.02544592524342804, 5.153800228976336051, 76.04057627198102409 ) ) ;
#163580 = CARTESIAN_POINT ( 'NONE',  ( -21.52544592524343514, 5.823673210054127303, 66.04057627198103830 ) ) ;
#163581 = CARTESIAN_POINT ( 'NONE',  ( -21.53943276465977519, -0.05219959533937600094, 98.75109039468568994 ) ) ;
#163582 = CARTESIAN_POINT ( 'NONE',  ( -5.049401038298153566, 19.05341960407611168, 75.20724293864769550 ) ) ;
#163583 = CARTESIAN_POINT ( 'NONE',  ( 18.67979575497194134, -10.72451020669871369, 30.83442372801902209 ) ) ;
#163584 = CARTESIAN_POINT ( 'NONE',  ( 5.153800228976335163, 19.02544592524342804, 114.7905762719810241 ) ) ;
#163585 = CARTESIAN_POINT ( 'NONE',  ( 12.14591786802327356, -12.06949235617739191, 95.62609039468568994 ) ) ;
#163586 = CARTESIAN_POINT ( 'NONE',  ( -0.05219959533937732626, 21.53943276465977519, 77.50109039468567573 ) ) ;
#163587 = CARTESIAN_POINT ( 'NONE',  ( -10.72451020669870658, -18.67979575497194134, 94.58442372801901854 ) ) ;
#163588 = CARTESIAN_POINT ( 'NONE',  ( -8.314922557961024197, 14.29746914071037800, 57.91775706135234714 ) ) ;
#163589 = CARTESIAN_POINT ( 'NONE',  ( -21.52544592524334988, -5.823673210054445271, 23.95942372801901143 ) ) ;
#163590 = CARTESIAN_POINT ( 'NONE',  ( 19.03943276465977164, -0.05219959533909143690, 113.7489096053143669 ) ) ;
#163591 = CARTESIAN_POINT ( 'NONE',  ( 18.62759615963255655, 10.81492255796105972, 91.66775706135234714 ) ) ;
#163592 = CARTESIAN_POINT ( 'NONE',  ( -9.564922557960796823, -16.46253265017161027, 87.08224293864769550 ) ) ;
#163593 = CARTESIAN_POINT ( 'NONE',  ( 21.52544592524344225, -5.823673210054117533, 83.54057627198102409 ) ) ;
#163594 = CARTESIAN_POINT ( 'NONE',  ( -13.89961937509957401, -13.97604488694547875, 59.37609039468566863 ) ) ;
#163596 = CARTESIAN_POINT ( 'NONE',  ( -5.823673210054116645, -21.52544592524344225, 57.29057627198103120 ) ) ;
#163595 = CARTESIAN_POINT ( 'NONE',  ( -13.57915378923026317, -35.22819508409138933, -29.39033328705865245 ) ) ;
#163598 = CARTESIAN_POINT ( 'NONE',  ( 4.483927247898545687, 16.52544592524342804, 39.79057627198103830 ) ) ;
#163597 = CARTESIAN_POINT ( 'NONE',  ( 16.51473224551069308, 9.474510206698969483, 89.16557627198103830 ) ) ;
#163599 = CARTESIAN_POINT ( 'NONE',  ( 21.82220748998222959, 8.288476145941624296, 169.3167957967150414 ) ) ;
#163600 = CARTESIAN_POINT ( 'NONE',  ( -9.564922557961040184, 16.46253265017147172, 72.91775706135233293 ) ) ;
#163601 = CARTESIAN_POINT ( 'NONE',  ( -17.26058549869090797, 6.457015423128532383, 103.6225416252393643 ) ) ;
#163602 = CARTESIAN_POINT ( 'NONE',  ( -4.379528057220086978, -16.55341960407618274, 19.79275706135235069 ) ) ;
#163603 = CARTESIAN_POINT ( 'NONE',  ( 21.53943276465977519, -0.05219959533907433946, 88.74890960531436690 ) ) ;
#163604 = CARTESIAN_POINT ( 'NONE',  ( 12.14591786802309770, 12.06949235617756955, 64.37390960531435269 ) ) ;
#163605 = CARTESIAN_POINT ( 'NONE',  ( -19.03943276465977164, 0.05219959533909376836, 106.2489096053143669 ) ) ;
#163606 = CARTESIAN_POINT ( 'NONE',  ( 0.05219959533934541429, -16.53943276465976808, 35.00109039468568284 ) ) ;
#163607 = CARTESIAN_POINT ( 'NONE',  ( 9.474510206698971260, -16.51473224551069308, 57.91557627198103120 ) ) ;
#163609 = CARTESIAN_POINT ( 'NONE',  ( 16.51473224551083163, -9.474510206698727899, 90.83442372801900433 ) ) ;
#163608 = CARTESIAN_POINT ( 'NONE',  ( -18.62759615963255300, -10.81492255796106328, 19.16775706135234714 ) ) ;
#163610 = CARTESIAN_POINT ( 'NONE',  ( 16.51473224551069308, 9.474510206698969483, 89.16557627198103830 ) ) ;
#163611 = CARTESIAN_POINT ( 'NONE',  ( 5.153800228976335163, 19.02544592524342804, 79.79057627198102409 ) ) ;
#163612 = CARTESIAN_POINT ( 'NONE',  ( 21.52544592524344225, -5.823673210054117533, 78.54057627198103830 ) ) ;
#163613 = CARTESIAN_POINT ( 'NONE',  ( -5.153800228976328057, -19.02544592524343514, 52.29057627198100988 ) ) ;
#163614 = DIRECTION ( 'NONE',  ( 0.000000000000000000, 0.000000000000000000, 1.000000000000000000 ) ) ;
#163615 = CARTESIAN_POINT ( 'NONE',  ( -12.06949235617756955, 12.14591786802309770, 50.62390960531435979 ) ) ;
#163616 = CARTESIAN_POINT ( 'NONE',  ( -19.02544592524342804, 5.153800228976336051, 106.0405762719810241 ) ) ;
#163617 = CARTESIAN_POINT ( 'NONE',  ( -18.22780087662119541, 5.500000000000102141, 41.01763182126894236 ) ) ;
#163618 = CARTESIAN_POINT ( 'NONE',  ( -9.474510206698720793, -16.51473224551083518, 69.58442372801901854 ) ) ;
#163619 = CARTESIAN_POINT ( 'NONE',  ( 10.72451020669898902, -18.67979575497178502, 72.91557627198103830 ) ) ;
#163620 = CARTESIAN_POINT ( 'NONE',  ( 19.05341960407617918, -5.049401038297876454, 51.04275706135231871 ) ) ;
#163621 = CARTESIAN_POINT ( 'NONE',  ( 5.153800228976335163, 19.02544592524342804, 104.7905762719809957 ) ) ;
#163622 = CARTESIAN_POINT ( 'NONE',  ( -17.49999999999999645, 4.640572885337594933, 115.6378816454884486 ) ) ;
#163623 = CARTESIAN_POINT ( 'NONE',  ( 21.53943276465977519, -0.05219959533907433946, 38.74890960531435979 ) ) ;
#163624 = CARTESIAN_POINT ( 'NONE',  ( -19.03943276465977164, 0.05219959533909376836, 71.24890960531435269 ) ) ;
#163625 = CARTESIAN_POINT ( 'NONE',  ( 10.81492255796106328, -18.62759615963255655, 65.41775706135234714 ) ) ;
#163626 = CARTESIAN_POINT ( 'NONE',  ( 16.51473224551069308, 9.474510206698969483, 34.16557627198102409 ) ) ;
#163628 = VERTEX_POINT ( 'NONE', #196152 ) ;
#163627 = CARTESIAN_POINT ( 'NONE',  ( 12.06949235617757843, -12.14591786802309237, 73.12390960531436690 ) ) ;
#163629 = CARTESIAN_POINT ( 'NONE',  ( 18.67979575497194134, -10.72451020669871369, 55.83442372801901854 ) ) ;
#163630 = ORIENTED_EDGE ( 'NONE', *, *, #158665, .T. ) ;
#163631 = CARTESIAN_POINT ( 'NONE',  ( 19.03943276465977164, -0.05219959533909143690, 108.7489096053143527 ) ) ;
#163633 = EDGE_CURVE ( 'NONE', #50923, #192458, #179033, .T. ) ;
#163632 = CARTESIAN_POINT ( 'NONE',  ( -5.153800228976607833, 19.02544592524334988, 62.70942372801899722 ) ) ;
#163634 = CARTESIAN_POINT ( 'NONE',  ( 20.41037832431316090, -34.40082058117813801, -24.99999999999991829 ) ) ;
#163635 = CARTESIAN_POINT ( 'NONE',  ( 5.823673210054125526, 21.52544592524343514, 114.7905762719810383 ) ) ;
#163636 = CARTESIAN_POINT ( 'NONE',  ( 19.05341960407611168, 5.049401038298154454, 53.95724293864770260 ) ) ;
#163637 = CARTESIAN_POINT ( 'NONE',  ( -16.53943276465976808, -0.05219959533934237506, 43.75109039468568284 ) ) ;
#163638 = CARTESIAN_POINT ( 'NONE',  ( -23.48529157249599919, -32.32473071737750558, -9.449999994537623849 ) ) ;
#163639 = CARTESIAN_POINT ( 'NONE',  ( -19.02544592524334988, -5.153800228976617603, 23.95942372801900078 ) ) ;
#163640 = CARTESIAN_POINT ( 'NONE',  ( -19.03943276465977164, 0.05219959533909376836, 46.24890960531435979 ) ) ;
#163641 = CARTESIAN_POINT ( 'NONE',  ( 19.02544592524334988, 5.153800228976608722, 21.45942372801899012 ) ) ;
#163642 = CARTESIAN_POINT ( 'NONE',  ( -8.224510206698735004, -14.34966873604973081, 94.58442372801901854 ) ) ;
#163644 = CARTESIAN_POINT ( 'NONE',  ( 15.80617190586769283, -15.72974639402175789, 55.62609039468568284 ) ) ;
#163643 = CARTESIAN_POINT ( 'NONE',  ( -19.03943276465977164, 0.05219959533909376836, 91.24890960531436690 ) ) ;
#163645 = CARTESIAN_POINT ( 'NONE',  ( 6.874011537017774565, -5.225144896384527726, -62.00632993653601233 ) ) ;
#163646 = CARTESIAN_POINT ( 'NONE',  ( 0.05219959533909260263, 19.03943276465977164, 109.9989096053143669 ) ) ;
#163647 = CARTESIAN_POINT ( 'NONE',  ( -17.50000000000017764, 3.417042746626915317, 30.17380396232480066 ) ) ;
#163649 = CARTESIAN_POINT ( 'NONE',  ( 18.62759615963255655, 10.81492255796105972, 76.66775706135234714 ) ) ;
#163648 = CARTESIAN_POINT ( 'NONE',  ( 0.05219959533934541429, -16.53943276465976808, 50.00109039468568994 ) ) ;
#163650 = CARTESIAN_POINT ( 'NONE',  ( 10.72451020669871369, 18.67979575497193778, 107.0844237280190043 ) ) ;
#163651 = CARTESIAN_POINT ( 'NONE',  ( -10.87998047749161046, 9.250641775538069211, -60.21451611132643222 ) ) ;
#163652 = CARTESIAN_POINT ( 'NONE',  ( 14.29746914071037800, 8.314922557961029526, 31.66775706135234358 ) ) ;
#163653 = CARTESIAN_POINT ( 'NONE',  ( -19.03943276465977164, 0.05219959533909376836, 81.24890960531436690 ) ) ;
#163654 = CARTESIAN_POINT ( 'NONE',  ( 16.51473224551069308, 9.474510206698969483, 114.1655762719810241 ) ) ;
#163655 = EDGE_LOOP ( 'NONE', ( #194739, #87840, #129341, #18476, #138150, #69076, #38830, #72270, #39547, #52898, #169475, #119699, #186860, #17420, #155496, #176360, #158675, #149919, #86238, #136602, #182040, #117699, #44604, #108910, #192216, #82532, #86285, #134610, #52095, #51727, #184322, #150004, #69070, #104319, #152646, #42658, #79018, #179042, #126519, #151394, #131169, #148117, #174107, #123126, #75353, #95796, #132119, #166389, #71110, #38129, #6243, #27504, #93975, #133116, #118016, #164629 ) ) ;
#163656 = DIRECTION ( 'NONE',  ( 0.000000000000000000, 0.000000000000000000, 1.000000000000000000 ) ) ;
#163657 = CARTESIAN_POINT ( 'NONE',  ( 13.89961937509977652, -13.97604488694527269, 28.12390960531435624 ) ) ;
#163658 = CARTESIAN_POINT ( 'NONE',  ( 15.80617190586746368, 15.72974639402197994, 44.37390960531435979 ) ) ;
#163659 = CARTESIAN_POINT ( 'NONE',  ( 8.224510206698742110, 14.34966873604972548, 107.0844237280190043 ) ) ;
#163661 = CARTESIAN_POINT ( 'NONE',  ( 16.46253265017160672, -9.564922557960803928, 73.33224293864769550 ) ) ;
#163660 = CARTESIAN_POINT ( 'NONE',  ( 4.379528057220339221, -16.55341960407611168, 82.70724293864770971 ) ) ;
#163662 = CARTESIAN_POINT ( 'NONE',  ( 5.719274019375673035, 21.55341960407619339, 102.2927570613523613 ) ) ;
#163663 = B_SPLINE_CURVE_WITH_KNOTS ( 'NONE', 3,
 ( #15063, #185915, #188905, #107057, #155560, #76723, #169735, #186926, #92879, #16062, #1873, #77720, #63554, #48396, #84673, #115029, #5846, #81671, #147371, #144359, #98842, #20029, #23028, #22026, #176722, #99851 ),
 .UNSPECIFIED., .F., .F.,
 ( 4, 2, 2, 2, 2, 2, 2, 2, 2, 2, 2, 2, 4 ),
 ( 1.964780709336654224E-07, 0.001036009418421648520, 0.001553915888597004469, 0.002071822358772360418, 0.003107635299123065378, 0.004143448239473769036, 0.006215074120175169414, 0.008286700000876570660, 0.01035832588157797017, 0.01139413882192866732, 0.01242995176227936274, 0.01450157764298075705, 0.01657320352368214789 ),
 .UNSPECIFIED. ) ;
#163664 = CARTESIAN_POINT ( 'NONE',  ( -4.379528057220086978, -16.55341960407618274, 19.79275706135235069 ) ) ;
#163665 = CARTESIAN_POINT ( 'NONE',  ( 12.06949235617757843, -12.14591786802309237, 93.12390960531436690 ) ) ;
#163666 = CARTESIAN_POINT ( 'NONE',  ( -15.72974639402176322, -15.80617190586768395, 44.37609039468567573 ) ) ;
#163667 = CARTESIAN_POINT ( 'NONE',  ( 15.72974639402199770, -15.80617190586745480, 78.12390960531436690 ) ) ;
#163668 = CARTESIAN_POINT ( 'NONE',  ( 13.97604488694548053, -13.89961937509957401, 55.62609039468566863 ) ) ;
#163669 = CARTESIAN_POINT ( 'NONE',  ( 16.51473224551069308, 9.474510206698969483, 44.16557627198103120 ) ) ;
#163670 = CARTESIAN_POINT ( 'NONE',  ( 5.153800228976335163, 19.02544592524342804, 94.79057627198103830 ) ) ;
#163671 = CARTESIAN_POINT ( 'NONE',  ( 8.224510206698953496, -14.34966873604960469, 67.91557627198102409 ) ) ;
#163672 = CARTESIAN_POINT ( 'NONE',  ( -16.52544592524342804, 4.483927247898546575, 51.04057627198103120 ) ) ;
#163673 = CARTESIAN_POINT ( 'NONE',  ( 4.379528057220339221, -16.55341960407611168, 22.70724293864769194 ) ) ;
#163674 = CARTESIAN_POINT ( 'NONE',  ( 16.46253265017146816, 9.564922557961045513, 71.66775706135233293 ) ) ;
#163675 = CARTESIAN_POINT ( 'NONE',  ( -19.48894818550246200, 5.499999999999919176, 85.10307310435239003 ) ) ;
#163676 = CARTESIAN_POINT ( 'NONE',  ( 5.719274019375991003, -21.55341960407610458, 22.70724293864769194 ) ) ;
#163677 = CARTESIAN_POINT ( 'NONE',  ( 16.53943276465976808, -0.05219959533910856209, 83.74890960531435269 ) ) ;
#163678 = CYLINDRICAL_SURFACE ( 'NONE', #23886, 5.000000000000000888 ) ;
#163680 = CARTESIAN_POINT ( 'NONE',  ( 18.67979575497178502, 10.72451020669898547, 54.16557627198103120 ) ) ;
#163679 = CARTESIAN_POINT ( 'NONE',  ( 9.564922557960805705, 16.46253265017160317, 44.58224293864769550 ) ) ;
#163681 = CARTESIAN_POINT ( 'NONE',  ( -18.62759615963270932, 10.81492255796079327, 75.83224293864769550 ) ) ;
#163682 = CARTESIAN_POINT ( 'NONE',  ( -14.34966873604960291, -8.224510206698953496, 111.6655762719810525 ) ) ;
#163684 = CARTESIAN_POINT ( 'NONE',  ( -9.474510206698964154, 16.51473224551069663, 60.41557627198102409 ) ) ;
#163683 = CARTESIAN_POINT ( 'NONE',  ( 4.483927247898790824, -16.52544592524335698, 70.20942372801904696 ) ) ;
#163685 = CARTESIAN_POINT ( 'NONE',  ( 19.05341960407617918, -5.049401038297876454, 36.04275706135234003 ) ) ;
#163686 = CARTESIAN_POINT ( 'NONE',  ( -5.823673210054431948, 21.52544592524334988, 52.70942372801902565 ) ) ;
#163687 = AXIS2_PLACEMENT_3D ( 'NONE', #125293, #40245, #178777 ) ;
#163688 = CARTESIAN_POINT ( 'NONE',  ( 12.14591786802309770, 12.06949235617756955, 104.3739096053143669 ) ) ;
#163689 = CARTESIAN_POINT ( 'NONE',  ( -19.05341960407617563, 5.049401038297882671, 93.54275706135234714 ) ) ;
#163690 = CARTESIAN_POINT ( 'NONE',  ( 3.556970738554034288E-15, -38.81732327939057114, -4.624999997268814056 ) ) ;
#163692 = CARTESIAN_POINT ( 'NONE',  ( -5.719274019375978568, 21.55341960407610458, 50.20724293864769550 ) ) ;
#163691 = CARTESIAN_POINT ( 'NONE',  ( 69.65682714487590488, -71.74905178543389184, -4.999999999999999112 ) ) ;
#163693 = CARTESIAN_POINT ( 'NONE',  ( -16.51473224551069308, -9.474510206698971260, 21.66557627198102765 ) ) ;
#163694 = CARTESIAN_POINT ( 'NONE',  ( 0.05219959533937995610, -21.53943276465977519, 90.00109039468567573 ) ) ;
#163695 = CARTESIAN_POINT ( 'NONE',  ( -8.314922557960811034, -14.29746914071050412, 27.08224293864769550 ) ) ;
#163697 = CARTESIAN_POINT ( 'NONE',  ( 14.34966873604960469, 8.224510206698951720, 59.16557627198103120 ) ) ;
#163696 = CARTESIAN_POINT ( 'NONE',  ( 16.53943276465976808, 0.05219959533934440121, 61.25109039468567573 ) ) ;
#163698 = B_SPLINE_CURVE_WITH_KNOTS ( 'NONE', 3,
 ( #17957, #79611, #20918, #37083, #173627, #129075 ),
 .UNSPECIFIED., .F., .F.,
 ( 4, 2, 4 ),
 ( 0.000000000000000000, 0.0003837532665553974615, 0.0007675065331107949231 ),
 .UNSPECIFIED. ) ;
#163699 = CARTESIAN_POINT ( 'NONE',  ( -21.53943276465977519, 0.05219959533907696930, 76.24890960531435269 ) ) ;
#163700 = CARTESIAN_POINT ( 'NONE',  ( -5.719274019375978568, 21.55341960407610458, 75.20724293864769550 ) ) ;
#163701 = CYLINDRICAL_SURFACE ( 'NONE', #140274, 28.82186960331498682 ) ;
#163703 = CARTESIAN_POINT ( 'NONE',  ( -9.474510206698964154, 16.51473224551069663, 115.4155762719810241 ) ) ;
#163702 = CARTESIAN_POINT ( 'NONE',  ( -13.89961937509957401, -13.97604488694547875, 79.37609039468567573 ) ) ;
#163704 = CARTESIAN_POINT ( 'NONE',  ( 19.03943276465977164, -0.05219959533909143690, 53.74890960531436690 ) ) ;
#163705 = CARTESIAN_POINT ( 'NONE',  ( -9.564922557960796823, -16.46253265017161027, 27.08224293864769550 ) ) ;
#163706 = CYLINDRICAL_SURFACE ( 'NONE', #2569, 1.000000000000000888 ) ;
#163707 = ORIENTED_EDGE ( 'NONE', *, *, #100813, .T. ) ;
#163708 = CARTESIAN_POINT ( 'NONE',  ( 16.55341960407618274, -4.379528057220086978, 86.04275706135236135 ) ) ;
#163709 = CARTESIAN_POINT ( 'NONE',  ( 0.05219959533907565091, 21.53943276465977519, 104.9989096053143669 ) ) ;
#163710 = CARTESIAN_POINT ( 'NONE',  ( -16.51473224551069308, -9.474510206698971260, 71.66557627198102409 ) ) ;
#163711 = CARTESIAN_POINT ( 'NONE',  ( 21.52544592524334988, 5.823673210054432836, 46.45942372801901854 ) ) ;
#163712 = CARTESIAN_POINT ( 'NONE',  ( -13.89961937509977652, 13.97604488694528158, 90.62390960531432427 ) ) ;
#163714 = EDGE_LOOP ( 'NONE', ( #78446, #107198, #32080, #10973 ) ) ;
#163713 = CARTESIAN_POINT ( 'NONE',  ( -21.14397880779349137, -35.31393329058855102, -18.60109459635327767 ) ) ;
#163715 = VERTEX_POINT ( 'NONE', #135464 ) ;
#163716 = CARTESIAN_POINT ( 'NONE',  ( 5.719274019375673035, 21.55341960407619339, 27.29275706135234358 ) ) ;
#163718 = CARTESIAN_POINT ( 'NONE',  ( 19.02544592524343514, -5.153800228976328945, 98.54057627198100988 ) ) ;
#163717 = CARTESIAN_POINT ( 'NONE',  ( -13.89961937509977652, 13.97604488694528158, 25.62390960531434558 ) ) ;
#163719 = CARTESIAN_POINT ( 'NONE',  ( -16.51473224551082808, 9.474510206698731452, 43.33442372801900433 ) ) ;
#163720 = CARTESIAN_POINT ( 'NONE',  ( -18.67979575497178146, -10.72451020669898902, 111.6655762719810525 ) ) ;
#163721 = CARTESIAN_POINT ( 'NONE',  ( 0.05219959533936267826, -19.03943276465977164, 50.00109039468566863 ) ) ;
#163722 = CARTESIAN_POINT ( 'NONE',  ( 0.05219959533936267826, -19.03943276465977164, 50.00109039468566863 ) ) ;
#163723 = CARTESIAN_POINT ( 'NONE',  ( -4.379528057220086978, -16.55341960407618274, 99.79275706135234714 ) ) ;
#163725 = ORIENTED_EDGE ( 'NONE', *, *, #187343, .T. ) ;
#163724 = CARTESIAN_POINT ( 'NONE',  ( -17.79613651744293890, -24.49428055684527550, 146.2843446568999752 ) ) ;
#163726 = CARTESIAN_POINT ( 'NONE',  ( -19.05341960407611168, -5.049401038298163336, 76.45724293864769550 ) ) ;
#163727 = VECTOR ( 'NONE', #9012, 1000.000000000000000 ) ;
#163728 = CARTESIAN_POINT ( 'NONE',  ( -21.53943276465977519, -0.05219959533937600094, 83.75109039468568994 ) ) ;
#163729 = CARTESIAN_POINT ( 'NONE',  ( -5.823673210054431948, 21.52544592524334988, 97.70942372801904696 ) ) ;
#163730 = CARTESIAN_POINT ( 'NONE',  ( -1.461319442807290869, -7.990187535671176455, -64.16708268805476223 ) ) ;
#163731 = CARTESIAN_POINT ( 'NONE',  ( -0.05219959533909027116, -19.03943276465977164, 92.49890960531436690 ) ) ;
#163732 = CARTESIAN_POINT ( 'NONE',  ( -15.80617190586768217, 15.72974639402176855, 58.12609039468568994 ) ) ;
#163733 = CARTESIAN_POINT ( 'NONE',  ( 8.224510206698742110, 14.34966873604972548, 22.08442372801901143 ) ) ;
#163734 = EDGE_CURVE ( 'NONE', #199255, #14026, #69855, .T. ) ;
#163735 = CARTESIAN_POINT ( 'NONE',  ( 19.02544592524343514, -5.153800228976328945, 63.54057627198103830 ) ) ;
#163736 = CARTESIAN_POINT ( 'NONE',  ( 13.89961937509977652, -13.97604488694527269, 113.1239096053143527 ) ) ;
#163737 = CARTESIAN_POINT ( 'NONE',  ( -9.564922557960796823, -16.46253265017161027, 87.08224293864769550 ) ) ;
#163738 = FACE_OUTER_BOUND ( 'NONE', #170283, .T. ) ;
#163739 = CARTESIAN_POINT ( 'NONE',  ( -5.049401038298153566, 19.05341960407611168, 65.20724293864765286 ) ) ;
#163740 = CARTESIAN_POINT ( 'NONE',  ( 19.05341960407611168, 5.049401038298154454, 53.95724293864770260 ) ) ;
#163741 = CARTESIAN_POINT ( 'NONE',  ( -5.719274019375978568, 21.55341960407610458, 110.2072429386477239 ) ) ;
#163742 = CARTESIAN_POINT ( 'NONE',  ( 14.34966873604972726, -8.224510206698740333, 105.8344237280190328 ) ) ;
#163743 = DIRECTION ( 'NONE',  ( -1.000000000000000000, 0.000000000000000000, -6.982962677686266711E-15 ) ) ;
#163744 = CARTESIAN_POINT ( 'NONE',  ( 16.46253265017146816, 9.564922557961045513, 61.66775706135234003 ) ) ;
#163745 = CARTESIAN_POINT ( 'NONE',  ( -16.51473224551069308, -9.474510206698971260, 91.66557627198103830 ) ) ;
#163746 = CARTESIAN_POINT ( 'NONE',  ( -12.14591786802309592, -12.06949235617757132, 76.87390960531439532 ) ) ;
#163747 = CARTESIAN_POINT ( 'NONE',  ( 4.379528057220339221, -16.55341960407611168, 102.7072429386476955 ) ) ;
#163748 = CARTESIAN_POINT ( 'NONE',  ( -15.72974639402197994, 15.80617190586746368, 30.62390960531436335 ) ) ;
#163749 = CARTESIAN_POINT ( 'NONE',  ( 5.153800228976335163, 19.02544592524342804, 114.7905762719810241 ) ) ;
#163750 = CARTESIAN_POINT ( 'NONE',  ( -14.34966873604960291, -8.224510206698953496, 91.66557627198103830 ) ) ;
#163751 = CARTESIAN_POINT ( 'NONE',  ( -17.50000000000001421, 5.622605283950871780, 53.68792689403890250 ) ) ;
#163752 = CARTESIAN_POINT ( 'NONE',  ( 16.51473224551083163, -9.474510206698727899, 40.83442372801900433 ) ) ;
#163753 = CARTESIAN_POINT ( 'NONE',  ( 4.483927247898790824, -16.52544592524335698, 100.2094237280190043 ) ) ;
#163754 = CARTESIAN_POINT ( 'NONE',  ( -19.05341960407611168, -5.049401038298163336, 91.45724293864766707 ) ) ;
#163755 = CARTESIAN_POINT ( 'NONE',  ( 18.67979575497194134, -10.72451020669871369, 50.83442372801901143 ) ) ;
#163756 = CARTESIAN_POINT ( 'NONE',  ( 15.80617190586746368, 15.72974639402197994, 49.37390960531436690 ) ) ;
#163757 = CARTESIAN_POINT ( 'NONE',  ( 21.53943276465977519, 0.05219959533937863772, 31.25109039468568639 ) ) ;
#163758 = CARTESIAN_POINT ( 'NONE',  ( -5.719274019375978568, 21.55341960407610458, 80.20724293864769550 ) ) ;
#163759 = CARTESIAN_POINT ( 'NONE',  ( 16.53943276465976808, -0.05219959533910856209, 108.7489096053143669 ) ) ;
#163760 = CARTESIAN_POINT ( 'NONE',  ( 5.049401038297881783, 19.05341960407617563, 62.29275706135234003 ) ) ;
#163761 = CARTESIAN_POINT ( 'NONE',  ( -16.51473224551069308, -9.474510206698971260, 46.66557627198102409 ) ) ;
#163762 = CARTESIAN_POINT ( 'NONE',  ( -19.03943276465977164, 0.05219959533909376836, 96.24890960531436690 ) ) ;
#163763 = CARTESIAN_POINT ( 'NONE',  ( 19.02544592524343514, -5.153800228976328945, 93.54057627198102409 ) ) ;
#163764 = CARTESIAN_POINT ( 'NONE',  ( 19.02544592524343514, -5.153800228976328945, 23.54057627198102054 ) ) ;
#163765 = CARTESIAN_POINT ( 'NONE',  ( 8.314922557960818139, 14.29746914071049879, 44.58224293864769550 ) ) ;
#163766 = CARTESIAN_POINT ( 'NONE',  ( 16.52544592524335698, 4.483927247898782831, 41.45942372801901143 ) ) ;
#163767 = CARTESIAN_POINT ( 'NONE',  ( -15.80617190586768217, 15.72974639402176855, 108.1260903946856757 ) ) ;
#163769 = CARTESIAN_POINT ( 'NONE',  ( 12.06949235617757843, -12.14591786802309237, 23.12390960531436335 ) ) ;
#163768 = CARTESIAN_POINT ( 'NONE',  ( -5.049401038298153566, 19.05341960407611168, 115.2072429386477097 ) ) ;
#163770 = CARTESIAN_POINT ( 'NONE',  ( -5.823673210054431948, 21.52544592524334988, 32.70942372801900433 ) ) ;
#163771 = CARTESIAN_POINT ( 'NONE',  ( 13.97604488694527802, 13.89961937509977652, 109.3739096053143669 ) ) ;
#163772 = CARTESIAN_POINT ( 'NONE',  ( 16.53943276465976808, 0.05219959533934440121, 56.25109039468568284 ) ) ;
#163773 = CARTESIAN_POINT ( 'NONE',  ( 4.379528057220092307, 16.55341960407617563, 102.2927570613523613 ) ) ;
#163774 = CARTESIAN_POINT ( 'NONE',  ( -12.06949235617739369, -12.14591786802326823, 99.37609039468568994 ) ) ;
#163775 = CARTESIAN_POINT ( 'NONE',  ( -4.483927247898782831, 16.52544592524335698, 22.70942372801901499 ) ) ;
#163776 = CARTESIAN_POINT ( 'NONE',  ( -9.474510206698964154, 16.51473224551069663, 45.41557627198103120 ) ) ;
#163777 = CARTESIAN_POINT ( 'NONE',  ( 12.06949235617757843, -12.14591786802309237, 113.1239096053143953 ) ) ;
#163778 = CARTESIAN_POINT ( 'NONE',  ( 0.05219959533937995610, -21.53943276465977519, 20.00109039468568639 ) ) ;
#163779 = CARTESIAN_POINT ( 'NONE',  ( -19.02544592524342804, 5.153800228976336051, 36.04057627198100988 ) ) ;
#163780 = CARTESIAN_POINT ( 'NONE',  ( -5.153800228976328057, -19.02544592524343514, 107.2905762719810383 ) ) ;
#163781 = CARTESIAN_POINT ( 'NONE',  ( 15.80617190586769283, -15.72974639402175789, 35.62609039468568994 ) ) ;
#163782 = CARTESIAN_POINT ( 'NONE',  ( -19.02544592524342804, 5.153800228976336051, 26.04057627198103120 ) ) ;
#163783 = CARTESIAN_POINT ( 'NONE',  ( 13.97604488694527802, 13.89961937509977652, 109.3739096053143669 ) ) ;
#163784 = CARTESIAN_POINT ( 'NONE',  ( 16.62475595723700650, -7.163666690055283226, 113.0271335181047050 ) ) ;
#163785 = CARTESIAN_POINT ( 'NONE',  ( 13.97604488694527802, 13.89961937509977652, 99.37390960531436690 ) ) ;
#163787 = CARTESIAN_POINT ( 'NONE',  ( 16.52544592524342804, -4.483927247898539470, 93.54057627198103830 ) ) ;
#163786 = CARTESIAN_POINT ( 'NONE',  ( -5.719274019375665041, -21.55341960407619695, 39.79275706135235424 ) ) ;
#163788 = CARTESIAN_POINT ( 'NONE',  ( -16.51473224551069308, -9.474510206698971260, 101.6655762719810241 ) ) ;
#163789 = CARTESIAN_POINT ( 'NONE',  ( 17.59860650958994555, -7.585241751806880650, 70.92337014262493256 ) ) ;
#163790 = CARTESIAN_POINT ( 'NONE',  ( -16.55341960407617563, 4.379528057220093196, 63.54275706135234003 ) ) ;
#163791 = CARTESIAN_POINT ( 'NONE',  ( 21.53943276465977519, 0.05219959533937863772, 81.25109039468568994 ) ) ;
#163792 = CARTESIAN_POINT ( 'NONE',  ( -4.483927247898782831, 16.52544592524335698, 37.70942372801900433 ) ) ;
#163793 = CARTESIAN_POINT ( 'NONE',  ( 5.049401038298161559, -19.05341960407611168, 82.70724293864770971 ) ) ;
#163794 = CARTESIAN_POINT ( 'NONE',  ( 13.89961937509957401, 13.97604488694547697, 106.8760903946856757 ) ) ;
#163795 = CARTESIAN_POINT ( 'NONE',  ( -4.483927247898782831, 16.52544592524335698, 67.70942372801901854 ) ) ;
#163796 = CARTESIAN_POINT ( 'NONE',  ( -16.46253265017146816, -9.564922557961047289, 19.16775706135233293 ) ) ;
#163797 = CARTESIAN_POINT ( 'NONE',  ( -13.97604488694547697, 13.89961937509957934, 93.12609039468566152 ) ) ;
#163798 = CARTESIAN_POINT ( 'NONE',  ( -19.03943276465977164, 0.05219959533909376836, 66.24890960531436690 ) ) ;
#163799 = CARTESIAN_POINT ( 'NONE',  ( -0.05219959533907301413, -21.53943276465977519, 82.49890960531436690 ) ) ;
#163801 = CARTESIAN_POINT ( 'NONE',  ( 9.564922557961047289, -16.46253265017146816, 95.41775706135233293 ) ) ;
#163800 = CARTESIAN_POINT ( 'NONE',  ( 14.34966873604960469, 8.224510206698951720, 94.16557627198103830 ) ) ;
#163802 = CARTESIAN_POINT ( 'NONE',  ( 4.483927247898790824, -16.52544592524335698, 65.20942372801901854 ) ) ;
#163803 = CARTESIAN_POINT ( 'NONE',  ( 24.20757866959953120, 5.698759791481088577, 172.9004493943157570 ) ) ;
#163804 = CARTESIAN_POINT ( 'NONE',  ( 9.474510206698729675, 16.51473224551082808, 52.08442372801900433 ) ) ;
#163805 = CARTESIAN_POINT ( 'NONE',  ( 16.52544592524342804, -4.483927247898539470, 33.54057627198102409 ) ) ;
#163806 = CARTESIAN_POINT ( 'NONE',  ( 16.53943276465976808, -0.05219959533910856209, 83.74890960531435269 ) ) ;
#163808 = CARTESIAN_POINT ( 'NONE',  ( 16.51473224551083163, -9.474510206698727899, 45.83442372801900433 ) ) ;
#163807 = CARTESIAN_POINT ( 'NONE',  ( 0.05219959533937995610, -21.53943276465977519, 110.0010903946856757 ) ) ;
#163809 = CARTESIAN_POINT ( 'NONE',  ( 18.67979575497194134, -10.72451020669871369, 25.83442372801901499 ) ) ;
#163810 = CARTESIAN_POINT ( 'NONE',  ( -5.049401038298153566, 19.05341960407611168, 95.20724293864770971 ) ) ;
#163811 = CARTESIAN_POINT ( 'NONE',  ( -5.153800228976328057, -19.02544592524343514, 77.29057627198099567 ) ) ;
#163812 = CARTESIAN_POINT ( 'NONE',  ( -15.72974639402176322, -15.80617190586768395, 94.37609039468568994 ) ) ;
#163813 = CARTESIAN_POINT ( 'NONE',  ( 19.05341960407611168, 5.049401038298154454, 78.95724293864769550 ) ) ;
#163814 = CARTESIAN_POINT ( 'NONE',  ( 18.67979575497178502, 10.72451020669898547, 39.16557627198102409 ) ) ;
#163815 = CARTESIAN_POINT ( 'NONE',  ( 16.52544592524342804, -4.483927247898539470, 83.54057627198102409 ) ) ;
#163816 = CARTESIAN_POINT ( 'NONE',  ( 19.02544592524343514, -5.153800228976328945, 58.54057627198102409 ) ) ;
#163817 = CARTESIAN_POINT ( 'NONE',  ( -12.06949235617756955, 12.14591786802309770, 100.6239096053143811 ) ) ;
#163818 = VECTOR ( 'NONE', #196805, 1000.000000000000000 ) ;
#163819 = CARTESIAN_POINT ( 'NONE',  ( -15.72974639402176322, -15.80617190586768395, 24.37609039468567573 ) ) ;
#163820 = CARTESIAN_POINT ( 'NONE',  ( 5.823673210054444382, -21.52544592524334988, 65.20942372801901854 ) ) ;
#163821 = CARTESIAN_POINT ( 'NONE',  ( -0.05219959533909027116, -19.03943276465977164, 47.49890960531435979 ) ) ;
#163822 = CARTESIAN_POINT ( 'NONE',  ( -12.06949235617739369, -12.14591786802326823, 59.37609039468568284 ) ) ;
#163823 = CARTESIAN_POINT ( 'NONE',  ( 18.67979575497178502, 10.72451020669898547, 114.1655762719810383 ) ) ;
#163824 = CARTESIAN_POINT ( 'NONE',  ( -21.55341960407610458, -5.719274019375992779, 111.4572429386476813 ) ) ;
#163826 = CARTESIAN_POINT ( 'NONE',  ( 9.474510206698971260, -16.51473224551069308, 62.91557627198102409 ) ) ;
#163825 = CARTESIAN_POINT ( 'NONE',  ( -9.564922557961040184, 16.46253265017147172, 42.91775706135234003 ) ) ;
#163827 = CARTESIAN_POINT ( 'NONE',  ( -30.00000000000000355, 3.181980515339468241, 1.110912703473986074 ) ) ;
#163828 = CARTESIAN_POINT ( 'NONE',  ( -21.53943276465977519, -0.05219959533937600094, 68.75109039468568994 ) ) ;
#163829 = CARTESIAN_POINT ( 'NONE',  ( -0.05219959533907301413, -21.53943276465977519, 57.49890960531435979 ) ) ;
#163830 = CARTESIAN_POINT ( 'NONE',  ( 14.34966873604960469, 8.224510206698951720, 44.16557627198103120 ) ) ;
#163832 = CARTESIAN_POINT ( 'NONE',  ( 16.51473224551083163, -9.474510206698727899, 20.83442372801899722 ) ) ;
#163831 = CARTESIAN_POINT ( 'NONE',  ( 21.53943276465977519, 0.05219959533937863772, 71.25109039468568994 ) ) ;
#163833 = CARTESIAN_POINT ( 'NONE',  ( 12.06949235617757843, -12.14591786802309237, 58.12390960531435979 ) ) ;
#163834 = CARTESIAN_POINT ( 'NONE',  ( 16.52544592524342804, -4.483927247898539470, 103.5405762719810383 ) ) ;
#163835 = CARTESIAN_POINT ( 'NONE',  ( -5.153800228976607833, 19.02544592524334988, 47.70942372801900433 ) ) ;
#163836 = CARTESIAN_POINT ( 'NONE',  ( -16.52544592524342804, 4.483927247898546575, 26.04057627198103475 ) ) ;
#163838 = ADVANCED_FACE ( 'NONE', ( #123235 ), #16080, .F. ) ;
#163837 = CARTESIAN_POINT ( 'NONE',  ( -5.823673210054431948, 21.52544592524334988, 72.70942372801901854 ) ) ;
#163839 = CARTESIAN_POINT ( 'NONE',  ( -19.02544592524342804, 5.153800228976336051, 61.04057627198103120 ) ) ;
#163840 = CARTESIAN_POINT ( 'NONE',  ( -16.51473224551082808, 9.474510206698731452, 28.33442372801900433 ) ) ;
#163841 = CARTESIAN_POINT ( 'NONE',  ( 5.823673210054125526, 21.52544592524343514, 34.79057627198103120 ) ) ;
#163842 = CARTESIAN_POINT ( 'NONE',  ( 21.53943276465977519, 0.05219959533937863772, 36.25109039468567573 ) ) ;
#163843 = CARTESIAN_POINT ( 'NONE',  ( 10.72451020669898902, -18.67979575497178502, 92.91557627198103830 ) ) ;
#163844 = CARTESIAN_POINT ( 'NONE',  ( 16.51473224551083163, -9.474510206698727899, 80.83442372801899012 ) ) ;
#163845 = CARTESIAN_POINT ( 'NONE',  ( 14.29746914071037800, 8.314922557961029526, 46.66775706135234714 ) ) ;
#163847 = CARTESIAN_POINT ( 'NONE',  ( 18.62759615963271287, -10.81492255796078972, 88.33224293864769550 ) ) ;
#163846 = CARTESIAN_POINT ( 'NONE',  ( 37.99626262588765258, 2.893932880411085066E-14, -5.002157773949823749 ) ) ;
#163848 = CARTESIAN_POINT ( 'NONE',  ( 16.52544592524342804, -4.483927247898539470, 93.54057627198103830 ) ) ;
#163849 = CARTESIAN_POINT ( 'NONE',  ( -30.07467525274877218, -23.10311534983929249, -22.45479934155870083 ) ) ;
#163850 = CARTESIAN_POINT ( 'NONE',  ( 12.14591786802327356, -12.06949235617739191, 25.62609039468567929 ) ) ;
#163851 = CARTESIAN_POINT ( 'NONE',  ( 10.72451020669898902, -18.67979575497178502, 47.91557627198102409 ) ) ;
#163853 = CARTESIAN_POINT ( 'NONE',  ( 12.06949235617739724, 12.14591786802326823, 91.87609039468568994 ) ) ;
#163852 = CIRCLE ( 'NONE', #134844, 28.02760797243269408 ) ;
#163854 = CARTESIAN_POINT ( 'NONE',  ( 19.05341960407611168, 5.049401038298154454, 23.95724293864769194 ) ) ;
#163855 = EDGE_CURVE ( 'NONE', #24501, #55198, #185933, .T. ) ;
#163856 = CARTESIAN_POINT ( 'NONE',  ( 14.34966873604972726, -8.224510206698740333, 55.83442372801901854 ) ) ;
#163857 = CARTESIAN_POINT ( 'NONE',  ( 21.52544592524334988, 5.823673210054432836, 31.45942372801901854 ) ) ;
#163858 = CARTESIAN_POINT ( 'NONE',  ( 10.72451020669898902, -18.67979575497178502, 47.91557627198102409 ) ) ;
#163859 = CARTESIAN_POINT ( 'NONE',  ( -0.05219959533934338120, 16.53943276465976808, 87.50109039468568994 ) ) ;
#163860 = CARTESIAN_POINT ( 'NONE',  ( 0.05219959533909260263, 19.03943276465977164, 99.99890960531436690 ) ) ;
#163862 = CARTESIAN_POINT ( 'NONE',  ( -13.89961937509977652, 13.97604488694528158, 25.62390960531434558 ) ) ;
#163861 = CARTESIAN_POINT ( 'NONE',  ( 15.72974639402176855, 15.80617190586768217, 61.87609039468568284 ) ) ;
#163863 = CARTESIAN_POINT ( 'NONE',  ( -10.72451020669898014, 18.67979575497178502, 45.41557627198103830 ) ) ;
#163864 = CARTESIAN_POINT ( 'NONE',  ( 0.05219959533909260263, 19.03943276465977164, 109.9989096053143669 ) ) ;
#163865 = EDGE_LOOP ( 'NONE', ( #100495, #175448, #93246, #15731, #44270, #156102, #141232, #118649, #35744, #65474 ) ) ;
#163866 = CARTESIAN_POINT ( 'NONE',  ( -0.05219959533936034679, 19.03943276465977164, 42.50109039468566152 ) ) ;
#163867 = CARTESIAN_POINT ( 'NONE',  ( 12.14591786802327356, -12.06949235617739191, 60.62609039468567573 ) ) ;
#163868 = CARTESIAN_POINT ( 'NONE',  ( 9.564922557960805705, 16.46253265017160317, 114.5822429386476955 ) ) ;
#163869 = ORIENTED_EDGE ( 'NONE', *, *, #134694, .T. ) ;
#163870 = CARTESIAN_POINT ( 'NONE',  ( 9.564922557960805705, 16.46253265017160317, 89.58224293864769550 ) ) ;
#163871 = CARTESIAN_POINT ( 'NONE',  ( 14.29746914071037800, 8.314922557961029526, 106.6677570613523756 ) ) ;
#163872 = CARTESIAN_POINT ( 'NONE',  ( 7.652493125987819944, -39.26116846142902261, -15.00000000000000000 ) ) ;
#163873 = CARTESIAN_POINT ( 'NONE',  ( -4.483927247898539470, -16.52544592524342804, 97.29057627198105251 ) ) ;
#163874 = CARTESIAN_POINT ( 'NONE',  ( 18.62759615963271287, -10.81492255796078972, 48.33224293864770260 ) ) ;
#163875 = CARTESIAN_POINT ( 'NONE',  ( 9.564922557960805705, 16.46253265017160317, 34.58224293864770260 ) ) ;
#163876 = CARTESIAN_POINT ( 'NONE',  ( -8.314922557961024197, 14.29746914071037800, 77.91775706135231871 ) ) ;
#163877 = CARTESIAN_POINT ( 'NONE',  ( 0.05219959533937995610, -21.53943276465977519, 35.00109039468568284 ) ) ;
#163878 = CARTESIAN_POINT ( 'NONE',  ( 19.03943276465977164, 0.05219959533936151252, 96.25109039468567573 ) ) ;
#163879 = CARTESIAN_POINT ( 'NONE',  ( 16.53943276465976808, -0.05219959533910856209, 88.74890960531436690 ) ) ;
#163880 = CARTESIAN_POINT ( 'NONE',  ( 9.474510206698971260, -16.51473224551069308, 42.91557627198103120 ) ) ;
#163881 = VECTOR ( 'NONE', #71599, 1000.000000000000000 ) ;
#163882 = CARTESIAN_POINT ( 'NONE',  ( 9.474510206698971260, -16.51473224551069308, 107.9155762719810383 ) ) ;
#163883 = CARTESIAN_POINT ( 'NONE',  ( 21.53943276465977519, 0.05219959533937863772, 101.2510903946856757 ) ) ;
#163884 = CARTESIAN_POINT ( 'NONE',  ( -9.564922557960796823, -16.46253265017161027, 72.08224293864770971 ) ) ;
#163885 = CARTESIAN_POINT ( 'NONE',  ( 14.29746914071037800, 8.314922557961029526, 61.66775706135235424 ) ) ;
#163886 = CARTESIAN_POINT ( 'NONE',  ( 10.81492255796106328, -18.62759615963255655, 95.41775706135234714 ) ) ;
#163887 = CARTESIAN_POINT ( 'NONE',  ( -16.52544592524335698, -4.483927247898792601, 58.95942372801902565 ) ) ;
#163888 = CARTESIAN_POINT ( 'NONE',  ( 19.03943276465977164, 0.05219959533936151252, 51.25109039468567573 ) ) ;
#163889 = EDGE_CURVE ( 'NONE', #152017, #78021, #39191, .T. ) ;
#163890 = CARTESIAN_POINT ( 'NONE',  ( 16.51473224551083163, -9.474510206698727899, 70.83442372801900433 ) ) ;
#163891 = VERTEX_POINT ( 'NONE', #151617 ) ;
#163892 = CARTESIAN_POINT ( 'NONE',  ( 21.55341960407619695, -5.719274019375665929, 61.04275706135234714 ) ) ;
#163893 = CARTESIAN_POINT ( 'NONE',  ( 9.474510206698971260, -16.51473224551069308, 67.91557627198102409 ) ) ;
#163894 = CARTESIAN_POINT ( 'NONE',  ( -9.564922557960796823, -16.46253265017161027, 22.08224293864768839 ) ) ;
#163895 = CARTESIAN_POINT ( 'NONE',  ( -9.564922557961040184, 16.46253265017147172, 57.91775706135233293 ) ) ;
#163896 = CARTESIAN_POINT ( 'NONE',  ( -16.46253265017160317, 9.564922557960807481, 110.8322429386476955 ) ) ;
#163897 = CARTESIAN_POINT ( 'NONE',  ( -0.05219959533909027116, -19.03943276465977164, 87.49890960531436690 ) ) ;
#163898 = CARTESIAN_POINT ( 'NONE',  ( 16.52544592524342804, -4.483927247898539470, 33.54057627198102409 ) ) ;
#163899 = CARTESIAN_POINT ( 'NONE',  ( -18.62759615963270932, 10.81492255796079327, 45.83224293864769550 ) ) ;
#163900 = CARTESIAN_POINT ( 'NONE',  ( -17.60779699588839264, -5.499999999999979572, 96.34981316670102558 ) ) ;
#163901 = CARTESIAN_POINT ( 'NONE',  ( 15.72974639402176855, 15.80617190586768217, 106.8760903946856899 ) ) ;
#163902 = CARTESIAN_POINT ( 'NONE',  ( -27.96779038917889793, 7.241162895362913687, 160.9774814432332164 ) ) ;
#163903 = CARTESIAN_POINT ( 'NONE',  ( 5.153800228976335163, 19.02544592524342804, 39.79057627198100988 ) ) ;
#163904 = CARTESIAN_POINT ( 'NONE',  ( 5.049401038298161559, -19.05341960407611168, 27.70724293864769550 ) ) ;
#163905 = CARTESIAN_POINT ( 'NONE',  ( -10.85402516922718874, -12.25173339339350775, -59.29444586289682206 ) ) ;
#163906 = CARTESIAN_POINT ( 'NONE',  ( 15.72974639402176855, 15.80617190586768217, 71.87609039468568994 ) ) ;
#163907 = CARTESIAN_POINT ( 'NONE',  ( -37.51207494968712552, -5.596088347520207229, -8.000000000000000000 ) ) ;
#163908 = CARTESIAN_POINT ( 'NONE',  ( -0.05219959533934338120, 16.53943276465976808, 57.50109039468568994 ) ) ;
#163909 = CARTESIAN_POINT ( 'NONE',  ( -18.67979575497178146, -10.72451020669898902, 81.66557627198103830 ) ) ;
#163910 = CARTESIAN_POINT ( 'NONE',  ( 12.14591786802309770, 12.06949235617756955, 54.37390960531435979 ) ) ;
#163912 = CARTESIAN_POINT ( 'NONE',  ( -0.05219959533909027116, -19.03943276465977164, 102.4989096053143669 ) ) ;
#163911 = CARTESIAN_POINT ( 'NONE',  ( 19.05341960407611168, 5.049401038298154454, 23.95724293864769194 ) ) ;
#163913 = CARTESIAN_POINT ( 'NONE',  ( 21.55341960407619695, -5.719274019375665929, 36.04275706135234714 ) ) ;
#163914 = CARTESIAN_POINT ( 'NONE',  ( -19.05341960407617563, 5.049401038297882671, 43.54275706135232582 ) ) ;
#163915 = CARTESIAN_POINT ( 'NONE',  ( -16.51473224551069308, -9.474510206698971260, 31.66557627198102054 ) ) ;
#163916 = CARTESIAN_POINT ( 'NONE',  ( 5.719274019375673035, 21.55341960407619339, 82.29275706135234714 ) ) ;
#163917 = CARTESIAN_POINT ( 'NONE',  ( 17.26172910966779384, -6.454744622555846689, 33.30646908649223548 ) ) ;
#163918 = CARTESIAN_POINT ( 'NONE',  ( -16.52544592524342804, 4.483927247898546575, 31.04057627198102409 ) ) ;
#163919 = CARTESIAN_POINT ( 'NONE',  ( 17.50000000000000355, 3.565345528327992231, 113.0750551319353292 ) ) ;
#163920 = CARTESIAN_POINT ( 'NONE',  ( -0.05219959533907301413, -21.53943276465977519, 37.49890960531436690 ) ) ;
#163921 = CARTESIAN_POINT ( 'NONE',  ( 3.503282210674363295, -48.86437366581479580, -23.00000000000000000 ) ) ;
#163922 = CARTESIAN_POINT ( 'NONE',  ( -19.05341960407611168, -5.049401038298163336, 91.45724293864766707 ) ) ;
#163923 = CARTESIAN_POINT ( 'NONE',  ( 4.379528057220339221, -16.55341960407611168, 92.70724293864770971 ) ) ;
#163924 = CARTESIAN_POINT ( 'NONE',  ( -19.05341960407617563, 5.049401038297882671, 108.5427570613523187 ) ) ;
#163925 = CARTESIAN_POINT ( 'NONE',  ( 18.62759615963271287, -10.81492255796078972, 58.33224293864768839 ) ) ;
#163926 = ORIENTED_EDGE ( 'NONE', *, *, #78587, .T. ) ;
#163927 = CARTESIAN_POINT ( 'NONE',  ( -19.02544592524342804, 5.153800228976336051, 36.04057627198100988 ) ) ;
#163929 = CARTESIAN_POINT ( 'NONE',  ( -15.80617190586745835, -15.72974639402198527, 86.87390960531438111 ) ) ;
#163928 = CARTESIAN_POINT ( 'NONE',  ( 19.05341960407611168, 5.049401038298154454, 83.95724293864766707 ) ) ;
#163931 = CARTESIAN_POINT ( 'NONE',  ( -13.97604488694527625, -13.89961937509977652, 101.8739096053143811 ) ) ;
#163930 = CARTESIAN_POINT ( 'NONE',  ( -12.14591786802326823, 12.06949235617739902, 108.1260903946856757 ) ) ;
#163932 = CARTESIAN_POINT ( 'NONE',  ( -5.049401038297874678, -19.05341960407617918, 84.79275706135233293 ) ) ;
#163933 = CARTESIAN_POINT ( 'NONE',  ( 0.05219959533937995610, -21.53943276465977519, 95.00109039468568994 ) ) ;
#163934 = CARTESIAN_POINT ( 'NONE',  ( 15.80617190586746368, 15.72974639402197994, 79.37390960531436690 ) ) ;
#163935 = CARTESIAN_POINT ( 'NONE',  ( 18.62759615963271287, -10.81492255796078972, 43.33224293864769550 ) ) ;
#163936 = CARTESIAN_POINT ( 'NONE',  ( 13.97604488694527802, 13.89961937509977652, 49.37390960531434558 ) ) ;
#163937 = CARTESIAN_POINT ( 'NONE',  ( 12.06949235617739724, 12.14591786802326823, 111.8760903946856615 ) ) ;
#163938 = CARTESIAN_POINT ( 'NONE',  ( -13.97604488694527625, -13.89961937509977652, 61.87390960531435979 ) ) ;
#163939 = EDGE_LOOP ( 'NONE', ( #55934, #55284, #67905, #104709, #43500 ) ) ;
#163940 = CARTESIAN_POINT ( 'NONE',  ( -31.27032343591157471, -7.501918430611450361, 95.46114142609054909 ) ) ;
#163941 = CARTESIAN_POINT ( 'NONE',  ( -0.05219959533936034679, 19.03943276465977164, 27.50109039468566507 ) ) ;
#163942 = CARTESIAN_POINT ( 'NONE',  ( -16.53943276465976808, 0.05219959533911058130, 76.24890960531435269 ) ) ;
#163943 = CARTESIAN_POINT ( 'NONE',  ( -21.53943276465977519, 0.05219959533907696930, 116.2489096053143669 ) ) ;
#163944 = CARTESIAN_POINT ( 'NONE',  ( 17.14385361876520264, -23.59649016807271238, 142.0750000027311444 ) ) ;
#163945 = CARTESIAN_POINT ( 'NONE',  ( 18.62759615963271287, -10.81492255796078972, 63.33224293864770260 ) ) ;
#163946 = CARTESIAN_POINT ( 'NONE',  ( -12.06949235617739369, -12.14591786802326823, 99.37609039468568994 ) ) ;
#163947 = CARTESIAN_POINT ( 'NONE',  ( -16.51473224551069308, -9.474510206698971260, 21.66557627198102765 ) ) ;
#163948 = CARTESIAN_POINT ( 'NONE',  ( 13.97604488694527802, 13.89961937509977652, 69.37390960531436690 ) ) ;
#163949 =( NAMED_UNIT ( * ) SI_UNIT ( $, .STERADIAN. ) SOLID_ANGLE_UNIT ( ) );
#163950 = FACE_OUTER_BOUND ( 'NONE', #120467, .T. ) ;
#163951 = CARTESIAN_POINT ( 'NONE',  ( -16.52544592524342804, 4.483927247898546575, 26.04057627198103475 ) ) ;
#163952 = CARTESIAN_POINT ( 'NONE',  ( 10.81492255796106328, -18.62759615963255655, 60.41775706135235424 ) ) ;
#163953 = CARTESIAN_POINT ( 'NONE',  ( 0.05219959533909260263, 19.03943276465977164, 114.9989096053143669 ) ) ;
#163954 = CARTESIAN_POINT ( 'NONE',  ( -5.719274019375665041, -21.55341960407619695, 99.79275706135234714 ) ) ;
#163955 = CARTESIAN_POINT ( 'NONE',  ( 9.564922557960805705, 16.46253265017160317, 34.58224293864770260 ) ) ;
#163956 = CARTESIAN_POINT ( 'NONE',  ( 13.89961937509977652, -13.97604488694527269, 33.12390960531434558 ) ) ;
#163957 = ORIENTED_EDGE ( 'NONE', *, *, #37951, .T. ) ;
#163958 = CARTESIAN_POINT ( 'NONE',  ( -15.72974639402176322, -15.80617190586768395, 94.37609039468568994 ) ) ;
#163959 = CARTESIAN_POINT ( 'NONE',  ( -8.314922557961024197, 14.29746914071037800, 52.91775706135235424 ) ) ;
#163960 = CARTESIAN_POINT ( 'NONE',  ( -21.53943276465977519, -0.05219959533937600094, 83.75109039468568994 ) ) ;
#163961 = CARTESIAN_POINT ( 'NONE',  ( -16.51473224551069308, -9.474510206698971260, 111.6655762719810383 ) ) ;
#163962 = CARTESIAN_POINT ( 'NONE',  ( -16.46253265017146816, -9.564922557961047289, 89.16775706135234714 ) ) ;
#163963 = CARTESIAN_POINT ( 'NONE',  ( -15.72974639402176322, -15.80617190586768395, 59.37609039468568284 ) ) ;
#163964 = CARTESIAN_POINT ( 'NONE',  ( -14.29746914071037622, -8.314922557961029526, 29.16775706135234003 ) ) ;
#163965 = CARTESIAN_POINT ( 'NONE',  ( -16.46253265017146816, -9.564922557961047289, 89.16775706135234714 ) ) ;
#163966 = CARTESIAN_POINT ( 'NONE',  ( -5.153800228976328057, -19.02544592524343514, 47.29057627198102409 ) ) ;
#163967 = CARTESIAN_POINT ( 'NONE',  ( 19.03943276465977164, 0.05219959533936151252, 101.2510903946856757 ) ) ;
#163968 = CARTESIAN_POINT ( 'NONE',  ( -16.46253265017146816, -9.564922557961047289, 89.16775706135234714 ) ) ;
#163969 = CARTESIAN_POINT ( 'NONE',  ( -14.34966873604960291, -8.224510206698953496, 51.66557627198102409 ) ) ;
#163970 = EDGE_CURVE ( 'NONE', #193478, #188443, #199031, .T. ) ;
#163971 = CARTESIAN_POINT ( 'NONE',  ( -19.05341960407617563, 5.049401038297882671, 73.54275706135233293 ) ) ;
#163972 = CARTESIAN_POINT ( 'NONE',  ( -8.224510206698735004, -14.34966873604973081, 59.58442372801901854 ) ) ;
#163973 = CARTESIAN_POINT ( 'NONE',  ( 0.05219959533936267826, -19.03943276465977164, 20.00109039468567218 ) ) ;
#163974 = CARTESIAN_POINT ( 'NONE',  ( -5.049401038298153566, 19.05341960407611168, 40.20724293864768839 ) ) ;
#163975 = CARTESIAN_POINT ( 'NONE',  ( -13.97604488694527625, -13.89961937509977652, 41.87390960531435979 ) ) ;
#163976 = CARTESIAN_POINT ( 'NONE',  ( -12.14591786802326823, 12.06949235617739902, 63.12609039468568994 ) ) ;
#163977 = CARTESIAN_POINT ( 'NONE',  ( 18.22780087662126647, 5.499999999999818812, 41.48236817873107185 ) ) ;
#163978 = CARTESIAN_POINT ( 'NONE',  ( -17.81289503416611097, -24.51734667627696496, 138.5500000054623229 ) ) ;
#163979 = CARTESIAN_POINT ( 'NONE',  ( 16.51473224551069308, 9.474510206698969483, 104.1655762719810241 ) ) ;
#163980 = CARTESIAN_POINT ( 'NONE',  ( 17.59860650958994555, -7.585241751806880650, 85.92337014262491834 ) ) ;
#163981 = VERTEX_POINT ( 'NONE', #13109 ) ;
#163982 = CARTESIAN_POINT ( 'NONE',  ( -5.153800228976607833, 19.02544592524334988, 92.70942372801901854 ) ) ;
#163983 = CARTESIAN_POINT ( 'NONE',  ( 15.72974639402199770, -15.80617190586745480, 38.12390960531436690 ) ) ;
#163985 = CARTESIAN_POINT ( 'NONE',  ( 16.46253265017146816, 9.564922557961045513, 106.6677570613523471 ) ) ;
#163984 = CARTESIAN_POINT ( 'NONE',  ( -16.51473224551082808, 9.474510206698731452, 28.33442372801900433 ) ) ;
#163986 = CARTESIAN_POINT ( 'NONE',  ( 9.474510206698971260, -16.51473224551069308, 27.91557627198103120 ) ) ;
#163987 = CARTESIAN_POINT ( 'NONE',  ( 19.03943276465977164, -0.05219959533909143690, 38.74890960531436690 ) ) ;
#163988 = CARTESIAN_POINT ( 'NONE',  ( -21.52544592524343514, 5.823673210054127303, 76.04057627198102409 ) ) ;
#163989 = CARTESIAN_POINT ( 'NONE',  ( -19.02544592524342804, 5.153800228976336051, 31.04057627198102409 ) ) ;
#163990 = CARTESIAN_POINT ( 'NONE',  ( -5.359611314223446995E-15, 29.16686587814335851, 144.8750000027311842 ) ) ;
#163991 = CARTESIAN_POINT ( 'NONE',  ( 9.474510206698729675, 16.51473224551082808, 87.08442372801900433 ) ) ;
#163992 = CARTESIAN_POINT ( 'NONE',  ( 16.55341960407611168, 4.379528057220329451, 58.95724293864770971 ) ) ;
#163993 = CARTESIAN_POINT ( 'NONE',  ( 18.62759615963271287, -10.81492255796078972, 33.33224293864769550 ) ) ;
#163994 = CARTESIAN_POINT ( 'NONE',  ( -10.72451020669870658, -18.67979575497194134, 104.5844237280190185 ) ) ;
#163995 = CARTESIAN_POINT ( 'NONE',  ( 21.52544592524344225, -5.823673210054117533, 78.54057627198103830 ) ) ;
#163996 = CARTESIAN_POINT ( 'NONE',  ( 5.823673210054444382, -21.52544592524334988, 70.20942372801904696 ) ) ;
#163997 = CARTESIAN_POINT ( 'NONE',  ( 21.55341960407619695, -5.719274019375665929, 61.04275706135234714 ) ) ;
#163998 = EDGE_CURVE ( 'NONE', #149545, #106915, #74774, .T. ) ;
#163999 = CARTESIAN_POINT ( 'NONE',  ( -9.564922557960796823, -16.46253265017161027, 107.0822429386476955 ) ) ;
#164001 = CARTESIAN_POINT ( 'NONE',  ( 10.72451020669871369, 18.67979575497193778, 57.08442372801901854 ) ) ;
#164000 = CARTESIAN_POINT ( 'NONE',  ( 14.34966873604972726, -8.224510206698740333, 100.8344237280190185 ) ) ;
#164002 = CARTESIAN_POINT ( 'NONE',  ( 13.89961937509977652, -13.97604488694527269, 53.12390960531434558 ) ) ;
#164003 = CARTESIAN_POINT ( 'NONE',  ( 5.153800228976615827, -19.02544592524334988, 30.20942372801900433 ) ) ;
#164004 = CARTESIAN_POINT ( 'NONE',  ( -21.52544592524334988, -5.823673210054445271, 23.95942372801901143 ) ) ;
#164005 = CARTESIAN_POINT ( 'NONE',  ( -19.03943276465977164, 0.05219959533909376836, 71.24890960531435269 ) ) ;
#164006 = CARTESIAN_POINT ( 'NONE',  ( -16.52544592524342804, 4.483927247898546575, 76.04057627198102409 ) ) ;
#164007 = CARTESIAN_POINT ( 'NONE',  ( -16.53943276465976808, 0.05219959533911058130, 51.24890960531436690 ) ) ;
#164008 = CARTESIAN_POINT ( 'NONE',  ( 15.72974639402199770, -15.80617190586745480, 63.12390960531435979 ) ) ;
#164009 = CARTESIAN_POINT ( 'NONE',  ( 9.564922557960805705, 16.46253265017160317, 54.58224293864769550 ) ) ;
#164010 = CARTESIAN_POINT ( 'NONE',  ( -10.72451020669898014, 18.67979575497178502, 70.41557627198102409 ) ) ;
#164011 = CARTESIAN_POINT ( 'NONE',  ( 16.46253265017146816, 9.564922557961045513, 56.66775706135233293 ) ) ;
#164013 = CARTESIAN_POINT ( 'NONE',  ( 8.224510206698953496, -14.34966873604960469, 57.91557627198103120 ) ) ;
#164012 = CARTESIAN_POINT ( 'NONE',  ( 25.25560589046783022, 4.310829775027161581, 167.9999999999999716 ) ) ;
#164014 = CARTESIAN_POINT ( 'NONE',  ( -21.52544592524343514, 5.823673210054127303, 41.04057627198103120 ) ) ;
#164015 = ORIENTED_EDGE ( 'NONE', *, *, #60978, .F. ) ;
#164016 = CARTESIAN_POINT ( 'NONE',  ( 17.48853670773245028, 5.747243402303093163, 103.8332870025000858 ) ) ;
#164018 = CARTESIAN_POINT ( 'NONE',  ( -8.571926809382601320, -26.38167802310801591, 147.2750000027311899 ) ) ;
#164017 = CARTESIAN_POINT ( 'NONE',  ( -14.29746914071037622, -8.314922557961029526, 84.16775706135234714 ) ) ;
#164019 = CARTESIAN_POINT ( 'NONE',  ( 19.05341960407617918, -5.049401038297876454, 91.04275706135234714 ) ) ;
#164020 = CARTESIAN_POINT ( 'NONE',  ( 4.483927247898545687, 16.52544592524342804, 54.79057627198104541 ) ) ;
#164021 = PLANE ( 'NONE',  #187160 ) ;
#164022 = CARTESIAN_POINT ( 'NONE',  ( 19.03943276465977164, -0.05219959533909143690, 43.74890960531435979 ) ) ;
#164023 = CARTESIAN_POINT ( 'NONE',  ( -8.224510206698948167, 14.34966873604960824, 45.41557627198103830 ) ) ;
#164024 = CARTESIAN_POINT ( 'NONE',  ( -19.02544592524342804, 5.153800228976336051, 86.04057627198103830 ) ) ;
#164025 = CARTESIAN_POINT ( 'NONE',  ( 5.153800228976335163, 19.02544592524342804, 54.79057627198103120 ) ) ;
#164026 = CARTESIAN_POINT ( 'NONE',  ( 0.05219959533937995610, -21.53943276465977519, 55.00109039468568284 ) ) ;
#164027 = CARTESIAN_POINT ( 'NONE',  ( -19.02544592524342804, 5.153800228976336051, 71.04057627198099567 ) ) ;
#164028 = CARTESIAN_POINT ( 'NONE',  ( 16.51473224551069308, 9.474510206698969483, 29.16557627198103475 ) ) ;
#164029 = CARTESIAN_POINT ( 'NONE',  ( 0.05219959533909260263, 19.03943276465977164, 69.99890960531435269 ) ) ;
#164030 = CARTESIAN_POINT ( 'NONE',  ( 10.72451020669898902, -18.67979575497178502, 52.91557627198103830 ) ) ;
#164031 = CARTESIAN_POINT ( 'NONE',  ( -19.03943276465977164, 0.05219959533909376836, 31.24890960531435979 ) ) ;
#164032 = CARTESIAN_POINT ( 'NONE',  ( -10.81492255796078084, -18.62759615963271287, 37.08224293864768129 ) ) ;
#164033 = CARTESIAN_POINT ( 'NONE',  ( -14.29746914071037622, -8.314922557961029526, 104.1677570613523471 ) ) ;
#164034 = CARTESIAN_POINT ( 'NONE',  ( 16.51473224551083163, -9.474510206698727899, 20.83442372801899722 ) ) ;
#164036 = CARTESIAN_POINT ( 'NONE',  ( 16.55341960407618274, -4.379528057220086978, 81.04275706135236135 ) ) ;
#164035 = CARTESIAN_POINT ( 'NONE',  ( 8.224510206698742110, 14.34966873604972548, 42.08442372801901854 ) ) ;
#164037 = CYLINDRICAL_SURFACE ( 'NONE', #37154, 28.82186960331498682 ) ;
#164038 = CARTESIAN_POINT ( 'NONE',  ( 16.55341960407618274, -4.379528057220086978, 61.04275706135234714 ) ) ;
#164039 = CARTESIAN_POINT ( 'NONE',  ( -5.049401038298153566, 19.05341960407611168, 105.2072429386476671 ) ) ;
#164040 = CARTESIAN_POINT ( 'NONE',  ( -19.02544592524342804, 5.153800228976336051, 36.04057627198100988 ) ) ;
#164041 = CARTESIAN_POINT ( 'NONE',  ( 4.379528057220092307, 16.55341960407617563, 42.29275706135235424 ) ) ;
#164042 = CARTESIAN_POINT ( 'NONE',  ( 5.049401038298161559, -19.05341960407611168, 42.70724293864767418 ) ) ;
#164043 = CARTESIAN_POINT ( 'NONE',  ( -15.72974639402176322, -15.80617190586768395, 24.37609039468567573 ) ) ;
#164044 = CARTESIAN_POINT ( 'NONE',  ( -14.29746914071037622, -8.314922557961029526, 39.16775706135235424 ) ) ;
#164045 = CARTESIAN_POINT ( 'NONE',  ( 16.52544592524335698, 4.483927247898782831, 101.4594237280190185 ) ) ;
#164046 = DIRECTION ( 'NONE',  ( 0.000000000000000000, 0.000000000000000000, 1.000000000000000000 ) ) ;
#164047 = CARTESIAN_POINT ( 'NONE',  ( -10.72451020669870658, -18.67979575497194134, 94.58442372801901854 ) ) ;
#164048 = CARTESIAN_POINT ( 'NONE',  ( 19.05341960407617918, -5.049401038297876454, 101.0427570613523045 ) ) ;
#164049 = CARTESIAN_POINT ( 'NONE',  ( 19.05341960407617918, -5.049401038297876454, 51.04275706135231871 ) ) ;
#164050 = CARTESIAN_POINT ( 'NONE',  ( -16.55341960407611168, -4.379528057220339221, 56.45724293864768839 ) ) ;
#164051 = CARTESIAN_POINT ( 'NONE',  ( 5.049401038298161559, -19.05341960407611168, 27.70724293864769550 ) ) ;
#164053 = CARTESIAN_POINT ( 'NONE',  ( -15.49999999999999822, 5.499999999999997335, 118.0000000000000142 ) ) ;
#164052 = CARTESIAN_POINT ( 'NONE',  ( 0.05219959533936267826, -19.03943276465977164, 60.00109039468566863 ) ) ;
#164054 = CARTESIAN_POINT ( 'NONE',  ( -21.55341960407619339, 5.719274019375674811, 63.54275706135234003 ) ) ;
#164055 = CARTESIAN_POINT ( 'NONE',  ( 16.55341960407618274, -4.379528057220086978, 21.04275706135234714 ) ) ;
#164056 = CARTESIAN_POINT ( 'NONE',  ( 19.48894818550242647, -5.500000000000105693, 57.60307310435242556 ) ) ;
#164057 = CARTESIAN_POINT ( 'NONE',  ( -9.474510206698964154, 16.51473224551069663, 115.4155762719810241 ) ) ;
#164058 = CARTESIAN_POINT ( 'NONE',  ( -19.05341960407617563, 5.049401038297882671, 103.5427570613523329 ) ) ;
#164059 = CARTESIAN_POINT ( 'NONE',  ( -0.05219959533909027116, -19.03943276465977164, 112.4989096053143669 ) ) ;
#164060 = CARTESIAN_POINT ( 'NONE',  ( -23.35043118190705869, 14.19381810411928235, 169.8796877288295946 ) ) ;
#164061 = CARTESIAN_POINT ( 'NONE',  ( -19.03943276465977164, 0.05219959533909376836, 21.24890960531436335 ) ) ;
#164062 = CARTESIAN_POINT ( 'NONE',  ( 0.05219959533937995610, -21.53943276465977519, 110.0010903946856757 ) ) ;
#164063 = CARTESIAN_POINT ( 'NONE',  ( -16.51473224551069308, -9.474510206698971260, 61.66557627198103120 ) ) ;
#164064 = CARTESIAN_POINT ( 'NONE',  ( -21.52544592524334988, -5.823673210054445271, 63.95942372801901854 ) ) ;
#164065 = CARTESIAN_POINT ( 'NONE',  ( 21.53943276465977519, 0.05219959533937863772, 106.2510903946856757 ) ) ;
#164066 = CARTESIAN_POINT ( 'NONE',  ( -0.05219959533934338120, 16.53943276465976808, 107.5010903946856899 ) ) ;
#164067 = CARTESIAN_POINT ( 'NONE',  ( 19.05341960407611168, 5.049401038298154454, 73.95724293864768129 ) ) ;
#164068 = CARTESIAN_POINT ( 'NONE',  ( 21.53943276465977519, 0.05219959533937863772, 56.25109039468568284 ) ) ;
#164069 = CARTESIAN_POINT ( 'NONE',  ( -15.72974639402176322, -15.80617190586768395, 59.37609039468568284 ) ) ;
#164071 = CARTESIAN_POINT ( 'NONE',  ( 5.049401038298161559, -19.05341960407611168, 102.7072429386476955 ) ) ;
#164070 = CARTESIAN_POINT ( 'NONE',  ( 19.03943276465977164, 0.05219959533936151252, 86.25109039468567573 ) ) ;
#164072 = CARTESIAN_POINT ( 'NONE',  ( -12.14591786802309592, -12.06949235617757132, 111.8739096053143669 ) ) ;
#164073 = CARTESIAN_POINT ( 'NONE',  ( 10.72451020669898902, -18.67979575497178502, 92.91557627198103830 ) ) ;
#164074 = CARTESIAN_POINT ( 'NONE',  ( 16.51473224551083163, -9.474510206698727899, 20.83442372801899722 ) ) ;
#164075 = CARTESIAN_POINT ( 'NONE',  ( 16.52544592524342804, -4.483927247898539470, 103.5405762719810383 ) ) ;
#164076 = CARTESIAN_POINT ( 'NONE',  ( 13.97604488694527802, 13.89961937509977652, 49.37390960531434558 ) ) ;
#164077 = CARTESIAN_POINT ( 'NONE',  ( -13.97604488694547697, 13.89961937509957934, 93.12609039468566152 ) ) ;
#164078 = CARTESIAN_POINT ( 'NONE',  ( 16.52544592524342804, -4.483927247898539470, 68.54057627198103830 ) ) ;
#164079 = CARTESIAN_POINT ( 'NONE',  ( 15.72974639402176855, 15.80617190586768217, 111.8760903946856615 ) ) ;
#164080 = CARTESIAN_POINT ( 'NONE',  ( 19.05341960407611168, 5.049401038298154454, 103.9572429386476671 ) ) ;
#164081 = CARTESIAN_POINT ( 'NONE',  ( 5.049401038297881783, 19.05341960407617563, 77.29275706135231871 ) ) ;
#164082 = CARTESIAN_POINT ( 'NONE',  ( 21.52544592524344225, -5.823673210054117533, 83.54057627198102409 ) ) ;
#164083 = CARTESIAN_POINT ( 'NONE',  ( -15.80617190586768217, 15.72974639402176855, 33.12609039468569705 ) ) ;
#164084 = CARTESIAN_POINT ( 'NONE',  ( -0.05219959533934338120, 16.53943276465976808, 37.50109039468568284 ) ) ;
#164085 = CARTESIAN_POINT ( 'NONE',  ( 16.53943276465976808, 0.05219959533934440121, 91.25109039468568994 ) ) ;
#164087 = CARTESIAN_POINT ( 'NONE',  ( -5.719274019375665041, -21.55341960407619695, 39.79275706135235424 ) ) ;
#164086 = CARTESIAN_POINT ( 'NONE',  ( 14.29746914071037800, 8.314922557961029526, 46.66775706135234714 ) ) ;
#164088 = CARTESIAN_POINT ( 'NONE',  ( 0.05219959533907565091, 21.53943276465977519, 39.99890960531436690 ) ) ;
#164089 = CARTESIAN_POINT ( 'NONE',  ( -16.51473224551069308, -9.474510206698971260, 31.66557627198102054 ) ) ;
#164090 = CARTESIAN_POINT ( 'NONE',  ( -38.00000000000000711, 2.428612866367529932E-14, -11.74999999453762634 ) ) ;
#164091 = CARTESIAN_POINT ( 'NONE',  ( 4.483927247898790824, -16.52544592524335698, 60.20942372801902565 ) ) ;
#164092 = CARTESIAN_POINT ( 'NONE',  ( -18.67979575497178146, -10.72451020669898902, 91.66557627198103830 ) ) ;
#164093 = CARTESIAN_POINT ( 'NONE',  ( -14.34966873604960291, -8.224510206698953496, 41.66557627198103120 ) ) ;
#164094 = CARTESIAN_POINT ( 'NONE',  ( -16.52544592524335698, -4.483927247898792601, 43.95942372801902565 ) ) ;
#164095 = CARTESIAN_POINT ( 'NONE',  ( -16.46253265017160317, 9.564922557960807481, 55.83224293864769550 ) ) ;
#164096 = CARTESIAN_POINT ( 'NONE',  ( 4.483927247898790824, -16.52544592524335698, 90.20942372801903275 ) ) ;
#164097 = CARTESIAN_POINT ( 'NONE',  ( 16.51473224551083163, -9.474510206698727899, 90.83442372801900433 ) ) ;
#164098 = CARTESIAN_POINT ( 'NONE',  ( 10.72451020669898902, -18.67979575497178502, 87.91557627198103830 ) ) ;
#164099 = CARTESIAN_POINT ( 'NONE',  ( 16.52544592524342804, -4.483927247898539470, 28.54057627198103120 ) ) ;
#164100 = ORIENTED_EDGE ( 'NONE', *, *, #133168, .F. ) ;
#164101 = CARTESIAN_POINT ( 'NONE',  ( 69.65682714487590488, -71.74905178543389184, -4.999999999999999112 ) ) ;
#164102 = CARTESIAN_POINT ( 'NONE',  ( -5.719274019375978568, 21.55341960407610458, 55.20724293864770260 ) ) ;
#164103 = CARTESIAN_POINT ( 'NONE',  ( 16.55341960407618274, -4.379528057220086978, 101.0427570613523756 ) ) ;
#164104 = ORIENTED_EDGE ( 'NONE', *, *, #13961, .T. ) ;
#164105 = CARTESIAN_POINT ( 'NONE',  ( 17.50000000000000711, -3.427582784585717413, 102.6734475746479092 ) ) ;
#164106 = CARTESIAN_POINT ( 'NONE',  ( 18.67979575497178502, 10.72451020669898547, 84.16557627198103830 ) ) ;
#164107 = CARTESIAN_POINT ( 'NONE',  ( 16.55341960407611168, 4.379528057220329451, 23.95724293864769550 ) ) ;
#164108 = CARTESIAN_POINT ( 'NONE',  ( -4.483927247898782831, 16.52544592524335698, 37.70942372801900433 ) ) ;
#164109 = VECTOR ( 'NONE', #161839, 1000.000000000000000 ) ;
#164110 = CARTESIAN_POINT ( 'NONE',  ( -0.05219959533909027116, -19.03943276465977164, 37.49890960531436690 ) ) ;
#164111 = CARTESIAN_POINT ( 'NONE',  ( 19.05341960407611168, 5.049401038298154454, 48.95724293864768129 ) ) ;
#164112 = CARTESIAN_POINT ( 'NONE',  ( -27.73933785331498925, 2.428612866367529932E-14, 139.3750000027311842 ) ) ;
#164113 = CARTESIAN_POINT ( 'NONE',  ( 10.81492255796078972, 18.62759615963270932, 24.58224293864768839 ) ) ;
#164114 = CARTESIAN_POINT ( 'NONE',  ( -9.248023074035629065, -10.74802307403544077, -62.40259441833023857 ) ) ;
#164115 = CARTESIAN_POINT ( 'NONE',  ( -8.314922557961024197, 14.29746914071037800, 97.91775706135236135 ) ) ;
#164116 = CARTESIAN_POINT ( 'NONE',  ( -9.474510206698720793, -16.51473224551083518, 104.5844237280190043 ) ) ;
#164117 = CARTESIAN_POINT ( 'NONE',  ( 19.03943276465977164, 0.05219959533936151252, 31.25109039468566863 ) ) ;
#164118 = CARTESIAN_POINT ( 'NONE',  ( -0.05219959533907301413, -21.53943276465977519, 87.49890960531436690 ) ) ;
#164119 = CARTESIAN_POINT ( 'NONE',  ( 12.14591786802327356, -12.06949235617739191, 110.6260903946857042 ) ) ;
#164120 = CARTESIAN_POINT ( 'NONE',  ( -0.05219959533907301413, -21.53943276465977519, 32.49890960531435979 ) ) ;
#164121 = CARTESIAN_POINT ( 'NONE',  ( -19.03943276465977164, -0.05219959533935918106, 103.7510903946856757 ) ) ;
#164122 = CARTESIAN_POINT ( 'NONE',  ( -13.89961937509977652, 13.97604488694528158, 110.6239096053143243 ) ) ;
#164123 = CARTESIAN_POINT ( 'NONE',  ( 10.81492255796106328, -18.62759615963255655, 60.41775706135235424 ) ) ;
#164124 = CARTESIAN_POINT ( 'NONE',  ( 19.05341960407611168, 5.049401038298154454, 53.95724293864770260 ) ) ;
#164125 = CARTESIAN_POINT ( 'NONE',  ( -14.29746914071049879, 8.314922557960819915, 95.83224293864770971 ) ) ;
#164126 = CARTESIAN_POINT ( 'NONE',  ( 31.24009710442676280, 7.113574878955725822, 97.38907943302065462 ) ) ;
#164127 = CARTESIAN_POINT ( 'NONE',  ( 9.564922557960805705, 16.46253265017160317, 74.58224293864769550 ) ) ;
#164128 = CARTESIAN_POINT ( 'NONE',  ( 14.34966873604960469, 8.224510206698951720, 74.16557627198102409 ) ) ;
#164129 = ORIENTED_EDGE ( 'NONE', *, *, #190442, .F. ) ;
#164130 = CARTESIAN_POINT ( 'NONE',  ( 19.03943276465977164, 0.05219959533936151252, 86.25109039468567573 ) ) ;
#164131 = CARTESIAN_POINT ( 'NONE',  ( 19.20446147854526231, 5.499999999999948486, 91.88999695167677828 ) ) ;
#164132 = CARTESIAN_POINT ( 'NONE',  ( -19.02544592524342804, 5.153800228976336051, 61.04057627198103120 ) ) ;
#164133 = CARTESIAN_POINT ( 'NONE',  ( 31.28611164036840364, -6.519914617504974252, 98.73992561365416520 ) ) ;
#164134 = VECTOR ( 'NONE', #116425, 1000.000000000000000 ) ;
#164136 = CARTESIAN_POINT ( 'NONE',  ( 5.153800228976335163, 19.02544592524342804, 99.79057627198102409 ) ) ;
#164135 = CARTESIAN_POINT ( 'NONE',  ( -19.05341960407611168, -5.049401038298163336, 71.45724293864766707 ) ) ;
#164137 = CARTESIAN_POINT ( 'NONE',  ( -8.224510206698735004, -14.34966873604973081, 59.58442372801901854 ) ) ;
#164138 = DIRECTION ( 'NONE',  ( -0.000000000000000000, -0.000000000000000000, 1.000000000000000000 ) ) ;
#164139 = CARTESIAN_POINT ( 'NONE',  ( 19.02544592524334988, 5.153800228976608722, 46.45942372801899012 ) ) ;
#164140 = CARTESIAN_POINT ( 'NONE',  ( 5.719274019375673035, 21.55341960407619339, 97.29275706135234714 ) ) ;
#164141 = CARTESIAN_POINT ( 'NONE',  ( 4.000000000000000888, -105.0000000000000000, 12.00000000000000355 ) ) ;
#164142 = CARTESIAN_POINT ( 'NONE',  ( -9.564922557960796823, -16.46253265017161027, 112.0822429386476955 ) ) ;
#164143 = CARTESIAN_POINT ( 'NONE',  ( -0.05219959533934338120, 16.53943276465976808, 102.5010903946856899 ) ) ;
#164144 = CARTESIAN_POINT ( 'NONE',  ( -34.78522506798723413, -4.592425496937305498E-15, 52.50000000000000000 ) ) ;
#164145 = CARTESIAN_POINT ( 'NONE',  ( -14.34966873604972548, 8.224510206698743886, 98.33442372801901854 ) ) ;
#164146 = CARTESIAN_POINT ( 'NONE',  ( -16.38665767535054485, 7.295008042176025498, 30.26400864214545905 ) ) ;
#164147 = CARTESIAN_POINT ( 'NONE',  ( 12.14591786802327356, -12.06949235617739191, 70.62609039468567573 ) ) ;
#164148 = VERTEX_POINT ( 'NONE', #59584 ) ;
#164149 = CARTESIAN_POINT ( 'NONE',  ( -18.62759615963255300, -10.81492255796106328, 74.16775706135231871 ) ) ;
#164150 = CARTESIAN_POINT ( 'NONE',  ( -19.05341960407617563, 5.049401038297882671, 83.54275706135233293 ) ) ;
#164151 = CARTESIAN_POINT ( 'NONE',  ( 19.05341960407617918, -5.049401038297876454, 31.04275706135232227 ) ) ;
#164152 = CARTESIAN_POINT ( 'NONE',  ( 16.51473224551069308, 9.474510206698969483, 64.16557627198102409 ) ) ;
#164153 = CARTESIAN_POINT ( 'NONE',  ( -16.51473224551069308, -9.474510206698971260, 51.66557627198102409 ) ) ;
#164154 = CARTESIAN_POINT ( 'NONE',  ( -17.07994770534405760, -36.17121603258436835, -9.645916067152393580 ) ) ;
#164155 = CARTESIAN_POINT ( 'NONE',  ( -15.72974639402197994, 15.80617190586746368, 80.62390960531438111 ) ) ;
#164156 = CARTESIAN_POINT ( 'NONE',  ( 5.823673210054125526, 21.52544592524343514, 39.79057627198103830 ) ) ;
#164157 = CARTESIAN_POINT ( 'NONE',  ( 16.51473224551069308, 9.474510206698969483, 39.16557627198103120 ) ) ;
#164158 = CARTESIAN_POINT ( 'NONE',  ( 14.34966873604972726, -8.224510206698740333, 60.83442372801901854 ) ) ;
#164159 = VERTEX_POINT ( 'NONE', #182952 ) ;
#164160 = CARTESIAN_POINT ( 'NONE',  ( 10.81492255796106328, -18.62759615963255655, 25.41775706135235779 ) ) ;
#164162 = CARTESIAN_POINT ( 'NONE',  ( -22.81625015709510507, 31.40387420917330275, -6.924999997268812990 ) ) ;
#164161 = CARTESIAN_POINT ( 'NONE',  ( 16.53943276465976808, -0.05219959533910856209, 63.74890960531435979 ) ) ;
#164163 = CARTESIAN_POINT ( 'NONE',  ( -4.379528057220086978, -16.55341960407618274, 19.79275706135235069 ) ) ;
#164164 = CARTESIAN_POINT ( 'NONE',  ( -19.03943276465977164, -0.05219959533935918106, 38.75109039468566152 ) ) ;
#164165 = CARTESIAN_POINT ( 'NONE',  ( 14.34966873604960469, 8.224510206698951720, 64.16557627198102409 ) ) ;
#164166 = CARTESIAN_POINT ( 'NONE',  ( 0.05219959533937995610, -21.53943276465977519, 25.00109039468567218 ) ) ;
#164168 = CARTESIAN_POINT ( 'NONE',  ( 21.52544592524344225, -5.823673210054117533, 73.54057627198102409 ) ) ;
#164167 = CARTESIAN_POINT ( 'NONE',  ( 1.491173228115779237, 15.38774048274545159, -59.71317227968791030 ) ) ;
#164169 = CARTESIAN_POINT ( 'NONE',  ( 9.564922557960805705, 16.46253265017160317, 94.58224293864769550 ) ) ;
#164170 = CARTESIAN_POINT ( 'NONE',  ( -12.06949235617756955, 12.14591786802309770, 60.62390960531437401 ) ) ;
#164171 = CARTESIAN_POINT ( 'NONE',  ( 33.12942481080231971, -22.41379292486335117, -24.08540372093460746 ) ) ;
#164172 = PLANE ( 'NONE',  #47247 ) ;
#164173 = CARTESIAN_POINT ( 'NONE',  ( -9.474510206698720793, -16.51473224551083518, 74.58442372801900433 ) ) ;
#164174 = CARTESIAN_POINT ( 'NONE',  ( -10.81492255796078084, -18.62759615963271287, 102.0822429386476955 ) ) ;
#164175 = CARTESIAN_POINT ( 'NONE',  ( -13.89961937509977652, 13.97604488694528158, 50.62390960531435979 ) ) ;
#164176 = CARTESIAN_POINT ( 'NONE',  ( -19.05341960407617563, 5.049401038297882671, 48.54275706135233293 ) ) ;
#164177 = CARTESIAN_POINT ( 'NONE',  ( -13.89961937509977652, 13.97604488694528158, 25.62390960531434558 ) ) ;
#164178 = CARTESIAN_POINT ( 'NONE',  ( -18.67979575497193778, 10.72451020669871902, 68.33442372801900433 ) ) ;
#164179 = CARTESIAN_POINT ( 'NONE',  ( -17.50000000000000000, -5.624438216177585659, 69.18329655085355512 ) ) ;
#164180 = CARTESIAN_POINT ( 'NONE',  ( -12.14591786802309592, -12.06949235617757132, 46.87390960531435979 ) ) ;
#164181 = CARTESIAN_POINT ( 'NONE',  ( 9.474510206698971260, -16.51473224551069308, 67.91557627198102409 ) ) ;
#164182 = CARTESIAN_POINT ( 'NONE',  ( 15.80617190586746368, 15.72974639402197994, 74.37390960531436690 ) ) ;
#164183 = CARTESIAN_POINT ( 'NONE',  ( 5.049401038298161559, -19.05341960407611168, 62.70724293864769550 ) ) ;
#164184 = ORIENTED_EDGE ( 'NONE', *, *, #140289, .F. ) ;
#164185 = CARTESIAN_POINT ( 'NONE',  ( 5.823673210054125526, 21.52544592524343514, 69.79057627198102409 ) ) ;
#164186 = CARTESIAN_POINT ( 'NONE',  ( -15.80617190586768217, 15.72974639402176855, 103.1260903946856757 ) ) ;
#164189 = CARTESIAN_POINT ( 'NONE',  ( 4.483927247898545687, 16.52544592524342804, 89.79057627198103830 ) ) ;
#164188 = CARTESIAN_POINT ( 'NONE',  ( 0.05219959533934541429, -16.53943276465976808, 95.00109039468568994 ) ) ;
#164187 = CARTESIAN_POINT ( 'NONE',  ( -4.000000000000000888, -105.0000000000000000, 12.00000000000000355 ) ) ;
#164190 = CARTESIAN_POINT ( 'NONE',  ( -0.05219959533936034679, 19.03943276465977164, 87.50109039468567573 ) ) ;
#164191 = ORIENTED_EDGE ( 'NONE', *, *, #179533, .T. ) ;
#164192 = CARTESIAN_POINT ( 'NONE',  ( -16.46253265017146816, -9.564922557961047289, 44.16775706135232582 ) ) ;
#164193 = CARTESIAN_POINT ( 'NONE',  ( -16.52544592524335698, -4.483927247898792601, 103.9594237280190185 ) ) ;
#164194 = CARTESIAN_POINT ( 'NONE',  ( -5.153800228976607833, 19.02544592524334988, 32.70942372801899722 ) ) ;
#164195 = CARTESIAN_POINT ( 'NONE',  ( -13.89961937509977652, 13.97604488694528158, 95.62390960531436690 ) ) ;
#164196 = CARTESIAN_POINT ( 'NONE',  ( -18.62759615963270932, 10.81492255796079327, 55.83224293864770260 ) ) ;
#164197 = CARTESIAN_POINT ( 'NONE',  ( -4.215739103160454526, -48.58376198229541387, -25.00000000000007105 ) ) ;
#164198 = CARTESIAN_POINT ( 'NONE',  ( -12.14591786802309592, -12.06949235617757132, 111.8739096053143669 ) ) ;
#164199 = CARTESIAN_POINT ( 'NONE',  ( 21.55341960407619695, -5.719274019375665929, 101.0427570613523756 ) ) ;
#164200 = CARTESIAN_POINT ( 'NONE',  ( 14.34966873604972726, -8.224510206698740333, 75.83442372801900433 ) ) ;
#164201 = CARTESIAN_POINT ( 'NONE',  ( -10.81492255796105439, 18.62759615963255655, 27.91775706135234358 ) ) ;
#164202 = CARTESIAN_POINT ( 'NONE',  ( -4.379528057220086978, -16.55341960407618274, 29.79275706135234358 ) ) ;
#164203 = CARTESIAN_POINT ( 'NONE',  ( 19.03943276465977164, -0.05219959533909143690, 93.74890960531435269 ) ) ;
#164204 = CARTESIAN_POINT ( 'NONE',  ( 13.97604488694527802, 13.89961937509977652, 39.37390960531435269 ) ) ;
#164205 = CARTESIAN_POINT ( 'NONE',  ( -9.564922557960796823, -16.46253265017161027, 47.08224293864769550 ) ) ;
#164206 = CARTESIAN_POINT ( 'NONE',  ( -4.379528057220086978, -16.55341960407618274, 29.79275706135234358 ) ) ;
#164207 = CARTESIAN_POINT ( 'NONE',  ( -14.29746914071049879, 8.314922557960819915, 90.83224293864769550 ) ) ;
#164208 = ADVANCED_FACE ( 'NONE', ( #5863 ), #97852, .F. ) ;
#164209 = CARTESIAN_POINT ( 'NONE',  ( 14.34966873604972726, -8.224510206698740333, 100.8344237280190185 ) ) ;
#164212 = CARTESIAN_POINT ( 'NONE',  ( -5.049401038298153566, 19.05341960407611168, 60.20724293864768129 ) ) ;
#164211 = CARTESIAN_POINT ( 'NONE',  ( 19.05341960407611168, 5.049401038298154454, 83.95724293864766707 ) ) ;
#164210 = CARTESIAN_POINT ( 'NONE',  ( -5.719274019375665041, -21.55341960407619695, 39.79275706135235424 ) ) ;
#164213 = CARTESIAN_POINT ( 'NONE',  ( -16.46253265017160317, 9.564922557960807481, 80.83224293864769550 ) ) ;
#164214 = CARTESIAN_POINT ( 'NONE',  ( 12.06949235617757843, -12.14591786802309237, 38.12390960531436690 ) ) ;
#164215 = CARTESIAN_POINT ( 'NONE',  ( 0.05219959533934541429, -16.53943276465976808, 105.0010903946856757 ) ) ;
#164216 = ORIENTED_EDGE ( 'NONE', *, *, #16052, .F. ) ;
#164217 = CARTESIAN_POINT ( 'NONE',  ( -19.02544592524334988, -5.153800228976617603, 48.95942372801900433 ) ) ;
#164218 = CARTESIAN_POINT ( 'NONE',  ( 22.73749492396215288, -155.7167183371838064, 0.000000000000000000 ) ) ;
#164219 = CARTESIAN_POINT ( 'NONE',  ( 9.564922557960805705, 16.46253265017160317, 44.58224293864769550 ) ) ;
#164220 = CARTESIAN_POINT ( 'NONE',  ( -5.049401038297874678, -19.05341960407617918, 34.79275706135233293 ) ) ;
#164221 = CARTESIAN_POINT ( 'NONE',  ( 11.40812507854755253, -35.11059874428192273, -6.024999997268814411 ) ) ;
#164222 = CARTESIAN_POINT ( 'NONE',  ( -16.55341960407617563, 4.379528057220093196, 43.54275706135235424 ) ) ;
#164224 = CARTESIAN_POINT ( 'NONE',  ( 12.14591786802327356, -12.06949235617739191, 50.62609039468568994 ) ) ;
#164223 = CARTESIAN_POINT ( 'NONE',  ( -16.46253265017146816, -9.564922557961047289, 74.16775706135234714 ) ) ;
#164225 = CARTESIAN_POINT ( 'NONE',  ( -28.28060372831499336, 2.428612866367529932E-14, 149.6875000013656063 ) ) ;
#164226 = CARTESIAN_POINT ( 'NONE',  ( 19.05341960407611168, 5.049401038298154454, 73.95724293864768129 ) ) ;
#164227 = CARTESIAN_POINT ( 'NONE',  ( 15.80617190586769283, -15.72974639402175789, 20.62609039468568639 ) ) ;
#164228 = CARTESIAN_POINT ( 'NONE',  ( 9.474510206698729675, 16.51473224551082808, 77.08442372801900433 ) ) ;
#164230 = CARTESIAN_POINT ( 'NONE',  ( 5.049401038298161559, -19.05341960407611168, 32.70724293864768129 ) ) ;
#164229 = CARTESIAN_POINT ( 'NONE',  ( -13.89961937509977652, 13.97604488694528158, 110.6239096053143243 ) ) ;
#164231 = B_SPLINE_CURVE_WITH_KNOTS ( 'NONE', 3,
 ( #138277, #126088, #91748, #199960, #61425, #185785 ),
 .UNSPECIFIED., .F., .F.,
 ( 4, 2, 4 ),
 ( 0.003715511750470261790, 0.004312155465044938130, 0.004908799179619614469 ),
 .UNSPECIFIED. ) ;
#164232 = CARTESIAN_POINT ( 'NONE',  ( -16.46253265017160317, 9.564922557960807481, 75.83224293864769550 ) ) ;
#164234 = CARTESIAN_POINT ( 'NONE',  ( 19.03943276465977164, -0.05219959533909143690, 33.74890960531435979 ) ) ;
#164233 = CARTESIAN_POINT ( 'NONE',  ( -12.06949235617756955, 12.14591786802309770, 40.62390960531435269 ) ) ;
#164235 = CARTESIAN_POINT ( 'NONE',  ( 13.97604488694548053, -13.89961937509957401, 55.62609039468566863 ) ) ;
#164236 = CARTESIAN_POINT ( 'NONE',  ( -16.55341960407611168, -4.379528057220339221, 91.45724293864769550 ) ) ;
#164237 = CARTESIAN_POINT ( 'NONE',  ( -16.51473224551082808, 9.474510206698731452, 23.33442372801900078 ) ) ;
#164238 = CARTESIAN_POINT ( 'NONE',  ( -13.89961937509977652, 13.97604488694528158, 50.62390960531435979 ) ) ;
#164239 = EDGE_CURVE ( 'NONE', #60981, #163981, #133164, .T. ) ;
#164240 = CARTESIAN_POINT ( 'NONE',  ( -10.81492255796078084, -18.62759615963271287, 52.08224293864768839 ) ) ;
#164242 = CARTESIAN_POINT ( 'NONE',  ( 5.719274019375673035, 21.55341960407619339, 102.2927570613523613 ) ) ;
#164241 = CARTESIAN_POINT ( 'NONE',  ( 16.53943276465976808, -0.05219959533910856209, 58.74890960531436690 ) ) ;
#164243 = CARTESIAN_POINT ( 'NONE',  ( 19.05341960407611168, 5.049401038298154454, 93.95724293864769550 ) ) ;
#164244 = CARTESIAN_POINT ( 'NONE',  ( -5.153800228976328057, -19.02544592524343514, 107.2905762719810383 ) ) ;
#164245 = CARTESIAN_POINT ( 'NONE',  ( 19.05341960407611168, 5.049401038298154454, 33.95724293864769550 ) ) ;
#164246 = CARTESIAN_POINT ( 'NONE',  ( -12.06949235617756955, 12.14591786802309770, 115.6239096053143669 ) ) ;
#164247 = CARTESIAN_POINT ( 'NONE',  ( 16.53943276465976808, -0.05219959533910856209, 93.74890960531436690 ) ) ;
#164248 = CARTESIAN_POINT ( 'NONE',  ( 15.72974639402199770, -15.80617190586745480, 103.1239096053143811 ) ) ;
#164249 = CARTESIAN_POINT ( 'NONE',  ( 16.46253265017160672, -9.564922557960803928, 98.33224293864769550 ) ) ;
#164250 = CARTESIAN_POINT ( 'NONE',  ( 15.80617190586746368, 15.72974639402197994, 109.3739096053143811 ) ) ;
#164251 = CARTESIAN_POINT ( 'NONE',  ( -13.89961937509977652, 13.97604488694528158, 90.62390960531432427 ) ) ;
#164253 = CARTESIAN_POINT ( 'NONE',  ( -12.14591786802309592, -12.06949235617757132, 106.8739096053143811 ) ) ;
#164252 = CARTESIAN_POINT ( 'NONE',  ( -24.40828949532295056, 2.848420800297980726, 173.9378174459542947 ) ) ;
#164254 = CARTESIAN_POINT ( 'NONE',  ( 0.05219959533909260263, 19.03943276465977164, 74.99890960531435269 ) ) ;
#164255 = CARTESIAN_POINT ( 'NONE',  ( 10.81492255796078972, 18.62759615963270932, 84.58224293864769550 ) ) ;
#164256 = LINE ( 'NONE', #93092, #150505 ) ;
#164257 = CARTESIAN_POINT ( 'NONE',  ( -20.09068217638366960, -11.70722341973408476, 168.0245402885401234 ) ) ;
#164259 = SURFACE_STYLE_FILL_AREA ( #102575 ) ;
#164258 = CARTESIAN_POINT ( 'NONE',  ( -5.719274019375978568, 21.55341960407610458, 30.20724293864769550 ) ) ;
#164260 = CARTESIAN_POINT ( 'NONE',  ( -12.06949235617739369, -12.14591786802326823, 39.37609039468567573 ) ) ;
#164261 = CARTESIAN_POINT ( 'NONE',  ( 16.53943276465976808, -0.05219959533910856209, 88.74890960531436690 ) ) ;
#164262 = CARTESIAN_POINT ( 'NONE',  ( 19.46398650005387410, -5.500000000000147438, 52.68269651486371430 ) ) ;
#164263 = CARTESIAN_POINT ( 'NONE',  ( -19.03943276465977164, 0.05219959533909376836, 86.24890960531436690 ) ) ;
#164264 = CARTESIAN_POINT ( 'NONE',  ( -19.02544592524342804, 5.153800228976336051, 46.04057627198101699 ) ) ;
#164265 = CARTESIAN_POINT ( 'NONE',  ( 8.314922557960818139, 14.29746914071049879, 84.58224293864769550 ) ) ;
#164266 = CARTESIAN_POINT ( 'NONE',  ( 10.72451020669898902, -18.67979575497178502, 27.91557627198103830 ) ) ;
#164267 = CARTESIAN_POINT ( 'NONE',  ( 16.55341960407611168, 4.379528057220329451, 48.95724293864770971 ) ) ;
#164268 = CARTESIAN_POINT ( 'NONE',  ( 9.474510206698729675, 16.51473224551082808, 102.0844237280190043 ) ) ;
#164269 = CARTESIAN_POINT ( 'NONE',  ( -18.67979575497193778, 10.72451020669871902, 73.33442372801901854 ) ) ;
#164270 = CARTESIAN_POINT ( 'NONE',  ( -22.44159573604010305, 16.30477369853692338, 144.6750000027311671 ) ) ;
#164271 = CARTESIAN_POINT ( 'NONE',  ( -21.55341960407610458, -5.719274019375992779, 21.45724293864769550 ) ) ;
#164272 = CARTESIAN_POINT ( 'NONE',  ( -16.53943276465976808, -0.05219959533934237506, 78.75109039468568994 ) ) ;
#164273 = CARTESIAN_POINT ( 'NONE',  ( 19.05341960407611168, 5.049401038298154454, 23.95724293864769194 ) ) ;
#164274 = CARTESIAN_POINT ( 'NONE',  ( -19.02544592524342804, 5.153800228976336051, 76.04057627198102409 ) ) ;
#164275 = CARTESIAN_POINT ( 'NONE',  ( 5.823673210054125526, 21.52544592524343514, 79.79057627198102409 ) ) ;
#164276 =( BOUNDED_SURFACE ( )  B_SPLINE_SURFACE ( 3, 2, ( 
 ( #195165, #119315, #26321, #12154, #87961, #27319, #118319, #181001, #180012, #88966, #41479, #103143, #150656, #73819, #110095, #199129, #92921, #908, #94921, #44460, #14104, #152614, #156606, #77760, #109097, #167798, #124261, #184948, #46433, #106114, #1916, #139426, #63595, #154607, #32266, #18101, #171773, #75772, #62583, #107099, #33262, #108092, #140426, #45446, #125270, #29298, #93923, #186968, #78749, #79755, #16102, #141426, #30272, #169776, #137450, #200120, #48438, #60596, #122271, #185956, #168769, #90928, #59610, #15106, #121283, #183959, #91917, #153610, #182976, #47440, #76767, #138439, #170776, #61589, #123257, #31270, #17096, #155601, #95913, #114051, #19089, #113064, #159565, #81710, #21063, #82718, #129220, #65574, #144400, #20067, #157597, #130213, #176763, #51404, #115071, #36221, #2912, #5886, #96894, #64591, #191908, #143396, #53393, #84714, #97873, #160578, #4885, #38235, #66567, #128232, #189929, #190917, #37227, #174756, #67562, #173774, #158577, #52394, #175750, #98884, #22067, #188948, #99890, #161575, #83718, #23068, #145396, #126255, #6879, #68557, #187952, #49421, #111083, #172773, #34254, #80737, #142416, #3895, #127234, #50425, #35240, #112084, #58393, #196926, #85726, #179769, #87722, #181748, #131233, #100884, #39228, #43229, #164584, #195937, #54399, #10902, #71565, #133230, #192921, #88728, #26078, #150423, #41238, #119084, #104896, #120060, #162567, #149407, #193929, #166585, #194921, #27081, #132237, #11918, #116071, #180765, #73582, #165583, #28085, #102899, #146392, #117062, #56397, #24071, #86725, #135254, #147413, #8901, #72576, #55392, #177759, #7881, #101900, #69566, #70569, #178757, #40223, #163582, #134250, #25082, #148410, #57411, #9905, #118079, #42241, #103902, #29065, #182742, #674, #105884, #199895, #46200, #168545, #107853, #169538, #15869, #152387, #31038, #106872, #44227, #16861, #63356, #138213, #1678, #123030, #89725, #92687, #183731, #151411, #78512, #30043, #140186, #171539, #184716, #47202, #91682, #125033, #153374, #14876, #76537, #77527, #124014, #61359, #154375, #60369, #45217, #186729, #74563, #167571, #90704, #48200, #139199, #62345, #197905, #185712, #108862, #170541, #136230, #32032, #93689, #155372, #109854, #12899, #59374, #121046, #13872, #75539, #137214, #198901, #122041, #113816, #18857, #36985, #2678, #5647, #98647, #52159, #83482, #127994, #53152, #3660, #158345, #49191, #173534, #21830, #126024, #172533, #97636, #142176, #64355, #175511, #188705, #114831, #17864, #187720, #80503, #145160, #66333, #65338, #156361, #112830, #35003, #110849, #96658, #190684, #34019, #95677, #144162, #157363, #143162, #189697, #111844, #51170, #174522, #159325, #126998, #35989, #50187, #19834, #160341, #6644, #81475, #68322, #20821, #33027, #82478, #4642, #94682, #129972, #67324, #191672, #79519, #128986, #141189, #193692, #103674, #116830, #55160, #163350, #102671, #10672, #178521, #39988, #147175, #132004, #101659, #24846, #117843, #162336, #165352, #88487, #164356, #26846, #194691, #60871, #56161, #86495, #179535, #148180, #72336, #9673, #25852, #69326, #41004, #150182, #133001, #11683, #8664, #73349, #135022, #196697, #115840, #71338, #87495, #176525, #149184, #134011, #38001, #99656, #146156, #195703, #57175, #161340, #177529, #118852, #180535, #22832, #84479, #130992, #192684, #7642, #42009, #54167, #38998, #100654, #23837, #85486, #70337, #64860, #140699, #126522, #17369, #95192, #157874, #173048, #77040, #63871, #170054, #34525, #47716, #3187, #108378, #188221, #92202, #156878, #49694, #141696, #96185, #79024, #142687, #93197, #109367, #138711, #62859, #111359, #15383, #61861, #187238, #31545, #153886, #19363, #78027, #4167, #107372, #192, #154882, #81012, #155872, #16380, #45719, #2189, #124541, #123530, #186238, #80027, #185224, #46715, #33530, #139696, #32539, #125542, #1182, #48708, #110361, #172043, #171049, #18375 ),
 ( #122548, #184238, #169044, #30550, #94192, #193201, #6163, #83003, #52673, #192199, #100174, #67843, #144678, #36498, #21345, #129498, #114336, #7161, #51679, #54674, #178037, #53681, #116348, #84000, #147700, #145679, #191198, #68844, #176039, #161856, #37507, #130503, #99169, #158849, #39505, #101165, #160859, #162853, #22349, #65845, #115358, #159852, #127515, #24360, #177048, #86011, #189219, #38518, #23350, #84995, #50697, #146676, #8171, #69847, #131515, #112356, #174047, #35516, #98152, #97164, #20337, #81986, #143679, #113341, #5160, #66843, #128506, #190201, #175033, #90967, #27360, #164869, #89006, #119360, #105173, #181044, #58663, #102185, #150697, #136499, #165864, #198179, #120329, #12195, #72865, #132522, #148700, #42519, #73860, #44499, #194211, #163873, #25372, #106155, #135529, #182024, #117350, #197200, #134534, #196222, #55676, #151681, #43507, #13173, #104182, #166859, #167837, #59649, #87014, #28361, #56689, #121323, #57692, #89999, #195209, #74836, #179046, #183015, #29338, #9188, #70853, #40514, #10188, #180056, #71848, #133517, #149692, #118363, #41525, #103188, #26364, #88004, #11190, #94957, #108132, #34288, #137489, #184001, #200158, #64627, #185995, #184988, #75811, #32306, #92960, #45484, #154646, #110131, #91956, #107139, #63633, #168809, #62620, #109135, #31307, #170813, #93960, #78787, #15144, #2948, #47478, #172807, #123296, #77796, #30313, #16141, #141464, #153649, #76806, #17135, #61628, #138477, #156641, #169816, #152654, #199169, #46472, #139465, #126289, #155640, #945, #60636, #140464, #124298, #1954, #125309, #171810, #187005, #48475, #33298, #18137, #79791, #187986, #49456, #111118, #14144, #122310, #158611, #37260, #113098, #188982, #23101, #69599, #144433, #7915, #129255, #95948, #175786, #189963, #157634, #84747, #174789, #146424, #177791, #190950, #53426, #36255, #131266, #97908, #159599, #82753, #22100, #130246, #21096, #5919, #66601, #51438, #67596, #52427, #98918, #81745, #192954, #54433, #83750, #116103, #114085, #19123, #160610, #145429, #6912, #68590, #191941, #115103, #176795, #50458, #38268, #80773, #99922, #142451, #161607, #3929, #65609, #127269, #35274, #112117, #173809, #96929, #20101, #143432, #4918, #128265, #57441, #88757, #147447, #103932, #164616, #26110, #85760, #181776, #119114, #43257, #134281, #11946, #74589, #89752, #193962, #180795, #86760, #151438, #87753, #120088, #25116, #104925, #8935, #73610, #166612, #58421, #42274, #28114, #195969, #12925, #150450, #165612, #102931, #162602, #178791, #72607, #27111, #136257, #24106, #55425, #132271, #197933, #135281, #196953, #70604, #59401, #149438, #10934, #117096, #121075, #39261, #100917, #40260, #101933, #163615, #148443, #9938, #71597, #133263, #194954, #56431, #118111, #179800, #41269, #152413, #155401, #186760, #1710, #33058, #77558, #2709, #153406, #107885, #198928, #123060, #171569, #75567, #122068, #47234, #91712, #13901, #125063, #138241, #64386, #167596, #137243, #30071, #94713, #15900, #14904, #105910, #62377, #184746, #60396, #46231, #140217, #183760, #45246, #93719, #106900, #92717, #139230, #61388, #705, #124047, #108893, #168573, #185746, #199925, #76566, #109885, #156391, #31069, #17895, #170572, #182769, #32063, #169572, #44253, #79549, #154406, #141218, #29091, #16891, #63386, #78542, #90730, #48230, #143195, #112863, #52190, #160373, #66367, #4675, #96690, #81507, #128027, #174554, #67357, #111876, #53187, #38032, #113848, #114862, #144195, #7673, #5681, #189729, #129017, #36021, #21864, #97670, #175544, #18888, #19867, #159359, #176557, #190717, #95707, #37019, #35035, #157395, #20856, #98680, #51202, #83514, #145191, #130003, #50222, #80534, #84510, #6674, #68352, #191703, #99688, #161372, #22863, #146188, #126054, #187751, #82513, #49221, #110879, #172564, #142208, #34050, #3691, #65370, #127030, #188737, #173566, #158378, #72368, #117875, #85518, #119865 ),
 ( #151210, #164389, #26878, #86526, #196729, #9704, #148210, #56192, #195735, #103705, #71368, #133032, #40018, #24877, #194722, #179565, #10705, #55192, #58197, #181550, #57208, #43029, #87527, #69357, #149214, #41035, #134042, #102701, #165385, #25882, #118883, #162366, #180567, #104695, #42041, #166383, #88521, #150217, #11714, #192715, #8697, #73381, #135053, #27879, #54199, #23867, #147206, #89520, #131026, #115871, #177560, #39029, #100684, #70367, #132035, #193724, #116861, #178552, #101691, #163380, #47994, #63141, #167367, #154170, #60164, #124820, #138003, #93474, #198698, #16653, #182538, #185503, #78300, #31824, #122824, #169326, #91476, #30833, #92481, #138988, #75338, #15661, #29839, #105681, #139974, #186520, #61152, #109648, #45994, #12698, #77320, #106670, #74364, #1463, #153164, #171330, #94469, #107649, #170331, #14665, #32818, #76326, #199687, #184514, #466, #46994, #62141, #123805, #183527, #168343, #108653, #155161, #136030, #121833, #197704, #59170, #120839, #44020, #28865, #90505, #152187, #13671, #137008, #45010, #51951, #66122, #5437, #48980, #174316, #83276, #112624, #144951, #67121, #35786, #19630, #79308, #95465, #189487, #97433, #191462, #140977, #110635, #172316, #52940, #159119, #128779, #64147, #20614, #81272, #142954, #2465, #98435, #82265, #160131, #50965, #190479, #114614, #6432, #33805, #143957, #3453, #68114, #4434, #36771, #141964, #21619, #125811, #113611, #129766, #175305, #176314, #37784, #156150, #126787, #127787, #157151, #96451, #17648, #18646, #80292, #187514, #65130, #188493, #49972, #111636, #173321, #34796, #158138, #146965, #11470, #132793, #131798, #22624, #179326, #39778, #130783, #101442, #56963, #38793, #192475, #10462, #115633, #53958, #134811, #117628, #148973, #7433, #164147, #24636, #86284, #145952, #41796, #40790, #103463, #194480, #72123, #196491, #149964, #177322, #102459, #8453, #73141, #147975, #180328, #85274, #165142, #69117, #133797, #26633, #118636, #57961, #55952, #119632, #70126, #9464, #100450, #163133, #88276, #162130, #23626, #25644, #193477, #54954, #181315, #116626, #99448, #84271, #178315, #71127, #161128, #87289, #195488, #166139, #122586, #183287, #74127, #44769, #229, #182298, #135798, #153925, #58935, #152922, #199442, #121592, #60910, #184273, #169081, #105443, #45756, #59924, #197469, #170088, #16415, #91232, #154917, #76082, #42794, #107408, #136767, #104456, #31582, #106422, #93232, #124577, #137758, #61897, #168103, #78062, #29600, #14418, #30587, #92239, #77078, #15419, #138747, #13436, #198453, #123567, #185262, #46754, #28627, #139730, #1219, #108413, #62897, #27641, #89282, #150972, #12466, #120604, #43778, #167127, #90264, #151947, #75100, #4202, #113375, #142722, #177827, #97197, #65880, #49730, #109406, #125577, #19397, #127554, #24145, #171085, #140736, #95229, #155910, #34562, #158883, #111398, #35550, #112390, #190235, #110398, #79063, #147483, #174081, #5195, #189255, #143716, #50731, #20373, #162639, #100954, #8973, #81046, #82021, #39297, #66877, #17406, #128539, #51712, #85797, #47752, #2225, #70642, #156915, #186273, #96218, #63907, #32576, #94229, #187275, #48745, #172080, #80061, #33567, #18412, #141731, #3221, #64895, #126556, #188256, #173083, #157907, #55462, #120124, #196990, #41306, #43294, #101971, #166649, #196004, #86796, #40297, #44290, #164652, #88793, #194000, #163652, #132308, #105948, #13937, #57477, #25154, #151474, #148483, #12964, #90768, #117133, #73646, #74628, #104962, #136294, #121113, #27146, #150486, #29130, #182807, #119149, #28150, #135317, #58456, #9974, #197970, #178827, #71634, #11981, #167633, #133300, #89790, #194991, #165648, #59440, #56468, #10970, #42308, #118146, #179836, #102967, #181815, #26147, #152452, #180831, #87789, #149474, #103969, #72643, #134318, #76602, #62415, #94750, #187785, #198965, #153444, #93757, #15937, #169609, #185786, #64420, #16928, #45283 ),
 ( #124087, #49255, #108930, #75604, #155438, #31107, #137283, #126089, #154443, #2743, #157429, #170610, #33094, #92755, #110913, #77596, #139267, #47273, #1747, #109924, #743, #32100, #46269, #78581, #140255, #63425, #125100, #61426, #172599, #34085, #186798, #95744, #48269, #60432, #171606, #156431, #17931, #79585, #141254, #122106, #183796, #168609, #106936, #30109, #91749, #14942, #138279, #199961, #123097, #184783, #107924, #52226, #160410, #54234, #3728, #173601, #111913, #115905, #37057, #68388, #127066, #83549, #144233, #5717, #65405, #161407, #98716, #22899, #113882, #191739, #177595, #69394, #35070, #21899, #66402, #131062, #67395, #99723, #4713, #84545, #188774, #53223, #146222, #38067, #192751, #175580, #39063, #189766, #129051, #96725, #159398, #7710, #158413, #19902, #145228, #128064, #50257, #100720, #174593, #18923, #81544, #143230, #51238, #80568, #6710, #112899, #142243, #130040, #20893, #36058, #82551, #176593, #97707, #190752, #114899, #178589, #179600, #72403, #166419, #197737, #163418, #149248, #181583, #74397, #85557, #40053, #180601, #102735, #56229, #134080, #151242, #103739, #132071, #150254, #71403, #193760, #10739, #135086, #87561, #11748, #88555, #27913, #86561, #55228, #120872, #73415, #43061, #42075, #119898, #165419, #196762, #136062, #59203, #182572, #195769, #26912, #12731, #58229, #116897, #57243, #104727, #89556, #23903, #101730, #44055, #133067, #162400, #118917, #24915, #147242, #8734, #70403, #148245, #9739, #117911, #194757, #41072, #164424, #25917, #16686, #94503, #105715, #124855, #63176, #28898, #93511, #170366, #14701, #78336, #75371, #140010, #169360, #60198, #13704, #17684, #138040, #62175, #167402, #137041, #90538, #79342, #187547, #30870, #198732, #186555, #121868, #48027, #64180, #152220, #47030, #109684, #1498, #171365, #156185, #503, #123839, #2499, #141012, #92516, #32853, #108688, #31858, #183560, #125846, #45046, #106704, #185537, #168378, #29873, #91510, #153197, #139023, #76363, #199721, #184547, #15695, #61187, #122859, #46027, #155197, #107683, #154206, #77356, #69147, #18678, #143989, #37817, #172349, #144983, #141997, #82298, #114647, #130814, #127817, #159149, #95498, #65162, #34827, #5470, #158170, #67152, #35817, #49014, #66154, #20645, #52970, #84302, #50004, #97463, #68144, #161159, #33838, #126821, #128810, #189522, #142987, #190509, #99478, #51983, #80324, #36803, #19662, #3485, #113641, #21653, #174347, #98468, #175336, #176345, #173357, #188527, #7463, #160162, #129795, #83306, #6463, #191492, #22655, #145981, #110669, #157184, #111669, #96482, #81303, #4465, #50995, #112656, #56992, #40819, #53989, #85303, #133828, #178345, #164176, #71157, #146995, #26664, #118666, #196520, #41826, #149994, #39807, #25674, #180357, #73171, #11500, #10492, #165171, #192505, #103493, #88306, #177352, #72152, #149003, #101473, #195519, #23655, #134841, #132823, #8482, #162159, #115662, #24666, #87319, #100480, #70157, #38822, #131827, #193508, #54985, #163163, #116654, #55982, #86316, #148004, #9494, #194509, #117659, #179356, #102489, #161813, #67805, #129460, #69804, #23308, #159810, #7118, #175998, #37468, #80972, #192156, #34487, #54631, #191159, #128464, #52632, #82962, #68800, #144639, #22307, #65806, #114296, #100132, #99129, #84952, #83958, #160819, #36455, #96145, #112314, #6122, #145638, #8126, #157834, #127474, #189180, #131472, #130459, #53637, #142648, #115314, #98113, #21305, #19325, #177006, #38475, #146634, #193159, #173008, #4127, #50653, #174004, #35475, #20296, #97124, #158807, #81944, #143635, #5119, #66801, #190160, #51636, #113300, #174991, #145849, #193376, #69015, #19531, #82161, #142858, #21516, #7331, #98329, #22522, #99345, #177220, #97334, #66021, #131695, #161028, #192375, #52840, #130681, #191362, #84169, #146858, #85170, #54852, #6334, #37680, #23524, #53858, #4337, #68014, #115532, #114509, #34696 ),
 ( #173220, #176211, #67020, #96353, #162028, #51851, #100349, #158040, #129666, #38693, #190376, #8351, #113510, #175205, #160029, #70026, #81176, #36670, #83177, #143857, #128679, #144851, #127689, #189389, #159020, #50866, #112524, #174218, #35686, #20513, #5336, #132694, #26533, #73036, #195385, #134708, #196391, #42691, #179222, #57859, #133692, #9362, #43676, #90163, #165040, #28527, #149861, #116526, #119532, #10362, #178214, #105338, #56863, #167025, #198348, #11366, #74026, #118538, #151846, #180227, #41697, #103362, #104352, #150869, #88177, #181215, #87190, #72019, #166036, #27536, #89177, #102357, #13336, #75001, #12363, #136666, #135696, #39678, #197368, #58833, #120500, #182191, #101340, #163029, #24535, #71027, #86186, #147876, #194383, #55850, #117524, #40688, #164047, #25546, #148871, #93132, #1120, #97839, #44668, #14320, #152826, #159527, #77965, #109305, #168007, #124475, #185159, #46649, #106321, #4848, #139632, #66533, #154817, #32477, #21025, #113030, #75985, #62794, #107307, #174722, #108309, #140637, #45656, #128196, #29503, #94130, #189894, #78962, #36185, #16315, #82679, #186172, #47654, #59822, #128, #51369, #137658, #199345, #170984, #168979, #91136, #144363, #15317, #121492, #60810, #122483, #30484, #183186, #155809, #92135, #184174, #17307, #61797, #153822, #123467, #76976, #138647, #169989, #31480, #39193, #38200, #129183, #85689, #146357, #37190, #7844, #163547, #145361, #98847, #117027, #22031, #116035, #162531, #84678, #24035, #147376, #132201, #68522, #8865, #23033, #160542, #133195, #179733, #54363, #118043, #100849, #5850, #70532, #99856, #67526, #194886, #69531, #56360, #87687, #193892, #25047, #131195, #41203, #192885, #177724, #55357, #178722, #40184, #101864, #86690, #176727, #161540, #148374, #9869, #71528, #191873, #102864, #164549, #26042, #190881, #52357, #114013, #175711, #83683, #6843, #130176, #53357, #115034, #198866, #42207, #167536, #76503, #105849, #138179, #60333, #29031, #12865, #72538, #88691, #182705, #90671, #184683, #134215, #103867, #165548, #46166, #152353, #122007, #57376, #13838, #74530, #136195, #195901, #91650, #75505, #153339, #44190, #183698, #107820, #199861, #27045, #137178, #196891, #61326, #197870, #30012, #135219, #14840, #119049, #45185, #122997, #168514, #169504, #106839, #31003, #149372, #10868, #180731, #89689, #150387, #11883, #73546, #58358, #120025, #181710, #43191, #104860, #166549, #28048, #151374, #59337, #121007, #143130, #187688, #51138, #18825, #49158, #92652, #32996, #81444, #185678, #31997, #157330, #1644, #123980, #34974, #48167, #174492, #77493, #47168, #140152, #4610, #125990, #125001, #15834, #172499, #94650, #108827, #156330, #50154, #93654, #170506, #3627, #155339, #2646, #110816, #171507, #33986, #95642, #80470, #16828, #142143, #109824, #78479, #19803, #66302, #141157, #127962, #65306, #154341, #126965, #186696, #139163, #189665, #17830, #112799, #640, #188674, #111813, #79488, #62310, #64323, #173501, #96627, #158315, #63322, #176493, #114800, #6613, #191642, #37969, #84449, #177500, #21800, #163321, #148152, #23807, #24818, #54136, #117814, #115810, #53122, #38969, #146127, #131976, #7612, #85458, #128954, #100625, #86467, #192653, #9644, #147147, #162307, #99627, #159294, #175482, #69297, #8635, #71310, #20791, #190654, #52130, #132973, #70307, #193661, #144134, #55132, #161309, #22803, #82446, #178494, #116802, #39960, #130963, #101631, #194663, #56132, #113787, #35959, #83452, #97606, #5616, #67295, #145130, #36954, #98616, #160310, #68292, #129943, #102644, #57146, #197645, #119807, #73320, #89461, #152129, #199624, #75279, #25823, #88457, #149155, #27819, #13611, #104633, #28804, #105620, #183465, #103647, #72306, #137940, #167308, #198638, #59111, #136949, #120776, #90444, #153102, #91415, #61091, #12640, #43958, #29779, #60104, #10645, #74307, #121772, #182477, #40975, #195675, #44951, #150153 ),
 ( #106607, #168282, #179507, #14606, #76262, #164329, #87468, #133984, #11654, #118823, #180508, #41981, #42970, #165325, #26817, #134991, #196670, #135974, #58139, #181492, #166322, #151149, #4375, #186455, #92419, #141902, #154105, #3393, #81212, #122764, #64081, #65068, #33742, #126725, #111573, #17585, #79245, #19568, #173257, #109585, #157088, #125751, #187451, #30772, #188429, #184453, #15599, #140916, #34732, #45933, #18584, #77257, #156088, #49907, #107588, #1400, #32756, #169266, #138926, #108591, #2403, #31762, #48919, #171268, #142893, #139910, #94407, #96390, #158077, #123743, #110573, #406, #172254, #62078, #185442, #170268, #95402, #93411, #80231, #46932, #155097, #63080, #16591, #78239, #124759, #47931, #52878, #85209, #178252, #189428, #143893, #84206, #6371, #160067, #176249, #38729, #86221, #162065, #112561, #175242, #35724, #114550, #100387, #191401, #115570, #192413, #70064, #190413, #159057, #24572, #53895, #146898, #145886, #23561, #7369, #177257, #39713, #101376, #147911, #99382, #130720, #116563, #8389, #97371, #161065, #131732, #69054, #127726, #82201, #193414, #36707, #54889, #37720, #5374, #163066, #66059, #50903, #174256, #20551, #21554, #67058, #128716, #51889, #113548, #98369, #83214, #144889, #68051, #129705, #22560, #197404, #74062, #118572, #120536, #179260, #43714, #73071, #164082, #117560, #121528, #41732, #166072, #71063, #40725, #9397, #183223, #91172, #134743, #102394, #28563, #25581, #90200, #168042, #132729, #150906, #151883, #182229, #13373, #198384, #104389, #27574, #106358, #59861, #196425, #105375, #12400, #135733, #87225, #75037, #194417, #148907, #89213, #44704, #55887, #167062, #10397, #42727, #136703, #72054, #88211, #133728, #195420, #58870, #149895, #103396, #119567, #29539, #56898, #180262, #165074, #26568, #11402, #57895, #181250, #78001, #2164, #78998, #156852, #77012, #45692, #111331, #63843, #165, #64835, #186210, #185196, #76021, #32514, #93170, #184210, #154855, #110335, #92172, #107343, #125515, #169016, #62831, #109341, #31517, #171023, #94166, #140672, #15356, #155845, #170027, #30521, #80002, #126497, #1156, #188195, #47691, #152861, #17342, #46687, #14356, #141671, #16353, #3162, #34500, #187212, #172016, #139668, #49667, #124514, #48683, #33505, #95164, #18347, #173021, #137696, #123503, #108347, #199381, #60845, #122520, #138684, #153858, #61833, #83970, #84965, #114309, #178008, #176011, #51649, #37480, #6134, #192170, #67817, #145650, #189193, #99142, #23321, #52645, #146647, #7131, #160831, #159823, #19339, #35488, #129472, #22319, #131485, #80986, #50667, #112327, #193172, #68814, #130473, #4140, #53650, #21318, #82976, #142661, #38488, #115328, #100145, #191171, #177019, #54644, #8141, #174017, #161826, #143649, #69818, #144652, #116319, #81957, #96158, #157847, #65819, #127488, #97138, #158821, #20309, #5132, #66815, #128477, #190173, #113313, #175005, #36469, #98126, #164838, #120302, #25342, #43477, #9158, #12165, #105145, #58636, #89971, #134504, #198151, #165834, #196190, #39475, #180025, #28332, #132493, #179015, #104152, #148670, #70824, #181995, #136471, #41493, #181015, #88977, #86983, #151651, #72834, #71818, #162822, #119329, #103157, #194182, #26334, #197171, #40483, #55646, #150667, #117319, #149662, #57662, #118332, #42489, #27331, #73830, #102155, #135500, #56659, #163841, #166831, #13146, #87974, #74809, #59621, #101136, #121294, #133486, #24331, #85981, #11160, #147670, #10158, #195178, #140437, #200131, #110106, #123269, #61600, #169788, #109108, #17108, #184960, #46444, #153621, #138450, #108104, #31281, #124272, #168781, #171785, #94932, #170787, #33273, #920, #64602, #62594, #92932, #185968, #154619, #78760, #16113, #32277, #75783, #47452, #156617, #139438, #18112, #93934, #155613, #77771, #106125, #122282, #1927, #63606, #79766, #167809, #137461, #199140, #141437, #125282, #186979, #90939, #2924, #182987 ),
 ( #48449, #44471, #152626, #29309, #14116, #60607, #183970, #45457, #107111, #30284, #91929, #15117, #76778, #176773, #80749, #67573, #173785, #38245, #51415, #6889, #112095, #130224, #95924, #98894, #191920, #145407, #99900, #21074, #84724, #52405, #82730, #126266, #66578, #115081, #19100, #65586, #190928, #35252, #157609, #68567, #23079, #128243, #129231, #175762, #96905, #161585, #159577, #158589, #49433, #5897, #189940, #142427, #113075, #83728, #127246, #3906, #37238, #188959, #36233, #144411, #4896, #114064, #160588, #22077, #50436, #53403, #143408, #20078, #146402, #7892, #174767, #187963, #111094, #172784, #34265, #81722, #97885, #61117, #148420, #199651, #154135, #164594, #29805, #86735, #122791, #9915, #71574, #56408, #195947, #106635, #133240, #194932, #40234, #25093, #118089, #179779, #10913, #55402, #184480, #45959, #60131, #107614, #87732, #69577, #149417, #41248, #72586, #102910, #168308, #26088, #121799, #162578, #134260, #169292, #30798, #183492, #92447, #44976, #91441, #131243, #153129, #192931, #24082, #8911, #14632, #178768, #100894, #76291, #54409, #137969, #116081, #177769, #117072, #39238, #85737, #101910, #147424, #70579, #132247, #193939, #163592, #173286, #155126, #108619, #126754, #31790, #125778, #172282, #94435, #33771, #95431, #141929, #78267, #157115, #32783, #170297, #142919, #189453, #64112, #127752, #48947, #15627, #18612, #109613, #77284, #4401, #156116, #66086, #97397, #110600, #34760, #17614, #50931, #79273, #140944, #2432, #3420, #49937, #187480, #80259, #186485, #171297, #65096, #188456, #111602, #1429, #112588, #174282, #96418, #35751, #158104, #138954, #19596, #81238, #433, #62107, #123770, #185470, #46960, #93439, #16619, #139939, #63108, #124786, #47961, #115599, #22588, #82230, #98399, #192442, #100415, #194444, #143920, #113575, #51916, #55915, #177288, #8420, #67085, #23591, #84236, #145914, #5401, #101405, #38758, #163099, #53924, #131761, #117589, #9425, #175269, #162096, #6399, #71090, #7399, #39743, #144916, #24602, #128744, #193443, #86249, #178280, #54919, #69083, #70092, #36735, #85239, #147939, #146930, #132757, #116591, #179290, #130750, #190440, #160096, #40755, #159083, #20578, #21582, #83241, #68078, #129732, #191429, #52905, #114581, #176279, #37750, #99411, #161093, #44736, #120567, #106392, #197435, #75068, #137730, #152892, #56929, #43746, #149927, #14388, #27606, #183255, #88242, #168073, #72086, #136734, #29571, #121560, #76054, #58901, #60878, #28594, #182261, #102424, #42758, #91202, #195455, #41762, #167093, #11434, #133760, #199414, #122555, #104421, #105409, #151915, #73105, #184245, #135764, #134774, #25609, #90231, #166104, #118604, #89246, #59893, #103427, #180294, #13404, #165106, #12431, #198416, #181281, #164111, #87253, #148938, #26599, #10428, #119598, #196457, #57927, #150938, #74094, #157881, #79031, #45726, #125549, #139703, #107379, #34533, #124548, #173056, #127523, #140707, #3194, #62866, #96192, #186245, #47723, #32546, #172050, #80034, #109374, #171056, #16387, #1189, #94199, #155879, #187245, #31552, #19370, #81019, #33537, #142694, #63878, #169051, #48715, #17376, #110368, #2197, #30557, #95200, #64867, #156886, #4174, #18383, #141703, #126529, #188228, #49701, #111367, #65852, #78034, #92209, #153894, #15390, #77047, #93204, #138718, #199, #61868, #123537, #185231, #46722, #108385, #170062, #154889, #99178, #85003, #160867, #38526, #81993, #7169, #116356, #145687, #178045, #100182, #68852, #52681, #112363, #128513, #22357, #130511, #24369, #174054, #143686, #5168, #86020, #192207, #161864, #97171, #53689, #114344, #176048, #35523, #131524, #115367, #193209, #84009, #23358, #147709, #39513, #66851, #177056, #36506, #101173, #37516, #69856, #175041, #54683, #158856, #146684, #162861, #8180, #9196, #70862, #189227, #50705, #20344, #190208, #129506, #51687, #113349, #98160, #159861, #21354, #83011 ) ),
 .UNSPECIFIED., .T., .F., .F. ) 
 B_SPLINE_SURFACE_WITH_KNOTS ( ( 4, 3, 4 ),
 ( 3, 2, 2, 2, 2, 2, 2, 2, 2, 2, 2, 2, 2, 2, 2, 2, 2, 2, 2, 2, 2, 2, 2, 2, 2, 2, 2, 2, 2, 2, 2, 2, 2, 2, 2, 2, 2, 2, 2, 2, 2, 2, 2, 2, 2, 2, 2, 2, 2, 2, 2, 2, 2, 2, 2, 2, 2, 2, 2, 2, 2, 2, 2, 2, 2, 2, 2, 2, 2, 2, 2, 2, 2, 2, 2, 2, 2, 2, 2, 2, 2, 2, 2, 2, 2, 2, 2, 2, 2, 2, 2, 2, 2, 2, 2, 2, 2, 2, 2, 2, 2, 2, 2, 2, 2, 2, 2, 2, 2, 2, 2, 2, 2, 2, 2, 2, 2, 2, 2, 2, 2, 2, 2, 2, 2, 2, 2, 2, 2, 2, 2, 2, 2, 2, 2, 2, 2, 2, 2, 2, 2, 2, 2, 2, 2, 2, 2, 2, 2, 2, 2, 2, 2, 2, 2, 2, 2, 2, 2, 2, 2, 2, 2, 2, 2, 2, 2, 2, 2, 2, 2, 2, 2, 2, 2, 2, 2, 2, 2, 2, 2, 2, 2, 2, 2, 2, 2, 2, 2, 2, 2, 2, 2, 2, 2, 2, 2, 2, 2, 2, 2, 2, 2, 2, 2, 2, 2, 2, 2, 2, 2, 2, 2, 2, 2, 2, 2, 2, 2, 2, 2, 2, 2, 2, 2, 2, 2, 2, 3 ),
 ( 0.000000000000000000, 0.5000000000000000000, 1.000000000000000000 ),
 ( 0.000000000000000000, 0.004385964912280701511, 0.008771929824561403022, 0.01315789473684210453, 0.01754385964912280604, 0.02192982456140350755, 0.02631578947368420907, 0.03070175438596491058, 0.03508771929824561209, 0.03947368421052631360, 0.04385964912280701511, 0.04824561403508771662, 0.05263157894736841813, 0.05701754385964911964, 0.06140350877192982115, 0.06578947368421052266, 0.07017543859649122417, 0.07456140350877192569, 0.07894736842105262720, 0.08333333333333332871, 0.08771929824561403022, 0.09210526315789473173, 0.09649122807017543324, 0.1008771929824561348, 0.1052631578947368363, 0.1096491228070175378, 0.1140350877192982393, 0.1184210526315789408, 0.1228070175438596423, 0.1271929824561403577, 0.1315789473684210453, 0.1359649122807017607, 0.1403508771929824483, 0.1447368421052631637, 0.1491228070175438514, 0.1535087719298245668, 0.1578947368421052544, 0.1622807017543859698, 0.1666666666666666574, 0.1710526315789473728, 0.1754385964912280604, 0.1798245614035087758, 0.1842105263157894635, 0.1885964912280701788, 0.1929824561403508665, 0.1973684210526315819, 0.2017543859649122695, 0.2061403508771929849, 0.2105263157894736725, 0.2149122807017543879, 0.2192982456140350755, 0.2236842105263157909, 0.2280701754385964786, 0.2324561403508771940, 0.2368421052631578816, 0.2412280701754385970, 0.2456140350877192846, 0.2500000000000000000, 0.2543859649122807154, 0.2587719298245614308, 0.2631578947368420907, 0.2675438596491228060, 0.2719298245614035214, 0.2763157894736842368, 0.2807017543859648967, 0.2850877192982456121, 0.2894736842105263275, 0.2938596491228070429, 0.2982456140350877027, 0.3026315789473684181, 0.3070175438596491335, 0.3114035087719298489, 0.3157894736842105088, 0.3201754385964912242, 0.3245614035087719396, 0.3289473684210526550, 0.3333333333333333148, 0.3377192982456140302, 0.3421052631578947456, 0.3464912280701754610, 0.3508771929824561209, 0.3552631578947368363, 0.3596491228070175517, 0.3640350877192982670, 0.3684210526315789269, 0.3728070175438596423, 0.3771929824561403577, 0.3815789473684210731, 0.3859649122807017330, 0.3903508771929824483, 0.3947368421052631637, 0.3991228070175438791, 0.4035087719298245390, 0.4078947368421052544, 0.4122807017543859698, 0.4166666666666666852, 0.4210526315789473450, 0.4254385964912280604, 0.4298245614035087758, 0.4342105263157894912, 0.4385964912280701511, 0.4429824561403508665, 0.4473684210526315819, 0.4517543859649122973, 0.4561403508771929571, 0.4605263157894736725, 0.4649122807017543879, 0.4692982456140351033, 0.4736842105263157632, 0.4780701754385964786, 0.4824561403508771940, 0.4868421052631579093, 0.4912280701754385692, 0.4956140350877192846, 0.5000000000000000000, 0.5043859649122807154, 0.5087719298245614308, 0.5131578947368421462, 0.5175438596491228616, 0.5219298245614034659, 0.5263157894736841813, 0.5307017543859648967, 0.5350877192982456121, 0.5394736842105263275, 0.5438596491228070429, 0.5482456140350877583, 0.5526315789473684736, 0.5570175438596490780, 0.5614035087719297934, 0.5657894736842105088, 0.5701754385964912242, 0.5745614035087719396, 0.5789473684210526550, 0.5833333333333333703, 0.5877192982456140857, 0.5921052631578946901, 0.5964912280701754055, 0.6008771929824561209, 0.6052631578947368363, 0.6096491228070175517, 0.6140350877192982670, 0.6184210526315789824, 0.6228070175438596978, 0.6271929824561403022, 0.6315789473684210176, 0.6359649122807017330, 0.6403508771929824483, 0.6447368421052631637, 0.6491228070175438791, 0.6535087719298245945, 0.6578947368421053099, 0.6622807017543859143, 0.6666666666666666297, 0.6710526315789473450, 0.6754385964912280604, 0.6798245614035087758, 0.6842105263157894912, 0.6885964912280702066, 0.6929824561403509220, 0.6973684210526315264, 0.7017543859649122417, 0.7061403508771929571, 0.7105263157894736725, 0.7149122807017543879, 0.7192982456140351033, 0.7236842105263158187, 0.7280701754385965341, 0.7324561403508771384, 0.7368421052631578538, 0.7412280701754385692, 0.7456140350877192846, 0.7500000000000000000, 0.7543859649122807154, 0.7587719298245614308, 0.7631578947368421462, 0.7675438596491228616, 0.7719298245614034659, 0.7763157894736841813, 0.7807017543859648967, 0.7850877192982456121, 0.7894736842105263275, 0.7938596491228070429, 0.7982456140350877583, 0.8026315789473684736, 0.8070175438596490780, 0.8114035087719297934, 0.8157894736842105088, 0.8201754385964912242, 0.8245614035087719396, 0.8289473684210526550, 0.8333333333333333703, 0.8377192982456140857, 0.8421052631578946901, 0.8464912280701754055, 0.8508771929824561209, 0.8552631578947368363, 0.8596491228070175517, 0.8640350877192982670, 0.8684210526315789824, 0.8728070175438596978, 0.8771929824561403022, 0.8815789473684210176, 0.8859649122807017330, 0.8903508771929824483, 0.8947368421052631637, 0.8991228070175438791, 0.9035087719298245945, 0.9078947368421053099, 0.9122807017543859143, 0.9166666666666666297, 0.9210526315789473450, 0.9254385964912280604, 0.9298245614035087758, 0.9342105263157894912, 0.9385964912280702066, 0.9429824561403509220, 0.9473684210526315264, 0.9517543859649122417, 0.9561403508771929571, 0.9605263157894736725, 0.9649122807017543879, 0.9692982456140351033, 0.9736842105263158187, 0.9780701754385965341, 0.9824561403508771384, 0.9868421052631578538, 0.9912280701754385692, 0.9956140350877192846, 1.000000000000000000 ),
 .UNSPECIFIED. ) 
 GEOMETRIC_REPRESENTATION_ITEM ( )  RATIONAL_B_SPLINE_SURFACE ( (
 ( 1.000000000000000000, 0.9659258262890683122, 1.000000000000000000, 0.9659258262890683122, 1.000000000000000000, 0.9659258262890683122, 1.000000000000000000, 0.9659258262890683122, 1.000000000000000000, 0.9659258262890683122, 1.000000000000000000, 0.9659258262890683122, 1.000000000000000000, 0.9659258262890683122, 1.000000000000000000, 0.9659258262890683122, 1.000000000000000000, 0.9659258262890683122, 1.000000000000000000, 0.9659258262890683122, 1.000000000000000000, 0.9659258262890683122, 1.000000000000000000, 0.9659258262890683122, 1.000000000000000000, 0.9659258262890683122, 1.000000000000000000, 0.9659258262890683122, 1.000000000000000000, 0.9659258262890683122, 1.000000000000000000, 0.9659258262890683122, 1.000000000000000000, 0.9659258262890683122, 1.000000000000000000, 0.9659258262890683122, 1.000000000000000000, 0.9659258262890683122, 1.000000000000000000, 0.9659258262890683122, 1.000000000000000000, 0.9659258262890683122, 1.000000000000000000, 0.9659258262890683122, 1.000000000000000000, 0.9659258262890683122, 1.000000000000000000, 0.9659258262890683122, 1.000000000000000000, 0.9659258262890683122, 1.000000000000000000, 0.9659258262890683122, 1.000000000000000000, 0.9659258262890683122, 1.000000000000000000, 0.9659258262890683122, 1.000000000000000000, 0.9659258262890683122, 1.000000000000000000, 0.9659258262890683122, 1.000000000000000000, 0.9659258262890683122, 1.000000000000000000, 0.9659258262890683122, 1.000000000000000000, 0.9659258262890683122, 1.000000000000000000, 0.9659258262890683122, 1.000000000000000000, 0.9659258262890683122, 1.000000000000000000, 0.9659258262890683122, 1.000000000000000000, 0.9659258262890683122, 1.000000000000000000, 0.9659258262890683122, 1.000000000000000000, 0.9659258262890683122, 1.000000000000000000, 0.9659258262890683122, 1.000000000000000000, 0.9659258262890683122, 1.000000000000000000, 0.9659258262890683122, 1.000000000000000000, 0.9659258262890683122, 1.000000000000000000, 0.9659258262890683122, 1.000000000000000000, 0.9659258262890683122, 1.000000000000000000, 0.9659258262890683122, 1.000000000000000000, 0.9659258262890683122, 1.000000000000000000, 0.9659258262890683122, 1.000000000000000000, 0.9659258262890683122, 1.000000000000000000, 0.9659258262890683122, 1.000000000000000000, 0.9659258262890683122, 1.000000000000000000, 0.9659258262890683122, 1.000000000000000000, 0.9659258262890683122, 1.000000000000000000, 0.9659258262890683122, 1.000000000000000000, 0.9659258262890683122, 1.000000000000000000, 0.9659258262890683122, 1.000000000000000000, 0.9659258262890683122, 1.000000000000000000, 0.9659258262890683122, 1.000000000000000000, 0.9659258262890683122, 1.000000000000000000, 0.9659258262890683122, 1.000000000000000000, 0.9659258262890683122, 1.000000000000000000, 0.9659258262890683122, 1.000000000000000000, 0.9659258262890683122, 1.000000000000000000, 0.9659258262890683122, 1.000000000000000000, 0.9659258262890683122, 1.000000000000000000, 0.9659258262890683122, 1.000000000000000000, 0.9659258262890683122, 1.000000000000000000, 0.9659258262890683122, 1.000000000000000000, 0.9659258262890683122, 1.000000000000000000, 0.9659258262890683122, 1.000000000000000000, 0.9659258262890683122, 1.000000000000000000, 0.9659258262890683122, 1.000000000000000000, 0.9659258262890683122, 1.000000000000000000, 0.9659258262890683122, 1.000000000000000000, 0.9659258262890683122, 1.000000000000000000, 0.9659258262890683122, 1.000000000000000000, 0.9659258262890683122, 1.000000000000000000, 0.9659258262890683122, 1.000000000000000000, 0.9659258262890683122, 1.000000000000000000, 0.9659258262890683122, 1.000000000000000000, 0.9659258262890683122, 1.000000000000000000, 0.9659258262890683122, 1.000000000000000000, 0.9659258262890683122, 1.000000000000000000, 0.9659258262890683122, 1.000000000000000000, 0.9659258262890683122, 1.000000000000000000, 0.9659258262890683122, 1.000000000000000000, 0.9659258262890683122, 1.000000000000000000, 0.9659258262890683122, 1.000000000000000000, 0.9659258262890683122, 1.000000000000000000, 0.9659258262890683122, 1.000000000000000000, 0.9659258262890683122, 1.000000000000000000, 0.9659258262890683122, 1.000000000000000000, 0.9659258262890683122, 1.000000000000000000, 0.9659258262890683122, 1.000000000000000000, 0.9659258262890683122, 1.000000000000000000, 0.9659258262890683122, 1.000000000000000000, 0.9659258262890683122, 1.000000000000000000, 0.9659258262890683122, 1.000000000000000000, 0.9659258262890683122, 1.000000000000000000, 0.9659258262890683122, 1.000000000000000000, 0.9659258262890683122, 1.000000000000000000, 0.9659258262890683122, 1.000000000000000000, 0.9659258262890683122, 1.000000000000000000, 0.9659258262890683122, 1.000000000000000000, 0.9659258262890683122, 1.000000000000000000, 0.9659258262890683122, 1.000000000000000000, 0.9659258262890683122, 1.000000000000000000, 0.9659258262890683122, 1.000000000000000000, 0.9659258262890683122, 1.000000000000000000, 0.9659258262890683122, 1.000000000000000000, 0.9659258262890683122, 1.000000000000000000, 0.9659258262890683122, 1.000000000000000000, 0.9659258262890683122, 1.000000000000000000, 0.9659258262890683122, 1.000000000000000000, 0.9659258262890683122, 1.000000000000000000, 0.9659258262890683122, 1.000000000000000000, 0.9659258262890683122, 1.000000000000000000, 0.9659258262890683122, 1.000000000000000000, 0.9659258262890683122, 1.000000000000000000, 0.9659258262890683122, 1.000000000000000000, 0.9659258262890683122, 1.000000000000000000, 0.9659258262890683122, 1.000000000000000000, 0.9659258262890683122, 1.000000000000000000, 0.9659258262890683122, 1.000000000000000000, 0.9659258262890683122, 1.000000000000000000, 0.9659258262890683122, 1.000000000000000000, 0.9659258262890683122, 1.000000000000000000, 0.9659258262890683122, 1.000000000000000000, 0.9659258262890683122, 1.000000000000000000, 0.9659258262890683122, 1.000000000000000000, 0.9659258262890683122, 1.000000000000000000, 0.9659258262890683122, 1.000000000000000000, 0.9659258262890683122, 1.000000000000000000, 0.9659258262890683122, 1.000000000000000000, 0.9659258262890683122, 1.000000000000000000, 0.9659258262890683122, 1.000000000000000000, 0.9659258262890683122, 1.000000000000000000, 0.9659258262890683122, 1.000000000000000000, 0.9659258262890683122, 1.000000000000000000, 0.9659258262890683122, 1.000000000000000000, 0.9659258262890683122, 1.000000000000000000, 0.9659258262890683122, 1.000000000000000000, 0.9659258262890683122, 1.000000000000000000, 0.9659258262890683122, 1.000000000000000000, 0.9659258262890683122, 1.000000000000000000, 0.9659258262890683122, 1.000000000000000000, 0.9659258262890683122, 1.000000000000000000, 0.9659258262890683122, 1.000000000000000000, 0.9659258262890683122, 1.000000000000000000, 0.9659258262890683122, 1.000000000000000000, 0.9659258262890683122, 1.000000000000000000, 0.9659258262890683122, 1.000000000000000000, 0.9659258262890683122, 1.000000000000000000, 0.9659258262890683122, 1.000000000000000000, 0.9659258262890683122, 1.000000000000000000, 0.9659258262890683122, 1.000000000000000000, 0.9659258262890683122, 1.000000000000000000, 0.9659258262890683122, 1.000000000000000000, 0.9659258262890683122, 1.000000000000000000, 0.9659258262890683122, 1.000000000000000000, 0.9659258262890683122, 1.000000000000000000, 0.9659258262890683122, 1.000000000000000000, 0.9659258262890683122, 1.000000000000000000, 0.9659258262890683122, 1.000000000000000000, 0.9659258262890683122, 1.000000000000000000, 0.9659258262890683122, 1.000000000000000000, 0.9659258262890683122, 1.000000000000000000, 0.9659258262890683122, 1.000000000000000000, 0.9659258262890683122, 1.000000000000000000, 0.9659258262890683122, 1.000000000000000000, 0.9659258262890683122, 1.000000000000000000, 0.9659258262890683122, 1.000000000000000000, 0.9659258262890683122, 1.000000000000000000, 0.9659258262890683122, 1.000000000000000000, 0.9659258262890683122, 1.000000000000000000, 0.9659258262890683122, 1.000000000000000000, 0.9659258262890683122, 1.000000000000000000, 0.9659258262890683122, 1.000000000000000000, 0.9659258262890683122, 1.000000000000000000, 0.9659258262890683122, 1.000000000000000000, 0.9659258262890683122, 1.000000000000000000, 0.9659258262890683122, 1.000000000000000000, 0.9659258262890683122, 1.000000000000000000, 0.9659258262890683122, 1.000000000000000000, 0.9659258262890683122, 1.000000000000000000, 0.9659258262890683122, 1.000000000000000000, 0.9659258262890683122, 1.000000000000000000, 0.9659258262890683122, 1.000000000000000000, 0.9659258262890683122, 1.000000000000000000, 0.9659258262890683122, 1.000000000000000000, 0.9659258262890683122, 1.000000000000000000, 0.9659258262890683122, 1.000000000000000000, 0.9659258262890683122, 1.000000000000000000, 0.9659258262890683122, 1.000000000000000000, 0.9659258262890683122, 1.000000000000000000, 0.9659258262890683122, 1.000000000000000000, 0.9659258262890683122, 1.000000000000000000, 0.9659258262890683122, 1.000000000000000000, 0.9659258262890683122, 1.000000000000000000, 0.9659258262890683122, 1.000000000000000000, 0.9659258262890683122, 1.000000000000000000, 0.9659258262890683122, 1.000000000000000000, 0.9659258262890683122, 1.000000000000000000, 0.9659258262890683122, 1.000000000000000000, 0.9659258262890683122, 1.000000000000000000, 0.9659258262890683122, 1.000000000000000000, 0.9659258262890683122, 1.000000000000000000, 0.9659258262890683122, 1.000000000000000000, 0.9659258262890683122, 1.000000000000000000, 0.9659258262890683122, 1.000000000000000000, 0.9659258262890683122, 1.000000000000000000, 0.9659258262890683122, 1.000000000000000000, 0.9659258262890683122, 1.000000000000000000, 0.9659258262890683122, 1.000000000000000000, 0.9659258262890683122, 1.000000000000000000, 0.9659258262890683122, 1.000000000000000000, 0.9659258262890683122, 1.000000000000000000, 0.9659258262890683122, 1.000000000000000000, 0.9659258262890683122, 1.000000000000000000, 0.9659258262890683122, 1.000000000000000000, 0.9659258262890683122, 1.000000000000000000, 0.9659258262890683122, 1.000000000000000000, 0.9659258262890683122, 1.000000000000000000, 0.9659258262890683122, 1.000000000000000000, 0.9659258262890683122, 1.000000000000000000, 0.9659258262890683122, 1.000000000000000000, 0.9659258262890683122, 1.000000000000000000, 0.9659258262890683122, 1.000000000000000000),
 ( 0.3333333333333333703, 0.3219752754296894559, 0.3333333333333333703, 0.3219752754296894559, 0.3333333333333333703, 0.3219752754296894559, 0.3333333333333333703, 0.3219752754296894559, 0.3333333333333333703, 0.3219752754296894559, 0.3333333333333333703, 0.3219752754296894559, 0.3333333333333333703, 0.3219752754296894559, 0.3333333333333333703, 0.3219752754296894559, 0.3333333333333333703, 0.3219752754296894559, 0.3333333333333333703, 0.3219752754296894559, 0.3333333333333333703, 0.3219752754296894559, 0.3333333333333333703, 0.3219752754296894559, 0.3333333333333333703, 0.3219752754296894559, 0.3333333333333333703, 0.3219752754296894559, 0.3333333333333333703, 0.3219752754296894559, 0.3333333333333333703, 0.3219752754296894559, 0.3333333333333333703, 0.3219752754296894559, 0.3333333333333333703, 0.3219752754296894559, 0.3333333333333333703, 0.3219752754296894559, 0.3333333333333333703, 0.3219752754296894559, 0.3333333333333333703, 0.3219752754296894559, 0.3333333333333333703, 0.3219752754296894559, 0.3333333333333333703, 0.3219752754296894559, 0.3333333333333333703, 0.3219752754296894559, 0.3333333333333333703, 0.3219752754296894559, 0.3333333333333333703, 0.3219752754296894559, 0.3333333333333333703, 0.3219752754296894559, 0.3333333333333333703, 0.3219752754296894559, 0.3333333333333333703, 0.3219752754296894559, 0.3333333333333333703, 0.3219752754296894559, 0.3333333333333333703, 0.3219752754296894559, 0.3333333333333333703, 0.3219752754296894559, 0.3333333333333333703, 0.3219752754296894559, 0.3333333333333333703, 0.3219752754296894559, 0.3333333333333333703, 0.3219752754296894559, 0.3333333333333333703, 0.3219752754296894559, 0.3333333333333333703, 0.3219752754296894559, 0.3333333333333333703, 0.3219752754296894559, 0.3333333333333333703, 0.3219752754296894559, 0.3333333333333333703, 0.3219752754296894559, 0.3333333333333333703, 0.3219752754296894559, 0.3333333333333333703, 0.3219752754296894559, 0.3333333333333333703, 0.3219752754296894559, 0.3333333333333333703, 0.3219752754296894559, 0.3333333333333333703, 0.3219752754296894559, 0.3333333333333333703, 0.3219752754296894559, 0.3333333333333333703, 0.3219752754296894559, 0.3333333333333333703, 0.3219752754296894559, 0.3333333333333333703, 0.3219752754296894559, 0.3333333333333333703, 0.3219752754296894559, 0.3333333333333333703, 0.3219752754296894559, 0.3333333333333333703, 0.3219752754296894559, 0.3333333333333333703, 0.3219752754296894559, 0.3333333333333333703, 0.3219752754296894559, 0.3333333333333333703, 0.3219752754296894559, 0.3333333333333333703, 0.3219752754296894559, 0.3333333333333333703, 0.3219752754296894559, 0.3333333333333333703, 0.3219752754296894559, 0.3333333333333333703, 0.3219752754296894559, 0.3333333333333333703, 0.3219752754296894559, 0.3333333333333333703, 0.3219752754296894559, 0.3333333333333333703, 0.3219752754296894559, 0.3333333333333333703, 0.3219752754296894559, 0.3333333333333333703, 0.3219752754296894559, 0.3333333333333333703, 0.3219752754296894559, 0.3333333333333333703, 0.3219752754296894559, 0.3333333333333333703, 0.3219752754296894559, 0.3333333333333333703, 0.3219752754296894559, 0.3333333333333333703, 0.3219752754296894559, 0.3333333333333333703, 0.3219752754296894559, 0.3333333333333333703, 0.3219752754296894559, 0.3333333333333333703, 0.3219752754296894559, 0.3333333333333333703, 0.3219752754296894559, 0.3333333333333333703, 0.3219752754296894559, 0.3333333333333333703, 0.3219752754296894559, 0.3333333333333333703, 0.3219752754296894559, 0.3333333333333333703, 0.3219752754296894559, 0.3333333333333333703, 0.3219752754296894559, 0.3333333333333333703, 0.3219752754296894559, 0.3333333333333333703, 0.3219752754296894559, 0.3333333333333333703, 0.3219752754296894559, 0.3333333333333333703, 0.3219752754296894559, 0.3333333333333333703, 0.3219752754296894559, 0.3333333333333333703, 0.3219752754296894559, 0.3333333333333333703, 0.3219752754296894559, 0.3333333333333333703, 0.3219752754296894559, 0.3333333333333333703, 0.3219752754296894559, 0.3333333333333333703, 0.3219752754296894559, 0.3333333333333333703, 0.3219752754296894559, 0.3333333333333333703, 0.3219752754296894559, 0.3333333333333333703, 0.3219752754296894559, 0.3333333333333333703, 0.3219752754296894559, 0.3333333333333333703, 0.3219752754296894559, 0.3333333333333333703, 0.3219752754296894559, 0.3333333333333333703, 0.3219752754296894559, 0.3333333333333333703, 0.3219752754296894559, 0.3333333333333333703, 0.3219752754296894559, 0.3333333333333333703, 0.3219752754296894559, 0.3333333333333333703, 0.3219752754296894559, 0.3333333333333333703, 0.3219752754296894559, 0.3333333333333333703, 0.3219752754296894559, 0.3333333333333333703, 0.3219752754296894559, 0.3333333333333333703, 0.3219752754296894559, 0.3333333333333333703, 0.3219752754296894559, 0.3333333333333333703, 0.3219752754296894559, 0.3333333333333333703, 0.3219752754296894559, 0.3333333333333333703, 0.3219752754296894559, 0.3333333333333333703, 0.3219752754296894559, 0.3333333333333333703, 0.3219752754296894559, 0.3333333333333333703, 0.3219752754296894559, 0.3333333333333333703, 0.3219752754296894559, 0.3333333333333333703, 0.3219752754296894559, 0.3333333333333333703, 0.3219752754296894559, 0.3333333333333333703, 0.3219752754296894559, 0.3333333333333333703, 0.3219752754296894559, 0.3333333333333333703, 0.3219752754296894559, 0.3333333333333333703, 0.3219752754296894559, 0.3333333333333333703, 0.3219752754296894559, 0.3333333333333333703, 0.3219752754296894559, 0.3333333333333333703, 0.3219752754296894559, 0.3333333333333333703, 0.3219752754296894559, 0.3333333333333333703, 0.3219752754296894559, 0.3333333333333333703, 0.3219752754296894559, 0.3333333333333333703, 0.3219752754296894559, 0.3333333333333333703, 0.3219752754296894559, 0.3333333333333333703, 0.3219752754296894559, 0.3333333333333333703, 0.3219752754296894559, 0.3333333333333333703, 0.3219752754296894559, 0.3333333333333333703, 0.3219752754296894559, 0.3333333333333333703, 0.3219752754296894559, 0.3333333333333333703, 0.3219752754296894559, 0.3333333333333333703, 0.3219752754296894559, 0.3333333333333333703, 0.3219752754296894559, 0.3333333333333333703, 0.3219752754296894559, 0.3333333333333333703, 0.3219752754296894559, 0.3333333333333333703, 0.3219752754296894559, 0.3333333333333333703, 0.3219752754296894559, 0.3333333333333333703, 0.3219752754296894559, 0.3333333333333333703, 0.3219752754296894559, 0.3333333333333333703, 0.3219752754296894559, 0.3333333333333333703, 0.3219752754296894559, 0.3333333333333333703, 0.3219752754296894559, 0.3333333333333333703, 0.3219752754296894559, 0.3333333333333333703, 0.3219752754296894559, 0.3333333333333333703, 0.3219752754296894559, 0.3333333333333333703, 0.3219752754296894559, 0.3333333333333333703, 0.3219752754296894559, 0.3333333333333333703, 0.3219752754296894559, 0.3333333333333333703, 0.3219752754296894559, 0.3333333333333333703, 0.3219752754296894559, 0.3333333333333333703, 0.3219752754296894559, 0.3333333333333333703, 0.3219752754296894559, 0.3333333333333333703, 0.3219752754296894559, 0.3333333333333333703, 0.3219752754296894559, 0.3333333333333333703, 0.3219752754296894559, 0.3333333333333333703, 0.3219752754296894559, 0.3333333333333333703, 0.3219752754296894559, 0.3333333333333333703, 0.3219752754296894559, 0.3333333333333333703, 0.3219752754296894559, 0.3333333333333333703, 0.3219752754296894559, 0.3333333333333333703, 0.3219752754296894559, 0.3333333333333333703, 0.3219752754296894559, 0.3333333333333333703, 0.3219752754296894559, 0.3333333333333333703, 0.3219752754296894559, 0.3333333333333333703, 0.3219752754296894559, 0.3333333333333333703, 0.3219752754296894559, 0.3333333333333333703, 0.3219752754296894559, 0.3333333333333333703, 0.3219752754296894559, 0.3333333333333333703, 0.3219752754296894559, 0.3333333333333333703, 0.3219752754296894559, 0.3333333333333333703, 0.3219752754296894559, 0.3333333333333333703, 0.3219752754296894559, 0.3333333333333333703, 0.3219752754296894559, 0.3333333333333333703, 0.3219752754296894559, 0.3333333333333333703, 0.3219752754296894559, 0.3333333333333333703, 0.3219752754296894559, 0.3333333333333333703, 0.3219752754296894559, 0.3333333333333333703, 0.3219752754296894559, 0.3333333333333333703, 0.3219752754296894559, 0.3333333333333333703, 0.3219752754296894559, 0.3333333333333333703, 0.3219752754296894559, 0.3333333333333333703, 0.3219752754296894559, 0.3333333333333333703, 0.3219752754296894559, 0.3333333333333333703, 0.3219752754296894559, 0.3333333333333333703, 0.3219752754296894559, 0.3333333333333333703, 0.3219752754296894559, 0.3333333333333333703, 0.3219752754296894559, 0.3333333333333333703, 0.3219752754296894559, 0.3333333333333333703, 0.3219752754296894559, 0.3333333333333333703, 0.3219752754296894559, 0.3333333333333333703, 0.3219752754296894559, 0.3333333333333333703, 0.3219752754296894559, 0.3333333333333333703, 0.3219752754296894559, 0.3333333333333333703, 0.3219752754296894559, 0.3333333333333333703, 0.3219752754296894559, 0.3333333333333333703, 0.3219752754296894559, 0.3333333333333333703, 0.3219752754296894559, 0.3333333333333333703, 0.3219752754296894559, 0.3333333333333333703, 0.3219752754296894559, 0.3333333333333333703, 0.3219752754296894559, 0.3333333333333333703, 0.3219752754296894559, 0.3333333333333333703, 0.3219752754296894559, 0.3333333333333333703, 0.3219752754296894559, 0.3333333333333333703, 0.3219752754296894559, 0.3333333333333333703, 0.3219752754296894559, 0.3333333333333333703, 0.3219752754296894559, 0.3333333333333333703, 0.3219752754296894559, 0.3333333333333333703, 0.3219752754296894559, 0.3333333333333333703, 0.3219752754296894559, 0.3333333333333333703, 0.3219752754296894559, 0.3333333333333333703, 0.3219752754296894559, 0.3333333333333333703, 0.3219752754296894559, 0.3333333333333333703, 0.3219752754296894559, 0.3333333333333333703, 0.3219752754296894559, 0.3333333333333333703, 0.3219752754296894559, 0.3333333333333333703, 0.3219752754296894559, 0.3333333333333333703, 0.3219752754296894559, 0.3333333333333333703, 0.3219752754296894559, 0.3333333333333333703, 0.3219752754296894559, 0.3333333333333333703, 0.3219752754296894559, 0.3333333333333333703, 0.3219752754296894559, 0.3333333333333333703, 0.3219752754296894559, 0.3333333333333333703, 0.3219752754296894559, 0.3333333333333333703, 0.3219752754296894559, 0.3333333333333333703, 0.3219752754296894559, 0.3333333333333333703, 0.3219752754296894559, 0.3333333333333333703, 0.3219752754296894559, 0.3333333333333333703, 0.3219752754296894559, 0.3333333333333333703),
 ( 0.3333333333333333703, 0.3219752754296894559, 0.3333333333333333703, 0.3219752754296894559, 0.3333333333333333703, 0.3219752754296894559, 0.3333333333333333703, 0.3219752754296894559, 0.3333333333333333703, 0.3219752754296894559, 0.3333333333333333703, 0.3219752754296894559, 0.3333333333333333703, 0.3219752754296894559, 0.3333333333333333703, 0.3219752754296894559, 0.3333333333333333703, 0.3219752754296894559, 0.3333333333333333703, 0.3219752754296894559, 0.3333333333333333703, 0.3219752754296894559, 0.3333333333333333703, 0.3219752754296894559, 0.3333333333333333703, 0.3219752754296894559, 0.3333333333333333703, 0.3219752754296894559, 0.3333333333333333703, 0.3219752754296894559, 0.3333333333333333703, 0.3219752754296894559, 0.3333333333333333703, 0.3219752754296894559, 0.3333333333333333703, 0.3219752754296894559, 0.3333333333333333703, 0.3219752754296894559, 0.3333333333333333703, 0.3219752754296894559, 0.3333333333333333703, 0.3219752754296894559, 0.3333333333333333703, 0.3219752754296894559, 0.3333333333333333703, 0.3219752754296894559, 0.3333333333333333703, 0.3219752754296894559, 0.3333333333333333703, 0.3219752754296894559, 0.3333333333333333703, 0.3219752754296894559, 0.3333333333333333703, 0.3219752754296894559, 0.3333333333333333703, 0.3219752754296894559, 0.3333333333333333703, 0.3219752754296894559, 0.3333333333333333703, 0.3219752754296894559, 0.3333333333333333703, 0.3219752754296894559, 0.3333333333333333703, 0.3219752754296894559, 0.3333333333333333703, 0.3219752754296894559, 0.3333333333333333703, 0.3219752754296894559, 0.3333333333333333703, 0.3219752754296894559, 0.3333333333333333703, 0.3219752754296894559, 0.3333333333333333703, 0.3219752754296894559, 0.3333333333333333703, 0.3219752754296894559, 0.3333333333333333703, 0.3219752754296894559, 0.3333333333333333703, 0.3219752754296894559, 0.3333333333333333703, 0.3219752754296894559, 0.3333333333333333703, 0.3219752754296894559, 0.3333333333333333703, 0.3219752754296894559, 0.3333333333333333703, 0.3219752754296894559, 0.3333333333333333703, 0.3219752754296894559, 0.3333333333333333703, 0.3219752754296894559, 0.3333333333333333703, 0.3219752754296894559, 0.3333333333333333703, 0.3219752754296894559, 0.3333333333333333703, 0.3219752754296894559, 0.3333333333333333703, 0.3219752754296894559, 0.3333333333333333703, 0.3219752754296894559, 0.3333333333333333703, 0.3219752754296894559, 0.3333333333333333703, 0.3219752754296894559, 0.3333333333333333703, 0.3219752754296894559, 0.3333333333333333703, 0.3219752754296894559, 0.3333333333333333703, 0.3219752754296894559, 0.3333333333333333703, 0.3219752754296894559, 0.3333333333333333703, 0.3219752754296894559, 0.3333333333333333703, 0.3219752754296894559, 0.3333333333333333703, 0.3219752754296894559, 0.3333333333333333703, 0.3219752754296894559, 0.3333333333333333703, 0.3219752754296894559, 0.3333333333333333703, 0.3219752754296894559, 0.3333333333333333703, 0.3219752754296894559, 0.3333333333333333703, 0.3219752754296894559, 0.3333333333333333703, 0.3219752754296894559, 0.3333333333333333703, 0.3219752754296894559, 0.3333333333333333703, 0.3219752754296894559, 0.3333333333333333703, 0.3219752754296894559, 0.3333333333333333703, 0.3219752754296894559, 0.3333333333333333703, 0.3219752754296894559, 0.3333333333333333703, 0.3219752754296894559, 0.3333333333333333703, 0.3219752754296894559, 0.3333333333333333703, 0.3219752754296894559, 0.3333333333333333703, 0.3219752754296894559, 0.3333333333333333703, 0.3219752754296894559, 0.3333333333333333703, 0.3219752754296894559, 0.3333333333333333703, 0.3219752754296894559, 0.3333333333333333703, 0.3219752754296894559, 0.3333333333333333703, 0.3219752754296894559, 0.3333333333333333703, 0.3219752754296894559, 0.3333333333333333703, 0.3219752754296894559, 0.3333333333333333703, 0.3219752754296894559, 0.3333333333333333703, 0.3219752754296894559, 0.3333333333333333703, 0.3219752754296894559, 0.3333333333333333703, 0.3219752754296894559, 0.3333333333333333703, 0.3219752754296894559, 0.3333333333333333703, 0.3219752754296894559, 0.3333333333333333703, 0.3219752754296894559, 0.3333333333333333703, 0.3219752754296894559, 0.3333333333333333703, 0.3219752754296894559, 0.3333333333333333703, 0.3219752754296894559, 0.3333333333333333703, 0.3219752754296894559, 0.3333333333333333703, 0.3219752754296894559, 0.3333333333333333703, 0.3219752754296894559, 0.3333333333333333703, 0.3219752754296894559, 0.3333333333333333703, 0.3219752754296894559, 0.3333333333333333703, 0.3219752754296894559, 0.3333333333333333703, 0.3219752754296894559, 0.3333333333333333703, 0.3219752754296894559, 0.3333333333333333703, 0.3219752754296894559, 0.3333333333333333703, 0.3219752754296894559, 0.3333333333333333703, 0.3219752754296894559, 0.3333333333333333703, 0.3219752754296894559, 0.3333333333333333703, 0.3219752754296894559, 0.3333333333333333703, 0.3219752754296894559, 0.3333333333333333703, 0.3219752754296894559, 0.3333333333333333703, 0.3219752754296894559, 0.3333333333333333703, 0.3219752754296894559, 0.3333333333333333703, 0.3219752754296894559, 0.3333333333333333703, 0.3219752754296894559, 0.3333333333333333703, 0.3219752754296894559, 0.3333333333333333703, 0.3219752754296894559, 0.3333333333333333703, 0.3219752754296894559, 0.3333333333333333703, 0.3219752754296894559, 0.3333333333333333703, 0.3219752754296894559, 0.3333333333333333703, 0.3219752754296894559, 0.3333333333333333703, 0.3219752754296894559, 0.3333333333333333703, 0.3219752754296894559, 0.3333333333333333703, 0.3219752754296894559, 0.3333333333333333703, 0.3219752754296894559, 0.3333333333333333703, 0.3219752754296894559, 0.3333333333333333703, 0.3219752754296894559, 0.3333333333333333703, 0.3219752754296894559, 0.3333333333333333703, 0.3219752754296894559, 0.3333333333333333703, 0.3219752754296894559, 0.3333333333333333703, 0.3219752754296894559, 0.3333333333333333703, 0.3219752754296894559, 0.3333333333333333703, 0.3219752754296894559, 0.3333333333333333703, 0.3219752754296894559, 0.3333333333333333703, 0.3219752754296894559, 0.3333333333333333703, 0.3219752754296894559, 0.3333333333333333703, 0.3219752754296894559, 0.3333333333333333703, 0.3219752754296894559, 0.3333333333333333703, 0.3219752754296894559, 0.3333333333333333703, 0.3219752754296894559, 0.3333333333333333703, 0.3219752754296894559, 0.3333333333333333703, 0.3219752754296894559, 0.3333333333333333703, 0.3219752754296894559, 0.3333333333333333703, 0.3219752754296894559, 0.3333333333333333703, 0.3219752754296894559, 0.3333333333333333703, 0.3219752754296894559, 0.3333333333333333703, 0.3219752754296894559, 0.3333333333333333703, 0.3219752754296894559, 0.3333333333333333703, 0.3219752754296894559, 0.3333333333333333703, 0.3219752754296894559, 0.3333333333333333703, 0.3219752754296894559, 0.3333333333333333703, 0.3219752754296894559, 0.3333333333333333703, 0.3219752754296894559, 0.3333333333333333703, 0.3219752754296894559, 0.3333333333333333703, 0.3219752754296894559, 0.3333333333333333703, 0.3219752754296894559, 0.3333333333333333703, 0.3219752754296894559, 0.3333333333333333703, 0.3219752754296894559, 0.3333333333333333703, 0.3219752754296894559, 0.3333333333333333703, 0.3219752754296894559, 0.3333333333333333703, 0.3219752754296894559, 0.3333333333333333703, 0.3219752754296894559, 0.3333333333333333703, 0.3219752754296894559, 0.3333333333333333703, 0.3219752754296894559, 0.3333333333333333703, 0.3219752754296894559, 0.3333333333333333703, 0.3219752754296894559, 0.3333333333333333703, 0.3219752754296894559, 0.3333333333333333703, 0.3219752754296894559, 0.3333333333333333703, 0.3219752754296894559, 0.3333333333333333703, 0.3219752754296894559, 0.3333333333333333703, 0.3219752754296894559, 0.3333333333333333703, 0.3219752754296894559, 0.3333333333333333703, 0.3219752754296894559, 0.3333333333333333703, 0.3219752754296894559, 0.3333333333333333703, 0.3219752754296894559, 0.3333333333333333703, 0.3219752754296894559, 0.3333333333333333703, 0.3219752754296894559, 0.3333333333333333703, 0.3219752754296894559, 0.3333333333333333703, 0.3219752754296894559, 0.3333333333333333703, 0.3219752754296894559, 0.3333333333333333703, 0.3219752754296894559, 0.3333333333333333703, 0.3219752754296894559, 0.3333333333333333703, 0.3219752754296894559, 0.3333333333333333703, 0.3219752754296894559, 0.3333333333333333703, 0.3219752754296894559, 0.3333333333333333703, 0.3219752754296894559, 0.3333333333333333703, 0.3219752754296894559, 0.3333333333333333703, 0.3219752754296894559, 0.3333333333333333703, 0.3219752754296894559, 0.3333333333333333703, 0.3219752754296894559, 0.3333333333333333703, 0.3219752754296894559, 0.3333333333333333703, 0.3219752754296894559, 0.3333333333333333703, 0.3219752754296894559, 0.3333333333333333703, 0.3219752754296894559, 0.3333333333333333703, 0.3219752754296894559, 0.3333333333333333703, 0.3219752754296894559, 0.3333333333333333703, 0.3219752754296894559, 0.3333333333333333703, 0.3219752754296894559, 0.3333333333333333703, 0.3219752754296894559, 0.3333333333333333703, 0.3219752754296894559, 0.3333333333333333703, 0.3219752754296894559, 0.3333333333333333703, 0.3219752754296894559, 0.3333333333333333703, 0.3219752754296894559, 0.3333333333333333703, 0.3219752754296894559, 0.3333333333333333703, 0.3219752754296894559, 0.3333333333333333703, 0.3219752754296894559, 0.3333333333333333703, 0.3219752754296894559, 0.3333333333333333703, 0.3219752754296894559, 0.3333333333333333703, 0.3219752754296894559, 0.3333333333333333703, 0.3219752754296894559, 0.3333333333333333703, 0.3219752754296894559, 0.3333333333333333703, 0.3219752754296894559, 0.3333333333333333703, 0.3219752754296894559, 0.3333333333333333703, 0.3219752754296894559, 0.3333333333333333703, 0.3219752754296894559, 0.3333333333333333703, 0.3219752754296894559, 0.3333333333333333703, 0.3219752754296894559, 0.3333333333333333703, 0.3219752754296894559, 0.3333333333333333703, 0.3219752754296894559, 0.3333333333333333703, 0.3219752754296894559, 0.3333333333333333703, 0.3219752754296894559, 0.3333333333333333703, 0.3219752754296894559, 0.3333333333333333703, 0.3219752754296894559, 0.3333333333333333703, 0.3219752754296894559, 0.3333333333333333703, 0.3219752754296894559, 0.3333333333333333703, 0.3219752754296894559, 0.3333333333333333703, 0.3219752754296894559, 0.3333333333333333703, 0.3219752754296894559, 0.3333333333333333703, 0.3219752754296894559, 0.3333333333333333703, 0.3219752754296894559, 0.3333333333333333703, 0.3219752754296894559, 0.3333333333333333703, 0.3219752754296894559, 0.3333333333333333703),
 ( 1.000000000000000000, 0.9659258262890683122, 1.000000000000000000, 0.9659258262890683122, 1.000000000000000000, 0.9659258262890683122, 1.000000000000000000, 0.9659258262890683122, 1.000000000000000000, 0.9659258262890683122, 1.000000000000000000, 0.9659258262890683122, 1.000000000000000000, 0.9659258262890683122, 1.000000000000000000, 0.9659258262890683122, 1.000000000000000000, 0.9659258262890683122, 1.000000000000000000, 0.9659258262890683122, 1.000000000000000000, 0.9659258262890683122, 1.000000000000000000, 0.9659258262890683122, 1.000000000000000000, 0.9659258262890683122, 1.000000000000000000, 0.9659258262890683122, 1.000000000000000000, 0.9659258262890683122, 1.000000000000000000, 0.9659258262890683122, 1.000000000000000000, 0.9659258262890683122, 1.000000000000000000, 0.9659258262890683122, 1.000000000000000000, 0.9659258262890683122, 1.000000000000000000, 0.9659258262890683122, 1.000000000000000000, 0.9659258262890683122, 1.000000000000000000, 0.9659258262890683122, 1.000000000000000000, 0.9659258262890683122, 1.000000000000000000, 0.9659258262890683122, 1.000000000000000000, 0.9659258262890683122, 1.000000000000000000, 0.9659258262890683122, 1.000000000000000000, 0.9659258262890683122, 1.000000000000000000, 0.9659258262890683122, 1.000000000000000000, 0.9659258262890683122, 1.000000000000000000, 0.9659258262890683122, 1.000000000000000000, 0.9659258262890683122, 1.000000000000000000, 0.9659258262890683122, 1.000000000000000000, 0.9659258262890683122, 1.000000000000000000, 0.9659258262890683122, 1.000000000000000000, 0.9659258262890683122, 1.000000000000000000, 0.9659258262890683122, 1.000000000000000000, 0.9659258262890683122, 1.000000000000000000, 0.9659258262890683122, 1.000000000000000000, 0.9659258262890683122, 1.000000000000000000, 0.9659258262890683122, 1.000000000000000000, 0.9659258262890683122, 1.000000000000000000, 0.9659258262890683122, 1.000000000000000000, 0.9659258262890683122, 1.000000000000000000, 0.9659258262890683122, 1.000000000000000000, 0.9659258262890683122, 1.000000000000000000, 0.9659258262890683122, 1.000000000000000000, 0.9659258262890683122, 1.000000000000000000, 0.9659258262890683122, 1.000000000000000000, 0.9659258262890683122, 1.000000000000000000, 0.9659258262890683122, 1.000000000000000000, 0.9659258262890683122, 1.000000000000000000, 0.9659258262890683122, 1.000000000000000000, 0.9659258262890683122, 1.000000000000000000, 0.9659258262890683122, 1.000000000000000000, 0.9659258262890683122, 1.000000000000000000, 0.9659258262890683122, 1.000000000000000000, 0.9659258262890683122, 1.000000000000000000, 0.9659258262890683122, 1.000000000000000000, 0.9659258262890683122, 1.000000000000000000, 0.9659258262890683122, 1.000000000000000000, 0.9659258262890683122, 1.000000000000000000, 0.9659258262890683122, 1.000000000000000000, 0.9659258262890683122, 1.000000000000000000, 0.9659258262890683122, 1.000000000000000000, 0.9659258262890683122, 1.000000000000000000, 0.9659258262890683122, 1.000000000000000000, 0.9659258262890683122, 1.000000000000000000, 0.9659258262890683122, 1.000000000000000000, 0.9659258262890683122, 1.000000000000000000, 0.9659258262890683122, 1.000000000000000000, 0.9659258262890683122, 1.000000000000000000, 0.9659258262890683122, 1.000000000000000000, 0.9659258262890683122, 1.000000000000000000, 0.9659258262890683122, 1.000000000000000000, 0.9659258262890683122, 1.000000000000000000, 0.9659258262890683122, 1.000000000000000000, 0.9659258262890683122, 1.000000000000000000, 0.9659258262890683122, 1.000000000000000000, 0.9659258262890683122, 1.000000000000000000, 0.9659258262890683122, 1.000000000000000000, 0.9659258262890683122, 1.000000000000000000, 0.9659258262890683122, 1.000000000000000000, 0.9659258262890683122, 1.000000000000000000, 0.9659258262890683122, 1.000000000000000000, 0.9659258262890683122, 1.000000000000000000, 0.9659258262890683122, 1.000000000000000000, 0.9659258262890683122, 1.000000000000000000, 0.9659258262890683122, 1.000000000000000000, 0.9659258262890683122, 1.000000000000000000, 0.9659258262890683122, 1.000000000000000000, 0.9659258262890683122, 1.000000000000000000, 0.9659258262890683122, 1.000000000000000000, 0.9659258262890683122, 1.000000000000000000, 0.9659258262890683122, 1.000000000000000000, 0.9659258262890683122, 1.000000000000000000, 0.9659258262890683122, 1.000000000000000000, 0.9659258262890683122, 1.000000000000000000, 0.9659258262890683122, 1.000000000000000000, 0.9659258262890683122, 1.000000000000000000, 0.9659258262890683122, 1.000000000000000000, 0.9659258262890683122, 1.000000000000000000, 0.9659258262890683122, 1.000000000000000000, 0.9659258262890683122, 1.000000000000000000, 0.9659258262890683122, 1.000000000000000000, 0.9659258262890683122, 1.000000000000000000, 0.9659258262890683122, 1.000000000000000000, 0.9659258262890683122, 1.000000000000000000, 0.9659258262890683122, 1.000000000000000000, 0.9659258262890683122, 1.000000000000000000, 0.9659258262890683122, 1.000000000000000000, 0.9659258262890683122, 1.000000000000000000, 0.9659258262890683122, 1.000000000000000000, 0.9659258262890683122, 1.000000000000000000, 0.9659258262890683122, 1.000000000000000000, 0.9659258262890683122, 1.000000000000000000, 0.9659258262890683122, 1.000000000000000000, 0.9659258262890683122, 1.000000000000000000, 0.9659258262890683122, 1.000000000000000000, 0.9659258262890683122, 1.000000000000000000, 0.9659258262890683122, 1.000000000000000000, 0.9659258262890683122, 1.000000000000000000, 0.9659258262890683122, 1.000000000000000000, 0.9659258262890683122, 1.000000000000000000, 0.9659258262890683122, 1.000000000000000000, 0.9659258262890683122, 1.000000000000000000, 0.9659258262890683122, 1.000000000000000000, 0.9659258262890683122, 1.000000000000000000, 0.9659258262890683122, 1.000000000000000000, 0.9659258262890683122, 1.000000000000000000, 0.9659258262890683122, 1.000000000000000000, 0.9659258262890683122, 1.000000000000000000, 0.9659258262890683122, 1.000000000000000000, 0.9659258262890683122, 1.000000000000000000, 0.9659258262890683122, 1.000000000000000000, 0.9659258262890683122, 1.000000000000000000, 0.9659258262890683122, 1.000000000000000000, 0.9659258262890683122, 1.000000000000000000, 0.9659258262890683122, 1.000000000000000000, 0.9659258262890683122, 1.000000000000000000, 0.9659258262890683122, 1.000000000000000000, 0.9659258262890683122, 1.000000000000000000, 0.9659258262890683122, 1.000000000000000000, 0.9659258262890683122, 1.000000000000000000, 0.9659258262890683122, 1.000000000000000000, 0.9659258262890683122, 1.000000000000000000, 0.9659258262890683122, 1.000000000000000000, 0.9659258262890683122, 1.000000000000000000, 0.9659258262890683122, 1.000000000000000000, 0.9659258262890683122, 1.000000000000000000, 0.9659258262890683122, 1.000000000000000000, 0.9659258262890683122, 1.000000000000000000, 0.9659258262890683122, 1.000000000000000000, 0.9659258262890683122, 1.000000000000000000, 0.9659258262890683122, 1.000000000000000000, 0.9659258262890683122, 1.000000000000000000, 0.9659258262890683122, 1.000000000000000000, 0.9659258262890683122, 1.000000000000000000, 0.9659258262890683122, 1.000000000000000000, 0.9659258262890683122, 1.000000000000000000, 0.9659258262890683122, 1.000000000000000000, 0.9659258262890683122, 1.000000000000000000, 0.9659258262890683122, 1.000000000000000000, 0.9659258262890683122, 1.000000000000000000, 0.9659258262890683122, 1.000000000000000000, 0.9659258262890683122, 1.000000000000000000, 0.9659258262890683122, 1.000000000000000000, 0.9659258262890683122, 1.000000000000000000, 0.9659258262890683122, 1.000000000000000000, 0.9659258262890683122, 1.000000000000000000, 0.9659258262890683122, 1.000000000000000000, 0.9659258262890683122, 1.000000000000000000, 0.9659258262890683122, 1.000000000000000000, 0.9659258262890683122, 1.000000000000000000, 0.9659258262890683122, 1.000000000000000000, 0.9659258262890683122, 1.000000000000000000, 0.9659258262890683122, 1.000000000000000000, 0.9659258262890683122, 1.000000000000000000, 0.9659258262890683122, 1.000000000000000000, 0.9659258262890683122, 1.000000000000000000, 0.9659258262890683122, 1.000000000000000000, 0.9659258262890683122, 1.000000000000000000, 0.9659258262890683122, 1.000000000000000000, 0.9659258262890683122, 1.000000000000000000, 0.9659258262890683122, 1.000000000000000000, 0.9659258262890683122, 1.000000000000000000, 0.9659258262890683122, 1.000000000000000000, 0.9659258262890683122, 1.000000000000000000, 0.9659258262890683122, 1.000000000000000000, 0.9659258262890683122, 1.000000000000000000, 0.9659258262890683122, 1.000000000000000000, 0.9659258262890683122, 1.000000000000000000, 0.9659258262890683122, 1.000000000000000000, 0.9659258262890683122, 1.000000000000000000, 0.9659258262890683122, 1.000000000000000000, 0.9659258262890683122, 1.000000000000000000, 0.9659258262890683122, 1.000000000000000000, 0.9659258262890683122, 1.000000000000000000, 0.9659258262890683122, 1.000000000000000000, 0.9659258262890683122, 1.000000000000000000, 0.9659258262890683122, 1.000000000000000000, 0.9659258262890683122, 1.000000000000000000, 0.9659258262890683122, 1.000000000000000000, 0.9659258262890683122, 1.000000000000000000, 0.9659258262890683122, 1.000000000000000000, 0.9659258262890683122, 1.000000000000000000, 0.9659258262890683122, 1.000000000000000000, 0.9659258262890683122, 1.000000000000000000, 0.9659258262890683122, 1.000000000000000000, 0.9659258262890683122, 1.000000000000000000, 0.9659258262890683122, 1.000000000000000000, 0.9659258262890683122, 1.000000000000000000, 0.9659258262890683122, 1.000000000000000000, 0.9659258262890683122, 1.000000000000000000, 0.9659258262890683122, 1.000000000000000000, 0.9659258262890683122, 1.000000000000000000, 0.9659258262890683122, 1.000000000000000000, 0.9659258262890683122, 1.000000000000000000, 0.9659258262890683122, 1.000000000000000000, 0.9659258262890683122, 1.000000000000000000, 0.9659258262890683122, 1.000000000000000000, 0.9659258262890683122, 1.000000000000000000, 0.9659258262890683122, 1.000000000000000000, 0.9659258262890683122, 1.000000000000000000, 0.9659258262890683122, 1.000000000000000000, 0.9659258262890683122, 1.000000000000000000, 0.9659258262890683122, 1.000000000000000000, 0.9659258262890683122, 1.000000000000000000, 0.9659258262890683122, 1.000000000000000000),
 ( 0.3333333333333333703, 0.3219752754296894559, 0.3333333333333333703, 0.3219752754296894559, 0.3333333333333333703, 0.3219752754296894559, 0.3333333333333333703, 0.3219752754296894559, 0.3333333333333333703, 0.3219752754296894559, 0.3333333333333333703, 0.3219752754296894559, 0.3333333333333333703, 0.3219752754296894559, 0.3333333333333333703, 0.3219752754296894559, 0.3333333333333333703, 0.3219752754296894559, 0.3333333333333333703, 0.3219752754296894559, 0.3333333333333333703, 0.3219752754296894559, 0.3333333333333333703, 0.3219752754296894559, 0.3333333333333333703, 0.3219752754296894559, 0.3333333333333333703, 0.3219752754296894559, 0.3333333333333333703, 0.3219752754296894559, 0.3333333333333333703, 0.3219752754296894559, 0.3333333333333333703, 0.3219752754296894559, 0.3333333333333333703, 0.3219752754296894559, 0.3333333333333333703, 0.3219752754296894559, 0.3333333333333333703, 0.3219752754296894559, 0.3333333333333333703, 0.3219752754296894559, 0.3333333333333333703, 0.3219752754296894559, 0.3333333333333333703, 0.3219752754296894559, 0.3333333333333333703, 0.3219752754296894559, 0.3333333333333333703, 0.3219752754296894559, 0.3333333333333333703, 0.3219752754296894559, 0.3333333333333333703, 0.3219752754296894559, 0.3333333333333333703, 0.3219752754296894559, 0.3333333333333333703, 0.3219752754296894559, 0.3333333333333333703, 0.3219752754296894559, 0.3333333333333333703, 0.3219752754296894559, 0.3333333333333333703, 0.3219752754296894559, 0.3333333333333333703, 0.3219752754296894559, 0.3333333333333333703, 0.3219752754296894559, 0.3333333333333333703, 0.3219752754296894559, 0.3333333333333333703, 0.3219752754296894559, 0.3333333333333333703, 0.3219752754296894559, 0.3333333333333333703, 0.3219752754296894559, 0.3333333333333333703, 0.3219752754296894559, 0.3333333333333333703, 0.3219752754296894559, 0.3333333333333333703, 0.3219752754296894559, 0.3333333333333333703, 0.3219752754296894559, 0.3333333333333333703, 0.3219752754296894559, 0.3333333333333333703, 0.3219752754296894559, 0.3333333333333333703, 0.3219752754296894559, 0.3333333333333333703, 0.3219752754296894559, 0.3333333333333333703, 0.3219752754296894559, 0.3333333333333333703, 0.3219752754296894559, 0.3333333333333333703, 0.3219752754296894559, 0.3333333333333333703, 0.3219752754296894559, 0.3333333333333333703, 0.3219752754296894559, 0.3333333333333333703, 0.3219752754296894559, 0.3333333333333333703, 0.3219752754296894559, 0.3333333333333333703, 0.3219752754296894559, 0.3333333333333333703, 0.3219752754296894559, 0.3333333333333333703, 0.3219752754296894559, 0.3333333333333333703, 0.3219752754296894559, 0.3333333333333333703, 0.3219752754296894559, 0.3333333333333333703, 0.3219752754296894559, 0.3333333333333333703, 0.3219752754296894559, 0.3333333333333333703, 0.3219752754296894559, 0.3333333333333333703, 0.3219752754296894559, 0.3333333333333333703, 0.3219752754296894559, 0.3333333333333333703, 0.3219752754296894559, 0.3333333333333333703, 0.3219752754296894559, 0.3333333333333333703, 0.3219752754296894559, 0.3333333333333333703, 0.3219752754296894559, 0.3333333333333333703, 0.3219752754296894559, 0.3333333333333333703, 0.3219752754296894559, 0.3333333333333333703, 0.3219752754296894559, 0.3333333333333333703, 0.3219752754296894559, 0.3333333333333333703, 0.3219752754296894559, 0.3333333333333333703, 0.3219752754296894559, 0.3333333333333333703, 0.3219752754296894559, 0.3333333333333333703, 0.3219752754296894559, 0.3333333333333333703, 0.3219752754296894559, 0.3333333333333333703, 0.3219752754296894559, 0.3333333333333333703, 0.3219752754296894559, 0.3333333333333333703, 0.3219752754296894559, 0.3333333333333333703, 0.3219752754296894559, 0.3333333333333333703, 0.3219752754296894559, 0.3333333333333333703, 0.3219752754296894559, 0.3333333333333333703, 0.3219752754296894559, 0.3333333333333333703, 0.3219752754296894559, 0.3333333333333333703, 0.3219752754296894559, 0.3333333333333333703, 0.3219752754296894559, 0.3333333333333333703, 0.3219752754296894559, 0.3333333333333333703, 0.3219752754296894559, 0.3333333333333333703, 0.3219752754296894559, 0.3333333333333333703, 0.3219752754296894559, 0.3333333333333333703, 0.3219752754296894559, 0.3333333333333333703, 0.3219752754296894559, 0.3333333333333333703, 0.3219752754296894559, 0.3333333333333333703, 0.3219752754296894559, 0.3333333333333333703, 0.3219752754296894559, 0.3333333333333333703, 0.3219752754296894559, 0.3333333333333333703, 0.3219752754296894559, 0.3333333333333333703, 0.3219752754296894559, 0.3333333333333333703, 0.3219752754296894559, 0.3333333333333333703, 0.3219752754296894559, 0.3333333333333333703, 0.3219752754296894559, 0.3333333333333333703, 0.3219752754296894559, 0.3333333333333333703, 0.3219752754296894559, 0.3333333333333333703, 0.3219752754296894559, 0.3333333333333333703, 0.3219752754296894559, 0.3333333333333333703, 0.3219752754296894559, 0.3333333333333333703, 0.3219752754296894559, 0.3333333333333333703, 0.3219752754296894559, 0.3333333333333333703, 0.3219752754296894559, 0.3333333333333333703, 0.3219752754296894559, 0.3333333333333333703, 0.3219752754296894559, 0.3333333333333333703, 0.3219752754296894559, 0.3333333333333333703, 0.3219752754296894559, 0.3333333333333333703, 0.3219752754296894559, 0.3333333333333333703, 0.3219752754296894559, 0.3333333333333333703, 0.3219752754296894559, 0.3333333333333333703, 0.3219752754296894559, 0.3333333333333333703, 0.3219752754296894559, 0.3333333333333333703, 0.3219752754296894559, 0.3333333333333333703, 0.3219752754296894559, 0.3333333333333333703, 0.3219752754296894559, 0.3333333333333333703, 0.3219752754296894559, 0.3333333333333333703, 0.3219752754296894559, 0.3333333333333333703, 0.3219752754296894559, 0.3333333333333333703, 0.3219752754296894559, 0.3333333333333333703, 0.3219752754296894559, 0.3333333333333333703, 0.3219752754296894559, 0.3333333333333333703, 0.3219752754296894559, 0.3333333333333333703, 0.3219752754296894559, 0.3333333333333333703, 0.3219752754296894559, 0.3333333333333333703, 0.3219752754296894559, 0.3333333333333333703, 0.3219752754296894559, 0.3333333333333333703, 0.3219752754296894559, 0.3333333333333333703, 0.3219752754296894559, 0.3333333333333333703, 0.3219752754296894559, 0.3333333333333333703, 0.3219752754296894559, 0.3333333333333333703, 0.3219752754296894559, 0.3333333333333333703, 0.3219752754296894559, 0.3333333333333333703, 0.3219752754296894559, 0.3333333333333333703, 0.3219752754296894559, 0.3333333333333333703, 0.3219752754296894559, 0.3333333333333333703, 0.3219752754296894559, 0.3333333333333333703, 0.3219752754296894559, 0.3333333333333333703, 0.3219752754296894559, 0.3333333333333333703, 0.3219752754296894559, 0.3333333333333333703, 0.3219752754296894559, 0.3333333333333333703, 0.3219752754296894559, 0.3333333333333333703, 0.3219752754296894559, 0.3333333333333333703, 0.3219752754296894559, 0.3333333333333333703, 0.3219752754296894559, 0.3333333333333333703, 0.3219752754296894559, 0.3333333333333333703, 0.3219752754296894559, 0.3333333333333333703, 0.3219752754296894559, 0.3333333333333333703, 0.3219752754296894559, 0.3333333333333333703, 0.3219752754296894559, 0.3333333333333333703, 0.3219752754296894559, 0.3333333333333333703, 0.3219752754296894559, 0.3333333333333333703, 0.3219752754296894559, 0.3333333333333333703, 0.3219752754296894559, 0.3333333333333333703, 0.3219752754296894559, 0.3333333333333333703, 0.3219752754296894559, 0.3333333333333333703, 0.3219752754296894559, 0.3333333333333333703, 0.3219752754296894559, 0.3333333333333333703, 0.3219752754296894559, 0.3333333333333333703, 0.3219752754296894559, 0.3333333333333333703, 0.3219752754296894559, 0.3333333333333333703, 0.3219752754296894559, 0.3333333333333333703, 0.3219752754296894559, 0.3333333333333333703, 0.3219752754296894559, 0.3333333333333333703, 0.3219752754296894559, 0.3333333333333333703, 0.3219752754296894559, 0.3333333333333333703, 0.3219752754296894559, 0.3333333333333333703, 0.3219752754296894559, 0.3333333333333333703, 0.3219752754296894559, 0.3333333333333333703, 0.3219752754296894559, 0.3333333333333333703, 0.3219752754296894559, 0.3333333333333333703, 0.3219752754296894559, 0.3333333333333333703, 0.3219752754296894559, 0.3333333333333333703, 0.3219752754296894559, 0.3333333333333333703, 0.3219752754296894559, 0.3333333333333333703, 0.3219752754296894559, 0.3333333333333333703, 0.3219752754296894559, 0.3333333333333333703, 0.3219752754296894559, 0.3333333333333333703, 0.3219752754296894559, 0.3333333333333333703, 0.3219752754296894559, 0.3333333333333333703, 0.3219752754296894559, 0.3333333333333333703, 0.3219752754296894559, 0.3333333333333333703, 0.3219752754296894559, 0.3333333333333333703, 0.3219752754296894559, 0.3333333333333333703, 0.3219752754296894559, 0.3333333333333333703, 0.3219752754296894559, 0.3333333333333333703, 0.3219752754296894559, 0.3333333333333333703, 0.3219752754296894559, 0.3333333333333333703, 0.3219752754296894559, 0.3333333333333333703, 0.3219752754296894559, 0.3333333333333333703, 0.3219752754296894559, 0.3333333333333333703, 0.3219752754296894559, 0.3333333333333333703, 0.3219752754296894559, 0.3333333333333333703, 0.3219752754296894559, 0.3333333333333333703, 0.3219752754296894559, 0.3333333333333333703, 0.3219752754296894559, 0.3333333333333333703, 0.3219752754296894559, 0.3333333333333333703, 0.3219752754296894559, 0.3333333333333333703, 0.3219752754296894559, 0.3333333333333333703, 0.3219752754296894559, 0.3333333333333333703, 0.3219752754296894559, 0.3333333333333333703, 0.3219752754296894559, 0.3333333333333333703, 0.3219752754296894559, 0.3333333333333333703, 0.3219752754296894559, 0.3333333333333333703, 0.3219752754296894559, 0.3333333333333333703, 0.3219752754296894559, 0.3333333333333333703, 0.3219752754296894559, 0.3333333333333333703, 0.3219752754296894559, 0.3333333333333333703, 0.3219752754296894559, 0.3333333333333333703, 0.3219752754296894559, 0.3333333333333333703, 0.3219752754296894559, 0.3333333333333333703, 0.3219752754296894559, 0.3333333333333333703, 0.3219752754296894559, 0.3333333333333333703, 0.3219752754296894559, 0.3333333333333333703, 0.3219752754296894559, 0.3333333333333333703, 0.3219752754296894559, 0.3333333333333333703, 0.3219752754296894559, 0.3333333333333333703, 0.3219752754296894559, 0.3333333333333333703, 0.3219752754296894559, 0.3333333333333333703, 0.3219752754296894559, 0.3333333333333333703, 0.3219752754296894559, 0.3333333333333333703, 0.3219752754296894559, 0.3333333333333333703, 0.3219752754296894559, 0.3333333333333333703),
 ( 0.3333333333333333703, 0.3219752754296894559, 0.3333333333333333703, 0.3219752754296894559, 0.3333333333333333703, 0.3219752754296894559, 0.3333333333333333703, 0.3219752754296894559, 0.3333333333333333703, 0.3219752754296894559, 0.3333333333333333703, 0.3219752754296894559, 0.3333333333333333703, 0.3219752754296894559, 0.3333333333333333703, 0.3219752754296894559, 0.3333333333333333703, 0.3219752754296894559, 0.3333333333333333703, 0.3219752754296894559, 0.3333333333333333703, 0.3219752754296894559, 0.3333333333333333703, 0.3219752754296894559, 0.3333333333333333703, 0.3219752754296894559, 0.3333333333333333703, 0.3219752754296894559, 0.3333333333333333703, 0.3219752754296894559, 0.3333333333333333703, 0.3219752754296894559, 0.3333333333333333703, 0.3219752754296894559, 0.3333333333333333703, 0.3219752754296894559, 0.3333333333333333703, 0.3219752754296894559, 0.3333333333333333703, 0.3219752754296894559, 0.3333333333333333703, 0.3219752754296894559, 0.3333333333333333703, 0.3219752754296894559, 0.3333333333333333703, 0.3219752754296894559, 0.3333333333333333703, 0.3219752754296894559, 0.3333333333333333703, 0.3219752754296894559, 0.3333333333333333703, 0.3219752754296894559, 0.3333333333333333703, 0.3219752754296894559, 0.3333333333333333703, 0.3219752754296894559, 0.3333333333333333703, 0.3219752754296894559, 0.3333333333333333703, 0.3219752754296894559, 0.3333333333333333703, 0.3219752754296894559, 0.3333333333333333703, 0.3219752754296894559, 0.3333333333333333703, 0.3219752754296894559, 0.3333333333333333703, 0.3219752754296894559, 0.3333333333333333703, 0.3219752754296894559, 0.3333333333333333703, 0.3219752754296894559, 0.3333333333333333703, 0.3219752754296894559, 0.3333333333333333703, 0.3219752754296894559, 0.3333333333333333703, 0.3219752754296894559, 0.3333333333333333703, 0.3219752754296894559, 0.3333333333333333703, 0.3219752754296894559, 0.3333333333333333703, 0.3219752754296894559, 0.3333333333333333703, 0.3219752754296894559, 0.3333333333333333703, 0.3219752754296894559, 0.3333333333333333703, 0.3219752754296894559, 0.3333333333333333703, 0.3219752754296894559, 0.3333333333333333703, 0.3219752754296894559, 0.3333333333333333703, 0.3219752754296894559, 0.3333333333333333703, 0.3219752754296894559, 0.3333333333333333703, 0.3219752754296894559, 0.3333333333333333703, 0.3219752754296894559, 0.3333333333333333703, 0.3219752754296894559, 0.3333333333333333703, 0.3219752754296894559, 0.3333333333333333703, 0.3219752754296894559, 0.3333333333333333703, 0.3219752754296894559, 0.3333333333333333703, 0.3219752754296894559, 0.3333333333333333703, 0.3219752754296894559, 0.3333333333333333703, 0.3219752754296894559, 0.3333333333333333703, 0.3219752754296894559, 0.3333333333333333703, 0.3219752754296894559, 0.3333333333333333703, 0.3219752754296894559, 0.3333333333333333703, 0.3219752754296894559, 0.3333333333333333703, 0.3219752754296894559, 0.3333333333333333703, 0.3219752754296894559, 0.3333333333333333703, 0.3219752754296894559, 0.3333333333333333703, 0.3219752754296894559, 0.3333333333333333703, 0.3219752754296894559, 0.3333333333333333703, 0.3219752754296894559, 0.3333333333333333703, 0.3219752754296894559, 0.3333333333333333703, 0.3219752754296894559, 0.3333333333333333703, 0.3219752754296894559, 0.3333333333333333703, 0.3219752754296894559, 0.3333333333333333703, 0.3219752754296894559, 0.3333333333333333703, 0.3219752754296894559, 0.3333333333333333703, 0.3219752754296894559, 0.3333333333333333703, 0.3219752754296894559, 0.3333333333333333703, 0.3219752754296894559, 0.3333333333333333703, 0.3219752754296894559, 0.3333333333333333703, 0.3219752754296894559, 0.3333333333333333703, 0.3219752754296894559, 0.3333333333333333703, 0.3219752754296894559, 0.3333333333333333703, 0.3219752754296894559, 0.3333333333333333703, 0.3219752754296894559, 0.3333333333333333703, 0.3219752754296894559, 0.3333333333333333703, 0.3219752754296894559, 0.3333333333333333703, 0.3219752754296894559, 0.3333333333333333703, 0.3219752754296894559, 0.3333333333333333703, 0.3219752754296894559, 0.3333333333333333703, 0.3219752754296894559, 0.3333333333333333703, 0.3219752754296894559, 0.3333333333333333703, 0.3219752754296894559, 0.3333333333333333703, 0.3219752754296894559, 0.3333333333333333703, 0.3219752754296894559, 0.3333333333333333703, 0.3219752754296894559, 0.3333333333333333703, 0.3219752754296894559, 0.3333333333333333703, 0.3219752754296894559, 0.3333333333333333703, 0.3219752754296894559, 0.3333333333333333703, 0.3219752754296894559, 0.3333333333333333703, 0.3219752754296894559, 0.3333333333333333703, 0.3219752754296894559, 0.3333333333333333703, 0.3219752754296894559, 0.3333333333333333703, 0.3219752754296894559, 0.3333333333333333703, 0.3219752754296894559, 0.3333333333333333703, 0.3219752754296894559, 0.3333333333333333703, 0.3219752754296894559, 0.3333333333333333703, 0.3219752754296894559, 0.3333333333333333703, 0.3219752754296894559, 0.3333333333333333703, 0.3219752754296894559, 0.3333333333333333703, 0.3219752754296894559, 0.3333333333333333703, 0.3219752754296894559, 0.3333333333333333703, 0.3219752754296894559, 0.3333333333333333703, 0.3219752754296894559, 0.3333333333333333703, 0.3219752754296894559, 0.3333333333333333703, 0.3219752754296894559, 0.3333333333333333703, 0.3219752754296894559, 0.3333333333333333703, 0.3219752754296894559, 0.3333333333333333703, 0.3219752754296894559, 0.3333333333333333703, 0.3219752754296894559, 0.3333333333333333703, 0.3219752754296894559, 0.3333333333333333703, 0.3219752754296894559, 0.3333333333333333703, 0.3219752754296894559, 0.3333333333333333703, 0.3219752754296894559, 0.3333333333333333703, 0.3219752754296894559, 0.3333333333333333703, 0.3219752754296894559, 0.3333333333333333703, 0.3219752754296894559, 0.3333333333333333703, 0.3219752754296894559, 0.3333333333333333703, 0.3219752754296894559, 0.3333333333333333703, 0.3219752754296894559, 0.3333333333333333703, 0.3219752754296894559, 0.3333333333333333703, 0.3219752754296894559, 0.3333333333333333703, 0.3219752754296894559, 0.3333333333333333703, 0.3219752754296894559, 0.3333333333333333703, 0.3219752754296894559, 0.3333333333333333703, 0.3219752754296894559, 0.3333333333333333703, 0.3219752754296894559, 0.3333333333333333703, 0.3219752754296894559, 0.3333333333333333703, 0.3219752754296894559, 0.3333333333333333703, 0.3219752754296894559, 0.3333333333333333703, 0.3219752754296894559, 0.3333333333333333703, 0.3219752754296894559, 0.3333333333333333703, 0.3219752754296894559, 0.3333333333333333703, 0.3219752754296894559, 0.3333333333333333703, 0.3219752754296894559, 0.3333333333333333703, 0.3219752754296894559, 0.3333333333333333703, 0.3219752754296894559, 0.3333333333333333703, 0.3219752754296894559, 0.3333333333333333703, 0.3219752754296894559, 0.3333333333333333703, 0.3219752754296894559, 0.3333333333333333703, 0.3219752754296894559, 0.3333333333333333703, 0.3219752754296894559, 0.3333333333333333703, 0.3219752754296894559, 0.3333333333333333703, 0.3219752754296894559, 0.3333333333333333703, 0.3219752754296894559, 0.3333333333333333703, 0.3219752754296894559, 0.3333333333333333703, 0.3219752754296894559, 0.3333333333333333703, 0.3219752754296894559, 0.3333333333333333703, 0.3219752754296894559, 0.3333333333333333703, 0.3219752754296894559, 0.3333333333333333703, 0.3219752754296894559, 0.3333333333333333703, 0.3219752754296894559, 0.3333333333333333703, 0.3219752754296894559, 0.3333333333333333703, 0.3219752754296894559, 0.3333333333333333703, 0.3219752754296894559, 0.3333333333333333703, 0.3219752754296894559, 0.3333333333333333703, 0.3219752754296894559, 0.3333333333333333703, 0.3219752754296894559, 0.3333333333333333703, 0.3219752754296894559, 0.3333333333333333703, 0.3219752754296894559, 0.3333333333333333703, 0.3219752754296894559, 0.3333333333333333703, 0.3219752754296894559, 0.3333333333333333703, 0.3219752754296894559, 0.3333333333333333703, 0.3219752754296894559, 0.3333333333333333703, 0.3219752754296894559, 0.3333333333333333703, 0.3219752754296894559, 0.3333333333333333703, 0.3219752754296894559, 0.3333333333333333703, 0.3219752754296894559, 0.3333333333333333703, 0.3219752754296894559, 0.3333333333333333703, 0.3219752754296894559, 0.3333333333333333703, 0.3219752754296894559, 0.3333333333333333703, 0.3219752754296894559, 0.3333333333333333703, 0.3219752754296894559, 0.3333333333333333703, 0.3219752754296894559, 0.3333333333333333703, 0.3219752754296894559, 0.3333333333333333703, 0.3219752754296894559, 0.3333333333333333703, 0.3219752754296894559, 0.3333333333333333703, 0.3219752754296894559, 0.3333333333333333703, 0.3219752754296894559, 0.3333333333333333703, 0.3219752754296894559, 0.3333333333333333703, 0.3219752754296894559, 0.3333333333333333703, 0.3219752754296894559, 0.3333333333333333703, 0.3219752754296894559, 0.3333333333333333703, 0.3219752754296894559, 0.3333333333333333703, 0.3219752754296894559, 0.3333333333333333703, 0.3219752754296894559, 0.3333333333333333703, 0.3219752754296894559, 0.3333333333333333703, 0.3219752754296894559, 0.3333333333333333703, 0.3219752754296894559, 0.3333333333333333703, 0.3219752754296894559, 0.3333333333333333703, 0.3219752754296894559, 0.3333333333333333703, 0.3219752754296894559, 0.3333333333333333703, 0.3219752754296894559, 0.3333333333333333703, 0.3219752754296894559, 0.3333333333333333703, 0.3219752754296894559, 0.3333333333333333703, 0.3219752754296894559, 0.3333333333333333703, 0.3219752754296894559, 0.3333333333333333703, 0.3219752754296894559, 0.3333333333333333703, 0.3219752754296894559, 0.3333333333333333703, 0.3219752754296894559, 0.3333333333333333703, 0.3219752754296894559, 0.3333333333333333703, 0.3219752754296894559, 0.3333333333333333703, 0.3219752754296894559, 0.3333333333333333703, 0.3219752754296894559, 0.3333333333333333703, 0.3219752754296894559, 0.3333333333333333703, 0.3219752754296894559, 0.3333333333333333703, 0.3219752754296894559, 0.3333333333333333703, 0.3219752754296894559, 0.3333333333333333703, 0.3219752754296894559, 0.3333333333333333703, 0.3219752754296894559, 0.3333333333333333703, 0.3219752754296894559, 0.3333333333333333703, 0.3219752754296894559, 0.3333333333333333703, 0.3219752754296894559, 0.3333333333333333703, 0.3219752754296894559, 0.3333333333333333703, 0.3219752754296894559, 0.3333333333333333703, 0.3219752754296894559, 0.3333333333333333703, 0.3219752754296894559, 0.3333333333333333703, 0.3219752754296894559, 0.3333333333333333703, 0.3219752754296894559, 0.3333333333333333703, 0.3219752754296894559, 0.3333333333333333703),
 ( 1.000000000000000000, 0.9659258262890683122, 1.000000000000000000, 0.9659258262890683122, 1.000000000000000000, 0.9659258262890683122, 1.000000000000000000, 0.9659258262890683122, 1.000000000000000000, 0.9659258262890683122, 1.000000000000000000, 0.9659258262890683122, 1.000000000000000000, 0.9659258262890683122, 1.000000000000000000, 0.9659258262890683122, 1.000000000000000000, 0.9659258262890683122, 1.000000000000000000, 0.9659258262890683122, 1.000000000000000000, 0.9659258262890683122, 1.000000000000000000, 0.9659258262890683122, 1.000000000000000000, 0.9659258262890683122, 1.000000000000000000, 0.9659258262890683122, 1.000000000000000000, 0.9659258262890683122, 1.000000000000000000, 0.9659258262890683122, 1.000000000000000000, 0.9659258262890683122, 1.000000000000000000, 0.9659258262890683122, 1.000000000000000000, 0.9659258262890683122, 1.000000000000000000, 0.9659258262890683122, 1.000000000000000000, 0.9659258262890683122, 1.000000000000000000, 0.9659258262890683122, 1.000000000000000000, 0.9659258262890683122, 1.000000000000000000, 0.9659258262890683122, 1.000000000000000000, 0.9659258262890683122, 1.000000000000000000, 0.9659258262890683122, 1.000000000000000000, 0.9659258262890683122, 1.000000000000000000, 0.9659258262890683122, 1.000000000000000000, 0.9659258262890683122, 1.000000000000000000, 0.9659258262890683122, 1.000000000000000000, 0.9659258262890683122, 1.000000000000000000, 0.9659258262890683122, 1.000000000000000000, 0.9659258262890683122, 1.000000000000000000, 0.9659258262890683122, 1.000000000000000000, 0.9659258262890683122, 1.000000000000000000, 0.9659258262890683122, 1.000000000000000000, 0.9659258262890683122, 1.000000000000000000, 0.9659258262890683122, 1.000000000000000000, 0.9659258262890683122, 1.000000000000000000, 0.9659258262890683122, 1.000000000000000000, 0.9659258262890683122, 1.000000000000000000, 0.9659258262890683122, 1.000000000000000000, 0.9659258262890683122, 1.000000000000000000, 0.9659258262890683122, 1.000000000000000000, 0.9659258262890683122, 1.000000000000000000, 0.9659258262890683122, 1.000000000000000000, 0.9659258262890683122, 1.000000000000000000, 0.9659258262890683122, 1.000000000000000000, 0.9659258262890683122, 1.000000000000000000, 0.9659258262890683122, 1.000000000000000000, 0.9659258262890683122, 1.000000000000000000, 0.9659258262890683122, 1.000000000000000000, 0.9659258262890683122, 1.000000000000000000, 0.9659258262890683122, 1.000000000000000000, 0.9659258262890683122, 1.000000000000000000, 0.9659258262890683122, 1.000000000000000000, 0.9659258262890683122, 1.000000000000000000, 0.9659258262890683122, 1.000000000000000000, 0.9659258262890683122, 1.000000000000000000, 0.9659258262890683122, 1.000000000000000000, 0.9659258262890683122, 1.000000000000000000, 0.9659258262890683122, 1.000000000000000000, 0.9659258262890683122, 1.000000000000000000, 0.9659258262890683122, 1.000000000000000000, 0.9659258262890683122, 1.000000000000000000, 0.9659258262890683122, 1.000000000000000000, 0.9659258262890683122, 1.000000000000000000, 0.9659258262890683122, 1.000000000000000000, 0.9659258262890683122, 1.000000000000000000, 0.9659258262890683122, 1.000000000000000000, 0.9659258262890683122, 1.000000000000000000, 0.9659258262890683122, 1.000000000000000000, 0.9659258262890683122, 1.000000000000000000, 0.9659258262890683122, 1.000000000000000000, 0.9659258262890683122, 1.000000000000000000, 0.9659258262890683122, 1.000000000000000000, 0.9659258262890683122, 1.000000000000000000, 0.9659258262890683122, 1.000000000000000000, 0.9659258262890683122, 1.000000000000000000, 0.9659258262890683122, 1.000000000000000000, 0.9659258262890683122, 1.000000000000000000, 0.9659258262890683122, 1.000000000000000000, 0.9659258262890683122, 1.000000000000000000, 0.9659258262890683122, 1.000000000000000000, 0.9659258262890683122, 1.000000000000000000, 0.9659258262890683122, 1.000000000000000000, 0.9659258262890683122, 1.000000000000000000, 0.9659258262890683122, 1.000000000000000000, 0.9659258262890683122, 1.000000000000000000, 0.9659258262890683122, 1.000000000000000000, 0.9659258262890683122, 1.000000000000000000, 0.9659258262890683122, 1.000000000000000000, 0.9659258262890683122, 1.000000000000000000, 0.9659258262890683122, 1.000000000000000000, 0.9659258262890683122, 1.000000000000000000, 0.9659258262890683122, 1.000000000000000000, 0.9659258262890683122, 1.000000000000000000, 0.9659258262890683122, 1.000000000000000000, 0.9659258262890683122, 1.000000000000000000, 0.9659258262890683122, 1.000000000000000000, 0.9659258262890683122, 1.000000000000000000, 0.9659258262890683122, 1.000000000000000000, 0.9659258262890683122, 1.000000000000000000, 0.9659258262890683122, 1.000000000000000000, 0.9659258262890683122, 1.000000000000000000, 0.9659258262890683122, 1.000000000000000000, 0.9659258262890683122, 1.000000000000000000, 0.9659258262890683122, 1.000000000000000000, 0.9659258262890683122, 1.000000000000000000, 0.9659258262890683122, 1.000000000000000000, 0.9659258262890683122, 1.000000000000000000, 0.9659258262890683122, 1.000000000000000000, 0.9659258262890683122, 1.000000000000000000, 0.9659258262890683122, 1.000000000000000000, 0.9659258262890683122, 1.000000000000000000, 0.9659258262890683122, 1.000000000000000000, 0.9659258262890683122, 1.000000000000000000, 0.9659258262890683122, 1.000000000000000000, 0.9659258262890683122, 1.000000000000000000, 0.9659258262890683122, 1.000000000000000000, 0.9659258262890683122, 1.000000000000000000, 0.9659258262890683122, 1.000000000000000000, 0.9659258262890683122, 1.000000000000000000, 0.9659258262890683122, 1.000000000000000000, 0.9659258262890683122, 1.000000000000000000, 0.9659258262890683122, 1.000000000000000000, 0.9659258262890683122, 1.000000000000000000, 0.9659258262890683122, 1.000000000000000000, 0.9659258262890683122, 1.000000000000000000, 0.9659258262890683122, 1.000000000000000000, 0.9659258262890683122, 1.000000000000000000, 0.9659258262890683122, 1.000000000000000000, 0.9659258262890683122, 1.000000000000000000, 0.9659258262890683122, 1.000000000000000000, 0.9659258262890683122, 1.000000000000000000, 0.9659258262890683122, 1.000000000000000000, 0.9659258262890683122, 1.000000000000000000, 0.9659258262890683122, 1.000000000000000000, 0.9659258262890683122, 1.000000000000000000, 0.9659258262890683122, 1.000000000000000000, 0.9659258262890683122, 1.000000000000000000, 0.9659258262890683122, 1.000000000000000000, 0.9659258262890683122, 1.000000000000000000, 0.9659258262890683122, 1.000000000000000000, 0.9659258262890683122, 1.000000000000000000, 0.9659258262890683122, 1.000000000000000000, 0.9659258262890683122, 1.000000000000000000, 0.9659258262890683122, 1.000000000000000000, 0.9659258262890683122, 1.000000000000000000, 0.9659258262890683122, 1.000000000000000000, 0.9659258262890683122, 1.000000000000000000, 0.9659258262890683122, 1.000000000000000000, 0.9659258262890683122, 1.000000000000000000, 0.9659258262890683122, 1.000000000000000000, 0.9659258262890683122, 1.000000000000000000, 0.9659258262890683122, 1.000000000000000000, 0.9659258262890683122, 1.000000000000000000, 0.9659258262890683122, 1.000000000000000000, 0.9659258262890683122, 1.000000000000000000, 0.9659258262890683122, 1.000000000000000000, 0.9659258262890683122, 1.000000000000000000, 0.9659258262890683122, 1.000000000000000000, 0.9659258262890683122, 1.000000000000000000, 0.9659258262890683122, 1.000000000000000000, 0.9659258262890683122, 1.000000000000000000, 0.9659258262890683122, 1.000000000000000000, 0.9659258262890683122, 1.000000000000000000, 0.9659258262890683122, 1.000000000000000000, 0.9659258262890683122, 1.000000000000000000, 0.9659258262890683122, 1.000000000000000000, 0.9659258262890683122, 1.000000000000000000, 0.9659258262890683122, 1.000000000000000000, 0.9659258262890683122, 1.000000000000000000, 0.9659258262890683122, 1.000000000000000000, 0.9659258262890683122, 1.000000000000000000, 0.9659258262890683122, 1.000000000000000000, 0.9659258262890683122, 1.000000000000000000, 0.9659258262890683122, 1.000000000000000000, 0.9659258262890683122, 1.000000000000000000, 0.9659258262890683122, 1.000000000000000000, 0.9659258262890683122, 1.000000000000000000, 0.9659258262890683122, 1.000000000000000000, 0.9659258262890683122, 1.000000000000000000, 0.9659258262890683122, 1.000000000000000000, 0.9659258262890683122, 1.000000000000000000, 0.9659258262890683122, 1.000000000000000000, 0.9659258262890683122, 1.000000000000000000, 0.9659258262890683122, 1.000000000000000000, 0.9659258262890683122, 1.000000000000000000, 0.9659258262890683122, 1.000000000000000000, 0.9659258262890683122, 1.000000000000000000, 0.9659258262890683122, 1.000000000000000000, 0.9659258262890683122, 1.000000000000000000, 0.9659258262890683122, 1.000000000000000000, 0.9659258262890683122, 1.000000000000000000, 0.9659258262890683122, 1.000000000000000000, 0.9659258262890683122, 1.000000000000000000, 0.9659258262890683122, 1.000000000000000000, 0.9659258262890683122, 1.000000000000000000, 0.9659258262890683122, 1.000000000000000000, 0.9659258262890683122, 1.000000000000000000, 0.9659258262890683122, 1.000000000000000000, 0.9659258262890683122, 1.000000000000000000, 0.9659258262890683122, 1.000000000000000000, 0.9659258262890683122, 1.000000000000000000, 0.9659258262890683122, 1.000000000000000000, 0.9659258262890683122, 1.000000000000000000, 0.9659258262890683122, 1.000000000000000000, 0.9659258262890683122, 1.000000000000000000, 0.9659258262890683122, 1.000000000000000000, 0.9659258262890683122, 1.000000000000000000, 0.9659258262890683122, 1.000000000000000000, 0.9659258262890683122, 1.000000000000000000, 0.9659258262890683122, 1.000000000000000000, 0.9659258262890683122, 1.000000000000000000, 0.9659258262890683122, 1.000000000000000000, 0.9659258262890683122, 1.000000000000000000, 0.9659258262890683122, 1.000000000000000000, 0.9659258262890683122, 1.000000000000000000, 0.9659258262890683122, 1.000000000000000000, 0.9659258262890683122, 1.000000000000000000, 0.9659258262890683122, 1.000000000000000000, 0.9659258262890683122, 1.000000000000000000, 0.9659258262890683122, 1.000000000000000000, 0.9659258262890683122, 1.000000000000000000, 0.9659258262890683122, 1.000000000000000000, 0.9659258262890683122, 1.000000000000000000, 0.9659258262890683122, 1.000000000000000000) ) ) 
 REPRESENTATION_ITEM ( '' )  SURFACE ( )  );
#164277 = CARTESIAN_POINT ( 'NONE',  ( 0.05219959533934541429, -16.53943276465976808, 25.00109039468567218 ) ) ;
#164279 = CARTESIAN_POINT ( 'NONE',  ( -15.72974639402176322, -15.80617190586768395, 79.37609039468567573 ) ) ;
#164278 = CARTESIAN_POINT ( 'NONE',  ( 8.314922557960818139, 14.29746914071049879, 49.58224293864769550 ) ) ;
#164280 = AXIS2_PLACEMENT_3D ( 'NONE', #121905, #138076, #169399 ) ;
#164282 = CARTESIAN_POINT ( 'NONE',  ( -18.62759615963270932, 10.81492255796079327, 25.83224293864769194 ) ) ;
#164281 = CARTESIAN_POINT ( 'NONE',  ( -8.314922557961024197, 14.29746914071037800, 87.91775706135234714 ) ) ;
#164283 = CARTESIAN_POINT ( 'NONE',  ( -19.05341960407611168, -5.049401038298164224, 111.4572429386476813 ) ) ;
#164284 = CARTESIAN_POINT ( 'NONE',  ( 37.66961640367472341, 5.000000000000023981, -18.00000000000000355 ) ) ;
#164285 = CARTESIAN_POINT ( 'NONE',  ( 0.05219959533934541429, -16.53943276465976808, 105.0010903946856757 ) ) ;
#164286 = CARTESIAN_POINT ( 'NONE',  ( 14.34966873604972726, -8.224510206698740333, 55.83442372801901854 ) ) ;
#164287 = CARTESIAN_POINT ( 'NONE',  ( -16.46253265017160317, 9.564922557960807481, 70.83224293864770971 ) ) ;
#164288 = CARTESIAN_POINT ( 'NONE',  ( 13.97604488694527802, 13.89961937509977652, 89.37390960531436690 ) ) ;
#164289 = CARTESIAN_POINT ( 'NONE',  ( 5.823673210054444382, -21.52544592524334988, 75.20942372801901854 ) ) ;
#164290 = CARTESIAN_POINT ( 'NONE',  ( -4.483927247898782831, 16.52544592524335698, 72.70942372801901854 ) ) ;
#164291 = CARTESIAN_POINT ( 'NONE',  ( 8.224510206698953496, -14.34966873604960469, 42.91557627198103120 ) ) ;
#164292 = CARTESIAN_POINT ( 'NONE',  ( -13.89961937509977652, 13.97604488694528158, 60.62390960531436690 ) ) ;
#164293 = CARTESIAN_POINT ( 'NONE',  ( 5.049401038298161559, -19.05341960407611168, 42.70724293864767418 ) ) ;
#164294 = ORIENTED_EDGE ( 'NONE', *, *, #89680, .F. ) ;
#164295 = CARTESIAN_POINT ( 'NONE',  ( 5.153800228976615827, -19.02544592524334988, 95.20942372801897591 ) ) ;
#164296 = CARTESIAN_POINT ( 'NONE',  ( -12.06949235617756955, 12.14591786802309770, 95.62390960531436690 ) ) ;
#164297 = CARTESIAN_POINT ( 'NONE',  ( -9.564922557960796823, -16.46253265017161027, 62.08224293864769550 ) ) ;
#164299 = CARTESIAN_POINT ( 'NONE',  ( -30.74264578624800492, 22.33583958711400186, -2.200000000000000178 ) ) ;
#164298 = CARTESIAN_POINT ( 'NONE',  ( -5.153800228976607833, 19.02544592524334988, 102.7094237280189759 ) ) ;
#164300 = CARTESIAN_POINT ( 'NONE',  ( 10.72451020669871369, 18.67979575497193778, 102.0844237280190185 ) ) ;
#164301 = CARTESIAN_POINT ( 'NONE',  ( 12.06949235617739724, 12.14591786802326823, 61.87609039468568284 ) ) ;
#164302 = CARTESIAN_POINT ( 'NONE',  ( 9.474510206698729675, 16.51473224551082808, 97.08442372801900433 ) ) ;
#164303 = CARTESIAN_POINT ( 'NONE',  ( -5.719274019375978568, 21.55341960407610458, 65.20724293864768129 ) ) ;
#164304 = CARTESIAN_POINT ( 'NONE',  ( 12.06949235617739724, 12.14591786802326823, 46.87609039468568994 ) ) ;
#164305 = CARTESIAN_POINT ( 'NONE',  ( -18.39443945427638738, 5.500000000000033751, 68.51745347608652992 ) ) ;
#164306 = CARTESIAN_POINT ( 'NONE',  ( 16.46253265017146816, 9.564922557961045513, 56.66775706135233293 ) ) ;
#164307 = CARTESIAN_POINT ( 'NONE',  ( -15.80617190586768217, 15.72974639402176855, 103.1260903946856757 ) ) ;
#164308 = CARTESIAN_POINT ( 'NONE',  ( -4.483927247898539470, -16.52544592524342804, 112.2905762719810241 ) ) ;
#164309 = CARTESIAN_POINT ( 'NONE',  ( 9.474510206698971260, -16.51473224551069308, 62.91557627198102409 ) ) ;
#164310 = CARTESIAN_POINT ( 'NONE',  ( 8.224510206698953496, -14.34966873604960469, 62.91557627198102409 ) ) ;
#164311 = CARTESIAN_POINT ( 'NONE',  ( -15.72974639402176322, -15.80617190586768395, 94.37609039468568994 ) ) ;
#164312 = CARTESIAN_POINT ( 'NONE',  ( -9.564922557961040184, 16.46253265017147172, 42.91775706135234003 ) ) ;
#164313 = CARTESIAN_POINT ( 'NONE',  ( -13.89961937509957401, -13.97604488694547875, 24.37609039468565442 ) ) ;
#164314 = CARTESIAN_POINT ( 'NONE',  ( 10.81492255796078972, 18.62759615963270932, 24.58224293864768839 ) ) ;
#164315 = CARTESIAN_POINT ( 'NONE',  ( -18.67979575497193778, 10.72451020669871902, 93.33442372801901854 ) ) ;
#164316 = CARTESIAN_POINT ( 'NONE',  ( -9.564922557960796823, -16.46253265017161027, 72.08224293864770971 ) ) ;
#164317 = CARTESIAN_POINT ( 'NONE',  ( -15.72974639402176322, -15.80617190586768395, 94.37609039468568994 ) ) ;
#164318 = CARTESIAN_POINT ( 'NONE',  ( 0.05219959533907565091, 21.53943276465977519, 49.99890960531437401 ) ) ;
#164319 = CARTESIAN_POINT ( 'NONE',  ( 19.03943276465977164, -0.05219959533909143690, 83.74890960531436690 ) ) ;
#164320 = CARTESIAN_POINT ( 'NONE',  ( -13.89961937509957401, -13.97604488694547875, 64.37609039468567573 ) ) ;
#164321 = CARTESIAN_POINT ( 'NONE',  ( 5.049401038298161559, -19.05341960407611168, 42.70724293864767418 ) ) ;
#164322 = CARTESIAN_POINT ( 'NONE',  ( -13.89961937509977652, 13.97604488694528158, 85.62390960531433848 ) ) ;
#164323 = CARTESIAN_POINT ( 'NONE',  ( 16.51473224551083163, -9.474510206698727899, 85.83442372801900433 ) ) ;
#164324 = CARTESIAN_POINT ( 'NONE',  ( 12.14591786802327356, -12.06949235617739191, 40.62609039468567573 ) ) ;
#164325 = CARTESIAN_POINT ( 'NONE',  ( -16.55341960407611168, -4.379528057220339221, 106.4572429386477097 ) ) ;
#164326 = CARTESIAN_POINT ( 'NONE',  ( 13.97604488694527802, 13.89961937509977652, 64.37390960531436690 ) ) ;
#164327 = CARTESIAN_POINT ( 'NONE',  ( 18.67979575497178502, 10.72451020669898547, 49.16557627198102409 ) ) ;
#164328 = CARTESIAN_POINT ( 'NONE',  ( 8.314922557961029526, -14.29746914071037800, 20.41775706135234714 ) ) ;
#164329 = CARTESIAN_POINT ( 'NONE',  ( -5.719274019375978568, 21.55341960407610458, 115.2072429386476955 ) ) ;
#164330 = CARTESIAN_POINT ( 'NONE',  ( -10.72451020669870658, -18.67979575497194134, 79.58442372801903275 ) ) ;
#164331 = CARTESIAN_POINT ( 'NONE',  ( -8.224510206698735004, -14.34966873604973081, 79.58442372801903275 ) ) ;
#164332 = CARTESIAN_POINT ( 'NONE',  ( 0.05219959533909260263, 19.03943276465977164, 79.99890960531436690 ) ) ;
#164333 = CARTESIAN_POINT ( 'NONE',  ( 8.314922557961029526, -14.29746914071037800, 105.4177570613523613 ) ) ;
#164334 = CARTESIAN_POINT ( 'NONE',  ( 13.89961937509957401, 13.97604488694547697, 61.87609039468566863 ) ) ;
#164335 = CARTESIAN_POINT ( 'NONE',  ( 21.52544592524334988, 5.823673210054432836, 31.45942372801901854 ) ) ;
#164336 = CARTESIAN_POINT ( 'NONE',  ( -4.379528057220328563, 16.55341960407611168, 75.20724293864769550 ) ) ;
#164337 = CARTESIAN_POINT ( 'NONE',  ( -16.51473224551069308, -9.474510206698971260, 101.6655762719810241 ) ) ;
#164338 = CARTESIAN_POINT ( 'NONE',  ( -14.34966873604972548, 8.224510206698743886, 93.33442372801901854 ) ) ;
#164339 = CARTESIAN_POINT ( 'NONE',  ( -21.53943276465977519, -0.05219959533937600094, 73.75109039468567573 ) ) ;
#164340 = CARTESIAN_POINT ( 'NONE',  ( -4.379528057220086978, -16.55341960407618274, 34.79275706135235424 ) ) ;
#164341 = CARTESIAN_POINT ( 'NONE',  ( -18.67979575497193778, 10.72451020669871902, 23.33442372801901499 ) ) ;
#164342 = CARTESIAN_POINT ( 'NONE',  ( -16.52544592524342804, 4.483927247898546575, 66.04057627198103830 ) ) ;
#164343 = ORIENTED_EDGE ( 'NONE', *, *, #164865, .T. ) ;
#164344 = CARTESIAN_POINT ( 'NONE',  ( 5.719274019375991003, -21.55341960407610458, 97.70724293864772392 ) ) ;
#164345 = CARTESIAN_POINT ( 'NONE',  ( 0.05219959533910956823, 16.53943276465976808, 49.99890960531437401 ) ) ;
#164346 = VERTEX_POINT ( 'NONE', #50401 ) ;
#164347 = CARTESIAN_POINT ( 'NONE',  ( -6.434671708797631950, -6.434671708797536027, -64.92279855667830191 ) ) ;
#164348 = CARTESIAN_POINT ( 'NONE',  ( 21.52544592524344225, -5.823673210054117533, 23.54057627198102765 ) ) ;
#164349 = CARTESIAN_POINT ( 'NONE',  ( -0.05219959533937732626, 21.53943276465977519, 52.50109039468567573 ) ) ;
#164350 = CARTESIAN_POINT ( 'NONE',  ( 16.52544592524342804, -4.483927247898539470, 58.54057627198103120 ) ) ;
#164351 = CARTESIAN_POINT ( 'NONE',  ( -5.823673210054116645, -21.52544592524344225, 62.29057627198102409 ) ) ;
#164352 = CARTESIAN_POINT ( 'NONE',  ( 19.02544592524343514, -5.153800228976328945, 68.54057627198103830 ) ) ;
#164354 = CARTESIAN_POINT ( 'NONE',  ( -9.564922557961040184, 16.46253265017147172, 77.91775706135234714 ) ) ;
#164353 = CARTESIAN_POINT ( 'NONE',  ( 19.05341960407611168, 5.049401038298154454, 23.95724293864769194 ) ) ;
#164355 = CARTESIAN_POINT ( 'NONE',  ( 5.823673210054125526, 21.52544592524343514, 59.79057627198103120 ) ) ;
#164356 = CARTESIAN_POINT ( 'NONE',  ( 13.89961937509977652, -13.97604488694527269, 43.12390960531434558 ) ) ;
#164357 = CARTESIAN_POINT ( 'NONE',  ( 5.049401038298161559, -19.05341960407611168, 67.70724293864769550 ) ) ;
#164358 = ORIENTED_EDGE ( 'NONE', *, *, #52799, .F. ) ;
#164359 = CARTESIAN_POINT ( 'NONE',  ( 4.483927247898790824, -16.52544592524335698, 55.20942372801902565 ) ) ;
#164360 = CARTESIAN_POINT ( 'NONE',  ( -10.72451020669870658, -18.67979575497194134, 34.58442372801900433 ) ) ;
#164361 = CARTESIAN_POINT ( 'NONE',  ( 5.823673210054444382, -21.52544592524334988, 60.20942372801902565 ) ) ;
#164362 = CARTESIAN_POINT ( 'NONE',  ( 16.46253265017160672, -9.564922557960803928, 103.3322429386476955 ) ) ;
#164363 = CARTESIAN_POINT ( 'NONE',  ( -5.719274019375978568, 21.55341960407610458, 90.20724293864770971 ) ) ;
#164365 = CARTESIAN_POINT ( 'NONE',  ( -8.224510206698735004, -14.34966873604973081, 54.58442372801901143 ) ) ;
#164364 = CARTESIAN_POINT ( 'NONE',  ( 15.72974639402199770, -15.80617190586745480, 103.1239096053143811 ) ) ;
#164366 = CARTESIAN_POINT ( 'NONE',  ( -21.55341960407610458, -5.719274019375992779, 56.45724293864768839 ) ) ;
#164367 = CARTESIAN_POINT ( 'NONE',  ( 15.72974639402176855, 15.80617190586768217, 101.8760903946857042 ) ) ;
#164368 = AXIS2_PLACEMENT_3D ( 'NONE', #143705, #38544, #145704 ) ;
#164369 = CARTESIAN_POINT ( 'NONE',  ( 9.474510206698971260, -16.51473224551069308, 52.91557627198102409 ) ) ;
#164370 = CARTESIAN_POINT ( 'NONE',  ( -13.97604488694527625, -13.89961937509977652, 106.8739096053143669 ) ) ;
#164371 = CARTESIAN_POINT ( 'NONE',  ( 5.153800228976335163, 19.02544592524342804, 79.79057627198102409 ) ) ;
#164372 = APPLICATION_CONTEXT ( 'automotive_design' ) ;
#164373 = CARTESIAN_POINT ( 'NONE',  ( -11.55487914182271147, -42.80721638308652643, -21.19679778042607410 ) ) ;
#164374 = EDGE_CURVE ( 'NONE', #22185, #117961, #2145, .T. ) ;
#164375 = CARTESIAN_POINT ( 'NONE',  ( 16.46253265017146816, 9.564922557961045513, 66.66775706135233293 ) ) ;
#164376 = CARTESIAN_POINT ( 'NONE',  ( -21.55341960407610458, -5.719274019375992779, 41.45724293864769550 ) ) ;
#164377 = CARTESIAN_POINT ( 'NONE',  ( -8.224510206698735004, -14.34966873604973081, 104.5844237280190185 ) ) ;
#164378 = CARTESIAN_POINT ( 'NONE',  ( -16.51473224551082808, 9.474510206698731452, 88.33442372801900433 ) ) ;
#164379 = CARTESIAN_POINT ( 'NONE',  ( 12.50000000000001066, -90.00000000000005684, -15.00000000000000178 ) ) ;
#164380 = CARTESIAN_POINT ( 'NONE',  ( 19.02544592524334988, 5.153800228976608722, 21.45942372801899012 ) ) ;
#164381 = CARTESIAN_POINT ( 'NONE',  ( -19.03943276465977164, -0.05219959533935918106, 88.75109039468567573 ) ) ;
#164382 = CARTESIAN_POINT ( 'NONE',  ( -13.97604488694547697, 13.89961937509957934, 48.12609039468566863 ) ) ;
#164383 = CARTESIAN_POINT ( 'NONE',  ( 17.26058549869091507, 6.457015423128556364, 108.8774583747606783 ) ) ;
#164384 = CARTESIAN_POINT ( 'NONE',  ( 19.03943276465977164, -0.05219959533909143690, 58.74890960531435979 ) ) ;
#164385 = CARTESIAN_POINT ( 'NONE',  ( -16.55341960407611168, -4.379528057220339221, 46.45724293864769550 ) ) ;
#164386 = CARTESIAN_POINT ( 'NONE',  ( 13.89961937509977652, -13.97604488694527269, 28.12390960531435624 ) ) ;
#164387 = CARTESIAN_POINT ( 'NONE',  ( -16.52544592524342804, 4.483927247898546575, 41.04057627198103120 ) ) ;
#164388 = CARTESIAN_POINT ( 'NONE',  ( 37.99626262588768810, 12.34573411038912027, -6.647842220587802942 ) ) ;
#164389 = CARTESIAN_POINT ( 'NONE',  ( -16.55341960407617563, 4.379528057220093196, 113.5427570613523756 ) ) ;
#164390 = CARTESIAN_POINT ( 'NONE',  ( -13.97604488694527625, -13.89961937509977652, 51.87390960531436690 ) ) ;
#164391 = CARTESIAN_POINT ( 'NONE',  ( -19.05341960407617563, 5.049401038297882671, 23.54275706135233648 ) ) ;
#164392 = CARTESIAN_POINT ( 'NONE',  ( -8.314922557961024197, 14.29746914071037800, 32.91775706135234714 ) ) ;
#164393 = CARTESIAN_POINT ( 'NONE',  ( -10.72451020669898014, 18.67979575497178502, 35.41557627198102409 ) ) ;
#164395 = ORIENTED_EDGE ( 'NONE', *, *, #126480, .F. ) ;
#164394 = CARTESIAN_POINT ( 'NONE',  ( -0.05219959533937732626, 21.53943276465977519, 92.50109039468567573 ) ) ;
#164396 = CARTESIAN_POINT ( 'NONE',  ( 13.89961937509977652, -13.97604488694527269, 63.12390960531435979 ) ) ;
#164397 = CARTESIAN_POINT ( 'NONE',  ( -16.46253265017160317, 9.564922557960807481, 105.8322429386476955 ) ) ;
#164398 = CARTESIAN_POINT ( 'NONE',  ( 19.02544592524343514, -5.153800228976328945, 93.54057627198102409 ) ) ;
#164399 = CARTESIAN_POINT ( 'NONE',  ( 22.81625015709510151, -31.40387420917324590, -7.924999997268812990 ) ) ;
#164400 = CARTESIAN_POINT ( 'NONE',  ( -5.719274019375665041, -21.55341960407619695, 19.79275706135235069 ) ) ;
#164401 = CARTESIAN_POINT ( 'NONE',  ( 8.314922557960818139, 14.29746914071049879, 74.58224293864768129 ) ) ;
#164403 = CARTESIAN_POINT ( 'NONE',  ( -13.97604488694527625, -13.89961937509977652, 66.87390960531436690 ) ) ;
#164402 = CARTESIAN_POINT ( 'NONE',  ( -5.719274019375978568, 21.55341960407610458, 70.20724293864769550 ) ) ;
#164404 = CARTESIAN_POINT ( 'NONE',  ( -13.97604488694527625, -13.89961937509977652, 76.87390960531433848 ) ) ;
#164405 = CARTESIAN_POINT ( 'NONE',  ( -21.53943276465977519, 0.05219959533907696930, 111.2489096053143669 ) ) ;
#164406 = VERTEX_POINT ( 'NONE', #66546 ) ;
#164407 = CARTESIAN_POINT ( 'NONE',  ( -19.02544592524342804, 5.153800228976336051, 56.04057627198100988 ) ) ;
#164409 = CARTESIAN_POINT ( 'NONE',  ( 29.82769333492476704, -26.65767662149077211, -16.82146015663694882 ) ) ;
#164408 = CARTESIAN_POINT ( 'NONE',  ( 8.314922557960818139, 14.29746914071049879, 104.5822429386477097 ) ) ;
#164410 = CARTESIAN_POINT ( 'NONE',  ( 19.03943276465977164, -0.05219959533909143690, 58.74890960531435979 ) ) ;
#164411 = CARTESIAN_POINT ( 'NONE',  ( 13.97604488694548053, -13.89961937509957401, 90.62609039468567573 ) ) ;
#164412 = CARTESIAN_POINT ( 'NONE',  ( 16.52544592524342804, -4.483927247898539470, 93.54057627198103830 ) ) ;
#164413 = CARTESIAN_POINT ( 'NONE',  ( 5.823673210054444382, -21.52544592524334988, 65.20942372801901854 ) ) ;
#164415 = CARTESIAN_POINT ( 'NONE',  ( 21.53943276465977519, -0.05219959533907433946, 113.7489096053143527 ) ) ;
#164414 = CARTESIAN_POINT ( 'NONE',  ( 19.03943276465977164, -0.05219959533909143690, 53.74890960531436690 ) ) ;
#164416 = CARTESIAN_POINT ( 'NONE',  ( 8.314922557960818139, 14.29746914071049879, 99.58224293864770971 ) ) ;
#164417 = CARTESIAN_POINT ( 'NONE',  ( -8.906447517083060816, 27.41122689804195645, 143.5999999999999943 ) ) ;
#164418 = CARTESIAN_POINT ( 'NONE',  ( 16.46253265017160672, -9.564922557960803928, 68.33224293864770971 ) ) ;
#164419 = CARTESIAN_POINT ( 'NONE',  ( 16.61371651742599553, 7.165104196376170798, 113.6458493000700543 ) ) ;
#164421 = CARTESIAN_POINT ( 'NONE',  ( 21.53943276465977519, -0.05219959533907433946, 28.74890960531435624 ) ) ;
#164420 = CARTESIAN_POINT ( 'NONE',  ( -16.46253265017146816, -9.564922557961047289, 109.1677570613523471 ) ) ;
#164422 = CARTESIAN_POINT ( 'NONE',  ( -10.81492255796105439, 18.62759615963255655, 47.91775706135234714 ) ) ;
#164423 = CARTESIAN_POINT ( 'NONE',  ( 5.049401038298161559, -19.05341960407611168, 102.7072429386476955 ) ) ;
#164424 = CARTESIAN_POINT ( 'NONE',  ( 13.89961937509957401, 13.97604488694547697, 76.87609039468566152 ) ) ;
#164425 = CARTESIAN_POINT ( 'NONE',  ( -9.474510206698964154, 16.51473224551069663, 75.41557627198103830 ) ) ;
#164426 = CARTESIAN_POINT ( 'NONE',  ( 12.14591786802309770, 12.06949235617756955, 79.37390960531436690 ) ) ;
#164427 = CARTESIAN_POINT ( 'NONE',  ( -16.51473224551069308, -9.474510206698971260, 101.6655762719810241 ) ) ;
#164428 = CARTESIAN_POINT ( 'NONE',  ( -16.52544592524342804, 4.483927247898546575, 76.04057627198102409 ) ) ;
#164429 = CARTESIAN_POINT ( 'NONE',  ( -13.97604488694527625, -13.89961937509977652, 101.8739096053143811 ) ) ;
#164432 = CARTESIAN_POINT ( 'NONE',  ( -9.474510206698964154, 16.51473224551069663, 30.41557627198102054 ) ) ;
#164431 = CARTESIAN_POINT ( 'NONE',  ( -14.34966873604960291, -8.224510206698953496, 41.66557627198103120 ) ) ;
#164430 = CARTESIAN_POINT ( 'NONE',  ( -19.05341960407611168, -5.049401038298163336, 51.45724293864770260 ) ) ;
#164433 = VERTEX_POINT ( 'NONE', #172748 ) ;
#164434 = CARTESIAN_POINT ( 'NONE',  ( -10.72451020669870658, -18.67979575497194134, 49.58442372801901143 ) ) ;
#164435 = CARTESIAN_POINT ( 'NONE',  ( 19.05341960407617918, -5.049401038297876454, 81.04275706135231871 ) ) ;
#164436 = CARTESIAN_POINT ( 'NONE',  ( -0.05219959533910754901, -16.53943276465976808, 52.49890960531435979 ) ) ;
#164437 = CARTESIAN_POINT ( 'NONE',  ( 10.72451020669898902, -18.67979575497178502, 92.91557627198103830 ) ) ;
#164438 = CARTESIAN_POINT ( 'NONE',  ( 18.67979575497178502, 10.72451020669898547, 29.16557627198103120 ) ) ;
#164439 = CARTESIAN_POINT ( 'NONE',  ( 16.53943276465976808, -0.05219959533910856209, 83.74890960531435269 ) ) ;
#164440 = CARTESIAN_POINT ( 'NONE',  ( 19.05341960407611168, 5.049401038298154454, 48.95724293864768129 ) ) ;
#164441 = CARTESIAN_POINT ( 'NONE',  ( -16.52544592524342804, 4.483927247898546575, 26.04057627198103475 ) ) ;
#164442 = CARTESIAN_POINT ( 'NONE',  ( -4.379528057220086978, -16.55341960407618274, 89.79275706135236135 ) ) ;
#164443 = CARTESIAN_POINT ( 'NONE',  ( 4.483927247898790824, -16.52544592524335698, 70.20942372801904696 ) ) ;
#164444 = CARTESIAN_POINT ( 'NONE',  ( -9.474510206698720793, -16.51473224551083518, 29.58442372801900433 ) ) ;
#164445 = CARTESIAN_POINT ( 'NONE',  ( -19.02544592524342804, 5.153800228976336051, 91.04057627198100988 ) ) ;
#164446 = CARTESIAN_POINT ( 'NONE',  ( 19.03943276465977164, -0.05219959533909143690, 78.74890960531436690 ) ) ;
#164447 = CARTESIAN_POINT ( 'NONE',  ( -4.483927247898782831, 16.52544592524335698, 77.70942372801900433 ) ) ;
#164448 = CARTESIAN_POINT ( 'NONE',  ( 19.05341960407611168, 5.049401038298154454, 43.95724293864769550 ) ) ;
#164449 = EDGE_CURVE ( 'NONE', #91848, #155866, #121204, .T. ) ;
#164450 = CARTESIAN_POINT ( 'NONE',  ( -8.224510206698948167, 14.34966873604960824, 50.41557627198103120 ) ) ;
#164451 = CARTESIAN_POINT ( 'NONE',  ( 19.05341960407611168, 5.049401038298154454, 98.95724293864766707 ) ) ;
#164452 = CARTESIAN_POINT ( 'NONE',  ( 10.81492255796078972, 18.62759615963270932, 29.58224293864769905 ) ) ;
#164453 = CARTESIAN_POINT ( 'NONE',  ( -8.314922557960811034, -14.29746914071050412, 67.08224293864770971 ) ) ;
#164454 = CARTESIAN_POINT ( 'NONE',  ( 8.314922557960818139, 14.29746914071049879, 69.58224293864769550 ) ) ;
#164455 = CARTESIAN_POINT ( 'NONE',  ( 17.50000000000018474, -3.292511757969704522, 32.56520270210548773 ) ) ;
#164456 = CARTESIAN_POINT ( 'NONE',  ( -13.89961937509957401, -13.97604488694547875, 64.37609039468567573 ) ) ;
#164457 = CARTESIAN_POINT ( 'NONE',  ( 0.05219959533909260263, 19.03943276465977164, 99.99890960531436690 ) ) ;
#164458 = CARTESIAN_POINT ( 'NONE',  ( 9.474510206698729675, 16.51473224551082808, 77.08442372801900433 ) ) ;
#164459 = CARTESIAN_POINT ( 'NONE',  ( -17.58332526062525147, -7.635886036038636249, 94.07665040441534643 ) ) ;
#164461 = CARTESIAN_POINT ( 'NONE',  ( 16.55341960407618274, -4.379528057220086978, 91.04275706135236135 ) ) ;
#164460 = CARTESIAN_POINT ( 'NONE',  ( -19.05341960407617563, 5.049401038297882671, 113.5427570613523471 ) ) ;
#164462 = CARTESIAN_POINT ( 'NONE',  ( 5.049401038298161559, -19.05341960407611168, 42.70724293864767418 ) ) ;
#164463 = CARTESIAN_POINT ( 'NONE',  ( 21.53943276465977519, -0.05219959533907433946, 38.74890960531435979 ) ) ;
#164464 = CARTESIAN_POINT ( 'NONE',  ( -18.67979575497193778, 10.72451020669871902, 53.33442372801901854 ) ) ;
#164465 = CARTESIAN_POINT ( 'NONE',  ( 8.224510206698742110, 14.34966873604972548, 27.08442372801901854 ) ) ;
#164467 = CARTESIAN_POINT ( 'NONE',  ( -9.474510206698964154, 16.51473224551069663, 80.41557627198103830 ) ) ;
#164466 = CARTESIAN_POINT ( 'NONE',  ( 1.486117417673710336E-14, -69.45644693201178654, -24.99410988519313648 ) ) ;
#164468 = CARTESIAN_POINT ( 'NONE',  ( 13.97604488694527802, 13.89961937509977652, 114.3739096053143669 ) ) ;
#164470 = CARTESIAN_POINT ( 'NONE',  ( 0.05219959533909260263, 19.03943276465977164, 79.99890960531436690 ) ) ;
#164469 = CARTESIAN_POINT ( 'NONE',  ( -12.06949235617756955, 12.14591786802309770, 80.62390960531438111 ) ) ;
#164471 = CARTESIAN_POINT ( 'NONE',  ( 13.89961937509977652, -13.97604488694527269, 83.12390960531436690 ) ) ;
#164472 = ORIENTED_EDGE ( 'NONE', *, *, #60352, .T. ) ;
#164473 = CARTESIAN_POINT ( 'NONE',  ( 5.049401038297881783, 19.05341960407617563, 87.29275706135234714 ) ) ;
#164474 = CARTESIAN_POINT ( 'NONE',  ( 21.52544592524344225, -5.823673210054117533, 58.54057627198103120 ) ) ;
#164475 = CARTESIAN_POINT ( 'NONE',  ( -19.02544592524342804, 5.153800228976336051, 31.04057627198102409 ) ) ;
#164476 = CARTESIAN_POINT ( 'NONE',  ( 19.02544592524334988, 5.153800228976608722, 61.45942372801900433 ) ) ;
#164477 = CARTESIAN_POINT ( 'NONE',  ( -13.89961937509977652, 13.97604488694528158, 60.62390960531436690 ) ) ;
#164478 = CARTESIAN_POINT ( 'NONE',  ( -16.51473224551069308, -9.474510206698971260, 86.66557627198102409 ) ) ;
#164479 = ORIENTED_EDGE ( 'NONE', *, *, #50912, .F. ) ;
#164480 = CARTESIAN_POINT ( 'NONE',  ( -10.72451020669898014, 18.67979575497178502, 85.41557627198102409 ) ) ;
#164482 = CARTESIAN_POINT ( 'NONE',  ( 5.153800228976615827, -19.02544592524334988, 50.20942372801897591 ) ) ;
#164481 = CARTESIAN_POINT ( 'NONE',  ( 14.34966873604960469, 8.224510206698951720, 94.16557627198103830 ) ) ;
#164483 = CARTESIAN_POINT ( 'NONE',  ( 21.55341960407610458, 5.719274019375980345, 93.95724293864770971 ) ) ;
#164484 = CARTESIAN_POINT ( 'NONE',  ( 21.53943276465977519, -0.05219959533907433946, 78.74890960531436690 ) ) ;
#164485 = CARTESIAN_POINT ( 'NONE',  ( -4.483927247898539470, -16.52544592524342804, 37.29057627198102409 ) ) ;
#164486 = CARTESIAN_POINT ( 'NONE',  ( 21.52544592524334988, 5.823673210054432836, 101.4594237280190185 ) ) ;
#164487 = CARTESIAN_POINT ( 'NONE',  ( -16.55341960407617563, 4.379528057220093196, 53.54275706135234714 ) ) ;
#164488 = CARTESIAN_POINT ( 'NONE',  ( 19.03943276465977164, -0.05219959533909143690, 78.74890960531436690 ) ) ;
#164489 = CARTESIAN_POINT ( 'NONE',  ( -16.51473224551069308, -9.474510206698971260, 26.66557627198103120 ) ) ;
#164490 = CARTESIAN_POINT ( 'NONE',  ( -5.719274019375665041, -21.55341960407619695, 44.79275706135234714 ) ) ;
#164491 = CARTESIAN_POINT ( 'NONE',  ( 10.72451020669871369, 18.67979575497193778, 52.08442372801901854 ) ) ;
#164492 = CARTESIAN_POINT ( 'NONE',  ( -13.89961937509977652, 13.97604488694528158, 50.62390960531435979 ) ) ;
#164493 = CARTESIAN_POINT ( 'NONE',  ( -10.72451020669898014, 18.67979575497178502, 115.4155762719810241 ) ) ;
#164494 = CARTESIAN_POINT ( 'NONE',  ( 9.474510206698729675, 16.51473224551082808, 67.08442372801900433 ) ) ;
#164495 = CARTESIAN_POINT ( 'NONE',  ( 19.05341960407611168, 5.049401038298154454, 38.95724293864767418 ) ) ;
#164496 = CARTESIAN_POINT ( 'NONE',  ( 0.05219959533934541429, -16.53943276465976808, 25.00109039468567218 ) ) ;
#164497 = CARTESIAN_POINT ( 'NONE',  ( -19.03943276465977164, 0.05219959533909376836, 26.24890960531435624 ) ) ;
#164498 = CARTESIAN_POINT ( 'NONE',  ( -4.483927247898782831, 16.52544592524335698, 72.70942372801901854 ) ) ;
#164499 = CARTESIAN_POINT ( 'NONE',  ( 9.564922557960805705, 16.46253265017160317, 44.58224293864769550 ) ) ;
#164500 = CARTESIAN_POINT ( 'NONE',  ( 24.04614410381781653, -5.408324479810879382, 174.2944578187869240 ) ) ;
#164501 = CARTESIAN_POINT ( 'NONE',  ( 13.89961937509977652, -13.97604488694527269, 88.12390960531438111 ) ) ;
#164502 = CARTESIAN_POINT ( 'NONE',  ( -0.05219959533909027116, -19.03943276465977164, 22.49890960531436690 ) ) ;
#164503 = CARTESIAN_POINT ( 'NONE',  ( 10.81492255796078972, 18.62759615963270932, 79.58224293864769550 ) ) ;
#164504 = CARTESIAN_POINT ( 'NONE',  ( 12.14591786802327356, -12.06949235617739191, 50.62609039468568994 ) ) ;
#164505 = CARTESIAN_POINT ( 'NONE',  ( -9.564922557961040184, 16.46253265017147172, 22.91775706135233648 ) ) ;
#164506 = CARTESIAN_POINT ( 'NONE',  ( -9.564922557960796823, -16.46253265017161027, 37.08224293864768839 ) ) ;
#164507 = CARTESIAN_POINT ( 'NONE',  ( 16.52544592524342804, -4.483927247898539470, 28.54057627198103120 ) ) ;
#164508 = CARTESIAN_POINT ( 'NONE',  ( 16.52544592524342804, -4.483927247898539470, 63.54057627198103830 ) ) ;
#164509 = CIRCLE ( 'NONE', #77300, 1.500000000000001332 ) ;
#164510 = CARTESIAN_POINT ( 'NONE',  ( -13.89961937509977652, 13.97604488694528158, 65.62390960531436690 ) ) ;
#164511 = CARTESIAN_POINT ( 'NONE',  ( -18.62759615963255300, -10.81492255796106328, 109.1677570613523613 ) ) ;
#164512 = CARTESIAN_POINT ( 'NONE',  ( 0.05219959533937995610, -21.53943276465977519, 30.00109039468568284 ) ) ;
#164513 = CARTESIAN_POINT ( 'NONE',  ( 16.51473224551069308, 9.474510206698969483, 74.16557627198103830 ) ) ;
#164514 = CARTESIAN_POINT ( 'NONE',  ( 21.55341960407619695, -5.719274019375665929, 81.04275706135236135 ) ) ;
#164515 = CARTESIAN_POINT ( 'NONE',  ( -0.05219959533934338120, 16.53943276465976808, 72.50109039468568994 ) ) ;
#164516 = CARTESIAN_POINT ( 'NONE',  ( 16.51473224551069308, 9.474510206698969483, 109.1655762719810383 ) ) ;
#164517 = CARTESIAN_POINT ( 'NONE',  ( 12.06949235617757843, -12.14591786802309237, 33.12390960531435979 ) ) ;
#164518 = CARTESIAN_POINT ( 'NONE',  ( -9.564922557960796823, -16.46253265017161027, 32.08224293864769550 ) ) ;
#164519 = CARTESIAN_POINT ( 'NONE',  ( -4.379528057220086978, -16.55341960407618274, 54.79275706135235424 ) ) ;
#164520 = CARTESIAN_POINT ( 'NONE',  ( 4.483927247898545687, 16.52544592524342804, 54.79057627198104541 ) ) ;
#164521 = CARTESIAN_POINT ( 'NONE',  ( -19.02544592524342804, 5.153800228976336051, 106.0405762719810241 ) ) ;
#164522 = CARTESIAN_POINT ( 'NONE',  ( 10.72451020669898902, -18.67979575497178502, 37.91557627198102409 ) ) ;
#164523 = CARTESIAN_POINT ( 'NONE',  ( 18.62759615963255655, 10.81492255796105972, 106.6677570613523756 ) ) ;
#164524 = CARTESIAN_POINT ( 'NONE',  ( -4.483927247898539470, -16.52544592524342804, 87.29057627198103830 ) ) ;
#164525 = CARTESIAN_POINT ( 'NONE',  ( -19.03943276465977164, 0.05219959533909376836, 96.24890960531436690 ) ) ;
#164526 = EDGE_LOOP ( 'NONE', ( #43847, #124149, #172147, #73004 ) ) ;
#164527 = CARTESIAN_POINT ( 'NONE',  ( 16.53943276465976808, 0.05219959533934440121, 56.25109039468568284 ) ) ;
#164528 = CARTESIAN_POINT ( 'NONE',  ( 16.46253265017160672, -9.564922557960803928, 58.33224293864769550 ) ) ;
#164529 = CARTESIAN_POINT ( 'NONE',  ( 13.89961937509957401, 13.97604488694547697, 51.87609039468566863 ) ) ;
#164530 = CARTESIAN_POINT ( 'NONE',  ( -16.51473224551069308, -9.474510206698971260, 51.66557627198102409 ) ) ;
#164531 = CARTESIAN_POINT ( 'NONE',  ( -14.34966873604972548, 8.224510206698743886, 78.33442372801901854 ) ) ;
#164532 = CARTESIAN_POINT ( 'NONE',  ( -5.049401038297874678, -19.05341960407617918, 94.79275706135230450 ) ) ;
#164533 = CARTESIAN_POINT ( 'NONE',  ( -0.05219959533937732626, 21.53943276465977519, 62.50109039468568284 ) ) ;
#164534 = CARTESIAN_POINT ( 'NONE',  ( -0.05219959533909027116, -19.03943276465977164, 57.49890960531435979 ) ) ;
#164535 = CARTESIAN_POINT ( 'NONE',  ( 0.05219959533907565091, 21.53943276465977519, 94.99890960531436690 ) ) ;
#164536 = CARTESIAN_POINT ( 'NONE',  ( 14.29746914071049879, -8.314922557960816363, 98.33224293864769550 ) ) ;
#164537 = VECTOR ( 'NONE', #147675, 1000.000000000000000 ) ;
#164538 = CARTESIAN_POINT ( 'NONE',  ( -13.89961937509957401, -13.97604488694547875, 69.37609039468564731 ) ) ;
#164539 = CARTESIAN_POINT ( 'NONE',  ( 5.823673210054125526, 21.52544592524343514, 64.79057627198103830 ) ) ;
#164540 = CARTESIAN_POINT ( 'NONE',  ( 19.02544592524334988, 5.153800228976608722, 36.45942372801900433 ) ) ;
#164541 = CARTESIAN_POINT ( 'NONE',  ( 18.22780087662123805, 5.499999999999960032, 96.48236817873105053 ) ) ;
#164542 = CARTESIAN_POINT ( 'NONE',  ( -18.67979575497178146, -10.72451020669898902, 91.66557627198103830 ) ) ;
#164543 = CARTESIAN_POINT ( 'NONE',  ( -19.02130022317638236, 5.499999999999601208, 55.78188669246575415 ) ) ;
#164544 = CARTESIAN_POINT ( 'NONE',  ( 4.483927247898790824, -16.52544592524335698, 20.20942372801900788 ) ) ;
#164545 = CARTESIAN_POINT ( 'NONE',  ( -4.379528057220086978, -16.55341960407618274, 24.79275706135235779 ) ) ;
#164546 = CARTESIAN_POINT ( 'NONE',  ( -19.02544592524342804, 5.153800228976336051, 46.04057627198101699 ) ) ;
#164547 = CARTESIAN_POINT ( 'NONE',  ( -16.46253265017160317, 9.564922557960807481, 110.8322429386476955 ) ) ;
#164548 = CARTESIAN_POINT ( 'NONE',  ( -5.719274019375978568, 21.55341960407610458, 85.20724293864770971 ) ) ;
#164549 = CARTESIAN_POINT ( 'NONE',  ( -10.72451020669870658, -18.67979575497194134, 69.58442372801900433 ) ) ;
#164551 = CARTESIAN_POINT ( 'NONE',  ( 5.049401038297881783, 19.05341960407617563, 22.29275706135233648 ) ) ;
#164550 = CARTESIAN_POINT ( 'NONE',  ( 8.224510206698742110, 14.34966873604972548, 27.08442372801901854 ) ) ;
#164552 = CARTESIAN_POINT ( 'NONE',  ( -16.52544592524342804, 4.483927247898546575, 31.04057627198102409 ) ) ;
#164553 = CARTESIAN_POINT ( 'NONE',  ( 5.719274019375991003, -21.55341960407610458, 112.7072429386476955 ) ) ;
#164554 = CARTESIAN_POINT ( 'NONE',  ( 0.05219959533910956823, 16.53943276465976808, 44.99890960531435979 ) ) ;
#164555 = CARTESIAN_POINT ( 'NONE',  ( 16.46253265017146816, 9.564922557961045513, 91.66775706135234714 ) ) ;
#164556 = CARTESIAN_POINT ( 'NONE',  ( -16.46253265017146816, -9.564922557961047289, 54.16775706135234003 ) ) ;
#164557 = CARTESIAN_POINT ( 'NONE',  ( -21.53943276465977519, -0.05219959533937600094, 68.75109039468568994 ) ) ;
#164558 = CARTESIAN_POINT ( 'NONE',  ( -16.46253265017146816, -9.564922557961047289, 54.16775706135234003 ) ) ;
#164559 = CARTESIAN_POINT ( 'NONE',  ( 5.153800228976335163, 19.02544592524342804, 29.79057627198102409 ) ) ;
#164560 = CARTESIAN_POINT ( 'NONE',  ( 21.55341960407610458, 5.719274019375980345, 43.95724293864769550 ) ) ;
#164561 = CARTESIAN_POINT ( 'NONE',  ( 12.06949235617757843, -12.14591786802309237, 48.12390960531436690 ) ) ;
#164562 = CARTESIAN_POINT ( 'NONE',  ( -16.79531203550646268, -7.028104445595714900, 26.25244988220445919 ) ) ;
#164563 = CARTESIAN_POINT ( 'NONE',  ( 13.97604488694548053, -13.89961937509957401, 20.62609039468567573 ) ) ;
#164564 = CARTESIAN_POINT ( 'NONE',  ( 16.55341960407618274, -4.379528057220086978, 71.04275706135234714 ) ) ;
#164565 = CARTESIAN_POINT ( 'NONE',  ( -8.224510206698948167, 14.34966873604960824, 45.41557627198103830 ) ) ;
#164566 = CARTESIAN_POINT ( 'NONE',  ( -5.823673210054431948, 21.52544592524334988, 77.70942372801900433 ) ) ;
#164567 = CARTESIAN_POINT ( 'NONE',  ( 10.81492255796106328, -18.62759615963255655, 70.41775706135236135 ) ) ;
#164568 = CARTESIAN_POINT ( 'NONE',  ( 10.81492255796078972, 18.62759615963270932, 84.58224293864769550 ) ) ;
#164569 = CARTESIAN_POINT ( 'NONE',  ( -19.05341960407611168, -5.049401038298163336, 36.45724293864766707 ) ) ;
#164570 = CARTESIAN_POINT ( 'NONE',  ( 10.81492255796106328, -18.62759615963255655, 40.41775706135234714 ) ) ;
#164571 = CARTESIAN_POINT ( 'NONE',  ( 16.46253265017160672, -9.564922557960803928, 23.33224293864769194 ) ) ;
#164572 = CARTESIAN_POINT ( 'NONE',  ( 5.153800228976335163, 19.02544592524342804, 34.79057627198102409 ) ) ;
#164573 = CARTESIAN_POINT ( 'NONE',  ( -12.14591786802309592, -12.06949235617757132, 96.87390960531436690 ) ) ;
#164574 = CARTESIAN_POINT ( 'NONE',  ( 0.05219959533909260263, 19.03943276465977164, 89.99890960531436690 ) ) ;
#164575 = CARTESIAN_POINT ( 'NONE',  ( 8.314922557960818139, 14.29746914071049879, 44.58224293864769550 ) ) ;
#164576 = CARTESIAN_POINT ( 'NONE',  ( -8.224510206698948167, 14.34966873604960824, 105.4155762719810383 ) ) ;
#164577 = CARTESIAN_POINT ( 'NONE',  ( 0.05219959533907565091, 21.53943276465977519, 64.99890960531435269 ) ) ;
#164578 = CARTESIAN_POINT ( 'NONE',  ( 21.53943276465977519, -0.05219959533907433946, 113.7489096053143527 ) ) ;
#164579 = CARTESIAN_POINT ( 'NONE',  ( -5.049401038298153566, 19.05341960407611168, 110.2072429386476671 ) ) ;
#164581 = CARTESIAN_POINT ( 'NONE',  ( 14.29746914071037800, 8.314922557961029526, 21.66775706135235069 ) ) ;
#164580 = CARTESIAN_POINT ( 'NONE',  ( -9.474510206698964154, 16.51473224551069663, 60.41557627198102409 ) ) ;
#164582 = CARTESIAN_POINT ( 'NONE',  ( 18.67979575497178502, 10.72451020669898547, 69.16557627198102409 ) ) ;
#164583 = CARTESIAN_POINT ( 'NONE',  ( 5.823673210054444382, -21.52544592524334988, 95.20942372801903275 ) ) ;
#164584 = CARTESIAN_POINT ( 'NONE',  ( 9.564922557960805705, 16.46253265017160317, 84.58224293864769550 ) ) ;
#164585 = CARTESIAN_POINT ( 'NONE',  ( 10.72451020669898902, -18.67979575497178502, 112.9155762719810383 ) ) ;
#164586 = CARTESIAN_POINT ( 'NONE',  ( -19.03943276465977164, 0.05219959533909376836, 111.2489096053143669 ) ) ;
#164587 = CARTESIAN_POINT ( 'NONE',  ( 12.14591786802327356, -12.06949235617739191, 85.62609039468568994 ) ) ;
#164588 = CARTESIAN_POINT ( 'NONE',  ( 21.52544592524334988, 5.823673210054432836, 71.45942372801901854 ) ) ;
#164589 = CARTESIAN_POINT ( 'NONE',  ( 15.80617190586769283, -15.72974639402175789, 105.6260903946856899 ) ) ;
#164590 = CARTESIAN_POINT ( 'NONE',  ( 12.14591786802327356, -12.06949235617739191, 55.62609039468568284 ) ) ;
#164591 = CARTESIAN_POINT ( 'NONE',  ( 21.53943276465977519, 0.05219959533937863772, 26.25109039468567573 ) ) ;
#164592 = CARTESIAN_POINT ( 'NONE',  ( -5.153800228976328057, -19.02544592524343514, 112.2905762719810099 ) ) ;
#164593 = CARTESIAN_POINT ( 'NONE',  ( -21.55341960407619339, 5.719274019375674811, 88.54275706135236135 ) ) ;
#164594 = CARTESIAN_POINT ( 'NONE',  ( 13.97604488694527802, 13.89961937509977652, 99.37390960531436690 ) ) ;
#164595 = CARTESIAN_POINT ( 'NONE',  ( -18.67979575497178146, -10.72451020669898902, 86.66557627198102409 ) ) ;
#164596 = CARTESIAN_POINT ( 'NONE',  ( -9.474510206698720793, -16.51473224551083518, 64.58442372801900433 ) ) ;
#164597 = CARTESIAN_POINT ( 'NONE',  ( -21.53943276465977519, 0.05219959533907696930, 56.24890960531436690 ) ) ;
#164599 = CARTESIAN_POINT ( 'NONE',  ( -8.224510206698948167, 14.34966873604960824, 35.41557627198102409 ) ) ;
#164598 = CARTESIAN_POINT ( 'NONE',  ( -5.153800228976328057, -19.02544592524343514, 92.29057627198099567 ) ) ;
#164600 = CARTESIAN_POINT ( 'NONE',  ( 21.96449396329681392, 6.689387493872144930, 170.9254202302468570 ) ) ;
#164601 = CARTESIAN_POINT ( 'NONE',  ( -19.05341960407617563, 5.049401038297882671, 83.54275706135233293 ) ) ;
#164602 = CARTESIAN_POINT ( 'NONE',  ( 1.464819237669550356, 14.82474175162738383, -59.95888713364202260 ) ) ;
#164603 = ADVANCED_FACE ( 'NONE', ( #159541 ), #94898, .T. ) ;
#164604 = CARTESIAN_POINT ( 'NONE',  ( 13.97604488694548053, -13.89961937509957401, 110.6260903946856615 ) ) ;
#164605 = CARTESIAN_POINT ( 'NONE',  ( -15.72974639402197994, 15.80617190586746368, 85.62390960531436690 ) ) ;
#164606 = CARTESIAN_POINT ( 'NONE',  ( -16.53943276465976808, 0.05219959533911058130, 71.24890960531435269 ) ) ;
#164607 = CARTESIAN_POINT ( 'NONE',  ( 12.14591786802327356, -12.06949235617739191, 35.62609039468568994 ) ) ;
#164608 = CARTESIAN_POINT ( 'NONE',  ( 16.46253265017160672, -9.564922557960803928, 43.33224293864769550 ) ) ;
#164610 = CARTESIAN_POINT ( 'NONE',  ( -5.049401038297874678, -19.05341960407617918, 89.79275706135230450 ) ) ;
#164609 = CARTESIAN_POINT ( 'NONE',  ( 5.823673210054125526, 21.52544592524343514, 109.7905762719810383 ) ) ;
#164611 = CARTESIAN_POINT ( 'NONE',  ( 19.05341960407611168, 5.049401038298154454, 98.95724293864766707 ) ) ;
#164612 = CARTESIAN_POINT ( 'NONE',  ( 19.05341960407611168, 5.049401038298154454, 68.95724293864769550 ) ) ;
#164613 = CARTESIAN_POINT ( 'NONE',  ( 15.80617190586746368, 15.72974639402197994, 79.37390960531436690 ) ) ;
#164614 = CARTESIAN_POINT ( 'NONE',  ( -13.89961937509977652, 13.97604488694528158, 40.62390960531435979 ) ) ;
#164615 = CARTESIAN_POINT ( 'NONE',  ( 5.714903183877464876, 37.05114278946271611, -8.000000000000000000 ) ) ;
#164616 = CARTESIAN_POINT ( 'NONE',  ( -16.52544592524342804, 4.483927247898546575, 61.04057627198103120 ) ) ;
#164617 = CARTESIAN_POINT ( 'NONE',  ( -19.03943276465977164, 0.05219959533909376836, 96.24890960531436690 ) ) ;
#164618 = CARTESIAN_POINT ( 'NONE',  ( -67.00000000000000000, -5.510910596163089556E-15, 39.49999999999996447 ) ) ;
#164619 = CARTESIAN_POINT ( 'NONE',  ( -13.97604488694547697, 13.89961937509957934, 68.12609039468563310 ) ) ;
#164620 = CARTESIAN_POINT ( 'NONE',  ( 21.53943276465977519, -0.05219959533907433946, 73.74890960531433848 ) ) ;
#164621 = CARTESIAN_POINT ( 'NONE',  ( -9.474510206698720793, -16.51473224551083518, 39.58442372801899722 ) ) ;
#164622 = CARTESIAN_POINT ( 'NONE',  ( 19.03943276465977164, -0.05219959533909143690, 103.7489096053143669 ) ) ;
#164623 = CARTESIAN_POINT ( 'NONE',  ( 12.24802307403560953, -10.59827931221447805, -59.37567494090387044 ) ) ;
#164624 = CARTESIAN_POINT ( 'NONE',  ( -21.52544592524343514, 5.823673210054127303, 41.04057627198103120 ) ) ;
#164625 = CARTESIAN_POINT ( 'NONE',  ( -19.03943276465977164, 0.05219959533909376836, 66.24890960531436690 ) ) ;
#164626 = CARTESIAN_POINT ( 'NONE',  ( -21.53943276465977519, -0.05219959533937600094, 68.75109039468568994 ) ) ;
#164627 = CARTESIAN_POINT ( 'NONE',  ( 5.049401038298161559, -19.05341960407611168, 27.70724293864769550 ) ) ;
#164629 = ORIENTED_EDGE ( 'NONE', *, *, #164449, .F. ) ;
#164628 = CARTESIAN_POINT ( 'NONE',  ( 21.52544592524344225, -5.823673210054117533, 108.5405762719810241 ) ) ;
#164630 = CARTESIAN_POINT ( 'NONE',  ( 18.62759615963255655, 10.81492255796105972, 51.66775706135234714 ) ) ;
#164631 = ORIENTED_EDGE ( 'NONE', *, *, #135020, .T. ) ;
#164632 = CARTESIAN_POINT ( 'NONE',  ( -22.11591546058419766, -17.92733262806552474, 140.0000000000000853 ) ) ;
#164633 = CARTESIAN_POINT ( 'NONE',  ( -16.46253265017146816, -9.564922557961047289, 64.16775706135233293 ) ) ;
#164634 = CARTESIAN_POINT ( 'NONE',  ( -21.65431292632188942, 8.856125861401146437, 168.9593721673316793 ) ) ;
#164635 = CARTESIAN_POINT ( 'NONE',  ( 0.05219959533907565091, 21.53943276465977519, 104.9989096053143669 ) ) ;
#164636 = CARTESIAN_POINT ( 'NONE',  ( -0.05219959533909027116, -19.03943276465977164, 62.49890960531435979 ) ) ;
#164637 = CARTESIAN_POINT ( 'NONE',  ( 4.483927247898790824, -16.52544592524335698, 40.20942372801901854 ) ) ;
#164638 = CARTESIAN_POINT ( 'NONE',  ( -38.00000000000000711, 2.428612866367529932E-14, -9.749999994537626336 ) ) ;
#164639 = CARTESIAN_POINT ( 'NONE',  ( 10.72451020669871369, 18.67979575497193778, 102.0844237280190185 ) ) ;
#164640 = CARTESIAN_POINT ( 'NONE',  ( -19.03943276465977164, 0.05219959533909376836, 36.24890960531436690 ) ) ;
#164641 = CARTESIAN_POINT ( 'NONE',  ( -21.53943276465977519, -0.05219959533937600094, 108.7510903946857042 ) ) ;
#164643 = CARTESIAN_POINT ( 'NONE',  ( -5.719274019375665041, -21.55341960407619695, 64.79275706135234714 ) ) ;
#164642 = CARTESIAN_POINT ( 'NONE',  ( -5.049401038298153566, 19.05341960407611168, 85.20724293864766707 ) ) ;
#164644 = CIRCLE ( 'NONE', #9776, 0.5000000000000004441 ) ;
#164645 = CARTESIAN_POINT ( 'NONE',  ( -22.44159573604010305, 16.30477369853692338, 149.1750000027311671 ) ) ;
#164646 = CARTESIAN_POINT ( 'NONE',  ( 16.46253265017160672, -9.564922557960803928, 113.3322429386476955 ) ) ;
#164647 = CARTESIAN_POINT ( 'NONE',  ( -17.49999999999998224, 3.512728167237041621, 30.22809995181128428 ) ) ;
#164649 = CARTESIAN_POINT ( 'NONE',  ( 10.72451020669871369, 18.67979575497193778, 72.08442372801899012 ) ) ;
#164648 = CARTESIAN_POINT ( 'NONE',  ( -16.55341960407617563, 4.379528057220093196, 58.54275706135235424 ) ) ;
#164650 = CARTESIAN_POINT ( 'NONE',  ( 18.67979575497194134, -10.72451020669871369, 90.83442372801901854 ) ) ;
#164651 = CARTESIAN_POINT ( 'NONE',  ( 26.58496454516998142, -7.626754437231455519, 167.9682100371138915 ) ) ;
#164652 = CARTESIAN_POINT ( 'NONE',  ( 4.379528057220092307, 16.55341960407617563, 32.29275706135235424 ) ) ;
#164653 = CARTESIAN_POINT ( 'NONE',  ( 5.153800228976335163, 19.02544592524342804, 89.79057627198102409 ) ) ;
#164654 = LINE ( 'NONE', #178829, #93083 ) ;
#164655 = ORIENTED_EDGE ( 'NONE', *, *, #96611, .T. ) ;
#164656 = CARTESIAN_POINT ( 'NONE',  ( -1.114265510929671077, -29.39134536520999319, -52.10946600208642820 ) ) ;
#164657 = CARTESIAN_POINT ( 'NONE',  ( -5.153800228976328057, -19.02544592524343514, 22.29057627198102765 ) ) ;
#164658 = CARTESIAN_POINT ( 'NONE',  ( -21.52544592524343514, 5.823673210054127303, 46.04057627198103830 ) ) ;
#164659 = CARTESIAN_POINT ( 'NONE',  ( 14.34966873604972726, -8.224510206698740333, 110.8344237280190043 ) ) ;
#164661 = CARTESIAN_POINT ( 'NONE',  ( 9.564922557960805705, 16.46253265017160317, 74.58224293864769550 ) ) ;
#164660 = CARTESIAN_POINT ( 'NONE',  ( 8.224510206698953496, -14.34966873604960469, 82.91557627198103830 ) ) ;
#164662 = CARTESIAN_POINT ( 'NONE',  ( 18.67979575497194134, -10.72451020669871369, 95.83442372801903275 ) ) ;
#164663 = CARTESIAN_POINT ( 'NONE',  ( 0.05219959533934541429, -16.53943276465976808, 30.00109039468568284 ) ) ;
#164664 = CARTESIAN_POINT ( 'NONE',  ( 12.14591786802309770, 12.06949235617756955, 89.37390960531435269 ) ) ;
#164665 = CARTESIAN_POINT ( 'NONE',  ( -5.823673210054431948, 21.52544592524334988, 42.70942372801901854 ) ) ;
#164666 = CARTESIAN_POINT ( 'NONE',  ( -21.53943276465977519, 0.05219959533907696930, 71.24890960531435269 ) ) ;
#164667 = CARTESIAN_POINT ( 'NONE',  ( 5.049401038297881783, 19.05341960407617563, 42.29275706135234003 ) ) ;
#164668 = FACE_OUTER_BOUND ( 'NONE', #64960, .T. ) ;
#164669 = CARTESIAN_POINT ( 'NONE',  ( -9.564922557960796823, -16.46253265017161027, 82.08224293864768129 ) ) ;
#164670 = CARTESIAN_POINT ( 'NONE',  ( -4.379528057220328563, 16.55341960407611168, 60.20724293864768839 ) ) ;
#164671 = AXIS2_PLACEMENT_3D ( 'NONE', #59804, #186152, #32458 ) ;
#164672 = CARTESIAN_POINT ( 'NONE',  ( -16.52544592524342804, 4.483927247898546575, 41.04057627198103120 ) ) ;
#164673 = CARTESIAN_POINT ( 'NONE',  ( -4.379528057220086978, -16.55341960407618274, 109.7927570613523613 ) ) ;
#164674 = CARTESIAN_POINT ( 'NONE',  ( 9.474510206698729675, 16.51473224551082808, 62.08442372801899722 ) ) ;
#164675 = CARTESIAN_POINT ( 'NONE',  ( 17.48847506799968698, 5.747544572773807481, 46.67302562156721280 ) ) ;
#164676 = CARTESIAN_POINT ( 'NONE',  ( -18.62759615963270932, 10.81492255796079327, 25.83224293864769194 ) ) ;
#164677 = EDGE_CURVE ( 'NONE', #15380, #192038, #166718, .T. ) ;
#164678 = CARTESIAN_POINT ( 'NONE',  ( 8.314922557960818139, 14.29746914071049879, 84.58224293864769550 ) ) ;
#164679 = CARTESIAN_POINT ( 'NONE',  ( 18.52568451169414843, -5.500000000000145661, 38.52123528320487367 ) ) ;
#164681 = CARTESIAN_POINT ( 'NONE',  ( -10.81492255796078084, -18.62759615963271287, 47.08224293864770260 ) ) ;
#164680 = CARTESIAN_POINT ( 'NONE',  ( -9.564922557960796823, -16.46253265017161027, 47.08224293864769550 ) ) ;
#164682 = CARTESIAN_POINT ( 'NONE',  ( 5.719274019375991003, -21.55341960407610458, 82.70724293864770971 ) ) ;
#164683 = CARTESIAN_POINT ( 'NONE',  ( 8.224510206698953496, -14.34966873604960469, 107.9155762719810241 ) ) ;
#164685 = CARTESIAN_POINT ( 'NONE',  ( -16.51473224551069308, -9.474510206698971260, 41.66557627198103120 ) ) ;
#164684 = CARTESIAN_POINT ( 'NONE',  ( -16.52544592524335698, -4.483927247898792601, 63.95942372801901854 ) ) ;
#164686 = CARTESIAN_POINT ( 'NONE',  ( 21.52544592524334988, 5.823673210054432836, 51.45942372801901854 ) ) ;
#164687 = CARTESIAN_POINT ( 'NONE',  ( -16.53943276465976808, 0.05219959533911058130, 101.2489096053143669 ) ) ;
#164688 = CARTESIAN_POINT ( 'NONE',  ( -9.474510206698720793, -16.51473224551083518, 84.58442372801900433 ) ) ;
#164689 = CARTESIAN_POINT ( 'NONE',  ( 22.81625015709510151, -31.40387420917324590, -4.424999997268812990 ) ) ;
#164691 = CARTESIAN_POINT ( 'NONE',  ( -15.72974639402197994, 15.80617190586746368, 50.62390960531435979 ) ) ;
#164690 = CYLINDRICAL_SURFACE ( 'NONE', #183062, 216.0437394197456342 ) ;
#164692 = CARTESIAN_POINT ( 'NONE',  ( 16.21995358207306737, -7.366697692864089042, 67.43551001512162202 ) ) ;
#164693 = CARTESIAN_POINT ( 'NONE',  ( -15.72974639402176322, -15.80617190586768395, 79.37609039468567573 ) ) ;
#164694 = CARTESIAN_POINT ( 'NONE',  ( 16.55341960407611168, 4.379528057220329451, 38.95724293864768839 ) ) ;
#164696 = CARTESIAN_POINT ( 'NONE',  ( 12.14591786802309770, 12.06949235617756955, 44.37390960531435979 ) ) ;
#164695 = CARTESIAN_POINT ( 'NONE',  ( -8.314922557961024197, 14.29746914071037800, 52.91775706135235424 ) ) ;
#164697 = CARTESIAN_POINT ( 'NONE',  ( 10.81492255796078972, 18.62759615963270932, 74.58224293864768129 ) ) ;
#164698 = CARTESIAN_POINT ( 'NONE',  ( 0.05219959533907565091, 21.53943276465977519, 69.99890960531435269 ) ) ;
#164699 = CARTESIAN_POINT ( 'NONE',  ( -21.92644707618962485, 9.078916001213697129, 171.2473621415418847 ) ) ;
#164701 = CARTESIAN_POINT ( 'NONE',  ( 21.55341960407610458, 5.719274019375980345, 23.95724293864769550 ) ) ;
#164700 = CARTESIAN_POINT ( 'NONE',  ( 5.153800228976615827, -19.02544592524334988, 90.20942372801900433 ) ) ;
#164702 = CARTESIAN_POINT ( 'NONE',  ( -19.05341960407611168, -5.049401038298163336, 51.45724293864770260 ) ) ;
#164703 = CARTESIAN_POINT ( 'NONE',  ( -16.51473224551069308, -9.474510206698971260, 21.66557627198102765 ) ) ;
#164704 = CARTESIAN_POINT ( 'NONE',  ( 0.000000000000000000, 0.000000000000000000, 0.000000000000000000 ) ) ;
#164705 = LINE ( 'NONE', #179891, #105784 ) ;
#164706 = ORIENTED_EDGE ( 'NONE', *, *, #33627, .T. ) ;
#164707 = CARTESIAN_POINT ( 'NONE',  ( -8.314922557961024197, 14.29746914071037800, 82.91775706135234714 ) ) ;
#164708 = CARTESIAN_POINT ( 'NONE',  ( 21.52544592524344225, -5.823673210054117533, 108.5405762719810241 ) ) ;
#164709 = CARTESIAN_POINT ( 'NONE',  ( -19.03943276465977164, 0.05219959533909376836, 66.24890960531436690 ) ) ;
#164710 = CARTESIAN_POINT ( 'NONE',  ( -18.67979575497193778, 10.72451020669871902, 43.33442372801901143 ) ) ;
#164711 = CARTESIAN_POINT ( 'NONE',  ( -0.05219959533909027116, -19.03943276465977164, 92.49890960531436690 ) ) ;
#164712 = CARTESIAN_POINT ( 'NONE',  ( -30.57338251523015771, -25.88377959333046974, -17.25078043576605680 ) ) ;
#164713 = ORIENTED_EDGE ( 'NONE', *, *, #117840, .F. ) ;
#164714 = CARTESIAN_POINT ( 'NONE',  ( -15.80617190586768217, 15.72974639402176855, 38.12609039468567573 ) ) ;
#164716 = CARTESIAN_POINT ( 'NONE',  ( -19.03943276465977164, -0.05219959533935918106, 93.75109039468566152 ) ) ;
#164715 = CARTESIAN_POINT ( 'NONE',  ( -9.564922557960796823, -16.46253265017161027, 27.08224293864769550 ) ) ;
#164717 = CARTESIAN_POINT ( 'NONE',  ( 5.049401038297881783, 19.05341960407617563, 37.29275706135232582 ) ) ;
#164718 = CARTESIAN_POINT ( 'NONE',  ( 21.55341960407610458, 5.719274019375980345, 108.9572429386476955 ) ) ;
#164719 = CARTESIAN_POINT ( 'NONE',  ( 9.474510206698729675, 16.51473224551082808, 47.08442372801900433 ) ) ;
#164720 = CARTESIAN_POINT ( 'NONE',  ( -16.46253265017146816, -9.564922557961047289, 49.16775706135233293 ) ) ;
#164721 = CARTESIAN_POINT ( 'NONE',  ( -0.05219959533934338120, 16.53943276465976808, 92.50109039468567573 ) ) ;
#164723 = EDGE_LOOP ( 'NONE', ( #40936, #118682, #195560, #134548 ) ) ;
#164722 = CARTESIAN_POINT ( 'NONE',  ( 2.649999999999999911, -105.0000000000000000, -15.00000000000000000 ) ) ;
#164724 = CARTESIAN_POINT ( 'NONE',  ( -0.05219959533909027116, -19.03943276465977164, 77.49890960531435269 ) ) ;
#164725 = CARTESIAN_POINT ( 'NONE',  ( -15.72974639402176322, -15.80617190586768395, 74.37609039468568994 ) ) ;
#164726 = CARTESIAN_POINT ( 'NONE',  ( 10.72451020669871369, 18.67979575497193778, 97.08442372801904696 ) ) ;
#164727 = CARTESIAN_POINT ( 'NONE',  ( 21.94965239947789826, -1.250870343808790031, -55.99511580764674790 ) ) ;
#164728 = CARTESIAN_POINT ( 'NONE',  ( 19.03943276465977164, -0.05219959533909143690, 93.74890960531435269 ) ) ;
#164729 = CARTESIAN_POINT ( 'NONE',  ( -5.823673210054431948, 21.52544592524334988, 67.70942372801901854 ) ) ;
#164730 = CARTESIAN_POINT ( 'NONE',  ( 19.02544592524334988, 5.153800228976608722, 96.45942372801897591 ) ) ;
#164731 = CARTESIAN_POINT ( 'NONE',  ( 0.05219959533909260263, 19.03943276465977164, 64.99890960531436690 ) ) ;
#164732 = CARTESIAN_POINT ( 'NONE',  ( -19.02544592524342804, 5.153800228976336051, 116.0405762719810383 ) ) ;
#164733 = CARTESIAN_POINT ( 'NONE',  ( 5.153800228976335163, 19.02544592524342804, 79.79057627198102409 ) ) ;
#164734 = LINE ( 'NONE', #129370, #91909 ) ;
#164735 = CARTESIAN_POINT ( 'NONE',  ( 19.03943276465977164, -0.05219959533909143690, 68.74890960531436690 ) ) ;
#164736 = CARTESIAN_POINT ( 'NONE',  ( 16.46253265017160672, -9.564922557960803928, 48.33224293864769550 ) ) ;
#164737 = CARTESIAN_POINT ( 'NONE',  ( 5.719274019375991003, -21.55341960407610458, 112.7072429386476955 ) ) ;
#164738 = CARTESIAN_POINT ( 'NONE',  ( 12.06949235617739724, 12.14591786802326823, 96.87609039468568994 ) ) ;
#164739 = CARTESIAN_POINT ( 'NONE',  ( -18.22780087662126647, -5.499999999999827693, 38.98236817873107185 ) ) ;
#164740 = CYLINDRICAL_SURFACE ( 'NONE', #191722, 5.000000000000000000 ) ;
#164741 = CARTESIAN_POINT ( 'NONE',  ( -9.474510206698720793, -16.51473224551083518, 54.58442372801899722 ) ) ;
#164742 = CARTESIAN_POINT ( 'NONE',  ( 5.049401038298161559, -19.05341960407611168, 82.70724293864770971 ) ) ;
#164743 = CARTESIAN_POINT ( 'NONE',  ( -0.05219959533910754901, -16.53943276465976808, 77.49890960531433848 ) ) ;
#164744 = CARTESIAN_POINT ( 'NONE',  ( 16.52544592524342804, -4.483927247898539470, 108.5405762719810241 ) ) ;
#164745 = CARTESIAN_POINT ( 'NONE',  ( 21.52544592524344225, -5.823673210054117533, 38.54057627198103120 ) ) ;
#164746 = CARTESIAN_POINT ( 'NONE',  ( 19.05341960407611168, 5.049401038298154454, 103.9572429386476671 ) ) ;
#164747 = CARTESIAN_POINT ( 'NONE',  ( 12.06949235617757843, -12.14591786802309237, 88.12390960531436690 ) ) ;
#164748 = CARTESIAN_POINT ( 'NONE',  ( 16.46253265017160672, -9.564922557960803928, 113.3322429386476955 ) ) ;
#164749 = CARTESIAN_POINT ( 'NONE',  ( -13.97604488694547697, 13.89961937509957934, 28.12609039468565797 ) ) ;
#164750 = CARTESIAN_POINT ( 'NONE',  ( 16.55341960407618274, -4.379528057220086978, 111.0427570613523613 ) ) ;
#164751 = CARTESIAN_POINT ( 'NONE',  ( -0.05219959533909027116, -19.03943276465977164, 92.49890960531436690 ) ) ;
#164752 = CARTESIAN_POINT ( 'NONE',  ( 5.719274019375673035, 21.55341960407619339, 47.29275706135234003 ) ) ;
#164753 = CARTESIAN_POINT ( 'NONE',  ( 0.05219959533907565091, 21.53943276465977519, 39.99890960531436690 ) ) ;
#164754 = CARTESIAN_POINT ( 'NONE',  ( 21.55341960407619695, -5.719274019375665929, 26.04275706135235779 ) ) ;
#164755 = CARTESIAN_POINT ( 'NONE',  ( 18.67979575497178502, 10.72451020669898547, 74.16557627198102409 ) ) ;
#164756 = CARTESIAN_POINT ( 'NONE',  ( -16.53943276465976808, 0.05219959533911058130, 91.24890960531436690 ) ) ;
#164757 = CARTESIAN_POINT ( 'NONE',  ( -0.05219959533936034679, 19.03943276465977164, 62.50109039468566863 ) ) ;
#164758 = CARTESIAN_POINT ( 'NONE',  ( 19.05341960407611168, 5.049401038298154454, 33.95724293864769550 ) ) ;
#164759 = CARTESIAN_POINT ( 'NONE',  ( -16.46253265017160317, 9.564922557960807481, 100.8322429386477097 ) ) ;
#164760 = CARTESIAN_POINT ( 'NONE',  ( 19.05341960407611168, 5.049401038298154454, 98.95724293864766707 ) ) ;
#164761 = CARTESIAN_POINT ( 'NONE',  ( 12.14591786802309770, 12.06949235617756955, 109.3739096053143811 ) ) ;
#164762 = CARTESIAN_POINT ( 'NONE',  ( 16.53943276465976808, -0.05219959533910856209, 33.74890960531436690 ) ) ;
#164763 = CARTESIAN_POINT ( 'NONE',  ( 0.05219959533934541429, -16.53943276465976808, 45.00109039468568284 ) ) ;
#164764 = CARTESIAN_POINT ( 'NONE',  ( 0.05219959533937995610, -21.53943276465977519, 110.0010903946856757 ) ) ;
#164766 = CARTESIAN_POINT ( 'NONE',  ( -16.53943276465976808, 0.05219959533911058130, 21.24890960531436690 ) ) ;
#164765 = CARTESIAN_POINT ( 'NONE',  ( -16.46253265017160317, 9.564922557960807481, 110.8322429386476955 ) ) ;
#164767 = CARTESIAN_POINT ( 'NONE',  ( 5.719274019375673035, 21.55341960407619339, 32.29275706135235424 ) ) ;
#164768 = CARTESIAN_POINT ( 'NONE',  ( -5.049401038298153566, 19.05341960407611168, 45.20724293864769550 ) ) ;
#164769 = CARTESIAN_POINT ( 'NONE',  ( -16.53943276465976808, -0.05219959533934237506, 48.75109039468568284 ) ) ;
#164770 = CARTESIAN_POINT ( 'NONE',  ( 14.34966873604972726, -8.224510206698740333, 105.8344237280190328 ) ) ;
#164771 = CARTESIAN_POINT ( 'NONE',  ( -4.379528057220086978, -16.55341960407618274, 94.79275706135234714 ) ) ;
#164772 = CARTESIAN_POINT ( 'NONE',  ( 9.564922557961047289, -16.46253265017146816, 110.4177570613523471 ) ) ;
#164773 = EDGE_CURVE ( 'NONE', #78133, #18983, #46129, .T. ) ;
#164774 = CARTESIAN_POINT ( 'NONE',  ( -5.049401038298153566, 19.05341960407611168, 40.20724293864768839 ) ) ;
#164775 = CARTESIAN_POINT ( 'NONE',  ( 12.14591786802309770, 12.06949235617756955, 94.37390960531436690 ) ) ;
#164776 = CARTESIAN_POINT ( 'NONE',  ( -10.81492255796078084, -18.62759615963271287, 102.0822429386476955 ) ) ;
#164777 = CARTESIAN_POINT ( 'NONE',  ( 5.049401038298161559, -19.05341960407611168, 37.70724293864768839 ) ) ;
#164778 = CARTESIAN_POINT ( 'NONE',  ( -9.564922557960796823, -16.46253265017161027, 107.0822429386476955 ) ) ;
#164779 = CARTESIAN_POINT ( 'NONE',  ( -5.719274019375665041, -21.55341960407619695, 29.79275706135234358 ) ) ;
#164780 = CARTESIAN_POINT ( 'NONE',  ( 3.678949249685231848, 1.601138781673192758E-19, 0.000000000000000000 ) ) ;
#164781 = CARTESIAN_POINT ( 'NONE',  ( 19.02544592524343514, -5.153800228976328945, 108.5405762719810383 ) ) ;
#164782 = CARTESIAN_POINT ( 'NONE',  ( 19.97888994334922685, -34.65319547504297759, -5.000000000000000000 ) ) ;
#164783 = CARTESIAN_POINT ( 'NONE',  ( -19.02544592524342804, 5.153800228976336051, 81.04057627198103830 ) ) ;
#164785 = CARTESIAN_POINT ( 'NONE',  ( -16.53943276465976808, 0.05219959533911058130, 86.24890960531436690 ) ) ;
#164784 = CARTESIAN_POINT ( 'NONE',  ( -21.55341960407619339, 5.719274019375674811, 28.54275706135234358 ) ) ;
#164786 = CARTESIAN_POINT ( 'NONE',  ( -13.89961937509977652, 13.97604488694528158, 100.6239096053143669 ) ) ;
#164787 = CARTESIAN_POINT ( 'NONE',  ( -27.96625882250065942, -7.271219613218503852, 160.9431592986335318 ) ) ;
#164788 = CARTESIAN_POINT ( 'NONE',  ( 12.14591786802327356, -12.06949235617739191, 60.62609039468567573 ) ) ;
#164789 = CARTESIAN_POINT ( 'NONE',  ( -5.719274019375665041, -21.55341960407619695, 74.79275706135234714 ) ) ;
#164790 = CARTESIAN_POINT ( 'NONE',  ( -12.06949235617739369, -12.14591786802326823, 44.37609039468567573 ) ) ;
#164791 = CARTESIAN_POINT ( 'NONE',  ( -19.05341960407611168, -5.049401038298163336, 81.45724293864769550 ) ) ;
#164792 = CARTESIAN_POINT ( 'NONE',  ( -19.03943276465977164, -0.05219959533935918106, 108.7510903946856615 ) ) ;
#164793 = CARTESIAN_POINT ( 'NONE',  ( -16.53943276465976808, -0.05219959533934237506, 63.75109039468568284 ) ) ;
#164794 = CARTESIAN_POINT ( 'NONE',  ( 19.02544592524334988, 5.153800228976608722, 21.45942372801899012 ) ) ;
#164795 = CARTESIAN_POINT ( 'NONE',  ( -9.564922557961040184, 16.46253265017147172, 87.91775706135233293 ) ) ;
#164796 = CARTESIAN_POINT ( 'NONE',  ( 9.564922557960805705, 16.46253265017160317, 64.58224293864769550 ) ) ;
#164797 = CARTESIAN_POINT ( 'NONE',  ( 15.72974639402199770, -15.80617190586745480, 88.12390960531436690 ) ) ;
#164799 = CARTESIAN_POINT ( 'NONE',  ( -5.153800228976607833, 19.02544592524334988, 87.70942372801897591 ) ) ;
#164798 = CARTESIAN_POINT ( 'NONE',  ( -4.483927247898539470, -16.52544592524342804, 87.29057627198103830 ) ) ;
#164800 = CARTESIAN_POINT ( 'NONE',  ( -14.29746914071037622, -8.314922557961029526, 64.16775706135234714 ) ) ;
#164801 = CARTESIAN_POINT ( 'NONE',  ( -19.36337904590693171, 5.499999999999953815, 80.41494137495621430 ) ) ;
#164802 = CARTESIAN_POINT ( 'NONE',  ( 9.474510206698729675, 16.51473224551082808, 62.08442372801899722 ) ) ;
#164803 = CARTESIAN_POINT ( 'NONE',  ( -14.34966873604960291, -8.224510206698953496, 26.66557627198103475 ) ) ;
#164804 = CARTESIAN_POINT ( 'NONE',  ( 16.52544592524342804, -4.483927247898539470, 78.54057627198103830 ) ) ;
#164806 = CARTESIAN_POINT ( 'NONE',  ( 18.22780087662122384, -5.500000000000022204, 46.01540105326107266 ) ) ;
#164805 = CARTESIAN_POINT ( 'NONE',  ( 9.564922557961047289, -16.46253265017146816, 25.41775706135234003 ) ) ;
#164807 = CARTESIAN_POINT ( 'NONE',  ( 5.823673210054444382, -21.52544592524334988, 30.20942372801902565 ) ) ;
#164808 = CARTESIAN_POINT ( 'NONE',  ( -16.51473224551069308, -9.474510206698971260, 96.66557627198102409 ) ) ;
#164809 = CARTESIAN_POINT ( 'NONE',  ( -19.02544592524342804, 5.153800228976336051, 81.04057627198103830 ) ) ;
#164810 = CARTESIAN_POINT ( 'NONE',  ( 18.67979575497194134, -10.72451020669871369, 90.83442372801901854 ) ) ;
#164811 = CARTESIAN_POINT ( 'NONE',  ( 13.97604488694527802, 13.89961937509977652, 79.37390960531435269 ) ) ;
#164812 = CARTESIAN_POINT ( 'NONE',  ( 10.72451020669898902, -18.67979575497178502, 32.91557627198102409 ) ) ;
#164813 = CARTESIAN_POINT ( 'NONE',  ( -12.06949235617756955, 12.14591786802309770, 85.62390960531436690 ) ) ;
#164814 = CARTESIAN_POINT ( 'NONE',  ( 19.02544592524343514, -5.153800228976328945, 48.54057627198103120 ) ) ;
#164815 = CARTESIAN_POINT ( 'NONE',  ( -12.14591786802309592, -12.06949235617757132, 96.87390960531436690 ) ) ;
#164816 = CARTESIAN_POINT ( 'NONE',  ( -15.72974639402197994, 15.80617190586746368, 105.6239096053143669 ) ) ;
#164817 = AXIS2_PLACEMENT_3D ( 'NONE', #121725, #46884, #124709 ) ;
#164818 = CARTESIAN_POINT ( 'NONE',  ( -10.72451020669870658, -18.67979575497194134, 64.58442372801900433 ) ) ;
#164819 = CARTESIAN_POINT ( 'NONE',  ( -9.564922557960796823, -16.46253265017161027, 27.08224293864769550 ) ) ;
#164820 = CARTESIAN_POINT ( 'NONE',  ( -14.29746914071037622, -8.314922557961029526, 64.16775706135234714 ) ) ;
#164821 = CARTESIAN_POINT ( 'NONE',  ( -15.80617190586745835, -15.72974639402198527, 101.8739096053143811 ) ) ;
#164822 = CARTESIAN_POINT ( 'NONE',  ( 10.72451020669898902, -18.67979575497178502, 112.9155762719810383 ) ) ;
#164824 = CARTESIAN_POINT ( 'NONE',  ( 0.05219959533909260263, 19.03943276465977164, 49.99890960531435979 ) ) ;
#164823 = CARTESIAN_POINT ( 'NONE',  ( -5.153800228976607833, 19.02544592524334988, 42.70942372801901143 ) ) ;
#164825 = CARTESIAN_POINT ( 'NONE',  ( 1.300000000000000044, 1.082531754730548856, -0.6250000000000003331 ) ) ;
#164826 = CARTESIAN_POINT ( 'NONE',  ( 10.81492255796106328, -18.62759615963255655, 55.41775706135234714 ) ) ;
#164827 = CARTESIAN_POINT ( 'NONE',  ( -0.05219959533907301413, -21.53943276465977519, 62.49890960531436690 ) ) ;
#164828 = CARTESIAN_POINT ( 'NONE',  ( 14.34966873604960469, 8.224510206698951720, 39.16557627198102409 ) ) ;
#164830 = CARTESIAN_POINT ( 'NONE',  ( 19.03943276465977164, 0.05219959533936151252, 21.25109039468565797 ) ) ;
#164829 = CARTESIAN_POINT ( 'NONE',  ( -15.80617190586768217, 15.72974639402176855, 73.12609039468567573 ) ) ;
#164831 = CARTESIAN_POINT ( 'NONE',  ( 16.53943276465976808, -0.05219959533910856209, 63.74890960531435979 ) ) ;
#164832 = CARTESIAN_POINT ( 'NONE',  ( -14.29746914071049879, 8.314922557960819915, 105.8322429386476955 ) ) ;
#164833 = CARTESIAN_POINT ( 'NONE',  ( 9.564922557961047289, -16.46253265017146816, 40.41775706135234003 ) ) ;
#164834 = CARTESIAN_POINT ( 'NONE',  ( 16.52544592524335698, 4.483927247898782831, 101.4594237280190185 ) ) ;
#164835 = CARTESIAN_POINT ( 'NONE',  ( -10.81492255796105439, 18.62759615963255655, 67.91775706135234714 ) ) ;
#164836 = CARTESIAN_POINT ( 'NONE',  ( 19.05341960407611168, 5.049401038298154454, 53.95724293864770260 ) ) ;
#164837 = CARTESIAN_POINT ( 'NONE',  ( -9.564922557961040184, 16.46253265017147172, 32.91775706135233293 ) ) ;
#164838 = CARTESIAN_POINT ( 'NONE',  ( 0.05219959533907565091, 21.53943276465977519, 44.99890960531435979 ) ) ;
#164839 = CARTESIAN_POINT ( 'NONE',  ( 18.67979575497194134, -10.72451020669871369, 25.83442372801901499 ) ) ;
#164840 = CARTESIAN_POINT ( 'NONE',  ( 21.53943276465977519, -0.05219959533907433946, 83.74890960531435269 ) ) ;
#164841 = CARTESIAN_POINT ( 'NONE',  ( -16.51473224551082808, 9.474510206698731452, 88.33442372801900433 ) ) ;
#164842 = CARTESIAN_POINT ( 'NONE',  ( -4.483927247898782831, 16.52544592524335698, 52.70942372801902565 ) ) ;
#164844 = CARTESIAN_POINT ( 'NONE',  ( 21.55341960407610458, 5.719274019375980345, 93.95724293864770971 ) ) ;
#164843 = CARTESIAN_POINT ( 'NONE',  ( -5.184702103851166477, 3.882744257519115560, -62.44399821614915425 ) ) ;
#164845 = CARTESIAN_POINT ( 'NONE',  ( 0.05219959533910956823, 16.53943276465976808, 79.99890960531435269 ) ) ;
#164846 = CARTESIAN_POINT ( 'NONE',  ( 17.60691670004651854, 5.500000000000061284, 41.63333313366439370 ) ) ;
#164847 = CARTESIAN_POINT ( 'NONE',  ( 8.314922557961029526, -14.29746914071037800, 25.41775706135235779 ) ) ;
#164848 = CARTESIAN_POINT ( 'NONE',  ( 18.67979575497178502, 10.72451020669898547, 34.16557627198102409 ) ) ;
#164849 = CARTESIAN_POINT ( 'NONE',  ( -0.05219959533934338120, 16.53943276465976808, 72.50109039468568994 ) ) ;
#164850 = CARTESIAN_POINT ( 'NONE',  ( -5.049401038298153566, 19.05341960407611168, 25.20724293864768484 ) ) ;
#164851 = CARTESIAN_POINT ( 'NONE',  ( -16.53943276465976808, -0.05219959533934237506, 53.75109039468568994 ) ) ;
#164852 = CARTESIAN_POINT ( 'NONE',  ( -10.81492255796105439, 18.62759615963255655, 22.91775706135235069 ) ) ;
#164853 = CARTESIAN_POINT ( 'NONE',  ( -21.53943276465977519, 0.05219959533907696930, 46.24890960531435979 ) ) ;
#164854 = CARTESIAN_POINT ( 'NONE',  ( -4.483927247898782831, 16.52544592524335698, 67.70942372801901854 ) ) ;
#164855 = CARTESIAN_POINT ( 'NONE',  ( -13.97604488694527625, -13.89961937509977652, 81.87390960531436690 ) ) ;
#164857 = CARTESIAN_POINT ( 'NONE',  ( -19.02544592524342804, 5.153800228976336051, 31.04057627198102409 ) ) ;
#164856 = CARTESIAN_POINT ( 'NONE',  ( 18.62759615963255655, 10.81492255796105972, 51.66775706135234714 ) ) ;
#164858 = CARTESIAN_POINT ( 'NONE',  ( 10.81492255796078972, 18.62759615963270932, 44.58224293864769550 ) ) ;
#164859 = CARTESIAN_POINT ( 'NONE',  ( 18.67979575497178502, 10.72451020669898547, 24.16557627198103120 ) ) ;
#164860 = ORIENTED_EDGE ( 'NONE', *, *, #192121, .T. ) ;
#164861 = CARTESIAN_POINT ( 'NONE',  ( -9.564922557961040184, 16.46253265017147172, 37.91775706135233293 ) ) ;
#164862 = CARTESIAN_POINT ( 'NONE',  ( 0.05219959533934541429, -16.53943276465976808, 50.00109039468568994 ) ) ;
#164863 = CARTESIAN_POINT ( 'NONE',  ( 9.474510206698971260, -16.51473224551069308, 112.9155762719810383 ) ) ;
#164864 = ORIENTED_EDGE ( 'NONE', *, *, #115833, .F. ) ;
#164865 = EDGE_CURVE ( 'NONE', #198671, #85061, #29325, .T. ) ;
#164866 = CARTESIAN_POINT ( 'NONE',  ( -13.89961937509977652, 13.97604488694528158, 90.62390960531432427 ) ) ;
#164867 = CARTESIAN_POINT ( 'NONE',  ( 8.314922557961029526, -14.29746914071037800, 100.4177570613523471 ) ) ;
#164868 = CARTESIAN_POINT ( 'NONE',  ( -18.22780087662122028, 5.500000000000031086, 93.51540105326107266 ) ) ;
#164869 = CARTESIAN_POINT ( 'NONE',  ( -16.55341960407611168, -4.379528057220339221, 101.4572429386476955 ) ) ;
#164870 = CARTESIAN_POINT ( 'NONE',  ( 10.81492255796078972, 18.62759615963270932, 44.58224293864769550 ) ) ;
#164871 = CARTESIAN_POINT ( 'NONE',  ( -9.474510206698964154, 16.51473224551069663, 35.41557627198102409 ) ) ;
#164872 = CARTESIAN_POINT ( 'NONE',  ( -4.379528057220086978, -16.55341960407618274, 79.79275706135236135 ) ) ;
#164873 = CARTESIAN_POINT ( 'NONE',  ( -18.62759615963270932, 10.81492255796079327, 115.8322429386477097 ) ) ;
#164874 = CARTESIAN_POINT ( 'NONE',  ( 19.03943276465977164, 0.05219959533936151252, 76.25109039468566152 ) ) ;
#164875 = CARTESIAN_POINT ( 'NONE',  ( 5.153800228976335163, 19.02544592524342804, 39.79057627198100988 ) ) ;
#164876 = CARTESIAN_POINT ( 'NONE',  ( -19.03943276465977164, 0.05219959533909376836, 106.2489096053143669 ) ) ;
#164877 = CARTESIAN_POINT ( 'NONE',  ( -18.67979575497193778, 10.72451020669871902, 103.3344237280190043 ) ) ;
#164878 = CARTESIAN_POINT ( 'NONE',  ( 16.51473224551069308, 9.474510206698969483, 64.16557627198102409 ) ) ;
#164879 = EDGE_CURVE ( 'NONE', #161202, #92863, #34321, .T. ) ;
#164880 = CARTESIAN_POINT ( 'NONE',  ( -4.483927247898782831, 16.52544592524335698, 52.70942372801902565 ) ) ;
#164881 = CARTESIAN_POINT ( 'NONE',  ( -21.52544592524334988, -5.823673210054445271, 88.95942372801901854 ) ) ;
#164882 = CARTESIAN_POINT ( 'NONE',  ( -16.51473224551082808, 9.474510206698731452, 53.33442372801900433 ) ) ;
#164883 = CARTESIAN_POINT ( 'NONE',  ( 0.05219959533936267826, -19.03943276465977164, 50.00109039468566863 ) ) ;
#164884 = ORIENTED_EDGE ( 'NONE', *, *, #1430, .T. ) ;
#164885 = CARTESIAN_POINT ( 'NONE',  ( 21.52544592524334988, 5.823673210054432836, 51.45942372801901854 ) ) ;
#164886 = AXIS2_PLACEMENT_3D ( 'NONE', #186511, #109638, #61143 ) ;
#164887 = DIRECTION ( 'NONE',  ( -1.000000000000000000, -0.000000000000000000, -3.709348145883536076E-20 ) ) ;
#164888 = CARTESIAN_POINT ( 'NONE',  ( -19.03943276465977164, -0.05219959533935918106, 43.75109039468566863 ) ) ;
#164889 = CARTESIAN_POINT ( 'NONE',  ( -19.02544592524342804, 5.153800228976336051, 106.0405762719810241 ) ) ;
#164890 = CARTESIAN_POINT ( 'NONE',  ( 19.03943276465977164, -0.05219959533909143690, 78.74890960531436690 ) ) ;
#164891 = CARTESIAN_POINT ( 'NONE',  ( 12.06949235617757843, -12.14591786802309237, 43.12390960531435269 ) ) ;
#164892 = CARTESIAN_POINT ( 'NONE',  ( 10.81492255796078972, 18.62759615963270932, 39.58224293864769550 ) ) ;
#164893 = CARTESIAN_POINT ( 'NONE',  ( 36.91746824999999177, 2.880721459617395097E-14, -4.124999997268813168 ) ) ;
#164894 = CARTESIAN_POINT ( 'NONE',  ( -18.22780087662122384, -5.500000000000025757, 96.48459894673894155 ) ) ;
#164895 = CARTESIAN_POINT ( 'NONE',  ( -10.81492255796105439, 18.62759615963255655, 107.9177570613523471 ) ) ;
#164896 = CARTESIAN_POINT ( 'NONE',  ( -27.77694149905213905, 7.633451960439542106, 161.4496143021112857 ) ) ;
#164897 = CARTESIAN_POINT ( 'NONE',  ( 19.02544592524343514, -5.153800228976328945, 43.54057627198103120 ) ) ;
#164898 = CARTESIAN_POINT ( 'NONE',  ( 0.05219959533909260263, 19.03943276465977164, 24.99890960531435269 ) ) ;
#164899 = CARTESIAN_POINT ( 'NONE',  ( -34.46475727851697002, -1.773375775694353562, 89.78131888620559664 ) ) ;
#164900 = DIRECTION ( 'NONE',  ( -0.000000000000000000, -0.7071067811865466846, -0.7071067811865484609 ) ) ;
#164901 = CARTESIAN_POINT ( 'NONE',  ( -16.53943276465976808, -0.05219959533934237506, 68.75109039468568994 ) ) ;
#164902 = CARTESIAN_POINT ( 'NONE',  ( 18.67979575497178502, 10.72451020669898547, 79.16557627198103830 ) ) ;
#164903 = CARTESIAN_POINT ( 'NONE',  ( -12.14591786802309592, -12.06949235617757132, 51.87390960531437401 ) ) ;
#164905 = CARTESIAN_POINT ( 'NONE',  ( 16.46253265017160672, -9.564922557960803928, 108.3322429386476955 ) ) ;
#164904 = CARTESIAN_POINT ( 'NONE',  ( -5.153800228976328057, -19.02544592524343514, 22.29057627198102765 ) ) ;
#164906 = CARTESIAN_POINT ( 'NONE',  ( -18.62759615963255300, -10.81492255796106328, 24.16775706135235424 ) ) ;
#164907 = CARTESIAN_POINT ( 'NONE',  ( -0.05219959533936034679, 19.03943276465977164, 32.50109039468566863 ) ) ;
#164908 = CARTESIAN_POINT ( 'NONE',  ( -0.05219959533909027116, -19.03943276465977164, 27.49890960531435624 ) ) ;
#164909 = CARTESIAN_POINT ( 'NONE',  ( -18.67979575497193778, 10.72451020669871902, 83.33442372801903275 ) ) ;
#164910 = LINE ( 'NONE', #26404, #143376 ) ;
#164911 = CARTESIAN_POINT ( 'NONE',  ( -14.34966873604960291, -8.224510206698953496, 26.66557627198103475 ) ) ;
#164912 = CARTESIAN_POINT ( 'NONE',  ( 17.50000000000001066, 3.850315288878835229, 113.2337086939655677 ) ) ;
#164913 = CARTESIAN_POINT ( 'NONE',  ( -10.81492255796078084, -18.62759615963271287, 42.08224293864769550 ) ) ;
#164914 = CARTESIAN_POINT ( 'NONE',  ( 16.52544592524342804, -4.483927247898539470, 98.54057627198105251 ) ) ;
#164915 = CARTESIAN_POINT ( 'NONE',  ( -5.070555798855037821, -6.850306330133427934, -64.08177057783885289 ) ) ;
#164916 = CARTESIAN_POINT ( 'NONE',  ( -0.05219959533909027116, -19.03943276465977164, 92.49890960531436690 ) ) ;
#164917 = CARTESIAN_POINT ( 'NONE',  ( -0.05219959533910754901, -16.53943276465976808, 92.49890960531436690 ) ) ;
#164918 = CARTESIAN_POINT ( 'NONE',  ( 19.02544592524334988, 5.153800228976608722, 101.4594237280189759 ) ) ;
#164919 = CARTESIAN_POINT ( 'NONE',  ( -18.67979575497178146, -10.72451020669898902, 66.66557627198102409 ) ) ;
#164920 = ORIENTED_EDGE ( 'NONE', *, *, #169778, .F. ) ;
#164921 = CARTESIAN_POINT ( 'NONE',  ( 9.474510206698971260, -16.51473224551069308, 32.91557627198102409 ) ) ;
#164922 = B_SPLINE_CURVE_WITH_KNOTS ( 'NONE', 3,
 ( #8696, #179564, #116860, #21862, #192714, #70366 ),
 .UNSPECIFIED., .F., .F.,
 ( 4, 2, 4 ),
 ( 0.003239945802372221333, 0.003620412082092075261, 0.004000878361811928755 ),
 .UNSPECIFIED. ) ;
#164924 = CARTESIAN_POINT ( 'NONE',  ( -15.80617190586745835, -15.72974639402198527, 91.87390960531436690 ) ) ;
#164923 = CARTESIAN_POINT ( 'NONE',  ( -9.564922557960796823, -16.46253265017161027, 92.08224293864769550 ) ) ;
#164926 = CARTESIAN_POINT ( 'NONE',  ( -5.153800228976328057, -19.02544592524343514, 87.29057627198103830 ) ) ;
#164925 = CARTESIAN_POINT ( 'NONE',  ( -12.14591786802326823, 12.06949235617739902, 103.1260903946856757 ) ) ;
#164927 = CARTESIAN_POINT ( 'NONE',  ( 9.474510206698729675, 16.51473224551082808, 82.08442372801899012 ) ) ;
#164928 = CARTESIAN_POINT ( 'NONE',  ( 10.81492255796106328, -18.62759615963255655, 100.4177570613523471 ) ) ;
#164929 = CARTESIAN_POINT ( 'NONE',  ( 0.05219959533907565091, 21.53943276465977519, 69.99890960531435269 ) ) ;
#164930 = CARTESIAN_POINT ( 'NONE',  ( -5.823673210054116645, -21.52544592524344225, 42.29057627198103120 ) ) ;
#164931 = CARTESIAN_POINT ( 'NONE',  ( -16.51473224551069308, -9.474510206698971260, 46.66557627198102409 ) ) ;
#164932 = CARTESIAN_POINT ( 'NONE',  ( 4.483927247898790824, -16.52544592524335698, 110.2094237280190185 ) ) ;
#164933 = CARTESIAN_POINT ( 'NONE',  ( 19.03943276465977164, -0.05219959533909143690, 68.74890960531436690 ) ) ;
#164934 = ORIENTED_EDGE ( 'NONE', *, *, #16286, .T. ) ;
#164935 = CARTESIAN_POINT ( 'NONE',  ( -32.33375351741885595, -3.966103829525452262, 88.62974963220463565 ) ) ;
#164936 = CARTESIAN_POINT ( 'NONE',  ( 13.97604488694548053, -13.89961937509957401, 30.62609039468566863 ) ) ;
#164937 = CARTESIAN_POINT ( 'NONE',  ( 4.379528057220339221, -16.55341960407611168, 67.70724293864769550 ) ) ;
#164938 = CARTESIAN_POINT ( 'NONE',  ( -21.55341960407619339, 5.719274019375674811, 28.54275706135234358 ) ) ;
#164939 = CARTESIAN_POINT ( 'NONE',  ( 1.784210473542230573E-15, -29.16686587814331588, 141.8750000027311842 ) ) ;
#164940 = CARTESIAN_POINT ( 'NONE',  ( 18.67979575497178502, 10.72451020669898547, 64.16557627198102409 ) ) ;
#164941 = CARTESIAN_POINT ( 'NONE',  ( 16.52544592524335698, 4.483927247898782831, 96.45942372801901854 ) ) ;
#164942 = CARTESIAN_POINT ( 'NONE',  ( 14.29746914071049879, -8.314922557960816363, 103.3322429386476955 ) ) ;
#164943 = CARTESIAN_POINT ( 'NONE',  ( 16.46253265017160672, -9.564922557960803928, 68.33224293864770971 ) ) ;
#164944 = CARTESIAN_POINT ( 'NONE',  ( -16.52544592524342804, 4.483927247898546575, 36.04057627198102409 ) ) ;
#164945 = CARTESIAN_POINT ( 'NONE',  ( 5.719274019375673035, 21.55341960407619339, 42.29275706135235424 ) ) ;
#164946 = CARTESIAN_POINT ( 'NONE',  ( 16.46253265017160672, -9.564922557960803928, 108.3322429386476955 ) ) ;
#164947 = CARTESIAN_POINT ( 'NONE',  ( 18.67979575497194134, -10.72451020669871369, 75.83442372801900433 ) ) ;
#164948 = CARTESIAN_POINT ( 'NONE',  ( 16.51473224551069308, 9.474510206698969483, 29.16557627198103475 ) ) ;
#164949 = CARTESIAN_POINT ( 'NONE',  ( 13.89961937509977652, -13.97604488694527269, 43.12390960531434558 ) ) ;
#164950 = ORIENTED_EDGE ( 'NONE', *, *, #125615, .T. ) ;
#164951 = CARTESIAN_POINT ( 'NONE',  ( 21.53943276465977519, 0.05219959533937863772, 91.25109039468568994 ) ) ;
#164952 = CARTESIAN_POINT ( 'NONE',  ( -16.55341960407617563, 4.379528057220093196, 48.54275706135234714 ) ) ;
#164953 = CARTESIAN_POINT ( 'NONE',  ( -21.55341960407619339, 5.719274019375674811, 73.54275706135234714 ) ) ;
#164954 = CARTESIAN_POINT ( 'NONE',  ( 9.474510206698971260, -16.51473224551069308, 97.91557627198102409 ) ) ;
#164955 = CARTESIAN_POINT ( 'NONE',  ( -16.46253265017146816, -9.564922557961047289, 84.16775706135233293 ) ) ;
#164956 = CARTESIAN_POINT ( 'NONE',  ( 21.53943276465977519, 0.05219959533937863772, 56.25109039468568284 ) ) ;
#164957 = CARTESIAN_POINT ( 'NONE',  ( -8.314922557961024197, 14.29746914071037800, 27.91775706135234358 ) ) ;
#164958 = CARTESIAN_POINT ( 'NONE',  ( 19.03943276465977164, 0.05219959533936151252, 91.25109039468566152 ) ) ;
#164959 = CARTESIAN_POINT ( 'NONE',  ( -9.474510206698964154, 16.51473224551069663, 45.41557627198103120 ) ) ;
#164960 = CARTESIAN_POINT ( 'NONE',  ( 5.049401038297881783, 19.05341960407617563, 92.29275706135234714 ) ) ;
#164961 = CARTESIAN_POINT ( 'NONE',  ( -16.55341960407611168, -4.379528057220339221, 21.45724293864769550 ) ) ;
#164962 = CARTESIAN_POINT ( 'NONE',  ( -9.474510206698720793, -16.51473224551083518, 84.58442372801900433 ) ) ;
#164963 = CARTESIAN_POINT ( 'NONE',  ( 8.224510206698953496, -14.34966873604960469, 42.91557627198103120 ) ) ;
#164964 = CARTESIAN_POINT ( 'NONE',  ( -0.05219959533936034679, 19.03943276465977164, 62.50109039468566863 ) ) ;
#164965 = CARTESIAN_POINT ( 'NONE',  ( -16.52544592524335698, -4.483927247898792601, 53.95942372801900433 ) ) ;
#164966 = CARTESIAN_POINT ( 'NONE',  ( 19.05341960407617918, -5.049401038297876454, 26.04275706135233293 ) ) ;
#164967 = CARTESIAN_POINT ( 'NONE',  ( -9.564922557960796823, -16.46253265017161027, 27.08224293864769550 ) ) ;
#164968 = CARTESIAN_POINT ( 'NONE',  ( 13.89961937509977652, -13.97604488694527269, 38.12390960531436690 ) ) ;
#164969 = CARTESIAN_POINT ( 'NONE',  ( 12.06949235617739724, 12.14591786802326823, 41.87609039468568284 ) ) ;
#164970 = DIRECTION ( 'NONE',  ( -3.491481338843133355E-15, 0.000000000000000000, 1.000000000000000000 ) ) ;
#164971 = CARTESIAN_POINT ( 'NONE',  ( -8.906447517083053711, -27.41122689804191026, 142.6500000054623740 ) ) ;
#164972 = CARTESIAN_POINT ( 'NONE',  ( -5.153800228976328057, -19.02544592524343514, 92.29057627198099567 ) ) ;
#164973 = EDGE_CURVE ( 'NONE', #71610, #94299, #137676, .T. ) ;
#164974 = CARTESIAN_POINT ( 'NONE',  ( -17.97058386085788584, -5.499999999999976019, 69.00390968646215129 ) ) ;
#164975 = CARTESIAN_POINT ( 'NONE',  ( -13.97604488694547697, 13.89961937509957934, 98.12609039468566152 ) ) ;
#164976 = CARTESIAN_POINT ( 'NONE',  ( 0.05219959533907565091, 21.53943276465977519, 29.99890960531435979 ) ) ;
#164978 = CARTESIAN_POINT ( 'NONE',  ( 13.89961937509957401, 13.97604488694547697, 111.8760903946856757 ) ) ;
#164977 = CARTESIAN_POINT ( 'NONE',  ( 19.02544592524334988, 5.153800228976608722, 36.45942372801900433 ) ) ;
#164979 = CARTESIAN_POINT ( 'NONE',  ( 14.34966873604960469, 8.224510206698951720, 114.1655762719810383 ) ) ;
#164980 = CARTESIAN_POINT ( 'NONE',  ( -5.049401038298153566, 19.05341960407611168, 35.20724293864768839 ) ) ;
#164981 = CARTESIAN_POINT ( 'NONE',  ( 15.80617190586746368, 15.72974639402197994, 74.37390960531436690 ) ) ;
#164982 = CARTESIAN_POINT ( 'NONE',  ( 9.474510206698971260, -16.51473224551069308, 42.91557627198103120 ) ) ;
#164983 = CARTESIAN_POINT ( 'NONE',  ( 11.30153831258470731, -180.0000000000000000, 0.000000000000000000 ) ) ;
#164984 = CARTESIAN_POINT ( 'NONE',  ( 16.51473224551083163, -9.474510206698727899, 75.83442372801900433 ) ) ;
#164985 = CARTESIAN_POINT ( 'NONE',  ( -0.05219959533910754901, -16.53943276465976808, 57.49890960531435979 ) ) ;
#164986 = CARTESIAN_POINT ( 'NONE',  ( 15.80617190586746368, 15.72974639402197994, 39.37390960531436690 ) ) ;
#164987 = CARTESIAN_POINT ( 'NONE',  ( -21.53943276465977519, -0.05219959533937600094, 93.75109039468567573 ) ) ;
#164988 = EDGE_CURVE ( 'NONE', #171657, #188443, #53370, .T. ) ;
#164989 = CARTESIAN_POINT ( 'NONE',  ( 5.719274019375991003, -21.55341960407610458, 77.70724293864770971 ) ) ;
#164990 = CARTESIAN_POINT ( 'NONE',  ( -15.72974639402176322, -15.80617190586768395, 74.37609039468568994 ) ) ;
#164991 = CARTESIAN_POINT ( 'NONE',  ( -5.719274019375665041, -21.55341960407619695, 69.79275706135234714 ) ) ;
#164992 = CARTESIAN_POINT ( 'NONE',  ( 16.46253265017160672, -9.564922557960803928, 98.33224293864769550 ) ) ;
#164994 = CARTESIAN_POINT ( 'NONE',  ( -0.05219959533937732626, 21.53943276465977519, 67.50109039468568994 ) ) ;
#164993 = CARTESIAN_POINT ( 'NONE',  ( -14.29746914071037622, -8.314922557961029526, 89.16775706135236135 ) ) ;
#164995 = CARTESIAN_POINT ( 'NONE',  ( -16.51473224551069308, -9.474510206698971260, 51.66557627198102409 ) ) ;
#164996 = CARTESIAN_POINT ( 'NONE',  ( -21.52544592524334988, -5.823673210054445271, 28.95942372801902209 ) ) ;
#164997 = CARTESIAN_POINT ( 'NONE',  ( -5.049401038298153566, 19.05341960407611168, 70.20724293864769550 ) ) ;
#164998 = CARTESIAN_POINT ( 'NONE',  ( -8.314922557960811034, -14.29746914071050412, 67.08224293864770971 ) ) ;
#164999 = CARTESIAN_POINT ( 'NONE',  ( -4.379528057220328563, 16.55341960407611168, 50.20724293864769550 ) ) ;
#165000 = CARTESIAN_POINT ( 'NONE',  ( -21.52544592524343514, 5.823673210054127303, 56.04057627198102409 ) ) ;
#165001 = CARTESIAN_POINT ( 'NONE',  ( -9.564922557960796823, -16.46253265017161027, 42.08224293864769550 ) ) ;
#165002 = CARTESIAN_POINT ( 'NONE',  ( -21.53943276465977519, 0.05219959533907696930, 56.24890960531436690 ) ) ;
#165003 = CARTESIAN_POINT ( 'NONE',  ( 5.049401038297881783, 19.05341960407617563, 57.29275706135231871 ) ) ;
#165005 = CARTESIAN_POINT ( 'NONE',  ( 12.06949235617757843, -12.14591786802309237, 68.12390960531436690 ) ) ;
#165004 = DIRECTION ( 'NONE',  ( 1.000000000000000000, 0.000000000000000000, 0.000000000000000000 ) ) ;
#165006 = CARTESIAN_POINT ( 'NONE',  ( 15.80617190586746368, 15.72974639402197994, 34.37390960531435979 ) ) ;
#165007 = VERTEX_POINT ( 'NONE', #8879 ) ;
#165008 = CARTESIAN_POINT ( 'NONE',  ( -3.573655867282028392E-15, 2.428612866367529932E-14, -15.00000000000000000 ) ) ;
#165009 = CARTESIAN_POINT ( 'NONE',  ( -12.06949235617739369, -12.14591786802326823, 84.37609039468570415 ) ) ;
#165010 = CARTESIAN_POINT ( 'NONE',  ( 5.049401038297881783, 19.05341960407617563, 92.29275706135234714 ) ) ;
#165011 = CARTESIAN_POINT ( 'NONE',  ( 16.53943276465976808, -0.05219959533910856209, 53.74890960531437401 ) ) ;
#165012 = CARTESIAN_POINT ( 'NONE',  ( -18.56399227203345959, -5.499999999999827693, 58.97830131249904184 ) ) ;
#165013 = CARTESIAN_POINT ( 'NONE',  ( 13.89961937509977652, -13.97604488694527269, 53.12390960531434558 ) ) ;
#165014 = CARTESIAN_POINT ( 'NONE',  ( -14.29746914071049879, 8.314922557960819915, 45.83224293864769550 ) ) ;
#165015 = EDGE_CURVE ( 'NONE', #159131, #174271, #59721, .T. ) ;
#165016 = CARTESIAN_POINT ( 'NONE',  ( 5.049401038298161559, -19.05341960407611168, 77.70724293864765286 ) ) ;
#165017 = CARTESIAN_POINT ( 'NONE',  ( -19.05341960407611168, -5.049401038298163336, 46.45724293864768129 ) ) ;
#165018 = CARTESIAN_POINT ( 'NONE',  ( -21.53943276465977519, -0.05219959533937600094, 53.75109039468568994 ) ) ;
#165019 = CARTESIAN_POINT ( 'NONE',  ( 16.46253265017160672, -9.564922557960803928, 73.33224293864769550 ) ) ;
#165020 = CARTESIAN_POINT ( 'NONE',  ( 16.46253265017160672, -9.564922557960803928, 33.33224293864770260 ) ) ;
#165021 = CARTESIAN_POINT ( 'NONE',  ( -19.03943276465977164, 0.05219959533909376836, 56.24890960531435979 ) ) ;
#165022 = CARTESIAN_POINT ( 'NONE',  ( 5.823673210054125526, 21.52544592524343514, 54.79057627198104541 ) ) ;
#165023 = CARTESIAN_POINT ( 'NONE',  ( -5.153800228976328057, -19.02544592524343514, 32.29057627198102409 ) ) ;
#165024 = CARTESIAN_POINT ( 'NONE',  ( -15.72974639402197994, 15.80617190586746368, 35.62390960531437401 ) ) ;
#165025 = CARTESIAN_POINT ( 'NONE',  ( -14.29746914071037622, -8.314922557961029526, 109.1677570613523613 ) ) ;
#165026 = CARTESIAN_POINT ( 'NONE',  ( -5.823673210054431948, 21.52544592524334988, 112.7094237280190328 ) ) ;
#165028 = CARTESIAN_POINT ( 'NONE',  ( 14.34966873604972726, -8.224510206698740333, 75.83442372801900433 ) ) ;
#165027 = CARTESIAN_POINT ( 'NONE',  ( 12.14591786802327356, -12.06949235617739191, 40.62609039468567573 ) ) ;
#165029 = CARTESIAN_POINT ( 'NONE',  ( 4.962140900324507164, 6.180203150055796790, 6.568406857878971827 ) ) ;
#165030 = CARTESIAN_POINT ( 'NONE',  ( 12.14591786802327356, -12.06949235617739191, 65.62609039468568994 ) ) ;
#165031 = CARTESIAN_POINT ( 'NONE',  ( -14.34966873604972548, 8.224510206698743886, 58.33442372801901143 ) ) ;
#165032 = CARTESIAN_POINT ( 'NONE',  ( -16.51473224551069308, -9.474510206698971260, 111.6655762719810383 ) ) ;
#165033 = CARTESIAN_POINT ( 'NONE',  ( 13.97604488694527802, 13.89961937509977652, 29.37390960531435979 ) ) ;
#165034 = CARTESIAN_POINT ( 'NONE',  ( -4.379528057220086978, -16.55341960407618274, 39.79275706135235424 ) ) ;
#165035 = CARTESIAN_POINT ( 'NONE',  ( -13.97604488694527625, -13.89961937509977652, 36.87390960531436690 ) ) ;
#165036 = CARTESIAN_POINT ( 'NONE',  ( 18.67979575497194134, -10.72451020669871369, 30.83442372801902209 ) ) ;
#165037 = CARTESIAN_POINT ( 'NONE',  ( 14.29746914071037800, 8.314922557961029526, 36.66775706135234714 ) ) ;
#165038 = CARTESIAN_POINT ( 'NONE',  ( -8.224510206698735004, -14.34966873604973081, 99.58442372801900433 ) ) ;
#165039 = CARTESIAN_POINT ( 'NONE',  ( 2.973862142520697471, -93.04182470242777470, -15.00000000000000178 ) ) ;
#165040 = CARTESIAN_POINT ( 'NONE',  ( -10.72451020669870658, -18.67979575497194134, 104.5844237280190185 ) ) ;
#165041 = CARTESIAN_POINT ( 'NONE',  ( -19.02544592524334988, -5.153800228976617603, 98.95942372801900433 ) ) ;
#165042 = CARTESIAN_POINT ( 'NONE',  ( -14.29746914071049879, 8.314922557960819915, 50.83224293864770971 ) ) ;
#165043 = CARTESIAN_POINT ( 'NONE',  ( -9.564922557960796823, -16.46253265017161027, 27.08224293864769550 ) ) ;
#165045 = CARTESIAN_POINT ( 'NONE',  ( 16.19135201231366139, 7.376712067591951083, 77.68680854052031748 ) ) ;
#165044 = CARTESIAN_POINT ( 'NONE',  ( 5.153800228976615827, -19.02544592524334988, 60.20942372801899012 ) ) ;
#165046 = CARTESIAN_POINT ( 'NONE',  ( -10.72451020669870658, -18.67979575497194134, 69.58442372801900433 ) ) ;
#165047 = CARTESIAN_POINT ( 'NONE',  ( -8.224510206698735004, -14.34966873604973081, 24.58442372801901499 ) ) ;
#165048 = CARTESIAN_POINT ( 'NONE',  ( 17.05587630539785593, 6.762274262135716363, 81.75819690962686082 ) ) ;
#165049 = CARTESIAN_POINT ( 'NONE',  ( -15.72974639402197994, 15.80617190586746368, 25.62390960531435624 ) ) ;
#165050 = CARTESIAN_POINT ( 'NONE',  ( -5.153800228976607833, 19.02544592524334988, 107.7094237280189759 ) ) ;
#165051 = CARTESIAN_POINT ( 'NONE',  ( 5.153800228976335163, 19.02544592524342804, 114.7905762719810241 ) ) ;
#165052 = CARTESIAN_POINT ( 'NONE',  ( -24.42783677680704102, 12.30119602009721014, 169.8172178118632587 ) ) ;
#165053 = CARTESIAN_POINT ( 'NONE',  ( 16.51473224551069308, 9.474510206698969483, 29.16557627198103475 ) ) ;
#165054 = CARTESIAN_POINT ( 'NONE',  ( 21.52544592524334988, 5.823673210054432836, 101.4594237280190185 ) ) ;
#165055 = CARTESIAN_POINT ( 'NONE',  ( 13.89961937509977652, -13.97604488694527269, 48.12390960531435979 ) ) ;
#165056 = CARTESIAN_POINT ( 'NONE',  ( -5.823673210054431948, 21.52544592524334988, 52.70942372801902565 ) ) ;
#165057 = CARTESIAN_POINT ( 'NONE',  ( -5.823673210054431948, 21.52544592524334988, 107.7094237280190328 ) ) ;
#165058 = CARTESIAN_POINT ( 'NONE',  ( -16.55341960407617563, 4.379528057220093196, 98.54275706135234714 ) ) ;
#165059 = CARTESIAN_POINT ( 'NONE',  ( -0.05219959533909027116, -19.03943276465977164, 72.49890960531435269 ) ) ;
#165060 = CARTESIAN_POINT ( 'NONE',  ( -18.62759615963255300, -10.81492255796106328, 59.16775706135234714 ) ) ;
#165061 = CARTESIAN_POINT ( 'NONE',  ( 18.67979575497194134, -10.72451020669871369, 55.83442372801901854 ) ) ;
#165063 = CARTESIAN_POINT ( 'NONE',  ( 19.05341960407611168, 5.049401038298154454, 88.95724293864769550 ) ) ;
#165062 = CARTESIAN_POINT ( 'NONE',  ( -19.05341960407617563, 5.049401038297882671, 83.54275706135233293 ) ) ;
#165064 = CARTESIAN_POINT ( 'NONE',  ( -9.564922557960796823, -16.46253265017161027, 27.08224293864769550 ) ) ;
#165065 = CARTESIAN_POINT ( 'NONE',  ( -0.05219959533907301413, -21.53943276465977519, 97.49890960531436690 ) ) ;
#165066 = CARTESIAN_POINT ( 'NONE',  ( -9.564922557961040184, 16.46253265017147172, 27.91775706135232582 ) ) ;
#165067 = CARTESIAN_POINT ( 'NONE',  ( 0.05219959533910956823, 16.53943276465976808, 99.99890960531436690 ) ) ;
#165068 = CARTESIAN_POINT ( 'NONE',  ( -19.05341960407611168, -5.049401038298163336, 51.45724293864770260 ) ) ;
#165069 = CARTESIAN_POINT ( 'NONE',  ( -19.05341960407617563, 5.049401038297882671, 78.54275706135233293 ) ) ;
#165070 = CARTESIAN_POINT ( 'NONE',  ( -0.05219959533910754901, -16.53943276465976808, 47.49890960531435979 ) ) ;
#165071 = CARTESIAN_POINT ( 'NONE',  ( 15.80617190586769283, -15.72974639402175789, 105.6260903946856899 ) ) ;
#165072 = CARTESIAN_POINT ( 'NONE',  ( -13.89961937509977652, 13.97604488694528158, 105.6239096053143527 ) ) ;
#165073 = CARTESIAN_POINT ( 'NONE',  ( 9.564922557961047289, -16.46253265017146816, 70.41775706135233293 ) ) ;
#165074 = CARTESIAN_POINT ( 'NONE',  ( 5.719274019375991003, -21.55341960407610458, 72.70724293864769550 ) ) ;
#165075 = CARTESIAN_POINT ( 'NONE',  ( -0.05219959533937732626, 21.53943276465977519, 32.50109039468568284 ) ) ;
#165076 = CARTESIAN_POINT ( 'NONE',  ( 16.55341960407618274, -4.379528057220086978, 36.04275706135234714 ) ) ;
#165077 = CARTESIAN_POINT ( 'NONE',  ( 12.06949235617739724, 12.14591786802326823, 91.87609039468568994 ) ) ;
#165079 = CARTESIAN_POINT ( 'NONE',  ( 18.67979575497194134, -10.72451020669871369, 40.83442372801901854 ) ) ;
#165078 = CARTESIAN_POINT ( 'NONE',  ( -16.46253265017160317, 9.564922557960807481, 30.83224293864769550 ) ) ;
#165080 = CARTESIAN_POINT ( 'NONE',  ( -15.72974639402197994, 15.80617190586746368, 40.62390960531435269 ) ) ;
#165081 = CARTESIAN_POINT ( 'NONE',  ( -9.564922557960796823, -16.46253265017161027, 22.08224293864768839 ) ) ;
#165082 = CARTESIAN_POINT ( 'NONE',  ( -22.81625015709509441, -31.40387420917324590, -2.824999997268812901 ) ) ;
#165083 = CARTESIAN_POINT ( 'NONE',  ( 8.224510206698742110, 14.34966873604972548, 62.08442372801901143 ) ) ;
#165084 = CARTESIAN_POINT ( 'NONE',  ( -12.14591786802309592, -12.06949235617757132, 96.87390960531436690 ) ) ;
#165085 = CARTESIAN_POINT ( 'NONE',  ( 0.05219959533907565091, 21.53943276465977519, 84.99890960531436690 ) ) ;
#165086 = CARTESIAN_POINT ( 'NONE',  ( -4.483927247898782831, 16.52544592524335698, 112.7094237280190328 ) ) ;
#165087 = CARTESIAN_POINT ( 'NONE',  ( 4.483927247898790824, -16.52544592524335698, 50.20942372801901854 ) ) ;
#165088 = CARTESIAN_POINT ( 'NONE',  ( -16.46253265017160317, 9.564922557960807481, 60.83224293864769550 ) ) ;
#165089 = CARTESIAN_POINT ( 'NONE',  ( 12.14591786802327356, -12.06949235617739191, 95.62609039468568994 ) ) ;
#165090 = CARTESIAN_POINT ( 'NONE',  ( 9.564922557961047289, -16.46253265017146816, 85.41775706135233293 ) ) ;
#165091 = CARTESIAN_POINT ( 'NONE',  ( 15.80617190586746368, 15.72974639402197994, 84.37390960531438111 ) ) ;
#165092 = CARTESIAN_POINT ( 'NONE',  ( 8.314922557960818139, 14.29746914071049879, 24.58224293864768839 ) ) ;
#165093 = ORIENTED_EDGE ( 'NONE', *, *, #126396, .F. ) ;
#165094 = CARTESIAN_POINT ( 'NONE',  ( 25.85392304583292145, 7.514126903508385524, 173.7688241862488212 ) ) ;
#165095 =( BOUNDED_SURFACE ( )  B_SPLINE_SURFACE ( 1, 2, ( 
 ( #177266, #93674, #36714, #128723, #160074, #142899, #192421, #35731, #4381, #21561, #82209, #193422, #114560, #112568, #158083, #66066, #7377, #115578, #37728, #100395, #19575, #22568, #97378, #99390, #51896, #189434, #127732, #81218, #161073, #50910, #174263, #38737, #84214, #162073, #145894, #190420, #129712, #68058, #69062, #113555, #143900, #131740, #83221, #108846, #144896, #159064, #20558, #70072, #6378, #130729, #53903, #32016, #191409, #5382, #67065, #52885, #23569, #85217, #8397, #133736, #72062, #9405, #101384, #163077, #120543, #24580, #132737, #102403, #134751, #167069, #42735, #43721, #73079, #136710, #71071, #26576, #194425, #74069, #166079, #147919, #58877, #89220, #57903, #27582, #54897, #86229, #116571, #55895, #117568, #75044, #87233, #196433, #103404, #11410, #39721, #179269, #40733, #90207, #119575, #104397, #164090 ),
 ( #181258, #13380, #195430, #10405, #151890, #150913, #12407, #25589, #56906, #148916, #118580, #135740, #178260, #149903, #180270, #197411, #41740, #165082, #28570, #88219, #182236, #105382, #106366, #169023, #17349, #109348, #172023, #33512, #31524, #44711, #184217, #152868, #95171, #45699, #171030, #156859, #93177, #78008, #107350, #80009, #91179, #62838, #61840, #18354, #154862, #138691, #123510, #198391, #32521, #94173, #139675, #79005, #16360, #59868, #14363, #155852, #30528, #76028, #153865, #63851, #1163, #140679, #124522, #186217, #172, #47698, #2171, #48689, #15363, #168049, #92181, #125522, #187219, #110342, #121535, #137703, #183230, #29546, #199388, #60852, #77019, #122527, #185203, #46694, #108355, #170034, #52654, #34507, #145658, #176019, #144660, #114317, #141678, #49674, #3169, #188202, #142668, #161834, #174025, #21326, #190182 ) ),
 .UNSPECIFIED., .F., .F., .F. ) 
 B_SPLINE_SURFACE_WITH_KNOTS ( ( 2, 2 ),
 ( 3, 2, 2, 2, 2, 2, 2, 2, 2, 2, 2, 2, 2, 2, 2, 2, 2, 2, 2, 2, 2, 2, 2, 2, 2, 2, 2, 2, 2, 2, 2, 2, 2, 2, 2, 2, 2, 2, 2, 2, 2, 2, 2, 2, 2, 2, 2, 2, 2, 2, 3 ),
 ( 0.000000000000000000, 1.000000000000000000 ),
 ( 0.000000000000000000, 0.02000000000000000042, 0.04000000000000000083, 0.05999999999999999778, 0.08000000000000000167, 0.1000000000000000056, 0.1199999999999999956, 0.1400000000000000133, 0.1600000000000000033, 0.1799999999999999933, 0.2000000000000000111, 0.2200000000000000011, 0.2399999999999999911, 0.2600000000000000089, 0.2800000000000000266, 0.2999999999999999889, 0.3200000000000000067, 0.3400000000000000244, 0.3599999999999999867, 0.3800000000000000044, 0.4000000000000000222, 0.4199999999999999845, 0.4400000000000000022, 0.4600000000000000200, 0.4799999999999999822, 0.5000000000000000000, 0.5200000000000000178, 0.5400000000000000355, 0.5600000000000000533, 0.5799999999999999600, 0.5999999999999999778, 0.6199999999999999956, 0.6400000000000000133, 0.6600000000000000311, 0.6800000000000000488, 0.6999999999999999556, 0.7199999999999999734, 0.7399999999999999911, 0.7600000000000000089, 0.7800000000000000266, 0.8000000000000000444, 0.8199999999999999512, 0.8399999999999999689, 0.8599999999999999867, 0.8800000000000000044, 0.9000000000000000222, 0.9200000000000000400, 0.9399999999999999467, 0.9599999999999999645, 0.9799999999999999822, 1.000000000000000000 ),
 .UNSPECIFIED. ) 
 GEOMETRIC_REPRESENTATION_ITEM ( )  RATIONAL_B_SPLINE_SURFACE ( (
 ( 1.000000000000000000, 0.9510565162951535312, 1.000000000000000000, 0.9510565162951535312, 1.000000000000000000, 0.9510565162951535312, 1.000000000000000000, 0.9510565162951535312, 1.000000000000000000, 0.9510565162951535312, 1.000000000000000000, 0.9510565162951535312, 1.000000000000000000, 0.9510565162951535312, 1.000000000000000000, 0.9510565162951535312, 1.000000000000000000, 0.9510565162951535312, 1.000000000000000000, 0.9510565162951535312, 1.000000000000000000, 0.9510565162951535312, 1.000000000000000000, 0.9510565162951535312, 1.000000000000000000, 0.9510565162951535312, 1.000000000000000000, 0.9510565162951535312, 1.000000000000000000, 0.9510565162951535312, 1.000000000000000000, 0.9510565162951535312, 1.000000000000000000, 0.9510565162951535312, 1.000000000000000000, 0.9510565162951535312, 1.000000000000000000, 0.9510565162951535312, 1.000000000000000000, 0.9510565162951535312, 1.000000000000000000, 0.9510565162951535312, 1.000000000000000000, 0.9510565162951535312, 1.000000000000000000, 0.9510565162951535312, 1.000000000000000000, 0.9510565162951535312, 1.000000000000000000, 0.9510565162951535312, 1.000000000000000000, 0.9510565162951535312, 1.000000000000000000, 0.9510565162951535312, 1.000000000000000000, 0.9510565162951535312, 1.000000000000000000, 0.9510565162951535312, 1.000000000000000000, 0.9510565162951535312, 1.000000000000000000, 0.9510565162951535312, 1.000000000000000000, 0.9510565162951535312, 1.000000000000000000, 0.9510565162951535312, 1.000000000000000000, 0.9510565162951535312, 1.000000000000000000, 0.9510565162951535312, 1.000000000000000000, 0.9510565162951535312, 1.000000000000000000, 0.9510565162951535312, 1.000000000000000000, 0.9510565162951535312, 1.000000000000000000, 0.9510565162951535312, 1.000000000000000000, 0.9510565162951535312, 1.000000000000000000, 0.9510565162951535312, 1.000000000000000000, 0.9510565162951535312, 1.000000000000000000, 0.9510565162951535312, 1.000000000000000000, 0.9510565162951535312, 1.000000000000000000, 0.9510565162951535312, 1.000000000000000000, 0.9510565162951535312, 1.000000000000000000, 0.9510565162951535312, 1.000000000000000000, 0.9510565162951535312, 1.000000000000000000, 0.9510565162951535312, 1.000000000000000000, 0.9510565162951535312, 1.000000000000000000),
 ( 1.000000000000000000, 0.9510565162951535312, 1.000000000000000000, 0.9510565162951535312, 1.000000000000000000, 0.9510565162951535312, 1.000000000000000000, 0.9510565162951535312, 1.000000000000000000, 0.9510565162951535312, 1.000000000000000000, 0.9510565162951535312, 1.000000000000000000, 0.9510565162951535312, 1.000000000000000000, 0.9510565162951535312, 1.000000000000000000, 0.9510565162951535312, 1.000000000000000000, 0.9510565162951535312, 1.000000000000000000, 0.9510565162951535312, 1.000000000000000000, 0.9510565162951535312, 1.000000000000000000, 0.9510565162951535312, 1.000000000000000000, 0.9510565162951535312, 1.000000000000000000, 0.9510565162951535312, 1.000000000000000000, 0.9510565162951535312, 1.000000000000000000, 0.9510565162951535312, 1.000000000000000000, 0.9510565162951535312, 1.000000000000000000, 0.9510565162951535312, 1.000000000000000000, 0.9510565162951535312, 1.000000000000000000, 0.9510565162951535312, 1.000000000000000000, 0.9510565162951535312, 1.000000000000000000, 0.9510565162951535312, 1.000000000000000000, 0.9510565162951535312, 1.000000000000000000, 0.9510565162951535312, 1.000000000000000000, 0.9510565162951535312, 1.000000000000000000, 0.9510565162951535312, 1.000000000000000000, 0.9510565162951535312, 1.000000000000000000, 0.9510565162951535312, 1.000000000000000000, 0.9510565162951535312, 1.000000000000000000, 0.9510565162951535312, 1.000000000000000000, 0.9510565162951535312, 1.000000000000000000, 0.9510565162951535312, 1.000000000000000000, 0.9510565162951535312, 1.000000000000000000, 0.9510565162951535312, 1.000000000000000000, 0.9510565162951535312, 1.000000000000000000, 0.9510565162951535312, 1.000000000000000000, 0.9510565162951535312, 1.000000000000000000, 0.9510565162951535312, 1.000000000000000000, 0.9510565162951535312, 1.000000000000000000, 0.9510565162951535312, 1.000000000000000000, 0.9510565162951535312, 1.000000000000000000, 0.9510565162951535312, 1.000000000000000000, 0.9510565162951535312, 1.000000000000000000, 0.9510565162951535312, 1.000000000000000000, 0.9510565162951535312, 1.000000000000000000, 0.9510565162951535312, 1.000000000000000000, 0.9510565162951535312, 1.000000000000000000, 0.9510565162951535312, 1.000000000000000000, 0.9510565162951535312, 1.000000000000000000) ) ) 
 REPRESENTATION_ITEM ( '' )  SURFACE ( )  );
#165096 = CARTESIAN_POINT ( 'NONE',  ( 15.72974639402199770, -15.80617190586745480, 63.12390960531435979 ) ) ;
#165097 = CARTESIAN_POINT ( 'NONE',  ( 12.06949235617739724, 12.14591786802326823, 91.87609039468568994 ) ) ;
#165098 = ORIENTED_EDGE ( 'NONE', *, *, #119454, .F. ) ;
#165099 = CARTESIAN_POINT ( 'NONE',  ( -21.52544592524343514, 5.823673210054127303, 36.04057627198102409 ) ) ;
#165100 = CARTESIAN_POINT ( 'NONE',  ( 18.56101223717332971, 5.499999999999949374, 88.94978406935679516 ) ) ;
#165101 = CARTESIAN_POINT ( 'NONE',  ( 10.81492255796078972, 18.62759615963270932, 89.58224293864768129 ) ) ;
#165102 = CARTESIAN_POINT ( 'NONE',  ( 16.53943276465976808, 0.05219959533934440121, 111.2510903946856899 ) ) ;
#165103 = CARTESIAN_POINT ( 'NONE',  ( 12.06949235617739724, 12.14591786802326823, 31.87609039468567929 ) ) ;
#165104 = CARTESIAN_POINT ( 'NONE',  ( 19.03943276465977164, -0.05219959533909143690, 28.74890960531435624 ) ) ;
#165105 = CARTESIAN_POINT ( 'NONE',  ( -4.379528057220086978, -16.55341960407618274, 34.79275706135235424 ) ) ;
#165106 = CARTESIAN_POINT ( 'NONE',  ( 5.153800228976335163, 19.02544592524342804, 49.79057627198100988 ) ) ;
#165107 = CARTESIAN_POINT ( 'NONE',  ( 22.44159573604009239, 16.30477369853692693, 140.5750000027311728 ) ) ;
#165108 = CARTESIAN_POINT ( 'NONE',  ( 9.474510206698971260, -16.51473224551069308, 107.9155762719810383 ) ) ;
#165109 = CARTESIAN_POINT ( 'NONE',  ( 9.474510206698971260, -16.51473224551069308, 112.9155762719810383 ) ) ;
#165110 = ADVANCED_FACE ( 'NONE', ( #36850 ), #35864, .T. ) ;
#165111 = CARTESIAN_POINT ( 'NONE',  ( -12.14591786802326823, 12.06949235617739902, 108.1260903946856757 ) ) ;
#165112 = CARTESIAN_POINT ( 'NONE',  ( -19.03943276465977164, -0.05219959533935918106, 98.75109039468567573 ) ) ;
#165113 = CARTESIAN_POINT ( 'NONE',  ( -19.03943276465977164, -0.05219959533935918106, 43.75109039468566863 ) ) ;
#165114 = CARTESIAN_POINT ( 'NONE',  ( 5.719274019375991003, -21.55341960407610458, 72.70724293864769550 ) ) ;
#165115 = CARTESIAN_POINT ( 'NONE',  ( -8.224510206698735004, -14.34966873604973081, 99.58442372801900433 ) ) ;
#165116 = CARTESIAN_POINT ( 'NONE',  ( 10.72451020669898902, -18.67979575497178502, 27.91557627198103830 ) ) ;
#165117 = CARTESIAN_POINT ( 'NONE',  ( -5.153800228976607833, 19.02544592524334988, 102.7094237280189759 ) ) ;
#165118 = CARTESIAN_POINT ( 'NONE',  ( 19.05341960407611168, 5.049401038298154454, 108.9572429386477097 ) ) ;
#165119 = CARTESIAN_POINT ( 'NONE',  ( -10.81492255796105439, 18.62759615963255655, 57.91775706135234714 ) ) ;
#165120 = CARTESIAN_POINT ( 'NONE',  ( -19.05341960407611168, -5.049401038298163336, 66.45724293864769550 ) ) ;
#165121 = CARTESIAN_POINT ( 'NONE',  ( 4.483927247898545687, 16.52544592524342804, 99.79057627198103830 ) ) ;
#165122 = LINE ( 'NONE', #92222, #166990 ) ;
#165123 = CARTESIAN_POINT ( 'NONE',  ( -14.29746914071049879, 8.314922557960819915, 75.83224293864769550 ) ) ;
#165124 = CARTESIAN_POINT ( 'NONE',  ( 15.72974639402199770, -15.80617190586745480, 78.12390960531436690 ) ) ;
#165125 = VERTEX_POINT ( 'NONE', #145030 ) ;
#165126 = CARTESIAN_POINT ( 'NONE',  ( 19.05341960407617918, -5.049401038297876454, 96.04275706135231871 ) ) ;
#165127 = DIRECTION ( 'NONE',  ( -0.4999999999999967248, 0.5000000000000019984, 0.7071067811865484609 ) ) ;
#165128 = CARTESIAN_POINT ( 'NONE',  ( -5.049401038298153566, 19.05341960407611168, 60.20724293864768129 ) ) ;
#165129 = CARTESIAN_POINT ( 'NONE',  ( 16.52216118717250026, -7.221426719304218089, 71.42400978952970547 ) ) ;
#165131 = CARTESIAN_POINT ( 'NONE',  ( 19.02544592524343514, -5.153800228976328945, 83.54057627198100988 ) ) ;
#165130 = CARTESIAN_POINT ( 'NONE',  ( 16.46253265017160672, -9.564922557960803928, 83.33224293864768129 ) ) ;
#165132 = CARTESIAN_POINT ( 'NONE',  ( -16.53943276465976808, -0.05219959533934237506, 58.75109039468568994 ) ) ;
#165133 = CARTESIAN_POINT ( 'NONE',  ( -16.29526858892876717, -7.335722546919996034, 50.79670597800200937 ) ) ;
#165134 = CARTESIAN_POINT ( 'NONE',  ( 9.474510206698729675, 16.51473224551082808, 37.08442372801899722 ) ) ;
#165135 = CARTESIAN_POINT ( 'NONE',  ( 16.52479559737576764, -14.65015464700936576, -58.35289975817769914 ) ) ;
#165136 = CARTESIAN_POINT ( 'NONE',  ( -9.564922557960796823, -16.46253265017161027, 107.0822429386476955 ) ) ;
#165137 = CARTESIAN_POINT ( 'NONE',  ( -12.14591786802326823, 12.06949235617739902, 103.1260903946856757 ) ) ;
#165138 = EDGE_CURVE ( 'NONE', #147212, #148543, #189351, .T. ) ;
#165139 = CARTESIAN_POINT ( 'NONE',  ( -34.61318912441601015, -7.252276964307558416, 43.02678305251433244 ) ) ;
#165140 = CARTESIAN_POINT ( 'NONE',  ( 16.52544592524335698, 4.483927247898782831, 91.45942372801901854 ) ) ;
#165141 = CARTESIAN_POINT ( 'NONE',  ( -16.18388926212241685, 7.379444403734382263, 29.56046848633847901 ) ) ;
#165142 = CARTESIAN_POINT ( 'NONE',  ( 12.06949235617739724, 12.14591786802326823, 66.87609039468568994 ) ) ;
#165143 = PLANE ( 'NONE',  #169261 ) ;
#165144 = CARTESIAN_POINT ( 'NONE',  ( 21.52544592524334988, 5.823673210054432836, 66.45942372801903275 ) ) ;
#165145 = CARTESIAN_POINT ( 'NONE',  ( 19.02544592524334988, 5.153800228976608722, 91.45942372801900433 ) ) ;
#165146 = CARTESIAN_POINT ( 'NONE',  ( 16.51473224551083163, -9.474510206698727899, 30.83442372801900433 ) ) ;
#165147 = CARTESIAN_POINT ( 'NONE',  ( -5.153800228976328057, -19.02544592524343514, 67.29057627198102409 ) ) ;
#165148 = CARTESIAN_POINT ( 'NONE',  ( 19.02544592524343514, -5.153800228976328945, 48.54057627198103120 ) ) ;
#165149 = CARTESIAN_POINT ( 'NONE',  ( 16.82725176010342949, -7.001296733591735766, 23.13668599133183079 ) ) ;
#165150 = CARTESIAN_POINT ( 'NONE',  ( -5.719274019375978568, 21.55341960407610458, 80.20724293864769550 ) ) ;
#165151 = CARTESIAN_POINT ( 'NONE',  ( -5.719274019375978568, 21.55341960407610458, 35.20724293864768839 ) ) ;
#165152 = CARTESIAN_POINT ( 'NONE',  ( 19.05341960407611168, 5.049401038298154454, 28.95724293864769550 ) ) ;
#165153 = CARTESIAN_POINT ( 'NONE',  ( 14.34966873604972726, -8.224510206698740333, 50.83442372801901143 ) ) ;
#165154 = ORIENTED_EDGE ( 'NONE', *, *, #150678, .F. ) ;
#165155 = CARTESIAN_POINT ( 'NONE',  ( 21.52544592524334988, 5.823673210054432836, 31.45942372801901854 ) ) ;
#165157 = CARTESIAN_POINT ( 'NONE',  ( -6.020228577223754586E-15, 39.95556452105416412, -0.4999999999999999445 ) ) ;
#165156 = CARTESIAN_POINT ( 'NONE',  ( -16.55341960407611168, -4.379528057220339221, 51.45724293864770260 ) ) ;
#165158 = CARTESIAN_POINT ( 'NONE',  ( 4.483927247898790824, -16.52544592524335698, 30.20942372801902565 ) ) ;
#165159 = CARTESIAN_POINT ( 'NONE',  ( -16.51473224551082808, 9.474510206698731452, 33.33442372801899722 ) ) ;
#165160 = CARTESIAN_POINT ( 'NONE',  ( -8.314922557960811034, -14.29746914071050412, 52.08224293864768839 ) ) ;
#165161 = CARTESIAN_POINT ( 'NONE',  ( -10.81492255796078084, -18.62759615963271287, 112.0822429386477097 ) ) ;
#165163 = CARTESIAN_POINT ( 'NONE',  ( 21.55341960407610458, 5.719274019375980345, 73.95724293864769550 ) ) ;
#165162 = DIRECTION ( 'NONE',  ( 1.000000000000000000, -0.000000000000000000, -0.000000000000000000 ) ) ;
#165164 = CARTESIAN_POINT ( 'NONE',  ( 9.474510206698971260, -16.51473224551069308, 87.91557627198102409 ) ) ;
#165165 = CARTESIAN_POINT ( 'NONE',  ( -14.34966873604960291, -8.224510206698953496, 61.66557627198103120 ) ) ;
#165166 = CARTESIAN_POINT ( 'NONE',  ( 19.05341960407611168, 5.049401038298154454, 108.9572429386477097 ) ) ;
#165167 = CARTESIAN_POINT ( 'NONE',  ( -37.24189295061466254, 4.138848244557342682, 41.36027101465353439 ) ) ;
#165168 = CARTESIAN_POINT ( 'NONE',  ( 5.049401038297881783, 19.05341960407617563, 62.29275706135234003 ) ) ;
#165169 = CARTESIAN_POINT ( 'NONE',  ( -10.81492255796078084, -18.62759615963271287, 107.0822429386476955 ) ) ;
#165170 = CARTESIAN_POINT ( 'NONE',  ( -13.97604488694527625, -13.89961937509977652, 51.87390960531436690 ) ) ;
#165171 = CARTESIAN_POINT ( 'NONE',  ( 13.97604488694548053, -13.89961937509957401, 45.62609039468566863 ) ) ;
#165172 = CARTESIAN_POINT ( 'NONE',  ( 8.224510206698953496, -14.34966873604960469, 112.9155762719810383 ) ) ;
#165173 = CARTESIAN_POINT ( 'NONE',  ( -15.80617190586768217, 15.72974639402176855, 68.12609039468567573 ) ) ;
#165174 = CARTESIAN_POINT ( 'NONE',  ( -16.38665767535051998, -7.295008042176176488, 69.73599135785454450 ) ) ;
#165175 = CARTESIAN_POINT ( 'NONE',  ( -4.379528057220328563, 16.55341960407611168, 35.20724293864768839 ) ) ;
#165176 = CARTESIAN_POINT ( 'NONE',  ( 5.049401038298161559, -19.05341960407611168, 52.70724293864767418 ) ) ;
#165177 = CARTESIAN_POINT ( 'NONE',  ( -5.823673210054116645, -21.52544592524344225, 72.29057627198102409 ) ) ;
#165178 = CARTESIAN_POINT ( 'NONE',  ( -22.44159573604010305, 16.30477369853692338, 142.6750000027311671 ) ) ;
#165179 = CARTESIAN_POINT ( 'NONE',  ( -19.03943276465977164, 0.05219959533909376836, 51.24890960531436690 ) ) ;
#165180 = VERTEX_POINT ( 'NONE', #49061 ) ;
#165181 = CARTESIAN_POINT ( 'NONE',  ( -21.55341960407610458, -5.719274019375992779, 66.45724293864768129 ) ) ;
#165182 = CARTESIAN_POINT ( 'NONE',  ( 21.52544592524334988, 5.823673210054432836, 91.45942372801901854 ) ) ;
#165185 = CARTESIAN_POINT ( 'NONE',  ( 12.06949235617757843, -12.14591786802309237, 83.12390960531436690 ) ) ;
#165184 = CARTESIAN_POINT ( 'NONE',  ( 14.34966873604972726, -8.224510206698740333, 100.8344237280190185 ) ) ;
#165183 = CARTESIAN_POINT ( 'NONE',  ( 7.282160400439392944, -46.44936954762798109, -22.53643251332693254 ) ) ;
#165186 = CARTESIAN_POINT ( 'NONE',  ( 5.153800228976335163, 19.02544592524342804, 64.79057627198100988 ) ) ;
#165187 = VERTEX_POINT ( 'NONE', #34873 ) ;
#165188 = CARTESIAN_POINT ( 'NONE',  ( 19.05341960407617918, -5.049401038297876454, 46.04275706135233293 ) ) ;
#165189 = CARTESIAN_POINT ( 'NONE',  ( -16.53943276465976808, -0.05219959533934237506, 88.75109039468567573 ) ) ;
#165190 = CARTESIAN_POINT ( 'NONE',  ( -5.823673210054431948, 21.52544592524334988, 107.7094237280190328 ) ) ;
#165191 = CARTESIAN_POINT ( 'NONE',  ( -19.03943276465977164, 0.05219959533909376836, 91.24890960531436690 ) ) ;
#165192 = CARTESIAN_POINT ( 'NONE',  ( 15.72974639402199770, -15.80617190586745480, 48.12390960531436690 ) ) ;
#165193 = CARTESIAN_POINT ( 'NONE',  ( 193.3062444957835453, -155.7167183371837496, -15.00000000000000000 ) ) ;
#165194 = CARTESIAN_POINT ( 'NONE',  ( -15.72974639402176322, -15.80617190586768395, 99.37609039468568994 ) ) ;
#165195 = CARTESIAN_POINT ( 'NONE',  ( -4.379528057220086978, -16.55341960407618274, 64.79275706135234714 ) ) ;
#165196 = CARTESIAN_POINT ( 'NONE',  ( 15.80617190586746368, 15.72974639402197994, 114.3739096053143527 ) ) ;
#165197 = CARTESIAN_POINT ( 'NONE',  ( 12.14591786802327356, -12.06949235617739191, 35.62609039468568994 ) ) ;
#165198 = CARTESIAN_POINT ( 'NONE',  ( 19.02544592524343514, -5.153800228976328945, 93.54057627198102409 ) ) ;
#165199 = CARTESIAN_POINT ( 'NONE',  ( -9.564922557960796823, -16.46253265017161027, 37.08224293864768839 ) ) ;
#165200 = CARTESIAN_POINT ( 'NONE',  ( 5.153800228976335163, 19.02544592524342804, 49.79057627198100988 ) ) ;
#165201 = CARTESIAN_POINT ( 'NONE',  ( -14.29746914071037622, -8.314922557961029526, 39.16775706135235424 ) ) ;
#165202 = CARTESIAN_POINT ( 'NONE',  ( 12.06949235617757843, -12.14591786802309237, 78.12390960531436690 ) ) ;
#165203 = CARTESIAN_POINT ( 'NONE',  ( -16.55341960407617563, 4.379528057220093196, 103.5427570613523613 ) ) ;
#165206 = CARTESIAN_POINT ( 'NONE',  ( -5.049401038298153566, 19.05341960407611168, 50.20724293864770260 ) ) ;
#165205 = CARTESIAN_POINT ( 'NONE',  ( 5.153800228976335163, 19.02544592524342804, 64.79057627198100988 ) ) ;
#165204 = CARTESIAN_POINT ( 'NONE',  ( -5.823673210054431948, 21.52544592524334988, 47.70942372801902565 ) ) ;
#165207 = CARTESIAN_POINT ( 'NONE',  ( 16.51473224551069308, 9.474510206698969483, 89.16557627198103830 ) ) ;
#165208 = CARTESIAN_POINT ( 'NONE',  ( -16.55341960407611168, -4.379528057220339221, 36.45724293864768839 ) ) ;
#165209 = CARTESIAN_POINT ( 'NONE',  ( 14.29746914071037800, 8.314922557961029526, 96.66775706135234714 ) ) ;
#165210 = VERTEX_POINT ( 'NONE', #33887 ) ;
#165211 = CARTESIAN_POINT ( 'NONE',  ( 19.02544592524334988, 5.153800228976608722, 26.45942372801899722 ) ) ;
#165212 = CARTESIAN_POINT ( 'NONE',  ( -19.03943276465977164, 0.05219959533909376836, 106.2489096053143669 ) ) ;
#165213 = EDGE_CURVE ( 'NONE', #123757, #132572, #21700, .T. ) ;
#165214 = CARTESIAN_POINT ( 'NONE',  ( 19.05341960407611168, 5.049401038298154454, 48.95724293864768129 ) ) ;
#165215 = CARTESIAN_POINT ( 'NONE',  ( 19.02544592524334988, 5.153800228976608722, 26.45942372801899722 ) ) ;
#165216 = CARTESIAN_POINT ( 'NONE',  ( 11.40812507854755253, -35.11059874428192273, -4.024999997268814411 ) ) ;
#165217 = CARTESIAN_POINT ( 'NONE',  ( -14.29746914071037622, -8.314922557961029526, 44.16775706135234714 ) ) ;
#165219 = CARTESIAN_POINT ( 'NONE',  ( -8.224510206698735004, -14.34966873604973081, 49.58442372801901143 ) ) ;
#165218 = CARTESIAN_POINT ( 'NONE',  ( 9.474510206698729675, 16.51473224551082808, 67.08442372801900433 ) ) ;
#165220 = CARTESIAN_POINT ( 'NONE',  ( 6.442614714193029890, -4.311334843530821637, -64.24190475577076143 ) ) ;
#165221 = CARTESIAN_POINT ( 'NONE',  ( 9.474510206698971260, -16.51473224551069308, 72.91557627198102409 ) ) ;
#165222 = CARTESIAN_POINT ( 'NONE',  ( -10.72451020669898014, 18.67979575497178502, 110.4155762719810383 ) ) ;
#165223 = CARTESIAN_POINT ( 'NONE',  ( 9.564922557961047289, -16.46253265017146816, 65.41775706135233293 ) ) ;
#165225 = CARTESIAN_POINT ( 'NONE',  ( -0.05219959533909027116, -19.03943276465977164, 32.49890960531435979 ) ) ;
#165224 = CARTESIAN_POINT ( 'NONE',  ( 5.049401038298161559, -19.05341960407611168, 102.7072429386476955 ) ) ;
#165226 = CARTESIAN_POINT ( 'NONE',  ( -19.02544592524342804, 5.153800228976336051, 71.04057627198099567 ) ) ;
#165228 = CARTESIAN_POINT ( 'NONE',  ( 9.474510206698971260, -16.51473224551069308, 37.91557627198102409 ) ) ;
#165227 = CARTESIAN_POINT ( 'NONE',  ( 4.483927247898545687, 16.52544592524342804, 34.79057627198103120 ) ) ;
#165229 = CARTESIAN_POINT ( 'NONE',  ( -13.89961937509957401, -13.97604488694547875, 34.37609039468566863 ) ) ;
#165230 = CARTESIAN_POINT ( 'NONE',  ( -16.53943276465976808, 0.05219959533911058130, 76.24890960531435269 ) ) ;
#165231 = CARTESIAN_POINT ( 'NONE',  ( 21.52544592524334988, 5.823673210054432836, 111.4594237280190328 ) ) ;
#165232 = CARTESIAN_POINT ( 'NONE',  ( -19.03943276465977164, 0.05219959533909376836, 56.24890960531435979 ) ) ;
#165233 = CARTESIAN_POINT ( 'NONE',  ( -21.53943276465977519, 0.05219959533907696930, 51.24890960531436690 ) ) ;
#165235 = CARTESIAN_POINT ( 'NONE',  ( -10.81492255796105439, 18.62759615963255655, 97.91775706135236135 ) ) ;
#165234 = CARTESIAN_POINT ( 'NONE',  ( 0.05219959533910956823, 16.53943276465976808, 49.99890960531437401 ) ) ;
#165236 = CARTESIAN_POINT ( 'NONE',  ( -16.51473224551069308, -9.474510206698971260, 96.66557627198102409 ) ) ;
#165237 = CARTESIAN_POINT ( 'NONE',  ( 13.89961937509977652, -13.97604488694527269, 103.1239096053143527 ) ) ;
#165238 = CARTESIAN_POINT ( 'NONE',  ( -19.03943276465977164, 0.05219959533909376836, 46.24890960531435979 ) ) ;
#165239 = CARTESIAN_POINT ( 'NONE',  ( -19.02544592524342804, 5.153800228976336051, 26.04057627198103120 ) ) ;
#165240 = CARTESIAN_POINT ( 'NONE',  ( -12.14591786802309592, -12.06949235617757132, 86.87390960531438111 ) ) ;
#165241 = CARTESIAN_POINT ( 'NONE',  ( -21.55341960407610458, -5.719274019375992779, 96.45724293864770971 ) ) ;
#165242 = CARTESIAN_POINT ( 'NONE',  ( -5.153800228976328057, -19.02544592524343514, 87.29057627198103830 ) ) ;
#165243 = CARTESIAN_POINT ( 'NONE',  ( -15.72974639402197994, 15.80617190586746368, 95.62390960531436690 ) ) ;
#165244 = CARTESIAN_POINT ( 'NONE',  ( 9.564922557960805705, 16.46253265017160317, 94.58224293864769550 ) ) ;
#165246 = CARTESIAN_POINT ( 'NONE',  ( -14.29746914071049879, 8.314922557960819915, 105.8322429386476955 ) ) ;
#165245 = DIRECTION ( 'NONE',  ( -1.000000000000000000, -0.000000000000000000, -0.000000000000000000 ) ) ;
#165247 = CARTESIAN_POINT ( 'NONE',  ( 5.049401038298161559, -19.05341960407611168, 67.70724293864769550 ) ) ;
#165248 = CARTESIAN_POINT ( 'NONE',  ( 21.53943276465977519, -0.05219959533907433946, 73.74890960531433848 ) ) ;
#165249 = CARTESIAN_POINT ( 'NONE',  ( -32.45668260148361384, 3.101559039593200673, 88.16695215365973581 ) ) ;
#165250 = CARTESIAN_POINT ( 'NONE',  ( -20.48593134815242323, -11.15862823513540825, 168.1084560298344854 ) ) ;
#165252 = CARTESIAN_POINT ( 'NONE',  ( 19.25663599770060941, -5.499999999999441336, 66.49419308057197497 ) ) ;
#165251 = CARTESIAN_POINT ( 'NONE',  ( -10.81492255796078084, -18.62759615963271287, 32.08224293864769550 ) ) ;
#165253 = CARTESIAN_POINT ( 'NONE',  ( 0.05219959533934541429, -16.53943276465976808, 30.00109039468568284 ) ) ;
#165254 = CARTESIAN_POINT ( 'NONE',  ( -14.34966873604960291, -8.224510206698953496, 91.66557627198103830 ) ) ;
#165255 = CARTESIAN_POINT ( 'NONE',  ( -17.44279575226823198, -5.990770900252464060, 94.16442432485685288 ) ) ;
#165256 = CARTESIAN_POINT ( 'NONE',  ( 19.03943276465977164, -0.05219959533909143690, 93.74890960531435269 ) ) ;
#165257 = CARTESIAN_POINT ( 'NONE',  ( -16.46253265017160317, 9.564922557960807481, 40.83224293864769550 ) ) ;
#165258 = CARTESIAN_POINT ( 'NONE',  ( 14.29746914071049879, -8.314922557960816363, 78.33224293864770971 ) ) ;
#165259 = CARTESIAN_POINT ( 'NONE',  ( 21.52544592524344225, -5.823673210054117533, 38.54057627198103120 ) ) ;
#165260 = CARTESIAN_POINT ( 'NONE',  ( 14.34966873604960469, 8.224510206698951720, 49.16557627198102409 ) ) ;
#165261 = CARTESIAN_POINT ( 'NONE',  ( -0.05219959533936034679, 19.03943276465977164, 97.50109039468567573 ) ) ;
#165262 = CARTESIAN_POINT ( 'NONE',  ( -15.72974639402176322, -15.80617190586768395, 64.37609039468568994 ) ) ;
#165263 = CARTESIAN_POINT ( 'NONE',  ( -8.571926809382601320, -26.38167802310801591, 147.2750000027311899 ) ) ;
#165264 = CARTESIAN_POINT ( 'NONE',  ( -0.05219959533909027116, -19.03943276465977164, 97.49890960531436690 ) ) ;
#165265 = CARTESIAN_POINT ( 'NONE',  ( -16.55341960407617563, 4.379528057220093196, 88.54275706135236135 ) ) ;
#165266 = CARTESIAN_POINT ( 'NONE',  ( -0.05219959533909027116, -19.03943276465977164, 27.49890960531435624 ) ) ;
#165267 = CARTESIAN_POINT ( 'NONE',  ( -9.474510206698964154, 16.51473224551069663, 75.41557627198103830 ) ) ;
#165268 = CARTESIAN_POINT ( 'NONE',  ( 0.05219959533907565091, 21.53943276465977519, 74.99890960531435269 ) ) ;
#165269 = CARTESIAN_POINT ( 'NONE',  ( -13.89961937509957401, -13.97604488694547875, 109.3760903946856331 ) ) ;
#165271 = CARTESIAN_POINT ( 'NONE',  ( 15.80617190586769283, -15.72974639402175789, 55.62609039468568284 ) ) ;
#165270 = CARTESIAN_POINT ( 'NONE',  ( 14.29746914071049879, -8.314922557960816363, 58.33224293864768839 ) ) ;
#165273 = CARTESIAN_POINT ( 'NONE',  ( 21.52544592524344225, -5.823673210054117533, 23.54057627198102765 ) ) ;
#165272 = CARTESIAN_POINT ( 'NONE',  ( 14.34966873604972726, -8.224510206698740333, 80.83442372801901854 ) ) ;
#165274 = CARTESIAN_POINT ( 'NONE',  ( 26.53515902489025535, 7.921333329385870314, 167.7790254135049111 ) ) ;
#165275 = CARTESIAN_POINT ( 'NONE',  ( -27.86273085795036408, -28.69962071417357663, -15.00000000000000178 ) ) ;
#165276 = CARTESIAN_POINT ( 'NONE',  ( -16.53943276465976808, -0.05219959533934237506, 113.7510903946856757 ) ) ;
#165277 = CARTESIAN_POINT ( 'NONE',  ( -16.52544592524335698, -4.483927247898792601, 58.95942372801902565 ) ) ;
#165279 = ORIENTED_EDGE ( 'NONE', *, *, #64977, .F. ) ;
#165278 = CARTESIAN_POINT ( 'NONE',  ( 16.51473224551069308, 9.474510206698969483, 74.16557627198103830 ) ) ;
#165280 = CARTESIAN_POINT ( 'NONE',  ( -19.02544592524342804, 5.153800228976336051, 86.04057627198103830 ) ) ;
#165281 = CARTESIAN_POINT ( 'NONE',  ( 15.80617190586769283, -15.72974639402175789, 70.62609039468567573 ) ) ;
#165282 = CARTESIAN_POINT ( 'NONE',  ( 16.52544592524335698, 4.483927247898782831, 81.45942372801900433 ) ) ;
#165283 = CARTESIAN_POINT ( 'NONE',  ( 16.53943276465976808, -0.05219959533910856209, 48.74890960531435979 ) ) ;
#165284 = CARTESIAN_POINT ( 'NONE',  ( -9.474510206698964154, 16.51473224551069663, 55.41557627198103120 ) ) ;
#165285 = CARTESIAN_POINT ( 'NONE',  ( 16.46253265017160672, -9.564922557960803928, 53.33224293864768839 ) ) ;
#165287 = ORIENTED_EDGE ( 'NONE', *, *, #135559, .T. ) ;
#165286 = CARTESIAN_POINT ( 'NONE',  ( 16.55341960407618274, -4.379528057220086978, 36.04275706135234714 ) ) ;
#165288 = CARTESIAN_POINT ( 'NONE',  ( -13.97604488694547697, 13.89961937509957934, 93.12609039468566152 ) ) ;
#165289 = CARTESIAN_POINT ( 'NONE',  ( -12.14591786802309592, -12.06949235617757132, 91.87390960531436690 ) ) ;
#165290 = CARTESIAN_POINT ( 'NONE',  ( 13.89961937509977652, -13.97604488694527269, 68.12390960531436690 ) ) ;
#165292 = CARTESIAN_POINT ( 'NONE',  ( 23.48529157249600630, -32.32473071737749137, -3.300000000000000266 ) ) ;
#165291 = CARTESIAN_POINT ( 'NONE',  ( -5.153800228976607833, 19.02544592524334988, 97.70942372801900433 ) ) ;
#165293 = CARTESIAN_POINT ( 'NONE',  ( -18.67979575497193778, 10.72451020669871902, 103.3344237280190043 ) ) ;
#165294 = CARTESIAN_POINT ( 'NONE',  ( 14.29746914071037800, 8.314922557961029526, 61.66775706135235424 ) ) ;
#165295 = CARTESIAN_POINT ( 'NONE',  ( -17.50000000000002842, 4.013004640162660230, 25.44605720994415066 ) ) ;
#165296 = CARTESIAN_POINT ( 'NONE',  ( 21.53943276465977519, -0.05219959533907433946, 68.74890960531435269 ) ) ;
#165297 = CARTESIAN_POINT ( 'NONE',  ( 14.34966873604972726, -8.224510206698740333, 55.83442372801901854 ) ) ;
#165298 = LINE ( 'NONE', #26791, #31316 ) ;
#165299 = CARTESIAN_POINT ( 'NONE',  ( -19.03943276465977164, -0.05219959533935918106, 58.75109039468566863 ) ) ;
#165300 = CARTESIAN_POINT ( 'NONE',  ( -0.05219959533909027116, -19.03943276465977164, 87.49890960531436690 ) ) ;
#165301 = CARTESIAN_POINT ( 'NONE',  ( 5.049401038298161559, -19.05341960407611168, 22.70724293864769194 ) ) ;
#165302 = CARTESIAN_POINT ( 'NONE',  ( -9.474510206698964154, 16.51473224551069663, 60.41557627198102409 ) ) ;
#165303 = CARTESIAN_POINT ( 'NONE',  ( 12.06949235617757843, -12.14591786802309237, 53.12390960531436690 ) ) ;
#165304 = CARTESIAN_POINT ( 'NONE',  ( 15.80617190586769283, -15.72974639402175789, 75.62609039468567573 ) ) ;
#165305 = CARTESIAN_POINT ( 'NONE',  ( 13.89961937509957401, 13.97604488694547697, 41.87609039468566152 ) ) ;
#165306 = CARTESIAN_POINT ( 'NONE',  ( 13.89961937509957401, 13.97604488694547697, 31.87609039468566863 ) ) ;
#165307 = CARTESIAN_POINT ( 'NONE',  ( 19.05341960407611168, 5.049401038298154454, 53.95724293864770260 ) ) ;
#165309 = B_SPLINE_CURVE_WITH_KNOTS ( 'NONE', 3,
 ( #63440, #124102, #94765, #76616, #107939, #61440, #138294, #111929, #171621, #80584, #14956, #187801, #46283, #33109, #157444, #91764, #142258, #169626, #123112, #156447, #153459, #17947, #64435, #77611, #154460, #15952, #65419, #139282, #759, #62430, #185802, #170626 ),
 .UNSPECIFIED., .F., .F.,
 ( 4, 2, 2, 2, 2, 2, 2, 2, 2, 2, 2, 2, 2, 2, 2, 4 ),
 ( 8.673617379884035472E-19, 0.0003712461730036752312, 0.0007424923460073495950, 0.001113738519011024013, 0.001484984692014698323, 0.002227477038022067542, 0.002598723211025740550, 0.002969969384029413993, 0.003341215557033087868, 0.003712461730036761311, 0.004083707903040434753, 0.004454954076044109063, 0.004826200249047782505, 0.005197446422051455947, 0.005568692595055130257, 0.005939938768058803699 ),
 .UNSPECIFIED. ) ;
#165308 = CARTESIAN_POINT ( 'NONE',  ( -15.80617190586745835, -15.72974639402198527, 21.87390960531436690 ) ) ;
#165310 = CARTESIAN_POINT ( 'NONE',  ( 5.823673210054444382, -21.52544592524334988, 95.20942372801903275 ) ) ;
#165311 = CARTESIAN_POINT ( 'NONE',  ( 16.46253265017160672, -9.564922557960803928, 58.33224293864769550 ) ) ;
#165312 = CARTESIAN_POINT ( 'NONE',  ( -0.05219959533937732626, 21.53943276465977519, 92.50109039468567573 ) ) ;
#165313 = CARTESIAN_POINT ( 'NONE',  ( -18.62759615963270932, 10.81492255796079327, 55.83224293864770260 ) ) ;
#165314 = AXIS2_PLACEMENT_3D ( 'NONE', #36600, #51780, #113440 ) ;
#165315 = CARTESIAN_POINT ( 'NONE',  ( 5.153800228976335163, 19.02544592524342804, 79.79057627198102409 ) ) ;
#165316 = CARTESIAN_POINT ( 'NONE',  ( 9.474510206698729675, 16.51473224551082808, 57.08442372801900433 ) ) ;
#165317 = CARTESIAN_POINT ( 'NONE',  ( -19.05341960407611168, -5.049401038298163336, 46.45724293864768129 ) ) ;
#165318 = CARTESIAN_POINT ( 'NONE',  ( 9.474510206698971260, -16.51473224551069308, 87.91557627198102409 ) ) ;
#165319 = CARTESIAN_POINT ( 'NONE',  ( -0.05219959533936034679, 19.03943276465977164, 87.50109039468567573 ) ) ;
#165320 = CARTESIAN_POINT ( 'NONE',  ( -16.53943276465976808, -0.05219959533934237506, 33.75109039468568284 ) ) ;
#165321 = CARTESIAN_POINT ( 'NONE',  ( -4.379528057220328563, 16.55341960407611168, 100.2072429386476955 ) ) ;
#165322 = CARTESIAN_POINT ( 'NONE',  ( -16.46253265017160317, 9.564922557960807481, 65.83224293864769550 ) ) ;
#165323 = CARTESIAN_POINT ( 'NONE',  ( 15.72974639402199770, -15.80617190586745480, 48.12390960531436690 ) ) ;
#165324 = CARTESIAN_POINT ( 'NONE',  ( -16.46253265017146816, -9.564922557961047289, 109.1677570613523471 ) ) ;
#165325 = CARTESIAN_POINT ( 'NONE',  ( 21.52544592524344225, -5.823673210054117533, 113.5405762719810383 ) ) ;
#165326 = CARTESIAN_POINT ( 'NONE',  ( 0.05219959533937995610, -21.53943276465977519, 65.00109039468568994 ) ) ;
#165327 = CARTESIAN_POINT ( 'NONE',  ( 8.314922557961029526, -14.29746914071037800, 65.41775706135234714 ) ) ;
#165328 = CARTESIAN_POINT ( 'NONE',  ( -16.46253265017160317, 9.564922557960807481, 70.83224293864770971 ) ) ;
#165329 = CARTESIAN_POINT ( 'NONE',  ( -14.34966873604972548, 8.224510206698743886, 103.3344237280190043 ) ) ;
#165330 = CARTESIAN_POINT ( 'NONE',  ( 19.02544592524334988, 5.153800228976608722, 46.45942372801899012 ) ) ;
#165331 = CARTESIAN_POINT ( 'NONE',  ( -15.72974639402176322, -15.80617190586768395, 29.37609039468568284 ) ) ;
#165332 = CARTESIAN_POINT ( 'NONE',  ( -12.06949235617756955, 12.14591786802309770, 80.62390960531438111 ) ) ;
#165333 = CARTESIAN_POINT ( 'NONE',  ( -9.474510206698964154, 16.51473224551069663, 95.41557627198102409 ) ) ;
#165334 = CARTESIAN_POINT ( 'NONE',  ( 8.314922557961029526, -14.29746914071037800, 85.41775706135236135 ) ) ;
#165335 = CARTESIAN_POINT ( 'NONE',  ( 15.72974639402176855, 15.80617190586768217, 66.87609039468568994 ) ) ;
#165336 = CARTESIAN_POINT ( 'NONE',  ( 4.379528057220092307, 16.55341960407617563, 27.29275706135234358 ) ) ;
#165337 = CARTESIAN_POINT ( 'NONE',  ( -21.52544592524334988, -5.823673210054445271, 28.95942372801902209 ) ) ;
#165338 = CARTESIAN_POINT ( 'NONE',  ( -12.06949235617756955, 12.14591786802309770, 65.62390960531436690 ) ) ;
#165339 = ORIENTED_EDGE ( 'NONE', *, *, #9292, .T. ) ;
#165340 = CARTESIAN_POINT ( 'NONE',  ( 5.719274019375991003, -21.55341960407610458, 107.7072429386476955 ) ) ;
#165341 = CARTESIAN_POINT ( 'NONE',  ( 12.06949235617757843, -12.14591786802309237, 48.12390960531436690 ) ) ;
#165342 = ORIENTED_EDGE ( 'NONE', *, *, #157548, .F. ) ;
#165343 = CARTESIAN_POINT ( 'NONE',  ( 19.02544592524343514, -5.153800228976328945, 23.54057627198102054 ) ) ;
#165344 = CARTESIAN_POINT ( 'NONE',  ( 10.81492255796078972, 18.62759615963270932, 34.58224293864770260 ) ) ;
#165345 = CARTESIAN_POINT ( 'NONE',  ( 5.823673210054444382, -21.52544592524334988, 40.20942372801901854 ) ) ;
#165346 = CARTESIAN_POINT ( 'NONE',  ( 4.483927247898545687, 16.52544592524342804, 69.79057627198102409 ) ) ;
#165347 = CARTESIAN_POINT ( 'NONE',  ( 0.05219959533907565091, 21.53943276465977519, 64.99890960531435269 ) ) ;
#165348 = CARTESIAN_POINT ( 'NONE',  ( 13.89961937509977652, -13.97604488694527269, 78.12390960531433848 ) ) ;
#165350 = CARTESIAN_POINT ( 'NONE',  ( -16.46253265017146816, -9.564922557961047289, 74.16775706135234714 ) ) ;
#165349 = CARTESIAN_POINT ( 'NONE',  ( 16.46253265017160672, -9.564922557960803928, 28.33224293864769550 ) ) ;
#165351 = CARTESIAN_POINT ( 'NONE',  ( -5.823673210054116645, -21.52544592524344225, 52.29057627198102409 ) ) ;
#165352 = CARTESIAN_POINT ( 'NONE',  ( 19.02544592524343514, -5.153800228976328945, 43.54057627198103120 ) ) ;
#165353 = CARTESIAN_POINT ( 'NONE',  ( -19.05341960407611168, -5.049401038298163336, 71.45724293864766707 ) ) ;
#165354 = ORIENTED_EDGE ( 'NONE', *, *, #43996, .T. ) ;
#165355 = CARTESIAN_POINT ( 'NONE',  ( 12.14591786802327356, -12.06949235617739191, 30.62609039468567929 ) ) ;
#165356 = CARTESIAN_POINT ( 'NONE',  ( 18.67979575497178502, 10.72451020669898547, 114.1655762719810383 ) ) ;
#165357 = CARTESIAN_POINT ( 'NONE',  ( 8.224510206698953496, -14.34966873604960469, 47.91557627198102409 ) ) ;
#165358 = CARTESIAN_POINT ( 'NONE',  ( -21.55341960407619339, 5.719274019375674811, 63.54275706135234003 ) ) ;
#165359 = CARTESIAN_POINT ( 'NONE',  ( -9.564922557960796823, -16.46253265017161027, 107.0822429386476955 ) ) ;
#165360 = CARTESIAN_POINT ( 'NONE',  ( 15.80617190586746368, 15.72974639402197994, 74.37390960531436690 ) ) ;
#165362 = CARTESIAN_POINT ( 'NONE',  ( -16.55341960407617563, 4.379528057220093196, 53.54275706135234714 ) ) ;
#165361 = CARTESIAN_POINT ( 'NONE',  ( 10.81492255796078972, 18.62759615963270932, 104.5822429386477097 ) ) ;
#165363 = CARTESIAN_POINT ( 'NONE',  ( -10.72451020669898014, 18.67979575497178502, 55.41557627198102409 ) ) ;
#165364 = CARTESIAN_POINT ( 'NONE',  ( -15.72974639402176322, -15.80617190586768395, 99.37609039468568994 ) ) ;
#165365 = CARTESIAN_POINT ( 'NONE',  ( -9.564922557960796823, -16.46253265017161027, 52.08224293864768839 ) ) ;
#165366 = CARTESIAN_POINT ( 'NONE',  ( 19.02544592524343514, -5.153800228976328945, 108.5405762719810383 ) ) ;
#165367 = CARTESIAN_POINT ( 'NONE',  ( -19.05341960407611168, -5.049401038298163336, 71.45724293864766707 ) ) ;
#165368 = CARTESIAN_POINT ( 'NONE',  ( -4.500000000000001776, -139.5000000000000000, 13.35010376910484098 ) ) ;
#165369 = CARTESIAN_POINT ( 'NONE',  ( -16.46253265017146816, -9.564922557961047289, 64.16775706135233293 ) ) ;
#165371 = CARTESIAN_POINT ( 'NONE',  ( -15.80617190586745835, -15.72974639402198527, 26.87390960531435979 ) ) ;
#165370 = CARTESIAN_POINT ( 'NONE',  ( -19.02544592524334988, -5.153800228976617603, 18.95942372801899722 ) ) ;
#165372 = CARTESIAN_POINT ( 'NONE',  ( 4.379528057220092307, 16.55341960407617563, 107.2927570613523471 ) ) ;
#165373 = CARTESIAN_POINT ( 'NONE',  ( 5.049401038297881783, 19.05341960407617563, 82.29275706135229029 ) ) ;
#165374 = CARTESIAN_POINT ( 'NONE',  ( -16.31925111598458855, 7.325300261831458215, 60.16424538967254421 ) ) ;
#165375 = CARTESIAN_POINT ( 'NONE',  ( -19.02544592524334988, -5.153800228976617603, 18.95942372801899722 ) ) ;
#165376 = CARTESIAN_POINT ( 'NONE',  ( 9.474510206698729675, 16.51473224551082808, 77.08442372801900433 ) ) ;
#165377 = CARTESIAN_POINT ( 'NONE',  ( 13.89961937509957401, 13.97604488694547697, 41.87609039468566152 ) ) ;
#165378 = CARTESIAN_POINT ( 'NONE',  ( -14.62203461105316826, -15.93943620433476838, -56.24376339824761573 ) ) ;
#165379 = CARTESIAN_POINT ( 'NONE',  ( -19.02544592524342804, 5.153800228976336051, 46.04057627198101699 ) ) ;
#165380 = CARTESIAN_POINT ( 'NONE',  ( 8.314922557960818139, 14.29746914071049879, 54.58224293864769550 ) ) ;
#165381 = ADVANCED_FACE ( 'NONE', ( #176393 ), #63641, .T. ) ;
#165382 = CARTESIAN_POINT ( 'NONE',  ( -13.89961937509977652, 13.97604488694528158, 40.62390960531435979 ) ) ;
#165383 = CARTESIAN_POINT ( 'NONE',  ( 8.224510206698953496, -14.34966873604960469, 37.91557627198102409 ) ) ;
#165384 = CARTESIAN_POINT ( 'NONE',  ( 18.10062525802554489, -5.500000000000022204, 46.01383468041920821 ) ) ;
#165385 = CARTESIAN_POINT ( 'NONE',  ( -8.314922557961024197, 14.29746914071037800, 107.9177570613523471 ) ) ;
#165386 = CARTESIAN_POINT ( 'NONE',  ( 0.05219959533909260263, 19.03943276465977164, 49.99890960531435979 ) ) ;
#165387 = CARTESIAN_POINT ( 'NONE',  ( -19.02544592524334988, -5.153800228976617603, 28.95942372801900433 ) ) ;
#165388 = CARTESIAN_POINT ( 'NONE',  ( -14.29746914071037622, -8.314922557961029526, 39.16775706135235424 ) ) ;
#165389 = CARTESIAN_POINT ( 'NONE',  ( -21.53943276465977519, 0.05219959533907696930, 41.24890960531435269 ) ) ;
#165391 = ORIENTED_EDGE ( 'NONE', *, *, #77460, .F. ) ;
#165390 = CARTESIAN_POINT ( 'NONE',  ( -21.52544592524334988, -5.823673210054445271, 88.95942372801901854 ) ) ;
#165392 = CARTESIAN_POINT ( 'NONE',  ( -13.89961937509977652, 13.97604488694528158, 105.6239096053143527 ) ) ;
#165393 = CARTESIAN_POINT ( 'NONE',  ( 5.049401038298161559, -19.05341960407611168, 82.70724293864770971 ) ) ;
#165394 = CARTESIAN_POINT ( 'NONE',  ( -31.58488912581707098, -24.54536626606730110, -19.09122180200634133 ) ) ;
#165395 = CARTESIAN_POINT ( 'NONE',  ( 10.72451020669898902, -18.67979575497178502, 112.9155762719810383 ) ) ;
#165396 = CARTESIAN_POINT ( 'NONE',  ( -4.379528057220328563, 16.55341960407611168, 75.20724293864769550 ) ) ;
#165398 = CARTESIAN_POINT ( 'NONE',  ( 19.05341960407611168, 5.049401038298154454, 68.95724293864769550 ) ) ;
#165397 = CARTESIAN_POINT ( 'NONE',  ( -21.55341960407610458, -5.719274019375992779, 71.45724293864769550 ) ) ;
#165399 = CARTESIAN_POINT ( 'NONE',  ( 9.564922557960805705, 16.46253265017160317, 79.58224293864769550 ) ) ;
#165400 = CARTESIAN_POINT ( 'NONE',  ( -21.52544592524343514, 5.823673210054127303, 91.04057627198103830 ) ) ;
#165401 = ORIENTED_EDGE ( 'NONE', *, *, #54823, .T. ) ;
#165402 = CARTESIAN_POINT ( 'NONE',  ( 16.51473224551069308, 9.474510206698969483, 64.16557627198102409 ) ) ;
#165404 = CARTESIAN_POINT ( 'NONE',  ( -16.46253265017160317, 9.564922557960807481, 25.83224293864769194 ) ) ;
#165403 = CARTESIAN_POINT ( 'NONE',  ( 4.483927247898545687, 16.52544592524342804, 94.79057627198105251 ) ) ;
#165405 = CARTESIAN_POINT ( 'NONE',  ( 5.153800228976335163, 19.02544592524342804, 59.79057627198100988 ) ) ;
#165406 = CARTESIAN_POINT ( 'NONE',  ( 19.05341960407617918, -5.049401038297876454, 81.04275706135231871 ) ) ;
#165407 = CARTESIAN_POINT ( 'NONE',  ( -14.34966873604960291, -8.224510206698953496, 91.66557627198103830 ) ) ;
#165408 = CARTESIAN_POINT ( 'NONE',  ( -15.80617190586768217, 15.72974639402176855, 53.12609039468568284 ) ) ;
#165410 = CARTESIAN_POINT ( 'NONE',  ( 15.72974639402176855, 15.80617190586768217, 21.87609039468567573 ) ) ;
#165409 = CARTESIAN_POINT ( 'NONE',  ( -19.03943276465977164, 0.05219959533909376836, 51.24890960531436690 ) ) ;
#165411 = CARTESIAN_POINT ( 'NONE',  ( -12.06949235617756955, 12.14591786802309770, 105.6239096053143669 ) ) ;
#165412 = CARTESIAN_POINT ( 'NONE',  ( 4.576660509524177911, -38.96431129323279663, -32.99999999890352598 ) ) ;
#165413 = CARTESIAN_POINT ( 'NONE',  ( 16.46253265017160672, -9.564922557960803928, 58.33224293864769550 ) ) ;
#165414 = DIRECTION ( 'NONE',  ( -0.000000000000000000, -0.000000000000000000, 1.000000000000000000 ) ) ;
#165416 = CARTESIAN_POINT ( 'NONE',  ( 5.719274019375991003, -21.55341960407610458, 22.70724293864769194 ) ) ;
#165415 = CARTESIAN_POINT ( 'NONE',  ( 9.474510206698729675, 16.51473224551082808, 107.0844237280190043 ) ) ;
#165417 = CARTESIAN_POINT ( 'NONE',  ( -21.53943276465977519, -0.05219959533937600094, 43.75109039468568284 ) ) ;
#165418 = CARTESIAN_POINT ( 'NONE',  ( 16.46253265017160672, -9.564922557960803928, 98.33224293864769550 ) ) ;
#165419 = CARTESIAN_POINT ( 'NONE',  ( -5.153800228976607833, 19.02544592524334988, 82.70942372801897591 ) ) ;
#165420 = CARTESIAN_POINT ( 'NONE',  ( 0.05219959533909260263, 19.03943276465977164, 59.99890960531436690 ) ) ;
#165421 = CARTESIAN_POINT ( 'NONE',  ( -16.52544592524342804, 4.483927247898546575, 81.04057627198102409 ) ) ;
#165422 = CARTESIAN_POINT ( 'NONE',  ( 19.03943276465977164, -0.05219959533909143690, 103.7489096053143669 ) ) ;
#165423 = CARTESIAN_POINT ( 'NONE',  ( -16.53943276465976808, 0.05219959533911058130, 81.24890960531436690 ) ) ;
#165424 = CARTESIAN_POINT ( 'NONE',  ( -9.564922557960796823, -16.46253265017161027, 97.08224293864769550 ) ) ;
#165425 = CARTESIAN_POINT ( 'NONE',  ( 9.474510206698729675, 16.51473224551082808, 47.08442372801900433 ) ) ;
#165428 = CARTESIAN_POINT ( 'NONE',  ( 16.51473224551069308, 9.474510206698969483, 34.16557627198102409 ) ) ;
#165427 = CARTESIAN_POINT ( 'NONE',  ( 14.29746914071049879, -8.314922557960816363, 43.33224293864769550 ) ) ;
#165426 = CARTESIAN_POINT ( 'NONE',  ( -9.564922557960796823, -16.46253265017161027, 52.08224293864768839 ) ) ;
#165429 = VERTEX_POINT ( 'NONE', #144035 ) ;
#165430 = CARTESIAN_POINT ( 'NONE',  ( -10.81492255796105439, 18.62759615963255655, 47.91775706135234714 ) ) ;
#165431 = CARTESIAN_POINT ( 'NONE',  ( -16.51473224551082808, 9.474510206698731452, 83.33442372801899012 ) ) ;
#165432 = CARTESIAN_POINT ( 'NONE',  ( -16.52544592524342804, 4.483927247898546575, 41.04057627198103120 ) ) ;
#165433 = CARTESIAN_POINT ( 'NONE',  ( -18.62759615963270932, 10.81492255796079327, 105.8322429386476955 ) ) ;
#165434 = CARTESIAN_POINT ( 'NONE',  ( -21.55341960407610458, -5.719274019375992779, 31.45724293864769550 ) ) ;
#165435 = CARTESIAN_POINT ( 'NONE',  ( 16.53943276465976808, -0.05219959533910856209, 78.74890960531436690 ) ) ;
#165436 = CARTESIAN_POINT ( 'NONE',  ( -5.153800228976328057, -19.02544592524343514, 37.29057627198102409 ) ) ;
#165437 = CARTESIAN_POINT ( 'NONE',  ( -16.55341960407617563, 4.379528057220093196, 98.54275706135234714 ) ) ;
#165438 = CARTESIAN_POINT ( 'NONE',  ( 16.55341960407618274, -4.379528057220086978, 71.04275706135234714 ) ) ;
#165439 = CARTESIAN_POINT ( 'NONE',  ( 0.05219959533936267826, -19.03943276465977164, 30.00109039468566863 ) ) ;
#165440 = CARTESIAN_POINT ( 'NONE',  ( -19.02544592524342804, 5.153800228976336051, 96.04057627198103830 ) ) ;
#165441 = CARTESIAN_POINT ( 'NONE',  ( 9.474510206698971260, -16.51473224551069308, 72.91557627198102409 ) ) ;
#165442 = CARTESIAN_POINT ( 'NONE',  ( -14.29746914071037622, -8.314922557961029526, 69.16775706135234714 ) ) ;
#165443 = CARTESIAN_POINT ( 'NONE',  ( 13.97604488694527802, 13.89961937509977652, 39.37390960531435269 ) ) ;
#165444 = CARTESIAN_POINT ( 'NONE',  ( 14.34966873604960469, 8.224510206698951720, 44.16557627198103120 ) ) ;
#165446 = CARTESIAN_POINT ( 'NONE',  ( 5.153800228976335163, 19.02544592524342804, 84.79057627198099567 ) ) ;
#165445 = CARTESIAN_POINT ( 'NONE',  ( 15.50000000000000355, 7.499999999999998224, 22.00000000000000711 ) ) ;
#165447 = CARTESIAN_POINT ( 'NONE',  ( 21.52544592524344225, -5.823673210054117533, 23.54057627198102765 ) ) ;
#165448 = CARTESIAN_POINT ( 'NONE',  ( 16.53943276465976808, -0.05219959533910856209, 73.74890960531433848 ) ) ;
#165449 = CARTESIAN_POINT ( 'NONE',  ( -16.53943276465976808, 0.05219959533911058130, 61.24890960531435979 ) ) ;
#165451 = CARTESIAN_POINT ( 'NONE',  ( 17.50000000000149569, -3.254303733634584361, 32.52395893071417277 ) ) ;
#165450 = CARTESIAN_POINT ( 'NONE',  ( -4.379528057220086978, -16.55341960407618274, 54.79275706135235424 ) ) ;
#165452 = CARTESIAN_POINT ( 'NONE',  ( -13.89961937509957401, -13.97604488694547875, 69.37609039468564731 ) ) ;
#165453 = CARTESIAN_POINT ( 'NONE',  ( -16.46253265017160317, 9.564922557960807481, 85.83224293864769550 ) ) ;
#165454 = CARTESIAN_POINT ( 'NONE',  ( -16.46253265017146816, -9.564922557961047289, 64.16775706135233293 ) ) ;
#165455 = CARTESIAN_POINT ( 'NONE',  ( 13.97604488694548053, -13.89961937509957401, 40.62609039468565442 ) ) ;
#165457 = CARTESIAN_POINT ( 'NONE',  ( 0.05219959533934541429, -16.53943276465976808, 95.00109039468568994 ) ) ;
#165456 = CARTESIAN_POINT ( 'NONE',  ( 4.483927247898790824, -16.52544592524335698, 20.20942372801900788 ) ) ;
#165458 = CARTESIAN_POINT ( 'NONE',  ( -16.46253265017160317, 9.564922557960807481, 40.83224293864769550 ) ) ;
#165459 =( BOUNDED_SURFACE ( )  B_SPLINE_SURFACE ( 3, 2, ( 
 ( #121950, #196838, #76444 ),
 ( #11827, #138121, #45125 ),
 ( #183643, #26991, #43138 ),
 ( #136142, #150332, #73492 ),
 ( #104807, #198812, #60277 ),
 ( #44136, #581, #153283 ),
 ( #47110, #135165, #59284 ),
 ( #14784, #166496, #154286 ),
 ( #77435, #106783, #27994 ),
 ( #197818, #46108, #89633 ),
 ( #169447, #15776, #30949 ),
 ( #119973, #199802, #139107 ),
 ( #168458, #61269, #62252 ),
 ( #165495, #29955, #88636 ),
 ( #122939, #151321, #90618 ),
 ( #12810, #184626, #105795 ),
 ( #137125, #120953, #91593 ),
 ( #123921, #13784, #107762 ),
 ( #185620, #74477, #182652 ),
 ( #167481, #28976, #152300 ),
 ( #75451, #79424, #93592 ),
 ( #128891, #35900, #124938 ),
 ( #48106, #156267, #190591 ),
 ( #19743, #65245, #31938 ) ),
 .UNSPECIFIED., .F., .F., .F. ) 
 B_SPLINE_SURFACE_WITH_KNOTS ( ( 4, 2, 2, 2, 2, 2, 2, 2, 2, 2, 2, 4 ),
 ( 3, 3 ),
 ( 0.000000000000000000, 0.001899702839891690993, 0.002849554259837536706, 0.003799405679783381985, 0.005699108519675073412, 0.006648959939620918691, 0.007598811359566763970, 0.008548662779512609250, 0.009498514199458456264, 0.01139821703935014682, 0.01329791987924183738, 0.01519762271913352794 ),
 ( 0.000000000000000000, 1.000000000000000000 ),
 .UNSPECIFIED. ) 
 GEOMETRIC_REPRESENTATION_ITEM ( )  RATIONAL_B_SPLINE_SURFACE ( (
 ( 1.000000000000000000, 0.7660444431189779024, 1.000000000000000000),
 ( 1.000000000000000000, 0.7753720600382123518, 1.000000000000000000),
 ( 1.000000000000000000, 0.7832595754286273415, 1.000000000000000000),
 ( 1.000000000000000000, 0.7928595458705296473, 1.000000000000000000),
 ( 1.000000000000000000, 0.7956872332516093937, 1.000000000000000000),
 ( 1.000000000000000000, 0.8005750596157590326, 1.000000000000000000),
 ( 1.000000000000000000, 0.8026302056541515517, 1.000000000000000000),
 ( 1.000000000000000000, 0.8075080643848789874, 1.000000000000000000),
 ( 1.000000000000000000, 0.8091143015809036942, 1.000000000000000000),
 ( 1.000000000000000000, 0.8093067629633434734, 1.000000000000000000),
 ( 1.000000000000000000, 0.8089952915731429828, 1.000000000000000000),
 ( 1.000000000000000000, 0.8076919994862520324, 1.000000000000000000),
 ( 1.000000000000000000, 0.8067078407649239669, 1.000000000000000000),
 ( 1.000000000000000000, 0.8041786842467097962, 1.000000000000000000),
 ( 1.000000000000000000, 0.8026334674877428910, 1.000000000000000000),
 ( 1.000000000000000000, 0.7990747329468967930, 1.000000000000000000),
 ( 1.000000000000000000, 0.7970509760942138255, 1.000000000000000000),
 ( 1.000000000000000000, 0.7904793850862680271, 1.000000000000000000),
 ( 1.000000000000000000, 0.7855040224314145947, 1.000000000000000000),
 ( 1.000000000000000000, 0.7751942650507163135, 1.000000000000000000),
 ( 1.000000000000000000, 0.7698260778211021282, 1.000000000000000000),
 ( 1.000000000000000000, 0.7598259884961480193, 1.000000000000000000),
 ( 1.000000000000000000, 0.7551428682219901711, 1.000000000000000000),
 ( 1.000000000000000000, 0.7510191126010862250, 1.000000000000000000) ) ) 
 REPRESENTATION_ITEM ( '' )  SURFACE ( )  );
#165460 = CARTESIAN_POINT ( 'NONE',  ( -21.53943276465977519, 0.05219959533907696930, 21.24890960531436690 ) ) ;
#165461 = CARTESIAN_POINT ( 'NONE',  ( 18.67979575497194134, -10.72451020669871369, 55.83442372801901854 ) ) ;
#165462 = CARTESIAN_POINT ( 'NONE',  ( -14.34966873604972548, 8.224510206698743886, 23.33442372801901499 ) ) ;
#165464 = CARTESIAN_POINT ( 'NONE',  ( -16.46253265017160317, 9.564922557960807481, 75.83224293864769550 ) ) ;
#165463 = CARTESIAN_POINT ( 'NONE',  ( -17.58332526062528345, -7.635886036038592728, 54.07665040441535353 ) ) ;
#165465 = CARTESIAN_POINT ( 'NONE',  ( -37.99626262588766679, 2.428612866367529932E-14, -0.002157773949821304490 ) ) ;
#165467 = CARTESIAN_POINT ( 'NONE',  ( 19.03943276465977164, -0.05219959533909143690, 78.74890960531436690 ) ) ;
#165466 = CARTESIAN_POINT ( 'NONE',  ( -16.52544592524342804, 4.483927247898546575, 81.04057627198102409 ) ) ;
#165468 = CARTESIAN_POINT ( 'NONE',  ( 9.474510206698971260, -16.51473224551069308, 67.91557627198102409 ) ) ;
#165469 = CARTESIAN_POINT ( 'NONE',  ( -0.05219959533936034679, 19.03943276465977164, 92.50109039468566152 ) ) ;
#165470 = CARTESIAN_POINT ( 'NONE',  ( -10.81492255796078084, -18.62759615963271287, 67.08224293864770971 ) ) ;
#165471 = CARTESIAN_POINT ( 'NONE',  ( 19.02544592524343514, -5.153800228976328945, 33.54057627198102409 ) ) ;
#165472 = CARTESIAN_POINT ( 'NONE',  ( 19.03943276465977164, 0.05219959533936151252, 56.25109039468566863 ) ) ;
#165473 = CARTESIAN_POINT ( 'NONE',  ( -9.474510206698964154, 16.51473224551069663, 60.41557627198102409 ) ) ;
#165474 = CARTESIAN_POINT ( 'NONE',  ( 13.97604488694527802, 13.89961937509977652, 94.37390960531436690 ) ) ;
#165475 = ORIENTED_EDGE ( 'NONE', *, *, #198827, .T. ) ;
#165476 = CARTESIAN_POINT ( 'NONE',  ( 10.72451020669898902, -18.67979575497178502, 87.91557627198103830 ) ) ;
#165478 = CARTESIAN_POINT ( 'NONE',  ( -9.564922557961040184, 16.46253265017147172, 52.91775706135233293 ) ) ;
#165477 = CARTESIAN_POINT ( 'NONE',  ( -16.52544592524342804, 4.483927247898546575, 91.04057627198103830 ) ) ;
#165479 = CARTESIAN_POINT ( 'NONE',  ( -18.62759615963270932, 10.81492255796079327, 80.83224293864769550 ) ) ;
#165480 = CARTESIAN_POINT ( 'NONE',  ( -0.05219959533907301413, -21.53943276465977519, 57.49890960531435979 ) ) ;
#165481 = CARTESIAN_POINT ( 'NONE',  ( -16.53943276465976808, 0.05219959533911058130, 36.24890960531435979 ) ) ;
#165482 = CARTESIAN_POINT ( 'NONE',  ( 5.719274019375673035, 21.55341960407619339, 107.2927570613523471 ) ) ;
#165483 = CARTESIAN_POINT ( 'NONE',  ( 19.03943276465977164, -0.05219959533909143690, 83.74890960531436690 ) ) ;
#165484 = CARTESIAN_POINT ( 'NONE',  ( 5.049401038298161559, -19.05341960407611168, 37.70724293864768839 ) ) ;
#165485 = CARTESIAN_POINT ( 'NONE',  ( 5.823673210054444382, -21.52544592524334988, 45.20942372801901854 ) ) ;
#165486 = CARTESIAN_POINT ( 'NONE',  ( -15.72974639402176322, -15.80617190586768395, 49.37609039468569705 ) ) ;
#165487 = CARTESIAN_POINT ( 'NONE',  ( 13.89961937509977652, -13.97604488694527269, 53.12390960531434558 ) ) ;
#165488 = CARTESIAN_POINT ( 'NONE',  ( -21.53943276465977519, -0.05219959533937600094, 28.75109039468567929 ) ) ;
#165489 = CARTESIAN_POINT ( 'NONE',  ( -19.05341960407617563, 5.049401038297882671, 63.54275706135234003 ) ) ;
#165490 = CARTESIAN_POINT ( 'NONE',  ( 5.049401038298161559, -19.05341960407611168, 32.70724293864768129 ) ) ;
#165491 = CARTESIAN_POINT ( 'NONE',  ( 14.29746914071037800, 8.314922557961029526, 26.66775706135235424 ) ) ;
#165492 = FACE_OUTER_BOUND ( 'NONE', #67683, .T. ) ;
#165493 = CARTESIAN_POINT ( 'NONE',  ( 14.29746914071037800, 8.314922557961029526, 76.66775706135234714 ) ) ;
#165494 = CARTESIAN_POINT ( 'NONE',  ( 19.05341960407611168, 5.049401038298154454, 33.95724293864769550 ) ) ;
#165495 = CARTESIAN_POINT ( 'NONE',  ( -21.93180397000192272, -9.000796715313676088, 171.3297436093443196 ) ) ;
#165496 = CARTESIAN_POINT ( 'NONE',  ( 19.05341960407611168, 5.049401038298154454, 83.95724293864766707 ) ) ;
#165497 = CARTESIAN_POINT ( 'NONE',  ( -19.03943276465977164, 0.05219959533909376836, 26.24890960531435624 ) ) ;
#165498 = CARTESIAN_POINT ( 'NONE',  ( 5.719274019375991003, -21.55341960407610458, 72.70724293864769550 ) ) ;
#165499 = CARTESIAN_POINT ( 'NONE',  ( 12.06949235617739724, 12.14591786802326823, 46.87609039468568994 ) ) ;
#165500 = CARTESIAN_POINT ( 'NONE',  ( 5.823673210054444382, -21.52544592524334988, 105.2094237280190328 ) ) ;
#165501 = CARTESIAN_POINT ( 'NONE',  ( 5.049401038298161559, -19.05341960407611168, 37.70724293864768839 ) ) ;
#165502 = CARTESIAN_POINT ( 'NONE',  ( 16.55341960407611168, 4.379528057220329451, 28.95724293864769905 ) ) ;
#165503 = CARTESIAN_POINT ( 'NONE',  ( -0.05219959533910754901, -16.53943276465976808, 67.49890960531436690 ) ) ;
#165504 = CARTESIAN_POINT ( 'NONE',  ( -13.97604488694527625, -13.89961937509977652, 61.87390960531435979 ) ) ;
#165505 = CARTESIAN_POINT ( 'NONE',  ( -18.67979575497193778, 10.72451020669871902, 103.3344237280190043 ) ) ;
#165506 = CARTESIAN_POINT ( 'NONE',  ( -21.53943276465977519, -0.05219959533937600094, 28.75109039468567929 ) ) ;
#165507 = CARTESIAN_POINT ( 'NONE',  ( -5.049401038298153566, 19.05341960407611168, 80.20724293864769550 ) ) ;
#165508 = CARTESIAN_POINT ( 'NONE',  ( -21.55341960407619339, 5.719274019375674811, 83.54275706135234714 ) ) ;
#165509 = CARTESIAN_POINT ( 'NONE',  ( 12.06949235617739724, 12.14591786802326823, 61.87609039468568284 ) ) ;
#165510 = CARTESIAN_POINT ( 'NONE',  ( 14.29746914071037800, 8.314922557961029526, 26.66775706135235424 ) ) ;
#165511 = EDGE_CURVE ( 'NONE', #99775, #162452, #198343, .T. ) ;
#165513 = CARTESIAN_POINT ( 'NONE',  ( -5.823673210054431948, 21.52544592524334988, 102.7094237280190185 ) ) ;
#165512 = CARTESIAN_POINT ( 'NONE',  ( -12.06949235617756955, 12.14591786802309770, 90.62390960531436690 ) ) ;
#165514 = CARTESIAN_POINT ( 'NONE',  ( 12.14591786802309770, 12.06949235617756955, 39.37390960531436690 ) ) ;
#165515 = CARTESIAN_POINT ( 'NONE',  ( -0.05219959533909027116, -19.03943276465977164, 27.49890960531435624 ) ) ;
#165516 = CARTESIAN_POINT ( 'NONE',  ( 8.224510206698742110, 14.34966873604972548, 57.08442372801901854 ) ) ;
#165517 = CARTESIAN_POINT ( 'NONE',  ( 0.05219959533910956823, 16.53943276465976808, 54.99890960531435269 ) ) ;
#165518 = CARTESIAN_POINT ( 'NONE',  ( 16.53943276465976808, 0.05219959533934440121, 101.2510903946856757 ) ) ;
#165519 = CARTESIAN_POINT ( 'NONE',  ( 5.719274019375991003, -21.55341960407610458, 22.70724293864769194 ) ) ;
#165520 = CARTESIAN_POINT ( 'NONE',  ( -10.81492255796078084, -18.62759615963271287, 32.08224293864769550 ) ) ;
#165521 = CARTESIAN_POINT ( 'NONE',  ( -19.05341960407617563, 5.049401038297882671, 23.54275706135233648 ) ) ;
#165522 = CARTESIAN_POINT ( 'NONE',  ( -12.06949235617756955, 12.14591786802309770, 80.62390960531438111 ) ) ;
#165523 = CARTESIAN_POINT ( 'NONE',  ( -9.564922557960796823, -16.46253265017161027, 97.08224293864769550 ) ) ;
#165524 = VERTEX_POINT ( 'NONE', #22703 ) ;
#165525 = CARTESIAN_POINT ( 'NONE',  ( 14.34966873604972726, -8.224510206698740333, 35.83442372801901143 ) ) ;
#165526 = CARTESIAN_POINT ( 'NONE',  ( -16.46253265017160317, 9.564922557960807481, 45.83224293864769550 ) ) ;
#165528 = FACE_OUTER_BOUND ( 'NONE', #81800, .T. ) ;
#165527 = CARTESIAN_POINT ( 'NONE',  ( -12.14591786802326823, 12.06949235617739902, 43.12609039468568284 ) ) ;
#165529 = CARTESIAN_POINT ( 'NONE',  ( -19.05341960407617563, 5.049401038297882671, 53.54275706135231871 ) ) ;
#165530 = CARTESIAN_POINT ( 'NONE',  ( 5.049401038298161559, -19.05341960407611168, 52.70724293864767418 ) ) ;
#165531 = CARTESIAN_POINT ( 'NONE',  ( 16.55341960407618274, -4.379528057220086978, 86.04275706135236135 ) ) ;
#165532 = CARTESIAN_POINT ( 'NONE',  ( -5.049401038297874678, -19.05341960407617918, 89.79275706135230450 ) ) ;
#165533 = CARTESIAN_POINT ( 'NONE',  ( -9.564922557961040184, 16.46253265017147172, 27.91775706135232582 ) ) ;
#165534 = CARTESIAN_POINT ( 'NONE',  ( -0.05219959533909027116, -19.03943276465977164, 67.49890960531436690 ) ) ;
#165535 = CARTESIAN_POINT ( 'NONE',  ( -4.379528057220328563, 16.55341960407611168, 105.2072429386477097 ) ) ;
#165536 = CARTESIAN_POINT ( 'NONE',  ( -9.474510206698720793, -16.51473224551083518, 74.58442372801900433 ) ) ;
#165537 = CARTESIAN_POINT ( 'NONE',  ( -15.80617190586745835, -15.72974639402198527, 66.87390960531436690 ) ) ;
#165538 = CARTESIAN_POINT ( 'NONE',  ( -19.05341960407617563, 5.049401038297882671, 43.54275706135232582 ) ) ;
#165539 = CARTESIAN_POINT ( 'NONE',  ( 19.02544592524343514, -5.153800228976328945, 98.54057627198100988 ) ) ;
#165540 = CARTESIAN_POINT ( 'NONE',  ( -21.53943276465977519, 0.05219959533907696930, 91.24890960531436690 ) ) ;
#165541 = CARTESIAN_POINT ( 'NONE',  ( -16.19135201231366139, 7.376712067591929767, 84.81319145947969673 ) ) ;
#165542 = CARTESIAN_POINT ( 'NONE',  ( -9.474510206698720793, -16.51473224551083518, 99.58442372801900433 ) ) ;
#165543 = CARTESIAN_POINT ( 'NONE',  ( -18.22780087662119541, 5.500000000000102141, 61.01763182126894947 ) ) ;
#165544 = CARTESIAN_POINT ( 'NONE',  ( 16.53943276465976808, 0.05219959533934440121, 26.25109039468567573 ) ) ;
#165545 = CARTESIAN_POINT ( 'NONE',  ( -19.02544592524342804, 5.153800228976336051, 51.04057627198103120 ) ) ;
#165546 = CARTESIAN_POINT ( 'NONE',  ( 19.03943276465977164, -0.05219959533909143690, 108.7489096053143527 ) ) ;
#165547 = CARTESIAN_POINT ( 'NONE',  ( -15.72974639402197994, 15.80617190586746368, 90.62390960531436690 ) ) ;
#165548 = CARTESIAN_POINT ( 'NONE',  ( -21.52544592524334988, -5.823673210054445271, 63.95942372801901854 ) ) ;
#165550 = CARTESIAN_POINT ( 'NONE',  ( 15.80617190586769283, -15.72974639402175789, 110.6260903946857042 ) ) ;
#165549 = CARTESIAN_POINT ( 'NONE',  ( 13.89961937509957401, 13.97604488694547697, 106.8760903946856757 ) ) ;
#165551 = CARTESIAN_POINT ( 'NONE',  ( 14.34966873604960469, 8.224510206698951720, 34.16557627198102409 ) ) ;
#165552 = CARTESIAN_POINT ( 'NONE',  ( 15.72974639402199770, -15.80617190586745480, 98.12390960531436690 ) ) ;
#165553 = CARTESIAN_POINT ( 'NONE',  ( -4.379528057220328563, 16.55341960407611168, 45.20724293864769550 ) ) ;
#165554 = CARTESIAN_POINT ( 'NONE',  ( -9.564922557961040184, 16.46253265017147172, 87.91775706135233293 ) ) ;
#165555 = CARTESIAN_POINT ( 'NONE',  ( 9.474510206698729675, 16.51473224551082808, 62.08442372801899722 ) ) ;
#165556 = CARTESIAN_POINT ( 'NONE',  ( 0.05219959533937995610, -21.53943276465977519, 70.00109039468568994 ) ) ;
#165557 = CARTESIAN_POINT ( 'NONE',  ( 9.474510206698729675, 16.51473224551082808, 42.08442372801900433 ) ) ;
#165558 = CARTESIAN_POINT ( 'NONE',  ( -0.05219959533909027116, -19.03943276465977164, 27.49890960531435624 ) ) ;
#165559 = CARTESIAN_POINT ( 'NONE',  ( 5.719274019375991003, -21.55341960407610458, 42.70724293864770260 ) ) ;
#165560 = CARTESIAN_POINT ( 'NONE',  ( 16.53943276465976808, -0.05219959533910856209, 33.74890960531436690 ) ) ;
#165561 = CARTESIAN_POINT ( 'NONE',  ( 19.05341960407617918, -5.049401038297876454, 21.04275706135232582 ) ) ;
#165562 = CARTESIAN_POINT ( 'NONE',  ( -16.53943276465976808, -0.05219959533934237506, 68.75109039468568994 ) ) ;
#165563 = CARTESIAN_POINT ( 'NONE',  ( 14.29746914071049879, -8.314922557960816363, 43.33224293864769550 ) ) ;
#165564 = CARTESIAN_POINT ( 'NONE',  ( -0.05219959533937732626, 21.53943276465977519, 82.50109039468568994 ) ) ;
#165565 = CARTESIAN_POINT ( 'NONE',  ( 15.72974639402176855, 15.80617190586768217, 71.87609039468568994 ) ) ;
#165566 = CARTESIAN_POINT ( 'NONE',  ( 21.55341960407610458, 5.719274019375980345, 68.95724293864769550 ) ) ;
#165567 = CARTESIAN_POINT ( 'NONE',  ( 9.474510206698971260, -16.51473224551069308, 22.91557627198102765 ) ) ;
#165568 = CARTESIAN_POINT ( 'NONE',  ( -15.72974639402176322, -15.80617190586768395, 44.37609039468567573 ) ) ;
#165569 = CARTESIAN_POINT ( 'NONE',  ( 13.89961937509977652, -13.97604488694527269, 23.12390960531436335 ) ) ;
#165570 = CARTESIAN_POINT ( 'NONE',  ( 19.02544592524343514, -5.153800228976328945, 33.54057627198102409 ) ) ;
#165571 = CARTESIAN_POINT ( 'NONE',  ( -0.05219959533910754901, -16.53943276465976808, 97.49890960531436690 ) ) ;
#165572 = CARTESIAN_POINT ( 'NONE',  ( -9.564922557960796823, -16.46253265017161027, 82.08224293864768129 ) ) ;
#165573 = CARTESIAN_POINT ( 'NONE',  ( 14.29746914071049879, -8.314922557960816363, 43.33224293864769550 ) ) ;
#165574 = CARTESIAN_POINT ( 'NONE',  ( 16.53943276465976808, -0.05219959533910856209, 103.7489096053143669 ) ) ;
#165575 = CARTESIAN_POINT ( 'NONE',  ( 18.67979575497178502, 10.72451020669898547, 69.16557627198102409 ) ) ;
#165576 = CARTESIAN_POINT ( 'NONE',  ( -21.52544592524343514, 5.823673210054127303, 101.0405762719810383 ) ) ;
#165577 = CARTESIAN_POINT ( 'NONE',  ( -13.89961937509977652, 13.97604488694528158, 110.6239096053143243 ) ) ;
#165578 = ADVANCED_FACE ( 'NONE', ( #4511 ), #190555, .T. ) ;
#165580 = CARTESIAN_POINT ( 'NONE',  ( -16.53943276465976808, -0.05219959533934237506, 23.75109039468567929 ) ) ;
#165579 = CARTESIAN_POINT ( 'NONE',  ( -16.46253265017160317, 9.564922557960807481, 60.83224293864769550 ) ) ;
#165581 = CARTESIAN_POINT ( 'NONE',  ( -21.55341960407610458, -5.719274019375992779, 56.45724293864768839 ) ) ;
#165582 = CARTESIAN_POINT ( 'NONE',  ( 15.80617190586769283, -15.72974639402175789, 80.62609039468567573 ) ) ;
#165583 = CARTESIAN_POINT ( 'NONE',  ( 13.97604488694527802, 13.89961937509977652, 79.37390960531435269 ) ) ;
#165584 = CARTESIAN_POINT ( 'NONE',  ( 15.80617190586769283, -15.72974639402175789, 20.62609039468568639 ) ) ;
#165585 = CARTESIAN_POINT ( 'NONE',  ( 13.89961937509977652, -13.97604488694527269, 113.1239096053143527 ) ) ;
#165586 = CARTESIAN_POINT ( 'NONE',  ( -4.379528057220086978, -16.55341960407618274, 79.79275706135236135 ) ) ;
#165587 = CARTESIAN_POINT ( 'NONE',  ( -5.823673210054431948, 21.52544592524334988, 72.70942372801901854 ) ) ;
#165588 = CARTESIAN_POINT ( 'NONE',  ( 15.80617190586769283, -15.72974639402175789, 100.6260903946857184 ) ) ;
#165589 = CARTESIAN_POINT ( 'NONE',  ( 0.05219959533934541429, -16.53943276465976808, 55.00109039468568284 ) ) ;
#165590 = CARTESIAN_POINT ( 'NONE',  ( -21.53943276465977519, 0.05219959533907696930, 116.2489096053143669 ) ) ;
#165591 = CARTESIAN_POINT ( 'NONE',  ( 16.51473224551069308, 9.474510206698969483, 114.1655762719810241 ) ) ;
#165592 = CARTESIAN_POINT ( 'NONE',  ( -0.05219959533937732626, 21.53943276465977519, 92.50109039468567573 ) ) ;
#165593 = CARTESIAN_POINT ( 'NONE',  ( 10.81492255796078972, 18.62759615963270932, 84.58224293864769550 ) ) ;
#165594 = CARTESIAN_POINT ( 'NONE',  ( 9.564922557961047289, -16.46253265017146816, 50.41775706135233293 ) ) ;
#165595 = CARTESIAN_POINT ( 'NONE',  ( -15.72974639402197994, 15.80617190586746368, 50.62390960531435979 ) ) ;
#165597 = CARTESIAN_POINT ( 'NONE',  ( 16.52544592524342804, -4.483927247898539470, 38.54057627198103120 ) ) ;
#165596 = CARTESIAN_POINT ( 'NONE',  ( 19.05341960407611168, 5.049401038298154454, 93.95724293864769550 ) ) ;
#165598 = CARTESIAN_POINT ( 'NONE',  ( -18.22780087662121673, -5.500000000000063061, 41.48459894673893444 ) ) ;
#165599 = CARTESIAN_POINT ( 'NONE',  ( 1.323952442993630241, 14.46947684450821647, -60.11301529061759652 ) ) ;
#165600 = CARTESIAN_POINT ( 'NONE',  ( 9.474510206698729675, 16.51473224551082808, 102.0844237280190043 ) ) ;
#165601 = CARTESIAN_POINT ( 'NONE',  ( 21.55341960407610458, 5.719274019375980345, 88.95724293864769550 ) ) ;
#165602 = CARTESIAN_POINT ( 'NONE',  ( -16.52544592524342804, 4.483927247898546575, 46.04057627198103830 ) ) ;
#165603 = CARTESIAN_POINT ( 'NONE',  ( 8.314922557961029526, -14.29746914071037800, 25.41775706135235779 ) ) ;
#165604 = CARTESIAN_POINT ( 'NONE',  ( 19.03943276465977164, -0.05219959533909143690, 38.74890960531436690 ) ) ;
#165606 = CARTESIAN_POINT ( 'NONE',  ( 9.564922557961047289, -16.46253265017146816, 80.41775706135234714 ) ) ;
#165605 = CARTESIAN_POINT ( 'NONE',  ( -15.72974639402197994, 15.80617190586746368, 110.6239096053143669 ) ) ;
#165607 = CARTESIAN_POINT ( 'NONE',  ( 9.474510206698971260, -16.51473224551069308, 82.91557627198103830 ) ) ;
#165608 = CARTESIAN_POINT ( 'NONE',  ( 0.05219959533909260263, 19.03943276465977164, 79.99890960531436690 ) ) ;
#165609 = CARTESIAN_POINT ( 'NONE',  ( 15.80617190586746368, 15.72974639402197994, 74.37390960531436690 ) ) ;
#165610 = CARTESIAN_POINT ( 'NONE',  ( 13.89961937509977652, -13.97604488694527269, 33.12390960531434558 ) ) ;
#165611 = CARTESIAN_POINT ( 'NONE',  ( -25.52603992809234157, 28.15638454425511839, -8.000000000000001776 ) ) ;
#165612 = CARTESIAN_POINT ( 'NONE',  ( -8.224510206698948167, 14.34966873604960824, 55.41557627198102409 ) ) ;
#165613 = CARTESIAN_POINT ( 'NONE',  ( 9.564922557960805705, 16.46253265017160317, 84.58224293864769550 ) ) ;
#165614 = DIRECTION ( 'NONE',  ( 0.000000000000000000, 0.000000000000000000, -1.000000000000000000 ) ) ;
#165615 = CARTESIAN_POINT ( 'NONE',  ( 9.564922557961047289, -16.46253265017146816, 60.41775706135233293 ) ) ;
#165616 = CARTESIAN_POINT ( 'NONE',  ( 21.52544592524344225, -5.823673210054117533, 78.54057627198103830 ) ) ;
#165617 = CARTESIAN_POINT ( 'NONE',  ( 13.97604488694548053, -13.89961937509957401, 40.62609039468564731 ) ) ;
#165618 = CARTESIAN_POINT ( 'NONE',  ( 16.46253265017160672, -9.564922557960803928, 103.3322429386476955 ) ) ;
#165619 = CARTESIAN_POINT ( 'NONE',  ( -17.49999999999999645, 3.805241302050293761, 115.3735247278259095 ) ) ;
#165620 = CARTESIAN_POINT ( 'NONE',  ( -21.52544592524343514, 5.823673210054127303, 26.04057627198103475 ) ) ;
#165621 = CARTESIAN_POINT ( 'NONE',  ( 9.564922557960805705, 16.46253265017160317, 74.58224293864769550 ) ) ;
#165622 = CARTESIAN_POINT ( 'NONE',  ( 21.55341960407619695, -5.719274019375665929, 51.04275706135234714 ) ) ;
#165623 = CARTESIAN_POINT ( 'NONE',  ( 19.03943276465977164, -0.05219959533909143690, 28.74890960531435624 ) ) ;
#165625 = EDGE_LOOP ( 'NONE', ( #170897, #106053, #10015, #179571 ) ) ;
#165624 = CARTESIAN_POINT ( 'NONE',  ( 21.52544592524334988, 5.823673210054432836, 21.45942372801901499 ) ) ;
#165626 = CARTESIAN_POINT ( 'NONE',  ( -21.53943276465977519, -0.05219959533937600094, 43.75109039468568284 ) ) ;
#165627 = ORIENTED_EDGE ( 'NONE', *, *, #119374, .T. ) ;
#165628 = CARTESIAN_POINT ( 'NONE',  ( -0.05219959533909027116, -19.03943276465977164, 97.49890960531436690 ) ) ;
#165629 = VECTOR ( 'NONE', #165245, 1000.000000000000000 ) ;
#165630 = CARTESIAN_POINT ( 'NONE',  ( -21.75476783670602288, 5.835674035550357353, 172.5278397751181387 ) ) ;
#165631 = CARTESIAN_POINT ( 'NONE',  ( 15.72974639402199770, -15.80617190586745480, 113.1239096053143953 ) ) ;
#165632 = CARTESIAN_POINT ( 'NONE',  ( 13.89961937509977652, -13.97604488694527269, 63.12390960531435979 ) ) ;
#165633 = CARTESIAN_POINT ( 'NONE',  ( 14.29746914071037800, 8.314922557961029526, 21.66775706135235069 ) ) ;
#165634 = CARTESIAN_POINT ( 'NONE',  ( -11.74264578624800670, 36.14014761921585972, -4.149999994537627579 ) ) ;
#165635 = CARTESIAN_POINT ( 'NONE',  ( 21.52544592524334988, 5.823673210054432836, 106.4594237280190328 ) ) ;
#165636 = CARTESIAN_POINT ( 'NONE',  ( -19.05341960407611168, -5.049401038298163336, 46.45724293864768129 ) ) ;
#165637 = CARTESIAN_POINT ( 'NONE',  ( -10.72451020669870658, -18.67979575497194134, 104.5844237280190185 ) ) ;
#165639 = CARTESIAN_POINT ( 'NONE',  ( -5.719274019375665041, -21.55341960407619695, 54.79275706135235424 ) ) ;
#165638 = CARTESIAN_POINT ( 'NONE',  ( -9.564922557960796823, -16.46253265017161027, 87.08224293864769550 ) ) ;
#165640 = CARTESIAN_POINT ( 'NONE',  ( -22.81625015709509441, -31.40387420917324590, -10.32499999726881157 ) ) ;
#165641 = CARTESIAN_POINT ( 'NONE',  ( 5.049401038298161559, -19.05341960407611168, 107.7072429386476955 ) ) ;
#165642 = CARTESIAN_POINT ( 'NONE',  ( -17.49999999999999645, 5.068104630630415386, 30.72818405340029813 ) ) ;
#165645 = CARTESIAN_POINT ( 'NONE',  ( -18.67979575497193778, 10.72451020669871902, 53.33442372801901854 ) ) ;
#165644 = CARTESIAN_POINT ( 'NONE',  ( 0.05219959533934541429, -16.53943276465976808, 75.00109039468568994 ) ) ;
#165643 = CARTESIAN_POINT ( 'NONE',  ( 4.483927247898790824, -16.52544592524335698, 55.20942372801902565 ) ) ;
#165646 = CARTESIAN_POINT ( 'NONE',  ( -18.62759615963255300, -10.81492255796106328, 94.16775706135237556 ) ) ;
#165647 = CARTESIAN_POINT ( 'NONE',  ( 25.82634036940374855, -7.758313425001082564, 169.9660385289634235 ) ) ;
#165648 = CARTESIAN_POINT ( 'NONE',  ( -4.379528057220086978, -16.55341960407618274, 24.79275706135235779 ) ) ;
#165649 = CARTESIAN_POINT ( 'NONE',  ( -19.02544592524342804, 5.153800228976336051, 76.04057627198102409 ) ) ;
#165650 = CARTESIAN_POINT ( 'NONE',  ( -16.46253265017160317, 9.564922557960807481, 105.8322429386476955 ) ) ;
#165651 = CARTESIAN_POINT ( 'NONE',  ( 16.31925111598457079, 7.325300261831479531, 42.33575461032752685 ) ) ;
#165652 = CARTESIAN_POINT ( 'NONE',  ( 19.02544592524343514, -5.153800228976328945, 28.54057627198102409 ) ) ;
#165653 = CARTESIAN_POINT ( 'NONE',  ( 18.67979575497178502, 10.72451020669898547, 39.16557627198102409 ) ) ;
#165654 = CARTESIAN_POINT ( 'NONE',  ( 4.379528057220092307, 16.55341960407617563, 92.29275706135236135 ) ) ;
#165656 = CARTESIAN_POINT ( 'NONE',  ( -13.89961937509977652, 13.97604488694528158, 65.62390960531436690 ) ) ;
#165655 = CARTESIAN_POINT ( 'NONE',  ( 12.06949235617757843, -12.14591786802309237, 78.12390960531436690 ) ) ;
#165657 = CARTESIAN_POINT ( 'NONE',  ( -15.72974639402176322, -15.80617190586768395, 84.37609039468570415 ) ) ;
#165658 = CARTESIAN_POINT ( 'NONE',  ( -23.94686256013568837, 0.9720251121417748941, -57.02522261278123494 ) ) ;
#165659 = CARTESIAN_POINT ( 'NONE',  ( 14.29746914071037800, 8.314922557961029526, 26.66775706135235424 ) ) ;
#165660 = CARTESIAN_POINT ( 'NONE',  ( -16.55341960407611168, -4.379528057220339221, 71.45724293864769550 ) ) ;
#165661 = CARTESIAN_POINT ( 'NONE',  ( -21.52544592524334988, -5.823673210054445271, 38.95942372801901854 ) ) ;
#165662 = CARTESIAN_POINT ( 'NONE',  ( 21.53943276465977519, -0.05219959533907433946, 78.74890960531436690 ) ) ;
#165663 = CARTESIAN_POINT ( 'NONE',  ( -9.474510206698720793, -16.51473224551083518, 44.58442372801900433 ) ) ;
#165664 = CARTESIAN_POINT ( 'NONE',  ( -34.91303292417841675, 6.360705039060875698, 41.01876028008880581 ) ) ;
#165665 = CARTESIAN_POINT ( 'NONE',  ( 5.049401038298161559, -19.05341960407611168, 77.70724293864765286 ) ) ;
#165666 = CARTESIAN_POINT ( 'NONE',  ( 12.06949235617757843, -12.14591786802309237, 68.12390960531436690 ) ) ;
#165667 = CARTESIAN_POINT ( 'NONE',  ( -8.224510206698948167, 14.34966873604960824, 30.41557627198101699 ) ) ;
#165668 = CARTESIAN_POINT ( 'NONE',  ( -16.55341960407617563, 4.379528057220093196, 113.5427570613523756 ) ) ;
#165669 = CARTESIAN_POINT ( 'NONE',  ( 9.564922557961047289, -16.46253265017146816, 65.41775706135233293 ) ) ;
#165670 = DIRECTION ( 'NONE',  ( 0.000000000000000000, 0.000000000000000000, 1.000000000000000000 ) ) ;
#165671 = CARTESIAN_POINT ( 'NONE',  ( 19.05341960407611168, 5.049401038298154454, 113.9572429386477097 ) ) ;
#165672 = CARTESIAN_POINT ( 'NONE',  ( 4.379528057220339221, -16.55341960407611168, 82.70724293864770971 ) ) ;
#165673 = CARTESIAN_POINT ( 'NONE',  ( -17.97182807773875268, 5.499999999999872990, 58.53038844047289047 ) ) ;
#165675 = CARTESIAN_POINT ( 'NONE',  ( 15.80617190586746368, 15.72974639402197994, 44.37390960531435979 ) ) ;
#165674 = CARTESIAN_POINT ( 'NONE',  ( -5.049401038298153566, 19.05341960407611168, 40.20724293864768839 ) ) ;
#165676 = CARTESIAN_POINT ( 'NONE',  ( 10.81492255796078972, 18.62759615963270932, 64.58224293864769550 ) ) ;
#165677 = CARTESIAN_POINT ( 'NONE',  ( -12.06949235617756955, 12.14591786802309770, 105.6239096053143669 ) ) ;
#165679 = CARTESIAN_POINT ( 'NONE',  ( 9.474510206698971260, -16.51473224551069308, 42.91557627198103120 ) ) ;
#165678 = CARTESIAN_POINT ( 'NONE',  ( 12.14591786802327356, -12.06949235617739191, 65.62609039468568994 ) ) ;
#165680 = CARTESIAN_POINT ( 'NONE',  ( -15.72974639402176322, -15.80617190586768395, 59.37609039468568284 ) ) ;
#165681 = ORIENTED_EDGE ( 'NONE', *, *, #179533, .F. ) ;
#165682 = CARTESIAN_POINT ( 'NONE',  ( 0.05219959533910956823, 16.53943276465976808, 104.9989096053143669 ) ) ;
#165683 = CARTESIAN_POINT ( 'NONE',  ( -13.89961937509957401, -13.97604488694547875, 94.37609039468566152 ) ) ;
#165684 = CARTESIAN_POINT ( 'NONE',  ( -22.81625015709510507, 31.40387420917330275, -5.424999997268812990 ) ) ;
#165686 = CARTESIAN_POINT ( 'NONE',  ( 21.52544592524344225, -5.823673210054117533, 38.54057627198103120 ) ) ;
#165685 = CARTESIAN_POINT ( 'NONE',  ( -17.60769864724391454, 5.499999999999988454, 38.65024842019165874 ) ) ;
#165687 = CARTESIAN_POINT ( 'NONE',  ( -13.97604488694527625, -13.89961937509977652, 26.87390960531434558 ) ) ;
#165688 = CARTESIAN_POINT ( 'NONE',  ( -18.62759615963255300, -10.81492255796106328, 74.16775706135231871 ) ) ;
#165690 = CARTESIAN_POINT ( 'NONE',  ( 14.29746914071049879, -8.314922557960816363, 48.33224293864770260 ) ) ;
#165689 = CARTESIAN_POINT ( 'NONE',  ( 14.34966873604972726, -8.224510206698740333, 60.83442372801901854 ) ) ;
#165691 = CARTESIAN_POINT ( 'NONE',  ( -21.55341960407610458, -5.719274019375992779, 71.45724293864769550 ) ) ;
#165692 = CARTESIAN_POINT ( 'NONE',  ( -5.823673210054116645, -21.52544592524344225, 67.29057627198103830 ) ) ;
#165693 = DIRECTION ( 'NONE',  ( -1.000000000000000000, 0.000000000000000000, -0.000000000000000000 ) ) ;
#165695 = CARTESIAN_POINT ( 'NONE',  ( 9.564922557960805705, 16.46253265017160317, 109.5822429386476955 ) ) ;
#165694 = CARTESIAN_POINT ( 'NONE',  ( 16.51473224551083163, -9.474510206698727899, 85.83442372801900433 ) ) ;
#165696 = EDGE_CURVE ( 'NONE', #45713, #159190, #99526, .T. ) ;
#165697 = CARTESIAN_POINT ( 'NONE',  ( 9.564922557960805705, 16.46253265017160317, 44.58224293864769550 ) ) ;
#165698 = CARTESIAN_POINT ( 'NONE',  ( -8.224510206698948167, 14.34966873604960824, 110.4155762719810383 ) ) ;
#165699 = SURFACE_SIDE_STYLE ('',( #104020 ) ) ;
#165700 = FACE_BOUND ( 'NONE', #85286, .T. ) ;
#165701 = ORIENTED_EDGE ( 'NONE', *, *, #82301, .T. ) ;
#165702 = CARTESIAN_POINT ( 'NONE',  ( 16.53943276465976808, 0.05219959533934440121, 71.25109039468568994 ) ) ;
#165703 = CARTESIAN_POINT ( 'NONE',  ( 21.55341960407610458, 5.719274019375980345, 98.95724293864770971 ) ) ;
#165704 = CARTESIAN_POINT ( 'NONE',  ( 19.05341960407611168, 5.049401038298154454, 63.95724293864769550 ) ) ;
#165705 = CARTESIAN_POINT ( 'NONE',  ( -5.719274019375665041, -21.55341960407619695, 44.79275706135234714 ) ) ;
#165706 = CARTESIAN_POINT ( 'NONE',  ( -13.89961937509977652, 13.97604488694528158, 100.6239096053143669 ) ) ;
#165707 = CARTESIAN_POINT ( 'NONE',  ( -27.14096102835633317, -28.70429377953645655, -18.51261060099007949 ) ) ;
#165708 = ORIENTED_EDGE ( 'NONE', *, *, #53785, .F. ) ;
#165709 = CARTESIAN_POINT ( 'NONE',  ( -21.53943276465977519, -0.05219959533937600094, 33.75109039468568284 ) ) ;
#165711 = CARTESIAN_POINT ( 'NONE',  ( -19.05341960407617563, 5.049401038297882671, 83.54275706135233293 ) ) ;
#165710 = CARTESIAN_POINT ( 'NONE',  ( -19.02544592524342804, 5.153800228976336051, 31.04057627198102409 ) ) ;
#165712 = CARTESIAN_POINT ( 'NONE',  ( -9.474510206698720793, -16.51473224551083518, 34.58442372801899722 ) ) ;
#165713 = CARTESIAN_POINT ( 'NONE',  ( 21.53943276465977519, -0.05219959533907433946, 113.7489096053143527 ) ) ;
#165714 = CARTESIAN_POINT ( 'NONE',  ( -19.02544592524334988, -5.153800228976617603, 33.95942372801897591 ) ) ;
#165715 = CARTESIAN_POINT ( 'NONE',  ( -16.46253265017146816, -9.564922557961047289, 54.16775706135234003 ) ) ;
#165716 = CARTESIAN_POINT ( 'NONE',  ( 8.224510206698742110, 14.34966873604972548, 87.08442372801901854 ) ) ;
#165718 = ORIENTED_EDGE ( 'NONE', *, *, #131252, .F. ) ;
#165717 = PLANE ( 'NONE',  #8709 ) ;
#165719 = CARTESIAN_POINT ( 'NONE',  ( 5.049401038298161559, -19.05341960407611168, 72.70724293864768129 ) ) ;
#165720 = CARTESIAN_POINT ( 'NONE',  ( 0.05219959533937995610, -21.53943276465977519, 80.00109039468568994 ) ) ;
#165721 = CARTESIAN_POINT ( 'NONE',  ( 21.53943276465977519, 0.05219959533937863772, 96.25109039468568994 ) ) ;
#165722 = CARTESIAN_POINT ( 'NONE',  ( 18.22780087662121673, 5.500000000000056843, 38.98459894673893444 ) ) ;
#165723 = CARTESIAN_POINT ( 'NONE',  ( -0.05219959533909027116, -19.03943276465977164, 82.49890960531436690 ) ) ;
#165724 = CARTESIAN_POINT ( 'NONE',  ( 5.719274019375673035, 21.55341960407619339, 57.29275706135234714 ) ) ;
#165725 = CARTESIAN_POINT ( 'NONE',  ( 16.51473224551083163, -9.474510206698727899, 105.8344237280190043 ) ) ;
#165726 = CARTESIAN_POINT ( 'NONE',  ( -13.89961937509977652, 13.97604488694528158, 70.62390960531432427 ) ) ;
#165727 = CARTESIAN_POINT ( 'NONE',  ( 5.719274019375991003, -21.55341960407610458, 22.70724293864769194 ) ) ;
#165728 = CARTESIAN_POINT ( 'NONE',  ( 9.474510206698971260, -16.51473224551069308, 72.91557627198102409 ) ) ;
#165729 = CARTESIAN_POINT ( 'NONE',  ( 17.49999999999997513, -3.905042442100252309, 22.90465208775962935 ) ) ;
#165730 = CARTESIAN_POINT ( 'NONE',  ( 9.474510206698971260, -16.51473224551069308, 67.91557627198102409 ) ) ;
#165731 = CARTESIAN_POINT ( 'NONE',  ( 9.474510206698971260, -16.51473224551069308, 52.91557627198102409 ) ) ;
#165732 = CARTESIAN_POINT ( 'NONE',  ( 10.81492255796106328, -18.62759615963255655, 20.41775706135234714 ) ) ;
#165733 = CARTESIAN_POINT ( 'NONE',  ( 14.29746914071037800, 8.314922557961029526, 86.66775706135234714 ) ) ;
#165734 = CARTESIAN_POINT ( 'NONE',  ( 11.80868324581538253, -11.80868324581533457, -59.13370768023891344 ) ) ;
#165735 = CARTESIAN_POINT ( 'NONE',  ( 6.941067294099604545, -1.351053078614634639, -64.37011660792191492 ) ) ;
#165736 = CARTESIAN_POINT ( 'NONE',  ( -5.049401038297874678, -19.05341960407617918, 54.79275706135234003 ) ) ;
#165737 = CARTESIAN_POINT ( 'NONE',  ( 19.02544592524343514, -5.153800228976328945, 73.54057627198103830 ) ) ;
#165738 = CARTESIAN_POINT ( 'NONE',  ( 16.55341960407611168, 4.379528057220329451, 73.95724293864769550 ) ) ;
#165739 = CARTESIAN_POINT ( 'NONE',  ( -12.14591786802309592, -12.06949235617757132, 101.8739096053143811 ) ) ;
#165740 = CARTESIAN_POINT ( 'NONE',  ( -21.52544592524343514, 5.823673210054127303, 26.04057627198103475 ) ) ;
#165741 = CARTESIAN_POINT ( 'NONE',  ( 19.05341960407611168, 5.049401038298154454, 98.95724293864766707 ) ) ;
#165742 = AXIS2_PLACEMENT_3D ( 'NONE', #22885, #114885, #71388 ) ;
#165743 = CARTESIAN_POINT ( 'NONE',  ( 4.379528057220339221, -16.55341960407611168, 92.70724293864770971 ) ) ;
#165744 = CARTESIAN_POINT ( 'NONE',  ( -16.46253265017160317, 9.564922557960807481, 115.8322429386477097 ) ) ;
#165745 = CARTESIAN_POINT ( 'NONE',  ( -16.46253265017146816, -9.564922557961047289, 34.16775706135233293 ) ) ;
#165746 = CARTESIAN_POINT ( 'NONE',  ( 16.53943276465976808, 0.05219959533934440121, 111.2510903946856899 ) ) ;
#165748 = EDGE_CURVE ( 'NONE', #24895, #109664, #159196, .T. ) ;
#165747 = CARTESIAN_POINT ( 'NONE',  ( 13.97604488694527802, 13.89961937509977652, 89.37390960531436690 ) ) ;
#165749 = CARTESIAN_POINT ( 'NONE',  ( -15.72974639402176322, -15.80617190586768395, 54.37609039468568994 ) ) ;
#165750 = CARTESIAN_POINT ( 'NONE',  ( 21.55341960407610458, 5.719274019375980345, 48.95724293864770971 ) ) ;
#165751 = CARTESIAN_POINT ( 'NONE',  ( 21.53943276465977519, -0.05219959533907433946, 113.7489096053143527 ) ) ;
#165752 = CARTESIAN_POINT ( 'NONE',  ( 21.52544592524344225, -5.823673210054117533, 73.54057627198102409 ) ) ;
#165753 = CARTESIAN_POINT ( 'NONE',  ( 16.53943276465976808, -0.05219959533910856209, 98.74890960531438111 ) ) ;
#165754 = CARTESIAN_POINT ( 'NONE',  ( 19.02544592524334988, 5.153800228976608722, 56.45942372801898301 ) ) ;
#165755 = CARTESIAN_POINT ( 'NONE',  ( -16.51473224551069308, -9.474510206698971260, 26.66557627198103120 ) ) ;
#165756 = CARTESIAN_POINT ( 'NONE',  ( 16.46253265017160672, -9.564922557960803928, 83.33224293864768129 ) ) ;
#165757 = CARTESIAN_POINT ( 'NONE',  ( -5.049401038298153566, 19.05341960407611168, 80.20724293864769550 ) ) ;
#165758 = CARTESIAN_POINT ( 'NONE',  ( 8.224510206698953496, -14.34966873604960469, 102.9155762719810383 ) ) ;
#165759 = VERTEX_POINT ( 'NONE', #18724 ) ;
#165760 = CARTESIAN_POINT ( 'NONE',  ( 8.314922557960818139, 14.29746914071049879, 29.58224293864769905 ) ) ;
#165761 = CARTESIAN_POINT ( 'NONE',  ( -14.29746914071037622, -8.314922557961029526, 34.16775706135234714 ) ) ;
#165762 = CARTESIAN_POINT ( 'NONE',  ( -0.05219959533937732626, 21.53943276465977519, 102.5010903946856899 ) ) ;
#165763 = CARTESIAN_POINT ( 'NONE',  ( 9.564922557960805705, 16.46253265017160317, 104.5822429386476955 ) ) ;
#165764 = CARTESIAN_POINT ( 'NONE',  ( -5.823673210054431948, 21.52544592524334988, 37.70942372801900433 ) ) ;
#165765 = CARTESIAN_POINT ( 'NONE',  ( 19.03943276465977164, -0.05219959533909143690, 43.74890960531435979 ) ) ;
#165766 = CARTESIAN_POINT ( 'NONE',  ( -12.14591786802326823, 12.06949235617739902, 43.12609039468568284 ) ) ;
#165767 = CARTESIAN_POINT ( 'NONE',  ( -12.14591786802326823, 12.06949235617739902, 98.12609039468570415 ) ) ;
#165768 = CARTESIAN_POINT ( 'NONE',  ( -9.474510206698720793, -16.51473224551083518, 109.5844237280190043 ) ) ;
#165769 = CARTESIAN_POINT ( 'NONE',  ( -19.02544592524342804, 5.153800228976336051, 41.04057627198103120 ) ) ;
#165770 = VECTOR ( 'NONE', #29707, 1000.000000000000000 ) ;
#165771 = CARTESIAN_POINT ( 'NONE',  ( 14.34966873604960469, 8.224510206698951720, 99.16557627198100988 ) ) ;
#165772 = CARTESIAN_POINT ( 'NONE',  ( 15.80617190586746368, 15.72974639402197994, 99.37390960531436690 ) ) ;
#165773 = CARTESIAN_POINT ( 'NONE',  ( 19.02544592524334988, 5.153800228976608722, 76.45942372801897591 ) ) ;
#165774 = CARTESIAN_POINT ( 'NONE',  ( -19.02544592524342804, 5.153800228976336051, 26.04057627198103120 ) ) ;
#165775 = CARTESIAN_POINT ( 'NONE',  ( 9.564922557960805705, 16.46253265017160317, 89.58224293864769550 ) ) ;
#165776 = CARTESIAN_POINT ( 'NONE',  ( 10.72451020669871369, 18.67979575497193778, 37.08442372801901143 ) ) ;
#165777 = CARTESIAN_POINT ( 'NONE',  ( -37.99626262588765968, 12.34573411038917179, -3.847842220587804007 ) ) ;
#165778 = CARTESIAN_POINT ( 'NONE',  ( -9.564922557960796823, -16.46253265017161027, 92.08224293864769550 ) ) ;
#165779 = CARTESIAN_POINT ( 'NONE',  ( -38.00000000000000711, 2.428612866367529932E-14, -5.749999994537626336 ) ) ;
#165780 = CARTESIAN_POINT ( 'NONE',  ( -5.049401038298153566, 19.05341960407611168, 90.20724293864766707 ) ) ;
#165782 = CARTESIAN_POINT ( 'NONE',  ( -12.06949235617756955, 12.14591786802309770, 90.62390960531436690 ) ) ;
#165781 = CARTESIAN_POINT ( 'NONE',  ( 18.67979575497194134, -10.72451020669871369, 25.83442372801901499 ) ) ;
#165783 = CARTESIAN_POINT ( 'NONE',  ( -9.474510206698964154, 16.51473224551069663, 90.41557627198103830 ) ) ;
#165784 = CARTESIAN_POINT ( 'NONE',  ( -9.564922557961040184, 16.46253265017147172, 27.91775706135232582 ) ) ;
#165785 = CARTESIAN_POINT ( 'NONE',  ( 12.06949235617739724, 12.14591786802326823, 56.87609039468568994 ) ) ;
#165786 = CARTESIAN_POINT ( 'NONE',  ( -10.81492255796105439, 18.62759615963255655, 77.91775706135231871 ) ) ;
#165787 = CARTESIAN_POINT ( 'NONE',  ( 0.05219959533934541429, -16.53943276465976808, 40.00109039468567573 ) ) ;
#165788 = CARTESIAN_POINT ( 'NONE',  ( -19.02544592524342804, 5.153800228976336051, 71.04057627198099567 ) ) ;
#165789 = CARTESIAN_POINT ( 'NONE',  ( 0.05219959533936267826, -19.03943276465977164, 95.00109039468567573 ) ) ;
#165790 = CARTESIAN_POINT ( 'NONE',  ( 8.314922557961029526, -14.29746914071037800, 75.41775706135233293 ) ) ;
#165791 = CARTESIAN_POINT ( 'NONE',  ( 0.05219959533936267826, -19.03943276465977164, 20.00109039468567218 ) ) ;
#165792 = CARTESIAN_POINT ( 'NONE',  ( -5.049401038297874678, -19.05341960407617918, 84.79275706135233293 ) ) ;
#165793 = CARTESIAN_POINT ( 'NONE',  ( -0.05219959533909027116, -19.03943276465977164, 67.49890960531436690 ) ) ;
#165794 = CARTESIAN_POINT ( 'NONE',  ( -5.823673210054116645, -21.52544592524344225, 87.29057627198103830 ) ) ;
#165796 = CARTESIAN_POINT ( 'NONE',  ( -9.474510206698720793, -16.51473224551083518, 94.58442372801900433 ) ) ;
#165795 = CARTESIAN_POINT ( 'NONE',  ( 12.06949235617757843, -12.14591786802309237, 73.12390960531436690 ) ) ;
#165797 = CARTESIAN_POINT ( 'NONE',  ( 24.85114155361847565, 5.582993631601034679, 168.8590791472286412 ) ) ;
#165798 = CARTESIAN_POINT ( 'NONE',  ( 5.049401038297881783, 19.05341960407617563, 57.29275706135231871 ) ) ;
#165799 = CARTESIAN_POINT ( 'NONE',  ( -14.34966873604972548, 8.224510206698743886, 113.3344237280190328 ) ) ;
#165800 = CARTESIAN_POINT ( 'NONE',  ( -4.379528057220328563, 16.55341960407611168, 75.20724293864769550 ) ) ;
#165802 = CARTESIAN_POINT ( 'NONE',  ( -17.40805194821983903, 6.112264579160790134, 40.83371272510607497 ) ) ;
#165801 = CARTESIAN_POINT ( 'NONE',  ( 5.049401038297881783, 19.05341960407617563, 27.29275706135232937 ) ) ;
#165803 = CARTESIAN_POINT ( 'NONE',  ( -0.05219959533907301413, -21.53943276465977519, 107.4989096053143669 ) ) ;
#165804 = CARTESIAN_POINT ( 'NONE',  ( 5.049401038298161559, -19.05341960407611168, 97.70724293864766707 ) ) ;
#165805 = CARTESIAN_POINT ( 'NONE',  ( 13.97604488694527802, 13.89961937509977652, 74.37390960531436690 ) ) ;
#165806 = CARTESIAN_POINT ( 'NONE',  ( -18.67979575497193778, 10.72451020669871902, 83.33442372801903275 ) ) ;
#165807 = CARTESIAN_POINT ( 'NONE',  ( 16.46253265017160672, -9.564922557960803928, 68.33224293864770971 ) ) ;
#165808 = CARTESIAN_POINT ( 'NONE',  ( 19.02544592524343514, -5.153800228976328945, 43.54057627198103120 ) ) ;
#165809 = CARTESIAN_POINT ( 'NONE',  ( -21.53943276465977519, 0.05219959533907696930, 26.24890960531435624 ) ) ;
#165810 = CARTESIAN_POINT ( 'NONE',  ( 16.53943276465976808, -0.05219959533910856209, 78.74890960531436690 ) ) ;
#165811 = CARTESIAN_POINT ( 'NONE',  ( 9.564922557960805705, 16.46253265017160317, 49.58224293864770260 ) ) ;
#165812 = CARTESIAN_POINT ( 'NONE',  ( -14.34966873604960291, -8.224510206698953496, 101.6655762719810383 ) ) ;
#165813 = CARTESIAN_POINT ( 'NONE',  ( 21.52544592524344225, -5.823673210054117533, 103.5405762719810383 ) ) ;
#165814 = CARTESIAN_POINT ( 'NONE',  ( 5.719274019375673035, 21.55341960407619339, 47.29275706135234003 ) ) ;
#165815 = CARTESIAN_POINT ( 'NONE',  ( -5.049401038298153566, 19.05341960407611168, 25.20724293864768484 ) ) ;
#165816 = EDGE_CURVE ( 'NONE', #115376, #157973, #127864, .T. ) ;
#165817 = CARTESIAN_POINT ( 'NONE',  ( 0.05219959533934541429, -16.53943276465976808, 70.00109039468568994 ) ) ;
#165818 = CARTESIAN_POINT ( 'NONE',  ( -10.81492255796078084, -18.62759615963271287, 97.08224293864770971 ) ) ;
#165819 = CARTESIAN_POINT ( 'NONE',  ( -21.55341960407610458, -5.719274019375992779, 101.4572429386476955 ) ) ;
#165821 = CARTESIAN_POINT ( 'NONE',  ( 19.03943276465977164, -0.05219959533909143690, 48.74890960531435979 ) ) ;
#165820 = CARTESIAN_POINT ( 'NONE',  ( 16.51473224551083163, -9.474510206698727899, 35.83442372801899722 ) ) ;
#165822 = DIRECTION ( 'NONE',  ( -0.000000000000000000, 0.000000000000000000, -1.000000000000000000 ) ) ;
#165823 = CARTESIAN_POINT ( 'NONE',  ( 21.55341960407619695, -5.719274019375665929, 51.04275706135234714 ) ) ;
#165824 = CARTESIAN_POINT ( 'NONE',  ( 10.72451020669898902, -18.67979575497178502, 52.91557627198103830 ) ) ;
#165825 = CARTESIAN_POINT ( 'NONE',  ( -8.314922557960811034, -14.29746914071050412, 42.08224293864769550 ) ) ;
#165827 = CARTESIAN_POINT ( 'NONE',  ( 21.52544592524334988, 5.823673210054432836, 106.4594237280190328 ) ) ;
#165826 = CARTESIAN_POINT ( 'NONE',  ( -15.72974639402176322, -15.80617190586768395, 79.37609039468567573 ) ) ;
#165828 = CARTESIAN_POINT ( 'NONE',  ( -16.53943276465976808, 0.05219959533911058130, 101.2489096053143669 ) ) ;
#165829 = CARTESIAN_POINT ( 'NONE',  ( -19.02544592524334988, -5.153800228976617603, 38.95942372801900433 ) ) ;
#165830 = CARTESIAN_POINT ( 'NONE',  ( 16.53943276465976808, 0.05219959533934440121, 106.2510903946856757 ) ) ;
#165831 = CARTESIAN_POINT ( 'NONE',  ( -21.53943276465977519, -0.05219959533937600094, 68.75109039468568994 ) ) ;
#165832 = CARTESIAN_POINT ( 'NONE',  ( 19.02544592524343514, -5.153800228976328945, 53.54057627198102409 ) ) ;
#165833 = CARTESIAN_POINT ( 'NONE',  ( -19.05341960407617563, 5.049401038297882671, 28.54275706135232937 ) ) ;
#165834 = CARTESIAN_POINT ( 'NONE',  ( 5.719274019375991003, -21.55341960407610458, 42.70724293864770260 ) ) ;
#165835 = CARTESIAN_POINT ( 'NONE',  ( 21.52544592524334988, 5.823673210054432836, 31.45942372801901854 ) ) ;
#165836 = CARTESIAN_POINT ( 'NONE',  ( 0.05219959533907565091, 21.53943276465977519, 94.99890960531436690 ) ) ;
#165837 = CARTESIAN_POINT ( 'NONE',  ( -19.03943276465977164, -0.05219959533935918106, 83.75109039468567573 ) ) ;
#165838 = CARTESIAN_POINT ( 'NONE',  ( 16.53943276465976808, 0.05219959533934440121, 56.25109039468568284 ) ) ;
#165840 = CARTESIAN_POINT ( 'NONE',  ( -21.52544592524343514, 5.823673210054127303, 96.04057627198102409 ) ) ;
#165839 = CARTESIAN_POINT ( 'NONE',  ( -6.673813065215404627, 4.619076279717873490, -62.12322917040971504 ) ) ;
#165842 = CARTESIAN_POINT ( 'NONE',  ( -14.29746914071049879, 8.314922557960819915, 75.83224293864769550 ) ) ;
#165841 = CARTESIAN_POINT ( 'NONE',  ( 16.52544592524335698, 4.483927247898782831, 81.45942372801900433 ) ) ;
#165843 = CARTESIAN_POINT ( 'NONE',  ( -17.49999999999998579, -5.499999999999973355, 101.2823096230356583 ) ) ;
#165844 = CARTESIAN_POINT ( 'NONE',  ( -5.153800228976607833, 19.02544592524334988, 107.7094237280189759 ) ) ;
#165845 = AXIS2_PLACEMENT_3D ( 'NONE', #22535, #147889, #192388 ) ;
#165846 = CARTESIAN_POINT ( 'NONE',  ( -18.67979575497178146, -10.72451020669898902, 31.66557627198102054 ) ) ;
#165847 = CARTESIAN_POINT ( 'NONE',  ( -32.00000000000000000, -5.510910596163089556E-15, 45.00000000000000000 ) ) ;
#165848 = CARTESIAN_POINT ( 'NONE',  ( 8.314922557961029526, -14.29746914071037800, 55.41775706135234714 ) ) ;
#165849 = CARTESIAN_POINT ( 'NONE',  ( -0.05219959533937732626, 21.53943276465977519, 32.50109039468568284 ) ) ;
#165850 = CARTESIAN_POINT ( 'NONE',  ( -18.62759615963270932, 10.81492255796079327, 40.83224293864769550 ) ) ;
#165851 = CARTESIAN_POINT ( 'NONE',  ( 12.06949235617739724, 12.14591786802326823, 76.87609039468567573 ) ) ;
#165852 = CARTESIAN_POINT ( 'NONE',  ( -19.03943276465977164, 0.05219959533909376836, 86.24890960531436690 ) ) ;
#165854 = CARTESIAN_POINT ( 'NONE',  ( -13.97604488694527625, -13.89961937509977652, 21.87390960531435979 ) ) ;
#165853 = CARTESIAN_POINT ( 'NONE',  ( -18.67979575497193778, 10.72451020669871902, 53.33442372801901854 ) ) ;
#165855 = CARTESIAN_POINT ( 'NONE',  ( -21.53943276465977519, 0.05219959533907696930, 36.24890960531435979 ) ) ;
#165856 = ORIENTED_EDGE ( 'NONE', *, *, #132474, .F. ) ;
#165857 = CARTESIAN_POINT ( 'NONE',  ( 16.51473224551083163, -9.474510206698727899, 35.83442372801899722 ) ) ;
#165858 = CARTESIAN_POINT ( 'NONE',  ( 14.34966873604972726, -8.224510206698740333, 55.83442372801901854 ) ) ;
#165859 = CARTESIAN_POINT ( 'NONE',  ( 10.72451020669898902, -18.67979575497178502, 22.91557627198102765 ) ) ;
#165860 = VERTEX_POINT ( 'NONE', #80371 ) ;
#165861 = CARTESIAN_POINT ( 'NONE',  ( -19.03943276465977164, 0.05219959533909376836, 91.24890960531436690 ) ) ;
#165862 = CARTESIAN_POINT ( 'NONE',  ( -0.05219959533934338120, 16.53943276465976808, 97.50109039468567573 ) ) ;
#165863 = CARTESIAN_POINT ( 'NONE',  ( -16.46253265017160317, 9.564922557960807481, 115.8322429386477097 ) ) ;
#165864 = CARTESIAN_POINT ( 'NONE',  ( 8.314922557960818139, 14.29746914071049879, 99.58224293864770971 ) ) ;
#165865 = CARTESIAN_POINT ( 'NONE',  ( 10.81492255796078972, 18.62759615963270932, 39.58224293864769550 ) ) ;
#165866 = CARTESIAN_POINT ( 'NONE',  ( 9.564922557960805705, 16.46253265017160317, 29.58224293864769550 ) ) ;
#165867 = CARTESIAN_POINT ( 'NONE',  ( 12.14591786802327356, -12.06949235617739191, 75.62609039468567573 ) ) ;
#165868 = CARTESIAN_POINT ( 'NONE',  ( -21.55341960407610458, -5.719274019375992779, 111.4572429386476813 ) ) ;
#165869 = CARTESIAN_POINT ( 'NONE',  ( 16.51473224551083163, -9.474510206698727899, 70.83442372801900433 ) ) ;
#165870 = CARTESIAN_POINT ( 'NONE',  ( -19.02544592524342804, 5.153800228976336051, 41.04057627198103120 ) ) ;
#165871 = CARTESIAN_POINT ( 'NONE',  ( -5.049401038298153566, 19.05341960407611168, 115.2072429386477097 ) ) ;
#165872 = CARTESIAN_POINT ( 'NONE',  ( -5.719274019375665041, -21.55341960407619695, 99.79275706135234714 ) ) ;
#165873 = CARTESIAN_POINT ( 'NONE',  ( 5.153800228976335163, 19.02544592524342804, 59.79057627198100988 ) ) ;
#165874 = CARTESIAN_POINT ( 'NONE',  ( -16.53943276465976808, -0.05219959533934237506, 48.75109039468568284 ) ) ;
#165875 = CARTESIAN_POINT ( 'NONE',  ( 15.72974639402176855, 15.80617190586768217, 91.87609039468568994 ) ) ;
#165876 = CARTESIAN_POINT ( 'NONE',  ( 5.049401038297881783, 19.05341960407617563, 37.29275706135232582 ) ) ;
#165877 = CARTESIAN_POINT ( 'NONE',  ( 5.049401038297881783, 19.05341960407617563, 57.29275706135231871 ) ) ;
#165878 = ORIENTED_EDGE ( 'NONE', *, *, #98431, .T. ) ;
#165879 = CARTESIAN_POINT ( 'NONE',  ( 0.05219959533937995610, -21.53943276465977519, 45.00109039468568284 ) ) ;
#165880 = CARTESIAN_POINT ( 'NONE',  ( -13.97604488694527625, -13.89961937509977830, 56.87390960531435269 ) ) ;
#165881 = CARTESIAN_POINT ( 'NONE',  ( -0.05219959533936034679, 19.03943276465977164, 47.50109039468566863 ) ) ;
#165882 = CARTESIAN_POINT ( 'NONE',  ( -16.51473224551069308, -9.474510206698971260, 106.6655762719810383 ) ) ;
#165883 = CARTESIAN_POINT ( 'NONE',  ( -19.02544592524342804, 5.153800228976336051, 81.04057627198103830 ) ) ;
#165884 = CARTESIAN_POINT ( 'NONE',  ( -16.53943276465976808, 0.05219959533911058130, 41.24890960531435269 ) ) ;
#165885 = CARTESIAN_POINT ( 'NONE',  ( 15.80617190586746368, 15.72974639402197994, 39.37390960531436690 ) ) ;
#165886 = CARTESIAN_POINT ( 'NONE',  ( -22.81625015709509441, -31.40387420917324590, -4.824999997268813345 ) ) ;
#165887 = DIRECTION ( 'NONE',  ( 1.000000000000000000, 8.881784197001252323E-16, 0.000000000000000000 ) ) ;
#165888 = CARTESIAN_POINT ( 'NONE',  ( -21.53943276465977519, -0.05219959533937600094, 98.75109039468568994 ) ) ;
#165889 = LINE ( 'NONE', #60666, #83121 ) ;
#165890 = CARTESIAN_POINT ( 'NONE',  ( -5.153800228976328057, -19.02544592524343514, 37.29057627198102409 ) ) ;
#165891 = CARTESIAN_POINT ( 'NONE',  ( -13.89961937509977652, 13.97604488694528158, 110.6239096053143243 ) ) ;
#165892 = CARTESIAN_POINT ( 'NONE',  ( -33.73406392173259150, -5.500497537618388222, 95.16330145977875077 ) ) ;
#165893 = LINE ( 'NONE', #39536, #150248 ) ;
#165894 = CARTESIAN_POINT ( 'NONE',  ( -8.224510206698735004, -14.34966873604973081, 64.58442372801900433 ) ) ;
#165895 = CARTESIAN_POINT ( 'NONE',  ( -0.05219959533907301413, -21.53943276465977519, 87.49890960531436690 ) ) ;
#165896 = CARTESIAN_POINT ( 'NONE',  ( 4.379528057220339221, -16.55341960407611168, 42.70724293864770260 ) ) ;
#165898 = CARTESIAN_POINT ( 'NONE',  ( -19.05341960407611168, -5.049401038298163336, 111.4572429386476671 ) ) ;
#165897 = CARTESIAN_POINT ( 'NONE',  ( 13.89961937509977652, -13.97604488694527269, 28.12390960531435624 ) ) ;
#165899 = CARTESIAN_POINT ( 'NONE',  ( -10.72451020669870658, -18.67979575497194134, 24.58442372801901499 ) ) ;
#165900 = CARTESIAN_POINT ( 'NONE',  ( -5.049401038297874678, -19.05341960407617918, 29.79275706135232227 ) ) ;
#165901 = CARTESIAN_POINT ( 'NONE',  ( 9.564922557960805705, 16.46253265017160317, 29.58224293864769550 ) ) ;
#165902 = CARTESIAN_POINT ( 'NONE',  ( 10.72451020669871369, 18.67979575497193778, 77.08442372801901854 ) ) ;
#165903 = CARTESIAN_POINT ( 'NONE',  ( -25.25560589046783733, -4.310829775027113620, 167.9999999999999716 ) ) ;
#165904 = CARTESIAN_POINT ( 'NONE',  ( -12.14591786802309592, -12.06949235617757132, 21.87390960531436690 ) ) ;
#165905 = CARTESIAN_POINT ( 'NONE',  ( -5.950531402560715689E-15, 38.81732327939063509, -1.624999997268813390 ) ) ;
#165906 = CARTESIAN_POINT ( 'NONE',  ( 10.81492255796078972, 18.62759615963270932, 29.58224293864769905 ) ) ;
#165907 = CARTESIAN_POINT ( 'NONE',  ( 14.34966873604960469, 8.224510206698951720, 104.1655762719810241 ) ) ;
#165908 = CARTESIAN_POINT ( 'NONE',  ( -17.97058386085787163, -5.500000000000058620, 39.00390968646216550 ) ) ;
#165909 = CARTESIAN_POINT ( 'NONE',  ( 9.564922557960805705, 16.46253265017160317, 94.58224293864769550 ) ) ;
#165910 = CARTESIAN_POINT ( 'NONE',  ( 4.379528057220339221, -16.55341960407611168, 77.70724293864770971 ) ) ;
#165911 = CARTESIAN_POINT ( 'NONE',  ( -5.049401038297874678, -19.05341960407617918, 99.79275706135234714 ) ) ;
#165912 = CARTESIAN_POINT ( 'NONE',  ( 21.53943276465977519, -0.05219959533907433946, 68.74890960531435269 ) ) ;
#165913 = ORIENTED_EDGE ( 'NONE', *, *, #97744, .F. ) ;
#165914 = CARTESIAN_POINT ( 'NONE',  ( 0.05219959533909260263, 19.03943276465977164, 34.99890960531435979 ) ) ;
#165915 = EDGE_CURVE ( 'NONE', #10420, #49922, #52028, .T. ) ;
#165917 = CARTESIAN_POINT ( 'NONE',  ( 10.81492255796078972, 18.62759615963270932, 89.58224293864768129 ) ) ;
#165916 = CARTESIAN_POINT ( 'NONE',  ( 19.05341960407611168, 5.049401038298154454, 88.95724293864769550 ) ) ;
#165918 = AXIS2_PLACEMENT_3D ( 'NONE', #117395, #136544, #87059 ) ;
#165920 = CARTESIAN_POINT ( 'NONE',  ( -9.564922557960796823, -16.46253265017161027, 82.08224293864768129 ) ) ;
#165919 = CARTESIAN_POINT ( 'NONE',  ( -4.379528057220086978, -16.55341960407618274, 99.79275706135234714 ) ) ;
#165921 = CARTESIAN_POINT ( 'NONE',  ( 0.05219959533936267826, -19.03943276465977164, 85.00109039468567573 ) ) ;
#165922 = CARTESIAN_POINT ( 'NONE',  ( -21.52544592524334988, -5.823673210054445271, 88.95942372801901854 ) ) ;
#165923 = CARTESIAN_POINT ( 'NONE',  ( -21.53943276465977519, 0.05219959533907696930, 76.24890960531435269 ) ) ;
#165924 = CARTESIAN_POINT ( 'NONE',  ( 5.719274019375991003, -21.55341960407610458, 32.70724293864770260 ) ) ;
#165925 = CARTESIAN_POINT ( 'NONE',  ( 16.51473224551069308, 9.474510206698969483, 49.16557627198102409 ) ) ;
#165926 = CARTESIAN_POINT ( 'NONE',  ( -16.55341960407611168, -4.379528057220339221, 26.45724293864768839 ) ) ;
#165927 = CARTESIAN_POINT ( 'NONE',  ( -9.474510206698964154, 16.51473224551069663, 70.41557627198102409 ) ) ;
#165928 = DIRECTION ( 'NONE',  ( 0.000000000000000000, 0.000000000000000000, 1.000000000000000000 ) ) ;
#165929 = CARTESIAN_POINT ( 'NONE',  ( -16.46253265017146816, -9.564922557961047289, 19.16775706135233293 ) ) ;
#165930 = CARTESIAN_POINT ( 'NONE',  ( 0.05219959533910956823, 16.53943276465976808, 69.99890960531435269 ) ) ;
#165931 = CARTESIAN_POINT ( 'NONE',  ( -5.823673210054116645, -21.52544592524344225, 107.2905762719810525 ) ) ;
#165932 = CARTESIAN_POINT ( 'NONE',  ( -21.55341960407610458, -5.719274019375992779, 111.4572429386476813 ) ) ;
#165933 = CARTESIAN_POINT ( 'NONE',  ( 17.14385361876520264, -23.59649016807271238, 140.0750000027311728 ) ) ;
#165934 = CARTESIAN_POINT ( 'NONE',  ( -18.67979575497178146, -10.72451020669898902, 61.66557627198103120 ) ) ;
#165935 = CARTESIAN_POINT ( 'NONE',  ( 8.314922557961029526, -14.29746914071037800, 90.41775706135236135 ) ) ;
#165936 = CARTESIAN_POINT ( 'NONE',  ( 16.53943276465976808, -0.05219959533910856209, 98.74890960531438111 ) ) ;
#165937 = CARTESIAN_POINT ( 'NONE',  ( -16.46253265017160317, 9.564922557960807481, 55.83224293864769550 ) ) ;
#165938 = CARTESIAN_POINT ( 'NONE',  ( -16.53943276465976808, 0.05219959533911058130, 36.24890960531435979 ) ) ;
#165939 = ORIENTED_EDGE ( 'NONE', *, *, #115128, .T. ) ;
#165940 = CARTESIAN_POINT ( 'NONE',  ( -5.823673210054431948, 21.52544592524334988, 42.70942372801901854 ) ) ;
#165941 = CARTESIAN_POINT ( 'NONE',  ( -19.05341960407611168, -5.049401038298163336, 111.4572429386476671 ) ) ;
#165942 = CARTESIAN_POINT ( 'NONE',  ( 15.80617190586769283, -15.72974639402175789, 75.62609039468567573 ) ) ;
#165943 = CARTESIAN_POINT ( 'NONE',  ( -16.51473224551069308, -9.474510206698971260, 26.66557627198103120 ) ) ;
#165944 = CARTESIAN_POINT ( 'NONE',  ( -19.05341960407611168, -5.049401038298163336, 41.45724293864769550 ) ) ;
#165945 = ORIENTED_EDGE ( 'NONE', *, *, #42863, .F. ) ;
#165946 = CARTESIAN_POINT ( 'NONE',  ( -5.823673210054431948, 21.52544592524334988, 82.70942372801900433 ) ) ;
#165947 = CARTESIAN_POINT ( 'NONE',  ( 16.53943276465976808, 0.05219959533934440121, 51.25109039468568994 ) ) ;
#165948 = CARTESIAN_POINT ( 'NONE',  ( -18.67979575497193778, 10.72451020669871902, 68.33442372801900433 ) ) ;
#165949 = CARTESIAN_POINT ( 'NONE',  ( 5.153800228976335163, 19.02544592524342804, 99.79057627198102409 ) ) ;
#165950 = CARTESIAN_POINT ( 'NONE',  ( 19.03943276465977164, 0.05219959533936151252, 81.25109039468567573 ) ) ;
#165951 = CARTESIAN_POINT ( 'NONE',  ( 5.823673210054444382, -21.52544592524334988, 55.20942372801902565 ) ) ;
#165952 = CARTESIAN_POINT ( 'NONE',  ( -0.05219959533934338120, 16.53943276465976808, 22.50109039468567573 ) ) ;
#165953 = CARTESIAN_POINT ( 'NONE',  ( 19.05341960407617918, -5.049401038297876454, 76.04275706135230450 ) ) ;
#165954 = CARTESIAN_POINT ( 'NONE',  ( -0.05219959533909027116, -19.03943276465977164, 57.49890960531435979 ) ) ;
#165955 = CARTESIAN_POINT ( 'NONE',  ( -5.049401038297874678, -19.05341960407617918, 89.79275706135230450 ) ) ;
#165956 = CARTESIAN_POINT ( 'NONE',  ( -4.483927247898539470, -16.52544592524342804, 27.29057627198103120 ) ) ;
#165957 = CARTESIAN_POINT ( 'NONE',  ( -13.89961937509957401, -13.97604488694547875, 89.37609039468563310 ) ) ;
#165958 = CARTESIAN_POINT ( 'NONE',  ( 16.52544592524342804, -4.483927247898539470, 33.54057627198102409 ) ) ;
#165959 = CARTESIAN_POINT ( 'NONE',  ( 19.05341960407617918, -5.049401038297876454, 61.04275706135232582 ) ) ;
#165960 = CARTESIAN_POINT ( 'NONE',  ( -16.55341960407617563, 4.379528057220093196, 48.54275706135234714 ) ) ;
#165961 = CARTESIAN_POINT ( 'NONE',  ( -9.474510206698720793, -16.51473224551083518, 29.58442372801900433 ) ) ;
#165962 = CARTESIAN_POINT ( 'NONE',  ( 19.05341960407611168, 5.049401038298154454, 48.95724293864768129 ) ) ;
#165963 = CARTESIAN_POINT ( 'NONE',  ( 4.483927247898790824, -16.52544592524335698, 40.20942372801901854 ) ) ;
#165964 = DIRECTION ( 'NONE',  ( 0.000000000000000000, -1.000000000000000000, 0.000000000000000000 ) ) ;
#165965 = CARTESIAN_POINT ( 'NONE',  ( -17.14385361876520619, 23.59649016807275856, 146.5750000027311444 ) ) ;
#165966 = CARTESIAN_POINT ( 'NONE',  ( 16.46253265017160672, -9.564922557960803928, 98.33224293864769550 ) ) ;
#165967 = CARTESIAN_POINT ( 'NONE',  ( 5.153800228976617603, -19.02544592524335343, 85.20942372801900433 ) ) ;
#165968 = EDGE_LOOP ( 'NONE', ( #59129, #31212 ) ) ;
#165969 = CARTESIAN_POINT ( 'NONE',  ( -13.89961937509957401, -13.97604488694547875, 94.37609039468566152 ) ) ;
#165970 = CARTESIAN_POINT ( 'NONE',  ( 21.55341960407610458, 5.719274019375980345, 28.95724293864769905 ) ) ;
#165972 = CARTESIAN_POINT ( 'NONE',  ( -16.53943276465976808, -0.05219959533934237506, 18.75109039468568639 ) ) ;
#165971 = CARTESIAN_POINT ( 'NONE',  ( -15.80617190586768217, 15.72974639402176855, 108.1260903946856757 ) ) ;
#165973 = CARTESIAN_POINT ( 'NONE',  ( -14.34966873604960291, -8.224510206698953496, 111.6655762719810525 ) ) ;
#165974 = CARTESIAN_POINT ( 'NONE',  ( -16.51473224551069308, -9.474510206698971260, 36.66557627198102409 ) ) ;
#165975 = CARTESIAN_POINT ( 'NONE',  ( 0.05219959533907565091, 21.53943276465977519, 74.99890960531435269 ) ) ;
#165976 = VECTOR ( 'NONE', #134335, 999.9999999999998863 ) ;
#165977 = CARTESIAN_POINT ( 'NONE',  ( 0.05219959533909260263, 19.03943276465977164, 39.99890960531436690 ) ) ;
#165978 = CARTESIAN_POINT ( 'NONE',  ( 0.000000000000000000, 0.000000000000000000, -52.65483682830183199 ) ) ;
#165979 = CARTESIAN_POINT ( 'NONE',  ( 19.05341960407617918, -5.049401038297876454, 66.04275706135233293 ) ) ;
#165980 = CARTESIAN_POINT ( 'NONE',  ( -12.14591786802309592, -12.06949235617757132, 56.87390960531436690 ) ) ;
#165982 = EDGE_CURVE ( 'NONE', #2008, #86900, #197917, .T. ) ;
#165981 = CARTESIAN_POINT ( 'NONE',  ( -5.719274019375978568, 21.55341960407610458, 30.20724293864769550 ) ) ;
#165983 = CARTESIAN_POINT ( 'NONE',  ( 15.72974639402176855, 15.80617190586768217, 86.87609039468568994 ) ) ;
#165984 = CARTESIAN_POINT ( 'NONE',  ( 21.55341960407610458, 5.719274019375980345, 88.95724293864769550 ) ) ;
#165985 = CARTESIAN_POINT ( 'NONE',  ( 5.719274019375673035, 21.55341960407619339, 57.29275706135234714 ) ) ;
#165986 = CARTESIAN_POINT ( 'NONE',  ( -15.80617190586768217, 15.72974639402176855, 58.12609039468568994 ) ) ;
#165987 = CARTESIAN_POINT ( 'NONE',  ( 9.474510206698971260, -16.51473224551069308, 102.9155762719810241 ) ) ;
#165989 = CARTESIAN_POINT ( 'NONE',  ( -5.719274019375665041, -21.55341960407619695, 69.79275706135234714 ) ) ;
#165988 = CARTESIAN_POINT ( 'NONE',  ( -0.05219959533934338120, 16.53943276465976808, 87.50109039468568994 ) ) ;
#165990 = CARTESIAN_POINT ( 'NONE',  ( 19.05341960407611168, 5.049401038298154454, 58.95724293864768129 ) ) ;
#165991 = CARTESIAN_POINT ( 'NONE',  ( -16.51473224551069308, -9.474510206698971260, 21.66557627198102765 ) ) ;
#165992 = CARTESIAN_POINT ( 'NONE',  ( 16.46253265017160672, -9.564922557960803928, 53.33224293864768839 ) ) ;
#165993 = CARTESIAN_POINT ( 'NONE',  ( 16.53943276465976808, -0.05219959533910856209, 63.74890960531435979 ) ) ;
#165994 = CARTESIAN_POINT ( 'NONE',  ( 14.29746914071049879, -8.314922557960816363, 38.33224293864768839 ) ) ;
#165995 = CARTESIAN_POINT ( 'NONE',  ( 15.80617190586746368, 15.72974639402197994, 44.37390960531435979 ) ) ;
#165996 = CARTESIAN_POINT ( 'NONE',  ( -13.89961937509977652, 13.97604488694528158, 50.62390960531435979 ) ) ;
#165997 = CARTESIAN_POINT ( 'NONE',  ( -15.72974639402197994, 15.80617190586746368, 55.62390960531436690 ) ) ;
#165999 = CIRCLE ( 'NONE', #107806, 2.649999999999999911 ) ;
#165998 = CARTESIAN_POINT ( 'NONE',  ( 9.564922557961047289, -16.46253265017146816, 55.41775706135234003 ) ) ;
#166001 = CARTESIAN_POINT ( 'NONE',  ( 4.483927247898545687, 16.52544592524342804, 49.79057627198102409 ) ) ;
#166000 = LINE ( 'NONE', #12327, #88107 ) ;
#166002 = CARTESIAN_POINT ( 'NONE',  ( -18.62759615963270932, 10.81492255796079327, 35.83224293864768839 ) ) ;
#166003 = EDGE_LOOP ( 'NONE', ( #10328, #14859 ) ) ;
#166004 = ORIENTED_EDGE ( 'NONE', *, *, #63061, .T. ) ;
#166005 = CARTESIAN_POINT ( 'NONE',  ( 24.30000000000003268, -9.712231019420881533E-14, -64.92279855667830191 ) ) ;
#166006 = CARTESIAN_POINT ( 'NONE',  ( -8.224510206698735004, -14.34966873604973081, 79.58442372801903275 ) ) ;
#166007 = CARTESIAN_POINT ( 'NONE',  ( -13.89961937509957401, -13.97604488694547875, 74.37609039468566152 ) ) ;
#166008 = EDGE_CURVE ( 'NONE', #196699, #104654, #130628, .T. ) ;
#166009 = CARTESIAN_POINT ( 'NONE',  ( 14.34966873604960469, 8.224510206698951720, 49.16557627198102409 ) ) ;
#166010 = CARTESIAN_POINT ( 'NONE',  ( 17.48847506799972251, -5.747544572773699123, 53.32697437843280852 ) ) ;
#166011 = CARTESIAN_POINT ( 'NONE',  ( -8.314922557960811034, -14.29746914071050412, 37.08224293864768129 ) ) ;
#166012 = CARTESIAN_POINT ( 'NONE',  ( 13.97604488694527802, 13.89961937509977652, 54.37390960531435979 ) ) ;
#166013 = CARTESIAN_POINT ( 'NONE',  ( -9.474510206698964154, 16.51473224551069663, 75.41557627198103830 ) ) ;
#166014 = CARTESIAN_POINT ( 'NONE',  ( 13.89961937509977652, -13.97604488694527269, 38.12390960531436690 ) ) ;
#166015 = CARTESIAN_POINT ( 'NONE',  ( 5.823673210054444382, -21.52544592524334988, 40.20942372801901854 ) ) ;
#166016 = CARTESIAN_POINT ( 'NONE',  ( 5.049401038298161559, -19.05341960407611168, 72.70724293864768129 ) ) ;
#166017 = CARTESIAN_POINT ( 'NONE',  ( -0.05219959533909027116, -19.03943276465977164, 22.49890960531436690 ) ) ;
#166018 = CARTESIAN_POINT ( 'NONE',  ( 13.97604488694527802, 13.89961937509977652, 54.37390960531435979 ) ) ;
#166019 = CARTESIAN_POINT ( 'NONE',  ( -21.53943276465977519, 0.05219959533907696930, 51.24890960531436690 ) ) ;
#166020 = CARTESIAN_POINT ( 'NONE',  ( 16.51473224551069308, 9.474510206698969483, 39.16557627198103120 ) ) ;
#166021 = CARTESIAN_POINT ( 'NONE',  ( 5.719274019375991003, -21.55341960407610458, 37.70724293864769550 ) ) ;
#166022 = CARTESIAN_POINT ( 'NONE',  ( -16.52544592524335698, -4.483927247898792601, 108.9594237280190185 ) ) ;
#166023 = CARTESIAN_POINT ( 'NONE',  ( -21.53943276465977519, -0.05219959533937600094, 113.7510903946856757 ) ) ;
#166025 = CARTESIAN_POINT ( 'NONE',  ( 0.05219959533934541429, -16.53943276465976808, 80.00109039468568994 ) ) ;
#166024 = CARTESIAN_POINT ( 'NONE',  ( 12.06949235617739724, 12.14591786802326823, 51.87609039468568284 ) ) ;
#166026 = DIRECTION ( 'NONE',  ( 0.000000000000000000, -0.9945218953682734009, 0.1045284632676537068 ) ) ;
#166027 = CARTESIAN_POINT ( 'NONE',  ( -16.55341960407617563, 4.379528057220093196, 63.54275706135234003 ) ) ;
#166028 = CARTESIAN_POINT ( 'NONE',  ( 16.53943276465976808, 0.05219959533934440121, 36.25109039468567573 ) ) ;
#166029 = CARTESIAN_POINT ( 'NONE',  ( -13.97604488694527625, -13.89961937509977652, 101.8739096053143811 ) ) ;
#166030 = CARTESIAN_POINT ( 'NONE',  ( 8.224510206698742110, 14.34966873604972548, 27.08442372801901854 ) ) ;
#166031 = CARTESIAN_POINT ( 'NONE',  ( 5.153800228976335163, 19.02544592524342804, 29.79057627198102409 ) ) ;
#166032 = CARTESIAN_POINT ( 'NONE',  ( 10.72451020669871369, 18.67979575497193778, 22.08442372801901143 ) ) ;
#166033 = CARTESIAN_POINT ( 'NONE',  ( 8.224510206698742110, 14.34966873604972548, 37.08442372801901143 ) ) ;
#166034 = CARTESIAN_POINT ( 'NONE',  ( -8.314922557961024197, 14.29746914071037800, 102.9177570613523756 ) ) ;
#166035 = CARTESIAN_POINT ( 'NONE',  ( 17.50000000000000000, -5.500000000000000888, 120.0000000000000142 ) ) ;
#166036 = CARTESIAN_POINT ( 'NONE',  ( -10.72451020669870658, -18.67979575497194134, 99.58442372801900433 ) ) ;
#166037 = CARTESIAN_POINT ( 'NONE',  ( -19.05341960407617563, 5.049401038297882671, 98.54275706135233293 ) ) ;
#166038 = CARTESIAN_POINT ( 'NONE',  ( -16.53943276465976808, 0.05219959533911058130, 56.24890960531436690 ) ) ;
#166039 = CARTESIAN_POINT ( 'NONE',  ( -13.89961937509977652, 13.97604488694528158, 25.62390960531434558 ) ) ;
#166041 = FACE_OUTER_BOUND ( 'NONE', #13686, .T. ) ;
#166040 = CARTESIAN_POINT ( 'NONE',  ( 9.564922557961047289, -16.46253265017146816, 65.41775706135233293 ) ) ;
#166042 = CARTESIAN_POINT ( 'NONE',  ( -21.53943276465977519, -0.05219959533937600094, 58.75109039468568994 ) ) ;
#166043 = CARTESIAN_POINT ( 'NONE',  ( 16.55341960407618274, -4.379528057220086978, 26.04275706135235779 ) ) ;
#166044 = DIRECTION ( 'NONE',  ( 0.06104853953485701173, 0.000000000000000000, -0.9981347984218670311 ) ) ;
#166045 = CARTESIAN_POINT ( 'NONE',  ( 15.72974639402199770, -15.80617190586745480, 23.12390960531436335 ) ) ;
#166046 = CARTESIAN_POINT ( 'NONE',  ( 10.72451020669898902, -18.67979575497178502, 77.91557627198102409 ) ) ;
#166047 = CARTESIAN_POINT ( 'NONE',  ( 19.05341960407617918, -5.049401038297876454, 106.0427570613523471 ) ) ;
#166048 = CARTESIAN_POINT ( 'NONE',  ( 9.474510206698971260, -16.51473224551069308, 107.9155762719810383 ) ) ;
#166049 = CARTESIAN_POINT ( 'NONE',  ( -25.82893184620927229, 8.167111171438236283, 172.3011985515803417 ) ) ;
#166050 = CARTESIAN_POINT ( 'NONE',  ( 14.34966873604960469, 8.224510206698951720, 114.1655762719810383 ) ) ;
#166051 = CARTESIAN_POINT ( 'NONE',  ( -18.62759615963255300, -10.81492255796106328, 109.1677570613523613 ) ) ;
#166052 = CARTESIAN_POINT ( 'NONE',  ( -9.564922557960796823, -16.46253265017161027, 47.08224293864769550 ) ) ;
#166053 = CARTESIAN_POINT ( 'NONE',  ( 15.72974639402176855, 15.80617190586768217, 56.87609039468568994 ) ) ;
#166054 = CARTESIAN_POINT ( 'NONE',  ( -18.67979575497193778, 10.72451020669871902, 83.33442372801903275 ) ) ;
#166055 = CARTESIAN_POINT ( 'NONE',  ( -16.52544592524335698, -4.483927247898792601, 108.9594237280190185 ) ) ;
#166056 = CARTESIAN_POINT ( 'NONE',  ( -0.05219959533909027116, -19.03943276465977164, 82.49890960531436690 ) ) ;
#166057 = CARTESIAN_POINT ( 'NONE',  ( 21.55341960407619695, -5.719274019375665929, 41.04275706135236135 ) ) ;
#166058 = CARTESIAN_POINT ( 'NONE',  ( -15.80617190586768217, 15.72974639402176855, 58.12609039468568994 ) ) ;
#166060 = CARTESIAN_POINT ( 'NONE',  ( 13.97604488694527802, 13.89961937509977652, 94.37390960531436690 ) ) ;
#166059 = CARTESIAN_POINT ( 'NONE',  ( 16.51473224551083163, -9.474510206698727899, 75.83442372801900433 ) ) ;
#166061 = CARTESIAN_POINT ( 'NONE',  ( 8.224510206698953496, -14.34966873604960469, 97.91557627198103830 ) ) ;
#166062 = CARTESIAN_POINT ( 'NONE',  ( -18.67979575497178146, -10.72451020669898902, 101.6655762719810383 ) ) ;
#166063 = CARTESIAN_POINT ( 'NONE',  ( -4.483927247898539470, -16.52544592524342804, 77.29057627198102409 ) ) ;
#166064 = CARTESIAN_POINT ( 'NONE',  ( 16.46253265017146816, 9.564922557961045513, 21.66775706135233648 ) ) ;
#166065 = CARTESIAN_POINT ( 'NONE',  ( 16.53943276465976808, -0.05219959533910856209, 103.7489096053143669 ) ) ;
#166066 = CARTESIAN_POINT ( 'NONE',  ( 5.153800228976335163, 19.02544592524342804, 49.79057627198100988 ) ) ;
#166067 = CARTESIAN_POINT ( 'NONE',  ( -13.97604488694547697, 13.89961937509957934, 88.12609039468563310 ) ) ;
#166068 = CARTESIAN_POINT ( 'NONE',  ( 4.483927247898545687, 16.52544592524342804, 54.79057627198104541 ) ) ;
#166069 = CARTESIAN_POINT ( 'NONE',  ( 10.81492255796106328, -18.62759615963255655, 110.4177570613523756 ) ) ;
#166070 = CARTESIAN_POINT ( 'NONE',  ( 16.46253265017160672, -9.564922557960803928, 103.3322429386476955 ) ) ;
#166071 = CARTESIAN_POINT ( 'NONE',  ( -9.564922557961040184, 16.46253265017147172, 77.91775706135234714 ) ) ;
#166072 = CARTESIAN_POINT ( 'NONE',  ( 5.719274019375991003, -21.55341960407610458, 82.70724293864770971 ) ) ;
#166073 = CARTESIAN_POINT ( 'NONE',  ( 21.53943276465977519, 0.05219959533937863772, 36.25109039468567573 ) ) ;
#166074 = CARTESIAN_POINT ( 'NONE',  ( -0.05219959533934338120, 16.53943276465976808, 27.50109039468567929 ) ) ;
#166075 = CARTESIAN_POINT ( 'NONE',  ( 16.52544592524335698, 4.483927247898782831, 91.45942372801901854 ) ) ;
#166077 = CARTESIAN_POINT ( 'NONE',  ( 21.52544592524334988, 5.823673210054432836, 31.45942372801901854 ) ) ;
#166076 = CARTESIAN_POINT ( 'NONE',  ( 17.26172910966779384, 6.454744622555874223, 61.69353091350775742 ) ) ;
#166078 = CARTESIAN_POINT ( 'NONE',  ( -16.53943276465976808, 0.05219959533911058130, 116.2489096053143669 ) ) ;
#166079 = CARTESIAN_POINT ( 'NONE',  ( -30.74264578624800492, -22.33583958711396278, -9.549999994537627046 ) ) ;
#166080 = CARTESIAN_POINT ( 'NONE',  ( 4.379528057220092307, 16.55341960407617563, 67.29275706135234714 ) ) ;
#166081 = CARTESIAN_POINT ( 'NONE',  ( 4.483927247898545687, 16.52544592524342804, 89.79057627198103830 ) ) ;
#166082 = CARTESIAN_POINT ( 'NONE',  ( -15.72974639402197994, 15.80617190586746368, 80.62390960531438111 ) ) ;
#166083 = CARTESIAN_POINT ( 'NONE',  ( 14.29746914071049879, -8.314922557960816363, 28.33224293864769550 ) ) ;
#166084 = CARTESIAN_POINT ( 'NONE',  ( -16.53943276465976808, -0.05219959533934237506, 48.75109039468568284 ) ) ;
#166085 = CARTESIAN_POINT ( 'NONE',  ( -16.46253265017160317, 9.564922557960807481, 45.83224293864769550 ) ) ;
#166086 = CARTESIAN_POINT ( 'NONE',  ( -4.379528057220086978, -16.55341960407618274, 94.79275706135234714 ) ) ;
#166087 = CARTESIAN_POINT ( 'NONE',  ( -9.564922557961040184, 16.46253265017147172, 87.91775706135233293 ) ) ;
#166088 = CARTESIAN_POINT ( 'NONE',  ( -18.62759615963270932, 10.81492255796079327, 90.83224293864769550 ) ) ;
#166089 = CARTESIAN_POINT ( 'NONE',  ( -12.06949235617739369, -12.14591786802326823, 104.3760903946856899 ) ) ;
#166090 = VERTEX_POINT ( 'NONE', #100526 ) ;
#166091 = CARTESIAN_POINT ( 'NONE',  ( 16.46253265017160672, -9.564922557960803928, 113.3322429386476955 ) ) ;
#166092 = CIRCLE ( 'NONE', #143521, 5.000000000000000888 ) ;
#166093 = CARTESIAN_POINT ( 'NONE',  ( 21.53943276465977519, -0.05219959533907433946, 58.74890960531436690 ) ) ;
#166094 = ORIENTED_EDGE ( 'NONE', *, *, #114637, .T. ) ;
#166095 = CARTESIAN_POINT ( 'NONE',  ( 4.483927247898790824, -16.52544592524335698, 95.20942372801903275 ) ) ;
#166096 = ORIENTED_EDGE ( 'NONE', *, *, #142697, .T. ) ;
#166097 = CARTESIAN_POINT ( 'NONE',  ( -21.55341960407610458, -5.719274019375992779, 36.45724293864768839 ) ) ;
#166098 = CARTESIAN_POINT ( 'NONE',  ( -18.22780087662122028, 5.500000000000031086, 73.51540105326107266 ) ) ;
#166099 = CARTESIAN_POINT ( 'NONE',  ( -5.719274019375978568, 21.55341960407610458, 80.20724293864769550 ) ) ;
#166100 = CARTESIAN_POINT ( 'NONE',  ( 4.379528057220339221, -16.55341960407611168, 22.70724293864769194 ) ) ;
#166101 = CARTESIAN_POINT ( 'NONE',  ( -4.483927247898782831, 16.52544592524335698, 27.70942372801901854 ) ) ;
#166102 = CARTESIAN_POINT ( 'NONE',  ( -19.05341960407611168, -5.049401038298163336, 31.45724293864769550 ) ) ;
#166103 = CARTESIAN_POINT ( 'NONE',  ( 12.06949235617739724, 12.14591786802326823, 26.87609039468567218 ) ) ;
#166104 = CARTESIAN_POINT ( 'NONE',  ( -19.03943276465977164, 0.05219959533909376836, 51.24890960531436690 ) ) ;
#166105 = CARTESIAN_POINT ( 'NONE',  ( -28.82186960331499392, 9.364793116373565596, 147.8999999999999488 ) ) ;
#166106 = CARTESIAN_POINT ( 'NONE',  ( -0.05219959533909027116, -19.03943276465977164, 107.4989096053143527 ) ) ;
#166107 = CARTESIAN_POINT ( 'NONE',  ( 19.05341960407611168, 5.049401038298154454, 103.9572429386476671 ) ) ;
#166108 = CARTESIAN_POINT ( 'NONE',  ( 12.14591786802327356, -12.06949235617739191, 85.62609039468568994 ) ) ;
#166109 = CARTESIAN_POINT ( 'NONE',  ( -13.97604488694547697, 13.89961937509957934, 93.12609039468566152 ) ) ;
#166110 = CARTESIAN_POINT ( 'NONE',  ( 19.02544592524334988, 5.153800228976608722, 41.45942372801900433 ) ) ;
#166111 = CARTESIAN_POINT ( 'NONE',  ( 10.81492255796078972, 18.62759615963270932, 79.58224293864769550 ) ) ;
#166112 = CARTESIAN_POINT ( 'NONE',  ( 14.34966873604972726, -8.224510206698740333, 95.83442372801903275 ) ) ;
#166113 = CARTESIAN_POINT ( 'NONE',  ( 15.72974639402199770, -15.80617190586745480, 38.12390960531436690 ) ) ;
#166114 = CARTESIAN_POINT ( 'NONE',  ( 9.564922557961047289, -16.46253265017146816, 90.41775706135234714 ) ) ;
#166115 = CARTESIAN_POINT ( 'NONE',  ( -19.05341960407611168, -5.049401038298163336, 51.45724293864770260 ) ) ;
#166117 = MECHANICAL_DESIGN_GEOMETRIC_PRESENTATION_REPRESENTATION (  '', ( #4699 ), #198430 ) ;
#166116 = CARTESIAN_POINT ( 'NONE',  ( 16.46253265017160672, -9.564922557960803928, 93.33224293864769550 ) ) ;
#166118 = CARTESIAN_POINT ( 'NONE',  ( -21.55341960407619339, 5.719274019375674811, 68.54275706135234714 ) ) ;
#166119 = CARTESIAN_POINT ( 'NONE',  ( -9.564922557960796823, -16.46253265017161027, 57.08224293864769550 ) ) ;
#166120 = CARTESIAN_POINT ( 'NONE',  ( 14.29746914071049879, -8.314922557960816363, 98.33224293864769550 ) ) ;
#166121 = CARTESIAN_POINT ( 'NONE',  ( 24.06609220500530100, -14.38661408136896114, 165.8682408874383896 ) ) ;
#166122 = CARTESIAN_POINT ( 'NONE',  ( 0.05219959533910956823, 16.53943276465976808, 74.99890960531435269 ) ) ;
#166123 = CARTESIAN_POINT ( 'NONE',  ( 21.55341960407610458, 5.719274019375980345, 73.95724293864769550 ) ) ;
#166124 = CARTESIAN_POINT ( 'NONE',  ( -19.03943276465977164, -0.05219959533935918106, 93.75109039468566152 ) ) ;
#166125 = STYLED_ITEM ( 'NONE', ( #199247 ), #107481 ) ;
#166126 = CARTESIAN_POINT ( 'NONE',  ( -16.46253265017160317, 9.564922557960807481, 55.83224293864769550 ) ) ;
#166127 = CARTESIAN_POINT ( 'NONE',  ( 18.22780087662121673, 5.500000000000056843, 68.98459894673892734 ) ) ;
#166129 = CARTESIAN_POINT ( 'NONE',  ( -16.51473224551069308, -9.474510206698971260, 86.66557627198102409 ) ) ;
#166128 = CARTESIAN_POINT ( 'NONE',  ( -19.03943276465977164, 0.05219959533909376836, 71.24890960531435269 ) ) ;
#166130 = CARTESIAN_POINT ( 'NONE',  ( -14.29746914071037622, -8.314922557961029526, 64.16775706135234714 ) ) ;
#166131 = CARTESIAN_POINT ( 'NONE',  ( -16.61371651742603817, -7.165104196376042900, 51.14584930007003294 ) ) ;
#166132 = CARTESIAN_POINT ( 'NONE',  ( 5.153800228976615827, -19.02544592524334988, 50.20942372801897591 ) ) ;
#166133 = CARTESIAN_POINT ( 'NONE',  ( 36.81592377195799060, 3.639597414954547805, 49.13916779353751707 ) ) ;
#166134 = CARTESIAN_POINT ( 'NONE',  ( -13.97604488694527625, -13.89961937509977652, 111.8739096053143243 ) ) ;
#166135 = CARTESIAN_POINT ( 'NONE',  ( 16.53943276465976808, 0.05219959533934440121, 101.2510903946856757 ) ) ;
#166136 = CARTESIAN_POINT ( 'NONE',  ( 13.70000000000000817, -0.2077008434174363316, -60.44446360152740993 ) ) ;
#166137 = CARTESIAN_POINT ( 'NONE',  ( 8.224510206698742110, 14.34966873604972548, 82.08442372801901854 ) ) ;
#166138 = CARTESIAN_POINT ( 'NONE',  ( 18.22780087662122384, -5.500000000000022204, 66.01540105326107266 ) ) ;
#166139 = CARTESIAN_POINT ( 'NONE',  ( 16.53943276465976808, 0.05219959533934440121, 61.25109039468567573 ) ) ;
#166140 = CARTESIAN_POINT ( 'NONE',  ( 35.00000000000000000, -3.889087296526014814, 1.818019484660534424 ) ) ;
#166141 = CARTESIAN_POINT ( 'NONE',  ( -0.05219959533937732626, 21.53943276465977519, 62.50109039468568284 ) ) ;
#166142 = CARTESIAN_POINT ( 'NONE',  ( -19.02544592524334988, -5.153800228976617603, 73.95942372801900433 ) ) ;
#166143 = CARTESIAN_POINT ( 'NONE',  ( -19.02544592524334988, -5.153800228976617603, 28.95942372801900433 ) ) ;
#166144 = CARTESIAN_POINT ( 'NONE',  ( 9.564922557960805705, 16.46253265017160317, 69.58224293864770971 ) ) ;
#166145 = CARTESIAN_POINT ( 'NONE',  ( 9.564922557960805705, 16.46253265017160317, 49.58224293864770260 ) ) ;
#166146 = CYLINDRICAL_SURFACE ( 'NONE', #172449, 7.999999999999998224 ) ;
#166147 = CARTESIAN_POINT ( 'NONE',  ( -21.52544592524343514, 5.823673210054127303, 71.04057627198103830 ) ) ;
#166148 = CIRCLE ( 'NONE', #40269, 0.5000000000000004441 ) ;
#166149 = CARTESIAN_POINT ( 'NONE',  ( -21.55341960407610458, -5.719274019375992779, 36.45724293864768839 ) ) ;
#166150 = CARTESIAN_POINT ( 'NONE',  ( 16.55341960407611168, 4.379528057220329451, 108.9572429386476955 ) ) ;
#166151 = CARTESIAN_POINT ( 'NONE',  ( 0.05219959533934541429, -16.53943276465976808, 50.00109039468568994 ) ) ;
#166152 = ORIENTED_EDGE ( 'NONE', *, *, #190234, .T. ) ;
#166153 = EDGE_CURVE ( 'NONE', #40748, #193517, #60740, .T. ) ;
#166154 = CARTESIAN_POINT ( 'NONE',  ( -18.62759615963255300, -10.81492255796106328, 29.16775706135234003 ) ) ;
#166156 = CARTESIAN_POINT ( 'NONE',  ( -38.00000000000001421, -12.34694845685042708, -3.899999999999999911 ) ) ;
#166155 = CARTESIAN_POINT ( 'NONE',  ( 16.55341960407611168, 4.379528057220329451, 48.95724293864770971 ) ) ;
#166157 = CARTESIAN_POINT ( 'NONE',  ( -4.483927247898782831, 16.52544592524335698, 22.70942372801901499 ) ) ;
#166158 = CARTESIAN_POINT ( 'NONE',  ( -19.05341960407617563, 5.049401038297882671, 38.54275706135233293 ) ) ;
#166159 = CARTESIAN_POINT ( 'NONE',  ( -4.379528057220328563, 16.55341960407611168, 45.20724293864769550 ) ) ;
#166160 = CARTESIAN_POINT ( 'NONE',  ( 0.05219959533907565091, 21.53943276465977519, 109.9989096053143527 ) ) ;
#166162 = CARTESIAN_POINT ( 'NONE',  ( -18.62759615963270932, 10.81492255796079327, 80.83224293864769550 ) ) ;
#166161 = CYLINDRICAL_SURFACE ( 'NONE', #43933, 2.649999999999999467 ) ;
#166163 = CARTESIAN_POINT ( 'NONE',  ( 13.97604488694527802, 13.89961937509977652, 94.37390960531436690 ) ) ;
#166164 = CARTESIAN_POINT ( 'NONE',  ( 14.34966873604960469, 8.224510206698951720, 64.16557627198102409 ) ) ;
#166165 = CARTESIAN_POINT ( 'NONE',  ( 0.05219959533909260263, 19.03943276465977164, 104.9989096053143669 ) ) ;
#166166 = CARTESIAN_POINT ( 'NONE',  ( -36.78335851983072047, 5.362873614019889601, 46.23361200806721882 ) ) ;
#166167 = CARTESIAN_POINT ( 'NONE',  ( -16.46253265017146816, -9.564922557961047289, 74.16775706135234714 ) ) ;
#166168 = CARTESIAN_POINT ( 'NONE',  ( 18.62759615963271287, -10.81492255796078972, 103.3322429386476955 ) ) ;
#166169 = CARTESIAN_POINT ( 'NONE',  ( -19.03943276465977164, 0.05219959533909376836, 61.24890960531436690 ) ) ;
#166170 = CARTESIAN_POINT ( 'NONE',  ( -19.03943276465977164, 0.05219959533909376836, 21.24890960531436335 ) ) ;
#166171 = CARTESIAN_POINT ( 'NONE',  ( 18.62759615963255655, 10.81492255796105972, 51.66775706135234714 ) ) ;
#166172 = CARTESIAN_POINT ( 'NONE',  ( 22.44159573604009239, 16.30477369853692693, 148.0750000027312012 ) ) ;
#166173 = CARTESIAN_POINT ( 'NONE',  ( 0.05219959533910956823, 16.53943276465976808, 44.99890960531435979 ) ) ;
#166174 = CARTESIAN_POINT ( 'NONE',  ( -5.049401038298153566, 19.05341960407611168, 45.20724293864769550 ) ) ;
#166175 = CARTESIAN_POINT ( 'NONE',  ( 5.153800228976335163, 19.02544592524342804, 99.79057627198102409 ) ) ;
#166176 = CARTESIAN_POINT ( 'NONE',  ( 10.72451020669898902, -18.67979575497178502, 67.91557627198102409 ) ) ;
#166177 = CARTESIAN_POINT ( 'NONE',  ( 1.784210473542230573E-15, -29.16686587814331588, 147.3750000027311842 ) ) ;
#166178 = CARTESIAN_POINT ( 'NONE',  ( 19.02544592524343514, -5.153800228976328945, 38.54057627198103120 ) ) ;
#166179 = CARTESIAN_POINT ( 'NONE',  ( -18.67979575497178146, -10.72451020669898902, 61.66557627198103120 ) ) ;
#166180 = CARTESIAN_POINT ( 'NONE',  ( 10.81492255796106328, -18.62759615963255655, 80.41775706135234714 ) ) ;
#166183 = CARTESIAN_POINT ( 'NONE',  ( -16.55341960407611168, -4.379528057220339221, 81.45724293864769550 ) ) ;
#166182 = CARTESIAN_POINT ( 'NONE',  ( -8.224510206698735004, -14.34966873604973081, 89.58442372801901854 ) ) ;
#166181 = DIRECTION ( 'NONE',  ( -0.000000000000000000, -0.000000000000000000, -1.000000000000000000 ) ) ;
#166184 = CARTESIAN_POINT ( 'NONE',  ( -0.05219959533909027116, -19.03943276465977164, 67.49890960531436690 ) ) ;
#166185 = VERTEX_POINT ( 'NONE', #45586 ) ;
#166186 = CARTESIAN_POINT ( 'NONE',  ( -9.564922557961040184, 16.46253265017147172, 32.91775706135233293 ) ) ;
#166187 = CARTESIAN_POINT ( 'NONE',  ( -12.06949235617739369, -12.14591786802326823, 94.37609039468568994 ) ) ;
#166188 = CARTESIAN_POINT ( 'NONE',  ( 5.719274019375673035, 21.55341960407619339, 107.2927570613523471 ) ) ;
#166189 = CARTESIAN_POINT ( 'NONE',  ( 19.05341960407611168, 5.049401038298154454, 88.95724293864769550 ) ) ;
#166190 = CARTESIAN_POINT ( 'NONE',  ( -21.55341960407610458, -5.719274019375992779, 46.45724293864769550 ) ) ;
#166191 = CARTESIAN_POINT ( 'NONE',  ( 18.67979575497194134, -10.72451020669871369, 95.83442372801903275 ) ) ;
#166192 = CARTESIAN_POINT ( 'NONE',  ( 4.379528057220092307, 16.55341960407617563, 57.29275706135234714 ) ) ;
#166193 = CARTESIAN_POINT ( 'NONE',  ( -21.53943276465977519, 0.05219959533907696930, 106.2489096053143811 ) ) ;
#166194 = CARTESIAN_POINT ( 'NONE',  ( 16.53943276465976808, 0.05219959533934440121, 26.25109039468567573 ) ) ;
#166195 = CARTESIAN_POINT ( 'NONE',  ( -19.05341960407611168, -5.049401038298163336, 86.45724293864769550 ) ) ;
#166196 = CARTESIAN_POINT ( 'NONE',  ( 0.05219959533934541429, -16.53943276465976808, 25.00109039468567218 ) ) ;
#166197 = CARTESIAN_POINT ( 'NONE',  ( -16.51473224551069308, -9.474510206698971260, 56.66557627198103120 ) ) ;
#166198 = CARTESIAN_POINT ( 'NONE',  ( -4.483927247898782831, 16.52544592524335698, 27.70942372801901854 ) ) ;
#166199 = CARTESIAN_POINT ( 'NONE',  ( -14.29746914071049879, 8.314922557960819915, 75.83224293864769550 ) ) ;
#166200 = CARTESIAN_POINT ( 'NONE',  ( 12.06949235617739724, 12.14591786802326823, 86.87609039468568994 ) ) ;
#166202 = CARTESIAN_POINT ( 'NONE',  ( -19.02544592524342804, 5.153800228976336051, 71.04057627198099567 ) ) ;
#166201 = CARTESIAN_POINT ( 'NONE',  ( -21.52544592524334988, -5.823673210054445271, 43.95942372801902565 ) ) ;
#166203 = CARTESIAN_POINT ( 'NONE',  ( 0.05219959533909260263, 19.03943276465977164, 84.99890960531436690 ) ) ;
#166204 = CARTESIAN_POINT ( 'NONE',  ( 16.55341960407611168, 4.379528057220329451, 28.95724293864769905 ) ) ;
#166205 = CARTESIAN_POINT ( 'NONE',  ( -4.379528057220086978, -16.55341960407618274, 79.79275706135236135 ) ) ;
#166206 = AXIS2_PLACEMENT_3D ( 'NONE', #57571, #151568, #28245 ) ;
#166207 = EDGE_LOOP ( 'NONE', ( #39818, #94483, #132126, #107954 ) ) ;
#166208 = CARTESIAN_POINT ( 'NONE',  ( 19.03943276465977164, 0.05219959533936151252, 36.25109039468567573 ) ) ;
#166209 = CARTESIAN_POINT ( 'NONE',  ( 5.153800228976335163, 19.02544592524342804, 104.7905762719809957 ) ) ;
#166210 = CARTESIAN_POINT ( 'NONE',  ( -9.474510206698964154, 16.51473224551069663, 55.41557627198103120 ) ) ;
#166211 = LINE ( 'NONE', #122660, #26913 ) ;
#166212 = CARTESIAN_POINT ( 'NONE',  ( 12.14591786802327356, -12.06949235617739191, 40.62609039468567573 ) ) ;
#166214 = CARTESIAN_POINT ( 'NONE',  ( -16.53943276465976808, -0.05219959533934237506, 53.75109039468568994 ) ) ;
#166213 = CARTESIAN_POINT ( 'NONE',  ( -13.89961937509957401, -13.97604488694547875, 74.37609039468566152 ) ) ;
#166215 = DIRECTION ( 'NONE',  ( 3.469446951953611033E-15, 0.000000000000000000, -1.000000000000000000 ) ) ;
#166216 = CARTESIAN_POINT ( 'NONE',  ( -0.05219959533909027116, -19.03943276465977164, 77.49890960531435269 ) ) ;
#166217 = CARTESIAN_POINT ( 'NONE',  ( 18.67979575497178502, 10.72451020669898547, 114.1655762719810383 ) ) ;
#166218 = CARTESIAN_POINT ( 'NONE',  ( -13.89961937509957401, -13.97604488694547875, 69.37609039468564731 ) ) ;
#166220 = CARTESIAN_POINT ( 'NONE',  ( -0.05219959533909027116, -19.03943276465977164, 27.49890960531435624 ) ) ;
#166219 = CARTESIAN_POINT ( 'NONE',  ( -16.46253265017160317, 9.564922557960807481, 100.8322429386477097 ) ) ;
#166221 = CARTESIAN_POINT ( 'NONE',  ( 16.46253265017160672, -9.564922557960803928, 78.33224293864769550 ) ) ;
#166223 = CARTESIAN_POINT ( 'NONE',  ( -5.153800228976328057, -19.02544592524343514, 22.29057627198102765 ) ) ;
#166222 = CARTESIAN_POINT ( 'NONE',  ( -0.05219959533910754901, -16.53943276465976808, 32.49890960531435979 ) ) ;
#166224 = CARTESIAN_POINT ( 'NONE',  ( 0.05219959533936267826, -19.03943276465977164, 40.00109039468566152 ) ) ;
#166225 = CARTESIAN_POINT ( 'NONE',  ( -0.05219959533910754901, -16.53943276465976808, 77.49890960531433848 ) ) ;
#166226 = CARTESIAN_POINT ( 'NONE',  ( -13.97604488694547697, 13.89961937509957934, 23.12609039468565442 ) ) ;
#166227 = CARTESIAN_POINT ( 'NONE',  ( 16.51473224551069308, 9.474510206698969483, 34.16557627198102409 ) ) ;
#166228 = CIRCLE ( 'NONE', #27393, 2.649999999999999467 ) ;
#166230 = CARTESIAN_POINT ( 'NONE',  ( -18.67979575497193778, 10.72451020669871902, 103.3344237280190043 ) ) ;
#166229 = CARTESIAN_POINT ( 'NONE',  ( -16.53943276465976808, 0.05219959533911058130, 46.24890960531435979 ) ) ;
#166231 = CARTESIAN_POINT ( 'NONE',  ( -16.46253265017160317, 9.564922557960807481, 95.83224293864769550 ) ) ;
#166232 = CARTESIAN_POINT ( 'NONE',  ( -0.05219959533909027116, -19.03943276465977164, 107.4989096053143527 ) ) ;
#166233 = CARTESIAN_POINT ( 'NONE',  ( -19.05341960407611168, -5.049401038298163336, 36.45724293864766707 ) ) ;
#166234 = CARTESIAN_POINT ( 'NONE',  ( -14.29746914071049879, 8.314922557960819915, 110.8322429386476955 ) ) ;
#166235 = CARTESIAN_POINT ( 'NONE',  ( -4.483927247898539470, -16.52544592524342804, 72.29057627198102409 ) ) ;
#166236 = CARTESIAN_POINT ( 'NONE',  ( -21.55341960407610458, -5.719274019375992779, 86.45724293864770971 ) ) ;
#166237 = CARTESIAN_POINT ( 'NONE',  ( 19.03943276465977164, -0.05219959533909143690, 83.74890960531436690 ) ) ;
#166238 = CARTESIAN_POINT ( 'NONE',  ( 15.72974639402199770, -15.80617190586745480, 98.12390960531436690 ) ) ;
#166239 = CARTESIAN_POINT ( 'NONE',  ( -19.05341960407611168, -5.049401038298163336, 96.45724293864769550 ) ) ;
#166241 = CARTESIAN_POINT ( 'NONE',  ( -8.314922557960811034, -14.29746914071050412, 107.0822429386476955 ) ) ;
#166240 = CARTESIAN_POINT ( 'NONE',  ( 19.35633801406907750, -5.499999999999772626, 46.63373818172765795 ) ) ;
#166242 = CARTESIAN_POINT ( 'NONE',  ( 19.02544592524343514, -5.153800228976328945, 68.54057627198103830 ) ) ;
#166243 = CARTESIAN_POINT ( 'NONE',  ( 10.72451020669898902, -18.67979575497178502, 77.91557627198102409 ) ) ;
#166244 = DIRECTION ( 'NONE',  ( 1.000000000000000000, 0.000000000000000000, 0.000000000000000000 ) ) ;
#166246 = CARTESIAN_POINT ( 'NONE',  ( 19.52217212775656563, -5.500000000000102141, 67.43993709005262360 ) ) ;
#166245 = CARTESIAN_POINT ( 'NONE',  ( 0.05219959533907565091, 21.53943276465977519, 29.99890960531435979 ) ) ;
#166247 = CARTESIAN_POINT ( 'NONE',  ( 19.03943276465977164, 0.05219959533936151252, 111.2510903946856757 ) ) ;
#166248 = EDGE_CURVE ( 'NONE', #133361, #132987, #107239, .T. ) ;
#166249 = CARTESIAN_POINT ( 'NONE',  ( 12.06949235617757843, -12.14591786802309237, 98.12390960531436690 ) ) ;
#166250 = CARTESIAN_POINT ( 'NONE',  ( -16.31925111598456368, -7.325300261831544368, 94.83575461032751264 ) ) ;
#166251 = CARTESIAN_POINT ( 'NONE',  ( -19.05341960407611168, -5.049401038298163336, 86.45724293864769550 ) ) ;
#166252 = CARTESIAN_POINT ( 'NONE',  ( 9.564922557960805705, 16.46253265017160317, 49.58224293864770260 ) ) ;
#166253 = CARTESIAN_POINT ( 'NONE',  ( 12.06949235617757843, -12.14591786802309237, 83.12390960531436690 ) ) ;
#166254 = CARTESIAN_POINT ( 'NONE',  ( 21.53943276465977519, -0.05219959533907433946, 23.74890960531435269 ) ) ;
#166255 = CARTESIAN_POINT ( 'NONE',  ( -16.52544592524342804, 4.483927247898546575, 51.04057627198103120 ) ) ;
#166256 = CARTESIAN_POINT ( 'NONE',  ( -16.46253265017146816, -9.564922557961047289, 104.1677570613523329 ) ) ;
#166257 = CARTESIAN_POINT ( 'NONE',  ( -5.823673210054431948, 21.52544592524334988, 62.70942372801902565 ) ) ;
#166258 =( GEOMETRIC_REPRESENTATION_CONTEXT ( 3 ) GLOBAL_UNCERTAINTY_ASSIGNED_CONTEXT ( ( #142968 ) ) GLOBAL_UNIT_ASSIGNED_CONTEXT ( ( #28026, #103847, #10848 ) ) REPRESENTATION_CONTEXT ( 'NONE', 'WORKASPACE' ) );
#166259 = CARTESIAN_POINT ( 'NONE',  ( 27.73933785331498569, 9.013057229001093518, 147.9750000027311501 ) ) ;
#166260 = CARTESIAN_POINT ( 'NONE',  ( 9.564922557960805705, 16.46253265017160317, 94.58224293864769550 ) ) ;
#166261 = CARTESIAN_POINT ( 'NONE',  ( -15.80617190586745835, -15.72974639402198527, 86.87390960531438111 ) ) ;
#166262 = CARTESIAN_POINT ( 'NONE',  ( 16.55341960407618274, -4.379528057220086978, 91.04275706135236135 ) ) ;
#166263 = CARTESIAN_POINT ( 'NONE',  ( 9.564922557960805705, 16.46253265017160317, 29.58224293864769550 ) ) ;
#166264 = CARTESIAN_POINT ( 'NONE',  ( -19.02544592524342804, 5.153800228976336051, 81.04057627198103830 ) ) ;
#166265 = CARTESIAN_POINT ( 'NONE',  ( -10.72451020669898014, 18.67979575497178502, 85.41557627198102409 ) ) ;
#166266 =( GEOMETRIC_REPRESENTATION_CONTEXT ( 3 ) GLOBAL_UNCERTAINTY_ASSIGNED_CONTEXT ( ( #51963 ) ) GLOBAL_UNIT_ASSIGNED_CONTEXT ( ( #93038, #1025, #174872 ) ) REPRESENTATION_CONTEXT ( 'NONE', 'WORKASPACE' ) );
#166267 = CARTESIAN_POINT ( 'NONE',  ( 0.05219959533936267826, -19.03943276465977164, 105.0010903946856615 ) ) ;
#166269 = CARTESIAN_POINT ( 'NONE',  ( 5.823673210054444382, -21.52544592524334988, 55.20942372801902565 ) ) ;
#166268 = CARTESIAN_POINT ( 'NONE',  ( -16.52544592524342804, 4.483927247898546575, 56.04057627198102409 ) ) ;
#166271 = CARTESIAN_POINT ( 'NONE',  ( 13.97604488694527802, 13.89961937509977652, 114.3739096053143669 ) ) ;
#166270 = CARTESIAN_POINT ( 'NONE',  ( -8.224510206698735004, -14.34966873604973081, 89.58442372801901854 ) ) ;
#166272 = CARTESIAN_POINT ( 'NONE',  ( -19.03943276465977164, 0.05219959533909376836, 111.2489096053143669 ) ) ;
#166273 = CARTESIAN_POINT ( 'NONE',  ( -16.62475595723700650, 7.163666690055234376, 80.52713351810471920 ) ) ;
#166274 = CARTESIAN_POINT ( 'NONE',  ( -16.52544592524335698, -4.483927247898792601, 108.9594237280190185 ) ) ;
#166275 = CARTESIAN_POINT ( 'NONE',  ( -16.55341960407617563, 4.379528057220093196, 63.54275706135234003 ) ) ;
#166276 = CARTESIAN_POINT ( 'NONE',  ( 19.03943276465977164, -0.05219959533909143690, 68.74890960531436690 ) ) ;
#166277 = CARTESIAN_POINT ( 'NONE',  ( 13.97604488694527802, 13.89961937509977652, 79.37390960531435269 ) ) ;
#166278 = CARTESIAN_POINT ( 'NONE',  ( 18.67979575497194134, -10.72451020669871369, 70.83442372801901854 ) ) ;
#166279 = EDGE_CURVE ( 'NONE', #122084, #99233, #144300, .T. ) ;
#166280 = CARTESIAN_POINT ( 'NONE',  ( -8.224510206698735004, -14.34966873604973081, 74.58442372801901854 ) ) ;
#166281 = CARTESIAN_POINT ( 'NONE',  ( -4.379528057220328563, 16.55341960407611168, 50.20724293864769550 ) ) ;
#166282 = CARTESIAN_POINT ( 'NONE',  ( -16.51473224551069308, -9.474510206698971260, 51.66557627198102409 ) ) ;
#166283 = CARTESIAN_POINT ( 'NONE',  ( 16.51473224551069308, 9.474510206698969483, 54.16557627198103120 ) ) ;
#166285 = ORIENTED_EDGE ( 'NONE', *, *, #191135, .T. ) ;
#166284 = CARTESIAN_POINT ( 'NONE',  ( 16.53943276465976808, 0.05219959533934440121, 41.25109039468568284 ) ) ;
#166287 = CARTESIAN_POINT ( 'NONE',  ( 13.89961937509957401, 13.97604488694547697, 91.87609039468567573 ) ) ;
#166286 =( BOUNDED_CURVE ( )  B_SPLINE_CURVE ( 2, ( #104211, #195236, #146707, #180085, #23380, #69879, #41554, #26393, #8204, #54706, #147730 ),
 .UNSPECIFIED., .F., .T. ) 
 B_SPLINE_CURVE_WITH_KNOTS ( ( 3, 2, 2, 2, 2, 3 ),
 ( 0.4000000000000000222, 0.4199999999999999845, 0.4400000000000000022, 0.4600000000000000200, 0.4799999999999999822, 0.5000000000000000000 ),
 .UNSPECIFIED. ) 
 CURVE ( )  GEOMETRIC_REPRESENTATION_ITEM ( )  RATIONAL_B_SPLINE_CURVE ( ( 1.000000000000000000, 0.9510565162951535312, 1.000000000000000000, 0.9510565162951535312, 1.000000000000000000, 0.9510565162951535312, 1.000000000000000000, 0.9510565162951535312, 1.000000000000000000, 0.9510565162951535312, 1.000000000000000000 ) ) 
 REPRESENTATION_ITEM ( '' )  );
#166288 = CARTESIAN_POINT ( 'NONE',  ( 4.379528057220339221, -16.55341960407611168, 102.7072429386476955 ) ) ;
#166289 = CARTESIAN_POINT ( 'NONE',  ( 13.97604488694527802, 13.89961937509977652, 64.37390960531436690 ) ) ;
#166291 = CARTESIAN_POINT ( 'NONE',  ( -6.020228577223754586E-15, 39.95556452105416412, -6.500000000000000000 ) ) ;
#166290 = CARTESIAN_POINT ( 'NONE',  ( -0.05219959533936034679, 19.03943276465977164, 97.50109039468567573 ) ) ;
#166292 = CARTESIAN_POINT ( 'NONE',  ( -5.719274019375665041, -21.55341960407619695, 99.79275706135234714 ) ) ;
#166293 = CARTESIAN_POINT ( 'NONE',  ( -14.34966873604972548, 8.224510206698743886, 68.33442372801900433 ) ) ;
#166294 = CARTESIAN_POINT ( 'NONE',  ( 0.000000000000000000, 0.000000000000000000, 10.00000000000000000 ) ) ;
#166295 = CARTESIAN_POINT ( 'NONE',  ( -21.53943276465977519, 0.05219959533907696930, 61.24890960531435979 ) ) ;
#166296 = CARTESIAN_POINT ( 'NONE',  ( -8.314922557961024197, 14.29746914071037800, 47.91775706135234714 ) ) ;
#166297 = CARTESIAN_POINT ( 'NONE',  ( -9.564922557960796823, -16.46253265017161027, 32.08224293864769550 ) ) ;
#166298 = CARTESIAN_POINT ( 'NONE',  ( 19.03943276465977164, 0.05219959533936151252, 46.25109039468566863 ) ) ;
#166299 = CARTESIAN_POINT ( 'NONE',  ( 19.02544592524343514, -5.153800228976328945, 93.54057627198102409 ) ) ;
#166300 = CARTESIAN_POINT ( 'NONE',  ( -4.379528057220328563, 16.55341960407611168, 115.2072429386476955 ) ) ;
#166301 = CARTESIAN_POINT ( 'NONE',  ( 0.05219959533909260263, 19.03943276465977164, 64.99890960531436690 ) ) ;
#166302 = AXIS2_PLACEMENT_3D ( 'NONE', #33802, #64144, #66119 ) ;
#166303 = CARTESIAN_POINT ( 'NONE',  ( -10.72451020669870658, -18.67979575497194134, 79.58442372801903275 ) ) ;
#166304 = CARTESIAN_POINT ( 'NONE',  ( -19.03943276465977164, -0.05219959533935918106, 48.75109039468566863 ) ) ;
#166305 = CARTESIAN_POINT ( 'NONE',  ( -19.05341960407617563, 5.049401038297882671, 33.54275706135231871 ) ) ;
#166306 = CARTESIAN_POINT ( 'NONE',  ( 9.474510206698971260, -16.51473224551069308, 57.91557627198103120 ) ) ;
#166307 = CARTESIAN_POINT ( 'NONE',  ( 0.05219959533907565091, 21.53943276465977519, 24.99890960531435624 ) ) ;
#166308 = CARTESIAN_POINT ( 'NONE',  ( -18.67979575497193778, 10.72451020669871902, 88.33442372801901854 ) ) ;
#166309 = CARTESIAN_POINT ( 'NONE',  ( -19.02544592524342804, 5.153800228976336051, 66.04057627198103830 ) ) ;
#166310 = CARTESIAN_POINT ( 'NONE',  ( -18.62759615963255300, -10.81492255796106328, 99.16775706135234714 ) ) ;
#166311 = CARTESIAN_POINT ( 'NONE',  ( 18.62759615963271287, -10.81492255796078972, 33.33224293864769550 ) ) ;
#166312 = CARTESIAN_POINT ( 'NONE',  ( 13.89961937509977652, -13.97604488694527269, 78.12390960531433848 ) ) ;
#166313 = CARTESIAN_POINT ( 'NONE',  ( 18.67979575497194134, -10.72451020669871369, 40.83442372801901854 ) ) ;
#166314 = CARTESIAN_POINT ( 'NONE',  ( 0.05219959533936267826, -19.03943276465977164, 60.00109039468566863 ) ) ;
#166315 = CARTESIAN_POINT ( 'NONE',  ( -13.97604488694527625, -13.89961937509977652, 41.87390960531435979 ) ) ;
#166316 = CARTESIAN_POINT ( 'NONE',  ( 0.05219959533909260263, 19.03943276465977164, 94.99890960531436690 ) ) ;
#166317 = CARTESIAN_POINT ( 'NONE',  ( -8.224510206698735004, -14.34966873604973081, 29.58442372801901854 ) ) ;
#166318 = CARTESIAN_POINT ( 'NONE',  ( 12.14591786802309770, 12.06949235617756955, 84.37390960531438111 ) ) ;
#166319 = CARTESIAN_POINT ( 'NONE',  ( -16.51473224551069308, -9.474510206698971260, 66.66557627198102409 ) ) ;
#166320 = CARTESIAN_POINT ( 'NONE',  ( 21.52544592524344225, -5.823673210054117533, 53.54057627198103120 ) ) ;
#166321 = CARTESIAN_POINT ( 'NONE',  ( -14.29746914071037622, -8.314922557961029526, 19.16775706135234714 ) ) ;
#166322 = CARTESIAN_POINT ( 'NONE',  ( -10.81492255796078084, -18.62759615963271287, 112.0822429386477097 ) ) ;
#166323 = CARTESIAN_POINT ( 'NONE',  ( 21.52544592524334988, 5.823673210054432836, 71.45942372801901854 ) ) ;
#166324 = CARTESIAN_POINT ( 'NONE',  ( -8.224510206698735004, -14.34966873604973081, 64.58442372801900433 ) ) ;
#166325 = CARTESIAN_POINT ( 'NONE',  ( -0.05219959533934338120, 16.53943276465976808, 72.50109039468568994 ) ) ;
#166326 = CARTESIAN_POINT ( 'NONE',  ( -0.05219959533909027116, -19.03943276465977164, 67.49890960531436690 ) ) ;
#166327 = CARTESIAN_POINT ( 'NONE',  ( 16.55341960407618274, -4.379528057220086978, 96.04275706135236135 ) ) ;
#166328 = CARTESIAN_POINT ( 'NONE',  ( 13.89961937509957401, 13.97604488694547697, 41.87609039468566152 ) ) ;
#166329 = CARTESIAN_POINT ( 'NONE',  ( -21.53943276465977519, 0.05219959533907696930, 116.2489096053143669 ) ) ;
#166330 = CARTESIAN_POINT ( 'NONE',  ( 8.224510206698953496, -14.34966873604960469, 62.91557627198102409 ) ) ;
#166331 = CARTESIAN_POINT ( 'NONE',  ( -5.049401038298153566, 19.05341960407611168, 80.20724293864769550 ) ) ;
#166332 = CARTESIAN_POINT ( 'NONE',  ( -8.224510206698735004, -14.34966873604973081, 84.58442372801903275 ) ) ;
#166333 = CARTESIAN_POINT ( 'NONE',  ( -21.55341960407619339, 5.719274019375674811, 53.54275706135234714 ) ) ;
#166334 = CARTESIAN_POINT ( 'NONE',  ( 4.483927247898790824, -16.52544592524335698, 25.20942372801901854 ) ) ;
#166335 = CARTESIAN_POINT ( 'NONE',  ( 18.62759615963255655, 10.81492255796105972, 21.66775706135235069 ) ) ;
#166336 = CARTESIAN_POINT ( 'NONE',  ( -12.14591786802309592, -12.06949235617757132, 51.87390960531437401 ) ) ;
#166337 = ORIENTED_EDGE ( 'NONE', *, *, #38962, .F. ) ;
#166338 = CARTESIAN_POINT ( 'NONE',  ( -10.81492255796078084, -18.62759615963271287, 97.08224293864770971 ) ) ;
#166339 = CARTESIAN_POINT ( 'NONE',  ( 16.52544592524342804, -4.483927247898539470, 33.54057627198102409 ) ) ;
#166340 = ORIENTED_EDGE ( 'NONE', *, *, #158246, .F. ) ;
#166341 = DIRECTION ( 'NONE',  ( -0.5000000000000002220, -0.4999999999999985012, 0.7071067811865483499 ) ) ;
#166342 = AXIS2_PLACEMENT_3D ( 'NONE', #51910, #156108, #2423 ) ;
#166343 = CARTESIAN_POINT ( 'NONE',  ( -15.72974639402197994, 15.80617190586746368, 35.62390960531437401 ) ) ;
#166344 = CARTESIAN_POINT ( 'NONE',  ( -5.719274019375665041, -21.55341960407619695, 39.79275706135235424 ) ) ;
#166345 = CARTESIAN_POINT ( 'NONE',  ( -4.483927247898539470, -16.52544592524342804, 62.29057627198102409 ) ) ;
#166346 = CARTESIAN_POINT ( 'NONE',  ( 15.80617190586746368, 15.72974639402197994, 69.37390960531436690 ) ) ;
#166347 = CARTESIAN_POINT ( 'NONE',  ( 9.474510206698971260, -16.51473224551069308, 72.91557627198102409 ) ) ;
#166349 = CARTESIAN_POINT ( 'NONE',  ( -9.564922557961040184, 16.46253265017147172, 67.91775706135233293 ) ) ;
#166348 = CARTESIAN_POINT ( 'NONE',  ( 5.153800228976335163, 19.02544592524342804, 29.79057627198102409 ) ) ;
#166350 = CARTESIAN_POINT ( 'NONE',  ( 10.72451020669898902, -18.67979575497178502, 52.91557627198103830 ) ) ;
#166351 = CARTESIAN_POINT ( 'NONE',  ( -16.46253265017160317, 9.564922557960807481, 55.83224293864769550 ) ) ;
#166352 = ORIENTED_EDGE ( 'NONE', *, *, #93254, .T. ) ;
#166353 = CARTESIAN_POINT ( 'NONE',  ( -16.55341960407617563, 4.379528057220093196, 33.54275706135234714 ) ) ;
#166354 = CARTESIAN_POINT ( 'NONE',  ( 15.80617190586769283, -15.72974639402175789, 20.62609039468568639 ) ) ;
#166355 = CARTESIAN_POINT ( 'NONE',  ( -16.55341960407611168, -4.379528057220339221, 41.45724293864769550 ) ) ;
#166356 = AXIS2_PLACEMENT_3D ( 'NONE', #117223, #180916, #11057 ) ;
#166357 = CARTESIAN_POINT ( 'NONE',  ( -0.05219959533909027116, -19.03943276465977164, 102.4989096053143669 ) ) ;
#166358 = CARTESIAN_POINT ( 'NONE',  ( -15.72974639402197994, 15.80617190586746368, 70.62390960531436690 ) ) ;
#166360 = CARTESIAN_POINT ( 'NONE',  ( -14.29746914071037622, -8.314922557961029526, 34.16775706135234714 ) ) ;
#166359 = CARTESIAN_POINT ( 'NONE',  ( -10.81492255796078084, -18.62759615963271287, 102.0822429386476955 ) ) ;
#166361 = EDGE_CURVE ( 'NONE', #163173, #112403, #128114, .T. ) ;
#166362 = CARTESIAN_POINT ( 'NONE',  ( -21.52544592524343514, 5.823673210054127303, 46.04057627198103830 ) ) ;
#166363 = CARTESIAN_POINT ( 'NONE',  ( -21.53943276465977519, -0.05219959533937600094, 98.75109039468568994 ) ) ;
#166364 = CARTESIAN_POINT ( 'NONE',  ( -9.474510206698964154, 16.51473224551069663, 35.41557627198102409 ) ) ;
#166365 = CARTESIAN_POINT ( 'NONE',  ( -5.153800228976328057, -19.02544592524343514, 102.2905762719810383 ) ) ;
#166366 = CARTESIAN_POINT ( 'NONE',  ( 5.049401038298161559, -19.05341960407611168, 77.70724293864765286 ) ) ;
#166367 = CARTESIAN_POINT ( 'NONE',  ( 17.50000000001358202, -5.500000000000038192, 88.29690382535061133 ) ) ;
#166368 = CARTESIAN_POINT ( 'NONE',  ( -13.97604488694547697, 13.89961937509957934, 53.12609039468565442 ) ) ;
#166370 = CARTESIAN_POINT ( 'NONE',  ( 10.72451020669898902, -18.67979575497178502, 32.91557627198102409 ) ) ;
#166369 = CARTESIAN_POINT ( 'NONE',  ( 18.62759615963255655, 10.81492255796105972, 106.6677570613523756 ) ) ;
#166372 = EDGE_CURVE ( 'NONE', #68158, #83853, #157144, .T. ) ;
#166371 = CARTESIAN_POINT ( 'NONE',  ( -16.53943276465976808, -0.05219959533934237506, 98.75109039468568994 ) ) ;
#166373 = CARTESIAN_POINT ( 'NONE',  ( -5.153800228976607833, 19.02544592524334988, 82.70942372801897591 ) ) ;
#166374 = CARTESIAN_POINT ( 'NONE',  ( -14.92453577844291424, -15.21309657316540509, -58.85011498497254934 ) ) ;
#166375 = CARTESIAN_POINT ( 'NONE',  ( -5.153800228976607833, 19.02544592524334988, 82.70942372801897591 ) ) ;
#166376 = CARTESIAN_POINT ( 'NONE',  ( 9.474510206698729675, 16.51473224551082808, 42.08442372801900433 ) ) ;
#166377 = FACE_OUTER_BOUND ( 'NONE', #105455, .T. ) ;
#166378 = CARTESIAN_POINT ( 'NONE',  ( 19.02544592524343514, -5.153800228976328945, 38.54057627198103120 ) ) ;
#166379 = CARTESIAN_POINT ( 'NONE',  ( 16.53943276465976808, -0.05219959533910856209, 53.74890960531437401 ) ) ;
#166380 = CARTESIAN_POINT ( 'NONE',  ( -16.46253265017160317, 9.564922557960807481, 35.83224293864768839 ) ) ;
#166381 = CARTESIAN_POINT ( 'NONE',  ( 16.53943276465976808, -0.05219959533910856209, 43.74890960531435979 ) ) ;
#166382 = CARTESIAN_POINT ( 'NONE',  ( 17.72696623605164845, -5.499999999999870326, 46.09811031808416715 ) ) ;
#166383 = CARTESIAN_POINT ( 'NONE',  ( 16.52544592524335698, 4.483927247898782831, 106.4594237280190328 ) ) ;
#166384 = CARTESIAN_POINT ( 'NONE',  ( -16.46253265017160317, 9.564922557960807481, 50.83224293864770260 ) ) ;
#166385 = CARTESIAN_POINT ( 'NONE',  ( -21.52544592524334988, -5.823673210054445271, 108.9594237280190185 ) ) ;
#166386 = CARTESIAN_POINT ( 'NONE',  ( -14.29746914071037622, -8.314922557961029526, 19.16775706135234714 ) ) ;
#166387 = CARTESIAN_POINT ( 'NONE',  ( -21.52544592524343514, 5.823673210054127303, 41.04057627198103120 ) ) ;
#166389 = ORIENTED_EDGE ( 'NONE', *, *, #187948, .F. ) ;
#166388 = CARTESIAN_POINT ( 'NONE',  ( 18.67979575497194134, -10.72451020669871369, 85.83442372801901854 ) ) ;
#166390 = CARTESIAN_POINT ( 'NONE',  ( -5.049401038298153566, 19.05341960407611168, 100.2072429386476955 ) ) ;
#166391 = CARTESIAN_POINT ( 'NONE',  ( 13.89961937509977652, -13.97604488694527269, 78.12390960531433848 ) ) ;
#166392 = CARTESIAN_POINT ( 'NONE',  ( 36.91746824999999177, 2.880721459617395097E-14, -9.624999997268814056 ) ) ;
#166393 = CARTESIAN_POINT ( 'NONE',  ( 18.67979575497178502, 10.72451020669898547, 109.1655762719810383 ) ) ;
#166394 = MECHANICAL_DESIGN_GEOMETRIC_PRESENTATION_REPRESENTATION (  '', ( #88862 ), #66184 ) ;
#166395 = CARTESIAN_POINT ( 'NONE',  ( -8.224510206698948167, 14.34966873604960824, 80.41557627198103830 ) ) ;
#166396 = CARTESIAN_POINT ( 'NONE',  ( 18.62759615963271287, -10.81492255796078972, 68.33224293864769550 ) ) ;
#166397 = CARTESIAN_POINT ( 'NONE',  ( 13.89961937509977652, -13.97604488694527269, 73.12390960531436690 ) ) ;
#166398 = CARTESIAN_POINT ( 'NONE',  ( -21.53943276465977519, 0.05219959533907696930, 96.24890960531435269 ) ) ;
#166399 = VERTEX_POINT ( 'NONE', #28321 ) ;
#166400 = CARTESIAN_POINT ( 'NONE',  ( -19.02544592524342804, 5.153800228976336051, 61.04057627198103120 ) ) ;
#166402 = CARTESIAN_POINT ( 'NONE',  ( -7.656827144875921753, -71.74905178543390605, -25.00000000000000000 ) ) ;
#166401 = CARTESIAN_POINT ( 'NONE',  ( 0.05219959533910956823, 16.53943276465976808, 89.99890960531438111 ) ) ;
#166403 = CARTESIAN_POINT ( 'NONE',  ( -19.03943276465977164, 0.05219959533909376836, 61.24890960531436690 ) ) ;
#166404 = CARTESIAN_POINT ( 'NONE',  ( 13.89961937509957401, 13.97604488694547697, 76.87609039468566152 ) ) ;
#166405 = AXIS2_PLACEMENT_3D ( 'NONE', #151851, #120505, #59827 ) ;
#166406 = CARTESIAN_POINT ( 'NONE',  ( 16.52544592524342804, -4.483927247898539470, 83.54057627198102409 ) ) ;
#166407 = CARTESIAN_POINT ( 'NONE',  ( -10.72451020669870658, -18.67979575497194134, 54.58442372801901143 ) ) ;
#166409 = CARTESIAN_POINT ( 'NONE',  ( 10.81492255796106328, -18.62759615963255655, 20.41775706135234714 ) ) ;
#166408 = CARTESIAN_POINT ( 'NONE',  ( -5.049401038298153566, 19.05341960407611168, 50.20724293864770260 ) ) ;
#166410 = CARTESIAN_POINT ( 'NONE',  ( 16.53943276465976808, -0.05219959533910856209, 103.7489096053143669 ) ) ;
#166411 = FACE_OUTER_BOUND ( 'NONE', #78257, .T. ) ;
#166412 = CARTESIAN_POINT ( 'NONE',  ( 5.153800228976335163, 19.02544592524342804, 54.79057627198103120 ) ) ;
#166413 = AXIS2_PLACEMENT_3D ( 'NONE', #103218, #193234, #27390 ) ;
#166414 = CARTESIAN_POINT ( 'NONE',  ( 16.18388926212238133, 7.379444403734521707, 112.9395315136614926 ) ) ;
#166416 = CARTESIAN_POINT ( 'NONE',  ( 19.02544592524343514, -5.153800228976328945, 108.5405762719810383 ) ) ;
#166415 = CARTESIAN_POINT ( 'NONE',  ( -9.564922557961040184, 16.46253265017147172, 102.9177570613523329 ) ) ;
#166417 = CARTESIAN_POINT ( 'NONE',  ( 18.67979575497194134, -10.72451020669871369, 50.83442372801901143 ) ) ;
#166418 = CARTESIAN_POINT ( 'NONE',  ( 13.97604488694527802, 13.89961937509977652, 94.37390960531436690 ) ) ;
#166419 = CARTESIAN_POINT ( 'NONE',  ( -16.46253265017146816, -9.564922557961047289, 89.16775706135234714 ) ) ;
#166420 = CARTESIAN_POINT ( 'NONE',  ( -5.153800228976328057, -19.02544592524343514, 52.29057627198100988 ) ) ;
#166421 = CARTESIAN_POINT ( 'NONE',  ( -8.314922557960811034, -14.29746914071050412, 87.08224293864769550 ) ) ;
#166422 = CARTESIAN_POINT ( 'NONE',  ( 13.89961937509977652, -13.97604488694527269, 93.12390960531436690 ) ) ;
#166423 = CARTESIAN_POINT ( 'NONE',  ( 14.34966873604960469, 8.224510206698951720, 84.16557627198103830 ) ) ;
#166424 = CARTESIAN_POINT ( 'NONE',  ( 19.02544592524343514, -5.153800228976328945, 88.54057627198102409 ) ) ;
#166425 = CARTESIAN_POINT ( 'NONE',  ( -19.05341960407617563, 5.049401038297882671, 28.54275706135232937 ) ) ;
#166428 = CARTESIAN_POINT ( 'NONE',  ( 19.02544592524343514, -5.153800228976328945, 33.54057627198102409 ) ) ;
#166427 = CARTESIAN_POINT ( 'NONE',  ( -16.53943276465976808, 0.05219959533911058130, 26.24890960531435624 ) ) ;
#166426 = CARTESIAN_POINT ( 'NONE',  ( 16.46253265017160672, -9.564922557960803928, 43.33224293864769550 ) ) ;
#166429 = ORIENTED_EDGE ( 'NONE', *, *, #174036, .T. ) ;
#166430 = CARTESIAN_POINT ( 'NONE',  ( 18.62759615963255655, 10.81492255796105972, 41.66775706135235424 ) ) ;
#166431 = CARTESIAN_POINT ( 'NONE',  ( -5.049401038297874678, -19.05341960407617918, 79.79275706135233293 ) ) ;
#166432 = CARTESIAN_POINT ( 'NONE',  ( -12.14591786802309592, -12.06949235617757132, 36.87390960531435979 ) ) ;
#166433 = CARTESIAN_POINT ( 'NONE',  ( -5.719274019375978568, 21.55341960407610458, 85.20724293864770971 ) ) ;
#166434 = CARTESIAN_POINT ( 'NONE',  ( 5.719274019375991003, -21.55341960407610458, 32.70724293864770260 ) ) ;
#166435 = CARTESIAN_POINT ( 'NONE',  ( -16.53943276465976808, 0.05219959533911058130, 66.24890960531436690 ) ) ;
#166436 = CARTESIAN_POINT ( 'NONE',  ( 5.049401038298161559, -19.05341960407611168, 42.70724293864767418 ) ) ;
#166437 = CARTESIAN_POINT ( 'NONE',  ( -0.05219959533934338120, 16.53943276465976808, 107.5010903946856899 ) ) ;
#166438 = CARTESIAN_POINT ( 'NONE',  ( -16.52544592524335698, -4.483927247898792601, 63.95942372801901854 ) ) ;
#166439 = CARTESIAN_POINT ( 'NONE',  ( -15.72974639402197994, 15.80617190586746368, 40.62390960531435269 ) ) ;
#166440 = CARTESIAN_POINT ( 'NONE',  ( 13.89961937509957401, 13.97604488694547697, 21.87609039468566152 ) ) ;
#166441 = CARTESIAN_POINT ( 'NONE',  ( -9.564922557960796823, -16.46253265017161027, 97.08224293864769550 ) ) ;
#166442 = CARTESIAN_POINT ( 'NONE',  ( 4.483927247898790824, -16.52544592524335698, 75.20942372801901854 ) ) ;
#166443 = CARTESIAN_POINT ( 'NONE',  ( 5.049401038298161559, -19.05341960407611168, 22.70724293864769194 ) ) ;
#166444 = CARTESIAN_POINT ( 'NONE',  ( -12.14591786802309592, -12.06949235617757132, 36.87390960531435979 ) ) ;
#166446 = CARTESIAN_POINT ( 'NONE',  ( 5.049401038298161559, -19.05341960407611168, 97.70724293864766707 ) ) ;
#166445 = CARTESIAN_POINT ( 'NONE',  ( -5.049401038298153566, 19.05341960407611168, 105.2072429386476671 ) ) ;
#166447 = CARTESIAN_POINT ( 'NONE',  ( -10.81492255796078084, -18.62759615963271287, 22.08224293864769194 ) ) ;
#166448 = CARTESIAN_POINT ( 'NONE',  ( -4.483927247898539470, -16.52544592524342804, 72.29057627198102409 ) ) ;
#166449 = ORIENTED_EDGE ( 'NONE', *, *, #114142, .T. ) ;
#166450 = CARTESIAN_POINT ( 'NONE',  ( 12.14591786802309770, 12.06949235617756955, 54.37390960531435979 ) ) ;
#166452 = CYLINDRICAL_SURFACE ( 'NONE', #135133, 8.000000000000000000 ) ;
#166451 = CARTESIAN_POINT ( 'NONE',  ( 4.483927247898790824, -16.52544592524335698, 50.20942372801901854 ) ) ;
#166453 = CARTESIAN_POINT ( 'NONE',  ( 16.46253265017146816, 9.564922557961045513, 56.66775706135233293 ) ) ;
#166454 = CARTESIAN_POINT ( 'NONE',  ( 9.474510206698971260, -16.51473224551069308, 87.91557627198102409 ) ) ;
#166455 = CARTESIAN_POINT ( 'NONE',  ( 9.474510206698729675, 16.51473224551082808, 72.08442372801900433 ) ) ;
#166456 = CARTESIAN_POINT ( 'NONE',  ( 22.44159573604009239, 16.30477369853692693, 142.5750000027311728 ) ) ;
#166458 = CARTESIAN_POINT ( 'NONE',  ( -8.224510206698735004, -14.34966873604973081, 99.58442372801900433 ) ) ;
#166457 = CARTESIAN_POINT ( 'NONE',  ( -16.53943276465976808, -0.05219959533934237506, 18.75109039468568639 ) ) ;
#166459 = CARTESIAN_POINT ( 'NONE',  ( -5.049401038298153566, 19.05341960407611168, 35.20724293864768839 ) ) ;
#166460 = CARTESIAN_POINT ( 'NONE',  ( -18.67979575497178146, -10.72451020669898902, 26.66557627198103475 ) ) ;
#166461 = CARTESIAN_POINT ( 'NONE',  ( 18.67979575497194134, -10.72451020669871369, 60.83442372801901854 ) ) ;
#166462 = CARTESIAN_POINT ( 'NONE',  ( -0.05219959533936034679, 19.03943276465977164, 102.5010903946856757 ) ) ;
#166464 = CARTESIAN_POINT ( 'NONE',  ( 9.564922557960805705, 16.46253265017160317, 79.58224293864769550 ) ) ;
#166463 = CYLINDRICAL_SURFACE ( 'NONE', #134820, 2.500000000000002220 ) ;
#166465 = CARTESIAN_POINT ( 'NONE',  ( -13.89961937509977652, 13.97604488694528158, 115.6239096053143669 ) ) ;
#166467 = CARTESIAN_POINT ( 'NONE',  ( 0.05219959533909260263, 19.03943276465977164, 59.99890960531436690 ) ) ;
#166466 = CARTESIAN_POINT ( 'NONE',  ( -4.379528057220328563, 16.55341960407611168, 70.20724293864769550 ) ) ;
#166468 = CARTESIAN_POINT ( 'NONE',  ( 5.049401038298161559, -19.05341960407611168, 77.70724293864765286 ) ) ;
#166469 = CARTESIAN_POINT ( 'NONE',  ( -13.97604488694547697, 13.89961937509957934, 73.12609039468568994 ) ) ;
#166470 = CARTESIAN_POINT ( 'NONE',  ( 0.05219959533907565091, 21.53943276465977519, 59.99890960531436690 ) ) ;
#166471 = CARTESIAN_POINT ( 'NONE',  ( 14.29746914071049879, -8.314922557960816363, 113.3322429386476955 ) ) ;
#166472 = CARTESIAN_POINT ( 'NONE',  ( 9.564922557961047289, -16.46253265017146816, 55.41775706135234003 ) ) ;
#166473 = CARTESIAN_POINT ( 'NONE',  ( -9.564922557960796823, -16.46253265017161027, 52.08224293864768839 ) ) ;
#166474 = CARTESIAN_POINT ( 'NONE',  ( 19.03943276465977164, -0.05219959533909143690, 98.74890960531436690 ) ) ;
#166475 = CARTESIAN_POINT ( 'NONE',  ( 15.80617190586746368, 15.72974639402197994, 94.37390960531436690 ) ) ;
#166477 = CARTESIAN_POINT ( 'NONE',  ( -0.05219959533936034679, 19.03943276465977164, 47.50109039468566863 ) ) ;
#166476 = CARTESIAN_POINT ( 'NONE',  ( 14.34966873604960469, 8.224510206698951720, 74.16557627198102409 ) ) ;
#166478 = CARTESIAN_POINT ( 'NONE',  ( -21.55341960407610458, -5.719274019375992779, 76.45724293864769550 ) ) ;
#166479 = CARTESIAN_POINT ( 'NONE',  ( -15.72974639402197994, 15.80617190586746368, 65.62390960531436690 ) ) ;
#166480 = VECTOR ( 'NONE', #1129, 1000.000000000000000 ) ;
#166481 = CARTESIAN_POINT ( 'NONE',  ( -12.06949235617756955, 12.14591786802309770, 30.62390960531436335 ) ) ;
#166482 = CARTESIAN_POINT ( 'NONE',  ( 18.62759615963255655, 10.81492255796105972, 91.66775706135234714 ) ) ;
#166483 = CARTESIAN_POINT ( 'NONE',  ( 19.03943276465977164, -0.05219959533909143690, 73.74890960531435269 ) ) ;
#166484 = CARTESIAN_POINT ( 'NONE',  ( 5.153800228976335163, 19.02544592524342804, 29.79057627198102409 ) ) ;
#166485 = CARTESIAN_POINT ( 'NONE',  ( 21.52544592524334988, 5.823673210054432836, 36.45942372801901143 ) ) ;
#166486 = ADVANCED_FACE ( 'NONE', ( #116306 ), #13135, .F. ) ;
#166487 = CARTESIAN_POINT ( 'NONE',  ( -21.52544592524334988, -5.823673210054445271, 38.95942372801901854 ) ) ;
#166488 = CARTESIAN_POINT ( 'NONE',  ( -5.049401038298153566, 19.05341960407611168, 45.20724293864769550 ) ) ;
#166489 = CARTESIAN_POINT ( 'NONE',  ( 21.52544592524344225, -5.823673210054117533, 113.5405762719810383 ) ) ;
#166490 = CARTESIAN_POINT ( 'NONE',  ( -19.02544592524334988, -5.153800228976617603, 58.95942372801900433 ) ) ;
#166491 = CARTESIAN_POINT ( 'NONE',  ( -9.474510206698964154, 16.51473224551069663, 40.41557627198103120 ) ) ;
#166492 = CARTESIAN_POINT ( 'NONE',  ( -14.34966873604972548, 8.224510206698743886, 33.33442372801900433 ) ) ;
#166493 = CARTESIAN_POINT ( 'NONE',  ( 0.05219959533909260263, 19.03943276465977164, 24.99890960531435269 ) ) ;
#166494 = CARTESIAN_POINT ( 'NONE',  ( -4.379528057220086978, -16.55341960407618274, 69.79275706135234714 ) ) ;
#166495 = CARTESIAN_POINT ( 'NONE',  ( 16.46253265017160672, -9.564922557960803928, 43.33224293864769550 ) ) ;
#166496 = CARTESIAN_POINT ( 'NONE',  ( -24.86475712555574802, -11.37215039200969890, 169.9824823118008226 ) ) ;
#166497 = CARTESIAN_POINT ( 'NONE',  ( -19.03943276465977164, 0.05219959533909376836, 86.24890960531436690 ) ) ;
#166498 = CARTESIAN_POINT ( 'NONE',  ( 9.474510206698971260, -16.51473224551069308, 22.91557627198102765 ) ) ;
#166499 = CARTESIAN_POINT ( 'NONE',  ( 5.823673210054125526, 21.52544592524343514, 64.79057627198103830 ) ) ;
#166500 = CARTESIAN_POINT ( 'NONE',  ( 12.06949235617739724, 12.14591786802326823, 51.87609039468568284 ) ) ;
#166501 = CARTESIAN_POINT ( 'NONE',  ( -5.823673210054431948, 21.52544592524334988, 97.70942372801904696 ) ) ;
#166502 = CARTESIAN_POINT ( 'NONE',  ( -16.46253265017160317, 9.564922557960807481, 35.83224293864768839 ) ) ;
#166503 = CARTESIAN_POINT ( 'NONE',  ( -12.06949235617756955, 12.14591786802309770, 30.62390960531436335 ) ) ;
#166504 = CARTESIAN_POINT ( 'NONE',  ( 4.379528057220339221, -16.55341960407611168, 67.70724293864769550 ) ) ;
#166505 = CARTESIAN_POINT ( 'NONE',  ( 5.049401038298161559, -19.05341960407611168, 67.70724293864769550 ) ) ;
#166506 = CARTESIAN_POINT ( 'NONE',  ( 18.62759615963255655, 10.81492255796105972, 111.6677570613523613 ) ) ;
#166507 = CARTESIAN_POINT ( 'NONE',  ( -0.05219959533937732626, 21.53943276465977519, 27.50109039468567929 ) ) ;
#166508 = CARTESIAN_POINT ( 'NONE',  ( 16.51473224551069308, 9.474510206698969483, 79.16557627198103830 ) ) ;
#166509 = CARTESIAN_POINT ( 'NONE',  ( -5.823673210054431948, 21.52544592524334988, 82.70942372801900433 ) ) ;
#166510 = CARTESIAN_POINT ( 'NONE',  ( -16.55341960407617563, 4.379528057220093196, 58.54275706135235424 ) ) ;
#166511 = CARTESIAN_POINT ( 'NONE',  ( 14.34966873604972726, -8.224510206698740333, 30.83442372801902209 ) ) ;
#166513 = CARTESIAN_POINT ( 'NONE',  ( -0.05219959533937732626, 21.53943276465977519, 97.50109039468567573 ) ) ;
#166512 = CARTESIAN_POINT ( 'NONE',  ( -16.52544592524342804, 4.483927247898546575, 91.04057627198103830 ) ) ;
#166514 = CARTESIAN_POINT ( 'NONE',  ( 12.14591786802309770, 12.06949235617756955, 34.37390960531435979 ) ) ;
#166515 = CARTESIAN_POINT ( 'NONE',  ( -9.564922557960796823, -16.46253265017161027, 27.08224293864769550 ) ) ;
#166516 = CARTESIAN_POINT ( 'NONE',  ( 0.05219959533934541429, -16.53943276465976808, 50.00109039468568994 ) ) ;
#166517 = CARTESIAN_POINT ( 'NONE',  ( 8.224510206698953496, -14.34966873604960469, 57.91557627198103120 ) ) ;
#166518 = CARTESIAN_POINT ( 'NONE',  ( 14.34966873604972726, -8.224510206698740333, 100.8344237280190185 ) ) ;
#166519 = CARTESIAN_POINT ( 'NONE',  ( -9.474510206698964154, 16.51473224551069663, 110.4155762719810383 ) ) ;
#166520 = CARTESIAN_POINT ( 'NONE',  ( -5.049401038298153566, 19.05341960407611168, 110.2072429386476671 ) ) ;
#166521 = CARTESIAN_POINT ( 'NONE',  ( 13.89961937509957401, 13.97604488694547697, 21.87609039468566152 ) ) ;
#166522 = EDGE_CURVE ( 'NONE', #116638, #199703, #85021, .T. ) ;
#166523 = CARTESIAN_POINT ( 'NONE',  ( -12.14591786802309592, -12.06949235617757132, 86.87390960531438111 ) ) ;
#166524 = CARTESIAN_POINT ( 'NONE',  ( -16.51473224551069308, -9.474510206698971260, 96.66557627198102409 ) ) ;
#166525 = ORIENTED_EDGE ( 'NONE', *, *, #128355, .T. ) ;
#166526 = CARTESIAN_POINT ( 'NONE',  ( 14.29746914071037800, 8.314922557961029526, 46.66775706135234714 ) ) ;
#166527 = CARTESIAN_POINT ( 'NONE',  ( -19.02544592524342804, 5.153800228976336051, 46.04057627198101699 ) ) ;
#166529 = DIRECTION ( 'NONE',  ( 0.000000000000000000, 0.000000000000000000, 1.000000000000000000 ) ) ;
#166528 = CARTESIAN_POINT ( 'NONE',  ( 14.29746914071037800, 8.314922557961029526, 51.66775706135234714 ) ) ;
#166530 = CARTESIAN_POINT ( 'NONE',  ( -0.05219959533936034679, 19.03943276465977164, 52.50109039468566863 ) ) ;
#166531 = CARTESIAN_POINT ( 'NONE',  ( 13.97604488694527802, 13.89961937509977652, 44.37390960531435269 ) ) ;
#166532 = CARTESIAN_POINT ( 'NONE',  ( -4.483927247898782831, 16.52544592524335698, 82.70942372801900433 ) ) ;
#166533 = CARTESIAN_POINT ( 'NONE',  ( 16.51473224551083163, -9.474510206698727899, 80.83442372801899012 ) ) ;
#166534 = CARTESIAN_POINT ( 'NONE',  ( 9.564922557961047289, -16.46253265017146816, 30.41775706135232937 ) ) ;
#166535 = CARTESIAN_POINT ( 'NONE',  ( 5.049401038298161559, -19.05341960407611168, 57.70724293864769550 ) ) ;
#166536 = CARTESIAN_POINT ( 'NONE',  ( -8.314922557960811034, -14.29746914071050412, 102.0822429386476955 ) ) ;
#166537 = CARTESIAN_POINT ( 'NONE',  ( 13.97604488694548053, -13.89961937509957401, 70.62609039468567573 ) ) ;
#166538 = CARTESIAN_POINT ( 'NONE',  ( 21.53943276465977519, -0.05219959533907433946, 63.74890960531435979 ) ) ;
#166539 = CARTESIAN_POINT ( 'NONE',  ( -13.97604488694547697, 13.89961937509957934, 23.12609039468565442 ) ) ;
#166540 = CARTESIAN_POINT ( 'NONE',  ( -0.05219959533909027116, -19.03943276465977164, 102.4989096053143669 ) ) ;
#166541 = CARTESIAN_POINT ( 'NONE',  ( 18.62759615963271287, -10.81492255796078972, 83.33224293864769550 ) ) ;
#166542 = DIRECTION ( 'NONE',  ( -0.000000000000000000, -0.000000000000000000, 1.000000000000000000 ) ) ;
#166543 = CARTESIAN_POINT ( 'NONE',  ( 0.05219959533936267826, -19.03943276465977164, 105.0010903946856615 ) ) ;
#166544 = CARTESIAN_POINT ( 'NONE',  ( 37.24135263299451992, -4.142047767899329713, 41.36355589474229788 ) ) ;
#166545 = CARTESIAN_POINT ( 'NONE',  ( 8.224510206698742110, 14.34966873604972548, 22.08442372801901143 ) ) ;
#166546 = CARTESIAN_POINT ( 'NONE',  ( 5.049401038298161559, -19.05341960407611168, 27.70724293864769550 ) ) ;
#166547 = CARTESIAN_POINT ( 'NONE',  ( -16.46253265017160317, 9.564922557960807481, 105.8322429386476955 ) ) ;
#166548 = CARTESIAN_POINT ( 'NONE',  ( 10.81492255796078972, 18.62759615963270932, 94.58224293864769550 ) ) ;
#166549 = CARTESIAN_POINT ( 'NONE',  ( 0.05219959533937995610, -21.53943276465977519, 55.00109039468568284 ) ) ;
#166551 = CARTESIAN_POINT ( 'NONE',  ( -21.52544592524334988, -5.823673210054445271, 108.9594237280190185 ) ) ;
#166550 = CARTESIAN_POINT ( 'NONE',  ( 13.97604488694548053, -13.89961937509957401, 110.6260903946856615 ) ) ;
#166552 = CARTESIAN_POINT ( 'NONE',  ( -14.29746914071037622, -8.314922557961029526, 104.1677570613523471 ) ) ;
#166553 = CARTESIAN_POINT ( 'NONE',  ( -10.72451020669898014, 18.67979575497178502, 95.41557627198102409 ) ) ;
#166554 = CARTESIAN_POINT ( 'NONE',  ( -8.224510206698948167, 14.34966873604960824, 50.41557627198103120 ) ) ;
#166555 = CARTESIAN_POINT ( 'NONE',  ( 5.153800228976615827, -19.02544592524334988, 80.20942372801901854 ) ) ;
#166556 = CARTESIAN_POINT ( 'NONE',  ( 13.89961937509957401, 13.97604488694547697, 61.87609039468566863 ) ) ;
#166557 = CARTESIAN_POINT ( 'NONE',  ( 18.67979575497194134, -10.72451020669871369, 70.83442372801901854 ) ) ;
#166558 = CARTESIAN_POINT ( 'NONE',  ( 19.05341960407617918, -5.049401038297876454, 41.04275706135233293 ) ) ;
#166559 = CARTESIAN_POINT ( 'NONE',  ( -4.379528057220328563, 16.55341960407611168, 105.2072429386477097 ) ) ;
#166560 = CARTESIAN_POINT ( 'NONE',  ( -5.823673210054116645, -21.52544592524344225, 42.29057627198103120 ) ) ;
#166561 = CARTESIAN_POINT ( 'NONE',  ( -12.06949235617756955, 12.14591786802309770, 30.62390960531436335 ) ) ;
#166562 = CARTESIAN_POINT ( 'NONE',  ( 10.81492255796106328, -18.62759615963255655, 100.4177570613523471 ) ) ;
#166563 = CARTESIAN_POINT ( 'NONE',  ( 14.34966873604972726, -8.224510206698740333, 70.83442372801901854 ) ) ;
#166564 = CARTESIAN_POINT ( 'NONE',  ( 8.224510206698953496, -14.34966873604960469, 22.91557627198102765 ) ) ;
#166565 = CARTESIAN_POINT ( 'NONE',  ( -15.72974639402176322, -15.80617190586768395, 59.37609039468568284 ) ) ;
#166566 = CARTESIAN_POINT ( 'NONE',  ( -18.67979575497193778, 10.72451020669871902, 63.33442372801900433 ) ) ;
#166567 = CARTESIAN_POINT ( 'NONE',  ( 5.823673210054125526, 21.52544592524343514, 74.79057627198105251 ) ) ;
#166568 = VERTEX_POINT ( 'NONE', #194169 ) ;
#166569 = CARTESIAN_POINT ( 'NONE',  ( 16.51473224551069308, 9.474510206698969483, 29.16557627198103475 ) ) ;
#166570 = CARTESIAN_POINT ( 'NONE',  ( 10.81492255796106328, -18.62759615963255655, 45.41775706135234003 ) ) ;
#166571 = CARTESIAN_POINT ( 'NONE',  ( -5.153800228976328057, -19.02544592524343514, 27.29057627198103120 ) ) ;
#166572 = CARTESIAN_POINT ( 'NONE',  ( 0.05219959533909260263, 19.03943276465977164, 39.99890960531436690 ) ) ;
#166573 = CARTESIAN_POINT ( 'NONE',  ( 16.52544592524342804, -4.483927247898539470, 83.54057627198102409 ) ) ;
#166574 = CARTESIAN_POINT ( 'NONE',  ( 19.03943276465977164, -0.05219959533909143690, 88.74890960531436690 ) ) ;
#166575 = CARTESIAN_POINT ( 'NONE',  ( 14.34966873604960469, 8.224510206698951720, 29.16557627198103120 ) ) ;
#166576 = CARTESIAN_POINT ( 'NONE',  ( 12.06949235617757843, -12.14591786802309237, 103.1239096053143811 ) ) ;
#166577 = CARTESIAN_POINT ( 'NONE',  ( 15.72974639402199770, -15.80617190586745480, 68.12390960531436690 ) ) ;
#166578 = VECTOR ( 'NONE', #140485, 1000.000000000000000 ) ;
#166579 = CARTESIAN_POINT ( 'NONE',  ( -10.81492255796078084, -18.62759615963271287, 102.0822429386476955 ) ) ;
#166580 = CARTESIAN_POINT ( 'NONE',  ( 13.89961937509977652, -13.97604488694527269, 108.1239096053143669 ) ) ;
#166582 = CARTESIAN_POINT ( 'NONE',  ( -14.34966873604972548, 8.224510206698743886, 28.33442372801902209 ) ) ;
#166581 = CARTESIAN_POINT ( 'NONE',  ( -19.02544592524342804, 5.153800228976336051, 71.04057627198099567 ) ) ;
#166583 = CARTESIAN_POINT ( 'NONE',  ( 21.53943276465977519, -0.05219959533907433946, 58.74890960531436690 ) ) ;
#166584 = CARTESIAN_POINT ( 'NONE',  ( -15.80617190586768217, 15.72974639402176855, 78.12609039468570415 ) ) ;
#166585 = CARTESIAN_POINT ( 'NONE',  ( -19.02544592524342804, 5.153800228976336051, 81.04057627198103830 ) ) ;
#166586 = CARTESIAN_POINT ( 'NONE',  ( -13.89961937509977652, 13.97604488694528158, 105.6239096053143527 ) ) ;
#166587 = CARTESIAN_POINT ( 'NONE',  ( -0.05219959533934338120, 16.53943276465976808, 77.50109039468567573 ) ) ;
#166588 = CARTESIAN_POINT ( 'NONE',  ( 21.52544592524334988, 5.823673210054432836, 51.45942372801901854 ) ) ;
#166589 = CARTESIAN_POINT ( 'NONE',  ( -21.52544592524334988, -5.823673210054445271, 98.95942372801903275 ) ) ;
#166590 = CARTESIAN_POINT ( 'NONE',  ( -4.379528057220086978, -16.55341960407618274, 59.79275706135234714 ) ) ;
#166591 = CARTESIAN_POINT ( 'NONE',  ( -5.719274019375665041, -21.55341960407619695, 19.79275706135235069 ) ) ;
#166592 = CARTESIAN_POINT ( 'NONE',  ( -5.153800228976328057, -19.02544592524343514, 22.29057627198102765 ) ) ;
#166593 = CARTESIAN_POINT ( 'NONE',  ( -21.53943276465977519, 0.05219959533907696930, 91.24890960531436690 ) ) ;
#166594 = CARTESIAN_POINT ( 'NONE',  ( -5.153800228976607833, 19.02544592524334988, 42.70942372801901143 ) ) ;
#166595 = CARTESIAN_POINT ( 'NONE',  ( 21.55341960407610458, 5.719274019375980345, 38.95724293864768839 ) ) ;
#166597 = CARTESIAN_POINT ( 'NONE',  ( -14.34966873604960291, -8.224510206698953496, 41.66557627198103120 ) ) ;
#166596 = CARTESIAN_POINT ( 'NONE',  ( 19.03943276465977164, -0.05219959533909143690, 78.74890960531436690 ) ) ;
#166598 = CARTESIAN_POINT ( 'NONE',  ( -16.20579543436675252, 7.371946100355232900, 64.43479165828124167 ) ) ;
#166599 = CARTESIAN_POINT ( 'NONE',  ( 0.000000000000000000, 0.000000000000000000, -64.92279855667830191 ) ) ;
#166600 = CARTESIAN_POINT ( 'NONE',  ( 5.153800228976615827, -19.02544592524334988, 95.20942372801897591 ) ) ;
#166601 = CARTESIAN_POINT ( 'NONE',  ( 10.72451020669898902, -18.67979575497178502, 67.91557627198102409 ) ) ;
#166602 = CARTESIAN_POINT ( 'NONE',  ( 14.34966873604960469, 8.224510206698951720, 54.16557627198103120 ) ) ;
#166603 = CARTESIAN_POINT ( 'NONE',  ( -4.379528057220086978, -16.55341960407618274, 29.79275706135234358 ) ) ;
#166604 = CARTESIAN_POINT ( 'NONE',  ( -19.05341960407611168, -5.049401038298163336, 51.45724293864770260 ) ) ;
#166606 = CARTESIAN_POINT ( 'NONE',  ( -16.51473224551082808, 9.474510206698731452, 78.33442372801900433 ) ) ;
#166605 = CARTESIAN_POINT ( 'NONE',  ( 18.62759615963255655, 10.81492255796105972, 21.66775706135235069 ) ) ;
#166607 = CARTESIAN_POINT ( 'NONE',  ( -13.97604488694527625, -13.89961937509977652, 76.87390960531433848 ) ) ;
#166608 = CARTESIAN_POINT ( 'NONE',  ( -13.97604488694527625, -13.89961937509977652, 71.87390960531433848 ) ) ;
#166609 = CARTESIAN_POINT ( 'NONE',  ( 5.719274019375991003, -21.55341960407610458, 82.70724293864770971 ) ) ;
#166610 = CARTESIAN_POINT ( 'NONE',  ( 0.05219959533909260263, 19.03943276465977164, 29.99890960531435979 ) ) ;
#166611 = CARTESIAN_POINT ( 'NONE',  ( -18.22780087662123094, -5.499999999999984901, 81.48459894673892734 ) ) ;
#166612 = CARTESIAN_POINT ( 'NONE',  ( -12.14591786802309592, -12.06949235617757132, 56.87390960531436690 ) ) ;
#166613 = CARTESIAN_POINT ( 'NONE',  ( 19.05341960407611168, 5.049401038298154454, 93.95724293864769550 ) ) ;
#166614 = CARTESIAN_POINT ( 'NONE',  ( 5.049401038297881783, 19.05341960407617563, 52.29275706135234003 ) ) ;
#166615 = VECTOR ( 'NONE', #128801, 1000.000000000000000 ) ;
#166616 = CARTESIAN_POINT ( 'NONE',  ( 5.719274019375991003, -21.55341960407610458, 72.70724293864769550 ) ) ;
#166617 = CARTESIAN_POINT ( 'NONE',  ( -5.049401038297874678, -19.05341960407617918, 39.79275706135232582 ) ) ;
#166618 = CARTESIAN_POINT ( 'NONE',  ( 19.03943276465977164, -0.05219959533909143690, 93.74890960531435269 ) ) ;
#166619 = CARTESIAN_POINT ( 'NONE',  ( -11.30153831258470731, -188.0000000000000000, -25.00000000000000000 ) ) ;
#166620 = CARTESIAN_POINT ( 'NONE',  ( 18.67979575497178502, 10.72451020669898547, 24.16557627198103120 ) ) ;
#166621 = CARTESIAN_POINT ( 'NONE',  ( -0.05219959533909027116, -19.03943276465977164, 77.49890960531435269 ) ) ;
#166622 = CARTESIAN_POINT ( 'NONE',  ( -21.55341960407619339, 5.719274019375674811, 53.54275706135234714 ) ) ;
#166623 = CARTESIAN_POINT ( 'NONE',  ( -12.06949235617756955, 12.14591786802309770, 115.6239096053143669 ) ) ;
#166626 = EDGE_LOOP ( 'NONE', ( #129600, #71174, #70645, #71199 ) ) ;
#166625 = CARTESIAN_POINT ( 'NONE',  ( 9.474510206698971260, -16.51473224551069308, 97.91557627198102409 ) ) ;
#166624 = CARTESIAN_POINT ( 'NONE',  ( 18.62759615963255655, 10.81492255796105972, 21.66775706135235069 ) ) ;
#166627 = CARTESIAN_POINT ( 'NONE',  ( 21.52544592524334988, 5.823673210054432836, 41.45942372801901143 ) ) ;
#166628 = ORIENTED_EDGE ( 'NONE', *, *, #52535, .T. ) ;
#166629 = CARTESIAN_POINT ( 'NONE',  ( -0.05219959533909027116, -19.03943276465977164, 102.4989096053143669 ) ) ;
#166630 = CARTESIAN_POINT ( 'NONE',  ( -37.99626262588766679, 2.428612866367529932E-14, -2.002157773949823305 ) ) ;
#166631 = CARTESIAN_POINT ( 'NONE',  ( -5.719274019375978568, 21.55341960407610458, 105.2072429386477097 ) ) ;
#166632 = CARTESIAN_POINT ( 'NONE',  ( 0.05219959533909260263, 19.03943276465977164, 49.99890960531435979 ) ) ;
#166633 = CARTESIAN_POINT ( 'NONE',  ( 14.34966873604972726, -8.224510206698740333, 30.83442372801902209 ) ) ;
#166634 = CARTESIAN_POINT ( 'NONE',  ( 36.91746824999999887, 11.99521256947799053, -2.024999997268813523 ) ) ;
#166635 = CARTESIAN_POINT ( 'NONE',  ( 0.05219959533937995610, -21.53943276465977519, 100.0010903946857042 ) ) ;
#166636 = CARTESIAN_POINT ( 'NONE',  ( 13.89961937509977652, -13.97604488694527269, 38.12390960531436690 ) ) ;
#166637 = CARTESIAN_POINT ( 'NONE',  ( -21.52544592524334988, -5.823673210054445271, 93.95942372801903275 ) ) ;
#166639 = CARTESIAN_POINT ( 'NONE',  ( 21.52544592524334988, 5.823673210054432836, 66.45942372801903275 ) ) ;
#166638 = CARTESIAN_POINT ( 'NONE',  ( -13.89961937509977652, 13.97604488694528158, 90.62390960531432427 ) ) ;
#166640 = CARTESIAN_POINT ( 'NONE',  ( -27.73933785331498925, 2.428612866367529932E-14, 147.3750000027311842 ) ) ;
#166641 = CARTESIAN_POINT ( 'NONE',  ( -9.474510206698964154, 16.51473224551069663, 100.4155762719810241 ) ) ;
#166642 = CARTESIAN_POINT ( 'NONE',  ( -17.50000000000017408, 3.292511757969708519, 30.06520270210541668 ) ) ;
#166645 = CARTESIAN_POINT ( 'NONE',  ( 5.719274019375673035, 21.55341960407619339, 62.29275706135236845 ) ) ;
#166644 = CARTESIAN_POINT ( 'NONE',  ( -4.379528057220086978, -16.55341960407618274, 69.79275706135234714 ) ) ;
#166643 = CARTESIAN_POINT ( 'NONE',  ( -8.224510206698735004, -14.34966873604973081, 49.58442372801901143 ) ) ;
#166646 = CARTESIAN_POINT ( 'NONE',  ( 10.81492255796106328, -18.62759615963255655, 85.41775706135236135 ) ) ;
#166647 = CARTESIAN_POINT ( 'NONE',  ( -12.20125963778088796, 10.33027487414774193, -59.47400725600234495 ) ) ;
#166648 =( BOUNDED_SURFACE ( )  B_SPLINE_SURFACE ( 3, 2, ( 
 ( #20971, #170925, #113963 ),
 ( #52306, #108252, #125421 ),
 ( #31423, #93076, #175662 ),
 ( #37136, #98796, #109245 ),
 ( #16258, #139576, #1061 ),
 ( #186111, #84628, #180679 ),
 ( #69478, #103815, #114982 ),
 ( #85638, #57320, #178669 ),
 ( #38151, #71479, #192832 ),
 ( #133144, #118996, #134159 ),
 ( #21980, #194835, #193841 ),
 ( #55305, #130126, #54313 ),
 ( #56308, #195847, #42155 ),
 ( #83632, #24996, #22979 ),
 ( #116977, #25993, #40132 ),
 ( #10816, #191823, #117990 ),
 ( #86640, #162480, #99805 ),
 ( #146306, #161491, #9818 ),
 ( #149322, #179680, #72486 ),
 ( #100797, #101810, #163498 ),
 ( #39142, #145309, #6792 ),
 ( #148323, #41152, #23982 ),
 ( #102815, #164500, #68471 ),
 ( #115985, #87636, #53303 ) ),
 .UNSPECIFIED., .F., .F., .T. ) 
 B_SPLINE_SURFACE_WITH_KNOTS ( ( 4, 2, 2, 2, 2, 2, 2, 2, 2, 2, 2, 4 ),
 ( 3, 3 ),
 ( -1.040834085586084257E-17, 0.001899702839891682536, 0.002849554259837528900, 0.003799405679783375480, 0.005699108519675068207, 0.006648959939620915222, 0.007598811359566761368, 0.008548662779512607515, 0.009498514199458454529, 0.01139821703935014682, 0.01329791987924184085, 0.01519762271913353315 ),
 ( 0.000000000000000000, 1.000000000000000000 ),
 .UNSPECIFIED. ) 
 GEOMETRIC_REPRESENTATION_ITEM ( )  RATIONAL_B_SPLINE_SURFACE ( (
 ( 1.000000000000000000, 0.7660444431189795678, 1.000000000000000000),
 ( 1.000000000000000000, 0.7753720600381870387, 1.000000000000000000),
 ( 1.000000000000000000, 0.7832595754286640899, 1.000000000000000000),
 ( 1.000000000000000000, 0.7928595458705136600, 1.000000000000000000),
 ( 1.000000000000000000, 0.7956872332516109481, 1.000000000000000000),
 ( 1.000000000000000000, 0.8005750596157605870, 1.000000000000000000),
 ( 1.000000000000000000, 0.8026302056541708696, 1.000000000000000000),
 ( 1.000000000000000000, 0.8075080643848453477, 1.000000000000000000),
 ( 1.000000000000000000, 0.8091143015810815520, 1.000000000000000000),
 ( 1.000000000000000000, 0.8093067629632570981, 1.000000000000000000),
 ( 1.000000000000000000, 0.8089952915731098981, 1.000000000000000000),
 ( 1.000000000000000000, 0.8076919994862900021, 1.000000000000000000),
 ( 1.000000000000000000, 0.8067078407648371474, 1.000000000000000000),
 ( 1.000000000000000000, 0.8041786842467988361, 1.000000000000000000),
 ( 1.000000000000000000, 0.8026334674876747233, 1.000000000000000000),
 ( 1.000000000000000000, 0.7990747329469696236, 1.000000000000000000),
 ( 1.000000000000000000, 0.7970509760941616451, 1.000000000000000000),
 ( 1.000000000000000000, 0.7904793850863758298, 1.000000000000000000),
 ( 1.000000000000000000, 0.7855040224314863151, 1.000000000000000000),
 ( 1.000000000000000000, 0.7751942650506468135, 1.000000000000000000),
 ( 1.000000000000000000, 0.7698260778211376554, 1.000000000000000000),
 ( 1.000000000000000000, 0.7598259884961129362, 1.000000000000000000),
 ( 1.000000000000000000, 0.7551428682220174826, 1.000000000000000000),
 ( 1.000000000000000000, 0.7510191126010865581, 1.000000000000000000) ) ) 
 REPRESENTATION_ITEM ( '' )  SURFACE ( )  );
#166649 = CARTESIAN_POINT ( 'NONE',  ( -14.34966873604972548, 8.224510206698743886, 33.33442372801900433 ) ) ;
#166650 = CARTESIAN_POINT ( 'NONE',  ( -9.474510206698964154, 16.51473224551069663, 70.41557627198102409 ) ) ;
#166651 = CARTESIAN_POINT ( 'NONE',  ( 9.564922557960805705, 16.46253265017160317, 99.58224293864770971 ) ) ;
#166652 = CARTESIAN_POINT ( 'NONE',  ( 17.49999999999999289, 5.500000000000063061, 41.70309617465829177 ) ) ;
#166653 = CARTESIAN_POINT ( 'NONE',  ( 9.564922557960805705, 16.46253265017160317, 24.58224293864769194 ) ) ;
#166654 = CARTESIAN_POINT ( 'NONE',  ( -21.52544592524343514, 5.823673210054127303, 31.04057627198102409 ) ) ;
#166655 = CARTESIAN_POINT ( 'NONE',  ( -0.05219959533934338120, 16.53943276465976808, 87.50109039468568994 ) ) ;
#166657 = CARTESIAN_POINT ( 'NONE',  ( -0.05219959533909027116, -19.03943276465977164, 67.49890960531436690 ) ) ;
#166656 = CARTESIAN_POINT ( 'NONE',  ( 12.14591786802309770, 12.06949235617756955, 89.37390960531435269 ) ) ;
#166658 = CARTESIAN_POINT ( 'NONE',  ( 21.53943276465977519, 0.05219959533937863772, 96.25109039468568994 ) ) ;
#166659 = CARTESIAN_POINT ( 'NONE',  ( -22.94331271462294808, -3.784814030245898575, 190.0000000000000000 ) ) ;
#166660 = CARTESIAN_POINT ( 'NONE',  ( 16.55341960407618274, -4.379528057220086978, 31.04275706135234714 ) ) ;
#166661 = CARTESIAN_POINT ( 'NONE',  ( -14.29746914071049879, 8.314922557960819915, 70.83224293864770971 ) ) ;
#166662 = CARTESIAN_POINT ( 'NONE',  ( -10.72451020669870658, -18.67979575497194134, 44.58442372801901854 ) ) ;
#166663 = CARTESIAN_POINT ( 'NONE',  ( 21.55341960407610458, 5.719274019375980345, 68.95724293864769550 ) ) ;
#166664 = CARTESIAN_POINT ( 'NONE',  ( -19.02544592524334988, -5.153800228976617603, 38.95942372801900433 ) ) ;
#166665 = CARTESIAN_POINT ( 'NONE',  ( -34.38695055765524700, 7.456135981908278865, 45.94887894546500462 ) ) ;
#166666 = CARTESIAN_POINT ( 'NONE',  ( 16.51473224551069308, 9.474510206698969483, 84.16557627198102409 ) ) ;
#166667 = CARTESIAN_POINT ( 'NONE',  ( 14.29746914071049879, -8.314922557960816363, 48.33224293864770260 ) ) ;
#166668 = CARTESIAN_POINT ( 'NONE',  ( 4.483927247898545687, 16.52544592524342804, 29.79057627198102409 ) ) ;
#166669 = CARTESIAN_POINT ( 'NONE',  ( 16.55341960407618274, -4.379528057220086978, 106.0427570613523471 ) ) ;
#166670 = CARTESIAN_POINT ( 'NONE',  ( -16.46253265017146816, -9.564922557961047289, 64.16775706135233293 ) ) ;
#166671 = CARTESIAN_POINT ( 'NONE',  ( 13.89961937509957579, 13.97604488694547520, 76.87609039468566152 ) ) ;
#166672 = CARTESIAN_POINT ( 'NONE',  ( 0.05219959533909260263, 19.03943276465977164, 114.9989096053143669 ) ) ;
#166673 = CARTESIAN_POINT ( 'NONE',  ( 16.53943276465976808, -0.05219959533910856209, 88.74890960531436690 ) ) ;
#166674 = B_SPLINE_CURVE_WITH_KNOTS ( 'NONE', 3,
 ( #61608, #74818, #75791, #182996, #1935, #137469, #139446, #186986, #123277, #108112, #199149, #110114, #121304, #92940 ),
 .UNSPECIFIED., .F., .F.,
 ( 4, 2, 2, 2, 2, 2, 4 ),
 ( 0.003265479109357864295, 0.004052109043202368685, 0.004445424010124612857, 0.004838738977046857029, 0.005625368910891345373, 0.006018683877813588677, 0.006411998844735832849 ),
 .UNSPECIFIED. ) ;
#166675 = DIRECTION ( 'NONE',  ( -0.7071067811865467956, 7.406550393246788537E-15, -0.7071067811865483499 ) ) ;
#166677 = CARTESIAN_POINT ( 'NONE',  ( -5.719274019375978568, 21.55341960407610458, 35.20724293864768839 ) ) ;
#166676 = CARTESIAN_POINT ( 'NONE',  ( 19.03943276465977164, -0.05219959533909143690, 28.74890960531435624 ) ) ;
#166678 = CARTESIAN_POINT ( 'NONE',  ( 5.823673210054125526, 21.52544592524343514, 64.79057627198103830 ) ) ;
#166679 = CARTESIAN_POINT ( 'NONE',  ( -16.53943276465976808, 0.05219959533911058130, 111.2489096053143669 ) ) ;
#166681 = CARTESIAN_POINT ( 'NONE',  ( -5.153800228976328057, -19.02544592524343514, 47.29057627198102409 ) ) ;
#166680 = CARTESIAN_POINT ( 'NONE',  ( -16.53943276465976808, -0.05219959533934237506, 68.75109039468568994 ) ) ;
#166682 = CARTESIAN_POINT ( 'NONE',  ( 18.62759615963255655, 10.81492255796105972, 61.66775706135235424 ) ) ;
#166683 = CARTESIAN_POINT ( 'NONE',  ( -8.224510206698948167, 14.34966873604960824, 105.4155762719810383 ) ) ;
#166684 = CARTESIAN_POINT ( 'NONE',  ( -13.97604488694547697, 13.89961937509957934, 88.12609039468563310 ) ) ;
#166685 = CARTESIAN_POINT ( 'NONE',  ( 29.86685920354754842, -21.69954338932559068, -4.324999997268814234 ) ) ;
#166687 = CARTESIAN_POINT ( 'NONE',  ( -15.72974639402197994, 15.80617190586746368, 30.62390960531436335 ) ) ;
#166686 = DIRECTION ( 'NONE',  ( -1.000000000000000000, 0.000000000000000000, 0.000000000000000000 ) ) ;
#166688 = CARTESIAN_POINT ( 'NONE',  ( 0.05219959533937995610, -21.53943276465977519, 75.00109039468568994 ) ) ;
#166690 = CARTESIAN_POINT ( 'NONE',  ( 0.05219959533910956823, 16.53943276465976808, 39.99890960531436690 ) ) ;
#166689 = CARTESIAN_POINT ( 'NONE',  ( -12.14591786802326823, 12.06949235617739902, 58.12609039468568994 ) ) ;
#166691 = CARTESIAN_POINT ( 'NONE',  ( 5.719274019375991003, -21.55341960407610458, 72.70724293864769550 ) ) ;
#166692 = CARTESIAN_POINT ( 'NONE',  ( -10.72451020669898014, 18.67979575497178502, 60.41557627198102409 ) ) ;
#166693 = CARTESIAN_POINT ( 'NONE',  ( -21.76075944043963872, -9.615265036675765487, 170.8440536485302061 ) ) ;
#166695 = CARTESIAN_POINT ( 'NONE',  ( -5.719274019375978568, 21.55341960407610458, 25.20724293864769550 ) ) ;
#166694 = CARTESIAN_POINT ( 'NONE',  ( -16.51473224551082808, 9.474510206698731452, 83.33442372801899012 ) ) ;
#166696 = CARTESIAN_POINT ( 'NONE',  ( -19.05341960407611168, -5.049401038298163336, 46.45724293864768129 ) ) ;
#166697 = CARTESIAN_POINT ( 'NONE',  ( 19.05341960407611168, 5.049401038298154454, 23.95724293864769194 ) ) ;
#166698 = FILL_AREA_STYLE_COLOUR ( '', #137089 ) ;
#166699 = FACE_BOUND ( 'NONE', #7931, .T. ) ;
#166700 = ORIENTED_EDGE ( 'NONE', *, *, #8154, .F. ) ;
#166701 = CARTESIAN_POINT ( 'NONE',  ( 0.05219959533934541429, -16.53943276465976808, 65.00109039468568994 ) ) ;
#166702 = CARTESIAN_POINT ( 'NONE',  ( -21.53943276465977519, 0.05219959533907696930, 106.2489096053143811 ) ) ;
#166703 = CARTESIAN_POINT ( 'NONE',  ( -9.564922557960796823, -16.46253265017161027, 52.08224293864768839 ) ) ;
#166704 = CARTESIAN_POINT ( 'NONE',  ( 5.823673210054444382, -21.52544592524334988, 40.20942372801901854 ) ) ;
#166705 = CARTESIAN_POINT ( 'NONE',  ( 16.51473224551069308, 9.474510206698969483, 94.16557627198103830 ) ) ;
#166706 = CARTESIAN_POINT ( 'NONE',  ( -21.50179914128360892, -34.93963825065945628, -18.44273973154475854 ) ) ;
#166707 = VERTEX_POINT ( 'NONE', #163827 ) ;
#166708 = CARTESIAN_POINT ( 'NONE',  ( -10.81492255796105439, 18.62759615963255655, 37.91775706135235424 ) ) ;
#166710 = CARTESIAN_POINT ( 'NONE',  ( -5.049401038297874678, -19.05341960407617918, 94.79275706135230450 ) ) ;
#166709 = CARTESIAN_POINT ( 'NONE',  ( -9.564922557960796823, -16.46253265017161027, 112.0822429386476955 ) ) ;
#166711 = CARTESIAN_POINT ( 'NONE',  ( -16.46253265017146816, -9.564922557961047289, 44.16775706135232582 ) ) ;
#166712 = CARTESIAN_POINT ( 'NONE',  ( -18.62759615963270932, 10.81492255796079327, 95.83224293864770971 ) ) ;
#166713 = CARTESIAN_POINT ( 'NONE',  ( 5.153800228976615827, -19.02544592524334988, 30.20942372801900433 ) ) ;
#166714 = CARTESIAN_POINT ( 'NONE',  ( 5.153800228976615827, -19.02544592524334988, 45.20942372801901143 ) ) ;
#166715 = CARTESIAN_POINT ( 'NONE',  ( -16.52544592524335698, -4.483927247898792601, 93.95942372801903275 ) ) ;
#166716 = CARTESIAN_POINT ( 'NONE',  ( -18.22780087662126647, -5.499999999999827693, 43.98236817873107185 ) ) ;
#166717 = CARTESIAN_POINT ( 'NONE',  ( -16.46253265017160317, 9.564922557960807481, 75.83224293864769550 ) ) ;
#166718 = CIRCLE ( 'NONE', #95669, 214.0437394197456911 ) ;
#166719 = CARTESIAN_POINT ( 'NONE',  ( 10.72451020669871369, 18.67979575497193778, 77.08442372801901854 ) ) ;
#166720 = CARTESIAN_POINT ( 'NONE',  ( 5.719274019375673035, 21.55341960407619339, 82.29275706135234714 ) ) ;
#166721 = CARTESIAN_POINT ( 'NONE',  ( 21.30000000000002913, 0.000000000000000000, -56.46919128290398504 ) ) ;
#166722 = CARTESIAN_POINT ( 'NONE',  ( -19.02544592524342804, 5.153800228976336051, 86.04057627198103830 ) ) ;
#166723 = CARTESIAN_POINT ( 'NONE',  ( 21.53943276465977519, 0.05219959533937863772, 56.25109039468568284 ) ) ;
#166724 = CARTESIAN_POINT ( 'NONE',  ( -5.049401038297874678, -19.05341960407617918, 104.7927570613523471 ) ) ;
#166725 = CARTESIAN_POINT ( 'NONE',  ( -9.474510206698964154, 16.51473224551069663, 70.41557627198102409 ) ) ;
#166726 = CARTESIAN_POINT ( 'NONE',  ( 16.46253265017160672, -9.564922557960803928, 108.3322429386476955 ) ) ;
#166727 = CARTESIAN_POINT ( 'NONE',  ( -0.05219959533909027116, -19.03943276465977164, 82.49890960531436690 ) ) ;
#166728 = CARTESIAN_POINT ( 'NONE',  ( -17.48853670773246805, -5.747243402303017668, 91.33328700250007159 ) ) ;
#166729 = CARTESIAN_POINT ( 'NONE',  ( 5.153800228976335163, 19.02544592524342804, 64.79057627198100988 ) ) ;
#166730 = CARTESIAN_POINT ( 'NONE',  ( 19.02544592524343514, -5.153800228976328945, 58.54057627198102409 ) ) ;
#166731 = CARTESIAN_POINT ( 'NONE',  ( -21.52544592524343514, 5.823673210054127303, 111.0405762719810525 ) ) ;
#166732 = CARTESIAN_POINT ( 'NONE',  ( -12.14591786802326823, 12.06949235617739902, 93.12609039468568994 ) ) ;
#166733 = CARTESIAN_POINT ( 'NONE',  ( -21.98685479826780309, 13.98560643873834231, 165.5209445330007725 ) ) ;
#166734 = CARTESIAN_POINT ( 'NONE',  ( 19.05341960407617918, -5.049401038297876454, 51.04275706135231871 ) ) ;
#166735 = CARTESIAN_POINT ( 'NONE',  ( -19.03943276465977164, 0.05219959533909376836, 81.24890960531436690 ) ) ;
#166736 = CARTESIAN_POINT ( 'NONE',  ( 14.29746914071049879, -8.314922557960816363, 73.33224293864769550 ) ) ;
#166737 = CARTESIAN_POINT ( 'NONE',  ( 12.14591786802309770, 12.06949235617756955, 104.3739096053143669 ) ) ;
#166738 = CARTESIAN_POINT ( 'NONE',  ( -5.049401038298153566, 19.05341960407611168, 110.2072429386476671 ) ) ;
#166739 = ORIENTED_EDGE ( 'NONE', *, *, #29683, .T. ) ;
#166740 = CARTESIAN_POINT ( 'NONE',  ( -13.97604488694527625, -13.89961937509977652, 101.8739096053143811 ) ) ;
#166741 = CARTESIAN_POINT ( 'NONE',  ( -16.52544592524342804, 4.483927247898546575, 76.04057627198102409 ) ) ;
#166742 = DIRECTION ( 'NONE',  ( 0.000000000000000000, 0.000000000000000000, -1.000000000000000000 ) ) ;
#166743 = CARTESIAN_POINT ( 'NONE',  ( 5.153800228976615827, -19.02544592524334988, 35.20942372801899722 ) ) ;
#166744 = CARTESIAN_POINT ( 'NONE',  ( -14.34966873604972548, 8.224510206698743886, 93.33442372801901854 ) ) ;
#166745 = CARTESIAN_POINT ( 'NONE',  ( 16.51473224551069308, 9.474510206698969483, 84.16557627198102409 ) ) ;
#166746 = CARTESIAN_POINT ( 'NONE',  ( -18.62759615963255300, -10.81492255796106328, 59.16775706135234714 ) ) ;
#166747 = CARTESIAN_POINT ( 'NONE',  ( -15.72974639402197994, 15.80617190586746368, 40.62390960531435269 ) ) ;
#166748 = CARTESIAN_POINT ( 'NONE',  ( -21.53943276465977519, 0.05219959533907696930, 116.2489096053143669 ) ) ;
#166749 = CARTESIAN_POINT ( 'NONE',  ( 0.05219959533907565091, 21.53943276465977519, 69.99890960531435269 ) ) ;
#166750 = CARTESIAN_POINT ( 'NONE',  ( -14.29746914071049879, 8.314922557960819915, 95.83224293864770971 ) ) ;
#166751 = CARTESIAN_POINT ( 'NONE',  ( 13.97604488694548053, -13.89961937509957401, 55.62609039468566863 ) ) ;
#166752 = EDGE_CURVE ( 'NONE', #188843, #123761, #196022, .T. ) ;
#166753 = CARTESIAN_POINT ( 'NONE',  ( -19.03943276465977164, 0.05219959533909376836, 31.24890960531435979 ) ) ;
#166754 = CARTESIAN_POINT ( 'NONE',  ( -13.89961937509977652, 13.97604488694528158, 85.62390960531433848 ) ) ;
#166755 = CARTESIAN_POINT ( 'NONE',  ( 5.049401038298161559, -19.05341960407611168, 87.70724293864769550 ) ) ;
#166756 = CARTESIAN_POINT ( 'NONE',  ( -0.05219959533910754901, -16.53943276465976808, 102.4989096053143811 ) ) ;
#166757 = ORIENTED_EDGE ( 'NONE', *, *, #55, .F. ) ;
#166758 = VECTOR ( 'NONE', #127087, 1000.000000000000000 ) ;
#166759 = CARTESIAN_POINT ( 'NONE',  ( 0.05219959533910956823, 16.53943276465976808, 24.99890960531435624 ) ) ;
#166760 = CARTESIAN_POINT ( 'NONE',  ( -16.53943276465976808, -0.05219959533934237506, 43.75109039468568284 ) ) ;
#166761 = CARTESIAN_POINT ( 'NONE',  ( 21.53943276465977519, 0.05219959533937863772, 106.2510903946856757 ) ) ;
#166762 = CARTESIAN_POINT ( 'NONE',  ( 13.97604488694527802, 13.89961937509977652, 104.3739096053143385 ) ) ;
#166763 = CARTESIAN_POINT ( 'NONE',  ( 18.62759615963271287, -10.81492255796078972, 113.3322429386476955 ) ) ;
#166764 = CARTESIAN_POINT ( 'NONE',  ( -0.05219959533909027116, -19.03943276465977164, 47.49890960531435979 ) ) ;
#166765 = VECTOR ( 'NONE', #178341, 1000.000000000000114 ) ;
#166766 = CARTESIAN_POINT ( 'NONE',  ( 12.14591786802327356, -12.06949235617739191, 40.62609039468567573 ) ) ;
#166767 = CARTESIAN_POINT ( 'NONE',  ( 9.474510206698729675, 16.51473224551082808, 102.0844237280190043 ) ) ;
#166768 = CARTESIAN_POINT ( 'NONE',  ( -19.03943276465977164, 0.05219959533909376836, 41.24890960531435269 ) ) ;
#166769 = CARTESIAN_POINT ( 'NONE',  ( -14.34966873604960291, -8.224510206698953496, 96.66557627198102409 ) ) ;
#166770 = CARTESIAN_POINT ( 'NONE',  ( -15.72974639402197994, 15.80617190586746368, 100.6239096053143811 ) ) ;
#166771 = CARTESIAN_POINT ( 'NONE',  ( 9.474510206698729675, 16.51473224551082808, 77.08442372801900433 ) ) ;
#166772 = DIRECTION ( 'NONE',  ( -1.000000000000000000, 0.000000000000000000, 0.000000000000000000 ) ) ;
#166773 = CARTESIAN_POINT ( 'NONE',  ( -16.46253265017160317, 9.564922557960807481, 85.83224293864769550 ) ) ;
#166774 = CARTESIAN_POINT ( 'NONE',  ( -21.53943276465977519, -0.05219959533937600094, 18.75109039468568639 ) ) ;
#166775 = CARTESIAN_POINT ( 'NONE',  ( -5.153800228976328057, -19.02544592524343514, 22.29057627198102765 ) ) ;
#166776 = CARTESIAN_POINT ( 'NONE',  ( 19.05341960407611168, 5.049401038298154454, 88.95724293864769550 ) ) ;
#166777 = CARTESIAN_POINT ( 'NONE',  ( -17.50000000000000711, -5.499999999999944045, 81.28230962303565832 ) ) ;
#166778 = CARTESIAN_POINT ( 'NONE',  ( -19.02544592524342804, 5.153800228976336051, 86.04057627198103830 ) ) ;
#166780 = CARTESIAN_POINT ( 'NONE',  ( -8.224510206698948167, 14.34966873604960824, 90.41557627198103830 ) ) ;
#166779 = CARTESIAN_POINT ( 'NONE',  ( -5.823673210054431948, 21.52544592524334988, 32.70942372801900433 ) ) ;
#166781 = CARTESIAN_POINT ( 'NONE',  ( -13.89961937509977652, 13.97604488694528158, 95.62390960531436690 ) ) ;
#166782 = CARTESIAN_POINT ( 'NONE',  ( -5.153800228976607833, 19.02544592524334988, 27.70942372801899722 ) ) ;
#166783 = CARTESIAN_POINT ( 'NONE',  ( 16.53943276465976808, 0.05219959533934440121, 46.25109039468567573 ) ) ;
#166784 = CARTESIAN_POINT ( 'NONE',  ( 21.55341960407619695, -5.719274019375665929, 71.04275706135234714 ) ) ;
#166785 = CARTESIAN_POINT ( 'NONE',  ( 4.483927247898790824, -16.52544592524335698, 25.20942372801901854 ) ) ;
#166786 = CARTESIAN_POINT ( 'NONE',  ( -16.51473224551069308, -9.474510206698971260, 66.66557627198102409 ) ) ;
#166787 = CARTESIAN_POINT ( 'NONE',  ( 19.05341960407617918, -5.049401038297876454, 101.0427570613523045 ) ) ;
#166788 = CARTESIAN_POINT ( 'NONE',  ( 16.53943276465976808, 0.05219959533934440121, 71.25109039468568994 ) ) ;
#166789 = CARTESIAN_POINT ( 'NONE',  ( -5.719274019375665041, -21.55341960407619695, 109.7927570613523613 ) ) ;
#166790 = CARTESIAN_POINT ( 'NONE',  ( 5.153800228976615827, -19.02544592524334988, 85.20942372801900433 ) ) ;
#166791 = CARTESIAN_POINT ( 'NONE',  ( 19.03943276465977164, -0.05219959533909143690, 48.74890960531435979 ) ) ;
#166792 = CARTESIAN_POINT ( 'NONE',  ( 21.53943276465977519, -0.05219959533907433946, 78.74890960531436690 ) ) ;
#166794 = CARTESIAN_POINT ( 'NONE',  ( -13.97604488694547697, 13.89961937509957934, 73.12609039468568994 ) ) ;
#166793 = CARTESIAN_POINT ( 'NONE',  ( -14.29746914071049879, 8.314922557960819915, 80.83224293864769550 ) ) ;
#166795 = CARTESIAN_POINT ( 'NONE',  ( -19.34837522270365895, -5.499999999999857003, 70.86337684832579953 ) ) ;
#166796 = CARTESIAN_POINT ( 'NONE',  ( 13.97604488694548053, -13.89961937509957401, 50.62609039468566152 ) ) ;
#166797 = CARTESIAN_POINT ( 'NONE',  ( -16.52544592524335698, -4.483927247898792601, 108.9594237280190185 ) ) ;
#166798 = CARTESIAN_POINT ( 'NONE',  ( -16.52544592524342804, 4.483927247898546575, 61.04057627198103120 ) ) ;
#166800 = CARTESIAN_POINT ( 'NONE',  ( 22.44159573604009594, -16.30477369853687364, 143.6750000027311671 ) ) ;
#166799 = CARTESIAN_POINT ( 'NONE',  ( 21.53943276465977519, 0.05219959533937863772, 106.2510903946856757 ) ) ;
#166801 = CARTESIAN_POINT ( 'NONE',  ( -5.823673210054116645, -21.52544592524344225, 107.2905762719810525 ) ) ;
#166802 = CARTESIAN_POINT ( 'NONE',  ( 9.474510206698971260, -16.51473224551069308, 107.9155762719810383 ) ) ;
#166803 = CARTESIAN_POINT ( 'NONE',  ( 13.97604488694527802, 13.89961937509977652, 64.37390960531436690 ) ) ;
#166804 = CARTESIAN_POINT ( 'NONE',  ( -21.53943276465977519, -0.05219959533937600094, 78.75109039468568994 ) ) ;
#166805 = CARTESIAN_POINT ( 'NONE',  ( 9.474510206698971260, -16.51473224551069308, 67.91557627198102409 ) ) ;
#166806 = VERTEX_POINT ( 'NONE', #55633 ) ;
#166807 = CARTESIAN_POINT ( 'NONE',  ( 19.03943276465977164, -0.05219959533909143690, 33.74890960531435979 ) ) ;
#166808 = CARTESIAN_POINT ( 'NONE',  ( 18.67979575497178502, 10.72451020669898547, 24.16557627198103120 ) ) ;
#166809 = CARTESIAN_POINT ( 'NONE',  ( -8.314922557960811034, -14.29746914071050412, 67.08224293864770971 ) ) ;
#166810 = CARTESIAN_POINT ( 'NONE',  ( -9.474510206698964154, 16.51473224551069663, 45.41557627198103120 ) ) ;
#166811 = CARTESIAN_POINT ( 'NONE',  ( 0.05219959533910956823, 16.53943276465976808, 94.99890960531436690 ) ) ;
#166812 = CARTESIAN_POINT ( 'NONE',  ( -10.72451020669898014, 18.67979575497178502, 110.4155762719810383 ) ) ;
#166813 = CARTESIAN_POINT ( 'NONE',  ( -15.72974639402176322, -15.80617190586768395, 49.37609039468569705 ) ) ;
#166814 = CARTESIAN_POINT ( 'NONE',  ( 5.049401038298161559, -19.05341960407611168, 27.70724293864769550 ) ) ;
#166815 = CARTESIAN_POINT ( 'NONE',  ( 14.29746914071037800, 8.314922557961029526, 66.66775706135234714 ) ) ;
#166816 = CARTESIAN_POINT ( 'NONE',  ( -10.72451020669898014, 18.67979575497178502, 105.4155762719810383 ) ) ;
#166817 = CARTESIAN_POINT ( 'NONE',  ( 18.67979575497178502, 10.72451020669898547, 94.16557627198103830 ) ) ;
#166819 = CARTESIAN_POINT ( 'NONE',  ( -19.03943276465977164, 0.05219959533909376836, 56.24890960531435979 ) ) ;
#166818 = CARTESIAN_POINT ( 'NONE',  ( -9.474510206698720793, -16.51473224551083518, 29.58442372801900433 ) ) ;
#166820 = CARTESIAN_POINT ( 'NONE',  ( -18.09805431107519880, 5.500000000000101252, 41.01606229291888894 ) ) ;
#166821 = CARTESIAN_POINT ( 'NONE',  ( -21.53943276465977519, -0.05219959533937600094, 58.75109039468568994 ) ) ;
#166822 = CARTESIAN_POINT ( 'NONE',  ( -15.80617190586745835, -15.72974639402198527, 56.87390960531436690 ) ) ;
#166823 = CARTESIAN_POINT ( 'NONE',  ( 16.53943276465976808, -0.05219959533910856209, 23.74890960531435269 ) ) ;
#166825 = CARTESIAN_POINT ( 'NONE',  ( -18.67979575497193778, 10.72451020669871902, 103.3344237280190043 ) ) ;
#166824 = CARTESIAN_POINT ( 'NONE',  ( -5.719274019375665041, -21.55341960407619695, 79.79275706135236135 ) ) ;
#166826 = CARTESIAN_POINT ( 'NONE',  ( 19.02544592524334988, 5.153800228976608722, 41.45942372801900433 ) ) ;
#166827 = CARTESIAN_POINT ( 'NONE',  ( 16.52544592524335698, 4.483927247898782831, 96.45942372801901854 ) ) ;
#166828 = CARTESIAN_POINT ( 'NONE',  ( 21.55341960407619695, -5.719274019375665929, 51.04275706135234714 ) ) ;
#166829 = CARTESIAN_POINT ( 'NONE',  ( 9.474510206698971260, -16.51473224551069308, 57.91557627198103120 ) ) ;
#166830 = CARTESIAN_POINT ( 'NONE',  ( -16.51473224551082808, 9.474510206698731452, 38.33442372801899722 ) ) ;
#166831 = CARTESIAN_POINT ( 'NONE',  ( 10.81492255796078972, 18.62759615963270932, 34.58224293864770260 ) ) ;
#166832 = CARTESIAN_POINT ( 'NONE',  ( -15.72974639402176322, -15.80617190586768395, 34.37609039468568284 ) ) ;
#166833 = CARTESIAN_POINT ( 'NONE',  ( -10.72451020669898014, 18.67979575497178502, 85.41557627198102409 ) ) ;
#166834 = CARTESIAN_POINT ( 'NONE',  ( 9.474510206698729675, 16.51473224551082808, 82.08442372801899012 ) ) ;
#166835 = CARTESIAN_POINT ( 'NONE',  ( 4.483927247898790824, -16.52544592524335698, 50.20942372801901854 ) ) ;
#166837 = CARTESIAN_POINT ( 'NONE',  ( 15.80617190586746368, 15.72974639402197994, 99.37390960531436690 ) ) ;
#166836 = CARTESIAN_POINT ( 'NONE',  ( -4.460769206500190265, 4.179973224035743229, -62.50518786092071366 ) ) ;
#166839 = CARTESIAN_POINT ( 'NONE',  ( -16.52544592524342804, 4.483927247898546575, 76.04057627198102409 ) ) ;
#166838 = CARTESIAN_POINT ( 'NONE',  ( -16.53943276465976808, -0.05219959533934237506, 83.75109039468568994 ) ) ;
#166840 = CARTESIAN_POINT ( 'NONE',  ( -16.29526858892875651, -7.335722546920136367, 100.7967059780020520 ) ) ;
#166841 = CARTESIAN_POINT ( 'NONE',  ( -16.46253265017146816, -9.564922557961047289, 104.1677570613523329 ) ) ;
#166842 = CARTESIAN_POINT ( 'NONE',  ( -5.719274019375978568, 21.55341960407610458, 35.20724293864768839 ) ) ;
#166843 = FACE_OUTER_BOUND ( 'NONE', #12053, .T. ) ;
#166844 = CARTESIAN_POINT ( 'NONE',  ( -16.55341960407617563, 4.379528057220093196, 48.54275706135234714 ) ) ;
#166845 = CARTESIAN_POINT ( 'NONE',  ( 0.05219959533907565091, 21.53943276465977519, 109.9989096053143527 ) ) ;
#166846 = CARTESIAN_POINT ( 'NONE',  ( -15.80617190586745835, -15.72974639402198527, 31.87390960531435979 ) ) ;
#166847 = CARTESIAN_POINT ( 'NONE',  ( 14.29746914071037800, 8.314922557961029526, 76.66775706135234714 ) ) ;
#166848 = CARTESIAN_POINT ( 'NONE',  ( 19.03943276465977164, -0.05219959533909143690, 78.74890960531436690 ) ) ;
#166850 = CARTESIAN_POINT ( 'NONE',  ( -13.97604488694527625, -13.89961937509977652, 31.87390960531435979 ) ) ;
#166849 = CARTESIAN_POINT ( 'NONE',  ( 21.52544592524334988, 5.823673210054432836, 61.45942372801901854 ) ) ;
#166851 = CARTESIAN_POINT ( 'NONE',  ( 18.67979575497178502, 10.72451020669898547, 24.16557627198103120 ) ) ;
#166852 = ORIENTED_EDGE ( 'NONE', *, *, #197067, .T. ) ;
#166853 = CARTESIAN_POINT ( 'NONE',  ( 16.51473224551083163, -9.474510206698727899, 40.83442372801900433 ) ) ;
#166854 = CARTESIAN_POINT ( 'NONE',  ( -4.379528057220086978, -16.55341960407618274, 54.79275706135235424 ) ) ;
#166855 = CARTESIAN_POINT ( 'NONE',  ( -16.51473224551069308, -9.474510206698971260, 111.6655762719810383 ) ) ;
#166856 = CARTESIAN_POINT ( 'NONE',  ( 5.049401038298161559, -19.05341960407611168, 72.70724293864768129 ) ) ;
#166857 = CARTESIAN_POINT ( 'NONE',  ( -14.34966873604972548, 8.224510206698743886, 103.3344237280190043 ) ) ;
#166858 = DIRECTION ( 'NONE',  ( -0.000000000000000000, 0.000000000000000000, -1.000000000000000000 ) ) ;
#166859 = CARTESIAN_POINT ( 'NONE',  ( 12.14591786802309770, 12.06949235617756955, 94.37390960531436690 ) ) ;
#166860 = CARTESIAN_POINT ( 'NONE',  ( -21.53943276465977519, 0.05219959533907696930, 41.24890960531435269 ) ) ;
#166861 = CARTESIAN_POINT ( 'NONE',  ( -9.474510206698964154, 16.51473224551069663, 25.41557627198103120 ) ) ;
#166862 = CARTESIAN_POINT ( 'NONE',  ( 4.483927247898790824, -16.52544592524335698, 65.20942372801901854 ) ) ;
#166863 = CARTESIAN_POINT ( 'NONE',  ( 0.05219959533937995610, -21.53943276465977519, 25.00109039468567218 ) ) ;
#166864 = CARTESIAN_POINT ( 'NONE',  ( 19.03943276465977164, 0.05219959533936151252, 71.25109039468566152 ) ) ;
#166865 = CARTESIAN_POINT ( 'NONE',  ( 16.51473224551069308, 9.474510206698969483, 39.16557627198103120 ) ) ;
#166866 = CARTESIAN_POINT ( 'NONE',  ( -21.52544592524343514, 5.823673210054127303, 71.04057627198103830 ) ) ;
#166867 = AXIS2_PLACEMENT_3D ( 'NONE', #7587, #102619, #39936 ) ;
#166868 = CARTESIAN_POINT ( 'NONE',  ( -16.51473224551069308, -9.474510206698971260, 111.6655762719810383 ) ) ;
#166869 = CARTESIAN_POINT ( 'NONE',  ( -15.80617190586768217, 15.72974639402176855, 98.12609039468570415 ) ) ;
#166870 = CARTESIAN_POINT ( 'NONE',  ( -19.05341960407611168, -5.049401038298163336, 66.45724293864769550 ) ) ;
#166871 = CARTESIAN_POINT ( 'NONE',  ( -8.314922557961024197, 14.29746914071037800, 52.91775706135235424 ) ) ;
#166872 = CARTESIAN_POINT ( 'NONE',  ( -5.719274019375665041, -21.55341960407619695, 84.79275706135234714 ) ) ;
#166873 = CARTESIAN_POINT ( 'NONE',  ( 9.564922557961047289, -16.46253265017146816, 35.41775706135233293 ) ) ;
#166874 = CARTESIAN_POINT ( 'NONE',  ( -19.03943276465977164, -0.05219959533935918106, 58.75109039468566863 ) ) ;
#166875 = EDGE_LOOP ( 'NONE', ( #110411, #114352, #19881, #57003 ) ) ;
#166876 = CARTESIAN_POINT ( 'NONE',  ( -21.53943276465977519, -0.05219959533937600094, 53.75109039468568994 ) ) ;
#166877 = CARTESIAN_POINT ( 'NONE',  ( -19.05341960407611168, -5.049401038298163336, 26.45724293864769550 ) ) ;
#166878 = CARTESIAN_POINT ( 'NONE',  ( 5.153800228976615827, -19.02544592524334988, 45.20942372801901143 ) ) ;
#166879 = CARTESIAN_POINT ( 'NONE',  ( 19.03943276465977164, -0.05219959533909143690, 93.74890960531435269 ) ) ;
#166880 = CARTESIAN_POINT ( 'NONE',  ( -9.564922557960796823, -16.46253265017161027, 77.08224293864769550 ) ) ;
#166881 = CARTESIAN_POINT ( 'NONE',  ( 14.34966873604960469, 8.224510206698951720, 39.16557627198102409 ) ) ;
#166882 = CARTESIAN_POINT ( 'NONE',  ( 0.05219959533907565091, 21.53943276465977519, 39.99890960531436690 ) ) ;
#166883 = CARTESIAN_POINT ( 'NONE',  ( -22.81625015709510507, 31.40387420917330275, -0.9249999972688132122 ) ) ;
#166884 = CARTESIAN_POINT ( 'NONE',  ( 17.31747979337948706, 6.344076630961012597, 58.87944868065186199 ) ) ;
#166885 = CARTESIAN_POINT ( 'NONE',  ( -0.05219959533937732626, 21.53943276465977519, 92.50109039468567573 ) ) ;
#166886 = LINE ( 'NONE', #28387, #86319 ) ;
#166887 = CARTESIAN_POINT ( 'NONE',  ( -16.46253265017160317, 9.564922557960807481, 35.83224293864768839 ) ) ;
#166888 = CARTESIAN_POINT ( 'NONE',  ( -19.03943276465977164, 0.05219959533909376836, 111.2489096053143669 ) ) ;
#166889 = EDGE_CURVE ( 'NONE', #74166, #137566, #177995, .T. ) ;
#166890 = CARTESIAN_POINT ( 'NONE',  ( 11.74149087413295156, -36.13659316521243881, -1.402157773949822550 ) ) ;
#166891 = CARTESIAN_POINT ( 'NONE',  ( 8.314922557961029526, -14.29746914071037800, 45.41775706135234003 ) ) ;
#166892 = CARTESIAN_POINT ( 'NONE',  ( 18.62759615963271287, -10.81492255796078972, 63.33224293864770260 ) ) ;
#166893 = CARTESIAN_POINT ( 'NONE',  ( -0.05219959533910754901, -16.53943276465976808, 37.49890960531436690 ) ) ;
#166895 = CARTESIAN_POINT ( 'NONE',  ( 5.153800228976335163, 19.02544592524342804, 109.7905762719810099 ) ) ;
#166894 = CARTESIAN_POINT ( 'NONE',  ( -9.564922557960796823, -16.46253265017161027, 27.08224293864769550 ) ) ;
#166896 = CARTESIAN_POINT ( 'NONE',  ( -21.52544592524334988, -5.823673210054445271, 28.95942372801902209 ) ) ;
#166897 = CARTESIAN_POINT ( 'NONE',  ( -5.153800228976607833, 19.02544592524334988, 37.70942372801899722 ) ) ;
#166898 = CARTESIAN_POINT ( 'NONE',  ( 13.89961937509977652, -13.97604488694527269, 23.12390960531436335 ) ) ;
#166899 = CARTESIAN_POINT ( 'NONE',  ( 21.53943276465977519, 0.05219959533937863772, 76.25109039468568994 ) ) ;
#166900 = CARTESIAN_POINT ( 'NONE',  ( 19.49401214000073779, -12.39993551617566503, 164.9999999999999716 ) ) ;
#166901 = CARTESIAN_POINT ( 'NONE',  ( -16.53943276465976808, 0.05219959533911058130, 31.24890960531435979 ) ) ;
#166902 = CARTESIAN_POINT ( 'NONE',  ( 17.50000000000014566, 3.292511757969652120, 112.4347972978947325 ) ) ;
#166903 = CARTESIAN_POINT ( 'NONE',  ( 0.05219959533907565091, 21.53943276465977519, 29.99890960531435979 ) ) ;
#166904 = CARTESIAN_POINT ( 'NONE',  ( 0.05219959533910956823, 16.53943276465976808, 84.99890960531436690 ) ) ;
#166905 = CARTESIAN_POINT ( 'NONE',  ( 4.790240017743697010, -48.14548474357627583, -22.95279619250844050 ) ) ;
#166906 = AXIS2_PLACEMENT_3D ( 'NONE', #143503, #4987, #25193 ) ;
#166907 = CARTESIAN_POINT ( 'NONE',  ( 5.049401038298161559, -19.05341960407611168, 72.70724293864768129 ) ) ;
#166908 = CARTESIAN_POINT ( 'NONE',  ( 12.14591786802309770, 12.06949235617756955, 74.37390960531436690 ) ) ;
#166909 = CARTESIAN_POINT ( 'NONE',  ( -5.049401038297874678, -19.05341960407617918, 104.7927570613523471 ) ) ;
#166910 = CARTESIAN_POINT ( 'NONE',  ( -15.80617190586745835, -15.72974639402198527, 61.87390960531436690 ) ) ;
#166911 = EDGE_LOOP ( 'NONE', ( #19463, #110973, #42414, #194678 ) ) ;
#166912 = CARTESIAN_POINT ( 'NONE',  ( -13.89961937509977652, 13.97604488694528158, 35.62390960531435269 ) ) ;
#166914 = CARTESIAN_POINT ( 'NONE',  ( -15.72974639402197994, 15.80617190586746368, 80.62390960531438111 ) ) ;
#166913 = CARTESIAN_POINT ( 'NONE',  ( 9.474510206698971260, -16.51473224551069308, 87.91557627198102409 ) ) ;
#166916 = CARTESIAN_POINT ( 'NONE',  ( -16.46253265017160317, 9.564922557960807481, 80.83224293864769550 ) ) ;
#166915 = CARTESIAN_POINT ( 'NONE',  ( 12.06949235617739724, 12.14591786802326823, 101.8760903946857042 ) ) ;
#166917 = CARTESIAN_POINT ( 'NONE',  ( 19.03943276465977164, 0.05219959533936151252, 61.25109039468566863 ) ) ;
#166918 = CARTESIAN_POINT ( 'NONE',  ( -10.81492255796105439, 18.62759615963255655, 97.91775706135236135 ) ) ;
#166919 = CARTESIAN_POINT ( 'NONE',  ( 10.81492255796078972, 18.62759615963270932, 79.58224293864769550 ) ) ;
#166920 = CARTESIAN_POINT ( 'NONE',  ( 19.05341960407611168, 5.049401038298154454, 113.9572429386477097 ) ) ;
#166921 = CARTESIAN_POINT ( 'NONE',  ( 5.049401038298161559, -19.05341960407611168, 52.70724293864767418 ) ) ;
#166922 = CARTESIAN_POINT ( 'NONE',  ( -16.55341960407617563, 4.379528057220093196, 113.5427570613523756 ) ) ;
#166923 = CARTESIAN_POINT ( 'NONE',  ( 0.05219959533909260263, 19.03943276465977164, 69.99890960531435269 ) ) ;
#166924 = CARTESIAN_POINT ( 'NONE',  ( -13.97604488694547520, 13.89961937509957934, 83.12609039468566152 ) ) ;
#166925 = CARTESIAN_POINT ( 'NONE',  ( -18.62759615963255300, -10.81492255796106328, 104.1677570613523471 ) ) ;
#166926 = CARTESIAN_POINT ( 'NONE',  ( 14.34966873604960469, 8.224510206698951720, 69.16557627198102409 ) ) ;
#166927 = CARTESIAN_POINT ( 'NONE',  ( 5.823673210054125526, 21.52544592524343514, 109.7905762719810383 ) ) ;
#166928 = CARTESIAN_POINT ( 'NONE',  ( 18.67979575497178502, 10.72451020669898547, 104.1655762719810241 ) ) ;
#166929 = DIRECTION ( 'NONE',  ( 1.000000000000000000, 0.000000000000000000, -0.000000000000000000 ) ) ;
#166930 = CARTESIAN_POINT ( 'NONE',  ( -15.72974639402197994, 15.80617190586746368, 60.62390960531437401 ) ) ;
#166931 = CARTESIAN_POINT ( 'NONE',  ( -16.55341960407617563, 4.379528057220093196, 83.54275706135234714 ) ) ;
#166932 = CARTESIAN_POINT ( 'NONE',  ( -14.29746914071049879, 8.314922557960819915, 110.8322429386476955 ) ) ;
#166933 = CARTESIAN_POINT ( 'NONE',  ( 13.89961937509977652, -13.97604488694527269, 53.12390960531434558 ) ) ;
#166934 = CARTESIAN_POINT ( 'NONE',  ( -14.34966873604960291, -8.224510206698953496, 21.66557627198102409 ) ) ;
#166935 = CARTESIAN_POINT ( 'NONE',  ( -10.81492255796105439, 18.62759615963255655, 47.91775706135234714 ) ) ;
#166936 = CARTESIAN_POINT ( 'NONE',  ( -9.474510206698964154, 16.51473224551069663, 110.4155762719810383 ) ) ;
#166937 = CARTESIAN_POINT ( 'NONE',  ( 21.53943276465977519, 0.05219959533937863772, 81.25109039468568994 ) ) ;
#166938 = CARTESIAN_POINT ( 'NONE',  ( 16.51473224551069308, 9.474510206698969483, 34.16557627198102409 ) ) ;
#166939 = CARTESIAN_POINT ( 'NONE',  ( 9.474510206698971260, -16.51473224551069308, 37.91557627198102409 ) ) ;
#166940 = ORIENTED_EDGE ( 'NONE', *, *, #101975, .F. ) ;
#166941 = CARTESIAN_POINT ( 'NONE',  ( 21.53943276465977519, 0.05219959533937863772, 66.25109039468567573 ) ) ;
#166942 = CARTESIAN_POINT ( 'NONE',  ( 16.51473224551069308, 9.474510206698969483, 104.1655762719810241 ) ) ;
#166943 = CARTESIAN_POINT ( 'NONE',  ( -19.03943276465977164, -0.05219959533935918106, 78.75109039468567573 ) ) ;
#166944 = CARTESIAN_POINT ( 'NONE',  ( 5.823673210054444382, -21.52544592524334988, 45.20942372801901854 ) ) ;
#166945 = CARTESIAN_POINT ( 'NONE',  ( -12.14591786802326823, 12.06949235617739902, 28.12609039468568284 ) ) ;
#166946 = CARTESIAN_POINT ( 'NONE',  ( 19.05341960407617918, -5.049401038297876454, 71.04275706135234714 ) ) ;
#166947 = CARTESIAN_POINT ( 'NONE',  ( -9.564922557960796823, -16.46253265017161027, 57.08224293864769550 ) ) ;
#166948 = CARTESIAN_POINT ( 'NONE',  ( 5.153800228976615827, -19.02544592524334988, 85.20942372801900433 ) ) ;
#166949 = CARTESIAN_POINT ( 'NONE',  ( -16.55341960407611168, -4.379528057220339221, 31.45724293864769550 ) ) ;
#166950 = CARTESIAN_POINT ( 'NONE',  ( -16.51473224551082808, 9.474510206698731452, 88.33442372801900433 ) ) ;
#166951 = CARTESIAN_POINT ( 'NONE',  ( -12.06949235617756955, 12.14591786802309770, 40.62390960531435269 ) ) ;
#166952 = CARTESIAN_POINT ( 'NONE',  ( 9.474510206698729675, 16.51473224551082808, 67.08442372801900433 ) ) ;
#166953 = CARTESIAN_POINT ( 'NONE',  ( 4.379528057220092307, 16.55341960407617563, 42.29275706135235424 ) ) ;
#166954 = CARTESIAN_POINT ( 'NONE',  ( -5.049401038297874678, -19.05341960407617918, 19.79275706135233293 ) ) ;
#166955 = ADVANCED_FACE ( 'NONE', ( #57649 ), #162809, .F. ) ;
#166956 = CARTESIAN_POINT ( 'NONE',  ( -9.474510206698964154, 16.51473224551069663, 40.41557627198103120 ) ) ;
#166957 = CARTESIAN_POINT ( 'NONE',  ( -4.999999999999999112, -140.0000000000000000, -15.00000000000000000 ) ) ;
#166958 = CARTESIAN_POINT ( 'NONE',  ( -16.53943276465976808, -0.05219959533934237506, 48.75109039468568284 ) ) ;
#166959 = DIRECTION ( 'NONE',  ( 0.000000000000000000, 0.000000000000000000, 1.000000000000000000 ) ) ;
#166960 = CARTESIAN_POINT ( 'NONE',  ( -17.14385361876520619, 23.59649016807275856, 144.5750000027312012 ) ) ;
#166961 = CARTESIAN_POINT ( 'NONE',  ( 0.05219959533909260263, 19.03943276465977164, 89.99890960531436690 ) ) ;
#166962 = CARTESIAN_POINT ( 'NONE',  ( 69.65682714487590488, -71.74905178543389184, -15.00000000000000178 ) ) ;
#166963 = CARTESIAN_POINT ( 'NONE',  ( 19.02544592524334988, 5.153800228976608722, 86.45942372801900433 ) ) ;
#166964 = EDGE_CURVE ( 'NONE', #94189, #159131, #10145, .T. ) ;
#166965 = CARTESIAN_POINT ( 'NONE',  ( -10.72451020669898014, 18.67979575497178502, 30.41557627198101699 ) ) ;
#166967 = CARTESIAN_POINT ( 'NONE',  ( -16.46253265017146816, -9.564922557961047289, 99.16775706135233293 ) ) ;
#166966 = CARTESIAN_POINT ( 'NONE',  ( 15.72974639402176855, 15.80617190586768217, 106.8760903946856899 ) ) ;
#166968 = CARTESIAN_POINT ( 'NONE',  ( -8.224510206698948167, 14.34966873604960824, 110.4155762719810383 ) ) ;
#166969 = CARTESIAN_POINT ( 'NONE',  ( 0.05219959533909260263, 19.03943276465977164, 39.99890960531436690 ) ) ;
#166970 = CARTESIAN_POINT ( 'NONE',  ( 21.55341960407610458, 5.719274019375980345, 58.95724293864770971 ) ) ;
#166971 = CARTESIAN_POINT ( 'NONE',  ( 9.474510206698971260, -16.51473224551069308, 22.91557627198102765 ) ) ;
#166972 = CARTESIAN_POINT ( 'NONE',  ( 27.73933785331498925, -9.013057229001034898, 140.2750000027311614 ) ) ;
#166973 = CARTESIAN_POINT ( 'NONE',  ( 19.02544592524334988, 5.153800228976608722, 76.45942372801897591 ) ) ;
#166974 = CARTESIAN_POINT ( 'NONE',  ( 4.483927247898545687, 16.52544592524342804, 49.79057627198102409 ) ) ;
#166975 = CARTESIAN_POINT ( 'NONE',  ( -15.80617190586745835, -15.72974639402198527, 31.87390960531435979 ) ) ;
#166976 = CARTESIAN_POINT ( 'NONE',  ( -15.80617190586768217, 15.72974639402176855, 98.12609039468570415 ) ) ;
#166977 = CARTESIAN_POINT ( 'NONE',  ( -15.80617190586745835, -15.72974639402198527, 86.87390960531438111 ) ) ;
#166978 = CARTESIAN_POINT ( 'NONE',  ( -15.80617190586768217, 15.72974639402176855, 53.12609039468568284 ) ) ;
#166979 = CARTESIAN_POINT ( 'NONE',  ( 15.80617190586769283, -15.72974639402175789, 70.62609039468567573 ) ) ;
#166980 = CARTESIAN_POINT ( 'NONE',  ( 5.049401038298161559, -19.05341960407611168, 102.7072429386476955 ) ) ;
#166982 = CARTESIAN_POINT ( 'NONE',  ( 10.81492255796106328, -18.62759615963255655, 65.41775706135234714 ) ) ;
#166981 = CARTESIAN_POINT ( 'NONE',  ( 0.05219959533934541429, -16.53943276465976808, 95.00109039468568994 ) ) ;
#166983 = CARTESIAN_POINT ( 'NONE',  ( -12.06949235617756955, 12.14591786802309770, 115.6239096053143669 ) ) ;
#166984 = CARTESIAN_POINT ( 'NONE',  ( 8.224510206698953496, -14.34966873604960469, 72.91557627198103830 ) ) ;
#166985 = CARTESIAN_POINT ( 'NONE',  ( -4.483927247898539470, -16.52544592524342804, 37.29057627198102409 ) ) ;
#166986 = CARTESIAN_POINT ( 'NONE',  ( 18.67979575497178502, 10.72451020669898547, 44.16557627198103120 ) ) ;
#166987 = CARTESIAN_POINT ( 'NONE',  ( 9.564922557960805705, 16.46253265017160317, 49.58224293864770260 ) ) ;
#166988 = CARTESIAN_POINT ( 'NONE',  ( 5.719274019375991003, -21.55341960407610458, 62.70724293864769550 ) ) ;
#166989 = CARTESIAN_POINT ( 'NONE',  ( 16.46253265017146816, 9.564922557961045513, 51.66775706135233293 ) ) ;
#166992 = CARTESIAN_POINT ( 'NONE',  ( -4.379528057220328563, 16.55341960407611168, 45.20724293864769550 ) ) ;
#166991 = CARTESIAN_POINT ( 'NONE',  ( -16.18388926212241330, -7.379444403734408908, 40.43953151366154231 ) ) ;
#166990 = VECTOR ( 'NONE', #122568, 1000.000000000000000 ) ;
#166993 = CARTESIAN_POINT ( 'NONE',  ( -10.81492255796078084, -18.62759615963271287, 27.08224293864769550 ) ) ;
#166994 = VERTEX_POINT ( 'NONE', #70811 ) ;
#166995 = VERTEX_POINT ( 'NONE', #164825 ) ;
#166996 = CARTESIAN_POINT ( 'NONE',  ( -27.91311885011354121, 2.086775749827418075E-14, 155.0000000000000000 ) ) ;
#166997 = CARTESIAN_POINT ( 'NONE',  ( 8.224510206698742110, 14.34966873604972548, 72.08442372801899012 ) ) ;
#166998 = CARTESIAN_POINT ( 'NONE',  ( 16.51473224551083163, -9.474510206698727899, 75.83442372801900433 ) ) ;
#166999 = CARTESIAN_POINT ( 'NONE',  ( 14.29746914071049879, -8.314922557960816363, 38.33224293864768839 ) ) ;
#167000 = CARTESIAN_POINT ( 'NONE',  ( 16.81555441253556893, -7.025013491695413670, 53.13685445334258617 ) ) ;
#167001 = CARTESIAN_POINT ( 'NONE',  ( 14.29746914071049879, -8.314922557960816363, 33.33224293864769550 ) ) ;
#167002 = CARTESIAN_POINT ( 'NONE',  ( -16.51473224551069308, -9.474510206698971260, 46.66557627198102409 ) ) ;
#167003 = CARTESIAN_POINT ( 'NONE',  ( -19.02544592524342804, 5.153800228976336051, 71.04057627198099567 ) ) ;
#167004 = CARTESIAN_POINT ( 'NONE',  ( -13.89961937509977652, 13.97604488694528158, 40.62390960531435979 ) ) ;
#167005 = CARTESIAN_POINT ( 'NONE',  ( 10.81492255796106328, -18.62759615963255655, 45.41775706135234003 ) ) ;
#167006 = CARTESIAN_POINT ( 'NONE',  ( -19.02544592524342804, 5.153800228976336051, 61.04057627198103120 ) ) ;
#167007 = FACE_BOUND ( 'NONE', #99220, .T. ) ;
#167008 = CIRCLE ( 'NONE', #79812, 40.00000000000002132 ) ;
#167009 = CARTESIAN_POINT ( 'NONE',  ( -5.153800228976328057, -19.02544592524343514, 62.29057627198100988 ) ) ;
#167010 = CARTESIAN_POINT ( 'NONE',  ( -5.719274019375978568, 21.55341960407610458, 40.20724293864769550 ) ) ;
#167011 = CARTESIAN_POINT ( 'NONE',  ( 19.05341960407611168, 5.049401038298154454, 38.95724293864767418 ) ) ;
#167012 = CARTESIAN_POINT ( 'NONE',  ( -5.823673210054116645, -21.52544592524344225, 37.29057627198102409 ) ) ;
#167013 = CARTESIAN_POINT ( 'NONE',  ( -16.52544592524335698, -4.483927247898792601, 93.95942372801903275 ) ) ;
#167014 = CARTESIAN_POINT ( 'NONE',  ( -15.80617190586768217, 15.72974639402176855, 113.1260903946856899 ) ) ;
#167015 = CARTESIAN_POINT ( 'NONE',  ( 8.224510206698742110, 14.34966873604972548, 72.08442372801899012 ) ) ;
#167016 = CARTESIAN_POINT ( 'NONE',  ( -5.049401038298153566, 19.05341960407611168, 105.2072429386476671 ) ) ;
#167017 = CARTESIAN_POINT ( 'NONE',  ( 14.34966873604972726, -8.224510206698740333, 60.83442372801901854 ) ) ;
#167018 = CARTESIAN_POINT ( 'NONE',  ( -12.14591786802326823, 12.06949235617739902, 38.12609039468567573 ) ) ;
#167019 = CARTESIAN_POINT ( 'NONE',  ( 5.153800228976335163, 19.02544592524342804, 104.7905762719809957 ) ) ;
#167020 = CARTESIAN_POINT ( 'NONE',  ( -0.05219959533934338120, 16.53943276465976808, 27.50109039468567929 ) ) ;
#167021 = CARTESIAN_POINT ( 'NONE',  ( -9.474510206698964154, 16.51473224551069663, 40.41557627198103120 ) ) ;
#167022 = CARTESIAN_POINT ( 'NONE',  ( 5.823673210054444382, -21.52544592524334988, 25.20942372801901854 ) ) ;
#167023 = CARTESIAN_POINT ( 'NONE',  ( -4.483927247898782831, 16.52544592524335698, 27.70942372801901854 ) ) ;
#167024 = CARTESIAN_POINT ( 'NONE',  ( 0.05219959533934541429, -16.53943276465976808, 105.0010903946856757 ) ) ;
#167025 = CARTESIAN_POINT ( 'NONE',  ( -5.823673210054431948, 21.52544592524334988, 102.7094237280190185 ) ) ;
#167026 = CARTESIAN_POINT ( 'NONE',  ( 9.474510206698729675, 16.51473224551082808, 102.0844237280190043 ) ) ;
#167027 = CARTESIAN_POINT ( 'NONE',  ( -8.224510206698948167, 14.34966873604960824, 55.41557627198102409 ) ) ;
#167028 = CARTESIAN_POINT ( 'NONE',  ( -16.51473224551069308, -9.474510206698971260, 31.66557627198102054 ) ) ;
#167030 = CARTESIAN_POINT ( 'NONE',  ( -8.349412516403756257, 1.313804288003871612, -64.09731636040744718 ) ) ;
#167029 = CARTESIAN_POINT ( 'NONE',  ( -9.474510206698720793, -16.51473224551083518, 54.58442372801899722 ) ) ;
#167031 = CARTESIAN_POINT ( 'NONE',  ( 18.67979575497194134, -10.72451020669871369, 50.83442372801901143 ) ) ;
#167032 = CARTESIAN_POINT ( 'NONE',  ( -14.34966873604972548, 8.224510206698743886, 23.33442372801901499 ) ) ;
#167033 = DIRECTION ( 'NONE',  ( 0.7071067811865466846, -7.406550393246786959E-15, 0.7071067811865484609 ) ) ;
#167034 = CARTESIAN_POINT ( 'NONE',  ( 19.02544592524343514, -5.153800228976328945, 108.5405762719810383 ) ) ;
#167035 = CARTESIAN_POINT ( 'NONE',  ( -0.05219959533907301413, -21.53943276465977519, 67.49890960531436690 ) ) ;
#167036 = CARTESIAN_POINT ( 'NONE',  ( 9.564922557961047289, -16.46253265017146816, 105.4177570613523471 ) ) ;
#167037 = CARTESIAN_POINT ( 'NONE',  ( -19.05341960407611168, -5.049401038298163336, 96.45724293864769550 ) ) ;
#167038 = CARTESIAN_POINT ( 'NONE',  ( -18.94301819075103310, -21.11311916587052906, 139.9999999999999716 ) ) ;
#167039 = CARTESIAN_POINT ( 'NONE',  ( 4.483927247898545687, 16.52544592524342804, 104.7905762719810241 ) ) ;
#167040 = CARTESIAN_POINT ( 'NONE',  ( -21.53943276465977519, -0.05219959533937600094, 93.75109039468567573 ) ) ;
#167041 = CARTESIAN_POINT ( 'NONE',  ( -16.46253265017160317, 9.564922557960807481, 45.83224293864769550 ) ) ;
#167043 = CARTESIAN_POINT ( 'NONE',  ( 21.53943276465977519, 0.05219959533937863772, 51.25109039468568994 ) ) ;
#167042 = AXIS2_PLACEMENT_3D ( 'NONE', #3693, #83516, #50224 ) ;
#167044 = CARTESIAN_POINT ( 'NONE',  ( 0.05219959533937995610, -21.53943276465977519, 95.00109039468568994 ) ) ;
#167045 = CARTESIAN_POINT ( 'NONE',  ( 12.06949235617739724, 12.14591786802326823, 106.8760903946856899 ) ) ;
#167046 = CARTESIAN_POINT ( 'NONE',  ( -16.51473224551069308, -9.474510206698971260, 76.66557627198103830 ) ) ;
#167047 = CARTESIAN_POINT ( 'NONE',  ( 0.05219959533937995610, -21.53943276465977519, 45.00109039468568284 ) ) ;
#167048 = CARTESIAN_POINT ( 'NONE',  ( 10.81492255796106328, -18.62759615963255655, 40.41775706135234714 ) ) ;
#167050 = CARTESIAN_POINT ( 'NONE',  ( -19.03943276465977164, 0.05219959533909376836, 86.24890960531436690 ) ) ;
#167049 = CARTESIAN_POINT ( 'NONE',  ( 9.474510206698729675, 16.51473224551082808, 72.08442372801900433 ) ) ;
#167051 = CARTESIAN_POINT ( 'NONE',  ( -14.29746914071049879, 8.314922557960819915, 110.8322429386476955 ) ) ;
#167052 = CARTESIAN_POINT ( 'NONE',  ( 15.80617190586746368, 15.72974639402197994, 94.37390960531436690 ) ) ;
#167053 = CARTESIAN_POINT ( 'NONE',  ( -8.224510206698948167, 14.34966873604960824, 60.41557627198102409 ) ) ;
#167054 = CARTESIAN_POINT ( 'NONE',  ( -9.564922557961040184, 16.46253265017147172, 22.91775706135233648 ) ) ;
#167055 = CARTESIAN_POINT ( 'NONE',  ( -4.379528057220328563, 16.55341960407611168, 100.2072429386476955 ) ) ;
#167056 = CARTESIAN_POINT ( 'NONE',  ( -5.153800228976328057, -19.02544592524343514, 32.29057627198102409 ) ) ;
#167057 = CARTESIAN_POINT ( 'NONE',  ( -16.51473224551082808, 9.474510206698731452, 83.33442372801899012 ) ) ;
#167058 = CARTESIAN_POINT ( 'NONE',  ( -4.483927247898539470, -16.52544592524342804, 42.29057627198103120 ) ) ;
#167059 = CARTESIAN_POINT ( 'NONE',  ( -5.823673210054431948, 21.52544592524334988, 92.70942372801901854 ) ) ;
#167060 = CARTESIAN_POINT ( 'NONE',  ( 9.564922557960805705, 16.46253265017160317, 104.5822429386476955 ) ) ;
#167061 = CARTESIAN_POINT ( 'NONE',  ( -19.02544592524334988, -5.153800228976617603, 68.95942372801896170 ) ) ;
#167062 = CARTESIAN_POINT ( 'NONE',  ( -18.62759615963270932, 10.81492255796079327, 75.83224293864769550 ) ) ;
#167063 = CARTESIAN_POINT ( 'NONE',  ( 21.55341960407619695, -5.719274019375665929, 36.04275706135234714 ) ) ;
#167064 = CARTESIAN_POINT ( 'NONE',  ( 4.483927247898790824, -16.52544592524335698, 30.20942372801902565 ) ) ;
#167065 = CARTESIAN_POINT ( 'NONE',  ( 12.14591786802327356, -12.06949235617739191, 90.62609039468567573 ) ) ;
#167067 = CARTESIAN_POINT ( 'NONE',  ( -0.05219959533937732626, 21.53943276465977519, 37.50109039468568284 ) ) ;
#167066 = CARTESIAN_POINT ( 'NONE',  ( -19.05341960407611168, -5.049401038298163336, 26.45724293864769550 ) ) ;
#167068 = CARTESIAN_POINT ( 'NONE',  ( -19.05341960407611168, -5.049401038298163336, 21.45724293864768839 ) ) ;
#167069 = CARTESIAN_POINT ( 'NONE',  ( 38.00000000000000000, 12.34694845685046616, -8.649999994537624914 ) ) ;
#167070 = CARTESIAN_POINT ( 'NONE',  ( -12.06949235617739369, -12.14591786802326823, 54.37609039468568994 ) ) ;
#167071 = CARTESIAN_POINT ( 'NONE',  ( 8.224510206698953496, -14.34966873604960469, 77.91557627198102409 ) ) ;
#167072 = CARTESIAN_POINT ( 'NONE',  ( -21.53943276465977519, 0.05219959533907696930, 71.24890960531435269 ) ) ;
#167073 = CARTESIAN_POINT ( 'NONE',  ( -14.29746914071049879, 8.314922557960819915, 30.83224293864770260 ) ) ;
#167074 = CARTESIAN_POINT ( 'NONE',  ( 12.14591786802327356, -12.06949235617739191, 55.62609039468568284 ) ) ;
#167075 = CARTESIAN_POINT ( 'NONE',  ( -13.97604488694527625, -13.89961937509977652, 46.87390960531435979 ) ) ;
#167076 = CARTESIAN_POINT ( 'NONE',  ( 0.05219959533934541429, -16.53943276465976808, 90.00109039468567573 ) ) ;
#167077 = CARTESIAN_POINT ( 'NONE',  ( -19.05341960407617563, 5.049401038297882671, 93.54275706135234714 ) ) ;
#167078 = CARTESIAN_POINT ( 'NONE',  ( 5.823673210054125526, 21.52544592524343514, 69.79057627198102409 ) ) ;
#167079 = CARTESIAN_POINT ( 'NONE',  ( 16.55341960407618274, -4.379528057220086978, 111.0427570613523613 ) ) ;
#167080 = ORIENTED_EDGE ( 'NONE', *, *, #27827, .F. ) ;
#167081 = DIRECTION ( 'NONE',  ( 0.000000000000000000, 0.000000000000000000, -1.000000000000000000 ) ) ;
#167082 = CARTESIAN_POINT ( 'NONE',  ( -21.55341960407610458, -5.719274019375992779, 61.45724293864770260 ) ) ;
#167083 = EDGE_LOOP ( 'NONE', ( #143694, #58527, #38751, #834 ) ) ;
#167084 = CARTESIAN_POINT ( 'NONE',  ( 12.14591786802327356, -12.06949235617739191, 95.62609039468568994 ) ) ;
#167085 = VERTEX_POINT ( 'NONE', #58624 ) ;
#167086 = CARTESIAN_POINT ( 'NONE',  ( 21.55341960407610458, 5.719274019375980345, 23.95724293864769550 ) ) ;
#167087 = CARTESIAN_POINT ( 'NONE',  ( 17.49999999999999289, 3.805241302050251573, 107.1264752721741615 ) ) ;
#167088 = CARTESIAN_POINT ( 'NONE',  ( -21.55341960407610458, -5.719274019375992779, 71.45724293864769550 ) ) ;
#167089 = CARTESIAN_POINT ( 'NONE',  ( -16.55341960407611168, -4.379528057220339221, 31.45724293864769550 ) ) ;
#167090 = CARTESIAN_POINT ( 'NONE',  ( -16.52544592524335698, -4.483927247898792601, 23.95942372801901143 ) ) ;
#167091 = CARTESIAN_POINT ( 'NONE',  ( -0.05219959533909027116, -19.03943276465977164, 27.49890960531435624 ) ) ;
#167092 = CARTESIAN_POINT ( 'NONE',  ( -0.05219959533934338120, 16.53943276465976808, 32.50109039468568284 ) ) ;
#167093 = CARTESIAN_POINT ( 'NONE',  ( 16.51473224551069308, 9.474510206698969483, 54.16557627198103120 ) ) ;
#167094 = CARTESIAN_POINT ( 'NONE',  ( 8.906447517083057264, -27.41122689804191026, 144.5999999999999943 ) ) ;
#167095 = CARTESIAN_POINT ( 'NONE',  ( -9.474510206698964154, 16.51473224551069663, 100.4155762719810241 ) ) ;
#167096 = CARTESIAN_POINT ( 'NONE',  ( 4.483927247898790824, -16.52544592524335698, 95.20942372801903275 ) ) ;
#167097 = CARTESIAN_POINT ( 'NONE',  ( -13.97604488694547697, 13.89961937509957934, 98.12609039468566152 ) ) ;
#167098 = CARTESIAN_POINT ( 'NONE',  ( 19.05341960407617918, -5.049401038297876454, 26.04275706135233293 ) ) ;
#167099 = CARTESIAN_POINT ( 'NONE',  ( -10.72451020669898014, 18.67979575497178502, 80.41557627198103830 ) ) ;
#167100 = CARTESIAN_POINT ( 'NONE',  ( -4.379528057220086978, -16.55341960407618274, 99.79275706135234714 ) ) ;
#167101 = CARTESIAN_POINT ( 'NONE',  ( -19.05341960407617563, 5.049401038297882671, 98.54275706135233293 ) ) ;
#167102 = CARTESIAN_POINT ( 'NONE',  ( -9.564922557960796823, -16.46253265017161027, 52.08224293864768839 ) ) ;
#167103 = CARTESIAN_POINT ( 'NONE',  ( -19.03943276465977164, 0.05219959533909376836, 86.24890960531436690 ) ) ;
#167104 = CARTESIAN_POINT ( 'NONE',  ( -15.80617190586768217, 15.72974639402176855, 63.12609039468568994 ) ) ;
#167105 = CARTESIAN_POINT ( 'NONE',  ( -5.049401038298153566, 19.05341960407611168, 60.20724293864768129 ) ) ;
#167106 = CARTESIAN_POINT ( 'NONE',  ( -16.52544592524342804, 4.483927247898546575, 86.04057627198102409 ) ) ;
#167107 = CARTESIAN_POINT ( 'NONE',  ( -17.26172910966779739, -6.454744622555837807, 84.19353091350780005 ) ) ;
#167108 = CARTESIAN_POINT ( 'NONE',  ( 12.06949235617757843, -12.14591786802309237, 78.12390960531436690 ) ) ;
#167109 = CARTESIAN_POINT ( 'NONE',  ( -10.72451020669898014, 18.67979575497178502, 80.41557627198103830 ) ) ;
#167110 = CARTESIAN_POINT ( 'NONE',  ( -19.02544592524334988, -5.153800228976617603, 93.95942372801900433 ) ) ;
#167111 = CARTESIAN_POINT ( 'NONE',  ( 17.05116617787825462, -6.768360034955811955, 81.15675553259195851 ) ) ;
#167112 = CARTESIAN_POINT ( 'NONE',  ( -19.02544592524334988, -5.153800228976617603, 38.95942372801900433 ) ) ;
#167113 = CARTESIAN_POINT ( 'NONE',  ( 31.69386653422658640, -1.706804019390332661, 102.3073255780427360 ) ) ;
#167115 = CARTESIAN_POINT ( 'NONE',  ( 9.474510206698971260, -16.51473224551069308, 87.91557627198102409 ) ) ;
#167114 = CARTESIAN_POINT ( 'NONE',  ( -9.474510206698964154, 16.51473224551069663, 75.41557627198103830 ) ) ;
#167116 = B_SPLINE_CURVE_WITH_KNOTS ( 'NONE', 3,
 ( #142210, #65372, #174556, #6676, #68354, #159361 ),
 .UNSPECIFIED., .F., .F.,
 ( 4, 2, 4 ),
 ( 0.000000000000000000, 0.0003837532665634982949, 0.0007675065331269965898 ),
 .UNSPECIFIED. ) ;
#167117 = EDGE_CURVE ( 'NONE', #198282, #95422, #117306, .T. ) ;
#167118 = CARTESIAN_POINT ( 'NONE',  ( 12.14591786802327356, -12.06949235617739191, 60.62609039468567573 ) ) ;
#167119 = CARTESIAN_POINT ( 'NONE',  ( -24.04960827311053606, 5.809912860844014482, 170.7323280178997891 ) ) ;
#167120 = CARTESIAN_POINT ( 'NONE',  ( -19.03943276465977164, -0.05219959533935918106, 38.75109039468566152 ) ) ;
#167121 = CARTESIAN_POINT ( 'NONE',  ( 17.62203461105334412, -15.97128521727769446, -57.16225127900796821 ) ) ;
#167122 = CARTESIAN_POINT ( 'NONE',  ( -19.02544592524342804, 5.153800228976336051, 111.0405762719810099 ) ) ;
#167123 = CARTESIAN_POINT ( 'NONE',  ( -4.483927247898782831, 16.52544592524335698, 107.7094237280190328 ) ) ;
#167124 = DIRECTION ( 'NONE',  ( 0.000000000000000000, 0.000000000000000000, -1.000000000000000000 ) ) ;
#167125 = CARTESIAN_POINT ( 'NONE',  ( -4.379528057220086978, -16.55341960407618274, 74.79275706135234714 ) ) ;
#167126 = CARTESIAN_POINT ( 'NONE',  ( -17.44270441346513678, 5.991230190323086013, 28.63664920735772057 ) ) ;
#167127 = CARTESIAN_POINT ( 'NONE',  ( -16.53943276465976808, -0.05219959533934237506, 48.75109039468568284 ) ) ;
#167128 = LINE ( 'NONE', #103464, #108359 ) ;
#167129 = CARTESIAN_POINT ( 'NONE',  ( 5.719274019375673035, 21.55341960407619339, 67.29275706135234714 ) ) ;
#167130 = CARTESIAN_POINT ( 'NONE',  ( 5.153800228976615827, -19.02544592524334988, 75.20942372801896170 ) ) ;
#167131 = CARTESIAN_POINT ( 'NONE',  ( -13.89961937509957401, -13.97604488694547875, 29.37609039468565797 ) ) ;
#167132 = CARTESIAN_POINT ( 'NONE',  ( -9.564922557960796823, -16.46253265017161027, 57.08224293864769550 ) ) ;
#167133 = CARTESIAN_POINT ( 'NONE',  ( 5.049401038298161559, -19.05341960407611168, 47.70724293864770260 ) ) ;
#167134 = CARTESIAN_POINT ( 'NONE',  ( -16.30299161242153971, -36.53133444124396334, -10.23071320450981680 ) ) ;
#167135 = CARTESIAN_POINT ( 'NONE',  ( -21.53943276465977519, 0.05219959533907696930, 66.24890960531436690 ) ) ;
#167136 = CIRCLE ( 'NONE', #89622, 5.000000000000000000 ) ;
#167137 = CARTESIAN_POINT ( 'NONE',  ( -21.53943276465977519, 0.05219959533907696930, 31.24890960531435979 ) ) ;
#167138 = CARTESIAN_POINT ( 'NONE',  ( 5.153800228976335163, 19.02544592524342804, 24.79057627198102765 ) ) ;
#167139 = CARTESIAN_POINT ( 'NONE',  ( 12.06949235617739724, 12.14591786802326823, 51.87609039468568284 ) ) ;
#167140 = EDGE_CURVE ( 'NONE', #11758, #16981, #102322, .T. ) ;
#167141 = ORIENTED_EDGE ( 'NONE', *, *, #62577, .F. ) ;
#167142 = CARTESIAN_POINT ( 'NONE',  ( -21.53943276465977519, -0.05219959533937600094, 28.75109039468567929 ) ) ;
#167144 = CARTESIAN_POINT ( 'NONE',  ( -23.48529157249599919, -32.32473071737750558, -7.699999999999999289 ) ) ;
#167143 = CARTESIAN_POINT ( 'NONE',  ( -4.483927247898539470, -16.52544592524342804, 57.29057627198103120 ) ) ;
#167145 = CARTESIAN_POINT ( 'NONE',  ( 13.97604488694548053, -13.89961937509957401, 110.6260903946856615 ) ) ;
#167146 = CARTESIAN_POINT ( 'NONE',  ( -19.02544592524334988, -5.153800228976617603, 38.95942372801900433 ) ) ;
#167147 = CARTESIAN_POINT ( 'NONE',  ( 14.29746914071049879, -8.314922557960816363, 48.33224293864770260 ) ) ;
#167148 = CARTESIAN_POINT ( 'NONE',  ( 10.81492255796106328, -18.62759615963255655, 25.41775706135235779 ) ) ;
#167150 = CARTESIAN_POINT ( 'NONE',  ( 21.55341960407610458, 5.719274019375980345, 58.95724293864770971 ) ) ;
#167149 = CARTESIAN_POINT ( 'NONE',  ( -3.573655867282028392E-15, 2.428612866367529932E-14, -25.00000000000000000 ) ) ;
#167151 = CARTESIAN_POINT ( 'NONE',  ( -5.153800228976328057, -19.02544592524343514, 92.29057627198099567 ) ) ;
#167152 = CARTESIAN_POINT ( 'NONE',  ( 16.52544592524342804, -4.483927247898539470, 63.54057627198103830 ) ) ;
#167153 = CARTESIAN_POINT ( 'NONE',  ( -5.049401038298153566, 19.05341960407611168, 110.2072429386476671 ) ) ;
#167154 = CARTESIAN_POINT ( 'NONE',  ( -17.49999999999999645, -5.500000000000000888, 120.0000000000000142 ) ) ;
#167155 = CARTESIAN_POINT ( 'NONE',  ( -9.474510206698720793, -16.51473224551083518, 49.58442372801899722 ) ) ;
#167156 = CARTESIAN_POINT ( 'NONE',  ( -5.719274019375978568, 21.55341960407610458, 105.2072429386477097 ) ) ;
#167157 = CARTESIAN_POINT ( 'NONE',  ( -13.89961937509977652, 13.97604488694528158, 40.62390960531435979 ) ) ;
#167158 = CARTESIAN_POINT ( 'NONE',  ( -13.97604488694527625, -13.89961937509977652, 21.87390960531435979 ) ) ;
#167159 = CARTESIAN_POINT ( 'NONE',  ( 15.80617190586769283, -15.72974639402175789, 50.62609039468568994 ) ) ;
#167160 = VECTOR ( 'NONE', #96960, 1000.000000000000000 ) ;
#167161 = CARTESIAN_POINT ( 'NONE',  ( 17.14385361876520264, -23.59649016807271238, 145.5750000027312012 ) ) ;
#167162 = CARTESIAN_POINT ( 'NONE',  ( 12.06949235617757843, -12.14591786802309237, 23.12390960531436335 ) ) ;
#167163 = CARTESIAN_POINT ( 'NONE',  ( -13.89961937509977652, 13.97604488694528158, 45.62390960531433848 ) ) ;
#167164 = CARTESIAN_POINT ( 'NONE',  ( 0.05219959533909260263, 19.03943276465977164, 94.99890960531436690 ) ) ;
#167165 = CARTESIAN_POINT ( 'NONE',  ( 0.05219959533907565091, 21.53943276465977519, 79.99890960531435269 ) ) ;
#167166 = CARTESIAN_POINT ( 'NONE',  ( 27.73933785331498214, 9.013057229001095294, 143.9750000027312069 ) ) ;
#167167 = CARTESIAN_POINT ( 'NONE',  ( -19.05341960407611168, -5.049401038298163336, 46.45724293864768129 ) ) ;
#167168 = CARTESIAN_POINT ( 'NONE',  ( -18.62759615963270932, 10.81492255796079327, 50.83224293864770971 ) ) ;
#167169 = CARTESIAN_POINT ( 'NONE',  ( -18.67979575497193778, 10.72451020669871902, 83.33442372801903275 ) ) ;
#167172 = CARTESIAN_POINT ( 'NONE',  ( -14.29746914071049879, 8.314922557960819915, 65.83224293864769550 ) ) ;
#167171 = CARTESIAN_POINT ( 'NONE',  ( -4.483927247898782831, 16.52544592524335698, 82.70942372801900433 ) ) ;
#167170 = CARTESIAN_POINT ( 'NONE',  ( 18.22780087662121673, 5.500000000000056843, 53.98459894673893444 ) ) ;
#167173 = CARTESIAN_POINT ( 'NONE',  ( -19.05341960407611168, -5.049401038298163336, 76.45724293864769550 ) ) ;
#167174 = EDGE_LOOP ( 'NONE', ( #122164, #108458, #125644, #70918, #105481, #64857 ) ) ;
#167175 = CARTESIAN_POINT ( 'NONE',  ( 19.02544592524334988, 5.153800228976608722, 21.45942372801899012 ) ) ;
#167176 = CARTESIAN_POINT ( 'NONE',  ( -12.14591786802326823, 12.06949235617739902, 93.12609039468568994 ) ) ;
#167177 = CARTESIAN_POINT ( 'NONE',  ( -15.80617190586768217, 15.72974639402176855, 108.1260903946856757 ) ) ;
#167178 = CARTESIAN_POINT ( 'NONE',  ( -0.05219959533909027116, -19.03943276465977164, 77.49890960531435269 ) ) ;
#167179 = CARTESIAN_POINT ( 'NONE',  ( -5.719274019375978568, 21.55341960407610458, 50.20724293864769550 ) ) ;
#167180 = CARTESIAN_POINT ( 'NONE',  ( 4.483927247898790824, -16.52544592524335698, 25.20942372801901854 ) ) ;
#167181 = CARTESIAN_POINT ( 'NONE',  ( -21.53943276465977519, -0.05219959533937600094, 93.75109039468567573 ) ) ;
#167182 = CARTESIAN_POINT ( 'NONE',  ( -14.29746914071037622, -8.314922557961029526, 69.16775706135234714 ) ) ;
#167183 = CARTESIAN_POINT ( 'NONE',  ( 10.81492255796106328, -18.62759615963255655, 20.41775706135234714 ) ) ;
#167184 = CARTESIAN_POINT ( 'NONE',  ( -16.46253265017146816, -9.564922557961047289, 109.1677570613523471 ) ) ;
#167185 = CARTESIAN_POINT ( 'NONE',  ( -13.89961937509977652, 13.97604488694528158, 95.62390960531436690 ) ) ;
#167186 = CARTESIAN_POINT ( 'NONE',  ( 4.483927247898790824, -16.52544592524335698, 30.20942372801902565 ) ) ;
#167187 = CARTESIAN_POINT ( 'NONE',  ( 0.05219959533909260263, 19.03943276465977164, 49.99890960531435979 ) ) ;
#167188 = AXIS2_PLACEMENT_3D ( 'NONE', #11945, #25115, #148442 ) ;
#167189 = CARTESIAN_POINT ( 'NONE',  ( 14.29746914071037800, 8.314922557961029526, 31.66775706135234358 ) ) ;
#167190 = CARTESIAN_POINT ( 'NONE',  ( 4.379528057220339221, -16.55341960407611168, 72.70724293864769550 ) ) ;
#167191 = CARTESIAN_POINT ( 'NONE',  ( 12.06949235617739724, 12.14591786802326823, 81.87609039468568994 ) ) ;
#167192 = EDGE_CURVE ( 'NONE', #166707, #178298, #56646, .T. ) ;
#167194 = CARTESIAN_POINT ( 'NONE',  ( -5.049401038298153566, 19.05341960407611168, 65.20724293864765286 ) ) ;
#167193 = CARTESIAN_POINT ( 'NONE',  ( -10.81492255796105439, 18.62759615963255655, 32.91775706135234714 ) ) ;
#167195 = CARTESIAN_POINT ( 'NONE',  ( -9.564922557960796823, -16.46253265017161027, 82.08224293864768129 ) ) ;
#167196 = CARTESIAN_POINT ( 'NONE',  ( -12.06949235617739369, -12.14591786802326823, 84.37609039468570415 ) ) ;
#167197 = CARTESIAN_POINT ( 'NONE',  ( -21.94905633995418270, -7.481063542987935300, 170.0146117665048848 ) ) ;
#167198 = ORIENTED_EDGE ( 'NONE', *, *, #82089, .F. ) ;
#167199 = CARTESIAN_POINT ( 'NONE',  ( -19.05341960407617563, 5.049401038297882671, 33.54275706135231871 ) ) ;
#167200 = CARTESIAN_POINT ( 'NONE',  ( -19.02544592524342804, 5.153800228976336051, 101.0405762719810241 ) ) ;
#167201 = CARTESIAN_POINT ( 'NONE',  ( -0.05219959533909027116, -19.03943276465977164, 52.49890960531436690 ) ) ;
#167202 = CARTESIAN_POINT ( 'NONE',  ( 0.9451604965124735802, 14.01865473875232304, -62.45165202555292439 ) ) ;
#167203 = CARTESIAN_POINT ( 'NONE',  ( -12.14591786802326823, 12.06949235617739902, 38.12609039468567573 ) ) ;
#167205 = CARTESIAN_POINT ( 'NONE',  ( 12.14591786802327356, -12.06949235617739191, 55.62609039468568284 ) ) ;
#167204 = CARTESIAN_POINT ( 'NONE',  ( -9.564922557961040184, 16.46253265017147172, 57.91775706135233293 ) ) ;
#167206 = CARTESIAN_POINT ( 'NONE',  ( -16.46253265017160317, 9.564922557960807481, 105.8322429386476955 ) ) ;
#167207 =( BOUNDED_CURVE ( )  B_SPLINE_CURVE ( 2, ( #92248, #17413, #140744, #107416, #47760, #111405, #18419, #172087, #173091, #125584, #33574 ),
 .UNSPECIFIED., .F., .T. ) 
 B_SPLINE_CURVE_WITH_KNOTS ( ( 3, 2, 2, 2, 2, 3 ),
 ( 0.2002265011048941501, 0.2199999999999999734, 0.2400000000000000189, 0.2600000000000000089, 0.2800000000000000822, 0.3000000000000000999 ),
 .UNSPECIFIED. ) 
 CURVE ( )  GEOMETRIC_REPRESENTATION_ITEM ( )  RATIONAL_B_SPLINE_CURVE ( ( 0.9989039793630181130, 0.9516108039519795003, 1.000000000000000000, 0.9510565162951535312, 1.000000000000000000, 0.9510565162951535312, 1.000000000000000000, 0.9510565162951535312, 1.000000000000000000, 0.9510565162951534202, 1.000000000000000222 ) ) 
 REPRESENTATION_ITEM ( '' )  );
#167208 = CARTESIAN_POINT ( 'NONE',  ( -5.153800228976328057, -19.02544592524343514, 82.29057627198103830 ) ) ;
#167209 = CARTESIAN_POINT ( 'NONE',  ( 0.05219959533907565091, 21.53943276465977519, 99.99890960531436690 ) ) ;
#167210 = CARTESIAN_POINT ( 'NONE',  ( -9.474510206698720793, -16.51473224551083518, 69.58442372801901854 ) ) ;
#167212 = DIRECTION ( 'NONE',  ( 0.000000000000000000, 0.000000000000000000, 1.000000000000000000 ) ) ;
#167211 = CARTESIAN_POINT ( 'NONE',  ( -0.05219959533909027116, -19.03943276465977164, 87.49890960531436690 ) ) ;
#167213 = CARTESIAN_POINT ( 'NONE',  ( 19.02544592524343514, -5.153800228976328945, 63.54057627198103830 ) ) ;
#167215 = CARTESIAN_POINT ( 'NONE',  ( 16.46253265017160672, -9.564922557960803928, 23.33224293864769194 ) ) ;
#167214 = CARTESIAN_POINT ( 'NONE',  ( 12.14591786802309770, 12.06949235617756955, 29.37390960531435269 ) ) ;
#167216 = CARTESIAN_POINT ( 'NONE',  ( 9.474510206698729675, 16.51473224551082808, 42.08442372801900433 ) ) ;
#167217 = CARTESIAN_POINT ( 'NONE',  ( 14.29746914071049879, -8.314922557960816363, 68.33224293864769550 ) ) ;
#167218 = CARTESIAN_POINT ( 'NONE',  ( -21.53943276465977519, -0.05219959533937600094, 98.75109039468568994 ) ) ;
#167219 = CARTESIAN_POINT ( 'NONE',  ( -19.03943276465977164, 0.05219959533909376836, 36.24890960531436690 ) ) ;
#167221 = CARTESIAN_POINT ( 'NONE',  ( 15.80617190586769283, -15.72974639402175789, 105.6260903946856899 ) ) ;
#167220 = CARTESIAN_POINT ( 'NONE',  ( -4.483927247898539470, -16.52544592524342804, 37.29057627198102409 ) ) ;
#167222 = CARTESIAN_POINT ( 'NONE',  ( -5.153800228976328057, -19.02544592524343514, 87.29057627198103830 ) ) ;
#167223 = CARTESIAN_POINT ( 'NONE',  ( 19.03943276465977164, -0.05219959533909143690, 88.74890960531436690 ) ) ;
#167224 = CARTESIAN_POINT ( 'NONE',  ( 19.02544592524343514, -5.153800228976328945, 23.54057627198102054 ) ) ;
#167225 = CARTESIAN_POINT ( 'NONE',  ( -4.483927247898539470, -16.52544592524342804, 112.2905762719810241 ) ) ;
#167226 = CARTESIAN_POINT ( 'NONE',  ( -16.53943276465976808, 0.05219959533911058130, 76.24890960531435269 ) ) ;
#167227 = CARTESIAN_POINT ( 'NONE',  ( 0.05219959533907565091, 21.53943276465977519, 89.99890960531438111 ) ) ;
#167228 = CARTESIAN_POINT ( 'NONE',  ( 5.153800228976335163, 19.02544592524342804, 84.79057627198099567 ) ) ;
#167229 = CARTESIAN_POINT ( 'NONE',  ( -5.719274019375978568, 21.55341960407610458, 100.2072429386476955 ) ) ;
#167230 = CARTESIAN_POINT ( 'NONE',  ( -19.05341960407611168, -5.049401038298163336, 91.45724293864766707 ) ) ;
#167232 = CARTESIAN_POINT ( 'NONE',  ( -14.29746914071049879, 8.314922557960819915, 85.83224293864768129 ) ) ;
#167231 = CARTESIAN_POINT ( 'NONE',  ( -5.049401038297874678, -19.05341960407618274, 64.79275706135233293 ) ) ;
#167233 = CARTESIAN_POINT ( 'NONE',  ( -9.474510206698964154, 16.51473224551069663, 65.41557627198102409 ) ) ;
#167234 = CARTESIAN_POINT ( 'NONE',  ( -18.67979575497178146, -10.72451020669898902, 71.66557627198100988 ) ) ;
#167235 = CARTESIAN_POINT ( 'NONE',  ( -40.00200000000003087, -1.163414459189985801E-14, 95.00000000000000000 ) ) ;
#167237 = CARTESIAN_POINT ( 'NONE',  ( -3.573655867282028392E-15, 2.428612866367529932E-14, 169.9999999999999716 ) ) ;
#167236 = CARTESIAN_POINT ( 'NONE',  ( -4.483927247898782831, 16.52544592524335698, 112.7094237280190328 ) ) ;
#167238 = CARTESIAN_POINT ( 'NONE',  ( 16.53943276465976808, 0.05219959533934440121, 26.25109039468567573 ) ) ;
#167239 = CARTESIAN_POINT ( 'NONE',  ( 12.06949235617757843, -12.14591786802309237, 93.12390960531436690 ) ) ;
#167240 = CARTESIAN_POINT ( 'NONE',  ( -17.50000000000000711, -5.622605283950870003, 96.31207310596111881 ) ) ;
#167241 = CARTESIAN_POINT ( 'NONE',  ( 16.46253265017160672, -9.564922557960803928, 83.33224293864768129 ) ) ;
#167242 = CARTESIAN_POINT ( 'NONE',  ( -13.89961937509977652, 13.97604488694528158, 50.62390960531435979 ) ) ;
#167243 = CARTESIAN_POINT ( 'NONE',  ( 4.379528057220339221, -16.55341960407611168, 67.70724293864769550 ) ) ;
#167244 = CARTESIAN_POINT ( 'NONE',  ( 19.03943276465977164, -0.05219959533909143690, 108.7489096053143527 ) ) ;
#167245 = CARTESIAN_POINT ( 'NONE',  ( 16.51473224551083163, -9.474510206698727899, 105.8344237280190043 ) ) ;
#167246 = CARTESIAN_POINT ( 'NONE',  ( -10.81492255796105439, 18.62759615963255655, 62.91775706135236135 ) ) ;
#167247 = CARTESIAN_POINT ( 'NONE',  ( 13.89961937509977652, -13.97604488694527269, 93.12390960531436690 ) ) ;
#167248 = CARTESIAN_POINT ( 'NONE',  ( -15.72974639402197994, 15.80617190586746368, 80.62390960531438111 ) ) ;
#167249 = CARTESIAN_POINT ( 'NONE',  ( 12.14591786802327356, -12.06949235617739191, 65.62609039468568994 ) ) ;
#167250 = CARTESIAN_POINT ( 'NONE',  ( 30.00000000000000000, 5.499999999999992895, 37.50000000000000000 ) ) ;
#167251 = CARTESIAN_POINT ( 'NONE',  ( -19.02544592524342804, 5.153800228976336051, 71.04057627198099567 ) ) ;
#167252 = CARTESIAN_POINT ( 'NONE',  ( -15.80617190586745835, -15.72974639402198527, 86.87390960531438111 ) ) ;
#167253 = CARTESIAN_POINT ( 'NONE',  ( -5.049401038297874678, -19.05341960407617918, 109.7927570613523187 ) ) ;
#167255 = CARTESIAN_POINT ( 'NONE',  ( -10.72451020669870658, -18.67979575497194134, 64.58442372801900433 ) ) ;
#167254 = CARTESIAN_POINT ( 'NONE',  ( 0.05219959533910956823, 16.53943276465976808, 34.99890960531435979 ) ) ;
#167257 = CARTESIAN_POINT ( 'NONE',  ( -18.67979575497178146, -10.72451020669898902, 26.66557627198103475 ) ) ;
#167256 = CARTESIAN_POINT ( 'NONE',  ( -14.34966873604972548, 8.224510206698743886, 88.33442372801901854 ) ) ;
#167258 = CARTESIAN_POINT ( 'NONE',  ( 5.049401038298163336, -19.05341960407611168, 107.7072429386476955 ) ) ;
#167259 = DIRECTION ( 'NONE',  ( 1.000000000000000000, 0.000000000000000000, 0.000000000000000000 ) ) ;
#167260 = CARTESIAN_POINT ( 'NONE',  ( 8.224510206698742110, 14.34966873604972548, 112.0844237280190185 ) ) ;
#167261 = CARTESIAN_POINT ( 'NONE',  ( 14.29746914071037800, 8.314922557961029526, 46.66775706135234714 ) ) ;
#167262 = CARTESIAN_POINT ( 'NONE',  ( -9.474510206698964154, 16.51473224551069663, 60.41557627198102409 ) ) ;
#167263 = CARTESIAN_POINT ( 'NONE',  ( 5.049401038298161559, -19.05341960407611168, 72.70724293864768129 ) ) ;
#167264 = CARTESIAN_POINT ( 'NONE',  ( 0.05219959533934541429, -16.53943276465976808, 70.00109039468568994 ) ) ;
#167265 = CARTESIAN_POINT ( 'NONE',  ( 12.06949235617757843, -12.14591786802309237, 43.12390960531435269 ) ) ;
#167266 = CARTESIAN_POINT ( 'NONE',  ( -9.564922557960796823, -16.46253265017161027, 52.08224293864768839 ) ) ;
#167267 = CARTESIAN_POINT ( 'NONE',  ( -13.89961937509977652, 13.97604488694528158, 45.62390960531433848 ) ) ;
#167268 = CARTESIAN_POINT ( 'NONE',  ( -12.06949235617739369, -12.14591786802326823, 39.37609039468567573 ) ) ;
#167269 = CARTESIAN_POINT ( 'NONE',  ( 19.05341960407617918, -5.049401038297876454, 91.04275706135234714 ) ) ;
#167270 = CARTESIAN_POINT ( 'NONE',  ( 14.29746914071049879, -8.314922557960816363, 103.3322429386476955 ) ) ;
#167271 = CARTESIAN_POINT ( 'NONE',  ( -9.474510206698964154, 16.51473224551069663, 70.41557627198102409 ) ) ;
#167273 = CARTESIAN_POINT ( 'NONE',  ( -38.00000000000001421, -12.34694845685042708, -1.899999999999999911 ) ) ;
#167272 = CARTESIAN_POINT ( 'NONE',  ( -16.46253265017146816, -9.564922557961047289, 104.1677570613523329 ) ) ;
#167274 = CARTESIAN_POINT ( 'NONE',  ( 15.80617190586769283, -15.72974639402175789, 85.62609039468568994 ) ) ;
#167275 = CARTESIAN_POINT ( 'NONE',  ( -8.314922557961024197, 14.29746914071037800, 62.91775706135236135 ) ) ;
#167276 = CARTESIAN_POINT ( 'NONE',  ( -17.50000000000000000, -5.500000000000000000, 106.2823096230357010 ) ) ;
#167277 = CARTESIAN_POINT ( 'NONE',  ( -10.72451020669898014, 18.67979575497178502, 65.41557627198102409 ) ) ;
#167278 = CARTESIAN_POINT ( 'NONE',  ( -12.06949235617739369, -12.14591786802326823, 49.37609039468569705 ) ) ;
#167279 = CARTESIAN_POINT ( 'NONE',  ( 19.03943276465977164, -0.05219959533909143690, 33.74890960531435979 ) ) ;
#167280 = CARTESIAN_POINT ( 'NONE',  ( -0.05219959533936034679, 19.03943276465977164, 47.50109039468566863 ) ) ;
#167281 = CARTESIAN_POINT ( 'NONE',  ( 19.03943276465977164, -0.05219959533909143690, 88.74890960531436690 ) ) ;
#167282 = CARTESIAN_POINT ( 'NONE',  ( 4.379528057220339221, -16.55341960407611168, 112.7072429386476955 ) ) ;
#167283 = CARTESIAN_POINT ( 'NONE',  ( 5.153800228976335163, 19.02544592524342804, 64.79057627198100988 ) ) ;
#167284 = VECTOR ( 'NONE', #117681, 1000.000000000000000 ) ;
#167285 = CARTESIAN_POINT ( 'NONE',  ( -17.49999999999999645, 5.499999999999992895, 53.71769037696436300 ) ) ;
#167286 = CARTESIAN_POINT ( 'NONE',  ( -18.62759615963255300, -10.81492255796106328, 74.16775706135231871 ) ) ;
#167287 = DIRECTION ( 'NONE',  ( 0.000000000000000000, 0.000000000000000000, 1.000000000000000000 ) ) ;
#167288 = CARTESIAN_POINT ( 'NONE',  ( -19.03943276465977164, -0.05219959533935918106, 33.75109039468566863 ) ) ;
#167289 = CARTESIAN_POINT ( 'NONE',  ( -9.564922557961040184, 16.46253265017147172, 27.91775706135232582 ) ) ;
#167290 = CARTESIAN_POINT ( 'NONE',  ( 4.379528057220339221, -16.55341960407611168, 57.70724293864770260 ) ) ;
#167291 = CARTESIAN_POINT ( 'NONE',  ( 5.049401038298161559, -19.05341960407611168, 57.70724293864769550 ) ) ;
#167292 = CARTESIAN_POINT ( 'NONE',  ( -10.72451020669898014, 18.67979575497178502, 25.41557627198103120 ) ) ;
#167293 = CARTESIAN_POINT ( 'NONE',  ( -21.53943276465977519, -0.05219959533937600094, 83.75109039468568994 ) ) ;
#167294 = CARTESIAN_POINT ( 'NONE',  ( 16.46253265017160672, -9.564922557960803928, 68.33224293864770971 ) ) ;
#167295 = ADVANCED_FACE ( 'NONE', ( #71805 ), #164276, .T. ) ;
#167296 = CARTESIAN_POINT ( 'NONE',  ( -21.53943276465977519, -0.05219959533937600094, 83.75109039468568994 ) ) ;
#167297 = CARTESIAN_POINT ( 'NONE',  ( -18.67979575497178146, -10.72451020669898902, 31.66557627198102054 ) ) ;
#167298 = CARTESIAN_POINT ( 'NONE',  ( -16.46253265017160317, 9.564922557960807481, 65.83224293864769550 ) ) ;
#167299 = CARTESIAN_POINT ( 'NONE',  ( 15.80617190586769283, -15.72974639402175789, 40.62609039468567573 ) ) ;
#167300 = CARTESIAN_POINT ( 'NONE',  ( -19.03943276465977164, -0.05219959533935918106, 63.75109039468566863 ) ) ;
#167301 = CARTESIAN_POINT ( 'NONE',  ( 19.02544592524343514, -5.153800228976328945, 38.54057627198103120 ) ) ;
#167302 = CARTESIAN_POINT ( 'NONE',  ( 5.049401038298161559, -19.05341960407611168, 72.70724293864768129 ) ) ;
#167303 = CARTESIAN_POINT ( 'NONE',  ( -16.55341960407617563, 4.379528057220093196, 28.54275706135234358 ) ) ;
#167304 = CARTESIAN_POINT ( 'NONE',  ( -8.224510206698948167, 14.34966873604960824, 90.41557627198103830 ) ) ;
#167305 = CARTESIAN_POINT ( 'NONE',  ( 16.46253265017160672, -9.564922557960803928, 53.33224293864768839 ) ) ;
#167306 = CARTESIAN_POINT ( 'NONE',  ( -21.55341960407610458, -5.719274019375992779, 51.45724293864770260 ) ) ;
#167307 = CARTESIAN_POINT ( 'NONE',  ( 4.483927247898790824, -16.52544592524335698, 20.20942372801900788 ) ) ;
#167308 = CARTESIAN_POINT ( 'NONE',  ( -10.81492255796105439, 18.62759615963255655, 22.91775706135235069 ) ) ;
#167309 = CARTESIAN_POINT ( 'NONE',  ( 18.67979575497194134, -10.72451020669871369, 70.83442372801901854 ) ) ;
#167310 = CARTESIAN_POINT ( 'NONE',  ( -16.52544592524335698, -4.483927247898792601, 73.95942372801901854 ) ) ;
#167311 = CARTESIAN_POINT ( 'NONE',  ( -16.52544592524335698, -4.483927247898792601, 73.95942372801901854 ) ) ;
#167312 = CARTESIAN_POINT ( 'NONE',  ( -13.89961937509977652, 13.97604488694528158, 55.62390960531434558 ) ) ;
#167313 = CARTESIAN_POINT ( 'NONE',  ( 8.224510206698742110, 14.34966873604972548, 92.08442372801901854 ) ) ;
#167314 = CARTESIAN_POINT ( 'NONE',  ( 9.564922557961047289, -16.46253265017146816, 40.41775706135234003 ) ) ;
#167315 = PRESENTATION_LAYER_ASSIGNMENT (  '', '', ( #121967 ) ) ;
#167316 = CARTESIAN_POINT ( 'NONE',  ( -5.823673210054431948, 21.52544592524334988, 22.70942372801901499 ) ) ;
#167317 = CARTESIAN_POINT ( 'NONE',  ( 4.379528057220339221, -16.55341960407611168, 67.70724293864769550 ) ) ;
#167318 = CARTESIAN_POINT ( 'NONE',  ( 13.97604488694527802, 13.89961937509977652, 84.37390960531433848 ) ) ;
#167319 = CARTESIAN_POINT ( 'NONE',  ( 4.483927247898790824, -16.52544592524335698, 90.20942372801903275 ) ) ;
#167320 = CARTESIAN_POINT ( 'NONE',  ( 18.67979575497194134, -10.72451020669871369, 60.83442372801901854 ) ) ;
#167321 = CARTESIAN_POINT ( 'NONE',  ( 16.53943276465976808, 0.05219959533934440121, 36.25109039468567573 ) ) ;
#167322 = CARTESIAN_POINT ( 'NONE',  ( -0.05219959533937732626, 21.53943276465977519, 32.50109039468568284 ) ) ;
#167323 = CARTESIAN_POINT ( 'NONE',  ( -4.483927247898539470, -16.52544592524342804, 57.29057627198103120 ) ) ;
#167324 = VERTEX_POINT ( 'NONE', #144686 ) ;
#167325 = CARTESIAN_POINT ( 'NONE',  ( 5.823673210054125526, 21.52544592524343514, 99.79057627198103830 ) ) ;
#167326 = CARTESIAN_POINT ( 'NONE',  ( 16.52544592524342804, -4.483927247898539470, 38.54057627198103120 ) ) ;
#167327 = VERTEX_POINT ( 'NONE', #6171 ) ;
#167328 = CARTESIAN_POINT ( 'NONE',  ( 34.38695055765521857, 7.456135981908276200, 45.94887894546498330 ) ) ;
#167329 = CARTESIAN_POINT ( 'NONE',  ( -18.62759615963270932, 10.81492255796079327, 25.83224293864769194 ) ) ;
#167330 = CARTESIAN_POINT ( 'NONE',  ( 5.719274019375673035, 21.55341960407619339, 42.29275706135235424 ) ) ;
#167331 = CARTESIAN_POINT ( 'NONE',  ( 14.34966873604960469, 8.224510206698951720, 69.16557627198102409 ) ) ;
#167332 = CARTESIAN_POINT ( 'NONE',  ( 16.51473224551069308, 9.474510206698969483, 74.16557627198103830 ) ) ;
#167334 = CARTESIAN_POINT ( 'NONE',  ( -9.474510206698720793, -16.51473224551083518, 69.58442372801901854 ) ) ;
#167333 = CARTESIAN_POINT ( 'NONE',  ( -16.51473224551069308, -9.474510206698971260, 26.66557627198103120 ) ) ;
#167335 = CARTESIAN_POINT ( 'NONE',  ( -5.823673210054116645, -21.52544592524344225, 47.29057627198103120 ) ) ;
#167336 = CARTESIAN_POINT ( 'NONE',  ( -11.44429459767042090, -35.82063519324131562, -30.53178620540835553 ) ) ;
#167337 = CARTESIAN_POINT ( 'NONE',  ( -19.05341960407611168, -5.049401038298163336, 56.45724293864768129 ) ) ;
#167338 = CARTESIAN_POINT ( 'NONE',  ( 4.379528057220092307, 16.55341960407617563, 42.29275706135235424 ) ) ;
#167339 = CARTESIAN_POINT ( 'NONE',  ( 21.52544592524344225, -5.823673210054117533, 113.5405762719810383 ) ) ;
#167340 = CARTESIAN_POINT ( 'NONE',  ( -4.379528057220328563, 16.55341960407611168, 50.20724293864769550 ) ) ;
#167341 = VERTEX_POINT ( 'NONE', #67851 ) ;
#167342 = CARTESIAN_POINT ( 'NONE',  ( -19.02544592524342804, 5.153800228976336051, 96.04057627198103830 ) ) ;
#167343 = CARTESIAN_POINT ( 'NONE',  ( 18.62759615963271287, -10.81492255796078972, 78.33224293864770971 ) ) ;
#167345 = CARTESIAN_POINT ( 'NONE',  ( 12.06949235617739724, 12.14591786802326823, 31.87609039468567929 ) ) ;
#167344 = CARTESIAN_POINT ( 'NONE',  ( 10.81492255796078972, 18.62759615963270932, 114.5822429386477097 ) ) ;
#167346 = CARTESIAN_POINT ( 'NONE',  ( -5.719274019375978568, 21.55341960407610458, 40.20724293864769550 ) ) ;
#167347 = CARTESIAN_POINT ( 'NONE',  ( -21.53943276465977519, -0.05219959533937600094, 108.7510903946857042 ) ) ;
#167348 = CARTESIAN_POINT ( 'NONE',  ( 9.564922557960805705, 16.46253265017160317, 104.5822429386476955 ) ) ;
#167349 = CARTESIAN_POINT ( 'NONE',  ( -19.02544592524342804, 5.153800228976336051, 36.04057627198100988 ) ) ;
#167350 = CARTESIAN_POINT ( 'NONE',  ( 9.474510206698971260, -16.51473224551069308, 97.91557627198102409 ) ) ;
#167351 = CARTESIAN_POINT ( 'NONE',  ( 5.153800228976335163, 19.02544592524342804, 74.79057627198103830 ) ) ;
#167352 = CARTESIAN_POINT ( 'NONE',  ( -27.39934578958840206, -26.16170490841989249, -16.57183124570353883 ) ) ;
#167353 = CARTESIAN_POINT ( 'NONE',  ( 13.97604488694548053, -13.89961937509957401, 50.62609039468566152 ) ) ;
#167355 = CARTESIAN_POINT ( 'NONE',  ( -15.72974639402197994, 15.80617190586746368, 25.62390960531435624 ) ) ;
#167354 = CARTESIAN_POINT ( 'NONE',  ( -18.67979575497193778, 10.72451020669871902, 108.3344237280190185 ) ) ;
#167356 = CARTESIAN_POINT ( 'NONE',  ( 16.53943276465976808, 0.05219959533934440121, 106.2510903946856757 ) ) ;
#167357 = CARTESIAN_POINT ( 'NONE',  ( 9.474510206698729675, 16.51473224551082808, 92.08442372801900433 ) ) ;
#167358 = CARTESIAN_POINT ( 'NONE',  ( -16.21995358207306737, 7.366697692864095259, 59.93551001512161491 ) ) ;
#167359 = CARTESIAN_POINT ( 'NONE',  ( -13.97604488694547697, 13.89961937509957934, 88.12609039468563310 ) ) ;
#167360 = CARTESIAN_POINT ( 'NONE',  ( 19.05341960407617918, -5.049401038297876454, 36.04275706135234003 ) ) ;
#167361 = CARTESIAN_POINT ( 'NONE',  ( -16.18388926212241330, -7.379444403734407132, 45.43953151366152809 ) ) ;
#167362 = CARTESIAN_POINT ( 'NONE',  ( 16.46253265017160672, -9.564922557960803928, 43.33224293864769550 ) ) ;
#167363 = CARTESIAN_POINT ( 'NONE',  ( 14.29746914071049879, -8.314922557960816363, 53.33224293864769550 ) ) ;
#167364 = CARTESIAN_POINT ( 'NONE',  ( -17.50000000000000711, -5.622605283950883326, 111.3120731059611330 ) ) ;
#167365 = CARTESIAN_POINT ( 'NONE',  ( 4.379528057220339221, -16.55341960407611168, 22.70724293864769194 ) ) ;
#167366 = CARTESIAN_POINT ( 'NONE',  ( 20.58216519391595156, -20.30265720351238201, -52.64392108347575316 ) ) ;
#167367 = CARTESIAN_POINT ( 'NONE',  ( 14.34966873604972726, -8.224510206698740333, 100.8344237280190185 ) ) ;
#167368 = CARTESIAN_POINT ( 'NONE',  ( -13.89961937509977652, 13.97604488694528158, 45.62390960531433848 ) ) ;
#167369 = EDGE_CURVE ( 'NONE', #101974, #67859, #191206, .T. ) ;
#167370 = CARTESIAN_POINT ( 'NONE',  ( -15.80617190586768217, 15.72974639402176855, 108.1260903946856757 ) ) ;
#167371 = CARTESIAN_POINT ( 'NONE',  ( 12.06949235617739724, 12.14591786802326823, 26.87609039468567218 ) ) ;
#167373 = ORIENTED_EDGE ( 'NONE', *, *, #60920, .T. ) ;
#167372 = CARTESIAN_POINT ( 'NONE',  ( -15.80617190586768217, 15.72974639402176855, 93.12609039468568994 ) ) ;
#167374 = CARTESIAN_POINT ( 'NONE',  ( -16.51473224551069308, -9.474510206698971260, 86.66557627198102409 ) ) ;
#167375 = CARTESIAN_POINT ( 'NONE',  ( 9.564922557960805705, 16.46253265017160317, 79.58224293864769550 ) ) ;
#167376 = CARTESIAN_POINT ( 'NONE',  ( 29.86685920354754487, 21.69954338932564752, -7.424999997268813878 ) ) ;
#167377 = CARTESIAN_POINT ( 'NONE',  ( -18.62759615963270932, 10.81492255796079327, 105.8322429386476955 ) ) ;
#167378 = CARTESIAN_POINT ( 'NONE',  ( 16.52544592524342804, -4.483927247898539470, 78.54057627198103830 ) ) ;
#167379 = CARTESIAN_POINT ( 'NONE',  ( 10.81492255796078972, 18.62759615963270932, 79.58224293864769550 ) ) ;
#167380 = CARTESIAN_POINT ( 'NONE',  ( 5.153800228976335163, 19.02544592524342804, 64.79057627198100988 ) ) ;
#167382 = CARTESIAN_POINT ( 'NONE',  ( 8.224510206698742110, 14.34966873604972548, 97.08442372801904696 ) ) ;
#167381 = CARTESIAN_POINT ( 'NONE',  ( 15.72974639402199770, -15.80617190586745480, 98.12390960531436690 ) ) ;
#167383 = ADVANCED_FACE ( 'NONE', ( #152662 ), #43515, .T. ) ;
#167384 = ORIENTED_EDGE ( 'NONE', *, *, #177829, .T. ) ;
#167385 = CARTESIAN_POINT ( 'NONE',  ( -19.03943276465977164, 0.05219959533909376836, 66.24890960531436690 ) ) ;
#167387 = CARTESIAN_POINT ( 'NONE',  ( 20.48541513753860954, -11.15937153969631979, 168.1083253156164119 ) ) ;
#167386 = CARTESIAN_POINT ( 'NONE',  ( -12.14591786802309592, -12.06949235617757132, 86.87390960531438111 ) ) ;
#167388 = CARTESIAN_POINT ( 'NONE',  ( 13.89961937509977652, -13.97604488694527269, 68.12390960531436690 ) ) ;
#167389 = CARTESIAN_POINT ( 'NONE',  ( 19.02544592524334988, 5.153800228976608722, 76.45942372801897591 ) ) ;
#167390 = CARTESIAN_POINT ( 'NONE',  ( -12.14591786802309592, -12.06949235617757132, 86.87390960531438111 ) ) ;
#167391 = CARTESIAN_POINT ( 'NONE',  ( -15.72974639402176322, -15.80617190586768395, 59.37609039468568284 ) ) ;
#167393 = CARTESIAN_POINT ( 'NONE',  ( -21.53943276465977519, 0.05219959533907696930, 116.2489096053143669 ) ) ;
#167392 = CARTESIAN_POINT ( 'NONE',  ( 0.05219959533909260263, 19.03943276465977164, 54.99890960531435979 ) ) ;
#167394 = CARTESIAN_POINT ( 'NONE',  ( 16.52544592524342804, -4.483927247898539470, 98.54057627198105251 ) ) ;
#167395 = CARTESIAN_POINT ( 'NONE',  ( 9.824205582582273166, -39.25481172344606762, -25.36904614590414297 ) ) ;
#167396 = CARTESIAN_POINT ( 'NONE',  ( 19.03943276465977164, -0.05219959533909143690, 53.74890960531436690 ) ) ;
#167397 = CYLINDRICAL_SURFACE ( 'NONE', #21534, 2.500000000000002220 ) ;
#167399 = CARTESIAN_POINT ( 'NONE',  ( 15.72974639402199770, -15.80617190586745480, 23.12390960531436335 ) ) ;
#167398 = CARTESIAN_POINT ( 'NONE',  ( 0.05219959533936267826, -19.03943276465977164, 100.0010903946856757 ) ) ;
#167400 = CARTESIAN_POINT ( 'NONE',  ( 21.53943276465977519, 0.05219959533937863772, 46.25109039468567573 ) ) ;
#167401 = CARTESIAN_POINT ( 'NONE',  ( -19.05341960407611168, -5.049401038298163336, 86.45724293864769550 ) ) ;
#167402 = CARTESIAN_POINT ( 'NONE',  ( -5.153800228976607833, 19.02544592524334988, 72.70942372801900433 ) ) ;
#167403 = CARTESIAN_POINT ( 'NONE',  ( 19.03943276465977164, -0.05219959533909143690, 58.74890960531435979 ) ) ;
#167404 = CARTESIAN_POINT ( 'NONE',  ( -4.483927247898539470, -16.52544592524342804, 82.29057627198103830 ) ) ;
#167405 = CARTESIAN_POINT ( 'NONE',  ( 8.224510206698953496, -14.34966873604960469, 77.91557627198102409 ) ) ;
#167406 = CARTESIAN_POINT ( 'NONE',  ( -19.02544592524342804, 5.153800228976336051, 91.04057627198100988 ) ) ;
#167407 = CARTESIAN_POINT ( 'NONE',  ( -8.314922557960811034, -14.29746914071050412, 77.08224293864769550 ) ) ;
#167408 = CARTESIAN_POINT ( 'NONE',  ( 5.153800228976335163, 19.02544592524342804, 84.79057627198099567 ) ) ;
#167409 = CARTESIAN_POINT ( 'NONE',  ( 9.564922557961047289, -16.46253265017146816, 25.41775706135234003 ) ) ;
#167412 = CARTESIAN_POINT ( 'NONE',  ( 12.06949235617757843, -12.14591786802309237, 108.1239096053143811 ) ) ;
#167411 = CARTESIAN_POINT ( 'NONE',  ( 14.34966873604960469, 8.224510206698951720, 24.16557627198103120 ) ) ;
#167410 = CARTESIAN_POINT ( 'NONE',  ( 16.46253265017160672, -9.564922557960803928, 53.33224293864768839 ) ) ;
#167413 = VERTEX_POINT ( 'NONE', #197208 ) ;
#167414 = CARTESIAN_POINT ( 'NONE',  ( 18.67979575497194134, -10.72451020669871369, 45.83442372801901854 ) ) ;
#167415 = CARTESIAN_POINT ( 'NONE',  ( -19.02544592524334988, -5.153800228976617603, 68.95942372801896170 ) ) ;
#167416 = CARTESIAN_POINT ( 'NONE',  ( -14.29746914071049879, 8.314922557960819915, 40.83224293864769550 ) ) ;
#167417 = CARTESIAN_POINT ( 'NONE',  ( -21.55341960407610458, -5.719274019375992779, 81.45724293864769550 ) ) ;
#167418 = CARTESIAN_POINT ( 'NONE',  ( 19.03943276465977164, -0.05219959533909143690, 113.7489096053143669 ) ) ;
#167419 = CARTESIAN_POINT ( 'NONE',  ( 12.14591786802309770, 12.06949235617756955, 69.37390960531436690 ) ) ;
#167420 = CARTESIAN_POINT ( 'NONE',  ( -9.564922557960796823, -16.46253265017161027, 42.08224293864769550 ) ) ;
#167421 = CARTESIAN_POINT ( 'NONE',  ( 16.51473224551083163, -9.474510206698727899, 45.83442372801900433 ) ) ;
#167422 = CARTESIAN_POINT ( 'NONE',  ( -16.52544592524335698, -4.483927247898792601, 103.9594237280190185 ) ) ;
#167423 = CARTESIAN_POINT ( 'NONE',  ( 12.06949235617739724, 12.14591786802326823, 61.87609039468568284 ) ) ;
#167424 = CARTESIAN_POINT ( 'NONE',  ( -15.72974639402197994, 15.80617190586746368, 35.62390960531437401 ) ) ;
#167425 = CARTESIAN_POINT ( 'NONE',  ( -18.67979575497193778, 10.72451020669871902, 108.3344237280190185 ) ) ;
#167426 = CARTESIAN_POINT ( 'NONE',  ( -16.51473224551069308, -9.474510206698971260, 91.66557627198103830 ) ) ;
#167427 = CARTESIAN_POINT ( 'NONE',  ( 14.29746914071037800, 8.314922557961029526, 71.66775706135234714 ) ) ;
#167428 = CARTESIAN_POINT ( 'NONE',  ( 19.05341960407611168, 5.049401038298154454, 23.95724293864769194 ) ) ;
#167429 = CARTESIAN_POINT ( 'NONE',  ( 0.05219959533910956823, 16.53943276465976808, 29.99890960531435979 ) ) ;
#167431 = CARTESIAN_POINT ( 'NONE',  ( -5.049401038298153566, 19.05341960407611168, 95.20724293864770971 ) ) ;
#167430 = CARTESIAN_POINT ( 'NONE',  ( 13.89961937509977652, -13.97604488694527269, 103.1239096053143527 ) ) ;
#167432 = CARTESIAN_POINT ( 'NONE',  ( -18.67979575497178146, -10.72451020669898902, 26.66557627198103475 ) ) ;
#167433 = CARTESIAN_POINT ( 'NONE',  ( 12.06949235617757843, -12.14591786802309237, 68.12390960531436690 ) ) ;
#167434 = CARTESIAN_POINT ( 'NONE',  ( 8.224510206698953496, -14.34966873604960469, 47.91557627198102409 ) ) ;
#167436 = CARTESIAN_POINT ( 'NONE',  ( -17.72662750342724891, -5.500000000000087041, 56.40179492283746043 ) ) ;
#167435 = CARTESIAN_POINT ( 'NONE',  ( -14.29746914071037622, -8.314922557961029526, 54.16775706135235424 ) ) ;
#167437 = CARTESIAN_POINT ( 'NONE',  ( 5.153800228976615827, -19.02544592524334988, 55.20942372801899722 ) ) ;
#167438 = CARTESIAN_POINT ( 'NONE',  ( 9.474510206698971260, -16.51473224551069308, 92.91557627198103830 ) ) ;
#167439 = CARTESIAN_POINT ( 'NONE',  ( 9.564922557961047289, -16.46253265017146816, 65.41775706135233293 ) ) ;
#167440 = CARTESIAN_POINT ( 'NONE',  ( 27.73933785331498569, 2.768321779492822058E-14, 144.3750000027311842 ) ) ;
#167441 = CARTESIAN_POINT ( 'NONE',  ( 9.474510206698729675, 16.51473224551082808, 52.08442372801900433 ) ) ;
#167443 = CARTESIAN_POINT ( 'NONE',  ( 4.379528057220092307, 16.55341960407617563, 92.29275706135236135 ) ) ;
#167442 = CARTESIAN_POINT ( 'NONE',  ( -9.564922557961040184, 16.46253265017147172, 102.9177570613523329 ) ) ;
#167444 = CARTESIAN_POINT ( 'NONE',  ( 27.73933785331498925, -9.013057229001033122, 144.2750000027311899 ) ) ;
#167445 = CARTESIAN_POINT ( 'NONE',  ( 19.05341960407611168, 5.049401038298154454, 38.95724293864767418 ) ) ;
#167446 = CARTESIAN_POINT ( 'NONE',  ( -5.823673210054116645, -21.52544592524344225, 27.29057627198103120 ) ) ;
#167447 = CARTESIAN_POINT ( 'NONE',  ( 15.80617190586769283, -15.72974639402175789, 50.62609039468568994 ) ) ;
#167448 = CARTESIAN_POINT ( 'NONE',  ( -16.51473224551082808, 9.474510206698731452, 103.3344237280190043 ) ) ;
#167450 = CARTESIAN_POINT ( 'NONE',  ( 16.51473224551069308, 9.474510206698969483, 59.16557627198102409 ) ) ;
#167449 = DIRECTION ( 'NONE',  ( 1.000000000000000000, 0.000000000000000000, 0.000000000000000000 ) ) ;
#167451 = AXIS2_PLACEMENT_3D ( 'NONE', #176630, #180639, #55264 ) ;
#167452 = PLANE ( 'NONE',  #1396 ) ;
#167454 = CARTESIAN_POINT ( 'NONE',  ( -9.564922557960796823, -16.46253265017161027, 62.08224293864769550 ) ) ;
#167453 = CARTESIAN_POINT ( 'NONE',  ( 4.379528057220339221, -16.55341960407611168, 72.70724293864769550 ) ) ;
#167455 = CARTESIAN_POINT ( 'NONE',  ( 19.02544592524343514, -5.153800228976328945, 78.54057627198099567 ) ) ;
#167456 = CARTESIAN_POINT ( 'NONE',  ( -9.474510206698720793, -16.51473224551083518, 84.58442372801900433 ) ) ;
#167457 = CARTESIAN_POINT ( 'NONE',  ( 18.67979575497178502, 10.72451020669898547, 69.16557627198102409 ) ) ;
#167458 = CARTESIAN_POINT ( 'NONE',  ( 14.34966873604960469, 8.224510206698951720, 109.1655762719810383 ) ) ;
#167459 = CARTESIAN_POINT ( 'NONE',  ( 5.153800228976615827, -19.02544592524334988, 45.20942372801901143 ) ) ;
#167460 = CARTESIAN_POINT ( 'NONE',  ( 19.02544592524343514, -5.153800228976328945, 73.54057627198103830 ) ) ;
#167461 =( BOUNDED_CURVE ( )  B_SPLINE_CURVE ( 2, ( #91788, #123135, #77634, #139303, #781, #114937, #19938, #81579, #141291, #50293, #95781 ),
 .UNSPECIFIED., .F., .T. ) 
 B_SPLINE_CURVE_WITH_KNOTS ( ( 3, 2, 2, 2, 2, 3 ),
 ( 0.7000000000000006217, 0.7200000000000006395, 0.7400000000000006573, 0.7600000000000006750, 0.7800000000000006928, 0.8000000000000007105 ),
 .UNSPECIFIED. ) 
 CURVE ( )  GEOMETRIC_REPRESENTATION_ITEM ( )  RATIONAL_B_SPLINE_CURVE ( ( 0.9999999999999983347, 0.9510565162951551965, 1.000000000000000000, 0.9510565162951535312, 1.000000000000000000, 0.9510565162951535312, 1.000000000000000000, 0.9510565162951535312, 1.000000000000000000, 0.9510565162951518658, 1.000000000000001554 ) ) 
 REPRESENTATION_ITEM ( '' )  );
#167462 = CARTESIAN_POINT ( 'NONE',  ( -18.67979575497178146, -10.72451020669898902, 86.66557627198102409 ) ) ;
#167464 = CARTESIAN_POINT ( 'NONE',  ( 19.02544592524334988, 5.153800228976608722, 51.45942372801900433 ) ) ;
#167463 = CARTESIAN_POINT ( 'NONE',  ( 16.55341960407611168, 4.379528057220329451, 73.95724293864769550 ) ) ;
#167465 = CARTESIAN_POINT ( 'NONE',  ( -10.81492255796078084, -18.62759615963271287, 77.08224293864769550 ) ) ;
#167466 = CARTESIAN_POINT ( 'NONE',  ( -21.55341960407610458, -5.719274019375992779, 61.45724293864770260 ) ) ;
#167467 = CARTESIAN_POINT ( 'NONE',  ( -15.72974639402197994, 15.80617190586746368, 35.62390960531437401 ) ) ;
#167468 = CARTESIAN_POINT ( 'NONE',  ( -15.80617190586768217, 15.72974639402176855, 88.12609039468570415 ) ) ;
#167469 = CARTESIAN_POINT ( 'NONE',  ( -9.474510206698964154, 16.51473224551069663, 80.41557627198103830 ) ) ;
#167470 = CARTESIAN_POINT ( 'NONE',  ( 12.14591786802309770, 12.06949235617756955, 114.3739096053143527 ) ) ;
#167471 = CARTESIAN_POINT ( 'NONE',  ( 21.55341960407619695, -5.719274019375665929, 26.04275706135235779 ) ) ;
#167472 = CARTESIAN_POINT ( 'NONE',  ( 5.719274019375673035, 21.55341960407619339, 37.29275706135235424 ) ) ;
#167473 = CARTESIAN_POINT ( 'NONE',  ( -16.51473224551069308, -9.474510206698971260, 31.66557627198102054 ) ) ;
#167474 = CARTESIAN_POINT ( 'NONE',  ( 18.67979575497194134, -10.72451020669871369, 20.83442372801901143 ) ) ;
#167475 = CARTESIAN_POINT ( 'NONE',  ( 16.46253265017146816, 9.564922557961045513, 66.66775706135233293 ) ) ;
#167476 = CARTESIAN_POINT ( 'NONE',  ( 13.97604488694527802, 13.89961937509977652, 39.37390960531435269 ) ) ;
#167477 = CARTESIAN_POINT ( 'NONE',  ( 16.52544592524335698, 4.483927247898782831, 31.45942372801901854 ) ) ;
#167478 = CARTESIAN_POINT ( 'NONE',  ( 17.50000000000000000, 5.499999999999997335, 120.0000000000000142 ) ) ;
#167479 = CARTESIAN_POINT ( 'NONE',  ( 4.483927247898790824, -16.52544592524335698, 65.20942372801901854 ) ) ;
#167480 = CARTESIAN_POINT ( 'NONE',  ( 9.564922557960805705, 16.46253265017160317, 39.58224293864768839 ) ) ;
#167481 = CARTESIAN_POINT ( 'NONE',  ( -21.81230582904511550, -7.807068725607987147, 172.9985625539908085 ) ) ;
#167482 = CARTESIAN_POINT ( 'NONE',  ( -16.51473224551069308, -9.474510206698971260, 86.66557627198102409 ) ) ;
#167483 = CARTESIAN_POINT ( 'NONE',  ( -19.03943276465977164, 0.05219959533909376836, 21.24890960531436335 ) ) ;
#167484 = CARTESIAN_POINT ( 'NONE',  ( -21.52544592524343514, 5.823673210054127303, 56.04057627198102409 ) ) ;
#167485 = CARTESIAN_POINT ( 'NONE',  ( -12.14591786802326823, 12.06949235617739902, 48.12609039468568284 ) ) ;
#167486 = CARTESIAN_POINT ( 'NONE',  ( -18.62759615963255300, -10.81492255796106328, 99.16775706135234714 ) ) ;
#167487 = EDGE_CURVE ( 'NONE', #120670, #116832, #53222, .T. ) ;
#167488 = CARTESIAN_POINT ( 'NONE',  ( 19.03943276465977164, -0.05219959533909143690, 43.74890960531435979 ) ) ;
#167489 = CARTESIAN_POINT ( 'NONE',  ( 16.53943276465976808, -0.05219959533910856209, 28.74890960531435624 ) ) ;
#167490 = CARTESIAN_POINT ( 'NONE',  ( -14.29746914071049879, 8.314922557960819915, 70.83224293864770971 ) ) ;
#167491 = CARTESIAN_POINT ( 'NONE',  ( -5.049401038298153566, 19.05341960407611168, 60.20724293864768129 ) ) ;
#167492 = CARTESIAN_POINT ( 'NONE',  ( 5.823673210054444382, -21.52544592524334988, 110.2094237280190185 ) ) ;
#167493 = CARTESIAN_POINT ( 'NONE',  ( -10.81492255796105439, 18.62759615963255655, 22.91775706135235069 ) ) ;
#167494 = CARTESIAN_POINT ( 'NONE',  ( 21.52544592524334988, 5.823673210054432836, 86.45942372801901854 ) ) ;
#167495 = CARTESIAN_POINT ( 'NONE',  ( -4.483927247898782831, 16.52544592524335698, 47.70942372801902565 ) ) ;
#167496 = CARTESIAN_POINT ( 'NONE',  ( 16.53943276465976808, 0.05219959533934440121, 26.25109039468567573 ) ) ;
#167498 = CARTESIAN_POINT ( 'NONE',  ( -10.72451020669870658, -18.67979575497194134, 94.58442372801901854 ) ) ;
#167497 = CARTESIAN_POINT ( 'NONE',  ( 14.34966873604960469, 8.224510206698951720, 89.16557627198102409 ) ) ;
#167499 = ADVANCED_FACE ( 'NONE', ( #27367 ), #80375, .T. ) ;
#167500 = CARTESIAN_POINT ( 'NONE',  ( 4.379528057220339221, -16.55341960407611168, 32.70724293864770260 ) ) ;
#167501 = CARTESIAN_POINT ( 'NONE',  ( -0.05219959533909027116, -19.03943276465977164, 32.49890960531435979 ) ) ;
#167502 = CARTESIAN_POINT ( 'NONE',  ( 14.34966873604972726, -8.224510206698740333, 45.83442372801901854 ) ) ;
#167503 = CARTESIAN_POINT ( 'NONE',  ( 12.06949235617757843, -12.14591786802309237, 58.12390960531435979 ) ) ;
#167504 = CARTESIAN_POINT ( 'NONE',  ( -4.483927247898782831, 16.52544592524335698, 92.70942372801901854 ) ) ;
#167505 = CARTESIAN_POINT ( 'NONE',  ( -13.97604488694527625, -13.89961937509977652, 96.87390960531433848 ) ) ;
#167506 = CARTESIAN_POINT ( 'NONE',  ( 10.72451020669898902, -18.67979575497178502, 22.91557627198102765 ) ) ;
#167507 = CARTESIAN_POINT ( 'NONE',  ( -15.72974639402176322, -15.80617190586768395, 109.3760903946857042 ) ) ;
#167508 = CARTESIAN_POINT ( 'NONE',  ( 16.55341960407611168, 4.379528057220329451, 83.95724293864770971 ) ) ;
#167509 = CARTESIAN_POINT ( 'NONE',  ( -13.89961937509977652, 13.97604488694528158, 100.6239096053143669 ) ) ;
#167510 = ORIENTED_EDGE ( 'NONE', *, *, #16720, .T. ) ;
#167511 = CARTESIAN_POINT ( 'NONE',  ( -16.52544592524335698, -4.483927247898792601, 38.95942372801901854 ) ) ;
#167512 = CARTESIAN_POINT ( 'NONE',  ( -5.153800228976328057, -19.02544592524343514, 42.29057627198101699 ) ) ;
#167513 = CARTESIAN_POINT ( 'NONE',  ( 13.89961937509977652, -13.97604488694527269, 103.1239096053143527 ) ) ;
#167515 = DIRECTION ( 'NONE',  ( 0.000000000000000000, 0.8164965809277232589, 0.5773502691896297279 ) ) ;
#167514 = CARTESIAN_POINT ( 'NONE',  ( 12.06949235617739724, 12.14591786802326823, 41.87609039468568284 ) ) ;
#167516 = CARTESIAN_POINT ( 'NONE',  ( 9.564922557961047289, -16.46253265017146816, 50.41775706135233293 ) ) ;
#167517 = CARTESIAN_POINT ( 'NONE',  ( 16.46253265017160672, -9.564922557960803928, 48.33224293864769550 ) ) ;
#167518 = CARTESIAN_POINT ( 'NONE',  ( -4.379528057220086978, -16.55341960407618274, 79.79275706135236135 ) ) ;
#167519 = CARTESIAN_POINT ( 'NONE',  ( 19.02544592524334988, 5.153800228976608722, 86.45942372801900433 ) ) ;
#167520 = CARTESIAN_POINT ( 'NONE',  ( -9.474510206698720793, -16.51473224551083518, 34.58442372801899722 ) ) ;
#167521 = CARTESIAN_POINT ( 'NONE',  ( -19.02544592524342804, 5.153800228976336051, 66.04057627198103830 ) ) ;
#167522 = CARTESIAN_POINT ( 'NONE',  ( -0.05219959533910754901, -16.53943276465976808, 97.49890960531436690 ) ) ;
#167523 = CARTESIAN_POINT ( 'NONE',  ( 19.03943276465977164, 0.05219959533936151252, 71.25109039468566152 ) ) ;
#167524 = CARTESIAN_POINT ( 'NONE',  ( 18.67979575497178502, 10.72451020669898547, 69.16557627198102409 ) ) ;
#167525 = CARTESIAN_POINT ( 'NONE',  ( 16.51473224551083163, -9.474510206698727899, 25.83442372801900078 ) ) ;
#167526 = CARTESIAN_POINT ( 'NONE',  ( -9.474510206698964154, 16.51473224551069663, 105.4155762719810383 ) ) ;
#167527 = EDGE_CURVE ( 'NONE', #187814, #37464, #99118, .T. ) ;
#167528 = CARTESIAN_POINT ( 'NONE',  ( -15.80617190586745835, -15.72974639402198527, 81.87390960531435269 ) ) ;
#167529 = CARTESIAN_POINT ( 'NONE',  ( -18.22780087662122028, 5.500000000000031086, 53.51540105326106556 ) ) ;
#167530 = CARTESIAN_POINT ( 'NONE',  ( -19.02544592524334988, -5.153800228976617603, 103.9594237280190043 ) ) ;
#167531 = CARTESIAN_POINT ( 'NONE',  ( -19.25663599770061296, 5.499999999999452882, 58.99419308057201050 ) ) ;
#167532 = CARTESIAN_POINT ( 'NONE',  ( 8.314922557961029526, -14.29746914071037800, 25.41775706135235779 ) ) ;
#167533 = CARTESIAN_POINT ( 'NONE',  ( 5.153800228976335163, 19.02544592524342804, 34.79057627198102409 ) ) ;
#167534 = CARTESIAN_POINT ( 'NONE',  ( 19.03943276465977164, -0.05219959533909143690, 103.7489096053143669 ) ) ;
#167535 = CARTESIAN_POINT ( 'NONE',  ( -15.80617190586745835, -15.72974639402198527, 91.87390960531436690 ) ) ;
#167536 = CARTESIAN_POINT ( 'NONE',  ( 15.72974639402176855, 15.80617190586768217, 66.87609039468568994 ) ) ;
#167538 = CARTESIAN_POINT ( 'NONE',  ( 15.72974639402176855, 15.80617190586768217, 106.8760903946856899 ) ) ;
#167537 = CARTESIAN_POINT ( 'NONE',  ( -13.89961937509957401, -13.97604488694547875, 109.3760903946856331 ) ) ;
#167539 = CARTESIAN_POINT ( 'NONE',  ( -0.05219959533910754901, -16.53943276465976808, 22.49890960531436335 ) ) ;
#167540 = CARTESIAN_POINT ( 'NONE',  ( -0.05219959533907301413, -21.53943276465977519, 97.49890960531436690 ) ) ;
#167541 = CARTESIAN_POINT ( 'NONE',  ( 12.06949235617757843, -12.14591786802309237, 53.12390960531436690 ) ) ;
#167542 = CARTESIAN_POINT ( 'NONE',  ( 19.03943276465977164, 0.05219959533936151252, 81.25109039468567573 ) ) ;
#167543 = CARTESIAN_POINT ( 'NONE',  ( 19.05341960407617918, -5.049401038297876454, 56.04275706135234714 ) ) ;
#167544 = CARTESIAN_POINT ( 'NONE',  ( 21.55341960407619695, -5.719274019375665929, 61.04275706135234714 ) ) ;
#167545 = CARTESIAN_POINT ( 'NONE',  ( 13.97604488694548053, -13.89961937509957401, 40.62609039468564731 ) ) ;
#167546 = CARTESIAN_POINT ( 'NONE',  ( -16.52544592524342804, 4.483927247898546575, 111.0405762719810525 ) ) ;
#167547 = CARTESIAN_POINT ( 'NONE',  ( 15.80617190586746368, 15.72974639402197994, 34.37390960531435979 ) ) ;
#167548 = CARTESIAN_POINT ( 'NONE',  ( -4.483927247898539470, -16.52544592524342804, 42.29057627198103120 ) ) ;
#167549 = CARTESIAN_POINT ( 'NONE',  ( 5.823673210054444382, -21.52544592524334988, 95.20942372801903275 ) ) ;
#167550 = CARTESIAN_POINT ( 'NONE',  ( 16.52544592524335698, 4.483927247898782831, 76.45942372801901854 ) ) ;
#167551 = CARTESIAN_POINT ( 'NONE',  ( -16.55341960407611168, -4.379528057220339221, 21.45724293864769550 ) ) ;
#167552 = CARTESIAN_POINT ( 'NONE',  ( 21.53943276465977519, 0.05219959533937863772, 56.25109039468568284 ) ) ;
#167553 = CARTESIAN_POINT ( 'NONE',  ( 5.823673210054444382, -21.52544592524334988, 70.20942372801904696 ) ) ;
#167554 = CARTESIAN_POINT ( 'NONE',  ( -21.53943276465977519, 0.05219959533907696930, 66.24890960531436690 ) ) ;
#167555 = EDGE_LOOP ( 'NONE', ( #109696, #187091, #91727 ) ) ;
#167556 = CARTESIAN_POINT ( 'NONE',  ( 19.03943276465977164, -0.05219959533909143690, 23.74890960531435269 ) ) ;
#167557 = CARTESIAN_POINT ( 'NONE',  ( -10.81492255796105439, 18.62759615963255655, 42.91775706135235424 ) ) ;
#167558 = CARTESIAN_POINT ( 'NONE',  ( -16.53943276465976808, 0.05219959533911058130, 116.2489096053143669 ) ) ;
#167559 = CARTESIAN_POINT ( 'NONE',  ( -13.89961937509977652, 13.97604488694528158, 45.62390960531433848 ) ) ;
#167560 = CARTESIAN_POINT ( 'NONE',  ( 4.483927247898545687, 16.52544592524342804, 79.79057627198102409 ) ) ;
#167561 = CARTESIAN_POINT ( 'NONE',  ( 13.97604488694527802, 13.89961937509977652, 89.37390960531436690 ) ) ;
#167562 = CARTESIAN_POINT ( 'NONE',  ( 16.55341960407611168, 4.379528057220329451, 23.95724293864769550 ) ) ;
#167563 = CARTESIAN_POINT ( 'NONE',  ( 14.34966873604960469, 8.224510206698951720, 104.1655762719810241 ) ) ;
#167564 = CARTESIAN_POINT ( 'NONE',  ( 5.823673210054125526, 21.52544592524343514, 74.79057627198105251 ) ) ;
#167565 = CARTESIAN_POINT ( 'NONE',  ( 10.81492255796078972, 18.62759615963270932, 109.5822429386476955 ) ) ;
#167566 = CARTESIAN_POINT ( 'NONE',  ( 19.02544592524343514, -5.153800228976328945, 108.5405762719810383 ) ) ;
#167568 = CARTESIAN_POINT ( 'NONE',  ( -19.02544592524334988, -5.153800228976617603, 108.9594237280189759 ) ) ;
#167567 = CARTESIAN_POINT ( 'NONE',  ( 19.02544592524343514, -5.153800228976328945, 63.54057627198103830 ) ) ;
#167569 = CARTESIAN_POINT ( 'NONE',  ( -21.53943276465977519, 0.05219959533907696930, 56.24890960531436690 ) ) ;
#167570 = CARTESIAN_POINT ( 'NONE',  ( -21.52544592524334988, -5.823673210054445271, 78.95942372801901854 ) ) ;
#167571 = CARTESIAN_POINT ( 'NONE',  ( 9.564922557960805705, 16.46253265017160317, 64.58224293864769550 ) ) ;
#167572 = CARTESIAN_POINT ( 'NONE',  ( 13.97604488694527802, 13.89961937509977652, 104.3739096053143385 ) ) ;
#167573 = CARTESIAN_POINT ( 'NONE',  ( 14.29746914071037800, 8.314922557961029526, 71.66775706135234714 ) ) ;
#167574 = CARTESIAN_POINT ( 'NONE',  ( 15.80617190586769283, -15.72974639402175789, 55.62609039468568284 ) ) ;
#167575 = CARTESIAN_POINT ( 'NONE',  ( 21.53943276465977519, 0.05219959533937863772, 106.2510903946856757 ) ) ;
#167576 = CARTESIAN_POINT ( 'NONE',  ( -21.52544592524343514, 5.823673210054127303, 111.0405762719810525 ) ) ;
#167577 = CARTESIAN_POINT ( 'NONE',  ( 21.52544592524344225, -5.823673210054117533, 78.54057627198103830 ) ) ;
#167578 = CARTESIAN_POINT ( 'NONE',  ( 13.97604488694548053, -13.89961937509957401, 45.62609039468566863 ) ) ;
#167579 = CARTESIAN_POINT ( 'NONE',  ( -5.823673210054116645, -21.52544592524344225, 42.29057627198103120 ) ) ;
#167581 = CARTESIAN_POINT ( 'NONE',  ( 16.55341960407611168, 4.379528057220329451, 33.95724293864769550 ) ) ;
#167580 = CARTESIAN_POINT ( 'NONE',  ( -13.97604488694527625, -13.89961937509977652, 76.87390960531433848 ) ) ;
#167582 = CARTESIAN_POINT ( 'NONE',  ( 2.500000000000000000, -2.357898499370432610, 3.252606517456513302E-15 ) ) ;
#167583 = CARTESIAN_POINT ( 'NONE',  ( 16.46253265017146816, 9.564922557961045513, 91.66775706135234714 ) ) ;
#167584 = CARTESIAN_POINT ( 'NONE',  ( -15.72974639402197994, 15.80617190586746368, 65.62390960531436690 ) ) ;
#167585 = CARTESIAN_POINT ( 'NONE',  ( 16.53943276465976808, -0.05219959533910856209, 48.74890960531435979 ) ) ;
#167586 = CARTESIAN_POINT ( 'NONE',  ( 16.55341960407618274, -4.379528057220086978, 31.04275706135234714 ) ) ;
#167587 = CARTESIAN_POINT ( 'NONE',  ( -0.05219959533909027116, -19.03943276465977164, 42.49890960531435269 ) ) ;
#167589 = CARTESIAN_POINT ( 'NONE',  ( -0.05219959533936034679, 19.03943276465977164, 82.50109039468567573 ) ) ;
#167588 = CARTESIAN_POINT ( 'NONE',  ( 5.719274019375991003, -21.55341960407610458, 97.70724293864772392 ) ) ;
#167590 = CARTESIAN_POINT ( 'NONE',  ( 19.05341960407611168, 5.049401038298154454, 78.95724293864769550 ) ) ;
#167591 = CARTESIAN_POINT ( 'NONE',  ( -14.29746914071049879, 8.314922557960819915, 90.83224293864769550 ) ) ;
#167592 = CARTESIAN_POINT ( 'NONE',  ( -16.51473224551069308, -9.474510206698971260, 66.66557627198102409 ) ) ;
#167593 = CARTESIAN_POINT ( 'NONE',  ( -4.483927247898539470, -16.52544592524342804, 67.29057627198103830 ) ) ;
#167594 = CARTESIAN_POINT ( 'NONE',  ( -5.153800228976328057, -19.02544592524343514, 37.29057627198102409 ) ) ;
#167595 = CARTESIAN_POINT ( 'NONE',  ( -36.77739090780051612, -5.326908766905468440, 46.41547615974453578 ) ) ;
#167596 = CARTESIAN_POINT ( 'NONE',  ( 12.14591786802309770, 12.06949235617756955, 44.37390960531435979 ) ) ;
#167597 = CARTESIAN_POINT ( 'NONE',  ( 16.46253265017160672, -9.564922557960803928, 88.33224293864769550 ) ) ;
#167598 = CARTESIAN_POINT ( 'NONE',  ( -1.324169127979094807, -14.46985881644524063, -60.11284999819413599 ) ) ;
#167599 = CARTESIAN_POINT ( 'NONE',  ( 5.049401038297881783, 19.05341960407617563, 57.29275706135231871 ) ) ;
#167600 = CARTESIAN_POINT ( 'NONE',  ( 14.34966873604972726, -8.224510206698740333, 65.83442372801900433 ) ) ;
#167601 = CARTESIAN_POINT ( 'NONE',  ( 15.80617190586746368, 15.72974639402197994, 74.37390960531436690 ) ) ;
#167602 = CARTESIAN_POINT ( 'NONE',  ( 0.05219959533936267826, -19.03943276465977164, 40.00109039468566152 ) ) ;
#167603 = CARTESIAN_POINT ( 'NONE',  ( 5.153800228976335163, 19.02544592524342804, 89.79057627198102409 ) ) ;
#167604 = CARTESIAN_POINT ( 'NONE',  ( 10.79449291341264328, -9.218202637343335226, -60.25055865658766407 ) ) ;
#167605 = CARTESIAN_POINT ( 'NONE',  ( 5.823673210054125526, 21.52544592524343514, 29.79057627198102409 ) ) ;
#167606 = CARTESIAN_POINT ( 'NONE',  ( -9.474510206698964154, 16.51473224551069663, 55.41557627198103120 ) ) ;
#167607 = CARTESIAN_POINT ( 'NONE',  ( 21.53943276465977519, 0.05219959533937863772, 56.25109039468568284 ) ) ;
#167608 = CARTESIAN_POINT ( 'NONE',  ( 16.46253265017160672, -9.564922557960803928, 28.33224293864769550 ) ) ;
#167611 = ORIENTED_EDGE ( 'NONE', *, *, #169440, .T. ) ;
#167610 = CARTESIAN_POINT ( 'NONE',  ( -5.049401038298153566, 19.05341960407611168, 90.20724293864766707 ) ) ;
#167609 = CARTESIAN_POINT ( 'NONE',  ( 15.80617190586769283, -15.72974639402175789, 20.62609039468568639 ) ) ;
#167612 = CARTESIAN_POINT ( 'NONE',  ( -15.72974639402176322, -15.80617190586768395, 44.37609039468567573 ) ) ;
#167613 = ORIENTED_EDGE ( 'NONE', *, *, #139743, .F. ) ;
#167614 = CARTESIAN_POINT ( 'NONE',  ( 9.564922557960805705, 16.46253265017160317, 94.58224293864769550 ) ) ;
#167615 = DIRECTION ( 'NONE',  ( 0.000000000000000000, 0.000000000000000000, 1.000000000000000000 ) ) ;
#167616 = CARTESIAN_POINT ( 'NONE',  ( -10.72451020669898014, 18.67979575497178502, 105.4155762719810383 ) ) ;
#167617 = CARTESIAN_POINT ( 'NONE',  ( -9.474510206698964154, 16.51473224551069663, 45.41557627198103120 ) ) ;
#167618 = CARTESIAN_POINT ( 'NONE',  ( 16.52544592524335698, 4.483927247898782831, 26.45942372801901854 ) ) ;
#167619 = CARTESIAN_POINT ( 'NONE',  ( 36.91746824999999887, 11.99521256947799053, -6.024999997268811747 ) ) ;
#167620 = CARTESIAN_POINT ( 'NONE',  ( 21.55341960407619695, -5.719274019375665929, 106.0427570613523471 ) ) ;
#167621 = CARTESIAN_POINT ( 'NONE',  ( 13.97604488694527802, 13.89961937509977652, 29.37390960531435979 ) ) ;
#167622 = CARTESIAN_POINT ( 'NONE',  ( 21.52544592524334988, 5.823673210054432836, 101.4594237280190185 ) ) ;
#167624 = CARTESIAN_POINT ( 'NONE',  ( 21.55341960407619695, -5.719274019375665929, 66.04275706135236135 ) ) ;
#167623 = CARTESIAN_POINT ( 'NONE',  ( -9.474510206698964154, 16.51473224551069663, 90.41557627198103830 ) ) ;
#167625 = CARTESIAN_POINT ( 'NONE',  ( -17.14385361876520619, 23.59649016807275856, 141.0750000027311728 ) ) ;
#167626 = CARTESIAN_POINT ( 'NONE',  ( -19.05341960407611168, -5.049401038298163336, 96.45724293864769550 ) ) ;
#167627 = CARTESIAN_POINT ( 'NONE',  ( -17.50000000000001421, 4.049696124445815393, 29.18039670665949004 ) ) ;
#167630 = CARTESIAN_POINT ( 'NONE',  ( 15.72974639402176855, 15.80617190586768217, 61.87609039468568284 ) ) ;
#167629 = CARTESIAN_POINT ( 'NONE',  ( 8.314922557961029526, -14.29746914071037800, 70.41775706135236135 ) ) ;
#167628 = CARTESIAN_POINT ( 'NONE',  ( 4.379528057220092307, 16.55341960407617563, 52.29275706135236135 ) ) ;
#167631 = CARTESIAN_POINT ( 'NONE',  ( 15.72974639402176855, 15.80617190586768217, 86.87609039468568994 ) ) ;
#167632 = LINE ( 'NONE', #152450, #38115 ) ;
#167633 = CARTESIAN_POINT ( 'NONE',  ( 12.14591786802327356, -12.06949235617739191, 25.62609039468567929 ) ) ;
#167634 = CARTESIAN_POINT ( 'NONE',  ( 16.51473224551069308, 9.474510206698969483, 79.16557627198103830 ) ) ;
#167635 = CARTESIAN_POINT ( 'NONE',  ( 5.153800228976335163, 19.02544592524342804, 99.79057627198102409 ) ) ;
#167636 = SPHERICAL_SURFACE ( 'NONE', #4547, 38.00000000000002132 ) ;
#167637 = CARTESIAN_POINT ( 'NONE',  ( -19.05341960407611168, -5.049401038298163336, 21.45724293864768839 ) ) ;
#167639 = ADVANCED_FACE ( 'NONE', ( #67273 ), #191619, .F. ) ;
#167638 = CARTESIAN_POINT ( 'NONE',  ( -0.05219959533907301413, -21.53943276465977519, 27.49890960531435269 ) ) ;
#167640 = CARTESIAN_POINT ( 'NONE',  ( -14.29746914071037622, -8.314922557961029526, 99.16775706135234714 ) ) ;
#167642 = CARTESIAN_POINT ( 'NONE',  ( 19.03943276465977164, -0.05219959533909143690, 73.74890960531435269 ) ) ;
#167641 = CARTESIAN_POINT ( 'NONE',  ( 12.14591786802309770, 12.06949235617756955, 69.37390960531436690 ) ) ;
#167643 = CARTESIAN_POINT ( 'NONE',  ( 21.53943276465977519, 0.05219959533937863772, 91.25109039468568994 ) ) ;
#167644 = CARTESIAN_POINT ( 'NONE',  ( 17.48464627749218536, 5.278740712515454625, 21.75031283919550162 ) ) ;
#167645 = CARTESIAN_POINT ( 'NONE',  ( 0.05219959533936267826, -19.03943276465977164, 105.0010903946856615 ) ) ;
#167646 = CARTESIAN_POINT ( 'NONE',  ( -4.483927247898539470, -16.52544592524342804, 82.29057627198103830 ) ) ;
#167647 = CARTESIAN_POINT ( 'NONE',  ( 0.05219959533937995610, -21.53943276465977519, 30.00109039468568284 ) ) ;
#167648 = CARTESIAN_POINT ( 'NONE',  ( 10.81492255796078972, 18.62759615963270932, 69.58224293864769550 ) ) ;
#167649 = CARTESIAN_POINT ( 'NONE',  ( -16.51473224551082808, 9.474510206698731452, 33.33442372801899722 ) ) ;
#167650 = CARTESIAN_POINT ( 'NONE',  ( -8.906447517083053711, -27.41122689804191026, 146.6500000054623740 ) ) ;
#167651 = CARTESIAN_POINT ( 'NONE',  ( 5.153800228976335163, 19.02544592524342804, 79.79057627198102409 ) ) ;
#167652 = CARTESIAN_POINT ( 'NONE',  ( -12.06949235617756955, 12.14591786802309770, 55.62390960531436690 ) ) ;
#167653 = CARTESIAN_POINT ( 'NONE',  ( 0.05219959533910956823, 16.53943276465976808, 34.99890960531435979 ) ) ;
#167654 = CARTESIAN_POINT ( 'NONE',  ( -12.06949235617739369, -12.14591786802326823, 104.3760903946856899 ) ) ;
#167655 = CARTESIAN_POINT ( 'NONE',  ( -5.049401038297874678, -19.05341960407617918, 59.79275706135231871 ) ) ;
#167656 = CARTESIAN_POINT ( 'NONE',  ( 19.34837522270366605, 5.499999999999732658, 53.36337684832579953 ) ) ;
#167657 = CARTESIAN_POINT ( 'NONE',  ( 13.97604488694527802, 13.89961937509977652, 109.3739096053143669 ) ) ;
#167658 = CARTESIAN_POINT ( 'NONE',  ( -8.224510206698948167, 14.34966873604960824, 70.41557627198102409 ) ) ;
#167659 = CARTESIAN_POINT ( 'NONE',  ( 19.42893418801164529, -5.499999999999810818, 37.78583261411539240 ) ) ;
#167661 = CARTESIAN_POINT ( 'NONE',  ( -5.719274019375978568, 21.55341960407610458, 30.20724293864769550 ) ) ;
#167660 = CARTESIAN_POINT ( 'NONE',  ( -16.46253265017160317, 9.564922557960807481, 25.83224293864769194 ) ) ;
#167662 = CARTESIAN_POINT ( 'NONE',  ( -15.80617190586745835, -15.72974639402198527, 66.87390960531436690 ) ) ;
#167663 = CARTESIAN_POINT ( 'NONE',  ( 16.53943276465976808, -0.05219959533910856209, 108.7489096053143669 ) ) ;
#167665 = CARTESIAN_POINT ( 'NONE',  ( 16.51473224551069308, 9.474510206698969483, 49.16557627198102409 ) ) ;
#167664 = CARTESIAN_POINT ( 'NONE',  ( 0.05219959533934541429, -16.53943276465976808, 65.00109039468568994 ) ) ;
#167666 = CARTESIAN_POINT ( 'NONE',  ( -15.80617190586768217, 15.72974639402176855, 43.12609039468568284 ) ) ;
#167667 = CARTESIAN_POINT ( 'NONE',  ( -4.379528057220328563, 16.55341960407611168, 90.20724293864770971 ) ) ;
#167668 = CARTESIAN_POINT ( 'NONE',  ( 17.31728774477274868, -6.344390552232389346, 38.31906651689320142 ) ) ;
#167669 = CARTESIAN_POINT ( 'NONE',  ( -22.81625015709510507, 31.40387420917330275, -9.424999997268812990 ) ) ;
#167670 = CARTESIAN_POINT ( 'NONE',  ( 10.81492255796078972, 18.62759615963270932, 29.58224293864769905 ) ) ;
#167671 = CARTESIAN_POINT ( 'NONE',  ( 18.09805431107249873, -5.499999999999975131, 78.51606229291886052 ) ) ;
#167672 = CARTESIAN_POINT ( 'NONE',  ( 11.74149087413295156, -36.13659316521243881, -7.147842220587802942 ) ) ;
#167673 = TOROIDAL_SURFACE ( 'NONE', #48165, 206.0437394197456911, 8.000000000000000000 ) ;
#167675 = CARTESIAN_POINT ( 'NONE',  ( -4.483927247898539470, -16.52544592524342804, 42.29057627198103120 ) ) ;
#167674 = CARTESIAN_POINT ( 'NONE',  ( -16.52544592524335698, -4.483927247898792601, 38.95942372801901854 ) ) ;
#167676 = CARTESIAN_POINT ( 'NONE',  ( 0.05219959533907565091, 21.53943276465977519, 69.99890960531435269 ) ) ;
#167677 = CARTESIAN_POINT ( 'NONE',  ( -15.80617190586745835, -15.72974639402198527, 61.87390960531436690 ) ) ;
#167678 = CARTESIAN_POINT ( 'NONE',  ( 5.000000000000000888, -140.0000000000000000, -15.00000000000000000 ) ) ;
#167680 = CARTESIAN_POINT ( 'NONE',  ( 9.564922557960805705, 16.46253265017160317, 104.5822429386476955 ) ) ;
#167679 = CARTESIAN_POINT ( 'NONE',  ( -9.564922557961040184, 16.46253265017147172, 77.91775706135234714 ) ) ;
#167682 = CARTESIAN_POINT ( 'NONE',  ( -13.89961937509977652, 13.97604488694528158, 50.62390960531435979 ) ) ;
#167681 = B_SPLINE_CURVE_WITH_KNOTS ( 'NONE', 3,
 ( #184621, #169442, #111747, #31933, #34905, #33919 ),
 .UNSPECIFIED., .F., .F.,
 ( 4, 2, 4 ),
 ( 0.003239945802372249956, 0.003620412082092100414, 0.004000878361811950439 ),
 .UNSPECIFIED. ) ;
#167683 = CARTESIAN_POINT ( 'NONE',  ( -0.05219959533909027116, -19.03943276465977164, 22.49890960531436690 ) ) ;
#167684 = PRODUCT_CONTEXT ( 'NONE', #183562, 'mechanical' ) ;
#167685 = FACE_BOUND ( 'NONE', #131032, .T. ) ;
#167686 = ORIENTED_EDGE ( 'NONE', *, *, #166752, .T. ) ;
#167687 = CARTESIAN_POINT ( 'NONE',  ( -4.379528057220086978, -16.55341960407618274, 69.79275706135234714 ) ) ;
#167688 = CARTESIAN_POINT ( 'NONE',  ( -0.05219959533907301413, -21.53943276465977519, 102.4989096053143811 ) ) ;
#167689 = CARTESIAN_POINT ( 'NONE',  ( -9.474510206698964154, 16.51473224551069663, 50.41557627198102409 ) ) ;
#167690 = CARTESIAN_POINT ( 'NONE',  ( 10.72451020669871369, 18.67979575497193778, 42.08442372801901854 ) ) ;
#167691 = CARTESIAN_POINT ( 'NONE',  ( -19.05341960407611168, -5.049401038298163336, 91.45724293864766707 ) ) ;
#167692 = CARTESIAN_POINT ( 'NONE',  ( 28.79475375365573697, 9.355982642739409272, 145.0843446569000434 ) ) ;
#167693 = VERTEX_POINT ( 'NONE', #52107 ) ;
#167694 = CARTESIAN_POINT ( 'NONE',  ( -0.05219959533937732626, 21.53943276465977519, 37.50109039468568284 ) ) ;
#167696 = CARTESIAN_POINT ( 'NONE',  ( -5.153800228976607833, 19.02544592524334988, 92.70942372801901854 ) ) ;
#167695 = CARTESIAN_POINT ( 'NONE',  ( 13.89961937509977652, -13.97604488694527269, 113.1239096053143527 ) ) ;
#167697 = CARTESIAN_POINT ( 'NONE',  ( 16.46253265017146816, 9.564922557961045513, 36.66775706135233293 ) ) ;
#167698 = CARTESIAN_POINT ( 'NONE',  ( -18.67979575497178146, -10.72451020669898902, 101.6655762719810383 ) ) ;
#167699 = CARTESIAN_POINT ( 'NONE',  ( -5.153800228976607833, 19.02544592524334988, 32.70942372801899722 ) ) ;
#167700 = CARTESIAN_POINT ( 'NONE',  ( 19.03943276465977164, 0.05219959533936151252, 41.25109039468566152 ) ) ;
#167701 = CARTESIAN_POINT ( 'NONE',  ( -12.14591786802326823, 12.06949235617739902, 93.12609039468568994 ) ) ;
#167702 = ORIENTED_EDGE ( 'NONE', *, *, #88386, .T. ) ;
#167703 = CARTESIAN_POINT ( 'NONE',  ( 13.97604488694527802, 13.89961937509977652, 64.37390960531436690 ) ) ;
#167704 = AXIS2_PLACEMENT_3D ( 'NONE', #168786, #88982, #181020 ) ;
#167705 = CARTESIAN_POINT ( 'NONE',  ( -15.72974639402176322, -15.80617190586768395, 64.37609039468568994 ) ) ;
#167706 = CARTESIAN_POINT ( 'NONE',  ( -18.67979575497193778, 10.72451020669871902, 83.33442372801903275 ) ) ;
#167707 = CARTESIAN_POINT ( 'NONE',  ( -17.49999999999999645, -5.499999999999992895, 54.20309617465830598 ) ) ;
#167708 = CARTESIAN_POINT ( 'NONE',  ( 9.474510206698971260, -16.51473224551069308, 92.91557627198103830 ) ) ;
#167709 = CARTESIAN_POINT ( 'NONE',  ( -18.67979575497193778, 10.72451020669871902, 68.33442372801900433 ) ) ;
#167710 = CARTESIAN_POINT ( 'NONE',  ( 9.474510206698729675, 16.51473224551082808, 102.0844237280190043 ) ) ;
#167711 = CARTESIAN_POINT ( 'NONE',  ( -16.51473224551069308, -9.474510206698971260, 61.66557627198103120 ) ) ;
#167712 = CARTESIAN_POINT ( 'NONE',  ( -0.05219959533909027116, -19.03943276465977164, 102.4989096053143669 ) ) ;
#167713 = CARTESIAN_POINT ( 'NONE',  ( -9.564922557960796823, -16.46253265017161027, 82.08224293864768129 ) ) ;
#167714 = CARTESIAN_POINT ( 'NONE',  ( -19.02544592524342804, 5.153800228976336051, 71.04057627198099567 ) ) ;
#167715 = CARTESIAN_POINT ( 'NONE',  ( 5.823673210054125526, 21.52544592524343514, 99.79057627198103830 ) ) ;
#167716 = CARTESIAN_POINT ( 'NONE',  ( 12.14591786802327356, -12.06949235617739191, 90.62609039468567573 ) ) ;
#167717 = CARTESIAN_POINT ( 'NONE',  ( 6.691186640346301395, -1.197302953328933883, -64.41832325557876970 ) ) ;
#167718 = CARTESIAN_POINT ( 'NONE',  ( 13.89961937509957401, 13.97604488694547697, 46.87609039468565442 ) ) ;
#167719 = CARTESIAN_POINT ( 'NONE',  ( 9.564922557960805705, 16.46253265017160317, 79.58224293864769550 ) ) ;
#167720 = CARTESIAN_POINT ( 'NONE',  ( -0.05219959533910754901, -16.53943276465976808, 72.49890960531435269 ) ) ;
#167721 = CARTESIAN_POINT ( 'NONE',  ( -14.29746914071049879, 8.314922557960819915, 110.8322429386476955 ) ) ;
#167722 = CARTESIAN_POINT ( 'NONE',  ( -13.89961937509977652, 13.97604488694528158, 115.6239096053143669 ) ) ;
#167723 = CARTESIAN_POINT ( 'NONE',  ( -9.474510206698964154, 16.51473224551069663, 100.4155762719810241 ) ) ;
#167724 = DIRECTION ( 'NONE',  ( -0.000000000000000000, -0.000000000000000000, -1.000000000000000000 ) ) ;
#167725 = CARTESIAN_POINT ( 'NONE',  ( 19.03943276465977164, 0.05219959533936151252, 31.25109039468566863 ) ) ;
#167726 = CARTESIAN_POINT ( 'NONE',  ( -12.06949235617739369, -12.14591786802326823, 99.37609039468568994 ) ) ;
#167727 = CARTESIAN_POINT ( 'NONE',  ( 19.02544592524343514, -5.153800228976328945, 78.54057627198099567 ) ) ;
#167728 = CARTESIAN_POINT ( 'NONE',  ( -15.80617190586768217, 15.72974639402176855, 58.12609039468568994 ) ) ;
#167729 = CARTESIAN_POINT ( 'NONE',  ( 10.72451020669898902, -18.67979575497178502, 47.91557627198102409 ) ) ;
#167730 = CARTESIAN_POINT ( 'NONE',  ( -5.719274019375665041, -21.55341960407619695, 19.79275706135235069 ) ) ;
#167731 = CARTESIAN_POINT ( 'NONE',  ( 10.72451020669898902, -18.67979575497178502, 67.91557627198102409 ) ) ;
#167732 = CARTESIAN_POINT ( 'NONE',  ( -16.52544592524342804, 4.483927247898546575, 91.04057627198103830 ) ) ;
#167733 = CARTESIAN_POINT ( 'NONE',  ( 16.46253265017146816, 9.564922557961045513, 61.66775706135234003 ) ) ;
#167734 = CARTESIAN_POINT ( 'NONE',  ( 0.05219959533909260263, 19.03943276465977164, 29.99890960531435979 ) ) ;
#167735 = CARTESIAN_POINT ( 'NONE',  ( 19.05341960407611168, 5.049401038298154454, 83.95724293864766707 ) ) ;
#167736 = CARTESIAN_POINT ( 'NONE',  ( -5.049401038298153566, 19.05341960407611168, 85.20724293864766707 ) ) ;
#167737 = CARTESIAN_POINT ( 'NONE',  ( -27.73933785331498925, 2.428612866367529932E-14, 139.3750000027311842 ) ) ;
#167738 = CARTESIAN_POINT ( 'NONE',  ( 0.05219959533910956823, 16.53943276465976808, 99.99890960531436690 ) ) ;
#167739 = ORIENTED_EDGE ( 'NONE', *, *, #186918, .F. ) ;
#167740 = CARTESIAN_POINT ( 'NONE',  ( -8.314922557960811034, -14.29746914071050412, 32.08224293864769550 ) ) ;
#167741 = CARTESIAN_POINT ( 'NONE',  ( 4.379528057220092307, 16.55341960407617563, 27.29275706135234358 ) ) ;
#167742 = CARTESIAN_POINT ( 'NONE',  ( 21.52544592524334988, 5.823673210054432836, 96.45942372801901854 ) ) ;
#167743 = CARTESIAN_POINT ( 'NONE',  ( -9.564922557960796823, -16.46253265017161027, 107.0822429386476955 ) ) ;
#167744 = CARTESIAN_POINT ( 'NONE',  ( 0.05219959533937995610, -21.53943276465977519, 20.00109039468568639 ) ) ;
#167745 = CARTESIAN_POINT ( 'NONE',  ( 0.05219959533909260263, 19.03943276465977164, 44.99890960531435979 ) ) ;
#167746 = CARTESIAN_POINT ( 'NONE',  ( -0.05219959533934338120, 16.53943276465976808, 42.50109039468567573 ) ) ;
#167747 = CARTESIAN_POINT ( 'NONE',  ( -13.97604488694547697, 13.89961937509957934, 113.1260903946856757 ) ) ;
#167748 = CARTESIAN_POINT ( 'NONE',  ( -5.153800228976328057, -19.02544592524343514, 32.29057627198102409 ) ) ;
#167749 = CARTESIAN_POINT ( 'NONE',  ( -16.53943276465976808, 0.05219959533911058130, 101.2489096053143669 ) ) ;
#167750 = CARTESIAN_POINT ( 'NONE',  ( -18.62759615963270932, 10.81492255796079327, 100.8322429386477097 ) ) ;
#167751 = CARTESIAN_POINT ( 'NONE',  ( -9.564922557961040184, 16.46253265017147172, 62.91775706135233293 ) ) ;
#167752 =( LENGTH_UNIT ( ) NAMED_UNIT ( * ) SI_UNIT ( .MILLI., .METRE. ) );
#167753 = CARTESIAN_POINT ( 'NONE',  ( 10.81492255796078972, 18.62759615963270932, 114.5822429386477097 ) ) ;
#167754 = CARTESIAN_POINT ( 'NONE',  ( 0.05219959533909260263, 19.03943276465977164, 24.99890960531435269 ) ) ;
#167755 = CARTESIAN_POINT ( 'NONE',  ( 5.049401038298161559, -19.05341960407611168, 97.70724293864766707 ) ) ;
#167756 = CARTESIAN_POINT ( 'NONE',  ( -17.79613651744293890, -24.49428055684527550, 142.2843446568999752 ) ) ;
#167757 = CARTESIAN_POINT ( 'NONE',  ( -5.049401038298153566, 19.05341960407611168, 85.20724293864766707 ) ) ;
#167759 = CARTESIAN_POINT ( 'NONE',  ( -8.314922557960811034, -14.29746914071050412, 77.08224293864769550 ) ) ;
#167758 = CARTESIAN_POINT ( 'NONE',  ( 21.52544592524334988, 5.823673210054432836, 31.45942372801901854 ) ) ;
#167760 = CARTESIAN_POINT ( 'NONE',  ( 5.153800228976335163, 19.02544592524342804, 79.79057627198102409 ) ) ;
#167761 = CARTESIAN_POINT ( 'NONE',  ( 9.564922557961047289, -16.46253265017146816, 30.41775706135232937 ) ) ;
#167763 = CARTESIAN_POINT ( 'NONE',  ( -19.05341960407617563, 5.049401038297882671, 53.54275706135231871 ) ) ;
#167762 = CARTESIAN_POINT ( 'NONE',  ( -4.379528057220086978, -16.55341960407618274, 54.79275706135235424 ) ) ;
#167764 = CARTESIAN_POINT ( 'NONE',  ( -21.53943276465977519, -0.05219959533937600094, 68.75109039468568994 ) ) ;
#167765 = CARTESIAN_POINT ( 'NONE',  ( -16.55341960407617563, 4.379528057220093196, 33.54275706135234714 ) ) ;
#167766 = CARTESIAN_POINT ( 'NONE',  ( 9.474510206698971260, -16.51473224551069308, 72.91557627198102409 ) ) ;
#167767 = CARTESIAN_POINT ( 'NONE',  ( -0.05219959533936034679, 19.03943276465977164, 92.50109039468566152 ) ) ;
#167768 = CARTESIAN_POINT ( 'NONE',  ( -12.06949235617739369, -12.14591786802326823, 74.37609039468568994 ) ) ;
#167769 = CARTESIAN_POINT ( 'NONE',  ( -15.72974639402176322, -15.80617190586768395, 94.37609039468568994 ) ) ;
#167770 = CARTESIAN_POINT ( 'NONE',  ( -13.97604488694547697, 13.89961937509957934, 78.12609039468567573 ) ) ;
#167771 = CARTESIAN_POINT ( 'NONE',  ( -5.153800228976328057, -19.02544592524343514, 47.29057627198102409 ) ) ;
#167772 = CARTESIAN_POINT ( 'NONE',  ( -10.81492255796078084, -18.62759615963271287, 77.08224293864769550 ) ) ;
#167774 = CARTESIAN_POINT ( 'NONE',  ( -16.51473224551082808, 9.474510206698731452, 83.33442372801899012 ) ) ;
#167773 = CARTESIAN_POINT ( 'NONE',  ( 16.53943276465976808, -0.05219959533910856209, 78.74890960531436690 ) ) ;
#167775 = CARTESIAN_POINT ( 'NONE',  ( 16.62475595723702781, -7.163666690055162434, 63.02713351810474052 ) ) ;
#167776 = CARTESIAN_POINT ( 'NONE',  ( 19.05341960407617918, -5.049401038297876454, 41.04275706135233293 ) ) ;
#167777 = CARTESIAN_POINT ( 'NONE',  ( 12.14591786802309770, 12.06949235617756955, 24.37390960531435979 ) ) ;
#167778 = CARTESIAN_POINT ( 'NONE',  ( -12.14591786802309592, -12.06949235617757132, 71.87390960531438111 ) ) ;
#167780 = CARTESIAN_POINT ( 'NONE',  ( -8.571926809382601320, -26.38167802310801591, 147.2750000027311899 ) ) ;
#167779 = CARTESIAN_POINT ( 'NONE',  ( -0.05219959533937732626, 21.53943276465977519, 107.5010903946856899 ) ) ;
#167781 = CARTESIAN_POINT ( 'NONE',  ( 21.52544592524344225, -5.823673210054117533, 108.5405762719810241 ) ) ;
#167782 = CARTESIAN_POINT ( 'NONE',  ( -16.46253265017160317, 9.564922557960807481, 65.83224293864769550 ) ) ;
#167783 = CARTESIAN_POINT ( 'NONE',  ( 15.72974639402176855, 15.80617190586768217, 86.87609039468568994 ) ) ;
#167784 = CARTESIAN_POINT ( 'NONE',  ( 16.46253265017160672, -9.564922557960803928, 63.33224293864769550 ) ) ;
#167785 = CARTESIAN_POINT ( 'NONE',  ( 0.05219959533909260263, 19.03943276465977164, 29.99890960531435979 ) ) ;
#167786 = CARTESIAN_POINT ( 'NONE',  ( -18.62759615963270932, 10.81492255796079327, 35.83224293864768839 ) ) ;
#167787 = CARTESIAN_POINT ( 'NONE',  ( 12.14591786802309770, 12.06949235617756955, 64.37390960531435269 ) ) ;
#167788 = CARTESIAN_POINT ( 'NONE',  ( -5.049401038298153566, 19.05341960407611168, 45.20724293864769550 ) ) ;
#167789 = CARTESIAN_POINT ( 'NONE',  ( 14.29746914071049879, -8.314922557960816363, 103.3322429386476955 ) ) ;
#167790 = CARTESIAN_POINT ( 'NONE',  ( 10.81492255796078972, 18.62759615963270932, 109.5822429386476955 ) ) ;
#167791 = CARTESIAN_POINT ( 'NONE',  ( -0.05219959533937732626, 21.53943276465977519, 52.50109039468567573 ) ) ;
#167792 = CARTESIAN_POINT ( 'NONE',  ( 9.474510206698971260, -16.51473224551069308, 32.91557627198102409 ) ) ;
#167793 = CARTESIAN_POINT ( 'NONE',  ( -8.314922557961024197, 14.29746914071037800, 52.91775706135235424 ) ) ;
#167794 = CARTESIAN_POINT ( 'NONE',  ( 10.72451020669898902, -18.67979575497178502, 102.9155762719810383 ) ) ;
#167795 = CARTESIAN_POINT ( 'NONE',  ( -21.55341960407610458, -5.719274019375992779, 91.45724293864769550 ) ) ;
#167797 = CARTESIAN_POINT ( 'NONE',  ( 19.02544592524343514, -5.153800228976328945, 53.54057627198102409 ) ) ;
#167796 = CARTESIAN_POINT ( 'NONE',  ( -5.049401038297874678, -19.05341960407617918, 19.79275706135233293 ) ) ;
#167798 = CARTESIAN_POINT ( 'NONE',  ( -19.02544592524342804, 5.153800228976336051, 111.0405762719810099 ) ) ;
#167799 = CARTESIAN_POINT ( 'NONE',  ( -5.823673210054431948, 21.52544592524334988, 52.70942372801902565 ) ) ;
#167800 = CARTESIAN_POINT ( 'NONE',  ( 21.53943276465977519, -0.05219959533907433946, 43.74890960531435979 ) ) ;
#167801 = CARTESIAN_POINT ( 'NONE',  ( 4.379528057220092307, 16.55341960407617563, 112.2927570613523471 ) ) ;
#167803 = CARTESIAN_POINT ( 'NONE',  ( 21.53943276465977519, 0.05219959533937863772, 96.25109039468568994 ) ) ;
#167802 = CARTESIAN_POINT ( 'NONE',  ( 15.72974639402176855, 15.80617190586768217, 61.87609039468568284 ) ) ;
#167804 = CARTESIAN_POINT ( 'NONE',  ( -19.05341960407617563, 5.049401038297882671, 38.54275706135233293 ) ) ;
#167805 = CARTESIAN_POINT ( 'NONE',  ( -16.53943276465976808, -0.05219959533934237506, 103.7510903946857042 ) ) ;
#167806 = CARTESIAN_POINT ( 'NONE',  ( 10.81492255796106328, -18.62759615963255655, 60.41775706135235424 ) ) ;
#167807 = CARTESIAN_POINT ( 'NONE',  ( -19.02544592524342804, 5.153800228976336051, 66.04057627198103830 ) ) ;
#167808 = CARTESIAN_POINT ( 'NONE',  ( 21.52544592524334988, 5.823673210054432836, 111.4594237280190328 ) ) ;
#167809 = CARTESIAN_POINT ( 'NONE',  ( 10.72451020669898902, -18.67979575497178502, 22.91557627198102765 ) ) ;
#167810 = CARTESIAN_POINT ( 'NONE',  ( 21.55341960407619695, -5.719274019375665929, 36.04275706135234714 ) ) ;
#167811 = AXIS2_PLACEMENT_3D ( 'NONE', #147849, #144822, #132669 ) ;
#167812 = CARTESIAN_POINT ( 'NONE',  ( 10.72451020669898902, -18.67979575497178502, 82.91557627198103830 ) ) ;
#167813 = CARTESIAN_POINT ( 'NONE',  ( -4.483927247898782831, 16.52544592524335698, 37.70942372801900433 ) ) ;
#167815 = CARTESIAN_POINT ( 'NONE',  ( -0.05219959533907301413, -21.53943276465977519, 77.49890960531433848 ) ) ;
#167814 = CARTESIAN_POINT ( 'NONE',  ( 18.09918380851993192, 5.500000000000035527, 63.98618307335613054 ) ) ;
#167817 = CARTESIAN_POINT ( 'NONE',  ( -12.06949235617756955, 12.14591786802309770, 75.62390960531439532 ) ) ;
#167816 = CARTESIAN_POINT ( 'NONE',  ( -12.06949235617739369, -12.14591786802326823, 59.37609039468568284 ) ) ;
#167818 = DIRECTION ( 'NONE',  ( -1.000000000000000000, -0.000000000000000000, -0.000000000000000000 ) ) ;
#167819 = CARTESIAN_POINT ( 'NONE',  ( 9.474510206698729675, 16.51473224551082808, 107.0844237280190043 ) ) ;
#167820 = CARTESIAN_POINT ( 'NONE',  ( 21.55341960407610458, 5.719274019375980345, 33.95724293864769550 ) ) ;
#167821 = CARTESIAN_POINT ( 'NONE',  ( 0.000000000000000000, 0.000000000000000000, -64.92279855667830191 ) ) ;
#167822 = CARTESIAN_POINT ( 'NONE',  ( 0.05219959533934541429, -16.53943276465976808, 40.00109039468567573 ) ) ;
#167823 = CARTESIAN_POINT ( 'NONE',  ( -21.55341960407610458, -5.719274019375992779, 106.4572429386477097 ) ) ;
#167824 = CARTESIAN_POINT ( 'NONE',  ( 15.80617190586746368, 15.72974639402197994, 34.37390960531435979 ) ) ;
#167825 = CARTESIAN_POINT ( 'NONE',  ( 4.483927247898790824, -16.52544592524335698, 65.20942372801901854 ) ) ;
#167826 = CARTESIAN_POINT ( 'NONE',  ( -9.474510206698964154, 16.51473224551069663, 90.41557627198103830 ) ) ;
#167828 = CARTESIAN_POINT ( 'NONE',  ( -5.049401038298153566, 19.05341960407611168, 25.20724293864768484 ) ) ;
#167827 = CARTESIAN_POINT ( 'NONE',  ( -10.81492255796105439, 18.62759615963255655, 52.91775706135235424 ) ) ;
#167829 = CARTESIAN_POINT ( 'NONE',  ( -5.049401038298153566, 19.05341960407611168, 115.2072429386477097 ) ) ;
#167830 = VERTEX_POINT ( 'NONE', #81424 ) ;
#167831 = CARTESIAN_POINT ( 'NONE',  ( -16.51473224551082808, 9.474510206698731452, 43.33442372801900433 ) ) ;
#167832 = CARTESIAN_POINT ( 'NONE',  ( 16.55341960407618274, -4.379528057220086978, 46.04275706135234714 ) ) ;
#167833 = CARTESIAN_POINT ( 'NONE',  ( 19.03943276465977164, -0.05219959533909143690, 113.7489096053143669 ) ) ;
#167834 = CARTESIAN_POINT ( 'NONE',  ( 13.89961937509977652, -13.97604488694527269, 78.12390960531433848 ) ) ;
#167835 = CARTESIAN_POINT ( 'NONE',  ( -16.52544592524335698, -4.483927247898792601, 93.95942372801903275 ) ) ;
#167836 = CARTESIAN_POINT ( 'NONE',  ( 25.22510128165246002, 6.326562104755751648, 165.8168824682948070 ) ) ;
#167837 = CARTESIAN_POINT ( 'NONE',  ( 14.34966873604960469, 8.224510206698951720, 94.16557627198103830 ) ) ;
#167838 = CARTESIAN_POINT ( 'NONE',  ( -21.55341960407610458, -5.719274019375992779, 41.45724293864769550 ) ) ;
#167839 = CARTESIAN_POINT ( 'NONE',  ( 16.46253265017160672, -9.564922557960803928, 28.33224293864769550 ) ) ;
#167840 = CARTESIAN_POINT ( 'NONE',  ( 8.224510206698742110, 14.34966873604972548, 67.08442372801901854 ) ) ;
#167841 = CARTESIAN_POINT ( 'NONE',  ( 18.67979575497194134, -10.72451020669871369, 20.83442372801901143 ) ) ;
#167842 = CARTESIAN_POINT ( 'NONE',  ( -0.05219959533936034679, 19.03943276465977164, 77.50109039468566152 ) ) ;
#167843 = CARTESIAN_POINT ( 'NONE',  ( 13.89961937509977652, -13.97604488694527269, 38.12390960531436690 ) ) ;
#167844 = CARTESIAN_POINT ( 'NONE',  ( 5.823673210054125526, 21.52544592524343514, 64.79057627198103830 ) ) ;
#167845 = CIRCLE ( 'NONE', #22632, 206.0437394197456911 ) ;
#167846 = CARTESIAN_POINT ( 'NONE',  ( 5.049401038298161559, -19.05341960407611168, 112.7072429386476813 ) ) ;
#167847 = CARTESIAN_POINT ( 'NONE',  ( -10.81492255796105439, 18.62759615963255655, 87.91775706135234714 ) ) ;
#167848 = CARTESIAN_POINT ( 'NONE',  ( 9.474510206698971260, -16.51473224551069308, 62.91557627198102409 ) ) ;
#167849 = CARTESIAN_POINT ( 'NONE',  ( 8.314922557961029526, -14.29746914071037800, 45.41775706135234003 ) ) ;
#167850 = CARTESIAN_POINT ( 'NONE',  ( -16.46253265017160317, 9.564922557960807481, 55.83224293864769550 ) ) ;
#167851 = CARTESIAN_POINT ( 'NONE',  ( -0.05219959533937732626, 21.53943276465977519, 77.50109039468567573 ) ) ;
#167852 = CARTESIAN_POINT ( 'NONE',  ( 5.153800228976615827, -19.02544592524334988, 40.20942372801898301 ) ) ;
#167853 = CARTESIAN_POINT ( 'NONE',  ( -19.03943276465977164, -0.05219959533935918106, 48.75109039468566863 ) ) ;
#167854 = CARTESIAN_POINT ( 'NONE',  ( -18.67979575497193778, 10.72451020669871902, 53.33442372801901854 ) ) ;
#167855 = CARTESIAN_POINT ( 'NONE',  ( 28.79475375365660028, 9.355982642738212007, 143.0843446568999582 ) ) ;
#167856 = CARTESIAN_POINT ( 'NONE',  ( -16.46253265017146816, -9.564922557961047289, 49.16775706135233293 ) ) ;
#167857 = CARTESIAN_POINT ( 'NONE',  ( -19.03943276465977164, 0.05219959533909376836, 96.24890960531436690 ) ) ;
#167858 = CARTESIAN_POINT ( 'NONE',  ( -19.02544592524342804, 5.153800228976336051, 66.04057627198103830 ) ) ;
#167859 = CARTESIAN_POINT ( 'NONE',  ( 4.483927247898545687, 16.52544592524342804, 29.79057627198102409 ) ) ;
#167861 = CARTESIAN_POINT ( 'NONE',  ( 21.52544592524334988, 5.823673210054432836, 106.4594237280190328 ) ) ;
#167860 = CARTESIAN_POINT ( 'NONE',  ( 15.80617190586746368, 15.72974639402197994, 29.37390960531435269 ) ) ;
#167862 = CARTESIAN_POINT ( 'NONE',  ( 11.40812507854755253, -35.11059874428192273, -2.024999997268813079 ) ) ;
#167863 = CARTESIAN_POINT ( 'NONE',  ( -34.40575365382724016, 2.434396366613705176, 90.06480789948632548 ) ) ;
#167864 = CARTESIAN_POINT ( 'NONE',  ( 21.52544592524334988, 5.823673210054432836, 96.45942372801901854 ) ) ;
#167865 = LINE ( 'NONE', #29365, #44482 ) ;
#167866 = CARTESIAN_POINT ( 'NONE',  ( 13.97604488694527802, 13.89961937509977652, 39.37390960531435269 ) ) ;
#167867 = DIRECTION ( 'NONE',  ( 1.000000000000000000, 0.000000000000000000, 0.000000000000000000 ) ) ;
#167868 = CARTESIAN_POINT ( 'NONE',  ( 34.29436769411893948, 3.356737774573909316, 90.62828869849683144 ) ) ;
#167869 = CARTESIAN_POINT ( 'NONE',  ( 16.52544592524335698, 4.483927247898782831, 46.45942372801901854 ) ) ;
#167871 = EDGE_CURVE ( 'NONE', #113699, #99783, #57168, .T. ) ;
#167870 = CARTESIAN_POINT ( 'NONE',  ( -15.80617190586745835, -15.72974639402198527, 66.87390960531436690 ) ) ;
#167872 = CARTESIAN_POINT ( 'NONE',  ( 16.53943276465976808, -0.05219959533910856209, 43.74890960531435979 ) ) ;
#167874 = CARTESIAN_POINT ( 'NONE',  ( -0.05219959533909027116, -19.03943276465977164, 107.4989096053143527 ) ) ;
#167873 = CARTESIAN_POINT ( 'NONE',  ( -0.05219959533910754901, -16.53943276465976808, 107.4989096053143669 ) ) ;
#167875 = CARTESIAN_POINT ( 'NONE',  ( -5.719274019375665041, -21.55341960407619695, 29.79275706135234358 ) ) ;
#167876 = CARTESIAN_POINT ( 'NONE',  ( 0.05219959533936267826, -19.03943276465977164, 40.00109039468566152 ) ) ;
#167877 = CARTESIAN_POINT ( 'NONE',  ( 16.52544592524342804, -4.483927247898539470, 113.5405762719810383 ) ) ;
#167878 = CARTESIAN_POINT ( 'NONE',  ( -10.72451020669870658, -18.67979575497194134, 74.58442372801901854 ) ) ;
#167879 = CARTESIAN_POINT ( 'NONE',  ( 17.44270441346514389, -5.991230190323083349, 31.13664920735773478 ) ) ;
#167880 = CARTESIAN_POINT ( 'NONE',  ( 4.379528057220339221, -16.55341960407611168, 22.70724293864769194 ) ) ;
#167881 = CARTESIAN_POINT ( 'NONE',  ( -36.91746825000000598, 2.428612866367529932E-14, -5.124999997268813168 ) ) ;
#167882 = CARTESIAN_POINT ( 'NONE',  ( -21.53943276465977519, 0.05219959533907696930, 31.24890960531435979 ) ) ;
#167883 = CARTESIAN_POINT ( 'NONE',  ( -8.224510206698948167, 14.34966873604960824, 95.41557627198102409 ) ) ;
#167884 = CARTESIAN_POINT ( 'NONE',  ( 27.93585545099115919, -25.65867777193838606, -16.61539413803383169 ) ) ;
#167885 = CARTESIAN_POINT ( 'NONE',  ( 5.153800228976335163, 19.02544592524342804, 74.79057627198103830 ) ) ;
#167886 = CARTESIAN_POINT ( 'NONE',  ( 14.29746914071049879, -8.314922557960816363, 78.33224293864770971 ) ) ;
#167887 = CARTESIAN_POINT ( 'NONE',  ( 16.46253265017146816, 9.564922557961045513, 111.6677570613523329 ) ) ;
#167888 = CARTESIAN_POINT ( 'NONE',  ( -21.52544592524343514, 5.823673210054127303, 51.04057627198103120 ) ) ;
#167889 = VERTEX_POINT ( 'NONE', #187668 ) ;
#167890 = CARTESIAN_POINT ( 'NONE',  ( -9.564922557960796823, -16.46253265017161027, 22.08224293864768839 ) ) ;
#167892 = CARTESIAN_POINT ( 'NONE',  ( -18.62759615963270932, 10.81492255796079327, 70.83224293864770971 ) ) ;
#167891 = CARTESIAN_POINT ( 'NONE',  ( 19.05341960407611168, 5.049401038298154454, 73.95724293864768129 ) ) ;
#167894 = CARTESIAN_POINT ( 'NONE',  ( 5.153800228976335163, 19.02544592524342804, 89.79057627198102409 ) ) ;
#167893 = CARTESIAN_POINT ( 'NONE',  ( -12.06949235617739369, -12.14591786802326823, 109.3760903946857042 ) ) ;
#167895 = CARTESIAN_POINT ( 'NONE',  ( 5.153800228976615827, -19.02544592524334988, 70.20942372801899012 ) ) ;
#167896 = CARTESIAN_POINT ( 'NONE',  ( -0.05219959533937732626, 21.53943276465977519, 92.50109039468567573 ) ) ;
#167897 = CARTESIAN_POINT ( 'NONE',  ( -21.55341960407610458, -5.719274019375992779, 66.45724293864768129 ) ) ;
#167898 = CARTESIAN_POINT ( 'NONE',  ( 9.474510206698971260, -16.51473224551069308, 112.9155762719810383 ) ) ;
#167899 = CARTESIAN_POINT ( 'NONE',  ( 19.03943276465977164, -0.05219959533909143690, 33.74890960531435979 ) ) ;
#167900 = CARTESIAN_POINT ( 'NONE',  ( 14.29746914071037800, 8.314922557961029526, 101.6677570613523613 ) ) ;
#167901 = CARTESIAN_POINT ( 'NONE',  ( -16.46253265017160317, 9.564922557960807481, 65.83224293864769550 ) ) ;
#167902 = CARTESIAN_POINT ( 'NONE',  ( 14.34966873604972726, -8.224510206698740333, 20.83442372801901143 ) ) ;
#167903 = CARTESIAN_POINT ( 'NONE',  ( 16.38665767535053774, 7.295008042176050367, 52.23599135785457293 ) ) ;
#167904 = CARTESIAN_POINT ( 'NONE',  ( 15.80617190586769283, -15.72974639402175789, 110.6260903946857042 ) ) ;
#167905 = CARTESIAN_POINT ( 'NONE',  ( -12.14591786802309592, -12.06949235617757132, 76.87390960531439532 ) ) ;
#167906 = CARTESIAN_POINT ( 'NONE',  ( 5.823673210054125526, 21.52544592524343514, 114.7905762719810383 ) ) ;
#167907 = CARTESIAN_POINT ( 'NONE',  ( 15.72974639402199770, -15.80617190586745480, 103.1239096053143811 ) ) ;
#167908 = CARTESIAN_POINT ( 'NONE',  ( -6.131632772416347521, 4.064918688780001510, -64.31816925299780507 ) ) ;
#167909 = CARTESIAN_POINT ( 'NONE',  ( 10.81492255796078972, 18.62759615963270932, 54.58224293864769550 ) ) ;
#167910 = CARTESIAN_POINT ( 'NONE',  ( 16.52544592524335698, 4.483927247898782831, 76.45942372801901854 ) ) ;
#167911 = CARTESIAN_POINT ( 'NONE',  ( 12.06949235617757843, -12.14591786802309237, 108.1239096053143811 ) ) ;
#167912 = CARTESIAN_POINT ( 'NONE',  ( 19.02544592524343514, -5.153800228976328945, 58.54057627198102409 ) ) ;
#167913 = CARTESIAN_POINT ( 'NONE',  ( 4.379528057220092307, 16.55341960407617563, 107.2927570613523471 ) ) ;
#167914 = CARTESIAN_POINT ( 'NONE',  ( 10.72451020669871369, 18.67979575497193778, 47.08442372801901854 ) ) ;
#167915 = CARTESIAN_POINT ( 'NONE',  ( -16.46253265017160317, 9.564922557960807481, 100.8322429386477097 ) ) ;
#167916 = CARTESIAN_POINT ( 'NONE',  ( -10.72451020669870658, -18.67979575497194134, 79.58442372801903275 ) ) ;
#167917 = CARTESIAN_POINT ( 'NONE',  ( -13.89961937509977652, 13.97604488694528158, 35.62390960531435269 ) ) ;
#167918 = CARTESIAN_POINT ( 'NONE',  ( 0.05219959533909260263, 19.03943276465977164, 39.99890960531436690 ) ) ;
#167919 = ORIENTED_EDGE ( 'NONE', *, *, #77460, .T. ) ;
#167920 = CARTESIAN_POINT ( 'NONE',  ( -10.72451020669870658, -18.67979575497194134, 74.58442372801901854 ) ) ;
#167921 = CARTESIAN_POINT ( 'NONE',  ( -19.02544592524342804, 5.153800228976336051, 106.0405762719810241 ) ) ;
#167922 = CARTESIAN_POINT ( 'NONE',  ( 19.02544592524334988, 5.153800228976608722, 76.45942372801897591 ) ) ;
#167923 = CARTESIAN_POINT ( 'NONE',  ( -10.81492255796105439, 18.62759615963255655, 37.91775706135235424 ) ) ;
#167924 = CARTESIAN_POINT ( 'NONE',  ( 12.14591786802327356, -12.06949235617739191, 20.62609039468568639 ) ) ;
#167925 = CARTESIAN_POINT ( 'NONE',  ( -5.153800228976607833, 19.02544592524334988, 67.70942372801900433 ) ) ;
#167926 = CARTESIAN_POINT ( 'NONE',  ( -13.89961937509977652, 13.97604488694528158, 50.62390960531435979 ) ) ;
#167927 = CARTESIAN_POINT ( 'NONE',  ( 5.153800228976615827, -19.02544592524334988, 80.20942372801901854 ) ) ;
#167928 = CARTESIAN_POINT ( 'NONE',  ( 16.52544592524342804, -4.483927247898539470, 28.54057627198103120 ) ) ;
#167929 = CARTESIAN_POINT ( 'NONE',  ( -9.564922557961040184, 16.46253265017147172, 72.91775706135233293 ) ) ;
#167930 = CARTESIAN_POINT ( 'NONE',  ( 16.55341960407611168, 4.379528057220329451, 43.95724293864769550 ) ) ;
#167931 = CARTESIAN_POINT ( 'NONE',  ( -5.049401038297874678, -19.05341960407617918, 69.79275706135233293 ) ) ;
#167932 = CARTESIAN_POINT ( 'NONE',  ( -4.379528057220086978, -16.55341960407618274, 44.79275706135234714 ) ) ;
#167933 = CARTESIAN_POINT ( 'NONE',  ( 16.51473224551083163, -9.474510206698727899, 25.83442372801900078 ) ) ;
#167934 = PRODUCT_DEFINITION_SHAPE ( 'NONE', 'NONE',  #183372 ) ;
#167935 = CARTESIAN_POINT ( 'NONE',  ( 13.89961937509977652, -13.97604488694527269, 33.12390960531434558 ) ) ;
#167936 = CARTESIAN_POINT ( 'NONE',  ( -16.19135201231369692, -7.376712067591814304, 65.18680854052030327 ) ) ;
#167937 = CARTESIAN_POINT ( 'NONE',  ( 12.14591786802327356, -12.06949235617739191, 45.62609039468567573 ) ) ;
#167938 = DIRECTION ( 'NONE',  ( 0.000000000000000000, 0.000000000000000000, 1.000000000000000000 ) ) ;
#167939 = CARTESIAN_POINT ( 'NONE',  ( 27.73933785331498569, 2.768321779492822058E-14, 145.8750000027311842 ) ) ;
#167940 = CARTESIAN_POINT ( 'NONE',  ( 9.474510206698971260, -16.51473224551069308, 92.91557627198103830 ) ) ;
#167941 = CARTESIAN_POINT ( 'NONE',  ( 13.97604488694548053, -13.89961937509957401, 85.62609039468567573 ) ) ;
#167942 = ORIENTED_EDGE ( 'NONE', *, *, #105746, .F. ) ;
#167943 = CARTESIAN_POINT ( 'NONE',  ( 5.153800228976615827, -19.02544592524334988, 90.20942372801900433 ) ) ;
#167945 = CARTESIAN_POINT ( 'NONE',  ( 10.81492255796078972, 18.62759615963270932, 24.58224293864768839 ) ) ;
#167944 = AXIS2_PLACEMENT_3D ( 'NONE', #79547, #188735, #35033 ) ;
#167947 = CARTESIAN_POINT ( 'NONE',  ( -13.89961937509957401, -13.97604488694547875, 104.3760903946856757 ) ) ;
#167946 = CARTESIAN_POINT ( 'NONE',  ( -9.474510206698720793, -16.51473224551083518, 19.58442372801899722 ) ) ;
#167948 = CARTESIAN_POINT ( 'NONE',  ( 12.06949235617757843, -12.14591786802309237, 108.1239096053143811 ) ) ;
#167949 = CARTESIAN_POINT ( 'NONE',  ( 9.474510206698971260, -16.51473224551069308, 32.91557627198102409 ) ) ;
#167950 = CARTESIAN_POINT ( 'NONE',  ( 21.52544592524344225, -5.823673210054117533, 53.54057627198103120 ) ) ;
#167951 = CARTESIAN_POINT ( 'NONE',  ( 19.03943276465977164, -0.05219959533909143690, 28.74890960531435624 ) ) ;
#167952 = DIRECTION ( 'NONE',  ( -0.000000000000000000, -0.000000000000000000, 1.000000000000000000 ) ) ;
#167953 = CARTESIAN_POINT ( 'NONE',  ( -16.51473224551082808, 9.474510206698731452, 73.33442372801900433 ) ) ;
#167954 = CARTESIAN_POINT ( 'NONE',  ( 4.483927247898545687, 16.52544592524342804, 34.79057627198103120 ) ) ;
#167955 = CARTESIAN_POINT ( 'NONE',  ( 19.05341960407611168, 5.049401038298154454, 108.9572429386477097 ) ) ;
#167956 = CARTESIAN_POINT ( 'NONE',  ( -18.67979575497193778, 10.72451020669871902, 93.33442372801901854 ) ) ;
#167957 = CARTESIAN_POINT ( 'NONE',  ( -10.72451020669898014, 18.67979575497178502, 80.41557627198103830 ) ) ;
#167958 = CARTESIAN_POINT ( 'NONE',  ( 5.823673210054444382, -21.52544592524334988, 55.20942372801902565 ) ) ;
#167959 = CARTESIAN_POINT ( 'NONE',  ( 21.53943276465977519, 0.05219959533937863772, 61.25109039468567573 ) ) ;
#167960 = CARTESIAN_POINT ( 'NONE',  ( -13.97604488694527625, -13.89961937509977652, 91.87390960531432427 ) ) ;
#167962 = CARTESIAN_POINT ( 'NONE',  ( 15.72974639402176855, 15.80617190586768217, 51.87609039468568284 ) ) ;
#167961 = CARTESIAN_POINT ( 'NONE',  ( -16.52544592524335698, -4.483927247898792601, 93.95942372801903275 ) ) ;
#167963 = CARTESIAN_POINT ( 'NONE',  ( -0.05219959533910754901, -16.53943276465976808, 112.4989096053143669 ) ) ;
#167964 = CARTESIAN_POINT ( 'NONE',  ( -12.06949235617756955, 12.14591786802309770, 70.62390960531436690 ) ) ;
#167965 = CARTESIAN_POINT ( 'NONE',  ( -8.314922557960811034, -14.29746914071050412, 32.08224293864769550 ) ) ;
#167966 = CARTESIAN_POINT ( 'NONE',  ( 15.72974639402199770, -15.80617190586745480, 43.12390960531435269 ) ) ;
#167967 = CARTESIAN_POINT ( 'NONE',  ( -19.05341960407611168, -5.049401038298163336, 61.45724293864769550 ) ) ;
#167968 = CARTESIAN_POINT ( 'NONE',  ( 5.153800228976335163, 19.02544592524342804, 49.79057627198100988 ) ) ;
#167969 = CARTESIAN_POINT ( 'NONE',  ( 5.719274019375991003, -21.55341960407610458, 57.70724293864770260 ) ) ;
#167970 = CARTESIAN_POINT ( 'NONE',  ( 19.02544592524334988, 5.153800228976608722, 41.45942372801900433 ) ) ;
#167972 = CARTESIAN_POINT ( 'NONE',  ( 8.224510206698953496, -14.34966873604960469, 47.91557627198102409 ) ) ;
#167971 = CARTESIAN_POINT ( 'NONE',  ( -17.05587630539784882, -6.762274262135712810, 39.25819690962689634 ) ) ;
#167974 = AXIS2_PLACEMENT_3D ( 'NONE', #7567, #69253, #51096 ) ;
#167973 = CARTESIAN_POINT ( 'NONE',  ( 10.81492255796078972, 18.62759615963270932, 24.58224293864768839 ) ) ;
#167975 = ORIENTED_EDGE ( 'NONE', *, *, #98443, .F. ) ;
#167976 = ORIENTED_EDGE ( 'NONE', *, *, #35293, .T. ) ;
#167977 = CARTESIAN_POINT ( 'NONE',  ( -28.82186960331499037, 2.428612866367529932E-14, 140.2500000054623683 ) ) ;
#167978 = CARTESIAN_POINT ( 'NONE',  ( 12.14591786802327356, -12.06949235617739191, 75.62609039468567573 ) ) ;
#167979 = CARTESIAN_POINT ( 'NONE',  ( 9.474510206698729675, 16.51473224551082808, 77.08442372801900433 ) ) ;
#167980 = CARTESIAN_POINT ( 'NONE',  ( -4.379528057220328563, 16.55341960407611168, 35.20724293864768839 ) ) ;
#167981 = DIRECTION ( 'NONE',  ( -1.000000000000000000, 0.000000000000000000, 0.000000000000000000 ) ) ;
#167982 = CARTESIAN_POINT ( 'NONE',  ( 12.06949235617757843, -12.14591786802309237, 23.12390960531436335 ) ) ;
#167983 = CARTESIAN_POINT ( 'NONE',  ( -19.02544592524342804, 5.153800228976336051, 46.04057627198101699 ) ) ;
#167984 = CARTESIAN_POINT ( 'NONE',  ( 16.51473224551069308, 9.474510206698969483, 79.16557627198103830 ) ) ;
#167985 = CARTESIAN_POINT ( 'NONE',  ( -19.03943276465977164, 0.05219959533909376836, 41.24890960531435269 ) ) ;
#167986 = CARTESIAN_POINT ( 'NONE',  ( 21.55341960407619695, -5.719274019375665929, 51.04275706135234714 ) ) ;
#167987 = CARTESIAN_POINT ( 'NONE',  ( -0.05219959533909027116, -19.03943276465977164, 52.49890960531436690 ) ) ;
#167988 = CARTESIAN_POINT ( 'NONE',  ( -22.96528548301343520, 5.795830589372932273, 190.0000000000000000 ) ) ;
#167989 = CARTESIAN_POINT ( 'NONE',  ( 9.564922557960805705, 16.46253265017160317, 54.58224293864769550 ) ) ;
#167990 = CARTESIAN_POINT ( 'NONE',  ( -15.80617190586745835, -15.72974639402198527, 41.87390960531435979 ) ) ;
#167991 = CARTESIAN_POINT ( 'NONE',  ( 8.224510206698953496, -14.34966873604960469, 112.9155762719810383 ) ) ;
#167992 = CARTESIAN_POINT ( 'NONE',  ( -5.719274019375978568, 21.55341960407610458, 30.20724293864769550 ) ) ;
#167993 = CARTESIAN_POINT ( 'NONE',  ( -8.224510206698735004, -14.34966873604973081, 94.58442372801901854 ) ) ;
#167994 = EDGE_CURVE ( 'NONE', #151167, #160176, #67962, .T. ) ;
#167995 = CARTESIAN_POINT ( 'NONE',  ( 18.67979575497194134, -10.72451020669871369, 110.8344237280190043 ) ) ;
#167996 = CARTESIAN_POINT ( 'NONE',  ( 4.483927247898790824, -16.52544592524335698, 65.20942372801901854 ) ) ;
#167997 = CARTESIAN_POINT ( 'NONE',  ( 13.97604488694527802, 13.89961937509977652, 109.3739096053143669 ) ) ;
#167998 = CARTESIAN_POINT ( 'NONE',  ( 12.14591786802327356, -12.06949235617739191, 50.62609039468568994 ) ) ;
#167999 = CARTESIAN_POINT ( 'NONE',  ( -16.55341960407617563, 4.379528057220093196, 43.54275706135235424 ) ) ;
#168000 = CARTESIAN_POINT ( 'NONE',  ( 5.049401038298161559, -19.05341960407611168, 112.7072429386476813 ) ) ;
#168001 = CARTESIAN_POINT ( 'NONE',  ( -16.53943276465976808, -0.05219959533934237506, 23.75109039468567929 ) ) ;
#168002 = CARTESIAN_POINT ( 'NONE',  ( 13.97604488694527802, 13.89961937509977652, 34.37390960531436690 ) ) ;
#168003 = CARTESIAN_POINT ( 'NONE',  ( -10.81492255796105439, 18.62759615963255655, 27.91775706135234358 ) ) ;
#168004 = CARTESIAN_POINT ( 'NONE',  ( -12.14591786802326823, 12.06949235617739902, 28.12609039468568284 ) ) ;
#168005 = CARTESIAN_POINT ( 'NONE',  ( -12.06949235617739369, -12.14591786802326823, 84.37609039468570415 ) ) ;
#168006 = CARTESIAN_POINT ( 'NONE',  ( -17.50000000001357847, 5.500000000000046185, 45.79690382535059001 ) ) ;
#168007 = CARTESIAN_POINT ( 'NONE',  ( 10.72451020669871369, 18.67979575497193778, 92.08442372801901854 ) ) ;
#168008 = CARTESIAN_POINT ( 'NONE',  ( -13.97604488694547697, 13.89961937509957934, 83.12609039468564731 ) ) ;
#168009 = CARTESIAN_POINT ( 'NONE',  ( -4.483927247898539470, -16.52544592524342804, 52.29057627198102409 ) ) ;
#168010 = CARTESIAN_POINT ( 'NONE',  ( 16.52544592524342804, -4.483927247898539470, 108.5405762719810241 ) ) ;
#168012 = CARTESIAN_POINT ( 'NONE',  ( -6.292920404648713273, 0.7621229312825712476, -64.49503546857650349 ) ) ;
#168011 = CARTESIAN_POINT ( 'NONE',  ( -19.03943276465977164, -0.05219959533935918106, 53.75109039468566863 ) ) ;
#168013 = CARTESIAN_POINT ( 'NONE',  ( -10.72451020669870658, -18.67979575497194134, 54.58442372801901143 ) ) ;
#168014 = CARTESIAN_POINT ( 'NONE',  ( 19.03943276465977164, 0.05219959533936151252, 111.2510903946856757 ) ) ;
#168015 = CARTESIAN_POINT ( 'NONE',  ( 17.44279575226823553, 5.990770900252481823, 81.66442432485685288 ) ) ;
#168016 = CARTESIAN_POINT ( 'NONE',  ( 19.03943276465977164, -0.05219959533909143690, 103.7489096053143669 ) ) ;
#168017 = CARTESIAN_POINT ( 'NONE',  ( -18.67979575497178146, -10.72451020669898902, 76.66557627198103830 ) ) ;
#168018 = CARTESIAN_POINT ( 'NONE',  ( -0.05219959533936034679, 19.03943276465977164, 97.50109039468567573 ) ) ;
#168019 = CARTESIAN_POINT ( 'NONE',  ( -0.05219959533909027116, -19.03943276465977164, 102.4989096053143669 ) ) ;
#168020 = CARTESIAN_POINT ( 'NONE',  ( -11.30073351558003480, -25.82347143560497926, 139.9999999999999716 ) ) ;
#168021 = CARTESIAN_POINT ( 'NONE',  ( -16.53943276465976808, 0.05219959533911058130, 101.2489096053143669 ) ) ;
#168022 = CARTESIAN_POINT ( 'NONE',  ( 5.823673210054444382, -21.52544592524334988, 95.20942372801903275 ) ) ;
#168023 = CARTESIAN_POINT ( 'NONE',  ( -5.153800228976328057, -19.02544592524343514, 42.29057627198101699 ) ) ;
#168024 = CARTESIAN_POINT ( 'NONE',  ( -21.53943276465977519, -0.05219959533937600094, 48.75109039468568284 ) ) ;
#168025 = CARTESIAN_POINT ( 'NONE',  ( -5.823673210054431948, 21.52544592524334988, 82.70942372801900433 ) ) ;
#168026 = CARTESIAN_POINT ( 'NONE',  ( -8.224510206698735004, -14.34966873604973081, 99.58442372801900433 ) ) ;
#168027 = CARTESIAN_POINT ( 'NONE',  ( -0.05219959533937732626, 21.53943276465977519, 37.50109039468568284 ) ) ;
#168028 = CARTESIAN_POINT ( 'NONE',  ( 15.72974639402176855, 15.80617190586768217, 41.87609039468568284 ) ) ;
#168030 = CARTESIAN_POINT ( 'NONE',  ( -19.02544592524342804, 5.153800228976336051, 96.04057627198103830 ) ) ;
#168029 = CARTESIAN_POINT ( 'NONE',  ( 5.153800228976615827, -19.02544592524334988, 65.20942372801900433 ) ) ;
#168031 = CARTESIAN_POINT ( 'NONE',  ( -12.06949235617756955, 12.14591786802309770, 105.6239096053143669 ) ) ;
#168032 = CARTESIAN_POINT ( 'NONE',  ( -21.52544592524343514, 5.823673210054127303, 81.04057627198102409 ) ) ;
#168033 = CARTESIAN_POINT ( 'NONE',  ( -12.06949235617756955, 12.14591786802309770, 70.62390960531436690 ) ) ;
#168034 = CARTESIAN_POINT ( 'NONE',  ( 21.52544592524334988, 5.823673210054432836, 111.4594237280190328 ) ) ;
#168035 = CARTESIAN_POINT ( 'NONE',  ( -4.483927247898539470, -16.52544592524342804, 82.29057627198103830 ) ) ;
#168036 = CARTESIAN_POINT ( 'NONE',  ( 0.05219959533909260263, 19.03943276465977164, 29.99890960531435979 ) ) ;
#168037 = CARTESIAN_POINT ( 'NONE',  ( 9.564922557961047289, -16.46253265017146816, 90.41775706135234714 ) ) ;
#168038 = CARTESIAN_POINT ( 'NONE',  ( -8.224510206698948167, 14.34966873604960824, 45.41557627198103830 ) ) ;
#168039 = CARTESIAN_POINT ( 'NONE',  ( 15.80617190586769283, -15.72974639402175789, 90.62609039468567573 ) ) ;
#168040 = CARTESIAN_POINT ( 'NONE',  ( 0.05219959533909260263, 19.03943276465977164, 89.99890960531436690 ) ) ;
#168041 = CARTESIAN_POINT ( 'NONE',  ( -5.153800228976607833, 19.02544592524334988, 62.70942372801899722 ) ) ;
#168042 = CARTESIAN_POINT ( 'NONE',  ( -10.72451020669898014, 18.67979575497178502, 80.41557627198103830 ) ) ;
#168043 = CARTESIAN_POINT ( 'NONE',  ( 18.62759615963255655, 10.81492255796105972, 26.66775706135235424 ) ) ;
#168044 = CARTESIAN_POINT ( 'NONE',  ( -16.52544592524335698, -4.483927247898792601, 33.95942372801901143 ) ) ;
#168045 = CARTESIAN_POINT ( 'NONE',  ( -16.55341960407617563, 4.379528057220093196, 83.54275706135234714 ) ) ;
#168047 = CARTESIAN_POINT ( 'NONE',  ( -10.72451020669898014, 18.67979575497178502, 115.4155762719810241 ) ) ;
#168046 = CARTESIAN_POINT ( 'NONE',  ( 13.97604488694527802, 13.89961937509977652, 29.37390960531435979 ) ) ;
#168048 = CARTESIAN_POINT ( 'NONE',  ( 16.53943276465976808, -0.05219959533910856209, 113.7489096053143527 ) ) ;
#168049 = CARTESIAN_POINT ( 'NONE',  ( 36.91746824999999887, 11.99521256947799053, -8.024999997268814411 ) ) ;
#168050 = CARTESIAN_POINT ( 'NONE',  ( -14.34966873604972548, 8.224510206698743886, 43.33442372801901143 ) ) ;
#168051 = CARTESIAN_POINT ( 'NONE',  ( 4.483927247898545687, 16.52544592524342804, 84.79057627198102409 ) ) ;
#168052 = CARTESIAN_POINT ( 'NONE',  ( -21.52544592524343514, 5.823673210054127303, 71.04057627198103830 ) ) ;
#168053 = CARTESIAN_POINT ( 'NONE',  ( -4.379528057220328563, 16.55341960407611168, 25.20724293864769550 ) ) ;
#168054 = CARTESIAN_POINT ( 'NONE',  ( 12.14591786802327356, -12.06949235617739191, 45.62609039468567573 ) ) ;
#168055 = CARTESIAN_POINT ( 'NONE',  ( 5.049401038298161559, -19.05341960407611168, 47.70724293864770260 ) ) ;
#168056 = CARTESIAN_POINT ( 'NONE',  ( -14.29746914071037622, -8.314922557961029526, 79.16775706135234714 ) ) ;
#168057 = CARTESIAN_POINT ( 'NONE',  ( -19.03943276465977164, -0.05219959533935918106, 68.75109039468566152 ) ) ;
#168058 = CARTESIAN_POINT ( 'NONE',  ( -10.81492255796078084, -18.62759615963271287, 67.08224293864770971 ) ) ;
#168059 = CARTESIAN_POINT ( 'NONE',  ( -14.34966873604972548, 8.224510206698743886, 108.3344237280190185 ) ) ;
#168060 = ORIENTED_EDGE ( 'NONE', *, *, #168230, .F. ) ;
#168061 = CARTESIAN_POINT ( 'NONE',  ( -19.02544592524342804, 5.153800228976336051, 116.0405762719810383 ) ) ;
#168062 = CARTESIAN_POINT ( 'NONE',  ( 0.05219959533907565091, 21.53943276465977519, 49.99890960531437401 ) ) ;
#168063 = VERTEX_POINT ( 'NONE', #149129 ) ;
#168064 = CARTESIAN_POINT ( 'NONE',  ( -16.53943276465976808, -0.05219959533934237506, 88.75109039468567573 ) ) ;
#168065 = ORIENTED_EDGE ( 'NONE', *, *, #85112, .F. ) ;
#168066 = CARTESIAN_POINT ( 'NONE',  ( -16.51473224551069308, -9.474510206698971260, 106.6655762719810383 ) ) ;
#168067 = CARTESIAN_POINT ( 'NONE',  ( 17.50000000000000000, 3.850315288878781050, 108.2337086939655109 ) ) ;
#168068 = CARTESIAN_POINT ( 'NONE',  ( 21.52544592524344225, -5.823673210054117533, 73.54057627198102409 ) ) ;
#168069 = CARTESIAN_POINT ( 'NONE',  ( 8.224510206698742110, 14.34966873604972548, 102.0844237280190185 ) ) ;
#168070 = CARTESIAN_POINT ( 'NONE',  ( -0.05219959533936034679, 19.03943276465977164, 112.5010903946856757 ) ) ;
#168071 = CARTESIAN_POINT ( 'NONE',  ( -9.564922557960796823, -16.46253265017161027, 27.08224293864769550 ) ) ;
#168072 = CARTESIAN_POINT ( 'NONE',  ( -14.29746914071037622, -8.314922557961029526, 24.16775706135235424 ) ) ;
#168073 = CARTESIAN_POINT ( 'NONE',  ( -5.153800228976328057, -19.02544592524343514, 57.29057627198103120 ) ) ;
#168074 = EDGE_CURVE ( 'NONE', #123524, #49927, #173330, .T. ) ;
#168075 = CARTESIAN_POINT ( 'NONE',  ( 16.70000000000003482, -0.1032682159774155756, -61.34707691135563579 ) ) ;
#168076 = CARTESIAN_POINT ( 'NONE',  ( 19.03943276465977164, -0.05219959533909143690, 98.74890960531436690 ) ) ;
#168077 = CARTESIAN_POINT ( 'NONE',  ( -8.314922557961024197, 14.29746914071037800, 87.91775706135234714 ) ) ;
#168078 = CARTESIAN_POINT ( 'NONE',  ( 16.51473224551083163, -9.474510206698727899, 85.83442372801900433 ) ) ;
#168079 = CARTESIAN_POINT ( 'NONE',  ( -21.53943276465977519, -0.05219959533937600094, 113.7510903946856757 ) ) ;
#168080 = CARTESIAN_POINT ( 'NONE',  ( 18.62759615963271287, -10.81492255796078972, 73.33224293864769550 ) ) ;
#168081 = CARTESIAN_POINT ( 'NONE',  ( 12.06949235617739724, 12.14591786802326823, 101.8760903946857042 ) ) ;
#168082 = CARTESIAN_POINT ( 'NONE',  ( 19.03943276465977164, 0.05219959533936151252, 96.25109039468567573 ) ) ;
#168083 = CARTESIAN_POINT ( 'NONE',  ( -13.97604488694527625, -13.89961937509977652, 46.87390960531435979 ) ) ;
#168084 = CARTESIAN_POINT ( 'NONE',  ( -5.153800228976328057, -19.02544592524343514, 97.29057627198099567 ) ) ;
#168085 = CARTESIAN_POINT ( 'NONE',  ( 21.52544592524334988, 5.823673210054432836, 66.45942372801903275 ) ) ;
#168086 = CARTESIAN_POINT ( 'NONE',  ( 19.05341960407611168, 5.049401038298154454, 43.95724293864769550 ) ) ;
#168087 = FACE_OUTER_BOUND ( 'NONE', #114100, .T. ) ;
#168088 = CARTESIAN_POINT ( 'NONE',  ( -14.34966873604960291, -8.224510206698953496, 76.66557627198103830 ) ) ;
#168089 = CARTESIAN_POINT ( 'NONE',  ( 21.55341960407610458, 5.719274019375980345, 78.95724293864769550 ) ) ;
#168090 = CARTESIAN_POINT ( 'NONE',  ( 38.00000000000002842, 12.34694845685041109, -6.649999994537624914 ) ) ;
#168091 = CARTESIAN_POINT ( 'NONE',  ( 19.03943276465977164, 0.05219959533936151252, 41.25109039468566152 ) ) ;
#168092 = CARTESIAN_POINT ( 'NONE',  ( 16.61371651742642186, -7.165104196375917667, 71.35415069992967574 ) ) ;
#168094 = CARTESIAN_POINT ( 'NONE',  ( 13.89961937509977652, -13.97604488694527269, 83.12390960531436690 ) ) ;
#168093 = CARTESIAN_POINT ( 'NONE',  ( -5.049401038298153566, 19.05341960407611168, 75.20724293864769550 ) ) ;
#168095 = CARTESIAN_POINT ( 'NONE',  ( 12.14591786802327356, -12.06949235617739191, 65.62609039468568994 ) ) ;
#168096 = CARTESIAN_POINT ( 'NONE',  ( 8.839334217631813928, -46.13630234914187156, -24.17074550867518923 ) ) ;
#168097 = CARTESIAN_POINT ( 'NONE',  ( -19.03943276465977164, -0.05219959533935918106, 23.75109039468566152 ) ) ;
#168098 = CARTESIAN_POINT ( 'NONE',  ( 17.49999999999999645, -5.500000000000031974, 93.29690382534172954 ) ) ;
#168099 = CARTESIAN_POINT ( 'NONE',  ( -8.224510206698735004, -14.34966873604973081, 84.58442372801903275 ) ) ;
#168100 = PLANE ( 'NONE',  #33912 ) ;
#168101 = CARTESIAN_POINT ( 'NONE',  ( 12.14591786802327356, -12.06949235617739191, 85.62609039468568994 ) ) ;
#168102 = CARTESIAN_POINT ( 'NONE',  ( -16.52216118717208460, 7.221426719304501418, 28.92400978953008561 ) ) ;
#168103 = CARTESIAN_POINT ( 'NONE',  ( -16.52544592524335698, -4.483927247898792601, 53.95942372801900433 ) ) ;
#168104 = CARTESIAN_POINT ( 'NONE',  ( -9.474510206698964154, 16.51473224551069663, 75.41557627198103830 ) ) ;
#168105 = CARTESIAN_POINT ( 'NONE',  ( 18.62759615963255655, 10.81492255796105972, 66.66775706135234714 ) ) ;
#168106 = CARTESIAN_POINT ( 'NONE',  ( -5.153800228976607833, 19.02544592524334988, 72.70942372801900433 ) ) ;
#168107 = CARTESIAN_POINT ( 'NONE',  ( -5.719274019375665041, -21.55341960407619695, 104.7927570613523898 ) ) ;
#168108 = CARTESIAN_POINT ( 'NONE',  ( -5.049401038298153566, 19.05341960407611168, 55.20724293864769550 ) ) ;
#168109 = CARTESIAN_POINT ( 'NONE',  ( -13.97604488694527625, -13.89961937509977652, 46.87390960531435979 ) ) ;
#168110 = CARTESIAN_POINT ( 'NONE',  ( 16.40734927747358540, 7.283318515949404492, 22.21415419577492045 ) ) ;
#168111 = CARTESIAN_POINT ( 'NONE',  ( -0.05219959533907301413, -21.53943276465977519, 62.49890960531436690 ) ) ;
#168112 = VECTOR ( 'NONE', #88922, 1000.000000000000000 ) ;
#168113 = CARTESIAN_POINT ( 'NONE',  ( -5.823673210054116645, -21.52544592524344225, 27.29057627198103120 ) ) ;
#168114 = CARTESIAN_POINT ( 'NONE',  ( 19.02544592524343514, -5.153800228976328945, 23.54057627198102054 ) ) ;
#168115 = CARTESIAN_POINT ( 'NONE',  ( -16.55341960407617563, 4.379528057220093196, 53.54275706135234714 ) ) ;
#168116 = ORIENTED_EDGE ( 'NONE', *, *, #116420, .F. ) ;
#168117 = CARTESIAN_POINT ( 'NONE',  ( 18.67979575497178502, 10.72451020669898547, 114.1655762719810383 ) ) ;
#168119 = CARTESIAN_POINT ( 'NONE',  ( 23.48529157249600630, -32.32473071737749137, -3.300000000000000266 ) ) ;
#168118 = CARTESIAN_POINT ( 'NONE',  ( 8.314922557960818139, 14.29746914071049879, 54.58224293864769550 ) ) ;
#168120 = CARTESIAN_POINT ( 'NONE',  ( 0.05219959533936267826, -19.03943276465977164, 105.0010903946856615 ) ) ;
#168121 = CARTESIAN_POINT ( 'NONE',  ( 5.153800228976615827, -19.02544592524334988, 45.20942372801901143 ) ) ;
#168122 = CARTESIAN_POINT ( 'NONE',  ( 16.53943276465976808, -0.05219959533910856209, 38.74890960531435979 ) ) ;
#168123 = CARTESIAN_POINT ( 'NONE',  ( -0.05219959533937732626, 21.53943276465977519, 22.50109039468567573 ) ) ;
#168125 = CARTESIAN_POINT ( 'NONE',  ( 10.72451020669898902, -18.67979575497178502, 62.91557627198102409 ) ) ;
#168124 = DIRECTION ( 'NONE',  ( -0.000000000000000000, -0.000000000000000000, 1.000000000000000000 ) ) ;
#168126 = CARTESIAN_POINT ( 'NONE',  ( 19.02544592524343514, -5.153800228976328945, 88.54057627198102409 ) ) ;
#168127 = CARTESIAN_POINT ( 'NONE',  ( 14.29746914071049879, -8.314922557960816363, 53.33224293864769550 ) ) ;
#168128 = CARTESIAN_POINT ( 'NONE',  ( -19.03943276465977164, 0.05219959533909376836, 101.2489096053143669 ) ) ;
#168129 = DIRECTION ( 'NONE',  ( 0.000000000000000000, 0.000000000000000000, -1.000000000000000000 ) ) ;
#168130 = CARTESIAN_POINT ( 'NONE',  ( -0.05219959533936034679, 19.03943276465977164, 57.50109039468566863 ) ) ;
#168131 = CARTESIAN_POINT ( 'NONE',  ( 18.67979575497178502, 10.72451020669898547, 99.16557627198100988 ) ) ;
#168132 = CARTESIAN_POINT ( 'NONE',  ( 9.564922557960805705, 16.46253265017160317, 49.58224293864770260 ) ) ;
#168133 = CARTESIAN_POINT ( 'NONE',  ( 13.89961937509977652, -13.97604488694527269, 23.12390960531436335 ) ) ;
#168134 = CARTESIAN_POINT ( 'NONE',  ( 18.62759615963255655, 10.81492255796105972, 56.66775706135235424 ) ) ;
#168135 = CARTESIAN_POINT ( 'NONE',  ( 27.73933785331498925, -9.013057229001033122, 145.7750000027311899 ) ) ;
#168136 = CARTESIAN_POINT ( 'NONE',  ( -8.314922557960811034, -14.29746914071050412, 22.08224293864769194 ) ) ;
#168137 = CARTESIAN_POINT ( 'NONE',  ( -5.049401038298153566, 19.05341960407611168, 50.20724293864770260 ) ) ;
#168138 = CARTESIAN_POINT ( 'NONE',  ( 19.05341960407611168, 5.049401038298154454, 98.95724293864766707 ) ) ;
#168139 = CARTESIAN_POINT ( 'NONE',  ( 0.05219959533907565091, 21.53943276465977519, 54.99890960531435269 ) ) ;
#168140 = CARTESIAN_POINT ( 'NONE',  ( 17.14385361876520264, -23.59649016807271238, 143.5750000027312012 ) ) ;
#168141 = CARTESIAN_POINT ( 'NONE',  ( 19.05341960407611168, 5.049401038298154454, 48.95724293864768129 ) ) ;
#168142 = CARTESIAN_POINT ( 'NONE',  ( -5.719274019375978568, 21.55341960407610458, 50.20724293864769550 ) ) ;
#168143 = CARTESIAN_POINT ( 'NONE',  ( 10.81492255796106328, -18.62759615963255655, 85.41775706135236135 ) ) ;
#168146 = CARTESIAN_POINT ( 'NONE',  ( -14.29746914071049879, 8.314922557960819915, 75.83224293864769550 ) ) ;
#168145 = CARTESIAN_POINT ( 'NONE',  ( 16.52544592524335698, 4.483927247898782831, 86.45942372801901854 ) ) ;
#168144 = CARTESIAN_POINT ( 'NONE',  ( 16.87022414722825303, -33.99382086345632104, -27.12615631800316507 ) ) ;
#168147 = CARTESIAN_POINT ( 'NONE',  ( 14.29746914071037800, 8.314922557961029526, 86.66775706135234714 ) ) ;
#168148 = CARTESIAN_POINT ( 'NONE',  ( 9.564922557960805705, 16.46253265017160317, 69.58224293864770971 ) ) ;
#168149 = ORIENTED_EDGE ( 'NONE', *, *, #113740, .F. ) ;
#168150 = CARTESIAN_POINT ( 'NONE',  ( 16.51473224551083163, -9.474510206698727899, 20.83442372801899722 ) ) ;
#168151 = CARTESIAN_POINT ( 'NONE',  ( 4.483927247898790824, -16.52544592524335698, 90.20942372801903275 ) ) ;
#168152 = CARTESIAN_POINT ( 'NONE',  ( 5.153800228976615827, -19.02544592524334988, 20.20942372801899722 ) ) ;
#168153 = CARTESIAN_POINT ( 'NONE',  ( -5.153800228976328057, -19.02544592524343514, 82.29057627198103830 ) ) ;
#168154 = CARTESIAN_POINT ( 'NONE',  ( -10.81492255796078084, -18.62759615963271287, 42.08224293864769550 ) ) ;
#168155 = CARTESIAN_POINT ( 'NONE',  ( 0.05219959533934541429, -16.53943276465976808, 30.00109039468568284 ) ) ;
#168156 = CARTESIAN_POINT ( 'NONE',  ( 5.719274019375673035, 21.55341960407619339, 87.29275706135236135 ) ) ;
#168157 = CARTESIAN_POINT ( 'NONE',  ( 16.52544592524335698, 4.483927247898782831, 66.45942372801903275 ) ) ;
#168158 = CARTESIAN_POINT ( 'NONE',  ( 0.05219959533907565091, 21.53943276465977519, 114.9989096053143669 ) ) ;
#168159 = CARTESIAN_POINT ( 'NONE',  ( 4.483927247898790824, -16.52544592524335698, 20.20942372801900788 ) ) ;
#168160 = CARTESIAN_POINT ( 'NONE',  ( 16.46253265017160672, -9.564922557960803928, 93.33224293864769550 ) ) ;
#168161 = CARTESIAN_POINT ( 'NONE',  ( -0.05219959533934338120, 16.53943276465976808, 27.50109039468567929 ) ) ;
#168162 = CARTESIAN_POINT ( 'NONE',  ( -9.474510206698964154, 16.51473224551069663, 40.41557627198103120 ) ) ;
#168163 = CARTESIAN_POINT ( 'NONE',  ( -12.06949235617739369, -12.14591786802326823, 39.37609039468567573 ) ) ;
#168164 = CARTESIAN_POINT ( 'NONE',  ( 4.483927247898545687, 16.52544592524342804, 74.79057627198105251 ) ) ;
#168165 = CARTESIAN_POINT ( 'NONE',  ( 4.379528057220092307, 16.55341960407617563, 82.29275706135234714 ) ) ;
#168167 = CARTESIAN_POINT ( 'NONE',  ( 5.049401038298161559, -19.05341960407611168, 67.70724293864769550 ) ) ;
#168166 = CARTESIAN_POINT ( 'NONE',  ( -15.72974639402176322, -15.80617190586768395, 24.37609039468567573 ) ) ;
#168168 = CARTESIAN_POINT ( 'NONE',  ( 19.03943276465977164, -0.05219959533909143690, 88.74890960531436690 ) ) ;
#168169 = CARTESIAN_POINT ( 'NONE',  ( 4.379528057220092307, 16.55341960407617563, 92.29275706135236135 ) ) ;
#168171 = ORIENTED_EDGE ( 'NONE', *, *, #154300, .T. ) ;
#168170 = CARTESIAN_POINT ( 'NONE',  ( 5.000000000000000000, -99.43240762267087973, 40.28936402012540441 ) ) ;
#168172 = ORIENTED_EDGE ( 'NONE', *, *, #47533, .F. ) ;
#168173 = CARTESIAN_POINT ( 'NONE',  ( -13.89961937509957401, -13.97604488694547875, 34.37609039468566863 ) ) ;
#168174 = CARTESIAN_POINT ( 'NONE',  ( -0.05219959533909027116, -19.03943276465977164, 92.49890960531436690 ) ) ;
#168175 = CARTESIAN_POINT ( 'NONE',  ( 13.97604488694527802, 13.89961937509977652, 54.37390960531435979 ) ) ;
#168177 = ORIENTED_EDGE ( 'NONE', *, *, #95827, .F. ) ;
#168176 = CARTESIAN_POINT ( 'NONE',  ( -5.153800228976328057, -19.02544592524343514, 112.2905762719810099 ) ) ;
#168178 = CARTESIAN_POINT ( 'NONE',  ( 4.483927247898790824, -16.52544592524335698, 25.20942372801901854 ) ) ;
#168180 = CARTESIAN_POINT ( 'NONE',  ( 16.55341960407618274, -4.379528057220086978, 36.04275706135234714 ) ) ;
#168179 = CARTESIAN_POINT ( 'NONE',  ( -16.51473224551082808, 9.474510206698731452, 53.33442372801900433 ) ) ;
#168181 = CARTESIAN_POINT ( 'NONE',  ( -19.02544592524342804, 5.153800228976336051, 106.0405762719810241 ) ) ;
#168182 = CARTESIAN_POINT ( 'NONE',  ( -13.89961937509977652, 13.97604488694528158, 80.62390960531436690 ) ) ;
#168183 = CARTESIAN_POINT ( 'NONE',  ( 21.55341960407610458, 5.719274019375980345, 93.95724293864770971 ) ) ;
#168184 = CARTESIAN_POINT ( 'NONE',  ( -13.89961937509957401, -13.97604488694547875, 59.37609039468566863 ) ) ;
#168186 = LINE ( 'NONE', #16497, #31074 ) ;
#168185 = CARTESIAN_POINT ( 'NONE',  ( 5.049401038298161559, -19.05341960407611168, 87.70724293864769550 ) ) ;
#168187 = CARTESIAN_POINT ( 'NONE',  ( 13.89961937509977652, -13.97604488694527269, 58.12390960531436690 ) ) ;
#168189 = CARTESIAN_POINT ( 'NONE',  ( -19.03943276465977164, 0.05219959533909376836, 26.24890960531435624 ) ) ;
#168188 = CARTESIAN_POINT ( 'NONE',  ( -0.05219959533934338120, 16.53943276465976808, 112.5010903946857042 ) ) ;
#168190 = EDGE_CURVE ( 'NONE', #87243, #124967, #86149, .T. ) ;
#168191 = CARTESIAN_POINT ( 'NONE',  ( -13.89961937509957401, -13.97604488694547875, 39.37609039468566152 ) ) ;
#168192 = CARTESIAN_POINT ( 'NONE',  ( -8.224510206698948167, 14.34966873604960824, 70.41557627198102409 ) ) ;
#168193 = CARTESIAN_POINT ( 'NONE',  ( 5.823673210054444382, -21.52544592524334988, 105.2094237280190328 ) ) ;
#168194 = CARTESIAN_POINT ( 'NONE',  ( -5.153800228976328057, -19.02544592524343514, 42.29057627198101699 ) ) ;
#168195 = CARTESIAN_POINT ( 'NONE',  ( -16.53943276465976808, -0.05219959533934237506, 53.75109039468568994 ) ) ;
#168197 = CARTESIAN_POINT ( 'NONE',  ( 15.80617190586769283, -15.72974639402175789, 90.62609039468567573 ) ) ;
#168196 = CARTESIAN_POINT ( 'NONE',  ( -14.34966873604960291, -8.224510206698953496, 41.66557627198103120 ) ) ;
#168198 = CARTESIAN_POINT ( 'NONE',  ( -13.97604488694527625, -13.89961937509977652, 86.87390960531436690 ) ) ;
#168199 = CARTESIAN_POINT ( 'NONE',  ( -13.89961937509977652, 13.97604488694528158, 100.6239096053143669 ) ) ;
#168200 = CARTESIAN_POINT ( 'NONE',  ( -14.29746914071049879, 8.314922557960819915, 105.8322429386476955 ) ) ;
#168201 = CARTESIAN_POINT ( 'NONE',  ( 16.53943276465976808, -0.05219959533910856209, 73.74890960531433848 ) ) ;
#168202 = CARTESIAN_POINT ( 'NONE',  ( 10.72451020669898902, -18.67979575497178502, 77.91557627198102409 ) ) ;
#168203 = CARTESIAN_POINT ( 'NONE',  ( 9.474510206698971260, -16.51473224551069308, 92.91557627198103830 ) ) ;
#168204 = CARTESIAN_POINT ( 'NONE',  ( -15.72974639402197994, 15.80617190586746368, 100.6239096053143811 ) ) ;
#168205 = CARTESIAN_POINT ( 'NONE',  ( 19.02544592524343514, -5.153800228976328945, 93.54057627198102409 ) ) ;
#168207 = CARTESIAN_POINT ( 'NONE',  ( -16.52544592524342804, 4.483927247898546575, 91.04057627198103830 ) ) ;
#168206 = CARTESIAN_POINT ( 'NONE',  ( -19.52851543214744368, -5.499999999999942268, 90.39357721762578990 ) ) ;
#168208 = CARTESIAN_POINT ( 'NONE',  ( -5.049401038298153566, 19.05341960407611168, 55.20724293864769550 ) ) ;
#168209 = CARTESIAN_POINT ( 'NONE',  ( -15.72974639402197994, 15.80617190586746368, 60.62390960531437401 ) ) ;
#168210 = CARTESIAN_POINT ( 'NONE',  ( -17.81289503416611097, -24.51734667627696496, 146.2999999999999829 ) ) ;
#168212 = LINE ( 'NONE', #44879, #179255 ) ;
#168211 = CARTESIAN_POINT ( 'NONE',  ( 16.52544592524342804, -4.483927247898539470, 23.54057627198102765 ) ) ;
#168213 = CARTESIAN_POINT ( 'NONE',  ( 4.379528057220092307, 16.55341960407617563, 22.29275706135235069 ) ) ;
#168214 = CARTESIAN_POINT ( 'NONE',  ( 8.224510206698953496, -14.34966873604960469, 82.91557627198103830 ) ) ;
#168215 = CARTESIAN_POINT ( 'NONE',  ( -16.38665767535051998, -7.295008042176110763, 94.73599135785453029 ) ) ;
#168216 = CARTESIAN_POINT ( 'NONE',  ( -19.03943276465977164, 0.05219959533909376836, 81.24890960531436690 ) ) ;
#168217 = CARTESIAN_POINT ( 'NONE',  ( 13.97604488694527802, 13.89961937509977652, 39.37390960531435269 ) ) ;
#168218 = CARTESIAN_POINT ( 'NONE',  ( 4.379528057220339221, -16.55341960407611168, 72.70724293864769550 ) ) ;
#168219 = CARTESIAN_POINT ( 'NONE',  ( 5.823673210054125526, 21.52544592524343514, 24.79057627198103120 ) ) ;
#168220 = CARTESIAN_POINT ( 'NONE',  ( -9.564922557961040184, 16.46253265017147172, 97.91775706135233293 ) ) ;
#168221 = CARTESIAN_POINT ( 'NONE',  ( -16.51473224551069308, -9.474510206698971260, 101.6655762719810241 ) ) ;
#168222 = CARTESIAN_POINT ( 'NONE',  ( -21.53943276465977519, 0.05219959533907696930, 76.24890960531435269 ) ) ;
#168223 = CARTESIAN_POINT ( 'NONE',  ( 16.52544592524335698, 4.483927247898782831, 76.45942372801901854 ) ) ;
#168224 = CARTESIAN_POINT ( 'NONE',  ( -16.61371651742643252, 7.165104196375864376, 93.85415069992970416 ) ) ;
#168225 = CARTESIAN_POINT ( 'NONE',  ( -13.89961937509977652, 13.97604488694528158, 75.62390960531438111 ) ) ;
#168226 = CARTESIAN_POINT ( 'NONE',  ( -15.80617190586745835, -15.72974639402198527, 76.87390960531439532 ) ) ;
#168227 = CARTESIAN_POINT ( 'NONE',  ( 19.05341960407617918, -5.049401038297876454, 106.0427570613523471 ) ) ;
#168229 = CARTESIAN_POINT ( 'NONE',  ( -18.67979575497193778, 10.72451020669871902, 53.33442372801901854 ) ) ;
#168228 = CARTESIAN_POINT ( 'NONE',  ( 8.314922557960818139, 14.29746914071049879, 34.58224293864770260 ) ) ;
#168230 = EDGE_CURVE ( 'NONE', #98258, #7157, #89484, .T. ) ;
#168231 = DIRECTION ( 'NONE',  ( 0.000000000000000000, 0.000000000000000000, -1.000000000000000000 ) ) ;
#168233 = CARTESIAN_POINT ( 'NONE',  ( -13.97604488694527625, -13.89961937509977652, 106.8739096053143669 ) ) ;
#168232 = CARTESIAN_POINT ( 'NONE',  ( 14.29746914071037800, 8.314922557961029526, 66.66775706135234714 ) ) ;
#168234 = DIRECTION ( 'NONE',  ( -1.000000000000000000, 0.000000000000000000, 0.000000000000000000 ) ) ;
#168235 = CARTESIAN_POINT ( 'NONE',  ( -17.31747979337950127, 6.344076630960996610, 78.62055131934819485 ) ) ;
#168236 = CARTESIAN_POINT ( 'NONE',  ( -12.14591786802326823, 12.06949235617739902, 93.12609039468568994 ) ) ;
#168237 = CARTESIAN_POINT ( 'NONE',  ( 12.06949235617739724, 12.14591786802326823, 41.87609039468568284 ) ) ;
#168238 = CARTESIAN_POINT ( 'NONE',  ( -16.51473224551069308, -9.474510206698971260, 56.66557627198103120 ) ) ;
#168239 = CARTESIAN_POINT ( 'NONE',  ( 16.51473224551069308, 9.474510206698969483, 79.16557627198103830 ) ) ;
#168240 = CARTESIAN_POINT ( 'NONE',  ( 10.81492255796106328, -18.62759615963255655, 60.41775706135235424 ) ) ;
#168241 = CARTESIAN_POINT ( 'NONE',  ( 16.52544592524335698, 4.483927247898782831, 61.45942372801901854 ) ) ;
#168242 = CARTESIAN_POINT ( 'NONE',  ( 4.379528057220339221, -16.55341960407611168, 37.70724293864769550 ) ) ;
#168243 = CARTESIAN_POINT ( 'NONE',  ( 9.474510206698971260, -16.51473224551069308, 42.91557627198103120 ) ) ;
#168244 = CARTESIAN_POINT ( 'NONE',  ( 9.474510206698971260, -16.51473224551069308, 52.91557627198102409 ) ) ;
#168245 = CARTESIAN_POINT ( 'NONE',  ( -12.06949235617739369, -12.14591786802326823, 44.37609039468567573 ) ) ;
#168246 = CARTESIAN_POINT ( 'NONE',  ( -9.564922557961040184, 16.46253265017147172, 97.91775706135233293 ) ) ;
#168247 = CARTESIAN_POINT ( 'NONE',  ( -0.05219959533910754901, -16.53943276465976808, 102.4989096053143811 ) ) ;
#168248 = CARTESIAN_POINT ( 'NONE',  ( 16.46253265017160672, -9.564922557960803928, 53.33224293864768839 ) ) ;
#168250 = CARTESIAN_POINT ( 'NONE',  ( 17.49999999999999645, -5.624438216177591876, 93.31670344914644488 ) ) ;
#168249 = CARTESIAN_POINT ( 'NONE',  ( -9.474510206698720793, -16.51473224551083518, 84.58442372801900433 ) ) ;
#168251 = CARTESIAN_POINT ( 'NONE',  ( 21.52544592524334988, 5.823673210054432836, 96.45942372801901854 ) ) ;
#168252 = CARTESIAN_POINT ( 'NONE',  ( -14.29746914071037622, -8.314922557961029526, 49.16775706135234003 ) ) ;
#168253 = LINE ( 'NONE', #119780, #47094 ) ;
#168254 = CARTESIAN_POINT ( 'NONE',  ( 15.72974639402199770, -15.80617190586745480, 48.12390960531436690 ) ) ;
#168255 = CARTESIAN_POINT ( 'NONE',  ( 12.14591786802327356, -12.06949235617739191, 45.62609039468567573 ) ) ;
#168256 = CARTESIAN_POINT ( 'NONE',  ( -19.49149378614661643, 5.499999999999580780, 69.43757513605359577 ) ) ;
#168257 = CARTESIAN_POINT ( 'NONE',  ( 19.02544592524334988, 5.153800228976608722, 46.45942372801899012 ) ) ;
#168258 = CARTESIAN_POINT ( 'NONE',  ( 16.46253265017160672, -9.564922557960803928, 88.33224293864769550 ) ) ;
#168259 = CARTESIAN_POINT ( 'NONE',  ( 16.46253265017160672, -9.564922557960803928, 23.33224293864769194 ) ) ;
#168260 = CARTESIAN_POINT ( 'NONE',  ( -16.46253265017160317, 9.564922557960807481, 55.83224293864769550 ) ) ;
#168261 = CARTESIAN_POINT ( 'NONE',  ( -21.91292544274605092, -22.94826072392755378, -49.35653942980806619 ) ) ;
#168262 = CARTESIAN_POINT ( 'NONE',  ( 5.719274019375673035, 21.55341960407619339, 82.29275706135234714 ) ) ;
#168263 = CARTESIAN_POINT ( 'NONE',  ( 17.58332526062529411, -7.635886036038496805, 93.42334959558465357 ) ) ;
#168264 = CARTESIAN_POINT ( 'NONE',  ( -19.02544592524334988, -5.153800228976617603, 33.95942372801897591 ) ) ;
#168265 = CARTESIAN_POINT ( 'NONE',  ( -21.53943276465977519, -0.05219959533937600094, 108.7510903946857042 ) ) ;
#168266 = CARTESIAN_POINT ( 'NONE',  ( 16.55341960407611168, 4.379528057220329451, 53.95724293864770260 ) ) ;
#168267 = CARTESIAN_POINT ( 'NONE',  ( -5.153800228976328057, -19.02544592524343514, 62.29057627198100988 ) ) ;
#168268 = CARTESIAN_POINT ( 'NONE',  ( -0.05219959533909027116, -19.03943276465977164, 102.4989096053143669 ) ) ;
#168269 = CARTESIAN_POINT ( 'NONE',  ( 18.62759615963255655, 10.81492255796105972, 76.66775706135234714 ) ) ;
#168270 = CARTESIAN_POINT ( 'NONE',  ( 5.049401038298161559, -19.05341960407611168, 62.70724293864769550 ) ) ;
#168271 = CARTESIAN_POINT ( 'NONE',  ( -21.53943276465977519, -0.05219959533937600094, 73.75109039468567573 ) ) ;
#168272 = CARTESIAN_POINT ( 'NONE',  ( -21.53943276465977519, 0.05219959533907696930, 36.24890960531435979 ) ) ;
#168273 = CARTESIAN_POINT ( 'NONE',  ( -10.72451020669870658, -18.67979575497194134, 34.58442372801900433 ) ) ;
#168274 = CARTESIAN_POINT ( 'NONE',  ( -0.05219959533936034679, 19.03943276465977164, 57.50109039468566863 ) ) ;
#168275 = CARTESIAN_POINT ( 'NONE',  ( 0.05219959533909260263, 19.03943276465977164, 29.99890960531435979 ) ) ;
#168276 = CARTESIAN_POINT ( 'NONE',  ( -5.049401038298153566, 19.05341960407611168, 75.20724293864769550 ) ) ;
#168277 = CARTESIAN_POINT ( 'NONE',  ( 0.05219959533934541429, -16.53943276465976808, 35.00109039468568284 ) ) ;
#168278 = CARTESIAN_POINT ( 'NONE',  ( 4.483927247898545687, 16.52544592524342804, 94.79057627198105251 ) ) ;
#168279 = CARTESIAN_POINT ( 'NONE',  ( 9.474510206698971260, -16.51473224551069308, 62.91557627198102409 ) ) ;
#168280 = CARTESIAN_POINT ( 'NONE',  ( -15.72974639402197994, 15.80617190586746368, 30.62390960531436335 ) ) ;
#168281 = CARTESIAN_POINT ( 'NONE',  ( -0.05219959533934338120, 16.53943276465976808, 22.50109039468567573 ) ) ;
#168282 = CARTESIAN_POINT ( 'NONE',  ( -21.52544592524343514, 5.823673210054127303, 116.0405762719810383 ) ) ;
#168283 = CARTESIAN_POINT ( 'NONE',  ( 21.53943276465977519, 0.05219959533937863772, 66.25109039468567573 ) ) ;
#168284 = CARTESIAN_POINT ( 'NONE',  ( 12.14591786802327356, -12.06949235617739191, 70.62609039468567573 ) ) ;
#168285 = CARTESIAN_POINT ( 'NONE',  ( -4.379528057220086978, -16.55341960407618274, 69.79275706135234714 ) ) ;
#168286 = EDGE_LOOP ( 'NONE', ( #177151, #118707, #124868, #179062, #99003, #135296, #153425, #9414 ) ) ;
#168287 = CARTESIAN_POINT ( 'NONE',  ( 9.474510206698971260, -16.51473224551069308, 62.91557627198102409 ) ) ;
#168288 = CARTESIAN_POINT ( 'NONE',  ( -0.05219959533934338120, 16.53943276465976808, 87.50109039468568994 ) ) ;
#168289 = CARTESIAN_POINT ( 'NONE',  ( -5.049401038297874678, -19.05341960407617918, 39.79275706135232582 ) ) ;
#168290 = CARTESIAN_POINT ( 'NONE',  ( -15.80617190586745835, -15.72974639402198527, 111.8739096053143669 ) ) ;
#168291 = CARTESIAN_POINT ( 'NONE',  ( -16.52544592524342804, 4.483927247898546575, 71.04057627198103830 ) ) ;
#168292 = CARTESIAN_POINT ( 'NONE',  ( 0.05219959533909260263, 19.03943276465977164, 89.99890960531436690 ) ) ;
#168293 = CARTESIAN_POINT ( 'NONE',  ( -8.314922557961024197, 14.29746914071037800, 92.91775706135236135 ) ) ;
#168294 = CARTESIAN_POINT ( 'NONE',  ( -21.53943276465977519, -0.05219959533937600094, 53.75109039468568994 ) ) ;
#168295 = CARTESIAN_POINT ( 'NONE',  ( -14.34966873604972548, 8.224510206698743886, 28.33442372801902209 ) ) ;
#168296 = CARTESIAN_POINT ( 'NONE',  ( 18.62759615963271287, -10.81492255796078972, 108.3322429386477097 ) ) ;
#168297 = CARTESIAN_POINT ( 'NONE',  ( 16.55341960407611168, 4.379528057220329451, 63.95724293864770260 ) ) ;
#168298 = ORIENTED_EDGE ( 'NONE', *, *, #72533, .T. ) ;
#168299 = CARTESIAN_POINT ( 'NONE',  ( 0.05219959533907565091, 21.53943276465977519, 94.99890960531436690 ) ) ;
#168300 = CARTESIAN_POINT ( 'NONE',  ( 8.224510206698953496, -14.34966873604960469, 37.91557627198102409 ) ) ;
#168301 = ORIENTED_EDGE ( 'NONE', *, *, #87134, .F. ) ;
#168302 = CARTESIAN_POINT ( 'NONE',  ( 35.44323460151742466, 3.757829821678515980, 38.50466947567800702 ) ) ;
#168303 = CARTESIAN_POINT ( 'NONE',  ( 9.474510206698971260, -16.51473224551069308, 112.9155762719810383 ) ) ;
#168304 = CARTESIAN_POINT ( 'NONE',  ( 0.05219959533937995610, -21.53943276465977519, 40.00109039468567573 ) ) ;
#168305 = CARTESIAN_POINT ( 'NONE',  ( -4.379528057220328563, 16.55341960407611168, 50.20724293864769550 ) ) ;
#168306 = CARTESIAN_POINT ( 'NONE',  ( -13.97604488694527625, -13.89961937509977652, 61.87390960531435979 ) ) ;
#168307 = CARTESIAN_POINT ( 'NONE',  ( 0.05219959533936267826, -19.03943276465977164, 65.00109039468567573 ) ) ;
#168308 = CARTESIAN_POINT ( 'NONE',  ( 19.03943276465977164, -0.05219959533909143690, 93.74890960531435269 ) ) ;
#168309 = EDGE_CURVE ( 'NONE', #82035, #12418, #86442, .T. ) ;
#168310 = CARTESIAN_POINT ( 'NONE',  ( 5.719274019375991003, -21.55341960407610458, 47.70724293864770260 ) ) ;
#168311 = CARTESIAN_POINT ( 'NONE',  ( -16.98531384170231817, -34.11756901830543143, -21.70785296103623452 ) ) ;
#168312 = CARTESIAN_POINT ( 'NONE',  ( 19.03943276465977164, -0.05219959533909143690, 53.74890960531436690 ) ) ;
#168313 = CARTESIAN_POINT ( 'NONE',  ( -16.52544592524335698, -4.483927247898792601, 38.95942372801901854 ) ) ;
#168314 = CARTESIAN_POINT ( 'NONE',  ( 13.97604488694548053, -13.89961937509957401, 60.62609039468564731 ) ) ;
#168315 = CARTESIAN_POINT ( 'NONE',  ( 5.823673210054444382, -21.52544592524334988, 20.20942372801900788 ) ) ;
#168316 = CARTESIAN_POINT ( 'NONE',  ( -8.224510206698948167, 14.34966873604960824, 50.41557627198103120 ) ) ;
#168317 = CARTESIAN_POINT ( 'NONE',  ( -9.564922557960796823, -16.46253265017161027, 87.08224293864769550 ) ) ;
#168318 = CARTESIAN_POINT ( 'NONE',  ( 15.80617190586746368, 15.72974639402197994, 79.37390960531436690 ) ) ;
#168320 = CARTESIAN_POINT ( 'NONE',  ( -0.05219959533934338120, 16.53943276465976808, 37.50109039468568284 ) ) ;
#168319 = CARTESIAN_POINT ( 'NONE',  ( -21.55341960407610458, -5.719274019375992779, 111.4572429386476813 ) ) ;
#168321 = CARTESIAN_POINT ( 'NONE',  ( 21.52544592524344225, -5.823673210054117533, 38.54057627198103120 ) ) ;
#168322 = CARTESIAN_POINT ( 'NONE',  ( -18.62759615963255300, -10.81492255796106328, 104.1677570613523471 ) ) ;
#168323 = CARTESIAN_POINT ( 'NONE',  ( 5.153800228976335163, 19.02544592524342804, 89.79057627198102409 ) ) ;
#168324 = CARTESIAN_POINT ( 'NONE',  ( -16.51473224551069308, -9.474510206698971260, 41.66557627198103120 ) ) ;
#168325 = CARTESIAN_POINT ( 'NONE',  ( -13.97604488694527625, -13.89961937509977652, 101.8739096053143811 ) ) ;
#168326 = B_SPLINE_CURVE_WITH_KNOTS ( 'NONE', 3,
 ( #176220, #38701, #115541, #114519, #25555, #100358, #102367, #132703, #130690, #52848, #116535, #164056, #162037, #87199, #22531, #144860, #98339, #85179, #192384, #5345 ),
 .UNSPECIFIED., .F., .F.,
 ( 4, 2, 2, 2, 2, 2, 2, 2, 2, 4 ),
 ( 0.004000878361811928755, 0.004499404418915952525, 0.004997930476019976295, 0.005496456533124000066, 0.005994982590228023836, 0.006244245618780026180, 0.006493508647332026790, 0.006992034704436006325, 0.007490560761539986727, 0.007989086818643966262 ),
 .UNSPECIFIED. ) ;
#168327 = CARTESIAN_POINT ( 'NONE',  ( 19.05341960407611168, 5.049401038298154454, 73.95724293864768129 ) ) ;
#168328 = CARTESIAN_POINT ( 'NONE',  ( -0.05219959533934338120, 16.53943276465976808, 27.50109039468567929 ) ) ;
#168329 = DIRECTION ( 'NONE',  ( 1.000000000000000000, 0.000000000000000000, -0.000000000000000000 ) ) ;
#168330 = CARTESIAN_POINT ( 'NONE',  ( 16.46253265017146816, 9.564922557961045513, 56.66775706135233293 ) ) ;
#168332 = CARTESIAN_POINT ( 'NONE',  ( -0.05219959533907301413, -21.53943276465977519, 37.49890960531436690 ) ) ;
#168331 = CARTESIAN_POINT ( 'NONE',  ( 5.823673210054444382, -21.52544592524334988, 105.2094237280190328 ) ) ;
#168333 = CARTESIAN_POINT ( 'NONE',  ( 16.55341960407618274, -4.379528057220086978, 101.0427570613523756 ) ) ;
#168334 = DIRECTION ( 'NONE',  ( -1.000000000000000000, 0.000000000000000000, 0.000000000000000000 ) ) ;
#168335 = CARTESIAN_POINT ( 'NONE',  ( -13.97604488694547697, 13.89961937509957934, 78.12609039468567573 ) ) ;
#168336 = CARTESIAN_POINT ( 'NONE',  ( -5.049401038297874678, -19.05341960407617918, 24.79275706135233648 ) ) ;
#168337 = FACE_OUTER_BOUND ( 'NONE', #176750, .T. ) ;
#168338 = CARTESIAN_POINT ( 'NONE',  ( 9.474510206698971260, -16.51473224551069308, 37.91557627198102409 ) ) ;
#168339 = CARTESIAN_POINT ( 'NONE',  ( -4.379528057220328563, 16.55341960407611168, 40.20724293864769550 ) ) ;
#168340 = CARTESIAN_POINT ( 'NONE',  ( -19.03943276465977164, 0.05219959533909376836, 26.24890960531435624 ) ) ;
#168341 = CARTESIAN_POINT ( 'NONE',  ( -16.53943276465976808, -0.05219959533934237506, 113.7510903946856757 ) ) ;
#168342 = CARTESIAN_POINT ( 'NONE',  ( 20.74300244486288847, -20.19516923136415443, -52.60240525300990555 ) ) ;
#168343 = CARTESIAN_POINT ( 'NONE',  ( 16.55341960407618274, -4.379528057220086978, 91.04275706135236135 ) ) ;
#168344 = CARTESIAN_POINT ( 'NONE',  ( -19.05341960407611168, -5.049401038298163336, 46.45724293864768129 ) ) ;
#168345 = CARTESIAN_POINT ( 'NONE',  ( 21.52544592524334988, 5.823673210054432836, 101.4594237280190185 ) ) ;
#168346 = CARTESIAN_POINT ( 'NONE',  ( 14.34966873604972726, -8.224510206698740333, 25.83442372801901499 ) ) ;
#168348 = ORIENTED_EDGE ( 'NONE', *, *, #58299, .F. ) ;
#168347 = CARTESIAN_POINT ( 'NONE',  ( 10.72451020669871369, 18.67979575497193778, 77.08442372801901854 ) ) ;
#168349 = CARTESIAN_POINT ( 'NONE',  ( 19.03943276465977164, 0.05219959533936151252, 61.25109039468566863 ) ) ;
#168350 = CARTESIAN_POINT ( 'NONE',  ( -19.03943276465977164, 0.05219959533909376836, 86.24890960531436690 ) ) ;
#168351 = CARTESIAN_POINT ( 'NONE',  ( 13.89961937509977652, -13.97604488694527269, 83.12390960531436690 ) ) ;
#168352 = CARTESIAN_POINT ( 'NONE',  ( 36.91746824999999177, 2.880721459617395097E-14, -5.624999997268813168 ) ) ;
#168353 = CARTESIAN_POINT ( 'NONE',  ( -5.719274019375978568, 21.55341960407610458, 115.2072429386476955 ) ) ;
#168354 = CARTESIAN_POINT ( 'NONE',  ( -14.34966873604960291, -8.224510206698953496, 71.66557627198100988 ) ) ;
#168355 = CARTESIAN_POINT ( 'NONE',  ( 21.53943276465977519, -0.05219959533907433946, 58.74890960531436690 ) ) ;
#168356 = CARTESIAN_POINT ( 'NONE',  ( -19.05341960407611168, -5.049401038298163336, 56.45724293864768129 ) ) ;
#168358 = CARTESIAN_POINT ( 'NONE',  ( -12.06949235617739369, -12.14591786802326823, 84.37609039468570415 ) ) ;
#168357 = CARTESIAN_POINT ( 'NONE',  ( 18.62759615963271287, -10.81492255796078972, 93.33224293864769550 ) ) ;
#168359 = EDGE_LOOP ( 'NONE', ( #89145, #17985, #77037, #133659, #178125 ) ) ;
#168360 = CARTESIAN_POINT ( 'NONE',  ( -5.153800228976328057, -19.02544592524343514, 57.29057627198103120 ) ) ;
#168362 = CARTESIAN_POINT ( 'NONE',  ( -6.434671708797631950, -6.434671708797536027, -63.95112321872120731 ) ) ;
#168361 = CARTESIAN_POINT ( 'NONE',  ( -8.224510206698948167, 14.34966873604960824, 95.41557627198102409 ) ) ;
#168363 = CARTESIAN_POINT ( 'NONE',  ( -16.51473224551069308, -9.474510206698971260, 51.66557627198102409 ) ) ;
#168364 = CARTESIAN_POINT ( 'NONE',  ( -0.05219959533936034679, 19.03943276465977164, 77.50109039468566152 ) ) ;
#168365 = CARTESIAN_POINT ( 'NONE',  ( 16.53943276465976808, -0.05219959533910856209, 78.74890960531436690 ) ) ;
#168366 = CARTESIAN_POINT ( 'NONE',  ( -10.72451020669870658, -18.67979575497194134, 64.58442372801900433 ) ) ;
#168368 = CARTESIAN_POINT ( 'NONE',  ( 5.719274019375991003, -21.55341960407610458, 102.7072429386476955 ) ) ;
#168367 = CARTESIAN_POINT ( 'NONE',  ( 0.05219959533909260263, 19.03943276465977164, 39.99890960531436690 ) ) ;
#168369 = CARTESIAN_POINT ( 'NONE',  ( 12.06949235617757843, -12.14591786802309237, 98.12390960531436690 ) ) ;
#168370 = CARTESIAN_POINT ( 'NONE',  ( 8.906447517083050158, 27.41122689804195645, 147.6500000054623740 ) ) ;
#168371 = CARTESIAN_POINT ( 'NONE',  ( 9.564922557960805705, 16.46253265017160317, 54.58224293864769550 ) ) ;
#168372 = CARTESIAN_POINT ( 'NONE',  ( -11.69814101308375065, -11.91922547854696113, -61.34707691135562158 ) ) ;
#168374 = CARTESIAN_POINT ( 'NONE',  ( 9.564922557960805705, 16.46253265017160317, 114.5822429386476955 ) ) ;
#168373 = CARTESIAN_POINT ( 'NONE',  ( -5.049401038297874678, -19.05341960407617918, 94.79275706135230450 ) ) ;
#168375 = CARTESIAN_POINT ( 'NONE',  ( -15.80617190586768217, 15.72974639402176855, 33.12609039468569705 ) ) ;
#168376 = CARTESIAN_POINT ( 'NONE',  ( -5.153800228976328057, -19.02544592524343514, 82.29057627198103830 ) ) ;
#168377 =( BOUNDED_CURVE ( )  B_SPLINE_CURVE ( 2, ( #162897, #24406, #197242, #135570, #147744, #165905, #194254, #104224, #196264, #56735, #55721, #41567, #102230, #117393, #72908, #179092, #27403, #40561, #25415, #180099, #148742, #134577, #26406, #58703, #89048, #57733, #73900, #43549, #991, #31354, #186040, #140510, #106197, #91999, #110174, #153693, #48520, #152697, #155683, #77841, #167881, #29380, #1999, #183058, #91011, #185033, #14186, #108179, #79838, #169860, #141508, #138519, #93005, #18181, #16186, #199213, #123340, #46520, #63678, #154691, #139508, #125353, #187050, #171853, #62665, #75855, #156687, #2993, #15189, #61671, #33341 ),
 .UNSPECIFIED., .F., .T. ) 
 B_SPLINE_CURVE_WITH_KNOTS ( ( 3, 2, 2, 2, 2, 2, 2, 2, 2, 2, 2, 2, 2, 2, 2, 2, 2, 2, 2, 2, 2, 2, 2, 2, 2, 2, 2, 2, 2, 2, 2, 2, 2, 2, 2, 3 ),
 ( 0.000000000000000000, 0.02000000000000000042, 0.04000000000000000083, 0.05999999999999999084, 0.08000000000000000167, 0.1000000000000000056, 0.1199999999999999817, 0.1400000000000000133, 0.1600000000000000033, 0.1799999999999999933, 0.2000000000000000111, 0.2200000000000000011, 0.2399999999999999634, 0.2600000000000000089, 0.2800000000000000266, 0.2999999999999999889, 0.3200000000000000067, 0.3400000000000000244, 0.3599999999999999867, 0.3799999999999999489, 0.4000000000000000222, 0.4199999999999999845, 0.4400000000000000022, 0.4600000000000000200, 0.4799999999999999267, 0.5000000000000000000, 0.5200000000000000178, 0.5400000000000000355, 0.5600000000000000533, 0.5799999999999999600, 0.5999999999999999778, 0.6199999999999999956, 0.6400000000000000133, 0.6600000000000000311, 0.6800000000000000488, 0.6875575298689686754 ),
 .UNSPECIFIED. ) 
 CURVE ( )  GEOMETRIC_REPRESENTATION_ITEM ( )  RATIONAL_B_SPLINE_CURVE ( ( 1.000000000000000000, 0.9510565162951535312, 1.000000000000000000, 0.9510565162951535312, 1.000000000000000000, 0.9510565162951535312, 1.000000000000000000, 0.9510565162951535312, 1.000000000000000000, 0.9510565162951535312, 1.000000000000000000, 0.9510565162951535312, 1.000000000000000000, 0.9510565162951535312, 1.000000000000000000, 0.9510565162951535312, 1.000000000000000000, 0.9510565162951535312, 1.000000000000000000, 0.9510565162951535312, 1.000000000000000000, 0.9510565162951535312, 1.000000000000000000, 0.9510565162951535312, 1.000000000000000000, 0.9510565162951535312, 1.000000000000000000, 0.9510565162951535312, 1.000000000000000000, 0.9510565162951535312, 1.000000000000000000, 0.9510565162951535312, 1.000000000000000000, 0.9510565162951535312, 1.000000000000000000, 0.9510565162951535312, 1.000000000000000000, 0.9510565162951535312, 1.000000000000000000, 0.9510565162951535312, 1.000000000000000000, 0.9510565162951535312, 1.000000000000000000, 0.9510565162951535312, 1.000000000000000000, 0.9510565162951535312, 1.000000000000000000, 0.9510565162951535312, 1.000000000000000000, 0.9510565162951535312, 1.000000000000000000, 0.9510565162951535312, 1.000000000000000000, 0.9510565162951535312, 1.000000000000000000, 0.9510565162951535312, 1.000000000000000000, 0.9510565162951535312, 1.000000000000000000, 0.9510565162951535312, 1.000000000000000000, 0.9510565162951535312, 1.000000000000000000, 0.9510565162951535312, 1.000000000000000000, 0.9510565162951535312, 1.000000000000000000, 0.9510565162951535312, 1.000000000000000000, 0.9815054080004621540, 0.9769881591460138903 ) ) 
 REPRESENTATION_ITEM ( '' )  );
#168378 = CARTESIAN_POINT ( 'NONE',  ( 19.02544592524334988, 5.153800228976608722, 66.45942372801899012 ) ) ;
#168379 = CARTESIAN_POINT ( 'NONE',  ( -19.03943276465977164, 0.05219959533909376836, 61.24890960531436690 ) ) ;
#168380 = CARTESIAN_POINT ( 'NONE',  ( 16.53943276465976808, -0.05219959533910856209, 78.74890960531436690 ) ) ;
#168381 = CARTESIAN_POINT ( 'NONE',  ( 14.29746914071049879, -8.314922557960816363, 68.33224293864769550 ) ) ;
#168382 = CARTESIAN_POINT ( 'NONE',  ( 19.03943276465977164, -0.05219959533909143690, 83.74890960531436690 ) ) ;
#168383 = CARTESIAN_POINT ( 'NONE',  ( 16.52544592524342804, -4.483927247898539470, 83.54057627198102409 ) ) ;
#168384 = CARTESIAN_POINT ( 'NONE',  ( 16.51473224551069308, 9.474510206698969483, 79.16557627198103830 ) ) ;
#168385 = CARTESIAN_POINT ( 'NONE',  ( -13.89961937509957401, -13.97604488694547875, 34.37609039468566863 ) ) ;
#168388 = CARTESIAN_POINT ( 'NONE',  ( -0.05219959533910754901, -16.53943276465976808, 107.4989096053143669 ) ) ;
#168387 = CARTESIAN_POINT ( 'NONE',  ( -16.53943276465976808, 0.05219959533911058130, 31.24890960531435979 ) ) ;
#168386 = CARTESIAN_POINT ( 'NONE',  ( 9.564922557960805705, 16.46253265017160317, 54.58224293864769550 ) ) ;
#168389 = ORIENTED_EDGE ( 'NONE', *, *, #65754, .T. ) ;
#168390 = CARTESIAN_POINT ( 'NONE',  ( -21.55341960407619339, 5.719274019375674811, 48.54275706135234714 ) ) ;
#168391 = CARTESIAN_POINT ( 'NONE',  ( -13.89961937509957401, -13.97604488694547875, 64.37609039468567573 ) ) ;
#168392 = CARTESIAN_POINT ( 'NONE',  ( -12.06949235617756955, 12.14591786802309770, 40.62390960531435269 ) ) ;
#168393 = CARTESIAN_POINT ( 'NONE',  ( 10.81492255796078972, 18.62759615963270932, 89.58224293864768129 ) ) ;
#168394 = CARTESIAN_POINT ( 'NONE',  ( -18.62759615963270932, 10.81492255796079327, 25.83224293864769194 ) ) ;
#168395 = CARTESIAN_POINT ( 'NONE',  ( -14.34966873604960291, -8.224510206698953496, 76.66557627198103830 ) ) ;
#168396 = CARTESIAN_POINT ( 'NONE',  ( -13.97604488694527625, -13.89961937509977652, 46.87390960531435979 ) ) ;
#168397 = CARTESIAN_POINT ( 'NONE',  ( -13.89961937509957401, -13.97604488694547875, 29.37609039468565797 ) ) ;
#168398 = CARTESIAN_POINT ( 'NONE',  ( -4.483927247898782831, 16.52544592524335698, 97.70942372801904696 ) ) ;
#168399 = CARTESIAN_POINT ( 'NONE',  ( 0.05219959533934541429, -16.53943276465976808, 55.00109039468568284 ) ) ;
#168400 = CARTESIAN_POINT ( 'NONE',  ( -5.719274019375978568, 21.55341960407610458, 30.20724293864769550 ) ) ;
#168401 = CARTESIAN_POINT ( 'NONE',  ( -0.05219959533937732626, 21.53943276465977519, 112.5010903946857042 ) ) ;
#168402 = CARTESIAN_POINT ( 'NONE',  ( 16.51473224551069308, 9.474510206698969483, 99.16557627198102409 ) ) ;
#168403 = CARTESIAN_POINT ( 'NONE',  ( -8.224510206698735004, -14.34966873604973081, 69.58442372801900433 ) ) ;
#168404 = CARTESIAN_POINT ( 'NONE',  ( -5.153800228976328057, -19.02544592524343514, 27.29057627198103120 ) ) ;
#168405 = CARTESIAN_POINT ( 'NONE',  ( 16.52544592524342804, -4.483927247898539470, 28.54057627198103120 ) ) ;
#168407 = CARTESIAN_POINT ( 'NONE',  ( 5.049401038298161559, -19.05341960407611168, 92.70724293864769550 ) ) ;
#168406 = CARTESIAN_POINT ( 'NONE',  ( 5.049401038298161559, -19.05341960407611168, 102.7072429386476955 ) ) ;
#168408 = CARTESIAN_POINT ( 'NONE',  ( -15.72974639402197994, 15.80617190586746368, 25.62390960531435624 ) ) ;
#168409 = CARTESIAN_POINT ( 'NONE',  ( -14.29746914071049879, 8.314922557960819915, 60.83224293864769550 ) ) ;
#168410 = EDGE_CURVE ( 'NONE', #193436, #162084, #118500, .T. ) ;
#168411 = CARTESIAN_POINT ( 'NONE',  ( -16.52544592524342804, 4.483927247898546575, 36.04057627198102409 ) ) ;
#168412 = CARTESIAN_POINT ( 'NONE',  ( -16.52544592524342804, 4.483927247898546575, 46.04057627198103830 ) ) ;
#168414 = CARTESIAN_POINT ( 'NONE',  ( -7.143419655154886527, -2.300691058039395553, 1.353258418600862045 ) ) ;
#168413 = CARTESIAN_POINT ( 'NONE',  ( 14.34966873604972726, -8.224510206698740333, 45.83442372801901854 ) ) ;
#168415 = CARTESIAN_POINT ( 'NONE',  ( 9.564922557961047289, -16.46253265017146816, 55.41775706135234003 ) ) ;
#168416 = CARTESIAN_POINT ( 'NONE',  ( 5.153800228976335163, 19.02544592524342804, 94.79057627198103830 ) ) ;
#168417 = CARTESIAN_POINT ( 'NONE',  ( -0.05219959533936034679, 19.03943276465977164, 67.50109039468566152 ) ) ;
#168418 = CARTESIAN_POINT ( 'NONE',  ( 1.784210473542230573E-15, -29.16686587814331588, 141.8750000027311842 ) ) ;
#168419 = CARTESIAN_POINT ( 'NONE',  ( -13.97604488694547697, 13.89961937509957934, 58.12609039468566863 ) ) ;
#168421 = CARTESIAN_POINT ( 'NONE',  ( 16.53943276465976808, 0.05219959533934440121, 81.25109039468568994 ) ) ;
#168420 = CARTESIAN_POINT ( 'NONE',  ( -0.05219959533936034679, 19.03943276465977164, 92.50109039468566152 ) ) ;
#168422 = CARTESIAN_POINT ( 'NONE',  ( 17.14385361876520264, -23.59649016807271238, 146.0750000027311728 ) ) ;
#168423 = CARTESIAN_POINT ( 'NONE',  ( 19.03943276465977164, -0.05219959533909143690, 23.74890960531435269 ) ) ;
#168424 = CARTESIAN_POINT ( 'NONE',  ( 19.02544592524343514, -5.153800228976328945, 113.5405762719810241 ) ) ;
#168425 = CARTESIAN_POINT ( 'NONE',  ( -10.72451020669870658, -18.67979575497194134, 39.58442372801901143 ) ) ;
#168426 = CARTESIAN_POINT ( 'NONE',  ( 19.03943276465977164, 0.05219959533936151252, 101.2510903946856757 ) ) ;
#168428 = CARTESIAN_POINT ( 'NONE',  ( 19.03943276465977164, -0.05219959533909143690, 58.74890960531435979 ) ) ;
#168427 = PLANE ( 'NONE',  #8803 ) ;
#168429 = CARTESIAN_POINT ( 'NONE',  ( 16.46253265017160672, -9.564922557960803928, 108.3322429386476955 ) ) ;
#168431 = CARTESIAN_POINT ( 'NONE',  ( 19.02544592524343514, -5.153800228976328945, 63.54057627198103830 ) ) ;
#168430 = CARTESIAN_POINT ( 'NONE',  ( -12.06949235617756955, 12.14591786802309770, 75.62390960531439532 ) ) ;
#168432 = CARTESIAN_POINT ( 'NONE',  ( 13.97604488694527802, 13.89961937509977652, 69.37390960531436690 ) ) ;
#168433 = CARTESIAN_POINT ( 'NONE',  ( 9.474510206698729675, 16.51473224551082808, 77.08442372801900433 ) ) ;
#168434 = CARTESIAN_POINT ( 'NONE',  ( 18.62759615963271287, -10.81492255796078972, 53.33224293864769550 ) ) ;
#168435 = CARTESIAN_POINT ( 'NONE',  ( 9.474510206698971260, -16.51473224551069308, 22.91557627198102765 ) ) ;
#168436 = CARTESIAN_POINT ( 'NONE',  ( 5.049401038297881783, 19.05341960407617563, 37.29275706135232582 ) ) ;
#168437 = CARTESIAN_POINT ( 'NONE',  ( 5.153800228976335163, 19.02544592524342804, 74.79057627198103830 ) ) ;
#168438 = CARTESIAN_POINT ( 'NONE',  ( -18.67979575497178146, -10.72451020669898902, 71.66557627198100988 ) ) ;
#168440 = CARTESIAN_POINT ( 'NONE',  ( 19.05341960407617918, -5.049401038297876454, 46.04275706135233293 ) ) ;
#168439 = CARTESIAN_POINT ( 'NONE',  ( -16.55341960407611168, -4.379528057220339221, 76.45724293864769550 ) ) ;
#168441 = CARTESIAN_POINT ( 'NONE',  ( -0.05219959533907301413, -21.53943276465977519, 72.49890960531435269 ) ) ;
#168442 = CARTESIAN_POINT ( 'NONE',  ( -21.52544592524343514, 5.823673210054127303, 61.04057627198103120 ) ) ;
#168443 = CARTESIAN_POINT ( 'NONE',  ( 18.62759615963271287, -10.81492255796078972, 33.33224293864769550 ) ) ;
#168444 = CARTESIAN_POINT ( 'NONE',  ( 21.53943276465977519, 0.05219959533937863772, 96.25109039468568994 ) ) ;
#168445 = CARTESIAN_POINT ( 'NONE',  ( -9.564922557960796823, -16.46253265017161027, 67.08224293864769550 ) ) ;
#168446 = CARTESIAN_POINT ( 'NONE',  ( 4.483927247898545687, 16.52544592524342804, 109.7905762719810383 ) ) ;
#168447 = EDGE_CURVE ( 'NONE', #147006, #65515, #140986, .T. ) ;
#168448 = CARTESIAN_POINT ( 'NONE',  ( -10.81492255796105439, 18.62759615963255655, 22.91775706135235069 ) ) ;
#168449 = CARTESIAN_POINT ( 'NONE',  ( -5.823673210054431948, 21.52544592524334988, 37.70942372801900433 ) ) ;
#168450 = CARTESIAN_POINT ( 'NONE',  ( -0.05219959533909027116, -19.03943276465977164, 37.49890960531436690 ) ) ;
#168451 = CARTESIAN_POINT ( 'NONE',  ( -18.62759615963270932, 10.81492255796079327, 105.8322429386476955 ) ) ;
#168452 = CARTESIAN_POINT ( 'NONE',  ( -16.51473224551082808, 9.474510206698731452, 48.33442372801900433 ) ) ;
#168453 = CARTESIAN_POINT ( 'NONE',  ( -9.474510206698964154, 16.51473224551069663, 35.41557627198102409 ) ) ;
#168454 = CARTESIAN_POINT ( 'NONE',  ( -19.03943276465977164, 0.05219959533909376836, 26.24890960531435624 ) ) ;
#168455 = CARTESIAN_POINT ( 'NONE',  ( 30.00000000000000000, -1.163414459189985801E-14, 95.00000000000000000 ) ) ;
#168456 = CARTESIAN_POINT ( 'NONE',  ( -16.52544592524335698, -4.483927247898792601, 58.95942372801902565 ) ) ;
#168457 = CARTESIAN_POINT ( 'NONE',  ( -16.46253265017160317, 9.564922557960807481, 25.83224293864769194 ) ) ;
#168458 = CARTESIAN_POINT ( 'NONE',  ( -21.88033147701211689, -9.239123595180315007, 171.1226046679803403 ) ) ;
#168459 = CARTESIAN_POINT ( 'NONE',  ( 5.153800228976335163, 19.02544592524342804, 79.79057627198102409 ) ) ;
#168460 = CARTESIAN_POINT ( 'NONE',  ( -12.14591786802309592, -12.06949235617757132, 101.8739096053143811 ) ) ;
#168461 = CARTESIAN_POINT ( 'NONE',  ( 18.67979575497178502, 10.72451020669898547, 54.16557627198103120 ) ) ;
#168462 = CARTESIAN_POINT ( 'NONE',  ( -0.05219959533934338120, 16.53943276465976808, 52.50109039468567573 ) ) ;
#168463 = CARTESIAN_POINT ( 'NONE',  ( -10.72451020669870658, -18.67979575497194134, 104.5844237280190185 ) ) ;
#168464 = CARTESIAN_POINT ( 'NONE',  ( 19.05341960407611168, 5.049401038298154454, 23.95724293864769194 ) ) ;
#168465 = CARTESIAN_POINT ( 'NONE',  ( 4.379528057220092307, 16.55341960407617563, 107.2927570613523471 ) ) ;
#168466 = CARTESIAN_POINT ( 'NONE',  ( 12.06949235617757843, -12.14591786802309237, 53.12390960531436690 ) ) ;
#168467 = CARTESIAN_POINT ( 'NONE',  ( -16.51473224551069308, -9.474510206698971260, 46.66557627198102409 ) ) ;
#168468 = CARTESIAN_POINT ( 'NONE',  ( -15.80617190586768217, 15.72974639402176855, 113.1260903946856899 ) ) ;
#168469 = CARTESIAN_POINT ( 'NONE',  ( -15.80617190586768217, 15.72974639402176855, 28.12609039468568284 ) ) ;
#168470 = CARTESIAN_POINT ( 'NONE',  ( -18.62759615963255300, -10.81492255796106328, 74.16775706135231871 ) ) ;
#168471 = CARTESIAN_POINT ( 'NONE',  ( -16.53943276465976808, -0.05219959533934237506, 53.75109039468568994 ) ) ;
#168472 = CARTESIAN_POINT ( 'NONE',  ( -4.379528057220086978, -16.55341960407618274, 34.79275706135235424 ) ) ;
#168474 = CARTESIAN_POINT ( 'NONE',  ( -21.52544592524334988, -5.823673210054445271, 103.9594237280190185 ) ) ;
#168473 = CARTESIAN_POINT ( 'NONE',  ( -12.06949235617756955, 12.14591786802309770, 75.62390960531439532 ) ) ;
#168475 = CARTESIAN_POINT ( 'NONE',  ( 14.34966873604960469, 8.224510206698951720, 29.16557627198103120 ) ) ;
#168476 = CARTESIAN_POINT ( 'NONE',  ( -16.21995358207305671, 7.366697692864169866, 114.9355100151216078 ) ) ;
#168477 = CARTESIAN_POINT ( 'NONE',  ( 8.314922557961029526, -14.29746914071037800, 35.41775706135234003 ) ) ;
#168478 = CARTESIAN_POINT ( 'NONE',  ( 12.06949235617757843, -12.14591786802309237, 48.12390960531436690 ) ) ;
#168479 = CARTESIAN_POINT ( 'NONE',  ( 12.06949235617739724, 12.14591786802326823, 81.87609039468568994 ) ) ;
#168480 = CARTESIAN_POINT ( 'NONE',  ( 16.51473224551069308, 9.474510206698969483, 99.16557627198102409 ) ) ;
#168481 = CARTESIAN_POINT ( 'NONE',  ( 13.89961937509977652, -13.97604488694527269, 113.1239096053143527 ) ) ;
#168482 = CARTESIAN_POINT ( 'NONE',  ( 21.53943276465977519, 0.05219959533937863772, 96.25109039468568994 ) ) ;
#168483 = CARTESIAN_POINT ( 'NONE',  ( -16.55341960407617563, 4.379528057220093196, 98.54275706135234714 ) ) ;
#168484 = CARTESIAN_POINT ( 'NONE',  ( -16.55341960407611168, -4.379528057220339221, 81.45724293864769550 ) ) ;
#168485 = CARTESIAN_POINT ( 'NONE',  ( 13.97604488694527802, 13.89961937509977652, 84.37390960531433848 ) ) ;
#168486 = VERTEX_POINT ( 'NONE', #8611 ) ;
#168487 = CARTESIAN_POINT ( 'NONE',  ( 16.52544592524335698, 4.483927247898782831, 41.45942372801901143 ) ) ;
#168488 = CARTESIAN_POINT ( 'NONE',  ( -13.89961937509977652, 13.97604488694528158, 45.62390960531433848 ) ) ;
#168489 = CARTESIAN_POINT ( 'NONE',  ( 16.46253265017160672, -9.564922557960803928, 103.3322429386476955 ) ) ;
#168491 = CARTESIAN_POINT ( 'NONE',  ( 11.40812507854755253, -35.11059874428192273, -2.024999997268813079 ) ) ;
#168490 = CARTESIAN_POINT ( 'NONE',  ( 8.224510206698742110, 14.34966873604972548, 27.08442372801901854 ) ) ;
#168492 = CARTESIAN_POINT ( 'NONE',  ( 19.02544592524334988, 5.153800228976608722, 41.45942372801900433 ) ) ;
#168493 = CARTESIAN_POINT ( 'NONE',  ( -16.55341960407617563, 4.379528057220093196, 103.5427570613523613 ) ) ;
#168494 = CARTESIAN_POINT ( 'NONE',  ( 16.51473224551069308, 9.474510206698969483, 29.16557627198103475 ) ) ;
#168495 = CARTESIAN_POINT ( 'NONE',  ( -14.34966873604972548, 8.224510206698743886, 73.33442372801901854 ) ) ;
#168496 = CARTESIAN_POINT ( 'NONE',  ( -5.049401038297874678, -19.05341960407617918, 79.79275706135233293 ) ) ;
#168497 = CARTESIAN_POINT ( 'NONE',  ( -9.564922557961040184, 16.46253265017147172, 32.91775706135233293 ) ) ;
#168498 = CARTESIAN_POINT ( 'NONE',  ( 19.03943276465977164, -0.05219959533909143690, 63.74890960531435979 ) ) ;
#168499 = CARTESIAN_POINT ( 'NONE',  ( -16.53943276465976808, 0.05219959533911058130, 101.2489096053143669 ) ) ;
#168500 = EDGE_CURVE ( 'NONE', #120670, #58517, #26096, .T. ) ;
#168501 = CARTESIAN_POINT ( 'NONE',  ( -0.05219959533936034679, 19.03943276465977164, 62.50109039468566863 ) ) ;
#168502 = CARTESIAN_POINT ( 'NONE',  ( -5.823673210054116645, -21.52544592524344225, 67.29057627198103830 ) ) ;
#168503 = CARTESIAN_POINT ( 'NONE',  ( 13.89961937509957401, 13.97604488694547697, 21.87609039468566152 ) ) ;
#168504 = CARTESIAN_POINT ( 'NONE',  ( 0.05219959533909260263, 19.03943276465977164, 109.9989096053143669 ) ) ;
#168505 = CARTESIAN_POINT ( 'NONE',  ( -21.52544592524343514, 5.823673210054127303, 71.04057627198103830 ) ) ;
#168506 = CARTESIAN_POINT ( 'NONE',  ( 0.05219959533909260263, 19.03943276465977164, 109.9989096053143669 ) ) ;
#168507 = CARTESIAN_POINT ( 'NONE',  ( -9.564922557961040184, 16.46253265017147172, 102.9177570613523329 ) ) ;
#168508 = CARTESIAN_POINT ( 'NONE',  ( -17.50000000000000355, 4.013004640162589176, 110.4460572099441009 ) ) ;
#168509 = CARTESIAN_POINT ( 'NONE',  ( 16.55341960407618274, -4.379528057220086978, 21.04275706135234714 ) ) ;
#168510 = CARTESIAN_POINT ( 'NONE',  ( -5.049401038298153566, 19.05341960407611168, 35.20724293864768839 ) ) ;
#168511 = CARTESIAN_POINT ( 'NONE',  ( -5.153800228976328057, -19.02544592524343514, 92.29057627198099567 ) ) ;
#168512 = CARTESIAN_POINT ( 'NONE',  ( -15.72974639402197994, 15.80617190586746368, 85.62390960531436690 ) ) ;
#168513 = CARTESIAN_POINT ( 'NONE',  ( -14.34966873604972548, 8.224510206698743886, 58.33442372801901143 ) ) ;
#168514 = CARTESIAN_POINT ( 'NONE',  ( -18.67979575497193778, 10.72451020669871902, 58.33442372801901143 ) ) ;
#168516 = CARTESIAN_POINT ( 'NONE',  ( -10.72451020669870658, -18.67979575497194134, 109.5844237280190328 ) ) ;
#168515 = CARTESIAN_POINT ( 'NONE',  ( 16.46253265017146816, 9.564922557961045513, 101.6677570613523329 ) ) ;
#168517 = CARTESIAN_POINT ( 'NONE',  ( -8.314922557960811034, -14.29746914071050412, 22.08224293864769194 ) ) ;
#168518 = CARTESIAN_POINT ( 'NONE',  ( 21.55341960407610458, 5.719274019375980345, 98.95724293864770971 ) ) ;
#168519 = CARTESIAN_POINT ( 'NONE',  ( -14.34966873604960291, -8.224510206698953496, 41.66557627198103120 ) ) ;
#168520 = CARTESIAN_POINT ( 'NONE',  ( -13.97604488694547697, 13.89961937509957934, 88.12609039468563310 ) ) ;
#168521 = CARTESIAN_POINT ( 'NONE',  ( -21.53943276465977519, -0.05219959533937600094, 53.75109039468568994 ) ) ;
#168522 = CARTESIAN_POINT ( 'NONE',  ( 19.05341960407617918, -5.049401038297876454, 46.04275706135233293 ) ) ;
#168523 = CARTESIAN_POINT ( 'NONE',  ( -14.29746914071049879, 8.314922557960819915, 110.8322429386476955 ) ) ;
#168524 = CARTESIAN_POINT ( 'NONE',  ( 18.62759615963271287, -10.81492255796078972, 28.33224293864769550 ) ) ;
#168525 = CARTESIAN_POINT ( 'NONE',  ( 16.53943276465976808, -0.05219959533910856209, 38.74890960531435979 ) ) ;
#168526 = CARTESIAN_POINT ( 'NONE',  ( 10.81492255796106328, -18.62759615963255655, 105.4177570613523613 ) ) ;
#168527 = CARTESIAN_POINT ( 'NONE',  ( -14.34966873604972548, 8.224510206698743886, 68.33442372801900433 ) ) ;
#168528 = CARTESIAN_POINT ( 'NONE',  ( 14.29746914071049879, -8.314922557960816363, 28.33224293864769550 ) ) ;
#168529 = CARTESIAN_POINT ( 'NONE',  ( -0.05219959533937732626, 21.53943276465977519, 62.50109039468568284 ) ) ;
#168530 = CARTESIAN_POINT ( 'NONE',  ( -21.55341960407619339, 5.719274019375674811, 53.54275706135234714 ) ) ;
#168531 = CARTESIAN_POINT ( 'NONE',  ( 13.97604488694527802, 13.89961937509977652, 29.37390960531435979 ) ) ;
#168532 = CARTESIAN_POINT ( 'NONE',  ( 0.05219959533937995610, -21.53943276465977519, 40.00109039468567573 ) ) ;
#168533 = CARTESIAN_POINT ( 'NONE',  ( 12.06949235617757843, -12.14591786802309237, 113.1239096053143953 ) ) ;
#168534 = CARTESIAN_POINT ( 'NONE',  ( -16.46253265017160317, 9.564922557960807481, 40.83224293864769550 ) ) ;
#168535 = CARTESIAN_POINT ( 'NONE',  ( -4.483927247898539470, -16.52544592524342804, 82.29057627198103830 ) ) ;
#168536 = CARTESIAN_POINT ( 'NONE',  ( -5.049401038298153566, 19.05341960407611168, 85.20724293864766707 ) ) ;
#168537 = CARTESIAN_POINT ( 'NONE',  ( -12.14591786802309592, -12.06949235617757132, 31.87390960531435979 ) ) ;
#168538 = CARTESIAN_POINT ( 'NONE',  ( 0.05219959533907565091, 21.53943276465977519, 54.99890960531435269 ) ) ;
#168539 = CARTESIAN_POINT ( 'NONE',  ( 5.823673210054125526, 21.52544592524343514, 104.7905762719810241 ) ) ;
#168540 = CARTESIAN_POINT ( 'NONE',  ( 13.97604488694527802, 13.89961937509977652, 99.37390960531436690 ) ) ;
#168542 = CARTESIAN_POINT ( 'NONE',  ( -5.049401038297874678, -19.05341960407617918, 99.79275706135234714 ) ) ;
#168541 = CARTESIAN_POINT ( 'NONE',  ( 5.049401038298161559, -19.05341960407611168, 62.70724293864769550 ) ) ;
#168543 = CARTESIAN_POINT ( 'NONE',  ( 15.72974639402199770, -15.80617190586745480, 63.12390960531435979 ) ) ;
#168544 = CARTESIAN_POINT ( 'NONE',  ( -15.80617190586768217, 15.72974639402176855, 83.12609039468568994 ) ) ;
#168545 = CARTESIAN_POINT ( 'NONE',  ( -9.564922557960796823, -16.46253265017161027, 72.08224293864770971 ) ) ;
#168546 = CARTESIAN_POINT ( 'NONE',  ( -9.564922557960796823, -16.46253265017161027, 92.08224293864769550 ) ) ;
#168547 = CARTESIAN_POINT ( 'NONE',  ( -14.34966873604972548, 8.224510206698743886, 73.33442372801901854 ) ) ;
#168548 = CARTESIAN_POINT ( 'NONE',  ( -5.719274019375665041, -21.55341960407619695, 59.79275706135234714 ) ) ;
#168549 = CARTESIAN_POINT ( 'NONE',  ( 21.52544592524334988, 5.823673210054432836, 91.45942372801901854 ) ) ;
#168550 = CARTESIAN_POINT ( 'NONE',  ( 21.52544592524344225, -5.823673210054117533, 108.5405762719810241 ) ) ;
#168551 = CARTESIAN_POINT ( 'NONE',  ( -8.224510206698735004, -14.34966873604973081, 79.58442372801903275 ) ) ;
#168552 = CARTESIAN_POINT ( 'NONE',  ( -15.72974639402197994, 15.80617190586746368, 70.62390960531436690 ) ) ;
#168553 = CARTESIAN_POINT ( 'NONE',  ( -9.564922557961040184, 16.46253265017147172, 47.91775706135233293 ) ) ;
#168554 = CARTESIAN_POINT ( 'NONE',  ( -10.72451020669898014, 18.67979575497178502, 40.41557627198103120 ) ) ;
#168556 = CARTESIAN_POINT ( 'NONE',  ( 16.53943276465976808, -0.05219959533910856209, 23.74890960531435269 ) ) ;
#168555 = CARTESIAN_POINT ( 'NONE',  ( -0.05219959533909027116, -19.03943276465977164, 87.49890960531436690 ) ) ;
#168557 = CARTESIAN_POINT ( 'NONE',  ( -17.31728774477274158, 6.344390552232390235, 65.81906651689320142 ) ) ;
#168558 = CARTESIAN_POINT ( 'NONE',  ( -0.05219959533907301413, -21.53943276465977519, 27.49890960531435269 ) ) ;
#168559 = CARTESIAN_POINT ( 'NONE',  ( -18.56399227203343472, -5.499999999999927169, 78.97830131249902763 ) ) ;
#168560 = CARTESIAN_POINT ( 'NONE',  ( 13.97604488694548053, -13.89961937509957401, 100.6260903946856615 ) ) ;
#168561 = CARTESIAN_POINT ( 'NONE',  ( 18.62759615963271287, -10.81492255796078972, 68.33224293864769550 ) ) ;
#168562 = CARTESIAN_POINT ( 'NONE',  ( -16.52544592524342804, 4.483927247898546575, 51.04057627198103120 ) ) ;
#168563 = CARTESIAN_POINT ( 'NONE',  ( 9.474510206698729675, 16.51473224551082808, 107.0844237280190043 ) ) ;
#168564 = CARTESIAN_POINT ( 'NONE',  ( 0.05219959533909260263, 19.03943276465977164, 39.99890960531436690 ) ) ;
#168566 = CARTESIAN_POINT ( 'NONE',  ( 9.474510206698729675, 16.51473224551082808, 72.08442372801900433 ) ) ;
#168565 = CARTESIAN_POINT ( 'NONE',  ( 15.72974639402199770, -15.80617190586745480, 103.1239096053143811 ) ) ;
#168567 = CARTESIAN_POINT ( 'NONE',  ( -5.049401038298153566, 19.05341960407611168, 80.20724293864769550 ) ) ;
#168568 = CARTESIAN_POINT ( 'NONE',  ( 14.34966873604960469, 8.224510206698951720, 94.16557627198103830 ) ) ;
#168569 = CARTESIAN_POINT ( 'NONE',  ( 0.05219959533909260263, 19.03943276465977164, 59.99890960531436690 ) ) ;
#168570 = CARTESIAN_POINT ( 'NONE',  ( 12.06949235617757843, -12.14591786802309237, 73.12390960531436690 ) ) ;
#168571 = CARTESIAN_POINT ( 'NONE',  ( 19.03943276465977164, -0.05219959533909143690, 33.74890960531435979 ) ) ;
#168572 = CARTESIAN_POINT ( 'NONE',  ( -36.95458794302616212, -5.320992724678917263, 43.56214547691710237 ) ) ;
#168573 = CARTESIAN_POINT ( 'NONE',  ( 4.483927247898545687, 16.52544592524342804, 39.79057627198103830 ) ) ;
#168574 = CARTESIAN_POINT ( 'NONE',  ( -9.474510206698964154, 16.51473224551069663, 90.41557627198103830 ) ) ;
#168575 = FACE_BOUND ( 'NONE', #118359, .T. ) ;
#168576 = CARTESIAN_POINT ( 'NONE',  ( -19.03943276465977164, -0.05219959533935918106, 48.75109039468566863 ) ) ;
#168577 = CARTESIAN_POINT ( 'NONE',  ( 16.55341960407618274, -4.379528057220086978, 66.04275706135236135 ) ) ;
#168578 = CARTESIAN_POINT ( 'NONE',  ( 0.05219959533907565091, 21.53943276465977519, 69.99890960531435269 ) ) ;
#168579 = CARTESIAN_POINT ( 'NONE',  ( 9.474510206698729675, 16.51473224551082808, 32.08442372801900433 ) ) ;
#168580 = CARTESIAN_POINT ( 'NONE',  ( -13.89961937509977652, 13.97604488694528158, 85.62390960531433848 ) ) ;
#168581 = CARTESIAN_POINT ( 'NONE',  ( -22.13758331326615902, -22.85500914106531312, -45.77467392966760684 ) ) ;
#168582 = CARTESIAN_POINT ( 'NONE',  ( -15.80617190586745835, -15.72974639402198527, 31.87390960531435979 ) ) ;
#168583 = CARTESIAN_POINT ( 'NONE',  ( -16.46253265017160317, 9.564922557960807481, 65.83224293864769550 ) ) ;
#168584 = CARTESIAN_POINT ( 'NONE',  ( -0.05219959533937732626, 21.53943276465977519, 47.50109039468568994 ) ) ;
#168585 = CARTESIAN_POINT ( 'NONE',  ( -16.52544592524342804, 4.483927247898546575, 116.0405762719810383 ) ) ;
#168588 = ORIENTED_EDGE ( 'NONE', *, *, #32959, .T. ) ;
#168587 = CARTESIAN_POINT ( 'NONE',  ( 16.51473224551069308, 9.474510206698969483, 89.16557627198103830 ) ) ;
#168586 = CARTESIAN_POINT ( 'NONE',  ( 5.823673210054125526, 21.52544592524343514, 109.7905762719810383 ) ) ;
#168589 = CARTESIAN_POINT ( 'NONE',  ( 15.80617190586769283, -15.72974639402175789, 45.62609039468567573 ) ) ;
#168590 = VERTEX_POINT ( 'NONE', #38944 ) ;
#168591 = CARTESIAN_POINT ( 'NONE',  ( -5.049401038298153566, 19.05341960407611168, 95.20724293864770971 ) ) ;
#168592 = CARTESIAN_POINT ( 'NONE',  ( 18.22780087662121673, 5.500000000000056843, 88.98459894673892734 ) ) ;
#168593 = CARTESIAN_POINT ( 'NONE',  ( -15.72974639402197994, 15.80617190586746368, 110.6239096053143669 ) ) ;
#168594 = CARTESIAN_POINT ( 'NONE',  ( 16.46253265017160672, -9.564922557960803928, 43.33224293864769550 ) ) ;
#168595 = CARTESIAN_POINT ( 'NONE',  ( 4.483927247898790824, -16.52544592524335698, 25.20942372801901854 ) ) ;
#168596 = CARTESIAN_POINT ( 'NONE',  ( 36.91746824999999887, 11.99521256947799053, -4.024999997268814411 ) ) ;
#168597 = CARTESIAN_POINT ( 'NONE',  ( -5.153800228976328057, -19.02544592524343514, 32.29057627198102409 ) ) ;
#168598 = CARTESIAN_POINT ( 'NONE',  ( -10.72451020669870658, -18.67979575497194134, 99.58442372801900433 ) ) ;
#168600 = CARTESIAN_POINT ( 'NONE',  ( 10.81492255796106328, -18.62759615963255655, 45.41775706135234003 ) ) ;
#168599 = CARTESIAN_POINT ( 'NONE',  ( -16.51473224551069308, -9.474510206698971260, 76.66557627198103830 ) ) ;
#168601 = CARTESIAN_POINT ( 'NONE',  ( 27.73933785331498214, 9.013057229001095294, 146.4750000027311501 ) ) ;
#168602 = CARTESIAN_POINT ( 'NONE',  ( 16.46253265017160672, -9.564922557960803928, 103.3322429386476955 ) ) ;
#168603 = CARTESIAN_POINT ( 'NONE',  ( 18.56101223717332616, 5.499999999999942268, 63.94978406935678095 ) ) ;
#168606 = CARTESIAN_POINT ( 'NONE',  ( 10.72451020669871369, 18.67979575497193778, 57.08442372801901854 ) ) ;
#168605 = CARTESIAN_POINT ( 'NONE',  ( 0.05219959533934541429, -16.53943276465976808, 70.00109039468568994 ) ) ;
#168604 = CARTESIAN_POINT ( 'NONE',  ( -4.379528057220086978, -16.55341960407618274, 39.79275706135235424 ) ) ;
#168607 = CARTESIAN_POINT ( 'NONE',  ( -15.72974639402176322, -15.80617190586768395, 94.37609039468568994 ) ) ;
#168608 = CARTESIAN_POINT ( 'NONE',  ( 6.293041912674292249, 6.576301504920881946, -61.89430850415822505 ) ) ;
#168609 = CARTESIAN_POINT ( 'NONE',  ( 5.153800228976615827, -19.02544592524334988, 105.2094237280190185 ) ) ;
#168610 = CARTESIAN_POINT ( 'NONE',  ( 9.474510206698971260, -16.51473224551069308, 72.91557627198102409 ) ) ;
#168611 = CARTESIAN_POINT ( 'NONE',  ( -13.97604488694527625, -13.89961937509977652, 96.87390960531433848 ) ) ;
#168612 = CARTESIAN_POINT ( 'NONE',  ( 14.29746914071049879, -8.314922557960816363, 108.3322429386477097 ) ) ;
#168613 = CARTESIAN_POINT ( 'NONE',  ( -21.53943276465977519, 0.05219959533907696930, 31.24890960531435979 ) ) ;
#168614 = CARTESIAN_POINT ( 'NONE',  ( -0.05219959533934338120, 16.53943276465976808, 97.50109039468567573 ) ) ;
#168616 = CARTESIAN_POINT ( 'NONE',  ( -19.05341960407611168, -5.049401038298163336, 56.45724293864768129 ) ) ;
#168615 = CARTESIAN_POINT ( 'NONE',  ( -12.14591786802309592, -12.06949235617757132, 76.87390960531439532 ) ) ;
#168617 = CARTESIAN_POINT ( 'NONE',  ( -10.81492255796105439, 18.62759615963255655, 92.91775706135236135 ) ) ;
#168618 = CARTESIAN_POINT ( 'NONE',  ( -22.98313974082795141, 1.499560036715340994, -57.70434786042496000 ) ) ;
#168619 = CARTESIAN_POINT ( 'NONE',  ( -0.05219959533936034679, 19.03943276465977164, 102.5010903946856757 ) ) ;
#168620 = CARTESIAN_POINT ( 'NONE',  ( -16.55341960407611168, -4.379528057220339221, 76.45724293864769550 ) ) ;
#168621 = CARTESIAN_POINT ( 'NONE',  ( 18.67979575497194134, -10.72451020669871369, 30.83442372801902209 ) ) ;
#168622 = CARTESIAN_POINT ( 'NONE',  ( 18.62759615963271287, -10.81492255796078972, 58.33224293864768839 ) ) ;
#168623 = CARTESIAN_POINT ( 'NONE',  ( -19.03943276465977164, -0.05219959533935918106, 33.75109039468566863 ) ) ;
#168624 = CARTESIAN_POINT ( 'NONE',  ( -35.50084720355936696, 3.323798168015720034, 38.27222404303020653 ) ) ;
#168625 = CARTESIAN_POINT ( 'NONE',  ( -16.46253265017160317, 9.564922557960807481, 85.83224293864769550 ) ) ;
#168626 = CARTESIAN_POINT ( 'NONE',  ( 14.29746914071049879, -8.314922557960816363, 53.33224293864769550 ) ) ;
#168627 = CARTESIAN_POINT ( 'NONE',  ( -12.06949235617756955, 12.14591786802309770, 35.62390960531437401 ) ) ;
#168628 = CARTESIAN_POINT ( 'NONE',  ( -4.379528057220086978, -16.55341960407618274, 94.79275706135234714 ) ) ;
#168629 = CARTESIAN_POINT ( 'NONE',  ( -5.153800228976607833, 19.02544592524334988, 47.70942372801900433 ) ) ;
#168630 = CARTESIAN_POINT ( 'NONE',  ( -0.05219959533936034679, 19.03943276465977164, 77.50109039468566152 ) ) ;
#168631 = CARTESIAN_POINT ( 'NONE',  ( 16.51473224551069308, 9.474510206698969483, 99.16557627198102409 ) ) ;
#168632 = CARTESIAN_POINT ( 'NONE',  ( 4.483927247898545687, 16.52544592524342804, 69.79057627198102409 ) ) ;
#168633 = CARTESIAN_POINT ( 'NONE',  ( 19.02544592524334988, 5.153800228976608722, 46.45942372801899012 ) ) ;
#168635 = CARTESIAN_POINT ( 'NONE',  ( 10.81492255796078972, 18.62759615963270932, 39.58224293864769550 ) ) ;
#168634 = CARTESIAN_POINT ( 'NONE',  ( -0.05219959533909027116, -19.03943276465977164, 37.49890960531436690 ) ) ;
#168636 = CARTESIAN_POINT ( 'NONE',  ( 15.72974639402199770, -15.80617190586745480, 63.12390960531435979 ) ) ;
#168637 = CARTESIAN_POINT ( 'NONE',  ( -12.14591786802309592, -12.06949235617757132, 101.8739096053143811 ) ) ;
#168638 = CARTESIAN_POINT ( 'NONE',  ( -14.34966873604972548, 8.224510206698743886, 53.33442372801901854 ) ) ;
#168639 = EDGE_CURVE ( 'NONE', #189747, #130647, #2283, .T. ) ;
#168640 = CARTESIAN_POINT ( 'NONE',  ( 5.719274019375673035, 21.55341960407619339, 37.29275706135235424 ) ) ;
#168641 = CARTESIAN_POINT ( 'NONE',  ( 16.52544592524342804, -4.483927247898539470, 88.54057627198103830 ) ) ;
#168642 = DIRECTION ( 'NONE',  ( 0.000000000000000000, 0.000000000000000000, 1.000000000000000000 ) ) ;
#168643 = CARTESIAN_POINT ( 'NONE',  ( 29.86685920354754842, -21.69954338932559068, -8.324999997268813345 ) ) ;
#168644 = CARTESIAN_POINT ( 'NONE',  ( -5.719274019375978568, 21.55341960407610458, 40.20724293864769550 ) ) ;
#168645 = DIRECTION ( 'NONE',  ( 0.000000000000000000, 0.000000000000000000, 1.000000000000000000 ) ) ;
#168646 = CARTESIAN_POINT ( 'NONE',  ( 0.4878707274068331268, 9.021887631461126489, -63.96636194779098616 ) ) ;
#168648 = CARTESIAN_POINT ( 'NONE',  ( 14.34966873604960469, 8.224510206698951720, 34.16557627198102409 ) ) ;
#168647 = CARTESIAN_POINT ( 'NONE',  ( -14.29746914071037622, -8.314922557961029526, 49.16775706135234003 ) ) ;
#168649 = CARTESIAN_POINT ( 'NONE',  ( -15.72974639402197994, 15.80617190586746368, 65.62390960531436690 ) ) ;
#168650 = CARTESIAN_POINT ( 'NONE',  ( 19.03943276465977164, 0.05219959533936151252, 91.25109039468566152 ) ) ;
#168651 = CARTESIAN_POINT ( 'NONE',  ( -21.52544592524343514, 5.823673210054127303, 61.04057627198103120 ) ) ;
#168652 = DIRECTION ( 'NONE',  ( 1.000000000000000000, 0.000000000000000000, 0.000000000000000000 ) ) ;
#168654 = CARTESIAN_POINT ( 'NONE',  ( -13.97604488694527625, -13.89961937509977652, 96.87390960531433848 ) ) ;
#168653 = CARTESIAN_POINT ( 'NONE',  ( -19.05341960407611168, -5.049401038298163336, 36.45724293864766707 ) ) ;
#168655 = CARTESIAN_POINT ( 'NONE',  ( -9.474510206698964154, 16.51473224551069663, 40.41557627198103120 ) ) ;
#168656 = CARTESIAN_POINT ( 'NONE',  ( 12.06949235617757843, -12.14591786802309237, 108.1239096053143811 ) ) ;
#168657 = DIRECTION ( 'NONE',  ( 1.000000000000000000, 0.000000000000000000, 0.000000000000000000 ) ) ;
#168658 = CARTESIAN_POINT ( 'NONE',  ( -9.564922557960796823, -16.46253265017161027, 112.0822429386476955 ) ) ;
#168659 = VERTEX_POINT ( 'NONE', #178469 ) ;
#168660 = CARTESIAN_POINT ( 'NONE',  ( 16.52544592524335698, 4.483927247898782831, 66.45942372801903275 ) ) ;
#168661 = CARTESIAN_POINT ( 'NONE',  ( -5.823673210054116645, -21.52544592524344225, 97.29057627198105251 ) ) ;
#168662 = CARTESIAN_POINT ( 'NONE',  ( 13.89961937509977652, -13.97604488694527269, 58.12390960531436690 ) ) ;
#168663 = CARTESIAN_POINT ( 'NONE',  ( -15.72974639402176322, -15.80617190586768395, 24.37609039468567573 ) ) ;
#168664 = CARTESIAN_POINT ( 'NONE',  ( 16.46253265017160672, -9.564922557960803928, 78.33224293864769550 ) ) ;
#168665 = CARTESIAN_POINT ( 'NONE',  ( -19.02544592524342804, 5.153800228976336051, 116.0405762719810383 ) ) ;
#168666 = ORIENTED_EDGE ( 'NONE', *, *, #39485, .T. ) ;
#168667 = CARTESIAN_POINT ( 'NONE',  ( -15.72974639402197994, 15.80617190586746368, 110.6239096053143669 ) ) ;
#168670 = CARTESIAN_POINT ( 'NONE',  ( 13.89961937509957401, 13.97604488694547697, 91.87609039468567573 ) ) ;
#168669 = CARTESIAN_POINT ( 'NONE',  ( -0.05219959533909027116, -19.03943276465977164, 102.4989096053143669 ) ) ;
#168668 = CARTESIAN_POINT ( 'NONE',  ( 16.53943276465976808, -0.05219959533910856209, 113.7489096053143527 ) ) ;
#168671 = CARTESIAN_POINT ( 'NONE',  ( -19.05341960407617563, 5.049401038297882671, 28.54275706135232937 ) ) ;
#168672 = CARTESIAN_POINT ( 'NONE',  ( 10.72451020669898902, -18.67979575497178502, 102.9155762719810383 ) ) ;
#168673 = CARTESIAN_POINT ( 'NONE',  ( 19.05341960407617918, -5.049401038297876454, 31.04275706135232227 ) ) ;
#168674 = CARTESIAN_POINT ( 'NONE',  ( 13.97604488694548053, -13.89961937509957401, 35.62609039468567573 ) ) ;
#168675 = CARTESIAN_POINT ( 'NONE',  ( -8.314922557961024197, 14.29746914071037800, 77.91775706135231871 ) ) ;
#168676 = CARTESIAN_POINT ( 'NONE',  ( 13.89961937509977652, -13.97604488694527269, 103.1239096053143527 ) ) ;
#168677 = CARTESIAN_POINT ( 'NONE',  ( -19.05341960407611168, -5.049401038298163336, 61.45724293864769550 ) ) ;
#168678 = CARTESIAN_POINT ( 'NONE',  ( -5.719274019375665041, -21.55341960407619695, 69.79275706135234714 ) ) ;
#168679 = CARTESIAN_POINT ( 'NONE',  ( 18.67979575497194134, -10.72451020669871369, 85.83442372801901854 ) ) ;
#168680 = CARTESIAN_POINT ( 'NONE',  ( -35.00000000000000000, 0.3535533905932707888, 5.353553390593270400 ) ) ;
#168681 = CARTESIAN_POINT ( 'NONE',  ( -16.51473224551069308, -9.474510206698971260, 76.66557627198103830 ) ) ;
#168682 = CARTESIAN_POINT ( 'NONE',  ( -18.67979575497193778, 10.72451020669871902, 53.33442372801901854 ) ) ;
#168683 = CARTESIAN_POINT ( 'NONE',  ( 16.46253265017146816, 9.564922557961045513, 96.66775706135233293 ) ) ;
#168684 = CARTESIAN_POINT ( 'NONE',  ( -19.05341960407611168, -5.049401038298163336, 56.45724293864768129 ) ) ;
#168685 = CARTESIAN_POINT ( 'NONE',  ( 19.02544592524343514, -5.153800228976328945, 93.54057627198102409 ) ) ;
#168686 = CARTESIAN_POINT ( 'NONE',  ( 16.46253265017160672, -9.564922557960803928, 83.33224293864768129 ) ) ;
#168687 = CARTESIAN_POINT ( 'NONE',  ( 17.50000000000000000, -5.500000000000000888, 23.29690382534171889 ) ) ;
#168688 = CARTESIAN_POINT ( 'NONE',  ( -16.46253265017160317, 9.564922557960807481, 55.83224293864769550 ) ) ;
#168689 = CARTESIAN_POINT ( 'NONE',  ( 21.55341960407610458, 5.719274019375980345, 103.9572429386476813 ) ) ;
#168690 = CARTESIAN_POINT ( 'NONE',  ( -14.34966873604972548, 8.224510206698743886, 88.33442372801901854 ) ) ;
#168691 = CARTESIAN_POINT ( 'NONE',  ( 1.251854463851703304E-30, -64.82615989628266107, -13.00000000000000000 ) ) ;
#168692 = CARTESIAN_POINT ( 'NONE',  ( 19.02544592524334988, 5.153800228976608722, 46.45942372801899012 ) ) ;
#168693 = CARTESIAN_POINT ( 'NONE',  ( -0.05219959533909027116, -19.03943276465977164, 82.49890960531436690 ) ) ;
#168694 = CARTESIAN_POINT ( 'NONE',  ( 12.14591786802309770, 12.06949235617756955, 64.37390960531435269 ) ) ;
#168695 = CARTESIAN_POINT ( 'NONE',  ( 16.52544592524342804, -4.483927247898539470, 98.54057627198105251 ) ) ;
#168696 = CARTESIAN_POINT ( 'NONE',  ( -15.72974639402197994, 15.80617190586746368, 25.62390960531435624 ) ) ;
#168697 = CARTESIAN_POINT ( 'NONE',  ( -16.51473224551069308, -9.474510206698971260, 111.6655762719810383 ) ) ;
#168698 = CARTESIAN_POINT ( 'NONE',  ( 19.05341960407611168, 5.049401038298154454, 113.9572429386477097 ) ) ;
#168699 = CARTESIAN_POINT ( 'NONE',  ( -5.049401038297874678, -19.05341960407617918, 34.79275706135233293 ) ) ;
#168700 = CARTESIAN_POINT ( 'NONE',  ( 16.52544592524335698, 4.483927247898782831, 91.45942372801901854 ) ) ;
#168701 = CARTESIAN_POINT ( 'NONE',  ( 16.51473224551069308, 9.474510206698969483, 79.16557627198103830 ) ) ;
#168702 = CARTESIAN_POINT ( 'NONE',  ( 21.52544592524334988, 5.823673210054432836, 46.45942372801901854 ) ) ;
#168703 = CARTESIAN_POINT ( 'NONE',  ( -21.55341960407610458, -5.719274019375992779, 31.45724293864769550 ) ) ;
#168704 = CARTESIAN_POINT ( 'NONE',  ( 5.823673210054444382, -21.52544592524334988, 20.20942372801900788 ) ) ;
#168705 = CARTESIAN_POINT ( 'NONE',  ( -18.67979575497178146, -10.72451020669898902, 71.66557627198100988 ) ) ;
#168706 = CARTESIAN_POINT ( 'NONE',  ( -4.379528057220328563, 16.55341960407611168, 95.20724293864769550 ) ) ;
#168707 = CARTESIAN_POINT ( 'NONE',  ( -16.51473224551082808, 9.474510206698731452, 38.33442372801899722 ) ) ;
#168708 = CARTESIAN_POINT ( 'NONE',  ( 9.474510206698971260, -16.51473224551069308, 27.91557627198103120 ) ) ;
#168709 = CARTESIAN_POINT ( 'NONE',  ( -19.03943276465977164, 0.05219959533909376836, 86.24890960531436690 ) ) ;
#168710 = CARTESIAN_POINT ( 'NONE',  ( 13.97604488694527802, 13.89961937509977652, 79.37390960531435269 ) ) ;
#168711 = CARTESIAN_POINT ( 'NONE',  ( -17.14385361876520975, 23.59649016807275856, 148.5750000027311728 ) ) ;
#168712 = CARTESIAN_POINT ( 'NONE',  ( -12.14591786802309592, -12.06949235617757132, 101.8739096053143811 ) ) ;
#168713 = EDGE_LOOP ( 'NONE', ( #25227, #73874, #59004, #87847, #40568 ) ) ;
#168714 = CARTESIAN_POINT ( 'NONE',  ( 16.53943276465976808, -0.05219959533910856209, 28.74890960531435624 ) ) ;
#168715 = CARTESIAN_POINT ( 'NONE',  ( -16.53943276465976808, -0.05219959533934237506, 33.75109039468568284 ) ) ;
#168716 = CARTESIAN_POINT ( 'NONE',  ( 10.81492255796106328, -18.62759615963255655, 95.41775706135234714 ) ) ;
#168717 = CARTESIAN_POINT ( 'NONE',  ( -0.05219959533909027116, -19.03943276465977164, 97.49890960531436690 ) ) ;
#168718 = CARTESIAN_POINT ( 'NONE',  ( -21.53943276465977519, 0.05219959533907696930, 111.2489096053143669 ) ) ;
#168719 = CARTESIAN_POINT ( 'NONE',  ( -19.02544592524342804, 5.153800228976336051, 41.04057627198103120 ) ) ;
#168720 = CARTESIAN_POINT ( 'NONE',  ( 4.379528057220092307, 16.55341960407617563, 42.29275706135235424 ) ) ;
#168721 = EDGE_CURVE ( 'NONE', #175496, #129810, #165298, .T. ) ;
#168722 = CARTESIAN_POINT ( 'NONE',  ( -8.224510206698735004, -14.34966873604973081, 19.58442372801901143 ) ) ;
#168723 = CARTESIAN_POINT ( 'NONE',  ( 4.379528057220339221, -16.55341960407611168, 92.70724293864770971 ) ) ;
#168724 = CARTESIAN_POINT ( 'NONE',  ( -21.55341960407610458, -5.719274019375992779, 101.4572429386476955 ) ) ;
#168725 = CARTESIAN_POINT ( 'NONE',  ( 13.89961937509957401, 13.97604488694547697, 61.87609039468566863 ) ) ;
#168726 = CARTESIAN_POINT ( 'NONE',  ( -18.67979575497178146, -10.72451020669898902, 111.6655762719810525 ) ) ;
#168727 = CARTESIAN_POINT ( 'NONE',  ( -16.46253265017160317, 9.564922557960807481, 90.83224293864769550 ) ) ;
#168728 = CARTESIAN_POINT ( 'NONE',  ( 37.99626262588765258, 2.893932880411085066E-14, -7.002157773949822861 ) ) ;
#168729 = CARTESIAN_POINT ( 'NONE',  ( -0.05219959533909027116, -19.03943276465977164, 87.49890960531436690 ) ) ;
#168731 = CARTESIAN_POINT ( 'NONE',  ( 12.14591786802309770, 12.06949235617756955, 74.37390960531436690 ) ) ;
#168730 = CARTESIAN_POINT ( 'NONE',  ( -15.80617190586768217, 15.72974639402176855, 28.12609039468568284 ) ) ;
#168732 = CARTESIAN_POINT ( 'NONE',  ( -16.51473224551069308, -9.474510206698971260, 81.66557627198103830 ) ) ;
#168734 = CARTESIAN_POINT ( 'NONE',  ( 5.049401038297881783, 19.05341960407617563, 57.29275706135231871 ) ) ;
#168733 = CARTESIAN_POINT ( 'NONE',  ( 16.53943276465976808, 0.05219959533934440121, 56.25109039468568284 ) ) ;
#168735 = CARTESIAN_POINT ( 'NONE',  ( 18.62759615963255655, 10.81492255796105972, 71.66775706135234714 ) ) ;
#168736 = CARTESIAN_POINT ( 'NONE',  ( 4.379528057220092307, 16.55341960407617563, 32.29275706135235424 ) ) ;
#168737 = CARTESIAN_POINT ( 'NONE',  ( -5.153800228976328057, -19.02544592524343514, 72.29057627198102409 ) ) ;
#168738 = CARTESIAN_POINT ( 'NONE',  ( -5.153800228976607833, 19.02544592524334988, 92.70942372801901854 ) ) ;
#168739 = CARTESIAN_POINT ( 'NONE',  ( -4.483927247898782831, 16.52544592524335698, 57.70942372801901143 ) ) ;
#168740 = CARTESIAN_POINT ( 'NONE',  ( 21.55341960407619695, -5.719274019375665929, 96.04275706135236135 ) ) ;
#168741 = CARTESIAN_POINT ( 'NONE',  ( -13.89961937509957401, -13.97604488694547875, 79.37609039468567573 ) ) ;
#168742 = CARTESIAN_POINT ( 'NONE',  ( 0.05219959533909260263, 19.03943276465977164, 44.99890960531435979 ) ) ;
#168743 = CARTESIAN_POINT ( 'NONE',  ( 21.55341960407610458, 5.719274019375980345, 73.95724293864769550 ) ) ;
#168745 = CARTESIAN_POINT ( 'NONE',  ( 0.05219959533936267826, -19.03943276465977164, 80.00109039468567573 ) ) ;
#168744 = CARTESIAN_POINT ( 'NONE',  ( -12.06949235617756955, 12.14591786802309770, 75.62390960531439532 ) ) ;
#168746 = DIRECTION ( 'NONE',  ( -5.204170427930421283E-16, 0.000000000000000000, -1.000000000000000000 ) ) ;
#168748 = ADVANCED_FACE ( 'NONE', ( #177475 ), #170150, .F. ) ;
#168747 = CARTESIAN_POINT ( 'NONE',  ( -19.05341960407617563, 5.049401038297882671, 48.54275706135233293 ) ) ;
#168749 = CARTESIAN_POINT ( 'NONE',  ( 8.314922557961029526, -14.29746914071037800, 110.4177570613523756 ) ) ;
#168750 = CARTESIAN_POINT ( 'NONE',  ( -4.483927247898539470, -16.52544592524342804, 67.29057627198103830 ) ) ;
#168752 = CARTESIAN_POINT ( 'NONE',  ( -22.44159573604009950, -16.30477369853688430, 143.0750000027311728 ) ) ;
#168751 = CARTESIAN_POINT ( 'NONE',  ( 5.823673210054444382, -21.52544592524334988, 105.2094237280190328 ) ) ;
#168753 = CARTESIAN_POINT ( 'NONE',  ( -18.62759615963270932, 10.81492255796079327, 105.8322429386476955 ) ) ;
#168754 = CARTESIAN_POINT ( 'NONE',  ( -9.474510206698964154, 16.51473224551069663, 60.41557627198102409 ) ) ;
#168755 = CARTESIAN_POINT ( 'NONE',  ( -10.72451020669870658, -18.67979575497194134, 89.58442372801901854 ) ) ;
#168756 = CARTESIAN_POINT ( 'NONE',  ( 9.564922557960805705, 16.46253265017160317, 64.58224293864769550 ) ) ;
#168757 = CARTESIAN_POINT ( 'NONE',  ( 5.153800228976335163, 19.02544592524342804, 24.79057627198102765 ) ) ;
#168758 = CARTESIAN_POINT ( 'NONE',  ( -21.55341960407610458, -5.719274019375992779, 31.45724293864769550 ) ) ;
#168759 = CARTESIAN_POINT ( 'NONE',  ( -12.14591786802309592, -12.06949235617757132, 61.87390960531436690 ) ) ;
#168760 = CARTESIAN_POINT ( 'NONE',  ( 19.03943276465977164, -0.05219959533909143690, 48.74890960531435979 ) ) ;
#168761 = CARTESIAN_POINT ( 'NONE',  ( -16.53943276465976808, 0.05219959533911058130, 81.24890960531436690 ) ) ;
#168762 = CARTESIAN_POINT ( 'NONE',  ( 15.80617190586746368, 15.72974639402197994, 109.3739096053143811 ) ) ;
#168763 = CARTESIAN_POINT ( 'NONE',  ( -18.67979575497193778, 10.72451020669871902, 48.33442372801902565 ) ) ;
#168764 = CARTESIAN_POINT ( 'NONE',  ( 9.564922557960805705, 16.46253265017160317, 34.58224293864770260 ) ) ;
#168765 = CARTESIAN_POINT ( 'NONE',  ( 14.29746914071037800, 8.314922557961029526, 46.66775706135234714 ) ) ;
#168766 = CARTESIAN_POINT ( 'NONE',  ( 21.52544592524344225, -5.823673210054117533, 93.54057627198103830 ) ) ;
#168768 = CARTESIAN_POINT ( 'NONE',  ( -0.05219959533909027116, -19.03943276465977164, 52.49890960531436690 ) ) ;
#168767 = CARTESIAN_POINT ( 'NONE',  ( 5.049401038297881783, 19.05341960407617563, 32.29275706135233293 ) ) ;
#168769 = CARTESIAN_POINT ( 'NONE',  ( 19.03943276465977164, -0.05219959533909143690, 103.7489096053143669 ) ) ;
#168770 = CARTESIAN_POINT ( 'NONE',  ( 10.81492255796106328, -18.62759615963255655, 60.41775706135235424 ) ) ;
#168771 = VECTOR ( 'NONE', #197569, 1000.000000000000000 ) ;
#168772 = CARTESIAN_POINT ( 'NONE',  ( 15.72974639402199770, -15.80617190586745480, 43.12390960531435269 ) ) ;
#168773 = CARTESIAN_POINT ( 'NONE',  ( 8.314922557960818139, 14.29746914071049879, 24.58224293864768839 ) ) ;
#168775 = CARTESIAN_POINT ( 'NONE',  ( 10.81492255796106328, -18.62759615963255655, 100.4177570613523471 ) ) ;
#168774 = CARTESIAN_POINT ( 'NONE',  ( 10.72451020669871369, 18.67979575497193778, 57.08442372801901854 ) ) ;
#168776 = CARTESIAN_POINT ( 'NONE',  ( -9.564922557961040184, 16.46253265017147172, 37.91775706135233293 ) ) ;
#168777 = CARTESIAN_POINT ( 'NONE',  ( -8.314922557961024197, 14.29746914071037800, 97.91775706135236135 ) ) ;
#168778 = CARTESIAN_POINT ( 'NONE',  ( 15.80617190586769283, -15.72974639402175789, 60.62609039468567573 ) ) ;
#168779 = CARTESIAN_POINT ( 'NONE',  ( -0.05219959533909027116, -19.03943276465977164, 52.49890960531436690 ) ) ;
#168780 = CARTESIAN_POINT ( 'NONE',  ( -9.564922557961040184, 16.46253265017147172, 22.91775706135233648 ) ) ;
#168781 = CARTESIAN_POINT ( 'NONE',  ( 21.52544592524344225, -5.823673210054117533, 28.54057627198103120 ) ) ;
#168783 = CARTESIAN_POINT ( 'NONE',  ( 5.719274019375991003, -21.55341960407610458, 112.7072429386476955 ) ) ;
#168782 = B_SPLINE_CURVE_WITH_KNOTS ( 'NONE', 3,
 ( #33282, #81731, #185978, #32289, #142436, #1937, #47462, #96915, #62604, #171794, #156626, #92944, #154630, #65595, #187972, #141447, #79776, #93944, #48459, #140447, #16125, #94942 ),
 .UNSPECIFIED., .F., .F.,
 ( 4, 2, 2, 2, 2, 2, 2, 2, 2, 2, 4 ),
 ( 1.967889508984713855E-07, 0.0003311341139581566229, 0.0006620714389654147689, 0.0009930087639726729691, 0.001323946088979931169, 0.002647695389008995412, 0.003309570039023526991, 0.003971444689038058570, 0.004633319339052590149, 0.004964256664059855939, 0.005295193989067121729 ),
 .UNSPECIFIED. ) ;
#168784 = CARTESIAN_POINT ( 'NONE',  ( -21.53943276465977519, 0.05219959533907696930, 81.24890960531436690 ) ) ;
#168785 = CARTESIAN_POINT ( 'NONE',  ( 14.34966873604972726, -8.224510206698740333, 45.83442372801901854 ) ) ;
#168787 = CARTESIAN_POINT ( 'NONE',  ( 21.52544592524344225, -5.823673210054117533, 78.54057627198103830 ) ) ;
#168786 = CARTESIAN_POINT ( 'NONE',  ( -19.99999999999998224, -180.0000000000000000, -4.999999999999999112 ) ) ;
#168789 = CARTESIAN_POINT ( 'NONE',  ( -12.06949235617756955, 12.14591786802309770, 70.62390960531436690 ) ) ;
#168788 = CARTESIAN_POINT ( 'NONE',  ( 12.14591786802327356, -12.06949235617739191, 70.62609039468567573 ) ) ;
#168790 = DIRECTION ( 'NONE',  ( 0.000000000000000000, 0.000000000000000000, 1.000000000000000000 ) ) ;
#168791 = CARTESIAN_POINT ( 'NONE',  ( 19.02544592524334988, 5.153800228976608722, 101.4594237280189759 ) ) ;
#168792 = CARTESIAN_POINT ( 'NONE',  ( -0.05219959533907301413, -21.53943276465977519, 37.49890960531436690 ) ) ;
#168793 = LINE ( 'NONE', #11172, #5458 ) ;
#168794 = CARTESIAN_POINT ( 'NONE',  ( 0.05219959533934541429, -16.53943276465976808, 45.00109039468568284 ) ) ;
#168795 = CARTESIAN_POINT ( 'NONE',  ( -21.53943276465977519, 0.05219959533907696930, 111.2489096053143669 ) ) ;
#168796 = CARTESIAN_POINT ( 'NONE',  ( -0.05219959533907301413, -21.53943276465977519, 37.49890960531436690 ) ) ;
#168797 = CARTESIAN_POINT ( 'NONE',  ( 12.14591786802327356, -12.06949235617739191, 70.62609039468567573 ) ) ;
#168798 = CARTESIAN_POINT ( 'NONE',  ( 5.049401038298161559, -19.05341960407611168, 82.70724293864770971 ) ) ;
#168800 = CARTESIAN_POINT ( 'NONE',  ( 14.29746914071037800, 8.314922557961029526, 21.66775706135235069 ) ) ;
#168799 = CARTESIAN_POINT ( 'NONE',  ( 10.72451020669871369, 18.67979575497193778, 47.08442372801901854 ) ) ;
#168801 = CARTESIAN_POINT ( 'NONE',  ( 18.67979575497178502, 10.72451020669898547, 29.16557627198103120 ) ) ;
#168802 = EDGE_LOOP ( 'NONE', ( #38304, #424, #38360, #37833 ) ) ;
#168803 = CARTESIAN_POINT ( 'NONE',  ( -13.97604488694547697, 13.89961937509957934, 28.12609039468565797 ) ) ;
#168804 = CARTESIAN_POINT ( 'NONE',  ( -16.53943276465976808, -0.05219959533934237506, 58.75109039468568994 ) ) ;
#168805 = CARTESIAN_POINT ( 'NONE',  ( -19.05341960407611168, -5.049401038298163336, 106.4572429386476955 ) ) ;
#168806 = CARTESIAN_POINT ( 'NONE',  ( 15.80617190586746368, 15.72974639402197994, 99.37390960531436690 ) ) ;
#168807 = CARTESIAN_POINT ( 'NONE',  ( -16.46253265017160317, 9.564922557960807481, 70.83224293864770971 ) ) ;
#168808 = CARTESIAN_POINT ( 'NONE',  ( -17.05116617787826883, 6.768360034955676952, 23.65675553259199759 ) ) ;
#168809 = CARTESIAN_POINT ( 'NONE',  ( 4.483927247898545687, 16.52544592524342804, 84.79057627198102409 ) ) ;
#168810 = CARTESIAN_POINT ( 'NONE',  ( 10.81492255796078972, 18.62759615963270932, 34.58224293864770260 ) ) ;
#168811 = CARTESIAN_POINT ( 'NONE',  ( 9.564922557960805705, 16.46253265017160317, 24.58224293864769194 ) ) ;
#168812 = CARTESIAN_POINT ( 'NONE',  ( -0.05219959533934338120, 16.53943276465976808, 67.50109039468568994 ) ) ;
#168813 = CARTESIAN_POINT ( 'NONE',  ( 18.67979575497178502, 10.72451020669898547, 114.1655762719810383 ) ) ;
#168814 = CARTESIAN_POINT ( 'NONE',  ( -19.05341960407617563, 5.049401038297882671, 78.54275706135233293 ) ) ;
#168815 = CARTESIAN_POINT ( 'NONE',  ( 19.03943276465977164, -0.05219959533909143690, 23.74890960531435269 ) ) ;
#168816 = CARTESIAN_POINT ( 'NONE',  ( 10.81492255796078972, 18.62759615963270932, 74.58224293864768129 ) ) ;
#168817 = CARTESIAN_POINT ( 'NONE',  ( 19.05341960407611168, 5.049401038298154454, 103.9572429386476671 ) ) ;
#168818 = CARTESIAN_POINT ( 'NONE',  ( -18.62759615963255300, -10.81492255796106328, 89.16775706135236135 ) ) ;
#168819 = CARTESIAN_POINT ( 'NONE',  ( 19.05341960407611168, 5.049401038298154454, 63.95724293864769550 ) ) ;
#168820 = CARTESIAN_POINT ( 'NONE',  ( -12.06949235617739369, -12.14591786802326823, 54.37609039468568994 ) ) ;
#168821 = CARTESIAN_POINT ( 'NONE',  ( 13.89961937509977652, -13.97604488694527269, 58.12390960531436690 ) ) ;
#168822 = CARTESIAN_POINT ( 'NONE',  ( 10.81492255796106328, -18.62759615963255655, 80.41775706135234714 ) ) ;
#168823 = ORIENTED_EDGE ( 'NONE', *, *, #70540, .F. ) ;
#168824 = CARTESIAN_POINT ( 'NONE',  ( 16.51473224551083163, -9.474510206698727899, 35.83442372801899722 ) ) ;
#168825 = CARTESIAN_POINT ( 'NONE',  ( 19.05341960407617918, -5.049401038297876454, 51.04275706135231871 ) ) ;
#168826 = CARTESIAN_POINT ( 'NONE',  ( 18.67979575497194134, -10.72451020669871369, 45.83442372801901854 ) ) ;
#168827 = EDGE_CURVE ( 'NONE', #197193, #43824, #115303, .T. ) ;
#168828 = CARTESIAN_POINT ( 'NONE',  ( -28.79475375365586842, 2.428612866367529932E-14, 143.9843446568999923 ) ) ;
#168829 = CARTESIAN_POINT ( 'NONE',  ( 5.153800228976615827, -19.02544592524334988, 50.20942372801897591 ) ) ;
#168830 = CARTESIAN_POINT ( 'NONE',  ( 0.05219959533909260263, 19.03943276465977164, 94.99890960531436690 ) ) ;
#168831 = CARTESIAN_POINT ( 'NONE',  ( -13.89961937509977652, 13.97604488694528158, 70.62390960531432427 ) ) ;
#168832 = CARTESIAN_POINT ( 'NONE',  ( -4.379528057220328563, 16.55341960407611168, 25.20724293864769550 ) ) ;
#168834 = CARTESIAN_POINT ( 'NONE',  ( 0.05219959533937995610, -21.53943276465977519, 100.0010903946857042 ) ) ;
#168833 = CARTESIAN_POINT ( 'NONE',  ( -21.52544592524343514, 5.823673210054127303, 36.04057627198102409 ) ) ;
#168835 = CARTESIAN_POINT ( 'NONE',  ( -36.91746825000001309, -11.99521256947794789, -7.024999997268812635 ) ) ;
#168836 = DIRECTION ( 'NONE',  ( -0.000000000000000000, -0.000000000000000000, -1.000000000000000000 ) ) ;
#168837 = CARTESIAN_POINT ( 'NONE',  ( -21.52544592524334988, -5.823673210054445271, 103.9594237280190185 ) ) ;
#168838 = CARTESIAN_POINT ( 'NONE',  ( 37.99626262588765258, 2.893932880411085066E-14, -2.747842220587803475 ) ) ;
#168839 = CARTESIAN_POINT ( 'NONE',  ( -16.51473224551069308, -9.474510206698971260, 21.66557627198102765 ) ) ;
#168840 = CARTESIAN_POINT ( 'NONE',  ( -19.02544592524342804, 5.153800228976336051, 116.0405762719810383 ) ) ;
#168841 = CARTESIAN_POINT ( 'NONE',  ( 33.79632059884288964, 5.461862605997787057, 94.26112944759007917 ) ) ;
#168842 = CARTESIAN_POINT ( 'NONE',  ( -12.14591786802326823, 12.06949235617739902, 53.12609039468568284 ) ) ;
#168843 = CARTESIAN_POINT ( 'NONE',  ( 15.80617190586746368, 15.72974639402197994, 64.37390960531435269 ) ) ;
#168844 = CARTESIAN_POINT ( 'NONE',  ( 16.55341960407611168, 4.379528057220329451, 43.95724293864769550 ) ) ;
#168846 = CARTESIAN_POINT ( 'NONE',  ( -13.89961937509977652, 13.97604488694528158, 95.62390960531436690 ) ) ;
#168845 = CARTESIAN_POINT ( 'NONE',  ( -16.53943276465976808, 0.05219959533911058130, 111.2489096053143669 ) ) ;
#168847 = CARTESIAN_POINT ( 'NONE',  ( -9.564922557961040184, 16.46253265017147172, 32.91775706135233293 ) ) ;
#168848 = CARTESIAN_POINT ( 'NONE',  ( -8.224510206698948167, 14.34966873604960824, 115.4155762719810241 ) ) ;
#168849 = CARTESIAN_POINT ( 'NONE',  ( 21.53943276465977519, 0.05219959533937863772, 71.25109039468568994 ) ) ;
#168850 = LINE ( 'NONE', #139505, #33704 ) ;
#168851 = CARTESIAN_POINT ( 'NONE',  ( 4.483927247898790824, -16.52544592524335698, 105.2094237280190328 ) ) ;
#168852 = DIRECTION ( 'NONE',  ( 0.000000000000000000, 0.000000000000000000, -1.000000000000000000 ) ) ;
#168853 = CARTESIAN_POINT ( 'NONE',  ( -5.719274019375978568, 21.55341960407610458, 30.20724293864769550 ) ) ;
#168854 = CARTESIAN_POINT ( 'NONE',  ( 16.52544592524342804, -4.483927247898539470, 88.54057627198103830 ) ) ;
#168855 = CARTESIAN_POINT ( 'NONE',  ( 5.049401038297881783, 19.05341960407617563, 57.29275706135231871 ) ) ;
#168856 = CARTESIAN_POINT ( 'NONE',  ( -19.05341960407611168, -5.049401038298163336, 71.45724293864766707 ) ) ;
#168857 = CARTESIAN_POINT ( 'NONE',  ( -12.06949235617756955, 12.14591786802309770, 75.62390960531439532 ) ) ;
#168858 = CARTESIAN_POINT ( 'NONE',  ( 16.46253265017146816, 9.564922557961045513, 86.66775706135233293 ) ) ;
#168859 = CARTESIAN_POINT ( 'NONE',  ( 21.53943276465977519, -0.05219959533907433946, 48.74890960531435979 ) ) ;
#168860 = ORIENTED_EDGE ( 'NONE', *, *, #102359, .F. ) ;
#168861 = CARTESIAN_POINT ( 'NONE',  ( -19.02544592524342804, 5.153800228976336051, 26.04057627198103120 ) ) ;
#168862 = CARTESIAN_POINT ( 'NONE',  ( -32.00000000000000000, -5.510910596163089556E-15, 45.00000000000000000 ) ) ;
#168864 = CARTESIAN_POINT ( 'NONE',  ( 15.80617190586746368, 15.72974639402197994, 74.37390960531436690 ) ) ;
#168863 = CARTESIAN_POINT ( 'NONE',  ( -5.153800228976328057, -19.02544592524343514, 72.29057627198102409 ) ) ;
#168866 = CARTESIAN_POINT ( 'NONE',  ( -9.474510206698964154, 16.51473224551069663, 90.41557627198103830 ) ) ;
#168865 = CARTESIAN_POINT ( 'NONE',  ( -16.55341960407617563, 4.379528057220093196, 98.54275706135234714 ) ) ;
#168867 = CARTESIAN_POINT ( 'NONE',  ( 19.03943276465977164, 0.05219959533936151252, 71.25109039468566152 ) ) ;
#168868 = CARTESIAN_POINT ( 'NONE',  ( -18.62759615963255300, -10.81492255796106328, 79.16775706135234714 ) ) ;
#168869 = CARTESIAN_POINT ( 'NONE',  ( 21.53943276465977519, -0.05219959533907433946, 58.74890960531436690 ) ) ;
#168870 = CARTESIAN_POINT ( 'NONE',  ( 5.823673210054125526, 21.52544592524343514, 29.79057627198102409 ) ) ;
#168871 = CARTESIAN_POINT ( 'NONE',  ( -19.02544592524342804, 5.153800228976336051, 41.04057627198103120 ) ) ;
#168872 = CARTESIAN_POINT ( 'NONE',  ( -4.379528057220086978, -16.55341960407618274, 104.7927570613523898 ) ) ;
#168873 = CARTESIAN_POINT ( 'NONE',  ( -13.97604488694527625, -13.89961937509977652, 56.87390960531434558 ) ) ;
#168874 = CARTESIAN_POINT ( 'NONE',  ( 4.379528057220092307, 16.55341960407617563, 27.29275706135234358 ) ) ;
#168875 = CARTESIAN_POINT ( 'NONE',  ( -31.51098639601627838, -4.378554692192621722, 101.0941514966583412 ) ) ;
#168876 = CARTESIAN_POINT ( 'NONE',  ( 13.97604488694548053, -13.89961937509957401, 20.62609039468567573 ) ) ;
#168877 = CARTESIAN_POINT ( 'NONE',  ( -4.483927247898539470, -16.52544592524342804, 62.29057627198102409 ) ) ;
#168878 = CARTESIAN_POINT ( 'NONE',  ( -10.81492255796078084, -18.62759615963271287, 112.0822429386477097 ) ) ;
#168879 = CARTESIAN_POINT ( 'NONE',  ( -15.80617190586745835, -15.72974639402198527, 101.8739096053143811 ) ) ;
#168880 = CARTESIAN_POINT ( 'NONE',  ( 17.49999999999999645, -5.624438216177592764, 98.31670344914645909 ) ) ;
#168881 = CARTESIAN_POINT ( 'NONE',  ( -15.72974639402197994, 15.80617190586746368, 45.62390960531436690 ) ) ;
#168882 = CARTESIAN_POINT ( 'NONE',  ( -12.14591786802326823, 12.06949235617739902, 78.12609039468570415 ) ) ;
#168883 = CARTESIAN_POINT ( 'NONE',  ( -4.379528057220328563, 16.55341960407611168, 110.2072429386477239 ) ) ;
#168884 = CARTESIAN_POINT ( 'NONE',  ( 16.46253265017160672, -9.564922557960803928, 63.33224293864769550 ) ) ;
#168885 = CARTESIAN_POINT ( 'NONE',  ( -19.70810511599105297, -36.80807878390137944, -19.26229262562157274 ) ) ;
#168886 = CARTESIAN_POINT ( 'NONE',  ( -8.314922557961024197, 14.29746914071037800, 112.9177570613523329 ) ) ;
#168887 = EDGE_LOOP ( 'NONE', ( #99658, #176176, #83992, #63156 ) ) ;
#168888 = CARTESIAN_POINT ( 'NONE',  ( 15.80617190586769283, -15.72974639402175789, 50.62609039468568994 ) ) ;
#168889 = CARTESIAN_POINT ( 'NONE',  ( 16.51473224551069308, 9.474510206698969483, 99.16557627198102409 ) ) ;
#168890 = CARTESIAN_POINT ( 'NONE',  ( -21.55341960407619339, 5.719274019375674811, 83.54275706135234714 ) ) ;
#168891 = CARTESIAN_POINT ( 'NONE',  ( 29.15849868437704728, -10.00000000000000000, 150.0000000000000000 ) ) ;
#168892 = CARTESIAN_POINT ( 'NONE',  ( -5.049401038298153566, 19.05341960407611168, 30.20724293864768839 ) ) ;
#168893 = VERTEX_POINT ( 'NONE', #22778 ) ;
#168894 = CARTESIAN_POINT ( 'NONE',  ( 21.52544592524334988, 5.823673210054432836, 66.45942372801903275 ) ) ;
#168895 = CARTESIAN_POINT ( 'NONE',  ( -19.05341960407611168, -5.049401038298163336, 51.45724293864770260 ) ) ;
#168896 = CARTESIAN_POINT ( 'NONE',  ( 19.05341960407611168, 5.049401038298154454, 98.95724293864766707 ) ) ;
#168897 = CARTESIAN_POINT ( 'NONE',  ( -13.97604488694547697, 13.89961937509957934, 78.12609039468567573 ) ) ;
#168898 = CARTESIAN_POINT ( 'NONE',  ( -15.72974639402176322, -15.80617190586768395, 39.37609039468567573 ) ) ;
#168899 = CARTESIAN_POINT ( 'NONE',  ( 0.05219959533936267826, -19.03943276465977164, 110.0010903946856757 ) ) ;
#168900 = CARTESIAN_POINT ( 'NONE',  ( -19.05341960407617563, 5.049401038297882671, 73.54275706135233293 ) ) ;
#168901 = CARTESIAN_POINT ( 'NONE',  ( 19.02544592524343514, -5.153800228976328945, 38.54057627198103120 ) ) ;
#168902 = CARTESIAN_POINT ( 'NONE',  ( -9.474510206698720793, -16.51473224551083518, 84.58442372801900433 ) ) ;
#168903 = CARTESIAN_POINT ( 'NONE',  ( -12.14591786802326823, 12.06949235617739902, 103.1260903946856757 ) ) ;
#168904 = CARTESIAN_POINT ( 'NONE',  ( 16.51473224551083163, -9.474510206698727899, 80.83442372801899012 ) ) ;
#168905 = CARTESIAN_POINT ( 'NONE',  ( -8.314922557960811034, -14.29746914071050412, 42.08224293864769550 ) ) ;
#168906 = CARTESIAN_POINT ( 'NONE',  ( 5.153800228976615827, -19.02544592524334988, 70.20942372801899012 ) ) ;
#168907 = CARTESIAN_POINT ( 'NONE',  ( 21.55341960407619695, -5.719274019375665929, 111.0427570613523613 ) ) ;
#168908 = CARTESIAN_POINT ( 'NONE',  ( -16.51473224551082808, 9.474510206698731452, 23.33442372801900078 ) ) ;
#168909 = CARTESIAN_POINT ( 'NONE',  ( -19.03943276465977164, 0.05219959533909376836, 26.24890960531435624 ) ) ;
#168910 = CARTESIAN_POINT ( 'NONE',  ( 5.000000000000001776, -120.0000000000000142, 0.0009999999999992653654 ) ) ;
#168911 = CARTESIAN_POINT ( 'NONE',  ( 14.29746914071037800, 8.314922557961029526, 41.66775706135235424 ) ) ;
#168912 = CARTESIAN_POINT ( 'NONE',  ( 13.97604488694527802, 13.89961937509977652, 94.37390960531436690 ) ) ;
#168913 = AXIS2_PLACEMENT_3D ( 'NONE', #24503, #86154, #118505 ) ;
#168914 = CARTESIAN_POINT ( 'NONE',  ( -27.73933785331498925, 9.013057229001089965, 142.7750000027311899 ) ) ;
#168915 = CARTESIAN_POINT ( 'NONE',  ( -19.05341960407611168, -5.049401038298163336, 91.45724293864766707 ) ) ;
#168916 = CARTESIAN_POINT ( 'NONE',  ( -17.31728774477210564, 6.344390552233735825, 100.8190665168930593 ) ) ;
#168917 = EDGE_LOOP ( 'NONE', ( #46487, #42134, #191674, #185041 ) ) ;
#168918 = CARTESIAN_POINT ( 'NONE',  ( 16.46253265017146816, 9.564922557961045513, 81.66775706135233293 ) ) ;
#168919 = CARTESIAN_POINT ( 'NONE',  ( -21.52544592524343514, 5.823673210054127303, 26.04057627198103475 ) ) ;
#168921 = CARTESIAN_POINT ( 'NONE',  ( 19.02544592524334988, 5.153800228976608722, 101.4594237280189759 ) ) ;
#168920 = CARTESIAN_POINT ( 'NONE',  ( 18.67979575497194134, -10.72451020669871369, 110.8344237280190043 ) ) ;
#168922 = CARTESIAN_POINT ( 'NONE',  ( -4.483927247898539470, -16.52544592524342804, 107.2905762719810525 ) ) ;
#168923 = CARTESIAN_POINT ( 'NONE',  ( -5.049401038298153566, 19.05341960407611168, 25.20724293864768484 ) ) ;
#168924 = CARTESIAN_POINT ( 'NONE',  ( 15.72974639402199770, -15.80617190586745480, 58.12390960531435979 ) ) ;
#168925 = CARTESIAN_POINT ( 'NONE',  ( 21.53943276465977519, -0.05219959533907433946, 43.74890960531435979 ) ) ;
#168926 = CARTESIAN_POINT ( 'NONE',  ( 19.02544592524343514, -5.153800228976328945, 28.54057627198102409 ) ) ;
#168927 = CARTESIAN_POINT ( 'NONE',  ( -8.906447517083053711, -27.41122689804191026, 142.6500000054623740 ) ) ;
#168928 = CARTESIAN_POINT ( 'NONE',  ( 0.05219959533936267826, -19.03943276465977164, 70.00109039468566152 ) ) ;
#168929 = CARTESIAN_POINT ( 'NONE',  ( -16.52544592524342804, 4.483927247898546575, 41.04057627198103120 ) ) ;
#168930 = CARTESIAN_POINT ( 'NONE',  ( 19.03943276465977164, -0.05219959533909143690, 108.7489096053143527 ) ) ;
#168931 = CARTESIAN_POINT ( 'NONE',  ( -21.55341960407619339, 5.719274019375674811, 98.54275706135234714 ) ) ;
#168932 = CARTESIAN_POINT ( 'NONE',  ( -18.62759615963270932, 10.81492255796079327, 70.83224293864770971 ) ) ;
#168933 = CARTESIAN_POINT ( 'NONE',  ( 10.72451020669871369, 18.67979575497193778, 52.08442372801901854 ) ) ;
#168934 = CARTESIAN_POINT ( 'NONE',  ( 18.62759615963255655, 10.81492255796105972, 46.66775706135234714 ) ) ;
#168935 = CARTESIAN_POINT ( 'NONE',  ( -19.03943276465977164, 0.05219959533909376836, 91.24890960531436690 ) ) ;
#168936 = CARTESIAN_POINT ( 'NONE',  ( -14.34966873604972548, 8.224510206698743886, 98.33442372801901854 ) ) ;
#168937 = CARTESIAN_POINT ( 'NONE',  ( 12.14591786802309770, 12.06949235617756955, 114.3739096053143527 ) ) ;
#168938 = CARTESIAN_POINT ( 'NONE',  ( -31.27056374934903715, 7.502136971886772088, 95.45648825569139717 ) ) ;
#168939 = CARTESIAN_POINT ( 'NONE',  ( -0.05219959533910754901, -16.53943276465976808, 67.49890960531436690 ) ) ;
#168940 = CARTESIAN_POINT ( 'NONE',  ( 14.29746914071049879, -8.314922557960816363, 33.33224293864769550 ) ) ;
#168941 = CARTESIAN_POINT ( 'NONE',  ( -0.05219959533909027116, -19.03943276465977164, 62.49890960531435979 ) ) ;
#168942 = CARTESIAN_POINT ( 'NONE',  ( -19.05341960407611168, -5.049401038298163336, 36.45724293864766707 ) ) ;
#168943 = CARTESIAN_POINT ( 'NONE',  ( 18.67979575497178502, 10.72451020669898547, 64.16557627198102409 ) ) ;
#168944 = CARTESIAN_POINT ( 'NONE',  ( -19.05341960407617563, 5.049401038297882671, 33.54275706135231871 ) ) ;
#168946 = CARTESIAN_POINT ( 'NONE',  ( -16.53943276465976808, 0.05219959533911058130, 56.24890960531436690 ) ) ;
#168945 = DIRECTION ( 'NONE',  ( 3.469446951953612217E-15, 0.000000000000000000, -1.000000000000000000 ) ) ;
#168947 = CARTESIAN_POINT ( 'NONE',  ( -10.81492255796078084, -18.62759615963271287, 32.08224293864769550 ) ) ;
#168948 = ORIENTED_EDGE ( 'NONE', *, *, #120571, .T. ) ;
#168949 = CARTESIAN_POINT ( 'NONE',  ( 17.49999999999999645, 3.242565516156353134, 37.49999999998637179 ) ) ;
#168950 = CARTESIAN_POINT ( 'NONE',  ( 8.224510206698742110, 14.34966873604972548, 77.08442372801901854 ) ) ;
#168951 = CARTESIAN_POINT ( 'NONE',  ( 16.46253265017146816, 9.564922557961045513, 71.66775706135233293 ) ) ;
#168952 = CARTESIAN_POINT ( 'NONE',  ( 16.52544592524342804, -4.483927247898539470, 38.54057627198103120 ) ) ;
#168953 = CARTESIAN_POINT ( 'NONE',  ( -18.22780087662124160, -5.499999999999927169, 73.98236817873106475 ) ) ;
#168954 = CARTESIAN_POINT ( 'NONE',  ( -14.34966873604960291, -8.224510206698953496, 31.66557627198102054 ) ) ;
#168955 = CARTESIAN_POINT ( 'NONE',  ( 16.46253265017160672, -9.564922557960803928, 58.33224293864769550 ) ) ;
#168956 = CARTESIAN_POINT ( 'NONE',  ( -13.97604488694527625, -13.89961937509977652, 71.87390960531433848 ) ) ;
#168957 = CARTESIAN_POINT ( 'NONE',  ( 13.97604488694527802, 13.89961937509977652, 39.37390960531435269 ) ) ;
#168958 = CARTESIAN_POINT ( 'NONE',  ( 10.72451020669871369, 18.67979575497193778, 42.08442372801901854 ) ) ;
#168959 = CARTESIAN_POINT ( 'NONE',  ( 13.97604488694527802, 13.89961937509977652, 59.37390960531434558 ) ) ;
#168960 = DIRECTION ( 'NONE',  ( -1.000000000000000000, 0.000000000000000000, 0.000000000000000000 ) ) ;
#168961 = CARTESIAN_POINT ( 'NONE',  ( 13.97604488694527802, 13.89961937509977652, 59.37390960531434558 ) ) ;
#168962 = CARTESIAN_POINT ( 'NONE',  ( 10.72451020669898902, -18.67979575497178502, 37.91557627198102409 ) ) ;
#168963 = CARTESIAN_POINT ( 'NONE',  ( 8.314922557960818139, 14.29746914071049879, 114.5822429386477097 ) ) ;
#168964 = CARTESIAN_POINT ( 'NONE',  ( 18.62759615963271287, -10.81492255796078972, 28.33224293864769550 ) ) ;
#168965 = AXIS2_PLACEMENT_3D ( 'NONE', #146872, #68028, #194395 ) ;
#168966 = CARTESIAN_POINT ( 'NONE',  ( -12.06949235617739369, -12.14591786802326823, 89.37609039468568994 ) ) ;
#168967 = CARTESIAN_POINT ( 'NONE',  ( 15.72974639402176855, 15.80617190586768217, 101.8760903946857042 ) ) ;
#168968 = CARTESIAN_POINT ( 'NONE',  ( 12.14591786802327356, -12.06949235617739191, 65.62609039468568994 ) ) ;
#168969 = CARTESIAN_POINT ( 'NONE',  ( 5.049401038298161559, -19.05341960407611168, 112.7072429386476813 ) ) ;
#168970 = CARTESIAN_POINT ( 'NONE',  ( 4.483927247898790824, -16.52544592524335698, 60.20942372801902565 ) ) ;
#168971 = CARTESIAN_POINT ( 'NONE',  ( -16.52544592524335698, -4.483927247898792601, 43.95942372801902565 ) ) ;
#168972 = CARTESIAN_POINT ( 'NONE',  ( -0.05219959533934338120, 16.53943276465976808, 92.50109039468567573 ) ) ;
#168973 = CARTESIAN_POINT ( 'NONE',  ( -8.314922557961024197, 14.29746914071037800, 27.91775706135234358 ) ) ;
#168974 = CARTESIAN_POINT ( 'NONE',  ( 16.46253265017160672, -9.564922557960803928, 33.33224293864770260 ) ) ;
#168975 = CARTESIAN_POINT ( 'NONE',  ( -18.62759615963255300, -10.81492255796106328, 19.16775706135234714 ) ) ;
#168976 = CARTESIAN_POINT ( 'NONE',  ( -4.379528057220086978, -16.55341960407618274, 24.79275706135235779 ) ) ;
#168977 = CARTESIAN_POINT ( 'NONE',  ( 8.224510206698742110, 14.34966873604972548, 82.08442372801901854 ) ) ;
#168978 = CARTESIAN_POINT ( 'NONE',  ( 23.48529157249599564, 32.32473071737754111, -4.449999994537627401 ) ) ;
#168979 = CARTESIAN_POINT ( 'NONE',  ( -5.719274019375665041, -21.55341960407619695, 84.79275706135234714 ) ) ;
#168981 = EDGE_CURVE ( 'NONE', #108968, #45388, #28169, .T. ) ;
#168980 = CARTESIAN_POINT ( 'NONE',  ( -16.51473224551082808, 9.474510206698731452, 78.33442372801900433 ) ) ;
#168982 = CARTESIAN_POINT ( 'NONE',  ( -16.52544592524342804, 4.483927247898546575, 56.04057627198102409 ) ) ;
#168983 = CARTESIAN_POINT ( 'NONE',  ( 4.379528057220339221, -16.55341960407611168, 42.70724293864770260 ) ) ;
#168984 = CARTESIAN_POINT ( 'NONE',  ( -16.53943276465976808, 0.05219959533911058130, 101.2489096053143669 ) ) ;
#168986 = CARTESIAN_POINT ( 'NONE',  ( -7.121805330552559710, 1.425084765988153368, -64.33521149768085934 ) ) ;
#168985 = CARTESIAN_POINT ( 'NONE',  ( 19.05341960407617918, -5.049401038297876454, 41.04275706135233293 ) ) ;
#168987 = CARTESIAN_POINT ( 'NONE',  ( 21.53943276465977519, 0.05219959533937863772, 56.25109039468568284 ) ) ;
#168988 = CARTESIAN_POINT ( 'NONE',  ( -13.97604488694547697, 13.89961937509957934, 113.1260903946856757 ) ) ;
#168989 = LINE ( 'NONE', #43684, #124584 ) ;
#168990 = CARTESIAN_POINT ( 'NONE',  ( 19.05341960407611168, 5.049401038298154454, 108.9572429386477097 ) ) ;
#168991 = CARTESIAN_POINT ( 'NONE',  ( 0.05219959533907565091, 21.53943276465977519, 69.99890960531435269 ) ) ;
#168992 = CARTESIAN_POINT ( 'NONE',  ( 9.474510206698729675, 16.51473224551082808, 97.08442372801900433 ) ) ;
#168993 = CARTESIAN_POINT ( 'NONE',  ( 19.05341960407611168, 5.049401038298154454, 108.9572429386477097 ) ) ;
#168994 = CARTESIAN_POINT ( 'NONE',  ( -19.78400068765821374, -20.35809916000442499, 140.0000000000000000 ) ) ;
#168995 = CARTESIAN_POINT ( 'NONE',  ( 16.52544592524342804, -4.483927247898539470, 103.5405762719810383 ) ) ;
#168996 = CARTESIAN_POINT ( 'NONE',  ( -10.81492255796105439, 18.62759615963255655, 97.91775706135236135 ) ) ;
#168997 = CARTESIAN_POINT ( 'NONE',  ( 9.564922557960805705, 16.46253265017160317, 29.58224293864769550 ) ) ;
#168998 = CARTESIAN_POINT ( 'NONE',  ( 0.05219959533937995610, -21.53943276465977519, 55.00109039468568284 ) ) ;
#168999 = CARTESIAN_POINT ( 'NONE',  ( 10.72451020669871369, 18.67979575497193778, 87.08442372801901854 ) ) ;
#169000 = CARTESIAN_POINT ( 'NONE',  ( -12.14591786802326823, 12.06949235617739902, 88.12609039468570415 ) ) ;
#169001 = CARTESIAN_POINT ( 'NONE',  ( 10.72451020669871369, 18.67979575497193778, 37.08442372801901143 ) ) ;
#169002 = CARTESIAN_POINT ( 'NONE',  ( -15.72974639402176322, -15.80617190586768395, 44.37609039468567573 ) ) ;
#169004 = CARTESIAN_POINT ( 'NONE',  ( 9.474510206698971260, -16.51473224551069308, 92.91557627198103830 ) ) ;
#169003 = CARTESIAN_POINT ( 'NONE',  ( 9.474510206698729675, 16.51473224551082808, 62.08442372801899722 ) ) ;
#169005 = CARTESIAN_POINT ( 'NONE',  ( -16.53943276465976808, 0.05219959533911058130, 101.2489096053143669 ) ) ;
#169006 = CARTESIAN_POINT ( 'NONE',  ( 5.719274019375991003, -21.55341960407610458, 87.70724293864769550 ) ) ;
#169007 = CARTESIAN_POINT ( 'NONE',  ( 14.29746914071049879, -8.314922557960816363, 63.33224293864770260 ) ) ;
#169008 = CARTESIAN_POINT ( 'NONE',  ( 10.72451020669871369, 18.67979575497193778, 107.0844237280190043 ) ) ;
#169009 = CARTESIAN_POINT ( 'NONE',  ( 8.224510206698953496, -14.34966873604960469, 77.91557627198102409 ) ) ;
#169010 = CARTESIAN_POINT ( 'NONE',  ( 19.05341960407611168, 5.049401038298154454, 33.95724293864769550 ) ) ;
#169011 = CARTESIAN_POINT ( 'NONE',  ( 16.46253265017146816, 9.564922557961045513, 86.66775706135233293 ) ) ;
#169012 = CARTESIAN_POINT ( 'NONE',  ( 0.05219959533910956823, 16.53943276465976808, 44.99890960531435979 ) ) ;
#169013 = CARTESIAN_POINT ( 'NONE',  ( -15.80617190586768217, 15.72974639402176855, 93.12609039468568994 ) ) ;
#169014 = CARTESIAN_POINT ( 'NONE',  ( -5.153800228976328057, -19.02544592524343514, 97.29057627198099567 ) ) ;
#169015 = CARTESIAN_POINT ( 'NONE',  ( 16.46253265017146816, 9.564922557961045513, 56.66775706135233293 ) ) ;
#169016 = CARTESIAN_POINT ( 'NONE',  ( -5.823673210054116645, -21.52544592524344225, 67.29057627198103830 ) ) ;
#169017 = CARTESIAN_POINT ( 'NONE',  ( -10.72451020669898014, 18.67979575497178502, 115.4155762719810241 ) ) ;
#169018 = CARTESIAN_POINT ( 'NONE',  ( 0.05219959533934541429, -16.53943276465976808, 25.00109039468567218 ) ) ;
#169019 = CARTESIAN_POINT ( 'NONE',  ( -12.06949235617739369, -12.14591786802326823, 79.37609039468567573 ) ) ;
#169021 = CARTESIAN_POINT ( 'NONE',  ( 15.80617190586769283, -15.72974639402175789, 20.62609039468568639 ) ) ;
#169020 = CARTESIAN_POINT ( 'NONE',  ( -16.51473224551069308, -9.474510206698971260, 31.66557627198102054 ) ) ;
#169022 = CARTESIAN_POINT ( 'NONE',  ( -12.06949235617756955, 12.14591786802309770, 115.6239096053143669 ) ) ;
#169023 = CARTESIAN_POINT ( 'NONE',  ( -22.81625015709510507, 31.40387420917330275, -3.424999997268813434 ) ) ;
#169024 = CARTESIAN_POINT ( 'NONE',  ( -16.53943276465976808, -0.05219959533934237506, 53.75109039468568994 ) ) ;
#169025 = CARTESIAN_POINT ( 'NONE',  ( -8.314922557960811034, -14.29746914071050412, 77.08224293864769550 ) ) ;
#169026 = CARTESIAN_POINT ( 'NONE',  ( 0.05219959533907565091, 21.53943276465977519, 74.99890960531435269 ) ) ;
#169027 = CARTESIAN_POINT ( 'NONE',  ( 0.05219959533910956823, 16.53943276465976808, 29.99890960531435979 ) ) ;
#169028 = CARTESIAN_POINT ( 'NONE',  ( 8.314922557961029526, -14.29746914071037800, 35.41775706135234003 ) ) ;
#169029 = CARTESIAN_POINT ( 'NONE',  ( 13.97604488694527802, 13.89961937509977652, 44.37390960531435269 ) ) ;
#169030 = CARTESIAN_POINT ( 'NONE',  ( -4.379528057220086978, -16.55341960407618274, 74.79275706135234714 ) ) ;
#169031 = CARTESIAN_POINT ( 'NONE',  ( -9.474510206698720793, -16.51473224551083518, 79.58442372801899012 ) ) ;
#169032 = CARTESIAN_POINT ( 'NONE',  ( 18.62759615963271287, -10.81492255796078972, 73.33224293864769550 ) ) ;
#169033 = CARTESIAN_POINT ( 'NONE',  ( -0.05219959533934338120, 16.53943276465976808, 107.5010903946856899 ) ) ;
#169034 = ORIENTED_EDGE ( 'NONE', *, *, #108503, .T. ) ;
#169035 = CARTESIAN_POINT ( 'NONE',  ( -18.62759615963255300, -10.81492255796106328, 79.16775706135234714 ) ) ;
#169036 = CARTESIAN_POINT ( 'NONE',  ( 10.72451020669898902, -18.67979575497178502, 42.91557627198103120 ) ) ;
#169037 = ORIENTED_EDGE ( 'NONE', *, *, #14709, .T. ) ;
#169038 = VERTEX_POINT ( 'NONE', #69273 ) ;
#169039 = CARTESIAN_POINT ( 'NONE',  ( 12.06949235617739724, 12.14591786802326823, 86.87609039468568994 ) ) ;
#169040 = CARTESIAN_POINT ( 'NONE',  ( -5.719274019375978568, 21.55341960407610458, 45.20724293864769550 ) ) ;
#169041 = ORIENTED_EDGE ( 'NONE', *, *, #126300, .T. ) ;
#169042 = CARTESIAN_POINT ( 'NONE',  ( -19.05341960407611168, -5.049401038298163336, 106.4572429386476955 ) ) ;
#169043 = DIRECTION ( 'NONE',  ( -0.8571673007021135549, 1.049727191138620175E-16, 0.5150380749100520461 ) ) ;
#169044 = CARTESIAN_POINT ( 'NONE',  ( -14.29746914071049879, 8.314922557960819915, 115.8322429386477097 ) ) ;
#169045 = CARTESIAN_POINT ( 'NONE',  ( -15.80617190586745835, -15.72974639402198527, 76.87390960531439532 ) ) ;
#169046 = CARTESIAN_POINT ( 'NONE',  ( 8.314922557961029526, -14.29746914071037800, 110.4177570613523756 ) ) ;
#169047 = CARTESIAN_POINT ( 'NONE',  ( -10.81492255796105439, 18.62759615963255655, 57.91775706135234714 ) ) ;
#169048 = CARTESIAN_POINT ( 'NONE',  ( 16.52544592524335698, 4.483927247898782831, 21.45942372801901499 ) ) ;
#169049 = CARTESIAN_POINT ( 'NONE',  ( 5.049401038298161559, -19.05341960407611168, 27.70724293864769550 ) ) ;
#169050 = CARTESIAN_POINT ( 'NONE',  ( 12.06949235617739724, 12.14591786802326823, 31.87609039468567929 ) ) ;
#169051 = CARTESIAN_POINT ( 'NONE',  ( -5.049401038298153566, 19.05341960407611168, 40.20724293864768839 ) ) ;
#169052 = CARTESIAN_POINT ( 'NONE',  ( 16.09882439466104032, -1.216645939406789445, -61.59766612755957738 ) ) ;
#169053 = CARTESIAN_POINT ( 'NONE',  ( -19.03943276465977164, 0.05219959533909376836, 106.2489096053143669 ) ) ;
#169054 = CARTESIAN_POINT ( 'NONE',  ( 4.483927247898790824, -16.52544592524335698, 85.20942372801901854 ) ) ;
#169055 = CARTESIAN_POINT ( 'NONE',  ( 13.97604488694548053, -13.89961937509957401, 75.62609039468564731 ) ) ;
#169056 = CARTESIAN_POINT ( 'NONE',  ( 16.46253265017146816, 9.564922557961045513, 21.66775706135233648 ) ) ;
#169057 = CARTESIAN_POINT ( 'NONE',  ( 0.05219959533907565091, 21.53943276465977519, 79.99890960531435269 ) ) ;
#169058 = CARTESIAN_POINT ( 'NONE',  ( 12.14591786802327356, -12.06949235617739191, 95.62609039468568994 ) ) ;
#169059 = AXIS2_PLACEMENT_3D ( 'NONE', #117158, #28176, #194025 ) ;
#169060 = CARTESIAN_POINT ( 'NONE',  ( -5.049401038297874678, -19.05341960407617918, 89.79275706135230450 ) ) ;
#169061 = CARTESIAN_POINT ( 'NONE',  ( 16.46253265017160672, -9.564922557960803928, 53.33224293864768839 ) ) ;
#169062 = CARTESIAN_POINT ( 'NONE',  ( 13.89961937509977652, -13.97604488694527269, 88.12390960531438111 ) ) ;
#169063 = CARTESIAN_POINT ( 'NONE',  ( -5.719274019375665041, -21.55341960407619695, 54.79275706135235424 ) ) ;
#169064 = CARTESIAN_POINT ( 'NONE',  ( 13.89961937509977652, -13.97604488694527269, 53.12390960531434558 ) ) ;
#169065 = CARTESIAN_POINT ( 'NONE',  ( -16.81555441253551919, -7.025013491695472290, 84.36314554665739252 ) ) ;
#169066 = CARTESIAN_POINT ( 'NONE',  ( -19.03943276465977164, 0.05219959533909376836, 111.2489096053143669 ) ) ;
#169067 = CARTESIAN_POINT ( 'NONE',  ( 14.34966873604960469, 8.224510206698951720, 64.16557627198102409 ) ) ;
#169068 = CARTESIAN_POINT ( 'NONE',  ( 21.53943276465977519, -0.05219959533907433946, 78.74890960531436690 ) ) ;
#169069 = CYLINDRICAL_SURFACE ( 'NONE', #90146, 16.70000000000002061 ) ;
#169070 = CARTESIAN_POINT ( 'NONE',  ( 16.51473224551083163, -9.474510206698727899, 40.83442372801900433 ) ) ;
#169071 = CARTESIAN_POINT ( 'NONE',  ( -11.30153831258470731, -180.0000000000000000, -15.00000000000000178 ) ) ;
#169073 = CARTESIAN_POINT ( 'NONE',  ( 13.89961937509977652, -13.97604488694527269, 88.12390960531438111 ) ) ;
#169072 = CARTESIAN_POINT ( 'NONE',  ( -16.51473224551069308, -9.474510206698971260, 66.66557627198102409 ) ) ;
#169074 = CARTESIAN_POINT ( 'NONE',  ( -16.55341960407617563, 4.379528057220093196, 48.54275706135234714 ) ) ;
#169075 = CARTESIAN_POINT ( 'NONE',  ( 22.72061570927962393, -33.65877872499203960, -17.91763856381927411 ) ) ;
#169076 = CARTESIAN_POINT ( 'NONE',  ( -19.02544592524334988, -5.153800228976617603, 33.95942372801897591 ) ) ;
#169077 = CARTESIAN_POINT ( 'NONE',  ( 11.30153831258470731, -180.0000000000000000, -25.00000000000000000 ) ) ;
#169078 = CARTESIAN_POINT ( 'NONE',  ( 14.34966873604972726, -8.224510206698740333, 95.83442372801903275 ) ) ;
#169079 = CARTESIAN_POINT ( 'NONE',  ( -0.9791052130474502402, -23.94081952771227151, -54.49391133501601558 ) ) ;
#169080 = CARTESIAN_POINT ( 'NONE',  ( -8.224510206698735004, -14.34966873604973081, 79.58442372801903275 ) ) ;
#169081 = CARTESIAN_POINT ( 'NONE',  ( -12.14591786802326823, 12.06949235617739902, 58.12609039468568994 ) ) ;
#169082 = CARTESIAN_POINT ( 'NONE',  ( -9.474510206698720793, -16.51473224551083518, 19.58442372801899722 ) ) ;
#169084 = CARTESIAN_POINT ( 'NONE',  ( -18.22780087662126647, -5.499999999999827693, 58.98236817873108606 ) ) ;
#169083 = CARTESIAN_POINT ( 'NONE',  ( 0.05219959533909260263, 19.03943276465977164, 54.99890960531435979 ) ) ;
#169085 = CARTESIAN_POINT ( 'NONE',  ( -21.55341960407619339, 5.719274019375674811, 73.54275706135234714 ) ) ;
#169086 = CARTESIAN_POINT ( 'NONE',  ( -19.05341960407617563, 5.049401038297882671, 78.54275706135233293 ) ) ;
#169087 = CARTESIAN_POINT ( 'NONE',  ( 18.67979575497194134, -10.72451020669871369, 105.8344237280190328 ) ) ;
#169088 = CARTESIAN_POINT ( 'NONE',  ( -5.153800228976328057, -19.02544592524343514, 32.29057627198102409 ) ) ;
#169089 = CARTESIAN_POINT ( 'NONE',  ( -16.39429727647829083, 14.63400850047063528, -58.42335914450119816 ) ) ;
#169090 = CARTESIAN_POINT ( 'NONE',  ( 21.52544592524344225, -5.823673210054117533, 68.54057627198103830 ) ) ;
#169091 = CARTESIAN_POINT ( 'NONE',  ( 5.153800228976335163, 19.02544592524342804, 114.7905762719810241 ) ) ;
#169092 = CARTESIAN_POINT ( 'NONE',  ( -8.314922557960811034, -14.29746914071050412, 112.0822429386477097 ) ) ;
#169093 = CARTESIAN_POINT ( 'NONE',  ( -12.14591786802326823, 12.06949235617739902, 43.12609039468568284 ) ) ;
#169094 = CARTESIAN_POINT ( 'NONE',  ( -16.55341960407611168, -4.379528057220339221, 26.45724293864768839 ) ) ;
#169095 = VERTEX_POINT ( 'NONE', #130939 ) ;
#169096 = CARTESIAN_POINT ( 'NONE',  ( -5.719274019375665041, -21.55341960407619695, 19.79275706135235069 ) ) ;
#169098 = CARTESIAN_POINT ( 'NONE',  ( 11.74264578624800315, -36.14014761921581709, -3.400000000000000355 ) ) ;
#169097 = CARTESIAN_POINT ( 'NONE',  ( -16.52544592524342804, 4.483927247898546575, 46.04057627198103830 ) ) ;
#169099 = CARTESIAN_POINT ( 'NONE',  ( -16.51473224551082808, 9.474510206698731452, 108.3344237280190043 ) ) ;
#169100 = CARTESIAN_POINT ( 'NONE',  ( 13.97604488694548053, -13.89961937509957401, 30.62609039468566863 ) ) ;
#169101 = CARTESIAN_POINT ( 'NONE',  ( 16.52544592524342804, -4.483927247898539470, 48.54057627198103120 ) ) ;
#169102 = CARTESIAN_POINT ( 'NONE',  ( -10.81492255796078084, -18.62759615963271287, 102.0822429386476955 ) ) ;
#169104 = CARTESIAN_POINT ( 'NONE',  ( 10.72451020669898902, -18.67979575497178502, 67.91557627198102409 ) ) ;
#169103 = CARTESIAN_POINT ( 'NONE',  ( 16.38665767535053064, 7.295008042176040597, 32.23599135785455871 ) ) ;
#169105 = CARTESIAN_POINT ( 'NONE',  ( -13.89961937509977652, 13.97604488694528158, 75.62390960531438111 ) ) ;
#169106 = CARTESIAN_POINT ( 'NONE',  ( -4.379528057220328563, 16.55341960407611168, 45.20724293864769550 ) ) ;
#169107 = CARTESIAN_POINT ( 'NONE',  ( 16.51473224551069308, 9.474510206698969483, 104.1655762719810241 ) ) ;
#169108 = CARTESIAN_POINT ( 'NONE',  ( 1.784589286804253661, -7.284589286804279418, 1.818019484660534424 ) ) ;
#169109 = CARTESIAN_POINT ( 'NONE',  ( 19.03943276465977164, 0.05219959533936151252, 56.25109039468566863 ) ) ;
#169110 = CARTESIAN_POINT ( 'NONE',  ( -15.80617190586745835, -15.72974639402198527, 91.87390960531436690 ) ) ;
#169111 = CARTESIAN_POINT ( 'NONE',  ( -5.153800228976328057, -19.02544592524343514, 42.29057627198101699 ) ) ;
#169112 = CARTESIAN_POINT ( 'NONE',  ( -14.29746914071049879, 8.314922557960819915, 115.8322429386477097 ) ) ;
#169113 = CIRCLE ( 'NONE', #162637, 10.00000000000000888 ) ;
#169114 = EDGE_CURVE ( 'NONE', #184086, #165860, #100601, .T. ) ;
#169115 = CARTESIAN_POINT ( 'NONE',  ( 21.52544592524334988, 5.823673210054432836, 51.45942372801901854 ) ) ;
#169116 = CARTESIAN_POINT ( 'NONE',  ( -27.73933785331498925, 9.013057229001089965, 148.7750000027311899 ) ) ;
#169117 = CARTESIAN_POINT ( 'NONE',  ( 12.14591786802309770, 12.06949235617756955, 24.37390960531435979 ) ) ;
#169118 = CARTESIAN_POINT ( 'NONE',  ( -13.97604488694527625, -13.89961937509977652, 46.87390960531435979 ) ) ;
#169119 = CARTESIAN_POINT ( 'NONE',  ( -16.46253265017160317, 9.564922557960807481, 105.8322429386476955 ) ) ;
#169120 = CARTESIAN_POINT ( 'NONE',  ( 5.719274019375991003, -21.55341960407610458, 57.70724293864770260 ) ) ;
#169121 = CARTESIAN_POINT ( 'NONE',  ( -13.97604488694547520, 13.89961937509957934, 93.12609039468566152 ) ) ;
#169122 = CARTESIAN_POINT ( 'NONE',  ( -13.89961937509977652, 13.97604488694528158, 40.62390960531435979 ) ) ;
#169123 = CARTESIAN_POINT ( 'NONE',  ( -21.53943276465977519, 0.05219959533907696930, 51.24890960531436690 ) ) ;
#169124 = ORIENTED_EDGE ( 'NONE', *, *, #91315, .T. ) ;
#169125 = CARTESIAN_POINT ( 'NONE',  ( -21.52544592524334988, -5.823673210054445271, 88.95942372801901854 ) ) ;
#169127 = CARTESIAN_POINT ( 'NONE',  ( 4.379528057220092307, 16.55341960407617563, 77.29275706135234714 ) ) ;
#169126 = CARTESIAN_POINT ( 'NONE',  ( 21.18879603623556918, -31.24179269221876254, -19.75583340878575456 ) ) ;
#169128 = CARTESIAN_POINT ( 'NONE',  ( 16.53943276465976808, 0.05219959533934440121, 91.25109039468568994 ) ) ;
#169129 = CARTESIAN_POINT ( 'NONE',  ( -13.89961937509977652, 13.97604488694528158, 65.62390960531436690 ) ) ;
#169130 = CARTESIAN_POINT ( 'NONE',  ( 13.97604488694527802, 13.89961937509977652, 69.37390960531436690 ) ) ;
#169131 = ORIENTED_EDGE ( 'NONE', *, *, #184219, .T. ) ;
#169132 = CARTESIAN_POINT ( 'NONE',  ( -9.564922557961040184, 16.46253265017147172, 27.91775706135232582 ) ) ;
#169133 = CARTESIAN_POINT ( 'NONE',  ( 8.314922557961029526, -14.29746914071037800, 75.41775706135233293 ) ) ;
#169134 = CARTESIAN_POINT ( 'NONE',  ( -13.89961937509957401, -13.97604488694547875, 19.37609039468566507 ) ) ;
#169135 = CARTESIAN_POINT ( 'NONE',  ( -19.03943276465977164, 0.05219959533909376836, 81.24890960531436690 ) ) ;
#169136 = CARTESIAN_POINT ( 'NONE',  ( -10.81492255796078084, -18.62759615963271287, 47.08224293864770260 ) ) ;
#169137 = CARTESIAN_POINT ( 'NONE',  ( -14.34966873604972548, 8.224510206698743886, 28.33442372801902209 ) ) ;
#169138 = CARTESIAN_POINT ( 'NONE',  ( 10.72451020669871369, 18.67979575497193778, 82.08442372801901854 ) ) ;
#169139 = CARTESIAN_POINT ( 'NONE',  ( -14.29746914071037622, -8.314922557961029526, 64.16775706135234714 ) ) ;
#169140 = CARTESIAN_POINT ( 'NONE',  ( 10.81492255796078972, 18.62759615963270932, 114.5822429386477097 ) ) ;
#169141 = CARTESIAN_POINT ( 'NONE',  ( 16.46253265017146816, 9.564922557961045513, 106.6677570613523471 ) ) ;
#169142 = CARTESIAN_POINT ( 'NONE',  ( -13.97604488694527625, -13.89961937509977652, 76.87390960531433848 ) ) ;
#169143 = CARTESIAN_POINT ( 'NONE',  ( 14.34966873604972726, -8.224510206698740333, 25.83442372801901499 ) ) ;
#169144 = CARTESIAN_POINT ( 'NONE',  ( -5.049401038298153566, 19.05341960407611168, 45.20724293864769550 ) ) ;
#169145 = AXIS2_PLACEMENT_3D ( 'NONE', #129177, #113024, #143352 ) ;
#169146 = CARTESIAN_POINT ( 'NONE',  ( -0.05219959533934338120, 16.53943276465976808, 22.50109039468567573 ) ) ;
#169147 = CARTESIAN_POINT ( 'NONE',  ( -14.34966873604960291, -8.224510206698953496, 76.66557627198103830 ) ) ;
#169148 = CARTESIAN_POINT ( 'NONE',  ( -4.379528057220086978, -16.55341960407618274, 84.79275706135234714 ) ) ;
#169150 = CARTESIAN_POINT ( 'NONE',  ( -9.474510206698964154, 16.51473224551069663, 60.41557627198102409 ) ) ;
#169149 = CARTESIAN_POINT ( 'NONE',  ( 15.80617190586769283, -15.72974639402175789, 35.62609039468568994 ) ) ;
#169151 = CARTESIAN_POINT ( 'NONE',  ( 13.97604488694527802, 13.89961937509977652, 74.37390960531436690 ) ) ;
#169152 = B_SPLINE_CURVE_WITH_KNOTS ( 'NONE', 3,
 ( #158889, #128544, #69891, #190241, #193244, #85038 ),
 .UNSPECIFIED., .F., .F.,
 ( 4, 2, 4 ),
 ( 0.003239945802372207456, 0.003620412082092024954, 0.004000878361811842886 ),
 .UNSPECIFIED. ) ;
#169153 = CARTESIAN_POINT ( 'NONE',  ( -14.29746914071037622, -8.314922557961029526, 89.16775706135236135 ) ) ;
#169155 = EDGE_LOOP ( 'NONE', ( #170588, #120557, #15618, #83108, #180810 ) ) ;
#169154 = CARTESIAN_POINT ( 'NONE',  ( -24.40828949532285463, -2.848420800298675282, 173.9378174459543516 ) ) ;
#169156 = EDGE_LOOP ( 'NONE', ( #8055, #59666, #163352, #39044, #104022, #81982 ) ) ;
#169157 = CARTESIAN_POINT ( 'NONE',  ( 19.02544592524334988, 5.153800228976608722, 36.45942372801900433 ) ) ;
#169158 = CARTESIAN_POINT ( 'NONE',  ( 5.049401038298161559, -19.05341960407611168, 32.70724293864768129 ) ) ;
#169160 = ORIENTED_EDGE ( 'NONE', *, *, #31320, .F. ) ;
#169159 = CARTESIAN_POINT ( 'NONE',  ( -29.86685920354755197, -21.69954338932560134, -10.42499999726881299 ) ) ;
#169161 = CARTESIAN_POINT ( 'NONE',  ( 0.05219959533934541429, -16.53943276465976808, 25.00109039468567218 ) ) ;
#169163 = CARTESIAN_POINT ( 'NONE',  ( 8.224510206698742110, 14.34966873604972548, 42.08442372801901854 ) ) ;
#169162 = CARTESIAN_POINT ( 'NONE',  ( 5.049401038297881783, 19.05341960407617563, 62.29275706135234003 ) ) ;
#169164 = CARTESIAN_POINT ( 'NONE',  ( -0.05219959533909027116, -19.03943276465977164, 112.4989096053143669 ) ) ;
#169165 = CARTESIAN_POINT ( 'NONE',  ( 19.03943276465977164, -0.05219959533909143690, 68.74890960531436690 ) ) ;
#169166 = CARTESIAN_POINT ( 'NONE',  ( -21.53943276465977519, 0.05219959533907696930, 96.24890960531435269 ) ) ;
#169168 = CARTESIAN_POINT ( 'NONE',  ( -19.02544592524342804, 5.153800228976336051, 26.04057627198103120 ) ) ;
#169167 = CARTESIAN_POINT ( 'NONE',  ( 13.97604488694527802, 13.89961937509977652, 94.37390960531436690 ) ) ;
#169169 = CARTESIAN_POINT ( 'NONE',  ( 19.05341960407611168, 5.049401038298154454, 68.95724293864769550 ) ) ;
#169171 = CARTESIAN_POINT ( 'NONE',  ( 5.153800228976335163, 19.02544592524342804, 69.79057627198102409 ) ) ;
#169170 = CARTESIAN_POINT ( 'NONE',  ( 8.224510206698953496, -14.34966873604960469, 22.91557627198102765 ) ) ;
#169172 = CARTESIAN_POINT ( 'NONE',  ( -16.46253265017146816, -9.564922557961047289, 44.16775706135232582 ) ) ;
#169173 = CARTESIAN_POINT ( 'NONE',  ( 16.55341960407611168, 4.379528057220329451, 63.95724293864770260 ) ) ;
#169174 = CARTESIAN_POINT ( 'NONE',  ( 10.72451020669871369, 18.67979575497193778, 92.08442372801901854 ) ) ;
#169175 = CARTESIAN_POINT ( 'NONE',  ( -19.05341960407611168, -5.049401038298163336, 36.45724293864766707 ) ) ;
#169176 = CARTESIAN_POINT ( 'NONE',  ( 14.29746914071037800, 8.314922557961029526, 56.66775706135235424 ) ) ;
#169178 = CARTESIAN_POINT ( 'NONE',  ( -15.80617190586768217, 15.72974639402176855, 93.12609039468568994 ) ) ;
#169177 = CARTESIAN_POINT ( 'NONE',  ( 16.52544592524342804, -4.483927247898539470, 43.54057627198103830 ) ) ;
#169179 = CARTESIAN_POINT ( 'NONE',  ( 13.97604488694527802, 13.89961937509977652, 74.37390960531436690 ) ) ;
#169180 = CARTESIAN_POINT ( 'NONE',  ( -19.02544592524342804, 5.153800228976336051, 91.04057627198100988 ) ) ;
#169181 = CARTESIAN_POINT ( 'NONE',  ( 12.06949235617757843, -12.14591786802309237, 108.1239096053143811 ) ) ;
#169182 = CARTESIAN_POINT ( 'NONE',  ( -4.379528057220328563, 16.55341960407611168, 75.20724293864769550 ) ) ;
#169183 = CARTESIAN_POINT ( 'NONE',  ( 18.67979575497178502, 10.72451020669898547, 89.16557627198102409 ) ) ;
#169184 = CARTESIAN_POINT ( 'NONE',  ( 13.89961937509977652, -13.97604488694527269, 93.12390960531436690 ) ) ;
#169185 = CARTESIAN_POINT ( 'NONE',  ( 10.72451020669898902, -18.67979575497178502, 102.9155762719810383 ) ) ;
#169186 = CARTESIAN_POINT ( 'NONE',  ( 19.03943276465977164, 0.05219959533936151252, 81.25109039468567573 ) ) ;
#169188 = CARTESIAN_POINT ( 'NONE',  ( -8.314922557960811034, -14.29746914071050412, 87.08224293864769550 ) ) ;
#169187 = CARTESIAN_POINT ( 'NONE',  ( -19.01529144963339846, -5.499999999999896083, 91.23431955728437970 ) ) ;
#169189 = CARTESIAN_POINT ( 'NONE',  ( -0.05219959533909027116, -19.03943276465977164, 52.49890960531436690 ) ) ;
#169190 = CARTESIAN_POINT ( 'NONE',  ( 21.55341960407610458, 5.719274019375980345, 68.95724293864769550 ) ) ;
#169191 = CARTESIAN_POINT ( 'NONE',  ( -26.45564479744090036, -7.620358626195407936, 168.5728521449592279 ) ) ;
#169193 = DIRECTION ( 'NONE',  ( -0.000000000000000000, -0.000000000000000000, -1.000000000000000000 ) ) ;
#169192 = CARTESIAN_POINT ( 'NONE',  ( 12.14591786802327356, -12.06949235617739191, 105.6260903946856899 ) ) ;
#169194 = CARTESIAN_POINT ( 'NONE',  ( -8.224510206698735004, -14.34966873604973081, 24.58442372801901499 ) ) ;
#169195 = CARTESIAN_POINT ( 'NONE',  ( -14.29746914071049879, 8.314922557960819915, 75.83224293864769550 ) ) ;
#169196 = CARTESIAN_POINT ( 'NONE',  ( -18.22780087662126647, -5.499999999999827693, 63.98236817873107185 ) ) ;
#169197 = CARTESIAN_POINT ( 'NONE',  ( 19.02544592524343514, -5.153800228976328945, 68.54057627198103830 ) ) ;
#169198 = CARTESIAN_POINT ( 'NONE',  ( 19.05341960407611168, 5.049401038298154454, 28.95724293864769550 ) ) ;
#169199 = CARTESIAN_POINT ( 'NONE',  ( 14.34966873604960469, 8.224510206698951720, 69.16557627198102409 ) ) ;
#169200 = AXIS2_PLACEMENT_3D ( 'NONE', #75686, #134406, #196093 ) ;
#169201 = CARTESIAN_POINT ( 'NONE',  ( 18.67979575497178502, 10.72451020669898547, 24.16557627198103120 ) ) ;
#169202 = CARTESIAN_POINT ( 'NONE',  ( -9.474510206698720793, -16.51473224551083518, 94.58442372801900433 ) ) ;
#169203 = CARTESIAN_POINT ( 'NONE',  ( 16.51473224551069308, 9.474510206698969483, 99.16557627198102409 ) ) ;
#169204 = CARTESIAN_POINT ( 'NONE',  ( -21.55341960407610458, -5.719274019375992779, 76.45724293864769550 ) ) ;
#169205 = CARTESIAN_POINT ( 'NONE',  ( 8.314922557961029526, -14.29746914071037800, 65.41775706135234714 ) ) ;
#169206 = CARTESIAN_POINT ( 'NONE',  ( 19.02544592524335343, 5.153800228976608722, 106.4594237280190043 ) ) ;
#169207 = CARTESIAN_POINT ( 'NONE',  ( 19.02544592524343514, -5.153800228976328945, 58.54057627198102409 ) ) ;
#169208 = CARTESIAN_POINT ( 'NONE',  ( -0.05219959533907301413, -21.53943276465977519, 62.49890960531436690 ) ) ;
#169209 = CARTESIAN_POINT ( 'NONE',  ( -9.564922557961040184, 16.46253265017147172, 112.9177570613523329 ) ) ;
#169211 = CARTESIAN_POINT ( 'NONE',  ( -18.62759615963255300, -10.81492255796106328, 64.16775706135234714 ) ) ;
#169210 = CARTESIAN_POINT ( 'NONE',  ( 8.224510206698953496, -14.34966873604960469, 32.91557627198102409 ) ) ;
#169212 = CARTESIAN_POINT ( 'NONE',  ( 17.97214573761830536, 5.500000000000079048, 83.96970049038658601 ) ) ;
#169214 = CARTESIAN_POINT ( 'NONE',  ( -9.474510206698964154, 16.51473224551069663, 110.4155762719810383 ) ) ;
#169213 = CARTESIAN_POINT ( 'NONE',  ( -16.52544592524335698, -4.483927247898792601, 68.95942372801901854 ) ) ;
#169215 = CARTESIAN_POINT ( 'NONE',  ( 32.00000000000000000, -1.163414459189985801E-14, 89.49999999999897682 ) ) ;
#169216 = CARTESIAN_POINT ( 'NONE',  ( 28.82186960331498327, 2.781578969918950771E-14, 139.2500000054623683 ) ) ;
#169217 = CARTESIAN_POINT ( 'NONE',  ( -14.34966873604972548, 8.224510206698743886, 98.33442372801901854 ) ) ;
#169218 = CARTESIAN_POINT ( 'NONE',  ( -16.55341960407617563, 4.379528057220093196, 48.54275706135234714 ) ) ;
#169219 = CARTESIAN_POINT ( 'NONE',  ( 19.02544592524343514, -5.153800228976328945, 53.54057627198102409 ) ) ;
#169220 = CARTESIAN_POINT ( 'NONE',  ( -9.564922557960796823, -16.46253265017161027, 77.08224293864769550 ) ) ;
#169221 = CARTESIAN_POINT ( 'NONE',  ( 15.80617190586769283, -15.72974639402175789, 55.62609039468568284 ) ) ;
#169222 = CARTESIAN_POINT ( 'NONE',  ( 0.05219959533934541429, -16.53943276465976808, 65.00109039468568994 ) ) ;
#169223 = CARTESIAN_POINT ( 'NONE',  ( 12.14591786802309770, 12.06949235617756955, 29.37390960531435269 ) ) ;
#169224 = CARTESIAN_POINT ( 'NONE',  ( -0.05219959533909027116, -19.03943276465977164, 37.49890960531436690 ) ) ;
#169225 = CARTESIAN_POINT ( 'NONE',  ( 5.049401038298161559, -19.05341960407611168, 32.70724293864768129 ) ) ;
#169227 = ADVANCED_FACE ( 'NONE', ( #23783 ), #24794, .T. ) ;
#169226 = CARTESIAN_POINT ( 'NONE',  ( -0.05219959533934338120, 16.53943276465976808, 32.50109039468568284 ) ) ;
#169228 = AXIS2_PLACEMENT_3D ( 'NONE', #188027, #107179, #110171 ) ;
#169229 = CARTESIAN_POINT ( 'NONE',  ( 13.97604488694548053, -13.89961937509957401, 85.62609039468568994 ) ) ;
#169230 = CARTESIAN_POINT ( 'NONE',  ( -16.53943276465976808, 0.05219959533911058130, 81.24890960531436690 ) ) ;
#169231 = CARTESIAN_POINT ( 'NONE',  ( 13.89961937509977652, -13.97604488694527269, 48.12390960531435979 ) ) ;
#169233 = FACE_OUTER_BOUND ( 'NONE', #27598, .T. ) ;
#169232 = CARTESIAN_POINT ( 'NONE',  ( 19.02544592524334988, 5.153800228976608722, 81.45942372801897591 ) ) ;
#169234 = CARTESIAN_POINT ( 'NONE',  ( 18.67979575497194134, -10.72451020669871369, 95.83442372801903275 ) ) ;
#169235 = CARTESIAN_POINT ( 'NONE',  ( 4.483927247898790824, -16.52544592524335698, 55.20942372801902565 ) ) ;
#169236 = DIRECTION ( 'NONE',  ( 0.7071067811865467956, -7.406550393246788537E-15, 0.7071067811865483499 ) ) ;
#169237 = CARTESIAN_POINT ( 'NONE',  ( -10.72451020669898014, 18.67979575497178502, 50.41557627198103120 ) ) ;
#169238 = CARTESIAN_POINT ( 'NONE',  ( 4.379528057220092307, 16.55341960407617563, 42.29275706135235424 ) ) ;
#169239 = CARTESIAN_POINT ( 'NONE',  ( -18.56453257813364388, 5.500000000000057732, 70.99000423690689843 ) ) ;
#169240 = CARTESIAN_POINT ( 'NONE',  ( -9.564922557961040184, 16.46253265017147172, 37.91775706135233293 ) ) ;
#169241 = CARTESIAN_POINT ( 'NONE',  ( -9.474510206698964154, 16.51473224551069663, 85.41557627198102409 ) ) ;
#169242 = CARTESIAN_POINT ( 'NONE',  ( -16.51473224551069308, -9.474510206698971260, 51.66557627198102409 ) ) ;
#169243 = CARTESIAN_POINT ( 'NONE',  ( 14.62261807015722859, 16.01221511231801031, -56.20577350945247730 ) ) ;
#169244 = CARTESIAN_POINT ( 'NONE',  ( 21.55341960407619695, -5.719274019375665929, 71.04275706135234714 ) ) ;
#169245 = CARTESIAN_POINT ( 'NONE',  ( 18.22780087662123805, -5.499999999999976019, 93.51763182126896368 ) ) ;
#169246 = CARTESIAN_POINT ( 'NONE',  ( -16.51473224551082808, 9.474510206698731452, 33.33442372801899722 ) ) ;
#169247 = CARTESIAN_POINT ( 'NONE',  ( 5.823673210054444382, -21.52544592524334988, 105.2094237280190328 ) ) ;
#169248 = CARTESIAN_POINT ( 'NONE',  ( -12.14591786802309592, -12.06949235617757132, 36.87390960531435979 ) ) ;
#169249 = CARTESIAN_POINT ( 'NONE',  ( 16.46253265017160672, -9.564922557960803928, 43.33224293864769550 ) ) ;
#169250 = AXIS2_PLACEMENT_3D ( 'NONE', #17675, #96474, #80316 ) ;
#169251 = CARTESIAN_POINT ( 'NONE',  ( -19.05341960407611168, -5.049401038298163336, 101.4572429386476955 ) ) ;
#169252 = CARTESIAN_POINT ( 'NONE',  ( 10.72451020669871369, 18.67979575497193778, 87.08442372801901854 ) ) ;
#169253 = CARTESIAN_POINT ( 'NONE',  ( 16.51473224551069308, 9.474510206698969483, 64.16557627198102409 ) ) ;
#169254 = CARTESIAN_POINT ( 'NONE',  ( 18.67979575497194134, -10.72451020669871369, 80.83442372801901854 ) ) ;
#169255 = CARTESIAN_POINT ( 'NONE',  ( -10.81492255796078084, -18.62759615963271287, 37.08224293864768129 ) ) ;
#169256 = CARTESIAN_POINT ( 'NONE',  ( 21.53943276465977519, 0.05219959533937863772, 21.25109039468567218 ) ) ;
#169257 = CARTESIAN_POINT ( 'NONE',  ( -16.46253265017146816, -9.564922557961047289, 44.16775706135232582 ) ) ;
#169258 = CARTESIAN_POINT ( 'NONE',  ( 16.51473224551069308, 9.474510206698969483, 24.16557627198102765 ) ) ;
#169259 = CARTESIAN_POINT ( 'NONE',  ( -5.153800228976328057, -19.02544592524343514, 77.29057627198099567 ) ) ;
#169261 = AXIS2_PLACEMENT_3D ( 'NONE', #181316, #137760, #104457 ) ;
#169260 = CARTESIAN_POINT ( 'NONE',  ( 14.29746914071037800, 8.314922557961029526, 31.66775706135234358 ) ) ;
#169262 = CARTESIAN_POINT ( 'NONE',  ( 8.314922557960818139, 14.29746914071049879, 84.58224293864769550 ) ) ;
#169263 = CARTESIAN_POINT ( 'NONE',  ( 5.049401038298161559, -19.05341960407611168, 62.70724293864769550 ) ) ;
#169264 = CARTESIAN_POINT ( 'NONE',  ( -21.55341960407610458, -5.719274019375992779, 31.45724293864769550 ) ) ;
#169265 = CARTESIAN_POINT ( 'NONE',  ( 16.46253265017146816, 9.564922557961045513, 96.66775706135233293 ) ) ;
#169266 = CARTESIAN_POINT ( 'NONE',  ( 15.80617190586746368, 15.72974639402197994, 104.3739096053143669 ) ) ;
#169267 = CARTESIAN_POINT ( 'NONE',  ( 5.719274019375673035, 21.55341960407619339, 77.29275706135234714 ) ) ;
#169268 = CARTESIAN_POINT ( 'NONE',  ( 0.05219959533934541429, -16.53943276465976808, 70.00109039468568994 ) ) ;
#169269 = CARTESIAN_POINT ( 'NONE',  ( -8.314922557961024197, 14.29746914071037800, 62.91775706135236135 ) ) ;
#169270 = CARTESIAN_POINT ( 'NONE',  ( 5.153800228976335163, 19.02544592524342804, 64.79057627198100988 ) ) ;
#169271 = CARTESIAN_POINT ( 'NONE',  ( -14.34966873604972548, 8.224510206698743886, 93.33442372801901854 ) ) ;
#169272 = CARTESIAN_POINT ( 'NONE',  ( -9.564922557961040184, 16.46253265017147172, 47.91775706135233293 ) ) ;
#169273 = CARTESIAN_POINT ( 'NONE',  ( 0.05219959533937995610, -21.53943276465977519, 20.00109039468568639 ) ) ;
#169274 = CARTESIAN_POINT ( 'NONE',  ( -14.29746914071049879, 8.314922557960819915, 70.83224293864770971 ) ) ;
#169275 = CARTESIAN_POINT ( 'NONE',  ( 16.51473224551069308, 9.474510206698969483, 89.16557627198103830 ) ) ;
#169276 = CARTESIAN_POINT ( 'NONE',  ( 4.379528057220092307, 16.55341960407617563, 77.29275706135234714 ) ) ;
#169277 = CARTESIAN_POINT ( 'NONE',  ( 15.80617190586769283, -15.72974639402175789, 55.62609039468568284 ) ) ;
#169278 = CARTESIAN_POINT ( 'NONE',  ( -14.29746914071037622, -8.314922557961029526, 19.16775706135234714 ) ) ;
#169279 = CARTESIAN_POINT ( 'NONE',  ( -18.67979575497178146, -10.72451020669898902, 111.6655762719810525 ) ) ;
#169280 = CARTESIAN_POINT ( 'NONE',  ( 16.52544592524342804, -4.483927247898539470, 53.54057627198103120 ) ) ;
#169281 = ORIENTED_EDGE ( 'NONE', *, *, #99796, .F. ) ;
#169282 = CARTESIAN_POINT ( 'NONE',  ( 21.52544592524344225, -5.823673210054117533, 93.54057627198103830 ) ) ;
#169283 = CARTESIAN_POINT ( 'NONE',  ( -4.379528057220328563, 16.55341960407611168, 40.20724293864769550 ) ) ;
#169284 = VERTEX_POINT ( 'NONE', #56107 ) ;
#169285 = CARTESIAN_POINT ( 'NONE',  ( 35.50084720355934564, 3.323798168015733800, 38.27222404303021364 ) ) ;
#169286 = CARTESIAN_POINT ( 'NONE',  ( 18.67979575497178502, 10.72451020669898547, 109.1655762719810383 ) ) ;
#169287 = CARTESIAN_POINT ( 'NONE',  ( -15.80617190586745835, -15.72974639402198527, 21.87390960531436690 ) ) ;
#169288 = CARTESIAN_POINT ( 'NONE',  ( 10.72451020669871369, 18.67979575497193778, 37.08442372801901143 ) ) ;
#169289 = CARTESIAN_POINT ( 'NONE',  ( -14.34966873604960291, -8.224510206698953496, 56.66557627198103830 ) ) ;
#169290 = CARTESIAN_POINT ( 'NONE',  ( -9.564922557960796823, -16.46253265017161027, 62.08224293864769550 ) ) ;
#169291 = CARTESIAN_POINT ( 'NONE',  ( 19.03943276465977164, 0.05219959533936151252, 66.25109039468567573 ) ) ;
#169292 = CARTESIAN_POINT ( 'NONE',  ( 5.049401038298161559, -19.05341960407611168, 92.70724293864769550 ) ) ;
#169293 = CARTESIAN_POINT ( 'NONE',  ( 0.05219959533907565091, 21.53943276465977519, 49.99890960531437401 ) ) ;
#169294 = CARTESIAN_POINT ( 'NONE',  ( -10.70342273063628014, -35.99563703666770920, -30.86961840752219288 ) ) ;
#169295 = CARTESIAN_POINT ( 'NONE',  ( 19.02544592524343514, -5.153800228976328945, 63.54057627198103830 ) ) ;
#169296 = CARTESIAN_POINT ( 'NONE',  ( -8.314922557961024197, 14.29746914071037800, 42.91775706135235424 ) ) ;
#169297 = CARTESIAN_POINT ( 'NONE',  ( 5.049401038297881783, 19.05341960407617563, 67.29275706135234714 ) ) ;
#169298 = CARTESIAN_POINT ( 'NONE',  ( 21.52544592524334988, 5.823673210054432836, 21.45942372801901499 ) ) ;
#169299 = CARTESIAN_POINT ( 'NONE',  ( 16.55341960407611168, 4.379528057220329451, 43.95724293864769550 ) ) ;
#169300 = CARTESIAN_POINT ( 'NONE',  ( -9.474510206698964154, 16.51473224551069663, 90.41557627198103830 ) ) ;
#169301 = CARTESIAN_POINT ( 'NONE',  ( 21.55341960407610458, 5.719274019375980345, 73.95724293864769550 ) ) ;
#169303 = CARTESIAN_POINT ( 'NONE',  ( -4.379528057220086978, -16.55341960407618274, 44.79275706135234714 ) ) ;
#169302 = CARTESIAN_POINT ( 'NONE',  ( 18.62759615963271287, -10.81492255796078972, 93.33224293864769550 ) ) ;
#169304 = CARTESIAN_POINT ( 'NONE',  ( 18.62759615963271287, -10.81492255796078972, 38.33224293864768839 ) ) ;
#169305 = CARTESIAN_POINT ( 'NONE',  ( -18.67979575497193778, 10.72451020669871902, 93.33442372801901854 ) ) ;
#169306 = CARTESIAN_POINT ( 'NONE',  ( -9.564922557960796823, -16.46253265017161027, 87.08224293864769550 ) ) ;
#169307 = CARTESIAN_POINT ( 'NONE',  ( -0.05219959533909027116, -19.03943276465977164, 47.49890960531435979 ) ) ;
#169308 = CARTESIAN_POINT ( 'NONE',  ( 0.05219959533909260263, 19.03943276465977164, 94.99890960531436690 ) ) ;
#169309 = CARTESIAN_POINT ( 'NONE',  ( -16.52544592524342804, 4.483927247898546575, 111.0405762719810525 ) ) ;
#169310 = CARTESIAN_POINT ( 'NONE',  ( 0.05219959533909260263, 19.03943276465977164, 59.99890960531436690 ) ) ;
#169311 = CARTESIAN_POINT ( 'NONE',  ( -12.06949235617739369, -12.14591786802326823, 19.37609039468568639 ) ) ;
#169312 = CARTESIAN_POINT ( 'NONE',  ( 17.50000000000147082, 3.254303733634585694, 32.47604106928593382 ) ) ;
#169313 = CARTESIAN_POINT ( 'NONE',  ( -19.05341960407617563, 5.049401038297882671, 58.54275706135234003 ) ) ;
#169315 = CARTESIAN_POINT ( 'NONE',  ( -15.72974639402197994, 15.80617190586746368, 30.62390960531436335 ) ) ;
#169314 = CARTESIAN_POINT ( 'NONE',  ( 15.72974639402176855, 15.80617190586768217, 111.8760903946856615 ) ) ;
#169316 = CARTESIAN_POINT ( 'NONE',  ( 12.06949235617739724, 12.14591786802326823, 96.87609039468568994 ) ) ;
#169317 = CARTESIAN_POINT ( 'NONE',  ( -23.48529157249599919, -32.32473071737749848, -9.699999999999999289 ) ) ;
#169318 = CARTESIAN_POINT ( 'NONE',  ( 16.51473224551083163, -9.474510206698727899, 65.83442372801900433 ) ) ;
#169319 = CARTESIAN_POINT ( 'NONE',  ( -5.153800228976607833, 19.02544592524334988, 32.70942372801899722 ) ) ;
#169320 = CARTESIAN_POINT ( 'NONE',  ( -17.05116617787826172, -6.768360034955700044, 46.34324446740803438 ) ) ;
#169321 = CARTESIAN_POINT ( 'NONE',  ( -19.03943276465977164, 0.05219959533909376836, 41.24890960531435269 ) ) ;
#169322 = CARTESIAN_POINT ( 'NONE',  ( -0.05219959533910754901, -16.53943276465976808, 37.49890960531436690 ) ) ;
#169323 = CARTESIAN_POINT ( 'NONE',  ( -9.564922557960796823, -16.46253265017161027, 27.08224293864769550 ) ) ;
#169324 = CARTESIAN_POINT ( 'NONE',  ( 16.53943276465976808, -0.05219959533910856209, 23.74890960531435269 ) ) ;
#169325 = CARTESIAN_POINT ( 'NONE',  ( -27.86273085795036408, -28.69962071417357663, -25.00000000000000000 ) ) ;
#169326 = CARTESIAN_POINT ( 'NONE',  ( -12.14591786802326823, 12.06949235617739902, 98.12609039468570415 ) ) ;
#169327 = CARTESIAN_POINT ( 'NONE',  ( 16.46253265017160672, -9.564922557960803928, 33.33224293864770260 ) ) ;
#169328 = CARTESIAN_POINT ( 'NONE',  ( 21.53943276465977519, 0.05219959533937863772, 101.2510903946856757 ) ) ;
#169329 = CARTESIAN_POINT ( 'NONE',  ( 0.05219959533934541429, -16.53943276465976808, 20.00109039468568639 ) ) ;
#169330 = CARTESIAN_POINT ( 'NONE',  ( -18.62759615963255300, -10.81492255796106328, 74.16775706135231871 ) ) ;
#169331 = CARTESIAN_POINT ( 'NONE',  ( -9.564922557961040184, 16.46253265017147172, 57.91775706135233293 ) ) ;
#169332 = CARTESIAN_POINT ( 'NONE',  ( -16.51473224551069308, -9.474510206698971260, 91.66557627198103830 ) ) ;
#169333 = CARTESIAN_POINT ( 'NONE',  ( 16.51473224551069308, 9.474510206698969483, 79.16557627198103830 ) ) ;
#169334 = CARTESIAN_POINT ( 'NONE',  ( 16.62475595723699939, 7.163666690055260133, 71.97286648189529501 ) ) ;
#169335 = CARTESIAN_POINT ( 'NONE',  ( 18.67979575497178502, 10.72451020669898547, 114.1655762719810383 ) ) ;
#169336 = CARTESIAN_POINT ( 'NONE',  ( -8.314922557960811034, -14.29746914071050412, 62.08224293864769550 ) ) ;
#169337 = CARTESIAN_POINT ( 'NONE',  ( 10.72451020669898902, -18.67979575497178502, 62.91557627198102409 ) ) ;
#169338 = CARTESIAN_POINT ( 'NONE',  ( 13.97604488694527802, 13.89961937509977652, 64.37390960531436690 ) ) ;
#169340 = CARTESIAN_POINT ( 'NONE',  ( -4.379528057220086978, -16.55341960407618274, 94.79275706135234714 ) ) ;
#169339 = CARTESIAN_POINT ( 'NONE',  ( 15.72974639402199770, -15.80617190586745480, 93.12390960531436690 ) ) ;
#169341 = ORIENTED_EDGE ( 'NONE', *, *, #42638, .F. ) ;
#169342 = CARTESIAN_POINT ( 'NONE',  ( 16.51473224551069308, 9.474510206698969483, 49.16557627198102409 ) ) ;
#169344 = CARTESIAN_POINT ( 'NONE',  ( 20.09035150276018555, -11.70762861043687053, 168.0245124264526453 ) ) ;
#169343 = CARTESIAN_POINT ( 'NONE',  ( -4.379528057220328563, 16.55341960407611168, 95.20724293864769550 ) ) ;
#169345 = CARTESIAN_POINT ( 'NONE',  ( 9.474510206698971260, -16.51473224551069308, 47.91557627198102409 ) ) ;
#169346 = CARTESIAN_POINT ( 'NONE',  ( -19.05341960407611168, -5.049401038298163336, 21.45724293864768839 ) ) ;
#169347 = CARTESIAN_POINT ( 'NONE',  ( -19.03943276465977164, -0.05219959533935918106, 78.75109039468567573 ) ) ;
#169348 = CARTESIAN_POINT ( 'NONE',  ( 8.314922557960818139, 14.29746914071049879, 84.58224293864769550 ) ) ;
#169349 = CARTESIAN_POINT ( 'NONE',  ( 10.81492255796106328, -18.62759615963255655, 50.41775706135235424 ) ) ;
#169351 = CARTESIAN_POINT ( 'NONE',  ( -15.72974639402197994, 15.80617190586746368, 110.6239096053143669 ) ) ;
#169350 = CARTESIAN_POINT ( 'NONE',  ( 16.46253265017160672, -9.564922557960803928, 38.33224293864768839 ) ) ;
#169352 = CARTESIAN_POINT ( 'NONE',  ( -8.224510206698948167, 14.34966873604960824, 90.41557627198103830 ) ) ;
#169353 = CARTESIAN_POINT ( 'NONE',  ( -4.647474457565486646E-15, 28.90000000000004476, -65.00100000000003320 ) ) ;
#169354 = CARTESIAN_POINT ( 'NONE',  ( -9.474510206698964154, 16.51473224551069663, 60.41557627198102409 ) ) ;
#169355 = CARTESIAN_POINT ( 'NONE',  ( 18.22780087662126647, 5.499999999999818812, 46.48236817873107185 ) ) ;
#169357 = CARTESIAN_POINT ( 'NONE',  ( 13.97604488694527802, 13.89961937509977652, 114.3739096053143669 ) ) ;
#169356 = CARTESIAN_POINT ( 'NONE',  ( 16.51473224551083163, -9.474510206698727899, 90.83442372801900433 ) ) ;
#169358 = CARTESIAN_POINT ( 'NONE',  ( 15.80617190586769283, -15.72974639402175789, 30.62609039468567929 ) ) ;
#169359 = CARTESIAN_POINT ( 'NONE',  ( 16.46253265017160672, -9.564922557960803928, 78.33224293864769550 ) ) ;
#169360 = CARTESIAN_POINT ( 'NONE',  ( -19.02544592524334988, -5.153800228976617603, 73.95942372801900433 ) ) ;
#169361 = CARTESIAN_POINT ( 'NONE',  ( 13.97604488694527802, 13.89961937509977652, 54.37390960531435979 ) ) ;
#169362 = EDGE_CURVE ( 'NONE', #49283, #105512, #157374, .T. ) ;
#169363 = CARTESIAN_POINT ( 'NONE',  ( -12.06949235617756955, 12.14591786802309770, 75.62390960531439532 ) ) ;
#169364 = CARTESIAN_POINT ( 'NONE',  ( -16.52544592524342804, 4.483927247898546575, 66.04057627198103830 ) ) ;
#169365 = CARTESIAN_POINT ( 'NONE',  ( -19.02544592524342804, 5.153800228976336051, 96.04057627198103830 ) ) ;
#169366 = CARTESIAN_POINT ( 'NONE',  ( 5.719274019375991003, -21.55341960407610458, 97.70724293864772392 ) ) ;
#169367 = CARTESIAN_POINT ( 'NONE',  ( -19.03943276465977164, 0.05219959533909376836, 86.24890960531436690 ) ) ;
#169368 = CIRCLE ( 'NONE', #30542, 0.2000000000000000944 ) ;
#169369 = CARTESIAN_POINT ( 'NONE',  ( 16.51473224551083163, -9.474510206698727899, 25.83442372801900078 ) ) ;
#169372 = CARTESIAN_POINT ( 'NONE',  ( -8.224510206698948167, 14.34966873604960824, 115.4155762719810241 ) ) ;
#169371 = CARTESIAN_POINT ( 'NONE',  ( 8.314922557960818139, 14.29746914071049879, 29.58224293864769905 ) ) ;
#169370 = CARTESIAN_POINT ( 'NONE',  ( 13.97604488694527802, 13.89961937509977652, 34.37390960531436690 ) ) ;
#169373 = ORIENTED_EDGE ( 'NONE', *, *, #161468, .F. ) ;
#169374 = CARTESIAN_POINT ( 'NONE',  ( -10.72451020669870658, -18.67979575497194134, 29.58442372801901854 ) ) ;
#169375 = CARTESIAN_POINT ( 'NONE',  ( 13.89961937509957401, 13.97604488694547697, 71.87609039468567573 ) ) ;
#169376 = CARTESIAN_POINT ( 'NONE',  ( -16.55341960407611168, -4.379528057220339221, 31.45724293864769550 ) ) ;
#169377 = CARTESIAN_POINT ( 'NONE',  ( -10.72451020669898014, 18.67979575497178502, 85.41557627198102409 ) ) ;
#169378 = CARTESIAN_POINT ( 'NONE',  ( 18.62759615963271287, -10.81492255796078972, 23.33224293864769194 ) ) ;
#169379 = CARTESIAN_POINT ( 'NONE',  ( 12.14591786802309770, 12.06949235617756955, 74.37390960531436690 ) ) ;
#169380 = CARTESIAN_POINT ( 'NONE',  ( -9.474510206698964154, 16.51473224551069663, 30.41557627198102054 ) ) ;
#169381 = CARTESIAN_POINT ( 'NONE',  ( -0.05219959533936034679, 19.03943276465977164, 22.50109039468566152 ) ) ;
#169382 = CARTESIAN_POINT ( 'NONE',  ( -8.314922557961024197, 14.29746914071037800, 102.9177570613523756 ) ) ;
#169383 = CARTESIAN_POINT ( 'NONE',  ( -16.55341960407617563, 4.379528057220093196, 53.54275706135234714 ) ) ;
#169384 = CARTESIAN_POINT ( 'NONE',  ( -18.67979575497178146, -10.72451020669898902, 36.66557627198103120 ) ) ;
#169385 = CARTESIAN_POINT ( 'NONE',  ( -21.55341960407619339, 5.719274019375674811, 113.5427570613523756 ) ) ;
#169386 = CARTESIAN_POINT ( 'NONE',  ( -13.89961937509977652, 13.97604488694528158, 85.62390960531433848 ) ) ;
#169387 = CARTESIAN_POINT ( 'NONE',  ( 8.314922557961029526, -14.29746914071037800, 55.41775706135234714 ) ) ;
#169388 = CARTESIAN_POINT ( 'NONE',  ( 9.564922557960805705, 16.46253265017160317, 24.58224293864769194 ) ) ;
#169389 = CARTESIAN_POINT ( 'NONE',  ( 14.29746914071049879, -8.314922557960816363, 33.33224293864769550 ) ) ;
#169391 = CARTESIAN_POINT ( 'NONE',  ( 13.89961937509977652, -13.97604488694527269, 93.12390960531436690 ) ) ;
#169390 = CARTESIAN_POINT ( 'NONE',  ( -9.564922557960796823, -16.46253265017161027, 107.0822429386476955 ) ) ;
#169392 = CARTESIAN_POINT ( 'NONE',  ( 19.05341960407611168, 5.049401038298154454, 103.9572429386476671 ) ) ;
#169393 = TOROIDAL_SURFACE ( 'NONE', #33725, 2.700000000000000622, 0.2000000000000000111 ) ;
#169394 = CARTESIAN_POINT ( 'NONE',  ( 12.06949235617757843, -12.14591786802309237, 58.12390960531435979 ) ) ;
#169396 = CARTESIAN_POINT ( 'NONE',  ( 14.34966873604960469, 8.224510206698951720, 39.16557627198102409 ) ) ;
#169395 = B_SPLINE_CURVE_WITH_KNOTS ( 'NONE', 3,
 ( #134747, #41736, #57899, #181254, #42731, #104393, #166076, #27579, #89217, #31521, #126501, #111335, #1160, #93174, #157851, #188199, #65823, #189197, #172020, #154859, #96162, #3166, #139672, #50672, #95168, #34504, #2168, #140676, #156856, #64839, #17346, #112332 ),
 .UNSPECIFIED., .F., .F.,
 ( 4, 2, 2, 2, 2, 2, 2, 2, 2, 2, 2, 2, 2, 2, 2, 4 ),
 ( 2.711112516444420852E-17, 0.0003712461730037074862, 0.0007424923460073878673, 0.001113738519011068248, 0.001484984692014748630, 0.002227477038022109609, 0.002598723211025793026, 0.002969969384029457361, 0.003341215557033121696, 0.003712461730036786031, 0.004083707903040450365, 0.004454954076044115134, 0.004826200249047779903, 0.005197446422051443804, 0.005568692595055108573, 0.005939938768058773341 ),
 .UNSPECIFIED. ) ;
#169397 = CARTESIAN_POINT ( 'NONE',  ( 14.29746914071049879, -8.314922557960816363, 48.33224293864770260 ) ) ;
#169400 = PRESENTATION_LAYER_ASSIGNMENT (  '', '', ( #179109 ) ) ;
#169399 = DIRECTION ( 'NONE',  ( 0.000000000000000000, -0.7071067811865483499, -0.7071067811865465735 ) ) ;
#169398 = CARTESIAN_POINT ( 'NONE',  ( 4.483927247898790824, -16.52544592524335698, 40.20942372801901854 ) ) ;
#169401 = CARTESIAN_POINT ( 'NONE',  ( 16.51473224551083163, -9.474510206698727899, 45.83442372801900433 ) ) ;
#169402 = CARTESIAN_POINT ( 'NONE',  ( 19.03943276465977164, -0.05219959533909143690, 83.74890960531436690 ) ) ;
#169403 = CARTESIAN_POINT ( 'NONE',  ( -13.97604488694547697, 13.89961937509957934, 68.12609039468563310 ) ) ;
#169404 = CARTESIAN_POINT ( 'NONE',  ( -27.73933785331498925, -9.013057229001049109, 145.4750000027311501 ) ) ;
#169405 = CARTESIAN_POINT ( 'NONE',  ( -5.049401038297874678, -19.05341960407617918, 54.79275706135234003 ) ) ;
#169407 = CARTESIAN_POINT ( 'NONE',  ( -0.05219959533934338120, 16.53943276465976808, 82.50109039468568994 ) ) ;
#169406 = CARTESIAN_POINT ( 'NONE',  ( 5.049401038297881783, 19.05341960407617563, 97.29275706135233293 ) ) ;
#169408 = CARTESIAN_POINT ( 'NONE',  ( 8.571926809382597767, 26.38167802310806209, 146.7750000027311899 ) ) ;
#169410 = LINE ( 'NONE', #2548, #98019 ) ;
#169409 = COLOUR_RGB ( '', 0.40784314, 0.44705882, 0.49803922) ;
#169411 = CARTESIAN_POINT ( 'NONE',  ( -5.823673210054116645, -21.52544592524344225, 22.29057627198102765 ) ) ;
#169412 = CARTESIAN_POINT ( 'NONE',  ( 15.72974639402176855, 15.80617190586768217, 36.87609039468568994 ) ) ;
#169413 = CARTESIAN_POINT ( 'NONE',  ( -5.153800228976607833, 19.02544592524334988, 107.7094237280189759 ) ) ;
#169415 = CARTESIAN_POINT ( 'NONE',  ( 5.153800228976335163, 19.02544592524342804, 64.79057627198100988 ) ) ;
#169414 = CARTESIAN_POINT ( 'NONE',  ( 15.50000000000000178, 5.499999999999998224, 22.00000000000000000 ) ) ;
#169416 = CARTESIAN_POINT ( 'NONE',  ( -0.05219959533909027116, -19.03943276465977164, 107.4989096053143527 ) ) ;
#169418 = CARTESIAN_POINT ( 'NONE',  ( -16.51473224551069308, -9.474510206698971260, 66.66557627198102409 ) ) ;
#169417 = CARTESIAN_POINT ( 'NONE',  ( -16.52544592524342804, 4.483927247898546575, 61.04057627198103120 ) ) ;
#169419 = CARTESIAN_POINT ( 'NONE',  ( -5.153800228976328057, -19.02544592524343514, 77.29057627198099567 ) ) ;
#169420 = CARTESIAN_POINT ( 'NONE',  ( 9.564922557961047289, -16.46253265017146816, 75.41775706135234714 ) ) ;
#169421 = CARTESIAN_POINT ( 'NONE',  ( -10.72451020669898014, 18.67979575497178502, 50.41557627198103120 ) ) ;
#169422 = CARTESIAN_POINT ( 'NONE',  ( -14.34966873604960291, -8.224510206698953496, 111.6655762719810525 ) ) ;
#169423 = CARTESIAN_POINT ( 'NONE',  ( 13.89961937509957401, 13.97604488694547697, 46.87609039468565442 ) ) ;
#169424 = CARTESIAN_POINT ( 'NONE',  ( 9.564922557960805705, 16.46253265017160317, 79.58224293864769550 ) ) ;
#169425 = CARTESIAN_POINT ( 'NONE',  ( -0.05219959533907301413, -21.53943276465977519, 82.49890960531436690 ) ) ;
#169427 = CARTESIAN_POINT ( 'NONE',  ( -19.03943276465977164, -0.05219959533935918106, 28.75109039468566507 ) ) ;
#169426 = CARTESIAN_POINT ( 'NONE',  ( -14.34966873604960291, -8.224510206698953496, 86.66557627198102409 ) ) ;
#169428 = CARTESIAN_POINT ( 'NONE',  ( -18.62759615963270932, 10.81492255796079327, 55.83224293864770260 ) ) ;
#169429 = ORIENTED_EDGE ( 'NONE', *, *, #93300, .T. ) ;
#169430 = CARTESIAN_POINT ( 'NONE',  ( 5.823673210054125526, 21.52544592524343514, 39.79057627198103830 ) ) ;
#169431 = CARTESIAN_POINT ( 'NONE',  ( 10.72451020669871369, 18.67979575497193778, 97.08442372801904696 ) ) ;
#169432 = CARTESIAN_POINT ( 'NONE',  ( -5.049401038298153566, 19.05341960407611168, 60.20724293864768129 ) ) ;
#169433 = CARTESIAN_POINT ( 'NONE',  ( -9.474510206698964154, 16.51473224551069663, 25.41557627198103120 ) ) ;
#169434 = VECTOR ( 'NONE', #15931, 1000.000000000000114 ) ;
#169435 = CARTESIAN_POINT ( 'NONE',  ( 10.81492255796106328, -18.62759615963255655, 25.41775706135235779 ) ) ;
#169436 = CARTESIAN_POINT ( 'NONE',  ( -19.35543954521081389, -5.499999999999585221, 39.58901960356453031 ) ) ;
#169437 = CARTESIAN_POINT ( 'NONE',  ( 15.72974639402176855, 15.80617190586768217, 46.87609039468568994 ) ) ;
#169438 = CARTESIAN_POINT ( 'NONE',  ( -13.89961937509977652, 13.97604488694528158, 40.62390960531435979 ) ) ;
#169439 = CARTESIAN_POINT ( 'NONE',  ( -21.53943276465977519, 0.05219959533907696930, 111.2489096053143669 ) ) ;
#169440 = EDGE_CURVE ( 'NONE', #38560, #16610, #155072, .T. ) ;
#169441 = CARTESIAN_POINT ( 'NONE',  ( 19.02544592524334988, 5.153800228976608722, 46.45942372801899012 ) ) ;
#169442 = CARTESIAN_POINT ( 'NONE',  ( 17.60769864724391098, -5.499999999999979572, 76.15024842019164453 ) ) ;
#169443 = CARTESIAN_POINT ( 'NONE',  ( 19.03943276465977164, -0.05219959533909143690, 28.74890960531435624 ) ) ;
#169444 = FACE_OUTER_BOUND ( 'NONE', #92735, .T. ) ;
#169445 = CARTESIAN_POINT ( 'NONE',  ( -4.483927247898782831, 16.52544592524335698, 57.70942372801901143 ) ) ;
#169446 = CARTESIAN_POINT ( 'NONE',  ( -5.049401038298153566, 19.05341960407611168, 25.20724293864768484 ) ) ;
#169447 = CARTESIAN_POINT ( 'NONE',  ( -21.75836449082842705, -9.620754668594841519, 170.8405250346321509 ) ) ;
#169448 = CARTESIAN_POINT ( 'NONE',  ( 9.474510206698971260, -16.51473224551069308, 72.91557627198102409 ) ) ;
#169449 = CARTESIAN_POINT ( 'NONE',  ( -8.314922557960811034, -14.29746914071050412, 112.0822429386477097 ) ) ;
#169450 = CARTESIAN_POINT ( 'NONE',  ( 15.72974639402199770, -15.80617190586745480, 58.12390960531435979 ) ) ;
#169451 = CARTESIAN_POINT ( 'NONE',  ( -14.29746914071037622, -8.314922557961029526, 39.16775706135235424 ) ) ;
#169452 = CARTESIAN_POINT ( 'NONE',  ( 15.80617190586769283, -15.72974639402175789, 100.6260903946857184 ) ) ;
#169453 = CARTESIAN_POINT ( 'NONE',  ( -5.153800228976328057, -19.02544592524343514, 22.29057627198102765 ) ) ;
#169454 = ADVANCED_FACE ( 'NONE', ( #16567 ), #185415, .T. ) ;
#169455 = CARTESIAN_POINT ( 'NONE',  ( -12.14591786802309592, -12.06949235617757132, 21.87390960531436690 ) ) ;
#169456 = CARTESIAN_POINT ( 'NONE',  ( 4.483927247898545687, 16.52544592524342804, 49.79057627198102409 ) ) ;
#169457 = CARTESIAN_POINT ( 'NONE',  ( -19.05341960407611168, -5.049401038298163336, 46.45724293864768129 ) ) ;
#169458 = CARTESIAN_POINT ( 'NONE',  ( 10.81492255796106328, -18.62759615963255655, 100.4177570613523471 ) ) ;
#169459 = CARTESIAN_POINT ( 'NONE',  ( -15.80617190586745835, -15.72974639402198527, 106.8739096053143811 ) ) ;
#169460 = CARTESIAN_POINT ( 'NONE',  ( 5.719274019375673035, 21.55341960407619339, 67.29275706135234714 ) ) ;
#169461 = CARTESIAN_POINT ( 'NONE',  ( -16.52544592524335698, -4.483927247898792601, 53.95942372801900433 ) ) ;
#169463 = CARTESIAN_POINT ( 'NONE',  ( 15.80617190586769283, -15.72974639402175789, 100.6260903946857184 ) ) ;
#169462 = CARTESIAN_POINT ( 'NONE',  ( -16.55341960407611168, -4.379528057220339221, 76.45724293864769550 ) ) ;
#169464 = CARTESIAN_POINT ( 'NONE',  ( -8.314922557960811034, -14.29746914071050412, 22.08224293864769194 ) ) ;
#169465 = CARTESIAN_POINT ( 'NONE',  ( -16.79531203550645557, 7.028104445595627858, 113.7475501177956119 ) ) ;
#169466 = CARTESIAN_POINT ( 'NONE',  ( 4.483927247898790824, -16.52544592524335698, 35.20942372801901854 ) ) ;
#169467 = CARTESIAN_POINT ( 'NONE',  ( 12.06949235617757843, -12.14591786802309237, 43.12390960531435269 ) ) ;
#169468 = CARTESIAN_POINT ( 'NONE',  ( 16.52544592524335698, 4.483927247898782831, 91.45942372801901854 ) ) ;
#169469 = CARTESIAN_POINT ( 'NONE',  ( 13.97604488694527802, 13.89961937509977652, 99.37390960531436690 ) ) ;
#169470 = CARTESIAN_POINT ( 'NONE',  ( 21.55341960407610458, 5.719274019375980345, 23.95724293864769550 ) ) ;
#169471 = CARTESIAN_POINT ( 'NONE',  ( -10.81492255796105439, 18.62759615963255655, 92.91775706135236135 ) ) ;
#169472 = CARTESIAN_POINT ( 'NONE',  ( -16.53943276465976808, -0.05219959533934237506, 98.75109039468568994 ) ) ;
#169473 = CARTESIAN_POINT ( 'NONE',  ( 12.14591786802309770, 12.06949235617756955, 74.37390960531436690 ) ) ;
#169474 = CARTESIAN_POINT ( 'NONE',  ( 19.05341960407611168, 5.049401038298154454, 78.95724293864769550 ) ) ;
#169475 = ORIENTED_EDGE ( 'NONE', *, *, #193154, .F. ) ;
#169476 = CARTESIAN_POINT ( 'NONE',  ( 16.55341960407618274, -4.379528057220086978, 26.04275706135235779 ) ) ;
#169477 = CARTESIAN_POINT ( 'NONE',  ( 16.46253265017160672, -9.564922557960803928, 43.33224293864769550 ) ) ;
#169478 = CARTESIAN_POINT ( 'NONE',  ( -19.02544592524342804, 5.153800228976336051, 96.04057627198103830 ) ) ;
#169480 = CARTESIAN_POINT ( 'NONE',  ( -11.40812507854755609, 35.11059874428196537, -1.024999997268813301 ) ) ;
#169479 = CARTESIAN_POINT ( 'NONE',  ( -0.05219959533934338120, 16.53943276465976808, 37.50109039468568284 ) ) ;
#169481 = CARTESIAN_POINT ( 'NONE',  ( -16.51473224551082808, 9.474510206698731452, 33.33442372801899722 ) ) ;
#169482 = CARTESIAN_POINT ( 'NONE',  ( 12.14591786802327356, -12.06949235617739191, 95.62609039468568994 ) ) ;
#169483 = CARTESIAN_POINT ( 'NONE',  ( 16.46253265017160672, -9.564922557960803928, 38.33224293864768839 ) ) ;
#169484 = CARTESIAN_POINT ( 'NONE',  ( 8.224510206698742110, 14.34966873604972548, 77.08442372801901854 ) ) ;
#169485 = CARTESIAN_POINT ( 'NONE',  ( -12.14591786802326823, 12.06949235617739902, 73.12609039468567573 ) ) ;
#169486 = CARTESIAN_POINT ( 'NONE',  ( -9.474510206698720793, -16.51473224551083518, 79.58442372801899012 ) ) ;
#169487 = CARTESIAN_POINT ( 'NONE',  ( -0.05219959533936034679, 19.03943276465977164, 22.50109039468566152 ) ) ;
#169488 = CARTESIAN_POINT ( 'NONE',  ( -16.51473224551069308, -9.474510206698971260, 51.66557627198102409 ) ) ;
#169489 = CARTESIAN_POINT ( 'NONE',  ( -8.224510206698948167, 14.34966873604960824, 85.41557627198102409 ) ) ;
#169490 = CARTESIAN_POINT ( 'NONE',  ( -19.03943276465977164, -0.05219959533935918106, 58.75109039468566863 ) ) ;
#169491 = CARTESIAN_POINT ( 'NONE',  ( -10.81492255796078084, -18.62759615963271287, 57.08224293864769550 ) ) ;
#169492 = CARTESIAN_POINT ( 'NONE',  ( 9.564922557961047289, -16.46253265017146816, 30.41775706135232937 ) ) ;
#169493 = CARTESIAN_POINT ( 'NONE',  ( -9.474510206698964154, 16.51473224551069663, 100.4155762719810241 ) ) ;
#169494 = CIRCLE ( 'NONE', #66136, 10.00000000000000888 ) ;
#169495 = CARTESIAN_POINT ( 'NONE',  ( -5.823673210054116645, -21.52544592524344225, 82.29057627198103830 ) ) ;
#169496 = CARTESIAN_POINT ( 'NONE',  ( 13.97604488694527802, 13.89961937509977652, 109.3739096053143669 ) ) ;
#169497 = CARTESIAN_POINT ( 'NONE',  ( -5.153800228976607833, 19.02544592524334988, 97.70942372801900433 ) ) ;
#169498 = CARTESIAN_POINT ( 'NONE',  ( -16.46253265017160317, 9.564922557960807481, 115.8322429386477097 ) ) ;
#169499 = CARTESIAN_POINT ( 'NONE',  ( -9.564922557961040184, 16.46253265017147172, 112.9177570613523329 ) ) ;
#169500 = CARTESIAN_POINT ( 'NONE',  ( -9.564922557960796823, -16.46253265017161027, 32.08224293864769550 ) ) ;
#169501 = CARTESIAN_POINT ( 'NONE',  ( 19.05341960407611168, 5.049401038298154454, 98.95724293864766707 ) ) ;
#169502 = CARTESIAN_POINT ( 'NONE',  ( 21.52544592524344225, -5.823673210054117533, 73.54057627198102409 ) ) ;
#169503 = CARTESIAN_POINT ( 'NONE',  ( -12.06949235617739369, -12.14591786802326823, 44.37609039468567573 ) ) ;
#169504 = CARTESIAN_POINT ( 'NONE',  ( -15.80617190586768217, 15.72974639402176855, 58.12609039468568994 ) ) ;
#169506 = CARTESIAN_POINT ( 'NONE',  ( -0.05219959533937732626, 21.53943276465977519, 107.5010903946856899 ) ) ;
#169505 = CARTESIAN_POINT ( 'NONE',  ( 9.564922557961047289, -16.46253265017146816, 100.4177570613523329 ) ) ;
#169507 = CARTESIAN_POINT ( 'NONE',  ( 16.52544592524342804, -4.483927247898539470, 23.54057627198102765 ) ) ;
#169508 = CARTESIAN_POINT ( 'NONE',  ( -21.52544592524343514, 5.823673210054127303, 106.0405762719810525 ) ) ;
#169509 = CARTESIAN_POINT ( 'NONE',  ( 8.224510206698953496, -14.34966873604960469, 37.91557627198102409 ) ) ;
#169510 = CARTESIAN_POINT ( 'NONE',  ( -13.97604488694547697, 13.89961937509957934, 78.12609039468567573 ) ) ;
#169511 = CARTESIAN_POINT ( 'NONE',  ( 10.81492255796106328, -18.62759615963255655, 55.41775706135234714 ) ) ;
#169512 = CARTESIAN_POINT ( 'NONE',  ( 0.05219959533936267826, -19.03943276465977164, 25.00109039468566152 ) ) ;
#169513 = CARTESIAN_POINT ( 'NONE',  ( 14.34966873604960469, 8.224510206698951720, 99.16557627198100988 ) ) ;
#169514 = CARTESIAN_POINT ( 'NONE',  ( -5.823673210054116645, -21.52544592524344225, 37.29057627198102409 ) ) ;
#169515 = CARTESIAN_POINT ( 'NONE',  ( -14.29746914071049879, 8.314922557960819915, 40.83224293864769550 ) ) ;
#169516 = CARTESIAN_POINT ( 'NONE',  ( -5.719274019375665041, -21.55341960407619695, 99.79275706135234714 ) ) ;
#169517 = CARTESIAN_POINT ( 'NONE',  ( 4.379528057220092307, 16.55341960407617563, 57.29275706135234714 ) ) ;
#169518 = CARTESIAN_POINT ( 'NONE',  ( -14.34966873604972548, 8.224510206698743886, 113.3344237280190328 ) ) ;
#169519 = CARTESIAN_POINT ( 'NONE',  ( -5.823673210054431948, 21.52544592524334988, 67.70942372801901854 ) ) ;
#169520 = CARTESIAN_POINT ( 'NONE',  ( 10.81492255796106328, -18.62759615963255655, 50.41775706135235424 ) ) ;
#169521 = EDGE_LOOP ( 'NONE', ( #149348, #16045, #78692, #111353 ) ) ;
#169522 = CARTESIAN_POINT ( 'NONE',  ( 16.46253265017160672, -9.564922557960803928, 28.33224293864769550 ) ) ;
#169523 = CARTESIAN_POINT ( 'NONE',  ( 18.62759615963255655, 10.81492255796105972, 36.66775706135234714 ) ) ;
#169524 = CARTESIAN_POINT ( 'NONE',  ( 8.314922557960818139, 14.29746914071049879, 109.5822429386476955 ) ) ;
#169525 = CARTESIAN_POINT ( 'NONE',  ( 9.564922557960805705, 16.46253265017160317, 24.58224293864769194 ) ) ;
#169526 = CARTESIAN_POINT ( 'NONE',  ( -14.34966873604960291, -8.224510206698953496, 81.66557627198103830 ) ) ;
#169527 = CARTESIAN_POINT ( 'NONE',  ( 0.05219959533909260263, 19.03943276465977164, 69.99890960531435269 ) ) ;
#169528 = CARTESIAN_POINT ( 'NONE',  ( 16.53943276465976808, -0.05219959533910856209, 23.74890960531435269 ) ) ;
#169529 = CARTESIAN_POINT ( 'NONE',  ( 18.67979575497178502, 10.72451020669898547, 59.16557627198103120 ) ) ;
#169530 = CARTESIAN_POINT ( 'NONE',  ( 4.379528057220339221, -16.55341960407611168, 87.70724293864769550 ) ) ;
#169531 = CIRCLE ( 'NONE', #75858, 40.00000000000002132 ) ;
#169532 = CARTESIAN_POINT ( 'NONE',  ( 10.72451020669898902, -18.67979575497178502, 97.91557627198103830 ) ) ;
#169533 = CARTESIAN_POINT ( 'NONE',  ( 16.51473224551069308, 9.474510206698969483, 104.1655762719810241 ) ) ;
#169535 = CARTESIAN_POINT ( 'NONE',  ( 9.564922557961047289, -16.46253265017146816, 110.4177570613523471 ) ) ;
#169534 = CARTESIAN_POINT ( 'NONE',  ( 19.02544592524343514, -5.153800228976328945, 58.54057627198102409 ) ) ;
#169536 = CARTESIAN_POINT ( 'NONE',  ( 10.72451020669898902, -18.67979575497178502, 52.91557627198103830 ) ) ;
#169537 = CARTESIAN_POINT ( 'NONE',  ( 10.72451020669871369, 18.67979575497193778, 87.08442372801901854 ) ) ;
#169538 = CARTESIAN_POINT ( 'NONE',  ( -16.51473224551069308, -9.474510206698971260, 71.66557627198102409 ) ) ;
#169539 = EDGE_CURVE ( 'NONE', #196449, #11730, #115229, .T. ) ;
#169540 = CARTESIAN_POINT ( 'NONE',  ( 19.03943276465977164, -0.05219959533909143690, 98.74890960531436690 ) ) ;
#169541 = CARTESIAN_POINT ( 'NONE',  ( 8.224510206698742110, 14.34966873604972548, 82.08442372801901854 ) ) ;
#169542 = CARTESIAN_POINT ( 'NONE',  ( -10.72451020669870658, -18.67979575497194134, 54.58442372801901143 ) ) ;
#169543 = CARTESIAN_POINT ( 'NONE',  ( 18.62759615963255655, 10.81492255796105972, 81.66775706135236135 ) ) ;
#169544 = CARTESIAN_POINT ( 'NONE',  ( 15.80617190586746368, 15.72974639402197994, 114.3739096053143527 ) ) ;
#169545 = CARTESIAN_POINT ( 'NONE',  ( 14.29746914071037800, 8.314922557961029526, 71.66775706135234714 ) ) ;
#169546 = CARTESIAN_POINT ( 'NONE',  ( 10.72451020669898902, -18.67979575497178502, 82.91557627198103830 ) ) ;
#169547 = CARTESIAN_POINT ( 'NONE',  ( 13.97604488694548053, -13.89961937509957401, 40.62609039468564731 ) ) ;
#169548 = CARTESIAN_POINT ( 'NONE',  ( -18.67979575497178146, -10.72451020669898902, 41.66557627198103120 ) ) ;
#169549 = AXIS2_PLACEMENT_3D ( 'NONE', #12692, #106664, #11708 ) ;
#169551 = CARTESIAN_POINT ( 'NONE',  ( -8.314922557960811034, -14.29746914071050412, 27.08224293864769550 ) ) ;
#169550 = CARTESIAN_POINT ( 'NONE',  ( -13.89961937509977652, 13.97604488694528158, 80.62390960531436690 ) ) ;
#169552 = CARTESIAN_POINT ( 'NONE',  ( -16.29526858892873875, 7.335722546920271370, 64.20329402199794799 ) ) ;
#169553 = PRODUCT_DEFINITION_FORMATION_WITH_SPECIFIED_SOURCE ( 'ANY', '', #29103, .NOT_KNOWN. ) ;
#169554 =( BOUNDED_SURFACE ( )  B_SPLINE_SURFACE ( 3, 2, ( 
 ( #142216, #127038, #20864, #188745, #7681, #50230, #111884, #35043, #129024, #69365, #131034, #96697, #81515, #143202, #66375, #174562, #82521, #144203, #190725, #179573, #194730, #40025, #72375, #9712, #135060, #70375, #134049, #27886, #162373, #196736, #132043, #195741, #104701, #120845, #117882, #149221, #85526, #100692, #57215, #59176, #181557, #23875, #118889, #41043, #133040, #10712, #147214, #116869, #119872, #102708, #164397, #165392, #180574, #71376, #8705, #24885, #193732, #12705, #86534, #150224, #197711, #42048, #136036, #56200, #178560, #55200, #103712, #25889, #39036, #26885, #101698, #87534, #163388, #58203, #148218, #43035, #88528, #166390, #11720, #73388, #89528, #151216, #74371, #64153, #1469, #16659, #63147, #47000, #15667, #122831, #106677, #124826, #14672, #182544, #92487, #61159, #44026, #76333, #186526, #79314, #75344, #62147, #138994, #60170, #17654, #138010, #170337, #199694, #473, #109654, #184520, #107655, #154176, #156156, #46000, #90511, #2471, #152193, #169332, #13677, #48000, #137013, #198703, #121839, #77326, #31830, #171336, #93480, #32824, #94475, #108659, #105687, #123811, #30840, #140983, #185509, #155167, #183533, #78307, #153170, #139980, #45017, #167374, #28870, #168350, #29846, #91483, #159124, #191466, #7437, #4440, #35792, #172322, #141970, #84275, #66128, #81278, #161132, #5442, #128784, #65136, #127793, #34802, #189493, #143962, #125817, #67126, #174322, #114619, #50971, #142960, #126793, #20620, #96457, #21624, #157157, #82270, #176318, #48986, #83281, #18652, #190484, #52944, #187520, #112630, #97439, #33811, #3459, #145956, #51956, #113616, #22628, #175310, #36776, #188499, #98441, #158144, #160136, #144955, #110641, #6436, #95471, #68118, #80298, #129770, #37788, #19636, #99452, #49978, #111642, #173327, #71132, #147980, #195494, #40795, #101447, #115637, #54959, #23630, #42799, #116631, #180333, #27647, #102464, #166144, #86290, #8458, #162134, #148978, #194485, #150977, #10467, #131803, #9469, #100454, #165147, #85278, #26638, #163139, #134816, #130788, #146970, #103468, #39783, #132798, #69121, #88281, #149969, #11475, #133802, #164152, #55957, #193482, #73146, #24642, #192479, #179332, #117633, #53962, #25649, #196496, #89286, #70131, #72128, #87294, #178320, #104461, #56968, #118641, #41801, #57966, #119637, #181320, #177326, #38797, #189016, #14424, #120609, #35309, #182303, #76089, #43784, #34322, #105448, #167132, #28632, #48509, #64660, #95984, #126322, #157669, #3963, #79827, #168108, #13441, #110163, #183292, #111153, #90269, #171842, #65643, #135803, #172842, #151952, #33330, #80806, #96963, #91237, #125341, #58940, #75105, #173843, #152927, #29605, #50490, #94990, #18170, #136772, #137764, #121597, #199448, #156675, #74132, #141497, #12471, #19158, #197474, #2981, #60916, #106427, #187039, #198458, #59930, #142485, #188019, #49491, #127305, #112153, #44774, #128299, #54472, #131305, #66636, #113135, #116142, #162644, #23140, #189998, #82788, #160645, #100959, #39301, #159637, #190987, #51473, #36289, #177833, #194005, #130284, #176835, #174825, #22137, #175823, #37296, #38306, #115142, #84785, #24151, #69639, #70647, #143467, #40301, #191978, #97945, #21133, #146464, #144470, #85802, #83787, #158643, #20135, #192995, #145466, #5954, #114121, #52463, #147488, #98955, #6948, #67631, #8979, #4951, #7956, #68628, #129291, #132313, #53465, #99961, #55468, #161645, #117138, #178832, #81780, #89795, #90771, #120128, #183799, #118151, #73650, #56472, #121117, #197974, #11986, #151478, #194995, #135322, #59444, #101977, #41312, #29134, #103973, #165652, #181819, #163657, #196994, #122110, #44294, #86802, #43298, #42312, #196008, #58461, #25160, #179841, #182811, #27150, #180835, #28154, #104966, #134322, #166653, #137286, #105953, #88797, #149479, #12969, #60435, #74633, #198968, #119153, #102972, #164657, #136299, #150490, #148488, #167637, #26152 ),
 ( #152455, #13941, #9979, #71639, #75607, #133306, #87794, #10975, #72648, #57483, #170614, #127069, #45286, #156434, #108933, #169613, #746, #139270, #79588, #124090, #62418, #14945, #49258, #30112, #171609, #185789, #199964, #187789, #47277, #61429, #33097, #76605, #91753, #123100, #106939, #94753, #34088, #63428, #168612, #184786, #16931, #46272, #64423, #141257, #155441, #17934, #138283, #78584, #2747, #153447, #107927, #172602, #32103, #3731, #126092, #77599, #125104, #93760, #1750, #31110, #92758, #154447, #80572, #186802, #110916, #15940, #109927, #140258, #48272, #95747, #157432, #18927, #142246, #65408, #174596, #6713, #188777, #176596, #114902, #177598, #37060, #192754, #7713, #39066, #83552, #98719, #8737, #159401, #21902, #84548, #20896, #129054, #190755, #158417, #146226, #161410, #96728, #143233, #69398, #54237, #53226, #19905, #112902, #52229, #131065, #115908, #189769, #82554, #81547, #66405, #100723, #23906, #160413, #68391, #4716, #113886, #5720, #67398, #130043, #145231, #38070, #162404, #99726, #85560, #173604, #70406, #191743, #128067, #51242, #22902, #36062, #147246, #175584, #50260, #111916, #35074, #97710, #144236, #87563, #25919, #166421, #10741, #149250, #101733, #136066, #116900, #58232, #72405, #86564, #74400, #134082, #148247, #119900, #163421, #178593, #9741, #13708, #181585, #120875, #150256, #132074, #71405, #103741, #133069, #151245, #27916, #42077, #43063, #24919, #165421, #89559, #193763, #194759, #59206, #195772, #90541, #104729, #164426, #11750, #180604, #88557, #40056, #56231, #117913, #167405, #73417, #12734, #179602, #196764, #57245, #118919, #41074, #197740, #102738, #182575, #44058, #26915, #135088, #55231, #105718, #28901, #152223, #156188, #141016, #140013, #171368, #108691, #17687, #76366, #107686, #183564, #153200, #32856, #110672, #47034, #93514, #106707, #77359, #92519, #154209, #155200, #31861, #1501, #79345, #186558, #187550, #60201, #157187, #170369, #45049, #168381, #63179, #14705, #2503, #506, #75374, #137044, #48030, #139027, #199724, #30873, #169364, #109687, #15698, #62178, #29876, #64183, #121871, #124859, #123842, #91514, #125849, #185540, #138043, #94506, #61190, #122862, #184550, #198736, #49017, #172352, #16689, #46031, #78339, #33841, #95501, #37822, #114651, #128813, #68148, #111673, #51986, #176349, #100484, #158174, #145985, #20648, #177356, #191498, #50998, #98472, #67156, #175339, #3488, #173360, #34830, #53993, #36806, #129799, #126824, #83309, #143992, #5473, #65165, #161163, #188530, #144986, #52974, #4468, #160166, #18681, #6467, #99482, #21656, #22659, #84306, #7468, #69152, #113645, #130818, #190512, #192509, #115667, #38826, #80328, #142000, #50007, #189526, #96485, #19665, #112659, #159152, #82302, #81306, #142990, #66157, #127820, #174350, #35821, #97467, #26669, #70162, #86321, #164180, #104491, #193513, #25678, #179360, #40823, #180362, #118671, #88310, #166173, #73175, #74160, #147000, #43812, #133832, #131831, #54989, #149998, #39812, #89314, #87323, #162163, #23660, #134846, #149008, #148008, #117663, #55987, #196524, #102495, #10496, #116658, #27674, #8486, #11504, #72157, #178349, #151007, #195523, #101477, #57995, #163167, #24671, #9498, #85308, #119665, #12498, #41830, #71162, #132827, #56996, #194513, #181347, #42826, #103497, #135832, #165175, #197501, #58968, #120636, #182334, #32610, #107443, #63940, #78097, #137795, #185296, #153959, #61932, #90296, #59959, #198486, #140768, #123601, #154952, #13469, #170122, #30622, #92275, #151980, #47787, #75132, #31617, #139766, #91265, #46787, #105475, #93267, #16448, #108446, #186306, #171121, #1254, #62931, #138783, #94264, #15457, #109438, #124611, #155943, #264, #77113, #125608, #76117, #17439, #79095, #199479, #45791, #169117, #136802, #2257, #187307, #121625, #183321, #167162, #28661, #44802, #106457, #29632, #168136, #152956, #14454, #60945, #122620 ),
 ( #184310, #144748, #21414, #156946, #3254, #6233, #52738, #113408, #18443, #173118, #50765, #191263, #129565, #49766, #81076, #80094, #126587, #67912, #84069, #20408, #66912, #141762, #112423, #65915, #127588, #128576, #5231, #175099, #114405, #159925, #160928, #33600, #130576, #82057, #64927, #188289, #36567, #111431, #176106, #174114, #48778, #110432, #83072, #35584, #34593, #4235, #142755, #37576, #189287, #97230, #96251, #99239, #95263, #98222, #158918, #157938, #22419, #143751, #19429, #145748, #190270, #51747, #7229, #172114, #68914, #181115, #10258, #73929, #8245, #163946, #146750, #11264, #88075, #102259, #41595, #85068, #25444, #149761, #192271, #131589, #119431, #194282, #150768, #164941, #24433, #71918, #40588, #148769, #177118, #69923, #193274, #27434, #133589, #103259, #100244, #56762, #117422, #179120, #38589, #134605, #161926, #118434, #26434, #178109, #195280, #53753, #180127, #72936, #196291, #57761, #42589, #104252, #165935, #87084, #89077, #12265, #115427, #23420, #54747, #116421, #39577, #101236, #162925, #86081, #147772, #9259, #70925, #132592, #55748, #43579, #105244, #123370, #13244, #62695, #60711, #17208, #135598, #46551, #199244, #59726, #91040, #29410, #169892, #14217, #152727, #166931, #139538, #120402, #61701, #75886, #90069, #77871, #137561, #151751, #185063, #28432, #182095, #74907, #197270, #108213, #124377, #153724, #58732, #136571, #107212, #198251, #154723, #31386, #45558, #93035, #121396, #168882, #16217, #183089, #44571, #186072, #122385, #94033, #1022, #167910, #15220, #184074, #92034, #106226, #30387, #76879, #170887, #138550, #47555, #27, #109208, #32379, #155712, #125384, #21178, #187081, #4998, #51517, #64704, #97007, #78861, #66682, #128344, #35356, #159682, #144514, #143511, #174869, #112197, #67678, #127350, #82834, #97988, #129336, #173887, #189063, #98999, #49533, #158689, #36335, #111195, #19203, #80852, #48550, #5999, #113179, #110204, #33372, #191031, #52506, #190043, #171884, #3028, #142529, #114166, #175869, #79870, #172886, #95030, #156720, #37341, #160689, #50535, #20178, #18212, #4007, #96027, #157713, #81824, #140541, #2029, #141539, #63709, #65686, #126366, #188062, #34366, #130327, #151276, #197772, #7998, #43094, #22180, #12765, #74429, #181615, #105749, #90573, #89589, #120907, #58261, #13739, #73446, #28932, #44091, #75408, #119930, #135119, #45081, #193037, #104762, #182606, #54514, #165450, #26947, #192024, #167435, #59238, #53508, #176878, #152254, #137078, #136096, #115185, #146508, #88588, #198767, #60233, #23185, #116187, #38348, #100003, #121904, #183597, #196793, #166451, #161690, #150287, #42109, #103771, #27948, #106738, #83830, #145511, #6992, #68673, #84828, #69682, #131349, #180634, #11782, #186594, #122894, #141053, #185575, #33880, #168413, #109722, #47067, #30905, #139061, #77391, #32892, #62211, #539, #138075, #2539, #153235, #48066, #123878, #61223, #79384, #108727, #184583, #171406, #199756, #14738, #46064, #29908, #94544, #187586, #140049, #91548, #169398, #1538, #92553, #64221, #125886, #78373, #156225, #107718, #63215, #49055, #76399, #170404, #154241, #17725, #15732, #31896, #110710, #93549, #155235, #16725, #172392, #124895, #41761, #184244, #58900, #195454, #165105, #107378, #89244, #104420, #45725, #28593, #151914, #88241, #150937, #57926, #12430, #167092, #10427, #43745, #169050, #91201, #133759, #90230, #74093, #42757, #120566, #72085, #26598, #29570, #135763, #27605, #75067, #182260, #181280, #105407, #30556, #152891, #197434, #196456, #59892, #148937, #13403, #56928, #166103, #149926, #103426, #136733, #198415, #118603, #121558, #11433, #183254, #180293, #44735, #73103, #106391, #168072, #14387, #134773, #119597, #76053, #137729, #199413, #60877, #122554, #126528, #111365, #156884, #173054, #142693, #80033, #170060, #19369, #17375, #174053, #92208, #3193, #155878, #16386, #47722, #186244, #188227, #171055 ),
 ( #112362, #198, #79030, #61867, #34531, #123536, #185230, #46721, #125548, #141702, #96191, #64866, #157880, #81018, #18381, #153892, #110367, #140705, #4173, #32545, #109373, #93203, #187244, #62865, #49700, #108384, #48714, #65851, #15389, #127521, #31551, #172049, #189225, #77046, #94198, #154888, #50703, #124547, #2195, #138717, #78033, #139702, #1188, #63877, #33536, #95198, #31671, #34638, #156992, #186360, #51793, #170178, #81121, #33647, #94316, #125659, #63989, #4282, #48826, #187356, #139818, #174161, #155005, #96298, #110479, #124664, #112468, #172162, #47840, #157984, #1306, #16502, #109492, #93321, #19475, #158964, #188335, #78150, #171175, #141809, #32662, #189333, #65962, #80139, #142801, #62985, #3302, #127633, #155994, #17490, #97276, #95308, #128623, #50810, #2308, #49813, #18491, #126633, #79147, #140819, #64974, #5280, #111478, #35631, #173163, #20455, #82105, #143797, #66962, #190316, #21458, #39623, #86128, #99285, #131636, #113452, #101283, #162973, #69970, #194327, #179165, #178158, #9305, #146799, #102302, #161970, #117467, #132639, #163991, #8292, #23466, #133636, #84114, #193320, #70971, #145793, #53798, #115473, #83119, #55795, #147819, #144796, #67957, #40633, #25488, #24478, #6279, #37623, #177162, #87130, #148815, #114452, #7276, #129612, #191307, #10305, #71962, #85115, #54794, #52783, #38635, #130622, #192318, #175145, #68960, #195327, #36613, #176153, #116469, #98269, #160972, #159971, #100292, #22466, #89123, #74949, #184122, #73973, #182138, #166973, #30434, #58776, #164984, #76923, #26479, #120444, #88121, #75932, #149805, #11311, #72981, #90110, #106268, #137607, #167953, #199290, #45604, #121438, #138594, #136612, #105285, #107257, #197312, #12307, #57804, #151794, #27480, #152771, #134650, #13285, #168928, #180171, #14263, #196336, #198293, #122430, #56807, #135642, #28476, #103305, #119475, #15265, #43621, #59770, #92081, #183131, #44614, #181158, #29452, #165979, #91084, #60757, #118481, #153770, #41640, #42634, #104297, #150811, #140583, #94076, #110245, #123414, #77914, #80895, #2073, #78906, #126408, #171927, #32421, #95075, #35398, #4051, #125426, #47597, #111240, #158731, #33416, #97049, #17253, #139581, #93081, #79910, #187122, #81869, #141581, #62741, #63752, #31428, #96068, #154765, #157757, #155755, #65728, #61746, #16263, #34410, #170930, #48594, #76, #19248, #142572, #109250, #156763, #18257, #169937, #173929, #1066, #3069, #64746, #188104, #49577, #172931, #127397, #189106, #50579, #112239, #20221, #185107, #108257, #46597, #124421, #186117, #113225, #162736, #174915, #36379, #98033, #176924, #193084, #24244, #54559, #85893, #132404, #8049, #25252, #161737, #192073, #194097, #83876, #99045, #144560, #38395, #114212, #39391, #159730, #100051, #55559, #66729, #101051, #21226, #23232, #9067, #143560, #22227, #53554, #190085, #82882, #102067, #145558, #160735, #178926, #84876, #146553, #6046, #7036, #52551, #68718, #69728, #5043, #131396, #163752, #147581, #128389, #116232, #130375, #37388, #115233, #51561, #67724, #70737, #177923, #117233, #40396, #129382, #175917, #191078, #122197, #90856, #12079, #134416, #198065, #45374, #120218, #183889, #104064, #26244, #179935, #166743, #73742, #168699, #28246, #149571, #165745, #118244, #182900, #41402, #44384, #119242, #152541, #148578, #103067, #121209, #57572, #88888, #86894, #106039, #167725, #196102, #27239, #197085, #56570, #60522, #87883, #150580, #180926, #58552, #135414, #10068, #42401, #29223, #107027, #164749, #89886, #43387, #11067, #71728, #181908, #74724, #105059, #72745, #151569, #13058, #14029, #136388, #59531, #75694, #137374, #133398, #199052, #195087, #184877, #172693, #32191, #46359, #156527, #61519, #15033, #108017, #112009, #18026, #19017, #48363, #30201, #169703, #1839, #31197, #49345, #126182, #140351, #79679, #123188, #63521, #187877, #91842, #92848, #157523, #93849 ),
 ( #94846, #155527, #17022, #76693, #34178, #138370, #141350, #2837, #16030, #110018, #153536, #64515, #111007, #186892, #95839, #80663, #142339, #3819, #125196, #65497, #78675, #127159, #188867, #50350, #171698, #33187, #200050, #837, #154533, #77688, #62510, #170702, #139356, #124182, #185883, #47368, #109023, #128158, #69491, #177686, #38163, #81637, #97802, #175675, #115997, #54325, #174686, #5813, #143319, #51332, #131156, #8825, #145322, #191835, #4806, #37149, #190843, #52319, #53316, #130138, #99818, #39154, #84641, #85651, #158506, #114994, #70494, #192845, #23994, #35166, #161503, #160502, #189858, #55318, #173698, #146318, #98808, #100810, #162494, #22993, #147338, #6805, #132161, #21992, #193853, #96821, #19993, #68483, #83645, #66495, #144324, #176688, #112992, #67488, #113977, #7807, #36150, #159491, #20985, #82641, #129146, #12824, #120965, #181672, #25008, #41165, #119009, #59297, #197831, #118004, #149335, #86652, #194849, #74490, #152312, #88649, #135178, #148336, #180692, #134173, #195861, #196852, #73506, #43152, #182664, #28007, #28990, #101822, #58318, #13798, #136156, #167494, #178683, #104820, #103828, #133157, #198824, #116989, #89647, #42168, #102828, #72499, #10830, #151335, #57333, #165508, #9831, #44148, #163510, #166509, #27005, #71491, #105807, #150345, #56321, #90630, #179693, #164514, #26007, #40145, #75464, #137137, #119986, #87649, #11841, #31951, #14796, #79437, #156281, #170460, #109776, #153295, #93606, #17782, #142095, #199814, #187640, #62266, #18775, #32947, #92608, #140105, #108782, #16781, #45139, #76456, #138133, #95595, #78430, #171459, #168470, #124952, #185632, #47124, #106796, #2596, #29968, #186648, #94602, #46121, #1596, #60289, #48119, #141108, #63272, #121962, #64275, #122952, #77448, #91607, #125942, #61282, #49111, #154298, #110768, #183655, #184640, #172450, #30961, #123934, #107775, #33937, #157279, #169460, #595, #155291, #15788, #80422, #139119, #8328, #115510, #116504, #85149, #65258, #100326, #25522, #103338, #96578, #86164, #163007, #81397, #41674, #38671, #194362, #162005, #24514, #133670, #23501, #131673, #178192, #180205, #70003, #111765, #26511, #173454, #193354, #34923, #87168, #158267, #19756, #143083, #39657, #55829, #148849, #117502, #10340, #195361, #71006, #88155, #147854, #54830, #56840, #146835, #101318, #4562, #9341, #177198, #102336, #66254, #132674, #118515, #126918, #164026, #127914, #179199, #71996, #3580, #40667, #165018, #50105, #189616, #188625, #53836, #105318, #185137, #29484, #152805, #89156, #90141, #58810, #151826, #167986, #11344, #44648, #169966, #92112, #134684, #91115, #13315, #43656, #59802, #73015, #27515, #30464, #74981, #28507, #75965, #121472, #182170, #106300, #46628, #153801, #136643, #197347, #60790, #108288, #183164, #31459, #167005, #150845, #42670, #14297, #198326, #149840, #137638, #199325, #57838, #122461, #184154, #45635, #196370, #15295, #119511, #107287, #168958, #135675, #76955, #181192, #138625, #106, #61776, #123444, #104331, #166015, #12341, #74005, #120479, #141614, #97080, #112268, #143591, #188138, #3101, #113254, #63786, #126440, #189137, #125458, #33448, #95107, #62773, #50609, #65760, #1097, #47629, #173960, #158761, #157789, #124454, #17285, #156796, #35427, #20252, #94109, #187155, #186150, #170962, #81898, #128418, #64779, #111272, #109284, #18289, #110279, #171960, #172963, #49609, #19279, #5074, #4082, #66757, #77944, #34441, #190114, #51589, #174945, #154796, #80926, #79944, #32456, #93111, #16294, #127429, #96100, #78939, #48627, #142603, #139611, #155788, #140615, #2105, #40422, #21256, #162761, #53588, #191108, #178952, #38426, #52583, #24270, #67753, #82911, #114242, #118271, #85919, #25279, #54585, #36407, #175949, #8079, #37418, #55585, #132430, #146585, #147607, #129411, #69755, #194122, #98062, #99078, #163778, #100082, #195114, #9095, #68750, #116258, #84906 ),
 ( #71756, #177949, #70762, #144589, #101076, #161767, #23262, #6075, #102093, #160768, #117260, #86922, #22258, #39417, #159761, #148604, #10096, #193111, #133426, #56597, #83907, #145590, #131425, #7068, #130407, #192105, #115264, #176957, #74748, #28271, #200074, #150607, #13083, #75722, #12103, #120242, #181933, #149599, #137398, #152566, #87912, #134442, #199079, #183913, #44410, #11096, #104089, #43414, #122222, #60547, #180950, #73766, #72772, #57598, #45398, #15057, #151592, #198091, #196127, #105084, #197109, #58576, #59556, #136411, #106064, #107051, #90882, #91867, #164776, #121234, #76717, #168724, #30225, #41428, #167750, #166770, #119267, #61542, #179961, #14055, #89910, #165772, #135439, #182927, #153560, #29248, #138393, #42427, #103094, #26270, #27266, #88915, #140379, #48389, #33214, #96847, #125221, #31223, #143346, #92872, #186919, #154559, #142367, #16055, #77713, #139379, #156554, #172722, #3846, #34204, #65525, #112037, #187904, #4834, #141377, #171726, #173725, #63547, #184901, #18054, #123211, #127185, #108043, #2865, #110046, #17047, #94874, #46385, #861, #188896, #79708, #1866, #49373, #64543, #155553, #126208, #158532, #50377, #111036, #170726, #95867, #81663, #157550, #20021, #19043, #62536, #124210, #80690, #35194, #169728, #185908, #47394, #109049, #32218, #93875, #78702, #162519, #98834, #132188, #128184, #82667, #100836, #37175, #68509, #148361, #85676, #24022, #114001, #6830, #176714, #36174, #40171, #5838, #130163, #175699, #38187, #145348, #189882, #160529, #147363, #163534, #159515, #146344, #144351, #22018, #117014, #83670, #54350, #191860, #84665, #193879, #53342, #115021, #99843, #101850, #161527, #174710, #86677, #97827, #23019, #21011, #8852, #67514, #129171, #190869, #7831, #116022, #70519, #177711, #55344, #178709, #131182, #66521, #69517, #192872, #25034, #39179, #51357, #52345, #113018, #180720, #105837, #41191, #104848, #198855, #133183, #167524, #102853, #43180, #75493, #91638, #88679, #120014, #56346, #26031, #168502, #150375, #165537, #45172, #89677, #12854, #149361, #11871, #119038, #73535, #28036, #151363, #164539, #135208, #27034, #196880, #74519, #166538, #136184, #13827, #120995, #121996, #194873, #197859, #106827, #29020, #60321, #71515, #59326, #58346, #87676, #9856, #118029, #182694, #181699, #134202, #44179, #103856, #90660, #10857, #152342, #30000, #137166, #179720, #183686, #72526, #195890, #57365, #42195, #169491, #79475, #184671, #138167, #107809, #34961, #141143, #142130, #171494, #153326, #30991, #124987, #92640, #172485, #49145, #63308, #2633, #46154, #186683, #110803, #14828, #154330, #80456, #155326, #111799, #125977, #185665, #32983, #1631, #109811, #199848, #15820, #77481, #188661, #94636, #64309, #61314, #17817, #78464, #140139, #122984, #95629, #139150, #187675, #33972, #627, #156316, #76490, #157316, #18812, #3614, #65293, #126952, #50140, #173488, #48153, #62298, #123968, #47156, #108815, #170494, #31984, #93641, #16814, #67280, #129929, #192639, #128939, #36940, #98602, #66289, #54122, #69283, #4597, #51125, #115795, #100610, #161293, #127948, #20777, #160296, #38954, #177485, #97592, #190640, #189651, #174479, #162293, #131961, #68278, #23793, #85443, #6599, #146113, #112785, #191628, #147133, #178478, #35946, #8621, #21786, #55118, #130949, #52116, #176479, #145114, #53108, #81431, #159280, #82432, #193646, #114786, #7597, #144120, #22788, #83437, #37955, #143117, #70293, #5601, #84435, #116787, #113772, #99613, #96613, #158302, #19790, #175468, #120761, #105605, #104618, #135959, #73306, #28789, #88443, #43943, #59095, #90428, #134977, #150138, #60090, #10629, #196654, #197629, #72290, #180493, #41965, #9628, #182462, #12625, #148137, #194646, #167292, #152114, #166307, #71295, #164314, #103632, #13597, #75264, #40957, #133968, #132958, #117799, #136935, #198624, #11639, #58123, #56116, #165308, #57131, #118807, #119792 ),
 ( #149139, #181476, #26802, #101616, #195660, #121758, #39945, #179492, #42954, #102629, #27803, #163305, #89444, #151134, #74290, #24803, #86452, #25807, #87453, #93398, #157074, #185428, #91399, #3379, #153088, #46918, #14592, #2388, #76248, #137926, #199610, #16578, #32741, #138911, #184439, #78225, #154091, #79231, #61076, #139896, #172240, #106592, #140902, #122748, #1385, #48905, #65054, #62064, #155084, #29765, #45919, #141888, #123729, #391, #18570, #63066, #186441, #107573, #108578, #92405, #170255, #124745, #44935, #47917, #183451, #125737, #168268, #109571, #31749, #77243, #171254, #169251, #30758, #64067, #94393, #156072, #17570, #187437, #15585, #110559, #80217, #33726, #95388, #174241, #37704, #85192, #160052, #23545, #143878, #66044, #19554, #6356, #51874, #8373, #68036, #189412, #5359, #158063, #22543, #81198, #84190, #159042, #192397, #188414, #142879, #161049, #97356, #128701, #126711, #145870, #7353, #35709, #67042, #36692, #96376, #100370, #127711, #190398, #20535, #98353, #113533, #49892, #82185, #69037, #146881, #4360, #129688, #50888, #175227, #177241, #21539, #114533, #83199, #144873, #53879, #191385, #52861, #176233, #162049, #99366, #34718, #111558, #112546, #130702, #115554, #38713, #173243, #101360, #39698, #103381, #119552, #150890, #181235, #12384, #58853, #134728, #151867, #88196, #118557, #120520, #10382, #24557, #166056, #74046, #196410, #178235, #194402, #72039, #135717, #197388, #71048, #102379, #163050, #147896, #27557, #105359, #41716, #149880, #86206, #133712, #87210, #148892, #11386, #26553, #57880, #182213, #42711, #43697, #54873, #73056, #167046, #89197, #28547, #131716, #104373, #56883, #9382, #70048, #193398, #90184, #195405, #55870, #25566, #164067, #116547, #132714, #117544, #179243, #40710, #180247, #165059, #33250, #170764, #158565, #18087, #32253, #142404, #44688, #198368, #93911, #97862, #3882, #4873, #34240, #13357, #155589, #187939, #17084, #35228, #112072, #126243, #65561, #106342, #49408, #173761, #75021, #78737, #143381, #79743, #174745, #188935, #48426, #95901, #64578, #172760, #59845, #140413, #1903, #51393, #157585, #127221, #121512, #80725, #141412, #2900, #183207, #20054, #63583, #50412, #96882, #125257, #19077, #136686, #81698, #66556, #128221, #189918, #113053, #36209, #186955, #111071, #110082, #171761, #94908, #156593, #9892, #54387, #7869, #179756, #130201, #192910, #55380, #191896, #99879, #161564, #129207, #117050, #132224, #67550, #144388, #114039, #41226, #147401, #148398, #177748, #159552, #175737, #131219, #37214, #178745, #40209, #69555, #8889, #52382, #116060, #101888, #21049, #98870, #86713, #23057, #118066, #193917, #53381, #39217, #100873, #162555, #5873, #160566, #22055, #194909, #24060, #70557, #190905, #85715, #84702, #146381, #83706, #163570, #145384, #25070, #71553, #6866, #133218, #82704, #56384, #68545, #115058, #176751, #38224, #167559, #198889, #136218, #91670, #151398, #106860, #122030, #153361, #197893, #12888, #123018, #73569, #59362, #60357, #135242, #43216, #104884, #72563, #183720, #75528, #10890, #57399, #45206, #168534, #29053, #134238, #27069, #166572, #30032, #14863, #103890, #196914, #195923, #180753, #76524, #138201, #74551, #121031, #119071, #28072, #120048, #181735, #182729, #44213, #90693, #199883, #13861, #61347, #87709, #105872, #184703, #102887, #164572, #26066, #152376, #89713, #42229, #149395, #165570, #137203, #88715, #150410, #58381, #11905, #80489, #185700, #172520, #143148, #173519, #31025, #34005, #63344, #662, #188692, #48187, #62332, #95662, #77515, #142163, #124002, #3647, #78500, #111830, #107841, #47189, #65325, #16849, #109842, #127980, #126985, #50173, #93677, #186717, #156349, #15857, #19821, #108849, #171527, #155360, #17850, #125021, #169525, #140173, #34990, #4629, #139187, #126011, #170529, #1666, #96644, #33015, #157349, #94670, #64342, #158332, #79506, #141175, #2665 ) ),
 .UNSPECIFIED., .T., .F., .T. ) 
 B_SPLINE_SURFACE_WITH_KNOTS ( ( 4, 3, 4 ),
 ( 3, 2, 2, 2, 2, 2, 2, 2, 2, 2, 2, 2, 2, 2, 2, 2, 2, 2, 2, 2, 2, 2, 2, 2, 2, 2, 2, 2, 2, 2, 2, 2, 2, 2, 2, 2, 2, 2, 2, 2, 2, 2, 2, 2, 2, 2, 2, 2, 2, 2, 2, 2, 2, 2, 2, 2, 2, 2, 2, 2, 2, 2, 2, 2, 2, 2, 2, 2, 2, 2, 2, 2, 2, 2, 2, 2, 2, 2, 2, 2, 2, 2, 2, 2, 2, 2, 2, 2, 2, 2, 2, 2, 2, 2, 2, 2, 2, 2, 2, 2, 2, 2, 2, 2, 2, 2, 2, 2, 2, 2, 2, 2, 2, 2, 2, 2, 2, 2, 2, 2, 2, 2, 2, 2, 2, 2, 2, 2, 2, 2, 2, 2, 2, 2, 2, 2, 2, 2, 2, 2, 2, 2, 2, 2, 2, 2, 2, 2, 2, 2, 2, 2, 2, 2, 2, 2, 2, 2, 2, 2, 2, 2, 2, 2, 2, 2, 2, 2, 2, 2, 2, 2, 2, 2, 2, 2, 2, 2, 2, 2, 2, 2, 2, 2, 2, 2, 2, 2, 2, 2, 2, 2, 2, 2, 2, 2, 2, 2, 2, 2, 2, 2, 2, 2, 2, 2, 2, 2, 2, 2, 2, 2, 2, 2, 2, 2, 2, 2, 2, 2, 2, 2, 2, 2, 2, 2, 2, 2, 3 ),
 ( 0.000000000000000000, 0.5000000000000000000, 1.000000000000000000 ),
 ( 0.000000000000000000, 0.004385964912280701511, 0.008771929824561403022, 0.01315789473684210453, 0.01754385964912280604, 0.02192982456140350755, 0.02631578947368420907, 0.03070175438596491058, 0.03508771929824561209, 0.03947368421052631360, 0.04385964912280701511, 0.04824561403508771662, 0.05263157894736841813, 0.05701754385964911964, 0.06140350877192982115, 0.06578947368421052266, 0.07017543859649122417, 0.07456140350877192569, 0.07894736842105262720, 0.08333333333333332871, 0.08771929824561403022, 0.09210526315789473173, 0.09649122807017543324, 0.1008771929824561348, 0.1052631578947368363, 0.1096491228070175378, 0.1140350877192982393, 0.1184210526315789408, 0.1228070175438596423, 0.1271929824561403577, 0.1315789473684210453, 0.1359649122807017607, 0.1403508771929824483, 0.1447368421052631637, 0.1491228070175438514, 0.1535087719298245668, 0.1578947368421052544, 0.1622807017543859698, 0.1666666666666666574, 0.1710526315789473728, 0.1754385964912280604, 0.1798245614035087758, 0.1842105263157894635, 0.1885964912280701788, 0.1929824561403508665, 0.1973684210526315819, 0.2017543859649122695, 0.2061403508771929849, 0.2105263157894736725, 0.2149122807017543879, 0.2192982456140350755, 0.2236842105263157909, 0.2280701754385964786, 0.2324561403508771940, 0.2368421052631578816, 0.2412280701754385970, 0.2456140350877192846, 0.2500000000000000000, 0.2543859649122807154, 0.2587719298245614308, 0.2631578947368420907, 0.2675438596491228060, 0.2719298245614035214, 0.2763157894736842368, 0.2807017543859648967, 0.2850877192982456121, 0.2894736842105263275, 0.2938596491228070429, 0.2982456140350877027, 0.3026315789473684181, 0.3070175438596491335, 0.3114035087719298489, 0.3157894736842105088, 0.3201754385964912242, 0.3245614035087719396, 0.3289473684210526550, 0.3333333333333333148, 0.3377192982456140302, 0.3421052631578947456, 0.3464912280701754610, 0.3508771929824561209, 0.3552631578947368363, 0.3596491228070175517, 0.3640350877192982670, 0.3684210526315789269, 0.3728070175438596423, 0.3771929824561403577, 0.3815789473684210731, 0.3859649122807017330, 0.3903508771929824483, 0.3947368421052631637, 0.3991228070175438791, 0.4035087719298245390, 0.4078947368421052544, 0.4122807017543859698, 0.4166666666666666852, 0.4210526315789473450, 0.4254385964912280604, 0.4298245614035087758, 0.4342105263157894912, 0.4385964912280701511, 0.4429824561403508665, 0.4473684210526315819, 0.4517543859649122973, 0.4561403508771929571, 0.4605263157894736725, 0.4649122807017543879, 0.4692982456140351033, 0.4736842105263157632, 0.4780701754385964786, 0.4824561403508771940, 0.4868421052631579093, 0.4912280701754385692, 0.4956140350877192846, 0.5000000000000000000, 0.5043859649122807154, 0.5087719298245614308, 0.5131578947368421462, 0.5175438596491228616, 0.5219298245614034659, 0.5263157894736841813, 0.5307017543859648967, 0.5350877192982456121, 0.5394736842105263275, 0.5438596491228070429, 0.5482456140350877583, 0.5526315789473684736, 0.5570175438596490780, 0.5614035087719297934, 0.5657894736842105088, 0.5701754385964912242, 0.5745614035087719396, 0.5789473684210526550, 0.5833333333333333703, 0.5877192982456140857, 0.5921052631578946901, 0.5964912280701754055, 0.6008771929824561209, 0.6052631578947368363, 0.6096491228070175517, 0.6140350877192982670, 0.6184210526315789824, 0.6228070175438596978, 0.6271929824561403022, 0.6315789473684210176, 0.6359649122807017330, 0.6403508771929824483, 0.6447368421052631637, 0.6491228070175438791, 0.6535087719298245945, 0.6578947368421053099, 0.6622807017543859143, 0.6666666666666666297, 0.6710526315789473450, 0.6754385964912280604, 0.6798245614035087758, 0.6842105263157894912, 0.6885964912280702066, 0.6929824561403509220, 0.6973684210526315264, 0.7017543859649122417, 0.7061403508771929571, 0.7105263157894736725, 0.7149122807017543879, 0.7192982456140351033, 0.7236842105263158187, 0.7280701754385965341, 0.7324561403508771384, 0.7368421052631578538, 0.7412280701754385692, 0.7456140350877192846, 0.7500000000000000000, 0.7543859649122807154, 0.7587719298245614308, 0.7631578947368421462, 0.7675438596491228616, 0.7719298245614034659, 0.7763157894736841813, 0.7807017543859648967, 0.7850877192982456121, 0.7894736842105263275, 0.7938596491228070429, 0.7982456140350877583, 0.8026315789473684736, 0.8070175438596490780, 0.8114035087719297934, 0.8157894736842105088, 0.8201754385964912242, 0.8245614035087719396, 0.8289473684210526550, 0.8333333333333333703, 0.8377192982456140857, 0.8421052631578946901, 0.8464912280701754055, 0.8508771929824561209, 0.8552631578947368363, 0.8596491228070175517, 0.8640350877192982670, 0.8684210526315789824, 0.8728070175438596978, 0.8771929824561403022, 0.8815789473684210176, 0.8859649122807017330, 0.8903508771929824483, 0.8947368421052631637, 0.8991228070175438791, 0.9035087719298245945, 0.9078947368421053099, 0.9122807017543859143, 0.9166666666666666297, 0.9210526315789473450, 0.9254385964912280604, 0.9298245614035087758, 0.9342105263157894912, 0.9385964912280702066, 0.9429824561403509220, 0.9473684210526315264, 0.9517543859649122417, 0.9561403508771929571, 0.9605263157894736725, 0.9649122807017543879, 0.9692982456140351033, 0.9736842105263158187, 0.9780701754385965341, 0.9824561403508771384, 0.9868421052631578538, 0.9912280701754385692, 0.9956140350877192846, 1.000000000000000000 ),
 .UNSPECIFIED. ) 
 GEOMETRIC_REPRESENTATION_ITEM ( )  RATIONAL_B_SPLINE_SURFACE ( (
 ( 1.000000000000000000, 0.9659258262890683122, 1.000000000000000000, 0.9659258262890683122, 1.000000000000000000, 0.9659258262890683122, 1.000000000000000000, 0.9659258262890683122, 1.000000000000000000, 0.9659258262890683122, 1.000000000000000000, 0.9659258262890683122, 1.000000000000000000, 0.9659258262890683122, 1.000000000000000000, 0.9659258262890683122, 1.000000000000000000, 0.9659258262890683122, 1.000000000000000000, 0.9659258262890683122, 1.000000000000000000, 0.9659258262890683122, 1.000000000000000000, 0.9659258262890683122, 1.000000000000000000, 0.9659258262890683122, 1.000000000000000000, 0.9659258262890683122, 1.000000000000000000, 0.9659258262890683122, 1.000000000000000000, 0.9659258262890683122, 1.000000000000000000, 0.9659258262890683122, 1.000000000000000000, 0.9659258262890683122, 1.000000000000000000, 0.9659258262890683122, 1.000000000000000000, 0.9659258262890683122, 1.000000000000000000, 0.9659258262890683122, 1.000000000000000000, 0.9659258262890683122, 1.000000000000000000, 0.9659258262890683122, 1.000000000000000000, 0.9659258262890683122, 1.000000000000000000, 0.9659258262890683122, 1.000000000000000000, 0.9659258262890683122, 1.000000000000000000, 0.9659258262890683122, 1.000000000000000000, 0.9659258262890683122, 1.000000000000000000, 0.9659258262890683122, 1.000000000000000000, 0.9659258262890683122, 1.000000000000000000, 0.9659258262890683122, 1.000000000000000000, 0.9659258262890683122, 1.000000000000000000, 0.9659258262890683122, 1.000000000000000000, 0.9659258262890683122, 1.000000000000000000, 0.9659258262890683122, 1.000000000000000000, 0.9659258262890683122, 1.000000000000000000, 0.9659258262890683122, 1.000000000000000000, 0.9659258262890683122, 1.000000000000000000, 0.9659258262890683122, 1.000000000000000000, 0.9659258262890683122, 1.000000000000000000, 0.9659258262890683122, 1.000000000000000000, 0.9659258262890683122, 1.000000000000000000, 0.9659258262890683122, 1.000000000000000000, 0.9659258262890683122, 1.000000000000000000, 0.9659258262890683122, 1.000000000000000000, 0.9659258262890683122, 1.000000000000000000, 0.9659258262890683122, 1.000000000000000000, 0.9659258262890683122, 1.000000000000000000, 0.9659258262890683122, 1.000000000000000000, 0.9659258262890683122, 1.000000000000000000, 0.9659258262890683122, 1.000000000000000000, 0.9659258262890683122, 1.000000000000000000, 0.9659258262890683122, 1.000000000000000000, 0.9659258262890683122, 1.000000000000000000, 0.9659258262890683122, 1.000000000000000000, 0.9659258262890683122, 1.000000000000000000, 0.9659258262890683122, 1.000000000000000000, 0.9659258262890683122, 1.000000000000000000, 0.9659258262890683122, 1.000000000000000000, 0.9659258262890683122, 1.000000000000000000, 0.9659258262890683122, 1.000000000000000000, 0.9659258262890683122, 1.000000000000000000, 0.9659258262890683122, 1.000000000000000000, 0.9659258262890683122, 1.000000000000000000, 0.9659258262890683122, 1.000000000000000000, 0.9659258262890683122, 1.000000000000000000, 0.9659258262890683122, 1.000000000000000000, 0.9659258262890683122, 1.000000000000000000, 0.9659258262890683122, 1.000000000000000000, 0.9659258262890683122, 1.000000000000000000, 0.9659258262890683122, 1.000000000000000000, 0.9659258262890683122, 1.000000000000000000, 0.9659258262890683122, 1.000000000000000000, 0.9659258262890683122, 1.000000000000000000, 0.9659258262890683122, 1.000000000000000000, 0.9659258262890683122, 1.000000000000000000, 0.9659258262890683122, 1.000000000000000000, 0.9659258262890683122, 1.000000000000000000, 0.9659258262890683122, 1.000000000000000000, 0.9659258262890683122, 1.000000000000000000, 0.9659258262890683122, 1.000000000000000000, 0.9659258262890683122, 1.000000000000000000, 0.9659258262890683122, 1.000000000000000000, 0.9659258262890683122, 1.000000000000000000, 0.9659258262890683122, 1.000000000000000000, 0.9659258262890683122, 1.000000000000000000, 0.9659258262890683122, 1.000000000000000000, 0.9659258262890683122, 1.000000000000000000, 0.9659258262890683122, 1.000000000000000000, 0.9659258262890683122, 1.000000000000000000, 0.9659258262890683122, 1.000000000000000000, 0.9659258262890683122, 1.000000000000000000, 0.9659258262890683122, 1.000000000000000000, 0.9659258262890683122, 1.000000000000000000, 0.9659258262890683122, 1.000000000000000000, 0.9659258262890683122, 1.000000000000000000, 0.9659258262890683122, 1.000000000000000000, 0.9659258262890683122, 1.000000000000000000, 0.9659258262890683122, 1.000000000000000000, 0.9659258262890683122, 1.000000000000000000, 0.9659258262890683122, 1.000000000000000000, 0.9659258262890683122, 1.000000000000000000, 0.9659258262890683122, 1.000000000000000000, 0.9659258262890683122, 1.000000000000000000, 0.9659258262890683122, 1.000000000000000000, 0.9659258262890683122, 1.000000000000000000, 0.9659258262890683122, 1.000000000000000000, 0.9659258262890683122, 1.000000000000000000, 0.9659258262890683122, 1.000000000000000000, 0.9659258262890683122, 1.000000000000000000, 0.9659258262890683122, 1.000000000000000000, 0.9659258262890683122, 1.000000000000000000, 0.9659258262890683122, 1.000000000000000000, 0.9659258262890683122, 1.000000000000000000, 0.9659258262890683122, 1.000000000000000000, 0.9659258262890683122, 1.000000000000000000, 0.9659258262890683122, 1.000000000000000000, 0.9659258262890683122, 1.000000000000000000, 0.9659258262890683122, 1.000000000000000000, 0.9659258262890683122, 1.000000000000000000, 0.9659258262890683122, 1.000000000000000000, 0.9659258262890683122, 1.000000000000000000, 0.9659258262890683122, 1.000000000000000000, 0.9659258262890683122, 1.000000000000000000, 0.9659258262890683122, 1.000000000000000000, 0.9659258262890683122, 1.000000000000000000, 0.9659258262890683122, 1.000000000000000000, 0.9659258262890683122, 1.000000000000000000, 0.9659258262890683122, 1.000000000000000000, 0.9659258262890683122, 1.000000000000000000, 0.9659258262890683122, 1.000000000000000000, 0.9659258262890683122, 1.000000000000000000, 0.9659258262890683122, 1.000000000000000000, 0.9659258262890683122, 1.000000000000000000, 0.9659258262890683122, 1.000000000000000000, 0.9659258262890683122, 1.000000000000000000, 0.9659258262890683122, 1.000000000000000000, 0.9659258262890683122, 1.000000000000000000, 0.9659258262890683122, 1.000000000000000000, 0.9659258262890683122, 1.000000000000000000, 0.9659258262890683122, 1.000000000000000000, 0.9659258262890683122, 1.000000000000000000, 0.9659258262890683122, 1.000000000000000000, 0.9659258262890683122, 1.000000000000000000, 0.9659258262890683122, 1.000000000000000000, 0.9659258262890683122, 1.000000000000000000, 0.9659258262890683122, 1.000000000000000000, 0.9659258262890683122, 1.000000000000000000, 0.9659258262890683122, 1.000000000000000000, 0.9659258262890683122, 1.000000000000000000, 0.9659258262890683122, 1.000000000000000000, 0.9659258262890683122, 1.000000000000000000, 0.9659258262890683122, 1.000000000000000000, 0.9659258262890683122, 1.000000000000000000, 0.9659258262890683122, 1.000000000000000000, 0.9659258262890683122, 1.000000000000000000, 0.9659258262890683122, 1.000000000000000000, 0.9659258262890683122, 1.000000000000000000, 0.9659258262890683122, 1.000000000000000000, 0.9659258262890683122, 1.000000000000000000, 0.9659258262890683122, 1.000000000000000000, 0.9659258262890683122, 1.000000000000000000, 0.9659258262890683122, 1.000000000000000000, 0.9659258262890683122, 1.000000000000000000, 0.9659258262890683122, 1.000000000000000000, 0.9659258262890683122, 1.000000000000000000, 0.9659258262890683122, 1.000000000000000000, 0.9659258262890683122, 1.000000000000000000, 0.9659258262890683122, 1.000000000000000000, 0.9659258262890683122, 1.000000000000000000, 0.9659258262890683122, 1.000000000000000000, 0.9659258262890683122, 1.000000000000000000, 0.9659258262890683122, 1.000000000000000000, 0.9659258262890683122, 1.000000000000000000, 0.9659258262890683122, 1.000000000000000000, 0.9659258262890683122, 1.000000000000000000, 0.9659258262890683122, 1.000000000000000000, 0.9659258262890683122, 1.000000000000000000, 0.9659258262890683122, 1.000000000000000000, 0.9659258262890683122, 1.000000000000000000, 0.9659258262890683122, 1.000000000000000000, 0.9659258262890683122, 1.000000000000000000, 0.9659258262890683122, 1.000000000000000000, 0.9659258262890683122, 1.000000000000000000, 0.9659258262890683122, 1.000000000000000000, 0.9659258262890683122, 1.000000000000000000, 0.9659258262890683122, 1.000000000000000000, 0.9659258262890683122, 1.000000000000000000, 0.9659258262890683122, 1.000000000000000000, 0.9659258262890683122, 1.000000000000000000, 0.9659258262890683122, 1.000000000000000000, 0.9659258262890683122, 1.000000000000000000, 0.9659258262890683122, 1.000000000000000000, 0.9659258262890683122, 1.000000000000000000, 0.9659258262890683122, 1.000000000000000000, 0.9659258262890683122, 1.000000000000000000, 0.9659258262890683122, 1.000000000000000000, 0.9659258262890683122, 1.000000000000000000, 0.9659258262890683122, 1.000000000000000000, 0.9659258262890683122, 1.000000000000000000, 0.9659258262890683122, 1.000000000000000000, 0.9659258262890683122, 1.000000000000000000, 0.9659258262890683122, 1.000000000000000000, 0.9659258262890683122, 1.000000000000000000, 0.9659258262890683122, 1.000000000000000000, 0.9659258262890683122, 1.000000000000000000, 0.9659258262890683122, 1.000000000000000000, 0.9659258262890683122, 1.000000000000000000, 0.9659258262890683122, 1.000000000000000000, 0.9659258262890683122, 1.000000000000000000, 0.9659258262890683122, 1.000000000000000000, 0.9659258262890683122, 1.000000000000000000, 0.9659258262890683122, 1.000000000000000000, 0.9659258262890683122, 1.000000000000000000, 0.9659258262890683122, 1.000000000000000000, 0.9659258262890683122, 1.000000000000000000, 0.9659258262890683122, 1.000000000000000000, 0.9659258262890683122, 1.000000000000000000, 0.9659258262890683122, 1.000000000000000000, 0.9659258262890683122, 1.000000000000000000, 0.9659258262890683122, 1.000000000000000000, 0.9659258262890683122, 1.000000000000000000, 0.9659258262890683122, 1.000000000000000000, 0.9659258262890683122, 1.000000000000000000, 0.9659258262890683122, 1.000000000000000000, 0.9659258262890683122, 1.000000000000000000, 0.9659258262890683122, 1.000000000000000000, 0.9659258262890683122, 1.000000000000000000),
 ( 0.3333333333333333703, 0.3219752754296894559, 0.3333333333333333703, 0.3219752754296894559, 0.3333333333333333703, 0.3219752754296894559, 0.3333333333333333703, 0.3219752754296894559, 0.3333333333333333703, 0.3219752754296894559, 0.3333333333333333703, 0.3219752754296894559, 0.3333333333333333703, 0.3219752754296894559, 0.3333333333333333703, 0.3219752754296894559, 0.3333333333333333703, 0.3219752754296894559, 0.3333333333333333703, 0.3219752754296894559, 0.3333333333333333703, 0.3219752754296894559, 0.3333333333333333703, 0.3219752754296894559, 0.3333333333333333703, 0.3219752754296894559, 0.3333333333333333703, 0.3219752754296894559, 0.3333333333333333703, 0.3219752754296894559, 0.3333333333333333703, 0.3219752754296894559, 0.3333333333333333703, 0.3219752754296894559, 0.3333333333333333703, 0.3219752754296894559, 0.3333333333333333703, 0.3219752754296894559, 0.3333333333333333703, 0.3219752754296894559, 0.3333333333333333703, 0.3219752754296894559, 0.3333333333333333703, 0.3219752754296894559, 0.3333333333333333703, 0.3219752754296894559, 0.3333333333333333703, 0.3219752754296894559, 0.3333333333333333703, 0.3219752754296894559, 0.3333333333333333703, 0.3219752754296894559, 0.3333333333333333703, 0.3219752754296894559, 0.3333333333333333703, 0.3219752754296894559, 0.3333333333333333703, 0.3219752754296894559, 0.3333333333333333703, 0.3219752754296894559, 0.3333333333333333703, 0.3219752754296894559, 0.3333333333333333703, 0.3219752754296894559, 0.3333333333333333703, 0.3219752754296894559, 0.3333333333333333703, 0.3219752754296894559, 0.3333333333333333703, 0.3219752754296894559, 0.3333333333333333703, 0.3219752754296894559, 0.3333333333333333703, 0.3219752754296894559, 0.3333333333333333703, 0.3219752754296894559, 0.3333333333333333703, 0.3219752754296894559, 0.3333333333333333703, 0.3219752754296894559, 0.3333333333333333703, 0.3219752754296894559, 0.3333333333333333703, 0.3219752754296894559, 0.3333333333333333703, 0.3219752754296894559, 0.3333333333333333703, 0.3219752754296894559, 0.3333333333333333703, 0.3219752754296894559, 0.3333333333333333703, 0.3219752754296894559, 0.3333333333333333703, 0.3219752754296894559, 0.3333333333333333703, 0.3219752754296894559, 0.3333333333333333703, 0.3219752754296894559, 0.3333333333333333703, 0.3219752754296894559, 0.3333333333333333703, 0.3219752754296894559, 0.3333333333333333703, 0.3219752754296894559, 0.3333333333333333703, 0.3219752754296894559, 0.3333333333333333703, 0.3219752754296894559, 0.3333333333333333703, 0.3219752754296894559, 0.3333333333333333703, 0.3219752754296894559, 0.3333333333333333703, 0.3219752754296894559, 0.3333333333333333703, 0.3219752754296894559, 0.3333333333333333703, 0.3219752754296894559, 0.3333333333333333703, 0.3219752754296894559, 0.3333333333333333703, 0.3219752754296894559, 0.3333333333333333703, 0.3219752754296894559, 0.3333333333333333703, 0.3219752754296894559, 0.3333333333333333703, 0.3219752754296894559, 0.3333333333333333703, 0.3219752754296894559, 0.3333333333333333703, 0.3219752754296894559, 0.3333333333333333703, 0.3219752754296894559, 0.3333333333333333703, 0.3219752754296894559, 0.3333333333333333703, 0.3219752754296894559, 0.3333333333333333703, 0.3219752754296894559, 0.3333333333333333703, 0.3219752754296894559, 0.3333333333333333703, 0.3219752754296894559, 0.3333333333333333703, 0.3219752754296894559, 0.3333333333333333703, 0.3219752754296894559, 0.3333333333333333703, 0.3219752754296894559, 0.3333333333333333703, 0.3219752754296894559, 0.3333333333333333703, 0.3219752754296894559, 0.3333333333333333703, 0.3219752754296894559, 0.3333333333333333703, 0.3219752754296894559, 0.3333333333333333703, 0.3219752754296894559, 0.3333333333333333703, 0.3219752754296894559, 0.3333333333333333703, 0.3219752754296894559, 0.3333333333333333703, 0.3219752754296894559, 0.3333333333333333703, 0.3219752754296894559, 0.3333333333333333703, 0.3219752754296894559, 0.3333333333333333703, 0.3219752754296894559, 0.3333333333333333703, 0.3219752754296894559, 0.3333333333333333703, 0.3219752754296894559, 0.3333333333333333703, 0.3219752754296894559, 0.3333333333333333703, 0.3219752754296894559, 0.3333333333333333703, 0.3219752754296894559, 0.3333333333333333703, 0.3219752754296894559, 0.3333333333333333703, 0.3219752754296894559, 0.3333333333333333703, 0.3219752754296894559, 0.3333333333333333703, 0.3219752754296894559, 0.3333333333333333703, 0.3219752754296894559, 0.3333333333333333703, 0.3219752754296894559, 0.3333333333333333703, 0.3219752754296894559, 0.3333333333333333703, 0.3219752754296894559, 0.3333333333333333703, 0.3219752754296894559, 0.3333333333333333703, 0.3219752754296894559, 0.3333333333333333703, 0.3219752754296894559, 0.3333333333333333703, 0.3219752754296894559, 0.3333333333333333703, 0.3219752754296894559, 0.3333333333333333703, 0.3219752754296894559, 0.3333333333333333703, 0.3219752754296894559, 0.3333333333333333703, 0.3219752754296894559, 0.3333333333333333703, 0.3219752754296894559, 0.3333333333333333703, 0.3219752754296894559, 0.3333333333333333703, 0.3219752754296894559, 0.3333333333333333703, 0.3219752754296894559, 0.3333333333333333703, 0.3219752754296894559, 0.3333333333333333703, 0.3219752754296894559, 0.3333333333333333703, 0.3219752754296894559, 0.3333333333333333703, 0.3219752754296894559, 0.3333333333333333703, 0.3219752754296894559, 0.3333333333333333703, 0.3219752754296894559, 0.3333333333333333703, 0.3219752754296894559, 0.3333333333333333703, 0.3219752754296894559, 0.3333333333333333703, 0.3219752754296894559, 0.3333333333333333703, 0.3219752754296894559, 0.3333333333333333703, 0.3219752754296894559, 0.3333333333333333703, 0.3219752754296894559, 0.3333333333333333703, 0.3219752754296894559, 0.3333333333333333703, 0.3219752754296894559, 0.3333333333333333703, 0.3219752754296894559, 0.3333333333333333703, 0.3219752754296894559, 0.3333333333333333703, 0.3219752754296894559, 0.3333333333333333703, 0.3219752754296894559, 0.3333333333333333703, 0.3219752754296894559, 0.3333333333333333703, 0.3219752754296894559, 0.3333333333333333703, 0.3219752754296894559, 0.3333333333333333703, 0.3219752754296894559, 0.3333333333333333703, 0.3219752754296894559, 0.3333333333333333703, 0.3219752754296894559, 0.3333333333333333703, 0.3219752754296894559, 0.3333333333333333703, 0.3219752754296894559, 0.3333333333333333703, 0.3219752754296894559, 0.3333333333333333703, 0.3219752754296894559, 0.3333333333333333703, 0.3219752754296894559, 0.3333333333333333703, 0.3219752754296894559, 0.3333333333333333703, 0.3219752754296894559, 0.3333333333333333703, 0.3219752754296894559, 0.3333333333333333703, 0.3219752754296894559, 0.3333333333333333703, 0.3219752754296894559, 0.3333333333333333703, 0.3219752754296894559, 0.3333333333333333703, 0.3219752754296894559, 0.3333333333333333703, 0.3219752754296894559, 0.3333333333333333703, 0.3219752754296894559, 0.3333333333333333703, 0.3219752754296894559, 0.3333333333333333703, 0.3219752754296894559, 0.3333333333333333703, 0.3219752754296894559, 0.3333333333333333703, 0.3219752754296894559, 0.3333333333333333703, 0.3219752754296894559, 0.3333333333333333703, 0.3219752754296894559, 0.3333333333333333703, 0.3219752754296894559, 0.3333333333333333703, 0.3219752754296894559, 0.3333333333333333703, 0.3219752754296894559, 0.3333333333333333703, 0.3219752754296894559, 0.3333333333333333703, 0.3219752754296894559, 0.3333333333333333703, 0.3219752754296894559, 0.3333333333333333703, 0.3219752754296894559, 0.3333333333333333703, 0.3219752754296894559, 0.3333333333333333703, 0.3219752754296894559, 0.3333333333333333703, 0.3219752754296894559, 0.3333333333333333703, 0.3219752754296894559, 0.3333333333333333703, 0.3219752754296894559, 0.3333333333333333703, 0.3219752754296894559, 0.3333333333333333703, 0.3219752754296894559, 0.3333333333333333703, 0.3219752754296894559, 0.3333333333333333703, 0.3219752754296894559, 0.3333333333333333703, 0.3219752754296894559, 0.3333333333333333703, 0.3219752754296894559, 0.3333333333333333703, 0.3219752754296894559, 0.3333333333333333703, 0.3219752754296894559, 0.3333333333333333703, 0.3219752754296894559, 0.3333333333333333703, 0.3219752754296894559, 0.3333333333333333703, 0.3219752754296894559, 0.3333333333333333703, 0.3219752754296894559, 0.3333333333333333703, 0.3219752754296894559, 0.3333333333333333703, 0.3219752754296894559, 0.3333333333333333703, 0.3219752754296894559, 0.3333333333333333703, 0.3219752754296894559, 0.3333333333333333703, 0.3219752754296894559, 0.3333333333333333703, 0.3219752754296894559, 0.3333333333333333703, 0.3219752754296894559, 0.3333333333333333703, 0.3219752754296894559, 0.3333333333333333703, 0.3219752754296894559, 0.3333333333333333703, 0.3219752754296894559, 0.3333333333333333703, 0.3219752754296894559, 0.3333333333333333703, 0.3219752754296894559, 0.3333333333333333703, 0.3219752754296894559, 0.3333333333333333703, 0.3219752754296894559, 0.3333333333333333703, 0.3219752754296894559, 0.3333333333333333703, 0.3219752754296894559, 0.3333333333333333703, 0.3219752754296894559, 0.3333333333333333703, 0.3219752754296894559, 0.3333333333333333703, 0.3219752754296894559, 0.3333333333333333703, 0.3219752754296894559, 0.3333333333333333703, 0.3219752754296894559, 0.3333333333333333703, 0.3219752754296894559, 0.3333333333333333703, 0.3219752754296894559, 0.3333333333333333703, 0.3219752754296894559, 0.3333333333333333703, 0.3219752754296894559, 0.3333333333333333703, 0.3219752754296894559, 0.3333333333333333703, 0.3219752754296894559, 0.3333333333333333703, 0.3219752754296894559, 0.3333333333333333703, 0.3219752754296894559, 0.3333333333333333703, 0.3219752754296894559, 0.3333333333333333703, 0.3219752754296894559, 0.3333333333333333703, 0.3219752754296894559, 0.3333333333333333703, 0.3219752754296894559, 0.3333333333333333703, 0.3219752754296894559, 0.3333333333333333703, 0.3219752754296894559, 0.3333333333333333703, 0.3219752754296894559, 0.3333333333333333703, 0.3219752754296894559, 0.3333333333333333703, 0.3219752754296894559, 0.3333333333333333703, 0.3219752754296894559, 0.3333333333333333703, 0.3219752754296894559, 0.3333333333333333703, 0.3219752754296894559, 0.3333333333333333703, 0.3219752754296894559, 0.3333333333333333703, 0.3219752754296894559, 0.3333333333333333703, 0.3219752754296894559, 0.3333333333333333703, 0.3219752754296894559, 0.3333333333333333703, 0.3219752754296894559, 0.3333333333333333703, 0.3219752754296894559, 0.3333333333333333703, 0.3219752754296894559, 0.3333333333333333703, 0.3219752754296894559, 0.3333333333333333703),
 ( 0.3333333333333333703, 0.3219752754296894559, 0.3333333333333333703, 0.3219752754296894559, 0.3333333333333333703, 0.3219752754296894559, 0.3333333333333333703, 0.3219752754296894559, 0.3333333333333333703, 0.3219752754296894559, 0.3333333333333333703, 0.3219752754296894559, 0.3333333333333333703, 0.3219752754296894559, 0.3333333333333333703, 0.3219752754296894559, 0.3333333333333333703, 0.3219752754296894559, 0.3333333333333333703, 0.3219752754296894559, 0.3333333333333333703, 0.3219752754296894559, 0.3333333333333333703, 0.3219752754296894559, 0.3333333333333333703, 0.3219752754296894559, 0.3333333333333333703, 0.3219752754296894559, 0.3333333333333333703, 0.3219752754296894559, 0.3333333333333333703, 0.3219752754296894559, 0.3333333333333333703, 0.3219752754296894559, 0.3333333333333333703, 0.3219752754296894559, 0.3333333333333333703, 0.3219752754296894559, 0.3333333333333333703, 0.3219752754296894559, 0.3333333333333333703, 0.3219752754296894559, 0.3333333333333333703, 0.3219752754296894559, 0.3333333333333333703, 0.3219752754296894559, 0.3333333333333333703, 0.3219752754296894559, 0.3333333333333333703, 0.3219752754296894559, 0.3333333333333333703, 0.3219752754296894559, 0.3333333333333333703, 0.3219752754296894559, 0.3333333333333333703, 0.3219752754296894559, 0.3333333333333333703, 0.3219752754296894559, 0.3333333333333333703, 0.3219752754296894559, 0.3333333333333333703, 0.3219752754296894559, 0.3333333333333333703, 0.3219752754296894559, 0.3333333333333333703, 0.3219752754296894559, 0.3333333333333333703, 0.3219752754296894559, 0.3333333333333333703, 0.3219752754296894559, 0.3333333333333333703, 0.3219752754296894559, 0.3333333333333333703, 0.3219752754296894559, 0.3333333333333333703, 0.3219752754296894559, 0.3333333333333333703, 0.3219752754296894559, 0.3333333333333333703, 0.3219752754296894559, 0.3333333333333333703, 0.3219752754296894559, 0.3333333333333333703, 0.3219752754296894559, 0.3333333333333333703, 0.3219752754296894559, 0.3333333333333333703, 0.3219752754296894559, 0.3333333333333333703, 0.3219752754296894559, 0.3333333333333333703, 0.3219752754296894559, 0.3333333333333333703, 0.3219752754296894559, 0.3333333333333333703, 0.3219752754296894559, 0.3333333333333333703, 0.3219752754296894559, 0.3333333333333333703, 0.3219752754296894559, 0.3333333333333333703, 0.3219752754296894559, 0.3333333333333333703, 0.3219752754296894559, 0.3333333333333333703, 0.3219752754296894559, 0.3333333333333333703, 0.3219752754296894559, 0.3333333333333333703, 0.3219752754296894559, 0.3333333333333333703, 0.3219752754296894559, 0.3333333333333333703, 0.3219752754296894559, 0.3333333333333333703, 0.3219752754296894559, 0.3333333333333333703, 0.3219752754296894559, 0.3333333333333333703, 0.3219752754296894559, 0.3333333333333333703, 0.3219752754296894559, 0.3333333333333333703, 0.3219752754296894559, 0.3333333333333333703, 0.3219752754296894559, 0.3333333333333333703, 0.3219752754296894559, 0.3333333333333333703, 0.3219752754296894559, 0.3333333333333333703, 0.3219752754296894559, 0.3333333333333333703, 0.3219752754296894559, 0.3333333333333333703, 0.3219752754296894559, 0.3333333333333333703, 0.3219752754296894559, 0.3333333333333333703, 0.3219752754296894559, 0.3333333333333333703, 0.3219752754296894559, 0.3333333333333333703, 0.3219752754296894559, 0.3333333333333333703, 0.3219752754296894559, 0.3333333333333333703, 0.3219752754296894559, 0.3333333333333333703, 0.3219752754296894559, 0.3333333333333333703, 0.3219752754296894559, 0.3333333333333333703, 0.3219752754296894559, 0.3333333333333333703, 0.3219752754296894559, 0.3333333333333333703, 0.3219752754296894559, 0.3333333333333333703, 0.3219752754296894559, 0.3333333333333333703, 0.3219752754296894559, 0.3333333333333333703, 0.3219752754296894559, 0.3333333333333333703, 0.3219752754296894559, 0.3333333333333333703, 0.3219752754296894559, 0.3333333333333333703, 0.3219752754296894559, 0.3333333333333333703, 0.3219752754296894559, 0.3333333333333333703, 0.3219752754296894559, 0.3333333333333333703, 0.3219752754296894559, 0.3333333333333333703, 0.3219752754296894559, 0.3333333333333333703, 0.3219752754296894559, 0.3333333333333333703, 0.3219752754296894559, 0.3333333333333333703, 0.3219752754296894559, 0.3333333333333333703, 0.3219752754296894559, 0.3333333333333333703, 0.3219752754296894559, 0.3333333333333333703, 0.3219752754296894559, 0.3333333333333333703, 0.3219752754296894559, 0.3333333333333333703, 0.3219752754296894559, 0.3333333333333333703, 0.3219752754296894559, 0.3333333333333333703, 0.3219752754296894559, 0.3333333333333333703, 0.3219752754296894559, 0.3333333333333333703, 0.3219752754296894559, 0.3333333333333333703, 0.3219752754296894559, 0.3333333333333333703, 0.3219752754296894559, 0.3333333333333333703, 0.3219752754296894559, 0.3333333333333333703, 0.3219752754296894559, 0.3333333333333333703, 0.3219752754296894559, 0.3333333333333333703, 0.3219752754296894559, 0.3333333333333333703, 0.3219752754296894559, 0.3333333333333333703, 0.3219752754296894559, 0.3333333333333333703, 0.3219752754296894559, 0.3333333333333333703, 0.3219752754296894559, 0.3333333333333333703, 0.3219752754296894559, 0.3333333333333333703, 0.3219752754296894559, 0.3333333333333333703, 0.3219752754296894559, 0.3333333333333333703, 0.3219752754296894559, 0.3333333333333333703, 0.3219752754296894559, 0.3333333333333333703, 0.3219752754296894559, 0.3333333333333333703, 0.3219752754296894559, 0.3333333333333333703, 0.3219752754296894559, 0.3333333333333333703, 0.3219752754296894559, 0.3333333333333333703, 0.3219752754296894559, 0.3333333333333333703, 0.3219752754296894559, 0.3333333333333333703, 0.3219752754296894559, 0.3333333333333333703, 0.3219752754296894559, 0.3333333333333333703, 0.3219752754296894559, 0.3333333333333333703, 0.3219752754296894559, 0.3333333333333333703, 0.3219752754296894559, 0.3333333333333333703, 0.3219752754296894559, 0.3333333333333333703, 0.3219752754296894559, 0.3333333333333333703, 0.3219752754296894559, 0.3333333333333333703, 0.3219752754296894559, 0.3333333333333333703, 0.3219752754296894559, 0.3333333333333333703, 0.3219752754296894559, 0.3333333333333333703, 0.3219752754296894559, 0.3333333333333333703, 0.3219752754296894559, 0.3333333333333333703, 0.3219752754296894559, 0.3333333333333333703, 0.3219752754296894559, 0.3333333333333333703, 0.3219752754296894559, 0.3333333333333333703, 0.3219752754296894559, 0.3333333333333333703, 0.3219752754296894559, 0.3333333333333333703, 0.3219752754296894559, 0.3333333333333333703, 0.3219752754296894559, 0.3333333333333333703, 0.3219752754296894559, 0.3333333333333333703, 0.3219752754296894559, 0.3333333333333333703, 0.3219752754296894559, 0.3333333333333333703, 0.3219752754296894559, 0.3333333333333333703, 0.3219752754296894559, 0.3333333333333333703, 0.3219752754296894559, 0.3333333333333333703, 0.3219752754296894559, 0.3333333333333333703, 0.3219752754296894559, 0.3333333333333333703, 0.3219752754296894559, 0.3333333333333333703, 0.3219752754296894559, 0.3333333333333333703, 0.3219752754296894559, 0.3333333333333333703, 0.3219752754296894559, 0.3333333333333333703, 0.3219752754296894559, 0.3333333333333333703, 0.3219752754296894559, 0.3333333333333333703, 0.3219752754296894559, 0.3333333333333333703, 0.3219752754296894559, 0.3333333333333333703, 0.3219752754296894559, 0.3333333333333333703, 0.3219752754296894559, 0.3333333333333333703, 0.3219752754296894559, 0.3333333333333333703, 0.3219752754296894559, 0.3333333333333333703, 0.3219752754296894559, 0.3333333333333333703, 0.3219752754296894559, 0.3333333333333333703, 0.3219752754296894559, 0.3333333333333333703, 0.3219752754296894559, 0.3333333333333333703, 0.3219752754296894559, 0.3333333333333333703, 0.3219752754296894559, 0.3333333333333333703, 0.3219752754296894559, 0.3333333333333333703, 0.3219752754296894559, 0.3333333333333333703, 0.3219752754296894559, 0.3333333333333333703, 0.3219752754296894559, 0.3333333333333333703, 0.3219752754296894559, 0.3333333333333333703, 0.3219752754296894559, 0.3333333333333333703, 0.3219752754296894559, 0.3333333333333333703, 0.3219752754296894559, 0.3333333333333333703, 0.3219752754296894559, 0.3333333333333333703, 0.3219752754296894559, 0.3333333333333333703, 0.3219752754296894559, 0.3333333333333333703, 0.3219752754296894559, 0.3333333333333333703, 0.3219752754296894559, 0.3333333333333333703, 0.3219752754296894559, 0.3333333333333333703, 0.3219752754296894559, 0.3333333333333333703, 0.3219752754296894559, 0.3333333333333333703, 0.3219752754296894559, 0.3333333333333333703, 0.3219752754296894559, 0.3333333333333333703, 0.3219752754296894559, 0.3333333333333333703, 0.3219752754296894559, 0.3333333333333333703, 0.3219752754296894559, 0.3333333333333333703, 0.3219752754296894559, 0.3333333333333333703, 0.3219752754296894559, 0.3333333333333333703, 0.3219752754296894559, 0.3333333333333333703, 0.3219752754296894559, 0.3333333333333333703, 0.3219752754296894559, 0.3333333333333333703, 0.3219752754296894559, 0.3333333333333333703, 0.3219752754296894559, 0.3333333333333333703, 0.3219752754296894559, 0.3333333333333333703, 0.3219752754296894559, 0.3333333333333333703, 0.3219752754296894559, 0.3333333333333333703, 0.3219752754296894559, 0.3333333333333333703, 0.3219752754296894559, 0.3333333333333333703, 0.3219752754296894559, 0.3333333333333333703, 0.3219752754296894559, 0.3333333333333333703, 0.3219752754296894559, 0.3333333333333333703, 0.3219752754296894559, 0.3333333333333333703, 0.3219752754296894559, 0.3333333333333333703, 0.3219752754296894559, 0.3333333333333333703, 0.3219752754296894559, 0.3333333333333333703, 0.3219752754296894559, 0.3333333333333333703, 0.3219752754296894559, 0.3333333333333333703, 0.3219752754296894559, 0.3333333333333333703, 0.3219752754296894559, 0.3333333333333333703, 0.3219752754296894559, 0.3333333333333333703, 0.3219752754296894559, 0.3333333333333333703, 0.3219752754296894559, 0.3333333333333333703, 0.3219752754296894559, 0.3333333333333333703, 0.3219752754296894559, 0.3333333333333333703, 0.3219752754296894559, 0.3333333333333333703, 0.3219752754296894559, 0.3333333333333333703, 0.3219752754296894559, 0.3333333333333333703, 0.3219752754296894559, 0.3333333333333333703, 0.3219752754296894559, 0.3333333333333333703, 0.3219752754296894559, 0.3333333333333333703, 0.3219752754296894559, 0.3333333333333333703, 0.3219752754296894559, 0.3333333333333333703, 0.3219752754296894559, 0.3333333333333333703, 0.3219752754296894559, 0.3333333333333333703, 0.3219752754296894559, 0.3333333333333333703),
 ( 1.000000000000000000, 0.9659258262890683122, 1.000000000000000000, 0.9659258262890683122, 1.000000000000000000, 0.9659258262890683122, 1.000000000000000000, 0.9659258262890683122, 1.000000000000000000, 0.9659258262890683122, 1.000000000000000000, 0.9659258262890683122, 1.000000000000000000, 0.9659258262890683122, 1.000000000000000000, 0.9659258262890683122, 1.000000000000000000, 0.9659258262890683122, 1.000000000000000000, 0.9659258262890683122, 1.000000000000000000, 0.9659258262890683122, 1.000000000000000000, 0.9659258262890683122, 1.000000000000000000, 0.9659258262890683122, 1.000000000000000000, 0.9659258262890683122, 1.000000000000000000, 0.9659258262890683122, 1.000000000000000000, 0.9659258262890683122, 1.000000000000000000, 0.9659258262890683122, 1.000000000000000000, 0.9659258262890683122, 1.000000000000000000, 0.9659258262890683122, 1.000000000000000000, 0.9659258262890683122, 1.000000000000000000, 0.9659258262890683122, 1.000000000000000000, 0.9659258262890683122, 1.000000000000000000, 0.9659258262890683122, 1.000000000000000000, 0.9659258262890683122, 1.000000000000000000, 0.9659258262890683122, 1.000000000000000000, 0.9659258262890683122, 1.000000000000000000, 0.9659258262890683122, 1.000000000000000000, 0.9659258262890683122, 1.000000000000000000, 0.9659258262890683122, 1.000000000000000000, 0.9659258262890683122, 1.000000000000000000, 0.9659258262890683122, 1.000000000000000000, 0.9659258262890683122, 1.000000000000000000, 0.9659258262890683122, 1.000000000000000000, 0.9659258262890683122, 1.000000000000000000, 0.9659258262890683122, 1.000000000000000000, 0.9659258262890683122, 1.000000000000000000, 0.9659258262890683122, 1.000000000000000000, 0.9659258262890683122, 1.000000000000000000, 0.9659258262890683122, 1.000000000000000000, 0.9659258262890683122, 1.000000000000000000, 0.9659258262890683122, 1.000000000000000000, 0.9659258262890683122, 1.000000000000000000, 0.9659258262890683122, 1.000000000000000000, 0.9659258262890683122, 1.000000000000000000, 0.9659258262890683122, 1.000000000000000000, 0.9659258262890683122, 1.000000000000000000, 0.9659258262890683122, 1.000000000000000000, 0.9659258262890683122, 1.000000000000000000, 0.9659258262890683122, 1.000000000000000000, 0.9659258262890683122, 1.000000000000000000, 0.9659258262890683122, 1.000000000000000000, 0.9659258262890683122, 1.000000000000000000, 0.9659258262890683122, 1.000000000000000000, 0.9659258262890683122, 1.000000000000000000, 0.9659258262890683122, 1.000000000000000000, 0.9659258262890683122, 1.000000000000000000, 0.9659258262890683122, 1.000000000000000000, 0.9659258262890683122, 1.000000000000000000, 0.9659258262890683122, 1.000000000000000000, 0.9659258262890683122, 1.000000000000000000, 0.9659258262890683122, 1.000000000000000000, 0.9659258262890683122, 1.000000000000000000, 0.9659258262890683122, 1.000000000000000000, 0.9659258262890683122, 1.000000000000000000, 0.9659258262890683122, 1.000000000000000000, 0.9659258262890683122, 1.000000000000000000, 0.9659258262890683122, 1.000000000000000000, 0.9659258262890683122, 1.000000000000000000, 0.9659258262890683122, 1.000000000000000000, 0.9659258262890683122, 1.000000000000000000, 0.9659258262890683122, 1.000000000000000000, 0.9659258262890683122, 1.000000000000000000, 0.9659258262890683122, 1.000000000000000000, 0.9659258262890683122, 1.000000000000000000, 0.9659258262890683122, 1.000000000000000000, 0.9659258262890683122, 1.000000000000000000, 0.9659258262890683122, 1.000000000000000000, 0.9659258262890683122, 1.000000000000000000, 0.9659258262890683122, 1.000000000000000000, 0.9659258262890683122, 1.000000000000000000, 0.9659258262890683122, 1.000000000000000000, 0.9659258262890683122, 1.000000000000000000, 0.9659258262890683122, 1.000000000000000000, 0.9659258262890683122, 1.000000000000000000, 0.9659258262890683122, 1.000000000000000000, 0.9659258262890683122, 1.000000000000000000, 0.9659258262890683122, 1.000000000000000000, 0.9659258262890683122, 1.000000000000000000, 0.9659258262890683122, 1.000000000000000000, 0.9659258262890683122, 1.000000000000000000, 0.9659258262890683122, 1.000000000000000000, 0.9659258262890683122, 1.000000000000000000, 0.9659258262890683122, 1.000000000000000000, 0.9659258262890683122, 1.000000000000000000, 0.9659258262890683122, 1.000000000000000000, 0.9659258262890683122, 1.000000000000000000, 0.9659258262890683122, 1.000000000000000000, 0.9659258262890683122, 1.000000000000000000, 0.9659258262890683122, 1.000000000000000000, 0.9659258262890683122, 1.000000000000000000, 0.9659258262890683122, 1.000000000000000000, 0.9659258262890683122, 1.000000000000000000, 0.9659258262890683122, 1.000000000000000000, 0.9659258262890683122, 1.000000000000000000, 0.9659258262890683122, 1.000000000000000000, 0.9659258262890683122, 1.000000000000000000, 0.9659258262890683122, 1.000000000000000000, 0.9659258262890683122, 1.000000000000000000, 0.9659258262890683122, 1.000000000000000000, 0.9659258262890683122, 1.000000000000000000, 0.9659258262890683122, 1.000000000000000000, 0.9659258262890683122, 1.000000000000000000, 0.9659258262890683122, 1.000000000000000000, 0.9659258262890683122, 1.000000000000000000, 0.9659258262890683122, 1.000000000000000000, 0.9659258262890683122, 1.000000000000000000, 0.9659258262890683122, 1.000000000000000000, 0.9659258262890683122, 1.000000000000000000, 0.9659258262890683122, 1.000000000000000000, 0.9659258262890683122, 1.000000000000000000, 0.9659258262890683122, 1.000000000000000000, 0.9659258262890683122, 1.000000000000000000, 0.9659258262890683122, 1.000000000000000000, 0.9659258262890683122, 1.000000000000000000, 0.9659258262890683122, 1.000000000000000000, 0.9659258262890683122, 1.000000000000000000, 0.9659258262890683122, 1.000000000000000000, 0.9659258262890683122, 1.000000000000000000, 0.9659258262890683122, 1.000000000000000000, 0.9659258262890683122, 1.000000000000000000, 0.9659258262890683122, 1.000000000000000000, 0.9659258262890683122, 1.000000000000000000, 0.9659258262890683122, 1.000000000000000000, 0.9659258262890683122, 1.000000000000000000, 0.9659258262890683122, 1.000000000000000000, 0.9659258262890683122, 1.000000000000000000, 0.9659258262890683122, 1.000000000000000000, 0.9659258262890683122, 1.000000000000000000, 0.9659258262890683122, 1.000000000000000000, 0.9659258262890683122, 1.000000000000000000, 0.9659258262890683122, 1.000000000000000000, 0.9659258262890683122, 1.000000000000000000, 0.9659258262890683122, 1.000000000000000000, 0.9659258262890683122, 1.000000000000000000, 0.9659258262890683122, 1.000000000000000000, 0.9659258262890683122, 1.000000000000000000, 0.9659258262890683122, 1.000000000000000000, 0.9659258262890683122, 1.000000000000000000, 0.9659258262890683122, 1.000000000000000000, 0.9659258262890683122, 1.000000000000000000, 0.9659258262890683122, 1.000000000000000000, 0.9659258262890683122, 1.000000000000000000, 0.9659258262890683122, 1.000000000000000000, 0.9659258262890683122, 1.000000000000000000, 0.9659258262890683122, 1.000000000000000000, 0.9659258262890683122, 1.000000000000000000, 0.9659258262890683122, 1.000000000000000000, 0.9659258262890683122, 1.000000000000000000, 0.9659258262890683122, 1.000000000000000000, 0.9659258262890683122, 1.000000000000000000, 0.9659258262890683122, 1.000000000000000000, 0.9659258262890683122, 1.000000000000000000, 0.9659258262890683122, 1.000000000000000000, 0.9659258262890683122, 1.000000000000000000, 0.9659258262890683122, 1.000000000000000000, 0.9659258262890683122, 1.000000000000000000, 0.9659258262890683122, 1.000000000000000000, 0.9659258262890683122, 1.000000000000000000, 0.9659258262890683122, 1.000000000000000000, 0.9659258262890683122, 1.000000000000000000, 0.9659258262890683122, 1.000000000000000000, 0.9659258262890683122, 1.000000000000000000, 0.9659258262890683122, 1.000000000000000000, 0.9659258262890683122, 1.000000000000000000, 0.9659258262890683122, 1.000000000000000000, 0.9659258262890683122, 1.000000000000000000, 0.9659258262890683122, 1.000000000000000000, 0.9659258262890683122, 1.000000000000000000, 0.9659258262890683122, 1.000000000000000000, 0.9659258262890683122, 1.000000000000000000, 0.9659258262890683122, 1.000000000000000000, 0.9659258262890683122, 1.000000000000000000, 0.9659258262890683122, 1.000000000000000000, 0.9659258262890683122, 1.000000000000000000, 0.9659258262890683122, 1.000000000000000000, 0.9659258262890683122, 1.000000000000000000, 0.9659258262890683122, 1.000000000000000000, 0.9659258262890683122, 1.000000000000000000, 0.9659258262890683122, 1.000000000000000000, 0.9659258262890683122, 1.000000000000000000, 0.9659258262890683122, 1.000000000000000000, 0.9659258262890683122, 1.000000000000000000, 0.9659258262890683122, 1.000000000000000000, 0.9659258262890683122, 1.000000000000000000, 0.9659258262890683122, 1.000000000000000000, 0.9659258262890683122, 1.000000000000000000, 0.9659258262890683122, 1.000000000000000000, 0.9659258262890683122, 1.000000000000000000, 0.9659258262890683122, 1.000000000000000000, 0.9659258262890683122, 1.000000000000000000, 0.9659258262890683122, 1.000000000000000000, 0.9659258262890683122, 1.000000000000000000, 0.9659258262890683122, 1.000000000000000000, 0.9659258262890683122, 1.000000000000000000, 0.9659258262890683122, 1.000000000000000000, 0.9659258262890683122, 1.000000000000000000, 0.9659258262890683122, 1.000000000000000000, 0.9659258262890683122, 1.000000000000000000, 0.9659258262890683122, 1.000000000000000000, 0.9659258262890683122, 1.000000000000000000, 0.9659258262890683122, 1.000000000000000000, 0.9659258262890683122, 1.000000000000000000, 0.9659258262890683122, 1.000000000000000000, 0.9659258262890683122, 1.000000000000000000, 0.9659258262890683122, 1.000000000000000000, 0.9659258262890683122, 1.000000000000000000, 0.9659258262890683122, 1.000000000000000000, 0.9659258262890683122, 1.000000000000000000, 0.9659258262890683122, 1.000000000000000000, 0.9659258262890683122, 1.000000000000000000, 0.9659258262890683122, 1.000000000000000000, 0.9659258262890683122, 1.000000000000000000, 0.9659258262890683122, 1.000000000000000000, 0.9659258262890683122, 1.000000000000000000, 0.9659258262890683122, 1.000000000000000000, 0.9659258262890683122, 1.000000000000000000, 0.9659258262890683122, 1.000000000000000000, 0.9659258262890683122, 1.000000000000000000),
 ( 0.3333333333333333703, 0.3219752754296894559, 0.3333333333333333703, 0.3219752754296894559, 0.3333333333333333703, 0.3219752754296894559, 0.3333333333333333703, 0.3219752754296894559, 0.3333333333333333703, 0.3219752754296894559, 0.3333333333333333703, 0.3219752754296894559, 0.3333333333333333703, 0.3219752754296894559, 0.3333333333333333703, 0.3219752754296894559, 0.3333333333333333703, 0.3219752754296894559, 0.3333333333333333703, 0.3219752754296894559, 0.3333333333333333703, 0.3219752754296894559, 0.3333333333333333703, 0.3219752754296894559, 0.3333333333333333703, 0.3219752754296894559, 0.3333333333333333703, 0.3219752754296894559, 0.3333333333333333703, 0.3219752754296894559, 0.3333333333333333703, 0.3219752754296894559, 0.3333333333333333703, 0.3219752754296894559, 0.3333333333333333703, 0.3219752754296894559, 0.3333333333333333703, 0.3219752754296894559, 0.3333333333333333703, 0.3219752754296894559, 0.3333333333333333703, 0.3219752754296894559, 0.3333333333333333703, 0.3219752754296894559, 0.3333333333333333703, 0.3219752754296894559, 0.3333333333333333703, 0.3219752754296894559, 0.3333333333333333703, 0.3219752754296894559, 0.3333333333333333703, 0.3219752754296894559, 0.3333333333333333703, 0.3219752754296894559, 0.3333333333333333703, 0.3219752754296894559, 0.3333333333333333703, 0.3219752754296894559, 0.3333333333333333703, 0.3219752754296894559, 0.3333333333333333703, 0.3219752754296894559, 0.3333333333333333703, 0.3219752754296894559, 0.3333333333333333703, 0.3219752754296894559, 0.3333333333333333703, 0.3219752754296894559, 0.3333333333333333703, 0.3219752754296894559, 0.3333333333333333703, 0.3219752754296894559, 0.3333333333333333703, 0.3219752754296894559, 0.3333333333333333703, 0.3219752754296894559, 0.3333333333333333703, 0.3219752754296894559, 0.3333333333333333703, 0.3219752754296894559, 0.3333333333333333703, 0.3219752754296894559, 0.3333333333333333703, 0.3219752754296894559, 0.3333333333333333703, 0.3219752754296894559, 0.3333333333333333703, 0.3219752754296894559, 0.3333333333333333703, 0.3219752754296894559, 0.3333333333333333703, 0.3219752754296894559, 0.3333333333333333703, 0.3219752754296894559, 0.3333333333333333703, 0.3219752754296894559, 0.3333333333333333703, 0.3219752754296894559, 0.3333333333333333703, 0.3219752754296894559, 0.3333333333333333703, 0.3219752754296894559, 0.3333333333333333703, 0.3219752754296894559, 0.3333333333333333703, 0.3219752754296894559, 0.3333333333333333703, 0.3219752754296894559, 0.3333333333333333703, 0.3219752754296894559, 0.3333333333333333703, 0.3219752754296894559, 0.3333333333333333703, 0.3219752754296894559, 0.3333333333333333703, 0.3219752754296894559, 0.3333333333333333703, 0.3219752754296894559, 0.3333333333333333703, 0.3219752754296894559, 0.3333333333333333703, 0.3219752754296894559, 0.3333333333333333703, 0.3219752754296894559, 0.3333333333333333703, 0.3219752754296894559, 0.3333333333333333703, 0.3219752754296894559, 0.3333333333333333703, 0.3219752754296894559, 0.3333333333333333703, 0.3219752754296894559, 0.3333333333333333703, 0.3219752754296894559, 0.3333333333333333703, 0.3219752754296894559, 0.3333333333333333703, 0.3219752754296894559, 0.3333333333333333703, 0.3219752754296894559, 0.3333333333333333703, 0.3219752754296894559, 0.3333333333333333703, 0.3219752754296894559, 0.3333333333333333703, 0.3219752754296894559, 0.3333333333333333703, 0.3219752754296894559, 0.3333333333333333703, 0.3219752754296894559, 0.3333333333333333703, 0.3219752754296894559, 0.3333333333333333703, 0.3219752754296894559, 0.3333333333333333703, 0.3219752754296894559, 0.3333333333333333703, 0.3219752754296894559, 0.3333333333333333703, 0.3219752754296894559, 0.3333333333333333703, 0.3219752754296894559, 0.3333333333333333703, 0.3219752754296894559, 0.3333333333333333703, 0.3219752754296894559, 0.3333333333333333703, 0.3219752754296894559, 0.3333333333333333703, 0.3219752754296894559, 0.3333333333333333703, 0.3219752754296894559, 0.3333333333333333703, 0.3219752754296894559, 0.3333333333333333703, 0.3219752754296894559, 0.3333333333333333703, 0.3219752754296894559, 0.3333333333333333703, 0.3219752754296894559, 0.3333333333333333703, 0.3219752754296894559, 0.3333333333333333703, 0.3219752754296894559, 0.3333333333333333703, 0.3219752754296894559, 0.3333333333333333703, 0.3219752754296894559, 0.3333333333333333703, 0.3219752754296894559, 0.3333333333333333703, 0.3219752754296894559, 0.3333333333333333703, 0.3219752754296894559, 0.3333333333333333703, 0.3219752754296894559, 0.3333333333333333703, 0.3219752754296894559, 0.3333333333333333703, 0.3219752754296894559, 0.3333333333333333703, 0.3219752754296894559, 0.3333333333333333703, 0.3219752754296894559, 0.3333333333333333703, 0.3219752754296894559, 0.3333333333333333703, 0.3219752754296894559, 0.3333333333333333703, 0.3219752754296894559, 0.3333333333333333703, 0.3219752754296894559, 0.3333333333333333703, 0.3219752754296894559, 0.3333333333333333703, 0.3219752754296894559, 0.3333333333333333703, 0.3219752754296894559, 0.3333333333333333703, 0.3219752754296894559, 0.3333333333333333703, 0.3219752754296894559, 0.3333333333333333703, 0.3219752754296894559, 0.3333333333333333703, 0.3219752754296894559, 0.3333333333333333703, 0.3219752754296894559, 0.3333333333333333703, 0.3219752754296894559, 0.3333333333333333703, 0.3219752754296894559, 0.3333333333333333703, 0.3219752754296894559, 0.3333333333333333703, 0.3219752754296894559, 0.3333333333333333703, 0.3219752754296894559, 0.3333333333333333703, 0.3219752754296894559, 0.3333333333333333703, 0.3219752754296894559, 0.3333333333333333703, 0.3219752754296894559, 0.3333333333333333703, 0.3219752754296894559, 0.3333333333333333703, 0.3219752754296894559, 0.3333333333333333703, 0.3219752754296894559, 0.3333333333333333703, 0.3219752754296894559, 0.3333333333333333703, 0.3219752754296894559, 0.3333333333333333703, 0.3219752754296894559, 0.3333333333333333703, 0.3219752754296894559, 0.3333333333333333703, 0.3219752754296894559, 0.3333333333333333703, 0.3219752754296894559, 0.3333333333333333703, 0.3219752754296894559, 0.3333333333333333703, 0.3219752754296894559, 0.3333333333333333703, 0.3219752754296894559, 0.3333333333333333703, 0.3219752754296894559, 0.3333333333333333703, 0.3219752754296894559, 0.3333333333333333703, 0.3219752754296894559, 0.3333333333333333703, 0.3219752754296894559, 0.3333333333333333703, 0.3219752754296894559, 0.3333333333333333703, 0.3219752754296894559, 0.3333333333333333703, 0.3219752754296894559, 0.3333333333333333703, 0.3219752754296894559, 0.3333333333333333703, 0.3219752754296894559, 0.3333333333333333703, 0.3219752754296894559, 0.3333333333333333703, 0.3219752754296894559, 0.3333333333333333703, 0.3219752754296894559, 0.3333333333333333703, 0.3219752754296894559, 0.3333333333333333703, 0.3219752754296894559, 0.3333333333333333703, 0.3219752754296894559, 0.3333333333333333703, 0.3219752754296894559, 0.3333333333333333703, 0.3219752754296894559, 0.3333333333333333703, 0.3219752754296894559, 0.3333333333333333703, 0.3219752754296894559, 0.3333333333333333703, 0.3219752754296894559, 0.3333333333333333703, 0.3219752754296894559, 0.3333333333333333703, 0.3219752754296894559, 0.3333333333333333703, 0.3219752754296894559, 0.3333333333333333703, 0.3219752754296894559, 0.3333333333333333703, 0.3219752754296894559, 0.3333333333333333703, 0.3219752754296894559, 0.3333333333333333703, 0.3219752754296894559, 0.3333333333333333703, 0.3219752754296894559, 0.3333333333333333703, 0.3219752754296894559, 0.3333333333333333703, 0.3219752754296894559, 0.3333333333333333703, 0.3219752754296894559, 0.3333333333333333703, 0.3219752754296894559, 0.3333333333333333703, 0.3219752754296894559, 0.3333333333333333703, 0.3219752754296894559, 0.3333333333333333703, 0.3219752754296894559, 0.3333333333333333703, 0.3219752754296894559, 0.3333333333333333703, 0.3219752754296894559, 0.3333333333333333703, 0.3219752754296894559, 0.3333333333333333703, 0.3219752754296894559, 0.3333333333333333703, 0.3219752754296894559, 0.3333333333333333703, 0.3219752754296894559, 0.3333333333333333703, 0.3219752754296894559, 0.3333333333333333703, 0.3219752754296894559, 0.3333333333333333703, 0.3219752754296894559, 0.3333333333333333703, 0.3219752754296894559, 0.3333333333333333703, 0.3219752754296894559, 0.3333333333333333703, 0.3219752754296894559, 0.3333333333333333703, 0.3219752754296894559, 0.3333333333333333703, 0.3219752754296894559, 0.3333333333333333703, 0.3219752754296894559, 0.3333333333333333703, 0.3219752754296894559, 0.3333333333333333703, 0.3219752754296894559, 0.3333333333333333703, 0.3219752754296894559, 0.3333333333333333703, 0.3219752754296894559, 0.3333333333333333703, 0.3219752754296894559, 0.3333333333333333703, 0.3219752754296894559, 0.3333333333333333703, 0.3219752754296894559, 0.3333333333333333703, 0.3219752754296894559, 0.3333333333333333703, 0.3219752754296894559, 0.3333333333333333703, 0.3219752754296894559, 0.3333333333333333703, 0.3219752754296894559, 0.3333333333333333703, 0.3219752754296894559, 0.3333333333333333703, 0.3219752754296894559, 0.3333333333333333703, 0.3219752754296894559, 0.3333333333333333703, 0.3219752754296894559, 0.3333333333333333703, 0.3219752754296894559, 0.3333333333333333703, 0.3219752754296894559, 0.3333333333333333703, 0.3219752754296894559, 0.3333333333333333703, 0.3219752754296894559, 0.3333333333333333703, 0.3219752754296894559, 0.3333333333333333703, 0.3219752754296894559, 0.3333333333333333703, 0.3219752754296894559, 0.3333333333333333703, 0.3219752754296894559, 0.3333333333333333703, 0.3219752754296894559, 0.3333333333333333703, 0.3219752754296894559, 0.3333333333333333703, 0.3219752754296894559, 0.3333333333333333703, 0.3219752754296894559, 0.3333333333333333703, 0.3219752754296894559, 0.3333333333333333703, 0.3219752754296894559, 0.3333333333333333703, 0.3219752754296894559, 0.3333333333333333703, 0.3219752754296894559, 0.3333333333333333703, 0.3219752754296894559, 0.3333333333333333703, 0.3219752754296894559, 0.3333333333333333703, 0.3219752754296894559, 0.3333333333333333703, 0.3219752754296894559, 0.3333333333333333703, 0.3219752754296894559, 0.3333333333333333703, 0.3219752754296894559, 0.3333333333333333703, 0.3219752754296894559, 0.3333333333333333703, 0.3219752754296894559, 0.3333333333333333703, 0.3219752754296894559, 0.3333333333333333703, 0.3219752754296894559, 0.3333333333333333703, 0.3219752754296894559, 0.3333333333333333703, 0.3219752754296894559, 0.3333333333333333703, 0.3219752754296894559, 0.3333333333333333703),
 ( 0.3333333333333333703, 0.3219752754296894559, 0.3333333333333333703, 0.3219752754296894559, 0.3333333333333333703, 0.3219752754296894559, 0.3333333333333333703, 0.3219752754296894559, 0.3333333333333333703, 0.3219752754296894559, 0.3333333333333333703, 0.3219752754296894559, 0.3333333333333333703, 0.3219752754296894559, 0.3333333333333333703, 0.3219752754296894559, 0.3333333333333333703, 0.3219752754296894559, 0.3333333333333333703, 0.3219752754296894559, 0.3333333333333333703, 0.3219752754296894559, 0.3333333333333333703, 0.3219752754296894559, 0.3333333333333333703, 0.3219752754296894559, 0.3333333333333333703, 0.3219752754296894559, 0.3333333333333333703, 0.3219752754296894559, 0.3333333333333333703, 0.3219752754296894559, 0.3333333333333333703, 0.3219752754296894559, 0.3333333333333333703, 0.3219752754296894559, 0.3333333333333333703, 0.3219752754296894559, 0.3333333333333333703, 0.3219752754296894559, 0.3333333333333333703, 0.3219752754296894559, 0.3333333333333333703, 0.3219752754296894559, 0.3333333333333333703, 0.3219752754296894559, 0.3333333333333333703, 0.3219752754296894559, 0.3333333333333333703, 0.3219752754296894559, 0.3333333333333333703, 0.3219752754296894559, 0.3333333333333333703, 0.3219752754296894559, 0.3333333333333333703, 0.3219752754296894559, 0.3333333333333333703, 0.3219752754296894559, 0.3333333333333333703, 0.3219752754296894559, 0.3333333333333333703, 0.3219752754296894559, 0.3333333333333333703, 0.3219752754296894559, 0.3333333333333333703, 0.3219752754296894559, 0.3333333333333333703, 0.3219752754296894559, 0.3333333333333333703, 0.3219752754296894559, 0.3333333333333333703, 0.3219752754296894559, 0.3333333333333333703, 0.3219752754296894559, 0.3333333333333333703, 0.3219752754296894559, 0.3333333333333333703, 0.3219752754296894559, 0.3333333333333333703, 0.3219752754296894559, 0.3333333333333333703, 0.3219752754296894559, 0.3333333333333333703, 0.3219752754296894559, 0.3333333333333333703, 0.3219752754296894559, 0.3333333333333333703, 0.3219752754296894559, 0.3333333333333333703, 0.3219752754296894559, 0.3333333333333333703, 0.3219752754296894559, 0.3333333333333333703, 0.3219752754296894559, 0.3333333333333333703, 0.3219752754296894559, 0.3333333333333333703, 0.3219752754296894559, 0.3333333333333333703, 0.3219752754296894559, 0.3333333333333333703, 0.3219752754296894559, 0.3333333333333333703, 0.3219752754296894559, 0.3333333333333333703, 0.3219752754296894559, 0.3333333333333333703, 0.3219752754296894559, 0.3333333333333333703, 0.3219752754296894559, 0.3333333333333333703, 0.3219752754296894559, 0.3333333333333333703, 0.3219752754296894559, 0.3333333333333333703, 0.3219752754296894559, 0.3333333333333333703, 0.3219752754296894559, 0.3333333333333333703, 0.3219752754296894559, 0.3333333333333333703, 0.3219752754296894559, 0.3333333333333333703, 0.3219752754296894559, 0.3333333333333333703, 0.3219752754296894559, 0.3333333333333333703, 0.3219752754296894559, 0.3333333333333333703, 0.3219752754296894559, 0.3333333333333333703, 0.3219752754296894559, 0.3333333333333333703, 0.3219752754296894559, 0.3333333333333333703, 0.3219752754296894559, 0.3333333333333333703, 0.3219752754296894559, 0.3333333333333333703, 0.3219752754296894559, 0.3333333333333333703, 0.3219752754296894559, 0.3333333333333333703, 0.3219752754296894559, 0.3333333333333333703, 0.3219752754296894559, 0.3333333333333333703, 0.3219752754296894559, 0.3333333333333333703, 0.3219752754296894559, 0.3333333333333333703, 0.3219752754296894559, 0.3333333333333333703, 0.3219752754296894559, 0.3333333333333333703, 0.3219752754296894559, 0.3333333333333333703, 0.3219752754296894559, 0.3333333333333333703, 0.3219752754296894559, 0.3333333333333333703, 0.3219752754296894559, 0.3333333333333333703, 0.3219752754296894559, 0.3333333333333333703, 0.3219752754296894559, 0.3333333333333333703, 0.3219752754296894559, 0.3333333333333333703, 0.3219752754296894559, 0.3333333333333333703, 0.3219752754296894559, 0.3333333333333333703, 0.3219752754296894559, 0.3333333333333333703, 0.3219752754296894559, 0.3333333333333333703, 0.3219752754296894559, 0.3333333333333333703, 0.3219752754296894559, 0.3333333333333333703, 0.3219752754296894559, 0.3333333333333333703, 0.3219752754296894559, 0.3333333333333333703, 0.3219752754296894559, 0.3333333333333333703, 0.3219752754296894559, 0.3333333333333333703, 0.3219752754296894559, 0.3333333333333333703, 0.3219752754296894559, 0.3333333333333333703, 0.3219752754296894559, 0.3333333333333333703, 0.3219752754296894559, 0.3333333333333333703, 0.3219752754296894559, 0.3333333333333333703, 0.3219752754296894559, 0.3333333333333333703, 0.3219752754296894559, 0.3333333333333333703, 0.3219752754296894559, 0.3333333333333333703, 0.3219752754296894559, 0.3333333333333333703, 0.3219752754296894559, 0.3333333333333333703, 0.3219752754296894559, 0.3333333333333333703, 0.3219752754296894559, 0.3333333333333333703, 0.3219752754296894559, 0.3333333333333333703, 0.3219752754296894559, 0.3333333333333333703, 0.3219752754296894559, 0.3333333333333333703, 0.3219752754296894559, 0.3333333333333333703, 0.3219752754296894559, 0.3333333333333333703, 0.3219752754296894559, 0.3333333333333333703, 0.3219752754296894559, 0.3333333333333333703, 0.3219752754296894559, 0.3333333333333333703, 0.3219752754296894559, 0.3333333333333333703, 0.3219752754296894559, 0.3333333333333333703, 0.3219752754296894559, 0.3333333333333333703, 0.3219752754296894559, 0.3333333333333333703, 0.3219752754296894559, 0.3333333333333333703, 0.3219752754296894559, 0.3333333333333333703, 0.3219752754296894559, 0.3333333333333333703, 0.3219752754296894559, 0.3333333333333333703, 0.3219752754296894559, 0.3333333333333333703, 0.3219752754296894559, 0.3333333333333333703, 0.3219752754296894559, 0.3333333333333333703, 0.3219752754296894559, 0.3333333333333333703, 0.3219752754296894559, 0.3333333333333333703, 0.3219752754296894559, 0.3333333333333333703, 0.3219752754296894559, 0.3333333333333333703, 0.3219752754296894559, 0.3333333333333333703, 0.3219752754296894559, 0.3333333333333333703, 0.3219752754296894559, 0.3333333333333333703, 0.3219752754296894559, 0.3333333333333333703, 0.3219752754296894559, 0.3333333333333333703, 0.3219752754296894559, 0.3333333333333333703, 0.3219752754296894559, 0.3333333333333333703, 0.3219752754296894559, 0.3333333333333333703, 0.3219752754296894559, 0.3333333333333333703, 0.3219752754296894559, 0.3333333333333333703, 0.3219752754296894559, 0.3333333333333333703, 0.3219752754296894559, 0.3333333333333333703, 0.3219752754296894559, 0.3333333333333333703, 0.3219752754296894559, 0.3333333333333333703, 0.3219752754296894559, 0.3333333333333333703, 0.3219752754296894559, 0.3333333333333333703, 0.3219752754296894559, 0.3333333333333333703, 0.3219752754296894559, 0.3333333333333333703, 0.3219752754296894559, 0.3333333333333333703, 0.3219752754296894559, 0.3333333333333333703, 0.3219752754296894559, 0.3333333333333333703, 0.3219752754296894559, 0.3333333333333333703, 0.3219752754296894559, 0.3333333333333333703, 0.3219752754296894559, 0.3333333333333333703, 0.3219752754296894559, 0.3333333333333333703, 0.3219752754296894559, 0.3333333333333333703, 0.3219752754296894559, 0.3333333333333333703, 0.3219752754296894559, 0.3333333333333333703, 0.3219752754296894559, 0.3333333333333333703, 0.3219752754296894559, 0.3333333333333333703, 0.3219752754296894559, 0.3333333333333333703, 0.3219752754296894559, 0.3333333333333333703, 0.3219752754296894559, 0.3333333333333333703, 0.3219752754296894559, 0.3333333333333333703, 0.3219752754296894559, 0.3333333333333333703, 0.3219752754296894559, 0.3333333333333333703, 0.3219752754296894559, 0.3333333333333333703, 0.3219752754296894559, 0.3333333333333333703, 0.3219752754296894559, 0.3333333333333333703, 0.3219752754296894559, 0.3333333333333333703, 0.3219752754296894559, 0.3333333333333333703, 0.3219752754296894559, 0.3333333333333333703, 0.3219752754296894559, 0.3333333333333333703, 0.3219752754296894559, 0.3333333333333333703, 0.3219752754296894559, 0.3333333333333333703, 0.3219752754296894559, 0.3333333333333333703, 0.3219752754296894559, 0.3333333333333333703, 0.3219752754296894559, 0.3333333333333333703, 0.3219752754296894559, 0.3333333333333333703, 0.3219752754296894559, 0.3333333333333333703, 0.3219752754296894559, 0.3333333333333333703, 0.3219752754296894559, 0.3333333333333333703, 0.3219752754296894559, 0.3333333333333333703, 0.3219752754296894559, 0.3333333333333333703, 0.3219752754296894559, 0.3333333333333333703, 0.3219752754296894559, 0.3333333333333333703, 0.3219752754296894559, 0.3333333333333333703, 0.3219752754296894559, 0.3333333333333333703, 0.3219752754296894559, 0.3333333333333333703, 0.3219752754296894559, 0.3333333333333333703, 0.3219752754296894559, 0.3333333333333333703, 0.3219752754296894559, 0.3333333333333333703, 0.3219752754296894559, 0.3333333333333333703, 0.3219752754296894559, 0.3333333333333333703, 0.3219752754296894559, 0.3333333333333333703, 0.3219752754296894559, 0.3333333333333333703, 0.3219752754296894559, 0.3333333333333333703, 0.3219752754296894559, 0.3333333333333333703, 0.3219752754296894559, 0.3333333333333333703, 0.3219752754296894559, 0.3333333333333333703, 0.3219752754296894559, 0.3333333333333333703, 0.3219752754296894559, 0.3333333333333333703, 0.3219752754296894559, 0.3333333333333333703, 0.3219752754296894559, 0.3333333333333333703, 0.3219752754296894559, 0.3333333333333333703, 0.3219752754296894559, 0.3333333333333333703, 0.3219752754296894559, 0.3333333333333333703, 0.3219752754296894559, 0.3333333333333333703, 0.3219752754296894559, 0.3333333333333333703, 0.3219752754296894559, 0.3333333333333333703, 0.3219752754296894559, 0.3333333333333333703, 0.3219752754296894559, 0.3333333333333333703, 0.3219752754296894559, 0.3333333333333333703, 0.3219752754296894559, 0.3333333333333333703, 0.3219752754296894559, 0.3333333333333333703, 0.3219752754296894559, 0.3333333333333333703, 0.3219752754296894559, 0.3333333333333333703, 0.3219752754296894559, 0.3333333333333333703, 0.3219752754296894559, 0.3333333333333333703, 0.3219752754296894559, 0.3333333333333333703, 0.3219752754296894559, 0.3333333333333333703, 0.3219752754296894559, 0.3333333333333333703, 0.3219752754296894559, 0.3333333333333333703, 0.3219752754296894559, 0.3333333333333333703, 0.3219752754296894559, 0.3333333333333333703, 0.3219752754296894559, 0.3333333333333333703, 0.3219752754296894559, 0.3333333333333333703, 0.3219752754296894559, 0.3333333333333333703, 0.3219752754296894559, 0.3333333333333333703),
 ( 1.000000000000000000, 0.9659258262890683122, 1.000000000000000000, 0.9659258262890683122, 1.000000000000000000, 0.9659258262890683122, 1.000000000000000000, 0.9659258262890683122, 1.000000000000000000, 0.9659258262890683122, 1.000000000000000000, 0.9659258262890683122, 1.000000000000000000, 0.9659258262890683122, 1.000000000000000000, 0.9659258262890683122, 1.000000000000000000, 0.9659258262890683122, 1.000000000000000000, 0.9659258262890683122, 1.000000000000000000, 0.9659258262890683122, 1.000000000000000000, 0.9659258262890683122, 1.000000000000000000, 0.9659258262890683122, 1.000000000000000000, 0.9659258262890683122, 1.000000000000000000, 0.9659258262890683122, 1.000000000000000000, 0.9659258262890683122, 1.000000000000000000, 0.9659258262890683122, 1.000000000000000000, 0.9659258262890683122, 1.000000000000000000, 0.9659258262890683122, 1.000000000000000000, 0.9659258262890683122, 1.000000000000000000, 0.9659258262890683122, 1.000000000000000000, 0.9659258262890683122, 1.000000000000000000, 0.9659258262890683122, 1.000000000000000000, 0.9659258262890683122, 1.000000000000000000, 0.9659258262890683122, 1.000000000000000000, 0.9659258262890683122, 1.000000000000000000, 0.9659258262890683122, 1.000000000000000000, 0.9659258262890683122, 1.000000000000000000, 0.9659258262890683122, 1.000000000000000000, 0.9659258262890683122, 1.000000000000000000, 0.9659258262890683122, 1.000000000000000000, 0.9659258262890683122, 1.000000000000000000, 0.9659258262890683122, 1.000000000000000000, 0.9659258262890683122, 1.000000000000000000, 0.9659258262890683122, 1.000000000000000000, 0.9659258262890683122, 1.000000000000000000, 0.9659258262890683122, 1.000000000000000000, 0.9659258262890683122, 1.000000000000000000, 0.9659258262890683122, 1.000000000000000000, 0.9659258262890683122, 1.000000000000000000, 0.9659258262890683122, 1.000000000000000000, 0.9659258262890683122, 1.000000000000000000, 0.9659258262890683122, 1.000000000000000000, 0.9659258262890683122, 1.000000000000000000, 0.9659258262890683122, 1.000000000000000000, 0.9659258262890683122, 1.000000000000000000, 0.9659258262890683122, 1.000000000000000000, 0.9659258262890683122, 1.000000000000000000, 0.9659258262890683122, 1.000000000000000000, 0.9659258262890683122, 1.000000000000000000, 0.9659258262890683122, 1.000000000000000000, 0.9659258262890683122, 1.000000000000000000, 0.9659258262890683122, 1.000000000000000000, 0.9659258262890683122, 1.000000000000000000, 0.9659258262890683122, 1.000000000000000000, 0.9659258262890683122, 1.000000000000000000, 0.9659258262890683122, 1.000000000000000000, 0.9659258262890683122, 1.000000000000000000, 0.9659258262890683122, 1.000000000000000000, 0.9659258262890683122, 1.000000000000000000, 0.9659258262890683122, 1.000000000000000000, 0.9659258262890683122, 1.000000000000000000, 0.9659258262890683122, 1.000000000000000000, 0.9659258262890683122, 1.000000000000000000, 0.9659258262890683122, 1.000000000000000000, 0.9659258262890683122, 1.000000000000000000, 0.9659258262890683122, 1.000000000000000000, 0.9659258262890683122, 1.000000000000000000, 0.9659258262890683122, 1.000000000000000000, 0.9659258262890683122, 1.000000000000000000, 0.9659258262890683122, 1.000000000000000000, 0.9659258262890683122, 1.000000000000000000, 0.9659258262890683122, 1.000000000000000000, 0.9659258262890683122, 1.000000000000000000, 0.9659258262890683122, 1.000000000000000000, 0.9659258262890683122, 1.000000000000000000, 0.9659258262890683122, 1.000000000000000000, 0.9659258262890683122, 1.000000000000000000, 0.9659258262890683122, 1.000000000000000000, 0.9659258262890683122, 1.000000000000000000, 0.9659258262890683122, 1.000000000000000000, 0.9659258262890683122, 1.000000000000000000, 0.9659258262890683122, 1.000000000000000000, 0.9659258262890683122, 1.000000000000000000, 0.9659258262890683122, 1.000000000000000000, 0.9659258262890683122, 1.000000000000000000, 0.9659258262890683122, 1.000000000000000000, 0.9659258262890683122, 1.000000000000000000, 0.9659258262890683122, 1.000000000000000000, 0.9659258262890683122, 1.000000000000000000, 0.9659258262890683122, 1.000000000000000000, 0.9659258262890683122, 1.000000000000000000, 0.9659258262890683122, 1.000000000000000000, 0.9659258262890683122, 1.000000000000000000, 0.9659258262890683122, 1.000000000000000000, 0.9659258262890683122, 1.000000000000000000, 0.9659258262890683122, 1.000000000000000000, 0.9659258262890683122, 1.000000000000000000, 0.9659258262890683122, 1.000000000000000000, 0.9659258262890683122, 1.000000000000000000, 0.9659258262890683122, 1.000000000000000000, 0.9659258262890683122, 1.000000000000000000, 0.9659258262890683122, 1.000000000000000000, 0.9659258262890683122, 1.000000000000000000, 0.9659258262890683122, 1.000000000000000000, 0.9659258262890683122, 1.000000000000000000, 0.9659258262890683122, 1.000000000000000000, 0.9659258262890683122, 1.000000000000000000, 0.9659258262890683122, 1.000000000000000000, 0.9659258262890683122, 1.000000000000000000, 0.9659258262890683122, 1.000000000000000000, 0.9659258262890683122, 1.000000000000000000, 0.9659258262890683122, 1.000000000000000000, 0.9659258262890683122, 1.000000000000000000, 0.9659258262890683122, 1.000000000000000000, 0.9659258262890683122, 1.000000000000000000, 0.9659258262890683122, 1.000000000000000000, 0.9659258262890683122, 1.000000000000000000, 0.9659258262890683122, 1.000000000000000000, 0.9659258262890683122, 1.000000000000000000, 0.9659258262890683122, 1.000000000000000000, 0.9659258262890683122, 1.000000000000000000, 0.9659258262890683122, 1.000000000000000000, 0.9659258262890683122, 1.000000000000000000, 0.9659258262890683122, 1.000000000000000000, 0.9659258262890683122, 1.000000000000000000, 0.9659258262890683122, 1.000000000000000000, 0.9659258262890683122, 1.000000000000000000, 0.9659258262890683122, 1.000000000000000000, 0.9659258262890683122, 1.000000000000000000, 0.9659258262890683122, 1.000000000000000000, 0.9659258262890683122, 1.000000000000000000, 0.9659258262890683122, 1.000000000000000000, 0.9659258262890683122, 1.000000000000000000, 0.9659258262890683122, 1.000000000000000000, 0.9659258262890683122, 1.000000000000000000, 0.9659258262890683122, 1.000000000000000000, 0.9659258262890683122, 1.000000000000000000, 0.9659258262890683122, 1.000000000000000000, 0.9659258262890683122, 1.000000000000000000, 0.9659258262890683122, 1.000000000000000000, 0.9659258262890683122, 1.000000000000000000, 0.9659258262890683122, 1.000000000000000000, 0.9659258262890683122, 1.000000000000000000, 0.9659258262890683122, 1.000000000000000000, 0.9659258262890683122, 1.000000000000000000, 0.9659258262890683122, 1.000000000000000000, 0.9659258262890683122, 1.000000000000000000, 0.9659258262890683122, 1.000000000000000000, 0.9659258262890683122, 1.000000000000000000, 0.9659258262890683122, 1.000000000000000000, 0.9659258262890683122, 1.000000000000000000, 0.9659258262890683122, 1.000000000000000000, 0.9659258262890683122, 1.000000000000000000, 0.9659258262890683122, 1.000000000000000000, 0.9659258262890683122, 1.000000000000000000, 0.9659258262890683122, 1.000000000000000000, 0.9659258262890683122, 1.000000000000000000, 0.9659258262890683122, 1.000000000000000000, 0.9659258262890683122, 1.000000000000000000, 0.9659258262890683122, 1.000000000000000000, 0.9659258262890683122, 1.000000000000000000, 0.9659258262890683122, 1.000000000000000000, 0.9659258262890683122, 1.000000000000000000, 0.9659258262890683122, 1.000000000000000000, 0.9659258262890683122, 1.000000000000000000, 0.9659258262890683122, 1.000000000000000000, 0.9659258262890683122, 1.000000000000000000, 0.9659258262890683122, 1.000000000000000000, 0.9659258262890683122, 1.000000000000000000, 0.9659258262890683122, 1.000000000000000000, 0.9659258262890683122, 1.000000000000000000, 0.9659258262890683122, 1.000000000000000000, 0.9659258262890683122, 1.000000000000000000, 0.9659258262890683122, 1.000000000000000000, 0.9659258262890683122, 1.000000000000000000, 0.9659258262890683122, 1.000000000000000000, 0.9659258262890683122, 1.000000000000000000, 0.9659258262890683122, 1.000000000000000000, 0.9659258262890683122, 1.000000000000000000, 0.9659258262890683122, 1.000000000000000000, 0.9659258262890683122, 1.000000000000000000, 0.9659258262890683122, 1.000000000000000000, 0.9659258262890683122, 1.000000000000000000, 0.9659258262890683122, 1.000000000000000000, 0.9659258262890683122, 1.000000000000000000, 0.9659258262890683122, 1.000000000000000000, 0.9659258262890683122, 1.000000000000000000, 0.9659258262890683122, 1.000000000000000000, 0.9659258262890683122, 1.000000000000000000, 0.9659258262890683122, 1.000000000000000000, 0.9659258262890683122, 1.000000000000000000, 0.9659258262890683122, 1.000000000000000000, 0.9659258262890683122, 1.000000000000000000, 0.9659258262890683122, 1.000000000000000000, 0.9659258262890683122, 1.000000000000000000, 0.9659258262890683122, 1.000000000000000000, 0.9659258262890683122, 1.000000000000000000, 0.9659258262890683122, 1.000000000000000000, 0.9659258262890683122, 1.000000000000000000, 0.9659258262890683122, 1.000000000000000000, 0.9659258262890683122, 1.000000000000000000, 0.9659258262890683122, 1.000000000000000000, 0.9659258262890683122, 1.000000000000000000, 0.9659258262890683122, 1.000000000000000000, 0.9659258262890683122, 1.000000000000000000, 0.9659258262890683122, 1.000000000000000000, 0.9659258262890683122, 1.000000000000000000, 0.9659258262890683122, 1.000000000000000000, 0.9659258262890683122, 1.000000000000000000, 0.9659258262890683122, 1.000000000000000000, 0.9659258262890683122, 1.000000000000000000, 0.9659258262890683122, 1.000000000000000000, 0.9659258262890683122, 1.000000000000000000, 0.9659258262890683122, 1.000000000000000000, 0.9659258262890683122, 1.000000000000000000, 0.9659258262890683122, 1.000000000000000000, 0.9659258262890683122, 1.000000000000000000, 0.9659258262890683122, 1.000000000000000000, 0.9659258262890683122, 1.000000000000000000, 0.9659258262890683122, 1.000000000000000000, 0.9659258262890683122, 1.000000000000000000, 0.9659258262890683122, 1.000000000000000000, 0.9659258262890683122, 1.000000000000000000, 0.9659258262890683122, 1.000000000000000000, 0.9659258262890683122, 1.000000000000000000, 0.9659258262890683122, 1.000000000000000000, 0.9659258262890683122, 1.000000000000000000) ) ) 
 REPRESENTATION_ITEM ( '' )  SURFACE ( )  );
#169555 = CARTESIAN_POINT ( 'NONE',  ( -9.474510206698964154, 16.51473224551069663, 110.4155762719810383 ) ) ;
#169556 = DIRECTION ( 'NONE',  ( -0.000000000000000000, -0.000000000000000000, 1.000000000000000000 ) ) ;
#169557 = CARTESIAN_POINT ( 'NONE',  ( 19.05341960407617918, -5.049401038297876454, 96.04275706135231871 ) ) ;
#169558 = CARTESIAN_POINT ( 'NONE',  ( 5.719274019375991003, -21.55341960407610458, 67.70724293864769550 ) ) ;
#169559 = CARTESIAN_POINT ( 'NONE',  ( 0.05219959533910956823, 16.53943276465976808, 54.99890960531435269 ) ) ;
#169560 = CARTESIAN_POINT ( 'NONE',  ( 0.05219959533934541429, -16.53943276465976808, 20.00109039468568639 ) ) ;
#169561 = CARTESIAN_POINT ( 'NONE',  ( 19.02544592524343514, -5.153800228976328945, 33.54057627198102409 ) ) ;
#169562 = CARTESIAN_POINT ( 'NONE',  ( 5.153800228976615827, -19.02544592524334988, 105.2094237280190185 ) ) ;
#169564 = CARTESIAN_POINT ( 'NONE',  ( -13.89961937509957401, -13.97604488694547875, 69.37609039468564731 ) ) ;
#169563 = CARTESIAN_POINT ( 'NONE',  ( 5.823673210054125526, 21.52544592524343514, 99.79057627198103830 ) ) ;
#169565 = CARTESIAN_POINT ( 'NONE',  ( -16.55341960407617563, 4.379528057220093196, 83.54275706135234714 ) ) ;
#169566 = CARTESIAN_POINT ( 'NONE',  ( -19.05341960407611168, -5.049401038298163336, 76.45724293864769550 ) ) ;
#169567 = CARTESIAN_POINT ( 'NONE',  ( 0.05219959533910956823, 16.53943276465976808, 79.99890960531435269 ) ) ;
#169568 = CARTESIAN_POINT ( 'NONE',  ( -13.97604488694527625, -13.89961937509977652, 61.87390960531435979 ) ) ;
#169569 = CARTESIAN_POINT ( 'NONE',  ( -14.34966873604960291, -8.224510206698953496, 66.66557627198102409 ) ) ;
#169570 = CARTESIAN_POINT ( 'NONE',  ( 16.51473224551069308, 9.474510206698969483, 34.16557627198102409 ) ) ;
#169571 = CARTESIAN_POINT ( 'NONE',  ( -36.81794758165438708, -5.500929263287721582, 45.34431116311557020 ) ) ;
#169572 = CARTESIAN_POINT ( 'NONE',  ( -0.05219959533910754901, -16.53943276465976808, 37.49890960531436690 ) ) ;
#169573 = CARTESIAN_POINT ( 'NONE',  ( -5.153800228976328057, -19.02544592524343514, 82.29057627198103830 ) ) ;
#169574 = CARTESIAN_POINT ( 'NONE',  ( -0.7844626028949902574, -13.90528855463213631, -60.35633530387644896 ) ) ;
#169575 = CARTESIAN_POINT ( 'NONE',  ( -5.049401038297874678, -19.05341960407617918, 54.79275706135234003 ) ) ;
#169576 = CARTESIAN_POINT ( 'NONE',  ( -0.05219959533934338120, 16.53943276465976808, 57.50109039468568994 ) ) ;
#169577 = CARTESIAN_POINT ( 'NONE',  ( 21.53943276465977519, -0.05219959533907433946, 58.74890960531436690 ) ) ;
#169578 = CARTESIAN_POINT ( 'NONE',  ( -19.02544592524334988, -5.153800228976617603, 28.95942372801900433 ) ) ;
#169579 = CARTESIAN_POINT ( 'NONE',  ( -16.51473224551069308, -9.474510206698971260, 86.66557627198102409 ) ) ;
#169580 = DIRECTION ( 'NONE',  ( 1.000000000000000000, 0.000000000000000000, 0.000000000000000000 ) ) ;
#169581 = CARTESIAN_POINT ( 'NONE',  ( 15.80617190586746368, 15.72974639402197994, 29.37390960531435269 ) ) ;
#169582 = CARTESIAN_POINT ( 'NONE',  ( -0.05219959533909027116, -19.03943276465977164, 57.49890960531435979 ) ) ;
#169583 = CARTESIAN_POINT ( 'NONE',  ( -5.823673210054431948, 21.52544592524334988, 52.70942372801902565 ) ) ;
#169584 = CARTESIAN_POINT ( 'NONE',  ( -0.05219959533910754901, -16.53943276465976808, 112.4989096053143669 ) ) ;
#169587 = ORIENTED_EDGE ( 'NONE', *, *, #118593, .F. ) ;
#169586 = CARTESIAN_POINT ( 'NONE',  ( -9.564922557960796823, -16.46253265017161027, 97.08224293864769550 ) ) ;
#169585 = CARTESIAN_POINT ( 'NONE',  ( 15.80617190586746368, 15.72974639402197994, 104.3739096053143669 ) ) ;
#169588 = CARTESIAN_POINT ( 'NONE',  ( -21.55341960407619339, 5.719274019375674811, 38.54275706135234714 ) ) ;
#169589 = ORIENTED_EDGE ( 'NONE', *, *, #185663, .T. ) ;
#169590 = CARTESIAN_POINT ( 'NONE',  ( 0.05219959533909260263, 19.03943276465977164, 99.99890960531436690 ) ) ;
#169591 = CARTESIAN_POINT ( 'NONE',  ( 0.000000000000000000, 0.000000000000000000, 0.000000000000000000 ) ) ;
#169592 = CARTESIAN_POINT ( 'NONE',  ( 21.53943276465977519, -0.05219959533907433946, 88.74890960531436690 ) ) ;
#169593 = CARTESIAN_POINT ( 'NONE',  ( -19.03943276465977164, 0.05219959533909376836, 51.24890960531436690 ) ) ;
#169594 = CARTESIAN_POINT ( 'NONE',  ( 8.224510206698742110, 14.34966873604972548, 27.08442372801901854 ) ) ;
#169595 = CARTESIAN_POINT ( 'NONE',  ( -36.91746825000001309, 11.99521256947798342, -5.224999997268811924 ) ) ;
#169596 = CARTESIAN_POINT ( 'NONE',  ( -13.89961937509977652, 13.97604488694528158, 35.62390960531435269 ) ) ;
#169597 = CARTESIAN_POINT ( 'NONE',  ( 5.719274019375673035, 21.55341960407619339, 97.29275706135234714 ) ) ;
#169599 = CARTESIAN_POINT ( 'NONE',  ( -21.52544592524334988, -5.823673210054445271, 48.95942372801902565 ) ) ;
#169598 = CARTESIAN_POINT ( 'NONE',  ( -0.05219959533909027116, -19.03943276465977164, 72.49890960531435269 ) ) ;
#169600 = CARTESIAN_POINT ( 'NONE',  ( 18.67979575497194134, -10.72451020669871369, 25.83442372801901499 ) ) ;
#169601 = CARTESIAN_POINT ( 'NONE',  ( -17.14385361876520619, 23.59649016807275856, 143.0750000027311444 ) ) ;
#169602 = CARTESIAN_POINT ( 'NONE',  ( 0.05219959533909260263, 19.03943276465977164, 99.99890960531436690 ) ) ;
#169603 = CARTESIAN_POINT ( 'NONE',  ( 14.78475781823265756, 23.88375075827561034, 139.9999999999999716 ) ) ;
#169606 = CARTESIAN_POINT ( 'NONE',  ( -10.72451020669870658, -18.67979575497194134, 59.58442372801901854 ) ) ;
#169605 = CARTESIAN_POINT ( 'NONE',  ( -4.483927247898782831, 16.52544592524335698, 72.70942372801901854 ) ) ;
#169604 = CARTESIAN_POINT ( 'NONE',  ( -16.53943276465976808, -0.05219959533934237506, 33.75109039468568284 ) ) ;
#169607 = CARTESIAN_POINT ( 'NONE',  ( -5.823673210054431948, 21.52544592524334988, 82.70942372801900433 ) ) ;
#169608 = CARTESIAN_POINT ( 'NONE',  ( 15.50000000000000178, -5.500000000000000888, 118.0000000000000142 ) ) ;
#169609 = CARTESIAN_POINT ( 'NONE',  ( -8.224510206698735004, -14.34966873604973081, 19.58442372801901143 ) ) ;
#169610 = CARTESIAN_POINT ( 'NONE',  ( -5.049401038298153566, 19.05341960407611168, 70.20724293864769550 ) ) ;
#169611 = CARTESIAN_POINT ( 'NONE',  ( -13.97604488694527625, -13.89961937509977652, 101.8739096053143811 ) ) ;
#169612 = EDGE_CURVE ( 'NONE', #66950, #87358, #183023, .T. ) ;
#169613 = CARTESIAN_POINT ( 'NONE',  ( 12.06949235617757843, -12.14591786802309237, 113.1239096053143953 ) ) ;
#169614 = CARTESIAN_POINT ( 'NONE',  ( -12.14591786802309592, -12.06949235617757132, 111.8739096053143669 ) ) ;
#169615 = CARTESIAN_POINT ( 'NONE',  ( 21.52544592524344225, -5.823673210054117533, 28.54057627198103120 ) ) ;
#169616 = CARTESIAN_POINT ( 'NONE',  ( 0.05219959533934541429, -16.53943276465976808, 75.00109039468568994 ) ) ;
#169618 = CARTESIAN_POINT ( 'NONE',  ( 13.89961937509977652, -13.97604488694527269, 53.12390960531434558 ) ) ;
#169617 = CARTESIAN_POINT ( 'NONE',  ( 4.483927247898545687, 16.52544592524342804, 69.79057627198102409 ) ) ;
#169619 = CARTESIAN_POINT ( 'NONE',  ( -18.67979575497193778, 10.72451020669871902, 73.33442372801901854 ) ) ;
#169620 = CARTESIAN_POINT ( 'NONE',  ( -21.35939100396076995, 0.4315818942740129449, -58.81718527612538594 ) ) ;
#169621 = CARTESIAN_POINT ( 'NONE',  ( 13.89961937509957401, 13.97604488694547697, 106.8760903946856757 ) ) ;
#169622 = CARTESIAN_POINT ( 'NONE',  ( 12.06949235617757843, -12.14591786802309237, 78.12390960531436690 ) ) ;
#169623 = CARTESIAN_POINT ( 'NONE',  ( -10.81492255796105439, 18.62759615963255655, 27.91775706135234358 ) ) ;
#169624 = CARTESIAN_POINT ( 'NONE',  ( -0.05219959533907301413, -21.53943276465977519, 57.49890960531435979 ) ) ;
#169626 = CARTESIAN_POINT ( 'NONE',  ( -16.29526858892874586, -7.335722546920136367, 105.7967059780020520 ) ) ;
#169625 = CIRCLE ( 'NONE', #21101, 31.90000000000003411 ) ;
#169627 = CARTESIAN_POINT ( 'NONE',  ( -35.59978325014670730, 2.421353778481746044, 37.88472941744216627 ) ) ;
#169628 = CARTESIAN_POINT ( 'NONE',  ( -13.89961937509977652, 13.97604488694528158, 75.62390960531438111 ) ) ;
#169629 = CARTESIAN_POINT ( 'NONE',  ( 8.224510206698953496, -14.34966873604960469, 47.91557627198102409 ) ) ;
#169630 = CARTESIAN_POINT ( 'NONE',  ( 8.224510206698953496, -14.34966873604960469, 27.91557627198103830 ) ) ;
#169631 = CARTESIAN_POINT ( 'NONE',  ( 12.06949235617739724, 12.14591786802326823, 91.87609039468568994 ) ) ;
#169632 = CARTESIAN_POINT ( 'NONE',  ( 19.05341960407617918, -5.049401038297876454, 46.04275706135233293 ) ) ;
#169633 = CARTESIAN_POINT ( 'NONE',  ( 17.31747979337950838, 6.344076630961018815, 48.87944868065186910 ) ) ;
#169634 = CARTESIAN_POINT ( 'NONE',  ( -16.51473224551069308, -9.474510206698971260, 111.6655762719810383 ) ) ;
#169635 = EDGE_CURVE ( 'NONE', #91449, #187465, #159486, .T. ) ;
#169636 = CARTESIAN_POINT ( 'NONE',  ( -12.14591786802309592, -12.06949235617757132, 71.87390960531438111 ) ) ;
#169637 = CARTESIAN_POINT ( 'NONE',  ( 5.049401038297881783, 19.05341960407617563, 42.29275706135234003 ) ) ;
#169639 = CARTESIAN_POINT ( 'NONE',  ( -0.05219959533907301413, -21.53943276465977519, 37.49890960531436690 ) ) ;
#169638 = CARTESIAN_POINT ( 'NONE',  ( -13.89961937509977652, 13.97604488694528158, 30.62390960531435269 ) ) ;
#169641 = ORIENTED_EDGE ( 'NONE', *, *, #67633, .T. ) ;
#169640 = CARTESIAN_POINT ( 'NONE',  ( 5.719274019375991003, -21.55341960407610458, 57.70724293864770260 ) ) ;
#169642 = CARTESIAN_POINT ( 'NONE',  ( 8.314922557960818139, 14.29746914071049879, 104.5822429386477097 ) ) ;
#169643 = CARTESIAN_POINT ( 'NONE',  ( 16.53943276465976808, 0.05219959533934440121, 51.25109039468568994 ) ) ;
#169644 = CARTESIAN_POINT ( 'NONE',  ( 4.379528057220339221, -16.55341960407611168, 92.70724293864770971 ) ) ;
#169645 = DIRECTION ( 'NONE',  ( 1.000000000000000000, -0.000000000000000000, -0.000000000000000000 ) ) ;
#169646 = CARTESIAN_POINT ( 'NONE',  ( -17.50000000000000000, 5.622605283950872668, 48.68792689403888829 ) ) ;
#169647 = CARTESIAN_POINT ( 'NONE',  ( -21.53943276465977519, 0.05219959533907696930, 31.24890960531435979 ) ) ;
#169648 = DIRECTION ( 'NONE',  ( -0.000000000000000000, -0.000000000000000000, 1.000000000000000000 ) ) ;
#169649 = CARTESIAN_POINT ( 'NONE',  ( -30.73962218707677962, -22.33364281372842441, -7.547842220587804185 ) ) ;
#169651 = CARTESIAN_POINT ( 'NONE',  ( -16.53943276465976808, 0.05219959533911058130, 26.24890960531435624 ) ) ;
#169650 = CARTESIAN_POINT ( 'NONE',  ( 12.06949235617739724, 12.14591786802326823, 36.87609039468568994 ) ) ;
#169652 = CARTESIAN_POINT ( 'NONE',  ( 21.53943276465977519, -0.05219959533907433946, 53.74890960531437401 ) ) ;
#169653 = CARTESIAN_POINT ( 'NONE',  ( -9.474510206698720793, -16.51473224551083518, 79.58442372801899012 ) ) ;
#169654 = CARTESIAN_POINT ( 'NONE',  ( -21.55341960407610458, -5.719274019375992779, 61.45724293864770260 ) ) ;
#169655 = CARTESIAN_POINT ( 'NONE',  ( 21.53943276465977519, 0.05219959533937863772, 76.25109039468568994 ) ) ;
#169656 = CARTESIAN_POINT ( 'NONE',  ( -11.95480631804128002, 11.66256017358944064, -61.34707691135564289 ) ) ;
#169657 = CARTESIAN_POINT ( 'NONE',  ( -12.14591786802326823, 12.06949235617739902, 43.12609039468568284 ) ) ;
#169659 = CARTESIAN_POINT ( 'NONE',  ( 13.97604488694527802, 13.89961937509977652, 99.37390960531436690 ) ) ;
#169658 = CARTESIAN_POINT ( 'NONE',  ( -16.51473224551069308, -9.474510206698971260, 31.66557627198102054 ) ) ;
#169660 = CARTESIAN_POINT ( 'NONE',  ( 5.049401038298161559, -19.05341960407611168, 32.70724293864768129 ) ) ;
#169661 = CARTESIAN_POINT ( 'NONE',  ( -4.483927247898539470, -16.52544592524342804, 97.29057627198105251 ) ) ;
#169662 = CARTESIAN_POINT ( 'NONE',  ( -37.00000000000000711, -1.163414459189985801E-14, 95.00000000000000000 ) ) ;
#169663 = CARTESIAN_POINT ( 'NONE',  ( 0.05219959533909260263, 19.03943276465977164, 114.9989096053143669 ) ) ;
#169664 = ORIENTED_EDGE ( 'NONE', *, *, #185663, .F. ) ;
#169665 = CARTESIAN_POINT ( 'NONE',  ( -4.379528057220086978, -16.55341960407618274, 74.79275706135234714 ) ) ;
#169666 = CARTESIAN_POINT ( 'NONE',  ( -21.55341960407610458, -5.719274019375992779, 86.45724293864770971 ) ) ;
#169667 = CARTESIAN_POINT ( 'NONE',  ( 9.474510206698971260, -16.51473224551069308, 62.91557627198102409 ) ) ;
#169668 = CARTESIAN_POINT ( 'NONE',  ( -21.53943276465977519, -0.05219959533937600094, 23.75109039468567929 ) ) ;
#169669 = CARTESIAN_POINT ( 'NONE',  ( 19.02544592524343514, -5.153800228976328945, 78.54057627198099567 ) ) ;
#169670 = EDGE_LOOP ( 'NONE', ( #88234, #190620, #148227, #156656, #195290 ) ) ;
#169671 = CARTESIAN_POINT ( 'NONE',  ( 15.80617190586746368, 15.72974639402197994, 114.3739096053143527 ) ) ;
#169674 = CARTESIAN_POINT ( 'NONE',  ( -16.51473224551082808, 9.474510206698731452, 73.33442372801900433 ) ) ;
#169673 = CARTESIAN_POINT ( 'NONE',  ( 19.05341960407611168, 5.049401038298154454, 108.9572429386477097 ) ) ;
#169672 = CARTESIAN_POINT ( 'NONE',  ( -5.049401038298153566, 19.05341960407611168, 30.20724293864768839 ) ) ;
#169675 = CARTESIAN_POINT ( 'NONE',  ( 9.564922557961047289, -16.46253265017146816, 30.41775706135232937 ) ) ;
#169676 = CARTESIAN_POINT ( 'NONE',  ( -15.80617190586745835, -15.72974639402198527, 101.8739096053143811 ) ) ;
#169677 = CARTESIAN_POINT ( 'NONE',  ( -19.05341960407617563, 5.049401038297882671, 38.54275706135233293 ) ) ;
#169678 = CARTESIAN_POINT ( 'NONE',  ( -16.52544592524335698, -4.483927247898792601, 78.95942372801901854 ) ) ;
#169679 = CARTESIAN_POINT ( 'NONE',  ( -19.02544592524342804, 5.153800228976336051, 111.0405762719810099 ) ) ;
#169680 = CARTESIAN_POINT ( 'NONE',  ( 9.564922557960805705, 16.46253265017160317, 64.58224293864769550 ) ) ;
#169681 = VECTOR ( 'NONE', #56733, 1000.000000000000000 ) ;
#169682 = CARTESIAN_POINT ( 'NONE',  ( -0.05219959533937732626, 21.53943276465977519, 67.50109039468568994 ) ) ;
#169683 = CARTESIAN_POINT ( 'NONE',  ( 15.72974639402176855, 15.80617190586768217, 86.87609039468568994 ) ) ;
#169684 = CARTESIAN_POINT ( 'NONE',  ( -16.46253265017160317, 9.564922557960807481, 70.83224293864770971 ) ) ;
#169685 = CARTESIAN_POINT ( 'NONE',  ( 0.05219959533937995610, -21.53943276465977519, 45.00109039468568284 ) ) ;
#169686 = CARTESIAN_POINT ( 'NONE',  ( -9.564922557961040184, 16.46253265017147172, 82.91775706135233293 ) ) ;
#169687 = CARTESIAN_POINT ( 'NONE',  ( 16.46253265017160672, -9.564922557960803928, 53.33224293864768839 ) ) ;
#169688 = CARTESIAN_POINT ( 'NONE',  ( 13.89961937509977652, -13.97604488694527269, 103.1239096053143527 ) ) ;
#169689 = CARTESIAN_POINT ( 'NONE',  ( -13.97604488694527625, -13.89961937509977652, 66.87390960531436690 ) ) ;
#169690 = CARTESIAN_POINT ( 'NONE',  ( 16.46253265017160672, -9.564922557960803928, 78.33224293864769550 ) ) ;
#169691 = CARTESIAN_POINT ( 'NONE',  ( -13.97604488694527625, -13.89961937509977652, 56.87390960531434558 ) ) ;
#169692 = CARTESIAN_POINT ( 'NONE',  ( -10.81492255796078084, -18.62759615963271287, 102.0822429386476955 ) ) ;
#169693 = CARTESIAN_POINT ( 'NONE',  ( -16.55341960407617563, 4.379528057220093196, 88.54275706135236135 ) ) ;
#169694 = CARTESIAN_POINT ( 'NONE',  ( -19.83802472612592993, 12.02135855755751059, 167.9999999999999716 ) ) ;
#169695 = CARTESIAN_POINT ( 'NONE',  ( 16.51473224551083163, -9.474510206698727899, 40.83442372801900433 ) ) ;
#169696 = CARTESIAN_POINT ( 'NONE',  ( -19.02544592524342804, 5.153800228976336051, 66.04057627198103830 ) ) ;
#169697 = CARTESIAN_POINT ( 'NONE',  ( 14.34966873604960469, 8.224510206698951720, 54.16557627198103120 ) ) ;
#169698 = CARTESIAN_POINT ( 'NONE',  ( 16.52544592524342804, -4.483927247898539470, 93.54057627198103830 ) ) ;
#169699 = AXIS2_PLACEMENT_3D ( 'NONE', #109216, #1031, #62703 ) ;
#169700 = CARTESIAN_POINT ( 'NONE',  ( -19.03943276465977164, 0.05219959533909376836, 111.2489096053143669 ) ) ;
#169701 = CARTESIAN_POINT ( 'NONE',  ( 9.564922557960805705, 16.46253265017160317, 94.58224293864769550 ) ) ;
#169702 = CARTESIAN_POINT ( 'NONE',  ( 13.89961937509977652, -13.97604488694527269, 103.1239096053143527 ) ) ;
#169703 = CARTESIAN_POINT ( 'NONE',  ( 19.02544592524334988, 5.153800228976608722, 21.45942372801899012 ) ) ;
#169704 = CARTESIAN_POINT ( 'NONE',  ( 16.55341960407618274, -4.379528057220086978, 96.04275706135236135 ) ) ;
#169705 = CARTESIAN_POINT ( 'NONE',  ( 5.049401038298161559, -19.05341960407611168, 72.70724293864768129 ) ) ;
#169706 = CARTESIAN_POINT ( 'NONE',  ( 15.72974639402176855, 15.80617190586768217, 41.87609039468568284 ) ) ;
#169707 = AXIS2_PLACEMENT_3D ( 'NONE', #24399, #51714, #21379 ) ;
#169708 = CARTESIAN_POINT ( 'NONE',  ( -0.05219959533907301413, -21.53943276465977519, 32.49890960531435979 ) ) ;
#169709 = CARTESIAN_POINT ( 'NONE',  ( -21.53943276465977519, -0.05219959533937600094, 23.75109039468567929 ) ) ;
#169710 = CARTESIAN_POINT ( 'NONE',  ( -4.483927247898539470, -16.52544592524342804, 62.29057627198102409 ) ) ;
#169711 = CARTESIAN_POINT ( 'NONE',  ( 16.51473224551069308, 9.474510206698969483, 59.16557627198102409 ) ) ;
#169712 = CARTESIAN_POINT ( 'NONE',  ( 0.05219959533910956823, 16.53943276465976808, 79.99890960531435269 ) ) ;
#169713 = CARTESIAN_POINT ( 'NONE',  ( -0.05219959533936034679, 19.03943276465977164, 47.50109039468566863 ) ) ;
#169714 = CARTESIAN_POINT ( 'NONE',  ( 5.049401038298161559, -19.05341960407611168, 22.70724293864769194 ) ) ;
#169715 = CARTESIAN_POINT ( 'NONE',  ( 9.474510206698971260, -16.51473224551069308, 82.91557627198103830 ) ) ;
#169716 = CARTESIAN_POINT ( 'NONE',  ( -13.97604488694527625, -13.89961937509977652, 86.87390960531436690 ) ) ;
#169717 = CARTESIAN_POINT ( 'NONE',  ( -27.73933785331498925, 9.013057229001088189, 142.7750000027311899 ) ) ;
#169718 = CARTESIAN_POINT ( 'NONE',  ( -12.14591786802309592, -12.06949235617757132, 106.8739096053143811 ) ) ;
#169719 = EDGE_LOOP ( 'NONE', ( #18792, #23367, #55953, #124651, #68895 ) ) ;
#169720 = CARTESIAN_POINT ( 'NONE',  ( 14.29746914071037800, 8.314922557961029526, 101.6677570613523613 ) ) ;
#169721 = CARTESIAN_POINT ( 'NONE',  ( 16.52544592524335698, 4.483927247898782831, 31.45942372801901854 ) ) ;
#169722 = CARTESIAN_POINT ( 'NONE',  ( -10.81492255796105439, 18.62759615963255655, 92.91775706135236135 ) ) ;
#169723 = CARTESIAN_POINT ( 'NONE',  ( 13.97604488694527802, 13.89961937509977652, 84.37390960531433848 ) ) ;
#169724 = CARTESIAN_POINT ( 'NONE',  ( 15.72974639402176855, 15.80617190586768217, 21.87609039468567573 ) ) ;
#169725 = CARTESIAN_POINT ( 'NONE',  ( -16.51473224551069308, -9.474510206698971260, 31.66557627198102054 ) ) ;
#169726 = CARTESIAN_POINT ( 'NONE',  ( 14.29746914071037800, 8.314922557961029526, 31.66775706135234358 ) ) ;
#169727 = CARTESIAN_POINT ( 'NONE',  ( 19.03943276465977164, 0.05219959533936151252, 96.25109039468567573 ) ) ;
#169728 = CARTESIAN_POINT ( 'NONE',  ( -5.719274019375978568, 21.55341960407610458, 85.20724293864770971 ) ) ;
#169729 = CARTESIAN_POINT ( 'NONE',  ( -5.153800228976607833, 19.02544592524334988, 67.70942372801900433 ) ) ;
#169730 = CARTESIAN_POINT ( 'NONE',  ( -13.97604488694527625, -13.89961937509977652, 21.87390960531435979 ) ) ;
#169731 = CARTESIAN_POINT ( 'NONE',  ( 5.823673210054444382, -21.52544592524334988, 25.20942372801901854 ) ) ;
#169732 = CARTESIAN_POINT ( 'NONE',  ( 23.48298174826589246, 32.32155151706776053, -4.447842220587801876 ) ) ;
#169733 = CARTESIAN_POINT ( 'NONE',  ( 16.46253265017160672, -9.564922557960803928, 88.33224293864769550 ) ) ;
#169734 = CARTESIAN_POINT ( 'NONE',  ( -0.05219959533934338120, 16.53943276465976808, 47.50109039468568994 ) ) ;
#169735 = CARTESIAN_POINT ( 'NONE',  ( 19.53216895467080860, -34.90705393983476768, -6.817813017276924015 ) ) ;
#169736 = CARTESIAN_POINT ( 'NONE',  ( 0.05219959533936267826, -19.03943276465977164, 55.00109039468566863 ) ) ;
#169738 = CARTESIAN_POINT ( 'NONE',  ( 0.05219959533910956823, 16.53943276465976808, 79.99890960531435269 ) ) ;
#169737 = CARTESIAN_POINT ( 'NONE',  ( -10.72451020669898014, 18.67979575497178502, 110.4155762719810383 ) ) ;
#169739 = CARTESIAN_POINT ( 'NONE',  ( 0.05219959533909260263, 19.03943276465977164, 84.99890960531436690 ) ) ;
#169741 = CARTESIAN_POINT ( 'NONE',  ( 9.564922557961047289, -16.46253265017146816, 55.41775706135234003 ) ) ;
#169740 = CARTESIAN_POINT ( 'NONE',  ( 12.06949235617739724, 12.14591786802326823, 46.87609039468568994 ) ) ;
#169742 = CARTESIAN_POINT ( 'NONE',  ( -18.62759615963255300, -10.81492255796106328, 69.16775706135234714 ) ) ;
#169743 = CARTESIAN_POINT ( 'NONE',  ( 16.55341960407618274, -4.379528057220086978, 21.04275706135234714 ) ) ;
#169744 = CARTESIAN_POINT ( 'NONE',  ( 19.03943276465977164, -0.05219959533909143690, 63.74890960531435979 ) ) ;
#169745 = CARTESIAN_POINT ( 'NONE',  ( 19.03943276465977164, 0.05219959533936151252, 101.2510903946856757 ) ) ;
#169746 = CARTESIAN_POINT ( 'NONE',  ( -8.224510206698735004, -14.34966873604973081, 49.58442372801901143 ) ) ;
#169747 = CARTESIAN_POINT ( 'NONE',  ( 21.53943276465977519, 0.05219959533937863772, 96.25109039468568994 ) ) ;
#169748 = CARTESIAN_POINT ( 'NONE',  ( -5.049401038297874678, -19.05341960407617918, 74.79275706135231871 ) ) ;
#169749 = CARTESIAN_POINT ( 'NONE',  ( 5.049401038298161559, -19.05341960407611168, 47.70724293864770260 ) ) ;
#169750 = CARTESIAN_POINT ( 'NONE',  ( -21.53943276465977519, 0.05219959533907696930, 66.24890960531436690 ) ) ;
#169752 = CARTESIAN_POINT ( 'NONE',  ( 16.51473224551083163, -9.474510206698727899, 75.83442372801900433 ) ) ;
#169751 = CARTESIAN_POINT ( 'NONE',  ( -12.14591786802309592, -12.06949235617757132, 71.87390960531438111 ) ) ;
#169753 = CARTESIAN_POINT ( 'NONE',  ( -19.25176906914649777, -5.499999999999856115, 70.99927264242278113 ) ) ;
#169754 = CARTESIAN_POINT ( 'NONE',  ( 5.153800228976615827, -19.02544592524334988, 50.20942372801897591 ) ) ;
#169755 = CARTESIAN_POINT ( 'NONE',  ( -12.06949235617756955, 12.14591786802309770, 25.62390960531435624 ) ) ;
#169756 = CARTESIAN_POINT ( 'NONE',  ( -14.34966873604960291, -8.224510206698953496, 71.66557627198100988 ) ) ;
#169758 = CARTESIAN_POINT ( 'NONE',  ( 27.73933785331498925, -9.013057229001033122, 143.7750000027311614 ) ) ;
#169757 = CARTESIAN_POINT ( 'NONE',  ( 10.72451020669871369, 18.67979575497193778, 107.0844237280190043 ) ) ;
#169759 = CARTESIAN_POINT ( 'NONE',  ( 15.80617190586746368, 15.72974639402197994, 109.3739096053143811 ) ) ;
#169760 = CARTESIAN_POINT ( 'NONE',  ( 0.05219959533909260263, 19.03943276465977164, 69.99890960531435269 ) ) ;
#169761 = CARTESIAN_POINT ( 'NONE',  ( -18.67979575497193778, 10.72451020669871902, 88.33442372801901854 ) ) ;
#169762 = CARTESIAN_POINT ( 'NONE',  ( 9.474510206698971260, -16.51473224551069308, 52.91557627198102409 ) ) ;
#169763 = EDGE_LOOP ( 'NONE', ( #87095, #42289, #133998, #176295 ) ) ;
#169764 = CARTESIAN_POINT ( 'NONE',  ( 19.05341960407611168, 5.049401038298154454, 23.95724293864769194 ) ) ;
#169765 = CARTESIAN_POINT ( 'NONE',  ( -16.51473224551069308, -9.474510206698971260, 111.6655762719810383 ) ) ;
#169766 = CIRCLE ( 'NONE', #98730, 0.4999999999999945044 ) ;
#169767 = CARTESIAN_POINT ( 'NONE',  ( -8.314922557960811034, -14.29746914071050412, 72.08224293864769550 ) ) ;
#169768 = CARTESIAN_POINT ( 'NONE',  ( -9.564922557960796823, -16.46253265017161027, 27.08224293864769550 ) ) ;
#169769 = CARTESIAN_POINT ( 'NONE',  ( -14.34966873604960291, -8.224510206698953496, 81.66557627198103830 ) ) ;
#169770 = CARTESIAN_POINT ( 'NONE',  ( -15.80617190586745835, -15.72974639402198527, 101.8739096053143811 ) ) ;
#169771 = CARTESIAN_POINT ( 'NONE',  ( -18.67979575497193778, 10.72451020669871902, 43.33442372801901143 ) ) ;
#169772 = CARTESIAN_POINT ( 'NONE',  ( 0.7625336781875722281, 6.293144983425331240, -62.46804555434153627 ) ) ;
#169773 = CARTESIAN_POINT ( 'NONE',  ( 16.55341960407618274, -4.379528057220086978, 51.04275706135234714 ) ) ;
#169774 = CARTESIAN_POINT ( 'NONE',  ( -5.719274019375978568, 21.55341960407610458, 100.2072429386476955 ) ) ;
#169775 = CARTESIAN_POINT ( 'NONE',  ( -0.05219959533936034679, 19.03943276465977164, 22.50109039468566152 ) ) ;
#169776 = CARTESIAN_POINT ( 'NONE',  ( -5.049401038298153566, 19.05341960407611168, 105.2072429386476671 ) ) ;
#169777 = CARTESIAN_POINT ( 'NONE',  ( 21.55341960407619695, -5.719274019375665929, 41.04275706135236135 ) ) ;
#169778 = EDGE_CURVE ( 'NONE', #11483, #85078, #101047, .T. ) ;
#169779 = CARTESIAN_POINT ( 'NONE',  ( 10.72451020669898902, -18.67979575497178502, 47.91557627198102409 ) ) ;
#169780 = CARTESIAN_POINT ( 'NONE',  ( 14.34966873604960469, 8.224510206698951720, 29.16557627198103120 ) ) ;
#169782 = CARTESIAN_POINT ( 'NONE',  ( 5.719274019375673035, 21.55341960407619339, 102.2927570613523613 ) ) ;
#169781 = CARTESIAN_POINT ( 'NONE',  ( -10.72451020669870658, -18.67979575497194134, 69.58442372801900433 ) ) ;
#169783 = CARTESIAN_POINT ( 'NONE',  ( -0.05219959533936034679, 19.03943276465977164, 27.50109039468566507 ) ) ;
#169784 = CARTESIAN_POINT ( 'NONE',  ( -4.483927247898782831, 16.52544592524335698, 82.70942372801900433 ) ) ;
#169785 = CARTESIAN_POINT ( 'NONE',  ( -5.719274019375665041, -21.55341960407619695, 54.79275706135235424 ) ) ;
#169786 = CARTESIAN_POINT ( 'NONE',  ( -9.474510206698964154, 16.51473224551069663, 50.41557627198102409 ) ) ;
#169787 = CARTESIAN_POINT ( 'NONE',  ( -19.05341960407617563, 5.049401038297882671, 23.54275706135233648 ) ) ;
#169788 = CARTESIAN_POINT ( 'NONE',  ( -15.72974639402197994, 15.80617190586746368, 30.62390960531436335 ) ) ;
#169789 = CARTESIAN_POINT ( 'NONE',  ( -10.81492255796105439, 18.62759615963255655, 22.91775706135235069 ) ) ;
#169790 = CARTESIAN_POINT ( 'NONE',  ( -18.67979575497178146, -10.72451020669898902, 81.66557627198103830 ) ) ;
#169791 = CARTESIAN_POINT ( 'NONE',  ( -8.314922557961024197, 14.29746914071037800, 42.91775706135235424 ) ) ;
#169793 = CARTESIAN_POINT ( 'NONE',  ( -21.55341960407610458, -5.719274019375992779, 81.45724293864769550 ) ) ;
#169792 = CARTESIAN_POINT ( 'NONE',  ( 69.65682714487590488, -71.74905178543389184, 0.000000000000000000 ) ) ;
#169795 = CARTESIAN_POINT ( 'NONE',  ( -8.314922557960811034, -14.29746914071050412, 62.08224293864769550 ) ) ;
#169794 = CARTESIAN_POINT ( 'NONE',  ( -12.06949235617739369, -12.14591786802326823, 69.37609039468567573 ) ) ;
#169796 = CARTESIAN_POINT ( 'NONE',  ( -22.34286686445884840, 20.24680444626648068, -48.12863666802710583 ) ) ;
#169797 = CARTESIAN_POINT ( 'NONE',  ( 9.564922557961047289, -16.46253265017146816, 100.4177570613523329 ) ) ;
#169798 = CARTESIAN_POINT ( 'NONE',  ( -9.564922557960796823, -16.46253265017161027, 112.0822429386476955 ) ) ;
#169799 = CYLINDRICAL_SURFACE ( 'NONE', #157591, 2.649999999999992806 ) ;
#169800 = CARTESIAN_POINT ( 'NONE',  ( 16.55341960407618274, -4.379528057220086978, 46.04275706135234714 ) ) ;
#169801 = CARTESIAN_POINT ( 'NONE',  ( -15.72974639402197994, 15.80617190586746368, 110.6239096053143669 ) ) ;
#169802 = CARTESIAN_POINT ( 'NONE',  ( -21.52544592524343514, 5.823673210054127303, 26.04057627198103475 ) ) ;
#169803 = CARTESIAN_POINT ( 'NONE',  ( 4.379528057220092307, 16.55341960407617563, 52.29275706135236135 ) ) ;
#169804 = CARTESIAN_POINT ( 'NONE',  ( 5.049401038298161559, -19.05341960407611168, 67.70724293864769550 ) ) ;
#169806 = CARTESIAN_POINT ( 'NONE',  ( 9.564922557961047289, -16.46253265017146816, 110.4177570613523471 ) ) ;
#169805 = CARTESIAN_POINT ( 'NONE',  ( -15.72974639402176322, -15.80617190586768395, 44.37609039468567573 ) ) ;
#169807 = CARTESIAN_POINT ( 'NONE',  ( -21.55341960407610458, -5.719274019375992779, 31.45724293864769550 ) ) ;
#169808 = ORIENTED_EDGE ( 'NONE', *, *, #167487, .F. ) ;
#169809 = CARTESIAN_POINT ( 'NONE',  ( 0.05219959533936267826, -19.03943276465977164, 30.00109039468566863 ) ) ;
#169810 =( BOUNDED_CURVE ( )  B_SPLINE_CURVE ( 2, ( #65242, #126902, #18759, #5551, #188608, #128888, #80406, #67230, #99560, #50089, #176428 ),
 .UNSPECIFIED., .F., .T. ) 
 B_SPLINE_CURVE_WITH_KNOTS ( ( 3, 2, 2, 2, 2, 3 ),
 ( 0.1000000000000000056, 0.1199999999999999956, 0.1400000000000000133, 0.1600000000000000033, 0.1799999999999999933, 0.2000000000000000111 ),
 .UNSPECIFIED. ) 
 CURVE ( )  GEOMETRIC_REPRESENTATION_ITEM ( )  RATIONAL_B_SPLINE_CURVE ( ( 1.000000000000000000, 0.9510565162951535312, 1.000000000000000000, 0.9510565162951535312, 1.000000000000000000, 0.9510565162951535312, 1.000000000000000000, 0.9510565162951535312, 1.000000000000000000, 0.9510565162951535312, 1.000000000000000000 ) ) 
 REPRESENTATION_ITEM ( '' )  );
#169811 = CARTESIAN_POINT ( 'NONE',  ( 16.52544592524335698, 4.483927247898782831, 36.45942372801901143 ) ) ;
#169812 = CARTESIAN_POINT ( 'NONE',  ( 19.03943276465977164, -0.05219959533909143690, 103.7489096053143669 ) ) ;
#169813 = CARTESIAN_POINT ( 'NONE',  ( 18.62759615963271287, -10.81492255796078972, 98.33224293864769550 ) ) ;
#169814 = CARTESIAN_POINT ( 'NONE',  ( -5.153800228976328057, -19.02544592524343514, 67.29057627198102409 ) ) ;
#169815 = CARTESIAN_POINT ( 'NONE',  ( -17.05587630539786304, 6.762274262135694158, 25.74180309037313208 ) ) ;
#169816 = CARTESIAN_POINT ( 'NONE',  ( -4.379528057220328563, 16.55341960407611168, 80.20724293864769550 ) ) ;
#169817 = CARTESIAN_POINT ( 'NONE',  ( 5.719274019375991003, -21.55341960407610458, 37.70724293864769550 ) ) ;
#169818 = CARTESIAN_POINT ( 'NONE',  ( -5.049401038298153566, 19.05341960407611168, 25.20724293864768484 ) ) ;
#169819 = CARTESIAN_POINT ( 'NONE',  ( -4.379528057220086978, -16.55341960407618274, 59.79275706135234714 ) ) ;
#169820 = CARTESIAN_POINT ( 'NONE',  ( -21.52544592524343514, 5.823673210054127303, 106.0405762719810525 ) ) ;
#169821 = CARTESIAN_POINT ( 'NONE',  ( 19.02544592524334988, 5.153800228976608722, 61.45942372801900433 ) ) ;
#169822 = CARTESIAN_POINT ( 'NONE',  ( 0.05219959533907565091, 21.53943276465977519, 29.99890960531435979 ) ) ;
#169823 = CARTESIAN_POINT ( 'NONE',  ( -0.05219959533909027116, -19.03943276465977164, 22.49890960531436690 ) ) ;
#169824 = CARTESIAN_POINT ( 'NONE',  ( 21.52544592524344225, -5.823673210054117533, 73.54057627198102409 ) ) ;
#169825 = CARTESIAN_POINT ( 'NONE',  ( -5.153800228976328057, -19.02544592524343514, 97.29057627198099567 ) ) ;
#169826 = CARTESIAN_POINT ( 'NONE',  ( -21.55341960407619339, 5.719274019375674811, 93.54275706135234714 ) ) ;
#169827 = CARTESIAN_POINT ( 'NONE',  ( 9.564922557960805705, 16.46253265017160317, 54.58224293864769550 ) ) ;
#169828 = CARTESIAN_POINT ( 'NONE',  ( 16.53943276465976808, 0.05219959533934440121, 36.25109039468567573 ) ) ;
#169829 = CARTESIAN_POINT ( 'NONE',  ( -16.46253265017160317, 9.564922557960807481, 60.83224293864769550 ) ) ;
#169830 = CARTESIAN_POINT ( 'NONE',  ( 21.55341960407619695, -5.719274019375665929, 76.04275706135237556 ) ) ;
#169831 = VERTEX_POINT ( 'NONE', #102370 ) ;
#169832 = CARTESIAN_POINT ( 'NONE',  ( -13.89961937509957401, -13.97604488694547875, 44.37609039468566863 ) ) ;
#169833 = CARTESIAN_POINT ( 'NONE',  ( 19.02544592524334988, 5.153800228976608722, 36.45942372801900433 ) ) ;
#169834 = CARTESIAN_POINT ( 'NONE',  ( 10.72451020669871369, 18.67979575497193778, 32.08442372801901854 ) ) ;
#169835 = DIRECTION ( 'NONE',  ( 0.000000000000000000, -0.3420201433256828127, -0.9396926207859033209 ) ) ;
#169836 = CARTESIAN_POINT ( 'NONE',  ( -19.03943276465977164, -0.05219959533935918106, 28.75109039468566507 ) ) ;
#169837 = CARTESIAN_POINT ( 'NONE',  ( 16.51473224551069308, 9.474510206698969483, 84.16557627198102409 ) ) ;
#169838 = CARTESIAN_POINT ( 'NONE',  ( -16.51473224551069308, -9.474510206698971260, 71.66557627198102409 ) ) ;
#169839 = CARTESIAN_POINT ( 'NONE',  ( 16.55341960407618274, -4.379528057220086978, 111.0427570613523613 ) ) ;
#169841 = CARTESIAN_POINT ( 'NONE',  ( 21.55341960407619695, -5.719274019375665929, 86.04275706135236135 ) ) ;
#169840 = CARTESIAN_POINT ( 'NONE',  ( 5.153800228976335163, 19.02544592524342804, 114.7905762719810241 ) ) ;
#169842 = CARTESIAN_POINT ( 'NONE',  ( 22.81625015709510151, -31.40387420917324590, -10.42499999726881477 ) ) ;
#169843 = CARTESIAN_POINT ( 'NONE',  ( -34.42157296979473813, 2.272259278789487968, 89.98812102125175727 ) ) ;
#169844 = CARTESIAN_POINT ( 'NONE',  ( -5.719274019375665041, -21.55341960407619695, 94.79275706135234714 ) ) ;
#169845 = CARTESIAN_POINT ( 'NONE',  ( 22.44763431097445761, -1.469699867061888376, -58.07555020237585097 ) ) ;
#169846 = CARTESIAN_POINT ( 'NONE',  ( 12.06949235617757843, -12.14591786802309237, 113.1239096053143953 ) ) ;
#169847 = CARTESIAN_POINT ( 'NONE',  ( -3.573655867282028392E-15, 2.428612866367529932E-14, 169.9999999999999716 ) ) ;
#169848 = CARTESIAN_POINT ( 'NONE',  ( 34.37139930337509952, 2.751904643975405573, 90.23455903727463578 ) ) ;
#169849 = CARTESIAN_POINT ( 'NONE',  ( 0.05219959533934541429, -16.53943276465976808, 55.00109039468568284 ) ) ;
#169850 = CARTESIAN_POINT ( 'NONE',  ( 10.81492255796078972, 18.62759615963270932, 69.58224293864769550 ) ) ;
#169851 = CARTESIAN_POINT ( 'NONE',  ( -4.483927247898539470, -16.52544592524342804, 37.29057627198102409 ) ) ;
#169853 = CARTESIAN_POINT ( 'NONE',  ( -9.474510206698964154, 16.51473224551069663, 90.41557627198103830 ) ) ;
#169852 = CARTESIAN_POINT ( 'NONE',  ( -8.314922557960811034, -14.29746914071050412, 112.0822429386477097 ) ) ;
#169854 = CARTESIAN_POINT ( 'NONE',  ( 5.153800228976615827, -19.02544592524334988, 20.20942372801899722 ) ) ;
#169855 = CARTESIAN_POINT ( 'NONE',  ( 16.53943276465976808, -0.05219959533910856209, 113.7489096053143527 ) ) ;
#169856 = CARTESIAN_POINT ( 'NONE',  ( -21.55341960407619339, 5.719274019375674811, 73.54275706135234714 ) ) ;
#169857 = CARTESIAN_POINT ( 'NONE',  ( -19.03943276465977164, 0.05219959533909376836, 111.2489096053143669 ) ) ;
#169858 = CARTESIAN_POINT ( 'NONE',  ( -14.29746914071037622, -8.314922557961029526, 109.1677570613523613 ) ) ;
#169859 = CARTESIAN_POINT ( 'NONE',  ( 16.46253265017146816, 9.564922557961045513, 61.66775706135234003 ) ) ;
#169860 = CARTESIAN_POINT ( 'NONE',  ( 36.91746824999999177, 11.99521256947799230, -6.024999997268812635 ) ) ;
#169861 = CARTESIAN_POINT ( 'NONE',  ( -5.823673210054116645, -21.52544592524344225, 27.29057627198103120 ) ) ;
#169862 = CARTESIAN_POINT ( 'NONE',  ( -4.483927247898539470, -16.52544592524342804, 87.29057627198103830 ) ) ;
#169864 = CARTESIAN_POINT ( 'NONE',  ( 13.89961937509957401, 13.97604488694547697, 56.87609039468564731 ) ) ;
#169863 = CIRCLE ( 'NONE', #111699, 216.0437394197456911 ) ;
#169865 = CARTESIAN_POINT ( 'NONE',  ( -16.46253265017160317, 9.564922557960807481, 70.83224293864770971 ) ) ;
#169866 = CARTESIAN_POINT ( 'NONE',  ( -16.52544592524342804, 4.483927247898546575, 71.04057627198103830 ) ) ;
#169867 = CARTESIAN_POINT ( 'NONE',  ( -13.97604488694547697, 13.89961937509957934, 98.12609039468566152 ) ) ;
#169868 = CARTESIAN_POINT ( 'NONE',  ( 10.81492255796078972, 18.62759615963270932, 49.58224293864769550 ) ) ;
#169869 = VERTEX_POINT ( 'NONE', #149872 ) ;
#169870 = EDGE_CURVE ( 'NONE', #81412, #191417, #54864, .T. ) ;
#169871 = CARTESIAN_POINT ( 'NONE',  ( -19.03943276465977164, 0.05219959533909376836, 21.24890960531436335 ) ) ;
#169872 = CARTESIAN_POINT ( 'NONE',  ( -17.26172910966778673, -6.454744622555875111, 29.19353091350778229 ) ) ;
#169874 = CARTESIAN_POINT ( 'NONE',  ( -10.81492255796078084, -18.62759615963271287, 72.08224293864769550 ) ) ;
#169873 = CARTESIAN_POINT ( 'NONE',  ( -13.97604488694527625, -13.89961937509977652, 71.87390960531433848 ) ) ;
#169876 = CARTESIAN_POINT ( 'NONE',  ( -19.05341960407611168, -5.049401038298163336, 71.45724293864766707 ) ) ;
#169875 = CARTESIAN_POINT ( 'NONE',  ( -14.29746914071037622, -8.314922557961029526, 89.16775706135236135 ) ) ;
#169877 = CARTESIAN_POINT ( 'NONE',  ( 19.02544592524334988, 5.153800228976608722, 66.45942372801899012 ) ) ;
#169878 = CARTESIAN_POINT ( 'NONE',  ( 21.55341960407619695, -5.719274019375665929, 76.04275706135237556 ) ) ;
#169879 = CARTESIAN_POINT ( 'NONE',  ( 21.53943276465977519, -0.05219959533907433946, 63.74890960531435979 ) ) ;
#169880 = CARTESIAN_POINT ( 'NONE',  ( -19.02544592524342804, 5.153800228976336051, 116.0405762719810383 ) ) ;
#169881 = CARTESIAN_POINT ( 'NONE',  ( -16.51473224551069308, -9.474510206698971260, 36.66557627198102409 ) ) ;
#169882 = CARTESIAN_POINT ( 'NONE',  ( 14.34966873604972726, -8.224510206698740333, 105.8344237280190328 ) ) ;
#169883 = CARTESIAN_POINT ( 'NONE',  ( 5.153800228976335163, 19.02544592524342804, 54.79057627198103120 ) ) ;
#169884 = CARTESIAN_POINT ( 'NONE',  ( -4.483927247898782831, 16.52544592524335698, 22.70942372801901499 ) ) ;
#169885 = CARTESIAN_POINT ( 'NONE',  ( 16.19135201231370047, 7.376712067591809863, 52.68680854052031748 ) ) ;
#169886 = CARTESIAN_POINT ( 'NONE',  ( 5.823673210054444382, -21.52544592524334988, 105.2094237280190328 ) ) ;
#169887 = CARTESIAN_POINT ( 'NONE',  ( 14.34966873604960469, 8.224510206698951720, 59.16557627198103120 ) ) ;
#169888 = CARTESIAN_POINT ( 'NONE',  ( 10.72451020669898902, -18.67979575497178502, 102.9155762719810383 ) ) ;
#169889 = CARTESIAN_POINT ( 'NONE',  ( -18.62759615963270932, 10.81492255796079327, 100.8322429386477097 ) ) ;
#169890 = CARTESIAN_POINT ( 'NONE',  ( -4.384086992840744657, 4.242615737635153650, -64.53213882399992940 ) ) ;
#169891 = CARTESIAN_POINT ( 'NONE',  ( 5.823673210054125526, 21.52544592524343514, 44.79057627198103120 ) ) ;
#169892 = CARTESIAN_POINT ( 'NONE',  ( -14.29746914071037622, -8.314922557961029526, 84.16775706135234714 ) ) ;
#169893 = CARTESIAN_POINT ( 'NONE',  ( -12.14591786802309592, -12.06949235617757132, 96.87390960531436690 ) ) ;
#169894 = CARTESIAN_POINT ( 'NONE',  ( 0.05219959533909260263, 19.03943276465977164, 64.99890960531436690 ) ) ;
#169895 =( NAMED_UNIT ( * ) PLANE_ANGLE_UNIT ( ) SI_UNIT ( $, .RADIAN. ) );
#169896 = CARTESIAN_POINT ( 'NONE',  ( -8.839334217631824586, -46.13630234914189288, -24.17074550867520344 ) ) ;
#169897 = CARTESIAN_POINT ( 'NONE',  ( -12.06949235617739369, -12.14591786802326823, 104.3760903946856899 ) ) ;
#169898 = CARTESIAN_POINT ( 'NONE',  ( -5.823673210054431948, 21.52544592524334988, 32.70942372801900433 ) ) ;
#169899 = CARTESIAN_POINT ( 'NONE',  ( -0.05219959533909027116, -19.03943276465977164, 92.49890960531436690 ) ) ;
#169900 = CARTESIAN_POINT ( 'NONE',  ( -10.81492255796105439, 18.62759615963255655, 62.91775706135236135 ) ) ;
#169901 = CARTESIAN_POINT ( 'NONE',  ( -30.00000000000000000, 5.499999999999992895, 102.5000000000000142 ) ) ;
#169902 = CARTESIAN_POINT ( 'NONE',  ( -28.82186960331499037, 2.428612866367529932E-14, 148.2500000054623683 ) ) ;
#169903 = ORIENTED_EDGE ( 'NONE', *, *, #166889, .F. ) ;
#169904 = CARTESIAN_POINT ( 'NONE',  ( -10.81492255796105439, 18.62759615963255655, 62.91775706135236135 ) ) ;
#169905 = CARTESIAN_POINT ( 'NONE',  ( -13.97604488694527625, -13.89961937509977652, 56.87390960531434558 ) ) ;
#169906 = CARTESIAN_POINT ( 'NONE',  ( 19.03943276465977164, -0.05219959533909143690, 83.74890960531436690 ) ) ;
#169907 = CARTESIAN_POINT ( 'NONE',  ( -16.46253265017146816, -9.564922557961047289, 69.16775706135233293 ) ) ;
#169908 = CARTESIAN_POINT ( 'NONE',  ( 21.55341960407619695, -5.719274019375665929, 46.04275706135234714 ) ) ;
#169909 = CARTESIAN_POINT ( 'NONE',  ( 19.03943276465977164, 0.05219959533936151252, 106.2510903946856615 ) ) ;
#169910 = CIRCLE ( 'NONE', #195786, 59.99999999999998579 ) ;
#169911 = CARTESIAN_POINT ( 'NONE',  ( 16.51473224551083163, -9.474510206698727899, 65.83442372801900433 ) ) ;
#169912 = CARTESIAN_POINT ( 'NONE',  ( 0.05219959533909260263, 19.03943276465977164, 34.99890960531435979 ) ) ;
#169913 = CARTESIAN_POINT ( 'NONE',  ( -8.314922557961024197, 14.29746914071037800, 107.9177570613523471 ) ) ;
#169914 = CARTESIAN_POINT ( 'NONE',  ( 13.89961937509957401, 13.97604488694547697, 81.87609039468564731 ) ) ;
#169915 = CARTESIAN_POINT ( 'NONE',  ( 0.05219959533910956823, 16.53943276465976808, 29.99890960531435979 ) ) ;
#169916 = CARTESIAN_POINT ( 'NONE',  ( 19.03943276465977164, 0.05219959533936151252, 46.25109039468566863 ) ) ;
#169917 = CARTESIAN_POINT ( 'NONE',  ( 0.05219959533937995610, -21.53943276465977519, 100.0010903946857042 ) ) ;
#169918 = CARTESIAN_POINT ( 'NONE',  ( 19.03943276465977164, 0.05219959533936151252, 26.25109039468566507 ) ) ;
#169919 = CARTESIAN_POINT ( 'NONE',  ( 16.46253265017160672, -9.564922557960803928, 23.33224293864769194 ) ) ;
#169920 = CARTESIAN_POINT ( 'NONE',  ( -5.823673210054431948, 21.52544592524334988, 87.70942372801901854 ) ) ;
#169921 = CARTESIAN_POINT ( 'NONE',  ( 8.314922557961029526, -14.29746914071037800, 35.41775706135234003 ) ) ;
#169922 = CARTESIAN_POINT ( 'NONE',  ( 0.05219959533909260263, 19.03943276465977164, 94.99890960531436690 ) ) ;
#169923 = CARTESIAN_POINT ( 'NONE',  ( -27.73933785331498925, 9.013057229001089965, 146.7750000027312183 ) ) ;
#169924 = CARTESIAN_POINT ( 'NONE',  ( 5.153800228976335163, 19.02544592524342804, 79.79057627198102409 ) ) ;
#169925 = DIRECTION ( 'NONE',  ( 1.000000000000000000, 0.000000000000000000, 0.000000000000000000 ) ) ;
#169926 = ORIENTED_EDGE ( 'NONE', *, *, #170997, .T. ) ;
#169927 = CARTESIAN_POINT ( 'NONE',  ( -19.05341960407617563, 5.049401038297882671, 83.54275706135233293 ) ) ;
#169928 = CARTESIAN_POINT ( 'NONE',  ( 13.97604488694527802, 13.89961937509977652, 109.3739096053143669 ) ) ;
#169930 = CARTESIAN_POINT ( 'NONE',  ( -19.03943276465977164, -0.05219959533935918106, 98.75109039468567573 ) ) ;
#169929 = CARTESIAN_POINT ( 'NONE',  ( 19.03943276465977164, 0.05219959533936151252, 21.25109039468565797 ) ) ;
#169931 = CARTESIAN_POINT ( 'NONE',  ( 4.379528057220339221, -16.55341960407611168, 92.70724293864770971 ) ) ;
#169932 = CARTESIAN_POINT ( 'NONE',  ( -5.153800228976328057, -19.02544592524343514, 27.29057627198103120 ) ) ;
#169933 = CARTESIAN_POINT ( 'NONE',  ( 15.72974639402199770, -15.80617190586745480, 63.12390960531435979 ) ) ;
#169934 = CARTESIAN_POINT ( 'NONE',  ( -5.823673210054116645, -21.52544592524344225, 42.29057627198103120 ) ) ;
#169935 = CARTESIAN_POINT ( 'NONE',  ( 16.55341960407611168, 4.379528057220329451, 113.9572429386477239 ) ) ;
#169936 = DIRECTION ( 'NONE',  ( -0.000000000000000000, 0.000000000000000000, 1.000000000000000000 ) ) ;
#169937 = CARTESIAN_POINT ( 'NONE',  ( -9.474510206698720793, -16.51473224551083518, 54.58442372801899722 ) ) ;
#169938 = CARTESIAN_POINT ( 'NONE',  ( -16.52544592524342804, 4.483927247898546575, 46.04057627198103830 ) ) ;
#169939 = CARTESIAN_POINT ( 'NONE',  ( -10.72451020669898014, 18.67979575497178502, 25.41557627198103120 ) ) ;
#169940 = CARTESIAN_POINT ( 'NONE',  ( 15.72974639402176855, 15.80617190586768217, 76.87609039468567573 ) ) ;
#169941 = CARTESIAN_POINT ( 'NONE',  ( -15.80617190586745835, -15.72974639402198527, 71.87390960531438111 ) ) ;
#169942 = CARTESIAN_POINT ( 'NONE',  ( -15.80617190586768217, 15.72974639402176855, 58.12609039468568994 ) ) ;
#169943 = CARTESIAN_POINT ( 'NONE',  ( -5.823673210054431948, 21.52544592524334988, 52.70942372801902565 ) ) ;
#169944 = CARTESIAN_POINT ( 'NONE',  ( 16.46253265017160672, -9.564922557960803928, 88.33224293864769550 ) ) ;
#169945 = CARTESIAN_POINT ( 'NONE',  ( -8.314922557961024197, 14.29746914071037800, 77.91775706135231871 ) ) ;
#169946 = CARTESIAN_POINT ( 'NONE',  ( 13.89961937509977652, -13.97604488694527269, 28.12390960531435624 ) ) ;
#169947 = CARTESIAN_POINT ( 'NONE',  ( -31.54545164052522566, 7.106679946642016077, 92.55365670706888181 ) ) ;
#169948 = CARTESIAN_POINT ( 'NONE',  ( 16.52544592524342804, -4.483927247898539470, 48.54057627198103120 ) ) ;
#169949 = CARTESIAN_POINT ( 'NONE',  ( 16.53943276465976808, -0.05219959533910856209, 28.74890960531435624 ) ) ;
#169950 = CARTESIAN_POINT ( 'NONE',  ( -5.153800228976328057, -19.02544592524343514, 72.29057627198102409 ) ) ;
#169951 = CARTESIAN_POINT ( 'NONE',  ( -16.51473224551069308, -9.474510206698971260, 36.66557627198102409 ) ) ;
#169952 = CARTESIAN_POINT ( 'NONE',  ( -21.52544592524343514, 5.823673210054127303, 51.04057627198103120 ) ) ;
#169953 = CARTESIAN_POINT ( 'NONE',  ( 16.46253265017146816, 9.564922557961045513, 31.66775706135232937 ) ) ;
#169955 = CARTESIAN_POINT ( 'NONE',  ( -8.314922557960811034, -14.29746914071050412, 52.08224293864768839 ) ) ;
#169954 = CARTESIAN_POINT ( 'NONE',  ( -28.90000000000004476, 2.980639576201346218E-13, -64.92279855667830191 ) ) ;
#169956 = CARTESIAN_POINT ( 'NONE',  ( -5.823673210054116645, -21.52544592524344225, 22.29057627198102765 ) ) ;
#169957 = DIRECTION ( 'NONE',  ( -0.000000000000000000, -0.000000000000000000, 1.000000000000000000 ) ) ;
#169958 = CARTESIAN_POINT ( 'NONE',  ( -12.14591786802326823, 12.06949235617739902, 78.12609039468570415 ) ) ;
#169959 = CARTESIAN_POINT ( 'NONE',  ( 9.564922557961047289, -16.46253265017146816, 70.41775706135233293 ) ) ;
#169960 = CARTESIAN_POINT ( 'NONE',  ( -12.06949235617756955, 12.14591786802309770, 40.62390960531435269 ) ) ;
#169961 = CARTESIAN_POINT ( 'NONE',  ( -19.20446147854525876, -5.500000000000005329, 74.38999695167674986 ) ) ;
#169962 = CARTESIAN_POINT ( 'NONE',  ( 4.483927247898545687, 16.52544592524342804, 29.79057627198102409 ) ) ;
#169963 = CARTESIAN_POINT ( 'NONE',  ( -9.564922557960796823, -16.46253265017161027, 57.08224293864769550 ) ) ;
#169964 = CARTESIAN_POINT ( 'NONE',  ( 19.05341960407611168, 5.049401038298154454, 63.95724293864769550 ) ) ;
#169965 = CARTESIAN_POINT ( 'NONE',  ( 0.05219959533909260263, 19.03943276465977164, 34.99890960531435979 ) ) ;
#169966 = CARTESIAN_POINT ( 'NONE',  ( 10.81492255796106328, -18.62759615963255655, 50.41775706135235424 ) ) ;
#169967 = CARTESIAN_POINT ( 'NONE',  ( 0.05219959533909260263, 19.03943276465977164, 59.99890960531436690 ) ) ;
#169968 = DIRECTION ( 'NONE',  ( -0.000000000000000000, -0.000000000000000000, -1.000000000000000000 ) ) ;
#169969 = CARTESIAN_POINT ( 'NONE',  ( -16.46253265017160317, 9.564922557960807481, 40.83224293864769550 ) ) ;
#169970 = EDGE_CURVE ( 'NONE', #132379, #95422, #96816, .T. ) ;
#169971 = CARTESIAN_POINT ( 'NONE',  ( 15.72974639402199770, -15.80617190586745480, 38.12390960531436690 ) ) ;
#169973 = CARTESIAN_POINT ( 'NONE',  ( -0.05219959533909027116, -19.03943276465977164, 27.49890960531435624 ) ) ;
#169972 = CARTESIAN_POINT ( 'NONE',  ( -21.52544592524334988, -5.823673210054445271, 63.95942372801901854 ) ) ;
#169974 = CARTESIAN_POINT ( 'NONE',  ( -0.05219959533907301413, -21.53943276465977519, 22.49890960531436335 ) ) ;
#169975 = CARTESIAN_POINT ( 'NONE',  ( 14.34966873604972726, -8.224510206698740333, 95.83442372801903275 ) ) ;
#169976 = CARTESIAN_POINT ( 'NONE',  ( 0.05219959533937995610, -21.53943276465977519, 110.0010903946856757 ) ) ;
#169977 = CARTESIAN_POINT ( 'NONE',  ( 16.55341960407618274, -4.379528057220086978, 71.04275706135234714 ) ) ;
#169978 = CARTESIAN_POINT ( 'NONE',  ( 19.02544592524343514, -5.153800228976328945, 103.5405762719809957 ) ) ;
#169979 = EDGE_CURVE ( 'NONE', #50285, #48134, #131707, .T. ) ;
#169980 = CARTESIAN_POINT ( 'NONE',  ( 8.314922557961029526, -14.29746914071037800, 55.41775706135234714 ) ) ;
#169981 = CARTESIAN_POINT ( 'NONE',  ( 16.53943276465976808, 0.05219959533934440121, 46.25109039468567573 ) ) ;
#169982 = CARTESIAN_POINT ( 'NONE',  ( 8.314922557961029526, -14.29746914071037800, 100.4177570613523471 ) ) ;
#169983 = CARTESIAN_POINT ( 'NONE',  ( -10.72451020669870658, -18.67979575497194134, 54.58442372801901143 ) ) ;
#169984 = CARTESIAN_POINT ( 'NONE',  ( 14.34966873604972726, -8.224510206698740333, 20.83442372801901143 ) ) ;
#169985 = CARTESIAN_POINT ( 'NONE',  ( 18.62759615963271287, -10.81492255796078972, 108.3322429386477097 ) ) ;
#169986 = CARTESIAN_POINT ( 'NONE',  ( -16.52544592524335698, -4.483927247898792601, 28.95942372801902209 ) ) ;
#169987 = CARTESIAN_POINT ( 'NONE',  ( -16.53943276465976808, -0.05219959533934237506, 88.75109039468567573 ) ) ;
#169988 = CARTESIAN_POINT ( 'NONE',  ( -16.38665767534995510, 7.295008042176403862, 45.26400864214468811 ) ) ;
#169989 = CARTESIAN_POINT ( 'NONE',  ( 21.55341960407619695, -5.719274019375665929, 81.04275706135236135 ) ) ;
#169990 = CARTESIAN_POINT ( 'NONE',  ( -19.02544592524334988, -5.153800228976617603, 83.95942372801901854 ) ) ;
#169991 = CARTESIAN_POINT ( 'NONE',  ( -12.14591786802309592, -12.06949235617757132, 56.87390960531436690 ) ) ;
#169992 = CARTESIAN_POINT ( 'NONE',  ( 0.05219959533910956823, 16.53943276465976808, 44.99890960531435979 ) ) ;
#169993 = CARTESIAN_POINT ( 'NONE',  ( 12.14591786802309770, 12.06949235617756955, 109.3739096053143811 ) ) ;
#169995 = CARTESIAN_POINT ( 'NONE',  ( 17.48853670773249291, -5.747243402302947501, 56.16671299749993551 ) ) ;
#169994 = CARTESIAN_POINT ( 'NONE',  ( 9.474510206698729675, 16.51473224551082808, 52.08442372801900433 ) ) ;
#169996 = CARTESIAN_POINT ( 'NONE',  ( 5.823673210054444382, -21.52544592524334988, 55.20942372801902565 ) ) ;
#169997 = CARTESIAN_POINT ( 'NONE',  ( -19.05341960407617563, 5.049401038297882671, 108.5427570613523187 ) ) ;
#169998 = PLANE ( 'NONE',  #14768 ) ;
#169999 = CARTESIAN_POINT ( 'NONE',  ( 16.46253265017160672, -9.564922557960803928, 103.3322429386476955 ) ) ;
#170000 = CARTESIAN_POINT ( 'NONE',  ( -15.72974639402197994, 15.80617190586746368, 70.62390960531436690 ) ) ;
#170001 = CARTESIAN_POINT ( 'NONE',  ( -13.89961937509957401, -13.97604488694547875, 94.37609039468566152 ) ) ;
#170002 = CARTESIAN_POINT ( 'NONE',  ( -5.049401038298153566, 19.05341960407611168, 100.2072429386476955 ) ) ;
#170003 = CARTESIAN_POINT ( 'NONE',  ( 21.53943276465977519, -0.05219959533907433946, 58.74890960531436690 ) ) ;
#170004 = CARTESIAN_POINT ( 'NONE',  ( 4.379528057220339221, -16.55341960407611168, 112.7072429386476955 ) ) ;
#170005 = CARTESIAN_POINT ( 'NONE',  ( -10.72451020669870658, -18.67979575497194134, 99.58442372801900433 ) ) ;
#170006 = CARTESIAN_POINT ( 'NONE',  ( 9.564922557960805705, 16.46253265017160317, 24.58224293864769194 ) ) ;
#170007 = CIRCLE ( 'NONE', #79512, 4.999999999999998224 ) ;
#170008 = CARTESIAN_POINT ( 'NONE',  ( -10.81492255796105439, 18.62759615963255655, 37.91775706135235424 ) ) ;
#170009 = CARTESIAN_POINT ( 'NONE',  ( -21.55341960407619339, 5.719274019375674811, 93.54275706135234714 ) ) ;
#170010 = CARTESIAN_POINT ( 'NONE',  ( -14.29746914071037622, -8.314922557961029526, 84.16775706135234714 ) ) ;
#170011 = CARTESIAN_POINT ( 'NONE',  ( -18.67979575497193778, 10.72451020669871902, 33.33442372801900433 ) ) ;
#170012 = CARTESIAN_POINT ( 'NONE',  ( 21.55341960407619695, -5.719274019375665929, 41.04275706135236135 ) ) ;
#170014 = CARTESIAN_POINT ( 'NONE',  ( 16.51473224551069308, 9.474510206698969483, 74.16557627198103830 ) ) ;
#170013 = CARTESIAN_POINT ( 'NONE',  ( -9.564922557961040184, 16.46253265017147172, 72.91775706135233293 ) ) ;
#170015 = CARTESIAN_POINT ( 'NONE',  ( -14.34966873604960291, -8.224510206698953496, 106.6655762719810383 ) ) ;
#170016 = EDGE_CURVE ( 'NONE', #196503, #14377, #37692, .T. ) ;
#170017 = CARTESIAN_POINT ( 'NONE',  ( -10.81492255796078084, -18.62759615963271287, 77.08224293864769550 ) ) ;
#170018 = CARTESIAN_POINT ( 'NONE',  ( 8.224510206698953496, -14.34966873604960469, 62.91557627198102409 ) ) ;
#170019 = CARTESIAN_POINT ( 'NONE',  ( 15.80617190586769283, -15.72974639402175789, 100.6260903946857184 ) ) ;
#170020 = CARTESIAN_POINT ( 'NONE',  ( 16.55341960407611168, 4.379528057220329451, 83.95724293864770971 ) ) ;
#170021 = CARTESIAN_POINT ( 'NONE',  ( 19.03943276465977164, -0.05219959533909143690, 33.74890960531435979 ) ) ;
#170022 = CARTESIAN_POINT ( 'NONE',  ( 9.474510206698729675, 16.51473224551082808, 77.08442372801900433 ) ) ;
#170023 = CARTESIAN_POINT ( 'NONE',  ( 16.55341960407611168, 4.379528057220329451, 28.95724293864769905 ) ) ;
#170024 = CARTESIAN_POINT ( 'NONE',  ( -0.05219959533937732626, 21.53943276465977519, 92.50109039468567573 ) ) ;
#170025 = CARTESIAN_POINT ( 'NONE',  ( -19.03943276465977164, 0.05219959533909376836, 96.24890960531436690 ) ) ;
#170026 = CARTESIAN_POINT ( 'NONE',  ( -16.46253265017146816, -9.564922557961047289, 64.16775706135233293 ) ) ;
#170027 = CARTESIAN_POINT ( 'NONE',  ( -10.72451020669898014, 18.67979575497178502, 65.41557627198102409 ) ) ;
#170028 = CARTESIAN_POINT ( 'NONE',  ( 21.55341960407610458, 5.719274019375980345, 113.9572429386477239 ) ) ;
#170029 = CARTESIAN_POINT ( 'NONE',  ( 19.05341960407617918, -5.049401038297876454, 111.0427570613523329 ) ) ;
#170030 = CARTESIAN_POINT ( 'NONE',  ( -12.06949235617739369, -12.14591786802326823, 84.37609039468570415 ) ) ;
#170032 = CARTESIAN_POINT ( 'NONE',  ( 5.719274019375673035, 21.55341960407619339, 27.29275706135234358 ) ) ;
#170031 = CARTESIAN_POINT ( 'NONE',  ( 2.310831529832237923E-15, -71.74905152827281540, -14.99410988490250496 ) ) ;
#170033 = CARTESIAN_POINT ( 'NONE',  ( -4.483927247898539470, -16.52544592524342804, 107.2905762719810525 ) ) ;
#170034 = CARTESIAN_POINT ( 'NONE',  ( -5.950531402560715689E-15, 38.81732327939063509, -9.624999997268815832 ) ) ;
#170035 = CARTESIAN_POINT ( 'NONE',  ( -14.29746914071037622, -8.314922557961029526, 44.16775706135234714 ) ) ;
#170036 = CARTESIAN_POINT ( 'NONE',  ( -12.14591786802309592, -12.06949235617757132, 81.87390960531435269 ) ) ;
#170037 = CARTESIAN_POINT ( 'NONE',  ( -15.72974639402197994, 15.80617190586746368, 70.62390960531436690 ) ) ;
#170038 = CARTESIAN_POINT ( 'NONE',  ( -12.14591786802326823, 12.06949235617739902, 108.1260903946856757 ) ) ;
#170039 = CARTESIAN_POINT ( 'NONE',  ( 8.224510206698742110, 14.34966873604972548, 32.08442372801901854 ) ) ;
#170040 = CARTESIAN_POINT ( 'NONE',  ( 0.05219959533909260263, 19.03943276465977164, 44.99890960531435979 ) ) ;
#170041 = CARTESIAN_POINT ( 'NONE',  ( -16.55341960407617563, 4.379528057220093196, 83.54275706135234714 ) ) ;
#170042 = CARTESIAN_POINT ( 'NONE',  ( 0.05219959533936267826, -19.03943276465977164, 75.00109039468566152 ) ) ;
#170043 = CARTESIAN_POINT ( 'NONE',  ( -18.67979575497178146, -10.72451020669898902, 76.66557627198103830 ) ) ;
#170044 = CARTESIAN_POINT ( 'NONE',  ( -16.53943276465976808, -0.05219959533934237506, 93.75109039468567573 ) ) ;
#170045 = CARTESIAN_POINT ( 'NONE',  ( -15.80617190586768217, 15.72974639402176855, 83.12609039468568994 ) ) ;
#170046 = CARTESIAN_POINT ( 'NONE',  ( -21.52544592524343514, 5.823673210054127303, 66.04057627198103830 ) ) ;
#170047 = CARTESIAN_POINT ( 'NONE',  ( -21.53943276465977519, 0.05219959533907696930, 41.24890960531435269 ) ) ;
#170048 = ORIENTED_EDGE ( 'NONE', *, *, #36780, .F. ) ;
#170049 = CARTESIAN_POINT ( 'NONE',  ( -4.379528057220086978, -16.55341960407618274, 84.79275706135234714 ) ) ;
#170050 = CARTESIAN_POINT ( 'NONE',  ( 18.67979575497178502, 10.72451020669898547, 49.16557627198102409 ) ) ;
#170051 = ORIENTED_EDGE ( 'NONE', *, *, #104283, .F. ) ;
#170052 = CARTESIAN_POINT ( 'NONE',  ( -19.03943276465977164, 0.05219959533909376836, 116.2489096053143669 ) ) ;
#170053 = LINE ( 'NONE', #91196, #79116 ) ;
#170054 = CARTESIAN_POINT ( 'NONE',  ( -19.05341960407611168, -5.049401038298163336, 31.45724293864769550 ) ) ;
#170055 = CARTESIAN_POINT ( 'NONE',  ( -15.72974639402197994, 15.80617190586746368, 75.62390960531439532 ) ) ;
#170056 = CARTESIAN_POINT ( 'NONE',  ( -4.379528057220086978, -16.55341960407618274, 109.7927570613523613 ) ) ;
#170057 = CARTESIAN_POINT ( 'NONE',  ( -0.05219959533937732626, 21.53943276465977519, 52.50109039468567573 ) ) ;
#170058 = CARTESIAN_POINT ( 'NONE',  ( -12.14591786802326823, 12.06949235617739902, 28.12609039468568284 ) ) ;
#170059 = CARTESIAN_POINT ( 'NONE',  ( -9.564922557960796823, -16.46253265017161027, 22.08224293864768839 ) ) ;
#170060 = CARTESIAN_POINT ( 'NONE',  ( 16.55341960407618274, -4.379528057220086978, 21.04275706135234714 ) ) ;
#170061 = AXIS2_PLACEMENT_3D ( 'NONE', #5989, #50527, #17200 ) ;
#170062 = CARTESIAN_POINT ( 'NONE',  ( 19.05341960407611168, 5.049401038298154454, 33.95724293864769550 ) ) ;
#170063 = CARTESIAN_POINT ( 'NONE',  ( -23.31738231874055600, 16.94106989632528837, 141.7999999999999829 ) ) ;
#170064 = CARTESIAN_POINT ( 'NONE',  ( -5.049401038298153566, 19.05341960407611168, 110.2072429386476671 ) ) ;
#170065 = CARTESIAN_POINT ( 'NONE',  ( -14.29746914071037622, -8.314922557961029526, 89.16775706135236135 ) ) ;
#170066 = CARTESIAN_POINT ( 'NONE',  ( 16.46253265017146816, 9.564922557961045513, 76.66775706135234714 ) ) ;
#170067 = CARTESIAN_POINT ( 'NONE',  ( 19.02544592524334988, 5.153800228976608722, 21.45942372801899012 ) ) ;
#170068 = CARTESIAN_POINT ( 'NONE',  ( -18.62759615963270932, 10.81492255796079327, 55.83224293864770260 ) ) ;
#170069 = CARTESIAN_POINT ( 'NONE',  ( -4.483927247898782831, 16.52544592524335698, 92.70942372801901854 ) ) ;
#170070 = CARTESIAN_POINT ( 'NONE',  ( 5.153800228976615827, -19.02544592524334988, 90.20942372801900433 ) ) ;
#170071 = CARTESIAN_POINT ( 'NONE',  ( 9.564922557960805705, 16.46253265017160317, 54.58224293864769550 ) ) ;
#170072 = CARTESIAN_POINT ( 'NONE',  ( -9.564922557960796823, -16.46253265017161027, 97.08224293864769550 ) ) ;
#170073 = CARTESIAN_POINT ( 'NONE',  ( -21.52544592524334988, -5.823673210054445271, 53.95942372801900433 ) ) ;
#170074 = CARTESIAN_POINT ( 'NONE',  ( -16.51473224551069308, -9.474510206698971260, 41.66557627198103120 ) ) ;
#170075 = CARTESIAN_POINT ( 'NONE',  ( 25.62062145120188816, -9.171473787276744005, 171.1688781158082691 ) ) ;
#170076 = CARTESIAN_POINT ( 'NONE',  ( 9.474510206698971260, -16.51473224551069308, 102.9155762719810241 ) ) ;
#170077 = CARTESIAN_POINT ( 'NONE',  ( 16.55341960407611168, 4.379528057220329451, 68.95724293864769550 ) ) ;
#170078 = CARTESIAN_POINT ( 'NONE',  ( -21.52544592524343514, 5.823673210054127303, 56.04057627198102409 ) ) ;
#170079 = CARTESIAN_POINT ( 'NONE',  ( 20.22402473803820300, -1.857821124618943331, 102.5000000000000284 ) ) ;
#170080 = CARTESIAN_POINT ( 'NONE',  ( -19.05341960407617563, 5.049401038297882671, 43.54275706135232582 ) ) ;
#170082 = CARTESIAN_POINT ( 'NONE',  ( 0.05219959533909260263, 19.03943276465977164, 74.99890960531435269 ) ) ;
#170081 = CARTESIAN_POINT ( 'NONE',  ( -19.05341960407611168, -5.049401038298163336, 61.45724293864769550 ) ) ;
#170083 = CARTESIAN_POINT ( 'NONE',  ( -16.53943276465976808, -0.05219959533934237506, 53.75109039468568994 ) ) ;
#170084 = CARTESIAN_POINT ( 'NONE',  ( -17.29957754486504129, -5.500000000000000888, 21.12734848878977445 ) ) ;
#170085 = CARTESIAN_POINT ( 'NONE',  ( -12.06949235617739369, -12.14591786802326823, 84.37609039468570415 ) ) ;
#170086 = CARTESIAN_POINT ( 'NONE',  ( 15.38830714838548452, -1.491100297015996556, -59.71292413584865244 ) ) ;
#170087 = CARTESIAN_POINT ( 'NONE',  ( -4.483927247898782831, 16.52544592524335698, 77.70942372801900433 ) ) ;
#170088 = CARTESIAN_POINT ( 'NONE',  ( 8.224510206698742110, 14.34966873604972548, 57.08442372801901854 ) ) ;
#170089 = CARTESIAN_POINT ( 'NONE',  ( 0.05219959533936267826, -19.03943276465977164, 20.00109039468567218 ) ) ;
#170091 = CARTESIAN_POINT ( 'NONE',  ( 0.000000000000000000, 5.795830589372932273, 190.0000000000000000 ) ) ;
#170090 = CARTESIAN_POINT ( 'NONE',  ( -19.02544592524342804, 5.153800228976336051, 51.04057627198103120 ) ) ;
#170092 = CARTESIAN_POINT ( 'NONE',  ( -21.52544592524334988, -5.823673210054445271, 58.95942372801902565 ) ) ;
#170093 = CARTESIAN_POINT ( 'NONE',  ( 16.46253265017146816, 9.564922557961045513, 61.66775706135234003 ) ) ;
#170094 = CARTESIAN_POINT ( 'NONE',  ( 15.72974639402176855, 15.80617190586768217, 111.8760903946856615 ) ) ;
#170095 = CARTESIAN_POINT ( 'NONE',  ( 9.474510206698971260, -16.51473224551069308, 27.91557627198103120 ) ) ;
#170096 = CARTESIAN_POINT ( 'NONE',  ( -17.06172130128252462, 14.93915603648724399, -57.95097928225586514 ) ) ;
#170097 = CARTESIAN_POINT ( 'NONE',  ( 21.53943276465977519, -0.05219959533907433946, 73.74890960531433848 ) ) ;
#170098 = EDGE_CURVE ( 'NONE', #22834, #44025, #88188, .T. ) ;
#170099 = CARTESIAN_POINT ( 'NONE',  ( -15.80617190586745835, -15.72974639402198527, 26.87390960531435979 ) ) ;
#170100 = CARTESIAN_POINT ( 'NONE',  ( -16.53943276465976808, 0.05219959533911058130, 116.2489096053143669 ) ) ;
#170101 = CARTESIAN_POINT ( 'NONE',  ( 14.29746914071037800, 8.314922557961029526, 31.66775706135234358 ) ) ;
#170102 = CARTESIAN_POINT ( 'NONE',  ( -16.53943276465976808, 0.05219959533911058130, 36.24890960531435979 ) ) ;
#170103 = ORIENTED_EDGE ( 'NONE', *, *, #167369, .F. ) ;
#170104 = CARTESIAN_POINT ( 'NONE',  ( -21.53943276465977519, 0.05219959533907696930, 111.2489096053143669 ) ) ;
#170106 = CARTESIAN_POINT ( 'NONE',  ( -13.89961937509977652, 13.97604488694528158, 110.6239096053143243 ) ) ;
#170105 = CARTESIAN_POINT ( 'NONE',  ( 12.06949235617757843, -12.14591786802309237, 43.12390960531435269 ) ) ;
#170107 = CARTESIAN_POINT ( 'NONE',  ( -13.97604488694547697, 13.89961937509957934, 103.1260903946856473 ) ) ;
#170108 = CARTESIAN_POINT ( 'NONE',  ( -13.97604488694547697, 13.89961937509957934, 23.12609039468565442 ) ) ;
#170109 = CARTESIAN_POINT ( 'NONE',  ( -16.52544592524342804, 4.483927247898546575, 41.04057627198103120 ) ) ;
#170110 = CARTESIAN_POINT ( 'NONE',  ( -0.05219959533907301413, -21.53943276465977519, 97.49890960531436690 ) ) ;
#170112 = CARTESIAN_POINT ( 'NONE',  ( 10.81492255796078972, 18.62759615963270932, 64.58224293864769550 ) ) ;
#170111 = CARTESIAN_POINT ( 'NONE',  ( -3.573655867282028392E-15, 12.39993551617566681, 175.0000000000000000 ) ) ;
#170113 = CARTESIAN_POINT ( 'NONE',  ( 0.05219959533909260263, 19.03943276465977164, 79.99890960531436690 ) ) ;
#170114 = CARTESIAN_POINT ( 'NONE',  ( -16.53943276465976808, 0.05219959533911058130, 51.24890960531436690 ) ) ;
#170115 = CARTESIAN_POINT ( 'NONE',  ( -13.97604488694527625, -13.89961937509977652, 86.87390960531436690 ) ) ;
#170116 = CARTESIAN_POINT ( 'NONE',  ( 37.99626262588765258, 2.893932880411085066E-14, -5.002157773949823749 ) ) ;
#170117 = CARTESIAN_POINT ( 'NONE',  ( 13.89961937509957401, 13.97604488694547697, 51.87609039468566863 ) ) ;
#170118 = CARTESIAN_POINT ( 'NONE',  ( -5.719274019375978568, 21.55341960407610458, 95.20724293864769550 ) ) ;
#170119 = CARTESIAN_POINT ( 'NONE',  ( -14.29746914071049879, 8.314922557960819915, 95.83224293864770971 ) ) ;
#170120 = CARTESIAN_POINT ( 'NONE',  ( 10.72451020669871369, 18.67979575497193778, 57.08442372801901854 ) ) ;
#170121 = CARTESIAN_POINT ( 'NONE',  ( -17.14385361876520619, 23.59649016807275856, 144.5750000027312012 ) ) ;
#170122 = CARTESIAN_POINT ( 'NONE',  ( -16.52544592524342804, 4.483927247898546575, 31.04057627198102409 ) ) ;
#170123 = CARTESIAN_POINT ( 'NONE',  ( 13.97604488694527802, 13.89961937509977652, 39.37390960531435269 ) ) ;
#170124 = CARTESIAN_POINT ( 'NONE',  ( -19.02544592524342804, 5.153800228976336051, 101.0405762719810241 ) ) ;
#170125 = CARTESIAN_POINT ( 'NONE',  ( 18.67979575497178502, 10.72451020669898547, 59.16557627198103120 ) ) ;
#170126 = CARTESIAN_POINT ( 'NONE',  ( -18.87075004821571866, 5.499999999999904077, 43.67408112101048090 ) ) ;
#170127 = CARTESIAN_POINT ( 'NONE',  ( -19.05341960407611168, -5.049401038298163336, 31.45724293864769550 ) ) ;
#170128 = CARTESIAN_POINT ( 'NONE',  ( 21.52544592524344225, -5.823673210054117533, 58.54057627198103120 ) ) ;
#170129 = ADVANCED_FACE ( 'NONE', ( #162040 ), #101352, .T. ) ;
#170130 = CARTESIAN_POINT ( 'NONE',  ( 18.62759615963255655, 10.81492255796105972, 71.66775706135234714 ) ) ;
#170132 = CARTESIAN_POINT ( 'NONE',  ( 14.34966873604972726, -8.224510206698740333, 80.83442372801901854 ) ) ;
#170131 = CARTESIAN_POINT ( 'NONE',  ( 12.97112549082123678, -41.39484261838032353, -20.61933656601679132 ) ) ;
#170133 = CARTESIAN_POINT ( 'NONE',  ( -19.02544592524342804, 5.153800228976336051, 56.04057627198100988 ) ) ;
#170134 = CARTESIAN_POINT ( 'NONE',  ( -19.05341960407611168, -5.049401038298163336, 71.45724293864766707 ) ) ;
#170135 = EDGE_LOOP ( 'NONE', ( #27596, #194316, #31085, #173370 ) ) ;
#170136 = CARTESIAN_POINT ( 'NONE',  ( 13.89961937509957401, 13.97604488694547697, 26.87609039468566507 ) ) ;
#170137 = CARTESIAN_POINT ( 'NONE',  ( -12.06949235617739369, -12.14591786802326823, 74.37609039468568994 ) ) ;
#170138 = CARTESIAN_POINT ( 'NONE',  ( 0.05219959533937995610, -21.53943276465977519, 95.00109039468568994 ) ) ;
#170139 = CARTESIAN_POINT ( 'NONE',  ( -9.474510206698964154, 16.51473224551069663, 70.41557627198102409 ) ) ;
#170140 = CARTESIAN_POINT ( 'NONE',  ( -0.05219959533907301413, -21.53943276465977519, 32.49890960531435979 ) ) ;
#170141 = CARTESIAN_POINT ( 'NONE',  ( 0.05219959533936267826, -19.03943276465977164, 110.0010903946856757 ) ) ;
#170142 = CARTESIAN_POINT ( 'NONE',  ( -21.52544592524334988, -5.823673210054445271, 83.95942372801900433 ) ) ;
#170143 = CARTESIAN_POINT ( 'NONE',  ( -4.379528057220086978, -16.55341960407618274, 49.79275706135234714 ) ) ;
#170144 = CARTESIAN_POINT ( 'NONE',  ( -10.72451020669898014, 18.67979575497178502, 95.41557627198102409 ) ) ;
#170145 = CARTESIAN_POINT ( 'NONE',  ( 19.05341960407617918, -5.049401038297876454, 106.0427570613523471 ) ) ;
#170147 = ADVANCED_FACE ( 'NONE', ( #11377 ), #4191, .T. ) ;
#170146 = CARTESIAN_POINT ( 'NONE',  ( 0.05219959533909260263, 19.03943276465977164, 84.99890960531436690 ) ) ;
#170148 = CARTESIAN_POINT ( 'NONE',  ( 12.06949235617739724, 12.14591786802326823, 26.87609039468567218 ) ) ;
#170149 = CARTESIAN_POINT ( 'NONE',  ( -16.51473224551069308, -9.474510206698971260, 36.66557627198102409 ) ) ;
#170150 = TOROIDAL_SURFACE ( 'NONE', #134669, 2.700000000000000622, 0.2000000000000000111 ) ;
#170151 = CARTESIAN_POINT ( 'NONE',  ( 13.97604488694548053, -13.89961937509957401, 110.6260903946856615 ) ) ;
#170152 = CARTESIAN_POINT ( 'NONE',  ( -16.55341960407611168, -4.379528057220339221, 71.45724293864769550 ) ) ;
#170153 = CARTESIAN_POINT ( 'NONE',  ( -0.05219959533934338120, 16.53943276465976808, 87.50109039468568994 ) ) ;
#170155 = CARTESIAN_POINT ( 'NONE',  ( 9.564922557960805705, 16.46253265017160317, 54.58224293864769550 ) ) ;
#170154 = CARTESIAN_POINT ( 'NONE',  ( 21.55341960407619695, -5.719274019375665929, 31.04275706135234714 ) ) ;
#170156 = CARTESIAN_POINT ( 'NONE',  ( -9.474510206698964154, 16.51473224551069663, 70.41557627198102409 ) ) ;
#170157 = CARTESIAN_POINT ( 'NONE',  ( 14.29746914071037800, 8.314922557961029526, 66.66775706135234714 ) ) ;
#170159 = VERTEX_POINT ( 'NONE', #169902 ) ;
#170158 = CARTESIAN_POINT ( 'NONE',  ( -21.47377332592085963, -5.474134792251713399, 173.8918256800992594 ) ) ;
#170160 = ORIENTED_EDGE ( 'NONE', *, *, #90984, .T. ) ;
#170161 = CARTESIAN_POINT ( 'NONE',  ( 21.55341960407619695, -5.719274019375665929, 111.0427570613523613 ) ) ;
#170162 = AXIS2_PLACEMENT_3D ( 'NONE', #174775, #95933, #126275 ) ;
#170163 = CARTESIAN_POINT ( 'NONE',  ( -5.153800228976328057, -19.02544592524343514, 37.29057627198102409 ) ) ;
#170165 = ORIENTED_EDGE ( 'NONE', *, *, #139917, .T. ) ;
#170164 = CARTESIAN_POINT ( 'NONE',  ( -9.474510206698964154, 16.51473224551069663, 110.4155762719810383 ) ) ;
#170166 = CARTESIAN_POINT ( 'NONE',  ( -8.224510206698735004, -14.34966873604973081, 34.58442372801900433 ) ) ;
#170168 = CARTESIAN_POINT ( 'NONE',  ( -12.14591786802326823, 12.06949235617739902, 43.12609039468568284 ) ) ;
#170167 = CARTESIAN_POINT ( 'NONE',  ( 9.474510206698729675, 16.51473224551082808, 62.08442372801899722 ) ) ;
#170169 = CARTESIAN_POINT ( 'NONE',  ( -5.049401038298153566, 19.05341960407611168, 40.20724293864768839 ) ) ;
#170170 = CARTESIAN_POINT ( 'NONE',  ( -16.51473224551069308, -9.474510206698971260, 106.6655762719810383 ) ) ;
#170171 = CARTESIAN_POINT ( 'NONE',  ( -13.97604488694527625, -13.89961937509977652, 61.87390960531435979 ) ) ;
#170172 = CARTESIAN_POINT ( 'NONE',  ( 15.80617190586746368, 15.72974639402197994, 104.3739096053143669 ) ) ;
#170174 = CARTESIAN_POINT ( 'NONE',  ( 5.153800228976335163, 19.02544592524342804, 24.79057627198102765 ) ) ;
#170173 = CARTESIAN_POINT ( 'NONE',  ( -13.89961937509977652, 13.97604488694528158, 95.62390960531436690 ) ) ;
#170175 = CARTESIAN_POINT ( 'NONE',  ( 0.05219959533909260263, 19.03943276465977164, 69.99890960531435269 ) ) ;
#170177 = CARTESIAN_POINT ( 'NONE',  ( 13.89961937509977652, -13.97604488694527269, 23.12390960531436335 ) ) ;
#170176 = CARTESIAN_POINT ( 'NONE',  ( 16.52544592524342804, -4.483927247898539470, 23.54057627198102765 ) ) ;
#170178 = CARTESIAN_POINT ( 'NONE',  ( -13.97604488694547697, 13.89961937509957934, 103.1260903946856473 ) ) ;
#170179 = CARTESIAN_POINT ( 'NONE',  ( -21.55341960407619339, 5.719274019375674811, 113.5427570613523756 ) ) ;
#170180 = CARTESIAN_POINT ( 'NONE',  ( -12.14591786802309592, -12.06949235617757132, 56.87390960531436690 ) ) ;
#170181 = CARTESIAN_POINT ( 'NONE',  ( -21.55341960407619339, 5.719274019375674811, 98.54275706135234714 ) ) ;
#170182 = CARTESIAN_POINT ( 'NONE',  ( 13.89961937509977652, -13.97604488694527269, 38.12390960531436690 ) ) ;
#170184 = CARTESIAN_POINT ( 'NONE',  ( 0.05219959533937995610, -21.53943276465977519, 85.00109039468568994 ) ) ;
#170183 = CARTESIAN_POINT ( 'NONE',  ( 8.314922557960818139, 14.29746914071049879, 39.58224293864769550 ) ) ;
#170185 = CARTESIAN_POINT ( 'NONE',  ( -9.564922557960796823, -16.46253265017161027, 82.08224293864768129 ) ) ;
#170186 = CARTESIAN_POINT ( 'NONE',  ( -5.049401038298153566, 19.05341960407611168, 95.20724293864770971 ) ) ;
#170187 = CARTESIAN_POINT ( 'NONE',  ( -14.34966873604960291, -8.224510206698953496, 106.6655762719810383 ) ) ;
#170188 = CARTESIAN_POINT ( 'NONE',  ( -12.06949235617756955, 12.14591786802309770, 80.62390960531438111 ) ) ;
#170189 = CARTESIAN_POINT ( 'NONE',  ( 10.72451020669898902, -18.67979575497178502, 82.91557627198103830 ) ) ;
#170190 = CARTESIAN_POINT ( 'NONE',  ( 19.05341960407611168, 5.049401038298154454, 68.95724293864769550 ) ) ;
#170191 = CARTESIAN_POINT ( 'NONE',  ( -21.53943276465977519, 0.05219959533907696930, 86.24890960531436690 ) ) ;
#170192 = CARTESIAN_POINT ( 'NONE',  ( 9.474510206698729675, 16.51473224551082808, 77.08442372801900433 ) ) ;
#170194 = CARTESIAN_POINT ( 'NONE',  ( -12.06949235617756955, 12.14591786802309770, 90.62390960531436690 ) ) ;
#170193 = CARTESIAN_POINT ( 'NONE',  ( -9.474510206698720793, -16.51473224551083518, 64.58442372801900433 ) ) ;
#170196 = CARTESIAN_POINT ( 'NONE',  ( 5.153800228976335163, 19.02544592524342804, 59.79057627198100988 ) ) ;
#170195 = VECTOR ( 'NONE', #170396, 1000.000000000000000 ) ;
#170197 = CARTESIAN_POINT ( 'NONE',  ( -5.719274019375978568, 21.55341960407610458, 65.20724293864768129 ) ) ;
#170198 = CARTESIAN_POINT ( 'NONE',  ( -17.49999999999999645, -5.499999999999992895, 84.20309617465829888 ) ) ;
#170200 = SPHERICAL_SURFACE ( 'NONE', #88735, 0.5000000000000000000 ) ;
#170199 = CARTESIAN_POINT ( 'NONE',  ( 16.55341960407611168, 4.379528057220329451, 23.95724293864769550 ) ) ;
#170201 = CARTESIAN_POINT ( 'NONE',  ( -16.53943276465976808, -0.05219959533934237506, 23.75109039468567929 ) ) ;
#170202 = CARTESIAN_POINT ( 'NONE',  ( 0.05219959533910956823, 16.53943276465976808, 79.99890960531435269 ) ) ;
#170203 = CARTESIAN_POINT ( 'NONE',  ( -18.22780087662122384, -5.500000000000025757, 96.48459894673894155 ) ) ;
#170204 = CARTESIAN_POINT ( 'NONE',  ( -19.05341960407611168, -5.049401038298163336, 76.45724293864769550 ) ) ;
#170205 = CARTESIAN_POINT ( 'NONE',  ( -5.049401038298153566, 19.05341960407611168, 35.20724293864768839 ) ) ;
#170206 = CARTESIAN_POINT ( 'NONE',  ( -4.379528057220328563, 16.55341960407611168, 65.20724293864768129 ) ) ;
#170207 = CARTESIAN_POINT ( 'NONE',  ( 21.52544592524344225, -5.823673210054117533, 23.54057627198102765 ) ) ;
#170209 = CARTESIAN_POINT ( 'NONE',  ( -19.02544592524342804, 5.153800228976336051, 76.04057627198102409 ) ) ;
#170208 = CARTESIAN_POINT ( 'NONE',  ( 13.89961937509957401, 13.97604488694547697, 86.87609039468567573 ) ) ;
#170210 = CARTESIAN_POINT ( 'NONE',  ( 13.97604488694527802, 13.89961937509977652, 84.37390960531433848 ) ) ;
#170211 = CARTESIAN_POINT ( 'NONE',  ( 10.72451020669898902, -18.67979575497178502, 82.91557627198103830 ) ) ;
#170212 = CARTESIAN_POINT ( 'NONE',  ( 0.05219959533934541429, -16.53943276465976808, 65.00109039468568994 ) ) ;
#170213 = CARTESIAN_POINT ( 'NONE',  ( -9.564922557961040184, 16.46253265017147172, 112.9177570613523329 ) ) ;
#170214 = CARTESIAN_POINT ( 'NONE',  ( 19.03943276465977164, -0.05219959533909143690, 68.74890960531436690 ) ) ;
#170215 = CARTESIAN_POINT ( 'NONE',  ( -10.81492255796078084, -18.62759615963271287, 72.08224293864769550 ) ) ;
#170216 = CARTESIAN_POINT ( 'NONE',  ( 13.97604488694548053, -13.89961937509957401, 90.62609039468567573 ) ) ;
#170218 = CARTESIAN_POINT ( 'NONE',  ( -18.62759615963255300, -10.81492255796106328, 49.16775706135234003 ) ) ;
#170217 = CARTESIAN_POINT ( 'NONE',  ( 16.53943276465976808, -0.05219959533910856209, 33.74890960531436690 ) ) ;
#170219 = FACE_OUTER_BOUND ( 'NONE', #56771, .T. ) ;
#170221 = CARTESIAN_POINT ( 'NONE',  ( 0.05219959533909260263, 19.03943276465977164, 99.99890960531436690 ) ) ;
#170220 = CARTESIAN_POINT ( 'NONE',  ( -16.52544592524335698, -4.483927247898792601, 73.95942372801901854 ) ) ;
#170222 = CARTESIAN_POINT ( 'NONE',  ( -17.59860650958990647, -7.585241751807021870, 101.5766298573750817 ) ) ;
#170223 = CARTESIAN_POINT ( 'NONE',  ( 0.5037075166051908637, 31.83037104268352024, -49.22065939777928634 ) ) ;
#170224 = CARTESIAN_POINT ( 'NONE',  ( 8.314922557961029526, -14.29746914071037800, 95.41775706135234714 ) ) ;
#170225 = CARTESIAN_POINT ( 'NONE',  ( -8.224510206698735004, -14.34966873604973081, 44.58442372801901854 ) ) ;
#170226 = CARTESIAN_POINT ( 'NONE',  ( 19.02544592524343514, -5.153800228976328945, 58.54057627198102409 ) ) ;
#170227 = CARTESIAN_POINT ( 'NONE',  ( -19.03943276465977164, 0.05219959533909376836, 76.24890960531435269 ) ) ;
#170228 = CARTESIAN_POINT ( 'NONE',  ( 0.05219959533937995610, -21.53943276465977519, 50.00109039468568994 ) ) ;
#170229 = CARTESIAN_POINT ( 'NONE',  ( -12.14591786802326823, 12.06949235617739902, 63.12609039468568994 ) ) ;
#170230 = CARTESIAN_POINT ( 'NONE',  ( 16.53943276465976808, -0.05219959533910856209, 33.74890960531436690 ) ) ;
#170231 = CARTESIAN_POINT ( 'NONE',  ( -9.564922557960796823, -16.46253265017161027, 42.08224293864769550 ) ) ;
#170232 = CARTESIAN_POINT ( 'NONE',  ( 13.97604488694527802, 13.89961937509977652, 29.37390960531435979 ) ) ;
#170233 = CARTESIAN_POINT ( 'NONE',  ( -4.483927247898782831, 16.52544592524335698, 22.70942372801901499 ) ) ;
#170234 = CARTESIAN_POINT ( 'NONE',  ( 19.02544592524334988, 5.153800228976608722, 81.45942372801897591 ) ) ;
#170235 = CARTESIAN_POINT ( 'NONE',  ( -0.05219959533910754901, -16.53943276465976808, 87.49890960531436690 ) ) ;
#170236 = CARTESIAN_POINT ( 'NONE',  ( -9.564922557960796823, -16.46253265017161027, 52.08224293864768839 ) ) ;
#170238 = DIRECTION ( 'NONE',  ( 1.000000000000000000, 0.000000000000000000, 0.000000000000000000 ) ) ;
#170237 = CARTESIAN_POINT ( 'NONE',  ( -5.049401038297874678, -19.05341960407617918, 89.79275706135230450 ) ) ;
#170239 = CARTESIAN_POINT ( 'NONE',  ( 15.80617190586769283, -15.72974639402175789, 90.62609039468567573 ) ) ;
#170240 = CARTESIAN_POINT ( 'NONE',  ( -12.06949235617739369, -12.14591786802326823, 49.37609039468569705 ) ) ;
#170241 = CARTESIAN_POINT ( 'NONE',  ( -17.49999999999999645, 3.512728167237046950, 25.22809995181131271 ) ) ;
#170242 = CARTESIAN_POINT ( 'NONE',  ( -0.05219959533907301413, -21.53943276465977519, 52.49890960531435979 ) ) ;
#170243 = CARTESIAN_POINT ( 'NONE',  ( 16.55341960407618274, -4.379528057220086978, 41.04275706135236135 ) ) ;
#170244 = CARTESIAN_POINT ( 'NONE',  ( 13.89961937509978007, -13.97604488694527269, 33.12390960531435269 ) ) ;
#170245 = CARTESIAN_POINT ( 'NONE',  ( 5.153800228976615827, -19.02544592524334988, 40.20942372801898301 ) ) ;
#170246 = CARTESIAN_POINT ( 'NONE',  ( -0.05219959533909027116, -19.03943276465977164, 82.49890960531436690 ) ) ;
#170247 = CARTESIAN_POINT ( 'NONE',  ( -9.474510206698964154, 16.51473224551069663, 55.41557627198103120 ) ) ;
#170248 = CARTESIAN_POINT ( 'NONE',  ( 4.500000000000000888, -126.1226662136678272, 8.481152457036388981 ) ) ;
#170249 = CARTESIAN_POINT ( 'NONE',  ( 19.03943276465977164, -0.05219959533909143690, 68.74890960531436690 ) ) ;
#170250 = CARTESIAN_POINT ( 'NONE',  ( 2.500000000000000000, 0.000000000000000000, -64.92179855667829713 ) ) ;
#170251 = CARTESIAN_POINT ( 'NONE',  ( -19.05341960407617563, 5.049401038297882671, 33.54275706135231871 ) ) ;
#170252 = CARTESIAN_POINT ( 'NONE',  ( 15.72974639402176855, 15.80617190586768217, 111.8760903946856615 ) ) ;
#170253 = CARTESIAN_POINT ( 'NONE',  ( 16.52544592524342804, -4.483927247898539470, 38.54057627198103120 ) ) ;
#170254 = CARTESIAN_POINT ( 'NONE',  ( -13.97604488694527625, -13.89961937509977652, 36.87390960531436690 ) ) ;
#170255 = CARTESIAN_POINT ( 'NONE',  ( 19.03943276465977164, -0.05219959533909143690, 103.7489096053143669 ) ) ;
#170256 = CARTESIAN_POINT ( 'NONE',  ( -21.52544592524334988, -5.823673210054445271, 78.95942372801901854 ) ) ;
#170257 = CARTESIAN_POINT ( 'NONE',  ( -5.049401038298153566, 19.05341960407611168, 50.20724293864770260 ) ) ;
#170258 = CARTESIAN_POINT ( 'NONE',  ( 15.80617190586769283, -15.72974639402175789, 80.62609039468567573 ) ) ;
#170259 = CARTESIAN_POINT ( 'NONE',  ( -15.80617190586745835, -15.72974639402198527, 26.87390960531435979 ) ) ;
#170260 = CARTESIAN_POINT ( 'NONE',  ( 5.823673210054444382, -21.52544592524334988, 20.20942372801900788 ) ) ;
#170261 = CARTESIAN_POINT ( 'NONE',  ( 16.51473224551083163, -9.474510206698727899, 45.83442372801900433 ) ) ;
#170262 = CARTESIAN_POINT ( 'NONE',  ( 19.02544592524343514, -5.153800228976328945, 33.54057627198102409 ) ) ;
#170263 = CARTESIAN_POINT ( 'NONE',  ( 19.02544592524343514, -5.153800228976328945, 78.54057627198099567 ) ) ;
#170264 = CARTESIAN_POINT ( 'NONE',  ( 4.379528057220092307, 16.55341960407617563, 22.29275706135235069 ) ) ;
#170265 = CARTESIAN_POINT ( 'NONE',  ( -16.55341960407611168, -4.379528057220339221, 86.45724293864770971 ) ) ;
#170266 = CARTESIAN_POINT ( 'NONE',  ( 18.67979575497178502, 10.72451020669898547, 39.16557627198102409 ) ) ;
#170267 = CARTESIAN_POINT ( 'NONE',  ( -5.153800228976607833, 19.02544592524334988, 102.7094237280189759 ) ) ;
#170268 = CARTESIAN_POINT ( 'NONE',  ( -15.72974639402197994, 15.80617190586746368, 100.6239096053143811 ) ) ;
#170269 = CARTESIAN_POINT ( 'NONE',  ( 21.52544592524334988, 5.823673210054432836, 51.45942372801901854 ) ) ;
#170270 = CARTESIAN_POINT ( 'NONE',  ( -4.483927247898782831, 16.52544592524335698, 62.70942372801902565 ) ) ;
#170271 = CARTESIAN_POINT ( 'NONE',  ( 8.224510206698742110, 14.34966873604972548, 67.08442372801901854 ) ) ;
#170272 = ORIENTED_EDGE ( 'NONE', *, *, #145481, .F. ) ;
#170273 = CARTESIAN_POINT ( 'NONE',  ( -9.564922557960796823, -16.46253265017161027, 57.08224293864769550 ) ) ;
#170274 = CARTESIAN_POINT ( 'NONE',  ( -14.29746914071037622, -8.314922557961029526, 89.16775706135236135 ) ) ;
#170275 = CARTESIAN_POINT ( 'NONE',  ( 5.719274019375991003, -21.55341960407610458, 112.7072429386476955 ) ) ;
#170276 = CARTESIAN_POINT ( 'NONE',  ( -12.06949235617756955, 12.14591786802309770, 50.62390960531435979 ) ) ;
#170277 = CARTESIAN_POINT ( 'NONE',  ( -13.89961937509977652, 13.97604488694528158, 80.62390960531436690 ) ) ;
#170278 = CARTESIAN_POINT ( 'NONE',  ( -8.314922557961024197, 14.29746914071037800, 72.91775706135234714 ) ) ;
#170279 = CARTESIAN_POINT ( 'NONE',  ( -10.81492255796105439, 18.62759615963255655, 52.91775706135235424 ) ) ;
#170280 = CARTESIAN_POINT ( 'NONE',  ( -13.89961937509957401, -13.97604488694547875, 109.3760903946856331 ) ) ;
#170281 = CARTESIAN_POINT ( 'NONE',  ( 15.72974639402199770, -15.80617190586745480, 108.1239096053143811 ) ) ;
#170282 = CARTESIAN_POINT ( 'NONE',  ( -4.483927247898539470, -16.52544592524342804, 52.29057627198102409 ) ) ;
#170283 = EDGE_LOOP ( 'NONE', ( #148780, #126801, #164395, #194463 ) ) ;
#170284 = CARTESIAN_POINT ( 'NONE',  ( -17.48853670773247515, 5.747243402303043425, 68.66671299749995683 ) ) ;
#170285 = CARTESIAN_POINT ( 'NONE',  ( -15.80617190586745835, -15.72974639402198527, 81.87390960531435269 ) ) ;
#170286 = CARTESIAN_POINT ( 'NONE',  ( 12.06949235617757843, -12.14591786802309237, 43.12390960531435269 ) ) ;
#170287 = VERTEX_POINT ( 'NONE', #47564 ) ;
#170288 = CARTESIAN_POINT ( 'NONE',  ( 34.72612402863278191, 2.419136457854856204, 52.10344399403046367 ) ) ;
#170289 = CARTESIAN_POINT ( 'NONE',  ( 21.55341960407610458, 5.719274019375980345, 108.9572429386476955 ) ) ;
#170290 = CARTESIAN_POINT ( 'NONE',  ( 5.719274019375991003, -21.55341960407610458, 22.70724293864769194 ) ) ;
#170291 = CARTESIAN_POINT ( 'NONE',  ( -10.81492255796105439, 18.62759615963255655, 27.91775706135234358 ) ) ;
#170292 = CARTESIAN_POINT ( 'NONE',  ( -8.314922557960811034, -14.29746914071050412, 52.08224293864768839 ) ) ;
#170293 = CARTESIAN_POINT ( 'NONE',  ( -12.06949235617739369, -12.14591786802326823, 59.37609039468568284 ) ) ;
#170294 = AXIS2_PLACEMENT_3D ( 'NONE', #63484, #106992, #199019 ) ;
#170295 = CARTESIAN_POINT ( 'NONE',  ( -0.05219959533909027116, -19.03943276465977164, 57.49890960531435979 ) ) ;
#170296 = CARTESIAN_POINT ( 'NONE',  ( -16.51473224551082808, 9.474510206698731452, 63.33442372801900433 ) ) ;
#170297 = CARTESIAN_POINT ( 'NONE',  ( 19.05341960407611168, 5.049401038298154454, 83.95724293864766707 ) ) ;
#170298 = CARTESIAN_POINT ( 'NONE',  ( 15.80617190586746368, 15.72974639402197994, 34.37390960531435979 ) ) ;
#170299 = CARTESIAN_POINT ( 'NONE',  ( -19.65168359646841978, -34.19331532915863647, -17.88087567707375314 ) ) ;
#170300 = CARTESIAN_POINT ( 'NONE',  ( -5.153800228976328057, -19.02544592524343514, 62.29057627198100988 ) ) ;
#170301 = CARTESIAN_POINT ( 'NONE',  ( -12.14591786802326823, 12.06949235617739902, 23.12609039468567573 ) ) ;
#170302 = CARTESIAN_POINT ( 'NONE',  ( -19.05341960407617563, 5.049401038297882671, 63.54275706135234003 ) ) ;
#170303 = CARTESIAN_POINT ( 'NONE',  ( 18.67979575497178502, 10.72451020669898547, 104.1655762719810241 ) ) ;
#170304 = CARTESIAN_POINT ( 'NONE',  ( 14.34966873604960469, 8.224510206698951720, 34.16557627198102409 ) ) ;
#170305 = CARTESIAN_POINT ( 'NONE',  ( -16.51473224551069308, -9.474510206698971260, 96.66557627198102409 ) ) ;
#170306 = CARTESIAN_POINT ( 'NONE',  ( -5.823673210054116645, -21.52544592524344225, 62.29057627198102409 ) ) ;
#170308 = CARTESIAN_POINT ( 'NONE',  ( -14.29746914071037622, -8.314922557961029526, 39.16775706135235424 ) ) ;
#170307 = CARTESIAN_POINT ( 'NONE',  ( -18.67979575497178146, -10.72451020669898902, 91.66557627198103830 ) ) ;
#170309 = CARTESIAN_POINT ( 'NONE',  ( -21.52544592524343514, 5.823673210054127303, 41.04057627198103120 ) ) ;
#170310 = CARTESIAN_POINT ( 'NONE',  ( 10.81492255796106328, -18.62759615963255655, 90.41775706135236135 ) ) ;
#170311 = CARTESIAN_POINT ( 'NONE',  ( -16.46253265017160317, 9.564922557960807481, 90.83224293864769550 ) ) ;
#170312 = CARTESIAN_POINT ( 'NONE',  ( -9.474510206698964154, 16.51473224551069663, 40.41557627198103120 ) ) ;
#170313 = CARTESIAN_POINT ( 'NONE',  ( -16.46253265017160317, 9.564922557960807481, 100.8322429386477097 ) ) ;
#170314 = CARTESIAN_POINT ( 'NONE',  ( 12.14591786802309770, 12.06949235617756955, 104.3739096053143669 ) ) ;
#170315 = CARTESIAN_POINT ( 'NONE',  ( -19.05341960407611168, -5.049401038298163336, 61.45724293864769550 ) ) ;
#170316 = CARTESIAN_POINT ( 'NONE',  ( -16.52544592524335698, -4.483927247898792601, 18.95942372801901143 ) ) ;
#170317 = CARTESIAN_POINT ( 'NONE',  ( 17.12812012977046905, -6.668231424565697729, 86.14051240676850796 ) ) ;
#170318 = COLOUR_RGB ( '', 0.72549020, 0.75294118, 0.79215686) ;
#170320 = CARTESIAN_POINT ( 'NONE',  ( 16.46253265017160672, -9.564922557960803928, 113.3322429386476955 ) ) ;
#170319 = CARTESIAN_POINT ( 'NONE',  ( 5.823673210054444382, -21.52544592524334988, 100.2094237280190043 ) ) ;
#170321 = CARTESIAN_POINT ( 'NONE',  ( 16.52544592524335698, 4.483927247898782831, 96.45942372801901854 ) ) ;
#170322 = CARTESIAN_POINT ( 'NONE',  ( -3.573655867282028392E-15, 2.428612866367529932E-14, 167.9999999999999716 ) ) ;
#170323 = CARTESIAN_POINT ( 'NONE',  ( -5.153800228976607833, 19.02544592524334988, 67.70942372801900433 ) ) ;
#170324 = CARTESIAN_POINT ( 'NONE',  ( 16.46253265017146816, 9.564922557961045513, 31.66775706135232937 ) ) ;
#170325 = CARTESIAN_POINT ( 'NONE',  ( 27.56318840656206248, 3.609252070617571473, 139.9999999999999716 ) ) ;
#170326 = CARTESIAN_POINT ( 'NONE',  ( -5.153800228976328057, -19.02544592524343514, 27.29057627198103120 ) ) ;
#170327 = CARTESIAN_POINT ( 'NONE',  ( 0.05219959533910956823, 16.53943276465976808, 39.99890960531436690 ) ) ;
#170328 = CARTESIAN_POINT ( 'NONE',  ( -17.49999999999999645, -5.500000000000000888, 109.2030961746582847 ) ) ;
#170329 = CARTESIAN_POINT ( 'NONE',  ( -16.53943276465976808, 0.05219959533911058130, 31.24890960531435979 ) ) ;
#170330 = CARTESIAN_POINT ( 'NONE',  ( 17.26172910966779028, 6.454744622555872446, 66.69353091350777163 ) ) ;
#170331 = CARTESIAN_POINT ( 'NONE',  ( -14.34966873604972548, 8.224510206698743886, 93.33442372801901854 ) ) ;
#170332 = CARTESIAN_POINT ( 'NONE',  ( -16.51473224551069308, -9.474510206698971260, 41.66557627198103120 ) ) ;
#170333 = CARTESIAN_POINT ( 'NONE',  ( -21.53943276465977519, -0.05219959533937600094, 108.7510903946857042 ) ) ;
#170334 = CARTESIAN_POINT ( 'NONE',  ( -0.05219959533936034679, 19.03943276465977164, 112.5010903946856757 ) ) ;
#170335 = CARTESIAN_POINT ( 'NONE',  ( -5.719274019375665041, -21.55341960407619695, 74.79275706135234714 ) ) ;
#170336 = CARTESIAN_POINT ( 'NONE',  ( -9.564922557961040184, 16.46253265017147172, 52.91775706135233293 ) ) ;
#170337 = CARTESIAN_POINT ( 'NONE',  ( 16.51473224551069308, 9.474510206698969483, 94.16557627198103830 ) ) ;
#170338 = CARTESIAN_POINT ( 'NONE',  ( 19.05341960407611168, 5.049401038298154454, 68.95724293864769550 ) ) ;
#170339 = CARTESIAN_POINT ( 'NONE',  ( 16.81555441253552274, 7.025013491695500711, 71.86314554665747778 ) ) ;
#170340 = CARTESIAN_POINT ( 'NONE',  ( -15.72974639402197994, 15.80617190586746368, 95.62390960531436690 ) ) ;
#170341 = VECTOR ( 'NONE', #148445, 1000.000000000000114 ) ;
#170342 = CARTESIAN_POINT ( 'NONE',  ( -16.53943276465976808, 0.05219959533911058130, 66.24890960531436690 ) ) ;
#170343 = CARTESIAN_POINT ( 'NONE',  ( -18.67979575497178146, -10.72451020669898902, 61.66557627198103120 ) ) ;
#170344 = CARTESIAN_POINT ( 'NONE',  ( -19.03943276465977164, 0.05219959533909376836, 66.24890960531436690 ) ) ;
#170346 = CARTESIAN_POINT ( 'NONE',  ( -4.483927247898782831, 16.52544592524335698, 72.70942372801901854 ) ) ;
#170345 = CARTESIAN_POINT ( 'NONE',  ( -18.67979575497178146, -10.72451020669898902, 81.66557627198103830 ) ) ;
#170347 = EDGE_LOOP ( 'NONE', ( #93302, #141756, #103721, #28585, #42985 ) ) ;
#170348 = CARTESIAN_POINT ( 'NONE',  ( -19.02544592524342804, 5.153800228976336051, 41.04057627198103120 ) ) ;
#170350 = CARTESIAN_POINT ( 'NONE',  ( 21.93187539022923715, -6.436421874423670531, 171.3066408880984852 ) ) ;
#170349 = CARTESIAN_POINT ( 'NONE',  ( -16.53943276465976808, 0.05219959533911058130, 76.24890960531435269 ) ) ;
#170351 = CARTESIAN_POINT ( 'NONE',  ( -16.46253265017160317, 9.564922557960807481, 50.83224293864770260 ) ) ;
#170352 = CARTESIAN_POINT ( 'NONE',  ( 4.379528057220339221, -16.55341960407611168, 112.7072429386476955 ) ) ;
#170353 = CARTESIAN_POINT ( 'NONE',  ( 13.97604488694548053, -13.89961937509957401, 60.62609039468564731 ) ) ;
#170354 = CARTESIAN_POINT ( 'NONE',  ( -4.483927247898539470, -16.52544592524342804, 87.29057627198103830 ) ) ;
#170355 = CARTESIAN_POINT ( 'NONE',  ( -10.81492255796105439, 18.62759615963255655, 42.91775706135235424 ) ) ;
#170357 = CARTESIAN_POINT ( 'NONE',  ( -5.823673210054116645, -21.52544592524344225, 102.2905762719810383 ) ) ;
#170356 = CARTESIAN_POINT ( 'NONE',  ( 19.05341960407611168, 5.049401038298154454, 38.95724293864767418 ) ) ;
#170358 = CARTESIAN_POINT ( 'NONE',  ( 12.14591786802309770, 12.06949235617756955, 89.37390960531435269 ) ) ;
#170359 = CARTESIAN_POINT ( 'NONE',  ( 25.17999522921048694, -30.53243704067885034, -18.89073929087368597 ) ) ;
#170360 = CARTESIAN_POINT ( 'NONE',  ( 16.51473224551069308, 9.474510206698969483, 49.16557627198102409 ) ) ;
#170361 = DIRECTION ( 'NONE',  ( 0.000000000000000000, 0.000000000000000000, 1.000000000000000000 ) ) ;
#170363 = CARTESIAN_POINT ( 'NONE',  ( 19.02544592524343514, -5.153800228976328945, 93.54057627198102409 ) ) ;
#170362 = CARTESIAN_POINT ( 'NONE',  ( 9.564922557961047289, -16.46253265017146816, 95.41775706135233293 ) ) ;
#170364 = CARTESIAN_POINT ( 'NONE',  ( -5.719274019375665041, -21.55341960407619695, 29.79275706135234358 ) ) ;
#170365 = CARTESIAN_POINT ( 'NONE',  ( 13.89961937509977652, -13.97604488694527269, 88.12390960531438111 ) ) ;
#170366 = CARTESIAN_POINT ( 'NONE',  ( 0.05219959533936267826, -19.03943276465977164, 75.00109039468566152 ) ) ;
#170367 = CARTESIAN_POINT ( 'NONE',  ( 13.97604488694527802, 13.89961937509977652, 44.37390960531435269 ) ) ;
#170368 = CARTESIAN_POINT ( 'NONE',  ( -8.314922557960811034, -14.29746914071050412, 72.08224293864769550 ) ) ;
#170369 = CARTESIAN_POINT ( 'NONE',  ( 16.53943276465976808, -0.05219959533910856209, 68.74890960531435269 ) ) ;
#170370 = CARTESIAN_POINT ( 'NONE',  ( 13.97604488694527802, 13.89961937509977652, 89.37390960531436690 ) ) ;
#170371 = CARTESIAN_POINT ( 'NONE',  ( -15.80617190586745835, -15.72974639402198527, 96.87390960531436690 ) ) ;
#170372 = CARTESIAN_POINT ( 'NONE',  ( 9.564922557960805705, 16.46253265017160317, 69.58224293864770971 ) ) ;
#170373 = EDGE_CURVE ( 'NONE', #64290, #30088, #107221, .T. ) ;
#170374 = CARTESIAN_POINT ( 'NONE',  ( 19.02544592524334988, 5.153800228976608722, 26.45942372801899722 ) ) ;
#170377 = CARTESIAN_POINT ( 'NONE',  ( 16.52544592524342804, -4.483927247898539470, 113.5405762719810383 ) ) ;
#170376 = CARTESIAN_POINT ( 'NONE',  ( -8.224510206698948167, 14.34966873604960824, 25.41557627198103120 ) ) ;
#170375 = CARTESIAN_POINT ( 'NONE',  ( 16.46253265017160672, -9.564922557960803928, 38.33224293864768839 ) ) ;
#170378 = CARTESIAN_POINT ( 'NONE',  ( 16.46253265017146816, 9.564922557961045513, 111.6677570613523329 ) ) ;
#170379 = ORIENTED_EDGE ( 'NONE', *, *, #73495, .F. ) ;
#170380 = CARTESIAN_POINT ( 'NONE',  ( -15.80617190586768217, 15.72974639402176855, 28.12609039468568284 ) ) ;
#170381 = CARTESIAN_POINT ( 'NONE',  ( -19.05341960407617563, 5.049401038297882671, 68.54275706135230450 ) ) ;
#170382 = CARTESIAN_POINT ( 'NONE',  ( 8.224510206698953496, -14.34966873604960469, 27.91557627198103830 ) ) ;
#170383 = CARTESIAN_POINT ( 'NONE',  ( 15.72974639402199770, -15.80617190586745480, 88.12390960531436690 ) ) ;
#170384 = CARTESIAN_POINT ( 'NONE',  ( -19.03943276465977164, 0.05219959533909376836, 111.2489096053143669 ) ) ;
#170385 = CARTESIAN_POINT ( 'NONE',  ( 8.224510206698953496, -14.34966873604960469, 62.91557627198102409 ) ) ;
#170386 = CARTESIAN_POINT ( 'NONE',  ( -16.46253265017160317, 9.564922557960807481, 30.83224293864769550 ) ) ;
#170387 = CARTESIAN_POINT ( 'NONE',  ( 5.049401038297881783, 19.05341960407617563, 32.29275706135233293 ) ) ;
#170388 = CARTESIAN_POINT ( 'NONE',  ( -8.224510206698735004, -14.34966873604973081, 84.58442372801903275 ) ) ;
#170389 = CARTESIAN_POINT ( 'NONE',  ( 14.29746914071037800, 8.314922557961029526, 61.66775706135235424 ) ) ;
#170390 = CARTESIAN_POINT ( 'NONE',  ( -0.05219959533909027116, -19.03943276465977164, 112.4989096053143669 ) ) ;
#170391 = CARTESIAN_POINT ( 'NONE',  ( -18.62759615963255300, -10.81492255796106328, 109.1677570613523613 ) ) ;
#170392 = CARTESIAN_POINT ( 'NONE',  ( 5.049401038298161559, -19.05341960407611168, 77.70724293864765286 ) ) ;
#170393 = CARTESIAN_POINT ( 'NONE',  ( 0.05219959533934541429, -16.53943276465976808, 55.00109039468568284 ) ) ;
#170394 = CARTESIAN_POINT ( 'NONE',  ( 19.02544592524343514, -5.153800228976328945, 28.54057627198102409 ) ) ;
#170395 = CARTESIAN_POINT ( 'NONE',  ( -16.55341960407611168, -4.379528057220339221, 31.45724293864769550 ) ) ;
#170396 = DIRECTION ( 'NONE',  ( -0.000000000000000000, -0.000000000000000000, 1.000000000000000000 ) ) ;
#170399 = CARTESIAN_POINT ( 'NONE',  ( -9.474510206698964154, 16.51473224551069663, 75.41557627198103830 ) ) ;
#170398 = CARTESIAN_POINT ( 'NONE',  ( 13.89961937509977652, -13.97604488694527269, 108.1239096053143669 ) ) ;
#170397 = CARTESIAN_POINT ( 'NONE',  ( 5.823673210054444382, -21.52544592524334988, 75.20942372801901854 ) ) ;
#170400 = CARTESIAN_POINT ( 'NONE',  ( 9.564922557960805705, 16.46253265017160317, 114.5822429386476955 ) ) ;
#170401 = CARTESIAN_POINT ( 'NONE',  ( 16.52544592524342804, -4.483927247898539470, 53.54057627198103120 ) ) ;
#170402 = CARTESIAN_POINT ( 'NONE',  ( 0.05219959533910956823, 16.53943276465976808, 34.99890960531435979 ) ) ;
#170403 = CARTESIAN_POINT ( 'NONE',  ( -14.34966873604960291, -8.224510206698953496, 56.66557627198103830 ) ) ;
#170405 = CARTESIAN_POINT ( 'NONE',  ( 5.153800228976617603, -19.02544592524335343, 60.20942372801899722 ) ) ;
#170404 = CARTESIAN_POINT ( 'NONE',  ( -8.314922557961024197, 14.29746914071037800, 37.91775706135235424 ) ) ;
#170406 = CARTESIAN_POINT ( 'NONE',  ( -16.46253265017146816, -9.564922557961047289, 49.16775706135233293 ) ) ;
#170407 = CARTESIAN_POINT ( 'NONE',  ( -9.474510206698964154, 16.51473224551069663, 70.41557627198102409 ) ) ;
#170408 = CARTESIAN_POINT ( 'NONE',  ( 13.97604488694548053, -13.89961937509957401, 55.62609039468566863 ) ) ;
#170409 = CARTESIAN_POINT ( 'NONE',  ( 16.46253265017146816, 9.564922557961045513, 51.66775706135233293 ) ) ;
#170411 = CARTESIAN_POINT ( 'NONE',  ( -16.55341960407617563, 4.379528057220093196, 88.54275706135236135 ) ) ;
#170410 = CARTESIAN_POINT ( 'NONE',  ( -5.153800228976607833, 19.02544592524334988, 92.70942372801901854 ) ) ;
#170412 = CARTESIAN_POINT ( 'NONE',  ( -27.73933785331498925, 9.013057229001089965, 145.2750000027311899 ) ) ;
#170413 = CARTESIAN_POINT ( 'NONE',  ( -5.153800228976328057, -19.02544592524343514, 22.29057627198102765 ) ) ;
#170414 = CARTESIAN_POINT ( 'NONE',  ( 9.474510206698971260, -16.51473224551069308, 97.91557627198102409 ) ) ;
#170415 = CARTESIAN_POINT ( 'NONE',  ( 21.53943276465977519, 0.05219959533937863772, 41.25109039468568284 ) ) ;
#170416 = CARTESIAN_POINT ( 'NONE',  ( -19.05341960407617563, 5.049401038297882671, 103.5427570613523329 ) ) ;
#170418 = CARTESIAN_POINT ( 'NONE',  ( -16.46253265017160317, 9.564922557960807481, 60.83224293864769550 ) ) ;
#170417 = CARTESIAN_POINT ( 'NONE',  ( -6.020228577223754586E-15, 39.95556452105416412, -2.500000000000000000 ) ) ;
#170419 = CARTESIAN_POINT ( 'NONE',  ( -13.89961937509977652, 13.97604488694528158, 105.6239096053143527 ) ) ;
#170421 = CARTESIAN_POINT ( 'NONE',  ( 19.02544592524343514, -5.153800228976328945, 68.54057627198103830 ) ) ;
#170420 = CARTESIAN_POINT ( 'NONE',  ( 12.06949235617757843, -12.14591786802309237, 58.12390960531435979 ) ) ;
#170422 = CARTESIAN_POINT ( 'NONE',  ( -9.564922557960796823, -16.46253265017161027, 57.08224293864769550 ) ) ;
#170423 = CARTESIAN_POINT ( 'NONE',  ( 5.049401038297881783, 19.05341960407617563, 77.29275706135231871 ) ) ;
#170424 = CARTESIAN_POINT ( 'NONE',  ( 21.53943276465977519, -0.05219959533907433946, 53.74890960531437401 ) ) ;
#170425 = CARTESIAN_POINT ( 'NONE',  ( -19.03943276465977164, -0.05219959533935918106, 43.75109039468566863 ) ) ;
#170426 = CARTESIAN_POINT ( 'NONE',  ( -13.89961937509977652, 13.97604488694528158, 80.62390960531436690 ) ) ;
#170427 = CARTESIAN_POINT ( 'NONE',  ( -15.80617190586745835, -15.72974639402198527, 76.87390960531439532 ) ) ;
#170429 = CARTESIAN_POINT ( 'NONE',  ( 5.049401038297881783, 19.05341960407617563, 37.29275706135232582 ) ) ;
#170428 = CARTESIAN_POINT ( 'NONE',  ( -12.14591786802309592, -12.06949235617757132, 81.87390960531435269 ) ) ;
#170430 = CARTESIAN_POINT ( 'NONE',  ( 5.823673210054125526, 21.52544592524343514, 44.79057627198103120 ) ) ;
#170431 = CARTESIAN_POINT ( 'NONE',  ( -18.67979575497178146, -10.72451020669898902, 36.66557627198103120 ) ) ;
#170432 = CARTESIAN_POINT ( 'NONE',  ( 0.05219959533909260263, 19.03943276465977164, 59.99890960531436690 ) ) ;
#170433 = CARTESIAN_POINT ( 'NONE',  ( 9.474510206698971260, -16.51473224551069308, 47.91557627198102409 ) ) ;
#170434 = CARTESIAN_POINT ( 'NONE',  ( 19.03943276465977164, -0.05219959533909143690, 23.74890960531435269 ) ) ;
#170435 = VECTOR ( 'NONE', #31, 1000.000000000000000 ) ;
#170436 = CARTESIAN_POINT ( 'NONE',  ( -0.05219959533937732626, 21.53943276465977519, 27.50109039468567929 ) ) ;
#170437 = CARTESIAN_POINT ( 'NONE',  ( -19.02544592524342804, 5.153800228976336051, 116.0405762719810383 ) ) ;
#170438 = CARTESIAN_POINT ( 'NONE',  ( 10.81492255796106328, -18.62759615963255655, 45.41775706135234003 ) ) ;
#170439 = CARTESIAN_POINT ( 'NONE',  ( 5.153800228976335163, 19.02544592524342804, 39.79057627198100988 ) ) ;
#170440 = CARTESIAN_POINT ( 'NONE',  ( 5.719274019375991003, -21.55341960407610458, 112.7072429386476955 ) ) ;
#170441 = CARTESIAN_POINT ( 'NONE',  ( 19.03943276465977164, 0.05219959533936151252, 46.25109039468566863 ) ) ;
#170442 = CARTESIAN_POINT ( 'NONE',  ( -5.049401038298153566, 19.05341960407611168, 25.20724293864768484 ) ) ;
#170443 = CARTESIAN_POINT ( 'NONE',  ( -0.05219959533909027116, -19.03943276465977164, 22.49890960531436690 ) ) ;
#170444 =( LENGTH_UNIT ( ) NAMED_UNIT ( * ) SI_UNIT ( .MILLI., .METRE. ) );
#170445 = CARTESIAN_POINT ( 'NONE',  ( -12.06949235617739369, -12.14591786802326823, 54.37609039468568994 ) ) ;
#170446 = CARTESIAN_POINT ( 'NONE',  ( 19.02544592524343514, -5.153800228976328945, 23.54057627198102054 ) ) ;
#170447 = CARTESIAN_POINT ( 'NONE',  ( 34.51794252349512249, -0.7246179257117796313, 89.53606970770105988 ) ) ;
#170448 = CARTESIAN_POINT ( 'NONE',  ( 19.05341960407611168, 5.049401038298154454, 73.95724293864768129 ) ) ;
#170449 = CARTESIAN_POINT ( 'NONE',  ( -4.483927247898539470, -16.52544592524342804, 112.2905762719810241 ) ) ;
#170450 = CARTESIAN_POINT ( 'NONE',  ( 21.55341960407610458, 5.719274019375980345, 58.95724293864770971 ) ) ;
#170451 = CARTESIAN_POINT ( 'NONE',  ( 16.52544592524342804, -4.483927247898539470, 73.54057627198102409 ) ) ;
#170452 = CARTESIAN_POINT ( 'NONE',  ( 14.29746914071037800, 8.314922557961029526, 31.66775706135234358 ) ) ;
#170453 = CARTESIAN_POINT ( 'NONE',  ( 18.67979575497194134, -10.72451020669871369, 90.83442372801901854 ) ) ;
#170454 = CARTESIAN_POINT ( 'NONE',  ( -19.05341960407611168, -5.049401038298163336, 26.45724293864769550 ) ) ;
#170455 = CARTESIAN_POINT ( 'NONE',  ( 8.314922557960818139, 14.29746914071049879, 24.58224293864768839 ) ) ;
#170456 = CARTESIAN_POINT ( 'NONE',  ( 8.314922557960818139, 14.29746914071049879, 54.58224293864769550 ) ) ;
#170457 = CARTESIAN_POINT ( 'NONE',  ( -9.474510206698964154, 16.51473224551069663, 50.41557627198102409 ) ) ;
#170458 = CARTESIAN_POINT ( 'NONE',  ( 15.80617190586769283, -15.72974639402175789, 90.62609039468567573 ) ) ;
#170459 = CARTESIAN_POINT ( 'NONE',  ( 18.62759615963271287, -10.81492255796078972, 103.3322429386476955 ) ) ;
#170460 = CARTESIAN_POINT ( 'NONE',  ( -21.55341960407619339, 5.719274019375674811, 78.54275706135236135 ) ) ;
#170461 = CARTESIAN_POINT ( 'NONE',  ( -8.314922557961024197, 14.29746914071037800, 47.91775706135234714 ) ) ;
#170463 = CARTESIAN_POINT ( 'NONE',  ( 0.05219959533937995610, -21.53943276465977519, 90.00109039468567573 ) ) ;
#170462 = CARTESIAN_POINT ( 'NONE',  ( 8.314922557960818139, 14.29746914071049879, 74.58224293864768129 ) ) ;
#170464 = AXIS2_PLACEMENT_3D ( 'NONE', #27145, #89789, #12963 ) ;
#170465 = CARTESIAN_POINT ( 'NONE',  ( -4.483927247898782831, 16.52544592524335698, 107.7094237280190328 ) ) ;
#170466 = DIRECTION ( 'NONE',  ( -0.000000000000000000, -0.000000000000000000, 1.000000000000000000 ) ) ;
#170467 = CARTESIAN_POINT ( 'NONE',  ( -4.483927247898782831, 16.52544592524335698, 42.70942372801901854 ) ) ;
#170468 = CARTESIAN_POINT ( 'NONE',  ( 8.224510206698953496, -14.34966873604960469, 47.91557627198102409 ) ) ;
#170469 = CARTESIAN_POINT ( 'NONE',  ( -16.52544592524335698, -4.483927247898792601, 88.95942372801901854 ) ) ;
#170470 = CARTESIAN_POINT ( 'NONE',  ( 0.05219959533909260263, 19.03943276465977164, 99.99890960531436690 ) ) ;
#170471 = CARTESIAN_POINT ( 'NONE',  ( 0.05219959533909260263, 19.03943276465977164, 114.9989096053143669 ) ) ;
#170472 = CARTESIAN_POINT ( 'NONE',  ( -0.05219959533937732626, 21.53943276465977519, 102.5010903946856899 ) ) ;
#170473 = CARTESIAN_POINT ( 'NONE',  ( -16.53943276465976808, -0.05219959533934237506, 103.7510903946857042 ) ) ;
#170474 = CARTESIAN_POINT ( 'NONE',  ( -16.52544592524342804, 4.483927247898546575, 76.04057627198102409 ) ) ;
#170475 = CARTESIAN_POINT ( 'NONE',  ( -13.89961937509977652, 13.97604488694528158, 75.62390960531438111 ) ) ;
#170476 = ORIENTED_EDGE ( 'NONE', *, *, #101839, .F. ) ;
#170477 = CARTESIAN_POINT ( 'NONE',  ( -0.05219959533934338120, 16.53943276465976808, 27.50109039468567929 ) ) ;
#170478 = CARTESIAN_POINT ( 'NONE',  ( -9.474510206698964154, 16.51473224551069663, 25.41557627198103120 ) ) ;
#170479 = CARTESIAN_POINT ( 'NONE',  ( 16.46253265017160672, -9.564922557960803928, 93.33224293864769550 ) ) ;
#170481 = CARTESIAN_POINT ( 'NONE',  ( -29.86685920354755552, 21.69954338932564397, -0.8249999972688133454 ) ) ;
#170480 = CARTESIAN_POINT ( 'NONE',  ( -12.14591786802326823, 12.06949235617739902, 28.12609039468568284 ) ) ;
#170482 = CARTESIAN_POINT ( 'NONE',  ( 9.564922557961047289, -16.46253265017146816, 40.41775706135234003 ) ) ;
#170483 = CARTESIAN_POINT ( 'NONE',  ( 8.314922557961029526, -14.29746914071037800, 100.4177570613523471 ) ) ;
#170484 = CARTESIAN_POINT ( 'NONE',  ( 13.97604488694527802, 13.89961937509977652, 39.37390960531435269 ) ) ;
#170485 = CARTESIAN_POINT ( 'NONE',  ( -4.379528057220086978, -16.55341960407618274, 84.79275706135234714 ) ) ;
#170486 = CARTESIAN_POINT ( 'NONE',  ( 0.05219959533934541429, -16.53943276465976808, 65.00109039468568994 ) ) ;
#170487 = CARTESIAN_POINT ( 'NONE',  ( -5.153800228976607833, 19.02544592524334988, 87.70942372801897591 ) ) ;
#170488 = CARTESIAN_POINT ( 'NONE',  ( 21.55341960407619695, -5.719274019375665929, 111.0427570613523613 ) ) ;
#170489 = CARTESIAN_POINT ( 'NONE',  ( 16.51473224551069308, 9.474510206698969483, 49.16557627198102409 ) ) ;
#170490 = CARTESIAN_POINT ( 'NONE',  ( 16.46253265017160672, -9.564922557960803928, 93.33224293864769550 ) ) ;
#170491 = CARTESIAN_POINT ( 'NONE',  ( -14.29746914071049879, 8.314922557960819915, 85.83224293864768129 ) ) ;
#170492 = B_SPLINE_CURVE_WITH_KNOTS ( 'NONE', 3,
 ( #183555, #45041, #152215, #140004, #106699, #185532, #62170, #13699, #91505, #124850, #186550, #61182, #77351, #139018, #168372, #121863 ),
 .UNSPECIFIED., .F., .F.,
 ( 4, 2, 2, 2, 2, 2, 2, 4 ),
 ( 0.001189573402565897910, 0.002113295908917162298, 0.002575157162092795576, 0.003037018415268428854, 0.003498879668444062133, 0.003960740921619694543, 0.004422602174795328689, 0.004884463427970961967 ),
 .UNSPECIFIED. ) ;
#170493 = CARTESIAN_POINT ( 'NONE',  ( 0.05219959533936267826, -19.03943276465977164, 50.00109039468566863 ) ) ;
#170494 = CARTESIAN_POINT ( 'NONE',  ( 10.81492255796078972, 18.62759615963270932, 44.58224293864769550 ) ) ;
#170495 = CARTESIAN_POINT ( 'NONE',  ( 13.89961937509957401, 13.97604488694547697, 26.87609039468566507 ) ) ;
#170496 = CARTESIAN_POINT ( 'NONE',  ( -9.474510206698964154, 16.51473224551069663, 85.41557627198102409 ) ) ;
#170497 = CARTESIAN_POINT ( 'NONE',  ( 15.80617190586746368, 15.72974639402197994, 79.37390960531436690 ) ) ;
#170498 = CARTESIAN_POINT ( 'NONE',  ( -19.03943276465977164, 0.05219959533909376836, 111.2489096053143669 ) ) ;
#170499 = CARTESIAN_POINT ( 'NONE',  ( -13.89961937509957401, -13.97604488694547875, 94.37609039468566152 ) ) ;
#170500 = CARTESIAN_POINT ( 'NONE',  ( -5.049401038298153566, 19.05341960407611168, 115.2072429386477097 ) ) ;
#170501 = CARTESIAN_POINT ( 'NONE',  ( 13.89961937509957401, 13.97604488694547697, 111.8760903946856757 ) ) ;
#170502 = CARTESIAN_POINT ( 'NONE',  ( 19.02544592524343514, -5.153800228976328945, 28.54057627198102409 ) ) ;
#170503 = CARTESIAN_POINT ( 'NONE',  ( -16.46253265017160317, 9.564922557960807481, 100.8322429386477097 ) ) ;
#170504 = CARTESIAN_POINT ( 'NONE',  ( -21.55341960407610458, -5.719274019375992779, 76.45724293864769550 ) ) ;
#170505 = CARTESIAN_POINT ( 'NONE',  ( -16.55341960407617563, 4.379528057220093196, 48.54275706135234714 ) ) ;
#170506 = CARTESIAN_POINT ( 'NONE',  ( -10.81492255796105439, 18.62759615963255655, 47.91775706135234714 ) ) ;
#170508 = CARTESIAN_POINT ( 'NONE',  ( -15.72974639402176322, -15.80617190586768395, 99.37609039468568994 ) ) ;
#170507 = CARTESIAN_POINT ( 'NONE',  ( 16.46253265017146816, 9.564922557961045513, 96.66775706135233293 ) ) ;
#170509 = CARTESIAN_POINT ( 'NONE',  ( -0.05219959533934338120, 16.53943276465976808, 102.5010903946856899 ) ) ;
#170510 = EDGE_CURVE ( 'NONE', #159084, #8650, #138559, .T. ) ;
#170511 = CARTESIAN_POINT ( 'NONE',  ( 13.89961937509977652, -13.97604488694527269, 103.1239096053143527 ) ) ;
#170512 = CARTESIAN_POINT ( 'NONE',  ( 8.314922557960818139, 14.29746914071049879, 89.58224293864768129 ) ) ;
#170513 = CARTESIAN_POINT ( 'NONE',  ( -12.06949235617756955, 12.14591786802309770, 40.62390960531435269 ) ) ;
#170514 = CARTESIAN_POINT ( 'NONE',  ( -19.03943276465977164, -0.05219959533935918106, 68.75109039468566152 ) ) ;
#170515 = EDGE_CURVE ( 'NONE', #198657, #22834, #167136, .T. ) ;
#170516 = CARTESIAN_POINT ( 'NONE',  ( -10.81492255796105439, 18.62759615963255655, 62.91775706135236135 ) ) ;
#170517 = CARTESIAN_POINT ( 'NONE',  ( 9.474510206698729675, 16.51473224551082808, 27.08442372801900433 ) ) ;
#170518 = CARTESIAN_POINT ( 'NONE',  ( -16.53943276465976808, 0.05219959533911058130, 111.2489096053143669 ) ) ;
#170519 = CARTESIAN_POINT ( 'NONE',  ( -15.72974639402197994, 15.80617190586746368, 30.62390960531436335 ) ) ;
#170520 = CARTESIAN_POINT ( 'NONE',  ( -14.29746914071049879, 8.314922557960819915, 25.83224293864769194 ) ) ;
#170521 = CARTESIAN_POINT ( 'NONE',  ( -15.80617190586768217, 15.72974639402176855, 98.12609039468570415 ) ) ;
#170522 = CARTESIAN_POINT ( 'NONE',  ( 8.314922557961029526, -14.29746914071037800, 55.41775706135234714 ) ) ;
#170523 = CARTESIAN_POINT ( 'NONE',  ( 4.483927247898545687, 16.52544592524342804, 29.79057627198102409 ) ) ;
#170524 = CARTESIAN_POINT ( 'NONE',  ( -15.80617190586768217, 15.72974639402176855, 63.12609039468568994 ) ) ;
#170525 = CARTESIAN_POINT ( 'NONE',  ( 10.72451020669871369, 18.67979575497193778, 57.08442372801901854 ) ) ;
#170526 = ORIENTED_EDGE ( 'NONE', *, *, #158176, .T. ) ;
#170527 = CARTESIAN_POINT ( 'NONE',  ( -21.52544592524334988, -5.823673210054445271, 23.95942372801901143 ) ) ;
#170528 = CARTESIAN_POINT ( 'NONE',  ( 8.314922557960818139, 14.29746914071049879, 104.5822429386477097 ) ) ;
#170529 = CARTESIAN_POINT ( 'NONE',  ( 16.46253265017160672, -9.564922557960803928, 23.33224293864769194 ) ) ;
#170530 = CARTESIAN_POINT ( 'NONE',  ( 8.314922557960818139, 14.29746914071049879, 79.58224293864769550 ) ) ;
#170531 = CARTESIAN_POINT ( 'NONE',  ( -13.97604488694527625, -13.89961937509977652, 66.87390960531436690 ) ) ;
#170532 = CARTESIAN_POINT ( 'NONE',  ( 16.52544592524335698, 4.483927247898782831, 101.4594237280190185 ) ) ;
#170533 = CARTESIAN_POINT ( 'NONE',  ( -5.719274019375978568, 21.55341960407610458, 50.20724293864769550 ) ) ;
#170534 = CARTESIAN_POINT ( 'NONE',  ( -4.483927247898539470, -16.52544592524342804, 87.29057627198103830 ) ) ;
#170535 = CARTESIAN_POINT ( 'NONE',  ( 18.67979575497178502, 10.72451020669898547, 94.16557627198103830 ) ) ;
#170536 = CARTESIAN_POINT ( 'NONE',  ( 19.05341960407611168, 5.049401038298154454, 98.95724293864766707 ) ) ;
#170538 = CARTESIAN_POINT ( 'NONE',  ( -16.51473224551082808, 9.474510206698731452, 108.3344237280190043 ) ) ;
#170537 = CARTESIAN_POINT ( 'NONE',  ( -9.564922557960796823, -16.46253265017161027, 57.08224293864769550 ) ) ;
#170539 = CARTESIAN_POINT ( 'NONE',  ( -15.72974639402197994, 15.80617190586746368, 45.62390960531436690 ) ) ;
#170540 = CARTESIAN_POINT ( 'NONE',  ( 18.62759615963255655, 10.81492255796105972, 71.66775706135234714 ) ) ;
#170541 = CARTESIAN_POINT ( 'NONE',  ( 9.474510206698971260, -16.51473224551069308, 62.91557627198102409 ) ) ;
#170542 = CARTESIAN_POINT ( 'NONE',  ( 16.51473224551069308, 9.474510206698969483, 99.16557627198102409 ) ) ;
#170543 = CARTESIAN_POINT ( 'NONE',  ( 4.379528057220092307, 16.55341960407617563, 67.29275706135234714 ) ) ;
#170544 = CARTESIAN_POINT ( 'NONE',  ( 18.62759615963255655, 10.81492255796105972, 56.66775706135235424 ) ) ;
#170545 = CARTESIAN_POINT ( 'NONE',  ( -10.72451020669870658, -18.67979575497194134, 89.58442372801901854 ) ) ;
#170546 = CARTESIAN_POINT ( 'NONE',  ( -10.72451020669898014, 18.67979575497178502, 95.41557627198102409 ) ) ;
#170548 = CARTESIAN_POINT ( 'NONE',  ( -8.314922557961024197, 14.29746914071037800, 82.91775706135234714 ) ) ;
#170547 = CARTESIAN_POINT ( 'NONE',  ( 5.823673210054444382, -21.52544592524334988, 40.20942372801901854 ) ) ;
#170550 = CARTESIAN_POINT ( 'NONE',  ( 21.53943276465977519, -0.05219959533907433946, 78.74890960531436690 ) ) ;
#170549 = B_SPLINE_CURVE_WITH_KNOTS ( 'NONE', 3,
 ( #153081, #61069, #142873, #50882, #19547, #190392, #6350, #84184, #96369, #35703 ),
 .UNSPECIFIED., .F., .F.,
 ( 4, 2, 2, 2, 4 ),
 ( 2.778238173776314926E-07, 0.0003233481720886709990, 0.0006464185203599643768, 0.0009694888686312577546, 0.001292559216902551241 ),
 .UNSPECIFIED. ) ;
#170551 = CARTESIAN_POINT ( 'NONE',  ( -19.03943276465977164, -0.05219959533935918106, 28.75109039468566507 ) ) ;
#170553 = CARTESIAN_POINT ( 'NONE',  ( -0.05219959533910754901, -16.53943276465976808, 22.49890960531436335 ) ) ;
#170552 = CARTESIAN_POINT ( 'NONE',  ( -16.46253265017160317, 9.564922557960807481, 85.83224293864769550 ) ) ;
#170554 = DIRECTION ( 'NONE',  ( 6.938893903907222067E-15, 0.000000000000000000, 1.000000000000000000 ) ) ;
#170555 = CARTESIAN_POINT ( 'NONE',  ( 9.564922557960805705, 16.46253265017160317, 99.58224293864770971 ) ) ;
#170556 = CARTESIAN_POINT ( 'NONE',  ( 17.60691670004651144, 5.500000000000063061, 81.63333313366442212 ) ) ;
#170557 = CARTESIAN_POINT ( 'NONE',  ( 9.474510206698729675, 16.51473224551082808, 92.08442372801900433 ) ) ;
#170558 = CARTESIAN_POINT ( 'NONE',  ( -10.72451020669898014, 18.67979575497178502, 70.41557627198102409 ) ) ;
#170559 = CARTESIAN_POINT ( 'NONE',  ( -12.06949235617756955, 12.14591786802309770, 40.62390960531435269 ) ) ;
#170560 = CARTESIAN_POINT ( 'NONE',  ( 13.89961937509957401, 13.97604488694547697, 106.8760903946856757 ) ) ;
#170561 = CARTESIAN_POINT ( 'NONE',  ( -19.05341960407611168, -5.049401038298163336, 36.45724293864766707 ) ) ;
#170562 = CARTESIAN_POINT ( 'NONE',  ( 14.29746914071037800, 8.314922557961029526, 21.66775706135235069 ) ) ;
#170564 = CARTESIAN_POINT ( 'NONE',  ( -9.564922557961040184, 16.46253265017147172, 77.91775706135234714 ) ) ;
#170563 = CARTESIAN_POINT ( 'NONE',  ( 10.72451020669898902, -18.67979575497178502, 97.91557627198103830 ) ) ;
#170565 = CARTESIAN_POINT ( 'NONE',  ( -4.379528057220086978, -16.55341960407618274, 79.79275706135236135 ) ) ;
#170566 = CARTESIAN_POINT ( 'NONE',  ( 13.97604488694527802, 13.89961937509977652, 74.37390960531436690 ) ) ;
#170567 = CARTESIAN_POINT ( 'NONE',  ( 14.29746914071049879, -8.314922557960816363, 78.33224293864770971 ) ) ;
#170568 = CARTESIAN_POINT ( 'NONE',  ( -5.049401038298153566, 19.05341960407611168, 60.20724293864768129 ) ) ;
#170569 = CARTESIAN_POINT ( 'NONE',  ( -16.52544592524342804, 4.483927247898546575, 66.04057627198103830 ) ) ;
#170570 = LINE ( 'NONE', #187749, #22603 ) ;
#170571 = CARTESIAN_POINT ( 'NONE',  ( -36.86570815857407979, -2.439361326604243096, 49.93277065412546278 ) ) ;
#170572 = CARTESIAN_POINT ( 'NONE',  ( 12.06949235617757843, -12.14591786802309237, 38.12390960531436690 ) ) ;
#170573 = CARTESIAN_POINT ( 'NONE',  ( -13.97604488694527625, -13.89961937509977652, 76.87390960531433848 ) ) ;
#170574 = FACE_BOUND ( 'NONE', #194805, .T. ) ;
#170575 = CARTESIAN_POINT ( 'NONE',  ( -5.153800228976607833, 19.02544592524334988, 57.70942372801899012 ) ) ;
#170576 = CARTESIAN_POINT ( 'NONE',  ( -14.34966873604972548, 8.224510206698743886, 58.33442372801901143 ) ) ;
#170577 = CARTESIAN_POINT ( 'NONE',  ( 18.67979575497178502, 10.72451020669898547, 64.16557627198102409 ) ) ;
#170578 = CARTESIAN_POINT ( 'NONE',  ( 19.02544592524334988, 5.153800228976608722, 21.45942372801899012 ) ) ;
#170579 = CARTESIAN_POINT ( 'NONE',  ( -16.51473224551069308, -9.474510206698971260, 81.66557627198103830 ) ) ;
#170580 = CARTESIAN_POINT ( 'NONE',  ( -7.600000000000007638, 7.873841278763511268E-14, -64.92279855667830191 ) ) ;
#170581 = CARTESIAN_POINT ( 'NONE',  ( -13.97604488694527625, -13.89961937509977652, 106.8739096053143669 ) ) ;
#170582 = CARTESIAN_POINT ( 'NONE',  ( -13.97604488694527625, -13.89961937509977652, 56.87390960531434558 ) ) ;
#170583 = CARTESIAN_POINT ( 'NONE',  ( 21.55341960407619695, -5.719274019375665929, 36.04275706135234714 ) ) ;
#170584 = CARTESIAN_POINT ( 'NONE',  ( -4.379528057220328563, 16.55341960407611168, 100.2072429386476955 ) ) ;
#170585 = ADVANCED_FACE ( 'NONE', ( #16228 ), #77880, .T. ) ;
#170588 = ORIENTED_EDGE ( 'NONE', *, *, #141481, .T. ) ;
#170587 = CARTESIAN_POINT ( 'NONE',  ( -19.03943276465977164, 0.05219959533909376836, 101.2489096053143669 ) ) ;
#170586 = CARTESIAN_POINT ( 'NONE',  ( 0.05219959533907565091, 21.53943276465977519, 104.9989096053143669 ) ) ;
#170589 = CARTESIAN_POINT ( 'NONE',  ( 5.823673210054444382, -21.52544592524334988, 25.20942372801901854 ) ) ;
#170590 = ORIENTED_EDGE ( 'NONE', *, *, #43224, .T. ) ;
#170591 = CARTESIAN_POINT ( 'NONE',  ( 19.02544592524343514, -5.153800228976328945, 83.54057627198100988 ) ) ;
#170592 = DIRECTION ( 'NONE',  ( -0.000000000000000000, -0.000000000000000000, 1.000000000000000000 ) ) ;
#170593 = CARTESIAN_POINT ( 'NONE',  ( -18.62759615963270932, 10.81492255796079327, 95.83224293864770971 ) ) ;
#170594 = CARTESIAN_POINT ( 'NONE',  ( -5.153800228976328057, -19.02544592524343514, 52.29057627198100988 ) ) ;
#170595 = CARTESIAN_POINT ( 'NONE',  ( 5.153800228976615827, -19.02544592524334988, 105.2094237280190185 ) ) ;
#170596 = CARTESIAN_POINT ( 'NONE',  ( 29.86685920354754487, 21.69954338932564752, -3.924999997268812990 ) ) ;
#170597 = CARTESIAN_POINT ( 'NONE',  ( -13.97604488694527625, -13.89961937509977652, 26.87390960531434558 ) ) ;
#170598 = CARTESIAN_POINT ( 'NONE',  ( 18.67979575497194134, -10.72451020669871369, 90.83442372801901854 ) ) ;
#170600 = CARTESIAN_POINT ( 'NONE',  ( -10.81492255796105439, 18.62759615963255655, 52.91775706135235424 ) ) ;
#170599 = CARTESIAN_POINT ( 'NONE',  ( 5.049401038298161559, -19.05341960407611168, 72.70724293864768129 ) ) ;
#170601 = CARTESIAN_POINT ( 'NONE',  ( -10.72451020669870658, -18.67979575497194134, 24.58442372801901499 ) ) ;
#170602 = CARTESIAN_POINT ( 'NONE',  ( 27.73933785331498925, -9.013057229001033122, 142.2750000027311899 ) ) ;
#170603 = CARTESIAN_POINT ( 'NONE',  ( -5.153800228976328057, -19.02544592524343514, 102.2905762719810383 ) ) ;
#170604 = CARTESIAN_POINT ( 'NONE',  ( 19.39720447994796615, 5.499999999999970690, 62.16317477297180716 ) ) ;
#170607 = CARTESIAN_POINT ( 'NONE',  ( 18.62759615963255655, 10.81492255796105972, 41.66775706135235424 ) ) ;
#170606 = CARTESIAN_POINT ( 'NONE',  ( 5.719274019375991003, -21.55341960407610458, 42.70724293864770260 ) ) ;
#170605 = CARTESIAN_POINT ( 'NONE',  ( -16.55341960407617563, 4.379528057220093196, 43.54275706135235424 ) ) ;
#170608 = CARTESIAN_POINT ( 'NONE',  ( 15.72974639402176855, 15.80617190586768217, 71.87609039468568994 ) ) ;
#170609 = CARTESIAN_POINT ( 'NONE',  ( 18.22780087662119897, -5.500000000000146549, 38.51763182126893525 ) ) ;
#170610 = CARTESIAN_POINT ( 'NONE',  ( 19.02544592524334988, 5.153800228976608722, 111.4594237280190043 ) ) ;
#170611 = CARTESIAN_POINT ( 'NONE',  ( 9.564922557960805705, 16.46253265017160317, 59.58224293864769550 ) ) ;
#170612 = CARTESIAN_POINT ( 'NONE',  ( -19.05341960407611168, -5.049401038298163336, 96.45724293864769550 ) ) ;
#170613 = VECTOR ( 'NONE', #179634, 1000.000000000000000 ) ;
#170614 = CARTESIAN_POINT ( 'NONE',  ( 14.34966873604960469, 8.224510206698951720, 114.1655762719810383 ) ) ;
#170615 = CARTESIAN_POINT ( 'NONE',  ( -4.483927247898539470, -16.52544592524342804, 107.2905762719810525 ) ) ;
#170616 = CARTESIAN_POINT ( 'NONE',  ( -10.72451020669898014, 18.67979575497178502, 25.41557627198103120 ) ) ;
#170617 = CARTESIAN_POINT ( 'NONE',  ( 14.34966873604972726, -8.224510206698740333, 80.83442372801901854 ) ) ;
#170619 = CARTESIAN_POINT ( 'NONE',  ( -9.564922557960796823, -16.46253265017161027, 52.08224293864768839 ) ) ;
#170618 = CARTESIAN_POINT ( 'NONE',  ( 0.05219959533910956823, 16.53943276465976808, 69.99890960531435269 ) ) ;
#170620 = CARTESIAN_POINT ( 'NONE',  ( 18.62759615963255655, 10.81492255796105972, 71.66775706135234714 ) ) ;
#170621 = CARTESIAN_POINT ( 'NONE',  ( -5.823673210054431948, 21.52544592524334988, 77.70942372801900433 ) ) ;
#170622 = CARTESIAN_POINT ( 'NONE',  ( -9.564922557961040184, 16.46253265017147172, 112.9177570613523329 ) ) ;
#170623 = CARTESIAN_POINT ( 'NONE',  ( -8.314922557960811034, -14.29746914071050412, 57.08224293864769550 ) ) ;
#170624 = CARTESIAN_POINT ( 'NONE',  ( -5.719274019375665041, -21.55341960407619695, 24.79275706135235779 ) ) ;
#170625 = CARTESIAN_POINT ( 'NONE',  ( 0.05219959533907565091, 21.53943276465977519, 54.99890960531435269 ) ) ;
#170626 = CARTESIAN_POINT ( 'NONE',  ( -17.50000000000000000, -5.500000000000000000, 106.2823096230357010 ) ) ;
#170627 = CARTESIAN_POINT ( 'NONE',  ( -17.81289503416611808, 24.51734667627700404, 147.9500000054623570 ) ) ;
#170628 = CARTESIAN_POINT ( 'NONE',  ( 0.05219959533909260263, 19.03943276465977164, 64.99890960531436690 ) ) ;
#170629 = CARTESIAN_POINT ( 'NONE',  ( -4.379528057220328563, 16.55341960407611168, 40.20724293864769550 ) ) ;
#170630 = CARTESIAN_POINT ( 'NONE',  ( -16.55341960407617563, 4.379528057220093196, 113.5427570613523756 ) ) ;
#170631 = CARTESIAN_POINT ( 'NONE',  ( 4.379528057220092307, 16.55341960407617563, 97.29275706135234714 ) ) ;
#170632 = CARTESIAN_POINT ( 'NONE',  ( 9.474510206698729675, 16.51473224551082808, 57.08442372801900433 ) ) ;
#170633 = CARTESIAN_POINT ( 'NONE',  ( -38.00000000000000711, 2.428612866367529932E-14, -8.000000000000000000 ) ) ;
#170634 = CARTESIAN_POINT ( 'NONE',  ( 9.474510206698971260, -16.51473224551069308, 107.9155762719810383 ) ) ;
#170635 = CARTESIAN_POINT ( 'NONE',  ( 14.34966873604960469, 8.224510206698951720, 69.16557627198102409 ) ) ;
#170636 = CARTESIAN_POINT ( 'NONE',  ( -19.03943276465977164, -0.05219959533935918106, 43.75109039468566863 ) ) ;
#170638 = CARTESIAN_POINT ( 'NONE',  ( 18.67979575497178502, 10.72451020669898547, 34.16557627198102409 ) ) ;
#170637 = CARTESIAN_POINT ( 'NONE',  ( 19.02544592524343514, -5.153800228976328945, 33.54057627198102409 ) ) ;
#170640 = ORIENTED_EDGE ( 'NONE', *, *, #103959, .F. ) ;
#170639 = CARTESIAN_POINT ( 'NONE',  ( -21.53943276465977519, 0.05219959533907696930, 56.24890960531436690 ) ) ;
#170641 = CARTESIAN_POINT ( 'NONE',  ( 14.34966873604960469, 8.224510206698951720, 99.16557627198100988 ) ) ;
#170642 = CARTESIAN_POINT ( 'NONE',  ( 14.34966873604972726, -8.224510206698740333, 50.83442372801901143 ) ) ;
#170643 = CARTESIAN_POINT ( 'NONE',  ( -16.53943276465976808, 0.05219959533911058130, 96.24890960531435269 ) ) ;
#170644 = CARTESIAN_POINT ( 'NONE',  ( -30.74264578624800492, -22.33583958711396278, -11.54999999453762527 ) ) ;
#170645 = CARTESIAN_POINT ( 'NONE',  ( -17.44279575226823198, 5.990770900252468500, 50.83557567514321818 ) ) ;
#170646 = CARTESIAN_POINT ( 'NONE',  ( -5.049401038298153566, 19.05341960407611168, 115.2072429386477097 ) ) ;
#170647 = CARTESIAN_POINT ( 'NONE',  ( -36.91746825000001309, 11.99521256947798342, -1.224999997268813035 ) ) ;
#170648 = DIRECTION ( 'NONE',  ( 0.000000000000000000, 0.000000000000000000, 1.000000000000000000 ) ) ;
#170649 = ORIENTED_EDGE ( 'NONE', *, *, #154768, .F. ) ;
#170651 = CARTESIAN_POINT ( 'NONE',  ( 14.34966873604960469, 8.224510206698951720, 24.16557627198103120 ) ) ;
#170650 = CARTESIAN_POINT ( 'NONE',  ( -12.14591786802326823, 12.06949235617739902, 43.12609039468568284 ) ) ;
#170652 = CARTESIAN_POINT ( 'NONE',  ( -18.67979575497178146, -10.72451020669898902, 51.66557627198102409 ) ) ;
#170653 = CARTESIAN_POINT ( 'NONE',  ( -13.97604488694547697, 13.89961937509957934, 83.12609039468564731 ) ) ;
#170654 = CARTESIAN_POINT ( 'NONE',  ( 5.823673210054125526, 21.52544592524343514, 54.79057627198104541 ) ) ;
#170655 = CARTESIAN_POINT ( 'NONE',  ( 5.823673210054444382, -21.52544592524334988, 75.20942372801901854 ) ) ;
#170656 = DIRECTION ( 'NONE',  ( 0.000000000000000000, 0.000000000000000000, -1.000000000000000000 ) ) ;
#170657 = CARTESIAN_POINT ( 'NONE',  ( 4.483927247898790824, -16.52544592524335698, 50.20942372801901854 ) ) ;
#170659 = CARTESIAN_POINT ( 'NONE',  ( 0.05219959533909260263, 19.03943276465977164, 104.9989096053143669 ) ) ;
#170658 = CARTESIAN_POINT ( 'NONE',  ( 19.02544592524343514, -5.153800228976328945, 33.54057627198102409 ) ) ;
#170660 = CARTESIAN_POINT ( 'NONE',  ( 13.97604488694527802, 13.89961937509977652, 29.37390960531435979 ) ) ;
#170661 = CARTESIAN_POINT ( 'NONE',  ( -16.55341960407611168, -4.379528057220339221, 96.45724293864770971 ) ) ;
#170662 = DIRECTION ( 'NONE',  ( -1.000000000000000000, 0.000000000000000000, -6.982962677686266711E-15 ) ) ;
#170663 = CARTESIAN_POINT ( 'NONE',  ( 0.05219959533909260263, 19.03943276465977164, 104.9989096053143669 ) ) ;
#170664 = ORIENTED_EDGE ( 'NONE', *, *, #27260, .T. ) ;
#170665 = CARTESIAN_POINT ( 'NONE',  ( 12.06949235617739724, 12.14591786802326823, 56.87609039468568994 ) ) ;
#170666 = CARTESIAN_POINT ( 'NONE',  ( 21.55341960407610458, 5.719274019375980345, 93.95724293864770971 ) ) ;
#170667 = CARTESIAN_POINT ( 'NONE',  ( -9.474510206698964154, 16.51473224551069663, 60.41557627198102409 ) ) ;
#170668 = CARTESIAN_POINT ( 'NONE',  ( 5.823673210054444382, -21.52544592524334988, 25.20942372801901854 ) ) ;
#170669 = CARTESIAN_POINT ( 'NONE',  ( -16.46253265017160317, 9.564922557960807481, 85.83224293864769550 ) ) ;
#170670 = CARTESIAN_POINT ( 'NONE',  ( -33.17138627372819570, -22.14683228596885911, -20.77970695691874070 ) ) ;
#170671 = ORIENTED_EDGE ( 'NONE', *, *, #10239, .T. ) ;
#170672 = CARTESIAN_POINT ( 'NONE',  ( -18.62759615963255300, -10.81492255796106328, 19.16775706135234714 ) ) ;
#170675 = CARTESIAN_POINT ( 'NONE',  ( 16.46253265017146816, 9.564922557961045513, 71.66775706135233293 ) ) ;
#170674 = CARTESIAN_POINT ( 'NONE',  ( -9.474510206698964154, 16.51473224551069663, 105.4155762719810383 ) ) ;
#170673 = CARTESIAN_POINT ( 'NONE',  ( 5.049401038298161559, -19.05341960407611168, 27.70724293864769550 ) ) ;
#170676 = CARTESIAN_POINT ( 'NONE',  ( -19.03943276465977164, -0.05219959533935918106, 33.75109039468566863 ) ) ;
#170677 = CARTESIAN_POINT ( 'NONE',  ( 21.55341960407610458, 5.719274019375980345, 98.95724293864770971 ) ) ;
#170678 = CARTESIAN_POINT ( 'NONE',  ( -19.02544592524334988, -5.153800228976617603, 33.95942372801897591 ) ) ;
#170679 = CARTESIAN_POINT ( 'NONE',  ( 8.224510206698742110, 14.34966873604972548, 72.08442372801899012 ) ) ;
#170680 = CARTESIAN_POINT ( 'NONE',  ( -19.05341960407611168, -5.049401038298163336, 111.4572429386476671 ) ) ;
#170681 = CARTESIAN_POINT ( 'NONE',  ( -9.474510206698964154, 16.51473224551069663, 55.41557627198103120 ) ) ;
#170682 = CARTESIAN_POINT ( 'NONE',  ( 18.62759615963255655, 10.81492255796105972, 66.66775706135234714 ) ) ;
#170683 = CARTESIAN_POINT ( 'NONE',  ( -21.55341960407619339, 5.719274019375674811, 78.54275706135236135 ) ) ;
#170684 = CARTESIAN_POINT ( 'NONE',  ( 19.02544592524343514, -5.153800228976328945, 73.54057627198103830 ) ) ;
#170685 = CARTESIAN_POINT ( 'NONE',  ( 15.80617190586769283, -15.72974639402175789, 50.62609039468568994 ) ) ;
#170686 = CARTESIAN_POINT ( 'NONE',  ( -19.05341960407617563, 5.049401038297882671, 83.54275706135233293 ) ) ;
#170687 = CARTESIAN_POINT ( 'NONE',  ( 13.89961937509977652, -13.97604488694527269, 58.12390960531436690 ) ) ;
#170688 = CARTESIAN_POINT ( 'NONE',  ( 13.97604488694527802, 13.89961937509977652, 104.3739096053143385 ) ) ;
#170689 = CARTESIAN_POINT ( 'NONE',  ( -16.51473224551069308, -9.474510206698971260, 61.66557627198103120 ) ) ;
#170690 = CARTESIAN_POINT ( 'NONE',  ( 19.05341960407611168, 5.049401038298154454, 113.9572429386477097 ) ) ;
#170691 = CARTESIAN_POINT ( 'NONE',  ( 5.153800228976335163, 19.02544592524342804, 49.79057627198100988 ) ) ;
#170692 = CARTESIAN_POINT ( 'NONE',  ( -0.05219959533907301413, -21.53943276465977519, 97.49890960531436690 ) ) ;
#170693 = CARTESIAN_POINT ( 'NONE',  ( 4.483927247898790824, -16.52544592524335698, 80.20942372801901854 ) ) ;
#170694 = CARTESIAN_POINT ( 'NONE',  ( -22.37486833544148368, 13.37560805684316101, 165.5209445320982695 ) ) ;
#170695 = CARTESIAN_POINT ( 'NONE',  ( -13.97604488694547697, 13.89961937509957934, 43.12609039468566152 ) ) ;
#170696 = CARTESIAN_POINT ( 'NONE',  ( 16.46253265017160672, -9.564922557960803928, 68.33224293864770971 ) ) ;
#170697 = CARTESIAN_POINT ( 'NONE',  ( -4.483927247898539470, -16.52544592524342804, 62.29057627198102409 ) ) ;
#170698 = CARTESIAN_POINT ( 'NONE',  ( 16.52544592524342804, -4.483927247898539470, 88.54057627198103830 ) ) ;
#170699 = CARTESIAN_POINT ( 'NONE',  ( 5.153800228976335163, 19.02544592524342804, 99.79057627198102409 ) ) ;
#170700 = CARTESIAN_POINT ( 'NONE',  ( 5.153800228976335163, 19.02544592524342804, 89.79057627198102409 ) ) ;
#170701 = CARTESIAN_POINT ( 'NONE',  ( -9.564922557960796823, -16.46253265017161027, 102.0822429386477097 ) ) ;
#170702 = CARTESIAN_POINT ( 'NONE',  ( 5.719274019375673035, 21.55341960407619339, 107.2927570613523471 ) ) ;
#170703 = CARTESIAN_POINT ( 'NONE',  ( -0.05219959533934338120, 16.53943276465976808, 97.50109039468567573 ) ) ;
#170704 = CARTESIAN_POINT ( 'NONE',  ( -19.02544592524342804, 5.153800228976336051, 81.04057627198103830 ) ) ;
#170705 = CARTESIAN_POINT ( 'NONE',  ( -5.719274019375665041, -21.55341960407619695, 44.79275706135234714 ) ) ;
#170706 = CARTESIAN_POINT ( 'NONE',  ( -10.81492255796078084, -18.62759615963271287, 27.08224293864769550 ) ) ;
#170707 = CARTESIAN_POINT ( 'NONE',  ( -10.72451020669898014, 18.67979575497178502, 105.4155762719810383 ) ) ;
#170708 = CARTESIAN_POINT ( 'NONE',  ( -16.53943276465976808, 0.05219959533911058130, 61.24890960531435979 ) ) ;
#170709 = CARTESIAN_POINT ( 'NONE',  ( -9.474510206698964154, 16.51473224551069663, 50.41557627198102409 ) ) ;
#170710 = CARTESIAN_POINT ( 'NONE',  ( -8.224510206698948167, 14.34966873604960824, 85.41557627198102409 ) ) ;
#170711 = CARTESIAN_POINT ( 'NONE',  ( 5.153800228976615827, -19.02544592524334988, 45.20942372801901143 ) ) ;
#170712 = CARTESIAN_POINT ( 'NONE',  ( -12.14591786802309592, -12.06949235617757132, 106.8739096053143811 ) ) ;
#170713 = CARTESIAN_POINT ( 'NONE',  ( 4.379528057220092307, 16.55341960407617563, 62.29275706135236845 ) ) ;
#170714 = CARTESIAN_POINT ( 'NONE',  ( -5.153800228976328057, -19.02544592524343514, 67.29057627198102409 ) ) ;
#170715 = CARTESIAN_POINT ( 'NONE',  ( 22.44159573604009239, 16.30477369853692693, 146.0750000027311728 ) ) ;
#170716 = CARTESIAN_POINT ( 'NONE',  ( 12.06949235617757843, -12.14591786802309237, 93.12390960531436690 ) ) ;
#170717 = CARTESIAN_POINT ( 'NONE',  ( -15.72974639402197994, 15.80617190586746368, 35.62390960531437401 ) ) ;
#170718 = CARTESIAN_POINT ( 'NONE',  ( 8.314922557961029526, -14.29746914071037800, 100.4177570613523471 ) ) ;
#170719 = CARTESIAN_POINT ( 'NONE',  ( 16.52544592524335698, 4.483927247898782831, 26.45942372801901854 ) ) ;
#170720 = CARTESIAN_POINT ( 'NONE',  ( -21.52544592524334988, -5.823673210054445271, 93.95942372801903275 ) ) ;
#170721 = CARTESIAN_POINT ( 'NONE',  ( -19.05341960407611168, -5.049401038298163336, 81.45724293864769550 ) ) ;
#170722 = CARTESIAN_POINT ( 'NONE',  ( 15.80617190586769283, -15.72974639402175789, 25.62609039468567929 ) ) ;
#170723 = CARTESIAN_POINT ( 'NONE',  ( 16.46253265017160672, -9.564922557960803928, 28.33224293864769550 ) ) ;
#170724 = CARTESIAN_POINT ( 'NONE',  ( 14.34966873604972726, -8.224510206698740333, 25.83442372801901499 ) ) ;
#170725 = CARTESIAN_POINT ( 'NONE',  ( 0.05219959533936267826, -19.03943276465977164, 90.00109039468567573 ) ) ;
#170726 = CARTESIAN_POINT ( 'NONE',  ( -5.823673210054116645, -21.52544592524344225, 87.29057627198103830 ) ) ;
#170727 = CARTESIAN_POINT ( 'NONE',  ( 16.51473224551083163, -9.474510206698727899, 70.83442372801900433 ) ) ;
#170728 = CARTESIAN_POINT ( 'NONE',  ( -17.72560187377285246, -5.500000000000056843, 64.07814504131322053 ) ) ;
#170729 = CARTESIAN_POINT ( 'NONE',  ( -18.62759615963255300, -10.81492255796106328, 19.16775706135234714 ) ) ;
#170730 = PLANE ( 'NONE',  #37014 ) ;
#170731 = CARTESIAN_POINT ( 'NONE',  ( 16.51473224551069308, 9.474510206698969483, 79.16557627198103830 ) ) ;
#170732 = CARTESIAN_POINT ( 'NONE',  ( 16.52544592524335698, 4.483927247898782831, 36.45942372801901143 ) ) ;
#170733 = CARTESIAN_POINT ( 'NONE',  ( -17.72517630441458891, 5.499999999999979572, 100.9217571925760097 ) ) ;
#170734 = CARTESIAN_POINT ( 'NONE',  ( 16.51473224551083163, -9.474510206698727899, 60.83442372801900433 ) ) ;
#170736 = CARTESIAN_POINT ( 'NONE',  ( 8.224510206698953496, -14.34966873604960469, 72.91557627198103830 ) ) ;
#170735 = CARTESIAN_POINT ( 'NONE',  ( 21.55341960407610458, 5.719274019375980345, 113.9572429386477239 ) ) ;
#170737 = CARTESIAN_POINT ( 'NONE',  ( -16.51473224551069308, -9.474510206698971260, 86.66557627198102409 ) ) ;
#170740 = CARTESIAN_POINT ( 'NONE',  ( 0.05219959533936267826, -19.03943276465977164, 50.00109039468566863 ) ) ;
#170739 = CARTESIAN_POINT ( 'NONE',  ( 16.55341960407618274, -4.379528057220086978, 41.04275706135236135 ) ) ;
#170738 =( BOUNDED_CURVE ( )  B_SPLINE_CURVE ( 2, ( #5700, #40037, #101710, #176577, #38051, #163401, #52210, #175564, #192736, #83533, #67377 ),
 .UNSPECIFIED., .F., .T. ) 
 B_SPLINE_CURVE_WITH_KNOTS ( ( 3, 2, 2, 2, 2, 3 ),
 ( 0.7000000000000006217, 0.7200000000000006395, 0.7400000000000006573, 0.7600000000000006750, 0.7800000000000006928, 0.8000000000000007105 ),
 .UNSPECIFIED. ) 
 CURVE ( )  GEOMETRIC_REPRESENTATION_ITEM ( )  RATIONAL_B_SPLINE_CURVE ( ( 0.9999999999999983347, 0.9510565162951551965, 1.000000000000000000, 0.9510565162951535312, 1.000000000000000000, 0.9510565162951535312, 1.000000000000000000, 0.9510565162951535312, 1.000000000000000000, 0.9510565162951518658, 1.000000000000001554 ) ) 
 REPRESENTATION_ITEM ( '' )  );
#170741 = CARTESIAN_POINT ( 'NONE',  ( 18.67979575497194134, -10.72451020669871369, 65.83442372801900433 ) ) ;
#170742 = CARTESIAN_POINT ( 'NONE',  ( 14.29746914071037800, 8.314922557961029526, 21.66775706135235069 ) ) ;
#170744 = EDGE_CURVE ( 'NONE', #139805, #41053, #161700, .T. ) ;
#170743 = CARTESIAN_POINT ( 'NONE',  ( 16.51473224551069308, 9.474510206698969483, 59.16557627198102409 ) ) ;
#170745 = CARTESIAN_POINT ( 'NONE',  ( -13.97604488694547697, 13.89961937509957934, 78.12609039468567573 ) ) ;
#170746 = CARTESIAN_POINT ( 'NONE',  ( -8.224510206698735004, -14.34966873604973081, 59.58442372801901854 ) ) ;
#170747 = CARTESIAN_POINT ( 'NONE',  ( 21.53943276465977519, 0.05219959533937863772, 101.2510903946856757 ) ) ;
#170748 = CARTESIAN_POINT ( 'NONE',  ( -13.89961937509957401, -13.97604488694547875, 69.37609039468564731 ) ) ;
#170749 = CARTESIAN_POINT ( 'NONE',  ( -19.02544592524342804, 5.153800228976336051, 51.04057627198103120 ) ) ;
#170750 = CARTESIAN_POINT ( 'NONE',  ( -0.05219959533907301413, -21.53943276465977519, 77.49890960531433848 ) ) ;
#170752 = CARTESIAN_POINT ( 'NONE',  ( -9.564922557961040184, 16.46253265017147172, 82.91775706135233293 ) ) ;
#170751 = CARTESIAN_POINT ( 'NONE',  ( 8.224510206698953496, -14.34966873604960469, 62.91557627198102409 ) ) ;
#170753 = CARTESIAN_POINT ( 'NONE',  ( -19.01529144963335582, -5.500000000000083489, 71.23431955728437970 ) ) ;
#170754 = CARTESIAN_POINT ( 'NONE',  ( 5.153800228976615827, -19.02544592524334988, 40.20942372801898301 ) ) ;
#170755 = CARTESIAN_POINT ( 'NONE',  ( -8.314922557961024197, 14.29746914071037800, 97.91775706135236135 ) ) ;
#170756 = CARTESIAN_POINT ( 'NONE',  ( -16.53943276465976808, 0.05219959533911058130, 71.24890960531435269 ) ) ;
#170758 = CARTESIAN_POINT ( 'NONE',  ( -17.14385361876520619, 23.59649016807275856, 148.5750000027311444 ) ) ;
#170757 = CARTESIAN_POINT ( 'NONE',  ( -18.67979575497193778, 10.72451020669871902, 98.33442372801901854 ) ) ;
#170759 = CARTESIAN_POINT ( 'NONE',  ( -15.72974639402197994, 15.80617190586746368, 90.62390960531436690 ) ) ;
#170760 = CARTESIAN_POINT ( 'NONE',  ( 19.02544592524343514, -5.153800228976328945, 58.54057627198102409 ) ) ;
#170761 = CARTESIAN_POINT ( 'NONE',  ( 15.80617190586769283, -15.72974639402175789, 65.62609039468568994 ) ) ;
#170762 = CARTESIAN_POINT ( 'NONE',  ( -16.51473224551069308, -9.474510206698971260, 46.66557627198102409 ) ) ;
#170763 = VERTEX_POINT ( 'NONE', #97998 ) ;
#170764 = CARTESIAN_POINT ( 'NONE',  ( -9.564922557960796823, -16.46253265017161027, 72.08224293864770971 ) ) ;
#170765 = CARTESIAN_POINT ( 'NONE',  ( -16.52544592524342804, 4.483927247898546575, 116.0405762719810383 ) ) ;
#170766 = CARTESIAN_POINT ( 'NONE',  ( 13.89961937509977652, -13.97604488694527269, 108.1239096053143669 ) ) ;
#170767 = CARTESIAN_POINT ( 'NONE',  ( 4.379528057220339221, -16.55341960407611168, 62.70724293864769550 ) ) ;
#170768 = CARTESIAN_POINT ( 'NONE',  ( -13.97604488694527625, -13.89961937509977652, 36.87390960531436690 ) ) ;
#170769 = CARTESIAN_POINT ( 'NONE',  ( 16.55341960407611168, 4.379528057220329451, 88.95724293864769550 ) ) ;
#170770 = CARTESIAN_POINT ( 'NONE',  ( 15.72974639402199770, -15.80617190586745480, 93.12390960531436690 ) ) ;
#170771 = CARTESIAN_POINT ( 'NONE',  ( 15.80617190586769283, -15.72974639402175789, 35.62609039468568994 ) ) ;
#170772 = CARTESIAN_POINT ( 'NONE',  ( 1.490396665426041878, 7.404744102125047966, -62.24188859777813576 ) ) ;
#170773 = CARTESIAN_POINT ( 'NONE',  ( -0.05219959533934338120, 16.53943276465976808, 52.50109039468567573 ) ) ;
#170774 = CARTESIAN_POINT ( 'NONE',  ( 18.62759615963271287, -10.81492255796078972, 78.33224293864770971 ) ) ;
#170775 = CARTESIAN_POINT ( 'NONE',  ( 19.05341960407617918, -5.049401038297876454, 31.04275706135232227 ) ) ;
#170776 = CARTESIAN_POINT ( 'NONE',  ( -19.03943276465977164, 0.05219959533909376836, 101.2489096053143669 ) ) ;
#170777 = CARTESIAN_POINT ( 'NONE',  ( 15.80617190586769283, -15.72974639402175789, 40.62609039468567573 ) ) ;
#170778 = CARTESIAN_POINT ( 'NONE',  ( 5.719274019375991003, -21.55341960407610458, 42.70724293864770260 ) ) ;
#170779 = CARTESIAN_POINT ( 'NONE',  ( -4.379528057220328563, 16.55341960407611168, 30.20724293864769550 ) ) ;
#170781 = CARTESIAN_POINT ( 'NONE',  ( -21.55341960407619339, 5.719274019375674811, 93.54275706135234714 ) ) ;
#170780 = CARTESIAN_POINT ( 'NONE',  ( -10.81492255796105439, 18.62759615963255655, 67.91775706135234714 ) ) ;
#170782 = CARTESIAN_POINT ( 'NONE',  ( 13.97604488694548053, -13.89961937509957401, 25.62609039468566507 ) ) ;
#170783 = CARTESIAN_POINT ( 'NONE',  ( 14.29746914071037800, 8.314922557961029526, 91.66775706135234714 ) ) ;
#170784 = CARTESIAN_POINT ( 'NONE',  ( -10.81492255796105439, 18.62759615963255655, 57.91775706135234714 ) ) ;
#170785 = CARTESIAN_POINT ( 'NONE',  ( 9.564922557960805705, 16.46253265017160317, 39.58224293864768839 ) ) ;
#170786 = CARTESIAN_POINT ( 'NONE',  ( 16.46253265017146816, 9.564922557961045513, 21.66775706135233648 ) ) ;
#170787 = CARTESIAN_POINT ( 'NONE',  ( 10.72451020669898902, -18.67979575497178502, 27.91557627198103830 ) ) ;
#170788 = CARTESIAN_POINT ( 'NONE',  ( 15.72974639402199770, -15.80617190586745480, 113.1239096053143953 ) ) ;
#170789 = CARTESIAN_POINT ( 'NONE',  ( -10.72451020669898014, 18.67979575497178502, 80.41557627198103830 ) ) ;
#170790 = CARTESIAN_POINT ( 'NONE',  ( 12.14591786802327356, -12.06949235617739191, 45.62609039468567573 ) ) ;
#170792 = CARTESIAN_POINT ( 'NONE',  ( -0.05219959533907301413, -21.53943276465977519, 82.49890960531436690 ) ) ;
#170791 = DIRECTION ( 'NONE',  ( 0.000000000000000000, -1.000000000000000000, 0.000000000000000000 ) ) ;
#170794 = CARTESIAN_POINT ( 'NONE',  ( 16.53943276465976808, -0.05219959533910856209, 58.74890960531436690 ) ) ;
#170793 = CARTESIAN_POINT ( 'NONE',  ( 14.29746914071037800, 8.314922557961029526, 61.66775706135235424 ) ) ;
#170795 = CARTESIAN_POINT ( 'NONE',  ( -27.60098488412539908, -5.861468761075184553, 164.8187539380755311 ) ) ;
#170796 = CARTESIAN_POINT ( 'NONE',  ( 13.89961937509957401, 13.97604488694547697, 91.87609039468567573 ) ) ;
#170797 = CARTESIAN_POINT ( 'NONE',  ( 6.575277882517920780, -6.294065535077253415, -61.89430850415822505 ) ) ;
#170798 = CARTESIAN_POINT ( 'NONE',  ( -16.53943276465976808, -0.05219959533934237506, 38.75109039468567573 ) ) ;
#170799 = CARTESIAN_POINT ( 'NONE',  ( 21.53943276465977519, -0.05219959533907433946, 113.7489096053143527 ) ) ;
#170800 = CARTESIAN_POINT ( 'NONE',  ( -18.62759615963270932, 10.81492255796079327, 80.83224293864769550 ) ) ;
#170801 = CARTESIAN_POINT ( 'NONE',  ( -18.67979575497178146, -10.72451020669898902, 36.66557627198103120 ) ) ;
#170802 = CARTESIAN_POINT ( 'NONE',  ( -12.06949235617739369, -12.14591786802326823, 59.37609039468568284 ) ) ;
#170803 = CARTESIAN_POINT ( 'NONE',  ( 13.97604488694527802, 13.89961937509977652, 74.37390960531436690 ) ) ;
#170805 = CARTESIAN_POINT ( 'NONE',  ( -5.049401038297874678, -19.05341960407617918, 104.7927570613523471 ) ) ;
#170804 = CARTESIAN_POINT ( 'NONE',  ( -5.823673210054431948, 21.52544592524334988, 47.70942372801902565 ) ) ;
#170806 = CARTESIAN_POINT ( 'NONE',  ( 21.53943276465977519, -0.05219959533907433946, 28.74890960531435624 ) ) ;
#170807 = CARTESIAN_POINT ( 'NONE',  ( -9.474510206698720793, -16.51473224551083518, 24.58442372801900078 ) ) ;
#170808 = CARTESIAN_POINT ( 'NONE',  ( 16.55341960407618274, -4.379528057220086978, 41.04275706135236135 ) ) ;
#170809 = CARTESIAN_POINT ( 'NONE',  ( -13.97604488694527625, -13.89961937509977652, 101.8739096053143811 ) ) ;
#170810 = CARTESIAN_POINT ( 'NONE',  ( -21.53943276465977519, 0.05219959533907696930, 101.2489096053143669 ) ) ;
#170811 = CARTESIAN_POINT ( 'NONE',  ( 19.02544592524343514, -5.153800228976328945, 68.54057627198103830 ) ) ;
#170812 = CARTESIAN_POINT ( 'NONE',  ( -16.21995358207306737, 7.366697692864093483, 24.93551001512159360 ) ) ;
#170814 = B_SPLINE_CURVE_WITH_KNOTS ( 'NONE', 3,
 ( #183919, #11103, #45404, #152572, #10102, #135446, #105091, #103101, #133432, #151599, #163784, #134448, #89917, #74755, #121239, #71762, #120248, #150614, #12110, #195121, #60553, #43422, #137404, #136418, #182933, #59564, #29254, #198098, #196133, #149605, #122228, #180956 ),
 .UNSPECIFIED., .F., .F.,
 ( 4, 2, 2, 2, 2, 2, 2, 2, 2, 2, 2, 2, 2, 2, 2, 4 ),
 ( 2.602085213965210256E-18, 0.0003712461730036788090, 0.0007424923460073550160, 0.001113738519011031386, 0.001484984692014707430, 0.002227477038022071879, 0.002598723211025736213, 0.002969969384029400548, 0.003341215557033064883, 0.003712461730036728785, 0.004083707903040393120, 0.004454954076044057888, 0.004826200249047722657, 0.005197446422051386558, 0.005568692595055051327, 0.005939938768058715228 ),
 .UNSPECIFIED. ) ;
#170813 = CARTESIAN_POINT ( 'NONE',  ( 16.55341960407611168, 4.379528057220329451, 83.95724293864770971 ) ) ;
#170815 = CARTESIAN_POINT ( 'NONE',  ( -18.62759615963270932, 10.81492255796079327, 25.83224293864769194 ) ) ;
#170816 = CARTESIAN_POINT ( 'NONE',  ( -17.05587630539785238, 6.762274262135689717, 35.74180309037312497 ) ) ;
#170817 = CARTESIAN_POINT ( 'NONE',  ( 18.62759615963271287, -10.81492255796078972, 103.3322429386476955 ) ) ;
#170818 = CARTESIAN_POINT ( 'NONE',  ( -19.03943276465977164, -0.05219959533935918106, 68.75109039468566152 ) ) ;
#170819 = CARTESIAN_POINT ( 'NONE',  ( 10.72451020669898902, -18.67979575497178502, 37.91557627198102409 ) ) ;
#170820 = CARTESIAN_POINT ( 'NONE',  ( 16.46253265017160672, -9.564922557960803928, 23.33224293864769194 ) ) ;
#170821 = CARTESIAN_POINT ( 'NONE',  ( 10.72451020669898902, -18.67979575497178502, 67.91557627198102409 ) ) ;
#170822 = CARTESIAN_POINT ( 'NONE',  ( -19.05341960407611168, -5.049401038298163336, 101.4572429386476955 ) ) ;
#170823 = CARTESIAN_POINT ( 'NONE',  ( -15.80617190586768217, 15.72974639402176855, 88.12609039468570415 ) ) ;
#170824 = CARTESIAN_POINT ( 'NONE',  ( 5.049401038298161559, -19.05341960407611168, 52.70724293864767418 ) ) ;
#170825 = ADVANCED_FACE ( 'NONE', ( #37351 ), #94553, .F. ) ;
#170826 = CARTESIAN_POINT ( 'NONE',  ( -14.34966873604960291, -8.224510206698953496, 86.66557627198102409 ) ) ;
#170827 = CARTESIAN_POINT ( 'NONE',  ( 16.53943276465976808, 0.05219959533934440121, 31.25109039468568639 ) ) ;
#170828 = CARTESIAN_POINT ( 'NONE',  ( 16.46253265017160672, -9.564922557960803928, 63.33224293864769550 ) ) ;
#170829 = CARTESIAN_POINT ( 'NONE',  ( -21.55341960407619339, 5.719274019375674811, 73.54275706135234714 ) ) ;
#170830 = VERTEX_POINT ( 'NONE', #140316 ) ;
#170831 = CARTESIAN_POINT ( 'NONE',  ( -19.03943276465977164, -0.05219959533935918106, 23.75109039468566152 ) ) ;
#170832 = CARTESIAN_POINT ( 'NONE',  ( 9.564922557961047289, -16.46253265017146816, 45.41775706135232582 ) ) ;
#170833 = CARTESIAN_POINT ( 'NONE',  ( 10.81492255796106328, -18.62759615963255655, 40.41775706135234714 ) ) ;
#170834 = CARTESIAN_POINT ( 'NONE',  ( -8.516083024820087388, 1.203758653825318881, -62.01440738234571626 ) ) ;
#170835 = CARTESIAN_POINT ( 'NONE',  ( -19.05341960407617563, 5.049401038297882671, 38.54275706135233293 ) ) ;
#170836 = CARTESIAN_POINT ( 'NONE',  ( -19.03943276465977164, 0.05219959533909376836, 81.24890960531436690 ) ) ;
#170837 = CARTESIAN_POINT ( 'NONE',  ( 19.02544592524343514, -5.153800228976328945, 68.54057627198103830 ) ) ;
#170838 = CARTESIAN_POINT ( 'NONE',  ( -16.52544592524342804, 4.483927247898546575, 26.04057627198103475 ) ) ;
#170840 = CARTESIAN_POINT ( 'NONE',  ( -10.72451020669870658, -18.67979575497194134, 89.58442372801901854 ) ) ;
#170839 = CARTESIAN_POINT ( 'NONE',  ( -9.474510206698964154, 16.51473224551069663, 110.4155762719810383 ) ) ;
#170841 = AXIS2_PLACEMENT_3D ( 'NONE', #109163, #198205, #59676 ) ;
#170842 = CARTESIAN_POINT ( 'NONE',  ( 29.86685920354754487, 21.69954338932564752, -1.424999997268813212 ) ) ;
#170843 = CARTESIAN_POINT ( 'NONE',  ( -34.52594549653173317, 2.005792002353502844E-14, 89.49999999999897682 ) ) ;
#170844 = CARTESIAN_POINT ( 'NONE',  ( -5.719274019375665041, -21.55341960407619695, 79.79275706135236135 ) ) ;
#170845 = CARTESIAN_POINT ( 'NONE',  ( 16.21995358207306737, -7.366697692864084601, 42.43551001512160781 ) ) ;
#170846 = CARTESIAN_POINT ( 'NONE',  ( 9.474510206698971260, -16.51473224551069308, 97.91557627198102409 ) ) ;
#170847 = DIRECTION ( 'NONE',  ( -1.000000000000000000, -0.000000000000000000, -0.000000000000000000 ) ) ;
#170848 = CARTESIAN_POINT ( 'NONE',  ( 10.72451020669898902, -18.67979575497178502, 72.91557627198103830 ) ) ;
#170849 = CARTESIAN_POINT ( 'NONE',  ( -14.34966873604960291, -8.224510206698953496, 21.66557627198102409 ) ) ;
#170851 = CARTESIAN_POINT ( 'NONE',  ( 16.51473224551069308, 9.474510206698969483, 99.16557627198102409 ) ) ;
#170850 = CARTESIAN_POINT ( 'NONE',  ( -14.34966873604960291, -8.224510206698953496, 111.6655762719810525 ) ) ;
#170852 = CARTESIAN_POINT ( 'NONE',  ( -9.564922557961040184, 16.46253265017147172, 27.91775706135232582 ) ) ;
#170853 = CARTESIAN_POINT ( 'NONE',  ( 8.314922557960818139, 14.29746914071049879, 109.5822429386476955 ) ) ;
#170854 = CARTESIAN_POINT ( 'NONE',  ( -21.55341960407619339, 5.719274019375674811, 63.54275706135234003 ) ) ;
#170855 = CARTESIAN_POINT ( 'NONE',  ( -13.89961937509977652, 13.97604488694528158, 110.6239096053143243 ) ) ;
#170856 = CARTESIAN_POINT ( 'NONE',  ( 12.14591786802327356, -12.06949235617739191, 110.6260903946857042 ) ) ;
#170857 = CARTESIAN_POINT ( 'NONE',  ( 13.89961937509957401, 13.97604488694547697, 66.87609039468567573 ) ) ;
#170858 = CARTESIAN_POINT ( 'NONE',  ( 9.474510206698729675, 16.51473224551082808, 67.08442372801900433 ) ) ;
#170859 = CARTESIAN_POINT ( 'NONE',  ( 0.05219959533909260263, 19.03943276465977164, 104.9989096053143669 ) ) ;
#170860 = CARTESIAN_POINT ( 'NONE',  ( 16.53943276465976808, -0.05219959533910856209, 93.74890960531436690 ) ) ;
#170861 = CARTESIAN_POINT ( 'NONE',  ( 19.05341960407617918, -5.049401038297876454, 56.04275706135234714 ) ) ;
#170862 = CARTESIAN_POINT ( 'NONE',  ( -19.03943276465977164, 0.05219959533909376836, 81.24890960531436690 ) ) ;
#170863 = CARTESIAN_POINT ( 'NONE',  ( 12.06949235617757843, -12.14591786802309237, 58.12390960531435979 ) ) ;
#170864 = CARTESIAN_POINT ( 'NONE',  ( -9.564922557961040184, 16.46253265017147172, 97.91775706135233293 ) ) ;
#170865 = CARTESIAN_POINT ( 'NONE',  ( 18.62759615963271287, -10.81492255796078972, 48.33224293864770260 ) ) ;
#170866 = ORIENTED_EDGE ( 'NONE', *, *, #98810, .T. ) ;
#170867 = CARTESIAN_POINT ( 'NONE',  ( -8.224510206698948167, 14.34966873604960824, 115.4155762719810241 ) ) ;
#170868 = CARTESIAN_POINT ( 'NONE',  ( -17.49999999999999289, -5.622605283950893984, 31.31207310596114013 ) ) ;
#170870 = CARTESIAN_POINT ( 'NONE',  ( 0.05219959533907565091, 21.53943276465977519, 74.99890960531435269 ) ) ;
#170869 = CARTESIAN_POINT ( 'NONE',  ( -0.05219959533909027116, -19.03943276465977164, 67.49890960531436690 ) ) ;
#170872 = CARTESIAN_POINT ( 'NONE',  ( 5.049401038298161559, -19.05341960407611168, 67.70724293864769550 ) ) ;
#170871 = CARTESIAN_POINT ( 'NONE',  ( -16.52544592524335698, -4.483927247898792601, 88.95942372801901854 ) ) ;
#170873 = CARTESIAN_POINT ( 'NONE',  ( -5.153800228976607833, 19.02544592524334988, 72.70942372801900433 ) ) ;
#170874 = CARTESIAN_POINT ( 'NONE',  ( 21.52544592524334988, 5.823673210054432836, 81.45942372801900433 ) ) ;
#170875 = CARTESIAN_POINT ( 'NONE',  ( 10.81492255796078972, 18.62759615963270932, 69.58224293864769550 ) ) ;
#170876 = CARTESIAN_POINT ( 'NONE',  ( -10.81492255796078084, -18.62759615963271287, 22.08224293864769194 ) ) ;
#170877 = CARTESIAN_POINT ( 'NONE',  ( -19.02544592524342804, 5.153800228976336051, 31.04057627198102409 ) ) ;
#170878 = CARTESIAN_POINT ( 'NONE',  ( -8.314922557961024197, 14.29746914071037800, 97.91775706135236135 ) ) ;
#170879 = CARTESIAN_POINT ( 'NONE',  ( -16.53943276465976808, -0.05219959533934237506, 23.75109039468567929 ) ) ;
#170880 = CARTESIAN_POINT ( 'NONE',  ( 17.31747979337948706, 6.344076630961017038, 53.87944868065186199 ) ) ;
#170881 = CARTESIAN_POINT ( 'NONE',  ( -18.62759615963255300, -10.81492255796106328, 94.16775706135237556 ) ) ;
#170882 = ORIENTED_EDGE ( 'NONE', *, *, #135545, .T. ) ;
#170883 = CARTESIAN_POINT ( 'NONE',  ( 16.52544592524342804, -4.483927247898539470, 53.54057627198103120 ) ) ;
#170884 = CARTESIAN_POINT ( 'NONE',  ( -21.52544592524343514, 5.823673210054127303, 91.04057627198103830 ) ) ;
#170885 = CARTESIAN_POINT ( 'NONE',  ( 21.52544592524344225, -5.823673210054117533, 103.5405762719810383 ) ) ;
#170886 = CARTESIAN_POINT ( 'NONE',  ( 21.52544592524344225, -5.823673210054117533, 43.54057627198103830 ) ) ;
#170887 = CARTESIAN_POINT ( 'NONE',  ( 0.05219959533934541429, -16.53943276465976808, 75.00109039468568994 ) ) ;
#170888 = CARTESIAN_POINT ( 'NONE',  ( -12.06949235617756955, 12.14591786802309770, 85.62390960531436690 ) ) ;
#170889 = CARTESIAN_POINT ( 'NONE',  ( -13.97604488694527625, -13.89961937509977652, 51.87390960531436690 ) ) ;
#170890 = CARTESIAN_POINT ( 'NONE',  ( 34.37176626784628297, -7.314009959508099179, 46.67821535514400466 ) ) ;
#170891 = CARTESIAN_POINT ( 'NONE',  ( 8.224510206698953496, -14.34966873604960469, 22.91557627198102765 ) ) ;
#170892 = CARTESIAN_POINT ( 'NONE',  ( -10.72451020669870658, -18.67979575497194134, 29.58442372801901854 ) ) ;
#170893 = CARTESIAN_POINT ( 'NONE',  ( -5.153800228976328057, -19.02544592524343514, 92.29057627198099567 ) ) ;
#170894 = CARTESIAN_POINT ( 'NONE',  ( 21.52544592524334988, 5.823673210054432836, 71.45942372801901854 ) ) ;
#170895 = CARTESIAN_POINT ( 'NONE',  ( -3.573655867282028392E-15, 2.428612866367529932E-14, 139.9999999999999716 ) ) ;
#170896 = CARTESIAN_POINT ( 'NONE',  ( -19.03943276465977164, 0.05219959533909376836, 26.24890960531435624 ) ) ;
#170897 = ORIENTED_EDGE ( 'NONE', *, *, #154166, .F. ) ;
#170898 = CARTESIAN_POINT ( 'NONE',  ( -5.823673210054431948, 21.52544592524334988, 52.70942372801902565 ) ) ;
#170900 = CARTESIAN_POINT ( 'NONE',  ( -19.03943276465977164, 0.05219959533909376836, 111.2489096053143669 ) ) ;
#170899 = CARTESIAN_POINT ( 'NONE',  ( 19.03943276465977164, -0.05219959533909143690, 48.74890960531435979 ) ) ;
#170901 = CARTESIAN_POINT ( 'NONE',  ( 0.05219959533909260263, 19.03943276465977164, 84.99890960531436690 ) ) ;
#170902 = CARTESIAN_POINT ( 'NONE',  ( -0.05219959533936034679, 19.03943276465977164, 67.50109039468566152 ) ) ;
#170903 = CARTESIAN_POINT ( 'NONE',  ( -5.719274019375665041, -21.55341960407619695, 44.79275706135234714 ) ) ;
#170904 = CARTESIAN_POINT ( 'NONE',  ( -13.97604488694547697, 13.89961937509957934, 63.12609039468566152 ) ) ;
#170905 = CARTESIAN_POINT ( 'NONE',  ( -19.05341960407611168, -5.049401038298163336, 36.45724293864766707 ) ) ;
#170906 = CARTESIAN_POINT ( 'NONE',  ( -4.379528057220086978, -16.55341960407618274, 104.7927570613523898 ) ) ;
#170907 = CARTESIAN_POINT ( 'NONE',  ( -19.03943276465977164, -0.05219959533935918106, 73.75109039468566152 ) ) ;
#170908 = CARTESIAN_POINT ( 'NONE',  ( -14.34966873604960291, -8.224510206698953496, 26.66557627198103475 ) ) ;
#170909 = CARTESIAN_POINT ( 'NONE',  ( -19.02544592524334988, -5.153800228976617603, 48.95942372801900433 ) ) ;
#170910 = CARTESIAN_POINT ( 'NONE',  ( -21.52544592524334988, -5.823673210054445271, 103.9594237280190185 ) ) ;
#170911 = CARTESIAN_POINT ( 'NONE',  ( 13.89961937509957401, 13.97604488694547697, 31.87609039468566863 ) ) ;
#170912 = CARTESIAN_POINT ( 'NONE',  ( 0.05219959533909260263, 19.03943276465977164, 29.99890960531435979 ) ) ;
#170913 = CARTESIAN_POINT ( 'NONE',  ( 0.05219959533937995610, -21.53943276465977519, 95.00109039468568994 ) ) ;
#170914 = CARTESIAN_POINT ( 'NONE',  ( 16.52544592524335698, 4.483927247898782831, 26.45942372801901854 ) ) ;
#170915 = CARTESIAN_POINT ( 'NONE',  ( -19.05341960407611168, -5.049401038298163336, 86.45724293864769550 ) ) ;
#170916 = EDGE_CURVE ( 'NONE', #52906, #58517, #184913, .T. ) ;
#170917 = CARTESIAN_POINT ( 'NONE',  ( 8.571926809382597767, 26.38167802310806209, 140.2750000027311899 ) ) ;
#170918 = CARTESIAN_POINT ( 'NONE',  ( -9.474510206698964154, 16.51473224551069663, 80.41557627198103830 ) ) ;
#170919 = CARTESIAN_POINT ( 'NONE',  ( -8.906447517083060816, 27.41122689804195645, 141.5999999999999943 ) ) ;
#170920 = CARTESIAN_POINT ( 'NONE',  ( -19.05341960407617563, 5.049401038297882671, 78.54275706135233293 ) ) ;
#170921 = B_SPLINE_CURVE_WITH_KNOTS ( 'NONE', 3,
 ( #6694, #22883, #193743, #190736, #161391, #145212, #114883, #98700, #130024, #84529, #82534, #20876, #68372, #177579, #39046, #8717, #191723, #129035, #144216, #131046 ),
 .UNSPECIFIED., .F., .F.,
 ( 4, 2, 2, 2, 2, 2, 2, 2, 2, 4 ),
 ( 0.004000878361811951306, 0.004499404418915963801, 0.004997930476019976295, 0.005496456533123988790, 0.005994982590228001285, 0.006244245618779987149, 0.006493508647331973013, 0.006992034704435948211, 0.007490560761539923409, 0.007989086818643898608 ),
 .UNSPECIFIED. ) ;
#170922 = CARTESIAN_POINT ( 'NONE',  ( -13.97604488694527625, -13.89961937509977652, 111.8739096053143243 ) ) ;
#170923 = CARTESIAN_POINT ( 'NONE',  ( 18.67979575497194134, -10.72451020669871369, 105.8344237280190328 ) ) ;
#170924 = CARTESIAN_POINT ( 'NONE',  ( 0.05219959533910956823, 16.53943276465976808, 99.99890960531436690 ) ) ;
#170925 = CARTESIAN_POINT ( 'NONE',  ( 21.61802400803982849, -13.75099706318440873, 167.9999999999999432 ) ) ;
#170926 = CARTESIAN_POINT ( 'NONE',  ( -10.72451020669898014, 18.67979575497178502, 55.41557627198102409 ) ) ;
#170927 = CARTESIAN_POINT ( 'NONE',  ( -10.81492255796078084, -18.62759615963271287, 32.08224293864769550 ) ) ;
#170928 = CARTESIAN_POINT ( 'NONE',  ( 19.05341960407611168, 5.049401038298154454, 28.95724293864769550 ) ) ;
#170929 = DIRECTION ( 'NONE',  ( 1.000000000000000000, 0.000000000000000000, 0.000000000000000000 ) ) ;
#170930 = CARTESIAN_POINT ( 'NONE',  ( 19.03943276465977164, 0.05219959533936151252, 56.25109039468566863 ) ) ;
#170931 = CARTESIAN_POINT ( 'NONE',  ( 8.224510206698953496, -14.34966873604960469, 42.91557627198103120 ) ) ;
#170932 = CARTESIAN_POINT ( 'NONE',  ( 19.02544592524343514, -5.153800228976328945, 113.5405762719810241 ) ) ;
#170933 = CARTESIAN_POINT ( 'NONE',  ( -21.52544592524334988, -5.823673210054445271, 73.95942372801901854 ) ) ;
#170934 = CARTESIAN_POINT ( 'NONE',  ( 5.719274019375991003, -21.55341960407610458, 67.70724293864769550 ) ) ;
#170935 = CARTESIAN_POINT ( 'NONE',  ( 15.80617190586769283, -15.72974639402175789, 45.62609039468567573 ) ) ;
#170936 = CARTESIAN_POINT ( 'NONE',  ( 18.67979575497178502, 10.72451020669898547, 94.16557627198103830 ) ) ;
#170937 = CARTESIAN_POINT ( 'NONE',  ( 0.05219959533937995610, -21.53943276465977519, 45.00109039468568284 ) ) ;
#170938 = CARTESIAN_POINT ( 'NONE',  ( 5.153800228976335163, 19.02544592524342804, 29.79057627198102409 ) ) ;
#170939 = CARTESIAN_POINT ( 'NONE',  ( 13.89961937509977652, -13.97604488694527269, 83.12390960531436690 ) ) ;
#170940 = CARTESIAN_POINT ( 'NONE',  ( 16.52544592524335698, 4.483927247898782831, 76.45942372801901854 ) ) ;
#170941 = CARTESIAN_POINT ( 'NONE',  ( 8.314922557960818139, 14.29746914071049879, 104.5822429386477097 ) ) ;
#170942 = CARTESIAN_POINT ( 'NONE',  ( -19.03943276465977164, 0.05219959533909376836, 116.2489096053143669 ) ) ;
#170943 = CARTESIAN_POINT ( 'NONE',  ( 16.53943276465976808, -0.05219959533910856209, 48.74890960531435979 ) ) ;
#170944 = CARTESIAN_POINT ( 'NONE',  ( 8.224510206698742110, 14.34966873604972548, 107.0844237280190043 ) ) ;
#170945 = CARTESIAN_POINT ( 'NONE',  ( -19.02544592524342804, 5.153800228976336051, 66.04057627198103830 ) ) ;
#170946 = CARTESIAN_POINT ( 'NONE',  ( 13.89961937509977652, -13.97604488694527269, 33.12390960531434558 ) ) ;
#170947 = CARTESIAN_POINT ( 'NONE',  ( 10.72451020669898902, -18.67979575497178502, 42.91557627198103120 ) ) ;
#170948 = CARTESIAN_POINT ( 'NONE',  ( -0.05219959533936034679, 19.03943276465977164, 42.50109039468566152 ) ) ;
#170950 = CARTESIAN_POINT ( 'NONE',  ( 12.06949235617757843, -12.14591786802309237, 38.12390960531436690 ) ) ;
#170949 = CYLINDRICAL_SURFACE ( 'NONE', #146256, 38.00000000000000000 ) ;
#170951 = CARTESIAN_POINT ( 'NONE',  ( 5.719274019375991003, -21.55341960407610458, 27.70724293864769905 ) ) ;
#170952 = CARTESIAN_POINT ( 'NONE',  ( 21.53943276465977519, 0.05219959533937863772, 61.25109039468567573 ) ) ;
#170953 = CARTESIAN_POINT ( 'NONE',  ( 23.29544513554940366, -16.92513159979222337, 140.7843446568999752 ) ) ;
#170954 = CARTESIAN_POINT ( 'NONE',  ( -8.224510206698735004, -14.34966873604973081, 69.58442372801900433 ) ) ;
#170955 = CARTESIAN_POINT ( 'NONE',  ( -19.03943276465977164, -0.05219959533935918106, 63.75109039468566863 ) ) ;
#170956 = CARTESIAN_POINT ( 'NONE',  ( -14.29746914071049879, 8.314922557960819915, 40.83224293864769550 ) ) ;
#170957 = CARTESIAN_POINT ( 'NONE',  ( -19.49671883438226416, -5.500000000000082601, 74.89279849105685116 ) ) ;
#170958 = CARTESIAN_POINT ( 'NONE',  ( 0.05219959533910956823, 16.53943276465976808, 24.99890960531435624 ) ) ;
#170959 = CARTESIAN_POINT ( 'NONE',  ( 9.474510206698971260, -16.51473224551069308, 37.91557627198102409 ) ) ;
#170960 = CARTESIAN_POINT ( 'NONE',  ( -19.02544592524342804, 5.153800228976336051, 56.04057627198100988 ) ) ;
#170961 = CARTESIAN_POINT ( 'NONE',  ( 0.05219959533910956823, 16.53943276465976808, 114.9989096053143669 ) ) ;
#170962 = CARTESIAN_POINT ( 'NONE',  ( -18.67979575497193778, 10.72451020669871902, 33.33442372801900433 ) ) ;
#170963 = CARTESIAN_POINT ( 'NONE',  ( 0.05219959533909260263, 19.03943276465977164, 54.99890960531435979 ) ) ;
#170964 = CARTESIAN_POINT ( 'NONE',  ( 17.50000000000000000, -5.499999999999992895, 81.21769037696435589 ) ) ;
#170965 = CARTESIAN_POINT ( 'NONE',  ( 19.03943276465977164, -0.05219959533909143690, 43.74890960531435979 ) ) ;
#170966 = CARTESIAN_POINT ( 'NONE',  ( 5.823673210054125526, 21.52544592524343514, 34.79057627198103120 ) ) ;
#170967 = VECTOR ( 'NONE', #181424, 1000.000000000000000 ) ;
#170969 = CARTESIAN_POINT ( 'NONE',  ( -14.34966873604960291, -8.224510206698953496, 111.6655762719810525 ) ) ;
#170968 = CARTESIAN_POINT ( 'NONE',  ( -10.72451020669870658, -18.67979575497194134, 59.58442372801901854 ) ) ;
#170970 = CARTESIAN_POINT ( 'NONE',  ( 15.72974639402199770, -15.80617190586745480, 28.12390960531435979 ) ) ;
#170971 = CARTESIAN_POINT ( 'NONE',  ( 8.224510206698742110, 14.34966873604972548, 97.08442372801904696 ) ) ;
#170972 = CARTESIAN_POINT ( 'NONE',  ( -15.80617190586768217, 15.72974639402176855, 108.1260903946856757 ) ) ;
#170973 = CARTESIAN_POINT ( 'NONE',  ( 4.483927247898790824, -16.52544592524335698, 70.20942372801904696 ) ) ;
#170974 = CARTESIAN_POINT ( 'NONE',  ( -9.474510206698964154, 16.51473224551069663, 105.4155762719810383 ) ) ;
#170975 = CARTESIAN_POINT ( 'NONE',  ( -16.55341960407617563, 4.379528057220093196, 58.54275706135235424 ) ) ;
#170976 = CARTESIAN_POINT ( 'NONE',  ( -12.06949235617739369, -12.14591786802326823, 24.37609039468567573 ) ) ;
#170977 = CARTESIAN_POINT ( 'NONE',  ( 4.483927247898790824, -16.52544592524335698, 90.20942372801903275 ) ) ;
#170978 = CARTESIAN_POINT ( 'NONE',  ( -5.823673210054431948, 21.52544592524334988, 47.70942372801902565 ) ) ;
#170979 = CARTESIAN_POINT ( 'NONE',  ( -13.97604488694547697, 13.89961937509957934, 113.1260903946856757 ) ) ;
#170980 = CARTESIAN_POINT ( 'NONE',  ( -15.80617190586745835, -15.72974639402198527, 111.8739096053143669 ) ) ;
#170981 = CARTESIAN_POINT ( 'NONE',  ( 16.55341960407618274, -4.379528057220086978, 26.04275706135235779 ) ) ;
#170982 = CARTESIAN_POINT ( 'NONE',  ( -12.06949235617739369, -12.14591786802326823, 89.37609039468568994 ) ) ;
#170983 = CARTESIAN_POINT ( 'NONE',  ( -37.99626262588766679, 2.428612866367529932E-14, 2.000000000000000000 ) ) ;
#170984 = CARTESIAN_POINT ( 'NONE',  ( 0.05219959533937995610, -21.53943276465977519, 85.00109039468568994 ) ) ;
#170985 = CARTESIAN_POINT ( 'NONE',  ( -9.564922557961040184, 16.46253265017147172, 82.91775706135233293 ) ) ;
#170986 = CARTESIAN_POINT ( 'NONE',  ( 8.314922557960818139, 14.29746914071049879, 49.58224293864769550 ) ) ;
#170987 = CARTESIAN_POINT ( 'NONE',  ( 16.55341960407611168, 4.379528057220329451, 43.95724293864769550 ) ) ;
#170988 = CARTESIAN_POINT ( 'NONE',  ( 16.53943276465976808, -0.05219959533910856209, 108.7489096053143669 ) ) ;
#170990 = CARTESIAN_POINT ( 'NONE',  ( 18.22780087662123805, 5.499999999999960032, 96.48236817873105053 ) ) ;
#170989 = CARTESIAN_POINT ( 'NONE',  ( 5.049401038297881783, 19.05341960407617563, 47.29275706135231161 ) ) ;
#170991 = CARTESIAN_POINT ( 'NONE',  ( -15.80617190586768217, 15.72974639402176855, 53.12609039468568284 ) ) ;
#170992 = CARTESIAN_POINT ( 'NONE',  ( -4.379528057220086978, -16.55341960407618274, 19.79275706135235069 ) ) ;
#170993 = CARTESIAN_POINT ( 'NONE',  ( -36.91128768240056246, 1.976579976310101802E-14, 50.50000000000002842 ) ) ;
#170994 = CARTESIAN_POINT ( 'NONE',  ( 16.51473224551069308, 9.474510206698969483, 99.16557627198102409 ) ) ;
#170995 = CARTESIAN_POINT ( 'NONE',  ( -18.62759615963270932, 10.81492255796079327, 65.83224293864769550 ) ) ;
#170996 = CARTESIAN_POINT ( 'NONE',  ( 5.153800228976615827, -19.02544592524334988, 95.20942372801897591 ) ) ;
#170997 = EDGE_CURVE ( 'NONE', #14496, #19466, #189649, .T. ) ;
#170998 = CARTESIAN_POINT ( 'NONE',  ( 0.05219959533909260263, 19.03943276465977164, 84.99890960531436690 ) ) ;
#170999 = CARTESIAN_POINT ( 'NONE',  ( -21.52544592524343514, 5.823673210054127303, 56.04057627198102409 ) ) ;
#171000 = CARTESIAN_POINT ( 'NONE',  ( -4.379528057220328563, 16.55341960407611168, 105.2072429386477097 ) ) ;
#171001 = CARTESIAN_POINT ( 'NONE',  ( 16.51473224551069308, 9.474510206698969483, 64.16557627198102409 ) ) ;
#171002 = CARTESIAN_POINT ( 'NONE',  ( -16.46253265017160317, 9.564922557960807481, 25.83224293864769194 ) ) ;
#171003 = CARTESIAN_POINT ( 'NONE',  ( -21.53943276465977519, -0.05219959533937600094, 33.75109039468568284 ) ) ;
#171004 = VECTOR ( 'NONE', #143354, 1000.000000000000114 ) ;
#171005 = CARTESIAN_POINT ( 'NONE',  ( 21.55341960407619695, -5.719274019375665929, 81.04275706135236135 ) ) ;
#171006 = CARTESIAN_POINT ( 'NONE',  ( -16.55341960407617563, 4.379528057220093196, 93.54275706135234714 ) ) ;
#171007 = EDGE_CURVE ( 'NONE', #9294, #33383, #185847, .T. ) ;
#171008 = CARTESIAN_POINT ( 'NONE',  ( 21.53943276465977519, 0.05219959533937863772, 26.25109039468567573 ) ) ;
#171009 = CARTESIAN_POINT ( 'NONE',  ( -5.719274019375665041, -21.55341960407619695, 39.79275706135235424 ) ) ;
#171011 = CARTESIAN_POINT ( 'NONE',  ( -19.03943276465977164, 0.05219959533909376836, 81.24890960531436690 ) ) ;
#171010 = CARTESIAN_POINT ( 'NONE',  ( 16.51473224551083163, -9.474510206698727899, 70.83442372801900433 ) ) ;
#171012 = CARTESIAN_POINT ( 'NONE',  ( -21.52544592524334988, -5.823673210054445271, 78.95942372801901854 ) ) ;
#171013 = CARTESIAN_POINT ( 'NONE',  ( -18.62759615963270932, 10.81492255796079327, 80.83224293864769550 ) ) ;
#171014 = CARTESIAN_POINT ( 'NONE',  ( 4.483927247898545687, 16.52544592524342804, 69.79057627198102409 ) ) ;
#171015 = CARTESIAN_POINT ( 'NONE',  ( 18.62759615963255655, 10.81492255796105972, 101.6677570613523613 ) ) ;
#171016 = CARTESIAN_POINT ( 'NONE',  ( -8.224510206698948167, 14.34966873604960824, 80.41557627198103830 ) ) ;
#171017 = CARTESIAN_POINT ( 'NONE',  ( 0.05219959533909260263, 19.03943276465977164, 39.99890960531436690 ) ) ;
#171018 = CARTESIAN_POINT ( 'NONE',  ( 16.46253265017146816, 9.564922557961045513, 71.66775706135233293 ) ) ;
#171019 = CARTESIAN_POINT ( 'NONE',  ( 12.06949235617757843, -12.14591786802309237, 38.12390960531436690 ) ) ;
#171020 = CARTESIAN_POINT ( 'NONE',  ( -10.72451020669870658, -18.67979575497194134, 89.58442372801901854 ) ) ;
#171021 = CARTESIAN_POINT ( 'NONE',  ( -5.049401038298153566, 19.05341960407611168, 95.20724293864770971 ) ) ;
#171022 = CARTESIAN_POINT ( 'NONE',  ( -13.97604488694547697, 13.89961937509957934, 63.12609039468566152 ) ) ;
#171023 = CARTESIAN_POINT ( 'NONE',  ( -21.55341960407610458, -5.719274019375992779, 66.45724293864768129 ) ) ;
#171024 = CARTESIAN_POINT ( 'NONE',  ( -5.719274019375665041, -21.55341960407619695, 19.79275706135235069 ) ) ;
#171025 = CARTESIAN_POINT ( 'NONE',  ( -19.03943276465977164, -0.05219959533935918106, 113.7510903946856757 ) ) ;
#171026 = CARTESIAN_POINT ( 'NONE',  ( 16.55341960407618274, -4.379528057220086978, 81.04275706135236135 ) ) ;
#171028 = CARTESIAN_POINT ( 'NONE',  ( -21.52544592524343514, 5.823673210054127303, 116.0405762719810383 ) ) ;
#171027 = CARTESIAN_POINT ( 'NONE',  ( -4.570733098192862111E-16, -74.04324336000735229, -12.99263613531267936 ) ) ;
#171029 = CARTESIAN_POINT ( 'NONE',  ( 14.29746914071049879, -8.314922557960816363, 98.33224293864769550 ) ) ;
#171030 = CARTESIAN_POINT ( 'NONE',  ( 11.40812507854755253, -35.11059874428192273, -4.524999997268813523 ) ) ;
#171031 = CARTESIAN_POINT ( 'NONE',  ( 4.483927247898790824, -16.52544592524335698, 50.20942372801901854 ) ) ;
#171032 = CARTESIAN_POINT ( 'NONE',  ( 10.81492255796078972, 18.62759615963270932, 64.58224293864769550 ) ) ;
#171033 = CARTESIAN_POINT ( 'NONE',  ( 16.55341960407618274, -4.379528057220086978, 111.0427570613523613 ) ) ;
#171034 = CARTESIAN_POINT ( 'NONE',  ( 16.52544592524335698, 4.483927247898782831, 31.45942372801901854 ) ) ;
#171035 = CARTESIAN_POINT ( 'NONE',  ( -9.474510206698964154, 16.51473224551069663, 25.41557627198103120 ) ) ;
#171036 = CARTESIAN_POINT ( 'NONE',  ( 14.34966873604972726, -8.224510206698740333, 85.83442372801901854 ) ) ;
#171037 = CARTESIAN_POINT ( 'NONE',  ( -5.049401038297874678, -19.05341960407617918, 79.79275706135233293 ) ) ;
#171038 = CARTESIAN_POINT ( 'NONE',  ( 21.52544592524344225, -5.823673210054117533, 68.54057627198103830 ) ) ;
#171039 = CARTESIAN_POINT ( 'NONE',  ( -8.314922557961024197, 14.29746914071037800, 97.91775706135236135 ) ) ;
#171040 = CARTESIAN_POINT ( 'NONE',  ( 10.72451020669871369, 18.67979575497193778, 82.08442372801901854 ) ) ;
#171041 = CARTESIAN_POINT ( 'NONE',  ( -10.72451020669898014, 18.67979575497178502, 65.41557627198102409 ) ) ;
#171042 = CARTESIAN_POINT ( 'NONE',  ( 21.53943276465977519, -0.05219959533907433946, 48.74890960531435979 ) ) ;
#171043 = ORIENTED_EDGE ( 'NONE', *, *, #182123, .F. ) ;
#171044 = CARTESIAN_POINT ( 'NONE',  ( 12.06949235617739724, 12.14591786802326823, 81.87609039468568994 ) ) ;
#171045 = CARTESIAN_POINT ( 'NONE',  ( 18.62759615963271287, -10.81492255796078972, 48.33224293864770260 ) ) ;
#171046 = ORIENTED_EDGE ( 'NONE', *, *, #134292, .F. ) ;
#171047 = CARTESIAN_POINT ( 'NONE',  ( 21.52544592524344225, -5.823673210054117533, 23.54057627198102765 ) ) ;
#171048 = CARTESIAN_POINT ( 'NONE',  ( -24.93942350307309752, -7.769968609432603479, 171.2173313942149662 ) ) ;
#171049 = CARTESIAN_POINT ( 'NONE',  ( -19.05341960407611168, -5.049401038298163336, 21.45724293864768839 ) ) ;
#171050 = CARTESIAN_POINT ( 'NONE',  ( -10.81492255796078084, -18.62759615963271287, 57.08224293864769550 ) ) ;
#171051 = CARTESIAN_POINT ( 'NONE',  ( 4.483927247898790824, -16.52544592524335698, 110.2094237280190185 ) ) ;
#171052 = CARTESIAN_POINT ( 'NONE',  ( 21.55341960407619695, -5.719274019375665929, 41.04275706135236135 ) ) ;
#171053 = CARTESIAN_POINT ( 'NONE',  ( -13.89961937509957401, -13.97604488694547875, 99.37609039468567573 ) ) ;
#171054 = CARTESIAN_POINT ( 'NONE',  ( 19.05341960407611168, 5.049401038298154454, 23.95724293864769194 ) ) ;
#171055 = CARTESIAN_POINT ( 'NONE',  ( -16.53943276465976808, -0.05219959533934237506, 18.75109039468568639 ) ) ;
#171056 = CARTESIAN_POINT ( 'NONE',  ( 5.049401038298161559, -19.05341960407611168, 42.70724293864767418 ) ) ;
#171057 = CARTESIAN_POINT ( 'NONE',  ( 28.82186960331499392, -9.364793116373510529, 140.9000000000000057 ) ) ;
#171058 = CARTESIAN_POINT ( 'NONE',  ( 19.05341960407611168, 5.049401038298154454, 93.95724293864769550 ) ) ;
#171059 = CARTESIAN_POINT ( 'NONE',  ( -4.379528057220086978, -16.55341960407618274, 79.79275706135236135 ) ) ;
#171060 = CARTESIAN_POINT ( 'NONE',  ( -16.51473224551082808, 9.474510206698731452, 73.33442372801900433 ) ) ;
#171061 = CARTESIAN_POINT ( 'NONE',  ( 5.049401038297881783, 19.05341960407617563, 27.29275706135232937 ) ) ;
#171062 = CARTESIAN_POINT ( 'NONE',  ( -18.67979575497178146, -10.72451020669898902, 61.66557627198103120 ) ) ;
#171063 = CARTESIAN_POINT ( 'NONE',  ( 8.224510206698742110, 14.34966873604972548, 82.08442372801901854 ) ) ;
#171064 = CARTESIAN_POINT ( 'NONE',  ( -19.05341960407617563, 5.049401038297882671, 78.54275706135233293 ) ) ;
#171065 = CARTESIAN_POINT ( 'NONE',  ( -13.89961937509977652, 13.97604488694528158, 40.62390960531435979 ) ) ;
#171066 = CARTESIAN_POINT ( 'NONE',  ( 16.46253265017160672, -9.564922557960803928, 73.33224293864769550 ) ) ;
#171067 = CARTESIAN_POINT ( 'NONE',  ( -15.72974639402176322, -15.80617190586768395, 54.37609039468568994 ) ) ;
#171068 = CARTESIAN_POINT ( 'NONE',  ( -16.46253265017160317, 9.564922557960807481, 40.83224293864769550 ) ) ;
#171069 = CARTESIAN_POINT ( 'NONE',  ( -13.97604488694547697, 13.89961937509957934, 73.12609039468568994 ) ) ;
#171070 = CARTESIAN_POINT ( 'NONE',  ( 25.70602947687970641, -7.354137148287276382, 175.2376750527030254 ) ) ;
#171071 = CARTESIAN_POINT ( 'NONE',  ( 19.03943276465977164, -0.05219959533909143690, 108.7489096053143527 ) ) ;
#171072 = CARTESIAN_POINT ( 'NONE',  ( 8.314922557960818139, 14.29746914071049879, 59.58224293864770260 ) ) ;
#171073 = CARTESIAN_POINT ( 'NONE',  ( 15.80617190586746368, 15.72974639402197994, 64.37390960531435269 ) ) ;
#171074 = CARTESIAN_POINT ( 'NONE',  ( 193.3062444957835453, -155.7167183371837496, -13.00000000000000000 ) ) ;
#171075 = CARTESIAN_POINT ( 'NONE',  ( -5.049401038297874678, -19.05341960407617918, 39.79275706135232582 ) ) ;
#171076 = FACE_OUTER_BOUND ( 'NONE', #8976, .T. ) ;
#171078 = CARTESIAN_POINT ( 'NONE',  ( 19.05341960407611168, 5.049401038298154454, 68.95724293864769550 ) ) ;
#171077 = CARTESIAN_POINT ( 'NONE',  ( 0.05219959533909260263, 19.03943276465977164, 59.99890960531436690 ) ) ;
#171079 = CARTESIAN_POINT ( 'NONE',  ( -8.224510206698735004, -14.34966873604973081, 54.58442372801901143 ) ) ;
#171080 = CARTESIAN_POINT ( 'NONE',  ( 17.59860650958994555, -7.585241751806880650, 80.92337014262491834 ) ) ;
#171081 = CARTESIAN_POINT ( 'NONE',  ( -28.82186960331499037, 2.428612866367529617E-14, 146.2500000054623683 ) ) ;
#171082 = CARTESIAN_POINT ( 'NONE',  ( 8.314922557961029526, -14.29746914071037800, 90.41775706135236135 ) ) ;
#171083 = CARTESIAN_POINT ( 'NONE',  ( -17.72696623605158806, 5.500000000000047962, 78.59811031808416715 ) ) ;
#171084 = CARTESIAN_POINT ( 'NONE',  ( -12.14591786802326823, 12.06949235617739902, 68.12609039468567573 ) ) ;
#171085 = CARTESIAN_POINT ( 'NONE',  ( 8.314922557961029526, -14.29746914071037800, 45.41775706135234003 ) ) ;
#171086 = CARTESIAN_POINT ( 'NONE',  ( -19.02544592524334988, -5.153800228976617603, 23.95942372801900078 ) ) ;
#171088 = CARTESIAN_POINT ( 'NONE',  ( 31.79999999999934346, 1.011436372600181938E-12, 95.00000000000021316 ) ) ;
#171087 = CARTESIAN_POINT ( 'NONE',  ( 19.02544592524343514, -5.153800228976328945, 48.54057627198103120 ) ) ;
#171089 = CARTESIAN_POINT ( 'NONE',  ( -18.67979575497193778, 10.72451020669871902, 53.33442372801901854 ) ) ;
#171090 = CARTESIAN_POINT ( 'NONE',  ( 19.03943276465977164, 0.05219959533936151252, 66.25109039468567573 ) ) ;
#171091 = CARTESIAN_POINT ( 'NONE',  ( 5.823673210054444382, -21.52544592524334988, 105.2094237280190328 ) ) ;
#171092 = CARTESIAN_POINT ( 'NONE',  ( -13.97604488694527625, -13.89961937509977652, 26.87390960531434558 ) ) ;
#171093 = CYLINDRICAL_SURFACE ( 'NONE', #30294, 38.00000000000000000 ) ;
#171094 = CARTESIAN_POINT ( 'NONE',  ( 18.67979575497178502, 10.72451020669898547, 54.16557627198103120 ) ) ;
#171095 = CARTESIAN_POINT ( 'NONE',  ( -10.72451020669898014, 18.67979575497178502, 25.41557627198103120 ) ) ;
#171096 = CARTESIAN_POINT ( 'NONE',  ( -8.314922557960811034, -14.29746914071050412, 97.08224293864770971 ) ) ;
#171097 = CARTESIAN_POINT ( 'NONE',  ( 14.34966873604972726, -8.224510206698740333, 40.83442372801901854 ) ) ;
#171098 = CARTESIAN_POINT ( 'NONE',  ( 14.34966873604960469, 8.224510206698951720, 34.16557627198102409 ) ) ;
#171099 = VERTEX_POINT ( 'NONE', #141313 ) ;
#171100 = CARTESIAN_POINT ( 'NONE',  ( -5.719274019375665041, -21.55341960407619695, 24.79275706135235779 ) ) ;
#171102 = CARTESIAN_POINT ( 'NONE',  ( 13.97604488694527802, 13.89961937509977652, 109.3739096053143669 ) ) ;
#171101 = CARTESIAN_POINT ( 'NONE',  ( -8.224510206698948167, 14.34966873604960824, 40.41557627198103120 ) ) ;
#171103 = CARTESIAN_POINT ( 'NONE',  ( 9.564922557961047289, -16.46253265017146816, 105.4177570613523471 ) ) ;
#171104 = CARTESIAN_POINT ( 'NONE',  ( 0.05219959533936267826, -19.03943276465977164, 20.00109039468567218 ) ) ;
#171105 = CARTESIAN_POINT ( 'NONE',  ( 4.379528057220339221, -16.55341960407611168, 27.70724293864769905 ) ) ;
#171107 = EDGE_CURVE ( 'NONE', #61621, #48040, #89266, .T. ) ;
#171106 = CARTESIAN_POINT ( 'NONE',  ( 10.72451020669898902, -18.67979575497178502, 107.9155762719810241 ) ) ;
#171109 = CARTESIAN_POINT ( 'NONE',  ( 18.67979575497178502, 10.72451020669898547, 64.16557627198102409 ) ) ;
#171108 = CARTESIAN_POINT ( 'NONE',  ( 16.81555441253550853, 7.025013491695496270, 31.86314554665743870 ) ) ;
#171110 = CARTESIAN_POINT ( 'NONE',  ( 13.89961937509977652, -13.97604488694527269, 83.12390960531436690 ) ) ;
#171111 = CARTESIAN_POINT ( 'NONE',  ( 16.53943276465976808, -0.05219959533910856209, 48.74890960531435979 ) ) ;
#171112 = CARTESIAN_POINT ( 'NONE',  ( 13.89961937509977652, -13.97604488694527269, 88.12390960531438111 ) ) ;
#171113 = VECTOR ( 'NONE', #47620, 1000.000000000000000 ) ;
#171114 = CARTESIAN_POINT ( 'NONE',  ( -18.22780087662123805, 5.499999999999981348, 81.01763182126896368 ) ) ;
#171115 = CARTESIAN_POINT ( 'NONE',  ( 13.97604488694548053, -13.89961937509957401, 55.62609039468566863 ) ) ;
#171116 = CARTESIAN_POINT ( 'NONE',  ( -10.81492255796078084, -18.62759615963271287, 97.08224293864770971 ) ) ;
#171117 = CARTESIAN_POINT ( 'NONE',  ( 4.483927247898545687, 16.52544592524342804, 104.7905762719810241 ) ) ;
#171118 = CARTESIAN_POINT ( 'NONE',  ( -15.80617190586768217, 15.72974639402176855, 43.12609039468568284 ) ) ;
#171119 = CARTESIAN_POINT ( 'NONE',  ( -22.44159573604009950, -16.30477369853688430, 139.0750000027311728 ) ) ;
#171120 = ADVANCED_FACE ( 'NONE', ( #200017, #93815 ), #139323, .F. ) ;
#171121 = CARTESIAN_POINT ( 'NONE',  ( 8.224510206698953496, -14.34966873604960469, 27.91557627198103830 ) ) ;
#171122 = CARTESIAN_POINT ( 'NONE',  ( -9.564922557960796823, -16.46253265017161027, 32.08224293864769550 ) ) ;
#171123 = CARTESIAN_POINT ( 'NONE',  ( 5.153800228976335163, 19.02544592524342804, 79.79057627198102409 ) ) ;
#171124 = CARTESIAN_POINT ( 'NONE',  ( 18.67979575497178502, 10.72451020669898547, 64.16557627198102409 ) ) ;
#171125 = CARTESIAN_POINT ( 'NONE',  ( -18.22780087662121673, -5.500000000000063061, 61.48459894673894155 ) ) ;
#171126 = CARTESIAN_POINT ( 'NONE',  ( 5.153800228976335163, 19.02544592524342804, 29.79057627198102409 ) ) ;
#171127 = CARTESIAN_POINT ( 'NONE',  ( 10.72451020669898902, -18.67979575497178502, 47.91557627198102409 ) ) ;
#171128 = CARTESIAN_POINT ( 'NONE',  ( 0.05219959533937995610, -21.53943276465977519, 75.00109039468568994 ) ) ;
#171130 = CARTESIAN_POINT ( 'NONE',  ( 4.379528057220092307, 16.55341960407617563, 72.29275706135236135 ) ) ;
#171129 = CARTESIAN_POINT ( 'NONE',  ( 21.90755247610641021, -31.73190472514349381, -17.16613178567241960 ) ) ;
#171131 = CARTESIAN_POINT ( 'NONE',  ( 19.02544592524343514, -5.153800228976328945, 58.54057627198102409 ) ) ;
#171132 = CARTESIAN_POINT ( 'NONE',  ( -5.153800228976328057, -19.02544592524343514, 67.29057627198102409 ) ) ;
#171133 = VERTEX_POINT ( 'NONE', #64480 ) ;
#171134 = CARTESIAN_POINT ( 'NONE',  ( 15.72974639402176855, 15.80617190586768217, 106.8760903946856899 ) ) ;
#171135 = CARTESIAN_POINT ( 'NONE',  ( -0.05219959533934338120, 16.53943276465976808, 72.50109039468568994 ) ) ;
#171136 = CARTESIAN_POINT ( 'NONE',  ( -15.80617190586768217, 15.72974639402176855, 93.12609039468568994 ) ) ;
#171137 = CARTESIAN_POINT ( 'NONE',  ( -16.51473224551069308, -9.474510206698971260, 81.66557627198103830 ) ) ;
#171138 = CARTESIAN_POINT ( 'NONE',  ( -21.53943276465977519, 0.05219959533907696930, 31.24890960531435979 ) ) ;
#171139 = CARTESIAN_POINT ( 'NONE',  ( -5.153800228976607833, 19.02544592524334988, 107.7094237280189759 ) ) ;
#171140 = CARTESIAN_POINT ( 'NONE',  ( 21.53943276465977519, 0.05219959533937863772, 81.25109039468568994 ) ) ;
#171141 = CARTESIAN_POINT ( 'NONE',  ( 8.314922557961029526, -14.29746914071037800, 50.41775706135235424 ) ) ;
#171142 = CARTESIAN_POINT ( 'NONE',  ( -10.72451020669898014, 18.67979575497178502, 105.4155762719810383 ) ) ;
#171143 = CARTESIAN_POINT ( 'NONE',  ( -9.474510206698720793, -16.51473224551083518, 109.5844237280190043 ) ) ;
#171144 = CARTESIAN_POINT ( 'NONE',  ( -19.03943276465977164, 0.05219959533909376836, 76.24890960531435269 ) ) ;
#171145 = CARTESIAN_POINT ( 'NONE',  ( -5.153800228976607833, 19.02544592524334988, 112.7094237280190043 ) ) ;
#171146 = CARTESIAN_POINT ( 'NONE',  ( -5.049401038298153566, 19.05341960407611168, 40.20724293864768839 ) ) ;
#171147 = CIRCLE ( 'NONE', #138810, 8.000000000000000000 ) ;
#171148 = CARTESIAN_POINT ( 'NONE',  ( 9.474510206698729675, 16.51473224551082808, 112.0844237280190043 ) ) ;
#171149 = CARTESIAN_POINT ( 'NONE',  ( -8.224510206698948167, 14.34966873604960824, 65.41557627198102409 ) ) ;
#171150 = CARTESIAN_POINT ( 'NONE',  ( 0.05219959533934541429, -16.53943276465976808, 70.00109039468568994 ) ) ;
#171152 = CARTESIAN_POINT ( 'NONE',  ( -13.89961937509977652, 13.97604488694528158, 45.62390960531433848 ) ) ;
#171151 = CARTESIAN_POINT ( 'NONE',  ( 10.81492255796106328, -18.62759615963255655, 25.41775706135235779 ) ) ;
#171153 = CARTESIAN_POINT ( 'NONE',  ( 19.05341960407611168, 5.049401038298154454, 73.95724293864768129 ) ) ;
#171154 = CARTESIAN_POINT ( 'NONE',  ( -8.314922557961024197, 14.29746914071037800, 67.91775706135234714 ) ) ;
#171155 = ADVANCED_FACE ( 'NONE', ( #108989 ), #122905, .T. ) ;
#171157 = ORIENTED_EDGE ( 'NONE', *, *, #89680, .T. ) ;
#171156 = CARTESIAN_POINT ( 'NONE',  ( -24.27957997113618305, -6.290849861786781183, 171.5443985711290793 ) ) ;
#171158 = VERTEX_POINT ( 'NONE', #192455 ) ;
#171159 = CARTESIAN_POINT ( 'NONE',  ( -5.719274019375665041, -21.55341960407619695, 109.7927570613523613 ) ) ;
#171160 = CARTESIAN_POINT ( 'NONE',  ( -19.02544592524342804, 5.153800228976336051, 41.04057627198103120 ) ) ;
#171162 = ORIENTED_EDGE ( 'NONE', *, *, #60543, .F. ) ;
#171161 = CARTESIAN_POINT ( 'NONE',  ( -19.05341960407611168, -5.049401038298163336, 96.45724293864769550 ) ) ;
#171163 = CARTESIAN_POINT ( 'NONE',  ( -4.379528057220086978, -16.55341960407618274, 29.79275706135234358 ) ) ;
#171165 = CARTESIAN_POINT ( 'NONE',  ( 12.06949235617739724, 12.14591786802326823, 36.87609039468568994 ) ) ;
#171164 = CARTESIAN_POINT ( 'NONE',  ( -16.51473224551082808, 9.474510206698731452, 43.33442372801900433 ) ) ;
#171166 = CARTESIAN_POINT ( 'NONE',  ( -9.564922557960796823, -16.46253265017161027, 47.08224293864769550 ) ) ;
#171167 = CARTESIAN_POINT ( 'NONE',  ( -5.049401038298153566, 19.05341960407611168, 110.2072429386476671 ) ) ;
#171168 = CARTESIAN_POINT ( 'NONE',  ( 16.46253265017160672, -9.564922557960803928, 63.33224293864769550 ) ) ;
#171169 = CARTESIAN_POINT ( 'NONE',  ( 21.53943276465977519, -0.05219959533907433946, 103.7489096053143669 ) ) ;
#171171 = DIRECTION ( 'NONE',  ( 0.000000000000000000, 0.000000000000000000, -1.000000000000000000 ) ) ;
#171170 = CARTESIAN_POINT ( 'NONE',  ( -19.02544592524342804, 5.153800228976336051, 91.04057627198100988 ) ) ;
#171172 = CARTESIAN_POINT ( 'NONE',  ( -16.46253265017160317, 9.564922557960807481, 60.83224293864769550 ) ) ;
#171174 = DIRECTION ( 'NONE',  ( 0.000000000000000000, 0.000000000000000000, -1.000000000000000000 ) ) ;
#171173 = CARTESIAN_POINT ( 'NONE',  ( 4.379528057220339221, -16.55341960407611168, 27.70724293864769905 ) ) ;
#171175 = CARTESIAN_POINT ( 'NONE',  ( -0.05219959533936034679, 19.03943276465977164, 97.50109039468567573 ) ) ;
#171176 = CARTESIAN_POINT ( 'NONE',  ( -13.89961937509957401, -13.97604488694547875, 29.37609039468565797 ) ) ;
#171177 = CARTESIAN_POINT ( 'NONE',  ( 14.29746914071049879, -8.314922557960816363, 63.33224293864770260 ) ) ;
#171178 = CARTESIAN_POINT ( 'NONE',  ( -10.72451020669870658, -18.67979575497194134, 104.5844237280190185 ) ) ;
#171179 = CARTESIAN_POINT ( 'NONE',  ( 5.153800228976335163, 19.02544592524342804, 29.79057627198102409 ) ) ;
#171181 = CARTESIAN_POINT ( 'NONE',  ( -21.53943276465977519, -0.05219959533937600094, 93.75109039468567573 ) ) ;
#171180 = CARTESIAN_POINT ( 'NONE',  ( -0.05219959533910754901, -16.53943276465976808, 22.49890960531436335 ) ) ;
#171182 = CARTESIAN_POINT ( 'NONE',  ( -16.46253265017160317, 9.564922557960807481, 75.83224293864769550 ) ) ;
#171183 = CARTESIAN_POINT ( 'NONE',  ( -9.474510206698964154, 16.51473224551069663, 95.41557627198102409 ) ) ;
#171184 = CARTESIAN_POINT ( 'NONE',  ( -4.483927247898539470, -16.52544592524342804, 97.29057627198105251 ) ) ;
#171185 = CARTESIAN_POINT ( 'NONE',  ( -0.05219959533910754901, -16.53943276465976808, 62.49890960531436690 ) ) ;
#171186 = CARTESIAN_POINT ( 'NONE',  ( 21.55341960407610458, 5.719274019375980345, 73.95724293864769550 ) ) ;
#171187 = CARTESIAN_POINT ( 'NONE',  ( 9.564922557960805705, 16.46253265017160317, 79.58224293864769550 ) ) ;
#171188 = CARTESIAN_POINT ( 'NONE',  ( -18.67979575497178146, -10.72451020669898902, 86.66557627198102409 ) ) ;
#171189 = CARTESIAN_POINT ( 'NONE',  ( 5.049401038297881783, 19.05341960407617563, 82.29275706135229029 ) ) ;
#171191 = CARTESIAN_POINT ( 'NONE',  ( -16.53943276465976808, 0.05219959533911058130, 86.24890960531436690 ) ) ;
#171190 = CARTESIAN_POINT ( 'NONE',  ( -9.564922557961040184, 16.46253265017147172, 32.91775706135233293 ) ) ;
#171192 = CARTESIAN_POINT ( 'NONE',  ( -0.05219959533909027116, -19.03943276465977164, 57.49890960531435979 ) ) ;
#171193 = CARTESIAN_POINT ( 'NONE',  ( -18.67979575497178146, -10.72451020669898902, 61.66557627198103120 ) ) ;
#171194 = CARTESIAN_POINT ( 'NONE',  ( 17.13100169013300444, -6.664070546373151771, 28.26789835699850428 ) ) ;
#171196 = CYLINDRICAL_SURFACE ( 'NONE', #104903, 4.500000000000000000 ) ;
#171195 = CARTESIAN_POINT ( 'NONE',  ( -16.52544592524335698, -4.483927247898792601, 108.9594237280190185 ) ) ;
#171197 = CARTESIAN_POINT ( 'NONE',  ( -16.51473224551082808, 9.474510206698731452, 108.3344237280190043 ) ) ;
#171198 = CARTESIAN_POINT ( 'NONE',  ( 4.483927247898545687, 16.52544592524342804, 84.79057627198102409 ) ) ;
#171199 = CARTESIAN_POINT ( 'NONE',  ( 6.941592873960390264, -1.351304681146071829, -62.33628431810817716 ) ) ;
#171200 = CARTESIAN_POINT ( 'NONE',  ( 5.153800228976335163, 19.02544592524342804, 74.79057627198103830 ) ) ;
#171201 = CARTESIAN_POINT ( 'NONE',  ( -19.03943276465977164, 0.05219959533909376836, 36.24890960531436690 ) ) ;
#171202 = CARTESIAN_POINT ( 'NONE',  ( 16.55341960407611168, 4.379528057220329451, 63.95724293864770260 ) ) ;
#171203 = CARTESIAN_POINT ( 'NONE',  ( 13.89961937509977652, -13.97604488694527269, 98.12390960531433848 ) ) ;
#171205 = CARTESIAN_POINT ( 'NONE',  ( 5.049401038298161559, -19.05341960407611168, 67.70724293864769550 ) ) ;
#171204 = CARTESIAN_POINT ( 'NONE',  ( -16.51473224551082808, 9.474510206698731452, 93.33442372801900433 ) ) ;
#171206 = CARTESIAN_POINT ( 'NONE',  ( -13.97604488694527625, -13.89961937509977652, 91.87390960531432427 ) ) ;
#171207 = CARTESIAN_POINT ( 'NONE',  ( 18.67979575497178502, 10.72451020669898547, 74.16557627198102409 ) ) ;
#171208 = CARTESIAN_POINT ( 'NONE',  ( 16.52544592524335698, 4.483927247898782831, 71.45942372801901854 ) ) ;
#171209 = CARTESIAN_POINT ( 'NONE',  ( -5.153800228976607833, 19.02544592524335343, 112.7094237280190043 ) ) ;
#171210 = CARTESIAN_POINT ( 'NONE',  ( -0.05219959533909027116, -19.03943276465977164, 67.49890960531436690 ) ) ;
#171211 = CARTESIAN_POINT ( 'NONE',  ( -5.719274019375978568, 21.55341960407610458, 70.20724293864769550 ) ) ;
#171212 = CARTESIAN_POINT ( 'NONE',  ( -5.049401038297874678, -19.05341960407617918, 89.79275706135230450 ) ) ;
#171214 = CARTESIAN_POINT ( 'NONE',  ( -21.53943276465977519, -0.05219959533937600094, 48.75109039468568284 ) ) ;
#171213 = CARTESIAN_POINT ( 'NONE',  ( 8.224510206698953496, -14.34966873604960469, 42.91557627198103120 ) ) ;
#171215 = CARTESIAN_POINT ( 'NONE',  ( 0.000000000000000000, 0.000000000000000000, -52.65483682830183199 ) ) ;
#171217 = CARTESIAN_POINT ( 'NONE',  ( -13.97604488694527625, -13.89961937509977652, 111.8739096053143243 ) ) ;
#171216 = CARTESIAN_POINT ( 'NONE',  ( 8.314922557961029526, -14.29746914071037800, 75.41775706135233293 ) ) ;
#171218 = CARTESIAN_POINT ( 'NONE',  ( 16.46253265017160672, -9.564922557960803928, 108.3322429386476955 ) ) ;
#171219 = CARTESIAN_POINT ( 'NONE',  ( -17.26058549869092218, 6.457015423128486198, 78.62254162523936429 ) ) ;
#171220 = CARTESIAN_POINT ( 'NONE',  ( 12.06949235617739724, 12.14591786802326823, 96.87609039468568994 ) ) ;
#171221 = CARTESIAN_POINT ( 'NONE',  ( 8.224510206698742110, 14.34966873604972548, 42.08442372801901854 ) ) ;
#171222 = CARTESIAN_POINT ( 'NONE',  ( 16.46253265017160672, -9.564922557960803928, 53.33224293864768839 ) ) ;
#171223 = CARTESIAN_POINT ( 'NONE',  ( 5.049401038298161559, -19.05341960407611168, 57.70724293864769550 ) ) ;
#171224 = CARTESIAN_POINT ( 'NONE',  ( -5.823673210054431948, 21.52544592524334988, 47.70942372801902565 ) ) ;
#171225 = CARTESIAN_POINT ( 'NONE',  ( -0.05219959533934338120, 16.53943276465976808, 62.50109039468568284 ) ) ;
#171226 = CARTESIAN_POINT ( 'NONE',  ( -16.52544592524342804, 4.483927247898546575, 31.04057627198102409 ) ) ;
#171227 = CARTESIAN_POINT ( 'NONE',  ( 16.51473224551069308, 9.474510206698969483, 44.16557627198103120 ) ) ;
#171228 = CARTESIAN_POINT ( 'NONE',  ( -0.05219959533909027116, -19.03943276465977164, 32.49890960531435979 ) ) ;
#171229 = CARTESIAN_POINT ( 'NONE',  ( 8.224510206698742110, 14.34966873604972548, 27.08442372801901854 ) ) ;
#171230 = CARTESIAN_POINT ( 'NONE',  ( -19.03943276465977164, -0.05219959533935918106, 88.75109039468567573 ) ) ;
#171231 = CARTESIAN_POINT ( 'NONE',  ( 14.29746914071049879, -8.314922557960816363, 83.33224293864769550 ) ) ;
#171232 = CARTESIAN_POINT ( 'NONE',  ( -5.153800228976328057, -19.02544592524343514, 57.29057627198103120 ) ) ;
#171234 = CARTESIAN_POINT ( 'NONE',  ( 17.44279575226823198, -5.990770900252456066, 93.33557567514314712 ) ) ;
#171233 = CARTESIAN_POINT ( 'NONE',  ( 0.05219959533936267826, -19.03943276465977164, 90.00109039468567573 ) ) ;
#171235 = CARTESIAN_POINT ( 'NONE',  ( -10.72451020669870658, -18.67979575497194134, 89.58442372801901854 ) ) ;
#171236 = CARTESIAN_POINT ( 'NONE',  ( -4.379528057220086978, -16.55341960407618274, 59.79275706135234714 ) ) ;
#171237 = CARTESIAN_POINT ( 'NONE',  ( 17.44279575226823553, 5.990770900252484488, 36.66442432485683156 ) ) ;
#171238 = CARTESIAN_POINT ( 'NONE',  ( 15.80617190586746368, 15.72974639402197994, 49.37390960531436690 ) ) ;
#171239 = CARTESIAN_POINT ( 'NONE',  ( -14.29746914071037622, -8.314922557961029526, 44.16775706135234714 ) ) ;
#171240 = CARTESIAN_POINT ( 'NONE',  ( -19.03943276465977164, 0.05219959533909376836, 21.24890960531436335 ) ) ;
#171241 = CARTESIAN_POINT ( 'NONE',  ( -13.89961937509957401, -13.97604488694547875, 34.37609039468566863 ) ) ;
#171242 = CARTESIAN_POINT ( 'NONE',  ( -16.46253265017160317, 9.564922557960807481, 70.83224293864770971 ) ) ;
#171243 = CARTESIAN_POINT ( 'NONE',  ( 30.74264578624800137, -22.33583958711395212, -7.200000000000001066 ) ) ;
#171244 = CARTESIAN_POINT ( 'NONE',  ( -13.89961937509977652, 13.97604488694528158, 55.62390960531434558 ) ) ;
#171245 = CARTESIAN_POINT ( 'NONE',  ( -20.10096181552316708, -22.06460587353105751, -51.62975016085093927 ) ) ;
#171246 = CARTESIAN_POINT ( 'NONE',  ( -5.049401038298153566, 19.05341960407611168, 75.20724293864769550 ) ) ;
#171247 = CARTESIAN_POINT ( 'NONE',  ( -19.19724070472091881, -5.500000000000170530, 56.06193348274384647 ) ) ;
#171248 = PRODUCT_DEFINITION_SHAPE ( 'NONE', 'NONE',  #200204 ) ;
#171249 = CARTESIAN_POINT ( 'NONE',  ( 19.03943276465977164, 0.05219959533936151252, 31.25109039468566863 ) ) ;
#171250 = CARTESIAN_POINT ( 'NONE',  ( -0.05219959533937732626, 21.53943276465977519, 107.5010903946856899 ) ) ;
#171251 = CARTESIAN_POINT ( 'NONE',  ( -4.483927247898539470, -16.52544592524342804, 42.29057627198103120 ) ) ;
#171252 = CARTESIAN_POINT ( 'NONE',  ( 13.89961937509977652, -13.97604488694527269, 43.12390960531434558 ) ) ;
#171253 = EDGE_CURVE ( 'NONE', #89861, #191417, #5133, .T. ) ;
#171254 = CARTESIAN_POINT ( 'NONE',  ( -16.51473224551069308, -9.474510206698971260, 101.6655762719810241 ) ) ;
#171255 = CARTESIAN_POINT ( 'NONE',  ( -15.80617190586768217, 15.72974639402176855, 73.12609039468567573 ) ) ;
#171256 = CARTESIAN_POINT ( 'NONE',  ( -0.05219959533909027116, -19.03943276465977164, 47.49890960531435979 ) ) ;
#171257 = CARTESIAN_POINT ( 'NONE',  ( -21.52544592524334988, -5.823673210054445271, 78.95942372801901854 ) ) ;
#171258 = CARTESIAN_POINT ( 'NONE',  ( -5.823673210054116645, -21.52544592524344225, 22.29057627198102765 ) ) ;
#171259 = CARTESIAN_POINT ( 'NONE',  ( -0.05219959533909027116, -19.03943276465977164, 32.49890960531435979 ) ) ;
#171260 = CARTESIAN_POINT ( 'NONE',  ( 0.05219959533937995610, -21.53943276465977519, 20.00109039468568639 ) ) ;
#171261 = CARTESIAN_POINT ( 'NONE',  ( -13.89961937509957401, -13.97604488694547875, 54.37609039468565442 ) ) ;
#171262 = CARTESIAN_POINT ( 'NONE',  ( -13.89961937509977652, 13.97604488694528158, 30.62390960531435269 ) ) ;
#171263 = CARTESIAN_POINT ( 'NONE',  ( 9.564922557960805705, 16.46253265017160317, 74.58224293864769550 ) ) ;
#171264 = CARTESIAN_POINT ( 'NONE',  ( -9.564922557961040184, 16.46253265017147172, 107.9177570613523471 ) ) ;
#171265 = CARTESIAN_POINT ( 'NONE',  ( -0.05219959533910754901, -16.53943276465976808, 77.49890960531433848 ) ) ;
#171266 = CARTESIAN_POINT ( 'NONE',  ( 10.81492255796078972, 18.62759615963270932, 39.58224293864769550 ) ) ;
#171267 = CARTESIAN_POINT ( 'NONE',  ( 19.05341960407617918, -5.049401038297876454, 101.0427570613523045 ) ) ;
#171268 = CARTESIAN_POINT ( 'NONE',  ( 15.72974639402199770, -15.80617190586745480, 103.1239096053143811 ) ) ;
#171269 = CARTESIAN_POINT ( 'NONE',  ( -0.05219959533937732626, 21.53943276465977519, 57.50109039468568994 ) ) ;
#171270 = CARTESIAN_POINT ( 'NONE',  ( 16.55341960407618274, -4.379528057220086978, 51.04275706135234714 ) ) ;
#171271 = CARTESIAN_POINT ( 'NONE',  ( -12.14591786802326823, 12.06949235617739902, 53.12609039468568284 ) ) ;
#171272 = CARTESIAN_POINT ( 'NONE',  ( 18.62759615963271287, -10.81492255796078972, 63.33224293864770260 ) ) ;
#171273 = CARTESIAN_POINT ( 'NONE',  ( 5.049401038298161559, -19.05341960407611168, 52.70724293864767418 ) ) ;
#171274 = CARTESIAN_POINT ( 'NONE',  ( -8.314922557961024197, 14.29746914071037800, 82.91775706135234714 ) ) ;
#171275 = CARTESIAN_POINT ( 'NONE',  ( -5.719274019375978568, 21.55341960407610458, 105.2072429386477097 ) ) ;
#171276 = CARTESIAN_POINT ( 'NONE',  ( -14.29746914071049879, 8.314922557960819915, 45.83224293864769550 ) ) ;
#171277 = CARTESIAN_POINT ( 'NONE',  ( 9.564922557960805705, 16.46253265017160317, 74.58224293864769550 ) ) ;
#171278 = CARTESIAN_POINT ( 'NONE',  ( 12.14591786802327356, -12.06949235617739191, 80.62609039468567573 ) ) ;
#171279 = CARTESIAN_POINT ( 'NONE',  ( -8.224510206698735004, -14.34966873604973081, 19.58442372801901143 ) ) ;
#171280 = CARTESIAN_POINT ( 'NONE',  ( 21.55341960407610458, 5.719274019375980345, 108.9572429386476955 ) ) ;
#171281 = CARTESIAN_POINT ( 'NONE',  ( -8.314922557960811034, -14.29746914071050412, 42.08224293864769550 ) ) ;
#171282 = EDGE_CURVE ( 'NONE', #16960, #179364, #128273, .T. ) ;
#171283 = VERTEX_POINT ( 'NONE', #129746 ) ;
#171284 = CARTESIAN_POINT ( 'NONE',  ( -16.31925111598454592, 7.325300261831593218, 70.16424538967251578 ) ) ;
#171285 = CARTESIAN_POINT ( 'NONE',  ( -21.53943276465977519, 0.05219959533907696930, 91.24890960531436690 ) ) ;
#171286 = CARTESIAN_POINT ( 'NONE',  ( 4.483927247898545687, 16.52544592524342804, 29.79057627198102409 ) ) ;
#171287 = ORIENTED_EDGE ( 'NONE', *, *, #17418, .T. ) ;
#171288 = CARTESIAN_POINT ( 'NONE',  ( -16.21995358207306381, -7.366697692864128122, 55.06448998487843483 ) ) ;
#171289 = CARTESIAN_POINT ( 'NONE',  ( 21.53943276465977519, 0.05219959533937863772, 21.25109039468567218 ) ) ;
#171290 = CARTESIAN_POINT ( 'NONE',  ( -5.049401038298153566, 19.05341960407611168, 115.2072429386477097 ) ) ;
#171291 = CARTESIAN_POINT ( 'NONE',  ( 0.05219959533937995610, -21.53943276465977519, 20.00109039468568639 ) ) ;
#171292 = CARTESIAN_POINT ( 'NONE',  ( 12.06949235617757843, -12.14591786802309237, 53.12390960531436690 ) ) ;
#171293 = CARTESIAN_POINT ( 'NONE',  ( 4.483927247898790824, -16.52544592524335698, 45.20942372801901854 ) ) ;
#171294 = CIRCLE ( 'NONE', #158300, 28.82186960331498682 ) ;
#171295 = CARTESIAN_POINT ( 'NONE',  ( -16.51473224551069308, -9.474510206698971260, 56.66557627198103120 ) ) ;
#171296 = CARTESIAN_POINT ( 'NONE',  ( -19.05341960407617563, 5.049401038297882671, 58.54275706135234003 ) ) ;
#171297 = CARTESIAN_POINT ( 'NONE',  ( 19.02544592524343514, -5.153800228976328945, 78.54057627198099567 ) ) ;
#171298 = CARTESIAN_POINT ( 'NONE',  ( 0.05219959533907565091, 21.53943276465977519, 39.99890960531436690 ) ) ;
#171299 = CARTESIAN_POINT ( 'NONE',  ( -28.03896471500539889, -25.30868469084938965, -20.82118626251310189 ) ) ;
#171300 = CARTESIAN_POINT ( 'NONE',  ( -16.46253265017160317, 9.564922557960807481, 40.83224293864769550 ) ) ;
#171301 = CARTESIAN_POINT ( 'NONE',  ( 8.314922557961029526, -14.29746914071037800, 20.41775706135234714 ) ) ;
#171302 = CARTESIAN_POINT ( 'NONE',  ( 16.46253265017146816, 9.564922557961045513, 61.66775706135234003 ) ) ;
#171303 = CARTESIAN_POINT ( 'NONE',  ( -18.67979575497178146, -10.72451020669898902, 106.6655762719810383 ) ) ;
#171304 = CARTESIAN_POINT ( 'NONE',  ( 12.06949235617757843, -12.14591786802309237, 28.12390960531435979 ) ) ;
#171305 = CARTESIAN_POINT ( 'NONE',  ( 0.05219959533909260263, 19.03943276465977164, 89.99890960531436690 ) ) ;
#171306 = CARTESIAN_POINT ( 'NONE',  ( -18.67979575497178146, -10.72451020669898902, 61.66557627198103120 ) ) ;
#171308 = CARTESIAN_POINT ( 'NONE',  ( -14.29746914071037622, -8.314922557961029526, 24.16775706135235424 ) ) ;
#171307 = CARTESIAN_POINT ( 'NONE',  ( 10.72451020669898902, -18.67979575497178502, 97.91557627198103830 ) ) ;
#171309 = CARTESIAN_POINT ( 'NONE',  ( -15.80617190586745835, -15.72974639402198527, 36.87390960531435979 ) ) ;
#171310 = CARTESIAN_POINT ( 'NONE',  ( 21.52544592524334988, 5.823673210054432836, 91.45942372801901854 ) ) ;
#171311 = CARTESIAN_POINT ( 'NONE',  ( 13.89961937509977652, -13.97604488694527269, 83.12390960531436690 ) ) ;
#171312 = CARTESIAN_POINT ( 'NONE',  ( 16.51473224551069308, 9.474510206698969483, 34.16557627198102409 ) ) ;
#171313 = CARTESIAN_POINT ( 'NONE',  ( 13.97604488694527802, 13.89961937509977652, 84.37390960531433848 ) ) ;
#171314 = CARTESIAN_POINT ( 'NONE',  ( -12.06949235617756955, 12.14591786802309770, 110.6239096053143669 ) ) ;
#171315 = CARTESIAN_POINT ( 'NONE',  ( 0.05219959533909260263, 19.03943276465977164, 64.99890960531436690 ) ) ;
#171316 = CARTESIAN_POINT ( 'NONE',  ( -8.224510206698735004, -14.34966873604973081, 19.58442372801901143 ) ) ;
#171317 = CARTESIAN_POINT ( 'NONE',  ( 0.000000000000000000, 0.000000000000000000, -64.92279855667830191 ) ) ;
#171319 = CARTESIAN_POINT ( 'NONE',  ( -10.81492255796078084, -18.62759615963271287, 22.08224293864769194 ) ) ;
#171318 = CARTESIAN_POINT ( 'NONE',  ( -21.53943276465977519, -0.05219959533937600094, 103.7510903946857042 ) ) ;
#171320 = CARTESIAN_POINT ( 'NONE',  ( -12.06949235617739369, -12.14591786802326823, 94.37609039468568994 ) ) ;
#171321 = CARTESIAN_POINT ( 'NONE',  ( 20.51075850018421676, -20.36001345239828808, -49.67367017693149478 ) ) ;
#171322 = CARTESIAN_POINT ( 'NONE',  ( 19.03943276465977164, 0.05219959533936151252, 66.25109039468567573 ) ) ;
#171323 = CARTESIAN_POINT ( 'NONE',  ( -5.153800228976607833, 19.02544592524334988, 27.70942372801899722 ) ) ;
#171324 = CARTESIAN_POINT ( 'NONE',  ( 20.91330281277714676, -18.31365339088606348, 140.0000000000000568 ) ) ;
#171325 = CARTESIAN_POINT ( 'NONE',  ( -16.51473224551069308, -9.474510206698971260, 26.66557627198103120 ) ) ;
#171326 = CARTESIAN_POINT ( 'NONE',  ( -16.53943276465976808, 0.05219959533911058130, 31.24890960531435979 ) ) ;
#171327 = CARTESIAN_POINT ( 'NONE',  ( 0.05219959533909260263, 19.03943276465977164, 24.99890960531435269 ) ) ;
#171328 = CARTESIAN_POINT ( 'NONE',  ( 8.314922557960818139, 14.29746914071049879, 24.58224293864768839 ) ) ;
#171329 = CARTESIAN_POINT ( 'NONE',  ( 6.434671708797586653, 6.434671708797580436, -61.89430850415821794 ) ) ;
#171330 = CARTESIAN_POINT ( 'NONE',  ( -16.52544592524335698, -4.483927247898792601, 93.95942372801903275 ) ) ;
#171331 = CARTESIAN_POINT ( 'NONE',  ( -16.46253265017160317, 9.564922557960807481, 30.83224293864769550 ) ) ;
#171332 = CARTESIAN_POINT ( 'NONE',  ( 0.05219959533937995610, -21.53943276465977519, 90.00109039468567573 ) ) ;
#171333 = CARTESIAN_POINT ( 'NONE',  ( -13.97604488694547697, 13.89961937509957934, 98.12609039468566152 ) ) ;
#171334 = CARTESIAN_POINT ( 'NONE',  ( 5.719274019375673035, 21.55341960407619339, 82.29275706135234714 ) ) ;
#171335 = CARTESIAN_POINT ( 'NONE',  ( -9.474510206698720793, -16.51473224551083518, 54.58442372801899722 ) ) ;
#171336 = CARTESIAN_POINT ( 'NONE',  ( 0.05219959533909260263, 19.03943276465977164, 89.99890960531436690 ) ) ;
#171337 = CARTESIAN_POINT ( 'NONE',  ( -5.153800228976328057, -19.02544592524343514, 67.29057627198102409 ) ) ;
#171338 = DIRECTION ( 'NONE',  ( 1.000000000000000000, 0.000000000000000000, 0.000000000000000000 ) ) ;
#171339 = CARTESIAN_POINT ( 'NONE',  ( 12.06949235617757843, -12.14591786802309237, 68.12390960531436690 ) ) ;
#171340 = CARTESIAN_POINT ( 'NONE',  ( -5.719274019375978568, 21.55341960407610458, 60.20724293864768839 ) ) ;
#171341 = CARTESIAN_POINT ( 'NONE',  ( -19.02544592524342804, 5.153800228976336051, 51.04057627198103120 ) ) ;
#171343 = CARTESIAN_POINT ( 'NONE',  ( -8.314922557961024197, 14.29746914071037800, 77.91775706135231871 ) ) ;
#171342 = CARTESIAN_POINT ( 'NONE',  ( 5.719274019375991003, -21.55341960407610458, 82.70724293864770971 ) ) ;
#171344 = ORIENTED_EDGE ( 'NONE', *, *, #143324, .T. ) ;
#171345 = CARTESIAN_POINT ( 'NONE',  ( -16.51473224551069308, -9.474510206698971260, 46.66557627198102409 ) ) ;
#171347 = CARTESIAN_POINT ( 'NONE',  ( 36.91746824999999887, 11.99521256947799053, -3.524999997268813079 ) ) ;
#171346 = CARTESIAN_POINT ( 'NONE',  ( 4.379528057220339221, -16.55341960407611168, 82.70724293864770971 ) ) ;
#171348 = CARTESIAN_POINT ( 'NONE',  ( -19.02544592524342804, 5.153800228976336051, 46.04057627198101699 ) ) ;
#171349 = CARTESIAN_POINT ( 'NONE',  ( -0.05219959533909027116, -19.03943276465977164, 27.49890960531435624 ) ) ;
#171350 = CARTESIAN_POINT ( 'NONE',  ( 19.03943276465977164, 0.05219959533936151252, 71.25109039468566152 ) ) ;
#171351 = CARTESIAN_POINT ( 'NONE',  ( 8.314922557960818139, 14.29746914071049879, 64.58224293864769550 ) ) ;
#171353 = ADVANCED_FACE ( 'NONE', ( #25624 ), #178295, .T. ) ;
#171352 = CARTESIAN_POINT ( 'NONE',  ( -21.52544592524334988, -5.823673210054445271, 38.95942372801901854 ) ) ;
#171355 = CARTESIAN_POINT ( 'NONE',  ( 18.67979575497178502, 10.72451020669898547, 104.1655762719810241 ) ) ;
#171354 = CARTESIAN_POINT ( 'NONE',  ( -16.46253265017160317, 9.564922557960807481, 40.83224293864769550 ) ) ;
#171356 = DIRECTION ( 'NONE',  ( -0.000000000000000000, -0.000000000000000000, 1.000000000000000000 ) ) ;
#171357 = CARTESIAN_POINT ( 'NONE',  ( 12.06949235617757843, -12.14591786802309237, 93.12390960531436690 ) ) ;
#171358 = CARTESIAN_POINT ( 'NONE',  ( 27.19415581439775664, -28.92630772671044070, -20.12198987529614058 ) ) ;
#171359 = CARTESIAN_POINT ( 'NONE',  ( 5.049401038298161559, -19.05341960407611168, 52.70724293864767418 ) ) ;
#171360 = CARTESIAN_POINT ( 'NONE',  ( 17.44270441346517231, 5.991230190323030946, 113.8633507926423079 ) ) ;
#171362 = CARTESIAN_POINT ( 'NONE',  ( 5.153800228976335163, 19.02544592524342804, 99.79057627198102409 ) ) ;
#171361 = CARTESIAN_POINT ( 'NONE',  ( -13.89961937509957401, -13.97604488694547875, 94.37609039468566152 ) ) ;
#171363 = CARTESIAN_POINT ( 'NONE',  ( -5.719274019375665041, -21.55341960407619695, 39.79275706135235424 ) ) ;
#171364 = CARTESIAN_POINT ( 'NONE',  ( -5.049401038298153566, 19.05341960407611168, 80.20724293864769550 ) ) ;
#171365 = CARTESIAN_POINT ( 'NONE',  ( -9.474510206698720793, -16.51473224551083518, 69.58442372801901854 ) ) ;
#171366 = CARTESIAN_POINT ( 'NONE',  ( 16.46253265017160672, -9.564922557960803928, 38.33224293864768839 ) ) ;
#171367 = CARTESIAN_POINT ( 'NONE',  ( -14.34966873604960291, -8.224510206698953496, 66.66557627198102409 ) ) ;
#171368 = CARTESIAN_POINT ( 'NONE',  ( 16.52544592524342804, -4.483927247898539470, 73.54057627198102409 ) ) ;
#171369 = CARTESIAN_POINT ( 'NONE',  ( -13.89961937509977652, 13.97604488694528158, 75.62390960531438111 ) ) ;
#171370 = CARTESIAN_POINT ( 'NONE',  ( 0.05219959533907565091, 21.53943276465977519, 99.99890960531436690 ) ) ;
#171371 = CARTESIAN_POINT ( 'NONE',  ( -19.05341960407611168, -5.049401038298163336, 66.45724293864769550 ) ) ;
#171372 = ADVANCED_FACE ( 'NONE', ( #6413 ), #50787, .T. ) ;
#171373 = CARTESIAN_POINT ( 'NONE',  ( 15.72974639402176855, 15.80617190586768217, 111.8760903946856615 ) ) ;
#171376 = CARTESIAN_POINT ( 'NONE',  ( -4.379528057220328563, 16.55341960407611168, 110.2072429386477239 ) ) ;
#171375 = CARTESIAN_POINT ( 'NONE',  ( 8.224510206698742110, 14.34966873604972548, 107.0844237280190043 ) ) ;
#171374 = CARTESIAN_POINT ( 'NONE',  ( -19.03943276465977164, 0.05219959533909376836, 36.24890960531436690 ) ) ;
#171377 = CARTESIAN_POINT ( 'NONE',  ( 19.03943276465977164, 0.05219959533936151252, 111.2510903946856757 ) ) ;
#171378 = ORIENTED_EDGE ( 'NONE', *, *, #78423, .F. ) ;
#171379 = CARTESIAN_POINT ( 'NONE',  ( 21.55341960407619695, -5.719274019375665929, 26.04275706135235779 ) ) ;
#171380 = CARTESIAN_POINT ( 'NONE',  ( 9.474510206698729675, 16.51473224551082808, 72.08442372801900433 ) ) ;
#171381 = CARTESIAN_POINT ( 'NONE',  ( 8.314922557961029526, -14.29746914071037800, 110.4177570613523756 ) ) ;
#171382 = CARTESIAN_POINT ( 'NONE',  ( 15.72974639402199770, -15.80617190586745480, 78.12390960531436690 ) ) ;
#171383 = CARTESIAN_POINT ( 'NONE',  ( 9.474510206698971260, -16.51473224551069308, 112.9155762719810383 ) ) ;
#171384 = CARTESIAN_POINT ( 'NONE',  ( -16.53943276465976808, 0.05219959533911058130, 51.24890960531436690 ) ) ;
#171385 = CARTESIAN_POINT ( 'NONE',  ( -9.564922557960796823, -16.46253265017161027, 32.08224293864769550 ) ) ;
#171386 = CARTESIAN_POINT ( 'NONE',  ( 16.46253265017160672, -9.564922557960803928, 43.33224293864769550 ) ) ;
#171387 = CARTESIAN_POINT ( 'NONE',  ( -13.97604488694547697, 13.89961937509957934, 28.12609039468565797 ) ) ;
#171388 = CARTESIAN_POINT ( 'NONE',  ( -16.53943276465976808, -0.05219959533934237506, 88.75109039468567573 ) ) ;
#171389 = CARTESIAN_POINT ( 'NONE',  ( -4.483927247898782831, 16.52544592524335698, 57.70942372801901143 ) ) ;
#171390 = CARTESIAN_POINT ( 'NONE',  ( 19.03943276465977164, -0.05219959533909143690, 113.7489096053143669 ) ) ;
#171392 = CARTESIAN_POINT ( 'NONE',  ( 10.81492255796106328, -18.62759615963255655, 110.4177570613523756 ) ) ;
#171391 = CARTESIAN_POINT ( 'NONE',  ( 9.474510206698971260, -16.51473224551069308, 47.91557627198102409 ) ) ;
#171393 = CARTESIAN_POINT ( 'NONE',  ( -9.564922557960796823, -16.46253265017161027, 77.08224293864769550 ) ) ;
#171394 = CARTESIAN_POINT ( 'NONE',  ( 4.379528057220092307, 16.55341960407617563, 57.29275706135234714 ) ) ;
#171395 = CARTESIAN_POINT ( 'NONE',  ( 0.05219959533910956823, 16.53943276465976808, 104.9989096053143669 ) ) ;
#171396 = CARTESIAN_POINT ( 'NONE',  ( 8.224510206698953496, -14.34966873604960469, 22.91557627198102765 ) ) ;
#171397 = CARTESIAN_POINT ( 'NONE',  ( 12.50000000000001066, -90.00000000000005684, -4.999999999999999112 ) ) ;
#171400 = CARTESIAN_POINT ( 'NONE',  ( -16.46253265017160317, 9.564922557960807481, 75.83224293864769550 ) ) ;
#171399 = CARTESIAN_POINT ( 'NONE',  ( -16.46253265017160317, 9.564922557960807481, 95.83224293864769550 ) ) ;
#171398 = CARTESIAN_POINT ( 'NONE',  ( -10.72451020669870658, -18.67979575497194134, 64.58442372801900433 ) ) ;
#171401 = CARTESIAN_POINT ( 'NONE',  ( -16.46253265017160317, 9.564922557960807481, 105.8322429386476955 ) ) ;
#171402 = CARTESIAN_POINT ( 'NONE',  ( -0.05219959533910754901, -16.53943276465976808, 52.49890960531435979 ) ) ;
#171403 = CARTESIAN_POINT ( 'NONE',  ( -16.53943276465976808, -0.05219959533934237506, 113.7510903946856757 ) ) ;
#171404 = ORIENTED_EDGE ( 'NONE', *, *, #136656, .F. ) ;
#171405 = CARTESIAN_POINT ( 'NONE',  ( 16.55341960407611168, 4.379528057220329451, 43.95724293864769550 ) ) ;
#171407 = PLANE ( 'NONE',  #51241 ) ;
#171406 = CARTESIAN_POINT ( 'NONE',  ( 8.224510206698742110, 14.34966873604972548, 42.08442372801901854 ) ) ;
#171408 = CARTESIAN_POINT ( 'NONE',  ( -13.89961937509957401, -13.97604488694547875, 39.37609039468566152 ) ) ;
#171409 = CARTESIAN_POINT ( 'NONE',  ( -19.05341960407611168, -5.049401038298163336, 81.45724293864769550 ) ) ;
#171410 = CARTESIAN_POINT ( 'NONE',  ( 16.51473224551083163, -9.474510206698727899, 45.83442372801900433 ) ) ;
#171411 = CARTESIAN_POINT ( 'NONE',  ( -19.02544592524334988, -5.153800228976617603, 53.95942372801898301 ) ) ;
#171413 = CARTESIAN_POINT ( 'NONE',  ( 8.314922557961029526, -14.29746914071037800, 80.41775706135234714 ) ) ;
#171412 = CARTESIAN_POINT ( 'NONE',  ( 19.05341960407617918, -5.049401038297876454, 96.04275706135231871 ) ) ;
#171414 = CARTESIAN_POINT ( 'NONE',  ( -13.97604488694527625, -13.89961937509977652, 31.87390960531435979 ) ) ;
#171415 = CARTESIAN_POINT ( 'NONE',  ( -5.153800228976328057, -19.02544592524343514, 102.2905762719810383 ) ) ;
#171416 = CARTESIAN_POINT ( 'NONE',  ( 10.81492255796106328, -18.62759615963255655, 35.41775706135234003 ) ) ;
#171417 = CARTESIAN_POINT ( 'NONE',  ( -16.46253265017146816, -9.564922557961047289, 84.16775706135233293 ) ) ;
#171419 = CARTESIAN_POINT ( 'NONE',  ( -19.03943276465977164, 0.05219959533909376836, 56.24890960531435979 ) ) ;
#171418 = CARTESIAN_POINT ( 'NONE',  ( 17.50000000000002487, 4.262806489437421575, 23.40424424251102664 ) ) ;
#171420 = CARTESIAN_POINT ( 'NONE',  ( 16.51473224551069308, 9.474510206698969483, 109.1655762719810383 ) ) ;
#171422 = CARTESIAN_POINT ( 'NONE',  ( -9.564922557960796823, -16.46253265017161027, 47.08224293864769550 ) ) ;
#171421 = CARTESIAN_POINT ( 'NONE',  ( 14.34966873604960469, 8.224510206698951720, 59.16557627198103120 ) ) ;
#171423 = CARTESIAN_POINT ( 'NONE',  ( -9.474510206698964154, 16.51473224551069663, 65.41557627198102409 ) ) ;
#171424 = CARTESIAN_POINT ( 'NONE',  ( 5.153800228976615827, -19.02544592524334988, 65.20942372801900433 ) ) ;
#171425 = CARTESIAN_POINT ( 'NONE',  ( 0.05219959533936267826, -19.03943276465977164, 50.00109039468566863 ) ) ;
#171426 = CARTESIAN_POINT ( 'NONE',  ( 16.51473224551069308, 9.474510206698969483, 79.16557627198103830 ) ) ;
#171427 = CARTESIAN_POINT ( 'NONE',  ( 15.72974639402199770, -15.80617190586745480, 78.12390960531436690 ) ) ;
#171429 = CARTESIAN_POINT ( 'NONE',  ( -5.049401038297874678, -19.05341960407617918, 34.79275706135233293 ) ) ;
#171428 = CARTESIAN_POINT ( 'NONE',  ( -14.29746914071049879, 8.314922557960819915, 70.83224293864770971 ) ) ;
#171430 = CARTESIAN_POINT ( 'NONE',  ( -15.72974639402197994, 15.80617190586746368, 40.62390960531435269 ) ) ;
#171431 = CARTESIAN_POINT ( 'NONE',  ( 15.72974639402199770, -15.80617190586745480, 43.12390960531435269 ) ) ;
#171432 = CARTESIAN_POINT ( 'NONE',  ( -5.153800228976328057, -19.02544592524343514, 72.29057627198102409 ) ) ;
#171433 = CARTESIAN_POINT ( 'NONE',  ( -19.02544592524342804, 5.153800228976336051, 41.04057627198103120 ) ) ;
#171434 = CARTESIAN_POINT ( 'NONE',  ( 19.05341960407611168, 5.049401038298154454, 23.95724293864769194 ) ) ;
#171435 = CARTESIAN_POINT ( 'NONE',  ( -18.67979575497193778, 10.72451020669871902, 23.33442372801901499 ) ) ;
#171436 = CARTESIAN_POINT ( 'NONE',  ( -16.46253265017160317, 9.564922557960807481, 115.8322429386477097 ) ) ;
#171437 = CARTESIAN_POINT ( 'NONE',  ( 21.55341960407619695, -5.719274019375665929, 21.04275706135234714 ) ) ;
#171438 = CARTESIAN_POINT ( 'NONE',  ( -16.51473224551069308, -9.474510206698971260, 36.66557627198102409 ) ) ;
#171439 = CARTESIAN_POINT ( 'NONE',  ( -5.719274019375978568, 21.55341960407610458, 100.2072429386476955 ) ) ;
#171440 = CARTESIAN_POINT ( 'NONE',  ( 13.97604488694548053, -13.89961937509957401, 45.62609039468566863 ) ) ;
#171441 = CARTESIAN_POINT ( 'NONE',  ( 5.153800228976335163, 19.02544592524342804, 24.79057627198102765 ) ) ;
#171442 = CARTESIAN_POINT ( 'NONE',  ( 19.05341960407611168, 5.049401038298154454, 23.95724293864769194 ) ) ;
#171443 = CARTESIAN_POINT ( 'NONE',  ( 16.86227489769508026, -6.785021502584605457, 21.28941672232436488 ) ) ;
#171444 = CARTESIAN_POINT ( 'NONE',  ( 14.34966873604972726, -8.224510206698740333, 55.83442372801901854 ) ) ;
#171445 = CARTESIAN_POINT ( 'NONE',  ( -19.05341960407611168, -5.049401038298163336, 26.45724293864769550 ) ) ;
#171446 = CARTESIAN_POINT ( 'NONE',  ( 33.90027759800518936, -5.214635694306275049, 93.21535130585120044 ) ) ;
#171447 = CARTESIAN_POINT ( 'NONE',  ( -16.46253265017160317, 9.564922557960807481, 70.83224293864770971 ) ) ;
#171448 = CARTESIAN_POINT ( 'NONE',  ( -12.14591786802309592, -12.06949235617757132, 106.8739096053143811 ) ) ;
#171449 = CARTESIAN_POINT ( 'NONE',  ( -15.80617190586745835, -15.72974639402198527, 41.87390960531435979 ) ) ;
#171450 = CARTESIAN_POINT ( 'NONE',  ( -0.05219959533910754901, -16.53943276465976808, 72.49890960531435269 ) ) ;
#171451 = CARTESIAN_POINT ( 'NONE',  ( -8.224510206698735004, -14.34966873604973081, 39.58442372801901143 ) ) ;
#171452 = CARTESIAN_POINT ( 'NONE',  ( 18.62759615963255655, 10.81492255796105972, 81.66775706135236135 ) ) ;
#171453 = CARTESIAN_POINT ( 'NONE',  ( -0.05219959533909027116, -19.03943276465977164, 32.49890960531435979 ) ) ;
#171454 = CARTESIAN_POINT ( 'NONE',  ( -14.34966873604972548, 8.224510206698743886, 108.3344237280190185 ) ) ;
#171455 = CARTESIAN_POINT ( 'NONE',  ( -0.05219959533910754901, -16.53943276465976808, 52.49890960531435979 ) ) ;
#171456 = CARTESIAN_POINT ( 'NONE',  ( -16.46253265017160317, 9.564922557960807481, 55.83224293864769550 ) ) ;
#171457 = CARTESIAN_POINT ( 'NONE',  ( 21.55341960407619695, -5.719274019375665929, 101.0427570613523756 ) ) ;
#171458 = CARTESIAN_POINT ( 'NONE',  ( 21.52544592524344225, -5.823673210054117533, 113.5405762719810383 ) ) ;
#171459 = CARTESIAN_POINT ( 'NONE',  ( -15.72974639402176322, -15.80617190586768395, 74.37609039468568994 ) ) ;
#171460 = CARTESIAN_POINT ( 'NONE',  ( -4.483927247898782831, 16.52544592524335698, 42.70942372801901854 ) ) ;
#171462 = CARTESIAN_POINT ( 'NONE',  ( 21.53943276465977519, 0.05219959533937863772, 81.25109039468568994 ) ) ;
#171461 = CARTESIAN_POINT ( 'NONE',  ( 16.55341960407611168, 4.379528057220329451, 78.95724293864769550 ) ) ;
#171463 = CARTESIAN_POINT ( 'NONE',  ( -14.29746914071049879, 8.314922557960819915, 25.83224293864769194 ) ) ;
#171464 = CARTESIAN_POINT ( 'NONE',  ( 17.97182807773873137, -5.500000000000077272, 61.03038844047286915 ) ) ;
#171465 = CARTESIAN_POINT ( 'NONE',  ( -12.14591786802326823, 12.06949235617739902, 38.12609039468567573 ) ) ;
#171466 = CARTESIAN_POINT ( 'NONE',  ( -8.224510206698948167, 14.34966873604960824, 45.41557627198103830 ) ) ;
#171467 = CARTESIAN_POINT ( 'NONE',  ( -16.55341960407617563, 4.379528057220093196, 93.54275706135234714 ) ) ;
#171468 = CARTESIAN_POINT ( 'NONE',  ( -16.46253265017160317, 9.564922557960807481, 95.83224293864769550 ) ) ;
#171469 = CARTESIAN_POINT ( 'NONE',  ( -13.97604488694527625, -13.89961937509977652, 106.8739096053143669 ) ) ;
#171470 = CARTESIAN_POINT ( 'NONE',  ( -18.67979575497193778, 10.72451020669871902, 93.33442372801901854 ) ) ;
#171471 = CARTESIAN_POINT ( 'NONE',  ( -16.52544592524335698, -4.483927247898792601, 103.9594237280190185 ) ) ;
#171472 = CARTESIAN_POINT ( 'NONE',  ( 14.34966873604960469, 8.224510206698951720, 79.16557627198103830 ) ) ;
#171473 = CARTESIAN_POINT ( 'NONE',  ( 5.049401038298161559, -19.05341960407611168, 77.70724293864765286 ) ) ;
#171474 = ORIENTED_EDGE ( 'NONE', *, *, #160051, .T. ) ;
#171475 = CARTESIAN_POINT ( 'NONE',  ( 12.14591786802327356, -12.06949235617739191, 20.62609039468568639 ) ) ;
#171476 = CARTESIAN_POINT ( 'NONE',  ( 9.474510206698971260, -16.51473224551069308, 27.91557627198103120 ) ) ;
#171477 = CARTESIAN_POINT ( 'NONE',  ( 5.153800228976335163, 19.02544592524342804, 94.79057627198103830 ) ) ;
#171479 = CARTESIAN_POINT ( 'NONE',  ( 36.91746824999999887, 11.99521256947799053, -3.524999997268813079 ) ) ;
#171478 = CARTESIAN_POINT ( 'NONE',  ( 4.379528057220092307, 16.55341960407617563, 32.29275706135235424 ) ) ;
#171480 = CARTESIAN_POINT ( 'NONE',  ( -5.049401038297874678, -19.05341960407617918, 34.79275706135233293 ) ) ;
#171481 = CARTESIAN_POINT ( 'NONE',  ( 12.06949235617739724, 12.14591786802326823, 91.87609039468568994 ) ) ;
#171482 = CARTESIAN_POINT ( 'NONE',  ( 16.51473224551083163, -9.474510206698727899, 110.8344237280190043 ) ) ;
#171483 = CARTESIAN_POINT ( 'NONE',  ( 0.05219959533909260263, 19.03943276465977164, 34.99890960531435979 ) ) ;
#171484 = CARTESIAN_POINT ( 'NONE',  ( 8.224510206698742110, 14.34966873604972548, 82.08442372801901854 ) ) ;
#171485 = CARTESIAN_POINT ( 'NONE',  ( 14.34966873604972726, -8.224510206698740333, 65.83442372801900433 ) ) ;
#171486 = CARTESIAN_POINT ( 'NONE',  ( -19.02544592524342804, 5.153800228976336051, 36.04057627198100988 ) ) ;
#171487 = CARTESIAN_POINT ( 'NONE',  ( -0.05219959533936034679, 19.03943276465977164, 72.50109039468566152 ) ) ;
#171488 = CARTESIAN_POINT ( 'NONE',  ( -19.03943276465977164, -0.05219959533935918106, 18.75109039468567218 ) ) ;
#171489 = CARTESIAN_POINT ( 'NONE',  ( -13.89961937509977652, 13.97604488694528158, 45.62390960531433848 ) ) ;
#171490 = CARTESIAN_POINT ( 'NONE',  ( -5.153800228976328057, -19.02544592524343514, 92.29057627198099567 ) ) ;
#171491 = CARTESIAN_POINT ( 'NONE',  ( -14.34966873604960291, -8.224510206698953496, 81.66557627198103830 ) ) ;
#171492 = EDGE_CURVE ( 'NONE', #54169, #34628, #99262, .T. ) ;
#171493 = CARTESIAN_POINT ( 'NONE',  ( -19.05341960407617563, 5.049401038297882671, 48.54275706135233293 ) ) ;
#171494 = CARTESIAN_POINT ( 'NONE',  ( -10.72451020669898014, 18.67979575497178502, 55.41557627198102409 ) ) ;
#171495 = CARTESIAN_POINT ( 'NONE',  ( -21.52544592524334988, -5.823673210054445271, 103.9594237280190185 ) ) ;
#171496 = CARTESIAN_POINT ( 'NONE',  ( 9.564922557960805705, 16.46253265017160317, 84.58224293864769550 ) ) ;
#171497 = CARTESIAN_POINT ( 'NONE',  ( -19.02544592524334988, -5.153800228976617603, 18.95942372801899722 ) ) ;
#171498 = CARTESIAN_POINT ( 'NONE',  ( 10.81492255796078972, 18.62759615963270932, 69.58224293864769550 ) ) ;
#171499 = CARTESIAN_POINT ( 'NONE',  ( -19.02544592524342804, 5.153800228976336051, 106.0405762719810241 ) ) ;
#171500 = CARTESIAN_POINT ( 'NONE',  ( 9.474510206698729675, 16.51473224551082808, 87.08442372801900433 ) ) ;
#171501 = CARTESIAN_POINT ( 'NONE',  ( -17.49999999999999289, 3.850315288878825903, 109.2662913060345460 ) ) ;
#171502 = CARTESIAN_POINT ( 'NONE',  ( 16.51473224551083163, -9.474510206698727899, 105.8344237280190043 ) ) ;
#171503 = CARTESIAN_POINT ( 'NONE',  ( 16.52544592524342804, -4.483927247898539470, 113.5405762719810383 ) ) ;
#171504 = CARTESIAN_POINT ( 'NONE',  ( 19.03943276465977164, -0.05219959533909143690, 98.74890960531436690 ) ) ;
#171505 = CARTESIAN_POINT ( 'NONE',  ( -18.67979575497178146, -10.72451020669898902, 81.66557627198103830 ) ) ;
#171506 = CARTESIAN_POINT ( 'NONE',  ( -8.314922557961024197, 14.29746914071037800, 42.91775706135235424 ) ) ;
#171507 = CARTESIAN_POINT ( 'NONE',  ( 15.72974639402176855, 15.80617190586768217, 46.87609039468568994 ) ) ;
#171508 = CARTESIAN_POINT ( 'NONE',  ( 5.719274019375673035, 21.55341960407619339, 92.29275706135236135 ) ) ;
#171509 = CARTESIAN_POINT ( 'NONE',  ( 8.314922557961029526, -14.29746914071037800, 90.41775706135236135 ) ) ;
#171510 = CARTESIAN_POINT ( 'NONE',  ( -16.51473224551069308, -9.474510206698971260, 86.66557627198102409 ) ) ;
#171511 = CARTESIAN_POINT ( 'NONE',  ( -4.483927247898539470, -16.52544592524342804, 92.29057627198103830 ) ) ;
#171512 = CARTESIAN_POINT ( 'NONE',  ( 8.314922557960818139, 14.29746914071049879, 39.58224293864769550 ) ) ;
#171513 = CARTESIAN_POINT ( 'NONE',  ( 0.05219959533936267826, -19.03943276465977164, 65.00109039468567573 ) ) ;
#171514 = CARTESIAN_POINT ( 'NONE',  ( 21.53943276465977519, 0.05219959533937863772, 51.25109039468568994 ) ) ;
#171515 = CARTESIAN_POINT ( 'NONE',  ( 9.564922557961047289, -16.46253265017146816, 20.41775706135233293 ) ) ;
#171516 = CARTESIAN_POINT ( 'NONE',  ( 8.314922557960818139, 14.29746914071049879, 94.58224293864769550 ) ) ;
#171517 = CARTESIAN_POINT ( 'NONE',  ( -21.53943276465977519, 0.05219959533907696930, 36.24890960531435979 ) ) ;
#171518 = CARTESIAN_POINT ( 'NONE',  ( 4.483927247898790824, -16.52544592524335698, 110.2094237280190185 ) ) ;
#171519 = CARTESIAN_POINT ( 'NONE',  ( 18.62759615963255655, 10.81492255796105972, 81.66775706135236135 ) ) ;
#171520 = CARTESIAN_POINT ( 'NONE',  ( 16.53943276465976808, 0.05219959533934440121, 56.25109039468568284 ) ) ;
#171521 = CARTESIAN_POINT ( 'NONE',  ( -16.52544592524335698, -4.483927247898792601, 108.9594237280190185 ) ) ;
#171522 = CARTESIAN_POINT ( 'NONE',  ( -5.823673210054431948, 21.52544592524334988, 52.70942372801902565 ) ) ;
#171523 = EDGE_CURVE ( 'NONE', #35595, #112207, #165122, .T. ) ;
#171524 = ORIENTED_EDGE ( 'NONE', *, *, #84815, .F. ) ;
#171525 = CARTESIAN_POINT ( 'NONE',  ( -21.55341960407619339, 5.719274019375674811, 33.54275706135234714 ) ) ;
#171526 = CARTESIAN_POINT ( 'NONE',  ( 16.52544592524342804, -4.483927247898539470, 98.54057627198105251 ) ) ;
#171527 = CARTESIAN_POINT ( 'NONE',  ( -9.474510206698964154, 16.51473224551069663, 25.41557627198103120 ) ) ;
#171528 = CARTESIAN_POINT ( 'NONE',  ( 4.483927247898545687, 16.52544592524342804, 64.79057627198103830 ) ) ;
#171529 = CARTESIAN_POINT ( 'NONE',  ( -19.05341960407611168, -5.049401038298163336, 71.45724293864766707 ) ) ;
#171530 = CARTESIAN_POINT ( 'NONE',  ( 14.34966873604972726, -8.224510206698740333, 105.8344237280190328 ) ) ;
#171531 = CARTESIAN_POINT ( 'NONE',  ( 5.719274019375991003, -21.55341960407610458, 52.70724293864769550 ) ) ;
#171532 = CARTESIAN_POINT ( 'NONE',  ( -12.06949235617756955, 12.14591786802309770, 90.62390960531436690 ) ) ;
#171533 = CARTESIAN_POINT ( 'NONE',  ( 5.823673210054125526, 21.52544592524343514, 99.79057627198103830 ) ) ;
#171534 = CARTESIAN_POINT ( 'NONE',  ( 9.564922557960805705, 16.46253265017160317, 99.58224293864770971 ) ) ;
#171536 = CARTESIAN_POINT ( 'NONE',  ( 5.049401038297881783, 19.05341960407617563, 102.2927570613523045 ) ) ;
#171535 = CARTESIAN_POINT ( 'NONE',  ( -5.153800228976328057, -19.02544592524343514, 57.29057627198103120 ) ) ;
#171537 = CARTESIAN_POINT ( 'NONE',  ( -10.81492255796078084, -18.62759615963271287, 47.08224293864770260 ) ) ;
#171538 = CARTESIAN_POINT ( 'NONE',  ( -10.72451020669870658, -18.67979575497194134, 64.58442372801900433 ) ) ;
#171539 = CARTESIAN_POINT ( 'NONE',  ( 9.474510206698971260, -16.51473224551069308, 67.91557627198102409 ) ) ;
#171540 = CARTESIAN_POINT ( 'NONE',  ( -16.51473224551069308, -9.474510206698971260, 81.66557627198103830 ) ) ;
#171541 = CARTESIAN_POINT ( 'NONE',  ( -4.379528057220086978, -16.55341960407618274, 69.79275706135234714 ) ) ;
#171542 = CARTESIAN_POINT ( 'NONE',  ( -15.80617190586768217, 15.72974639402176855, 48.12609039468568284 ) ) ;
#171543 = CARTESIAN_POINT ( 'NONE',  ( 0.05219959533937995610, -21.53943276465977519, 90.00109039468567573 ) ) ;
#171544 = CARTESIAN_POINT ( 'NONE',  ( 10.81492255796078972, 18.62759615963270932, 99.58224293864770971 ) ) ;
#171546 = CARTESIAN_POINT ( 'NONE',  ( -12.14591786802326823, 12.06949235617739902, 78.12609039468570415 ) ) ;
#171545 = CARTESIAN_POINT ( 'NONE',  ( 15.72974639402176855, 15.80617190586768217, 36.87609039468568994 ) ) ;
#171547 = CARTESIAN_POINT ( 'NONE',  ( 21.55341960407610458, 5.719274019375980345, 73.95724293864769550 ) ) ;
#171548 = CARTESIAN_POINT ( 'NONE',  ( -5.153800228976607833, 19.02544592524334988, 27.70942372801899722 ) ) ;
#171550 = CARTESIAN_POINT ( 'NONE',  ( -12.06949235617756955, 12.14591786802309770, 25.62390960531435624 ) ) ;
#171549 = CARTESIAN_POINT ( 'NONE',  ( -5.153800228976328057, -19.02544592524343514, 72.29057627198102409 ) ) ;
#171551 = CARTESIAN_POINT ( 'NONE',  ( -30.74264578624800492, -22.33583958711396278, -5.800000000000000711 ) ) ;
#171552 = CARTESIAN_POINT ( 'NONE',  ( 9.564922557960805705, 16.46253265017160317, 104.5822429386476955 ) ) ;
#171553 = CARTESIAN_POINT ( 'NONE',  ( -16.51473224551082808, 9.474510206698731452, 88.33442372801900433 ) ) ;
#171554 = CARTESIAN_POINT ( 'NONE',  ( -10.81492255796078084, -18.62759615963271287, 57.08224293864769550 ) ) ;
#171555 = CARTESIAN_POINT ( 'NONE',  ( 8.224510206698953496, -14.34966873604960469, 42.91557627198103120 ) ) ;
#171556 = CARTESIAN_POINT ( 'NONE',  ( 19.02544592524334988, 5.153800228976608722, 111.4594237280190043 ) ) ;
#171557 = CARTESIAN_POINT ( 'NONE',  ( 5.049401038298161559, -19.05341960407611168, 37.70724293864768839 ) ) ;
#171558 = CARTESIAN_POINT ( 'NONE',  ( -19.03943276465977164, -0.05219959533935918106, 103.7510903946856757 ) ) ;
#171560 = CARTESIAN_POINT ( 'NONE',  ( -16.46253265017146816, -9.564922557961047289, 74.16775706135234714 ) ) ;
#171559 = CARTESIAN_POINT ( 'NONE',  ( 0.05219959533907565091, 21.53943276465977519, 99.99890960531436690 ) ) ;
#171561 = CARTESIAN_POINT ( 'NONE',  ( -8.224510206698735004, -14.34966873604973081, 79.58442372801903275 ) ) ;
#171562 = CARTESIAN_POINT ( 'NONE',  ( -13.97604488694527625, -13.89961937509977652, 61.87390960531435979 ) ) ;
#171563 = CARTESIAN_POINT ( 'NONE',  ( -16.53943276465976808, 0.05219959533911058130, 76.24890960531435269 ) ) ;
#171564 =( BOUNDED_SURFACE ( )  B_SPLINE_SURFACE ( 3, 2, ( 
 ( #28891, #92509, #27906 ),
 ( #90531, #30862, #165412 ),
 ( #61180, #495, #122852 ),
 ( #182565, #184540, #59196 ),
 ( #152213, #88548, #44048 ),
 ( #46020, #154198, #15688 ),
 ( #77349, #62168, #196755 ),
 ( #123832, #103732, #42068 ),
 ( #119891, #167395, #43054 ),
 ( #104720, #89549, #151235 ),
 ( #12724, #13697, #75364 ),
 ( #137034, #4459, #142981 ),
 ( #33832, #155190, #158164 ),
 ( #34821, #93504, #49998 ),
 ( #156178, #49008, #5465 ),
 ( #185530, #67147, #17677 ),
 ( #32846, #110663, #48020 ),
 ( #157178, #111663, #96476 ),
 ( #159143, #16680, #47022 ),
 ( #141991, #1491, #78329 ),
 ( #20640, #35811, #82293 ),
 ( #19656, #3479, #81297 ),
 ( #173350, #140002, #79335 ),
 ( #18672, #126815, #141005 ),
 ( #143984, #172343, #66148 ),
 ( #65156, #2493, #108681 ),
 ( #95492, #170359, #31851 ),
 ( #80318, #97457, #63169 ),
 ( #124848, #188521, #186548 ),
 ( #127811, #109677, #171358 ),
 ( #125839, #189516, #94496 ),
 ( #50989, #64174, #187541 ),
 ( #112649, #174341, #117654 ),
 ( #9488, #163158, #113636 ),
 ( #160157, #193502, #38817 ),
 ( #36798, #55977, #130809 ),
 ( #70152, #98463, #131822 ),
 ( #51978, #83301, #179351 ),
 ( #162154, #24661, #7458 ),
 ( #54980, #114642, #21648 ),
 ( #85298, #8477, #40814 ),
 ( #102484, #175331, #164171 ),
 ( #25669, #86310, #177346 ),
 ( #147999, #145976, #144977 ) ),
 .UNSPECIFIED., .F., .F., .T. ) 
 B_SPLINE_SURFACE_WITH_KNOTS ( ( 4, 2, 2, 2, 2, 2, 2, 2, 2, 2, 2, 2, 2, 2, 2, 2, 2, 2, 2, 2, 2, 4 ),
 ( 3, 3 ),
 ( 0.1334715276261013994, 0.1400397817209069751, 0.1416818452446083620, 0.1433239087683097490, 0.1466080358157125230, 0.1498921628631152969, 0.1531762899105180986, 0.1564604169579209003, 0.1597445440053236743, 0.1630286710527264482, 0.1646707345764278352, 0.1663127981001292222, 0.1679548616238306091, 0.1695969251475319961, 0.1712389886712333831, 0.1720600204330841043, 0.1728810521949347978, 0.1745231157186362125, 0.1761651792423375995, 0.1794493062897403735, 0.1827334333371431474, 0.1860175603845459213 ),
 ( 0.000000000000000000, 1.000000000000000000 ),
 .UNSPECIFIED. ) 
 GEOMETRIC_REPRESENTATION_ITEM ( )  RATIONAL_B_SPLINE_SURFACE ( (
 ( 1.000000000000000000, 0.7745966692414832933, 1.000000000000000000),
 ( 1.000000000000000000, 0.7873173169476441746, 1.000000000000000000),
 ( 1.000000000000000000, 0.8012080269091598206, 1.000000000000000000),
 ( 1.000000000000000000, 0.8197272276933330604, 1.000000000000000000),
 ( 1.000000000000000000, 0.8234885421912105929, 1.000000000000000000),
 ( 1.000000000000000000, 0.8311157573376537488, 1.000000000000000000),
 ( 1.000000000000000000, 0.8349728938257902078, 1.000000000000000000),
 ( 1.000000000000000000, 0.8465302108188730301, 1.000000000000000000),
 ( 1.000000000000000000, 0.8542644918355096761, 1.000000000000000000),
 ( 1.000000000000000000, 0.8696747091110100802, 1.000000000000000000),
 ( 1.000000000000000000, 0.8773507960691678820, 1.000000000000000000),
 ( 1.000000000000000000, 0.8925002889089019842, 1.000000000000000000),
 ( 1.000000000000000000, 0.8999891582782626465, 1.000000000000000000),
 ( 1.000000000000000000, 0.9145203485640005514, 1.000000000000000000),
 ( 1.000000000000000000, 0.9215166741120213167, 1.000000000000000000),
 ( 1.000000000000000000, 0.9348196634156189511, 1.000000000000000000),
 ( 1.000000000000000000, 0.9411264847296241243, 1.000000000000000000),
 ( 1.000000000000000000, 0.9528821887672445090, 1.000000000000000000),
 ( 1.000000000000000000, 0.9583320463343933948, 1.000000000000000000),
 ( 1.000000000000000000, 0.9657141226242612619, 1.000000000000000000),
 ( 1.000000000000000000, 0.9680424144921332408, 1.000000000000000000),
 ( 1.000000000000000000, 0.9724014971077671321, 1.000000000000000000),
 ( 1.000000000000000000, 0.9744334801158450743, 1.000000000000000000),
 ( 1.000000000000000000, 0.9781204877085362126, 1.000000000000000000),
 ( 1.000000000000000000, 0.9797809101336113491, 1.000000000000000000),
 ( 1.000000000000000000, 0.9826818083352578670, 1.000000000000000000),
 ( 1.000000000000000000, 0.9839230189806438265, 1.000000000000000000),
 ( 1.000000000000000000, 0.9859013487405716702, 1.000000000000000000),
 ( 1.000000000000000000, 0.9866146582094302842, 1.000000000000000000),
 ( 1.000000000000000000, 0.9872250220265940124, 1.000000000000000000),
 ( 1.000000000000000000, 0.9873522598263766437, 1.000000000000000000),
 ( 1.000000000000000000, 0.9874472609175324322, 1.000000000000000000),
 ( 1.000000000000000000, 0.9874138636738800656, 1.000000000000000000),
 ( 1.000000000000000000, 0.9870735186574125519, 1.000000000000000000),
 ( 1.000000000000000000, 0.9865315217160959271, 1.000000000000000000),
 ( 1.000000000000000000, 0.9848873008857480515, 1.000000000000000000),
 ( 1.000000000000000000, 0.9837743821442975767, 1.000000000000000000),
 ( 1.000000000000000000, 0.9797976954002131089, 1.000000000000000000),
 ( 1.000000000000000000, 0.9763000371664239951, 1.000000000000000000),
 ( 1.000000000000000000, 0.9680363503267302994, 1.000000000000000000),
 ( 1.000000000000000000, 0.9632464763794107432, 1.000000000000000000),
 ( 1.000000000000000000, 0.9526889542240987163, 1.000000000000000000),
 ( 1.000000000000000000, 0.9469283804591228648, 1.000000000000000000),
 ( 1.000000000000000000, 0.9407878411039234390, 1.000000000000000000) ) ) 
 REPRESENTATION_ITEM ( '' )  SURFACE ( )  );
#171565 = CARTESIAN_POINT ( 'NONE',  ( -13.89961937509977652, 13.97604488694528158, 55.62390960531434558 ) ) ;
#171566 = CARTESIAN_POINT ( 'NONE',  ( -0.05219959533910754901, -16.53943276465976808, 62.49890960531436690 ) ) ;
#171567 = FACE_BOUND ( 'NONE', #53787, .T. ) ;
#171568 = CARTESIAN_POINT ( 'NONE',  ( -36.77186724307693311, -4.769522647520278547, 47.74487706083468197 ) ) ;
#171569 = CARTESIAN_POINT ( 'NONE',  ( -16.53943276465976808, 0.05219959533911058130, 46.24890960531435979 ) ) ;
#171570 = CARTESIAN_POINT ( 'NONE',  ( 16.46253265017160672, -9.564922557960803928, 78.33224293864769550 ) ) ;
#171571 = DIRECTION ( 'NONE',  ( -1.000000000000000000, 0.000000000000000000, 0.000000000000000000 ) ) ;
#171572 = CARTESIAN_POINT ( 'NONE',  ( 19.02544592524334988, 5.153800228976608722, 41.45942372801900433 ) ) ;
#171573 = CARTESIAN_POINT ( 'NONE',  ( 12.06949235617739724, 12.14591786802326823, 41.87609039468568284 ) ) ;
#171574 = CARTESIAN_POINT ( 'NONE',  ( -18.67979575497178146, -10.72451020669898902, 61.66557627198103120 ) ) ;
#171575 = CARTESIAN_POINT ( 'NONE',  ( -0.05219959533936034679, 19.03943276465977164, 27.50109039468566507 ) ) ;
#171576 = CARTESIAN_POINT ( 'NONE',  ( 5.153800228976335163, 19.02544592524342804, 79.79057627198102409 ) ) ;
#171577 = FACE_OUTER_BOUND ( 'NONE', #23191, .T. ) ;
#171578 = CARTESIAN_POINT ( 'NONE',  ( -0.05219959533909027116, -19.03943276465977164, 112.4989096053143669 ) ) ;
#171579 = CARTESIAN_POINT ( 'NONE',  ( -19.02544592524342804, 5.153800228976336051, 56.04057627198100988 ) ) ;
#171580 = CARTESIAN_POINT ( 'NONE',  ( 21.52544592524334988, 5.823673210054432836, 41.45942372801901143 ) ) ;
#171581 = CARTESIAN_POINT ( 'NONE',  ( 4.379528057220339221, -16.55341960407611168, 102.7072429386476955 ) ) ;
#171584 = ORIENTED_EDGE ( 'NONE', *, *, #60477, .T. ) ;
#171583 = CARTESIAN_POINT ( 'NONE',  ( -0.05219959533909027116, -19.03943276465977164, 82.49890960531436690 ) ) ;
#171582 = CARTESIAN_POINT ( 'NONE',  ( -5.823673210054116645, -21.52544592524344225, 107.2905762719810525 ) ) ;
#171585 = CARTESIAN_POINT ( 'NONE',  ( 5.823673210054444382, -21.52544592524334988, 30.20942372801902565 ) ) ;
#171586 = ORIENTED_EDGE ( 'NONE', *, *, #116496, .T. ) ;
#171587 = CARTESIAN_POINT ( 'NONE',  ( -9.474510206698964154, 16.51473224551069663, 85.41557627198102409 ) ) ;
#171588 = CARTESIAN_POINT ( 'NONE',  ( 0.000000000000000000, 0.000000000000000000, -64.92279855667830191 ) ) ;
#171589 = CARTESIAN_POINT ( 'NONE',  ( 21.55341960407610458, 5.719274019375980345, 93.95724293864770971 ) ) ;
#171590 = CARTESIAN_POINT ( 'NONE',  ( 9.564922557960805705, 16.46253265017160317, 39.58224293864768839 ) ) ;
#171591 = CARTESIAN_POINT ( 'NONE',  ( 13.97604488694548053, -13.89961937509957401, 100.6260903946856615 ) ) ;
#171592 = CARTESIAN_POINT ( 'NONE',  ( -36.91746825000001309, -11.99521256947794789, -11.02499999726881263 ) ) ;
#171593 = CARTESIAN_POINT ( 'NONE',  ( -9.474510206698964154, 16.51473224551069663, 35.41557627198102409 ) ) ;
#171594 = CARTESIAN_POINT ( 'NONE',  ( -15.72974639402176322, -15.80617190586768395, 79.37609039468567573 ) ) ;
#171596 = CARTESIAN_POINT ( 'NONE',  ( 15.80617190586769283, -15.72974639402175789, 50.62609039468568994 ) ) ;
#171595 = CARTESIAN_POINT ( 'NONE',  ( -16.51473224551069308, -9.474510206698971260, 71.66557627198102409 ) ) ;
#171597 = CARTESIAN_POINT ( 'NONE',  ( 10.72451020669871369, 18.67979575497193778, 22.08442372801901143 ) ) ;
#171598 = CARTESIAN_POINT ( 'NONE',  ( 23.31738231874054534, 16.94106989632529192, 149.1999999999999886 ) ) ;
#171599 = CARTESIAN_POINT ( 'NONE',  ( 9.564922557960805705, 16.46253265017160317, 89.58224293864769550 ) ) ;
#171600 = CARTESIAN_POINT ( 'NONE',  ( 2.107141108080088809, 28.27445460515380304, 140.0000000000000284 ) ) ;
#171603 = CARTESIAN_POINT ( 'NONE',  ( -0.05219959533937732626, 21.53943276465977519, 42.50109039468567573 ) ) ;
#171602 = CARTESIAN_POINT ( 'NONE',  ( 21.53943276465977519, -0.05219959533907433946, 43.74890960531435979 ) ) ;
#171601 = CARTESIAN_POINT ( 'NONE',  ( -8.224510206698735004, -14.34966873604973081, 34.58442372801900433 ) ) ;
#171604 = CARTESIAN_POINT ( 'NONE',  ( 10.81492255796106328, -18.62759615963255655, 70.41775706135236135 ) ) ;
#171605 = CARTESIAN_POINT ( 'NONE',  ( 17.50000000000000000, -5.499999999999992895, 38.29690382534171533 ) ) ;
#171606 = CARTESIAN_POINT ( 'NONE',  ( 16.46253265017146816, 9.564922557961045513, 106.6677570613523471 ) ) ;
#171607 = CARTESIAN_POINT ( 'NONE',  ( -19.03943276465977164, 0.05219959533909376836, 56.24890960531435979 ) ) ;
#171608 = CARTESIAN_POINT ( 'NONE',  ( 19.05341960407611168, 5.049401038298154454, 78.95724293864769550 ) ) ;
#171609 = CARTESIAN_POINT ( 'NONE',  ( -16.53943276465976808, 0.05219959533911058130, 111.2489096053143669 ) ) ;
#171610 = CARTESIAN_POINT ( 'NONE',  ( 14.34966873604960469, 8.224510206698951720, 99.16557627198100988 ) ) ;
#171611 = CARTESIAN_POINT ( 'NONE',  ( -19.02544592524342804, 5.153800228976336051, 111.0405762719810099 ) ) ;
#171612 = CARTESIAN_POINT ( 'NONE',  ( 4.483927247898790824, -16.52544592524335698, 85.20942372801901854 ) ) ;
#171614 = CARTESIAN_POINT ( 'NONE',  ( 0.05219959533909260263, 19.03943276465977164, 49.99890960531435979 ) ) ;
#171613 = CARTESIAN_POINT ( 'NONE',  ( 16.55341960407611168, 4.379528057220329451, 68.95724293864769550 ) ) ;
#171615 = CARTESIAN_POINT ( 'NONE',  ( 21.52544592524334988, 5.823673210054432836, 76.45942372801901854 ) ) ;
#171616 = CARTESIAN_POINT ( 'NONE',  ( 15.80617190586769283, -15.72974639402175789, 75.62609039468567573 ) ) ;
#171617 = CARTESIAN_POINT ( 'NONE',  ( -13.97604488694547697, 13.89961937509957934, 113.1260903946856757 ) ) ;
#171618 = CARTESIAN_POINT ( 'NONE',  ( -8.314922557960811034, -14.29746914071050412, 62.08224293864769550 ) ) ;
#171619 = CARTESIAN_POINT ( 'NONE',  ( 21.52544592524344225, -5.823673210054117533, 108.5405762719810241 ) ) ;
#171620 = CARTESIAN_POINT ( 'NONE',  ( -5.719274019375978568, 21.55341960407610458, 60.20724293864768839 ) ) ;
#171621 = CARTESIAN_POINT ( 'NONE',  ( -17.05587630539787369, -6.762274262135686165, 104.2581969096269319 ) ) ;
#171622 = CARTESIAN_POINT ( 'NONE',  ( -23.31738231874055245, -16.94106989632524574, 146.4500000054623854 ) ) ;
#171623 = CARTESIAN_POINT ( 'NONE',  ( 9.564922557960805705, 16.46253265017160317, 69.58224293864770971 ) ) ;
#171624 = CARTESIAN_POINT ( 'NONE',  ( -14.29746914071049879, 8.314922557960819915, 35.83224293864768839 ) ) ;
#171625 = CARTESIAN_POINT ( 'NONE',  ( -16.53943276465976808, 0.05219959533911058130, 26.24890960531435624 ) ) ;
#171626 = CARTESIAN_POINT ( 'NONE',  ( 4.379528057220092307, 16.55341960407617563, 92.29275706135236135 ) ) ;
#171627 = CARTESIAN_POINT ( 'NONE',  ( 5.153800228976615827, -19.02544592524334988, 50.20942372801897591 ) ) ;
#171628 = CARTESIAN_POINT ( 'NONE',  ( 16.61371651742604882, 7.165104196376036683, 48.64584930007006136 ) ) ;
#171629 = CARTESIAN_POINT ( 'NONE',  ( -19.03943276465977164, 0.05219959533909376836, 106.2489096053143669 ) ) ;
#171630 = CARTESIAN_POINT ( 'NONE',  ( -4.379528057220328563, 16.55341960407611168, 65.20724293864768129 ) ) ;
#171632 = CARTESIAN_POINT ( 'NONE',  ( 5.049401038298161559, -19.05341960407611168, 112.7072429386476813 ) ) ;
#171631 = CARTESIAN_POINT ( 'NONE',  ( 17.44279575226826395, -5.990770900252401887, 103.3355756751432040 ) ) ;
#171633 = CARTESIAN_POINT ( 'NONE',  ( 21.55341960407610458, 5.719274019375980345, 48.95724293864770971 ) ) ;
#171634 = CARTESIAN_POINT ( 'NONE',  ( -12.06949235617756955, 12.14591786802309770, 95.62390960531436690 ) ) ;
#171635 = CARTESIAN_POINT ( 'NONE',  ( -0.05219959533934338120, 16.53943276465976808, 57.50109039468568994 ) ) ;
#171636 = CARTESIAN_POINT ( 'NONE',  ( 16.55341960407611168, 4.379528057220329451, 88.95724293864769550 ) ) ;
#171637 = CARTESIAN_POINT ( 'NONE',  ( -4.500000000000001776, -120.6140767358124180, 14.26817184396703198 ) ) ;
#171638 = CARTESIAN_POINT ( 'NONE',  ( 19.05341960407617918, -5.049401038297876454, 71.04275706135234714 ) ) ;
#171639 = CARTESIAN_POINT ( 'NONE',  ( -19.03943276465977164, 0.05219959533909376836, 116.2489096053143669 ) ) ;
#171640 = CARTESIAN_POINT ( 'NONE',  ( -11.40812507854755609, 35.11059874428196537, -7.524999997268813523 ) ) ;
#171641 = CARTESIAN_POINT ( 'NONE',  ( 37.99626262588760994, -12.34573411038917357, -6.847842220587804007 ) ) ;
#171643 = CARTESIAN_POINT ( 'NONE',  ( -4.379528057220328563, 16.55341960407611168, 35.20724293864768839 ) ) ;
#171642 = CARTESIAN_POINT ( 'NONE',  ( -8.224510206698735004, -14.34966873604973081, 49.58442372801901143 ) ) ;
#171644 = CARTESIAN_POINT ( 'NONE',  ( -15.72974639402197994, 15.80617190586746368, 60.62390960531437401 ) ) ;
#171645 = CARTESIAN_POINT ( 'NONE',  ( -13.89961937509957401, -13.97604488694547875, 89.37609039468563310 ) ) ;
#171646 = CARTESIAN_POINT ( 'NONE',  ( 15.72974639402199770, -15.80617190586745480, 48.12390960531436690 ) ) ;
#171647 = CARTESIAN_POINT ( 'NONE',  ( -10.72451020669870658, -18.67979575497194134, 79.58442372801903275 ) ) ;
#171648 = CARTESIAN_POINT ( 'NONE',  ( -9.687362902255733488, 9.687362902255692632, -62.58071313852362039 ) ) ;
#171649 = CARTESIAN_POINT ( 'NONE',  ( -8.224510206698735004, -14.34966873604973081, 39.58442372801901143 ) ) ;
#171652 = EDGE_CURVE ( 'NONE', #170830, #129803, #60662, .T. ) ;
#171651 = CARTESIAN_POINT ( 'NONE',  ( -19.03943276465977164, 0.05219959533909376836, 101.2489096053143669 ) ) ;
#171650 = CARTESIAN_POINT ( 'NONE',  ( 0.05219959533909260263, 19.03943276465977164, 34.99890960531435979 ) ) ;
#171653 = CARTESIAN_POINT ( 'NONE',  ( -9.564922557960796823, -16.46253265017161027, 37.08224293864768839 ) ) ;
#171654 = CARTESIAN_POINT ( 'NONE',  ( -16.53943276465976808, 0.05219959533911058130, 96.24890960531435269 ) ) ;
#171655 = DIRECTION ( 'NONE',  ( 5.551115123125774690E-17, 9.714451465470120961E-17, -1.000000000000000000 ) ) ;
#171656 = CARTESIAN_POINT ( 'NONE',  ( -16.46253265017160317, 9.564922557960807481, 100.8322429386477097 ) ) ;
#171657 = VERTEX_POINT ( 'NONE', #106405 ) ;
#171658 = CARTESIAN_POINT ( 'NONE',  ( 4.483927247898790824, -16.52544592524335698, 50.20942372801901854 ) ) ;
#171659 = CARTESIAN_POINT ( 'NONE',  ( 10.72451020669898902, -18.67979575497178502, 87.91557627198103830 ) ) ;
#171660 = CARTESIAN_POINT ( 'NONE',  ( 16.46253265017160672, -9.564922557960803928, 43.33224293864769550 ) ) ;
#171661 = CARTESIAN_POINT ( 'NONE',  ( -0.05219959533937732626, 21.53943276465977519, 32.50109039468568284 ) ) ;
#171662 = CARTESIAN_POINT ( 'NONE',  ( -19.05341960407611168, -5.049401038298163336, 81.45724293864769550 ) ) ;
#171663 = CARTESIAN_POINT ( 'NONE',  ( -17.79613651744294600, 24.49428055684532524, 145.6843446568999809 ) ) ;
#171664 = VERTEX_POINT ( 'NONE', #14403 ) ;
#171665 = CARTESIAN_POINT ( 'NONE',  ( -4.483927247898782831, 16.52544592524335698, 52.70942372801902565 ) ) ;
#171666 = CARTESIAN_POINT ( 'NONE',  ( 18.67979575497178502, 10.72451020669898547, 114.1655762719810383 ) ) ;
#171669 = CARTESIAN_POINT ( 'NONE',  ( 16.46253265017146816, 9.564922557961045513, 81.66775706135233293 ) ) ;
#171668 = CARTESIAN_POINT ( 'NONE',  ( -5.049401038298153566, 19.05341960407611168, 100.2072429386476955 ) ) ;
#171667 = CARTESIAN_POINT ( 'NONE',  ( 19.02544592524343514, -5.153800228976328945, 28.54057627198102409 ) ) ;
#171670 = CARTESIAN_POINT ( 'NONE',  ( 5.153800228976615827, -19.02544592524334988, 25.20942372801900433 ) ) ;
#171671 = CARTESIAN_POINT ( 'NONE',  ( 21.52544592524344225, -5.823673210054117533, 83.54057627198102409 ) ) ;
#171672 = CARTESIAN_POINT ( 'NONE',  ( 19.03943276465977164, 0.05219959533936151252, 31.25109039468566863 ) ) ;
#171673 = CARTESIAN_POINT ( 'NONE',  ( 8.224510206698742110, 14.34966873604972548, 82.08442372801901854 ) ) ;
#171674 = CARTESIAN_POINT ( 'NONE',  ( 19.05341960407611168, 5.049401038298154454, 108.9572429386477097 ) ) ;
#171675 = CARTESIAN_POINT ( 'NONE',  ( -9.564922557960796823, -16.46253265017161027, 57.08224293864769550 ) ) ;
#171676 = CARTESIAN_POINT ( 'NONE',  ( -10.72451020669870658, -18.67979575497194134, 64.58442372801900433 ) ) ;
#171677 = CARTESIAN_POINT ( 'NONE',  ( 10.81492255796106328, -18.62759615963255655, 70.41775706135236135 ) ) ;
#171678 = CARTESIAN_POINT ( 'NONE',  ( 19.03943276465977164, -0.05219959533909143690, 78.74890960531436690 ) ) ;
#171679 = CARTESIAN_POINT ( 'NONE',  ( -10.72451020669870658, -18.67979575497194134, 44.58442372801901854 ) ) ;
#171680 = CARTESIAN_POINT ( 'NONE',  ( 5.153800228976615827, -19.02544592524334988, 85.20942372801900433 ) ) ;
#171681 = B_SPLINE_CURVE_WITH_KNOTS ( 'NONE', 3,
 ( #147560, #40372, #196079, #134393, #88866, #43365, #9045, #72720, #104042, #132383, #55539, #163730, #148556, #195065, #56545, #12058, #197063, #135393, #41379, #58531, #95563, #19726, #143051, #172418, #80391, #81367 ),
 .UNSPECIFIED., .F., .F.,
 ( 4, 2, 2, 2, 2, 2, 2, 2, 2, 2, 2, 2, 4 ),
 ( 1.971416326048476669E-07, 0.0002960211146592905160, 0.0005918450876859761246, 0.0008876690607126617874, 0.001183493033739347559, 0.001775140979792719318, 0.002366788925846091077, 0.002662612898872771753, 0.002958436871899451995, 0.003254260844926132237, 0.003550084817952812912, 0.004141732764006173829, 0.004733380710059535181 ),
 .UNSPECIFIED. ) ;
#171682 = CARTESIAN_POINT ( 'NONE',  ( 9.474510206698971260, -16.51473224551069308, 52.91557627198102409 ) ) ;
#171683 = CARTESIAN_POINT ( 'NONE',  ( -19.03943276465977164, 0.05219959533909376836, 96.24890960531436690 ) ) ;
#171684 = CARTESIAN_POINT ( 'NONE',  ( -0.05219959533909027116, -19.03943276465977164, 67.49890960531436690 ) ) ;
#171685 = CARTESIAN_POINT ( 'NONE',  ( -5.049401038298153566, 19.05341960407611168, 110.2072429386476671 ) ) ;
#171686 = CARTESIAN_POINT ( 'NONE',  ( 13.89961937509977652, -13.97604488694527269, 53.12390960531434558 ) ) ;
#171687 = CARTESIAN_POINT ( 'NONE',  ( 0.05219959533907565091, 21.53943276465977519, 104.9989096053143669 ) ) ;
#171688 = CARTESIAN_POINT ( 'NONE',  ( 14.29746914071037800, 8.314922557961029526, 71.66775706135234714 ) ) ;
#171689 = CARTESIAN_POINT ( 'NONE',  ( -21.95653654802609722, 6.613221094984321979, 171.0358100525039902 ) ) ;
#171690 = CARTESIAN_POINT ( 'NONE',  ( 5.049401038297881783, 19.05341960407617563, 27.29275706135232937 ) ) ;
#171691 = CARTESIAN_POINT ( 'NONE',  ( -9.564922557960796823, -16.46253265017161027, 67.08224293864769550 ) ) ;
#171692 = CARTESIAN_POINT ( 'NONE',  ( 14.34966873604960469, 8.224510206698951720, 59.16557627198103120 ) ) ;
#171693 = CARTESIAN_POINT ( 'NONE',  ( 16.53943276465976808, -0.05219959533910856209, 98.74890960531438111 ) ) ;
#171694 = CARTESIAN_POINT ( 'NONE',  ( 19.02544592524343514, -5.153800228976328945, 103.5405762719809957 ) ) ;
#171695 = CARTESIAN_POINT ( 'NONE',  ( 19.03943276465977164, -0.05219959533909143690, 93.74890960531435269 ) ) ;
#171696 = CARTESIAN_POINT ( 'NONE',  ( -10.72451020669870658, -18.67979575497194134, 54.58442372801901143 ) ) ;
#171697 = CARTESIAN_POINT ( 'NONE',  ( -9.564922557960796823, -16.46253265017161027, 107.0822429386476955 ) ) ;
#171698 = CARTESIAN_POINT ( 'NONE',  ( -21.53943276465977519, -0.05219959533937600094, 108.7510903946857042 ) ) ;
#171699 = CARTESIAN_POINT ( 'NONE',  ( -8.224510206698735004, -14.34966873604973081, 84.58442372801903275 ) ) ;
#171700 = CARTESIAN_POINT ( 'NONE',  ( -10.72451020669870658, -18.67979575497194134, 39.58442372801901143 ) ) ;
#171701 = CARTESIAN_POINT ( 'NONE',  ( -21.52544592524343514, 5.823673210054127303, 26.04057627198103475 ) ) ;
#171702 = CARTESIAN_POINT ( 'NONE',  ( -18.62759615963270932, 10.81492255796079327, 100.8322429386477097 ) ) ;
#171703 = CARTESIAN_POINT ( 'NONE',  ( -8.314922557960811034, -14.29746914071050412, 67.08224293864770971 ) ) ;
#171704 = CARTESIAN_POINT ( 'NONE',  ( 19.05341960407611168, 5.049401038298154454, 53.95724293864770260 ) ) ;
#171705 = CARTESIAN_POINT ( 'NONE',  ( -12.06949235617756955, 12.14591786802309770, 80.62390960531438111 ) ) ;
#171706 = CARTESIAN_POINT ( 'NONE',  ( 21.53943276465977519, -0.05219959533907433946, 38.74890960531435979 ) ) ;
#171707 = CARTESIAN_POINT ( 'NONE',  ( 9.474510206698729675, 16.51473224551082808, 47.08442372801900433 ) ) ;
#171708 = CARTESIAN_POINT ( 'NONE',  ( -14.29746914071049879, 8.314922557960819915, 115.8322429386477097 ) ) ;
#171709 = ORIENTED_EDGE ( 'NONE', *, *, #153149, .T. ) ;
#171710 = CARTESIAN_POINT ( 'NONE',  ( 0.05219959533934541429, -16.53943276465976808, 70.00109039468568994 ) ) ;
#171711 = CARTESIAN_POINT ( 'NONE',  ( -16.51473224551069308, -9.474510206698971260, 66.66557627198102409 ) ) ;
#171712 = CARTESIAN_POINT ( 'NONE',  ( 1.784210473542230573E-15, -29.16686587814331588, 145.3750000027311842 ) ) ;
#171713 = CARTESIAN_POINT ( 'NONE',  ( 4.483927247898545687, 16.52544592524342804, 84.79057627198102409 ) ) ;
#171714 = CARTESIAN_POINT ( 'NONE',  ( 15.72974639402199770, -15.80617190586745480, 33.12390960531435979 ) ) ;
#171715 = VERTEX_POINT ( 'NONE', #29584 ) ;
#171716 = CARTESIAN_POINT ( 'NONE',  ( -12.14591786802326823, 12.06949235617739902, 108.1260903946856757 ) ) ;
#171717 = CARTESIAN_POINT ( 'NONE',  ( -14.34966873604972548, 8.224510206698743886, 23.33442372801901499 ) ) ;
#171718 = CARTESIAN_POINT ( 'NONE',  ( 18.67979575497194134, -10.72451020669871369, 95.83442372801903275 ) ) ;
#171719 = CARTESIAN_POINT ( 'NONE',  ( 19.03943276465977164, -0.05219959533909143690, 83.74890960531436690 ) ) ;
#171720 = CARTESIAN_POINT ( 'NONE',  ( -18.62759615963270932, 10.81492255796079327, 105.8322429386476955 ) ) ;
#171721 = CARTESIAN_POINT ( 'NONE',  ( 12.14591786802327356, -12.06949235617739191, 50.62609039468568994 ) ) ;
#171722 = CARTESIAN_POINT ( 'NONE',  ( -9.474510206698964154, 16.51473224551069663, 35.41557627198102409 ) ) ;
#171723 = ADVANCED_FACE ( 'NONE', ( #168087 ), #212, .T. ) ;
#171724 = CARTESIAN_POINT ( 'NONE',  ( -16.55341960407617563, 4.379528057220093196, 28.54275706135234358 ) ) ;
#171725 = CARTESIAN_POINT ( 'NONE',  ( 13.97604488694548053, -13.89961937509957401, 100.6260903946856615 ) ) ;
#171726 = CARTESIAN_POINT ( 'NONE',  ( -5.823673210054116645, -21.52544592524344225, 92.29057627198103830 ) ) ;
#171727 = CARTESIAN_POINT ( 'NONE',  ( -19.02544592524334988, -5.153800228976617603, 73.95942372801900433 ) ) ;
#171728 = CARTESIAN_POINT ( 'NONE',  ( 18.56197773271728124, -5.500000000000076383, 86.05066217314454491 ) ) ;
#171729 = CARTESIAN_POINT ( 'NONE',  ( 21.52544592524344225, -5.823673210054117533, 108.5405762719810241 ) ) ;
#171730 = CARTESIAN_POINT ( 'NONE',  ( -28.82186960331499037, 2.428612866367530248E-14, 142.2500000054623683 ) ) ;
#171731 = CARTESIAN_POINT ( 'NONE',  ( -13.89961937509977652, 13.97604488694528158, 80.62390960531436690 ) ) ;
#171732 = CARTESIAN_POINT ( 'NONE',  ( 4.379528057220092307, 16.55341960407617563, 32.29275706135235424 ) ) ;
#171733 = CARTESIAN_POINT ( 'NONE',  ( -21.46320343559653665, -25.04568634023494056, 8.240304736541400388 ) ) ;
#171734 = CARTESIAN_POINT ( 'NONE',  ( -13.97604488694547697, 13.89961937509957934, 58.12609039468566863 ) ) ;
#171736 = CARTESIAN_POINT ( 'NONE',  ( -0.05219959533910754901, -16.53943276465976808, 72.49890960531435269 ) ) ;
#171735 = CARTESIAN_POINT ( 'NONE',  ( 0.05219959533937995610, -21.53943276465977519, 25.00109039468567218 ) ) ;
#171737 = CARTESIAN_POINT ( 'NONE',  ( 16.51473224551069308, 9.474510206698969483, 89.16557627198103830 ) ) ;
#171739 = CARTESIAN_POINT ( 'NONE',  ( 5.049401038297881783, 19.05341960407617563, 42.29275706135234003 ) ) ;
#171738 = CARTESIAN_POINT ( 'NONE',  ( -8.314922557961024197, 14.29746914071037800, 32.91775706135234714 ) ) ;
#171740 = CARTESIAN_POINT ( 'NONE',  ( -0.05219959533937732626, 21.53943276465977519, 52.50109039468567573 ) ) ;
#171741 = CARTESIAN_POINT ( 'NONE',  ( -16.51473224551082808, 9.474510206698731452, 108.3344237280190043 ) ) ;
#171742 = CARTESIAN_POINT ( 'NONE',  ( 19.05341960407611168, 5.049401038298154454, 53.95724293864770260 ) ) ;
#171743 = CARTESIAN_POINT ( 'NONE',  ( -0.05219959533936034679, 19.03943276465977164, 77.50109039468566152 ) ) ;
#171744 = CARTESIAN_POINT ( 'NONE',  ( 4.379528057220092307, 16.55341960407617563, 52.29275706135236135 ) ) ;
#171745 = CARTESIAN_POINT ( 'NONE',  ( -15.80617190586768217, 15.72974639402176855, 103.1260903946856757 ) ) ;
#171746 = CARTESIAN_POINT ( 'NONE',  ( 19.05341960407617918, -5.049401038297876454, 66.04275706135233293 ) ) ;
#171747 = CARTESIAN_POINT ( 'NONE',  ( -5.153800228976328057, -19.02544592524343514, 32.29057627198102409 ) ) ;
#171748 = CARTESIAN_POINT ( 'NONE',  ( -18.67979575497178146, -10.72451020669898902, 76.66557627198103830 ) ) ;
#171750 = CARTESIAN_POINT ( 'NONE',  ( -19.03943276465977164, -0.05219959533935918106, 68.75109039468566152 ) ) ;
#171749 = CARTESIAN_POINT ( 'NONE',  ( -8.314922557960811034, -14.29746914071050412, 67.08224293864770971 ) ) ;
#171751 = CARTESIAN_POINT ( 'NONE',  ( 21.57728377622143512, 10.02787190051641453, 170.5958156194642186 ) ) ;
#171752 = CARTESIAN_POINT ( 'NONE',  ( 9.474510206698729675, 16.51473224551082808, 47.08442372801900433 ) ) ;
#171753 = CARTESIAN_POINT ( 'NONE',  ( -4.379528057220086978, -16.55341960407618274, 104.7927570613523898 ) ) ;
#171754 = CARTESIAN_POINT ( 'NONE',  ( 12.14591786802309770, 12.06949235617756955, 49.37390960531436690 ) ) ;
#171756 = CARTESIAN_POINT ( 'NONE',  ( -8.571926809382608425, 26.38167802310805854, 140.4750000027312069 ) ) ;
#171755 = CARTESIAN_POINT ( 'NONE',  ( -10.81492255796105439, 18.62759615963255655, 92.91775706135236135 ) ) ;
#171757 = CARTESIAN_POINT ( 'NONE',  ( -18.67979575497178146, -10.72451020669898902, 96.66557627198102409 ) ) ;
#171758 = CARTESIAN_POINT ( 'NONE',  ( -19.02544592524342804, 5.153800228976336051, 56.04057627198100988 ) ) ;
#171759 = CARTESIAN_POINT ( 'NONE',  ( 5.823673210054444382, -21.52544592524334988, 75.20942372801901854 ) ) ;
#171760 = CARTESIAN_POINT ( 'NONE',  ( -19.02544592524342804, 5.153800228976336051, 51.04057627198103120 ) ) ;
#171761 = CARTESIAN_POINT ( 'NONE',  ( 9.564922557960805705, 16.46253265017160317, 59.58224293864769550 ) ) ;
#171762 = CARTESIAN_POINT ( 'NONE',  ( 4.483927247898545687, 16.52544592524342804, 99.79057627198103830 ) ) ;
#171763 = CARTESIAN_POINT ( 'NONE',  ( 13.97604488694527802, 13.89961937509977652, 114.3739096053143669 ) ) ;
#171764 = CARTESIAN_POINT ( 'NONE',  ( 8.314922557960818139, 14.29746914071049879, 54.58224293864769550 ) ) ;
#171765 = CARTESIAN_POINT ( 'NONE',  ( -19.03943276465977164, 0.05219959533909376836, 31.24890960531435979 ) ) ;
#171766 = CARTESIAN_POINT ( 'NONE',  ( -4.483927247898539470, -16.52544592524342804, 87.29057627198103830 ) ) ;
#171767 = CARTESIAN_POINT ( 'NONE',  ( -18.62759615963270932, 10.81492255796079327, 95.83224293864770971 ) ) ;
#171768 = CARTESIAN_POINT ( 'NONE',  ( 0.05219959533937995610, -21.53943276465977519, 30.00109039468568284 ) ) ;
#171769 = CARTESIAN_POINT ( 'NONE',  ( 19.03943276465977164, -0.05219959533909143690, 23.74890960531435269 ) ) ;
#171770 = CARTESIAN_POINT ( 'NONE',  ( -4.379528057220086978, -16.55341960407618274, 44.79275706135234714 ) ) ;
#171771 = CARTESIAN_POINT ( 'NONE',  ( 21.55341960407610458, 5.719274019375980345, 88.95724293864769550 ) ) ;
#171772 = CARTESIAN_POINT ( 'NONE',  ( 18.62759615963255655, 10.81492255796105972, 111.6677570613523613 ) ) ;
#171773 = CARTESIAN_POINT ( 'NONE',  ( 19.03943276465977164, -0.05219959533909143690, 108.7489096053143527 ) ) ;
#171774 = CARTESIAN_POINT ( 'NONE',  ( -21.52544592524334988, -5.823673210054445271, 43.95942372801902565 ) ) ;
#171775 = CARTESIAN_POINT ( 'NONE',  ( 10.72451020669898902, -18.67979575497178502, 37.91557627198102409 ) ) ;
#171776 = CARTESIAN_POINT ( 'NONE',  ( -0.05219959533934338120, 16.53943276465976808, 97.50109039468567573 ) ) ;
#171777 = AXIS2_PLACEMENT_3D ( 'NONE', #68710, #192064, #69720 ) ;
#171779 = CARTESIAN_POINT ( 'NONE',  ( -10.72451020669870658, -18.67979575497194134, 89.58442372801901854 ) ) ;
#171778 = CARTESIAN_POINT ( 'NONE',  ( -18.67979575497193778, 10.72451020669871902, 58.33442372801901143 ) ) ;
#171780 = CARTESIAN_POINT ( 'NONE',  ( 9.564922557961047289, -16.46253265017146816, 30.41775706135232937 ) ) ;
#171781 = CARTESIAN_POINT ( 'NONE',  ( 12.06949235617739724, 12.14591786802326823, 91.87609039468568994 ) ) ;
#171782 = CARTESIAN_POINT ( 'NONE',  ( 5.719274019375673035, 21.55341960407619339, 47.29275706135234003 ) ) ;
#171783 = CARTESIAN_POINT ( 'NONE',  ( -13.89961937509977652, 13.97604488694528158, 45.62390960531433848 ) ) ;
#171784 = CARTESIAN_POINT ( 'NONE',  ( 13.89961937509957401, 13.97604488694547697, 26.87609039468566507 ) ) ;
#171785 = CARTESIAN_POINT ( 'NONE',  ( 18.62759615963271287, -10.81492255796078972, 28.33224293864769550 ) ) ;
#171786 = CARTESIAN_POINT ( 'NONE',  ( -21.52544592524334988, -5.823673210054445271, 18.95942372801901143 ) ) ;
#171787 = CARTESIAN_POINT ( 'NONE',  ( 15.80617190586746368, 15.72974639402197994, 69.37390960531436690 ) ) ;
#171789 = CARTESIAN_POINT ( 'NONE',  ( 18.62759615963271287, -10.81492255796078972, 78.33224293864770971 ) ) ;
#171788 = DIRECTION ( 'NONE',  ( -1.000000000000000000, 0.000000000000000000, 0.000000000000000000 ) ) ;
#171791 = CARTESIAN_POINT ( 'NONE',  ( 0.05219959533910956823, 16.53943276465976808, 59.99890960531436690 ) ) ;
#171790 = CARTESIAN_POINT ( 'NONE',  ( -8.224510206698735004, -14.34966873604973081, 59.58442372801901854 ) ) ;
#171792 = CARTESIAN_POINT ( 'NONE',  ( 37.87393738558668588, 2.428612866367529932E-14, 2.000000000000000000 ) ) ;
#171793 = CARTESIAN_POINT ( 'NONE',  ( 19.02544592524334988, 5.153800228976608722, 91.45942372801900433 ) ) ;
#171794 = CARTESIAN_POINT ( 'NONE',  ( -23.51385019162032819, 1.374935097489404123, -54.82293943248598822 ) ) ;
#171795 = CARTESIAN_POINT ( 'NONE',  ( -0.05219959533934338120, 16.53943276465976808, 42.50109039468567573 ) ) ;
#171796 = CARTESIAN_POINT ( 'NONE',  ( 10.81492255796078972, 18.62759615963270932, 99.58224293864770971 ) ) ;
#171797 = CARTESIAN_POINT ( 'NONE',  ( 18.62759615963271287, -10.81492255796078972, 78.33224293864770971 ) ) ;
#171798 = CARTESIAN_POINT ( 'NONE',  ( -19.03943276465977164, 0.05219959533909376836, 111.2489096053143669 ) ) ;
#171799 = CARTESIAN_POINT ( 'NONE',  ( 14.29746914071037800, 8.314922557961029526, 61.66775706135235424 ) ) ;
#171800 = CARTESIAN_POINT ( 'NONE',  ( 16.51473224551069308, 9.474510206698969483, 69.16557627198102409 ) ) ;
#171802 = CARTESIAN_POINT ( 'NONE',  ( -5.153800228976607833, 19.02544592524334988, 112.7094237280190043 ) ) ;
#171801 = CARTESIAN_POINT ( 'NONE',  ( 21.53943276465977519, 0.05219959533937863772, 41.25109039468568284 ) ) ;
#171803 = CARTESIAN_POINT ( 'NONE',  ( 0.05219959533909260263, 19.03943276465977164, 104.9989096053143669 ) ) ;
#171804 = CARTESIAN_POINT ( 'NONE',  ( 9.564922557961047289, -16.46253265017146816, 30.41775706135232937 ) ) ;
#171805 = CARTESIAN_POINT ( 'NONE',  ( -16.55341960407617563, 4.379528057220093196, 38.54275706135234714 ) ) ;
#171806 = CARTESIAN_POINT ( 'NONE',  ( 5.049401038298161559, -19.05341960407611168, 107.7072429386476955 ) ) ;
#171807 = CARTESIAN_POINT ( 'NONE',  ( -15.72974639402197994, 15.80617190586746368, 105.6239096053143669 ) ) ;
#171808 = CARTESIAN_POINT ( 'NONE',  ( -9.474510206698964154, 16.51473224551069663, 65.41557627198102409 ) ) ;
#171809 = CARTESIAN_POINT ( 'NONE',  ( -16.88567814943165502, 6.947325034625575491, 23.70998877347416922 ) ) ;
#171810 = CARTESIAN_POINT ( 'NONE',  ( -0.05219959533910754901, -16.53943276465976808, 77.49890960531433848 ) ) ;
#171811 = CARTESIAN_POINT ( 'NONE',  ( 19.05341960407611168, 5.049401038298154454, 113.9572429386477097 ) ) ;
#171812 = CARTESIAN_POINT ( 'NONE',  ( 16.46253265017160672, -9.564922557960803928, 23.33224293864769194 ) ) ;
#171813 = CARTESIAN_POINT ( 'NONE',  ( -0.05219959533907301413, -21.53943276465977519, 107.4989096053143669 ) ) ;
#171814 = CARTESIAN_POINT ( 'NONE',  ( 13.97604488694548053, -13.89961937509957401, 60.62609039468564731 ) ) ;
#171815 = CARTESIAN_POINT ( 'NONE',  ( 0.05219959533909260263, 19.03943276465977164, 109.9989096053143669 ) ) ;
#171816 = CARTESIAN_POINT ( 'NONE',  ( -5.153800228976328057, -19.02544592524343514, 22.29057627198102765 ) ) ;
#171817 = CARTESIAN_POINT ( 'NONE',  ( -5.823673210054116645, -21.52544592524344225, 57.29057627198103120 ) ) ;
#171818 = CARTESIAN_POINT ( 'NONE',  ( -9.564922557960796823, -16.46253265017161027, 97.08224293864769550 ) ) ;
#171819 = CARTESIAN_POINT ( 'NONE',  ( -21.52544592524334988, -5.823673210054445271, 73.95942372801901854 ) ) ;
#171820 = CARTESIAN_POINT ( 'NONE',  ( 13.89961937509977652, -13.97604488694527269, 53.12390960531434558 ) ) ;
#171821 = CARTESIAN_POINT ( 'NONE',  ( -14.29746914071049879, 8.314922557960819915, 85.83224293864768129 ) ) ;
#171822 = CARTESIAN_POINT ( 'NONE',  ( -12.06949235617739369, -12.14591786802326823, 29.37609039468568284 ) ) ;
#171823 = CARTESIAN_POINT ( 'NONE',  ( -18.67979575497193778, 10.72451020669871902, 63.33442372801900433 ) ) ;
#171824 = VERTEX_POINT ( 'NONE', #105424 ) ;
#171825 = CARTESIAN_POINT ( 'NONE',  ( 19.05341960407617918, -5.049401038297876454, 21.04275706135232582 ) ) ;
#171826 = CARTESIAN_POINT ( 'NONE',  ( -19.03943276465977164, -0.05219959533935918106, 78.75109039468567573 ) ) ;
#171827 = CARTESIAN_POINT ( 'NONE',  ( -5.153800228976607833, 19.02544592524334988, 42.70942372801901143 ) ) ;
#171828 = DIRECTION ( 'NONE',  ( 0.000000000000000000, 1.000000000000000000, 0.000000000000000000 ) ) ;
#171829 = CARTESIAN_POINT ( 'NONE',  ( -15.72974639402176322, -15.80617190586768395, 39.37609039468567573 ) ) ;
#171830 = CARTESIAN_POINT ( 'NONE',  ( -19.05341960407617563, 5.049401038297882671, 28.54275706135232937 ) ) ;
#171831 = CARTESIAN_POINT ( 'NONE',  ( -16.46253265017160317, 9.564922557960807481, 70.83224293864770971 ) ) ;
#171832 = CARTESIAN_POINT ( 'NONE',  ( -12.14591786802309592, -12.06949235617757132, 21.87390960531436690 ) ) ;
#171835 = B_SPLINE_CURVE_WITH_KNOTS ( 'NONE', 3,
 ( #187094, #33386, #156734, #155725, #77884, #19216 ),
 .UNSPECIFIED., .F., .F.,
 ( 4, 2, 4 ),
 ( 0.000000000000000000, 0.0003837532665554015815, 0.0007675065331108031630 ),
 .UNSPECIFIED. ) ;
#171834 = CARTESIAN_POINT ( 'NONE',  ( 15.80617190586769283, -15.72974639402175789, 85.62609039468568994 ) ) ;
#171833 = CARTESIAN_POINT ( 'NONE',  ( -16.46253265017160317, 9.564922557960807481, 115.8322429386477097 ) ) ;
#171836 = CARTESIAN_POINT ( 'NONE',  ( -11.40812507854755609, 35.11059874428196537, -7.024999997268813523 ) ) ;
#171837 = DIRECTION ( 'NONE',  ( 0.000000000000000000, 0.000000000000000000, 1.000000000000000000 ) ) ;
#171838 = CARTESIAN_POINT ( 'NONE',  ( 15.80617190586769283, -15.72974639402175789, 90.62609039468567573 ) ) ;
#171839 = CARTESIAN_POINT ( 'NONE',  ( 17.26172910966779384, -6.454744622555847577, 43.30646908649224258 ) ) ;
#171840 = CARTESIAN_POINT ( 'NONE',  ( -5.049401038298153566, 19.05341960407611168, 100.2072429386476955 ) ) ;
#171841 = CARTESIAN_POINT ( 'NONE',  ( -24.84792715949104291, -12.91290060751520130, 166.0205615092969822 ) ) ;
#171842 = CARTESIAN_POINT ( 'NONE',  ( 19.05341960407611168, 5.049401038298154454, 53.95724293864770260 ) ) ;
#171843 = CARTESIAN_POINT ( 'NONE',  ( 5.719274019375991003, -21.55341960407610458, 62.70724293864769550 ) ) ;
#171844 = CARTESIAN_POINT ( 'NONE',  ( -12.14591786802326823, 12.06949235617739902, 113.1260903946856899 ) ) ;
#171846 = CARTESIAN_POINT ( 'NONE',  ( 9.564922557960805705, 16.46253265017160317, 94.58224293864769550 ) ) ;
#171845 = CARTESIAN_POINT ( 'NONE',  ( -19.05341960407611168, -5.049401038298163336, 21.45724293864768839 ) ) ;
#171847 = CARTESIAN_POINT ( 'NONE',  ( 13.89961937509957401, 13.97604488694547697, 26.87609039468566507 ) ) ;
#171848 = CARTESIAN_POINT ( 'NONE',  ( -0.05219959533910754901, -16.53943276465976808, 102.4989096053143811 ) ) ;
#171849 = CARTESIAN_POINT ( 'NONE',  ( -15.72974639402176322, -15.80617190586768395, 74.37609039468568994 ) ) ;
#171850 = LINE ( 'NONE', #153691, #20707 ) ;
#171851 = CARTESIAN_POINT ( 'NONE',  ( 16.52544592524335698, 4.483927247898782831, 106.4594237280190328 ) ) ;
#171852 = CARTESIAN_POINT ( 'NONE',  ( -9.474510206698720793, -16.51473224551083518, 59.58442372801900433 ) ) ;
#171853 = CARTESIAN_POINT ( 'NONE',  ( -22.81625015709510507, 31.40387420917330275, -7.424999997268812102 ) ) ;
#171854 = CARTESIAN_POINT ( 'NONE',  ( 16.46253265017160672, -9.564922557960803928, 113.3322429386476955 ) ) ;
#171855 = CARTESIAN_POINT ( 'NONE',  ( -14.34966873604960291, -8.224510206698953496, 81.66557627198103830 ) ) ;
#171856 = CARTESIAN_POINT ( 'NONE',  ( -16.51473224551082808, 9.474510206698731452, 53.33442372801900433 ) ) ;
#171857 = CARTESIAN_POINT ( 'NONE',  ( 0.05219959533909260263, 19.03943276465977164, 59.99890960531436690 ) ) ;
#171858 = CARTESIAN_POINT ( 'NONE',  ( -0.05219959533910754901, -16.53943276465976808, 57.49890960531435979 ) ) ;
#171859 = CARTESIAN_POINT ( 'NONE',  ( -0.05219959533936034679, 19.03943276465977164, 87.50109039468567573 ) ) ;
#171860 = CARTESIAN_POINT ( 'NONE',  ( 18.62759615963271287, -10.81492255796078972, 53.33224293864769550 ) ) ;
#171861 = EDGE_LOOP ( 'NONE', ( #6118, #89294, #58891, #33636 ) ) ;
#171862 = CARTESIAN_POINT ( 'NONE',  ( 4.483927247898545687, 16.52544592524342804, 109.7905762719810383 ) ) ;
#171864 = CARTESIAN_POINT ( 'NONE',  ( -18.62759615963270932, 10.81492255796079327, 60.83224293864769550 ) ) ;
#171863 = CARTESIAN_POINT ( 'NONE',  ( 16.46253265017160672, -9.564922557960803928, 63.33224293864769550 ) ) ;
#171866 = CARTESIAN_POINT ( 'NONE',  ( -13.97604488694527625, -13.89961937509977652, 76.87390960531433848 ) ) ;
#171865 = CARTESIAN_POINT ( 'NONE',  ( 14.29746914071037800, 8.314922557961029526, 96.66775706135234714 ) ) ;
#171867 = CARTESIAN_POINT ( 'NONE',  ( 19.03943276465977164, 0.05219959533936151252, 51.25109039468567573 ) ) ;
#171868 = CARTESIAN_POINT ( 'NONE',  ( -5.823673210054431948, 21.52544592524334988, 82.70942372801900433 ) ) ;
#171869 = CARTESIAN_POINT ( 'NONE',  ( 5.719274019375991003, -21.55341960407610458, 67.70724293864769550 ) ) ;
#171870 = CARTESIAN_POINT ( 'NONE',  ( -0.05219959533909027116, -19.03943276465977164, 112.4989096053143669 ) ) ;
#171871 = CARTESIAN_POINT ( 'NONE',  ( 19.02544592524343514, -5.153800228976328945, 43.54057627198103120 ) ) ;
#171872 = CARTESIAN_POINT ( 'NONE',  ( 16.53943276465976808, 0.05219959533934440121, 96.25109039468568994 ) ) ;
#171873 = CARTESIAN_POINT ( 'NONE',  ( -19.05341960407617563, 5.049401038297882671, 113.5427570613523471 ) ) ;
#171874 = CARTESIAN_POINT ( 'NONE',  ( 17.40861289039002813, 6.110651285853275994, 53.87232470827435549 ) ) ;
#171875 = CARTESIAN_POINT ( 'NONE',  ( 5.823673210054444382, -21.52544592524334988, 90.20942372801903275 ) ) ;
#171876 = VERTEX_POINT ( 'NONE', #90246 ) ;
#171877 = CARTESIAN_POINT ( 'NONE',  ( 16.55341960407611168, 4.379528057220329451, 58.95724293864770971 ) ) ;
#171878 = CARTESIAN_POINT ( 'NONE',  ( -14.34966873604960291, -8.224510206698953496, 71.66557627198100988 ) ) ;
#171879 = CARTESIAN_POINT ( 'NONE',  ( 21.55341960407610458, 5.719274019375980345, 88.95724293864769550 ) ) ;
#171880 = CARTESIAN_POINT ( 'NONE',  ( -21.52544592524343514, 5.823673210054127303, 91.04057627198103830 ) ) ;
#171881 = CARTESIAN_POINT ( 'NONE',  ( 16.21995358207302473, -7.366697692864217828, 97.43551001512156517 ) ) ;
#171883 = EDGE_CURVE ( 'NONE', #145198, #166185, #83094, .T. ) ;
#171882 = CARTESIAN_POINT ( 'NONE',  ( 5.719274019375991003, -21.55341960407610458, 52.70724293864769550 ) ) ;
#171884 = CARTESIAN_POINT ( 'NONE',  ( 12.14591786802327356, -12.06949235617739191, 65.62609039468568994 ) ) ;
#171885 = CARTESIAN_POINT ( 'NONE',  ( -4.483927247898539470, -16.52544592524342804, 97.29057627198105251 ) ) ;
#171886 = CARTESIAN_POINT ( 'NONE',  ( -5.153800228976328057, -19.02544592524343514, 47.29057627198102409 ) ) ;
#171887 =( NAMED_UNIT ( * ) SI_UNIT ( $, .STERADIAN. ) SOLID_ANGLE_UNIT ( ) );
#171888 = CARTESIAN_POINT ( 'NONE',  ( 15.50000000000000178, -5.500000000000000888, 118.0000000000000142 ) ) ;
#171889 = CARTESIAN_POINT ( 'NONE',  ( 16.55341960407618274, -4.379528057220086978, 101.0427570613523756 ) ) ;
#171890 = CARTESIAN_POINT ( 'NONE',  ( -21.52544592524334988, -5.823673210054445271, 33.95942372801901143 ) ) ;
#171891 = CARTESIAN_POINT ( 'NONE',  ( 13.89961937509977652, -13.97604488694527269, 103.1239096053143527 ) ) ;
#171892 = CARTESIAN_POINT ( 'NONE',  ( 21.52544592524334988, 5.823673210054432836, 61.45942372801901854 ) ) ;
#171893 = DIRECTION ( 'NONE',  ( 0.9974398506828145994, 0.07151044867601362431, 4.325705812135698390E-17 ) ) ;
#171894 = CARTESIAN_POINT ( 'NONE',  ( -9.564922557960796823, -16.46253265017161027, 22.08224293864768839 ) ) ;
#171895 = ORIENTED_EDGE ( 'NONE', *, *, #39003, .F. ) ;
#171896 = CARTESIAN_POINT ( 'NONE',  ( -21.53943276465977519, -0.05219959533937600094, 53.75109039468568994 ) ) ;
#171898 = DIRECTION ( 'NONE',  ( 0.000000000000000000, 0.000000000000000000, -1.000000000000000000 ) ) ;
#171897 = CARTESIAN_POINT ( 'NONE',  ( 5.153800228976335163, 19.02544592524342804, 44.79057627198103830 ) ) ;
#171899 = CARTESIAN_POINT ( 'NONE',  ( 9.564922557960805705, 16.46253265017160317, 94.58224293864769550 ) ) ;
#171900 = CARTESIAN_POINT ( 'NONE',  ( 16.46253265017146816, 9.564922557961045513, 71.66775706135233293 ) ) ;
#171901 = CARTESIAN_POINT ( 'NONE',  ( 18.62759615963255655, 10.81492255796105972, 26.66775706135235424 ) ) ;
#171902 = CARTESIAN_POINT ( 'NONE',  ( 13.97604488694548053, -13.89961937509957401, 55.62609039468566863 ) ) ;
#171903 = CARTESIAN_POINT ( 'NONE',  ( 9.474510206698971260, -16.51473224551069308, 32.91557627198102409 ) ) ;
#171904 = CARTESIAN_POINT ( 'NONE',  ( 16.52544592524335698, 4.483927247898782831, 106.4594237280190328 ) ) ;
#171905 = CARTESIAN_POINT ( 'NONE',  ( 13.97604488694548053, -13.89961937509957401, 70.62609039468567573 ) ) ;
#171906 = CARTESIAN_POINT ( 'NONE',  ( -8.224510206698948167, 14.34966873604960824, 25.41557627198103120 ) ) ;
#171907 = CARTESIAN_POINT ( 'NONE',  ( -0.05219959533936034679, 19.03943276465977164, 47.50109039468566863 ) ) ;
#171908 = CARTESIAN_POINT ( 'NONE',  ( -13.97604488694527625, -13.89961937509977652, 101.8739096053143811 ) ) ;
#171909 = CARTESIAN_POINT ( 'NONE',  ( -0.05219959533937732626, 21.53943276465977519, 102.5010903946856899 ) ) ;
#171910 = CARTESIAN_POINT ( 'NONE',  ( 9.564922557961047289, -16.46253265017146816, 20.41775706135233293 ) ) ;
#171911 = CARTESIAN_POINT ( 'NONE',  ( 9.564922557960805705, 16.46253265017160317, 29.58224293864769550 ) ) ;
#171912 = CARTESIAN_POINT ( 'NONE',  ( -5.823673210054431948, 21.52544592524334988, 92.70942372801901854 ) ) ;
#171913 = CARTESIAN_POINT ( 'NONE',  ( 12.14591786802327356, -12.06949235617739191, 35.62609039468568994 ) ) ;
#171914 = CARTESIAN_POINT ( 'NONE',  ( -9.474510206698964154, 16.51473224551069663, 90.41557627198103830 ) ) ;
#171915 = DIRECTION ( 'NONE',  ( 0.000000000000000000, 0.000000000000000000, -1.000000000000000000 ) ) ;
#171916 = CARTESIAN_POINT ( 'NONE',  ( 16.46253265017160672, -9.564922557960803928, 78.33224293864769550 ) ) ;
#171917 = DIRECTION ( 'NONE',  ( 0.000000000000000000, 0.000000000000000000, 1.000000000000000000 ) ) ;
#171918 = CARTESIAN_POINT ( 'NONE',  ( 19.03943276465977164, 0.05219959533936151252, 66.25109039468567573 ) ) ;
#171919 = CARTESIAN_POINT ( 'NONE',  ( 5.153800228976335163, 19.02544592524342804, 99.79057627198102409 ) ) ;
#171920 = CARTESIAN_POINT ( 'NONE',  ( 21.52544592524334988, 5.823673210054432836, 96.45942372801901854 ) ) ;
#171921 = CARTESIAN_POINT ( 'NONE',  ( -16.55341960407611168, -4.379528057220339221, 96.45724293864770971 ) ) ;
#171922 = CARTESIAN_POINT ( 'NONE',  ( 5.719274019375991003, -21.55341960407610458, 42.70724293864770260 ) ) ;
#171923 =( BOUNDED_SURFACE ( )  B_SPLINE_SURFACE ( 3, 2, ( 
 ( #35458, #69787, #67786, #100114, #98094, #114278, #113284, #131455, #160802, #101107, #174975, #36439, #97109, #159792, #193142, #6105, #37449, #20281, #177979, #162793, #82944, #175981, #145621, #5103, #9128, #21287, #22290, #144622, #7100, #83941, #81927, #129443, #24302, #130439, #192138, #161797, #23292, #84936, #147639, #146617, #166802, #11129, #197140, #108831, #196159, #104122, #88948, #155343, #180982, #86954, #1648, #148638, #42458, #10128, #644, #71789, #133458, #195148, #12135, #31007, #62314, #92656, #123984, #170511, #43448, #63326, #58607, #27301, #32001, #119299, #134474, #179995, #73799, #149631, #77497, #56629, #135472, #93658, #102126, #139167, #118303, #120273, #47172, #178985, #57633, #150639, #25312, #41462, #72804, #165804, #105116, #103127, #181965, #154345, #164808, #15838, #87943, #185682, #16832, #40452, #78483, #163810, #140156, #26303, #143134, #65309, #18828, #34977, #48170, #2649, #5619, #126969, #175485, #96630, #33989, #145133, #19806, #160313, #128957, #50157, #172502, #35962, #83455, #158318, #21803, #142146, #64326, #17833, #4613, #111816, #6616, #66305, #36957, #109827, #127965, #125004, #144137, #98619, #186699, #189668, #173504, #141160, #171510, #32999, #97609, #188677, #49161, #80473, #3630, #159298, #125993, #51141, #94653, #52133, #156333, #112802, #81447, #79491, #67298, #174495, #187691, #20794, #110820, #95645, #157333, #82449, #190657, #113790, #86470, #150157, #84452, #39964, #22806, #87471, #164332, #178497, #117817, #161312, #101634, #25826, #68295, #7616, #195678, #70310, #26820, #40978, #100629, #148155, #116805, #24821, #53125, #146130, #69300, #103650, #9647, #179510, #176496, #132976, #193664, #55135, #114803, #10648, #149158, #129946, #130966, #192656, #71313, #191646, #56136, #194666, #102647, #72310, #133987, #57149, #118827, #163325, #180511, #41984, #165328, #88461, #37972, #99630, #54139, #115813, #38972, #177503, #162310, #23811, #85461, #147150, #8638, #131979, #184457, #119811, #166326, #107592, #15603, #76267, #181496, #135978, #13616, #154110, #92424, #12644, #43962, #42974, #89465, #169270, #46936, #183470, #185446, #91419, #121777, #151154, #90449, #29783, #168287, #137945, #77261, #122768, #27823, #199628, #104639, #196674, #74311, #93415, #61095, #410, #153106, #11658, #197649, #44955, #59115, #30777, #138930, #106612, #45937, #120781, #14610, #62083, #73324, #182481, #123747, #75283, #170273, #108596, #105624, #31766, #60109, #134995, #58143, #167312, #28808, #152133, #136954, #198643, #63084, #19574, #80236, #141907, #1405, #97377, #112567, #16595, #156093, #171273, #173262, #155102, #142898, #81217, #111578, #35730, #20557, #4380, #50909, #188434, #143899, #3398, #159063, #174262, #5381, #49913, #65073, #175248, #125756, #34737, #32761, #187456, #82208, #36713, #124763, #67064, #127731, #186460, #109590, #128722, #190419, #66065, #47938, #79250, #157093, #51895, #113554, #17590, #48924, #94413, #140922, #78243, #139915, #126731, #2408, #96395, #158082, #64087, #33749, #189433, #110578, #172259, #95407, #18589, #10404, #83220, #178259, #195429, #117567, #148915, #160073, #163076, #85216, #114559, #180269, #98376, #9404, #162072, #22567, #53902, #192420, #132736, #37727, #24579, #56905, #25588, #144895, #86228, #115577, #52884, #40732, #100394, #177265, #23568, #8396, #72061, #146907, #6377, #118579, #68057, #70071, #129711, #179268, #191408, #176256, #99389, #131739, #147918, #102402, #71070, #164089, #87232, #194424, #21560, #116570, #193421, #133735, #38736, #54896, #161072, #39720, #69061, #55894, #84213, #101383, #145893, #7376, #130728, #134750, #75043, #107349, #123509, #120542, #151889, #88218, #57902, #74068, #135739, #106365, #196432, #121534, #44710, #181257, #182235, #150912, #43720, #59867, #103403, #136709, #61839, #184216, #26575, #183229, #105381, #197410, #13379, #165081, #119574, #122526, #167068, #92180 ),
 ( #166078, #28569, #45698, #169022, #42734, #58876, #149902, #104396, #199387, #77018, #198390, #15362, #168048, #29545, #27581, #90206, #91178, #152867, #14362, #30527, #76027, #153864, #11409, #137702, #138690, #60851, #171, #73078, #41739, #89219, #12406, #66822, #185202, #96164, #48688, #109347, #140678, #79004, #19344, #124521, #111337, #81964, #112334, #170033, #173027, #2170, #4146, #16359, #78007, #154861, #18353, #34506, #65825, #157853, #127494, #174024, #49673, #46693, #3168, #33511, #35495, #125521, #63850, #186216, #80008, #155851, #80992, #139674, #141677, #97145, #108354, #142667, #1162, #64841, #50674, #31523, #187218, #95170, #93176, #62837, #17348, #110341, #189199, #47697, #126503, #188201, #171029, #172022, #94172, #156858, #158828, #32520, #20316, #5140, #143656, #113320, #146654, #68821, #22327, #38496, #51656, #6142, #9165, #130480, #179022, #100152, #37487, #148677, #23328, #163848, #132500, #53658, #176018, #39482, #86990, #161833, #25349, #145657, #67824, #21325, #8148, #115335, #10165, #69825, #191178, #7138, #159830, #24338, #177026, #194189, #144659, #82983, #190181, #129479, #162829, #99149, #192177, #128485, #147677, #85988, #160838, #84971, #131492, #98133, #102162, #52652, #193179, #83977, #54652, #116326, #175012, #178015, #70832, #36476, #114316, #101143, #55654, #117326, #40490, #42497, #59629, #104161, #89979, #199148, #88985, #197179, #182003, #45464, #73838, #180032, #91936, #41501, #135509, #103165, #164845, #90946, #26341, #87981, #149669, #105153, #121303, #152633, #182995, #14123, #60614, #136479, #153629, #151660, #120310, #122289, #12173, #27339, #72842, #166839, #165842, #167817, #11167, #28340, #183978, #195185, #29316, #134512, #13154, #137468, #71825, #150675, #43486, #118339, #196198, #58644, #74817, #198159, #57670, #44478, #106133, #119337, #75790, #181023, #107118, #168789, #133493, #30291, #56666, #157615, #200138, #33279, #155620, #109115, #125288, #138457, #92939, #95930, #17116, #65592, #186985, #124279, #35257, #110113, #50441, #19106, #140444, #62601, #126272, #173790, #48456, #112100, #32286, #154627, #108111, #94938, #1934, #96911, #156623, #77777, #93941, #46451, #111100, #63613, #80756, #31288, #169795, #76786, #16122, #49439, #185975, #78767, #15124, #34271, #172790, #47459, #171791, #18118, #184967, #188965, #139445, #79773, #170794, #141443, #2930, #61607, #64609, #142433, #123276, #927, #187969, #3912, #127252, #8917, #129237, #146407, #190933, #176778, #85743, #175767, #83733, #68572, #132254, #160593, #66584, #178774, #128248, #22082, #51420, #38250, #174772, #114069, #70585, #52410, #7897, #37243, #99905, #147430, #98899, #145412, #130229, #193945, #6894, #189945, #40240, #113080, #191924, #36238, #177774, #97890, #159582, #21079, #53408, #69582, #39244, #131248, #100900, #55408, #23084, #158594, #161590, #115086, #117078, #84729, #192937, #82735, #54414, #116086, #162584, #144416, #24088, #20083, #81728, #143413, #5902, #4901, #67579, #183742, #180780, #11930, #148426, #118094, #134265, #195952, #166597, #56414, #181760, #104909, #41253, #42255, #10918, #103917, #120072, #163598, #196938, #122051, #44237, #86741, #43242, #165597, #57425, #73594, #25099, #179784, #182753, #27095, #88741, #90714, #194938, #102915, #71580, #197915, #74573, #9921, #164599, #59385, #105894, #28097, #133246, #26093, #150435, #167581, #29075, #87737, #119098, #149422, #72591, #121059, #137226, #135267, #75550, #89736, #58406, #151422, #12909, #136241, #152397, #13883, #198911, #60379, #101916, #30054, #125044, #142188, #64366, #95688, #106883, #109865, #32043, #61370, #127010, #45229, #156372, #108873, #169551, #686, #155383, #91695, #123041, #77539, #139211, #171550, #199906, #186740, #48211, #184727, #185726, #154386, #47215, #63367, #168556, #140197, #65350, #187731, #153387, #33039, #170553, #62357, #16872, #14887, #46211, #126035, #93700 ),
 ( #124027, #107865, #138224, #94694, #78523, #76548, #17876, #31049, #1691, #92698, #141200, #79530, #49202, #15881, #2689, #110860, #172545, #34030, #157376, #18869, #80515, #3672, #25613, #36002, #128999, #98660, #158359, #165111, #128008, #190697, #97649, #160354, #67337, #50202, #82492, #10432, #88246, #81488, #71094, #4655, #144175, #41766, #159338, #179295, #20835, #9429, #118608, #5661, #113829, #21844, #26603, #52172, #96671, #11438, #19847, #175524, #143175, #72090, #66346, #189710, #51183, #86253, #40759, #133764, #102428, #195459, #180298, #55919, #73109, #132761, #36999, #103431, #147943, #194448, #112843, #117594, #164115, #87257, #174535, #148942, #149931, #111857, #56934, #188718, #173547, #35016, #16390, #13407, #150942, #167096, #28597, #199417, #89250, #14392, #137733, #74098, #75071, #43749, #136737, #152895, #196461, #29574, #154892, #77050, #119602, #76058, #198421, #90235, #44739, #57931, #12436, #15393, #59896, #105412, #104425, #183258, #107382, #91205, #170065, #138721, #121563, #182266, #45730, #93207, #168077, #31556, #151918, #135768, #27610, #60881, #106395, #134779, #122558, #197439, #184248, #166108, #30561, #169054, #202, #58905, #120572, #181285, #92212, #153898, #61871, #123541, #42763, #185234, #46726, #108388, #18386, #188231, #47726, #51690, #17379, #80037, #187249, #49704, #156890, #139706, #172053, #97174, #175044, #171059, #157884, #94202, #33540, #128516, #48718, #65855, #110371, #96195, #5171, #95203, #3197, #111370, #113352, #141706, #186248, #98164, #109378, #64871, #32549, #158859, #155882, #79035, #140710, #173059, #127526, #20348, #189230, #81996, #66854, #142698, #159864, #19373, #126532, #190211, #34536, #81022, #2200, #4177, #50708, #174057, #63881, #112366, #36509, #1193, #35526, #125552, #143689, #78037, #62870, #124551, #131528, #67854, #10198, #161867, #177059, #22360, #54686, #192210, #117361, #52684, #116359, #71858, #144689, #179057, #114347, #178048, #87025, #103199, #100185, #193212, #129509, #37519, #53693, #115370, #86023, #176052, #101176, #24372, #160870, #23361, #130514, #85006, #39516, #83014, #162864, #41535, #163885, #6174, #147712, #146687, #38529, #9200, #191209, #99181, #102197, #8183, #69859, #84012, #70865, #194222, #132533, #56700, #25382, #55687, #68855, #40526, #180067, #148710, #118373, #133527, #145690, #7172, #195219, #21357, #46484, #44510, #27370, #182036, #196233, #60647, #90010, #168820, #181054, #119371, #26375, #42530, #199181, #135540, #166871, #164880, #184013, #122321, #12207, #105184, #74847, #134544, #138488, #104193, #28372, #73870, #136510, #43518, #88014, #58674, #45495, #61639, #57702, #106166, #165874, #120341, #15157, #197211, #152665, #151694, #183027, #91967, #13184, #198191, #59661, #200170, #121334, #72876, #185000, #89017, #167849, #150708, #107150, #29349, #90978, #14155, #75823, #137501, #30325, #153661, #76817, #123307, #149702, #11200, #126302, #156654, #18150, #157646, #959, #141476, #65621, #189975, #47491, #35286, #110143, #66614, #80786, #140478, #187998, #79804, #64640, #92973, #62635, #124311, #143445, #49468, #19135, #16154, #172820, #33310, #94970, #154658, #50470, #127281, #169828, #109148, #186009, #111131, #108144, #95962, #34300, #142464, #188994, #173821, #3942, #112130, #2960, #96942, #158623, #20114, #81758, #4931, #128278, #31321, #77808, #78800, #139477, #48489, #170827, #32319, #93972, #155652, #17147, #1966, #63646, #125321, #187018, #171822, #84760, #97922, #52440, #145443, #100932, #39275, #129269, #98931, #159615, #5932, #116116, #132285, #115116, #70619, #161621, #53441, #67608, #83763, #23115, #38281, #146438, #162616, #131279, #8951, #174801, #7929, #193977, #177805, #147461, #51450, #69613, #191955, #190963, #113111, #36267, #24121, #99935, #22113, #130259, #68603, #85774, #37274, #55439, #21111, #117110, #114098, #82766, #176809, #175801, #144447, #160622 ),
 ( #6925, #192967, #54446, #35935, #51114, #82420, #126941, #80445, #52103, #2621, #65282, #172473, #20765, #124975, #171482, #1619, #127937, #4585, #140128, #186672, #189639, #97581, #96601, #63295, #156304, #33960, #174466, #112773, #32971, #64298, #48142, #109799, #159269, #67269, #3603, #5589, #111788, #142118, #94625, #110792, #50128, #188649, #158290, #144109, #143106, #128927, #16804, #173476, #190628, #113760, #31974, #93630, #19779, #18800, #17805, #155315, #78454, #66278, #95618, #79462, #187663, #125965, #141131, #49134, #81420, #157303, #34949, #160283, #101602, #192627, #129915, #117785, #177472, #191615, #163290, #6585, #21774, #53094, #57119, #24791, #164302, #193633, #175456, #114772, #147121, #176466, #194634, #71281, #85430, #86439, #68264, #8608, #132946, #36927, #37939, #102616, #38941, #133955, #148125, #7584, #55105, #23780, #131949, #83425, #99600, #161280, #10617, #116775, #9616, #145102, #39933, #100598, #162280, #22775, #179479, #56104, #98589, #84423, #146100, #178466, #69270, #40944, #25795, #87441, #149126, #72278, #195646, #130936, #70281, #54109, #115783, #83767, #64644, #37278, #145447, #65625, #188002, #141480, #128282, #173826, #130263, #189979, #111135, #127285, #79808, #144451, #35290, #52444, #126306, #2964, #110147, #49472, #82770, #19139, #50474, #48493, #67612, #5936, #95966, #188998, #158627, #18154, #22117, #172824, #112134, #157650, #20118, #96946, #171826, #142468, #129273, #6929, #34304, #51454, #80790, #3946, #98935, #81762, #36271, #143449, #66618, #175805, #4935, #113115, #174805, #68607, #97926, #156658, #33314, #159619, #21115, #190967, #114102, #160626, #94974, #161625, #25135, #41287, #72625, #102949, #134300, #183532, #56450, #76332, #9955, #40278, #45016, #132289, #147465, #192971, #86777, #162620, #87770, #23119, #148462, #106676, #115120, #149455, #84764, #71614, #60169, #191959, #70623, #101951, #38285, #7933, #24126, #85778, #118129, #146441, #133280, #194971, #131283, #193981, #100936, #55443, #179817, #53445, #164633, #14671, #195986, #176813, #26128, #117114, #8955, #163632, #99939, #69617, #121838, #178808, #10951, #54450, #168349, #29845, #91482, #153169, #116120, #177809, #39279, #65135, #122830, #64152, #155166, #92486, #80297, #139979, #154175, #125816, #169331, #184519, #15666, #19635, #187519, #126792, #156155, #138009, #77325, #109653, #138993, #157156, #33810, #47999, #48985, #30839, #171335, #95470, #199693, #472, #188498, #1468, #96456, #110640, #170336, #17653, #186525, #94474, #45999, #62146, #123810, #173326, #79313, #172321, #107654, #2470, #63146, #124825, #185508, #141969, #18651, #61158, #46999, #108658, #140982, #31829, #3458, #49977, #111641, #34801, #158143, #93479, #16658, #32823, #78306, #129769, #85277, #100453, #131802, #176317, #191465, #101446, #51955, #114617, #21623, #70130, #174321, #20619, #50970, #177325, #53961, #189492, #115636, #68117, #112629, #35791, #97438, #5441, #83280, #23629, #162133, #82269, #113615, #159123, #143961, #38796, #116630, #52943, #54958, #161131, #37787, #67125, #160135, #99451, #22627, #7436, #146968, #192478, #193481, #66127, #84274, #178319, #8457, #39782, #142959, #145955, #69120, #128783, #163137, #81277, #4439, #144954, #190483, #36775, #175309, #127792, #98440, #130786, #6435, #103467, #134815, #71131, #40794, #56967, #118640, #89285, #179330, #104460, #27645, #164151, #165146, #133801, #26637, #42798, #86289, #119636, #44773, #167131, #9468, #166143, #88280, #180332, #196495, #147979, #102463, #105447, #149968, #195492, #194484, #73145, #197473, #181319, #59928, #28631, #11474, #182302, #121596, #25648, #13440, #183291, #41800, #87293, #117632, #150976, #57965, #106426, #12470, #148977, #74131, #55956, #120608, #135802, #90268, #10466, #72127, #132797, #58939, #43782, #151951, #75104, #24641, #136771, #198457, #15425, #108418, #78068, #137763, #141736, #107414 ),
 ( #138753, #155916, #235, #186279, #95234, #185268, #93238, #139736, #3226, #170094, #76087, #188261, #199447, #31588, #60915, #187280, #122591, #184279, #45762, #1225, #17411, #48750, #79068, #110403, #156920, #32582, #18417, #124583, #80066, #64900, #154923, #126561, #140741, #61902, #47758, #16421, #109412, #152926, #169087, #30593, #49735, #171091, #2230, #168107, #62903, #92245, #29604, #153931, #94235, #77084, #172085, #123573, #46760, #63912, #125582, #33572, #91236, #14423, #192242, #100215, #6203, #67883, #8214, #161895, #23391, #51717, #66882, #112395, #144717, #82025, #7200, #142727, #129536, #85037, #34567, #68884, #4207, #191236, #177087, #193243, #190240, #21383, #157912, #127559, #143721, #5200, #176078, #65885, #52710, #114374, #50736, #113380, #20378, #175070, #37546, #173088, #99210, #131558, #53722, #96223, #160898, #36536, #128543, #83042, #19402, #189260, #115399, #98192, #159895, #81051, #22390, #84040, #145719, #146718, #38558, #130544, #69889, #111403, #174086, #35555, #97202, #158888, #194251, #147741, #134574, #180096, #136538, #196261, #117390, #71887, #86052, #150735, #41564, #58700, #70895, #9228, #116388, #132562, #89045, #25412, #56732, #54716, #73897, #12235, #102227, #195248, #164909, #24403, #28399, #55718, #118402, #163916, #26403, #133557, #178078, #148739, #135567, #151720, #179089, #57730, #40558, #10227, #105212, #87054, #42558, #103227, #72905, #182063, #88042, #149730, #11231, #119400, #197239, #181083, #120370, #104221, #165902, #39545, #27400, #43546, #166899, #90038, #101204, #13213, #74876, #162894, #138516, #108175, #167878, #171849, #137528, #46876, #107178, #169856, #76845, #59691, #91996, #17174, #94997, #91008, #77837, #14183, #153690, #48516, #168849, #186037, #30354, #16182, #125349, #15186, #123336, #31350, #33337, #61667, #106194, #18177, #29377, #185029, #152694, #78828, #75852, #199210, #60677, #93001, #47519, #140506, #109175, #1995, #187046, #154687, #139504, #156683, #110170, #79834, #46516, #987, #122352, #62662, #124341, #93998, #184041, #170854, #198219, #121362, #155679, #45524, #32345, #63674, #183055, #44539, #51481, #188026, #157676, #173851, #35317, #5962, #95991, #21141, #144478, #80815, #81788, #50498, #143475, #159645, #2989, #36298, #161653, #83795, #126329, #82796, #4959, #96971, #113143, #64667, #19166, #22145, #66644, #112162, #111160, #190007, #114130, #97953, #176843, #145475, #128307, #98963, #38314, #142493, #130292, #99969, #158652, #3971, #34330, #67640, #174833, #23149, #129299, #65651, #20143, #141504, #49498, #190995, #172849, #160653, #127313, #189024, #52471, #175831, #37304, #6956, #68636, #191986, #53473, #115150, #41320, #181828, #135331, #73659, #25168, #40309, #85810, #118159, #55476, #180844, #116150, #179849, #197004, #7964, #42321, #177841, #102980, #150499, #166662, #163666, #195003, #131313, #100968, #117146, #178841, #149488, #39309, #164665, #87802, #24159, #86810, #194013, #148496, #26161, #146472, #10984, #104975, #27159, #69647, #72657, #9987, #101985, #56481, #193003, #162653, #165661, #71647, #133314, #54480, #134332, #57492, #196016, #120137, #88806, #119161, #103982, #43307, #147496, #58470, #84793, #11996, #8987, #70655, #132321, #153456, #109937, #107937, #90780, #45296, #59453, #124100, #14954, #32113, #44303, #182821, #89805, #105962, #62428, #198977, #30121, #28163, #47287, #185799, #75616, #168621, #138292, #197983, #1760, #167647, #91762, #137295, #199973, #106948, #151487, #122119, #108943, #125114, #121126, #169623, #29143, #183808, #78595, #60444, #15950, #76614, #46281, #155451, #61438, #123110, #184795, #63438, #31120, #136308, #170624, #92768, #154458, #12978, #93770, #16941, #77609, #139280, #757, #152464, #186812, #13950, #140268, #48282, #74642, #50269, #33107, #65417, #190763, #68400, #64433, #51250, #187799, #127078, #21911, #142256, #159409, #3740, #189778, #98728 ),
 ( #49268, #143241, #126103, #52238, #67407, #81555, #20904, #110926, #112910, #160422, #128075, #83562, #145241, #173613, #130052, #144244, #188786, #174604, #19913, #36070, #156445, #172612, #34099, #6722, #97719, #82562, #79598, #5728, #96736, #158425, #17944, #113895, #129062, #94763, #95757, #157442, #175593, #171619, #37069, #191752, #53235, #141267, #2757, #18937, #80582, #4724, #111927, #66413, #35083, #134094, #165433, #9751, #163431, #135100, #85570, #148258, #55242, #103754, #7722, #54246, #84557, #10753, #87574, #22911, #149261, #101743, #146235, #69408, #131074, #39076, #116910, #57257, #195784, #115918, #147256, #192763, #177608, #72417, #150268, #86574, #88570, #194769, #24929, #100733, #193773, #133079, #99735, #56243, #11762, #118931, #26928, #176605, #179613, #71415, #162414, #196776, #114911, #25931, #178603, #23916, #70417, #8747, #180616, #132084, #41086, #73429, #42089, #161419, #102749, #40066, #117924, #38079, #164437, #74412, #184562, #89571, #43075, #12747, #140026, #46043, #47047, #76378, #58244, #136078, #29888, #197752, #77371, #154221, #168393, #107698, #151257, #138055, #185553, #14718, #108704, #170383, #60213, #16702, #30885, #90553, #199736, #106719, #61202, #104742, #59219, #120888, #93528, #122874, #169377, #166433, #92532, #183576, #45061, #27928, #519, #15711, #119912, #182587, #44070, #139039, #181598, #62191, #123855, #31874, #155213, #78352, #105730, #167417, #91526, #28913, #153213, #152235, #13720, #75386, #137058, #198748, #121883, #172365, #34844, #142014, #193273, #94519, #141029, #171382, #100243, #177117, #109700, #38587, #188544, #32869, #156201, #17701, #125863, #3503, #146749, #85067, #2516, #33855, #79358, #64196, #161925, #39576, #173374, #178108, #81321, #111687, #187563, #80342, #19679, #158189, #127834, #8244, #112673, #116419, #101235, #96499, #162924, #143004, #4482, #49030, #65179, #66172, #189540, #51012, #69922, #23419, #24432, #186571, #131588, #86080, #54746, #1515, #63192, #124872, #50022, #110685, #48044, #95515, #157201, #126838, #18695, #103258, #41594, #182094, #87083, #73928, #44570, #74906, #132591, #135597, #164940, #102258, #90068, #149759, #163945, #197269, #179119, #194280, #25443, #29409, #58731, #136570, #165934, #147771, #148768, #119430, #10257, #166930, #43578, #57760, #120401, #40587, #27432, #198250, #104251, #59725, #121395, #11263, #106225, #105242, #180126, #89076, #196290, #150767, #55747, #71916, #133588, #183087, #12264, #28431, #117421, #151750, #72935, #134604, #195279, #13243, #167909, #9258, #56761, #118433, #70924, #26433, #88074, #181114, #42588, #171882, #156719, #155711, #187080, #124376, #79869, #139537, #95029, #110203, #141538, #186071, #1021, #111194, #61700, #47554, #31385, #3027, #184073, #30386, #60709, #48549, #63708, #199243, #125383, #77870, #122384, #45557, #107211, #15219, #93034, #33371, #18211, #92033, #123369, #168881, #153723, #64703, #62694, #169891, #152726, #185062, #126365, #188061, #76878, #170886, #138548, #46550, #49531, #108212, #78860, #154722, #109207, #172885, #16215, #32378, #94031, #91039, #17207, #26, #14216, #140540, #2028, #75885, #137560, #65685, #127348, #4006, #67677, #83829, #115184, #145510, #176877, #23184, #129335, #191030, #131348, #84827, #146507, #174868, #190042, #35355, #52505, #4996, #130326, #189062, #114165, #7997, #157712, #192023, #50534, #175868, #100002, #116185, #113178, #144513, #80851, #112196, #66681, #128343, #98998, #173886, #37340, #160687, #97006, #36334, #143510, #97987, #22179, #96026, #6991, #54513, #38346, #19202, #68672, #159681, #51516, #5998, #142528, #158688, #161689, #21177, #82832, #20177, #53507, #69681, #193036, #34365, #81823, #103018, #135367, #13012, #194049, #166695, #74676, #195040, #117183, #70691, #57526, #164701, #59487, #119195, #40345, #56517, #9022, #73695, #26197, #181862, #55513, #132357, #39344, #178878, #12032 ),
 ( #87836, #85844, #102020, #147534, #163703, #179886, #120171, #58505, #25205, #10023, #86847, #148532, #197038, #136343, #149522, #151521, #180880, #11019, #71682, #118195, #196051, #134367, #104017, #43341, #88840, #89840, #162688, #42355, #198018, #105009, #28198, #101003, #165695, #72692, #133349, #177876, #24194, #150532, #41354, #27193, #76647, #14987, #155484, #60476, #47323, #17979, #48317, #105994, #108978, #138325, #75650, #63474, #123144, #137328, #170659, #152496, #167680, #199009, #2791, #32147, #109972, #139313, #121161, #122152, #92803, #183841, #140305, #16976, #31155, #93804, #13984, #792, #171651, #77644, #33141, #94799, #184831, #79633, #78630, #153491, #62464, #169659, #124137, #29177, #45330, #106980, #156478, #185836, #1796, #90813, #125149, #46317, #107972, #168654, #186848, #141301, #182854, #30154, #91797, #44337, #200007, #61473, #154491, #15985, #145275, #130088, #129096, #160454, #97754, #53268, #112944, #68435, #83595, #114946, #159442, #174637, #84591, #35117, #20937, #4757, #176639, #157477, #3773, #34132, #21945, #37102, #172644, #98761, #36102, #161454, #126137, #190796, #51283, #80616, #146271, #64470, #175628, #128107, #188819, #19947, #158458, #6756, #65450, #52270, #22945, #191787, #49301, #113928, #81588, #18970, #38114, #66446, #142293, #99769, #95791, #110960, #127112, #187832, #50302, #111959, #82594, #173648, #96769, #144276, #143274, #189811, #5763, #67439, #57287, #100765, #25961, #135132, #164467, #196806, #58274, #9784, #166464, #180647, #40098, #87604, #56273, #149290, #192797, #162447, #23948, #43108, #10784, #118961, #115952, #72451, #133111, #194800, #54279, #150299, #165464, #69441, #8779, #85602, #134126, #7757, #195815, #42122, #103784, #88603, #73459, #26960, #11795, #41116, #119943, #117956, #181628, #104776, #27961, #102780, #179647, #89602, #178635, #131109, #148290, #177641, #147289, #70448, #39109, #132114, #193807, #55273, #116942, #101776, #163463, #24961, #86607, #71446, #153251, #93563, #31910, #152269, #183612, #59253, #28947, #108742, #186607, #122910, #124909, #30920, #61238, #90588, #29923, #169415, #107733, #77406, #155249, #62225, #63229, #136111, #138090, #140063, #91563, #106753, #13754, #184598, #121919, #47081, #182621, #46079, #1554, #74444, #170418, #44106, #92568, #16738, #32905, #14753, #154256, #197787, #167450, #45096, #168428, #15747, #105764, #139076, #554, #75422, #76414, #60248, #199771, #123893, #12779, #185591, #171419, #78387, #120922, #48079, #109735, #151290, #137096, #198782, #172406, #175390, #96535, #3538, #64235, #143041, #67205, #189576, #129851, #98525, #19715, #52037, #191550, #110725, #83362, #53027, #111724, #33895, #187600, #174402, #81357, #176401, #35872, #157239, #173410, #125900, #190563, #4519, #160218, #95552, #49069, #156238, #18732, #128863, #65216, #158225, #94559, #113694, #36858, #159205, #68199, #80380, #51048, #114708, #142052, #66212, #126876, #127872, #34881, #17740, #188582, #21708, #79397, #50063, #97518, #112710, #20699, #145038, #82355, #144043, #5525, #6520, #141067, #2553, #163220, #148056, #11558, #39863, #146036, #58042, #7519, #101529, #69204, #57048, #130872, #192562, #54045, #71213, #87373, #118722, #149058, #180411, #26720, #132876, #194565, #134895, #88359, #162214, #24722, #41883, #103550, #38878, #70215, #115719, #177407, #195575, #73224, #9547, #196571, #117713, #56035, #100535, #116709, #179409, #40873, #164230, #165225, #10546, #150052, #22711, #86371, #23713, #102547, #119712, #99534, #25727, #72210, #85360, #37876, #161216, #133884, #84358, #147053, #193567, #131882, #8536, #55039, #178399, #78146, #108495, #166220, #107490, #198538, #135878, #123647, #183371, #197549, #169168, #12544, #27721, #59017, #62980, #30672, #170174, #199528, #181396, #120684, #153006, #182383, #313, #77163, #91314, #92325, #74209, #60996, #31667, #137847, #93317, #155001, #44853, #139814 ) ),
 .UNSPECIFIED., .T., .F., .F. ) 
 B_SPLINE_SURFACE_WITH_KNOTS ( ( 4, 3, 4 ),
 ( 3, 2, 2, 2, 2, 2, 2, 2, 2, 2, 2, 2, 2, 2, 2, 2, 2, 2, 2, 2, 2, 2, 2, 2, 2, 2, 2, 2, 2, 2, 2, 2, 2, 2, 2, 2, 2, 2, 2, 2, 2, 2, 2, 2, 2, 2, 2, 2, 2, 2, 2, 2, 2, 2, 2, 2, 2, 2, 2, 2, 2, 2, 2, 2, 2, 2, 2, 2, 2, 2, 2, 2, 2, 2, 2, 2, 2, 2, 2, 2, 2, 2, 2, 2, 2, 2, 2, 2, 2, 2, 2, 2, 2, 2, 2, 2, 2, 2, 2, 2, 2, 2, 2, 2, 2, 2, 2, 2, 2, 2, 2, 2, 2, 2, 2, 2, 2, 2, 2, 2, 2, 2, 2, 2, 2, 2, 2, 2, 2, 2, 2, 2, 2, 2, 2, 2, 2, 2, 2, 2, 2, 2, 2, 2, 2, 2, 2, 2, 2, 2, 2, 2, 2, 2, 2, 2, 2, 2, 2, 2, 2, 2, 2, 2, 2, 2, 2, 2, 2, 2, 2, 2, 2, 2, 2, 2, 2, 2, 2, 2, 2, 2, 2, 2, 2, 2, 2, 2, 2, 2, 2, 2, 2, 2, 2, 2, 2, 2, 2, 2, 2, 2, 2, 2, 2, 2, 2, 2, 2, 2, 2, 2, 2, 2, 2, 2, 2, 2, 2, 2, 2, 2, 2, 2, 2, 2, 2, 2, 3 ),
 ( 0.000000000000000000, 0.5000000000000000000, 1.000000000000000000 ),
 ( 0.000000000000000000, 0.004385964912280701511, 0.008771929824561403022, 0.01315789473684210453, 0.01754385964912280604, 0.02192982456140350755, 0.02631578947368420907, 0.03070175438596491058, 0.03508771929824561209, 0.03947368421052631360, 0.04385964912280701511, 0.04824561403508771662, 0.05263157894736841813, 0.05701754385964911964, 0.06140350877192982115, 0.06578947368421052266, 0.07017543859649122417, 0.07456140350877192569, 0.07894736842105262720, 0.08333333333333332871, 0.08771929824561403022, 0.09210526315789473173, 0.09649122807017543324, 0.1008771929824561348, 0.1052631578947368363, 0.1096491228070175378, 0.1140350877192982393, 0.1184210526315789408, 0.1228070175438596423, 0.1271929824561403577, 0.1315789473684210453, 0.1359649122807017607, 0.1403508771929824483, 0.1447368421052631637, 0.1491228070175438514, 0.1535087719298245668, 0.1578947368421052544, 0.1622807017543859698, 0.1666666666666666574, 0.1710526315789473728, 0.1754385964912280604, 0.1798245614035087758, 0.1842105263157894635, 0.1885964912280701788, 0.1929824561403508665, 0.1973684210526315819, 0.2017543859649122695, 0.2061403508771929849, 0.2105263157894736725, 0.2149122807017543879, 0.2192982456140350755, 0.2236842105263157909, 0.2280701754385964786, 0.2324561403508771940, 0.2368421052631578816, 0.2412280701754385970, 0.2456140350877192846, 0.2500000000000000000, 0.2543859649122807154, 0.2587719298245614308, 0.2631578947368420907, 0.2675438596491228060, 0.2719298245614035214, 0.2763157894736842368, 0.2807017543859648967, 0.2850877192982456121, 0.2894736842105263275, 0.2938596491228070429, 0.2982456140350877027, 0.3026315789473684181, 0.3070175438596491335, 0.3114035087719298489, 0.3157894736842105088, 0.3201754385964912242, 0.3245614035087719396, 0.3289473684210526550, 0.3333333333333333148, 0.3377192982456140302, 0.3421052631578947456, 0.3464912280701754610, 0.3508771929824561209, 0.3552631578947368363, 0.3596491228070175517, 0.3640350877192982670, 0.3684210526315789269, 0.3728070175438596423, 0.3771929824561403577, 0.3815789473684210731, 0.3859649122807017330, 0.3903508771929824483, 0.3947368421052631637, 0.3991228070175438791, 0.4035087719298245390, 0.4078947368421052544, 0.4122807017543859698, 0.4166666666666666852, 0.4210526315789473450, 0.4254385964912280604, 0.4298245614035087758, 0.4342105263157894912, 0.4385964912280701511, 0.4429824561403508665, 0.4473684210526315819, 0.4517543859649122973, 0.4561403508771929571, 0.4605263157894736725, 0.4649122807017543879, 0.4692982456140351033, 0.4736842105263157632, 0.4780701754385964786, 0.4824561403508771940, 0.4868421052631579093, 0.4912280701754385692, 0.4956140350877192846, 0.5000000000000000000, 0.5043859649122807154, 0.5087719298245614308, 0.5131578947368421462, 0.5175438596491228616, 0.5219298245614034659, 0.5263157894736841813, 0.5307017543859648967, 0.5350877192982456121, 0.5394736842105263275, 0.5438596491228070429, 0.5482456140350877583, 0.5526315789473684736, 0.5570175438596490780, 0.5614035087719297934, 0.5657894736842105088, 0.5701754385964912242, 0.5745614035087719396, 0.5789473684210526550, 0.5833333333333333703, 0.5877192982456140857, 0.5921052631578946901, 0.5964912280701754055, 0.6008771929824561209, 0.6052631578947368363, 0.6096491228070175517, 0.6140350877192982670, 0.6184210526315789824, 0.6228070175438596978, 0.6271929824561403022, 0.6315789473684210176, 0.6359649122807017330, 0.6403508771929824483, 0.6447368421052631637, 0.6491228070175438791, 0.6535087719298245945, 0.6578947368421053099, 0.6622807017543859143, 0.6666666666666666297, 0.6710526315789473450, 0.6754385964912280604, 0.6798245614035087758, 0.6842105263157894912, 0.6885964912280702066, 0.6929824561403509220, 0.6973684210526315264, 0.7017543859649122417, 0.7061403508771929571, 0.7105263157894736725, 0.7149122807017543879, 0.7192982456140351033, 0.7236842105263158187, 0.7280701754385965341, 0.7324561403508771384, 0.7368421052631578538, 0.7412280701754385692, 0.7456140350877192846, 0.7500000000000000000, 0.7543859649122807154, 0.7587719298245614308, 0.7631578947368421462, 0.7675438596491228616, 0.7719298245614034659, 0.7763157894736841813, 0.7807017543859648967, 0.7850877192982456121, 0.7894736842105263275, 0.7938596491228070429, 0.7982456140350877583, 0.8026315789473684736, 0.8070175438596490780, 0.8114035087719297934, 0.8157894736842105088, 0.8201754385964912242, 0.8245614035087719396, 0.8289473684210526550, 0.8333333333333333703, 0.8377192982456140857, 0.8421052631578946901, 0.8464912280701754055, 0.8508771929824561209, 0.8552631578947368363, 0.8596491228070175517, 0.8640350877192982670, 0.8684210526315789824, 0.8728070175438596978, 0.8771929824561403022, 0.8815789473684210176, 0.8859649122807017330, 0.8903508771929824483, 0.8947368421052631637, 0.8991228070175438791, 0.9035087719298245945, 0.9078947368421053099, 0.9122807017543859143, 0.9166666666666666297, 0.9210526315789473450, 0.9254385964912280604, 0.9298245614035087758, 0.9342105263157894912, 0.9385964912280702066, 0.9429824561403509220, 0.9473684210526315264, 0.9517543859649122417, 0.9561403508771929571, 0.9605263157894736725, 0.9649122807017543879, 0.9692982456140351033, 0.9736842105263158187, 0.9780701754385965341, 0.9824561403508771384, 0.9868421052631578538, 0.9912280701754385692, 0.9956140350877192846, 1.000000000000000000 ),
 .UNSPECIFIED. ) 
 GEOMETRIC_REPRESENTATION_ITEM ( )  RATIONAL_B_SPLINE_SURFACE ( (
 ( 1.000000000000000000, 0.9659258262890683122, 1.000000000000000000, 0.9659258262890683122, 1.000000000000000000, 0.9659258262890683122, 1.000000000000000000, 0.9659258262890683122, 1.000000000000000000, 0.9659258262890683122, 1.000000000000000000, 0.9659258262890683122, 1.000000000000000000, 0.9659258262890683122, 1.000000000000000000, 0.9659258262890683122, 1.000000000000000000, 0.9659258262890683122, 1.000000000000000000, 0.9659258262890683122, 1.000000000000000000, 0.9659258262890683122, 1.000000000000000000, 0.9659258262890683122, 1.000000000000000000, 0.9659258262890683122, 1.000000000000000000, 0.9659258262890683122, 1.000000000000000000, 0.9659258262890683122, 1.000000000000000000, 0.9659258262890683122, 1.000000000000000000, 0.9659258262890683122, 1.000000000000000000, 0.9659258262890683122, 1.000000000000000000, 0.9659258262890683122, 1.000000000000000000, 0.9659258262890683122, 1.000000000000000000, 0.9659258262890683122, 1.000000000000000000, 0.9659258262890683122, 1.000000000000000000, 0.9659258262890683122, 1.000000000000000000, 0.9659258262890683122, 1.000000000000000000, 0.9659258262890683122, 1.000000000000000000, 0.9659258262890683122, 1.000000000000000000, 0.9659258262890683122, 1.000000000000000000, 0.9659258262890683122, 1.000000000000000000, 0.9659258262890683122, 1.000000000000000000, 0.9659258262890683122, 1.000000000000000000, 0.9659258262890683122, 1.000000000000000000, 0.9659258262890683122, 1.000000000000000000, 0.9659258262890683122, 1.000000000000000000, 0.9659258262890683122, 1.000000000000000000, 0.9659258262890683122, 1.000000000000000000, 0.9659258262890683122, 1.000000000000000000, 0.9659258262890683122, 1.000000000000000000, 0.9659258262890683122, 1.000000000000000000, 0.9659258262890683122, 1.000000000000000000, 0.9659258262890683122, 1.000000000000000000, 0.9659258262890683122, 1.000000000000000000, 0.9659258262890683122, 1.000000000000000000, 0.9659258262890683122, 1.000000000000000000, 0.9659258262890683122, 1.000000000000000000, 0.9659258262890683122, 1.000000000000000000, 0.9659258262890683122, 1.000000000000000000, 0.9659258262890683122, 1.000000000000000000, 0.9659258262890683122, 1.000000000000000000, 0.9659258262890683122, 1.000000000000000000, 0.9659258262890683122, 1.000000000000000000, 0.9659258262890683122, 1.000000000000000000, 0.9659258262890683122, 1.000000000000000000, 0.9659258262890683122, 1.000000000000000000, 0.9659258262890683122, 1.000000000000000000, 0.9659258262890683122, 1.000000000000000000, 0.9659258262890683122, 1.000000000000000000, 0.9659258262890683122, 1.000000000000000000, 0.9659258262890683122, 1.000000000000000000, 0.9659258262890683122, 1.000000000000000000, 0.9659258262890683122, 1.000000000000000000, 0.9659258262890683122, 1.000000000000000000, 0.9659258262890683122, 1.000000000000000000, 0.9659258262890683122, 1.000000000000000000, 0.9659258262890683122, 1.000000000000000000, 0.9659258262890683122, 1.000000000000000000, 0.9659258262890683122, 1.000000000000000000, 0.9659258262890683122, 1.000000000000000000, 0.9659258262890683122, 1.000000000000000000, 0.9659258262890683122, 1.000000000000000000, 0.9659258262890683122, 1.000000000000000000, 0.9659258262890683122, 1.000000000000000000, 0.9659258262890683122, 1.000000000000000000, 0.9659258262890683122, 1.000000000000000000, 0.9659258262890683122, 1.000000000000000000, 0.9659258262890683122, 1.000000000000000000, 0.9659258262890683122, 1.000000000000000000, 0.9659258262890683122, 1.000000000000000000, 0.9659258262890683122, 1.000000000000000000, 0.9659258262890683122, 1.000000000000000000, 0.9659258262890683122, 1.000000000000000000, 0.9659258262890683122, 1.000000000000000000, 0.9659258262890683122, 1.000000000000000000, 0.9659258262890683122, 1.000000000000000000, 0.9659258262890683122, 1.000000000000000000, 0.9659258262890683122, 1.000000000000000000, 0.9659258262890683122, 1.000000000000000000, 0.9659258262890683122, 1.000000000000000000, 0.9659258262890683122, 1.000000000000000000, 0.9659258262890683122, 1.000000000000000000, 0.9659258262890683122, 1.000000000000000000, 0.9659258262890683122, 1.000000000000000000, 0.9659258262890683122, 1.000000000000000000, 0.9659258262890683122, 1.000000000000000000, 0.9659258262890683122, 1.000000000000000000, 0.9659258262890683122, 1.000000000000000000, 0.9659258262890683122, 1.000000000000000000, 0.9659258262890683122, 1.000000000000000000, 0.9659258262890683122, 1.000000000000000000, 0.9659258262890683122, 1.000000000000000000, 0.9659258262890683122, 1.000000000000000000, 0.9659258262890683122, 1.000000000000000000, 0.9659258262890683122, 1.000000000000000000, 0.9659258262890683122, 1.000000000000000000, 0.9659258262890683122, 1.000000000000000000, 0.9659258262890683122, 1.000000000000000000, 0.9659258262890683122, 1.000000000000000000, 0.9659258262890683122, 1.000000000000000000, 0.9659258262890683122, 1.000000000000000000, 0.9659258262890683122, 1.000000000000000000, 0.9659258262890683122, 1.000000000000000000, 0.9659258262890683122, 1.000000000000000000, 0.9659258262890683122, 1.000000000000000000, 0.9659258262890683122, 1.000000000000000000, 0.9659258262890683122, 1.000000000000000000, 0.9659258262890683122, 1.000000000000000000, 0.9659258262890683122, 1.000000000000000000, 0.9659258262890683122, 1.000000000000000000, 0.9659258262890683122, 1.000000000000000000, 0.9659258262890683122, 1.000000000000000000, 0.9659258262890683122, 1.000000000000000000, 0.9659258262890683122, 1.000000000000000000, 0.9659258262890683122, 1.000000000000000000, 0.9659258262890683122, 1.000000000000000000, 0.9659258262890683122, 1.000000000000000000, 0.9659258262890683122, 1.000000000000000000, 0.9659258262890683122, 1.000000000000000000, 0.9659258262890683122, 1.000000000000000000, 0.9659258262890683122, 1.000000000000000000, 0.9659258262890683122, 1.000000000000000000, 0.9659258262890683122, 1.000000000000000000, 0.9659258262890683122, 1.000000000000000000, 0.9659258262890683122, 1.000000000000000000, 0.9659258262890683122, 1.000000000000000000, 0.9659258262890683122, 1.000000000000000000, 0.9659258262890683122, 1.000000000000000000, 0.9659258262890683122, 1.000000000000000000, 0.9659258262890683122, 1.000000000000000000, 0.9659258262890683122, 1.000000000000000000, 0.9659258262890683122, 1.000000000000000000, 0.9659258262890683122, 1.000000000000000000, 0.9659258262890683122, 1.000000000000000000, 0.9659258262890683122, 1.000000000000000000, 0.9659258262890683122, 1.000000000000000000, 0.9659258262890683122, 1.000000000000000000, 0.9659258262890683122, 1.000000000000000000, 0.9659258262890683122, 1.000000000000000000, 0.9659258262890683122, 1.000000000000000000, 0.9659258262890683122, 1.000000000000000000, 0.9659258262890683122, 1.000000000000000000, 0.9659258262890683122, 1.000000000000000000, 0.9659258262890683122, 1.000000000000000000, 0.9659258262890683122, 1.000000000000000000, 0.9659258262890683122, 1.000000000000000000, 0.9659258262890683122, 1.000000000000000000, 0.9659258262890683122, 1.000000000000000000, 0.9659258262890683122, 1.000000000000000000, 0.9659258262890683122, 1.000000000000000000, 0.9659258262890683122, 1.000000000000000000, 0.9659258262890683122, 1.000000000000000000, 0.9659258262890683122, 1.000000000000000000, 0.9659258262890683122, 1.000000000000000000, 0.9659258262890683122, 1.000000000000000000, 0.9659258262890683122, 1.000000000000000000, 0.9659258262890683122, 1.000000000000000000, 0.9659258262890683122, 1.000000000000000000, 0.9659258262890683122, 1.000000000000000000, 0.9659258262890683122, 1.000000000000000000, 0.9659258262890683122, 1.000000000000000000, 0.9659258262890683122, 1.000000000000000000, 0.9659258262890683122, 1.000000000000000000, 0.9659258262890683122, 1.000000000000000000, 0.9659258262890683122, 1.000000000000000000, 0.9659258262890683122, 1.000000000000000000, 0.9659258262890683122, 1.000000000000000000, 0.9659258262890683122, 1.000000000000000000, 0.9659258262890683122, 1.000000000000000000, 0.9659258262890683122, 1.000000000000000000, 0.9659258262890683122, 1.000000000000000000, 0.9659258262890683122, 1.000000000000000000, 0.9659258262890683122, 1.000000000000000000, 0.9659258262890683122, 1.000000000000000000, 0.9659258262890683122, 1.000000000000000000, 0.9659258262890683122, 1.000000000000000000, 0.9659258262890683122, 1.000000000000000000, 0.9659258262890683122, 1.000000000000000000, 0.9659258262890683122, 1.000000000000000000, 0.9659258262890683122, 1.000000000000000000, 0.9659258262890683122, 1.000000000000000000, 0.9659258262890683122, 1.000000000000000000, 0.9659258262890683122, 1.000000000000000000, 0.9659258262890683122, 1.000000000000000000, 0.9659258262890683122, 1.000000000000000000, 0.9659258262890683122, 1.000000000000000000, 0.9659258262890683122, 1.000000000000000000, 0.9659258262890683122, 1.000000000000000000, 0.9659258262890683122, 1.000000000000000000, 0.9659258262890683122, 1.000000000000000000, 0.9659258262890683122, 1.000000000000000000, 0.9659258262890683122, 1.000000000000000000, 0.9659258262890683122, 1.000000000000000000, 0.9659258262890683122, 1.000000000000000000, 0.9659258262890683122, 1.000000000000000000, 0.9659258262890683122, 1.000000000000000000, 0.9659258262890683122, 1.000000000000000000, 0.9659258262890683122, 1.000000000000000000, 0.9659258262890683122, 1.000000000000000000, 0.9659258262890683122, 1.000000000000000000, 0.9659258262890683122, 1.000000000000000000, 0.9659258262890683122, 1.000000000000000000, 0.9659258262890683122, 1.000000000000000000, 0.9659258262890683122, 1.000000000000000000, 0.9659258262890683122, 1.000000000000000000, 0.9659258262890683122, 1.000000000000000000, 0.9659258262890683122, 1.000000000000000000, 0.9659258262890683122, 1.000000000000000000, 0.9659258262890683122, 1.000000000000000000, 0.9659258262890683122, 1.000000000000000000, 0.9659258262890683122, 1.000000000000000000, 0.9659258262890683122, 1.000000000000000000, 0.9659258262890683122, 1.000000000000000000, 0.9659258262890683122, 1.000000000000000000, 0.9659258262890683122, 1.000000000000000000, 0.9659258262890683122, 1.000000000000000000, 0.9659258262890683122, 1.000000000000000000, 0.9659258262890683122, 1.000000000000000000, 0.9659258262890683122, 1.000000000000000000, 0.9659258262890683122, 1.000000000000000000, 0.9659258262890683122, 1.000000000000000000),
 ( 0.3333333333333333703, 0.3219752754296894559, 0.3333333333333333703, 0.3219752754296894559, 0.3333333333333333703, 0.3219752754296894559, 0.3333333333333333703, 0.3219752754296894559, 0.3333333333333333703, 0.3219752754296894559, 0.3333333333333333703, 0.3219752754296894559, 0.3333333333333333703, 0.3219752754296894559, 0.3333333333333333703, 0.3219752754296894559, 0.3333333333333333703, 0.3219752754296894559, 0.3333333333333333703, 0.3219752754296894559, 0.3333333333333333703, 0.3219752754296894559, 0.3333333333333333703, 0.3219752754296894559, 0.3333333333333333703, 0.3219752754296894559, 0.3333333333333333703, 0.3219752754296894559, 0.3333333333333333703, 0.3219752754296894559, 0.3333333333333333703, 0.3219752754296894559, 0.3333333333333333703, 0.3219752754296894559, 0.3333333333333333703, 0.3219752754296894559, 0.3333333333333333703, 0.3219752754296894559, 0.3333333333333333703, 0.3219752754296894559, 0.3333333333333333703, 0.3219752754296894559, 0.3333333333333333703, 0.3219752754296894559, 0.3333333333333333703, 0.3219752754296894559, 0.3333333333333333703, 0.3219752754296894559, 0.3333333333333333703, 0.3219752754296894559, 0.3333333333333333703, 0.3219752754296894559, 0.3333333333333333703, 0.3219752754296894559, 0.3333333333333333703, 0.3219752754296894559, 0.3333333333333333703, 0.3219752754296894559, 0.3333333333333333703, 0.3219752754296894559, 0.3333333333333333703, 0.3219752754296894559, 0.3333333333333333703, 0.3219752754296894559, 0.3333333333333333703, 0.3219752754296894559, 0.3333333333333333703, 0.3219752754296894559, 0.3333333333333333703, 0.3219752754296894559, 0.3333333333333333703, 0.3219752754296894559, 0.3333333333333333703, 0.3219752754296894559, 0.3333333333333333703, 0.3219752754296894559, 0.3333333333333333703, 0.3219752754296894559, 0.3333333333333333703, 0.3219752754296894559, 0.3333333333333333703, 0.3219752754296894559, 0.3333333333333333703, 0.3219752754296894559, 0.3333333333333333703, 0.3219752754296894559, 0.3333333333333333703, 0.3219752754296894559, 0.3333333333333333703, 0.3219752754296894559, 0.3333333333333333703, 0.3219752754296894559, 0.3333333333333333703, 0.3219752754296894559, 0.3333333333333333703, 0.3219752754296894559, 0.3333333333333333703, 0.3219752754296894559, 0.3333333333333333703, 0.3219752754296894559, 0.3333333333333333703, 0.3219752754296894559, 0.3333333333333333703, 0.3219752754296894559, 0.3333333333333333703, 0.3219752754296894559, 0.3333333333333333703, 0.3219752754296894559, 0.3333333333333333703, 0.3219752754296894559, 0.3333333333333333703, 0.3219752754296894559, 0.3333333333333333703, 0.3219752754296894559, 0.3333333333333333703, 0.3219752754296894559, 0.3333333333333333703, 0.3219752754296894559, 0.3333333333333333703, 0.3219752754296894559, 0.3333333333333333703, 0.3219752754296894559, 0.3333333333333333703, 0.3219752754296894559, 0.3333333333333333703, 0.3219752754296894559, 0.3333333333333333703, 0.3219752754296894559, 0.3333333333333333703, 0.3219752754296894559, 0.3333333333333333703, 0.3219752754296894559, 0.3333333333333333703, 0.3219752754296894559, 0.3333333333333333703, 0.3219752754296894559, 0.3333333333333333703, 0.3219752754296894559, 0.3333333333333333703, 0.3219752754296894559, 0.3333333333333333703, 0.3219752754296894559, 0.3333333333333333703, 0.3219752754296894559, 0.3333333333333333703, 0.3219752754296894559, 0.3333333333333333703, 0.3219752754296894559, 0.3333333333333333703, 0.3219752754296894559, 0.3333333333333333703, 0.3219752754296894559, 0.3333333333333333703, 0.3219752754296894559, 0.3333333333333333703, 0.3219752754296894559, 0.3333333333333333703, 0.3219752754296894559, 0.3333333333333333703, 0.3219752754296894559, 0.3333333333333333703, 0.3219752754296894559, 0.3333333333333333703, 0.3219752754296894559, 0.3333333333333333703, 0.3219752754296894559, 0.3333333333333333703, 0.3219752754296894559, 0.3333333333333333703, 0.3219752754296894559, 0.3333333333333333703, 0.3219752754296894559, 0.3333333333333333703, 0.3219752754296894559, 0.3333333333333333703, 0.3219752754296894559, 0.3333333333333333703, 0.3219752754296894559, 0.3333333333333333703, 0.3219752754296894559, 0.3333333333333333703, 0.3219752754296894559, 0.3333333333333333703, 0.3219752754296894559, 0.3333333333333333703, 0.3219752754296894559, 0.3333333333333333703, 0.3219752754296894559, 0.3333333333333333703, 0.3219752754296894559, 0.3333333333333333703, 0.3219752754296894559, 0.3333333333333333703, 0.3219752754296894559, 0.3333333333333333703, 0.3219752754296894559, 0.3333333333333333703, 0.3219752754296894559, 0.3333333333333333703, 0.3219752754296894559, 0.3333333333333333703, 0.3219752754296894559, 0.3333333333333333703, 0.3219752754296894559, 0.3333333333333333703, 0.3219752754296894559, 0.3333333333333333703, 0.3219752754296894559, 0.3333333333333333703, 0.3219752754296894559, 0.3333333333333333703, 0.3219752754296894559, 0.3333333333333333703, 0.3219752754296894559, 0.3333333333333333703, 0.3219752754296894559, 0.3333333333333333703, 0.3219752754296894559, 0.3333333333333333703, 0.3219752754296894559, 0.3333333333333333703, 0.3219752754296894559, 0.3333333333333333703, 0.3219752754296894559, 0.3333333333333333703, 0.3219752754296894559, 0.3333333333333333703, 0.3219752754296894559, 0.3333333333333333703, 0.3219752754296894559, 0.3333333333333333703, 0.3219752754296894559, 0.3333333333333333703, 0.3219752754296894559, 0.3333333333333333703, 0.3219752754296894559, 0.3333333333333333703, 0.3219752754296894559, 0.3333333333333333703, 0.3219752754296894559, 0.3333333333333333703, 0.3219752754296894559, 0.3333333333333333703, 0.3219752754296894559, 0.3333333333333333703, 0.3219752754296894559, 0.3333333333333333703, 0.3219752754296894559, 0.3333333333333333703, 0.3219752754296894559, 0.3333333333333333703, 0.3219752754296894559, 0.3333333333333333703, 0.3219752754296894559, 0.3333333333333333703, 0.3219752754296894559, 0.3333333333333333703, 0.3219752754296894559, 0.3333333333333333703, 0.3219752754296894559, 0.3333333333333333703, 0.3219752754296894559, 0.3333333333333333703, 0.3219752754296894559, 0.3333333333333333703, 0.3219752754296894559, 0.3333333333333333703, 0.3219752754296894559, 0.3333333333333333703, 0.3219752754296894559, 0.3333333333333333703, 0.3219752754296894559, 0.3333333333333333703, 0.3219752754296894559, 0.3333333333333333703, 0.3219752754296894559, 0.3333333333333333703, 0.3219752754296894559, 0.3333333333333333703, 0.3219752754296894559, 0.3333333333333333703, 0.3219752754296894559, 0.3333333333333333703, 0.3219752754296894559, 0.3333333333333333703, 0.3219752754296894559, 0.3333333333333333703, 0.3219752754296894559, 0.3333333333333333703, 0.3219752754296894559, 0.3333333333333333703, 0.3219752754296894559, 0.3333333333333333703, 0.3219752754296894559, 0.3333333333333333703, 0.3219752754296894559, 0.3333333333333333703, 0.3219752754296894559, 0.3333333333333333703, 0.3219752754296894559, 0.3333333333333333703, 0.3219752754296894559, 0.3333333333333333703, 0.3219752754296894559, 0.3333333333333333703, 0.3219752754296894559, 0.3333333333333333703, 0.3219752754296894559, 0.3333333333333333703, 0.3219752754296894559, 0.3333333333333333703, 0.3219752754296894559, 0.3333333333333333703, 0.3219752754296894559, 0.3333333333333333703, 0.3219752754296894559, 0.3333333333333333703, 0.3219752754296894559, 0.3333333333333333703, 0.3219752754296894559, 0.3333333333333333703, 0.3219752754296894559, 0.3333333333333333703, 0.3219752754296894559, 0.3333333333333333703, 0.3219752754296894559, 0.3333333333333333703, 0.3219752754296894559, 0.3333333333333333703, 0.3219752754296894559, 0.3333333333333333703, 0.3219752754296894559, 0.3333333333333333703, 0.3219752754296894559, 0.3333333333333333703, 0.3219752754296894559, 0.3333333333333333703, 0.3219752754296894559, 0.3333333333333333703, 0.3219752754296894559, 0.3333333333333333703, 0.3219752754296894559, 0.3333333333333333703, 0.3219752754296894559, 0.3333333333333333703, 0.3219752754296894559, 0.3333333333333333703, 0.3219752754296894559, 0.3333333333333333703, 0.3219752754296894559, 0.3333333333333333703, 0.3219752754296894559, 0.3333333333333333703, 0.3219752754296894559, 0.3333333333333333703, 0.3219752754296894559, 0.3333333333333333703, 0.3219752754296894559, 0.3333333333333333703, 0.3219752754296894559, 0.3333333333333333703, 0.3219752754296894559, 0.3333333333333333703, 0.3219752754296894559, 0.3333333333333333703, 0.3219752754296894559, 0.3333333333333333703, 0.3219752754296894559, 0.3333333333333333703, 0.3219752754296894559, 0.3333333333333333703, 0.3219752754296894559, 0.3333333333333333703, 0.3219752754296894559, 0.3333333333333333703, 0.3219752754296894559, 0.3333333333333333703, 0.3219752754296894559, 0.3333333333333333703, 0.3219752754296894559, 0.3333333333333333703, 0.3219752754296894559, 0.3333333333333333703, 0.3219752754296894559, 0.3333333333333333703, 0.3219752754296894559, 0.3333333333333333703, 0.3219752754296894559, 0.3333333333333333703, 0.3219752754296894559, 0.3333333333333333703, 0.3219752754296894559, 0.3333333333333333703, 0.3219752754296894559, 0.3333333333333333703, 0.3219752754296894559, 0.3333333333333333703, 0.3219752754296894559, 0.3333333333333333703, 0.3219752754296894559, 0.3333333333333333703, 0.3219752754296894559, 0.3333333333333333703, 0.3219752754296894559, 0.3333333333333333703, 0.3219752754296894559, 0.3333333333333333703, 0.3219752754296894559, 0.3333333333333333703, 0.3219752754296894559, 0.3333333333333333703, 0.3219752754296894559, 0.3333333333333333703, 0.3219752754296894559, 0.3333333333333333703, 0.3219752754296894559, 0.3333333333333333703, 0.3219752754296894559, 0.3333333333333333703, 0.3219752754296894559, 0.3333333333333333703, 0.3219752754296894559, 0.3333333333333333703, 0.3219752754296894559, 0.3333333333333333703, 0.3219752754296894559, 0.3333333333333333703, 0.3219752754296894559, 0.3333333333333333703, 0.3219752754296894559, 0.3333333333333333703, 0.3219752754296894559, 0.3333333333333333703, 0.3219752754296894559, 0.3333333333333333703, 0.3219752754296894559, 0.3333333333333333703, 0.3219752754296894559, 0.3333333333333333703, 0.3219752754296894559, 0.3333333333333333703, 0.3219752754296894559, 0.3333333333333333703, 0.3219752754296894559, 0.3333333333333333703, 0.3219752754296894559, 0.3333333333333333703, 0.3219752754296894559, 0.3333333333333333703, 0.3219752754296894559, 0.3333333333333333703, 0.3219752754296894559, 0.3333333333333333703, 0.3219752754296894559, 0.3333333333333333703, 0.3219752754296894559, 0.3333333333333333703),
 ( 0.3333333333333333703, 0.3219752754296894559, 0.3333333333333333703, 0.3219752754296894559, 0.3333333333333333703, 0.3219752754296894559, 0.3333333333333333703, 0.3219752754296894559, 0.3333333333333333703, 0.3219752754296894559, 0.3333333333333333703, 0.3219752754296894559, 0.3333333333333333703, 0.3219752754296894559, 0.3333333333333333703, 0.3219752754296894559, 0.3333333333333333703, 0.3219752754296894559, 0.3333333333333333703, 0.3219752754296894559, 0.3333333333333333703, 0.3219752754296894559, 0.3333333333333333703, 0.3219752754296894559, 0.3333333333333333703, 0.3219752754296894559, 0.3333333333333333703, 0.3219752754296894559, 0.3333333333333333703, 0.3219752754296894559, 0.3333333333333333703, 0.3219752754296894559, 0.3333333333333333703, 0.3219752754296894559, 0.3333333333333333703, 0.3219752754296894559, 0.3333333333333333703, 0.3219752754296894559, 0.3333333333333333703, 0.3219752754296894559, 0.3333333333333333703, 0.3219752754296894559, 0.3333333333333333703, 0.3219752754296894559, 0.3333333333333333703, 0.3219752754296894559, 0.3333333333333333703, 0.3219752754296894559, 0.3333333333333333703, 0.3219752754296894559, 0.3333333333333333703, 0.3219752754296894559, 0.3333333333333333703, 0.3219752754296894559, 0.3333333333333333703, 0.3219752754296894559, 0.3333333333333333703, 0.3219752754296894559, 0.3333333333333333703, 0.3219752754296894559, 0.3333333333333333703, 0.3219752754296894559, 0.3333333333333333703, 0.3219752754296894559, 0.3333333333333333703, 0.3219752754296894559, 0.3333333333333333703, 0.3219752754296894559, 0.3333333333333333703, 0.3219752754296894559, 0.3333333333333333703, 0.3219752754296894559, 0.3333333333333333703, 0.3219752754296894559, 0.3333333333333333703, 0.3219752754296894559, 0.3333333333333333703, 0.3219752754296894559, 0.3333333333333333703, 0.3219752754296894559, 0.3333333333333333703, 0.3219752754296894559, 0.3333333333333333703, 0.3219752754296894559, 0.3333333333333333703, 0.3219752754296894559, 0.3333333333333333703, 0.3219752754296894559, 0.3333333333333333703, 0.3219752754296894559, 0.3333333333333333703, 0.3219752754296894559, 0.3333333333333333703, 0.3219752754296894559, 0.3333333333333333703, 0.3219752754296894559, 0.3333333333333333703, 0.3219752754296894559, 0.3333333333333333703, 0.3219752754296894559, 0.3333333333333333703, 0.3219752754296894559, 0.3333333333333333703, 0.3219752754296894559, 0.3333333333333333703, 0.3219752754296894559, 0.3333333333333333703, 0.3219752754296894559, 0.3333333333333333703, 0.3219752754296894559, 0.3333333333333333703, 0.3219752754296894559, 0.3333333333333333703, 0.3219752754296894559, 0.3333333333333333703, 0.3219752754296894559, 0.3333333333333333703, 0.3219752754296894559, 0.3333333333333333703, 0.3219752754296894559, 0.3333333333333333703, 0.3219752754296894559, 0.3333333333333333703, 0.3219752754296894559, 0.3333333333333333703, 0.3219752754296894559, 0.3333333333333333703, 0.3219752754296894559, 0.3333333333333333703, 0.3219752754296894559, 0.3333333333333333703, 0.3219752754296894559, 0.3333333333333333703, 0.3219752754296894559, 0.3333333333333333703, 0.3219752754296894559, 0.3333333333333333703, 0.3219752754296894559, 0.3333333333333333703, 0.3219752754296894559, 0.3333333333333333703, 0.3219752754296894559, 0.3333333333333333703, 0.3219752754296894559, 0.3333333333333333703, 0.3219752754296894559, 0.3333333333333333703, 0.3219752754296894559, 0.3333333333333333703, 0.3219752754296894559, 0.3333333333333333703, 0.3219752754296894559, 0.3333333333333333703, 0.3219752754296894559, 0.3333333333333333703, 0.3219752754296894559, 0.3333333333333333703, 0.3219752754296894559, 0.3333333333333333703, 0.3219752754296894559, 0.3333333333333333703, 0.3219752754296894559, 0.3333333333333333703, 0.3219752754296894559, 0.3333333333333333703, 0.3219752754296894559, 0.3333333333333333703, 0.3219752754296894559, 0.3333333333333333703, 0.3219752754296894559, 0.3333333333333333703, 0.3219752754296894559, 0.3333333333333333703, 0.3219752754296894559, 0.3333333333333333703, 0.3219752754296894559, 0.3333333333333333703, 0.3219752754296894559, 0.3333333333333333703, 0.3219752754296894559, 0.3333333333333333703, 0.3219752754296894559, 0.3333333333333333703, 0.3219752754296894559, 0.3333333333333333703, 0.3219752754296894559, 0.3333333333333333703, 0.3219752754296894559, 0.3333333333333333703, 0.3219752754296894559, 0.3333333333333333703, 0.3219752754296894559, 0.3333333333333333703, 0.3219752754296894559, 0.3333333333333333703, 0.3219752754296894559, 0.3333333333333333703, 0.3219752754296894559, 0.3333333333333333703, 0.3219752754296894559, 0.3333333333333333703, 0.3219752754296894559, 0.3333333333333333703, 0.3219752754296894559, 0.3333333333333333703, 0.3219752754296894559, 0.3333333333333333703, 0.3219752754296894559, 0.3333333333333333703, 0.3219752754296894559, 0.3333333333333333703, 0.3219752754296894559, 0.3333333333333333703, 0.3219752754296894559, 0.3333333333333333703, 0.3219752754296894559, 0.3333333333333333703, 0.3219752754296894559, 0.3333333333333333703, 0.3219752754296894559, 0.3333333333333333703, 0.3219752754296894559, 0.3333333333333333703, 0.3219752754296894559, 0.3333333333333333703, 0.3219752754296894559, 0.3333333333333333703, 0.3219752754296894559, 0.3333333333333333703, 0.3219752754296894559, 0.3333333333333333703, 0.3219752754296894559, 0.3333333333333333703, 0.3219752754296894559, 0.3333333333333333703, 0.3219752754296894559, 0.3333333333333333703, 0.3219752754296894559, 0.3333333333333333703, 0.3219752754296894559, 0.3333333333333333703, 0.3219752754296894559, 0.3333333333333333703, 0.3219752754296894559, 0.3333333333333333703, 0.3219752754296894559, 0.3333333333333333703, 0.3219752754296894559, 0.3333333333333333703, 0.3219752754296894559, 0.3333333333333333703, 0.3219752754296894559, 0.3333333333333333703, 0.3219752754296894559, 0.3333333333333333703, 0.3219752754296894559, 0.3333333333333333703, 0.3219752754296894559, 0.3333333333333333703, 0.3219752754296894559, 0.3333333333333333703, 0.3219752754296894559, 0.3333333333333333703, 0.3219752754296894559, 0.3333333333333333703, 0.3219752754296894559, 0.3333333333333333703, 0.3219752754296894559, 0.3333333333333333703, 0.3219752754296894559, 0.3333333333333333703, 0.3219752754296894559, 0.3333333333333333703, 0.3219752754296894559, 0.3333333333333333703, 0.3219752754296894559, 0.3333333333333333703, 0.3219752754296894559, 0.3333333333333333703, 0.3219752754296894559, 0.3333333333333333703, 0.3219752754296894559, 0.3333333333333333703, 0.3219752754296894559, 0.3333333333333333703, 0.3219752754296894559, 0.3333333333333333703, 0.3219752754296894559, 0.3333333333333333703, 0.3219752754296894559, 0.3333333333333333703, 0.3219752754296894559, 0.3333333333333333703, 0.3219752754296894559, 0.3333333333333333703, 0.3219752754296894559, 0.3333333333333333703, 0.3219752754296894559, 0.3333333333333333703, 0.3219752754296894559, 0.3333333333333333703, 0.3219752754296894559, 0.3333333333333333703, 0.3219752754296894559, 0.3333333333333333703, 0.3219752754296894559, 0.3333333333333333703, 0.3219752754296894559, 0.3333333333333333703, 0.3219752754296894559, 0.3333333333333333703, 0.3219752754296894559, 0.3333333333333333703, 0.3219752754296894559, 0.3333333333333333703, 0.3219752754296894559, 0.3333333333333333703, 0.3219752754296894559, 0.3333333333333333703, 0.3219752754296894559, 0.3333333333333333703, 0.3219752754296894559, 0.3333333333333333703, 0.3219752754296894559, 0.3333333333333333703, 0.3219752754296894559, 0.3333333333333333703, 0.3219752754296894559, 0.3333333333333333703, 0.3219752754296894559, 0.3333333333333333703, 0.3219752754296894559, 0.3333333333333333703, 0.3219752754296894559, 0.3333333333333333703, 0.3219752754296894559, 0.3333333333333333703, 0.3219752754296894559, 0.3333333333333333703, 0.3219752754296894559, 0.3333333333333333703, 0.3219752754296894559, 0.3333333333333333703, 0.3219752754296894559, 0.3333333333333333703, 0.3219752754296894559, 0.3333333333333333703, 0.3219752754296894559, 0.3333333333333333703, 0.3219752754296894559, 0.3333333333333333703, 0.3219752754296894559, 0.3333333333333333703, 0.3219752754296894559, 0.3333333333333333703, 0.3219752754296894559, 0.3333333333333333703, 0.3219752754296894559, 0.3333333333333333703, 0.3219752754296894559, 0.3333333333333333703, 0.3219752754296894559, 0.3333333333333333703, 0.3219752754296894559, 0.3333333333333333703, 0.3219752754296894559, 0.3333333333333333703, 0.3219752754296894559, 0.3333333333333333703, 0.3219752754296894559, 0.3333333333333333703, 0.3219752754296894559, 0.3333333333333333703, 0.3219752754296894559, 0.3333333333333333703, 0.3219752754296894559, 0.3333333333333333703, 0.3219752754296894559, 0.3333333333333333703, 0.3219752754296894559, 0.3333333333333333703, 0.3219752754296894559, 0.3333333333333333703, 0.3219752754296894559, 0.3333333333333333703, 0.3219752754296894559, 0.3333333333333333703, 0.3219752754296894559, 0.3333333333333333703, 0.3219752754296894559, 0.3333333333333333703, 0.3219752754296894559, 0.3333333333333333703, 0.3219752754296894559, 0.3333333333333333703, 0.3219752754296894559, 0.3333333333333333703, 0.3219752754296894559, 0.3333333333333333703, 0.3219752754296894559, 0.3333333333333333703, 0.3219752754296894559, 0.3333333333333333703, 0.3219752754296894559, 0.3333333333333333703, 0.3219752754296894559, 0.3333333333333333703, 0.3219752754296894559, 0.3333333333333333703, 0.3219752754296894559, 0.3333333333333333703, 0.3219752754296894559, 0.3333333333333333703, 0.3219752754296894559, 0.3333333333333333703, 0.3219752754296894559, 0.3333333333333333703, 0.3219752754296894559, 0.3333333333333333703, 0.3219752754296894559, 0.3333333333333333703, 0.3219752754296894559, 0.3333333333333333703, 0.3219752754296894559, 0.3333333333333333703, 0.3219752754296894559, 0.3333333333333333703, 0.3219752754296894559, 0.3333333333333333703, 0.3219752754296894559, 0.3333333333333333703, 0.3219752754296894559, 0.3333333333333333703, 0.3219752754296894559, 0.3333333333333333703, 0.3219752754296894559, 0.3333333333333333703, 0.3219752754296894559, 0.3333333333333333703, 0.3219752754296894559, 0.3333333333333333703, 0.3219752754296894559, 0.3333333333333333703, 0.3219752754296894559, 0.3333333333333333703, 0.3219752754296894559, 0.3333333333333333703, 0.3219752754296894559, 0.3333333333333333703, 0.3219752754296894559, 0.3333333333333333703, 0.3219752754296894559, 0.3333333333333333703, 0.3219752754296894559, 0.3333333333333333703, 0.3219752754296894559, 0.3333333333333333703),
 ( 1.000000000000000000, 0.9659258262890683122, 1.000000000000000000, 0.9659258262890683122, 1.000000000000000000, 0.9659258262890683122, 1.000000000000000000, 0.9659258262890683122, 1.000000000000000000, 0.9659258262890683122, 1.000000000000000000, 0.9659258262890683122, 1.000000000000000000, 0.9659258262890683122, 1.000000000000000000, 0.9659258262890683122, 1.000000000000000000, 0.9659258262890683122, 1.000000000000000000, 0.9659258262890683122, 1.000000000000000000, 0.9659258262890683122, 1.000000000000000000, 0.9659258262890683122, 1.000000000000000000, 0.9659258262890683122, 1.000000000000000000, 0.9659258262890683122, 1.000000000000000000, 0.9659258262890683122, 1.000000000000000000, 0.9659258262890683122, 1.000000000000000000, 0.9659258262890683122, 1.000000000000000000, 0.9659258262890683122, 1.000000000000000000, 0.9659258262890683122, 1.000000000000000000, 0.9659258262890683122, 1.000000000000000000, 0.9659258262890683122, 1.000000000000000000, 0.9659258262890683122, 1.000000000000000000, 0.9659258262890683122, 1.000000000000000000, 0.9659258262890683122, 1.000000000000000000, 0.9659258262890683122, 1.000000000000000000, 0.9659258262890683122, 1.000000000000000000, 0.9659258262890683122, 1.000000000000000000, 0.9659258262890683122, 1.000000000000000000, 0.9659258262890683122, 1.000000000000000000, 0.9659258262890683122, 1.000000000000000000, 0.9659258262890683122, 1.000000000000000000, 0.9659258262890683122, 1.000000000000000000, 0.9659258262890683122, 1.000000000000000000, 0.9659258262890683122, 1.000000000000000000, 0.9659258262890683122, 1.000000000000000000, 0.9659258262890683122, 1.000000000000000000, 0.9659258262890683122, 1.000000000000000000, 0.9659258262890683122, 1.000000000000000000, 0.9659258262890683122, 1.000000000000000000, 0.9659258262890683122, 1.000000000000000000, 0.9659258262890683122, 1.000000000000000000, 0.9659258262890683122, 1.000000000000000000, 0.9659258262890683122, 1.000000000000000000, 0.9659258262890683122, 1.000000000000000000, 0.9659258262890683122, 1.000000000000000000, 0.9659258262890683122, 1.000000000000000000, 0.9659258262890683122, 1.000000000000000000, 0.9659258262890683122, 1.000000000000000000, 0.9659258262890683122, 1.000000000000000000, 0.9659258262890683122, 1.000000000000000000, 0.9659258262890683122, 1.000000000000000000, 0.9659258262890683122, 1.000000000000000000, 0.9659258262890683122, 1.000000000000000000, 0.9659258262890683122, 1.000000000000000000, 0.9659258262890683122, 1.000000000000000000, 0.9659258262890683122, 1.000000000000000000, 0.9659258262890683122, 1.000000000000000000, 0.9659258262890683122, 1.000000000000000000, 0.9659258262890683122, 1.000000000000000000, 0.9659258262890683122, 1.000000000000000000, 0.9659258262890683122, 1.000000000000000000, 0.9659258262890683122, 1.000000000000000000, 0.9659258262890683122, 1.000000000000000000, 0.9659258262890683122, 1.000000000000000000, 0.9659258262890683122, 1.000000000000000000, 0.9659258262890683122, 1.000000000000000000, 0.9659258262890683122, 1.000000000000000000, 0.9659258262890683122, 1.000000000000000000, 0.9659258262890683122, 1.000000000000000000, 0.9659258262890683122, 1.000000000000000000, 0.9659258262890683122, 1.000000000000000000, 0.9659258262890683122, 1.000000000000000000, 0.9659258262890683122, 1.000000000000000000, 0.9659258262890683122, 1.000000000000000000, 0.9659258262890683122, 1.000000000000000000, 0.9659258262890683122, 1.000000000000000000, 0.9659258262890683122, 1.000000000000000000, 0.9659258262890683122, 1.000000000000000000, 0.9659258262890683122, 1.000000000000000000, 0.9659258262890683122, 1.000000000000000000, 0.9659258262890683122, 1.000000000000000000, 0.9659258262890683122, 1.000000000000000000, 0.9659258262890683122, 1.000000000000000000, 0.9659258262890683122, 1.000000000000000000, 0.9659258262890683122, 1.000000000000000000, 0.9659258262890683122, 1.000000000000000000, 0.9659258262890683122, 1.000000000000000000, 0.9659258262890683122, 1.000000000000000000, 0.9659258262890683122, 1.000000000000000000, 0.9659258262890683122, 1.000000000000000000, 0.9659258262890683122, 1.000000000000000000, 0.9659258262890683122, 1.000000000000000000, 0.9659258262890683122, 1.000000000000000000, 0.9659258262890683122, 1.000000000000000000, 0.9659258262890683122, 1.000000000000000000, 0.9659258262890683122, 1.000000000000000000, 0.9659258262890683122, 1.000000000000000000, 0.9659258262890683122, 1.000000000000000000, 0.9659258262890683122, 1.000000000000000000, 0.9659258262890683122, 1.000000000000000000, 0.9659258262890683122, 1.000000000000000000, 0.9659258262890683122, 1.000000000000000000, 0.9659258262890683122, 1.000000000000000000, 0.9659258262890683122, 1.000000000000000000, 0.9659258262890683122, 1.000000000000000000, 0.9659258262890683122, 1.000000000000000000, 0.9659258262890683122, 1.000000000000000000, 0.9659258262890683122, 1.000000000000000000, 0.9659258262890683122, 1.000000000000000000, 0.9659258262890683122, 1.000000000000000000, 0.9659258262890683122, 1.000000000000000000, 0.9659258262890683122, 1.000000000000000000, 0.9659258262890683122, 1.000000000000000000, 0.9659258262890683122, 1.000000000000000000, 0.9659258262890683122, 1.000000000000000000, 0.9659258262890683122, 1.000000000000000000, 0.9659258262890683122, 1.000000000000000000, 0.9659258262890683122, 1.000000000000000000, 0.9659258262890683122, 1.000000000000000000, 0.9659258262890683122, 1.000000000000000000, 0.9659258262890683122, 1.000000000000000000, 0.9659258262890683122, 1.000000000000000000, 0.9659258262890683122, 1.000000000000000000, 0.9659258262890683122, 1.000000000000000000, 0.9659258262890683122, 1.000000000000000000, 0.9659258262890683122, 1.000000000000000000, 0.9659258262890683122, 1.000000000000000000, 0.9659258262890683122, 1.000000000000000000, 0.9659258262890683122, 1.000000000000000000, 0.9659258262890683122, 1.000000000000000000, 0.9659258262890683122, 1.000000000000000000, 0.9659258262890683122, 1.000000000000000000, 0.9659258262890683122, 1.000000000000000000, 0.9659258262890683122, 1.000000000000000000, 0.9659258262890683122, 1.000000000000000000, 0.9659258262890683122, 1.000000000000000000, 0.9659258262890683122, 1.000000000000000000, 0.9659258262890683122, 1.000000000000000000, 0.9659258262890683122, 1.000000000000000000, 0.9659258262890683122, 1.000000000000000000, 0.9659258262890683122, 1.000000000000000000, 0.9659258262890683122, 1.000000000000000000, 0.9659258262890683122, 1.000000000000000000, 0.9659258262890683122, 1.000000000000000000, 0.9659258262890683122, 1.000000000000000000, 0.9659258262890683122, 1.000000000000000000, 0.9659258262890683122, 1.000000000000000000, 0.9659258262890683122, 1.000000000000000000, 0.9659258262890683122, 1.000000000000000000, 0.9659258262890683122, 1.000000000000000000, 0.9659258262890683122, 1.000000000000000000, 0.9659258262890683122, 1.000000000000000000, 0.9659258262890683122, 1.000000000000000000, 0.9659258262890683122, 1.000000000000000000, 0.9659258262890683122, 1.000000000000000000, 0.9659258262890683122, 1.000000000000000000, 0.9659258262890683122, 1.000000000000000000, 0.9659258262890683122, 1.000000000000000000, 0.9659258262890683122, 1.000000000000000000, 0.9659258262890683122, 1.000000000000000000, 0.9659258262890683122, 1.000000000000000000, 0.9659258262890683122, 1.000000000000000000, 0.9659258262890683122, 1.000000000000000000, 0.9659258262890683122, 1.000000000000000000, 0.9659258262890683122, 1.000000000000000000, 0.9659258262890683122, 1.000000000000000000, 0.9659258262890683122, 1.000000000000000000, 0.9659258262890683122, 1.000000000000000000, 0.9659258262890683122, 1.000000000000000000, 0.9659258262890683122, 1.000000000000000000, 0.9659258262890683122, 1.000000000000000000, 0.9659258262890683122, 1.000000000000000000, 0.9659258262890683122, 1.000000000000000000, 0.9659258262890683122, 1.000000000000000000, 0.9659258262890683122, 1.000000000000000000, 0.9659258262890683122, 1.000000000000000000, 0.9659258262890683122, 1.000000000000000000, 0.9659258262890683122, 1.000000000000000000, 0.9659258262890683122, 1.000000000000000000, 0.9659258262890683122, 1.000000000000000000, 0.9659258262890683122, 1.000000000000000000, 0.9659258262890683122, 1.000000000000000000, 0.9659258262890683122, 1.000000000000000000, 0.9659258262890683122, 1.000000000000000000, 0.9659258262890683122, 1.000000000000000000, 0.9659258262890683122, 1.000000000000000000, 0.9659258262890683122, 1.000000000000000000, 0.9659258262890683122, 1.000000000000000000, 0.9659258262890683122, 1.000000000000000000, 0.9659258262890683122, 1.000000000000000000, 0.9659258262890683122, 1.000000000000000000, 0.9659258262890683122, 1.000000000000000000, 0.9659258262890683122, 1.000000000000000000, 0.9659258262890683122, 1.000000000000000000, 0.9659258262890683122, 1.000000000000000000, 0.9659258262890683122, 1.000000000000000000, 0.9659258262890683122, 1.000000000000000000, 0.9659258262890683122, 1.000000000000000000, 0.9659258262890683122, 1.000000000000000000, 0.9659258262890683122, 1.000000000000000000, 0.9659258262890683122, 1.000000000000000000, 0.9659258262890683122, 1.000000000000000000, 0.9659258262890683122, 1.000000000000000000, 0.9659258262890683122, 1.000000000000000000, 0.9659258262890683122, 1.000000000000000000, 0.9659258262890683122, 1.000000000000000000, 0.9659258262890683122, 1.000000000000000000, 0.9659258262890683122, 1.000000000000000000, 0.9659258262890683122, 1.000000000000000000, 0.9659258262890683122, 1.000000000000000000, 0.9659258262890683122, 1.000000000000000000, 0.9659258262890683122, 1.000000000000000000, 0.9659258262890683122, 1.000000000000000000, 0.9659258262890683122, 1.000000000000000000, 0.9659258262890683122, 1.000000000000000000, 0.9659258262890683122, 1.000000000000000000, 0.9659258262890683122, 1.000000000000000000, 0.9659258262890683122, 1.000000000000000000, 0.9659258262890683122, 1.000000000000000000, 0.9659258262890683122, 1.000000000000000000, 0.9659258262890683122, 1.000000000000000000, 0.9659258262890683122, 1.000000000000000000, 0.9659258262890683122, 1.000000000000000000, 0.9659258262890683122, 1.000000000000000000, 0.9659258262890683122, 1.000000000000000000, 0.9659258262890683122, 1.000000000000000000, 0.9659258262890683122, 1.000000000000000000, 0.9659258262890683122, 1.000000000000000000),
 ( 0.3333333333333333703, 0.3219752754296894559, 0.3333333333333333703, 0.3219752754296894559, 0.3333333333333333703, 0.3219752754296894559, 0.3333333333333333703, 0.3219752754296894559, 0.3333333333333333703, 0.3219752754296894559, 0.3333333333333333703, 0.3219752754296894559, 0.3333333333333333703, 0.3219752754296894559, 0.3333333333333333703, 0.3219752754296894559, 0.3333333333333333703, 0.3219752754296894559, 0.3333333333333333703, 0.3219752754296894559, 0.3333333333333333703, 0.3219752754296894559, 0.3333333333333333703, 0.3219752754296894559, 0.3333333333333333703, 0.3219752754296894559, 0.3333333333333333703, 0.3219752754296894559, 0.3333333333333333703, 0.3219752754296894559, 0.3333333333333333703, 0.3219752754296894559, 0.3333333333333333703, 0.3219752754296894559, 0.3333333333333333703, 0.3219752754296894559, 0.3333333333333333703, 0.3219752754296894559, 0.3333333333333333703, 0.3219752754296894559, 0.3333333333333333703, 0.3219752754296894559, 0.3333333333333333703, 0.3219752754296894559, 0.3333333333333333703, 0.3219752754296894559, 0.3333333333333333703, 0.3219752754296894559, 0.3333333333333333703, 0.3219752754296894559, 0.3333333333333333703, 0.3219752754296894559, 0.3333333333333333703, 0.3219752754296894559, 0.3333333333333333703, 0.3219752754296894559, 0.3333333333333333703, 0.3219752754296894559, 0.3333333333333333703, 0.3219752754296894559, 0.3333333333333333703, 0.3219752754296894559, 0.3333333333333333703, 0.3219752754296894559, 0.3333333333333333703, 0.3219752754296894559, 0.3333333333333333703, 0.3219752754296894559, 0.3333333333333333703, 0.3219752754296894559, 0.3333333333333333703, 0.3219752754296894559, 0.3333333333333333703, 0.3219752754296894559, 0.3333333333333333703, 0.3219752754296894559, 0.3333333333333333703, 0.3219752754296894559, 0.3333333333333333703, 0.3219752754296894559, 0.3333333333333333703, 0.3219752754296894559, 0.3333333333333333703, 0.3219752754296894559, 0.3333333333333333703, 0.3219752754296894559, 0.3333333333333333703, 0.3219752754296894559, 0.3333333333333333703, 0.3219752754296894559, 0.3333333333333333703, 0.3219752754296894559, 0.3333333333333333703, 0.3219752754296894559, 0.3333333333333333703, 0.3219752754296894559, 0.3333333333333333703, 0.3219752754296894559, 0.3333333333333333703, 0.3219752754296894559, 0.3333333333333333703, 0.3219752754296894559, 0.3333333333333333703, 0.3219752754296894559, 0.3333333333333333703, 0.3219752754296894559, 0.3333333333333333703, 0.3219752754296894559, 0.3333333333333333703, 0.3219752754296894559, 0.3333333333333333703, 0.3219752754296894559, 0.3333333333333333703, 0.3219752754296894559, 0.3333333333333333703, 0.3219752754296894559, 0.3333333333333333703, 0.3219752754296894559, 0.3333333333333333703, 0.3219752754296894559, 0.3333333333333333703, 0.3219752754296894559, 0.3333333333333333703, 0.3219752754296894559, 0.3333333333333333703, 0.3219752754296894559, 0.3333333333333333703, 0.3219752754296894559, 0.3333333333333333703, 0.3219752754296894559, 0.3333333333333333703, 0.3219752754296894559, 0.3333333333333333703, 0.3219752754296894559, 0.3333333333333333703, 0.3219752754296894559, 0.3333333333333333703, 0.3219752754296894559, 0.3333333333333333703, 0.3219752754296894559, 0.3333333333333333703, 0.3219752754296894559, 0.3333333333333333703, 0.3219752754296894559, 0.3333333333333333703, 0.3219752754296894559, 0.3333333333333333703, 0.3219752754296894559, 0.3333333333333333703, 0.3219752754296894559, 0.3333333333333333703, 0.3219752754296894559, 0.3333333333333333703, 0.3219752754296894559, 0.3333333333333333703, 0.3219752754296894559, 0.3333333333333333703, 0.3219752754296894559, 0.3333333333333333703, 0.3219752754296894559, 0.3333333333333333703, 0.3219752754296894559, 0.3333333333333333703, 0.3219752754296894559, 0.3333333333333333703, 0.3219752754296894559, 0.3333333333333333703, 0.3219752754296894559, 0.3333333333333333703, 0.3219752754296894559, 0.3333333333333333703, 0.3219752754296894559, 0.3333333333333333703, 0.3219752754296894559, 0.3333333333333333703, 0.3219752754296894559, 0.3333333333333333703, 0.3219752754296894559, 0.3333333333333333703, 0.3219752754296894559, 0.3333333333333333703, 0.3219752754296894559, 0.3333333333333333703, 0.3219752754296894559, 0.3333333333333333703, 0.3219752754296894559, 0.3333333333333333703, 0.3219752754296894559, 0.3333333333333333703, 0.3219752754296894559, 0.3333333333333333703, 0.3219752754296894559, 0.3333333333333333703, 0.3219752754296894559, 0.3333333333333333703, 0.3219752754296894559, 0.3333333333333333703, 0.3219752754296894559, 0.3333333333333333703, 0.3219752754296894559, 0.3333333333333333703, 0.3219752754296894559, 0.3333333333333333703, 0.3219752754296894559, 0.3333333333333333703, 0.3219752754296894559, 0.3333333333333333703, 0.3219752754296894559, 0.3333333333333333703, 0.3219752754296894559, 0.3333333333333333703, 0.3219752754296894559, 0.3333333333333333703, 0.3219752754296894559, 0.3333333333333333703, 0.3219752754296894559, 0.3333333333333333703, 0.3219752754296894559, 0.3333333333333333703, 0.3219752754296894559, 0.3333333333333333703, 0.3219752754296894559, 0.3333333333333333703, 0.3219752754296894559, 0.3333333333333333703, 0.3219752754296894559, 0.3333333333333333703, 0.3219752754296894559, 0.3333333333333333703, 0.3219752754296894559, 0.3333333333333333703, 0.3219752754296894559, 0.3333333333333333703, 0.3219752754296894559, 0.3333333333333333703, 0.3219752754296894559, 0.3333333333333333703, 0.3219752754296894559, 0.3333333333333333703, 0.3219752754296894559, 0.3333333333333333703, 0.3219752754296894559, 0.3333333333333333703, 0.3219752754296894559, 0.3333333333333333703, 0.3219752754296894559, 0.3333333333333333703, 0.3219752754296894559, 0.3333333333333333703, 0.3219752754296894559, 0.3333333333333333703, 0.3219752754296894559, 0.3333333333333333703, 0.3219752754296894559, 0.3333333333333333703, 0.3219752754296894559, 0.3333333333333333703, 0.3219752754296894559, 0.3333333333333333703, 0.3219752754296894559, 0.3333333333333333703, 0.3219752754296894559, 0.3333333333333333703, 0.3219752754296894559, 0.3333333333333333703, 0.3219752754296894559, 0.3333333333333333703, 0.3219752754296894559, 0.3333333333333333703, 0.3219752754296894559, 0.3333333333333333703, 0.3219752754296894559, 0.3333333333333333703, 0.3219752754296894559, 0.3333333333333333703, 0.3219752754296894559, 0.3333333333333333703, 0.3219752754296894559, 0.3333333333333333703, 0.3219752754296894559, 0.3333333333333333703, 0.3219752754296894559, 0.3333333333333333703, 0.3219752754296894559, 0.3333333333333333703, 0.3219752754296894559, 0.3333333333333333703, 0.3219752754296894559, 0.3333333333333333703, 0.3219752754296894559, 0.3333333333333333703, 0.3219752754296894559, 0.3333333333333333703, 0.3219752754296894559, 0.3333333333333333703, 0.3219752754296894559, 0.3333333333333333703, 0.3219752754296894559, 0.3333333333333333703, 0.3219752754296894559, 0.3333333333333333703, 0.3219752754296894559, 0.3333333333333333703, 0.3219752754296894559, 0.3333333333333333703, 0.3219752754296894559, 0.3333333333333333703, 0.3219752754296894559, 0.3333333333333333703, 0.3219752754296894559, 0.3333333333333333703, 0.3219752754296894559, 0.3333333333333333703, 0.3219752754296894559, 0.3333333333333333703, 0.3219752754296894559, 0.3333333333333333703, 0.3219752754296894559, 0.3333333333333333703, 0.3219752754296894559, 0.3333333333333333703, 0.3219752754296894559, 0.3333333333333333703, 0.3219752754296894559, 0.3333333333333333703, 0.3219752754296894559, 0.3333333333333333703, 0.3219752754296894559, 0.3333333333333333703, 0.3219752754296894559, 0.3333333333333333703, 0.3219752754296894559, 0.3333333333333333703, 0.3219752754296894559, 0.3333333333333333703, 0.3219752754296894559, 0.3333333333333333703, 0.3219752754296894559, 0.3333333333333333703, 0.3219752754296894559, 0.3333333333333333703, 0.3219752754296894559, 0.3333333333333333703, 0.3219752754296894559, 0.3333333333333333703, 0.3219752754296894559, 0.3333333333333333703, 0.3219752754296894559, 0.3333333333333333703, 0.3219752754296894559, 0.3333333333333333703, 0.3219752754296894559, 0.3333333333333333703, 0.3219752754296894559, 0.3333333333333333703, 0.3219752754296894559, 0.3333333333333333703, 0.3219752754296894559, 0.3333333333333333703, 0.3219752754296894559, 0.3333333333333333703, 0.3219752754296894559, 0.3333333333333333703, 0.3219752754296894559, 0.3333333333333333703, 0.3219752754296894559, 0.3333333333333333703, 0.3219752754296894559, 0.3333333333333333703, 0.3219752754296894559, 0.3333333333333333703, 0.3219752754296894559, 0.3333333333333333703, 0.3219752754296894559, 0.3333333333333333703, 0.3219752754296894559, 0.3333333333333333703, 0.3219752754296894559, 0.3333333333333333703, 0.3219752754296894559, 0.3333333333333333703, 0.3219752754296894559, 0.3333333333333333703, 0.3219752754296894559, 0.3333333333333333703, 0.3219752754296894559, 0.3333333333333333703, 0.3219752754296894559, 0.3333333333333333703, 0.3219752754296894559, 0.3333333333333333703, 0.3219752754296894559, 0.3333333333333333703, 0.3219752754296894559, 0.3333333333333333703, 0.3219752754296894559, 0.3333333333333333703, 0.3219752754296894559, 0.3333333333333333703, 0.3219752754296894559, 0.3333333333333333703, 0.3219752754296894559, 0.3333333333333333703, 0.3219752754296894559, 0.3333333333333333703, 0.3219752754296894559, 0.3333333333333333703, 0.3219752754296894559, 0.3333333333333333703, 0.3219752754296894559, 0.3333333333333333703, 0.3219752754296894559, 0.3333333333333333703, 0.3219752754296894559, 0.3333333333333333703, 0.3219752754296894559, 0.3333333333333333703, 0.3219752754296894559, 0.3333333333333333703, 0.3219752754296894559, 0.3333333333333333703, 0.3219752754296894559, 0.3333333333333333703, 0.3219752754296894559, 0.3333333333333333703, 0.3219752754296894559, 0.3333333333333333703, 0.3219752754296894559, 0.3333333333333333703, 0.3219752754296894559, 0.3333333333333333703, 0.3219752754296894559, 0.3333333333333333703, 0.3219752754296894559, 0.3333333333333333703, 0.3219752754296894559, 0.3333333333333333703, 0.3219752754296894559, 0.3333333333333333703, 0.3219752754296894559, 0.3333333333333333703, 0.3219752754296894559, 0.3333333333333333703, 0.3219752754296894559, 0.3333333333333333703, 0.3219752754296894559, 0.3333333333333333703, 0.3219752754296894559, 0.3333333333333333703, 0.3219752754296894559, 0.3333333333333333703, 0.3219752754296894559, 0.3333333333333333703, 0.3219752754296894559, 0.3333333333333333703, 0.3219752754296894559, 0.3333333333333333703),
 ( 0.3333333333333333703, 0.3219752754296894559, 0.3333333333333333703, 0.3219752754296894559, 0.3333333333333333703, 0.3219752754296894559, 0.3333333333333333703, 0.3219752754296894559, 0.3333333333333333703, 0.3219752754296894559, 0.3333333333333333703, 0.3219752754296894559, 0.3333333333333333703, 0.3219752754296894559, 0.3333333333333333703, 0.3219752754296894559, 0.3333333333333333703, 0.3219752754296894559, 0.3333333333333333703, 0.3219752754296894559, 0.3333333333333333703, 0.3219752754296894559, 0.3333333333333333703, 0.3219752754296894559, 0.3333333333333333703, 0.3219752754296894559, 0.3333333333333333703, 0.3219752754296894559, 0.3333333333333333703, 0.3219752754296894559, 0.3333333333333333703, 0.3219752754296894559, 0.3333333333333333703, 0.3219752754296894559, 0.3333333333333333703, 0.3219752754296894559, 0.3333333333333333703, 0.3219752754296894559, 0.3333333333333333703, 0.3219752754296894559, 0.3333333333333333703, 0.3219752754296894559, 0.3333333333333333703, 0.3219752754296894559, 0.3333333333333333703, 0.3219752754296894559, 0.3333333333333333703, 0.3219752754296894559, 0.3333333333333333703, 0.3219752754296894559, 0.3333333333333333703, 0.3219752754296894559, 0.3333333333333333703, 0.3219752754296894559, 0.3333333333333333703, 0.3219752754296894559, 0.3333333333333333703, 0.3219752754296894559, 0.3333333333333333703, 0.3219752754296894559, 0.3333333333333333703, 0.3219752754296894559, 0.3333333333333333703, 0.3219752754296894559, 0.3333333333333333703, 0.3219752754296894559, 0.3333333333333333703, 0.3219752754296894559, 0.3333333333333333703, 0.3219752754296894559, 0.3333333333333333703, 0.3219752754296894559, 0.3333333333333333703, 0.3219752754296894559, 0.3333333333333333703, 0.3219752754296894559, 0.3333333333333333703, 0.3219752754296894559, 0.3333333333333333703, 0.3219752754296894559, 0.3333333333333333703, 0.3219752754296894559, 0.3333333333333333703, 0.3219752754296894559, 0.3333333333333333703, 0.3219752754296894559, 0.3333333333333333703, 0.3219752754296894559, 0.3333333333333333703, 0.3219752754296894559, 0.3333333333333333703, 0.3219752754296894559, 0.3333333333333333703, 0.3219752754296894559, 0.3333333333333333703, 0.3219752754296894559, 0.3333333333333333703, 0.3219752754296894559, 0.3333333333333333703, 0.3219752754296894559, 0.3333333333333333703, 0.3219752754296894559, 0.3333333333333333703, 0.3219752754296894559, 0.3333333333333333703, 0.3219752754296894559, 0.3333333333333333703, 0.3219752754296894559, 0.3333333333333333703, 0.3219752754296894559, 0.3333333333333333703, 0.3219752754296894559, 0.3333333333333333703, 0.3219752754296894559, 0.3333333333333333703, 0.3219752754296894559, 0.3333333333333333703, 0.3219752754296894559, 0.3333333333333333703, 0.3219752754296894559, 0.3333333333333333703, 0.3219752754296894559, 0.3333333333333333703, 0.3219752754296894559, 0.3333333333333333703, 0.3219752754296894559, 0.3333333333333333703, 0.3219752754296894559, 0.3333333333333333703, 0.3219752754296894559, 0.3333333333333333703, 0.3219752754296894559, 0.3333333333333333703, 0.3219752754296894559, 0.3333333333333333703, 0.3219752754296894559, 0.3333333333333333703, 0.3219752754296894559, 0.3333333333333333703, 0.3219752754296894559, 0.3333333333333333703, 0.3219752754296894559, 0.3333333333333333703, 0.3219752754296894559, 0.3333333333333333703, 0.3219752754296894559, 0.3333333333333333703, 0.3219752754296894559, 0.3333333333333333703, 0.3219752754296894559, 0.3333333333333333703, 0.3219752754296894559, 0.3333333333333333703, 0.3219752754296894559, 0.3333333333333333703, 0.3219752754296894559, 0.3333333333333333703, 0.3219752754296894559, 0.3333333333333333703, 0.3219752754296894559, 0.3333333333333333703, 0.3219752754296894559, 0.3333333333333333703, 0.3219752754296894559, 0.3333333333333333703, 0.3219752754296894559, 0.3333333333333333703, 0.3219752754296894559, 0.3333333333333333703, 0.3219752754296894559, 0.3333333333333333703, 0.3219752754296894559, 0.3333333333333333703, 0.3219752754296894559, 0.3333333333333333703, 0.3219752754296894559, 0.3333333333333333703, 0.3219752754296894559, 0.3333333333333333703, 0.3219752754296894559, 0.3333333333333333703, 0.3219752754296894559, 0.3333333333333333703, 0.3219752754296894559, 0.3333333333333333703, 0.3219752754296894559, 0.3333333333333333703, 0.3219752754296894559, 0.3333333333333333703, 0.3219752754296894559, 0.3333333333333333703, 0.3219752754296894559, 0.3333333333333333703, 0.3219752754296894559, 0.3333333333333333703, 0.3219752754296894559, 0.3333333333333333703, 0.3219752754296894559, 0.3333333333333333703, 0.3219752754296894559, 0.3333333333333333703, 0.3219752754296894559, 0.3333333333333333703, 0.3219752754296894559, 0.3333333333333333703, 0.3219752754296894559, 0.3333333333333333703, 0.3219752754296894559, 0.3333333333333333703, 0.3219752754296894559, 0.3333333333333333703, 0.3219752754296894559, 0.3333333333333333703, 0.3219752754296894559, 0.3333333333333333703, 0.3219752754296894559, 0.3333333333333333703, 0.3219752754296894559, 0.3333333333333333703, 0.3219752754296894559, 0.3333333333333333703, 0.3219752754296894559, 0.3333333333333333703, 0.3219752754296894559, 0.3333333333333333703, 0.3219752754296894559, 0.3333333333333333703, 0.3219752754296894559, 0.3333333333333333703, 0.3219752754296894559, 0.3333333333333333703, 0.3219752754296894559, 0.3333333333333333703, 0.3219752754296894559, 0.3333333333333333703, 0.3219752754296894559, 0.3333333333333333703, 0.3219752754296894559, 0.3333333333333333703, 0.3219752754296894559, 0.3333333333333333703, 0.3219752754296894559, 0.3333333333333333703, 0.3219752754296894559, 0.3333333333333333703, 0.3219752754296894559, 0.3333333333333333703, 0.3219752754296894559, 0.3333333333333333703, 0.3219752754296894559, 0.3333333333333333703, 0.3219752754296894559, 0.3333333333333333703, 0.3219752754296894559, 0.3333333333333333703, 0.3219752754296894559, 0.3333333333333333703, 0.3219752754296894559, 0.3333333333333333703, 0.3219752754296894559, 0.3333333333333333703, 0.3219752754296894559, 0.3333333333333333703, 0.3219752754296894559, 0.3333333333333333703, 0.3219752754296894559, 0.3333333333333333703, 0.3219752754296894559, 0.3333333333333333703, 0.3219752754296894559, 0.3333333333333333703, 0.3219752754296894559, 0.3333333333333333703, 0.3219752754296894559, 0.3333333333333333703, 0.3219752754296894559, 0.3333333333333333703, 0.3219752754296894559, 0.3333333333333333703, 0.3219752754296894559, 0.3333333333333333703, 0.3219752754296894559, 0.3333333333333333703, 0.3219752754296894559, 0.3333333333333333703, 0.3219752754296894559, 0.3333333333333333703, 0.3219752754296894559, 0.3333333333333333703, 0.3219752754296894559, 0.3333333333333333703, 0.3219752754296894559, 0.3333333333333333703, 0.3219752754296894559, 0.3333333333333333703, 0.3219752754296894559, 0.3333333333333333703, 0.3219752754296894559, 0.3333333333333333703, 0.3219752754296894559, 0.3333333333333333703, 0.3219752754296894559, 0.3333333333333333703, 0.3219752754296894559, 0.3333333333333333703, 0.3219752754296894559, 0.3333333333333333703, 0.3219752754296894559, 0.3333333333333333703, 0.3219752754296894559, 0.3333333333333333703, 0.3219752754296894559, 0.3333333333333333703, 0.3219752754296894559, 0.3333333333333333703, 0.3219752754296894559, 0.3333333333333333703, 0.3219752754296894559, 0.3333333333333333703, 0.3219752754296894559, 0.3333333333333333703, 0.3219752754296894559, 0.3333333333333333703, 0.3219752754296894559, 0.3333333333333333703, 0.3219752754296894559, 0.3333333333333333703, 0.3219752754296894559, 0.3333333333333333703, 0.3219752754296894559, 0.3333333333333333703, 0.3219752754296894559, 0.3333333333333333703, 0.3219752754296894559, 0.3333333333333333703, 0.3219752754296894559, 0.3333333333333333703, 0.3219752754296894559, 0.3333333333333333703, 0.3219752754296894559, 0.3333333333333333703, 0.3219752754296894559, 0.3333333333333333703, 0.3219752754296894559, 0.3333333333333333703, 0.3219752754296894559, 0.3333333333333333703, 0.3219752754296894559, 0.3333333333333333703, 0.3219752754296894559, 0.3333333333333333703, 0.3219752754296894559, 0.3333333333333333703, 0.3219752754296894559, 0.3333333333333333703, 0.3219752754296894559, 0.3333333333333333703, 0.3219752754296894559, 0.3333333333333333703, 0.3219752754296894559, 0.3333333333333333703, 0.3219752754296894559, 0.3333333333333333703, 0.3219752754296894559, 0.3333333333333333703, 0.3219752754296894559, 0.3333333333333333703, 0.3219752754296894559, 0.3333333333333333703, 0.3219752754296894559, 0.3333333333333333703, 0.3219752754296894559, 0.3333333333333333703, 0.3219752754296894559, 0.3333333333333333703, 0.3219752754296894559, 0.3333333333333333703, 0.3219752754296894559, 0.3333333333333333703, 0.3219752754296894559, 0.3333333333333333703, 0.3219752754296894559, 0.3333333333333333703, 0.3219752754296894559, 0.3333333333333333703, 0.3219752754296894559, 0.3333333333333333703, 0.3219752754296894559, 0.3333333333333333703, 0.3219752754296894559, 0.3333333333333333703, 0.3219752754296894559, 0.3333333333333333703, 0.3219752754296894559, 0.3333333333333333703, 0.3219752754296894559, 0.3333333333333333703, 0.3219752754296894559, 0.3333333333333333703, 0.3219752754296894559, 0.3333333333333333703, 0.3219752754296894559, 0.3333333333333333703, 0.3219752754296894559, 0.3333333333333333703, 0.3219752754296894559, 0.3333333333333333703, 0.3219752754296894559, 0.3333333333333333703, 0.3219752754296894559, 0.3333333333333333703, 0.3219752754296894559, 0.3333333333333333703, 0.3219752754296894559, 0.3333333333333333703, 0.3219752754296894559, 0.3333333333333333703, 0.3219752754296894559, 0.3333333333333333703, 0.3219752754296894559, 0.3333333333333333703, 0.3219752754296894559, 0.3333333333333333703, 0.3219752754296894559, 0.3333333333333333703, 0.3219752754296894559, 0.3333333333333333703, 0.3219752754296894559, 0.3333333333333333703, 0.3219752754296894559, 0.3333333333333333703, 0.3219752754296894559, 0.3333333333333333703, 0.3219752754296894559, 0.3333333333333333703, 0.3219752754296894559, 0.3333333333333333703, 0.3219752754296894559, 0.3333333333333333703, 0.3219752754296894559, 0.3333333333333333703, 0.3219752754296894559, 0.3333333333333333703, 0.3219752754296894559, 0.3333333333333333703, 0.3219752754296894559, 0.3333333333333333703, 0.3219752754296894559, 0.3333333333333333703, 0.3219752754296894559, 0.3333333333333333703, 0.3219752754296894559, 0.3333333333333333703, 0.3219752754296894559, 0.3333333333333333703, 0.3219752754296894559, 0.3333333333333333703),
 ( 1.000000000000000000, 0.9659258262890683122, 1.000000000000000000, 0.9659258262890683122, 1.000000000000000000, 0.9659258262890683122, 1.000000000000000000, 0.9659258262890683122, 1.000000000000000000, 0.9659258262890683122, 1.000000000000000000, 0.9659258262890683122, 1.000000000000000000, 0.9659258262890683122, 1.000000000000000000, 0.9659258262890683122, 1.000000000000000000, 0.9659258262890683122, 1.000000000000000000, 0.9659258262890683122, 1.000000000000000000, 0.9659258262890683122, 1.000000000000000000, 0.9659258262890683122, 1.000000000000000000, 0.9659258262890683122, 1.000000000000000000, 0.9659258262890683122, 1.000000000000000000, 0.9659258262890683122, 1.000000000000000000, 0.9659258262890683122, 1.000000000000000000, 0.9659258262890683122, 1.000000000000000000, 0.9659258262890683122, 1.000000000000000000, 0.9659258262890683122, 1.000000000000000000, 0.9659258262890683122, 1.000000000000000000, 0.9659258262890683122, 1.000000000000000000, 0.9659258262890683122, 1.000000000000000000, 0.9659258262890683122, 1.000000000000000000, 0.9659258262890683122, 1.000000000000000000, 0.9659258262890683122, 1.000000000000000000, 0.9659258262890683122, 1.000000000000000000, 0.9659258262890683122, 1.000000000000000000, 0.9659258262890683122, 1.000000000000000000, 0.9659258262890683122, 1.000000000000000000, 0.9659258262890683122, 1.000000000000000000, 0.9659258262890683122, 1.000000000000000000, 0.9659258262890683122, 1.000000000000000000, 0.9659258262890683122, 1.000000000000000000, 0.9659258262890683122, 1.000000000000000000, 0.9659258262890683122, 1.000000000000000000, 0.9659258262890683122, 1.000000000000000000, 0.9659258262890683122, 1.000000000000000000, 0.9659258262890683122, 1.000000000000000000, 0.9659258262890683122, 1.000000000000000000, 0.9659258262890683122, 1.000000000000000000, 0.9659258262890683122, 1.000000000000000000, 0.9659258262890683122, 1.000000000000000000, 0.9659258262890683122, 1.000000000000000000, 0.9659258262890683122, 1.000000000000000000, 0.9659258262890683122, 1.000000000000000000, 0.9659258262890683122, 1.000000000000000000, 0.9659258262890683122, 1.000000000000000000, 0.9659258262890683122, 1.000000000000000000, 0.9659258262890683122, 1.000000000000000000, 0.9659258262890683122, 1.000000000000000000, 0.9659258262890683122, 1.000000000000000000, 0.9659258262890683122, 1.000000000000000000, 0.9659258262890683122, 1.000000000000000000, 0.9659258262890683122, 1.000000000000000000, 0.9659258262890683122, 1.000000000000000000, 0.9659258262890683122, 1.000000000000000000, 0.9659258262890683122, 1.000000000000000000, 0.9659258262890683122, 1.000000000000000000, 0.9659258262890683122, 1.000000000000000000, 0.9659258262890683122, 1.000000000000000000, 0.9659258262890683122, 1.000000000000000000, 0.9659258262890683122, 1.000000000000000000, 0.9659258262890683122, 1.000000000000000000, 0.9659258262890683122, 1.000000000000000000, 0.9659258262890683122, 1.000000000000000000, 0.9659258262890683122, 1.000000000000000000, 0.9659258262890683122, 1.000000000000000000, 0.9659258262890683122, 1.000000000000000000, 0.9659258262890683122, 1.000000000000000000, 0.9659258262890683122, 1.000000000000000000, 0.9659258262890683122, 1.000000000000000000, 0.9659258262890683122, 1.000000000000000000, 0.9659258262890683122, 1.000000000000000000, 0.9659258262890683122, 1.000000000000000000, 0.9659258262890683122, 1.000000000000000000, 0.9659258262890683122, 1.000000000000000000, 0.9659258262890683122, 1.000000000000000000, 0.9659258262890683122, 1.000000000000000000, 0.9659258262890683122, 1.000000000000000000, 0.9659258262890683122, 1.000000000000000000, 0.9659258262890683122, 1.000000000000000000, 0.9659258262890683122, 1.000000000000000000, 0.9659258262890683122, 1.000000000000000000, 0.9659258262890683122, 1.000000000000000000, 0.9659258262890683122, 1.000000000000000000, 0.9659258262890683122, 1.000000000000000000, 0.9659258262890683122, 1.000000000000000000, 0.9659258262890683122, 1.000000000000000000, 0.9659258262890683122, 1.000000000000000000, 0.9659258262890683122, 1.000000000000000000, 0.9659258262890683122, 1.000000000000000000, 0.9659258262890683122, 1.000000000000000000, 0.9659258262890683122, 1.000000000000000000, 0.9659258262890683122, 1.000000000000000000, 0.9659258262890683122, 1.000000000000000000, 0.9659258262890683122, 1.000000000000000000, 0.9659258262890683122, 1.000000000000000000, 0.9659258262890683122, 1.000000000000000000, 0.9659258262890683122, 1.000000000000000000, 0.9659258262890683122, 1.000000000000000000, 0.9659258262890683122, 1.000000000000000000, 0.9659258262890683122, 1.000000000000000000, 0.9659258262890683122, 1.000000000000000000, 0.9659258262890683122, 1.000000000000000000, 0.9659258262890683122, 1.000000000000000000, 0.9659258262890683122, 1.000000000000000000, 0.9659258262890683122, 1.000000000000000000, 0.9659258262890683122, 1.000000000000000000, 0.9659258262890683122, 1.000000000000000000, 0.9659258262890683122, 1.000000000000000000, 0.9659258262890683122, 1.000000000000000000, 0.9659258262890683122, 1.000000000000000000, 0.9659258262890683122, 1.000000000000000000, 0.9659258262890683122, 1.000000000000000000, 0.9659258262890683122, 1.000000000000000000, 0.9659258262890683122, 1.000000000000000000, 0.9659258262890683122, 1.000000000000000000, 0.9659258262890683122, 1.000000000000000000, 0.9659258262890683122, 1.000000000000000000, 0.9659258262890683122, 1.000000000000000000, 0.9659258262890683122, 1.000000000000000000, 0.9659258262890683122, 1.000000000000000000, 0.9659258262890683122, 1.000000000000000000, 0.9659258262890683122, 1.000000000000000000, 0.9659258262890683122, 1.000000000000000000, 0.9659258262890683122, 1.000000000000000000, 0.9659258262890683122, 1.000000000000000000, 0.9659258262890683122, 1.000000000000000000, 0.9659258262890683122, 1.000000000000000000, 0.9659258262890683122, 1.000000000000000000, 0.9659258262890683122, 1.000000000000000000, 0.9659258262890683122, 1.000000000000000000, 0.9659258262890683122, 1.000000000000000000, 0.9659258262890683122, 1.000000000000000000, 0.9659258262890683122, 1.000000000000000000, 0.9659258262890683122, 1.000000000000000000, 0.9659258262890683122, 1.000000000000000000, 0.9659258262890683122, 1.000000000000000000, 0.9659258262890683122, 1.000000000000000000, 0.9659258262890683122, 1.000000000000000000, 0.9659258262890683122, 1.000000000000000000, 0.9659258262890683122, 1.000000000000000000, 0.9659258262890683122, 1.000000000000000000, 0.9659258262890683122, 1.000000000000000000, 0.9659258262890683122, 1.000000000000000000, 0.9659258262890683122, 1.000000000000000000, 0.9659258262890683122, 1.000000000000000000, 0.9659258262890683122, 1.000000000000000000, 0.9659258262890683122, 1.000000000000000000, 0.9659258262890683122, 1.000000000000000000, 0.9659258262890683122, 1.000000000000000000, 0.9659258262890683122, 1.000000000000000000, 0.9659258262890683122, 1.000000000000000000, 0.9659258262890683122, 1.000000000000000000, 0.9659258262890683122, 1.000000000000000000, 0.9659258262890683122, 1.000000000000000000, 0.9659258262890683122, 1.000000000000000000, 0.9659258262890683122, 1.000000000000000000, 0.9659258262890683122, 1.000000000000000000, 0.9659258262890683122, 1.000000000000000000, 0.9659258262890683122, 1.000000000000000000, 0.9659258262890683122, 1.000000000000000000, 0.9659258262890683122, 1.000000000000000000, 0.9659258262890683122, 1.000000000000000000, 0.9659258262890683122, 1.000000000000000000, 0.9659258262890683122, 1.000000000000000000, 0.9659258262890683122, 1.000000000000000000, 0.9659258262890683122, 1.000000000000000000, 0.9659258262890683122, 1.000000000000000000, 0.9659258262890683122, 1.000000000000000000, 0.9659258262890683122, 1.000000000000000000, 0.9659258262890683122, 1.000000000000000000, 0.9659258262890683122, 1.000000000000000000, 0.9659258262890683122, 1.000000000000000000, 0.9659258262890683122, 1.000000000000000000, 0.9659258262890683122, 1.000000000000000000, 0.9659258262890683122, 1.000000000000000000, 0.9659258262890683122, 1.000000000000000000, 0.9659258262890683122, 1.000000000000000000, 0.9659258262890683122, 1.000000000000000000, 0.9659258262890683122, 1.000000000000000000, 0.9659258262890683122, 1.000000000000000000, 0.9659258262890683122, 1.000000000000000000, 0.9659258262890683122, 1.000000000000000000, 0.9659258262890683122, 1.000000000000000000, 0.9659258262890683122, 1.000000000000000000, 0.9659258262890683122, 1.000000000000000000, 0.9659258262890683122, 1.000000000000000000, 0.9659258262890683122, 1.000000000000000000, 0.9659258262890683122, 1.000000000000000000, 0.9659258262890683122, 1.000000000000000000, 0.9659258262890683122, 1.000000000000000000, 0.9659258262890683122, 1.000000000000000000, 0.9659258262890683122, 1.000000000000000000, 0.9659258262890683122, 1.000000000000000000, 0.9659258262890683122, 1.000000000000000000, 0.9659258262890683122, 1.000000000000000000, 0.9659258262890683122, 1.000000000000000000, 0.9659258262890683122, 1.000000000000000000, 0.9659258262890683122, 1.000000000000000000, 0.9659258262890683122, 1.000000000000000000, 0.9659258262890683122, 1.000000000000000000, 0.9659258262890683122, 1.000000000000000000, 0.9659258262890683122, 1.000000000000000000, 0.9659258262890683122, 1.000000000000000000, 0.9659258262890683122, 1.000000000000000000, 0.9659258262890683122, 1.000000000000000000, 0.9659258262890683122, 1.000000000000000000, 0.9659258262890683122, 1.000000000000000000, 0.9659258262890683122, 1.000000000000000000, 0.9659258262890683122, 1.000000000000000000, 0.9659258262890683122, 1.000000000000000000, 0.9659258262890683122, 1.000000000000000000, 0.9659258262890683122, 1.000000000000000000, 0.9659258262890683122, 1.000000000000000000, 0.9659258262890683122, 1.000000000000000000, 0.9659258262890683122, 1.000000000000000000, 0.9659258262890683122, 1.000000000000000000, 0.9659258262890683122, 1.000000000000000000, 0.9659258262890683122, 1.000000000000000000, 0.9659258262890683122, 1.000000000000000000, 0.9659258262890683122, 1.000000000000000000, 0.9659258262890683122, 1.000000000000000000, 0.9659258262890683122, 1.000000000000000000, 0.9659258262890683122, 1.000000000000000000, 0.9659258262890683122, 1.000000000000000000, 0.9659258262890683122, 1.000000000000000000, 0.9659258262890683122, 1.000000000000000000) ) ) 
 REPRESENTATION_ITEM ( '' )  SURFACE ( )  );
#171924 = CARTESIAN_POINT ( 'NONE',  ( 5.719274019375991003, -21.55341960407610458, 42.70724293864770260 ) ) ;
#171925 = CARTESIAN_POINT ( 'NONE',  ( -4.379528057220328563, 16.55341960407611168, 110.2072429386477239 ) ) ;
#171926 = CARTESIAN_POINT ( 'NONE',  ( -31.72709406046301339, 2.040068635034919209E-14, 102.5000000000000142 ) ) ;
#171927 = CARTESIAN_POINT ( 'NONE',  ( 5.049401038297881783, 19.05341960407617563, 62.29275706135234003 ) ) ;
#171928 = CARTESIAN_POINT ( 'NONE',  ( 16.53943276465976808, -0.05219959533910856209, 38.74890960531435979 ) ) ;
#171929 = CARTESIAN_POINT ( 'NONE',  ( -19.02544592524342804, 5.153800228976336051, 111.0405762719810099 ) ) ;
#171930 = CARTESIAN_POINT ( 'NONE',  ( -10.72451020669870658, -18.67979575497194134, 84.58442372801903275 ) ) ;
#171931 = CARTESIAN_POINT ( 'NONE',  ( 5.719274019375991003, -21.55341960407610458, 72.70724293864769550 ) ) ;
#171932 = CARTESIAN_POINT ( 'NONE',  ( 21.55341960407619695, -5.719274019375665929, 41.04275706135236135 ) ) ;
#171933 = CARTESIAN_POINT ( 'NONE',  ( -15.80617190586745835, -15.72974639402198527, 96.87390960531436690 ) ) ;
#171934 = CARTESIAN_POINT ( 'NONE',  ( -18.62759615963255300, -10.81492255796106328, 54.16775706135235424 ) ) ;
#171935 = CARTESIAN_POINT ( 'NONE',  ( -0.05219959533909027116, -19.03943276465977164, 22.49890960531436690 ) ) ;
#171936 = CARTESIAN_POINT ( 'NONE',  ( 0.05219959533909260263, 19.03943276465977164, 84.99890960531436690 ) ) ;
#171937 = CARTESIAN_POINT ( 'NONE',  ( -8.314922557961024197, 14.29746914071037800, 82.91775706135234714 ) ) ;
#171938 = CARTESIAN_POINT ( 'NONE',  ( -14.29746914071049879, 8.314922557960819915, 110.8322429386476955 ) ) ;
#171939 = CARTESIAN_POINT ( 'NONE',  ( -16.51473224551069308, -9.474510206698971260, 106.6655762719810383 ) ) ;
#171940 = CARTESIAN_POINT ( 'NONE',  ( -14.29746914071049879, 8.314922557960819915, 60.83224293864769550 ) ) ;
#171941 = CARTESIAN_POINT ( 'NONE',  ( -16.53943276465976808, 0.05219959533911058130, 26.24890960531435624 ) ) ;
#171942 = CARTESIAN_POINT ( 'NONE',  ( -0.05219959533909027116, -19.03943276465977164, 67.49890960531436690 ) ) ;
#171943 = CARTESIAN_POINT ( 'NONE',  ( 19.02544592524343514, -5.153800228976328945, 28.54057627198102409 ) ) ;
#171944 = CARTESIAN_POINT ( 'NONE',  ( -21.53943276465977519, 0.05219959533907696930, 46.24890960531435979 ) ) ;
#171945 = CARTESIAN_POINT ( 'NONE',  ( 5.049401038297881783, 19.05341960407617563, 42.29275706135234003 ) ) ;
#171947 = CARTESIAN_POINT ( 'NONE',  ( -0.05219959533910754901, -16.53943276465976808, 32.49890960531435979 ) ) ;
#171946 = CARTESIAN_POINT ( 'NONE',  ( 30.00000000000000000, 40.00100000000004741, 37.49999999999999289 ) ) ;
#171948 = CARTESIAN_POINT ( 'NONE',  ( -5.153800228976328057, -19.02544592524343514, 102.2905762719810383 ) ) ;
#171949 = CARTESIAN_POINT ( 'NONE',  ( -21.55341960407619339, 5.719274019375674811, 53.54275706135234714 ) ) ;
#171950 = CARTESIAN_POINT ( 'NONE',  ( 13.89961937509977652, -13.97604488694527269, 113.1239096053143527 ) ) ;
#171951 = CARTESIAN_POINT ( 'NONE',  ( 14.29746914071037800, 8.314922557961029526, 56.66775706135235424 ) ) ;
#171952 = EDGE_CURVE ( 'NONE', #85047, #195827, #92774, .T. ) ;
#171953 = CARTESIAN_POINT ( 'NONE',  ( -0.05219959533936034679, 19.03943276465977164, 62.50109039468566863 ) ) ;
#171954 = CARTESIAN_POINT ( 'NONE',  ( 12.14591786802309770, 12.06949235617756955, 34.37390960531435979 ) ) ;
#171955 = CARTESIAN_POINT ( 'NONE',  ( -19.39056639909674828, -5.499999999999968026, 75.78948781074343799 ) ) ;
#171956 = CARTESIAN_POINT ( 'NONE',  ( 12.06949235617739724, 12.14591786802326823, 106.8760903946856899 ) ) ;
#171957 = CARTESIAN_POINT ( 'NONE',  ( -9.474510206698964154, 16.51473224551069663, 35.41557627198102409 ) ) ;
#171958 = CARTESIAN_POINT ( 'NONE',  ( -13.97604488694527625, -13.89961937509977652, 61.87390960531435979 ) ) ;
#171959 = CARTESIAN_POINT ( 'NONE',  ( 13.97604488694527802, 13.89961937509977652, 24.37390960531435624 ) ) ;
#171960 = CARTESIAN_POINT ( 'NONE',  ( 18.62759615963255655, 10.81492255796105972, 31.66775706135234358 ) ) ;
#171961 = CARTESIAN_POINT ( 'NONE',  ( -19.03943276465977164, 0.05219959533909376836, 46.24890960531435979 ) ) ;
#171962 = CARTESIAN_POINT ( 'NONE',  ( -5.801314085210285576, -6.819390806090331658, -61.93051126003076945 ) ) ;
#171963 = CARTESIAN_POINT ( 'NONE',  ( -13.97604488694527625, -13.89961937509977652, 51.87390960531436690 ) ) ;
#171964 = CARTESIAN_POINT ( 'NONE',  ( 10.81492255796078972, 18.62759615963270932, 24.58224293864768839 ) ) ;
#171965 = ADVANCED_FACE ( 'NONE', ( #13418 ), #121718, .T. ) ;
#171967 = CARTESIAN_POINT ( 'NONE',  ( 9.474510206698971260, -16.51473224551069308, 27.91557627198103120 ) ) ;
#171966 = CARTESIAN_POINT ( 'NONE',  ( -10.81492255796105439, 18.62759615963255655, 52.91775706135235424 ) ) ;
#171968 = CARTESIAN_POINT ( 'NONE',  ( 10.81492255796078972, 18.62759615963270932, 34.58224293864770260 ) ) ;
#171969 = CARTESIAN_POINT ( 'NONE',  ( -12.14591786802326823, 12.06949235617739902, 73.12609039468567573 ) ) ;
#171970 = CARTESIAN_POINT ( 'NONE',  ( -10.72451020669870658, -18.67979575497194134, 109.5844237280190328 ) ) ;
#171971 = CARTESIAN_POINT ( 'NONE',  ( -12.14591786802326823, 12.06949235617739902, 53.12609039468568284 ) ) ;
#171972 = CARTESIAN_POINT ( 'NONE',  ( -19.05341960407611168, -5.049401038298163336, 91.45724293864766707 ) ) ;
#171973 = CARTESIAN_POINT ( 'NONE',  ( 8.224510206698742110, 14.34966873604972548, 47.08442372801901854 ) ) ;
#171974 = CARTESIAN_POINT ( 'NONE',  ( 16.55341960407618274, -4.379528057220086978, 21.04275706135234714 ) ) ;
#171975 = CARTESIAN_POINT ( 'NONE',  ( 0.05219959533934541429, -16.53943276465976808, 90.00109039468567573 ) ) ;
#171976 = CARTESIAN_POINT ( 'NONE',  ( 18.67979575497194134, -10.72451020669871369, 50.83442372801901143 ) ) ;
#171977 = CARTESIAN_POINT ( 'NONE',  ( 9.474510206698729675, 16.51473224551082808, 102.0844237280190043 ) ) ;
#171978 = CARTESIAN_POINT ( 'NONE',  ( -15.72974639402176322, -15.80617190586768395, 19.37609039468568639 ) ) ;
#171980 = CARTESIAN_POINT ( 'NONE',  ( -16.51473224551082808, 9.474510206698731452, 103.3344237280190043 ) ) ;
#171979 = CARTESIAN_POINT ( 'NONE',  ( -8.224510206698948167, 14.34966873604960824, 100.4155762719810241 ) ) ;
#171981 = CARTESIAN_POINT ( 'NONE',  ( 4.483927247898790824, -16.52544592524335698, 85.20942372801901854 ) ) ;
#171982 = CARTESIAN_POINT ( 'NONE',  ( 24.57691432906749540, 7.727872488968289488, 167.2019946024467743 ) ) ;
#171983 = CARTESIAN_POINT ( 'NONE',  ( 16.46253265017146816, 9.564922557961045513, 86.66775706135233293 ) ) ;
#171984 = CARTESIAN_POINT ( 'NONE',  ( 4.379528057220339221, -16.55341960407611168, 47.70724293864770260 ) ) ;
#171985 = CARTESIAN_POINT ( 'NONE',  ( -4.483927247898539470, -16.52544592524342804, 42.29057627198103120 ) ) ;
#171986 = CARTESIAN_POINT ( 'NONE',  ( -16.55341960407611168, -4.379528057220339221, 106.4572429386477097 ) ) ;
#171988 = CARTESIAN_POINT ( 'NONE',  ( -17.49999999999999645, 5.499999999999992895, 88.71769037696435589 ) ) ;
#171987 = CARTESIAN_POINT ( 'NONE',  ( -16.46253265017146816, -9.564922557961047289, 39.16775706135234003 ) ) ;
#171989 = CARTESIAN_POINT ( 'NONE',  ( 21.53943276465977519, 0.05219959533937863772, 41.25109039468568284 ) ) ;
#171990 = CARTESIAN_POINT ( 'NONE',  ( 5.153800228976615827, -19.02544592524334988, 105.2094237280190185 ) ) ;
#171991 = CARTESIAN_POINT ( 'NONE',  ( -24.30000000000003268, 2.668083032619853614E-13, -56.77278709839600879 ) ) ;
#171992 = CARTESIAN_POINT ( 'NONE',  ( -19.02544592524342804, 5.153800228976336051, 91.04057627198100988 ) ) ;
#171993 = CARTESIAN_POINT ( 'NONE',  ( 16.46253265017160672, -9.564922557960803928, 83.33224293864768129 ) ) ;
#171994 = CARTESIAN_POINT ( 'NONE',  ( 5.823673210054125526, 21.52544592524343514, 59.79057627198103120 ) ) ;
#171995 = CARTESIAN_POINT ( 'NONE',  ( -8.224510206698948167, 14.34966873604960824, 95.41557627198102409 ) ) ;
#171996 = CARTESIAN_POINT ( 'NONE',  ( -5.049401038298153566, 19.05341960407611168, 65.20724293864765286 ) ) ;
#171997 = CARTESIAN_POINT ( 'NONE',  ( -19.03943276465977164, 0.05219959533909376836, 36.24890960531436690 ) ) ;
#171998 = CARTESIAN_POINT ( 'NONE',  ( -5.823673210054431948, 21.52544592524334988, 42.70942372801901854 ) ) ;
#171999 = CARTESIAN_POINT ( 'NONE',  ( 21.53943276465977519, 0.05219959533937863772, 71.25109039468568994 ) ) ;
#172000 = CARTESIAN_POINT ( 'NONE',  ( 4.483927247898790824, -16.52544592524335698, 95.20942372801903275 ) ) ;
#172001 = CARTESIAN_POINT ( 'NONE',  ( 21.55341960407619695, -5.719274019375665929, 26.04275706135235779 ) ) ;
#172002 = CARTESIAN_POINT ( 'NONE',  ( 10.72451020669871369, 18.67979575497193778, 22.08442372801901143 ) ) ;
#172004 = CARTESIAN_POINT ( 'NONE',  ( -5.153800228976328057, -19.02544592524343514, 82.29057627198103830 ) ) ;
#172003 = CARTESIAN_POINT ( 'NONE',  ( -9.474510206698720793, -16.51473224551083518, 59.58442372801900433 ) ) ;
#172005 = CARTESIAN_POINT ( 'NONE',  ( -18.67979575497193778, 10.72451020669871902, 83.33442372801903275 ) ) ;
#172006 = CARTESIAN_POINT ( 'NONE',  ( -21.55341960407610458, -5.719274019375992779, 81.45724293864769550 ) ) ;
#172007 = CARTESIAN_POINT ( 'NONE',  ( -12.14591786802309592, -12.06949235617757132, 56.87390960531436690 ) ) ;
#172008 = CARTESIAN_POINT ( 'NONE',  ( 21.52544592524334988, 5.823673210054432836, 106.4594237280190328 ) ) ;
#172009 = CARTESIAN_POINT ( 'NONE',  ( -16.52544592524342804, 4.483927247898546575, 66.04057627198103830 ) ) ;
#172010 = CARTESIAN_POINT ( 'NONE',  ( -0.05219959533909027116, -19.03943276465977164, 27.49890960531435624 ) ) ;
#172011 = CARTESIAN_POINT ( 'NONE',  ( 19.03943276465977164, 0.05219959533936151252, 76.25109039468566152 ) ) ;
#172012 = CARTESIAN_POINT ( 'NONE',  ( 8.224510206698953496, -14.34966873604960469, 32.91557627198102409 ) ) ;
#172013 = CARTESIAN_POINT ( 'NONE',  ( 15.72974639402176855, 15.80617190586768217, 81.87609039468568994 ) ) ;
#172014 = CARTESIAN_POINT ( 'NONE',  ( -19.02544592524342804, 5.153800228976336051, 86.04057627198103830 ) ) ;
#172015 = CARTESIAN_POINT ( 'NONE',  ( -13.97604488694547697, 13.89961937509957934, 58.12609039468566863 ) ) ;
#172016 = CARTESIAN_POINT ( 'NONE',  ( -10.81492255796078084, -18.62759615963271287, 62.08224293864769550 ) ) ;
#172017 = CARTESIAN_POINT ( 'NONE',  ( -18.62759615963270932, 10.81492255796079327, 110.8322429386476955 ) ) ;
#172018 = CARTESIAN_POINT ( 'NONE',  ( 12.14591786802327356, -12.06949235617739191, 20.62609039468568639 ) ) ;
#172019 = CARTESIAN_POINT ( 'NONE',  ( 8.314922557961029526, -14.29746914071037800, 85.41775706135236135 ) ) ;
#172021 = CARTESIAN_POINT ( 'NONE',  ( -18.67979575497193778, 10.72451020669871902, 28.33442372801902209 ) ) ;
#172020 = CARTESIAN_POINT ( 'NONE',  ( 16.36317988757058117, 7.306389748694948949, 63.40210391636776421 ) ) ;
#172022 = CARTESIAN_POINT ( 'NONE',  ( 12.06949235617757843, -12.14591786802309237, 98.12390960531436690 ) ) ;
#172023 = CARTESIAN_POINT ( 'NONE',  ( 11.40812507854754365, 35.11059874428196537, -3.724999997268813701 ) ) ;
#172024 = CARTESIAN_POINT ( 'NONE',  ( 8.224510206698742110, 14.34966873604972548, 42.08442372801901854 ) ) ;
#172025 = APPLICATION_CONTEXT ( 'automotive_design' ) ;
#172026 = CARTESIAN_POINT ( 'NONE',  ( -21.53943276465977519, 0.05219959533907696930, 56.24890960531436690 ) ) ;
#172027 = CARTESIAN_POINT ( 'NONE',  ( -8.224510206698735004, -14.34966873604973081, 109.5844237280190328 ) ) ;
#172028 = CARTESIAN_POINT ( 'NONE',  ( 12.14591786802327356, -12.06949235617739191, 40.62609039468567573 ) ) ;
#172029 = CARTESIAN_POINT ( 'NONE',  ( 16.51473224551069308, 9.474510206698969483, 34.16557627198102409 ) ) ;
#172030 = CARTESIAN_POINT ( 'NONE',  ( -0.05219959533934338120, 16.53943276465976808, 82.50109039468568994 ) ) ;
#172031 = CARTESIAN_POINT ( 'NONE',  ( 9.474510206698729675, 16.51473224551082808, 77.08442372801900433 ) ) ;
#172032 = CARTESIAN_POINT ( 'NONE',  ( 15.72974639402199770, -15.80617190586745480, 63.12390960531435979 ) ) ;
#172033 = CARTESIAN_POINT ( 'NONE',  ( 14.29746914071037800, 8.314922557961029526, 96.66775706135234714 ) ) ;
#172034 = CARTESIAN_POINT ( 'NONE',  ( 21.53943276465977519, 0.05219959533937863772, 81.25109039468568994 ) ) ;
#172035 = CARTESIAN_POINT ( 'NONE',  ( 18.67979575497178502, 10.72451020669898547, 59.16557627198103120 ) ) ;
#172036 = CARTESIAN_POINT ( 'NONE',  ( -10.72451020669898014, 18.67979575497178502, 45.41557627198103830 ) ) ;
#172037 = ORIENTED_EDGE ( 'NONE', *, *, #80739, .F. ) ;
#172038 = CARTESIAN_POINT ( 'NONE',  ( -16.55341960407617563, 4.379528057220093196, 83.54275706135234714 ) ) ;
#172039 = CARTESIAN_POINT ( 'NONE',  ( -15.72974639402197994, 15.80617190586746368, 45.62390960531436690 ) ) ;
#172040 = VERTEX_POINT ( 'NONE', #79047 ) ;
#172041 = CARTESIAN_POINT ( 'NONE',  ( -19.02544592524342804, 5.153800228976336051, 96.04057627198103830 ) ) ;
#172042 = CARTESIAN_POINT ( 'NONE',  ( -26.53317239408749373, 7.611579847057692305, 168.2742808015845526 ) ) ;
#172043 = CARTESIAN_POINT ( 'NONE',  ( -16.51473224551069308, -9.474510206698971260, 21.66557627198102765 ) ) ;
#172044 = CARTESIAN_POINT ( 'NONE',  ( 5.823673210054125526, 21.52544592524343514, 64.79057627198103830 ) ) ;
#172045 = CARTESIAN_POINT ( 'NONE',  ( -8.314922557961024197, 14.29746914071037800, 97.91775706135236135 ) ) ;
#172046 = CARTESIAN_POINT ( 'NONE',  ( -10.72451020669870658, -18.67979575497194134, 44.58442372801901854 ) ) ;
#172047 = CARTESIAN_POINT ( 'NONE',  ( 5.049401038297881783, 19.05341960407617563, 97.29275706135233293 ) ) ;
#172048 = CARTESIAN_POINT ( 'NONE',  ( 8.314922557960818139, 14.29746914071049879, 104.5822429386477097 ) ) ;
#172049 = CARTESIAN_POINT ( 'NONE',  ( 5.049401038297881783, 19.05341960407617563, 107.2927570613523187 ) ) ;
#172050 = CARTESIAN_POINT ( 'NONE',  ( 16.46253265017160672, -9.564922557960803928, 43.33224293864769550 ) ) ;
#172051 = CARTESIAN_POINT ( 'NONE',  ( 1.227931366032057224E-14, 24.30000000000003268, -54.21489346206828230 ) ) ;
#172052 = CARTESIAN_POINT ( 'NONE',  ( -9.474510206698964154, 16.51473224551069663, 95.41557627198102409 ) ) ;
#172053 = CARTESIAN_POINT ( 'NONE',  ( 8.314922557961029526, -14.29746914071037800, 80.41775706135234714 ) ) ;
#172054 = CARTESIAN_POINT ( 'NONE',  ( -9.564922557961040184, 16.46253265017147172, 72.91775706135233293 ) ) ;
#172055 = CARTESIAN_POINT ( 'NONE',  ( -10.81492255796105439, 18.62759615963255655, 102.9177570613523756 ) ) ;
#172056 = CARTESIAN_POINT ( 'NONE',  ( -18.62759615963270932, 10.81492255796079327, 65.83224293864769550 ) ) ;
#172057 = EDGE_CURVE ( 'NONE', #72076, #27411, #63892, .T. ) ;
#172058 = CARTESIAN_POINT ( 'NONE',  ( -4.379528057220086978, -16.55341960407618274, 84.79275706135234714 ) ) ;
#172059 = CARTESIAN_POINT ( 'NONE',  ( 16.46253265017146816, 9.564922557961045513, 76.66775706135234714 ) ) ;
#172060 = CARTESIAN_POINT ( 'NONE',  ( -13.97604488694527625, -13.89961937509977652, 31.87390960531435979 ) ) ;
#172061 = CARTESIAN_POINT ( 'NONE',  ( -13.97604488694527625, -13.89961937509977652, 71.87390960531433848 ) ) ;
#172062 = CARTESIAN_POINT ( 'NONE',  ( -18.67979575497193778, 10.72451020669871902, 53.33442372801901854 ) ) ;
#172063 = CARTESIAN_POINT ( 'NONE',  ( 13.97604488694527802, 13.89961937509977652, 49.37390960531434558 ) ) ;
#172064 = CARTESIAN_POINT ( 'NONE',  ( -5.153800228976607833, 19.02544592524334988, 67.70942372801900433 ) ) ;
#172065 = CARTESIAN_POINT ( 'NONE',  ( 21.70479006154364043, -9.754118203517492702, 170.7545476126473147 ) ) ;
#172066 = CARTESIAN_POINT ( 'NONE',  ( 13.89961937509977652, -13.97604488694527269, 108.1239096053143669 ) ) ;
#172067 = CARTESIAN_POINT ( 'NONE',  ( -16.55341960407611168, -4.379528057220339221, 66.45724293864768129 ) ) ;
#172068 = CARTESIAN_POINT ( 'NONE',  ( -5.823673210054116645, -21.52544592524344225, 57.29057627198103120 ) ) ;
#172069 = FACE_OUTER_BOUND ( 'NONE', #196300, .T. ) ;
#172070 = CARTESIAN_POINT ( 'NONE',  ( 19.03943276465977164, 0.05219959533936151252, 36.25109039468567573 ) ) ;
#172071 = CARTESIAN_POINT ( 'NONE',  ( 21.38418241377623019, -7.427326039334300134, 174.4773576836617224 ) ) ;
#172073 = CARTESIAN_POINT ( 'NONE',  ( 13.89961937509977652, -13.97604488694527269, 78.12390960531433848 ) ) ;
#172072 = CARTESIAN_POINT ( 'NONE',  ( 19.02544592524343514, -5.153800228976328945, 63.54057627198103830 ) ) ;
#172074 = CARTESIAN_POINT ( 'NONE',  ( -14.34966873604972548, 8.224510206698743886, 53.33442372801901854 ) ) ;
#172075 = CARTESIAN_POINT ( 'NONE',  ( 28.82186960331518222, 9.364793116373306248, 143.0999999999999943 ) ) ;
#172076 = CARTESIAN_POINT ( 'NONE',  ( -17.05587630539787725, 6.762274262135673730, 110.7418030903731534 ) ) ;
#172077 = CARTESIAN_POINT ( 'NONE',  ( 12.14591786802327356, -12.06949235617739191, 90.62609039468567573 ) ) ;
#172078 = CARTESIAN_POINT ( 'NONE',  ( 3.735172737399431091E-16, 6.100000000000006750, -65.00100000000003320 ) ) ;
#172079 = CARTESIAN_POINT ( 'NONE',  ( -0.05219959533934338120, 16.53943276465976808, 62.50109039468568284 ) ) ;
#172080 = CARTESIAN_POINT ( 'NONE',  ( 12.06949235617739724, 12.14591786802326823, 36.87609039468568994 ) ) ;
#172082 = CARTESIAN_POINT ( 'NONE',  ( 17.62203461105333702, -16.21435693443512704, -57.04011861108771342 ) ) ;
#172081 = CARTESIAN_POINT ( 'NONE',  ( -19.05341960407611168, -5.049401038298163336, 56.45724293864768129 ) ) ;
#172083 = CARTESIAN_POINT ( 'NONE',  ( -10.81492255796105439, 18.62759615963255655, 47.91775706135234714 ) ) ;
#172084 = CARTESIAN_POINT ( 'NONE',  ( 19.05341960407617918, -5.049401038297876454, 61.04275706135232582 ) ) ;
#172085 = CARTESIAN_POINT ( 'NONE',  ( -18.67979575497193778, 10.72451020669871902, 103.3344237280190043 ) ) ;
#172086 = CARTESIAN_POINT ( 'NONE',  ( -9.474510206698964154, 16.51473224551069663, 35.41557627198102409 ) ) ;
#172087 = CARTESIAN_POINT ( 'NONE',  ( 23.48298174826590667, -32.32155151706770368, -7.302157773949821795 ) ) ;
#172088 = CARTESIAN_POINT ( 'NONE',  ( 18.62759615963271287, -10.81492255796078972, 48.33224293864770260 ) ) ;
#172089 = CARTESIAN_POINT ( 'NONE',  ( -13.97604488694527625, -13.89961937509977652, 111.8739096053143243 ) ) ;
#172090 = CARTESIAN_POINT ( 'NONE',  ( -12.06949235617756955, 12.14591786802309770, 95.62390960531436690 ) ) ;
#172091 = CARTESIAN_POINT ( 'NONE',  ( -4.379528057220086978, -16.55341960407618274, 39.79275706135235424 ) ) ;
#172092 = CARTESIAN_POINT ( 'NONE',  ( 0.05219959533910956823, 16.53943276465976808, 34.99890960531435979 ) ) ;
#172093 = ORIENTED_EDGE ( 'NONE', *, *, #41117, .F. ) ;
#172094 = CARTESIAN_POINT ( 'NONE',  ( 21.52544592524344225, -5.823673210054117533, 103.5405762719810383 ) ) ;
#172095 = AXIS2_PLACEMENT_3D ( 'NONE', #31687, #107511, #139833 ) ;
#172097 = CARTESIAN_POINT ( 'NONE',  ( 30.74264578624800137, -22.33583958711395212, -9.199999999999999289 ) ) ;
#172096 = CARTESIAN_POINT ( 'NONE',  ( 14.34966873604960469, 8.224510206698951720, 34.16557627198102409 ) ) ;
#172098 = CARTESIAN_POINT ( 'NONE',  ( -9.564922557961040184, 16.46253265017147172, 92.91775706135233293 ) ) ;
#172099 = CARTESIAN_POINT ( 'NONE',  ( -9.564922557961040184, 16.46253265017147172, 27.91775706135232582 ) ) ;
#172100 = CARTESIAN_POINT ( 'NONE',  ( 0.05219959533910956823, 16.53943276465976808, 29.99890960531435979 ) ) ;
#172101 = CARTESIAN_POINT ( 'NONE',  ( 10.72451020669898902, -18.67979575497178502, 97.91557627198103830 ) ) ;
#172102 = CARTESIAN_POINT ( 'NONE',  ( -18.62759615963270932, 10.81492255796079327, 55.83224293864770260 ) ) ;
#172103 = CARTESIAN_POINT ( 'NONE',  ( 19.03943276465977164, -0.05219959533909143690, 78.74890960531436690 ) ) ;
#172104 = CARTESIAN_POINT ( 'NONE',  ( -16.53943276465976808, 0.05219959533911058130, 46.24890960531435979 ) ) ;
#172105 = CARTESIAN_POINT ( 'NONE',  ( 5.153800228976335163, 19.02544592524342804, 94.79057627198103830 ) ) ;
#172106 = ORIENTED_EDGE ( 'NONE', *, *, #58993, .T. ) ;
#172107 = DIRECTION ( 'NONE',  ( -1.000000000000000000, -0.000000000000000000, -0.000000000000000000 ) ) ;
#172108 = CARTESIAN_POINT ( 'NONE',  ( 16.51473224551083163, -9.474510206698727899, 35.83442372801899722 ) ) ;
#172109 = CARTESIAN_POINT ( 'NONE',  ( 10.81492255796078972, 18.62759615963270932, 99.58224293864770971 ) ) ;
#172110 = CARTESIAN_POINT ( 'NONE',  ( 4.483927247898545687, 16.52544592524342804, 94.79057627198105251 ) ) ;
#172111 = CARTESIAN_POINT ( 'NONE',  ( 10.72451020669871369, 18.67979575497193778, 32.08442372801901854 ) ) ;
#172112 = CARTESIAN_POINT ( 'NONE',  ( -27.73933785331498925, 9.013057229001089965, 142.7750000027311899 ) ) ;
#172113 = EDGE_CURVE ( 'NONE', #183247, #62967, #79799, .T. ) ;
#172114 = CARTESIAN_POINT ( 'NONE',  ( 12.14591786802327356, -12.06949235617739191, 100.6260903946857184 ) ) ;
#172115 = CARTESIAN_POINT ( 'NONE',  ( -13.89961937509977652, 13.97604488694528158, 30.62390960531435269 ) ) ;
#172116 = CARTESIAN_POINT ( 'NONE',  ( -19.02544592524342804, 5.153800228976336051, 86.04057627198103830 ) ) ;
#172117 = CARTESIAN_POINT ( 'NONE',  ( -17.14385361876520619, 23.59649016807275856, 140.5750000027311728 ) ) ;
#172118 = CARTESIAN_POINT ( 'NONE',  ( -19.05341960407611168, -5.049401038298163336, 36.45724293864766707 ) ) ;
#172119 = CARTESIAN_POINT ( 'NONE',  ( -14.29746914071049879, 8.314922557960819915, 40.83224293864769550 ) ) ;
#172120 = CARTESIAN_POINT ( 'NONE',  ( -15.72974639402176322, -15.80617190586768395, 69.37609039468567573 ) ) ;
#172122 = CARTESIAN_POINT ( 'NONE',  ( 12.06949235617739724, 12.14591786802326823, 71.87609039468568994 ) ) ;
#172121 = CARTESIAN_POINT ( 'NONE',  ( 10.70342273063187122, -35.99563703666952819, -30.86961840751871478 ) ) ;
#172123 = CARTESIAN_POINT ( 'NONE',  ( 16.46253265017160672, -9.564922557960803928, 58.33224293864769550 ) ) ;
#172124 = CARTESIAN_POINT ( 'NONE',  ( -5.049401038298153566, 19.05341960407611168, 65.20724293864765286 ) ) ;
#172125 = ORIENTED_EDGE ( 'NONE', *, *, #46506, .F. ) ;
#172126 = CARTESIAN_POINT ( 'NONE',  ( 0.05219959533937995610, -21.53943276465977519, 105.0010903946856757 ) ) ;
#172127 = CARTESIAN_POINT ( 'NONE',  ( 4.483927247898790824, -16.52544592524335698, 75.20942372801901854 ) ) ;
#172128 = CARTESIAN_POINT ( 'NONE',  ( -18.62759615963255300, -10.81492255796106328, 104.1677570613523471 ) ) ;
#172129 = CARTESIAN_POINT ( 'NONE',  ( -0.05219959533909027116, -19.03943276465977164, 67.49890960531436690 ) ) ;
#172130 = CARTESIAN_POINT ( 'NONE',  ( -21.55341960407610458, -5.719274019375992779, 41.45724293864769550 ) ) ;
#172131 = CARTESIAN_POINT ( 'NONE',  ( -9.474510206698720793, -16.51473224551083518, 104.5844237280190043 ) ) ;
#172132 = CARTESIAN_POINT ( 'NONE',  ( 10.72451020669871369, 18.67979575497193778, 87.08442372801901854 ) ) ;
#172133 = CARTESIAN_POINT ( 'NONE',  ( -16.52544592524335698, -4.483927247898792601, 53.95942372801900433 ) ) ;
#172134 = CARTESIAN_POINT ( 'NONE',  ( 0.05219959533907565091, 21.53943276465977519, 104.9989096053143669 ) ) ;
#172135 = CARTESIAN_POINT ( 'NONE',  ( 16.46253265017146816, 9.564922557961045513, 96.66775706135233293 ) ) ;
#172136 = CARTESIAN_POINT ( 'NONE',  ( 19.05341960407611168, 5.049401038298154454, 78.95724293864769550 ) ) ;
#172137 = CARTESIAN_POINT ( 'NONE',  ( -0.05219959533936034679, 19.03943276465977164, 112.5010903946856757 ) ) ;
#172138 = CARTESIAN_POINT ( 'NONE',  ( 16.52544592524335698, 4.483927247898782831, 26.45942372801901854 ) ) ;
#172139 = CARTESIAN_POINT ( 'NONE',  ( 0.05219959533910956823, 16.53943276465976808, 64.99890960531435269 ) ) ;
#172140 = CARTESIAN_POINT ( 'NONE',  ( 12.14591786802327356, -12.06949235617739191, 80.62609039468567573 ) ) ;
#172142 = CARTESIAN_POINT ( 'NONE',  ( 9.474510206698971260, -16.51473224551069308, 47.91557627198102409 ) ) ;
#172141 = CARTESIAN_POINT ( 'NONE',  ( -18.62759615963270932, 10.81492255796079327, 115.8322429386477097 ) ) ;
#172144 = EDGE_CURVE ( 'NONE', #93307, #122542, #118714, .T. ) ;
#172143 = CARTESIAN_POINT ( 'NONE',  ( 16.51473224551069308, 9.474510206698969483, 64.16557627198102409 ) ) ;
#172145 = CARTESIAN_POINT ( 'NONE',  ( 14.29746914071037800, 8.314922557961029526, 76.66775706135234714 ) ) ;
#172146 = CARTESIAN_POINT ( 'NONE',  ( -28.82186960331499392, -9.364793116373526516, 144.3500000054623627 ) ) ;
#172147 = ORIENTED_EDGE ( 'NONE', *, *, #113016, .T. ) ;
#172148 = CARTESIAN_POINT ( 'NONE',  ( 18.62759615963255655, 10.81492255796105972, 106.6677570613523756 ) ) ;
#172149 = CARTESIAN_POINT ( 'NONE',  ( -19.05341960407611168, -5.049401038298163336, 36.45724293864766707 ) ) ;
#172150 = ORIENTED_EDGE ( 'NONE', *, *, #185592, .F. ) ;
#172151 = CARTESIAN_POINT ( 'NONE',  ( 8.224510206698742110, 14.34966873604972548, 32.08442372801901854 ) ) ;
#172153 = CARTESIAN_POINT ( 'NONE',  ( 8.314922557961029526, -14.29746914071037800, 35.41775706135234003 ) ) ;
#172152 = CARTESIAN_POINT ( 'NONE',  ( 19.05341960407617918, -5.049401038297876454, 41.04275706135233293 ) ) ;
#172154 = CARTESIAN_POINT ( 'NONE',  ( -0.05219959533909027116, -19.03943276465977164, 42.49890960531435269 ) ) ;
#172155 = CARTESIAN_POINT ( 'NONE',  ( -0.05219959533909027116, -19.03943276465977164, 62.49890960531435979 ) ) ;
#172156 = CARTESIAN_POINT ( 'NONE',  ( -15.80617190586745835, -15.72974639402198527, 81.87390960531435269 ) ) ;
#172158 = CARTESIAN_POINT ( 'NONE',  ( -16.51473224551069308, -9.474510206698971260, 106.6655762719810383 ) ) ;
#172157 = CARTESIAN_POINT ( 'NONE',  ( 19.02544592524343514, -5.153800228976328945, 78.54057627198099567 ) ) ;
#172159 = CIRCLE ( 'NONE', #1105, 7.500000000000007105 ) ;
#172160 = CARTESIAN_POINT ( 'NONE',  ( -19.03943276465977164, 0.05219959533909376836, 51.24890960531436690 ) ) ;
#172161 = CARTESIAN_POINT ( 'NONE',  ( -5.359611314223446995E-15, 29.16686587814335851, 148.8750000027311842 ) ) ;
#172162 = CARTESIAN_POINT ( 'NONE',  ( -5.049401038297874678, -19.05341960407617918, 99.79275706135234714 ) ) ;
#172163 = CARTESIAN_POINT ( 'NONE',  ( 21.52544592524344225, -5.823673210054117533, 78.54057627198103830 ) ) ;
#172164 = CARTESIAN_POINT ( 'NONE',  ( -16.46253265017146816, -9.564922557961047289, 19.16775706135233293 ) ) ;
#172165 = CARTESIAN_POINT ( 'NONE',  ( 12.14591786802309770, 12.06949235617756955, 64.37390960531435269 ) ) ;
#172166 = CARTESIAN_POINT ( 'NONE',  ( 10.72451020669871369, 18.67979575497193778, 87.08442372801901854 ) ) ;
#172167 = CARTESIAN_POINT ( 'NONE',  ( 0.05219959533910956823, 16.53943276465976808, 114.9989096053143669 ) ) ;
#172169 = CARTESIAN_POINT ( 'NONE',  ( 15.72974639402176855, 15.80617190586768217, 91.87609039468568994 ) ) ;
#172168 = CARTESIAN_POINT ( 'NONE',  ( 14.34966873604960469, 8.224510206698951720, 24.16557627198103120 ) ) ;
#172170 = CARTESIAN_POINT ( 'NONE',  ( -16.51473224551069308, -9.474510206698971260, 81.66557627198103830 ) ) ;
#172171 = CARTESIAN_POINT ( 'NONE',  ( -21.53943276465977519, -0.05219959533937600094, 43.75109039468568284 ) ) ;
#172172 = CARTESIAN_POINT ( 'NONE',  ( -16.46253265017160317, 9.564922557960807481, 80.83224293864769550 ) ) ;
#172173 = CARTESIAN_POINT ( 'NONE',  ( 16.53943276465976808, -0.05219959533910856209, 98.74890960531438111 ) ) ;
#172174 = CARTESIAN_POINT ( 'NONE',  ( 14.34966873604960469, 8.224510206698951720, 64.16557627198102409 ) ) ;
#172175 = CARTESIAN_POINT ( 'NONE',  ( -5.823673210054116645, -21.52544592524344225, 72.29057627198102409 ) ) ;
#172176 = CARTESIAN_POINT ( 'NONE',  ( 9.564922557960805705, 16.46253265017160317, 69.58224293864770971 ) ) ;
#172177 = CARTESIAN_POINT ( 'NONE',  ( 18.67979575497178502, 10.72451020669898547, 89.16557627198102409 ) ) ;
#172178 = CARTESIAN_POINT ( 'NONE',  ( -19.05341960407617563, 5.049401038297882671, 78.54275706135233293 ) ) ;
#172180 = CARTESIAN_POINT ( 'NONE',  ( -4.483927247898539470, -16.52544592524342804, 77.29057627198102409 ) ) ;
#172179 = CARTESIAN_POINT ( 'NONE',  ( -5.153800228976607833, 19.02544592524335343, 32.70942372801899012 ) ) ;
#172181 = CARTESIAN_POINT ( 'NONE',  ( 21.55341960407610458, 5.719274019375980345, 53.95724293864770260 ) ) ;
#172182 = CARTESIAN_POINT ( 'NONE',  ( 16.62475595723697808, -7.163666690055227271, 28.02713351810468723 ) ) ;
#172184 = CARTESIAN_POINT ( 'NONE',  ( 8.571926809382597767, 26.38167802310806209, 144.7750000027311899 ) ) ;
#172183 = CARTESIAN_POINT ( 'NONE',  ( -16.53943276465976808, -0.05219959533934237506, 103.7510903946857042 ) ) ;
#172185 = CARTESIAN_POINT ( 'NONE',  ( -19.05341960407617563, 5.049401038297882671, 108.5427570613523187 ) ) ;
#172186 = CARTESIAN_POINT ( 'NONE',  ( -0.05219959533910754901, -16.53943276465976808, 77.49890960531433848 ) ) ;
#172187 = CARTESIAN_POINT ( 'NONE',  ( 9.090072183657238014, -0.1985533113405552330, -61.89635373339111624 ) ) ;
#172188 = CARTESIAN_POINT ( 'NONE',  ( -9.474510206698964154, 16.51473224551069663, 75.41557627198103830 ) ) ;
#172189 = CARTESIAN_POINT ( 'NONE',  ( 13.89961937509977652, -13.97604488694527269, 38.12390960531436690 ) ) ;
#172190 = CARTESIAN_POINT ( 'NONE',  ( -16.52544592524342804, 4.483927247898546575, 51.04057627198103120 ) ) ;
#172191 = CARTESIAN_POINT ( 'NONE',  ( -13.97604488694527625, -13.89961937509977652, 101.8739096053143811 ) ) ;
#172193 = CARTESIAN_POINT ( 'NONE',  ( -5.153800228976328057, -19.02544592524343514, 67.29057627198102409 ) ) ;
#172192 = CARTESIAN_POINT ( 'NONE',  ( -19.05341960407617563, 5.049401038297882671, 88.54275706135230450 ) ) ;
#172194 = CARTESIAN_POINT ( 'NONE',  ( 14.34966873604972726, -8.224510206698740333, 25.83442372801901499 ) ) ;
#172195 = CARTESIAN_POINT ( 'NONE',  ( -13.89961937509977652, 13.97604488694528158, 85.62390960531433848 ) ) ;
#172196 = CARTESIAN_POINT ( 'NONE',  ( 21.53943276465977519, -0.05219959533907433946, 68.74890960531435269 ) ) ;
#172197 = CARTESIAN_POINT ( 'NONE',  ( 16.55341960407618274, -4.379528057220086978, 56.04275706135235424 ) ) ;
#172198 = CARTESIAN_POINT ( 'NONE',  ( -13.89961937509957401, -13.97604488694547697, 109.3760903946856615 ) ) ;
#172199 = CARTESIAN_POINT ( 'NONE',  ( -9.564922557960796823, -16.46253265017161027, 67.08224293864769550 ) ) ;
#172200 = CARTESIAN_POINT ( 'NONE',  ( -5.719274019375978568, 21.55341960407610458, 65.20724293864768129 ) ) ;
#172201 = CARTESIAN_POINT ( 'NONE',  ( 9.564922557961047289, -16.46253265017146816, 90.41775706135234714 ) ) ;
#172203 = CARTESIAN_POINT ( 'NONE',  ( 0.05219959533937995610, -21.53943276465977519, 45.00109039468568284 ) ) ;
#172202 = CARTESIAN_POINT ( 'NONE',  ( 12.06949235617739724, 12.14591786802326823, 111.8760903946856615 ) ) ;
#172204 = PLANE ( 'NONE',  #18510 ) ;
#172206 = CARTESIAN_POINT ( 'NONE',  ( 13.89961937509977652, -13.97604488694527269, 108.1239096053143669 ) ) ;
#172205 = CARTESIAN_POINT ( 'NONE',  ( 8.224510206698742110, 14.34966873604972548, 77.08442372801901854 ) ) ;
#172207 = CARTESIAN_POINT ( 'NONE',  ( 19.35633801406903842, -5.499999999999758415, 41.63373818172757979 ) ) ;
#172208 = CARTESIAN_POINT ( 'NONE',  ( 0.000000000000000000, -165.0000000000000000, 12.00000000000000355 ) ) ;
#172209 = CARTESIAN_POINT ( 'NONE',  ( 8.224510206698742110, 14.34966873604972548, 97.08442372801904696 ) ) ;
#172210 = CARTESIAN_POINT ( 'NONE',  ( -16.55341960407617563, 4.379528057220093196, 38.54275706135234714 ) ) ;
#172211 = CARTESIAN_POINT ( 'NONE',  ( -16.46253265017160317, 9.564922557960807481, 45.83224293864769550 ) ) ;
#172212 = CARTESIAN_POINT ( 'NONE',  ( -16.51473224551069308, -9.474510206698971260, 56.66557627198103120 ) ) ;
#172213 = CARTESIAN_POINT ( 'NONE',  ( 9.564922557960805705, 16.46253265017160317, 54.58224293864769550 ) ) ;
#172214 = CARTESIAN_POINT ( 'NONE',  ( -0.05219959533937732626, 21.53943276465977519, 47.50109039468568994 ) ) ;
#172215 = CARTESIAN_POINT ( 'NONE',  ( 4.379528057220092307, 16.55341960407617563, 52.29275706135236135 ) ) ;
#172216 = CARTESIAN_POINT ( 'NONE',  ( -14.34966873604960291, -8.224510206698953496, 31.66557627198102054 ) ) ;
#172217 = CARTESIAN_POINT ( 'NONE',  ( -13.97604488694527625, -13.89961937509977652, 46.87390960531435979 ) ) ;
#172218 = CARTESIAN_POINT ( 'NONE',  ( 13.89961937509977652, -13.97604488694527269, 38.12390960531436690 ) ) ;
#172219 = CARTESIAN_POINT ( 'NONE',  ( -12.14591786802326823, 12.06949235617739902, 33.12609039468569705 ) ) ;
#172220 = CARTESIAN_POINT ( 'NONE',  ( -9.474510206698720793, -16.51473224551083518, 84.58442372801900433 ) ) ;
#172221 = CARTESIAN_POINT ( 'NONE',  ( 8.314922557960818139, 14.29746914071049879, 84.58224293864769550 ) ) ;
#172222 = CARTESIAN_POINT ( 'NONE',  ( -9.564922557960796823, -16.46253265017161027, 57.08224293864769550 ) ) ;
#172224 = CARTESIAN_POINT ( 'NONE',  ( -6.020228577223754586E-15, 39.95556452105416412, -8.500000000000001776 ) ) ;
#172223 = CARTESIAN_POINT ( 'NONE',  ( -0.05219959533936034679, 19.03943276465977164, 87.50109039468567573 ) ) ;
#172225 = CARTESIAN_POINT ( 'NONE',  ( 21.55341960407619695, -5.719274019375665929, 71.04275706135234714 ) ) ;
#172226 = CARTESIAN_POINT ( 'NONE',  ( -12.06949235617739369, -12.14591786802326823, 54.37609039468568994 ) ) ;
#172227 = CARTESIAN_POINT ( 'NONE',  ( 17.48847506799968698, 5.747544572773807481, 36.67302562156721990 ) ) ;
#172228 = CARTESIAN_POINT ( 'NONE',  ( -18.62759615963270932, 10.81492255796079327, 45.83224293864769550 ) ) ;
#172229 = CARTESIAN_POINT ( 'NONE',  ( -4.483927247898782831, 16.52544592524335698, 37.70942372801900433 ) ) ;
#172230 = CARTESIAN_POINT ( 'NONE',  ( -9.564922557960796823, -16.46253265017161027, 22.08224293864768839 ) ) ;
#172231 = CARTESIAN_POINT ( 'NONE',  ( -16.46253265017146816, -9.564922557961047289, 29.16775706135232937 ) ) ;
#172232 = CARTESIAN_POINT ( 'NONE',  ( 37.99999999999996447, -12.34694845685046793, -7.100000000000002309 ) ) ;
#172233 = CARTESIAN_POINT ( 'NONE',  ( 9.564922557960805705, 16.46253265017160317, 54.58224293864769550 ) ) ;
#172234 = CARTESIAN_POINT ( 'NONE',  ( 4.999999999999999112, 5.000000000000000888, -18.00000000000000000 ) ) ;
#172235 = CARTESIAN_POINT ( 'NONE',  ( 19.02544592524343514, -5.153800228976328945, 73.54057627198103830 ) ) ;
#172236 = CARTESIAN_POINT ( 'NONE',  ( -19.49149378614659511, 5.499999999999674039, 99.43757513605360998 ) ) ;
#172237 = CARTESIAN_POINT ( 'NONE',  ( 21.52544592524334988, 5.823673210054432836, 111.4594237280190328 ) ) ;
#172238 = CARTESIAN_POINT ( 'NONE',  ( 4.379528057220339221, -16.55341960407611168, 32.70724293864770260 ) ) ;
#172239 = CARTESIAN_POINT ( 'NONE',  ( -13.97604488694527625, -13.89961937509977652, 46.87390960531435979 ) ) ;
#172240 = CARTESIAN_POINT ( 'NONE',  ( 9.474510206698971260, -16.51473224551069308, 107.9155762719810383 ) ) ;
#172241 = CARTESIAN_POINT ( 'NONE',  ( 18.62759615963255655, 10.81492255796105972, 66.66775706135234714 ) ) ;
#172242 = CARTESIAN_POINT ( 'NONE',  ( -9.474510206698964154, 16.51473224551069663, 45.41557627198103120 ) ) ;
#172243 = CARTESIAN_POINT ( 'NONE',  ( -21.53943276465977519, -0.05219959533937600094, 63.75109039468568284 ) ) ;
#172244 = CARTESIAN_POINT ( 'NONE',  ( 16.51473224551069308, 9.474510206698969483, 114.1655762719810241 ) ) ;
#172245 = CARTESIAN_POINT ( 'NONE',  ( -13.89961937509977652, 13.97604488694528158, 30.62390960531435269 ) ) ;
#172246 = CARTESIAN_POINT ( 'NONE',  ( 10.72451020669871369, 18.67979575497193778, 22.08442372801901143 ) ) ;
#172247 = CARTESIAN_POINT ( 'NONE',  ( -19.05341960407617563, 5.049401038297882671, 43.54275706135232582 ) ) ;
#172248 = CARTESIAN_POINT ( 'NONE',  ( -19.05341960407611168, -5.049401038298163336, 26.45724293864769550 ) ) ;
#172249 = CARTESIAN_POINT ( 'NONE',  ( -16.46253265017160317, 9.564922557960807481, 60.83224293864769550 ) ) ;
#172250 = CARTESIAN_POINT ( 'NONE',  ( -5.049401038297874678, -19.05341960407617918, 109.7927570613523187 ) ) ;
#172251 = CARTESIAN_POINT ( 'NONE',  ( 14.34966873604960469, 8.224510206698951720, 69.16557627198102409 ) ) ;
#172252 = CARTESIAN_POINT ( 'NONE',  ( -15.80617190586745835, -15.72974639402198527, 41.87390960531435979 ) ) ;
#172253 = CARTESIAN_POINT ( 'NONE',  ( 13.97604488694548053, -13.89961937509957401, 105.6260903946856757 ) ) ;
#172254 = CARTESIAN_POINT ( 'NONE',  ( -21.53943276465977519, 0.05219959533907696930, 101.2489096053143669 ) ) ;
#172255 = CARTESIAN_POINT ( 'NONE',  ( -15.80617190586768217, 15.72974639402176855, 53.12609039468568284 ) ) ;
#172256 = CARTESIAN_POINT ( 'NONE',  ( -0.05219959533934338120, 16.53943276465976808, 52.50109039468567573 ) ) ;
#172257 = CARTESIAN_POINT ( 'NONE',  ( -12.14591786802326823, 12.06949235617739902, 58.12609039468568994 ) ) ;
#172258 = CARTESIAN_POINT ( 'NONE',  ( -0.05219959533907301413, -21.53943276465977519, 62.49890960531436690 ) ) ;
#172259 = CARTESIAN_POINT ( 'NONE',  ( -13.97604488694527625, -13.89961937509977652, 41.87390960531435979 ) ) ;
#172260 = CARTESIAN_POINT ( 'NONE',  ( -0.05219959533934338120, 16.53943276465976808, 72.50109039468568994 ) ) ;
#172261 = CARTESIAN_POINT ( 'NONE',  ( -10.81492255796078084, -18.62759615963271287, 97.08224293864770971 ) ) ;
#172262 = CARTESIAN_POINT ( 'NONE',  ( -8.314922557960811034, -14.29746914071050412, 52.08224293864768839 ) ) ;
#172263 = CARTESIAN_POINT ( 'NONE',  ( 16.46253265017160672, -9.564922557960803928, 78.33224293864769550 ) ) ;
#172264 = CARTESIAN_POINT ( 'NONE',  ( -16.55341960407617563, 4.379528057220093196, 73.54275706135234714 ) ) ;
#172265 = CARTESIAN_POINT ( 'NONE',  ( 19.05341960407617918, -5.049401038297876454, 111.0427570613523329 ) ) ;
#172266 = CARTESIAN_POINT ( 'NONE',  ( -5.719274019375665041, -21.55341960407619695, 19.79275706135235069 ) ) ;
#172267 = CARTESIAN_POINT ( 'NONE',  ( 12.14591786802309770, 12.06949235617756955, 49.37390960531436690 ) ) ;
#172268 = ORIENTED_EDGE ( 'NONE', *, *, #17592, .F. ) ;
#172269 = CARTESIAN_POINT ( 'NONE',  ( -16.88567814943163370, 6.947325034625699836, 68.70998877347419409 ) ) ;
#172270 = CARTESIAN_POINT ( 'NONE',  ( -10.72451020669898014, 18.67979575497178502, 90.41557627198103830 ) ) ;
#172271 = ORIENTED_EDGE ( 'NONE', *, *, #162246, .F. ) ;
#172272 = CARTESIAN_POINT ( 'NONE',  ( -16.55341960407611168, -4.379528057220339221, 21.45724293864769550 ) ) ;
#172273 = ORIENTED_EDGE ( 'NONE', *, *, #88289, .T. ) ;
#172274 = CARTESIAN_POINT ( 'NONE',  ( -17.48853670773242541, -5.747243402303178428, 56.33328700250010002 ) ) ;
#172275 = CARTESIAN_POINT ( 'NONE',  ( 15.72974639402199770, -15.80617190586745480, 98.12390960531436690 ) ) ;
#172276 = CARTESIAN_POINT ( 'NONE',  ( -13.89961937509977652, 13.97604488694528158, 115.6239096053143669 ) ) ;
#172277 = CARTESIAN_POINT ( 'NONE',  ( 0.05219959533907565091, 21.53943276465977519, 114.9989096053143669 ) ) ;
#172278 = CARTESIAN_POINT ( 'NONE',  ( 4.379528057220339221, -16.55341960407611168, 47.70724293864770260 ) ) ;
#172279 = CARTESIAN_POINT ( 'NONE',  ( -8.224510206698735004, -14.34966873604973081, 54.58442372801901143 ) ) ;
#172280 = CARTESIAN_POINT ( 'NONE',  ( -13.89961937509977652, 13.97604488694528158, 55.62390960531434558 ) ) ;
#172281 = CARTESIAN_POINT ( 'NONE',  ( 9.564922557961047289, -16.46253265017146816, 50.41775706135233293 ) ) ;
#172282 = CARTESIAN_POINT ( 'NONE',  ( -13.89961937509977652, 13.97604488694528158, 85.62390960531433848 ) ) ;
#172283 = CARTESIAN_POINT ( 'NONE',  ( -21.55341960407610458, -5.719274019375992779, 41.45724293864769550 ) ) ;
#172284 = CARTESIAN_POINT ( 'NONE',  ( 13.97604488694527802, 13.89961937509977830, 64.37390960531436690 ) ) ;
#172285 = CARTESIAN_POINT ( 'NONE',  ( -16.52544592524335698, -4.483927247898792601, 23.95942372801901143 ) ) ;
#172286 = CARTESIAN_POINT ( 'NONE',  ( 16.51473224551083163, -9.474510206698727899, 70.83442372801900433 ) ) ;
#172287 = CARTESIAN_POINT ( 'NONE',  ( -10.72451020669898014, 18.67979575497178502, 100.4155762719810241 ) ) ;
#172288 = EDGE_CURVE ( 'NONE', #38560, #67444, #141273, .T. ) ;
#172289 = CARTESIAN_POINT ( 'NONE',  ( -12.14591786802309592, -12.06949235617757132, 31.87390960531435979 ) ) ;
#172290 = CARTESIAN_POINT ( 'NONE',  ( 13.97604488694527802, 13.89961937509977652, 79.37390960531435269 ) ) ;
#172291 = CARTESIAN_POINT ( 'NONE',  ( -21.53943276465977519, 0.05219959533907696930, 61.24890960531435979 ) ) ;
#172293 = CARTESIAN_POINT ( 'NONE',  ( 16.53943276465976808, 0.05219959533934440121, 21.25109039468567218 ) ) ;
#172292 = CARTESIAN_POINT ( 'NONE',  ( 5.719274019375991003, -21.55341960407610458, 97.70724293864772392 ) ) ;
#172294 = CARTESIAN_POINT ( 'NONE',  ( 5.719274019375991003, -21.55341960407610458, 22.70724293864769194 ) ) ;
#172295 = CARTESIAN_POINT ( 'NONE',  ( 5.823673210054444382, -21.52544592524334988, 95.20942372801903275 ) ) ;
#172296 = CARTESIAN_POINT ( 'NONE',  ( 13.89961937509977652, -13.97604488694527269, 93.12390960531436690 ) ) ;
#172297 = CARTESIAN_POINT ( 'NONE',  ( -16.46253265017160317, 9.564922557960807481, 30.83224293864769550 ) ) ;
#172298 = CARTESIAN_POINT ( 'NONE',  ( 9.474510206698971260, -16.51473224551069308, 77.91557627198103830 ) ) ;
#172299 = CARTESIAN_POINT ( 'NONE',  ( -14.34966873604960291, -8.224510206698953496, 106.6655762719810383 ) ) ;
#172300 = CARTESIAN_POINT ( 'NONE',  ( 13.89961937509977652, -13.97604488694527269, 68.12390960531436690 ) ) ;
#172301 = CARTESIAN_POINT ( 'NONE',  ( -12.14591786802326823, 12.06949235617739902, 23.12609039468567573 ) ) ;
#172302 = CARTESIAN_POINT ( 'NONE',  ( 17.50000000000015987, 3.417042746626929528, 32.32619603767522420 ) ) ;
#172303 = CARTESIAN_POINT ( 'NONE',  ( -9.564922557960796823, -16.46253265017161027, 67.08224293864769550 ) ) ;
#172305 = CARTESIAN_POINT ( 'NONE',  ( 9.564922557960805705, 16.46253265017160317, 114.5822429386476955 ) ) ;
#172304 = CARTESIAN_POINT ( 'NONE',  ( 18.62759615963255655, 10.81492255796105972, 96.66775706135234714 ) ) ;
#172306 = CARTESIAN_POINT ( 'NONE',  ( 4.483927247898790824, -16.52544592524335698, 90.20942372801903275 ) ) ;
#172307 = CARTESIAN_POINT ( 'NONE',  ( 8.388830574159379737E-16, 13.70000000000001528, -62.58071313852362039 ) ) ;
#172308 = CARTESIAN_POINT ( 'NONE',  ( 13.97604488694548053, -13.89961937509957401, 65.62609039468567573 ) ) ;
#172309 = CARTESIAN_POINT ( 'NONE',  ( 19.02544592524334988, 5.153800228976608722, 21.45942372801899012 ) ) ;
#172310 = CARTESIAN_POINT ( 'NONE',  ( 3.948644494436277075, 4.896406352259362826, -64.50244604205114740 ) ) ;
#172311 = CARTESIAN_POINT ( 'NONE',  ( 5.153800228976335163, 19.02544592524342804, 24.79057627198102765 ) ) ;
#172312 = CARTESIAN_POINT ( 'NONE',  ( -14.34966873604960291, -8.224510206698953496, 31.66557627198102054 ) ) ;
#172313 = CARTESIAN_POINT ( 'NONE',  ( -35.68964480816960361, -0.9792624367684957809, 37.54765762180190336 ) ) ;
#172314 = CARTESIAN_POINT ( 'NONE',  ( 16.55341960407618274, -4.379528057220086978, 106.0427570613523471 ) ) ;
#172315 = DIRECTION ( 'NONE',  ( 0.000000000000000000, 1.000000000000000000, 0.000000000000000000 ) ) ;
#172316 = CARTESIAN_POINT ( 'NONE',  ( -14.29746914071037622, -8.314922557961029526, 84.16775706135234714 ) ) ;
#172317 = CARTESIAN_POINT ( 'NONE',  ( 9.474510206698971260, -16.51473224551069308, 32.91557627198102409 ) ) ;
#172318 = CARTESIAN_POINT ( 'NONE',  ( -15.72974639402176322, -15.80617190586768395, 94.37609039468568994 ) ) ;
#172319 = CARTESIAN_POINT ( 'NONE',  ( 5.049401038297881783, 19.05341960407617563, 107.2927570613523187 ) ) ;
#172320 = CARTESIAN_POINT ( 'NONE',  ( 18.62759615963255655, 10.81492255796105972, 76.66775706135234714 ) ) ;
#172321 = CARTESIAN_POINT ( 'NONE',  ( 19.05341960407617918, -5.049401038297876454, 51.04275706135231871 ) ) ;
#172322 = CARTESIAN_POINT ( 'NONE',  ( 9.564922557960805705, 16.46253265017160317, 84.58224293864769550 ) ) ;
#172323 = CARTESIAN_POINT ( 'NONE',  ( -13.97604488694527625, -13.89961937509977652, 76.87390960531433848 ) ) ;
#172324 = CARTESIAN_POINT ( 'NONE',  ( -37.66961640367473052, -4.999999999999976019, -25.00000000000000000 ) ) ;
#172325 = CARTESIAN_POINT ( 'NONE',  ( 14.34966873604960469, 8.224510206698951720, 64.16557627198102409 ) ) ;
#172326 = CARTESIAN_POINT ( 'NONE',  ( 18.67979575497178502, 10.72451020669898547, 64.16557627198102409 ) ) ;
#172327 = CARTESIAN_POINT ( 'NONE',  ( 19.02544592524343514, -5.153800228976328945, 48.54057627198103120 ) ) ;
#172329 = CARTESIAN_POINT ( 'NONE',  ( -14.29746914071037622, -8.314922557961029526, 79.16775706135234714 ) ) ;
#172328 = CARTESIAN_POINT ( 'NONE',  ( -10.72451020669898014, 18.67979575497178502, 90.41557627198103830 ) ) ;
#172330 = ORIENTED_EDGE ( 'NONE', *, *, #76057, .T. ) ;
#172331 = CARTESIAN_POINT ( 'NONE',  ( 19.02544592524343514, -5.153800228976328945, 53.54057627198102409 ) ) ;
#172333 = CARTESIAN_POINT ( 'NONE',  ( 3.556970738554033499E-15, -38.81732327939057825, -6.124999997268812280 ) ) ;
#172332 = CARTESIAN_POINT ( 'NONE',  ( 12.06949235617757843, -12.14591786802309237, 83.12390960531436690 ) ) ;
#172334 = CARTESIAN_POINT ( 'NONE',  ( -5.153800228976328057, -19.02544592524343514, 57.29057627198103120 ) ) ;
#172335 = CARTESIAN_POINT ( 'NONE',  ( 8.224510206698953496, -14.34966873604960469, 112.9155762719810383 ) ) ;
#172336 = CARTESIAN_POINT ( 'NONE',  ( -19.02544592524334988, -5.153800228976617603, 63.95942372801899012 ) ) ;
#172337 = CARTESIAN_POINT ( 'NONE',  ( 12.06949235617757843, -12.14591786802309237, 68.12390960531436690 ) ) ;
#172338 = CARTESIAN_POINT ( 'NONE',  ( 10.81492255796106328, -18.62759615963255655, 40.41775706135234714 ) ) ;
#172340 = CARTESIAN_POINT ( 'NONE',  ( 0.05219959533907565091, 21.53943276465977519, 104.9989096053143669 ) ) ;
#172339 = CARTESIAN_POINT ( 'NONE',  ( 0.05219959533909260263, 19.03943276465977164, 34.99890960531435979 ) ) ;
#172341 = CARTESIAN_POINT ( 'NONE',  ( -9.474510206698964154, 16.51473224551069663, 115.4155762719810241 ) ) ;
#172342 = CARTESIAN_POINT ( 'NONE',  ( -8.314922557960811034, -14.29746914071050412, 82.08224293864768129 ) ) ;
#172343 = CARTESIAN_POINT ( 'NONE',  ( 24.05628303387030797, -31.51879896406492065, -19.31700871831125710 ) ) ;
#172344 = CARTESIAN_POINT ( 'NONE',  ( 19.05341960407611168, 5.049401038298154454, 43.95724293864769550 ) ) ;
#172345 = CARTESIAN_POINT ( 'NONE',  ( 36.91746824999999177, 2.880721459617395097E-14, -1.624999997268813390 ) ) ;
#172346 = CARTESIAN_POINT ( 'NONE',  ( -5.153800228976607833, 19.02544592524334988, 82.70942372801897591 ) ) ;
#172347 = CARTESIAN_POINT ( 'NONE',  ( -15.80617190586768217, 15.72974639402176855, 38.12609039468567573 ) ) ;
#172348 = CARTESIAN_POINT ( 'NONE',  ( -0.05219959533909027116, -19.03943276465977164, 72.49890960531435269 ) ) ;
#172349 = CARTESIAN_POINT ( 'NONE',  ( 5.049401038297881783, 19.05341960407617563, 62.29275706135234003 ) ) ;
#172350 = CARTESIAN_POINT ( 'NONE',  ( -19.02544592524342804, 5.153800228976336051, 46.04057627198101699 ) ) ;
#172351 = CARTESIAN_POINT ( 'NONE',  ( 12.14591786802309770, 12.06949235617756955, 59.37390960531436690 ) ) ;
#172352 = CARTESIAN_POINT ( 'NONE',  ( -8.314922557960811034, -14.29746914071050412, 62.08224293864769550 ) ) ;
#172353 = CARTESIAN_POINT ( 'NONE',  ( 0.05219959533909260263, 19.03943276465977164, 69.99890960531435269 ) ) ;
#172354 = CARTESIAN_POINT ( 'NONE',  ( -5.823673210054116645, -21.52544592524344225, 102.2905762719810383 ) ) ;
#172355 = CARTESIAN_POINT ( 'NONE',  ( -19.03943276465977164, 0.05219959533909376836, 76.24890960531435269 ) ) ;
#172356 = CARTESIAN_POINT ( 'NONE',  ( 5.719274019375673035, 21.55341960407619339, 107.2927570613523471 ) ) ;
#172359 = CARTESIAN_POINT ( 'NONE',  ( -4.483927247898539470, -16.52544592524342804, 97.29057627198105251 ) ) ;
#172358 = CARTESIAN_POINT ( 'NONE',  ( 16.53943276465976808, 0.05219959533934440121, 111.2510903946856899 ) ) ;
#172357 = CARTESIAN_POINT ( 'NONE',  ( 5.049401038298161559, -19.05341960407611168, 42.70724293864767418 ) ) ;
#172360 = CARTESIAN_POINT ( 'NONE',  ( 5.049401038297881783, 19.05341960407617563, 112.2927570613523471 ) ) ;
#172361 = ORIENTED_EDGE ( 'NONE', *, *, #45144, .T. ) ;
#172362 = CARTESIAN_POINT ( 'NONE',  ( -21.55341960407619339, 5.719274019375674811, 33.54275706135234714 ) ) ;
#172363 = CARTESIAN_POINT ( 'NONE',  ( -5.049401038297874678, -19.05341960407617918, 49.79275706135231871 ) ) ;
#172364 = CARTESIAN_POINT ( 'NONE',  ( -8.314922557961024197, 14.29746914071037800, 112.9177570613523329 ) ) ;
#172365 = CARTESIAN_POINT ( 'NONE',  ( 15.80617190586746368, 15.72974639402197994, 79.37390960531436690 ) ) ;
#172366 = CARTESIAN_POINT ( 'NONE',  ( 9.564922557960805705, 16.46253265017160317, 104.5822429386476955 ) ) ;
#172367 = CARTESIAN_POINT ( 'NONE',  ( -14.29746914071049879, 8.314922557960819915, 55.83224293864770260 ) ) ;
#172368 = CARTESIAN_POINT ( 'NONE',  ( -19.02544592524342804, 5.153800228976336051, 31.04057627198102409 ) ) ;
#172369 = CARTESIAN_POINT ( 'NONE',  ( -5.153800228976328057, -19.02544592524343514, 32.29057627198102409 ) ) ;
#172370 = CARTESIAN_POINT ( 'NONE',  ( 19.03943276465977164, 0.05219959533936151252, 26.25109039468566507 ) ) ;
#172371 = CARTESIAN_POINT ( 'NONE',  ( -14.29746914071037622, -8.314922557961029526, 89.16775706135236135 ) ) ;
#172372 = CARTESIAN_POINT ( 'NONE',  ( 10.72451020669871369, 18.67979575497193778, 37.08442372801901143 ) ) ;
#172373 = CARTESIAN_POINT ( 'NONE',  ( -0.05219959533934338120, 16.53943276465976808, 37.50109039468568284 ) ) ;
#172374 = CARTESIAN_POINT ( 'NONE',  ( 9.564922557960805705, 16.46253265017160317, 114.5822429386476955 ) ) ;
#172376 = CARTESIAN_POINT ( 'NONE',  ( -15.72974639402176322, -15.80617190586768395, 94.37609039468568994 ) ) ;
#172375 = CARTESIAN_POINT ( 'NONE',  ( -9.474510206698964154, 16.51473224551069663, 55.41557627198103120 ) ) ;
#172377 = CARTESIAN_POINT ( 'NONE',  ( -19.03943276465977164, 0.05219959533909376836, 76.24890960531435269 ) ) ;
#172378 = CARTESIAN_POINT ( 'NONE',  ( -8.224510206698735004, -14.34966873604973081, 59.58442372801901854 ) ) ;
#172379 = CARTESIAN_POINT ( 'NONE',  ( -8.314922557960811034, -14.29746914071050412, 102.0822429386476955 ) ) ;
#172380 = CARTESIAN_POINT ( 'NONE',  ( -12.06949235617756955, 12.14591786802309770, 25.62390960531435624 ) ) ;
#172381 = LINE ( 'NONE', #17716, #186378 ) ;
#172384 = CARTESIAN_POINT ( 'NONE',  ( 19.05341960407611168, 5.049401038298154454, 78.95724293864769550 ) ) ;
#172383 = CARTESIAN_POINT ( 'NONE',  ( -19.02544592524342804, 5.153800228976336051, 86.04057627198103830 ) ) ;
#172382 = CARTESIAN_POINT ( 'NONE',  ( 0.05219959533937995610, -21.53943276465977519, 70.00109039468568994 ) ) ;
#172386 = ADVANCED_FACE ( 'NONE', ( #71867 ), #60897, .T. ) ;
#172385 = CARTESIAN_POINT ( 'NONE',  ( -19.03943276465977164, 0.05219959533909376836, 106.2489096053143669 ) ) ;
#172387 = CARTESIAN_POINT ( 'NONE',  ( -14.29746914071049879, 8.314922557960819915, 55.83224293864770260 ) ) ;
#172388 = CARTESIAN_POINT ( 'NONE',  ( -14.29746914071049879, 8.314922557960819915, 25.83224293864769194 ) ) ;
#172389 = AXIS2_PLACEMENT_3D ( 'NONE', #178436, #42910, #180450 ) ;
#172390 = VERTEX_POINT ( 'NONE', #84590 ) ;
#172391 = CARTESIAN_POINT ( 'NONE',  ( 4.379528057220339221, -16.55341960407611168, 42.70724293864770260 ) ) ;
#172393 = CARTESIAN_POINT ( 'NONE',  ( -17.18269478283327345, -17.18269478283298568, -54.21489346206828230 ) ) ;
#172392 = CARTESIAN_POINT ( 'NONE',  ( 16.55341960407618274, -4.379528057220086978, 36.04275706135234714 ) ) ;
#172394 = CARTESIAN_POINT ( 'NONE',  ( 5.049401038297881783, 19.05341960407617563, 42.29275706135234003 ) ) ;
#172395 = CARTESIAN_POINT ( 'NONE',  ( 16.46253265017160672, -9.564922557960803928, 78.33224293864769550 ) ) ;
#172396 = CARTESIAN_POINT ( 'NONE',  ( -13.89961937509957401, -13.97604488694547875, 49.37609039468567573 ) ) ;
#172397 = CARTESIAN_POINT ( 'NONE',  ( -11.40812507854755609, 35.11059874428196537, -3.024999997268813523 ) ) ;
#172398 = CARTESIAN_POINT ( 'NONE',  ( 30.74264578624799782, 22.33583958711400541, -2.549999994537626602 ) ) ;
#172400 = CARTESIAN_POINT ( 'NONE',  ( 12.06949235617739724, 12.14591786802326823, 86.87609039468568994 ) ) ;
#172399 = CARTESIAN_POINT ( 'NONE',  ( -9.564922557961040184, 16.46253265017147172, 87.91775706135233293 ) ) ;
#172401 = CARTESIAN_POINT ( 'NONE',  ( 19.02544592524343514, -5.153800228976328945, 28.54057627198102409 ) ) ;
#172402 = CARTESIAN_POINT ( 'NONE',  ( -16.46253265017160317, 9.564922557960807481, 100.8322429386477097 ) ) ;
#172403 = CARTESIAN_POINT ( 'NONE',  ( -18.62759615963255300, -10.81492255796106328, 24.16775706135235424 ) ) ;
#172404 = CARTESIAN_POINT ( 'NONE',  ( 16.46253265017146816, 9.564922557961045513, 91.66775706135234714 ) ) ;
#172406 = CARTESIAN_POINT ( 'NONE',  ( 9.564922557960805705, 16.46253265017160317, 54.58224293864769550 ) ) ;
#172405 = CARTESIAN_POINT ( 'NONE',  ( 17.50000000000000000, 5.622605283950890431, 88.81207310596111881 ) ) ;
#172407 = CARTESIAN_POINT ( 'NONE',  ( -13.97604488694527625, -13.89961937509977652, 101.8739096053143811 ) ) ;
#172409 = CARTESIAN_POINT ( 'NONE',  ( -0.05219959533909027116, -19.03943276465977164, 52.49890960531436690 ) ) ;
#172408 = CARTESIAN_POINT ( 'NONE',  ( 4.379528057220339221, -16.55341960407611168, 57.70724293864770260 ) ) ;
#172410 = CARTESIAN_POINT ( 'NONE',  ( 13.97604488694527802, 13.89961937509977652, 64.37390960531436690 ) ) ;
#172411 = CARTESIAN_POINT ( 'NONE',  ( 16.46253265017146816, 9.564922557961045513, 66.66775706135233293 ) ) ;
#172412 = VERTEX_POINT ( 'NONE', #96768 ) ;
#172413 = CARTESIAN_POINT ( 'NONE',  ( -16.46253265017146816, -9.564922557961047289, 34.16775706135233293 ) ) ;
#172414 = CARTESIAN_POINT ( 'NONE',  ( -19.02544592524342804, 5.153800228976336051, 71.04057627198099567 ) ) ;
#172415 = CARTESIAN_POINT ( 'NONE',  ( -18.67979575497178146, -10.72451020669898902, 81.66557627198103830 ) ) ;
#172417 = CARTESIAN_POINT ( 'NONE',  ( 13.97604488694548053, -13.89961937509957401, 30.62609039468566863 ) ) ;
#172416 = CARTESIAN_POINT ( 'NONE',  ( 0.05219959533910956823, 16.53943276465976808, 69.99890960531435269 ) ) ;
#172418 = CARTESIAN_POINT ( 'NONE',  ( -0.3964520562363653688, -6.139823915386825703, -64.52448473163052256 ) ) ;
#172419 = CARTESIAN_POINT ( 'NONE',  ( 15.72974639402199770, -15.80617190586745480, 53.12390960531436690 ) ) ;
#172420 = CARTESIAN_POINT ( 'NONE',  ( -15.80617190586745835, -15.72974639402198527, 31.87390960531435979 ) ) ;
#172421 = CARTESIAN_POINT ( 'NONE',  ( 19.02544592524343514, -5.153800228976328945, 68.54057627198103830 ) ) ;
#172422 = CARTESIAN_POINT ( 'NONE',  ( 5.049401038298161559, -19.05341960407611168, 37.70724293864768839 ) ) ;
#172423 = CARTESIAN_POINT ( 'NONE',  ( -8.314922557960811034, -14.29746914071050412, 107.0822429386476955 ) ) ;
#172424 = CARTESIAN_POINT ( 'NONE',  ( 18.67979575497178502, 10.72451020669898547, 114.1655762719810383 ) ) ;
#172425 = CARTESIAN_POINT ( 'NONE',  ( -19.03943276465977164, 0.05219959533909376836, 116.2489096053143669 ) ) ;
#172426 = CARTESIAN_POINT ( 'NONE',  ( -10.81492255796105439, 18.62759615963255655, 32.91775706135234714 ) ) ;
#172427 = CARTESIAN_POINT ( 'NONE',  ( -5.049401038298153566, 19.05341960407611168, 25.20724293864768484 ) ) ;
#172428 = CARTESIAN_POINT ( 'NONE',  ( -10.81492255796078084, -18.62759615963271287, 107.0822429386476955 ) ) ;
#172429 = CARTESIAN_POINT ( 'NONE',  ( -16.51473224551082808, 9.474510206698731452, 43.33442372801900433 ) ) ;
#172430 = CARTESIAN_POINT ( 'NONE',  ( -5.000000000000000888, -131.0000000000000000, -13.99999999999999822 ) ) ;
#172431 = CARTESIAN_POINT ( 'NONE',  ( -19.05341960407611168, -5.049401038298163336, 26.45724293864769550 ) ) ;
#172432 = CARTESIAN_POINT ( 'NONE',  ( 12.06170956654727355, -11.49862171186262039, -61.36395269087611126 ) ) ;
#172433 = CARTESIAN_POINT ( 'NONE',  ( -14.34966873604972548, 8.224510206698743886, 43.33442372801901143 ) ) ;
#172434 = CARTESIAN_POINT ( 'NONE',  ( -16.52544592524342804, 4.483927247898546575, 116.0405762719810383 ) ) ;
#172435 = B_SPLINE_CURVE_WITH_KNOTS ( 'NONE', 3,
 ( #190107, #95098, #50601, #145582, #52575, #98054, #83899, #33439, #66750, #128411, #172954, #189129, #188128, #111263 ),
 .UNSPECIFIED., .F., .F.,
 ( 4, 2, 2, 2, 2, 2, 4 ),
 ( 0.000000000000000000, 0.05072380597786523698, 0.1014476119557304740, 0.2028952239114615863, 0.4057904478229238943, 0.6086856717343860357, 0.8115808956458483436 ),
 .UNSPECIFIED. ) ;
#172436 = CARTESIAN_POINT ( 'NONE',  ( 33.80700117934222249, -2.275881256356157234, 100.0103016164005254 ) ) ;
#172437 = CARTESIAN_POINT ( 'NONE',  ( 9.564922557960805705, 16.46253265017160317, 69.58224293864770971 ) ) ;
#172438 = CARTESIAN_POINT ( 'NONE',  ( 4.483927247898545687, 16.52544592524342804, 104.7905762719810241 ) ) ;
#172439 = CARTESIAN_POINT ( 'NONE',  ( 21.55341960407610458, 5.719274019375980345, 43.95724293864769550 ) ) ;
#172440 = CARTESIAN_POINT ( 'NONE',  ( -12.06949235617756955, 12.14591786802309770, 75.62390960531439532 ) ) ;
#172441 = CARTESIAN_POINT ( 'NONE',  ( -16.53943276465976808, -0.05219959533934237506, 33.75109039468568284 ) ) ;
#172442 = CARTESIAN_POINT ( 'NONE',  ( -5.719274019375665041, -21.55341960407619695, 89.79275706135236135 ) ) ;
#172443 = CARTESIAN_POINT ( 'NONE',  ( 19.03943276465977164, -0.05219959533909143690, 28.74890960531435624 ) ) ;
#172444 = CARTESIAN_POINT ( 'NONE',  ( -16.53943276465976808, -0.05219959533934237506, 113.7510903946856757 ) ) ;
#172445 = CARTESIAN_POINT ( 'NONE',  ( -12.06949235617756955, 12.14591786802309770, 45.62390960531436690 ) ) ;
#172446 = CARTESIAN_POINT ( 'NONE',  ( 5.049401038298161559, -19.05341960407611168, 47.70724293864770260 ) ) ;
#172447 = CARTESIAN_POINT ( 'NONE',  ( -10.81492255796105439, 18.62759615963255655, 102.9177570613523756 ) ) ;
#172448 = CARTESIAN_POINT ( 'NONE',  ( 5.719274019375991003, -21.55341960407610458, 107.7072429386476955 ) ) ;
#172449 = AXIS2_PLACEMENT_3D ( 'NONE', #119639, #150979, #135805 ) ;
#172450 = CARTESIAN_POINT ( 'NONE',  ( -21.55341960407619339, 5.719274019375674811, 68.54275706135234714 ) ) ;
#172451 = CARTESIAN_POINT ( 'NONE',  ( 14.29746914071037800, 8.314922557961029526, 41.66775706135235424 ) ) ;
#172453 = CARTESIAN_POINT ( 'NONE',  ( 15.72974639402176855, 15.80617190586768217, 81.87609039468568994 ) ) ;
#172452 = CARTESIAN_POINT ( 'NONE',  ( -4.483927247898539470, -16.52544592524342804, 77.29057627198102409 ) ) ;
#172454 = CARTESIAN_POINT ( 'NONE',  ( 4.379528057220092307, 16.55341960407617563, 112.2927570613523471 ) ) ;
#172455 = CARTESIAN_POINT ( 'NONE',  ( 28.79475375365586132, 2.781246896534039337E-14, 141.2656553485623760 ) ) ;
#172456 = CARTESIAN_POINT ( 'NONE',  ( -19.39056639909674118, -5.500000000000057732, 65.78948781074339536 ) ) ;
#172457 = CARTESIAN_POINT ( 'NONE',  ( 14.29746914071049879, -8.314922557960816363, 38.33224293864768839 ) ) ;
#172458 = CARTESIAN_POINT ( 'NONE',  ( -4.379528057220086978, -16.55341960407618274, 74.79275706135234714 ) ) ;
#172459 = CARTESIAN_POINT ( 'NONE',  ( -19.05341960407611168, -5.049401038298163336, 86.45724293864769550 ) ) ;
#172460 = CARTESIAN_POINT ( 'NONE',  ( 13.89961937509977652, -13.97604488694527269, 98.12390960531433848 ) ) ;
#172461 = CARTESIAN_POINT ( 'NONE',  ( 21.53943276465977519, 0.05219959533937863772, 101.2510903946856757 ) ) ;
#172462 = CARTESIAN_POINT ( 'NONE',  ( 0.05219959533934541429, -16.53943276465976808, 105.0010903946856757 ) ) ;
#172463 = CARTESIAN_POINT ( 'NONE',  ( 4.379528057220339221, -16.55341960407611168, 67.70724293864769550 ) ) ;
#172464 = CARTESIAN_POINT ( 'NONE',  ( 16.46253265017160672, -9.564922557960803928, 88.33224293864769550 ) ) ;
#172465 = VERTEX_POINT ( 'NONE', #21944 ) ;
#172466 = CARTESIAN_POINT ( 'NONE',  ( 4.379528057220092307, 16.55341960407617563, 27.29275706135234358 ) ) ;
#172467 = CARTESIAN_POINT ( 'NONE',  ( 9.564922557960805705, 16.46253265017160317, 24.58224293864769194 ) ) ;
#172468 = CARTESIAN_POINT ( 'NONE',  ( 19.02544592524343514, -5.153800228976328945, 93.54057627198102409 ) ) ;
#172470 = CARTESIAN_POINT ( 'NONE',  ( -36.91746825000001309, 11.99521256947798342, -2.724999997268813701 ) ) ;
#172469 = CARTESIAN_POINT ( 'NONE',  ( 16.55341960407618274, -4.379528057220086978, 36.04275706135234714 ) ) ;
#172471 = CARTESIAN_POINT ( 'NONE',  ( -18.67979575497193778, 10.72451020669871902, 113.3344237280190328 ) ) ;
#172472 = CARTESIAN_POINT ( 'NONE',  ( 4.379528057220092307, 16.55341960407617563, 92.29275706135236135 ) ) ;
#172473 = CARTESIAN_POINT ( 'NONE',  ( 19.02544592524334988, 5.153800228976608722, 111.4594237280190043 ) ) ;
#172474 = CARTESIAN_POINT ( 'NONE',  ( 16.46253265017160672, -9.564922557960803928, 33.33224293864770260 ) ) ;
#172475 = CARTESIAN_POINT ( 'NONE',  ( 8.314922557961029526, -14.29746914071037800, 80.41775706135234714 ) ) ;
#172476 = CARTESIAN_POINT ( 'NONE',  ( -8.314922557961024197, 14.29746914071037800, 67.91775706135234714 ) ) ;
#172477 = CARTESIAN_POINT ( 'NONE',  ( 5.049401038298161559, -19.05341960407611168, 27.70724293864769550 ) ) ;
#172478 = CARTESIAN_POINT ( 'NONE',  ( 9.474510206698729675, 16.51473224551082808, 72.08442372801900433 ) ) ;
#172479 = CARTESIAN_POINT ( 'NONE',  ( 10.81492255796106328, -18.62759615963255655, 105.4177570613523613 ) ) ;
#172480 = CARTESIAN_POINT ( 'NONE',  ( -9.474510206698964154, 16.51473224551069663, 50.41557627198102409 ) ) ;
#172481 = CARTESIAN_POINT ( 'NONE',  ( 16.46253265017160672, -9.564922557960803928, 98.33224293864769550 ) ) ;
#172482 = CARTESIAN_POINT ( 'NONE',  ( 14.34966873604960469, 8.224510206698951720, 79.16557627198103830 ) ) ;
#172483 = VECTOR ( 'NONE', #189250, 1000.000000000000000 ) ;
#172484 = CARTESIAN_POINT ( 'NONE',  ( -16.46253265017146816, -9.564922557961047289, 54.16775706135234003 ) ) ;
#172485 = CARTESIAN_POINT ( 'NONE',  ( 15.80617190586746368, 15.72974639402197994, 54.37390960531435979 ) ) ;
#172486 = CARTESIAN_POINT ( 'NONE',  ( 0.05219959533937995610, -21.53943276465977519, 105.0010903946856757 ) ) ;
#172487 = CARTESIAN_POINT ( 'NONE',  ( 16.51473224551069308, 9.474510206698969483, 89.16557627198103830 ) ) ;
#172488 = CARTESIAN_POINT ( 'NONE',  ( 21.52544592524334988, 5.823673210054432836, 106.4594237280190328 ) ) ;
#172489 = CARTESIAN_POINT ( 'NONE',  ( -5.719274019375978568, 21.55341960407610458, 70.20724293864769550 ) ) ;
#172490 = CARTESIAN_POINT ( 'NONE',  ( -9.564922557960796823, -16.46253265017161027, 107.0822429386476955 ) ) ;
#172491 = CARTESIAN_POINT ( 'NONE',  ( -5.153800228976607833, 19.02544592524334988, 82.70942372801897591 ) ) ;
#172492 = CARTESIAN_POINT ( 'NONE',  ( -0.05219959533909027116, -19.03943276465977164, 112.4989096053143669 ) ) ;
#172493 = EDGE_CURVE ( 'NONE', #115498, #58678, #113927, .T. ) ;
#172494 = CARTESIAN_POINT ( 'NONE',  ( -9.564922557961040184, 16.46253265017147172, 107.9177570613523471 ) ) ;
#172495 = CARTESIAN_POINT ( 'NONE',  ( 19.02544592524343514, -5.153800228976328945, 23.54057627198102054 ) ) ;
#172496 = CARTESIAN_POINT ( 'NONE',  ( -5.153800228976328057, -19.02544592524343514, 82.29057627198103830 ) ) ;
#172497 = CARTESIAN_POINT ( 'NONE',  ( 0.05219959533907565091, 21.53943276465977519, 79.99890960531435269 ) ) ;
#172498 = CARTESIAN_POINT ( 'NONE',  ( 8.314922557961029526, -14.29746914071037800, 40.41775706135234714 ) ) ;
#172499 = CARTESIAN_POINT ( 'NONE',  ( -18.62759615963255300, -10.81492255796106328, 49.16775706135234003 ) ) ;
#172500 = CARTESIAN_POINT ( 'NONE',  ( -10.72451020669870658, -18.67979575497194134, 94.58442372801901854 ) ) ;
#172501 = CARTESIAN_POINT ( 'NONE',  ( -4.483927247898782831, 16.52544592524335698, 97.70942372801904696 ) ) ;
#172502 = CARTESIAN_POINT ( 'NONE',  ( -19.03943276465977164, 0.05219959533909376836, 91.24890960531436690 ) ) ;
#172503 = CARTESIAN_POINT ( 'NONE',  ( -14.34966873604960291, -8.224510206698953496, 96.66557627198102409 ) ) ;
#172504 = CARTESIAN_POINT ( 'NONE',  ( -8.224510206698948167, 14.34966873604960824, 30.41557627198101699 ) ) ;
#172505 = CARTESIAN_POINT ( 'NONE',  ( 19.05341960407617918, -5.049401038297876454, 71.04275706135234714 ) ) ;
#172506 = CARTESIAN_POINT ( 'NONE',  ( 10.72451020669871369, 18.67979575497193778, 47.08442372801901854 ) ) ;
#172508 = ADVANCED_FACE ( 'NONE', ( #20936 ), #145274, .T. ) ;
#172507 = CARTESIAN_POINT ( 'NONE',  ( -0.05219959533936034679, 19.03943276465977164, 27.50109039468566507 ) ) ;
#172510 = CARTESIAN_POINT ( 'NONE',  ( -12.14591786802309592, -12.06949235617757132, 86.87390960531438111 ) ) ;
#172509 = VECTOR ( 'NONE', #87397, 1000.000000000000000 ) ;
#172511 = CARTESIAN_POINT ( 'NONE',  ( 21.55341960407610458, 5.719274019375980345, 23.95724293864769550 ) ) ;
#172512 = CARTESIAN_POINT ( 'NONE',  ( -4.483927247898539470, -16.52544592524342804, 22.29057627198102765 ) ) ;
#172513 = CARTESIAN_POINT ( 'NONE',  ( 18.67979575497194134, -10.72451020669871369, 80.83442372801901854 ) ) ;
#172514 = CARTESIAN_POINT ( 'NONE',  ( -8.314922557961024197, 14.29746914071037800, 52.91775706135235424 ) ) ;
#172515 = CARTESIAN_POINT ( 'NONE',  ( 14.34966873604972726, -8.224510206698740333, 100.8344237280190185 ) ) ;
#172516 = CARTESIAN_POINT ( 'NONE',  ( -5.823673210054431948, 21.52544592524334988, 47.70942372801902565 ) ) ;
#172517 = ORIENTED_EDGE ( 'NONE', *, *, #91512, .F. ) ;
#172518 = CARTESIAN_POINT ( 'NONE',  ( 5.823673210054444382, -21.52544592524334988, 35.20942372801901854 ) ) ;
#172519 = CARTESIAN_POINT ( 'NONE',  ( -16.53943276465976808, 0.05219959533911058130, 106.2489096053143811 ) ) ;
#172520 = CARTESIAN_POINT ( 'NONE',  ( -13.97604488694527625, -13.89961937509977652, 31.87390960531435979 ) ) ;
#172521 = CARTESIAN_POINT ( 'NONE',  ( -0.05219959533910754901, -16.53943276465976808, 72.49890960531435269 ) ) ;
#172522 = CARTESIAN_POINT ( 'NONE',  ( -9.564922557960796823, -16.46253265017161027, 72.08224293864770971 ) ) ;
#172523 = CARTESIAN_POINT ( 'NONE',  ( -8.224510206698735004, -14.34966873604973081, 109.5844237280190328 ) ) ;
#172524 = CARTESIAN_POINT ( 'NONE',  ( 9.564922557960805705, 16.46253265017160317, 34.58224293864770260 ) ) ;
#172525 = CARTESIAN_POINT ( 'NONE',  ( -5.823673210054116645, -21.52544592524344225, 57.29057627198103120 ) ) ;
#172526 = CARTESIAN_POINT ( 'NONE',  ( 12.14591786802309770, 12.06949235617756955, 94.37390960531436690 ) ) ;
#172527 = CARTESIAN_POINT ( 'NONE',  ( 18.67979575497178502, 10.72451020669898547, 99.16557627198100988 ) ) ;
#172528 = CARTESIAN_POINT ( 'NONE',  ( 19.03943276465977164, -0.05219959533909143690, 98.74890960531436690 ) ) ;
#172530 = CARTESIAN_POINT ( 'NONE',  ( 9.474510206698729675, 16.51473224551082808, 97.08442372801900433 ) ) ;
#172529 = CARTESIAN_POINT ( 'NONE',  ( -19.03943276465977164, 0.05219959533909376836, 51.24890960531436690 ) ) ;
#172531 = CARTESIAN_POINT ( 'NONE',  ( 10.81492255796078972, 18.62759615963270932, 49.58224293864769550 ) ) ;
#172532 = CARTESIAN_POINT ( 'NONE',  ( 21.53943276465977519, 0.05219959533937863772, 66.25109039468567573 ) ) ;
#172533 = CARTESIAN_POINT ( 'NONE',  ( -16.51473224551069308, -9.474510206698971260, 56.66557627198103120 ) ) ;
#172534 = CARTESIAN_POINT ( 'NONE',  ( -13.89961937509977652, 13.97604488694528158, 80.62390960531436690 ) ) ;
#172535 = CARTESIAN_POINT ( 'NONE',  ( -16.55341960407617563, 4.379528057220093196, 63.54275706135234003 ) ) ;
#172536 = CARTESIAN_POINT ( 'NONE',  ( -21.53943276465977519, -0.05219959533937600094, 38.75109039468567573 ) ) ;
#172537 = EDGE_CURVE ( 'NONE', #135811, #159561, #131108, .T. ) ;
#172538 = CARTESIAN_POINT ( 'NONE',  ( -18.67979575497193778, 10.72451020669871902, 88.33442372801901854 ) ) ;
#172539 = CARTESIAN_POINT ( 'NONE',  ( -10.81492255796078084, -18.62759615963271287, 97.08224293864770971 ) ) ;
#172541 = CARTESIAN_POINT ( 'NONE',  ( 4.483927247898790824, -16.52544592524335698, 65.20942372801901854 ) ) ;
#172540 = CARTESIAN_POINT ( 'NONE',  ( 18.67979575497194134, -10.72451020669871369, 40.83442372801901854 ) ) ;
#172542 = CARTESIAN_POINT ( 'NONE',  ( 18.62759615963271287, -10.81492255796078972, 68.33224293864769550 ) ) ;
#172543 = CARTESIAN_POINT ( 'NONE',  ( 9.474510206698729675, 16.51473224551082808, 37.08442372801899722 ) ) ;
#172545 = CARTESIAN_POINT ( 'NONE',  ( 8.314922557961029526, -14.29746914071037800, 110.4177570613523756 ) ) ;
#172544 = CARTESIAN_POINT ( 'NONE',  ( -9.474510206698964154, 16.51473224551069663, 65.41557627198102409 ) ) ;
#172546 = CARTESIAN_POINT ( 'NONE',  ( 23.48529157249600630, -32.32473071737748427, -5.299999999999999822 ) ) ;
#172547 = CARTESIAN_POINT ( 'NONE',  ( 16.51473224551069308, 9.474510206698969483, 99.16557627198102409 ) ) ;
#172548 = DIRECTION ( 'NONE',  ( -0.4999999999999967248, 0.5000000000000019984, 0.7071067811865484609 ) ) ;
#172549 = CARTESIAN_POINT ( 'NONE',  ( -9.474510206698720793, -16.51473224551083518, 79.58442372801899012 ) ) ;
#172550 = CARTESIAN_POINT ( 'NONE',  ( 21.55341960407610458, 5.719274019375980345, 58.95724293864770971 ) ) ;
#172551 = CARTESIAN_POINT ( 'NONE',  ( -4.483927247898539470, -16.52544592524342804, 37.29057627198102409 ) ) ;
#172552 = CARTESIAN_POINT ( 'NONE',  ( -16.53943276465976808, -0.05219959533934237506, 23.75109039468567929 ) ) ;
#172553 = CARTESIAN_POINT ( 'NONE',  ( -0.05219959533909027116, -19.03943276465977164, 32.49890960531435979 ) ) ;
#172554 = CARTESIAN_POINT ( 'NONE',  ( -19.02544592524334988, -5.153800228976617603, 108.9594237280189759 ) ) ;
#172556 = CARTESIAN_POINT ( 'NONE',  ( -16.46253265017146816, -9.564922557961047289, 69.16775706135233293 ) ) ;
#172555 = CARTESIAN_POINT ( 'NONE',  ( -15.72974639402197994, 15.80617190586746368, 90.62390960531436690 ) ) ;
#172557 = CARTESIAN_POINT ( 'NONE',  ( 16.55341960407618274, -4.379528057220086978, 86.04275706135236135 ) ) ;
#172558 = CARTESIAN_POINT ( 'NONE',  ( 19.03943276465977164, -0.05219959533909143690, 73.74890960531435269 ) ) ;
#172559 = CARTESIAN_POINT ( 'NONE',  ( -4.483927247898539470, -16.52544592524342804, 77.29057627198102409 ) ) ;
#172560 = CARTESIAN_POINT ( 'NONE',  ( -9.564922557960796823, -16.46253265017161027, 42.08224293864769550 ) ) ;
#172561 = CARTESIAN_POINT ( 'NONE',  ( 4.483927247898545687, 16.52544592524342804, 54.79057627198104541 ) ) ;
#172562 = CARTESIAN_POINT ( 'NONE',  ( -23.48298174826590667, 32.32155151706776053, -6.047842220587802409 ) ) ;
#172563 = CARTESIAN_POINT ( 'NONE',  ( 32.45678934495597900, -3.100610132747068093, 88.16656412605026105 ) ) ;
#172564 = CARTESIAN_POINT ( 'NONE',  ( 16.53943276465976808, -0.05219959533910856209, 23.74890960531435269 ) ) ;
#172565 = CARTESIAN_POINT ( 'NONE',  ( -13.97604488694527625, -13.89961937509977652, 81.87390960531436690 ) ) ;
#172566 = CARTESIAN_POINT ( 'NONE',  ( 0.000000000000000000, 0.000000000000000000, -25.00000000000000000 ) ) ;
#172567 = CARTESIAN_POINT ( 'NONE',  ( -13.89961937509957401, -13.97604488694547875, 44.37609039468566863 ) ) ;
#172568 = CARTESIAN_POINT ( 'NONE',  ( -8.314922557961024197, 14.29746914071037800, 42.91775706135235424 ) ) ;
#172569 = CARTESIAN_POINT ( 'NONE',  ( 21.52544592524344225, -5.823673210054117533, 58.54057627198103120 ) ) ;
#172570 = CARTESIAN_POINT ( 'NONE',  ( 0.05219959533936267826, -19.03943276465977164, 30.00109039468566863 ) ) ;
#172571 = CARTESIAN_POINT ( 'NONE',  ( 16.46253265017160672, -9.564922557960803928, 68.33224293864770971 ) ) ;
#172572 = CARTESIAN_POINT ( 'NONE',  ( 1.500000000000335065, 22.62084519560232465, -57.95595451695638900 ) ) ;
#172573 = CARTESIAN_POINT ( 'NONE',  ( 19.02544592524343514, -5.153800228976328945, 113.5405762719810241 ) ) ;
#172574 = CARTESIAN_POINT ( 'NONE',  ( -21.53943276465977519, -0.05219959533937600094, 33.75109039468568284 ) ) ;
#172575 = CARTESIAN_POINT ( 'NONE',  ( -16.55341960407611168, -4.379528057220339221, 106.4572429386477097 ) ) ;
#172578 = CARTESIAN_POINT ( 'NONE',  ( 18.22780087662119897, -5.500000000000096811, 68.51763182126893525 ) ) ;
#172577 = CARTESIAN_POINT ( 'NONE',  ( -16.46253265017160317, 9.564922557960807481, 75.83224293864769550 ) ) ;
#172576 = CARTESIAN_POINT ( 'NONE',  ( 21.52544592524344225, -5.823673210054117533, 103.5405762719810383 ) ) ;
#172579 = CARTESIAN_POINT ( 'NONE',  ( -10.72451020669870658, -18.67979575497194134, 24.58442372801901499 ) ) ;
#172580 = ORIENTED_EDGE ( 'NONE', *, *, #140897, .F. ) ;
#172581 = CARTESIAN_POINT ( 'NONE',  ( -19.03943276465977164, 0.05219959533909376836, 86.24890960531436690 ) ) ;
#172582 = LINE ( 'NONE', #35053, #188332 ) ;
#172583 = CARTESIAN_POINT ( 'NONE',  ( 16.46253265017160672, -9.564922557960803928, 38.33224293864768839 ) ) ;
#172584 = CARTESIAN_POINT ( 'NONE',  ( 0.05219959533936267826, -19.03943276465977164, 110.0010903946856757 ) ) ;
#172585 = CARTESIAN_POINT ( 'NONE',  ( 22.81625015709510151, -31.40387420917324590, -8.424999997268812990 ) ) ;
#172586 = AXIS2_PLACEMENT_3D ( 'NONE', #86398, #151078, #41911 ) ;
#172587 = CARTESIAN_POINT ( 'NONE',  ( -12.14591786802309592, -12.06949235617757132, 111.8739096053143669 ) ) ;
#172588 = CARTESIAN_POINT ( 'NONE',  ( -5.719274019375665041, -21.55341960407619695, 84.79275706135234714 ) ) ;
#172590 = CARTESIAN_POINT ( 'NONE',  ( 21.52544592524334988, 5.823673210054432836, 46.45942372801901854 ) ) ;
#172589 = CARTESIAN_POINT ( 'NONE',  ( 0.05219959533909260263, 19.03943276465977164, 74.99890960531435269 ) ) ;
#172591 = CARTESIAN_POINT ( 'NONE',  ( 5.719274019375673035, 21.55341960407619339, 22.29275706135235069 ) ) ;
#172592 = CARTESIAN_POINT ( 'NONE',  ( 27.73933785331498214, 9.013057229001095294, 140.4750000027311785 ) ) ;
#172593 = CARTESIAN_POINT ( 'NONE',  ( -0.05219959533909027116, -19.03943276465977164, 82.49890960531436690 ) ) ;
#172594 = CARTESIAN_POINT ( 'NONE',  ( 19.25918095147781983, 5.499999999999580780, 61.95284276293936898 ) ) ;
#172596 = CARTESIAN_POINT ( 'NONE',  ( 5.823673210054125526, 21.52544592524343514, 39.79057627198103830 ) ) ;
#172595 = CARTESIAN_POINT ( 'NONE',  ( 4.483927247898790824, -16.52544592524335698, 45.20942372801901854 ) ) ;
#172597 = CARTESIAN_POINT ( 'NONE',  ( 18.62759615963255655, 10.81492255796105972, 76.66775706135234714 ) ) ;
#172598 = CARTESIAN_POINT ( 'NONE',  ( 17.60689202196055447, -5.500000000000023981, 38.36665076390895024 ) ) ;
#172599 = CARTESIAN_POINT ( 'NONE',  ( -9.564922557961040184, 16.46253265017147172, 107.9177570613523471 ) ) ;
#172600 = CARTESIAN_POINT ( 'NONE',  ( -5.049401038298153566, 19.05341960407611168, 55.20724293864769550 ) ) ;
#172601 = CARTESIAN_POINT ( 'NONE',  ( 16.46253265017160672, -9.564922557960803928, 78.33224293864769550 ) ) ;
#172602 = CARTESIAN_POINT ( 'NONE',  ( -12.06949235617756955, 12.14591786802309770, 105.6239096053143669 ) ) ;
#172603 = CARTESIAN_POINT ( 'NONE',  ( 12.06949235617757843, -12.14591786802309237, 108.1239096053143811 ) ) ;
#172604 = CARTESIAN_POINT ( 'NONE',  ( 5.153800228976335163, 19.02544592524342804, 114.7905762719810241 ) ) ;
#172605 = CARTESIAN_POINT ( 'NONE',  ( 0.05219959533934541429, -16.53943276465976808, 80.00109039468568994 ) ) ;
#172607 = CARTESIAN_POINT ( 'NONE',  ( 16.51473224551069308, 9.474510206698969483, 59.16557627198102409 ) ) ;
#172606 = CARTESIAN_POINT ( 'NONE',  ( 8.224510206698953496, -14.34966873604960469, 62.91557627198102409 ) ) ;
#172608 = CARTESIAN_POINT ( 'NONE',  ( 0.05219959533937995610, -21.53943276465977519, 80.00109039468568994 ) ) ;
#172609 = CARTESIAN_POINT ( 'NONE',  ( -0.05219959533937732626, 21.53943276465977519, 72.50109039468568994 ) ) ;
#172610 = CARTESIAN_POINT ( 'NONE',  ( -13.89961937509957401, -13.97604488694547875, 89.37609039468563310 ) ) ;
#172611 = CARTESIAN_POINT ( 'NONE',  ( 12.06949235617757843, -12.14591786802309237, 63.12390960531435979 ) ) ;
#172612 = CARTESIAN_POINT ( 'NONE',  ( -15.80617190586745835, -15.72974639402198527, 111.8739096053143669 ) ) ;
#172613 = CARTESIAN_POINT ( 'NONE',  ( 21.55341960407610458, 5.719274019375980345, 63.95724293864770260 ) ) ;
#172614 = LINE ( 'NONE', #49270, #196981 ) ;
#172615 = CARTESIAN_POINT ( 'NONE',  ( 17.14385361876520264, 23.59649016807275856, 148.1750000027311955 ) ) ;
#172616 = CARTESIAN_POINT ( 'NONE',  ( 9.474510206698971260, -16.51473224551069308, 72.91557627198102409 ) ) ;
#172617 = CARTESIAN_POINT ( 'NONE',  ( 16.52544592524342804, -4.483927247898539470, 38.54057627198103120 ) ) ;
#172618 = AXIS2_PLACEMENT_3D ( 'NONE', #155743, #20209, #171915 ) ;
#172619 = CARTESIAN_POINT ( 'NONE',  ( 8.314922557961029526, -14.29746914071037800, 110.4177570613523756 ) ) ;
#172620 = CARTESIAN_POINT ( 'NONE',  ( 16.53943276465976808, 0.05219959533934440121, 86.25109039468568994 ) ) ;
#172621 = CARTESIAN_POINT ( 'NONE',  ( -0.05219959533936034679, 19.03943276465977164, 37.50109039468567573 ) ) ;
#172622 = CARTESIAN_POINT ( 'NONE',  ( -9.474510206698964154, 16.51473224551069663, 95.41557627198102409 ) ) ;
#172623 = CARTESIAN_POINT ( 'NONE',  ( -16.53943276465976808, 0.05219959533911058130, 61.24890960531435979 ) ) ;
#172625 = CARTESIAN_POINT ( 'NONE',  ( -18.62759615963270932, 10.81492255796079327, 25.83224293864769194 ) ) ;
#172624 = CARTESIAN_POINT ( 'NONE',  ( 19.03943276465977164, -0.05219959533909143690, 23.74890960531435269 ) ) ;
#172626 = CARTESIAN_POINT ( 'NONE',  ( -21.52544592524343514, 5.823673210054127303, 56.04057627198102409 ) ) ;
#172627 = CARTESIAN_POINT ( 'NONE',  ( 16.53943276465976808, -0.05219959533910856209, 103.7489096053143669 ) ) ;
#172628 = CARTESIAN_POINT ( 'NONE',  ( 14.29746914071037800, 8.314922557961029526, 51.66775706135234714 ) ) ;
#172629 = CARTESIAN_POINT ( 'NONE',  ( 16.53943276465976808, -0.05219959533910856209, 83.74890960531435269 ) ) ;
#172630 = CARTESIAN_POINT ( 'NONE',  ( -18.56197773271732032, 5.499999999999902300, 63.55066217314450938 ) ) ;
#172631 = CARTESIAN_POINT ( 'NONE',  ( 9.474510206698729675, 16.51473224551082808, 77.08442372801900433 ) ) ;
#172632 = CARTESIAN_POINT ( 'NONE',  ( -10.72451020669898014, 18.67979575497178502, 25.41557627198103120 ) ) ;
#172633 = CARTESIAN_POINT ( 'NONE',  ( -36.91746825000001309, -11.99521256947794789, -5.024999997268813523 ) ) ;
#172634 = CARTESIAN_POINT ( 'NONE',  ( 9.474510206698971260, -16.51473224551069308, 42.91557627198103120 ) ) ;
#172636 = CARTESIAN_POINT ( 'NONE',  ( -8.224510206698948167, 14.34966873604960824, 35.41557627198102409 ) ) ;
#172635 = CARTESIAN_POINT ( 'NONE',  ( -12.14591786802326823, 12.06949235617739902, 33.12609039468569705 ) ) ;
#172637 = CARTESIAN_POINT ( 'NONE',  ( -0.05219959533907301413, -21.53943276465977519, 52.49890960531435979 ) ) ;
#172638 = CARTESIAN_POINT ( 'NONE',  ( -19.02544592524334988, -5.153800228976617603, 88.95942372801897591 ) ) ;
#172639 = CARTESIAN_POINT ( 'NONE',  ( 5.823673210054125526, 21.52544592524343514, 44.79057627198103120 ) ) ;
#172640 = CARTESIAN_POINT ( 'NONE',  ( -21.53943276465977519, -0.05219959533937600094, 83.75109039468568994 ) ) ;
#172641 = CARTESIAN_POINT ( 'NONE',  ( -11.94381442052175757, 9.822853212439014214, -61.89036147510174146 ) ) ;
#172642 = CARTESIAN_POINT ( 'NONE',  ( 14.34966873604972726, -8.224510206698740333, 35.83442372801901143 ) ) ;
#172644 = CARTESIAN_POINT ( 'NONE',  ( 0.05219959533909260263, 19.03943276465977164, 89.99890960531436690 ) ) ;
#172643 = CARTESIAN_POINT ( 'NONE',  ( -13.97604488694527625, -13.89961937509977652, 41.87390960531435979 ) ) ;
#172645 = CARTESIAN_POINT ( 'NONE',  ( -13.97604488694527625, -13.89961937509977652, 31.87390960531435979 ) ) ;
#172646 = CARTESIAN_POINT ( 'NONE',  ( 4.379528057220339221, -16.55341960407611168, 102.7072429386476955 ) ) ;
#172647 = APPLICATION_PROTOCOL_DEFINITION ( 'draft international standard', 'automotive_design', 1998, #129482 ) ;
#172648 = CARTESIAN_POINT ( 'NONE',  ( 19.02544592524343514, -5.153800228976328945, 103.5405762719809957 ) ) ;
#172649 = ORIENTED_EDGE ( 'NONE', *, *, #19336, .T. ) ;
#172650 = CARTESIAN_POINT ( 'NONE',  ( 16.53943276465976808, 0.05219959533934440121, 61.25109039468567573 ) ) ;
#172651 = CARTESIAN_POINT ( 'NONE',  ( 5.823673210054125526, 21.52544592524343514, 84.79057627198102409 ) ) ;
#172652 = CARTESIAN_POINT ( 'NONE',  ( 19.05341960407611168, 5.049401038298154454, 38.95724293864767418 ) ) ;
#172654 = CARTESIAN_POINT ( 'NONE',  ( -15.72974639402176322, -15.80617190586768395, 34.37609039468568284 ) ) ;
#172653 = CARTESIAN_POINT ( 'NONE',  ( -19.05341960407617563, 5.049401038297882671, 78.54275706135233293 ) ) ;
#172655 = CARTESIAN_POINT ( 'NONE',  ( 19.02544592524343514, -5.153800228976328945, 88.54057627198102409 ) ) ;
#172657 = EDGE_CURVE ( 'NONE', #66839, #46248, #24914, .T. ) ;
#172656 = CARTESIAN_POINT ( 'NONE',  ( -19.03943276465977164, 0.05219959533909376836, 106.2489096053143669 ) ) ;
#172658 = VERTEX_POINT ( 'NONE', #136110 ) ;
#172659 = CARTESIAN_POINT ( 'NONE',  ( 8.224510206698742110, 14.34966873604972548, 37.08442372801901143 ) ) ;
#172660 = CARTESIAN_POINT ( 'NONE',  ( -10.72451020669898014, 18.67979575497178502, 110.4155762719810383 ) ) ;
#172663 = CARTESIAN_POINT ( 'NONE',  ( -9.474510206698720793, -16.51473224551083518, 79.58442372801899012 ) ) ;
#172662 = CARTESIAN_POINT ( 'NONE',  ( -16.46253265017160317, 9.564922557960807481, 90.83224293864769550 ) ) ;
#172661 = CARTESIAN_POINT ( 'NONE',  ( -0.05219959533910754901, -16.53943276465976808, 102.4989096053143811 ) ) ;
#172664 = CARTESIAN_POINT ( 'NONE',  ( 5.153800228976615827, -19.02544592524334988, 30.20942372801900433 ) ) ;
#172665 = CARTESIAN_POINT ( 'NONE',  ( 5.719274019375991003, -21.55341960407610458, 87.70724293864769550 ) ) ;
#172666 = CARTESIAN_POINT ( 'NONE',  ( -5.049401038297874678, -19.05341960407617918, 19.79275706135233293 ) ) ;
#172667 = CARTESIAN_POINT ( 'NONE',  ( 16.52544592524335698, 4.483927247898782831, 76.45942372801901854 ) ) ;
#172668 = ADVANCED_FACE ( 'NONE', ( #72450 ), #41115, .F. ) ;
#172669 = CARTESIAN_POINT ( 'NONE',  ( 5.049401038298161559, -19.05341960407611168, 107.7072429386476955 ) ) ;
#172670 = CARTESIAN_POINT ( 'NONE',  ( -5.153800228976328057, -19.02544592524343514, 52.29057627198100988 ) ) ;
#172671 = CARTESIAN_POINT ( 'NONE',  ( -18.62759615963255300, -10.81492255796106328, 59.16775706135234714 ) ) ;
#172672 = CARTESIAN_POINT ( 'NONE',  ( -21.55341960407619339, 5.719274019375674811, 73.54275706135234714 ) ) ;
#172673 = CARTESIAN_POINT ( 'NONE',  ( 5.153800228976335163, 19.02544592524342804, 69.79057627198103830 ) ) ;
#172674 = CARTESIAN_POINT ( 'NONE',  ( 5.719274019375673035, 21.55341960407619339, 52.29275706135236135 ) ) ;
#172675 = CARTESIAN_POINT ( 'NONE',  ( 19.02544592524334988, 5.153800228976608722, 91.45942372801900433 ) ) ;
#172676 = CARTESIAN_POINT ( 'NONE',  ( 5.049401038298161559, -19.05341960407611168, 47.70724293864770260 ) ) ;
#172677 = CARTESIAN_POINT ( 'NONE',  ( 16.52544592524335698, 4.483927247898782831, 91.45942372801901854 ) ) ;
#172678 = CARTESIAN_POINT ( 'NONE',  ( 19.05341960407611168, 5.049401038298154454, 68.95724293864769550 ) ) ;
#172679 = CARTESIAN_POINT ( 'NONE',  ( -16.46253265017160317, 9.564922557960807481, 115.8322429386477097 ) ) ;
#172680 = CARTESIAN_POINT ( 'NONE',  ( 19.05341960407611168, 5.049401038298154454, 48.95724293864768129 ) ) ;
#172681 = VECTOR ( 'NONE', #22226, 1000.000000000000000 ) ;
#172682 = CARTESIAN_POINT ( 'NONE',  ( 5.719274019375991003, -21.55341960407610458, 87.70724293864769550 ) ) ;
#172683 = CARTESIAN_POINT ( 'NONE',  ( 16.52544592524335698, 4.483927247898782831, 71.45942372801901854 ) ) ;
#172684 = CARTESIAN_POINT ( 'NONE',  ( -24.06756124613724168, 8.142616467497040489, 169.4332804344609542 ) ) ;
#172685 = CARTESIAN_POINT ( 'NONE',  ( -19.05341960407617563, 5.049401038297882671, 33.54275706135231871 ) ) ;
#172686 = CARTESIAN_POINT ( 'NONE',  ( 5.049401038298161559, -19.05341960407611168, 72.70724293864768129 ) ) ;
#172687 = CARTESIAN_POINT ( 'NONE',  ( -4.483927247898539470, -16.52544592524342804, 57.29057627198103120 ) ) ;
#172688 = CARTESIAN_POINT ( 'NONE',  ( -16.53943276465976808, 0.05219959533911058130, 96.24890960531435269 ) ) ;
#172689 = CARTESIAN_POINT ( 'NONE',  ( -16.46253265017160317, 9.564922557960807481, 105.8322429386476955 ) ) ;
#172690 = CARTESIAN_POINT ( 'NONE',  ( 13.97604488694527802, 13.89961937509977652, 89.37390960531436690 ) ) ;
#172691 = CARTESIAN_POINT ( 'NONE',  ( -15.72974639402176322, -15.80617190586768395, 44.37609039468567573 ) ) ;
#172692 = CARTESIAN_POINT ( 'NONE',  ( 5.153800228976335163, 19.02544592524342804, 99.79057627198102409 ) ) ;
#172693 = CARTESIAN_POINT ( 'NONE',  ( -19.02544592524334988, -5.153800228976617603, 23.95942372801900078 ) ) ;
#172694 = CARTESIAN_POINT ( 'NONE',  ( -16.55341960407617563, 4.379528057220093196, 73.54275706135234714 ) ) ;
#172695 = CARTESIAN_POINT ( 'NONE',  ( -21.53943276465977519, -0.05219959533937600094, 38.75109039468567573 ) ) ;
#172696 = CARTESIAN_POINT ( 'NONE',  ( 18.62759615963271287, -10.81492255796078972, 23.33224293864769194 ) ) ;
#172697 = CARTESIAN_POINT ( 'NONE',  ( -21.55341960407610458, -5.719274019375992779, 96.45724293864770971 ) ) ;
#172698 = CARTESIAN_POINT ( 'NONE',  ( 4.483927247898545687, 16.52544592524342804, 64.79057627198103830 ) ) ;
#172700 = CARTESIAN_POINT ( 'NONE',  ( -0.05219959533909027116, -19.03943276465977164, 57.49890960531435979 ) ) ;
#172699 = AXIS2_PLACEMENT_3D ( 'NONE', #51095, #188630, #98571 ) ;
#172701 = CARTESIAN_POINT ( 'NONE',  ( -14.29746914071049879, 8.314922557960819915, 75.83224293864769550 ) ) ;
#172702 = CARTESIAN_POINT ( 'NONE',  ( 10.72451020669898902, -18.67979575497178502, 42.91557627198103120 ) ) ;
#172703 = CARTESIAN_POINT ( 'NONE',  ( -16.46253265017146816, -9.564922557961047289, 39.16775706135234003 ) ) ;
#172704 = CARTESIAN_POINT ( 'NONE',  ( 16.51473224551069308, 9.474510206698969483, 24.16557627198102765 ) ) ;
#172705 = ORIENTED_EDGE ( 'NONE', *, *, #73810, .T. ) ;
#172706 = CARTESIAN_POINT ( 'NONE',  ( 16.52544592524335698, 4.483927247898782831, 71.45942372801901854 ) ) ;
#172707 = CARTESIAN_POINT ( 'NONE',  ( 5.153800228976335163, 19.02544592524342804, 74.79057627198103830 ) ) ;
#172708 = CARTESIAN_POINT ( 'NONE',  ( 1.784210473542230573E-15, -29.16686587814331588, 141.3750000027311557 ) ) ;
#172709 = CARTESIAN_POINT ( 'NONE',  ( 8.314922557960818139, 14.29746914071049879, 89.58224293864768129 ) ) ;
#172710 = CARTESIAN_POINT ( 'NONE',  ( -10.72451020669898014, 18.67979575497178502, 35.41557627198102409 ) ) ;
#172711 = ORIENTED_EDGE ( 'NONE', *, *, #167994, .F. ) ;
#172712 = CARTESIAN_POINT ( 'NONE',  ( 14.34966873604972726, -8.224510206698740333, 105.8344237280190328 ) ) ;
#172713 = CARTESIAN_POINT ( 'NONE',  ( -13.97604488694547697, 13.89961937509957934, 103.1260903946856473 ) ) ;
#172714 = CARTESIAN_POINT ( 'NONE',  ( -5.719274019375665041, -21.55341960407619695, 84.79275706135234714 ) ) ;
#172715 = CARTESIAN_POINT ( 'NONE',  ( -16.46253265017160317, 9.564922557960807481, 90.83224293864769550 ) ) ;
#172716 = CARTESIAN_POINT ( 'NONE',  ( 5.823673210054125526, 21.52544592524343514, 104.7905762719810241 ) ) ;
#172717 = CARTESIAN_POINT ( 'NONE',  ( -14.34966873604972548, 8.224510206698743886, 53.33442372801901854 ) ) ;
#172719 = CARTESIAN_POINT ( 'NONE',  ( -13.89961937509977652, 13.97604488694528158, 25.62390960531434558 ) ) ;
#172718 = AXIS2_PLACEMENT_3D ( 'NONE', #21105, #52434, #37267 ) ;
#172720 = CARTESIAN_POINT ( 'NONE',  ( 4.483927247898790824, -16.52544592524335698, 30.20942372801902565 ) ) ;
#172721 = CARTESIAN_POINT ( 'NONE',  ( 9.474510206698729675, 16.51473224551082808, 97.08442372801900433 ) ) ;
#172722 = CARTESIAN_POINT ( 'NONE',  ( 21.55341960407610458, 5.719274019375980345, 93.95724293864770971 ) ) ;
#172723 = CARTESIAN_POINT ( 'NONE',  ( -9.564922557961040184, 16.46253265017147172, 57.91775706135233293 ) ) ;
#172724 = DIRECTION ( 'NONE',  ( 1.000000000000000000, 0.000000000000000000, 0.000000000000000000 ) ) ;
#172725 = CARTESIAN_POINT ( 'NONE',  ( -5.719274019375978568, 21.55341960407610458, 100.2072429386476955 ) ) ;
#172726 = DIRECTION ( 'NONE',  ( -0.000000000000000000, -0.000000000000000000, 1.000000000000000000 ) ) ;
#172727 = CARTESIAN_POINT ( 'NONE',  ( -19.02544592524342804, 5.153800228976336051, 81.04057627198103830 ) ) ;
#172728 = CIRCLE ( 'NONE', #150240, 59.99999999999998579 ) ;
#172729 = CARTESIAN_POINT ( 'NONE',  ( 16.53943276465976808, 0.05219959533934440121, 36.25109039468567573 ) ) ;
#172730 = CARTESIAN_POINT ( 'NONE',  ( 0.000000000000000000, 0.000000000000000000, 190.0000000000000000 ) ) ;
#172731 = CARTESIAN_POINT ( 'NONE',  ( -19.05341960407617563, 5.049401038297882671, 63.54275706135234003 ) ) ;
#172733 = CARTESIAN_POINT ( 'NONE',  ( -4.379528057220328563, 16.55341960407611168, 60.20724293864768839 ) ) ;
#172732 = CARTESIAN_POINT ( 'NONE',  ( -18.67979575497193778, 10.72451020669871902, 23.33442372801901499 ) ) ;
#172734 = CARTESIAN_POINT ( 'NONE',  ( -19.03943276465977164, 0.05219959533909376836, 71.24890960531435269 ) ) ;
#172735 = AXIS2_PLACEMENT_3D ( 'NONE', #162124, #98427, #82258 ) ;
#172737 = CARTESIAN_POINT ( 'NONE',  ( -13.97604488694547697, 13.89961937509957934, 38.12609039468566152 ) ) ;
#172736 = CARTESIAN_POINT ( 'NONE',  ( 4.379528057220092307, 16.55341960407617563, 42.29275706135235424 ) ) ;
#172738 = CARTESIAN_POINT ( 'NONE',  ( -0.05219959533937732626, 21.53943276465977519, 57.50109039468568994 ) ) ;
#172739 = CARTESIAN_POINT ( 'NONE',  ( -9.564922557961040184, 16.46253265017147172, 112.9177570613523329 ) ) ;
#172740 = CARTESIAN_POINT ( 'NONE',  ( 19.05341960407611168, 5.049401038298154454, 48.95724293864768129 ) ) ;
#172741 = CARTESIAN_POINT ( 'NONE',  ( -19.05341960407617563, 5.049401038297882671, 78.54275706135233293 ) ) ;
#172742 = CARTESIAN_POINT ( 'NONE',  ( 15.80617190586769283, -15.72974639402175789, 85.62609039468568994 ) ) ;
#172743 = CARTESIAN_POINT ( 'NONE',  ( -13.97604488694547697, 13.89961937509957934, 68.12609039468563310 ) ) ;
#172744 = CARTESIAN_POINT ( 'NONE',  ( -9.474510206698964154, 16.51473224551069663, 40.41557627198103120 ) ) ;
#172745 = CARTESIAN_POINT ( 'NONE',  ( 21.53943276465977519, -0.05219959533907433946, 63.74890960531435979 ) ) ;
#172747 = CARTESIAN_POINT ( 'NONE',  ( -5.049401038297874678, -19.05341960407617918, 69.79275706135233293 ) ) ;
#172746 = CARTESIAN_POINT ( 'NONE',  ( 12.14591786802309770, 12.06949235617756955, 64.37390960531435269 ) ) ;
#172748 = CARTESIAN_POINT ( 'NONE',  ( -11.30153831258470731, -190.0000000000000000, -4.999999999999999112 ) ) ;
#172749 = CARTESIAN_POINT ( 'NONE',  ( 5.153800228976615827, -19.02544592524334988, 35.20942372801899722 ) ) ;
#172750 = CARTESIAN_POINT ( 'NONE',  ( 14.29746914071037800, 8.314922557961029526, 101.6677570613523613 ) ) ;
#172751 = CARTESIAN_POINT ( 'NONE',  ( 12.06949235617757843, -12.14591786802309237, 53.12390960531436690 ) ) ;
#172753 = CARTESIAN_POINT ( 'NONE',  ( 27.73933785331498569, 2.768321779492822058E-14, 139.8750000027311842 ) ) ;
#172752 = CARTESIAN_POINT ( 'NONE',  ( 18.67979575497194134, -10.72451020669871369, 95.83442372801903275 ) ) ;
#172754 = CARTESIAN_POINT ( 'NONE',  ( -10.72451020669898014, 18.67979575497178502, 95.41557627198102409 ) ) ;
#172755 =( BOUNDED_CURVE ( )  B_SPLINE_CURVE ( 3, ( #88787, #118141, #13931, #71629 ),
 .UNSPECIFIED., .F., .T. ) 
 B_SPLINE_CURVE_WITH_KNOTS ( ( 4, 4 ),
 ( 2.008945357379066987, 2.115944711806982070 ),
 .UNSPECIFIED. ) 
 CURVE ( )  GEOMETRIC_REPRESENTATION_ITEM ( )  RATIONAL_B_SPLINE_CURVE ( ( 1.000000000000000000, 0.9990461557208837329, 0.9990461557208837329, 1.000000000000000000 ) ) 
 REPRESENTATION_ITEM ( '' )  );
#172756 = CARTESIAN_POINT ( 'NONE',  ( -19.03943276465977164, 0.05219959533909376836, 46.24890960531435979 ) ) ;
#172757 = CARTESIAN_POINT ( 'NONE',  ( 21.53943276465977519, 0.05219959533937863772, 71.25109039468568994 ) ) ;
#172758 = CARTESIAN_POINT ( 'NONE',  ( 13.89961937509977652, -13.97604488694527269, 43.12390960531434558 ) ) ;
#172759 = ORIENTED_EDGE ( 'NONE', *, *, #64962, .T. ) ;
#172760 = CARTESIAN_POINT ( 'NONE',  ( -9.474510206698964154, 16.51473224551069663, 65.41557627198102409 ) ) ;
#172761 = CARTESIAN_POINT ( 'NONE',  ( -8.224510206698948167, 14.34966873604960824, 110.4155762719810383 ) ) ;
#172762 = CARTESIAN_POINT ( 'NONE',  ( -13.97604488694527625, -13.89961937509977652, 106.8739096053143669 ) ) ;
#172763 = CARTESIAN_POINT ( 'NONE',  ( -14.29746914071049879, 8.314922557960819915, 50.83224293864770971 ) ) ;
#172764 = CARTESIAN_POINT ( 'NONE',  ( 16.51473224551069308, 9.474510206698969483, 29.16557627198103475 ) ) ;
#172765 = CARTESIAN_POINT ( 'NONE',  ( 14.29746914071049879, -8.314922557960816363, 83.33224293864769550 ) ) ;
#172766 = AXIS2_PLACEMENT_3D ( 'NONE', #140974, #2462, #51948 ) ;
#172767 = CARTESIAN_POINT ( 'NONE',  ( -21.55341960407610458, -5.719274019375992779, 96.45724293864770971 ) ) ;
#172768 = CARTESIAN_POINT ( 'NONE',  ( -21.52544592524334988, -5.823673210054445271, 38.95942372801901854 ) ) ;
#172769 = CARTESIAN_POINT ( 'NONE',  ( -19.03943276465977164, 0.05219959533909376836, 21.24890960531436335 ) ) ;
#172770 = CARTESIAN_POINT ( 'NONE',  ( 14.34966873604972726, -8.224510206698740333, 40.83442372801901854 ) ) ;
#172771 = CARTESIAN_POINT ( 'NONE',  ( 15.72974639402199770, -15.80617190586745480, 78.12390960531436690 ) ) ;
#172772 = CARTESIAN_POINT ( 'NONE',  ( -18.67979575497193778, 10.72451020669871902, 113.3344237280190328 ) ) ;
#172773 = CARTESIAN_POINT ( 'NONE',  ( 19.02544592524343514, -5.153800228976328945, 88.54057627198102409 ) ) ;
#172774 = CARTESIAN_POINT ( 'NONE',  ( 21.52544592524334988, 5.823673210054432836, 46.45942372801901854 ) ) ;
#172775 = CARTESIAN_POINT ( 'NONE',  ( 15.72974639402199770, -15.80617190586745480, 28.12390960531435979 ) ) ;
#172776 = CARTESIAN_POINT ( 'NONE',  ( 0.05219959533934541429, -16.53943276465976808, 100.0010903946857042 ) ) ;
#172778 = CARTESIAN_POINT ( 'NONE',  ( 5.823673210054444382, -21.52544592524334988, 80.20942372801901854 ) ) ;
#172777 = CARTESIAN_POINT ( 'NONE',  ( 18.62759615963255655, 10.81492255796105972, 56.66775706135235424 ) ) ;
#172779 = CARTESIAN_POINT ( 'NONE',  ( -5.153800228976607833, 19.02544592524334988, 27.70942372801899722 ) ) ;
#172780 = CARTESIAN_POINT ( 'NONE',  ( -16.53943276465976808, -0.05219959533934237506, 88.75109039468567573 ) ) ;
#172781 = CARTESIAN_POINT ( 'NONE',  ( 21.53943276465977519, 0.05219959533937863772, 46.25109039468567573 ) ) ;
#172782 = CARTESIAN_POINT ( 'NONE',  ( 5.153800228976335163, 19.02544592524342804, 49.79057627198100988 ) ) ;
#172783 = CARTESIAN_POINT ( 'NONE',  ( -15.72974639402176322, -15.80617190586768395, 99.37609039468568994 ) ) ;
#172784 = CARTESIAN_POINT ( 'NONE',  ( -19.02544592524342804, 5.153800228976336051, 101.0405762719810241 ) ) ;
#172785 = CARTESIAN_POINT ( 'NONE',  ( -21.52544592524343514, 5.823673210054127303, 106.0405762719810525 ) ) ;
#172786 = CARTESIAN_POINT ( 'NONE',  ( -21.52544592524343514, 5.823673210054127303, 81.04057627198102409 ) ) ;
#172788 = CARTESIAN_POINT ( 'NONE',  ( -21.53943276465977519, 0.05219959533907696930, 71.24890960531435269 ) ) ;
#172787 = CARTESIAN_POINT ( 'NONE',  ( -6.412877669190332419, -3.889087296526017479, 8.181980515339454030 ) ) ;
#172790 = CARTESIAN_POINT ( 'NONE',  ( -8.224510206698948167, 14.34966873604960824, 60.41557627198102409 ) ) ;
#172789 = CARTESIAN_POINT ( 'NONE',  ( 4.379528057220092307, 16.55341960407617563, 52.29275706135236135 ) ) ;
#172791 = CARTESIAN_POINT ( 'NONE',  ( 23.88378066561468316, 7.642901331109205998, 172.4262957903898723 ) ) ;
#172792 = CARTESIAN_POINT ( 'NONE',  ( 0.05219959533936267826, -19.03943276465977164, 95.00109039468567573 ) ) ;
#172793 = CARTESIAN_POINT ( 'NONE',  ( -9.616112110649096323, -9.758613693862333349, -60.44446360152742415 ) ) ;
#172794 = CARTESIAN_POINT ( 'NONE',  ( 8.224510206698742110, 14.34966873604972548, 22.08442372801901143 ) ) ;
#172795 = CARTESIAN_POINT ( 'NONE',  ( 18.67979575497178502, 10.72451020669898547, 94.16557627198103830 ) ) ;
#172796 = CARTESIAN_POINT ( 'NONE',  ( -15.72974639402197994, 15.80617190586746368, 80.62390960531438111 ) ) ;
#172797 = CARTESIAN_POINT ( 'NONE',  ( -10.81492255796078084, -18.62759615963271287, 22.08224293864769194 ) ) ;
#172798 = CARTESIAN_POINT ( 'NONE',  ( 12.14591786802327356, -12.06949235617739191, 55.62609039468568284 ) ) ;
#172799 = CARTESIAN_POINT ( 'NONE',  ( -9.474510206698964154, 16.51473224551069663, 65.41557627198102409 ) ) ;
#172801 = CARTESIAN_POINT ( 'NONE',  ( 9.474510206698729675, 16.51473224551082808, 107.0844237280190043 ) ) ;
#172800 = CARTESIAN_POINT ( 'NONE',  ( -18.67979575497193778, 10.72451020669871902, 38.33442372801900433 ) ) ;
#172802 = CARTESIAN_POINT ( 'NONE',  ( 5.153800228976335163, 19.02544592524342804, 104.7905762719809957 ) ) ;
#172803 = CARTESIAN_POINT ( 'NONE',  ( 16.46253265017160672, -9.564922557960803928, 98.33224293864769550 ) ) ;
#172804 = CARTESIAN_POINT ( 'NONE',  ( -0.05219959533907301413, -21.53943276465977519, 102.4989096053143811 ) ) ;
#172805 = CARTESIAN_POINT ( 'NONE',  ( 16.46253265017160672, -9.564922557960803928, 53.33224293864768839 ) ) ;
#172806 = CARTESIAN_POINT ( 'NONE',  ( -17.40861289039003523, 6.110651285853257342, 23.62767529172569070 ) ) ;
#172807 = CARTESIAN_POINT ( 'NONE',  ( 4.379528057220339221, -16.55341960407611168, 82.70724293864770971 ) ) ;
#172808 = CARTESIAN_POINT ( 'NONE',  ( 15.72974639402199770, -15.80617190586745480, 23.12390960531436335 ) ) ;
#172809 = CARTESIAN_POINT ( 'NONE',  ( -16.38665767535054130, 7.295008042176027274, 35.26400864214546260 ) ) ;
#172810 = VECTOR ( 'NONE', #76282, 1000.000000000000000 ) ;
#172811 = CARTESIAN_POINT ( 'NONE',  ( 0.05219959533907565091, 21.53943276465977519, 99.99890960531436690 ) ) ;
#172812 = CARTESIAN_POINT ( 'NONE',  ( -0.05219959533936034679, 19.03943276465977164, 67.50109039468566152 ) ) ;
#172813 = CARTESIAN_POINT ( 'NONE',  ( 5.719274019375991003, -21.55341960407610458, 22.70724293864769194 ) ) ;
#172814 = CARTESIAN_POINT ( 'NONE',  ( 9.474510206698971260, -16.51473224551069308, 22.91557627198102765 ) ) ;
#172815 = CARTESIAN_POINT ( 'NONE',  ( 21.55341960407610458, 5.719274019375980345, 48.95724293864770971 ) ) ;
#172816 = CARTESIAN_POINT ( 'NONE',  ( 19.03943276465977164, -0.05219959533909143690, 103.7489096053143669 ) ) ;
#172817 = CARTESIAN_POINT ( 'NONE',  ( 5.719274019375673035, 21.55341960407619339, 72.29275706135236135 ) ) ;
#172818 = CARTESIAN_POINT ( 'NONE',  ( 19.05341960407611168, 5.049401038298154454, 53.95724293864770260 ) ) ;
#172819 = CARTESIAN_POINT ( 'NONE',  ( 16.53943276465976808, -0.05219959533910856209, 83.74890960531435269 ) ) ;
#172820 = CARTESIAN_POINT ( 'NONE',  ( -0.05219959533934338120, 16.53943276465976808, 37.50109039468568284 ) ) ;
#172821 = CARTESIAN_POINT ( 'NONE',  ( 18.67979575497194134, -10.72451020669871369, 70.83442372801901854 ) ) ;
#172822 = ORIENTED_EDGE ( 'NONE', *, *, #162596, .F. ) ;
#172823 = CARTESIAN_POINT ( 'NONE',  ( 19.02544592524334988, 5.153800228976608722, 31.45942372801900433 ) ) ;
#172824 = CARTESIAN_POINT ( 'NONE',  ( -5.049401038297874678, -19.05341960407617918, 79.79275706135233293 ) ) ;
#172825 = CIRCLE ( 'NONE', #72676, 12.00000000000000178 ) ;
#172826 = CARTESIAN_POINT ( 'NONE',  ( -19.03943276465977164, -0.05219959533935918106, 43.75109039468566863 ) ) ;
#172827 = LINE ( 'NONE', #144452, #144018 ) ;
#172828 = CARTESIAN_POINT ( 'NONE',  ( -21.52544592524334988, -5.823673210054445271, 33.95942372801901143 ) ) ;
#172829 = CARTESIAN_POINT ( 'NONE',  ( 38.00000000000000000, 12.34694845685046616, -2.649999994537626247 ) ) ;
#172830 = CARTESIAN_POINT ( 'NONE',  ( 19.02544592524334988, 5.153800228976608722, 31.45942372801900433 ) ) ;
#172831 = CARTESIAN_POINT ( 'NONE',  ( 13.97604488694527802, 13.89961937509977652, 54.37390960531435979 ) ) ;
#172832 = CARTESIAN_POINT ( 'NONE',  ( 19.03943276465977164, 0.05219959533936151252, 31.25109039468566863 ) ) ;
#172833 = CARTESIAN_POINT ( 'NONE',  ( 0.05219959533934541429, -16.53943276465976808, 110.0010903946856757 ) ) ;
#172835 = CARTESIAN_POINT ( 'NONE',  ( 0.05219959533937995610, -21.53943276465977519, 80.00109039468568994 ) ) ;
#172834 = CARTESIAN_POINT ( 'NONE',  ( 21.53943276465977519, -0.05219959533907433946, 23.74890960531435269 ) ) ;
#172836 = CARTESIAN_POINT ( 'NONE',  ( -36.91746825000001309, -11.99521256947794789, -4.524999997268813523 ) ) ;
#172837 = DIRECTION ( 'NONE',  ( 0.000000000000000000, 0.000000000000000000, 1.000000000000000000 ) ) ;
#172838 = CARTESIAN_POINT ( 'NONE',  ( 21.53943276465977519, 0.05219959533937863772, 86.25109039468568994 ) ) ;
#172839 = CARTESIAN_POINT ( 'NONE',  ( 23.16108095314134019, -1.467328942210885279, -57.58004187413772712 ) ) ;
#172840 = CARTESIAN_POINT ( 'NONE',  ( 5.153800228976335163, 19.02544592524342804, 94.79057627198103830 ) ) ;
#172841 = CARTESIAN_POINT ( 'NONE',  ( -1.355922687059376797, -31.06299995236813416, -50.16575868250043868 ) ) ;
#172842 = CARTESIAN_POINT ( 'NONE',  ( 16.46253265017160672, -9.564922557960803928, 53.33224293864768839 ) ) ;
#172843 = CARTESIAN_POINT ( 'NONE',  ( -5.719274019375978568, 21.55341960407610458, 50.20724293864769550 ) ) ;
#172844 = CARTESIAN_POINT ( 'NONE',  ( -16.53943276465976808, -0.05219959533934237506, 113.7510903946856757 ) ) ;
#172846 = CARTESIAN_POINT ( 'NONE',  ( 13.97604488694527802, 13.89961937509977652, 99.37390960531436690 ) ) ;
#172845 = CARTESIAN_POINT ( 'NONE',  ( -0.05219959533910754901, -16.53943276465976808, 97.49890960531436690 ) ) ;
#172847 = CARTESIAN_POINT ( 'NONE',  ( 19.05341960407617918, -5.049401038297876454, 21.04275706135232582 ) ) ;
#172848 = CARTESIAN_POINT ( 'NONE',  ( -0.05219959533910754901, -16.53943276465976808, 107.4989096053143669 ) ) ;
#172849 = CARTESIAN_POINT ( 'NONE',  ( 18.67979575497194134, -10.72451020669871369, 50.83442372801901143 ) ) ;
#172850 = CARTESIAN_POINT ( 'NONE',  ( 16.52544592524335698, 4.483927247898782831, 101.4594237280190185 ) ) ;
#172851 = CARTESIAN_POINT ( 'NONE',  ( -9.474510206698720793, -16.51473224551083518, 64.58442372801900433 ) ) ;
#172852 = CYLINDRICAL_SURFACE ( 'NONE', #39963, 2.000000000000000000 ) ;
#172853 = CARTESIAN_POINT ( 'NONE',  ( -5.049401038298153566, 19.05341960407611168, 115.2072429386477097 ) ) ;
#172854 = CARTESIAN_POINT ( 'NONE',  ( 4.483927247898545687, 16.52544592524342804, 79.79057627198102409 ) ) ;
#172855 = CIRCLE ( 'NONE', #30398, 3.799999999999999378 ) ;
#172856 = CARTESIAN_POINT ( 'NONE',  ( -19.03943276465977164, -0.05219959533935918106, 58.75109039468566863 ) ) ;
#172857 = CARTESIAN_POINT ( 'NONE',  ( 19.02544592524343514, -5.153800228976328945, 63.54057627198103830 ) ) ;
#172858 = CARTESIAN_POINT ( 'NONE',  ( 4.483927247898545687, 16.52544592524342804, 64.79057627198103830 ) ) ;
#172859 = CARTESIAN_POINT ( 'NONE',  ( -16.51473224551082808, 9.474510206698731452, 98.33442372801900433 ) ) ;
#172860 = CARTESIAN_POINT ( 'NONE',  ( -21.53943276465977519, 0.05219959533907696930, 31.24890960531435979 ) ) ;
#172861 = ORIENTED_EDGE ( 'NONE', *, *, #120148, .F. ) ;
#172862 = CARTESIAN_POINT ( 'NONE',  ( -12.14591786802309592, -12.06949235617757132, 96.87390960531436690 ) ) ;
#172863 = CARTESIAN_POINT ( 'NONE',  ( 7.656827144875921753, -71.74905178543389184, -4.999999999999999112 ) ) ;
#172865 = CARTESIAN_POINT ( 'NONE',  ( -10.81492255796078084, -18.62759615963271287, 67.08224293864770971 ) ) ;
#172864 = CARTESIAN_POINT ( 'NONE',  ( -13.89961937509977652, 13.97604488694528158, 65.62390960531436690 ) ) ;
#172866 = CARTESIAN_POINT ( 'NONE',  ( -9.564922557960796823, -16.46253265017161027, 47.08224293864769550 ) ) ;
#172868 = CARTESIAN_POINT ( 'NONE',  ( 19.02544592524343514, -5.153800228976328945, 68.54057627198103830 ) ) ;
#172867 = CARTESIAN_POINT ( 'NONE',  ( 0.05219959533934541429, -16.53943276465976808, 95.00109039468568994 ) ) ;
#172869 = CARTESIAN_POINT ( 'NONE',  ( 19.02544592524334988, 5.153800228976608722, 51.45942372801900433 ) ) ;
#172870 = CARTESIAN_POINT ( 'NONE',  ( -18.62759615963255300, -10.81492255796106328, 84.16775706135234714 ) ) ;
#172871 = CARTESIAN_POINT ( 'NONE',  ( 15.80617190586746368, 15.72974639402197994, 54.37390960531435979 ) ) ;
#172872 = CARTESIAN_POINT ( 'NONE',  ( -19.03943276465977164, 0.05219959533909376836, 111.2489096053143669 ) ) ;
#172873 = CARTESIAN_POINT ( 'NONE',  ( 5.153800228976335163, 19.02544592524342804, 24.79057627198102765 ) ) ;
#172874 = CARTESIAN_POINT ( 'NONE',  ( -14.29746914071037622, -8.314922557961029526, 84.16775706135234714 ) ) ;
#172875 = CARTESIAN_POINT ( 'NONE',  ( -19.05341960407617563, 5.049401038297882671, 108.5427570613523187 ) ) ;
#172876 = CARTESIAN_POINT ( 'NONE',  ( 9.564922557960805705, 16.46253265017160317, 24.58224293864769194 ) ) ;
#172877 = CARTESIAN_POINT ( 'NONE',  ( 17.60728821186566861, -5.500000000000026645, 43.36690927743004664 ) ) ;
#172878 = CARTESIAN_POINT ( 'NONE',  ( -0.05219959533937732626, 21.53943276465977519, 102.5010903946856899 ) ) ;
#172879 = CIRCLE ( 'NONE', #14695, 10.00000000000000000 ) ;
#172880 = CARTESIAN_POINT ( 'NONE',  ( 12.06949235617757843, -12.14591786802309237, 58.12390960531435979 ) ) ;
#172881 = CARTESIAN_POINT ( 'NONE',  ( -14.34966873604960291, -8.224510206698953496, 66.66557627198102409 ) ) ;
#172882 = CARTESIAN_POINT ( 'NONE',  ( 18.62759615963271287, -10.81492255796078972, 98.33224293864769550 ) ) ;
#172883 = CARTESIAN_POINT ( 'NONE',  ( -15.80617190586745835, -15.72974639402198527, 91.87390960531436690 ) ) ;
#172884 = CARTESIAN_POINT ( 'NONE',  ( 16.18388926212238133, -7.379444403734519042, 97.06046848633849322 ) ) ;
#172885 = CARTESIAN_POINT ( 'NONE',  ( -15.80617190586745835, -15.72974639402198527, 41.87390960531435979 ) ) ;
#172887 = VECTOR ( 'NONE', #27642, 1000.000000000000000 ) ;
#172886 = CARTESIAN_POINT ( 'NONE',  ( -12.06949235617739369, -12.14591786802326823, 64.37609039468568994 ) ) ;
#172888 = CARTESIAN_POINT ( 'NONE',  ( 14.29746914071049879, -8.314922557960816363, 93.33224293864769550 ) ) ;
#172889 = CARTESIAN_POINT ( 'NONE',  ( 13.97604488694527802, 13.89961937509977652, 44.37390960531435269 ) ) ;
#172890 =( LENGTH_UNIT ( ) NAMED_UNIT ( * ) SI_UNIT ( .MILLI., .METRE. ) );
#172891 = CARTESIAN_POINT ( 'NONE',  ( 35.09697802211634610, -5.650142709571455590, 40.04346530744799537 ) ) ;
#172892 = CARTESIAN_POINT ( 'NONE',  ( 14.29746914071037800, 8.314922557961029526, 91.66775706135234714 ) ) ;
#172893 = CARTESIAN_POINT ( 'NONE',  ( -15.80617190586768217, 15.72974639402176855, 28.12609039468568284 ) ) ;
#172894 = CARTESIAN_POINT ( 'NONE',  ( 19.02544592524343514, -5.153800228976328945, 83.54057627198100988 ) ) ;
#172895 = CARTESIAN_POINT ( 'NONE',  ( 18.62759615963255655, 10.81492255796105972, 66.66775706135234714 ) ) ;
#172896 = CARTESIAN_POINT ( 'NONE',  ( 69.65682714487590488, -71.74905178543389184, -25.00000000000000000 ) ) ;
#172898 = EDGE_CURVE ( 'NONE', #143487, #36546, #135131, .T. ) ;
#172897 = CARTESIAN_POINT ( 'NONE',  ( 0.05219959533909260263, 19.03943276465977164, 29.99890960531435979 ) ) ;
#172899 = ORIENTED_EDGE ( 'NONE', *, *, #13466, .T. ) ;
#172900 = CARTESIAN_POINT ( 'NONE',  ( -21.55341960407619339, 5.719274019375674811, 58.54275706135235424 ) ) ;
#172902 = CARTESIAN_POINT ( 'NONE',  ( -16.51473224551069308, -9.474510206698971260, 111.6655762719810383 ) ) ;
#172901 = CARTESIAN_POINT ( 'NONE',  ( -19.03943276465977164, 0.05219959533909376836, 31.24890960531435979 ) ) ;
#172903 = CARTESIAN_POINT ( 'NONE',  ( -19.03943276465977164, 0.05219959533909376836, 96.24890960531436690 ) ) ;
#172904 = CARTESIAN_POINT ( 'NONE',  ( 9.474510206698729675, 16.51473224551082808, 62.08442372801899722 ) ) ;
#172905 = CARTESIAN_POINT ( 'NONE',  ( -18.67979575497193778, 10.72451020669871902, 23.33442372801901499 ) ) ;
#172906 = CARTESIAN_POINT ( 'NONE',  ( -16.51473224551082808, 9.474510206698731452, 53.33442372801900433 ) ) ;
#172907 = CARTESIAN_POINT ( 'NONE',  ( -13.89961937509977652, 13.97604488694528158, 40.62390960531435979 ) ) ;
#172908 = CARTESIAN_POINT ( 'NONE',  ( 4.483927247898790824, -16.52544592524335698, 105.2094237280190328 ) ) ;
#172909 = CARTESIAN_POINT ( 'NONE',  ( 9.474510206698729675, 16.51473224551082808, 67.08442372801900433 ) ) ;
#172910 = CARTESIAN_POINT ( 'NONE',  ( -16.55341960407611168, -4.379528057220339221, 31.45724293864769550 ) ) ;
#172912 = ORIENTED_EDGE ( 'NONE', *, *, #1987, .F. ) ;
#172911 = CARTESIAN_POINT ( 'NONE',  ( 19.02544592524334988, 5.153800228976608722, 51.45942372801900433 ) ) ;
#172913 = CARTESIAN_POINT ( 'NONE',  ( -13.89961937509977652, 13.97604488694528158, 95.62390960531436690 ) ) ;
#172914 = CARTESIAN_POINT ( 'NONE',  ( -0.05219959533937732626, 21.53943276465977519, 112.5010903946857042 ) ) ;
#172915 = CARTESIAN_POINT ( 'NONE',  ( -5.823673210054431948, 21.52544592524334988, 102.7094237280190185 ) ) ;
#172916 = CARTESIAN_POINT ( 'NONE',  ( -6.019987952026120409E-15, 39.95163481335720235, -4.502157773949821973 ) ) ;
#172917 = CARTESIAN_POINT ( 'NONE',  ( -18.67979575497193778, 10.72451020669871902, 83.33442372801903275 ) ) ;
#172918 = CARTESIAN_POINT ( 'NONE',  ( 12.06949235617739724, 12.14591786802326823, 26.87609039468567218 ) ) ;
#172919 = CARTESIAN_POINT ( 'NONE',  ( 9.564922557960805705, 16.46253265017160317, 89.58224293864769550 ) ) ;
#172920 = CARTESIAN_POINT ( 'NONE',  ( 27.73933785331498214, 9.013057229001095294, 139.9750000027311501 ) ) ;
#172921 = CARTESIAN_POINT ( 'NONE',  ( 19.05341960407611168, 5.049401038298154454, 73.95724293864768129 ) ) ;
#172922 = CARTESIAN_POINT ( 'NONE',  ( 17.81289503416610742, 24.51734667627700404, 141.3000000000000114 ) ) ;
#172923 = CARTESIAN_POINT ( 'NONE',  ( -16.46253265017146816, -9.564922557961047289, 69.16775706135233293 ) ) ;
#172924 = CARTESIAN_POINT ( 'NONE',  ( -0.05219959533909027116, -19.03943276465977164, 107.4989096053143527 ) ) ;
#172925 = CARTESIAN_POINT ( 'NONE',  ( 18.62759615963255655, 10.81492255796105972, 106.6677570613523756 ) ) ;
#172926 = CARTESIAN_POINT ( 'NONE',  ( 14.29746914071049879, -8.314922557960816363, 93.33224293864769550 ) ) ;
#172927 = CARTESIAN_POINT ( 'NONE',  ( -10.81492255796078084, -18.62759615963271287, 47.08224293864770260 ) ) ;
#172928 = CARTESIAN_POINT ( 'NONE',  ( -21.52544592524343514, 5.823673210054127303, 41.04057627198103120 ) ) ;
#172929 = CARTESIAN_POINT ( 'NONE',  ( -12.06949235617756955, 12.14591786802309770, 105.6239096053143669 ) ) ;
#172930 = FACE_OUTER_BOUND ( 'NONE', #91430, .T. ) ;
#172931 = CARTESIAN_POINT ( 'NONE',  ( -13.97604488694547697, 13.89961937509957934, 53.12609039468565442 ) ) ;
#172932 = CARTESIAN_POINT ( 'NONE',  ( -0.05219959533910754901, -16.53943276465976808, 32.49890960531435979 ) ) ;
#172933 = CARTESIAN_POINT ( 'NONE',  ( 9.474510206698971260, -16.51473224551069308, 97.91557627198102409 ) ) ;
#172934 = CARTESIAN_POINT ( 'NONE',  ( 10.81492255796106328, -18.62759615963255655, 85.41775706135236135 ) ) ;
#172935 = CARTESIAN_POINT ( 'NONE',  ( -0.05219959533907301413, -21.53943276465977519, 72.49890960531435269 ) ) ;
#172936 = CARTESIAN_POINT ( 'NONE',  ( -18.67979575497193778, 10.72451020669871902, 48.33442372801902565 ) ) ;
#172937 = CARTESIAN_POINT ( 'NONE',  ( -10.72451020669898014, 18.67979575497178502, 100.4155762719810241 ) ) ;
#172938 = CARTESIAN_POINT ( 'NONE',  ( -5.823673210054431948, 21.52544592524334988, 57.70942372801901143 ) ) ;
#172939 = CARTESIAN_POINT ( 'NONE',  ( 13.97604488694527802, 13.89961937509977652, 29.37390960531435979 ) ) ;
#172940 = CARTESIAN_POINT ( 'NONE',  ( -5.153800228976328057, -19.02544592524343514, 82.29057627198103830 ) ) ;
#172941 = CARTESIAN_POINT ( 'NONE',  ( -8.224510206698735004, -14.34966873604973081, 79.58442372801903275 ) ) ;
#172942 = CARTESIAN_POINT ( 'NONE',  ( 14.34966873604960469, 8.224510206698951720, 104.1655762719810241 ) ) ;
#172943 = CARTESIAN_POINT ( 'NONE',  ( 9.474510206698971260, -16.51473224551069308, 102.9155762719810241 ) ) ;
#172944 = CIRCLE ( 'NONE', #92246, 9.100000000000001421 ) ;
#172945 = CARTESIAN_POINT ( 'NONE',  ( 8.224510206698953496, -14.34966873604960469, 52.91557627198103830 ) ) ;
#172946 = CARTESIAN_POINT ( 'NONE',  ( -8.314922557961024197, 14.29746914071037800, 107.9177570613523471 ) ) ;
#172947 = CARTESIAN_POINT ( 'NONE',  ( 9.474510206698971260, -16.51473224551069308, 57.91557627198103120 ) ) ;
#172948 = CARTESIAN_POINT ( 'NONE',  ( -9.474510206698964154, 16.51473224551069663, 40.41557627198103120 ) ) ;
#172949 = CARTESIAN_POINT ( 'NONE',  ( 10.81492255796078972, 18.62759615963270932, 39.58224293864769550 ) ) ;
#172950 = CARTESIAN_POINT ( 'NONE',  ( 0.05219959533936267826, -19.03943276465977164, 25.00109039468566152 ) ) ;
#172952 = CARTESIAN_POINT ( 'NONE',  ( -4.379528057220328563, 16.55341960407611168, 35.20724293864768839 ) ) ;
#172951 = CARTESIAN_POINT ( 'NONE',  ( 13.70000000000001528, -4.867217739956692332E-14, -62.58071313852362039 ) ) ;
#172953 = CARTESIAN_POINT ( 'NONE',  ( 10.81492255796106328, -18.62759615963255655, 40.41775706135234714 ) ) ;
#172954 = CARTESIAN_POINT ( 'NONE',  ( 24.27707668318813816, -5.858708095980206920, 170.2635530474734367 ) ) ;
#172955 = CARTESIAN_POINT ( 'NONE',  ( 8.314922557961029526, -14.29746914071037800, 60.41775706135235424 ) ) ;
#172956 = CARTESIAN_POINT ( 'NONE',  ( -16.51473224551082808, 9.474510206698731452, 63.33442372801900433 ) ) ;
#172957 = CARTESIAN_POINT ( 'NONE',  ( 8.224510206698953496, -14.34966873604960469, 22.91557627198102765 ) ) ;
#172958 = CARTESIAN_POINT ( 'NONE',  ( -19.01529144963334872, -5.500000000000082601, 76.23431955728440812 ) ) ;
#172959 = CARTESIAN_POINT ( 'NONE',  ( 16.52544592524335698, 4.483927247898782831, 111.4594237280190328 ) ) ;
#172960 = CARTESIAN_POINT ( 'NONE',  ( -13.89961937509977652, 13.97604488694528158, 35.62390960531435269 ) ) ;
#172961 = CARTESIAN_POINT ( 'NONE',  ( -9.474510206698964154, 16.51473224551069663, 60.41557627198102409 ) ) ;
#172962 = CARTESIAN_POINT ( 'NONE',  ( -9.564922557960796823, -16.46253265017161027, 22.08224293864768839 ) ) ;
#172963 = CARTESIAN_POINT ( 'NONE',  ( 21.52544592524334988, 5.823673210054432836, 31.45942372801901854 ) ) ;
#172964 = CARTESIAN_POINT ( 'NONE',  ( -19.05341960407611168, -5.049401038298163336, 51.45724293864770260 ) ) ;
#172965 = CARTESIAN_POINT ( 'NONE',  ( -24.95432927374998044, 3.806786798636383917, 190.0000000000000000 ) ) ;
#172966 = CARTESIAN_POINT ( 'NONE',  ( -16.51473224551069308, -9.474510206698971260, 51.66557627198102409 ) ) ;
#172967 = CARTESIAN_POINT ( 'NONE',  ( -19.03943276465977164, 0.05219959533909376836, 116.2489096053143669 ) ) ;
#172969 = CARTESIAN_POINT ( 'NONE',  ( -8.224510206698948167, 14.34966873604960824, 105.4155762719810383 ) ) ;
#172968 = CARTESIAN_POINT ( 'NONE',  ( 18.62759615963255655, 10.81492255796105972, 56.66775706135235424 ) ) ;
#172970 = CARTESIAN_POINT ( 'NONE',  ( 19.02544592524343514, -5.153800228976328945, 113.5405762719810241 ) ) ;
#172971 = CARTESIAN_POINT ( 'NONE',  ( -12.14591786802326823, 12.06949235617739902, 83.12609039468568994 ) ) ;
#172972 = CARTESIAN_POINT ( 'NONE',  ( 21.55341960407619695, -5.719274019375665929, 91.04275706135236135 ) ) ;
#172973 = CARTESIAN_POINT ( 'NONE',  ( 8.314922557961029526, -14.29746914071037800, 55.41775706135234714 ) ) ;
#172974 = CARTESIAN_POINT ( 'NONE',  ( 19.02544592524343514, -5.153800228976328945, 93.54057627198102409 ) ) ;
#172975 = CARTESIAN_POINT ( 'NONE',  ( 4.379528057220092307, 16.55341960407617563, 37.29275706135235424 ) ) ;
#172976 = CARTESIAN_POINT ( 'NONE',  ( -16.53943276465976808, -0.05219959533934237506, 28.75109039468567929 ) ) ;
#172977 = CARTESIAN_POINT ( 'NONE',  ( 14.34966873604972726, -8.224510206698740333, 95.83442372801903275 ) ) ;
#172978 = CARTESIAN_POINT ( 'NONE',  ( -15.80617190586768217, 15.72974639402176855, 58.12609039468568994 ) ) ;
#172979 = CARTESIAN_POINT ( 'NONE',  ( 0.05219959533936267826, -19.03943276465977164, 100.0010903946856757 ) ) ;
#172980 = CARTESIAN_POINT ( 'NONE',  ( -5.719274019375978568, 21.55341960407610458, 115.2072429386476955 ) ) ;
#172982 = CARTESIAN_POINT ( 'NONE',  ( -9.564922557961040184, 16.46253265017147172, 107.9177570613523471 ) ) ;
#172981 = CARTESIAN_POINT ( 'NONE',  ( 12.06949235617757843, -12.14591786802309237, 103.1239096053143811 ) ) ;
#172983 = CARTESIAN_POINT ( 'NONE',  ( 4.483927247898790824, -16.52544592524335698, 75.20942372801901854 ) ) ;
#172984 = CARTESIAN_POINT ( 'NONE',  ( 21.75836449082842705, 8.509082329563685931, 169.1767350484841472 ) ) ;
#172985 = CARTESIAN_POINT ( 'NONE',  ( -0.05219959533936034679, 19.03943276465977164, 67.50109039468566152 ) ) ;
#172986 = CARTESIAN_POINT ( 'NONE',  ( 8.314922557960818139, 14.29746914071049879, 39.58224293864769550 ) ) ;
#172987 = CARTESIAN_POINT ( 'NONE',  ( 16.52544592524342804, -4.483927247898539470, 38.54057627198103120 ) ) ;
#172988 = CARTESIAN_POINT ( 'NONE',  ( 8.314922557960818139, 14.29746914071049879, 94.58224293864769550 ) ) ;
#172990 = CARTESIAN_POINT ( 'NONE',  ( -17.31728774477273447, 6.344390552232388458, 90.81906651689320142 ) ) ;
#172989 = CARTESIAN_POINT ( 'NONE',  ( -19.02544592524334988, -5.153800228976617603, 28.95942372801900433 ) ) ;
#172991 = CARTESIAN_POINT ( 'NONE',  ( 21.53943276465977519, 0.05219959533937863772, 36.25109039468567573 ) ) ;
#172992 = CARTESIAN_POINT ( 'NONE',  ( 5.049401038297881783, 19.05341960407617563, 97.29275706135233293 ) ) ;
#172993 = CARTESIAN_POINT ( 'NONE',  ( -0.3431728551240714742, -71.74905178543389184, -15.00000000000000178 ) ) ;
#172994 = CARTESIAN_POINT ( 'NONE',  ( -19.02544592524342804, 5.153800228976336051, 86.04057627198103830 ) ) ;
#172995 = CARTESIAN_POINT ( 'NONE',  ( -9.564922557960796823, -16.46253265017161027, 87.08224293864769550 ) ) ;
#172996 = CARTESIAN_POINT ( 'NONE',  ( 10.72451020669898902, -18.67979575497178502, 62.91557627198102409 ) ) ;
#172997 = CARTESIAN_POINT ( 'NONE',  ( 0.05219959533910956823, 16.53943276465976808, 89.99890960531438111 ) ) ;
#172998 = CARTESIAN_POINT ( 'NONE',  ( -0.05219959533909027116, -19.03943276465977164, 72.49890960531435269 ) ) ;
#172999 = CARTESIAN_POINT ( 'NONE',  ( -19.02544592524342804, 5.153800228976336051, 36.04057627198100988 ) ) ;
#173000 = CARTESIAN_POINT ( 'NONE',  ( 0.05219959533937995610, -21.53943276465977519, 45.00109039468568284 ) ) ;
#173001 = CARTESIAN_POINT ( 'NONE',  ( -10.72451020669870658, -18.67979575497194134, 69.58442372801900433 ) ) ;
#173002 = CARTESIAN_POINT ( 'NONE',  ( -5.153800228976328057, -19.02544592524343514, 62.29057627198100988 ) ) ;
#173003 = CARTESIAN_POINT ( 'NONE',  ( 12.14591786802327356, -12.06949235617739191, 85.62609039468568994 ) ) ;
#173004 = CARTESIAN_POINT ( 'NONE',  ( 21.53943276465977519, 0.05219959533937863772, 31.25109039468568639 ) ) ;
#173005 = CARTESIAN_POINT ( 'NONE',  ( -18.62759615963255300, -10.81492255796106328, 29.16775706135234003 ) ) ;
#173007 = CARTESIAN_POINT ( 'NONE',  ( 13.97604488694527802, 13.89961937509977652, 74.37390960531436690 ) ) ;
#173006 = CARTESIAN_POINT ( 'NONE',  ( -5.049401038297874678, -19.05341960407617918, 49.79275706135231871 ) ) ;
#173008 = CARTESIAN_POINT ( 'NONE',  ( -19.03943276465977164, -0.05219959533935918106, 28.75109039468566507 ) ) ;
#173009 = CARTESIAN_POINT ( 'NONE',  ( -18.62759615963255300, -10.81492255796106328, 79.16775706135234714 ) ) ;
#173010 = CARTESIAN_POINT ( 'NONE',  ( -5.719274019375978568, 21.55341960407610458, 75.20724293864769550 ) ) ;
#173011 = CARTESIAN_POINT ( 'NONE',  ( -4.379528057220328563, 16.55341960407611168, 45.20724293864769550 ) ) ;
#173013 = CARTESIAN_POINT ( 'NONE',  ( -5.153800228976607833, 19.02544592524334988, 27.70942372801899722 ) ) ;
#173012 = CARTESIAN_POINT ( 'NONE',  ( -18.62759615963255300, -10.81492255796106328, 104.1677570613523471 ) ) ;
#173014 = CARTESIAN_POINT ( 'NONE',  ( -16.55341960407611168, -4.379528057220339221, 76.45724293864769550 ) ) ;
#173015 = CARTESIAN_POINT ( 'NONE',  ( -12.14591786802309592, -12.06949235617757132, 111.8739096053143669 ) ) ;
#173016 = CARTESIAN_POINT ( 'NONE',  ( 13.89961937509957401, 13.97604488694547697, 71.87609039468567573 ) ) ;
#173017 = CARTESIAN_POINT ( 'NONE',  ( 14.29746914071049879, -8.314922557960816363, 33.33224293864769550 ) ) ;
#173018 = CARTESIAN_POINT ( 'NONE',  ( -21.52544592524334988, -5.823673210054445271, 83.95942372801900433 ) ) ;
#173019 = CARTESIAN_POINT ( 'NONE',  ( 5.153800228976335163, 19.02544592524342804, 74.79057627198103830 ) ) ;
#173020 = CARTESIAN_POINT ( 'NONE',  ( 0.05219959533936267826, -19.03943276465977164, 50.00109039468566863 ) ) ;
#173021 = CARTESIAN_POINT ( 'NONE',  ( -10.72451020669898014, 18.67979575497178502, 60.41557627198102409 ) ) ;
#173022 = CARTESIAN_POINT ( 'NONE',  ( 21.52544592524334988, 5.823673210054432836, 21.45942372801901499 ) ) ;
#173023 = CARTESIAN_POINT ( 'NONE',  ( 9.474510206698729675, 16.51473224551082808, 107.0844237280190043 ) ) ;
#173024 = CARTESIAN_POINT ( 'NONE',  ( 8.224510206698742110, 14.34966873604972548, 72.08442372801899012 ) ) ;
#173026 = CARTESIAN_POINT ( 'NONE',  ( 0.05219959533907565091, 21.53943276465977519, 104.9989096053143669 ) ) ;
#173025 = CARTESIAN_POINT ( 'NONE',  ( -4.500000000000001776, -139.2199041982123617, 21.73825240834792893 ) ) ;
#173027 = CARTESIAN_POINT ( 'NONE',  ( -8.314922557960811034, -14.29746914071050412, 107.0822429386476955 ) ) ;
#173028 = CARTESIAN_POINT ( 'NONE',  ( -17.49999999999999645, -4.013004640162675329, 29.55394279005589198 ) ) ;
#173029 = CARTESIAN_POINT ( 'NONE',  ( -8.224510206698735004, -14.34966873604973081, 39.58442372801901143 ) ) ;
#173030 = EDGE_CURVE ( 'NONE', #168590, #166995, #133110, .T. ) ;
#173031 = CARTESIAN_POINT ( 'NONE',  ( 21.53943276465977519, -0.05219959533907433946, 58.74890960531436690 ) ) ;
#173032 = CARTESIAN_POINT ( 'NONE',  ( -16.52544592524335698, -4.483927247898792601, 103.9594237280190185 ) ) ;
#173033 = CARTESIAN_POINT ( 'NONE',  ( -5.049401038298153566, 19.05341960407611168, 35.20724293864768839 ) ) ;
#173034 = CARTESIAN_POINT ( 'NONE',  ( 8.224510206698742110, 14.34966873604972548, 72.08442372801899012 ) ) ;
#173035 = CARTESIAN_POINT ( 'NONE',  ( 16.46253265017146816, 9.564922557961045513, 66.66775706135233293 ) ) ;
#173036 = CARTESIAN_POINT ( 'NONE',  ( -21.55341960407619339, 5.719274019375674811, 43.54275706135235424 ) ) ;
#173037 = CARTESIAN_POINT ( 'NONE',  ( -21.55341960407610458, -5.719274019375992779, 61.45724293864770260 ) ) ;
#173038 = CARTESIAN_POINT ( 'NONE',  ( -4.379528057220086978, -16.55341960407618274, 99.79275706135234714 ) ) ;
#173039 = CARTESIAN_POINT ( 'NONE',  ( -10.72451020669870658, -18.67979575497194134, 89.58442372801901854 ) ) ;
#173040 = CARTESIAN_POINT ( 'NONE',  ( -21.53943276465977519, 0.05219959533907696930, 51.24890960531436690 ) ) ;
#173041 = CARTESIAN_POINT ( 'NONE',  ( -5.719274019375978568, 21.55341960407610458, 30.20724293864769550 ) ) ;
#173042 = ORIENTED_EDGE ( 'NONE', *, *, #192356, .F. ) ;
#173043 = CARTESIAN_POINT ( 'NONE',  ( -8.314922557961024197, 14.29746914071037800, 82.91775706135234714 ) ) ;
#173044 = CARTESIAN_POINT ( 'NONE',  ( -21.53943276465977519, 0.05219959533907696930, 46.24890960531435979 ) ) ;
#173045 = EDGE_LOOP ( 'NONE', ( #7202, #196214, #161469, #66335 ) ) ;
#173046 = CARTESIAN_POINT ( 'NONE',  ( -5.049401038298153566, 19.05341960407611168, 95.20724293864770971 ) ) ;
#173047 = DIRECTION ( 'NONE',  ( -1.000000000000000000, 0.000000000000000000, -5.204170427930421283E-16 ) ) ;
#173048 = CARTESIAN_POINT ( 'NONE',  ( -9.564922557960796823, -16.46253265017161027, 32.08224293864769550 ) ) ;
#173049 = CARTESIAN_POINT ( 'NONE',  ( -21.53943276465977519, 0.05219959533907696930, 56.24890960531436690 ) ) ;
#173050 = CARTESIAN_POINT ( 'NONE',  ( -16.53943276465976808, -0.05219959533934237506, 88.75109039468567573 ) ) ;
#173051 = CARTESIAN_POINT ( 'NONE',  ( 5.719274019375673035, 21.55341960407619339, 42.29275706135235424 ) ) ;
#173052 = CARTESIAN_POINT ( 'NONE',  ( -5.049401038297874678, -19.05341960407617918, 99.79275706135234714 ) ) ;
#173053 = CARTESIAN_POINT ( 'NONE',  ( -14.34966873604960291, -8.224510206698953496, 96.66557627198102409 ) ) ;
#173054 = CARTESIAN_POINT ( 'NONE',  ( 14.29746914071037800, 8.314922557961029526, 21.66775706135235069 ) ) ;
#173055 = CIRCLE ( 'NONE', #53532, 2.055000000000000160 ) ;
#173056 = CARTESIAN_POINT ( 'NONE',  ( -5.049401038298153566, 19.05341960407611168, 45.20724293864769550 ) ) ;
#173057 = CARTESIAN_POINT ( 'NONE',  ( 13.74234921310041457, -0.4081324879001385630, -62.56359473395606585 ) ) ;
#173058 = CARTESIAN_POINT ( 'NONE',  ( -5.049401038298153566, 19.05341960407611168, 95.20724293864770971 ) ) ;
#173059 = CARTESIAN_POINT ( 'NONE',  ( -4.379528057220086978, -16.55341960407618274, 74.79275706135234714 ) ) ;
#173060 = CARTESIAN_POINT ( 'NONE',  ( -5.719274019375665041, -21.55341960407619695, 104.7927570613523898 ) ) ;
#173061 = CARTESIAN_POINT ( 'NONE',  ( -15.72974639402197994, 15.80617190586746368, 60.62390960531437401 ) ) ;
#173062 = CARTESIAN_POINT ( 'NONE',  ( -14.34966873604972548, 8.224510206698743886, 93.33442372801901854 ) ) ;
#173063 = CARTESIAN_POINT ( 'NONE',  ( -16.46253265017146816, -9.564922557961047289, 74.16775706135234714 ) ) ;
#173064 = CARTESIAN_POINT ( 'NONE',  ( -19.05341960407611168, -5.049401038298163336, 36.45724293864766707 ) ) ;
#173065 = CARTESIAN_POINT ( 'NONE',  ( 19.03943276465977164, -0.05219959533909143690, 78.74890960531436690 ) ) ;
#173066 = CARTESIAN_POINT ( 'NONE',  ( 19.05341960407611168, 5.049401038298154454, 33.95724293864769550 ) ) ;
#173067 = CARTESIAN_POINT ( 'NONE',  ( 16.51473224551083163, -9.474510206698727899, 70.83442372801900433 ) ) ;
#173068 = CARTESIAN_POINT ( 'NONE',  ( 25.52568752982154265, -9.519068727184667011, 170.8917780290425412 ) ) ;
#173069 = CARTESIAN_POINT ( 'NONE',  ( 16.51473224551069308, 9.474510206698969483, 114.1655762719810241 ) ) ;
#173070 = CARTESIAN_POINT ( 'NONE',  ( -16.52544592524342804, 4.483927247898546575, 61.04057627198103120 ) ) ;
#173071 = CARTESIAN_POINT ( 'NONE',  ( 10.72451020669898902, -18.67979575497178502, 57.91557627198103120 ) ) ;
#173072 = DIRECTION ( 'NONE',  ( 0.000000000000000000, 0.000000000000000000, -1.000000000000000000 ) ) ;
#173073 = CARTESIAN_POINT ( 'NONE',  ( 13.97604488694548053, -13.89961937509957401, 35.62609039468567573 ) ) ;
#173074 = CARTESIAN_POINT ( 'NONE',  ( 21.59135963187072349, -7.527667041516026281, 173.8290201207856285 ) ) ;
#173076 = CARTESIAN_POINT ( 'NONE',  ( 5.153800228976335163, 19.02544592524342804, 69.79057627198103830 ) ) ;
#173075 = CARTESIAN_POINT ( 'NONE',  ( 5.049401038298161559, -19.05341960407611168, 62.70724293864769550 ) ) ;
#173077 = CARTESIAN_POINT ( 'NONE',  ( -0.05219959533934338120, 16.53943276465976808, 47.50109039468568994 ) ) ;
#173078 = CARTESIAN_POINT ( 'NONE',  ( -19.20446147854527297, -5.499999999999958256, 99.38999695167676407 ) ) ;
#173079 = CYLINDRICAL_SURFACE ( 'NONE', #146899, 5.500000000000032863 ) ;
#173080 = CARTESIAN_POINT ( 'NONE',  ( 14.29746914071037800, 8.314922557961029526, 81.66775706135236135 ) ) ;
#173081 = CARTESIAN_POINT ( 'NONE',  ( -17.60769864724390388, 5.499999999999982236, 78.65024842019167295 ) ) ;
#173082 = CARTESIAN_POINT ( 'NONE',  ( 16.52544592524335698, 4.483927247898782831, 61.45942372801901854 ) ) ;
#173083 = CARTESIAN_POINT ( 'NONE',  ( 0.05219959533934541429, -16.53943276465976808, 35.00109039468568284 ) ) ;
#173085 = FACE_BOUND ( 'NONE', #14992, .T. ) ;
#173084 = CARTESIAN_POINT ( 'NONE',  ( -5.153800228976328057, -19.02544592524343514, 57.29057627198103120 ) ) ;
#173086 = CARTESIAN_POINT ( 'NONE',  ( -10.72451020669870658, -18.67979575497194134, 59.58442372801901854 ) ) ;
#173087 = CARTESIAN_POINT ( 'NONE',  ( -16.46253265017146816, -9.564922557961047289, 59.16775706135233293 ) ) ;
#173088 = CARTESIAN_POINT ( 'NONE',  ( -21.52544592524334988, -5.823673210054445271, 93.95942372801903275 ) ) ;
#173089 = AXIS2_PLACEMENT_3D ( 'NONE', #104984, #45306, #13959 ) ;
#173090 = CARTESIAN_POINT ( 'NONE',  ( -16.51473224551069308, -9.474510206698971260, 31.66557627198102054 ) ) ;
#173091 = CARTESIAN_POINT ( 'NONE',  ( 30.73962218707677962, -22.33364281372841376, -7.202157773949823927 ) ) ;
#173092 = CARTESIAN_POINT ( 'NONE',  ( 21.55341960407610458, 5.719274019375980345, 58.95724293864770971 ) ) ;
#173093 = CARTESIAN_POINT ( 'NONE',  ( 19.03943276465977164, -0.05219959533909143690, 103.7489096053143669 ) ) ;
#173094 = CARTESIAN_POINT ( 'NONE',  ( 8.314922557960818139, 14.29746914071049879, 99.58224293864770971 ) ) ;
#173095 = CARTESIAN_POINT ( 'NONE',  ( 16.52544592524335698, 4.483927247898782831, 36.45942372801901143 ) ) ;
#173096 = EDGE_CURVE ( 'NONE', #25364, #11205, #24984, .T. ) ;
#173097 = CARTESIAN_POINT ( 'NONE',  ( -16.55341960407611168, -4.379528057220339221, 36.45724293864768839 ) ) ;
#173098 = EDGE_LOOP ( 'NONE', ( #157102, #192252, #39816, #18904, #46768, #173909, #134388, #30423, #115591, #103611, #103511, #105399, #4228 ) ) ;
#173099 = CARTESIAN_POINT ( 'NONE',  ( -15.72974639402197994, 15.80617190586746368, 100.6239096053143811 ) ) ;
#173101 = CARTESIAN_POINT ( 'NONE',  ( 0.05219959533909260263, 19.03943276465977164, 114.9989096053143669 ) ) ;
#173100 = CARTESIAN_POINT ( 'NONE',  ( 8.314922557960818139, 14.29746914071049879, 34.58224293864770260 ) ) ;
#173102 = CARTESIAN_POINT ( 'NONE',  ( -19.02544592524334988, -5.153800228976617603, 88.95942372801897591 ) ) ;
#173103 = CARTESIAN_POINT ( 'NONE',  ( 19.05341960407617918, -5.049401038297876454, 26.04275706135233293 ) ) ;
#173104 = CARTESIAN_POINT ( 'NONE',  ( -4.483927247898539470, -16.52544592524342804, 37.29057627198102409 ) ) ;
#173105 = CARTESIAN_POINT ( 'NONE',  ( 10.81492255796078972, 18.62759615963270932, 99.58224293864770971 ) ) ;
#173106 = CARTESIAN_POINT ( 'NONE',  ( -18.67979575497178146, -10.72451020669898902, 46.66557627198102409 ) ) ;
#173107 = CARTESIAN_POINT ( 'NONE',  ( -9.474510206698964154, 16.51473224551069663, 80.41557627198103830 ) ) ;
#173108 = CARTESIAN_POINT ( 'NONE',  ( -4.483927247898539470, -16.52544592524342804, 37.29057627198102409 ) ) ;
#173109 = CARTESIAN_POINT ( 'NONE',  ( 16.46253265017160672, -9.564922557960803928, 88.33224293864769550 ) ) ;
#173110 = EDGE_LOOP ( 'NONE', ( #23413, #23489 ) ) ;
#173111 = CARTESIAN_POINT ( 'NONE',  ( 19.49671883438229969, 5.499999999999974243, 57.39279849105685827 ) ) ;
#173112 = CARTESIAN_POINT ( 'NONE',  ( 16.46253265017146816, 9.564922557961045513, 41.66775706135234003 ) ) ;
#173113 = CARTESIAN_POINT ( 'NONE',  ( -18.67979575497178146, -10.72451020669898902, 86.66557627198102409 ) ) ;
#173114 = CARTESIAN_POINT ( 'NONE',  ( 12.06949235617757843, -12.14591786802309237, 103.1239096053143811 ) ) ;
#173115 =( BOUNDED_CURVE ( )  B_SPLINE_CURVE ( 2, ( #181432, #87411, #57087, #86409, #133925, #116746, #25765, #195615, #196608, #166259, #89401, #103588, #151090, #11594, #24762, #10586, #165263, #193604, #27758, #39904, #118761, #163260, #197586, #88397, #41922, #26757, #12581, #73262, #74246, #135915, #55076, #102586, #56074, #71251, #148094, #9585, #132915, #194602, #117755, #72247, #179447, #40913, #164270, #143727, #144722, #37552, #194256, #190245, #84046, #68890, #116394, #115404, #21389, #99215, #36541, #159901, #193248, #147746, #83048, #66887, #9233, #20383, #160903, #24408, #82030, #161901, #70900, #177092, #51722, #38564, #85042, #132567, #55723, #7206, #114379, #100220, #158893, #175075, #6208, #174090, #69896, #35559, #97207, #67888, #176083, #129541, #54721, #8220, #5206, #191241, #146723 ),
 .UNSPECIFIED., .F., .F. ) 
 B_SPLINE_CURVE_WITH_KNOTS ( ( 3, 2, 2, 2, 2, 2, 2, 2, 2, 2, 2, 2, 2, 2, 2, 2, 2, 2, 2, 2, 2, 2, 2, 2, 2, 2, 2, 2, 2, 2, 2, 2, 2, 2, 2, 2, 2, 2, 2, 2, 2, 2, 2, 2, 2, 3 ),
 ( 0.000000000000000000, 0.02000000000000000042, 0.04000000000000000083, 0.06000000000000000472, 0.08000000000000000167, 0.1000000000000000056, 0.1200000000000000094, 0.1400000000000000133, 0.1600000000000000033, 0.1799999999999999933, 0.2000000000000000111, 0.2200000000000000011, 0.2400000000000000189, 0.2600000000000000089, 0.2800000000000000266, 0.2999999999999999889, 0.3200000000000000067, 0.3400000000000000244, 0.3599999999999999867, 0.3800000000000000044, 0.4000000000000000222, 0.4199999999999999845, 0.4400000000000000022, 0.4600000000000000200, 0.4800000000000000377, 0.5000000000000000000, 0.5200000000000000178, 0.5400000000000000355, 0.5600000000000000533, 0.5799999999999999600, 0.5999999999999999778, 0.6199999999999999956, 0.6400000000000000133, 0.6600000000000000311, 0.6800000000000000488, 0.6999999999999999556, 0.7199999999999999734, 0.7399999999999999911, 0.7600000000000000089, 0.7800000000000000266, 0.8000000000000000444, 0.8199999999999999512, 0.8399999999999999689, 0.8599999999999999867, 0.8800000000000000044, 0.8875575298689686310 ),
 .UNSPECIFIED. ) 
 CURVE ( )  GEOMETRIC_REPRESENTATION_ITEM ( )  RATIONAL_B_SPLINE_CURVE ( ( 1.000000000000000000, 0.9510565162951535312, 1.000000000000000000, 0.9510565162951535312, 1.000000000000000000, 0.9510565162951535312, 1.000000000000000000, 0.9510565162951535312, 1.000000000000000000, 0.9510565162951535312, 1.000000000000000000, 0.9510565162951535312, 1.000000000000000000, 0.9510565162951535312, 1.000000000000000000, 0.9510565162951535312, 1.000000000000000000, 0.9510565162951535312, 1.000000000000000000, 0.9510565162951535312, 1.000000000000000000, 0.9510565162951535312, 1.000000000000000000, 0.9510565162951535312, 1.000000000000000000, 0.9510565162951535312, 1.000000000000000000, 0.9510565162951535312, 1.000000000000000000, 0.9510565162951535312, 1.000000000000000000, 0.9510565162951535312, 1.000000000000000000, 0.9510565162951535312, 1.000000000000000000, 0.9510565162951535312, 1.000000000000000000, 0.9510565162951535312, 1.000000000000000000, 0.9510565162951535312, 1.000000000000000000, 0.9510565162951535312, 1.000000000000000000, 0.9510565162951535312, 1.000000000000000000, 0.9510565162951535312, 1.000000000000000000, 0.9510565162951535312, 1.000000000000000000, 0.9510565162951535312, 1.000000000000000000, 0.9510565162951535312, 1.000000000000000000, 0.9510565162951535312, 1.000000000000000000, 0.9510565162951535312, 1.000000000000000000, 0.9510565162951535312, 1.000000000000000000, 0.9510565162951535312, 1.000000000000000000, 0.9510565162951535312, 1.000000000000000000, 0.9510565162951535312, 1.000000000000000000, 0.9510565162951535312, 1.000000000000000000, 0.9510565162951535312, 1.000000000000000000, 0.9510565162951535312, 1.000000000000000000, 0.9510565162951535312, 1.000000000000000000, 0.9510565162951535312, 1.000000000000000000, 0.9510565162951535312, 1.000000000000000000, 0.9510565162951535312, 1.000000000000000000, 0.9510565162951535312, 1.000000000000000000, 0.9510565162951535312, 1.000000000000000000, 0.9510565162951535312, 1.000000000000000000, 0.9510565162951535312, 1.000000000000000000, 0.9510565162951535312, 1.000000000000000000, 0.9815054080004621540, 0.9769881591460138903 ) ) 
 REPRESENTATION_ITEM ( '' )  );
#173116 = CARTESIAN_POINT ( 'NONE',  ( -5.823673210054431948, 21.52544592524334988, 37.70942372801900433 ) ) ;
#173117 = CARTESIAN_POINT ( 'NONE',  ( 17.14385361876520264, -23.59649016807271238, 139.5750000027311444 ) ) ;
#173118 = CARTESIAN_POINT ( 'NONE',  ( 12.06949235617739724, 12.14591786802326823, 111.8760903946856615 ) ) ;
#173119 = CARTESIAN_POINT ( 'NONE',  ( -16.46253265017160317, 9.564922557960807481, 40.83224293864769550 ) ) ;
#173120 = CARTESIAN_POINT ( 'NONE',  ( -9.474510206698964154, 16.51473224551069663, 80.41557627198103830 ) ) ;
#173121 = CARTESIAN_POINT ( 'NONE',  ( -18.39635199886966532, 5.500000000000103029, 46.01967076360001840 ) ) ;
#173122 = CARTESIAN_POINT ( 'NONE',  ( -16.51473224551069308, -9.474510206698971260, 36.66557627198102409 ) ) ;
#173123 = CARTESIAN_POINT ( 'NONE',  ( -8.314922557960811034, -14.29746914071050412, 37.08224293864768129 ) ) ;
#173124 = CARTESIAN_POINT ( 'NONE',  ( -5.719274019375665041, -21.55341960407619695, 69.79275706135234714 ) ) ;
#173126 = CARTESIAN_POINT ( 'NONE',  ( -0.05219959533934338120, 16.53943276465976808, 67.50109039468568994 ) ) ;
#173125 = CARTESIAN_POINT ( 'NONE',  ( 29.33118895280741256, -23.95254016166647304, -21.73655181066850162 ) ) ;
#173127 = CARTESIAN_POINT ( 'NONE',  ( -16.46253265017160317, 9.564922557960807481, 55.83224293864769550 ) ) ;
#173128 = CARTESIAN_POINT ( 'NONE',  ( -13.89961937509977652, 13.97604488694528158, 70.62390960531432427 ) ) ;
#173129 = ORIENTED_EDGE ( 'NONE', *, *, #50044, .F. ) ;
#173130 = CARTESIAN_POINT ( 'NONE',  ( 21.55341960407619695, -5.719274019375665929, 111.0427570613523613 ) ) ;
#173131 = CARTESIAN_POINT ( 'NONE',  ( -8.224510206698735004, -14.34966873604973081, 79.58442372801903275 ) ) ;
#173132 = CARTESIAN_POINT ( 'NONE',  ( 18.67979575497194134, -10.72451020669871369, 95.83442372801903275 ) ) ;
#173133 = CARTESIAN_POINT ( 'NONE',  ( 13.89961937509977652, -13.97604488694527269, 58.12390960531436690 ) ) ;
#173134 = CARTESIAN_POINT ( 'NONE',  ( 15.80617190586746368, 15.72974639402197994, 29.37390960531435269 ) ) ;
#173135 = CARTESIAN_POINT ( 'NONE',  ( -19.03943276465977164, -0.05219959533935918106, 103.7510903946856757 ) ) ;
#173136 = CARTESIAN_POINT ( 'NONE',  ( 0.05219959533937995610, -21.53943276465977519, 70.00109039468568994 ) ) ;
#173137 = CARTESIAN_POINT ( 'NONE',  ( 12.14591786802327356, -12.06949235617739191, 55.62609039468568284 ) ) ;
#173138 = CARTESIAN_POINT ( 'NONE',  ( -0.05219959533907301413, -21.53943276465977519, 97.49890960531436690 ) ) ;
#173139 = CARTESIAN_POINT ( 'NONE',  ( -16.46253265017146816, -9.564922557961047289, 94.16775706135233293 ) ) ;
#173140 = CARTESIAN_POINT ( 'NONE',  ( 9.564922557960805705, 16.46253265017160317, 84.58224293864769550 ) ) ;
#173141 = CARTESIAN_POINT ( 'NONE',  ( 0.05219959533936267826, -19.03943276465977164, 110.0010903946856757 ) ) ;
#173142 = CARTESIAN_POINT ( 'NONE',  ( -13.97604488694547697, 13.89961937509957934, 113.1260903946856757 ) ) ;
#173143 = CARTESIAN_POINT ( 'NONE',  ( -8.314922557960811034, -14.29746914071050412, 72.08224293864769550 ) ) ;
#173144 = CARTESIAN_POINT ( 'NONE',  ( 16.53943276465976808, 0.05219959533934440121, 76.25109039468568994 ) ) ;
#173146 = CARTESIAN_POINT ( 'NONE',  ( 13.97604488694527802, 13.89961937509977652, 54.37390960531435979 ) ) ;
#173145 = CARTESIAN_POINT ( 'NONE',  ( -21.53943276465977519, 0.05219959533907696930, 111.2489096053143669 ) ) ;
#173147 = CARTESIAN_POINT ( 'NONE',  ( -16.51473224551069308, -9.474510206698971260, 51.66557627198102409 ) ) ;
#173148 = CARTESIAN_POINT ( 'NONE',  ( 16.52544592524335698, 4.483927247898782831, 66.45942372801903275 ) ) ;
#173149 = CARTESIAN_POINT ( 'NONE',  ( -17.81289503416611808, 24.51734667627700404, 145.9500000054623854 ) ) ;
#173150 = EDGE_LOOP ( 'NONE', ( #159869, #61406, #176901, #188268 ) ) ;
#173151 = CARTESIAN_POINT ( 'NONE',  ( -10.81492255796105439, 18.62759615963255655, 112.9177570613523329 ) ) ;
#173152 = CARTESIAN_POINT ( 'NONE',  ( 13.97604488694527802, 13.89961937509977652, 34.37390960531436690 ) ) ;
#173153 = VERTEX_POINT ( 'NONE', #101775 ) ;
#173154 = CARTESIAN_POINT ( 'NONE',  ( 5.049401038297881783, 19.05341960407617563, 107.2927570613523187 ) ) ;
#173156 = CARTESIAN_POINT ( 'NONE',  ( 4.379528057220092307, 16.55341960407617563, 27.29275706135234358 ) ) ;
#173155 = CARTESIAN_POINT ( 'NONE',  ( -19.02544592524334988, -5.153800228976617603, 38.95942372801900433 ) ) ;
#173157 = CARTESIAN_POINT ( 'NONE',  ( 13.97604488694527802, 13.89961937509977652, 49.37390960531434558 ) ) ;
#173158 = CARTESIAN_POINT ( 'NONE',  ( 9.474510206698971260, -16.51473224551069308, 62.91557627198102409 ) ) ;
#173159 = CARTESIAN_POINT ( 'NONE',  ( 10.81492255796078972, 18.62759615963270932, 79.58224293864769550 ) ) ;
#173160 = CARTESIAN_POINT ( 'NONE',  ( -0.05219959533909027116, -19.03943276465977164, 112.4989096053143669 ) ) ;
#173161 = CARTESIAN_POINT ( 'NONE',  ( -13.97604488694527625, -13.89961937509977652, 51.87390960531436690 ) ) ;
#173162 = LINE ( 'NONE', #126632, #153329 ) ;
#173163 = CARTESIAN_POINT ( 'NONE',  ( 9.474510206698729675, 16.51473224551082808, 92.08442372801900433 ) ) ;
#173164 = CARTESIAN_POINT ( 'NONE',  ( 8.314922557960818139, 14.29746914071049879, 69.58224293864769550 ) ) ;
#173165 = CARTESIAN_POINT ( 'NONE',  ( -9.474510206698720793, -16.51473224551083518, 24.58442372801900078 ) ) ;
#173166 = CARTESIAN_POINT ( 'NONE',  ( 16.52544592524342804, -4.483927247898539470, 58.54057627198103120 ) ) ;
#173167 = CARTESIAN_POINT ( 'NONE',  ( 5.719274019375673035, 21.55341960407619339, 87.29275706135236135 ) ) ;
#173168 = CARTESIAN_POINT ( 'NONE',  ( -9.564922557960796823, -16.46253265017161027, 27.08224293864769550 ) ) ;
#173169 = CARTESIAN_POINT ( 'NONE',  ( 18.62759615963255655, 10.81492255796105972, 86.66775706135234714 ) ) ;
#173171 = CARTESIAN_POINT ( 'NONE',  ( -0.05219959533937732626, 21.53943276465977519, 72.50109039468568994 ) ) ;
#173170 = CARTESIAN_POINT ( 'NONE',  ( -16.55341960407611168, -4.379528057220339221, 31.45724293864769550 ) ) ;
#173172 = CARTESIAN_POINT ( 'NONE',  ( -19.05341960407611168, -5.049401038298163336, 81.45724293864769550 ) ) ;
#173173 = CARTESIAN_POINT ( 'NONE',  ( -5.823673210054431948, 21.52544592524334988, 37.70942372801900433 ) ) ;
#173174 = CARTESIAN_POINT ( 'NONE',  ( -9.474510206698964154, 16.51473224551069663, 75.41557627198103830 ) ) ;
#173175 = CARTESIAN_POINT ( 'NONE',  ( -14.34966873604960291, -8.224510206698953496, 91.66557627198103830 ) ) ;
#173176 = CARTESIAN_POINT ( 'NONE',  ( -0.05219959533910754901, -16.53943276465976808, 57.49890960531435979 ) ) ;
#173177 = CARTESIAN_POINT ( 'NONE',  ( 21.52544592524344225, -5.823673210054117533, 68.54057627198103830 ) ) ;
#173178 = CARTESIAN_POINT ( 'NONE',  ( -19.05341960407611168, -5.049401038298163336, 71.45724293864766707 ) ) ;
#173179 = CARTESIAN_POINT ( 'NONE',  ( -5.719274019375978568, 21.55341960407610458, 90.20724293864770971 ) ) ;
#173180 = CARTESIAN_POINT ( 'NONE',  ( -5.049401038297874678, -19.05341960407617918, 74.79275706135231871 ) ) ;
#173183 = CARTESIAN_POINT ( 'NONE',  ( -14.34966873604960291, -8.224510206698953496, 76.66557627198103830 ) ) ;
#173182 = CARTESIAN_POINT ( 'NONE',  ( -18.89770734986048240, -5.500000000000011546, 89.10214472496642202 ) ) ;
#173181 = AXIS2_PLACEMENT_3D ( 'NONE', #74025, #195384, #162027 ) ;
#173184 = CARTESIAN_POINT ( 'NONE',  ( -5.719274019375978568, 21.55341960407610458, 55.20724293864770260 ) ) ;
#173185 = CARTESIAN_POINT ( 'NONE',  ( -4.999999999999996447, 5.000000000000003553, -18.00000000000000000 ) ) ;
#173187 = CARTESIAN_POINT ( 'NONE',  ( -27.73933785331498925, 9.013057229001088189, 147.2750000027311614 ) ) ;
#173186 = CARTESIAN_POINT ( 'NONE',  ( -8.224510206698735004, -14.34966873604973081, 94.58442372801901854 ) ) ;
#173188 = CARTESIAN_POINT ( 'NONE',  ( 9.564922557961047289, -16.46253265017146816, 105.4177570613523471 ) ) ;
#173189 = CARTESIAN_POINT ( 'NONE',  ( 14.34966873604960469, 8.224510206698951720, 74.16557627198102409 ) ) ;
#173190 = CARTESIAN_POINT ( 'NONE',  ( -19.52851543214743657, -5.499999999999989342, 95.39357721762576148 ) ) ;
#173191 = CARTESIAN_POINT ( 'NONE',  ( -9.474510206698964154, 16.51473224551069663, 65.41557627198102409 ) ) ;
#173192 = CARTESIAN_POINT ( 'NONE',  ( 8.314922557960818139, 14.29746914071049879, 49.58224293864769550 ) ) ;
#173193 = CARTESIAN_POINT ( 'NONE',  ( -5.153800228976328057, -19.02544592524343514, 97.29057627198099567 ) ) ;
#173195 = CARTESIAN_POINT ( 'NONE',  ( 5.049401038298161559, -19.05341960407611168, 72.70724293864768129 ) ) ;
#173194 = CARTESIAN_POINT ( 'NONE',  ( 19.03943276465977164, 0.05219959533936151252, 91.25109039468566152 ) ) ;
#173196 = CARTESIAN_POINT ( 'NONE',  ( 0.05219959533909260263, 19.03943276465977164, 79.99890960531436690 ) ) ;
#173197 = CARTESIAN_POINT ( 'NONE',  ( -16.51473224551069308, -9.474510206698971260, 81.66557627198103830 ) ) ;
#173198 = CARTESIAN_POINT ( 'NONE',  ( 18.62759615963271287, -10.81492255796078972, 58.33224293864768839 ) ) ;
#173199 = CARTESIAN_POINT ( 'NONE',  ( 4.483927247898790824, -16.52544592524335698, 55.20942372801902565 ) ) ;
#173200 = CARTESIAN_POINT ( 'NONE',  ( -0.05219959533936034679, 19.03943276465977164, 102.5010903946856757 ) ) ;
#173201 = CARTESIAN_POINT ( 'NONE',  ( -13.97604488694527625, -13.89961937509977652, 66.87390960531436690 ) ) ;
#173202 = CARTESIAN_POINT ( 'NONE',  ( -15.72974639402197994, 15.80617190586746368, 70.62390960531436690 ) ) ;
#173203 = CARTESIAN_POINT ( 'NONE',  ( -9.474510206698720793, -16.51473224551083518, 94.58442372801900433 ) ) ;
#173204 = APPLICATION_CONTEXT ( 'automotive_design' ) ;
#173206 = CARTESIAN_POINT ( 'NONE',  ( -18.67979575497193778, 10.72451020669871902, 43.33442372801901143 ) ) ;
#173205 = CARTESIAN_POINT ( 'NONE',  ( -0.05219959533910754901, -16.53943276465976808, 22.49890960531436335 ) ) ;
#173207 = CARTESIAN_POINT ( 'NONE',  ( 5.049401038297881783, 19.05341960407617563, 42.29275706135234003 ) ) ;
#173209 = CARTESIAN_POINT ( 'NONE',  ( -12.14591786802326823, 12.06949235617739902, 93.12609039468568994 ) ) ;
#173208 = CARTESIAN_POINT ( 'NONE',  ( 4.379528057220092307, 16.55341960407617563, 57.29275706135234714 ) ) ;
#173210 = CARTESIAN_POINT ( 'NONE',  ( -19.97888994334924817, -34.65319547504298470, -5.000000000000000000 ) ) ;
#173211 = CARTESIAN_POINT ( 'NONE',  ( 4.379528057220092307, 16.55341960407617563, 82.29275706135234714 ) ) ;
#173212 = CARTESIAN_POINT ( 'NONE',  ( -0.05219959533934338120, 16.53943276465976808, 37.50109039468568284 ) ) ;
#173213 = CARTESIAN_POINT ( 'NONE',  ( -0.05219959533909027116, -19.03943276465977164, 47.49890960531435979 ) ) ;
#173214 = CARTESIAN_POINT ( 'NONE',  ( -13.97604488694527625, -13.89961937509977652, 51.87390960531436690 ) ) ;
#173215 = CARTESIAN_POINT ( 'NONE',  ( -16.46253265017160317, 9.564922557960807481, 60.83224293864769550 ) ) ;
#173216 = CARTESIAN_POINT ( 'NONE',  ( -5.719274019375665041, -21.55341960407619695, 54.79275706135235424 ) ) ;
#173217 = CARTESIAN_POINT ( 'NONE',  ( -4.483927247898782831, 16.52544592524335698, 47.70942372801902565 ) ) ;
#173218 = CARTESIAN_POINT ( 'NONE',  ( 8.224510206698953496, -14.34966873604960469, 22.91557627198102765 ) ) ;
#173219 = CARTESIAN_POINT ( 'NONE',  ( 19.02544592524343514, -5.153800228976328945, 33.54057627198102409 ) ) ;
#173220 = CARTESIAN_POINT ( 'NONE',  ( -21.53943276465977519, -0.05219959533937600094, 113.7510903946856757 ) ) ;
#173221 = CARTESIAN_POINT ( 'NONE',  ( -14.29746914071037622, -8.314922557961029526, 24.16775706135235424 ) ) ;
#173222 = CARTESIAN_POINT ( 'NONE',  ( 19.05341960407617918, -5.049401038297876454, 81.04275706135231871 ) ) ;
#173223 = CARTESIAN_POINT ( 'NONE',  ( 4.483927247898545687, 16.52544592524342804, 84.79057627198102409 ) ) ;
#173224 = CARTESIAN_POINT ( 'NONE',  ( 9.474510206698971260, -16.51473224551069308, 42.91557627198103120 ) ) ;
#173226 = CARTESIAN_POINT ( 'NONE',  ( 16.21995358207304250, -7.366697692864150326, 92.43551001512157939 ) ) ;
#173225 = CARTESIAN_POINT ( 'NONE',  ( -5.153800228976607833, 19.02544592524334988, 77.70942372801900433 ) ) ;
#173227 = CARTESIAN_POINT ( 'NONE',  ( -18.62759615963255300, -10.81492255796106328, 74.16775706135231871 ) ) ;
#173228 = CARTESIAN_POINT ( 'NONE',  ( 14.34966873604972726, -8.224510206698740333, 35.83442372801901143 ) ) ;
#173229 = CARTESIAN_POINT ( 'NONE',  ( -17.49999999999998579, 3.850315288878732201, 24.26629130603454954 ) ) ;
#173230 = CARTESIAN_POINT ( 'NONE',  ( -5.719274019375978568, 21.55341960407610458, 40.20724293864769550 ) ) ;
#173231 = CARTESIAN_POINT ( 'NONE',  ( 8.314922557961029526, -14.29746914071037800, 20.41775706135234714 ) ) ;
#173232 = CARTESIAN_POINT ( 'NONE',  ( 5.049401038298163336, -19.05341960407611168, 27.70724293864769550 ) ) ;
#173233 = CARTESIAN_POINT ( 'NONE',  ( 5.049401038297881783, 19.05341960407617563, 32.29275706135233293 ) ) ;
#173234 = CARTESIAN_POINT ( 'NONE',  ( -23.48529157249599919, -32.32473071737749848, -7.699999999999999289 ) ) ;
#173235 = CARTESIAN_POINT ( 'NONE',  ( 19.02544592524343514, -5.153800228976328945, 43.54057627198103120 ) ) ;
#173236 = CARTESIAN_POINT ( 'NONE',  ( -18.22780087662122028, 5.500000000000031086, 58.51540105326107977 ) ) ;
#173237 = CARTESIAN_POINT ( 'NONE',  ( 0.05219959533909260263, 19.03943276465977164, 69.99890960531435269 ) ) ;
#173239 = CARTESIAN_POINT ( 'NONE',  ( -18.56197773271729190, 5.499999999999996447, 98.55066217314453070 ) ) ;
#173238 = VECTOR ( 'NONE', #73921, 1000.000000000000000 ) ;
#173240 = CARTESIAN_POINT ( 'NONE',  ( -15.72974639402176322, -15.80617190586768395, 109.3760903946857042 ) ) ;
#173241 = CARTESIAN_POINT ( 'NONE',  ( 16.55341960407611168, 4.379528057220329451, 43.95724293864769550 ) ) ;
#173242 = CARTESIAN_POINT ( 'NONE',  ( -19.03943276465977164, 0.05219959533909376836, 46.24890960531435979 ) ) ;
#173243 = CARTESIAN_POINT ( 'NONE',  ( -16.46253265017160317, 9.564922557960807481, 85.83224293864769550 ) ) ;
#173244 = CARTESIAN_POINT ( 'NONE',  ( -10.72451020669870658, -18.67979575497194134, 64.58442372801900433 ) ) ;
#173245 = CARTESIAN_POINT ( 'NONE',  ( -5.049401038298153566, 19.05341960407611168, 45.20724293864769550 ) ) ;
#173246 = CARTESIAN_POINT ( 'NONE',  ( -15.80617190586768217, 15.72974639402176855, 73.12609039468567573 ) ) ;
#173247 = CARTESIAN_POINT ( 'NONE',  ( 21.52544592524344225, -5.823673210054117533, 23.54057627198102765 ) ) ;
#173248 = CARTESIAN_POINT ( 'NONE',  ( -16.46253265017160317, 9.564922557960807481, 40.83224293864769550 ) ) ;
#173249 = CARTESIAN_POINT ( 'NONE',  ( 15.72974639402176855, 15.80617190586768217, 21.87609039468567573 ) ) ;
#173250 = CARTESIAN_POINT ( 'NONE',  ( -13.97604488694547697, 13.89961937509957934, 48.12609039468566863 ) ) ;
#173251 = CARTESIAN_POINT ( 'NONE',  ( -0.05219959533910754901, -16.53943276465976808, 112.4989096053143669 ) ) ;
#173252 = CARTESIAN_POINT ( 'NONE',  ( -13.97604488694527625, -13.89961937509977652, 56.87390960531434558 ) ) ;
#173253 = CARTESIAN_POINT ( 'NONE',  ( 13.97604488694548053, -13.89961937509957401, 110.6260903946856615 ) ) ;
#173254 = CARTESIAN_POINT ( 'NONE',  ( -12.14591786802309592, -12.06949235617757132, 81.87390960531435269 ) ) ;
#173255 = CARTESIAN_POINT ( 'NONE',  ( -10.81492255796078084, -18.62759615963271287, 27.08224293864769550 ) ) ;
#173256 = CARTESIAN_POINT ( 'NONE',  ( -19.03943276465977164, -0.05219959533935918106, 103.7510903946856757 ) ) ;
#173257 = CARTESIAN_POINT ( 'NONE',  ( 18.62759615963271287, -10.81492255796078972, 108.3322429386477097 ) ) ;
#173258 = CARTESIAN_POINT ( 'NONE',  ( 21.53943276465977519, 0.05219959533937863772, 56.25109039468568284 ) ) ;
#173259 = CARTESIAN_POINT ( 'NONE',  ( -8.314922557961024197, 14.29746914071037800, 62.91775706135236135 ) ) ;
#173260 = CARTESIAN_POINT ( 'NONE',  ( -14.29746914071037622, -8.314922557961029526, 54.16775706135235424 ) ) ;
#173261 = CARTESIAN_POINT ( 'NONE',  ( 21.52544592524344225, -5.823673210054117533, 53.54057627198103120 ) ) ;
#173262 = CARTESIAN_POINT ( 'NONE',  ( -0.05219959533909027116, -19.03943276465977164, 52.49890960531436690 ) ) ;
#173263 = CARTESIAN_POINT ( 'NONE',  ( -16.53943276465976808, -0.05219959533934237506, 73.75109039468567573 ) ) ;
#173264 = EDGE_CURVE ( 'NONE', #15377, #190965, #54118, .T. ) ;
#173265 = CARTESIAN_POINT ( 'NONE',  ( 21.55341960407610458, 5.719274019375980345, 103.9572429386476813 ) ) ;
#173266 = CARTESIAN_POINT ( 'NONE',  ( -14.29746914071049879, 8.314922557960819915, 55.83224293864770260 ) ) ;
#173267 = CARTESIAN_POINT ( 'NONE',  ( -9.564922557960796823, -16.46253265017161027, 67.08224293864769550 ) ) ;
#173268 = CARTESIAN_POINT ( 'NONE',  ( 16.55341960407618274, -4.379528057220086978, 76.04275706135237556 ) ) ;
#173269 = CARTESIAN_POINT ( 'NONE',  ( -8.314922557961024197, 14.29746914071037800, 22.91775706135235069 ) ) ;
#173270 = CARTESIAN_POINT ( 'NONE',  ( 18.62759615963271287, -10.81492255796078972, 98.33224293864769550 ) ) ;
#173271 = CARTESIAN_POINT ( 'NONE',  ( -14.34966873604960291, -8.224510206698953496, 46.66557627198102409 ) ) ;
#173272 = ORIENTED_EDGE ( 'NONE', *, *, #90391, .T. ) ;
#173273 = CARTESIAN_POINT ( 'NONE',  ( -16.52216118717207749, 7.221426719304494313, 73.92400978953011759 ) ) ;
#173274 = CARTESIAN_POINT ( 'NONE',  ( 0.05219959533907565091, 21.53943276465977519, 89.99890960531438111 ) ) ;
#173275 = ORIENTED_EDGE ( 'NONE', *, *, #68275, .F. ) ;
#173276 = CARTESIAN_POINT ( 'NONE',  ( -0.05219959533910754901, -16.53943276465976808, 27.49890960531435269 ) ) ;
#173277 = ORIENTED_EDGE ( 'NONE', *, *, #154401, .F. ) ;
#173278 = CARTESIAN_POINT ( 'NONE',  ( -16.88567814943164436, -6.947325034625596807, 56.29001122652586986 ) ) ;
#173279 = CARTESIAN_POINT ( 'NONE',  ( 18.67979575497178502, 10.72451020669898547, 104.1655762719810241 ) ) ;
#173280 = CARTESIAN_POINT ( 'NONE',  ( -13.89961937509977652, 13.97604488694528158, 95.62390960531436690 ) ) ;
#173281 = CARTESIAN_POINT ( 'NONE',  ( -15.80617190586768217, 15.72974639402176855, 28.12609039468568284 ) ) ;
#173282 = CARTESIAN_POINT ( 'NONE',  ( -16.52544592524342804, 4.483927247898546575, 36.04057627198102409 ) ) ;
#173283 = CARTESIAN_POINT ( 'NONE',  ( -16.55341960407617563, 4.379528057220093196, 43.54275706135235424 ) ) ;
#173284 = CARTESIAN_POINT ( 'NONE',  ( 16.46253265017160672, -9.564922557960803928, 48.33224293864769550 ) ) ;
#173285 = CARTESIAN_POINT ( 'NONE',  ( 0.05219959533936267826, -19.03943276465977164, 55.00109039468566863 ) ) ;
#173286 = CARTESIAN_POINT ( 'NONE',  ( -13.97604488694527625, -13.89961937509977652, 86.87390960531436690 ) ) ;
#173287 = ORIENTED_EDGE ( 'NONE', *, *, #34324, .F. ) ;
#173288 = EDGE_CURVE ( 'NONE', #76043, #58799, #138033, .T. ) ;
#173289 = CARTESIAN_POINT ( 'NONE',  ( -5.823673210054116645, -21.52544592524344225, 37.29057627198102409 ) ) ;
#173290 = CARTESIAN_POINT ( 'NONE',  ( -25.66183622254775898, -27.84411637527858119, -16.56099493762688724 ) ) ;
#173291 = CARTESIAN_POINT ( 'NONE',  ( -16.55341960407617563, 4.379528057220093196, 28.54275706135234358 ) ) ;
#173292 = CARTESIAN_POINT ( 'NONE',  ( -0.05219959533936034679, 19.03943276465977164, 52.50109039468566863 ) ) ;
#173293 = CARTESIAN_POINT ( 'NONE',  ( -10.72451020669898014, 18.67979575497178502, 105.4155762719810383 ) ) ;
#173294 = CARTESIAN_POINT ( 'NONE',  ( -4.379528057220328563, 16.55341960407611168, 30.20724293864769550 ) ) ;
#173295 = CARTESIAN_POINT ( 'NONE',  ( 19.02544592524343514, -5.153800228976328945, 73.54057627198103830 ) ) ;
#173296 = CARTESIAN_POINT ( 'NONE',  ( 0.05219959533907565091, 21.53943276465977519, 54.99890960531435269 ) ) ;
#173298 = CARTESIAN_POINT ( 'NONE',  ( -16.55341960407617563, 4.379528057220093196, 23.54275706135235424 ) ) ;
#173297 = CARTESIAN_POINT ( 'NONE',  ( 10.81492255796078972, 18.62759615963270932, 89.58224293864768129 ) ) ;
#173299 = CARTESIAN_POINT ( 'NONE',  ( -0.05219959533907301413, -21.53943276465977519, 27.49890960531435269 ) ) ;
#173300 = CARTESIAN_POINT ( 'NONE',  ( 10.81492255796106328, -18.62759615963255655, 85.41775706135236135 ) ) ;
#173301 = CARTESIAN_POINT ( 'NONE',  ( -5.049401038298153566, 19.05341960407611168, 75.20724293864769550 ) ) ;
#173302 = CARTESIAN_POINT ( 'NONE',  ( -19.03943276465977164, 0.05219959533909376836, 26.24890960531435624 ) ) ;
#173303 = CARTESIAN_POINT ( 'NONE',  ( -5.049401038298153566, 19.05341960407611168, 85.20724293864766707 ) ) ;
#173304 = CARTESIAN_POINT ( 'NONE',  ( 0.05219959533910956823, 16.53943276465976808, 109.9989096053143527 ) ) ;
#173305 = CARTESIAN_POINT ( 'NONE',  ( -9.564922557960796823, -16.46253265017161027, 62.08224293864769550 ) ) ;
#173306 = CARTESIAN_POINT ( 'NONE',  ( 19.05341960407617918, -5.049401038297876454, 101.0427570613523045 ) ) ;
#173307 = CARTESIAN_POINT ( 'NONE',  ( 7.500000000000000000, 9.184850993605147944E-16, 10.00000000000000000 ) ) ;
#173308 = CARTESIAN_POINT ( 'NONE',  ( 13.89961937509977652, -13.97604488694527269, 73.12390960531436690 ) ) ;
#173310 = CARTESIAN_POINT ( 'NONE',  ( -5.049401038298153566, 19.05341960407611168, 115.2072429386477097 ) ) ;
#173309 = CARTESIAN_POINT ( 'NONE',  ( -10.72451020669870658, -18.67979575497194134, 99.58442372801900433 ) ) ;
#173311 = CARTESIAN_POINT ( 'NONE',  ( -8.314922557961024197, 14.29746914071037800, 92.91775706135236135 ) ) ;
#173312 = CARTESIAN_POINT ( 'NONE',  ( -17.31728774477273447, -6.344390552232371583, 74.18093348310682700 ) ) ;
#173313 = CARTESIAN_POINT ( 'NONE',  ( 5.049401038297881783, 19.05341960407617563, 62.29275706135234003 ) ) ;
#173314 = CARTESIAN_POINT ( 'NONE',  ( -13.97604488694547697, 13.89961937509957934, 23.12609039468565442 ) ) ;
#173315 = CARTESIAN_POINT ( 'NONE',  ( -16.36317988757056696, -7.306389748694947173, 45.90210391636773579 ) ) ;
#173316 = CARTESIAN_POINT ( 'NONE',  ( 19.05341960407611168, 5.049401038298154454, 33.95724293864769550 ) ) ;
#173317 = CARTESIAN_POINT ( 'NONE',  ( -0.05219959533910754901, -16.53943276465976808, 22.49890960531436335 ) ) ;
#173318 = CARTESIAN_POINT ( 'NONE',  ( -35.41276914313063173, -3.966036006072681364, 38.62970943314355310 ) ) ;
#173319 = CARTESIAN_POINT ( 'NONE',  ( -16.52544592524335698, -4.483927247898792601, 108.9594237280190185 ) ) ;
#173320 = CARTESIAN_POINT ( 'NONE',  ( 22.84593195647081387, -20.82949652188557010, -50.38176470501583992 ) ) ;
#173321 = CARTESIAN_POINT ( 'NONE',  ( 4.483927247898790824, -16.52544592524335698, 75.20942372801901854 ) ) ;
#173322 = CARTESIAN_POINT ( 'NONE',  ( -13.97604488694527625, -13.89961937509977652, 36.87390960531436690 ) ) ;
#173323 = CARTESIAN_POINT ( 'NONE',  ( -10.72451020669870658, -18.67979575497194134, 89.58442372801901854 ) ) ;
#173324 = CARTESIAN_POINT ( 'NONE',  ( 19.03943276465977164, 0.05219959533936151252, 101.2510903946856757 ) ) ;
#173325 = CARTESIAN_POINT ( 'NONE',  ( -0.05219959533937732626, 21.53943276465977519, 67.50109039468568994 ) ) ;
#173326 = CARTESIAN_POINT ( 'NONE',  ( 19.02544592524334988, 5.153800228976608722, 51.45942372801900433 ) ) ;
#173327 = CARTESIAN_POINT ( 'NONE',  ( -0.05219959533909027116, -19.03943276465977164, 72.49890960531435269 ) ) ;
#173328 = CARTESIAN_POINT ( 'NONE',  ( -19.05341960407611168, -5.049401038298163336, 71.45724293864766707 ) ) ;
#173329 = CARTESIAN_POINT ( 'NONE',  ( 16.19135201231366139, 7.376712067591956412, 72.68680854052027485 ) ) ;
#173330 = CIRCLE ( 'NONE', #189496, 0.4999999999999972800 ) ;
#173331 = CARTESIAN_POINT ( 'NONE',  ( -8.314922557960811034, -14.29746914071050412, 52.08224293864768839 ) ) ;
#173332 = CARTESIAN_POINT ( 'NONE',  ( -21.53943276465977519, 0.05219959533907696930, 46.24890960531435979 ) ) ;
#173333 = CARTESIAN_POINT ( 'NONE',  ( 16.46253265017160672, -9.564922557960803928, 43.33224293864769550 ) ) ;
#173335 = CARTESIAN_POINT ( 'NONE',  ( -16.52544592524335698, -4.483927247898792601, 83.95942372801900433 ) ) ;
#173334 = CARTESIAN_POINT ( 'NONE',  ( -21.55341960407610458, -5.719274019375992779, 81.45724293864769550 ) ) ;
#173336 = EDGE_CURVE ( 'NONE', #120616, #66922, #150298, .T. ) ;
#173337 = ORIENTED_EDGE ( 'NONE', *, *, #77698, .F. ) ;
#173339 = CARTESIAN_POINT ( 'NONE',  ( -5.950531402560715689E-15, 38.81732327939063509, -3.124999997268813168 ) ) ;
#173338 = CARTESIAN_POINT ( 'NONE',  ( 4.483927247898545687, 16.52544592524342804, 84.79057627198102409 ) ) ;
#173340 = CARTESIAN_POINT ( 'NONE',  ( -0.05219959533934338120, 16.53943276465976808, 32.50109039468568284 ) ) ;
#173341 = CARTESIAN_POINT ( 'NONE',  ( -19.03943276465977164, 0.05219959533909376836, 26.24890960531435624 ) ) ;
#173342 = CARTESIAN_POINT ( 'NONE',  ( 16.51473224551083163, -9.474510206698727899, 70.83442372801900433 ) ) ;
#173343 = CIRCLE ( 'NONE', #86167, 5.000000000000000888 ) ;
#173344 = CARTESIAN_POINT ( 'NONE',  ( -14.34966873604960291, -8.224510206698953496, 76.66557627198103830 ) ) ;
#173345 = CARTESIAN_POINT ( 'NONE',  ( 5.719274019375673035, 21.55341960407619339, 47.29275706135234003 ) ) ;
#173347 = CARTESIAN_POINT ( 'NONE',  ( 10.81492255796078972, 18.62759615963270932, 89.58224293864768129 ) ) ;
#173346 = CARTESIAN_POINT ( 'NONE',  ( 9.564922557960805705, 16.46253265017160317, 24.58224293864769194 ) ) ;
#173348 = CARTESIAN_POINT ( 'NONE',  ( -0.05219959533909027116, -19.03943276465977164, 112.4989096053143669 ) ) ;
#173349 = CARTESIAN_POINT ( 'NONE',  ( 4.483927247898545687, 16.52544592524342804, 89.79057627198103830 ) ) ;
#173350 = CARTESIAN_POINT ( 'NONE',  ( 22.61240241994758904, -33.77560033877482937, -17.98683046886793591 ) ) ;
#173351 = CARTESIAN_POINT ( 'NONE',  ( -5.153800228976328057, -19.02544592524343514, 42.29057627198101699 ) ) ;
#173352 = CARTESIAN_POINT ( 'NONE',  ( -36.91746825000000598, -11.99521256947794789, -6.524999997268811747 ) ) ;
#173353 = CARTESIAN_POINT ( 'NONE',  ( -13.97604488694547697, 13.89961937509957934, 78.12609039468567573 ) ) ;
#173354 = CARTESIAN_POINT ( 'NONE',  ( -5.823673210054431948, 21.52544592524334988, 22.70942372801901499 ) ) ;
#173355 = CARTESIAN_POINT ( 'NONE',  ( 16.51473224551069308, 9.474510206698969483, 74.16557627198103830 ) ) ;
#173356 = B_SPLINE_CURVE_WITH_KNOTS ( 'NONE', 3,
 ( #96851, #98838, #115025, #146348, #176718, #7835 ),
 .UNSPECIFIED., .F., .F.,
 ( 4, 2, 4 ),
 ( 0.003989672132298079273, 0.004372778065220507722, 0.004755883998142936171 ),
 .UNSPECIFIED. ) ;
#173357 = CARTESIAN_POINT ( 'NONE',  ( -19.05341960407617563, 5.049401038297882671, 53.54275706135231871 ) ) ;
#173358 = CARTESIAN_POINT ( 'NONE',  ( 5.153800228976335163, 19.02544592524342804, 44.79057627198103830 ) ) ;
#173359 = CARTESIAN_POINT ( 'NONE',  ( 4.483927247898545687, 16.52544592524342804, 59.79057627198103120 ) ) ;
#173360 = CARTESIAN_POINT ( 'NONE',  ( -8.314922557960811034, -14.29746914071050412, 57.08224293864769550 ) ) ;
#173361 = CARTESIAN_POINT ( 'NONE',  ( -13.97604488694527625, -13.89961937509977652, 81.87390960531436690 ) ) ;
#173362 = CARTESIAN_POINT ( 'NONE',  ( 18.67979575497178502, 10.72451020669898547, 104.1655762719810241 ) ) ;
#173363 = CARTESIAN_POINT ( 'NONE',  ( 16.46253265017160672, -9.564922557960803928, 73.33224293864769550 ) ) ;
#173364 = CARTESIAN_POINT ( 'NONE',  ( -21.52544592524343514, 5.823673210054127303, 81.04057627198102409 ) ) ;
#173365 = CARTESIAN_POINT ( 'NONE',  ( -10.72451020669870658, -18.67979575497194134, 109.5844237280190328 ) ) ;
#173368 = CARTESIAN_POINT ( 'NONE',  ( -14.34966873604960291, -8.224510206698953496, 101.6655762719810383 ) ) ;
#173367 = CARTESIAN_POINT ( 'NONE',  ( 14.29746914071049879, -8.314922557960816363, 23.33224293864769194 ) ) ;
#173366 = CARTESIAN_POINT ( 'NONE',  ( 19.02544592524343514, -5.153800228976328945, 38.54057627198103120 ) ) ;
#173369 = CARTESIAN_POINT ( 'NONE',  ( 9.474510206698729675, 16.51473224551082808, 112.0844237280190043 ) ) ;
#173370 = ORIENTED_EDGE ( 'NONE', *, *, #1347, .F. ) ;
#173371 = CARTESIAN_POINT ( 'NONE',  ( 5.719274019375673035, 21.55341960407619339, 37.29275706135235424 ) ) ;
#173372 = CARTESIAN_POINT ( 'NONE',  ( -16.51473224551082808, 9.474510206698731452, 53.33442372801900433 ) ) ;
#173373 = CARTESIAN_POINT ( 'NONE',  ( -16.55341960407617563, 4.379528057220093196, 108.5427570613523756 ) ) ;
#173374 = CARTESIAN_POINT ( 'NONE',  ( 18.67979575497178502, 10.72451020669898547, 74.16557627198102409 ) ) ;
#173375 = CARTESIAN_POINT ( 'NONE',  ( 0.05219959533909260263, 19.03943276465977164, 104.9989096053143669 ) ) ;
#173376 = CARTESIAN_POINT ( 'NONE',  ( 0.05219959533910956823, 16.53943276465976808, 54.99890960531435269 ) ) ;
#173377 = CARTESIAN_POINT ( 'NONE',  ( 13.89961937509977652, -13.97604488694527269, 28.12390960531435624 ) ) ;
#173378 = CARTESIAN_POINT ( 'NONE',  ( -16.46253265017160317, 9.564922557960807481, 35.83224293864768839 ) ) ;
#173379 = CARTESIAN_POINT ( 'NONE',  ( 18.67979575497194134, -10.72451020669871369, 105.8344237280190328 ) ) ;
#173380 = CARTESIAN_POINT ( 'NONE',  ( -8.314922557961024197, 14.29746914071037800, 87.91775706135234714 ) ) ;
#173381 = CARTESIAN_POINT ( 'NONE',  ( -0.05219959533937732626, 21.53943276465977519, 47.50109039468568994 ) ) ;
#173382 = CARTESIAN_POINT ( 'NONE',  ( 4.379528057220092307, 16.55341960407617563, 47.29275706135234003 ) ) ;
#173383 = CARTESIAN_POINT ( 'NONE',  ( -10.81492255796078084, -18.62759615963271287, 27.08224293864769550 ) ) ;
#173384 = CARTESIAN_POINT ( 'NONE',  ( 13.97604488694527802, 13.89961937509977652, 59.37390960531434558 ) ) ;
#173385 = CARTESIAN_POINT ( 'NONE',  ( -9.474510206698964154, 16.51473224551069663, 60.41557627198102409 ) ) ;
#173386 = CARTESIAN_POINT ( 'NONE',  ( -4.483927247898782831, 16.52544592524335698, 62.70942372801902565 ) ) ;
#173387 = CARTESIAN_POINT ( 'NONE',  ( -8.224510206698948167, 14.34966873604960824, 100.4155762719810241 ) ) ;
#173388 = CARTESIAN_POINT ( 'NONE',  ( 4.379528057220339221, -16.55341960407611168, 27.70724293864769905 ) ) ;
#173389 = DIRECTION ( 'NONE',  ( 0.000000000000000000, -1.000000000000000000, 0.000000000000000000 ) ) ;
#173392 = CARTESIAN_POINT ( 'NONE',  ( 5.049401038298161559, -19.05341960407611168, 82.70724293864770971 ) ) ;
#173391 = CARTESIAN_POINT ( 'NONE',  ( -13.89961937509977652, 13.97604488694528158, 90.62390960531432427 ) ) ;
#173390 = CARTESIAN_POINT ( 'NONE',  ( 15.80617190586769283, -15.72974639402175789, 60.62609039468567573 ) ) ;
#173393 = CARTESIAN_POINT ( 'NONE',  ( 9.474510206698971260, -16.51473224551069308, 107.9155762719810383 ) ) ;
#173394 = CARTESIAN_POINT ( 'NONE',  ( 16.53943276465976808, -0.05219959533910856209, 48.74890960531435979 ) ) ;
#173395 = CARTESIAN_POINT ( 'NONE',  ( -16.55341960407617563, 4.379528057220093196, 108.5427570613523756 ) ) ;
#173396 = CARTESIAN_POINT ( 'NONE',  ( 16.52544592524342804, -4.483927247898539470, 38.54057627198103120 ) ) ;
#173397 = LINE ( 'NONE', #33881, #60900 ) ;
#173398 = CARTESIAN_POINT ( 'NONE',  ( -16.46253265017146816, -9.564922557961047289, 34.16775706135233293 ) ) ;
#173399 = CARTESIAN_POINT ( 'NONE',  ( -19.02544592524342804, 5.153800228976336051, 76.04057627198102409 ) ) ;
#173400 = CARTESIAN_POINT ( 'NONE',  ( 13.89961937509957401, 13.97604488694547697, 51.87609039468566863 ) ) ;
#173401 = CARTESIAN_POINT ( 'NONE',  ( -29.86685920354755197, -21.69954338932560134, -8.924999997268812990 ) ) ;
#173402 = CARTESIAN_POINT ( 'NONE',  ( -6.020228577223754586E-15, 39.95556452105416412, -2.249999994537626336 ) ) ;
#173404 = CARTESIAN_POINT ( 'NONE',  ( 0.05219959533934541429, -16.53943276465976808, 75.00109039468568994 ) ) ;
#173403 = CARTESIAN_POINT ( 'NONE',  ( 19.05341960407617918, -5.049401038297876454, 86.04275706135233293 ) ) ;
#173405 = CARTESIAN_POINT ( 'NONE',  ( 17.50000000000000000, 5.499999999999992895, 91.70309617465828467 ) ) ;
#173406 = CARTESIAN_POINT ( 'NONE',  ( -19.05341960407611168, -5.049401038298163336, 101.4572429386476955 ) ) ;
#173407 = CARTESIAN_POINT ( 'NONE',  ( 5.719274019375673035, 21.55341960407619339, 22.29275706135235069 ) ) ;
#173408 = CARTESIAN_POINT ( 'NONE',  ( 16.46253265017146816, 9.564922557961045513, 96.66775706135233293 ) ) ;
#173410 = CARTESIAN_POINT ( 'NONE',  ( 9.564922557960805705, 16.46253265017160317, 49.58224293864770260 ) ) ;
#173409 = CARTESIAN_POINT ( 'NONE',  ( -19.02544592524342804, 5.153800228976336051, 116.0405762719810383 ) ) ;
#173411 = CARTESIAN_POINT ( 'NONE',  ( -19.02544592524342804, 5.153800228976336051, 91.04057627198100988 ) ) ;
#173413 = CARTESIAN_POINT ( 'NONE',  ( 19.02544592524343514, -5.153800228976328945, 53.54057627198102409 ) ) ;
#173412 = CARTESIAN_POINT ( 'NONE',  ( 14.29746914071049879, -8.314922557960816363, 58.33224293864768839 ) ) ;
#173414 = CARTESIAN_POINT ( 'NONE',  ( -19.03943276465977164, 0.05219959533909376836, 61.24890960531436690 ) ) ;
#173415 = CARTESIAN_POINT ( 'NONE',  ( -19.02544592524334988, -5.153800228976617603, 68.95942372801896170 ) ) ;
#173416 = ORIENTED_EDGE ( 'NONE', *, *, #53677, .F. ) ;
#173417 = CARTESIAN_POINT ( 'NONE',  ( 5.049401038297881783, 19.05341960407617563, 27.29275706135232937 ) ) ;
#173418 = CARTESIAN_POINT ( 'NONE',  ( 5.049401038298161559, -19.05341960407611168, 67.70724293864769550 ) ) ;
#173419 = CARTESIAN_POINT ( 'NONE',  ( -10.81492255796078084, -18.62759615963271287, 62.08224293864769550 ) ) ;
#173421 = CARTESIAN_POINT ( 'NONE',  ( -19.03943276465977164, -0.05219959533935918106, 33.75109039468566863 ) ) ;
#173420 = CARTESIAN_POINT ( 'NONE',  ( 16.53943276465976808, -0.05219959533910856209, 63.74890960531435979 ) ) ;
#173422 = CARTESIAN_POINT ( 'NONE',  ( 5.153800228976335163, 19.02544592524342804, 114.7905762719810241 ) ) ;
#173423 = CARTESIAN_POINT ( 'NONE',  ( -21.53943276465977519, 0.05219959533907696930, 46.24890960531435979 ) ) ;
#173424 = CARTESIAN_POINT ( 'NONE',  ( -5.719274019375978568, 21.55341960407610458, 25.20724293864769550 ) ) ;
#173425 = CARTESIAN_POINT ( 'NONE',  ( -13.97604488694527625, -13.89961937509977652, 51.87390960531436690 ) ) ;
#173426 = CARTESIAN_POINT ( 'NONE',  ( 16.46253265017160672, -9.564922557960803928, 43.33224293864769550 ) ) ;
#173427 = CARTESIAN_POINT ( 'NONE',  ( -4.379528057220328563, 16.55341960407611168, 100.2072429386476955 ) ) ;
#173428 = CARTESIAN_POINT ( 'NONE',  ( -21.52544592524343514, 5.823673210054127303, 116.0405762719810383 ) ) ;
#173429 = DIRECTION ( 'NONE',  ( 1.000000000000000000, 0.000000000000000000, 0.000000000000000000 ) ) ;
#173430 = CARTESIAN_POINT ( 'NONE',  ( 10.81492255796106328, -18.62759615963255655, 30.41775706135234358 ) ) ;
#173431 = CARTESIAN_POINT ( 'NONE',  ( 16.52544592524342804, -4.483927247898539470, 113.5405762719810383 ) ) ;
#173432 = CARTESIAN_POINT ( 'NONE',  ( 15.80617190586769283, -15.72974639402175789, 75.62609039468567573 ) ) ;
#173433 = CARTESIAN_POINT ( 'NONE',  ( -5.719274019375978568, 21.55341960407610458, 95.20724293864769550 ) ) ;
#173434 = CARTESIAN_POINT ( 'NONE',  ( 5.153800228976615827, -19.02544592524334988, 35.20942372801899722 ) ) ;
#173435 = CARTESIAN_POINT ( 'NONE',  ( 5.153800228976335163, 19.02544592524342804, 29.79057627198102409 ) ) ;
#173436 = CARTESIAN_POINT ( 'NONE',  ( -3.573655867282028392E-15, 2.428612866367529932E-14, 150.0000000000000000 ) ) ;
#173437 = CARTESIAN_POINT ( 'NONE',  ( 31.06299995236814837, -1.355922687059476051, -50.16575868250042447 ) ) ;
#173438 = CARTESIAN_POINT ( 'NONE',  ( -0.05219959533934338120, 16.53943276465976808, 47.50109039468568994 ) ) ;
#173439 = CARTESIAN_POINT ( 'NONE',  ( 12.14591786802309770, 12.06949235617756955, 104.3739096053143669 ) ) ;
#173440 = CARTESIAN_POINT ( 'NONE',  ( -3.573655867282028392E-15, 2.428612866367529932E-14, 155.0000000000000000 ) ) ;
#173441 = CARTESIAN_POINT ( 'NONE',  ( -19.03943276465977164, 0.05219959533909376836, 66.24890960531436690 ) ) ;
#173443 = ADVANCED_FACE ( 'NONE', ( #56272 ), #166463, .F. ) ;
#173442 = CARTESIAN_POINT ( 'NONE',  ( -16.55341960407611168, -4.379528057220339221, 91.45724293864769550 ) ) ;
#173444 = CARTESIAN_POINT ( 'NONE',  ( -21.52544592524343514, 5.823673210054127303, 46.04057627198103830 ) ) ;
#173445 = CARTESIAN_POINT ( 'NONE',  ( 4.483927247898545687, 16.52544592524342804, 64.79057627198103830 ) ) ;
#173446 = CARTESIAN_POINT ( 'NONE',  ( 16.52544592524335698, 4.483927247898782831, 31.45942372801901854 ) ) ;
#173447 = CARTESIAN_POINT ( 'NONE',  ( -21.52544592524334988, -5.823673210054445271, 88.95942372801901854 ) ) ;
#173448 = CARTESIAN_POINT ( 'NONE',  ( -3.735172737399431091E-16, -6.100000000000006750, -64.53213882399991519 ) ) ;
#173449 = CARTESIAN_POINT ( 'NONE',  ( 4.379528057220092307, 16.55341960407617563, 97.29275706135234714 ) ) ;
#173450 = CARTESIAN_POINT ( 'NONE',  ( 14.29746914071049879, -8.314922557960816363, 43.33224293864769550 ) ) ;
#173451 = CARTESIAN_POINT ( 'NONE',  ( -5.153800228976328057, -19.02544592524343514, 42.29057627198101699 ) ) ;
#173452 = CARTESIAN_POINT ( 'NONE',  ( 21.52544592524334988, 5.823673210054432836, 96.45942372801901854 ) ) ;
#173453 = CARTESIAN_POINT ( 'NONE',  ( 0.05219959533907565091, 21.53943276465977519, 109.9989096053143527 ) ) ;
#173454 = CARTESIAN_POINT ( 'NONE',  ( 18.67979575497194134, -10.72451020669871369, 60.83442372801901854 ) ) ;
#173455 = CARTESIAN_POINT ( 'NONE',  ( -8.224510206698735004, -14.34966873604973081, 39.58442372801901143 ) ) ;
#173457 = CARTESIAN_POINT ( 'NONE',  ( -21.55341960407619339, 5.719274019375674811, 83.54275706135234714 ) ) ;
#173456 = CARTESIAN_POINT ( 'NONE',  ( 12.14591786802309770, 12.06949235617756955, 64.37390960531435269 ) ) ;
#173458 = CARTESIAN_POINT ( 'NONE',  ( 4.379528057220339221, -16.55341960407611168, 22.70724293864769194 ) ) ;
#173459 = FACE_OUTER_BOUND ( 'NONE', #69902, .T. ) ;
#173460 = CARTESIAN_POINT ( 'NONE',  ( 4.483927247898545687, 16.52544592524342804, 29.79057627198102409 ) ) ;
#173461 = CARTESIAN_POINT ( 'NONE',  ( -16.52544592524335698, -4.483927247898792601, 73.95942372801901854 ) ) ;
#173462 = CARTESIAN_POINT ( 'NONE',  ( 0.05219959533909260263, 19.03943276465977164, 79.99890960531436690 ) ) ;
#173463 = CARTESIAN_POINT ( 'NONE',  ( 9.564922557960805705, 16.46253265017160317, 104.5822429386476955 ) ) ;
#173464 = CARTESIAN_POINT ( 'NONE',  ( 15.80617190586769283, -15.72974639402175789, 80.62609039468567573 ) ) ;
#173465 = CARTESIAN_POINT ( 'NONE',  ( -12.14591786802326823, 12.06949235617739902, 83.12609039468568994 ) ) ;
#173466 = CARTESIAN_POINT ( 'NONE',  ( 8.224510206698953496, -14.34966873604960469, 72.91557627198103830 ) ) ;
#173467 = CARTESIAN_POINT ( 'NONE',  ( -5.049401038298153566, 19.05341960407611168, 65.20724293864765286 ) ) ;
#173468 = ORIENTED_EDGE ( 'NONE', *, *, #159157, .T. ) ;
#173469 = CARTESIAN_POINT ( 'NONE',  ( 14.34966873604972726, -8.224510206698740333, 30.83442372801902209 ) ) ;
#173470 = CARTESIAN_POINT ( 'NONE',  ( -13.97604488694527625, -13.89961937509977652, 21.87390960531435979 ) ) ;
#173471 = CARTESIAN_POINT ( 'NONE',  ( -5.153800228976328057, -19.02544592524343514, 92.29057627198099567 ) ) ;
#173473 = CARTESIAN_POINT ( 'NONE',  ( 11.40812507854755253, -35.11059874428192273, -8.024999997268814411 ) ) ;
#173472 = CARTESIAN_POINT ( 'NONE',  ( -16.55341960407617563, 4.379528057220093196, 23.54275706135235424 ) ) ;
#173474 = CARTESIAN_POINT ( 'NONE',  ( -13.97604488694547697, 13.89961937509957934, 28.12609039468565797 ) ) ;
#173475 = CARTESIAN_POINT ( 'NONE',  ( 0.05219959533934541429, -16.53943276465976808, 100.0010903946857042 ) ) ;
#173476 = CARTESIAN_POINT ( 'NONE',  ( -19.02544592524334988, -5.153800228976617603, 103.9594237280190043 ) ) ;
#173477 = CARTESIAN_POINT ( 'NONE',  ( -12.06949235617756955, 12.14591786802309770, 115.6239096053143669 ) ) ;
#173478 = CARTESIAN_POINT ( 'NONE',  ( 4.379528057220092307, 16.55341960407617563, 67.29275706135234714 ) ) ;
#173479 = CARTESIAN_POINT ( 'NONE',  ( -16.53943276465976808, -0.05219959533934237506, 53.75109039468568994 ) ) ;
#173480 = CARTESIAN_POINT ( 'NONE',  ( 17.38119043544336506, -36.03980009027800691, -12.45558932256932039 ) ) ;
#173481 = CARTESIAN_POINT ( 'NONE',  ( 9.564922557961047289, -16.46253265017146816, 65.41775706135233293 ) ) ;
#173482 = CARTESIAN_POINT ( 'NONE',  ( 21.53943276465977519, 0.05219959533937863772, 111.2510903946856899 ) ) ;
#173483 = CARTESIAN_POINT ( 'NONE',  ( -19.05341960407611168, -5.049401038298163336, 46.45724293864768129 ) ) ;
#173484 = CARTESIAN_POINT ( 'NONE',  ( 5.153800228976335163, 19.02544592524342804, 84.79057627198099567 ) ) ;
#173485 = CARTESIAN_POINT ( 'NONE',  ( -12.14591786802309592, -12.06949235617757132, 66.87390960531436690 ) ) ;
#173486 = VECTOR ( 'NONE', #131539, 1000.000000000000000 ) ;
#173487 = CARTESIAN_POINT ( 'NONE',  ( -5.049401038297874678, -19.05341960407617918, 54.79275706135234003 ) ) ;
#173488 = CARTESIAN_POINT ( 'NONE',  ( -18.62759615963270932, 10.81492255796079327, 45.83224293864769550 ) ) ;
#173489 = CARTESIAN_POINT ( 'NONE',  ( -18.67979575497193778, 10.72451020669871902, 103.3344237280190043 ) ) ;
#173490 = CARTESIAN_POINT ( 'NONE',  ( -0.05219959533909027116, -19.03943276465977164, 97.49890960531436690 ) ) ;
#173491 = CARTESIAN_POINT ( 'NONE',  ( -21.55341960407619339, 5.719274019375674811, 108.5427570613523756 ) ) ;
#173492 = CARTESIAN_POINT ( 'NONE',  ( 5.719274019375991003, -21.55341960407610458, 62.70724293864769550 ) ) ;
#173493 = CARTESIAN_POINT ( 'NONE',  ( 13.97604488694527802, 13.89961937509977652, 94.37390960531436690 ) ) ;
#173494 = CARTESIAN_POINT ( 'NONE',  ( -5.049401038297874678, -19.05341960407617918, 94.79275706135230450 ) ) ;
#173495 = CARTESIAN_POINT ( 'NONE',  ( 19.05341960407611168, 5.049401038298154454, 108.9572429386477097 ) ) ;
#173496 = CARTESIAN_POINT ( 'NONE',  ( -5.153800228976607833, 19.02544592524334988, 112.7094237280190043 ) ) ;
#173497 = CARTESIAN_POINT ( 'NONE',  ( 16.55341960407611168, 4.379528057220329451, 108.9572429386476955 ) ) ;
#173498 = CARTESIAN_POINT ( 'NONE',  ( 5.153800228976335163, 19.02544592524342804, 89.79057627198102409 ) ) ;
#173499 = CARTESIAN_POINT ( 'NONE',  ( -10.72451020669898014, 18.67979575497178502, 65.41557627198102409 ) ) ;
#173500 = CARTESIAN_POINT ( 'NONE',  ( 16.52544592524335698, 4.483927247898782831, 51.45942372801901854 ) ) ;
#173501 = CARTESIAN_POINT ( 'NONE',  ( 21.52544592524334988, 5.823673210054432836, 41.45942372801901143 ) ) ;
#173502 = CARTESIAN_POINT ( 'NONE',  ( 18.67979575497194134, -10.72451020669871369, 100.8344237280190185 ) ) ;
#173503 = CARTESIAN_POINT ( 'NONE',  ( 16.53943276465976808, 0.05219959533934440121, 101.2510903946856757 ) ) ;
#173504 = CARTESIAN_POINT ( 'NONE',  ( -9.564922557960796823, -16.46253265017161027, 87.08224293864769550 ) ) ;
#173505 = CARTESIAN_POINT ( 'NONE',  ( -16.53943276465976808, 0.05219959533911058130, 86.24890960531436690 ) ) ;
#173506 = CARTESIAN_POINT ( 'NONE',  ( 0.05219959533910956823, 16.53943276465976808, 24.99890960531435624 ) ) ;
#173507 = CARTESIAN_POINT ( 'NONE',  ( -5.153800228976607833, 19.02544592524334988, 67.70942372801900433 ) ) ;
#173508 = CARTESIAN_POINT ( 'NONE',  ( 15.80617190586769283, -15.72974639402175789, 40.62609039468567573 ) ) ;
#173509 = CARTESIAN_POINT ( 'NONE',  ( -16.53943276465976808, 0.05219959533911058130, 86.24890960531436690 ) ) ;
#173510 = CARTESIAN_POINT ( 'NONE',  ( -0.05219959533909027116, -19.03943276465977164, 107.4989096053143527 ) ) ;
#173511 = CARTESIAN_POINT ( 'NONE',  ( -8.314922557960811034, -14.29746914071050412, 22.08224293864769194 ) ) ;
#173512 = CARTESIAN_POINT ( 'NONE',  ( -15.80617190586768217, 15.72974639402176855, 88.12609039468570415 ) ) ;
#173513 = CARTESIAN_POINT ( 'NONE',  ( 8.224510206698742110, 14.34966873604972548, 52.08442372801901854 ) ) ;
#173514 = CARTESIAN_POINT ( 'NONE',  ( 10.81492255796106328, -18.62759615963255655, 45.41775706135234003 ) ) ;
#173515 = ORIENTED_EDGE ( 'NONE', *, *, #83344, .T. ) ;
#173516 = CARTESIAN_POINT ( 'NONE',  ( -10.72451020669870658, -18.67979575497194134, 29.58442372801901854 ) ) ;
#173517 = CARTESIAN_POINT ( 'NONE',  ( -4.483927247898539470, -16.52544592524342804, 107.2905762719810525 ) ) ;
#173518 = EDGE_CURVE ( 'NONE', #166707, #46039, #193806, .T. ) ;
#173519 = CARTESIAN_POINT ( 'NONE',  ( -19.05341960407611168, -5.049401038298163336, 31.45724293864769550 ) ) ;
#173520 = CARTESIAN_POINT ( 'NONE',  ( -12.06949235617756955, 12.14591786802309770, 65.62390960531436690 ) ) ;
#173521 = CARTESIAN_POINT ( 'NONE',  ( 13.97604488694527802, 13.89961937509977652, 59.37390960531434558 ) ) ;
#173522 = CARTESIAN_POINT ( 'NONE',  ( -16.53943276465976808, -0.05219959533934237506, 108.7510903946857042 ) ) ;
#173523 = CARTESIAN_POINT ( 'NONE',  ( 19.03943276465977164, -0.05219959533909143690, 43.74890960531435979 ) ) ;
#173524 = CARTESIAN_POINT ( 'NONE',  ( 18.62759615963271287, -10.81492255796078972, 38.33224293864768839 ) ) ;
#173525 = CARTESIAN_POINT ( 'NONE',  ( 14.29746914071049879, -8.314922557960816363, 73.33224293864769550 ) ) ;
#173526 = AXIS2_PLACEMENT_3D ( 'NONE', #189965, #82755, #144435 ) ;
#173527 = CARTESIAN_POINT ( 'NONE',  ( 18.67979575497178502, 10.72451020669898547, 89.16557627198102409 ) ) ;
#173528 = CARTESIAN_POINT ( 'NONE',  ( -5.153800228976328057, -19.02544592524343514, 92.29057627198099567 ) ) ;
#173530 = CARTESIAN_POINT ( 'NONE',  ( 13.97604488694548053, -13.89961937509957401, 90.62609039468567573 ) ) ;
#173529 = CARTESIAN_POINT ( 'NONE',  ( -0.05219959533909027116, -19.03943276465977164, 52.49890960531436690 ) ) ;
#173531 = EDGE_CURVE ( 'NONE', #159561, #16134, #496, .T. ) ;
#173532 = CARTESIAN_POINT ( 'NONE',  ( -21.53943276465977519, 0.05219959533907696930, 46.24890960531435979 ) ) ;
#173533 = CARTESIAN_POINT ( 'NONE',  ( -0.05219959533937732626, 21.53943276465977519, 72.50109039468568994 ) ) ;
#173534 = CARTESIAN_POINT ( 'NONE',  ( -5.153800228976328057, -19.02544592524343514, 57.29057627198103120 ) ) ;
#173535 = CARTESIAN_POINT ( 'NONE',  ( 19.03943276465977164, -0.05219959533909143690, 78.74890960531436690 ) ) ;
#173536 = ORIENTED_EDGE ( 'NONE', *, *, #101580, .T. ) ;
#173537 = CARTESIAN_POINT ( 'NONE',  ( -16.55341960407617563, 4.379528057220093196, 68.54275706135234714 ) ) ;
#173538 = CARTESIAN_POINT ( 'NONE',  ( 10.72451020669871369, 18.67979575497193778, 42.08442372801901854 ) ) ;
#173539 = CARTESIAN_POINT ( 'NONE',  ( -21.52544592524334988, -5.823673210054445271, 78.95942372801901854 ) ) ;
#173540 = CARTESIAN_POINT ( 'NONE',  ( -18.67979575497178146, -10.72451020669898902, 26.66557627198103475 ) ) ;
#173541 = CARTESIAN_POINT ( 'NONE',  ( 21.55341960407610458, 5.719274019375980345, 93.95724293864770971 ) ) ;
#173543 = CARTESIAN_POINT ( 'NONE',  ( -12.06949235617739369, -12.14591786802326823, 64.37609039468568994 ) ) ;
#173542 = CARTESIAN_POINT ( 'NONE',  ( 5.823673210054444382, -21.52544592524334988, 35.20942372801901854 ) ) ;
#173544 = CARTESIAN_POINT ( 'NONE',  ( 21.53943276465977519, -0.05219959533907433946, 58.74890960531436690 ) ) ;
#173545 = CARTESIAN_POINT ( 'NONE',  ( -19.02544592524334988, -5.153800228976617603, 33.95942372801897591 ) ) ;
#173547 = CARTESIAN_POINT ( 'NONE',  ( 16.53943276465976808, 0.05219959533934440121, 96.25109039468568994 ) ) ;
#173546 = CARTESIAN_POINT ( 'NONE',  ( 19.02544592524343514, -5.153800228976328945, 68.54057627198103830 ) ) ;
#173548 = CARTESIAN_POINT ( 'NONE',  ( -30.00000000000000355, -0.3535533905932735643, 4.646446609406718942 ) ) ;
#173549 = CARTESIAN_POINT ( 'NONE',  ( 16.46253265017160672, -9.564922557960803928, 103.3322429386476955 ) ) ;
#173550 = DIRECTION ( 'NONE',  ( 0.000000000000000000, 0.000000000000000000, -1.000000000000000000 ) ) ;
#173551 = CARTESIAN_POINT ( 'NONE',  ( 13.89961937509957401, 13.97604488694547697, 81.87609039468564731 ) ) ;
#173552 = CARTESIAN_POINT ( 'NONE',  ( 5.719274019375991003, -21.55341960407610458, 62.70724293864769550 ) ) ;
#173553 = CARTESIAN_POINT ( 'NONE',  ( 4.379528057220339221, -16.55341960407611168, 37.70724293864769550 ) ) ;
#173554 = CARTESIAN_POINT ( 'NONE',  ( -16.51473224551082808, 9.474510206698731452, 98.33442372801900433 ) ) ;
#173555 = CARTESIAN_POINT ( 'NONE',  ( -9.564922557960796823, -16.46253265017161027, 27.08224293864769550 ) ) ;
#173556 = CARTESIAN_POINT ( 'NONE',  ( 16.55341960407618274, -4.379528057220086978, 21.04275706135234714 ) ) ;
#173558 = CARTESIAN_POINT ( 'NONE',  ( 9.474510206698729675, 16.51473224551082808, 62.08442372801899722 ) ) ;
#173557 = CARTESIAN_POINT ( 'NONE',  ( 21.53943276465977519, -0.05219959533907433946, 83.74890960531435269 ) ) ;
#173559 = CARTESIAN_POINT ( 'NONE',  ( -8.224510206698735004, -14.34966873604973081, 84.58442372801903275 ) ) ;
#173560 = CARTESIAN_POINT ( 'NONE',  ( 5.153800228976335163, 19.02544592524342804, 64.79057627198100988 ) ) ;
#173561 = CARTESIAN_POINT ( 'NONE',  ( -12.14591786802309592, -12.06949235617757132, 71.87390960531438111 ) ) ;
#173562 = CARTESIAN_POINT ( 'NONE',  ( 13.97604488694527802, 13.89961937509977652, 54.37390960531435979 ) ) ;
#173563 = CARTESIAN_POINT ( 'NONE',  ( -16.52544592524342804, 4.483927247898546575, 56.04057627198102409 ) ) ;
#173564 = CARTESIAN_POINT ( 'NONE',  ( 0.000000000000000000, 0.000000000000000000, -62.50719930893269805 ) ) ;
#173565 = CARTESIAN_POINT ( 'NONE',  ( 31.37911219714120037, -7.435064219939697239, 93.98466263399201637 ) ) ;
#173566 = CARTESIAN_POINT ( 'NONE',  ( -4.483927247898539470, -16.52544592524342804, 22.29057627198102765 ) ) ;
#173567 = CARTESIAN_POINT ( 'NONE',  ( -16.51473224551069308, -9.474510206698971260, 71.66557627198102409 ) ) ;
#173568 = FACE_BOUND ( 'NONE', #129102, .T. ) ;
#173569 = CARTESIAN_POINT ( 'NONE',  ( -9.564922557961040184, 16.46253265017147172, 42.91775706135234003 ) ) ;
#173570 = CARTESIAN_POINT ( 'NONE',  ( 14.29746914071037800, 8.314922557961029526, 51.66775706135234714 ) ) ;
#173571 = CARTESIAN_POINT ( 'NONE',  ( 21.52544592524344225, -5.823673210054117533, 48.54057627198103120 ) ) ;
#173572 = CARTESIAN_POINT ( 'NONE',  ( 0.05219959533936267826, -19.03943276465977164, 25.00109039468566152 ) ) ;
#173573 = CARTESIAN_POINT ( 'NONE',  ( -19.05341960407611168, -5.049401038298163336, 76.45724293864769550 ) ) ;
#173574 = CARTESIAN_POINT ( 'NONE',  ( 7.086465707319022428E-15, -78.65691688641808810, -25.00000000000000000 ) ) ;
#173575 = CARTESIAN_POINT ( 'NONE',  ( -9.564922557960796823, -16.46253265017161027, 107.0822429386476955 ) ) ;
#173576 = CARTESIAN_POINT ( 'NONE',  ( -15.80617190586768217, 15.72974639402176855, 43.12609039468568284 ) ) ;
#173577 = CARTESIAN_POINT ( 'NONE',  ( -8.314922557960811034, -14.29746914071050412, 107.0822429386476955 ) ) ;
#173580 = EDGE_LOOP ( 'NONE', ( #191709, #137263, #175803, #2512 ) ) ;
#173579 = CARTESIAN_POINT ( 'NONE',  ( 5.153800228976335163, 19.02544592524342804, 79.79057627198102409 ) ) ;
#173578 = CARTESIAN_POINT ( 'NONE',  ( -5.823673210054116645, -21.52544592524344225, 82.29057627198103830 ) ) ;
#173581 = CARTESIAN_POINT ( 'NONE',  ( -18.62759615963255300, -10.81492255796106328, 24.16775706135235424 ) ) ;
#173582 = ORIENTED_EDGE ( 'NONE', *, *, #17418, .F. ) ;
#173583 = CARTESIAN_POINT ( 'NONE',  ( 19.03943276465977164, -0.05219959533909143690, 88.74890960531436690 ) ) ;
#173584 = CARTESIAN_POINT ( 'NONE',  ( -17.60779699588843883, -5.499999999999954703, 76.34981316670108242 ) ) ;
#173586 = CARTESIAN_POINT ( 'NONE',  ( 19.05341960407611168, 5.049401038298154454, 33.95724293864769550 ) ) ;
#173585 = CARTESIAN_POINT ( 'NONE',  ( -4.379528057220328563, 16.55341960407611168, 115.2072429386476955 ) ) ;
#173587 = CARTESIAN_POINT ( 'NONE',  ( -19.02544592524334988, -5.153800228976617603, 108.9594237280189759 ) ) ;
#173588 = CARTESIAN_POINT ( 'NONE',  ( -22.81625015709510507, 31.40387420917330275, -7.424999997268812990 ) ) ;
#173589 = CARTESIAN_POINT ( 'NONE',  ( 4.379528057220339221, -16.55341960407611168, 107.7072429386476955 ) ) ;
#173590 = CARTESIAN_POINT ( 'NONE',  ( 5.823673210054444382, -21.52544592524334988, 90.20942372801903275 ) ) ;
#173592 = CARTESIAN_POINT ( 'NONE',  ( -15.72974639402176322, -15.80617190586768395, 34.37609039468568284 ) ) ;
#173591 = CARTESIAN_POINT ( 'NONE',  ( 0.05219959533909260263, 19.03943276465977164, 64.99890960531436690 ) ) ;
#173593 = CARTESIAN_POINT ( 'NONE',  ( 15.80617190586769283, -15.72974639402175789, 20.62609039468568639 ) ) ;
#173594 = CARTESIAN_POINT ( 'NONE',  ( -22.44159573604009950, -16.30477369853688430, 139.5750000027311728 ) ) ;
#173595 = CARTESIAN_POINT ( 'NONE',  ( -16.51473224551069308, -9.474510206698971260, 81.66557627198103830 ) ) ;
#173596 = DIRECTION ( 'NONE',  ( -1.000000000000000000, -4.336808689942018352E-17, 3.574525976782710619E-31 ) ) ;
#173598 = CARTESIAN_POINT ( 'NONE',  ( 21.53943276465977519, -0.05219959533907433946, 48.74890960531435979 ) ) ;
#173597 = CARTESIAN_POINT ( 'NONE',  ( 16.53943276465976808, 0.05219959533934440121, 26.25109039468567573 ) ) ;
#173599 = CARTESIAN_POINT ( 'NONE',  ( -10.72451020669870658, -18.67979575497194134, 74.58442372801901854 ) ) ;
#173600 = CARTESIAN_POINT ( 'NONE',  ( -9.474510206698964154, 16.51473224551069663, 115.4155762719810241 ) ) ;
#173601 = CARTESIAN_POINT ( 'NONE',  ( 5.049401038297881783, 19.05341960407617563, 102.2927570613523045 ) ) ;
#173602 = CARTESIAN_POINT ( 'NONE',  ( 16.46253265017160672, -9.564922557960803928, 58.33224293864769550 ) ) ;
#173603 = CARTESIAN_POINT ( 'NONE',  ( 19.03943276465977164, -0.05219959533909143690, 83.74890960531436690 ) ) ;
#173604 = CARTESIAN_POINT ( 'NONE',  ( -8.224510206698948167, 14.34966873604960824, 90.41557627198103830 ) ) ;
#173605 = CARTESIAN_POINT ( 'NONE',  ( -12.06949235617756955, 12.14591786802309770, 100.6239096053143811 ) ) ;
#173606 = CARTESIAN_POINT ( 'NONE',  ( 0.05219959533909260263, 19.03943276465977164, 104.9989096053143669 ) ) ;
#173607 = CARTESIAN_POINT ( 'NONE',  ( 8.314922557961029526, -14.29746914071037800, 75.41775706135233293 ) ) ;
#173609 = CARTESIAN_POINT ( 'NONE',  ( 9.564922557960805705, 16.46253265017160317, 39.58224293864768839 ) ) ;
#173608 = CARTESIAN_POINT ( 'NONE',  ( 16.55341960407611168, 4.379528057220329451, 53.95724293864770260 ) ) ;
#173610 = CARTESIAN_POINT ( 'NONE',  ( 21.55341960407619695, -5.719274019375665929, 66.04275706135236135 ) ) ;
#173611 = CARTESIAN_POINT ( 'NONE',  ( -13.89961937509957401, -13.97604488694547875, 94.37609039468566152 ) ) ;
#173612 = CARTESIAN_POINT ( 'NONE',  ( 12.14591786802309770, 12.06949235617756955, 59.37390960531436690 ) ) ;
#173613 = CARTESIAN_POINT ( 'NONE',  ( 21.52544592524344225, -5.823673210054117533, 113.5405762719810383 ) ) ;
#173614 = CARTESIAN_POINT ( 'NONE',  ( 21.53943276465977519, -0.05219959533907433946, 43.74890960531435979 ) ) ;
#173615 = DIRECTION ( 'NONE',  ( -0.000000000000000000, -0.000000000000000000, 1.000000000000000000 ) ) ;
#173616 = CARTESIAN_POINT ( 'NONE',  ( -28.82186960331499392, 9.364793116373565596, 140.1500000054623740 ) ) ;
#173617 = CARTESIAN_POINT ( 'NONE',  ( 19.03943276465977164, -0.05219959533909143690, 68.74890960531436690 ) ) ;
#173618 = CARTESIAN_POINT ( 'NONE',  ( 4.483927247898545687, 16.52544592524342804, 34.79057627198103120 ) ) ;
#173619 = VECTOR ( 'NONE', #144993, 1000.000000000000000 ) ;
#173620 = CARTESIAN_POINT ( 'NONE',  ( 12.14591786802327356, -12.06949235617739191, 110.6260903946857042 ) ) ;
#173621 = CARTESIAN_POINT ( 'NONE',  ( -4.379528057220086978, -16.55341960407618274, 84.79275706135234714 ) ) ;
#173622 = CARTESIAN_POINT ( 'NONE',  ( -16.46253265017146816, -9.564922557961047289, 34.16775706135233293 ) ) ;
#173623 = CARTESIAN_POINT ( 'NONE',  ( -30.74264578624800492, 22.33583958711400186, -8.200000000000001066 ) ) ;
#173624 = CARTESIAN_POINT ( 'NONE',  ( -16.51473224551069308, -9.474510206698971260, 91.66557627198103830 ) ) ;
#173625 = CARTESIAN_POINT ( 'NONE',  ( 9.564922557960805705, 16.46253265017160317, 44.58224293864769550 ) ) ;
#173626 = CARTESIAN_POINT ( 'NONE',  ( -16.52544592524342804, 4.483927247898546575, 66.04057627198103830 ) ) ;
#173628 = CARTESIAN_POINT ( 'NONE',  ( -0.05219959533907301413, -21.53943276465977519, 27.49890960531435269 ) ) ;
#173627 = CARTESIAN_POINT ( 'NONE',  ( 17.60728821187776916, -5.500000000000037303, 48.36690927743607915 ) ) ;
#173629 = CARTESIAN_POINT ( 'NONE',  ( -10.81492255796078084, -18.62759615963271287, 57.08224293864769550 ) ) ;
#173630 = CARTESIAN_POINT ( 'NONE',  ( 4.483927247898545687, 16.52544592524342804, 89.79057627198103830 ) ) ;
#173631 = CARTESIAN_POINT ( 'NONE',  ( -4.483927247898782831, 16.52544592524335698, 42.70942372801901854 ) ) ;
#173632 = EDGE_LOOP ( 'NONE', ( #94804, #143761, #156538, #67922, #126148 ) ) ;
#173633 = CARTESIAN_POINT ( 'NONE',  ( 12.14591786802309770, 12.06949235617756955, 74.37390960531436690 ) ) ;
#173634 = ADVANCED_FACE ( 'NONE', ( #2552 ), #168427, .F. ) ;
#173635 = DIRECTION ( 'NONE',  ( 0.000000000000000000, 0.000000000000000000, 1.000000000000000000 ) ) ;
#173636 = CARTESIAN_POINT ( 'NONE',  ( -5.153800228976607833, 19.02544592524334988, 77.70942372801900433 ) ) ;
#173637 = CARTESIAN_POINT ( 'NONE',  ( -10.81492255796078084, -18.62759615963271287, 22.08224293864769194 ) ) ;
#173638 = CARTESIAN_POINT ( 'NONE',  ( 36.91746825000000598, -11.99521256947793546, -4.224999997268812812 ) ) ;
#173639 = CARTESIAN_POINT ( 'NONE',  ( 17.50000000000000000, -5.500000000000000888, 28.29690382534172244 ) ) ;
#173641 = CARTESIAN_POINT ( 'NONE',  ( -12.14591786802326823, 12.06949235617739902, 113.1260903946856899 ) ) ;
#173640 = CARTESIAN_POINT ( 'NONE',  ( 14.29746914071037800, 8.314922557961029526, 26.66775706135235424 ) ) ;
#173642 = CARTESIAN_POINT ( 'NONE',  ( 16.51473224551083163, -9.474510206698727899, 65.83442372801900433 ) ) ;
#173643 = CARTESIAN_POINT ( 'NONE',  ( -0.05219959533907301413, -21.53943276465977519, 52.49890960531435979 ) ) ;
#173644 = CARTESIAN_POINT ( 'NONE',  ( 5.823673210054444382, -21.52544592524334988, 65.20942372801901854 ) ) ;
#173645 = FACE_OUTER_BOUND ( 'NONE', #161959, .T. ) ;
#173646 = CARTESIAN_POINT ( 'NONE',  ( 12.14591786802327356, -12.06949235617739191, 35.62609039468568994 ) ) ;
#173648 = CARTESIAN_POINT ( 'NONE',  ( 5.049401038298161559, -19.05341960407611168, 82.70724293864770971 ) ) ;
#173647 = CARTESIAN_POINT ( 'NONE',  ( 13.89961937509977652, -13.97604488694527269, 23.12390960531436335 ) ) ;
#173649 = AXIS2_PLACEMENT_3D ( 'NONE', #94749, #156430, #17930 ) ;
#173650 = CARTESIAN_POINT ( 'NONE',  ( 13.89961937509977652, -13.97604488694527269, 28.12390960531435624 ) ) ;
#173652 = ADVANCED_FACE ( 'NONE', ( #183611 ), #147647, .T. ) ;
#173651 = CARTESIAN_POINT ( 'NONE',  ( 8.224510206698953496, -14.34966873604960469, 107.9155762719810241 ) ) ;
#173653 = CONTEXT_DEPENDENT_SHAPE_REPRESENTATION ( #141014, #93731 ) ;
#173654 = CARTESIAN_POINT ( 'NONE',  ( -19.02544592524342804, 5.153800228976336051, 106.0405762719810241 ) ) ;
#173655 = VERTEX_POINT ( 'NONE', #48078 ) ;
#173656 = CARTESIAN_POINT ( 'NONE',  ( -16.52544592524335698, -4.483927247898792601, 53.95942372801900433 ) ) ;
#173657 = CARTESIAN_POINT ( 'NONE',  ( 5.049401038297881783, 19.05341960407617563, 107.2927570613523187 ) ) ;
#173658 = CARTESIAN_POINT ( 'NONE',  ( -0.05219959533907301413, -21.53943276465977519, 72.49890960531435269 ) ) ;
#173659 = CARTESIAN_POINT ( 'NONE',  ( 19.02544592524343514, -5.153800228976328945, 43.54057627198103120 ) ) ;
#173661 = CARTESIAN_POINT ( 'NONE',  ( 21.52544592524344225, -5.823673210054117533, 113.5405762719810383 ) ) ;
#173660 = CARTESIAN_POINT ( 'NONE',  ( 5.153800228976615827, -19.02544592524334988, 70.20942372801899012 ) ) ;
#173662 = CARTESIAN_POINT ( 'NONE',  ( 5.153800228976335163, 19.02544592524342804, 74.79057627198103830 ) ) ;
#173663 = CARTESIAN_POINT ( 'NONE',  ( 0.05219959533909260263, 19.03943276465977164, 99.99890960531436690 ) ) ;
#173664 = ORIENTED_EDGE ( 'NONE', *, *, #24864, .T. ) ;
#173665 = CARTESIAN_POINT ( 'NONE',  ( -14.34966873604972548, 8.224510206698743886, 33.33442372801900433 ) ) ;
#173666 = CARTESIAN_POINT ( 'NONE',  ( 18.67979575497178502, 10.72451020669898547, 109.1655762719810383 ) ) ;
#173669 = CARTESIAN_POINT ( 'NONE',  ( 0.05219959533936267826, -19.03943276465977164, 80.00109039468567573 ) ) ;
#173668 = CARTESIAN_POINT ( 'NONE',  ( -16.51473224551069308, -9.474510206698971260, 96.66557627198102409 ) ) ;
#173667 = CARTESIAN_POINT ( 'NONE',  ( 4.379528057220339221, -16.55341960407611168, 107.7072429386476955 ) ) ;
#173670 = CARTESIAN_POINT ( 'NONE',  ( -10.72451020669898014, 18.67979575497178502, 80.41557627198103830 ) ) ;
#173671 = CARTESIAN_POINT ( 'NONE',  ( -16.53943276465976808, 0.05219959533911058130, 51.24890960531436690 ) ) ;
#173672 = CARTESIAN_POINT ( 'NONE',  ( 16.51473224551083163, -9.474510206698727899, 25.83442372801900078 ) ) ;
#173673 = CARTESIAN_POINT ( 'NONE',  ( 16.53943276465976808, 0.05219959533934440121, 71.25109039468568994 ) ) ;
#173674 = CARTESIAN_POINT ( 'NONE',  ( 9.474510206698971260, -16.51473224551069308, 87.91557627198102409 ) ) ;
#173675 = CARTESIAN_POINT ( 'NONE',  ( -16.51473224551069308, -9.474510206698971260, 51.66557627198102409 ) ) ;
#173676 = CARTESIAN_POINT ( 'NONE',  ( 21.53943276465977519, 0.05219959533937863772, 56.25109039468568284 ) ) ;
#173677 = CARTESIAN_POINT ( 'NONE',  ( 21.55341960407619695, -5.719274019375665929, 66.04275706135236135 ) ) ;
#173678 = CARTESIAN_POINT ( 'NONE',  ( 19.02544592524343514, -5.153800228976328945, 58.54057627198102409 ) ) ;
#173679 = CARTESIAN_POINT ( 'NONE',  ( 0.05219959533937995610, -21.53943276465977519, 40.00109039468567573 ) ) ;
#173680 = CARTESIAN_POINT ( 'NONE',  ( -9.474510206698720793, -16.51473224551083518, 69.58442372801901854 ) ) ;
#173681 = CARTESIAN_POINT ( 'NONE',  ( 16.51473224551069308, 9.474510206698969483, 39.16557627198103120 ) ) ;
#173682 = CARTESIAN_POINT ( 'NONE',  ( -16.55341960407617563, 4.379528057220093196, 83.54275706135234714 ) ) ;
#173683 = CARTESIAN_POINT ( 'NONE',  ( -19.03943276465977164, 0.05219959533909376836, 71.24890960531435269 ) ) ;
#173684 = CARTESIAN_POINT ( 'NONE',  ( -5.049401038298153566, 19.05341960407611168, 115.2072429386477097 ) ) ;
#173686 = ADVANCED_FACE ( 'NONE', ( #28946 ), #79396, .T. ) ;
#173685 = CARTESIAN_POINT ( 'NONE',  ( -16.46253265017160317, 9.564922557960807481, 35.83224293864768839 ) ) ;
#173687 = CARTESIAN_POINT ( 'NONE',  ( -10.72451020669898014, 18.67979575497178502, 85.41557627198102409 ) ) ;
#173688 = CARTESIAN_POINT ( 'NONE',  ( -16.52544592524335698, -4.483927247898792601, 68.95942372801901854 ) ) ;
#173689 = CARTESIAN_POINT ( 'NONE',  ( -21.35462415990441087, 9.648971641164905577, 168.5494316893069140 ) ) ;
#173690 = CARTESIAN_POINT ( 'NONE',  ( -13.97604488694547697, 13.89961937509957934, 28.12609039468565797 ) ) ;
#173691 = CARTESIAN_POINT ( 'NONE',  ( 13.89961937509977652, -13.97604488694527269, 63.12390960531435979 ) ) ;
#173692 = CARTESIAN_POINT ( 'NONE',  ( 16.52544592524342804, -4.483927247898539470, 38.54057627198103120 ) ) ;
#173693 = CARTESIAN_POINT ( 'NONE',  ( -16.52544592524342804, 4.483927247898546575, 81.04057627198102409 ) ) ;
#173694 = CARTESIAN_POINT ( 'NONE',  ( 9.474510206698971260, -16.51473224551069308, 107.9155762719810383 ) ) ;
#173695 = CARTESIAN_POINT ( 'NONE',  ( 19.05341960407611168, 5.049401038298154454, 93.95724293864769550 ) ) ;
#173696 = CARTESIAN_POINT ( 'NONE',  ( -15.80617190586768217, 15.72974639402176855, 53.12609039468568284 ) ) ;
#173697 = CARTESIAN_POINT ( 'NONE',  ( -0.05219959533909027116, -19.03943276465977164, 107.4989096053143527 ) ) ;
#173698 = CARTESIAN_POINT ( 'NONE',  ( -18.67979575497193778, 10.72451020669871902, 98.33442372801901854 ) ) ;
#173699 = CARTESIAN_POINT ( 'NONE',  ( -14.34966873604972548, 8.224510206698743886, 73.33442372801901854 ) ) ;
#173700 = CARTESIAN_POINT ( 'NONE',  ( 21.52544592524334988, 5.823673210054432836, 26.45942372801901854 ) ) ;
#173701 = CARTESIAN_POINT ( 'NONE',  ( -0.05219959533909027116, -19.03943276465977164, 107.4989096053143527 ) ) ;
#173702 = CARTESIAN_POINT ( 'NONE',  ( 10.81492255796078972, 18.62759615963270932, 99.58224293864770971 ) ) ;
#173703 = CARTESIAN_POINT ( 'NONE',  ( 16.52544592524342804, -4.483927247898539470, 63.54057627198103830 ) ) ;
#173704 = CARTESIAN_POINT ( 'NONE',  ( -16.51473224551069308, -9.474510206698971260, 46.66557627198102409 ) ) ;
#173705 = CARTESIAN_POINT ( 'NONE',  ( -4.379528057220328563, 16.55341960407611168, 75.20724293864769550 ) ) ;
#173706 = CARTESIAN_POINT ( 'NONE',  ( -18.67979575497178146, -10.72451020669898902, 31.66557627198102054 ) ) ;
#173707 = CARTESIAN_POINT ( 'NONE',  ( 13.97604488694548053, -13.89961937509957401, 25.62609039468566507 ) ) ;
#173708 = CARTESIAN_POINT ( 'NONE',  ( 14.34966873604960469, 8.224510206698951720, 109.1655762719810383 ) ) ;
#173709 = ORIENTED_EDGE ( 'NONE', *, *, #182333, .T. ) ;
#173710 = CARTESIAN_POINT ( 'NONE',  ( 16.52544592524335698, 4.483927247898782831, 66.45942372801903275 ) ) ;
#173711 = CARTESIAN_POINT ( 'NONE',  ( 19.05341960407611168, 5.049401038298154454, 73.95724293864768129 ) ) ;
#173712 = DIRECTION ( 'NONE',  ( 0.000000000000000000, -1.000000000000000000, 0.000000000000000000 ) ) ;
#173713 = CARTESIAN_POINT ( 'NONE',  ( 12.06949235617757843, -12.14591786802309237, 88.12390960531436690 ) ) ;
#173714 = CARTESIAN_POINT ( 'NONE',  ( -18.62759615963270932, 10.81492255796079327, 35.83224293864768839 ) ) ;
#173715 = ORIENTED_EDGE ( 'NONE', *, *, #40462, .F. ) ;
#173716 = CARTESIAN_POINT ( 'NONE',  ( 12.06949235617739724, 12.14591786802326823, 111.8760903946856615 ) ) ;
#173717 = CARTESIAN_POINT ( 'NONE',  ( -19.02544592524334988, -5.153800228976617603, 108.9594237280189759 ) ) ;
#173718 = CARTESIAN_POINT ( 'NONE',  ( -18.67979575497193778, 10.72451020669871902, 83.33442372801903275 ) ) ;
#173719 = CARTESIAN_POINT ( 'NONE',  ( -0.05219959533909027116, -19.03943276465977164, 82.49890960531436690 ) ) ;
#173720 = CARTESIAN_POINT ( 'NONE',  ( -21.53943276465977519, 0.05219959533907696930, 106.2489096053143811 ) ) ;
#173721 = CARTESIAN_POINT ( 'NONE',  ( -8.224510206698735004, -14.34966873604973081, 54.58442372801901143 ) ) ;
#173722 = CARTESIAN_POINT ( 'NONE',  ( 5.049401038298161559, -19.05341960407611168, 27.70724293864769550 ) ) ;
#173723 = CARTESIAN_POINT ( 'NONE',  ( 16.55341960407618274, -4.379528057220086978, 26.04275706135235779 ) ) ;
#173724 = CARTESIAN_POINT ( 'NONE',  ( 9.474510206698729675, 16.51473224551082808, 92.08442372801900433 ) ) ;
#173725 = CARTESIAN_POINT ( 'NONE',  ( -10.81492255796078084, -18.62759615963271287, 92.08224293864769550 ) ) ;
#173726 = CARTESIAN_POINT ( 'NONE',  ( 9.474510206698729675, 16.51473224551082808, 52.08442372801900433 ) ) ;
#173727 = CARTESIAN_POINT ( 'NONE',  ( 18.56453257813364388, -5.500000000000048850, 88.49000423690685579 ) ) ;
#173728 = CARTESIAN_POINT ( 'NONE',  ( -0.05219959533907301413, -21.53943276465977519, 107.4989096053143669 ) ) ;
#173729 = CARTESIAN_POINT ( 'NONE',  ( 17.50000000000000000, 5.499999999999997335, 26.70309617465829888 ) ) ;
#173730 = CARTESIAN_POINT ( 'NONE',  ( -13.97604488694527625, -13.89961937509977652, 81.87390960531436690 ) ) ;
#173731 = CARTESIAN_POINT ( 'NONE',  ( 5.000000000000000000, -140.0000000000000000, 12.99999999999998224 ) ) ;
#173732 = CARTESIAN_POINT ( 'NONE',  ( 16.55341960407618274, -4.379528057220086978, 36.04275706135234714 ) ) ;
#173733 = CARTESIAN_POINT ( 'NONE',  ( 36.77423900702710569, -4.677204790287845526, 47.89930394225363841 ) ) ;
#173735 = CARTESIAN_POINT ( 'NONE',  ( -8.224510206698948167, 14.34966873604960824, 65.41557627198102409 ) ) ;
#173734 = CARTESIAN_POINT ( 'NONE',  ( 15.72974639402199770, -15.80617190586745480, 113.1239096053143953 ) ) ;
#173736 = CARTESIAN_POINT ( 'NONE',  ( -5.153800228976328057, -19.02544592524343514, 72.29057627198102409 ) ) ;
#173738 = CARTESIAN_POINT ( 'NONE',  ( -5.153800228976607833, 19.02544592524334988, 47.70942372801900433 ) ) ;
#173737 = CARTESIAN_POINT ( 'NONE',  ( 14.34966873604972726, -8.224510206698740333, 35.83442372801901143 ) ) ;
#173739 = CARTESIAN_POINT ( 'NONE',  ( -15.72974639402176322, -15.80617190586768395, 54.37609039468568994 ) ) ;
#173740 = CARTESIAN_POINT ( 'NONE',  ( -0.05219959533936034679, 19.03943276465977164, 107.5010903946856615 ) ) ;
#173741 = CARTESIAN_POINT ( 'NONE',  ( -16.46253265017160317, 9.564922557960807481, 55.83224293864769550 ) ) ;
#173742 = CARTESIAN_POINT ( 'NONE',  ( 13.97604488694548053, -13.89961937509957401, 80.62609039468567573 ) ) ;
#173743 = CARTESIAN_POINT ( 'NONE',  ( -15.72974639402176322, -15.80617190586768395, 84.37609039468570415 ) ) ;
#173744 = CARTESIAN_POINT ( 'NONE',  ( 16.51473224551083163, -9.474510206698727899, 60.83442372801900433 ) ) ;
#173745 = CARTESIAN_POINT ( 'NONE',  ( -16.51473224551069308, -9.474510206698971260, 36.66557627198102409 ) ) ;
#173746 = CARTESIAN_POINT ( 'NONE',  ( -10.81492255796078084, -18.62759615963271287, 57.08224293864769550 ) ) ;
#173748 = CARTESIAN_POINT ( 'NONE',  ( -5.153800228976607833, 19.02544592524334988, 67.70942372801900433 ) ) ;
#173747 = CARTESIAN_POINT ( 'NONE',  ( 16.55341960407611168, 4.379528057220329451, 63.95724293864770260 ) ) ;
#173749 = CARTESIAN_POINT ( 'NONE',  ( 20.51359854606069177, 11.49117151696134442, 170.0775129446642495 ) ) ;
#173750 = CARTESIAN_POINT ( 'NONE',  ( 16.51473224551083163, -9.474510206698727899, 35.83442372801899722 ) ) ;
#173751 = CARTESIAN_POINT ( 'NONE',  ( 8.224510206698742110, 14.34966873604972548, 97.08442372801904696 ) ) ;
#173752 = CARTESIAN_POINT ( 'NONE',  ( 4.379528057220339221, -16.55341960407611168, 52.70724293864769550 ) ) ;
#173754 = CARTESIAN_POINT ( 'NONE',  ( 17.14385361876520264, 23.59649016807275856, 140.1750000027311955 ) ) ;
#173753 = CARTESIAN_POINT ( 'NONE',  ( -18.62759615963255300, -10.81492255796106328, 89.16775706135236135 ) ) ;
#173755 = CARTESIAN_POINT ( 'NONE',  ( -21.52544592524334988, -5.823673210054445271, 88.95942372801901854 ) ) ;
#173756 = CARTESIAN_POINT ( 'NONE',  ( 15.80617190586746368, 15.72974639402197994, 89.37390960531435269 ) ) ;
#173757 = CARTESIAN_POINT ( 'NONE',  ( 19.02544592524343514, -5.153800228976328945, 48.54057627198103120 ) ) ;
#173758 = CARTESIAN_POINT ( 'NONE',  ( 15.72974639402176855, 15.80617190586768217, 71.87609039468568994 ) ) ;
#173759 = CARTESIAN_POINT ( 'NONE',  ( -13.97604488694527625, -13.89961937509977652, 46.87390960531435979 ) ) ;
#173760 = EDGE_LOOP ( 'NONE', ( #142010, #6478, #147274, #96593, #105926 ) ) ;
#173761 = CARTESIAN_POINT ( 'NONE',  ( -0.05219959533909027116, -19.03943276465977164, 67.49890960531436690 ) ) ;
#173762 = CARTESIAN_POINT ( 'NONE',  ( -12.14591786802309592, -12.06949235617757132, 101.8739096053143811 ) ) ;
#173763 = CARTESIAN_POINT ( 'NONE',  ( 5.049401038298161559, -19.05341960407611168, 107.7072429386476955 ) ) ;
#173764 = CARTESIAN_POINT ( 'NONE',  ( 14.34966873604960469, 8.224510206698951720, 54.16557627198103120 ) ) ;
#173765 = CARTESIAN_POINT ( 'NONE',  ( -16.46253265017160317, 9.564922557960807481, 30.83224293864769550 ) ) ;
#173766 = CARTESIAN_POINT ( 'NONE',  ( 12.06949235617757843, -12.14591786802309237, 78.12390960531436690 ) ) ;
#173767 = TOROIDAL_SURFACE ( 'NONE', #70422, 23.10356920737165254, 3.000000000000000000 ) ;
#173768 = CARTESIAN_POINT ( 'NONE',  ( 10.72451020669898902, -18.67979575497178502, 92.91557627198103830 ) ) ;
#173769 = CARTESIAN_POINT ( 'NONE',  ( 5.823673210054444382, -21.52544592524334988, 40.20942372801901854 ) ) ;
#173770 = CARTESIAN_POINT ( 'NONE',  ( 30.00000000000000000, 5.499999999999992895, 102.5000000000000142 ) ) ;
#173771 = CARTESIAN_POINT ( 'NONE',  ( -4.483927247898782831, 16.52544592524335698, 32.70942372801900433 ) ) ;
#173772 = CARTESIAN_POINT ( 'NONE',  ( -5.719274019375978568, 21.55341960407610458, 85.20724293864770971 ) ) ;
#173773 = CARTESIAN_POINT ( 'NONE',  ( -21.53943276465977519, -0.05219959533937600094, 103.7510903946857042 ) ) ;
#173774 = CARTESIAN_POINT ( 'NONE',  ( -5.153800228976328057, -19.02544592524343514, 92.29057627198099567 ) ) ;
#173775 = CARTESIAN_POINT ( 'NONE',  ( -18.62759615963255300, -10.81492255796106328, 44.16775706135234714 ) ) ;
#173776 = CARTESIAN_POINT ( 'NONE',  ( -10.72451020669898014, 18.67979575497178502, 35.41557627198102409 ) ) ;
#173777 = CARTESIAN_POINT ( 'NONE',  ( 12.06949235617739724, 12.14591786802326823, 106.8760903946856899 ) ) ;
#173779 = CARTESIAN_POINT ( 'NONE',  ( -15.72974639402176322, -15.80617190586768395, 84.37609039468570415 ) ) ;
#173778 = CARTESIAN_POINT ( 'NONE',  ( 21.55341960407619695, -5.719274019375665929, 46.04275706135234714 ) ) ;
#173780 = CARTESIAN_POINT ( 'NONE',  ( -21.52544592524334988, -5.823673210054445271, 108.9594237280190185 ) ) ;
#173781 = CARTESIAN_POINT ( 'NONE',  ( -14.34966873604972548, 8.224510206698743886, 88.33442372801901854 ) ) ;
#173782 = CARTESIAN_POINT ( 'NONE',  ( 18.67979575497194134, -10.72451020669871369, 45.83442372801901854 ) ) ;
#173783 = CARTESIAN_POINT ( 'NONE',  ( -19.03943276465977164, 0.05219959533909376836, 36.24890960531436690 ) ) ;
#173784 = CARTESIAN_POINT ( 'NONE',  ( -21.52544592524334988, -5.823673210054445271, 98.95942372801903275 ) ) ;
#173785 = CARTESIAN_POINT ( 'NONE',  ( 9.474510206698971260, -16.51473224551069308, 112.9155762719810383 ) ) ;
#173786 = CARTESIAN_POINT ( 'NONE',  ( 21.52544592524344225, -5.823673210054117533, 108.5405762719810241 ) ) ;
#173788 = CARTESIAN_POINT ( 'NONE',  ( -15.72974639402197994, 15.80617190586746368, 70.62390960531436690 ) ) ;
#173787 = CARTESIAN_POINT ( 'NONE',  ( -193.3062444957834884, -155.7167183371838064, -15.00000000000000178 ) ) ;
#173790 = CARTESIAN_POINT ( 'NONE',  ( -12.06949235617756955, 12.14591786802309770, 65.62390960531436690 ) ) ;
#173789 = CARTESIAN_POINT ( 'NONE',  ( -8.314922557961024197, 14.29746914071037800, 52.91775706135235424 ) ) ;
#173791 = CARTESIAN_POINT ( 'NONE',  ( 19.53392245597579802, -5.499999999999960032, 102.1255887859039291 ) ) ;
#173792 = CARTESIAN_POINT ( 'NONE',  ( 5.049401038297881783, 19.05341960407617563, 92.29275706135234714 ) ) ;
#173793 = AXIS2_PLACEMENT_3D ( 'NONE', #179123, #113411, #144752 ) ;
#173794 = CARTESIAN_POINT ( 'NONE',  ( -9.248023074035629065, -10.55781631604391890, -60.31354024882315912 ) ) ;
#173795 = CARTESIAN_POINT ( 'NONE',  ( -4.483927247898782831, 16.52544592524335698, 32.70942372801900433 ) ) ;
#173796 = CARTESIAN_POINT ( 'NONE',  ( -10.81492255796078084, -18.62759615963271287, 102.0822429386476955 ) ) ;
#173797 = CARTESIAN_POINT ( 'NONE',  ( -5.823673210054116645, -21.52544592524344225, 77.29057627198102409 ) ) ;
#173798 = CARTESIAN_POINT ( 'NONE',  ( 5.719274019375991003, -21.55341960407610458, 22.70724293864769194 ) ) ;
#173799 = CARTESIAN_POINT ( 'NONE',  ( -0.05219959533934338120, 16.53943276465976808, 52.50109039468567573 ) ) ;
#173800 = CARTESIAN_POINT ( 'NONE',  ( 0.05219959533909260263, 19.03943276465977164, 74.99890960531435269 ) ) ;
#173802 = CARTESIAN_POINT ( 'NONE',  ( -13.89961937509957401, -13.97604488694547875, 99.37609039468567573 ) ) ;
#173801 = CARTESIAN_POINT ( 'NONE',  ( 21.53943276465977519, 0.05219959533937863772, 36.25109039468567573 ) ) ;
#173803 = EDGE_CURVE ( 'NONE', #11421, #167693, #150098, .T. ) ;
#173804 = CARTESIAN_POINT ( 'NONE',  ( 13.97604488694527802, 13.89961937509977652, 109.3739096053143669 ) ) ;
#173805 = CARTESIAN_POINT ( 'NONE',  ( 16.51473224551069308, 9.474510206698969483, 89.16557627198103830 ) ) ;
#173806 = CARTESIAN_POINT ( 'NONE',  ( 21.53943276465977519, -0.05219959533907433946, 83.74890960531435269 ) ) ;
#173807 = CARTESIAN_POINT ( 'NONE',  ( -16.46253265017160317, 9.564922557960807481, 55.83224293864769550 ) ) ;
#173808 = CARTESIAN_POINT ( 'NONE',  ( -17.49999999999999645, 5.499999999999992895, 78.71769037696437010 ) ) ;
#173809 = CARTESIAN_POINT ( 'NONE',  ( 12.06949235617757843, -12.14591786802309237, 63.12390960531435979 ) ) ;
#173810 = CARTESIAN_POINT ( 'NONE',  ( -15.80617190586745835, -15.72974639402198527, 26.87390960531435979 ) ) ;
#173811 = CARTESIAN_POINT ( 'NONE',  ( 15.06137443927351072, -15.06137443927345210, -56.46919128290398504 ) ) ;
#173812 = CARTESIAN_POINT ( 'NONE',  ( 21.53943276465977519, -0.05219959533907433946, 103.7489096053143669 ) ) ;
#173813 = CARTESIAN_POINT ( 'NONE',  ( -13.89961937509957401, -13.97604488694547875, 64.37609039468567573 ) ) ;
#173814 = CARTESIAN_POINT ( 'NONE',  ( -13.89961937509977652, 13.97604488694528158, 110.6239096053143243 ) ) ;
#173815 = SURFACE_SIDE_STYLE ('',( #24113 ) ) ;
#173816 = CARTESIAN_POINT ( 'NONE',  ( -18.62759615963270932, 10.81492255796079327, 55.83224293864770260 ) ) ;
#173817 = CARTESIAN_POINT ( 'NONE',  ( -16.51473224551069308, -9.474510206698971260, 86.66557627198102409 ) ) ;
#173818 = CARTESIAN_POINT ( 'NONE',  ( 15.72974639402176855, 15.80617190586768217, 76.87609039468567573 ) ) ;
#173819 = CARTESIAN_POINT ( 'NONE',  ( -19.05341960407611168, -5.049401038298163336, 51.45724293864770260 ) ) ;
#173820 = CARTESIAN_POINT ( 'NONE',  ( -16.55341960407611168, -4.379528057220339221, 86.45724293864770971 ) ) ;
#173822 = B_SPLINE_CURVE_WITH_KNOTS ( 'NONE', 3,
 ( #4656, #186741, #35017, #34031, #97650, #94695 ),
 .UNSPECIFIED., .F., .F.,
 ( 4, 2, 4 ),
 ( 0.000000000000000000, 0.0003837532665635174311, 0.0007675065331270348621 ),
 .UNSPECIFIED. ) ;
#173821 = CARTESIAN_POINT ( 'NONE',  ( -12.06949235617739369, -12.14591786802326823, 34.37609039468568284 ) ) ;
#173823 = CARTESIAN_POINT ( 'NONE',  ( -10.81492255796105439, 18.62759615963255655, 67.91775706135234714 ) ) ;
#173824 = ORIENTED_EDGE ( 'NONE', *, *, #94772, .T. ) ;
#173825 = CARTESIAN_POINT ( 'NONE',  ( 16.46253265017146816, 9.564922557961045513, 21.66775706135233648 ) ) ;
#173826 = CARTESIAN_POINT ( 'NONE',  ( -5.049401038297874678, -19.05341960407617918, 84.79275706135233293 ) ) ;
#173827 = CARTESIAN_POINT ( 'NONE',  ( 31.65755289763031044, -24.31906878930446680, -22.32084141216706286 ) ) ;
#173828 = CARTESIAN_POINT ( 'NONE',  ( 15.80617190586769283, -15.72974639402175789, 40.62609039468567573 ) ) ;
#173829 = CARTESIAN_POINT ( 'NONE',  ( 27.05641397906351386, -3.631740835637518927, 169.9999999999999716 ) ) ;
#173830 = CARTESIAN_POINT ( 'NONE',  ( -13.97604488694547697, 13.89961937509957934, 38.12609039468566152 ) ) ;
#173831 = CARTESIAN_POINT ( 'NONE',  ( -9.474510206698964154, 16.51473224551069663, 60.41557627198102409 ) ) ;
#173832 = CARTESIAN_POINT ( 'NONE',  ( 16.46253265017146816, 9.564922557961045513, 26.66775706135234003 ) ) ;
#173833 = CARTESIAN_POINT ( 'NONE',  ( -12.06949235617739369, -12.14591786802326823, 99.37609039468568994 ) ) ;
#173835 = CARTESIAN_POINT ( 'NONE',  ( -21.53943276465977519, -0.05219959533937600094, 88.75109039468567573 ) ) ;
#173834 = CARTESIAN_POINT ( 'NONE',  ( -19.02544592524342804, 5.153800228976336051, 101.0405762719810241 ) ) ;
#173836 = CARTESIAN_POINT ( 'NONE',  ( 36.91746824999999177, 2.880721459617395097E-14, -7.624999997268813168 ) ) ;
#173837 = CARTESIAN_POINT ( 'NONE',  ( -17.49999999999999289, -4.013004640162506576, 34.55394279005599145 ) ) ;
#173838 = CARTESIAN_POINT ( 'NONE',  ( 0.05219959533937995610, -21.53943276465977519, 85.00109039468568994 ) ) ;
#173839 = CARTESIAN_POINT ( 'NONE',  ( 16.88567814943166923, -6.947325034625572826, 41.20998877347414435 ) ) ;
#173840 = CARTESIAN_POINT ( 'NONE',  ( 0.05219959533909260263, 19.03943276465977164, 94.99890960531436690 ) ) ;
#173841 = VERTEX_POINT ( 'NONE', #124908 ) ;
#173842 = CARTESIAN_POINT ( 'NONE',  ( 30.07467525274878994, -23.10311534983925696, -22.45479934155872215 ) ) ;
#173843 = CARTESIAN_POINT ( 'NONE',  ( -19.05341960407611168, -5.049401038298163336, 51.45724293864770260 ) ) ;
#173844 = CARTESIAN_POINT ( 'NONE',  ( -21.55341960407610458, -5.719274019375992779, 56.45724293864768839 ) ) ;
#173845 = CARTESIAN_POINT ( 'NONE',  ( 12.14591786802309770, 12.06949235617756955, 29.37390960531435269 ) ) ;
#173847 = CARTESIAN_POINT ( 'NONE',  ( -19.05341960407611168, -5.049401038298163336, 76.45724293864769550 ) ) ;
#173846 = CARTESIAN_POINT ( 'NONE',  ( 14.29746914071049879, -8.314922557960816363, 93.33224293864769550 ) ) ;
#173848 = CARTESIAN_POINT ( 'NONE',  ( 9.564922557961047289, -16.46253265017146816, 20.41775706135233293 ) ) ;
#173849 = CARTESIAN_POINT ( 'NONE',  ( 5.049401038298161559, -19.05341960407611168, 32.70724293864768129 ) ) ;
#173850 = CARTESIAN_POINT ( 'NONE',  ( 8.224510206698953496, -14.34966873604960469, 97.91557627198103830 ) ) ;
#173851 = CARTESIAN_POINT ( 'NONE',  ( 21.55341960407619695, -5.719274019375665929, 61.04275706135234714 ) ) ;
#173852 = CARTESIAN_POINT ( 'NONE',  ( -5.719274019375978568, 21.55341960407610458, 85.20724293864770971 ) ) ;
#173853 = CARTESIAN_POINT ( 'NONE',  ( 16.46253265017146816, 9.564922557961045513, 66.66775706135233293 ) ) ;
#173854 = DIRECTION ( 'NONE',  ( 0.000000000000000000, 0.7071067811865483499, -0.7071067811865467956 ) ) ;
#173855 = CARTESIAN_POINT ( 'NONE',  ( -0.05219959533909027116, -19.03943276465977164, 112.4989096053143669 ) ) ;
#173856 = CARTESIAN_POINT ( 'NONE',  ( 0.05219959533910956823, 16.53943276465976808, 79.99890960531435269 ) ) ;
#173857 = CARTESIAN_POINT ( 'NONE',  ( -13.97604488694547697, 13.89961937509957934, 48.12609039468566863 ) ) ;
#173858 = CARTESIAN_POINT ( 'NONE',  ( -9.564922557960796823, -16.46253265017161027, 67.08224293864769550 ) ) ;
#173859 = CARTESIAN_POINT ( 'NONE',  ( 8.224510206698953496, -14.34966873604960469, 62.91557627198102409 ) ) ;
#173860 = CARTESIAN_POINT ( 'NONE',  ( -19.05341960407617563, 5.049401038297882671, 78.54275706135233293 ) ) ;
#173861 = CARTESIAN_POINT ( 'NONE',  ( -21.52544592524343514, 5.823673210054127303, 41.04057627198103120 ) ) ;
#173862 = ORIENTED_EDGE ( 'NONE', *, *, #59844, .F. ) ;
#173863 = CARTESIAN_POINT ( 'NONE',  ( -8.224510206698948167, 14.34966873604960824, 105.4155762719810383 ) ) ;
#173864 = CARTESIAN_POINT ( 'NONE',  ( -17.50000000000001066, -5.068104630630400287, 24.27181594659972319 ) ) ;
#173866 = CARTESIAN_POINT ( 'NONE',  ( -5.823673210054116645, -21.52544592524344225, 57.29057627198103120 ) ) ;
#173865 = CARTESIAN_POINT ( 'NONE',  ( 16.46253265017160672, -9.564922557960803928, 53.33224293864768839 ) ) ;
#173867 = CARTESIAN_POINT ( 'NONE',  ( 5.049401038298161559, -19.05341960407611168, 37.70724293864768839 ) ) ;
#173869 = CARTESIAN_POINT ( 'NONE',  ( -5.049401038298153566, 19.05341960407611168, 70.20724293864769550 ) ) ;
#173868 = CARTESIAN_POINT ( 'NONE',  ( -4.379528057220086978, -16.55341960407618274, 79.79275706135236135 ) ) ;
#173870 = CARTESIAN_POINT ( 'NONE',  ( -16.46253265017146816, -9.564922557961047289, 49.16775706135233293 ) ) ;
#173871 = CARTESIAN_POINT ( 'NONE',  ( -10.72451020669870658, -18.67979575497194134, 64.58442372801900433 ) ) ;
#173872 = CARTESIAN_POINT ( 'NONE',  ( -10.81492255796078084, -18.62759615963271287, 47.08224293864770260 ) ) ;
#173873 = CARTESIAN_POINT ( 'NONE',  ( 0.05219959533909260263, 19.03943276465977164, 24.99890960531435269 ) ) ;
#173874 = CARTESIAN_POINT ( 'NONE',  ( 14.34966873604972726, -8.224510206698740333, 80.83442372801901854 ) ) ;
#173875 = CARTESIAN_POINT ( 'NONE',  ( 13.97604488694548053, -13.89961937509957401, 105.6260903946856757 ) ) ;
#173876 = DIRECTION ( 'NONE',  ( 0.9945218953682734009, 0.000000000000000000, 0.1045284632676537068 ) ) ;
#173877 = DIRECTION ( 'NONE',  ( 0.000000000000000000, 0.000000000000000000, 1.000000000000000000 ) ) ;
#173878 = CARTESIAN_POINT ( 'NONE',  ( 10.81492255796106328, -18.62759615963255655, 100.4177570613523471 ) ) ;
#173879 = ORIENTED_EDGE ( 'NONE', *, *, #174237, .F. ) ;
#173880 = CARTESIAN_POINT ( 'NONE',  ( -4.483927247898539470, -16.52544592524342804, 47.29057627198103120 ) ) ;
#173881 = CARTESIAN_POINT ( 'NONE',  ( -12.06949235617756955, 12.14591786802309770, 75.62390960531439532 ) ) ;
#173882 = CARTESIAN_POINT ( 'NONE',  ( -15.80617190586745835, -15.72974639402198527, 96.87390960531436690 ) ) ;
#173883 = CARTESIAN_POINT ( 'NONE',  ( -0.05219959533907301413, -21.53943276465977519, 92.49890960531436690 ) ) ;
#173884 = CARTESIAN_POINT ( 'NONE',  ( 11.30153831258470021, -180.0000000000000000, -4.999999999999999112 ) ) ;
#173885 = B_SPLINE_CURVE_WITH_KNOTS ( 'NONE', 3,
 ( #138737, #218, #110389, #49721, #93223, #156906, #1210, #62888, #111388, #46745, #4193, #3212, #124568, #47743, #77066, #173074, #155900, #172071 ),
 .UNSPECIFIED., .F., .F.,
 ( 4, 2, 2, 2, 2, 2, 2, 2, 4 ),
 ( 0.000000000000000000, 0.001023866006848666178, 0.002047732013697332355, 0.003071598020545998533, 0.004095464027394664711, 0.005119330034243330455, 0.006143196041091997066, 0.007167062047940663677, 0.008190928054789329421 ),
 .UNSPECIFIED. ) ;
#173886 = CARTESIAN_POINT ( 'NONE',  ( -15.80617190586745835, -15.72974639402198527, 31.87390960531435979 ) ) ;
#173887 = CARTESIAN_POINT ( 'NONE',  ( -14.29746914071037622, -8.314922557961029526, 69.16775706135234714 ) ) ;
#173888 = CARTESIAN_POINT ( 'NONE',  ( -4.483927247898539470, -16.52544592524342804, 87.29057627198103830 ) ) ;
#173889 = CARTESIAN_POINT ( 'NONE',  ( -19.05341960407611168, -5.049401038298163336, 51.45724293864770260 ) ) ;
#173890 = DIRECTION ( 'NONE',  ( 1.000000000000000000, 0.000000000000000000, 0.000000000000000000 ) ) ;
#173891 = CARTESIAN_POINT ( 'NONE',  ( 8.314922557961029526, -14.29746914071037800, 95.41775706135234714 ) ) ;
#173892 = CARTESIAN_POINT ( 'NONE',  ( -15.72974639402176322, -15.80617190586768395, 29.37609039468568284 ) ) ;
#173893 = CARTESIAN_POINT ( 'NONE',  ( -9.474510206698964154, 16.51473224551069663, 80.41557627198103830 ) ) ;
#173894 = CARTESIAN_POINT ( 'NONE',  ( 21.55341960407619695, -5.719274019375665929, 66.04275706135236135 ) ) ;
#173895 = CARTESIAN_POINT ( 'NONE',  ( 19.03943276465977164, -0.05219959533909143690, 113.7489096053143669 ) ) ;
#173896 = CARTESIAN_POINT ( 'NONE',  ( -7.587788125975658993, -46.88744275388931726, -24.49805083758699098 ) ) ;
#173897 = EDGE_LOOP ( 'NONE', ( #116140, #55438, #142522 ) ) ;
#173898 = CARTESIAN_POINT ( 'NONE',  ( 21.55341960407619695, -5.719274019375665929, 56.04275706135235424 ) ) ;
#173900 = CARTESIAN_POINT ( 'NONE',  ( -23.96320343559652599, -18.46320343559629862, 1.818019484660532648 ) ) ;
#173899 = CARTESIAN_POINT ( 'NONE',  ( 13.89961937509977652, -13.97604488694527269, 33.12390960531434558 ) ) ;
#173901 = CARTESIAN_POINT ( 'NONE',  ( 16.51473224551083163, -9.474510206698727899, 70.83442372801900433 ) ) ;
#173902 = CARTESIAN_POINT ( 'NONE',  ( -21.53943276465977519, -0.05219959533937600094, 23.75109039468567929 ) ) ;
#173903 = CARTESIAN_POINT ( 'NONE',  ( 5.153800228976615827, -19.02544592524334988, 60.20942372801899012 ) ) ;
#173904 = CARTESIAN_POINT ( 'NONE',  ( 19.03943276465977164, -0.05219959533909143690, 23.74890960531435269 ) ) ;
#173905 = CARTESIAN_POINT ( 'NONE',  ( 8.314922557961029526, -14.29746914071037800, 90.41775706135236135 ) ) ;
#173906 = CARTESIAN_POINT ( 'NONE',  ( 19.03943276465977164, 0.05219959533936151252, 66.25109039468567573 ) ) ;
#173907 = CARTESIAN_POINT ( 'NONE',  ( 8.314922557960818139, 14.29746914071049879, 24.58224293864768839 ) ) ;
#173909 = ORIENTED_EDGE ( 'NONE', *, *, #191135, .F. ) ;
#173908 = CARTESIAN_POINT ( 'NONE',  ( 9.614343725828573994, 9.760382078682853901, -62.58071313852360618 ) ) ;
#173910 = CARTESIAN_POINT ( 'NONE',  ( -13.89961937509977652, 13.97604488694528158, 85.62390960531433848 ) ) ;
#173911 = CARTESIAN_POINT ( 'NONE',  ( 21.55341960407619695, -5.719274019375665929, 91.04275706135236135 ) ) ;
#173912 = CARTESIAN_POINT ( 'NONE',  ( -18.62759615963255300, -10.81492255796106328, 104.1677570613523471 ) ) ;
#173913 = CARTESIAN_POINT ( 'NONE',  ( -5.153800228976328057, -19.02544592524343514, 22.29057627198102765 ) ) ;
#173914 = CARTESIAN_POINT ( 'NONE',  ( 21.53943276465977519, 0.05219959533937863772, 81.25109039468568994 ) ) ;
#173915 = CARTESIAN_POINT ( 'NONE',  ( -16.55341960407617563, 4.379528057220093196, 28.54275706135234358 ) ) ;
#173916 = CARTESIAN_POINT ( 'NONE',  ( 13.97604488694527802, 13.89961937509977652, 84.37390960531433848 ) ) ;
#173917 = CARTESIAN_POINT ( 'NONE',  ( 21.53943276465977519, -0.05219959533907433946, 23.74890960531435269 ) ) ;
#173918 = FACE_BOUND ( 'NONE', #74971, .T. ) ;
#173919 = CARTESIAN_POINT ( 'NONE',  ( -16.51473224551069308, -9.474510206698971260, 76.66557627198103830 ) ) ;
#173920 = CARTESIAN_POINT ( 'NONE',  ( -17.31747979337959720, 6.344076630960796770, 98.62055131934816643 ) ) ;
#173921 = CARTESIAN_POINT ( 'NONE',  ( 19.05341960407617918, -5.049401038297876454, 71.04275706135234714 ) ) ;
#173922 = CARTESIAN_POINT ( 'NONE',  ( -13.97604488694527625, -13.89961937509977652, 106.8739096053143669 ) ) ;
#173923 = CARTESIAN_POINT ( 'NONE',  ( 15.80617190586769283, -15.72974639402175789, 100.6260903946857184 ) ) ;
#173924 = CARTESIAN_POINT ( 'NONE',  ( 16.55341960407611168, 4.379528057220329451, 103.9572429386476813 ) ) ;
#173925 = CARTESIAN_POINT ( 'NONE',  ( 15.80617190586746368, 15.72974639402197994, 49.37390960531436690 ) ) ;
#173926 = CARTESIAN_POINT ( 'NONE',  ( -15.80617190586745835, -15.72974639402198527, 31.87390960531435979 ) ) ;
#173927 = CARTESIAN_POINT ( 'NONE',  ( -16.52544592524342804, 4.483927247898546575, 106.0405762719810525 ) ) ;
#173928 = CARTESIAN_POINT ( 'NONE',  ( -15.38891197842625225, 1.491051326733042082, -61.89130710690761106 ) ) ;
#173929 = CARTESIAN_POINT ( 'NONE',  ( -13.89961937509957401, -13.97604488694547875, 54.37609039468565442 ) ) ;
#173931 = TOROIDAL_SURFACE ( 'NONE', #161616, 23.10356920737165254, 5.000000000000000000 ) ;
#173930 = CARTESIAN_POINT ( 'NONE',  ( 8.224510206698953496, -14.34966873604960469, 27.91557627198103830 ) ) ;
#173932 = CARTESIAN_POINT ( 'NONE',  ( -13.89961937509977652, 13.97604488694528158, 95.62390960531436690 ) ) ;
#173933 = CARTESIAN_POINT ( 'NONE',  ( -21.55341960407619339, 5.719274019375674811, 83.54275706135234714 ) ) ;
#173934 = CARTESIAN_POINT ( 'NONE',  ( -5.719274019375978568, 21.55341960407610458, 55.20724293864770260 ) ) ;
#173935 = CARTESIAN_POINT ( 'NONE',  ( -0.05219959533937732626, 21.53943276465977519, 47.50109039468568994 ) ) ;
#173936 = CARTESIAN_POINT ( 'NONE',  ( 18.62759615963271287, -10.81492255796078972, 98.33224293864769550 ) ) ;
#173937 = CARTESIAN_POINT ( 'NONE',  ( -18.62759615963255300, -10.81492255796106328, 44.16775706135234714 ) ) ;
#173938 = CARTESIAN_POINT ( 'NONE',  ( 13.89961937509977652, -13.97604488694527269, 23.12390960531436335 ) ) ;
#173939 = CARTESIAN_POINT ( 'NONE',  ( 13.89961937509977652, -13.97604488694527269, 88.12390960531438111 ) ) ;
#173940 =( BOUNDED_CURVE ( )  B_SPLINE_CURVE ( 3, ( #64222, #50048, #156226, #142039 ),
 .UNSPECIFIED., .F., .F. ) 
 B_SPLINE_CURVE_WITH_KNOTS ( ( 4, 4 ),
 ( 1.132647296210726351, 2.115944711806983403 ),
 .UNSPECIFIED. ) 
 CURVE ( )  GEOMETRIC_REPRESENTATION_ITEM ( )  RATIONAL_B_SPLINE_CURVE ( ( 1.000000000000000000, 0.9210371567966660900, 0.9210371567966660900, 1.000000000000000000 ) ) 
 REPRESENTATION_ITEM ( '' )  );
#173941 = CARTESIAN_POINT ( 'NONE',  ( 12.06949235617757843, -12.14591786802309237, 108.1239096053143811 ) ) ;
#173942 = CARTESIAN_POINT ( 'NONE',  ( -16.51473224551069308, -9.474510206698971260, 111.6655762719810383 ) ) ;
#173943 = CARTESIAN_POINT ( 'NONE',  ( 8.314922557960818139, 14.29746914071049879, 54.58224293864769550 ) ) ;
#173944 = CARTESIAN_POINT ( 'NONE',  ( 4.379528057220339221, -16.55341960407611168, 22.70724293864769194 ) ) ;
#173945 = CARTESIAN_POINT ( 'NONE',  ( -5.153800228976328057, -19.02544592524343514, 47.29057627198102409 ) ) ;
#173946 = CARTESIAN_POINT ( 'NONE',  ( -13.97604488694527625, -13.89961937509977652, 21.87390960531435979 ) ) ;
#173947 = CARTESIAN_POINT ( 'NONE',  ( 5.719274019375991003, -21.55341960407610458, 47.70724293864770260 ) ) ;
#173948 = CARTESIAN_POINT ( 'NONE',  ( 5.153800228976615827, -19.02544592524334988, 20.20942372801899722 ) ) ;
#173950 = CARTESIAN_POINT ( 'NONE',  ( 4.483927247898545687, 16.52544592524342804, 39.79057627198103830 ) ) ;
#173949 = DIRECTION ( 'NONE',  ( 3.709348145883536076E-20, 0.000000000000000000, -1.000000000000000000 ) ) ;
#173951 = CARTESIAN_POINT ( 'NONE',  ( -0.05219959533937732626, 21.53943276465977519, 52.50109039468567573 ) ) ;
#173952 = CARTESIAN_POINT ( 'NONE',  ( 9.564922557960805705, 16.46253265017160317, 114.5822429386476955 ) ) ;
#173953 = CARTESIAN_POINT ( 'NONE',  ( -4.379528057220086978, -16.55341960407618274, 59.79275706135234714 ) ) ;
#173954 = CARTESIAN_POINT ( 'NONE',  ( 5.153800228976615827, -19.02544592524334988, 65.20942372801900433 ) ) ;
#173955 = CARTESIAN_POINT ( 'NONE',  ( 16.52544592524342804, -4.483927247898539470, 33.54057627198102409 ) ) ;
#173956 = CARTESIAN_POINT ( 'NONE',  ( 16.53943276465976808, 0.05219959533934440121, 111.2510903946856899 ) ) ;
#173957 = CARTESIAN_POINT ( 'NONE',  ( -0.05219959533909027116, -19.03943276465977164, 42.49890960531435269 ) ) ;
#173958 = CARTESIAN_POINT ( 'NONE',  ( -5.049401038298153566, 19.05341960407611168, 65.20724293864765286 ) ) ;
#173959 = CARTESIAN_POINT ( 'NONE',  ( 19.02544592524343514, -5.153800228976328945, 28.54057627198102409 ) ) ;
#173960 = CARTESIAN_POINT ( 'NONE',  ( 15.80617190586769283, -15.72974639402175789, 35.62609039468568994 ) ) ;
#173961 = CARTESIAN_POINT ( 'NONE',  ( -5.049401038298153566, 19.05341960407611168, 45.20724293864769550 ) ) ;
#173962 = CARTESIAN_POINT ( 'NONE',  ( 13.97604488694527802, 13.89961937509977652, 114.3739096053143669 ) ) ;
#173963 = CARTESIAN_POINT ( 'NONE',  ( -5.049401038298153566, 19.05341960407611168, 50.20724293864770260 ) ) ;
#173964 = CARTESIAN_POINT ( 'NONE',  ( 19.03943276465977164, -0.05219959533909143690, 113.7489096053143669 ) ) ;
#173966 = CARTESIAN_POINT ( 'NONE',  ( 0.05219959533910956823, 16.53943276465976808, 109.9989096053143527 ) ) ;
#173965 = CARTESIAN_POINT ( 'NONE',  ( 21.52544592524334988, 5.823673210054432836, 56.45942372801902565 ) ) ;
#173967 = CARTESIAN_POINT ( 'NONE',  ( -19.03943276465977164, 0.05219959533909376836, 106.2489096053143669 ) ) ;
#173968 = CARTESIAN_POINT ( 'NONE',  ( 16.55341960407618274, -4.379528057220086978, 81.04275706135236135 ) ) ;
#173969 = CARTESIAN_POINT ( 'NONE',  ( 21.55341960407619695, -5.719274019375665929, 86.04275706135236135 ) ) ;
#173970 = CARTESIAN_POINT ( 'NONE',  ( -8.314922557961024197, 14.29746914071037800, 47.91775706135234714 ) ) ;
#173971 = CARTESIAN_POINT ( 'NONE',  ( 16.51473224551069308, 9.474510206698969483, 94.16557627198103830 ) ) ;
#173972 = CARTESIAN_POINT ( 'NONE',  ( 4.379528057220092307, 16.55341960407617563, 47.29275706135234003 ) ) ;
#173973 = CARTESIAN_POINT ( 'NONE',  ( -12.14591786802326823, 12.06949235617739902, 33.12609039468569705 ) ) ;
#173974 = CARTESIAN_POINT ( 'NONE',  ( -14.34966873604972548, 8.224510206698743886, 83.33442372801903275 ) ) ;
#173975 = CARTESIAN_POINT ( 'NONE',  ( -16.51473224551082808, 9.474510206698731452, 108.3344237280190043 ) ) ;
#173976 = CARTESIAN_POINT ( 'NONE',  ( -10.81492255796078084, -18.62759615963271287, 92.08224293864769550 ) ) ;
#173978 = CARTESIAN_POINT ( 'NONE',  ( -0.05219959533936034679, 19.03943276465977164, 107.5010903946856615 ) ) ;
#173977 = CARTESIAN_POINT ( 'NONE',  ( 8.314922557960818139, 14.29746914071049879, 104.5822429386477097 ) ) ;
#173979 = CARTESIAN_POINT ( 'NONE',  ( -14.29746914071037622, -8.314922557961029526, 79.16775706135234714 ) ) ;
#173980 = CARTESIAN_POINT ( 'NONE',  ( -17.26058549869106429, 6.457015423128173559, 43.62254162523933587 ) ) ;
#173981 = CARTESIAN_POINT ( 'NONE',  ( -9.474510206698720793, -16.51473224551083518, 64.58442372801900433 ) ) ;
#173982 = CARTESIAN_POINT ( 'NONE',  ( 14.29746914071049879, -8.314922557960816363, 43.33224293864769550 ) ) ;
#173983 = CARTESIAN_POINT ( 'NONE',  ( -8.314922557960811034, -14.29746914071050412, 32.08224293864769550 ) ) ;
#173984 = CARTESIAN_POINT ( 'NONE',  ( -8.224510206698948167, 14.34966873604960824, 90.41557627198103830 ) ) ;
#173986 = CARTESIAN_POINT ( 'NONE',  ( -19.25663599770060941, 5.499999999999449329, 88.99419308057201761 ) ) ;
#173985 = CARTESIAN_POINT ( 'NONE',  ( 16.51473224551083163, -9.474510206698727899, 30.83442372801900433 ) ) ;
#173987 = CARTESIAN_POINT ( 'NONE',  ( 15.72974639402176855, 15.80617190586768217, 31.87609039468567929 ) ) ;
#173988 = CARTESIAN_POINT ( 'NONE',  ( 16.46253265017146816, 9.564922557961045513, 101.6677570613523329 ) ) ;
#173989 = CARTESIAN_POINT ( 'NONE',  ( -11.02000550219323216, -37.94488912280210968, -31.28304700362893698 ) ) ;
#173990 = CARTESIAN_POINT ( 'NONE',  ( -9.474510206698964154, 16.51473224551069663, 90.41557627198103830 ) ) ;
#173991 = CARTESIAN_POINT ( 'NONE',  ( -19.02544592524342804, 5.153800228976336051, 96.04057627198103830 ) ) ;
#173992 = CARTESIAN_POINT ( 'NONE',  ( -10.81492255796078084, -18.62759615963271287, 62.08224293864769550 ) ) ;
#173993 = CARTESIAN_POINT ( 'NONE',  ( -14.29746914071049879, 8.314922557960819915, 95.83224293864770971 ) ) ;
#173994 = CARTESIAN_POINT ( 'NONE',  ( 5.049401038298161559, -19.05341960407611168, 67.70724293864769550 ) ) ;
#173995 = CARTESIAN_POINT ( 'NONE',  ( 16.53943276465976808, -0.05219959533910856209, 113.7489096053143527 ) ) ;
#173996 = CARTESIAN_POINT ( 'NONE',  ( 10.81492255796106328, -18.62759615963255655, 40.41775706135234714 ) ) ;
#173997 = CARTESIAN_POINT ( 'NONE',  ( 0.05219959533937995610, -21.53943276465977519, 80.00109039468568994 ) ) ;
#173998 = CARTESIAN_POINT ( 'NONE',  ( 13.89961937509977652, -13.97604488694527269, 63.12390960531435979 ) ) ;
#173999 = CARTESIAN_POINT ( 'NONE',  ( 16.53943276465976808, 0.05219959533934440121, 81.25109039468568994 ) ) ;
#174000 = CARTESIAN_POINT ( 'NONE',  ( 21.52544592524334988, 5.823673210054432836, 26.45942372801901854 ) ) ;
#174001 = CARTESIAN_POINT ( 'NONE',  ( -15.72974639402176322, -15.80617190586768395, 24.37609039468567573 ) ) ;
#174003 = CARTESIAN_POINT ( 'NONE',  ( 16.46253265017160672, -9.564922557960803928, 73.33224293864769550 ) ) ;
#174002 = CARTESIAN_POINT ( 'NONE',  ( -0.05219959533936034679, 19.03943276465977164, 57.50109039468566863 ) ) ;
#174004 = CARTESIAN_POINT ( 'NONE',  ( -13.97604488694547697, 13.89961937509957934, 28.12609039468565797 ) ) ;
#174005 = CARTESIAN_POINT ( 'NONE',  ( -21.53943276465977519, -0.05219959533937600094, 83.75109039468568994 ) ) ;
#174006 = CARTESIAN_POINT ( 'NONE',  ( -18.67979575497178146, -10.72451020669898902, 66.66557627198102409 ) ) ;
#174007 = CARTESIAN_POINT ( 'NONE',  ( 8.314922557960818139, 14.29746914071049879, 54.58224293864769550 ) ) ;
#174009 = CARTESIAN_POINT ( 'NONE',  ( 9.564922557961047289, -16.46253265017146816, 35.41775706135233293 ) ) ;
#174008 = CARTESIAN_POINT ( 'NONE',  ( 15.80617190586769283, -15.72974639402175789, 90.62609039468567573 ) ) ;
#174010 = CARTESIAN_POINT ( 'NONE',  ( 8.314922557960818139, 14.29746914071049879, 64.58224293864769550 ) ) ;
#174011 = CARTESIAN_POINT ( 'NONE',  ( 5.153800228976335163, 19.02544592524342804, 24.79057627198102765 ) ) ;
#174012 = CARTESIAN_POINT ( 'NONE',  ( -13.97604488694547697, 13.89961937509957934, 68.12609039468563310 ) ) ;
#174013 = CARTESIAN_POINT ( 'NONE',  ( -14.29746914071049879, 8.314922557960819915, 35.83224293864768839 ) ) ;
#174014 = CARTESIAN_POINT ( 'NONE',  ( 10.72451020669871369, 18.67979575497193778, 87.08442372801901854 ) ) ;
#174015 = CARTESIAN_POINT ( 'NONE',  ( -13.89961937509977652, 13.97604488694528158, 80.62390960531436690 ) ) ;
#174016 = CARTESIAN_POINT ( 'NONE',  ( -16.46253265017146816, -9.564922557961047289, 54.16775706135234003 ) ) ;
#174017 = CARTESIAN_POINT ( 'NONE',  ( 10.81492255796078972, 18.62759615963270932, 49.58224293864769550 ) ) ;
#174018 = CARTESIAN_POINT ( 'NONE',  ( -15.80617190586768217, 15.72974639402176855, 48.12609039468568284 ) ) ;
#174019 = CARTESIAN_POINT ( 'NONE',  ( -15.80617190586745835, -15.72974639402198527, 96.87390960531436690 ) ) ;
#174020 = CARTESIAN_POINT ( 'NONE',  ( 5.153800228976615827, -19.02544592524334988, 95.20942372801897591 ) ) ;
#174021 = CARTESIAN_POINT ( 'NONE',  ( -4.379528057220086978, -16.55341960407618274, 64.79275706135234714 ) ) ;
#174023 = CARTESIAN_POINT ( 'NONE',  ( -18.67979575497178146, -10.72451020669898902, 101.6655762719810383 ) ) ;
#174022 = CYLINDRICAL_SURFACE ( 'NONE', #80496, 1.499999999999994449 ) ;
#174024 = CARTESIAN_POINT ( 'NONE',  ( 4.483927247898545687, 16.52544592524342804, 104.7905762719810241 ) ) ;
#174025 = CARTESIAN_POINT ( 'NONE',  ( -29.86685920354755197, -21.69954338932560134, -10.92499999726881299 ) ) ;
#174026 = CARTESIAN_POINT ( 'NONE',  ( 8.314922557961029526, -14.29746914071037800, 35.41775706135234003 ) ) ;
#174027 = CARTESIAN_POINT ( 'NONE',  ( -15.72974639402197994, 15.80617190586746368, 60.62390960531437401 ) ) ;
#174028 = CARTESIAN_POINT ( 'NONE',  ( -14.29746914071037622, -8.314922557961029526, 104.1677570613523471 ) ) ;
#174029 = CARTESIAN_POINT ( 'NONE',  ( 0.05219959533909260263, 19.03943276465977164, 29.99890960531435979 ) ) ;
#174030 = CARTESIAN_POINT ( 'NONE',  ( -12.06949235617739369, -12.14591786802326823, 69.37609039468567573 ) ) ;
#174031 = CARTESIAN_POINT ( 'NONE',  ( -5.153800228976607833, 19.02544592524334988, 57.70942372801899012 ) ) ;
#174032 = CARTESIAN_POINT ( 'NONE',  ( 18.67979575497194134, -10.72451020669871369, 45.83442372801901854 ) ) ;
#174033 = CARTESIAN_POINT ( 'NONE',  ( 15.80617190586746368, 15.72974639402197994, 54.37390960531435979 ) ) ;
#174034 = CARTESIAN_POINT ( 'NONE',  ( 12.14591786802327356, -12.06949235617739191, 95.62609039468568994 ) ) ;
#174035 = CARTESIAN_POINT ( 'NONE',  ( -18.62759615963255300, -10.81492255796106328, 69.16775706135234714 ) ) ;
#174036 = EDGE_CURVE ( 'NONE', #179099, #64402, #43853, .T. ) ;
#174037 = CARTESIAN_POINT ( 'NONE',  ( 15.80617190586746368, 15.72974639402197994, 54.37390960531435979 ) ) ;
#174038 = CARTESIAN_POINT ( 'NONE',  ( 5.823673210054125526, 21.52544592524343514, 29.79057627198102409 ) ) ;
#174039 = ORIENTED_EDGE ( 'NONE', *, *, #43478, .T. ) ;
#174040 = VERTEX_POINT ( 'NONE', #107732 ) ;
#174041 = CARTESIAN_POINT ( 'NONE',  ( -0.05219959533934338120, 16.53943276465976808, 77.50109039468567573 ) ) ;
#174042 = CARTESIAN_POINT ( 'NONE',  ( -21.55341960407610458, -5.719274019375992779, 31.45724293864769550 ) ) ;
#174043 = ORIENTED_EDGE ( 'NONE', *, *, #107988, .F. ) ;
#174044 = CARTESIAN_POINT ( 'NONE',  ( -5.153800228976328057, -19.02544592524343514, 97.29057627198099567 ) ) ;
#174045 = CARTESIAN_POINT ( 'NONE',  ( -14.34966873604960291, -8.224510206698953496, 26.66557627198103475 ) ) ;
#174046 = CARTESIAN_POINT ( 'NONE',  ( 21.46320343559639099, -20.96320343559646915, 4.646446609406719830 ) ) ;
#174047 = CARTESIAN_POINT ( 'NONE',  ( 8.314922557960818139, 14.29746914071049879, 104.5822429386477097 ) ) ;
#174048 = CARTESIAN_POINT ( 'NONE',  ( 10.72451020669898902, -18.67979575497178502, 67.91557627198102409 ) ) ;
#174049 = CARTESIAN_POINT ( 'NONE',  ( -16.55341960407617563, 4.379528057220093196, 93.54275706135234714 ) ) ;
#174050 = CARTESIAN_POINT ( 'NONE',  ( 21.52544592524334988, 5.823673210054432836, 41.45942372801901143 ) ) ;
#174051 = CARTESIAN_POINT ( 'NONE',  ( 19.03943276465977164, 0.05219959533936151252, 101.2510903946856757 ) ) ;
#174052 = CARTESIAN_POINT ( 'NONE',  ( 14.29746914071049879, -8.314922557960816363, 108.3322429386477097 ) ) ;
#174053 = CARTESIAN_POINT ( 'NONE',  ( 8.314922557961029526, -14.29746914071037800, 20.41775706135234714 ) ) ;
#174054 = CARTESIAN_POINT ( 'NONE',  ( 0.05219959533909260263, 19.03943276465977164, 29.99890960531435979 ) ) ;
#174055 = CARTESIAN_POINT ( 'NONE',  ( 0.000000000000000000, 0.7216878364870328300, -1.250000000000000000 ) ) ;
#174056 = CARTESIAN_POINT ( 'NONE',  ( -0.05219959533909027116, -19.03943276465977164, 87.49890960531436690 ) ) ;
#174057 = CARTESIAN_POINT ( 'NONE',  ( 16.52544592524335698, 4.483927247898782831, 71.45942372801901854 ) ) ;
#174058 = CARTESIAN_POINT ( 'NONE',  ( 10.81492255796106328, -18.62759615963255655, 105.4177570613523613 ) ) ;
#174059 = CARTESIAN_POINT ( 'NONE',  ( 15.72974639402199770, -15.80617190586745480, 58.12390960531435979 ) ) ;
#174061 = B_SPLINE_CURVE_WITH_KNOTS ( 'NONE', 3,
 ( #178439, #149099, #10589, #13555, #72250, #133928, #195618, #134934, #32699, #183408, #107529, #29721, #63022, #108534, #91353, #106548, #125695, #350, #17526, #139852, #168224, #92362, #154048, #121715, #153045, #48862, #31706, #93355, #94350, #77201, #185383, #109527 ),
 .UNSPECIFIED., .F., .F.,
 ( 4, 2, 2, 2, 2, 2, 2, 2, 2, 2, 2, 2, 2, 2, 2, 4 ),
 ( 1.652208230918760859E-15, 0.0003712461730052253150, 0.0007424923460087984144, 0.001113738519012371459, 0.001484984692015944505, 0.002227477038023091029, 0.002598723211026663857, 0.002969969384030237119, 0.003341215557033810381, 0.003712461730037383209, 0.004083707903040956037, 0.004454954076044529733, 0.004826200249048102561, 0.005197446422051675390, 0.005568692595055249085, 0.005939938768058821913 ),
 .UNSPECIFIED. ) ;
#174060 = CARTESIAN_POINT ( 'NONE',  ( -16.52544592524335698, -4.483927247898792601, 83.95942372801900433 ) ) ;
#174062 = CARTESIAN_POINT ( 'NONE',  ( -16.51473224551082808, 9.474510206698731452, 78.33442372801900433 ) ) ;
#174063 = CARTESIAN_POINT ( 'NONE',  ( -5.049401038298153566, 19.05341960407611168, 30.20724293864768839 ) ) ;
#174064 = CARTESIAN_POINT ( 'NONE',  ( -5.153800228976328057, -19.02544592524343514, 82.29057627198103830 ) ) ;
#174065 = CARTESIAN_POINT ( 'NONE',  ( 16.46253265017160672, -9.564922557960803928, 33.33224293864770260 ) ) ;
#174066 = CARTESIAN_POINT ( 'NONE',  ( -16.51473224551082808, 9.474510206698731452, 78.33442372801900433 ) ) ;
#174067 = CARTESIAN_POINT ( 'NONE',  ( 20.56371838171487809, -11.43208494587337043, 170.0924998638764976 ) ) ;
#174068 = CARTESIAN_POINT ( 'NONE',  ( 0.05219959533909260263, 19.03943276465977164, 99.99890960531436690 ) ) ;
#174069 = CARTESIAN_POINT ( 'NONE',  ( 16.52544592524342804, -4.483927247898539470, 53.54057627198103120 ) ) ;
#174070 = CARTESIAN_POINT ( 'NONE',  ( 21.52544592524344225, -5.823673210054117533, 63.54057627198103830 ) ) ;
#174071 = CARTESIAN_POINT ( 'NONE',  ( 9.687362902255724606, 9.687362902255701513, -60.44446360152740993 ) ) ;
#174072 = CARTESIAN_POINT ( 'NONE',  ( -0.05219959533936034679, 19.03943276465977164, 27.50109039468566507 ) ) ;
#174073 = PLANE ( 'NONE',  #12177 ) ;
#174075 = CARTESIAN_POINT ( 'NONE',  ( -0.05219959533909027116, -19.03943276465977164, 77.49890960531435269 ) ) ;
#174074 = CARTESIAN_POINT ( 'NONE',  ( 16.51473224551069308, 9.474510206698969483, 49.16557627198102409 ) ) ;
#174076 = CARTESIAN_POINT ( 'NONE',  ( 12.14591786802327356, -12.06949235617739191, 40.62609039468567573 ) ) ;
#174077 = CARTESIAN_POINT ( 'NONE',  ( 29.09442113371785865, -27.25731168736310295, -16.99878707713621395 ) ) ;
#174078 = CARTESIAN_POINT ( 'NONE',  ( 5.000000000000000000, -120.9970989573719038, 14.58956564881029649 ) ) ;
#174079 = CARTESIAN_POINT ( 'NONE',  ( 0.05219959533934541429, -16.53943276465976808, 70.00109039468568994 ) ) ;
#174080 = CARTESIAN_POINT ( 'NONE',  ( -10.81492255796078084, -18.62759615963271287, 92.08224293864769550 ) ) ;
#174081 = CARTESIAN_POINT ( 'NONE',  ( -4.483927247898782831, 16.52544592524335698, 42.70942372801901854 ) ) ;
#174083 = CARTESIAN_POINT ( 'NONE',  ( 17.43248706301297091, -16.85888939060687264, -56.81032385587572264 ) ) ;
#174082 = CARTESIAN_POINT ( 'NONE',  ( 9.474510206698971260, -16.51473224551069308, 42.91557627198103120 ) ) ;
#174084 = CARTESIAN_POINT ( 'NONE',  ( 0.05219959533937995610, -21.53943276465977519, 50.00109039468568994 ) ) ;
#174085 = CARTESIAN_POINT ( 'NONE',  ( 5.049401038297881783, 19.05341960407617563, 67.29275706135234714 ) ) ;
#174086 = CARTESIAN_POINT ( 'NONE',  ( -18.62759615963255300, -10.81492255796106328, 89.16775706135236135 ) ) ;
#174087 = CARTESIAN_POINT ( 'NONE',  ( 17.48847506799968698, 5.747544572773780835, 96.67302562156719148 ) ) ;
#174088 = CARTESIAN_POINT ( 'NONE',  ( 3.889087296525994830, -6.412877669190346630, 8.181980515339454030 ) ) ;
#174089 = CARTESIAN_POINT ( 'NONE',  ( 21.52544592524344225, -5.823673210054117533, 58.54057627198103120 ) ) ;
#174090 = CARTESIAN_POINT ( 'NONE',  ( -27.73933785331498925, -9.013057229001049109, 140.9750000027311785 ) ) ;
#174091 = CARTESIAN_POINT ( 'NONE',  ( 5.049401038298161559, -19.05341960407611168, 97.70724293864766707 ) ) ;
#174092 = CARTESIAN_POINT ( 'NONE',  ( -14.34966873604960291, -8.224510206698953496, 101.6655762719810383 ) ) ;
#174093 = CARTESIAN_POINT ( 'NONE',  ( -16.53943276465976808, -0.05219959533934237506, 23.75109039468567929 ) ) ;
#174094 = CARTESIAN_POINT ( 'NONE',  ( 16.55341960407618274, -4.379528057220086978, 106.0427570613523471 ) ) ;
#174095 = ORIENTED_EDGE ( 'NONE', *, *, #120673, .T. ) ;
#174096 = CARTESIAN_POINT ( 'NONE',  ( -21.53943276465977519, 0.05219959533907696930, 101.2489096053143669 ) ) ;
#174098 = CARTESIAN_POINT ( 'NONE',  ( -13.89961937509977652, 13.97604488694528158, 115.6239096053143669 ) ) ;
#174097 = CARTESIAN_POINT ( 'NONE',  ( 0.05219959533910956823, 16.53943276465976808, 44.99890960531435979 ) ) ;
#174099 = CARTESIAN_POINT ( 'NONE',  ( -9.564922557961040184, 16.46253265017147172, 87.91775706135233293 ) ) ;
#174100 = CARTESIAN_POINT ( 'NONE',  ( -18.62759615963255300, -10.81492255796106328, 104.1677570613523471 ) ) ;
#174101 = CARTESIAN_POINT ( 'NONE',  ( 14.29746914071049879, -8.314922557960816363, 33.33224293864769550 ) ) ;
#174102 = CARTESIAN_POINT ( 'NONE',  ( -5.719274019375978568, 21.55341960407610458, 90.20724293864770971 ) ) ;
#174103 = CARTESIAN_POINT ( 'NONE',  ( -21.52544592524343514, 5.823673210054127303, 51.04057627198103120 ) ) ;
#174104 = CARTESIAN_POINT ( 'NONE',  ( 19.02544592524343514, -5.153800228976328945, 68.54057627198103830 ) ) ;
#174105 = CARTESIAN_POINT ( 'NONE',  ( 4.379528057220339221, -16.55341960407611168, 32.70724293864770260 ) ) ;
#174106 = CARTESIAN_POINT ( 'NONE',  ( -9.564922557960796823, -16.46253265017161027, 92.08224293864769550 ) ) ;
#174107 = ORIENTED_EDGE ( 'NONE', *, *, #121605, .F. ) ;
#174108 = CARTESIAN_POINT ( 'NONE',  ( 19.35633801406910237, -5.499999999999588773, 61.63373818172762952 ) ) ;
#174109 = CARTESIAN_POINT ( 'NONE',  ( 0.05219959533936267826, -19.03943276465977164, 45.00109039468566863 ) ) ;
#174110 = CARTESIAN_POINT ( 'NONE',  ( 5.823673210054125526, 21.52544592524343514, 74.79057627198105251 ) ) ;
#174111 = CARTESIAN_POINT ( 'NONE',  ( 16.55341960407611168, 4.379528057220329451, 103.9572429386476813 ) ) ;
#174112 = CARTESIAN_POINT ( 'NONE',  ( 10.81492255796106328, -18.62759615963255655, 40.41775706135234714 ) ) ;
#174113 = CARTESIAN_POINT ( 'NONE',  ( -22.44159573604010305, 16.30477369853692338, 149.1750000027311671 ) ) ;
#174114 = CARTESIAN_POINT ( 'NONE',  ( 12.14591786802327356, -12.06949235617739191, 105.6260903946856899 ) ) ;
#174115 = CARTESIAN_POINT ( 'NONE',  ( 19.02544592524343514, -5.153800228976328945, 33.54057627198102409 ) ) ;
#174116 = CARTESIAN_POINT ( 'NONE',  ( 9.474510206698971260, -16.51473224551069308, 82.91557627198103830 ) ) ;
#174117 = CARTESIAN_POINT ( 'NONE',  ( -19.02544592524342804, 5.153800228976336051, 26.04057627198103120 ) ) ;
#174118 = CARTESIAN_POINT ( 'NONE',  ( 12.06949235617757843, -12.14591786802309237, 38.12390960531436690 ) ) ;
#174119 = CARTESIAN_POINT ( 'NONE',  ( -21.55341960407619339, 5.719274019375674811, 78.54275706135236135 ) ) ;
#174121 = CARTESIAN_POINT ( 'NONE',  ( 12.06949235617739724, 12.14591786802326823, 66.87609039468568994 ) ) ;
#174120 = CARTESIAN_POINT ( 'NONE',  ( 27.75745401094703269, -25.59313184531724161, -20.67669038789624736 ) ) ;
#174122 = CARTESIAN_POINT ( 'NONE',  ( 19.03943276465977164, -0.05219959533909143690, 43.74890960531435979 ) ) ;
#174123 = CARTESIAN_POINT ( 'NONE',  ( -9.564922557960796823, -16.46253265017161027, 47.08224293864769550 ) ) ;
#174124 = ORIENTED_EDGE ( 'NONE', *, *, #91138, .F. ) ;
#174125 = CARTESIAN_POINT ( 'NONE',  ( 21.55341960407619695, -5.719274019375665929, 106.0427570613523471 ) ) ;
#174126 = CARTESIAN_POINT ( 'NONE',  ( -14.29746914071037622, -8.314922557961029526, 64.16775706135234714 ) ) ;
#174127 = CARTESIAN_POINT ( 'NONE',  ( 5.823673210054444382, -21.52544592524334988, 100.2094237280190043 ) ) ;
#174128 = CARTESIAN_POINT ( 'NONE',  ( 21.52544592524344225, -5.823673210054117533, 33.54057627198102409 ) ) ;
#174129 = CARTESIAN_POINT ( 'NONE',  ( -5.153800228976607833, 19.02544592524334988, 112.7094237280190043 ) ) ;
#174130 = CARTESIAN_POINT ( 'NONE',  ( 5.823673210054444382, -21.52544592524334988, 65.20942372801901854 ) ) ;
#174131 = CARTESIAN_POINT ( 'NONE',  ( 12.06949235617739724, 12.14591786802326823, 41.87609039468568284 ) ) ;
#174132 = CARTESIAN_POINT ( 'NONE',  ( 5.719274019375991003, -21.55341960407610458, 102.7072429386476955 ) ) ;
#174133 = CARTESIAN_POINT ( 'NONE',  ( -9.474510206698720793, -16.51473224551083518, 99.58442372801900433 ) ) ;
#174134 = CARTESIAN_POINT ( 'NONE',  ( 19.03943276465977164, -0.05219959533909143690, 63.74890960531435979 ) ) ;
#174135 = CARTESIAN_POINT ( 'NONE',  ( -12.06949235617739369, -12.14591786802326823, 19.37609039468568639 ) ) ;
#174136 = CARTESIAN_POINT ( 'NONE',  ( -19.05341960407617563, 5.049401038297882671, 108.5427570613523187 ) ) ;
#174137 = CARTESIAN_POINT ( 'NONE',  ( 16.52544592524342804, -4.483927247898539470, 63.54057627198103830 ) ) ;
#174138 = CARTESIAN_POINT ( 'NONE',  ( -12.06949235617739369, -12.14591786802326823, 74.37609039468568994 ) ) ;
#174140 = CARTESIAN_POINT ( 'NONE',  ( -5.049401038298153566, 19.05341960407611168, 50.20724293864770260 ) ) ;
#174139 = CARTESIAN_POINT ( 'NONE',  ( 10.72451020669898902, -18.67979575497178502, 112.9155762719810383 ) ) ;
#174141 = CARTESIAN_POINT ( 'NONE',  ( -19.03943276465977164, 0.05219959533909376836, 56.24890960531435979 ) ) ;
#174142 = CARTESIAN_POINT ( 'NONE',  ( 4.379528057220092307, 16.55341960407617563, 72.29275706135236135 ) ) ;
#174143 = CARTESIAN_POINT ( 'NONE',  ( -5.359611314223446995E-15, 29.16686587814335496, 144.8750000027311557 ) ) ;
#174144 = CARTESIAN_POINT ( 'NONE',  ( 28.82186960331498327, 2.781578969918950771E-14, 145.2500000054623683 ) ) ;
#174145 = ORIENTED_EDGE ( 'NONE', *, *, #149169, .T. ) ;
#174146 = CARTESIAN_POINT ( 'NONE',  ( -18.67979575497193778, 10.72451020669871902, 108.3344237280190185 ) ) ;
#174147 = CARTESIAN_POINT ( 'NONE',  ( 13.89961937509977652, -13.97604488694527269, 28.12390960531435624 ) ) ;
#174148 = ORIENTED_EDGE ( 'NONE', *, *, #144467, .T. ) ;
#174149 = CARTESIAN_POINT ( 'NONE',  ( -5.049401038297874678, -19.05341960407617918, 104.7927570613523471 ) ) ;
#174151 = CARTESIAN_POINT ( 'NONE',  ( -15.80617190586745835, -15.72974639402198527, 46.87390960531435979 ) ) ;
#174150 = CIRCLE ( 'NONE', #35432, 7.500000000000007105 ) ;
#174153 = CARTESIAN_POINT ( 'NONE',  ( 14.34966873604972726, -8.224510206698740333, 25.83442372801901499 ) ) ;
#174152 = CARTESIAN_POINT ( 'NONE',  ( 13.97604488694548053, -13.89961937509957401, 45.62609039468566863 ) ) ;
#174154 = CARTESIAN_POINT ( 'NONE',  ( -13.89961937509977652, 13.97604488694528158, 45.62390960531433848 ) ) ;
#174155 = CARTESIAN_POINT ( 'NONE',  ( -19.03943276465977164, 0.05219959533909376836, 56.24890960531435979 ) ) ;
#174156 = CARTESIAN_POINT ( 'NONE',  ( -21.53943276465977519, 0.05219959533907696930, 81.24890960531436690 ) ) ;
#174157 = CARTESIAN_POINT ( 'NONE',  ( -13.97604488694527625, -13.89961937509977652, 106.8739096053143669 ) ) ;
#174158 = EDGE_CURVE ( 'NONE', #142736, #127046, #199309, .T. ) ;
#174159 = CARTESIAN_POINT ( 'NONE',  ( -13.89961937509977652, 13.97604488694528158, 45.62390960531433848 ) ) ;
#174160 = DIRECTION ( 'NONE',  ( 0.000000000000000000, 0.000000000000000000, -1.000000000000000000 ) ) ;
#174161 = CARTESIAN_POINT ( 'NONE',  ( 19.05341960407617918, -5.049401038297876454, 101.0427570613523045 ) ) ;
#174162 = CARTESIAN_POINT ( 'NONE',  ( 12.06949235617757843, -12.14591786802309237, 63.12390960531435979 ) ) ;
#174163 = CARTESIAN_POINT ( 'NONE',  ( 16.51473224551083163, -9.474510206698727899, 30.83442372801900433 ) ) ;
#174164 = CARTESIAN_POINT ( 'NONE',  ( -10.81492255796078084, -18.62759615963271287, 97.08224293864770971 ) ) ;
#174165 = CARTESIAN_POINT ( 'NONE',  ( 10.81492255796106328, -18.62759615963255655, 80.41775706135234714 ) ) ;
#174166 = CARTESIAN_POINT ( 'NONE',  ( 0.05219959533909260263, 19.03943276465977164, 24.99890960531435269 ) ) ;
#174167 = CARTESIAN_POINT ( 'NONE',  ( 5.823673210054444382, -21.52544592524334988, 75.20942372801901854 ) ) ;
#174169 = CARTESIAN_POINT ( 'NONE',  ( 21.55341960407619695, -5.719274019375665929, 81.04275706135236135 ) ) ;
#174168 = CARTESIAN_POINT ( 'NONE',  ( -4.483927247898539470, -16.52544592524342804, 22.29057627198102765 ) ) ;
#174170 = CARTESIAN_POINT ( 'NONE',  ( 5.049401038298161559, -19.05341960407611168, 67.70724293864769550 ) ) ;
#174171 = CARTESIAN_POINT ( 'NONE',  ( 5.719274019375673035, 21.55341960407619339, 47.29275706135234003 ) ) ;
#174172 = CARTESIAN_POINT ( 'NONE',  ( 13.89961937509977652, -13.97604488694527269, 83.12390960531436690 ) ) ;
#174173 = CARTESIAN_POINT ( 'NONE',  ( 8.314922557960818139, 14.29746914071049879, 99.58224293864770971 ) ) ;
#174174 = CARTESIAN_POINT ( 'NONE',  ( -16.52544592524342804, 4.483927247898546575, 56.04057627198102409 ) ) ;
#174175 = CARTESIAN_POINT ( 'NONE',  ( -18.62759615963270932, 10.81492255796079327, 65.83224293864769550 ) ) ;
#174176 = CARTESIAN_POINT ( 'NONE',  ( 5.153800228976335163, 19.02544592524342804, 79.79057627198102409 ) ) ;
#174177 = CARTESIAN_POINT ( 'NONE',  ( -15.80617190586745835, -15.72974639402198527, 81.87390960531435269 ) ) ;
#174178 = CARTESIAN_POINT ( 'NONE',  ( -19.03943276465977164, -0.05219959533935918106, 63.75109039468566863 ) ) ;
#174180 = CARTESIAN_POINT ( 'NONE',  ( -16.52544592524342804, 4.483927247898546575, 71.04057627198103830 ) ) ;
#174179 = CARTESIAN_POINT ( 'NONE',  ( -19.05341960407617918, 5.049401038297883559, 33.54275706135232582 ) ) ;
#174182 = CIRCLE ( 'NONE', #45021, 214.0437394197456342 ) ;
#174181 = CARTESIAN_POINT ( 'NONE',  ( 10.81492255796078972, 18.62759615963270932, 49.58224293864769550 ) ) ;
#174183 = CARTESIAN_POINT ( 'NONE',  ( 0.000000000000000000, 0.000000000000000000, 0.000000000000000000 ) ) ;
#174185 = CARTESIAN_POINT ( 'NONE',  ( -22.44159573604009950, -16.30477369853688430, 145.5750000027311728 ) ) ;
#174184 = CARTESIAN_POINT ( 'NONE',  ( 14.29746914071037800, 8.314922557961029526, 101.6677570613523613 ) ) ;
#174186 = CARTESIAN_POINT ( 'NONE',  ( 9.474510206698729675, 16.51473224551082808, 102.0844237280190043 ) ) ;
#174187 = CARTESIAN_POINT ( 'NONE',  ( -16.52544592524342804, 4.483927247898546575, 71.04057627198103830 ) ) ;
#174188 = CARTESIAN_POINT ( 'NONE',  ( -17.49999999999996447, 3.805241302050396346, 35.37352472782593082 ) ) ;
#174189 = CARTESIAN_POINT ( 'NONE',  ( 19.03943276465977164, -0.05219959533909143690, 58.74890960531435979 ) ) ;
#174190 = CARTESIAN_POINT ( 'NONE',  ( 4.379528057220339221, -16.55341960407611168, 47.70724293864770260 ) ) ;
#174191 = CARTESIAN_POINT ( 'NONE',  ( 9.564922557960805705, 16.46253265017160317, 104.5822429386476955 ) ) ;
#174193 = CARTESIAN_POINT ( 'NONE',  ( 19.02544592524343514, -5.153800228976328945, 63.54057627198103830 ) ) ;
#174192 = CARTESIAN_POINT ( 'NONE',  ( 13.89961937509957401, 13.97604488694547697, 81.87609039468564731 ) ) ;
#174194 = CARTESIAN_POINT ( 'NONE',  ( -16.46253265017160317, 9.564922557960807481, 80.83224293864769550 ) ) ;
#174195 = CARTESIAN_POINT ( 'NONE',  ( 5.049401038298161559, -19.05341960407611168, 87.70724293864769550 ) ) ;
#174196 = CARTESIAN_POINT ( 'NONE',  ( -21.52544592524343514, 5.823673210054127303, 66.04057627198103830 ) ) ;
#174197 = CARTESIAN_POINT ( 'NONE',  ( 16.52544592524335698, 4.483927247898782831, 61.45942372801901854 ) ) ;
#174198 = CARTESIAN_POINT ( 'NONE',  ( 16.46253265017146816, 9.564922557961045513, 101.6677570613523329 ) ) ;
#174199 = CARTESIAN_POINT ( 'NONE',  ( 13.97604488694527802, 13.89961937509977652, 54.37390960531435979 ) ) ;
#174200 = CARTESIAN_POINT ( 'NONE',  ( -0.05219959533907301413, -21.53943276465977519, 57.49890960531435979 ) ) ;
#174201 = CARTESIAN_POINT ( 'NONE',  ( -13.89961937509957401, -13.97604488694547875, 94.37609039468566152 ) ) ;
#174203 = CARTESIAN_POINT ( 'NONE',  ( -0.05219959533937732626, 21.53943276465977519, 42.50109039468567573 ) ) ;
#174202 = CARTESIAN_POINT ( 'NONE',  ( 16.53943276465976808, -0.05219959533910856209, 23.74890960531435269 ) ) ;
#174204 = CARTESIAN_POINT ( 'NONE',  ( -9.474510206698720793, -16.51473224551083518, 34.58442372801899722 ) ) ;
#174206 = CARTESIAN_POINT ( 'NONE',  ( 16.55341960407618274, -4.379528057220086978, 96.04275706135236135 ) ) ;
#174205 = CARTESIAN_POINT ( 'NONE',  ( 16.52544592524335698, 4.483927247898782831, 56.45942372801902565 ) ) ;
#174207 = CARTESIAN_POINT ( 'NONE',  ( 28.79475375365588619, 9.355982642739197885, 147.3656553485623704 ) ) ;
#174208 = CARTESIAN_POINT ( 'NONE',  ( -4.379528057220086978, -16.55341960407618274, 74.79275706135234714 ) ) ;
#174210 = CARTESIAN_POINT ( 'NONE',  ( 14.29746914071037800, 8.314922557961029526, 31.66775706135234358 ) ) ;
#174209 = CARTESIAN_POINT ( 'NONE',  ( 0.05219959533907565091, 21.53943276465977519, 24.99890960531435624 ) ) ;
#174211 = CARTESIAN_POINT ( 'NONE',  ( -13.97604488694527625, -13.89961937509977652, 41.87390960531435979 ) ) ;
#174212 = CARTESIAN_POINT ( 'NONE',  ( -0.05219959533909027116, -19.03943276465977164, 52.49890960531436690 ) ) ;
#174213 = CARTESIAN_POINT ( 'NONE',  ( 19.05341960407611168, 5.049401038298154454, 58.95724293864768129 ) ) ;
#174214 = CARTESIAN_POINT ( 'NONE',  ( 15.72974639402176855, 15.80617190586768217, 41.87609039468568284 ) ) ;
#174215 = CARTESIAN_POINT ( 'NONE',  ( 12.14591786802327356, -12.06949235617739191, 45.62609039468567573 ) ) ;
#174216 = CARTESIAN_POINT ( 'NONE',  ( 16.52544592524335698, 4.483927247898782831, 111.4594237280190328 ) ) ;
#174217 = CARTESIAN_POINT ( 'NONE',  ( -9.564922557960796823, -16.46253265017161027, 32.08224293864769550 ) ) ;
#174218 = CARTESIAN_POINT ( 'NONE',  ( -15.80617190586768217, 15.72974639402176855, 108.1260903946856757 ) ) ;
#174219 = CARTESIAN_POINT ( 'NONE',  ( 13.89961937509957401, 13.97604488694547697, 111.8760903946856757 ) ) ;
#174220 = CARTESIAN_POINT ( 'NONE',  ( -13.89961937509957401, -13.97604488694547875, 74.37609039468566152 ) ) ;
#174221 = CARTESIAN_POINT ( 'NONE',  ( 12.14591786802309770, 12.06949235617756955, 69.37390960531436690 ) ) ;
#174222 = CARTESIAN_POINT ( 'NONE',  ( 5.049401038298161559, -19.05341960407611168, 37.70724293864768839 ) ) ;
#174224 = LINE ( 'NONE', #51857, #182418 ) ;
#174223 = CARTESIAN_POINT ( 'NONE',  ( -9.564922557961040184, 16.46253265017147172, 77.91775706135234714 ) ) ;
#174225 = CARTESIAN_POINT ( 'NONE',  ( -21.55341960407619339, 5.719274019375674811, 73.54275706135234714 ) ) ;
#174226 = CARTESIAN_POINT ( 'NONE',  ( -12.14591786802326823, 12.06949235617739902, 38.12609039468567573 ) ) ;
#174227 = CARTESIAN_POINT ( 'NONE',  ( 16.36317988757058828, 7.306389748694952502, 38.40210391636775711 ) ) ;
#174228 = CARTESIAN_POINT ( 'NONE',  ( 10.81492255796078972, 18.62759615963270932, 34.58224293864770260 ) ) ;
#174229 = CARTESIAN_POINT ( 'NONE',  ( 0.05219959533934541429, -16.53943276465976808, 20.00109039468568639 ) ) ;
#174230 = CARTESIAN_POINT ( 'NONE',  ( -5.000000000000000000, -116.8122400552013431, 54.87277500418469600 ) ) ;
#174231 = CARTESIAN_POINT ( 'NONE',  ( -0.05219959533936034679, 19.03943276465977164, 27.50109039468566507 ) ) ;
#174232 = DIRECTION ( 'NONE',  ( -3.709348145883536076E-20, 0.000000000000000000, 1.000000000000000000 ) ) ;
#174233 = CARTESIAN_POINT ( 'NONE',  ( -5.049401038298153566, 19.05341960407611168, 45.20724293864769550 ) ) ;
#174234 = CARTESIAN_POINT ( 'NONE',  ( 1.300000000000000044, -0.7216878364870319418, 1.249999999999999778 ) ) ;
#174235 = CARTESIAN_POINT ( 'NONE',  ( 5.153800228976335163, 19.02544592524342804, 64.79057627198100988 ) ) ;
#174236 = CARTESIAN_POINT ( 'NONE',  ( -19.36337904590693526, 5.499999999999952927, 100.4149413749561859 ) ) ;
#174237 = EDGE_CURVE ( 'NONE', #28437, #123075, #154255, .T. ) ;
#174238 = CARTESIAN_POINT ( 'NONE',  ( -16.46253265017146816, -9.564922557961047289, 19.16775706135233293 ) ) ;
#174239 = CARTESIAN_POINT ( 'NONE',  ( -14.34966873604972548, 8.224510206698743886, 113.3344237280190328 ) ) ;
#174240 = CARTESIAN_POINT ( 'NONE',  ( -19.05341960407611168, -5.049401038298163336, 36.45724293864766707 ) ) ;
#174241 = CARTESIAN_POINT ( 'NONE',  ( 19.05341960407611168, 5.049401038298154454, 98.95724293864766707 ) ) ;
#174242 = CARTESIAN_POINT ( 'NONE',  ( -21.53943276465977519, -0.05219959533937600094, 73.75109039468567573 ) ) ;
#174243 = CARTESIAN_POINT ( 'NONE',  ( 13.97604488694527802, 13.89961937509977652, 44.37390960531435269 ) ) ;
#174244 = CARTESIAN_POINT ( 'NONE',  ( 0.05219959533937995610, -21.53943276465977519, 60.00109039468568284 ) ) ;
#174246 = CARTESIAN_POINT ( 'NONE',  ( 18.67979575497178502, 10.72451020669898547, 24.16557627198103120 ) ) ;
#174245 = CARTESIAN_POINT ( 'NONE',  ( -0.05219959533936034679, 19.03943276465977164, 97.50109039468567573 ) ) ;
#174247 = CARTESIAN_POINT ( 'NONE',  ( 13.89961937509977652, -13.97604488694527269, 38.12390960531436690 ) ) ;
#174248 = CARTESIAN_POINT ( 'NONE',  ( 18.62759615963271287, -10.81492255796078972, 108.3322429386477097 ) ) ;
#174249 = CARTESIAN_POINT ( 'NONE',  ( 13.97604488694548053, -13.89961937509957401, 40.62609039468564731 ) ) ;
#174250 = CARTESIAN_POINT ( 'NONE',  ( 4.379528057220339221, -16.55341960407611168, 107.7072429386476955 ) ) ;
#174251 = CARTESIAN_POINT ( 'NONE',  ( 5.153800228976335163, 19.02544592524342804, 64.79057627198100988 ) ) ;
#174252 = CARTESIAN_POINT ( 'NONE',  ( -4.379528057220086978, -16.55341960407618274, 19.79275706135235069 ) ) ;
#174253 = CARTESIAN_POINT ( 'NONE',  ( 16.53943276465976808, -0.05219959533910856209, 73.74890960531433848 ) ) ;
#174254 = CARTESIAN_POINT ( 'NONE',  ( 13.97604488694527802, 13.89961937509977652, 114.3739096053143669 ) ) ;
#174255 = CARTESIAN_POINT ( 'NONE',  ( 16.46253265017146816, 9.564922557961045513, 91.66775706135234714 ) ) ;
#174256 = CARTESIAN_POINT ( 'NONE',  ( 5.719274019375991003, -21.55341960407610458, 87.70724293864769550 ) ) ;
#174257 = CARTESIAN_POINT ( 'NONE',  ( -21.55341960407619339, 5.719274019375674811, 58.54275706135235424 ) ) ;
#174258 = CARTESIAN_POINT ( 'NONE',  ( -12.14591786802326823, 12.06949235617739902, 53.12609039468568284 ) ) ;
#174260 = CARTESIAN_POINT ( 'NONE',  ( 18.67979575497194134, -10.72451020669871369, 45.83442372801901854 ) ) ;
#174259 = CARTESIAN_POINT ( 'NONE',  ( -12.06949235617739369, -12.14591786802326823, 54.37609039468568994 ) ) ;
#174261 = CARTESIAN_POINT ( 'NONE',  ( 21.52544592524344225, -5.823673210054117533, 58.54057627198103120 ) ) ;
#174262 = CARTESIAN_POINT ( 'NONE',  ( 5.153800228976335163, 19.02544592524342804, 49.79057627198100988 ) ) ;
#174263 = CARTESIAN_POINT ( 'NONE',  ( 37.99999999999999289, 2.893978650043524126E-14, -4.749999994537627224 ) ) ;
#174264 = CARTESIAN_POINT ( 'NONE',  ( -8.314922557961024197, 14.29746914071037800, 72.91775706135234714 ) ) ;
#174265 = CARTESIAN_POINT ( 'NONE',  ( -0.05219959533907301413, -21.53943276465977519, 107.4989096053143669 ) ) ;
#174266 = CARTESIAN_POINT ( 'NONE',  ( -4.379528057220328563, 16.55341960407611168, 55.20724293864770260 ) ) ;
#174267 = CARTESIAN_POINT ( 'NONE',  ( -16.52544592524335698, -4.483927247898792601, 58.95942372801902565 ) ) ;
#174268 = CARTESIAN_POINT ( 'NONE',  ( 9.474510206698729675, 16.51473224551082808, 97.08442372801900433 ) ) ;
#174269 = CARTESIAN_POINT ( 'NONE',  ( 10.81492255796078972, 18.62759615963270932, 94.58224293864769550 ) ) ;
#174270 = CARTESIAN_POINT ( 'NONE',  ( 0.05219959533910956823, 16.53943276465976808, 44.99890960531435979 ) ) ;
#174271 = VERTEX_POINT ( 'NONE', #128862 ) ;
#174272 = CARTESIAN_POINT ( 'NONE',  ( 18.22780087662122384, -5.500000000000022204, 91.01540105326107266 ) ) ;
#174273 = CARTESIAN_POINT ( 'NONE',  ( 18.67979575497178502, 10.72451020669898547, 74.16557627198102409 ) ) ;
#174274 = CARTESIAN_POINT ( 'NONE',  ( 12.14591786802309770, 12.06949235617756955, 29.37390960531435269 ) ) ;
#174275 = VERTEX_POINT ( 'NONE', #33894 ) ;
#174276 = CARTESIAN_POINT ( 'NONE',  ( -17.49999999999998934, -5.500000000000015987, 56.28230962303566542 ) ) ;
#174277 = CARTESIAN_POINT ( 'NONE',  ( -0.05219959533907301413, -21.53943276465977519, 107.4989096053143669 ) ) ;
#174278 = CARTESIAN_POINT ( 'NONE',  ( -21.52544592524334988, -5.823673210054445271, 23.95942372801901143 ) ) ;
#174279 = CARTESIAN_POINT ( 'NONE',  ( -14.29746914071049879, 8.314922557960819915, 35.83224293864768839 ) ) ;
#174280 = CARTESIAN_POINT ( 'NONE',  ( -4.379528057220086978, -16.55341960407618274, 44.79275706135234714 ) ) ;
#174281 = CARTESIAN_POINT ( 'NONE',  ( -19.02544592524342804, 5.153800228976336051, 51.04057627198103120 ) ) ;
#174282 = CARTESIAN_POINT ( 'NONE',  ( -5.153800228976328057, -19.02544592524343514, 77.29057627198099567 ) ) ;
#174283 = CARTESIAN_POINT ( 'NONE',  ( 21.55341960407610458, 5.719274019375980345, 28.95724293864769905 ) ) ;
#174284 = CARTESIAN_POINT ( 'NONE',  ( -24.48191864108932592, -29.02791343562081394, -16.65471697698749409 ) ) ;
#174285 = CARTESIAN_POINT ( 'NONE',  ( -8.224510206698735004, -14.34966873604973081, 29.58442372801901854 ) ) ;
#174286 = CARTESIAN_POINT ( 'NONE',  ( -5.049401038297874678, -19.05341960407617918, 49.79275706135231871 ) ) ;
#174287 = CARTESIAN_POINT ( 'NONE',  ( -18.62759615963270932, 10.81492255796079327, 95.83224293864770971 ) ) ;
#174288 = CARTESIAN_POINT ( 'NONE',  ( 8.314922557960818139, 14.29746914071049879, 29.58224293864769905 ) ) ;
#174289 = CARTESIAN_POINT ( 'NONE',  ( 9.474510206698971260, -16.51473224551069308, 82.91557627198103830 ) ) ;
#174290 = CARTESIAN_POINT ( 'NONE',  ( -10.81492255796078084, -18.62759615963271287, 62.08224293864769550 ) ) ;
#174292 = CARTESIAN_POINT ( 'NONE',  ( 14.29746914071037800, 8.314922557961029526, 21.66775706135235069 ) ) ;
#174291 = CARTESIAN_POINT ( 'NONE',  ( 15.72974639402199770, -15.80617190586745480, 88.12390960531436690 ) ) ;
#174293 = CARTESIAN_POINT ( 'NONE',  ( 0.05219959533907565091, 21.53943276465977519, 24.99890960531435624 ) ) ;
#174294 = CARTESIAN_POINT ( 'NONE',  ( -21.55341960407619339, 5.719274019375674811, 73.54275706135234714 ) ) ;
#174295 = CARTESIAN_POINT ( 'NONE',  ( 16.51473224551069308, 9.474510206698969483, 74.16557627198103830 ) ) ;
#174296 = VECTOR ( 'NONE', #180566, 999.9999999999997726 ) ;
#174297 = CARTESIAN_POINT ( 'NONE',  ( 13.89961937509977652, -13.97604488694527269, 23.12390960531436335 ) ) ;
#174298 = CARTESIAN_POINT ( 'NONE',  ( -16.46253265017160317, 9.564922557960807481, 80.83224293864769550 ) ) ;
#174299 = CARTESIAN_POINT ( 'NONE',  ( -16.55341960407611168, -4.379528057220339221, 96.45724293864770971 ) ) ;
#174300 = EDGE_LOOP ( 'NONE', ( #184936, #195638, #185696, #1266 ) ) ;
#174301 = CARTESIAN_POINT ( 'NONE',  ( -19.02544592524334988, -5.153800228976617603, 98.95942372801900433 ) ) ;
#174302 = LINE ( 'NONE', #35771, #163392 ) ;
#174303 = CARTESIAN_POINT ( 'NONE',  ( 13.97604488694527802, 13.89961937509977652, 79.37390960531435269 ) ) ;
#174305 = CARTESIAN_POINT ( 'NONE',  ( 13.89961937509977652, -13.97604488694527269, 113.1239096053143527 ) ) ;
#174304 = CARTESIAN_POINT ( 'NONE',  ( -18.67979575497193778, 10.72451020669871902, 83.33442372801903275 ) ) ;
#174306 = CARTESIAN_POINT ( 'NONE',  ( 8.314922557961029526, -14.29746914071037800, 80.41775706135234714 ) ) ;
#174307 = CARTESIAN_POINT ( 'NONE',  ( -29.03295818733087330, 0.6278704076488079711, -49.50940399778497181 ) ) ;
#174308 = CARTESIAN_POINT ( 'NONE',  ( 5.153800228976615827, -19.02544592524334988, 60.20942372801899012 ) ) ;
#174309 = CARTESIAN_POINT ( 'NONE',  ( -9.474510206698720793, -16.51473224551083518, 19.58442372801899722 ) ) ;
#174310 = CARTESIAN_POINT ( 'NONE',  ( 37.07039049082555948, 4.937524616431669067, 42.55055737136174088 ) ) ;
#174311 = CARTESIAN_POINT ( 'NONE',  ( 13.89961937509977652, -13.97604488694527269, 28.12390960531435624 ) ) ;
#174312 = CARTESIAN_POINT ( 'NONE',  ( 8.314922557960818139, 14.29746914071049879, 29.58224293864769905 ) ) ;
#174313 = CARTESIAN_POINT ( 'NONE',  ( -35.09697802211634610, -5.650142709571460031, 40.04346530744797406 ) ) ;
#174314 = CARTESIAN_POINT ( 'NONE',  ( 8.314922557961029526, -14.29746914071037800, 100.4177570613523471 ) ) ;
#174315 = CARTESIAN_POINT ( 'NONE',  ( 22.44948314067158890, -20.33105923352922773, -51.12866626710398776 ) ) ;
#174316 = CARTESIAN_POINT ( 'NONE',  ( 8.224510206698742110, 14.34966873604972548, 87.08442372801901854 ) ) ;
#174317 = CARTESIAN_POINT ( 'NONE',  ( -16.51473224551069308, -9.474510206698971260, 21.66557627198102765 ) ) ;
#174318 = CARTESIAN_POINT ( 'NONE',  ( 15.72974639402176855, 15.80617190586768217, 96.87609039468568994 ) ) ;
#174319 = CARTESIAN_POINT ( 'NONE',  ( -19.05341960407617563, 5.049401038297882671, 103.5427570613523329 ) ) ;
#174320 = CARTESIAN_POINT ( 'NONE',  ( 21.53943276465977519, 0.05219959533937863772, 71.25109039468568994 ) ) ;
#174321 = CARTESIAN_POINT ( 'NONE',  ( -16.46253265017146816, -9.564922557961047289, 44.16775706135232582 ) ) ;
#174322 = CARTESIAN_POINT ( 'NONE',  ( -19.05341960407611168, -5.049401038298163336, 81.45724293864769550 ) ) ;
#174323 = CARTESIAN_POINT ( 'NONE',  ( 5.153800228976335163, 19.02544592524342804, 74.79057627198103830 ) ) ;
#174324 = CARTESIAN_POINT ( 'NONE',  ( -7.220908937439997288, 2.044528755335752734, 8.410814283099849575 ) ) ;
#174325 = CIRCLE ( 'NONE', #125975, 69.99999999999997158 ) ;
#174326 = CARTESIAN_POINT ( 'NONE',  ( -10.81492255796078084, -18.62759615963271287, 42.08224293864769550 ) ) ;
#174327 = CARTESIAN_POINT ( 'NONE',  ( -19.05341960407611168, -5.049401038298163336, 46.45724293864768129 ) ) ;
#174328 = CARTESIAN_POINT ( 'NONE',  ( -4.483927247898782831, 16.52544592524335698, 82.70942372801900433 ) ) ;
#174329 = ORIENTED_EDGE ( 'NONE', *, *, #152669, .T. ) ;
#174331 = CARTESIAN_POINT ( 'NONE',  ( -36.91746825000001309, 11.99521256947798342, -4.724999997268811924 ) ) ;
#174330 = CARTESIAN_POINT ( 'NONE',  ( 14.29746914071049879, -8.314922557960816363, 83.33224293864769550 ) ) ;
#174332 = CARTESIAN_POINT ( 'NONE',  ( -8.224510206698735004, -14.34966873604973081, 34.58442372801900433 ) ) ;
#174333 = CARTESIAN_POINT ( 'NONE',  ( 16.55341960407611168, 4.379528057220329451, 108.9572429386476955 ) ) ;
#174334 = CARTESIAN_POINT ( 'NONE',  ( -13.97604488694547697, 13.89961937509957934, 73.12609039468568994 ) ) ;
#174335 = CARTESIAN_POINT ( 'NONE',  ( -14.29746914071049879, 8.314922557960819915, 75.83224293864769550 ) ) ;
#174336 = CARTESIAN_POINT ( 'NONE',  ( -15.80617190586768217, 15.72974639402176855, 28.12609039468568284 ) ) ;
#174338 = CARTESIAN_POINT ( 'NONE',  ( -10.72451020669898014, 18.67979575497178502, 95.41557627198102409 ) ) ;
#174337 = DIRECTION ( 'NONE',  ( -1.000000000000000000, -0.000000000000000000, -0.000000000000000000 ) ) ;
#174339 = CARTESIAN_POINT ( 'NONE',  ( 0.05219959533909260263, 19.03943276465977164, 109.9989096053143669 ) ) ;
#174340 = CARTESIAN_POINT ( 'NONE',  ( 16.53943276465976808, -0.05219959533910856209, 73.74890960531433848 ) ) ;
#174341 = CARTESIAN_POINT ( 'NONE',  ( 27.73791293434951655, -28.12602025316063603, -18.50562026186076992 ) ) ;
#174342 = CARTESIAN_POINT ( 'NONE',  ( -19.02544592524342804, 5.153800228976336051, 41.04057627198103120 ) ) ;
#174343 = CARTESIAN_POINT ( 'NONE',  ( -36.91746825000000598, 2.428612866367529932E-14, -2.624999997268813168 ) ) ;
#174344 = CARTESIAN_POINT ( 'NONE',  ( 19.03943276465977164, 0.05219959533936151252, 81.25109039468567573 ) ) ;
#174345 = CARTESIAN_POINT ( 'NONE',  ( -15.72974639402176322, -15.80617190586768395, 19.37609039468568639 ) ) ;
#174346 = CARTESIAN_POINT ( 'NONE',  ( -16.46253265017160317, 9.564922557960807481, 75.83224293864769550 ) ) ;
#174347 = CARTESIAN_POINT ( 'NONE',  ( -13.89961937509957401, -13.97604488694547875, 54.37609039468565442 ) ) ;
#174348 = CARTESIAN_POINT ( 'NONE',  ( -16.51473224551069308, -9.474510206698971260, 46.66557627198102409 ) ) ;
#174349 = CARTESIAN_POINT ( 'NONE',  ( 16.52544592524342804, -4.483927247898539470, 63.54057627198103830 ) ) ;
#174350 = CARTESIAN_POINT ( 'NONE',  ( 12.06949235617757843, -12.14591786802309237, 48.12390960531436690 ) ) ;
#174351 = CARTESIAN_POINT ( 'NONE',  ( 9.474510206698971260, -16.51473224551069308, 77.91557627198103830 ) ) ;
#174352 = CARTESIAN_POINT ( 'NONE',  ( -15.80617190586745835, -15.72974639402198527, 81.87390960531435269 ) ) ;
#174354 = CARTESIAN_POINT ( 'NONE',  ( 16.51473224551069308, 9.474510206698969483, 69.16557627198102409 ) ) ;
#174353 = B_SPLINE_CURVE_WITH_KNOTS ( 'NONE', 3,
 ( #98391, #36729, #113569, #64103, #158097, #4395, #160089, #47953, #140936, #125770, #21576, #81232, #112582, #171288, #127745, #188448, #49928, #109604, #128738, #82223, #32775, #187470, #173278, #83234, #80251, #19589, #110592, #142913, #63099, #172274, #143913, #174276 ),
 .UNSPECIFIED., .F., .F.,
 ( 4, 2, 2, 2, 2, 2, 2, 2, 2, 2, 2, 2, 2, 2, 2, 4 ),
 ( 2.969368287472575283E-17, 0.0003712461730037064562, 0.0007424923460073832053, 0.001113738519011060009, 0.001484984692014736703, 0.002227477038022087925, 0.002598723211025753127, 0.002969969384029418763, 0.003341215557033083098, 0.003712461730036748734, 0.004083707903040413069, 0.004454954076044077838, 0.004826200249047743474, 0.005197446422051408242, 0.005568692595055073011, 0.005939938768058737779 ),
 .UNSPECIFIED. ) ;
#174355 = CARTESIAN_POINT ( 'NONE',  ( -5.823673210054116645, -21.52544592524344225, 77.29057627198102409 ) ) ;
#174356 = CARTESIAN_POINT ( 'NONE',  ( 18.62759615963255655, 10.81492255796105972, 111.6677570613523613 ) ) ;
#174359 = CARTESIAN_POINT ( 'NONE',  ( -4.379528057220328563, 16.55341960407611168, 90.20724293864770971 ) ) ;
#174358 = CARTESIAN_POINT ( 'NONE',  ( 14.29746914071037800, 8.314922557961029526, 111.6677570613523613 ) ) ;
#174357 = CARTESIAN_POINT ( 'NONE',  ( -19.05341960407611168, -5.049401038298163336, 21.45724293864768839 ) ) ;
#174360 = CARTESIAN_POINT ( 'NONE',  ( -5.153800228976607833, 19.02544592524334988, 102.7094237280189759 ) ) ;
#174361 = EDGE_LOOP ( 'NONE', ( #50361, #194861, #78872, #120905 ) ) ;
#174362 = CARTESIAN_POINT ( 'NONE',  ( -5.823673210054431948, 21.52544592524334988, 22.70942372801901499 ) ) ;
#174363 = CARTESIAN_POINT ( 'NONE',  ( 19.03943276465977164, 0.05219959533936151252, 51.25109039468567573 ) ) ;
#174364 = CARTESIAN_POINT ( 'NONE',  ( -0.05219959533934338120, 16.53943276465976808, 112.5010903946857042 ) ) ;
#174365 = CARTESIAN_POINT ( 'NONE',  ( -19.05341960407617563, 5.049401038297882671, 48.54275706135233293 ) ) ;
#174366 = CARTESIAN_POINT ( 'NONE',  ( -9.474510206698964154, 16.51473224551069663, 105.4155762719810383 ) ) ;
#174367 = CARTESIAN_POINT ( 'NONE',  ( -12.06949235617756955, 12.14591786802309770, 60.62390960531437401 ) ) ;
#174368 = CARTESIAN_POINT ( 'NONE',  ( 17.50000000000000000, -5.500000000000000888, 120.0000000000000142 ) ) ;
#174369 = CARTESIAN_POINT ( 'NONE',  ( 5.049401038298161559, -19.05341960407611168, 37.70724293864768839 ) ) ;
#174370 = CARTESIAN_POINT ( 'NONE',  ( -10.81492255796105439, 18.62759615963255655, 112.9177570613523329 ) ) ;
#174371 = CARTESIAN_POINT ( 'NONE',  ( -16.55341960407617563, 4.379528057220093196, 93.54275706135234714 ) ) ;
#174372 = CARTESIAN_POINT ( 'NONE',  ( 10.81492255796106328, -18.62759615963255655, 45.41775706135234003 ) ) ;
#174373 = CARTESIAN_POINT ( 'NONE',  ( 4.379528057220092307, 16.55341960407617563, 37.29275706135235424 ) ) ;
#174374 = CARTESIAN_POINT ( 'NONE',  ( 18.67979575497178502, 10.72451020669898547, 24.16557627198103120 ) ) ;
#174375 = CARTESIAN_POINT ( 'NONE',  ( 19.02544592524343514, -5.153800228976328945, 58.54057627198102409 ) ) ;
#174376 = CARTESIAN_POINT ( 'NONE',  ( 0.05219959533909260263, 19.03943276465977164, 59.99890960531436690 ) ) ;
#174377 = CARTESIAN_POINT ( 'NONE',  ( -0.05219959533934338120, 16.53943276465976808, 52.50109039468567573 ) ) ;
#174378 = CARTESIAN_POINT ( 'NONE',  ( 8.314922557960818139, 14.29746914071049879, 99.58224293864770971 ) ) ;
#174379 = CARTESIAN_POINT ( 'NONE',  ( 14.29746914071049879, -8.314922557960816363, 23.33224293864769194 ) ) ;
#174380 = LINE ( 'NONE', #54535, #99023 ) ;
#174383 = CARTESIAN_POINT ( 'NONE',  ( -13.97604488694527625, -13.89961937509977652, 76.87390960531433848 ) ) ;
#174382 = CARTESIAN_POINT ( 'NONE',  ( -16.51473224551069308, -9.474510206698971260, 91.66557627198103830 ) ) ;
#174381 = CARTESIAN_POINT ( 'NONE',  ( -21.53943276465977519, -0.05219959533937600094, 58.75109039468568994 ) ) ;
#174384 = CARTESIAN_POINT ( 'NONE',  ( -19.02544592524342804, 5.153800228976336051, 96.04057627198103830 ) ) ;
#174385 = CARTESIAN_POINT ( 'NONE',  ( -12.06949235617756955, 12.14591786802309770, 40.62390960531435269 ) ) ;
#174386 = CARTESIAN_POINT ( 'NONE',  ( -12.14591786802326823, 12.06949235617739902, 108.1260903946856757 ) ) ;
#174387 = CARTESIAN_POINT ( 'NONE',  ( -0.05219959533910754901, -16.53943276465976808, 32.49890960531435979 ) ) ;
#174388 = EDGE_LOOP ( 'NONE', ( #133075, #68495, #162845, #111019 ) ) ;
#174389 = DIRECTION ( 'NONE',  ( -0.000000000000000000, -0.000000000000000000, 1.000000000000000000 ) ) ;
#174390 = CARTESIAN_POINT ( 'NONE',  ( -16.51473224551082808, 9.474510206698731452, 43.33442372801900433 ) ) ;
#174391 = CARTESIAN_POINT ( 'NONE',  ( 19.02544592524343514, -5.153800228976328945, 68.54057627198103830 ) ) ;
#174392 = CARTESIAN_POINT ( 'NONE',  ( -19.03943276465977164, -0.05219959533935918106, 58.75109039468566863 ) ) ;
#174393 = CARTESIAN_POINT ( 'NONE',  ( 36.91746824999999177, 2.880721459617395097E-14, -10.12499999726881583 ) ) ;
#174394 = CARTESIAN_POINT ( 'NONE',  ( -3.573655867282028392E-15, 2.428612866367529932E-14, 0.000000000000000000 ) ) ;
#174396 = CARTESIAN_POINT ( 'NONE',  ( -16.52544592524335698, -4.483927247898792601, 63.95942372801901854 ) ) ;
#174395 = CARTESIAN_POINT ( 'NONE',  ( 19.03943276465977164, 0.05219959533936151252, 86.25109039468567573 ) ) ;
#174397 = CARTESIAN_POINT ( 'NONE',  ( 17.12812012977026654, 6.668231424565988164, 93.85948759323144941 ) ) ;
#174398 = CARTESIAN_POINT ( 'NONE',  ( 5.153800228976335163, 19.02544592524342804, 99.79057627198102409 ) ) ;
#174399 = CARTESIAN_POINT ( 'NONE',  ( 0.05219959533937995610, -21.53943276465977519, 35.00109039468568284 ) ) ;
#174400 = CARTESIAN_POINT ( 'NONE',  ( -13.97604488694547697, 13.89961937509957934, 93.12609039468566152 ) ) ;
#174402 = CARTESIAN_POINT ( 'NONE',  ( -13.89961937509977652, 13.97604488694528158, 50.62390960531435979 ) ) ;
#174401 = CARTESIAN_POINT ( 'NONE',  ( 19.02544592524343514, -5.153800228976328945, 113.5405762719810241 ) ) ;
#174403 = EDGE_CURVE ( 'NONE', #194062, #91449, #147333, .T. ) ;
#174404 = CARTESIAN_POINT ( 'NONE',  ( -5.049401038298153566, 19.05341960407611168, 90.20724293864766707 ) ) ;
#174406 = CARTESIAN_POINT ( 'NONE',  ( 13.97604488694527802, 13.89961937509977652, 49.37390960531434558 ) ) ;
#174405 = CARTESIAN_POINT ( 'NONE',  ( 16.53943276465976808, -0.05219959533910856209, 53.74890960531437401 ) ) ;
#174407 = CARTESIAN_POINT ( 'NONE',  ( 16.51473224551083163, -9.474510206698727899, 60.83442372801900433 ) ) ;
#174408 = CARTESIAN_POINT ( 'NONE',  ( -9.564922557961040184, 16.46253265017147172, 27.91775706135232582 ) ) ;
#174409 = CARTESIAN_POINT ( 'NONE',  ( -0.05219959533909027116, -19.03943276465977164, 72.49890960531435269 ) ) ;
#174410 = CARTESIAN_POINT ( 'NONE',  ( 21.52544592524344225, -5.823673210054117533, 58.54057627198103120 ) ) ;
#174412 = CARTESIAN_POINT ( 'NONE',  ( 21.52544592524334988, 5.823673210054432836, 111.4594237280190328 ) ) ;
#174411 = CARTESIAN_POINT ( 'NONE',  ( 4.483927247898545687, 16.52544592524342804, 64.79057627198103830 ) ) ;
#174413 = CARTESIAN_POINT ( 'NONE',  ( 28.81842663310012753, -24.98430004053103559, -10.97651405319417783 ) ) ;
#174414 = CARTESIAN_POINT ( 'NONE',  ( -0.05219959533907301413, -21.53943276465977519, 32.49890960531435979 ) ) ;
#174415 = CARTESIAN_POINT ( 'NONE',  ( -9.474510206698964154, 16.51473224551069663, 50.41557627198102409 ) ) ;
#174416 = CARTESIAN_POINT ( 'NONE',  ( -19.05341960407611168, -5.049401038298163336, 36.45724293864766707 ) ) ;
#174417 = CARTESIAN_POINT ( 'NONE',  ( -4.483927247898539470, -16.52544592524342804, 102.2905762719810383 ) ) ;
#174418 = CARTESIAN_POINT ( 'NONE',  ( 15.80617190586746368, 15.72974639402197994, 109.3739096053143811 ) ) ;
#174419 = CARTESIAN_POINT ( 'NONE',  ( 19.02544592524343514, -5.153800228976328945, 113.5405762719810241 ) ) ;
#174420 = CARTESIAN_POINT ( 'NONE',  ( -10.72451020669870658, -18.67979575497194134, 24.58442372801901499 ) ) ;
#174421 = CARTESIAN_POINT ( 'NONE',  ( -16.46253265017160317, 9.564922557960807481, 105.8322429386476955 ) ) ;
#174422 = CARTESIAN_POINT ( 'NONE',  ( -16.46253265017160317, 9.564922557960807481, 25.83224293864769194 ) ) ;
#174423 = CARTESIAN_POINT ( 'NONE',  ( -18.67979575497193778, 10.72451020669871902, 73.33442372801901854 ) ) ;
#174424 = CARTESIAN_POINT ( 'NONE',  ( -21.52544592524343514, 5.823673210054127303, 96.04057627198102409 ) ) ;
#174425 = CARTESIAN_POINT ( 'NONE',  ( 16.19135201231366139, -7.376712067591912003, 107.3131914594796825 ) ) ;
#174426 = CARTESIAN_POINT ( 'NONE',  ( 16.46253265017160672, -9.564922557960803928, 53.33224293864768839 ) ) ;
#174427 = CARTESIAN_POINT ( 'NONE',  ( 0.000000000000000000, -165.0000000000000000, 12.00000000000000355 ) ) ;
#174428 = CARTESIAN_POINT ( 'NONE',  ( -4.379528057220086978, -16.55341960407618274, 44.79275706135234714 ) ) ;
#174429 = CARTESIAN_POINT ( 'NONE',  ( 4.379528057220339221, -16.55341960407611168, 107.7072429386476955 ) ) ;
#174430 = CARTESIAN_POINT ( 'NONE',  ( 33.79565148458099344, -5.463178417057489966, 94.26852713616585788 ) ) ;
#174431 = CARTESIAN_POINT ( 'NONE',  ( -19.03943276465977164, 0.05219959533909376836, 56.24890960531435979 ) ) ;
#174432 = CARTESIAN_POINT ( 'NONE',  ( -12.14591786802309592, -12.06949235617757132, 96.87390960531436690 ) ) ;
#174433 = CARTESIAN_POINT ( 'NONE',  ( -18.62759615963270932, 10.81492255796079327, 45.83224293864769550 ) ) ;
#174434 = CARTESIAN_POINT ( 'NONE',  ( 4.379528057220339221, -16.55341960407611168, 67.70724293864769550 ) ) ;
#174435 = CARTESIAN_POINT ( 'NONE',  ( -5.049401038297874678, -19.05341960407617918, 109.7927570613523187 ) ) ;
#174436 = CARTESIAN_POINT ( 'NONE',  ( -21.55341960407619339, 5.719274019375674811, 88.54275706135236135 ) ) ;
#174437 = CARTESIAN_POINT ( 'NONE',  ( 16.79531203550647689, -7.028104445595604766, 76.24755011779559766 ) ) ;
#174438 = CARTESIAN_POINT ( 'NONE',  ( -12.06949235617739369, -12.14591786802326823, 94.37609039468568994 ) ) ;
#174439 = CARTESIAN_POINT ( 'NONE',  ( 4.379528057220339221, -16.55341960407611168, 42.70724293864770260 ) ) ;
#174440 = VECTOR ( 'NONE', #104694, 1000.000000000000000 ) ;
#174441 = CARTESIAN_POINT ( 'NONE',  ( -5.049401038298153566, 19.05341960407611168, 35.20724293864768839 ) ) ;
#174442 = CARTESIAN_POINT ( 'NONE',  ( 16.46253265017160672, -9.564922557960803928, 93.33224293864769550 ) ) ;
#174443 = CARTESIAN_POINT ( 'NONE',  ( -15.80617190586745835, -15.72974639402198527, 91.87390960531436690 ) ) ;
#174444 = CARTESIAN_POINT ( 'NONE',  ( -16.53943276465976808, -0.05219959533934237506, 33.75109039468568284 ) ) ;
#174446 = CARTESIAN_POINT ( 'NONE',  ( 0.05219959533937995610, -21.53943276465977519, 80.00109039468568994 ) ) ;
#174445 = CARTESIAN_POINT ( 'NONE',  ( -14.34966873604960291, -8.224510206698953496, 71.66557627198100988 ) ) ;
#174447 = CARTESIAN_POINT ( 'NONE',  ( 8.224510206698742110, 14.34966873604972548, 97.08442372801904696 ) ) ;
#174448 = CARTESIAN_POINT ( 'NONE',  ( -19.49401214000077331, 12.39993551617566681, 169.9999999999999716 ) ) ;
#174449 = CARTESIAN_POINT ( 'NONE',  ( -19.34837522270365895, -5.499999999999739764, 65.86337684832577111 ) ) ;
#174450 = CARTESIAN_POINT ( 'NONE',  ( -16.53943276465976808, 0.05219959533911058130, 26.24890960531435624 ) ) ;
#174451 = CARTESIAN_POINT ( 'NONE',  ( 0.05219959533934541429, -16.53943276465976808, 70.00109039468568994 ) ) ;
#174452 = CARTESIAN_POINT ( 'NONE',  ( 16.46253265017160672, -9.564922557960803928, 83.33224293864768129 ) ) ;
#174453 = CARTESIAN_POINT ( 'NONE',  ( 19.05341960407611168, 5.049401038298154454, 103.9572429386476671 ) ) ;
#174454 = CARTESIAN_POINT ( 'NONE',  ( 10.72451020669871369, 18.67979575497193778, 92.08442372801901854 ) ) ;
#174455 = CARTESIAN_POINT ( 'NONE',  ( -16.55341960407617563, 4.379528057220093196, 88.54275706135236135 ) ) ;
#174456 = CARTESIAN_POINT ( 'NONE',  ( 8.314922557960818139, 14.29746914071049879, 59.58224293864770260 ) ) ;
#174457 = CARTESIAN_POINT ( 'NONE',  ( 19.05341960407611168, 5.049401038298154454, 63.95724293864769550 ) ) ;
#174458 = ORIENTED_EDGE ( 'NONE', *, *, #140456, .T. ) ;
#174459 = CARTESIAN_POINT ( 'NONE',  ( -16.51473224551082808, 9.474510206698731452, 103.3344237280190043 ) ) ;
#174460 = CARTESIAN_POINT ( 'NONE',  ( 16.51473224551069308, 9.474510206698969483, 29.16557627198103475 ) ) ;
#174461 = CARTESIAN_POINT ( 'NONE',  ( 16.51473224551069308, 9.474510206698969483, 84.16557627198102409 ) ) ;
#174463 = CARTESIAN_POINT ( 'NONE',  ( -36.91746825000000598, 2.428612866367529932E-14, -6.624999997268814056 ) ) ;
#174462 = CARTESIAN_POINT ( 'NONE',  ( 9.564922557961047289, -16.46253265017146816, 110.4177570613523471 ) ) ;
#174464 = CARTESIAN_POINT ( 'NONE',  ( -5.049401038297874678, -19.05341960407617918, 19.79275706135233293 ) ) ;
#174465 = CARTESIAN_POINT ( 'NONE',  ( 14.34966873604972726, -8.224510206698740333, 75.83442372801900433 ) ) ;
#174466 = CARTESIAN_POINT ( 'NONE',  ( -16.51473224551082808, 9.474510206698731452, 108.3344237280190043 ) ) ;
#174467 = CARTESIAN_POINT ( 'NONE',  ( 4.379528057220339221, -16.55341960407611168, 112.7072429386476955 ) ) ;
#174468 = CARTESIAN_POINT ( 'NONE',  ( 14.34966873604972726, -8.224510206698740333, 65.83442372801900433 ) ) ;
#174469 = CARTESIAN_POINT ( 'NONE',  ( -16.53943276465976808, -0.05219959533934237506, 48.75109039468568284 ) ) ;
#174470 = CARTESIAN_POINT ( 'NONE',  ( -9.564922557960796823, -16.46253265017161027, 22.08224293864768839 ) ) ;
#174471 = CARTESIAN_POINT ( 'NONE',  ( 19.02544592524334988, 5.153800228976608722, 71.45942372801900433 ) ) ;
#174472 = CARTESIAN_POINT ( 'NONE',  ( 15.80617190586769283, -15.72974639402175789, 105.6260903946856899 ) ) ;
#174473 = CARTESIAN_POINT ( 'NONE',  ( 5.153800228976335163, 19.02544592524342804, 29.79057627198102409 ) ) ;
#174474 = CARTESIAN_POINT ( 'NONE',  ( -5.049401038298153566, 19.05341960407611168, 75.20724293864769550 ) ) ;
#174475 = CARTESIAN_POINT ( 'NONE',  ( 12.14591786802309770, 12.06949235617756955, 69.37390960531436690 ) ) ;
#174476 = TOROIDAL_SURFACE ( 'NONE', #19453, 2.700000000000000622, 0.2000000000000000111 ) ;
#174477 = ADVANCED_FACE ( 'NONE', ( #6519 ), #160217, .F. ) ;
#174478 = CARTESIAN_POINT ( 'NONE',  ( 9.474510206698729675, 16.51473224551082808, 37.08442372801899722 ) ) ;
#174479 = CARTESIAN_POINT ( 'NONE',  ( 18.67979575497178502, 10.72451020669898547, 39.16557627198102409 ) ) ;
#174480 = CARTESIAN_POINT ( 'NONE',  ( 5.153800228976615827, -19.02544592524334988, 20.20942372801899722 ) ) ;
#174481 = CARTESIAN_POINT ( 'NONE',  ( -9.564922557960796823, -16.46253265017161027, 92.08224293864769550 ) ) ;
#174482 = CARTESIAN_POINT ( 'NONE',  ( 10.72451020669871369, 18.67979575497193778, 102.0844237280190185 ) ) ;
#174483 = CARTESIAN_POINT ( 'NONE',  ( -5.823673210054116645, -21.52544592524344225, 57.29057627198103120 ) ) ;
#174484 = CARTESIAN_POINT ( 'NONE',  ( -19.05341960407611168, -5.049401038298163336, 91.45724293864766707 ) ) ;
#174485 = CARTESIAN_POINT ( 'NONE',  ( 16.51473224551083163, -9.474510206698727899, 75.83442372801900433 ) ) ;
#174486 = CARTESIAN_POINT ( 'NONE',  ( 16.46253265017160672, -9.564922557960803928, 98.33224293864769550 ) ) ;
#174487 = CARTESIAN_POINT ( 'NONE',  ( -16.46253265017146816, -9.564922557961047289, 94.16775706135233293 ) ) ;
#174488 = CARTESIAN_POINT ( 'NONE',  ( 5.049401038298161559, -19.05341960407611168, 22.70724293864769194 ) ) ;
#174489 = CARTESIAN_POINT ( 'NONE',  ( 16.46253265017160672, -9.564922557960803928, 83.33224293864768129 ) ) ;
#174490 = CARTESIAN_POINT ( 'NONE',  ( -10.72451020669898014, 18.67979575497178502, 60.41557627198102409 ) ) ;
#174491 = CARTESIAN_POINT ( 'NONE',  ( 8.314922557961029526, -14.29746914071037800, 30.41775706135234358 ) ) ;
#174492 = CARTESIAN_POINT ( 'NONE',  ( 18.67979575497194134, -10.72451020669871369, 50.83442372801901143 ) ) ;
#174493 = CARTESIAN_POINT ( 'NONE',  ( -21.53943276465977519, -0.05219959533937600094, 93.75109039468567573 ) ) ;
#174494 = CARTESIAN_POINT ( 'NONE',  ( 8.224510206698742110, 14.34966873604972548, 102.0844237280190185 ) ) ;
#174495 = CARTESIAN_POINT ( 'NONE',  ( 13.89961937509977652, -13.97604488694527269, 83.12390960531436690 ) ) ;
#174496 = CARTESIAN_POINT ( 'NONE',  ( -16.55341960407611168, -4.379528057220339221, 91.45724293864769550 ) ) ;
#174497 = CARTESIAN_POINT ( 'NONE',  ( -8.314922557961024197, 14.29746914071037800, 112.9177570613523329 ) ) ;
#174498 = CARTESIAN_POINT ( 'NONE',  ( 16.51473224551083163, -9.474510206698727899, 70.83442372801900433 ) ) ;
#174499 = CARTESIAN_POINT ( 'NONE',  ( -15.72974639402176322, -15.80617190586768395, 39.37609039468567573 ) ) ;
#174500 = CARTESIAN_POINT ( 'NONE',  ( 14.34966873604960469, 8.224510206698951720, 89.16557627198102409 ) ) ;
#174501 = CARTESIAN_POINT ( 'NONE',  ( -19.02544592524342804, 5.153800228976336051, 116.0405762719810383 ) ) ;
#174502 = CARTESIAN_POINT ( 'NONE',  ( -0.05219959533910754901, -16.53943276465976808, 27.49890960531435269 ) ) ;
#174503 = CARTESIAN_POINT ( 'NONE',  ( 15.80617190586769283, -15.72974639402175789, 85.62609039468568994 ) ) ;
#174504 = CARTESIAN_POINT ( 'NONE',  ( 16.53943276465976808, 0.05219959533934440121, 51.25109039468568994 ) ) ;
#174505 = CARTESIAN_POINT ( 'NONE',  ( 21.55341960407619695, -5.719274019375665929, 36.04275706135234714 ) ) ;
#174506 = EDGE_LOOP ( 'NONE', ( #27124, #165401, #14999, #91106, #143447, #43736, #145162, #80126 ) ) ;
#174507 = CARTESIAN_POINT ( 'NONE',  ( 21.52544592524344225, -5.823673210054117533, 113.5405762719810383 ) ) ;
#174508 = CARTESIAN_POINT ( 'NONE',  ( 16.55341960407611168, 4.379528057220329451, 88.95724293864769550 ) ) ;
#174509 = CARTESIAN_POINT ( 'NONE',  ( -18.89770734986052148, -5.499999999999913847, 49.10214472496641491 ) ) ;
#174510 = CARTESIAN_POINT ( 'NONE',  ( 16.55341960407611168, 4.379528057220329451, 68.95724293864769550 ) ) ;
#174511 = CARTESIAN_POINT ( 'NONE',  ( -16.51473224551069308, -9.474510206698971260, 61.66557627198103120 ) ) ;
#174512 = CARTESIAN_POINT ( 'NONE',  ( 14.29746914071037800, 8.314922557961029526, 101.6677570613523613 ) ) ;
#174513 = CARTESIAN_POINT ( 'NONE',  ( -19.05341960407611168, -5.049401038298163336, 36.45724293864766707 ) ) ;
#174514 = CARTESIAN_POINT ( 'NONE',  ( -0.05219959533907301413, -21.53943276465977519, 47.49890960531435979 ) ) ;
#174515 = CARTESIAN_POINT ( 'NONE',  ( -12.06949235617756955, 12.14591786802309770, 75.62390960531439532 ) ) ;
#174516 = CARTESIAN_POINT ( 'NONE',  ( -15.72974639402197994, 15.80617190586746368, 85.62390960531436690 ) ) ;
#174517 = CARTESIAN_POINT ( 'NONE',  ( -19.02544592524342804, 5.153800228976336051, 91.04057627198100988 ) ) ;
#174519 = CARTESIAN_POINT ( 'NONE',  ( -16.51473224551082808, 9.474510206698731452, 98.33442372801900433 ) ) ;
#174518 = CARTESIAN_POINT ( 'NONE',  ( 19.03943276465977164, -0.05219959533909143690, 33.74890960531435979 ) ) ;
#174520 = CARTESIAN_POINT ( 'NONE',  ( 0.05219959533907565091, 21.53943276465977519, 44.99890960531435979 ) ) ;
#174521 = CARTESIAN_POINT ( 'NONE',  ( 10.81492255796106328, -18.62759615963255655, 70.41775706135236135 ) ) ;
#174522 = CARTESIAN_POINT ( 'NONE',  ( -19.02544592524342804, 5.153800228976336051, 51.04057627198103120 ) ) ;
#174523 = CARTESIAN_POINT ( 'NONE',  ( -19.03943276465977164, 0.05219959533909376836, 91.24890960531436690 ) ) ;
#174524 = ORIENTED_EDGE ( 'NONE', *, *, #134338, .F. ) ;
#174525 = CARTESIAN_POINT ( 'NONE',  ( -8.224510206698735004, -14.34966873604973081, 59.58442372801901854 ) ) ;
#174526 = CARTESIAN_POINT ( 'NONE',  ( -18.67979575497193778, 10.72451020669871902, 43.33442372801901143 ) ) ;
#174527 = CARTESIAN_POINT ( 'NONE',  ( 18.67979575497194134, -10.72451020669871369, 75.83442372801900433 ) ) ;
#174528 = CARTESIAN_POINT ( 'NONE',  ( -15.80617190586745835, -15.72974639402198527, 26.87390960531435979 ) ) ;
#174529 = CARTESIAN_POINT ( 'NONE',  ( 5.719274019375991003, -21.55341960407610458, 102.7072429386476955 ) ) ;
#174531 = CARTESIAN_POINT ( 'NONE',  ( 14.34966873604972726, -8.224510206698740333, 60.83442372801901854 ) ) ;
#174530 = CARTESIAN_POINT ( 'NONE',  ( 0.05219959533937995610, -21.53943276465977519, 40.00109039468567573 ) ) ;
#174532 = CARTESIAN_POINT ( 'NONE',  ( -0.05219959533907301413, -21.53943276465977519, 67.49890960531436690 ) ) ;
#174533 = CARTESIAN_POINT ( 'NONE',  ( 5.049401038297881783, 19.05341960407617563, 27.29275706135232937 ) ) ;
#174535 = CARTESIAN_POINT ( 'NONE',  ( -0.05219959533934338120, 16.53943276465976808, 97.50109039468567573 ) ) ;
#174534 = CARTESIAN_POINT ( 'NONE',  ( -13.89961937509977652, 13.97604488694528158, 70.62390960531432427 ) ) ;
#174536 = CARTESIAN_POINT ( 'NONE',  ( 3.766062262543149401E-15, -39.95556452105413570, -5.500000000000000000 ) ) ;
#174537 = CARTESIAN_POINT ( 'NONE',  ( 19.03943276465977164, -0.05219959533909143690, 103.7489096053143669 ) ) ;
#174538 = CARTESIAN_POINT ( 'NONE',  ( 20.13181022538189779, 20.85937581585698553, -49.56857446948049528 ) ) ;
#174539 = CARTESIAN_POINT ( 'NONE',  ( -0.05219959533936034679, 19.03943276465977164, 82.50109039468567573 ) ) ;
#174540 = CARTESIAN_POINT ( 'NONE',  ( -21.55341960407610458, -5.719274019375992779, 61.45724293864770260 ) ) ;
#174541 = CARTESIAN_POINT ( 'NONE',  ( 8.314922557960818139, 14.29746914071049879, 39.58224293864769550 ) ) ;
#174542 = CARTESIAN_POINT ( 'NONE',  ( -0.05219959533936034679, 19.03943276465977164, 102.5010903946856757 ) ) ;
#174543 = DIRECTION ( 'NONE',  ( 0.000000000000000000, -0.7071067811865467956, -0.7071067811865483499 ) ) ;
#174544 = CARTESIAN_POINT ( 'NONE',  ( 19.05341960407617918, -5.049401038297876454, 101.0427570613523045 ) ) ;
#174546 = CARTESIAN_POINT ( 'NONE',  ( 5.153800228976615827, -19.02544592524334988, 60.20942372801899012 ) ) ;
#174545 = CARTESIAN_POINT ( 'NONE',  ( -18.62759615963270932, 10.81492255796079327, 80.83224293864769550 ) ) ;
#174547 = CARTESIAN_POINT ( 'NONE',  ( 17.50000000000000000, 5.499999999999997335, 106.7030961746582847 ) ) ;
#174548 = CARTESIAN_POINT ( 'NONE',  ( 5.049401038298161559, -19.05341960407611168, 62.70724293864769550 ) ) ;
#174549 = CARTESIAN_POINT ( 'NONE',  ( -12.06949235617756955, 12.14591786802309770, 60.62390960531437401 ) ) ;
#174550 = CARTESIAN_POINT ( 'NONE',  ( 16.46253265017160672, -9.564922557960803928, 53.33224293864768839 ) ) ;
#174551 = CARTESIAN_POINT ( 'NONE',  ( -0.05219959533910754901, -16.53943276465976808, 47.49890960531435979 ) ) ;
#174552 = CARTESIAN_POINT ( 'NONE',  ( -9.474510206698964154, 16.51473224551069663, 25.41557627198103120 ) ) ;
#174553 = CARTESIAN_POINT ( 'NONE',  ( 31.40318257579880523, -7.397807925419288999, 93.74221852110635211 ) ) ;
#174554 = CARTESIAN_POINT ( 'NONE',  ( 14.29746914071049879, -8.314922557960816363, 33.33224293864769550 ) ) ;
#174555 = CARTESIAN_POINT ( 'NONE',  ( 9.474510206698971260, -16.51473224551069308, 67.91557627198102409 ) ) ;
#174556 = CARTESIAN_POINT ( 'NONE',  ( -17.97161686093721400, 5.500000000000146549, 50.99637206859166838 ) ) ;
#174557 = CARTESIAN_POINT ( 'NONE',  ( -16.51473224551082808, 9.474510206698731452, 33.33442372801899722 ) ) ;
#174558 = CARTESIAN_POINT ( 'NONE',  ( -14.29746914071037622, -8.314922557961029526, 49.16775706135234003 ) ) ;
#174559 = CARTESIAN_POINT ( 'NONE',  ( -5.719274019375978568, 21.55341960407610458, 45.20724293864769550 ) ) ;
#174560 = CARTESIAN_POINT ( 'NONE',  ( 10.72451020669871369, 18.67979575497193778, 107.0844237280190043 ) ) ;
#174561 = CARTESIAN_POINT ( 'NONE',  ( -16.46253265017160317, 9.564922557960807481, 75.83224293864769550 ) ) ;
#174562 = CARTESIAN_POINT ( 'NONE',  ( 13.89961937509977652, -13.97604488694527269, 113.1239096053143527 ) ) ;
#174563 = CARTESIAN_POINT ( 'NONE',  ( 0.05219959533909260263, 19.03943276465977164, 109.9989096053143669 ) ) ;
#174564 = CARTESIAN_POINT ( 'NONE',  ( 29.86685920354754842, -21.69954338932559068, -3.824999997268813345 ) ) ;
#174565 = CARTESIAN_POINT ( 'NONE',  ( -0.05219959533937732626, 21.53943276465977519, 37.50109039468568284 ) ) ;
#174567 = CARTESIAN_POINT ( 'NONE',  ( 0.05219959533910956823, 16.53943276465976808, 99.99890960531436690 ) ) ;
#174566 = PRODUCT_DEFINITION_SHAPE ( 'NONE', 'NONE',  #200202 ) ;
#174570 = CARTESIAN_POINT ( 'NONE',  ( 17.72517630440430025, -5.500000000000136779, 68.42175719257211597 ) ) ;
#174569 = CARTESIAN_POINT ( 'NONE',  ( 5.049401038298161559, -19.05341960407611168, 77.70724293864765286 ) ) ;
#174568 = CARTESIAN_POINT ( 'NONE',  ( 21.53943276465977519, -0.05219959533907433946, 93.74890960531436690 ) ) ;
#174571 = CARTESIAN_POINT ( 'NONE',  ( 9.474510206698971260, -16.51473224551069308, 92.91557627198103830 ) ) ;
#174572 = CARTESIAN_POINT ( 'NONE',  ( -15.80617190586768217, 15.72974639402176855, 28.12609039468568284 ) ) ;
#174573 = ORIENTED_EDGE ( 'NONE', *, *, #57594, .F. ) ;
#174574 = CARTESIAN_POINT ( 'NONE',  ( -19.02544592524342804, 5.153800228976336051, 91.04057627198100988 ) ) ;
#174575 = ADVANCED_FACE ( 'NONE', ( #51047 ), #116416, .T. ) ;
#174576 = DIRECTION ( 'NONE',  ( 1.000000000000000000, 0.000000000000000000, 0.000000000000000000 ) ) ;
#174578 = CARTESIAN_POINT ( 'NONE',  ( -9.564922557960796823, -16.46253265017161027, 32.08224293864769550 ) ) ;
#174577 = CARTESIAN_POINT ( 'NONE',  ( 14.34966873604960469, 8.224510206698951720, 114.1655762719810383 ) ) ;
#174579 = CARTESIAN_POINT ( 'NONE',  ( -16.46253265017146816, -9.564922557961047289, 109.1677570613523471 ) ) ;
#174580 = CARTESIAN_POINT ( 'NONE',  ( -36.91746825000000598, 2.428612866367529932E-14, -9.124999997268814056 ) ) ;
#174581 = CARTESIAN_POINT ( 'NONE',  ( -16.52544592524342804, 4.483927247898546575, 116.0405762719810383 ) ) ;
#174582 = CARTESIAN_POINT ( 'NONE',  ( 21.53943276465977519, 0.05219959533937863772, 81.25109039468568994 ) ) ;
#174584 = CARTESIAN_POINT ( 'NONE',  ( 18.62759615963255655, 10.81492255796105972, 26.66775706135235424 ) ) ;
#174583 = CARTESIAN_POINT ( 'NONE',  ( -19.03943276465977164, 0.05219959533909376836, 66.24890960531436690 ) ) ;
#174585 = CARTESIAN_POINT ( 'NONE',  ( 15.80617190586746368, 15.72974639402197994, 109.3739096053143811 ) ) ;
#174586 = CARTESIAN_POINT ( 'NONE',  ( 28.82186960331498327, 9.364793116373570925, 147.0999999999999943 ) ) ;
#174587 = CARTESIAN_POINT ( 'NONE',  ( 19.03943276465977164, -0.05219959533909143690, 83.74890960531436690 ) ) ;
#174588 = FACE_OUTER_BOUND ( 'NONE', #119500, .T. ) ;
#174590 = CARTESIAN_POINT ( 'NONE',  ( -15.72974639402197994, 15.80617190586746368, 40.62390960531435269 ) ) ;
#174589 = CARTESIAN_POINT ( 'NONE',  ( 4.483927247898790824, -16.52544592524335698, 20.20942372801900788 ) ) ;
#174591 = CARTESIAN_POINT ( 'NONE',  ( -21.52544592524334988, -5.823673210054445271, 58.95942372801902565 ) ) ;
#174592 = CARTESIAN_POINT ( 'NONE',  ( 16.51473224551069308, 9.474510206698969483, 109.1655762719810383 ) ) ;
#174593 = CARTESIAN_POINT ( 'NONE',  ( -16.51473224551082808, 9.474510206698731452, 93.33442372801900433 ) ) ;
#174594 = CARTESIAN_POINT ( 'NONE',  ( -13.89961937509977652, 13.97604488694528158, 65.62390960531436690 ) ) ;
#174595 = CARTESIAN_POINT ( 'NONE',  ( -13.89961937509977652, 13.97604488694528158, 90.62390960531432427 ) ) ;
#174596 = CARTESIAN_POINT ( 'NONE',  ( -14.29746914071049879, 8.314922557960819915, 100.8322429386477097 ) ) ;
#174597 = CARTESIAN_POINT ( 'NONE',  ( 4.379528057220339221, -16.55341960407611168, 87.70724293864769550 ) ) ;
#174598 = CARTESIAN_POINT ( 'NONE',  ( -5.049401038298153566, 19.05341960407611168, 115.2072429386477097 ) ) ;
#174600 = CARTESIAN_POINT ( 'NONE',  ( -5.153800228976328057, -19.02544592524343514, 42.29057627198101699 ) ) ;
#174599 = CARTESIAN_POINT ( 'NONE',  ( 16.53943276465976808, -0.05219959533910856209, 53.74890960531437401 ) ) ;
#174601 = CARTESIAN_POINT ( 'NONE',  ( -15.80617190586768217, 15.72974639402176855, 73.12609039468567573 ) ) ;
#174602 = CARTESIAN_POINT ( 'NONE',  ( 5.049401038297881783, 19.05341960407617563, 87.29275706135234714 ) ) ;
#174603 = CARTESIAN_POINT ( 'NONE',  ( -16.53943276465976808, 0.05219959533911058130, 56.24890960531436690 ) ) ;
#174604 = CARTESIAN_POINT ( 'NONE',  ( 5.719274019375991003, -21.55341960407610458, 112.7072429386476955 ) ) ;
#174605 = CARTESIAN_POINT ( 'NONE',  ( -21.53943276465977519, 0.05219959533907696930, 41.24890960531435269 ) ) ;
#174606 = CARTESIAN_POINT ( 'NONE',  ( 19.39056639909673407, 5.500000000000047962, 73.28948781074340957 ) ) ;
#174607 = CARTESIAN_POINT ( 'NONE',  ( 23.31738231874054890, -16.94106989632523508, 143.0500000054623513 ) ) ;
#174608 = CARTESIAN_POINT ( 'NONE',  ( -5.153800228976328057, -19.02544592524343514, 62.29057627198100988 ) ) ;
#174609 = CARTESIAN_POINT ( 'NONE',  ( -4.483927247898539470, -16.52544592524342804, 42.29057627198103120 ) ) ;
#174610 = ADVANCED_FACE ( 'NONE', ( #102668 ), #130573, .T. ) ;
#174611 = CARTESIAN_POINT ( 'NONE',  ( -14.34966873604972548, 8.224510206698743886, 98.33442372801901854 ) ) ;
#174612 = CARTESIAN_POINT ( 'NONE',  ( -8.314922557961024197, 14.29746914071037800, 77.91775706135231871 ) ) ;
#174613 = CARTESIAN_POINT ( 'NONE',  ( -19.03943276465977164, -0.05219959533935918106, 43.75109039468566863 ) ) ;
#174614 = CARTESIAN_POINT ( 'NONE',  ( -17.49999999999999289, 5.624438216177594541, 70.81670344914645909 ) ) ;
#174615 = CARTESIAN_POINT ( 'NONE',  ( 9.564922557960805705, 16.46253265017160317, 94.58224293864769550 ) ) ;
#174616 = CARTESIAN_POINT ( 'NONE',  ( -19.02544592524342804, 5.153800228976336051, 46.04057627198101699 ) ) ;
#174617 = CARTESIAN_POINT ( 'NONE',  ( 8.224510206698953496, -14.34966873604960469, 62.91557627198102409 ) ) ;
#174619 = CARTESIAN_POINT ( 'NONE',  ( -21.55341960407610458, -5.719274019375992779, 26.45724293864768839 ) ) ;
#174618 = CARTESIAN_POINT ( 'NONE',  ( 17.05116617787825106, -6.768360034955805737, 101.1567555325920011 ) ) ;
#174620 = CARTESIAN_POINT ( 'NONE',  ( 18.67979575497178502, 10.72451020669898547, 44.16557627198103120 ) ) ;
#174621 = CARTESIAN_POINT ( 'NONE',  ( 8.314922557960818139, 14.29746914071049879, 79.58224293864769550 ) ) ;
#174622 = CARTESIAN_POINT ( 'NONE',  ( 14.34966873604972726, -8.224510206698740333, 35.83442372801901143 ) ) ;
#174623 = CARTESIAN_POINT ( 'NONE',  ( -14.29746914071049879, 8.314922557960819915, 75.83224293864769550 ) ) ;
#174624 = CARTESIAN_POINT ( 'NONE',  ( -18.22780087662119541, 5.500000000000102141, 66.01763182126894947 ) ) ;
#174625 = CARTESIAN_POINT ( 'NONE',  ( 9.564922557961047289, -16.46253265017146816, 75.41775706135234714 ) ) ;
#174626 = CARTESIAN_POINT ( 'NONE',  ( -18.67979575497178146, -10.72451020669898902, 21.66557627198102409 ) ) ;
#174627 = CARTESIAN_POINT ( 'NONE',  ( -36.91746825000001309, -11.99521256947794789, -3.024999997268812635 ) ) ;
#174628 = CARTESIAN_POINT ( 'NONE',  ( -21.47640361312193491, 19.98428748653489961, -52.19293734151715825 ) ) ;
#174630 = CARTESIAN_POINT ( 'NONE',  ( -12.14591786802326823, 12.06949235617739902, 108.1260903946856757 ) ) ;
#174629 = CARTESIAN_POINT ( 'NONE',  ( 8.224510206698742110, 14.34966873604972548, 32.08442372801901854 ) ) ;
#174631 = CARTESIAN_POINT ( 'NONE',  ( 5.153800228976615827, -19.02544592524334988, 65.20942372801900433 ) ) ;
#174632 = CARTESIAN_POINT ( 'NONE',  ( -18.62759615963270932, 10.81492255796079327, 50.83224293864770971 ) ) ;
#174633 = CARTESIAN_POINT ( 'NONE',  ( -0.05219959533937732626, 21.53943276465977519, 72.50109039468568994 ) ) ;
#174634 = FACE_OUTER_BOUND ( 'NONE', #63403, .T. ) ;
#174635 = CARTESIAN_POINT ( 'NONE',  ( -16.53943276465976808, -0.05219959533934237506, 28.75109039468567929 ) ) ;
#174637 = CARTESIAN_POINT ( 'NONE',  ( -5.153800228976328057, -19.02544592524343514, 92.29057627198099567 ) ) ;
#174636 = CARTESIAN_POINT ( 'NONE',  ( -19.03943276465977164, 0.05219959533909376836, 21.24890960531436335 ) ) ;
#174638 = CARTESIAN_POINT ( 'NONE',  ( -5.153800228976328057, -19.02544592524343514, 27.29057627198103120 ) ) ;
#174639 = CARTESIAN_POINT ( 'NONE',  ( -8.314922557960811034, -14.29746914071050412, 92.08224293864769550 ) ) ;
#174640 = SHAPE_DEFINITION_REPRESENTATION ( #16244, #92179 ) ;
#174641 = CARTESIAN_POINT ( 'NONE',  ( -19.05341960407611168, -5.049401038298163336, 96.45724293864769550 ) ) ;
#174642 = ORIENTED_EDGE ( 'NONE', *, *, #99297, .F. ) ;
#174643 = CARTESIAN_POINT ( 'NONE',  ( -16.46253265017146816, -9.564922557961047289, 99.16775706135233293 ) ) ;
#174644 = CARTESIAN_POINT ( 'NONE',  ( 5.823673210054125526, 21.52544592524343514, 79.79057627198102409 ) ) ;
#174645 = CARTESIAN_POINT ( 'NONE',  ( -9.474510206698964154, 16.51473224551069663, 45.41557627198103120 ) ) ;
#174647 = CARTESIAN_POINT ( 'NONE',  ( -21.53943276465977519, 0.05219959533907696930, 116.2489096053143669 ) ) ;
#174646 = CARTESIAN_POINT ( 'NONE',  ( -9.474510206698720793, -16.51473224551083518, 64.58442372801900433 ) ) ;
#174648 = CARTESIAN_POINT ( 'NONE',  ( 19.05341960407611168, 5.049401038298154454, 63.95724293864769550 ) ) ;
#174649 = CARTESIAN_POINT ( 'NONE',  ( 13.97604488694527802, 13.89961937509977652, 104.3739096053143385 ) ) ;
#174650 = ORIENTED_EDGE ( 'NONE', *, *, #111919, .F. ) ;
#174651 = CARTESIAN_POINT ( 'NONE',  ( -0.05219959533934338120, 16.53943276465976808, 32.50109039468568284 ) ) ;
#174652 = CARTESIAN_POINT ( 'NONE',  ( -5.823673210054116645, -21.52544592524344225, 97.29057627198105251 ) ) ;
#174655 = CARTESIAN_POINT ( 'NONE',  ( 16.46253265017146816, 9.564922557961045513, 56.66775706135233293 ) ) ;
#174654 = CARTESIAN_POINT ( 'NONE',  ( 16.46253265017160672, -9.564922557960803928, 93.33224293864769550 ) ) ;
#174653 = CARTESIAN_POINT ( 'NONE',  ( 14.29746914071049879, -8.314922557960816363, 108.3322429386477097 ) ) ;
#174656 = CARTESIAN_POINT ( 'NONE',  ( 15.80617190586746368, 15.72974639402197994, 84.37390960531438111 ) ) ;
#174657 = CARTESIAN_POINT ( 'NONE',  ( 12.06949235617757843, -12.14591786802309237, 43.12390960531435269 ) ) ;
#174658 = CARTESIAN_POINT ( 'NONE',  ( 19.05341960407617918, -5.049401038297876454, 21.04275706135232582 ) ) ;
#174659 = CARTESIAN_POINT ( 'NONE',  ( 8.224510206698742110, 14.34966873604972548, 67.08442372801901854 ) ) ;
#174660 = CARTESIAN_POINT ( 'NONE',  ( -19.05341960407611168, -5.049401038298163336, 91.45724293864766707 ) ) ;
#174661 = CARTESIAN_POINT ( 'NONE',  ( 9.474510206698971260, -16.51473224551069308, 42.91557627198103120 ) ) ;
#174662 = CARTESIAN_POINT ( 'NONE',  ( -10.81492255796105439, 18.62759615963255655, 57.91775706135234714 ) ) ;
#174663 = CARTESIAN_POINT ( 'NONE',  ( 18.67979575497194134, -10.72451020669871369, 70.83442372801901854 ) ) ;
#174664 = CARTESIAN_POINT ( 'NONE',  ( -13.97604488694527625, -13.89961937509977652, 56.87390960531434558 ) ) ;
#174665 = CARTESIAN_POINT ( 'NONE',  ( -21.55341960407619339, 5.719274019375674811, 38.54275706135234714 ) ) ;
#174666 = CARTESIAN_POINT ( 'NONE',  ( -5.049401038297874678, -19.05341960407617918, 69.79275706135233293 ) ) ;
#174667 = EDGE_CURVE ( 'NONE', #87616, #4972, #85327, .T. ) ;
#174668 = CARTESIAN_POINT ( 'NONE',  ( 13.97604488694527802, 13.89961937509977652, 34.37390960531436690 ) ) ;
#174669 = CARTESIAN_POINT ( 'NONE',  ( -14.29746914071037622, -8.314922557961029526, 84.16775706135234714 ) ) ;
#174670 = CARTESIAN_POINT ( 'NONE',  ( -9.474510206698964154, 16.51473224551069663, 50.41557627198102409 ) ) ;
#174671 = CARTESIAN_POINT ( 'NONE',  ( -13.97604488694527625, -13.89961937509977652, 21.87390960531435979 ) ) ;
#174672 = CARTESIAN_POINT ( 'NONE',  ( 9.474510206698971260, -16.51473224551069308, 112.9155762719810383 ) ) ;
#174673 = CARTESIAN_POINT ( 'NONE',  ( 19.02544592524343514, -5.153800228976328945, 33.54057627198102409 ) ) ;
#174674 = CARTESIAN_POINT ( 'NONE',  ( -21.55341960407610458, -5.719274019375992779, 86.45724293864770971 ) ) ;
#174675 = CARTESIAN_POINT ( 'NONE',  ( 12.14591786802327356, -12.06949235617739191, 75.62609039468567573 ) ) ;
#174676 = CARTESIAN_POINT ( 'NONE',  ( 2.500000000000000000, 2.357898499370431722, -2.818925648462311528E-15 ) ) ;
#174677 = CARTESIAN_POINT ( 'NONE',  ( -5.153800228976607833, 19.02544592524334988, 37.70942372801899722 ) ) ;
#174678 = CARTESIAN_POINT ( 'NONE',  ( -9.564922557960796823, -16.46253265017161027, 47.08224293864769550 ) ) ;
#174679 = CARTESIAN_POINT ( 'NONE',  ( -16.55341960407611168, -4.379528057220339221, 46.45724293864769550 ) ) ;
#174680 = CARTESIAN_POINT ( 'NONE',  ( -4.379528057220328563, 16.55341960407611168, 75.20724293864769550 ) ) ;
#174681 = CARTESIAN_POINT ( 'NONE',  ( 9.474510206698971260, -16.51473224551069308, 97.91557627198102409 ) ) ;
#174682 = CARTESIAN_POINT ( 'NONE',  ( -13.89961937509977652, 13.97604488694528158, 80.62390960531436690 ) ) ;
#174683 = CARTESIAN_POINT ( 'NONE',  ( -21.53943276465977519, -0.05219959533937600094, 48.75109039468568284 ) ) ;
#174684 = CARTESIAN_POINT ( 'NONE',  ( 16.51473224551069308, 9.474510206698969483, 94.16557627198103830 ) ) ;
#174685 =( REPRESENTATION_RELATIONSHIP ('NONE','NONE', #154205, #9542 ) REPRESENTATION_RELATIONSHIP_WITH_TRANSFORMATION ( #73463 )SHAPE_REPRESENTATION_RELATIONSHIP( ) );
#174686 = CARTESIAN_POINT ( 'NONE',  ( -18.62759615963255300, -10.81492255796106328, 104.1677570613523471 ) ) ;
#174687 = CARTESIAN_POINT ( 'NONE',  ( 12.06949235617739724, 12.14591786802326823, 76.87609039468567573 ) ) ;
#174688 = CARTESIAN_POINT ( 'NONE',  ( -5.719274019375665041, -21.55341960407619695, 24.79275706135235779 ) ) ;
#174689 = CARTESIAN_POINT ( 'NONE',  ( -15.72974639402197994, 15.80617190586746368, 100.6239096053143811 ) ) ;
#174690 = CARTESIAN_POINT ( 'NONE',  ( 8.314922557960818139, 14.29746914071049879, 49.58224293864769550 ) ) ;
#174691 = CARTESIAN_POINT ( 'NONE',  ( -19.03943276465977164, 0.05219959533909376836, 46.24890960531435979 ) ) ;
#174692 = CARTESIAN_POINT ( 'NONE',  ( 8.314922557960818139, 14.29746914071049879, 74.58224293864768129 ) ) ;
#174693 = CARTESIAN_POINT ( 'NONE',  ( 15.72974639402199770, -15.80617190586745480, 33.12390960531435979 ) ) ;
#174694 = CARTESIAN_POINT ( 'NONE',  ( -19.02544592524334988, -5.153800228976617603, 23.95942372801900078 ) ) ;
#174695 = CARTESIAN_POINT ( 'NONE',  ( 8.314922557960818139, 14.29746914071049879, 99.58224293864770971 ) ) ;
#174696 = ORIENTED_EDGE ( 'NONE', *, *, #120476, .T. ) ;
#174697 = CARTESIAN_POINT ( 'NONE',  ( -12.14591786802326823, 12.06949235617739902, 73.12609039468567573 ) ) ;
#174698 = CARTESIAN_POINT ( 'NONE',  ( 19.02544592524343514, -5.153800228976328945, 73.54057627198103830 ) ) ;
#174699 = CARTESIAN_POINT ( 'NONE',  ( -16.66605195848753240, -6.777442124193050255, 20.99343749471847786 ) ) ;
#174700 = CARTESIAN_POINT ( 'NONE',  ( 10.81492255796078972, 18.62759615963270932, 39.58224293864769550 ) ) ;
#174701 = CARTESIAN_POINT ( 'NONE',  ( 0.05219959533934541429, -16.53943276465976808, 100.0010903946857042 ) ) ;
#174702 = CARTESIAN_POINT ( 'NONE',  ( 16.51473224551083163, -9.474510206698727899, 110.8344237280190043 ) ) ;
#174703 = CARTESIAN_POINT ( 'NONE',  ( 5.823673210054444382, -21.52544592524334988, 85.20942372801901854 ) ) ;
#174704 = CARTESIAN_POINT ( 'NONE',  ( 16.46253265017160672, -9.564922557960803928, 68.33224293864770971 ) ) ;
#174705 = CARTESIAN_POINT ( 'NONE',  ( -5.719274019375978568, 21.55341960407610458, 105.2072429386477097 ) ) ;
#174706 = CARTESIAN_POINT ( 'NONE',  ( -8.224510206698735004, -14.34966873604973081, 59.58442372801901854 ) ) ;
#174707 = CARTESIAN_POINT ( 'NONE',  ( -9.564922557960796823, -16.46253265017161027, 22.08224293864768839 ) ) ;
#174708 = CARTESIAN_POINT ( 'NONE',  ( -14.29746914071037622, -8.314922557961029526, 24.16775706135235424 ) ) ;
#174709 = CARTESIAN_POINT ( 'NONE',  ( 19.05341960407617918, -5.049401038297876454, 86.04275706135233293 ) ) ;
#174710 = CARTESIAN_POINT ( 'NONE',  ( -10.72451020669898014, 18.67979575497178502, 75.41557627198102409 ) ) ;
#174711 = CARTESIAN_POINT ( 'NONE',  ( 9.564922557961047289, -16.46253265017146816, 60.41775706135233293 ) ) ;
#174712 = CARTESIAN_POINT ( 'NONE',  ( -40.00000000000002842, 1.938754146708588393E-14, 0.000000000000000000 ) ) ;
#174713 = CARTESIAN_POINT ( 'NONE',  ( 10.81492255796078972, 18.62759615963270932, 99.58224293864770971 ) ) ;
#174714 = DIRECTION ( 'NONE',  ( -0.000000000000000000, 1.000000000000000000, -0.000000000000000000 ) ) ;
#174715 = CARTESIAN_POINT ( 'NONE',  ( 13.97604488694527802, 13.89961937509977652, 79.37390960531435269 ) ) ;
#174716 = CARTESIAN_POINT ( 'NONE',  ( -19.03943276465977164, -0.05219959533935946555, 113.7510903946856757 ) ) ;
#174717 = CARTESIAN_POINT ( 'NONE',  ( -12.14591786802326823, 12.06949235617739902, 28.12609039468568284 ) ) ;
#174718 = CARTESIAN_POINT ( 'NONE',  ( -18.22780087662119541, 5.500000000000102141, 51.01763182126894947 ) ) ;
#174720 = CARTESIAN_POINT ( 'NONE',  ( -8.314922557960811034, -14.29746914071050412, 67.08224293864770971 ) ) ;
#174719 = CARTESIAN_POINT ( 'NONE',  ( -0.05219959533907301413, -21.53943276465977519, 102.4989096053143811 ) ) ;
#174721 = CARTESIAN_POINT ( 'NONE',  ( -5.049401038298153566, 19.05341960407611168, 65.20724293864765286 ) ) ;
#174722 = CARTESIAN_POINT ( 'NONE',  ( -21.52544592524334988, -5.823673210054445271, 88.95942372801901854 ) ) ;
#174724 = CARTESIAN_POINT ( 'NONE',  ( -16.51473224551082808, 9.474510206698731452, 43.33442372801900433 ) ) ;
#174723 = CARTESIAN_POINT ( 'NONE',  ( 12.06949235617739724, 12.14591786802326823, 36.87609039468568994 ) ) ;
#174725 = CARTESIAN_POINT ( 'NONE',  ( -10.72451020669870658, -18.67979575497194134, 49.58442372801901143 ) ) ;
#174726 = CARTESIAN_POINT ( 'NONE',  ( 5.719274019375991003, -21.55341960407610458, 52.70724293864769550 ) ) ;
#174727 = CARTESIAN_POINT ( 'NONE',  ( -19.05341960407617563, 5.049401038297882671, 103.5427570613523329 ) ) ;
#174728 = CARTESIAN_POINT ( 'NONE',  ( -16.51473224551069308, -9.474510206698971260, 51.66557627198102409 ) ) ;
#174729 = CARTESIAN_POINT ( 'NONE',  ( 13.89961937509957401, 13.97604488694547697, 66.87609039468567573 ) ) ;
#174730 = CARTESIAN_POINT ( 'NONE',  ( -18.67979575497193778, 10.72451020669871902, 83.33442372801903275 ) ) ;
#174731 = CARTESIAN_POINT ( 'NONE',  ( 5.049401038297881783, 19.05341960407617563, 62.29275706135234003 ) ) ;
#174732 = CARTESIAN_POINT ( 'NONE',  ( -13.97604488694527625, -13.89961937509977652, 41.87390960531435979 ) ) ;
#174733 = CARTESIAN_POINT ( 'NONE',  ( 5.719274019375991003, -21.55341960407610458, 57.70724293864770260 ) ) ;
#174734 = CARTESIAN_POINT ( 'NONE',  ( -4.483927247898539470, -16.52544592524342804, 57.29057627198103120 ) ) ;
#174735 = CARTESIAN_POINT ( 'NONE',  ( 21.91636330721480874, 8.102911641865347292, 172.4379571683062409 ) ) ;
#174736 = CARTESIAN_POINT ( 'NONE',  ( 5.049401038297881783, 19.05341960407617563, 27.29275706135232937 ) ) ;
#174737 = CARTESIAN_POINT ( 'NONE',  ( 14.34966873604972726, -8.224510206698740333, 100.8344237280190185 ) ) ;
#174738 = CARTESIAN_POINT ( 'NONE',  ( 8.314922557960818139, 14.29746914071049879, 49.58224293864769550 ) ) ;
#174739 = CARTESIAN_POINT ( 'NONE',  ( -15.72974639402176322, -15.80617190586768395, 89.37609039468568994 ) ) ;
#174740 = CARTESIAN_POINT ( 'NONE',  ( 18.62759615963255655, 10.81492255796105972, 81.66775706135236135 ) ) ;
#174741 = CARTESIAN_POINT ( 'NONE',  ( -10.72451020669898014, 18.67979575497178502, 100.4155762719810241 ) ) ;
#174742 = CARTESIAN_POINT ( 'NONE',  ( -19.05341960407611168, -5.049401038298163336, 51.45724293864770260 ) ) ;
#174743 = CARTESIAN_POINT ( 'NONE',  ( 15.80617190586769283, -15.72974639402175789, 70.62609039468567573 ) ) ;
#174744 = CARTESIAN_POINT ( 'NONE',  ( -0.05219959533909027116, -19.03943276465977164, 42.49890960531435269 ) ) ;
#174745 = CARTESIAN_POINT ( 'NONE',  ( -19.05341960407611168, -5.049401038298163336, 66.45724293864769550 ) ) ;
#174746 = CARTESIAN_POINT ( 'NONE',  ( -8.314922557960811034, -14.29746914071050412, 112.0822429386477097 ) ) ;
#174747 = CARTESIAN_POINT ( 'NONE',  ( -9.474510206698964154, 16.51473224551069663, 100.4155762719810241 ) ) ;
#174748 = CARTESIAN_POINT ( 'NONE',  ( -4.379528057220328563, 16.55341960407611168, 55.20724293864770260 ) ) ;
#174749 = CARTESIAN_POINT ( 'NONE',  ( -16.55341960407611168, -4.379528057220339221, 111.4572429386476813 ) ) ;
#174750 = CARTESIAN_POINT ( 'NONE',  ( -15.80617190586745835, -15.72974639402198527, 86.87390960531438111 ) ) ;
#174751 = CARTESIAN_POINT ( 'NONE',  ( 0.05219959533937995610, -21.53943276465977519, 40.00109039468567573 ) ) ;
#174752 = CARTESIAN_POINT ( 'NONE',  ( 26.58496454516998142, -7.626754437231455519, 167.9682100371138915 ) ) ;
#174753 = CARTESIAN_POINT ( 'NONE',  ( 12.14591786802327356, -12.06949235617739191, 40.62609039468567573 ) ) ;
#174754 = CARTESIAN_POINT ( 'NONE',  ( 0.05219959533907565091, 21.53943276465977519, 79.99890960531435269 ) ) ;
#174755 = CARTESIAN_POINT ( 'NONE',  ( 10.72451020669871369, 18.67979575497193778, 102.0844237280190185 ) ) ;
#174756 = CARTESIAN_POINT ( 'NONE',  ( 5.049401038298161559, -19.05341960407611168, 92.70724293864769550 ) ) ;
#174757 = CARTESIAN_POINT ( 'NONE',  ( 5.823673210054444382, -21.52544592524334988, 30.20942372801902565 ) ) ;
#174758 = CARTESIAN_POINT ( 'NONE',  ( 18.67979575497178502, 10.72451020669898547, 34.16557627198102409 ) ) ;
#174759 = CARTESIAN_POINT ( 'NONE',  ( -16.53943276465976808, -0.05219959533934237506, 103.7510903946857042 ) ) ;
#174761 = CARTESIAN_POINT ( 'NONE',  ( -15.72974639402176322, -15.80617190586768395, 79.37609039468567573 ) ) ;
#174760 = CARTESIAN_POINT ( 'NONE',  ( -10.72451020669870658, -18.67979575497194134, 49.58442372801901143 ) ) ;
#174762 = CARTESIAN_POINT ( 'NONE',  ( 9.474510206698729675, 16.51473224551082808, 22.08442372801899722 ) ) ;
#174763 = CARTESIAN_POINT ( 'NONE',  ( -8.314922557961024197, 14.29746914071037800, 77.91775706135231871 ) ) ;
#174764 = CARTESIAN_POINT ( 'NONE',  ( 5.719274019375673035, 21.55341960407619339, 37.29275706135235424 ) ) ;
#174765 = CARTESIAN_POINT ( 'NONE',  ( -19.05341960407611168, -5.049401038298163336, 31.45724293864769550 ) ) ;
#174766 = CARTESIAN_POINT ( 'NONE',  ( 5.823673210054444382, -21.52544592524334988, 105.2094237280190328 ) ) ;
#174767 = CARTESIAN_POINT ( 'NONE',  ( -16.51473224551069308, -9.474510206698971260, 101.6655762719810241 ) ) ;
#174768 = CARTESIAN_POINT ( 'NONE',  ( 5.823673210054125526, 21.52544592524343514, 104.7905762719810241 ) ) ;
#174770 = CARTESIAN_POINT ( 'NONE',  ( -15.72974639402197994, 15.80617190586746368, 65.62390960531436690 ) ) ;
#174769 = CARTESIAN_POINT ( 'NONE',  ( -2.802625768539475093, -39.09149893265184517, -22.99999999999999289 ) ) ;
#174772 = CARTESIAN_POINT ( 'NONE',  ( 8.224510206698953496, -14.34966873604960469, 52.91557627198103830 ) ) ;
#174771 = CARTESIAN_POINT ( 'NONE',  ( 8.314922557961029526, -14.29746914071037800, 45.41775706135234003 ) ) ;
#174773 = CARTESIAN_POINT ( 'NONE',  ( -67.00000000000000000, -1.163414459189985801E-14, 95.00000000000000000 ) ) ;
#174774 = CARTESIAN_POINT ( 'NONE',  ( -9.564922557961040184, 16.46253265017147172, 92.91775706135233293 ) ) ;
#174775 = CARTESIAN_POINT ( 'NONE',  ( -26.97479053218977896, 7.816291847812730786, 151.6430507545553894 ) ) ;
#174776 = CARTESIAN_POINT ( 'NONE',  ( -4.379528057220086978, -16.55341960407618274, 24.79275706135235779 ) ) ;
#174777 = CARTESIAN_POINT ( 'NONE',  ( 18.67979575497178502, 10.72451020669898547, 99.16557627198100988 ) ) ;
#174778 = CARTESIAN_POINT ( 'NONE',  ( 0.05219959533907565091, 21.53943276465977519, 69.99890960531435269 ) ) ;
#174779 = CARTESIAN_POINT ( 'NONE',  ( 9.474510206698971260, -16.51473224551069308, 112.9155762719810383 ) ) ;
#174780 = CARTESIAN_POINT ( 'NONE',  ( 12.14591786802327356, -12.06949235617739191, 40.62609039468567573 ) ) ;
#174781 = CARTESIAN_POINT ( 'NONE',  ( 9.564922557960805705, 16.46253265017160317, 64.58224293864769550 ) ) ;
#174783 = CARTESIAN_POINT ( 'NONE',  ( -19.02544592524334988, -5.153800228976617603, 103.9594237280190043 ) ) ;
#174782 = CARTESIAN_POINT ( 'NONE',  ( -10.72451020669870658, -18.67979575497194134, 29.58442372801901854 ) ) ;
#174784 = CARTESIAN_POINT ( 'NONE',  ( -16.46253265017160317, 9.564922557960807481, 105.8322429386476955 ) ) ;
#174785 = CARTESIAN_POINT ( 'NONE',  ( 9.474510206698971260, -16.51473224551069308, 92.91557627198103830 ) ) ;
#174786 = CARTESIAN_POINT ( 'NONE',  ( 15.72974639402199770, -15.80617190586745480, 93.12390960531436690 ) ) ;
#174787 = CARTESIAN_POINT ( 'NONE',  ( -0.05219959533909027116, -19.03943276465977164, 62.49890960531435979 ) ) ;
#174788 = CARTESIAN_POINT ( 'NONE',  ( -17.48853670773243252, -5.747243402303183757, 61.33328700250010002 ) ) ;
#174789 = CARTESIAN_POINT ( 'NONE',  ( -4.483927247898539470, -16.52544592524342804, 72.29057627198102409 ) ) ;
#174790 = CARTESIAN_POINT ( 'NONE',  ( 18.62759615963271287, -10.81492255796078972, 23.33224293864769194 ) ) ;
#174791 = CARTESIAN_POINT ( 'NONE',  ( -28.82186960331499037, 2.781578969918950771E-14, 139.9999999999999716 ) ) ;
#174792 = CARTESIAN_POINT ( 'NONE',  ( -10.72451020669898014, 18.67979575497178502, 90.41557627198103830 ) ) ;
#174793 = CARTESIAN_POINT ( 'NONE',  ( 19.02544592524334988, 5.153800228976608722, 51.45942372801900433 ) ) ;
#174794 = CARTESIAN_POINT ( 'NONE',  ( -19.05341960407611168, -5.049401038298163336, 111.4572429386476671 ) ) ;
#174795 = CYLINDRICAL_SURFACE ( 'NONE', #8179, 1.500000000000001332 ) ;
#174796 = CARTESIAN_POINT ( 'NONE',  ( 0.05219959533907565091, 21.53943276465977519, 59.99890960531436690 ) ) ;
#174797 = CARTESIAN_POINT ( 'NONE',  ( 5.153800228976335163, 19.02544592524342804, 79.79057627198102409 ) ) ;
#174798 = CARTESIAN_POINT ( 'NONE',  ( -21.52544592524334988, -5.823673210054445271, 83.95942372801900433 ) ) ;
#174799 = CARTESIAN_POINT ( 'NONE',  ( 9.474510206698971260, -16.51473224551069308, 37.91557627198102409 ) ) ;
#174800 = CARTESIAN_POINT ( 'NONE',  ( 0.05219959533910956823, 16.53943276465976808, 74.99890960531435269 ) ) ;
#174801 = CARTESIAN_POINT ( 'NONE',  ( -14.29746914071037622, -8.314922557961029526, 24.16775706135235424 ) ) ;
#174802 = CARTESIAN_POINT ( 'NONE',  ( -10.81492255796105439, 18.62759615963255655, 62.91775706135236135 ) ) ;
#174803 = ORIENTED_EDGE ( 'NONE', *, *, #143563, .F. ) ;
#174804 = CARTESIAN_POINT ( 'NONE',  ( 9.474510206698729675, 16.51473224551082808, 27.08442372801900433 ) ) ;
#174806 = ADVANCED_FACE ( 'NONE', ( #97484 ), #129817, .T. ) ;
#174805 = CARTESIAN_POINT ( 'NONE',  ( 9.564922557961047289, -16.46253265017146816, 75.41775706135234714 ) ) ;
#174807 = CARTESIAN_POINT ( 'NONE',  ( 27.81822689058061115, -28.32190533958846856, -20.09416750255128292 ) ) ;
#174808 = CARTESIAN_POINT ( 'NONE',  ( 21.53943276465977519, 0.05219959533937863772, 21.25109039468567218 ) ) ;
#174809 = CARTESIAN_POINT ( 'NONE',  ( -3.889087296526137383, -34.99999999999999289, 1.818019484660534424 ) ) ;
#174810 = CARTESIAN_POINT ( 'NONE',  ( -18.62759615963255300, -10.81492255796106328, 109.1677570613523613 ) ) ;
#174811 = CARTESIAN_POINT ( 'NONE',  ( -16.46253265017160317, 9.564922557960807481, 55.83224293864769550 ) ) ;
#174812 = CARTESIAN_POINT ( 'NONE',  ( 0.05219959533936267826, -19.03943276465977164, 30.00109039468566863 ) ) ;
#174813 = CARTESIAN_POINT ( 'NONE',  ( -0.05219959533934338120, 16.53943276465976808, 107.5010903946856899 ) ) ;
#174815 = CARTESIAN_POINT ( 'NONE',  ( 5.823673210054444382, -21.52544592524334988, 70.20942372801904696 ) ) ;
#174814 = CARTESIAN_POINT ( 'NONE',  ( -16.51473224551069308, -9.474510206698971260, 101.6655762719810241 ) ) ;
#174816 = CARTESIAN_POINT ( 'NONE',  ( -11.40812507854754720, -35.11059874428192273, -8.224999997268813701 ) ) ;
#174817 = CARTESIAN_POINT ( 'NONE',  ( -17.49999999999999645, -5.500000000000000888, 34.20309617465829177 ) ) ;
#174818 = CARTESIAN_POINT ( 'NONE',  ( 5.719274019375673035, 21.55341960407619339, 87.29275706135236135 ) ) ;
#174819 = CARTESIAN_POINT ( 'NONE',  ( -5.823673210054431948, 21.52544592524334988, 102.7094237280190185 ) ) ;
#174820 = CARTESIAN_POINT ( 'NONE',  ( 17.50000000000001066, -5.622605283950867339, 41.18792689403890250 ) ) ;
#174821 = CARTESIAN_POINT ( 'NONE',  ( 5.049401038298161559, -19.05341960407611168, 102.7072429386476955 ) ) ;
#174822 = CARTESIAN_POINT ( 'NONE',  ( 5.049401038297881783, 19.05341960407617563, 22.29275706135233648 ) ) ;
#174823 = B_SPLINE_CURVE_WITH_KNOTS ( 'NONE', 3,
 ( #35895, #130896, #38901, #161240, #189598, #192586, #177430, #23737, #163246, #53052, #193591, #146059, #116734, #54069, #174425, #55062, #22734, #83385, #145062, #68223, #129875, #84382, #100558, #115743, #70239, #191574, #159228, #162237, #114732, #85386, #131907, #190586 ),
 .UNSPECIFIED., .F., .F.,
 ( 4, 2, 2, 2, 2, 2, 2, 2, 2, 2, 2, 2, 2, 2, 2, 4 ),
 ( 2.602085213965210642E-18, 0.0003712461730036887837, 0.0007424923460073749653, 0.001113738519011061310, 0.001484984692014747329, 0.002227477038022114813, 0.002598723211025784352, 0.002969969384029453891, 0.003341215557033123430, 0.003712461730036792969, 0.004083707903040462509, 0.004454954076044132481, 0.004826200249047802454, 0.005197446422051472427, 0.005568692595055141532, 0.005939938768058811505 ),
 .UNSPECIFIED. ) ;
#174824 = DIRECTION ( 'NONE',  ( -0.000000000000000000, -0.000000000000000000, 1.000000000000000000 ) ) ;
#174825 = CARTESIAN_POINT ( 'NONE',  ( -19.03943276465977164, 0.05219959533909376836, 41.24890960531435269 ) ) ;
#174826 = CARTESIAN_POINT ( 'NONE',  ( -18.62759615963270932, 10.81492255796079327, 60.83224293864769550 ) ) ;
#174827 = CARTESIAN_POINT ( 'NONE',  ( -16.55341960407611168, -4.379528057220339221, 21.45724293864769550 ) ) ;
#174829 = CARTESIAN_POINT ( 'NONE',  ( -0.05219959533909027116, -19.03943276465977164, 87.49890960531436690 ) ) ;
#174828 = CARTESIAN_POINT ( 'NONE',  ( -14.29746914071049879, 8.314922557960819915, 90.83224293864769550 ) ) ;
#174830 = CARTESIAN_POINT ( 'NONE',  ( -21.52544592524334988, -5.823673210054445271, 98.95942372801903275 ) ) ;
#174831 = CARTESIAN_POINT ( 'NONE',  ( -9.564922557960796823, -16.46253265017161027, 42.08224293864769550 ) ) ;
#174832 = CARTESIAN_POINT ( 'NONE',  ( 16.52544592524342804, -4.483927247898539470, 98.54057627198105251 ) ) ;
#174833 = CARTESIAN_POINT ( 'NONE',  ( -0.05219959533937732626, 21.53943276465977519, 52.50109039468567573 ) ) ;
#174834 = CARTESIAN_POINT ( 'NONE',  ( -18.67979575497178146, -10.72451020669898902, 91.66557627198103830 ) ) ;
#174835 = CARTESIAN_POINT ( 'NONE',  ( 19.05341960407617918, -5.049401038297876454, 56.04275706135234714 ) ) ;
#174836 = CARTESIAN_POINT ( 'NONE',  ( -5.000000000000000888, -130.0000000000000000, 12.49999999999999645 ) ) ;
#174837 = CARTESIAN_POINT ( 'NONE',  ( -9.474510206698964154, 16.51473224551069663, 115.4155762719810241 ) ) ;
#174838 = CARTESIAN_POINT ( 'NONE',  ( 14.34966873604960469, 8.224510206698951720, 74.16557627198102409 ) ) ;
#174839 = CARTESIAN_POINT ( 'NONE',  ( -19.05341960407617563, 5.049401038297882671, 38.54275706135233293 ) ) ;
#174840 = CARTESIAN_POINT ( 'NONE',  ( -0.05219959533909027116, -19.03943276465977164, 62.49890960531435979 ) ) ;
#174841 = CARTESIAN_POINT ( 'NONE',  ( 16.53943276465976808, -0.05219959533910856209, 48.74890960531435979 ) ) ;
#174842 = CARTESIAN_POINT ( 'NONE',  ( -0.05219959533936034679, 19.03943276465977164, 77.50109039468566152 ) ) ;
#174843 = CARTESIAN_POINT ( 'NONE',  ( 0.000000000000000000, -78.67194367458512261, -23.00000000000000000 ) ) ;
#174844 = CARTESIAN_POINT ( 'NONE',  ( -15.72974639402197994, 15.80617190586746368, 35.62390960531437401 ) ) ;
#174845 = CARTESIAN_POINT ( 'NONE',  ( 8.224510206698953496, -14.34966873604960469, 97.91557627198103830 ) ) ;
#174846 = PLANE ( 'NONE',  #3142 ) ;
#174848 = CARTESIAN_POINT ( 'NONE',  ( 10.72451020669898902, -18.67979575497178502, 62.91557627198102409 ) ) ;
#174847 = CARTESIAN_POINT ( 'NONE',  ( -5.153800228976328057, -19.02544592524343514, 62.29057627198100988 ) ) ;
#174849 = CARTESIAN_POINT ( 'NONE',  ( 5.153800228976335163, 19.02544592524342804, 24.79057627198102765 ) ) ;
#174851 = CARTESIAN_POINT ( 'NONE',  ( -9.564922557960796823, -16.46253265017161027, 62.08224293864769550 ) ) ;
#174850 = CARTESIAN_POINT ( 'NONE',  ( -8.224510206698735004, -14.34966873604973081, 74.58442372801901854 ) ) ;
#174852 = CARTESIAN_POINT ( 'NONE',  ( 16.51473224551083163, -9.474510206698727899, 50.83442372801899722 ) ) ;
#174853 = CARTESIAN_POINT ( 'NONE',  ( 10.72451020669871369, 18.67979575497193778, 67.08442372801901854 ) ) ;
#174854 = CARTESIAN_POINT ( 'NONE',  ( 21.53943276465977519, -0.05219959533907433946, 43.74890960531435979 ) ) ;
#174855 = CARTESIAN_POINT ( 'NONE',  ( -4.483927247898539470, -16.52544592524342804, 112.2905762719810241 ) ) ;
#174856 = CARTESIAN_POINT ( 'NONE',  ( -8.314922557961024197, 14.29746914071037800, 92.91775706135236135 ) ) ;
#174857 = CARTESIAN_POINT ( 'NONE',  ( 0.05219959533936267826, -19.03943276465977164, 105.0010903946856615 ) ) ;
#174858 = DIRECTION ( 'NONE',  ( 1.000000000000000000, 0.000000000000000000, 0.000000000000000000 ) ) ;
#174860 = CARTESIAN_POINT ( 'NONE',  ( 10.72451020669898902, -18.67979575497178502, 62.91557627198102409 ) ) ;
#174859 = CARTESIAN_POINT ( 'NONE',  ( 17.49999999999999645, 5.500000000000010658, 53.78230962303567964 ) ) ;
#174861 = CARTESIAN_POINT ( 'NONE',  ( -5.823673210054431948, 21.52544592524334988, 97.70942372801904696 ) ) ;
#174862 = CARTESIAN_POINT ( 'NONE',  ( 8.224510206698953496, -14.34966873604960469, 52.91557627198103830 ) ) ;
#174864 = CARTESIAN_POINT ( 'NONE',  ( -14.29746914071049879, 8.314922557960819915, 60.83224293864769550 ) ) ;
#174863 =( BOUNDED_CURVE ( )  B_SPLINE_CURVE ( 2, ( #4351, #172232, #171243, #143871, #109562, #2380, #5350, #173234, #139887, #19545, #95379 ),
 .UNSPECIFIED., .F., .T. ) 
 B_SPLINE_CURVE_WITH_KNOTS ( ( 3, 2, 2, 2, 2, 3 ),
 ( 0.7000000000000000666, 0.7200000000000000844, 0.7400000000000001021, 0.7600000000000000089, 0.7800000000000000266, 0.8000000000000000444 ),
 .UNSPECIFIED. ) 
 CURVE ( )  GEOMETRIC_REPRESENTATION_ITEM ( )  RATIONAL_B_SPLINE_CURVE ( ( 0.9999999999999997780, 0.9510565162951537532, 1.000000000000000000, 0.9510565162951535312, 1.000000000000000000, 0.9510565162951535312, 1.000000000000000000, 0.9510565162951535312, 1.000000000000000000, 0.9510565162951535312, 1.000000000000000000 ) ) 
 REPRESENTATION_ITEM ( '' )  );
#174865 = CARTESIAN_POINT ( 'NONE',  ( 10.72451020669898902, -18.67979575497178502, 92.91557627198103830 ) ) ;
#174866 = CARTESIAN_POINT ( 'NONE',  ( -15.80617190586745835, -15.72974639402198527, 86.87390960531438111 ) ) ;
#174867 = LINE ( 'NONE', #191029, #133655 ) ;
#174868 = CARTESIAN_POINT ( 'NONE',  ( -21.55341960407610458, -5.719274019375992779, 36.45724293864768839 ) ) ;
#174869 = CARTESIAN_POINT ( 'NONE',  ( 12.14591786802327356, -12.06949235617739191, 70.62609039468567573 ) ) ;
#174870 = CARTESIAN_POINT ( 'NONE',  ( 8.314922557960818139, 14.29746914071049879, 74.58224293864768129 ) ) ;
#174871 = CARTESIAN_POINT ( 'NONE',  ( 9.564922557960805705, 16.46253265017160317, 49.58224293864770260 ) ) ;
#174872 =( NAMED_UNIT ( * ) SI_UNIT ( $, .STERADIAN. ) SOLID_ANGLE_UNIT ( ) );
#174873 = CARTESIAN_POINT ( 'NONE',  ( 35.63774670715082493, -1.952809719854257775, 37.74170157406051374 ) ) ;
#174874 = CARTESIAN_POINT ( 'NONE',  ( -16.55341960407617563, 4.379528057220093196, 93.54275706135234714 ) ) ;
#174875 = CARTESIAN_POINT ( 'NONE',  ( 21.52544592524334988, 5.823673210054432836, 21.45942372801901499 ) ) ;
#174876 = CARTESIAN_POINT ( 'NONE',  ( -19.02544592524342804, 5.153800228976336051, 81.04057627198103830 ) ) ;
#174877 = CARTESIAN_POINT ( 'NONE',  ( 18.67979575497194134, -10.72451020669871369, 60.83442372801901854 ) ) ;
#174878 = CARTESIAN_POINT ( 'NONE',  ( -19.02544592524342804, 5.153800228976336051, 111.0405762719810099 ) ) ;
#174879 = CARTESIAN_POINT ( 'NONE',  ( -19.41322597532237637, -37.10879518268991006, -19.41738833682087062 ) ) ;
#174880 = EDGE_LOOP ( 'NONE', ( #106237, #28820, #57770, #139549 ) ) ;
#174881 = CARTESIAN_POINT ( 'NONE',  ( 15.80617190586769283, -15.72974639402175789, 45.62609039468567573 ) ) ;
#174883 = CARTESIAN_POINT ( 'NONE',  ( -13.97604488694527625, -13.89961937509977652, 111.8739096053143243 ) ) ;
#174882 = CARTESIAN_POINT ( 'NONE',  ( 16.51473224551069308, 9.474510206698969483, 44.16557627198103120 ) ) ;
#174884 = CARTESIAN_POINT ( 'NONE',  ( -16.46253265017146816, -9.564922557961047289, 59.16775706135233293 ) ) ;
#174885 = CARTESIAN_POINT ( 'NONE',  ( 15.72974639402176855, 15.80617190586768217, 31.87609039468567929 ) ) ;
#174886 = CARTESIAN_POINT ( 'NONE',  ( -16.46253265017146816, -9.564922557961047289, 59.16775706135233293 ) ) ;
#174887 = CARTESIAN_POINT ( 'NONE',  ( -16.51473224551069308, -9.474510206698971260, 26.66557627198103120 ) ) ;
#174888 = CARTESIAN_POINT ( 'NONE',  ( 8.224510206698742110, 14.34966873604972548, 87.08442372801901854 ) ) ;
#174889 = CARTESIAN_POINT ( 'NONE',  ( -9.564922557961040184, 16.46253265017147172, 57.91775706135233293 ) ) ;
#174890 = CARTESIAN_POINT ( 'NONE',  ( -12.14591786802326823, 12.06949235617739902, 103.1260903946856757 ) ) ;
#174891 = CARTESIAN_POINT ( 'NONE',  ( 9.561620553927779653, 11.67072985713511102, -62.04564570087489983 ) ) ;
#174892 = CARTESIAN_POINT ( 'NONE',  ( -19.03943276465977164, 0.05219959533909376836, 91.24890960531436690 ) ) ;
#174893 = CARTESIAN_POINT ( 'NONE',  ( 15.72974639402176855, 15.80617190586768217, 86.87609039468568994 ) ) ;
#174894 = CARTESIAN_POINT ( 'NONE',  ( 10.72451020669871369, 18.67979575497193778, 102.0844237280190185 ) ) ;
#174895 = CYLINDRICAL_SURFACE ( 'NONE', #72872, 16.70000000000002061 ) ;
#174896 = CARTESIAN_POINT ( 'NONE',  ( -13.97604488694527625, -13.89961937509977652, 101.8739096053143811 ) ) ;
#174897 = CARTESIAN_POINT ( 'NONE',  ( 15.80617190586769283, -15.72974639402175789, 70.62609039468567573 ) ) ;
#174898 = CARTESIAN_POINT ( 'NONE',  ( -0.05219959533934338120, 16.53943276465976808, 22.50109039468567573 ) ) ;
#174899 = EDGE_CURVE ( 'NONE', #169869, #163628, #84324, .T. ) ;
#174900 = CARTESIAN_POINT ( 'NONE',  ( 19.02544592524343514, -5.153800228976328945, 83.54057627198100988 ) ) ;
#174901 = CARTESIAN_POINT ( 'NONE',  ( 15.72974639402199770, -15.80617190586745480, 28.12390960531435979 ) ) ;
#174902 = CARTESIAN_POINT ( 'NONE',  ( 19.02544592524343514, -5.153800228976328945, 88.54057627198102409 ) ) ;
#174903 = CARTESIAN_POINT ( 'NONE',  ( 30.74264578624800137, -22.33583958711395212, -8.949999994537627401 ) ) ;
#174904 = B_SPLINE_CURVE_WITH_KNOTS ( 'NONE', 3,
 ( #1217, #27638, #152920, #91229, #74124, #93230, #183284, #169079, #46752, #89279, #150969, #29598, #124575, #184271, #42791, #135795, #60908, #30585, #136764, #120601, #45754, #154915 ),
 .UNSPECIFIED., .F., .F.,
 ( 4, 2, 2, 2, 2, 2, 2, 2, 2, 2, 4 ),
 ( 1.967889508672852735E-07, 0.0003311341139581320116, 0.0006620714389653966627, 0.0009930087639726614766, 0.001323946088979925748, 0.002647695389008988473, 0.003309570039023513113, 0.003971444689038037754, 0.004633319339052562394, 0.004964256664059822979, 0.005295193989067083565 ),
 .UNSPECIFIED. ) ;
#174905 = CARTESIAN_POINT ( 'NONE',  ( -5.153800228976328057, -19.02544592524343514, 72.29057627198102409 ) ) ;
#174906 = CARTESIAN_POINT ( 'NONE',  ( 16.53943276465976808, 0.05219959533934440121, 111.2510903946856899 ) ) ;
#174907 = CARTESIAN_POINT ( 'NONE',  ( -16.79531203550684282, 7.028104445595293015, 98.74755011779544134 ) ) ;
#174908 = CARTESIAN_POINT ( 'NONE',  ( -19.02544592524334988, -5.153800228976617603, 73.95942372801900433 ) ) ;
#174909 = CARTESIAN_POINT ( 'NONE',  ( 16.51473224551069308, 9.474510206698969483, 99.16557627198102409 ) ) ;
#174910 = CARTESIAN_POINT ( 'NONE',  ( -4.483927247898539470, -16.52544592524342804, 87.29057627198103830 ) ) ;
#174911 = CARTESIAN_POINT ( 'NONE',  ( -10.72451020669898014, 18.67979575497178502, 45.41557627198103830 ) ) ;
#174912 = CARTESIAN_POINT ( 'NONE',  ( -15.72974639402197994, 15.80617190586746368, 25.62390960531435624 ) ) ;
#174913 = CARTESIAN_POINT ( 'NONE',  ( -16.55341960407611168, -4.379528057220339221, 111.4572429386476813 ) ) ;
#174914 = CARTESIAN_POINT ( 'NONE',  ( -17.49999999999999289, 5.624438216177590100, 55.81670344914646620 ) ) ;
#174915 = CARTESIAN_POINT ( 'NONE',  ( 9.564922557961047289, -16.46253265017146816, 50.41775706135233293 ) ) ;
#174916 = CARTESIAN_POINT ( 'NONE',  ( 4.379528057220339221, -16.55341960407611168, 27.70724293864769905 ) ) ;
#174917 = CARTESIAN_POINT ( 'NONE',  ( -16.51473224551069308, -9.474510206698971260, 106.6655762719810383 ) ) ;
#174918 = CARTESIAN_POINT ( 'NONE',  ( -15.72974639402176322, -15.80617190586768395, 64.37609039468568994 ) ) ;
#174919 = CARTESIAN_POINT ( 'NONE',  ( 10.72451020669898902, -18.67979575497178502, 52.91557627198103830 ) ) ;
#174920 = CARTESIAN_POINT ( 'NONE',  ( 5.719274019375673035, 21.55341960407619339, 42.29275706135235424 ) ) ;
#174921 = CARTESIAN_POINT ( 'NONE',  ( -15.72974639402197994, 15.80617190586746368, 100.6239096053143811 ) ) ;
#174922 = CARTESIAN_POINT ( 'NONE',  ( 10.72451020669871369, 18.67979575497193778, 37.08442372801901143 ) ) ;
#174923 = CARTESIAN_POINT ( 'NONE',  ( -12.14591786802309592, -12.06949235617757132, 106.8739096053143811 ) ) ;
#174924 = EDGE_CURVE ( 'NONE', #166806, #63287, #31445, .T. ) ;
#174925 = CARTESIAN_POINT ( 'NONE',  ( 13.97604488694548053, -13.89961937509957401, 75.62609039468564731 ) ) ;
#174926 = CARTESIAN_POINT ( 'NONE',  ( -19.05341960407611168, -5.049401038298163336, 51.45724293864770260 ) ) ;
#174927 = CARTESIAN_POINT ( 'NONE',  ( 14.34966873604960469, 8.224510206698951720, 109.1655762719810383 ) ) ;
#174928 = CARTESIAN_POINT ( 'NONE',  ( -19.02544592524342804, 5.153800228976336051, 106.0405762719810241 ) ) ;
#174929 = CARTESIAN_POINT ( 'NONE',  ( 0.05219959533910956823, 16.53943276465976808, 39.99890960531436690 ) ) ;
#174930 = CARTESIAN_POINT ( 'NONE',  ( -4.483927247898539470, -16.52544592524342804, 27.29057627198103120 ) ) ;
#174931 = CARTESIAN_POINT ( 'NONE',  ( -9.474510206698964154, 16.51473224551069663, 55.41557627198103120 ) ) ;
#174932 = CARTESIAN_POINT ( 'NONE',  ( 14.29746914071049879, -8.314922557960816363, 113.3322429386476955 ) ) ;
#174933 = CARTESIAN_POINT ( 'NONE',  ( 9.564922557961047289, -16.46253265017146816, 30.41775706135232937 ) ) ;
#174935 = CARTESIAN_POINT ( 'NONE',  ( -14.29746914071049879, 8.314922557960819915, 30.83224293864770260 ) ) ;
#174934 = CARTESIAN_POINT ( 'NONE',  ( -17.26058549869088665, -6.457015423128629195, 41.37745837476068544 ) ) ;
#174936 = CARTESIAN_POINT ( 'NONE',  ( -21.55341960407619339, 5.719274019375674811, 43.54275706135235424 ) ) ;
#174937 = CARTESIAN_POINT ( 'NONE',  ( -2.662494480112493012, -37.13692398601925504, -32.59999999999999432 ) ) ;
#174938 = CARTESIAN_POINT ( 'NONE',  ( -14.34966873604972548, 8.224510206698743886, 63.33442372801900433 ) ) ;
#174939 = CARTESIAN_POINT ( 'NONE',  ( -16.53943276465976808, 0.05219959533911058130, 26.24890960531435624 ) ) ;
#174940 = CARTESIAN_POINT ( 'NONE',  ( -4.379528057220086978, -16.55341960407618274, 104.7927570613523898 ) ) ;
#174941 = B_SPLINE_CURVE_WITH_KNOTS ( 'NONE', 3,
 ( #132901, #194590, #27745, #43885, #56060, #8565, #70240, #131908, #39888, #42897, #180437, #104562, #117739, #89388, #101555, #12567, #165250, #164257, #163247, #118748 ),
 .UNSPECIFIED., .F., .F.,
 ( 4, 2, 2, 2, 2, 2, 2, 2, 2, 4 ),
 ( 0.000000000000000000, 0.001368201656092175042, 0.002736403312184350085, 0.004104604968276525344, 0.005472806624368700169, 0.006841008280460872393, 0.008209209936553043749, 0.008893310764599119886, 0.009577411592645196023, 0.01094561324873732922 ),
 .UNSPECIFIED. ) ;
#174942 = CARTESIAN_POINT ( 'NONE',  ( 16.53943276465976808, 0.05219959533934440121, 21.25109039468567218 ) ) ;
#174943 = CARTESIAN_POINT ( 'NONE',  ( -9.564922557960796823, -16.46253265017161027, 42.08224293864769550 ) ) ;
#174944 = CARTESIAN_POINT ( 'NONE',  ( 19.03943276465977164, -0.05219959533909143690, 28.74890960531435624 ) ) ;
#174945 = CARTESIAN_POINT ( 'NONE',  ( -15.72974639402176322, -15.80617190586768395, 29.37609039468568284 ) ) ;
#174946 = CARTESIAN_POINT ( 'NONE',  ( 9.474510206698971260, -16.51473224551069308, 47.91557627198102409 ) ) ;
#174947 = VECTOR ( 'NONE', #89111, 1000.000000000000000 ) ;
#174948 = CARTESIAN_POINT ( 'NONE',  ( -13.89961937509977652, 13.97604488694528158, 115.6239096053143669 ) ) ;
#174949 = CARTESIAN_POINT ( 'NONE',  ( 9.564922557960805705, 16.46253265017160317, 34.58224293864770260 ) ) ;
#174950 = CARTESIAN_POINT ( 'NONE',  ( -21.52544592524343514, 5.823673210054127303, 26.04057627198103475 ) ) ;
#174952 = CARTESIAN_POINT ( 'NONE',  ( 4.483927247898545687, 16.52544592524342804, 109.7905762719810383 ) ) ;
#174951 = CARTESIAN_POINT ( 'NONE',  ( -21.53943276465977519, -0.05219959533937600094, 48.75109039468568284 ) ) ;
#174953 = CARTESIAN_POINT ( 'NONE',  ( 9.564922557960805705, 16.46253265017160317, 104.5822429386476955 ) ) ;
#174954 = CARTESIAN_POINT ( 'NONE',  ( 12.06949235617739724, 12.14591786802326823, 76.87609039468567573 ) ) ;
#174955 = CARTESIAN_POINT ( 'NONE',  ( 21.53943276465977519, 0.05219959533937863772, 96.25109039468568994 ) ) ;
#174956 = CARTESIAN_POINT ( 'NONE',  ( -8.224510206698735004, -14.34966873604973081, 59.58442372801901854 ) ) ;
#174957 = CARTESIAN_POINT ( 'NONE',  ( -5.153800228976328057, -19.02544592524343514, 92.29057627198099567 ) ) ;
#174958 = CARTESIAN_POINT ( 'NONE',  ( -14.34966873604972548, 8.224510206698743886, 43.33442372801901143 ) ) ;
#174959 = CARTESIAN_POINT ( 'NONE',  ( 16.55341960407618274, -4.379528057220086978, 26.04275706135235779 ) ) ;
#174960 = CARTESIAN_POINT ( 'NONE',  ( -16.52544592524335698, -4.483927247898792601, 83.95942372801900433 ) ) ;
#174961 = CARTESIAN_POINT ( 'NONE',  ( -19.02544592524334988, -5.153800228976617603, 103.9594237280190043 ) ) ;
#174962 = CARTESIAN_POINT ( 'NONE',  ( -16.46253265017160317, 9.564922557960807481, 75.83224293864769550 ) ) ;
#174963 = CARTESIAN_POINT ( 'NONE',  ( 21.53943276465977519, -0.05219959533907433946, 93.74890960531436690 ) ) ;
#174965 = CARTESIAN_POINT ( 'NONE',  ( -9.564922557961040184, 16.46253265017147172, 102.9177570613523329 ) ) ;
#174964 = CARTESIAN_POINT ( 'NONE',  ( 0.05219959533910956823, 16.53943276465976808, 99.99890960531436690 ) ) ;
#174966 = CARTESIAN_POINT ( 'NONE',  ( 8.314922557961029526, -14.29746914071037800, 70.41775706135236135 ) ) ;
#174967 = CARTESIAN_POINT ( 'NONE',  ( 23.34492853952160374, 11.48509598731698667, 165.7658222004386062 ) ) ;
#174968 = CARTESIAN_POINT ( 'NONE',  ( 19.03943276465977164, 0.05219959533936151252, 66.25109039468567573 ) ) ;
#174969 = CARTESIAN_POINT ( 'NONE',  ( -12.06949235617756955, 12.14591786802309770, 50.62390960531435979 ) ) ;
#174970 = CARTESIAN_POINT ( 'NONE',  ( -0.05219959533910754901, -16.53943276465976808, 97.49890960531436690 ) ) ;
#174972 = CARTESIAN_POINT ( 'NONE',  ( -17.49999999999998579, 5.500000000000031974, 90.79690382534171533 ) ) ;
#174971 = CARTESIAN_POINT ( 'NONE',  ( -0.05219959533936034679, 19.03943276465977164, 37.50109039468567573 ) ) ;
#174973 = CARTESIAN_POINT ( 'NONE',  ( -21.52544592524334988, -5.823673210054445271, 38.95942372801901854 ) ) ;
#174974 = CARTESIAN_POINT ( 'NONE',  ( -5.049401038297874678, -19.05341960407617918, 94.79275706135230450 ) ) ;
#174975 = CARTESIAN_POINT ( 'NONE',  ( 16.51473224551069308, 9.474510206698969483, 114.1655762719810241 ) ) ;
#174976 = CARTESIAN_POINT ( 'NONE',  ( -19.05341960407611168, -5.049401038298163336, 91.45724293864766707 ) ) ;
#174977 = CARTESIAN_POINT ( 'NONE',  ( -9.474510206698720793, -16.51473224551083518, 19.58442372801899722 ) ) ;
#174978 = CARTESIAN_POINT ( 'NONE',  ( -13.89961937509977652, 13.97604488694528158, 85.62390960531433848 ) ) ;
#174979 = CARTESIAN_POINT ( 'NONE',  ( -0.05219959533907301413, -21.53943276465977519, 37.49890960531436690 ) ) ;
#174980 = CARTESIAN_POINT ( 'NONE',  ( 14.34966873604960469, 8.224510206698951720, 94.16557627198103830 ) ) ;
#174981 = CARTESIAN_POINT ( 'NONE',  ( 5.153800228976335163, 19.02544592524342804, 59.79057627198100988 ) ) ;
#174982 = CARTESIAN_POINT ( 'NONE',  ( -19.05341960407611168, -5.049401038298163336, 21.45724293864768839 ) ) ;
#174983 = CARTESIAN_POINT ( 'NONE',  ( 18.67979575497194134, -10.72451020669871369, 25.83442372801901499 ) ) ;
#174984 = CARTESIAN_POINT ( 'NONE',  ( -5.823673210054431948, 21.52544592524334988, 77.70942372801900433 ) ) ;
#174985 = CARTESIAN_POINT ( 'NONE',  ( 19.02544592524343514, -5.153800228976328945, 43.54057627198103120 ) ) ;
#174986 = CARTESIAN_POINT ( 'NONE',  ( -12.14591786802326823, 12.06949235617739902, 78.12609039468570415 ) ) ;
#174987 = CARTESIAN_POINT ( 'NONE',  ( 5.719274019375991003, -21.55341960407610458, 112.7072429386476955 ) ) ;
#174988 = CARTESIAN_POINT ( 'NONE',  ( -10.72451020669870658, -18.67979575497194134, 24.58442372801901499 ) ) ;
#174990 = CARTESIAN_POINT ( 'NONE',  ( -5.153800228976328057, -19.02544592524343514, 72.29057627198102409 ) ) ;
#174989 = CARTESIAN_POINT ( 'NONE',  ( -19.02544592524334988, -5.153800228976617603, 58.95942372801900433 ) ) ;
#174991 = CARTESIAN_POINT ( 'NONE',  ( 13.97604488694548053, -13.89961937509957401, 25.62609039468566507 ) ) ;
#174992 = CARTESIAN_POINT ( 'NONE',  ( 18.62759615963255655, 10.81492255796105972, 66.66775706135234714 ) ) ;
#174993 = CARTESIAN_POINT ( 'NONE',  ( -15.80617190586745835, -15.72974639402198527, 71.87390960531438111 ) ) ;
#174994 = CARTESIAN_POINT ( 'NONE',  ( 16.55341960407611168, 4.379528057220329451, 48.95724293864770971 ) ) ;
#174996 = CARTESIAN_POINT ( 'NONE',  ( -9.564922557961040184, 16.46253265017147172, 22.91775706135233648 ) ) ;
#174995 = CARTESIAN_POINT ( 'NONE',  ( 21.53943276465977519, 0.05219959533937863772, 96.25109039468568994 ) ) ;
#174997 = CARTESIAN_POINT ( 'NONE',  ( -16.53943276465976808, 0.05219959533911058130, 71.24890960531435269 ) ) ;
#174998 = CARTESIAN_POINT ( 'NONE',  ( 13.89961937509977652, -13.97604488694527269, 28.12390960531435624 ) ) ;
#174999 = CARTESIAN_POINT ( 'NONE',  ( -13.89961937509957401, -13.97604488694547875, 54.37609039468565442 ) ) ;
#175000 = CARTESIAN_POINT ( 'NONE',  ( -4.483927247898539470, -16.52544592524342804, 27.29057627198103120 ) ) ;
#175002 = EDGE_CURVE ( 'NONE', #101974, #15498, #137091, .T. ) ;
#175001 = CARTESIAN_POINT ( 'NONE',  ( -10.81492255796105439, 18.62759615963255655, 82.91775706135234714 ) ) ;
#175003 = CARTESIAN_POINT ( 'NONE',  ( 9.474510206698971260, -16.51473224551069308, 77.91557627198103830 ) ) ;
#175004 = CARTESIAN_POINT ( 'NONE',  ( -19.05341960407617563, 5.049401038297882671, 48.54275706135233293 ) ) ;
#175005 = CARTESIAN_POINT ( 'NONE',  ( -15.72974639402197994, 15.80617190586746368, 45.62390960531436690 ) ) ;
#175006 = CARTESIAN_POINT ( 'NONE',  ( 10.72451020669871369, 18.67979575497193778, 52.08442372801901854 ) ) ;
#175007 = CARTESIAN_POINT ( 'NONE',  ( -21.52544592524343514, 5.823673210054127303, 101.0405762719810383 ) ) ;
#175008 = CARTESIAN_POINT ( 'NONE',  ( -9.564922557961040184, 16.46253265017147172, 92.91775706135233293 ) ) ;
#175009 = CARTESIAN_POINT ( 'NONE',  ( -0.05219959533934338120, 16.53943276465976808, 72.50109039468568994 ) ) ;
#175011 = CARTESIAN_POINT ( 'NONE',  ( -10.72451020669898014, 18.67979575497178502, 110.4155762719810383 ) ) ;
#175010 = CARTESIAN_POINT ( 'NONE',  ( -16.47688973148989788, -17.58748242838617060, -56.92523117286675927 ) ) ;
#175012 = CARTESIAN_POINT ( 'NONE',  ( 0.05219959533910956823, 16.53943276465976808, 84.99890960531436690 ) ) ;
#175013 = CARTESIAN_POINT ( 'NONE',  ( -17.48847506799967277, -5.747544572773784388, 99.17302562156720569 ) ) ;
#175014 = CARTESIAN_POINT ( 'NONE',  ( 8.314922557961029526, -14.29746914071037800, 30.41775706135234358 ) ) ;
#175015 = CARTESIAN_POINT ( 'NONE',  ( -18.62759615963270932, 10.81492255796079327, 60.83224293864769550 ) ) ;
#175016 = CARTESIAN_POINT ( 'NONE',  ( 16.52544592524335698, 4.483927247898782831, 91.45942372801901854 ) ) ;
#175017 = CARTESIAN_POINT ( 'NONE',  ( -13.97604488694527625, -13.89961937509977652, 26.87390960531434558 ) ) ;
#175018 = EDGE_CURVE ( 'NONE', #2773, #63582, #115808, .T. ) ;
#175019 = CARTESIAN_POINT ( 'NONE',  ( -12.14591786802326823, 12.06949235617739902, 73.12609039468567573 ) ) ;
#175020 = CARTESIAN_POINT ( 'NONE',  ( 13.97604488694548053, -13.89961937509957401, 60.62609039468564731 ) ) ;
#175021 = CARTESIAN_POINT ( 'NONE',  ( 5.823673210054444382, -21.52544592524334988, 40.20942372801901854 ) ) ;
#175022 = CARTESIAN_POINT ( 'NONE',  ( -0.05219959533907301413, -21.53943276465977519, 62.49890960531436690 ) ) ;
#175023 = CARTESIAN_POINT ( 'NONE',  ( -4.483927247898782831, 16.52544592524335698, 77.70942372801900433 ) ) ;
#175024 = CARTESIAN_POINT ( 'NONE',  ( 21.52544592524334988, 5.823673210054432836, 66.45942372801903275 ) ) ;
#175025 = CARTESIAN_POINT ( 'NONE',  ( 15.80617190586746368, 15.72974639402197994, 59.37390960531436690 ) ) ;
#175026 = CARTESIAN_POINT ( 'NONE',  ( 5.823673210054125526, 21.52544592524343514, 34.79057627198103120 ) ) ;
#175027 = CARTESIAN_POINT ( 'NONE',  ( 14.34966873604972726, -8.224510206698740333, 65.83442372801900433 ) ) ;
#175028 = CARTESIAN_POINT ( 'NONE',  ( 5.719274019375991003, -21.55341960407610458, 32.70724293864770260 ) ) ;
#175029 = ORIENTED_EDGE ( 'NONE', *, *, #119720, .F. ) ;
#175030 = CARTESIAN_POINT ( 'NONE',  ( 9.564922557960805705, 16.46253265017160317, 104.5822429386476955 ) ) ;
#175031 = CARTESIAN_POINT ( 'NONE',  ( 4.379528057220092307, 16.55341960407617563, 107.2927570613523471 ) ) ;
#175032 = CARTESIAN_POINT ( 'NONE',  ( -22.67087683854552793, -7.530304285672279718, 173.4975851171454053 ) ) ;
#175033 = CARTESIAN_POINT ( 'NONE',  ( -8.314922557960811034, -14.29746914071050412, 102.0822429386476955 ) ) ;
#175034 = CARTESIAN_POINT ( 'NONE',  ( -5.719274019375978568, 21.55341960407610458, 60.20724293864768839 ) ) ;
#175035 = CARTESIAN_POINT ( 'NONE',  ( 0.05219959533909260263, 19.03943276465977164, 39.99890960531436690 ) ) ;
#175036 = CARTESIAN_POINT ( 'NONE',  ( -8.224510206698735004, -14.34966873604973081, 94.58442372801901854 ) ) ;
#175037 = CARTESIAN_POINT ( 'NONE',  ( -5.823673210054431948, 21.52544592524334988, 32.70942372801900433 ) ) ;
#175038 = CARTESIAN_POINT ( 'NONE',  ( 19.02544592524334988, 5.153800228976608722, 101.4594237280189759 ) ) ;
#175039 = CARTESIAN_POINT ( 'NONE',  ( -0.05219959533910754901, -16.53943276465976808, 102.4989096053143811 ) ) ;
#175040 = CARTESIAN_POINT ( 'NONE',  ( -19.02544592524342804, 5.153800228976336051, 51.04057627198103120 ) ) ;
#175041 = CARTESIAN_POINT ( 'NONE',  ( 0.05219959533909260263, 19.03943276465977164, 24.99890960531435269 ) ) ;
#175042 = CARTESIAN_POINT ( 'NONE',  ( 17.44279575226824264, -5.990770900252460507, 38.33557567514319686 ) ) ;
#175043 = CARTESIAN_POINT ( 'NONE',  ( -19.02544592524342804, 5.153800228976336051, 96.04057627198103830 ) ) ;
#175044 = CARTESIAN_POINT ( 'NONE',  ( 0.05219959533934541429, -16.53943276465976808, 80.00109039468568994 ) ) ;
#175045 = CARTESIAN_POINT ( 'NONE',  ( 0.05219959533937995610, -21.53943276465977519, 100.0010903946857042 ) ) ;
#175046 = CARTESIAN_POINT ( 'NONE',  ( 15.72974639402199770, -15.80617190586745480, 53.12390960531436690 ) ) ;
#175047 = CARTESIAN_POINT ( 'NONE',  ( 16.53943276465976808, 0.05219959533934440121, 71.25109039468568994 ) ) ;
#175048 = CARTESIAN_POINT ( 'NONE',  ( 19.05341960407617918, -5.049401038297876454, 76.04275706135230450 ) ) ;
#175049 = ORIENTED_EDGE ( 'NONE', *, *, #24639, .F. ) ;
#175050 = CARTESIAN_POINT ( 'NONE',  ( -13.89961937509977652, 13.97604488694528158, 35.62390960531435269 ) ) ;
#175051 = CARTESIAN_POINT ( 'NONE',  ( 19.05341960407611168, 5.049401038298154454, 73.95724293864768129 ) ) ;
#175052 = CARTESIAN_POINT ( 'NONE',  ( -19.03943276465977164, 0.05219959533909376836, 36.24890960531436690 ) ) ;
#175053 = CARTESIAN_POINT ( 'NONE',  ( -5.153800228976607833, 19.02544592524334988, 72.70942372801900433 ) ) ;
#175054 = CARTESIAN_POINT ( 'NONE',  ( -9.564922557960796823, -16.46253265017161027, 112.0822429386476955 ) ) ;
#175055 = CARTESIAN_POINT ( 'NONE',  ( -16.51473224551069308, -9.474510206698971260, 96.66557627198102409 ) ) ;
#175056 = CARTESIAN_POINT ( 'NONE',  ( 12.14591786802309770, 12.06949235617756955, 54.37390960531435979 ) ) ;
#175057 = CARTESIAN_POINT ( 'NONE',  ( -18.67979575497178146, -10.72451020669898902, 51.66557627198102409 ) ) ;
#175058 = DIRECTION ( 'NONE',  ( -0.1736481776669307198, -2.126576849575776229E-17, -0.9848077530122080203 ) ) ;
#175059 = CARTESIAN_POINT ( 'NONE',  ( -13.89961937509957401, -13.97604488694547875, 29.37609039468565797 ) ) ;
#175060 = CARTESIAN_POINT ( 'NONE',  ( -13.89961937509977652, 13.97604488694528158, 45.62390960531433848 ) ) ;
#175061 = CARTESIAN_POINT ( 'NONE',  ( -8.224510206698735004, -14.34966873604973081, 34.58442372801900433 ) ) ;
#175062 = DIRECTION ( 'NONE',  ( 0.000000000000000000, 0.000000000000000000, -1.000000000000000000 ) ) ;
#175063 = CARTESIAN_POINT ( 'NONE',  ( 24.69864643647408187, -7.736333414721475954, 171.5373488951853176 ) ) ;
#175064 = CARTESIAN_POINT ( 'NONE',  ( -14.34966873604972548, 8.224510206698743886, 78.33442372801901854 ) ) ;
#175065 = CARTESIAN_POINT ( 'NONE',  ( -10.72451020669898014, 18.67979575497178502, 95.41557627198102409 ) ) ;
#175067 = CARTESIAN_POINT ( 'NONE',  ( -26.58496454517000629, 7.626754437231443084, 167.9682100371138915 ) ) ;
#175066 = CARTESIAN_POINT ( 'NONE',  ( 19.02544592524343514, -5.153800228976328945, 38.54057627198103120 ) ) ;
#175068 = CARTESIAN_POINT ( 'NONE',  ( -10.81492255796105439, 18.62759615963255655, 42.91775706135235424 ) ) ;
#175069 = CARTESIAN_POINT ( 'NONE',  ( -13.89961937509957401, -13.97604488694547875, 54.37609039468565442 ) ) ;
#175070 = CARTESIAN_POINT ( 'NONE',  ( -15.72974639402176322, -15.80617190586768395, 94.37609039468568994 ) ) ;
#175071 = CARTESIAN_POINT ( 'NONE',  ( 17.26172910966779739, 6.454744622555850242, 96.69353091350775742 ) ) ;
#175072 = CARTESIAN_POINT ( 'NONE',  ( 16.52544592524342804, -4.483927247898539470, 38.54057627198103120 ) ) ;
#175073 = CARTESIAN_POINT ( 'NONE',  ( -16.37811251030163717, 0.9487569900775056908, -59.27680374464310376 ) ) ;
#175074 = CARTESIAN_POINT ( 'NONE',  ( 5.823673210054125526, 21.52544592524343514, 49.79057627198102409 ) ) ;
#175075 = CARTESIAN_POINT ( 'NONE',  ( -17.14385361876520264, -23.59649016807271238, 141.1750000027311671 ) ) ;
#175076 = CARTESIAN_POINT ( 'NONE',  ( -9.474510206698964154, 16.51473224551069663, 105.4155762719810383 ) ) ;
#175077 = CARTESIAN_POINT ( 'NONE',  ( 12.06949235617757843, -12.14591786802309237, 98.12390960531436690 ) ) ;
#175078 = CARTESIAN_POINT ( 'NONE',  ( -9.564922557961040184, 16.46253265017147172, 112.9177570613523329 ) ) ;
#175079 = CARTESIAN_POINT ( 'NONE',  ( 16.52544592524335698, 4.483927247898782831, 106.4594237280190328 ) ) ;
#175080 = EDGE_LOOP ( 'NONE', ( #195259, #26181, #161173, #76153, #105023, #49743 ) ) ;
#175082 = CARTESIAN_POINT ( 'NONE',  ( 21.53943276465977519, -0.05219959533907433946, 108.7489096053143669 ) ) ;
#175081 = CARTESIAN_POINT ( 'NONE',  ( 13.89961937509977652, -13.97604488694527269, 98.12390960531433848 ) ) ;
#175084 = CARTESIAN_POINT ( 'NONE',  ( -9.474510206698964154, 16.51473224551069663, 100.4155762719810241 ) ) ;
#175083 = CARTESIAN_POINT ( 'NONE',  ( 14.34966873604960469, 8.224510206698951720, 24.16557627198103120 ) ) ;
#175085 = CARTESIAN_POINT ( 'NONE',  ( 5.049401038297881783, 19.05341960407617563, 92.29275706135234714 ) ) ;
#175086 = CARTESIAN_POINT ( 'NONE',  ( 5.823673210054444382, -21.52544592524334988, 110.2094237280190185 ) ) ;
#175087 = CARTESIAN_POINT ( 'NONE',  ( 5.823673210054125526, 21.52544592524343514, 84.79057627198102409 ) ) ;
#175088 = CARTESIAN_POINT ( 'NONE',  ( -5.823673210054116645, -21.52544592524344225, 52.29057627198102409 ) ) ;
#175089 = CARTESIAN_POINT ( 'NONE',  ( 9.564922557960805705, 16.46253265017160317, 59.58224293864769550 ) ) ;
#175090 = CARTESIAN_POINT ( 'NONE',  ( -16.53943276465976808, 0.05219959533911058130, 36.24890960531435979 ) ) ;
#175091 = CARTESIAN_POINT ( 'NONE',  ( 19.03943276465977164, -0.05219959533909143690, 78.74890960531436690 ) ) ;
#175092 = CARTESIAN_POINT ( 'NONE',  ( -32.00000000000000000, -4.837354856632041508E-15, 50.50000000000002842 ) ) ;
#175093 = CARTESIAN_POINT ( 'NONE',  ( 19.03943276465977164, 0.05219959533936151252, 46.25109039468566863 ) ) ;
#175094 = CARTESIAN_POINT ( 'NONE',  ( 18.67979575497178502, 10.72451020669898547, 84.16557627198103830 ) ) ;
#175095 = B_SPLINE_CURVE_WITH_KNOTS ( 'NONE', 3,
 ( #154010, #29682, #28709, #152030, #13516, #15506, #14505, #136853, #60009, #121676 ),
 .UNSPECIFIED., .F., .F.,
 ( 4, 2, 2, 2, 4 ),
 ( 8.673617379884035472E-19, 0.001083413406193705275, 0.001625120109290555202, 0.001895973460838981358, 0.002166826812387407080 ),
 .UNSPECIFIED. ) ;
#175096 = CARTESIAN_POINT ( 'NONE',  ( -4.483927247898539470, -16.52544592524342804, 87.29057627198103830 ) ) ;
#175097 = CARTESIAN_POINT ( 'NONE',  ( 0.05219959533937995610, -21.53943276465977519, 35.00109039468568284 ) ) ;
#175098 = CARTESIAN_POINT ( 'NONE',  ( 22.44159573604009239, 16.30477369853692693, 148.5750000027312012 ) ) ;
#175099 = CARTESIAN_POINT ( 'NONE',  ( -12.14591786802326823, 12.06949235617739902, 108.1260903946856757 ) ) ;
#175100 = CARTESIAN_POINT ( 'NONE',  ( -9.564922557960796823, -16.46253265017161027, 22.08224293864768839 ) ) ;
#175101 = CARTESIAN_POINT ( 'NONE',  ( -5.049401038298153566, 19.05341960407611168, 85.20724293864766707 ) ) ;
#175102 = CARTESIAN_POINT ( 'NONE',  ( 5.153800228976335163, 19.02544592524342804, 24.79057627198102765 ) ) ;
#175103 = CARTESIAN_POINT ( 'NONE',  ( -8.224510206698948167, 14.34966873604960824, 40.41557627198103120 ) ) ;
#175104 = CARTESIAN_POINT ( 'NONE',  ( 15.80617190586769283, -15.72974639402175789, 55.62609039468568284 ) ) ;
#175105 = CARTESIAN_POINT ( 'NONE',  ( 36.30973463497186060, -18.33876584756081130, -18.81039752657306252 ) ) ;
#175106 = CARTESIAN_POINT ( 'NONE',  ( -16.51473224551069308, -9.474510206698971260, 46.66557627198102409 ) ) ;
#175107 = CARTESIAN_POINT ( 'NONE',  ( -5.153800228976328057, -19.02544592524343514, 52.29057627198100988 ) ) ;
#175108 =( BOUNDED_SURFACE ( )  B_SPLINE_SURFACE ( 3, 2, ( 
 ( #185335, #78136, #75172, #14495, #90336, #30663, #42865, #44843, #93306, #106499, #136844, #151045, #59999, #92316, #104530, #121666, #154001, #77153, #183361, #168176, #12535, #199518, #91304, #74200, #152021, #76157, #154991, #138824, #170164, #137837, #304, #135869, #61972, #123638, #46825, #31657, #197540, #120675, #43851, #182374, #192054, #54540, #144542, #131376, #6027, #146534, #24222, #68700, #23214, #160717, #37369, #94302, #83858, #129364, #155980, #47826, #7018, #38377, #113208, #99027, #32648, #53536, #130355, #21207, #115213, #193064, #100033, #175897, #69709, #174896, #128372, #109477, #36362, #176906, #145539, #67706, #85872, #51544, #98014, #161719, #116213, #17477, #191060, #84857, #22209, #8027, #186346, #66711, #177904, #162716, #39372, #101031, #147561, #9046, #70716, #171161, #79134, #52532, #114193, #159708, #190068, #143539, #5026, #82864, #73721, #102047, #151548, #28226, #164728, #182881, #120198, #181888, #167708, #56546, #163731, #42380, #118223, #179914, #89866, #59511, #104043, #105038, #25232, #86873, #57551, #103046, #12059, #121188, #135394, #88867, #41380, #87862, #148557, #150560, #44364, #13038, #74704, #136368, #198045, #197064, #71708, #119220, #43366, #26222, #11045, #166722, #58532, #149550, #106021, #132384, #72721, #178905, #40373, #29204, #134394, #55540, #10048, #90838, #180905, #196080, #133376, #152522, #165723, #195066, #14010, #194077, #117212, #27219, #122179, #124162, #109998, #153517, #48344, #32173, #46341, #64496, #75676, #154515, #183871, #45356, #171678, #200033, #199034, #30181, #140331, #62491, #107997, #15014, #186874, #109005, #168681, #79660, #126163, #187858, #60504, #107008, #185863, #33168, #76675, #92830, #94827, #110988, #155509, #156504, #47349, #170684, #91824, #93829, #16012, #138351, #137355, #17004, #125177, #61501, #78656, #123170, #1821, #63502, #169684, #18006, #141329, #2817, #49327, #172673, #184858, #31179, #77669, #139338, #34158, #95819, #817, #157504, #81617, #66476, #130118, #84620, #50331, #36129, #113955, #5793, #176668, #18997, #96799, #37129, #192825, #190823, #7787, #177667, #146299, #69470, #191815, #68464, #20964, #82621, #128138, #158486, #127140, #98789, #161484, #160483, #188847, #38144, #114975, #51311, #131137, #6785, #53296, #54306, #143300, #111987, #129125, #4786, #189838, #99798, #115978, #52298, #22972, #173678, #35145, #144303, #112972, #21973, #39135, #83625, #175655, #174664, #97781, #19974, #145302, #100790, #80643, #142320, #3800, #65478, #159469, #67466, #149314, #11819, #71471, #41143, #102806, #196829, #44128, #165487, #26983, #147316, #117982, #9810, #118987, #180670, #89625, #182644, #74468, #25985, #151313, #164492, #42147, #135156, #134151, #163489, #73484, #88628, #8806, #87628, #150324, #57312, #24987, #103807, #59275, #162473, #178661, #58297, #70475, #86632, #119965, #43130, #116970, #104799, #136133, #181651, #55298, #166488, #133136, #132141, #195839, #23975, #120945, #101802, #27986, #197809, #12802, #10808, #40124, #193834, #85630, #148315, #194827, #56300, #179672, #72478, #2573, #107755, #156258, #169438, #76436, #28968, #122931, #170439, #64254, #199794, #123913, #93584, #46100, #184618, #125921, #62244, #92589, #187619, #168450, #77428, #17761, #140083, #171438, #15768, #108762, #79417, #185612, #29946, #91584, #78407, #90610, #138113, #106775, #152291, #31930, #32925, #61261, #48098, #139099, #1575, #153275, #105787, #186627, #141087, #30942, #75443, #167473, #155270, #573, #47101, #13775, #94580, #154278, #14776, #109754, #16759, #137118, #63250, #124929, #198804, #60269, #121942, #183635, #45117, #98546, #49089, #161237, #110746, #22731, #189595, #19734, #190583, #4538, #176422, #174422, #37897, #160239, #172427, #84379, #33916, #127892, #83382, #130893, #52059, #113715, #95573, #66232, #96556, #5546, #67225, #99555, #69225, #146056, #112729, #7540, #51068, #128883 ),
 ( #6540, #157259, #175412, #145059, #20720, #97538, #18754, #144065, #35891, #80400, #142072, #36880, #21729, #173431, #159225, #3558, #68220, #129872, #81375, #191570, #53049, #114729, #82377, #65236, #34901, #188602, #126896, #158243, #50083, #111743, #143060, #89384, #55059, #39884, #103571, #58062, #23734, #9568, #87394, #179430, #150073, #192583, #70236, #10567, #166241, #164253, #181416, #151073, #119733, #42894, #165246, #41905, #194586, #56056, #101551, #131904, #100555, #72231, #134915, #133906, #162234, #11578, #88379, #24743, #104559, #180432, #26740, #27742, #116731, #85383, #102568, #178420, #163243, #73244, #12564, #25748, #196592, #147076, #8560, #117735, #86393, #195597, #74230, #57069, #149079, #148077, #71234, #54066, #115740, #177427, #38898, #132897, #193588, #118744, #40895, #60030, #93337, #63003, #107512, #108516, #28730, #105546, #61017, #106530, #15526, #124681, #138853, #92346, #44874, #91335, #90367, #154031, #47856, #155022, #16518, #78166, #139834, #333, #75203, #122689, #185364, #168207, #14527, #170194, #77183, #29704, #186377, #135898, #76188, #182403, #43882, #31688, #121696, #59037, #152052, #62001, #184378, #153027, #13537, #46856, #169188, #136874, #1323, #109509, #171191, #120704, #167232, #45859, #32680, #198560, #137867, #94333, #156011, #123667, #17508, #30695, #197570, #183392, #199547, #19495, #187375, #140837, #97297, #128642, #3321, #127653, #125677, #82125, #158983, #111497, #20475, #21479, #190336, #65983, #159992, #64994, #18509, #2325, #126652, #143818, #35649, #34658, #176174, #141828, #188355, #51813, #113472, #172180, #5299, #37644, #173183, #66982, #175167, #81140, #96317, #99307, #36633, #189353, #160992, #49833, #50830, #129631, #98290, #144815, #112487, #83139, #52804, #6298, #158003, #142821, #67977, #64007, #4301, #80157, #191326, #114471, #48844, #174180, #79166, #110498, #33665, #95327, #157012, #104317, #38656, #148836, #7296, #85136, #10326, #103325, #177183, #165005, #134671, #87153, #115495, #71982, #193341, #68980, #194348, #22486, #181178, #161991, #26499, #57824, #55816, #9327, #100312, #130645, #88141, #196356, #54815, #117489, #8315, #25509, #119496, #24499, #73002, #178179, #133657, #56827, #23487, #195347, #42655, #116490, #40654, #118502, #162994, #39644, #84134, #179186, #70992, #145813, #146820, #102323, #192339, #180192, #149826, #132660, #41662, #53821, #164013, #69991, #131659, #11331, #101305, #86151, #147841, #89143, #168946, #31447, #121458, #108277, #137626, #61764, #13303, #186138, #46616, #77933, #91104, #135662, #47617, #92100, #75952, #107275, #150832, #93100, #152792, #74968, #169955, #30453, #139600, #106287, #136630, #153788, #183150, #154784, #14284, #16281, #15284, #166001, #1086, #27501, #44635, #94, #12328, #76943, #138612, #73993, #167972, #198312, #122449, #184141, #62762, #197334, #124442, #29471, #58797, #199311, #45623, #123432, #60777, #166992, #185125, #120465, #182157, #43641, #105304, #28494, #59790, #90128, #151812, #21247, #34430, #78927, #129402, #35417, #19269, #50599, #32442, #36398, #96090, #18277, #51580, #112258, #82901, #49597, #79931, #173950, #64766, #98052, #157778, #159752, #158751, #109271, #144580, #170950, #188126, #143581, #191098, #97069, #20240, #94096, #126429, #156784, #65749, #127418, #6066, #155775, #67744, #172952, #17273, #111261, #189127, #81888, #80915, #110266, #5063, #66748, #140603, #142592, #128409, #4072, #171947, #190105, #2093, #63774, #125446, #113244, #187142, #33436, #174935, #48614, #95095, #141603, #3090, #117251, #145580, #102085, #23253, #37410, #24262, #134433, #11086, #192095, #195105, #87902, #85911, #39408, #7057, #160757, #56588, #26261, #84896, #147599, #38416, #55577, #149588, #54577, #103085, #8070, #178943, #86912, #68739, #40414, #72763, #146575, #70754, #163769, #193103, #69746, #52573, #9085, #101068, #114233, #115254, #132422, #164766 ),
 ( #194113, #148595, #100073, #175939, #133416, #99068, #177941, #22248, #83897, #25270, #162753, #10087, #130397, #179952, #71745, #161758, #118262, #41419, #53577, #116249, #131415, #176947, #154311, #125954, #123946, #187652, #48131, #198838, #110781, #60302, #77461, #32960, #80434, #1608, #63284, #183668, #15800, #46134, #155304, #16793, #49123, #18789, #172462, #62278, #33949, #139131, #78443, #171471, #170473, #199828, #109788, #124964, #45153, #185644, #186661, #93618, #61295, #140117, #95607, #121977, #14809, #94614, #106809, #122965, #156293, #79450, #153308, #141120, #157292, #17794, #91620, #2610, #169472, #168483, #31963, #29981, #76470, #138147, #64287, #184652, #107787, #47136, #30973, #92620, #608, #108794, #112762, #113749, #127926, #145091, #38930, #144098, #192616, #97570, #6574, #176455, #34938, #68253, #100587, #35924, #160272, #129904, #82409, #159258, #162269, #98578, #128916, #23769, #4574, #175445, #54098, #37928, #7573, #52092, #191604, #115772, #21763, #66267, #189628, #114761, #65270, #174455, #143095, #126930, #53083, #69259, #20754, #84412, #5578, #142107, #51102, #67258, #96590, #177461, #190617, #83414, #36915, #99589, #161269, #3592, #19768, #22763, #188638, #146089, #130925, #50117, #111777, #173465, #158279, #81409, #87429, #149114, #194621, #24780, #193622, #165282, #27777, #26775, #55094, #104593, #181451, #117773, #135934, #73280, #134950, #120737, #9604, #116764, #195633, #71269, #132934, #42929, #12600, #57106, #58097, #178455, #39922, #10605, #56092, #88417, #74264, #150111, #41940, #179467, #40932, #101591, #103606, #197604, #166280, #89419, #151108, #59070, #11612, #86427, #72266, #196628, #102604, #164290, #119767, #182436, #25783, #43916, #85419, #133943, #131938, #163279, #105578, #118780, #8596, #148113, #167264, #180468, #147110, #70270, #139869, #62037, #121731, #32714, #79203, #140872, #13570, #75237, #77217, #63037, #106564, #45893, #186413, #64042, #108550, #124715, #366, #138886, #136908, #123701, #169222, #198595, #90400, #46890, #78199, #153061, #185399, #60063, #31722, #170229, #61050, #93370, #171225, #1358, #15559, #109543, #14563, #168241, #152085, #76221, #155057, #16552, #47890, #94366, #125712, #137900, #183423, #156045, #199582, #122722, #17542, #2361, #187411, #48879, #44907, #29737, #154064, #184412, #110534, #28763, #91370, #107546, #30731, #92378, #126685, #128676, #84166, #129663, #191359, #114506, #176208, #36667, #111532, #159017, #21513, #81173, #50863, #144848, #190373, #142855, #161025, #172215, #112521, #18544, #80191, #6331, #96350, #95362, #188389, #98326, #20510, #4334, #49866, #83174, #5333, #65029, #37677, #22519, #145846, #157047, #141863, #82158, #68011, #173217, #189386, #52837, #7328, #51848, #99342, #143854, #67017, #3354, #113507, #174215, #34693, #33699, #175202, #69012, #158037, #160026, #19528, #130678, #192372, #66018, #53855, #127686, #35683, #97331, #196388, #39675, #54849, #177217, #163026, #56860, #72016, #71024, #12360, #178211, #24532, #70023, #150866, #102355, #118535, #10359, #164044, #73033, #115529, #193373, #133689, #89174, #87187, #104349, #74023, #181212, #166033, #26530, #165037, #117521, #179219, #86183, #116523, #23521, #195382, #57857, #180224, #85167, #134705, #11363, #147873, #27533, #9359, #41694, #103359, #132692, #135693, #101337, #194380, #131692, #197365, #25543, #88174, #149858, #148868, #119529, #38690, #55847, #42688, #100346, #162025, #146855, #8348, #40685, #109302, #169986, #108306, #60807, #122480, #168004, #198345, #167023, #138644, #1117, #125, #28524, #77962, #154814, #91133, #170981, #46646, #31477, #94127, #183183, #90160, #168976, #44665, #106318, #16312, #186169, #30481, #93129, #151843, #13333, #184171, #29500, #61794, #47651, #123464, #15314, #152823, #14317, #74998, #76973, #32474, #139629, #62791, #124472, #155806, #185156, #59819, #45653, #17304, #75982, #137655 ),
 ( #78959, #199342, #140634, #58830, #92132, #121489, #120497, #182188, #43673, #107304, #105335, #153819, #136663, #20270, #99100, #83931, #18308, #128437, #187175, #64798, #190134, #82934, #156816, #144612, #114267, #66776, #95126, #51609, #172982, #48646, #173978, #2124, #160792, #141633, #6097, #37440, #35446, #189154, #79964, #110298, #67776, #175971, #34460, #97098, #126459, #81916, #22280, #63806, #3123, #113273, #171980, #188157, #174965, #129433, #49630, #191131, #125479, #36429, #111293, #98084, #96119, #33468, #158782, #157807, #19298, #80946, #52605, #142621, #143609, #50627, #4100, #65779, #127448, #112288, #5093, #159782, #21277, #148629, #42450, #147630, #196150, #101098, #10119, #179985, #38449, #71779, #104114, #39438, #163801, #133449, #85941, #162784, #165796, #102116, #132453, #27293, #8100, #117282, #57622, #41453, #11120, #55608, #195139, #119290, #25303, #69778, #131446, #118294, #68772, #116280, #146607, #130430, #56620, #72795, #24292, #87935, #178976, #103118, #193133, #145612, #26294, #180973, #70785, #115286, #7091, #164799, #40443, #86945, #192129, #134465, #194144, #54606, #149622, #53610, #176979, #9118, #177970, #100104, #161788, #23283, #84927, #77737, #138417, #88940, #885, #150631, #167774, #123234, #170752, #91892, #153583, #73791, #44434, #136435, #45421, #107074, #16079, #109073, #62560, #152589, #139403, #29272, #168745, #61565, #60570, #89935, #200097, #15081, #135463, #14080, #76742, #184925, #183936, #151616, #30249, #185932, #12127, #105108, #46409, #197132, #13108, #108068, #169752, #43439, #31247, #124236, #92897, #181957, #154583, #59583, #58599, #122246, #120265, #47417, #28295, #166794, #74773, #198116, #75746, #121257, #182951, #106088, #90903, #137423, #199103, #48414, #111059, #50400, #156581, #127208, #33239, #172747, #157573, #140402, #34228, #112060, #171750, #126232, #95890, #18076, #94897, #173748, #187927, #141400, #32241, #186943, #64567, #188922, #19066, #65549, #49396, #80713, #93899, #142391, #110070, #79731, #3870, #17072, #2888, #155577, #1890, #78726, #63571, #125245, #155240, #184589, #108732, #60239, #32897, #93554, #124900, #138081, #182612, #94549, #139067, #122900, #154247, #136102, #140054, #199762, #121910, #16730, #15738, #186599, #153241, #183603, #77397, #168419, #1544, #61229, #63220, #62216, #12771, #48071, #74435, #91554, #47072, #197778, #545, #123884, #59244, #29914, #45087, #169405, #30911, #109727, #120913, #171411, #76405, #44097, #106744, #90579, #185582, #46070, #105755, #78378, #167441, #28938, #170409, #31901, #152260, #13745, #75413, #137085, #107724, #198773, #14744, #92559, #94219, #138736, #217, #120590, #91220, #183274, #92227, #153913, #62887, #139721, #78052, #61886, #106410, #76071, #15408, #108403, #107397, #136754, #185251, #123556, #182285, #60898, #46744, #30576, #198439, #77065, #32566, #17396, #151934, #170080, #43765, #59911, #31571, #16406, #90251, #1209, #47742, #93222, #28613, #154907, #168091, #105429, #169070, #135785, #155899, #75087, #124567, #171075, #186264, #122573, #13423, #167112, #109395, #197456, #29589, #58922, #121579, #44754, #152911, #137747, #14407, #199431, #184263, #45745, #172070, #143707, #176067, #173073, #97188, #66868, #19387, #96209, #99197, #35541, #65870, #160885, #141721, #50722, #129524, #113367, #144703, #189244, #82011, #52698, #158874, #3211, #64885, #51704, #2216, #49720, #80052, #63897, #5187, #6189, #34550, #21371, #112380, #175059, #126546, #79053, #159882, #191224, #4192, #48734, #140726, #128531, #174072, #20364, #125568, #67869, #127544, #188246, #83029, #190226, #114362, #81036, #111387, #36524, #142712, #157898, #18402, #187265, #98178, #37534, #110388, #33557, #95219, #156905, #54702, #72891, #10212, #71872, #57716, #146703, #53709, #132548, #8200, #69875, #180081, #149716, #194236, #195232, #115386, #192228, #147726, #193228, #102212, #11215, #25397 ),
 ( #133541, #87039, #56715, #118387, #119386, #116375, #134559, #22376, #101190, #68871, #130530, #41550, #131544, #177074, #38545, #39531, #100201, #178063, #161883, #103213, #55702, #23377, #26389, #196247, #181069, #7187, #85023, #70880, #164895, #162880, #24389, #88028, #42544, #163901, #104207, #117375, #179072, #86039, #40542, #9213, #148724, #84027, #145705, #15174, #90024, #14170, #12221, #168837, #184029, #198206, #45511, #108162, #76833, #152681, #46502, #151707, #105198, #27385, #13200, #107166, #122338, #121349, #62651, #28386, #74863, #120356, #975, #75838, #30342, #60665, #137516, #123323, #165888, #43533, #91983, #139493, #199197, #154675, #124328, #31338, #16170, #138505, #200186, #167864, #153677, #73884, #61655, #106181, #135554, #89031, #185016, #169844, #136525, #92989, #197226, #77824, #186026, #59677, #47508, #150722, #58688, #182050, #166885, #183042, #44525, #29364, #90995, #50486, #65638, #64656, #5948, #171838, #156671, #63664, #144463, #95980, #112146, #3959, #157664, #66630, #109164, #187035, #127298, #82782, #80803, #97938, #67625, #174818, #159631, #20130, #158639, #111148, #172838, #18166, #48505, #17164, #189011, #51467, #173838, #78817, #128294, #4946, #141493, #21127, #96959, #81774, #129285, #33325, #140496, #19154, #94986, #79822, #189992, #36283, #142481, #143461, #1984, #125337, #34317, #2977, #35304, #190980, #113128, #170844, #126318, #188015, #110159, #32335, #93988, #155668, #49485, #194987, #56465, #117130, #191972, #39294, #101968, #55459, #163649, #148480, #87786, #23133, #41303, #52457, #131298, #98949, #160639, #25151, #176827, #83781, #145460, #69632, #22130, #84778, #130277, #86793, #85794, #6942, #118143, #102964, #164649, #37290, #68621, #100951, #9971, #53459, #192987, #71631, #149471, #132305, #133297, #24142, #99953, #8970, #70639, #179833, #26144, #10966, #178823, #146456, #54465, #193997, #72640, #147480, #115135, #134315, #40294, #38299, #177824, #114114, #175817, #161639, #7949, #116135, #162635, #11978, #122103, #180827, #58453, #183793, #76599, #150483, #138275, #107921, #60429, #88790, #45280, #166645, #42305, #167630, #77593, #154440, #135314, #199958, #31104, #29127, #182804, #73643, #103966, #61423, #169606, #28147, #90765, #181812, #198962, #92752, #197967, #46266, #151472, #106933, #30106, #196987, #168606, #15934, #89787, #13934, #91746, #136291, #12961, #196001, #152448, #44287, #57474, #120121, #75601, #119146, #153441, #123094, #105945, #14939, #165645, #137280, #43290, #104959, #184780, #27143, #74625, #59437, #121110, #144965, #7446, #94747, #84285, #113624, #37798, #186795, #162143, #22638, #53972, #67135, #108927, #23639, #68127, #51965, #83289, #62412, #69130, #128793, #48266, #145964, #6446, #115645, #82279, #109920, #129778, #156427, #130797, #190493, #192489, #191475, #139264, #177335, #740, #99461, #52953, #100464, #114629, #176328, #124082, #17928, #161141, #185783, #171603, #140252, #47270, #38806, #170607, #143972, #32097, #175319, #93754, #33091, #155435, #16925, #78578, #36785, #1744, #63422, #125097, #98451, #5452, #160144, #21635, #72136, #194493, #27655, #88290, #58949, #25658, #55966, #26647, #40803, #12479, #10476, #74140, #134825, #85287, #197482, #146979, #42807, #196504, #43793, #149978, #11484, #70140, #102473, #132807, #41809, #103477, #135812, #89295, #150987, #73155, #117643, #87303, #165155, #57974, #56976, #86299, #119646, #181328, #131811, #133812, #104469, #180341, #147988, #166154, #182313, #167142, #101456, #120617, #193490, #9477, #105456, #8466, #39792, #54969, #116639, #178329, #163147, #24650, #179340, #71141, #118650, #164160, #148986, #195503, #171100, #63922, #244, #15435, #183301, #136781, #32593, #2239, #199459, #61912, #14435, #31598, #125591, #30603, #79078, #184290, #93247, #62913, #121606, #154933, #187288, #122600, #46769, #16430, #169096, #45771, #48759, #185277, #77094, #110413 ),
 ( #1234, #152936, #59938, #44783, #107423, #75113, #60926, #106436, #139746, #123582, #168117, #94245, #140751, #28641, #13449, #198467, #138763, #124593, #29613, #92256, #186288, #90277, #108428, #47768, #170104, #78078, #91245, #109421, #153940, #76098, #151961, #155925, #17421, #137773, #20389, #18426, #175082, #190252, #4216, #51729, #114388, #21397, #158899, #52722, #96233, #111413, #33581, #19411, #113392, #128557, #127569, #68897, #34576, #81060, #126570, #7213, #82037, #36549, #66894, #143734, #129548, #172094, #49744, #98204, #145732, #5213, #160910, #130557, #37560, #22403, #83055, #144729, #174096, #35565, #142737, #173099, #80076, #159908, #176090, #6216, #141745, #191248, #67895, #65895, #84054, #99223, #192255, #53737, #157921, #3235, #95244, #189270, #50746, #156929, #64909, #188270, #112404, #97213, #85050, #40571, #86065, #195262, #42572, #118417, #71900, #24416, #70908, #69906, #133571, #27414, #72920, #134589, #57744, #119414, #180110, #54730, #102241, #164924, #41578, #26417, #11246, #150751, #147755, #104235, #115411, #194264, #56746, #103242, #165917, #181098, #89060, #88057, #9241, #55731, #149744, #196275, #87067, #116402, #12249, #73911, #100227, #163929, #135581, #10241, #178091, #197253, #177100, #38571, #131572, #161909, #23403, #39561, #146732, #8228, #193256, #101218, #162908, #132576, #117404, #179102, #25426, #148752, #30369, #140522, #17190, #198233, #1003, #94014, #92013, #45539, #13227, #166914, #62677, #32361, #29392, #153706, #44553, #61683, #155695, #60691, #109191, #14198, #123352, #93017, #151734, #185045, #78844, #152708, #76861, #46532, #199226, #75867, #58715, #15202, #107193, #120384, #121378, #138531, #170870, #154705, #124358, #168864, #108192, #182077, #9, #183070, #106208, #31367, #43561, #91022, #59705, #105226, #169874, #186053, #137543, #47537, #16198, #77853, #167892, #28415, #139520, #90052, #184056, #74890, #136553, #122367, #112178, #143491, #125366, #129314, #189040, #111175, #144494, #4976, #175847, #142508, #172865, #66662, #157691, #191010, #127328, #52486, #51498, #2012, #114146, #63691, #159660, #113158, #160668, #128325, #190024, #187062, #19182, #49512, #141520, #50515, #174848, #36314, #97968, #21157, #37320, #34346, #98978, #48532, #80831, #110186, #171864, #82812, #126345, #33353, #95012, #3986, #156700, #96007, #79851, #5977, #35334, #18194, #67657, #22160, #83811, #3007, #64683, #173866, #188042, #65666, #96987, #158669, #20159, #81804, #179864, #117160, #194027, #53488, #40322, #85824, #115165, #6971, #163680, #195019, #69661, #55490, #192002, #148511, #25183, #177855, #86825, #87816, #56495, #132336, #26175, #131328, #84807, #68651, #193016, #10001, #101998, #100983, #42336, #7977, #54493, #99983, #180860, #178856, #71661, #133328, #118173, #102995, #145491, #23164, #41334, #119175, #164681, #134348, #103997, #10999, #196030, #149502, #72671, #147512, #9002, #116165, #146486, #176858, #57506, #165675, #27174, #38327, #130307, #161668, #39324, #162667, #24173, #70669, #124115, #12993, #120152, #198991, #74656, #136323, #46295, #15964, #60459, #61454, #181842, #58485, #13965, #59468, #168635, #77624, #91778, #45311, #197998, #44317, #43322, #106961, #771, #107952, #169639, #31135, #92783, #153472, #185815, #75632, #30135, #183821, #137310, #154472, #88821, #166677, #14968, #62441, #76628, #122134, #170638, #151501, #138306, #139294, #123124, #47302, #199987, #184809, #108959, #150514, #121141, #182835, #12012, #73673, #105976, #89820, #135345, #197019, #104989, #167661, #28178, #29157, #90794, #152478, #52252, #112924, #144258, #157456, #1775, #113909, #158440, #142271, #173628, #155465, #159423, #18950, #141281, #174619, #35098, #5745, #172625, #2771, #96750, #187812, #20919, #80596, #82577, #81569, #32127, #67421, #93784, #189793, #143255, #190777, #19928, #4739, #16955, #49281, #79612, #188800, #50283, #129076, #36084 ),
 ( #78609, #3753, #66428, #109952, #110939, #51264, #140283, #111941, #128089, #65430, #127091, #63453, #97734, #34113, #125130, #186827, #48296, #171632, #156459, #33120, #94777, #17958, #64447, #126117, #95770, #117939, #24942, #162428, #56256, #99751, #114928, #37084, #22927, #116923, #132096, #131090, #72431, #38096, #84573, #130068, #21926, #83577, #148273, #161435, #6737, #68415, #192778, #145256, #146251, #53250, #86590, #8761, #191767, #179628, #25945, #87588, #160436, #176621, #23929, #9765, #7737, #54261, #133093, #10767, #55255, #71429, #147270, #85584, #69423, #70430, #115933, #177623, #98743, #193786, #194783, #39091, #178616, #100747, #40079, #101757, #163445, #41099, #102764, #164451, #149274, #134109, #195798, #57270, #175608, #166446, #60228, #75401, #74425, #15726, #181611, #27942, #73442, #154236, #105744, #121897, #13734, #167431, #76393, #118945, #28927, #29902, #153228, #77386, #107712, #139054, #184576, #169391, #91540, #168407, #120901, #182601, #89584, #58257, #26941, #198762, #61216, #183590, #88583, #138069, #14732, #151270, #30900, #106733, #199750, #534, #43089, #150281, #90567, #104756, #12760, #122888, #46057, #152249, #92547, #11778, #135113, #44086, #136091, #45075, #180630, #42103, #137072, #197766, #59232, #196789, #103767, #165446, #119926, #19697, #4500, #66191, #126857, #1531, #49049, #111706, #65198, #173392, #158207, #97499, #32887, #51030, #62206, #141048, #3522, #18714, #17719, #159185, #124890, #109717, #16718, #20680, #110704, #188563, #157221, #172384, #81339, #123870, #33875, #34862, #96517, #82335, #112691, #144025, #127853, #174383, #143022, #189558, #64215, #125881, #171400, #63210, #170399, #142034, #35853, #50042, #31890, #185568, #47062, #94537, #108722, #93544, #155229, #78368, #186589, #140042, #95534, #48061, #156219, #79377, #2534, #80361, #187581, #98504, #175371, #130851, #176382, #85341, #132858, #8518, #162195, #114687, #161196, #160199, #23693, #117695, #163200, #24704, #148039, #9528, #70196, #145019, #192543, #55020, #131863, #116690, #101510, #40855, #37856, #194546, #5506, #84339, #52018, #113677, #178380, #129832, #36839, #21689, #22692, #83342, #99515, #6500, #39844, #38859, #68180, #71194, #56017, #179392, #190544, #191531, #54026, #86353, #53008, #146018, #102529, #164212, #147034, #25709, #177388, #115699, #7501, #100516, #69185, #193547, #67188, #87354, #128845, #73207, #40, #195556, #154735, #169905, #184088, #31398, #94046, #1035, #138562, #32391, #134878, #88341, #10528, #199257, #62708, #16231, #124390, #47568, #187093, #122398, #140553, #149040, #30401, #57030, #118703, #186085, #60724, #180394, #41865, #168895, #103531, #45571, #26701, #109220, #185075, #165206, #155724, #2041, #63721, #133865, #150032, #61715, #170899, #11539, #92047, #17222, #48563, #93048, #78874, #123383, #46564, #107224, #108225, #153736, #15232, #72191, #77883, #125396, #76891, #139551, #110216, #171897, #33385, #127364, #174882, #37354, #144527, #81836, #175883, #19215, #34379, #156733, #142541, #36348, #51530, #50549, #192040, #157726, #4020, #49546, #130341, #143524, #98001, #190054, #5012, #52518, #95044, #66694, #6013, #129350, #53521, #83843, #115199, #160703, #145525, #67692, #191045, #97020, #158701, #65698, #96039, #3040, #159695, #99012, #21192, #64716, #114179, #22194, #189076, #7004, #82848, #68686, #176891, #80865, #126378, #128358, #112209, #173899, #18226, #79882, #113193, #141551, #188075, #111209, #20190, #35368, #172901, #165710, #41367, #195054, #147546, #194064, #193051, #56532, #150546, #196066, #57539, #180893, #42368, #103033, #177890, #25219, #27207, #86861, #9034, #104031, #164715, #12045, #178891, #70703, #179901, #55525, #88853, #163717, #73709, #87849, #38362, #135381, #100017, #119208, #149537, #197051, #26210, #11032, #23200, #117199, #85857, #118210, #72708, #58519, #120185, #161704, #134380, #132371, #40359 ) ),
 .UNSPECIFIED., .T., .F., .T. ) 
 B_SPLINE_SURFACE_WITH_KNOTS ( ( 4, 3, 4 ),
 ( 3, 2, 2, 2, 2, 2, 2, 2, 2, 2, 2, 2, 2, 2, 2, 2, 2, 2, 2, 2, 2, 2, 2, 2, 2, 2, 2, 2, 2, 2, 2, 2, 2, 2, 2, 2, 2, 2, 2, 2, 2, 2, 2, 2, 2, 2, 2, 2, 2, 2, 2, 2, 2, 2, 2, 2, 2, 2, 2, 2, 2, 2, 2, 2, 2, 2, 2, 2, 2, 2, 2, 2, 2, 2, 2, 2, 2, 2, 2, 2, 2, 2, 2, 2, 2, 2, 2, 2, 2, 2, 2, 2, 2, 2, 2, 2, 2, 2, 2, 2, 2, 2, 2, 2, 2, 2, 2, 2, 2, 2, 2, 2, 2, 2, 2, 2, 2, 2, 2, 2, 2, 2, 2, 2, 2, 2, 2, 2, 2, 2, 2, 2, 2, 2, 2, 2, 2, 2, 2, 2, 2, 2, 2, 2, 2, 2, 2, 2, 2, 2, 2, 2, 2, 2, 2, 2, 2, 2, 2, 2, 2, 2, 2, 2, 2, 2, 2, 2, 2, 2, 2, 2, 2, 2, 2, 2, 2, 2, 2, 2, 2, 2, 2, 2, 2, 2, 2, 2, 2, 2, 2, 2, 2, 2, 2, 2, 2, 2, 2, 2, 2, 2, 2, 2, 2, 2, 2, 2, 2, 2, 2, 2, 2, 2, 2, 2, 2, 2, 2, 2, 2, 2, 2, 2, 2, 2, 2, 2, 3 ),
 ( 0.000000000000000000, 0.5000000000000000000, 1.000000000000000000 ),
 ( 0.000000000000000000, 0.004385964912280701511, 0.008771929824561403022, 0.01315789473684210453, 0.01754385964912280604, 0.02192982456140350755, 0.02631578947368420907, 0.03070175438596491058, 0.03508771929824561209, 0.03947368421052631360, 0.04385964912280701511, 0.04824561403508771662, 0.05263157894736841813, 0.05701754385964911964, 0.06140350877192982115, 0.06578947368421052266, 0.07017543859649122417, 0.07456140350877192569, 0.07894736842105262720, 0.08333333333333332871, 0.08771929824561403022, 0.09210526315789473173, 0.09649122807017543324, 0.1008771929824561348, 0.1052631578947368363, 0.1096491228070175378, 0.1140350877192982393, 0.1184210526315789408, 0.1228070175438596423, 0.1271929824561403577, 0.1315789473684210453, 0.1359649122807017607, 0.1403508771929824483, 0.1447368421052631637, 0.1491228070175438514, 0.1535087719298245668, 0.1578947368421052544, 0.1622807017543859698, 0.1666666666666666574, 0.1710526315789473728, 0.1754385964912280604, 0.1798245614035087758, 0.1842105263157894635, 0.1885964912280701788, 0.1929824561403508665, 0.1973684210526315819, 0.2017543859649122695, 0.2061403508771929849, 0.2105263157894736725, 0.2149122807017543879, 0.2192982456140350755, 0.2236842105263157909, 0.2280701754385964786, 0.2324561403508771940, 0.2368421052631578816, 0.2412280701754385970, 0.2456140350877192846, 0.2500000000000000000, 0.2543859649122807154, 0.2587719298245614308, 0.2631578947368420907, 0.2675438596491228060, 0.2719298245614035214, 0.2763157894736842368, 0.2807017543859648967, 0.2850877192982456121, 0.2894736842105263275, 0.2938596491228070429, 0.2982456140350877027, 0.3026315789473684181, 0.3070175438596491335, 0.3114035087719298489, 0.3157894736842105088, 0.3201754385964912242, 0.3245614035087719396, 0.3289473684210526550, 0.3333333333333333148, 0.3377192982456140302, 0.3421052631578947456, 0.3464912280701754610, 0.3508771929824561209, 0.3552631578947368363, 0.3596491228070175517, 0.3640350877192982670, 0.3684210526315789269, 0.3728070175438596423, 0.3771929824561403577, 0.3815789473684210731, 0.3859649122807017330, 0.3903508771929824483, 0.3947368421052631637, 0.3991228070175438791, 0.4035087719298245390, 0.4078947368421052544, 0.4122807017543859698, 0.4166666666666666852, 0.4210526315789473450, 0.4254385964912280604, 0.4298245614035087758, 0.4342105263157894912, 0.4385964912280701511, 0.4429824561403508665, 0.4473684210526315819, 0.4517543859649122973, 0.4561403508771929571, 0.4605263157894736725, 0.4649122807017543879, 0.4692982456140351033, 0.4736842105263157632, 0.4780701754385964786, 0.4824561403508771940, 0.4868421052631579093, 0.4912280701754385692, 0.4956140350877192846, 0.5000000000000000000, 0.5043859649122807154, 0.5087719298245614308, 0.5131578947368421462, 0.5175438596491228616, 0.5219298245614034659, 0.5263157894736841813, 0.5307017543859648967, 0.5350877192982456121, 0.5394736842105263275, 0.5438596491228070429, 0.5482456140350877583, 0.5526315789473684736, 0.5570175438596490780, 0.5614035087719297934, 0.5657894736842105088, 0.5701754385964912242, 0.5745614035087719396, 0.5789473684210526550, 0.5833333333333333703, 0.5877192982456140857, 0.5921052631578946901, 0.5964912280701754055, 0.6008771929824561209, 0.6052631578947368363, 0.6096491228070175517, 0.6140350877192982670, 0.6184210526315789824, 0.6228070175438596978, 0.6271929824561403022, 0.6315789473684210176, 0.6359649122807017330, 0.6403508771929824483, 0.6447368421052631637, 0.6491228070175438791, 0.6535087719298245945, 0.6578947368421053099, 0.6622807017543859143, 0.6666666666666666297, 0.6710526315789473450, 0.6754385964912280604, 0.6798245614035087758, 0.6842105263157894912, 0.6885964912280702066, 0.6929824561403509220, 0.6973684210526315264, 0.7017543859649122417, 0.7061403508771929571, 0.7105263157894736725, 0.7149122807017543879, 0.7192982456140351033, 0.7236842105263158187, 0.7280701754385965341, 0.7324561403508771384, 0.7368421052631578538, 0.7412280701754385692, 0.7456140350877192846, 0.7500000000000000000, 0.7543859649122807154, 0.7587719298245614308, 0.7631578947368421462, 0.7675438596491228616, 0.7719298245614034659, 0.7763157894736841813, 0.7807017543859648967, 0.7850877192982456121, 0.7894736842105263275, 0.7938596491228070429, 0.7982456140350877583, 0.8026315789473684736, 0.8070175438596490780, 0.8114035087719297934, 0.8157894736842105088, 0.8201754385964912242, 0.8245614035087719396, 0.8289473684210526550, 0.8333333333333333703, 0.8377192982456140857, 0.8421052631578946901, 0.8464912280701754055, 0.8508771929824561209, 0.8552631578947368363, 0.8596491228070175517, 0.8640350877192982670, 0.8684210526315789824, 0.8728070175438596978, 0.8771929824561403022, 0.8815789473684210176, 0.8859649122807017330, 0.8903508771929824483, 0.8947368421052631637, 0.8991228070175438791, 0.9035087719298245945, 0.9078947368421053099, 0.9122807017543859143, 0.9166666666666666297, 0.9210526315789473450, 0.9254385964912280604, 0.9298245614035087758, 0.9342105263157894912, 0.9385964912280702066, 0.9429824561403509220, 0.9473684210526315264, 0.9517543859649122417, 0.9561403508771929571, 0.9605263157894736725, 0.9649122807017543879, 0.9692982456140351033, 0.9736842105263158187, 0.9780701754385965341, 0.9824561403508771384, 0.9868421052631578538, 0.9912280701754385692, 0.9956140350877192846, 1.000000000000000000 ),
 .UNSPECIFIED. ) 
 GEOMETRIC_REPRESENTATION_ITEM ( )  RATIONAL_B_SPLINE_SURFACE ( (
 ( 1.000000000000000000, 0.9659258262890683122, 1.000000000000000000, 0.9659258262890683122, 1.000000000000000000, 0.9659258262890683122, 1.000000000000000000, 0.9659258262890683122, 1.000000000000000000, 0.9659258262890683122, 1.000000000000000000, 0.9659258262890683122, 1.000000000000000000, 0.9659258262890683122, 1.000000000000000000, 0.9659258262890683122, 1.000000000000000000, 0.9659258262890683122, 1.000000000000000000, 0.9659258262890683122, 1.000000000000000000, 0.9659258262890683122, 1.000000000000000000, 0.9659258262890683122, 1.000000000000000000, 0.9659258262890683122, 1.000000000000000000, 0.9659258262890683122, 1.000000000000000000, 0.9659258262890683122, 1.000000000000000000, 0.9659258262890683122, 1.000000000000000000, 0.9659258262890683122, 1.000000000000000000, 0.9659258262890683122, 1.000000000000000000, 0.9659258262890683122, 1.000000000000000000, 0.9659258262890683122, 1.000000000000000000, 0.9659258262890683122, 1.000000000000000000, 0.9659258262890683122, 1.000000000000000000, 0.9659258262890683122, 1.000000000000000000, 0.9659258262890683122, 1.000000000000000000, 0.9659258262890683122, 1.000000000000000000, 0.9659258262890683122, 1.000000000000000000, 0.9659258262890683122, 1.000000000000000000, 0.9659258262890683122, 1.000000000000000000, 0.9659258262890683122, 1.000000000000000000, 0.9659258262890683122, 1.000000000000000000, 0.9659258262890683122, 1.000000000000000000, 0.9659258262890683122, 1.000000000000000000, 0.9659258262890683122, 1.000000000000000000, 0.9659258262890683122, 1.000000000000000000, 0.9659258262890683122, 1.000000000000000000, 0.9659258262890683122, 1.000000000000000000, 0.9659258262890683122, 1.000000000000000000, 0.9659258262890683122, 1.000000000000000000, 0.9659258262890683122, 1.000000000000000000, 0.9659258262890683122, 1.000000000000000000, 0.9659258262890683122, 1.000000000000000000, 0.9659258262890683122, 1.000000000000000000, 0.9659258262890683122, 1.000000000000000000, 0.9659258262890683122, 1.000000000000000000, 0.9659258262890683122, 1.000000000000000000, 0.9659258262890683122, 1.000000000000000000, 0.9659258262890683122, 1.000000000000000000, 0.9659258262890683122, 1.000000000000000000, 0.9659258262890683122, 1.000000000000000000, 0.9659258262890683122, 1.000000000000000000, 0.9659258262890683122, 1.000000000000000000, 0.9659258262890683122, 1.000000000000000000, 0.9659258262890683122, 1.000000000000000000, 0.9659258262890683122, 1.000000000000000000, 0.9659258262890683122, 1.000000000000000000, 0.9659258262890683122, 1.000000000000000000, 0.9659258262890683122, 1.000000000000000000, 0.9659258262890683122, 1.000000000000000000, 0.9659258262890683122, 1.000000000000000000, 0.9659258262890683122, 1.000000000000000000, 0.9659258262890683122, 1.000000000000000000, 0.9659258262890683122, 1.000000000000000000, 0.9659258262890683122, 1.000000000000000000, 0.9659258262890683122, 1.000000000000000000, 0.9659258262890683122, 1.000000000000000000, 0.9659258262890683122, 1.000000000000000000, 0.9659258262890683122, 1.000000000000000000, 0.9659258262890683122, 1.000000000000000000, 0.9659258262890683122, 1.000000000000000000, 0.9659258262890683122, 1.000000000000000000, 0.9659258262890683122, 1.000000000000000000, 0.9659258262890683122, 1.000000000000000000, 0.9659258262890683122, 1.000000000000000000, 0.9659258262890683122, 1.000000000000000000, 0.9659258262890683122, 1.000000000000000000, 0.9659258262890683122, 1.000000000000000000, 0.9659258262890683122, 1.000000000000000000, 0.9659258262890683122, 1.000000000000000000, 0.9659258262890683122, 1.000000000000000000, 0.9659258262890683122, 1.000000000000000000, 0.9659258262890683122, 1.000000000000000000, 0.9659258262890683122, 1.000000000000000000, 0.9659258262890683122, 1.000000000000000000, 0.9659258262890683122, 1.000000000000000000, 0.9659258262890683122, 1.000000000000000000, 0.9659258262890683122, 1.000000000000000000, 0.9659258262890683122, 1.000000000000000000, 0.9659258262890683122, 1.000000000000000000, 0.9659258262890683122, 1.000000000000000000, 0.9659258262890683122, 1.000000000000000000, 0.9659258262890683122, 1.000000000000000000, 0.9659258262890683122, 1.000000000000000000, 0.9659258262890683122, 1.000000000000000000, 0.9659258262890683122, 1.000000000000000000, 0.9659258262890683122, 1.000000000000000000, 0.9659258262890683122, 1.000000000000000000, 0.9659258262890683122, 1.000000000000000000, 0.9659258262890683122, 1.000000000000000000, 0.9659258262890683122, 1.000000000000000000, 0.9659258262890683122, 1.000000000000000000, 0.9659258262890683122, 1.000000000000000000, 0.9659258262890683122, 1.000000000000000000, 0.9659258262890683122, 1.000000000000000000, 0.9659258262890683122, 1.000000000000000000, 0.9659258262890683122, 1.000000000000000000, 0.9659258262890683122, 1.000000000000000000, 0.9659258262890683122, 1.000000000000000000, 0.9659258262890683122, 1.000000000000000000, 0.9659258262890683122, 1.000000000000000000, 0.9659258262890683122, 1.000000000000000000, 0.9659258262890683122, 1.000000000000000000, 0.9659258262890683122, 1.000000000000000000, 0.9659258262890683122, 1.000000000000000000, 0.9659258262890683122, 1.000000000000000000, 0.9659258262890683122, 1.000000000000000000, 0.9659258262890683122, 1.000000000000000000, 0.9659258262890683122, 1.000000000000000000, 0.9659258262890683122, 1.000000000000000000, 0.9659258262890683122, 1.000000000000000000, 0.9659258262890683122, 1.000000000000000000, 0.9659258262890683122, 1.000000000000000000, 0.9659258262890683122, 1.000000000000000000, 0.9659258262890683122, 1.000000000000000000, 0.9659258262890683122, 1.000000000000000000, 0.9659258262890683122, 1.000000000000000000, 0.9659258262890683122, 1.000000000000000000, 0.9659258262890683122, 1.000000000000000000, 0.9659258262890683122, 1.000000000000000000, 0.9659258262890683122, 1.000000000000000000, 0.9659258262890683122, 1.000000000000000000, 0.9659258262890683122, 1.000000000000000000, 0.9659258262890683122, 1.000000000000000000, 0.9659258262890683122, 1.000000000000000000, 0.9659258262890683122, 1.000000000000000000, 0.9659258262890683122, 1.000000000000000000, 0.9659258262890683122, 1.000000000000000000, 0.9659258262890683122, 1.000000000000000000, 0.9659258262890683122, 1.000000000000000000, 0.9659258262890683122, 1.000000000000000000, 0.9659258262890683122, 1.000000000000000000, 0.9659258262890683122, 1.000000000000000000, 0.9659258262890683122, 1.000000000000000000, 0.9659258262890683122, 1.000000000000000000, 0.9659258262890683122, 1.000000000000000000, 0.9659258262890683122, 1.000000000000000000, 0.9659258262890683122, 1.000000000000000000, 0.9659258262890683122, 1.000000000000000000, 0.9659258262890683122, 1.000000000000000000, 0.9659258262890683122, 1.000000000000000000, 0.9659258262890683122, 1.000000000000000000, 0.9659258262890683122, 1.000000000000000000, 0.9659258262890683122, 1.000000000000000000, 0.9659258262890683122, 1.000000000000000000, 0.9659258262890683122, 1.000000000000000000, 0.9659258262890683122, 1.000000000000000000, 0.9659258262890683122, 1.000000000000000000, 0.9659258262890683122, 1.000000000000000000, 0.9659258262890683122, 1.000000000000000000, 0.9659258262890683122, 1.000000000000000000, 0.9659258262890683122, 1.000000000000000000, 0.9659258262890683122, 1.000000000000000000, 0.9659258262890683122, 1.000000000000000000, 0.9659258262890683122, 1.000000000000000000, 0.9659258262890683122, 1.000000000000000000, 0.9659258262890683122, 1.000000000000000000, 0.9659258262890683122, 1.000000000000000000, 0.9659258262890683122, 1.000000000000000000, 0.9659258262890683122, 1.000000000000000000, 0.9659258262890683122, 1.000000000000000000, 0.9659258262890683122, 1.000000000000000000, 0.9659258262890683122, 1.000000000000000000, 0.9659258262890683122, 1.000000000000000000, 0.9659258262890683122, 1.000000000000000000, 0.9659258262890683122, 1.000000000000000000, 0.9659258262890683122, 1.000000000000000000, 0.9659258262890683122, 1.000000000000000000, 0.9659258262890683122, 1.000000000000000000, 0.9659258262890683122, 1.000000000000000000, 0.9659258262890683122, 1.000000000000000000, 0.9659258262890683122, 1.000000000000000000, 0.9659258262890683122, 1.000000000000000000, 0.9659258262890683122, 1.000000000000000000, 0.9659258262890683122, 1.000000000000000000, 0.9659258262890683122, 1.000000000000000000, 0.9659258262890683122, 1.000000000000000000, 0.9659258262890683122, 1.000000000000000000, 0.9659258262890683122, 1.000000000000000000, 0.9659258262890683122, 1.000000000000000000, 0.9659258262890683122, 1.000000000000000000, 0.9659258262890683122, 1.000000000000000000, 0.9659258262890683122, 1.000000000000000000, 0.9659258262890683122, 1.000000000000000000, 0.9659258262890683122, 1.000000000000000000, 0.9659258262890683122, 1.000000000000000000, 0.9659258262890683122, 1.000000000000000000, 0.9659258262890683122, 1.000000000000000000, 0.9659258262890683122, 1.000000000000000000, 0.9659258262890683122, 1.000000000000000000, 0.9659258262890683122, 1.000000000000000000, 0.9659258262890683122, 1.000000000000000000, 0.9659258262890683122, 1.000000000000000000, 0.9659258262890683122, 1.000000000000000000, 0.9659258262890683122, 1.000000000000000000, 0.9659258262890683122, 1.000000000000000000, 0.9659258262890683122, 1.000000000000000000, 0.9659258262890683122, 1.000000000000000000, 0.9659258262890683122, 1.000000000000000000, 0.9659258262890683122, 1.000000000000000000, 0.9659258262890683122, 1.000000000000000000, 0.9659258262890683122, 1.000000000000000000, 0.9659258262890683122, 1.000000000000000000, 0.9659258262890683122, 1.000000000000000000, 0.9659258262890683122, 1.000000000000000000, 0.9659258262890683122, 1.000000000000000000, 0.9659258262890683122, 1.000000000000000000, 0.9659258262890683122, 1.000000000000000000, 0.9659258262890683122, 1.000000000000000000, 0.9659258262890683122, 1.000000000000000000, 0.9659258262890683122, 1.000000000000000000, 0.9659258262890683122, 1.000000000000000000, 0.9659258262890683122, 1.000000000000000000, 0.9659258262890683122, 1.000000000000000000, 0.9659258262890683122, 1.000000000000000000, 0.9659258262890683122, 1.000000000000000000, 0.9659258262890683122, 1.000000000000000000, 0.9659258262890683122, 1.000000000000000000, 0.9659258262890683122, 1.000000000000000000, 0.9659258262890683122, 1.000000000000000000),
 ( 0.3333333333333333703, 0.3219752754296894559, 0.3333333333333333703, 0.3219752754296894559, 0.3333333333333333703, 0.3219752754296894559, 0.3333333333333333703, 0.3219752754296894559, 0.3333333333333333703, 0.3219752754296894559, 0.3333333333333333703, 0.3219752754296894559, 0.3333333333333333703, 0.3219752754296894559, 0.3333333333333333703, 0.3219752754296894559, 0.3333333333333333703, 0.3219752754296894559, 0.3333333333333333703, 0.3219752754296894559, 0.3333333333333333703, 0.3219752754296894559, 0.3333333333333333703, 0.3219752754296894559, 0.3333333333333333703, 0.3219752754296894559, 0.3333333333333333703, 0.3219752754296894559, 0.3333333333333333703, 0.3219752754296894559, 0.3333333333333333703, 0.3219752754296894559, 0.3333333333333333703, 0.3219752754296894559, 0.3333333333333333703, 0.3219752754296894559, 0.3333333333333333703, 0.3219752754296894559, 0.3333333333333333703, 0.3219752754296894559, 0.3333333333333333703, 0.3219752754296894559, 0.3333333333333333703, 0.3219752754296894559, 0.3333333333333333703, 0.3219752754296894559, 0.3333333333333333703, 0.3219752754296894559, 0.3333333333333333703, 0.3219752754296894559, 0.3333333333333333703, 0.3219752754296894559, 0.3333333333333333703, 0.3219752754296894559, 0.3333333333333333703, 0.3219752754296894559, 0.3333333333333333703, 0.3219752754296894559, 0.3333333333333333703, 0.3219752754296894559, 0.3333333333333333703, 0.3219752754296894559, 0.3333333333333333703, 0.3219752754296894559, 0.3333333333333333703, 0.3219752754296894559, 0.3333333333333333703, 0.3219752754296894559, 0.3333333333333333703, 0.3219752754296894559, 0.3333333333333333703, 0.3219752754296894559, 0.3333333333333333703, 0.3219752754296894559, 0.3333333333333333703, 0.3219752754296894559, 0.3333333333333333703, 0.3219752754296894559, 0.3333333333333333703, 0.3219752754296894559, 0.3333333333333333703, 0.3219752754296894559, 0.3333333333333333703, 0.3219752754296894559, 0.3333333333333333703, 0.3219752754296894559, 0.3333333333333333703, 0.3219752754296894559, 0.3333333333333333703, 0.3219752754296894559, 0.3333333333333333703, 0.3219752754296894559, 0.3333333333333333703, 0.3219752754296894559, 0.3333333333333333703, 0.3219752754296894559, 0.3333333333333333703, 0.3219752754296894559, 0.3333333333333333703, 0.3219752754296894559, 0.3333333333333333703, 0.3219752754296894559, 0.3333333333333333703, 0.3219752754296894559, 0.3333333333333333703, 0.3219752754296894559, 0.3333333333333333703, 0.3219752754296894559, 0.3333333333333333703, 0.3219752754296894559, 0.3333333333333333703, 0.3219752754296894559, 0.3333333333333333703, 0.3219752754296894559, 0.3333333333333333703, 0.3219752754296894559, 0.3333333333333333703, 0.3219752754296894559, 0.3333333333333333703, 0.3219752754296894559, 0.3333333333333333703, 0.3219752754296894559, 0.3333333333333333703, 0.3219752754296894559, 0.3333333333333333703, 0.3219752754296894559, 0.3333333333333333703, 0.3219752754296894559, 0.3333333333333333703, 0.3219752754296894559, 0.3333333333333333703, 0.3219752754296894559, 0.3333333333333333703, 0.3219752754296894559, 0.3333333333333333703, 0.3219752754296894559, 0.3333333333333333703, 0.3219752754296894559, 0.3333333333333333703, 0.3219752754296894559, 0.3333333333333333703, 0.3219752754296894559, 0.3333333333333333703, 0.3219752754296894559, 0.3333333333333333703, 0.3219752754296894559, 0.3333333333333333703, 0.3219752754296894559, 0.3333333333333333703, 0.3219752754296894559, 0.3333333333333333703, 0.3219752754296894559, 0.3333333333333333703, 0.3219752754296894559, 0.3333333333333333703, 0.3219752754296894559, 0.3333333333333333703, 0.3219752754296894559, 0.3333333333333333703, 0.3219752754296894559, 0.3333333333333333703, 0.3219752754296894559, 0.3333333333333333703, 0.3219752754296894559, 0.3333333333333333703, 0.3219752754296894559, 0.3333333333333333703, 0.3219752754296894559, 0.3333333333333333703, 0.3219752754296894559, 0.3333333333333333703, 0.3219752754296894559, 0.3333333333333333703, 0.3219752754296894559, 0.3333333333333333703, 0.3219752754296894559, 0.3333333333333333703, 0.3219752754296894559, 0.3333333333333333703, 0.3219752754296894559, 0.3333333333333333703, 0.3219752754296894559, 0.3333333333333333703, 0.3219752754296894559, 0.3333333333333333703, 0.3219752754296894559, 0.3333333333333333703, 0.3219752754296894559, 0.3333333333333333703, 0.3219752754296894559, 0.3333333333333333703, 0.3219752754296894559, 0.3333333333333333703, 0.3219752754296894559, 0.3333333333333333703, 0.3219752754296894559, 0.3333333333333333703, 0.3219752754296894559, 0.3333333333333333703, 0.3219752754296894559, 0.3333333333333333703, 0.3219752754296894559, 0.3333333333333333703, 0.3219752754296894559, 0.3333333333333333703, 0.3219752754296894559, 0.3333333333333333703, 0.3219752754296894559, 0.3333333333333333703, 0.3219752754296894559, 0.3333333333333333703, 0.3219752754296894559, 0.3333333333333333703, 0.3219752754296894559, 0.3333333333333333703, 0.3219752754296894559, 0.3333333333333333703, 0.3219752754296894559, 0.3333333333333333703, 0.3219752754296894559, 0.3333333333333333703, 0.3219752754296894559, 0.3333333333333333703, 0.3219752754296894559, 0.3333333333333333703, 0.3219752754296894559, 0.3333333333333333703, 0.3219752754296894559, 0.3333333333333333703, 0.3219752754296894559, 0.3333333333333333703, 0.3219752754296894559, 0.3333333333333333703, 0.3219752754296894559, 0.3333333333333333703, 0.3219752754296894559, 0.3333333333333333703, 0.3219752754296894559, 0.3333333333333333703, 0.3219752754296894559, 0.3333333333333333703, 0.3219752754296894559, 0.3333333333333333703, 0.3219752754296894559, 0.3333333333333333703, 0.3219752754296894559, 0.3333333333333333703, 0.3219752754296894559, 0.3333333333333333703, 0.3219752754296894559, 0.3333333333333333703, 0.3219752754296894559, 0.3333333333333333703, 0.3219752754296894559, 0.3333333333333333703, 0.3219752754296894559, 0.3333333333333333703, 0.3219752754296894559, 0.3333333333333333703, 0.3219752754296894559, 0.3333333333333333703, 0.3219752754296894559, 0.3333333333333333703, 0.3219752754296894559, 0.3333333333333333703, 0.3219752754296894559, 0.3333333333333333703, 0.3219752754296894559, 0.3333333333333333703, 0.3219752754296894559, 0.3333333333333333703, 0.3219752754296894559, 0.3333333333333333703, 0.3219752754296894559, 0.3333333333333333703, 0.3219752754296894559, 0.3333333333333333703, 0.3219752754296894559, 0.3333333333333333703, 0.3219752754296894559, 0.3333333333333333703, 0.3219752754296894559, 0.3333333333333333703, 0.3219752754296894559, 0.3333333333333333703, 0.3219752754296894559, 0.3333333333333333703, 0.3219752754296894559, 0.3333333333333333703, 0.3219752754296894559, 0.3333333333333333703, 0.3219752754296894559, 0.3333333333333333703, 0.3219752754296894559, 0.3333333333333333703, 0.3219752754296894559, 0.3333333333333333703, 0.3219752754296894559, 0.3333333333333333703, 0.3219752754296894559, 0.3333333333333333703, 0.3219752754296894559, 0.3333333333333333703, 0.3219752754296894559, 0.3333333333333333703, 0.3219752754296894559, 0.3333333333333333703, 0.3219752754296894559, 0.3333333333333333703, 0.3219752754296894559, 0.3333333333333333703, 0.3219752754296894559, 0.3333333333333333703, 0.3219752754296894559, 0.3333333333333333703, 0.3219752754296894559, 0.3333333333333333703, 0.3219752754296894559, 0.3333333333333333703, 0.3219752754296894559, 0.3333333333333333703, 0.3219752754296894559, 0.3333333333333333703, 0.3219752754296894559, 0.3333333333333333703, 0.3219752754296894559, 0.3333333333333333703, 0.3219752754296894559, 0.3333333333333333703, 0.3219752754296894559, 0.3333333333333333703, 0.3219752754296894559, 0.3333333333333333703, 0.3219752754296894559, 0.3333333333333333703, 0.3219752754296894559, 0.3333333333333333703, 0.3219752754296894559, 0.3333333333333333703, 0.3219752754296894559, 0.3333333333333333703, 0.3219752754296894559, 0.3333333333333333703, 0.3219752754296894559, 0.3333333333333333703, 0.3219752754296894559, 0.3333333333333333703, 0.3219752754296894559, 0.3333333333333333703, 0.3219752754296894559, 0.3333333333333333703, 0.3219752754296894559, 0.3333333333333333703, 0.3219752754296894559, 0.3333333333333333703, 0.3219752754296894559, 0.3333333333333333703, 0.3219752754296894559, 0.3333333333333333703, 0.3219752754296894559, 0.3333333333333333703, 0.3219752754296894559, 0.3333333333333333703, 0.3219752754296894559, 0.3333333333333333703, 0.3219752754296894559, 0.3333333333333333703, 0.3219752754296894559, 0.3333333333333333703, 0.3219752754296894559, 0.3333333333333333703, 0.3219752754296894559, 0.3333333333333333703, 0.3219752754296894559, 0.3333333333333333703, 0.3219752754296894559, 0.3333333333333333703, 0.3219752754296894559, 0.3333333333333333703, 0.3219752754296894559, 0.3333333333333333703, 0.3219752754296894559, 0.3333333333333333703, 0.3219752754296894559, 0.3333333333333333703, 0.3219752754296894559, 0.3333333333333333703, 0.3219752754296894559, 0.3333333333333333703, 0.3219752754296894559, 0.3333333333333333703, 0.3219752754296894559, 0.3333333333333333703, 0.3219752754296894559, 0.3333333333333333703, 0.3219752754296894559, 0.3333333333333333703, 0.3219752754296894559, 0.3333333333333333703, 0.3219752754296894559, 0.3333333333333333703, 0.3219752754296894559, 0.3333333333333333703, 0.3219752754296894559, 0.3333333333333333703, 0.3219752754296894559, 0.3333333333333333703, 0.3219752754296894559, 0.3333333333333333703, 0.3219752754296894559, 0.3333333333333333703, 0.3219752754296894559, 0.3333333333333333703, 0.3219752754296894559, 0.3333333333333333703, 0.3219752754296894559, 0.3333333333333333703, 0.3219752754296894559, 0.3333333333333333703, 0.3219752754296894559, 0.3333333333333333703, 0.3219752754296894559, 0.3333333333333333703, 0.3219752754296894559, 0.3333333333333333703, 0.3219752754296894559, 0.3333333333333333703, 0.3219752754296894559, 0.3333333333333333703, 0.3219752754296894559, 0.3333333333333333703, 0.3219752754296894559, 0.3333333333333333703, 0.3219752754296894559, 0.3333333333333333703, 0.3219752754296894559, 0.3333333333333333703, 0.3219752754296894559, 0.3333333333333333703, 0.3219752754296894559, 0.3333333333333333703, 0.3219752754296894559, 0.3333333333333333703, 0.3219752754296894559, 0.3333333333333333703, 0.3219752754296894559, 0.3333333333333333703, 0.3219752754296894559, 0.3333333333333333703, 0.3219752754296894559, 0.3333333333333333703, 0.3219752754296894559, 0.3333333333333333703, 0.3219752754296894559, 0.3333333333333333703, 0.3219752754296894559, 0.3333333333333333703),
 ( 0.3333333333333333703, 0.3219752754296894559, 0.3333333333333333703, 0.3219752754296894559, 0.3333333333333333703, 0.3219752754296894559, 0.3333333333333333703, 0.3219752754296894559, 0.3333333333333333703, 0.3219752754296894559, 0.3333333333333333703, 0.3219752754296894559, 0.3333333333333333703, 0.3219752754296894559, 0.3333333333333333703, 0.3219752754296894559, 0.3333333333333333703, 0.3219752754296894559, 0.3333333333333333703, 0.3219752754296894559, 0.3333333333333333703, 0.3219752754296894559, 0.3333333333333333703, 0.3219752754296894559, 0.3333333333333333703, 0.3219752754296894559, 0.3333333333333333703, 0.3219752754296894559, 0.3333333333333333703, 0.3219752754296894559, 0.3333333333333333703, 0.3219752754296894559, 0.3333333333333333703, 0.3219752754296894559, 0.3333333333333333703, 0.3219752754296894559, 0.3333333333333333703, 0.3219752754296894559, 0.3333333333333333703, 0.3219752754296894559, 0.3333333333333333703, 0.3219752754296894559, 0.3333333333333333703, 0.3219752754296894559, 0.3333333333333333703, 0.3219752754296894559, 0.3333333333333333703, 0.3219752754296894559, 0.3333333333333333703, 0.3219752754296894559, 0.3333333333333333703, 0.3219752754296894559, 0.3333333333333333703, 0.3219752754296894559, 0.3333333333333333703, 0.3219752754296894559, 0.3333333333333333703, 0.3219752754296894559, 0.3333333333333333703, 0.3219752754296894559, 0.3333333333333333703, 0.3219752754296894559, 0.3333333333333333703, 0.3219752754296894559, 0.3333333333333333703, 0.3219752754296894559, 0.3333333333333333703, 0.3219752754296894559, 0.3333333333333333703, 0.3219752754296894559, 0.3333333333333333703, 0.3219752754296894559, 0.3333333333333333703, 0.3219752754296894559, 0.3333333333333333703, 0.3219752754296894559, 0.3333333333333333703, 0.3219752754296894559, 0.3333333333333333703, 0.3219752754296894559, 0.3333333333333333703, 0.3219752754296894559, 0.3333333333333333703, 0.3219752754296894559, 0.3333333333333333703, 0.3219752754296894559, 0.3333333333333333703, 0.3219752754296894559, 0.3333333333333333703, 0.3219752754296894559, 0.3333333333333333703, 0.3219752754296894559, 0.3333333333333333703, 0.3219752754296894559, 0.3333333333333333703, 0.3219752754296894559, 0.3333333333333333703, 0.3219752754296894559, 0.3333333333333333703, 0.3219752754296894559, 0.3333333333333333703, 0.3219752754296894559, 0.3333333333333333703, 0.3219752754296894559, 0.3333333333333333703, 0.3219752754296894559, 0.3333333333333333703, 0.3219752754296894559, 0.3333333333333333703, 0.3219752754296894559, 0.3333333333333333703, 0.3219752754296894559, 0.3333333333333333703, 0.3219752754296894559, 0.3333333333333333703, 0.3219752754296894559, 0.3333333333333333703, 0.3219752754296894559, 0.3333333333333333703, 0.3219752754296894559, 0.3333333333333333703, 0.3219752754296894559, 0.3333333333333333703, 0.3219752754296894559, 0.3333333333333333703, 0.3219752754296894559, 0.3333333333333333703, 0.3219752754296894559, 0.3333333333333333703, 0.3219752754296894559, 0.3333333333333333703, 0.3219752754296894559, 0.3333333333333333703, 0.3219752754296894559, 0.3333333333333333703, 0.3219752754296894559, 0.3333333333333333703, 0.3219752754296894559, 0.3333333333333333703, 0.3219752754296894559, 0.3333333333333333703, 0.3219752754296894559, 0.3333333333333333703, 0.3219752754296894559, 0.3333333333333333703, 0.3219752754296894559, 0.3333333333333333703, 0.3219752754296894559, 0.3333333333333333703, 0.3219752754296894559, 0.3333333333333333703, 0.3219752754296894559, 0.3333333333333333703, 0.3219752754296894559, 0.3333333333333333703, 0.3219752754296894559, 0.3333333333333333703, 0.3219752754296894559, 0.3333333333333333703, 0.3219752754296894559, 0.3333333333333333703, 0.3219752754296894559, 0.3333333333333333703, 0.3219752754296894559, 0.3333333333333333703, 0.3219752754296894559, 0.3333333333333333703, 0.3219752754296894559, 0.3333333333333333703, 0.3219752754296894559, 0.3333333333333333703, 0.3219752754296894559, 0.3333333333333333703, 0.3219752754296894559, 0.3333333333333333703, 0.3219752754296894559, 0.3333333333333333703, 0.3219752754296894559, 0.3333333333333333703, 0.3219752754296894559, 0.3333333333333333703, 0.3219752754296894559, 0.3333333333333333703, 0.3219752754296894559, 0.3333333333333333703, 0.3219752754296894559, 0.3333333333333333703, 0.3219752754296894559, 0.3333333333333333703, 0.3219752754296894559, 0.3333333333333333703, 0.3219752754296894559, 0.3333333333333333703, 0.3219752754296894559, 0.3333333333333333703, 0.3219752754296894559, 0.3333333333333333703, 0.3219752754296894559, 0.3333333333333333703, 0.3219752754296894559, 0.3333333333333333703, 0.3219752754296894559, 0.3333333333333333703, 0.3219752754296894559, 0.3333333333333333703, 0.3219752754296894559, 0.3333333333333333703, 0.3219752754296894559, 0.3333333333333333703, 0.3219752754296894559, 0.3333333333333333703, 0.3219752754296894559, 0.3333333333333333703, 0.3219752754296894559, 0.3333333333333333703, 0.3219752754296894559, 0.3333333333333333703, 0.3219752754296894559, 0.3333333333333333703, 0.3219752754296894559, 0.3333333333333333703, 0.3219752754296894559, 0.3333333333333333703, 0.3219752754296894559, 0.3333333333333333703, 0.3219752754296894559, 0.3333333333333333703, 0.3219752754296894559, 0.3333333333333333703, 0.3219752754296894559, 0.3333333333333333703, 0.3219752754296894559, 0.3333333333333333703, 0.3219752754296894559, 0.3333333333333333703, 0.3219752754296894559, 0.3333333333333333703, 0.3219752754296894559, 0.3333333333333333703, 0.3219752754296894559, 0.3333333333333333703, 0.3219752754296894559, 0.3333333333333333703, 0.3219752754296894559, 0.3333333333333333703, 0.3219752754296894559, 0.3333333333333333703, 0.3219752754296894559, 0.3333333333333333703, 0.3219752754296894559, 0.3333333333333333703, 0.3219752754296894559, 0.3333333333333333703, 0.3219752754296894559, 0.3333333333333333703, 0.3219752754296894559, 0.3333333333333333703, 0.3219752754296894559, 0.3333333333333333703, 0.3219752754296894559, 0.3333333333333333703, 0.3219752754296894559, 0.3333333333333333703, 0.3219752754296894559, 0.3333333333333333703, 0.3219752754296894559, 0.3333333333333333703, 0.3219752754296894559, 0.3333333333333333703, 0.3219752754296894559, 0.3333333333333333703, 0.3219752754296894559, 0.3333333333333333703, 0.3219752754296894559, 0.3333333333333333703, 0.3219752754296894559, 0.3333333333333333703, 0.3219752754296894559, 0.3333333333333333703, 0.3219752754296894559, 0.3333333333333333703, 0.3219752754296894559, 0.3333333333333333703, 0.3219752754296894559, 0.3333333333333333703, 0.3219752754296894559, 0.3333333333333333703, 0.3219752754296894559, 0.3333333333333333703, 0.3219752754296894559, 0.3333333333333333703, 0.3219752754296894559, 0.3333333333333333703, 0.3219752754296894559, 0.3333333333333333703, 0.3219752754296894559, 0.3333333333333333703, 0.3219752754296894559, 0.3333333333333333703, 0.3219752754296894559, 0.3333333333333333703, 0.3219752754296894559, 0.3333333333333333703, 0.3219752754296894559, 0.3333333333333333703, 0.3219752754296894559, 0.3333333333333333703, 0.3219752754296894559, 0.3333333333333333703, 0.3219752754296894559, 0.3333333333333333703, 0.3219752754296894559, 0.3333333333333333703, 0.3219752754296894559, 0.3333333333333333703, 0.3219752754296894559, 0.3333333333333333703, 0.3219752754296894559, 0.3333333333333333703, 0.3219752754296894559, 0.3333333333333333703, 0.3219752754296894559, 0.3333333333333333703, 0.3219752754296894559, 0.3333333333333333703, 0.3219752754296894559, 0.3333333333333333703, 0.3219752754296894559, 0.3333333333333333703, 0.3219752754296894559, 0.3333333333333333703, 0.3219752754296894559, 0.3333333333333333703, 0.3219752754296894559, 0.3333333333333333703, 0.3219752754296894559, 0.3333333333333333703, 0.3219752754296894559, 0.3333333333333333703, 0.3219752754296894559, 0.3333333333333333703, 0.3219752754296894559, 0.3333333333333333703, 0.3219752754296894559, 0.3333333333333333703, 0.3219752754296894559, 0.3333333333333333703, 0.3219752754296894559, 0.3333333333333333703, 0.3219752754296894559, 0.3333333333333333703, 0.3219752754296894559, 0.3333333333333333703, 0.3219752754296894559, 0.3333333333333333703, 0.3219752754296894559, 0.3333333333333333703, 0.3219752754296894559, 0.3333333333333333703, 0.3219752754296894559, 0.3333333333333333703, 0.3219752754296894559, 0.3333333333333333703, 0.3219752754296894559, 0.3333333333333333703, 0.3219752754296894559, 0.3333333333333333703, 0.3219752754296894559, 0.3333333333333333703, 0.3219752754296894559, 0.3333333333333333703, 0.3219752754296894559, 0.3333333333333333703, 0.3219752754296894559, 0.3333333333333333703, 0.3219752754296894559, 0.3333333333333333703, 0.3219752754296894559, 0.3333333333333333703, 0.3219752754296894559, 0.3333333333333333703, 0.3219752754296894559, 0.3333333333333333703, 0.3219752754296894559, 0.3333333333333333703, 0.3219752754296894559, 0.3333333333333333703, 0.3219752754296894559, 0.3333333333333333703, 0.3219752754296894559, 0.3333333333333333703, 0.3219752754296894559, 0.3333333333333333703, 0.3219752754296894559, 0.3333333333333333703, 0.3219752754296894559, 0.3333333333333333703, 0.3219752754296894559, 0.3333333333333333703, 0.3219752754296894559, 0.3333333333333333703, 0.3219752754296894559, 0.3333333333333333703, 0.3219752754296894559, 0.3333333333333333703, 0.3219752754296894559, 0.3333333333333333703, 0.3219752754296894559, 0.3333333333333333703, 0.3219752754296894559, 0.3333333333333333703, 0.3219752754296894559, 0.3333333333333333703, 0.3219752754296894559, 0.3333333333333333703, 0.3219752754296894559, 0.3333333333333333703, 0.3219752754296894559, 0.3333333333333333703, 0.3219752754296894559, 0.3333333333333333703, 0.3219752754296894559, 0.3333333333333333703, 0.3219752754296894559, 0.3333333333333333703, 0.3219752754296894559, 0.3333333333333333703, 0.3219752754296894559, 0.3333333333333333703, 0.3219752754296894559, 0.3333333333333333703, 0.3219752754296894559, 0.3333333333333333703, 0.3219752754296894559, 0.3333333333333333703, 0.3219752754296894559, 0.3333333333333333703, 0.3219752754296894559, 0.3333333333333333703, 0.3219752754296894559, 0.3333333333333333703, 0.3219752754296894559, 0.3333333333333333703, 0.3219752754296894559, 0.3333333333333333703, 0.3219752754296894559, 0.3333333333333333703, 0.3219752754296894559, 0.3333333333333333703, 0.3219752754296894559, 0.3333333333333333703, 0.3219752754296894559, 0.3333333333333333703, 0.3219752754296894559, 0.3333333333333333703, 0.3219752754296894559, 0.3333333333333333703),
 ( 1.000000000000000000, 0.9659258262890683122, 1.000000000000000000, 0.9659258262890683122, 1.000000000000000000, 0.9659258262890683122, 1.000000000000000000, 0.9659258262890683122, 1.000000000000000000, 0.9659258262890683122, 1.000000000000000000, 0.9659258262890683122, 1.000000000000000000, 0.9659258262890683122, 1.000000000000000000, 0.9659258262890683122, 1.000000000000000000, 0.9659258262890683122, 1.000000000000000000, 0.9659258262890683122, 1.000000000000000000, 0.9659258262890683122, 1.000000000000000000, 0.9659258262890683122, 1.000000000000000000, 0.9659258262890683122, 1.000000000000000000, 0.9659258262890683122, 1.000000000000000000, 0.9659258262890683122, 1.000000000000000000, 0.9659258262890683122, 1.000000000000000000, 0.9659258262890683122, 1.000000000000000000, 0.9659258262890683122, 1.000000000000000000, 0.9659258262890683122, 1.000000000000000000, 0.9659258262890683122, 1.000000000000000000, 0.9659258262890683122, 1.000000000000000000, 0.9659258262890683122, 1.000000000000000000, 0.9659258262890683122, 1.000000000000000000, 0.9659258262890683122, 1.000000000000000000, 0.9659258262890683122, 1.000000000000000000, 0.9659258262890683122, 1.000000000000000000, 0.9659258262890683122, 1.000000000000000000, 0.9659258262890683122, 1.000000000000000000, 0.9659258262890683122, 1.000000000000000000, 0.9659258262890683122, 1.000000000000000000, 0.9659258262890683122, 1.000000000000000000, 0.9659258262890683122, 1.000000000000000000, 0.9659258262890683122, 1.000000000000000000, 0.9659258262890683122, 1.000000000000000000, 0.9659258262890683122, 1.000000000000000000, 0.9659258262890683122, 1.000000000000000000, 0.9659258262890683122, 1.000000000000000000, 0.9659258262890683122, 1.000000000000000000, 0.9659258262890683122, 1.000000000000000000, 0.9659258262890683122, 1.000000000000000000, 0.9659258262890683122, 1.000000000000000000, 0.9659258262890683122, 1.000000000000000000, 0.9659258262890683122, 1.000000000000000000, 0.9659258262890683122, 1.000000000000000000, 0.9659258262890683122, 1.000000000000000000, 0.9659258262890683122, 1.000000000000000000, 0.9659258262890683122, 1.000000000000000000, 0.9659258262890683122, 1.000000000000000000, 0.9659258262890683122, 1.000000000000000000, 0.9659258262890683122, 1.000000000000000000, 0.9659258262890683122, 1.000000000000000000, 0.9659258262890683122, 1.000000000000000000, 0.9659258262890683122, 1.000000000000000000, 0.9659258262890683122, 1.000000000000000000, 0.9659258262890683122, 1.000000000000000000, 0.9659258262890683122, 1.000000000000000000, 0.9659258262890683122, 1.000000000000000000, 0.9659258262890683122, 1.000000000000000000, 0.9659258262890683122, 1.000000000000000000, 0.9659258262890683122, 1.000000000000000000, 0.9659258262890683122, 1.000000000000000000, 0.9659258262890683122, 1.000000000000000000, 0.9659258262890683122, 1.000000000000000000, 0.9659258262890683122, 1.000000000000000000, 0.9659258262890683122, 1.000000000000000000, 0.9659258262890683122, 1.000000000000000000, 0.9659258262890683122, 1.000000000000000000, 0.9659258262890683122, 1.000000000000000000, 0.9659258262890683122, 1.000000000000000000, 0.9659258262890683122, 1.000000000000000000, 0.9659258262890683122, 1.000000000000000000, 0.9659258262890683122, 1.000000000000000000, 0.9659258262890683122, 1.000000000000000000, 0.9659258262890683122, 1.000000000000000000, 0.9659258262890683122, 1.000000000000000000, 0.9659258262890683122, 1.000000000000000000, 0.9659258262890683122, 1.000000000000000000, 0.9659258262890683122, 1.000000000000000000, 0.9659258262890683122, 1.000000000000000000, 0.9659258262890683122, 1.000000000000000000, 0.9659258262890683122, 1.000000000000000000, 0.9659258262890683122, 1.000000000000000000, 0.9659258262890683122, 1.000000000000000000, 0.9659258262890683122, 1.000000000000000000, 0.9659258262890683122, 1.000000000000000000, 0.9659258262890683122, 1.000000000000000000, 0.9659258262890683122, 1.000000000000000000, 0.9659258262890683122, 1.000000000000000000, 0.9659258262890683122, 1.000000000000000000, 0.9659258262890683122, 1.000000000000000000, 0.9659258262890683122, 1.000000000000000000, 0.9659258262890683122, 1.000000000000000000, 0.9659258262890683122, 1.000000000000000000, 0.9659258262890683122, 1.000000000000000000, 0.9659258262890683122, 1.000000000000000000, 0.9659258262890683122, 1.000000000000000000, 0.9659258262890683122, 1.000000000000000000, 0.9659258262890683122, 1.000000000000000000, 0.9659258262890683122, 1.000000000000000000, 0.9659258262890683122, 1.000000000000000000, 0.9659258262890683122, 1.000000000000000000, 0.9659258262890683122, 1.000000000000000000, 0.9659258262890683122, 1.000000000000000000, 0.9659258262890683122, 1.000000000000000000, 0.9659258262890683122, 1.000000000000000000, 0.9659258262890683122, 1.000000000000000000, 0.9659258262890683122, 1.000000000000000000, 0.9659258262890683122, 1.000000000000000000, 0.9659258262890683122, 1.000000000000000000, 0.9659258262890683122, 1.000000000000000000, 0.9659258262890683122, 1.000000000000000000, 0.9659258262890683122, 1.000000000000000000, 0.9659258262890683122, 1.000000000000000000, 0.9659258262890683122, 1.000000000000000000, 0.9659258262890683122, 1.000000000000000000, 0.9659258262890683122, 1.000000000000000000, 0.9659258262890683122, 1.000000000000000000, 0.9659258262890683122, 1.000000000000000000, 0.9659258262890683122, 1.000000000000000000, 0.9659258262890683122, 1.000000000000000000, 0.9659258262890683122, 1.000000000000000000, 0.9659258262890683122, 1.000000000000000000, 0.9659258262890683122, 1.000000000000000000, 0.9659258262890683122, 1.000000000000000000, 0.9659258262890683122, 1.000000000000000000, 0.9659258262890683122, 1.000000000000000000, 0.9659258262890683122, 1.000000000000000000, 0.9659258262890683122, 1.000000000000000000, 0.9659258262890683122, 1.000000000000000000, 0.9659258262890683122, 1.000000000000000000, 0.9659258262890683122, 1.000000000000000000, 0.9659258262890683122, 1.000000000000000000, 0.9659258262890683122, 1.000000000000000000, 0.9659258262890683122, 1.000000000000000000, 0.9659258262890683122, 1.000000000000000000, 0.9659258262890683122, 1.000000000000000000, 0.9659258262890683122, 1.000000000000000000, 0.9659258262890683122, 1.000000000000000000, 0.9659258262890683122, 1.000000000000000000, 0.9659258262890683122, 1.000000000000000000, 0.9659258262890683122, 1.000000000000000000, 0.9659258262890683122, 1.000000000000000000, 0.9659258262890683122, 1.000000000000000000, 0.9659258262890683122, 1.000000000000000000, 0.9659258262890683122, 1.000000000000000000, 0.9659258262890683122, 1.000000000000000000, 0.9659258262890683122, 1.000000000000000000, 0.9659258262890683122, 1.000000000000000000, 0.9659258262890683122, 1.000000000000000000, 0.9659258262890683122, 1.000000000000000000, 0.9659258262890683122, 1.000000000000000000, 0.9659258262890683122, 1.000000000000000000, 0.9659258262890683122, 1.000000000000000000, 0.9659258262890683122, 1.000000000000000000, 0.9659258262890683122, 1.000000000000000000, 0.9659258262890683122, 1.000000000000000000, 0.9659258262890683122, 1.000000000000000000, 0.9659258262890683122, 1.000000000000000000, 0.9659258262890683122, 1.000000000000000000, 0.9659258262890683122, 1.000000000000000000, 0.9659258262890683122, 1.000000000000000000, 0.9659258262890683122, 1.000000000000000000, 0.9659258262890683122, 1.000000000000000000, 0.9659258262890683122, 1.000000000000000000, 0.9659258262890683122, 1.000000000000000000, 0.9659258262890683122, 1.000000000000000000, 0.9659258262890683122, 1.000000000000000000, 0.9659258262890683122, 1.000000000000000000, 0.9659258262890683122, 1.000000000000000000, 0.9659258262890683122, 1.000000000000000000, 0.9659258262890683122, 1.000000000000000000, 0.9659258262890683122, 1.000000000000000000, 0.9659258262890683122, 1.000000000000000000, 0.9659258262890683122, 1.000000000000000000, 0.9659258262890683122, 1.000000000000000000, 0.9659258262890683122, 1.000000000000000000, 0.9659258262890683122, 1.000000000000000000, 0.9659258262890683122, 1.000000000000000000, 0.9659258262890683122, 1.000000000000000000, 0.9659258262890683122, 1.000000000000000000, 0.9659258262890683122, 1.000000000000000000, 0.9659258262890683122, 1.000000000000000000, 0.9659258262890683122, 1.000000000000000000, 0.9659258262890683122, 1.000000000000000000, 0.9659258262890683122, 1.000000000000000000, 0.9659258262890683122, 1.000000000000000000, 0.9659258262890683122, 1.000000000000000000, 0.9659258262890683122, 1.000000000000000000, 0.9659258262890683122, 1.000000000000000000, 0.9659258262890683122, 1.000000000000000000, 0.9659258262890683122, 1.000000000000000000, 0.9659258262890683122, 1.000000000000000000, 0.9659258262890683122, 1.000000000000000000, 0.9659258262890683122, 1.000000000000000000, 0.9659258262890683122, 1.000000000000000000, 0.9659258262890683122, 1.000000000000000000, 0.9659258262890683122, 1.000000000000000000, 0.9659258262890683122, 1.000000000000000000, 0.9659258262890683122, 1.000000000000000000, 0.9659258262890683122, 1.000000000000000000, 0.9659258262890683122, 1.000000000000000000, 0.9659258262890683122, 1.000000000000000000, 0.9659258262890683122, 1.000000000000000000, 0.9659258262890683122, 1.000000000000000000, 0.9659258262890683122, 1.000000000000000000, 0.9659258262890683122, 1.000000000000000000, 0.9659258262890683122, 1.000000000000000000, 0.9659258262890683122, 1.000000000000000000, 0.9659258262890683122, 1.000000000000000000, 0.9659258262890683122, 1.000000000000000000, 0.9659258262890683122, 1.000000000000000000, 0.9659258262890683122, 1.000000000000000000, 0.9659258262890683122, 1.000000000000000000, 0.9659258262890683122, 1.000000000000000000, 0.9659258262890683122, 1.000000000000000000, 0.9659258262890683122, 1.000000000000000000, 0.9659258262890683122, 1.000000000000000000, 0.9659258262890683122, 1.000000000000000000, 0.9659258262890683122, 1.000000000000000000, 0.9659258262890683122, 1.000000000000000000, 0.9659258262890683122, 1.000000000000000000, 0.9659258262890683122, 1.000000000000000000, 0.9659258262890683122, 1.000000000000000000, 0.9659258262890683122, 1.000000000000000000, 0.9659258262890683122, 1.000000000000000000, 0.9659258262890683122, 1.000000000000000000, 0.9659258262890683122, 1.000000000000000000, 0.9659258262890683122, 1.000000000000000000),
 ( 0.3333333333333333703, 0.3219752754296894559, 0.3333333333333333703, 0.3219752754296894559, 0.3333333333333333703, 0.3219752754296894559, 0.3333333333333333703, 0.3219752754296894559, 0.3333333333333333703, 0.3219752754296894559, 0.3333333333333333703, 0.3219752754296894559, 0.3333333333333333703, 0.3219752754296894559, 0.3333333333333333703, 0.3219752754296894559, 0.3333333333333333703, 0.3219752754296894559, 0.3333333333333333703, 0.3219752754296894559, 0.3333333333333333703, 0.3219752754296894559, 0.3333333333333333703, 0.3219752754296894559, 0.3333333333333333703, 0.3219752754296894559, 0.3333333333333333703, 0.3219752754296894559, 0.3333333333333333703, 0.3219752754296894559, 0.3333333333333333703, 0.3219752754296894559, 0.3333333333333333703, 0.3219752754296894559, 0.3333333333333333703, 0.3219752754296894559, 0.3333333333333333703, 0.3219752754296894559, 0.3333333333333333703, 0.3219752754296894559, 0.3333333333333333703, 0.3219752754296894559, 0.3333333333333333703, 0.3219752754296894559, 0.3333333333333333703, 0.3219752754296894559, 0.3333333333333333703, 0.3219752754296894559, 0.3333333333333333703, 0.3219752754296894559, 0.3333333333333333703, 0.3219752754296894559, 0.3333333333333333703, 0.3219752754296894559, 0.3333333333333333703, 0.3219752754296894559, 0.3333333333333333703, 0.3219752754296894559, 0.3333333333333333703, 0.3219752754296894559, 0.3333333333333333703, 0.3219752754296894559, 0.3333333333333333703, 0.3219752754296894559, 0.3333333333333333703, 0.3219752754296894559, 0.3333333333333333703, 0.3219752754296894559, 0.3333333333333333703, 0.3219752754296894559, 0.3333333333333333703, 0.3219752754296894559, 0.3333333333333333703, 0.3219752754296894559, 0.3333333333333333703, 0.3219752754296894559, 0.3333333333333333703, 0.3219752754296894559, 0.3333333333333333703, 0.3219752754296894559, 0.3333333333333333703, 0.3219752754296894559, 0.3333333333333333703, 0.3219752754296894559, 0.3333333333333333703, 0.3219752754296894559, 0.3333333333333333703, 0.3219752754296894559, 0.3333333333333333703, 0.3219752754296894559, 0.3333333333333333703, 0.3219752754296894559, 0.3333333333333333703, 0.3219752754296894559, 0.3333333333333333703, 0.3219752754296894559, 0.3333333333333333703, 0.3219752754296894559, 0.3333333333333333703, 0.3219752754296894559, 0.3333333333333333703, 0.3219752754296894559, 0.3333333333333333703, 0.3219752754296894559, 0.3333333333333333703, 0.3219752754296894559, 0.3333333333333333703, 0.3219752754296894559, 0.3333333333333333703, 0.3219752754296894559, 0.3333333333333333703, 0.3219752754296894559, 0.3333333333333333703, 0.3219752754296894559, 0.3333333333333333703, 0.3219752754296894559, 0.3333333333333333703, 0.3219752754296894559, 0.3333333333333333703, 0.3219752754296894559, 0.3333333333333333703, 0.3219752754296894559, 0.3333333333333333703, 0.3219752754296894559, 0.3333333333333333703, 0.3219752754296894559, 0.3333333333333333703, 0.3219752754296894559, 0.3333333333333333703, 0.3219752754296894559, 0.3333333333333333703, 0.3219752754296894559, 0.3333333333333333703, 0.3219752754296894559, 0.3333333333333333703, 0.3219752754296894559, 0.3333333333333333703, 0.3219752754296894559, 0.3333333333333333703, 0.3219752754296894559, 0.3333333333333333703, 0.3219752754296894559, 0.3333333333333333703, 0.3219752754296894559, 0.3333333333333333703, 0.3219752754296894559, 0.3333333333333333703, 0.3219752754296894559, 0.3333333333333333703, 0.3219752754296894559, 0.3333333333333333703, 0.3219752754296894559, 0.3333333333333333703, 0.3219752754296894559, 0.3333333333333333703, 0.3219752754296894559, 0.3333333333333333703, 0.3219752754296894559, 0.3333333333333333703, 0.3219752754296894559, 0.3333333333333333703, 0.3219752754296894559, 0.3333333333333333703, 0.3219752754296894559, 0.3333333333333333703, 0.3219752754296894559, 0.3333333333333333703, 0.3219752754296894559, 0.3333333333333333703, 0.3219752754296894559, 0.3333333333333333703, 0.3219752754296894559, 0.3333333333333333703, 0.3219752754296894559, 0.3333333333333333703, 0.3219752754296894559, 0.3333333333333333703, 0.3219752754296894559, 0.3333333333333333703, 0.3219752754296894559, 0.3333333333333333703, 0.3219752754296894559, 0.3333333333333333703, 0.3219752754296894559, 0.3333333333333333703, 0.3219752754296894559, 0.3333333333333333703, 0.3219752754296894559, 0.3333333333333333703, 0.3219752754296894559, 0.3333333333333333703, 0.3219752754296894559, 0.3333333333333333703, 0.3219752754296894559, 0.3333333333333333703, 0.3219752754296894559, 0.3333333333333333703, 0.3219752754296894559, 0.3333333333333333703, 0.3219752754296894559, 0.3333333333333333703, 0.3219752754296894559, 0.3333333333333333703, 0.3219752754296894559, 0.3333333333333333703, 0.3219752754296894559, 0.3333333333333333703, 0.3219752754296894559, 0.3333333333333333703, 0.3219752754296894559, 0.3333333333333333703, 0.3219752754296894559, 0.3333333333333333703, 0.3219752754296894559, 0.3333333333333333703, 0.3219752754296894559, 0.3333333333333333703, 0.3219752754296894559, 0.3333333333333333703, 0.3219752754296894559, 0.3333333333333333703, 0.3219752754296894559, 0.3333333333333333703, 0.3219752754296894559, 0.3333333333333333703, 0.3219752754296894559, 0.3333333333333333703, 0.3219752754296894559, 0.3333333333333333703, 0.3219752754296894559, 0.3333333333333333703, 0.3219752754296894559, 0.3333333333333333703, 0.3219752754296894559, 0.3333333333333333703, 0.3219752754296894559, 0.3333333333333333703, 0.3219752754296894559, 0.3333333333333333703, 0.3219752754296894559, 0.3333333333333333703, 0.3219752754296894559, 0.3333333333333333703, 0.3219752754296894559, 0.3333333333333333703, 0.3219752754296894559, 0.3333333333333333703, 0.3219752754296894559, 0.3333333333333333703, 0.3219752754296894559, 0.3333333333333333703, 0.3219752754296894559, 0.3333333333333333703, 0.3219752754296894559, 0.3333333333333333703, 0.3219752754296894559, 0.3333333333333333703, 0.3219752754296894559, 0.3333333333333333703, 0.3219752754296894559, 0.3333333333333333703, 0.3219752754296894559, 0.3333333333333333703, 0.3219752754296894559, 0.3333333333333333703, 0.3219752754296894559, 0.3333333333333333703, 0.3219752754296894559, 0.3333333333333333703, 0.3219752754296894559, 0.3333333333333333703, 0.3219752754296894559, 0.3333333333333333703, 0.3219752754296894559, 0.3333333333333333703, 0.3219752754296894559, 0.3333333333333333703, 0.3219752754296894559, 0.3333333333333333703, 0.3219752754296894559, 0.3333333333333333703, 0.3219752754296894559, 0.3333333333333333703, 0.3219752754296894559, 0.3333333333333333703, 0.3219752754296894559, 0.3333333333333333703, 0.3219752754296894559, 0.3333333333333333703, 0.3219752754296894559, 0.3333333333333333703, 0.3219752754296894559, 0.3333333333333333703, 0.3219752754296894559, 0.3333333333333333703, 0.3219752754296894559, 0.3333333333333333703, 0.3219752754296894559, 0.3333333333333333703, 0.3219752754296894559, 0.3333333333333333703, 0.3219752754296894559, 0.3333333333333333703, 0.3219752754296894559, 0.3333333333333333703, 0.3219752754296894559, 0.3333333333333333703, 0.3219752754296894559, 0.3333333333333333703, 0.3219752754296894559, 0.3333333333333333703, 0.3219752754296894559, 0.3333333333333333703, 0.3219752754296894559, 0.3333333333333333703, 0.3219752754296894559, 0.3333333333333333703, 0.3219752754296894559, 0.3333333333333333703, 0.3219752754296894559, 0.3333333333333333703, 0.3219752754296894559, 0.3333333333333333703, 0.3219752754296894559, 0.3333333333333333703, 0.3219752754296894559, 0.3333333333333333703, 0.3219752754296894559, 0.3333333333333333703, 0.3219752754296894559, 0.3333333333333333703, 0.3219752754296894559, 0.3333333333333333703, 0.3219752754296894559, 0.3333333333333333703, 0.3219752754296894559, 0.3333333333333333703, 0.3219752754296894559, 0.3333333333333333703, 0.3219752754296894559, 0.3333333333333333703, 0.3219752754296894559, 0.3333333333333333703, 0.3219752754296894559, 0.3333333333333333703, 0.3219752754296894559, 0.3333333333333333703, 0.3219752754296894559, 0.3333333333333333703, 0.3219752754296894559, 0.3333333333333333703, 0.3219752754296894559, 0.3333333333333333703, 0.3219752754296894559, 0.3333333333333333703, 0.3219752754296894559, 0.3333333333333333703, 0.3219752754296894559, 0.3333333333333333703, 0.3219752754296894559, 0.3333333333333333703, 0.3219752754296894559, 0.3333333333333333703, 0.3219752754296894559, 0.3333333333333333703, 0.3219752754296894559, 0.3333333333333333703, 0.3219752754296894559, 0.3333333333333333703, 0.3219752754296894559, 0.3333333333333333703, 0.3219752754296894559, 0.3333333333333333703, 0.3219752754296894559, 0.3333333333333333703, 0.3219752754296894559, 0.3333333333333333703, 0.3219752754296894559, 0.3333333333333333703, 0.3219752754296894559, 0.3333333333333333703, 0.3219752754296894559, 0.3333333333333333703, 0.3219752754296894559, 0.3333333333333333703, 0.3219752754296894559, 0.3333333333333333703, 0.3219752754296894559, 0.3333333333333333703, 0.3219752754296894559, 0.3333333333333333703, 0.3219752754296894559, 0.3333333333333333703, 0.3219752754296894559, 0.3333333333333333703, 0.3219752754296894559, 0.3333333333333333703, 0.3219752754296894559, 0.3333333333333333703, 0.3219752754296894559, 0.3333333333333333703, 0.3219752754296894559, 0.3333333333333333703, 0.3219752754296894559, 0.3333333333333333703, 0.3219752754296894559, 0.3333333333333333703, 0.3219752754296894559, 0.3333333333333333703, 0.3219752754296894559, 0.3333333333333333703, 0.3219752754296894559, 0.3333333333333333703, 0.3219752754296894559, 0.3333333333333333703, 0.3219752754296894559, 0.3333333333333333703, 0.3219752754296894559, 0.3333333333333333703, 0.3219752754296894559, 0.3333333333333333703, 0.3219752754296894559, 0.3333333333333333703, 0.3219752754296894559, 0.3333333333333333703, 0.3219752754296894559, 0.3333333333333333703, 0.3219752754296894559, 0.3333333333333333703, 0.3219752754296894559, 0.3333333333333333703, 0.3219752754296894559, 0.3333333333333333703, 0.3219752754296894559, 0.3333333333333333703, 0.3219752754296894559, 0.3333333333333333703, 0.3219752754296894559, 0.3333333333333333703, 0.3219752754296894559, 0.3333333333333333703, 0.3219752754296894559, 0.3333333333333333703, 0.3219752754296894559, 0.3333333333333333703, 0.3219752754296894559, 0.3333333333333333703, 0.3219752754296894559, 0.3333333333333333703, 0.3219752754296894559, 0.3333333333333333703, 0.3219752754296894559, 0.3333333333333333703, 0.3219752754296894559, 0.3333333333333333703, 0.3219752754296894559, 0.3333333333333333703),
 ( 0.3333333333333333703, 0.3219752754296894559, 0.3333333333333333703, 0.3219752754296894559, 0.3333333333333333703, 0.3219752754296894559, 0.3333333333333333703, 0.3219752754296894559, 0.3333333333333333703, 0.3219752754296894559, 0.3333333333333333703, 0.3219752754296894559, 0.3333333333333333703, 0.3219752754296894559, 0.3333333333333333703, 0.3219752754296894559, 0.3333333333333333703, 0.3219752754296894559, 0.3333333333333333703, 0.3219752754296894559, 0.3333333333333333703, 0.3219752754296894559, 0.3333333333333333703, 0.3219752754296894559, 0.3333333333333333703, 0.3219752754296894559, 0.3333333333333333703, 0.3219752754296894559, 0.3333333333333333703, 0.3219752754296894559, 0.3333333333333333703, 0.3219752754296894559, 0.3333333333333333703, 0.3219752754296894559, 0.3333333333333333703, 0.3219752754296894559, 0.3333333333333333703, 0.3219752754296894559, 0.3333333333333333703, 0.3219752754296894559, 0.3333333333333333703, 0.3219752754296894559, 0.3333333333333333703, 0.3219752754296894559, 0.3333333333333333703, 0.3219752754296894559, 0.3333333333333333703, 0.3219752754296894559, 0.3333333333333333703, 0.3219752754296894559, 0.3333333333333333703, 0.3219752754296894559, 0.3333333333333333703, 0.3219752754296894559, 0.3333333333333333703, 0.3219752754296894559, 0.3333333333333333703, 0.3219752754296894559, 0.3333333333333333703, 0.3219752754296894559, 0.3333333333333333703, 0.3219752754296894559, 0.3333333333333333703, 0.3219752754296894559, 0.3333333333333333703, 0.3219752754296894559, 0.3333333333333333703, 0.3219752754296894559, 0.3333333333333333703, 0.3219752754296894559, 0.3333333333333333703, 0.3219752754296894559, 0.3333333333333333703, 0.3219752754296894559, 0.3333333333333333703, 0.3219752754296894559, 0.3333333333333333703, 0.3219752754296894559, 0.3333333333333333703, 0.3219752754296894559, 0.3333333333333333703, 0.3219752754296894559, 0.3333333333333333703, 0.3219752754296894559, 0.3333333333333333703, 0.3219752754296894559, 0.3333333333333333703, 0.3219752754296894559, 0.3333333333333333703, 0.3219752754296894559, 0.3333333333333333703, 0.3219752754296894559, 0.3333333333333333703, 0.3219752754296894559, 0.3333333333333333703, 0.3219752754296894559, 0.3333333333333333703, 0.3219752754296894559, 0.3333333333333333703, 0.3219752754296894559, 0.3333333333333333703, 0.3219752754296894559, 0.3333333333333333703, 0.3219752754296894559, 0.3333333333333333703, 0.3219752754296894559, 0.3333333333333333703, 0.3219752754296894559, 0.3333333333333333703, 0.3219752754296894559, 0.3333333333333333703, 0.3219752754296894559, 0.3333333333333333703, 0.3219752754296894559, 0.3333333333333333703, 0.3219752754296894559, 0.3333333333333333703, 0.3219752754296894559, 0.3333333333333333703, 0.3219752754296894559, 0.3333333333333333703, 0.3219752754296894559, 0.3333333333333333703, 0.3219752754296894559, 0.3333333333333333703, 0.3219752754296894559, 0.3333333333333333703, 0.3219752754296894559, 0.3333333333333333703, 0.3219752754296894559, 0.3333333333333333703, 0.3219752754296894559, 0.3333333333333333703, 0.3219752754296894559, 0.3333333333333333703, 0.3219752754296894559, 0.3333333333333333703, 0.3219752754296894559, 0.3333333333333333703, 0.3219752754296894559, 0.3333333333333333703, 0.3219752754296894559, 0.3333333333333333703, 0.3219752754296894559, 0.3333333333333333703, 0.3219752754296894559, 0.3333333333333333703, 0.3219752754296894559, 0.3333333333333333703, 0.3219752754296894559, 0.3333333333333333703, 0.3219752754296894559, 0.3333333333333333703, 0.3219752754296894559, 0.3333333333333333703, 0.3219752754296894559, 0.3333333333333333703, 0.3219752754296894559, 0.3333333333333333703, 0.3219752754296894559, 0.3333333333333333703, 0.3219752754296894559, 0.3333333333333333703, 0.3219752754296894559, 0.3333333333333333703, 0.3219752754296894559, 0.3333333333333333703, 0.3219752754296894559, 0.3333333333333333703, 0.3219752754296894559, 0.3333333333333333703, 0.3219752754296894559, 0.3333333333333333703, 0.3219752754296894559, 0.3333333333333333703, 0.3219752754296894559, 0.3333333333333333703, 0.3219752754296894559, 0.3333333333333333703, 0.3219752754296894559, 0.3333333333333333703, 0.3219752754296894559, 0.3333333333333333703, 0.3219752754296894559, 0.3333333333333333703, 0.3219752754296894559, 0.3333333333333333703, 0.3219752754296894559, 0.3333333333333333703, 0.3219752754296894559, 0.3333333333333333703, 0.3219752754296894559, 0.3333333333333333703, 0.3219752754296894559, 0.3333333333333333703, 0.3219752754296894559, 0.3333333333333333703, 0.3219752754296894559, 0.3333333333333333703, 0.3219752754296894559, 0.3333333333333333703, 0.3219752754296894559, 0.3333333333333333703, 0.3219752754296894559, 0.3333333333333333703, 0.3219752754296894559, 0.3333333333333333703, 0.3219752754296894559, 0.3333333333333333703, 0.3219752754296894559, 0.3333333333333333703, 0.3219752754296894559, 0.3333333333333333703, 0.3219752754296894559, 0.3333333333333333703, 0.3219752754296894559, 0.3333333333333333703, 0.3219752754296894559, 0.3333333333333333703, 0.3219752754296894559, 0.3333333333333333703, 0.3219752754296894559, 0.3333333333333333703, 0.3219752754296894559, 0.3333333333333333703, 0.3219752754296894559, 0.3333333333333333703, 0.3219752754296894559, 0.3333333333333333703, 0.3219752754296894559, 0.3333333333333333703, 0.3219752754296894559, 0.3333333333333333703, 0.3219752754296894559, 0.3333333333333333703, 0.3219752754296894559, 0.3333333333333333703, 0.3219752754296894559, 0.3333333333333333703, 0.3219752754296894559, 0.3333333333333333703, 0.3219752754296894559, 0.3333333333333333703, 0.3219752754296894559, 0.3333333333333333703, 0.3219752754296894559, 0.3333333333333333703, 0.3219752754296894559, 0.3333333333333333703, 0.3219752754296894559, 0.3333333333333333703, 0.3219752754296894559, 0.3333333333333333703, 0.3219752754296894559, 0.3333333333333333703, 0.3219752754296894559, 0.3333333333333333703, 0.3219752754296894559, 0.3333333333333333703, 0.3219752754296894559, 0.3333333333333333703, 0.3219752754296894559, 0.3333333333333333703, 0.3219752754296894559, 0.3333333333333333703, 0.3219752754296894559, 0.3333333333333333703, 0.3219752754296894559, 0.3333333333333333703, 0.3219752754296894559, 0.3333333333333333703, 0.3219752754296894559, 0.3333333333333333703, 0.3219752754296894559, 0.3333333333333333703, 0.3219752754296894559, 0.3333333333333333703, 0.3219752754296894559, 0.3333333333333333703, 0.3219752754296894559, 0.3333333333333333703, 0.3219752754296894559, 0.3333333333333333703, 0.3219752754296894559, 0.3333333333333333703, 0.3219752754296894559, 0.3333333333333333703, 0.3219752754296894559, 0.3333333333333333703, 0.3219752754296894559, 0.3333333333333333703, 0.3219752754296894559, 0.3333333333333333703, 0.3219752754296894559, 0.3333333333333333703, 0.3219752754296894559, 0.3333333333333333703, 0.3219752754296894559, 0.3333333333333333703, 0.3219752754296894559, 0.3333333333333333703, 0.3219752754296894559, 0.3333333333333333703, 0.3219752754296894559, 0.3333333333333333703, 0.3219752754296894559, 0.3333333333333333703, 0.3219752754296894559, 0.3333333333333333703, 0.3219752754296894559, 0.3333333333333333703, 0.3219752754296894559, 0.3333333333333333703, 0.3219752754296894559, 0.3333333333333333703, 0.3219752754296894559, 0.3333333333333333703, 0.3219752754296894559, 0.3333333333333333703, 0.3219752754296894559, 0.3333333333333333703, 0.3219752754296894559, 0.3333333333333333703, 0.3219752754296894559, 0.3333333333333333703, 0.3219752754296894559, 0.3333333333333333703, 0.3219752754296894559, 0.3333333333333333703, 0.3219752754296894559, 0.3333333333333333703, 0.3219752754296894559, 0.3333333333333333703, 0.3219752754296894559, 0.3333333333333333703, 0.3219752754296894559, 0.3333333333333333703, 0.3219752754296894559, 0.3333333333333333703, 0.3219752754296894559, 0.3333333333333333703, 0.3219752754296894559, 0.3333333333333333703, 0.3219752754296894559, 0.3333333333333333703, 0.3219752754296894559, 0.3333333333333333703, 0.3219752754296894559, 0.3333333333333333703, 0.3219752754296894559, 0.3333333333333333703, 0.3219752754296894559, 0.3333333333333333703, 0.3219752754296894559, 0.3333333333333333703, 0.3219752754296894559, 0.3333333333333333703, 0.3219752754296894559, 0.3333333333333333703, 0.3219752754296894559, 0.3333333333333333703, 0.3219752754296894559, 0.3333333333333333703, 0.3219752754296894559, 0.3333333333333333703, 0.3219752754296894559, 0.3333333333333333703, 0.3219752754296894559, 0.3333333333333333703, 0.3219752754296894559, 0.3333333333333333703, 0.3219752754296894559, 0.3333333333333333703, 0.3219752754296894559, 0.3333333333333333703, 0.3219752754296894559, 0.3333333333333333703, 0.3219752754296894559, 0.3333333333333333703, 0.3219752754296894559, 0.3333333333333333703, 0.3219752754296894559, 0.3333333333333333703, 0.3219752754296894559, 0.3333333333333333703, 0.3219752754296894559, 0.3333333333333333703, 0.3219752754296894559, 0.3333333333333333703, 0.3219752754296894559, 0.3333333333333333703, 0.3219752754296894559, 0.3333333333333333703, 0.3219752754296894559, 0.3333333333333333703, 0.3219752754296894559, 0.3333333333333333703, 0.3219752754296894559, 0.3333333333333333703, 0.3219752754296894559, 0.3333333333333333703, 0.3219752754296894559, 0.3333333333333333703, 0.3219752754296894559, 0.3333333333333333703, 0.3219752754296894559, 0.3333333333333333703, 0.3219752754296894559, 0.3333333333333333703, 0.3219752754296894559, 0.3333333333333333703, 0.3219752754296894559, 0.3333333333333333703, 0.3219752754296894559, 0.3333333333333333703, 0.3219752754296894559, 0.3333333333333333703, 0.3219752754296894559, 0.3333333333333333703, 0.3219752754296894559, 0.3333333333333333703, 0.3219752754296894559, 0.3333333333333333703, 0.3219752754296894559, 0.3333333333333333703, 0.3219752754296894559, 0.3333333333333333703, 0.3219752754296894559, 0.3333333333333333703, 0.3219752754296894559, 0.3333333333333333703, 0.3219752754296894559, 0.3333333333333333703, 0.3219752754296894559, 0.3333333333333333703, 0.3219752754296894559, 0.3333333333333333703, 0.3219752754296894559, 0.3333333333333333703, 0.3219752754296894559, 0.3333333333333333703, 0.3219752754296894559, 0.3333333333333333703, 0.3219752754296894559, 0.3333333333333333703, 0.3219752754296894559, 0.3333333333333333703, 0.3219752754296894559, 0.3333333333333333703, 0.3219752754296894559, 0.3333333333333333703, 0.3219752754296894559, 0.3333333333333333703, 0.3219752754296894559, 0.3333333333333333703, 0.3219752754296894559, 0.3333333333333333703),
 ( 1.000000000000000000, 0.9659258262890683122, 1.000000000000000000, 0.9659258262890683122, 1.000000000000000000, 0.9659258262890683122, 1.000000000000000000, 0.9659258262890683122, 1.000000000000000000, 0.9659258262890683122, 1.000000000000000000, 0.9659258262890683122, 1.000000000000000000, 0.9659258262890683122, 1.000000000000000000, 0.9659258262890683122, 1.000000000000000000, 0.9659258262890683122, 1.000000000000000000, 0.9659258262890683122, 1.000000000000000000, 0.9659258262890683122, 1.000000000000000000, 0.9659258262890683122, 1.000000000000000000, 0.9659258262890683122, 1.000000000000000000, 0.9659258262890683122, 1.000000000000000000, 0.9659258262890683122, 1.000000000000000000, 0.9659258262890683122, 1.000000000000000000, 0.9659258262890683122, 1.000000000000000000, 0.9659258262890683122, 1.000000000000000000, 0.9659258262890683122, 1.000000000000000000, 0.9659258262890683122, 1.000000000000000000, 0.9659258262890683122, 1.000000000000000000, 0.9659258262890683122, 1.000000000000000000, 0.9659258262890683122, 1.000000000000000000, 0.9659258262890683122, 1.000000000000000000, 0.9659258262890683122, 1.000000000000000000, 0.9659258262890683122, 1.000000000000000000, 0.9659258262890683122, 1.000000000000000000, 0.9659258262890683122, 1.000000000000000000, 0.9659258262890683122, 1.000000000000000000, 0.9659258262890683122, 1.000000000000000000, 0.9659258262890683122, 1.000000000000000000, 0.9659258262890683122, 1.000000000000000000, 0.9659258262890683122, 1.000000000000000000, 0.9659258262890683122, 1.000000000000000000, 0.9659258262890683122, 1.000000000000000000, 0.9659258262890683122, 1.000000000000000000, 0.9659258262890683122, 1.000000000000000000, 0.9659258262890683122, 1.000000000000000000, 0.9659258262890683122, 1.000000000000000000, 0.9659258262890683122, 1.000000000000000000, 0.9659258262890683122, 1.000000000000000000, 0.9659258262890683122, 1.000000000000000000, 0.9659258262890683122, 1.000000000000000000, 0.9659258262890683122, 1.000000000000000000, 0.9659258262890683122, 1.000000000000000000, 0.9659258262890683122, 1.000000000000000000, 0.9659258262890683122, 1.000000000000000000, 0.9659258262890683122, 1.000000000000000000, 0.9659258262890683122, 1.000000000000000000, 0.9659258262890683122, 1.000000000000000000, 0.9659258262890683122, 1.000000000000000000, 0.9659258262890683122, 1.000000000000000000, 0.9659258262890683122, 1.000000000000000000, 0.9659258262890683122, 1.000000000000000000, 0.9659258262890683122, 1.000000000000000000, 0.9659258262890683122, 1.000000000000000000, 0.9659258262890683122, 1.000000000000000000, 0.9659258262890683122, 1.000000000000000000, 0.9659258262890683122, 1.000000000000000000, 0.9659258262890683122, 1.000000000000000000, 0.9659258262890683122, 1.000000000000000000, 0.9659258262890683122, 1.000000000000000000, 0.9659258262890683122, 1.000000000000000000, 0.9659258262890683122, 1.000000000000000000, 0.9659258262890683122, 1.000000000000000000, 0.9659258262890683122, 1.000000000000000000, 0.9659258262890683122, 1.000000000000000000, 0.9659258262890683122, 1.000000000000000000, 0.9659258262890683122, 1.000000000000000000, 0.9659258262890683122, 1.000000000000000000, 0.9659258262890683122, 1.000000000000000000, 0.9659258262890683122, 1.000000000000000000, 0.9659258262890683122, 1.000000000000000000, 0.9659258262890683122, 1.000000000000000000, 0.9659258262890683122, 1.000000000000000000, 0.9659258262890683122, 1.000000000000000000, 0.9659258262890683122, 1.000000000000000000, 0.9659258262890683122, 1.000000000000000000, 0.9659258262890683122, 1.000000000000000000, 0.9659258262890683122, 1.000000000000000000, 0.9659258262890683122, 1.000000000000000000, 0.9659258262890683122, 1.000000000000000000, 0.9659258262890683122, 1.000000000000000000, 0.9659258262890683122, 1.000000000000000000, 0.9659258262890683122, 1.000000000000000000, 0.9659258262890683122, 1.000000000000000000, 0.9659258262890683122, 1.000000000000000000, 0.9659258262890683122, 1.000000000000000000, 0.9659258262890683122, 1.000000000000000000, 0.9659258262890683122, 1.000000000000000000, 0.9659258262890683122, 1.000000000000000000, 0.9659258262890683122, 1.000000000000000000, 0.9659258262890683122, 1.000000000000000000, 0.9659258262890683122, 1.000000000000000000, 0.9659258262890683122, 1.000000000000000000, 0.9659258262890683122, 1.000000000000000000, 0.9659258262890683122, 1.000000000000000000, 0.9659258262890683122, 1.000000000000000000, 0.9659258262890683122, 1.000000000000000000, 0.9659258262890683122, 1.000000000000000000, 0.9659258262890683122, 1.000000000000000000, 0.9659258262890683122, 1.000000000000000000, 0.9659258262890683122, 1.000000000000000000, 0.9659258262890683122, 1.000000000000000000, 0.9659258262890683122, 1.000000000000000000, 0.9659258262890683122, 1.000000000000000000, 0.9659258262890683122, 1.000000000000000000, 0.9659258262890683122, 1.000000000000000000, 0.9659258262890683122, 1.000000000000000000, 0.9659258262890683122, 1.000000000000000000, 0.9659258262890683122, 1.000000000000000000, 0.9659258262890683122, 1.000000000000000000, 0.9659258262890683122, 1.000000000000000000, 0.9659258262890683122, 1.000000000000000000, 0.9659258262890683122, 1.000000000000000000, 0.9659258262890683122, 1.000000000000000000, 0.9659258262890683122, 1.000000000000000000, 0.9659258262890683122, 1.000000000000000000, 0.9659258262890683122, 1.000000000000000000, 0.9659258262890683122, 1.000000000000000000, 0.9659258262890683122, 1.000000000000000000, 0.9659258262890683122, 1.000000000000000000, 0.9659258262890683122, 1.000000000000000000, 0.9659258262890683122, 1.000000000000000000, 0.9659258262890683122, 1.000000000000000000, 0.9659258262890683122, 1.000000000000000000, 0.9659258262890683122, 1.000000000000000000, 0.9659258262890683122, 1.000000000000000000, 0.9659258262890683122, 1.000000000000000000, 0.9659258262890683122, 1.000000000000000000, 0.9659258262890683122, 1.000000000000000000, 0.9659258262890683122, 1.000000000000000000, 0.9659258262890683122, 1.000000000000000000, 0.9659258262890683122, 1.000000000000000000, 0.9659258262890683122, 1.000000000000000000, 0.9659258262890683122, 1.000000000000000000, 0.9659258262890683122, 1.000000000000000000, 0.9659258262890683122, 1.000000000000000000, 0.9659258262890683122, 1.000000000000000000, 0.9659258262890683122, 1.000000000000000000, 0.9659258262890683122, 1.000000000000000000, 0.9659258262890683122, 1.000000000000000000, 0.9659258262890683122, 1.000000000000000000, 0.9659258262890683122, 1.000000000000000000, 0.9659258262890683122, 1.000000000000000000, 0.9659258262890683122, 1.000000000000000000, 0.9659258262890683122, 1.000000000000000000, 0.9659258262890683122, 1.000000000000000000, 0.9659258262890683122, 1.000000000000000000, 0.9659258262890683122, 1.000000000000000000, 0.9659258262890683122, 1.000000000000000000, 0.9659258262890683122, 1.000000000000000000, 0.9659258262890683122, 1.000000000000000000, 0.9659258262890683122, 1.000000000000000000, 0.9659258262890683122, 1.000000000000000000, 0.9659258262890683122, 1.000000000000000000, 0.9659258262890683122, 1.000000000000000000, 0.9659258262890683122, 1.000000000000000000, 0.9659258262890683122, 1.000000000000000000, 0.9659258262890683122, 1.000000000000000000, 0.9659258262890683122, 1.000000000000000000, 0.9659258262890683122, 1.000000000000000000, 0.9659258262890683122, 1.000000000000000000, 0.9659258262890683122, 1.000000000000000000, 0.9659258262890683122, 1.000000000000000000, 0.9659258262890683122, 1.000000000000000000, 0.9659258262890683122, 1.000000000000000000, 0.9659258262890683122, 1.000000000000000000, 0.9659258262890683122, 1.000000000000000000, 0.9659258262890683122, 1.000000000000000000, 0.9659258262890683122, 1.000000000000000000, 0.9659258262890683122, 1.000000000000000000, 0.9659258262890683122, 1.000000000000000000, 0.9659258262890683122, 1.000000000000000000, 0.9659258262890683122, 1.000000000000000000, 0.9659258262890683122, 1.000000000000000000, 0.9659258262890683122, 1.000000000000000000, 0.9659258262890683122, 1.000000000000000000, 0.9659258262890683122, 1.000000000000000000, 0.9659258262890683122, 1.000000000000000000, 0.9659258262890683122, 1.000000000000000000, 0.9659258262890683122, 1.000000000000000000, 0.9659258262890683122, 1.000000000000000000, 0.9659258262890683122, 1.000000000000000000, 0.9659258262890683122, 1.000000000000000000, 0.9659258262890683122, 1.000000000000000000, 0.9659258262890683122, 1.000000000000000000, 0.9659258262890683122, 1.000000000000000000, 0.9659258262890683122, 1.000000000000000000, 0.9659258262890683122, 1.000000000000000000, 0.9659258262890683122, 1.000000000000000000, 0.9659258262890683122, 1.000000000000000000, 0.9659258262890683122, 1.000000000000000000, 0.9659258262890683122, 1.000000000000000000, 0.9659258262890683122, 1.000000000000000000, 0.9659258262890683122, 1.000000000000000000, 0.9659258262890683122, 1.000000000000000000, 0.9659258262890683122, 1.000000000000000000, 0.9659258262890683122, 1.000000000000000000, 0.9659258262890683122, 1.000000000000000000, 0.9659258262890683122, 1.000000000000000000, 0.9659258262890683122, 1.000000000000000000, 0.9659258262890683122, 1.000000000000000000, 0.9659258262890683122, 1.000000000000000000, 0.9659258262890683122, 1.000000000000000000, 0.9659258262890683122, 1.000000000000000000, 0.9659258262890683122, 1.000000000000000000, 0.9659258262890683122, 1.000000000000000000, 0.9659258262890683122, 1.000000000000000000, 0.9659258262890683122, 1.000000000000000000, 0.9659258262890683122, 1.000000000000000000, 0.9659258262890683122, 1.000000000000000000, 0.9659258262890683122, 1.000000000000000000, 0.9659258262890683122, 1.000000000000000000, 0.9659258262890683122, 1.000000000000000000, 0.9659258262890683122, 1.000000000000000000, 0.9659258262890683122, 1.000000000000000000, 0.9659258262890683122, 1.000000000000000000, 0.9659258262890683122, 1.000000000000000000, 0.9659258262890683122, 1.000000000000000000, 0.9659258262890683122, 1.000000000000000000, 0.9659258262890683122, 1.000000000000000000, 0.9659258262890683122, 1.000000000000000000, 0.9659258262890683122, 1.000000000000000000, 0.9659258262890683122, 1.000000000000000000, 0.9659258262890683122, 1.000000000000000000, 0.9659258262890683122, 1.000000000000000000, 0.9659258262890683122, 1.000000000000000000) ) ) 
 REPRESENTATION_ITEM ( '' )  SURFACE ( )  );
#175109 = EDGE_LOOP ( 'NONE', ( #54526, #23455, #111587, #161086 ) ) ;
#175110 = CARTESIAN_POINT ( 'NONE',  ( -18.67979575497193778, 10.72451020669871902, 113.3344237280190328 ) ) ;
#175111 = CARTESIAN_POINT ( 'NONE',  ( 12.06949235617739724, 12.14591786802326823, 61.87609039468568284 ) ) ;
#175112 = CARTESIAN_POINT ( 'NONE',  ( 18.62759615963255655, 10.81492255796105972, 91.66775706135234714 ) ) ;
#175113 = CARTESIAN_POINT ( 'NONE',  ( -18.67979575497178146, -10.72451020669898902, 21.66557627198102409 ) ) ;
#175114 = CARTESIAN_POINT ( 'NONE',  ( -0.05219959533936034679, 19.03943276465977164, 97.50109039468567573 ) ) ;
#175115 = CARTESIAN_POINT ( 'NONE',  ( 0.05219959533937995610, -21.53943276465977519, 65.00109039468568994 ) ) ;
#175116 = CARTESIAN_POINT ( 'NONE',  ( 12.14591786802327356, -12.06949235617739191, 30.62609039468567929 ) ) ;
#175117 = CARTESIAN_POINT ( 'NONE',  ( 15.80617190586746368, 15.72974639402197994, 84.37390960531438111 ) ) ;
#175118 = CARTESIAN_POINT ( 'NONE',  ( 5.153800228976615827, -19.02544592524334988, 95.20942372801897591 ) ) ;
#175119 = CARTESIAN_POINT ( 'NONE',  ( -13.97604488694527625, -13.89961937509977652, 61.87390960531435979 ) ) ;
#175120 = CARTESIAN_POINT ( 'NONE',  ( -16.46253265017146816, -9.564922557961047289, 109.1677570613523471 ) ) ;
#175121 = CARTESIAN_POINT ( 'NONE',  ( 0.05219959533936267826, -19.03943276465977164, 100.0010903946856757 ) ) ;
#175122 = CARTESIAN_POINT ( 'NONE',  ( 4.379528057220339221, -16.55341960407611168, 57.70724293864770260 ) ) ;
#175123 = ADVANCED_FACE ( 'NONE', ( #113662 ), #81324, .F. ) ;
#175124 = CARTESIAN_POINT ( 'NONE',  ( -0.05219959533936034679, 19.03943276465977164, 82.50109039468567573 ) ) ;
#175125 = CARTESIAN_POINT ( 'NONE',  ( 16.53943276465976808, 0.05219959533934440121, 56.25109039468568284 ) ) ;
#175127 = CARTESIAN_POINT ( 'NONE',  ( -0.05219959533909027116, -19.03943276465977164, 32.49890960531435979 ) ) ;
#175126 = CARTESIAN_POINT ( 'NONE',  ( -10.81492255796078084, -18.62759615963271287, 112.0822429386477097 ) ) ;
#175128 = CARTESIAN_POINT ( 'NONE',  ( -13.89961937509977652, 13.97604488694528158, 50.62390960531435979 ) ) ;
#175129 = CARTESIAN_POINT ( 'NONE',  ( 8.224510206698742110, 14.34966873604972548, 62.08442372801901143 ) ) ;
#175130 = DIRECTION ( 'NONE',  ( -6.982962677686266711E-15, 0.000000000000000000, 1.000000000000000000 ) ) ;
#175131 = CARTESIAN_POINT ( 'NONE',  ( -17.81289503416611097, -24.51734667627696496, 146.5500000054623229 ) ) ;
#175132 = CARTESIAN_POINT ( 'NONE',  ( -19.05341960407611168, -5.049401038298163336, 101.4572429386476955 ) ) ;
#175133 = CARTESIAN_POINT ( 'NONE',  ( 16.46253265017160672, -9.564922557960803928, 23.33224293864769194 ) ) ;
#175134 = ORIENTED_EDGE ( 'NONE', *, *, #175799, .T. ) ;
#175135 = CARTESIAN_POINT ( 'NONE',  ( -9.474510206698720793, -16.51473224551083518, 109.5844237280190043 ) ) ;
#175136 = CARTESIAN_POINT ( 'NONE',  ( 5.823673210054125526, 21.52544592524343514, 44.79057627198103120 ) ) ;
#175138 = CARTESIAN_POINT ( 'NONE',  ( -8.314922557961024197, 14.29746914071037800, 27.91775706135234358 ) ) ;
#175137 = CARTESIAN_POINT ( 'NONE',  ( -5.049401038297874678, -19.05341960407617918, 49.79275706135231871 ) ) ;
#175139 = CARTESIAN_POINT ( 'NONE',  ( -16.51473224551069308, -9.474510206698971260, 26.66557627198103120 ) ) ;
#175140 = CARTESIAN_POINT ( 'NONE',  ( 16.46253265017160672, -9.564922557960803928, 53.33224293864768839 ) ) ;
#175141 = CARTESIAN_POINT ( 'NONE',  ( -10.72451020669898014, 18.67979575497178502, 85.41557627198102409 ) ) ;
#175142 = CARTESIAN_POINT ( 'NONE',  ( -13.89961937509977652, 13.97604488694528158, 105.6239096053143527 ) ) ;
#175143 = CARTESIAN_POINT ( 'NONE',  ( -16.51473224551069308, -9.474510206698971260, 56.66557627198103120 ) ) ;
#175144 = CARTESIAN_POINT ( 'NONE',  ( 8.571926809382603096, -26.38167802310801235, 147.9750000027311785 ) ) ;
#175145 = CARTESIAN_POINT ( 'NONE',  ( -5.049401038297874678, -19.05341960407617918, 79.79275706135233293 ) ) ;
#175146 = CARTESIAN_POINT ( 'NONE',  ( -0.05219959533910754901, -16.53943276465976808, 62.49890960531436690 ) ) ;
#175147 = CARTESIAN_POINT ( 'NONE',  ( 15.72974639402176855, 15.80617190586768217, 101.8760903946857042 ) ) ;
#175148 = CARTESIAN_POINT ( 'NONE',  ( -15.80617190586745835, -15.72974639402198527, 91.87390960531436690 ) ) ;
#175149 = CARTESIAN_POINT ( 'NONE',  ( 21.53943276465977519, 0.05219959533937863772, 91.25109039468568994 ) ) ;
#175150 = CARTESIAN_POINT ( 'NONE',  ( -19.03943276465977164, 0.05219959533909376836, 21.24890960531436335 ) ) ;
#175151 = CARTESIAN_POINT ( 'NONE',  ( -15.80617190586768217, 15.72974639402176855, 73.12609039468567573 ) ) ;
#175152 = EDGE_CURVE ( 'NONE', #147783, #5512, #112676, .T. ) ;
#175153 = CARTESIAN_POINT ( 'NONE',  ( -9.564922557960796823, -16.46253265017161027, 112.0822429386476955 ) ) ;
#175155 = CARTESIAN_POINT ( 'NONE',  ( -10.72451020669870658, -18.67979575497194134, 79.58442372801903275 ) ) ;
#175154 = CARTESIAN_POINT ( 'NONE',  ( -14.29746914071049879, 8.314922557960819915, 30.83224293864770260 ) ) ;
#175156 = CARTESIAN_POINT ( 'NONE',  ( 5.049401038298161559, -19.05341960407611168, 62.70724293864769550 ) ) ;
#175157 = CARTESIAN_POINT ( 'NONE',  ( 15.80617190586769283, -15.72974639402175789, 45.62609039468567573 ) ) ;
#175158 = CARTESIAN_POINT ( 'NONE',  ( -19.03943276465977164, 0.05219959533909376836, 76.24890960531435269 ) ) ;
#175159 = CARTESIAN_POINT ( 'NONE',  ( -8.224510206698948167, 14.34966873604960824, 90.41557627198103830 ) ) ;
#175160 = CARTESIAN_POINT ( 'NONE',  ( -16.52544592524342804, 4.483927247898546575, 61.04057627198103120 ) ) ;
#175161 = CARTESIAN_POINT ( 'NONE',  ( -15.80617190586745835, -15.72974639402198527, 71.87390960531438111 ) ) ;
#175162 = EDGE_CURVE ( 'NONE', #59793, #93191, #98945, .T. ) ;
#175163 = CARTESIAN_POINT ( 'NONE',  ( -19.02544592524342804, 5.153800228976336051, 61.04057627198103120 ) ) ;
#175164 = CARTESIAN_POINT ( 'NONE',  ( -5.719274019375978568, 21.55341960407610458, 75.20724293864769550 ) ) ;
#175165 = CARTESIAN_POINT ( 'NONE',  ( -9.474510206698720793, -16.51473224551083518, 59.58442372801900433 ) ) ;
#175167 = CARTESIAN_POINT ( 'NONE',  ( -16.53943276465976808, 0.05219959533911058130, 76.24890960531435269 ) ) ;
#175166 = CARTESIAN_POINT ( 'NONE',  ( -9.474510206698720793, -16.51473224551083518, 29.58442372801900433 ) ) ;
#175168 = CARTESIAN_POINT ( 'NONE',  ( -15.80617190586745835, -15.72974639402198527, 56.87390960531436690 ) ) ;
#175169 = CARTESIAN_POINT ( 'NONE',  ( -17.60779699588837843, -5.500000000000011546, 41.34981316670104690 ) ) ;
#175171 = CARTESIAN_POINT ( 'NONE',  ( -17.14385361876520264, -23.59649016807271238, 147.6750000027311671 ) ) ;
#175170 = CARTESIAN_POINT ( 'NONE',  ( -14.29746914071037622, -8.314922557961029526, 94.16775706135237556 ) ) ;
#175172 = CARTESIAN_POINT ( 'NONE',  ( -9.564922557961040184, 16.46253265017147172, 97.91775706135233293 ) ) ;
#175173 = CARTESIAN_POINT ( 'NONE',  ( 12.14591786802309770, 12.06949235617756955, 69.37390960531436690 ) ) ;
#175174 = FACE_OUTER_BOUND ( 'NONE', #42047, .T. ) ;
#175175 = CARTESIAN_POINT ( 'NONE',  ( 13.97604488694527802, 13.89961937509977652, 59.37390960531434558 ) ) ;
#175176 = CARTESIAN_POINT ( 'NONE',  ( -16.55341960407611168, -4.379528057220339221, 56.45724293864768839 ) ) ;
#175177 = CARTESIAN_POINT ( 'NONE',  ( -9.564922557960796823, -16.46253265017161027, 102.0822429386477097 ) ) ;
#175179 = CARTESIAN_POINT ( 'NONE',  ( 19.03943276465977164, -0.05219959533909143690, 63.74890960531435979 ) ) ;
#175178 = CARTESIAN_POINT ( 'NONE',  ( 5.049401038297881783, 19.05341960407617563, 82.29275706135229029 ) ) ;
#175180 = CARTESIAN_POINT ( 'NONE',  ( 9.564922557960805705, 16.46253265017160317, 89.58224293864769550 ) ) ;
#175181 = CARTESIAN_POINT ( 'NONE',  ( 13.97604488694527802, 13.89961937509977652, 69.37390960531436690 ) ) ;
#175182 = CARTESIAN_POINT ( 'NONE',  ( 10.81492255796078972, 18.62759615963270932, 64.58224293864769550 ) ) ;
#175183 = CARTESIAN_POINT ( 'NONE',  ( -12.06949235617739369, -12.14591786802326823, 54.37609039468568994 ) ) ;
#175184 = B_SPLINE_CURVE_WITH_KNOTS ( 'NONE', 3,
 ( #146753, #112426, #98225, #116424, #159928, #54750 ),
 .UNSPECIFIED., .F., .F.,
 ( 4, 2, 4 ),
 ( 0.003239945802372313274, 0.003620412082092175007, 0.004000878361812037175 ),
 .UNSPECIFIED. ) ;
#175185 = CARTESIAN_POINT ( 'NONE',  ( 16.51473224551083163, -9.474510206698727899, 105.8344237280190043 ) ) ;
#175186 = CARTESIAN_POINT ( 'NONE',  ( 9.474510206698971260, -16.51473224551069308, 47.91557627198102409 ) ) ;
#175187 = CARTESIAN_POINT ( 'NONE',  ( -10.72451020669898014, 18.67979575497178502, 60.41557627198102409 ) ) ;
#175188 = CARTESIAN_POINT ( 'NONE',  ( -16.46253265017146816, -9.564922557961047289, 84.16775706135233293 ) ) ;
#175190 = CARTESIAN_POINT ( 'NONE',  ( -18.67979575497193778, 10.72451020669871902, 33.33442372801900433 ) ) ;
#175189 = CARTESIAN_POINT ( 'NONE',  ( 12.06949235617757843, -12.14591786802309237, 28.12390960531435979 ) ) ;
#175191 = CARTESIAN_POINT ( 'NONE',  ( 0.05219959533936267826, -19.03943276465977164, 40.00109039468566152 ) ) ;
#175193 = CARTESIAN_POINT ( 'NONE',  ( -4.483927247898782831, 16.52544592524335698, 87.70942372801901854 ) ) ;
#175192 = CARTESIAN_POINT ( 'NONE',  ( -16.53943276465976808, -0.05219959533934237506, 63.75109039468568284 ) ) ;
#175194 = CARTESIAN_POINT ( 'NONE',  ( 18.22780087662119897, -5.500000000000096811, 43.51763182126894236 ) ) ;
#175195 = CARTESIAN_POINT ( 'NONE',  ( 14.34966873604972726, -8.224510206698740333, 75.83442372801900433 ) ) ;
#175197 = CARTESIAN_POINT ( 'NONE',  ( -4.379528057220086978, -16.55341960407618274, 39.79275706135235424 ) ) ;
#175196 = CARTESIAN_POINT ( 'NONE',  ( -0.05219959533907301413, -21.53943276465977519, 22.49890960531436335 ) ) ;
#175198 = CARTESIAN_POINT ( 'NONE',  ( 19.03943276465977164, -0.05219959533909143690, 43.74890960531435979 ) ) ;
#175199 = CARTESIAN_POINT ( 'NONE',  ( -13.89961937509977652, 13.97604488694528158, 50.62390960531435979 ) ) ;
#175200 = CARTESIAN_POINT ( 'NONE',  ( -5.049401038298153566, 19.05341960407611168, 60.20724293864768129 ) ) ;
#175201 = CARTESIAN_POINT ( 'NONE',  ( 21.52544592524334988, 5.823673210054432836, 36.45942372801901143 ) ) ;
#175202 = CARTESIAN_POINT ( 'NONE',  ( 0.05219959533934541429, -16.53943276465976808, 45.00109039468568284 ) ) ;
#175203 = CARTESIAN_POINT ( 'NONE',  ( 16.52544592524342804, -4.483927247898539470, 23.54057627198102765 ) ) ;
#175204 = CARTESIAN_POINT ( 'NONE',  ( 0.05219959533909260263, 19.03943276465977164, 29.99890960531435979 ) ) ;
#175205 = CARTESIAN_POINT ( 'NONE',  ( 21.55341960407619695, -5.719274019375665929, 111.0427570613523613 ) ) ;
#175206 = CARTESIAN_POINT ( 'NONE',  ( 8.314922557961029526, -14.29746914071037800, 20.41775706135234714 ) ) ;
#175207 = CARTESIAN_POINT ( 'NONE',  ( -5.153800228976607833, 19.02544592524334988, 67.70942372801900433 ) ) ;
#175208 = CARTESIAN_POINT ( 'NONE',  ( 14.29746914071049879, -8.314922557960816363, 73.33224293864769550 ) ) ;
#175209 = CARTESIAN_POINT ( 'NONE',  ( 9.474510206698971260, -16.51473224551069308, 32.91557627198102409 ) ) ;
#175211 = CARTESIAN_POINT ( 'NONE',  ( 17.48847506799967988, 5.747544572773808369, 76.67302562156720569 ) ) ;
#175210 = CARTESIAN_POINT ( 'NONE',  ( -5.049401038297874678, -19.05341960407617918, 74.79275706135231871 ) ) ;
#175212 = CARTESIAN_POINT ( 'NONE',  ( 5.823673210054444382, -21.52544592524334988, 75.20942372801901854 ) ) ;
#175213 = CARTESIAN_POINT ( 'NONE',  ( 8.314922557961029526, -14.29746914071037800, 40.41775706135234714 ) ) ;
#175214 = CARTESIAN_POINT ( 'NONE',  ( 15.50000000000000178, -7.500000000000000888, 22.00000000000000711 ) ) ;
#175215 = CARTESIAN_POINT ( 'NONE',  ( -0.05219959533907301413, -21.53943276465977519, 37.49890960531436690 ) ) ;
#175216 = CARTESIAN_POINT ( 'NONE',  ( -14.34966873604972548, 8.224510206698743886, 28.33442372801902209 ) ) ;
#175217 = CARTESIAN_POINT ( 'NONE',  ( -16.46253265017160317, 9.564922557960807481, 25.83224293864769194 ) ) ;
#175218 = CARTESIAN_POINT ( 'NONE',  ( -5.049401038297874678, -19.05341960407617918, 29.79275706135232227 ) ) ;
#175219 = CARTESIAN_POINT ( 'NONE',  ( 9.304348965730421028, 11.16651649332241192, -60.11051939825534873 ) ) ;
#175220 = CARTESIAN_POINT ( 'NONE',  ( -0.05219959533909027116, -19.03943276465977164, 32.49890960531435979 ) ) ;
#175221 = DIRECTION ( 'NONE',  ( 1.000000000000000000, 0.000000000000000000, 0.000000000000000000 ) ) ;
#175222 = CARTESIAN_POINT ( 'NONE',  ( 19.03943276465977164, -0.05219959533909143690, 58.74890960531435979 ) ) ;
#175223 = CARTESIAN_POINT ( 'NONE',  ( -19.48894818550245844, 5.499999999999918288, 100.1030731043523616 ) ) ;
#175224 = CARTESIAN_POINT ( 'NONE',  ( 19.05341960407617918, -5.049401038297876454, 21.04275706135232582 ) ) ;
#175225 = CARTESIAN_POINT ( 'NONE',  ( 14.34966873604972726, -8.224510206698740333, 110.8344237280190043 ) ) ;
#175226 = CARTESIAN_POINT ( 'NONE',  ( -19.03943276465977164, 0.05219959533909376836, 26.24890960531435624 ) ) ;
#175227 = CARTESIAN_POINT ( 'NONE',  ( 9.564922557960805705, 16.46253265017160317, 89.58224293864769550 ) ) ;
#175228 = CARTESIAN_POINT ( 'NONE',  ( -21.53943276465977519, -0.05219959533937600094, 63.75109039468568284 ) ) ;
#175229 = CARTESIAN_POINT ( 'NONE',  ( -13.97604488694527625, -13.89961937509977652, 41.87390960531435979 ) ) ;
#175230 = CARTESIAN_POINT ( 'NONE',  ( -21.53943276465977519, -0.05219959533937600094, 68.75109039468568994 ) ) ;
#175232 = CARTESIAN_POINT ( 'NONE',  ( -13.97604488694527625, -13.89961937509977652, 101.8739096053143811 ) ) ;
#175231 = CARTESIAN_POINT ( 'NONE',  ( -9.564922557961040184, 16.46253265017147172, 92.91775706135233293 ) ) ;
#175233 = CARTESIAN_POINT ( 'NONE',  ( -0.05219959533909027116, -19.03943276465977164, 37.49890960531436690 ) ) ;
#175234 = CARTESIAN_POINT ( 'NONE',  ( 15.80617190586746368, 15.72974639402197994, 104.3739096053143669 ) ) ;
#175235 = CARTESIAN_POINT ( 'NONE',  ( -13.89961937509957401, -13.97604488694547875, 34.37609039468566863 ) ) ;
#175236 = CARTESIAN_POINT ( 'NONE',  ( 4.379528057220339221, -16.55341960407611168, 112.7072429386476955 ) ) ;
#175237 = CARTESIAN_POINT ( 'NONE',  ( 5.049401038298161559, -19.05341960407611168, 67.70724293864769550 ) ) ;
#175238 = CARTESIAN_POINT ( 'NONE',  ( 9.474510206698729675, 16.51473224551082808, 92.08442372801900433 ) ) ;
#175239 = CARTESIAN_POINT ( 'NONE',  ( -16.52544592524342804, 4.483927247898546575, 71.04057627198103830 ) ) ;
#175240 = CARTESIAN_POINT ( 'NONE',  ( -15.80617190586745835, -15.72974639402198527, 26.87390960531435979 ) ) ;
#175241 = CARTESIAN_POINT ( 'NONE',  ( 13.89961937509957401, 13.97604488694547697, 81.87609039468564731 ) ) ;
#175242 = CARTESIAN_POINT ( 'NONE',  ( -15.72974639402197994, 15.80617190586746368, 95.62390960531436690 ) ) ;
#175243 = CARTESIAN_POINT ( 'NONE',  ( 21.55341960407619695, -5.719274019375665929, 41.04275706135236135 ) ) ;
#175244 = CARTESIAN_POINT ( 'NONE',  ( -8.224510206698735004, -14.34966873604973081, 44.58442372801901854 ) ) ;
#175246 = CARTESIAN_POINT ( 'NONE',  ( -0.05219959533937732626, 21.53943276465977519, 52.50109039468567573 ) ) ;
#175245 = CARTESIAN_POINT ( 'NONE',  ( -16.52544592524335698, -4.483927247898792601, 48.95942372801902565 ) ) ;
#175247 = CARTESIAN_POINT ( 'NONE',  ( 5.823673210054125526, 21.52544592524343514, 59.79057627198103120 ) ) ;
#175248 = CARTESIAN_POINT ( 'NONE',  ( 19.05341960407611168, 5.049401038298154454, 48.95724293864768129 ) ) ;
#175249 = DIRECTION ( 'NONE',  ( 0.000000000000000000, 0.000000000000000000, 1.000000000000000000 ) ) ;
#175250 = CARTESIAN_POINT ( 'NONE',  ( 8.224510206698742110, 14.34966873604972548, 72.08442372801899012 ) ) ;
#175251 = CARTESIAN_POINT ( 'NONE',  ( -21.55341960407610458, -5.719274019375992779, 96.45724293864770971 ) ) ;
#175252 = CARTESIAN_POINT ( 'NONE',  ( 16.55341960407611168, 4.379528057220329451, 38.95724293864768839 ) ) ;
#175253 = CARTESIAN_POINT ( 'NONE',  ( -4.379528057220086978, -16.55341960407618274, 64.79275706135234714 ) ) ;
#175254 = CARTESIAN_POINT ( 'NONE',  ( -0.05219959533936034679, 19.03943276465977164, 102.5010903946856757 ) ) ;
#175255 = CARTESIAN_POINT ( 'NONE',  ( -21.55341960407610458, -5.719274019375992779, 96.45724293864770971 ) ) ;
#175256 = CARTESIAN_POINT ( 'NONE',  ( -12.14591786802309592, -12.06949235617757132, 26.87390960531435979 ) ) ;
#175257 = ORIENTED_EDGE ( 'NONE', *, *, #188177, .T. ) ;
#175258 = CARTESIAN_POINT ( 'NONE',  ( -14.34966873604972548, 8.224510206698743886, 73.33442372801901854 ) ) ;
#175259 = DIRECTION ( 'NONE',  ( -1.000000000000000000, 0.000000000000000000, 0.000000000000000000 ) ) ;
#175260 = CARTESIAN_POINT ( 'NONE',  ( -15.80617190586745835, -15.72974639402198527, 76.87390960531439532 ) ) ;
#175261 = CARTESIAN_POINT ( 'NONE',  ( -12.06949235617739369, -12.14591786802326823, 104.3760903946856899 ) ) ;
#175262 = ORIENTED_EDGE ( 'NONE', *, *, #21485, .F. ) ;
#175263 = CARTESIAN_POINT ( 'NONE',  ( 17.50000000000000000, -5.500000000000000888, 120.0000000000000142 ) ) ;
#175264 = CARTESIAN_POINT ( 'NONE',  ( 15.80617190586746368, 15.72974639402197994, 99.37390960531436690 ) ) ;
#175265 = CARTESIAN_POINT ( 'NONE',  ( 21.53943276465977519, -0.05219959533907433946, 108.7489096053143669 ) ) ;
#175266 = CARTESIAN_POINT ( 'NONE',  ( -12.14591786802309592, -12.06949235617757132, 31.87390960531435979 ) ) ;
#175267 = CARTESIAN_POINT ( 'NONE',  ( -12.14591786802326823, 12.06949235617739902, 43.12609039468568284 ) ) ;
#175268 = CARTESIAN_POINT ( 'NONE',  ( -16.46253265017160317, 9.564922557960807481, 50.83224293864770260 ) ) ;
#175269 = CARTESIAN_POINT ( 'NONE',  ( 16.46253265017160672, -9.564922557960803928, 68.33224293864770971 ) ) ;
#175270 = VERTEX_POINT ( 'NONE', #92038 ) ;
#175271 = CARTESIAN_POINT ( 'NONE',  ( 18.67979575497178502, 10.72451020669898547, 24.16557627198103120 ) ) ;
#175272 = CARTESIAN_POINT ( 'NONE',  ( -26.39110954545251886, -27.12960848547384884, -16.54511501588637046 ) ) ;
#175273 = CARTESIAN_POINT ( 'NONE',  ( 19.05341960407617918, -5.049401038297876454, 106.0427570613523471 ) ) ;
#175274 = CARTESIAN_POINT ( 'NONE',  ( -16.51473224551082808, 9.474510206698731452, 48.33442372801900433 ) ) ;
#175275 = CARTESIAN_POINT ( 'NONE',  ( -15.72974639402197994, 15.80617190586746368, 90.62390960531436690 ) ) ;
#175276 = CARTESIAN_POINT ( 'NONE',  ( -16.53943276465976808, -0.05219959533934237506, 108.7510903946857042 ) ) ;
#175277 = AXIS2_PLACEMENT_3D ( 'NONE', #192094, #132421, #100072 ) ;
#175278 = CARTESIAN_POINT ( 'NONE',  ( 16.51473224551069308, 9.474510206698969483, 74.16557627198103830 ) ) ;
#175279 = CARTESIAN_POINT ( 'NONE',  ( -15.72974639402197994, 15.80617190586746368, 40.62390960531435269 ) ) ;
#175281 = CARTESIAN_POINT ( 'NONE',  ( 12.14591786802327356, -12.06949235617739191, 30.62609039468567929 ) ) ;
#175280 = CARTESIAN_POINT ( 'NONE',  ( 15.72974639402199770, -15.80617190586745480, 78.12390960531436690 ) ) ;
#175282 = CARTESIAN_POINT ( 'NONE',  ( -15.72974639402197994, 15.80617190586746368, 25.62390960531435624 ) ) ;
#175283 = CARTESIAN_POINT ( 'NONE',  ( 18.67979575497194134, -10.72451020669871369, 75.83442372801900433 ) ) ;
#175284 = CARTESIAN_POINT ( 'NONE',  ( 0.05219959533909260263, 19.03943276465977164, 79.99890960531436690 ) ) ;
#175285 = CARTESIAN_POINT ( 'NONE',  ( 5.049401038298161559, -19.05341960407611168, 22.70724293864769194 ) ) ;
#175286 = CARTESIAN_POINT ( 'NONE',  ( -5.153800228976328057, -19.02544592524343514, 67.29057627198102409 ) ) ;
#175287 = CARTESIAN_POINT ( 'NONE',  ( 14.29746914071049879, -8.314922557960816363, 93.33224293864769550 ) ) ;
#175288 = ORIENTED_EDGE ( 'NONE', *, *, #26049, .F. ) ;
#175289 = CARTESIAN_POINT ( 'NONE',  ( -16.46253265017146816, -9.564922557961047289, 99.16775706135233293 ) ) ;
#175290 = CARTESIAN_POINT ( 'NONE',  ( 17.40805194822031865, -6.112264579159332634, 83.33371272510612471 ) ) ;
#175291 = CARTESIAN_POINT ( 'NONE',  ( -9.474510206698964154, 16.51473224551069663, 75.41557627198103830 ) ) ;
#175293 = CARTESIAN_POINT ( 'NONE',  ( 19.03943276465977164, -0.05219959533909143690, 98.74890960531436690 ) ) ;
#175292 = CARTESIAN_POINT ( 'NONE',  ( 10.81492255796106328, -18.62759615963255655, 85.41775706135236135 ) ) ;
#175294 = CARTESIAN_POINT ( 'NONE',  ( -12.06949235617739369, -12.14591786802326823, 74.37609039468568994 ) ) ;
#175295 = CARTESIAN_POINT ( 'NONE',  ( -31.90000000000002700, 0.1356448107286085669, -45.64921306006598201 ) ) ;
#175296 = CARTESIAN_POINT ( 'NONE',  ( 19.02544592524334988, 5.153800228976608722, 51.45942372801900433 ) ) ;
#175297 = CARTESIAN_POINT ( 'NONE',  ( -0.05219959533937732626, 21.53943276465977519, 112.5010903946857042 ) ) ;
#175298 = CARTESIAN_POINT ( 'NONE',  ( 6.434671708797586653, 6.434671708797580436, -63.95112321872120731 ) ) ;
#175299 = DIRECTION ( 'NONE',  ( 1.000000000000000000, 0.000000000000000000, 0.000000000000000000 ) ) ;
#175300 = CARTESIAN_POINT ( 'NONE',  ( 29.86685920354754487, 21.69954338932564752, -5.924999997268813878 ) ) ;
#175301 = CARTESIAN_POINT ( 'NONE',  ( -16.55341960407617563, 4.379528057220093196, 113.5427570613523756 ) ) ;
#175302 = CARTESIAN_POINT ( 'NONE',  ( 30.00000000000000000, 5.499999999999992895, 102.5000000000000142 ) ) ;
#175303 = CARTESIAN_POINT ( 'NONE',  ( 16.53943276465976808, 0.05219959533934440121, 111.2510903946856899 ) ) ;
#175304 = CARTESIAN_POINT ( 'NONE',  ( 28.79475375365586132, 2.781246896534039337E-14, 145.2656553485623760 ) ) ;
#175305 = CARTESIAN_POINT ( 'NONE',  ( -16.55341960407617563, 4.379528057220093196, 78.54275706135236135 ) ) ;
#175306 = CARTESIAN_POINT ( 'NONE',  ( 21.53943276465977519, 0.05219959533937863772, 81.25109039468568994 ) ) ;
#175307 = CARTESIAN_POINT ( 'NONE',  ( 16.51473224551083163, -9.474510206698727899, 105.8344237280190043 ) ) ;
#175308 = CARTESIAN_POINT ( 'NONE',  ( 18.62759615963255655, 10.81492255796105972, 71.66775706135234714 ) ) ;
#175309 = CARTESIAN_POINT ( 'NONE',  ( -16.46253265017146816, -9.564922557961047289, 34.16775706135233293 ) ) ;
#175310 = CARTESIAN_POINT ( 'NONE',  ( -19.03943276465977164, 0.05219959533909376836, 76.24890960531435269 ) ) ;
#175311 = CARTESIAN_POINT ( 'NONE',  ( -19.02544592524342804, 5.153800228976336051, 61.04057627198103120 ) ) ;
#175312 = CARTESIAN_POINT ( 'NONE',  ( -13.16448406242845159, -37.77297734889211966, -11.88662703519201180 ) ) ;
#175313 = CARTESIAN_POINT ( 'NONE',  ( 5.823673210054125526, 21.52544592524343514, 94.79057627198105251 ) ) ;
#175314 = CARTESIAN_POINT ( 'NONE',  ( -0.05219959533907301413, -21.53943276465977519, 47.49890960531435979 ) ) ;
#175315 = CARTESIAN_POINT ( 'NONE',  ( 13.89961937509977652, -13.97604488694527269, 53.12390960531434558 ) ) ;
#175316 = CARTESIAN_POINT ( 'NONE',  ( -12.06949235617739369, -12.14591786802326823, 59.37609039468568284 ) ) ;
#175317 = UNCERTAINTY_MEASURE_WITH_UNIT (LENGTH_MEASURE( 1.000000000000000082E-05 ), #66915, 'distance_accuracy_value', 'NONE');
#175318 = VERTEX_POINT ( 'NONE', #16222 ) ;
#175319 = CARTESIAN_POINT ( 'NONE',  ( 21.55341960407619695, -5.719274019375665929, 41.04275706135236135 ) ) ;
#175321 = CARTESIAN_POINT ( 'NONE',  ( -11.40812507854754720, -35.11059874428192273, -4.224999997268813701 ) ) ;
#175320 = CARTESIAN_POINT ( 'NONE',  ( 12.06949235617757843, -12.14591786802309237, 68.12390960531436690 ) ) ;
#175322 = CARTESIAN_POINT ( 'NONE',  ( -12.06949235617739369, -12.14591786802326823, 34.37609039468568284 ) ) ;
#175323 = CARTESIAN_POINT ( 'NONE',  ( 8.224510206698953496, -14.34966873604960469, 97.91557627198103830 ) ) ;
#175324 = CARTESIAN_POINT ( 'NONE',  ( -5.153800228976607833, 19.02544592524334988, 47.70942372801900433 ) ) ;
#175325 = CARTESIAN_POINT ( 'NONE',  ( -8.224510206698948167, 14.34966873604960824, 70.41557627198102409 ) ) ;
#175326 = CARTESIAN_POINT ( 'NONE',  ( -10.72451020669870658, -18.67979575497194134, 34.58442372801900433 ) ) ;
#175328 = CARTESIAN_POINT ( 'NONE',  ( -0.05219959533907301413, -21.53943276465977519, 87.49890960531436690 ) ) ;
#175327 = CARTESIAN_POINT ( 'NONE',  ( -5.049401038298153566, 19.05341960407611168, 25.20724293864768484 ) ) ;
#175329 = CARTESIAN_POINT ( 'NONE',  ( -9.564922557960796823, -16.46253265017161027, 102.0822429386477097 ) ) ;
#175330 = CARTESIAN_POINT ( 'NONE',  ( -16.55341960407611168, -4.379528057220339221, 71.45724293864769550 ) ) ;
#175331 = CARTESIAN_POINT ( 'NONE',  ( 34.17105881114488852, -20.77207671795054011, -21.54825371331146044 ) ) ;
#175332 = CARTESIAN_POINT ( 'NONE',  ( -29.86685920354755197, -21.69954338932560134, -4.424999997268812990 ) ) ;
#175333 = CARTESIAN_POINT ( 'NONE',  ( -9.474510206698720793, -16.51473224551083518, 79.58442372801899012 ) ) ;
#175334 = CARTESIAN_POINT ( 'NONE',  ( -0.05219959533937732626, 21.53943276465977519, 27.50109039468567929 ) ) ;
#175335 = CARTESIAN_POINT ( 'NONE',  ( -16.46253265017160317, 9.564922557960807481, 65.83224293864769550 ) ) ;
#175336 = CARTESIAN_POINT ( 'NONE',  ( -19.02544592524334988, -5.153800228976617603, 53.95942372801898301 ) ) ;
#175337 = CARTESIAN_POINT ( 'NONE',  ( 9.564922557960805705, 16.46253265017160317, 34.58224293864770260 ) ) ;
#175338 = CARTESIAN_POINT ( 'NONE',  ( -16.53943276465976808, 0.05219959533911058130, 61.24890960531435979 ) ) ;
#175339 = CARTESIAN_POINT ( 'NONE',  ( -0.05219959533910754901, -16.53943276465976808, 57.49890960531435979 ) ) ;
#175340 = CARTESIAN_POINT ( 'NONE',  ( 9.474510206698971260, -16.51473224551069308, 62.91557627198102409 ) ) ;
#175341 = CARTESIAN_POINT ( 'NONE',  ( 15.72974639402199770, -15.80617190586745480, 93.12390960531436690 ) ) ;
#175342 = CARTESIAN_POINT ( 'NONE',  ( 0.05219959533909260263, 19.03943276465977164, 59.99890960531436690 ) ) ;
#175343 = CARTESIAN_POINT ( 'NONE',  ( 15.80617190586746368, 15.72974639402197994, 84.37390960531438111 ) ) ;
#175344 = CARTESIAN_POINT ( 'NONE',  ( 5.823673210054444382, -21.52544592524334988, 110.2094237280190185 ) ) ;
#175347 = CARTESIAN_POINT ( 'NONE',  ( -12.14591786802309592, -12.06949235617757132, 96.87390960531436690 ) ) ;
#175346 = CARTESIAN_POINT ( 'NONE',  ( 4.379528057220092307, 16.55341960407617563, 107.2927570613523471 ) ) ;
#175345 = CARTESIAN_POINT ( 'NONE',  ( 9.474510206698971260, -16.51473224551069308, 27.91557627198103120 ) ) ;
#175348 = CARTESIAN_POINT ( 'NONE',  ( 19.02544592524334988, 5.153800228976608722, 86.45942372801900433 ) ) ;
#175349 = ORIENTED_EDGE ( 'NONE', *, *, #48406, .F. ) ;
#175350 = CARTESIAN_POINT ( 'NONE',  ( -21.52544592524343514, 5.823673210054127303, 116.0405762719810383 ) ) ;
#175351 = CARTESIAN_POINT ( 'NONE',  ( -5.153800228976607833, 19.02544592524334988, 47.70942372801900433 ) ) ;
#175352 = CARTESIAN_POINT ( 'NONE',  ( 16.55341960407618274, -4.379528057220086978, 106.0427570613523471 ) ) ;
#175353 = CARTESIAN_POINT ( 'NONE',  ( -19.03943276465977164, -0.05219959533935918106, 38.75109039468566152 ) ) ;
#175354 = CARTESIAN_POINT ( 'NONE',  ( -19.02544592524342804, 5.153800228976336051, 106.0405762719810241 ) ) ;
#175355 = CARTESIAN_POINT ( 'NONE',  ( -10.81492255796078084, -18.62759615963271287, 62.08224293864769550 ) ) ;
#175356 = CARTESIAN_POINT ( 'NONE',  ( -23.64874990377915509, 15.04272038711346049, 165.8682408883346397 ) ) ;
#175357 = CARTESIAN_POINT ( 'NONE',  ( 13.97604488694527802, 13.89961937509977652, 39.37390960531435269 ) ) ;
#175358 = CARTESIAN_POINT ( 'NONE',  ( 15.72974639402176855, 15.80617190586768217, 111.8760903946856615 ) ) ;
#175359 = CARTESIAN_POINT ( 'NONE',  ( 8.224510206698742110, 14.34966873604972548, 72.08442372801899012 ) ) ;
#175360 = CARTESIAN_POINT ( 'NONE',  ( -5.823673210054431948, 21.52544592524334988, 32.70942372801900433 ) ) ;
#175361 = CARTESIAN_POINT ( 'NONE',  ( -0.05219959533934338120, 16.53943276465976808, 47.50109039468568994 ) ) ;
#175362 = CARTESIAN_POINT ( 'NONE',  ( 19.03943276465977164, -0.05219959533909143690, 108.7489096053143527 ) ) ;
#175363 = CARTESIAN_POINT ( 'NONE',  ( 16.46253265017160672, -9.564922557960803928, 53.33224293864768839 ) ) ;
#175364 = CARTESIAN_POINT ( 'NONE',  ( 19.02544592524343514, -5.153800228976328945, 63.54057627198103830 ) ) ;
#175365 = CARTESIAN_POINT ( 'NONE',  ( -8.224510206698735004, -14.34966873604973081, 49.58442372801901143 ) ) ;
#175366 = CARTESIAN_POINT ( 'NONE',  ( -0.05219959533910754901, -16.53943276465976808, 107.4989096053143669 ) ) ;
#175367 = CARTESIAN_POINT ( 'NONE',  ( 4.483927247898790824, -16.52544592524335698, 110.2094237280190185 ) ) ;
#175368 = CARTESIAN_POINT ( 'NONE',  ( 17.50000000000000000, -5.499999999999992895, 86.21769037696435589 ) ) ;
#175371 = CARTESIAN_POINT ( 'NONE',  ( -16.46253265017160317, 9.564922557960807481, 70.83224293864770971 ) ) ;
#175370 = CARTESIAN_POINT ( 'NONE',  ( 16.46253265017160672, -9.564922557960803928, 73.33224293864769550 ) ) ;
#175369 = CARTESIAN_POINT ( 'NONE',  ( 10.72451020669871369, 18.67979575497193778, 57.08442372801901854 ) ) ;
#175372 = CARTESIAN_POINT ( 'NONE',  ( -16.51473224551069308, -9.474510206698971260, 91.66557627198103830 ) ) ;
#175373 = CARTESIAN_POINT ( 'NONE',  ( 8.224510206698953496, -14.34966873604960469, 47.91557627198102409 ) ) ;
#175374 = CARTESIAN_POINT ( 'NONE',  ( 16.52544592524335698, 4.483927247898782831, 106.4594237280190328 ) ) ;
#175375 = CARTESIAN_POINT ( 'NONE',  ( -8.314922557960811034, -14.29746914071050412, 42.08224293864769550 ) ) ;
#175376 = ORIENTED_EDGE ( 'NONE', *, *, #22002, .F. ) ;
#175377 = CARTESIAN_POINT ( 'NONE',  ( 2.500000000000000000, -2.357898499370432610, 3.252606517456513302E-15 ) ) ;
#175378 = CARTESIAN_POINT ( 'NONE',  ( -5.153800228976328057, -19.02544592524343514, 62.29057627198100988 ) ) ;
#175379 = CARTESIAN_POINT ( 'NONE',  ( -5.049401038297874678, -19.05341960407617918, 44.79275706135232582 ) ) ;
#175380 = CARTESIAN_POINT ( 'NONE',  ( 36.91746824999999887, 11.99521256947799053, -1.524999997268813745 ) ) ;
#175381 = CARTESIAN_POINT ( 'NONE',  ( 5.049401038298163336, -19.05341960407611168, 67.70724293864768129 ) ) ;
#175383 = CARTESIAN_POINT ( 'NONE',  ( -16.53943276465976808, -0.05219959533934237506, 68.75109039468568994 ) ) ;
#175382 = CARTESIAN_POINT ( 'NONE',  ( 16.51473224551083163, -9.474510206698727899, 80.83442372801899012 ) ) ;
#175384 = FACE_OUTER_BOUND ( 'NONE', #35617, .T. ) ;
#175385 = CARTESIAN_POINT ( 'NONE',  ( 0.05219959533909260263, 19.03943276465977164, 94.99890960531436690 ) ) ;
#175386 = CARTESIAN_POINT ( 'NONE',  ( 18.62759615963255655, 10.81492255796105972, 31.66775706135234358 ) ) ;
#175387 = VECTOR ( 'NONE', #60183, 1000.000000000000114 ) ;
#175388 = CARTESIAN_POINT ( 'NONE',  ( 13.89961937509957401, 13.97604488694547697, 71.87609039468567573 ) ) ;
#175390 = CARTESIAN_POINT ( 'NONE',  ( 13.97604488694527802, 13.89961937509977652, 54.37390960531435979 ) ) ;
#175389 = CARTESIAN_POINT ( 'NONE',  ( 16.52216118717209525, 7.221426719304533393, 88.57599021046995347 ) ) ;
#175391 = CARTESIAN_POINT ( 'NONE',  ( 9.564922557960805705, 16.46253265017160317, 84.58224293864769550 ) ) ;
#175393 = CARTESIAN_POINT ( 'NONE',  ( -5.049401038298153566, 19.05341960407611168, 50.20724293864770260 ) ) ;
#175392 = CARTESIAN_POINT ( 'NONE',  ( -16.55341960407611168, -4.379528057220339221, 41.45724293864769550 ) ) ;
#175394 = CARTESIAN_POINT ( 'NONE',  ( -0.05219959533936034679, 19.03943276465977164, 62.50109039468566863 ) ) ;
#175395 = ORIENTED_EDGE ( 'NONE', *, *, #42622, .F. ) ;
#175396 = CARTESIAN_POINT ( 'NONE',  ( -8.314922557960811034, -14.29746914071050412, 92.08224293864769550 ) ) ;
#175397 = CARTESIAN_POINT ( 'NONE',  ( 5.049401038297881783, 19.05341960407617563, 32.29275706135233293 ) ) ;
#175398 = CARTESIAN_POINT ( 'NONE',  ( -19.03943276465977164, 0.05219959533909376836, 61.24890960531436690 ) ) ;
#175399 = EDGE_CURVE ( 'NONE', #119464, #84310, #183509, .T. ) ;
#175400 = CARTESIAN_POINT ( 'NONE',  ( 5.719274019375991003, -21.55341960407610458, 57.70724293864770260 ) ) ;
#175402 = CARTESIAN_POINT ( 'NONE',  ( -19.03943276465977164, -0.05219959533935918106, 23.75109039468566152 ) ) ;
#175401 = CARTESIAN_POINT ( 'NONE',  ( -16.55341960407611168, -4.379528057220339221, 61.45724293864770260 ) ) ;
#175403 = CARTESIAN_POINT ( 'NONE',  ( -19.03943276465977164, 0.05219959533909376836, 111.2489096053143669 ) ) ;
#175404 = CARTESIAN_POINT ( 'NONE',  ( 10.72451020669898902, -18.67979575497178502, 32.91557627198102409 ) ) ;
#175405 = CARTESIAN_POINT ( 'NONE',  ( 0.05219959533909260263, 19.03943276465977164, 54.99890960531435979 ) ) ;
#175406 = CARTESIAN_POINT ( 'NONE',  ( -5.049401038298153566, 19.05341960407611168, 45.20724293864769550 ) ) ;
#175407 = CARTESIAN_POINT ( 'NONE',  ( 14.34966873604960469, 8.224510206698951720, 99.16557627198100988 ) ) ;
#175408 = CARTESIAN_POINT ( 'NONE',  ( 0.05219959533907565091, 21.53943276465977519, 109.9989096053143527 ) ) ;
#175409 = CARTESIAN_POINT ( 'NONE',  ( 5.153800228976335163, 19.02544592524342804, 99.79057627198102409 ) ) ;
#175410 = CARTESIAN_POINT ( 'NONE',  ( -5.823673210054431948, 21.52544592524334988, 22.70942372801901499 ) ) ;
#175411 = CARTESIAN_POINT ( 'NONE',  ( -13.89961937509977652, 13.97604488694528158, 100.6239096053143669 ) ) ;
#175412 = CARTESIAN_POINT ( 'NONE',  ( -14.29746914071049879, 8.314922557960819915, 115.8322429386477097 ) ) ;
#175413 = CARTESIAN_POINT ( 'NONE',  ( -21.55341960407619339, 5.719274019375674811, 78.54275706135236135 ) ) ;
#175414 = CARTESIAN_POINT ( 'NONE',  ( 21.53943276465977519, -0.05219959533907433946, 98.74890960531438111 ) ) ;
#175415 = FACE_OUTER_BOUND ( 'NONE', #158092, .T. ) ;
#175416 = DIRECTION ( 'NONE',  ( 0.000000000000000000, 0.000000000000000000, -1.000000000000000000 ) ) ;
#175417 = CARTESIAN_POINT ( 'NONE',  ( 29.77433414031399650, -1.366177905283701532, -51.67655205196556523 ) ) ;
#175418 = CARTESIAN_POINT ( 'NONE',  ( 16.52544592524335698, 4.483927247898782831, 51.45942372801901854 ) ) ;
#175419 = CARTESIAN_POINT ( 'NONE',  ( 12.06949235617757843, -12.14591786802309237, 113.1239096053143953 ) ) ;
#175420 = CARTESIAN_POINT ( 'NONE',  ( 19.36337904590688197, -5.500000000000146549, 52.91494137495617878 ) ) ;
#175421 = CARTESIAN_POINT ( 'NONE',  ( -9.474510206698964154, 16.51473224551069663, 60.41557627198102409 ) ) ;
#175422 = CARTESIAN_POINT ( 'NONE',  ( -8.314922557960811034, -14.29746914071050412, 92.08224293864769550 ) ) ;
#175423 = AXIS2_PLACEMENT_3D ( 'NONE', #71238, #73248, #25752 ) ;
#175424 = CARTESIAN_POINT ( 'NONE',  ( 15.72974639402199770, -15.80617190586745480, 48.12390960531436690 ) ) ;
#175425 = CARTESIAN_POINT ( 'NONE',  ( -16.53943276465976808, 0.05219959533911058130, 66.24890960531436690 ) ) ;
#175426 = CARTESIAN_POINT ( 'NONE',  ( -16.55341960407617563, 4.379528057220093196, 23.54275706135235424 ) ) ;
#175427 = CARTESIAN_POINT ( 'NONE',  ( 5.719274019375673035, 21.55341960407619339, 72.29275706135236135 ) ) ;
#175428 = CARTESIAN_POINT ( 'NONE',  ( 18.22780087662126647, 5.499999999999818812, 61.48236817873107896 ) ) ;
#175429 = CARTESIAN_POINT ( 'NONE',  ( -0.05219959533934338120, 16.53943276465976808, 92.50109039468567573 ) ) ;
#175430 = CARTESIAN_POINT ( 'NONE',  ( -0.05219959533910754901, -16.53943276465976808, 47.49890960531435979 ) ) ;
#175431 = CARTESIAN_POINT ( 'NONE',  ( -16.46253265017160317, 9.564922557960807481, 40.83224293864769550 ) ) ;
#175432 = CARTESIAN_POINT ( 'NONE',  ( -19.03943276465977164, 0.05219959533909376836, 86.24890960531436690 ) ) ;
#175433 = CARTESIAN_POINT ( 'NONE',  ( -18.62759615963270932, 10.81492255796079327, 95.83224293864770971 ) ) ;
#175434 = CARTESIAN_POINT ( 'NONE',  ( 8.224510206698742110, 14.34966873604972548, 42.08442372801901854 ) ) ;
#175436 = CARTESIAN_POINT ( 'NONE',  ( 10.81492255796106328, -18.62759615963255655, 70.41775706135236135 ) ) ;
#175435 = CARTESIAN_POINT ( 'NONE',  ( 16.53943276465976808, -0.05219959533910856209, 68.74890960531435269 ) ) ;
#175437 = CARTESIAN_POINT ( 'NONE',  ( 14.34966873604972726, -8.224510206698740333, 100.8344237280190185 ) ) ;
#175438 = CARTESIAN_POINT ( 'NONE',  ( 17.44270441346523981, -5.991230190322817784, 46.13664920735775610 ) ) ;
#175439 = PLANE ( 'NONE',  #167974 ) ;
#175440 = CARTESIAN_POINT ( 'NONE',  ( 14.34966873604960469, 8.224510206698951720, 29.16557627198103120 ) ) ;
#175441 = CARTESIAN_POINT ( 'NONE',  ( -16.52544592524335698, -4.483927247898792601, 68.95942372801901854 ) ) ;
#175442 = CARTESIAN_POINT ( 'NONE',  ( 5.153800228976335163, 19.02544592524342804, 89.79057627198102409 ) ) ;
#175443 = CARTESIAN_POINT ( 'NONE',  ( 13.89961937509977652, -13.97604488694527269, 103.1239096053143527 ) ) ;
#175444 = CARTESIAN_POINT ( 'NONE',  ( 10.72451020669871369, 18.67979575497193778, 82.08442372801901854 ) ) ;
#175445 = CARTESIAN_POINT ( 'NONE',  ( 16.55341960407618274, -4.379528057220086978, 91.04275706135236135 ) ) ;
#175446 = CARTESIAN_POINT ( 'NONE',  ( -4.483927247898539470, -16.52544592524342804, 62.29057627198102409 ) ) ;
#175447 = CARTESIAN_POINT ( 'NONE',  ( -16.46253265017160317, 9.564922557960807481, 70.83224293864770971 ) ) ;
#175448 = ORIENTED_EDGE ( 'NONE', *, *, #198419, .T. ) ;
#175449 = CARTESIAN_POINT ( 'NONE',  ( -16.46253265017146816, -9.564922557961047289, 109.1677570613523471 ) ) ;
#175450 = CARTESIAN_POINT ( 'NONE',  ( -19.05341960407611168, -5.049401038298163336, 21.45724293864768839 ) ) ;
#175451 = CARTESIAN_POINT ( 'NONE',  ( -9.474510206698964154, 16.51473224551069663, 80.41557627198103830 ) ) ;
#175453 = CARTESIAN_POINT ( 'NONE',  ( 22.81625015709509441, 31.40387420917330275, -7.324999997268812457 ) ) ;
#175452 = CARTESIAN_POINT ( 'NONE',  ( -19.03943276465977164, -0.05219959533935918106, 108.7510903946856615 ) ) ;
#175454 = CARTESIAN_POINT ( 'NONE',  ( 16.51473224551083163, -9.474510206698727899, 25.83442372801900078 ) ) ;
#175455 = CARTESIAN_POINT ( 'NONE',  ( 16.52544592524335698, 4.483927247898782831, 81.45942372801900433 ) ) ;
#175456 = CARTESIAN_POINT ( 'NONE',  ( 16.46253265017146816, 9.564922557961045513, 96.66775706135233293 ) ) ;
#175457 = CARTESIAN_POINT ( 'NONE',  ( 8.314922557960818139, 14.29746914071049879, 109.5822429386476955 ) ) ;
#175458 = CARTESIAN_POINT ( 'NONE',  ( -4.379528057220086978, -16.55341960407618274, 69.79275706135234714 ) ) ;
#175459 = CARTESIAN_POINT ( 'NONE',  ( -12.06949235617739369, -12.14591786802326823, 59.37609039468568284 ) ) ;
#175460 = DIRECTION ( 'NONE',  ( 1.000000000000000000, 0.000000000000000000, 0.000000000000000000 ) ) ;
#175461 = CARTESIAN_POINT ( 'NONE',  ( -16.51473224551082808, 9.474510206698731452, 68.33442372801900433 ) ) ;
#175462 = CARTESIAN_POINT ( 'NONE',  ( 5.823673210054444382, -21.52544592524334988, 95.20942372801903275 ) ) ;
#175463 = CARTESIAN_POINT ( 'NONE',  ( -19.02544592524342804, 5.153800228976336051, 41.04057627198103120 ) ) ;
#175464 = CARTESIAN_POINT ( 'NONE',  ( -5.153800228976328057, -19.02544592524343514, 72.29057627198102409 ) ) ;
#175465 = CARTESIAN_POINT ( 'NONE',  ( -8.224510206698948167, 14.34966873604960824, 70.41557627198102409 ) ) ;
#175466 = CARTESIAN_POINT ( 'NONE',  ( -15.72974639402176322, -15.80617190586768395, 89.37609039468568994 ) ) ;
#175467 = CARTESIAN_POINT ( 'NONE',  ( -9.474510206698720793, -16.51473224551083518, 44.58442372801900433 ) ) ;
#175468 = CARTESIAN_POINT ( 'NONE',  ( -15.72974639402197994, 15.80617190586746368, 30.62390960531436335 ) ) ;
#175469 = CARTESIAN_POINT ( 'NONE',  ( -10.81492255796105439, 18.62759615963255655, 112.9177570613523329 ) ) ;
#175470 = CARTESIAN_POINT ( 'NONE',  ( 19.05341960407611168, 5.049401038298154454, 78.95724293864769550 ) ) ;
#175471 = CARTESIAN_POINT ( 'NONE',  ( 0.05219959533937995610, -21.53943276465977519, 100.0010903946857042 ) ) ;
#175472 = CARTESIAN_POINT ( 'NONE',  ( -10.72451020669898014, 18.67979575497178502, 65.41557627198102409 ) ) ;
#175473 = CARTESIAN_POINT ( 'NONE',  ( -5.153800228976328057, -19.02544592524343514, 102.2905762719810383 ) ) ;
#175474 = CARTESIAN_POINT ( 'NONE',  ( 19.02544592524334988, 5.153800228976608722, 71.45942372801900433 ) ) ;
#175475 = CARTESIAN_POINT ( 'NONE',  ( -13.97604488694527625, -13.89961937509977652, 96.87390960531433848 ) ) ;
#175476 = CARTESIAN_POINT ( 'NONE',  ( -5.153800228976607833, 19.02544592524334988, 102.7094237280189759 ) ) ;
#175477 = CARTESIAN_POINT ( 'NONE',  ( 8.314922557961029526, -14.29746914071037800, 55.41775706135234714 ) ) ;
#175478 = CARTESIAN_POINT ( 'NONE',  ( -5.049401038298153566, 19.05341960407611168, 25.20724293864768484 ) ) ;
#175479 = CARTESIAN_POINT ( 'NONE',  ( 16.51473224551069308, 9.474510206698969483, 84.16557627198102409 ) ) ;
#175480 = CARTESIAN_POINT ( 'NONE',  ( -18.67979575497178146, -10.72451020669898902, 61.66557627198103120 ) ) ;
#175481 = CARTESIAN_POINT ( 'NONE',  ( -8.314922557961024197, 14.29746914071037800, 27.91775706135234358 ) ) ;
#175482 = CARTESIAN_POINT ( 'NONE',  ( -15.72974639402176322, -15.80617190586768395, 34.37609039468568284 ) ) ;
#175483 = CARTESIAN_POINT ( 'NONE',  ( -21.55341960407619339, 5.719274019375674811, 88.54275706135236135 ) ) ;
#175484 = CARTESIAN_POINT ( 'NONE',  ( 14.34966873604972726, -8.224510206698740333, 85.83442372801901854 ) ) ;
#175485 = CARTESIAN_POINT ( 'NONE',  ( 9.474510206698971260, -16.51473224551069308, 92.91557627198103830 ) ) ;
#175486 = CARTESIAN_POINT ( 'NONE',  ( 16.55341960407611168, 4.379528057220329451, 73.95724293864769550 ) ) ;
#175487 = CARTESIAN_POINT ( 'NONE',  ( -14.34966873604960291, -8.224510206698953496, 21.66557627198102409 ) ) ;
#175488 = CARTESIAN_POINT ( 'NONE',  ( 16.51473224551083163, -9.474510206698727899, 55.83442372801899722 ) ) ;
#175489 = CARTESIAN_POINT ( 'NONE',  ( -21.55341960407619339, 5.719274019375674811, 38.54275706135234714 ) ) ;
#175490 = CARTESIAN_POINT ( 'NONE',  ( -4.379528057220328563, 16.55341960407611168, 90.20724293864770971 ) ) ;
#175491 = CARTESIAN_POINT ( 'NONE',  ( 18.67979575497178502, 10.72451020669898547, 24.16557627198103120 ) ) ;
#175492 = CARTESIAN_POINT ( 'NONE',  ( 0.05219959533934541429, -16.53943276465976808, 100.0010903946857042 ) ) ;
#175493 = CARTESIAN_POINT ( 'NONE',  ( 15.72974639402176855, 15.80617190586768217, 81.87609039468568994 ) ) ;
#175494 = CARTESIAN_POINT ( 'NONE',  ( 12.06949235617739724, 12.14591786802326823, 41.87609039468568284 ) ) ;
#175495 = CARTESIAN_POINT ( 'NONE',  ( 5.823673210054444382, -21.52544592524334988, 35.20942372801901854 ) ) ;
#175496 = VERTEX_POINT ( 'NONE', #179378 ) ;
#175497 = CARTESIAN_POINT ( 'NONE',  ( 10.72451020669898902, -18.67979575497178502, 107.9155762719810241 ) ) ;
#175498 = CARTESIAN_POINT ( 'NONE',  ( 8.314922557960818139, 14.29746914071049879, 89.58224293864768129 ) ) ;
#175499 = CARTESIAN_POINT ( 'NONE',  ( 17.50000000000148148, -3.254303733634558160, 27.52395893071405908 ) ) ;
#175500 = CARTESIAN_POINT ( 'NONE',  ( -8.224510206698948167, 14.34966873604960824, 60.41557627198102409 ) ) ;
#175501 = CARTESIAN_POINT ( 'NONE',  ( -4.379528057220086978, -16.55341960407618274, 99.79275706135234714 ) ) ;
#175502 = CARTESIAN_POINT ( 'NONE',  ( -5.049401038298153566, 19.05341960407611168, 45.20724293864769550 ) ) ;
#175503 = CARTESIAN_POINT ( 'NONE',  ( -18.67979575497178146, -10.72451020669898902, 46.66557627198102409 ) ) ;
#175504 = CARTESIAN_POINT ( 'NONE',  ( 16.53943276465976808, -0.05219959533910856209, 83.74890960531435269 ) ) ;
#175505 = CARTESIAN_POINT ( 'NONE',  ( -5.823673210054116645, -21.52544592524344225, 77.29057627198102409 ) ) ;
#175506 = CARTESIAN_POINT ( 'NONE',  ( -0.05219959533909027116, -19.03943276465977164, 92.49890960531436690 ) ) ;
#175508 = CARTESIAN_POINT ( 'NONE',  ( -13.89961937509957401, -13.97604488694547875, 89.37609039468563310 ) ) ;
#175507 = CARTESIAN_POINT ( 'NONE',  ( 13.89961937509977652, -13.97604488694527269, 38.12390960531436690 ) ) ;
#175509 = CARTESIAN_POINT ( 'NONE',  ( 21.53943276465977519, -0.05219959533907433946, 28.74890960531435624 ) ) ;
#175510 = CARTESIAN_POINT ( 'NONE',  ( -0.05219959533937732626, 21.53943276465977519, 57.50109039468568994 ) ) ;
#175511 = CARTESIAN_POINT ( 'NONE',  ( -16.46253265017160317, 9.564922557960807481, 55.83224293864769550 ) ) ;
#175512 = CARTESIAN_POINT ( 'NONE',  ( 5.153800228976335163, 19.02544592524342804, 84.79057627198099567 ) ) ;
#175513 = ORIENTED_EDGE ( 'NONE', *, *, #44938, .F. ) ;
#175514 = CARTESIAN_POINT ( 'NONE',  ( 14.29746914071037800, 8.314922557961029526, 46.66775706135234714 ) ) ;
#175515 = CARTESIAN_POINT ( 'NONE',  ( -5.823673210054431948, 21.52544592524334988, 47.70942372801902565 ) ) ;
#175516 = CARTESIAN_POINT ( 'NONE',  ( -15.80617190586768217, 15.72974639402176855, 78.12609039468570415 ) ) ;
#175517 = CARTESIAN_POINT ( 'NONE',  ( -0.05219959533907301413, -21.53943276465977519, 27.49890960531435269 ) ) ;
#175518 = CARTESIAN_POINT ( 'NONE',  ( 21.52544592524344225, -5.823673210054117533, 83.54057627198102409 ) ) ;
#175520 = CARTESIAN_POINT ( 'NONE',  ( -12.14591786802326823, 12.06949235617739902, 63.12609039468568994 ) ) ;
#175519 = CARTESIAN_POINT ( 'NONE',  ( 5.823673210054444382, -21.52544592524334988, 20.20942372801900788 ) ) ;
#175521 = CARTESIAN_POINT ( 'NONE',  ( -10.72451020669898014, 18.67979575497178502, 65.41557627198102409 ) ) ;
#175522 = CARTESIAN_POINT ( 'NONE',  ( -18.67979575497193778, 10.72451020669871902, 113.3344237280190328 ) ) ;
#175524 = CARTESIAN_POINT ( 'NONE',  ( 4.379528057220092307, 16.55341960407617563, 102.2927570613523613 ) ) ;
#175523 = CARTESIAN_POINT ( 'NONE',  ( -16.51473224551069308, -9.474510206698971260, 71.66557627198102409 ) ) ;
#175525 = DIRECTION ( 'NONE',  ( 0.000000000000000000, 0.000000000000000000, -1.000000000000000000 ) ) ;
#175526 = CARTESIAN_POINT ( 'NONE',  ( 9.564922557960805705, 16.46253265017160317, 84.58224293864769550 ) ) ;
#175527 = CARTESIAN_POINT ( 'NONE',  ( 17.50000000000000355, 5.499999999999989342, 103.7823096230356867 ) ) ;
#175528 = EDGE_CURVE ( 'NONE', #144964, #199519, #54252, .T. ) ;
#175529 = CARTESIAN_POINT ( 'NONE',  ( -13.97604488694547697, 13.89961937509957934, 83.12609039468564731 ) ) ;
#175530 = CARTESIAN_POINT ( 'NONE',  ( -10.72451020669898014, 18.67979575497178502, 55.41557627198102409 ) ) ;
#175531 = CARTESIAN_POINT ( 'NONE',  ( -4.483927247898782831, 16.52544592524335698, 112.7094237280190328 ) ) ;
#175532 = CARTESIAN_POINT ( 'NONE',  ( 5.153800228976615827, -19.02544592524334988, 105.2094237280190185 ) ) ;
#175533 = LINE ( 'NONE', #100674, #23998 ) ;
#175534 = CARTESIAN_POINT ( 'NONE',  ( 13.89961937509957401, 13.97604488694547697, 96.87609039468566152 ) ) ;
#175536 = CARTESIAN_POINT ( 'NONE',  ( 19.05341960407617918, -5.049401038297876454, 56.04275706135234714 ) ) ;
#175535 = CARTESIAN_POINT ( 'NONE',  ( -15.80617190586745835, -15.72974639402198527, 91.87390960531436690 ) ) ;
#175537 = DIRECTION ( 'NONE',  ( 0.000000000000000000, 0.000000000000000000, 1.000000000000000000 ) ) ;
#175538 = CARTESIAN_POINT ( 'NONE',  ( -0.05219959533909027116, -19.03943276465977164, 57.49890960531435979 ) ) ;
#175539 = CARTESIAN_POINT ( 'NONE',  ( -8.314922557960811034, -14.29746914071050412, 57.08224293864769550 ) ) ;
#175540 = CARTESIAN_POINT ( 'NONE',  ( -5.049401038298153566, 19.05341960407611168, 50.20724293864770260 ) ) ;
#175541 = CARTESIAN_POINT ( 'NONE',  ( 4.379528057220339221, -16.55341960407611168, 57.70724293864770260 ) ) ;
#175542 = CARTESIAN_POINT ( 'NONE',  ( -24.54195369798066295, -31.38977029645269212, -21.36864394644175746 ) ) ;
#175543 = CARTESIAN_POINT ( 'NONE',  ( 31.24012740013091616, -7.112679799535560399, 97.39185870086457442 ) ) ;
#175544 = CARTESIAN_POINT ( 'NONE',  ( -4.379528057220328563, 16.55341960407611168, 30.20724293864769550 ) ) ;
#175545 = CARTESIAN_POINT ( 'NONE',  ( -9.564922557960796823, -16.46253265017161027, 57.08224293864769550 ) ) ;
#175546 = SPHERICAL_SURFACE ( 'NONE', #141182, 40.00000000000002132 ) ;
#175547 = CARTESIAN_POINT ( 'NONE',  ( -19.02544592524334988, -5.153800228976617603, 38.95942372801900433 ) ) ;
#175548 = CARTESIAN_POINT ( 'NONE',  ( 8.314922557961029526, -14.29746914071037800, 45.41775706135234003 ) ) ;
#175549 = CARTESIAN_POINT ( 'NONE',  ( -15.80617190586745835, -15.72974639402198527, 56.87390960531436690 ) ) ;
#175550 = CARTESIAN_POINT ( 'NONE',  ( 21.52544592524334988, 5.823673210054432836, 106.4594237280190328 ) ) ;
#175551 = CARTESIAN_POINT ( 'NONE',  ( -0.05219959533909027116, -19.03943276465977164, 72.49890960531435269 ) ) ;
#175552 = DIRECTION ( 'NONE',  ( -0.000000000000000000, -0.000000000000000000, 1.000000000000000000 ) ) ;
#175553 = CARTESIAN_POINT ( 'NONE',  ( -19.03943276465977164, 0.05219959533909376836, 91.24890960531436690 ) ) ;
#175554 = CARTESIAN_POINT ( 'NONE',  ( -11.40812507854755609, 35.11059874428196537, -5.024999997268813523 ) ) ;
#175555 = CARTESIAN_POINT ( 'NONE',  ( -10.72451020669870658, -18.67979575497194134, 29.58442372801901854 ) ) ;
#175556 = CARTESIAN_POINT ( 'NONE',  ( 12.06949235617757843, -12.14591786802309237, 88.12390960531436690 ) ) ;
#175558 = CARTESIAN_POINT ( 'NONE',  ( -19.05341960407611168, -5.049401038298163336, 86.45724293864769550 ) ) ;
#175557 = CARTESIAN_POINT ( 'NONE',  ( -5.719274019375978568, 21.55341960407610458, 90.20724293864770971 ) ) ;
#175559 = CARTESIAN_POINT ( 'NONE',  ( 19.03943276465977164, -0.05219959533909143690, 83.74890960531436690 ) ) ;
#175560 = CARTESIAN_POINT ( 'NONE',  ( 15.80617190586746368, 15.72974639402197994, 114.3739096053143527 ) ) ;
#175561 = ORIENTED_EDGE ( 'NONE', *, *, #93872, .T. ) ;
#175562 = CARTESIAN_POINT ( 'NONE',  ( -0.05219959533909027116, -19.03943276465977164, 77.49890960531435269 ) ) ;
#175563 = CIRCLE ( 'NONE', #40036, 0.5000000000000004441 ) ;
#175564 = CARTESIAN_POINT ( 'NONE',  ( -17.79613651744294600, 24.49428055684532524, 147.6843446569000093 ) ) ;
#175566 = CARTESIAN_POINT ( 'NONE',  ( 0.05219959533909260263, 19.03943276465977164, 34.99890960531435979 ) ) ;
#175565 = CARTESIAN_POINT ( 'NONE',  ( -5.153800228976328057, -19.02544592524343514, 22.29057627198102765 ) ) ;
#175567 = CARTESIAN_POINT ( 'NONE',  ( 16.51473224551083163, -9.474510206698727899, 95.83442372801900433 ) ) ;
#175568 = CARTESIAN_POINT ( 'NONE',  ( -12.14591786802309592, -12.06949235617757132, 106.8739096053143811 ) ) ;
#175569 = CARTESIAN_POINT ( 'NONE',  ( -0.05219959533937732626, 21.53943276465977519, 67.50109039468568994 ) ) ;
#175571 = CARTESIAN_POINT ( 'NONE',  ( 18.67979575497194134, -10.72451020669871369, 35.83442372801901143 ) ) ;
#175570 = CARTESIAN_POINT ( 'NONE',  ( -19.02544592524342804, 5.153800228976336051, 61.04057627198103120 ) ) ;
#175572 = CARTESIAN_POINT ( 'NONE',  ( 15.72974639402199770, -15.80617190586745480, 113.1239096053143953 ) ) ;
#175573 = CARTESIAN_POINT ( 'NONE',  ( -17.81289503416611808, 24.51734667627700404, 147.6999999999999886 ) ) ;
#175574 = CARTESIAN_POINT ( 'NONE',  ( 0.05219959533909260263, 19.03943276465977164, 84.99890960531436690 ) ) ;
#175575 = CARTESIAN_POINT ( 'NONE',  ( -3.573655867282028392E-15, -12.39993551617566503, 169.9999999999999716 ) ) ;
#175577 = CARTESIAN_POINT ( 'NONE',  ( -15.72974639402197994, 15.80617190586746368, 25.62390960531435624 ) ) ;
#175576 = CARTESIAN_POINT ( 'NONE',  ( 12.14591786802327356, -12.06949235617739191, 25.62609039468567929 ) ) ;
#175578 = CARTESIAN_POINT ( 'NONE',  ( -10.72451020669870658, -18.67979575497194134, 64.58442372801900433 ) ) ;
#175579 = CARTESIAN_POINT ( 'NONE',  ( -5.049401038298153566, 19.05341960407611168, 110.2072429386476671 ) ) ;
#175580 = CARTESIAN_POINT ( 'NONE',  ( 19.05341960407617918, -5.049401038297876454, 96.04275706135231871 ) ) ;
#175581 = CARTESIAN_POINT ( 'NONE',  ( 5.049401038298161559, -19.05341960407611168, 42.70724293864767418 ) ) ;
#175582 = CARTESIAN_POINT ( 'NONE',  ( -19.02544592524342804, 5.153800228976336051, 81.04057627198103830 ) ) ;
#175583 = B_SPLINE_CURVE_WITH_KNOTS ( 'NONE', 3,
 ( #108485, #152996, #45830, #16487, #184348, #167202, #28700, #15497, #89355, #13507 ),
 .UNSPECIFIED., .F., .F.,
 ( 4, 2, 2, 2, 4 ),
 ( 0.002442800151708459776, 0.003053169662661163030, 0.003663539173613866284, 0.004273908684566569971, 0.004884278195519273225 ),
 .UNSPECIFIED. ) ;
#175584 = CARTESIAN_POINT ( 'NONE',  ( 16.53943276465976808, -0.05219959533910856209, 88.74890960531436690 ) ) ;
#175585 = CARTESIAN_POINT ( 'NONE',  ( 19.02544592524343514, -5.153800228976328945, 113.5405762719810241 ) ) ;
#175586 = CARTESIAN_POINT ( 'NONE',  ( 14.34966873604960469, 8.224510206698951720, 94.16557627198103830 ) ) ;
#175587 = CARTESIAN_POINT ( 'NONE',  ( -5.153800228976328057, -19.02544592524343514, 112.2905762719810099 ) ) ;
#175589 = CARTESIAN_POINT ( 'NONE',  ( -16.51473224551069308, -9.474510206698971260, 46.66557627198102409 ) ) ;
#175588 = CARTESIAN_POINT ( 'NONE',  ( -8.224510206698948167, 14.34966873604960824, 55.41557627198102409 ) ) ;
#175590 = CARTESIAN_POINT ( 'NONE',  ( -15.80617190586768217, 15.72974639402176855, 58.12609039468568994 ) ) ;
#175591 = CARTESIAN_POINT ( 'NONE',  ( -16.46253265017146816, -9.564922557961047289, 99.16775706135233293 ) ) ;
#175592 = CARTESIAN_POINT ( 'NONE',  ( 12.06949235617757843, -12.14591786802309237, 53.12390960531436690 ) ) ;
#175593 = CARTESIAN_POINT ( 'NONE',  ( 21.53943276465977519, -0.05219959533907433946, 108.7489096053143669 ) ) ;
#175594 = CARTESIAN_POINT ( 'NONE',  ( 18.62759615963271287, -10.81492255796078972, 48.33224293864770260 ) ) ;
#175595 = CARTESIAN_POINT ( 'NONE',  ( 5.153800228976335163, 19.02544592524342804, 114.7905762719810241 ) ) ;
#175596 = CARTESIAN_POINT ( 'NONE',  ( 28.82186960331499392, -9.364793116373510529, 141.1500000054623740 ) ) ;
#175597 = CARTESIAN_POINT ( 'NONE',  ( -9.564922557960796823, -16.46253265017161027, 52.08224293864768839 ) ) ;
#175598 = CARTESIAN_POINT ( 'NONE',  ( 12.06949235617739724, 12.14591786802326823, 111.8760903946856615 ) ) ;
#175599 = CARTESIAN_POINT ( 'NONE',  ( 8.224510206698742110, 14.34966873604972548, 107.0844237280190043 ) ) ;
#175600 = CARTESIAN_POINT ( 'NONE',  ( -12.06949235617739369, -12.14591786802326823, 89.37609039468568994 ) ) ;
#175601 = CARTESIAN_POINT ( 'NONE',  ( 13.89961937509957401, 13.97604488694547697, 41.87609039468566152 ) ) ;
#175602 = CARTESIAN_POINT ( 'NONE',  ( -17.31728774477273447, 6.344390552232387570, 70.81906651689320142 ) ) ;
#175603 = CARTESIAN_POINT ( 'NONE',  ( -5.049401038298153566, 19.05341960407611168, 90.20724293864766707 ) ) ;
#175604 = CARTESIAN_POINT ( 'NONE',  ( -5.049401038298153566, 19.05341960407611168, 50.20724293864770260 ) ) ;
#175605 = EDGE_CURVE ( 'NONE', #34941, #193436, #7265, .T. ) ;
#175606 = CARTESIAN_POINT ( 'NONE',  ( -16.55341960407611168, -4.379528057220339221, 66.45724293864768129 ) ) ;
#175608 = CARTESIAN_POINT ( 'NONE',  ( 9.474510206698971260, -16.51473224551069308, 97.91557627198102409 ) ) ;
#175607 = CARTESIAN_POINT ( 'NONE',  ( 17.12812012977028076, -6.668231424565989052, 101.1405124067685932 ) ) ;
#175609 = CARTESIAN_POINT ( 'NONE',  ( 18.62759615963271287, -10.81492255796078972, 38.33224293864768839 ) ) ;
#175610 = CARTESIAN_POINT ( 'NONE',  ( -4.483927247898539470, -16.52544592524342804, 87.29057627198103830 ) ) ;
#175611 = CARTESIAN_POINT ( 'NONE',  ( -12.14591786802326823, 12.06949235617739902, 43.12609039468568284 ) ) ;
#175612 = CARTESIAN_POINT ( 'NONE',  ( 16.55341960407611168, 4.379528057220329451, 78.95724293864769550 ) ) ;
#175613 = CARTESIAN_POINT ( 'NONE',  ( 26.45564479744089326, 7.620358626195402607, 168.5728521449592847 ) ) ;
#175614 = CARTESIAN_POINT ( 'NONE',  ( -5.049401038297874678, -19.05341960407617918, 79.79275706135233293 ) ) ;
#175615 = CARTESIAN_POINT ( 'NONE',  ( 5.049401038298161559, -19.05341960407611168, 97.70724293864766707 ) ) ;
#175617 = EDGE_CURVE ( 'NONE', #139778, #80788, #154726, .T. ) ;
#175616 = CARTESIAN_POINT ( 'NONE',  ( -16.46253265017146816, -9.564922557961047289, 79.16775706135234714 ) ) ;
#175618 = CARTESIAN_POINT ( 'NONE',  ( 18.22780087662123805, 5.499999999999960032, 101.4823681787310647 ) ) ;
#175620 = CARTESIAN_POINT ( 'NONE',  ( 16.55341960407618274, -4.379528057220086978, 111.0427570613523613 ) ) ;
#175619 = CARTESIAN_POINT ( 'NONE',  ( 8.314922557961029526, -14.29746914071037800, 35.41775706135234003 ) ) ;
#175622 = CARTESIAN_POINT ( 'NONE',  ( -5.049401038297874678, -19.05341960407617918, 74.79275706135231871 ) ) ;
#175621 = AXIS2_PLACEMENT_3D ( 'NONE', #22537, #82177, #3373 ) ;
#175623 = CARTESIAN_POINT ( 'NONE',  ( -15.72974639402197994, 15.80617190586746368, 35.62390960531437401 ) ) ;
#175624 = CARTESIAN_POINT ( 'NONE',  ( -21.53943276465977519, -0.05219959533937600094, 63.75109039468568284 ) ) ;
#175625 = CARTESIAN_POINT ( 'NONE',  ( -22.78714015945949356, -11.73760554535633105, 167.9671921004704416 ) ) ;
#175626 = CARTESIAN_POINT ( 'NONE',  ( 8.224510206698742110, 14.34966873604972548, 32.08442372801901854 ) ) ;
#175628 = CARTESIAN_POINT ( 'NONE',  ( 9.474510206698971260, -16.51473224551069308, 87.91557627198102409 ) ) ;
#175627 = CARTESIAN_POINT ( 'NONE',  ( -19.02544592524342804, 5.153800228976336051, 26.04057627198103120 ) ) ;
#175629 = CARTESIAN_POINT ( 'NONE',  ( 15.34147874640870590, 17.41603567004569797, -57.57865799245707450 ) ) ;
#175630 = CARTESIAN_POINT ( 'NONE',  ( 14.29746914071049879, -8.314922557960816363, 83.33224293864769550 ) ) ;
#175631 = CARTESIAN_POINT ( 'NONE',  ( -19.02544592524342804, 5.153800228976336051, 86.04057627198103830 ) ) ;
#175632 = ORIENTED_EDGE ( 'NONE', *, *, #150856, .F. ) ;
#175633 = CARTESIAN_POINT ( 'NONE',  ( -19.02544592524334988, -5.153800228976617603, 103.9594237280190043 ) ) ;
#175634 = CARTESIAN_POINT ( 'NONE',  ( -21.55341960407610458, -5.719274019375992779, 71.45724293864769550 ) ) ;
#175635 = CARTESIAN_POINT ( 'NONE',  ( -19.05341960407611168, -5.049401038298163336, 46.45724293864768129 ) ) ;
#175637 = CARTESIAN_POINT ( 'NONE',  ( 18.67979575497178502, 10.72451020669898547, 114.1655762719810383 ) ) ;
#175636 = CARTESIAN_POINT ( 'NONE',  ( 19.05341960407617918, -5.049401038297876454, 76.04275706135230450 ) ) ;
#175638 = CARTESIAN_POINT ( 'NONE',  ( 19.05341960407611168, 5.049401038298154454, 73.95724293864768129 ) ) ;
#175639 = CARTESIAN_POINT ( 'NONE',  ( 19.05341960407611168, 5.049401038298154454, 108.9572429386477097 ) ) ;
#175640 = EDGE_LOOP ( 'NONE', ( #99398, #162382, #153702, #54726 ) ) ;
#175641 = CARTESIAN_POINT ( 'NONE',  ( -4.379528057220086978, -16.55341960407618274, 34.79275706135235424 ) ) ;
#175642 = CARTESIAN_POINT ( 'NONE',  ( -21.52544592524343514, 5.823673210054127303, 106.0405762719810525 ) ) ;
#175645 = CARTESIAN_POINT ( 'NONE',  ( 5.153800228976615827, -19.02544592524334988, 65.20942372801900433 ) ) ;
#175644 = CARTESIAN_POINT ( 'NONE',  ( -0.05219959533909027116, -19.03943276465977164, 97.49890960531436690 ) ) ;
#175643 = CARTESIAN_POINT ( 'NONE',  ( 4.379528057220339221, -16.55341960407611168, 112.7072429386476955 ) ) ;
#175646 = CARTESIAN_POINT ( 'NONE',  ( -15.80617190586745835, -15.72974639402198527, 91.87390960531436690 ) ) ;
#175647 = CARTESIAN_POINT ( 'NONE',  ( 0.05219959533910956823, 16.53943276465976808, 44.99890960531435979 ) ) ;
#175648 = CARTESIAN_POINT ( 'NONE',  ( 9.564922557961047289, -16.46253265017146816, 20.41775706135233293 ) ) ;
#175649 = CARTESIAN_POINT ( 'NONE',  ( -4.483927247898782831, 16.52544592524335698, 62.70942372801902565 ) ) ;
#175650 = CARTESIAN_POINT ( 'NONE',  ( -9.564922557960796823, -16.46253265017161027, 87.08224293864769550 ) ) ;
#175651 = CARTESIAN_POINT ( 'NONE',  ( -16.46253265017160317, 9.564922557960807481, 40.83224293864769550 ) ) ;
#175652 = AXIS2_PLACEMENT_3D ( 'NONE', #135596, #105241, #27431 ) ;
#175653 = CARTESIAN_POINT ( 'NONE',  ( -21.52544592524334988, -5.823673210054445271, 48.95942372801902565 ) ) ;
#175654 = CARTESIAN_POINT ( 'NONE',  ( -15.72974639402176322, -15.80617190586768395, 69.37609039468567573 ) ) ;
#175655 = CARTESIAN_POINT ( 'NONE',  ( -9.564922557960796823, -16.46253265017161027, 57.08224293864769550 ) ) ;
#175656 = CARTESIAN_POINT ( 'NONE',  ( 5.823673210054444382, -21.52544592524334988, 30.20942372801902565 ) ) ;
#175657 = CARTESIAN_POINT ( 'NONE',  ( 9.564922557961047289, -16.46253265017146816, 80.41775706135234714 ) ) ;
#175658 = CARTESIAN_POINT ( 'NONE',  ( -9.474510206698720793, -16.51473224551083518, 79.58442372801899012 ) ) ;
#175659 = CARTESIAN_POINT ( 'NONE',  ( 0.05219959533909260263, 19.03943276465977164, 44.99890960531435979 ) ) ;
#175660 = CARTESIAN_POINT ( 'NONE',  ( -8.224510206698735004, -14.34966873604973081, 89.58442372801901854 ) ) ;
#175661 = CARTESIAN_POINT ( 'NONE',  ( 16.46253265017160672, -9.564922557960803928, 58.33224293864769550 ) ) ;
#175662 = CARTESIAN_POINT ( 'NONE',  ( 20.14845677604719043, -11.63499142542172571, 168.0304984204096286 ) ) ;
#175663 = CARTESIAN_POINT ( 'NONE',  ( -9.474510206698964154, 16.51473224551069663, 100.4155762719810241 ) ) ;
#175664 = CARTESIAN_POINT ( 'NONE',  ( 16.46253265017160672, -9.564922557960803928, 33.33224293864770260 ) ) ;
#175665 = CARTESIAN_POINT ( 'NONE',  ( 21.53943276465977519, -0.05219959533907433946, 83.74890960531435269 ) ) ;
#175666 = CARTESIAN_POINT ( 'NONE',  ( 16.53943276465976808, 0.05219959533934440121, 56.25109039468568284 ) ) ;
#175667 = CARTESIAN_POINT ( 'NONE',  ( -9.564922557961040184, 16.46253265017147172, 37.91775706135233293 ) ) ;
#175668 = CARTESIAN_POINT ( 'NONE',  ( 5.049401038298161559, -19.05341960407611168, 52.70724293864767418 ) ) ;
#175669 = CARTESIAN_POINT ( 'NONE',  ( -16.52544592524342804, 4.483927247898546575, 51.04057627198103120 ) ) ;
#175670 = CARTESIAN_POINT ( 'NONE',  ( 12.14591786802309770, 12.06949235617756955, 79.37390960531436690 ) ) ;
#175671 = CARTESIAN_POINT ( 'NONE',  ( -0.05219959533909027116, -19.03943276465977164, 87.49890960531436690 ) ) ;
#175672 = CARTESIAN_POINT ( 'NONE',  ( -9.474510206698964154, 16.51473224551069663, 75.41557627198103830 ) ) ;
#175673 = CARTESIAN_POINT ( 'NONE',  ( -21.52544592524334988, -5.823673210054445271, 38.95942372801901854 ) ) ;
#175674 = CARTESIAN_POINT ( 'NONE',  ( -19.03943276465977164, 0.05219959533909376836, 96.24890960531436690 ) ) ;
#175675 = CARTESIAN_POINT ( 'NONE',  ( -5.719274019375665041, -21.55341960407619695, 104.7927570613523898 ) ) ;
#175676 = CARTESIAN_POINT ( 'NONE',  ( -12.06949235617739369, -12.14591786802326823, 84.37609039468570415 ) ) ;
#175677 = CARTESIAN_POINT ( 'NONE',  ( -15.80617190586768217, 15.72974639402176855, 33.12609039468569705 ) ) ;
#175678 = CARTESIAN_POINT ( 'NONE',  ( 21.55341960407610458, 5.719274019375980345, 93.95724293864770971 ) ) ;
#175679 = CARTESIAN_POINT ( 'NONE',  ( 16.52544592524342804, -4.483927247898539470, 53.54057627198103120 ) ) ;
#175680 = CARTESIAN_POINT ( 'NONE',  ( 19.02544592524343514, -5.153800228976328945, 38.54057627198103120 ) ) ;
#175681 = CARTESIAN_POINT ( 'NONE',  ( -16.52544592524342804, 4.483927247898546575, 66.04057627198103830 ) ) ;
#175682 = CARTESIAN_POINT ( 'NONE',  ( 21.55341960407610458, 5.719274019375980345, 28.95724293864769905 ) ) ;
#175683 = CARTESIAN_POINT ( 'NONE',  ( 19.05341960407617918, -5.049401038297876454, 36.04275706135234003 ) ) ;
#175684 = CARTESIAN_POINT ( 'NONE',  ( 14.29746914071049879, -8.314922557960816363, 103.3322429386476955 ) ) ;
#175685 = CARTESIAN_POINT ( 'NONE',  ( -16.51473224551069308, -9.474510206698971260, 111.6655762719810383 ) ) ;
#175686 = ORIENTED_EDGE ( 'NONE', *, *, #197763, .F. ) ;
#175687 = CARTESIAN_POINT ( 'NONE',  ( -16.52544592524335698, -4.483927247898792601, 48.95942372801902565 ) ) ;
#175688 = CARTESIAN_POINT ( 'NONE',  ( -16.46253265017160317, 9.564922557960807481, 55.83224293864769550 ) ) ;
#175689 = CARTESIAN_POINT ( 'NONE',  ( -16.63550798202463099, -6.755536848170410558, 20.93280403780605781 ) ) ;
#175690 = CARTESIAN_POINT ( 'NONE',  ( -12.14591786802326823, 12.06949235617739902, 93.12609039468568994 ) ) ;
#175691 = CARTESIAN_POINT ( 'NONE',  ( -14.29746914071037622, -8.314922557961029526, 19.16775706135234714 ) ) ;
#175692 = CARTESIAN_POINT ( 'NONE',  ( 15.72974639402176855, 15.80617190586768217, 76.87609039468567573 ) ) ;
#175693 = CARTESIAN_POINT ( 'NONE',  ( 0.05219959533909260263, 19.03943276465977164, 79.99890960531436690 ) ) ;
#175694 = CARTESIAN_POINT ( 'NONE',  ( 18.67979575497178502, 10.72451020669898547, 104.1655762719810241 ) ) ;
#175695 = CARTESIAN_POINT ( 'NONE',  ( -4.379528057220086978, -16.55341960407618274, 54.79275706135235424 ) ) ;
#175696 = CARTESIAN_POINT ( 'NONE',  ( 8.224510206698953496, -14.34966873604960469, 107.9155762719810241 ) ) ;
#175697 = CARTESIAN_POINT ( 'NONE',  ( 12.14591786802327356, -12.06949235617739191, 20.62609039468568639 ) ) ;
#175698 = CARTESIAN_POINT ( 'NONE',  ( 19.05341960407617918, -5.049401038297876454, 81.04275706135231871 ) ) ;
#175699 = CARTESIAN_POINT ( 'NONE',  ( 0.05219959533907565091, 21.53943276465977519, 79.99890960531435269 ) ) ;
#175700 = CARTESIAN_POINT ( 'NONE',  ( 13.89961937509957401, 13.97604488694547697, 51.87609039468566863 ) ) ;
#175701 = CARTESIAN_POINT ( 'NONE',  ( 19.46398650005389896, -5.499999999999943157, 87.68269651486372140 ) ) ;
#175702 = CARTESIAN_POINT ( 'NONE',  ( -21.53943276465977519, 0.05219959533907696930, 101.2489096053143669 ) ) ;
#175703 = DIRECTION ( 'NONE',  ( 0.000000000000000000, 0.000000000000000000, -1.000000000000000000 ) ) ;
#175704 = CARTESIAN_POINT ( 'NONE',  ( 19.05341960407611168, 5.049401038298154454, 68.95724293864769550 ) ) ;
#175705 = FACE_OUTER_BOUND ( 'NONE', #193284, .T. ) ;
#175706 = CARTESIAN_POINT ( 'NONE',  ( -14.34966873604972548, 8.224510206698743886, 23.33442372801901499 ) ) ;
#175707 = CARTESIAN_POINT ( 'NONE',  ( 36.89003987753539349, -5.463308683677074562, 44.27017301194418764 ) ) ;
#175709 = CARTESIAN_POINT ( 'NONE',  ( -8.224510206698948167, 14.34966873604960824, 70.41557627198102409 ) ) ;
#175708 = CARTESIAN_POINT ( 'NONE',  ( 21.53943276465977519, -0.05219959533907433946, 103.7489096053143669 ) ) ;
#175710 = CARTESIAN_POINT ( 'NONE',  ( -13.89961937509977652, 13.97604488694528158, 75.62390960531438111 ) ) ;
#175711 = CARTESIAN_POINT ( 'NONE',  ( -21.55341960407619339, 5.719274019375674811, 68.54275706135234714 ) ) ;
#175713 = CARTESIAN_POINT ( 'NONE',  ( -19.02544592524334988, -5.153800228976617603, 23.95942372801900078 ) ) ;
#175712 = CARTESIAN_POINT ( 'NONE',  ( 4.483927247898790824, -16.52544592524335698, 25.20942372801901854 ) ) ;
#175714 = CARTESIAN_POINT ( 'NONE',  ( 10.81492255796106328, -18.62759615963255655, 55.41775706135234714 ) ) ;
#175715 = CARTESIAN_POINT ( 'NONE',  ( 15.80617190586746368, 15.72974639402197994, 109.3739096053143811 ) ) ;
#175716 = CARTESIAN_POINT ( 'NONE',  ( 10.72451020669898902, -18.67979575497178502, 62.91557627198102409 ) ) ;
#175717 = CARTESIAN_POINT ( 'NONE',  ( -16.52544592524335698, -4.483927247898792601, 18.95942372801901143 ) ) ;
#175718 = CARTESIAN_POINT ( 'NONE',  ( 5.049401038298161559, -19.05341960407611168, 47.70724293864770260 ) ) ;
#175719 = CARTESIAN_POINT ( 'NONE',  ( -5.153800228976607833, 19.02544592524334988, 67.70942372801900433 ) ) ;
#175720 = CARTESIAN_POINT ( 'NONE',  ( -10.81492255796105439, 18.62759615963255655, 77.91775706135231871 ) ) ;
#175721 = CARTESIAN_POINT ( 'NONE',  ( 19.05341960407617918, -5.049401038297876454, 56.04275706135234714 ) ) ;
#175722 = CARTESIAN_POINT ( 'NONE',  ( 9.564922557960805705, 16.46253265017160317, 39.58224293864768839 ) ) ;
#175723 = CARTESIAN_POINT ( 'NONE',  ( -5.719274019375978568, 21.55341960407610458, 55.20724293864770260 ) ) ;
#175724 = CARTESIAN_POINT ( 'NONE',  ( -16.53943276465976808, 0.05219959533911058130, 56.24890960531436690 ) ) ;
#175725 = CARTESIAN_POINT ( 'NONE',  ( -17.50000000000000711, -5.624438216177558125, 24.18329655085356933 ) ) ;
#175726 = CARTESIAN_POINT ( 'NONE',  ( 13.89961937509957401, 13.97604488694547697, 26.87609039468566507 ) ) ;
#175727 = CARTESIAN_POINT ( 'NONE',  ( 0.05219959533934541429, -16.53943276465976808, 90.00109039468567573 ) ) ;
#175728 = CARTESIAN_POINT ( 'NONE',  ( 0.05219959533910956823, 16.53943276465976808, 59.99890960531436690 ) ) ;
#175729 = CARTESIAN_POINT ( 'NONE',  ( -18.62759615963255300, -10.81492255796106328, 84.16775706135234714 ) ) ;
#175730 = CARTESIAN_POINT ( 'NONE',  ( 21.53943276465977519, 0.05219959533937863772, 76.25109039468568994 ) ) ;
#175731 = CARTESIAN_POINT ( 'NONE',  ( -15.72974639402197994, 15.80617190586746368, 80.62390960531438111 ) ) ;
#175732 = VECTOR ( 'NONE', #175703, 1000.000000000000000 ) ;
#175733 = CARTESIAN_POINT ( 'NONE',  ( -16.46253265017160317, 9.564922557960807481, 45.83224293864769550 ) ) ;
#175734 = CARTESIAN_POINT ( 'NONE',  ( -21.55341960407619339, 5.719274019375674811, 58.54275706135235424 ) ) ;
#175735 = CARTESIAN_POINT ( 'NONE',  ( 13.89961937509977652, -13.97604488694527269, 33.12390960531434558 ) ) ;
#175736 = ORIENTED_EDGE ( 'NONE', *, *, #163855, .T. ) ;
#175737 = CARTESIAN_POINT ( 'NONE',  ( 9.564922557960805705, 16.46253265017160317, 54.58224293864769550 ) ) ;
#175738 = CARTESIAN_POINT ( 'NONE',  ( -14.34966873604960291, -8.224510206698953496, 111.6655762719810525 ) ) ;
#175739 = CARTESIAN_POINT ( 'NONE',  ( 5.153800228976335163, 19.02544592524342804, 99.79057627198102409 ) ) ;
#175740 = CARTESIAN_POINT ( 'NONE',  ( -4.379528057220328563, 16.55341960407611168, 50.20724293864769550 ) ) ;
#175741 = CARTESIAN_POINT ( 'NONE',  ( -16.53943276465976808, 0.05219959533911058130, 106.2489096053143811 ) ) ;
#175742 = CARTESIAN_POINT ( 'NONE',  ( 21.52544592524344225, -5.823673210054117533, 88.54057627198103830 ) ) ;
#175743 = CARTESIAN_POINT ( 'NONE',  ( 10.72451020669871369, 18.67979575497193778, 27.08442372801901854 ) ) ;
#175744 = FACE_OUTER_BOUND ( 'NONE', #101484, .T. ) ;
#175745 = CARTESIAN_POINT ( 'NONE',  ( 16.53943276465976808, 0.05219959533934440121, 36.25109039468567573 ) ) ;
#175746 = ORIENTED_EDGE ( 'NONE', *, *, #36547, .F. ) ;
#175747 = CARTESIAN_POINT ( 'NONE',  ( 0.05219959533907565091, 21.53943276465977519, 69.99890960531435269 ) ) ;
#175749 = CARTESIAN_POINT ( 'NONE',  ( -5.823673210054431948, 21.52544592524334988, 102.7094237280190185 ) ) ;
#175748 = UNCERTAINTY_MEASURE_WITH_UNIT (LENGTH_MEASURE( 1.000000000000000082E-05 ), #795, 'distance_accuracy_value', 'NONE');
#175750 = CARTESIAN_POINT ( 'NONE',  ( -16.51473224551069308, -9.474510206698971260, 91.66557627198103830 ) ) ;
#175751 = CARTESIAN_POINT ( 'NONE',  ( 21.52544592524334988, 5.823673210054432836, 26.45942372801901854 ) ) ;
#175752 = CARTESIAN_POINT ( 'NONE',  ( 10.81492255796078972, 18.62759615963270932, 29.58224293864769905 ) ) ;
#175753 = CARTESIAN_POINT ( 'NONE',  ( -16.52544592524335698, -4.483927247898792601, 108.9594237280190185 ) ) ;
#175755 = CARTESIAN_POINT ( 'NONE',  ( -18.67979575497193778, 10.72451020669871902, 83.33442372801903275 ) ) ;
#175754 = CARTESIAN_POINT ( 'NONE',  ( 21.55341960407619695, -5.719274019375665929, 56.04275706135235424 ) ) ;
#175756 = CARTESIAN_POINT ( 'NONE',  ( 15.72974639402176855, 15.80617190586768217, 106.8760903946856899 ) ) ;
#175757 = CARTESIAN_POINT ( 'NONE',  ( -16.52544592524335698, -4.483927247898792601, 68.95942372801901854 ) ) ;
#175758 = CARTESIAN_POINT ( 'NONE',  ( -18.62759615963255300, -10.81492255796106328, 34.16775706135234714 ) ) ;
#175759 = AXIS2_PLACEMENT_3D ( 'NONE', #138118, #139104, #153280 ) ;
#175760 = CARTESIAN_POINT ( 'NONE',  ( 0.05219959533909260263, 19.03943276465977164, 34.99890960531435979 ) ) ;
#175761 = CARTESIAN_POINT ( 'NONE',  ( 21.55341960407619695, -5.719274019375665929, 101.0427570613523756 ) ) ;
#175762 = CARTESIAN_POINT ( 'NONE',  ( -5.153800228976328057, -19.02544592524343514, 107.2905762719810383 ) ) ;
#175763 = CARTESIAN_POINT ( 'NONE',  ( 21.55341960407610458, 5.719274019375980345, 103.9572429386476813 ) ) ;
#175765 = CARTESIAN_POINT ( 'NONE',  ( 21.53943276465977519, -0.05219959533907433946, 63.74890960531435979 ) ) ;
#175764 = CARTESIAN_POINT ( 'NONE',  ( -6.310639553376649502, -38.36010752037731208, -23.94295717419116443 ) ) ;
#175767 = CARTESIAN_POINT ( 'NONE',  ( -4.379528057220328563, 16.55341960407611168, 55.20724293864770260 ) ) ;
#175766 = CARTESIAN_POINT ( 'NONE',  ( -14.29746914071037622, -8.314922557961029526, 54.16775706135235424 ) ) ;
#175768 = CARTESIAN_POINT ( 'NONE',  ( 22.19348515620995954, 7.491027558428855038, 173.8712782147084965 ) ) ;
#175769 = CARTESIAN_POINT ( 'NONE',  ( -19.03943276465977164, -0.05219959533935918106, 73.75109039468566152 ) ) ;
#175770 = PRESENTATION_LAYER_ASSIGNMENT (  '', '', ( #149949 ) ) ;
#175771 = CARTESIAN_POINT ( 'NONE',  ( -0.4033639900674926282, -16.64831001466045279, -61.36868776158050309 ) ) ;
#175772 = EDGE_CURVE ( 'NONE', #48994, #97685, #137564, .T. ) ;
#175773 = CARTESIAN_POINT ( 'NONE',  ( 4.379528057220092307, 16.55341960407617563, 27.29275706135234358 ) ) ;
#175774 = CARTESIAN_POINT ( 'NONE',  ( -21.53943276465977519, 0.05219959533907696930, 96.24890960531435269 ) ) ;
#175775 = CARTESIAN_POINT ( 'NONE',  ( -12.14591786802309592, -12.06949235617757132, 71.87390960531438111 ) ) ;
#175776 = CARTESIAN_POINT ( 'NONE',  ( -0.05219959533909027116, -19.03943276465977164, 112.4989096053143669 ) ) ;
#175777 = CARTESIAN_POINT ( 'NONE',  ( -16.53943276465976808, -0.05219959533934237506, 43.75109039468568284 ) ) ;
#175778 = CARTESIAN_POINT ( 'NONE',  ( -19.05341960407611168, -5.049401038298163336, 56.45724293864768129 ) ) ;
#175780 = CARTESIAN_POINT ( 'NONE',  ( -13.89961937509957401, -13.97604488694547875, 104.3760903946856757 ) ) ;
#175779 = CARTESIAN_POINT ( 'NONE',  ( 18.67979575497194134, -10.72451020669871369, 25.83442372801901499 ) ) ;
#175781 = CARTESIAN_POINT ( 'NONE',  ( 19.02544592524343514, -5.153800228976328945, 88.54057627198102409 ) ) ;
#175782 = CARTESIAN_POINT ( 'NONE',  ( -5.153800228976328057, -19.02544592524343514, 92.29057627198099567 ) ) ;
#175783 = CARTESIAN_POINT ( 'NONE',  ( -18.62759615963270932, 10.81492255796079327, 90.83224293864769550 ) ) ;
#175784 = CARTESIAN_POINT ( 'NONE',  ( -13.97604488694527625, -13.89961937509977652, 56.87390960531434558 ) ) ;
#175785 = CARTESIAN_POINT ( 'NONE',  ( -17.05587630539785238, -6.762274262135718139, 59.25819690962690345 ) ) ;
#175786 = CARTESIAN_POINT ( 'NONE',  ( 12.06949235617757843, -12.14591786802309237, 73.12390960531436690 ) ) ;
#175787 = CARTESIAN_POINT ( 'NONE',  ( 13.89961937509977652, -13.97604488694527269, 98.12390960531433848 ) ) ;
#175788 = CARTESIAN_POINT ( 'NONE',  ( 2.500000000000000000, -105.0000000000000000, 7.000000000000003553 ) ) ;
#175789 = CARTESIAN_POINT ( 'NONE',  ( -9.564922557961040184, 16.46253265017147172, 77.91775706135234714 ) ) ;
#175790 = CARTESIAN_POINT ( 'NONE',  ( 18.67979575497178502, 10.72451020669898547, 94.16557627198103830 ) ) ;
#175791 = CARTESIAN_POINT ( 'NONE',  ( -19.02544592524334988, -5.153800228976617603, 53.95942372801898301 ) ) ;
#175792 = CARTESIAN_POINT ( 'NONE',  ( -9.474510206698964154, 16.51473224551069663, 110.4155762719810383 ) ) ;
#175793 = LINE ( 'NONE', #146432, #105034 ) ;
#175794 = CARTESIAN_POINT ( 'NONE',  ( -15.72974639402197994, 15.80617190586746368, 50.62390960531435979 ) ) ;
#175795 = CIRCLE ( 'NONE', #114428, 4.999999999999998224 ) ;
#175796 = CARTESIAN_POINT ( 'NONE',  ( 5.049401038298161559, -19.05341960407611168, 92.70724293864769550 ) ) ;
#175797 = CARTESIAN_POINT ( 'NONE',  ( -18.67979575497193778, 10.72451020669871902, 78.33442372801901854 ) ) ;
#175798 = CARTESIAN_POINT ( 'NONE',  ( 19.03943276465977164, -0.05219959533909143690, 43.74890960531435979 ) ) ;
#175799 = EDGE_CURVE ( 'NONE', #15380, #19836, #149026, .T. ) ;
#175800 = CARTESIAN_POINT ( 'NONE',  ( -0.05219959533910754901, -16.53943276465976808, 67.49890960531436690 ) ) ;
#175801 = CARTESIAN_POINT ( 'NONE',  ( -14.29746914071037622, -8.314922557961029526, 19.16775706135234714 ) ) ;
#175802 = CARTESIAN_POINT ( 'NONE',  ( 5.719274019375673035, 21.55341960407619339, 67.29275706135234714 ) ) ;
#175803 = ORIENTED_EDGE ( 'NONE', *, *, #46060, .T. ) ;
#175804 = CARTESIAN_POINT ( 'NONE',  ( 19.05341960407611168, 5.049401038298154454, 108.9572429386477097 ) ) ;
#175805 = CARTESIAN_POINT ( 'NONE',  ( 19.05341960407617918, -5.049401038297876454, 76.04275706135230450 ) ) ;
#175806 = CYLINDRICAL_SURFACE ( 'NONE', #182735, 1.499999999999997780 ) ;
#175807 = CARTESIAN_POINT ( 'NONE',  ( 10.81492255796078972, 18.62759615963270932, 114.5822429386477097 ) ) ;
#175808 = LINE ( 'NONE', #6932, #191645 ) ;
#175809 = CARTESIAN_POINT ( 'NONE',  ( 13.97604488694548053, -13.89961937509957401, 25.62609039468566507 ) ) ;
#175810 = CARTESIAN_POINT ( 'NONE',  ( -9.564922557960796823, -16.46253265017161027, 57.08224293864769550 ) ) ;
#175811 = CARTESIAN_POINT ( 'NONE',  ( -19.02544592524334988, -5.153800228976617603, 18.95942372801899722 ) ) ;
#175812 = CARTESIAN_POINT ( 'NONE',  ( 12.14591786802327356, -12.06949235617739191, 110.6260903946857042 ) ) ;
#175814 = CARTESIAN_POINT ( 'NONE',  ( 18.62759615963255655, 10.81492255796105972, 71.66775706135234714 ) ) ;
#175813 = CARTESIAN_POINT ( 'NONE',  ( -19.02544592524342804, 5.153800228976336051, 106.0405762719810241 ) ) ;
#175815 = CARTESIAN_POINT ( 'NONE',  ( -36.91746825000000598, 2.428612866367529932E-14, -6.624999997268814056 ) ) ;
#175816 = CARTESIAN_POINT ( 'NONE',  ( -17.60769864724391098, 5.499999999999987566, 98.65024842019163032 ) ) ;
#175817 = CARTESIAN_POINT ( 'NONE',  ( 18.67979575497194134, -10.72451020669871369, 65.83442372801900433 ) ) ;
#175818 = CARTESIAN_POINT ( 'NONE',  ( -10.72451020669870658, -18.67979575497194134, 104.5844237280190185 ) ) ;
#175819 = CARTESIAN_POINT ( 'NONE',  ( 17.26058549869090797, -6.457015423128605214, 41.12254162523932877 ) ) ;
#175820 = CARTESIAN_POINT ( 'NONE',  ( 16.46253265017160672, -9.564922557960803928, 93.33224293864769550 ) ) ;
#175821 = CARTESIAN_POINT ( 'NONE',  ( 9.564922557961047289, -16.46253265017146816, 25.41775706135234003 ) ) ;
#175822 = CARTESIAN_POINT ( 'NONE',  ( -0.1282610754043937429, -31.90000000000003411, -49.13275782002543934 ) ) ;
#175823 = CARTESIAN_POINT ( 'NONE',  ( -16.46253265017160317, 9.564922557960807481, 40.83224293864769550 ) ) ;
#175824 = CARTESIAN_POINT ( 'NONE',  ( -5.823673210054116645, -21.52544592524344225, 57.29057627198103120 ) ) ;
#175825 = CARTESIAN_POINT ( 'NONE',  ( 12.06949235617739724, 12.14591786802326823, 101.8760903946857042 ) ) ;
#175827 = CARTESIAN_POINT ( 'NONE',  ( 13.89961937509977652, -13.97604488694527269, 83.12390960531436690 ) ) ;
#175826 = CARTESIAN_POINT ( 'NONE',  ( -16.53943276465976808, 0.05219959533911058130, 101.2489096053143669 ) ) ;
#175828 = CARTESIAN_POINT ( 'NONE',  ( 10.72451020669871369, 18.67979575497193778, 107.0844237280190043 ) ) ;
#175829 = CARTESIAN_POINT ( 'NONE',  ( -13.89961937509977652, 13.97604488694528158, 40.62390960531435979 ) ) ;
#175830 = CARTESIAN_POINT ( 'NONE',  ( 0.05219959533910956823, 16.53943276465976808, 104.9989096053143669 ) ) ;
#175831 = CARTESIAN_POINT ( 'NONE',  ( -5.719274019375665041, -21.55341960407619695, 49.79275706135234714 ) ) ;
#175832 = CARTESIAN_POINT ( 'NONE',  ( -21.53943276465977519, 0.05219959533907696930, 86.24890960531436690 ) ) ;
#175833 = CARTESIAN_POINT ( 'NONE',  ( 19.05341960407617918, -5.049401038297876454, 51.04275706135231871 ) ) ;
#175834 = CARTESIAN_POINT ( 'NONE',  ( 13.89961937509978007, -13.97604488694527269, 48.12390960531435979 ) ) ;
#175835 = CARTESIAN_POINT ( 'NONE',  ( 0.05219959533909260263, 19.03943276465977164, 99.99890960531436690 ) ) ;
#175836 = CARTESIAN_POINT ( 'NONE',  ( 4.483927247898545687, 16.52544592524342804, 74.79057627198105251 ) ) ;
#175837 = CARTESIAN_POINT ( 'NONE',  ( 19.03943276465977164, 0.05219959533936151252, 51.25109039468567573 ) ) ;
#175838 = CARTESIAN_POINT ( 'NONE',  ( 19.02544592524343514, -5.153800228976328945, 58.54057627198102409 ) ) ;
#175839 = CARTESIAN_POINT ( 'NONE',  ( 8.314922557960818139, 14.29746914071049879, 44.58224293864769550 ) ) ;
#175840 = CARTESIAN_POINT ( 'NONE',  ( -13.89961937509957401, -13.97604488694547875, 79.37609039468567573 ) ) ;
#175841 = CARTESIAN_POINT ( 'NONE',  ( -19.25663599770060941, 5.499999999999451994, 83.99419308057203182 ) ) ;
#175842 = CARTESIAN_POINT ( 'NONE',  ( -10.81492255796078084, -18.62759615963271287, 37.08224293864768129 ) ) ;
#175843 = EDGE_CURVE ( 'NONE', #98417, #3830, #99409, .T. ) ;
#175844 = CARTESIAN_POINT ( 'NONE',  ( 12.14591786802309770, 12.06949235617756955, 104.3739096053143669 ) ) ;
#175845 = CARTESIAN_POINT ( 'NONE',  ( -17.50000000000000355, -3.345213924137174555, 25.41231376905639294 ) ) ;
#175847 = CARTESIAN_POINT ( 'NONE',  ( -0.05219959533907301413, -21.53943276465977519, 67.49890960531436690 ) ) ;
#175846 = CARTESIAN_POINT ( 'NONE',  ( -19.03943276465977164, 0.05219959533909376836, 61.24890960531436690 ) ) ;
#175848 = CARTESIAN_POINT ( 'NONE',  ( 0.05219959533909260263, 19.03943276465977164, 24.99890960531435269 ) ) ;
#175850 = CARTESIAN_POINT ( 'NONE',  ( 9.474510206698971260, -16.51473224551069308, 57.91557627198103120 ) ) ;
#175849 = CARTESIAN_POINT ( 'NONE',  ( 0.05219959533934541429, -16.53943276465976808, 75.00109039468568994 ) ) ;
#175851 = CARTESIAN_POINT ( 'NONE',  ( -16.51473224551082808, 9.474510206698731452, 53.33442372801900433 ) ) ;
#175852 = AXIS2_PLACEMENT_3D ( 'NONE', #145557, #7035, #43386 ) ;
#175853 = CARTESIAN_POINT ( 'NONE',  ( -5.823673210054431948, 21.52544592524334988, 67.70942372801901854 ) ) ;
#175854 = CARTESIAN_POINT ( 'NONE',  ( -21.55341960407610458, -5.719274019375992779, 46.45724293864769550 ) ) ;
#175855 = CARTESIAN_POINT ( 'NONE',  ( 13.97604488694527802, 13.89961937509977652, 24.37390960531435624 ) ) ;
#175856 = CARTESIAN_POINT ( 'NONE',  ( -16.53943276465976808, -0.05219959533934237506, 83.75109039468568994 ) ) ;
#175857 = CARTESIAN_POINT ( 'NONE',  ( 19.03943276465977164, 0.05219959533936151252, 101.2510903946856757 ) ) ;
#175858 = CARTESIAN_POINT ( 'NONE',  ( -13.89961937509977652, 13.97604488694528158, 25.62390960531434558 ) ) ;
#175860 = CARTESIAN_POINT ( 'NONE',  ( 15.72974639402199770, -15.80617190586745480, 48.12390960531436690 ) ) ;
#175859 = FACE_OUTER_BOUND ( 'NONE', #134090, .T. ) ;
#175861 = CARTESIAN_POINT ( 'NONE',  ( 15.80617190586769283, -15.72974639402175789, 85.62609039468568994 ) ) ;
#175862 = CARTESIAN_POINT ( 'NONE',  ( -8.224510206698948167, 14.34966873604960824, 45.41557627198103830 ) ) ;
#175863 = CARTESIAN_POINT ( 'NONE',  ( 14.29746914071049879, -8.314922557960816363, 53.33224293864769550 ) ) ;
#175864 = CARTESIAN_POINT ( 'NONE',  ( 21.53943276465977519, -0.05219959533907433946, 78.74890960531436690 ) ) ;
#175865 = APPLICATION_CONTEXT ( 'automotive_design' ) ;
#175866 = CARTESIAN_POINT ( 'NONE',  ( -21.55341960407610458, -5.719274019375992779, 91.45724293864769550 ) ) ;
#175867 = CARTESIAN_POINT ( 'NONE',  ( 4.647474457565486646E-15, -28.90000000000004476, -49.67367017693150189 ) ) ;
#175868 = CARTESIAN_POINT ( 'NONE',  ( 21.55341960407610458, 5.719274019375980345, 33.95724293864769550 ) ) ;
#175869 = CARTESIAN_POINT ( 'NONE',  ( -4.379528057220086978, -16.55341960407618274, 64.79275706135234714 ) ) ;
#175870 = CARTESIAN_POINT ( 'NONE',  ( -8.224510206698948167, 14.34966873604960824, 75.41557627198102409 ) ) ;
#175871 = CARTESIAN_POINT ( 'NONE',  ( -9.474510206698964154, 16.51473224551069663, 30.41557627198102054 ) ) ;
#175872 =( LENGTH_UNIT ( ) NAMED_UNIT ( * ) SI_UNIT ( .MILLI., .METRE. ) );
#175873 = CARTESIAN_POINT ( 'NONE',  ( 17.50000000000000000, -7.500000000000000888, 37.49999999999999289 ) ) ;
#175874 = CARTESIAN_POINT ( 'NONE',  ( -14.34966873604972548, 8.224510206698743886, 98.33442372801901854 ) ) ;
#175875 = CARTESIAN_POINT ( 'NONE',  ( 18.67979575497194134, -10.72451020669871369, 20.83442372801901143 ) ) ;
#175876 = CARTESIAN_POINT ( 'NONE',  ( -9.474510206698964154, 16.51473224551069663, 85.41557627198102409 ) ) ;
#175877 = CARTESIAN_POINT ( 'NONE',  ( 15.80617190586769283, -15.72974639402175789, 60.62609039468567573 ) ) ;
#175878 = CARTESIAN_POINT ( 'NONE',  ( -5.049401038298153566, 19.05341960407611168, 115.2072429386477097 ) ) ;
#175879 = CARTESIAN_POINT ( 'NONE',  ( -9.816778487192582503, -45.49549017958077712, -23.86159105743509556 ) ) ;
#175880 = CONICAL_SURFACE ( 'NONE', #192037, 1732.050807568856271, 1.047197551196592524 ) ;
#175881 = ORIENTED_EDGE ( 'NONE', *, *, #151864, .T. ) ;
#175882 = CARTESIAN_POINT ( 'NONE',  ( 21.55341960407619695, -5.719274019375665929, 41.04275706135236135 ) ) ;
#175884 = CARTESIAN_POINT ( 'NONE',  ( -0.05219959533909027116, -19.03943276465977164, 102.4989096053143669 ) ) ;
#175883 = CARTESIAN_POINT ( 'NONE',  ( 16.46253265017160672, -9.564922557960803928, 43.33224293864769550 ) ) ;
#175885 = CARTESIAN_POINT ( 'NONE',  ( -19.03943276465977164, -0.05219959533935918106, 48.75109039468566863 ) ) ;
#175886 = CARTESIAN_POINT ( 'NONE',  ( -21.52544592524334988, -5.823673210054445271, 28.95942372801902209 ) ) ;
#175887 = CARTESIAN_POINT ( 'NONE',  ( -16.46253265017146816, -9.564922557961047289, 49.16775706135233293 ) ) ;
#175888 = CARTESIAN_POINT ( 'NONE',  ( -19.02544592524342804, 5.153800228976336051, 26.04057627198103120 ) ) ;
#175889 = CARTESIAN_POINT ( 'NONE',  ( 4.379528057220092307, 16.55341960407617563, 97.29275706135234714 ) ) ;
#175890 = CARTESIAN_POINT ( 'NONE',  ( -13.89961937509957401, -13.97604488694547875, 64.37609039468567573 ) ) ;
#175891 = CARTESIAN_POINT ( 'NONE',  ( -8.224510206698735004, -14.34966873604973081, 99.58442372801900433 ) ) ;
#175892 = DIRECTION ( 'NONE',  ( 0.000000000000000000, -0.000000000000000000, -1.000000000000000000 ) ) ;
#175893 = CARTESIAN_POINT ( 'NONE',  ( -13.89961937509977652, 13.97604488694528158, 90.62390960531432427 ) ) ;
#175894 = CARTESIAN_POINT ( 'NONE',  ( -15.72974639402176322, -15.80617190586768395, 94.37609039468568994 ) ) ;
#175895 = CARTESIAN_POINT ( 'NONE',  ( 10.72451020669871369, 18.67979575497193778, 112.0844237280190185 ) ) ;
#175896 = CARTESIAN_POINT ( 'NONE',  ( 193.3062444957835453, -155.7167183371837496, -15.00000000000000000 ) ) ;
#175897 = CARTESIAN_POINT ( 'NONE',  ( -5.153800228976328057, -19.02544592524343514, 102.2905762719810383 ) ) ;
#175898 = CARTESIAN_POINT ( 'NONE',  ( -15.80617190586768217, 15.72974639402176855, 78.12609039468570415 ) ) ;
#175899 = CARTESIAN_POINT ( 'NONE',  ( -8.314922557961024197, 14.29746914071037800, 22.91775706135235069 ) ) ;
#175900 = AXIS2_PLACEMENT_3D ( 'NONE', #88515, #60158, #197698 ) ;
#175901 = CARTESIAN_POINT ( 'NONE',  ( 19.05341960407611168, 5.049401038298154454, 73.95724293864768129 ) ) ;
#175902 = CARTESIAN_POINT ( 'NONE',  ( 18.62759615963271287, -10.81492255796078972, 33.33224293864769550 ) ) ;
#175903 = CARTESIAN_POINT ( 'NONE',  ( 9.564922557960805705, 16.46253265017160317, 94.58224293864769550 ) ) ;
#175904 = CARTESIAN_POINT ( 'NONE',  ( -17.50000000000000000, -5.624438216177582106, 89.18329655085356933 ) ) ;
#175905 = CARTESIAN_POINT ( 'NONE',  ( 5.049401038298161559, -19.05341960407611168, 72.70724293864768129 ) ) ;
#175906 = CARTESIAN_POINT ( 'NONE',  ( -16.46253265017160317, 9.564922557960807481, 70.83224293864770971 ) ) ;
#175907 = CARTESIAN_POINT ( 'NONE',  ( 12.06949235617739724, 12.14591786802326823, 106.8760903946856899 ) ) ;
#175908 = CARTESIAN_POINT ( 'NONE',  ( -17.48853670773246805, 5.747243402303015003, 98.66671299749995683 ) ) ;
#175909 = AXIS2_PLACEMENT_3D ( 'NONE', #148291, #13755, #88604 ) ;
#175910 = CARTESIAN_POINT ( 'NONE',  ( -9.564922557961040184, 16.46253265017147172, 67.91775706135233293 ) ) ;
#175911 = CARTESIAN_POINT ( 'NONE',  ( -19.05341960407611168, -5.049401038298163336, 91.45724293864766707 ) ) ;
#175912 = CARTESIAN_POINT ( 'NONE',  ( -8.224510206698948167, 14.34966873604960824, 80.41557627198103830 ) ) ;
#175913 = CARTESIAN_POINT ( 'NONE',  ( 21.52544592524344225, -5.823673210054117533, 28.54057627198103120 ) ) ;
#175914 = CARTESIAN_POINT ( 'NONE',  ( -21.55341960407610458, -5.719274019375992779, 21.45724293864769550 ) ) ;
#175915 = CARTESIAN_POINT ( 'NONE',  ( 4.483927247898545687, 16.52544592524342804, 104.7905762719810241 ) ) ;
#175916 = CARTESIAN_POINT ( 'NONE',  ( -17.49999999999999645, 5.499999999999992895, 53.71769037696436300 ) ) ;
#175917 = CARTESIAN_POINT ( 'NONE',  ( -9.564922557961040184, 16.46253265017147172, 37.91775706135233293 ) ) ;
#175918 = CARTESIAN_POINT ( 'NONE',  ( -4.483927247898539470, -16.52544592524342804, 32.29057627198102409 ) ) ;
#175919 = CARTESIAN_POINT ( 'NONE',  ( -0.05219959533909027116, -19.03943276465977164, 97.49890960531436690 ) ) ;
#175920 = CARTESIAN_POINT ( 'NONE',  ( 10.81492255796106328, -18.62759615963255655, 60.41775706135235424 ) ) ;
#175921 = CARTESIAN_POINT ( 'NONE',  ( 10.72451020669898902, -18.67979575497178502, 57.91557627198103120 ) ) ;
#175922 = CARTESIAN_POINT ( 'NONE',  ( 21.55341960407619695, -5.719274019375665929, 36.04275706135234714 ) ) ;
#175923 = CARTESIAN_POINT ( 'NONE',  ( -15.80617190586745835, -15.72974639402198527, 81.87390960531435269 ) ) ;
#175924 = CARTESIAN_POINT ( 'NONE',  ( 21.53943276465977519, 0.05219959533937863772, 41.25109039468568284 ) ) ;
#175925 = CARTESIAN_POINT ( 'NONE',  ( 4.483927247898545687, 16.52544592524342804, 109.7905762719810383 ) ) ;
#175926 = CARTESIAN_POINT ( 'NONE',  ( -5.153800228976607833, 19.02544592524334988, 67.70942372801900433 ) ) ;
#175927 = CARTESIAN_POINT ( 'NONE',  ( -13.97604488694527625, -13.89961937509977652, 46.87390960531435979 ) ) ;
#175929 = CARTESIAN_POINT ( 'NONE',  ( -9.474510206698964154, 16.51473224551069663, 95.41557627198102409 ) ) ;
#175928 = CARTESIAN_POINT ( 'NONE',  ( 12.14591786802309770, 12.06949235617756955, 94.37390960531436690 ) ) ;
#175930 = CARTESIAN_POINT ( 'NONE',  ( 0.05219959533909260263, 19.03943276465977164, 109.9989096053143669 ) ) ;
#175931 = CARTESIAN_POINT ( 'NONE',  ( -13.89961937509977652, 13.97604488694528158, 30.62390960531435269 ) ) ;
#175932 = CARTESIAN_POINT ( 'NONE',  ( -14.34966873604960291, -8.224510206698953496, 46.66557627198102409 ) ) ;
#175933 = CARTESIAN_POINT ( 'NONE',  ( 16.53943276465976808, 0.05219959533934440121, 96.25109039468568994 ) ) ;
#175934 = CARTESIAN_POINT ( 'NONE',  ( -13.89961937509977652, 13.97604488694528158, 50.62390960531435979 ) ) ;
#175935 = CARTESIAN_POINT ( 'NONE',  ( 4.483927247898545687, 16.52544592524342804, 114.7905762719810383 ) ) ;
#175937 = CIRCLE ( 'NONE', #85575, 2.649999999999992806 ) ;
#175936 = CARTESIAN_POINT ( 'NONE',  ( 9.474510206698729675, 16.51473224551082808, 22.08442372801899722 ) ) ;
#175939 = CARTESIAN_POINT ( 'NONE',  ( -12.14591786802326823, 12.06949235617739902, 113.1260903946856899 ) ) ;
#175938 = CARTESIAN_POINT ( 'NONE',  ( -13.97604488694527625, -13.89961937509977652, 111.8739096053143243 ) ) ;
#175940 = CARTESIAN_POINT ( 'NONE',  ( 10.72451020669871369, 18.67979575497193778, 52.08442372801901854 ) ) ;
#175941 = CARTESIAN_POINT ( 'NONE',  ( -26.46959431505283789, -27.26463967846487435, -10.00000000000000000 ) ) ;
#175942 = CARTESIAN_POINT ( 'NONE',  ( -8.314922557961024197, 14.29746914071037800, 52.91775706135235424 ) ) ;
#175943 = CARTESIAN_POINT ( 'NONE',  ( -8.314922557960811034, -14.29746914071050412, 22.08224293864769194 ) ) ;
#175944 = CARTESIAN_POINT ( 'NONE',  ( 4.379528057220092307, 16.55341960407617563, 112.2927570613523471 ) ) ;
#175945 = CARTESIAN_POINT ( 'NONE',  ( -12.14591786802326823, 12.06949235617739902, 23.12609039468567573 ) ) ;
#175946 = ADVANCED_FACE ( 'NONE', ( #118688 ), #103517, .F. ) ;
#175947 = CARTESIAN_POINT ( 'NONE',  ( -9.564922557960796823, -16.46253265017161027, 47.08224293864769550 ) ) ;
#175948 = CARTESIAN_POINT ( 'NONE',  ( 16.52544592524342804, -4.483927247898539470, 113.5405762719810383 ) ) ;
#175949 = CARTESIAN_POINT ( 'NONE',  ( -0.05219959533937732626, 21.53943276465977519, 22.50109039468567573 ) ) ;
#175950 = CARTESIAN_POINT ( 'NONE',  ( 13.97604488694527802, 13.89961937509977652, 49.37390960531434558 ) ) ;
#175951 = DIRECTION ( 'NONE',  ( 0.000000000000000000, 0.000000000000000000, 1.000000000000000000 ) ) ;
#175952 = CARTESIAN_POINT ( 'NONE',  ( -13.97604488694527625, -13.89961937509977652, 26.87390960531434558 ) ) ;
#175953 = CARTESIAN_POINT ( 'NONE',  ( 5.719274019375991003, -21.55341960407610458, 22.70724293864769194 ) ) ;
#175954 = CARTESIAN_POINT ( 'NONE',  ( -17.50000000000000711, -5.499999999999956479, 36.28230962303565121 ) ) ;
#175955 = CARTESIAN_POINT ( 'NONE',  ( -5.049401038298153566, 19.05341960407611168, 95.20724293864770971 ) ) ;
#175957 = CARTESIAN_POINT ( 'NONE',  ( 8.224510206698953496, -14.34966873604960469, 102.9155762719810383 ) ) ;
#175956 = CARTESIAN_POINT ( 'NONE',  ( 21.52544592524334988, 5.823673210054432836, 41.45942372801901143 ) ) ;
#175958 = CARTESIAN_POINT ( 'NONE',  ( -0.05219959533909027116, -19.03943276465977164, 112.4989096053143669 ) ) ;
#175959 = DIRECTION ( 'NONE',  ( -1.000000000000000000, 0.000000000000000000, 0.000000000000000000 ) ) ;
#175960 = CARTESIAN_POINT ( 'NONE',  ( -14.34966873604972548, 8.224510206698743886, 83.33442372801903275 ) ) ;
#175961 = CARTESIAN_POINT ( 'NONE',  ( 10.81492255796106328, -18.62759615963255655, 90.41775706135236135 ) ) ;
#175962 = CARTESIAN_POINT ( 'NONE',  ( 0.05219959533934541429, -16.53943276465976808, 60.00109039468568284 ) ) ;
#175963 = CARTESIAN_POINT ( 'NONE',  ( 19.03943276465977164, -0.05219959533909143690, 98.74890960531436690 ) ) ;
#175964 = CARTESIAN_POINT ( 'NONE',  ( -4.483927247898782831, 16.52544592524335698, 42.70942372801901854 ) ) ;
#175965 = CARTESIAN_POINT ( 'NONE',  ( -0.05219959533936034679, 19.03943276465977164, 112.5010903946856757 ) ) ;
#175966 = CARTESIAN_POINT ( 'NONE',  ( 8.224510206698742110, 14.34966873604972548, 77.08442372801901854 ) ) ;
#175967 = CARTESIAN_POINT ( 'NONE',  ( 19.02544592524334988, 5.153800228976608722, 96.45942372801897591 ) ) ;
#175968 = CARTESIAN_POINT ( 'NONE',  ( -19.03943276465977164, 0.05219959533909376836, 71.24890960531435269 ) ) ;
#175969 = CARTESIAN_POINT ( 'NONE',  ( -21.55341960407610458, -5.719274019375992779, 96.45724293864770971 ) ) ;
#175971 = CARTESIAN_POINT ( 'NONE',  ( 5.153800228976615827, -19.02544592524334988, 105.2094237280190185 ) ) ;
#175970 = CARTESIAN_POINT ( 'NONE',  ( -8.224510206698948167, 14.34966873604960824, 95.41557627198102409 ) ) ;
#175972 = CARTESIAN_POINT ( 'NONE',  ( -12.14591786802326823, 12.06949235617739902, 73.12609039468567573 ) ) ;
#175973 = CARTESIAN_POINT ( 'NONE',  ( 23.91168844458708875, 8.792376985860574479, 168.9858545422794691 ) ) ;
#175974 = CARTESIAN_POINT ( 'NONE',  ( 16.46253265017146816, 9.564922557961045513, 71.66775706135233293 ) ) ;
#175975 = CARTESIAN_POINT ( 'NONE',  ( -14.34966873604960291, -8.224510206698953496, 36.66557627198103120 ) ) ;
#175976 = CARTESIAN_POINT ( 'NONE',  ( 16.52544592524342804, -4.483927247898539470, 98.54057627198105251 ) ) ;
#175978 = CARTESIAN_POINT ( 'NONE',  ( -17.48847506799967988, 5.747544572773787941, 90.82697437843279431 ) ) ;
#175977 = CARTESIAN_POINT ( 'NONE',  ( 0.05219959533936267826, -19.03943276465977164, 30.00109039468566863 ) ) ;
#175979 = CARTESIAN_POINT ( 'NONE',  ( -10.72451020669870658, -18.67979575497194134, 19.58442372801901143 ) ) ;
#175980 = CARTESIAN_POINT ( 'NONE',  ( 13.89961937509957401, 13.97604488694547697, 96.87609039468566152 ) ) ;
#175981 = CARTESIAN_POINT ( 'NONE',  ( -13.97604488694527625, -13.89961937509977652, 111.8739096053143243 ) ) ;
#175982 = CARTESIAN_POINT ( 'NONE',  ( -5.153800228976328057, -19.02544592524343514, 87.29057627198103830 ) ) ;
#175983 = CARTESIAN_POINT ( 'NONE',  ( -10.72451020669870658, -18.67979575497194134, 99.58442372801900433 ) ) ;
#175984 = CARTESIAN_POINT ( 'NONE',  ( 16.51473224551069308, 9.474510206698969483, 74.16557627198103830 ) ) ;
#175985 = CARTESIAN_POINT ( 'NONE',  ( -10.72451020669898014, 18.67979575497178502, 40.41557627198103120 ) ) ;
#175986 = CARTESIAN_POINT ( 'NONE',  ( -16.55341960407611168, -4.379528057220339221, 91.45724293864769550 ) ) ;
#175987 = CARTESIAN_POINT ( 'NONE',  ( -5.153800228976328057, -19.02544592524343514, 57.29057627198103120 ) ) ;
#175988 = CARTESIAN_POINT ( 'NONE',  ( -8.224510206698948167, 14.34966873604960824, 115.4155762719810241 ) ) ;
#175989 = CARTESIAN_POINT ( 'NONE',  ( 10.81492255796106328, -18.62759615963255655, 25.41775706135235779 ) ) ;
#175990 = CARTESIAN_POINT ( 'NONE',  ( 18.67979575497194134, -10.72451020669871369, 65.83442372801900433 ) ) ;
#175991 = CARTESIAN_POINT ( 'NONE',  ( 19.03943276465977164, -0.05219959533909143690, 43.74890960531435979 ) ) ;
#175992 = CARTESIAN_POINT ( 'NONE',  ( 4.379528057220092307, 16.55341960407617563, 82.29275706135234714 ) ) ;
#175993 = CARTESIAN_POINT ( 'NONE',  ( 10.81492255796106328, -18.62759615963255655, 20.41775706135234714 ) ) ;
#175994 = VERTEX_POINT ( 'NONE', #82838 ) ;
#175995 = CARTESIAN_POINT ( 'NONE',  ( -21.52544592524343514, 5.823673210054127303, 106.0405762719810525 ) ) ;
#175997 = CARTESIAN_POINT ( 'NONE',  ( 19.05341960407611168, 5.049401038298154454, 63.95724293864769550 ) ) ;
#175996 = CARTESIAN_POINT ( 'NONE',  ( -19.02544592524334988, -5.153800228976617603, 48.95942372801900433 ) ) ;
#175998 = CARTESIAN_POINT ( 'NONE',  ( 5.049401038297881783, 19.05341960407617563, 37.29275706135232582 ) ) ;
#175999 = CARTESIAN_POINT ( 'NONE',  ( 18.67979575497194134, -10.72451020669871369, 75.83442372801900433 ) ) ;
#176000 = VECTOR ( 'NONE', #147572, 1000.000000000000000 ) ;
#176001 = CARTESIAN_POINT ( 'NONE',  ( -18.67979575497178146, -10.72451020669898902, 76.66557627198103830 ) ) ;
#176002 = CARTESIAN_POINT ( 'NONE',  ( -16.52544592524342804, 4.483927247898546575, 51.04057627198103120 ) ) ;
#176004 = CARTESIAN_POINT ( 'NONE',  ( 19.02544592524334988, 5.153800228976608722, 26.45942372801899722 ) ) ;
#176003 = CARTESIAN_POINT ( 'NONE',  ( -18.67979575497193778, 10.72451020669871902, 88.33442372801901854 ) ) ;
#176005 = CARTESIAN_POINT ( 'NONE',  ( 0.05219959533910956823, 16.53943276465976808, 74.99890960531435269 ) ) ;
#176006 = CARTESIAN_POINT ( 'NONE',  ( 8.314922557960818139, 14.29746914071049879, 114.5822429386477097 ) ) ;
#176007 = CARTESIAN_POINT ( 'NONE',  ( 5.049401038297881783, 19.05341960407617563, 52.29275706135234003 ) ) ;
#176008 = CARTESIAN_POINT ( 'NONE',  ( 8.314922557961029526, -14.29746914071037800, 110.4177570613523756 ) ) ;
#176009 = CARTESIAN_POINT ( 'NONE',  ( 21.52544592524334988, 5.823673210054432836, 76.45942372801901854 ) ) ;
#176010 = CARTESIAN_POINT ( 'NONE',  ( -5.153800228976607833, 19.02544592524334988, 42.70942372801901143 ) ) ;
#176011 = CARTESIAN_POINT ( 'NONE',  ( -0.05219959533907301413, -21.53943276465977519, 57.49890960531435979 ) ) ;
#176012 = CARTESIAN_POINT ( 'NONE',  ( 10.81492255796106328, -18.62759615963255655, 50.41775706135235424 ) ) ;
#176013 = CARTESIAN_POINT ( 'NONE',  ( -21.55341960407610458, -5.719274019375992779, 101.4572429386476955 ) ) ;
#176014 = CARTESIAN_POINT ( 'NONE',  ( 13.89961937509957401, 13.97604488694547697, 91.87609039468567573 ) ) ;
#176015 = CARTESIAN_POINT ( 'NONE',  ( 14.29746914071037800, 8.314922557961029526, 66.66775706135234714 ) ) ;
#176017 = CARTESIAN_POINT ( 'NONE',  ( -21.52544592524343514, 5.823673210054127303, 111.0405762719810525 ) ) ;
#176016 = CARTESIAN_POINT ( 'NONE',  ( -14.93859650326285227, -17.05398664991142255, -57.95493304017681169 ) ) ;
#176018 = CARTESIAN_POINT ( 'NONE',  ( 8.224510206698953496, -14.34966873604960469, 92.91557627198103830 ) ) ;
#176019 = CARTESIAN_POINT ( 'NONE',  ( 36.91746824999999887, 11.99521256947799053, -10.02499999726881086 ) ) ;
#176020 = CARTESIAN_POINT ( 'NONE',  ( -4.379528057220086978, -16.55341960407618274, 34.79275706135235424 ) ) ;
#176021 = CARTESIAN_POINT ( 'NONE',  ( -21.52544592524343514, 5.823673210054127303, 51.04057627198103120 ) ) ;
#176022 = CARTESIAN_POINT ( 'NONE',  ( -0.05219959533934338120, 16.53943276465976808, 87.50109039468568994 ) ) ;
#176023 = CYLINDRICAL_SURFACE ( 'NONE', #9083, 28.82186960331498682 ) ;
#176024 = CARTESIAN_POINT ( 'NONE',  ( 14.34966873604972726, -8.224510206698740333, 70.83442372801901854 ) ) ;
#176025 = CARTESIAN_POINT ( 'NONE',  ( -15.80617190586768217, 15.72974639402176855, 38.12609039468567573 ) ) ;
#176026 = AXIS2_PLACEMENT_3D ( 'NONE', #159559, #69562, #116067 ) ;
#176027 = CARTESIAN_POINT ( 'NONE',  ( -15.72974639402197994, 15.80617190586746368, 55.62390960531436690 ) ) ;
#176028 = CARTESIAN_POINT ( 'NONE',  ( -12.14591786802326823, 12.06949235617739902, 78.12609039468570415 ) ) ;
#176029 = CARTESIAN_POINT ( 'NONE',  ( 21.55341960407619695, -5.719274019375665929, 76.04275706135237556 ) ) ;
#176030 = CARTESIAN_POINT ( 'NONE',  ( 15.72974639402199770, -15.80617190586745480, 48.12390960531436690 ) ) ;
#176031 = CARTESIAN_POINT ( 'NONE',  ( 15.80617190586746368, 15.72974639402197994, 34.37390960531435979 ) ) ;
#176032 = VERTEX_POINT ( 'NONE', #140544 ) ;
#176033 = CARTESIAN_POINT ( 'NONE',  ( 8.314922557961029526, -14.29746914071037800, 70.41775706135236135 ) ) ;
#176034 = CARTESIAN_POINT ( 'NONE',  ( -15.80617190586745835, -15.72974639402198527, 31.87390960531435979 ) ) ;
#176035 = VERTEX_POINT ( 'NONE', #78864 ) ;
#176036 = CARTESIAN_POINT ( 'NONE',  ( 0.05219959533909260263, 19.03943276465977164, 99.99890960531436690 ) ) ;
#176037 = CARTESIAN_POINT ( 'NONE',  ( -16.53943276465976808, 0.05219959533911058130, 26.24890960531435624 ) ) ;
#176038 = CARTESIAN_POINT ( 'NONE',  ( 17.60779699588839264, 5.500000000000008882, 73.84981316670106821 ) ) ;
#176039 = CARTESIAN_POINT ( 'NONE',  ( -8.224510206698948167, 14.34966873604960824, 110.4155762719810383 ) ) ;
#176040 = CARTESIAN_POINT ( 'NONE',  ( 15.72974639402199770, -15.80617190586745480, 43.12390960531435269 ) ) ;
#176041 = CARTESIAN_POINT ( 'NONE',  ( 19.05341960407611168, 5.049401038298154454, 43.95724293864769550 ) ) ;
#176042 = CARTESIAN_POINT ( 'NONE',  ( 16.55341960407618274, -4.379528057220086978, 91.04275706135236135 ) ) ;
#176043 = CARTESIAN_POINT ( 'NONE',  ( -21.55341960407619339, 5.719274019375674811, 28.54275706135234358 ) ) ;
#176044 = CARTESIAN_POINT ( 'NONE',  ( 19.02544592524334988, 5.153800228976608722, 96.45942372801897591 ) ) ;
#176045 = CARTESIAN_POINT ( 'NONE',  ( -8.314922557960811034, -14.29746914071050412, 97.08224293864770971 ) ) ;
#176046 = CARTESIAN_POINT ( 'NONE',  ( 9.474510206698971260, -16.51473224551069308, 57.91557627198103120 ) ) ;
#176047 = PRESENTATION_LAYER_ASSIGNMENT (  '', '', ( #179239 ) ) ;
#176048 = CARTESIAN_POINT ( 'NONE',  ( 13.89961937509977652, -13.97604488694527269, 28.12390960531435624 ) ) ;
#176049 = CARTESIAN_POINT ( 'NONE',  ( 17.72517630440434644, -5.499999999999995559, 63.42175719257210886 ) ) ;
#176050 = CARTESIAN_POINT ( 'NONE',  ( 19.03943276465977164, -0.05219959533909143690, 83.74890960531436690 ) ) ;
#176051 = EDGE_CURVE ( 'NONE', #134298, #186418, #89762, .T. ) ;
#176052 = CARTESIAN_POINT ( 'NONE',  ( -16.52544592524335698, -4.483927247898792601, 63.95942372801901854 ) ) ;
#176053 = CARTESIAN_POINT ( 'NONE',  ( 5.823673210054444382, -21.52544592524334988, 100.2094237280190043 ) ) ;
#176054 = CARTESIAN_POINT ( 'NONE',  ( -10.72451020669898014, 18.67979575497178502, 50.41557627198103120 ) ) ;
#176055 = CARTESIAN_POINT ( 'NONE',  ( 4.379528057220092307, 16.55341960407617563, 72.29275706135236135 ) ) ;
#176056 = CARTESIAN_POINT ( 'NONE',  ( -0.05219959533936034679, 19.03943276465977164, 67.50109039468566152 ) ) ;
#176057 = CARTESIAN_POINT ( 'NONE',  ( -15.80617190586768217, 15.72974639402176855, 58.12609039468568994 ) ) ;
#176059 = MECHANICAL_DESIGN_GEOMETRIC_PRESENTATION_REPRESENTATION (  '', ( #124365 ), #166258 ) ;
#176058 = CARTESIAN_POINT ( 'NONE',  ( 13.89961937509977652, -13.97604488694527269, 63.12390960531435979 ) ) ;
#176060 = CARTESIAN_POINT ( 'NONE',  ( 19.02544592524343514, -5.153800228976328945, 33.54057627198102409 ) ) ;
#176061 = CARTESIAN_POINT ( 'NONE',  ( 19.03943276465977164, 0.05219959533936151252, 56.25109039468566863 ) ) ;
#176062 = CARTESIAN_POINT ( 'NONE',  ( 19.03943276465977164, -0.05219959533909143690, 108.7489096053143527 ) ) ;
#176063 = CARTESIAN_POINT ( 'NONE',  ( -13.89961937509977652, 13.97604488694528158, 100.6239096053143669 ) ) ;
#176064 = CARTESIAN_POINT ( 'NONE',  ( 8.314922557960818139, 14.29746914071049879, 54.58224293864769550 ) ) ;
#176065 = CARTESIAN_POINT ( 'NONE',  ( -15.72974639402197994, 15.80617190586746368, 45.62390960531436690 ) ) ;
#176066 = DIRECTION ( 'NONE',  ( 1.000000000000000000, -0.000000000000000000, 0.000000000000000000 ) ) ;
#176067 = CARTESIAN_POINT ( 'NONE',  ( 16.51473224551083163, -9.474510206698727899, 35.83442372801899722 ) ) ;
#176068 = CARTESIAN_POINT ( 'NONE',  ( -13.89961937509977652, 13.97604488694528158, 55.62390960531434558 ) ) ;
#176069 = CARTESIAN_POINT ( 'NONE',  ( -11.30153831258470731, -180.0000000000000000, -4.999999999999999112 ) ) ;
#176070 = CARTESIAN_POINT ( 'NONE',  ( -17.49999999999999645, 5.622605283950888655, 108.6879268940389096 ) ) ;
#176071 = CARTESIAN_POINT ( 'NONE',  ( -16.53943276465976808, -0.05219959533934237506, 73.75109039468567573 ) ) ;
#176072 = CARTESIAN_POINT ( 'NONE',  ( 18.62759615963271287, -10.81492255796078972, 98.33224293864769550 ) ) ;
#176074 = CARTESIAN_POINT ( 'NONE',  ( 37.99999999999998579, -12.34694845685043951, -4.849999994537626868 ) ) ;
#176073 = CARTESIAN_POINT ( 'NONE',  ( -5.153800228976328057, -19.02544592524343514, 47.29057627198102409 ) ) ;
#176075 = CARTESIAN_POINT ( 'NONE',  ( -21.52544592524334988, -5.823673210054445271, 38.95942372801901854 ) ) ;
#176076 = CARTESIAN_POINT ( 'NONE',  ( -9.564922557961040184, 16.46253265017147172, 42.91775706135234003 ) ) ;
#176077 = CARTESIAN_POINT ( 'NONE',  ( 16.51473224551069308, 9.474510206698969483, 44.16557627198103120 ) ) ;
#176078 = CARTESIAN_POINT ( 'NONE',  ( 18.67979575497194134, -10.72451020669871369, 95.83442372801903275 ) ) ;
#176079 = CARTESIAN_POINT ( 'NONE',  ( -24.45434260692611517, -5.907237110200219021, 169.8064932912610914 ) ) ;
#176080 = CARTESIAN_POINT ( 'NONE',  ( -16.52544592524342804, 4.483927247898546575, 46.04057627198103830 ) ) ;
#176081 = CARTESIAN_POINT ( 'NONE',  ( 19.52851543214742591, 5.500000000000025757, 42.89357721762583253 ) ) ;
#176082 = CARTESIAN_POINT ( 'NONE',  ( -10.81492255796078084, -18.62759615963271287, 37.08224293864768129 ) ) ;
#176083 = CARTESIAN_POINT ( 'NONE',  ( -8.571926809382608425, 26.38167802310805854, 140.4750000027312069 ) ) ;
#176084 = CARTESIAN_POINT ( 'NONE',  ( 16.51473224551069308, 9.474510206698969483, 104.1655762719810241 ) ) ;
#176085 = CARTESIAN_POINT ( 'NONE',  ( 12.14591786802309770, 12.06949235617756955, 94.37390960531436690 ) ) ;
#176086 = CARTESIAN_POINT ( 'NONE',  ( 8.314922557961029526, -14.29746914071037800, 20.41775706135234714 ) ) ;
#176087 = CARTESIAN_POINT ( 'NONE',  ( -12.14591786802326823, 12.06949235617739902, 103.1260903946856757 ) ) ;
#176088 = ORIENTED_EDGE ( 'NONE', *, *, #168309, .F. ) ;
#176090 = CARTESIAN_POINT ( 'NONE',  ( 0.05219959533907565091, 21.53943276465977519, 99.99890960531436690 ) ) ;
#176089 = CARTESIAN_POINT ( 'NONE',  ( -13.89961937509977652, 13.97604488694528158, 95.62390960531436690 ) ) ;
#176092 = CARTESIAN_POINT ( 'NONE',  ( -16.46253265017160317, 9.564922557960807481, 95.83224293864769550 ) ) ;
#176091 = CARTESIAN_POINT ( 'NONE',  ( -12.14591786802326823, 12.06949235617739902, 113.1260903946856899 ) ) ;
#176093 = CARTESIAN_POINT ( 'NONE',  ( 13.97604488694548053, -13.89961937509957401, 95.62609039468563310 ) ) ;
#176094 = CARTESIAN_POINT ( 'NONE',  ( 21.52544592524334988, 5.823673210054432836, 111.4594237280190328 ) ) ;
#176095 = CARTESIAN_POINT ( 'NONE',  ( 21.53943276465977519, -0.05219959533907433946, 83.74890960531435269 ) ) ;
#176096 = CARTESIAN_POINT ( 'NONE',  ( -5.719274019375978568, 21.55341960407610458, 45.20724293864769550 ) ) ;
#176097 = CARTESIAN_POINT ( 'NONE',  ( 16.51473224551069308, 9.474510206698969483, 59.16557627198102409 ) ) ;
#176098 = CARTESIAN_POINT ( 'NONE',  ( -8.224510206698948167, 14.34966873604960824, 40.41557627198103120 ) ) ;
#176099 = CARTESIAN_POINT ( 'NONE',  ( 9.564922557960805705, 16.46253265017160317, 74.58224293864769550 ) ) ;
#176100 = EDGE_LOOP ( 'NONE', ( #177044, #2292, #6416, #108147 ) ) ;
#176101 = CARTESIAN_POINT ( 'NONE',  ( 18.56453257813367586, -5.499999999999872102, 63.49000423690685579 ) ) ;
#176102 = CARTESIAN_POINT ( 'NONE',  ( -5.049401038297874678, -19.05341960407617918, 39.79275706135232582 ) ) ;
#176103 = CARTESIAN_POINT ( 'NONE',  ( -16.55341960407611168, -4.379528057220339221, 81.45724293864769550 ) ) ;
#176104 = CARTESIAN_POINT ( 'NONE',  ( -21.53943276465977519, -0.05219959533937600094, 28.75109039468567929 ) ) ;
#176105 = CARTESIAN_POINT ( 'NONE',  ( -8.571926809382601320, -26.38167802310801591, 145.7750000027311899 ) ) ;
#176106 = CARTESIAN_POINT ( 'NONE',  ( 14.34966873604972726, -8.224510206698740333, 105.8344237280190328 ) ) ;
#176107 = CARTESIAN_POINT ( 'NONE',  ( 13.97604488694527802, 13.89961937509977652, 29.37390960531435979 ) ) ;
#176108 = CARTESIAN_POINT ( 'NONE',  ( -19.03943276465977164, 0.05219959533909376836, 66.24890960531436690 ) ) ;
#176109 =( NAMED_UNIT ( * ) SI_UNIT ( $, .STERADIAN. ) SOLID_ANGLE_UNIT ( ) );
#176110 = CARTESIAN_POINT ( 'NONE',  ( 19.02544592524343514, -5.153800228976328945, 23.54057627198102054 ) ) ;
#176111 = CARTESIAN_POINT ( 'NONE',  ( -16.55341960407611168, -4.379528057220339221, 46.45724293864769550 ) ) ;
#176112 = CARTESIAN_POINT ( 'NONE',  ( 0.05219959533937995610, -21.53943276465977519, 55.00109039468568284 ) ) ;
#176113 = CARTESIAN_POINT ( 'NONE',  ( 31.73299246115101724, -20.69072564976797324, -20.42656251077089991 ) ) ;
#176114 = CARTESIAN_POINT ( 'NONE',  ( 15.80617190586769283, -15.72974639402175789, 100.6260903946857184 ) ) ;
#176115 = CARTESIAN_POINT ( 'NONE',  ( -9.564922557960796823, -16.46253265017161027, 37.08224293864768839 ) ) ;
#176116 = CARTESIAN_POINT ( 'NONE',  ( -9.474510206698964154, 16.51473224551069663, 45.41557627198103120 ) ) ;
#176117 = ORIENTED_EDGE ( 'NONE', *, *, #95241, .F. ) ;
#176118 = CARTESIAN_POINT ( 'NONE',  ( 5.719274019375673035, 21.55341960407619339, 92.29275706135236135 ) ) ;
#176119 = CARTESIAN_POINT ( 'NONE',  ( -4.483927247898782831, 16.52544592524335698, 57.70942372801901143 ) ) ;
#176120 = CARTESIAN_POINT ( 'NONE',  ( 21.53943276465977519, 0.05219959533937863772, 86.25109039468568994 ) ) ;
#176121 = CARTESIAN_POINT ( 'NONE',  ( -21.55341960407610458, -5.719274019375992779, 26.45724293864768839 ) ) ;
#176122 = CARTESIAN_POINT ( 'NONE',  ( 16.51473224551083163, -9.474510206698727899, 95.83442372801900433 ) ) ;
#176123 = CARTESIAN_POINT ( 'NONE',  ( -21.55341960407619339, 5.719274019375674811, 68.54275706135234714 ) ) ;
#176124 = CARTESIAN_POINT ( 'NONE',  ( -14.29746914071037622, -8.314922557961029526, 39.16775706135235424 ) ) ;
#176126 = CARTESIAN_POINT ( 'NONE',  ( -5.719274019375978568, 21.55341960407610458, 85.20724293864770971 ) ) ;
#176125 = AXIS2_PLACEMENT_3D ( 'NONE', #67074, #175259, #68068 ) ;
#176127 = CARTESIAN_POINT ( 'NONE',  ( 13.89961937509957401, 13.97604488694547697, 91.87609039468567573 ) ) ;
#176128 = CARTESIAN_POINT ( 'NONE',  ( 13.89961937509977652, -13.97604488694527269, 63.12390960531435979 ) ) ;
#176129 = CARTESIAN_POINT ( 'NONE',  ( -5.153800228976607833, 19.02544592524334988, 102.7094237280189759 ) ) ;
#176130 = CARTESIAN_POINT ( 'NONE',  ( -19.02544592524334988, -5.153800228976617603, 103.9594237280190043 ) ) ;
#176131 = CARTESIAN_POINT ( 'NONE',  ( -12.14591786802309592, -12.06949235617757132, 56.87390960531436690 ) ) ;
#176132 = CARTESIAN_POINT ( 'NONE',  ( 19.03943276465977164, 0.05219959533936151252, 81.25109039468567573 ) ) ;
#176133 = CARTESIAN_POINT ( 'NONE',  ( 14.34966873604972726, -8.224510206698740333, 65.83442372801900433 ) ) ;
#176135 = CARTESIAN_POINT ( 'NONE',  ( -16.46253265017160317, 9.564922557960807481, 35.83224293864768839 ) ) ;
#176134 = CARTESIAN_POINT ( 'NONE',  ( 15.80617190586746368, 15.72974639402197994, 114.3739096053143527 ) ) ;
#176136 = CARTESIAN_POINT ( 'NONE',  ( 9.474510206698971260, -16.51473224551069308, 52.91557627198102409 ) ) ;
#176137 = CARTESIAN_POINT ( 'NONE',  ( 4.379528057220092307, 16.55341960407617563, 62.29275706135236845 ) ) ;
#176138 = CARTESIAN_POINT ( 'NONE',  ( -8.571926809382601320, -26.38167802310801591, 141.7750000027311899 ) ) ;
#176139 = FACE_OUTER_BOUND ( 'NONE', #145043, .T. ) ;
#176140 = CARTESIAN_POINT ( 'NONE',  ( 13.97604488694527802, 13.89961937509977652, 99.37390960531436690 ) ) ;
#176141 = EDGE_CURVE ( 'NONE', #144387, #24966, #47762, .T. ) ;
#176142 = CARTESIAN_POINT ( 'NONE',  ( 9.474510206698971260, -16.51473224551069308, 22.91557627198102765 ) ) ;
#176143 = CARTESIAN_POINT ( 'NONE',  ( -9.564922557961040184, 16.46253265017147172, 107.9177570613523471 ) ) ;
#176144 = CARTESIAN_POINT ( 'NONE',  ( -10.72451020669898014, 18.67979575497178502, 40.41557627198103120 ) ) ;
#176146 = CARTESIAN_POINT ( 'NONE',  ( -0.05219959533934338120, 16.53943276465976808, 27.50109039468567929 ) ) ;
#176145 = CARTESIAN_POINT ( 'NONE',  ( 19.05341960407617918, -5.049401038297876454, 26.04275706135233293 ) ) ;
#176147 = CARTESIAN_POINT ( 'NONE',  ( 9.564922557960805705, 16.46253265017160317, 29.58224293864769550 ) ) ;
#176148 = CARTESIAN_POINT ( 'NONE',  ( 16.46253265017160672, -9.564922557960803928, 48.33224293864769550 ) ) ;
#176149 = CARTESIAN_POINT ( 'NONE',  ( -21.55341960407610458, -5.719274019375992779, 81.45724293864769550 ) ) ;
#176150 = CARTESIAN_POINT ( 'NONE',  ( 19.02544592524343514, -5.153800228976328945, 103.5405762719809957 ) ) ;
#176151 = CARTESIAN_POINT ( 'NONE',  ( -19.02544592524342804, 5.153800228976336051, 46.04057627198101699 ) ) ;
#176152 = CARTESIAN_POINT ( 'NONE',  ( 27.73933785331498925, -9.013057229001034898, 146.2750000027311899 ) ) ;
#176153 = CARTESIAN_POINT ( 'NONE',  ( -19.02544592524334988, -5.153800228976617603, 78.95942372801900433 ) ) ;
#176154 = CARTESIAN_POINT ( 'NONE',  ( 16.53943276465976808, -0.05219959533910856209, 68.74890960531435269 ) ) ;
#176155 = CARTESIAN_POINT ( 'NONE',  ( -21.52544592524334988, -5.823673210054445271, 103.9594237280190185 ) ) ;
#176156 = EDGE_CURVE ( 'NONE', #168659, #60925, #101468, .T. ) ;
#176157 = CARTESIAN_POINT ( 'NONE',  ( 15.80617190586746368, 15.72974639402197994, 99.37390960531436690 ) ) ;
#176158 = CARTESIAN_POINT ( 'NONE',  ( -18.62759615963255300, -10.81492255796106328, 79.16775706135234714 ) ) ;
#176159 = CARTESIAN_POINT ( 'NONE',  ( 15.80617190586769283, -15.72974639402175789, 75.62609039468567573 ) ) ;
#176160 = CARTESIAN_POINT ( 'NONE',  ( 5.049401038298161559, -19.05341960407611168, 112.7072429386476813 ) ) ;
#176162 = CARTESIAN_POINT ( 'NONE',  ( -21.52544592524334988, -5.823673210054445271, 78.95942372801901854 ) ) ;
#176161 = CARTESIAN_POINT ( 'NONE',  ( -8.314922557961024197, 14.29746914071037800, 112.9177570613523329 ) ) ;
#176163 = CARTESIAN_POINT ( 'NONE',  ( -13.89961937509977652, 13.97604488694528158, 60.62390960531436690 ) ) ;
#176164 = CARTESIAN_POINT ( 'NONE',  ( -10.72451020669870658, -18.67979575497194134, 29.58442372801901854 ) ) ;
#176165 = CARTESIAN_POINT ( 'NONE',  ( -19.02544592524342804, 5.153800228976336051, 86.04057627198103830 ) ) ;
#176166 = CARTESIAN_POINT ( 'NONE',  ( 14.29746914071049879, -8.314922557960816363, 78.33224293864770971 ) ) ;
#176167 = CARTESIAN_POINT ( 'NONE',  ( -4.483927247898539470, -16.52544592524342804, 47.29057627198103120 ) ) ;
#176168 = CARTESIAN_POINT ( 'NONE',  ( -10.72451020669898014, 18.67979575497178502, 60.41557627198102409 ) ) ;
#176169 = CARTESIAN_POINT ( 'NONE',  ( 0.05219959533909260263, 19.03943276465977164, 54.99890960531435979 ) ) ;
#176170 = CARTESIAN_POINT ( 'NONE',  ( -21.53943276465977519, 0.05219959533907696930, 66.24890960531436690 ) ) ;
#176171 = CIRCLE ( 'NONE', #89013, 13.70000000000001528 ) ;
#176172 = CARTESIAN_POINT ( 'NONE',  ( -16.51473224551082808, 9.474510206698731452, 63.33442372801900433 ) ) ;
#176174 = CARTESIAN_POINT ( 'NONE',  ( 14.29746914071049879, -8.314922557960816363, 78.33224293864770971 ) ) ;
#176173 = CARTESIAN_POINT ( 'NONE',  ( 16.51473224551083163, -9.474510206698727899, 25.83442372801900078 ) ) ;
#176175 = CARTESIAN_POINT ( 'NONE',  ( 21.53943276465977519, -0.05219959533907433946, 53.74890960531437401 ) ) ;
#176176 = ORIENTED_EDGE ( 'NONE', *, *, #4069, .F. ) ;
#176177 = CARTESIAN_POINT ( 'NONE',  ( -3.573655867282028392E-15, 2.428612866367529932E-14, -25.00000000000000000 ) ) ;
#176179 = CARTESIAN_POINT ( 'NONE',  ( -8.571926809382601320, -26.38167802310801591, 145.7750000027311899 ) ) ;
#176178 = CARTESIAN_POINT ( 'NONE',  ( 4.483927247898790824, -16.52544592524335698, 100.2094237280190043 ) ) ;
#176180 = CARTESIAN_POINT ( 'NONE',  ( 16.51473224551083163, -9.474510206698727899, 90.83442372801900433 ) ) ;
#176181 = CARTESIAN_POINT ( 'NONE',  ( 16.53943276465976808, -0.05219959533910856209, 63.74890960531435979 ) ) ;
#176182 = DIRECTION ( 'NONE',  ( 0.000000000000000000, 0.000000000000000000, 1.000000000000000000 ) ) ;
#176183 = CARTESIAN_POINT ( 'NONE',  ( 5.153800228976335163, 19.02544592524342804, 64.79057627198100988 ) ) ;
#176184 = CARTESIAN_POINT ( 'NONE',  ( 16.55341960407611168, 4.379528057220329451, 58.95724293864770971 ) ) ;
#176185 = EDGE_CURVE ( 'NONE', #100590, #4163, #5002, .T. ) ;
#176186 = CARTESIAN_POINT ( 'NONE',  ( 19.03943276465977164, -0.05219959533909143690, 88.74890960531436690 ) ) ;
#176188 = CARTESIAN_POINT ( 'NONE',  ( 19.02544592524343514, -5.153800228976328945, 58.54057627198102409 ) ) ;
#176187 = CARTESIAN_POINT ( 'NONE',  ( -0.05219959533936034679, 19.03943276465977164, 77.50109039468566152 ) ) ;
#176189 = CARTESIAN_POINT ( 'NONE',  ( 9.564922557960805705, 16.46253265017160317, 84.58224293864769550 ) ) ;
#176190 = CARTESIAN_POINT ( 'NONE',  ( -9.474510206698964154, 16.51473224551069663, 75.41557627198103830 ) ) ;
#176191 = CARTESIAN_POINT ( 'NONE',  ( -10.72451020669898014, 18.67979575497178502, 60.41557627198102409 ) ) ;
#176192 = CARTESIAN_POINT ( 'NONE',  ( 0.05219959533934541429, -16.53943276465976808, 60.00109039468568284 ) ) ;
#176193 = CARTESIAN_POINT ( 'NONE',  ( 18.22780087662123805, 5.499999999999960032, 101.4823681787310647 ) ) ;
#176194 = CARTESIAN_POINT ( 'NONE',  ( -9.564922557960796823, -16.46253265017161027, 52.08224293864768839 ) ) ;
#176195 = CARTESIAN_POINT ( 'NONE',  ( -21.52544592524343514, 5.823673210054127303, 51.04057627198103120 ) ) ;
#176196 = CARTESIAN_POINT ( 'NONE',  ( 0.05219959533936267826, -19.03943276465977164, 75.00109039468566152 ) ) ;
#176197 = CARTESIAN_POINT ( 'NONE',  ( -16.52544592524342804, 4.483927247898546575, 26.04057627198103475 ) ) ;
#176198 = CARTESIAN_POINT ( 'NONE',  ( 5.153800228976615827, -19.02544592524334988, 35.20942372801899722 ) ) ;
#176200 = CARTESIAN_POINT ( 'NONE',  ( 16.53943276465976808, 0.05219959533934440121, 91.25109039468568994 ) ) ;
#176199 = CARTESIAN_POINT ( 'NONE',  ( -16.55341960407617563, 4.379528057220093196, 58.54275706135235424 ) ) ;
#176201 = CARTESIAN_POINT ( 'NONE',  ( -18.22780087662123805, -5.499999999999968026, 93.98236817873105053 ) ) ;
#176202 = CARTESIAN_POINT ( 'NONE',  ( -16.55341960407617563, 4.379528057220093196, 83.54275706135234714 ) ) ;
#176203 = CARTESIAN_POINT ( 'NONE',  ( -19.02544592524342804, 5.153800228976336051, 116.0405762719810383 ) ) ;
#176204 = CARTESIAN_POINT ( 'NONE',  ( 0.05219959533909260263, 19.03943276465977164, 39.99890960531436690 ) ) ;
#176205 = CARTESIAN_POINT ( 'NONE',  ( 16.51473224551069308, 9.474510206698969483, 44.16557627198103120 ) ) ;
#176206 = CARTESIAN_POINT ( 'NONE',  ( -19.03943276465977164, 0.05219959533909376836, 41.24890960531435269 ) ) ;
#176207 = CARTESIAN_POINT ( 'NONE',  ( -21.52544592524334988, -5.823673210054445271, 33.95942372801901143 ) ) ;
#176208 = CARTESIAN_POINT ( 'NONE',  ( -8.224510206698735004, -14.34966873604973081, 54.58442372801901143 ) ) ;
#176209 = CARTESIAN_POINT ( 'NONE',  ( 8.224510206698742110, 14.34966873604972548, 112.0844237280190185 ) ) ;
#176210 = CARTESIAN_POINT ( 'NONE',  ( -16.46253265017160317, 9.564922557960807481, 30.83224293864769550 ) ) ;
#176211 = CARTESIAN_POINT ( 'NONE',  ( -21.55341960407619339, 5.719274019375674811, 113.5427570613523756 ) ) ;
#176212 = CARTESIAN_POINT ( 'NONE',  ( -9.564922557961040184, 16.46253265017147172, 107.9177570613523471 ) ) ;
#176213 = CARTESIAN_POINT ( 'NONE',  ( -16.46253265017146816, -9.564922557961047289, 74.16775706135234714 ) ) ;
#176214 = CARTESIAN_POINT ( 'NONE',  ( -16.55341960407611168, -4.379528057220339221, 71.45724293864769550 ) ) ;
#176215 = CARTESIAN_POINT ( 'NONE',  ( -9.564922557960796823, -16.46253265017161027, 37.08224293864768839 ) ) ;
#176217 = DIRECTION ( 'NONE',  ( -1.000000000000000000, 0.000000000000000000, 0.000000000000000000 ) ) ;
#176216 = CARTESIAN_POINT ( 'NONE',  ( -0.05219959533936034679, 19.03943276465977164, 77.50109039468566152 ) ) ;
#176218 = CARTESIAN_POINT ( 'NONE',  ( -21.52544592524334988, -5.823673210054445271, 78.95942372801901854 ) ) ;
#176219 = CARTESIAN_POINT ( 'NONE',  ( 14.29746914071037800, 8.314922557961029526, 41.66775706135235424 ) ) ;
#176220 = CARTESIAN_POINT ( 'NONE',  ( 18.22780087662122384, -5.500000000000022204, 56.01540105326107977 ) ) ;
#176221 = CARTESIAN_POINT ( 'NONE',  ( -5.719274019375978568, 21.55341960407610458, 35.20724293864768839 ) ) ;
#176222 = CARTESIAN_POINT ( 'NONE',  ( -4.483927247898782831, 16.52544592524335698, 32.70942372801900433 ) ) ;
#176223 = DIRECTION ( 'NONE',  ( -0.06104853953485701173, -7.476289853398329258E-18, -0.9981347984218670311 ) ) ;
#176224 = CARTESIAN_POINT ( 'NONE',  ( -21.55341960407619339, 5.719274019375674811, 108.5427570613523756 ) ) ;
#176225 = CARTESIAN_POINT ( 'NONE',  ( -21.93180397000028492, 9.000796715316637275, 171.3297436093417900 ) ) ;
#176226 = CARTESIAN_POINT ( 'NONE',  ( -9.474510206698964154, 16.51473224551069663, 40.41557627198103120 ) ) ;
#176227 = CARTESIAN_POINT ( 'NONE',  ( 9.474510206698729675, 16.51473224551082808, 57.08442372801900433 ) ) ;
#176228 = CARTESIAN_POINT ( 'NONE',  ( -19.02544592524342804, 5.153800228976336051, 56.04057627198100988 ) ) ;
#176229 = CARTESIAN_POINT ( 'NONE',  ( 10.81492255796106328, -18.62759615963255655, 60.41775706135235424 ) ) ;
#176230 = CARTESIAN_POINT ( 'NONE',  ( 19.03943276465977164, 0.05219959533936151252, 26.25109039468566507 ) ) ;
#176231 = CARTESIAN_POINT ( 'NONE',  ( -14.34966873604960291, -8.224510206698953496, 21.66557627198102409 ) ) ;
#176232 = CARTESIAN_POINT ( 'NONE',  ( 5.153800228976335163, 19.02544592524342804, 34.79057627198102409 ) ) ;
#176233 = CARTESIAN_POINT ( 'NONE',  ( 5.049401038298161559, -19.05341960407611168, 87.70724293864769550 ) ) ;
#176234 = CARTESIAN_POINT ( 'NONE',  ( 18.67979575497194134, -10.72451020669871369, 55.83442372801901854 ) ) ;
#176235 = CARTESIAN_POINT ( 'NONE',  ( 5.153800228976335163, 19.02544592524342804, 39.79057627198100988 ) ) ;
#176236 = CARTESIAN_POINT ( 'NONE',  ( -0.05219959533937732626, 21.53943276465977519, 72.50109039468568994 ) ) ;
#176238 = CARTESIAN_POINT ( 'NONE',  ( -0.05219959533909027116, -19.03943276465977164, 107.4989096053143527 ) ) ;
#176237 = CARTESIAN_POINT ( 'NONE',  ( -16.46253265017146816, -9.564922557961047289, 89.16775706135234714 ) ) ;
#176239 = CARTESIAN_POINT ( 'NONE',  ( -16.52544592524342804, 4.483927247898546575, 111.0405762719810525 ) ) ;
#176240 = CARTESIAN_POINT ( 'NONE',  ( 15.80617190586746368, 15.72974639402197994, 109.3739096053143811 ) ) ;
#176241 = CARTESIAN_POINT ( 'NONE',  ( 19.05341960407617918, -5.049401038297876454, 41.04275706135233293 ) ) ;
#176242 = CARTESIAN_POINT ( 'NONE',  ( 12.14591786802309770, 12.06949235617756955, 109.3739096053143811 ) ) ;
#176243 = CARTESIAN_POINT ( 'NONE',  ( 9.564922557960805705, 16.46253265017160317, 69.58224293864770971 ) ) ;
#176244 = CARTESIAN_POINT ( 'NONE',  ( -5.049401038297874678, -19.05341960407617918, 99.79275706135234714 ) ) ;
#176245 = CARTESIAN_POINT ( 'NONE',  ( -0.05219959533910754901, -16.53943276465976808, 62.49890960531436690 ) ) ;
#176246 = CARTESIAN_POINT ( 'NONE',  ( -13.89961937509957401, -13.97604488694547875, 24.37609039468565442 ) ) ;
#176247 = CARTESIAN_POINT ( 'NONE',  ( 21.52544592524344225, -5.823673210054117533, 23.54057627198102765 ) ) ;
#176248 = CARTESIAN_POINT ( 'NONE',  ( 5.049401038297881783, 19.05341960407617563, 92.29275706135234714 ) ) ;
#176249 = CARTESIAN_POINT ( 'NONE',  ( -18.67979575497178146, -10.72451020669898902, 96.66557627198102409 ) ) ;
#176250 = CARTESIAN_POINT ( 'NONE',  ( -21.55341960407619339, 5.719274019375674811, 43.54275706135235424 ) ) ;
#176251 = CARTESIAN_POINT ( 'NONE',  ( 12.14591786802327356, -12.06949235617739191, 40.62609039468567573 ) ) ;
#176252 = CARTESIAN_POINT ( 'NONE',  ( -4.379528057220086978, -16.55341960407618274, 109.7927570613523613 ) ) ;
#176254 = CARTESIAN_POINT ( 'NONE',  ( 18.62759615963255655, 10.81492255796105972, 46.66775706135234714 ) ) ;
#176253 = CARTESIAN_POINT ( 'NONE',  ( 8.224510206698742110, 14.34966873604972548, 37.08442372801901143 ) ) ;
#176255 = CARTESIAN_POINT ( 'NONE',  ( -18.62759615963270932, 10.81492255796079327, 60.83224293864769550 ) ) ;
#176256 = CARTESIAN_POINT ( 'NONE',  ( 9.474510206698971260, -16.51473224551069308, 32.91557627198102409 ) ) ;
#176257 = CARTESIAN_POINT ( 'NONE',  ( 0.000000000000000000, -165.0000000000000000, 12.00000000000000355 ) ) ;
#176258 = CARTESIAN_POINT ( 'NONE',  ( -8.224510206698735004, -14.34966873604973081, 69.58442372801900433 ) ) ;
#176259 = CARTESIAN_POINT ( 'NONE',  ( 18.62759615963271287, -10.81492255796078972, 88.33224293864769550 ) ) ;
#176260 = CARTESIAN_POINT ( 'NONE',  ( -8.314922557960811034, -14.29746914071050412, 37.08224293864768129 ) ) ;
#176261 = CARTESIAN_POINT ( 'NONE',  ( 8.224510206698742110, 14.34966873604972548, 62.08442372801901143 ) ) ;
#176262 = CARTESIAN_POINT ( 'NONE',  ( -5.049401038297874678, -19.05341960407617918, 94.79275706135230450 ) ) ;
#176263 = CARTESIAN_POINT ( 'NONE',  ( 21.53943276465977519, -0.05219959533907433946, 98.74890960531438111 ) ) ;
#176264 = CARTESIAN_POINT ( 'NONE',  ( -16.53943276465976808, 0.05219959533911058130, 26.24890960531435624 ) ) ;
#176265 = ORIENTED_EDGE ( 'NONE', *, *, #140456, .F. ) ;
#176266 = CARTESIAN_POINT ( 'NONE',  ( -0.05219959533934338120, 16.53943276465976808, 82.50109039468568994 ) ) ;
#176267 = CARTESIAN_POINT ( 'NONE',  ( 20.56371838171434874, 11.43208494587337043, 170.0924998638764976 ) ) ;
#176268 = CARTESIAN_POINT ( 'NONE',  ( 10.72451020669898902, -18.67979575497178502, 72.91557627198103830 ) ) ;
#176269 = EDGE_LOOP ( 'NONE', ( #189471, #108486, #47313, #169037, #61713, #149257 ) ) ;
#176270 = CARTESIAN_POINT ( 'NONE',  ( 12.14591786802327356, -12.06949235617739191, 100.6260903946857184 ) ) ;
#176271 = ORIENTED_EDGE ( 'NONE', *, *, #109281, .T. ) ;
#176272 = CARTESIAN_POINT ( 'NONE',  ( -11.30153831258470731, -190.0000000000000000, 0.000000000000000000 ) ) ;
#176273 = CARTESIAN_POINT ( 'NONE',  ( 5.719274019375991003, -21.55341960407610458, 102.7072429386476955 ) ) ;
#176274 = CIRCLE ( 'NONE', #21240, 24.30000000000003268 ) ;
#176275 = CARTESIAN_POINT ( 'NONE',  ( -21.55341960407610458, -5.719274019375992779, 111.4572429386476813 ) ) ;
#176276 = CARTESIAN_POINT ( 'NONE',  ( 8.314922557960818139, 14.29746914071049879, 44.58224293864769550 ) ) ;
#176277 = CARTESIAN_POINT ( 'NONE',  ( 14.29746914071037800, 8.314922557961029526, 31.66775706135234358 ) ) ;
#176278 = CARTESIAN_POINT ( 'NONE',  ( 16.51473224551069308, 9.474510206698969483, 54.16557627198103120 ) ) ;
#176279 = CARTESIAN_POINT ( 'NONE',  ( -19.02544592524342804, 5.153800228976336051, 61.04057627198103120 ) ) ;
#176280 = CARTESIAN_POINT ( 'NONE',  ( 10.72451020669898902, -18.67979575497178502, 22.91557627198102765 ) ) ;
#176281 = CARTESIAN_POINT ( 'NONE',  ( 17.50000000000000355, 5.500000000000011546, 78.78230962303567253 ) ) ;
#176282 = CARTESIAN_POINT ( 'NONE',  ( -9.474510206698720793, -16.51473224551083518, 99.58442372801900433 ) ) ;
#176283 = CARTESIAN_POINT ( 'NONE',  ( -19.03943276465977164, -0.05219959533935918106, 53.75109039468566863 ) ) ;
#176284 = CARTESIAN_POINT ( 'NONE',  ( -5.823673210054116645, -21.52544592524344225, 82.29057627198103830 ) ) ;
#176285 = CARTESIAN_POINT ( 'NONE',  ( -16.52544592524342804, 4.483927247898546575, 26.04057627198103475 ) ) ;
#176286 = CARTESIAN_POINT ( 'NONE',  ( -18.67979575497178146, -10.72451020669898902, 41.66557627198103120 ) ) ;
#176288 = CARTESIAN_POINT ( 'NONE',  ( 16.51473224551083163, -9.474510206698727899, 100.8344237280190043 ) ) ;
#176287 = CARTESIAN_POINT ( 'NONE',  ( 15.80617190586746368, 15.72974639402197994, 79.37390960531436690 ) ) ;
#176289 = CARTESIAN_POINT ( 'NONE',  ( -16.46253265017160317, 9.564922557960807481, 110.8322429386476955 ) ) ;
#176290 = CARTESIAN_POINT ( 'NONE',  ( 21.55341960407619695, -5.719274019375665929, 81.04275706135236135 ) ) ;
#176291 = CARTESIAN_POINT ( 'NONE',  ( 5.049401038298161559, -19.05341960407611168, 77.70724293864765286 ) ) ;
#176292 = DIRECTION ( 'NONE',  ( -1.000000000000000000, 0.000000000000000000, 0.000000000000000000 ) ) ;
#176293 = CARTESIAN_POINT ( 'NONE',  ( -16.46253265017160317, 9.564922557960807481, 75.83224293864769550 ) ) ;
#176294 = CARTESIAN_POINT ( 'NONE',  ( 4.483927247898545687, 16.52544592524342804, 94.79057627198105251 ) ) ;
#176295 = ORIENTED_EDGE ( 'NONE', *, *, #76288, .T. ) ;
#176296 = CARTESIAN_POINT ( 'NONE',  ( -5.153800228976607833, 19.02544592524334988, 107.7094237280189759 ) ) ;
#176297 = DIRECTION ( 'NONE',  ( -1.000000000000000000, 0.000000000000000000, -4.336808689942016750E-16 ) ) ;
#176298 = CARTESIAN_POINT ( 'NONE',  ( 19.03943276465977164, -0.05219959533909143690, 78.74890960531436690 ) ) ;
#176300 = CARTESIAN_POINT ( 'NONE',  ( 16.51473224551069308, 9.474510206698969483, 94.16557627198103830 ) ) ;
#176299 = CARTESIAN_POINT ( 'NONE',  ( 21.53943276465977519, 0.05219959533937863772, 86.25109039468568994 ) ) ;
#176301 = CARTESIAN_POINT ( 'NONE',  ( 14.29746914071037800, 8.314922557961029526, 76.66775706135234714 ) ) ;
#176302 = CARTESIAN_POINT ( 'NONE',  ( -31.20457203169703675, 1.278449583442399451, -46.64972497815392671 ) ) ;
#176303 = CARTESIAN_POINT ( 'NONE',  ( 16.51473224551083163, -9.474510206698727899, 55.83442372801899722 ) ) ;
#176304 = CARTESIAN_POINT ( 'NONE',  ( -19.02544592524334988, -5.153800228976617603, 18.95942372801899722 ) ) ;
#176305 = CARTESIAN_POINT ( 'NONE',  ( -30.00000000000000000, -5.510910596163089556E-15, 45.00000000000000000 ) ) ;
#176306 = DIRECTION ( 'NONE',  ( 0.000000000000000000, 0.000000000000000000, 1.000000000000000000 ) ) ;
#176307 = CARTESIAN_POINT ( 'NONE',  ( -5.950531402560715689E-15, 38.81732327939063509, -3.624999997268813168 ) ) ;
#176308 = CARTESIAN_POINT ( 'NONE',  ( 8.224510206698742110, 14.34966873604972548, 112.0844237280190185 ) ) ;
#176309 = EDGE_CURVE ( 'NONE', #71928, #84310, #109090, .T. ) ;
#176310 = CARTESIAN_POINT ( 'NONE',  ( 32.00000000000000000, -5.510910596163089556E-15, 45.00000000000000000 ) ) ;
#176311 = CARTESIAN_POINT ( 'NONE',  ( -16.53943276465976808, -0.05219959533934237506, 103.7510903946857042 ) ) ;
#176312 = CARTESIAN_POINT ( 'NONE',  ( 17.49999999999999645, 5.622605283950886879, 68.81207310596114723 ) ) ;
#176313 =( BOUNDED_SURFACE ( )  B_SPLINE_SURFACE ( 3, 2, ( 
 ( #85033, #131554, #86048, #160894, #84036, #5197, #70891, #66879, #181079, #197235, #13209, #89041, #56728, #10223, #44535, #75849, #72901, #73893, #88038, #105208, #199207, #104217, #152690, #165898, #134570, #25408, #119396, #196257, #42554, #27396, #29373, #166895, #106190, #198215, #57726, #58696, #150731, #184038, #164905, #135563, #14179, #136534, #167874, #121358, #71883, #133553, #148735, #41560, #91004, #12231, #120366, #182059, #103223, #87050, #28395, #137525, #43542, #60674, #90034, #151716, #122349, #59687, #74872, #102223, #183051, #195244, #163912, #118398, #180092, #26399, #149726, #11227, #140503, #107175, #93995, #126326, #49495, #127309, #186034, #187043, #984, #172846, #170851, #109172, #123333, #65647, #188023, #111157, #62659, #1992, #34327, #48513, #110167, #30351, #124338, #76842, #45521, #185026, #33334, #168846, #157673, #32342, #95988, #142489, #171846, #91993, #47516, #15183, #19162, #80810, #94994, #3967, #155676, #153687, #17171, #138513, #92029, #154684, #61664, #156680, #46513, #108172, #18174, #79831, #169853, #77834, #31347, #78825, #92998, #63671, #16179, #141501, #139501, #2985, #125345, #64664, #130288, #5958, #174829, #68632, #23145, #160649, #37300, #189020, #51477, #115146, #112158, #84789, #98959, #162649, #22141, #131309, #24155, #38310, #144474, #83791, #176839, #129295, #145471, #175827, #69643, #113139, #128303, #50494, #36293, #191982, #6952, #67636, #85806, #97949, #159641, #99965, #54476, #20139, #190991, #52467, #158647, #147492, #53469, #161649, #146468, #192999, #190003, #177837, #8983, #116146, #39305, #7960, #100964, #114125, #70651, #173847, #35313, #96967, #81784, #143471, #4955, #21137, #66640, #82792, #164661, #182816, #120132, #181823, #167642, #56477, #163661, #148492, #55472, #26156, #73654, #59448, #103977, #104970, #25164, #194009, #29138, #117142, #178837, #40305, #87798, #121121, #101981, #44298, #194999, #196999, #118155, #89800, #151482, #74637, #136303, #43302, #86806, #9983, #166657, #90775, #197978, #105957, #102976, #149483, #152459, #132317, #10979, #165656, #179845, #13945, #88801, #71643, #133310, #58465, #119157, #41316, #72652, #134327, #42316, #196012, #57487, #180839, #28158, #12973, #27154, #150494, #135326, #11991, #60439, #31115, #106943, #75611, #14949, #63433, #95752, #187794, #139275, #64428, #172607, #78590, #198972, #154453, #45291, #79593, #110921, #140263, #126098, #92763, #34094, #47282, #49263, #168616, #184790, #157437, #1755, #122114, #138287, #125109, #186807, #137290, #107932, #183803, #108938, #30116, #93765, #153451, #48277, #169618, #91757, #141262, #76609, #15945, #170619, #109932, #62423, #199968, #61433, #17939, #123105, #46276, #32108, #77604, #171614, #752, #124095, #185794, #155446, #16936, #33102, #94758, #156440, #2752, #20900, #146231, #83558, #22907, #114907, #189774, #175589, #5724, #100728, #81551, #190759, #69404, #53231, #84553, #38075, #188782, #50265, #65413, #158421, #7718, #51246, #36066, #112906, #19909, #142251, #21907, #131070, #174600, #161415, #52234, #82558, #177603, #176601, #37065, #192759, #144240, #111923, #39071, #35079, #113891, #173609, #96732, #145237, #98724, #80577, #67403, #99731, #54242, #18932, #159405, #160418, #97715, #115913, #129058, #6718, #143237, #3736, #127074, #4720, #68396, #130048, #66409, #191748, #128071, #180611, #40061, #165428, #56238, #23911, #166428, #59214, #41081, #57252, #73424, #149256, #116905, #70412, #104737, #136073, #133074, #134089, #148253, #26923, #120883, #164432, #12742, #25926, #194764, #85565, #179608, #117919, #102744, #87569, #89566, #88565, #27923, #58239, #10748, #118926, #72412, #44065, #24924, #195779, #74407, #196771, #151252, #181593, #132079, #193768, #8742, #101738, #197747, #42084, #103749, #150263, #163426, #147251, #11757, #182582, #135095, #162409, #119907, #43070, #55237, #178598, #86569, #9746, #71410, #75381 ),
 ( #47041, #61197, #32863, #30880, #169372, #183571, #125857, #48038, #186565, #122869, #513, #109694, #108698, #170377, #90548, #184557, #137053, #105725, #45056, #93522, #187557, #17695, #92527, #94513, #2510, #31868, #28908, #46038, #198743, #171376, #141023, #155207, #156195, #107693, #64190, #77366, #79352, #60208, #14713, #167412, #16696, #152230, #168388, #78346, #140020, #13715, #1509, #63186, #121878, #29883, #106714, #91521, #153208, #199731, #124866, #76373, #139034, #138050, #154216, #15706, #62185, #123849, #185547, #157195, #4476, #176358, #33849, #37831, #111681, #113653, #173368, #6476, #68156, #191507, #52983, #160174, #18689, #3497, #36815, #7477, #114662, #99491, #19673, #81315, #161171, #49024, #127828, #82310, #96493, #69161, #5481, #172359, #65173, #175347, #35829, #22668, #50016, #84315, #159161, #34838, #145994, #158183, #98481, #21664, #142998, #144995, #130828, #66166, #190520, #189534, #51006, #128821, #83318, #20656, #97475, #110679, #112667, #129808, #95509, #80336, #144000, #142008, #67164, #126832, #188538, #174359, #51994, #164189, #118680, #132836, #25687, #179370, #73186, #116667, #131840, #54002, #39822, #133843, #149018, #148017, #89325, #54998, #101488, #103509, #58005, #23670, #9506, #55995, #162172, #27684, #40832, #87332, #195533, #134857, #193523, #181358, #151017, #119675, #42837, #165185, #41841, #194523, #117673, #12508, #26680, #88320, #104502, #166183, #102505, #178358, #10506, #150010, #24681, #74172, #115676, #71172, #85318, #196535, #192519, #57007, #177364, #72168, #38835, #180372, #100493, #147010, #163177, #8495, #11516, #70172, #86330, #64699, #188057, #112192, #168146, #173881, #110199, #97002, #156715, #13478, #141534, #29643, #197511, #142524, #35351, #14465, #33367, #49527, #125379, #90306, #43822, #80847, #158684, #106467, #171878, #121636, #3023, #20173, #137805, #189058, #199489, #91275, #58979, #152966, #76127, #63704, #187076, #65681, #126361, #4002, #34361, #48545, #95025, #18207, #135842, #198498, #79865, #50530, #172881, #127344, #157708, #105486, #167172, #182344, #75143, #120646, #111190, #96022, #19198, #136814, #28671, #151992, #59969, #183331, #44812, #53503, #83825, #40340, #116181, #99998, #194044, #6987, #51512, #102015, #97983, #115180, #174864, #36330, #84823, #176873, #143506, #130322, #162684, #85840, #163697, #22175, #23180, #37336, #9018, #68667, #145506, #159677, #81819, #24190, #147530, #98994, #38342, #70686, #146503, #7993, #66677, #160683, #113174, #4992, #21173, #69677, #128339, #55508, #192019, #132352, #178873, #131344, #175863, #190038, #117178, #82828, #161683, #193032, #54509, #177872, #144509, #5994, #67673, #129331, #52501, #39340, #191026, #100999, #114161, #27188, #75645, #88835, #196046, #148527, #42350, #57521, #165690, #150528, #152491, #89835, #29172, #121156, #119190, #181857, #12027, #106974, #87831, #197033, #137323, #59482, #90808, #44332, #195035, #56512, #71677, #164696, #13978, #180874, #104012, #73690, #26191, #10018, #28193, #199004, #135362, #167675, #58500, #120166, #183835, #182849, #43336, #60470, #105004, #118190, #45324, #41349, #166690, #179881, #103012, #151516, #13007, #86842, #74671, #105989, #122146, #25199, #136338, #198012, #133344, #149517, #11014, #72687, #134362, #188811, #110951, #49293, #124129, #63466, #172636, #171643, #33133, #153484, #185828, #200000, #168648, #107964, #156470, #50295, #80608, #32139, #157469, #65442, #94790, #91790, #47315, #138318, #34124, #3765, #17971, #18962, #108970, #127103, #140297, #142285, #61466, #77636, #30147, #79625, #14980, #31147, #141293, #2783, #76640, #784, #123137, #1788, #184823, #186840, #46308, #64461, #95783, #126129, #169651, #187824, #139305, #125141, #155476, #92795, #154483, #48309, #15977, #62455, #170651, #93796, #16968, #78621, #109964, #51276, #115945, #144269, #129089, #82588, #112937, #35110, #114939, #177635, #67432 ),
 ( #66439, #176632, #6749, #173641, #160447, #192790, #39102, #193799, #52263, #53262, #190789, #100758, #37095, #175620, #189804, #132107, #54272, #162440, #113921, #68428, #23941, #38107, #99762, #96762, #98754, #143266, #111952, #174630, #161447, #158451, #85595, #21937, #147282, #8772, #22938, #19940, #83588, #81581, #70441, #4750, #84584, #128100, #145268, #36095, #130081, #97747, #159434, #20930, #5756, #146264, #191779, #7748, #69434, #131102, #28940, #87598, #90581, #26954, #13747, #73453, #133105, #58268, #149284, #116935, #59246, #152262, #134120, #150293, #166458, #42116, #9778, #163456, #197780, #75415, #25955, #88596, #41110, #119937, #137087, #57281, #105757, #118955, #10778, #178628, #72444, #195809, #180641, #103778, #120915, #182614, #165457, #11789, #44099, #55266, #135126, #196800, #102774, #40091, #181622, #101769, #71440, #43102, #104770, #167443, #56267, #24954, #27955, #117950, #86601, #164461, #89596, #151283, #12773, #74437, #148284, #136104, #194794, #179640, #184591, #78380, #32899, #170411, #47074, #198775, #61231, #124902, #121912, #94551, #108734, #172400, #31903, #141061, #33890, #48073, #154249, #93556, #186601, #139069, #155242, #185584, #79391, #122902, #138083, #60241, #46072, #140056, #16732, #15740, #95546, #107726, #169407, #109729, #64229, #29916, #77399, #62218, #168421, #157234, #1546, #63222, #171413, #2547, #199764, #187594, #18726, #125894, #49063, #156232, #17733, #547, #123886, #80373, #110718, #183605, #45089, #106746, #91556, #30913, #153243, #14746, #92561, #76407, #129845, #191544, #177401, #66204, #173404, #158219, #65210, #35866, #83356, #69198, #113688, #114702, #34875, #3533, #38873, #126869, #188576, #50056, #97512, #130866, #111718, #192556, #4513, #6514, #127866, #99528, #161210, #84352, #146030, #53021, #96529, #19709, #176395, #100529, #175383, #190557, #142046, #189570, #68193, #81351, #37869, #52030, #115713, #36852, #7513, #162208, #22705, #159198, #98519, #54039, #82348, #160212, #128857, #23706, #51042, #143035, #112704, #174396, #145032, #21702, #20693, #144037, #5519, #67199, #196565, #151048, #116703, #102541, #149052, #55033, #120678, #133878, #57042, #26714, #27715, #86365, #74203, #43855, #12538, #135872, #58036, #134889, #87367, #10540, #182377, #119706, #181389, #197543, #59011, #25721, #9540, #118716, #42868, #117707, #105520, #73218, #104533, #167205, #71207, #178393, #101523, #8531, #179403, #88353, #85354, #180405, #166214, #39857, #147047, #70209, #131876, #193561, #163214, #40867, #24716, #148050, #132870, #194559, #150046, #56029, #89358, #164224, #72204, #195569, #41877, #103544, #165219, #11552, #187348, #94306, #155984, #199522, #60990, #17481, #28703, #107485, #61976, #76161, #48818, #185339, #152024, #183365, #93311, #15501, #79138, #29676, #140809, #138828, #91308, #63981, #137841, #16491, #154995, #14499, #124654, #110471, #122664, #170168, #45834, #184352, #108489, #62974, #169163, #2299, #90339, #30667, #123642, #92320, #13510, #46829, #75175, #44847, #78140, #77158, #125651, #153000, #136847, #308, #154005, #198532, #31661, #139808, #1296, #186350, #47830, #60003, #109482, #171165, #32652, #121670, #106503, #168180, #143790, #20447, #172153, #34631, #98262, #95301, #67950, #82098, #145786, #5273, #114445, #7268, #21451, #127626, #66954, #159964, #112461, #128616, #158957, #52776, #96290, #111471, #33639, #19469, #113445, #190309, #189326, #68952, #157977, #81114, #83112, #37616, #3295, #50803, #35624, #141802, #130615, #51785, #175138, #36605, #176146, #173156, #160965, #192311, #99278, #22459, #144789, #6272, #174153, #97269, #53791, #129604, #191300, #84107, #156985, #18483, #142794, #80132, #64967, #4274, #126626, #188327, #49806, #65955, #39616, #146792, #131629, #38628, #9298, #56801, #42627, #87124, #88115, #8285, #177155, #150805, #100285, #161963, #23459, #70964, #104291, #85106, #165972 ),
 ( #10299, #119469, #69963, #11305, #25482, #89117, #148809, #57798, #12301, #164978, #132632, #71956, #41634, #55788, #133629, #102296, #196330, #101275, #54787, #193313, #162965, #118474, #195321, #194320, #73967, #178151, #24471, #26473, #181152, #116462, #117459, #179158, #86121, #135636, #163985, #180164, #103299, #27474, #147812, #197306, #115466, #40626, #149799, #72975, #134644, #167947, #29445, #46589, #107250, #92074, #138587, #68, #106263, #136606, #75925, #153763, #121432, #61739, #45597, #168921, #185100, #74943, #105279, #90104, #120438, #183125, #60750, #123407, #14254, #30427, #166967, #58770, #169930, #43615, #28469, #151788, #91077, #108250, #13279, #182131, #137600, #198286, #199283, #59764, #44608, #152764, #122423, #184115, #15258, #76916, #76663, #166710, #90827, #59501, #182870, #44351, #164716, #135382, #11033, #179902, #119209, #167696, #200022, #91814, #43355, #168670, #138342, #106010, #103034, #58520, #149538, #183858, #15003, #29193, #30170, #197052, #61490, #151537, #153506, #72709, #88854, #41368, #152510, #26211, #42369, #13999, #75666, #87850, #12046, #134381, #120186, #13026, #137343, #181876, #74691, #28214, #60492, #104032, #180894, #196067, #27208, #121176, #136357, #105026, #57540, #165711, #150547, #199023, #45345, #73710, #89854, #198033, #122168, #106997, #171669, #94817, #64486, #65468, #124153, #111977, #81607, #188837, #173669, #34150, #172663, #125166, #186865, #19965, #95809, #18988, #50322, #35136, #63490, #47339, #156495, #80634, #155500, #96788, #110978, #157495, #158477, #108994, #154506, #139329, #46332, #16993, #126153, #143291, #17997, #142311, #16002, #184848, #4777, #107987, #169674, #31170, #78647, #123160, #92820, #77660, #185852, #187849, #170675, #3791, #127131, #808, #62481, #32163, #93820, #140322, #1812, #48334, #109989, #33158, #79650, #141319, #2808, #49318, #145292, #99787, #113946, #86622, #22962, #189829, #20955, #131126, #53285, #193823, #67457, #55288, #176657, #129115, #101791, #175645, #54296, #192814, #52289, #162463, #148305, #37119, #7776, #83614, #98778, #146289, #100780, #38134, #114964, #66465, #190814, #115968, #51301, #23964, #161473, #40113, #84610, #8795, #163479, #177656, #116960, #39125, #85619, #68454, #130108, #24976, #147306, #70465, #132130, #178651, #6775, #160472, #69459, #128127, #21963, #112962, #174655, #36120, #97772, #191804, #159459, #82612, #144293, #5783, #151304, #137108, #181642, #182634, #102796, #71461, #45108, #133126, #194816, #117971, #165478, #198794, #56289, #60260, #72468, #74458, #134141, #167464, #28959, #152282, #13766, #120935, #179662, #164482, #197800, #183626, #149305, #90600, #119956, #180661, #121931, #9799, #88617, #43121, #57301, #29936, #166477, #41132, #25976, #136124, #196820, #106765, #10799, #168440, #104789, #195830, #91575, #118978, #59266, #44118, #42137, #105777, #87619, #103798, #12793, #26974, #150314, #89615, #75434, #27976, #58287, #11810, #73474, #135147, #76426, #49079, #63240, #126886, #186617, #95562, #188592, #2563, #108753, #124920, #79407, #93575, #48089, #140074, #33905, #77418, #92580, #14765, #565, #94571, #109745, #170429, #50073, #15759, #62236, #64245, #18743, #184610, #31921, #16750, #122922, #111734, #1565, #171429, #156249, #157249, #154268, #142062, #173421, #80390, #34891, #123904, #141078, #125912, #139090, #110736, #153264, #185603, #17751, #155260, #47092, #32916, #187610, #172417, #3548, #138102, #78398, #65226, #199783, #61251, #46091, #107746, #169427, #30932, #70225, #146046, #52049, #68210, #22721, #36870, #129862, #83372, #177417, #20710, #35881, #158234, #144054, #37887, #53039, #113705, #193577, #159215, #5536, #7530, #162224, #127881, #175402, #160228, #66221, #131893, #145049, #191560, #99545, #38888, #97528, #85372, #55049, #23723, #147065, #69215, #130883, #98535, #21719, #116720, #192572, #54056, #8548, #178409, #6530, #82366, #114719 ),
 ( #176411, #115730, #189585, #19725, #96547, #81366, #143050, #4529, #161227, #51057, #112719, #174412, #67215, #84369, #128873, #100545, #190573, #182392, #43870, #151062, #9557, #194575, #27730, #13526, #179419, #197559, #150062, #10556, #28719, #39873, #118733, #73233, #87383, #60019, #196581, #163232, #56045, #104548, #26729, #167221, #40884, #90356, #11567, #102557, #134904, #105535, #75192, #89373, #195586, #58051, #166230, #180421, #119722, #88368, #120693, #164242, #25737, #101540, #149068, #181405, #42883, #57058, #136863, #72220, #133895, #12553, #152041, #71223, #41894, #103560, #132886, #198549, #74219, #135887, #59026, #121686, #165235, #24732, #86382, #148066, #117724, #94322, #32669, #185354, #46845, #80146, #156000, #79154, #48833, #110486, #123657, #107502, #16508, #140825, #15516, #33654, #171181, #17497, #18498, #169178, #14516, #199537, #106519, #77173, #124670, #172169, #155012, #2314, #76177, #44864, #141817, #168197, #29694, #91325, #138843, #95315, #153017, #157000, #45849, #47846, #30684, #63996, #125666, #187364, #3310, #64983, #137857, #61007, #183382, #122679, #184368, #92335, #93327, #154021, #323, #61991, #108505, #78156, #170184, #31678, #139824, #1313, #62992, #109499, #186367, #53808, #127641, #115483, #36622, #189341, #161979, #35639, #114460, #52792, #112476, #22475, #146808, #174169, #67966, #143805, #97285, #6287, #160981, #98279, #175155, #126641, #50819, #176162, #49822, #84123, #159980, #100301, #65971, #145802, #21466, #158972, #177171, #188343, #5288, #83128, #20464, #8302, #144804, #111486, #81129, #191315, #113461, #38644, #82114, #23475, #129620, #66971, #85124, #128631, #37632, #99295, #190325, #7285, #173171, #51802, #68969, #130633, #192327, #34647, #96306, #157992, #19484, #142810, #4290, #196345, #193329, #165989, #180181, #43631, #103314, #12317, #105294, #119485, #25497, #41650, #57813, #10314, #164994, #56816, #150820, #194336, #9315, #131647, #117476, #11320, #26488, #87140, #166982, #132648, #179174, #181167, #135651, #101292, #148824, #133645, #39632, #28485, #118490, #88130, #72990, #73982, #70980, #58785, #90119, #197322, #120454, #42644, #104306, #71971, #195336, #151803, #27489, #89132, #182147, #69979, #149814, #55804, #134659, #54803, #102311, #116478, #178167, #162982, #24487, #40642, #86138, #147829, #164001, #110015, #157521, #143317, #187875, #188865, #106277, #74959, #51330, #136621, #198302, #121448, #171696, #4804, #59779, #66493, #75941, #80661, #137616, #173696, #35164, #158504, #19991, #127157, #183140, #167962, #3817, #189856, #18024, #79677, #112990, #65495, #112007, #81634, #128156, #156525, #199300, #49343, #96819, #48361, #174683, #50348, #36148, #97800, #60767, #44624, #29461, #91093, #33185, #19015, #13294, #111005, #152781, #14272, #122439, #184131, #94844, #141348, #2835, #64513, #126180, #172691, #34176, #95837, #142337, #83643, #116987, #178680, #101820, #163508, #70492, #129144, #113975, #147336, #133155, #98806, #40143, #69489, #130136, #148334, #159489, #38161, #192843, #6803, #179691, #115995, #82639, #175673, #23992, #146316, #86650, #160500, #9829, #131154, #21990, #194846, #68481, #8823, #85649, #145320, #55316, #41163, #191833, #100808, #176686, #53314, #39152, #193851, #54323, #7805, #20982, #114992, #132159, #144322, #25006, #177684, #56319, #162491, #71489, #118002, #5811, #99816, #67486, #190841, #161501, #52317, #37147, #22991, #84639, #42166, #164512, #150343, #44147, #59295, #58316, #199813, #165506, #11839, #13797, #168469, #134171, #119984, #166507, #72497, #138132, #151333, #74488, #105806, #45138, #103826, #91605, #61281, #29967, #153294, #75462, #152311, #43149, #136154, #89645, #183654, #27002, #88647, #26005, #73504, #167493, #120964, #181670, #122951, #135176, #196850, #137136, #14795, #195859, #104818, #28005, #57331, #184639, #12822, #197829, #28989, #106795, #182663, #76455, #102826, #87647 ),
 ( #90629, #198823, #149333, #60288, #10827, #121961, #119007, #180690, #48118, #4561, #80421, #64274, #158266, #171458, #15787, #66253, #62265, #79436, #139118, #594, #49109, #141107, #107773, #94601, #126917, #50104, #127913, #186647, #187639, #1595, #173453, #32946, #109775, #123933, #46120, #188623, #143082, #156280, #157278, #125941, #110767, #172448, #30960, #63270, #77447, #169459, #185631, #33936, #92607, #19755, #17781, #34921, #154297, #95594, #47123, #124951, #108781, #111764, #81396, #18774, #96577, #2595, #170459, #142094, #31950, #93605, #155290, #16780, #3579, #78429, #140104, #65257, #38918, #163265, #21750, #24767, #161257, #148099, #7561, #67245, #192603, #83401, #51089, #193609, #86414, #68239, #55081, #9591, #129892, #84400, #100575, #176443, #144085, #97558, #131925, #71256, #160260, #22751, #175433, #54086, #189615, #191592, #39909, #53071, #145079, #112749, #6561, #114749, #37916, #99575, #116751, #115760, #178441, #85406, #146076, #69247, #130913, #174443, #52080, #177448, #101575, #23756, #35912, #8583, #159246, #20741, #82397, #128904, #5566, #162257, #147098, #70257, #190604, #113736, #36902, #98566, #88402, #75223, #104581, #134936, #91355, #167252, #151096, #44893, #58084, #102591, #153047, #149101, #166265, #25770, #87416, #135921, #27764, #194607, #181437, #13557, #136895, #14548, #73267, #74252, #150096, #60050, #119754, #196614, #10591, #132920, #198582, #29723, #42915, #43903, #12587, #197592, #59058, #117760, #11599, #164275, #56079, #72252, #120725, #179452, #106550, #89407, #121717, #40918, #182425, #133930, #105566, #195620, #183410, #168226, #28751, #57092, #90387, #118766, #152072, #180455, #41927, #103593, #165268, #26762, #61036, #138872, #2346, #125697, #49852, #108536, #111517, #47876, #34678, #94352, #154050, #79187, #170215, #137886, #15545, #140857, #31708, #199567, #80177, #173202, #155043, #171211, #187396, #63024, #30716, #184398, #18530, #96336, #46875, #109529, #62022, #64027, #158023, #78185, #126671, #139854, #93357, #122708, #16538, #1343, #124702, #186399, #3340, #48864, #141849, #172200, #32701, #156031, #17528, #76207, #352, #110519, #188375, #33685, #65014, #95348, #45878, #107531, #169208, #77203, #92364, #157032, #123686, #185385, #20495, #142841, #22506, #85155, #175187, #162011, #191346, #21499, #178198, #53842, #37664, #131679, #144834, #189372, #39663, #35668, #52824, #112506, #174200, #84153, #114493, #81159, #67997, #100333, #23507, #101324, #160011, #161012, #36653, #146841, #6318, #83160, #97316, #19514, #8334, #116510, #129650, #130665, #99329, #145832, #7314, #4320, #98311, #50849, #66003, #159002, #68999, #127672, #193360, #176195, #70010, #82143, #192359, #143839, #115516, #5318, #54836, #67002, #177204, #128661, #38677, #190356, #51833, #113492, #194368, #72002, #121478, #89162, #147861, #25530, #150853, #12347, #136650, #195367, #198332, #134691, #183171, #181199, #87174, #74011, #86171, #58817, #73021, #59808, #196376, #105324, #44654, #135681, #118522, #57845, #197353, #103345, #119517, #149846, #43662, #148855, #102343, #24520, #10346, #104337, #42676, #180211, #163013, #133676, #56846, #120485, #28513, #55835, #41681, #26517, #132680, #9347, #11350, #166021, #27521, #167012, #164032, #151832, #71012, #90148, #13322, #182176, #74987, #165024, #88161, #117508, #179205, #40673, #171968, #33455, #46635, #30470, #139618, #2112, #138633, #156803, #94116, #155795, #141621, #92120, #137644, #122468, #29489, #114, #47637, #95114, #77951, #78946, #199331, #167992, #3110, #91122, #152811, #14304, #61783, #18296, #75971, #79951, #168964, #170970, #153808, #63793, #125466, #48634, #110286, #17292, #60796, #184160, #140622, #64786, #45641, #187163, #16301, #76962, #126447, #106307, #185144, #1104, #15302, #188145, #62780, #107293, #123452, #32463, #93118, #108295, #169974, #31466, #124461, #154803, #186158, #109291, #37427 ),
 ( #52592, #34448, #5082, #80934, #49617, #189143, #99087, #69765, #161776, #113261, #38436, #146594, #114252, #172970, #128425, #19287, #53597, #84915, #175958, #100092, #66764, #8088, #21265, #23271, #142610, #158770, #131434, #160778, #96107, #112275, #22267, #83917, #111280, #81905, #157796, #82921, #4089, #67763, #127437, #145599, #143598, #65767, #115273, #50616, #190121, #144598, #7078, #36416, #173967, #35435, #192115, #97087, #20259, #6084, #51597, #68759, #174953, #98070, #159770, #129420, #191118, #130416, #176966, #25289, #133436, #195125, #120252, #57608, #197119, #88926, #163788, #149609, #179972, #74760, #55595, #164786, #43426, #27278, #58586, #12114, #162771, #24280, #39426, #132441, #181943, #86932, #10106, #148615, #194132, #116268, #196137, #105095, #71766, #135450, #26280, #56607, #151603, #150618, #11107, #166781, #118281, #85929, #13094, #9105, #87922, #147618, #70772, #119277, #72782, #54594, #41438, #73777, #28282, #193120, #103105, #134452, #180960, #89921, #42437, #104100, #117270, #177958, #101086, #178963, #165783, #40432, #102103, #139390, #46396, #137409, #171737, #45408, #124222, #62547, #122232, #32228, #156566, #183923, #77724, #153570, #107061, #16066, #170737, #108054, #184911, #136422, #199089, #185919, #59568, #93886, #169739, #110057, #31234, #78713, #33225, #47404, #91878, #92883, #109060, #76728, #154570, #123221, #17058, #60557, #75733, #198102, #168732, #872, #155564, #15067, #94885, #30236, #138403, #140389, #1877, #167760, #200084, #61552, #106073, #18064, #63558, #125232, #186930, #48400, #121243, #182937, #44420, #29258, #90890, #152576, #14066, #81674, #143357, #176726, #129182, #175710, #145360, #6842, #20032, #3857, #113029, #37188, #112048, #130175, #67525, #190880, #115033, #65536, #111047, #95878, #2876, #173736, #21023, #68521, #51368, #52356, #172734, #141388, #38199, #64555, #126219, #187915, #35205, #191872, #49384, #53355, #142378, #144362, #127196, #98846, #160541, #22030, #83682, #114012, #34215, #157561, #99855, #161539, #19054, #79719, #189893, #50388, #80701, #188908, #158542, #174721, #96858, #4846, #36184, #66532, #128195, #5849, #97838, #159526, #82678, #14591, #28788, #91398, #181475, #168267, #197628, #27802, #184438, #60089, #43942, #137925, #151133, #192884, #45918, #39192, #59094, #116034, #177723, #90427, #120760, #84677, #74289, #106591, #29764, #107572, #166306, #167291, #42953, #153087, #12624, #89443, #103631, #23032, #76247, #122747, #135958, #136934, #105604, #152113, #13596, #7843, #104617, #54362, #146356, #165307, #75263, #69529, #199609, #182461, #61075, #131194, #198623, #26801, #121757, #88442, #150137, #11638, #183450, #73305, #44934, #134976, #196653, #58122, #119791, #78224, #127710, #95387, #154090, #31748, #157073, #18569, #142878, #1384, #4358, #140901, #189411, #187436, #46917, #172239, #63065, #30757, #173242, #66043, #47916, #64066, #80216, #156071, #123728, #77242, #111557, #50887, #139895, #2387, #155083, #33724, #169249, #171252, #19553, #32740, #124744, #92404, #186440, #109570, #94392, #17569, #96375, #141887, #34717, #65053, #79230, #125736, #48903, #15584, #93396, #110558, #81197, #3378, #158062, #188413, #138910, #390, #62063, #108577, #185426, #126709, #49890, #170254, #16577, #174240, #35708, #51873, #69036, #130701, #131715, #98351, #193396, #176232, #54872, #161048, #67041, #84189, #160050, #112545, #8372, #97355, #191384, #145869, #38712, #99365, #190397, #5358, #70047, #178234, #144872, #22542, #21538, #192396, #159041, #114531, #116546, #37702, #6355, #143877, #52860, #68035, #7352, #53878, #20534, #177240, #82182, #128700, #115552, #100369, #162048, #113532, #23544, #85191, #175226, #36691, #83198, #129687, #146880, #124391, #139552, #32392, #97021, #125397, #110217, #63722, #94047, #16232, #96040, #158702, #48564, #35369, #64717, #95045, #51531, #127365, #111210, #5013, #18227 ) ),
 .UNSPECIFIED., .T., .F., .T. ) 
 B_SPLINE_SURFACE_WITH_KNOTS ( ( 4, 3, 4 ),
 ( 3, 2, 2, 2, 2, 2, 2, 2, 2, 2, 2, 2, 2, 2, 2, 2, 2, 2, 2, 2, 2, 2, 2, 2, 2, 2, 2, 2, 2, 2, 2, 2, 2, 2, 2, 2, 2, 2, 2, 2, 2, 2, 2, 2, 2, 2, 2, 2, 2, 2, 2, 2, 2, 2, 2, 2, 2, 2, 2, 2, 2, 2, 2, 2, 2, 2, 2, 2, 2, 2, 2, 2, 2, 2, 2, 2, 2, 2, 2, 2, 2, 2, 2, 2, 2, 2, 2, 2, 2, 2, 2, 2, 2, 2, 2, 2, 2, 2, 2, 2, 2, 2, 2, 2, 2, 2, 2, 2, 2, 2, 2, 2, 2, 2, 2, 2, 2, 2, 2, 2, 2, 2, 2, 2, 2, 2, 2, 2, 2, 2, 2, 2, 2, 2, 2, 2, 2, 2, 2, 2, 2, 2, 2, 2, 2, 2, 2, 2, 2, 2, 2, 2, 2, 2, 2, 2, 2, 2, 2, 2, 2, 2, 2, 2, 2, 2, 2, 2, 2, 2, 2, 2, 2, 2, 2, 2, 2, 2, 2, 2, 2, 2, 2, 2, 2, 2, 2, 2, 2, 2, 2, 2, 2, 2, 2, 2, 2, 2, 2, 2, 2, 2, 2, 2, 2, 2, 2, 2, 2, 2, 2, 2, 2, 2, 2, 2, 2, 2, 2, 2, 2, 2, 2, 2, 2, 2, 2, 2, 3 ),
 ( 0.000000000000000000, 0.5000000000000000000, 1.000000000000000000 ),
 ( 0.000000000000000000, 0.004385964912280701511, 0.008771929824561403022, 0.01315789473684210453, 0.01754385964912280604, 0.02192982456140350755, 0.02631578947368420907, 0.03070175438596491058, 0.03508771929824561209, 0.03947368421052631360, 0.04385964912280701511, 0.04824561403508771662, 0.05263157894736841813, 0.05701754385964911964, 0.06140350877192982115, 0.06578947368421052266, 0.07017543859649122417, 0.07456140350877192569, 0.07894736842105262720, 0.08333333333333332871, 0.08771929824561403022, 0.09210526315789473173, 0.09649122807017543324, 0.1008771929824561348, 0.1052631578947368363, 0.1096491228070175378, 0.1140350877192982393, 0.1184210526315789408, 0.1228070175438596423, 0.1271929824561403577, 0.1315789473684210453, 0.1359649122807017607, 0.1403508771929824483, 0.1447368421052631637, 0.1491228070175438514, 0.1535087719298245668, 0.1578947368421052544, 0.1622807017543859698, 0.1666666666666666574, 0.1710526315789473728, 0.1754385964912280604, 0.1798245614035087758, 0.1842105263157894635, 0.1885964912280701788, 0.1929824561403508665, 0.1973684210526315819, 0.2017543859649122695, 0.2061403508771929849, 0.2105263157894736725, 0.2149122807017543879, 0.2192982456140350755, 0.2236842105263157909, 0.2280701754385964786, 0.2324561403508771940, 0.2368421052631578816, 0.2412280701754385970, 0.2456140350877192846, 0.2500000000000000000, 0.2543859649122807154, 0.2587719298245614308, 0.2631578947368420907, 0.2675438596491228060, 0.2719298245614035214, 0.2763157894736842368, 0.2807017543859648967, 0.2850877192982456121, 0.2894736842105263275, 0.2938596491228070429, 0.2982456140350877027, 0.3026315789473684181, 0.3070175438596491335, 0.3114035087719298489, 0.3157894736842105088, 0.3201754385964912242, 0.3245614035087719396, 0.3289473684210526550, 0.3333333333333333148, 0.3377192982456140302, 0.3421052631578947456, 0.3464912280701754610, 0.3508771929824561209, 0.3552631578947368363, 0.3596491228070175517, 0.3640350877192982670, 0.3684210526315789269, 0.3728070175438596423, 0.3771929824561403577, 0.3815789473684210731, 0.3859649122807017330, 0.3903508771929824483, 0.3947368421052631637, 0.3991228070175438791, 0.4035087719298245390, 0.4078947368421052544, 0.4122807017543859698, 0.4166666666666666852, 0.4210526315789473450, 0.4254385964912280604, 0.4298245614035087758, 0.4342105263157894912, 0.4385964912280701511, 0.4429824561403508665, 0.4473684210526315819, 0.4517543859649122973, 0.4561403508771929571, 0.4605263157894736725, 0.4649122807017543879, 0.4692982456140351033, 0.4736842105263157632, 0.4780701754385964786, 0.4824561403508771940, 0.4868421052631579093, 0.4912280701754385692, 0.4956140350877192846, 0.5000000000000000000, 0.5043859649122807154, 0.5087719298245614308, 0.5131578947368421462, 0.5175438596491228616, 0.5219298245614034659, 0.5263157894736841813, 0.5307017543859648967, 0.5350877192982456121, 0.5394736842105263275, 0.5438596491228070429, 0.5482456140350877583, 0.5526315789473684736, 0.5570175438596490780, 0.5614035087719297934, 0.5657894736842105088, 0.5701754385964912242, 0.5745614035087719396, 0.5789473684210526550, 0.5833333333333333703, 0.5877192982456140857, 0.5921052631578946901, 0.5964912280701754055, 0.6008771929824561209, 0.6052631578947368363, 0.6096491228070175517, 0.6140350877192982670, 0.6184210526315789824, 0.6228070175438596978, 0.6271929824561403022, 0.6315789473684210176, 0.6359649122807017330, 0.6403508771929824483, 0.6447368421052631637, 0.6491228070175438791, 0.6535087719298245945, 0.6578947368421053099, 0.6622807017543859143, 0.6666666666666666297, 0.6710526315789473450, 0.6754385964912280604, 0.6798245614035087758, 0.6842105263157894912, 0.6885964912280702066, 0.6929824561403509220, 0.6973684210526315264, 0.7017543859649122417, 0.7061403508771929571, 0.7105263157894736725, 0.7149122807017543879, 0.7192982456140351033, 0.7236842105263158187, 0.7280701754385965341, 0.7324561403508771384, 0.7368421052631578538, 0.7412280701754385692, 0.7456140350877192846, 0.7500000000000000000, 0.7543859649122807154, 0.7587719298245614308, 0.7631578947368421462, 0.7675438596491228616, 0.7719298245614034659, 0.7763157894736841813, 0.7807017543859648967, 0.7850877192982456121, 0.7894736842105263275, 0.7938596491228070429, 0.7982456140350877583, 0.8026315789473684736, 0.8070175438596490780, 0.8114035087719297934, 0.8157894736842105088, 0.8201754385964912242, 0.8245614035087719396, 0.8289473684210526550, 0.8333333333333333703, 0.8377192982456140857, 0.8421052631578946901, 0.8464912280701754055, 0.8508771929824561209, 0.8552631578947368363, 0.8596491228070175517, 0.8640350877192982670, 0.8684210526315789824, 0.8728070175438596978, 0.8771929824561403022, 0.8815789473684210176, 0.8859649122807017330, 0.8903508771929824483, 0.8947368421052631637, 0.8991228070175438791, 0.9035087719298245945, 0.9078947368421053099, 0.9122807017543859143, 0.9166666666666666297, 0.9210526315789473450, 0.9254385964912280604, 0.9298245614035087758, 0.9342105263157894912, 0.9385964912280702066, 0.9429824561403509220, 0.9473684210526315264, 0.9517543859649122417, 0.9561403508771929571, 0.9605263157894736725, 0.9649122807017543879, 0.9692982456140351033, 0.9736842105263158187, 0.9780701754385965341, 0.9824561403508771384, 0.9868421052631578538, 0.9912280701754385692, 0.9956140350877192846, 1.000000000000000000 ),
 .UNSPECIFIED. ) 
 GEOMETRIC_REPRESENTATION_ITEM ( )  RATIONAL_B_SPLINE_SURFACE ( (
 ( 1.000000000000000000, 0.9659258262890683122, 1.000000000000000000, 0.9659258262890683122, 1.000000000000000000, 0.9659258262890683122, 1.000000000000000000, 0.9659258262890683122, 1.000000000000000000, 0.9659258262890683122, 1.000000000000000000, 0.9659258262890683122, 1.000000000000000000, 0.9659258262890683122, 1.000000000000000000, 0.9659258262890683122, 1.000000000000000000, 0.9659258262890683122, 1.000000000000000000, 0.9659258262890683122, 1.000000000000000000, 0.9659258262890683122, 1.000000000000000000, 0.9659258262890683122, 1.000000000000000000, 0.9659258262890683122, 1.000000000000000000, 0.9659258262890683122, 1.000000000000000000, 0.9659258262890683122, 1.000000000000000000, 0.9659258262890683122, 1.000000000000000000, 0.9659258262890683122, 1.000000000000000000, 0.9659258262890683122, 1.000000000000000000, 0.9659258262890683122, 1.000000000000000000, 0.9659258262890683122, 1.000000000000000000, 0.9659258262890683122, 1.000000000000000000, 0.9659258262890683122, 1.000000000000000000, 0.9659258262890683122, 1.000000000000000000, 0.9659258262890683122, 1.000000000000000000, 0.9659258262890683122, 1.000000000000000000, 0.9659258262890683122, 1.000000000000000000, 0.9659258262890683122, 1.000000000000000000, 0.9659258262890683122, 1.000000000000000000, 0.9659258262890683122, 1.000000000000000000, 0.9659258262890683122, 1.000000000000000000, 0.9659258262890683122, 1.000000000000000000, 0.9659258262890683122, 1.000000000000000000, 0.9659258262890683122, 1.000000000000000000, 0.9659258262890683122, 1.000000000000000000, 0.9659258262890683122, 1.000000000000000000, 0.9659258262890683122, 1.000000000000000000, 0.9659258262890683122, 1.000000000000000000, 0.9659258262890683122, 1.000000000000000000, 0.9659258262890683122, 1.000000000000000000, 0.9659258262890683122, 1.000000000000000000, 0.9659258262890683122, 1.000000000000000000, 0.9659258262890683122, 1.000000000000000000, 0.9659258262890683122, 1.000000000000000000, 0.9659258262890683122, 1.000000000000000000, 0.9659258262890683122, 1.000000000000000000, 0.9659258262890683122, 1.000000000000000000, 0.9659258262890683122, 1.000000000000000000, 0.9659258262890683122, 1.000000000000000000, 0.9659258262890683122, 1.000000000000000000, 0.9659258262890683122, 1.000000000000000000, 0.9659258262890683122, 1.000000000000000000, 0.9659258262890683122, 1.000000000000000000, 0.9659258262890683122, 1.000000000000000000, 0.9659258262890683122, 1.000000000000000000, 0.9659258262890683122, 1.000000000000000000, 0.9659258262890683122, 1.000000000000000000, 0.9659258262890683122, 1.000000000000000000, 0.9659258262890683122, 1.000000000000000000, 0.9659258262890683122, 1.000000000000000000, 0.9659258262890683122, 1.000000000000000000, 0.9659258262890683122, 1.000000000000000000, 0.9659258262890683122, 1.000000000000000000, 0.9659258262890683122, 1.000000000000000000, 0.9659258262890683122, 1.000000000000000000, 0.9659258262890683122, 1.000000000000000000, 0.9659258262890683122, 1.000000000000000000, 0.9659258262890683122, 1.000000000000000000, 0.9659258262890683122, 1.000000000000000000, 0.9659258262890683122, 1.000000000000000000, 0.9659258262890683122, 1.000000000000000000, 0.9659258262890683122, 1.000000000000000000, 0.9659258262890683122, 1.000000000000000000, 0.9659258262890683122, 1.000000000000000000, 0.9659258262890683122, 1.000000000000000000, 0.9659258262890683122, 1.000000000000000000, 0.9659258262890683122, 1.000000000000000000, 0.9659258262890683122, 1.000000000000000000, 0.9659258262890683122, 1.000000000000000000, 0.9659258262890683122, 1.000000000000000000, 0.9659258262890683122, 1.000000000000000000, 0.9659258262890683122, 1.000000000000000000, 0.9659258262890683122, 1.000000000000000000, 0.9659258262890683122, 1.000000000000000000, 0.9659258262890683122, 1.000000000000000000, 0.9659258262890683122, 1.000000000000000000, 0.9659258262890683122, 1.000000000000000000, 0.9659258262890683122, 1.000000000000000000, 0.9659258262890683122, 1.000000000000000000, 0.9659258262890683122, 1.000000000000000000, 0.9659258262890683122, 1.000000000000000000, 0.9659258262890683122, 1.000000000000000000, 0.9659258262890683122, 1.000000000000000000, 0.9659258262890683122, 1.000000000000000000, 0.9659258262890683122, 1.000000000000000000, 0.9659258262890683122, 1.000000000000000000, 0.9659258262890683122, 1.000000000000000000, 0.9659258262890683122, 1.000000000000000000, 0.9659258262890683122, 1.000000000000000000, 0.9659258262890683122, 1.000000000000000000, 0.9659258262890683122, 1.000000000000000000, 0.9659258262890683122, 1.000000000000000000, 0.9659258262890683122, 1.000000000000000000, 0.9659258262890683122, 1.000000000000000000, 0.9659258262890683122, 1.000000000000000000, 0.9659258262890683122, 1.000000000000000000, 0.9659258262890683122, 1.000000000000000000, 0.9659258262890683122, 1.000000000000000000, 0.9659258262890683122, 1.000000000000000000, 0.9659258262890683122, 1.000000000000000000, 0.9659258262890683122, 1.000000000000000000, 0.9659258262890683122, 1.000000000000000000, 0.9659258262890683122, 1.000000000000000000, 0.9659258262890683122, 1.000000000000000000, 0.9659258262890683122, 1.000000000000000000, 0.9659258262890683122, 1.000000000000000000, 0.9659258262890683122, 1.000000000000000000, 0.9659258262890683122, 1.000000000000000000, 0.9659258262890683122, 1.000000000000000000, 0.9659258262890683122, 1.000000000000000000, 0.9659258262890683122, 1.000000000000000000, 0.9659258262890683122, 1.000000000000000000, 0.9659258262890683122, 1.000000000000000000, 0.9659258262890683122, 1.000000000000000000, 0.9659258262890683122, 1.000000000000000000, 0.9659258262890683122, 1.000000000000000000, 0.9659258262890683122, 1.000000000000000000, 0.9659258262890683122, 1.000000000000000000, 0.9659258262890683122, 1.000000000000000000, 0.9659258262890683122, 1.000000000000000000, 0.9659258262890683122, 1.000000000000000000, 0.9659258262890683122, 1.000000000000000000, 0.9659258262890683122, 1.000000000000000000, 0.9659258262890683122, 1.000000000000000000, 0.9659258262890683122, 1.000000000000000000, 0.9659258262890683122, 1.000000000000000000, 0.9659258262890683122, 1.000000000000000000, 0.9659258262890683122, 1.000000000000000000, 0.9659258262890683122, 1.000000000000000000, 0.9659258262890683122, 1.000000000000000000, 0.9659258262890683122, 1.000000000000000000, 0.9659258262890683122, 1.000000000000000000, 0.9659258262890683122, 1.000000000000000000, 0.9659258262890683122, 1.000000000000000000, 0.9659258262890683122, 1.000000000000000000, 0.9659258262890683122, 1.000000000000000000, 0.9659258262890683122, 1.000000000000000000, 0.9659258262890683122, 1.000000000000000000, 0.9659258262890683122, 1.000000000000000000, 0.9659258262890683122, 1.000000000000000000, 0.9659258262890683122, 1.000000000000000000, 0.9659258262890683122, 1.000000000000000000, 0.9659258262890683122, 1.000000000000000000, 0.9659258262890683122, 1.000000000000000000, 0.9659258262890683122, 1.000000000000000000, 0.9659258262890683122, 1.000000000000000000, 0.9659258262890683122, 1.000000000000000000, 0.9659258262890683122, 1.000000000000000000, 0.9659258262890683122, 1.000000000000000000, 0.9659258262890683122, 1.000000000000000000, 0.9659258262890683122, 1.000000000000000000, 0.9659258262890683122, 1.000000000000000000, 0.9659258262890683122, 1.000000000000000000, 0.9659258262890683122, 1.000000000000000000, 0.9659258262890683122, 1.000000000000000000, 0.9659258262890683122, 1.000000000000000000, 0.9659258262890683122, 1.000000000000000000, 0.9659258262890683122, 1.000000000000000000, 0.9659258262890683122, 1.000000000000000000, 0.9659258262890683122, 1.000000000000000000, 0.9659258262890683122, 1.000000000000000000, 0.9659258262890683122, 1.000000000000000000, 0.9659258262890683122, 1.000000000000000000, 0.9659258262890683122, 1.000000000000000000, 0.9659258262890683122, 1.000000000000000000, 0.9659258262890683122, 1.000000000000000000, 0.9659258262890683122, 1.000000000000000000, 0.9659258262890683122, 1.000000000000000000, 0.9659258262890683122, 1.000000000000000000, 0.9659258262890683122, 1.000000000000000000, 0.9659258262890683122, 1.000000000000000000, 0.9659258262890683122, 1.000000000000000000, 0.9659258262890683122, 1.000000000000000000, 0.9659258262890683122, 1.000000000000000000, 0.9659258262890683122, 1.000000000000000000, 0.9659258262890683122, 1.000000000000000000, 0.9659258262890683122, 1.000000000000000000, 0.9659258262890683122, 1.000000000000000000, 0.9659258262890683122, 1.000000000000000000, 0.9659258262890683122, 1.000000000000000000, 0.9659258262890683122, 1.000000000000000000, 0.9659258262890683122, 1.000000000000000000, 0.9659258262890683122, 1.000000000000000000, 0.9659258262890683122, 1.000000000000000000, 0.9659258262890683122, 1.000000000000000000, 0.9659258262890683122, 1.000000000000000000, 0.9659258262890683122, 1.000000000000000000, 0.9659258262890683122, 1.000000000000000000, 0.9659258262890683122, 1.000000000000000000, 0.9659258262890683122, 1.000000000000000000, 0.9659258262890683122, 1.000000000000000000, 0.9659258262890683122, 1.000000000000000000, 0.9659258262890683122, 1.000000000000000000, 0.9659258262890683122, 1.000000000000000000, 0.9659258262890683122, 1.000000000000000000, 0.9659258262890683122, 1.000000000000000000, 0.9659258262890683122, 1.000000000000000000, 0.9659258262890683122, 1.000000000000000000, 0.9659258262890683122, 1.000000000000000000, 0.9659258262890683122, 1.000000000000000000, 0.9659258262890683122, 1.000000000000000000, 0.9659258262890683122, 1.000000000000000000, 0.9659258262890683122, 1.000000000000000000, 0.9659258262890683122, 1.000000000000000000, 0.9659258262890683122, 1.000000000000000000, 0.9659258262890683122, 1.000000000000000000, 0.9659258262890683122, 1.000000000000000000, 0.9659258262890683122, 1.000000000000000000, 0.9659258262890683122, 1.000000000000000000, 0.9659258262890683122, 1.000000000000000000, 0.9659258262890683122, 1.000000000000000000, 0.9659258262890683122, 1.000000000000000000, 0.9659258262890683122, 1.000000000000000000, 0.9659258262890683122, 1.000000000000000000, 0.9659258262890683122, 1.000000000000000000, 0.9659258262890683122, 1.000000000000000000, 0.9659258262890683122, 1.000000000000000000, 0.9659258262890683122, 1.000000000000000000, 0.9659258262890683122, 1.000000000000000000),
 ( 0.3333333333333333703, 0.3219752754296894559, 0.3333333333333333703, 0.3219752754296894559, 0.3333333333333333703, 0.3219752754296894559, 0.3333333333333333703, 0.3219752754296894559, 0.3333333333333333703, 0.3219752754296894559, 0.3333333333333333703, 0.3219752754296894559, 0.3333333333333333703, 0.3219752754296894559, 0.3333333333333333703, 0.3219752754296894559, 0.3333333333333333703, 0.3219752754296894559, 0.3333333333333333703, 0.3219752754296894559, 0.3333333333333333703, 0.3219752754296894559, 0.3333333333333333703, 0.3219752754296894559, 0.3333333333333333703, 0.3219752754296894559, 0.3333333333333333703, 0.3219752754296894559, 0.3333333333333333703, 0.3219752754296894559, 0.3333333333333333703, 0.3219752754296894559, 0.3333333333333333703, 0.3219752754296894559, 0.3333333333333333703, 0.3219752754296894559, 0.3333333333333333703, 0.3219752754296894559, 0.3333333333333333703, 0.3219752754296894559, 0.3333333333333333703, 0.3219752754296894559, 0.3333333333333333703, 0.3219752754296894559, 0.3333333333333333703, 0.3219752754296894559, 0.3333333333333333703, 0.3219752754296894559, 0.3333333333333333703, 0.3219752754296894559, 0.3333333333333333703, 0.3219752754296894559, 0.3333333333333333703, 0.3219752754296894559, 0.3333333333333333703, 0.3219752754296894559, 0.3333333333333333703, 0.3219752754296894559, 0.3333333333333333703, 0.3219752754296894559, 0.3333333333333333703, 0.3219752754296894559, 0.3333333333333333703, 0.3219752754296894559, 0.3333333333333333703, 0.3219752754296894559, 0.3333333333333333703, 0.3219752754296894559, 0.3333333333333333703, 0.3219752754296894559, 0.3333333333333333703, 0.3219752754296894559, 0.3333333333333333703, 0.3219752754296894559, 0.3333333333333333703, 0.3219752754296894559, 0.3333333333333333703, 0.3219752754296894559, 0.3333333333333333703, 0.3219752754296894559, 0.3333333333333333703, 0.3219752754296894559, 0.3333333333333333703, 0.3219752754296894559, 0.3333333333333333703, 0.3219752754296894559, 0.3333333333333333703, 0.3219752754296894559, 0.3333333333333333703, 0.3219752754296894559, 0.3333333333333333703, 0.3219752754296894559, 0.3333333333333333703, 0.3219752754296894559, 0.3333333333333333703, 0.3219752754296894559, 0.3333333333333333703, 0.3219752754296894559, 0.3333333333333333703, 0.3219752754296894559, 0.3333333333333333703, 0.3219752754296894559, 0.3333333333333333703, 0.3219752754296894559, 0.3333333333333333703, 0.3219752754296894559, 0.3333333333333333703, 0.3219752754296894559, 0.3333333333333333703, 0.3219752754296894559, 0.3333333333333333703, 0.3219752754296894559, 0.3333333333333333703, 0.3219752754296894559, 0.3333333333333333703, 0.3219752754296894559, 0.3333333333333333703, 0.3219752754296894559, 0.3333333333333333703, 0.3219752754296894559, 0.3333333333333333703, 0.3219752754296894559, 0.3333333333333333703, 0.3219752754296894559, 0.3333333333333333703, 0.3219752754296894559, 0.3333333333333333703, 0.3219752754296894559, 0.3333333333333333703, 0.3219752754296894559, 0.3333333333333333703, 0.3219752754296894559, 0.3333333333333333703, 0.3219752754296894559, 0.3333333333333333703, 0.3219752754296894559, 0.3333333333333333703, 0.3219752754296894559, 0.3333333333333333703, 0.3219752754296894559, 0.3333333333333333703, 0.3219752754296894559, 0.3333333333333333703, 0.3219752754296894559, 0.3333333333333333703, 0.3219752754296894559, 0.3333333333333333703, 0.3219752754296894559, 0.3333333333333333703, 0.3219752754296894559, 0.3333333333333333703, 0.3219752754296894559, 0.3333333333333333703, 0.3219752754296894559, 0.3333333333333333703, 0.3219752754296894559, 0.3333333333333333703, 0.3219752754296894559, 0.3333333333333333703, 0.3219752754296894559, 0.3333333333333333703, 0.3219752754296894559, 0.3333333333333333703, 0.3219752754296894559, 0.3333333333333333703, 0.3219752754296894559, 0.3333333333333333703, 0.3219752754296894559, 0.3333333333333333703, 0.3219752754296894559, 0.3333333333333333703, 0.3219752754296894559, 0.3333333333333333703, 0.3219752754296894559, 0.3333333333333333703, 0.3219752754296894559, 0.3333333333333333703, 0.3219752754296894559, 0.3333333333333333703, 0.3219752754296894559, 0.3333333333333333703, 0.3219752754296894559, 0.3333333333333333703, 0.3219752754296894559, 0.3333333333333333703, 0.3219752754296894559, 0.3333333333333333703, 0.3219752754296894559, 0.3333333333333333703, 0.3219752754296894559, 0.3333333333333333703, 0.3219752754296894559, 0.3333333333333333703, 0.3219752754296894559, 0.3333333333333333703, 0.3219752754296894559, 0.3333333333333333703, 0.3219752754296894559, 0.3333333333333333703, 0.3219752754296894559, 0.3333333333333333703, 0.3219752754296894559, 0.3333333333333333703, 0.3219752754296894559, 0.3333333333333333703, 0.3219752754296894559, 0.3333333333333333703, 0.3219752754296894559, 0.3333333333333333703, 0.3219752754296894559, 0.3333333333333333703, 0.3219752754296894559, 0.3333333333333333703, 0.3219752754296894559, 0.3333333333333333703, 0.3219752754296894559, 0.3333333333333333703, 0.3219752754296894559, 0.3333333333333333703, 0.3219752754296894559, 0.3333333333333333703, 0.3219752754296894559, 0.3333333333333333703, 0.3219752754296894559, 0.3333333333333333703, 0.3219752754296894559, 0.3333333333333333703, 0.3219752754296894559, 0.3333333333333333703, 0.3219752754296894559, 0.3333333333333333703, 0.3219752754296894559, 0.3333333333333333703, 0.3219752754296894559, 0.3333333333333333703, 0.3219752754296894559, 0.3333333333333333703, 0.3219752754296894559, 0.3333333333333333703, 0.3219752754296894559, 0.3333333333333333703, 0.3219752754296894559, 0.3333333333333333703, 0.3219752754296894559, 0.3333333333333333703, 0.3219752754296894559, 0.3333333333333333703, 0.3219752754296894559, 0.3333333333333333703, 0.3219752754296894559, 0.3333333333333333703, 0.3219752754296894559, 0.3333333333333333703, 0.3219752754296894559, 0.3333333333333333703, 0.3219752754296894559, 0.3333333333333333703, 0.3219752754296894559, 0.3333333333333333703, 0.3219752754296894559, 0.3333333333333333703, 0.3219752754296894559, 0.3333333333333333703, 0.3219752754296894559, 0.3333333333333333703, 0.3219752754296894559, 0.3333333333333333703, 0.3219752754296894559, 0.3333333333333333703, 0.3219752754296894559, 0.3333333333333333703, 0.3219752754296894559, 0.3333333333333333703, 0.3219752754296894559, 0.3333333333333333703, 0.3219752754296894559, 0.3333333333333333703, 0.3219752754296894559, 0.3333333333333333703, 0.3219752754296894559, 0.3333333333333333703, 0.3219752754296894559, 0.3333333333333333703, 0.3219752754296894559, 0.3333333333333333703, 0.3219752754296894559, 0.3333333333333333703, 0.3219752754296894559, 0.3333333333333333703, 0.3219752754296894559, 0.3333333333333333703, 0.3219752754296894559, 0.3333333333333333703, 0.3219752754296894559, 0.3333333333333333703, 0.3219752754296894559, 0.3333333333333333703, 0.3219752754296894559, 0.3333333333333333703, 0.3219752754296894559, 0.3333333333333333703, 0.3219752754296894559, 0.3333333333333333703, 0.3219752754296894559, 0.3333333333333333703, 0.3219752754296894559, 0.3333333333333333703, 0.3219752754296894559, 0.3333333333333333703, 0.3219752754296894559, 0.3333333333333333703, 0.3219752754296894559, 0.3333333333333333703, 0.3219752754296894559, 0.3333333333333333703, 0.3219752754296894559, 0.3333333333333333703, 0.3219752754296894559, 0.3333333333333333703, 0.3219752754296894559, 0.3333333333333333703, 0.3219752754296894559, 0.3333333333333333703, 0.3219752754296894559, 0.3333333333333333703, 0.3219752754296894559, 0.3333333333333333703, 0.3219752754296894559, 0.3333333333333333703, 0.3219752754296894559, 0.3333333333333333703, 0.3219752754296894559, 0.3333333333333333703, 0.3219752754296894559, 0.3333333333333333703, 0.3219752754296894559, 0.3333333333333333703, 0.3219752754296894559, 0.3333333333333333703, 0.3219752754296894559, 0.3333333333333333703, 0.3219752754296894559, 0.3333333333333333703, 0.3219752754296894559, 0.3333333333333333703, 0.3219752754296894559, 0.3333333333333333703, 0.3219752754296894559, 0.3333333333333333703, 0.3219752754296894559, 0.3333333333333333703, 0.3219752754296894559, 0.3333333333333333703, 0.3219752754296894559, 0.3333333333333333703, 0.3219752754296894559, 0.3333333333333333703, 0.3219752754296894559, 0.3333333333333333703, 0.3219752754296894559, 0.3333333333333333703, 0.3219752754296894559, 0.3333333333333333703, 0.3219752754296894559, 0.3333333333333333703, 0.3219752754296894559, 0.3333333333333333703, 0.3219752754296894559, 0.3333333333333333703, 0.3219752754296894559, 0.3333333333333333703, 0.3219752754296894559, 0.3333333333333333703, 0.3219752754296894559, 0.3333333333333333703, 0.3219752754296894559, 0.3333333333333333703, 0.3219752754296894559, 0.3333333333333333703, 0.3219752754296894559, 0.3333333333333333703, 0.3219752754296894559, 0.3333333333333333703, 0.3219752754296894559, 0.3333333333333333703, 0.3219752754296894559, 0.3333333333333333703, 0.3219752754296894559, 0.3333333333333333703, 0.3219752754296894559, 0.3333333333333333703, 0.3219752754296894559, 0.3333333333333333703, 0.3219752754296894559, 0.3333333333333333703, 0.3219752754296894559, 0.3333333333333333703, 0.3219752754296894559, 0.3333333333333333703, 0.3219752754296894559, 0.3333333333333333703, 0.3219752754296894559, 0.3333333333333333703, 0.3219752754296894559, 0.3333333333333333703, 0.3219752754296894559, 0.3333333333333333703, 0.3219752754296894559, 0.3333333333333333703, 0.3219752754296894559, 0.3333333333333333703, 0.3219752754296894559, 0.3333333333333333703, 0.3219752754296894559, 0.3333333333333333703, 0.3219752754296894559, 0.3333333333333333703, 0.3219752754296894559, 0.3333333333333333703, 0.3219752754296894559, 0.3333333333333333703, 0.3219752754296894559, 0.3333333333333333703, 0.3219752754296894559, 0.3333333333333333703, 0.3219752754296894559, 0.3333333333333333703, 0.3219752754296894559, 0.3333333333333333703, 0.3219752754296894559, 0.3333333333333333703, 0.3219752754296894559, 0.3333333333333333703, 0.3219752754296894559, 0.3333333333333333703, 0.3219752754296894559, 0.3333333333333333703, 0.3219752754296894559, 0.3333333333333333703, 0.3219752754296894559, 0.3333333333333333703, 0.3219752754296894559, 0.3333333333333333703, 0.3219752754296894559, 0.3333333333333333703, 0.3219752754296894559, 0.3333333333333333703, 0.3219752754296894559, 0.3333333333333333703, 0.3219752754296894559, 0.3333333333333333703, 0.3219752754296894559, 0.3333333333333333703, 0.3219752754296894559, 0.3333333333333333703, 0.3219752754296894559, 0.3333333333333333703),
 ( 0.3333333333333333703, 0.3219752754296894559, 0.3333333333333333703, 0.3219752754296894559, 0.3333333333333333703, 0.3219752754296894559, 0.3333333333333333703, 0.3219752754296894559, 0.3333333333333333703, 0.3219752754296894559, 0.3333333333333333703, 0.3219752754296894559, 0.3333333333333333703, 0.3219752754296894559, 0.3333333333333333703, 0.3219752754296894559, 0.3333333333333333703, 0.3219752754296894559, 0.3333333333333333703, 0.3219752754296894559, 0.3333333333333333703, 0.3219752754296894559, 0.3333333333333333703, 0.3219752754296894559, 0.3333333333333333703, 0.3219752754296894559, 0.3333333333333333703, 0.3219752754296894559, 0.3333333333333333703, 0.3219752754296894559, 0.3333333333333333703, 0.3219752754296894559, 0.3333333333333333703, 0.3219752754296894559, 0.3333333333333333703, 0.3219752754296894559, 0.3333333333333333703, 0.3219752754296894559, 0.3333333333333333703, 0.3219752754296894559, 0.3333333333333333703, 0.3219752754296894559, 0.3333333333333333703, 0.3219752754296894559, 0.3333333333333333703, 0.3219752754296894559, 0.3333333333333333703, 0.3219752754296894559, 0.3333333333333333703, 0.3219752754296894559, 0.3333333333333333703, 0.3219752754296894559, 0.3333333333333333703, 0.3219752754296894559, 0.3333333333333333703, 0.3219752754296894559, 0.3333333333333333703, 0.3219752754296894559, 0.3333333333333333703, 0.3219752754296894559, 0.3333333333333333703, 0.3219752754296894559, 0.3333333333333333703, 0.3219752754296894559, 0.3333333333333333703, 0.3219752754296894559, 0.3333333333333333703, 0.3219752754296894559, 0.3333333333333333703, 0.3219752754296894559, 0.3333333333333333703, 0.3219752754296894559, 0.3333333333333333703, 0.3219752754296894559, 0.3333333333333333703, 0.3219752754296894559, 0.3333333333333333703, 0.3219752754296894559, 0.3333333333333333703, 0.3219752754296894559, 0.3333333333333333703, 0.3219752754296894559, 0.3333333333333333703, 0.3219752754296894559, 0.3333333333333333703, 0.3219752754296894559, 0.3333333333333333703, 0.3219752754296894559, 0.3333333333333333703, 0.3219752754296894559, 0.3333333333333333703, 0.3219752754296894559, 0.3333333333333333703, 0.3219752754296894559, 0.3333333333333333703, 0.3219752754296894559, 0.3333333333333333703, 0.3219752754296894559, 0.3333333333333333703, 0.3219752754296894559, 0.3333333333333333703, 0.3219752754296894559, 0.3333333333333333703, 0.3219752754296894559, 0.3333333333333333703, 0.3219752754296894559, 0.3333333333333333703, 0.3219752754296894559, 0.3333333333333333703, 0.3219752754296894559, 0.3333333333333333703, 0.3219752754296894559, 0.3333333333333333703, 0.3219752754296894559, 0.3333333333333333703, 0.3219752754296894559, 0.3333333333333333703, 0.3219752754296894559, 0.3333333333333333703, 0.3219752754296894559, 0.3333333333333333703, 0.3219752754296894559, 0.3333333333333333703, 0.3219752754296894559, 0.3333333333333333703, 0.3219752754296894559, 0.3333333333333333703, 0.3219752754296894559, 0.3333333333333333703, 0.3219752754296894559, 0.3333333333333333703, 0.3219752754296894559, 0.3333333333333333703, 0.3219752754296894559, 0.3333333333333333703, 0.3219752754296894559, 0.3333333333333333703, 0.3219752754296894559, 0.3333333333333333703, 0.3219752754296894559, 0.3333333333333333703, 0.3219752754296894559, 0.3333333333333333703, 0.3219752754296894559, 0.3333333333333333703, 0.3219752754296894559, 0.3333333333333333703, 0.3219752754296894559, 0.3333333333333333703, 0.3219752754296894559, 0.3333333333333333703, 0.3219752754296894559, 0.3333333333333333703, 0.3219752754296894559, 0.3333333333333333703, 0.3219752754296894559, 0.3333333333333333703, 0.3219752754296894559, 0.3333333333333333703, 0.3219752754296894559, 0.3333333333333333703, 0.3219752754296894559, 0.3333333333333333703, 0.3219752754296894559, 0.3333333333333333703, 0.3219752754296894559, 0.3333333333333333703, 0.3219752754296894559, 0.3333333333333333703, 0.3219752754296894559, 0.3333333333333333703, 0.3219752754296894559, 0.3333333333333333703, 0.3219752754296894559, 0.3333333333333333703, 0.3219752754296894559, 0.3333333333333333703, 0.3219752754296894559, 0.3333333333333333703, 0.3219752754296894559, 0.3333333333333333703, 0.3219752754296894559, 0.3333333333333333703, 0.3219752754296894559, 0.3333333333333333703, 0.3219752754296894559, 0.3333333333333333703, 0.3219752754296894559, 0.3333333333333333703, 0.3219752754296894559, 0.3333333333333333703, 0.3219752754296894559, 0.3333333333333333703, 0.3219752754296894559, 0.3333333333333333703, 0.3219752754296894559, 0.3333333333333333703, 0.3219752754296894559, 0.3333333333333333703, 0.3219752754296894559, 0.3333333333333333703, 0.3219752754296894559, 0.3333333333333333703, 0.3219752754296894559, 0.3333333333333333703, 0.3219752754296894559, 0.3333333333333333703, 0.3219752754296894559, 0.3333333333333333703, 0.3219752754296894559, 0.3333333333333333703, 0.3219752754296894559, 0.3333333333333333703, 0.3219752754296894559, 0.3333333333333333703, 0.3219752754296894559, 0.3333333333333333703, 0.3219752754296894559, 0.3333333333333333703, 0.3219752754296894559, 0.3333333333333333703, 0.3219752754296894559, 0.3333333333333333703, 0.3219752754296894559, 0.3333333333333333703, 0.3219752754296894559, 0.3333333333333333703, 0.3219752754296894559, 0.3333333333333333703, 0.3219752754296894559, 0.3333333333333333703, 0.3219752754296894559, 0.3333333333333333703, 0.3219752754296894559, 0.3333333333333333703, 0.3219752754296894559, 0.3333333333333333703, 0.3219752754296894559, 0.3333333333333333703, 0.3219752754296894559, 0.3333333333333333703, 0.3219752754296894559, 0.3333333333333333703, 0.3219752754296894559, 0.3333333333333333703, 0.3219752754296894559, 0.3333333333333333703, 0.3219752754296894559, 0.3333333333333333703, 0.3219752754296894559, 0.3333333333333333703, 0.3219752754296894559, 0.3333333333333333703, 0.3219752754296894559, 0.3333333333333333703, 0.3219752754296894559, 0.3333333333333333703, 0.3219752754296894559, 0.3333333333333333703, 0.3219752754296894559, 0.3333333333333333703, 0.3219752754296894559, 0.3333333333333333703, 0.3219752754296894559, 0.3333333333333333703, 0.3219752754296894559, 0.3333333333333333703, 0.3219752754296894559, 0.3333333333333333703, 0.3219752754296894559, 0.3333333333333333703, 0.3219752754296894559, 0.3333333333333333703, 0.3219752754296894559, 0.3333333333333333703, 0.3219752754296894559, 0.3333333333333333703, 0.3219752754296894559, 0.3333333333333333703, 0.3219752754296894559, 0.3333333333333333703, 0.3219752754296894559, 0.3333333333333333703, 0.3219752754296894559, 0.3333333333333333703, 0.3219752754296894559, 0.3333333333333333703, 0.3219752754296894559, 0.3333333333333333703, 0.3219752754296894559, 0.3333333333333333703, 0.3219752754296894559, 0.3333333333333333703, 0.3219752754296894559, 0.3333333333333333703, 0.3219752754296894559, 0.3333333333333333703, 0.3219752754296894559, 0.3333333333333333703, 0.3219752754296894559, 0.3333333333333333703, 0.3219752754296894559, 0.3333333333333333703, 0.3219752754296894559, 0.3333333333333333703, 0.3219752754296894559, 0.3333333333333333703, 0.3219752754296894559, 0.3333333333333333703, 0.3219752754296894559, 0.3333333333333333703, 0.3219752754296894559, 0.3333333333333333703, 0.3219752754296894559, 0.3333333333333333703, 0.3219752754296894559, 0.3333333333333333703, 0.3219752754296894559, 0.3333333333333333703, 0.3219752754296894559, 0.3333333333333333703, 0.3219752754296894559, 0.3333333333333333703, 0.3219752754296894559, 0.3333333333333333703, 0.3219752754296894559, 0.3333333333333333703, 0.3219752754296894559, 0.3333333333333333703, 0.3219752754296894559, 0.3333333333333333703, 0.3219752754296894559, 0.3333333333333333703, 0.3219752754296894559, 0.3333333333333333703, 0.3219752754296894559, 0.3333333333333333703, 0.3219752754296894559, 0.3333333333333333703, 0.3219752754296894559, 0.3333333333333333703, 0.3219752754296894559, 0.3333333333333333703, 0.3219752754296894559, 0.3333333333333333703, 0.3219752754296894559, 0.3333333333333333703, 0.3219752754296894559, 0.3333333333333333703, 0.3219752754296894559, 0.3333333333333333703, 0.3219752754296894559, 0.3333333333333333703, 0.3219752754296894559, 0.3333333333333333703, 0.3219752754296894559, 0.3333333333333333703, 0.3219752754296894559, 0.3333333333333333703, 0.3219752754296894559, 0.3333333333333333703, 0.3219752754296894559, 0.3333333333333333703, 0.3219752754296894559, 0.3333333333333333703, 0.3219752754296894559, 0.3333333333333333703, 0.3219752754296894559, 0.3333333333333333703, 0.3219752754296894559, 0.3333333333333333703, 0.3219752754296894559, 0.3333333333333333703, 0.3219752754296894559, 0.3333333333333333703, 0.3219752754296894559, 0.3333333333333333703, 0.3219752754296894559, 0.3333333333333333703, 0.3219752754296894559, 0.3333333333333333703, 0.3219752754296894559, 0.3333333333333333703, 0.3219752754296894559, 0.3333333333333333703, 0.3219752754296894559, 0.3333333333333333703, 0.3219752754296894559, 0.3333333333333333703, 0.3219752754296894559, 0.3333333333333333703, 0.3219752754296894559, 0.3333333333333333703, 0.3219752754296894559, 0.3333333333333333703, 0.3219752754296894559, 0.3333333333333333703, 0.3219752754296894559, 0.3333333333333333703, 0.3219752754296894559, 0.3333333333333333703, 0.3219752754296894559, 0.3333333333333333703, 0.3219752754296894559, 0.3333333333333333703, 0.3219752754296894559, 0.3333333333333333703, 0.3219752754296894559, 0.3333333333333333703, 0.3219752754296894559, 0.3333333333333333703, 0.3219752754296894559, 0.3333333333333333703, 0.3219752754296894559, 0.3333333333333333703, 0.3219752754296894559, 0.3333333333333333703, 0.3219752754296894559, 0.3333333333333333703, 0.3219752754296894559, 0.3333333333333333703, 0.3219752754296894559, 0.3333333333333333703, 0.3219752754296894559, 0.3333333333333333703, 0.3219752754296894559, 0.3333333333333333703, 0.3219752754296894559, 0.3333333333333333703, 0.3219752754296894559, 0.3333333333333333703, 0.3219752754296894559, 0.3333333333333333703, 0.3219752754296894559, 0.3333333333333333703, 0.3219752754296894559, 0.3333333333333333703, 0.3219752754296894559, 0.3333333333333333703, 0.3219752754296894559, 0.3333333333333333703, 0.3219752754296894559, 0.3333333333333333703, 0.3219752754296894559, 0.3333333333333333703, 0.3219752754296894559, 0.3333333333333333703, 0.3219752754296894559, 0.3333333333333333703, 0.3219752754296894559, 0.3333333333333333703, 0.3219752754296894559, 0.3333333333333333703, 0.3219752754296894559, 0.3333333333333333703, 0.3219752754296894559, 0.3333333333333333703),
 ( 1.000000000000000000, 0.9659258262890683122, 1.000000000000000000, 0.9659258262890683122, 1.000000000000000000, 0.9659258262890683122, 1.000000000000000000, 0.9659258262890683122, 1.000000000000000000, 0.9659258262890683122, 1.000000000000000000, 0.9659258262890683122, 1.000000000000000000, 0.9659258262890683122, 1.000000000000000000, 0.9659258262890683122, 1.000000000000000000, 0.9659258262890683122, 1.000000000000000000, 0.9659258262890683122, 1.000000000000000000, 0.9659258262890683122, 1.000000000000000000, 0.9659258262890683122, 1.000000000000000000, 0.9659258262890683122, 1.000000000000000000, 0.9659258262890683122, 1.000000000000000000, 0.9659258262890683122, 1.000000000000000000, 0.9659258262890683122, 1.000000000000000000, 0.9659258262890683122, 1.000000000000000000, 0.9659258262890683122, 1.000000000000000000, 0.9659258262890683122, 1.000000000000000000, 0.9659258262890683122, 1.000000000000000000, 0.9659258262890683122, 1.000000000000000000, 0.9659258262890683122, 1.000000000000000000, 0.9659258262890683122, 1.000000000000000000, 0.9659258262890683122, 1.000000000000000000, 0.9659258262890683122, 1.000000000000000000, 0.9659258262890683122, 1.000000000000000000, 0.9659258262890683122, 1.000000000000000000, 0.9659258262890683122, 1.000000000000000000, 0.9659258262890683122, 1.000000000000000000, 0.9659258262890683122, 1.000000000000000000, 0.9659258262890683122, 1.000000000000000000, 0.9659258262890683122, 1.000000000000000000, 0.9659258262890683122, 1.000000000000000000, 0.9659258262890683122, 1.000000000000000000, 0.9659258262890683122, 1.000000000000000000, 0.9659258262890683122, 1.000000000000000000, 0.9659258262890683122, 1.000000000000000000, 0.9659258262890683122, 1.000000000000000000, 0.9659258262890683122, 1.000000000000000000, 0.9659258262890683122, 1.000000000000000000, 0.9659258262890683122, 1.000000000000000000, 0.9659258262890683122, 1.000000000000000000, 0.9659258262890683122, 1.000000000000000000, 0.9659258262890683122, 1.000000000000000000, 0.9659258262890683122, 1.000000000000000000, 0.9659258262890683122, 1.000000000000000000, 0.9659258262890683122, 1.000000000000000000, 0.9659258262890683122, 1.000000000000000000, 0.9659258262890683122, 1.000000000000000000, 0.9659258262890683122, 1.000000000000000000, 0.9659258262890683122, 1.000000000000000000, 0.9659258262890683122, 1.000000000000000000, 0.9659258262890683122, 1.000000000000000000, 0.9659258262890683122, 1.000000000000000000, 0.9659258262890683122, 1.000000000000000000, 0.9659258262890683122, 1.000000000000000000, 0.9659258262890683122, 1.000000000000000000, 0.9659258262890683122, 1.000000000000000000, 0.9659258262890683122, 1.000000000000000000, 0.9659258262890683122, 1.000000000000000000, 0.9659258262890683122, 1.000000000000000000, 0.9659258262890683122, 1.000000000000000000, 0.9659258262890683122, 1.000000000000000000, 0.9659258262890683122, 1.000000000000000000, 0.9659258262890683122, 1.000000000000000000, 0.9659258262890683122, 1.000000000000000000, 0.9659258262890683122, 1.000000000000000000, 0.9659258262890683122, 1.000000000000000000, 0.9659258262890683122, 1.000000000000000000, 0.9659258262890683122, 1.000000000000000000, 0.9659258262890683122, 1.000000000000000000, 0.9659258262890683122, 1.000000000000000000, 0.9659258262890683122, 1.000000000000000000, 0.9659258262890683122, 1.000000000000000000, 0.9659258262890683122, 1.000000000000000000, 0.9659258262890683122, 1.000000000000000000, 0.9659258262890683122, 1.000000000000000000, 0.9659258262890683122, 1.000000000000000000, 0.9659258262890683122, 1.000000000000000000, 0.9659258262890683122, 1.000000000000000000, 0.9659258262890683122, 1.000000000000000000, 0.9659258262890683122, 1.000000000000000000, 0.9659258262890683122, 1.000000000000000000, 0.9659258262890683122, 1.000000000000000000, 0.9659258262890683122, 1.000000000000000000, 0.9659258262890683122, 1.000000000000000000, 0.9659258262890683122, 1.000000000000000000, 0.9659258262890683122, 1.000000000000000000, 0.9659258262890683122, 1.000000000000000000, 0.9659258262890683122, 1.000000000000000000, 0.9659258262890683122, 1.000000000000000000, 0.9659258262890683122, 1.000000000000000000, 0.9659258262890683122, 1.000000000000000000, 0.9659258262890683122, 1.000000000000000000, 0.9659258262890683122, 1.000000000000000000, 0.9659258262890683122, 1.000000000000000000, 0.9659258262890683122, 1.000000000000000000, 0.9659258262890683122, 1.000000000000000000, 0.9659258262890683122, 1.000000000000000000, 0.9659258262890683122, 1.000000000000000000, 0.9659258262890683122, 1.000000000000000000, 0.9659258262890683122, 1.000000000000000000, 0.9659258262890683122, 1.000000000000000000, 0.9659258262890683122, 1.000000000000000000, 0.9659258262890683122, 1.000000000000000000, 0.9659258262890683122, 1.000000000000000000, 0.9659258262890683122, 1.000000000000000000, 0.9659258262890683122, 1.000000000000000000, 0.9659258262890683122, 1.000000000000000000, 0.9659258262890683122, 1.000000000000000000, 0.9659258262890683122, 1.000000000000000000, 0.9659258262890683122, 1.000000000000000000, 0.9659258262890683122, 1.000000000000000000, 0.9659258262890683122, 1.000000000000000000, 0.9659258262890683122, 1.000000000000000000, 0.9659258262890683122, 1.000000000000000000, 0.9659258262890683122, 1.000000000000000000, 0.9659258262890683122, 1.000000000000000000, 0.9659258262890683122, 1.000000000000000000, 0.9659258262890683122, 1.000000000000000000, 0.9659258262890683122, 1.000000000000000000, 0.9659258262890683122, 1.000000000000000000, 0.9659258262890683122, 1.000000000000000000, 0.9659258262890683122, 1.000000000000000000, 0.9659258262890683122, 1.000000000000000000, 0.9659258262890683122, 1.000000000000000000, 0.9659258262890683122, 1.000000000000000000, 0.9659258262890683122, 1.000000000000000000, 0.9659258262890683122, 1.000000000000000000, 0.9659258262890683122, 1.000000000000000000, 0.9659258262890683122, 1.000000000000000000, 0.9659258262890683122, 1.000000000000000000, 0.9659258262890683122, 1.000000000000000000, 0.9659258262890683122, 1.000000000000000000, 0.9659258262890683122, 1.000000000000000000, 0.9659258262890683122, 1.000000000000000000, 0.9659258262890683122, 1.000000000000000000, 0.9659258262890683122, 1.000000000000000000, 0.9659258262890683122, 1.000000000000000000, 0.9659258262890683122, 1.000000000000000000, 0.9659258262890683122, 1.000000000000000000, 0.9659258262890683122, 1.000000000000000000, 0.9659258262890683122, 1.000000000000000000, 0.9659258262890683122, 1.000000000000000000, 0.9659258262890683122, 1.000000000000000000, 0.9659258262890683122, 1.000000000000000000, 0.9659258262890683122, 1.000000000000000000, 0.9659258262890683122, 1.000000000000000000, 0.9659258262890683122, 1.000000000000000000, 0.9659258262890683122, 1.000000000000000000, 0.9659258262890683122, 1.000000000000000000, 0.9659258262890683122, 1.000000000000000000, 0.9659258262890683122, 1.000000000000000000, 0.9659258262890683122, 1.000000000000000000, 0.9659258262890683122, 1.000000000000000000, 0.9659258262890683122, 1.000000000000000000, 0.9659258262890683122, 1.000000000000000000, 0.9659258262890683122, 1.000000000000000000, 0.9659258262890683122, 1.000000000000000000, 0.9659258262890683122, 1.000000000000000000, 0.9659258262890683122, 1.000000000000000000, 0.9659258262890683122, 1.000000000000000000, 0.9659258262890683122, 1.000000000000000000, 0.9659258262890683122, 1.000000000000000000, 0.9659258262890683122, 1.000000000000000000, 0.9659258262890683122, 1.000000000000000000, 0.9659258262890683122, 1.000000000000000000, 0.9659258262890683122, 1.000000000000000000, 0.9659258262890683122, 1.000000000000000000, 0.9659258262890683122, 1.000000000000000000, 0.9659258262890683122, 1.000000000000000000, 0.9659258262890683122, 1.000000000000000000, 0.9659258262890683122, 1.000000000000000000, 0.9659258262890683122, 1.000000000000000000, 0.9659258262890683122, 1.000000000000000000, 0.9659258262890683122, 1.000000000000000000, 0.9659258262890683122, 1.000000000000000000, 0.9659258262890683122, 1.000000000000000000, 0.9659258262890683122, 1.000000000000000000, 0.9659258262890683122, 1.000000000000000000, 0.9659258262890683122, 1.000000000000000000, 0.9659258262890683122, 1.000000000000000000, 0.9659258262890683122, 1.000000000000000000, 0.9659258262890683122, 1.000000000000000000, 0.9659258262890683122, 1.000000000000000000, 0.9659258262890683122, 1.000000000000000000, 0.9659258262890683122, 1.000000000000000000, 0.9659258262890683122, 1.000000000000000000, 0.9659258262890683122, 1.000000000000000000, 0.9659258262890683122, 1.000000000000000000, 0.9659258262890683122, 1.000000000000000000, 0.9659258262890683122, 1.000000000000000000, 0.9659258262890683122, 1.000000000000000000, 0.9659258262890683122, 1.000000000000000000, 0.9659258262890683122, 1.000000000000000000, 0.9659258262890683122, 1.000000000000000000, 0.9659258262890683122, 1.000000000000000000, 0.9659258262890683122, 1.000000000000000000, 0.9659258262890683122, 1.000000000000000000, 0.9659258262890683122, 1.000000000000000000, 0.9659258262890683122, 1.000000000000000000, 0.9659258262890683122, 1.000000000000000000, 0.9659258262890683122, 1.000000000000000000, 0.9659258262890683122, 1.000000000000000000, 0.9659258262890683122, 1.000000000000000000, 0.9659258262890683122, 1.000000000000000000, 0.9659258262890683122, 1.000000000000000000, 0.9659258262890683122, 1.000000000000000000, 0.9659258262890683122, 1.000000000000000000, 0.9659258262890683122, 1.000000000000000000, 0.9659258262890683122, 1.000000000000000000, 0.9659258262890683122, 1.000000000000000000, 0.9659258262890683122, 1.000000000000000000, 0.9659258262890683122, 1.000000000000000000, 0.9659258262890683122, 1.000000000000000000, 0.9659258262890683122, 1.000000000000000000, 0.9659258262890683122, 1.000000000000000000, 0.9659258262890683122, 1.000000000000000000, 0.9659258262890683122, 1.000000000000000000, 0.9659258262890683122, 1.000000000000000000, 0.9659258262890683122, 1.000000000000000000, 0.9659258262890683122, 1.000000000000000000, 0.9659258262890683122, 1.000000000000000000, 0.9659258262890683122, 1.000000000000000000, 0.9659258262890683122, 1.000000000000000000, 0.9659258262890683122, 1.000000000000000000, 0.9659258262890683122, 1.000000000000000000, 0.9659258262890683122, 1.000000000000000000),
 ( 0.3333333333333333703, 0.3219752754296894559, 0.3333333333333333703, 0.3219752754296894559, 0.3333333333333333703, 0.3219752754296894559, 0.3333333333333333703, 0.3219752754296894559, 0.3333333333333333703, 0.3219752754296894559, 0.3333333333333333703, 0.3219752754296894559, 0.3333333333333333703, 0.3219752754296894559, 0.3333333333333333703, 0.3219752754296894559, 0.3333333333333333703, 0.3219752754296894559, 0.3333333333333333703, 0.3219752754296894559, 0.3333333333333333703, 0.3219752754296894559, 0.3333333333333333703, 0.3219752754296894559, 0.3333333333333333703, 0.3219752754296894559, 0.3333333333333333703, 0.3219752754296894559, 0.3333333333333333703, 0.3219752754296894559, 0.3333333333333333703, 0.3219752754296894559, 0.3333333333333333703, 0.3219752754296894559, 0.3333333333333333703, 0.3219752754296894559, 0.3333333333333333703, 0.3219752754296894559, 0.3333333333333333703, 0.3219752754296894559, 0.3333333333333333703, 0.3219752754296894559, 0.3333333333333333703, 0.3219752754296894559, 0.3333333333333333703, 0.3219752754296894559, 0.3333333333333333703, 0.3219752754296894559, 0.3333333333333333703, 0.3219752754296894559, 0.3333333333333333703, 0.3219752754296894559, 0.3333333333333333703, 0.3219752754296894559, 0.3333333333333333703, 0.3219752754296894559, 0.3333333333333333703, 0.3219752754296894559, 0.3333333333333333703, 0.3219752754296894559, 0.3333333333333333703, 0.3219752754296894559, 0.3333333333333333703, 0.3219752754296894559, 0.3333333333333333703, 0.3219752754296894559, 0.3333333333333333703, 0.3219752754296894559, 0.3333333333333333703, 0.3219752754296894559, 0.3333333333333333703, 0.3219752754296894559, 0.3333333333333333703, 0.3219752754296894559, 0.3333333333333333703, 0.3219752754296894559, 0.3333333333333333703, 0.3219752754296894559, 0.3333333333333333703, 0.3219752754296894559, 0.3333333333333333703, 0.3219752754296894559, 0.3333333333333333703, 0.3219752754296894559, 0.3333333333333333703, 0.3219752754296894559, 0.3333333333333333703, 0.3219752754296894559, 0.3333333333333333703, 0.3219752754296894559, 0.3333333333333333703, 0.3219752754296894559, 0.3333333333333333703, 0.3219752754296894559, 0.3333333333333333703, 0.3219752754296894559, 0.3333333333333333703, 0.3219752754296894559, 0.3333333333333333703, 0.3219752754296894559, 0.3333333333333333703, 0.3219752754296894559, 0.3333333333333333703, 0.3219752754296894559, 0.3333333333333333703, 0.3219752754296894559, 0.3333333333333333703, 0.3219752754296894559, 0.3333333333333333703, 0.3219752754296894559, 0.3333333333333333703, 0.3219752754296894559, 0.3333333333333333703, 0.3219752754296894559, 0.3333333333333333703, 0.3219752754296894559, 0.3333333333333333703, 0.3219752754296894559, 0.3333333333333333703, 0.3219752754296894559, 0.3333333333333333703, 0.3219752754296894559, 0.3333333333333333703, 0.3219752754296894559, 0.3333333333333333703, 0.3219752754296894559, 0.3333333333333333703, 0.3219752754296894559, 0.3333333333333333703, 0.3219752754296894559, 0.3333333333333333703, 0.3219752754296894559, 0.3333333333333333703, 0.3219752754296894559, 0.3333333333333333703, 0.3219752754296894559, 0.3333333333333333703, 0.3219752754296894559, 0.3333333333333333703, 0.3219752754296894559, 0.3333333333333333703, 0.3219752754296894559, 0.3333333333333333703, 0.3219752754296894559, 0.3333333333333333703, 0.3219752754296894559, 0.3333333333333333703, 0.3219752754296894559, 0.3333333333333333703, 0.3219752754296894559, 0.3333333333333333703, 0.3219752754296894559, 0.3333333333333333703, 0.3219752754296894559, 0.3333333333333333703, 0.3219752754296894559, 0.3333333333333333703, 0.3219752754296894559, 0.3333333333333333703, 0.3219752754296894559, 0.3333333333333333703, 0.3219752754296894559, 0.3333333333333333703, 0.3219752754296894559, 0.3333333333333333703, 0.3219752754296894559, 0.3333333333333333703, 0.3219752754296894559, 0.3333333333333333703, 0.3219752754296894559, 0.3333333333333333703, 0.3219752754296894559, 0.3333333333333333703, 0.3219752754296894559, 0.3333333333333333703, 0.3219752754296894559, 0.3333333333333333703, 0.3219752754296894559, 0.3333333333333333703, 0.3219752754296894559, 0.3333333333333333703, 0.3219752754296894559, 0.3333333333333333703, 0.3219752754296894559, 0.3333333333333333703, 0.3219752754296894559, 0.3333333333333333703, 0.3219752754296894559, 0.3333333333333333703, 0.3219752754296894559, 0.3333333333333333703, 0.3219752754296894559, 0.3333333333333333703, 0.3219752754296894559, 0.3333333333333333703, 0.3219752754296894559, 0.3333333333333333703, 0.3219752754296894559, 0.3333333333333333703, 0.3219752754296894559, 0.3333333333333333703, 0.3219752754296894559, 0.3333333333333333703, 0.3219752754296894559, 0.3333333333333333703, 0.3219752754296894559, 0.3333333333333333703, 0.3219752754296894559, 0.3333333333333333703, 0.3219752754296894559, 0.3333333333333333703, 0.3219752754296894559, 0.3333333333333333703, 0.3219752754296894559, 0.3333333333333333703, 0.3219752754296894559, 0.3333333333333333703, 0.3219752754296894559, 0.3333333333333333703, 0.3219752754296894559, 0.3333333333333333703, 0.3219752754296894559, 0.3333333333333333703, 0.3219752754296894559, 0.3333333333333333703, 0.3219752754296894559, 0.3333333333333333703, 0.3219752754296894559, 0.3333333333333333703, 0.3219752754296894559, 0.3333333333333333703, 0.3219752754296894559, 0.3333333333333333703, 0.3219752754296894559, 0.3333333333333333703, 0.3219752754296894559, 0.3333333333333333703, 0.3219752754296894559, 0.3333333333333333703, 0.3219752754296894559, 0.3333333333333333703, 0.3219752754296894559, 0.3333333333333333703, 0.3219752754296894559, 0.3333333333333333703, 0.3219752754296894559, 0.3333333333333333703, 0.3219752754296894559, 0.3333333333333333703, 0.3219752754296894559, 0.3333333333333333703, 0.3219752754296894559, 0.3333333333333333703, 0.3219752754296894559, 0.3333333333333333703, 0.3219752754296894559, 0.3333333333333333703, 0.3219752754296894559, 0.3333333333333333703, 0.3219752754296894559, 0.3333333333333333703, 0.3219752754296894559, 0.3333333333333333703, 0.3219752754296894559, 0.3333333333333333703, 0.3219752754296894559, 0.3333333333333333703, 0.3219752754296894559, 0.3333333333333333703, 0.3219752754296894559, 0.3333333333333333703, 0.3219752754296894559, 0.3333333333333333703, 0.3219752754296894559, 0.3333333333333333703, 0.3219752754296894559, 0.3333333333333333703, 0.3219752754296894559, 0.3333333333333333703, 0.3219752754296894559, 0.3333333333333333703, 0.3219752754296894559, 0.3333333333333333703, 0.3219752754296894559, 0.3333333333333333703, 0.3219752754296894559, 0.3333333333333333703, 0.3219752754296894559, 0.3333333333333333703, 0.3219752754296894559, 0.3333333333333333703, 0.3219752754296894559, 0.3333333333333333703, 0.3219752754296894559, 0.3333333333333333703, 0.3219752754296894559, 0.3333333333333333703, 0.3219752754296894559, 0.3333333333333333703, 0.3219752754296894559, 0.3333333333333333703, 0.3219752754296894559, 0.3333333333333333703, 0.3219752754296894559, 0.3333333333333333703, 0.3219752754296894559, 0.3333333333333333703, 0.3219752754296894559, 0.3333333333333333703, 0.3219752754296894559, 0.3333333333333333703, 0.3219752754296894559, 0.3333333333333333703, 0.3219752754296894559, 0.3333333333333333703, 0.3219752754296894559, 0.3333333333333333703, 0.3219752754296894559, 0.3333333333333333703, 0.3219752754296894559, 0.3333333333333333703, 0.3219752754296894559, 0.3333333333333333703, 0.3219752754296894559, 0.3333333333333333703, 0.3219752754296894559, 0.3333333333333333703, 0.3219752754296894559, 0.3333333333333333703, 0.3219752754296894559, 0.3333333333333333703, 0.3219752754296894559, 0.3333333333333333703, 0.3219752754296894559, 0.3333333333333333703, 0.3219752754296894559, 0.3333333333333333703, 0.3219752754296894559, 0.3333333333333333703, 0.3219752754296894559, 0.3333333333333333703, 0.3219752754296894559, 0.3333333333333333703, 0.3219752754296894559, 0.3333333333333333703, 0.3219752754296894559, 0.3333333333333333703, 0.3219752754296894559, 0.3333333333333333703, 0.3219752754296894559, 0.3333333333333333703, 0.3219752754296894559, 0.3333333333333333703, 0.3219752754296894559, 0.3333333333333333703, 0.3219752754296894559, 0.3333333333333333703, 0.3219752754296894559, 0.3333333333333333703, 0.3219752754296894559, 0.3333333333333333703, 0.3219752754296894559, 0.3333333333333333703, 0.3219752754296894559, 0.3333333333333333703, 0.3219752754296894559, 0.3333333333333333703, 0.3219752754296894559, 0.3333333333333333703, 0.3219752754296894559, 0.3333333333333333703, 0.3219752754296894559, 0.3333333333333333703, 0.3219752754296894559, 0.3333333333333333703, 0.3219752754296894559, 0.3333333333333333703, 0.3219752754296894559, 0.3333333333333333703, 0.3219752754296894559, 0.3333333333333333703, 0.3219752754296894559, 0.3333333333333333703, 0.3219752754296894559, 0.3333333333333333703, 0.3219752754296894559, 0.3333333333333333703, 0.3219752754296894559, 0.3333333333333333703, 0.3219752754296894559, 0.3333333333333333703, 0.3219752754296894559, 0.3333333333333333703, 0.3219752754296894559, 0.3333333333333333703, 0.3219752754296894559, 0.3333333333333333703, 0.3219752754296894559, 0.3333333333333333703, 0.3219752754296894559, 0.3333333333333333703, 0.3219752754296894559, 0.3333333333333333703, 0.3219752754296894559, 0.3333333333333333703, 0.3219752754296894559, 0.3333333333333333703, 0.3219752754296894559, 0.3333333333333333703, 0.3219752754296894559, 0.3333333333333333703, 0.3219752754296894559, 0.3333333333333333703, 0.3219752754296894559, 0.3333333333333333703, 0.3219752754296894559, 0.3333333333333333703, 0.3219752754296894559, 0.3333333333333333703, 0.3219752754296894559, 0.3333333333333333703, 0.3219752754296894559, 0.3333333333333333703, 0.3219752754296894559, 0.3333333333333333703, 0.3219752754296894559, 0.3333333333333333703, 0.3219752754296894559, 0.3333333333333333703, 0.3219752754296894559, 0.3333333333333333703, 0.3219752754296894559, 0.3333333333333333703, 0.3219752754296894559, 0.3333333333333333703, 0.3219752754296894559, 0.3333333333333333703, 0.3219752754296894559, 0.3333333333333333703, 0.3219752754296894559, 0.3333333333333333703, 0.3219752754296894559, 0.3333333333333333703, 0.3219752754296894559, 0.3333333333333333703, 0.3219752754296894559, 0.3333333333333333703, 0.3219752754296894559, 0.3333333333333333703, 0.3219752754296894559, 0.3333333333333333703, 0.3219752754296894559, 0.3333333333333333703, 0.3219752754296894559, 0.3333333333333333703, 0.3219752754296894559, 0.3333333333333333703),
 ( 0.3333333333333333703, 0.3219752754296894559, 0.3333333333333333703, 0.3219752754296894559, 0.3333333333333333703, 0.3219752754296894559, 0.3333333333333333703, 0.3219752754296894559, 0.3333333333333333703, 0.3219752754296894559, 0.3333333333333333703, 0.3219752754296894559, 0.3333333333333333703, 0.3219752754296894559, 0.3333333333333333703, 0.3219752754296894559, 0.3333333333333333703, 0.3219752754296894559, 0.3333333333333333703, 0.3219752754296894559, 0.3333333333333333703, 0.3219752754296894559, 0.3333333333333333703, 0.3219752754296894559, 0.3333333333333333703, 0.3219752754296894559, 0.3333333333333333703, 0.3219752754296894559, 0.3333333333333333703, 0.3219752754296894559, 0.3333333333333333703, 0.3219752754296894559, 0.3333333333333333703, 0.3219752754296894559, 0.3333333333333333703, 0.3219752754296894559, 0.3333333333333333703, 0.3219752754296894559, 0.3333333333333333703, 0.3219752754296894559, 0.3333333333333333703, 0.3219752754296894559, 0.3333333333333333703, 0.3219752754296894559, 0.3333333333333333703, 0.3219752754296894559, 0.3333333333333333703, 0.3219752754296894559, 0.3333333333333333703, 0.3219752754296894559, 0.3333333333333333703, 0.3219752754296894559, 0.3333333333333333703, 0.3219752754296894559, 0.3333333333333333703, 0.3219752754296894559, 0.3333333333333333703, 0.3219752754296894559, 0.3333333333333333703, 0.3219752754296894559, 0.3333333333333333703, 0.3219752754296894559, 0.3333333333333333703, 0.3219752754296894559, 0.3333333333333333703, 0.3219752754296894559, 0.3333333333333333703, 0.3219752754296894559, 0.3333333333333333703, 0.3219752754296894559, 0.3333333333333333703, 0.3219752754296894559, 0.3333333333333333703, 0.3219752754296894559, 0.3333333333333333703, 0.3219752754296894559, 0.3333333333333333703, 0.3219752754296894559, 0.3333333333333333703, 0.3219752754296894559, 0.3333333333333333703, 0.3219752754296894559, 0.3333333333333333703, 0.3219752754296894559, 0.3333333333333333703, 0.3219752754296894559, 0.3333333333333333703, 0.3219752754296894559, 0.3333333333333333703, 0.3219752754296894559, 0.3333333333333333703, 0.3219752754296894559, 0.3333333333333333703, 0.3219752754296894559, 0.3333333333333333703, 0.3219752754296894559, 0.3333333333333333703, 0.3219752754296894559, 0.3333333333333333703, 0.3219752754296894559, 0.3333333333333333703, 0.3219752754296894559, 0.3333333333333333703, 0.3219752754296894559, 0.3333333333333333703, 0.3219752754296894559, 0.3333333333333333703, 0.3219752754296894559, 0.3333333333333333703, 0.3219752754296894559, 0.3333333333333333703, 0.3219752754296894559, 0.3333333333333333703, 0.3219752754296894559, 0.3333333333333333703, 0.3219752754296894559, 0.3333333333333333703, 0.3219752754296894559, 0.3333333333333333703, 0.3219752754296894559, 0.3333333333333333703, 0.3219752754296894559, 0.3333333333333333703, 0.3219752754296894559, 0.3333333333333333703, 0.3219752754296894559, 0.3333333333333333703, 0.3219752754296894559, 0.3333333333333333703, 0.3219752754296894559, 0.3333333333333333703, 0.3219752754296894559, 0.3333333333333333703, 0.3219752754296894559, 0.3333333333333333703, 0.3219752754296894559, 0.3333333333333333703, 0.3219752754296894559, 0.3333333333333333703, 0.3219752754296894559, 0.3333333333333333703, 0.3219752754296894559, 0.3333333333333333703, 0.3219752754296894559, 0.3333333333333333703, 0.3219752754296894559, 0.3333333333333333703, 0.3219752754296894559, 0.3333333333333333703, 0.3219752754296894559, 0.3333333333333333703, 0.3219752754296894559, 0.3333333333333333703, 0.3219752754296894559, 0.3333333333333333703, 0.3219752754296894559, 0.3333333333333333703, 0.3219752754296894559, 0.3333333333333333703, 0.3219752754296894559, 0.3333333333333333703, 0.3219752754296894559, 0.3333333333333333703, 0.3219752754296894559, 0.3333333333333333703, 0.3219752754296894559, 0.3333333333333333703, 0.3219752754296894559, 0.3333333333333333703, 0.3219752754296894559, 0.3333333333333333703, 0.3219752754296894559, 0.3333333333333333703, 0.3219752754296894559, 0.3333333333333333703, 0.3219752754296894559, 0.3333333333333333703, 0.3219752754296894559, 0.3333333333333333703, 0.3219752754296894559, 0.3333333333333333703, 0.3219752754296894559, 0.3333333333333333703, 0.3219752754296894559, 0.3333333333333333703, 0.3219752754296894559, 0.3333333333333333703, 0.3219752754296894559, 0.3333333333333333703, 0.3219752754296894559, 0.3333333333333333703, 0.3219752754296894559, 0.3333333333333333703, 0.3219752754296894559, 0.3333333333333333703, 0.3219752754296894559, 0.3333333333333333703, 0.3219752754296894559, 0.3333333333333333703, 0.3219752754296894559, 0.3333333333333333703, 0.3219752754296894559, 0.3333333333333333703, 0.3219752754296894559, 0.3333333333333333703, 0.3219752754296894559, 0.3333333333333333703, 0.3219752754296894559, 0.3333333333333333703, 0.3219752754296894559, 0.3333333333333333703, 0.3219752754296894559, 0.3333333333333333703, 0.3219752754296894559, 0.3333333333333333703, 0.3219752754296894559, 0.3333333333333333703, 0.3219752754296894559, 0.3333333333333333703, 0.3219752754296894559, 0.3333333333333333703, 0.3219752754296894559, 0.3333333333333333703, 0.3219752754296894559, 0.3333333333333333703, 0.3219752754296894559, 0.3333333333333333703, 0.3219752754296894559, 0.3333333333333333703, 0.3219752754296894559, 0.3333333333333333703, 0.3219752754296894559, 0.3333333333333333703, 0.3219752754296894559, 0.3333333333333333703, 0.3219752754296894559, 0.3333333333333333703, 0.3219752754296894559, 0.3333333333333333703, 0.3219752754296894559, 0.3333333333333333703, 0.3219752754296894559, 0.3333333333333333703, 0.3219752754296894559, 0.3333333333333333703, 0.3219752754296894559, 0.3333333333333333703, 0.3219752754296894559, 0.3333333333333333703, 0.3219752754296894559, 0.3333333333333333703, 0.3219752754296894559, 0.3333333333333333703, 0.3219752754296894559, 0.3333333333333333703, 0.3219752754296894559, 0.3333333333333333703, 0.3219752754296894559, 0.3333333333333333703, 0.3219752754296894559, 0.3333333333333333703, 0.3219752754296894559, 0.3333333333333333703, 0.3219752754296894559, 0.3333333333333333703, 0.3219752754296894559, 0.3333333333333333703, 0.3219752754296894559, 0.3333333333333333703, 0.3219752754296894559, 0.3333333333333333703, 0.3219752754296894559, 0.3333333333333333703, 0.3219752754296894559, 0.3333333333333333703, 0.3219752754296894559, 0.3333333333333333703, 0.3219752754296894559, 0.3333333333333333703, 0.3219752754296894559, 0.3333333333333333703, 0.3219752754296894559, 0.3333333333333333703, 0.3219752754296894559, 0.3333333333333333703, 0.3219752754296894559, 0.3333333333333333703, 0.3219752754296894559, 0.3333333333333333703, 0.3219752754296894559, 0.3333333333333333703, 0.3219752754296894559, 0.3333333333333333703, 0.3219752754296894559, 0.3333333333333333703, 0.3219752754296894559, 0.3333333333333333703, 0.3219752754296894559, 0.3333333333333333703, 0.3219752754296894559, 0.3333333333333333703, 0.3219752754296894559, 0.3333333333333333703, 0.3219752754296894559, 0.3333333333333333703, 0.3219752754296894559, 0.3333333333333333703, 0.3219752754296894559, 0.3333333333333333703, 0.3219752754296894559, 0.3333333333333333703, 0.3219752754296894559, 0.3333333333333333703, 0.3219752754296894559, 0.3333333333333333703, 0.3219752754296894559, 0.3333333333333333703, 0.3219752754296894559, 0.3333333333333333703, 0.3219752754296894559, 0.3333333333333333703, 0.3219752754296894559, 0.3333333333333333703, 0.3219752754296894559, 0.3333333333333333703, 0.3219752754296894559, 0.3333333333333333703, 0.3219752754296894559, 0.3333333333333333703, 0.3219752754296894559, 0.3333333333333333703, 0.3219752754296894559, 0.3333333333333333703, 0.3219752754296894559, 0.3333333333333333703, 0.3219752754296894559, 0.3333333333333333703, 0.3219752754296894559, 0.3333333333333333703, 0.3219752754296894559, 0.3333333333333333703, 0.3219752754296894559, 0.3333333333333333703, 0.3219752754296894559, 0.3333333333333333703, 0.3219752754296894559, 0.3333333333333333703, 0.3219752754296894559, 0.3333333333333333703, 0.3219752754296894559, 0.3333333333333333703, 0.3219752754296894559, 0.3333333333333333703, 0.3219752754296894559, 0.3333333333333333703, 0.3219752754296894559, 0.3333333333333333703, 0.3219752754296894559, 0.3333333333333333703, 0.3219752754296894559, 0.3333333333333333703, 0.3219752754296894559, 0.3333333333333333703, 0.3219752754296894559, 0.3333333333333333703, 0.3219752754296894559, 0.3333333333333333703, 0.3219752754296894559, 0.3333333333333333703, 0.3219752754296894559, 0.3333333333333333703, 0.3219752754296894559, 0.3333333333333333703, 0.3219752754296894559, 0.3333333333333333703, 0.3219752754296894559, 0.3333333333333333703, 0.3219752754296894559, 0.3333333333333333703, 0.3219752754296894559, 0.3333333333333333703, 0.3219752754296894559, 0.3333333333333333703, 0.3219752754296894559, 0.3333333333333333703, 0.3219752754296894559, 0.3333333333333333703, 0.3219752754296894559, 0.3333333333333333703, 0.3219752754296894559, 0.3333333333333333703, 0.3219752754296894559, 0.3333333333333333703, 0.3219752754296894559, 0.3333333333333333703, 0.3219752754296894559, 0.3333333333333333703, 0.3219752754296894559, 0.3333333333333333703, 0.3219752754296894559, 0.3333333333333333703, 0.3219752754296894559, 0.3333333333333333703, 0.3219752754296894559, 0.3333333333333333703, 0.3219752754296894559, 0.3333333333333333703, 0.3219752754296894559, 0.3333333333333333703, 0.3219752754296894559, 0.3333333333333333703, 0.3219752754296894559, 0.3333333333333333703, 0.3219752754296894559, 0.3333333333333333703, 0.3219752754296894559, 0.3333333333333333703, 0.3219752754296894559, 0.3333333333333333703, 0.3219752754296894559, 0.3333333333333333703, 0.3219752754296894559, 0.3333333333333333703, 0.3219752754296894559, 0.3333333333333333703, 0.3219752754296894559, 0.3333333333333333703, 0.3219752754296894559, 0.3333333333333333703, 0.3219752754296894559, 0.3333333333333333703, 0.3219752754296894559, 0.3333333333333333703, 0.3219752754296894559, 0.3333333333333333703, 0.3219752754296894559, 0.3333333333333333703, 0.3219752754296894559, 0.3333333333333333703, 0.3219752754296894559, 0.3333333333333333703, 0.3219752754296894559, 0.3333333333333333703, 0.3219752754296894559, 0.3333333333333333703, 0.3219752754296894559, 0.3333333333333333703, 0.3219752754296894559, 0.3333333333333333703, 0.3219752754296894559, 0.3333333333333333703, 0.3219752754296894559, 0.3333333333333333703, 0.3219752754296894559, 0.3333333333333333703, 0.3219752754296894559, 0.3333333333333333703),
 ( 1.000000000000000000, 0.9659258262890683122, 1.000000000000000000, 0.9659258262890683122, 1.000000000000000000, 0.9659258262890683122, 1.000000000000000000, 0.9659258262890683122, 1.000000000000000000, 0.9659258262890683122, 1.000000000000000000, 0.9659258262890683122, 1.000000000000000000, 0.9659258262890683122, 1.000000000000000000, 0.9659258262890683122, 1.000000000000000000, 0.9659258262890683122, 1.000000000000000000, 0.9659258262890683122, 1.000000000000000000, 0.9659258262890683122, 1.000000000000000000, 0.9659258262890683122, 1.000000000000000000, 0.9659258262890683122, 1.000000000000000000, 0.9659258262890683122, 1.000000000000000000, 0.9659258262890683122, 1.000000000000000000, 0.9659258262890683122, 1.000000000000000000, 0.9659258262890683122, 1.000000000000000000, 0.9659258262890683122, 1.000000000000000000, 0.9659258262890683122, 1.000000000000000000, 0.9659258262890683122, 1.000000000000000000, 0.9659258262890683122, 1.000000000000000000, 0.9659258262890683122, 1.000000000000000000, 0.9659258262890683122, 1.000000000000000000, 0.9659258262890683122, 1.000000000000000000, 0.9659258262890683122, 1.000000000000000000, 0.9659258262890683122, 1.000000000000000000, 0.9659258262890683122, 1.000000000000000000, 0.9659258262890683122, 1.000000000000000000, 0.9659258262890683122, 1.000000000000000000, 0.9659258262890683122, 1.000000000000000000, 0.9659258262890683122, 1.000000000000000000, 0.9659258262890683122, 1.000000000000000000, 0.9659258262890683122, 1.000000000000000000, 0.9659258262890683122, 1.000000000000000000, 0.9659258262890683122, 1.000000000000000000, 0.9659258262890683122, 1.000000000000000000, 0.9659258262890683122, 1.000000000000000000, 0.9659258262890683122, 1.000000000000000000, 0.9659258262890683122, 1.000000000000000000, 0.9659258262890683122, 1.000000000000000000, 0.9659258262890683122, 1.000000000000000000, 0.9659258262890683122, 1.000000000000000000, 0.9659258262890683122, 1.000000000000000000, 0.9659258262890683122, 1.000000000000000000, 0.9659258262890683122, 1.000000000000000000, 0.9659258262890683122, 1.000000000000000000, 0.9659258262890683122, 1.000000000000000000, 0.9659258262890683122, 1.000000000000000000, 0.9659258262890683122, 1.000000000000000000, 0.9659258262890683122, 1.000000000000000000, 0.9659258262890683122, 1.000000000000000000, 0.9659258262890683122, 1.000000000000000000, 0.9659258262890683122, 1.000000000000000000, 0.9659258262890683122, 1.000000000000000000, 0.9659258262890683122, 1.000000000000000000, 0.9659258262890683122, 1.000000000000000000, 0.9659258262890683122, 1.000000000000000000, 0.9659258262890683122, 1.000000000000000000, 0.9659258262890683122, 1.000000000000000000, 0.9659258262890683122, 1.000000000000000000, 0.9659258262890683122, 1.000000000000000000, 0.9659258262890683122, 1.000000000000000000, 0.9659258262890683122, 1.000000000000000000, 0.9659258262890683122, 1.000000000000000000, 0.9659258262890683122, 1.000000000000000000, 0.9659258262890683122, 1.000000000000000000, 0.9659258262890683122, 1.000000000000000000, 0.9659258262890683122, 1.000000000000000000, 0.9659258262890683122, 1.000000000000000000, 0.9659258262890683122, 1.000000000000000000, 0.9659258262890683122, 1.000000000000000000, 0.9659258262890683122, 1.000000000000000000, 0.9659258262890683122, 1.000000000000000000, 0.9659258262890683122, 1.000000000000000000, 0.9659258262890683122, 1.000000000000000000, 0.9659258262890683122, 1.000000000000000000, 0.9659258262890683122, 1.000000000000000000, 0.9659258262890683122, 1.000000000000000000, 0.9659258262890683122, 1.000000000000000000, 0.9659258262890683122, 1.000000000000000000, 0.9659258262890683122, 1.000000000000000000, 0.9659258262890683122, 1.000000000000000000, 0.9659258262890683122, 1.000000000000000000, 0.9659258262890683122, 1.000000000000000000, 0.9659258262890683122, 1.000000000000000000, 0.9659258262890683122, 1.000000000000000000, 0.9659258262890683122, 1.000000000000000000, 0.9659258262890683122, 1.000000000000000000, 0.9659258262890683122, 1.000000000000000000, 0.9659258262890683122, 1.000000000000000000, 0.9659258262890683122, 1.000000000000000000, 0.9659258262890683122, 1.000000000000000000, 0.9659258262890683122, 1.000000000000000000, 0.9659258262890683122, 1.000000000000000000, 0.9659258262890683122, 1.000000000000000000, 0.9659258262890683122, 1.000000000000000000, 0.9659258262890683122, 1.000000000000000000, 0.9659258262890683122, 1.000000000000000000, 0.9659258262890683122, 1.000000000000000000, 0.9659258262890683122, 1.000000000000000000, 0.9659258262890683122, 1.000000000000000000, 0.9659258262890683122, 1.000000000000000000, 0.9659258262890683122, 1.000000000000000000, 0.9659258262890683122, 1.000000000000000000, 0.9659258262890683122, 1.000000000000000000, 0.9659258262890683122, 1.000000000000000000, 0.9659258262890683122, 1.000000000000000000, 0.9659258262890683122, 1.000000000000000000, 0.9659258262890683122, 1.000000000000000000, 0.9659258262890683122, 1.000000000000000000, 0.9659258262890683122, 1.000000000000000000, 0.9659258262890683122, 1.000000000000000000, 0.9659258262890683122, 1.000000000000000000, 0.9659258262890683122, 1.000000000000000000, 0.9659258262890683122, 1.000000000000000000, 0.9659258262890683122, 1.000000000000000000, 0.9659258262890683122, 1.000000000000000000, 0.9659258262890683122, 1.000000000000000000, 0.9659258262890683122, 1.000000000000000000, 0.9659258262890683122, 1.000000000000000000, 0.9659258262890683122, 1.000000000000000000, 0.9659258262890683122, 1.000000000000000000, 0.9659258262890683122, 1.000000000000000000, 0.9659258262890683122, 1.000000000000000000, 0.9659258262890683122, 1.000000000000000000, 0.9659258262890683122, 1.000000000000000000, 0.9659258262890683122, 1.000000000000000000, 0.9659258262890683122, 1.000000000000000000, 0.9659258262890683122, 1.000000000000000000, 0.9659258262890683122, 1.000000000000000000, 0.9659258262890683122, 1.000000000000000000, 0.9659258262890683122, 1.000000000000000000, 0.9659258262890683122, 1.000000000000000000, 0.9659258262890683122, 1.000000000000000000, 0.9659258262890683122, 1.000000000000000000, 0.9659258262890683122, 1.000000000000000000, 0.9659258262890683122, 1.000000000000000000, 0.9659258262890683122, 1.000000000000000000, 0.9659258262890683122, 1.000000000000000000, 0.9659258262890683122, 1.000000000000000000, 0.9659258262890683122, 1.000000000000000000, 0.9659258262890683122, 1.000000000000000000, 0.9659258262890683122, 1.000000000000000000, 0.9659258262890683122, 1.000000000000000000, 0.9659258262890683122, 1.000000000000000000, 0.9659258262890683122, 1.000000000000000000, 0.9659258262890683122, 1.000000000000000000, 0.9659258262890683122, 1.000000000000000000, 0.9659258262890683122, 1.000000000000000000, 0.9659258262890683122, 1.000000000000000000, 0.9659258262890683122, 1.000000000000000000, 0.9659258262890683122, 1.000000000000000000, 0.9659258262890683122, 1.000000000000000000, 0.9659258262890683122, 1.000000000000000000, 0.9659258262890683122, 1.000000000000000000, 0.9659258262890683122, 1.000000000000000000, 0.9659258262890683122, 1.000000000000000000, 0.9659258262890683122, 1.000000000000000000, 0.9659258262890683122, 1.000000000000000000, 0.9659258262890683122, 1.000000000000000000, 0.9659258262890683122, 1.000000000000000000, 0.9659258262890683122, 1.000000000000000000, 0.9659258262890683122, 1.000000000000000000, 0.9659258262890683122, 1.000000000000000000, 0.9659258262890683122, 1.000000000000000000, 0.9659258262890683122, 1.000000000000000000, 0.9659258262890683122, 1.000000000000000000, 0.9659258262890683122, 1.000000000000000000, 0.9659258262890683122, 1.000000000000000000, 0.9659258262890683122, 1.000000000000000000, 0.9659258262890683122, 1.000000000000000000, 0.9659258262890683122, 1.000000000000000000, 0.9659258262890683122, 1.000000000000000000, 0.9659258262890683122, 1.000000000000000000, 0.9659258262890683122, 1.000000000000000000, 0.9659258262890683122, 1.000000000000000000, 0.9659258262890683122, 1.000000000000000000, 0.9659258262890683122, 1.000000000000000000, 0.9659258262890683122, 1.000000000000000000, 0.9659258262890683122, 1.000000000000000000, 0.9659258262890683122, 1.000000000000000000, 0.9659258262890683122, 1.000000000000000000, 0.9659258262890683122, 1.000000000000000000, 0.9659258262890683122, 1.000000000000000000, 0.9659258262890683122, 1.000000000000000000, 0.9659258262890683122, 1.000000000000000000, 0.9659258262890683122, 1.000000000000000000, 0.9659258262890683122, 1.000000000000000000, 0.9659258262890683122, 1.000000000000000000, 0.9659258262890683122, 1.000000000000000000, 0.9659258262890683122, 1.000000000000000000, 0.9659258262890683122, 1.000000000000000000, 0.9659258262890683122, 1.000000000000000000, 0.9659258262890683122, 1.000000000000000000, 0.9659258262890683122, 1.000000000000000000, 0.9659258262890683122, 1.000000000000000000, 0.9659258262890683122, 1.000000000000000000, 0.9659258262890683122, 1.000000000000000000, 0.9659258262890683122, 1.000000000000000000, 0.9659258262890683122, 1.000000000000000000, 0.9659258262890683122, 1.000000000000000000, 0.9659258262890683122, 1.000000000000000000, 0.9659258262890683122, 1.000000000000000000, 0.9659258262890683122, 1.000000000000000000, 0.9659258262890683122, 1.000000000000000000, 0.9659258262890683122, 1.000000000000000000, 0.9659258262890683122, 1.000000000000000000, 0.9659258262890683122, 1.000000000000000000, 0.9659258262890683122, 1.000000000000000000, 0.9659258262890683122, 1.000000000000000000, 0.9659258262890683122, 1.000000000000000000, 0.9659258262890683122, 1.000000000000000000, 0.9659258262890683122, 1.000000000000000000, 0.9659258262890683122, 1.000000000000000000, 0.9659258262890683122, 1.000000000000000000, 0.9659258262890683122, 1.000000000000000000, 0.9659258262890683122, 1.000000000000000000, 0.9659258262890683122, 1.000000000000000000, 0.9659258262890683122, 1.000000000000000000, 0.9659258262890683122, 1.000000000000000000, 0.9659258262890683122, 1.000000000000000000, 0.9659258262890683122, 1.000000000000000000, 0.9659258262890683122, 1.000000000000000000, 0.9659258262890683122, 1.000000000000000000, 0.9659258262890683122, 1.000000000000000000, 0.9659258262890683122, 1.000000000000000000, 0.9659258262890683122, 1.000000000000000000, 0.9659258262890683122, 1.000000000000000000) ) ) 
 REPRESENTATION_ITEM ( '' )  SURFACE ( )  );
#176314 = CARTESIAN_POINT ( 'NONE',  ( -14.34966873604972548, 8.224510206698743886, 78.33442372801901854 ) ) ;
#176315 = CARTESIAN_POINT ( 'NONE',  ( -21.55341960407619339, 5.719274019375674811, 78.54275706135236135 ) ) ;
#176316 = CARTESIAN_POINT ( 'NONE',  ( -13.89961937509957401, -13.97604488694547875, 94.37609039468566152 ) ) ;
#176317 = CARTESIAN_POINT ( 'NONE',  ( 13.97604488694548053, -13.89961937509957401, 45.62609039468566863 ) ) ;
#176318 = CARTESIAN_POINT ( 'NONE',  ( 13.97604488694527802, 13.89961937509977652, 79.37390960531435269 ) ) ;
#176319 = CARTESIAN_POINT ( 'NONE',  ( -9.564922557960796823, -16.46253265017161027, 62.08224293864769550 ) ) ;
#176320 = AXIS2_PLACEMENT_3D ( 'NONE', #186130, #179433, #77925 ) ;
#176321 = EDGE_CURVE ( 'NONE', #55000, #17723, #157448, .T. ) ;
#176322 = CARTESIAN_POINT ( 'NONE',  ( 17.58332526062529411, -7.635886036038496805, 88.42334959558466778 ) ) ;
#176323 = CARTESIAN_POINT ( 'NONE',  ( -10.72451020669898014, 18.67979575497178502, 95.41557627198102409 ) ) ;
#176324 = CARTESIAN_POINT ( 'NONE',  ( -18.62759615963270932, 10.81492255796079327, 45.83224293864769550 ) ) ;
#176325 = CARTESIAN_POINT ( 'NONE',  ( -5.153800228976328057, -19.02544592524343514, 27.29057627198103120 ) ) ;
#176326 = CARTESIAN_POINT ( 'NONE',  ( 0.05219959533934541429, -16.53943276465976808, 60.00109039468568284 ) ) ;
#176327 = ORIENTED_EDGE ( 'NONE', *, *, #83071, .F. ) ;
#176328 = CARTESIAN_POINT ( 'NONE',  ( -21.55341960407619339, 5.719274019375674811, 43.54275706135235424 ) ) ;
#176330 = CARTESIAN_POINT ( 'NONE',  ( 29.86685920354754487, 21.69954338932564752, -7.424999997268813878 ) ) ;
#176329 = CARTESIAN_POINT ( 'NONE',  ( -12.14591786802309592, -12.06949235617757132, 61.87390960531436690 ) ) ;
#176331 = CARTESIAN_POINT ( 'NONE',  ( -8.314922557961024197, 14.29746914071037800, 32.91775706135234714 ) ) ;
#176332 = CARTESIAN_POINT ( 'NONE',  ( -16.52544592524342804, 4.483927247898546575, 101.0405762719810383 ) ) ;
#176333 = CARTESIAN_POINT ( 'NONE',  ( -9.564922557961040184, 16.46253265017147172, 52.91775706135233293 ) ) ;
#176334 = CARTESIAN_POINT ( 'NONE',  ( 4.379528057220339221, -16.55341960407611168, 57.70724293864770260 ) ) ;
#176335 = CARTESIAN_POINT ( 'NONE',  ( 15.72974639402176855, 15.80617190586768217, 31.87609039468567929 ) ) ;
#176337 = CARTESIAN_POINT ( 'NONE',  ( 10.81492255796078972, 18.62759615963270932, 84.58224293864769550 ) ) ;
#176336 = CARTESIAN_POINT ( 'NONE',  ( 5.049401038298161559, -19.05341960407611168, 22.70724293864769194 ) ) ;
#176338 = CARTESIAN_POINT ( 'NONE',  ( -0.05219959533909027116, -19.03943276465977164, 107.4989096053143527 ) ) ;
#176339 = CARTESIAN_POINT ( 'NONE',  ( 8.314922557960818139, 14.29746914071049879, 79.58224293864769550 ) ) ;
#176340 = CARTESIAN_POINT ( 'NONE',  ( 5.049401038298161559, -19.05341960407611168, 112.7072429386476813 ) ) ;
#176341 = CARTESIAN_POINT ( 'NONE',  ( 11.40812507854754365, 35.11059874428196537, -3.224999997268813701 ) ) ;
#176342 = CARTESIAN_POINT ( 'NONE',  ( 0.05219959533936267826, -19.03943276465977164, 85.00109039468567573 ) ) ;
#176343 = CARTESIAN_POINT ( 'NONE',  ( -5.823673210054431948, 21.52544592524334988, 27.70942372801901854 ) ) ;
#176344 = CARTESIAN_POINT ( 'NONE',  ( 13.89961937509977652, -13.97604488694527269, 73.12390960531436690 ) ) ;
#176345 = CARTESIAN_POINT ( 'NONE',  ( -19.03943276465977164, -0.05219959533935918106, 53.75109039468566863 ) ) ;
#176346 = CARTESIAN_POINT ( 'NONE',  ( -19.03943276465977164, 0.05219959533909376836, 36.24890960531436690 ) ) ;
#176347 = CARTESIAN_POINT ( 'NONE',  ( -5.823673210054431948, 21.52544592524334988, 67.70942372801901854 ) ) ;
#176348 = DIRECTION ( 'NONE',  ( -0.000000000000000000, 0.000000000000000000, -1.000000000000000000 ) ) ;
#176349 = CARTESIAN_POINT ( 'NONE',  ( 8.314922557960818139, 14.29746914071049879, 59.58224293864770260 ) ) ;
#176350 = CARTESIAN_POINT ( 'NONE',  ( 16.51473224551069308, 9.474510206698969483, 69.16557627198102409 ) ) ;
#176351 = CARTESIAN_POINT ( 'NONE',  ( -21.53943276465977519, 0.05219959533907696930, 86.24890960531436690 ) ) ;
#176352 = CARTESIAN_POINT ( 'NONE',  ( 13.89961937509977652, -13.97604488694527269, 53.12390960531434558 ) ) ;
#176353 = ORIENTED_EDGE ( 'NONE', *, *, #152778, .F. ) ;
#176354 = CARTESIAN_POINT ( 'NONE',  ( 18.62759615963271287, -10.81492255796078972, 83.33224293864769550 ) ) ;
#176355 = CARTESIAN_POINT ( 'NONE',  ( 21.55341960407619695, -5.719274019375665929, 96.04275706135236135 ) ) ;
#176358 = CARTESIAN_POINT ( 'NONE',  ( 4.379528057220339221, -16.55341960407611168, 102.7072429386476955 ) ) ;
#176357 = CARTESIAN_POINT ( 'NONE',  ( -8.224510206698735004, -14.34966873604973081, 94.58442372801901854 ) ) ;
#176356 = CARTESIAN_POINT ( 'NONE',  ( -13.97604488694527625, -13.89961937509977652, 26.87390960531434558 ) ) ;
#176359 = CARTESIAN_POINT ( 'NONE',  ( -0.05219959533936034679, 19.03943276465977164, 97.50109039468567573 ) ) ;
#176360 = ORIENTED_EDGE ( 'NONE', *, *, #164865, .F. ) ;
#176361 = CARTESIAN_POINT ( 'NONE',  ( 21.53943276465977519, 0.05219959533937863772, 21.25109039468567218 ) ) ;
#176362 = CARTESIAN_POINT ( 'NONE',  ( -0.05219959533936034679, 19.03943276465977164, 57.50109039468566863 ) ) ;
#176363 = CARTESIAN_POINT ( 'NONE',  ( 14.29746914071037800, 8.314922557961029526, 106.6677570613523756 ) ) ;
#176364 = CARTESIAN_POINT ( 'NONE',  ( 9.474510206698729675, 16.51473224551082808, 27.08442372801900433 ) ) ;
#176365 = CARTESIAN_POINT ( 'NONE',  ( -9.474510206698964154, 16.51473224551069663, 100.4155762719810241 ) ) ;
#176366 = CARTESIAN_POINT ( 'NONE',  ( -0.05219959533907301413, -21.53943276465977519, 57.49890960531435979 ) ) ;
#176367 = CARTESIAN_POINT ( 'NONE',  ( -26.26083487095749902, 9.141127703660897552, 167.1337248662267996 ) ) ;
#176368 = CARTESIAN_POINT ( 'NONE',  ( -8.224510206698948167, 14.34966873604960824, 115.4155762719810241 ) ) ;
#176369 = CARTESIAN_POINT ( 'NONE',  ( 9.564922557961047289, -16.46253265017146816, 20.41775706135233293 ) ) ;
#176370 = CARTESIAN_POINT ( 'NONE',  ( 0.05219959533934541429, -16.53943276465976808, 70.00109039468568994 ) ) ;
#176371 = CARTESIAN_POINT ( 'NONE',  ( 21.52544592524334988, 5.823673210054432836, 31.45942372801901854 ) ) ;
#176372 = CARTESIAN_POINT ( 'NONE',  ( 16.52544592524335698, 4.483927247898782831, 46.45942372801901854 ) ) ;
#176373 = CARTESIAN_POINT ( 'NONE',  ( 19.03943276465977164, -0.05219959533909143690, 98.74890960531436690 ) ) ;
#176374 = CARTESIAN_POINT ( 'NONE',  ( 5.153800228976335163, 19.02544592524342804, 44.79057627198103830 ) ) ;
#176375 = CARTESIAN_POINT ( 'NONE',  ( -0.05219959533909027116, -19.03943276465977164, 62.49890960531435979 ) ) ;
#176376 = CARTESIAN_POINT ( 'NONE',  ( 16.53943276465976808, 0.05219959533934440121, 46.25109039468567573 ) ) ;
#176377 = CARTESIAN_POINT ( 'NONE',  ( -12.14591786802309592, -12.06949235617757132, 96.87390960531436690 ) ) ;
#176378 = CARTESIAN_POINT ( 'NONE',  ( -14.29746914071037622, -8.314922557961029526, 99.16775706135234714 ) ) ;
#176379 = FACE_OUTER_BOUND ( 'NONE', #169719, .T. ) ;
#176382 = CARTESIAN_POINT ( 'NONE',  ( -9.474510206698964154, 16.51473224551069663, 70.41557627198102409 ) ) ;
#176381 = CARTESIAN_POINT ( 'NONE',  ( -5.049401038298153566, 19.05341960407611168, 75.20724293864769550 ) ) ;
#176380 = CARTESIAN_POINT ( 'NONE',  ( -5.823673210054431948, 21.52544592524334988, 52.70942372801902565 ) ) ;
#176383 = CARTESIAN_POINT ( 'NONE',  ( -19.05341960407611168, -5.049401038298163336, 96.45724293864769550 ) ) ;
#176384 = CARTESIAN_POINT ( 'NONE',  ( -16.52544592524342804, 4.483927247898546575, 51.04057627198103120 ) ) ;
#176385 = CARTESIAN_POINT ( 'NONE',  ( -8.224510206698735004, -14.34966873604973081, 99.58442372801900433 ) ) ;
#176386 = CARTESIAN_POINT ( 'NONE',  ( -14.34966873604960291, -8.224510206698953496, 21.66557627198102409 ) ) ;
#176387 = ORIENTED_EDGE ( 'NONE', *, *, #82183, .F. ) ;
#176388 = CARTESIAN_POINT ( 'NONE',  ( 9.564922557961047289, -16.46253265017146816, 45.41775706135232582 ) ) ;
#176389 = CARTESIAN_POINT ( 'NONE',  ( -9.564922557960796823, -16.46253265017161027, 112.0822429386476955 ) ) ;
#176390 = CARTESIAN_POINT ( 'NONE',  ( 13.97604488694527802, 13.89961937509977652, 59.37390960531434558 ) ) ;
#176391 = CARTESIAN_POINT ( 'NONE',  ( -5.153800228976607833, 19.02544592524334988, 37.70942372801899722 ) ) ;
#176392 = CARTESIAN_POINT ( 'NONE',  ( 22.81625015709510151, -31.40387420917324590, -1.924999997268813434 ) ) ;
#176393 = FACE_OUTER_BOUND ( 'NONE', #60863, .T. ) ;
#176395 = CARTESIAN_POINT ( 'NONE',  ( -14.29746914071037622, -8.314922557961029526, 69.16775706135234714 ) ) ;
#176394 = CARTESIAN_POINT ( 'NONE',  ( -13.89961937509957401, -13.97604488694547875, 84.37609039468567573 ) ) ;
#176396 = CARTESIAN_POINT ( 'NONE',  ( 17.13100169013300444, 6.664070546373150883, 91.73210164300154190 ) ) ;
#176397 = CARTESIAN_POINT ( 'NONE',  ( -16.46253265017160317, 9.564922557960807481, 85.83224293864769550 ) ) ;
#176398 = CARTESIAN_POINT ( 'NONE',  ( 21.52544592524334988, 5.823673210054432836, 26.45942372801901854 ) ) ;
#176399 = CARTESIAN_POINT ( 'NONE',  ( 19.05341960407617918, -5.049401038297876454, 71.04275706135234714 ) ) ;
#176401 = CARTESIAN_POINT ( 'NONE',  ( -5.049401038298153566, 19.05341960407611168, 50.20724293864770260 ) ) ;
#176400 = CARTESIAN_POINT ( 'NONE',  ( 16.81555441253551209, 7.025013491695498047, 86.86314554665750620 ) ) ;
#176402 = CARTESIAN_POINT ( 'NONE',  ( -9.474510206698964154, 16.51473224551069663, 90.41557627198103830 ) ) ;
#176404 = CARTESIAN_POINT ( 'NONE',  ( -5.153800228976328057, -19.02544592524343514, 37.29057627198102409 ) ) ;
#176403 = CARTESIAN_POINT ( 'NONE',  ( 8.314922557960818139, 14.29746914071049879, 44.58224293864769550 ) ) ;
#176405 = CARTESIAN_POINT ( 'NONE',  ( -16.46253265017146816, -9.564922557961047289, 54.16775706135234003 ) ) ;
#176406 = CARTESIAN_POINT ( 'NONE',  ( -0.05219959533910754901, -16.53943276465976808, 82.49890960531436690 ) ) ;
#176407 = CARTESIAN_POINT ( 'NONE',  ( -5.049401038297874678, -19.05341960407617918, 29.79275706135232227 ) ) ;
#176408 = CARTESIAN_POINT ( 'NONE',  ( 16.46253265017160672, -9.564922557960803928, 63.33224293864769550 ) ) ;
#176409 = CARTESIAN_POINT ( 'NONE',  ( -0.05219959533907301413, -21.53943276465977519, 62.49890960531436690 ) ) ;
#176411 = CARTESIAN_POINT ( 'NONE',  ( -21.53943276465977519, -0.05219959533937600094, 113.7510903946856757 ) ) ;
#176410 = CARTESIAN_POINT ( 'NONE',  ( 14.34966873604960469, 8.224510206698951720, 54.16557627198103120 ) ) ;
#176412 = CARTESIAN_POINT ( 'NONE',  ( -5.153800228976328057, -19.02544592524343514, 107.2905762719810383 ) ) ;
#176413 = AXIS2_PLACEMENT_3D ( 'NONE', #29620, #76105, #185284 ) ;
#176414 = CARTESIAN_POINT ( 'NONE',  ( 10.72451020669898902, -18.67979575497178502, 22.91557627198102765 ) ) ;
#176415 = CARTESIAN_POINT ( 'NONE',  ( -19.03943276465977164, 0.05219959533909376836, 51.24890960531436690 ) ) ;
#176416 = CARTESIAN_POINT ( 'NONE',  ( -19.03943276465977164, 0.05219959533909376836, 31.24890960531435979 ) ) ;
#176417 = CARTESIAN_POINT ( 'NONE',  ( -16.53943276465976808, 0.05219959533911058130, 96.24890960531435269 ) ) ;
#176418 = CARTESIAN_POINT ( 'NONE',  ( -10.72451020669898014, 18.67979575497178502, 105.4155762719810383 ) ) ;
#176419 = CARTESIAN_POINT ( 'NONE',  ( -9.474510206698964154, 16.51473224551069663, 95.41557627198102409 ) ) ;
#176420 = CARTESIAN_POINT ( 'NONE',  ( -21.55341960407610458, -5.719274019375992779, 106.4572429386477097 ) ) ;
#176421 = CARTESIAN_POINT ( 'NONE',  ( 13.89961937509977652, -13.97604488694527269, 108.1239096053143669 ) ) ;
#176422 = CARTESIAN_POINT ( 'NONE',  ( -19.02544592524342804, 5.153800228976336051, 26.04057627198103120 ) ) ;
#176424 = CARTESIAN_POINT ( 'NONE',  ( 15.72974639402176855, 15.80617190586768217, 76.87609039468567573 ) ) ;
#176423 = AXIS2_PLACEMENT_3D ( 'NONE', #67906, #172107, #33593 ) ;
#176425 = CARTESIAN_POINT ( 'NONE',  ( 15.80617190586746368, 15.72974639402197994, 89.37390960531435269 ) ) ;
#176426 = DIRECTION ( 'NONE',  ( 0.000000000000000000, 0.000000000000000000, 1.000000000000000000 ) ) ;
#176427 = FACE_OUTER_BOUND ( 'NONE', #28465, .T. ) ;
#176428 = CARTESIAN_POINT ( 'NONE',  ( -38.00000000000000711, 2.428612866367529932E-14, -2.000000000000000000 ) ) ;
#176429 = CARTESIAN_POINT ( 'NONE',  ( -0.05219959533934338120, 16.53943276465976808, 42.50109039468567573 ) ) ;
#176430 = CARTESIAN_POINT ( 'NONE',  ( -16.55341960407611168, -4.379528057220339221, 106.4572429386477097 ) ) ;
#176431 = CARTESIAN_POINT ( 'NONE',  ( 0.000000000000000000, 0.000000000000000000, -54.21489346206828230 ) ) ;
#176432 = CARTESIAN_POINT ( 'NONE',  ( -13.97604488694527625, -13.89961937509977652, 56.87390960531434558 ) ) ;
#176433 = CARTESIAN_POINT ( 'NONE',  ( 16.52544592524342804, -4.483927247898539470, 98.54057627198105251 ) ) ;
#176434 = CARTESIAN_POINT ( 'NONE',  ( -21.53943276465977519, 0.05219959533907696930, 36.24890960531435979 ) ) ;
#176435 = CARTESIAN_POINT ( 'NONE',  ( -4.483927247898539470, -16.52544592524342804, 67.29057627198103830 ) ) ;
#176436 = CARTESIAN_POINT ( 'NONE',  ( -14.29746914071037622, -8.314922557961029526, 24.16775706135235424 ) ) ;
#176437 = CARTESIAN_POINT ( 'NONE',  ( 18.67979575497194134, -10.72451020669871369, 70.83442372801901854 ) ) ;
#176438 = CARTESIAN_POINT ( 'NONE',  ( 9.474510206698729675, 16.51473224551082808, 62.08442372801899722 ) ) ;
#176439 = CARTESIAN_POINT ( 'NONE',  ( 14.29746914071037800, 8.314922557961029526, 91.66775706135234714 ) ) ;
#176440 = CARTESIAN_POINT ( 'NONE',  ( 4.379528057220339221, -16.55341960407611168, 37.70724293864769550 ) ) ;
#176441 = CARTESIAN_POINT ( 'NONE',  ( 16.51473224551069308, 9.474510206698969483, 44.16557627198103120 ) ) ;
#176442 = CARTESIAN_POINT ( 'NONE',  ( -13.97604488694527625, -13.89961937509977652, 91.87390960531432427 ) ) ;
#176443 = CARTESIAN_POINT ( 'NONE',  ( -5.823673210054116645, -21.52544592524344225, 97.29057627198105251 ) ) ;
#176444 = CARTESIAN_POINT ( 'NONE',  ( 16.55341960407618274, -4.379528057220086978, 31.04275706135234714 ) ) ;
#176446 = CARTESIAN_POINT ( 'NONE',  ( -21.55341960407619339, 5.719274019375674811, 68.54275706135234714 ) ) ;
#176445 = CARTESIAN_POINT ( 'NONE',  ( 8.314922557960818139, 14.29746914071049879, 59.58224293864770260 ) ) ;
#176447 = CARTESIAN_POINT ( 'NONE',  ( 12.14591786802327356, -12.06949235617739191, 100.6260903946857184 ) ) ;
#176448 = CARTESIAN_POINT ( 'NONE',  ( 16.81555441253551564, 7.025013491695498935, 26.86314554665745646 ) ) ;
#176449 = CARTESIAN_POINT ( 'NONE',  ( -18.22780087662126647, -5.499999999999827693, 63.98236817873107185 ) ) ;
#176450 = CARTESIAN_POINT ( 'NONE',  ( 14.29746914071049879, -8.314922557960816363, 33.33224293864769550 ) ) ;
#176451 = CARTESIAN_POINT ( 'NONE',  ( -0.05219959533934338120, 16.53943276465976808, 72.50109039468568994 ) ) ;
#176452 = CARTESIAN_POINT ( 'NONE',  ( -19.03943276465977164, 0.05219959533909376836, 81.24890960531436690 ) ) ;
#176453 = CARTESIAN_POINT ( 'NONE',  ( -16.51473224551069308, -9.474510206698971260, 81.66557627198103830 ) ) ;
#176454 = CARTESIAN_POINT ( 'NONE',  ( 5.719274019375673035, 21.55341960407619339, 82.29275706135234714 ) ) ;
#176455 = CARTESIAN_POINT ( 'NONE',  ( -16.52544592524335698, -4.483927247898792601, 93.95942372801903275 ) ) ;
#176456 = CARTESIAN_POINT ( 'NONE',  ( -8.314922557960811034, -14.29746914071050412, 62.08224293864769550 ) ) ;
#176457 = CARTESIAN_POINT ( 'NONE',  ( -5.153800228976328057, -19.02544592524343514, 62.29057627198100988 ) ) ;
#176458 = ORIENTED_EDGE ( 'NONE', *, *, #165982, .F. ) ;
#176459 = CARTESIAN_POINT ( 'NONE',  ( 13.89961937509957401, 13.97604488694547697, 111.8760903946856757 ) ) ;
#176460 = CARTESIAN_POINT ( 'NONE',  ( -4.379528057220328563, 16.55341960407611168, 105.2072429386477097 ) ) ;
#176461 = CARTESIAN_POINT ( 'NONE',  ( 5.153800228976335163, 19.02544592524342804, 84.79057627198099567 ) ) ;
#176463 = CARTESIAN_POINT ( 'NONE',  ( 11.74264578624799427, 36.14014761921585972, -0.5999999999999999778 ) ) ;
#176462 = CARTESIAN_POINT ( 'NONE',  ( 9.474510206698729675, 16.51473224551082808, 112.0844237280190043 ) ) ;
#176464 = CARTESIAN_POINT ( 'NONE',  ( 0.05219959533936267826, -19.03943276465977164, 25.00109039468566152 ) ) ;
#176465 = CARTESIAN_POINT ( 'NONE',  ( 0.05219959533934541429, -16.53943276465976808, 85.00109039468568994 ) ) ;
#176466 = CARTESIAN_POINT ( 'NONE',  ( 19.05341960407617918, -5.049401038297876454, 96.04275706135231871 ) ) ;
#176467 = CARTESIAN_POINT ( 'NONE',  ( 16.51473224551069308, 9.474510206698969483, 24.16557627198102765 ) ) ;
#176468 = CARTESIAN_POINT ( 'NONE',  ( 16.53943276465976808, 0.05219959533934440121, 61.25109039468567573 ) ) ;
#176469 = CARTESIAN_POINT ( 'NONE',  ( 12.14591786802327356, -12.06949235617739191, 55.62609039468568284 ) ) ;
#176470 = CARTESIAN_POINT ( 'NONE',  ( 13.97604488694527802, 13.89961937509977652, 24.37390960531435624 ) ) ;
#176471 = CARTESIAN_POINT ( 'NONE',  ( -9.564922557961040184, 16.46253265017147172, 52.91775706135233293 ) ) ;
#176472 = CARTESIAN_POINT ( 'NONE',  ( -0.05219959533937732626, 21.53943276465977519, 102.5010903946856899 ) ) ;
#176473 = CARTESIAN_POINT ( 'NONE',  ( -9.564922557960796823, -16.46253265017161027, 37.08224293864768839 ) ) ;
#176474 = CARTESIAN_POINT ( 'NONE',  ( 5.153800228976335163, 19.02544592524342804, 79.79057627198102409 ) ) ;
#176475 = CARTESIAN_POINT ( 'NONE',  ( 16.55341960407611168, 4.379528057220329451, 78.95724293864769550 ) ) ;
#176476 = CARTESIAN_POINT ( 'NONE',  ( 21.52544592524334988, 5.823673210054432836, 86.45942372801901854 ) ) ;
#176477 = CARTESIAN_POINT ( 'NONE',  ( -16.46253265017146816, -9.564922557961047289, 59.16775706135233293 ) ) ;
#176478 = CARTESIAN_POINT ( 'NONE',  ( -13.89961937509957401, -13.97604488694547875, 44.37609039468566863 ) ) ;
#176479 = CARTESIAN_POINT ( 'NONE',  ( -10.72451020669898014, 18.67979575497178502, 35.41557627198102409 ) ) ;
#176480 = CARTESIAN_POINT ( 'NONE',  ( 0.05219959533937995610, -21.53943276465977519, 100.0010903946857042 ) ) ;
#176481 = CARTESIAN_POINT ( 'NONE',  ( -19.02544592524342804, 5.153800228976336051, 71.04057627198099567 ) ) ;
#176482 = CARTESIAN_POINT ( 'NONE',  ( -5.823673210054431948, 21.52544592524334988, 102.7094237280190185 ) ) ;
#176483 = CARTESIAN_POINT ( 'NONE',  ( 5.719274019375991003, -21.55341960407610458, 52.70724293864769550 ) ) ;
#176484 = CARTESIAN_POINT ( 'NONE',  ( 13.97604488694527802, 13.89961937509977652, 99.37390960531436690 ) ) ;
#176485 = CARTESIAN_POINT ( 'NONE',  ( 19.05341960407617918, -5.049401038297876454, 81.04275706135231871 ) ) ;
#176486 = CARTESIAN_POINT ( 'NONE',  ( -5.153800228976328057, -19.02544592524343514, 102.2905762719810383 ) ) ;
#176487 = CARTESIAN_POINT ( 'NONE',  ( -5.049401038297874678, -19.05341960407617918, 99.79275706135234714 ) ) ;
#176488 = CARTESIAN_POINT ( 'NONE',  ( -16.52544592524335698, -4.483927247898792601, 38.95942372801901854 ) ) ;
#176489 = CARTESIAN_POINT ( 'NONE',  ( -14.29746914071049879, 8.314922557960819915, 105.8322429386476955 ) ) ;
#176490 = CARTESIAN_POINT ( 'NONE',  ( 19.05341960407611168, 5.049401038298154454, 88.95724293864769550 ) ) ;
#176491 = CARTESIAN_POINT ( 'NONE',  ( 21.53943276465977519, -0.05219959533907433946, 68.74890960531435269 ) ) ;
#176492 = CARTESIAN_POINT ( 'NONE',  ( -12.06949235617739369, -12.14591786802326823, 39.37609039468567573 ) ) ;
#176493 = CARTESIAN_POINT ( 'NONE',  ( 15.80617190586769283, -15.72974639402175789, 40.62609039468567573 ) ) ;
#176494 = CARTESIAN_POINT ( 'NONE',  ( 18.67979575497194134, -10.72451020669871369, 85.83442372801901854 ) ) ;
#176495 = CARTESIAN_POINT ( 'NONE',  ( -16.52544592524335698, -4.483927247898792601, 78.95942372801901854 ) ) ;
#176496 = CARTESIAN_POINT ( 'NONE',  ( -9.474510206698964154, 16.51473224551069663, 75.41557627198103830 ) ) ;
#176497 = CARTESIAN_POINT ( 'NONE',  ( -12.14591786802309592, -12.06949235617757132, 81.87390960531435269 ) ) ;
#176498 = CARTESIAN_POINT ( 'NONE',  ( 16.53943276465976808, -0.05219959533910856209, 28.74890960531435624 ) ) ;
#176499 = CARTESIAN_POINT ( 'NONE',  ( 9.474510206698729675, 16.51473224551082808, 52.08442372801900433 ) ) ;
#176500 = CARTESIAN_POINT ( 'NONE',  ( -10.81492255796105439, 18.62759615963255655, 37.91775706135235424 ) ) ;
#176501 = CARTESIAN_POINT ( 'NONE',  ( -8.314922557960811034, -14.29746914071050412, 82.08224293864768129 ) ) ;
#176502 = CARTESIAN_POINT ( 'NONE',  ( 5.153800228976335163, 19.02544592524342804, 114.7905762719810241 ) ) ;
#176503 = CARTESIAN_POINT ( 'NONE',  ( -8.314922557961024197, 14.29746914071037800, 102.9177570613523756 ) ) ;
#176504 = CARTESIAN_POINT ( 'NONE',  ( 21.52544592524334988, 5.823673210054432836, 76.45942372801901854 ) ) ;
#176505 = CARTESIAN_POINT ( 'NONE',  ( 14.34966873604972726, -8.224510206698740333, 40.83442372801901854 ) ) ;
#176506 = CARTESIAN_POINT ( 'NONE',  ( -21.52544592524334988, -5.823673210054445271, 38.95942372801901854 ) ) ;
#176507 = ORIENTED_EDGE ( 'NONE', *, *, #4359, .F. ) ;
#176508 = CARTESIAN_POINT ( 'NONE',  ( -15.80617190586745835, -15.72974639402198527, 111.8739096053143669 ) ) ;
#176509 = CARTESIAN_POINT ( 'NONE',  ( -4.379528057220328563, 16.55341960407611168, 85.20724293864770971 ) ) ;
#176510 = CARTESIAN_POINT ( 'NONE',  ( 17.50000000000148503, -3.202012800152207461, 27.42822416027260246 ) ) ;
#176511 = CARTESIAN_POINT ( 'NONE',  ( -8.314922557960811034, -14.29746914071050412, 57.08224293864769550 ) ) ;
#176512 = CARTESIAN_POINT ( 'NONE',  ( 12.06949235617739724, 12.14591786802326823, 91.87609039468568994 ) ) ;
#176513 = CARTESIAN_POINT ( 'NONE',  ( -13.97604488694527625, -13.89961937509977652, 26.87390960531434558 ) ) ;
#176514 = CARTESIAN_POINT ( 'NONE',  ( 21.55341960407610458, 5.719274019375980345, 43.95724293864769550 ) ) ;
#176515 = CARTESIAN_POINT ( 'NONE',  ( -16.52544592524342804, 4.483927247898546575, 76.04057627198102409 ) ) ;
#176516 = AXIS2_PLACEMENT_3D ( 'NONE', #109304, #106320, #63808 ) ;
#176517 = CARTESIAN_POINT ( 'NONE',  ( 18.62759615963271287, -10.81492255796078972, 73.33224293864769550 ) ) ;
#176519 = EDGE_CURVE ( 'NONE', #86852, #110081, #9826, .T. ) ;
#176518 = CARTESIAN_POINT ( 'NONE',  ( -0.05219959533909027116, -19.03943276465977164, 87.49890960531436690 ) ) ;
#176521 = CARTESIAN_POINT ( 'NONE',  ( 19.02544592524334988, 5.153800228976608722, 91.45942372801900433 ) ) ;
#176520 = CARTESIAN_POINT ( 'NONE',  ( -5.153800228976328057, -19.02544592524343514, 42.29057627198101699 ) ) ;
#176522 = CARTESIAN_POINT ( 'NONE',  ( 10.72451020669898902, -18.67979575497178502, 32.91557627198102409 ) ) ;
#176524 = CARTESIAN_POINT ( 'NONE',  ( -10.81492255796078084, -18.62759615963271287, 57.08224293864769550 ) ) ;
#176523 = CARTESIAN_POINT ( 'NONE',  ( 10.81492255796106328, -18.62759615963255655, 50.41775706135235424 ) ) ;
#176525 = CARTESIAN_POINT ( 'NONE',  ( 16.46253265017160672, -9.564922557960803928, 38.33224293864768839 ) ) ;
#176526 = CARTESIAN_POINT ( 'NONE',  ( 13.89961937509977652, -13.97604488694527269, 78.12390960531433848 ) ) ;
#176527 = ORIENTED_EDGE ( 'NONE', *, *, #151903, .T. ) ;
#176528 = CARTESIAN_POINT ( 'NONE',  ( -14.29746914071037622, -8.314922557961029526, 44.16775706135234714 ) ) ;
#176529 = CARTESIAN_POINT ( 'NONE',  ( -10.72451020669870658, -18.67979575497194134, 29.58442372801901854 ) ) ;
#176530 = CARTESIAN_POINT ( 'NONE',  ( -10.72451020669870658, -18.67979575497194134, 74.58442372801901854 ) ) ;
#176531 = CARTESIAN_POINT ( 'NONE',  ( 16.46253265017160672, -9.564922557960803928, 113.3322429386476955 ) ) ;
#176532 = CARTESIAN_POINT ( 'NONE',  ( -10.81492255796078084, -18.62759615963271287, 92.08224293864769550 ) ) ;
#176534 = CARTESIAN_POINT ( 'NONE',  ( 0.05219959533934541429, -16.53943276465976808, 55.00109039468568284 ) ) ;
#176533 = CARTESIAN_POINT ( 'NONE',  ( -21.55341960407619339, 5.719274019375674811, 23.54275706135235424 ) ) ;
#176535 = CARTESIAN_POINT ( 'NONE',  ( -15.80617190586745835, -15.72974639402198527, 56.87390960531436690 ) ) ;
#176536 = CARTESIAN_POINT ( 'NONE',  ( -5.049401038297874678, -19.05341960407617918, 24.79275706135233648 ) ) ;
#176537 = CARTESIAN_POINT ( 'NONE',  ( -16.46253265017160317, 9.564922557960807481, 50.83224293864770260 ) ) ;
#176538 = CARTESIAN_POINT ( 'NONE',  ( -19.02544592524342804, 5.153800228976336051, 116.0405762719810383 ) ) ;
#176539 = CARTESIAN_POINT ( 'NONE',  ( 5.153800228976335163, 19.02544592524342804, 94.79057627198103830 ) ) ;
#176540 = CARTESIAN_POINT ( 'NONE',  ( 17.50000000000000355, 3.210308386893693466, 102.5489375733106812 ) ) ;
#176541 = CARTESIAN_POINT ( 'NONE',  ( -5.153800228976607833, 19.02544592524334988, 72.70942372801900433 ) ) ;
#176542 = CARTESIAN_POINT ( 'NONE',  ( 15.80617190586746368, 15.72974639402197994, 39.37390960531436690 ) ) ;
#176543 = CARTESIAN_POINT ( 'NONE',  ( -8.314922557961024197, 14.29746914071037800, 112.9177570613523329 ) ) ;
#176544 = CARTESIAN_POINT ( 'NONE',  ( 13.89961937509957401, 13.97604488694547697, 96.87609039468566152 ) ) ;
#176545 = CARTESIAN_POINT ( 'NONE',  ( 13.97604488694527802, 13.89961937509977652, 24.37390960531435624 ) ) ;
#176546 = CARTESIAN_POINT ( 'NONE',  ( 9.564922557961047289, -16.46253265017146816, 25.41775706135234003 ) ) ;
#176547 = CARTESIAN_POINT ( 'NONE',  ( 13.97604488694548053, -13.89961937509957401, 100.6260903946856615 ) ) ;
#176549 = CARTESIAN_POINT ( 'NONE',  ( -19.03943276465977164, -0.05219959533935918106, 53.75109039468566863 ) ) ;
#176548 = CARTESIAN_POINT ( 'NONE',  ( 21.53943276465977519, -0.05219959533907433946, 88.74890960531436690 ) ) ;
#176550 = CARTESIAN_POINT ( 'NONE',  ( 16.20579543436677739, 7.371946100355104114, 108.0652083417187583 ) ) ;
#176551 = CARTESIAN_POINT ( 'NONE',  ( 5.153800228976335163, 19.02544592524342804, 59.79057627198100988 ) ) ;
#176552 = CARTESIAN_POINT ( 'NONE',  ( -16.52544592524342804, 4.483927247898546575, 66.04057627198103830 ) ) ;
#176553 = EDGE_CURVE ( 'NONE', #24966, #119129, #95033, .T. ) ;
#176554 = CARTESIAN_POINT ( 'NONE',  ( -0.05219959533909027116, -19.03943276465977164, 42.49890960531435269 ) ) ;
#176555 = CARTESIAN_POINT ( 'NONE',  ( 8.314922557960818139, 14.29746914071049879, 54.58224293864769550 ) ) ;
#176556 = DIRECTION ( 'NONE',  ( 0.000000000000000000, 0.000000000000000000, 1.000000000000000000 ) ) ;
#176557 = CARTESIAN_POINT ( 'NONE',  ( 12.14591786802309770, 12.06949235617756955, 29.37390960531435269 ) ) ;
#176558 = CARTESIAN_POINT ( 'NONE',  ( -5.049401038298153566, 19.05341960407611168, 60.20724293864768129 ) ) ;
#176559 = CARTESIAN_POINT ( 'NONE',  ( -5.049401038297874678, -19.05341960407617918, 29.79275706135232227 ) ) ;
#176560 = CARTESIAN_POINT ( 'NONE',  ( -16.52544592524335698, -4.483927247898792601, 28.95942372801902209 ) ) ;
#176561 = CARTESIAN_POINT ( 'NONE',  ( -21.52544592524343514, 5.823673210054127303, 51.04057627198103120 ) ) ;
#176563 = ORIENTED_EDGE ( 'NONE', *, *, #121704, .F. ) ;
#176562 = CARTESIAN_POINT ( 'NONE',  ( -21.52544592524334988, -5.823673210054445271, 98.95942372801903275 ) ) ;
#176564 = CARTESIAN_POINT ( 'NONE',  ( -19.02544592524342804, 5.153800228976336051, 66.04057627198103830 ) ) ;
#176565 = DIRECTION ( 'NONE',  ( -0.000000000000000000, -0.000000000000000000, 1.000000000000000000 ) ) ;
#176566 = CARTESIAN_POINT ( 'NONE',  ( -9.474510206698964154, 16.51473224551069663, 95.41557627198102409 ) ) ;
#176567 = CARTESIAN_POINT ( 'NONE',  ( -17.49999999999999645, -5.499999999999992895, 44.20309617465829888 ) ) ;
#176568 = CARTESIAN_POINT ( 'NONE',  ( 21.53943276465977519, 0.05219959533937863772, 31.25109039468568639 ) ) ;
#176569 = AXIS2_PLACEMENT_3D ( 'NONE', #67701, #83852, #192049 ) ;
#176570 = CARTESIAN_POINT ( 'NONE',  ( 4.379528057220339221, -16.55341960407611168, 97.70724293864772392 ) ) ;
#176572 = CARTESIAN_POINT ( 'NONE',  ( 5.049401038298161559, -19.05341960407611168, 67.70724293864769550 ) ) ;
#176571 = CARTESIAN_POINT ( 'NONE',  ( -21.53943276465977519, 0.05219959533907696930, 86.24890960531436690 ) ) ;
#176573 = CARTESIAN_POINT ( 'NONE',  ( 5.049401038298161559, -19.05341960407611168, 82.70724293864770971 ) ) ;
#176574 = CARTESIAN_POINT ( 'NONE',  ( -21.53943276465977519, 0.05219959533907696930, 116.2489096053143669 ) ) ;
#176575 = EDGE_LOOP ( 'NONE', ( #102745, #108125, #51152 ) ) ;
#176576 = CARTESIAN_POINT ( 'NONE',  ( 5.049401038298161559, -19.05341960407611168, 72.70724293864768129 ) ) ;
#176577 = CARTESIAN_POINT ( 'NONE',  ( 17.79613651744293534, 24.49428055684532524, 147.2843446568999752 ) ) ;
#176579 = CARTESIAN_POINT ( 'NONE',  ( 7.500000000000000000, 9.184850993605147944E-16, 4.292893218813446765 ) ) ;
#176578 = CARTESIAN_POINT ( 'NONE',  ( -14.34966873604960291, -8.224510206698953496, 101.6655762719810383 ) ) ;
#176580 = CARTESIAN_POINT ( 'NONE',  ( 19.05341960407617918, -5.049401038297876454, 96.04275706135231871 ) ) ;
#176581 = CARTESIAN_POINT ( 'NONE',  ( 8.314922557960818139, 14.29746914071049879, 114.5822429386477097 ) ) ;
#176582 = CARTESIAN_POINT ( 'NONE',  ( -15.72974639402176322, -15.80617190586768395, 74.37609039468568994 ) ) ;
#176584 = CARTESIAN_POINT ( 'NONE',  ( -5.719274019375665041, -21.55341960407619695, 34.79275706135235424 ) ) ;
#176583 = CARTESIAN_POINT ( 'NONE',  ( 9.564922557960805705, 16.46253265017160317, 64.58224293864769550 ) ) ;
#176585 = CARTESIAN_POINT ( 'NONE',  ( -15.72974639402197994, 15.80617190586746368, 110.6239096053143669 ) ) ;
#176586 = CARTESIAN_POINT ( 'NONE',  ( -28.82186960331499392, -9.364793116373526516, 144.0999999999999659 ) ) ;
#176587 = CARTESIAN_POINT ( 'NONE',  ( 13.89961937509977652, -13.97604488694527269, 68.12390960531436690 ) ) ;
#176588 = CARTESIAN_POINT ( 'NONE',  ( 27.86188877291512611, 7.554847477543872536, 161.1024127393341132 ) ) ;
#176590 = CARTESIAN_POINT ( 'NONE',  ( 5.719274019375991003, -21.55341960407610458, 27.70724293864769905 ) ) ;
#176589 = CARTESIAN_POINT ( 'NONE',  ( 8.224510206698742110, 14.34966873604972548, 27.08442372801901854 ) ) ;
#176591 = CARTESIAN_POINT ( 'NONE',  ( 18.67979575497194134, -10.72451020669871369, 65.83442372801900433 ) ) ;
#176592 = CARTESIAN_POINT ( 'NONE',  ( -9.564922557960796823, -16.46253265017161027, 112.0822429386476955 ) ) ;
#176593 = CARTESIAN_POINT ( 'NONE',  ( 13.97604488694548053, -13.89961937509957401, 90.62609039468567573 ) ) ;
#176594 = CARTESIAN_POINT ( 'NONE',  ( -5.153800228976328057, -19.02544592524343514, 52.29057627198100988 ) ) ;
#176595 = CARTESIAN_POINT ( 'NONE',  ( -0.05219959533909027116, -19.03943276465977164, 72.49890960531435269 ) ) ;
#176596 = CARTESIAN_POINT ( 'NONE',  ( -4.379528057220328563, 16.55341960407611168, 100.2072429386476955 ) ) ;
#176597 = CARTESIAN_POINT ( 'NONE',  ( -13.89961937509977652, 13.97604488694528158, 100.6239096053143669 ) ) ;
#176598 = CARTESIAN_POINT ( 'NONE',  ( -14.29746914071049879, 8.314922557960819915, 95.83224293864770971 ) ) ;
#176599 = CARTESIAN_POINT ( 'NONE',  ( -9.474510206698964154, 16.51473224551069663, 100.4155762719810241 ) ) ;
#176601 = CARTESIAN_POINT ( 'NONE',  ( -19.03943276465977164, 0.05219959533909376836, 41.24890960531435269 ) ) ;
#176600 = CARTESIAN_POINT ( 'NONE',  ( 4.379528057220339221, -16.55341960407611168, 57.70724293864770260 ) ) ;
#176602 = CARTESIAN_POINT ( 'NONE',  ( 10.72451020669871369, 18.67979575497193778, 52.08442372801901854 ) ) ;
#176603 = CARTESIAN_POINT ( 'NONE',  ( 9.474510206698729675, 16.51473224551082808, 92.08442372801900433 ) ) ;
#176604 = CARTESIAN_POINT ( 'NONE',  ( -4.379528057220328563, 16.55341960407611168, 45.20724293864769550 ) ) ;
#176605 = CARTESIAN_POINT ( 'NONE',  ( -5.823673210054116645, -21.52544592524344225, 97.29057627198105251 ) ) ;
#176606 = CARTESIAN_POINT ( 'NONE',  ( 5.719274019375991003, -21.55341960407610458, 47.70724293864770260 ) ) ;
#176608 = CARTESIAN_POINT ( 'NONE',  ( 4.379528057220339221, -16.55341960407611168, 87.70724293864769550 ) ) ;
#176607 = CARTESIAN_POINT ( 'NONE',  ( 19.25918095147778786, 5.499999999999571898, 71.95284276293934056 ) ) ;
#176609 = CARTESIAN_POINT ( 'NONE',  ( -23.31738231874055245, -16.94106989632524574, 142.4500000054623854 ) ) ;
#176610 = CARTESIAN_POINT ( 'NONE',  ( 5.153800228976335163, 19.02544592524342804, 59.79057627198100988 ) ) ;
#176611 = CARTESIAN_POINT ( 'NONE',  ( 0.05219959533934541429, -16.53943276465976808, 110.0010903946856757 ) ) ;
#176612 = CARTESIAN_POINT ( 'NONE',  ( 0.05219959533934541429, -16.53943276465976808, 95.00109039468568994 ) ) ;
#176613 = CARTESIAN_POINT ( 'NONE',  ( 12.14591786802327356, -12.06949235617739191, 85.62609039468568994 ) ) ;
#176614 = CARTESIAN_POINT ( 'NONE',  ( -5.049401038297874678, -19.05341960407617918, 39.79275706135232582 ) ) ;
#176616 = CARTESIAN_POINT ( 'NONE',  ( -9.564922557960796823, -16.46253265017161027, 112.0822429386476955 ) ) ;
#176615 = CARTESIAN_POINT ( 'NONE',  ( -17.50000000001357847, 5.500000000000046185, 45.79690382535059001 ) ) ;
#176617 = CARTESIAN_POINT ( 'NONE',  ( -5.153800228976328057, -19.02544592524343514, 87.29057627198103830 ) ) ;
#176618 = CARTESIAN_POINT ( 'NONE',  ( 5.049401038298161559, -19.05341960407611168, 37.70724293864768839 ) ) ;
#176619 = CARTESIAN_POINT ( 'NONE',  ( 14.34966873604960469, 8.224510206698951720, 54.16557627198103120 ) ) ;
#176621 = CARTESIAN_POINT ( 'NONE',  ( 13.97604488694527802, 13.89961937509977652, 104.3739096053143385 ) ) ;
#176620 = CARTESIAN_POINT ( 'NONE',  ( -5.049401038298153566, 19.05341960407611168, 115.2072429386477097 ) ) ;
#176622 = CARTESIAN_POINT ( 'NONE',  ( -21.55341960407610458, -5.719274019375992779, 46.45724293864769550 ) ) ;
#176623 = CARTESIAN_POINT ( 'NONE',  ( 16.52544592524342804, -4.483927247898539470, 88.54057627198103830 ) ) ;
#176624 = CARTESIAN_POINT ( 'NONE',  ( 14.29746914071037800, 8.314922557961029526, 41.66775706135235424 ) ) ;
#176625 = CARTESIAN_POINT ( 'NONE',  ( 16.53943276465976808, -0.05219959533910856209, 73.74890960531433848 ) ) ;
#176626 = LINE ( 'NONE', #177628, #170613 ) ;
#176627 = CARTESIAN_POINT ( 'NONE',  ( -13.97604488694547697, 13.89961937509957934, 63.12609039468566152 ) ) ;
#176628 = CARTESIAN_POINT ( 'NONE',  ( -13.97604488694527625, -13.89961937509977652, 96.87390960531433848 ) ) ;
#176629 = CARTESIAN_POINT ( 'NONE',  ( 19.05341960407617918, -5.049401038297876454, 81.04275706135231871 ) ) ;
#176630 = CARTESIAN_POINT ( 'NONE',  ( -69.65682714487590488, -71.74905178543390605, -4.999999999999999112 ) ) ;
#176632 = CARTESIAN_POINT ( 'NONE',  ( -16.55341960407617563, 4.379528057220093196, 113.5427570613523756 ) ) ;
#176631 = CARTESIAN_POINT ( 'NONE',  ( 0.05219959533934541429, -16.53943276465976808, 30.00109039468568284 ) ) ;
#176633 = CARTESIAN_POINT ( 'NONE',  ( 19.02544592524334988, 5.153800228976608722, 76.45942372801897591 ) ) ;
#176634 = CARTESIAN_POINT ( 'NONE',  ( -10.81492255796078084, -18.62759615963271287, 42.08224293864769550 ) ) ;
#176635 = CARTESIAN_POINT ( 'NONE',  ( -21.52544592524334988, -5.823673210054445271, 68.95942372801901854 ) ) ;
#176636 = CARTESIAN_POINT ( 'NONE',  ( 28.82186960331498327, 2.781578969918950771E-14, 147.2500000054623683 ) ) ;
#176637 = CARTESIAN_POINT ( 'NONE',  ( -16.55341960407617563, 4.379528057220093196, 23.54275706135235424 ) ) ;
#176639 = CARTESIAN_POINT ( 'NONE',  ( -19.03943276465977164, 0.05219959533909376836, 91.24890960531436690 ) ) ;
#176638 = CARTESIAN_POINT ( 'NONE',  ( -16.51473224551069308, -9.474510206698971260, 26.66557627198103120 ) ) ;
#176640 = CARTESIAN_POINT ( 'NONE',  ( 16.46253265017160672, -9.564922557960803928, 28.33224293864769550 ) ) ;
#176642 = CARTESIAN_POINT ( 'NONE',  ( -16.46253265017160317, 9.564922557960807481, 75.83224293864769550 ) ) ;
#176641 = CARTESIAN_POINT ( 'NONE',  ( -14.29746914071049879, 8.314922557960819915, 85.83224293864768129 ) ) ;
#176643 = SHAPE_DEFINITION_REPRESENTATION ( #61400, #65015 ) ;
#176644 = CARTESIAN_POINT ( 'NONE',  ( -13.89961937509977652, 13.97604488694528158, 90.62390960531432427 ) ) ;
#176645 = ORIENTED_EDGE ( 'NONE', *, *, #97058, .T. ) ;
#176646 = CARTESIAN_POINT ( 'NONE',  ( -19.03943276465977164, -0.05219959533935918106, 93.75109039468566152 ) ) ;
#176647 = CARTESIAN_POINT ( 'NONE',  ( 15.80617190586746368, 15.72974639402197994, 74.37390960531436690 ) ) ;
#176648 = CARTESIAN_POINT ( 'NONE',  ( -13.89961937509977652, 13.97604488694528158, 35.62390960531435269 ) ) ;
#176650 = CARTESIAN_POINT ( 'NONE',  ( -5.719274019375978568, 21.55341960407610458, 115.2072429386476955 ) ) ;
#176649 = CARTESIAN_POINT ( 'NONE',  ( -13.89961937509957401, -13.97604488694547875, 74.37609039468566152 ) ) ;
#176651 = CARTESIAN_POINT ( 'NONE',  ( 16.51473224551069308, 9.474510206698969483, 74.16557627198103830 ) ) ;
#176652 = CARTESIAN_POINT ( 'NONE',  ( 9.474510206698971260, -16.51473224551069308, 107.9155762719810383 ) ) ;
#176653 = VERTEX_POINT ( 'NONE', #53512 ) ;
#176654 = CARTESIAN_POINT ( 'NONE',  ( -21.53943276465977519, 0.05219959533907696930, 101.2489096053143669 ) ) ;
#176657 = CARTESIAN_POINT ( 'NONE',  ( 16.51473224551083163, -9.474510206698727899, 65.83442372801900433 ) ) ;
#176656 = CARTESIAN_POINT ( 'NONE',  ( -9.564922557960796823, -16.46253265017161027, 82.08224293864768129 ) ) ;
#176655 = CARTESIAN_POINT ( 'NONE',  ( -14.34966873604960291, -8.224510206698953496, 111.6655762719810525 ) ) ;
#176658 = CARTESIAN_POINT ( 'NONE',  ( 21.52544592524344225, -5.823673210054117533, 88.54057627198103830 ) ) ;
#176659 = CARTESIAN_POINT ( 'NONE',  ( -10.72451020669898014, 18.67979575497178502, 75.41557627198102409 ) ) ;
#176660 = CARTESIAN_POINT ( 'NONE',  ( 16.53943276465976808, -0.05219959533910856209, 43.74890960531435979 ) ) ;
#176661 = CARTESIAN_POINT ( 'NONE',  ( 21.53943276465977519, 0.05219959533937863772, 111.2510903946856899 ) ) ;
#176662 = CARTESIAN_POINT ( 'NONE',  ( 12.06949235617739724, 12.14591786802326823, 71.87609039468568994 ) ) ;
#176663 = CARTESIAN_POINT ( 'NONE',  ( 16.46253265017160672, -9.564922557960803928, 93.33224293864769550 ) ) ;
#176664 = CARTESIAN_POINT ( 'NONE',  ( -19.03943276465977164, 0.05219959533909376836, 46.24890960531435979 ) ) ;
#176665 = AXIS2_PLACEMENT_3D ( 'NONE', #161284, #145106, #53098 ) ;
#176666 = CARTESIAN_POINT ( 'NONE',  ( 18.62759615963255655, 10.81492255796105972, 51.66775706135234714 ) ) ;
#176667 = CARTESIAN_POINT ( 'NONE',  ( -21.52544592524334988, -5.823673210054445271, 53.95942372801900433 ) ) ;
#176668 = CARTESIAN_POINT ( 'NONE',  ( -19.03943276465977164, 0.05219959533909376836, 66.24890960531436690 ) ) ;
#176669 = CARTESIAN_POINT ( 'NONE',  ( -18.62759615963255300, -10.81492255796106328, 34.16775706135234714 ) ) ;
#176670 = CARTESIAN_POINT ( 'NONE',  ( -16.46253265017146816, -9.564922557961047289, 79.16775706135234714 ) ) ;
#176671 = CARTESIAN_POINT ( 'NONE',  ( -19.03943276465977164, -0.05219959533935918106, 73.75109039468566152 ) ) ;
#176672 = CARTESIAN_POINT ( 'NONE',  ( -13.97604488694527625, -13.89961937509977652, 41.87390960531435979 ) ) ;
#176673 = CARTESIAN_POINT ( 'NONE',  ( 12.14591786802327356, -12.06949235617739191, 80.62609039468567573 ) ) ;
#176674 = CARTESIAN_POINT ( 'NONE',  ( -5.153800228976328057, -19.02544592524343514, 57.29057627198103120 ) ) ;
#176675 = CARTESIAN_POINT ( 'NONE',  ( -11.30153831258470731, -190.0000000000000000, -15.00000000000000178 ) ) ;
#176676 = CARTESIAN_POINT ( 'NONE',  ( 13.97604488694527802, 13.89961937509977652, 94.37390960531436690 ) ) ;
#176677 = CARTESIAN_POINT ( 'NONE',  ( -9.564922557960796823, -16.46253265017161027, 42.08224293864769550 ) ) ;
#176678 = CARTESIAN_POINT ( 'NONE',  ( -21.55341960407610458, -5.719274019375992779, 81.45724293864769550 ) ) ;
#176679 = CARTESIAN_POINT ( 'NONE',  ( -14.29746914071037622, -8.314922557961029526, 54.16775706135235424 ) ) ;
#176680 = CIRCLE ( 'NONE', #102339, 4.000000000000000000 ) ;
#176681 = CARTESIAN_POINT ( 'NONE',  ( -16.51473224551082808, 9.474510206698731452, 23.33442372801900078 ) ) ;
#176682 = CARTESIAN_POINT ( 'NONE',  ( -16.51473224551069308, -9.474510206698971260, 51.66557627198102409 ) ) ;
#176683 = CARTESIAN_POINT ( 'NONE',  ( 8.314922557960818139, 14.29746914071049879, 49.58224293864769550 ) ) ;
#176684 = CARTESIAN_POINT ( 'NONE',  ( 4.379528057220339221, -16.55341960407611168, 82.70724293864770971 ) ) ;
#176685 = CARTESIAN_POINT ( 'NONE',  ( 5.049401038298161559, -19.05341960407611168, 72.70724293864768129 ) ) ;
#176686 = CARTESIAN_POINT ( 'NONE',  ( 10.81492255796106328, -18.62759615963255655, 35.41775706135234003 ) ) ;
#176687 = CARTESIAN_POINT ( 'NONE',  ( 16.51473224551069308, 9.474510206698969483, 89.16557627198103830 ) ) ;
#176688 = CARTESIAN_POINT ( 'NONE',  ( -5.719274019375665041, -21.55341960407619695, 94.79275706135234714 ) ) ;
#176689 = CARTESIAN_POINT ( 'NONE',  ( 12.14591786802327356, -12.06949235617739191, 65.62609039468568994 ) ) ;
#176690 = EDGE_CURVE ( 'NONE', #47139, #27411, #55647, .T. ) ;
#176691 = CARTESIAN_POINT ( 'NONE',  ( -18.67979575497193778, 10.72451020669871902, 28.33442372801902209 ) ) ;
#176692 = CARTESIAN_POINT ( 'NONE',  ( -19.02544592524342804, 5.153800228976336051, 111.0405762719810099 ) ) ;
#176693 = CARTESIAN_POINT ( 'NONE',  ( -18.62759615963270932, 10.81492255796079327, 95.83224293864770971 ) ) ;
#176694 = CARTESIAN_POINT ( 'NONE',  ( -12.14591786802309592, -12.06949235617757132, 51.87390960531437401 ) ) ;
#176695 = CARTESIAN_POINT ( 'NONE',  ( 13.97604488694527802, 13.89961937509977652, 39.37390960531435269 ) ) ;
#176696 = CARTESIAN_POINT ( 'NONE',  ( -12.14591786802309592, -12.06949235617757132, 71.87390960531438111 ) ) ;
#176697 = CARTESIAN_POINT ( 'NONE',  ( -5.719274019375978568, 21.55341960407610458, 25.20724293864769550 ) ) ;
#176698 = CARTESIAN_POINT ( 'NONE',  ( -0.05219959533936034679, 19.03943276465977164, 32.50109039468566863 ) ) ;
#176699 = CARTESIAN_POINT ( 'NONE',  ( -8.224510206698948167, 14.34966873604960824, 100.4155762719810241 ) ) ;
#176700 = CARTESIAN_POINT ( 'NONE',  ( 19.05341960407611168, 5.049401038298154454, 113.9572429386477097 ) ) ;
#176701 = ORIENTED_EDGE ( 'NONE', *, *, #28409, .F. ) ;
#176702 = CARTESIAN_POINT ( 'NONE',  ( -14.34966873604972548, 8.224510206698743886, 48.33442372801902565 ) ) ;
#176703 = CARTESIAN_POINT ( 'NONE',  ( -19.03943276465977164, 0.05219959533909376836, 61.24890960531436690 ) ) ;
#176704 = CARTESIAN_POINT ( 'NONE',  ( -8.571926809382608425, 26.38167802310805854, 140.4750000027312069 ) ) ;
#176705 = CARTESIAN_POINT ( 'NONE',  ( 14.34966873604972726, -8.224510206698740333, 90.83442372801901854 ) ) ;
#176706 = CARTESIAN_POINT ( 'NONE',  ( 16.46253265017146816, 9.564922557961045513, 96.66775706135233293 ) ) ;
#176707 = CARTESIAN_POINT ( 'NONE',  ( 10.81492255796106328, -18.62759615963255655, 75.41775706135233293 ) ) ;
#176708 = CARTESIAN_POINT ( 'NONE',  ( -5.153800228976328057, -19.02544592524343514, 72.29057627198102409 ) ) ;
#176709 = CARTESIAN_POINT ( 'NONE',  ( 5.719274019375991003, -21.55341960407610458, 87.70724293864769550 ) ) ;
#176710 = CARTESIAN_POINT ( 'NONE',  ( 14.29746914071037800, 8.314922557961029526, 41.66775706135235424 ) ) ;
#176711 = CARTESIAN_POINT ( 'NONE',  ( 14.29746914071049879, -8.314922557960816363, 108.3322429386477097 ) ) ;
#176712 = AXIS2_PLACEMENT_3D ( 'NONE', #77798, #46474, #62622 ) ;
#176713 = CARTESIAN_POINT ( 'NONE',  ( -16.51473224551082808, 9.474510206698731452, 78.33442372801900433 ) ) ;
#176714 = CARTESIAN_POINT ( 'NONE',  ( -21.52544592524343514, 5.823673210054127303, 81.04057627198102409 ) ) ;
#176715 = CARTESIAN_POINT ( 'NONE',  ( -19.05341960407617563, 5.049401038297882671, 48.54275706135233293 ) ) ;
#176716 = CARTESIAN_POINT ( 'NONE',  ( -19.02544592524342804, 5.153800228976336051, 111.0405762719810099 ) ) ;
#176717 = CARTESIAN_POINT ( 'NONE',  ( 10.81492255796078972, 18.62759615963270932, 84.58224293864769550 ) ) ;
#176718 = CARTESIAN_POINT ( 'NONE',  ( 17.60691670004651499, 5.500000000000063061, 61.63333313366440080 ) ) ;
#176719 = CARTESIAN_POINT ( 'NONE',  ( 16.51473224551069308, 9.474510206698969483, 64.16557627198102409 ) ) ;
#176720 = CARTESIAN_POINT ( 'NONE',  ( -11.57021340674615928, -12.01197775448600247, -59.14478828020191514 ) ) ;
#176721 = CARTESIAN_POINT ( 'NONE',  ( -13.89961937509957401, -13.97604488694547875, 109.3760903946856331 ) ) ;
#176722 = CARTESIAN_POINT ( 'NONE',  ( 8.334387768958743337, -39.12825866091939986, -13.00000000000000000 ) ) ;
#176723 = CARTESIAN_POINT ( 'NONE',  ( -15.72974639402176322, -15.80617190586768395, 59.37609039468568284 ) ) ;
#176725 = CARTESIAN_POINT ( 'NONE',  ( -12.06949235617756955, 12.14591786802309770, 65.62390960531436690 ) ) ;
#176724 = CARTESIAN_POINT ( 'NONE',  ( 21.52544592524344225, -5.823673210054117533, 108.5405762719810241 ) ) ;
#176726 = CARTESIAN_POINT ( 'NONE',  ( -19.02544592524342804, 5.153800228976336051, 76.04057627198102409 ) ) ;
#176727 = CARTESIAN_POINT ( 'NONE',  ( 21.55341960407619695, -5.719274019375665929, 71.04275706135234714 ) ) ;
#176729 = CARTESIAN_POINT ( 'NONE',  ( 9.564922557961047289, -16.46253265017146816, 35.41775706135233293 ) ) ;
#176728 = CARTESIAN_POINT ( 'NONE',  ( -16.52544592524335698, -4.483927247898792601, 18.95942372801901143 ) ) ;
#176730 = CARTESIAN_POINT ( 'NONE',  ( 21.53943276465977519, 0.05219959533937863772, 41.25109039468568284 ) ) ;
#176731 = CARTESIAN_POINT ( 'NONE',  ( 5.719274019375991003, -21.55341960407610458, 107.7072429386476955 ) ) ;
#176732 = CARTESIAN_POINT ( 'NONE',  ( -15.72974639402197994, 15.80617190586746368, 55.62390960531436690 ) ) ;
#176733 = CARTESIAN_POINT ( 'NONE',  ( 13.89961937509957401, 13.97604488694547697, 91.87609039468567573 ) ) ;
#176734 = CARTESIAN_POINT ( 'NONE',  ( -19.05341960407617563, 5.049401038297882671, 63.54275706135234003 ) ) ;
#176735 = CARTESIAN_POINT ( 'NONE',  ( 10.72451020669871369, 18.67979575497193778, 87.08442372801901854 ) ) ;
#176736 = CARTESIAN_POINT ( 'NONE',  ( -13.97604488694547697, 13.89961937509957934, 58.12609039468566863 ) ) ;
#176737 = CARTESIAN_POINT ( 'NONE',  ( -19.05341960407611168, -5.049401038298163336, 26.45724293864769550 ) ) ;
#176738 = CARTESIAN_POINT ( 'NONE',  ( -18.67979575497178146, -10.72451020669898902, 56.66557627198103830 ) ) ;
#176739 = CARTESIAN_POINT ( 'NONE',  ( 4.483927247898545687, 16.52544592524342804, 44.79057627198103120 ) ) ;
#176740 = CARTESIAN_POINT ( 'NONE',  ( -16.36317988757060959, -7.306389748694900099, 25.90210391636776777 ) ) ;
#176741 = CARTESIAN_POINT ( 'NONE',  ( 9.564922557961047289, -16.46253265017146816, 35.41775706135233293 ) ) ;
#176742 = CARTESIAN_POINT ( 'NONE',  ( 16.55341960407618274, -4.379528057220086978, 91.04275706135236135 ) ) ;
#176743 = CARTESIAN_POINT ( 'NONE',  ( -16.52544592524342804, 4.483927247898546575, 41.04057627198103120 ) ) ;
#176744 = CARTESIAN_POINT ( 'NONE',  ( 15.72974639402176855, 15.80617190586768217, 76.87609039468567573 ) ) ;
#176745 = CARTESIAN_POINT ( 'NONE',  ( 5.719274019375673035, 21.55341960407619339, 77.29275706135234714 ) ) ;
#176746 = CARTESIAN_POINT ( 'NONE',  ( 0.05219959533907565091, 21.53943276465977519, 74.99890960531435269 ) ) ;
#176747 = CARTESIAN_POINT ( 'NONE',  ( -16.51473224551069308, -9.474510206698971260, 41.66557627198103120 ) ) ;
#176748 = CARTESIAN_POINT ( 'NONE',  ( 15.80617190586769283, -15.72974639402175789, 50.62609039468568994 ) ) ;
#176749 = CARTESIAN_POINT ( 'NONE',  ( -19.05341960407611168, -5.049401038298163336, 36.45724293864766707 ) ) ;
#176750 = EDGE_LOOP ( 'NONE', ( #89231, #40110, #75167 ) ) ;
#176751 = CARTESIAN_POINT ( 'NONE',  ( -19.02544592524342804, 5.153800228976336051, 46.04057627198101699 ) ) ;
#176752 = CARTESIAN_POINT ( 'NONE',  ( -16.55341960407611168, -4.379528057220339221, 96.45724293864770971 ) ) ;
#176753 = CARTESIAN_POINT ( 'NONE',  ( -19.03943276465977164, 0.05219959533909376836, 101.2489096053143669 ) ) ;
#176754 = CARTESIAN_POINT ( 'NONE',  ( -16.53943276465976808, 0.05219959533911058130, 36.24890960531435979 ) ) ;
#176755 = CARTESIAN_POINT ( 'NONE',  ( 14.34966873604960469, 8.224510206698951720, 114.1655762719810383 ) ) ;
#176756 = CARTESIAN_POINT ( 'NONE',  ( 15.80617190586746368, 15.72974639402197994, 84.37390960531438111 ) ) ;
#176757 = CARTESIAN_POINT ( 'NONE',  ( 15.80617190586769283, -15.72974639402175789, 25.62609039468567929 ) ) ;
#176758 = CARTESIAN_POINT ( 'NONE',  ( 27.95720134624915687, -7.331398113984718634, 160.9065205403411198 ) ) ;
#176759 = ADVANCED_FACE ( 'NONE', ( #133353 ), #163706, .T. ) ;
#176760 = CARTESIAN_POINT ( 'NONE',  ( -16.53943276465976808, -0.05219959533934237506, 33.75109039468568284 ) ) ;
#176761 = CARTESIAN_POINT ( 'NONE',  ( 15.80617190586746368, 15.72974639402197994, 64.37390960531435269 ) ) ;
#176762 = CARTESIAN_POINT ( 'NONE',  ( -18.62759615963255300, -10.81492255796106328, 99.16775706135234714 ) ) ;
#176763 = CARTESIAN_POINT ( 'NONE',  ( -9.564922557960796823, -16.46253265017161027, 97.08224293864769550 ) ) ;
#176764 = CARTESIAN_POINT ( 'NONE',  ( 18.62759615963255655, 10.81492255796105972, 31.66775706135234358 ) ) ;
#176765 = CARTESIAN_POINT ( 'NONE',  ( -5.823673210054116645, -21.52544592524344225, 32.29057627198102409 ) ) ;
#176766 = CARTESIAN_POINT ( 'NONE',  ( -16.55341960407617563, 4.379528057220093196, 93.54275706135234714 ) ) ;
#176767 = CARTESIAN_POINT ( 'NONE',  ( 21.52544592524334988, 5.823673210054432836, 66.45942372801903275 ) ) ;
#176768 = CARTESIAN_POINT ( 'NONE',  ( 15.72974639402176855, 15.80617190586768217, 111.8760903946856615 ) ) ;
#176769 = CARTESIAN_POINT ( 'NONE',  ( -14.29746914071037622, -8.314922557961029526, 74.16775706135231871 ) ) ;
#176770 = CARTESIAN_POINT ( 'NONE',  ( 15.72974639402176855, 15.80617190586768217, 21.87609039468567573 ) ) ;
#176771 = CARTESIAN_POINT ( 'NONE',  ( -5.049401038298153566, 19.05341960407611168, 30.20724293864768839 ) ) ;
#176772 = CARTESIAN_POINT ( 'NONE',  ( -21.55341960407619339, 5.719274019375674811, 108.5427570613523756 ) ) ;
#176773 = CARTESIAN_POINT ( 'NONE',  ( 19.02544592524343514, -5.153800228976328945, 113.5405762719810241 ) ) ;
#176774 = CARTESIAN_POINT ( 'NONE',  ( -0.05219959533907301413, -21.53943276465977519, 97.49890960531436690 ) ) ;
#176776 = CARTESIAN_POINT ( 'NONE',  ( -21.52544592524343514, 5.823673210054127303, 61.04057627198103120 ) ) ;
#176775 = CYLINDRICAL_SURFACE ( 'NONE', #187332, 1.499999999999997780 ) ;
#176778 = CARTESIAN_POINT ( 'NONE',  ( -12.06949235617756955, 12.14591786802309770, 55.62390960531436690 ) ) ;
#176777 = CARTESIAN_POINT ( 'NONE',  ( 8.314922557961029526, -14.29746914071037800, 55.41775706135234714 ) ) ;
#176779 = CARTESIAN_POINT ( 'NONE',  ( 28.82186960331498327, 2.781578969918950771E-14, 145.0000000000000000 ) ) ;
#176780 = CARTESIAN_POINT ( 'NONE',  ( -5.153800228976607833, 19.02544592524334988, 82.70942372801897591 ) ) ;
#176781 = CARTESIAN_POINT ( 'NONE',  ( -17.48847506799968698, 5.747544572773742644, 105.8269743784328227 ) ) ;
#176782 = CARTESIAN_POINT ( 'NONE',  ( -16.46253265017146816, -9.564922557961047289, 109.1677570613523471 ) ) ;
#176783 = CARTESIAN_POINT ( 'NONE',  ( -21.52544592524343514, 5.823673210054127303, 81.04057627198102409 ) ) ;
#176784 = CARTESIAN_POINT ( 'NONE',  ( -4.483927247898539470, -16.52544592524342804, 62.29057627198102409 ) ) ;
#176785 = CARTESIAN_POINT ( 'NONE',  ( -9.564922557960796823, -16.46253265017161027, 102.0822429386477097 ) ) ;
#176786 = CARTESIAN_POINT ( 'NONE',  ( -16.53943276465976808, -0.05219959533934237506, 48.75109039468568284 ) ) ;
#176787 = CARTESIAN_POINT ( 'NONE',  ( 13.97604488694527802, 13.89961937509977652, 64.37390960531436690 ) ) ;
#176789 = CARTESIAN_POINT ( 'NONE',  ( -9.564922557961040184, 16.46253265017147172, 92.91775706135233293 ) ) ;
#176788 = CARTESIAN_POINT ( 'NONE',  ( -10.72451020669870658, -18.67979575497194134, 34.58442372801900433 ) ) ;
#176790 = CARTESIAN_POINT ( 'NONE',  ( 16.51473224551069308, 9.474510206698969483, 99.16557627198102409 ) ) ;
#176791 = CARTESIAN_POINT ( 'NONE',  ( 5.049401038298161559, -19.05341960407611168, 92.70724293864769550 ) ) ;
#176792 = CARTESIAN_POINT ( 'NONE',  ( -18.67979575497178146, -10.72451020669898902, 86.66557627198102409 ) ) ;
#176793 = CARTESIAN_POINT ( 'NONE',  ( 16.46253265017160672, -9.564922557960803928, 43.33224293864769550 ) ) ;
#176794 = CARTESIAN_POINT ( 'NONE',  ( -16.36317988757058473, -7.306389748694956054, 60.90210391636778553 ) ) ;
#176795 = CARTESIAN_POINT ( 'NONE',  ( -12.06949235617756955, 12.14591786802309770, 65.62390960531436690 ) ) ;
#176796 = CARTESIAN_POINT ( 'NONE',  ( 13.97604488694527802, 13.89961937509977652, 104.3739096053143385 ) ) ;
#176797 = CARTESIAN_POINT ( 'NONE',  ( -31.42649584489976178, 1.097581692000625386, -49.72218688481379445 ) ) ;
#176798 = CARTESIAN_POINT ( 'NONE',  ( -19.05341960407617563, 5.049401038297882671, 68.54275706135230450 ) ) ;
#176799 = CARTESIAN_POINT ( 'NONE',  ( 10.81492255796078972, 18.62759615963270932, 89.58224293864768129 ) ) ;
#176800 = CARTESIAN_POINT ( 'NONE',  ( -19.05341960407617563, 5.049401038297882671, 48.54275706135233293 ) ) ;
#176801 = CARTESIAN_POINT ( 'NONE',  ( 13.97604488694527802, 13.89961937509977652, 99.37390960531436690 ) ) ;
#176802 =( LENGTH_UNIT ( ) NAMED_UNIT ( * ) SI_UNIT ( .MILLI., .METRE. ) );
#176803 = CARTESIAN_POINT ( 'NONE',  ( 15.72974639402199770, -15.80617190586745480, 38.12390960531436690 ) ) ;
#176804 = VECTOR ( 'NONE', #18223, 1000.000000000000000 ) ;
#176805 = CARTESIAN_POINT ( 'NONE',  ( 0.05219959533909260263, 19.03943276465977164, 79.99890960531436690 ) ) ;
#176806 = CARTESIAN_POINT ( 'NONE',  ( -18.67979575497193778, 10.72451020669871902, 63.33442372801900433 ) ) ;
#176807 = CARTESIAN_POINT ( 'NONE',  ( 5.049401038298161559, -19.05341960407611168, 32.70724293864768129 ) ) ;
#176808 = CARTESIAN_POINT ( 'NONE',  ( 4.379528057220339221, -16.55341960407611168, 77.70724293864770971 ) ) ;
#176809 = CARTESIAN_POINT ( 'NONE',  ( -12.06949235617739369, -12.14591786802326823, 19.37609039468568639 ) ) ;
#176810 = CARTESIAN_POINT ( 'NONE',  ( 10.81492255796106328, -18.62759615963255655, 50.41775706135235424 ) ) ;
#176811 = ORIENTED_EDGE ( 'NONE', *, *, #18367, .T. ) ;
#176812 = DIRECTION ( 'NONE',  ( 1.000000000000000000, 0.000000000000000000, 0.000000000000000000 ) ) ;
#176813 = CARTESIAN_POINT ( 'NONE',  ( -19.05341960407617563, 5.049401038297882671, 63.54275706135234003 ) ) ;
#176814 = CARTESIAN_POINT ( 'NONE',  ( -8.673617379884035472E-16, 7.600000000000007638, -65.00100000000003320 ) ) ;
#176815 = CARTESIAN_POINT ( 'NONE',  ( -10.81492255796105439, 18.62759615963255655, 22.91775706135235069 ) ) ;
#176816 = CARTESIAN_POINT ( 'NONE',  ( 23.48529157249599919, 32.32473071737754111, -8.449999994537625625 ) ) ;
#176817 = CARTESIAN_POINT ( 'NONE',  ( 16.51473224551083163, -9.474510206698727899, 25.83442372801900078 ) ) ;
#176818 = CARTESIAN_POINT ( 'NONE',  ( 19.02544592524343514, -5.153800228976328945, 58.54057627198102409 ) ) ;
#176819 = CARTESIAN_POINT ( 'NONE',  ( 13.89961937509957401, 13.97604488694547697, 21.87609039468566152 ) ) ;
#176820 = CARTESIAN_POINT ( 'NONE',  ( -4.379528057220086978, -16.55341960407618274, 109.7927570613523613 ) ) ;
#176822 = CARTESIAN_POINT ( 'NONE',  ( -15.72974639402176322, -15.80617190586768395, 79.37609039468567573 ) ) ;
#176821 = CARTESIAN_POINT ( 'NONE',  ( 5.153800228976335163, 19.02544592524342804, 104.7905762719809957 ) ) ;
#176823 = CARTESIAN_POINT ( 'NONE',  ( 4.313351365237961588, -4.313351365237934054, -62.50719930893269805 ) ) ;
#176824 = CARTESIAN_POINT ( 'NONE',  ( 9.474510206698971260, -16.51473224551069308, 112.9155762719810383 ) ) ;
#176825 = CARTESIAN_POINT ( 'NONE',  ( 22.71027669145893668, -22.38345232661798079, -45.66972496404596882 ) ) ;
#176827 = CARTESIAN_POINT ( 'NONE',  ( -10.72451020669870658, -18.67979575497194134, 74.58442372801901854 ) ) ;
#176826 = CARTESIAN_POINT ( 'NONE',  ( 14.29746914071037800, 8.314922557961029526, 61.66775706135235424 ) ) ;
#176828 = CARTESIAN_POINT ( 'NONE',  ( -15.72974639402176322, -15.80617190586768395, 109.3760903946857042 ) ) ;
#176829 = CARTESIAN_POINT ( 'NONE',  ( 0.000000000000000000, 0.000000000000000000, -18.00000000000000000 ) ) ;
#176830 = CARTESIAN_POINT ( 'NONE',  ( 9.564922557960805705, 16.46253265017160317, 84.58224293864769550 ) ) ;
#176831 = CARTESIAN_POINT ( 'NONE',  ( -0.05219959533909027116, -19.03943276465977164, 107.4989096053143527 ) ) ;
#176832 = VERTEX_POINT ( 'NONE', #37344 ) ;
#176833 =( GEOMETRIC_REPRESENTATION_CONTEXT ( 3 ) GLOBAL_UNCERTAINTY_ASSIGNED_CONTEXT ( ( #68125 ) ) GLOBAL_UNIT_ASSIGNED_CONTEXT ( ( #63898, #154908, #185252 ) ) REPRESENTATION_CONTEXT ( 'NONE', 'WORKASPACE' ) );
#176834 = CARTESIAN_POINT ( 'NONE',  ( 27.03637221620040876, -26.30952996081074957, -20.42959548696013528 ) ) ;
#176835 = CARTESIAN_POINT ( 'NONE',  ( -19.05341960407611168, -5.049401038298163336, 41.45724293864769550 ) ) ;
#176836 = CARTESIAN_POINT ( 'NONE',  ( 5.823673210054125526, 21.52544592524343514, 39.79057627198103830 ) ) ;
#176837 = CARTESIAN_POINT ( 'NONE',  ( -0.05219959533934338120, 16.53943276465976808, 112.5010903946857042 ) ) ;
#176839 = CARTESIAN_POINT ( 'NONE',  ( 19.03943276465977164, -0.05219959533909143690, 83.74890960531436690 ) ) ;
#176838 = CARTESIAN_POINT ( 'NONE',  ( 14.29746914071049879, -8.314922557960816363, 103.3322429386476955 ) ) ;
#176840 = CARTESIAN_POINT ( 'NONE',  ( -21.53943276465977519, -0.05219959533937600094, 108.7510903946857042 ) ) ;
#176841 = CARTESIAN_POINT ( 'NONE',  ( 5.153800228976335163, 19.02544592524342804, 34.79057627198102409 ) ) ;
#176842 = CARTESIAN_POINT ( 'NONE',  ( 14.34966873604960469, 8.224510206698951720, 94.16557627198103830 ) ) ;
#176843 = CARTESIAN_POINT ( 'NONE',  ( 0.05219959533937995610, -21.53943276465977519, 55.00109039468568284 ) ) ;
#176844 = CARTESIAN_POINT ( 'NONE',  ( 21.53943276465977519, -0.05219959533907433946, 93.74890960531436690 ) ) ;
#176845 = CARTESIAN_POINT ( 'NONE',  ( 13.97604488694548053, -13.89961937509957401, 45.62609039468566863 ) ) ;
#176846 = CARTESIAN_POINT ( 'NONE',  ( -17.59860650958989936, -7.585241751807033417, 46.57662985737508166 ) ) ;
#176847 = CARTESIAN_POINT ( 'NONE',  ( -19.02544592524342804, 5.153800228976336051, 91.04057627198100988 ) ) ;
#176848 = CARTESIAN_POINT ( 'NONE',  ( -16.53943276465976808, 0.05219959533911058130, 66.24890960531436690 ) ) ;
#176849 = CARTESIAN_POINT ( 'NONE',  ( 19.03943276465977164, 0.05219959533936151252, 41.25109039468566152 ) ) ;
#176850 = CIRCLE ( 'NONE', #54160, 28.90000000000004476 ) ;
#176851 = CARTESIAN_POINT ( 'NONE',  ( 4.379528057220339221, -16.55341960407611168, 42.70724293864770260 ) ) ;
#176852 = CARTESIAN_POINT ( 'NONE',  ( -13.97604488694547697, 13.89961937509957934, 78.12609039468567573 ) ) ;
#176853 = CARTESIAN_POINT ( 'NONE',  ( -19.35633801406909527, 5.499999999999579892, 84.13373818172762242 ) ) ;
#176854 = CARTESIAN_POINT ( 'NONE',  ( -21.53943276465977519, 0.05219959533907696930, 36.24890960531435979 ) ) ;
#176855 = CARTESIAN_POINT ( 'NONE',  ( -16.53943276465976808, 0.05219959533911058130, 96.24890960531435269 ) ) ;
#176856 = CARTESIAN_POINT ( 'NONE',  ( -17.49999999999997158, -3.189878218039251756, 25.12948562571230227 ) ) ;
#176858 = CARTESIAN_POINT ( 'NONE',  ( 5.823673210054125526, 21.52544592524343514, 44.79057627198103120 ) ) ;
#176857 = CARTESIAN_POINT ( 'NONE',  ( -19.03943276465977164, 0.05219959533909376836, 46.24890960531435979 ) ) ;
#176859 = CARTESIAN_POINT ( 'NONE',  ( 9.564922557960805705, 16.46253265017160317, 34.58224293864770260 ) ) ;
#176861 = CARTESIAN_POINT ( 'NONE',  ( -0.05219959533909027116, -19.03943276465977164, 57.49890960531435979 ) ) ;
#176860 = CARTESIAN_POINT ( 'NONE',  ( -12.06949235617739369, -12.14591786802326823, 74.37609039468568994 ) ) ;
#176862 = CARTESIAN_POINT ( 'NONE',  ( 9.474510206698729675, 16.51473224551082808, 42.08442372801900433 ) ) ;
#176863 = CARTESIAN_POINT ( 'NONE',  ( 18.67979575497194134, -10.72451020669871369, 65.83442372801900433 ) ) ;
#176864 = CARTESIAN_POINT ( 'NONE',  ( 15.72974639402199770, -15.80617190586745480, 53.12390960531436690 ) ) ;
#176865 = CARTESIAN_POINT ( 'NONE',  ( 14.34966873604960469, 8.224510206698951720, 114.1655762719810383 ) ) ;
#176866 = CARTESIAN_POINT ( 'NONE',  ( -19.05341960407617563, 5.049401038297882671, 98.54275706135233293 ) ) ;
#176867 = CARTESIAN_POINT ( 'NONE',  ( 19.03943276465977164, -0.05219959533909143690, 23.74890960531435269 ) ) ;
#176869 = CARTESIAN_POINT ( 'NONE',  ( 18.67979575497178502, 10.72451020669898547, 54.16557627198103120 ) ) ;
#176868 = CARTESIAN_POINT ( 'NONE',  ( -0.2180554607492796448, -24.28797299941338395, -56.78142080721293894 ) ) ;
#176870 = CARTESIAN_POINT ( 'NONE',  ( 16.88567814943165857, -6.947325034625565721, 66.20998877347417988 ) ) ;
#176871 = CARTESIAN_POINT ( 'NONE',  ( 21.55341960407619695, -5.719274019375665929, 81.04275706135236135 ) ) ;
#176872 = CARTESIAN_POINT ( 'NONE',  ( -4.379528057220328563, 16.55341960407611168, 50.20724293864769550 ) ) ;
#176873 = CARTESIAN_POINT ( 'NONE',  ( -4.379528057220328563, 16.55341960407611168, 60.20724293864768839 ) ) ;
#176874 = CARTESIAN_POINT ( 'NONE',  ( 10.72451020669898902, -18.67979575497178502, 82.91557627198103830 ) ) ;
#176875 = CARTESIAN_POINT ( 'NONE',  ( 18.67979575497178502, 10.72451020669898547, 79.16557627198103830 ) ) ;
#176876 = CARTESIAN_POINT ( 'NONE',  ( -18.22780087662119541, 5.500000000000102141, 61.01763182126894947 ) ) ;
#176877 = CARTESIAN_POINT ( 'NONE',  ( 10.72451020669898902, -18.67979575497178502, 37.91557627198102409 ) ) ;
#176878 = CARTESIAN_POINT ( 'NONE',  ( -16.55341960407617563, 4.379528057220093196, 53.54275706135234714 ) ) ;
#176879 = CARTESIAN_POINT ( 'NONE',  ( -0.05219959533910754901, -16.53943276465976808, 77.49890960531433848 ) ) ;
#176880 = CARTESIAN_POINT ( 'NONE',  ( 5.153800228976335163, 19.02544592524342804, 59.79057627198100988 ) ) ;
#176881 = CARTESIAN_POINT ( 'NONE',  ( 16.51473224551069308, 9.474510206698969483, 39.16557627198103120 ) ) ;
#176882 = CARTESIAN_POINT ( 'NONE',  ( -17.49999999999999289, 5.500000000000036415, 75.79690382534175797 ) ) ;
#176883 = CARTESIAN_POINT ( 'NONE',  ( 16.52544592524335698, 4.483927247898782831, 81.45942372801900433 ) ) ;
#176884 = CARTESIAN_POINT ( 'NONE',  ( 10.81492255796106328, -18.62759615963255655, 25.41775706135235779 ) ) ;
#176885 = CARTESIAN_POINT ( 'NONE',  ( 5.153800228976335163, 19.02544592524342804, 79.79057627198102409 ) ) ;
#176886 = CARTESIAN_POINT ( 'NONE',  ( -15.72974639402176322, -15.80617190586768395, 59.37609039468568284 ) ) ;
#176887 = CARTESIAN_POINT ( 'NONE',  ( 13.89961937509977652, -13.97604488694527269, 108.1239096053143669 ) ) ;
#176888 = CARTESIAN_POINT ( 'NONE',  ( -16.14548778791224137, -40.33029071462993187, -21.07572238977526169 ) ) ;
#176889 = VERTEX_POINT ( 'NONE', #24197 ) ;
#176890 = CARTESIAN_POINT ( 'NONE',  ( -10.72451020669870658, -18.67979575497194134, 39.58442372801901143 ) ) ;
#176892 = CARTESIAN_POINT ( 'NONE',  ( 19.02544592524343514, -5.153800228976328945, 103.5405762719809957 ) ) ;
#176891 = CARTESIAN_POINT ( 'NONE',  ( 16.51473224551069308, 9.474510206698969483, 34.16557627198102409 ) ) ;
#176893 = CARTESIAN_POINT ( 'NONE',  ( -5.049401038297874678, -19.05341960407617918, 49.79275706135231871 ) ) ;
#176894 = CARTESIAN_POINT ( 'NONE',  ( -5.719274019375978568, 21.55341960407610458, 110.2072429386477239 ) ) ;
#176895 = CARTESIAN_POINT ( 'NONE',  ( 13.97604488694548053, -13.89961937509957401, 50.62609039468566152 ) ) ;
#176896 = CARTESIAN_POINT ( 'NONE',  ( -16.51473224551069308, -9.474510206698971260, 21.66557627198102765 ) ) ;
#176897 = CARTESIAN_POINT ( 'NONE',  ( 14.29746914071037800, 8.314922557961029526, 91.66775706135234714 ) ) ;
#176898 = CARTESIAN_POINT ( 'NONE',  ( 16.46253265017146816, 9.564922557961045513, 56.66775706135233293 ) ) ;
#176899 = CARTESIAN_POINT ( 'NONE',  ( 12.06949235617739724, 12.14591786802326823, 101.8760903946857042 ) ) ;
#176901 = ORIENTED_EDGE ( 'NONE', *, *, #58459, .F. ) ;
#176900 = CARTESIAN_POINT ( 'NONE',  ( 9.295088167215988406, 11.16688150046370964, -62.26853652665833749 ) ) ;
#176902 = CARTESIAN_POINT ( 'NONE',  ( -19.05341960407611168, -5.049401038298163336, 91.45724293864766707 ) ) ;
#176903 = CARTESIAN_POINT ( 'NONE',  ( -18.62759615963255300, -10.81492255796106328, 94.16775706135237556 ) ) ;
#176904 = CARTESIAN_POINT ( 'NONE',  ( 21.52544592524334988, 5.823673210054432836, 106.4594237280190328 ) ) ;
#176905 = CARTESIAN_POINT ( 'NONE',  ( -19.03943276465977164, 0.05219959533909376836, 21.24890960531436335 ) ) ;
#176906 = CARTESIAN_POINT ( 'NONE',  ( -19.02544592524342804, 5.153800228976336051, 101.0405762719810241 ) ) ;
#176907 = CARTESIAN_POINT ( 'NONE',  ( 21.55341960407619695, -5.719274019375665929, 76.04275706135237556 ) ) ;
#176908 = CARTESIAN_POINT ( 'NONE',  ( -16.52544592524335698, -4.483927247898792601, 23.95942372801901143 ) ) ;
#176909 = CARTESIAN_POINT ( 'NONE',  ( 9.564922557960805705, 16.46253265017160317, 84.58224293864769550 ) ) ;
#176910 = CARTESIAN_POINT ( 'NONE',  ( -18.62759615963270932, 10.81492255796079327, 35.83224293864768839 ) ) ;
#176911 = CARTESIAN_POINT ( 'NONE',  ( -13.97604488694527625, -13.89961937509977652, 96.87390960531433848 ) ) ;
#176912 = CARTESIAN_POINT ( 'NONE',  ( -16.19135201231366850, -7.376712067591933319, 90.18680854052031748 ) ) ;
#176913 = CARTESIAN_POINT ( 'NONE',  ( -13.89961937509977652, 13.97604488694528158, 75.62390960531438111 ) ) ;
#176914 = CARTESIAN_POINT ( 'NONE',  ( 19.03943276465977164, -0.05219959533909143690, 68.74890960531436690 ) ) ;
#176915 = CARTESIAN_POINT ( 'NONE',  ( -4.379528057220086978, -16.55341960407618274, 94.79275706135234714 ) ) ;
#176916 = DIRECTION ( 'NONE',  ( 0.000000000000000000, 0.000000000000000000, -1.000000000000000000 ) ) ;
#176917 = CARTESIAN_POINT ( 'NONE',  ( -9.474510206698720793, -16.51473224551083518, 59.58442372801900433 ) ) ;
#176918 = CARTESIAN_POINT ( 'NONE',  ( 13.97604488694527802, 13.89961937509977652, 99.37390960531436690 ) ) ;
#176919 = CARTESIAN_POINT ( 'NONE',  ( 16.52544592524342804, -4.483927247898539470, 78.54057627198103830 ) ) ;
#176920 = CARTESIAN_POINT ( 'NONE',  ( 21.55341960407610458, 5.719274019375980345, 28.95724293864769905 ) ) ;
#176921 = CARTESIAN_POINT ( 'NONE',  ( -5.049401038298153566, 19.05341960407611168, 115.2072429386477097 ) ) ;
#176922 = CARTESIAN_POINT ( 'NONE',  ( 14.34966873604960469, 8.224510206698951720, 94.16557627198103830 ) ) ;
#176923 = CARTESIAN_POINT ( 'NONE',  ( -17.13100169013299023, 6.664070546373147330, 55.76789835699847941 ) ) ;
#176924 = CARTESIAN_POINT ( 'NONE',  ( -5.049401038297874678, -19.05341960407617918, 49.79275706135231871 ) ) ;
#176925 = CARTESIAN_POINT ( 'NONE',  ( -16.55341960407611168, -4.379528057220339221, 21.45724293864769550 ) ) ;
#176927 = EDGE_CURVE ( 'NONE', #147212, #51307, #164705, .T. ) ;
#176926 = CARTESIAN_POINT ( 'NONE',  ( -9.474510206698964154, 16.51473224551069663, 100.4155762719810241 ) ) ;
#176928 = CARTESIAN_POINT ( 'NONE',  ( 10.72451020669871369, 18.67979575497193778, 62.08442372801901143 ) ) ;
#176929 = CARTESIAN_POINT ( 'NONE',  ( -18.62759615963270932, 10.81492255796079327, 55.83224293864770260 ) ) ;
#176930 = CARTESIAN_POINT ( 'NONE',  ( -18.67979575497193778, 10.72451020669871902, 38.33442372801900433 ) ) ;
#176931 = CARTESIAN_POINT ( 'NONE',  ( -21.55341960407610458, -5.719274019375992779, 81.45724293864769550 ) ) ;
#176932 = CARTESIAN_POINT ( 'NONE',  ( -5.719274019375665041, -21.55341960407619695, 39.79275706135235424 ) ) ;
#176933 = CARTESIAN_POINT ( 'NONE',  ( 14.34966873604960469, 8.224510206698951720, 114.1655762719810383 ) ) ;
#176934 = CARTESIAN_POINT ( 'NONE',  ( 16.51473224551083163, -9.474510206698727899, 65.83442372801900433 ) ) ;
#176935 = CARTESIAN_POINT ( 'NONE',  ( 19.03943276465977164, -0.05219959533909143690, 38.74890960531436690 ) ) ;
#176937 = CARTESIAN_POINT ( 'NONE',  ( -13.89961937509977652, 13.97604488694528158, 90.62390960531432427 ) ) ;
#176936 = CARTESIAN_POINT ( 'NONE',  ( -8.224510206698948167, 14.34966873604960824, 90.41557627198103830 ) ) ;
#176938 = CARTESIAN_POINT ( 'NONE',  ( 13.97604488694527802, 13.89961937509977652, 99.37390960531436690 ) ) ;
#176939 = CARTESIAN_POINT ( 'NONE',  ( -9.474510206698964154, 16.51473224551069663, 25.41557627198103120 ) ) ;
#176940 = CARTESIAN_POINT ( 'NONE',  ( -12.06949235617756955, 12.14591786802309770, 35.62390960531437401 ) ) ;
#176941 = CARTESIAN_POINT ( 'NONE',  ( -16.52544592524335698, -4.483927247898792601, 103.9594237280190185 ) ) ;
#176942 = CARTESIAN_POINT ( 'NONE',  ( -5.049401038298153566, 19.05341960407611168, 55.20724293864769550 ) ) ;
#176943 = CARTESIAN_POINT ( 'NONE',  ( -5.049401038298153566, 19.05341960407611168, 25.20724293864768484 ) ) ;
#176944 = CARTESIAN_POINT ( 'NONE',  ( 0.05219959533936267826, -19.03943276465977164, 30.00109039468566863 ) ) ;
#176947 = CARTESIAN_POINT ( 'NONE',  ( -12.06949235617739369, -12.14591786802326823, 109.3760903946857042 ) ) ;
#176946 = CARTESIAN_POINT ( 'NONE',  ( 26.79475375365586132, 2.756753960551091991E-14, 139.9999999999999716 ) ) ;
#176945 = VECTOR ( 'NONE', #147537, 1000.000000000000000 ) ;
#176948 = CARTESIAN_POINT ( 'NONE',  ( -5.823673210054431948, 21.52544592524334988, 52.70942372801902565 ) ) ;
#176949 = CARTESIAN_POINT ( 'NONE',  ( -19.05341960407611168, -5.049401038298163336, 101.4572429386476955 ) ) ;
#176950 = CARTESIAN_POINT ( 'NONE',  ( -16.53943276465976808, -0.05219959533934237506, 43.75109039468568284 ) ) ;
#176951 = CARTESIAN_POINT ( 'NONE',  ( 16.53943276465976808, 0.05219959533934440121, 106.2510903946856757 ) ) ;
#176952 = CARTESIAN_POINT ( 'NONE',  ( 9.474510206698971260, -16.51473224551069308, 47.91557627198102409 ) ) ;
#176953 = CARTESIAN_POINT ( 'NONE',  ( -8.314922557961024197, 14.29746914071037800, 87.91775706135234714 ) ) ;
#176954 = CARTESIAN_POINT ( 'NONE',  ( 8.224510206698742110, 14.34966873604972548, 27.08442372801901854 ) ) ;
#176955 = CARTESIAN_POINT ( 'NONE',  ( 16.51473224551069308, 9.474510206698969483, 49.16557627198102409 ) ) ;
#176956 = CARTESIAN_POINT ( 'NONE',  ( 4.483927247898545687, 16.52544592524342804, 104.7905762719810241 ) ) ;
#176957 = CARTESIAN_POINT ( 'NONE',  ( -15.72974639402197994, 15.80617190586746368, 110.6239096053143669 ) ) ;
#176958 = CARTESIAN_POINT ( 'NONE',  ( 19.05341960407611168, 5.049401038298154454, 33.95724293864769550 ) ) ;
#176959 = CARTESIAN_POINT ( 'NONE',  ( -5.049401038298153566, 19.05341960407611168, 100.2072429386476955 ) ) ;
#176960 = CARTESIAN_POINT ( 'NONE',  ( -16.51473224551069308, -9.474510206698971260, 31.66557627198102054 ) ) ;
#176961 = CARTESIAN_POINT ( 'NONE',  ( -5.153800228976328057, -19.02544592524343514, 102.2905762719810383 ) ) ;
#176962 = DIRECTION ( 'NONE',  ( -0.000000000000000000, -0.000000000000000000, 1.000000000000000000 ) ) ;
#176963 = CARTESIAN_POINT ( 'NONE',  ( 9.474510206698971260, -16.51473224551069308, 92.91557627198103830 ) ) ;
#176965 = CARTESIAN_POINT ( 'NONE',  ( -16.55341960407611168, -4.379528057220339221, 101.4572429386476955 ) ) ;
#176964 = CARTESIAN_POINT ( 'NONE',  ( 5.719274019375673035, 21.55341960407619339, 42.29275706135235424 ) ) ;
#176966 = CARTESIAN_POINT ( 'NONE',  ( 16.46253265017160672, -9.564922557960803928, 103.3322429386476955 ) ) ;
#176967 = CARTESIAN_POINT ( 'NONE',  ( -27.40250423668980417, -7.751724348666604314, 163.3149731962997748 ) ) ;
#176968 = CARTESIAN_POINT ( 'NONE',  ( 4.483927247898790824, -16.52544592524335698, 70.20942372801904696 ) ) ;
#176969 = CARTESIAN_POINT ( 'NONE',  ( 15.80617190586769283, -15.72974639402175789, 95.62609039468568994 ) ) ;
#176970 = AXIS2_PLACEMENT_3D ( 'NONE', #133299, #194990, #29129 ) ;
#176971 = CARTESIAN_POINT ( 'NONE',  ( 12.06949235617739724, 12.14591786802326823, 36.87609039468568994 ) ) ;
#176972 = CARTESIAN_POINT ( 'NONE',  ( 13.97604488694527802, 13.89961937509977652, 84.37390960531433848 ) ) ;
#176973 = CARTESIAN_POINT ( 'NONE',  ( -5.049401038297874678, -19.05341960407617918, 109.7927570613523187 ) ) ;
#176974 = CARTESIAN_POINT ( 'NONE',  ( 14.29746914071037800, 8.314922557961029526, 76.66775706135234714 ) ) ;
#176975 = CARTESIAN_POINT ( 'NONE',  ( -13.97604488694547697, 13.89961937509957934, 88.12609039468563310 ) ) ;
#176976 = CARTESIAN_POINT ( 'NONE',  ( 19.03943276465977164, -0.05219959533909143690, 78.74890960531436690 ) ) ;
#176977 = CARTESIAN_POINT ( 'NONE',  ( 21.55341960407610458, 5.719274019375980345, 98.95724293864770971 ) ) ;
#176979 = CARTESIAN_POINT ( 'NONE',  ( 16.51473224551083163, -9.474510206698727899, 85.83442372801900433 ) ) ;
#176978 = CARTESIAN_POINT ( 'NONE',  ( -12.14591786802309592, -12.06949235617757132, 91.87390960531436690 ) ) ;
#176980 = CARTESIAN_POINT ( 'NONE',  ( -8.314922557961024197, 14.29746914071037800, 77.91775706135231871 ) ) ;
#176981 = CARTESIAN_POINT ( 'NONE',  ( -18.87075004821565472, 5.500000000000083489, 78.67408112101043116 ) ) ;
#176982 = CARTESIAN_POINT ( 'NONE',  ( 0.05219959533936267826, -19.03943276465977164, 70.00109039468566152 ) ) ;
#176983 = CARTESIAN_POINT ( 'NONE',  ( 16.55341960407611168, 4.379528057220329451, 33.95724293864769550 ) ) ;
#176984 = CARTESIAN_POINT ( 'NONE',  ( -8.314922557960811034, -14.29746914071050412, 92.08224293864769550 ) ) ;
#176986 = CARTESIAN_POINT ( 'NONE',  ( -16.46253265017146816, -9.564922557961047289, 44.16775706135232582 ) ) ;
#176985 = CARTESIAN_POINT ( 'NONE',  ( -19.03943276465977164, -0.05219959533935918106, 23.75109039468566152 ) ) ;
#176987 = CARTESIAN_POINT ( 'NONE',  ( 10.81492255796106328, -18.62759615963255655, 30.41775706135234358 ) ) ;
#176988 = CARTESIAN_POINT ( 'NONE',  ( 3.181980515339446924, -6.791538853603077186, 8.889087296526001936 ) ) ;
#176989 = CARTESIAN_POINT ( 'NONE',  ( -16.51473224551069308, -9.474510206698971260, 76.66557627198103830 ) ) ;
#176990 = CARTESIAN_POINT ( 'NONE',  ( 15.80617190586769283, -15.72974639402175789, 100.6260903946857184 ) ) ;
#176991 = CARTESIAN_POINT ( 'NONE',  ( 5.049401038298161559, -19.05341960407611168, 82.70724293864770971 ) ) ;
#176992 = CARTESIAN_POINT ( 'NONE',  ( -15.72974639402197994, 15.80617190586746368, 40.62390960531435269 ) ) ;
#176993 = CARTESIAN_POINT ( 'NONE',  ( -0.05219959533910754901, -16.53943276465976808, 82.49890960531436690 ) ) ;
#176994 = CARTESIAN_POINT ( 'NONE',  ( -5.153800228976328057, -19.02544592524343514, 52.29057627198100988 ) ) ;
#176995 = CARTESIAN_POINT ( 'NONE',  ( 0.05219959533910956823, 16.53943276465976808, 104.9989096053143669 ) ) ;
#176996 = CARTESIAN_POINT ( 'NONE',  ( -21.53943276465977519, -0.05219959533937600094, 28.75109039468567929 ) ) ;
#176997 = CARTESIAN_POINT ( 'NONE',  ( -5.823673210054431948, 21.52544592524334988, 57.70942372801901143 ) ) ;
#176998 = CARTESIAN_POINT ( 'NONE',  ( 13.89961937509977652, -13.97604488694527269, 43.12390960531434558 ) ) ;
#176999 = EDGE_CURVE ( 'NONE', #116956, #155416, #83239, .T. ) ;
#177000 = CARTESIAN_POINT ( 'NONE',  ( -8.224510206698735004, -14.34966873604973081, 74.58442372801901854 ) ) ;
#177001 = CARTESIAN_POINT ( 'NONE',  ( -21.52544592524334988, -5.823673210054445271, 18.95942372801901143 ) ) ;
#177002 = ORIENTED_EDGE ( 'NONE', *, *, #168410, .T. ) ;
#177003 = CARTESIAN_POINT ( 'NONE',  ( 18.62759615963271287, -10.81492255796078972, 113.3322429386476955 ) ) ;
#177005 = CARTESIAN_POINT ( 'NONE',  ( -9.474510206698964154, 16.51473224551069663, 65.41557627198102409 ) ) ;
#177004 = CARTESIAN_POINT ( 'NONE',  ( -5.153800228976607833, 19.02544592524334988, 37.70942372801899722 ) ) ;
#177006 = CARTESIAN_POINT ( 'NONE',  ( -9.474510206698720793, -16.51473224551083518, 29.58442372801900433 ) ) ;
#177007 = CARTESIAN_POINT ( 'NONE',  ( -15.72974639402176322, -15.80617190586768395, 74.37609039468568994 ) ) ;
#177008 = CARTESIAN_POINT ( 'NONE',  ( -18.62759615963270932, 10.81492255796079327, 65.83224293864769550 ) ) ;
#177009 = CARTESIAN_POINT ( 'NONE',  ( 8.224510206698953496, -14.34966873604960469, 42.91557627198103120 ) ) ;
#177011 = CARTESIAN_POINT ( 'NONE',  ( -16.51473224551082808, 9.474510206698731452, 28.33442372801900433 ) ) ;
#177010 = CARTESIAN_POINT ( 'NONE',  ( 21.52544592524334988, 5.823673210054432836, 96.45942372801901854 ) ) ;
#177012 = CARTESIAN_POINT ( 'NONE',  ( -0.05219959533910754901, -16.53943276465976808, 62.49890960531436690 ) ) ;
#177013 = CARTESIAN_POINT ( 'NONE',  ( -12.14591786802309592, -12.06949235617757132, 106.8739096053143811 ) ) ;
#177014 = CARTESIAN_POINT ( 'NONE',  ( 5.153800228976615827, -19.02544592524334988, 55.20942372801899722 ) ) ;
#177015 = CARTESIAN_POINT ( 'NONE',  ( -8.314922557960811034, -14.29746914071050412, 27.08224293864769550 ) ) ;
#177016 = CARTESIAN_POINT ( 'NONE',  ( -18.62759615963255300, -10.81492255796106328, 64.16775706135234714 ) ) ;
#177017 = CARTESIAN_POINT ( 'NONE',  ( 13.97604488694527802, 13.89961937509977652, 79.37390960531435269 ) ) ;
#177018 = CARTESIAN_POINT ( 'NONE',  ( 9.564922557961047289, -16.46253265017146816, 50.41775706135233293 ) ) ;
#177019 = CARTESIAN_POINT ( 'NONE',  ( -5.719274019375978568, 21.55341960407610458, 50.20724293864769550 ) ) ;
#177020 = CARTESIAN_POINT ( 'NONE',  ( 5.719274019375673035, 21.55341960407619339, 47.29275706135234003 ) ) ;
#177021 = CARTESIAN_POINT ( 'NONE',  ( -5.823673210054116645, -21.52544592524344225, 102.2905762719810383 ) ) ;
#177022 = CARTESIAN_POINT ( 'NONE',  ( 9.564922557961047289, -16.46253265017146816, 95.41775706135233293 ) ) ;
#177023 = CARTESIAN_POINT ( 'NONE',  ( -12.06949235617739369, -12.14591786802326823, 64.37609039468568994 ) ) ;
#177025 = CARTESIAN_POINT ( 'NONE',  ( 10.81492255796078972, 18.62759615963270932, 104.5822429386477097 ) ) ;
#177024 = CARTESIAN_POINT ( 'NONE',  ( -16.63275618507867293, -17.54166085810596343, -56.86956483720373257 ) ) ;
#177026 = CARTESIAN_POINT ( 'NONE',  ( 8.314922557960818139, 14.29746914071049879, 89.58224293864768129 ) ) ;
#177027 = CARTESIAN_POINT ( 'NONE',  ( -16.21995358207305316, -7.366697692864184965, 100.0644899848783922 ) ) ;
#177028 = CARTESIAN_POINT ( 'NONE',  ( -12.06949235617739369, -12.14591786802326823, 19.37609039468568639 ) ) ;
#177029 = CARTESIAN_POINT ( 'NONE',  ( 10.72451020669898902, -18.67979575497178502, 42.91557627198103120 ) ) ;
#177030 = CARTESIAN_POINT ( 'NONE',  ( 4.379528057220092307, 16.55341960407617563, 92.29275706135236135 ) ) ;
#177031 = CARTESIAN_POINT ( 'NONE',  ( 33.13409719347311722, -16.32441212556909349, -7.999999999999998224 ) ) ;
#177032 = CARTESIAN_POINT ( 'NONE',  ( 4.379528057220092307, 16.55341960407617563, 72.29275706135236135 ) ) ;
#177033 = CARTESIAN_POINT ( 'NONE',  ( -10.72451020669870658, -18.67979575497194134, 34.58442372801900433 ) ) ;
#177034 = CARTESIAN_POINT ( 'NONE',  ( -21.55341960407610458, -5.719274019375992779, 41.45724293864769550 ) ) ;
#177035 = CARTESIAN_POINT ( 'NONE',  ( 0.05219959533934541429, -16.53943276465976808, 90.00109039468567573 ) ) ;
#177036 = CARTESIAN_POINT ( 'NONE',  ( -9.564922557960796823, -16.46253265017161027, 92.08224293864769550 ) ) ;
#177037 = CARTESIAN_POINT ( 'NONE',  ( 21.55341960407619695, -5.719274019375665929, 66.04275706135236135 ) ) ;
#177038 = CARTESIAN_POINT ( 'NONE',  ( 5.823673210054125526, 21.52544592524343514, 34.79057627198103120 ) ) ;
#177039 = CARTESIAN_POINT ( 'NONE',  ( 5.719274019375991003, -21.55341960407610458, 37.70724293864769550 ) ) ;
#177040 = ORIENTED_EDGE ( 'NONE', *, *, #71047, .T. ) ;
#177041 = CARTESIAN_POINT ( 'NONE',  ( 5.049401038297881783, 19.05341960407617563, 47.29275706135231161 ) ) ;
#177042 = CARTESIAN_POINT ( 'NONE',  ( 12.06949235617739724, 12.14591786802326823, 61.87609039468568284 ) ) ;
#177043 = CARTESIAN_POINT ( 'NONE',  ( 0.05219959533907565091, 21.53943276465977519, 29.99890960531435979 ) ) ;
#177044 = ORIENTED_EDGE ( 'NONE', *, *, #28742, .T. ) ;
#177045 = CARTESIAN_POINT ( 'NONE',  ( -19.02544592524342804, 5.153800228976336051, 91.04057627198100988 ) ) ;
#177046 = CARTESIAN_POINT ( 'NONE',  ( -12.14591786802309592, -12.06949235617757132, 26.87390960531435979 ) ) ;
#177047 = CARTESIAN_POINT ( 'NONE',  ( 19.23457310888372973, -35.06695140040304182, -26.03237767043686546 ) ) ;
#177048 = CARTESIAN_POINT ( 'NONE',  ( -8.314922557960811034, -14.29746914071050412, 107.0822429386476955 ) ) ;
#177049 = CARTESIAN_POINT ( 'NONE',  ( 10.72451020669898902, -18.67979575497178502, 47.91557627198102409 ) ) ;
#177050 = CARTESIAN_POINT ( 'NONE',  ( 9.474510206698971260, -16.51473224551069308, 47.91557627198102409 ) ) ;
#177051 = CARTESIAN_POINT ( 'NONE',  ( 16.52544592524335698, 4.483927247898782831, 71.45942372801901854 ) ) ;
#177052 = CARTESIAN_POINT ( 'NONE',  ( 5.719274019375673035, 21.55341960407619339, 27.29275706135234358 ) ) ;
#177053 = CARTESIAN_POINT ( 'NONE',  ( 16.51473224551083163, -9.474510206698727899, 90.83442372801900433 ) ) ;
#177054 = CARTESIAN_POINT ( 'NONE',  ( 14.29746914071049879, -8.314922557960816363, 88.33224293864769550 ) ) ;
#177055 = CARTESIAN_POINT ( 'NONE',  ( -9.474510206698964154, 16.51473224551069663, 55.41557627198103120 ) ) ;
#177056 = CARTESIAN_POINT ( 'NONE',  ( -19.02544592524342804, 5.153800228976336051, 26.04057627198103120 ) ) ;
#177057 = CARTESIAN_POINT ( 'NONE',  ( -15.80617190586768217, 15.72974639402176855, 103.1260903946856757 ) ) ;
#177058 = CARTESIAN_POINT ( 'NONE',  ( 5.049401038298161559, -19.05341960407611168, 82.70724293864770971 ) ) ;
#177059 = CARTESIAN_POINT ( 'NONE',  ( -14.34966873604972548, 8.224510206698743886, 68.33442372801900433 ) ) ;
#177060 = CARTESIAN_POINT ( 'NONE',  ( 10.72451020669871369, 18.67979575497193778, 87.08442372801901854 ) ) ;
#177061 = CARTESIAN_POINT ( 'NONE',  ( 15.80617190586746368, 15.72974639402197994, 44.37390960531435979 ) ) ;
#177062 = CARTESIAN_POINT ( 'NONE',  ( 16.53943276465976808, 0.05219959533934440121, 76.25109039468568994 ) ) ;
#177063 = CARTESIAN_POINT ( 'NONE',  ( 9.474510206698729675, 16.51473224551082808, 57.08442372801900433 ) ) ;
#177064 = CARTESIAN_POINT ( 'NONE',  ( 19.02544592524334988, 5.153800228976608722, 71.45942372801900433 ) ) ;
#177065 = CARTESIAN_POINT ( 'NONE',  ( 10.72451020669871369, 18.67979575497193778, 57.08442372801901854 ) ) ;
#177066 = CARTESIAN_POINT ( 'NONE',  ( 5.049401038298161559, -19.05341960407611168, 62.70724293864769550 ) ) ;
#177067 = CARTESIAN_POINT ( 'NONE',  ( 0.05219959533909260263, 19.03943276465977164, 29.99890960531435979 ) ) ;
#177068 = CARTESIAN_POINT ( 'NONE',  ( -9.474510206698720793, -16.51473224551083518, 64.58442372801900433 ) ) ;
#177069 = CARTESIAN_POINT ( 'NONE',  ( 0.05219959533909260263, 19.03943276465977164, 114.9989096053143669 ) ) ;
#177070 = CARTESIAN_POINT ( 'NONE',  ( 16.51473224551069308, 9.474510206698969483, 94.16557627198103830 ) ) ;
#177071 = CARTESIAN_POINT ( 'NONE',  ( -4.483927247898539470, -16.52544592524342804, 52.29057627198102409 ) ) ;
#177072 = CARTESIAN_POINT ( 'NONE',  ( -10.72451020669898014, 18.67979575497178502, 45.41557627198103830 ) ) ;
#177073 = CARTESIAN_POINT ( 'NONE',  ( 18.10062525802554134, -5.500000000000022204, 91.01383468041920821 ) ) ;
#177074 = CARTESIAN_POINT ( 'NONE',  ( 21.55341960407619695, -5.719274019375665929, 111.0427570613523613 ) ) ;
#177075 = CARTESIAN_POINT ( 'NONE',  ( -16.79531203550646268, -7.028104445595595884, 81.25244988220444498 ) ) ;
#177076 = CARTESIAN_POINT ( 'NONE',  ( -9.564922557960796823, -16.46253265017161027, 47.08224293864769550 ) ) ;
#177077 = CARTESIAN_POINT ( 'NONE',  ( -19.01529144963336293, -5.500000000000031086, 101.2343195572844081 ) ) ;
#177078 = CARTESIAN_POINT ( 'NONE',  ( -17.44270441346516876, 5.991230190323032723, 108.6366492073577632 ) ) ;
#177079 = CARTESIAN_POINT ( 'NONE',  ( -12.06949235617739369, -12.14591786802326823, 74.37609039468568994 ) ) ;
#177080 = CARTESIAN_POINT ( 'NONE',  ( 5.719274019375991003, -21.55341960407610458, 92.70724293864770971 ) ) ;
#177081 = CARTESIAN_POINT ( 'NONE',  ( -0.05219959533910754901, -16.53943276465976808, 52.49890960531435979 ) ) ;
#177083 = CARTESIAN_POINT ( 'NONE',  ( -6.791538853603066528, -3.181980515339470905, 8.889087296526001936 ) ) ;
#177082 = CARTESIAN_POINT ( 'NONE',  ( 5.153800228976335163, 19.02544592524342804, 44.79057627198103830 ) ) ;
#177084 = CARTESIAN_POINT ( 'NONE',  ( -10.72451020669870658, -18.67979575497194134, 44.58442372801901854 ) ) ;
#177085 = CARTESIAN_POINT ( 'NONE',  ( -13.97604488694547697, 13.89961937509957934, 53.12609039468565442 ) ) ;
#177086 = CARTESIAN_POINT ( 'NONE',  ( -9.474510206698964154, 16.51473224551069663, 35.41557627198102409 ) ) ;
#177087 = CARTESIAN_POINT ( 'NONE',  ( -0.05219959533937732626, 21.53943276465977519, 97.50109039468567573 ) ) ;
#177088 = CARTESIAN_POINT ( 'NONE',  ( -24.81835718235489097, -6.052279806424480491, 168.4265042179603427 ) ) ;
#177089 = CARTESIAN_POINT ( 'NONE',  ( 8.224510206698953496, -14.34966873604960469, 37.91557627198102409 ) ) ;
#177090 = CARTESIAN_POINT ( 'NONE',  ( -15.38830714838546854, 1.491100297016104470, -59.71292413584863823 ) ) ;
#177091 = CARTESIAN_POINT ( 'NONE',  ( -18.67979575497178146, -10.72451020669898902, 41.66557627198103120 ) ) ;
#177092 = CARTESIAN_POINT ( 'NONE',  ( 17.14385361876520264, 23.59649016807275856, 142.1750000027311671 ) ) ;
#177093 = CARTESIAN_POINT ( 'NONE',  ( -9.474510206698964154, 16.51473224551069663, 95.41557627198102409 ) ) ;
#177094 = CARTESIAN_POINT ( 'NONE',  ( 14.29746914071049879, -8.314922557960816363, 93.33224293864769550 ) ) ;
#177095 = CARTESIAN_POINT ( 'NONE',  ( 4.379528057220092307, 16.55341960407617563, 27.29275706135234358 ) ) ;
#177096 = CARTESIAN_POINT ( 'NONE',  ( -12.14591786802309592, -12.06949235617757132, 21.87390960531436690 ) ) ;
#177097 = ORIENTED_EDGE ( 'NONE', *, *, #47442, .T. ) ;
#177098 = EDGE_CURVE ( 'NONE', #86773, #102413, #25209, .T. ) ;
#177100 = CARTESIAN_POINT ( 'NONE',  ( -18.62759615963270932, 10.81492255796079327, 85.83224293864768129 ) ) ;
#177099 = CARTESIAN_POINT ( 'NONE',  ( 5.153800228976335163, 19.02544592524342804, 104.7905762719809957 ) ) ;
#177102 = CARTESIAN_POINT ( 'NONE',  ( -5.049401038298153566, 19.05341960407611168, 95.20724293864770971 ) ) ;
#177101 = CARTESIAN_POINT ( 'NONE',  ( -4.379528057220328563, 16.55341960407611168, 25.20724293864769550 ) ) ;
#177103 = CARTESIAN_POINT ( 'NONE',  ( 5.153800228976615827, -19.02544592524334988, 75.20942372801896170 ) ) ;
#177104 = CARTESIAN_POINT ( 'NONE',  ( -18.67979575497193778, 10.72451020669871902, 113.3344237280190328 ) ) ;
#177105 = CARTESIAN_POINT ( 'NONE',  ( -18.67979575497178146, -10.72451020669898902, 91.66557627198103830 ) ) ;
#177106 = CARTESIAN_POINT ( 'NONE',  ( 5.823673210054125526, 21.52544592524343514, 39.79057627198103830 ) ) ;
#177107 = CARTESIAN_POINT ( 'NONE',  ( 19.03943276465977164, -0.05219959533909143690, 63.74890960531435979 ) ) ;
#177108 = CARTESIAN_POINT ( 'NONE',  ( -16.53943276465976808, 0.05219959533911058130, 31.24890960531435979 ) ) ;
#177109 = CARTESIAN_POINT ( 'NONE',  ( -13.89961937509977652, 13.97604488694528158, 75.62390960531438111 ) ) ;
#177110 = EDGE_LOOP ( 'NONE', ( #154502, #199319, #8666, #21881 ) ) ;
#177111 = CYLINDRICAL_SURFACE ( 'NONE', #105408, 39.99999999999999289 ) ;
#177112 = CARTESIAN_POINT ( 'NONE',  ( -5.153800228976607833, 19.02544592524334988, 27.70942372801899722 ) ) ;
#177113 = CARTESIAN_POINT ( 'NONE',  ( -14.34966873604960291, -8.224510206698953496, 86.66557627198102409 ) ) ;
#177114 = CARTESIAN_POINT ( 'NONE',  ( -21.52544592524334988, -5.823673210054445271, 23.95942372801901143 ) ) ;
#177115 = AXIS2_PLACEMENT_3D ( 'NONE', #105984, #44325, #184817 ) ;
#177116 = CARTESIAN_POINT ( 'NONE',  ( -27.73933785331498925, 2.428612866367529932E-14, 141.3750000027311842 ) ) ;
#177117 = CARTESIAN_POINT ( 'NONE',  ( 5.719274019375991003, -21.55341960407610458, 77.70724293864770971 ) ) ;
#177118 = CARTESIAN_POINT ( 'NONE',  ( 8.314922557961029526, -14.29746914071037800, 95.41775706135234714 ) ) ;
#177119 = CARTESIAN_POINT ( 'NONE',  ( -5.153800228976328057, -19.02544592524343514, 22.29057627198102765 ) ) ;
#177120 = CARTESIAN_POINT ( 'NONE',  ( -9.474510206698964154, 16.51473224551069663, 70.41557627198102409 ) ) ;
#177121 = CARTESIAN_POINT ( 'NONE',  ( 30.74264578624799782, 22.33583958711400541, -10.54999999453762705 ) ) ;
#177122 = CARTESIAN_POINT ( 'NONE',  ( -0.05219959533910754901, -16.53943276465976808, 27.49890960531435269 ) ) ;
#177123 = CARTESIAN_POINT ( 'NONE',  ( 21.52544592524334988, 5.823673210054432836, 66.45942372801903275 ) ) ;
#177124 = CARTESIAN_POINT ( 'NONE',  ( 26.39110954545158805, -27.12960848547524151, -16.54511501588457634 ) ) ;
#177125 = CARTESIAN_POINT ( 'NONE',  ( 5.823673210054444382, -21.52544592524334988, 100.2094237280190043 ) ) ;
#177126 = CARTESIAN_POINT ( 'NONE',  ( 16.46253265017160672, -9.564922557960803928, 48.33224293864769550 ) ) ;
#177127 = CARTESIAN_POINT ( 'NONE',  ( -13.97604488694527625, -13.89961937509977652, 56.87390960531434558 ) ) ;
#177128 = ORIENTED_EDGE ( 'NONE', *, *, #190970, .F. ) ;
#177129 = CARTESIAN_POINT ( 'NONE',  ( -21.52544592524334988, -5.823673210054445271, 93.95942372801903275 ) ) ;
#177130 = CARTESIAN_POINT ( 'NONE',  ( -14.34966873604972548, 8.224510206698743886, 58.33442372801901143 ) ) ;
#177131 = CARTESIAN_POINT ( 'NONE',  ( -15.72974639402176322, -15.80617190586768395, 84.37609039468570415 ) ) ;
#177132 = CARTESIAN_POINT ( 'NONE',  ( -13.89961937509977652, 13.97604488694528158, 110.6239096053143243 ) ) ;
#177133 = CARTESIAN_POINT ( 'NONE',  ( -0.05219959533936034679, 19.03943276465977164, 87.50109039468567573 ) ) ;
#177134 = CARTESIAN_POINT ( 'NONE',  ( 15.72974639402176855, 15.80617190586768217, 71.87609039468568994 ) ) ;
#177135 = CARTESIAN_POINT ( 'NONE',  ( 8.314922557961029526, -14.29746914071037800, 35.41775706135234003 ) ) ;
#177136 = CARTESIAN_POINT ( 'NONE',  ( -21.52544592524343514, 5.823673210054127303, 86.04057627198102409 ) ) ;
#177137 = CARTESIAN_POINT ( 'NONE',  ( -13.89961937509957401, -13.97604488694547875, 89.37609039468563310 ) ) ;
#177138 = CARTESIAN_POINT ( 'NONE',  ( -19.02544592524342804, 5.153800228976336051, 66.04057627198103830 ) ) ;
#177139 = CARTESIAN_POINT ( 'NONE',  ( 19.02544592524334988, 5.153800228976608722, 91.45942372801900433 ) ) ;
#177140 = CARTESIAN_POINT ( 'NONE',  ( -16.51473224551082808, 9.474510206698731452, 103.3344237280190043 ) ) ;
#177141 = CARTESIAN_POINT ( 'NONE',  ( -8.314922557960811034, -14.29746914071050412, 47.08224293864770260 ) ) ;
#177142 = CARTESIAN_POINT ( 'NONE',  ( 9.474510206698729675, 16.51473224551082808, 82.08442372801899012 ) ) ;
#177143 = CARTESIAN_POINT ( 'NONE',  ( 14.34966873604972726, -8.224510206698740333, 60.83442372801901854 ) ) ;
#177144 = CARTESIAN_POINT ( 'NONE',  ( -13.97604488694527625, -13.89961937509977652, 41.87390960531435979 ) ) ;
#177145 = CARTESIAN_POINT ( 'NONE',  ( -19.05341960407611168, -5.049401038298163336, 61.45724293864769550 ) ) ;
#177146 = CARTESIAN_POINT ( 'NONE',  ( 14.34966873604972726, -8.224510206698740333, 55.83442372801901854 ) ) ;
#177147 = DIRECTION ( 'NONE',  ( 0.000000000000000000, 0.000000000000000000, 1.000000000000000000 ) ) ;
#177148 = CARTESIAN_POINT ( 'NONE',  ( 17.81289503416611453, -24.51734667627695785, 140.9500000054623285 ) ) ;
#177149 = CARTESIAN_POINT ( 'NONE',  ( 0.05219959533909260263, 19.03943276465977164, 109.9989096053143669 ) ) ;
#177150 = CARTESIAN_POINT ( 'NONE',  ( -19.03943276465977164, -1.327063459122257427E-13, 115.0000000000000142 ) ) ;
#177151 = ORIENTED_EDGE ( 'NONE', *, *, #109880, .F. ) ;
#177152 = CARTESIAN_POINT ( 'NONE',  ( -0.05219959533936034679, 19.03943276465977164, 112.5010903946856757 ) ) ;
#177153 = CARTESIAN_POINT ( 'NONE',  ( -18.67979575497178146, -10.72451020669898902, 31.66557627198102054 ) ) ;
#177155 = CARTESIAN_POINT ( 'NONE',  ( 8.314922557961029526, -14.29746914071037800, 20.41775706135234714 ) ) ;
#177154 = CARTESIAN_POINT ( 'NONE',  ( -19.05341960407617563, 5.049401038297882671, 28.54275706135232937 ) ) ;
#177156 = CARTESIAN_POINT ( 'NONE',  ( -16.46253265017160317, 9.564922557960807481, 35.83224293864768839 ) ) ;
#177157 = CARTESIAN_POINT ( 'NONE',  ( 13.89961937509977652, -13.97604488694527269, 53.12390960531434558 ) ) ;
#177158 = CARTESIAN_POINT ( 'NONE',  ( 21.52544592524344225, -5.823673210054117533, 73.54057627198102409 ) ) ;
#177159 = CARTESIAN_POINT ( 'NONE',  ( -5.153800228976328057, -19.02544592524343514, 102.2905762719810383 ) ) ;
#177160 = CARTESIAN_POINT ( 'NONE',  ( 19.02544592524343514, -5.153800228976328945, 38.54057627198103120 ) ) ;
#177161 = CARTESIAN_POINT ( 'NONE',  ( 1.784210473542230573E-15, -29.16686587814331588, 141.8750000027311842 ) ) ;
#177162 = CARTESIAN_POINT ( 'NONE',  ( -9.564922557961040184, 16.46253265017147172, 82.91775706135233293 ) ) ;
#177163 = CARTESIAN_POINT ( 'NONE',  ( 14.34966873604960469, 8.224510206698951720, 64.16557627198102409 ) ) ;
#177164 = CARTESIAN_POINT ( 'NONE',  ( 21.53943276465977519, -0.05219959533907433946, 48.74890960531435979 ) ) ;
#177165 = CARTESIAN_POINT ( 'NONE',  ( -21.53943276465977519, -0.05219959533937600094, 108.7510903946857042 ) ) ;
#177166 = CARTESIAN_POINT ( 'NONE',  ( 10.81492255796078972, 18.62759615963270932, 99.58224293864770971 ) ) ;
#177167 = CARTESIAN_POINT ( 'NONE',  ( -5.719274019375665041, -21.55341960407619695, 69.79275706135234714 ) ) ;
#177168 = CARTESIAN_POINT ( 'NONE',  ( 21.52544592524334988, 5.823673210054432836, 76.45942372801901854 ) ) ;
#177169 = CARTESIAN_POINT ( 'NONE',  ( 5.153800228976335163, 19.02544592524342804, 104.7905762719809957 ) ) ;
#177171 = CARTESIAN_POINT ( 'NONE',  ( 10.72451020669871369, 18.67979575497193778, 77.08442372801901854 ) ) ;
#177170 = CARTESIAN_POINT ( 'NONE',  ( 0.05219959533934541429, -16.53943276465976808, 105.0010903946856757 ) ) ;
#177172 = CARTESIAN_POINT ( 'NONE',  ( -19.02544592524342804, 5.153800228976336051, 71.04057627198099567 ) ) ;
#177173 = CARTESIAN_POINT ( 'NONE',  ( 19.03943276465977164, 0.05219959533936151252, 36.25109039468567573 ) ) ;
#177174 = CARTESIAN_POINT ( 'NONE',  ( 5.719274019375673035, 21.55341960407619339, 27.29275706135234358 ) ) ;
#177175 = CARTESIAN_POINT ( 'NONE',  ( 19.03943276465977164, -0.05219959533909143690, 68.74890960531436690 ) ) ;
#177176 = CARTESIAN_POINT ( 'NONE',  ( -14.34966873604960291, -8.224510206698953496, 81.66557627198103830 ) ) ;
#177177 = CARTESIAN_POINT ( 'NONE',  ( -8.224510206698948167, 14.34966873604960824, 45.41557627198103830 ) ) ;
#177178 = CARTESIAN_POINT ( 'NONE',  ( -21.53943276465977519, 0.05219959533907696930, 56.24890960531436690 ) ) ;
#177179 = CARTESIAN_POINT ( 'NONE',  ( 16.46253265017160672, -9.564922557960803928, 58.33224293864769550 ) ) ;
#177180 = CARTESIAN_POINT ( 'NONE',  ( 21.53943276465977519, -0.05219959533907433946, 73.74890960531433848 ) ) ;
#177181 = CARTESIAN_POINT ( 'NONE',  ( -16.51473224551082808, 9.474510206698731452, 58.33442372801900433 ) ) ;
#177183 = CARTESIAN_POINT ( 'NONE',  ( 14.29746914071049879, -8.314922557960816363, 68.33224293864769550 ) ) ;
#177182 = CARTESIAN_POINT ( 'NONE',  ( 9.564922557961047289, -16.46253265017146816, 25.41775706135234003 ) ) ;
#177184 = CARTESIAN_POINT ( 'NONE',  ( -21.55341960407610458, -5.719274019375992779, 36.45724293864768839 ) ) ;
#177185 = ORIENTED_EDGE ( 'NONE', *, *, #31131, .F. ) ;
#177186 = CARTESIAN_POINT ( 'NONE',  ( -5.000000000000003553, -4.999999999999996447, -15.00000000000000000 ) ) ;
#177188 = CARTESIAN_POINT ( 'NONE',  ( 8.571926809382597767, 26.38167802310806209, 140.7750000027311899 ) ) ;
#177187 = CARTESIAN_POINT ( 'NONE',  ( 16.55341960407618274, -4.379528057220086978, 91.04275706135236135 ) ) ;
#177189 = CARTESIAN_POINT ( 'NONE',  ( -19.05341960407617563, 5.049401038297882671, 83.54275706135233293 ) ) ;
#177190 = EDGE_CURVE ( 'NONE', #33758, #163981, #103022, .T. ) ;
#177191 = CARTESIAN_POINT ( 'NONE',  ( -4.483927247898539470, -16.52544592524342804, 67.29057627198103830 ) ) ;
#177192 = CARTESIAN_POINT ( 'NONE',  ( -17.50000000000000355, 5.076555817581239971, 33.82048507950225513 ) ) ;
#177193 = CARTESIAN_POINT ( 'NONE',  ( -19.02544592524342804, 5.153800228976336051, 56.04057627198100988 ) ) ;
#177194 = CARTESIAN_POINT ( 'NONE',  ( -4.483927247898539470, -16.52544592524342804, 42.29057627198103120 ) ) ;
#177195 = CARTESIAN_POINT ( 'NONE',  ( -5.153800228976328057, -19.02544592524343514, 87.29057627198103830 ) ) ;
#177197 = CARTESIAN_POINT ( 'NONE',  ( 16.46253265017160672, -9.564922557960803928, 48.33224293864769550 ) ) ;
#177196 = CARTESIAN_POINT ( 'NONE',  ( 9.564922557961047289, -16.46253265017146816, 80.41775706135234714 ) ) ;
#177198 = CARTESIAN_POINT ( 'NONE',  ( 21.53943276465977519, 0.05219959533937863772, 56.25109039468568284 ) ) ;
#177199 = CARTESIAN_POINT ( 'NONE',  ( 19.05341960407611168, 5.049401038298154454, 88.95724293864769550 ) ) ;
#177200 = CARTESIAN_POINT ( 'NONE',  ( -5.049401038298153566, 19.05341960407611168, 25.20724293864768484 ) ) ;
#177201 = CARTESIAN_POINT ( 'NONE',  ( 9.564922557960805705, 16.46253265017160317, 74.58224293864769550 ) ) ;
#177202 = CARTESIAN_POINT ( 'NONE',  ( -5.719274019375978568, 21.55341960407610458, 45.20724293864769550 ) ) ;
#177203 = CARTESIAN_POINT ( 'NONE',  ( -0.05219959533909027116, -19.03943276465977164, 47.49890960531435979 ) ) ;
#177204 = CARTESIAN_POINT ( 'NONE',  ( 18.67979575497178502, 10.72451020669898547, 49.16557627198102409 ) ) ;
#177205 = CARTESIAN_POINT ( 'NONE',  ( -5.049401038297874678, -19.05341960407617918, 74.79275706135231871 ) ) ;
#177206 = CARTESIAN_POINT ( 'NONE',  ( 4.483927247898790824, -16.52544592524335698, 105.2094237280190328 ) ) ;
#177207 = CARTESIAN_POINT ( 'NONE',  ( 13.89961937509957401, 13.97604488694547697, 31.87609039468566863 ) ) ;
#177209 = CARTESIAN_POINT ( 'NONE',  ( 12.06949235617739724, 12.14591786802326823, 91.87609039468568994 ) ) ;
#177208 = CARTESIAN_POINT ( 'NONE',  ( -4.379528057220086978, -16.55341960407618274, 59.79275706135234714 ) ) ;
#177210 = CARTESIAN_POINT ( 'NONE',  ( 40.00000000000001421, 2.428612866367529932E-14, 0.000000000000000000 ) ) ;
#177211 = CARTESIAN_POINT ( 'NONE',  ( 16.52544592524335698, 4.483927247898782831, 76.45942372801901854 ) ) ;
#177212 = CARTESIAN_POINT ( 'NONE',  ( 18.62759615963271287, -10.81492255796078972, 28.33224293864769550 ) ) ;
#177213 = CARTESIAN_POINT ( 'NONE',  ( 0.05219959533909260263, 19.03943276465977164, 34.99890960531435979 ) ) ;
#177214 = CARTESIAN_POINT ( 'NONE',  ( 12.06949235617739724, 12.14591786802326823, 31.87609039468567929 ) ) ;
#177215 = CARTESIAN_POINT ( 'NONE',  ( -19.02544592524342804, 5.153800228976336051, 46.04057627198101699 ) ) ;
#177216 = CARTESIAN_POINT ( 'NONE',  ( 0.05219959533937995610, -21.53943276465977519, 40.00109039468567573 ) ) ;
#177217 = CARTESIAN_POINT ( 'NONE',  ( 12.06949235617739724, 12.14591786802326823, 41.87609039468568284 ) ) ;
#177218 = CARTESIAN_POINT ( 'NONE',  ( -4.483927247898782831, 16.52544592524335698, 107.7094237280190328 ) ) ;
#177219 = CARTESIAN_POINT ( 'NONE',  ( -5.153800228976328057, -19.02544592524343514, 32.29057627198102409 ) ) ;
#177220 = CARTESIAN_POINT ( 'NONE',  ( -13.97604488694547697, 13.89961937509957934, 23.12609039468565442 ) ) ;
#177221 = CARTESIAN_POINT ( 'NONE',  ( 16.46253265017146816, 9.564922557961045513, 111.6677570613523329 ) ) ;
#177222 = CARTESIAN_POINT ( 'NONE',  ( 9.474510206698729675, 16.51473224551082808, 72.08442372801900433 ) ) ;
#177223 = CARTESIAN_POINT ( 'NONE',  ( -4.379528057220328563, 16.55341960407611168, 65.20724293864768129 ) ) ;
#177224 = CARTESIAN_POINT ( 'NONE',  ( -5.153800228976328057, -19.02544592524343514, 37.29057627198102409 ) ) ;
#177226 = CARTESIAN_POINT ( 'NONE',  ( 11.74264578624800315, -36.14014761921581709, -3.149999994537626247 ) ) ;
#177225 = CARTESIAN_POINT ( 'NONE',  ( 5.153800228976615827, -19.02544592524334988, 75.20942372801896170 ) ) ;
#177227 = CARTESIAN_POINT ( 'NONE',  ( 21.52544592524334988, 5.823673210054432836, 66.45942372801903275 ) ) ;
#177228 = CARTESIAN_POINT ( 'NONE',  ( -16.55341960407617563, 4.379528057220093196, 38.54275706135234714 ) ) ;
#177229 = CARTESIAN_POINT ( 'NONE',  ( 17.60728821187777271, -5.500000000000039968, 73.36690927743606494 ) ) ;
#177230 = CARTESIAN_POINT ( 'NONE',  ( 0.05219959533907565091, 21.53943276465977519, 39.99890960531436690 ) ) ;
#177231 = CARTESIAN_POINT ( 'NONE',  ( 8.224510206698742110, 14.34966873604972548, 22.08442372801901143 ) ) ;
#177232 = CARTESIAN_POINT ( 'NONE',  ( 19.02544592524343514, -5.153800228976328945, 113.5405762719810241 ) ) ;
#177233 = CARTESIAN_POINT ( 'NONE',  ( -24.18299921989881440, 12.77492350451764125, 169.7822198539310250 ) ) ;
#177234 = CARTESIAN_POINT ( 'NONE',  ( -19.03943276465977164, 0.05219959533909376836, 41.24890960531435269 ) ) ;
#177235 = CARTESIAN_POINT ( 'NONE',  ( 5.823673210054444382, -21.52544592524334988, 110.2094237280190185 ) ) ;
#177236 = CARTESIAN_POINT ( 'NONE',  ( -5.049401038298153566, 19.05341960407611168, 60.20724293864768129 ) ) ;
#177237 = CARTESIAN_POINT ( 'NONE',  ( -21.52544592524334988, -5.823673210054445271, 58.95942372801902565 ) ) ;
#177238 = CARTESIAN_POINT ( 'NONE',  ( 15.72974639402176855, 15.80617190586768217, 106.8760903946856899 ) ) ;
#177239 = CARTESIAN_POINT ( 'NONE',  ( 4.379528057220339221, -16.55341960407611168, 27.70724293864769905 ) ) ;
#177240 = CARTESIAN_POINT ( 'NONE',  ( 13.89961937509977652, -13.97604488694527269, 28.12390960531435624 ) ) ;
#177241 = CARTESIAN_POINT ( 'NONE',  ( 13.97604488694527802, 13.89961937509977652, 89.37390960531436690 ) ) ;
#177242 = CARTESIAN_POINT ( 'NONE',  ( 0.05219959533937995610, -21.53943276465977519, 50.00109039468568994 ) ) ;
#177243 = CARTESIAN_POINT ( 'NONE',  ( -16.51473224551069308, -9.474510206698971260, 31.66557627198102054 ) ) ;
#177244 = CARTESIAN_POINT ( 'NONE',  ( -5.823673210054431948, 21.52544592524334988, 57.70942372801901143 ) ) ;
#177246 = CARTESIAN_POINT ( 'NONE',  ( -9.474510206698964154, 16.51473224551069663, 100.4155762719810241 ) ) ;
#177245 = CARTESIAN_POINT ( 'NONE',  ( -19.03943276465977164, -0.05219959533935918106, 88.75109039468567573 ) ) ;
#177247 = CARTESIAN_POINT ( 'NONE',  ( 5.049401038298161559, -19.05341960407611168, 22.70724293864769194 ) ) ;
#177248 = CARTESIAN_POINT ( 'NONE',  ( -10.81492255796078084, -18.62759615963271287, 112.0822429386477097 ) ) ;
#177249 = CARTESIAN_POINT ( 'NONE',  ( 16.46253265017146816, 9.564922557961045513, 41.66775706135234003 ) ) ;
#177250 = CARTESIAN_POINT ( 'NONE',  ( 12.14591786802309770, 12.06949235617756955, 114.3739096053143527 ) ) ;
#177251 = CARTESIAN_POINT ( 'NONE',  ( -19.02544592524342804, 5.153800228976336051, 56.04057627198100988 ) ) ;
#177252 = CARTESIAN_POINT ( 'NONE',  ( 9.564922557961047289, -16.46253265017146816, 95.41775706135233293 ) ) ;
#177253 = CARTESIAN_POINT ( 'NONE',  ( 8.314922557960818139, 14.29746914071049879, 64.58224293864769550 ) ) ;
#177254 = CARTESIAN_POINT ( 'NONE',  ( -10.81492255796105439, 18.62759615963255655, 107.9177570613523471 ) ) ;
#177255 = CARTESIAN_POINT ( 'NONE',  ( -15.80617190586745835, -15.72974639402198527, 21.87390960531436690 ) ) ;
#177256 = CARTESIAN_POINT ( 'NONE',  ( 13.89961937509957401, 13.97604488694547697, 86.87609039468567573 ) ) ;
#177257 = CARTESIAN_POINT ( 'NONE',  ( -5.823673210054116645, -21.52544592524344225, 92.29057627198103830 ) ) ;
#177258 = CARTESIAN_POINT ( 'NONE',  ( -18.67979575497193778, 10.72451020669871902, 43.33442372801901143 ) ) ;
#177259 = CARTESIAN_POINT ( 'NONE',  ( 16.53943276465976808, 0.05219959533934440121, 41.25109039468568284 ) ) ;
#177260 = CARTESIAN_POINT ( 'NONE',  ( -14.29746914071037622, -8.314922557961029526, 109.1677570613523613 ) ) ;
#177262 = CARTESIAN_POINT ( 'NONE',  ( 10.81492255796106328, -18.62759615963255655, 45.41775706135234003 ) ) ;
#177261 = CARTESIAN_POINT ( 'NONE',  ( -14.29746914071037622, -8.314922557961029526, 39.16775706135235424 ) ) ;
#177263 = CARTESIAN_POINT ( 'NONE',  ( 0.05219959533907565091, 21.53943276465977519, 54.99890960531435269 ) ) ;
#177264 =( BOUNDED_CURVE ( )  B_SPLINE_CURVE ( 3, ( #56862, #105337, #59821, #77964 ),
 .UNSPECIFIED., .F., .T. ) 
 B_SPLINE_CURVE_WITH_KNOTS ( ( 4, 4 ),
 ( 1.025647941782809491, 2.008945357379068319 ),
 .UNSPECIFIED. ) 
 CURVE ( )  GEOMETRIC_REPRESENTATION_ITEM ( )  RATIONAL_B_SPLINE_CURVE ( ( 1.000000000000000000, 0.9210371567966657569, 0.9210371567966657569, 1.000000000000000000 ) ) 
 REPRESENTATION_ITEM ( '' )  );
#177265 = CARTESIAN_POINT ( 'NONE',  ( -9.474510206698964154, 16.51473224551069663, 35.41557627198102409 ) ) ;
#177266 = CARTESIAN_POINT ( 'NONE',  ( -38.00000000000000711, 2.428612866367529932E-14, -1.749999994537626558 ) ) ;
#177267 = CARTESIAN_POINT ( 'NONE',  ( -8.314922557961024197, 14.29746914071037800, 57.91775706135234714 ) ) ;
#177268 = CARTESIAN_POINT ( 'NONE',  ( -10.81492255796078084, -18.62759615963271287, 87.08224293864769550 ) ) ;
#177269 = CARTESIAN_POINT ( 'NONE',  ( -16.53943276465976808, 0.05219959533911058130, 41.24890960531435269 ) ) ;
#177270 = CARTESIAN_POINT ( 'NONE',  ( 4.379528057220092307, 16.55341960407617563, 57.29275706135234714 ) ) ;
#177271 = CARTESIAN_POINT ( 'NONE',  ( 19.05341960407617918, -5.049401038297876454, 101.0427570613523045 ) ) ;
#177272 = CARTESIAN_POINT ( 'NONE',  ( 5.823673210054125526, 21.52544592524343514, 104.7905762719810241 ) ) ;
#177273 = CARTESIAN_POINT ( 'NONE',  ( 12.06949235617757843, -12.14591786802309237, 38.12390960531436690 ) ) ;
#177274 = ORIENTED_EDGE ( 'NONE', *, *, #88626, .T. ) ;
#177275 = CARTESIAN_POINT ( 'NONE',  ( 8.224510206698742110, 14.34966873604972548, 72.08442372801899012 ) ) ;
#177276 = CARTESIAN_POINT ( 'NONE',  ( 31.79999999999967031, 4.791014396527177230E-13, 47.70000000000022311 ) ) ;
#177277 = CARTESIAN_POINT ( 'NONE',  ( 21.52544592524344225, -5.823673210054117533, 73.54057627198102409 ) ) ;
#177278 = VERTEX_POINT ( 'NONE', #26200 ) ;
#177279 = CARTESIAN_POINT ( 'NONE',  ( -14.29746914071037622, -8.314922557961029526, 99.16775706135234714 ) ) ;
#177280 = VERTEX_POINT ( 'NONE', #85847 ) ;
#177281 = CARTESIAN_POINT ( 'NONE',  ( 19.49190055781010500, 5.500000000000051514, 88.06116087098783396 ) ) ;
#177282 = CARTESIAN_POINT ( 'NONE',  ( 5.823673210054125526, 21.52544592524343514, 89.79057627198103830 ) ) ;
#177283 = CARTESIAN_POINT ( 'NONE',  ( 10.81492255796078972, 18.62759615963270932, 114.5822429386477097 ) ) ;
#177284 = CARTESIAN_POINT ( 'NONE',  ( 16.53943276465976808, -0.05219959533910856209, 38.74890960531435979 ) ) ;
#177285 = CARTESIAN_POINT ( 'NONE',  ( 12.14591786802327356, -12.06949235617739191, 30.62609039468567929 ) ) ;
#177286 = CARTESIAN_POINT ( 'NONE',  ( -13.97604488694527625, -13.89961937509977652, 36.87390960531436690 ) ) ;
#177287 = B_SPLINE_CURVE_WITH_KNOTS ( 'NONE', 3,
 ( #42375, #104038, #152517, #58526, #178899, #43361, #14005, #40367, #73716, #181882, #199029, #102041, #119215, #118217 ),
 .UNSPECIFIED., .F., .F.,
 ( 4, 2, 2, 2, 2, 2, 4 ),
 ( 0.1559601203333471908, 0.1570958510570473199, 0.1582315817807474767, 0.1605030432281477348, 0.1616387739518478917, 0.1627745046755480207, 0.1650459661229483066 ),
 .UNSPECIFIED. ) ;
#177288 = CARTESIAN_POINT ( 'NONE',  ( -19.03943276465977164, 0.05219959533909376836, 71.24890960531435269 ) ) ;
#177289 = CARTESIAN_POINT ( 'NONE',  ( 21.55341960407610458, 5.719274019375980345, 23.95724293864769550 ) ) ;
#177290 = CARTESIAN_POINT ( 'NONE',  ( 13.97604488694527802, 13.89961937509977652, 114.3739096053143669 ) ) ;
#177291 = CARTESIAN_POINT ( 'NONE',  ( -13.97604488694547697, 13.89961937509957934, 103.1260903946856473 ) ) ;
#177292 = CARTESIAN_POINT ( 'NONE',  ( 13.89961937509957401, 13.97604488694547697, 56.87609039468564731 ) ) ;
#177293 = CARTESIAN_POINT ( 'NONE',  ( 21.55341960407610458, 5.719274019375980345, 88.95724293864769550 ) ) ;
#177294 = CARTESIAN_POINT ( 'NONE',  ( -14.34966873604972548, 8.224510206698743886, 113.3344237280190328 ) ) ;
#177295 = CARTESIAN_POINT ( 'NONE',  ( 21.53943276465977519, -0.05219959533907433946, 48.74890960531435979 ) ) ;
#177297 = CARTESIAN_POINT ( 'NONE',  ( 13.89961937509957401, 13.97604488694547697, 106.8760903946856757 ) ) ;
#177296 = CARTESIAN_POINT ( 'NONE',  ( 0.05219959533907565091, 21.53943276465977519, 84.99890960531436690 ) ) ;
#177298 = CARTESIAN_POINT ( 'NONE',  ( -13.89961937509977652, 13.97604488694528158, 105.6239096053143527 ) ) ;
#177299 = CARTESIAN_POINT ( 'NONE',  ( -21.52544592524334988, -5.823673210054445271, 78.95942372801901854 ) ) ;
#177300 = CARTESIAN_POINT ( 'NONE',  ( -19.05341960407611168, -5.049401038298163336, 76.45724293864769550 ) ) ;
#177301 = CARTESIAN_POINT ( 'NONE',  ( -8.224510206698948167, 14.34966873604960824, 105.4155762719810383 ) ) ;
#177302 = CARTESIAN_POINT ( 'NONE',  ( 4.500000000000000888, -139.5000000000000000, 54.87277500418469600 ) ) ;
#177303 = CARTESIAN_POINT ( 'NONE',  ( -19.02544592524342804, 5.153800228976336051, 66.04057627198103830 ) ) ;
#177304 = CARTESIAN_POINT ( 'NONE',  ( -16.55341960407611168, -4.379528057220339221, 91.45724293864769550 ) ) ;
#177305 = ORIENTED_EDGE ( 'NONE', *, *, #115703, .F. ) ;
#177306 = CARTESIAN_POINT ( 'NONE',  ( 5.049401038297881783, 19.05341960407617563, 102.2927570613523045 ) ) ;
#177307 = CARTESIAN_POINT ( 'NONE',  ( 16.21995358207301763, -7.366697692864224045, 82.43551001512155096 ) ) ;
#177308 = CARTESIAN_POINT ( 'NONE',  ( -9.474510206698964154, 16.51473224551069663, 55.41557627198103120 ) ) ;
#177310 = CARTESIAN_POINT ( 'NONE',  ( -16.51473224551069308, -9.474510206698971260, 101.6655762719810241 ) ) ;
#177309 = CARTESIAN_POINT ( 'NONE',  ( -10.72451020669870658, -18.67979575497194134, 89.58442372801901854 ) ) ;
#177312 = EDGE_CURVE ( 'NONE', #73688, #165524, #193041, .T. ) ;
#177311 = CARTESIAN_POINT ( 'NONE',  ( 4.379528057220092307, 16.55341960407617563, 82.29275706135234714 ) ) ;
#177313 = FACE_OUTER_BOUND ( 'NONE', #154314, .T. ) ;
#177314 = CARTESIAN_POINT ( 'NONE',  ( -9.474510206698720793, -16.51473224551083518, 54.58442372801899722 ) ) ;
#177315 = CARTESIAN_POINT ( 'NONE',  ( -21.52544592524334988, -5.823673210054445271, 93.95942372801903275 ) ) ;
#177316 = CARTESIAN_POINT ( 'NONE',  ( 37.51279278323692523, 1.941191203875218596, 39.85083793614483483 ) ) ;
#177317 = FACE_OUTER_BOUND ( 'NONE', #13016, .T. ) ;
#177318 = CARTESIAN_POINT ( 'NONE',  ( 14.29746914071049879, -8.314922557960816363, 28.33224293864769550 ) ) ;
#177319 = CARTESIAN_POINT ( 'NONE',  ( -34.36947210329395119, -7.112397586384673787, 47.39260519897412394 ) ) ;
#177320 = CARTESIAN_POINT ( 'NONE',  ( -8.224510206698735004, -14.34966873604973081, 89.58442372801901854 ) ) ;
#177321 = DIRECTION ( 'NONE',  ( 0.000000000000000000, 0.7071067811865466846, 0.7071067811865484609 ) ) ;
#177322 = CARTESIAN_POINT ( 'NONE',  ( -14.34966873604972548, 8.224510206698743886, 68.33442372801900433 ) ) ;
#177323 = CARTESIAN_POINT ( 'NONE',  ( -21.52544592524334988, -5.823673210054445271, 83.95942372801900433 ) ) ;
#177324 = CARTESIAN_POINT ( 'NONE',  ( -19.05341960407617563, 5.049401038297882671, 88.54275706135230450 ) ) ;
#177325 = CARTESIAN_POINT ( 'NONE',  ( -19.05341960407617563, 5.049401038297882671, 43.54275706135232582 ) ) ;
#177326 = CARTESIAN_POINT ( 'NONE',  ( 13.97604488694527802, 13.89961937509977652, 59.37390960531434558 ) ) ;
#177327 = CARTESIAN_POINT ( 'NONE',  ( -5.153800228976328057, -19.02544592524343514, 52.29057627198100988 ) ) ;
#177328 = CARTESIAN_POINT ( 'NONE',  ( -4.313351365237979351, -4.313351365237916291, -64.53213882399992940 ) ) ;
#177329 = CARTESIAN_POINT ( 'NONE',  ( 21.53943276465977519, -0.05219959533907433946, 78.74890960531436690 ) ) ;
#177330 = CARTESIAN_POINT ( 'NONE',  ( 18.62759615963271287, -10.81492255796078972, 43.33224293864769550 ) ) ;
#177331 = CARTESIAN_POINT ( 'NONE',  ( 16.46253265017160672, -9.564922557960803928, 38.33224293864768839 ) ) ;
#177332 = CARTESIAN_POINT ( 'NONE',  ( 4.483927247898790824, -16.52544592524335698, 65.20942372801901854 ) ) ;
#177333 = EDGE_LOOP ( 'NONE', ( #149014, #106644, #64400, #32078 ) ) ;
#177334 = EDGE_CURVE ( 'NONE', #30166, #158898, #111, .T. ) ;
#177335 = CARTESIAN_POINT ( 'NONE',  ( -5.719274019375665041, -21.55341960407619695, 44.79275706135234714 ) ) ;
#177337 = CARTESIAN_POINT ( 'NONE',  ( -36.91746825000001309, -11.99521256947794789, -8.524999997268812635 ) ) ;
#177336 = CARTESIAN_POINT ( 'NONE',  ( -8.314922557960811034, -14.29746914071050412, 62.08224293864769550 ) ) ;
#177338 = CARTESIAN_POINT ( 'NONE',  ( 16.55341960407618274, -4.379528057220086978, 36.04275706135234714 ) ) ;
#177339 = CARTESIAN_POINT ( 'NONE',  ( -9.474510206698720793, -16.51473224551083518, 49.58442372801899722 ) ) ;
#177340 = CARTESIAN_POINT ( 'NONE',  ( -16.52544592524342804, 4.483927247898546575, 56.04057627198102409 ) ) ;
#177341 = CARTESIAN_POINT ( 'NONE',  ( 5.719274019375673035, 21.55341960407619339, 27.29275706135234358 ) ) ;
#177343 = CARTESIAN_POINT ( 'NONE',  ( 10.81492255796078972, 18.62759615963270932, 94.58224293864769550 ) ) ;
#177342 = DIRECTION ( 'NONE',  ( 1.000000000000000000, 0.000000000000000000, 0.000000000000000000 ) ) ;
#177344 = CARTESIAN_POINT ( 'NONE',  ( 9.564922557960805705, 16.46253265017160317, 104.5822429386476955 ) ) ;
#177345 = CARTESIAN_POINT ( 'NONE',  ( 12.14591786802309770, 12.06949235617756955, 79.37390960531436690 ) ) ;
#177346 = CARTESIAN_POINT ( 'NONE',  ( 33.52048507002423605, -21.84028095222489796, -24.62089730557384826 ) ) ;
#177347 = AXIS2_PLACEMENT_3D ( 'NONE', #18400, #64884, #112379 ) ;
#177348 = CARTESIAN_POINT ( 'NONE',  ( -19.97888994334924107, -34.65319547504297759, -7.500000000000000000 ) ) ;
#177349 = CARTESIAN_POINT ( 'NONE',  ( 13.89961937509957401, 13.97604488694547697, 71.87609039468567573 ) ) ;
#177350 = CARTESIAN_POINT ( 'NONE',  ( 5.823673210054125526, 21.52544592524343514, 114.7905762719810383 ) ) ;
#177351 = CARTESIAN_POINT ( 'NONE',  ( 9.564922557960805705, 16.46253265017160317, 54.58224293864769550 ) ) ;
#177352 = CARTESIAN_POINT ( 'NONE',  ( -5.049401038297874678, -19.05341960407617918, 44.79275706135232582 ) ) ;
#177353 = CARTESIAN_POINT ( 'NONE',  ( 5.049401038298161559, -19.05341960407611168, 32.70724293864768129 ) ) ;
#177354 = CARTESIAN_POINT ( 'NONE',  ( 0.05219959533937995610, -21.53943276465977519, 70.00109039468568994 ) ) ;
#177355 = CARTESIAN_POINT ( 'NONE',  ( -16.19135201231366139, -7.376712067591931543, 70.18680854052036011 ) ) ;
#177356 = CARTESIAN_POINT ( 'NONE',  ( 16.52544592524342804, -4.483927247898539470, 58.54057627198103120 ) ) ;
#177357 = CARTESIAN_POINT ( 'NONE',  ( 9.564922557960805705, 16.46253265017160317, 59.58224293864769550 ) ) ;
#177358 = CARTESIAN_POINT ( 'NONE',  ( -15.72974639402197994, 15.80617190586746368, 90.62390960531436690 ) ) ;
#177359 = CARTESIAN_POINT ( 'NONE',  ( 19.02544592524343514, -5.153800228976328945, 53.54057627198102409 ) ) ;
#177360 = CARTESIAN_POINT ( 'NONE',  ( -15.72974639402197994, 15.80617190586746368, 70.62390960531436690 ) ) ;
#177361 = CARTESIAN_POINT ( 'NONE',  ( -10.81492255796105439, 18.62759615963255655, 97.91775706135236135 ) ) ;
#177364 = CARTESIAN_POINT ( 'NONE',  ( 16.53943276465976808, -0.05219959533910856209, 78.74890960531436690 ) ) ;
#177363 = CARTESIAN_POINT ( 'NONE',  ( 4.379528057220092307, 16.55341960407617563, 92.29275706135236135 ) ) ;
#177362 = CARTESIAN_POINT ( 'NONE',  ( -16.46253265017160317, 9.564922557960807481, 25.83224293864769194 ) ) ;
#177365 = CARTESIAN_POINT ( 'NONE',  ( -9.564922557961040184, 16.46253265017147172, 92.91775706135233293 ) ) ;
#177366 = VERTEX_POINT ( 'NONE', #100007 ) ;
#177367 = CARTESIAN_POINT ( 'NONE',  ( -0.05219959533937732626, 21.53943276465977519, 22.50109039468567573 ) ) ;
#177368 = CARTESIAN_POINT ( 'NONE',  ( 16.51473224551083163, -9.474510206698727899, 35.83442372801899722 ) ) ;
#177369 = CARTESIAN_POINT ( 'NONE',  ( -0.05219959533934338120, 16.53943276465976808, 107.5010903946856899 ) ) ;
#177370 = CARTESIAN_POINT ( 'NONE',  ( 19.02544592524334988, 5.153800228976608722, 31.45942372801900433 ) ) ;
#177371 = CARTESIAN_POINT ( 'NONE',  ( 9.474510206698971260, -16.51473224551069308, 87.91557627198102409 ) ) ;
#177372 = CARTESIAN_POINT ( 'NONE',  ( -15.80617190586745835, -15.72974639402198527, 56.87390960531436690 ) ) ;
#177373 = CARTESIAN_POINT ( 'NONE',  ( -19.03943276465977164, 0.05219959533909376836, 21.24890960531436335 ) ) ;
#177374 = CARTESIAN_POINT ( 'NONE',  ( 13.89961937509977652, -13.97604488694527269, 23.12390960531436335 ) ) ;
#177375 = CARTESIAN_POINT ( 'NONE',  ( -15.80617190586768217, 15.72974639402176855, 113.1260903946856899 ) ) ;
#177376 = CARTESIAN_POINT ( 'NONE',  ( -4.483927247898782831, 16.52544592524335698, 82.70942372801900433 ) ) ;
#177377 = CARTESIAN_POINT ( 'NONE',  ( 15.72974639402176855, 15.80617190586768217, 21.87609039468567573 ) ) ;
#177378 = CARTESIAN_POINT ( 'NONE',  ( 16.53943276465976808, 0.05219959533934440121, 31.25109039468568639 ) ) ;
#177379 = CARTESIAN_POINT ( 'NONE',  ( -13.89961937509977652, 13.97604488694528158, 110.6239096053143243 ) ) ;
#177380 = CARTESIAN_POINT ( 'NONE',  ( 19.02544592524343514, -5.153800228976328945, 38.54057627198103120 ) ) ;
#177381 = CARTESIAN_POINT ( 'NONE',  ( 19.05341960407611168, 5.049401038298154454, 68.95724293864769550 ) ) ;
#177382 = VECTOR ( 'NONE', #105379, 1000.000000000000000 ) ;
#177383 = CARTESIAN_POINT ( 'NONE',  ( -4.483927247898782831, 16.52544592524335698, 42.70942372801901854 ) ) ;
#177384 = CARTESIAN_POINT ( 'NONE',  ( -16.55341960407611168, -4.379528057220339221, 86.45724293864770971 ) ) ;
#177385 = CARTESIAN_POINT ( 'NONE',  ( -8.314922557961024197, 14.29746914071037800, 97.91775706135236135 ) ) ;
#177388 = CARTESIAN_POINT ( 'NONE',  ( 9.564922557960805705, 16.46253265017160317, 59.58224293864769550 ) ) ;
#177387 = CARTESIAN_POINT ( 'NONE',  ( -13.89961937509977652, 13.97604488694528158, 75.62390960531438111 ) ) ;
#177386 = CARTESIAN_POINT ( 'NONE',  ( 15.80617190586769283, -15.72974639402175789, 55.62609039468568284 ) ) ;
#177389 = CARTESIAN_POINT ( 'NONE',  ( 19.03943276465977164, -0.05219959533909143690, 98.74890960531436690 ) ) ;
#177390 = CARTESIAN_POINT ( 'NONE',  ( 8.314922557960818139, 14.29746914071049879, 39.58224293864769550 ) ) ;
#177391 = CARTESIAN_POINT ( 'NONE',  ( -4.379528057220086978, -16.55341960407618274, 99.79275706135234714 ) ) ;
#177392 = ORIENTED_EDGE ( 'NONE', *, *, #153999, .F. ) ;
#177393 = CARTESIAN_POINT ( 'NONE',  ( 19.05341960407617918, -5.049401038297876454, 41.04275706135233293 ) ) ;
#177394 = CARTESIAN_POINT ( 'NONE',  ( 16.51473224551069308, 9.474510206698969483, 109.1655762719810383 ) ) ;
#177395 = CARTESIAN_POINT ( 'NONE',  ( -5.049401038298153566, 19.05341960407611168, 60.20724293864768129 ) ) ;
#177396 = CARTESIAN_POINT ( 'NONE',  ( 0.05219959533936267826, -19.03943276465977164, 40.00109039468566152 ) ) ;
#177397 = CARTESIAN_POINT ( 'NONE',  ( 36.91746824999999177, 2.880721459617395097E-14, -9.624999997268814056 ) ) ;
#177398 = CARTESIAN_POINT ( 'NONE',  ( -17.40861289039003168, -6.110651285853283987, 66.37232470827431996 ) ) ;
#177399 = CARTESIAN_POINT ( 'NONE',  ( 16.52544592524335698, 4.483927247898782831, 51.45942372801901854 ) ) ;
#177401 = CARTESIAN_POINT ( 'NONE',  ( 8.314922557961029526, -14.29746914071037800, 75.41775706135233293 ) ) ;
#177400 = CARTESIAN_POINT ( 'NONE',  ( -5.153800228976607833, 19.02544592524334988, 72.70942372801900433 ) ) ;
#177402 = CARTESIAN_POINT ( 'NONE',  ( -7.500000000000000000, 0.000000000000000000, 4.292893218813445877 ) ) ;
#177403 = CARTESIAN_POINT ( 'NONE',  ( -9.474510206698964154, 16.51473224551069663, 95.41557627198102409 ) ) ;
#177404 = CARTESIAN_POINT ( 'NONE',  ( 10.81492255796106328, -18.62759615963255655, 20.41775706135234714 ) ) ;
#177405 = CARTESIAN_POINT ( 'NONE',  ( 19.03943276465977164, 0.05219959533936151252, 76.25109039468566152 ) ) ;
#177407 = CARTESIAN_POINT ( 'NONE',  ( 0.05219959533909260263, 19.03943276465977164, 34.99890960531435979 ) ) ;
#177406 = CARTESIAN_POINT ( 'NONE',  ( 5.153800228976335163, 19.02544592524342804, 99.79057627198102409 ) ) ;
#177408 = CARTESIAN_POINT ( 'NONE',  ( -19.03943276465977164, 0.05219959533909376836, 96.24890960531436690 ) ) ;
#177410 = CARTESIAN_POINT ( 'NONE',  ( 19.03943276465977164, -0.05219959533909143690, 38.74890960531436690 ) ) ;
#177409 = CARTESIAN_POINT ( 'NONE',  ( -14.29746914071049879, 8.314922557960819915, 50.83224293864770971 ) ) ;
#177411 = CARTESIAN_POINT ( 'NONE',  ( 0.05219959533936267826, -19.03943276465977164, 45.00109039468566863 ) ) ;
#177412 = CARTESIAN_POINT ( 'NONE',  ( 14.29746914071049879, -8.314922557960816363, 93.33224293864769550 ) ) ;
#177413 = CARTESIAN_POINT ( 'NONE',  ( 13.97604488694548053, -13.89961937509957401, 20.62609039468567573 ) ) ;
#177414 = CARTESIAN_POINT ( 'NONE',  ( 16.51473224551069308, 9.474510206698969483, 54.16557627198103120 ) ) ;
#177415 = CARTESIAN_POINT ( 'NONE',  ( 21.53943276465977519, -0.05219959533907433946, 63.74890960531435979 ) ) ;
#177417 = CARTESIAN_POINT ( 'NONE',  ( 16.46253265017146816, 9.564922557961045513, 26.66775706135234003 ) ) ;
#177416 = CARTESIAN_POINT ( 'NONE',  ( 16.52544592524342804, -4.483927247898539470, 48.54057627198103120 ) ) ;
#177418 = CARTESIAN_POINT ( 'NONE',  ( -16.46253265017160317, 9.564922557960807481, 110.8322429386476955 ) ) ;
#177419 = CARTESIAN_POINT ( 'NONE',  ( 5.049401038298161559, -19.05341960407611168, 107.7072429386476955 ) ) ;
#177420 = CARTESIAN_POINT ( 'NONE',  ( -13.97604488694527625, -13.89961937509977652, 36.87390960531436690 ) ) ;
#177421 = CARTESIAN_POINT ( 'NONE',  ( 13.97604488694527802, 13.89961937509977652, 29.37390960531435979 ) ) ;
#177422 = CARTESIAN_POINT ( 'NONE',  ( 12.14591786802309770, 12.06949235617756955, 84.37390960531438111 ) ) ;
#177423 = CARTESIAN_POINT ( 'NONE',  ( 0.05219959533907565091, 21.53943276465977519, 94.99890960531436690 ) ) ;
#177424 = CARTESIAN_POINT ( 'NONE',  ( -9.564922557960796823, -16.46253265017161027, 97.08224293864769550 ) ) ;
#177425 = CARTESIAN_POINT ( 'NONE',  ( -0.05219959533907301413, -21.53943276465977519, 112.4989096053143669 ) ) ;
#177426 = CARTESIAN_POINT ( 'NONE',  ( -5.049401038298153566, 19.05341960407611168, 110.2072429386476671 ) ) ;
#177427 = CARTESIAN_POINT ( 'NONE',  ( 4.379528057220339221, -16.55341960407611168, 97.70724293864772392 ) ) ;
#177428 = CARTESIAN_POINT ( 'NONE',  ( 0.05219959533937995610, -21.53943276465977519, 80.00109039468568994 ) ) ;
#177429 = CARTESIAN_POINT ( 'NONE',  ( 5.719274019375991003, -21.55341960407610458, 77.70724293864770971 ) ) ;
#177430 = CARTESIAN_POINT ( 'NONE',  ( 17.26172910966779739, -6.454744622555833367, 108.3064690864922284 ) ) ;
#177431 = DIRECTION ( 'NONE',  ( 0.000000000000000000, -0.04175967627138118393, -0.9991276842514721368 ) ) ;
#177432 = LINE ( 'NONE', #89390, #111231 ) ;
#177433 = CARTESIAN_POINT ( 'NONE',  ( -0.05219959533934338120, 16.53943276465976808, 37.50109039468568284 ) ) ;
#177434 = EDGE_CURVE ( 'NONE', #12418, #100015, #50929, .T. ) ;
#177435 = CARTESIAN_POINT ( 'NONE',  ( 16.53943276465976808, -0.05219959533910856209, 113.7489096053143527 ) ) ;
#177436 = CARTESIAN_POINT ( 'NONE',  ( -17.49999999999997513, -4.013004640162659342, 109.5539427900558991 ) ) ;
#177437 = CARTESIAN_POINT ( 'NONE',  ( 19.05341960407611168, 5.049401038298154454, 58.95724293864768129 ) ) ;
#177438 = CARTESIAN_POINT ( 'NONE',  ( 16.53943276465976808, -0.05219959533910856209, 88.74890960531436690 ) ) ;
#177439 = CARTESIAN_POINT ( 'NONE',  ( 18.62759615963271287, -10.81492255796078972, 33.33224293864769550 ) ) ;
#177440 = CARTESIAN_POINT ( 'NONE',  ( 16.52544592524342804, -4.483927247898539470, 68.54057627198103830 ) ) ;
#177441 = CARTESIAN_POINT ( 'NONE',  ( 4.379528057220092307, 16.55341960407617563, 22.29275706135235069 ) ) ;
#177442 = CARTESIAN_POINT ( 'NONE',  ( -5.719274019375665041, -21.55341960407619695, 79.79275706135236135 ) ) ;
#177443 = DIRECTION ( 'NONE',  ( -1.734723475976805122E-15, 0.1033298494363120712, 0.9946471445771455366 ) ) ;
#177444 = CARTESIAN_POINT ( 'NONE',  ( -13.89961937509977652, 13.97604488694528158, 110.6239096053143243 ) ) ;
#177445 = CARTESIAN_POINT ( 'NONE',  ( -16.53943276465976808, -0.05219959533934237506, 98.75109039468568994 ) ) ;
#177446 = CARTESIAN_POINT ( 'NONE',  ( 9.564922557960805705, 16.46253265017160317, 34.58224293864770260 ) ) ;
#177447 = CARTESIAN_POINT ( 'NONE',  ( 19.03943276465977164, -0.05219959533909143690, 83.74890960531436690 ) ) ;
#177448 = CARTESIAN_POINT ( 'NONE',  ( -21.55341960407610458, -5.719274019375992779, 91.45724293864769550 ) ) ;
#177449 = CARTESIAN_POINT ( 'NONE',  ( 4.483927247898790824, -16.52544592524335698, 25.20942372801901854 ) ) ;
#177451 = CARTESIAN_POINT ( 'NONE',  ( 18.62759615963255655, 10.81492255796105972, 66.66775706135234714 ) ) ;
#177450 = CARTESIAN_POINT ( 'NONE',  ( -0.05219959533910754901, -16.53943276465976808, 67.49890960531436690 ) ) ;
#177452 = CARTESIAN_POINT ( 'NONE',  ( 16.53943276465976808, 0.05219959533934440121, 106.2510903946856757 ) ) ;
#177453 = CARTESIAN_POINT ( 'NONE',  ( 16.62475595723611477, -7.163666690055880082, 48.02713351810404419 ) ) ;
#177454 = CARTESIAN_POINT ( 'NONE',  ( -17.49999999999999289, 5.500000000000037303, 80.79690382534172954 ) ) ;
#177455 = CARTESIAN_POINT ( 'NONE',  ( 16.52544592524342804, -4.483927247898539470, 33.54057627198102409 ) ) ;
#177456 = CARTESIAN_POINT ( 'NONE',  ( 16.53943276465976808, 0.05219959533934440121, 56.25109039468568284 ) ) ;
#177457 = CARTESIAN_POINT ( 'NONE',  ( -19.02544592524342804, 5.153800228976336051, 76.04057627198102409 ) ) ;
#177458 = CARTESIAN_POINT ( 'NONE',  ( 16.46253265017160672, -9.564922557960803928, 88.33224293864769550 ) ) ;
#177459 = CARTESIAN_POINT ( 'NONE',  ( -15.80617190586768217, 15.72974639402176855, 83.12609039468568994 ) ) ;
#177460 = EDGE_CURVE ( 'NONE', #93735, #40506, #38086, .T. ) ;
#177461 = CARTESIAN_POINT ( 'NONE',  ( 16.55341960407618274, -4.379528057220086978, 86.04275706135236135 ) ) ;
#177462 = CARTESIAN_POINT ( 'NONE',  ( 12.14591786802309770, 12.06949235617756955, 54.37390960531435979 ) ) ;
#177463 = CARTESIAN_POINT ( 'NONE',  ( -19.02544592524342804, 5.153800228976336051, 66.04057627198103830 ) ) ;
#177464 = VERTEX_POINT ( 'NONE', #72696 ) ;
#177465 = CARTESIAN_POINT ( 'NONE',  ( -19.03943276465977164, -0.05219959533935918106, 113.7510903946856757 ) ) ;
#177466 = CARTESIAN_POINT ( 'NONE',  ( -12.06949235617756955, 12.14591786802309770, 115.6239096053143669 ) ) ;
#177467 = CARTESIAN_POINT ( 'NONE',  ( -16.46253265017160317, 9.564922557960807481, 75.83224293864769550 ) ) ;
#177469 = CARTESIAN_POINT ( 'NONE',  ( 29.86685920354754842, -21.69954338932559068, -7.824999997268813345 ) ) ;
#177468 = CARTESIAN_POINT ( 'NONE',  ( 4.483927247898790824, -16.52544592524335698, 20.20942372801900788 ) ) ;
#177470 = CARTESIAN_POINT ( 'NONE',  ( 10.72451020669871369, 18.67979575497193778, 107.0844237280190043 ) ) ;
#177471 = CARTESIAN_POINT ( 'NONE',  ( 14.29746914071037800, 8.314922557961029526, 76.66775706135234714 ) ) ;
#177472 = CARTESIAN_POINT ( 'NONE',  ( -19.03943276465977164, -0.05219959533935918106, 98.75109039468567573 ) ) ;
#177473 = CARTESIAN_POINT ( 'NONE',  ( 19.05341960407611168, 5.049401038298154454, 23.95724293864769194 ) ) ;
#177474 = CARTESIAN_POINT ( 'NONE',  ( -14.34966873604972548, 8.224510206698743886, 68.33442372801900433 ) ) ;
#177475 = FACE_OUTER_BOUND ( 'NONE', #64474, .T. ) ;
#177476 = CARTESIAN_POINT ( 'NONE',  ( -13.89961937509957401, -13.97604488694547875, 49.37609039468567573 ) ) ;
#177477 = CARTESIAN_POINT ( 'NONE',  ( -21.52544592524334988, -5.823673210054445271, 103.9594237280190185 ) ) ;
#177478 = CARTESIAN_POINT ( 'NONE',  ( -13.89961937509977652, 13.97604488694528158, 40.62390960531435979 ) ) ;
#177479 = CARTESIAN_POINT ( 'NONE',  ( -19.02544592524342804, 5.153800228976336051, 76.04057627198102409 ) ) ;
#177480 = CARTESIAN_POINT ( 'NONE',  ( -0.05219959533910754901, -16.53943276465976808, 67.49890960531436690 ) ) ;
#177481 = CARTESIAN_POINT ( 'NONE',  ( -18.62759615963255300, -10.81492255796106328, 84.16775706135234714 ) ) ;
#177482 = PRODUCT ( 'socket button head screw_iso_ISO 7380 - M4 x 8 - 8N', 'socket button head screw_iso_ISO 7380 - M4 x 8 - 8N', '', ( #167684 ) ) ;
#177483 = CARTESIAN_POINT ( 'NONE',  ( 9.474510206698729675, 16.51473224551082808, 47.08442372801900433 ) ) ;
#177484 = CARTESIAN_POINT ( 'NONE',  ( -19.02544592524334988, -5.153800228976617603, 38.95942372801900433 ) ) ;
#177485 = CARTESIAN_POINT ( 'NONE',  ( 0.05219959533907565091, 21.53943276465977519, 39.99890960531436690 ) ) ;
#177486 = CARTESIAN_POINT ( 'NONE',  ( -18.62759615963255300, -10.81492255796106328, 99.16775706135234714 ) ) ;
#177487 = CARTESIAN_POINT ( 'NONE',  ( -9.474510206698964154, 16.51473224551069663, 80.41557627198103830 ) ) ;
#177488 = CARTESIAN_POINT ( 'NONE',  ( -15.80617190586768217, 15.72974639402176855, 88.12609039468570415 ) ) ;
#177489 = CARTESIAN_POINT ( 'NONE',  ( 18.67979575497178502, 10.72451020669898547, 54.16557627198103120 ) ) ;
#177490 = CARTESIAN_POINT ( 'NONE',  ( -13.97604488694527625, -13.89961937509977652, 101.8739096053143811 ) ) ;
#177491 = CARTESIAN_POINT ( 'NONE',  ( -16.51473224551082808, 9.474510206698731452, 78.33442372801900433 ) ) ;
#177492 = CARTESIAN_POINT ( 'NONE',  ( 9.564922557960805705, 16.46253265017160317, 99.58224293864770971 ) ) ;
#177493 = CARTESIAN_POINT ( 'NONE',  ( -16.51473224551082808, 9.474510206698731452, 93.33442372801900433 ) ) ;
#177494 = CARTESIAN_POINT ( 'NONE',  ( -14.34966873604972548, 8.224510206698743886, 38.33442372801900433 ) ) ;
#177495 = CARTESIAN_POINT ( 'NONE',  ( -16.53943276465976808, 0.05219959533911058130, 96.24890960531435269 ) ) ;
#177496 = CARTESIAN_POINT ( 'NONE',  ( 0.05219959533909260263, 19.03943276465977164, 69.99890960531435269 ) ) ;
#177497 = CARTESIAN_POINT ( 'NONE',  ( -0.05219959533907301413, -21.53943276465977519, 67.49890960531436690 ) ) ;
#177498 = CIRCLE ( 'NONE', #141943, 59.99999999999998579 ) ;
#177499 = CARTESIAN_POINT ( 'NONE',  ( 14.29746914071037800, 8.314922557961029526, 36.66775706135234714 ) ) ;
#177500 = CARTESIAN_POINT ( 'NONE',  ( -15.72974639402176322, -15.80617190586768395, 39.37609039468567573 ) ) ;
#177501 = CARTESIAN_POINT ( 'NONE',  ( 0.05219959533937995610, -21.53943276465977519, 90.00109039468567573 ) ) ;
#177502 = CARTESIAN_POINT ( 'NONE',  ( 12.06949235617739724, 12.14591786802326823, 76.87609039468567573 ) ) ;
#177503 = CARTESIAN_POINT ( 'NONE',  ( 13.97604488694527802, 13.89961937509977652, 69.37390960531436690 ) ) ;
#177504 = CARTESIAN_POINT ( 'NONE',  ( -4.483927247898539470, -16.52544592524342804, 72.29057627198102409 ) ) ;
#177505 = CARTESIAN_POINT ( 'NONE',  ( 16.53943276465976808, 0.05219959533934440121, 101.2510903946856757 ) ) ;
#177506 = CARTESIAN_POINT ( 'NONE',  ( 13.97604488694548053, -13.89961937509957401, 50.62609039468566152 ) ) ;
#177507 = CARTESIAN_POINT ( 'NONE',  ( 10.81492255796106328, -18.62759615963255655, 30.41775706135234358 ) ) ;
#177508 = CARTESIAN_POINT ( 'NONE',  ( 0.05219959533910956823, 16.53943276465976808, 74.99890960531435269 ) ) ;
#177509 = CARTESIAN_POINT ( 'NONE',  ( 19.02544592524343514, -5.153800228976328945, 98.54057627198100988 ) ) ;
#177510 = CARTESIAN_POINT ( 'NONE',  ( 16.55341960407618274, -4.379528057220086978, 101.0427570613523756 ) ) ;
#177511 = CARTESIAN_POINT ( 'NONE',  ( 15.80617190586769283, -15.72974639402175789, 65.62609039468568994 ) ) ;
#177512 = CARTESIAN_POINT ( 'NONE',  ( -8.224510206698735004, -14.34966873604973081, 44.58442372801901854 ) ) ;
#177513 = CARTESIAN_POINT ( 'NONE',  ( 15.72974639402176855, 15.80617190586768217, 41.87609039468568284 ) ) ;
#177514 = CARTESIAN_POINT ( 'NONE',  ( -16.53943276465976808, 0.05219959533911058130, 76.24890960531435269 ) ) ;
#177515 = VERTEX_POINT ( 'NONE', #39349 ) ;
#177516 = CARTESIAN_POINT ( 'NONE',  ( -21.53943276465977519, 0.05219959533907696930, 116.2489096053143669 ) ) ;
#177517 = CARTESIAN_POINT ( 'NONE',  ( 17.50000000000001421, -3.471454075611625445, 26.98332581144362052 ) ) ;
#177518 = CARTESIAN_POINT ( 'NONE',  ( 16.55341960407611168, 4.379528057220329451, 48.95724293864770971 ) ) ;
#177519 = CARTESIAN_POINT ( 'NONE',  ( -16.51473224551069308, -9.474510206698971260, 21.66557627198102765 ) ) ;
#177520 = CARTESIAN_POINT ( 'NONE',  ( 10.81492255796078972, 18.62759615963270932, 44.58224293864769550 ) ) ;
#177521 = CARTESIAN_POINT ( 'NONE',  ( -4.483927247898539470, -16.52544592524342804, 82.29057627198103830 ) ) ;
#177522 = CIRCLE ( 'NONE', #190338, 69.99999999999998579 ) ;
#177523 = CARTESIAN_POINT ( 'NONE',  ( 5.719274019375991003, -21.55341960407610458, 82.70724293864770971 ) ) ;
#177524 = CARTESIAN_POINT ( 'NONE',  ( 16.46253265017160672, -9.564922557960803928, 88.33224293864769550 ) ) ;
#177526 = CARTESIAN_POINT ( 'NONE',  ( 9.564922557961047289, -16.46253265017146816, 80.41775706135234714 ) ) ;
#177525 = CARTESIAN_POINT ( 'NONE',  ( 5.049401038298161559, -19.05341960407611168, 42.70724293864767418 ) ) ;
#177528 = CARTESIAN_POINT ( 'NONE',  ( -5.823673210054116645, -21.52544592524344225, 67.29057627198103830 ) ) ;
#177527 = CARTESIAN_POINT ( 'NONE',  ( -5.823673210054431948, 21.52544592524334988, 57.70942372801901143 ) ) ;
#177529 = CARTESIAN_POINT ( 'NONE',  ( -19.05341960407611168, -5.049401038298163336, 36.45724293864766707 ) ) ;
#177530 = CARTESIAN_POINT ( 'NONE',  ( 9.564922557960805705, 16.46253265017160317, 74.58224293864769550 ) ) ;
#177531 = ORIENTED_EDGE ( 'NONE', *, *, #150034, .T. ) ;
#177532 = CARTESIAN_POINT ( 'NONE',  ( 0.05219959533934541429, -16.53943276465976808, 55.00109039468568284 ) ) ;
#177533 = CARTESIAN_POINT ( 'NONE',  ( -21.52544592524334988, -5.823673210054445271, 33.95942372801901143 ) ) ;
#177534 = CARTESIAN_POINT ( 'NONE',  ( 21.55341960407619695, -5.719274019375665929, 76.04275706135237556 ) ) ;
#177535 = CARTESIAN_POINT ( 'NONE',  ( -16.46253265017160317, 9.564922557960807481, 100.8322429386477097 ) ) ;
#177536 = CARTESIAN_POINT ( 'NONE',  ( 18.62759615963271287, -10.81492255796078972, 83.33224293864769550 ) ) ;
#177538 = CARTESIAN_POINT ( 'NONE',  ( -8.314922557961024197, 14.29746914071037800, 52.91775706135235424 ) ) ;
#177537 = CARTESIAN_POINT ( 'NONE',  ( -18.62759615963255300, -10.81492255796106328, 24.16775706135235424 ) ) ;
#177539 = EDGE_CURVE ( 'NONE', #68554, #129957, #151128, .T. ) ;
#177540 = CARTESIAN_POINT ( 'NONE',  ( -15.72974639402197994, 15.80617190586746368, 45.62390960531436690 ) ) ;
#177541 = CARTESIAN_POINT ( 'NONE',  ( 9.564922557961047289, -16.46253265017146816, 25.41775706135234003 ) ) ;
#177542 = CARTESIAN_POINT ( 'NONE',  ( 19.02544592524343514, -5.153800228976328945, 48.54057627198103120 ) ) ;
#177543 = CARTESIAN_POINT ( 'NONE',  ( 19.03943276465977164, -0.05219959533909143690, 108.7489096053143527 ) ) ;
#177544 = CARTESIAN_POINT ( 'NONE',  ( 13.97604488694527802, 13.89961937509977652, 94.37390960531436690 ) ) ;
#177545 = CARTESIAN_POINT ( 'NONE',  ( 19.98452092126598245, 21.51070015259071155, -49.12424573582180898 ) ) ;
#177546 = CARTESIAN_POINT ( 'NONE',  ( -0.05219959533936034679, 19.03943276465977164, 67.50109039468566152 ) ) ;
#177547 = CARTESIAN_POINT ( 'NONE',  ( 0.05219959533907565091, 21.53943276465977519, 39.99890960531436690 ) ) ;
#177548 = CARTESIAN_POINT ( 'NONE',  ( 12.14591786802309770, 12.06949235617756955, 24.37390960531435979 ) ) ;
#177549 = CARTESIAN_POINT ( 'NONE',  ( -19.03943276465977164, -0.05219959533935918106, 103.7510903946856757 ) ) ;
#177550 = DIRECTION ( 'NONE',  ( -0.000000000000000000, -0.000000000000000000, 1.000000000000000000 ) ) ;
#177551 = CARTESIAN_POINT ( 'NONE',  ( -15.80617190586768217, 15.72974639402176855, 113.1260903946856899 ) ) ;
#177552 = CARTESIAN_POINT ( 'NONE',  ( -5.049401038297874678, -19.05341960407617918, 94.79275706135230450 ) ) ;
#177553 = CARTESIAN_POINT ( 'NONE',  ( -13.97604488694547697, 13.89961937509957934, 63.12609039468566152 ) ) ;
#177554 = CARTESIAN_POINT ( 'NONE',  ( 17.50000000000000000, -5.499999999999992895, 91.21769037696437010 ) ) ;
#177555 = CARTESIAN_POINT ( 'NONE',  ( 9.564922557960805705, 16.46253265017160317, 54.58224293864769550 ) ) ;
#177556 = CARTESIAN_POINT ( 'NONE',  ( -4.379528057220328563, 16.55341960407611168, 65.20724293864768129 ) ) ;
#177557 = CARTESIAN_POINT ( 'NONE',  ( 16.46253265017160672, -9.564922557960803928, 38.33224293864768839 ) ) ;
#177558 = CARTESIAN_POINT ( 'NONE',  ( -8.224510206698948167, 14.34966873604960824, 35.41557627198102409 ) ) ;
#177559 = DIRECTION ( 'NONE',  ( 6.716189716306310304E-15, -0.9991276842514723588, 0.04175967627138119781 ) ) ;
#177560 = CARTESIAN_POINT ( 'NONE',  ( -14.34966873604972548, 8.224510206698743886, 103.3344237280190043 ) ) ;
#177561 = CARTESIAN_POINT ( 'NONE',  ( -5.153800228976328057, -19.02544592524343514, 67.29057627198102409 ) ) ;
#177562 = CARTESIAN_POINT ( 'NONE',  ( -16.46253265017146816, -9.564922557961047289, 24.16775706135233648 ) ) ;
#177563 = CARTESIAN_POINT ( 'NONE',  ( -16.55341960407617563, 4.379528057220093196, 28.54275706135234358 ) ) ;
#177564 = CARTESIAN_POINT ( 'NONE',  ( 5.719274019375991003, -21.55341960407610458, 52.70724293864769550 ) ) ;
#177566 = VERTEX_POINT ( 'NONE', #23190 ) ;
#177565 = CARTESIAN_POINT ( 'NONE',  ( -10.81492255796105439, 18.62759615963255655, 102.9177570613523756 ) ) ;
#177567 = CARTESIAN_POINT ( 'NONE',  ( 0.05219959533909260263, 19.03943276465977164, 64.99890960531436690 ) ) ;
#177568 = CARTESIAN_POINT ( 'NONE',  ( -1.304248841091933035E-15, -21.30000000000002913, -56.46919128290398504 ) ) ;
#177569 = CARTESIAN_POINT ( 'NONE',  ( -19.02544592524342804, 5.153800228976336051, 101.0405762719810241 ) ) ;
#177570 = CARTESIAN_POINT ( 'NONE',  ( -36.91746825000000598, -11.99521256947794789, -2.524999997268813523 ) ) ;
#177571 = CARTESIAN_POINT ( 'NONE',  ( -5.823673210054431948, 21.52544592524334988, 27.70942372801901854 ) ) ;
#177572 = CARTESIAN_POINT ( 'NONE',  ( -0.05219959533910754901, -16.53943276465976808, 92.49890960531436690 ) ) ;
#177574 = CARTESIAN_POINT ( 'NONE',  ( 9.474510206698971260, -16.51473224551069308, 62.91557627198102409 ) ) ;
#177573 = CARTESIAN_POINT ( 'NONE',  ( 0.05219959533907565091, 21.53943276465977519, 84.99890960531436690 ) ) ;
#177575 = CARTESIAN_POINT ( 'NONE',  ( 16.46253265017160672, -9.564922557960803928, 78.33224293864769550 ) ) ;
#177576 = CARTESIAN_POINT ( 'NONE',  ( 10.81492255796078972, 18.62759615963270932, 114.5822429386477097 ) ) ;
#177577 = ORIENTED_EDGE ( 'NONE', *, *, #136064, .F. ) ;
#177578 = CARTESIAN_POINT ( 'NONE',  ( -19.02544592524342804, 5.153800228976336051, 71.04057627198099567 ) ) ;
#177579 = CARTESIAN_POINT ( 'NONE',  ( 19.36337904590688552, -5.500000000000036415, 97.91494137495618588 ) ) ;
#177581 = DIRECTION ( 'NONE',  ( 1.000000000000000000, -0.000000000000000000, 6.982962677686266711E-15 ) ) ;
#177580 = CARTESIAN_POINT ( 'NONE',  ( -12.06949235617756955, 12.14591786802309770, 105.6239096053143669 ) ) ;
#177582 = CARTESIAN_POINT ( 'NONE',  ( -13.89961937509957401, -13.97604488694547875, 94.37609039468566152 ) ) ;
#177583 = CARTESIAN_POINT ( 'NONE',  ( -12.14591786802309592, -12.06949235617757132, 91.87390960531436690 ) ) ;
#177584 = CARTESIAN_POINT ( 'NONE',  ( 0.05219959533937995610, -21.53943276465977519, 70.00109039468568994 ) ) ;
#177586 = CARTESIAN_POINT ( 'NONE',  ( -15.72974639402176322, -15.80617190586768395, 29.37609039468568284 ) ) ;
#177585 = CARTESIAN_POINT ( 'NONE',  ( -16.46253265017160317, 9.564922557960807481, 60.83224293864769550 ) ) ;
#177587 = CARTESIAN_POINT ( 'NONE',  ( -10.72451020669898014, 18.67979575497178502, 110.4155762719810383 ) ) ;
#177588 = CARTESIAN_POINT ( 'NONE',  ( 11.30153831258471797, -180.0000000000000000, -4.999999999999999112 ) ) ;
#177589 = CARTESIAN_POINT ( 'NONE',  ( -0.05219959533909027116, -19.03943276465977164, 67.49890960531436690 ) ) ;
#177590 = CARTESIAN_POINT ( 'NONE',  ( 27.40250423669326096, 7.751724348666389375, 163.3149731962813860 ) ) ;
#177592 = CARTESIAN_POINT ( 'NONE',  ( -18.67979575497178146, -10.72451020669898902, 36.66557627198103120 ) ) ;
#177591 = CARTESIAN_POINT ( 'NONE',  ( -14.34966873604972548, 8.224510206698743886, 23.33442372801901499 ) ) ;
#177593 = CARTESIAN_POINT ( 'NONE',  ( -10.81492255796105439, 18.62759615963255655, 57.91775706135234714 ) ) ;
#177594 = CARTESIAN_POINT ( 'NONE',  ( 16.51473224551069308, 9.474510206698969483, 104.1655762719810241 ) ) ;
#177595 = CARTESIAN_POINT ( 'NONE',  ( -16.46253265017146816, -9.564922557961047289, 99.16775706135233293 ) ) ;
#177596 = CARTESIAN_POINT ( 'NONE',  ( -16.46253265017160317, 9.564922557960807481, 45.83224293864769550 ) ) ;
#177597 = CARTESIAN_POINT ( 'NONE',  ( 13.89961937509977652, -13.97604488694527269, 73.12390960531436690 ) ) ;
#177598 = CARTESIAN_POINT ( 'NONE',  ( 4.483927247898545687, 16.52544592524342804, 99.79057627198103830 ) ) ;
#177599 = CARTESIAN_POINT ( 'NONE',  ( 19.03943276465977164, -0.05219959533909143690, 98.74890960531436690 ) ) ;
#177600 = CARTESIAN_POINT ( 'NONE',  ( -0.05219959533910754901, -16.53943276465976808, 92.49890960531436690 ) ) ;
#177601 = CARTESIAN_POINT ( 'NONE',  ( -19.02544592524342804, 5.153800228976336051, 96.04057627198103830 ) ) ;
#177603 = CARTESIAN_POINT ( 'NONE',  ( -19.05341960407611168, -5.049401038298163336, 41.45724293864769550 ) ) ;
#177602 = CARTESIAN_POINT ( 'NONE',  ( -4.379528057220328563, 16.55341960407611168, 45.20724293864769550 ) ) ;
#177604 = VERTEX_POINT ( 'NONE', #194054 ) ;
#177605 = CARTESIAN_POINT ( 'NONE',  ( 21.52544592524334988, 5.823673210054432836, 51.45942372801901854 ) ) ;
#177606 = CARTESIAN_POINT ( 'NONE',  ( -19.02544592524334988, -5.153800228976617603, 83.95942372801901854 ) ) ;
#177607 = CARTESIAN_POINT ( 'NONE',  ( 16.55341960407611168, 4.379528057220329451, 53.95724293864770260 ) ) ;
#177608 = CARTESIAN_POINT ( 'NONE',  ( -10.72451020669898014, 18.67979575497178502, 100.4155762719810241 ) ) ;
#177609 = CARTESIAN_POINT ( 'NONE',  ( 21.53943276465977519, -0.05219959533907433946, 53.74890960531437401 ) ) ;
#177611 = CARTESIAN_POINT ( 'NONE',  ( 12.06949235617757843, -12.14591786802309237, 78.12390960531436690 ) ) ;
#177610 = CARTESIAN_POINT ( 'NONE',  ( 5.049401038298161559, -19.05341960407611168, 107.7072429386476955 ) ) ;
#177612 = CARTESIAN_POINT ( 'NONE',  ( -13.97604488694527625, -13.89961937509977652, 56.87390960531434558 ) ) ;
#177613 = CARTESIAN_POINT ( 'NONE',  ( 12.06949235617757843, -12.14591786802309237, 28.12390960531435979 ) ) ;
#177614 = CARTESIAN_POINT ( 'NONE',  ( -16.53943276465976808, -0.05219959533934237506, 98.75109039468568994 ) ) ;
#177615 = CARTESIAN_POINT ( 'NONE',  ( -16.53943276465976808, -0.05219959533934237506, 73.75109039468567573 ) ) ;
#177616 = CARTESIAN_POINT ( 'NONE',  ( 9.564922557961047289, -16.46253265017146816, 30.41775706135232937 ) ) ;
#177618 = CARTESIAN_POINT ( 'NONE',  ( -16.46253265017160317, 9.564922557960807481, 110.8322429386476955 ) ) ;
#177617 = FACE_OUTER_BOUND ( 'NONE', #134853, .T. ) ;
#177619 = CARTESIAN_POINT ( 'NONE',  ( -0.05219959533909027116, -19.03943276465977164, 72.49890960531435269 ) ) ;
#177620 = CARTESIAN_POINT ( 'NONE',  ( -9.564922557960796823, -16.46253265017161027, 37.08224293864768839 ) ) ;
#177621 = CARTESIAN_POINT ( 'NONE',  ( 16.55341960407611168, 4.379528057220329451, 43.95724293864769550 ) ) ;
#177623 = CARTESIAN_POINT ( 'NONE',  ( -19.05341960407611168, -5.049401038298163336, 101.4572429386476955 ) ) ;
#177622 = CARTESIAN_POINT ( 'NONE',  ( -5.153800228976328057, -19.02544592524343514, 112.2905762719810099 ) ) ;
#177624 = CARTESIAN_POINT ( 'NONE',  ( -18.67979575497178146, -10.72451020669898902, 46.66557627198102409 ) ) ;
#177625 = CARTESIAN_POINT ( 'NONE',  ( 12.14591786802309770, 12.06949235617756955, 84.37390960531438111 ) ) ;
#177626 = CARTESIAN_POINT ( 'NONE',  ( 12.14591786802327356, -12.06949235617739191, 35.62609039468568994 ) ) ;
#177627 = CARTESIAN_POINT ( 'NONE',  ( -4.379528057220328563, 16.55341960407611168, 65.20724293864768129 ) ) ;
#177628 = CARTESIAN_POINT ( 'NONE',  ( -17.49999999999999645, -5.499999999999992895, 120.0000000000000142 ) ) ;
#177629 = CARTESIAN_POINT ( 'NONE',  ( 0.05219959533936267826, -19.03943276465977164, 60.00109039468566863 ) ) ;
#177630 = CARTESIAN_POINT ( 'NONE',  ( -16.51473224551069308, -9.474510206698971260, 101.6655762719810241 ) ) ;
#177631 = CARTESIAN_POINT ( 'NONE',  ( 16.51473224551083163, -9.474510206698727899, 75.83442372801900433 ) ) ;
#177632 = CARTESIAN_POINT ( 'NONE',  ( 1.784210473542230573E-15, -29.16686587814331588, 147.8750000027311273 ) ) ;
#177633 = CIRCLE ( 'NONE', #61417, 40.00000000000000000 ) ;
#177635 = CARTESIAN_POINT ( 'NONE',  ( -16.55341960407611168, -4.379528057220339221, 21.45724293864769550 ) ) ;
#177634 = CARTESIAN_POINT ( 'NONE',  ( -9.474510206698720793, -16.51473224551083518, 109.5844237280190043 ) ) ;
#177636 = CARTESIAN_POINT ( 'NONE',  ( 13.97604488694548053, -13.89961937509957401, 75.62609039468564731 ) ) ;
#177637 = CARTESIAN_POINT ( 'NONE',  ( -18.62759615963270932, 10.81492255796079327, 30.83224293864770260 ) ) ;
#177638 = CARTESIAN_POINT ( 'NONE',  ( -5.823673210054431948, 21.52544592524334988, 72.70942372801901854 ) ) ;
#177639 = CARTESIAN_POINT ( 'NONE',  ( 19.08440550902512811, 5.499999999999857003, 38.67052153706850959 ) ) ;
#177640 = CARTESIAN_POINT ( 'NONE',  ( -9.564922557961040184, 16.46253265017147172, 112.9177570613523329 ) ) ;
#177641 = CARTESIAN_POINT ( 'NONE',  ( -13.89961937509977652, 13.97604488694528158, 70.62390960531432427 ) ) ;
#177642 = CARTESIAN_POINT ( 'NONE',  ( 14.63400850047069213, 16.39429727647822688, -58.42335914450117684 ) ) ;
#177644 = CARTESIAN_POINT ( 'NONE',  ( -13.89961937509977652, 13.97604488694528158, 80.62390960531436690 ) ) ;
#177643 = CARTESIAN_POINT ( 'NONE',  ( -14.34966873604960291, -8.224510206698953496, 81.66557627198103830 ) ) ;
#177645 = CARTESIAN_POINT ( 'NONE',  ( -9.474510206698964154, 16.51473224551069663, 90.41557627198103830 ) ) ;
#177646 = CARTESIAN_POINT ( 'NONE',  ( 13.97604488694548053, -13.89961937509957401, 90.62609039468567573 ) ) ;
#177647 = CARTESIAN_POINT ( 'NONE',  ( -18.62759615963270932, 10.81492255796079327, 80.83224293864769550 ) ) ;
#177648 = CARTESIAN_POINT ( 'NONE',  ( -9.474510206698964154, 16.51473224551069663, 25.41557627198103120 ) ) ;
#177649 = CARTESIAN_POINT ( 'NONE',  ( 16.46253265017146816, 9.564922557961045513, 51.66775706135233293 ) ) ;
#177650 = CARTESIAN_POINT ( 'NONE',  ( 16.51473224551069308, 9.474510206698969483, 59.16557627198102409 ) ) ;
#177651 = CARTESIAN_POINT ( 'NONE',  ( -19.03943276465977164, 0.05219959533909376836, 96.24890960531436690 ) ) ;
#177652 = VERTEX_POINT ( 'NONE', #146512 ) ;
#177653 = CARTESIAN_POINT ( 'NONE',  ( -10.81492255796078084, -18.62759615963271287, 102.0822429386476955 ) ) ;
#177656 = CARTESIAN_POINT ( 'NONE',  ( 5.153800228976615827, -19.02544592524334988, 60.20942372801899012 ) ) ;
#177655 = CARTESIAN_POINT ( 'NONE',  ( 19.05341960407611168, 5.049401038298154454, 83.95724293864766707 ) ) ;
#177654 = CARTESIAN_POINT ( 'NONE',  ( 8.224510206698953496, -14.34966873604960469, 87.91557627198103830 ) ) ;
#177657 = CARTESIAN_POINT ( 'NONE',  ( 21.55341960407610458, 5.719274019375980345, 88.95724293864769550 ) ) ;
#177658 = CARTESIAN_POINT ( 'NONE',  ( -0.05219959533907301413, -21.53943276465977519, 67.49890960531436690 ) ) ;
#177659 = CARTESIAN_POINT ( 'NONE',  ( 8.314922557960818139, 14.29746914071049879, 39.58224293864769550 ) ) ;
#177660 = CARTESIAN_POINT ( 'NONE',  ( -5.719274019375665041, -21.55341960407619695, 104.7927570613523898 ) ) ;
#177661 = CARTESIAN_POINT ( 'NONE',  ( 16.52544592524335698, 4.483927247898782831, 66.45942372801903275 ) ) ;
#177662 = CARTESIAN_POINT ( 'NONE',  ( -9.564922557960796823, -16.46253265017161027, 97.08224293864769550 ) ) ;
#177663 = CARTESIAN_POINT ( 'NONE',  ( 0.05219959533909260263, 19.03943276465977164, 34.99890960531435979 ) ) ;
#177664 = CARTESIAN_POINT ( 'NONE',  ( -0.05219959533937732626, 21.53943276465977519, 37.50109039468568284 ) ) ;
#177665 = EDGE_CURVE ( 'NONE', #111207, #58211, #69686, .T. ) ;
#177666 = CARTESIAN_POINT ( 'NONE',  ( 5.823673210054444382, -21.52544592524334988, 50.20942372801901854 ) ) ;
#177667 = CARTESIAN_POINT ( 'NONE',  ( 5.153800228976335163, 19.02544592524342804, 64.79057627198100988 ) ) ;
#177668 = CARTESIAN_POINT ( 'NONE',  ( 21.52544592524334988, 5.823673210054432836, 41.45942372801901143 ) ) ;
#177669 = CARTESIAN_POINT ( 'NONE',  ( -19.03943276465977164, -0.05219959533935918106, 73.75109039468566152 ) ) ;
#177670 = CARTESIAN_POINT ( 'NONE',  ( -13.89961937509957401, -13.97604488694547875, 79.37609039468567573 ) ) ;
#177671 = CARTESIAN_POINT ( 'NONE',  ( -5.153800228976328057, -19.02544592524343514, 42.29057627198101699 ) ) ;
#177672 = CARTESIAN_POINT ( 'NONE',  ( -8.314922557961024197, 14.29746914071037800, 72.91775706135234714 ) ) ;
#177673 = CARTESIAN_POINT ( 'NONE',  ( 19.02544592524343514, -5.153800228976328945, 53.54057627198102409 ) ) ;
#177674 = LINE ( 'NONE', #7795, #141800 ) ;
#177675 = CARTESIAN_POINT ( 'NONE',  ( 16.46253265017160672, -9.564922557960803928, 93.33224293864769550 ) ) ;
#177676 = CARTESIAN_POINT ( 'NONE',  ( 13.97604488694527802, 13.89961937509977652, 39.37390960531435269 ) ) ;
#177677 = CARTESIAN_POINT ( 'NONE',  ( 15.72974639402199770, -15.80617190586745480, 78.12390960531436690 ) ) ;
#177678 = CARTESIAN_POINT ( 'NONE',  ( 12.06949235617739724, 12.14591786802326823, 66.87609039468568994 ) ) ;
#177679 = CARTESIAN_POINT ( 'NONE',  ( -10.81492255796105439, 18.62759615963255655, 112.9177570613523329 ) ) ;
#177680 = CARTESIAN_POINT ( 'NONE',  ( 5.049401038298161559, -19.05341960407611168, 47.70724293864770260 ) ) ;
#177681 = CARTESIAN_POINT ( 'NONE',  ( -12.14591786802309592, -12.06949235617757132, 41.87390960531435979 ) ) ;
#177682 = CARTESIAN_POINT ( 'NONE',  ( -14.29746914071049879, 8.314922557960819915, 75.83224293864769550 ) ) ;
#177683 = CARTESIAN_POINT ( 'NONE',  ( 9.564922557960805705, 16.46253265017160317, 84.58224293864769550 ) ) ;
#177684 = CARTESIAN_POINT ( 'NONE',  ( -15.80617190586768217, 15.72974639402176855, 33.12609039468569705 ) ) ;
#177685 = CARTESIAN_POINT ( 'NONE',  ( 19.05341960407611168, 5.049401038298154454, 88.95724293864769550 ) ) ;
#177686 = CARTESIAN_POINT ( 'NONE',  ( 15.80617190586769283, -15.72974639402175789, 105.6260903946856899 ) ) ;
#177687 = CARTESIAN_POINT ( 'NONE',  ( -8.224510206698735004, -14.34966873604973081, 64.58442372801900433 ) ) ;
#177688 = CARTESIAN_POINT ( 'NONE',  ( 9.564922557960805705, 16.46253265017160317, 109.5822429386476955 ) ) ;
#177689 = CARTESIAN_POINT ( 'NONE',  ( 18.67979575497178502, 10.72451020669898547, 89.16557627198102409 ) ) ;
#177690 = CARTESIAN_POINT ( 'NONE',  ( 16.55341960407611168, 4.379528057220329451, 48.95724293864770971 ) ) ;
#177691 = CARTESIAN_POINT ( 'NONE',  ( -13.97604488694527625, -13.89961937509977652, 41.87390960531435979 ) ) ;
#177692 = CARTESIAN_POINT ( 'NONE',  ( -4.379528057220328563, 16.55341960407611168, 70.20724293864769550 ) ) ;
#177693 = CARTESIAN_POINT ( 'NONE',  ( -15.80617190586745835, -15.72974639402198527, 36.87390960531435979 ) ) ;
#177694 = CARTESIAN_POINT ( 'NONE',  ( 21.55341960407610458, 5.719274019375980345, 28.95724293864769905 ) ) ;
#177695 = CARTESIAN_POINT ( 'NONE',  ( -0.05219959533936034679, 19.03943276465977164, 27.50109039468566507 ) ) ;
#177696 = EDGE_CURVE ( 'NONE', #83841, #139003, #131611, .T. ) ;
#177697 = CARTESIAN_POINT ( 'NONE',  ( 16.55341960407611168, 4.379528057220329451, 98.95724293864770971 ) ) ;
#177698 = CARTESIAN_POINT ( 'NONE',  ( 16.51473224551069308, 9.474510206698969483, 104.1655762719810241 ) ) ;
#177699 = ORIENTED_EDGE ( 'NONE', *, *, #68776, .F. ) ;
#177700 = CARTESIAN_POINT ( 'NONE',  ( 16.52544592524335698, 4.483927247898782831, 51.45942372801901854 ) ) ;
#177701 = CARTESIAN_POINT ( 'NONE',  ( -16.46253265017160317, 9.564922557960807481, 60.83224293864769550 ) ) ;
#177702 = CARTESIAN_POINT ( 'NONE',  ( 17.14385361876520264, 23.59649016807275856, 140.1750000027311671 ) ) ;
#177703 = CARTESIAN_POINT ( 'NONE',  ( -13.97604488694547697, 13.89961937509957934, 58.12609039468566863 ) ) ;
#177704 = CARTESIAN_POINT ( 'NONE',  ( 4.379528057220092307, 16.55341960407617563, 87.29275706135236135 ) ) ;
#177705 = CARTESIAN_POINT ( 'NONE',  ( -0.05219959533936034679, 19.03943276465977164, 92.50109039468566152 ) ) ;
#177706 = CARTESIAN_POINT ( 'NONE',  ( -18.67979575497193778, 10.72451020669871902, 63.33442372801900433 ) ) ;
#177707 = CARTESIAN_POINT ( 'NONE',  ( 19.05341960407611168, 5.049401038298154454, 78.95724293864769550 ) ) ;
#177708 = CARTESIAN_POINT ( 'NONE',  ( 10.72451020669898902, -18.67979575497178502, 92.91557627198103830 ) ) ;
#177709 = CARTESIAN_POINT ( 'NONE',  ( 14.29746914071049879, -8.314922557960816363, 113.3322429386476955 ) ) ;
#177710 = CARTESIAN_POINT ( 'NONE',  ( 16.51473224551083163, -9.474510206698727899, 75.83442372801900433 ) ) ;
#177711 = CARTESIAN_POINT ( 'NONE',  ( 10.72451020669898902, -18.67979575497178502, 72.91557627198103830 ) ) ;
#177712 = CARTESIAN_POINT ( 'NONE',  ( 9.474510206698729675, 16.51473224551082808, 47.08442372801900433 ) ) ;
#177713 = CARTESIAN_POINT ( 'NONE',  ( 18.87255363501904526, 5.500000000000004441, 98.82513748171830059 ) ) ;
#177714 = CARTESIAN_POINT ( 'NONE',  ( 18.62759615963271287, -10.81492255796078972, 93.33224293864769550 ) ) ;
#177715 = CARTESIAN_POINT ( 'NONE',  ( 17.50000000000003553, 4.049696124445843814, 28.31960329334057391 ) ) ;
#177716 = CARTESIAN_POINT ( 'NONE',  ( -19.03943276465977164, 0.05219959533909376836, 66.24890960531436690 ) ) ;
#177717 = DIRECTION ( 'NONE',  ( 0.000000000000000000, 1.000000000000000000, 0.000000000000000000 ) ) ;
#177718 = CARTESIAN_POINT ( 'NONE',  ( 19.03943276465977164, 0.05219959533936151252, 111.2510903946856757 ) ) ;
#177719 = CARTESIAN_POINT ( 'NONE',  ( 36.86570815857407268, -2.439361326604236879, 49.93277065412544857 ) ) ;
#177720 = CARTESIAN_POINT ( 'NONE',  ( -16.51473224551069308, -9.474510206698971260, 46.66557627198102409 ) ) ;
#177722 = CARTESIAN_POINT ( 'NONE',  ( -16.55341960407611168, -4.379528057220339221, 51.45724293864770260 ) ) ;
#177721 = CARTESIAN_POINT ( 'NONE',  ( -5.823673210054116645, -21.52544592524344225, 102.2905762719810383 ) ) ;
#177723 = CARTESIAN_POINT ( 'NONE',  ( 9.564922557960805705, 16.46253265017160317, 59.58224293864769550 ) ) ;
#177724 = CARTESIAN_POINT ( 'NONE',  ( 5.719274019375673035, 21.55341960407619339, 72.29275706135236135 ) ) ;
#177726 = CARTESIAN_POINT ( 'NONE',  ( 16.46253265017146816, 9.564922557961045513, 26.66775706135234003 ) ) ;
#177725 = CARTESIAN_POINT ( 'NONE',  ( -0.05219959533934338120, 16.53943276465976808, 22.50109039468567573 ) ) ;
#177727 = CARTESIAN_POINT ( 'NONE',  ( 8.314922557960818139, 14.29746914071049879, 24.58224293864768839 ) ) ;
#177728 = CARTESIAN_POINT ( 'NONE',  ( -15.80617190586768217, 15.72974639402176855, 43.12609039468568284 ) ) ;
#177729 = CARTESIAN_POINT ( 'NONE',  ( -10.72451020669870658, -18.67979575497194134, 19.58442372801901143 ) ) ;
#177730 = CARTESIAN_POINT ( 'NONE',  ( 10.81492255796078972, 18.62759615963270932, 59.58224293864770260 ) ) ;
#177731 = CARTESIAN_POINT ( 'NONE',  ( 16.51473224551083163, -9.474510206698727899, 95.83442372801900433 ) ) ;
#177732 = CARTESIAN_POINT ( 'NONE',  ( -16.51473224551082808, 9.474510206698731452, 73.33442372801900433 ) ) ;
#177733 = CARTESIAN_POINT ( 'NONE',  ( 21.53943276465977519, 0.05219959533937863772, 66.25109039468567573 ) ) ;
#177734 = CARTESIAN_POINT ( 'NONE',  ( -19.03943276465977164, -0.05219959533935918106, 58.75109039468566863 ) ) ;
#177735 = CARTESIAN_POINT ( 'NONE',  ( -14.29746914071049879, 8.314922557960819915, 115.8322429386477097 ) ) ;
#177736 = CARTESIAN_POINT ( 'NONE',  ( -10.72451020669898014, 18.67979575497178502, 45.41557627198103830 ) ) ;
#177737 = CARTESIAN_POINT ( 'NONE',  ( 16.53943276465976808, -0.05219959533910856209, 53.74890960531437401 ) ) ;
#177738 = CARTESIAN_POINT ( 'NONE',  ( -19.01533133064923575, 5.499999999999444000, 93.76586590595742621 ) ) ;
#177739 = CARTESIAN_POINT ( 'NONE',  ( 18.67979575497194134, -10.72451020669871369, 110.8344237280190043 ) ) ;
#177740 = CARTESIAN_POINT ( 'NONE',  ( -12.06949235617739369, -12.14591786802326823, 89.37609039468568994 ) ) ;
#177741 = CARTESIAN_POINT ( 'NONE',  ( 16.53943276465976808, -0.05219959533910856209, 43.74890960531435979 ) ) ;
#177742 = CARTESIAN_POINT ( 'NONE',  ( 15.80617190586769283, -15.72974639402175789, 80.62609039468567573 ) ) ;
#177743 = CARTESIAN_POINT ( 'NONE',  ( -5.719274019375665041, -21.55341960407619695, 84.79275706135234714 ) ) ;
#177744 = CARTESIAN_POINT ( 'NONE',  ( -18.62759615963270932, 10.81492255796079327, 80.83224293864769550 ) ) ;
#177745 = CARTESIAN_POINT ( 'NONE',  ( 16.46253265017160672, -9.564922557960803928, 33.33224293864770260 ) ) ;
#177746 = CARTESIAN_POINT ( 'NONE',  ( -18.62759615963255300, -10.81492255796106328, 59.16775706135234714 ) ) ;
#177747 = CARTESIAN_POINT ( 'NONE',  ( 5.153800228976335163, 19.02544592524342804, 39.79057627198100988 ) ) ;
#177748 = CARTESIAN_POINT ( 'NONE',  ( 0.05219959533909260263, 19.03943276465977164, 54.99890960531435979 ) ) ;
#177749 = CARTESIAN_POINT ( 'NONE',  ( 12.14591786802309770, 12.06949235617756955, 89.37390960531435269 ) ) ;
#177750 = CARTESIAN_POINT ( 'NONE',  ( 0.05219959533909260263, 19.03943276465977164, 99.99890960531436690 ) ) ;
#177751 = CARTESIAN_POINT ( 'NONE',  ( 16.55341960407611168, 4.379528057220329451, 38.95724293864768839 ) ) ;
#177752 = CARTESIAN_POINT ( 'NONE',  ( -12.06949235617756955, 12.14591786802309770, 115.6239096053143669 ) ) ;
#177753 = CARTESIAN_POINT ( 'NONE',  ( 10.72451020669898902, -18.67979575497178502, 77.91557627198102409 ) ) ;
#177754 = CARTESIAN_POINT ( 'NONE',  ( 5.719274019375673035, 21.55341960407619339, 22.29275706135235069 ) ) ;
#177755 = CARTESIAN_POINT ( 'NONE',  ( 27.96779038917892279, -7.241162895362543317, 160.9774814432333869 ) ) ;
#177756 = CARTESIAN_POINT ( 'NONE',  ( 12.06949235617739724, 12.14591786802326823, 26.87609039468567218 ) ) ;
#177757 = CARTESIAN_POINT ( 'NONE',  ( -10.81492255796078084, -18.62759615963271287, 72.08224293864769550 ) ) ;
#177758 = CARTESIAN_POINT ( 'NONE',  ( 15.72974639402176855, 15.80617190586768217, 96.87609039468568994 ) ) ;
#177759 = CARTESIAN_POINT ( 'NONE',  ( -16.51473224551069308, -9.474510206698971260, 76.66557627198103830 ) ) ;
#177760 = CARTESIAN_POINT ( 'NONE',  ( 18.67979575497194134, -10.72451020669871369, 35.83442372801901143 ) ) ;
#177761 = CARTESIAN_POINT ( 'NONE',  ( -16.51473224551069308, -9.474510206698971260, 111.6655762719810383 ) ) ;
#177762 = CARTESIAN_POINT ( 'NONE',  ( 4.483927247898790824, -16.52544592524335698, 95.20942372801903275 ) ) ;
#177763 = CARTESIAN_POINT ( 'NONE',  ( -15.72974639402176322, -15.80617190586768395, 69.37609039468567573 ) ) ;
#177764 = CARTESIAN_POINT ( 'NONE',  ( -13.97604488694547697, 13.89961937509957934, 23.12609039468565442 ) ) ;
#177765 = CARTESIAN_POINT ( 'NONE',  ( -4.379528057220086978, -16.55341960407618274, 69.79275706135234714 ) ) ;
#177766 = CARTESIAN_POINT ( 'NONE',  ( -15.72974639402176322, -15.80617190586768395, 29.37609039468568284 ) ) ;
#177767 = CARTESIAN_POINT ( 'NONE',  ( 9.474510206698971260, -16.51473224551069308, 37.91557627198102409 ) ) ;
#177768 = CARTESIAN_POINT ( 'NONE',  ( 15.80617190586769283, -15.72974639402175789, 95.62609039468568994 ) ) ;
#177769 = CARTESIAN_POINT ( 'NONE',  ( 19.05341960407611168, 5.049401038298154454, 88.95724293864769550 ) ) ;
#177770 = CARTESIAN_POINT ( 'NONE',  ( 18.67979575497178502, 10.72451020669898547, 94.16557627198103830 ) ) ;
#177772 = CARTESIAN_POINT ( 'NONE',  ( 5.823673210054125526, 21.52544592524343514, 49.79057627198102409 ) ) ;
#177771 = FACE_OUTER_BOUND ( 'NONE', #55997, .T. ) ;
#177774 = CARTESIAN_POINT ( 'NONE',  ( 14.34966873604960469, 8.224510206698951720, 49.16557627198102409 ) ) ;
#177773 = CARTESIAN_POINT ( 'NONE',  ( 13.97604488694527802, 13.89961937509977652, 94.37390960531436690 ) ) ;
#177775 = CARTESIAN_POINT ( 'NONE',  ( 21.94566984220702466, 7.593969325705130835, 169.8906363267649056 ) ) ;
#177776 = CARTESIAN_POINT ( 'NONE',  ( -13.97604488694547697, 13.89961937509957934, 83.12609039468564731 ) ) ;
#177777 = CARTESIAN_POINT ( 'NONE',  ( -17.40805194822031510, 6.112264579159328193, 105.8337127251061105 ) ) ;
#177778 = CARTESIAN_POINT ( 'NONE',  ( -13.97604488694547697, 13.89961937509957934, 108.1260903946856331 ) ) ;
#177779 = CARTESIAN_POINT ( 'NONE',  ( 10.81492255796078972, 18.62759615963270932, 79.58224293864769550 ) ) ;
#177780 = CARTESIAN_POINT ( 'NONE',  ( -16.52544592524342804, 4.483927247898546575, 61.04057627198103120 ) ) ;
#177781 = CARTESIAN_POINT ( 'NONE',  ( 9.474510206698971260, -16.51473224551069308, 102.9155762719810241 ) ) ;
#177782 = CARTESIAN_POINT ( 'NONE',  ( 8.224510206698742110, 14.34966873604972548, 47.08442372801901854 ) ) ;
#177783 = CARTESIAN_POINT ( 'NONE',  ( -13.97604488694527625, -13.89961937509977652, 61.87390960531435979 ) ) ;
#177785 = CARTESIAN_POINT ( 'NONE',  ( -13.89961937509957401, -13.97604488694547875, 94.37609039468566152 ) ) ;
#177784 = CARTESIAN_POINT ( 'NONE',  ( -18.62759615963255300, -10.81492255796106328, 29.16775706135234003 ) ) ;
#177786 = CARTESIAN_POINT ( 'NONE',  ( 19.03943276465977164, -0.05219959533909143690, 93.74890960531435269 ) ) ;
#177787 = CARTESIAN_POINT ( 'NONE',  ( 5.049401038298161559, -19.05341960407611168, 82.70724293864770971 ) ) ;
#177788 = CARTESIAN_POINT ( 'NONE',  ( 21.52544592524344225, -5.823673210054117533, 73.54057627198102409 ) ) ;
#177789 = CARTESIAN_POINT ( 'NONE',  ( 5.153800228976335163, 19.02544592524342804, 49.79057627198100988 ) ) ;
#177790 = CARTESIAN_POINT ( 'NONE',  ( 22.93331243197825131, 29.30057843794256911, -8.000000000000003553 ) ) ;
#177791 = CARTESIAN_POINT ( 'NONE',  ( -12.14591786802309592, -12.06949235617757132, 71.87390960531438111 ) ) ;
#177792 = CARTESIAN_POINT ( 'NONE',  ( -5.049401038298153566, 19.05341960407611168, 100.2072429386476955 ) ) ;
#177793 = CARTESIAN_POINT ( 'NONE',  ( 28.82186960331498327, 2.781578969918950771E-14, 145.0000000000000000 ) ) ;
#177794 = CARTESIAN_POINT ( 'NONE',  ( -16.46253265017146816, -9.564922557961047289, 69.16775706135233293 ) ) ;
#177795 = CARTESIAN_POINT ( 'NONE',  ( -5.823673210054116645, -21.52544592524344225, 92.29057627198103830 ) ) ;
#177796 = CARTESIAN_POINT ( 'NONE',  ( -9.564922557961040184, 16.46253265017147172, 47.91775706135233293 ) ) ;
#177797 = CARTESIAN_POINT ( 'NONE',  ( -19.03943276465977164, 0.05219959533909376836, 96.24890960531436690 ) ) ;
#177798 = CARTESIAN_POINT ( 'NONE',  ( 19.39056639909674473, 5.500000000000053291, 68.28948781074343799 ) ) ;
#177799 = CARTESIAN_POINT ( 'NONE',  ( -5.823673210054116645, -21.52544592524344225, 47.29057627198103120 ) ) ;
#177800 = VECTOR ( 'NONE', #159252, 1000.000000000000000 ) ;
#177801 = CARTESIAN_POINT ( 'NONE',  ( -9.474510206698964154, 16.51473224551069663, 90.41557627198103830 ) ) ;
#177802 = CARTESIAN_POINT ( 'NONE',  ( 21.52544592524334988, 5.823673210054432836, 66.45942372801903275 ) ) ;
#177803 = CARTESIAN_POINT ( 'NONE',  ( -9.564922557960796823, -16.46253265017161027, 42.08224293864769550 ) ) ;
#177804 = CARTESIAN_POINT ( 'NONE',  ( 16.52544592524342804, -4.483927247898539470, 68.54057627198103830 ) ) ;
#177805 = CARTESIAN_POINT ( 'NONE',  ( -16.55341960407617563, 4.379528057220093196, 23.54275706135235424 ) ) ;
#177806 = CARTESIAN_POINT ( 'NONE',  ( -0.05219959533937732626, 21.53943276465977519, 57.50109039468568994 ) ) ;
#177807 = ORIENTED_EDGE ( 'NONE', *, *, #130358, .F. ) ;
#177808 = CARTESIAN_POINT ( 'NONE',  ( -5.153800228976328057, -19.02544592524343514, 112.2905762719810099 ) ) ;
#177809 = CARTESIAN_POINT ( 'NONE',  ( 5.153800228976615827, -19.02544592524334988, 60.20942372801899012 ) ) ;
#177810 = DIRECTION ( 'NONE',  ( -6.938893903907246521E-15, -0.000000000000000000, -1.000000000000000000 ) ) ;
#177811 = CARTESIAN_POINT ( 'NONE',  ( 18.67979575497194134, -10.72451020669871369, 25.83442372801901499 ) ) ;
#177812 = CARTESIAN_POINT ( 'NONE',  ( -9.474510206698964154, 16.51473224551069663, 55.41557627198103120 ) ) ;
#177813 = CARTESIAN_POINT ( 'NONE',  ( -11.74264578624800670, 36.14014761921585972, -8.149999994537626691 ) ) ;
#177814 = CARTESIAN_POINT ( 'NONE',  ( -5.049401038297874678, -19.05341960407617918, 19.79275706135233293 ) ) ;
#177815 = CARTESIAN_POINT ( 'NONE',  ( -19.02544592524342804, 5.153800228976336051, 46.04057627198101699 ) ) ;
#177816 = CARTESIAN_POINT ( 'NONE',  ( 15.80617190586769283, -15.72974639402175789, 105.6260903946856899 ) ) ;
#177817 = CARTESIAN_POINT ( 'NONE',  ( 4.379528057220092307, 16.55341960407617563, 97.29275706135234714 ) ) ;
#177819 = CARTESIAN_POINT ( 'NONE',  ( 15.80617190586769283, -15.72974639402175789, 75.62609039468567573 ) ) ;
#177818 = CARTESIAN_POINT ( 'NONE',  ( -9.474510206698964154, 16.51473224551069663, 100.4155762719810241 ) ) ;
#177820 = CARTESIAN_POINT ( 'NONE',  ( 27.73933785331498569, 2.768321779492822058E-14, 148.3750000027311842 ) ) ;
#177821 = CARTESIAN_POINT ( 'NONE',  ( -5.153800228976328057, -19.02544592524343514, 107.2905762719810383 ) ) ;
#177822 = CARTESIAN_POINT ( 'NONE',  ( 69.65682714487590488, -71.74905178543389184, -23.00000000000000000 ) ) ;
#177824 = CARTESIAN_POINT ( 'NONE',  ( 21.53943276465977519, 0.05219959533937863772, 66.25109039468567573 ) ) ;
#177823 = CARTESIAN_POINT ( 'NONE',  ( 14.29746914071037800, 8.314922557961029526, 66.66775706135234714 ) ) ;
#177825 = CARTESIAN_POINT ( 'NONE',  ( 0.05219959533937995610, -21.53943276465977519, 100.0010903946857042 ) ) ;
#177826 = CARTESIAN_POINT ( 'NONE',  ( -24.30000000000003268, 2.668083032619853614E-13, -64.92279855667830191 ) ) ;
#177827 = CARTESIAN_POINT ( 'NONE',  ( 4.379528057220092307, 16.55341960407617563, 47.29275706135234003 ) ) ;
#177828 = CARTESIAN_POINT ( 'NONE',  ( -16.51473224551069308, -9.474510206698971260, 86.66557627198102409 ) ) ;
#177829 = EDGE_CURVE ( 'NONE', #185456, #114656, #148535, .T. ) ;
#177830 = CARTESIAN_POINT ( 'NONE',  ( -5.049401038298153566, 19.05341960407611168, 115.2072429386477097 ) ) ;
#177831 = ORIENTED_EDGE ( 'NONE', *, *, #74445, .F. ) ;
#177832 = DIRECTION ( 'NONE',  ( 0.000000000000000000, 0.000000000000000000, 1.000000000000000000 ) ) ;
#177833 = CARTESIAN_POINT ( 'NONE',  ( -9.564922557960796823, -16.46253265017161027, 42.08224293864769550 ) ) ;
#177834 = CARTESIAN_POINT ( 'NONE',  ( -5.719274019375978568, 21.55341960407610458, 45.20724293864769550 ) ) ;
#177835 = CARTESIAN_POINT ( 'NONE',  ( -8.224510206698735004, -14.34966873604973081, 99.58442372801900433 ) ) ;
#177837 = CARTESIAN_POINT ( 'NONE',  ( 13.89961937509977652, -13.97604488694527269, 78.12390960531433848 ) ) ;
#177836 = CARTESIAN_POINT ( 'NONE',  ( -0.05219959533910754901, -16.53943276465976808, 82.49890960531436690 ) ) ;
#177838 = CARTESIAN_POINT ( 'NONE',  ( 10.72451020669871369, 18.67979575497193778, 102.0844237280190185 ) ) ;
#177839 = CARTESIAN_POINT ( 'NONE',  ( -0.05219959533909027116, -19.03943276465977164, 32.49890960531435979 ) ) ;
#177840 = CARTESIAN_POINT ( 'NONE',  ( 16.53943276465976808, -0.05219959533910856209, 88.74890960531436690 ) ) ;
#177841 = CARTESIAN_POINT ( 'NONE',  ( 5.823673210054444382, -21.52544592524334988, 45.20942372801901854 ) ) ;
#177842 = CARTESIAN_POINT ( 'NONE',  ( 5.823673210054125526, 21.52544592524343514, 89.79057627198103830 ) ) ;
#177843 = CARTESIAN_POINT ( 'NONE',  ( -16.51473224551082808, 9.474510206698731452, 48.33442372801900433 ) ) ;
#177844 = CARTESIAN_POINT ( 'NONE',  ( 30.82560697742735201, 2.428612866367529932E-14, 150.0000000000000000 ) ) ;
#177845 = CARTESIAN_POINT ( 'NONE',  ( -9.474510206698964154, 16.51473224551069663, 95.41557627198102409 ) ) ;
#177846 = CARTESIAN_POINT ( 'NONE',  ( 4.379528057220339221, -16.55341960407611168, 57.70724293864770260 ) ) ;
#177847 = CARTESIAN_POINT ( 'NONE',  ( 14.29746914071049879, -8.314922557960816363, 53.33224293864769550 ) ) ;
#177848 = CARTESIAN_POINT ( 'NONE',  ( 16.53943276465976808, -0.05219959533910856209, 28.74890960531435624 ) ) ;
#177849 = CARTESIAN_POINT ( 'NONE',  ( 19.02544592524334988, 5.153800228976608722, 76.45942372801897591 ) ) ;
#177850 = CARTESIAN_POINT ( 'NONE',  ( -19.02130022317637525, 5.499999999999802824, 85.78188669246577547 ) ) ;
#177851 = CARTESIAN_POINT ( 'NONE',  ( 21.53943276465977519, -0.05219959533907433946, 28.74890960531435624 ) ) ;
#177852 = CARTESIAN_POINT ( 'NONE',  ( -8.224510206698948167, 14.34966873604960824, 90.41557627198103830 ) ) ;
#177853 = CARTESIAN_POINT ( 'NONE',  ( -17.50000000000004619, -4.049696124445705259, 25.81960329334050641 ) ) ;
#177855 = CARTESIAN_POINT ( 'NONE',  ( 5.719274019375991003, -21.55341960407610458, 52.70724293864769550 ) ) ;
#177854 = CARTESIAN_POINT ( 'NONE',  ( -19.02544592524342804, 5.153800228976336051, 46.04057627198101699 ) ) ;
#177856 = CARTESIAN_POINT ( 'NONE',  ( -9.564922557960796823, -16.46253265017161027, 32.08224293864769550 ) ) ;
#177858 = CARTESIAN_POINT ( 'NONE',  ( 9.564922557960805705, 16.46253265017160317, 59.58224293864769550 ) ) ;
#177857 = CARTESIAN_POINT ( 'NONE',  ( 0.05219959533934541429, -16.53943276465976808, 80.00109039468568994 ) ) ;
#177859 = CARTESIAN_POINT ( 'NONE',  ( -19.02544592524334988, -5.153800228976617603, 33.95942372801897591 ) ) ;
#177860 = CARTESIAN_POINT ( 'NONE',  ( 5.823673210054444382, -21.52544592524334988, 65.20942372801901854 ) ) ;
#177861 = CARTESIAN_POINT ( 'NONE',  ( 0.05219959533907565091, 21.53943276465977519, 29.99890960531435979 ) ) ;
#177862 = CARTESIAN_POINT ( 'NONE',  ( -8.314922557960811034, -14.29746914071050412, 112.0822429386477097 ) ) ;
#177863 = CARTESIAN_POINT ( 'NONE',  ( 0.05219959533936267826, -19.03943276465977164, 90.00109039468567573 ) ) ;
#177864 = CARTESIAN_POINT ( 'NONE',  ( -36.91746825000000598, -11.99521256947794789, -3.024999997268813079 ) ) ;
#177866 = CARTESIAN_POINT ( 'NONE',  ( 5.823673210054125526, 21.52544592524343514, 49.79057627198102409 ) ) ;
#177865 = CYLINDRICAL_SURFACE ( 'NONE', #73392, 7.500000000000007105 ) ;
#177867 = CARTESIAN_POINT ( 'NONE',  ( 9.564922557960805705, 16.46253265017160317, 24.58224293864769194 ) ) ;
#177868 = CARTESIAN_POINT ( 'NONE',  ( -18.62759615963255300, -10.81492255796106328, 84.16775706135234714 ) ) ;
#177869 = ORIENTED_EDGE ( 'NONE', *, *, #79473, .T. ) ;
#177870 = CARTESIAN_POINT ( 'NONE',  ( -14.34966873604960291, -8.224510206698953496, 51.66557627198102409 ) ) ;
#177872 = CARTESIAN_POINT ( 'NONE',  ( -12.14591786802309592, -12.06949235617757132, 51.87390960531437401 ) ) ;
#177871 = CARTESIAN_POINT ( 'NONE',  ( 14.34966873604972726, -8.224510206698740333, 65.83442372801900433 ) ) ;
#177873 = CARTESIAN_POINT ( 'NONE',  ( -10.81492255796078084, -18.62759615963271287, 77.08224293864769550 ) ) ;
#177874 = CARTESIAN_POINT ( 'NONE',  ( -10.81492255796078084, -18.62759615963271287, 77.08224293864769550 ) ) ;
#177875 = CARTESIAN_POINT ( 'NONE',  ( 0.000000000000000000, 0.000000000000000000, -59.13370768023891344 ) ) ;
#177876 = CARTESIAN_POINT ( 'NONE',  ( 19.05341960407611168, 5.049401038298154454, 108.9572429386477097 ) ) ;
#177877 = CARTESIAN_POINT ( 'NONE',  ( -8.314922557960811034, -14.29746914071050412, 77.08224293864769550 ) ) ;
#177878 = CARTESIAN_POINT ( 'NONE',  ( -0.05219959533909027116, -19.03943276465977164, 62.49890960531435979 ) ) ;
#177879 = CARTESIAN_POINT ( 'NONE',  ( -19.02544592524342804, 5.153800228976336051, 36.04057627198100988 ) ) ;
#177880 =( LENGTH_UNIT ( ) NAMED_UNIT ( * ) SI_UNIT ( .MILLI., .METRE. ) );
#177881 = CARTESIAN_POINT ( 'NONE',  ( -3.573655867282028392E-15, 2.428612866367529932E-14, 6.432029388270255055E-14 ) ) ;
#177882 = CARTESIAN_POINT ( 'NONE',  ( 16.52544592524335698, 4.483927247898782831, 76.45942372801901854 ) ) ;
#177883 = CARTESIAN_POINT ( 'NONE',  ( -10.72451020669898014, 18.67979575497178502, 115.4155762719810241 ) ) ;
#177884 = CARTESIAN_POINT ( 'NONE',  ( -16.46253265017160317, 9.564922557960807481, 70.83224293864770971 ) ) ;
#177885 = CARTESIAN_POINT ( 'NONE',  ( -18.67979575497193778, 10.72451020669871902, 58.33442372801901143 ) ) ;
#177886 = CARTESIAN_POINT ( 'NONE',  ( -19.05341960407611168, -5.049401038298163336, 111.4572429386476671 ) ) ;
#177887 = CARTESIAN_POINT ( 'NONE',  ( -9.128739734652899784, -39.45218800495356248, -25.46847458086992333 ) ) ;
#177888 = ORIENTED_EDGE ( 'NONE', *, *, #135199, .F. ) ;
#177889 = CARTESIAN_POINT ( 'NONE',  ( 15.72974639402176855, 15.80617190586768217, 46.87609039468568994 ) ) ;
#177891 = CARTESIAN_POINT ( 'NONE',  ( 9.474510206698971260, -16.51473224551069308, 107.9155762719810383 ) ) ;
#177890 = CARTESIAN_POINT ( 'NONE',  ( 16.46253265017160672, -9.564922557960803928, 28.33224293864769550 ) ) ;
#177892 = CARTESIAN_POINT ( 'NONE',  ( -13.97604488694547697, 13.89961937509957934, 53.12609039468565442 ) ) ;
#177893 = CARTESIAN_POINT ( 'NONE',  ( 18.62759615963271287, -10.81492255796078972, 113.3322429386476955 ) ) ;
#177894 = CARTESIAN_POINT ( 'NONE',  ( 0.05219959533936267826, -19.03943276465977164, 40.00109039468566152 ) ) ;
#177895 = CARTESIAN_POINT ( 'NONE',  ( 16.51473224551083163, -9.474510206698727899, 50.83442372801899722 ) ) ;
#177896 = CARTESIAN_POINT ( 'NONE',  ( 8.314922557961029526, -14.29746914071037800, 100.4177570613523471 ) ) ;
#177898 = ORIENTED_EDGE ( 'NONE', *, *, #149044, .T. ) ;
#177897 = DIRECTION ( 'NONE',  ( 0.000000000000000000, 0.000000000000000000, -1.000000000000000000 ) ) ;
#177899 = CARTESIAN_POINT ( 'NONE',  ( -5.153800228976328057, -19.02544592524343514, 82.29057627198103830 ) ) ;
#177900 = CARTESIAN_POINT ( 'NONE',  ( -18.67979575497193778, 10.72451020669871902, 73.33442372801901854 ) ) ;
#177902 = EDGE_CURVE ( 'NONE', #82312, #67859, #57450, .T. ) ;
#177901 = CARTESIAN_POINT ( 'NONE',  ( -15.80617190586768217, 15.72974639402176855, 88.12609039468570415 ) ) ;
#177903 = CARTESIAN_POINT ( 'NONE',  ( 23.94081952771230704, -0.9791052130474939830, -54.49391133501600137 ) ) ;
#177904 = CARTESIAN_POINT ( 'NONE',  ( 9.474510206698971260, -16.51473224551069308, 97.91557627198102409 ) ) ;
#177905 = CARTESIAN_POINT ( 'NONE',  ( 21.55341960407619695, -5.719274019375665929, 71.04275706135234714 ) ) ;
#177906 = CARTESIAN_POINT ( 'NONE',  ( -14.29746914071037622, -8.314922557961029526, 24.16775706135235424 ) ) ;
#177907 = CARTESIAN_POINT ( 'NONE',  ( -19.03943276465977164, 0.05219959533909376836, 76.24890960531435269 ) ) ;
#177908 = CARTESIAN_POINT ( 'NONE',  ( -5.719274019375978568, 21.55341960407610458, 25.20724293864769550 ) ) ;
#177909 = CARTESIAN_POINT ( 'NONE',  ( 19.05341960407611168, 5.049401038298154454, 98.95724293864766707 ) ) ;
#177910 = CARTESIAN_POINT ( 'NONE',  ( 9.474510206698729675, 16.51473224551082808, 87.08442372801900433 ) ) ;
#177911 = CARTESIAN_POINT ( 'NONE',  ( -9.564922557960796823, -16.46253265017161027, 77.08224293864769550 ) ) ;
#177912 = CARTESIAN_POINT ( 'NONE',  ( 9.564922557960805705, 16.46253265017160317, 64.58224293864769550 ) ) ;
#177913 = CARTESIAN_POINT ( 'NONE',  ( 18.62759615963271287, -10.81492255796078972, 108.3322429386477097 ) ) ;
#177914 = CARTESIAN_POINT ( 'NONE',  ( 16.53943276465976808, 0.05219959533934440121, 96.25109039468568994 ) ) ;
#177915 = CARTESIAN_POINT ( 'NONE',  ( 7.220908937440010611, -2.044528755335700776, 8.410814283099846023 ) ) ;
#177916 = CARTESIAN_POINT ( 'NONE',  ( 13.89961937509957401, 13.97604488694547697, 51.87609039468566863 ) ) ;
#177917 = CARTESIAN_POINT ( 'NONE',  ( -0.05219959533909027116, -19.03943276465977164, 97.49890960531436690 ) ) ;
#177918 = CARTESIAN_POINT ( 'NONE',  ( -16.52544592524342804, 4.483927247898546575, 91.04057627198103830 ) ) ;
#177919 = CARTESIAN_POINT ( 'NONE',  ( 15.72974639402199770, -15.80617190586745480, 33.12390960531435979 ) ) ;
#177920 = CARTESIAN_POINT ( 'NONE',  ( -0.05219959533907301413, -21.53943276465977519, 27.49890960531435269 ) ) ;
#177921 = CARTESIAN_POINT ( 'NONE',  ( -12.14591786802309592, -12.06949235617757132, 91.87390960531436690 ) ) ;
#177922 = CARTESIAN_POINT ( 'NONE',  ( -16.36317988757058473, 7.306389748694923192, 54.09789608363225000 ) ) ;
#177923 = CARTESIAN_POINT ( 'NONE',  ( -19.03943276465977164, -0.05219959533935918106, 38.75109039468566152 ) ) ;
#177924 = CARTESIAN_POINT ( 'NONE',  ( -8.224510206698735004, -14.34966873604973081, 104.5844237280190185 ) ) ;
#177925 = CARTESIAN_POINT ( 'NONE',  ( 5.153800228976335163, 19.02544592524342804, 84.79057627198099567 ) ) ;
#177926 = CARTESIAN_POINT ( 'NONE',  ( -18.67979575497193778, 10.72451020669871902, 68.33442372801900433 ) ) ;
#177927 = CARTESIAN_POINT ( 'NONE',  ( 10.72451020669898902, -18.67979575497178502, 62.91557627198102409 ) ) ;
#177929 = EDGE_LOOP ( 'NONE', ( #112174, #180573, #5451, #68097 ) ) ;
#177928 = CARTESIAN_POINT ( 'NONE',  ( 21.52544592524334988, 5.823673210054432836, 36.45942372801901143 ) ) ;
#177930 = CARTESIAN_POINT ( 'NONE',  ( 21.55341960407610458, 5.719274019375980345, 83.95724293864770971 ) ) ;
#177931 = CARTESIAN_POINT ( 'NONE',  ( 14.29746914071049879, -8.314922557960816363, 103.3322429386476955 ) ) ;
#177932 = CARTESIAN_POINT ( 'NONE',  ( -16.46253265017146816, -9.564922557961047289, 74.16775706135234714 ) ) ;
#177933 = CARTESIAN_POINT ( 'NONE',  ( -19.03943276465977164, 0.05219959533909376836, 51.24890960531436690 ) ) ;
#177934 = CARTESIAN_POINT ( 'NONE',  ( -16.51473224551069308, -9.474510206698971260, 101.6655762719810241 ) ) ;
#177935 = CARTESIAN_POINT ( 'NONE',  ( -19.02544592524342804, 5.153800228976336051, 91.04057627198100988 ) ) ;
#177936 = CARTESIAN_POINT ( 'NONE',  ( -16.51473224551069308, -9.474510206698971260, 21.66557627198102765 ) ) ;
#177937 = CARTESIAN_POINT ( 'NONE',  ( -0.05219959533910754901, -16.53943276465976808, 37.49890960531436690 ) ) ;
#177938 = CARTESIAN_POINT ( 'NONE',  ( 16.53943276465976808, 0.05219959533934440121, 46.25109039468567573 ) ) ;
#177939 = CARTESIAN_POINT ( 'NONE',  ( 15.72974639402176855, 15.80617190586768217, 101.8760903946857042 ) ) ;
#177941 = CARTESIAN_POINT ( 'NONE',  ( -0.05219959533934338120, 16.53943276465976808, 112.5010903946857042 ) ) ;
#177940 = CARTESIAN_POINT ( 'NONE',  ( 19.02544592524343514, -5.153800228976328945, 113.5405762719810241 ) ) ;
#177942 = CARTESIAN_POINT ( 'NONE',  ( -10.81492255796105439, 18.62759615963255655, 32.91775706135234714 ) ) ;
#177943 = CARTESIAN_POINT ( 'NONE',  ( 19.03943276465977164, -0.05219959533909143690, 98.74890960531436690 ) ) ;
#177944 = CARTESIAN_POINT ( 'NONE',  ( 16.52544592524335698, 4.483927247898782831, 101.4594237280190185 ) ) ;
#177945 = CARTESIAN_POINT ( 'NONE',  ( -14.29746914071037622, -8.314922557961029526, 99.16775706135234714 ) ) ;
#177946 = CARTESIAN_POINT ( 'NONE',  ( 12.06949235617739724, 12.14591786802326823, 26.87609039468567218 ) ) ;
#177947 = CARTESIAN_POINT ( 'NONE',  ( 19.02544592524343514, -5.153800228976328945, 48.54057627198103120 ) ) ;
#177948 = CARTESIAN_POINT ( 'NONE',  ( -14.29746914071049879, 8.314922557960819915, 105.8322429386476955 ) ) ;
#177949 = CARTESIAN_POINT ( 'NONE',  ( -21.52544592524343514, 5.823673210054127303, 116.0405762719810383 ) ) ;
#177950 = CARTESIAN_POINT ( 'NONE',  ( -13.97604488694527625, -13.89961937509977652, 26.87390960531434558 ) ) ;
#177951 = CARTESIAN_POINT ( 'NONE',  ( -13.89961937509977652, 13.97604488694528158, 110.6239096053143243 ) ) ;
#177952 = CARTESIAN_POINT ( 'NONE',  ( -13.89961937509977652, 13.97604488694528158, 30.62390960531435269 ) ) ;
#177953 = CARTESIAN_POINT ( 'NONE',  ( 19.03943276465977164, -0.05219959533909143690, 103.7489096053143669 ) ) ;
#177954 = CARTESIAN_POINT ( 'NONE',  ( -17.48847506799970120, -5.747544572773717775, 34.17302562156721990 ) ) ;
#177955 = CARTESIAN_POINT ( 'NONE',  ( -9.474510206698964154, 16.51473224551069663, 100.4155762719810241 ) ) ;
#177957 = CARTESIAN_POINT ( 'NONE',  ( -8.314922557960811034, -14.29746914071050412, 92.08224293864769550 ) ) ;
#177956 = CARTESIAN_POINT ( 'NONE',  ( -10.72451020669870658, -18.67979575497194134, 49.58442372801901143 ) ) ;
#177958 = CARTESIAN_POINT ( 'NONE',  ( -19.02544592524342804, 5.153800228976336051, 91.04057627198100988 ) ) ;
#177959 = LINE ( 'NONE', #195126, #122466 ) ;
#177960 = CARTESIAN_POINT ( 'NONE',  ( 4.379528057220092307, 16.55341960407617563, 62.29275706135236845 ) ) ;
#177961 = CARTESIAN_POINT ( 'NONE',  ( -21.55341960407619339, 5.719274019375674811, 78.54275706135236135 ) ) ;
#177962 = CARTESIAN_POINT ( 'NONE',  ( -14.34966873604972548, 8.224510206698743886, 43.33442372801901143 ) ) ;
#177963 = CARTESIAN_POINT ( 'NONE',  ( 0.05219959533909260263, 19.03943276465977164, 84.99890960531436690 ) ) ;
#177964 = CARTESIAN_POINT ( 'NONE',  ( -13.97604488694547697, 13.89961937509957934, 113.1260903946856757 ) ) ;
#177965 = CARTESIAN_POINT ( 'NONE',  ( 14.29746914071037800, 8.314922557961029526, 86.66775706135234714 ) ) ;
#177966 = CARTESIAN_POINT ( 'NONE',  ( 16.51473224551083163, -9.474510206698727899, 95.83442372801900433 ) ) ;
#177967 = CARTESIAN_POINT ( 'NONE',  ( -0.05219959533909027116, -19.03943276465977164, 62.49890960531435979 ) ) ;
#177968 = CARTESIAN_POINT ( 'NONE',  ( 10.72451020669898902, -18.67979575497178502, 102.9155762719810383 ) ) ;
#177970 = CARTESIAN_POINT ( 'NONE',  ( 9.564922557961047289, -16.46253265017146816, 85.41775706135233293 ) ) ;
#177969 = CARTESIAN_POINT ( 'NONE',  ( -12.06949235617756955, 12.14591786802309770, 90.62390960531436690 ) ) ;
#177971 = CARTESIAN_POINT ( 'NONE',  ( 8.224510206698742110, 14.34966873604972548, 57.08442372801901854 ) ) ;
#177972 = CARTESIAN_POINT ( 'NONE',  ( 24.17640770809979855, 7.553848413212524981, 169.9412368235690565 ) ) ;
#177973 = CARTESIAN_POINT ( 'NONE',  ( -9.474510206698720793, -16.51473224551083518, 59.58442372801900433 ) ) ;
#177974 = CARTESIAN_POINT ( 'NONE',  ( -14.29746914071049879, 8.314922557960819915, 25.83224293864769194 ) ) ;
#177975 = CARTESIAN_POINT ( 'NONE',  ( -16.53943276465976808, 0.05219959533911058130, 81.24890960531436690 ) ) ;
#177977 = CARTESIAN_POINT ( 'NONE',  ( -18.39635199886970085, 5.499999999999980460, 91.01967076360000419 ) ) ;
#177976 = CARTESIAN_POINT ( 'NONE',  ( 21.53943276465977519, 0.05219959533937863772, 111.2510903946856899 ) ) ;
#177978 = CARTESIAN_POINT ( 'NONE',  ( 21.52544592524334988, 5.823673210054432836, 26.45942372801901854 ) ) ;
#177979 = CARTESIAN_POINT ( 'NONE',  ( -0.05219959533909027116, -19.03943276465977164, 112.4989096053143669 ) ) ;
#177980 = CARTESIAN_POINT ( 'NONE',  ( 5.153800228976335163, 19.02544592524342804, 74.79057627198103830 ) ) ;
#177981 = CARTESIAN_POINT ( 'NONE',  ( 0.05219959533937995610, -21.53943276465977519, 100.0010903946857042 ) ) ;
#177982 = CARTESIAN_POINT ( 'NONE',  ( -19.05341960407611168, -5.049401038298163336, 76.45724293864769550 ) ) ;
#177983 = CARTESIAN_POINT ( 'NONE',  ( -0.05219959533907301413, -21.53943276465977519, 47.49890960531435979 ) ) ;
#177984 = CARTESIAN_POINT ( 'NONE',  ( 16.55341960407611168, 4.379528057220329451, 83.95724293864770971 ) ) ;
#177985 = CARTESIAN_POINT ( 'NONE',  ( -19.03943276465977164, 0.05219959533909376836, 51.24890960531436690 ) ) ;
#177986 = CARTESIAN_POINT ( 'NONE',  ( 8.314922557960818139, 14.29746914071049879, 114.5822429386477097 ) ) ;
#177987 = CARTESIAN_POINT ( 'NONE',  ( 21.55341960407619695, -5.719274019375665929, 26.04275706135235779 ) ) ;
#177988 = CARTESIAN_POINT ( 'NONE',  ( 21.53943276465977519, 0.05219959533937863772, 61.25109039468567573 ) ) ;
#177989 = CARTESIAN_POINT ( 'NONE',  ( 16.46253265017160672, -9.564922557960803928, 43.33224293864769550 ) ) ;
#177990 = CARTESIAN_POINT ( 'NONE',  ( -12.06949235617739369, -12.14591786802326823, 79.37609039468567573 ) ) ;
#177991 = CARTESIAN_POINT ( 'NONE',  ( -18.62759615963255300, -10.81492255796106328, 19.16775706135234714 ) ) ;
#177992 = CARTESIAN_POINT ( 'NONE',  ( -21.52544592524343514, 5.823673210054127303, 116.0405762719810383 ) ) ;
#177994 = CARTESIAN_POINT ( 'NONE',  ( -16.46253265017160317, 9.564922557960807481, 60.83224293864769550 ) ) ;
#177993 = CARTESIAN_POINT ( 'NONE',  ( -19.02544592524334988, -5.153800228976617603, 33.95942372801897591 ) ) ;
#177995 = LINE ( 'NONE', #39462, #150830 ) ;
#177996 = CARTESIAN_POINT ( 'NONE',  ( 10.81492255796106328, -18.62759615963255655, 75.41775706135233293 ) ) ;
#177997 = CARTESIAN_POINT ( 'NONE',  ( -21.52544592524343514, 5.823673210054127303, 61.04057627198103120 ) ) ;
#177998 = CARTESIAN_POINT ( 'NONE',  ( -0.05219959533910754901, -16.53943276465976808, 37.49890960531436690 ) ) ;
#178000 = CARTESIAN_POINT ( 'NONE',  ( 10.72451020669871369, 18.67979575497193778, 107.0844237280190043 ) ) ;
#177999 = CARTESIAN_POINT ( 'NONE',  ( -21.55341960407619339, 5.719274019375674811, 78.54275706135236135 ) ) ;
#178001 = CARTESIAN_POINT ( 'NONE',  ( -4.379528057220328563, 16.55341960407611168, 55.20724293864770260 ) ) ;
#178002 = CARTESIAN_POINT ( 'NONE',  ( -8.224510206698948167, 14.34966873604960824, 100.4155762719810241 ) ) ;
#178003 = CARTESIAN_POINT ( 'NONE',  ( 9.564922557961047289, -16.46253265017146816, 60.41775706135233293 ) ) ;
#178004 = CARTESIAN_POINT ( 'NONE',  ( 16.53943276465976808, -0.05219959533910856209, 23.74890960531435269 ) ) ;
#178005 = CARTESIAN_POINT ( 'NONE',  ( -15.72974639402176322, -15.80617190586768395, 64.37609039468568994 ) ) ;
#178006 = CARTESIAN_POINT ( 'NONE',  ( -13.89961937509977652, 13.97604488694528158, 70.62390960531432427 ) ) ;
#178007 = CARTESIAN_POINT ( 'NONE',  ( 13.97604488694548053, -13.89961937509957401, 30.62609039468566863 ) ) ;
#178008 = CARTESIAN_POINT ( 'NONE',  ( 5.719274019375991003, -21.55341960407610458, 57.70724293864770260 ) ) ;
#178009 = CARTESIAN_POINT ( 'NONE',  ( 21.52544592524334988, 5.823673210054432836, 41.45942372801901143 ) ) ;
#178010 = CARTESIAN_POINT ( 'NONE',  ( -15.72974639402197994, 15.80617190586746368, 105.6239096053143669 ) ) ;
#178011 = CARTESIAN_POINT ( 'NONE',  ( -19.02544592524334988, -5.153800228976617603, 98.95942372801900433 ) ) ;
#178012 = CARTESIAN_POINT ( 'NONE',  ( -8.224510206698735004, -14.34966873604973081, 49.58442372801901143 ) ) ;
#178014 = CARTESIAN_POINT ( 'NONE',  ( -21.53943276465977519, 0.05219959533907696930, 96.24890960531435269 ) ) ;
#178013 = CARTESIAN_POINT ( 'NONE',  ( -15.23577778804332539, -17.33993248393032616, -57.66841858811282862 ) ) ;
#178015 = CARTESIAN_POINT ( 'NONE',  ( 4.483927247898545687, 16.52544592524342804, 84.79057627198102409 ) ) ;
#178016 = CARTESIAN_POINT ( 'NONE',  ( -23.31485601308163780, -29.82028178163005450, -21.55021174911970050 ) ) ;
#178017 = CARTESIAN_POINT ( 'NONE',  ( 14.34966873604972726, -8.224510206698740333, 25.83442372801901499 ) ) ;
#178018 = CARTESIAN_POINT ( 'NONE',  ( -15.80617190586745835, -15.72974639402198527, 51.87390960531437401 ) ) ;
#178019 = CARTESIAN_POINT ( 'NONE',  ( 12.06949235617739724, 12.14591786802326823, 96.87609039468568994 ) ) ;
#178020 = CARTESIAN_POINT ( 'NONE',  ( 27.79211460164531999, -24.33005135171561051, -8.000000000000005329 ) ) ;
#178021 = CARTESIAN_POINT ( 'NONE',  ( 12.14591786802327356, -12.06949235617739191, 50.62609039468568994 ) ) ;
#178022 = CARTESIAN_POINT ( 'NONE',  ( 18.62759615963255655, 10.81492255796105972, 21.66775706135235069 ) ) ;
#178023 = CARTESIAN_POINT ( 'NONE',  ( 21.55341960407610458, 5.719274019375980345, 38.95724293864768839 ) ) ;
#178024 = CARTESIAN_POINT ( 'NONE',  ( -14.34966873604972548, 8.224510206698743886, 88.33442372801901854 ) ) ;
#178025 = CARTESIAN_POINT ( 'NONE',  ( -19.02544592524342804, 5.153800228976336051, 101.0405762719810241 ) ) ;
#178026 = CARTESIAN_POINT ( 'NONE',  ( -21.52544592524334988, -5.823673210054445271, 63.95942372801901854 ) ) ;
#178027 = CARTESIAN_POINT ( 'NONE',  ( 15.80617190586746368, 15.72974639402197994, 34.37390960531435979 ) ) ;
#178028 = CARTESIAN_POINT ( 'NONE',  ( -5.823673210054116645, -21.52544592524344225, 22.29057627198102765 ) ) ;
#178029 = ORIENTED_EDGE ( 'NONE', *, *, #144097, .T. ) ;
#178030 = CARTESIAN_POINT ( 'NONE',  ( 19.02544592524334988, 5.153800228976608722, 46.45942372801899012 ) ) ;
#178031 = CARTESIAN_POINT ( 'NONE',  ( -8.224510206698735004, -14.34966873604973081, 69.58442372801900433 ) ) ;
#178032 = CARTESIAN_POINT ( 'NONE',  ( -5.823673210054116645, -21.52544592524344225, 27.29057627198103120 ) ) ;
#178033 = VERTEX_POINT ( 'NONE', #12035 ) ;
#178034 = CARTESIAN_POINT ( 'NONE',  ( -16.46253265017160317, 9.564922557960807481, 80.83224293864769550 ) ) ;
#178035 = CARTESIAN_POINT ( 'NONE',  ( -16.55341960407617563, 4.379528057220093196, 108.5427570613523756 ) ) ;
#178036 = CARTESIAN_POINT ( 'NONE',  ( 4.521720347981165844, -38.96825017273093295, -33.00000000000000711 ) ) ;
#178037 = CARTESIAN_POINT ( 'NONE',  ( -8.314922557960811034, -14.29746914071050412, 112.0822429386477097 ) ) ;
#178038 = CARTESIAN_POINT ( 'NONE',  ( 15.72974639402199770, -15.80617190586745480, 53.12390960531436690 ) ) ;
#178039 = CARTESIAN_POINT ( 'NONE',  ( -16.51473224551069308, -9.474510206698971260, 51.66557627198102409 ) ) ;
#178040 = CARTESIAN_POINT ( 'NONE',  ( 16.55341960407618274, -4.379528057220086978, 81.04275706135236135 ) ) ;
#178041 = CARTESIAN_POINT ( 'NONE',  ( -10.72451020669870658, -18.67979575497194134, 34.58442372801900433 ) ) ;
#178042 = CARTESIAN_POINT ( 'NONE',  ( -16.51473224551082808, 9.474510206698731452, 88.33442372801900433 ) ) ;
#178043 = CARTESIAN_POINT ( 'NONE',  ( 12.06949235617757843, -12.14591786802309237, 93.12390960531436690 ) ) ;
#178044 = CARTESIAN_POINT ( 'NONE',  ( -19.02544592524342804, 5.153800228976336051, 56.04057627198100988 ) ) ;
#178045 = CARTESIAN_POINT ( 'NONE',  ( -13.97604488694527625, -13.89961937509977652, 31.87390960531435979 ) ) ;
#178046 = CARTESIAN_POINT ( 'NONE',  ( -21.53943276465977519, -0.05219959533937600094, 98.75109039468568994 ) ) ;
#178047 = CARTESIAN_POINT ( 'NONE',  ( -16.46253265017160317, 9.564922557960807481, 80.83224293864769550 ) ) ;
#178048 = CARTESIAN_POINT ( 'NONE',  ( 16.55341960407618274, -4.379528057220086978, 66.04275706135236135 ) ) ;
#178049 = CARTESIAN_POINT ( 'NONE',  ( -18.67979575497193778, 10.72451020669871902, 98.33442372801901854 ) ) ;
#178050 = CARTESIAN_POINT ( 'NONE',  ( -21.52544592524343514, 5.823673210054127303, 51.04057627198103120 ) ) ;
#178051 = CARTESIAN_POINT ( 'NONE',  ( 12.06949235617739724, 12.14591786802326823, 71.87609039468568994 ) ) ;
#178052 = CARTESIAN_POINT ( 'NONE',  ( 5.049401038297881783, 19.05341960407617563, 52.29275706135234003 ) ) ;
#178053 = CARTESIAN_POINT ( 'NONE',  ( 19.03943276465977164, 0.05219959533936151252, 71.25109039468566152 ) ) ;
#178054 = CARTESIAN_POINT ( 'NONE',  ( 10.81492255796106328, -18.62759615963255655, 60.41775706135235424 ) ) ;
#178055 = CARTESIAN_POINT ( 'NONE',  ( 16.51473224551069308, 9.474510206698969483, 69.16557627198102409 ) ) ;
#178056 = CARTESIAN_POINT ( 'NONE',  ( 19.02544592524343514, -5.153800228976328945, 23.54057627198102054 ) ) ;
#178057 = CARTESIAN_POINT ( 'NONE',  ( -19.02544592524334988, -5.153800228976617603, 53.95942372801898301 ) ) ;
#178058 = DIRECTION ( 'NONE',  ( 1.000000000000000000, 0.000000000000000000, 0.000000000000000000 ) ) ;
#178059 = CARTESIAN_POINT ( 'NONE',  ( 9.564922557960805705, 16.46253265017160317, 99.58224293864770971 ) ) ;
#178060 = CARTESIAN_POINT ( 'NONE',  ( -16.53943276465976808, 0.05219959533911058130, 51.24890960531436690 ) ) ;
#178061 = CARTESIAN_POINT ( 'NONE',  ( 0.05219959533907565091, 21.53943276465977519, 49.99890960531437401 ) ) ;
#178062 = CARTESIAN_POINT ( 'NONE',  ( 22.36433501015068259, 22.72511982729788471, -49.15411784021381436 ) ) ;
#178063 = CARTESIAN_POINT ( 'NONE',  ( 5.823673210054444382, -21.52544592524334988, 110.2094237280190185 ) ) ;
#178064 = PRESENTATION_STYLE_ASSIGNMENT (( #190227 ) ) ;
#178065 = CARTESIAN_POINT ( 'NONE',  ( -13.97604488694527625, -13.89961937509977652, 46.87390960531435979 ) ) ;
#178066 = CARTESIAN_POINT ( 'NONE',  ( -19.03943276465977164, 0.05219959533909376836, 26.24890960531435624 ) ) ;
#178067 = EDGE_CURVE ( 'NONE', #19466, #6627, #136346, .T. ) ;
#178068 = CARTESIAN_POINT ( 'NONE',  ( -33.86249154851668663, -5.319940558880595027, 93.55791698674944712 ) ) ;
#178069 = CARTESIAN_POINT ( 'NONE',  ( 37.99626262588765258, -12.34573411038911672, -1.102157773949822506 ) ) ;
#178070 = CARTESIAN_POINT ( 'NONE',  ( 8.224510206698742110, 14.34966873604972548, 62.08442372801901143 ) ) ;
#178071 = CARTESIAN_POINT ( 'NONE',  ( -21.55341960407610458, -5.719274019375992779, 81.45724293864769550 ) ) ;
#178072 = CARTESIAN_POINT ( 'NONE',  ( 4.379528057220339221, -16.55341960407611168, 52.70724293864769550 ) ) ;
#178074 = CARTESIAN_POINT ( 'NONE',  ( 5.000000000000000000, -130.0000000000000000, 13.99999999999999822 ) ) ;
#178073 = CARTESIAN_POINT ( 'NONE',  ( 5.049401038298161559, -19.05341960407611168, 37.70724293864768839 ) ) ;
#178075 = CARTESIAN_POINT ( 'NONE',  ( -15.72974639402176322, -15.80617190586768395, 44.37609039468567573 ) ) ;
#178076 = CARTESIAN_POINT ( 'NONE',  ( -16.51473224551082808, 9.474510206698731452, 48.33442372801900433 ) ) ;
#178077 = CARTESIAN_POINT ( 'NONE',  ( -13.89961937509977652, 13.97604488694528158, 30.62390960531435269 ) ) ;
#178078 = CARTESIAN_POINT ( 'NONE',  ( 18.62759615963255655, 10.81492255796105972, 81.66775706135236135 ) ) ;
#178079 = CARTESIAN_POINT ( 'NONE',  ( 19.02544592524343514, -5.153800228976328945, 23.54057627198102054 ) ) ;
#178080 = CARTESIAN_POINT ( 'NONE',  ( -8.224510206698948167, 14.34966873604960824, 35.41557627198102409 ) ) ;
#178081 = CARTESIAN_POINT ( 'NONE',  ( 17.49999999999999645, 3.189878218039145619, 112.6294856257125900 ) ) ;
#178082 = CARTESIAN_POINT ( 'NONE',  ( -15.72974639402197994, 15.80617190586746368, 40.62390960531435269 ) ) ;
#178083 = DIRECTION ( 'NONE',  ( -1.000000000000000000, -0.000000000000000000, -0.000000000000000000 ) ) ;
#178084 = CARTESIAN_POINT ( 'NONE',  ( 5.049401038298161559, -19.05341960407611168, 92.70724293864769550 ) ) ;
#178085 = CARTESIAN_POINT ( 'NONE',  ( 8.314922557960818139, 14.29746914071049879, 89.58224293864768129 ) ) ;
#178086 = CARTESIAN_POINT ( 'NONE',  ( -14.29746914071037622, -8.314922557961029526, 29.16775706135234003 ) ) ;
#178087 = CARTESIAN_POINT ( 'NONE',  ( -12.14591786802326823, 12.06949235617739902, 113.1260903946856899 ) ) ;
#178088 = ORIENTED_EDGE ( 'NONE', *, *, #149044, .F. ) ;
#178089 = CARTESIAN_POINT ( 'NONE',  ( 19.05341960407611168, 5.049401038298154454, 28.95724293864769550 ) ) ;
#178091 = CARTESIAN_POINT ( 'NONE',  ( -21.53943276465977519, 0.05219959533907696930, 86.24890960531436690 ) ) ;
#178090 = CARTESIAN_POINT ( 'NONE',  ( 0.05219959533909260263, 19.03943276465977164, 89.99890960531436690 ) ) ;
#178093 = CARTESIAN_POINT ( 'NONE',  ( 19.05341960407611168, 5.049401038298154454, 103.9572429386476671 ) ) ;
#178092 = CARTESIAN_POINT ( 'NONE',  ( 4.379528057220339221, -16.55341960407611168, 22.70724293864769194 ) ) ;
#178094 = CARTESIAN_POINT ( 'NONE',  ( 16.46253265017146816, 9.564922557961045513, 81.66775706135233293 ) ) ;
#178095 = CARTESIAN_POINT ( 'NONE',  ( -5.823673210054431948, 21.52544592524334988, 107.7094237280190328 ) ) ;
#178096 = CARTESIAN_POINT ( 'NONE',  ( 15.80617190586746368, 15.72974639402197994, 89.37390960531435269 ) ) ;
#178097 = CARTESIAN_POINT ( 'NONE',  ( -15.80617190586745835, -15.72974639402198527, 41.87390960531435979 ) ) ;
#178098 = CARTESIAN_POINT ( 'NONE',  ( 5.049401038298161559, -19.05341960407611168, 67.70724293864769550 ) ) ;
#178099 = CARTESIAN_POINT ( 'NONE',  ( -12.06949235617756955, 12.14591786802309770, 25.62390960531435624 ) ) ;
#178100 = CARTESIAN_POINT ( 'NONE',  ( -19.02544592524342804, 5.153800228976336051, 81.04057627198103830 ) ) ;
#178101 = B_SPLINE_CURVE_WITH_KNOTS ( 'NONE', 3,
 ( #63055, #48896, #156063, #124735, #128693, #51865, #113525, #96367, #79221, #175219, #140891, #157065, #3371, #36684, #64059, #125729, #97348, #18561, #187428, #126702, #188406, #49884, #111549, #23537 ),
 .UNSPECIFIED., .F., .F.,
 ( 4, 2, 2, 2, 2, 2, 2, 2, 2, 2, 2, 4 ),
 ( 2.787091051215036154E-07, 0.0003070612385125908827, 0.0006138437679200602071, 0.001227408826735002434, 0.001534191356142473005, 0.001840973885549943576, 0.002147756414957414147, 0.002454538944364884935, 0.003068104003179817837, 0.003681669061994749872, 0.004295234120809682775, 0.004908799179624614810 ),
 .UNSPECIFIED. ) ;
#178102 = ORIENTED_EDGE ( 'NONE', *, *, #123966, .F. ) ;
#178103 = CARTESIAN_POINT ( 'NONE',  ( -31.91599925174812213, -5.957486376704252962, 90.41819350476903594 ) ) ;
#178104 = CARTESIAN_POINT ( 'NONE',  ( 9.474510206698729675, 16.51473224551082808, 22.08442372801899722 ) ) ;
#178105 = CARTESIAN_POINT ( 'NONE',  ( -4.483927247898539470, -16.52544592524342804, 92.29057627198103830 ) ) ;
#178106 = CARTESIAN_POINT ( 'NONE',  ( -18.62759615963255300, -10.81492255796106328, 29.16775706135234003 ) ) ;
#178107 = CARTESIAN_POINT ( 'NONE',  ( -22.44159573604009950, -16.30477369853688430, 143.5750000027311728 ) ) ;
#178108 = CARTESIAN_POINT ( 'NONE',  ( 21.55341960407610458, 5.719274019375980345, 73.95724293864769550 ) ) ;
#178109 = CARTESIAN_POINT ( 'NONE',  ( 4.379528057220092307, 16.55341960407617563, 92.29275706135236135 ) ) ;
#178110 = CARTESIAN_POINT ( 'NONE',  ( 4.483927247898545687, 16.52544592524342804, 114.7905762719810383 ) ) ;
#178111 = CARTESIAN_POINT ( 'NONE',  ( -0.05219959533909027116, -19.03943276465977164, 77.49890960531435269 ) ) ;
#178112 = CARTESIAN_POINT ( 'NONE',  ( 13.89961937509957579, 13.97604488694547520, 91.87609039468566152 ) ) ;
#178113 = CARTESIAN_POINT ( 'NONE',  ( 3.765340386950246872E-15, -39.95163481335715971, -5.247842220587802586 ) ) ;
#178114 = CARTESIAN_POINT ( 'NONE',  ( -16.53943276465976808, 0.05219959533911058130, 26.24890960531435624 ) ) ;
#178115 = CARTESIAN_POINT ( 'NONE',  ( 5.823673210054444382, -21.52544592524334988, 60.20942372801902565 ) ) ;
#178116 = CARTESIAN_POINT ( 'NONE',  ( 5.153800228976335163, 19.02544592524342804, 104.7905762719809957 ) ) ;
#178117 = CARTESIAN_POINT ( 'NONE',  ( 18.67979575497194134, -10.72451020669871369, 90.83442372801901854 ) ) ;
#178118 = CARTESIAN_POINT ( 'NONE',  ( 13.89961937509977652, -13.97604488694527269, 38.12390960531436690 ) ) ;
#178119 = CARTESIAN_POINT ( 'NONE',  ( 9.564922557960805705, 16.46253265017160317, 49.58224293864770260 ) ) ;
#178120 = ORIENTED_EDGE ( 'NONE', *, *, #100803, .T. ) ;
#178121 = CARTESIAN_POINT ( 'NONE',  ( -0.05219959533937732626, 21.53943276465977519, 92.50109039468567573 ) ) ;
#178122 = CARTESIAN_POINT ( 'NONE',  ( 4.483927247898790824, -16.52544592524335698, 55.20942372801902565 ) ) ;
#178123 = CARTESIAN_POINT ( 'NONE',  ( 15.72974639402176855, 15.80617190586768217, 91.87609039468568994 ) ) ;
#178124 = CARTESIAN_POINT ( 'NONE',  ( 19.05341960407611168, 5.049401038298154454, 113.9572429386477097 ) ) ;
#178125 = ORIENTED_EDGE ( 'NONE', *, *, #80593, .T. ) ;
#178126 = CARTESIAN_POINT ( 'NONE',  ( -5.049401038297874678, -19.05341960407617918, 94.79275706135230450 ) ) ;
#178127 = CARTESIAN_POINT ( 'NONE',  ( -10.81492255796105439, 18.62759615963255655, 57.91775706135234714 ) ) ;
#178128 = CARTESIAN_POINT ( 'NONE',  ( -4.483927247898782831, 16.52544592524335698, 32.70942372801900433 ) ) ;
#178129 = CARTESIAN_POINT ( 'NONE',  ( -5.823673210054116645, -21.52544592524344225, 87.29057627198103830 ) ) ;
#178130 = CARTESIAN_POINT ( 'NONE',  ( -9.564922557961040184, 16.46253265017147172, 82.91775706135233293 ) ) ;
#178131 = CARTESIAN_POINT ( 'NONE',  ( 5.153800228976335163, 19.02544592524342804, 69.79057627198103830 ) ) ;
#178132 = CARTESIAN_POINT ( 'NONE',  ( -5.153800228976607833, 19.02544592524334988, 92.70942372801901854 ) ) ;
#178133 = CARTESIAN_POINT ( 'NONE',  ( 13.89961937509957401, 13.97604488694547697, 101.8760903946856331 ) ) ;
#178134 = CARTESIAN_POINT ( 'NONE',  ( 8.224510206698953496, -14.34966873604960469, 52.91557627198103830 ) ) ;
#178135 = CARTESIAN_POINT ( 'NONE',  ( -13.97604488694547697, 13.89961937509957934, 83.12609039468564731 ) ) ;
#178136 = CARTESIAN_POINT ( 'NONE',  ( -8.224510206698735004, -14.34966873604973081, 64.58442372801900433 ) ) ;
#178137 = CARTESIAN_POINT ( 'NONE',  ( -19.05341960407617563, 5.049401038297882671, 43.54275706135232582 ) ) ;
#178138 = ADVANCED_FACE ( 'NONE', ( #165700, #92808, #183845, #166699, #46321, #107976, #77648, #89843, #59490, #180883, #167685, #152499, #29182, #28202 ), #157753, .T. ) ;
#178139 = CARTESIAN_POINT ( 'NONE',  ( -5.153800228976328057, -19.02544592524343514, 37.29057627198102409 ) ) ;
#178140 = CARTESIAN_POINT ( 'NONE',  ( 9.474510206698971260, -16.51473224551069308, 37.91557627198102409 ) ) ;
#178141 = CARTESIAN_POINT ( 'NONE',  ( 8.314922557961029526, -14.29746914071037800, 60.41775706135235424 ) ) ;
#178142 = DIRECTION ( 'NONE',  ( -0.000000000000000000, -0.000000000000000000, 1.000000000000000000 ) ) ;
#178143 = CARTESIAN_POINT ( 'NONE',  ( -17.81289503416611808, 24.51734667627700404, 139.9500000054623285 ) ) ;
#178144 = CARTESIAN_POINT ( 'NONE',  ( -13.97604488694527625, -13.89961937509977652, 106.8739096053143669 ) ) ;
#178145 = CARTESIAN_POINT ( 'NONE',  ( 4.999999999999996447, 5.000000000000003553, -15.00000000000000000 ) ) ;
#178146 = VERTEX_POINT ( 'NONE', #145992 ) ;
#178147 = CARTESIAN_POINT ( 'NONE',  ( -9.564922557961040184, 16.46253265017147172, 97.91775706135233293 ) ) ;
#178148 = EDGE_CURVE ( 'NONE', #193619, #46374, #192517, .T. ) ;
#178149 = CARTESIAN_POINT ( 'NONE',  ( 15.72974639402199770, -15.80617190586745480, 33.12390960531435979 ) ) ;
#178151 = CARTESIAN_POINT ( 'NONE',  ( -19.05341960407617563, 5.049401038297882671, 108.5427570613523187 ) ) ;
#178150 = CARTESIAN_POINT ( 'NONE',  ( 19.03943276465977164, 0.05219959533936151252, 26.25109039468566507 ) ) ;
#178152 = CARTESIAN_POINT ( 'NONE',  ( -5.153800228976328057, -19.02544592524343514, 27.29057627198103120 ) ) ;
#178153 = CARTESIAN_POINT ( 'NONE',  ( -5.049401038298153566, 19.05341960407611168, 55.20724293864769550 ) ) ;
#178154 = CARTESIAN_POINT ( 'NONE',  ( -5.823673210054116645, -21.52544592524344225, 67.29057627198103830 ) ) ;
#178155 = CARTESIAN_POINT ( 'NONE',  ( -13.97604488694527625, -13.89961937509977652, 101.8739096053143811 ) ) ;
#178156 = CARTESIAN_POINT ( 'NONE',  ( -16.46253265017160317, 9.564922557960807481, 40.83224293864769550 ) ) ;
#178157 = CARTESIAN_POINT ( 'NONE',  ( 8.571926809382603096, -26.38167802310801235, 145.9750000027311785 ) ) ;
#178158 = CARTESIAN_POINT ( 'NONE',  ( -19.05341960407617563, 5.049401038297882671, 88.54275706135230450 ) ) ;
#178159 = CARTESIAN_POINT ( 'NONE',  ( -12.06949235617756955, 12.14591786802309770, 50.62390960531435979 ) ) ;
#178160 = CARTESIAN_POINT ( 'NONE',  ( 15.72974639402199770, -15.80617190586745480, 28.12390960531435979 ) ) ;
#178161 = CARTESIAN_POINT ( 'NONE',  ( 15.72974639402176855, 15.80617190586768217, 106.8760903946856899 ) ) ;
#178162 = CARTESIAN_POINT ( 'NONE',  ( -10.72451020669898014, 18.67979575497178502, 95.41557627198102409 ) ) ;
#178163 = CARTESIAN_POINT ( 'NONE',  ( 0.05219959533937995610, -21.53943276465977519, 75.00109039468568994 ) ) ;
#178164 = CARTESIAN_POINT ( 'NONE',  ( -21.53943276465977519, -0.05219959533937600094, 78.75109039468568994 ) ) ;
#178165 = CARTESIAN_POINT ( 'NONE',  ( 5.153800228976335163, 19.02544592524342804, 114.7905762719810241 ) ) ;
#178167 = CARTESIAN_POINT ( 'NONE',  ( -18.67979575497193778, 10.72451020669871902, 58.33442372801901143 ) ) ;
#178166 = CARTESIAN_POINT ( 'NONE',  ( 8.224510206698742110, 14.34966873604972548, 102.0844237280190185 ) ) ;
#178168 = CARTESIAN_POINT ( 'NONE',  ( 13.97604488694527802, 13.89961937509977652, 64.37390960531436690 ) ) ;
#178169 = CARTESIAN_POINT ( 'NONE',  ( -19.03943276465977164, -0.05219959533935918106, 38.75109039468566152 ) ) ;
#178170 = CARTESIAN_POINT ( 'NONE',  ( -18.62759615963255300, -10.81492255796106328, 29.16775706135234003 ) ) ;
#178171 = CARTESIAN_POINT ( 'NONE',  ( 19.03943276465977164, -0.05219959533909143690, 63.74890960531435979 ) ) ;
#178172 = CARTESIAN_POINT ( 'NONE',  ( 0.05219959533910956823, 16.53943276465976808, 84.99890960531436690 ) ) ;
#178173 = CARTESIAN_POINT ( 'NONE',  ( -8.224510206698948167, 14.34966873604960824, 50.41557627198103120 ) ) ;
#178174 = CARTESIAN_POINT ( 'NONE',  ( -21.53943276465977519, 0.05219959533907696930, 51.24890960531436690 ) ) ;
#178175 = CARTESIAN_POINT ( 'NONE',  ( 16.51473224551069308, 9.474510206698969483, 64.16557627198102409 ) ) ;
#178176 = CARTESIAN_POINT ( 'NONE',  ( -10.81492255796078084, -18.62759615963271287, 77.08224293864769550 ) ) ;
#178177 = CARTESIAN_POINT ( 'NONE',  ( -9.564922557961040184, 16.46253265017147172, 67.91775706135233293 ) ) ;
#178179 = CARTESIAN_POINT ( 'NONE',  ( 4.379528057220339221, -16.55341960407611168, 62.70724293864769550 ) ) ;
#178178 = CARTESIAN_POINT ( 'NONE',  ( 19.03943276465977164, 0.05219959533936151252, 21.25109039468565797 ) ) ;
#178180 = CARTESIAN_POINT ( 'NONE',  ( -21.52544592524343514, 5.823673210054127303, 36.04057627198102409 ) ) ;
#178181 = EDGE_LOOP ( 'NONE', ( #59995, #107246, #9951, #5268 ) ) ;
#178182 = PLANE ( 'NONE',  #143072 ) ;
#178184 = CARTESIAN_POINT ( 'NONE',  ( 0.3963287095611701671, 6.139799388069159036, -64.52448944440712353 ) ) ;
#178183 = CARTESIAN_POINT ( 'NONE',  ( 12.14591786802327356, -12.06949235617739191, 90.62609039468567573 ) ) ;
#178185 = CARTESIAN_POINT ( 'NONE',  ( 5.049401038297881783, 19.05341960407617563, 87.29275706135234714 ) ) ;
#178186 = CARTESIAN_POINT ( 'NONE',  ( 16.52544592524342804, -4.483927247898539470, 53.54057627198103120 ) ) ;
#178187 = DIRECTION ( 'NONE',  ( -0.5000000000000044409, 0.000000000000000000, 0.8660254037844360431 ) ) ;
#178188 = CARTESIAN_POINT ( 'NONE',  ( 16.46253265017160672, -9.564922557960803928, 48.33224293864769550 ) ) ;
#178189 = CARTESIAN_POINT ( 'NONE',  ( 14.29746914071049879, -8.314922557960816363, 38.33224293864768839 ) ) ;
#178190 = CARTESIAN_POINT ( 'NONE',  ( -19.02544592524342804, 5.153800228976336051, 91.04057627198100988 ) ) ;
#178191 = CARTESIAN_POINT ( 'NONE',  ( 0.05219959533909260263, 19.03943276465977164, 54.99890960531435979 ) ) ;
#178192 = CARTESIAN_POINT ( 'NONE',  ( 15.72974639402176855, 15.80617190586768217, 61.87609039468568284 ) ) ;
#178193 = CARTESIAN_POINT ( 'NONE',  ( 19.02544592524343514, -5.153800228976328945, 73.54057627198103830 ) ) ;
#178194 = CYLINDRICAL_SURFACE ( 'NONE', #141973, 5.500000000000032863 ) ;
#178195 = CARTESIAN_POINT ( 'NONE',  ( -16.51473224551069308, -9.474510206698971260, 71.66557627198102409 ) ) ;
#178196 = CARTESIAN_POINT ( 'NONE',  ( 15.72974639402199770, -15.80617190586745480, 48.12390960531436690 ) ) ;
#178197 = CARTESIAN_POINT ( 'NONE',  ( 19.02544592524343514, -5.153800228976328945, 38.54057627198103120 ) ) ;
#178198 = CARTESIAN_POINT ( 'NONE',  ( 10.81492255796078972, 18.62759615963270932, 59.58224293864770260 ) ) ;
#178199 = CARTESIAN_POINT ( 'NONE',  ( -13.97604488694547697, 13.89961937509957934, 78.12609039468567573 ) ) ;
#178200 = CARTESIAN_POINT ( 'NONE',  ( -16.53943276465976808, -0.05219959533934237506, 108.7510903946857042 ) ) ;
#178201 = CARTESIAN_POINT ( 'NONE',  ( 19.02544592524334988, 5.153800228976608722, 21.45942372801899012 ) ) ;
#178203 = CARTESIAN_POINT ( 'NONE',  ( 14.29746914071037800, 8.314922557961029526, 81.66775706135236135 ) ) ;
#178202 = CARTESIAN_POINT ( 'NONE',  ( 14.34966873604972726, -8.224510206698740333, 50.83442372801901143 ) ) ;
#178204 = CARTESIAN_POINT ( 'NONE',  ( -19.03943276465977164, 0.05219959533909376836, 116.2489096053143669 ) ) ;
#178205 = CARTESIAN_POINT ( 'NONE',  ( -16.52544592524335698, -4.483927247898792601, 63.95942372801901854 ) ) ;
#178206 = CARTESIAN_POINT ( 'NONE',  ( -21.55341960407610458, -5.719274019375992779, 31.45724293864769550 ) ) ;
#178207 = CARTESIAN_POINT ( 'NONE',  ( 13.89961937509977652, -13.97604488694527269, 28.12390960531435624 ) ) ;
#178208 = CARTESIAN_POINT ( 'NONE',  ( -8.314922557961024197, 14.29746914071037800, 42.91775706135235424 ) ) ;
#178209 = CARTESIAN_POINT ( 'NONE',  ( -9.474510206698964154, 16.51473224551069663, 50.41557627198102409 ) ) ;
#178210 = CARTESIAN_POINT ( 'NONE',  ( 21.53943276465977519, 0.05219959533937863772, 36.25109039468567573 ) ) ;
#178211 = CARTESIAN_POINT ( 'NONE',  ( 12.14591786802327356, -12.06949235617739191, 40.62609039468567573 ) ) ;
#178212 = CARTESIAN_POINT ( 'NONE',  ( 14.29746914071037800, 8.314922557961029526, 96.66775706135234714 ) ) ;
#178213 = LINE ( 'NONE', #117523, #157010 ) ;
#178214 = CARTESIAN_POINT ( 'NONE',  ( -18.67979575497193778, 10.72451020669871902, 103.3344237280190043 ) ) ;
#178215 = CARTESIAN_POINT ( 'NONE',  ( 14.34966873604972726, -8.224510206698740333, 20.83442372801901143 ) ) ;
#178216 = CARTESIAN_POINT ( 'NONE',  ( -16.51473224551082808, 9.474510206698731452, 68.33442372801900433 ) ) ;
#178217 = CARTESIAN_POINT ( 'NONE',  ( -4.379528057220328563, 16.55341960407611168, 75.20724293864769550 ) ) ;
#178218 = CARTESIAN_POINT ( 'NONE',  ( -16.51473224551069308, -9.474510206698971260, 26.66557627198103120 ) ) ;
#178220 = CARTESIAN_POINT ( 'NONE',  ( 16.61371651742640765, -7.165104196375916779, 56.35415069992969705 ) ) ;
#178219 = CARTESIAN_POINT ( 'NONE',  ( 19.02544592524334988, 5.153800228976608722, 66.45942372801899012 ) ) ;
#178221 = CARTESIAN_POINT ( 'NONE',  ( 5.823673210054444382, -21.52544592524334988, 65.20942372801901854 ) ) ;
#178222 = CARTESIAN_POINT ( 'NONE',  ( -0.05219959533934338120, 16.53943276465976808, 27.50109039468567929 ) ) ;
#178223 = CARTESIAN_POINT ( 'NONE',  ( 17.50000000001358913, -5.500000000000039968, 73.29690382535059712 ) ) ;
#178224 = CARTESIAN_POINT ( 'NONE',  ( 18.62759615963271287, -10.81492255796078972, 23.33224293864769194 ) ) ;
#178225 = CARTESIAN_POINT ( 'NONE',  ( 19.02544592524334988, 5.153800228976608722, 111.4594237280190043 ) ) ;
#178226 = CARTESIAN_POINT ( 'NONE',  ( -16.46253265017160317, 9.564922557960807481, 110.8322429386476955 ) ) ;
#178227 = CARTESIAN_POINT ( 'NONE',  ( -20.69372460268670011, 11.29034304323151794, 170.1224388339879567 ) ) ;
#178228 = CARTESIAN_POINT ( 'NONE',  ( 19.05341960407611168, 5.049401038298154454, 23.95724293864769194 ) ) ;
#178229 = CARTESIAN_POINT ( 'NONE',  ( 18.67979575497194134, -10.72451020669871369, 105.8344237280190328 ) ) ;
#178230 = CARTESIAN_POINT ( 'NONE',  ( -5.049401038298153566, 19.05341960407611168, 50.20724293864770260 ) ) ;
#178231 = CARTESIAN_POINT ( 'NONE',  ( 15.80617190586769283, -15.72974639402175789, 70.62609039468567573 ) ) ;
#178232 = CARTESIAN_POINT ( 'NONE',  ( -10.81492255796105439, 18.62759615963255655, 102.9177570613523756 ) ) ;
#178233 = CARTESIAN_POINT ( 'NONE',  ( -8.314922557960811034, -14.29746914071050412, 22.08224293864769194 ) ) ;
#178234 = CARTESIAN_POINT ( 'NONE',  ( -19.05341960407611168, -5.049401038298163336, 31.45724293864769550 ) ) ;
#178235 = CARTESIAN_POINT ( 'NONE',  ( -13.97604488694527625, -13.89961937509977652, 81.87390960531436690 ) ) ;
#178236 = CARTESIAN_POINT ( 'NONE',  ( 10.81492255796106328, -18.62759615963255655, 60.41775706135235424 ) ) ;
#178237 = CARTESIAN_POINT ( 'NONE',  ( 19.02544592524343514, -5.153800228976328945, 38.54057627198103120 ) ) ;
#178238 = ADVANCED_FACE ( 'NONE', ( #6474, #116665, #178356 ), #143998, .F. ) ;
#178239 = CARTESIAN_POINT ( 'NONE',  ( 21.53943276465977519, 0.05219959533937863772, 51.25109039468568994 ) ) ;
#178241 = CARTESIAN_POINT ( 'NONE',  ( -19.02544592524342804, 5.153800228976336051, 106.0405762719810241 ) ) ;
#178240 = CARTESIAN_POINT ( 'NONE',  ( -5.049401038297874678, -19.05341960407617918, 84.79275706135233293 ) ) ;
#178242 = CARTESIAN_POINT ( 'NONE',  ( -0.05219959533909027116, -19.03943276465977164, 27.49890960531435624 ) ) ;
#178243 = CARTESIAN_POINT ( 'NONE',  ( -18.62759615963270932, 10.81492255796079327, 105.8322429386476955 ) ) ;
#178244 = CARTESIAN_POINT ( 'NONE',  ( 5.153800228976615827, -19.02544592524334988, 35.20942372801899722 ) ) ;
#178245 = CARTESIAN_POINT ( 'NONE',  ( -16.53943276465976808, 0.05219959533911058130, 91.24890960531436690 ) ) ;
#178246 = CARTESIAN_POINT ( 'NONE',  ( 19.03943276465977164, -0.05219959533909143690, 43.74890960531435979 ) ) ;
#178247 = CARTESIAN_POINT ( 'NONE',  ( 16.51473224551083163, -9.474510206698727899, 95.83442372801900433 ) ) ;
#178248 = CARTESIAN_POINT ( 'NONE',  ( 12.14591786802309770, 12.06949235617756955, 59.37390960531436690 ) ) ;
#178249 = CARTESIAN_POINT ( 'NONE',  ( 5.823673210054444382, -21.52544592524334988, 105.2094237280190328 ) ) ;
#178250 = CARTESIAN_POINT ( 'NONE',  ( 19.03943276465977164, -0.05219959533909143690, 103.7489096053143669 ) ) ;
#178251 = CARTESIAN_POINT ( 'NONE',  ( -16.51473224551082808, 9.474510206698731452, 88.33442372801900433 ) ) ;
#178252 = CARTESIAN_POINT ( 'NONE',  ( 10.72451020669898902, -18.67979575497178502, 97.91557627198103830 ) ) ;
#178253 = CARTESIAN_POINT ( 'NONE',  ( 18.67979575497194134, -10.72451020669871369, 40.83442372801901854 ) ) ;
#178254 = CARTESIAN_POINT ( 'NONE',  ( 12.06949235617739724, 12.14591786802326823, 41.87609039468568284 ) ) ;
#178255 = CARTESIAN_POINT ( 'NONE',  ( 12.06949235617739724, 12.14591786802326823, 106.8760903946856899 ) ) ;
#178257 = CARTESIAN_POINT ( 'NONE',  ( 0.05219959533937995610, -21.53943276465977519, 35.00109039468568284 ) ) ;
#178256 = CARTESIAN_POINT ( 'NONE',  ( 8.314922557961029526, -14.29746914071037800, 45.41775706135234003 ) ) ;
#178258 = CARTESIAN_POINT ( 'NONE',  ( -0.05219959533907301413, -21.53943276465977519, 47.49890960531435979 ) ) ;
#178259 = CARTESIAN_POINT ( 'NONE',  ( -16.46253265017160317, 9.564922557960807481, 40.83224293864769550 ) ) ;
#178260 = CARTESIAN_POINT ( 'NONE',  ( 29.86685920354754842, -21.69954338932559068, -2.324999997268813345 ) ) ;
#178261 = CARTESIAN_POINT ( 'NONE',  ( 14.29746914071037800, 8.314922557961029526, 61.66775706135235424 ) ) ;
#178262 = CARTESIAN_POINT ( 'NONE',  ( -21.52544592524343514, 5.823673210054127303, 86.04057627198102409 ) ) ;
#178263 = CARTESIAN_POINT ( 'NONE',  ( -12.14591786802309592, -12.06949235617757132, 36.87390960531435979 ) ) ;
#178264 = CARTESIAN_POINT ( 'NONE',  ( 14.34966873604972726, -8.224510206698740333, 60.83442372801901854 ) ) ;
#178265 = CARTESIAN_POINT ( 'NONE',  ( -5.153800228976328057, -19.02544592524343514, 57.29057627198103120 ) ) ;
#178266 = CARTESIAN_POINT ( 'NONE',  ( 0.05219959533936267826, -19.03943276465977164, 100.0010903946856757 ) ) ;
#178267 = CARTESIAN_POINT ( 'NONE',  ( 10.81492255796078972, 18.62759615963270932, 79.58224293864769550 ) ) ;
#178268 = CARTESIAN_POINT ( 'NONE',  ( -8.224510206698948167, 14.34966873604960824, 30.41557627198101699 ) ) ;
#178269 = ORIENTED_EDGE ( 'NONE', *, *, #52114, .T. ) ;
#178270 = CARTESIAN_POINT ( 'NONE',  ( 25.41223161463591396, 11.66315983254869693, 166.2610598689586254 ) ) ;
#178271 = CARTESIAN_POINT ( 'NONE',  ( -10.81492255796078084, -18.62759615963271287, 77.08224293864769550 ) ) ;
#178272 = CARTESIAN_POINT ( 'NONE',  ( -4.483927247898782831, 16.52544592524335698, 107.7094237280190328 ) ) ;
#178273 = EDGE_LOOP ( 'NONE', ( #182493, #114692, #15803, #7263 ) ) ;
#178274 = CARTESIAN_POINT ( 'NONE',  ( 17.49999999999999645, -3.556738311674189301, 102.7527116387158941 ) ) ;
#178275 = CARTESIAN_POINT ( 'NONE',  ( 21.55341960407610458, 5.719274019375980345, 88.95724293864769550 ) ) ;
#178276 = CARTESIAN_POINT ( 'NONE',  ( 21.52544592524344225, -5.823673210054117533, 103.5405762719810383 ) ) ;
#178277 = CARTESIAN_POINT ( 'NONE',  ( -4.379528057220328563, 16.55341960407611168, 25.20724293864769550 ) ) ;
#178278 = CARTESIAN_POINT ( 'NONE',  ( -0.05219959533934338120, 16.53943276465976808, 37.50109039468568284 ) ) ;
#178279 = CARTESIAN_POINT ( 'NONE',  ( 19.05341960407611168, 5.049401038298154454, 28.95724293864769550 ) ) ;
#178280 = CARTESIAN_POINT ( 'NONE',  ( -19.02544592524342804, 5.153800228976336051, 66.04057627198103830 ) ) ;
#178281 = CARTESIAN_POINT ( 'NONE',  ( -28.82186960331499392, -9.364793116373526516, 148.0999999999999943 ) ) ;
#178282 = CARTESIAN_POINT ( 'NONE',  ( -21.53943276465977519, 0.05219959533907696930, 26.24890960531435624 ) ) ;
#178283 = CARTESIAN_POINT ( 'NONE',  ( 0.8806672422397930911, 29.18146119162907581, -52.34378264204461573 ) ) ;
#178284 = CARTESIAN_POINT ( 'NONE',  ( -5.049401038297874678, -19.05341960407617918, 104.7927570613523471 ) ) ;
#178285 = CARTESIAN_POINT ( 'NONE',  ( 13.97604488694548053, -13.89961937509957401, 40.62609039468564731 ) ) ;
#178286 = CARTESIAN_POINT ( 'NONE',  ( 10.81492255796078972, 18.62759615963270932, 84.58224293864769550 ) ) ;
#178287 = CARTESIAN_POINT ( 'NONE',  ( 16.53943276465976808, 0.05219959533934440121, 111.2510903946856899 ) ) ;
#178288 = CARTESIAN_POINT ( 'NONE',  ( 15.72974639402199770, -15.80617190586745480, 43.12390960531435269 ) ) ;
#178290 = CARTESIAN_POINT ( 'NONE',  ( 16.46253265017146816, 9.564922557961045513, 111.6677570613523329 ) ) ;
#178289 = CARTESIAN_POINT ( 'NONE',  ( 18.62759615963271287, -10.81492255796078972, 78.33224293864770971 ) ) ;
#178291 = CARTESIAN_POINT ( 'NONE',  ( -19.03943276465977164, 0.05219959533909376836, 106.2489096053143669 ) ) ;
#178292 = CARTESIAN_POINT ( 'NONE',  ( 5.719274019375673035, 21.55341960407619339, 72.29275706135236135 ) ) ;
#178293 = CARTESIAN_POINT ( 'NONE',  ( -16.51473224551069308, -9.474510206698971260, 56.66557627198103120 ) ) ;
#178294 = CARTESIAN_POINT ( 'NONE',  ( -12.14591786802309592, -12.06949235617757132, 96.87390960531436690 ) ) ;
#178295 = CYLINDRICAL_SURFACE ( 'NONE', #125120, 0.5000000000000004441 ) ;
#178296 = CARTESIAN_POINT ( 'NONE',  ( -19.02544592524342804, 5.153800228976336051, 76.04057627198102409 ) ) ;
#178297 = CARTESIAN_POINT ( 'NONE',  ( 14.29746914071049879, -8.314922557960816363, 88.33224293864769550 ) ) ;
#178298 = VERTEX_POINT ( 'NONE', #162170 ) ;
#178299 = CARTESIAN_POINT ( 'NONE',  ( 19.05341960407617918, -5.049401038297876454, 91.04275706135234714 ) ) ;
#178300 = CARTESIAN_POINT ( 'NONE',  ( -193.3062444957834884, -155.7167183371838064, -25.00000000000000000 ) ) ;
#178301 = CARTESIAN_POINT ( 'NONE',  ( 16.51473224551069308, 9.474510206698969483, 64.16557627198102409 ) ) ;
#178303 = CARTESIAN_POINT ( 'NONE',  ( -5.049401038298153566, 19.05341960407611168, 100.2072429386476955 ) ) ;
#178302 = CARTESIAN_POINT ( 'NONE',  ( -15.80617190586768217, 15.72974639402176855, 78.12609039468570415 ) ) ;
#178304 = EDGE_CURVE ( 'NONE', #22637, #19836, #183296, .T. ) ;
#178305 = CARTESIAN_POINT ( 'NONE',  ( -4.483927247898782831, 16.52544592524335698, 77.70942372801900433 ) ) ;
#178306 = CARTESIAN_POINT ( 'NONE',  ( -16.38665767535054485, -7.295008042176060137, 49.73599135785455161 ) ) ;
#178307 = CARTESIAN_POINT ( 'NONE',  ( -9.564922557961040184, 16.46253265017147172, 47.91775706135233293 ) ) ;
#178308 = CARTESIAN_POINT ( 'NONE',  ( -21.53943276465977519, -0.05219959533937600094, 93.75109039468567573 ) ) ;
#178309 = CARTESIAN_POINT ( 'NONE',  ( 17.50000000000000000, 5.499999999999997335, 23.78230962303566542 ) ) ;
#178310 = CARTESIAN_POINT ( 'NONE',  ( 0.000000000000000000, 0.000000000000000000, -62.50719930893269805 ) ) ;
#178311 = CARTESIAN_POINT ( 'NONE',  ( -16.55341960407617563, 4.379528057220093196, 98.54275706135234714 ) ) ;
#178312 = CARTESIAN_POINT ( 'NONE',  ( -34.40547513665163848, -6.508760260264954134, 48.73452191691475832 ) ) ;
#178313 = CARTESIAN_POINT ( 'NONE',  ( -12.14591786802326823, 12.06949235617739902, 88.12609039468570415 ) ) ;
#178314 = CARTESIAN_POINT ( 'NONE',  ( 16.52216118717207038, 7.221426719304515629, 68.57599021046993926 ) ) ;
#178315 = CARTESIAN_POINT ( 'NONE',  ( 4.379528057220092307, 16.55341960407617563, 62.29275706135236845 ) ) ;
#178316 = ORIENTED_EDGE ( 'NONE', *, *, #121295, .T. ) ;
#178317 = CARTESIAN_POINT ( 'NONE',  ( -15.72974639402176322, -15.80617190586768395, 84.37609039468570415 ) ) ;
#178318 = CARTESIAN_POINT ( 'NONE',  ( -16.46253265017146816, -9.564922557961047289, 84.16775706135233293 ) ) ;
#178319 = CARTESIAN_POINT ( 'NONE',  ( 13.89961937509957401, 13.97604488694547697, 36.87609039468565442 ) ) ;
#178320 = CARTESIAN_POINT ( 'NONE',  ( -19.02544592524342804, 5.153800228976336051, 61.04057627198103120 ) ) ;
#178321 = CARTESIAN_POINT ( 'NONE',  ( 9.564922557960805705, 16.46253265017160317, 54.58224293864769550 ) ) ;
#178322 = CARTESIAN_POINT ( 'NONE',  ( 18.22780087662119897, -5.500000000000146549, 38.51763182126893525 ) ) ;
#178323 = CARTESIAN_POINT ( 'NONE',  ( -10.72451020669898014, 18.67979575497178502, 75.41557627198102409 ) ) ;
#178324 = CARTESIAN_POINT ( 'NONE',  ( 10.81492255796078972, 18.62759615963270932, 39.58224293864769550 ) ) ;
#178325 = CARTESIAN_POINT ( 'NONE',  ( 5.049401038298161559, -19.05341960407611168, 37.70724293864768839 ) ) ;
#178326 = CARTESIAN_POINT ( 'NONE',  ( 8.224510206698742110, 14.34966873604972548, 62.08442372801901143 ) ) ;
#178327 = ADVANCED_FACE ( 'NONE', ( #70170 ), #82308, .F. ) ;
#178328 = ORIENTED_EDGE ( 'NONE', *, *, #171492, .F. ) ;
#178329 = CARTESIAN_POINT ( 'NONE',  ( 18.62759615963255655, 10.81492255796105972, 26.66775706135235424 ) ) ;
#178331 = CARTESIAN_POINT ( 'NONE',  ( -30.74264578624800492, -22.33583958711396278, -1.800000000000000044 ) ) ;
#178330 = CARTESIAN_POINT ( 'NONE',  ( -8.224510206698948167, 14.34966873604960824, 65.41557627198102409 ) ) ;
#178332 = CARTESIAN_POINT ( 'NONE',  ( 4.379528057220092307, 16.55341960407617563, 22.29275706135235069 ) ) ;
#178333 = CARTESIAN_POINT ( 'NONE',  ( 19.03943276465977164, 0.05219959533936151252, 51.25109039468567573 ) ) ;
#178334 = CARTESIAN_POINT ( 'NONE',  ( 8.224510206698953496, -14.34966873604960469, 57.91557627198103120 ) ) ;
#178335 = CARTESIAN_POINT ( 'NONE',  ( 18.67979575497194134, -10.72451020669871369, 30.83442372801902209 ) ) ;
#178337 = CARTESIAN_POINT ( 'NONE',  ( -21.52544592524343514, 5.823673210054127303, 81.04057627198102409 ) ) ;
#178336 = CARTESIAN_POINT ( 'NONE',  ( 16.51473224551069308, 9.474510206698969483, 99.16557627198102409 ) ) ;
#178338 = CARTESIAN_POINT ( 'NONE',  ( 13.89961937509977652, -13.97604488694527269, 108.1239096053143669 ) ) ;
#178339 = CARTESIAN_POINT ( 'NONE',  ( 8.224510206698953496, -14.34966873604960469, 77.91557627198102409 ) ) ;
#178340 = CARTESIAN_POINT ( 'NONE',  ( 17.18269478283316332, -17.18269478283309226, -54.21489346206828230 ) ) ;
#178341 = DIRECTION ( 'NONE',  ( 0.1039620511844979306, -0.1039620511844979306, 0.9891328443778538704 ) ) ;
#178342 = CARTESIAN_POINT ( 'NONE',  ( -19.02544592524334988, -5.153800228976617603, 68.95942372801896170 ) ) ;
#178343 = CARTESIAN_POINT ( 'NONE',  ( 15.80617190586746368, 15.72974639402197994, 109.3739096053143811 ) ) ;
#178344 = CARTESIAN_POINT ( 'NONE',  ( 5.153800228976335163, 19.02544592524342804, 54.79057627198103120 ) ) ;
#178345 = CARTESIAN_POINT ( 'NONE',  ( -19.03943276465977164, -0.05219959533935918106, 48.75109039468566863 ) ) ;
#178346 = CARTESIAN_POINT ( 'NONE',  ( 5.049401038298161559, -19.05341960407611168, 27.70724293864769550 ) ) ;
#178347 = CARTESIAN_POINT ( 'NONE',  ( -5.719274019375665041, -21.55341960407619695, 64.79275706135234714 ) ) ;
#178348 = CARTESIAN_POINT ( 'NONE',  ( 4.313351365237961588, -4.313351365237934942, -64.92279855667830191 ) ) ;
#178349 = CARTESIAN_POINT ( 'NONE',  ( 12.14591786802309770, 12.06949235617756955, 39.37390960531436690 ) ) ;
#178350 = CARTESIAN_POINT ( 'NONE',  ( -9.564922557960796823, -16.46253265017161027, 67.08224293864769550 ) ) ;
#178351 = CARTESIAN_POINT ( 'NONE',  ( 5.719274019375991003, -21.55341960407610458, 87.70724293864769550 ) ) ;
#178352 = CARTESIAN_POINT ( 'NONE',  ( -16.51473224551069308, -9.474510206698971260, 56.66557627198103120 ) ) ;
#178353 = ORIENTED_EDGE ( 'NONE', *, *, #172057, .F. ) ;
#178354 = CARTESIAN_POINT ( 'NONE',  ( -5.719274019375978568, 21.55341960407610458, 60.20724293864768839 ) ) ;
#178355 = CARTESIAN_POINT ( 'NONE',  ( -21.55341960407619339, 5.719274019375674811, 103.5427570613523613 ) ) ;
#178358 = CARTESIAN_POINT ( 'NONE',  ( -16.52544592524342804, 4.483927247898546575, 81.04057627198102409 ) ) ;
#178357 = CARTESIAN_POINT ( 'NONE',  ( 4.483927247898790824, -16.52544592524335698, 90.20942372801903275 ) ) ;
#178356 = FACE_OUTER_BOUND ( 'NONE', #38121, .T. ) ;
#178359 = CARTESIAN_POINT ( 'NONE',  ( -9.474510206698720793, -16.51473224551083518, 94.58442372801900433 ) ) ;
#178360 = ORIENTED_EDGE ( 'NONE', *, *, #175162, .F. ) ;
#178361 = CARTESIAN_POINT ( 'NONE',  ( -13.89961937509957401, -13.97604488694547875, 34.37609039468566863 ) ) ;
#178362 = CARTESIAN_POINT ( 'NONE',  ( 8.314922557961029526, -14.29746914071037800, 95.41775706135234714 ) ) ;
#178363 = CARTESIAN_POINT ( 'NONE',  ( -0.05219959533936034679, 19.03943276465977164, 32.50109039468566863 ) ) ;
#178364 = CARTESIAN_POINT ( 'NONE',  ( 9.564922557960805705, 16.46253265017160317, 84.58224293864769550 ) ) ;
#178365 = CARTESIAN_POINT ( 'NONE',  ( -18.62759615963270932, 10.81492255796079327, 60.83224293864769550 ) ) ;
#178366 = CARTESIAN_POINT ( 'NONE',  ( -26.33854305698159592, 8.833284547248199559, 167.2806188263833747 ) ) ;
#178367 = CARTESIAN_POINT ( 'NONE',  ( -4.483927247898539470, -16.52544592524342804, 112.2905762719810241 ) ) ;
#178368 = CARTESIAN_POINT ( 'NONE',  ( 10.72451020669871369, 18.67979575497193778, 97.08442372801904696 ) ) ;
#178369 = CARTESIAN_POINT ( 'NONE',  ( 14.34966873604972726, -8.224510206698740333, 80.83442372801901854 ) ) ;
#178370 = CARTESIAN_POINT ( 'NONE',  ( 5.719274019375673035, 21.55341960407619339, 32.29275706135235424 ) ) ;
#178371 = CARTESIAN_POINT ( 'NONE',  ( -14.29746914071037622, -8.314922557961029526, 34.16775706135234714 ) ) ;
#178372 = CARTESIAN_POINT ( 'NONE',  ( -16.46253265017160317, 9.564922557960807481, 105.8322429386476955 ) ) ;
#178373 = CARTESIAN_POINT ( 'NONE',  ( 19.02544592524343514, -5.153800228976328945, 43.54057627198103120 ) ) ;
#178374 = CARTESIAN_POINT ( 'NONE',  ( 13.89961937509977652, -13.97604488694527269, 58.12390960531436690 ) ) ;
#178375 = CARTESIAN_POINT ( 'NONE',  ( -12.14591786802326823, 12.06949235617739902, 43.12609039468568284 ) ) ;
#178376 = CARTESIAN_POINT ( 'NONE',  ( -16.53943276465976808, 0.05219959533911058130, 86.24890960531436690 ) ) ;
#178377 = CARTESIAN_POINT ( 'NONE',  ( -8.314922557961024197, 14.29746914071037800, 102.9177570613523756 ) ) ;
#178380 = CARTESIAN_POINT ( 'NONE',  ( 9.564922557960805705, 16.46253265017160317, 64.58224293864769550 ) ) ;
#178379 = CARTESIAN_POINT ( 'NONE',  ( 13.89961937509977652, -13.97604488694527269, 83.12390960531436690 ) ) ;
#178378 = CARTESIAN_POINT ( 'NONE',  ( 21.55341960407619695, -5.719274019375665929, 46.04275706135234714 ) ) ;
#178381 = CARTESIAN_POINT ( 'NONE',  ( -9.474510206698964154, 16.51473224551069663, 95.41557627198102409 ) ) ;
#178382 = CARTESIAN_POINT ( 'NONE',  ( 12.14591786802309770, 12.06949235617756955, 29.37390960531435269 ) ) ;
#178383 = CARTESIAN_POINT ( 'NONE',  ( -14.34966873604972548, 8.224510206698743886, 98.33442372801901854 ) ) ;
#178384 = ORIENTED_EDGE ( 'NONE', *, *, #34091, .T. ) ;
#178385 = CARTESIAN_POINT ( 'NONE',  ( -5.153800228976607833, 19.02544592524334988, 42.70942372801901143 ) ) ;
#178386 = CARTESIAN_POINT ( 'NONE',  ( -9.474510206698964154, 16.51473224551069663, 115.4155762719810241 ) ) ;
#178387 = CARTESIAN_POINT ( 'NONE',  ( -13.89961937509977652, 13.97604488694528158, 65.62390960531436690 ) ) ;
#178388 = CARTESIAN_POINT ( 'NONE',  ( -0.05219959533936034679, 19.03943276465977164, 37.50109039468567573 ) ) ;
#178389 = CARTESIAN_POINT ( 'NONE',  ( 22.81625015709509441, 31.40387420917330275, -7.324999997268812457 ) ) ;
#178390 = CARTESIAN_POINT ( 'NONE',  ( 19.46398650005391673, -5.499999999999944933, 72.68269651486370719 ) ) ;
#178391 = CARTESIAN_POINT ( 'NONE',  ( -4.483927247898782831, 16.52544592524335698, 47.70942372801902565 ) ) ;
#178393 = CARTESIAN_POINT ( 'NONE',  ( 4.483927247898790824, -16.52544592524335698, 55.20942372801902565 ) ) ;
#178392 = CARTESIAN_POINT ( 'NONE',  ( 19.05341960407617918, -5.049401038297876454, 66.04275706135233293 ) ) ;
#178394 = CARTESIAN_POINT ( 'NONE',  ( 9.564922557960805705, 16.46253265017160317, 114.5822429386476955 ) ) ;
#178395 = CARTESIAN_POINT ( 'NONE',  ( -19.03943276465977164, 0.05219959533909376836, 91.24890960531436690 ) ) ;
#178396 = CARTESIAN_POINT ( 'NONE',  ( -5.719274019375978568, 21.55341960407610458, 115.2072429386476955 ) ) ;
#178397 = CARTESIAN_POINT ( 'NONE',  ( -5.153800228976607833, 19.02544592524334988, 77.70942372801900433 ) ) ;
#178399 = CARTESIAN_POINT ( 'NONE',  ( 13.89961937509977652, -13.97604488694527269, 28.12390960531435624 ) ) ;
#178398 = CARTESIAN_POINT ( 'NONE',  ( -19.02544592524342804, 5.153800228976336051, 111.0405762719810099 ) ) ;
#178400 = CARTESIAN_POINT ( 'NONE',  ( 19.03943276465977164, -0.05219959533909143690, 78.74890960531436690 ) ) ;
#178402 = CARTESIAN_POINT ( 'NONE',  ( 16.46253265017160672, -9.564922557960803928, 38.33224293864768839 ) ) ;
#178401 = CARTESIAN_POINT ( 'NONE',  ( -4.379528057220328563, 16.55341960407611168, 45.20724293864769550 ) ) ;
#178403 = CARTESIAN_POINT ( 'NONE',  ( 9.474510206698729675, 16.51473224551082808, 57.08442372801900433 ) ) ;
#178404 = CARTESIAN_POINT ( 'NONE',  ( -8.224510206698948167, 14.34966873604960824, 90.41557627198103830 ) ) ;
#178405 = CARTESIAN_POINT ( 'NONE',  ( 21.55341960407619695, -5.719274019375665929, 106.0427570613523471 ) ) ;
#178406 = CARTESIAN_POINT ( 'NONE',  ( -13.97604488694527625, -13.89961937509977652, 51.87390960531436690 ) ) ;
#178407 = CARTESIAN_POINT ( 'NONE',  ( 5.719274019375991003, -21.55341960407610458, 52.70724293864769550 ) ) ;
#178409 = CARTESIAN_POINT ( 'NONE',  ( -13.89961937509957401, -13.97604488694547875, 19.37609039468566507 ) ) ;
#178408 = CARTESIAN_POINT ( 'NONE',  ( 16.52544592524342804, -4.483927247898539470, 58.54057627198103120 ) ) ;
#178410 = CARTESIAN_POINT ( 'NONE',  ( -13.89961937509977652, 13.97604488694528158, 100.6239096053143669 ) ) ;
#178411 = CARTESIAN_POINT ( 'NONE',  ( -19.03943276465977164, 0.05219959533909376836, 111.2489096053143669 ) ) ;
#178412 = CARTESIAN_POINT ( 'NONE',  ( 9.564922557960805705, 16.46253265017160317, 34.58224293864770260 ) ) ;
#178413 = CARTESIAN_POINT ( 'NONE',  ( -19.05341960407611168, -5.049401038298163336, 31.45724293864769550 ) ) ;
#178414 = CARTESIAN_POINT ( 'NONE',  ( -14.34966873604960291, -8.224510206698953496, 86.66557627198102409 ) ) ;
#178415 = CARTESIAN_POINT ( 'NONE',  ( 18.67979575497178502, 10.72451020669898547, 94.16557627198103830 ) ) ;
#178416 = CARTESIAN_POINT ( 'NONE',  ( 5.049401038298161559, -19.05341960407611168, 97.70724293864766707 ) ) ;
#178417 = CARTESIAN_POINT ( 'NONE',  ( 18.67979575497194134, -10.72451020669871369, 20.83442372801901143 ) ) ;
#178418 = CARTESIAN_POINT ( 'NONE',  ( -13.89961937509977652, 13.97604488694528158, 110.6239096053143243 ) ) ;
#178420 = CARTESIAN_POINT ( 'NONE',  ( -16.55341960407611168, -4.379528057220339221, 101.4572429386476955 ) ) ;
#178419 = CARTESIAN_POINT ( 'NONE',  ( -37.99626262588766679, 2.428612866367529932E-14, -7.747842220587803475 ) ) ;
#178421 = CARTESIAN_POINT ( 'NONE',  ( -5.153800228976328057, -19.02544592524343514, 77.29057627198099567 ) ) ;
#178422 = CARTESIAN_POINT ( 'NONE',  ( 21.52544592524344225, -5.823673210054117533, 83.54057627198102409 ) ) ;
#178423 = CARTESIAN_POINT ( 'NONE',  ( 37.99999999999999289, 2.893978650043524126E-14, -6.749999994537627224 ) ) ;
#178424 = CYLINDRICAL_SURFACE ( 'NONE', #198089, 5.000000000000000000 ) ;
#178426 = LINE ( 'NONE', #117741, #24079 ) ;
#178425 = CARTESIAN_POINT ( 'NONE',  ( -18.67979575497178146, -10.72451020669898902, 26.66557627198103475 ) ) ;
#178427 = CARTESIAN_POINT ( 'NONE',  ( 4.379528057220092307, 16.55341960407617563, 32.29275706135235424 ) ) ;
#178428 = CARTESIAN_POINT ( 'NONE',  ( -16.52544592524342804, 4.483927247898546575, 91.04057627198103830 ) ) ;
#178429 = CARTESIAN_POINT ( 'NONE',  ( 10.59477242850415024, -90.60836494048558620, -15.00000000000000178 ) ) ;
#178430 = CARTESIAN_POINT ( 'NONE',  ( 5.153800228976335163, 19.02544592524342804, 59.79057627198100988 ) ) ;
#178431 = CARTESIAN_POINT ( 'NONE',  ( 4.379528057220339221, -16.55341960407611168, 82.70724293864770971 ) ) ;
#178432 = CARTESIAN_POINT ( 'NONE',  ( -18.67979575497178146, -10.72451020669898902, 36.66557627198103120 ) ) ;
#178433 = CARTESIAN_POINT ( 'NONE',  ( 8.314922557960818139, 14.29746914071049879, 54.58224293864769550 ) ) ;
#178434 = CARTESIAN_POINT ( 'NONE',  ( 5.153800228976615827, -19.02544592524334988, 110.2094237280189901 ) ) ;
#178435 = CARTESIAN_POINT ( 'NONE',  ( 10.81492255796106328, -18.62759615963255655, 70.41775706135236135 ) ) ;
#178436 = CARTESIAN_POINT ( 'NONE',  ( 0.000000000000000000, 0.000000000000000000, -10.00000000000000000 ) ) ;
#178437 = CARTESIAN_POINT ( 'NONE',  ( -9.564922557960796823, -16.46253265017161027, 112.0822429386476955 ) ) ;
#178438 = CARTESIAN_POINT ( 'NONE',  ( -16.55341960407617563, 4.379528057220093196, 78.54275706135236135 ) ) ;
#178439 = CARTESIAN_POINT ( 'NONE',  ( -17.50000000001354294, 5.500000000000027534, 95.79690382535056870 ) ) ;
#178440 = CARTESIAN_POINT ( 'NONE',  ( -16.51473224551069308, -9.474510206698971260, 91.66557627198103830 ) ) ;
#178441 = CARTESIAN_POINT ( 'NONE',  ( 10.72451020669898902, -18.67979575497178502, 92.91557627198103830 ) ) ;
#178442 =( BOUNDED_CURVE ( )  B_SPLINE_CURVE ( 2, ( #104094, #165777, #88920, #150612, #12108, #73771, #108047, #169732, #93879, #200078, #31227 ),
 .UNSPECIFIED., .F., .T. ) 
 B_SPLINE_CURVE_WITH_KNOTS ( ( 3, 2, 2, 2, 2, 3 ),
 ( 0.2000000000000000111, 0.2200000000000000289, 0.2400000000000000466, 0.2600000000000000644, 0.2800000000000001377, 0.3000000000000000999 ),
 .UNSPECIFIED. ) 
 CURVE ( )  GEOMETRIC_REPRESENTATION_ITEM ( )  RATIONAL_B_SPLINE_CURVE ( ( 1.000000000000000000, 0.9510565162951535312, 1.000000000000000000, 0.9510565162951535312, 1.000000000000000000, 0.9510565162951535312, 1.000000000000000000, 0.9510565162951535312, 1.000000000000000000, 0.9510565162951533091, 1.000000000000000222 ) ) 
 REPRESENTATION_ITEM ( '' )  );
#178443 = CARTESIAN_POINT ( 'NONE',  ( 16.52544592524335698, 4.483927247898782831, 31.45942372801901854 ) ) ;
#178445 = CARTESIAN_POINT ( 'NONE',  ( 21.53943276465977519, 0.05219959533937863772, 71.25109039468568994 ) ) ;
#178444 = CARTESIAN_POINT ( 'NONE',  ( -4.379528057220328563, 16.55341960407611168, 55.20724293864770260 ) ) ;
#178447 = CARTESIAN_POINT ( 'NONE',  ( -18.67979575497178146, -10.72451020669898902, 21.66557627198102409 ) ) ;
#178446 = CARTESIAN_POINT ( 'NONE',  ( 14.29746914071037800, 8.314922557961029526, 101.6677570613523613 ) ) ;
#178448 = CARTESIAN_POINT ( 'NONE',  ( -16.46253265017160317, 9.564922557960807481, 115.8322429386477097 ) ) ;
#178449 = CARTESIAN_POINT ( 'NONE',  ( -22.96528548301343520, -5.795830589372932273, 190.0000000000000000 ) ) ;
#178450 = CARTESIAN_POINT ( 'NONE',  ( -14.29746914071037622, -8.314922557961029526, 109.1677570613523613 ) ) ;
#178451 = CARTESIAN_POINT ( 'NONE',  ( -14.29746914071037622, -8.314922557961029526, 54.16775706135235424 ) ) ;
#178452 = CARTESIAN_POINT ( 'NONE',  ( -16.51473224551069308, -9.474510206698971260, 76.66557627198103830 ) ) ;
#178453 = CARTESIAN_POINT ( 'NONE',  ( 13.89961937509977652, -13.97604488694527269, 83.12390960531436690 ) ) ;
#178454 = CARTESIAN_POINT ( 'NONE',  ( 5.823673210054444382, -21.52544592524334988, 70.20942372801904696 ) ) ;
#178455 = CARTESIAN_POINT ( 'NONE',  ( 4.379528057220092307, 16.55341960407617563, 77.29275706135234714 ) ) ;
#178456 = CARTESIAN_POINT ( 'NONE',  ( 12.06949235617757843, -12.14591786802309237, 48.12390960531436690 ) ) ;
#178457 = CARTESIAN_POINT ( 'NONE',  ( 16.51473224551069308, 9.474510206698969483, 49.16557627198102409 ) ) ;
#178458 = VERTEX_POINT ( 'NONE', #52981 ) ;
#178459 = CARTESIAN_POINT ( 'NONE',  ( -9.474510206698720793, -16.51473224551083518, 104.5844237280190043 ) ) ;
#178460 = CARTESIAN_POINT ( 'NONE',  ( -12.06949235617756955, 12.14591786802309770, 105.6239096053143669 ) ) ;
#178461 = CARTESIAN_POINT ( 'NONE',  ( 13.97604488694527802, 13.89961937509977652, 74.37390960531436690 ) ) ;
#178463 = CARTESIAN_POINT ( 'NONE',  ( -30.74264578624800492, -22.33583958711396278, -5.800000000000000711 ) ) ;
#178462 = CARTESIAN_POINT ( 'NONE',  ( 5.049401038297881783, 19.05341960407617563, 97.29275706135233293 ) ) ;
#178464 = CARTESIAN_POINT ( 'NONE',  ( -15.80617190586768217, 15.72974639402176855, 98.12609039468570415 ) ) ;
#178465 = CARTESIAN_POINT ( 'NONE',  ( -8.314922557961024197, 14.29746914071037800, 77.91775706135231871 ) ) ;
#178466 = CARTESIAN_POINT ( 'NONE',  ( -19.02544592524334988, -5.153800228976617603, 88.95942372801897591 ) ) ;
#178467 = CARTESIAN_POINT ( 'NONE',  ( -0.05219959533907301413, -21.53943276465977519, 67.49890960531436690 ) ) ;
#178468 = CARTESIAN_POINT ( 'NONE',  ( -12.14591786802326823, 12.06949235617739902, 58.12609039468568994 ) ) ;
#178469 = CARTESIAN_POINT ( 'NONE',  ( 35.70266437024449147, 2.428612576286966776E-14, 37.50000000000000000 ) ) ;
#178470 = CARTESIAN_POINT ( 'NONE',  ( -9.564922557961040184, 16.46253265017147172, 57.91775706135233293 ) ) ;
#178471 = CARTESIAN_POINT ( 'NONE',  ( -10.81492255796105439, 18.62759615963255655, 92.91775706135236135 ) ) ;
#178472 = CARTESIAN_POINT ( 'NONE',  ( 5.049401038298161559, -19.05341960407611168, 32.70724293864768129 ) ) ;
#178473 = CARTESIAN_POINT ( 'NONE',  ( 9.564922557960805705, 16.46253265017160317, 69.58224293864770971 ) ) ;
#178474 = CARTESIAN_POINT ( 'NONE',  ( 4.483927247898545687, 16.52544592524342804, 59.79057627198103120 ) ) ;
#178475 = CARTESIAN_POINT ( 'NONE',  ( -21.55341960407619339, 5.719274019375674811, 88.54275706135236135 ) ) ;
#178476 = CARTESIAN_POINT ( 'NONE',  ( -9.564922557961040184, 16.46253265017147172, 47.91775706135233293 ) ) ;
#178477 = CARTESIAN_POINT ( 'NONE',  ( 5.049401038297881783, 19.05341960407617563, 22.29275706135233648 ) ) ;
#178478 = CARTESIAN_POINT ( 'NONE',  ( -15.80617190586745835, -15.72974639402198527, 36.87390960531435979 ) ) ;
#178479 = CARTESIAN_POINT ( 'NONE',  ( 21.52544592524334988, 5.823673210054432836, 91.45942372801901854 ) ) ;
#178480 = CARTESIAN_POINT ( 'NONE',  ( 13.97604488694527802, 13.89961937509977652, 79.37390960531435269 ) ) ;
#178481 = EDGE_CURVE ( 'NONE', #148543, #51216, #37829, .T. ) ;
#178482 = CARTESIAN_POINT ( 'NONE',  ( 15.80617190586769283, -15.72974639402175789, 95.62609039468568994 ) ) ;
#178483 = CARTESIAN_POINT ( 'NONE',  ( 5.719274019375991003, -21.55341960407610458, 47.70724293864770260 ) ) ;
#178484 = CARTESIAN_POINT ( 'NONE',  ( -19.02544592524342804, 5.153800228976336051, 86.04057627198103830 ) ) ;
#178485 = CARTESIAN_POINT ( 'NONE',  ( 9.564922557961047289, -16.46253265017146816, 75.41775706135234714 ) ) ;
#178486 = CARTESIAN_POINT ( 'NONE',  ( -19.05341960407611168, -5.049401038298163336, 91.45724293864766707 ) ) ;
#178487 = CARTESIAN_POINT ( 'NONE',  ( -16.46253265017146816, -9.564922557961047289, 99.16775706135233293 ) ) ;
#178488 = CARTESIAN_POINT ( 'NONE',  ( -4.379528057220086978, -16.55341960407618274, 39.79275706135235424 ) ) ;
#178489 = CARTESIAN_POINT ( 'NONE',  ( -16.52544592524342804, 4.483927247898546575, 106.0405762719810525 ) ) ;
#178490 = CARTESIAN_POINT ( 'NONE',  ( -0.05219959533909027116, -19.03943276465977164, 77.49890960531435269 ) ) ;
#178491 = CARTESIAN_POINT ( 'NONE',  ( -21.52544592524343514, 5.823673210054127303, 56.04057627198102409 ) ) ;
#178492 = B_SPLINE_CURVE_WITH_KNOTS ( 'NONE', 3,
 ( #166367, #41020, #91462, #57192, #43013, #74349, #44996, #183513, #105666, #90490, #152172, #181534, #104680, #13655, #42024, #75322, #27864, #106656, #25867, #29825, #9688, #118867, #180551, #103689, #170317, #63128, #49958, #47981, #30818, #155147, #16640, #33791 ),
 .UNSPECIFIED., .F., .F.,
 ( 4, 2, 2, 2, 2, 2, 2, 2, 2, 2, 2, 2, 2, 2, 2, 4 ),
 ( 1.643959876789974123E-15, 0.0003712461730052138767, 0.0007424923460087837776, 0.001113738519012353462, 0.001484984692015923471, 0.002227477038023074982, 0.002598723211026647811, 0.002969969384030220205, 0.003341215557033792600, 0.003712461730037365428, 0.004083707903040937823, 0.004454954076044509784, 0.004826200249048082612, 0.005197446422051654573, 0.005568692595055228269, 0.005939938768058800229 ),
 .UNSPECIFIED. ) ;
#178493 = CARTESIAN_POINT ( 'NONE',  ( 4.379528057220092307, 16.55341960407617563, 37.29275706135235424 ) ) ;
#178494 = CARTESIAN_POINT ( 'NONE',  ( 21.53943276465977519, 0.05219959533937863772, 31.25109039468568639 ) ) ;
#178495 = CARTESIAN_POINT ( 'NONE',  ( 18.67979575497194134, -10.72451020669871369, 80.83442372801901854 ) ) ;
#178496 = CARTESIAN_POINT ( 'NONE',  ( -12.06949235617739369, -12.14591786802326823, 89.37609039468568994 ) ) ;
#178497 = CARTESIAN_POINT ( 'NONE',  ( 5.153800228976335163, 19.02544592524342804, 79.79057627198102409 ) ) ;
#178498 = CARTESIAN_POINT ( 'NONE',  ( 8.314922557960818139, 14.29746914071049879, 74.58224293864768129 ) ) ;
#178499 = CARTESIAN_POINT ( 'NONE',  ( -8.314922557961024197, 14.29746914071037800, 107.9177570613523471 ) ) ;
#178500 = CARTESIAN_POINT ( 'NONE',  ( 19.03943276465977164, 0.05219959533936151252, 61.25109039468566863 ) ) ;
#178501 = CARTESIAN_POINT ( 'NONE',  ( 15.72974639402176855, 15.80617190586768217, 36.87609039468568994 ) ) ;
#178502 = CARTESIAN_POINT ( 'NONE',  ( -16.53943276465976808, 0.05219959533911058130, 76.24890960531435269 ) ) ;
#178503 = CARTESIAN_POINT ( 'NONE',  ( -0.05219959533909027116, -19.03943276465977164, 102.4989096053143669 ) ) ;
#178504 = CARTESIAN_POINT ( 'NONE',  ( 14.29746914071037800, 8.314922557961029526, 96.66775706135234714 ) ) ;
#178505 = CARTESIAN_POINT ( 'NONE',  ( 10.72451020669871369, 18.67979575497193778, 72.08442372801899012 ) ) ;
#178506 = CARTESIAN_POINT ( 'NONE',  ( 12.14591786802327356, -12.06949235617739191, 45.62609039468567573 ) ) ;
#178507 = CARTESIAN_POINT ( 'NONE',  ( 15.72974639402176855, 15.80617190586768217, 26.87609039468567218 ) ) ;
#178508 = CARTESIAN_POINT ( 'NONE',  ( -16.55341960407611168, -4.379528057220339221, 76.45724293864769550 ) ) ;
#178509 = EDGE_LOOP ( 'NONE', ( #62487, #143000 ) ) ;
#178510 = CARTESIAN_POINT ( 'NONE',  ( -21.53943276465977519, 0.05219959533907696930, 111.2489096053143669 ) ) ;
#178511 = CARTESIAN_POINT ( 'NONE',  ( -0.05219959533910754901, -16.53943276465976808, 52.49890960531435979 ) ) ;
#178512 = FACE_OUTER_BOUND ( 'NONE', #15434, .T. ) ;
#178513 = CARTESIAN_POINT ( 'NONE',  ( -0.05219959533907301413, -21.53943276465977519, 32.49890960531435979 ) ) ;
#178514 = CARTESIAN_POINT ( 'NONE',  ( -16.53943276465976808, 0.05219959533911058130, 61.24890960531435979 ) ) ;
#178515 = CARTESIAN_POINT ( 'NONE',  ( 10.81492255796078972, 18.62759615963270932, 84.58224293864769550 ) ) ;
#178516 = CARTESIAN_POINT ( 'NONE',  ( -9.564922557960796823, -16.46253265017161027, 72.08224293864770971 ) ) ;
#178518 = CARTESIAN_POINT ( 'NONE',  ( 0.05219959533936267826, -19.03943276465977164, 75.00109039468566152 ) ) ;
#178517 = CARTESIAN_POINT ( 'NONE',  ( 0.05219959533909260263, 19.03943276465977164, 44.99890960531435979 ) ) ;
#178520 = CARTESIAN_POINT ( 'NONE',  ( -21.52544592524343514, 5.823673210054127303, 56.04057627198102409 ) ) ;
#178519 = CARTESIAN_POINT ( 'NONE',  ( 21.53943276465977519, 0.05219959533937863772, 61.25109039468567573 ) ) ;
#178521 = CARTESIAN_POINT ( 'NONE',  ( -5.049401038298153566, 19.05341960407611168, 45.20724293864769550 ) ) ;
#178522 = CARTESIAN_POINT ( 'NONE',  ( 9.474510206698971260, -16.51473224551069308, 67.91557627198102409 ) ) ;
#178523 = ORIENTED_EDGE ( 'NONE', *, *, #94296, .F. ) ;
#178524 = CARTESIAN_POINT ( 'NONE',  ( -14.29746914071037622, -8.314922557961029526, 49.16775706135234003 ) ) ;
#178525 = CARTESIAN_POINT ( 'NONE',  ( 21.52544592524334988, 5.823673210054432836, 31.45942372801901854 ) ) ;
#178526 = CARTESIAN_POINT ( 'NONE',  ( -0.05219959533937732626, 21.53943276465977519, 57.50109039468568994 ) ) ;
#178527 = CARTESIAN_POINT ( 'NONE',  ( 19.03943276465977164, -0.05219959533909143690, 103.7489096053143669 ) ) ;
#178528 = CARTESIAN_POINT ( 'NONE',  ( 18.62759615963271287, -10.81492255796078972, 88.33224293864769550 ) ) ;
#178530 = CARTESIAN_POINT ( 'NONE',  ( -14.34966873604972548, 8.224510206698743886, 48.33442372801902565 ) ) ;
#178529 = CARTESIAN_POINT ( 'NONE',  ( 15.72974639402176855, 15.80617190586768217, 26.87609039468567218 ) ) ;
#178531 = CARTESIAN_POINT ( 'NONE',  ( 5.719274019375991003, -21.55341960407610458, 52.70724293864769550 ) ) ;
#178532 = CARTESIAN_POINT ( 'NONE',  ( -5.153800228976607833, 19.02544592524334988, 22.70942372801899012 ) ) ;
#178533 = CARTESIAN_POINT ( 'NONE',  ( 5.153800228976335163, 19.02544592524342804, 49.79057627198100988 ) ) ;
#178534 = FACE_OUTER_BOUND ( 'NONE', #26501, .T. ) ;
#178535 = CARTESIAN_POINT ( 'NONE',  ( -16.51473224551069308, -9.474510206698971260, 86.66557627198102409 ) ) ;
#178536 =( REPRESENTATION_RELATIONSHIP ('NONE','NONE', #154205, #65015 ) REPRESENTATION_RELATIONSHIP_WITH_TRANSFORMATION ( #36105 )SHAPE_REPRESENTATION_RELATIONSHIP( ) );
#178537 = CARTESIAN_POINT ( 'NONE',  ( 20.34442274205741796, 22.47021661561673156, -47.91864530057671345 ) ) ;
#178538 = CARTESIAN_POINT ( 'NONE',  ( -19.02544592524334988, -5.153800228976617603, 68.95942372801896170 ) ) ;
#178539 = CARTESIAN_POINT ( 'NONE',  ( -21.53943276465977519, 0.05219959533907696930, 51.24890960531436690 ) ) ;
#178540 = CARTESIAN_POINT ( 'NONE',  ( 16.55341960407611168, 4.379528057220329451, 28.95724293864769905 ) ) ;
#178541 = CARTESIAN_POINT ( 'NONE',  ( 13.89961937509957401, 13.97604488694547697, 86.87609039468567573 ) ) ;
#178542 = CARTESIAN_POINT ( 'NONE',  ( 17.50000000000000000, -5.499999999999992895, 51.21769037696435589 ) ) ;
#178543 = CARTESIAN_POINT ( 'NONE',  ( 18.67979575497194134, -10.72451020669871369, 110.8344237280190043 ) ) ;
#178544 = CARTESIAN_POINT ( 'NONE',  ( -19.05341960407617563, 5.049401038297882671, 103.5427570613523329 ) ) ;
#178545 = CARTESIAN_POINT ( 'NONE',  ( 9.564922557961047289, -16.46253265017146816, 50.41775706135233293 ) ) ;
#178546 = CARTESIAN_POINT ( 'NONE',  ( 16.18388926212239198, 7.379444403734514601, 107.9395315136615920 ) ) ;
#178547 = CARTESIAN_POINT ( 'NONE',  ( 9.474510206698971260, -16.51473224551069308, 52.91557627198102409 ) ) ;
#178548 = CARTESIAN_POINT ( 'NONE',  ( 14.29746914071049879, -8.314922557960816363, 68.33224293864769550 ) ) ;
#178549 = CARTESIAN_POINT ( 'NONE',  ( 0.05219959533909260263, 19.03943276465977164, 34.99890960531435979 ) ) ;
#178550 = CARTESIAN_POINT ( 'NONE',  ( -14.29746914071049879, 8.314922557960819915, 40.83224293864769550 ) ) ;
#178551 = CARTESIAN_POINT ( 'NONE',  ( -27.00987238947304547, -29.10436634937588707, -20.14159902729970852 ) ) ;
#178552 = CARTESIAN_POINT ( 'NONE',  ( 12.06949235617739724, 12.14591786802326823, 101.8760903946857042 ) ) ;
#178553 = CARTESIAN_POINT ( 'NONE',  ( 5.153800228976335163, 19.02544592524342804, 69.79057627198103830 ) ) ;
#178554 = CARTESIAN_POINT ( 'NONE',  ( -9.474510206698720793, -16.51473224551083518, 24.58442372801900078 ) ) ;
#178555 = CARTESIAN_POINT ( 'NONE',  ( 4.379528057220092307, 16.55341960407617563, 32.29275706135235424 ) ) ;
#178556 = CARTESIAN_POINT ( 'NONE',  ( -5.823673210054116645, -21.52544592524344225, 42.29057627198103120 ) ) ;
#178558 = ORIENTED_EDGE ( 'NONE', *, *, #174924, .T. ) ;
#178557 = CARTESIAN_POINT ( 'NONE',  ( 5.719274019375673035, 21.55341960407619339, 102.2927570613523613 ) ) ;
#178559 = CARTESIAN_POINT ( 'NONE',  ( 19.03943276465977164, -0.05219959533909143690, 63.74890960531435979 ) ) ;
#178560 = CARTESIAN_POINT ( 'NONE',  ( 9.474510206698971260, -16.51473224551069308, 102.9155762719810241 ) ) ;
#178561 = CARTESIAN_POINT ( 'NONE',  ( -5.049401038298153566, 19.05341960407611168, 100.2072429386476955 ) ) ;
#178562 = CARTESIAN_POINT ( 'NONE',  ( 36.91746824999999177, 11.99521256947799230, -3.524999997268813079 ) ) ;
#178563 = CARTESIAN_POINT ( 'NONE',  ( 15.80617190586769283, -15.72974639402175789, 25.62609039468567929 ) ) ;
#178564 = CARTESIAN_POINT ( 'NONE',  ( -16.52544592524342804, 4.483927247898546575, 96.04057627198102409 ) ) ;
#178566 = CARTESIAN_POINT ( 'NONE',  ( -5.049401038298153566, 19.05341960407611168, 70.20724293864769550 ) ) ;
#178565 = CARTESIAN_POINT ( 'NONE',  ( 5.823673210054125526, 21.52544592524343514, 69.79057627198102409 ) ) ;
#178567 = CARTESIAN_POINT ( 'NONE',  ( 13.97604488694527802, 13.89961937509977652, 79.37390960531435269 ) ) ;
#178568 = CARTESIAN_POINT ( 'NONE',  ( -0.05219959533907301413, -21.53943276465977519, 112.4989096053143669 ) ) ;
#178569 = EDGE_CURVE ( 'NONE', #122302, #107085, #144786, .T. ) ;
#178570 = ORIENTED_EDGE ( 'NONE', *, *, #195656, .T. ) ;
#178571 = CARTESIAN_POINT ( 'NONE',  ( 5.049401038298161559, -19.05341960407611168, 77.70724293864765286 ) ) ;
#178572 = CARTESIAN_POINT ( 'NONE',  ( -37.66961640367473052, -4.999999999999976019, -18.00000000000000355 ) ) ;
#178574 = CARTESIAN_POINT ( 'NONE',  ( 28.66576453816018244, -27.89900116845191391, -15.73147987472289167 ) ) ;
#178573 = CARTESIAN_POINT ( 'NONE',  ( 16.52544592524342804, -4.483927247898539470, 103.5405762719810383 ) ) ;
#178575 = CARTESIAN_POINT ( 'NONE',  ( 13.97604488694527802, 13.89961937509977652, 64.37390960531436690 ) ) ;
#178576 = CARTESIAN_POINT ( 'NONE',  ( -19.03943276465977164, -0.05219959533935918106, 88.75109039468567573 ) ) ;
#178577 = CARTESIAN_POINT ( 'NONE',  ( -16.52544592524342804, 4.483927247898546575, 96.04057627198102409 ) ) ;
#178578 = CARTESIAN_POINT ( 'NONE',  ( -15.72974639402176322, -15.80617190586768395, 69.37609039468567573 ) ) ;
#178580 = CARTESIAN_POINT ( 'NONE',  ( 21.55341960407619695, -5.719274019375665929, 21.04275706135234714 ) ) ;
#178579 = CARTESIAN_POINT ( 'NONE',  ( -0.05219959533909027116, -19.03943276465977164, 52.49890960531436690 ) ) ;
#178581 = CARTESIAN_POINT ( 'NONE',  ( 5.719274019375991003, -21.55341960407610458, 112.7072429386476955 ) ) ;
#178582 = SPHERICAL_SURFACE ( 'NONE', #94873, 10.00000000000000000 ) ;
#178583 = CARTESIAN_POINT ( 'NONE',  ( -19.03943276465977164, 0.05219959533909376836, 76.24890960531435269 ) ) ;
#178584 = CARTESIAN_POINT ( 'NONE',  ( 17.40805194822031865, 6.112264579159319311, 111.6662872748938895 ) ) ;
#178586 = CARTESIAN_POINT ( 'NONE',  ( -15.72974639402197994, 15.80617190586746368, 35.62390960531437401 ) ) ;
#178585 = CARTESIAN_POINT ( 'NONE',  ( -16.51473224551082808, 9.474510206698731452, 113.3344237280190043 ) ) ;
#178587 = CARTESIAN_POINT ( 'NONE',  ( -21.53943276465977519, -0.05219959533937600094, 63.75109039468568284 ) ) ;
#178588 = CARTESIAN_POINT ( 'NONE',  ( -0.05219959533909027116, -19.03943276465977164, 102.4989096053143669 ) ) ;
#178589 = CARTESIAN_POINT ( 'NONE',  ( -5.049401038297874678, -19.05341960407617918, 89.79275706135230450 ) ) ;
#178590 = AXIS2_PLACEMENT_3D ( 'NONE', #199001, #91787, #62451 ) ;
#178591 = CARTESIAN_POINT ( 'NONE',  ( 19.03943276465977164, -0.05219959533909143690, 48.74890960531435979 ) ) ;
#178592 = CARTESIAN_POINT ( 'NONE',  ( 5.153800228976335163, 19.02544592524342804, 69.79057627198103830 ) ) ;
#178593 = CARTESIAN_POINT ( 'NONE',  ( 14.34966873604960469, 8.224510206698951720, 84.16557627198103830 ) ) ;
#178594 = CARTESIAN_POINT ( 'NONE',  ( 9.474510206698971260, -16.51473224551069308, 107.9155762719810383 ) ) ;
#178595 = CARTESIAN_POINT ( 'NONE',  ( 16.52544592524342804, -4.483927247898539470, 98.54057627198105251 ) ) ;
#178596 = CARTESIAN_POINT ( 'NONE',  ( 9.474510206698971260, -16.51473224551069308, 97.91557627198102409 ) ) ;
#178598 = CARTESIAN_POINT ( 'NONE',  ( -9.564922557960796823, -16.46253265017161027, 22.08224293864768839 ) ) ;
#178597 = CARTESIAN_POINT ( 'NONE',  ( 16.53943276465976808, -0.05219959533910856209, 43.74890960531435979 ) ) ;
#178599 = ORIENTED_EDGE ( 'NONE', *, *, #119036, .T. ) ;
#178600 = CARTESIAN_POINT ( 'NONE',  ( -0.05219959533937732626, 21.53943276465977519, 62.50109039468568284 ) ) ;
#178601 = CARTESIAN_POINT ( 'NONE',  ( -16.46253265017146816, -9.564922557961047289, 74.16775706135234714 ) ) ;
#178602 = CARTESIAN_POINT ( 'NONE',  ( 14.29746914071049879, -8.314922557960816363, 43.33224293864769550 ) ) ;
#178603 = CARTESIAN_POINT ( 'NONE',  ( -18.62759615963270932, 10.81492255796079327, 95.83224293864770971 ) ) ;
#178604 = CARTESIAN_POINT ( 'NONE',  ( -21.53943276465977519, 0.05219959533907696930, 31.24890960531435979 ) ) ;
#178605 = CARTESIAN_POINT ( 'NONE',  ( -12.06949235617756955, 12.14591786802309770, 85.62390960531436690 ) ) ;
#178606 = CARTESIAN_POINT ( 'NONE',  ( -13.97604488694527625, -13.89961937509977652, 51.87390960531436690 ) ) ;
#178607 = CARTESIAN_POINT ( 'NONE',  ( 16.53943276465976808, -0.05219959533910856209, 23.74890960531435269 ) ) ;
#178608 = CARTESIAN_POINT ( 'NONE',  ( 14.29746914071037800, 8.314922557961029526, 96.66775706135234714 ) ) ;
#178609 = CARTESIAN_POINT ( 'NONE',  ( -14.34966873604972548, 8.224510206698743886, 73.33442372801901854 ) ) ;
#178610 = CARTESIAN_POINT ( 'NONE',  ( 16.51473224551083163, -9.474510206698727899, 25.83442372801900078 ) ) ;
#178611 = CARTESIAN_POINT ( 'NONE',  ( 9.564922557960805705, 16.46253265017160317, 99.58224293864770971 ) ) ;
#178612 = CARTESIAN_POINT ( 'NONE',  ( 9.474510206698971260, -16.51473224551069308, 77.91557627198103830 ) ) ;
#178613 = CARTESIAN_POINT ( 'NONE',  ( -9.474510206698964154, 16.51473224551069663, 35.41557627198102409 ) ) ;
#178614 = CARTESIAN_POINT ( 'NONE',  ( -14.29746914071049879, 8.314922557960819915, 45.83224293864769550 ) ) ;
#178616 = CARTESIAN_POINT ( 'NONE',  ( -9.474510206698964154, 16.51473224551069663, 100.4155762719810241 ) ) ;
#178615 = CARTESIAN_POINT ( 'NONE',  ( 9.564922557960805705, 16.46253265017160317, 114.5822429386476955 ) ) ;
#178617 = CARTESIAN_POINT ( 'NONE',  ( -10.81492255796078084, -18.62759615963271287, 37.08224293864768129 ) ) ;
#178618 = CARTESIAN_POINT ( 'NONE',  ( 8.224510206698953496, -14.34966873604960469, 72.91557627198103830 ) ) ;
#178619 = CARTESIAN_POINT ( 'NONE',  ( -16.53943276465976808, -0.05219959533934237506, 23.75109039468567929 ) ) ;
#178620 = AXIS2_PLACEMENT_3D ( 'NONE', #68738, #102084, #56587 ) ;
#178621 = CARTESIAN_POINT ( 'NONE',  ( -12.14591786802309592, -12.06949235617757132, 66.87390960531436690 ) ) ;
#178622 = LINE ( 'NONE', #133099, #38253 ) ;
#178623 = CARTESIAN_POINT ( 'NONE',  ( 13.89961937509957401, 13.97604488694547697, 61.87609039468566863 ) ) ;
#178624 = CARTESIAN_POINT ( 'NONE',  ( -19.02544592524342804, 5.153800228976336051, 101.0405762719810241 ) ) ;
#178625 = CARTESIAN_POINT ( 'NONE',  ( -5.153800228976607833, 19.02544592524334988, 82.70942372801897591 ) ) ;
#178626 = CARTESIAN_POINT ( 'NONE',  ( -9.474510206698720793, -16.51473224551083518, 94.58442372801900433 ) ) ;
#178628 = CARTESIAN_POINT ( 'NONE',  ( 16.52544592524335698, 4.483927247898782831, 96.45942372801901854 ) ) ;
#178627 = CARTESIAN_POINT ( 'NONE',  ( 14.34966873604972726, -8.224510206698740333, 20.83442372801901143 ) ) ;
#178629 = CARTESIAN_POINT ( 'NONE',  ( 19.03943276465977164, -0.05219959533909143690, 38.74890960531436690 ) ) ;
#178630 = CARTESIAN_POINT ( 'NONE',  ( -10.72451020669898014, 18.67979575497178502, 30.41557627198101699 ) ) ;
#178631 = CARTESIAN_POINT ( 'NONE',  ( 0.05219959533937995610, -21.53943276465977519, 50.00109039468568994 ) ) ;
#178632 = CARTESIAN_POINT ( 'NONE',  ( 19.53392245597576604, 5.500000000000095035, 37.87441121409608513 ) ) ;
#178633 = CARTESIAN_POINT ( 'NONE',  ( 14.34966873604972726, -8.224510206698740333, 20.83442372801901143 ) ) ;
#178635 = CARTESIAN_POINT ( 'NONE',  ( -19.03943276465977164, 0.05219959533909376836, 71.24890960531435269 ) ) ;
#178634 = CARTESIAN_POINT ( 'NONE',  ( 17.49999999999998934, 3.215008338131321697, 22.54447599092367227 ) ) ;
#178636 = LINE ( 'NONE', #105765, #91873 ) ;
#178638 = CARTESIAN_POINT ( 'NONE',  ( -9.564922557960796823, -16.46253265017161027, 82.08224293864768129 ) ) ;
#178637 = CARTESIAN_POINT ( 'NONE',  ( -14.29746914071049879, 8.314922557960819915, 90.83224293864769550 ) ) ;
#178639 = CARTESIAN_POINT ( 'NONE',  ( 9.474510206698971260, -16.51473224551069308, 82.91557627198103830 ) ) ;
#178640 = ORIENTED_EDGE ( 'NONE', *, *, #66709, .T. ) ;
#178641 = CARTESIAN_POINT ( 'NONE',  ( 19.03943276465977164, 0.05219959533936151252, 86.25109039468567573 ) ) ;
#178642 = CARTESIAN_POINT ( 'NONE',  ( -10.81492255796078084, -18.62759615963271287, 62.08224293864769550 ) ) ;
#178643 = CARTESIAN_POINT ( 'NONE',  ( 19.03943276465977164, -0.05219959533909143690, 23.74890960531435269 ) ) ;
#178644 = CARTESIAN_POINT ( 'NONE',  ( 19.02544592524334988, 5.153800228976608722, 51.45942372801900433 ) ) ;
#178645 = CARTESIAN_POINT ( 'NONE',  ( -19.02544592524342804, 5.153800228976336051, 56.04057627198100988 ) ) ;
#178646 = CARTESIAN_POINT ( 'NONE',  ( 19.05341960407611168, 5.049401038298154454, 93.95724293864769550 ) ) ;
#178647 = ORIENTED_EDGE ( 'NONE', *, *, #112783, .F. ) ;
#178648 = CARTESIAN_POINT ( 'NONE',  ( -5.719274019375978568, 21.55341960407610458, 90.20724293864770971 ) ) ;
#178651 = CARTESIAN_POINT ( 'NONE',  ( -13.97604488694547697, 13.89961937509957934, 58.12609039468566863 ) ) ;
#178650 = CARTESIAN_POINT ( 'NONE',  ( 13.89961937509977652, -13.97604488694527269, 83.12390960531436690 ) ) ;
#178649 = CARTESIAN_POINT ( 'NONE',  ( 16.53943276465976808, -0.05219959533910856209, 93.74890960531436690 ) ) ;
#178652 = CARTESIAN_POINT ( 'NONE',  ( -21.53943276465977519, 0.05219959533907696930, 86.24890960531436690 ) ) ;
#178653 = CARTESIAN_POINT ( 'NONE',  ( -0.05219959533907301413, -21.53943276465977519, 72.49890960531435269 ) ) ;
#178654 = CARTESIAN_POINT ( 'NONE',  ( 14.34966873604960469, 8.224510206698951720, 29.16557627198103120 ) ) ;
#178655 = CARTESIAN_POINT ( 'NONE',  ( 18.67979575497194134, -10.72451020669871369, 110.8344237280190043 ) ) ;
#178656 = CARTESIAN_POINT ( 'NONE',  ( -14.34966873604972548, 8.224510206698743886, 58.33442372801901143 ) ) ;
#178657 = CARTESIAN_POINT ( 'NONE',  ( -9.474510206698964154, 16.51473224551069663, 75.41557627198103830 ) ) ;
#178658 = CARTESIAN_POINT ( 'NONE',  ( -0.05219959533909027116, -19.03943276465977164, 27.49890960531435624 ) ) ;
#178659 = CARTESIAN_POINT ( 'NONE',  ( 18.67979575497194134, -10.72451020669871369, 45.83442372801901854 ) ) ;
#178660 = CARTESIAN_POINT ( 'NONE',  ( 15.72974639402176855, 15.80617190586768217, 51.87609039468568284 ) ) ;
#178661 = CARTESIAN_POINT ( 'NONE',  ( -0.05219959533909027116, -19.03943276465977164, 47.49890960531435979 ) ) ;
#178662 = CARTESIAN_POINT ( 'NONE',  ( -18.62759615963270932, 10.81492255796079327, 115.8322429386477097 ) ) ;
#178663 = CARTESIAN_POINT ( 'NONE',  ( 13.97604488694548053, -13.89961937509957401, 65.62609039468567573 ) ) ;
#178664 = CARTESIAN_POINT ( 'NONE',  ( -5.049401038297874678, -19.05341960407617918, 69.79275706135233293 ) ) ;
#178665 = CARTESIAN_POINT ( 'NONE',  ( 12.06949235617739724, 12.14591786802326823, 31.87609039468567929 ) ) ;
#178666 = CARTESIAN_POINT ( 'NONE',  ( -9.474510206698964154, 16.51473224551069663, 25.41557627198103120 ) ) ;
#178667 = CARTESIAN_POINT ( 'NONE',  ( -8.314922557961024197, 14.29746914071037800, 67.91775706135234714 ) ) ;
#178668 = CARTESIAN_POINT ( 'NONE',  ( 16.51473224551069308, 9.474510206698969483, 49.16557627198102409 ) ) ;
#178669 = CARTESIAN_POINT ( 'NONE',  ( 21.35462415990328111, -9.648971641164415303, 168.5494316893070845 ) ) ;
#178670 = CARTESIAN_POINT ( 'NONE',  ( -19.02544592524342804, 5.153800228976336051, 96.04057627198103830 ) ) ;
#178671 = CARTESIAN_POINT ( 'NONE',  ( 5.153800228976335163, 19.02544592524342804, 29.79057627198102409 ) ) ;
#178672 = CARTESIAN_POINT ( 'NONE',  ( -18.67979575497178146, -10.72451020669898902, 66.66557627198102409 ) ) ;
#178673 = CARTESIAN_POINT ( 'NONE',  ( 16.55341960407618274, -4.379528057220086978, 66.04275706135236135 ) ) ;
#178674 = CARTESIAN_POINT ( 'NONE',  ( -5.049401038297874678, -19.05341960407617918, 19.79275706135233293 ) ) ;
#178675 = EDGE_CURVE ( 'NONE', #14026, #15707, #154274, .T. ) ;
#178676 = CARTESIAN_POINT ( 'NONE',  ( -5.153800228976328057, -19.02544592524343514, 47.29057627198102409 ) ) ;
#178677 = CARTESIAN_POINT ( 'NONE',  ( -0.05219959533910754901, -16.53943276465976808, 32.49890960531435979 ) ) ;
#178678 = CARTESIAN_POINT ( 'NONE',  ( -14.34966873604960291, -8.224510206698953496, 66.66557627198102409 ) ) ;
#178679 = CARTESIAN_POINT ( 'NONE',  ( 13.97604488694527802, 13.89961937509977652, 74.37390960531436690 ) ) ;
#178680 = CARTESIAN_POINT ( 'NONE',  ( -15.80617190586768217, 15.72974639402176855, 43.12609039468568284 ) ) ;
#178681 = CARTESIAN_POINT ( 'NONE',  ( -19.05341960407611168, -5.049401038298163336, 91.45724293864766707 ) ) ;
#178682 = VECTOR ( 'NONE', #167615, 1000.000000000000000 ) ;
#178683 = CARTESIAN_POINT ( 'NONE',  ( 21.53943276465977519, 0.05219959533937863772, 86.25109039468568994 ) ) ;
#178684 = CARTESIAN_POINT ( 'NONE',  ( 8.314922557961029526, -14.29746914071037800, 60.41775706135235424 ) ) ;
#178685 = CARTESIAN_POINT ( 'NONE',  ( -0.05219959533909027116, -19.03943276465977164, 107.4989096053143527 ) ) ;
#178686 = EDGE_CURVE ( 'NONE', #126933, #23953, #199452, .T. ) ;
#178687 = CARTESIAN_POINT ( 'NONE',  ( 21.53943276465977519, -0.05219959533907433946, 88.74890960531436690 ) ) ;
#178688 = CARTESIAN_POINT ( 'NONE',  ( 12.06949235617757843, -12.14591786802309237, 43.12390960531435269 ) ) ;
#178689 = CARTESIAN_POINT ( 'NONE',  ( 19.05341960407611168, 5.049401038298154454, 28.95724293864769550 ) ) ;
#178690 = CARTESIAN_POINT ( 'NONE',  ( 4.379528057220092307, 16.55341960407617563, 52.29275706135236135 ) ) ;
#178691 = CARTESIAN_POINT ( 'NONE',  ( -12.06949235617756955, 12.14591786802309770, 70.62390960531436690 ) ) ;
#178692 = CARTESIAN_POINT ( 'NONE',  ( 18.62759615963271287, -10.81492255796078972, 23.33224293864769194 ) ) ;
#178693 = CARTESIAN_POINT ( 'NONE',  ( 21.55341960407610458, 5.719274019375980345, 33.95724293864769550 ) ) ;
#178694 = CARTESIAN_POINT ( 'NONE',  ( -5.823673210054431948, 21.52544592524334988, 112.7094237280190328 ) ) ;
#178695 = CARTESIAN_POINT ( 'NONE',  ( 16.52544592524342804, -4.483927247898539470, 98.54057627198105251 ) ) ;
#178696 = CARTESIAN_POINT ( 'NONE',  ( -0.05219959533909027116, -19.03943276465977164, 107.4989096053143527 ) ) ;
#178697 = VERTEX_POINT ( 'NONE', #12506 ) ;
#178698 = CARTESIAN_POINT ( 'NONE',  ( 4.483927247898790824, -16.52544592524335698, 50.20942372801901854 ) ) ;
#178699 = CARTESIAN_POINT ( 'NONE',  ( 19.02544592524343514, -5.153800228976328945, 53.54057627198102409 ) ) ;
#178700 = CARTESIAN_POINT ( 'NONE',  ( -30.00000000000000000, -1.163414459189985801E-14, 95.00000000000000000 ) ) ;
#178701 = CARTESIAN_POINT ( 'NONE',  ( 9.564922557961047289, -16.46253265017146816, 45.41775706135232582 ) ) ;
#178702 = CARTESIAN_POINT ( 'NONE',  ( -16.52544592524335698, -4.483927247898792601, 93.95942372801903275 ) ) ;
#178703 = CARTESIAN_POINT ( 'NONE',  ( -13.89961937509957401, -13.97604488694547875, 89.37609039468563310 ) ) ;
#178704 = CARTESIAN_POINT ( 'NONE',  ( 18.62759615963255655, 10.81492255796105972, 71.66775706135234714 ) ) ;
#178705 = CARTESIAN_POINT ( 'NONE',  ( 19.05341960407611168, 5.049401038298154454, 68.95724293864769550 ) ) ;
#178706 = CARTESIAN_POINT ( 'NONE',  ( -15.80617190586745835, -15.72974639402198527, 96.87390960531436690 ) ) ;
#178707 = CARTESIAN_POINT ( 'NONE',  ( -0.05219959533909027116, -19.03943276465977164, 22.49890960531436690 ) ) ;
#178708 = CARTESIAN_POINT ( 'NONE',  ( -0.05219959533936034679, 19.03943276465977164, 77.50109039468566152 ) ) ;
#178709 = CARTESIAN_POINT ( 'NONE',  ( -0.05219959533907301413, -21.53943276465977519, 72.49890960531435269 ) ) ;
#178710 = CARTESIAN_POINT ( 'NONE',  ( 5.049401038297881783, 19.05341960407617563, 37.29275706135232582 ) ) ;
#178711 = CARTESIAN_POINT ( 'NONE',  ( 19.19724070472095434, 5.500000000000029310, 98.56193348274383936 ) ) ;
#178712 = EDGE_CURVE ( 'NONE', #142504, #153137, #121634, .T. ) ;
#178713 = CARTESIAN_POINT ( 'NONE',  ( 15.80617190586746368, 15.72974639402197994, 84.37390960531438111 ) ) ;
#178714 = CARTESIAN_POINT ( 'NONE',  ( 13.89961937509977652, -13.97604488694527269, 68.12390960531436690 ) ) ;
#178715 = CARTESIAN_POINT ( 'NONE',  ( -18.22780087662123094, -5.499999999999984901, 91.48459894673894155 ) ) ;
#178716 = CARTESIAN_POINT ( 'NONE',  ( 0.05219959533934541429, -16.53943276465976808, 25.00109039468567218 ) ) ;
#178717 = CARTESIAN_POINT ( 'NONE',  ( -0.05219959533936034679, 19.03943276465977164, 97.50109039468567573 ) ) ;
#178718 = CARTESIAN_POINT ( 'NONE',  ( 13.89961937509977652, -13.97604488694527269, 43.12390960531434558 ) ) ;
#178719 = CARTESIAN_POINT ( 'NONE',  ( 9.564922557960805705, 16.46253265017160317, 109.5822429386476955 ) ) ;
#178721 = CARTESIAN_POINT ( 'NONE',  ( 4.483927247898545687, 16.52544592524342804, 44.79057627198103120 ) ) ;
#178720 = CARTESIAN_POINT ( 'NONE',  ( 15.72974639402199770, -15.80617190586745480, 108.1239096053143811 ) ) ;
#178722 = CARTESIAN_POINT ( 'NONE',  ( 15.72974639402176855, 15.80617190586768217, 71.87609039468568994 ) ) ;
#178724 = CARTESIAN_POINT ( 'NONE',  ( 9.474510206698729675, 16.51473224551082808, 27.08442372801900433 ) ) ;
#178723 = CARTESIAN_POINT ( 'NONE',  ( -8.224510206698735004, -14.34966873604973081, 24.58442372801901499 ) ) ;
#178725 = CARTESIAN_POINT ( 'NONE',  ( -12.14591786802309592, -12.06949235617757132, 31.87390960531435979 ) ) ;
#178726 = CARTESIAN_POINT ( 'NONE',  ( -15.80617190586745835, -15.72974639402198527, 111.8739096053143669 ) ) ;
#178727 = CARTESIAN_POINT ( 'NONE',  ( -8.314922557960811034, -14.29746914071050412, 52.08224293864768839 ) ) ;
#178728 = CARTESIAN_POINT ( 'NONE',  ( -19.03943276465977164, -0.05219959533935918106, 93.75109039468566152 ) ) ;
#178729 = CARTESIAN_POINT ( 'NONE',  ( 5.049401038297881783, 19.05341960407617563, 67.29275706135234714 ) ) ;
#178730 = CARTESIAN_POINT ( 'NONE',  ( 15.80617190586769283, -15.72974639402175789, 65.62609039468568994 ) ) ;
#178731 = CARTESIAN_POINT ( 'NONE',  ( 13.89961937509957401, 13.97604488694547697, 56.87609039468564731 ) ) ;
#178732 = CARTESIAN_POINT ( 'NONE',  ( 16.53943276465976808, -0.05219959533910856209, 113.7489096053143527 ) ) ;
#178733 = CARTESIAN_POINT ( 'NONE',  ( -5.719274019375978568, 21.55341960407610458, 40.20724293864769550 ) ) ;
#178734 = CARTESIAN_POINT ( 'NONE',  ( 16.55341960407611168, 4.379528057220329451, 48.95724293864770971 ) ) ;
#178735 = CARTESIAN_POINT ( 'NONE',  ( -17.50000000000003197, -5.622605283950793620, 26.31207310596111171 ) ) ;
#178736 = CARTESIAN_POINT ( 'NONE',  ( -19.05341960407617563, 5.049401038297882671, 23.54275706135233648 ) ) ;
#178737 = CARTESIAN_POINT ( 'NONE',  ( -8.224510206698735004, -14.34966873604973081, 79.58442372801903275 ) ) ;
#178738 = CARTESIAN_POINT ( 'NONE',  ( 16.55341960407611168, 4.379528057220329451, 33.95724293864769550 ) ) ;
#178739 = CARTESIAN_POINT ( 'NONE',  ( 10.72451020669871369, 18.67979575497193778, 82.08442372801901854 ) ) ;
#178740 = CARTESIAN_POINT ( 'NONE',  ( 21.55341960407619695, -5.719274019375665929, 81.04275706135236135 ) ) ;
#178741 = CARTESIAN_POINT ( 'NONE',  ( 18.67979575497178502, 10.72451020669898547, 84.16557627198103830 ) ) ;
#178742 = CARTESIAN_POINT ( 'NONE',  ( 13.89961937509977652, -13.97604488694527269, 38.12390960531436690 ) ) ;
#178743 = CARTESIAN_POINT ( 'NONE',  ( -5.719274019375665041, -21.55341960407619695, 59.79275706135234714 ) ) ;
#178744 = CARTESIAN_POINT ( 'NONE',  ( 16.46253265017160672, -9.564922557960803928, 38.33224293864768839 ) ) ;
#178745 = CARTESIAN_POINT ( 'NONE',  ( 19.05341960407611168, 5.049401038298154454, 53.95724293864770260 ) ) ;
#178746 = CARTESIAN_POINT ( 'NONE',  ( 8.314922557960818139, 14.29746914071049879, 89.58224293864768129 ) ) ;
#178747 = CARTESIAN_POINT ( 'NONE',  ( 19.03943276465977164, -0.05219959533909143690, 93.74890960531435269 ) ) ;
#178748 = CARTESIAN_POINT ( 'NONE',  ( -4.483927247898539470, -16.52544592524342804, 42.29057627198103120 ) ) ;
#178749 = CARTESIAN_POINT ( 'NONE',  ( 16.53943276465976808, -0.05219959533910856209, 113.7489096053143527 ) ) ;
#178750 = CARTESIAN_POINT ( 'NONE',  ( 0.05219959533907565091, 21.53943276465977519, 84.99890960531436690 ) ) ;
#178751 = CARTESIAN_POINT ( 'NONE',  ( -21.55341960407619339, 5.719274019375674811, 28.54275706135234358 ) ) ;
#178752 = CARTESIAN_POINT ( 'NONE',  ( -17.34149035984848553, 17.02389920581777005, -54.21489346206831073 ) ) ;
#178754 = CARTESIAN_POINT ( 'NONE',  ( -16.51473224551082808, 9.474510206698731452, 113.3344237280190043 ) ) ;
#178753 = CARTESIAN_POINT ( 'NONE',  ( 19.02544592524343514, -5.153800228976328945, 78.54057627198099567 ) ) ;
#178755 = CARTESIAN_POINT ( 'NONE',  ( 21.53943276465977519, -0.05219959533907433946, 73.74890960531433848 ) ) ;
#178756 = CARTESIAN_POINT ( 'NONE',  ( 21.55341960407619695, -5.719274019375665929, 91.04275706135236135 ) ) ;
#178757 = CARTESIAN_POINT ( 'NONE',  ( -13.89961937509977652, 13.97604488694528158, 75.62390960531438111 ) ) ;
#178758 = CARTESIAN_POINT ( 'NONE',  ( -18.67979575497193778, 10.72451020669871902, 28.33442372801902209 ) ) ;
#178759 = AXIS2_PLACEMENT_3D ( 'NONE', #173185, #19497, #81142 ) ;
#178760 = CARTESIAN_POINT ( 'NONE',  ( -0.05219959533909027116, -19.03943276465977164, 112.4989096053143669 ) ) ;
#178761 = CARTESIAN_POINT ( 'NONE',  ( 8.314922557961029526, -14.29746914071037800, 95.41775706135234714 ) ) ;
#178762 = CARTESIAN_POINT ( 'NONE',  ( 5.719274019375673035, 21.55341960407619339, 77.29275706135234714 ) ) ;
#178763 = CARTESIAN_POINT ( 'NONE',  ( -5.719274019375665041, -21.55341960407619695, 104.7927570613523898 ) ) ;
#178764 = CARTESIAN_POINT ( 'NONE',  ( -8.224510206698735004, -14.34966873604973081, 74.58442372801901854 ) ) ;
#178765 = CARTESIAN_POINT ( 'NONE',  ( 21.53943276465977519, 0.05219959533937863772, 31.25109039468568639 ) ) ;
#178766 = CARTESIAN_POINT ( 'NONE',  ( -19.02544592524342804, 5.153800228976336051, 116.0405762719810383 ) ) ;
#178767 = CARTESIAN_POINT ( 'NONE',  ( 21.55341960407619695, -5.719274019375665929, 96.04275706135236135 ) ) ;
#178768 = CARTESIAN_POINT ( 'NONE',  ( -5.049401038298153566, 19.05341960407611168, 90.20724293864766707 ) ) ;
#178769 = CARTESIAN_POINT ( 'NONE',  ( -18.62759615963270932, 10.81492255796079327, 95.83224293864770971 ) ) ;
#178770 = CARTESIAN_POINT ( 'NONE',  ( -16.46253265017146816, -9.564922557961047289, 64.16775706135233293 ) ) ;
#178772 = CARTESIAN_POINT ( 'NONE',  ( -5.823673210054116645, -21.52544592524344225, 47.29057627198103120 ) ) ;
#178771 = CARTESIAN_POINT ( 'NONE',  ( 19.49190055781010855, 5.500000000000050626, 83.06116087098779133 ) ) ;
#178774 = CARTESIAN_POINT ( 'NONE',  ( 16.55341960407611168, 4.379528057220329451, 53.95724293864770260 ) ) ;
#178773 = CARTESIAN_POINT ( 'NONE',  ( -19.02544592524342804, 5.153800228976336051, 101.0405762719810241 ) ) ;
#178775 = CARTESIAN_POINT ( 'NONE',  ( 10.20000000000000107, 1.971681346627238735E-16, -1.610000000000000098 ) ) ;
#178776 = CARTESIAN_POINT ( 'NONE',  ( 13.97604488694548053, -13.89961937509957401, 80.62609039468567573 ) ) ;
#178777 = DIRECTION ( 'NONE',  ( 1.000000000000000000, 0.000000000000000000, 0.000000000000000000 ) ) ;
#178778 = CARTESIAN_POINT ( 'NONE',  ( -19.02544592524334988, -5.153800228976617603, 103.9594237280190043 ) ) ;
#178779 = CARTESIAN_POINT ( 'NONE',  ( 18.62759615963271287, -10.81492255796078972, 83.33224293864769550 ) ) ;
#178780 = CARTESIAN_POINT ( 'NONE',  ( -4.379528057220328563, 16.55341960407611168, 65.20724293864768129 ) ) ;
#178781 = CARTESIAN_POINT ( 'NONE',  ( -19.05341960407611168, -5.049401038298163336, 101.4572429386476955 ) ) ;
#178782 = CARTESIAN_POINT ( 'NONE',  ( -8.314922557961024197, 14.29746914071037800, 32.91775706135234714 ) ) ;
#178783 = CARTESIAN_POINT ( 'NONE',  ( -5.049401038298153566, 19.05341960407611168, 55.20724293864769550 ) ) ;
#178785 = CARTESIAN_POINT ( 'NONE',  ( 19.03943276465977164, 0.05219959533936151252, 86.25109039468567573 ) ) ;
#178784 = CARTESIAN_POINT ( 'NONE',  ( 10.72451020669898902, -18.67979575497178502, 112.9155762719810383 ) ) ;
#178786 = CARTESIAN_POINT ( 'NONE',  ( -9.564922557960796823, -16.46253265017161027, 92.08224293864769550 ) ) ;
#178787 = CARTESIAN_POINT ( 'NONE',  ( -19.05341960407611168, -5.049401038298163336, 71.45724293864766707 ) ) ;
#178788 = CARTESIAN_POINT ( 'NONE',  ( 5.719274019375991003, -21.55341960407610458, 72.70724293864769550 ) ) ;
#178789 = CARTESIAN_POINT ( 'NONE',  ( 9.564922557960805705, 16.46253265017160317, 49.58224293864770260 ) ) ;
#178790 = CARTESIAN_POINT ( 'NONE',  ( 32.91334004812880920, 16.89252633786550817, -8.000000000000000000 ) ) ;
#178791 = CARTESIAN_POINT ( 'NONE',  ( 4.483927247898545687, 16.52544592524342804, 54.79057627198104541 ) ) ;
#178792 = CARTESIAN_POINT ( 'NONE',  ( -9.474510206698964154, 16.51473224551069663, 100.4155762719810241 ) ) ;
#178793 = CARTESIAN_POINT ( 'NONE',  ( 17.81289503416611453, -24.51734667627695785, 144.6999999999999886 ) ) ;
#178794 = CARTESIAN_POINT ( 'NONE',  ( 13.97604488694548053, -13.89961937509957401, 65.62609039468567573 ) ) ;
#178795 = CARTESIAN_POINT ( 'NONE',  ( 21.52544592524344225, -5.823673210054117533, 93.54057627198103830 ) ) ;
#178796 = CARTESIAN_POINT ( 'NONE',  ( 16.51473224551083163, -9.474510206698727899, 55.83442372801899722 ) ) ;
#178797 = CARTESIAN_POINT ( 'NONE',  ( -19.03943276465977164, 0.05219959533909376836, 101.2489096053143669 ) ) ;
#178798 = CARTESIAN_POINT ( 'NONE',  ( -17.50000000000003197, 4.658240926743175692, 113.9447041781680667 ) ) ;
#178799 = CARTESIAN_POINT ( 'NONE',  ( 18.67979575497178502, 10.72451020669898547, 44.16557627198103120 ) ) ;
#178800 = CARTESIAN_POINT ( 'NONE',  ( 0.05219959533909260263, 19.03943276465977164, 69.99890960531435269 ) ) ;
#178801 = CARTESIAN_POINT ( 'NONE',  ( -21.53943276465977519, -0.05219959533937600094, 58.75109039468568994 ) ) ;
#178802 = CARTESIAN_POINT ( 'NONE',  ( 9.564922557960805705, 16.46253265017160317, 34.58224293864770260 ) ) ;
#178804 = VERTEX_POINT ( 'NONE', #40830 ) ;
#178803 = CARTESIAN_POINT ( 'NONE',  ( -16.55341960407611168, -4.379528057220339221, 76.45724293864769550 ) ) ;
#178805 = CARTESIAN_POINT ( 'NONE',  ( 21.55341960407619695, -5.719274019375665929, 51.04275706135234714 ) ) ;
#178806 = ORIENTED_EDGE ( 'NONE', *, *, #110020, .T. ) ;
#178807 = CARTESIAN_POINT ( 'NONE',  ( 5.153800228976335163, 19.02544592524342804, 109.7905762719810099 ) ) ;
#178808 = CARTESIAN_POINT ( 'NONE',  ( 13.89961937509957401, 13.97604488694547697, 61.87609039468566863 ) ) ;
#178809 = CARTESIAN_POINT ( 'NONE',  ( 1.227931366032057224E-14, 24.30000000000003268, -54.21489346206828230 ) ) ;
#178810 = CARTESIAN_POINT ( 'NONE',  ( -21.52544592524334988, -5.823673210054445271, 18.95942372801901143 ) ) ;
#178811 = CARTESIAN_POINT ( 'NONE',  ( 16.46253265017160672, -9.564922557960803928, 63.33224293864769550 ) ) ;
#178812 = CARTESIAN_POINT ( 'NONE',  ( -12.14591786802326823, 12.06949235617739902, 43.12609039468568284 ) ) ;
#178813 = CARTESIAN_POINT ( 'NONE',  ( -23.48529157249599919, -32.32473071737750558, -7.449999994537624737 ) ) ;
#178814 = CARTESIAN_POINT ( 'NONE',  ( 19.05341960407617918, -5.049401038297876454, 21.04275706135232582 ) ) ;
#178815 = CARTESIAN_POINT ( 'NONE',  ( -19.03943276465977164, 0.05219959533909376836, 41.24890960531435269 ) ) ;
#178816 = CARTESIAN_POINT ( 'NONE',  ( -15.80617190586768217, 15.72974639402176855, 113.1260903946856899 ) ) ;
#178817 = CARTESIAN_POINT ( 'NONE',  ( -14.29746914071037622, -8.314922557961029526, 94.16775706135237556 ) ) ;
#178819 = CARTESIAN_POINT ( 'NONE',  ( 15.72974639402176855, 15.80617190586768217, 71.87609039468568994 ) ) ;
#178818 = CARTESIAN_POINT ( 'NONE',  ( 0.05219959533909260263, 19.03943276465977164, 84.99890960531436690 ) ) ;
#178820 = DIRECTION ( 'NONE',  ( 0.000000000000000000, 0.000000000000000000, -1.000000000000000000 ) ) ;
#178821 = CARTESIAN_POINT ( 'NONE',  ( 5.049401038298161559, -19.05341960407611168, 112.7072429386476813 ) ) ;
#178823 = CARTESIAN_POINT ( 'NONE',  ( -18.67979575497193778, 10.72451020669871902, 68.33442372801900433 ) ) ;
#178822 = CARTESIAN_POINT ( 'NONE',  ( -12.14591786802326823, 12.06949235617739902, 58.12609039468568994 ) ) ;
#178824 = CARTESIAN_POINT ( 'NONE',  ( 10.72451020669871369, 18.67979575497193778, 97.08442372801904696 ) ) ;
#178825 = AXIS2_PLACEMENT_3D ( 'NONE', #174234, #127705, #113527 ) ;
#178826 = CARTESIAN_POINT ( 'NONE',  ( 26.45595770381629563, -7.620359626981993983, 168.5711898564603359 ) ) ;
#178827 = CARTESIAN_POINT ( 'NONE',  ( 16.53943276465976808, 0.05219959533934440121, 26.25109039468567573 ) ) ;
#178828 = CARTESIAN_POINT ( 'NONE',  ( 0.05219959533909260263, 19.03943276465977164, 89.99890960531436690 ) ) ;
#178829 = CARTESIAN_POINT ( 'NONE',  ( -14.62203461105344005, -16.12203461105316649, -64.92279855667830191 ) ) ;
#178830 = ORIENTED_EDGE ( 'NONE', *, *, #14195, .F. ) ;
#178831 = CARTESIAN_POINT ( 'NONE',  ( -1.399641368455697865, -29.85394078251579941, -51.58569050288881641 ) ) ;
#178832 = CARTESIAN_POINT ( 'NONE',  ( 5.049401038298161559, -19.05341960407611168, 32.70724293864768129 ) ) ;
#178834 = EDGE_CURVE ( 'NONE', #44725, #15991, #58977, .T. ) ;
#178833 = CARTESIAN_POINT ( 'NONE',  ( -21.55341960407610458, -5.719274019375992779, 36.45724293864768839 ) ) ;
#178835 = CARTESIAN_POINT ( 'NONE',  ( -16.52544592524335698, -4.483927247898792601, 103.9594237280190185 ) ) ;
#178837 = CARTESIAN_POINT ( 'NONE',  ( -16.46253265017160317, 9.564922557960807481, 70.83224293864770971 ) ) ;
#178836 = CARTESIAN_POINT ( 'NONE',  ( 14.29746914071049879, -8.314922557960816363, 83.33224293864769550 ) ) ;
#178838 = CARTESIAN_POINT ( 'NONE',  ( 15.80617190586769283, -15.72974639402175789, 105.6260903946856899 ) ) ;
#178839 = CARTESIAN_POINT ( 'NONE',  ( 12.14591786802327356, -12.06949235617739191, 30.62609039468567929 ) ) ;
#178840 = CARTESIAN_POINT ( 'NONE',  ( -14.34966873604960291, -8.224510206698953496, 91.66557627198103830 ) ) ;
#178841 = CARTESIAN_POINT ( 'NONE',  ( -18.67979575497193778, 10.72451020669871902, 43.33442372801901143 ) ) ;
#178842 = CARTESIAN_POINT ( 'NONE',  ( 15.72974639402199770, -15.80617190586745480, 68.12390960531436690 ) ) ;
#178843 = CARTESIAN_POINT ( 'NONE',  ( 9.564922557961047289, -16.46253265017146816, 50.41775706135233293 ) ) ;
#178844 = CARTESIAN_POINT ( 'NONE',  ( -34.59574315510281650, 4.379613810579283673, 51.09339236891209168 ) ) ;
#178845 = CARTESIAN_POINT ( 'NONE',  ( -13.97604488694527625, -13.89961937509977652, 101.8739096053143811 ) ) ;
#178846 = CARTESIAN_POINT ( 'NONE',  ( -16.53943276465976808, 0.05219959533911058130, 61.24890960531435979 ) ) ;
#178847 = ADVANCED_FACE ( 'NONE', ( #197509 ), #39820, .F. ) ;
#178848 = CARTESIAN_POINT ( 'NONE',  ( 12.06949235617757843, -12.14591786802309237, 48.12390960531436690 ) ) ;
#178849 = CARTESIAN_POINT ( 'NONE',  ( 14.29746914071037800, 8.314922557961029526, 106.6677570613523756 ) ) ;
#178850 = CARTESIAN_POINT ( 'NONE',  ( -0.05219959533936034679, 19.03943276465977164, 72.50109039468566152 ) ) ;
#178851 = CARTESIAN_POINT ( 'NONE',  ( 7.500000000000000000, 9.184850993605147944E-16, 5.707106781186540800 ) ) ;
#178852 = CARTESIAN_POINT ( 'NONE',  ( -0.05219959533909027116, -19.03943276465977164, 112.4989096053143669 ) ) ;
#178853 = CARTESIAN_POINT ( 'NONE',  ( -4.379528057220328563, 16.55341960407611168, 85.20724293864770971 ) ) ;
#178854 = DIRECTION ( 'NONE',  ( -1.000000000000000000, 1.246178594180516623E-14, 0.000000000000000000 ) ) ;
#178856 = CARTESIAN_POINT ( 'NONE',  ( 21.55341960407610458, 5.719274019375980345, 48.95724293864770971 ) ) ;
#178855 = CARTESIAN_POINT ( 'NONE',  ( 16.51473224551069308, 9.474510206698969483, 39.16557627198103120 ) ) ;
#178857 = CARTESIAN_POINT ( 'NONE',  ( 21.52544592524344225, -5.823673210054117533, 83.54057627198102409 ) ) ;
#178858 = CARTESIAN_POINT ( 'NONE',  ( 16.51473224551069308, 9.474510206698969483, 24.16557627198102765 ) ) ;
#178860 = CARTESIAN_POINT ( 'NONE',  ( -19.05341960407611168, -5.049401038298163336, 56.45724293864768129 ) ) ;
#178859 = CARTESIAN_POINT ( 'NONE',  ( 16.52544592524335698, 4.483927247898782831, 66.45942372801903275 ) ) ;
#178861 = CARTESIAN_POINT ( 'NONE',  ( 19.02544592524334988, 5.153800228976608722, 46.45942372801899012 ) ) ;
#178862 = CARTESIAN_POINT ( 'NONE',  ( -21.52544592524334988, -5.823673210054445271, 48.95942372801902565 ) ) ;
#178863 = CARTESIAN_POINT ( 'NONE',  ( -15.80617190586745835, -15.72974639402198527, 41.87390960531435979 ) ) ;
#178864 = CARTESIAN_POINT ( 'NONE',  ( 14.34966873604960469, 8.224510206698951720, 104.1655762719810241 ) ) ;
#178865 = CARTESIAN_POINT ( 'NONE',  ( -19.05341960407617563, 5.049401038297882671, 88.54275706135230450 ) ) ;
#178866 = CARTESIAN_POINT ( 'NONE',  ( 22.81625015709509441, 31.40387420917330275, -3.824999997268813345 ) ) ;
#178868 = CARTESIAN_POINT ( 'NONE',  ( -5.719274019375978568, 21.55341960407610458, 45.20724293864769550 ) ) ;
#178867 = DIRECTION ( 'NONE',  ( 0.000000000000000000, 0.000000000000000000, -1.000000000000000000 ) ) ;
#178869 = CARTESIAN_POINT ( 'NONE',  ( 13.97604488694527802, 13.89961937509977652, 24.37390960531435624 ) ) ;
#178870 = CARTESIAN_POINT ( 'NONE',  ( -0.05219959533937732626, 21.53943276465977519, 82.50109039468568994 ) ) ;
#178871 = CARTESIAN_POINT ( 'NONE',  ( -16.55341960407611168, -4.379528057220339221, 36.45724293864768839 ) ) ;
#178873 = CARTESIAN_POINT ( 'NONE',  ( 16.53943276465976808, -0.05219959533910856209, 53.74890960531437401 ) ) ;
#178872 = CARTESIAN_POINT ( 'NONE',  ( 4.483927247898790824, -16.52544592524335698, 60.20942372801902565 ) ) ;
#178874 = CARTESIAN_POINT ( 'NONE',  ( -15.80617190586745835, -15.72974639402198527, 76.87390960531439532 ) ) ;
#178875 = CARTESIAN_POINT ( 'NONE',  ( 21.55341960407610458, 5.719274019375980345, 73.95724293864769550 ) ) ;
#178876 = CARTESIAN_POINT ( 'NONE',  ( 2.662494480112515660, -37.13692398601924793, -32.59999999999999432 ) ) ;
#178878 = CARTESIAN_POINT ( 'NONE',  ( -21.55341960407610458, -5.719274019375992779, 21.45724293864769550 ) ) ;
#178877 = CARTESIAN_POINT ( 'NONE',  ( 13.89961937509957401, 13.97604488694547697, 81.87609039468564731 ) ) ;
#178879 = CARTESIAN_POINT ( 'NONE',  ( -13.89961937509977652, 13.97604488694528158, 65.62390960531436690 ) ) ;
#178880 = CARTESIAN_POINT ( 'NONE',  ( 9.474510206698971260, -16.51473224551069308, 27.91557627198103120 ) ) ;
#178881 = PRESENTATION_STYLE_ASSIGNMENT (( #28201 ) ) ;
#178882 = CARTESIAN_POINT ( 'NONE',  ( 11.30153831258470731, -180.0000000000000000, 0.000000000000000000 ) ) ;
#178883 = CARTESIAN_POINT ( 'NONE',  ( 16.52544592524335698, 4.483927247898782831, 86.45942372801901854 ) ) ;
#178884 = CARTESIAN_POINT ( 'NONE',  ( 0.05219959533907565091, 21.53943276465977519, 114.9989096053143669 ) ) ;
#178885 = CARTESIAN_POINT ( 'NONE',  ( 13.97604488694527802, 13.89961937509977652, 74.37390960531436690 ) ) ;
#178886 = CARTESIAN_POINT ( 'NONE',  ( 18.62759615963255655, 10.81492255796105972, 41.66775706135235424 ) ) ;
#178887 = CARTESIAN_POINT ( 'NONE',  ( 13.89961937509977652, -13.97604488694527269, 103.1239096053143527 ) ) ;
#178888 = CARTESIAN_POINT ( 'NONE',  ( -20.47811964340476365, -34.28713832285652785, -21.14919058558906784 ) ) ;
#178889 = ORIENTED_EDGE ( 'NONE', *, *, #82905, .F. ) ;
#178890 = CARTESIAN_POINT ( 'NONE',  ( -18.67979575497193778, 10.72451020669871902, 48.33442372801902565 ) ) ;
#178892 = CARTESIAN_POINT ( 'NONE',  ( 5.153800228976335163, 19.02544592524342804, 104.7905762719809957 ) ) ;
#178891 = CARTESIAN_POINT ( 'NONE',  ( -16.51473224551069308, -9.474510206698971260, 26.66557627198103120 ) ) ;
#178893 = CARTESIAN_POINT ( 'NONE',  ( 5.049401038297881783, 19.05341960407617563, 47.29275706135231161 ) ) ;
#178894 = CARTESIAN_POINT ( 'NONE',  ( 10.81492255796106328, -18.62759615963255655, 20.41775706135234714 ) ) ;
#178895 = CARTESIAN_POINT ( 'NONE',  ( 9.474510206698729675, 16.51473224551082808, 52.08442372801900433 ) ) ;
#178896 = CARTESIAN_POINT ( 'NONE',  ( -19.02544592524334988, -5.153800228976617603, 53.95942372801898301 ) ) ;
#178898 = ORIENTED_EDGE ( 'NONE', *, *, #16838, .F. ) ;
#178897 = CARTESIAN_POINT ( 'NONE',  ( 14.29746914071037800, 8.314922557961029526, 106.6677570613523756 ) ) ;
#178900 = ORIENTED_EDGE ( 'NONE', *, *, #47633, .F. ) ;
#178899 = CARTESIAN_POINT ( 'NONE',  ( 24.60782808046175774, -7.576750539519846228, 167.2921137806583829 ) ) ;
#178901 = CARTESIAN_POINT ( 'NONE',  ( -5.049401038298153566, 19.05341960407611168, 70.20724293864769550 ) ) ;
#178902 = CARTESIAN_POINT ( 'NONE',  ( -10.72451020669870658, -18.67979575497194134, 74.58442372801901854 ) ) ;
#178903 = CARTESIAN_POINT ( 'NONE',  ( 0.05219959533937995610, -21.53943276465977519, 95.00109039468568994 ) ) ;
#178904 = DIRECTION ( 'NONE',  ( 1.000000000000000000, 0.000000000000000000, 0.000000000000000000 ) ) ;
#178905 = CARTESIAN_POINT ( 'NONE',  ( 5.153800228976335163, 19.02544592524342804, 84.79057627198099567 ) ) ;
#178906 = CARTESIAN_POINT ( 'NONE',  ( -21.55341960407619339, 5.719274019375674811, 58.54275706135235424 ) ) ;
#178907 = CARTESIAN_POINT ( 'NONE',  ( -16.51473224551082808, 9.474510206698731452, 108.3344237280190043 ) ) ;
#178908 = CARTESIAN_POINT ( 'NONE',  ( 13.97604488694527802, 13.89961937509977652, 69.37390960531436690 ) ) ;
#178909 = CARTESIAN_POINT ( 'NONE',  ( -18.67979575497178146, -10.72451020669898902, 21.66557627198102409 ) ) ;
#178910 = AXIS2_PLACEMENT_3D ( 'NONE', #104534, #25722, #166215 ) ;
#178911 = CARTESIAN_POINT ( 'NONE',  ( 13.89961937509977652, -13.97604488694527269, 88.12390960531438111 ) ) ;
#178912 = CARTESIAN_POINT ( 'NONE',  ( 21.46320343559639099, -20.96320343559646915, 4.646446609406719830 ) ) ;
#178913 = CARTESIAN_POINT ( 'NONE',  ( 19.05341960407611168, 5.049401038298154454, 83.95724293864766707 ) ) ;
#178914 = CARTESIAN_POINT ( 'NONE',  ( -19.02544592524342804, 5.153800228976336051, 71.04057627198099567 ) ) ;
#178915 = CARTESIAN_POINT ( 'NONE',  ( -21.53943276465977519, 0.05219959533907696930, 116.2489096053143669 ) ) ;
#178916 = CARTESIAN_POINT ( 'NONE',  ( 16.55341960407618274, -4.379528057220086978, 101.0427570613523756 ) ) ;
#178917 = CARTESIAN_POINT ( 'NONE',  ( 1.491112435928470425, 15.38843874529032618, -61.89150209872707364 ) ) ;
#178918 = CARTESIAN_POINT ( 'NONE',  ( -13.97604488694547697, 13.89961937509957934, 58.12609039468566863 ) ) ;
#178919 = CARTESIAN_POINT ( 'NONE',  ( -16.46253265017160317, 9.564922557960807481, 95.83224293864769550 ) ) ;
#178920 = CARTESIAN_POINT ( 'NONE',  ( 12.06949235617757843, -12.14591786802309237, 83.12390960531436690 ) ) ;
#178921 = CARTESIAN_POINT ( 'NONE',  ( 4.379528057220339221, -16.55341960407611168, 107.7072429386476955 ) ) ;
#178922 = CARTESIAN_POINT ( 'NONE',  ( 21.53943276465977519, -0.05219959533907433946, 38.74890960531435979 ) ) ;
#178923 = CARTESIAN_POINT ( 'NONE',  ( -5.823673210054116645, -21.52544592524344225, 22.29057627198102765 ) ) ;
#178924 = CARTESIAN_POINT ( 'NONE',  ( -16.52544592524342804, 4.483927247898546575, 91.04057627198103830 ) ) ;
#178925 = CARTESIAN_POINT ( 'NONE',  ( -17.40805194822031865, 6.112264579159341515, 55.83371272510613181 ) ) ;
#178926 = CARTESIAN_POINT ( 'NONE',  ( -9.564922557961040184, 16.46253265017147172, 42.91775706135234003 ) ) ;
#178927 = CARTESIAN_POINT ( 'NONE',  ( 0.05219959533934541429, -16.53943276465976808, 110.0010903946856757 ) ) ;
#178928 = CARTESIAN_POINT ( 'NONE',  ( 5.153800228976335163, 19.02544592524342804, 89.79057627198102409 ) ) ;
#178929 = CARTESIAN_POINT ( 'NONE',  ( -21.52544592524334988, -5.823673210054445271, 68.95942372801901854 ) ) ;
#178930 = CARTESIAN_POINT ( 'NONE',  ( -21.53943276465977519, 0.05219959533907696930, 46.24890960531435979 ) ) ;
#178931 = CARTESIAN_POINT ( 'NONE',  ( -15.72974639402176322, -15.80617190586768395, 29.37609039468568284 ) ) ;
#178932 = CARTESIAN_POINT ( 'NONE',  ( -18.67979575497178146, -10.72451020669898902, 81.66557627198103830 ) ) ;
#178933 = CARTESIAN_POINT ( 'NONE',  ( -12.06949235617756955, 12.14591786802309770, 105.6239096053143669 ) ) ;
#178934 = CARTESIAN_POINT ( 'NONE',  ( -9.474510206698720793, -16.51473224551083518, 74.58442372801900433 ) ) ;
#178935 = CARTESIAN_POINT ( 'NONE',  ( -9.474510206698964154, 16.51473224551069663, 45.41557627198103120 ) ) ;
#178936 = CARTESIAN_POINT ( 'NONE',  ( 9.564922557960805705, 16.46253265017160317, 99.58224293864770971 ) ) ;
#178937 = CARTESIAN_POINT ( 'NONE',  ( -16.46253265017160317, 9.564922557960807481, 90.83224293864769550 ) ) ;
#178938 = CARTESIAN_POINT ( 'NONE',  ( 5.049401038298161559, -19.05341960407611168, 22.70724293864769194 ) ) ;
#178939 = CARTESIAN_POINT ( 'NONE',  ( -8.224510206698948167, 14.34966873604960824, 40.41557627198103120 ) ) ;
#178940 = CARTESIAN_POINT ( 'NONE',  ( -4.483927247898782831, 16.52544592524335698, 42.70942372801901854 ) ) ;
#178941 = CARTESIAN_POINT ( 'NONE',  ( 10.72451020669871369, 18.67979575497193778, 107.0844237280190043 ) ) ;
#178943 = CARTESIAN_POINT ( 'NONE',  ( 8.314922557960818139, 14.29746914071049879, 24.58224293864768839 ) ) ;
#178942 = CARTESIAN_POINT ( 'NONE',  ( -13.89961937509977652, 13.97604488694528158, 115.6239096053143669 ) ) ;
#178944 = CARTESIAN_POINT ( 'NONE',  ( -21.55341960407619339, 5.719274019375674811, 33.54275706135234714 ) ) ;
#178945 = CARTESIAN_POINT ( 'NONE',  ( -5.049401038298153566, 19.05341960407611168, 100.2072429386476955 ) ) ;
#178946 = CARTESIAN_POINT ( 'NONE',  ( -8.314922557961024197, 14.29746914071037800, 102.9177570613523756 ) ) ;
#178947 = CARTESIAN_POINT ( 'NONE',  ( -8.314922557961024197, 14.29746914071037800, 97.91775706135236135 ) ) ;
#178948 = CIRCLE ( 'NONE', #127670, 2.500000000000002220 ) ;
#178949 = CARTESIAN_POINT ( 'NONE',  ( -12.06949235617739369, -12.14591786802326823, 24.37609039468567573 ) ) ;
#178950 = CARTESIAN_POINT ( 'NONE',  ( 19.05341960407611168, 5.049401038298154454, 43.95724293864769550 ) ) ;
#178951 = CARTESIAN_POINT ( 'NONE',  ( -12.14591786802309592, -12.06949235617757132, 101.8739096053143811 ) ) ;
#178952 = CARTESIAN_POINT ( 'NONE',  ( 0.05219959533937995610, -21.53943276465977519, 25.00109039468567218 ) ) ;
#178953 = CARTESIAN_POINT ( 'NONE',  ( -13.89961937509977652, 13.97604488694528158, 25.62390960531434558 ) ) ;
#178954 = CARTESIAN_POINT ( 'NONE',  ( -5.049401038298153566, 19.05341960407611168, 110.2072429386476671 ) ) ;
#178955 = CARTESIAN_POINT ( 'NONE',  ( 10.81492255796106328, -18.62759615963255655, 35.41775706135234003 ) ) ;
#178956 = CARTESIAN_POINT ( 'NONE',  ( 37.99626262588756731, 12.34573411038929436, -2.902157773949821884 ) ) ;
#178957 = CARTESIAN_POINT ( 'NONE',  ( 9.564922557960805705, 16.46253265017160317, 104.5822429386476955 ) ) ;
#178958 = CIRCLE ( 'NONE', #162766, 8.000000000000000000 ) ;
#178959 = CARTESIAN_POINT ( 'NONE',  ( -17.12812012977028076, -6.668231424566004151, 36.35948759323144941 ) ) ;
#178960 = CARTESIAN_POINT ( 'NONE',  ( -19.02544592524342804, 5.153800228976336051, 101.0405762719810241 ) ) ;
#178962 = CARTESIAN_POINT ( 'NONE',  ( -4.483927247898539470, -16.52544592524342804, 92.29057627198103830 ) ) ;
#178961 = CARTESIAN_POINT ( 'NONE',  ( -0.05219959533937732626, 21.53943276465977519, 47.50109039468568994 ) ) ;
#178963 = CARTESIAN_POINT ( 'NONE',  ( -13.89961937509977652, 13.97604488694528158, 90.62390960531432427 ) ) ;
#178964 = CARTESIAN_POINT ( 'NONE',  ( -27.93407901760531686, -7.419329114331087993, 160.9060561962049860 ) ) ;
#178965 = PRESENTATION_LAYER_ASSIGNMENT (  '', '', ( #7900 ) ) ;
#178966 = CARTESIAN_POINT ( 'NONE',  ( 12.14591786802327356, -12.06949235617739191, 65.62609039468568994 ) ) ;
#178967 = CARTESIAN_POINT ( 'NONE',  ( 21.52544592524334988, 5.823673210054432836, 76.45942372801901854 ) ) ;
#178968 = CARTESIAN_POINT ( 'NONE',  ( 14.34966873604972726, -8.224510206698740333, 45.83442372801901854 ) ) ;
#178969 = CARTESIAN_POINT ( 'NONE',  ( -16.46253265017160317, 9.564922557960807481, 80.83224293864769550 ) ) ;
#178970 = CARTESIAN_POINT ( 'NONE',  ( 16.46253265017146816, 9.564922557961045513, 106.6677570613523471 ) ) ;
#178971 = CARTESIAN_POINT ( 'NONE',  ( 16.52544592524335698, 4.483927247898782831, 71.45942372801901854 ) ) ;
#178972 = CARTESIAN_POINT ( 'NONE',  ( -0.05219959533936034679, 19.03943276465977164, 92.50109039468566152 ) ) ;
#178973 = CARTESIAN_POINT ( 'NONE',  ( -13.97604488694527625, -13.89961937509977652, 66.87390960531436690 ) ) ;
#178974 = CARTESIAN_POINT ( 'NONE',  ( 18.67979575497178502, 10.72451020669898547, 84.16557627198103830 ) ) ;
#178976 = CARTESIAN_POINT ( 'NONE',  ( -9.474510206698720793, -16.51473224551083518, 89.58442372801900433 ) ) ;
#178975 = CARTESIAN_POINT ( 'NONE',  ( 0.05219959533910956823, 16.53943276465976808, 94.99890960531436690 ) ) ;
#178977 = CARTESIAN_POINT ( 'NONE',  ( 4.379528057220092307, 16.55341960407617563, 57.29275706135234714 ) ) ;
#178978 = CARTESIAN_POINT ( 'NONE',  ( 17.44279575226826751, -5.990770900252369024, 63.33557567514322528 ) ) ;
#178979 = CARTESIAN_POINT ( 'NONE',  ( -16.46253265017146816, -9.564922557961047289, 54.16775706135234003 ) ) ;
#178980 = CARTESIAN_POINT ( 'NONE',  ( -8.224510206698948167, 14.34966873604960824, 35.41557627198102409 ) ) ;
#178981 = CARTESIAN_POINT ( 'NONE',  ( 12.06949235617757843, -12.14591786802309237, 78.12390960531436690 ) ) ;
#178983 = CARTESIAN_POINT ( 'NONE',  ( -18.22780087662123805, 5.499999999999981348, 91.01763182126894947 ) ) ;
#178982 = CARTESIAN_POINT ( 'NONE',  ( 18.67979575497194134, -10.72451020669871369, 110.8344237280190043 ) ) ;
#178984 = CARTESIAN_POINT ( 'NONE',  ( -21.53943276465977519, -0.05219959533937600094, 28.75109039468567929 ) ) ;
#178985 = CARTESIAN_POINT ( 'NONE',  ( 19.05341960407611168, 5.049401038298154454, 98.95724293864766707 ) ) ;
#178986 = CARTESIAN_POINT ( 'NONE',  ( 5.049401038298161559, -19.05341960407611168, 72.70724293864768129 ) ) ;
#178987 = CARTESIAN_POINT ( 'NONE',  ( 21.53943276465977519, 0.05219959533937863772, 91.25109039468568994 ) ) ;
#178988 = CARTESIAN_POINT ( 'NONE',  ( -13.97604488694527625, -13.89961937509977652, 81.87390960531436690 ) ) ;
#178989 = CARTESIAN_POINT ( 'NONE',  ( -10.81492255796078084, -18.62759615963271287, 42.08224293864769550 ) ) ;
#178990 = CARTESIAN_POINT ( 'NONE',  ( -14.29746914071049879, 8.314922557960819915, 75.83224293864769550 ) ) ;
#178991 = CARTESIAN_POINT ( 'NONE',  ( -13.97604488694527625, -13.89961937509977652, 51.87390960531436690 ) ) ;
#178992 = CARTESIAN_POINT ( 'NONE',  ( -0.05219959533910754901, -16.53943276465976808, 92.49890960531436690 ) ) ;
#178993 = VECTOR ( 'NONE', #146350, 1000.000000000000000 ) ;
#178994 = CARTESIAN_POINT ( 'NONE',  ( -21.52544592524334988, -5.823673210054445271, 28.95942372801902209 ) ) ;
#178995 = CARTESIAN_POINT ( 'NONE',  ( 21.55341960407619695, -5.719274019375665929, 61.04275706135234714 ) ) ;
#178996 = CARTESIAN_POINT ( 'NONE',  ( -19.02544592524342804, 5.153800228976336051, 41.04057627198103120 ) ) ;
#178997 = CARTESIAN_POINT ( 'NONE',  ( -0.05219959533934338120, 16.53943276465976808, 62.50109039468568284 ) ) ;
#178998 = CARTESIAN_POINT ( 'NONE',  ( -5.719274019375978568, 21.55341960407610458, 110.2072429386477239 ) ) ;
#178999 = CARTESIAN_POINT ( 'NONE',  ( -10.81492255796078084, -18.62759615963271287, 112.0822429386477097 ) ) ;
#179001 = CARTESIAN_POINT ( 'NONE',  ( -19.03943276465977164, 0.05219959533909376836, 66.24890960531436690 ) ) ;
#179000 = CARTESIAN_POINT ( 'NONE',  ( 5.153800228976615827, -19.02544592524334988, 45.20942372801901143 ) ) ;
#179002 = DIRECTION ( 'NONE',  ( 0.000000000000000000, 0.000000000000000000, -1.000000000000000000 ) ) ;
#179003 = CARTESIAN_POINT ( 'NONE',  ( 18.62759615963255655, 10.81492255796105972, 76.66775706135234714 ) ) ;
#179004 = CARTESIAN_POINT ( 'NONE',  ( -21.53943276465977519, 0.05219959533907696930, 51.24890960531436690 ) ) ;
#179005 = CARTESIAN_POINT ( 'NONE',  ( 16.55341960407611168, 4.379528057220329451, 38.95724293864768839 ) ) ;
#179007 = CARTESIAN_POINT ( 'NONE',  ( -5.049401038297874678, -19.05341960407617918, 19.79275706135233293 ) ) ;
#179006 = CARTESIAN_POINT ( 'NONE',  ( -18.67979575497193778, 10.72451020669871902, 78.33442372801901854 ) ) ;
#179008 = CARTESIAN_POINT ( 'NONE',  ( -16.55341960407611168, -4.379528057220339221, 56.45724293864768839 ) ) ;
#179009 = CARTESIAN_POINT ( 'NONE',  ( 16.55341960407611168, 4.379528057220329451, 98.95724293864770971 ) ) ;
#179010 = CARTESIAN_POINT ( 'NONE',  ( 5.049401038297881783, 19.05341960407617563, 57.29275706135231871 ) ) ;
#179011 = CARTESIAN_POINT ( 'NONE',  ( 16.53943276465976808, 0.05219959533934440121, 111.2510903946856899 ) ) ;
#179012 = CARTESIAN_POINT ( 'NONE',  ( 0.05219959533937995610, -21.53943276465977519, 70.00109039468568994 ) ) ;
#179013 = CARTESIAN_POINT ( 'NONE',  ( -9.564922557960796823, -16.46253265017161027, 57.08224293864769550 ) ) ;
#179014 = CARTESIAN_POINT ( 'NONE',  ( 9.564922557961047289, -16.46253265017146816, 35.41775706135233293 ) ) ;
#179015 = CARTESIAN_POINT ( 'NONE',  ( -21.55341960407610458, -5.719274019375992779, 41.45724293864769550 ) ) ;
#179016 = CARTESIAN_POINT ( 'NONE',  ( -5.823673210054431948, 21.52544592524334988, 37.70942372801900433 ) ) ;
#179017 = CARTESIAN_POINT ( 'NONE',  ( -10.72451020669898014, 18.67979575497178502, 90.41557627198103830 ) ) ;
#179018 = CARTESIAN_POINT ( 'NONE',  ( 16.46253265017146816, 9.564922557961045513, 81.66775706135233293 ) ) ;
#179019 = CARTESIAN_POINT ( 'NONE',  ( -0.05219959533934338120, 16.53943276465976808, 47.50109039468568994 ) ) ;
#179021 = CARTESIAN_POINT ( 'NONE',  ( 21.52544592524344225, -5.823673210054117533, 88.54057627198103830 ) ) ;
#179020 = CARTESIAN_POINT ( 'NONE',  ( -6.020228577223754586E-15, 39.95556452105416412, -6.500000000000000000 ) ) ;
#179022 = CARTESIAN_POINT ( 'NONE',  ( 8.314922557960818139, 14.29746914071049879, 94.58224293864769550 ) ) ;
#179023 = CARTESIAN_POINT ( 'NONE',  ( -28.61453998622349104, -24.72048905145116038, -21.14736193440031897 ) ) ;
#179024 = CARTESIAN_POINT ( 'NONE',  ( -12.06949235617739369, -12.14591786802326823, 24.37609039468567573 ) ) ;
#179025 = CARTESIAN_POINT ( 'NONE',  ( 15.72974639402199770, -15.80617190586745480, 53.12390960531436690 ) ) ;
#179026 = CARTESIAN_POINT ( 'NONE',  ( -8.314922557961024197, 14.29746914071037800, 97.91775706135236135 ) ) ;
#179027 = CARTESIAN_POINT ( 'NONE',  ( -19.03943276465977164, 0.05219959533909376836, 21.24890960531436335 ) ) ;
#179028 = CARTESIAN_POINT ( 'NONE',  ( 14.29746914071037800, 8.314922557961029526, 46.66775706135234714 ) ) ;
#179029 = VECTOR ( 'NONE', #176306, 1000.000000000000000 ) ;
#179030 = CARTESIAN_POINT ( 'NONE',  ( -18.62759615963255300, -10.81492255796106328, 24.16775706135235424 ) ) ;
#179031 = CARTESIAN_POINT ( 'NONE',  ( -21.52544592524343514, 5.823673210054127303, 51.04057627198103120 ) ) ;
#179032 = CARTESIAN_POINT ( 'NONE',  ( -16.55341960407617563, 4.379528057220093196, 83.54275706135234714 ) ) ;
#179033 = B_SPLINE_CURVE_WITH_KNOTS ( 'NONE', 3,
 ( #57624, #24294, #69780, #178978, #54608, #116282, #194146, #55610, #117284, #102118, #167775, #138418, #154584, #32242, #109074, #184926, #62561, #73792, #92898, #31248, #197133, #90904, #886, #14081, #152590, #60571, #200098, #108069, #75747, #137424, #44435, #29273 ),
 .UNSPECIFIED., .F., .F.,
 ( 4, 2, 2, 2, 2, 2, 2, 2, 2, 2, 2, 2, 2, 2, 2, 4 ),
 ( 8.184972452126140780E-17, 0.0003712461730037761704, 0.0007424923460074704835, 0.001113738519011164526, 0.001484984692014859001, 0.002227477038022250121, 0.002598723211025934406, 0.002969969384029600909, 0.003341215557033246162, 0.003712461730036892282, 0.004083707903040537102, 0.004454954076044181921, 0.004826200249047828475, 0.005197446422051473294, 0.005568692595055118981, 0.005939938768058764668 ),
 .UNSPECIFIED. ) ;
#179034 = CARTESIAN_POINT ( 'NONE',  ( -16.51473224551069308, -9.474510206698971260, 101.6655762719810241 ) ) ;
#179035 = CARTESIAN_POINT ( 'NONE',  ( 0.05219959533937995610, -21.53943276465977519, 50.00109039468568994 ) ) ;
#179036 = CARTESIAN_POINT ( 'NONE',  ( 18.67979575497178502, 10.72451020669898547, 39.16557627198102409 ) ) ;
#179037 = CARTESIAN_POINT ( 'NONE',  ( -5.049401038298153566, 19.05341960407611168, 110.2072429386476671 ) ) ;
#179038 = EDGE_LOOP ( 'NONE', ( #103415, #55818, #87077 ) ) ;
#179039 = CARTESIAN_POINT ( 'NONE',  ( -19.05341960407617563, 5.049401038297882671, 33.54275706135231871 ) ) ;
#179040 = CARTESIAN_POINT ( 'NONE',  ( 14.34966873604972726, -8.224510206698740333, 60.83442372801901854 ) ) ;
#179041 = CARTESIAN_POINT ( 'NONE',  ( -9.564922557960796823, -16.46253265017161027, 112.0822429386476955 ) ) ;
#179042 = ORIENTED_EDGE ( 'NONE', *, *, #160526, .F. ) ;
#179043 = CARTESIAN_POINT ( 'NONE',  ( 5.153800228976335163, 19.02544592524342804, 79.79057627198102409 ) ) ;
#179044 = CARTESIAN_POINT ( 'NONE',  ( -8.314922557961024197, 14.29746914071037800, 97.91775706135236135 ) ) ;
#179045 = FACE_OUTER_BOUND ( 'NONE', #94515, .T. ) ;
#179046 = CARTESIAN_POINT ( 'NONE',  ( -8.314922557960811034, -14.29746914071050412, 92.08224293864769550 ) ) ;
#179047 = CARTESIAN_POINT ( 'NONE',  ( 10.81492255796078972, 18.62759615963270932, 54.58224293864769550 ) ) ;
#179048 = CARTESIAN_POINT ( 'NONE',  ( 0.05219959533909260263, 19.03943276465977164, 29.99890960531435979 ) ) ;
#179049 = CARTESIAN_POINT ( 'NONE',  ( 8.314922557961029526, -14.29746914071037800, 80.41775706135234714 ) ) ;
#179050 = CARTESIAN_POINT ( 'NONE',  ( -21.55341960407619339, 5.719274019375674811, 33.54275706135234714 ) ) ;
#179051 = CARTESIAN_POINT ( 'NONE',  ( 9.474510206698729675, 16.51473224551082808, 87.08442372801900433 ) ) ;
#179052 = CARTESIAN_POINT ( 'NONE',  ( -12.06949235617756955, 12.14591786802309770, 95.62390960531436690 ) ) ;
#179053 = CARTESIAN_POINT ( 'NONE',  ( 13.97604488694527802, 13.89961937509977652, 39.37390960531435269 ) ) ;
#179054 = CARTESIAN_POINT ( 'NONE',  ( 16.46253265017160672, -9.564922557960803928, 108.3322429386476955 ) ) ;
#179055 = CARTESIAN_POINT ( 'NONE',  ( 15.80617190586769283, -15.72974639402175789, 110.6260903946857042 ) ) ;
#179056 = CARTESIAN_POINT ( 'NONE',  ( 16.46253265017160672, -9.564922557960803928, 73.33224293864769550 ) ) ;
#179057 = CARTESIAN_POINT ( 'NONE',  ( 16.52544592524335698, 4.483927247898782831, 66.45942372801903275 ) ) ;
#179058 = CARTESIAN_POINT ( 'NONE',  ( 5.719274019375673035, 21.55341960407619339, 97.29275706135234714 ) ) ;
#179059 = CARTESIAN_POINT ( 'NONE',  ( -14.29746914071037622, -8.314922557961029526, 74.16775706135231871 ) ) ;
#179060 = CARTESIAN_POINT ( 'NONE',  ( -19.03943276465977164, -0.05219959533935918106, 53.75109039468566863 ) ) ;
#179061 = CARTESIAN_POINT ( 'NONE',  ( -5.049401038297874678, -19.05341960407617918, 69.79275706135233293 ) ) ;
#179062 = ORIENTED_EDGE ( 'NONE', *, *, #50316, .T. ) ;
#179063 = CARTESIAN_POINT ( 'NONE',  ( -21.55341960407619339, 5.719274019375674811, 58.54275706135235424 ) ) ;
#179064 = CARTESIAN_POINT ( 'NONE',  ( 19.03943276465977164, -0.05219959533909143690, 68.74890960531436690 ) ) ;
#179065 = CARTESIAN_POINT ( 'NONE',  ( 16.51473224551069308, 9.474510206698969483, 24.16557627198102765 ) ) ;
#179066 = CARTESIAN_POINT ( 'NONE',  ( -19.03943276465977164, -0.05219959533935918106, 53.75109039468566863 ) ) ;
#179067 = CARTESIAN_POINT ( 'NONE',  ( -19.03943276465977164, 0.05219959533909376836, 111.2489096053143669 ) ) ;
#179068 = CARTESIAN_POINT ( 'NONE',  ( -5.153800228976328057, -19.02544592524343514, 82.29057627198103830 ) ) ;
#179069 = CARTESIAN_POINT ( 'NONE',  ( 0.05219959533910956823, 16.53943276465976808, 34.99890960531435979 ) ) ;
#179070 = CARTESIAN_POINT ( 'NONE',  ( 21.52544592524344225, -5.823673210054117533, 43.54057627198103830 ) ) ;
#179071 = CARTESIAN_POINT ( 'NONE',  ( -28.79475375365593592, 9.355982642739137489, 141.8843446568999980 ) ) ;
#179072 = CARTESIAN_POINT ( 'NONE',  ( 21.53943276465977519, 0.05219959533937863772, 106.2510903946856757 ) ) ;
#179073 = CARTESIAN_POINT ( 'NONE',  ( -16.36317988757057762, -7.306389748694919639, 80.90210391636773579 ) ) ;
#179074 = CARTESIAN_POINT ( 'NONE',  ( 13.89961937509977652, -13.97604488694527269, 43.12390960531434558 ) ) ;
#179075 = LINE ( 'NONE', #102215, #159721 ) ;
#179076 = CARTESIAN_POINT ( 'NONE',  ( -9.669289179520820454, -11.80006683339779805, -59.80355761763873801 ) ) ;
#179077 = CARTESIAN_POINT ( 'NONE',  ( 21.52544592524334988, 5.823673210054432836, 71.45942372801901854 ) ) ;
#179078 = CARTESIAN_POINT ( 'NONE',  ( -13.41967750377774848, -34.84915157265046304, -8.000000000000001776 ) ) ;
#179079 = CARTESIAN_POINT ( 'NONE',  ( 4.379528057220092307, 16.55341960407617563, 62.29275706135236845 ) ) ;
#179081 = ADVANCED_FACE ( 'NONE', ( #59967 ), #11514, .F. ) ;
#179080 = CARTESIAN_POINT ( 'NONE',  ( -15.80617190586745835, -15.72974639402198527, 81.87390960531435269 ) ) ;
#179082 = AXIS2_PLACEMENT_3D ( 'NONE', #157854, #97146, #7139 ) ;
#179083 = CARTESIAN_POINT ( 'NONE',  ( -12.06949235617756955, 12.14591786802309770, 50.62390960531435979 ) ) ;
#179085 = CYLINDRICAL_SURFACE ( 'NONE', #56719, 59.99999999999998579 ) ;
#179084 = CARTESIAN_POINT ( 'NONE',  ( 5.049401038298161559, -19.05341960407611168, 27.70724293864769550 ) ) ;
#179086 = CARTESIAN_POINT ( 'NONE',  ( 21.52544592524334988, 5.823673210054432836, 36.45942372801901143 ) ) ;
#179087 = CARTESIAN_POINT ( 'NONE',  ( -16.46253265017146816, -9.564922557961047289, 44.16775706135232582 ) ) ;
#179088 = CARTESIAN_POINT ( 'NONE',  ( -5.049401038298153566, 19.05341960407611168, 35.20724293864768839 ) ) ;
#179089 = CARTESIAN_POINT ( 'NONE',  ( 18.67979575497194134, -10.72451020669871369, 80.83442372801901854 ) ) ;
#179090 = CARTESIAN_POINT ( 'NONE',  ( 8.388830574159379737E-16, 13.70000000000001528, -65.00100000000003320 ) ) ;
#179091 = CARTESIAN_POINT ( 'NONE',  ( -14.29746914071049879, 8.314922557960819915, 45.83224293864769550 ) ) ;
#179092 = CARTESIAN_POINT ( 'NONE',  ( 3.556970738554034288E-15, -38.81732327939057114, -2.624999997268812724 ) ) ;
#179093 = CARTESIAN_POINT ( 'NONE',  ( 18.62759615963271287, -10.81492255796078972, 43.33224293864769550 ) ) ;
#179094 = CARTESIAN_POINT ( 'NONE',  ( -18.22780087662126647, -5.499999999999827693, 38.98236817873107185 ) ) ;
#179095 = CARTESIAN_POINT ( 'NONE',  ( -19.05341960407611168, -5.049401038298163336, 96.45724293864769550 ) ) ;
#179096 = CARTESIAN_POINT ( 'NONE',  ( -8.314922557960811034, -14.29746914071050412, 82.08224293864768129 ) ) ;
#179097 = CARTESIAN_POINT ( 'NONE',  ( -9.564922557961040184, 16.46253265017147172, 102.9177570613523329 ) ) ;
#179098 = CARTESIAN_POINT ( 'NONE',  ( 21.52544592524344225, -5.823673210054117533, 58.54057627198103120 ) ) ;
#179099 = VERTEX_POINT ( 'NONE', #196533 ) ;
#179100 = CARTESIAN_POINT ( 'NONE',  ( 16.46253265017160672, -9.564922557960803928, 33.33224293864770260 ) ) ;
#179102 = CARTESIAN_POINT ( 'NONE',  ( 15.72974639402199770, -15.80617190586745480, 83.12390960531436690 ) ) ;
#179101 = CARTESIAN_POINT ( 'NONE',  ( -19.02544592524342804, 5.153800228976336051, 91.04057627198100988 ) ) ;
#179104 = CARTESIAN_POINT ( 'NONE',  ( -16.46253265017160317, 9.564922557960807481, 105.8322429386476955 ) ) ;
#179103 = CARTESIAN_POINT ( 'NONE',  ( -4.483927247898539470, -16.52544592524342804, 27.29057627198103120 ) ) ;
#179105 = CARTESIAN_POINT ( 'NONE',  ( 5.153800228976615827, -19.02544592524334988, 85.20942372801900433 ) ) ;
#179106 = CARTESIAN_POINT ( 'NONE',  ( -15.80617190586768217, 15.72974639402176855, 93.12609039468568994 ) ) ;
#179107 = CARTESIAN_POINT ( 'NONE',  ( -21.55341960407610458, -5.719274019375992779, 76.45724293864769550 ) ) ;
#179108 = CARTESIAN_POINT ( 'NONE',  ( -18.67979575497178146, -10.72451020669898902, 31.66557627198102054 ) ) ;
#179109 = STYLED_ITEM ( 'NONE', ( #90372 ), #7058 ) ;
#179110 = CARTESIAN_POINT ( 'NONE',  ( 9.474510206698971260, -16.51473224551069308, 47.91557627198102409 ) ) ;
#179111 = CARTESIAN_POINT ( 'NONE',  ( 12.14591786802327356, -12.06949235617739191, 110.6260903946857042 ) ) ;
#179112 = CARTESIAN_POINT ( 'NONE',  ( 13.89961937509977652, -13.97604488694527269, 83.12390960531436690 ) ) ;
#179113 = ORIENTED_EDGE ( 'NONE', *, *, #170916, .T. ) ;
#179114 = CARTESIAN_POINT ( 'NONE',  ( -32.50820986112750433, -2.649538386493586639, 87.97934651352352375 ) ) ;
#179115 = CARTESIAN_POINT ( 'NONE',  ( -19.02544592524334988, -5.153800228976617603, 33.95942372801897591 ) ) ;
#179116 = CARTESIAN_POINT ( 'NONE',  ( -16.53943276465976808, 0.05219959533911058130, 91.24890960531436690 ) ) ;
#179117 = CARTESIAN_POINT ( 'NONE',  ( -21.52544592524334988, -5.823673210054445271, 18.95942372801901143 ) ) ;
#179118 = CARTESIAN_POINT ( 'NONE',  ( -22.44159573604010305, 16.30477369853692338, 147.1750000027311671 ) ) ;
#179119 = CARTESIAN_POINT ( 'NONE',  ( 10.72451020669898902, -18.67979575497178502, 62.91557627198102409 ) ) ;
#179120 = CARTESIAN_POINT ( 'NONE',  ( -16.55341960407617563, 4.379528057220093196, 93.54275706135234714 ) ) ;
#179121 = CARTESIAN_POINT ( 'NONE',  ( 5.049401038298161559, -19.05341960407611168, 22.70724293864769194 ) ) ;
#179122 = CARTESIAN_POINT ( 'NONE',  ( -16.51473224551069308, -9.474510206698971260, 76.66557627198103830 ) ) ;
#179123 = CARTESIAN_POINT ( 'NONE',  ( 69.65682714487590488, -71.74905178543389184, -15.00000000000000000 ) ) ;
#179124 = CARTESIAN_POINT ( 'NONE',  ( -8.314922557960811034, -14.29746914071050412, 32.08224293864769550 ) ) ;
#179125 = CARTESIAN_POINT ( 'NONE',  ( 18.62759615963255655, 10.81492255796105972, 61.66775706135235424 ) ) ;
#179126 = CARTESIAN_POINT ( 'NONE',  ( 0.05219959533909260263, 19.03943276465977164, 104.9989096053143669 ) ) ;
#179127 = CARTESIAN_POINT ( 'NONE',  ( -10.81492255796105439, 18.62759615963255655, 97.91775706135236135 ) ) ;
#179128 = CARTESIAN_POINT ( 'NONE',  ( -5.049401038298153566, 19.05341960407611168, 25.20724293864768484 ) ) ;
#179129 = CARTESIAN_POINT ( 'NONE',  ( 19.05341960407611168, 5.049401038298154454, 33.95724293864769550 ) ) ;
#179130 = ORIENTED_EDGE ( 'NONE', *, *, #120571, .F. ) ;
#179131 = CARTESIAN_POINT ( 'NONE',  ( 5.823673210054444382, -21.52544592524334988, 100.2094237280190043 ) ) ;
#179132 = CARTESIAN_POINT ( 'NONE',  ( -12.14591786802326823, 12.06949235617739902, 48.12609039468568284 ) ) ;
#179133 = CARTESIAN_POINT ( 'NONE',  ( -10.81492255796105439, 18.62759615963255655, 87.91775706135234714 ) ) ;
#179134 = CARTESIAN_POINT ( 'NONE',  ( 21.52544592524344225, -5.823673210054117533, 23.54057627198102765 ) ) ;
#179135 = CARTESIAN_POINT ( 'NONE',  ( 19.02544592524334988, 5.153800228976608722, 96.45942372801897591 ) ) ;
#179136 = CARTESIAN_POINT ( 'NONE',  ( 21.55341960407619695, -5.719274019375665929, 56.04275706135235424 ) ) ;
#179137 = CARTESIAN_POINT ( 'NONE',  ( 16.53943276465976808, 0.05219959533934440121, 21.25109039468567218 ) ) ;
#179138 = CARTESIAN_POINT ( 'NONE',  ( 9.564922557961047289, -16.46253265017146816, 90.41775706135234714 ) ) ;
#179139 = CARTESIAN_POINT ( 'NONE',  ( 16.51473224551069308, 9.474510206698969483, 49.16557627198102409 ) ) ;
#179140 = CARTESIAN_POINT ( 'NONE',  ( -16.51473224551082808, 9.474510206698731452, 103.3344237280190043 ) ) ;
#179141 = AXIS2_PLACEMENT_3D ( 'NONE', #25203, #100001, #161687 ) ;
#179142 = CARTESIAN_POINT ( 'NONE',  ( 19.02544592524334988, 5.153800228976608722, 86.45942372801900433 ) ) ;
#179143 = CARTESIAN_POINT ( 'NONE',  ( -14.29746914071049879, 8.314922557960819915, 50.83224293864770971 ) ) ;
#179144 = CARTESIAN_POINT ( 'NONE',  ( -19.05341960407617563, 5.049401038297882671, 78.54275706135233293 ) ) ;
#179145 = CARTESIAN_POINT ( 'NONE',  ( 12.14591786802327356, -12.06949235617739191, 65.62609039468568994 ) ) ;
#179146 = CARTESIAN_POINT ( 'NONE',  ( 13.97604488694548053, -13.89961937509957401, 30.62609039468566863 ) ) ;
#179147 = CARTESIAN_POINT ( 'NONE',  ( -16.46253265017160317, 9.564922557960807481, 40.83224293864769550 ) ) ;
#179148 = CARTESIAN_POINT ( 'NONE',  ( -9.564922557960796823, -16.46253265017161027, 42.08224293864769550 ) ) ;
#179149 = CARTESIAN_POINT ( 'NONE',  ( 14.29746914071037800, 8.314922557961029526, 56.66775706135235424 ) ) ;
#179150 = CARTESIAN_POINT ( 'NONE',  ( 1.784210473542230573E-15, -29.16686587814331588, 139.8750000027311842 ) ) ;
#179151 = CARTESIAN_POINT ( 'NONE',  ( -28.82186960331499392, -9.364793116373526516, 138.3500000054623911 ) ) ;
#179152 = CARTESIAN_POINT ( 'NONE',  ( 19.03943276465977164, -0.05219959533909143690, 108.7489096053143527 ) ) ;
#179153 = CARTESIAN_POINT ( 'NONE',  ( -17.49999999999999645, -5.499999999999992895, 69.20309617465828467 ) ) ;
#179154 = ORIENTED_EDGE ( 'NONE', *, *, #39357, .T. ) ;
#179155 = CARTESIAN_POINT ( 'NONE',  ( 9.474510206698729675, 16.51473224551082808, 92.08442372801900433 ) ) ;
#179156 = CARTESIAN_POINT ( 'NONE',  ( 21.52544592524344225, -5.823673210054117533, 33.54057627198102409 ) ) ;
#179158 = CARTESIAN_POINT ( 'NONE',  ( 5.049401038297881783, 19.05341960407617563, 107.2927570613523187 ) ) ;
#179157 = CARTESIAN_POINT ( 'NONE',  ( -13.89961937509957401, -13.97604488694547875, 34.37609039468566863 ) ) ;
#179159 = CARTESIAN_POINT ( 'NONE',  ( -16.51473224551069308, -9.474510206698971260, 31.66557627198102054 ) ) ;
#179160 = CARTESIAN_POINT ( 'NONE',  ( -19.03943276465977164, 0.05219959533909376836, 31.24890960531435979 ) ) ;
#179161 = CARTESIAN_POINT ( 'NONE',  ( 18.62759615963271287, -10.81492255796078972, 68.33224293864769550 ) ) ;
#179162 = CARTESIAN_POINT ( 'NONE',  ( -5.049401038298153566, 19.05341960407611168, 105.2072429386476671 ) ) ;
#179163 = CARTESIAN_POINT ( 'NONE',  ( -13.97604488694527625, -13.89961937509977652, 31.87390960531435979 ) ) ;
#179164 = CARTESIAN_POINT ( 'NONE',  ( 1.784210473542230573E-15, -29.16686587814331588, 143.8750000027311842 ) ) ;
#179165 = CARTESIAN_POINT ( 'NONE',  ( -19.03943276465977164, -0.05219959533935918106, 88.75109039468567573 ) ) ;
#179166 = CARTESIAN_POINT ( 'NONE',  ( 14.29746914071049879, -8.314922557960816363, 53.33224293864769550 ) ) ;
#179167 = CARTESIAN_POINT ( 'NONE',  ( 5.719274019375991003, -21.55341960407610458, 37.70724293864769550 ) ) ;
#179168 = CARTESIAN_POINT ( 'NONE',  ( 10.81492255796106328, -18.62759615963255655, 110.4177570613523756 ) ) ;
#179169 = CARTESIAN_POINT ( 'NONE',  ( 18.62759615963271287, -10.81492255796078972, 83.33224293864769550 ) ) ;
#179170 = CARTESIAN_POINT ( 'NONE',  ( -10.81492255796105439, 18.62759615963255655, 72.91775706135234714 ) ) ;
#179171 = CARTESIAN_POINT ( 'NONE',  ( 15.72974639402176855, 15.80617190586768217, 61.87609039468568284 ) ) ;
#179172 = CARTESIAN_POINT ( 'NONE',  ( 13.89961937509977652, -13.97604488694527269, 108.1239096053143669 ) ) ;
#179174 = CARTESIAN_POINT ( 'NONE',  ( 0.05219959533937995610, -21.53943276465977519, 65.00109039468568994 ) ) ;
#179173 = CARTESIAN_POINT ( 'NONE',  ( -12.14591786802326823, 12.06949235617739902, 108.1260903946856757 ) ) ;
#179175 = CARTESIAN_POINT ( 'NONE',  ( 16.46253265017160672, -9.564922557960803928, 58.33224293864769550 ) ) ;
#179176 = CARTESIAN_POINT ( 'NONE',  ( -9.564922557961040184, 16.46253265017147172, 32.91775706135233293 ) ) ;
#179177 = CARTESIAN_POINT ( 'NONE',  ( -5.719274019375665041, -21.55341960407619695, 24.79275706135235779 ) ) ;
#179178 = CARTESIAN_POINT ( 'NONE',  ( 16.46253265017160672, -9.564922557960803928, 68.33224293864770971 ) ) ;
#179179 = CARTESIAN_POINT ( 'NONE',  ( -16.53943276465976808, 0.05219959533911058130, 86.24890960531436690 ) ) ;
#179180 = CARTESIAN_POINT ( 'NONE',  ( -16.52544592524342804, 4.483927247898546575, 46.04057627198103830 ) ) ;
#179181 = CARTESIAN_POINT ( 'NONE',  ( -21.53943276465977519, 0.05219959533907696930, 61.24890960531435979 ) ) ;
#179182 = CARTESIAN_POINT ( 'NONE',  ( -13.97604488694527625, -13.89961937509977652, 61.87390960531435979 ) ) ;
#179183 = CARTESIAN_POINT ( 'NONE',  ( -5.823673210054116645, -21.52544592524344225, 72.29057627198102409 ) ) ;
#179184 = CARTESIAN_POINT ( 'NONE',  ( -16.51473224551082808, 9.474510206698731452, 53.33442372801900433 ) ) ;
#179186 = CARTESIAN_POINT ( 'NONE',  ( -4.379528057220328563, 16.55341960407611168, 60.20724293864768839 ) ) ;
#179185 = CARTESIAN_POINT ( 'NONE',  ( 1.300000000000000044, -0.7216878364870319418, 1.249999999999999778 ) ) ;
#179187 = CARTESIAN_POINT ( 'NONE',  ( 10.81492255796078972, 18.62759615963270932, 34.58224293864770260 ) ) ;
#179188 = ORIENTED_EDGE ( 'NONE', *, *, #182692, .T. ) ;
#179189 = CARTESIAN_POINT ( 'NONE',  ( -193.3062444957834884, -155.7167183371838064, 0.000000000000000000 ) ) ;
#179191 = CARTESIAN_POINT ( 'NONE',  ( 17.14385361876520264, 23.59649016807275856, 148.1750000027311671 ) ) ;
#179190 = CARTESIAN_POINT ( 'NONE',  ( 8.224510206698742110, 14.34966873604972548, 87.08442372801901854 ) ) ;
#179192 = CARTESIAN_POINT ( 'NONE',  ( -13.89961937509957401, -13.97604488694547875, 89.37609039468563310 ) ) ;
#179193 = CARTESIAN_POINT ( 'NONE',  ( 4.379528057220339221, -16.55341960407611168, 57.70724293864770260 ) ) ;
#179194 = DIRECTION ( 'NONE',  ( -0.000000000000000000, -0.000000000000000000, -1.000000000000000000 ) ) ;
#179195 = CARTESIAN_POINT ( 'NONE',  ( -5.049401038298153566, 19.05341960407611168, 45.20724293864769550 ) ) ;
#179196 = CARTESIAN_POINT ( 'NONE',  ( 16.52544592524342804, -4.483927247898539470, 38.54057627198103120 ) ) ;
#179197 = CARTESIAN_POINT ( 'NONE',  ( -16.51473224551069308, -9.474510206698971260, 91.66557627198103830 ) ) ;
#179198 = CARTESIAN_POINT ( 'NONE',  ( 5.049401038298161559, -19.05341960407611168, 52.70724293864767418 ) ) ;
#179199 = CARTESIAN_POINT ( 'NONE',  ( -10.72451020669870658, -18.67979575497194134, 54.58442372801901143 ) ) ;
#179200 = CARTESIAN_POINT ( 'NONE',  ( 19.05341960407611168, 5.049401038298154454, 68.95724293864769550 ) ) ;
#179201 = CARTESIAN_POINT ( 'NONE',  ( -13.97604488694527625, -13.89961937509977652, 26.87390960531434558 ) ) ;
#179202 = CARTESIAN_POINT ( 'NONE',  ( -19.02544592524342804, 5.153800228976336051, 71.04057627198099567 ) ) ;
#179203 = CARTESIAN_POINT ( 'NONE',  ( 21.53943276465977519, -0.05219959533907433946, 43.74890960531435979 ) ) ;
#179204 = CARTESIAN_POINT ( 'NONE',  ( -13.97604488694527625, -13.89961937509977652, 36.87390960531436690 ) ) ;
#179205 = CARTESIAN_POINT ( 'NONE',  ( 0.05219959533907565091, 21.53943276465977519, 34.99890960531435979 ) ) ;
#179206 = CARTESIAN_POINT ( 'NONE',  ( -4.379528057220086978, -16.55341960407618274, 109.7927570613523613 ) ) ;
#179207 = ADVANCED_FACE ( 'NONE', ( #104500 ), #24679, .T. ) ;
#179208 = CARTESIAN_POINT ( 'NONE',  ( 19.02544592524334988, 5.153800228976608722, 26.45942372801899722 ) ) ;
#179210 = CARTESIAN_POINT ( 'NONE',  ( -4.379528057220086978, -16.55341960407618274, 84.79275706135234714 ) ) ;
#179209 = CARTESIAN_POINT ( 'NONE',  ( -14.34966873604972548, 8.224510206698743886, 43.33442372801901143 ) ) ;
#179211 = CARTESIAN_POINT ( 'NONE',  ( -17.72560187377285601, -5.500000000000015987, 94.07814504131322053 ) ) ;
#179212 = CARTESIAN_POINT ( 'NONE',  ( 14.29746914071037800, 8.314922557961029526, 61.66775706135235424 ) ) ;
#179213 = CARTESIAN_POINT ( 'NONE',  ( -16.51473224551069308, -9.474510206698971260, 106.6655762719810383 ) ) ;
#179214 = VECTOR ( 'NONE', #142848, 1000.000000000000000 ) ;
#179215 = CARTESIAN_POINT ( 'NONE',  ( -16.46253265017160317, 9.564922557960807481, 35.83224293864768839 ) ) ;
#179216 = CARTESIAN_POINT ( 'NONE',  ( -14.34966873604972548, 8.224510206698743886, 33.33442372801900433 ) ) ;
#179217 = CARTESIAN_POINT ( 'NONE',  ( 16.46253265017160672, -9.564922557960803928, 43.33224293864769550 ) ) ;
#179218 = CARTESIAN_POINT ( 'NONE',  ( 0.05219959533937995610, -21.53943276465977519, 30.00109039468568284 ) ) ;
#179219 = CARTESIAN_POINT ( 'NONE',  ( 16.53943276465976808, 0.05219959533934440121, 36.25109039468567573 ) ) ;
#179220 = CARTESIAN_POINT ( 'NONE',  ( -16.53943276465976808, -0.05219959533934237506, 93.75109039468567573 ) ) ;
#179221 = DIRECTION ( 'NONE',  ( 4.336808689942018352E-17, -1.000000000000000000, 0.000000000000000000 ) ) ;
#179222 = CARTESIAN_POINT ( 'NONE',  ( 18.67979575497194134, -10.72451020669871369, 105.8344237280190328 ) ) ;
#179223 = CARTESIAN_POINT ( 'NONE',  ( -5.049401038297874678, -19.05341960407617918, 99.79275706135234714 ) ) ;
#179224 = CARTESIAN_POINT ( 'NONE',  ( -13.97604488694547697, 13.89961937509957934, 58.12609039468566863 ) ) ;
#179225 = CARTESIAN_POINT ( 'NONE',  ( 14.34966873604960469, 8.224510206698951720, 59.16557627198103120 ) ) ;
#179226 = CARTESIAN_POINT ( 'NONE',  ( 14.34966873604960469, 8.224510206698951720, 114.1655762719810383 ) ) ;
#179228 = CARTESIAN_POINT ( 'NONE',  ( 17.50000000000000355, -5.624438216177559902, 58.31670344914645909 ) ) ;
#179227 = CARTESIAN_POINT ( 'NONE',  ( 19.03943276465977164, 0.05219959533936151252, 61.25109039468566863 ) ) ;
#179229 = CARTESIAN_POINT ( 'NONE',  ( 21.55341960407619695, -5.719274019375665929, 66.04275706135236135 ) ) ;
#179230 = CARTESIAN_POINT ( 'NONE',  ( 14.29746914071037800, 8.314922557961029526, 21.66775706135235069 ) ) ;
#179231 = CARTESIAN_POINT ( 'NONE',  ( 69.65682714487590488, -71.74905178543389184, -15.00000000000000000 ) ) ;
#179232 = CARTESIAN_POINT ( 'NONE',  ( 21.52544592524344225, -5.823673210054117533, 23.54057627198102765 ) ) ;
#179233 = CARTESIAN_POINT ( 'NONE',  ( -9.564922557961040184, 16.46253265017147172, 107.9177570613523471 ) ) ;
#179234 = CARTESIAN_POINT ( 'NONE',  ( 17.50000000000000000, -5.500000000000031086, 98.29690382534174375 ) ) ;
#179235 = CARTESIAN_POINT ( 'NONE',  ( -26.62494319856312686, 7.396441074661496806, 168.1134502243650104 ) ) ;
#179236 = CARTESIAN_POINT ( 'NONE',  ( 12.14591786802309770, 12.06949235617756955, 114.3739096053143527 ) ) ;
#179237 = CARTESIAN_POINT ( 'NONE',  ( -21.55341960407619339, 5.719274019375674811, 108.5427570613523756 ) ) ;
#179238 = CARTESIAN_POINT ( 'NONE',  ( -13.97604488694527625, -13.89961937509977652, 51.87390960531436690 ) ) ;
#179239 = STYLED_ITEM ( 'NONE', ( #53434 ), #143056 ) ;
#179240 = CARTESIAN_POINT ( 'NONE',  ( 0.05219959533937995610, -21.53943276465977519, 60.00109039468568284 ) ) ;
#179241 = CARTESIAN_POINT ( 'NONE',  ( -21.52544592524334988, -5.823673210054445271, 98.95942372801903275 ) ) ;
#179242 = CARTESIAN_POINT ( 'NONE',  ( 16.52544592524335698, 4.483927247898782831, 106.4594237280190328 ) ) ;
#179244 = B_SPLINE_CURVE_WITH_KNOTS ( 'NONE', 3,
 ( #154039, #182411, #42902, #15534, #75211, #104567 ),
 .UNSPECIFIED., .F., .F.,
 ( 4, 2, 4 ),
 ( 0.007228050697041515406, 0.007608510107494982286, 0.007988969517948450033 ),
 .UNSPECIFIED. ) ;
#179243 = CARTESIAN_POINT ( 'NONE',  ( 13.89961937509977652, -13.97604488694527269, 73.12390960531436690 ) ) ;
#179245 = CARTESIAN_POINT ( 'NONE',  ( -21.55341960407619339, 5.719274019375674811, 58.54275706135235424 ) ) ;
#179246 = CARTESIAN_POINT ( 'NONE',  ( 15.72974639402176855, 15.80617190586768217, 51.87609039468568284 ) ) ;
#179248 = CARTESIAN_POINT ( 'NONE',  ( 13.89961937509977652, -13.97604488694527269, 103.1239096053143527 ) ) ;
#179247 = CARTESIAN_POINT ( 'NONE',  ( 16.51473224551083163, -9.474510206698727899, 85.83442372801900433 ) ) ;
#179249 = CARTESIAN_POINT ( 'NONE',  ( -5.153800228976328057, -19.02544592524343514, 22.29057627198102765 ) ) ;
#179250 = CARTESIAN_POINT ( 'NONE',  ( 21.52544592524344225, -5.823673210054117533, 93.54057627198103830 ) ) ;
#179251 = CARTESIAN_POINT ( 'NONE',  ( 19.05341960407617918, -5.049401038297876454, 26.04275706135233293 ) ) ;
#179252 = CARTESIAN_POINT ( 'NONE',  ( -8.314922557960811034, -14.29746914071050412, 102.0822429386476955 ) ) ;
#179253 = CARTESIAN_POINT ( 'NONE',  ( 9.564922557960805705, 16.46253265017160317, 44.58224293864769550 ) ) ;
#179255 = VECTOR ( 'NONE', #29709, 1000.000000000000000 ) ;
#179254 = CARTESIAN_POINT ( 'NONE',  ( -13.97604488694547697, 13.89961937509957934, 98.12609039468566152 ) ) ;
#179256 = CARTESIAN_POINT ( 'NONE',  ( -4.483927247898539470, -16.52544592524342804, 62.29057627198102409 ) ) ;
#179257 = CARTESIAN_POINT ( 'NONE',  ( -0.05219959533937732626, 21.53943276465977519, 107.5010903946856899 ) ) ;
#179258 = CARTESIAN_POINT ( 'NONE',  ( -9.564922557960796823, -16.46253265017161027, 107.0822429386476955 ) ) ;
#179259 = CARTESIAN_POINT ( 'NONE',  ( -16.51473224551082808, 9.474510206698731452, 78.33442372801900433 ) ) ;
#179260 = CARTESIAN_POINT ( 'NONE',  ( 18.67979575497178502, 10.72451020669898547, 84.16557627198103830 ) ) ;
#179261 = CARTESIAN_POINT ( 'NONE',  ( -5.719274019375665041, -21.55341960407619695, 34.79275706135235424 ) ) ;
#179262 = CARTESIAN_POINT ( 'NONE',  ( -8.314922557961024197, 14.29746914071037800, 42.91775706135235424 ) ) ;
#179263 = CARTESIAN_POINT ( 'NONE',  ( 8.224510206698742110, 14.34966873604972548, 87.08442372801901854 ) ) ;
#179265 = CARTESIAN_POINT ( 'NONE',  ( 21.53943276465977519, 0.05219959533937863772, 31.25109039468568639 ) ) ;
#179264 = CARTESIAN_POINT ( 'NONE',  ( -8.314922557961024197, 14.29746914071037800, 37.91775706135235424 ) ) ;
#179266 = CARTESIAN_POINT ( 'NONE',  ( -15.80617190586745835, -15.72974639402198527, 41.87390960531435979 ) ) ;
#179267 = PRODUCT_DEFINITION_FORMATION_WITH_SPECIFIED_SOURCE ( 'ANY', '', #155079, .NOT_KNOWN. ) ;
#179268 = CARTESIAN_POINT ( 'NONE',  ( 16.46253265017160672, -9.564922557960803928, 33.33224293864770260 ) ) ;
#179269 = CARTESIAN_POINT ( 'NONE',  ( 3.766062262543149401E-15, -39.95556452105413570, -11.24999999453762278 ) ) ;
#179270 = CARTESIAN_POINT ( 'NONE',  ( 12.06949235617739724, 12.14591786802326823, 66.87609039468568994 ) ) ;
#179271 = CARTESIAN_POINT ( 'NONE',  ( -0.05219959533907301413, -21.53943276465977519, 87.49890960531436690 ) ) ;
#179272 = CARTESIAN_POINT ( 'NONE',  ( 0.05219959533910956823, 16.53943276465976808, 44.99890960531435979 ) ) ;
#179273 = CARTESIAN_POINT ( 'NONE',  ( 0.05219959533934541429, -16.53943276465976808, 55.00109039468568284 ) ) ;
#179274 = CARTESIAN_POINT ( 'NONE',  ( 9.474510206698971260, -16.51473224551069308, 57.91557627198103120 ) ) ;
#179275 = CARTESIAN_POINT ( 'NONE',  ( 9.474510206698729675, 16.51473224551082808, 82.08442372801899012 ) ) ;
#179276 = CARTESIAN_POINT ( 'NONE',  ( 21.55341960407610458, 5.719274019375980345, 88.95724293864769550 ) ) ;
#179277 = CARTESIAN_POINT ( 'NONE',  ( 14.34966873604960469, 8.224510206698951720, 34.16557627198102409 ) ) ;
#179278 = EDGE_LOOP ( 'NONE', ( #163926, #174039, #133746, #84136, #142748, #73738 ) ) ;
#179279 = CARTESIAN_POINT ( 'NONE',  ( 21.35462415990330243, 10.43496131973800090, 170.3924512066482748 ) ) ;
#179280 =( BOUNDED_CURVE ( )  B_SPLINE_CURVE ( 2, ( #187543, #105710, #158166, #34823, #110665, #82294, #52966, #98464, #49010, #67148, #172345, #191488, #141993, #143985, #5466, #128806, #84298, #7459, #188523, #21649, #174343, #69143, #6459, #114643, #190505, #65158, #176341, #18674, #37813, #51979, #50991, #112652, #96478, #50000, #113637, #145977, #142983, #97459, #175332, #111665, #3481, #36799, #99474, #126817, #33834, #159145, #19658, #35813, #160158, #68140, #95494, #127813, #129791, #20641, #83302, #81299, #144979, #161155, #130810, #173352, #22651, #157180, #80320, #4461, #66150, #189518, #195515, #89307, #86311, #40815, #148999, #131823, #146991, #116650, #134837 ),
 .UNSPECIFIED., .F., .F. ) 
 B_SPLINE_CURVE_WITH_KNOTS ( ( 3, 2, 2, 2, 2, 2, 2, 2, 2, 2, 2, 2, 2, 2, 2, 2, 2, 2, 2, 2, 2, 2, 2, 2, 2, 2, 2, 2, 2, 2, 2, 2, 2, 2, 2, 2, 2, 3 ),
 ( 0.000000000000000000, 0.02000000000000000042, 0.04000000000000000083, 0.05999999999999999778, 0.08000000000000000167, 0.1000000000000000056, 0.1199999999999999956, 0.1400000000000000133, 0.1600000000000000033, 0.1799999999999999933, 0.2000000000000000111, 0.2200000000000000011, 0.2399999999999999911, 0.2600000000000000089, 0.2800000000000000266, 0.2999999999999999889, 0.3200000000000000067, 0.3400000000000000244, 0.3599999999999999867, 0.3800000000000000044, 0.4000000000000000222, 0.4199999999999999845, 0.4400000000000000022, 0.4600000000000000200, 0.4799999999999999822, 0.5000000000000000000, 0.5200000000000000178, 0.5400000000000000355, 0.5600000000000000533, 0.5799999999999999600, 0.5999999999999999778, 0.6199999999999999956, 0.6400000000000000133, 0.6600000000000000311, 0.6800000000000000488, 0.6999999999999999556, 0.7199999999999999734, 0.7374174419963606120 ),
 .UNSPECIFIED. ) 
 CURVE ( )  GEOMETRIC_REPRESENTATION_ITEM ( )  RATIONAL_B_SPLINE_CURVE ( ( 1.000000000000000000, 0.9510565162951535312, 1.000000000000000000, 0.9510565162951535312, 1.000000000000000000, 0.9510565162951535312, 1.000000000000000000, 0.9510565162951535312, 1.000000000000000000, 0.9510565162951535312, 1.000000000000000000, 0.9510565162951535312, 1.000000000000000000, 0.9510565162951535312, 1.000000000000000000, 0.9510565162951535312, 1.000000000000000000, 0.9510565162951535312, 1.000000000000000000, 0.9510565162951535312, 1.000000000000000000, 0.9510565162951535312, 1.000000000000000000, 0.9510565162951535312, 1.000000000000000000, 0.9510565162951535312, 1.000000000000000000, 0.9510565162951535312, 1.000000000000000000, 0.9510565162951535312, 1.000000000000000000, 0.9510565162951535312, 1.000000000000000000, 0.9510565162951535312, 1.000000000000000000, 0.9510565162951535312, 1.000000000000000000, 0.9510565162951535312, 1.000000000000000000, 0.9510565162951535312, 1.000000000000000000, 0.9510565162951535312, 1.000000000000000000, 0.9510565162951535312, 1.000000000000000000, 0.9510565162951535312, 1.000000000000000000, 0.9510565162951535312, 1.000000000000000000, 0.9510565162951535312, 1.000000000000000000, 0.9510565162951535312, 1.000000000000000000, 0.9510565162951535312, 1.000000000000000000, 0.9510565162951535312, 1.000000000000000000, 0.9510565162951535312, 1.000000000000000000, 0.9510565162951535312, 1.000000000000000000, 0.9510565162951535312, 1.000000000000000000, 0.9510565162951535312, 1.000000000000000000, 0.9510565162951535312, 1.000000000000000000, 0.9510565162951535312, 1.000000000000000000, 0.9510565162951535312, 1.000000000000000000, 0.9510565162951535312, 1.000000000000000000, 0.9573764855735508172, 0.9889922301674735072 ) ) 
 REPRESENTATION_ITEM ( '' )  );
#179281 = CARTESIAN_POINT ( 'NONE',  ( -15.80617190586745835, -15.72974639402198527, 61.87390960531436690 ) ) ;
#179282 = CARTESIAN_POINT ( 'NONE',  ( -8.314922557961024197, 14.29746914071037800, 102.9177570613523756 ) ) ;
#179283 = ORIENTED_EDGE ( 'NONE', *, *, #47103, .T. ) ;
#179284 = CARTESIAN_POINT ( 'NONE',  ( 17.50000000000000000, -5.500000000000000888, 103.2969038253417153 ) ) ;
#179285 = CARTESIAN_POINT ( 'NONE',  ( 15.80617190586746368, 15.72974639402197994, 84.37390960531438111 ) ) ;
#179286 = CARTESIAN_POINT ( 'NONE',  ( 14.29746914071049879, -8.314922557960816363, 28.33224293864769550 ) ) ;
#179288 = CARTESIAN_POINT ( 'NONE',  ( -4.379528057220086978, -16.55341960407618274, 29.79275706135234358 ) ) ;
#179287 = VECTOR ( 'NONE', #86791, 1000.000000000000000 ) ;
#179289 = CARTESIAN_POINT ( 'NONE',  ( -9.564922557960796823, -16.46253265017161027, 32.08224293864769550 ) ) ;
#179290 = CARTESIAN_POINT ( 'NONE',  ( 19.05341960407611168, 5.049401038298154454, 63.95724293864769550 ) ) ;
#179291 = EDGE_CURVE ( 'NONE', #138197, #85313, #132834, .T. ) ;
#179292 = CARTESIAN_POINT ( 'NONE',  ( -23.31738231874055600, 16.94106989632528837, 147.7999999999999829 ) ) ;
#179293 = CARTESIAN_POINT ( 'NONE',  ( -15.80617190586745835, -15.72974639402198527, 21.87390960531436690 ) ) ;
#179294 = DIRECTION ( 'NONE',  ( 0.000000000000000000, 0.000000000000000000, -1.000000000000000000 ) ) ;
#179295 = CARTESIAN_POINT ( 'NONE',  ( -4.379528057220086978, -16.55341960407618274, 104.7927570613523898 ) ) ;
#179296 = CARTESIAN_POINT ( 'NONE',  ( 9.564922557961047289, -16.46253265017146816, 105.4177570613523471 ) ) ;
#179297 = CARTESIAN_POINT ( 'NONE',  ( -19.02544592524334988, -5.153800228976617603, 38.95942372801900433 ) ) ;
#179298 = CARTESIAN_POINT ( 'NONE',  ( -18.62759615963270932, 10.81492255796079327, 85.83224293864768129 ) ) ;
#179299 = CARTESIAN_POINT ( 'NONE',  ( -4.483927247898539470, -16.52544592524342804, 22.29057627198102765 ) ) ;
#179300 = CARTESIAN_POINT ( 'NONE',  ( -10.81492255796078084, -18.62759615963271287, 37.08224293864768129 ) ) ;
#179301 = CARTESIAN_POINT ( 'NONE',  ( 9.564922557961047289, -16.46253265017146816, 105.4177570613523471 ) ) ;
#179302 = CARTESIAN_POINT ( 'NONE',  ( -16.46253265017160317, 9.564922557960807481, 105.8322429386476955 ) ) ;
#179303 = CARTESIAN_POINT ( 'NONE',  ( 21.53943276465977519, 0.05219959533937863772, 61.25109039468567573 ) ) ;
#179304 = CARTESIAN_POINT ( 'NONE',  ( -0.05219959533909027116, -19.03943276465977164, 57.49890960531435979 ) ) ;
#179305 = CARTESIAN_POINT ( 'NONE',  ( -16.53943276465976808, 0.05219959533911058130, 106.2489096053143811 ) ) ;
#179306 = CARTESIAN_POINT ( 'NONE',  ( 32.57470439124677597, 1.954246231034476811, 87.74243420032607332 ) ) ;
#179307 = CARTESIAN_POINT ( 'NONE',  ( 0.05219959533909260263, 19.03943276465977164, 74.99890960531435269 ) ) ;
#179308 = CARTESIAN_POINT ( 'NONE',  ( 4.379528057220339221, -16.55341960407611168, 77.70724293864770971 ) ) ;
#179309 = VERTEX_POINT ( 'NONE', #57005 ) ;
#179310 = CARTESIAN_POINT ( 'NONE',  ( 5.049401038297881783, 19.05341960407617563, 97.29275706135233293 ) ) ;
#179311 = CARTESIAN_POINT ( 'NONE',  ( 17.48853670773246449, -5.747243402303036319, 81.16671299749991420 ) ) ;
#179312 = CARTESIAN_POINT ( 'NONE',  ( 9.564922557960805705, 16.46253265017160317, 64.58224293864769550 ) ) ;
#179313 = CARTESIAN_POINT ( 'NONE',  ( 31.33613174426653458, -7.485780765379337787, 94.47638157584336227 ) ) ;
#179315 = CARTESIAN_POINT ( 'NONE',  ( -13.97604488694527625, -13.89961937509977652, 101.8739096053143811 ) ) ;
#179314 = CARTESIAN_POINT ( 'NONE',  ( -9.564922557960796823, -16.46253265017161027, 77.08224293864769550 ) ) ;
#179316 = CARTESIAN_POINT ( 'NONE',  ( -8.224510206698735004, -14.34966873604973081, 64.58442372801900433 ) ) ;
#179317 = CARTESIAN_POINT ( 'NONE',  ( 193.3062444957835453, -155.7167183371837496, -15.00000000000000178 ) ) ;
#179318 = CARTESIAN_POINT ( 'NONE',  ( -5.049401038297874678, -19.05341960407617918, 44.79275706135232582 ) ) ;
#179319 = CARTESIAN_POINT ( 'NONE',  ( -15.80617190586768217, 15.72974639402176855, 98.12609039468570415 ) ) ;
#179320 = CARTESIAN_POINT ( 'NONE',  ( 36.89064505505185565, 5.462148823192609193, 44.26314855211815313 ) ) ;
#179321 = CARTESIAN_POINT ( 'NONE',  ( 5.153800228976335163, 19.02544592524342804, 114.7905762719810241 ) ) ;
#179322 = CARTESIAN_POINT ( 'NONE',  ( 4.379528057220092307, 16.55341960407617563, 97.29275706135234714 ) ) ;
#179323 = DIRECTION ( 'NONE',  ( 0.000000000000000000, 0.000000000000000000, 1.000000000000000000 ) ) ;
#179324 = CARTESIAN_POINT ( 'NONE',  ( -0.05219959533934338120, 16.53943276465976808, 87.50109039468568994 ) ) ;
#179325 = CARTESIAN_POINT ( 'NONE',  ( -8.898068258721474777, 27.38543819252877398, 145.8656553485623704 ) ) ;
#179326 = CARTESIAN_POINT ( 'NONE',  ( -16.55341960407617563, 4.379528057220093196, 73.54275706135234714 ) ) ;
#179327 = ORIENTED_EDGE ( 'NONE', *, *, #109403, .T. ) ;
#179328 = CARTESIAN_POINT ( 'NONE',  ( -18.67979575497193778, 10.72451020669871902, 78.33442372801901854 ) ) ;
#179329 = CARTESIAN_POINT ( 'NONE',  ( -16.51473224551082808, 9.474510206698731452, 88.33442372801900433 ) ) ;
#179330 = CARTESIAN_POINT ( 'NONE',  ( 16.46253265017146816, 9.564922557961045513, 31.66775706135232937 ) ) ;
#179331 = VECTOR ( 'NONE', #153121, 1000.000000000000000 ) ;
#179332 = CARTESIAN_POINT ( 'NONE',  ( 9.474510206698971260, -16.51473224551069308, 62.91557627198102409 ) ) ;
#179333 = CARTESIAN_POINT ( 'NONE',  ( -19.03943276465977164, 0.05219959533909376836, 61.24890960531436690 ) ) ;
#179334 = CARTESIAN_POINT ( 'NONE',  ( -19.60206085084869443, -34.86781819333700838, -6.670742825288880518 ) ) ;
#179335 = CARTESIAN_POINT ( 'NONE',  ( -21.55341960407610458, -5.719274019375992779, 86.45724293864770971 ) ) ;
#179336 = CARTESIAN_POINT ( 'NONE',  ( 18.67979575497178502, 10.72451020669898547, 29.16557627198103120 ) ) ;
#179337 = CARTESIAN_POINT ( 'NONE',  ( -9.564922557960796823, -16.46253265017161027, 32.08224293864769550 ) ) ;
#179338 = CARTESIAN_POINT ( 'NONE',  ( 12.14591786802327356, -12.06949235617739191, 70.62609039468567573 ) ) ;
#179339 = ORIENTED_EDGE ( 'NONE', *, *, #89272, .F. ) ;
#179340 = CARTESIAN_POINT ( 'NONE',  ( 21.55341960407619695, -5.719274019375665929, 26.04275706135235779 ) ) ;
#179342 = CARTESIAN_POINT ( 'NONE',  ( 29.86685920354754487, 21.69954338932564752, -9.424999997268814766 ) ) ;
#179341 = CARTESIAN_POINT ( 'NONE',  ( 12.14591786802309770, 12.06949235617756955, 64.37390960531435269 ) ) ;
#179343 = CARTESIAN_POINT ( 'NONE',  ( 8.314922557961029526, -14.29746914071037800, 20.41775706135234714 ) ) ;
#179344 = CARTESIAN_POINT ( 'NONE',  ( -19.03943276465977164, -0.05219959533935918106, 53.75109039468566863 ) ) ;
#179345 = CARTESIAN_POINT ( 'NONE',  ( -14.34966873604960291, -8.224510206698953496, 51.66557627198102409 ) ) ;
#179346 = CARTESIAN_POINT ( 'NONE',  ( -21.55341960407619339, 5.719274019375674811, 23.54275706135235424 ) ) ;
#179348 = CARTESIAN_POINT ( 'NONE',  ( 21.55341960407610458, 5.719274019375980345, 78.95724293864769550 ) ) ;
#179347 = CARTESIAN_POINT ( 'NONE',  ( 18.22780087662122384, 5.500000000000018652, 98.98459894673892734 ) ) ;
#179349 = CARTESIAN_POINT ( 'NONE',  ( 5.049401038298161559, -19.05341960407611168, 92.70724293864769550 ) ) ;
#179350 = CARTESIAN_POINT ( 'NONE',  ( -14.34966873604960291, -8.224510206698953496, 56.66557627198103830 ) ) ;
#179351 = CARTESIAN_POINT ( 'NONE',  ( 30.36026264928092999, -25.76863830327009453, -21.12575414591866974 ) ) ;
#179352 = CARTESIAN_POINT ( 'NONE',  ( 2.500000000000000000, 0.000000000000000000, -62.91767397929362460 ) ) ;
#179353 = CARTESIAN_POINT ( 'NONE',  ( 9.474510206698729675, 16.51473224551082808, 72.08442372801900433 ) ) ;
#179354 = CARTESIAN_POINT ( 'NONE',  ( -5.823673210054116645, -21.52544592524344225, 107.2905762719810525 ) ) ;
#179355 = CARTESIAN_POINT ( 'NONE',  ( 19.02544592524343514, -5.153800228976328945, 53.54057627198102409 ) ) ;
#179356 = CARTESIAN_POINT ( 'NONE',  ( -16.46253265017146816, -9.564922557961047289, 39.16775706135234003 ) ) ;
#179357 = CARTESIAN_POINT ( 'NONE',  ( -9.564922557960796823, -16.46253265017161027, 32.08224293864769550 ) ) ;
#179358 = CARTESIAN_POINT ( 'NONE',  ( 0.05219959533937995610, -21.53943276465977519, 60.00109039468568284 ) ) ;
#179359 = DIRECTION ( 'NONE',  ( -1.000000000000000000, 0.000000000000000000, 0.000000000000000000 ) ) ;
#179360 = CARTESIAN_POINT ( 'NONE',  ( -16.52544592524342804, 4.483927247898546575, 46.04057627198103830 ) ) ;
#179361 = CARTESIAN_POINT ( 'NONE',  ( 19.02544592524343514, -5.153800228976328945, 68.54057627198103830 ) ) ;
#179362 = CARTESIAN_POINT ( 'NONE',  ( -21.52544592524343514, 5.823673210054127303, 71.04057627198103830 ) ) ;
#179363 = CARTESIAN_POINT ( 'NONE',  ( -16.46253265017160317, 9.564922557960807481, 55.83224293864769550 ) ) ;
#179364 = VERTEX_POINT ( 'NONE', #164187 ) ;
#179365 = CARTESIAN_POINT ( 'NONE',  ( -18.67979575497178146, -10.72451020669898902, 66.66557627198102409 ) ) ;
#179366 = VERTEX_POINT ( 'NONE', #74170 ) ;
#179367 = CARTESIAN_POINT ( 'NONE',  ( 0.05219959533937995610, -21.53943276465977519, 95.00109039468568994 ) ) ;
#179370 = CARTESIAN_POINT ( 'NONE',  ( 16.55341960407611168, 4.379528057220329451, 88.95724293864769550 ) ) ;
#179369 = CARTESIAN_POINT ( 'NONE',  ( 8.224510206698742110, 14.34966873604972548, 102.0844237280190185 ) ) ;
#179368 = DIRECTION ( 'NONE',  ( -0.000000000000000000, -0.000000000000000000, 1.000000000000000000 ) ) ;
#179371 = CARTESIAN_POINT ( 'NONE',  ( -16.46253265017146816, -9.564922557961047289, 89.16775706135234714 ) ) ;
#179372 = VERTEX_POINT ( 'NONE', #71170 ) ;
#179373 = CARTESIAN_POINT ( 'NONE',  ( 5.049401038297881783, 19.05341960407617563, 37.29275706135232582 ) ) ;
#179374 = CARTESIAN_POINT ( 'NONE',  ( 8.224510206698742110, 14.34966873604972548, 97.08442372801904696 ) ) ;
#179375 = CARTESIAN_POINT ( 'NONE',  ( -0.05219959533936034679, 19.03943276465977164, 27.50109039468566507 ) ) ;
#179376 = CARTESIAN_POINT ( 'NONE',  ( 5.049401038298161559, -19.05341960407611168, 87.70724293864769550 ) ) ;
#179377 = CARTESIAN_POINT ( 'NONE',  ( 10.81492255796078972, 18.62759615963270932, 64.58224293864769550 ) ) ;
#179378 = CARTESIAN_POINT ( 'NONE',  ( 3.889087296526328785, 29.99999999999996092, 1.818019484660534424 ) ) ;
#179379 = CARTESIAN_POINT ( 'NONE',  ( -16.53943276465976808, 0.05219959533911058130, 116.2489096053143669 ) ) ;
#179380 = CARTESIAN_POINT ( 'NONE',  ( -5.719274019375665041, -21.55341960407619695, 89.79275706135236135 ) ) ;
#179381 = CARTESIAN_POINT ( 'NONE',  ( 4.379528057220092307, 16.55341960407617563, 82.29275706135234714 ) ) ;
#179382 = CARTESIAN_POINT ( 'NONE',  ( -15.80617190586768217, 15.72974639402176855, 28.12609039468568284 ) ) ;
#179383 = CARTESIAN_POINT ( 'NONE',  ( 12.14591786802327356, -12.06949235617739191, 25.62609039468567929 ) ) ;
#179384 = CARTESIAN_POINT ( 'NONE',  ( -13.89961937509977652, 13.97604488694528158, 105.6239096053143527 ) ) ;
#179385 = CARTESIAN_POINT ( 'NONE',  ( -19.02544592524342804, 5.153800228976336051, 46.04057627198101699 ) ) ;
#179386 = CARTESIAN_POINT ( 'NONE',  ( -13.89961937509977652, 13.97604488694528158, 50.62390960531435979 ) ) ;
#179387 = CARTESIAN_POINT ( 'NONE',  ( -8.314922557961024197, 14.29746914071037800, 32.91775706135234714 ) ) ;
#179388 = CARTESIAN_POINT ( 'NONE',  ( 8.224510206698953496, -14.34966873604960469, 97.91557627198103830 ) ) ;
#179389 = CARTESIAN_POINT ( 'NONE',  ( 4.483927247898790824, -16.52544592524335698, 100.2094237280190043 ) ) ;
#179392 = CARTESIAN_POINT ( 'NONE',  ( -13.97604488694527625, -13.89961937509977652, 61.87390960531435979 ) ) ;
#179391 = CARTESIAN_POINT ( 'NONE',  ( 13.97604488694527802, 13.89961937509977652, 84.37390960531433848 ) ) ;
#179390 = CARTESIAN_POINT ( 'NONE',  ( -0.05219959533937732626, 21.53943276465977519, 37.50109039468568284 ) ) ;
#179393 = CARTESIAN_POINT ( 'NONE',  ( 13.97604488694527802, 13.89961937509977652, 84.37390960531433848 ) ) ;
#179394 = CARTESIAN_POINT ( 'NONE',  ( 4.379528057220339221, -16.55341960407611168, 27.70724293864769905 ) ) ;
#179395 = CARTESIAN_POINT ( 'NONE',  ( 12.06949235617739724, 12.14591786802326823, 101.8760903946857042 ) ) ;
#179396 = EDGE_LOOP ( 'NONE', ( #58510, #79131 ) ) ;
#179397 = CARTESIAN_POINT ( 'NONE',  ( -9.564922557961040184, 16.46253265017147172, 37.91775706135233293 ) ) ;
#179398 = CARTESIAN_POINT ( 'NONE',  ( -13.97604488694527625, -13.89961937509977652, 46.87390960531435979 ) ) ;
#179399 = CARTESIAN_POINT ( 'NONE',  ( 9.564922557961047289, -16.46253265017146816, 35.41775706135233293 ) ) ;
#179400 = CARTESIAN_POINT ( 'NONE',  ( -22.81625015709510507, 31.40387420917330275, -8.924999997268814766 ) ) ;
#179401 = CARTESIAN_POINT ( 'NONE',  ( -16.52544592524335698, -4.483927247898792601, 38.95942372801901854 ) ) ;
#179403 = CARTESIAN_POINT ( 'NONE',  ( -8.224510206698735004, -14.34966873604973081, 54.58442372801901143 ) ) ;
#179402 = CARTESIAN_POINT ( 'NONE',  ( -13.97604488694547697, 13.89961937509957934, 68.12609039468563310 ) ) ;
#179404 = CARTESIAN_POINT ( 'NONE',  ( 19.02544592524343514, -5.153800228976328945, 113.5405762719810241 ) ) ;
#179405 = CARTESIAN_POINT ( 'NONE',  ( -5.153800228976328057, -19.02544592524343514, 87.29057627198103830 ) ) ;
#179406 = CARTESIAN_POINT ( 'NONE',  ( 21.55341960407619695, -5.719274019375665929, 21.04275706135234714 ) ) ;
#179407 = CARTESIAN_POINT ( 'NONE',  ( -9.564922557961040184, 16.46253265017147172, 82.91775706135233293 ) ) ;
#179409 = CARTESIAN_POINT ( 'NONE',  ( 13.89961937509977652, -13.97604488694527269, 33.12390960531434558 ) ) ;
#179408 = CARTESIAN_POINT ( 'NONE',  ( 16.51473224551069308, 9.474510206698969483, 99.16557627198102409 ) ) ;
#179410 = CARTESIAN_POINT ( 'NONE',  ( 9.474510206698971260, -16.51473224551069308, 77.91557627198103830 ) ) ;
#179412 = CARTESIAN_POINT ( 'NONE',  ( -5.153800228976328057, -19.02544592524343514, 32.29057627198102409 ) ) ;
#179411 = CARTESIAN_POINT ( 'NONE',  ( -4.379528057220328563, 16.55341960407611168, 30.20724293864769550 ) ) ;
#179413 = CARTESIAN_POINT ( 'NONE',  ( 19.05341960407617918, -5.049401038297876454, 51.04275706135231871 ) ) ;
#179414 = CARTESIAN_POINT ( 'NONE',  ( -14.34966873604960291, -8.224510206698953496, 81.66557627198103830 ) ) ;
#179415 = CARTESIAN_POINT ( 'NONE',  ( -21.53943276465977519, -0.05219959533937600094, 108.7510903946857042 ) ) ;
#179416 = CARTESIAN_POINT ( 'NONE',  ( 16.46253265017160672, -9.564922557960803928, 53.33224293864768839 ) ) ;
#179417 = CARTESIAN_POINT ( 'NONE',  ( -10.72451020669898014, 18.67979575497178502, 45.41557627198103830 ) ) ;
#179419 = CARTESIAN_POINT ( 'NONE',  ( -21.53943276465977519, -0.05219959533937600094, 108.7510903946857042 ) ) ;
#179418 = CARTESIAN_POINT ( 'NONE',  ( 12.14591786802309770, 12.06949235617756955, 54.37390960531435979 ) ) ;
#179420 = CARTESIAN_POINT ( 'NONE',  ( -19.02544592524342804, 5.153800228976336051, 96.04057627198103830 ) ) ;
#179421 = CARTESIAN_POINT ( 'NONE',  ( -5.153800228976328057, -19.02544592524343514, 112.2905762719810099 ) ) ;
#179422 = CARTESIAN_POINT ( 'NONE',  ( 13.89961937509977652, -13.97604488694527269, 33.12390960531434558 ) ) ;
#179423 = CARTESIAN_POINT ( 'NONE',  ( 19.03943276465977164, -0.05219959533909143690, 28.74890960531435624 ) ) ;
#179424 = CARTESIAN_POINT ( 'NONE',  ( -16.52544592524342804, 4.483927247898546575, 86.04057627198102409 ) ) ;
#179425 = CARTESIAN_POINT ( 'NONE',  ( -18.62759615963270932, 10.81492255796079327, 90.83224293864769550 ) ) ;
#179426 = CARTESIAN_POINT ( 'NONE',  ( 9.474510206698971260, -16.51473224551069308, 102.9155762719810241 ) ) ;
#179427 = CARTESIAN_POINT ( 'NONE',  ( 15.72974639402199770, -15.80617190586745480, 108.1239096053143811 ) ) ;
#179428 = CARTESIAN_POINT ( 'NONE',  ( 9.474510206698971260, -16.51473224551069308, 92.91557627198103830 ) ) ;
#179430 = CARTESIAN_POINT ( 'NONE',  ( 12.06949235617757843, -12.14591786802309237, 108.1239096053143811 ) ) ;
#179429 = DIRECTION ( 'NONE',  ( -1.000000000000000000, -0.000000000000000000, -0.000000000000000000 ) ) ;
#179431 = CARTESIAN_POINT ( 'NONE',  ( -16.46253265017160317, 9.564922557960807481, 75.83224293864769550 ) ) ;
#179432 = CARTESIAN_POINT ( 'NONE',  ( 18.67979575497178502, 10.72451020669898547, 74.16557627198102409 ) ) ;
#179433 = DIRECTION ( 'NONE',  ( -0.3041824702427711746, 0.9526137857479314297, 1.533086186985162281E-15 ) ) ;
#179434 = DIRECTION ( 'NONE',  ( 0.000000000000000000, 0.000000000000000000, -1.000000000000000000 ) ) ;
#179436 = LINE ( 'NONE', #93342, #146893 ) ;
#179435 = CARTESIAN_POINT ( 'NONE',  ( 5.719274019375991003, -21.55341960407610458, 27.70724293864769905 ) ) ;
#179437 = CARTESIAN_POINT ( 'NONE',  ( 4.483927247898790824, -16.52544592524335698, 35.20942372801901854 ) ) ;
#179438 = CARTESIAN_POINT ( 'NONE',  ( -16.52544592524342804, 4.483927247898546575, 101.0405762719810383 ) ) ;
#179439 = CARTESIAN_POINT ( 'NONE',  ( 19.48894818550245489, -5.499999999999918288, 52.60307310435240424 ) ) ;
#179440 = CARTESIAN_POINT ( 'NONE',  ( 9.474510206698971260, -16.51473224551069308, 92.91557627198103830 ) ) ;
#179441 = CARTESIAN_POINT ( 'NONE',  ( 5.049401038298161559, -19.05341960407611168, 47.70724293864770260 ) ) ;
#179442 = CARTESIAN_POINT ( 'NONE',  ( 4.483927247898545687, 16.52544592524342804, 74.79057627198105251 ) ) ;
#179443 = CARTESIAN_POINT ( 'NONE',  ( -5.823673210054116645, -21.52544592524344225, 27.29057627198103120 ) ) ;
#179444 = CARTESIAN_POINT ( 'NONE',  ( 8.224510206698953496, -14.34966873604960469, 52.91557627198103830 ) ) ;
#179445 = CARTESIAN_POINT ( 'NONE',  ( 19.02544592524334988, 5.153800228976608722, 106.4594237280190185 ) ) ;
#179446 = CARTESIAN_POINT ( 'NONE',  ( -21.52544592524334988, -5.823673210054445271, 68.95942372801901854 ) ) ;
#179447 = CARTESIAN_POINT ( 'NONE',  ( -27.73933785331498925, 2.428612866367529932E-14, 144.8750000027311842 ) ) ;
#179448 = CARTESIAN_POINT ( 'NONE',  ( -16.51473224551069308, -9.474510206698971260, 111.6655762719810383 ) ) ;
#179449 = CARTESIAN_POINT ( 'NONE',  ( 16.52544592524335698, 4.483927247898782831, 81.45942372801900433 ) ) ;
#179450 = CARTESIAN_POINT ( 'NONE',  ( 9.474510206698971260, -16.51473224551069308, 27.91557627198103120 ) ) ;
#179451 = CARTESIAN_POINT ( 'NONE',  ( 19.02544592524343514, -5.153800228976328945, 73.54057627198103830 ) ) ;
#179452 = CARTESIAN_POINT ( 'NONE',  ( 21.55341960407610458, 5.719274019375980345, 78.95724293864769550 ) ) ;
#179453 = CARTESIAN_POINT ( 'NONE',  ( -8.224510206698735004, -14.34966873604973081, 29.58442372801901854 ) ) ;
#179455 = CARTESIAN_POINT ( 'NONE',  ( -18.67979575497193778, 10.72451020669871902, 73.33442372801901854 ) ) ;
#179454 = CARTESIAN_POINT ( 'NONE',  ( 4.379528057220339221, -16.55341960407611168, 57.70724293864770260 ) ) ;
#179456 = ADVANCED_FACE ( 'NONE', ( #151990 ), #19573, .T. ) ;
#179458 = CARTESIAN_POINT ( 'NONE',  ( -10.72451020669898014, 18.67979575497178502, 30.41557627198101699 ) ) ;
#179457 = CARTESIAN_POINT ( 'NONE',  ( -12.14591786802326823, 12.06949235617739902, 93.12609039468568994 ) ) ;
#179459 = CARTESIAN_POINT ( 'NONE',  ( 9.564922557960805705, 16.46253265017160317, 114.5822429386476955 ) ) ;
#179460 = DIRECTION ( 'NONE',  ( 0.000000000000000000, 0.000000000000000000, 1.000000000000000000 ) ) ;
#179461 = CARTESIAN_POINT ( 'NONE',  ( -0.05219959533934338120, 16.53943276465976808, 102.5010903946856899 ) ) ;
#179462 = CARTESIAN_POINT ( 'NONE',  ( -4.379528057220086978, -16.55341960407618274, 64.79275706135234714 ) ) ;
#179464 = ORIENTED_EDGE ( 'NONE', *, *, #39318, .T. ) ;
#179463 = CARTESIAN_POINT ( 'NONE',  ( 13.89961937509977652, -13.97604488694527269, 73.12390960531436690 ) ) ;
#179465 = CARTESIAN_POINT ( 'NONE',  ( 9.564922557960805705, 16.46253265017160317, 89.58224293864769550 ) ) ;
#179466 = CARTESIAN_POINT ( 'NONE',  ( 15.72974639402176855, 15.80617190586768217, 71.87609039468568994 ) ) ;
#179467 = CARTESIAN_POINT ( 'NONE',  ( 12.14591786802327356, -12.06949235617739191, 75.62609039468567573 ) ) ;
#179468 = CARTESIAN_POINT ( 'NONE',  ( -14.29746914071049879, 8.314922557960819915, 40.83224293864769550 ) ) ;
#179469 = CARTESIAN_POINT ( 'NONE',  ( -16.46253265017160317, 9.564922557960807481, 55.83224293864769550 ) ) ;
#179470 = CARTESIAN_POINT ( 'NONE',  ( 16.46253265017160672, -9.564922557960803928, 43.33224293864769550 ) ) ;
#179471 = VERTEX_POINT ( 'NONE', #99246 ) ;
#179472 = CARTESIAN_POINT ( 'NONE',  ( 19.05341960407617918, -5.049401038297876454, 101.0427570613523045 ) ) ;
#179473 = CARTESIAN_POINT ( 'NONE',  ( -8.224510206698948167, 14.34966873604960824, 110.4155762719810383 ) ) ;
#179474 = CARTESIAN_POINT ( 'NONE',  ( -0.05219959533909027116, -19.03943276465977164, 62.49890960531435979 ) ) ;
#179476 = CARTESIAN_POINT ( 'NONE',  ( 38.00000000000000000, 12.34694845685046616, -4.900000000000000355 ) ) ;
#179475 = CARTESIAN_POINT ( 'NONE',  ( -13.97604488694547697, 13.89961937509957934, 103.1260903946856473 ) ) ;
#179477 = CARTESIAN_POINT ( 'NONE',  ( 5.719274019375673035, 21.55341960407619339, 97.29275706135234714 ) ) ;
#179478 = CARTESIAN_POINT ( 'NONE',  ( -12.14591786802326823, 12.06949235617739902, 63.12609039468568994 ) ) ;
#179479 = CARTESIAN_POINT ( 'NONE',  ( 0.05219959533936267826, -19.03943276465977164, 90.00109039468567573 ) ) ;
#179480 = CARTESIAN_POINT ( 'NONE',  ( -18.67979575497178146, -10.72451020669898902, 56.66557627198103830 ) ) ;
#179481 = CARTESIAN_POINT ( 'NONE',  ( -14.29746914071037622, -8.314922557961029526, 59.16775706135234714 ) ) ;
#179482 = DIRECTION ( 'NONE',  ( -1.000000000000000000, -0.000000000000000000, -0.000000000000000000 ) ) ;
#179483 = CARTESIAN_POINT ( 'NONE',  ( -9.474510206698720793, -16.51473224551083518, 59.58442372801900433 ) ) ;
#179484 = AXIS2_PLACEMENT_3D ( 'NONE', #121743, #58110, #59082 ) ;
#179485 = CARTESIAN_POINT ( 'NONE',  ( -5.719274019375665041, -21.55341960407619695, 94.79275706135234714 ) ) ;
#179486 = CARTESIAN_POINT ( 'NONE',  ( 19.05341960407611168, 5.049401038298154454, 23.95724293864769194 ) ) ;
#179487 = CARTESIAN_POINT ( 'NONE',  ( 13.97604488694527802, 13.89961937509977652, 64.37390960531436690 ) ) ;
#179488 = CARTESIAN_POINT ( 'NONE',  ( 16.52544592524342804, -4.483927247898539470, 63.54057627198103830 ) ) ;
#179489 = CARTESIAN_POINT ( 'NONE',  ( -15.80617190586768217, 15.72974639402176855, 88.12609039468570415 ) ) ;
#179490 = CARTESIAN_POINT ( 'NONE',  ( -19.02544592524334988, -5.153800228976617603, 48.95942372801900433 ) ) ;
#179491 = CARTESIAN_POINT ( 'NONE',  ( 9.564922557961047289, -16.46253265017146816, 25.41775706135234003 ) ) ;
#179492 = CARTESIAN_POINT ( 'NONE',  ( 5.153800228976335163, 19.02544592524342804, 114.7905762719810241 ) ) ;
#179493 = CARTESIAN_POINT ( 'NONE',  ( -5.823673210054431948, 21.52544592524334988, 102.7094237280190185 ) ) ;
#179494 = CARTESIAN_POINT ( 'NONE',  ( 5.049401038298161559, -19.05341960407611168, 72.70724293864768129 ) ) ;
#179495 = CARTESIAN_POINT ( 'NONE',  ( -18.62759615963255300, -10.81492255796106328, 89.16775706135236135 ) ) ;
#179496 = CARTESIAN_POINT ( 'NONE',  ( 0.05219959533907565091, 21.53943276465977519, 54.99890960531435269 ) ) ;
#179497 = CARTESIAN_POINT ( 'NONE',  ( -9.564922557960796823, -16.46253265017161027, 87.08224293864769550 ) ) ;
#179498 = CARTESIAN_POINT ( 'NONE',  ( 13.89961937509957401, 13.97604488694547697, 66.87609039468567573 ) ) ;
#179499 = CARTESIAN_POINT ( 'NONE',  ( -13.97604488694527625, -13.89961937509977652, 36.87390960531436690 ) ) ;
#179500 = CARTESIAN_POINT ( 'NONE',  ( -13.97604488694527625, -13.89961937509977652, 91.87390960531432427 ) ) ;
#179501 = CARTESIAN_POINT ( 'NONE',  ( -16.46253265017146816, -9.564922557961047289, 84.16775706135233293 ) ) ;
#179502 = CARTESIAN_POINT ( 'NONE',  ( 16.55341960407618274, -4.379528057220086978, 46.04275706135234714 ) ) ;
#179503 = CARTESIAN_POINT ( 'NONE',  ( 4.379528057220339221, -16.55341960407611168, 102.7072429386476955 ) ) ;
#179504 = CARTESIAN_POINT ( 'NONE',  ( -13.89961937509977652, 13.97604488694528158, 75.62390960531438111 ) ) ;
#179505 = CARTESIAN_POINT ( 'NONE',  ( 5.719274019375991003, -21.55341960407610458, 52.70724293864769550 ) ) ;
#179506 = CARTESIAN_POINT ( 'NONE',  ( 16.52544592524335698, 4.483927247898782831, 21.45942372801901499 ) ) ;
#179507 = CARTESIAN_POINT ( 'NONE',  ( -18.62759615963270932, 10.81492255796079327, 115.8322429386477097 ) ) ;
#179508 = CARTESIAN_POINT ( 'NONE',  ( 21.53943276465977519, 0.05219959533937863772, 86.25109039468568994 ) ) ;
#179509 = CARTESIAN_POINT ( 'NONE',  ( -12.14591786802326823, 12.06949235617739902, 83.12609039468568994 ) ) ;
#179510 = CARTESIAN_POINT ( 'NONE',  ( -13.89961937509977652, 13.97604488694528158, 75.62390960531438111 ) ) ;
#179511 = CARTESIAN_POINT ( 'NONE',  ( 16.53943276465976808, 0.05219959533934440121, 96.25109039468568994 ) ) ;
#179512 = CARTESIAN_POINT ( 'NONE',  ( 13.97604488694548053, -13.89961937509957401, 55.62609039468566863 ) ) ;
#179513 = CARTESIAN_POINT ( 'NONE',  ( -10.72451020669870658, -18.67979575497194134, 34.58442372801900433 ) ) ;
#179514 = CARTESIAN_POINT ( 'NONE',  ( -14.29746914071049879, 8.314922557960819915, 80.83224293864769550 ) ) ;
#179515 = CARTESIAN_POINT ( 'NONE',  ( 13.97604488694527802, 13.89961937509977652, 104.3739096053143385 ) ) ;
#179516 = CARTESIAN_POINT ( 'NONE',  ( 14.34966873604972726, -8.224510206698740333, 90.83442372801901854 ) ) ;
#179517 = CARTESIAN_POINT ( 'NONE',  ( 10.81492255796106328, -18.62759615963255655, 75.41775706135233293 ) ) ;
#179518 = CARTESIAN_POINT ( 'NONE',  ( 16.53943276465976808, 0.05219959533934440121, 31.25109039468568639 ) ) ;
#179519 = CARTESIAN_POINT ( 'NONE',  ( -10.81492255796105439, 18.62759615963255655, 27.91775706135234358 ) ) ;
#179520 = CARTESIAN_POINT ( 'NONE',  ( -0.05219959533910754901, -16.53943276465976808, 67.49890960531436690 ) ) ;
#179521 = ORIENTED_EDGE ( 'NONE', *, *, #69397, .T. ) ;
#179522 = CARTESIAN_POINT ( 'NONE',  ( 0.05219959533907565091, 21.53943276465977519, 104.9989096053143669 ) ) ;
#179523 = CARTESIAN_POINT ( 'NONE',  ( 4.379528057220339221, -16.55341960407611168, 57.70724293864770260 ) ) ;
#179524 = ORIENTED_EDGE ( 'NONE', *, *, #125471, .F. ) ;
#179525 = CARTESIAN_POINT ( 'NONE',  ( 13.89961937509977652, -13.97604488694527269, 28.12390960531435624 ) ) ;
#179526 = CARTESIAN_POINT ( 'NONE',  ( 5.823673210054125526, 21.52544592524343514, 24.79057627198103120 ) ) ;
#179527 = CARTESIAN_POINT ( 'NONE',  ( 5.823673210054444382, -21.52544592524334988, 55.20942372801902565 ) ) ;
#179528 = CARTESIAN_POINT ( 'NONE',  ( 16.55341960407611168, 4.379528057220329451, 58.95724293864770971 ) ) ;
#179529 = CARTESIAN_POINT ( 'NONE',  ( -21.53943276465977519, 0.05219959533907696930, 71.24890960531435269 ) ) ;
#179530 = CARTESIAN_POINT ( 'NONE',  ( -19.02544592524342804, 5.153800228976336051, 71.04057627198099567 ) ) ;
#179532 = CARTESIAN_POINT ( 'NONE',  ( 9.474510206698729675, 16.51473224551082808, 82.08442372801899012 ) ) ;
#179531 = CARTESIAN_POINT ( 'NONE',  ( -0.05219959533909027116, -19.03943276465977164, 27.49890960531435624 ) ) ;
#179533 = EDGE_CURVE ( 'NONE', #22834, #198657, #102625, .T. ) ;
#179534 = CARTESIAN_POINT ( 'NONE',  ( -10.72451020669898014, 18.67979575497178502, 55.41557627198102409 ) ) ;
#179535 = CARTESIAN_POINT ( 'NONE',  ( -13.97604488694527625, -13.89961937509977652, 41.87390960531435979 ) ) ;
#179536 = CARTESIAN_POINT ( 'NONE',  ( -16.46253265017160317, 9.564922557960807481, 65.83224293864769550 ) ) ;
#179537 = ORIENTED_EDGE ( 'NONE', *, *, #158923, .F. ) ;
#179538 = CARTESIAN_POINT ( 'NONE',  ( 16.52544592524335698, 4.483927247898782831, 51.45942372801901854 ) ) ;
#179539 = CARTESIAN_POINT ( 'NONE',  ( 10.72451020669871369, 18.67979575497193778, 27.08442372801901854 ) ) ;
#179540 = CARTESIAN_POINT ( 'NONE',  ( 10.81492255796106328, -18.62759615963255655, 65.41775706135234714 ) ) ;
#179541 = CARTESIAN_POINT ( 'NONE',  ( 19.02544592524343514, -5.153800228976328945, 98.54057627198100988 ) ) ;
#179542 = CARTESIAN_POINT ( 'NONE',  ( -21.55341960407610458, -5.719274019375992779, 81.45724293864769550 ) ) ;
#179544 = CARTESIAN_POINT ( 'NONE',  ( 16.55341960407618274, -4.379528057220086978, 56.04275706135235424 ) ) ;
#179543 = CARTESIAN_POINT ( 'NONE',  ( -21.53943276465977519, -0.05219959533937600094, 23.75109039468567929 ) ) ;
#179545 = CARTESIAN_POINT ( 'NONE',  ( 15.80617190586746368, 15.72974639402197994, 54.37390960531435979 ) ) ;
#179546 = CARTESIAN_POINT ( 'NONE',  ( -13.89961937509957401, -13.97604488694547875, 24.37609039468565442 ) ) ;
#179547 = CARTESIAN_POINT ( 'NONE',  ( -19.02544592524342804, 5.153800228976336051, 56.04057627198100988 ) ) ;
#179548 = CARTESIAN_POINT ( 'NONE',  ( 0.05219959533909260263, 19.03943276465977164, 109.9989096053143669 ) ) ;
#179549 = CARTESIAN_POINT ( 'NONE',  ( 16.46253265017160672, -9.564922557960803928, 93.33224293864769550 ) ) ;
#179550 = CARTESIAN_POINT ( 'NONE',  ( -4.158454644149600199, -48.51789971941261825, -23.00000000000039435 ) ) ;
#179551 = CARTESIAN_POINT ( 'NONE',  ( 13.89961937509957401, 13.97604488694547697, 66.87609039468567573 ) ) ;
#179552 = CARTESIAN_POINT ( 'NONE',  ( 10.72451020669898902, -18.67979575497178502, 42.91557627198103120 ) ) ;
#179553 = CARTESIAN_POINT ( 'NONE',  ( 14.34966873604960469, 8.224510206698951720, 24.16557627198103120 ) ) ;
#179554 = CARTESIAN_POINT ( 'NONE',  ( 9.474510206698729675, 16.51473224551082808, 82.08442372801899012 ) ) ;
#179555 = CARTESIAN_POINT ( 'NONE',  ( -17.50000000000001776, 5.622605283950873556, 58.68792689403890250 ) ) ;
#179556 = CARTESIAN_POINT ( 'NONE',  ( -19.03943276465977164, -0.05219959533935918106, 23.75109039468566152 ) ) ;
#179557 = CARTESIAN_POINT ( 'NONE',  ( 5.153800228976615827, -19.02544592524334988, 80.20942372801901854 ) ) ;
#179558 = CARTESIAN_POINT ( 'NONE',  ( -13.89961937509957401, -13.97604488694547875, 44.37609039468566863 ) ) ;
#179559 = CARTESIAN_POINT ( 'NONE',  ( -15.49999999999999822, 5.499999999999998224, 120.0000000000000142 ) ) ;
#179560 = CARTESIAN_POINT ( 'NONE',  ( -0.05219959533909027116, -19.03943276465977164, 52.49890960531436690 ) ) ;
#179561 = CARTESIAN_POINT ( 'NONE',  ( 0.05219959533910956823, 16.53943276465976808, 44.99890960531435979 ) ) ;
#179562 = CARTESIAN_POINT ( 'NONE',  ( 0.05219959533909260263, 19.03943276465977164, 39.99890960531436690 ) ) ;
#179563 = CARTESIAN_POINT ( 'NONE',  ( 16.55341960407611168, 4.379528057220329451, 43.95724293864769550 ) ) ;
#179564 = CARTESIAN_POINT ( 'NONE',  ( 17.60769864724391098, -5.499999999999977796, 56.15024842019168005 ) ) ;
#179565 = CARTESIAN_POINT ( 'NONE',  ( 12.14591786802327356, -12.06949235617739191, 110.6260903946857042 ) ) ;
#179566 = CARTESIAN_POINT ( 'NONE',  ( 19.03943276465977164, -0.05219959533909143690, 43.74890960531435979 ) ) ;
#179567 = CARTESIAN_POINT ( 'NONE',  ( 16.51473224551083163, -9.474510206698727899, 25.83442372801900078 ) ) ;
#179568 = CARTESIAN_POINT ( 'NONE',  ( 16.53943276465976808, 0.05219959533934440121, 31.25109039468568639 ) ) ;
#179569 = CARTESIAN_POINT ( 'NONE',  ( 21.55341960407610458, 5.719274019375980345, 33.95724293864769550 ) ) ;
#179571 = ORIENTED_EDGE ( 'NONE', *, *, #109656, .T. ) ;
#179570 = CARTESIAN_POINT ( 'NONE',  ( -15.72974639402176322, -15.80617190586768395, 89.37609039468568994 ) ) ;
#179572 = CARTESIAN_POINT ( 'NONE',  ( -5.153800228976328057, -19.02544592524343514, 62.29057627198100988 ) ) ;
#179573 = CARTESIAN_POINT ( 'NONE',  ( -5.153800228976328057, -19.02544592524343514, 112.2905762719810099 ) ) ;
#179574 = CARTESIAN_POINT ( 'NONE',  ( -13.89961937509977652, 13.97604488694528158, 100.6239096053143669 ) ) ;
#179575 = CARTESIAN_POINT ( 'NONE',  ( -33.78191506369886810, -21.41920200728862511, -24.99999999999999289 ) ) ;
#179576 = CARTESIAN_POINT ( 'NONE',  ( 10.72451020669871369, 18.67979575497193778, 27.08442372801901854 ) ) ;
#179577 = CARTESIAN_POINT ( 'NONE',  ( 4.483927247898545687, 16.52544592524342804, 74.79057627198105251 ) ) ;
#179579 = CARTESIAN_POINT ( 'NONE',  ( 9.474510206698971260, -16.51473224551069308, 72.91557627198102409 ) ) ;
#179578 = CARTESIAN_POINT ( 'NONE',  ( 21.52544592524344225, -5.823673210054117533, 78.54057627198103830 ) ) ;
#179580 = CARTESIAN_POINT ( 'NONE',  ( 9.474510206698971260, -16.51473224551069308, 72.91557627198102409 ) ) ;
#179581 = CARTESIAN_POINT ( 'NONE',  ( -5.719274019375978568, 21.55341960407610458, 105.2072429386477097 ) ) ;
#179582 = EDGE_LOOP ( 'NONE', ( #197710, #300, #147692, #179659 ) ) ;
#179583 = CARTESIAN_POINT ( 'NONE',  ( -16.46253265017160317, 9.564922557960807481, 75.83224293864769550 ) ) ;
#179585 = CARTESIAN_POINT ( 'NONE',  ( -16.51473224551069308, -9.474510206698971260, 26.66557627198103120 ) ) ;
#179584 = CARTESIAN_POINT ( 'NONE',  ( -12.06949235617756955, 12.14591786802309770, 100.6239096053143811 ) ) ;
#179586 = CARTESIAN_POINT ( 'NONE',  ( -13.97604488694527625, -13.89961937509977652, 66.87390960531436690 ) ) ;
#179587 = CARTESIAN_POINT ( 'NONE',  ( -5.049401038297874678, -19.05341960407617918, 99.79275706135234714 ) ) ;
#179588 = CARTESIAN_POINT ( 'NONE',  ( -4.483927247898539470, -16.52544592524342804, 97.29057627198105251 ) ) ;
#179589 = CARTESIAN_POINT ( 'NONE',  ( 15.80617190586769283, -15.72974639402175789, 60.62609039468567573 ) ) ;
#179591 = CARTESIAN_POINT ( 'NONE',  ( 21.53943276465977519, 0.05219959533937863772, 26.25109039468567573 ) ) ;
#179590 = CARTESIAN_POINT ( 'NONE',  ( -0.05219959533909027116, -19.03943276465977164, 47.49890960531435979 ) ) ;
#179592 = CARTESIAN_POINT ( 'NONE',  ( -4.379528057220328563, 16.55341960407611168, 100.2072429386476955 ) ) ;
#179593 = CARTESIAN_POINT ( 'NONE',  ( -8.906447517083053711, -27.41122689804191026, 142.4000000000000057 ) ) ;
#179594 = CARTESIAN_POINT ( 'NONE',  ( -9.474510206698964154, 16.51473224551069663, 75.41557627198103830 ) ) ;
#179595 = CARTESIAN_POINT ( 'NONE',  ( 17.05587630539788080, 6.762274262135663960, 111.7581969096268892 ) ) ;
#179597 = CARTESIAN_POINT ( 'NONE',  ( 21.55341960407610458, 5.719274019375980345, 28.95724293864769905 ) ) ;
#179596 = CARTESIAN_POINT ( 'NONE',  ( 16.51473224551083163, -9.474510206698727899, 110.8344237280190043 ) ) ;
#179598 = CARTESIAN_POINT ( 'NONE',  ( -0.05219959533937732626, 21.53943276465977519, 52.50109039468567573 ) ) ;
#179599 = CARTESIAN_POINT ( 'NONE',  ( -13.97604488694527625, -13.89961937509977652, 101.8739096053143811 ) ) ;
#179600 = CARTESIAN_POINT ( 'NONE',  ( -9.474510206698720793, -16.51473224551083518, 89.58442372801900433 ) ) ;
#179601 = CARTESIAN_POINT ( 'NONE',  ( 16.51473224551069308, 9.474510206698969483, 69.16557627198102409 ) ) ;
#179602 = CARTESIAN_POINT ( 'NONE',  ( -4.483927247898539470, -16.52544592524342804, 77.29057627198102409 ) ) ;
#179603 = CARTESIAN_POINT ( 'NONE',  ( -0.05219959533909027116, -19.03943276465977164, 102.4989096053143669 ) ) ;
#179604 = CARTESIAN_POINT ( 'NONE',  ( -16.55341960407611168, -4.379528057220339221, 81.45724293864769550 ) ) ;
#179605 = CARTESIAN_POINT ( 'NONE',  ( -13.97604488694527625, -13.89961937509977652, 96.87390960531433848 ) ) ;
#179608 = CARTESIAN_POINT ( 'NONE',  ( 13.97604488694527802, 13.89961937509977652, 29.37390960531435979 ) ) ;
#179607 = CARTESIAN_POINT ( 'NONE',  ( -0.05219959533910754901, -16.53943276465976808, 47.49890960531435979 ) ) ;
#179606 = CARTESIAN_POINT ( 'NONE',  ( -9.474510206698964154, 16.51473224551069663, 50.41557627198102409 ) ) ;
#179609 = EDGE_LOOP ( 'NONE', ( #42934, #12510, #73908, #132776 ) ) ;
#179610 = CARTESIAN_POINT ( 'NONE',  ( -5.823673210054431948, 21.52544592524334988, 42.70942372801901854 ) ) ;
#179611 = CARTESIAN_POINT ( 'NONE',  ( 16.46253265017146816, 9.564922557961045513, 81.66775706135233293 ) ) ;
#179612 = CARTESIAN_POINT ( 'NONE',  ( -12.14591786802309592, -12.06949235617757132, 46.87390960531435979 ) ) ;
#179613 = CARTESIAN_POINT ( 'NONE',  ( -10.81492255796078084, -18.62759615963271287, 97.08224293864770971 ) ) ;
#179614 = CARTESIAN_POINT ( 'NONE',  ( 21.53943276465977519, -0.05219959533907433946, 33.74890960531436690 ) ) ;
#179616 = CARTESIAN_POINT ( 'NONE',  ( -16.55341960407611168, -4.379528057220339221, 81.45724293864769550 ) ) ;
#179615 = AXIS2_PLACEMENT_3D ( 'NONE', #104539, #43861, #61981 ) ;
#179617 = CARTESIAN_POINT ( 'NONE',  ( 13.89961937509977652, -13.97604488694527269, 38.12390960531436690 ) ) ;
#179618 = CARTESIAN_POINT ( 'NONE',  ( -4.483927247898782831, 16.52544592524335698, 112.7094237280190328 ) ) ;
#179619 = CARTESIAN_POINT ( 'NONE',  ( -16.52544592524335698, -4.483927247898792601, 88.95942372801901854 ) ) ;
#179620 = CARTESIAN_POINT ( 'NONE',  ( -8.314922557961024197, 14.29746914071037800, 72.91775706135234714 ) ) ;
#179621 = CARTESIAN_POINT ( 'NONE',  ( 19.05341960407617918, -5.049401038297876454, 21.04275706135232582 ) ) ;
#179622 = CARTESIAN_POINT ( 'NONE',  ( 13.89961937509977652, -13.97604488694527269, 93.12390960531436690 ) ) ;
#179623 = CARTESIAN_POINT ( 'NONE',  ( 9.474510206698971260, -16.51473224551069308, 82.91557627198103830 ) ) ;
#179624 = CARTESIAN_POINT ( 'NONE',  ( 4.379528057220092307, 16.55341960407617563, 92.29275706135236135 ) ) ;
#179625 = CARTESIAN_POINT ( 'NONE',  ( 16.46253265017160672, -9.564922557960803928, 38.33224293864768839 ) ) ;
#179626 = CARTESIAN_POINT ( 'NONE',  ( 0.05219959533910956823, 16.53943276465976808, 44.99890960531435979 ) ) ;
#179628 = CARTESIAN_POINT ( 'NONE',  ( -5.049401038298153566, 19.05341960407611168, 105.2072429386476671 ) ) ;
#179627 = FILL_AREA_STYLE ('',( #87587 ) ) ;
#179629 = CARTESIAN_POINT ( 'NONE',  ( -10.81492255796078084, -18.62759615963271287, 27.08224293864769550 ) ) ;
#179630 = CARTESIAN_POINT ( 'NONE',  ( 16.52544592524342804, -4.483927247898539470, 68.54057627198103830 ) ) ;
#179631 = B_SPLINE_CURVE_WITH_KNOTS ( 'NONE', 3,
 ( #66121, #19629, #94468, #3452, #65129, #126786, #127786, #112623, #50964, #47993, #155160, #188492, #78299, #124819, #35785, #187513, #97432, #62140, #109647, #15660 ),
 .UNSPECIFIED., .F., .F.,
 ( 4, 2, 2, 2, 2, 2, 2, 2, 2, 4 ),
 ( 0.000000000000000000, 0.0004987090165372566565, 0.0009974180330745133129, 0.001246772541343138009, 0.001496127049611762488, 0.001994836066149011881, 0.002493545082686261273, 0.002742899590954883584, 0.002992254099223505895, 0.003989672132298080140 ),
 .UNSPECIFIED. ) ;
#179632 = EDGE_CURVE ( 'NONE', #196966, #41517, #73924, .T. ) ;
#179633 = CARTESIAN_POINT ( 'NONE',  ( -8.314922557960811034, -14.29746914071050412, 67.08224293864770971 ) ) ;
#179634 = DIRECTION ( 'NONE',  ( 0.000000000000000000, 0.000000000000000000, -1.000000000000000000 ) ) ;
#179635 = CARTESIAN_POINT ( 'NONE',  ( 16.46253265017146816, 9.564922557961045513, 66.66775706135233293 ) ) ;
#179636 = CARTESIAN_POINT ( 'NONE',  ( -0.05219959533909027116, -19.03943276465977164, 102.4989096053143669 ) ) ;
#179637 = CARTESIAN_POINT ( 'NONE',  ( 19.02544592524334988, 5.153800228976608722, 76.45942372801897591 ) ) ;
#179638 = CARTESIAN_POINT ( 'NONE',  ( -22.44159573604010305, 16.30477369853692338, 147.1750000027311671 ) ) ;
#179640 = CARTESIAN_POINT ( 'NONE',  ( -12.06949235617739369, -12.14591786802326823, 89.37609039468568994 ) ) ;
#179639 = CARTESIAN_POINT ( 'NONE',  ( 14.29746914071037800, 8.314922557961029526, 21.66775706135235069 ) ) ;
#179641 = CARTESIAN_POINT ( 'NONE',  ( -13.89961937509977652, 13.97604488694528158, 40.62390960531435979 ) ) ;
#179642 =( BOUNDED_CURVE ( )  B_SPLINE_CURVE ( 3, ( #148509, #9999, #121139, #10997 ),
 .UNSPECIFIED., .F., .F. ) 
 B_SPLINE_CURVE_WITH_KNOTS ( ( 4, 4 ),
 ( 5.503250352303675541, 7.063120262055496923 ),
 .UNSPECIFIED. ) 
 CURVE ( )  GEOMETRIC_REPRESENTATION_ITEM ( )  RATIONAL_B_SPLINE_CURVE ( ( 1.000000000000000000, 0.8073061876036304874, 0.8073061876036304874, 1.000000000000000000 ) ) 
 REPRESENTATION_ITEM ( '' )  );
#179643 = CARTESIAN_POINT ( 'NONE',  ( -18.62759615963270932, 10.81492255796079327, 35.83224293864768839 ) ) ;
#179644 = CARTESIAN_POINT ( 'NONE',  ( 15.72974639402176855, 15.80617190586768217, 56.87609039468568994 ) ) ;
#179645 = CARTESIAN_POINT ( 'NONE',  ( -5.153800228976607833, 19.02544592524334988, 112.7094237280190043 ) ) ;
#179647 = CARTESIAN_POINT ( 'NONE',  ( -16.51473224551069308, -9.474510206698971260, 71.66557627198102409 ) ) ;
#179646 = DIRECTION ( 'NONE',  ( -9.445700745138859830E-17, 1.000000000000000000, 0.000000000000000000 ) ) ;
#179648 = CARTESIAN_POINT ( 'NONE',  ( 19.05341960407611168, 5.049401038298154454, 113.9572429386477097 ) ) ;
#179650 = CARTESIAN_POINT ( 'NONE',  ( -19.05341960407611168, -5.049401038298163336, 81.45724293864769550 ) ) ;
#179649 = CARTESIAN_POINT ( 'NONE',  ( 16.53943276465976808, -0.05219959533910856209, 73.74890960531433848 ) ) ;
#179651 = CARTESIAN_POINT ( 'NONE',  ( -19.05341960407611168, -5.049401038298163336, 91.45724293864766707 ) ) ;
#179652 = ORIENTED_EDGE ( 'NONE', *, *, #134205, .F. ) ;
#179653 = CARTESIAN_POINT ( 'NONE',  ( -19.05341960407617563, 5.049401038297882671, 93.54275706135234714 ) ) ;
#179654 = CARTESIAN_POINT ( 'NONE',  ( 21.55341960407610458, 5.719274019375980345, 58.95724293864770971 ) ) ;
#179655 = CARTESIAN_POINT ( 'NONE',  ( -9.564922557960796823, -16.46253265017161027, 27.08224293864769550 ) ) ;
#179656 = CARTESIAN_POINT ( 'NONE',  ( -0.05219959533936034679, 19.03943276465977164, 57.50109039468566863 ) ) ;
#179657 = CARTESIAN_POINT ( 'NONE',  ( -0.05219959533909027116, -19.03943276465977164, 62.49890960531435979 ) ) ;
#179658 = CARTESIAN_POINT ( 'NONE',  ( 5.153800228976335163, 19.02544592524342804, 94.79057627198103830 ) ) ;
#179659 = ORIENTED_EDGE ( 'NONE', *, *, #61925, .T. ) ;
#179660 = CARTESIAN_POINT ( 'NONE',  ( -21.52544592524343514, 5.823673210054127303, 96.04057627198102409 ) ) ;
#179662 = CARTESIAN_POINT ( 'NONE',  ( 9.564922557961047289, -16.46253265017146816, 50.41775706135233293 ) ) ;
#179661 = CARTESIAN_POINT ( 'NONE',  ( -14.34966873604960291, -8.224510206698953496, 96.66557627198102409 ) ) ;
#179663 = CARTESIAN_POINT ( 'NONE',  ( 5.719274019375991003, -21.55341960407610458, 92.70724293864770971 ) ) ;
#179664 = CARTESIAN_POINT ( 'NONE',  ( 21.55341960407610458, 5.719274019375980345, 73.95724293864769550 ) ) ;
#179665 = CARTESIAN_POINT ( 'NONE',  ( 12.14591786802309770, 12.06949235617756955, 29.37390960531435269 ) ) ;
#179666 = CARTESIAN_POINT ( 'NONE',  ( -21.52544592524334988, -5.823673210054445271, 108.9594237280190185 ) ) ;
#179667 = CARTESIAN_POINT ( 'NONE',  ( -14.29746914071037622, -8.314922557961029526, 49.16775706135234003 ) ) ;
#179668 = CARTESIAN_POINT ( 'NONE',  ( -13.89961937509977652, 13.97604488694528158, 75.62390960531438111 ) ) ;
#179669 = CARTESIAN_POINT ( 'NONE',  ( 19.05341960407611168, 5.049401038298154454, 33.95724293864769550 ) ) ;
#179670 = CARTESIAN_POINT ( 'NONE',  ( 10.72451020669871369, 18.67979575497193778, 42.08442372801901854 ) ) ;
#179671 = CARTESIAN_POINT ( 'NONE',  ( -10.81492255796105439, 18.62759615963255655, 52.91775706135235424 ) ) ;
#179672 = CARTESIAN_POINT ( 'NONE',  ( -16.51473224551069308, -9.474510206698971260, 41.66557627198103120 ) ) ;
#179673 = CARTESIAN_POINT ( 'NONE',  ( 18.67979575497194134, -10.72451020669871369, 25.83442372801901499 ) ) ;
#179674 = CARTESIAN_POINT ( 'NONE',  ( -13.97604488694547697, 13.89961937509957934, 63.12609039468566152 ) ) ;
#179675 = CARTESIAN_POINT ( 'NONE',  ( 0.05219959533936267826, -19.03943276465977164, 80.00109039468567573 ) ) ;
#179676 = CARTESIAN_POINT ( 'NONE',  ( -4.379528057220086978, -16.55341960407618274, 29.79275706135234358 ) ) ;
#179677 = CARTESIAN_POINT ( 'NONE',  ( 9.564922557960805705, 16.46253265017160317, 24.58224293864769194 ) ) ;
#179678 = CARTESIAN_POINT ( 'NONE',  ( -0.05219959533934338120, 16.53943276465976808, 67.50109039468568994 ) ) ;
#179679 = CARTESIAN_POINT ( 'NONE',  ( 19.02544592524343514, -5.153800228976328945, 38.54057627198103120 ) ) ;
#179680 = CARTESIAN_POINT ( 'NONE',  ( 24.27957997113507815, -6.290849861785656749, 171.5443985711291361 ) ) ;
#179681 = CARTESIAN_POINT ( 'NONE',  ( -13.97604488694527625, -13.89961937509977652, 101.8739096053143811 ) ) ;
#179682 = CARTESIAN_POINT ( 'NONE',  ( -9.474510206698964154, 16.51473224551069663, 30.41557627198102054 ) ) ;
#179683 = CARTESIAN_POINT ( 'NONE',  ( -0.05219959533907301413, -21.53943276465977519, 72.49890960531435269 ) ) ;
#179684 = CARTESIAN_POINT ( 'NONE',  ( -12.14591786802326823, 12.06949235617739902, 63.12609039468568994 ) ) ;
#179685 = CARTESIAN_POINT ( 'NONE',  ( -5.823673210054431948, 21.52544592524334988, 107.7094237280190328 ) ) ;
#179686 = CARTESIAN_POINT ( 'NONE',  ( 5.049401038298161559, -19.05341960407611168, 42.70724293864767418 ) ) ;
#179687 = CARTESIAN_POINT ( 'NONE',  ( 12.14591786802309770, 12.06949235617756955, 34.37390960531435979 ) ) ;
#179688 = CARTESIAN_POINT ( 'NONE',  ( -16.55341960407611168, -4.379528057220339221, 71.45724293864769550 ) ) ;
#179689 = CARTESIAN_POINT ( 'NONE',  ( -0.05219959533909027116, -19.03943276465977164, 67.49890960531436690 ) ) ;
#179690 = CARTESIAN_POINT ( 'NONE',  ( -15.80617190586768217, 15.72974639402176855, 108.1260903946856757 ) ) ;
#179691 = CARTESIAN_POINT ( 'NONE',  ( -10.72451020669870658, -18.67979575497194134, 39.58442372801901143 ) ) ;
#179692 = CARTESIAN_POINT ( 'NONE',  ( -13.89961937509977652, 13.97604488694528158, 75.62390960531438111 ) ) ;
#179693 = CARTESIAN_POINT ( 'NONE',  ( 21.53943276465977519, 0.05219959533937863772, 81.25109039468568994 ) ) ;
#179694 = CARTESIAN_POINT ( 'NONE',  ( -16.52544592524335698, -4.483927247898792601, 63.95942372801901854 ) ) ;
#179695 = CARTESIAN_POINT ( 'NONE',  ( 19.05341960407611168, 5.049401038298154454, 113.9572429386477097 ) ) ;
#179696 = CARTESIAN_POINT ( 'NONE',  ( 14.29746914071049879, -8.314922557960816363, 28.33224293864769550 ) ) ;
#179697 = CARTESIAN_POINT ( 'NONE',  ( 19.05341960407611168, 5.049401038298154454, 23.95724293864769194 ) ) ;
#179698 = CARTESIAN_POINT ( 'NONE',  ( -14.29746914071037622, -8.314922557961029526, 54.16775706135235424 ) ) ;
#179699 = CARTESIAN_POINT ( 'NONE',  ( 16.55341960407611168, 4.379528057220329451, 58.95724293864770971 ) ) ;
#179700 = CARTESIAN_POINT ( 'NONE',  ( 16.51473224551069308, 9.474510206698969483, 109.1655762719810383 ) ) ;
#179701 = CARTESIAN_POINT ( 'NONE',  ( 18.62759615963271287, -10.81492255796078972, 33.33224293864769550 ) ) ;
#179702 = CARTESIAN_POINT ( 'NONE',  ( 10.72451020669871369, 18.67979575497193778, 107.0844237280190043 ) ) ;
#179703 = CARTESIAN_POINT ( 'NONE',  ( -12.06949235617756955, 12.14591786802309770, 90.62390960531436690 ) ) ;
#179704 = CARTESIAN_POINT ( 'NONE',  ( 16.51473224551069308, 9.474510206698969483, 99.16557627198102409 ) ) ;
#179705 = ORIENTED_EDGE ( 'NONE', *, *, #187016, .T. ) ;
#179706 = CARTESIAN_POINT ( 'NONE',  ( -14.29746914071037622, -8.314922557961029526, 54.16775706135235424 ) ) ;
#179707 = CARTESIAN_POINT ( 'NONE',  ( -5.049401038298153566, 19.05341960407611168, 50.20724293864770260 ) ) ;
#179708 = CARTESIAN_POINT ( 'NONE',  ( 24.95432927374997334, -3.806786798636382141, 190.0000000000000000 ) ) ;
#179709 = CARTESIAN_POINT ( 'NONE',  ( 5.049401038297881783, 19.05341960407617563, 42.29275706135234003 ) ) ;
#179710 = EDGE_CURVE ( 'NONE', #9032, #1947, #145754, .T. ) ;
#179711 = CARTESIAN_POINT ( 'NONE',  ( 12.06949235617739724, 12.14591786802326823, 81.87609039468568994 ) ) ;
#179712 = CARTESIAN_POINT ( 'NONE',  ( 19.02544592524334988, 5.153800228976608722, 96.45942372801897591 ) ) ;
#179713 = CARTESIAN_POINT ( 'NONE',  ( 0.05219959533937995610, -21.53943276465977519, 70.00109039468568994 ) ) ;
#179714 = CARTESIAN_POINT ( 'NONE',  ( -19.02544592524342804, 5.153800228976336051, 61.04057627198103120 ) ) ;
#179715 = CARTESIAN_POINT ( 'NONE',  ( 18.62759615963271287, -10.81492255796078972, 88.33224293864769550 ) ) ;
#179716 = CARTESIAN_POINT ( 'NONE',  ( 12.14591786802309770, 12.06949235617756955, 104.3739096053143669 ) ) ;
#179717 = AXIS2_PLACEMENT_3D ( 'NONE', #165039, #181214, #11365 ) ;
#179718 = ADVANCED_FACE ( 'NONE', ( #35591 ), #46743, .T. ) ;
#179719 = CARTESIAN_POINT ( 'NONE',  ( -5.153800228976607833, 19.02544592524334988, 72.70942372801900433 ) ) ;
#179720 = CARTESIAN_POINT ( 'NONE',  ( 18.62759615963271287, -10.81492255796078972, 58.33224293864768839 ) ) ;
#179721 = CARTESIAN_POINT ( 'NONE',  ( -16.51473224551082808, 9.474510206698731452, 38.33442372801899722 ) ) ;
#179722 = CARTESIAN_POINT ( 'NONE',  ( 19.02544592524343514, -5.153800228976328945, 113.5405762719810241 ) ) ;
#179723 = CARTESIAN_POINT ( 'NONE',  ( 15.80617190586746368, 15.72974639402197994, 89.37390960531435269 ) ) ;
#179724 = DIRECTION ( 'NONE',  ( -0.1039620511844979306, 0.1039620511844979306, 0.9891328443778538704 ) ) ;
#179725 = CARTESIAN_POINT ( 'NONE',  ( -3.573655867282028392E-15, 2.428612866367529932E-14, -25.00000000000000000 ) ) ;
#179726 = CARTESIAN_POINT ( 'NONE',  ( -19.02544592524334988, -5.153800228976617603, 108.9594237280189759 ) ) ;
#179727 = CARTESIAN_POINT ( 'NONE',  ( 37.42090987696015247, -2.907880681671514367, 40.32815749938561112 ) ) ;
#179728 = CARTESIAN_POINT ( 'NONE',  ( -16.55341960407617563, 4.379528057220093196, 28.54275706135234358 ) ) ;
#179729 = CARTESIAN_POINT ( 'NONE',  ( 19.05341960407611168, 5.049401038298154454, 48.95724293864768129 ) ) ;
#179730 = CARTESIAN_POINT ( 'NONE',  ( -19.03943276465977164, 0.05219959533909376836, 106.2489096053143669 ) ) ;
#179732 = CARTESIAN_POINT ( 'NONE',  ( -4.483927247898539470, -16.52544592524342804, 52.29057627198102409 ) ) ;
#179731 = CARTESIAN_POINT ( 'NONE',  ( 10.81492255796078972, 18.62759615963270932, 84.58224293864769550 ) ) ;
#179733 = CARTESIAN_POINT ( 'NONE',  ( 18.67979575497194134, -10.72451020669871369, 75.83442372801900433 ) ) ;
#179735 = CARTESIAN_POINT ( 'NONE',  ( -13.97604488694547697, 13.89961937509957934, 28.12609039468565797 ) ) ;
#179734 = CARTESIAN_POINT ( 'NONE',  ( 8.314922557961029526, -14.29746914071037800, 20.41775706135234714 ) ) ;
#179736 = CARTESIAN_POINT ( 'NONE',  ( -16.55341960407611168, -4.379528057220339221, 36.45724293864768839 ) ) ;
#179737 = CARTESIAN_POINT ( 'NONE',  ( -0.05219959533937732626, 21.53943276465977519, 22.50109039468567573 ) ) ;
#179738 = CARTESIAN_POINT ( 'NONE',  ( -14.29746914071049879, 8.314922557960819915, 45.83224293864769550 ) ) ;
#179739 = CARTESIAN_POINT ( 'NONE',  ( -0.05219959533936034679, 19.03943276465977164, 97.50109039468567573 ) ) ;
#179740 = CARTESIAN_POINT ( 'NONE',  ( 16.46253265017146816, 9.564922557961045513, 61.66775706135234003 ) ) ;
#179741 = CARTESIAN_POINT ( 'NONE',  ( 5.719274019375673035, 21.55341960407619339, 77.29275706135234714 ) ) ;
#179742 = CARTESIAN_POINT ( 'NONE',  ( -16.46253265017146816, -9.564922557961047289, 49.16775706135233293 ) ) ;
#179743 = CARTESIAN_POINT ( 'NONE',  ( -16.51473224551069308, -9.474510206698971260, 26.66557627198103120 ) ) ;
#179744 = CARTESIAN_POINT ( 'NONE',  ( -18.67979575497178146, -10.72451020669898902, 46.66557627198102409 ) ) ;
#179745 = CARTESIAN_POINT ( 'NONE',  ( 16.52544592524342804, -4.483927247898539470, 53.54057627198103120 ) ) ;
#179746 = CARTESIAN_POINT ( 'NONE',  ( -4.500000000000001776, -139.5000000000000000, 21.32407087589996308 ) ) ;
#179747 = CARTESIAN_POINT ( 'NONE',  ( -19.02544592524334988, -5.153800228976617603, 18.95942372801899722 ) ) ;
#179748 = CARTESIAN_POINT ( 'NONE',  ( -8.224510206698735004, -14.34966873604973081, 74.58442372801901854 ) ) ;
#179749 = CARTESIAN_POINT ( 'NONE',  ( 14.34966873604960469, 8.224510206698951720, 39.16557627198102409 ) ) ;
#179750 = CARTESIAN_POINT ( 'NONE',  ( -21.52544592524334988, -5.823673210054445271, 78.95942372801901854 ) ) ;
#179751 = CARTESIAN_POINT ( 'NONE',  ( 21.52544592524334988, 5.823673210054432836, 66.45942372801903275 ) ) ;
#179752 = CARTESIAN_POINT ( 'NONE',  ( -21.53943276465977519, 0.05219959533907696930, 76.24890960531435269 ) ) ;
#179753 = CARTESIAN_POINT ( 'NONE',  ( -5.049401038298153566, 19.05341960407611168, 40.20724293864768839 ) ) ;
#179754 = CARTESIAN_POINT ( 'NONE',  ( -5.719274019375665041, -21.55341960407619695, 54.79275706135235424 ) ) ;
#179755 = CARTESIAN_POINT ( 'NONE',  ( 19.03943276465977164, -0.05219959533909143690, 28.74890960531435624 ) ) ;
#179756 = CARTESIAN_POINT ( 'NONE',  ( 16.46253265017160672, -9.564922557960803928, 58.33224293864769550 ) ) ;
#179757 = CARTESIAN_POINT ( 'NONE',  ( -8.224510206698948167, 14.34966873604960824, 90.41557627198103830 ) ) ;
#179758 = CARTESIAN_POINT ( 'NONE',  ( -5.049401038298153566, 19.05341960407611168, 80.20724293864769550 ) ) ;
#179759 = CARTESIAN_POINT ( 'NONE',  ( -16.55341960407611168, -4.379528057220339221, 41.45724293864769550 ) ) ;
#179760 = CARTESIAN_POINT ( 'NONE',  ( 12.14591786802309770, 12.06949235617756955, 99.37390960531436690 ) ) ;
#179761 = CARTESIAN_POINT ( 'NONE',  ( -21.53943276465977519, 0.05219959533907696930, 76.24890960531435269 ) ) ;
#179762 = AXIS2_PLACEMENT_3D ( 'NONE', #3999, #97979, #144505 ) ;
#179763 = CARTESIAN_POINT ( 'NONE',  ( 10.81492255796078972, 18.62759615963270932, 114.5822429386477097 ) ) ;
#179764 = LINE ( 'NONE', #42236, #114970 ) ;
#179766 = CARTESIAN_POINT ( 'NONE',  ( -12.06949235617739369, -12.14591786802326823, 29.37609039468568284 ) ) ;
#179765 = CARTESIAN_POINT ( 'NONE',  ( 13.97604488694527802, 13.89961937509977652, 64.37390960531436690 ) ) ;
#179767 = CARTESIAN_POINT ( 'NONE',  ( -5.719274019375978568, 21.55341960407610458, 70.20724293864769550 ) ) ;
#179768 = CARTESIAN_POINT ( 'NONE',  ( 10.81492255796106328, -18.62759615963255655, 90.41775706135236135 ) ) ;
#179769 = CARTESIAN_POINT ( 'NONE',  ( -19.02544592524342804, 5.153800228976336051, 86.04057627198103830 ) ) ;
#179770 = CARTESIAN_POINT ( 'NONE',  ( 21.52544592524344225, -5.823673210054117533, 113.5405762719810383 ) ) ;
#179771 = CARTESIAN_POINT ( 'NONE',  ( 13.89961937509977652, -13.97604488694527269, 108.1239096053143669 ) ) ;
#179772 = CARTESIAN_POINT ( 'NONE',  ( -16.55341960407617563, 4.379528057220093196, 88.54275706135236135 ) ) ;
#179773 = CARTESIAN_POINT ( 'NONE',  ( -18.67979575497193778, 10.72451020669871902, 68.33442372801900433 ) ) ;
#179774 = CARTESIAN_POINT ( 'NONE',  ( -18.67979575497193778, 10.72451020669871902, 93.33442372801901854 ) ) ;
#179775 = CARTESIAN_POINT ( 'NONE',  ( 16.53943276465976808, 0.05219959533934440121, 56.25109039468568284 ) ) ;
#179776 = CARTESIAN_POINT ( 'NONE',  ( -21.53943276465977519, -0.05219959533937600094, 33.75109039468568284 ) ) ;
#179777 = CARTESIAN_POINT ( 'NONE',  ( 0.05219959533909260263, 19.03943276465977164, 24.99890960531435269 ) ) ;
#179778 = CARTESIAN_POINT ( 'NONE',  ( 21.52544592524334988, 5.823673210054432836, 91.45942372801901854 ) ) ;
#179779 = CARTESIAN_POINT ( 'NONE',  ( -19.05341960407611168, -5.049401038298163336, 96.45724293864769550 ) ) ;
#179780 = CARTESIAN_POINT ( 'NONE',  ( 15.72974639402199770, -15.80617190586745480, 88.12390960531436690 ) ) ;
#179781 = CARTESIAN_POINT ( 'NONE',  ( 19.02544592524334988, 5.153800228976608722, 56.45942372801898301 ) ) ;
#179782 = CARTESIAN_POINT ( 'NONE',  ( -18.67979575497178146, -10.72451020669898902, 56.66557627198103830 ) ) ;
#179784 = CARTESIAN_POINT ( 'NONE',  ( 4.379528057220339221, -16.55341960407611168, 37.70724293864769550 ) ) ;
#179783 = CARTESIAN_POINT ( 'NONE',  ( 5.049401038298161559, -19.05341960407611168, 97.70724293864766707 ) ) ;
#179785 = CARTESIAN_POINT ( 'NONE',  ( 12.14253177836985564, -10.17673712963189381, -61.72896360825912865 ) ) ;
#179786 = CARTESIAN_POINT ( 'NONE',  ( -13.89961937509957401, -13.97604488694547875, 79.37609039468567573 ) ) ;
#179787 = CARTESIAN_POINT ( 'NONE',  ( -19.35543954521082810, -5.499999999999488409, 79.58901960356450900 ) ) ;
#179788 = CARTESIAN_POINT ( 'NONE',  ( -5.049401038297874678, -19.05341960407617918, 109.7927570613523187 ) ) ;
#179789 = CARTESIAN_POINT ( 'NONE',  ( -15.72974639402197994, 15.80617190586746368, 90.62390960531436690 ) ) ;
#179790 = CARTESIAN_POINT ( 'NONE',  ( 0.05219959533910956823, 16.53943276465976808, 59.99890960531436690 ) ) ;
#179791 = CARTESIAN_POINT ( 'NONE',  ( -8.224510206698735004, -14.34966873604973081, 34.58442372801900433 ) ) ;
#179792 = CARTESIAN_POINT ( 'NONE',  ( -13.97604488694527625, -13.89961937509977652, 46.87390960531435979 ) ) ;
#179794 = CARTESIAN_POINT ( 'NONE',  ( -19.05341960407617563, 5.049401038297882671, 78.54275706135233293 ) ) ;
#179793 = CARTESIAN_POINT ( 'NONE',  ( 0.05219959533907565091, 21.53943276465977519, 114.9989096053143669 ) ) ;
#179795 = CARTESIAN_POINT ( 'NONE',  ( 5.049401038298161559, -19.05341960407611168, 97.70724293864766707 ) ) ;
#179796 = CARTESIAN_POINT ( 'NONE',  ( 5.049401038298161559, -19.05341960407611168, 77.70724293864765286 ) ) ;
#179797 = CARTESIAN_POINT ( 'NONE',  ( -5.719274019375978568, 21.55341960407610458, 70.20724293864769550 ) ) ;
#179798 = CARTESIAN_POINT ( 'NONE',  ( 19.05341960407611168, 5.049401038298154454, 43.95724293864769550 ) ) ;
#179799 = CARTESIAN_POINT ( 'NONE',  ( 31.44458473636817075, 19.57661126282215491, -8.000000000000001776 ) ) ;
#179800 = CARTESIAN_POINT ( 'NONE',  ( 16.55341960407611168, 4.379528057220329451, 48.95724293864770971 ) ) ;
#179801 = CARTESIAN_POINT ( 'NONE',  ( -9.564922557960796823, -16.46253265017161027, 107.0822429386476955 ) ) ;
#179802 = CARTESIAN_POINT ( 'NONE',  ( -5.000000000000003553, 37.66961640367474473, -25.00000000000000000 ) ) ;
#179803 = CARTESIAN_POINT ( 'NONE',  ( 5.153800228976615827, -19.02544592524334988, 65.20942372801900433 ) ) ;
#179804 = CARTESIAN_POINT ( 'NONE',  ( 21.55341960407610458, 5.719274019375980345, 73.95724293864769550 ) ) ;
#179805 = CARTESIAN_POINT ( 'NONE',  ( -0.05219959533936034679, 19.03943276465977164, 42.50109039468566152 ) ) ;
#179806 = CARTESIAN_POINT ( 'NONE',  ( 5.049401038298161559, -19.05341960407611168, 107.7072429386476955 ) ) ;
#179807 = CARTESIAN_POINT ( 'NONE',  ( -18.22780087662124160, -5.499999999999927169, 73.98236817873106475 ) ) ;
#179808 = CARTESIAN_POINT ( 'NONE',  ( 10.72451020669898902, -18.67979575497178502, 37.91557627198102409 ) ) ;
#179809 = CARTESIAN_POINT ( 'NONE',  ( -13.97604488694527625, -13.89961937509977652, 66.87390960531436690 ) ) ;
#179810 = CARTESIAN_POINT ( 'NONE',  ( 21.52544592524334988, 5.823673210054432836, 61.45942372801901854 ) ) ;
#179811 = CARTESIAN_POINT ( 'NONE',  ( 8.314922557960818139, 14.29746914071049879, 114.5822429386477097 ) ) ;
#179813 = VERTEX_POINT ( 'NONE', #147683 ) ;
#179812 = CARTESIAN_POINT ( 'NONE',  ( 21.53943276465977519, -0.05219959533907433946, 108.7489096053143669 ) ) ;
#179814 = CARTESIAN_POINT ( 'NONE',  ( -21.53943276465977519, -0.05219959533937600094, 58.75109039468568994 ) ) ;
#179815 = ORIENTED_EDGE ( 'NONE', *, *, #75719, .F. ) ;
#179816 = CARTESIAN_POINT ( 'NONE',  ( -24.13384886353222214, -15.22194871136943206, 140.0000000000000000 ) ) ;
#179817 = CARTESIAN_POINT ( 'NONE',  ( -9.474510206698720793, -16.51473224551083518, 64.58442372801900433 ) ) ;
#179818 = CARTESIAN_POINT ( 'NONE',  ( -20.09035150276022463, 11.70762861043687764, 168.0245124264526453 ) ) ;
#179819 = CARTESIAN_POINT ( 'NONE',  ( 18.67979575497178502, 10.72451020669898547, 109.1655762719810383 ) ) ;
#179820 = CARTESIAN_POINT ( 'NONE',  ( -16.46253265017160317, 9.564922557960807481, 60.83224293864769550 ) ) ;
#179822 = EDGE_CURVE ( 'NONE', #129974, #63497, #56671, .T. ) ;
#179821 = CARTESIAN_POINT ( 'NONE',  ( -12.14591786802326823, 12.06949235617739902, 33.12609039468569705 ) ) ;
#179823 = CARTESIAN_POINT ( 'NONE',  ( 23.48529157249600630, -32.32473071737749137, -7.049999994537626158 ) ) ;
#179824 = CARTESIAN_POINT ( 'NONE',  ( -10.81492255796105439, 18.62759615963255655, 107.9177570613523471 ) ) ;
#179825 = CARTESIAN_POINT ( 'NONE',  ( -5.049401038298153566, 19.05341960407611168, 40.20724293864768839 ) ) ;
#179826 = CARTESIAN_POINT ( 'NONE',  ( -21.52544592524334988, -5.823673210054445271, 108.9594237280190185 ) ) ;
#179828 = CARTESIAN_POINT ( 'NONE',  ( -0.05219959533937732626, 21.53943276465977519, 57.50109039468568994 ) ) ;
#179827 = CARTESIAN_POINT ( 'NONE',  ( 5.153800228976335163, 19.02544592524342804, 89.79057627198102409 ) ) ;
#179829 = CARTESIAN_POINT ( 'NONE',  ( 6.703997108180972830, -4.665206786362193547, -62.11218654135820572 ) ) ;
#179830 = CARTESIAN_POINT ( 'NONE',  ( 9.564922557960805705, 16.46253265017160317, 109.5822429386476955 ) ) ;
#179831 = CARTESIAN_POINT ( 'NONE',  ( -0.3535533905929611476, 30.00000000000000711, 4.646446609406721606 ) ) ;
#179833 = CARTESIAN_POINT ( 'NONE',  ( -21.52544592524334988, -5.823673210054445271, 68.95942372801901854 ) ) ;
#179832 = CARTESIAN_POINT ( 'NONE',  ( -12.06949235617739369, -12.14591786802326823, 49.37609039468569705 ) ) ;
#179834 = CARTESIAN_POINT ( 'NONE',  ( 10.81492255796106328, -18.62759615963255655, 90.41775706135236135 ) ) ;
#179835 = CARTESIAN_POINT ( 'NONE',  ( -10.58667710475869939, 9.243954752495751492, -60.30599866924266905 ) ) ;
#179836 = CARTESIAN_POINT ( 'NONE',  ( -16.55341960407617563, 4.379528057220093196, 23.54275706135235424 ) ) ;
#179837 = CARTESIAN_POINT ( 'NONE',  ( 19.03943276465977164, -0.05219959533909143690, 88.74890960531436690 ) ) ;
#179838 = CARTESIAN_POINT ( 'NONE',  ( -5.153800228976328057, -19.02544592524343514, 107.2905762719810383 ) ) ;
#179839 = EDGE_CURVE ( 'NONE', #175270, #121093, #34897, .T. ) ;
#179840 = CARTESIAN_POINT ( 'NONE',  ( 17.44270441346512968, 5.991230190323100224, 43.86335079264229364 ) ) ;
#179841 = CARTESIAN_POINT ( 'NONE',  ( -19.02544592524342804, 5.153800228976336051, 26.04057627198103120 ) ) ;
#179842 = CARTESIAN_POINT ( 'NONE',  ( -15.80617190586745835, -15.72974639402198527, 46.87390960531435979 ) ) ;
#179843 = CARTESIAN_POINT ( 'NONE',  ( 8.224510206698742110, 14.34966873604972548, 112.0844237280190185 ) ) ;
#179845 = CARTESIAN_POINT ( 'NONE',  ( -9.474510206698964154, 16.51473224551069663, 65.41557627198102409 ) ) ;
#179844 = CARTESIAN_POINT ( 'NONE',  ( 16.53943276465976808, -0.05219959533910856209, 78.74890960531436690 ) ) ;
#179846 = CARTESIAN_POINT ( 'NONE',  ( 21.52544592524334988, 5.823673210054432836, 96.45942372801901854 ) ) ;
#179847 = CARTESIAN_POINT ( 'NONE',  ( 4.379528057220092307, 16.55341960407617563, 22.29275706135235069 ) ) ;
#179848 = CARTESIAN_POINT ( 'NONE',  ( 0.05219959533910956823, 16.53943276465976808, 84.99890960531436690 ) ) ;
#179849 = CARTESIAN_POINT ( 'NONE',  ( 21.55341960407619695, -5.719274019375665929, 46.04275706135234714 ) ) ;
#179850 = CARTESIAN_POINT ( 'NONE',  ( 5.719274019375991003, -21.55341960407610458, 67.70724293864769550 ) ) ;
#179851 = CARTESIAN_POINT ( 'NONE',  ( -16.46253265017146816, -9.564922557961047289, 44.16775706135232582 ) ) ;
#179852 = CARTESIAN_POINT ( 'NONE',  ( -34.72612402863279613, 2.419136457854829558, 52.10344399403046367 ) ) ;
#179853 = CARTESIAN_POINT ( 'NONE',  ( -13.97604488694527625, -13.89961937509977652, 96.87390960531433848 ) ) ;
#179854 = CARTESIAN_POINT ( 'NONE',  ( -8.314922557960811034, -14.29746914071050412, 67.08224293864770971 ) ) ;
#179855 = AXIS2_PLACEMENT_3D ( 'NONE', #148707, #42526, #89014 ) ;
#179856 = CARTESIAN_POINT ( 'NONE',  ( 12.06949235617757843, -12.14591786802309237, 38.12390960531436690 ) ) ;
#179857 = CARTESIAN_POINT ( 'NONE',  ( -0.05219959533934338120, 16.53943276465976808, 112.5010903946857042 ) ) ;
#179858 = CARTESIAN_POINT ( 'NONE',  ( 5.153800228976615827, -19.02544592524334988, 65.20942372801900433 ) ) ;
#179859 = CARTESIAN_POINT ( 'NONE',  ( 17.58332526062524437, 7.635886036038643354, 76.57665040441536064 ) ) ;
#179860 = CARTESIAN_POINT ( 'NONE',  ( -10.81492255796078084, -18.62759615963271287, 27.08224293864769550 ) ) ;
#179861 = CARTESIAN_POINT ( 'NONE',  ( -12.14591786802309592, -12.06949235617757132, 81.87390960531435269 ) ) ;
#179862 = DIRECTION ( 'NONE',  ( 1.000000000000000000, 0.000000000000000000, 0.000000000000000000 ) ) ;
#179864 = CARTESIAN_POINT ( 'NONE',  ( -18.62759615963270932, 10.81492255796079327, 55.83224293864770260 ) ) ;
#179863 = CARTESIAN_POINT ( 'NONE',  ( 5.049401038298161559, -19.05341960407611168, 42.70724293864767418 ) ) ;
#179865 = CARTESIAN_POINT ( 'NONE',  ( 21.52544592524344225, -5.823673210054117533, 78.54057627198103830 ) ) ;
#179866 = CARTESIAN_POINT ( 'NONE',  ( 12.06949235617757843, -12.14591786802309237, 108.1239096053143811 ) ) ;
#179868 = CARTESIAN_POINT ( 'NONE',  ( 13.89961937509977652, -13.97604488694527269, 48.12390960531435979 ) ) ;
#179867 = CARTESIAN_POINT ( 'NONE',  ( 16.53943276465976808, 0.05219959533934440121, 61.25109039468567573 ) ) ;
#179869 = EDGE_CURVE ( 'NONE', #8593, #155176, #102754, .T. ) ;
#179870 = CARTESIAN_POINT ( 'NONE',  ( 15.80617190586769283, -15.72974639402175789, 55.62609039468568284 ) ) ;
#179871 = AXIS2_PLACEMENT_3D ( 'NONE', #63370, #111860, #15884 ) ;
#179872 = CARTESIAN_POINT ( 'NONE',  ( 8.314922557960818139, 14.29746914071049879, 109.5822429386476955 ) ) ;
#179873 = CARTESIAN_POINT ( 'NONE',  ( 5.153800228976615827, -19.02544592524334988, 85.20942372801900433 ) ) ;
#179874 = CARTESIAN_POINT ( 'NONE',  ( -36.91746825000000598, 2.428612866367529932E-14, -7.124999997268813168 ) ) ;
#179876 = CARTESIAN_POINT ( 'NONE',  ( -18.62759615963270932, 10.81492255796079327, 50.83224293864770971 ) ) ;
#179875 = CARTESIAN_POINT ( 'NONE',  ( -1.340157125434632501, -22.10131684062752555, -58.31342218742629768 ) ) ;
#179877 = CARTESIAN_POINT ( 'NONE',  ( 17.44279575226823908, -5.990770900252462283, 68.33557567514318976 ) ) ;
#179878 = CARTESIAN_POINT ( 'NONE',  ( -0.05219959533937732626, 21.53943276465977519, 87.50109039468568994 ) ) ;
#179879 = CARTESIAN_POINT ( 'NONE',  ( 16.52544592524342804, -4.483927247898539470, 33.54057627198102409 ) ) ;
#179881 = CARTESIAN_POINT ( 'NONE',  ( 4.483927247898545687, 16.52544592524342804, 39.79057627198103830 ) ) ;
#179880 = CARTESIAN_POINT ( 'NONE',  ( 14.29746914071037800, 8.314922557961029526, 51.66775706135234714 ) ) ;
#179882 = CARTESIAN_POINT ( 'NONE',  ( -21.52544592524343514, 5.823673210054127303, 71.04057627198103830 ) ) ;
#179883 = CARTESIAN_POINT ( 'NONE',  ( -21.53943276465977519, 0.05219959533907696930, 71.24890960531435269 ) ) ;
#179884 = CARTESIAN_POINT ( 'NONE',  ( -21.34799762026588255, 10.44447989802408827, 170.3878604776606096 ) ) ;
#179886 = CARTESIAN_POINT ( 'NONE',  ( -5.049401038298153566, 19.05341960407611168, 115.2072429386477097 ) ) ;
#179885 = CARTESIAN_POINT ( 'NONE',  ( 19.02544592524334988, 5.153800228976608722, 81.45942372801897591 ) ) ;
#179888 = CARTESIAN_POINT ( 'NONE',  ( 5.049401038298161559, -19.05341960407611168, 42.70724293864767418 ) ) ;
#179887 = B_SPLINE_CURVE_WITH_KNOTS ( 'NONE', 3,
 ( #52085, #99581, #22756, #192609, #144090, #5571, #115766, #160265, #80427, #145084, #177453, #142100, #53076, #3585, #189621, #4567, #50110, #128909, #161262, #65263, #38923, #37921, #7566, #97563, #18781, #190610, #35917, #6567, #175438, #21755, #126923, #146082 ),
 .UNSPECIFIED., .F., .F.,
 ( 4, 2, 2, 2, 2, 2, 2, 2, 2, 2, 2, 2, 2, 2, 2, 4 ),
 ( 1.645181051943004889E-15, 0.0003712461730052120336, 0.0007424923460087788987, 0.001113738519012345655, 0.001484984692015912629, 0.002227477038023061105, 0.002598723211026641739, 0.002969969384030222374, 0.003341215557033802575, 0.003712461730037383643, 0.004083707903040963844, 0.004454954076044545346, 0.004826200249048125113, 0.005197446422051706615, 0.005568692595055287249, 0.005939938768058867884 ),
 .UNSPECIFIED. ) ;
#179889 = CARTESIAN_POINT ( 'NONE',  ( 19.03943276465977164, -0.05219959533909143690, 28.74890960531435624 ) ) ;
#179890 = DIRECTION ( 'NONE',  ( 0.000000000000000000, 0.000000000000000000, 1.000000000000000000 ) ) ;
#179891 = CARTESIAN_POINT ( 'NONE',  ( -28.79475375365586842, 2.428612866367529932E-14, 155.0000000000000000 ) ) ;
#179892 = VERTEX_POINT ( 'NONE', #102167 ) ;
#179893 = CARTESIAN_POINT ( 'NONE',  ( -14.29746914071037622, -8.314922557961029526, 84.16775706135234714 ) ) ;
#179894 = CARTESIAN_POINT ( 'NONE',  ( 18.62759615963271287, -10.81492255796078972, 103.3322429386476955 ) ) ;
#179895 = CARTESIAN_POINT ( 'NONE',  ( -5.049401038298153566, 19.05341960407611168, 75.20724293864769550 ) ) ;
#179896 = CARTESIAN_POINT ( 'NONE',  ( 10.81492255796106328, -18.62759615963255655, 35.41775706135234003 ) ) ;
#179897 = CARTESIAN_POINT ( 'NONE',  ( 16.51473224551069308, 9.474510206698969483, 99.16557627198102409 ) ) ;
#179898 = CARTESIAN_POINT ( 'NONE',  ( -29.51469970000582066, -26.64072072720978923, -20.60124869738260855 ) ) ;
#179899 = EDGE_LOOP ( 'NONE', ( #30328, #192191, #112949, #160467 ) ) ;
#179900 = CARTESIAN_POINT ( 'NONE',  ( 0.05219959533937995610, -21.53943276465977519, 35.00109039468568284 ) ) ;
#179902 = CARTESIAN_POINT ( 'NONE',  ( -13.97604488694547697, 13.89961937509957934, 93.12609039468566152 ) ) ;
#179901 = CARTESIAN_POINT ( 'NONE',  ( -19.03943276465977164, 0.05219959533909376836, 26.24890960531435624 ) ) ;
#179903 = CARTESIAN_POINT ( 'NONE',  ( -13.89961937509957401, -13.97604488694547875, 44.37609039468566863 ) ) ;
#179904 = CARTESIAN_POINT ( 'NONE',  ( 5.719274019375991003, -21.55341960407610458, 107.7072429386476955 ) ) ;
#179905 = CARTESIAN_POINT ( 'NONE',  ( 5.153800228976615827, -19.02544592524334988, 40.20942372801898301 ) ) ;
#179906 = CARTESIAN_POINT ( 'NONE',  ( 13.97604488694548053, -13.89961937509957401, 50.62609039468566152 ) ) ;
#179907 = CARTESIAN_POINT ( 'NONE',  ( 0.05219959533934541429, -16.53943276465976808, 95.00109039468568994 ) ) ;
#179909 = VERTEX_POINT ( 'NONE', #37492 ) ;
#179908 = DIRECTION ( 'NONE',  ( 0.000000000000000000, -1.000000000000000000, 0.000000000000000000 ) ) ;
#179910 = CARTESIAN_POINT ( 'NONE',  ( 5.153800228976335163, 19.02544592524342804, 69.79057627198103830 ) ) ;
#179911 = CARTESIAN_POINT ( 'NONE',  ( 15.72974639402176855, 15.80617190586768217, 76.87609039468567573 ) ) ;
#179912 = CARTESIAN_POINT ( 'NONE',  ( 18.62759615963255655, 10.81492255796105972, 96.66775706135234714 ) ) ;
#179913 = CARTESIAN_POINT ( 'NONE',  ( 5.000000000000001776, -120.0000000000000142, -13.00000000000000000 ) ) ;
#179914 = CARTESIAN_POINT ( 'NONE',  ( -13.97604488694527625, -13.89961937509977652, 91.87390960531432427 ) ) ;
#179915 = CARTESIAN_POINT ( 'NONE',  ( 10.81492255796106328, -18.62759615963255655, 60.41775706135235424 ) ) ;
#179916 = CARTESIAN_POINT ( 'NONE',  ( 19.03943276465977164, 0.05219959533936151252, 101.2510903946856757 ) ) ;
#179917 = CARTESIAN_POINT ( 'NONE',  ( -19.05341960407611168, -5.049401038298163336, 71.45724293864766707 ) ) ;
#179918 = CARTESIAN_POINT ( 'NONE',  ( -19.02544592524342804, 5.153800228976336051, 106.0405762719810241 ) ) ;
#179919 = CARTESIAN_POINT ( 'NONE',  ( 9.474510206698971260, -16.51473224551069308, 82.91557627198103830 ) ) ;
#179920 = CARTESIAN_POINT ( 'NONE',  ( 69.65682714487590488, -71.74905178543389184, -4.999999999999999112 ) ) ;
#179921 = CARTESIAN_POINT ( 'NONE',  ( -19.05341960407611168, -5.049401038298163336, 66.45724293864769550 ) ) ;
#179922 = CARTESIAN_POINT ( 'NONE',  ( 0.05219959533909260263, 19.03943276465977164, 49.99890960531435979 ) ) ;
#179923 = CARTESIAN_POINT ( 'NONE',  ( 15.80617190586769283, -15.72974639402175789, 20.62609039468568639 ) ) ;
#179924 = CARTESIAN_POINT ( 'NONE',  ( 16.53943276465976808, 0.05219959533934440121, 106.2510903946856757 ) ) ;
#179925 = DIRECTION ( 'NONE',  ( -0.07151044867601408228, 0.9974398506828143773, 0.000000000000000000 ) ) ;
#179926 = CARTESIAN_POINT ( 'NONE',  ( -2.285367203649863287E-16, -64.83960026421343059, -13.00000000000000000 ) ) ;
#179927 = CARTESIAN_POINT ( 'NONE',  ( 13.97604488694548053, -13.89961937509957401, 55.62609039468566863 ) ) ;
#179928 = CARTESIAN_POINT ( 'NONE',  ( -5.049401038298153566, 19.05341960407611168, 85.20724293864766707 ) ) ;
#179929 = CARTESIAN_POINT ( 'NONE',  ( -8.224510206698948167, 14.34966873604960824, 65.41557627198102409 ) ) ;
#179930 = CARTESIAN_POINT ( 'NONE',  ( 8.224510206698953496, -14.34966873604960469, 102.9155762719810383 ) ) ;
#179931 = CARTESIAN_POINT ( 'NONE',  ( 21.52544592524344225, -5.823673210054117533, 33.54057627198102409 ) ) ;
#179932 = CARTESIAN_POINT ( 'NONE',  ( 13.89961937509977652, -13.97604488694527269, 108.1239096053143669 ) ) ;
#179933 = CARTESIAN_POINT ( 'NONE',  ( 8.224510206698953496, -14.34966873604960469, 92.91557627198103830 ) ) ;
#179934 = CARTESIAN_POINT ( 'NONE',  ( 13.89961937509977652, -13.97604488694527269, 113.1239096053143527 ) ) ;
#179935 = CARTESIAN_POINT ( 'NONE',  ( 9.564922557961047289, -16.46253265017146816, 35.41775706135233293 ) ) ;
#179936 = CARTESIAN_POINT ( 'NONE',  ( 16.53943276465976808, 0.05219959533934440121, 106.2510903946856757 ) ) ;
#179937 = CARTESIAN_POINT ( 'NONE',  ( 9.474510206698971260, -16.51473224551069308, 82.91557627198103830 ) ) ;
#179938 = CARTESIAN_POINT ( 'NONE',  ( -5.823673210054431948, 21.52544592524334988, 47.70942372801902565 ) ) ;
#179939 = CARTESIAN_POINT ( 'NONE',  ( -21.52544592524343514, 5.823673210054127303, 41.04057627198103120 ) ) ;
#179940 = CARTESIAN_POINT ( 'NONE',  ( -0.05219959533937732626, 21.53943276465977519, 32.50109039468568284 ) ) ;
#179941 = CARTESIAN_POINT ( 'NONE',  ( -18.62759615963270932, 10.81492255796079327, 85.83224293864768129 ) ) ;
#179942 = CARTESIAN_POINT ( 'NONE',  ( 12.06949235617757843, -12.14591786802309237, 93.12390960531436690 ) ) ;
#179943 = CARTESIAN_POINT ( 'NONE',  ( -19.05341960407617563, 5.049401038297882671, 63.54275706135234003 ) ) ;
#179944 = CARTESIAN_POINT ( 'NONE',  ( -19.03943276465977164, 0.05219959533909376836, 36.24890960531436690 ) ) ;
#179945 = CARTESIAN_POINT ( 'NONE',  ( -13.97604488694527625, -13.89961937509977652, 101.8739096053143811 ) ) ;
#179946 = CARTESIAN_POINT ( 'NONE',  ( -13.97604488694527625, -13.89961937509977652, 91.87390960531432427 ) ) ;
#179947 = CARTESIAN_POINT ( 'NONE',  ( -4.379528057220328563, 16.55341960407611168, 110.2072429386477239 ) ) ;
#179948 = CARTESIAN_POINT ( 'NONE',  ( -14.34966873604960291, -8.224510206698953496, 21.66557627198102409 ) ) ;
#179949 = CARTESIAN_POINT ( 'NONE',  ( -12.14591786802326823, 12.06949235617739902, 43.12609039468568284 ) ) ;
#179950 = CARTESIAN_POINT ( 'NONE',  ( 21.52544592524334988, 5.823673210054432836, 111.4594237280190328 ) ) ;
#179952 = CARTESIAN_POINT ( 'NONE',  ( 16.55341960407618274, -4.379528057220086978, 111.0427570613523613 ) ) ;
#179951 = CARTESIAN_POINT ( 'NONE',  ( -16.51473224551069308, -9.474510206698971260, 111.6655762719810383 ) ) ;
#179953 = CARTESIAN_POINT ( 'NONE',  ( -15.72974639402176322, -15.80617190586768395, 34.37609039468568284 ) ) ;
#179954 = CARTESIAN_POINT ( 'NONE',  ( 19.03943276465977164, -0.05219959533909143690, 38.74890960531436690 ) ) ;
#179955 = CARTESIAN_POINT ( 'NONE',  ( -8.314922557961024197, 14.29746914071037800, 37.91775706135235424 ) ) ;
#179956 = CARTESIAN_POINT ( 'NONE',  ( -16.52544592524335698, -4.483927247898792601, 108.9594237280190185 ) ) ;
#179957 = CARTESIAN_POINT ( 'NONE',  ( -8.224510206698735004, -14.34966873604973081, 89.58442372801901854 ) ) ;
#179958 = CARTESIAN_POINT ( 'NONE',  ( -0.05219959533936034679, 19.03943276465977164, 107.5010903946856615 ) ) ;
#179959 = CARTESIAN_POINT ( 'NONE',  ( 5.153800228976335163, 19.02544592524342804, 29.79057627198102409 ) ) ;
#179960 = CARTESIAN_POINT ( 'NONE',  ( 8.224510206698953496, -14.34966873604960469, 112.9155762719810383 ) ) ;
#179961 = CARTESIAN_POINT ( 'NONE',  ( 0.05219959533907565091, 21.53943276465977519, 99.99890960531436690 ) ) ;
#179962 = CARTESIAN_POINT ( 'NONE',  ( -16.46253265017160317, 9.564922557960807481, 30.83224293864769550 ) ) ;
#179963 = B_SPLINE_CURVE_WITH_KNOTS ( 'NONE', 3,
 ( #180878, #42353, #76644, #75648, #183839, #198016, #134365, #45328, #87834, #106978, #74674, #120169 ),
 .UNSPECIFIED., .F., .F.,
 ( 4, 2, 2, 2, 2, 4 ),
 ( 0.000000000000000000, 0.002596730589505801597, 0.003895095884258703480, 0.005193461179011606664, 0.007790191768517405226, 0.01038692235802320812 ),
 .UNSPECIFIED. ) ;
#179964 = CARTESIAN_POINT ( 'NONE',  ( -0.05219959533909027116, -19.03943276465977164, 102.4989096053143669 ) ) ;
#179965 = CARTESIAN_POINT ( 'NONE',  ( 18.62759615963255655, 10.81492255796105972, 36.66775706135234714 ) ) ;
#179966 = CARTESIAN_POINT ( 'NONE',  ( -6.019987952026120409E-15, 39.95163481335720235, -2.502157773949823305 ) ) ;
#179967 = CARTESIAN_POINT ( 'NONE',  ( -16.51473224551069308, -9.474510206698971260, 101.6655762719810241 ) ) ;
#179968 = CARTESIAN_POINT ( 'NONE',  ( 25.25560589046783022, 2.428612866367529932E-14, 167.9999999999999716 ) ) ;
#179969 = CARTESIAN_POINT ( 'NONE',  ( 19.02544592524343514, -5.153800228976328945, 93.54057627198102409 ) ) ;
#179971 = CARTESIAN_POINT ( 'NONE',  ( 16.53943276465976808, -0.05219959533910856209, 88.74890960531436690 ) ) ;
#179970 = CARTESIAN_POINT ( 'NONE',  ( 21.55341960407619695, -5.719274019375665929, 31.04275706135234714 ) ) ;
#179972 = CARTESIAN_POINT ( 'NONE',  ( -19.03943276465977164, 0.05219959533909376836, 101.2489096053143669 ) ) ;
#179973 = CARTESIAN_POINT ( 'NONE',  ( -27.96111904526444292, -7.044650443050448629, 161.2906300811048368 ) ) ;
#179974 = CARTESIAN_POINT ( 'NONE',  ( -8.224510206698735004, -14.34966873604973081, 69.58442372801900433 ) ) ;
#179975 = CARTESIAN_POINT ( 'NONE',  ( -15.80617190586768217, 15.72974639402176855, 78.12609039468570415 ) ) ;
#179976 = CARTESIAN_POINT ( 'NONE',  ( 12.14591786802327356, -12.06949235617739191, 40.62609039468567573 ) ) ;
#179977 = CARTESIAN_POINT ( 'NONE',  ( 9.474510206698971260, -16.51473224551069308, 77.91557627198103830 ) ) ;
#179978 = CARTESIAN_POINT ( 'NONE',  ( -19.05341960407617563, 5.049401038297882671, 103.5427570613523329 ) ) ;
#179979 = CARTESIAN_POINT ( 'NONE',  ( 8.224510206698742110, 14.34966873604972548, 67.08442372801901854 ) ) ;
#179980 = CARTESIAN_POINT ( 'NONE',  ( 5.823673210054444382, -21.52544592524334988, 110.2094237280190185 ) ) ;
#179981 = CARTESIAN_POINT ( 'NONE',  ( 19.02544592524334988, 5.153800228976608722, 91.45942372801900433 ) ) ;
#179982 = CARTESIAN_POINT ( 'NONE',  ( 13.97604488694527802, 13.89961937509977652, 64.37390960531436690 ) ) ;
#179983 = CARTESIAN_POINT ( 'NONE',  ( -21.55341960407610458, -5.719274019375992779, 81.45724293864769550 ) ) ;
#179985 = CARTESIAN_POINT ( 'NONE',  ( 19.02544592524334988, 5.153800228976608722, 96.45942372801897591 ) ) ;
#179984 = CARTESIAN_POINT ( 'NONE',  ( -14.34966873604960291, -8.224510206698953496, 91.66557627198103830 ) ) ;
#179986 = CARTESIAN_POINT ( 'NONE',  ( -8.224510206698735004, -14.34966873604973081, 64.58442372801900433 ) ) ;
#179987 = CARTESIAN_POINT ( 'NONE',  ( 21.81230582904511550, 5.969922009377570227, 172.1979875755936860 ) ) ;
#179989 = EDGE_CURVE ( 'NONE', #115310, #90405, #148682, .T. ) ;
#179988 = CARTESIAN_POINT ( 'NONE',  ( 9.474510206698729675, 16.51473224551082808, 57.08442372801900433 ) ) ;
#179990 = CARTESIAN_POINT ( 'NONE',  ( 4.379528057220339221, -16.55341960407611168, 32.70724293864770260 ) ) ;
#179991 = CARTESIAN_POINT ( 'NONE',  ( -12.14591786802309592, -12.06949235617757132, 81.87390960531435269 ) ) ;
#179993 = CARTESIAN_POINT ( 'NONE',  ( 13.97604488694548053, -13.89961937509957401, 45.62609039468566863 ) ) ;
#179992 = CARTESIAN_POINT ( 'NONE',  ( 16.51473224551083163, -9.474510206698727899, 25.83442372801900078 ) ) ;
#179994 = CARTESIAN_POINT ( 'NONE',  ( -10.81492255796105439, 18.62759615963255655, 27.91775706135234358 ) ) ;
#179995 = CARTESIAN_POINT ( 'NONE',  ( -19.05341960407611168, -5.049401038298163336, 101.4572429386476955 ) ) ;
#179996 = CARTESIAN_POINT ( 'NONE',  ( 13.89961937509977652, -13.97604488694527269, 83.12390960531436690 ) ) ;
#179997 = CARTESIAN_POINT ( 'NONE',  ( 15.80617190586769283, -15.72974639402175789, 95.62609039468568994 ) ) ;
#179998 = CARTESIAN_POINT ( 'NONE',  ( -13.97604488694527625, -13.89961937509977652, 76.87390960531433848 ) ) ;
#179999 = CARTESIAN_POINT ( 'NONE',  ( 5.823673210054125526, 21.52544592524343514, 34.79057627198103120 ) ) ;
#180000 = CARTESIAN_POINT ( 'NONE',  ( -4.379528057220328563, 16.55341960407611168, 85.20724293864770971 ) ) ;
#180001 = CARTESIAN_POINT ( 'NONE',  ( 9.474510206698971260, -16.51473224551069308, 37.91557627198102409 ) ) ;
#180002 = CARTESIAN_POINT ( 'NONE',  ( -16.53943276465976808, 0.05219959533911058130, 101.2489096053143669 ) ) ;
#180003 = VECTOR ( 'NONE', #124148, 1000.000000000000000 ) ;
#180004 = CARTESIAN_POINT ( 'NONE',  ( -5.719274019375978568, 21.55341960407610458, 105.2072429386477097 ) ) ;
#180005 = CARTESIAN_POINT ( 'NONE',  ( 15.72974639402176855, 15.80617190586768217, 66.87609039468568994 ) ) ;
#180006 = CARTESIAN_POINT ( 'NONE',  ( 19.05341960407611168, 5.049401038298154454, 28.95724293864769550 ) ) ;
#180007 = CARTESIAN_POINT ( 'NONE',  ( -12.14591786802326823, 12.06949235617739902, 68.12609039468567573 ) ) ;
#180008 = CARTESIAN_POINT ( 'NONE',  ( -18.67979575497178146, -10.72451020669898902, 101.6655762719810383 ) ) ;
#180009 = CARTESIAN_POINT ( 'NONE',  ( -21.53943276465977519, 0.05219959533907696930, 116.2489096053143669 ) ) ;
#180011 = CARTESIAN_POINT ( 'NONE',  ( -9.564922557960796823, -16.46253265017161027, 57.08224293864769550 ) ) ;
#180010 = CARTESIAN_POINT ( 'NONE',  ( -5.049401038297874678, -19.05341960407617918, 39.79275706135232582 ) ) ;
#180012 = CARTESIAN_POINT ( 'NONE',  ( 9.564922557960805705, 16.46253265017160317, 114.5822429386476955 ) ) ;
#180013 = CARTESIAN_POINT ( 'NONE',  ( 15.72974639402176855, 15.80617190586768217, 51.87609039468568284 ) ) ;
#180014 = CARTESIAN_POINT ( 'NONE',  ( -18.67979575497178146, -10.72451020669898902, 61.66557627198103120 ) ) ;
#180015 = CARTESIAN_POINT ( 'NONE',  ( -0.05219959533910754901, -16.53943276465976808, 42.49890960531435979 ) ) ;
#180017 = CARTESIAN_POINT ( 'NONE',  ( 15.72974639402176855, 15.80617190586768217, 106.8760903946856899 ) ) ;
#180016 = CARTESIAN_POINT ( 'NONE',  ( -5.823673210054431948, 21.52544592524334988, 72.70942372801901854 ) ) ;
#180018 = CARTESIAN_POINT ( 'NONE',  ( -4.483927247898539470, -16.52544592524342804, 57.29057627198103120 ) ) ;
#180019 = CARTESIAN_POINT ( 'NONE',  ( -4.483927247898539470, -16.52544592524342804, 107.2905762719810525 ) ) ;
#180020 = CARTESIAN_POINT ( 'NONE',  ( -5.153800228976607833, 19.02544592524334988, 42.70942372801901143 ) ) ;
#180021 = CARTESIAN_POINT ( 'NONE',  ( 4.379528057220092307, 16.55341960407617563, 102.2927570613523613 ) ) ;
#180022 = CARTESIAN_POINT ( 'NONE',  ( 21.52544592524334988, 5.823673210054432836, 71.45942372801901854 ) ) ;
#180023 = CARTESIAN_POINT ( 'NONE',  ( 13.97604488694527802, 13.89961937509977652, 59.37390960531434558 ) ) ;
#180024 = CARTESIAN_POINT ( 'NONE',  ( -13.89961937509957401, -13.97604488694547875, 34.37609039468566863 ) ) ;
#180025 = CARTESIAN_POINT ( 'NONE',  ( -10.81492255796078084, -18.62759615963271287, 42.08224293864769550 ) ) ;
#180026 = CARTESIAN_POINT ( 'NONE',  ( -21.53943276465977519, -0.05219959533937600094, 28.75109039468567929 ) ) ;
#180027 = CARTESIAN_POINT ( 'NONE',  ( 5.823673210054125526, 21.52544592524343514, 94.79057627198105251 ) ) ;
#180028 = CARTESIAN_POINT ( 'NONE',  ( -9.564922557961040184, 16.46253265017147172, 87.91775706135233293 ) ) ;
#180029 = CARTESIAN_POINT ( 'NONE',  ( -16.53943276465976808, -0.05219959533934237506, 53.75109039468568994 ) ) ;
#180031 = CARTESIAN_POINT ( 'NONE',  ( 18.62759615963271287, -10.81492255796078972, 98.33224293864769550 ) ) ;
#180030 = CARTESIAN_POINT ( 'NONE',  ( 17.97214573761831247, 5.500000000000080824, 63.96970049038658601 ) ) ;
#180032 = CARTESIAN_POINT ( 'NONE',  ( -16.52544592524342804, 4.483927247898546575, 81.04057627198102409 ) ) ;
#180033 = CARTESIAN_POINT ( 'NONE',  ( -31.73029476377070424, -20.92000799991019022, -24.48145274275711003 ) ) ;
#180034 = CARTESIAN_POINT ( 'NONE',  ( 19.03943276465977164, 0.05219959533936151252, 111.2510903946856757 ) ) ;
#180035 = CARTESIAN_POINT ( 'NONE',  ( -10.72451020669898014, 18.67979575497178502, 50.41557627198103120 ) ) ;
#180037 = CARTESIAN_POINT ( 'NONE',  ( 0.05219959533934541429, -16.53943276465976808, 75.00109039468568994 ) ) ;
#180036 = VECTOR ( 'NONE', #137748, 1000.000000000000000 ) ;
#180038 = DIRECTION ( 'NONE',  ( 0.000000000000000000, 0.000000000000000000, 1.000000000000000000 ) ) ;
#180039 = CARTESIAN_POINT ( 'NONE',  ( -16.53943276465976808, -0.05219959533934237506, 58.75109039468568994 ) ) ;
#180040 = CARTESIAN_POINT ( 'NONE',  ( 15.80617190586769283, -15.72974639402175789, 30.62609039468567929 ) ) ;
#180041 = CARTESIAN_POINT ( 'NONE',  ( 21.53943276465977519, -0.05219959533907433946, 43.74890960531435979 ) ) ;
#180042 = CARTESIAN_POINT ( 'NONE',  ( 8.224510206698742110, 14.34966873604972548, 72.08442372801899012 ) ) ;
#180043 = CARTESIAN_POINT ( 'NONE',  ( 19.03943276465977164, -0.05219959533909143690, 93.74890960531435269 ) ) ;
#180045 = CARTESIAN_POINT ( 'NONE',  ( -9.564922557960796823, -16.46253265017161027, 32.08224293864769550 ) ) ;
#180044 = CARTESIAN_POINT ( 'NONE',  ( 15.80617190586769283, -15.72974639402175789, 55.62609039468568284 ) ) ;
#180046 = CARTESIAN_POINT ( 'NONE',  ( -18.62759615963270932, 10.81492255796079327, 45.83224293864769550 ) ) ;
#180047 = CARTESIAN_POINT ( 'NONE',  ( -15.80617190586745835, -15.72974639402198527, 21.87390960531436690 ) ) ;
#180048 = ORIENTED_EDGE ( 'NONE', *, *, #193551, .T. ) ;
#180049 = CARTESIAN_POINT ( 'NONE',  ( -5.153800228976607833, 19.02544592524334988, 32.70942372801899722 ) ) ;
#180050 = CARTESIAN_POINT ( 'NONE',  ( -14.34966873604972548, 8.224510206698743886, 53.33442372801901854 ) ) ;
#180051 = CARTESIAN_POINT ( 'NONE',  ( 5.153800228976335163, 19.02544592524342804, 109.7905762719810099 ) ) ;
#180052 = ORIENTED_EDGE ( 'NONE', *, *, #4454, .T. ) ;
#180053 = CARTESIAN_POINT ( 'NONE',  ( -0.05219959533909027116, -19.03943276465977164, 87.49890960531436690 ) ) ;
#180054 = CARTESIAN_POINT ( 'NONE',  ( -14.29746914071037622, -8.314922557961029526, 104.1677570613523471 ) ) ;
#180055 = FACE_OUTER_BOUND ( 'NONE', #53273, .T. ) ;
#180056 = CARTESIAN_POINT ( 'NONE',  ( -12.06949235617756955, 12.14591786802309770, 90.62390960531436690 ) ) ;
#180057 = CARTESIAN_POINT ( 'NONE',  ( 18.67979575497178502, 10.72451020669898547, 49.16557627198102409 ) ) ;
#180058 = CARTESIAN_POINT ( 'NONE',  ( -9.564922557960796823, -16.46253265017161027, 27.08224293864769550 ) ) ;
#180059 = CARTESIAN_POINT ( 'NONE',  ( -4.483927247898782831, 16.52544592524335698, 82.70942372801900433 ) ) ;
#180060 = CARTESIAN_POINT ( 'NONE',  ( -5.823673210054431948, 21.52544592524334988, 22.70942372801901499 ) ) ;
#180061 = CARTESIAN_POINT ( 'NONE',  ( -13.89961937509957401, -13.97604488694547875, 94.37609039468566152 ) ) ;
#180062 = CARTESIAN_POINT ( 'NONE',  ( -0.05219959533909027116, -19.03943276465977164, 42.49890960531435269 ) ) ;
#180063 = CIRCLE ( 'NONE', #138014, 28.90000000000004476 ) ;
#180064 = CARTESIAN_POINT ( 'NONE',  ( -19.05341960407611168, -5.049401038298163336, 106.4572429386476955 ) ) ;
#180065 = CARTESIAN_POINT ( 'NONE',  ( -0.05219959533937732626, 21.53943276465977519, 107.5010903946856899 ) ) ;
#180066 = CARTESIAN_POINT ( 'NONE',  ( 5.049401038298161559, -19.05341960407611168, 77.70724293864765286 ) ) ;
#180067 = CARTESIAN_POINT ( 'NONE',  ( -0.05219959533934338120, 16.53943276465976808, 57.50109039468568994 ) ) ;
#180068 = CARTESIAN_POINT ( 'NONE',  ( -18.62759615963255300, -10.81492255796106328, 94.16775706135237556 ) ) ;
#180069 = CARTESIAN_POINT ( 'NONE',  ( 19.02544592524334988, 5.153800228976608722, 56.45942372801898301 ) ) ;
#180070 = CARTESIAN_POINT ( 'NONE',  ( -16.46253265017146816, -9.564922557961047289, 49.16775706135233293 ) ) ;
#180071 = ORIENTED_EDGE ( 'NONE', *, *, #71324, .F. ) ;
#180072 = CARTESIAN_POINT ( 'NONE',  ( 15.72974639402176855, 15.80617190586768217, 61.87609039468568284 ) ) ;
#180073 = CARTESIAN_POINT ( 'NONE',  ( 0.05219959533909260263, 19.03943276465977164, 24.99890960531435269 ) ) ;
#180074 = CARTESIAN_POINT ( 'NONE',  ( -0.05219959533936034679, 19.03943276465977164, 62.50109039468566863 ) ) ;
#180075 = CARTESIAN_POINT ( 'NONE',  ( -13.89961937509977652, 13.97604488694528158, 100.6239096053143669 ) ) ;
#180076 = CARTESIAN_POINT ( 'NONE',  ( -19.03943276465977164, 0.05219959533909376836, 86.24890960531436690 ) ) ;
#180077 = CARTESIAN_POINT ( 'NONE',  ( -4.483927247898539470, -16.52544592524342804, 37.29057627198102409 ) ) ;
#180078 = CARTESIAN_POINT ( 'NONE',  ( -10.72451020669898014, 18.67979575497178502, 30.41557627198101699 ) ) ;
#180079 = CARTESIAN_POINT ( 'NONE',  ( 11.40812507854754365, 35.11059874428196537, -1.724999997268813479 ) ) ;
#180080 = CARTESIAN_POINT ( 'NONE',  ( 22.04895058596758517, 22.89469264416797856, -49.28358967601002405 ) ) ;
#180081 = CARTESIAN_POINT ( 'NONE',  ( 16.51473224551083163, -9.474510206698727899, 20.83442372801899722 ) ) ;
#180082 = CARTESIAN_POINT ( 'NONE',  ( -27.86147134968503991, 7.555459793078377118, 161.1037931155424303 ) ) ;
#180083 = CARTESIAN_POINT ( 'NONE',  ( -19.05341960407611168, -5.049401038298163336, 36.45724293864766707 ) ) ;
#180084 = CARTESIAN_POINT ( 'NONE',  ( 5.049401038298161559, -19.05341960407611168, 22.70724293864769194 ) ) ;
#180085 = CARTESIAN_POINT ( 'NONE',  ( -23.48529157249600985, 32.32473071737754111, -4.299999999999999822 ) ) ;
#180086 = CARTESIAN_POINT ( 'NONE',  ( 0.05219959533937995610, -21.53943276465977519, 70.00109039468568994 ) ) ;
#180087 = CARTESIAN_POINT ( 'NONE',  ( 3.765340386950246872E-15, -39.95163481335715971, -1.502157773949822639 ) ) ;
#180088 = CARTESIAN_POINT ( 'NONE',  ( -16.52544592524335698, -4.483927247898792601, 58.95942372801902565 ) ) ;
#180089 = CARTESIAN_POINT ( 'NONE',  ( -21.52544592524343514, 5.823673210054127303, 81.04057627198102409 ) ) ;
#180090 = CARTESIAN_POINT ( 'NONE',  ( 8.224510206698953496, -14.34966873604960469, 47.91557627198102409 ) ) ;
#180092 = CARTESIAN_POINT ( 'NONE',  ( -9.564922557960796823, -16.46253265017161027, 102.0822429386477097 ) ) ;
#180091 = CARTESIAN_POINT ( 'NONE',  ( 9.474510206698971260, -16.51473224551069308, 22.91557627198102765 ) ) ;
#180093 = CARTESIAN_POINT ( 'NONE',  ( -10.72451020669870658, -18.67979575497194134, 29.58442372801901854 ) ) ;
#180094 = CARTESIAN_POINT ( 'NONE',  ( 19.05341960407617918, -5.049401038297876454, 31.04275706135232227 ) ) ;
#180095 = CARTESIAN_POINT ( 'NONE',  ( -5.049401038298153566, 19.05341960407611168, 30.20724293864768839 ) ) ;
#180096 = CARTESIAN_POINT ( 'NONE',  ( -5.823673210054431948, 21.52544592524334988, 87.70942372801901854 ) ) ;
#180097 = DIRECTION ( 'NONE',  ( 0.8437662581494459468, -0.5367108174878556515, 0.000000000000000000 ) ) ;
#180098 = CARTESIAN_POINT ( 'NONE',  ( 4.379528057220339221, -16.55341960407611168, 32.70724293864770260 ) ) ;
#180099 = CARTESIAN_POINT ( 'NONE',  ( -36.91746825000000598, -11.99521256947794789, -3.024999997268813079 ) ) ;
#180100 = CARTESIAN_POINT ( 'NONE',  ( -15.80617190586745835, -15.72974639402198527, 41.87390960531435979 ) ) ;
#180101 = CARTESIAN_POINT ( 'NONE',  ( -12.06949235617756955, 12.14591786802309770, 100.6239096053143811 ) ) ;
#180102 = CARTESIAN_POINT ( 'NONE',  ( 6.613545406318523945, -46.94410406412048786, -22.68594355512400895 ) ) ;
#180103 = CARTESIAN_POINT ( 'NONE',  ( 19.02544592524343514, -5.153800228976328945, 88.54057627198102409 ) ) ;
#180104 = CARTESIAN_POINT ( 'NONE',  ( -14.34966873604960291, -8.224510206698953496, 86.66557627198102409 ) ) ;
#180105 = CARTESIAN_POINT ( 'NONE',  ( -16.51473224551082808, 9.474510206698731452, 103.3344237280190043 ) ) ;
#180106 = CARTESIAN_POINT ( 'NONE',  ( -15.72974639402197994, 15.80617190586746368, 60.62390960531437401 ) ) ;
#180107 = ORIENTED_EDGE ( 'NONE', *, *, #186506, .F. ) ;
#180108 = CARTESIAN_POINT ( 'NONE',  ( 19.05341960407611168, 5.049401038298154454, 38.95724293864767418 ) ) ;
#180110 = CARTESIAN_POINT ( 'NONE',  ( -0.05219959533907301413, -21.53943276465977519, 92.49890960531436690 ) ) ;
#180109 = CARTESIAN_POINT ( 'NONE',  ( -13.89961937509977652, 13.97604488694528158, 85.62390960531433848 ) ) ;
#180112 = CARTESIAN_POINT ( 'NONE',  ( -16.51473224551069308, -9.474510206698971260, 81.66557627198103830 ) ) ;
#180111 = CARTESIAN_POINT ( 'NONE',  ( 4.379528057220092307, 16.55341960407617563, 102.2927570613523613 ) ) ;
#180113 = CARTESIAN_POINT ( 'NONE',  ( 13.97604488694548053, -13.89961937509957401, 80.62609039468567573 ) ) ;
#180114 = CARTESIAN_POINT ( 'NONE',  ( -18.67979575497193778, 10.72451020669871902, 93.33442372801901854 ) ) ;
#180115 = CARTESIAN_POINT ( 'NONE',  ( -21.52544592524343514, 5.823673210054127303, 71.04057627198103830 ) ) ;
#180116 = CARTESIAN_POINT ( 'NONE',  ( 10.72451020669898902, -18.67979575497178502, 37.91557627198102409 ) ) ;
#180117 = CARTESIAN_POINT ( 'NONE',  ( -16.46253265017160317, 9.564922557960807481, 50.83224293864770260 ) ) ;
#180118 = CARTESIAN_POINT ( 'NONE',  ( 8.224510206698953496, -14.34966873604960469, 27.91557627198103830 ) ) ;
#180119 = CARTESIAN_POINT ( 'NONE',  ( -13.97604488694527625, -13.89961937509977652, 66.87390960531436690 ) ) ;
#180120 = ORIENTED_EDGE ( 'NONE', *, *, #103099, .F. ) ;
#180121 = CARTESIAN_POINT ( 'NONE',  ( -31.28611164036841785, -6.519914617504969812, 98.73992561365416520 ) ) ;
#180122 = CARTESIAN_POINT ( 'NONE',  ( -19.05341960407617563, 5.049401038297882671, 28.54275706135232937 ) ) ;
#180123 = CARTESIAN_POINT ( 'NONE',  ( 12.06949235617757843, -12.14591786802309237, 78.12390960531436690 ) ) ;
#180124 = CARTESIAN_POINT ( 'NONE',  ( 10.81492255796106328, -18.62759615963255655, 20.41775706135234714 ) ) ;
#180125 = CARTESIAN_POINT ( 'NONE',  ( 8.571926809382597767, 26.38167802310806209, 146.7750000027311899 ) ) ;
#180126 = CARTESIAN_POINT ( 'NONE',  ( 10.72451020669898902, -18.67979575497178502, 57.91557627198103120 ) ) ;
#180127 = CARTESIAN_POINT ( 'NONE',  ( 14.29746914071037800, 8.314922557961029526, 91.66775706135234714 ) ) ;
#180128 = CARTESIAN_POINT ( 'NONE',  ( 14.34966873604960469, 8.224510206698951720, 104.1655762719810241 ) ) ;
#180129 = CARTESIAN_POINT ( 'NONE',  ( 9.564922557960805705, 16.46253265017160317, 69.58224293864770971 ) ) ;
#180130 = CARTESIAN_POINT ( 'NONE',  ( -8.314922557960811034, -14.29746914071050412, 27.08224293864769550 ) ) ;
#180131 = CARTESIAN_POINT ( 'NONE',  ( 5.719274019375673035, 21.55341960407619339, 52.29275706135236135 ) ) ;
#180132 = CARTESIAN_POINT ( 'NONE',  ( 19.03943276465977164, -0.05219959533909143690, 113.7489096053143669 ) ) ;
#180133 = CARTESIAN_POINT ( 'NONE',  ( -21.52544592524334988, -5.823673210054445271, 78.95942372801901854 ) ) ;
#180134 = CARTESIAN_POINT ( 'NONE',  ( -16.46253265017160317, 9.564922557960807481, 35.83224293864768839 ) ) ;
#180135 = CARTESIAN_POINT ( 'NONE',  ( -9.564922557960796823, -16.46253265017161027, 32.08224293864769550 ) ) ;
#180136 = ORIENTED_EDGE ( 'NONE', *, *, #119131, .F. ) ;
#180137 = CARTESIAN_POINT ( 'NONE',  ( 0.05219959533937995610, -21.53943276465977519, 100.0010903946857042 ) ) ;
#180138 = CARTESIAN_POINT ( 'NONE',  ( 0.05219959533934541429, -16.53943276465976808, 45.00109039468568284 ) ) ;
#180139 = CARTESIAN_POINT ( 'NONE',  ( 15.72974639402176855, 15.80617190586768217, 76.87609039468567573 ) ) ;
#180140 = CARTESIAN_POINT ( 'NONE',  ( 19.03943276465977164, -0.05219959533909143690, 98.74890960531436690 ) ) ;
#180141 = CARTESIAN_POINT ( 'NONE',  ( 16.51473224551083163, -9.474510206698727899, 80.83442372801899012 ) ) ;
#180142 = CARTESIAN_POINT ( 'NONE',  ( 18.67979575497194134, -10.72451020669871369, 60.83442372801901854 ) ) ;
#180143 = CARTESIAN_POINT ( 'NONE',  ( -16.53943276465976808, -0.05219959533934237506, 23.75109039468567929 ) ) ;
#180144 = CARTESIAN_POINT ( 'NONE',  ( 5.049401038297881783, 19.05341960407617563, 82.29275706135229029 ) ) ;
#180145 = CARTESIAN_POINT ( 'NONE',  ( -16.46253265017160317, 9.564922557960807481, 45.83224293864769550 ) ) ;
#180146 = CARTESIAN_POINT ( 'NONE',  ( -9.564922557961040184, 16.46253265017147172, 92.91775706135233293 ) ) ;
#180147 = VECTOR ( 'NONE', #179368, 1000.000000000000000 ) ;
#180148 = CARTESIAN_POINT ( 'NONE',  ( 4.379528057220339221, -16.55341960407611168, 27.70724293864769905 ) ) ;
#180149 = CARTESIAN_POINT ( 'NONE',  ( -13.97604488694547697, 13.89961937509957934, 83.12609039468564731 ) ) ;
#180150 = CARTESIAN_POINT ( 'NONE',  ( -4.379528057220328563, 16.55341960407611168, 45.20724293864769550 ) ) ;
#180151 = CARTESIAN_POINT ( 'NONE',  ( 9.564922557961047289, -16.46253265017146816, 70.41775706135233293 ) ) ;
#180152 = CARTESIAN_POINT ( 'NONE',  ( 14.34966873604972726, -8.224510206698740333, 45.83442372801901854 ) ) ;
#180153 = CARTESIAN_POINT ( 'NONE',  ( -13.89961937509957401, -13.97604488694547875, 29.37609039468565797 ) ) ;
#180154 = CARTESIAN_POINT ( 'NONE',  ( 9.474510206698971260, -16.51473224551069308, 27.91557627198103120 ) ) ;
#180155 = CARTESIAN_POINT ( 'NONE',  ( 16.51473224551069308, 9.474510206698969483, 39.16557627198103120 ) ) ;
#180156 = CARTESIAN_POINT ( 'NONE',  ( -14.29746914071037622, -8.314922557961029526, 44.16775706135234714 ) ) ;
#180157 = CARTESIAN_POINT ( 'NONE',  ( -8.906447517083060816, 27.41122689804195645, 139.8500000054623911 ) ) ;
#180158 = CARTESIAN_POINT ( 'NONE',  ( 8.571926809382603096, -26.38167802310801235, 147.4750000027311785 ) ) ;
#180159 = CARTESIAN_POINT ( 'NONE',  ( 16.46253265017160672, -9.564922557960803928, 88.33224293864769550 ) ) ;
#180160 = EDGE_LOOP ( 'NONE', ( #172268, #134882, #95295, #48246, #161907, #114441 ) ) ;
#180161 = CARTESIAN_POINT ( 'NONE',  ( -5.153800228976607833, 19.02544592524334988, 97.70942372801900433 ) ) ;
#180162 = CARTESIAN_POINT ( 'NONE',  ( -10.81492255796078084, -18.62759615963271287, 32.08224293864769550 ) ) ;
#180164 = CARTESIAN_POINT ( 'NONE',  ( 19.02544592524334988, 5.153800228976608722, 106.4594237280190185 ) ) ;
#180163 = CARTESIAN_POINT ( 'NONE',  ( 13.89961937509957401, 13.97604488694547697, 36.87609039468565442 ) ) ;
#180165 = CARTESIAN_POINT ( 'NONE',  ( -16.52544592524342804, 4.483927247898546575, 106.0405762719810525 ) ) ;
#180166 = B_SPLINE_CURVE_WITH_KNOTS ( 'NONE', 3,
 ( #159073, #156103, #187466, #123758, #155113, #109600, #32771, #141917, #31778, #157103, #3408, #78254, #79260, #124774, #48935, #138941, #108607, #94423, #126742, #173273, #111588, #189443, #96406, #50920, #33759, #421, #140932, #64098, #139927, #125766, #112578, #1416 ),
 .UNSPECIFIED., .F., .F.,
 ( 4, 2, 2, 2, 2, 2, 2, 2, 2, 2, 2, 2, 2, 2, 2, 4 ),
 ( 2.711112516444420852E-17, 0.0003712461730036983247, 0.0007424923460073695443, 0.001113738519011040710, 0.001484984692014711984, 0.002227477038022072746, 0.002598723211025739249, 0.002969969384029405319, 0.003341215557033071389, 0.003712461730036737025, 0.004083707903040402661, 0.004454954076044068297, 0.004826200249047734800, 0.005197446422051400436, 0.005568692595055066939, 0.005939938768058731708 ),
 .UNSPECIFIED. ) ;
#180167 = CARTESIAN_POINT ( 'NONE',  ( -19.02544592524342804, 5.153800228976336051, 41.04057627198103120 ) ) ;
#180168 = CARTESIAN_POINT ( 'NONE',  ( -21.55341960407610458, -5.719274019375992779, 71.45724293864769550 ) ) ;
#180169 = CARTESIAN_POINT ( 'NONE',  ( 19.05341960407611168, 5.049401038298154454, 33.95724293864769550 ) ) ;
#180170 = CARTESIAN_POINT ( 'NONE',  ( -28.82186960331499037, 2.428612866367529932E-14, 142.2500000054623683 ) ) ;
#180171 = CARTESIAN_POINT ( 'NONE',  ( -5.049401038297874678, -19.05341960407617918, 69.79275706135233293 ) ) ;
#180173 = VECTOR ( 'NONE', #36176, 1000.000000000000114 ) ;
#180172 = CARTESIAN_POINT ( 'NONE',  ( 12.06949235617757843, -12.14591786802309237, 58.12390960531435979 ) ) ;
#180174 = CARTESIAN_POINT ( 'NONE',  ( 18.67979575497178502, 10.72451020669898547, 34.16557627198102409 ) ) ;
#180175 = CARTESIAN_POINT ( 'NONE',  ( -5.719274019375665041, -21.55341960407619695, 99.79275706135234714 ) ) ;
#180176 = CARTESIAN_POINT ( 'NONE',  ( 15.72974639402199770, -15.80617190586745480, 78.12390960531436690 ) ) ;
#180177 = CARTESIAN_POINT ( 'NONE',  ( 18.62759615963255655, 10.81492255796105972, 71.66775706135234714 ) ) ;
#180178 = CARTESIAN_POINT ( 'NONE',  ( -21.52544592524334988, -5.823673210054445271, 58.95942372801902565 ) ) ;
#180179 = CARTESIAN_POINT ( 'NONE',  ( 5.049401038298161559, -19.05341960407611168, 92.70724293864769550 ) ) ;
#180181 = CARTESIAN_POINT ( 'NONE',  ( -10.72451020669870658, -18.67979575497194134, 69.58442372801900433 ) ) ;
#180180 = CARTESIAN_POINT ( 'NONE',  ( 12.06949235617739724, 12.14591786802326823, 101.8760903946857042 ) ) ;
#180182 = CARTESIAN_POINT ( 'NONE',  ( -5.153800228976328057, -19.02544592524343514, 52.29057627198100988 ) ) ;
#180183 = CARTESIAN_POINT ( 'NONE',  ( -5.719274019375665041, -21.55341960407619695, 34.79275706135235424 ) ) ;
#180184 = CARTESIAN_POINT ( 'NONE',  ( 19.02544592524343514, -5.153800228976328945, 63.54057627198103830 ) ) ;
#180185 = CARTESIAN_POINT ( 'NONE',  ( -14.34966873604960291, -8.224510206698953496, 76.66557627198103830 ) ) ;
#180186 = CARTESIAN_POINT ( 'NONE',  ( -0.05219959533910754901, -16.53943276465976808, 52.49890960531435979 ) ) ;
#180187 = CARTESIAN_POINT ( 'NONE',  ( -5.719274019375978568, 21.55341960407610458, 55.20724293864770260 ) ) ;
#180188 = CARTESIAN_POINT ( 'NONE',  ( 5.049401038298161559, -19.05341960407611168, 42.70724293864767418 ) ) ;
#180189 = CARTESIAN_POINT ( 'NONE',  ( 21.55341960407610458, 5.719274019375980345, 58.95724293864770971 ) ) ;
#180190 = CARTESIAN_POINT ( 'NONE',  ( -5.153800228976607833, 19.02544592524334988, 52.70942372801900433 ) ) ;
#180192 = CARTESIAN_POINT ( 'NONE',  ( 16.55341960407611168, 4.379528057220329451, 58.95724293864770971 ) ) ;
#180191 = CARTESIAN_POINT ( 'NONE',  ( -1.784589286804288299, -7.284589286804248331, 8.181980515339454030 ) ) ;
#180193 = CARTESIAN_POINT ( 'NONE',  ( 10.72451020669898902, -18.67979575497178502, 37.91557627198102409 ) ) ;
#180194 = ORIENTED_EDGE ( 'NONE', *, *, #176519, .F. ) ;
#180195 = CARTESIAN_POINT ( 'NONE',  ( 17.12812012977026654, 6.668231424565988164, 103.8594875932314068 ) ) ;
#180197 = CARTESIAN_POINT ( 'NONE',  ( -27.73933785331498925, -9.013057229001049109, 141.4750000027312069 ) ) ;
#180196 = CARTESIAN_POINT ( 'NONE',  ( 8.224510206698742110, 14.34966873604972548, 82.08442372801901854 ) ) ;
#180198 = CARTESIAN_POINT ( 'NONE',  ( -9.564922557961040184, 16.46253265017147172, 92.91775706135233293 ) ) ;
#180199 = CARTESIAN_POINT ( 'NONE',  ( -12.06949235617756955, 12.14591786802309770, 60.62390960531437401 ) ) ;
#180200 = DIRECTION ( 'NONE',  ( 0.000000000000000000, 0.000000000000000000, -1.000000000000000000 ) ) ;
#180201 = CARTESIAN_POINT ( 'NONE',  ( 0.05219959533909260263, 19.03943276465977164, 44.99890960531435979 ) ) ;
#180202 = CARTESIAN_POINT ( 'NONE',  ( 12.14591786802309770, 12.06949235617756955, 44.37390960531435979 ) ) ;
#180203 = CARTESIAN_POINT ( 'NONE',  ( -0.05219959533909027116, -19.03943276465977164, 87.49890960531436690 ) ) ;
#180204 = CARTESIAN_POINT ( 'NONE',  ( 9.474510206698971260, -16.51473224551069308, 52.91557627198102409 ) ) ;
#180205 = CARTESIAN_POINT ( 'NONE',  ( 18.62759615963255655, 10.81492255796105972, 61.66775706135235424 ) ) ;
#180206 = CARTESIAN_POINT ( 'NONE',  ( -16.46253265017160317, 9.564922557960807481, 70.83224293864770971 ) ) ;
#180207 = CARTESIAN_POINT ( 'NONE',  ( 19.05341960407611168, 5.049401038298154454, 23.95724293864769194 ) ) ;
#180208 = CARTESIAN_POINT ( 'NONE',  ( 5.153800228976335163, 19.02544592524342804, 64.79057627198100988 ) ) ;
#180209 = CARTESIAN_POINT ( 'NONE',  ( 18.67979575497178502, 10.72451020669898547, 54.16557627198103120 ) ) ;
#180210 = CARTESIAN_POINT ( 'NONE',  ( -5.153800228976328057, -19.02544592524343514, 42.29057627198101699 ) ) ;
#180211 = CARTESIAN_POINT ( 'NONE',  ( -5.719274019375978568, 21.55341960407610458, 40.20724293864769550 ) ) ;
#180212 = CARTESIAN_POINT ( 'NONE',  ( 16.52544592524335698, 4.483927247898782831, 101.4594237280190185 ) ) ;
#180213 = CARTESIAN_POINT ( 'NONE',  ( -9.564922557961040184, 16.46253265017147172, 22.91775706135233648 ) ) ;
#180215 = CARTESIAN_POINT ( 'NONE',  ( 16.53943276465976808, 0.05219959533934440121, 76.25109039468568994 ) ) ;
#180214 = CARTESIAN_POINT ( 'NONE',  ( -12.14591786802326823, 12.06949235617739902, 53.12609039468568284 ) ) ;
#180216 = CARTESIAN_POINT ( 'NONE',  ( -18.10062525802553424, 5.500000000000031974, 68.51383468041923663 ) ) ;
#180217 = CARTESIAN_POINT ( 'NONE',  ( -14.29746914071037622, -8.314922557961029526, 74.16775706135231871 ) ) ;
#180218 = CARTESIAN_POINT ( 'NONE',  ( 14.29746914071037800, 8.314922557961029526, 51.66775706135234714 ) ) ;
#180219 = CARTESIAN_POINT ( 'NONE',  ( 16.51473224551069308, 9.474510206698969483, 104.1655762719810241 ) ) ;
#180220 = CARTESIAN_POINT ( 'NONE',  ( 5.153800228976335163, 19.02544592524342804, 29.79057627198102409 ) ) ;
#180221 = CARTESIAN_POINT ( 'NONE',  ( -0.05219959533934338120, 16.53943276465976808, 37.50109039468568284 ) ) ;
#180222 = CARTESIAN_POINT ( 'NONE',  ( -13.97604488694527625, -13.89961937509977652, 51.87390960531436690 ) ) ;
#180223 = CARTESIAN_POINT ( 'NONE',  ( 15.72974639402176855, 15.80617190586768217, 21.87609039468567573 ) ) ;
#180224 = CARTESIAN_POINT ( 'NONE',  ( 0.05219959533934541429, -16.53943276465976808, 35.00109039468568284 ) ) ;
#180225 = CARTESIAN_POINT ( 'NONE',  ( 4.483927247898790824, -16.52544592524335698, 100.2094237280190043 ) ) ;
#180226 = CARTESIAN_POINT ( 'NONE',  ( -17.50000000000001421, -5.499999999999944045, 71.28230962303567253 ) ) ;
#180227 = CARTESIAN_POINT ( 'NONE',  ( 21.52544592524334988, 5.823673210054432836, 101.4594237280190185 ) ) ;
#180229 = EDGE_CURVE ( 'NONE', #193812, #134824, #10170, .T. ) ;
#180228 = CARTESIAN_POINT ( 'NONE',  ( -0.05219959533936034679, 19.03943276465977164, 102.5010903946856757 ) ) ;
#180230 = CARTESIAN_POINT ( 'NONE',  ( -0.05219959533910754901, -16.53943276465976808, 52.49890960531435979 ) ) ;
#180231 = CARTESIAN_POINT ( 'NONE',  ( 19.03943276465977164, -0.05219959533909143690, 28.74890960531435624 ) ) ;
#180233 = CARTESIAN_POINT ( 'NONE',  ( 16.38665767534995865, -7.295008042176402085, 57.76400864214468811 ) ) ;
#180232 = CARTESIAN_POINT ( 'NONE',  ( 19.03943276465977164, 0.05219959533936151252, 66.25109039468567573 ) ) ;
#180234 = CARTESIAN_POINT ( 'NONE',  ( -10.81492255796105439, 18.62759615963255655, 67.91775706135234714 ) ) ;
#180235 = CARTESIAN_POINT ( 'NONE',  ( 4.483927247898790824, -16.52544592524335698, 25.20942372801901854 ) ) ;
#180236 = DIRECTION ( 'NONE',  ( 0.7071067811865483499, 0.000000000000000000, -0.7071067811865465735 ) ) ;
#180237 = CARTESIAN_POINT ( 'NONE',  ( 15.80617190586746368, 15.72974639402197994, 29.37390960531435269 ) ) ;
#180238 = CARTESIAN_POINT ( 'NONE',  ( -5.153800228976607833, 19.02544592524334988, 112.7094237280190043 ) ) ;
#180239 = CARTESIAN_POINT ( 'NONE',  ( 17.60728821186568638, -5.500000000000035527, 98.36690927743006796 ) ) ;
#180240 = CARTESIAN_POINT ( 'NONE',  ( -24.05407591190764549, 13.01182159662891635, 169.7785964492052244 ) ) ;
#180241 = CARTESIAN_POINT ( 'NONE',  ( 9.564922557960805705, 16.46253265017160317, 24.58224293864769194 ) ) ;
#180242 = CARTESIAN_POINT ( 'NONE',  ( 15.72974639402176855, 15.80617190586768217, 101.8760903946857042 ) ) ;
#180243 = CARTESIAN_POINT ( 'NONE',  ( -9.564922557960796823, -16.46253265017161027, 37.08224293864768839 ) ) ;
#180244 = CARTESIAN_POINT ( 'NONE',  ( -10.81492255796105439, 18.62759615963255655, 57.91775706135234714 ) ) ;
#180245 = CARTESIAN_POINT ( 'NONE',  ( -18.67979575497193778, 10.72451020669871902, 108.3344237280190185 ) ) ;
#180246 = CARTESIAN_POINT ( 'NONE',  ( -4.483927247898782831, 16.52544592524335698, 97.70942372801904696 ) ) ;
#180247 = CARTESIAN_POINT ( 'NONE',  ( 5.049401038298161559, -19.05341960407611168, 72.70724293864768129 ) ) ;
#180248 = CARTESIAN_POINT ( 'NONE',  ( 10.81492255796106328, -18.62759615963255655, 50.41775706135235424 ) ) ;
#180249 = CARTESIAN_POINT ( 'NONE',  ( 21.52544592524334988, 5.823673210054432836, 51.45942372801901854 ) ) ;
#180251 = CARTESIAN_POINT ( 'NONE',  ( -5.153800228976328057, -19.02544592524343514, 92.29057627198099567 ) ) ;
#180250 = CARTESIAN_POINT ( 'NONE',  ( -9.474510206698720793, -16.51473224551083518, 79.58442372801899012 ) ) ;
#180252 = CARTESIAN_POINT ( 'NONE',  ( -8.224510206698948167, 14.34966873604960824, 115.4155762719810241 ) ) ;
#180253 = CARTESIAN_POINT ( 'NONE',  ( -15.80617190586745835, -15.72974639402198527, 91.87390960531436690 ) ) ;
#180254 = CARTESIAN_POINT ( 'NONE',  ( 10.72451020669871369, 18.67979575497193778, 112.0844237280190185 ) ) ;
#180255 = CARTESIAN_POINT ( 'NONE',  ( 12.06949235617757843, -12.14591786802309237, 93.12390960531436690 ) ) ;
#180256 = CARTESIAN_POINT ( 'NONE',  ( -16.51473224551069308, -9.474510206698971260, 51.66557627198102409 ) ) ;
#180257 = CARTESIAN_POINT ( 'NONE',  ( -13.89961937509957401, -13.97604488694547875, 84.37609039468567573 ) ) ;
#180258 = CARTESIAN_POINT ( 'NONE',  ( -14.29746914071049879, 8.314922557960819915, 55.83224293864770260 ) ) ;
#180259 = CARTESIAN_POINT ( 'NONE',  ( -13.89961937509957401, -13.97604488694547875, 19.37609039468566507 ) ) ;
#180260 = CARTESIAN_POINT ( 'NONE',  ( -13.97604488694527625, -13.89961937509977652, 111.8739096053143243 ) ) ;
#180261 = CARTESIAN_POINT ( 'NONE',  ( 9.564922557961047289, -16.46253265017146816, 75.41775706135234714 ) ) ;
#180262 = CARTESIAN_POINT ( 'NONE',  ( 10.72451020669898902, -18.67979575497178502, 72.91557627198103830 ) ) ;
#180263 = CARTESIAN_POINT ( 'NONE',  ( 18.62759615963255655, 10.81492255796105972, 31.66775706135234358 ) ) ;
#180264 = CARTESIAN_POINT ( 'NONE',  ( 14.29746914071037800, 8.314922557961029526, 31.66775706135234358 ) ) ;
#180265 = CARTESIAN_POINT ( 'NONE',  ( -16.52544592524335698, -4.483927247898792601, 93.95942372801903275 ) ) ;
#180267 = CARTESIAN_POINT ( 'NONE',  ( 18.62759615963255655, 10.81492255796105972, 41.66775706135235424 ) ) ;
#180266 = CARTESIAN_POINT ( 'NONE',  ( -17.49999999999999645, -7.500000000000000888, 102.5000000000000142 ) ) ;
#180268 = CARTESIAN_POINT ( 'NONE',  ( -0.05219959533907301413, -21.53943276465977519, 37.49890960531436690 ) ) ;
#180269 = CARTESIAN_POINT ( 'NONE',  ( 16.51473224551069308, 9.474510206698969483, 39.16557627198103120 ) ) ;
#180270 = CARTESIAN_POINT ( 'NONE',  ( 11.40812507854755253, -35.11059874428192273, -2.524999997268813523 ) ) ;
#180271 = CARTESIAN_POINT ( 'NONE',  ( 4.379528057220092307, 16.55341960407617563, 57.29275706135234714 ) ) ;
#180272 = CARTESIAN_POINT ( 'NONE',  ( -16.52544592524342804, 4.483927247898546575, 96.04057627198102409 ) ) ;
#180273 = CARTESIAN_POINT ( 'NONE',  ( 5.823673210054125526, 21.52544592524343514, 89.79057627198103830 ) ) ;
#180274 = CARTESIAN_POINT ( 'NONE',  ( -14.34966873604960291, -8.224510206698953496, 26.66557627198103475 ) ) ;
#180275 = CARTESIAN_POINT ( 'NONE',  ( -16.55341960407617563, 4.379528057220093196, 53.54275706135234714 ) ) ;
#180276 = CARTESIAN_POINT ( 'NONE',  ( 5.153800228976335163, 19.02544592524342804, 64.79057627198100988 ) ) ;
#180277 = CARTESIAN_POINT ( 'NONE',  ( -16.53943276465976808, -0.05219959533934237506, 93.75109039468567573 ) ) ;
#180278 = CARTESIAN_POINT ( 'NONE',  ( 19.05341960407617918, -5.049401038297876454, 86.04275706135233293 ) ) ;
#180279 = CARTESIAN_POINT ( 'NONE',  ( -15.80617190586745835, -15.72974639402198527, 86.87390960531438111 ) ) ;
#180280 = CARTESIAN_POINT ( 'NONE',  ( -14.34966873604960291, -8.224510206698953496, 21.66557627198102409 ) ) ;
#180281 = ORIENTED_EDGE ( 'NONE', *, *, #91586, .F. ) ;
#180282 = CARTESIAN_POINT ( 'NONE',  ( 21.96844466259091533, 8.667631922777363940, 171.6690673070886533 ) ) ;
#180283 = CARTESIAN_POINT ( 'NONE',  ( -0.05219959533907301413, -21.53943276465977519, 67.49890960531436690 ) ) ;
#180284 = ORIENTED_EDGE ( 'NONE', *, *, #97731, .T. ) ;
#180285 = CARTESIAN_POINT ( 'NONE',  ( -12.06949235617739369, -12.14591786802326823, 94.37609039468568994 ) ) ;
#180286 = EDGE_LOOP ( 'NONE', ( #39358, #101215, #137261, #115462 ) ) ;
#180287 = CARTESIAN_POINT ( 'NONE',  ( 0.05219959533907565091, 21.53943276465977519, 24.99890960531435624 ) ) ;
#180288 = LINE ( 'NONE', #54913, #46953 ) ;
#180289 = CARTESIAN_POINT ( 'NONE',  ( 5.719274019375991003, -21.55341960407610458, 87.70724293864769550 ) ) ;
#180290 = CARTESIAN_POINT ( 'NONE',  ( 4.379528057220339221, -16.55341960407611168, 27.70724293864769905 ) ) ;
#180291 = CARTESIAN_POINT ( 'NONE',  ( 16.55341960407618274, -4.379528057220086978, 41.04275706135236135 ) ) ;
#180292 = CARTESIAN_POINT ( 'NONE',  ( 19.05341960407611168, 5.049401038298154454, 33.95724293864769550 ) ) ;
#180293 = CARTESIAN_POINT ( 'NONE',  ( 0.05219959533934541429, -16.53943276465976808, 25.00109039468567218 ) ) ;
#180294 = CARTESIAN_POINT ( 'NONE',  ( -5.049401038298153566, 19.05341960407611168, 50.20724293864770260 ) ) ;
#180295 = CARTESIAN_POINT ( 'NONE',  ( -5.429308488886486681E-15, 30.30510711980690175, 149.5000000000000000 ) ) ;
#180296 = CARTESIAN_POINT ( 'NONE',  ( -13.89961937509977652, 13.97604488694528158, 105.6239096053143527 ) ) ;
#180297 = CARTESIAN_POINT ( 'NONE',  ( 17.72662750342724891, 5.500000000000081712, 78.90179492283748175 ) ) ;
#180298 = CARTESIAN_POINT ( 'NONE',  ( 0.05219959533934541429, -16.53943276465976808, 100.0010903946857042 ) ) ;
#180299 = CARTESIAN_POINT ( 'NONE',  ( 19.05341960407617918, -5.049401038297876454, 96.04275706135231871 ) ) ;
#180300 = CARTESIAN_POINT ( 'NONE',  ( -16.51473224551082808, 9.474510206698731452, 38.33442372801899722 ) ) ;
#180301 = CARTESIAN_POINT ( 'NONE',  ( -21.55341960407610458, -5.719274019375992779, 76.45724293864769550 ) ) ;
#180302 = CARTESIAN_POINT ( 'NONE',  ( -14.34966873604972548, 8.224510206698743886, 103.3344237280190043 ) ) ;
#180303 = CARTESIAN_POINT ( 'NONE',  ( -21.53943276465977519, 0.05219959533907696930, 26.24890960531435624 ) ) ;
#180304 = CARTESIAN_POINT ( 'NONE',  ( -13.89961937509957401, -13.97604488694547875, 109.3760903946856331 ) ) ;
#180305 = CARTESIAN_POINT ( 'NONE',  ( 19.02544592524343514, -5.153800228976328945, 108.5405762719810383 ) ) ;
#180306 = CARTESIAN_POINT ( 'NONE',  ( -15.72974639402176322, -15.80617190586768395, 59.37609039468568284 ) ) ;
#180307 = CARTESIAN_POINT ( 'NONE',  ( -16.46253265017160317, 9.564922557960807481, 60.83224293864769550 ) ) ;
#180308 = CARTESIAN_POINT ( 'NONE',  ( 14.34966873604960469, 8.224510206698951720, 99.16557627198100988 ) ) ;
#180309 = CARTESIAN_POINT ( 'NONE',  ( 32.36630342937671401, 3.758454152357569633, 88.50505952879542804 ) ) ;
#180310 = CARTESIAN_POINT ( 'NONE',  ( 16.53943276465976808, -0.05219959533910856209, 83.74890960531435269 ) ) ;
#180311 = CARTESIAN_POINT ( 'NONE',  ( -21.52544592524343514, 5.823673210054127303, 76.04057627198102409 ) ) ;
#180312 = ORIENTED_EDGE ( 'NONE', *, *, #91138, .T. ) ;
#180313 = CARTESIAN_POINT ( 'NONE',  ( -5.153800228976607833, 19.02544592524334988, 97.70942372801900433 ) ) ;
#180314 = CARTESIAN_POINT ( 'NONE',  ( 19.01529144963337359, 5.500000000000033751, 93.73431955728439391 ) ) ;
#180315 = CARTESIAN_POINT ( 'NONE',  ( -13.97604488694527625, -13.89961937509977652, 56.87390960531434558 ) ) ;
#180316 = CARTESIAN_POINT ( 'NONE',  ( 17.26058549869104652, -6.457015423128295240, 71.12254162523932166 ) ) ;
#180318 = CARTESIAN_POINT ( 'NONE',  ( 13.97604488694527802, 13.89961937509977652, 89.37390960531436690 ) ) ;
#180317 = CARTESIAN_POINT ( 'NONE',  ( -16.51473224551069308, -9.474510206698971260, 81.66557627198103830 ) ) ;
#180319 = CARTESIAN_POINT ( 'NONE',  ( 8.224510206698742110, 14.34966873604972548, 67.08442372801901854 ) ) ;
#180320 = CARTESIAN_POINT ( 'NONE',  ( -16.81555441253550853, -7.025013491695501600, 49.36314554665745646 ) ) ;
#180321 = CARTESIAN_POINT ( 'NONE',  ( 5.049401038297881783, 19.05341960407617563, 37.29275706135232582 ) ) ;
#180322 = CARTESIAN_POINT ( 'NONE',  ( 17.62203461105333702, -16.12203461105326951, -57.08650645001478097 ) ) ;
#180323 = CARTESIAN_POINT ( 'NONE',  ( -19.03943276465977164, 0.05219959533909376836, 106.2489096053143669 ) ) ;
#180324 = CARTESIAN_POINT ( 'NONE',  ( -0.05219959533934338120, 16.53943276465976808, 107.5010903946856899 ) ) ;
#180325 = CARTESIAN_POINT ( 'NONE',  ( -18.22780087662124160, -5.499999999999927169, 73.98236817873106475 ) ) ;
#180326 = CARTESIAN_POINT ( 'NONE',  ( -12.06949235617739369, -12.14591786802326823, 94.37609039468568994 ) ) ;
#180327 = CARTESIAN_POINT ( 'NONE',  ( -16.31925111598457434, 7.325300261831451110, 30.16424538967251578 ) ) ;
#180328 = CARTESIAN_POINT ( 'NONE',  ( 4.379528057220092307, 16.55341960407617563, 67.29275706135234714 ) ) ;
#180329 = DIRECTION ( 'NONE',  ( 0.000000000000000000, 0.000000000000000000, 1.000000000000000000 ) ) ;
#180330 = CARTESIAN_POINT ( 'NONE',  ( 5.823673210054444382, -21.52544592524334988, 70.20942372801904696 ) ) ;
#180331 = CARTESIAN_POINT ( 'NONE',  ( -9.564922557961040184, 16.46253265017147172, 82.91775706135233293 ) ) ;
#180332 = CARTESIAN_POINT ( 'NONE',  ( -19.05341960407617563, 5.049401038297882671, 28.54275706135232937 ) ) ;
#180333 = CARTESIAN_POINT ( 'NONE',  ( -5.049401038298153566, 19.05341960407611168, 70.20724293864769550 ) ) ;
#180334 = CARTESIAN_POINT ( 'NONE',  ( -9.474510206698964154, 16.51473224551069663, 50.41557627198102409 ) ) ;
#180335 = CARTESIAN_POINT ( 'NONE',  ( -7.500000000000000000, 0.000000000000000000, 5.707106781186540800 ) ) ;
#180336 = CARTESIAN_POINT ( 'NONE',  ( 5.719274019375991003, -21.55341960407610458, 87.70724293864769550 ) ) ;
#180337 = CARTESIAN_POINT ( 'NONE',  ( -21.53943276465977519, 0.05219959533907696930, 41.24890960531435269 ) ) ;
#180338 = CARTESIAN_POINT ( 'NONE',  ( 16.46253265017160672, -9.564922557960803928, 28.33224293864769550 ) ) ;
#180339 = CARTESIAN_POINT ( 'NONE',  ( -14.34966873604972548, 8.224510206698743886, 53.33442372801901854 ) ) ;
#180340 = VERTEX_POINT ( 'NONE', #52658 ) ;
#180341 = CARTESIAN_POINT ( 'NONE',  ( -10.72451020669870658, -18.67979575497194134, 29.58442372801901854 ) ) ;
#180343 = CARTESIAN_POINT ( 'NONE',  ( -36.91746825000001309, -11.99521256947794789, -10.52499999726881441 ) ) ;
#180342 = CARTESIAN_POINT ( 'NONE',  ( 0.05219959533910956823, 16.53943276465976808, 54.99890960531435269 ) ) ;
#180344 = CARTESIAN_POINT ( 'NONE',  ( -12.14591786802326823, 12.06949235617739902, 28.12609039468568284 ) ) ;
#180345 = CARTESIAN_POINT ( 'NONE',  ( 13.97604488694548053, -13.89961937509957401, 45.62609039468566863 ) ) ;
#180346 = CARTESIAN_POINT ( 'NONE',  ( 14.29746914071049879, -8.314922557960816363, 58.33224293864768839 ) ) ;
#180347 = CARTESIAN_POINT ( 'NONE',  ( -15.80617190586745835, -15.72974639402198527, 111.8739096053143669 ) ) ;
#180349 = CARTESIAN_POINT ( 'NONE',  ( -21.53943276465977519, 0.05219959533907696930, 81.24890960531436690 ) ) ;
#180348 = CARTESIAN_POINT ( 'NONE',  ( 0.000000000000000000, 0.000000000000000000, 0.000000000000000000 ) ) ;
#180350 = CARTESIAN_POINT ( 'NONE',  ( -19.05341960407611168, -5.049401038298163336, 91.45724293864766707 ) ) ;
#180351 = CARTESIAN_POINT ( 'NONE',  ( 0.05219959533910956823, 16.53943276465976808, 59.99890960531436690 ) ) ;
#180352 = CARTESIAN_POINT ( 'NONE',  ( -5.153800228976328057, -19.02544592524343514, 102.2905762719810383 ) ) ;
#180353 = CARTESIAN_POINT ( 'NONE',  ( -37.52489844900624405, 1.772207303729224970, 39.79021962610335095 ) ) ;
#180354 = CARTESIAN_POINT ( 'NONE',  ( 13.97604488694548053, -13.89961937509957401, 65.62609039468567573 ) ) ;
#180355 = CARTESIAN_POINT ( 'NONE',  ( 18.67979575497178502, 10.72451020669898547, 109.1655762719810383 ) ) ;
#180356 = CARTESIAN_POINT ( 'NONE',  ( 13.97604488694527802, 13.89961937509977652, 54.37390960531435979 ) ) ;
#180357 = CARTESIAN_POINT ( 'NONE',  ( 19.02544592524334988, 5.153800228976608722, 46.45942372801899012 ) ) ;
#180358 = CARTESIAN_POINT ( 'NONE',  ( 4.379528057220339221, -16.55341960407611168, 107.7072429386476955 ) ) ;
#180359 = ADVANCED_FACE ( 'NONE', ( #133499 ), #176023, .F. ) ;
#180360 = CARTESIAN_POINT ( 'NONE',  ( -10.72451020669870658, -18.67979575497194134, 59.58442372801901854 ) ) ;
#180361 = CARTESIAN_POINT ( 'NONE',  ( -17.40861289039004234, -6.110651285853239578, 71.37232470827430575 ) ) ;
#180362 = CARTESIAN_POINT ( 'NONE',  ( -12.06949235617756955, 12.14591786802309770, 45.62390960531436690 ) ) ;
#180363 = CARTESIAN_POINT ( 'NONE',  ( -5.049401038298153566, 19.05341960407611168, 55.20724293864769550 ) ) ;
#180364 = CARTESIAN_POINT ( 'NONE',  ( -21.52544592524343514, 5.823673210054127303, 76.04057627198102409 ) ) ;
#180365 = CARTESIAN_POINT ( 'NONE',  ( 27.73933785331498925, -9.013057229001033122, 145.7750000027311899 ) ) ;
#180366 = CARTESIAN_POINT ( 'NONE',  ( -9.564922557960796823, -16.46253265017161027, 42.08224293864769550 ) ) ;
#180367 = EDGE_LOOP ( 'NONE', ( #177002, #182312, #47767 ) ) ;
#180368 = CARTESIAN_POINT ( 'NONE',  ( -15.80617190586745835, -15.72974639402198527, 66.87390960531436690 ) ) ;
#180369 = CARTESIAN_POINT ( 'NONE',  ( 5.823673210054444382, -21.52544592524334988, 90.20942372801903275 ) ) ;
#180372 = CARTESIAN_POINT ( 'NONE',  ( 12.06949235617757843, -12.14591786802309237, 78.12390960531436690 ) ) ;
#180371 = CARTESIAN_POINT ( 'NONE',  ( -4.379528057220086978, -16.55341960407618274, 94.79275706135234714 ) ) ;
#180370 = CARTESIAN_POINT ( 'NONE',  ( 4.562484170618506418, -48.30423733473406145, -23.00000000000000355 ) ) ;
#180373 = CARTESIAN_POINT ( 'NONE',  ( -5.153800228976328057, -19.02544592524343514, 72.29057627198102409 ) ) ;
#180374 = ORIENTED_EDGE ( 'NONE', *, *, #67646, .T. ) ;
#180375 = CARTESIAN_POINT ( 'NONE',  ( 9.564922557961047289, -16.46253265017146816, 45.41775706135232582 ) ) ;
#180376 = CARTESIAN_POINT ( 'NONE',  ( -14.34966873604972548, 8.224510206698743886, 88.33442372801901854 ) ) ;
#180377 = CARTESIAN_POINT ( 'NONE',  ( -19.02544592524334988, -5.153800228976617603, 28.95942372801900433 ) ) ;
#180378 = CARTESIAN_POINT ( 'NONE',  ( -5.153800228976328057, -19.02544592524343514, 92.29057627198099567 ) ) ;
#180379 = CARTESIAN_POINT ( 'NONE',  ( -21.55341960407610458, -5.719274019375992779, 51.45724293864770260 ) ) ;
#180380 = CARTESIAN_POINT ( 'NONE',  ( 27.88129983271663903, -6.733757357602863536, 162.1517353552116560 ) ) ;
#180381 = CARTESIAN_POINT ( 'NONE',  ( 5.049401038298161559, -19.05341960407611168, 22.70724293864769194 ) ) ;
#180382 = CARTESIAN_POINT ( 'NONE',  ( -18.62759615963255300, -10.81492255796106328, 89.16775706135236135 ) ) ;
#180383 = CARTESIAN_POINT ( 'NONE',  ( 4.483927247898790824, -16.52544592524335698, 60.20942372801902565 ) ) ;
#180384 = CARTESIAN_POINT ( 'NONE',  ( 0.05219959533937995610, -21.53943276465977519, 20.00109039468568639 ) ) ;
#180385 = CARTESIAN_POINT ( 'NONE',  ( -8.314922557961024197, 14.29746914071037800, 27.91775706135234358 ) ) ;
#180386 = CARTESIAN_POINT ( 'NONE',  ( 13.89961937509977652, -13.97604488694527269, 93.12390960531436690 ) ) ;
#180387 = CARTESIAN_POINT ( 'NONE',  ( -13.89961937509977652, 13.97604488694528158, 45.62390960531433848 ) ) ;
#180388 = CARTESIAN_POINT ( 'NONE',  ( 13.97604488694527802, 13.89961937509977652, 59.37390960531434558 ) ) ;
#180389 = CARTESIAN_POINT ( 'NONE',  ( 8.224510206698742110, 14.34966873604972548, 37.08442372801901143 ) ) ;
#180390 = CARTESIAN_POINT ( 'NONE',  ( 12.14591786802309770, 12.06949235617756955, 89.37390960531435269 ) ) ;
#180391 = CARTESIAN_POINT ( 'NONE',  ( 12.06949235617739724, 12.14591786802326823, 101.8760903946857042 ) ) ;
#180394 = CARTESIAN_POINT ( 'NONE',  ( -13.97604488694527625, -13.89961937509977652, 51.87390960531436690 ) ) ;
#180393 = CARTESIAN_POINT ( 'NONE',  ( -13.97604488694527625, -13.89961937509977652, 66.87390960531436690 ) ) ;
#180392 = CARTESIAN_POINT ( 'NONE',  ( -18.67979575497193778, 10.72451020669871902, 48.33442372801902565 ) ) ;
#180395 = CARTESIAN_POINT ( 'NONE',  ( 13.89961937509977652, -13.97604488694527269, 78.12390960531433848 ) ) ;
#180396 = CARTESIAN_POINT ( 'NONE',  ( -4.379528057220328563, 16.55341960407611168, 35.20724293864768839 ) ) ;
#180397 = CARTESIAN_POINT ( 'NONE',  ( -8.224510206698735004, -14.34966873604973081, 94.58442372801901854 ) ) ;
#180398 = CARTESIAN_POINT ( 'NONE',  ( 5.153800228976615827, -19.02544592524334988, 45.20942372801901143 ) ) ;
#180399 = CARTESIAN_POINT ( 'NONE',  ( 19.03943276465977164, -0.05219959533909143690, 108.7489096053143527 ) ) ;
#180400 = CARTESIAN_POINT ( 'NONE',  ( -13.89961937509977652, 13.97604488694528158, 45.62390960531433848 ) ) ;
#180401 = CARTESIAN_POINT ( 'NONE',  ( 5.153800228976615827, -19.02544592524334988, 30.20942372801900433 ) ) ;
#180402 = CARTESIAN_POINT ( 'NONE',  ( -36.91746825000001309, 11.99521256947798342, -4.724999997268811924 ) ) ;
#180403 = CARTESIAN_POINT ( 'NONE',  ( -8.314922557961024197, 14.29746914071037800, 42.91775706135235424 ) ) ;
#180405 = CARTESIAN_POINT ( 'NONE',  ( -16.52544592524335698, -4.483927247898792601, 53.95942372801900433 ) ) ;
#180404 = CARTESIAN_POINT ( 'NONE',  ( -16.51473224551082808, 9.474510206698731452, 73.33442372801900433 ) ) ;
#180406 = DIRECTION ( 'NONE',  ( 0.000000000000000000, 0.000000000000000000, 1.000000000000000000 ) ) ;
#180407 = CARTESIAN_POINT ( 'NONE',  ( 19.02544592524343514, -5.153800228976328945, 73.54057627198103830 ) ) ;
#180408 = CARTESIAN_POINT ( 'NONE',  ( 10.72451020669898902, -18.67979575497178502, 112.9155762719810383 ) ) ;
#180409 = CARTESIAN_POINT ( 'NONE',  ( 13.89961937509957401, 13.97604488694547697, 66.87609039468567573 ) ) ;
#180411 = CARTESIAN_POINT ( 'NONE',  ( 5.049401038298161559, -19.05341960407611168, 37.70724293864768839 ) ) ;
#180410 = CARTESIAN_POINT ( 'NONE',  ( 5.153800228976335163, 19.02544592524342804, 104.7905762719809957 ) ) ;
#180412 = CARTESIAN_POINT ( 'NONE',  ( 19.05341960407611168, 5.049401038298154454, 73.95724293864768129 ) ) ;
#180414 = CARTESIAN_POINT ( 'NONE',  ( -5.049401038298153566, 19.05341960407611168, 30.20724293864768839 ) ) ;
#180413 = CARTESIAN_POINT ( 'NONE',  ( 16.53943276465976808, -0.05219959533910856209, 38.74890960531435979 ) ) ;
#180415 = CARTESIAN_POINT ( 'NONE',  ( -19.03943276465977164, -0.05219959533935918106, 38.75109039468566152 ) ) ;
#180416 = CARTESIAN_POINT ( 'NONE',  ( 0.05219959533910956823, 16.53943276465976808, 79.99890960531435269 ) ) ;
#180417 = CARTESIAN_POINT ( 'NONE',  ( -21.53943276465977519, -0.05219959533937600094, 113.7510903946856757 ) ) ;
#180418 = CARTESIAN_POINT ( 'NONE',  ( -19.02544592524342804, 5.153800228976336051, 56.04057627198100988 ) ) ;
#180419 = CARTESIAN_POINT ( 'NONE',  ( 15.80617190586746368, 15.72974639402197994, 44.37390960531435979 ) ) ;
#180421 = CARTESIAN_POINT ( 'NONE',  ( -15.80617190586768217, 15.72974639402176855, 103.1260903946856757 ) ) ;
#180420 = CARTESIAN_POINT ( 'NONE',  ( -12.06949235617756955, 12.14591786802309770, 50.62390960531435979 ) ) ;
#180422 = CARTESIAN_POINT ( 'NONE',  ( -16.46253265017160317, 9.564922557960807481, 90.83224293864769550 ) ) ;
#180423 = CARTESIAN_POINT ( 'NONE',  ( 9.474510206698971260, -16.51473224551069308, 107.9155762719810383 ) ) ;
#180424 = CARTESIAN_POINT ( 'NONE',  ( -19.02544592524342804, 5.153800228976336051, 46.04057627198101699 ) ) ;
#180425 = CARTESIAN_POINT ( 'NONE',  ( 16.51473224551069308, 9.474510206698969483, 29.16557627198103475 ) ) ;
#180426 = CARTESIAN_POINT ( 'NONE',  ( 14.29746914071049879, -8.314922557960816363, 88.33224293864769550 ) ) ;
#180427 = CARTESIAN_POINT ( 'NONE',  ( 21.52544592524344225, -5.823673210054117533, 98.54057627198105251 ) ) ;
#180428 = CARTESIAN_POINT ( 'NONE',  ( -5.153800228976328057, -19.02544592524343514, 82.29057627198103830 ) ) ;
#180429 = CARTESIAN_POINT ( 'NONE',  ( -10.81492255796078084, -18.62759615963271287, 112.0822429386477097 ) ) ;
#180430 = CARTESIAN_POINT ( 'NONE',  ( -19.02544592524342804, 5.153800228976336051, 86.04057627198103830 ) ) ;
#180432 = CARTESIAN_POINT ( 'NONE',  ( 4.379528057220339221, -16.55341960407611168, 102.7072429386476955 ) ) ;
#180431 = FACE_OUTER_BOUND ( 'NONE', #155538, .T. ) ;
#180433 = CARTESIAN_POINT ( 'NONE',  ( -0.05219959533909027116, -19.03943276465977164, 72.49890960531435269 ) ) ;
#180434 = CARTESIAN_POINT ( 'NONE',  ( -5.823673210054116645, -21.52544592524344225, 77.29057627198102409 ) ) ;
#180435 = EDGE_CURVE ( 'NONE', #21447, #43523, #192787, .T. ) ;
#180436 = CARTESIAN_POINT ( 'NONE',  ( -31.26591117326541536, 6.741338443544420578, 98.29621977100285335 ) ) ;
#180437 = CARTESIAN_POINT ( 'NONE',  ( -21.72193145969974992, -8.667250440200811923, 169.0624054586918987 ) ) ;
#180439 = CARTESIAN_POINT ( 'NONE',  ( 19.48894818550241581, -5.500000000000102141, 67.60307310435240424 ) ) ;
#180438 = CARTESIAN_POINT ( 'NONE',  ( -15.72974639402197994, 15.80617190586746368, 30.62390960531436335 ) ) ;
#180440 = CARTESIAN_POINT ( 'NONE',  ( 16.53943276465976808, 0.05219959533934440121, 36.25109039468567573 ) ) ;
#180441 = CARTESIAN_POINT ( 'NONE',  ( 14.34966873604960469, 8.224510206698951720, 99.16557627198100988 ) ) ;
#180442 = LINE ( 'NONE', #92353, #109628 ) ;
#180443 = CARTESIAN_POINT ( 'NONE',  ( 0.05219959533909260263, 19.03943276465977164, 84.99890960531436690 ) ) ;
#180444 = CARTESIAN_POINT ( 'NONE',  ( -13.89961937509977652, 13.97604488694528158, 40.62390960531435979 ) ) ;
#180445 = CARTESIAN_POINT ( 'NONE',  ( 0.05219959533910956823, 16.53943276465976808, 84.99890960531436690 ) ) ;
#180446 = CARTESIAN_POINT ( 'NONE',  ( 5.823673210054125526, 21.52544592524343514, 34.79057627198103120 ) ) ;
#180447 = CARTESIAN_POINT ( 'NONE',  ( 4.483927247898545687, 16.52544592524342804, 54.79057627198104541 ) ) ;
#180448 = CARTESIAN_POINT ( 'NONE',  ( -19.05341960407617563, 5.049401038297882671, 98.54275706135233293 ) ) ;
#180449 = CARTESIAN_POINT ( 'NONE',  ( -21.53943276465977519, -0.05219959533937600094, 63.75109039468568284 ) ) ;
#180450 = DIRECTION ( 'NONE',  ( 1.000000000000000000, 0.000000000000000000, 0.000000000000000000 ) ) ;
#180451 = CARTESIAN_POINT ( 'NONE',  ( 0.05219959533909260263, 19.03943276465977164, 94.99890960531436690 ) ) ;
#180452 = CARTESIAN_POINT ( 'NONE',  ( -8.224510206698735004, -14.34966873604973081, 79.58442372801903275 ) ) ;
#180453 = CARTESIAN_POINT ( 'NONE',  ( -0.05219959533909027116, -19.03943276465977164, 22.49890960531436690 ) ) ;
#180454 = CARTESIAN_POINT ( 'NONE',  ( -16.51473224551069308, -9.474510206698971260, 71.66557627198102409 ) ) ;
#180455 = CARTESIAN_POINT ( 'NONE',  ( -15.72974639402197994, 15.80617190586746368, 75.62390960531439532 ) ) ;
#180456 = CARTESIAN_POINT ( 'NONE',  ( -0.05219959533934338120, 16.53943276465976808, 32.50109039468568284 ) ) ;
#180458 = CARTESIAN_POINT ( 'NONE',  ( 15.72974639402176855, 15.80617190586768217, 61.87609039468568284 ) ) ;
#180457 = CARTESIAN_POINT ( 'NONE',  ( -16.55341960407611168, -4.379528057220339221, 56.45724293864768839 ) ) ;
#180460 = CARTESIAN_POINT ( 'NONE',  ( -5.823673210054116645, -21.52544592524344225, 27.29057627198103120 ) ) ;
#180459 = CARTESIAN_POINT ( 'NONE',  ( -16.53943276465976808, -0.05219959533934237506, 83.75109039468568994 ) ) ;
#180461 = CARTESIAN_POINT ( 'NONE',  ( 25.79025989231048399, 10.69883710965548929, 166.5180000355202310 ) ) ;
#180462 = CARTESIAN_POINT ( 'NONE',  ( -17.26172910966779384, 6.454744622555854683, 80.80646908649224258 ) ) ;
#180463 = CARTESIAN_POINT ( 'NONE',  ( 8.314922557961029526, -14.29746914071037800, 105.4177570613523613 ) ) ;
#180464 = CARTESIAN_POINT ( 'NONE',  ( -12.14591786802326823, 12.06949235617739902, 63.12609039468568994 ) ) ;
#180465 = CARTESIAN_POINT ( 'NONE',  ( -0.05219959533909027116, -19.03943276465977164, 77.49890960531435269 ) ) ;
#180466 = CARTESIAN_POINT ( 'NONE',  ( 19.02544592524343514, -5.153800228976328945, 93.54057627198102409 ) ) ;
#180467 = CARTESIAN_POINT ( 'NONE',  ( -10.72451020669870658, -18.67979575497194134, 69.58442372801900433 ) ) ;
#180468 = CARTESIAN_POINT ( 'NONE',  ( -4.379528057220086978, -16.55341960407618274, 69.79275706135234714 ) ) ;
#180469 = CARTESIAN_POINT ( 'NONE',  ( 14.29746914071049879, -8.314922557960816363, 43.33224293864769550 ) ) ;
#180470 = CARTESIAN_POINT ( 'NONE',  ( -19.05341960407611168, -5.049401038298163336, 61.45724293864769550 ) ) ;
#180471 = CARTESIAN_POINT ( 'NONE',  ( 19.05341960407611168, 5.049401038298154454, 53.95724293864770260 ) ) ;
#180473 = VERTEX_POINT ( 'NONE', #90950 ) ;
#180472 = CARTESIAN_POINT ( 'NONE',  ( 14.29746914071037800, 8.314922557961029526, 36.66775706135234714 ) ) ;
#180475 = CARTESIAN_POINT ( 'NONE',  ( 19.02544592524334988, 5.153800228976608722, 96.45942372801897591 ) ) ;
#180474 =( BOUNDED_CURVE ( )  B_SPLINE_CURVE ( 2, ( #67916, #191266, #51750, #70928, #190274, #84072, #69927, #129569, #177121, #130580, #131592 ),
 .UNSPECIFIED., .F., .F. ) 
 B_SPLINE_CURVE_WITH_KNOTS ( ( 3, 2, 2, 2, 2, 3 ),
 ( 0.8000000000000000444, 0.8199999999999999512, 0.8399999999999999689, 0.8599999999999999867, 0.8800000000000000044, 0.9000000000000000222 ),
 .UNSPECIFIED. ) 
 CURVE ( )  GEOMETRIC_REPRESENTATION_ITEM ( )  RATIONAL_B_SPLINE_CURVE ( ( 1.000000000000000000, 0.9510565162951535312, 1.000000000000000000, 0.9510565162951535312, 1.000000000000000000, 0.9510565162951535312, 1.000000000000000000, 0.9510565162951535312, 1.000000000000000000, 0.9510565162951535312, 1.000000000000000000 ) ) 
 REPRESENTATION_ITEM ( '' )  );
#180476 = CARTESIAN_POINT ( 'NONE',  ( 14.34966873604960469, 8.224510206698951720, 99.16557627198100988 ) ) ;
#180477 = CARTESIAN_POINT ( 'NONE',  ( 19.02544592524343514, -5.153800228976328945, 58.54057627198102409 ) ) ;
#180479 = CARTESIAN_POINT ( 'NONE',  ( -38.00000000000000711, 2.428612866367529932E-14, -4.000000000000000000 ) ) ;
#180478 = CARTESIAN_POINT ( 'NONE',  ( 9.564922557961047289, -16.46253265017146816, 100.4177570613523329 ) ) ;
#180480 = CARTESIAN_POINT ( 'NONE',  ( 21.55341960407619695, -5.719274019375665929, 106.0427570613523471 ) ) ;
#180481 = CARTESIAN_POINT ( 'NONE',  ( -8.314922557961024197, 14.29746914071037800, 72.91775706135234714 ) ) ;
#180482 = DIRECTION ( 'NONE',  ( 0.000000000000000000, 1.000000000000000000, 0.000000000000000000 ) ) ;
#180483 = CARTESIAN_POINT ( 'NONE',  ( 5.823673210054125526, 21.52544592524343514, 59.79057627198103120 ) ) ;
#180484 = CARTESIAN_POINT ( 'NONE',  ( 8.224510206698742110, 14.34966873604972548, 52.08442372801901854 ) ) ;
#180485 = CARTESIAN_POINT ( 'NONE',  ( 19.03943276465977164, 0.05219959533936151252, 61.25109039468566863 ) ) ;
#180486 = CARTESIAN_POINT ( 'NONE',  ( -5.153800228976328057, -19.02544592524343514, 87.29057627198103830 ) ) ;
#180487 = CARTESIAN_POINT ( 'NONE',  ( -4.379528057220328563, 16.55341960407611168, 110.2072429386477239 ) ) ;
#180488 = CARTESIAN_POINT ( 'NONE',  ( -19.05341960407611168, -5.049401038298163336, 61.45724293864769550 ) ) ;
#180489 = CARTESIAN_POINT ( 'NONE',  ( -8.314922557960811034, -14.29746914071050412, 62.08224293864769550 ) ) ;
#180490 = CARTESIAN_POINT ( 'NONE',  ( 15.80617190586769283, -15.72974639402175789, 80.62609039468567573 ) ) ;
#180491 = CARTESIAN_POINT ( 'NONE',  ( 19.02544592524334988, 5.153800228976608722, 46.45942372801899012 ) ) ;
#180492 = CARTESIAN_POINT ( 'NONE',  ( 19.05341960407617918, -5.049401038297876454, 26.04275706135233293 ) ) ;
#180493 = CARTESIAN_POINT ( 'NONE',  ( -15.80617190586745835, -15.72974639402198527, 26.87390960531435979 ) ) ;
#180494 = CARTESIAN_POINT ( 'NONE',  ( 15.72974639402176855, 15.80617190586768217, 101.8760903946857042 ) ) ;
#180495 = CARTESIAN_POINT ( 'NONE',  ( 16.51473224551069308, 9.474510206698969483, 69.16557627198102409 ) ) ;
#180496 = CARTESIAN_POINT ( 'NONE',  ( 10.81492255796106328, -18.62759615963255655, 90.41775706135236135 ) ) ;
#180497 = CARTESIAN_POINT ( 'NONE',  ( -10.72451020669898014, 18.67979575497178502, 45.41557627198103830 ) ) ;
#180498 = CARTESIAN_POINT ( 'NONE',  ( 19.05341960407611168, 5.049401038298154454, 83.95724293864766707 ) ) ;
#180499 = CARTESIAN_POINT ( 'NONE',  ( -13.97604488694547697, 13.89961937509957934, 58.12609039468566863 ) ) ;
#180500 = CARTESIAN_POINT ( 'NONE',  ( 19.05341960407611168, 5.049401038298154454, 43.95724293864769550 ) ) ;
#180501 = CARTESIAN_POINT ( 'NONE',  ( 9.564922557960805705, 16.46253265017160317, 89.58224293864769550 ) ) ;
#180502 = CARTESIAN_POINT ( 'NONE',  ( 19.02544592524334988, 5.153800228976608722, 86.45942372801900433 ) ) ;
#180503 = CARTESIAN_POINT ( 'NONE',  ( -14.29746914071037622, -8.314922557961029526, 34.16775706135234714 ) ) ;
#180504 = CARTESIAN_POINT ( 'NONE',  ( -8.314922557960811034, -14.29746914071050412, 97.08224293864770971 ) ) ;
#180505 = CARTESIAN_POINT ( 'NONE',  ( -5.153800228976328057, -19.02544592524343514, 72.29057627198102409 ) ) ;
#180506 = CARTESIAN_POINT ( 'NONE',  ( -10.72451020669898014, 18.67979575497178502, 50.41557627198103120 ) ) ;
#180507 = CARTESIAN_POINT ( 'NONE',  ( -13.97604488694547697, 13.89961937509957934, 108.1260903946856331 ) ) ;
#180508 = CARTESIAN_POINT ( 'NONE',  ( 18.67979575497178502, 10.72451020669898547, 114.1655762719810383 ) ) ;
#180509 = CARTESIAN_POINT ( 'NONE',  ( 15.72974639402176855, 15.80617190586768217, 66.87609039468568994 ) ) ;
#180510 = CARTESIAN_POINT ( 'NONE',  ( 14.34966873604972726, -8.224510206698740333, 75.83442372801900433 ) ) ;
#180511 = CARTESIAN_POINT ( 'NONE',  ( -19.03943276465977164, 0.05219959533909376836, 71.24890960531435269 ) ) ;
#180512 = CARTESIAN_POINT ( 'NONE',  ( 0.05219959533934541429, -16.53943276465976808, 100.0010903946857042 ) ) ;
#180513 = CARTESIAN_POINT ( 'NONE',  ( -16.51473224551082808, 9.474510206698731452, 38.33442372801899722 ) ) ;
#180514 = CARTESIAN_POINT ( 'NONE',  ( -5.719274019375665041, -21.55341960407619695, 29.79275706135234358 ) ) ;
#180515 = CARTESIAN_POINT ( 'NONE',  ( 16.52544592524342804, -4.483927247898539470, 73.54057627198102409 ) ) ;
#180516 = CARTESIAN_POINT ( 'NONE',  ( 19.03943276465977164, -0.05219959533909143690, 93.74890960531435269 ) ) ;
#180517 = CARTESIAN_POINT ( 'NONE',  ( 16.52544592524335698, 4.483927247898782831, 86.45942372801901854 ) ) ;
#180518 = CARTESIAN_POINT ( 'NONE',  ( -15.80617190586768217, 15.72974639402176855, 68.12609039468567573 ) ) ;
#180519 = CARTESIAN_POINT ( 'NONE',  ( -12.06949235617739369, -12.14591786802326823, 34.37609039468568284 ) ) ;
#180520 = CARTESIAN_POINT ( 'NONE',  ( -21.53943276465977519, -0.05219959533937600094, 28.75109039468567929 ) ) ;
#180521 = CARTESIAN_POINT ( 'NONE',  ( 0.05219959533910956823, 16.53943276465976808, 69.99890960531435269 ) ) ;
#180522 = EDGE_LOOP ( 'NONE', ( #194350, #75524, #184529, #61478 ) ) ;
#180523 = CARTESIAN_POINT ( 'NONE',  ( 21.53943276465977519, -0.05219959533907433946, 98.74890960531438111 ) ) ;
#180524 = CARTESIAN_POINT ( 'NONE',  ( 12.14591786802309770, 12.06949235617756955, 49.37390960531436690 ) ) ;
#180525 = EDGE_LOOP ( 'NONE', ( #53971, #158699, #144336, #106500, #91949, #150169, #305, #147463, #136580, #39166, #180707, #166429, #124535, #163630 ) ) ;
#180526 = CARTESIAN_POINT ( 'NONE',  ( -5.153800228976328057, -19.02544592524343514, 27.29057627198103120 ) ) ;
#180527 = CARTESIAN_POINT ( 'NONE',  ( 21.55341960407610458, 5.719274019375980345, 28.95724293864769905 ) ) ;
#180528 = CARTESIAN_POINT ( 'NONE',  ( 15.80617190586769283, -15.72974639402175789, 35.62609039468568994 ) ) ;
#180529 = CARTESIAN_POINT ( 'NONE',  ( 16.53943276465976808, -0.05219959533910856209, 63.74890960531435979 ) ) ;
#180530 = CARTESIAN_POINT ( 'NONE',  ( -15.72974639402197994, 15.80617190586746368, 70.62390960531436690 ) ) ;
#180531 = CARTESIAN_POINT ( 'NONE',  ( -9.474510206698964154, 16.51473224551069663, 75.41557627198103830 ) ) ;
#180533 = CARTESIAN_POINT ( 'NONE',  ( 9.564922557961047289, -16.46253265017146816, 75.41775706135234714 ) ) ;
#180532 = CARTESIAN_POINT ( 'NONE',  ( 0.05219959533909260263, 19.03943276465977164, 29.99890960531435979 ) ) ;
#180534 = CARTESIAN_POINT ( 'NONE',  ( -15.80617190586745835, -15.72974639402198527, 56.87390960531436690 ) ) ;
#180535 = CARTESIAN_POINT ( 'NONE',  ( -19.02544592524342804, 5.153800228976336051, 36.04057627198100988 ) ) ;
#180536 = CARTESIAN_POINT ( 'NONE',  ( 19.03943276465977164, -0.05219959533909143690, 73.74890960531435269 ) ) ;
#180537 = ORIENTED_EDGE ( 'NONE', *, *, #118352, .F. ) ;
#180538 = CARTESIAN_POINT ( 'NONE',  ( 4.379528057220092307, 16.55341960407617563, 32.29275706135235424 ) ) ;
#180539 = CARTESIAN_POINT ( 'NONE',  ( -5.823673210054431948, 21.52544592524334988, 27.70942372801901854 ) ) ;
#180540 = CARTESIAN_POINT ( 'NONE',  ( 18.67979575497194134, -10.72451020669871369, 60.83442372801901854 ) ) ;
#180541 = CARTESIAN_POINT ( 'NONE',  ( 19.05341960407611168, 5.049401038298154454, 108.9572429386477097 ) ) ;
#180542 = CARTESIAN_POINT ( 'NONE',  ( -18.67979575497178146, -10.72451020669898902, 71.66557627198100988 ) ) ;
#180544 = CARTESIAN_POINT ( 'NONE',  ( -0.05219959533934338120, 16.53943276465976808, 52.50109039468567573 ) ) ;
#180543 = CARTESIAN_POINT ( 'NONE',  ( -18.62759615963270932, 10.81492255796079327, 105.8322429386476955 ) ) ;
#180545 = CARTESIAN_POINT ( 'NONE',  ( 21.55341960407610458, 5.719274019375980345, 48.95724293864770971 ) ) ;
#180546 = CARTESIAN_POINT ( 'NONE',  ( 21.55341960407619695, -5.719274019375665929, 101.0427570613523756 ) ) ;
#180547 = AXIS2_PLACEMENT_3D ( 'NONE', #69766, #100093, #161777 ) ;
#180548 = CARTESIAN_POINT ( 'NONE',  ( 16.51473224551069308, 9.474510206698969483, 59.16557627198102409 ) ) ;
#180549 = CARTESIAN_POINT ( 'NONE',  ( 9.564922557960805705, 16.46253265017160317, 104.5822429386476955 ) ) ;
#180550 = CARTESIAN_POINT ( 'NONE',  ( -13.89961937509977652, 13.97604488694528158, 75.62390960531438111 ) ) ;
#180551 = CARTESIAN_POINT ( 'NONE',  ( 16.88567814943193568, -6.947325034625396967, 86.20998877347402356 ) ) ;
#180552 = CARTESIAN_POINT ( 'NONE',  ( 5.049401038297881783, 19.05341960407617563, 67.29275706135234714 ) ) ;
#180554 = CARTESIAN_POINT ( 'NONE',  ( 21.53943276465977519, -0.05219959533907433946, 43.74890960531435979 ) ) ;
#180553 = CARTESIAN_POINT ( 'NONE',  ( -0.05219959533936034679, 19.03943276465977164, 22.50109039468566152 ) ) ;
#180555 = CARTESIAN_POINT ( 'NONE',  ( -4.379528057220086978, -16.55341960407618274, 104.7927570613523898 ) ) ;
#180556 = CARTESIAN_POINT ( 'NONE',  ( 16.51473224551083163, -9.474510206698727899, 85.83442372801900433 ) ) ;
#180557 = CARTESIAN_POINT ( 'NONE',  ( 25.04568634023502582, -21.46320343559646560, 8.240304736541396835 ) ) ;
#180558 = CARTESIAN_POINT ( 'NONE',  ( -16.46253265017146816, -9.564922557961047289, 24.16775706135233648 ) ) ;
#180559 = CARTESIAN_POINT ( 'NONE',  ( 13.89961937509957401, 13.97604488694547697, 86.87609039468567573 ) ) ;
#180560 = CARTESIAN_POINT ( 'NONE',  ( 13.97604488694548053, -13.89961937509957401, 45.62609039468566863 ) ) ;
#180561 = CARTESIAN_POINT ( 'NONE',  ( 17.50000000000000355, 5.622605283950878885, 108.8120731059611188 ) ) ;
#180562 = CARTESIAN_POINT ( 'NONE',  ( 13.89961937509977652, -13.97604488694527269, 38.12390960531436690 ) ) ;
#180563 = CARTESIAN_POINT ( 'NONE',  ( 12.06949235617757843, -12.14591786802309237, 48.12390960531436690 ) ) ;
#180564 = CARTESIAN_POINT ( 'NONE',  ( 16.51473224551069308, 9.474510206698969483, 34.16557627198102409 ) ) ;
#180565 = CARTESIAN_POINT ( 'NONE',  ( 16.52544592524342804, -4.483927247898539470, 38.54057627198103120 ) ) ;
#180566 = DIRECTION ( 'NONE',  ( 0.000000000000000000, -0.5000000000000013323, -0.8660254037844380415 ) ) ;
#180567 = CARTESIAN_POINT ( 'NONE',  ( 8.224510206698742110, 14.34966873604972548, 107.0844237280190043 ) ) ;
#180568 = CARTESIAN_POINT ( 'NONE',  ( 19.05341960407611168, 5.049401038298154454, 43.95724293864769550 ) ) ;
#180569 = CARTESIAN_POINT ( 'NONE',  ( 5.153800228976615827, -19.02544592524334988, 25.20942372801900433 ) ) ;
#180570 = CARTESIAN_POINT ( 'NONE',  ( 12.14591786802327356, -12.06949235617739191, 35.62609039468568994 ) ) ;
#180571 = CARTESIAN_POINT ( 'NONE',  ( 18.67979575497178502, 10.72451020669898547, 44.16557627198103120 ) ) ;
#180573 = ORIENTED_EDGE ( 'NONE', *, *, #44361, .T. ) ;
#180572 = CARTESIAN_POINT ( 'NONE',  ( 21.55341960407619695, -5.719274019375665929, 91.04275706135236135 ) ) ;
#180574 = CARTESIAN_POINT ( 'NONE',  ( -9.474510206698964154, 16.51473224551069663, 105.4155762719810383 ) ) ;
#180575 = CARTESIAN_POINT ( 'NONE',  ( -9.474510206698964154, 16.51473224551069663, 90.41557627198103830 ) ) ;
#180576 = CARTESIAN_POINT ( 'NONE',  ( 22.81625015709510151, -31.40387420917324590, -9.924999997268814766 ) ) ;
#180577 = CARTESIAN_POINT ( 'NONE',  ( -18.67979575497178146, -10.72451020669898902, 106.6655762719810383 ) ) ;
#180578 = CARTESIAN_POINT ( 'NONE',  ( 4.483927247898545687, 16.52544592524342804, 84.79057627198102409 ) ) ;
#180580 = CARTESIAN_POINT ( 'NONE',  ( 16.46253265017160672, -9.564922557960803928, 73.33224293864769550 ) ) ;
#180579 = CARTESIAN_POINT ( 'NONE',  ( -15.80617190586745835, -15.72974639402198527, 71.87390960531438111 ) ) ;
#180581 = CARTESIAN_POINT ( 'NONE',  ( -19.03943276465977164, 0.05219959533909376836, 71.24890960531435269 ) ) ;
#180582 = CARTESIAN_POINT ( 'NONE',  ( 5.823673210054125526, 21.52544592524343514, 94.79057627198105251 ) ) ;
#180583 = ORIENTED_EDGE ( 'NONE', *, *, #172288, .T. ) ;
#180584 = CARTESIAN_POINT ( 'NONE',  ( -13.89961937509977652, 13.97604488694528158, 55.62390960531434558 ) ) ;
#180586 = CARTESIAN_POINT ( 'NONE',  ( -4.999999999999999112, -140.0000000000000000, 0.0009999999999992653654 ) ) ;
#180585 = CARTESIAN_POINT ( 'NONE',  ( -12.14591786802309592, -12.06949235617757132, 96.87390960531436690 ) ) ;
#180587 = CARTESIAN_POINT ( 'NONE',  ( 5.049401038298161559, -19.05341960407611168, 57.70724293864769550 ) ) ;
#180588 = CARTESIAN_POINT ( 'NONE',  ( 16.46253265017146816, 9.564922557961045513, 76.66775706135234714 ) ) ;
#180589 = CARTESIAN_POINT ( 'NONE',  ( 4.379528057220339221, -16.55341960407611168, 92.70724293864770971 ) ) ;
#180590 = CARTESIAN_POINT ( 'NONE',  ( 5.719274019375673035, 21.55341960407619339, 57.29275706135234714 ) ) ;
#180592 = CARTESIAN_POINT ( 'NONE',  ( 21.53943276465977519, 0.05219959533937863772, 21.25109039468567218 ) ) ;
#180591 = CARTESIAN_POINT ( 'NONE',  ( 0.05219959533909260263, 19.03943276465977164, 44.99890960531435979 ) ) ;
#180593 = CARTESIAN_POINT ( 'NONE',  ( -16.53943276465976808, 0.05219959533911058130, 101.2489096053143669 ) ) ;
#180594 = CARTESIAN_POINT ( 'NONE',  ( -23.31738231874055245, -16.94106989632524574, 142.1999999999999886 ) ) ;
#180595 = CARTESIAN_POINT ( 'NONE',  ( -0.05219959533909027116, -19.03943276465977164, 72.49890960531435269 ) ) ;
#180596 = CARTESIAN_POINT ( 'NONE',  ( 16.19135201231367560, 7.376712067591920885, 112.6868085405202748 ) ) ;
#180598 = CARTESIAN_POINT ( 'NONE',  ( 21.52544592524344225, -5.823673210054117533, 23.54057627198102765 ) ) ;
#180597 = CARTESIAN_POINT ( 'NONE',  ( -16.52544592524335698, -4.483927247898792601, 18.95942372801901143 ) ) ;
#180599 = CARTESIAN_POINT ( 'NONE',  ( -10.72451020669870658, -18.67979575497194134, 49.58442372801901143 ) ) ;
#180600 = CARTESIAN_POINT ( 'NONE',  ( 13.89961937509977652, -13.97604488694527269, 93.12390960531436690 ) ) ;
#180601 = CARTESIAN_POINT ( 'NONE',  ( -0.05219959533936034679, 19.03943276465977164, 87.50109039468567573 ) ) ;
#180602 = CARTESIAN_POINT ( 'NONE',  ( -19.02544592524342804, 5.153800228976336051, 76.04057627198102409 ) ) ;
#180603 = ADVANCED_FACE ( 'NONE', ( #166843 ), #173767, .F. ) ;
#180604 = CARTESIAN_POINT ( 'NONE',  ( 16.55341960407611168, 4.379528057220329451, 78.95724293864769550 ) ) ;
#180605 = CARTESIAN_POINT ( 'NONE',  ( -16.46253265017160317, 9.564922557960807481, 105.8322429386476955 ) ) ;
#180606 = CARTESIAN_POINT ( 'NONE',  ( -16.52544592524342804, 4.483927247898546575, 81.04057627198102409 ) ) ;
#180607 = CARTESIAN_POINT ( 'NONE',  ( -5.049401038298153566, 19.05341960407611168, 100.2072429386476955 ) ) ;
#180608 = CARTESIAN_POINT ( 'NONE',  ( 19.05341960407617918, -5.049401038297876454, 46.04275706135233293 ) ) ;
#180611 = CARTESIAN_POINT ( 'NONE',  ( 9.564922557960805705, 16.46253265017160317, 34.58224293864770260 ) ) ;
#180610 = CARTESIAN_POINT ( 'NONE',  ( 12.06949235617757843, -12.14591786802309237, 48.12390960531436690 ) ) ;
#180609 = CARTESIAN_POINT ( 'NONE',  ( 5.153800228976335163, 19.02544592524342804, 44.79057627198103830 ) ) ;
#180612 = ORIENTED_EDGE ( 'NONE', *, *, #23142, .T. ) ;
#180613 = CARTESIAN_POINT ( 'NONE',  ( -5.719274019375665041, -21.55341960407619695, 49.79275706135234714 ) ) ;
#180614 = CARTESIAN_POINT ( 'NONE',  ( 5.153800228976615827, -19.02544592524334988, 85.20942372801900433 ) ) ;
#180615 = CARTESIAN_POINT ( 'NONE',  ( -14.29746914071049879, 8.314922557960819915, 35.83224293864768839 ) ) ;
#180616 = CARTESIAN_POINT ( 'NONE',  ( 0.05219959533907565091, 21.53943276465977519, 94.99890960531436690 ) ) ;
#180617 = CARTESIAN_POINT ( 'NONE',  ( 10.81492255796078972, 18.62759615963270932, 39.58224293864769550 ) ) ;
#180618 = CARTESIAN_POINT ( 'NONE',  ( -8.314922557960811034, -14.29746914071050412, 82.08224293864768129 ) ) ;
#180619 = CARTESIAN_POINT ( 'NONE',  ( -19.05341960407611168, -5.049401038298163336, 46.45724293864768129 ) ) ;
#180620 = CARTESIAN_POINT ( 'NONE',  ( -8.224510206698735004, -14.34966873604973081, 99.58442372801900433 ) ) ;
#180621 = CARTESIAN_POINT ( 'NONE',  ( 16.55341960407618274, -4.379528057220086978, 91.04275706135236135 ) ) ;
#180622 = CARTESIAN_POINT ( 'NONE',  ( 12.14591786802327356, -12.06949235617739191, 70.62609039468567573 ) ) ;
#180623 = CARTESIAN_POINT ( 'NONE',  ( 16.46253265017146816, 9.564922557961045513, 26.66775706135234003 ) ) ;
#180624 = CARTESIAN_POINT ( 'NONE',  ( 9.564922557960805705, 16.46253265017160317, 94.58224293864769550 ) ) ;
#180625 = CARTESIAN_POINT ( 'NONE',  ( 16.51473224551069308, 9.474510206698969483, 74.16557627198103830 ) ) ;
#180626 = CARTESIAN_POINT ( 'NONE',  ( 12.14591786802327356, -12.06949235617739191, 75.62609039468567573 ) ) ;
#180627 = CARTESIAN_POINT ( 'NONE',  ( 16.46253265017160672, -9.564922557960803928, 33.33224293864770260 ) ) ;
#180628 = CARTESIAN_POINT ( 'NONE',  ( -0.05219959533910754901, -16.53943276465976808, 47.49890960531435979 ) ) ;
#180630 = CARTESIAN_POINT ( 'NONE',  ( -19.03943276465977164, 0.05219959533909376836, 86.24890960531436690 ) ) ;
#180629 = DIRECTION ( 'NONE',  ( 1.000000000000000000, -0.000000000000000000, -0.000000000000000000 ) ) ;
#180631 = CARTESIAN_POINT ( 'NONE',  ( 10.81492255796078972, 18.62759615963270932, 24.58224293864768839 ) ) ;
#180632 = CARTESIAN_POINT ( 'NONE',  ( 12.06949235617757843, -12.14591786802309237, 73.12390960531436690 ) ) ;
#180633 = CARTESIAN_POINT ( 'NONE',  ( -4.379528057220328563, 16.55341960407611168, 60.20724293864768839 ) ) ;
#180635 = CARTESIAN_POINT ( 'NONE',  ( 17.50000000000001776, -4.640572885337594045, 33.13788164548843440 ) ) ;
#180634 = CARTESIAN_POINT ( 'NONE',  ( 4.379528057220092307, 16.55341960407617563, 47.29275706135234003 ) ) ;
#180636 = CARTESIAN_POINT ( 'NONE',  ( -13.97604488694547697, 13.89961937509957934, 68.12609039468563310 ) ) ;
#180637 = CARTESIAN_POINT ( 'NONE',  ( -13.97604488694527625, -13.89961937509977652, 86.87390960531436690 ) ) ;
#180638 = CARTESIAN_POINT ( 'NONE',  ( 13.89961937509957401, 13.97604488694547697, 66.87609039468567573 ) ) ;
#180639 = DIRECTION ( 'NONE',  ( -0.000000000000000000, -0.000000000000000000, -1.000000000000000000 ) ) ;
#180641 = CARTESIAN_POINT ( 'NONE',  ( 14.34966873604972726, -8.224510206698740333, 95.83442372801903275 ) ) ;
#180640 = CARTESIAN_POINT ( 'NONE',  ( 16.53943276465976808, 0.05219959533934440121, 21.25109039468567218 ) ) ;
#180642 = CARTESIAN_POINT ( 'NONE',  ( 19.05341960407611168, 5.049401038298154454, 43.95724293864769550 ) ) ;
#180643 = CARTESIAN_POINT ( 'NONE',  ( -0.05219959533907301413, -21.53943276465977519, 27.49890960531435269 ) ) ;
#180644 = CARTESIAN_POINT ( 'NONE',  ( 21.55341960407619695, -5.719274019375665929, 51.04275706135234714 ) ) ;
#180645 = CARTESIAN_POINT ( 'NONE',  ( 9.474510206698729675, 16.51473224551082808, 112.0844237280190043 ) ) ;
#180647 = CARTESIAN_POINT ( 'NONE',  ( 13.97604488694527802, 13.89961937509977652, 79.37390960531435269 ) ) ;
#180646 = CARTESIAN_POINT ( 'NONE',  ( -16.46253265017146816, -9.564922557961047289, 54.16775706135234003 ) ) ;
#180648 = CARTESIAN_POINT ( 'NONE',  ( -17.50000000000000000, 5.499999999999992895, 23.71769037696436300 ) ) ;
#180650 = CARTESIAN_POINT ( 'NONE',  ( 16.46253265017160672, -9.564922557960803928, 73.33224293864769550 ) ) ;
#180649 = CARTESIAN_POINT ( 'NONE',  ( 16.55341960407611168, 4.379528057220329451, 78.95724293864769550 ) ) ;
#180651 = CARTESIAN_POINT ( 'NONE',  ( 5.153800228976335163, 19.02544592524342804, 69.79057627198103830 ) ) ;
#180652 = CARTESIAN_POINT ( 'NONE',  ( -19.02544592524334988, -5.153800228976617603, 88.95942372801897591 ) ) ;
#180653 = CARTESIAN_POINT ( 'NONE',  ( 21.53943276465977519, -0.05219959533907433946, 68.74890960531435269 ) ) ;
#180654 = CARTESIAN_POINT ( 'NONE',  ( 13.89961937509977652, -13.97604488694527269, 28.12390960531435624 ) ) ;
#180655 = CARTESIAN_POINT ( 'NONE',  ( 19.02544592524334988, 5.153800228976608722, 56.45942372801898301 ) ) ;
#180656 = CARTESIAN_POINT ( 'NONE',  ( 9.474510206698971260, -16.51473224551069308, 62.91557627198102409 ) ) ;
#180657 = CARTESIAN_POINT ( 'NONE',  ( 19.02544592524343514, -5.153800228976328945, 98.54057627198100988 ) ) ;
#180658 = ORIENTED_EDGE ( 'NONE', *, *, #184085, .F. ) ;
#180659 = CARTESIAN_POINT ( 'NONE',  ( -10.81492255796078084, -18.62759615963271287, 87.08224293864769550 ) ) ;
#180661 = CARTESIAN_POINT ( 'NONE',  ( -19.02544592524334988, -5.153800228976617603, 48.95942372801900433 ) ) ;
#180660 = CARTESIAN_POINT ( 'NONE',  ( 12.14591786802309770, 12.06949235617756955, 94.37390960531436690 ) ) ;
#180662 = CARTESIAN_POINT ( 'NONE',  ( -5.719274019375978568, 21.55341960407610458, 70.20724293864769550 ) ) ;
#180663 = CARTESIAN_POINT ( 'NONE',  ( -15.72974639402197994, 15.80617190586746368, 75.62390960531439532 ) ) ;
#180664 = CARTESIAN_POINT ( 'NONE',  ( -14.34966873604960291, -8.224510206698953496, 36.66557627198103120 ) ) ;
#180665 = CARTESIAN_POINT ( 'NONE',  ( -15.80617190586768217, 15.72974639402176855, 103.1260903946856757 ) ) ;
#180666 = CARTESIAN_POINT ( 'NONE',  ( 0.05219959533909260263, 19.03943276465977164, 74.99890960531435269 ) ) ;
#180667 = CARTESIAN_POINT ( 'NONE',  ( -16.46253265017160317, 9.564922557960807481, 30.83224293864769550 ) ) ;
#180668 = CARTESIAN_POINT ( 'NONE',  ( 15.72974639402176855, 15.80617190586768217, 41.87609039468568284 ) ) ;
#180669 = CARTESIAN_POINT ( 'NONE',  ( -21.53943276465977519, -0.05219959533937600094, 58.75109039468568994 ) ) ;
#180670 = CARTESIAN_POINT ( 'NONE',  ( -13.97604488694527625, -13.89961937509977652, 51.87390960531436690 ) ) ;
#180671 = CARTESIAN_POINT ( 'NONE',  ( -5.719274019375665041, -21.55341960407619695, 24.79275706135235779 ) ) ;
#180672 = ADVANCED_FACE ( 'NONE', ( #134517 ), #196203, .F. ) ;
#180673 = CARTESIAN_POINT ( 'NONE',  ( -13.89961937509957401, -13.97604488694547875, 59.37609039468566863 ) ) ;
#180674 = CARTESIAN_POINT ( 'NONE',  ( 19.03943276465977164, -0.05219959533909143690, 33.74890960531435979 ) ) ;
#180675 = CARTESIAN_POINT ( 'NONE',  ( 8.224510206698742110, 14.34966873604972548, 22.08442372801901143 ) ) ;
#180676 = CARTESIAN_POINT ( 'NONE',  ( -13.97604488694527625, -13.89961937509977652, 21.87390960531435979 ) ) ;
#180677 = CARTESIAN_POINT ( 'NONE',  ( 0.05219959533934541429, -16.53943276465976808, 80.00109039468568994 ) ) ;
#180678 = CARTESIAN_POINT ( 'NONE',  ( 13.97604488694527802, 13.89961937509977652, 34.37390960531436690 ) ) ;
#180679 = CARTESIAN_POINT ( 'NONE',  ( 20.93662873023546211, -10.44628751056279015, 168.2749732860603444 ) ) ;
#180680 = CARTESIAN_POINT ( 'NONE',  ( -19.05341960407611168, -5.049401038298163336, 91.45724293864766707 ) ) ;
#180681 = CARTESIAN_POINT ( 'NONE',  ( 19.03943276465977164, -0.05219959533909143690, 23.74890960531435269 ) ) ;
#180682 = CARTESIAN_POINT ( 'NONE',  ( 10.72451020669898902, -18.67979575497178502, 72.91557627198103830 ) ) ;
#180683 = CARTESIAN_POINT ( 'NONE',  ( 8.224510206698742110, 14.34966873604972548, 52.08442372801901854 ) ) ;
#180684 = CARTESIAN_POINT ( 'NONE',  ( -9.474510206698720793, -16.51473224551083518, 24.58442372801900078 ) ) ;
#180685 = CARTESIAN_POINT ( 'NONE',  ( 9.564922557960805705, 16.46253265017160317, 39.58224293864768839 ) ) ;
#180686 = CARTESIAN_POINT ( 'NONE',  ( -0.05219959533910754901, -16.53943276465976808, 37.49890960531436690 ) ) ;
#180687 = CARTESIAN_POINT ( 'NONE',  ( 14.29746914071049879, -8.314922557960816363, 73.33224293864769550 ) ) ;
#180688 = CARTESIAN_POINT ( 'NONE',  ( 13.97604488694527802, 13.89961937509977652, 59.37390960531434558 ) ) ;
#180689 = CARTESIAN_POINT ( 'NONE',  ( 10.81492255796106328, -18.62759615963255655, 105.4177570613523613 ) ) ;
#180690 = CARTESIAN_POINT ( 'NONE',  ( 5.823673210054125526, 21.52544592524343514, 114.7905762719810383 ) ) ;
#180691 = CARTESIAN_POINT ( 'NONE',  ( 16.46253265017160672, -9.564922557960803928, 73.33224293864769550 ) ) ;
#180692 = CARTESIAN_POINT ( 'NONE',  ( -18.62759615963255300, -10.81492255796106328, 89.16775706135236135 ) ) ;
#180693 = CARTESIAN_POINT ( 'NONE',  ( -4.483927247898782831, 16.52544592524335698, 72.70942372801901854 ) ) ;
#180694 = CARTESIAN_POINT ( 'NONE',  ( -4.379528057220086978, -16.55341960407618274, 29.79275706135234358 ) ) ;
#180696 = CARTESIAN_POINT ( 'NONE',  ( 5.153800228976335163, 19.02544592524342804, 109.7905762719810099 ) ) ;
#180695 = CARTESIAN_POINT ( 'NONE',  ( 4.483927247898545687, 16.52544592524342804, 94.79057627198105251 ) ) ;
#180697 = CARTESIAN_POINT ( 'NONE',  ( -0.05219959533910754901, -16.53943276465976808, 27.49890960531435269 ) ) ;
#180698 = CARTESIAN_POINT ( 'NONE',  ( 19.02544592524343514, -5.153800228976328945, 23.54057627198102054 ) ) ;
#180699 = CARTESIAN_POINT ( 'NONE',  ( -14.34966873604972548, 8.224510206698743886, 58.33442372801901143 ) ) ;
#180700 = CARTESIAN_POINT ( 'NONE',  ( 16.55341960407611168, 4.379528057220329451, 48.95724293864770971 ) ) ;
#180701 = CARTESIAN_POINT ( 'NONE',  ( 14.34966873604972726, -8.224510206698740333, 105.8344237280190328 ) ) ;
#180702 = CARTESIAN_POINT ( 'NONE',  ( -5.049401038298153566, 19.05341960407611168, 110.2072429386476671 ) ) ;
#180703 = CARTESIAN_POINT ( 'NONE',  ( 5.719274019375991003, -21.55341960407610458, 27.70724293864769905 ) ) ;
#180704 = CARTESIAN_POINT ( 'NONE',  ( 18.67979575497194134, -10.72451020669871369, 105.8344237280190328 ) ) ;
#180705 = CARTESIAN_POINT ( 'NONE',  ( 16.52544592524342804, -4.483927247898539470, 83.54057627198102409 ) ) ;
#180706 = CARTESIAN_POINT ( 'NONE',  ( 16.51473224551069308, 9.474510206698969483, 89.16557627198103830 ) ) ;
#180707 = ORIENTED_EDGE ( 'NONE', *, *, #31222, .T. ) ;
#180708 = CARTESIAN_POINT ( 'NONE',  ( -16.53943276465976808, -0.05219959533934237506, 43.75109039468568284 ) ) ;
#180709 = CARTESIAN_POINT ( 'NONE',  ( -19.02544592524342804, 5.153800228976336051, 41.04057627198103120 ) ) ;
#180711 = SURFACE_SIDE_STYLE ('',( #133174 ) ) ;
#180710 = CARTESIAN_POINT ( 'NONE',  ( -4.379528057220086978, -16.55341960407618274, 39.79275706135235424 ) ) ;
#180712 = CARTESIAN_POINT ( 'NONE',  ( 9.474510206698729675, 16.51473224551082808, 47.08442372801900433 ) ) ;
#180713 = CARTESIAN_POINT ( 'NONE',  ( -9.474510206698964154, 16.51473224551069663, 50.41557627198102409 ) ) ;
#180714 = CARTESIAN_POINT ( 'NONE',  ( -8.314922557961024197, 14.29746914071037800, 77.91775706135231871 ) ) ;
#180715 = CARTESIAN_POINT ( 'NONE',  ( 0.05219959533936267826, -19.03943276465977164, 90.00109039468567573 ) ) ;
#180716 = CARTESIAN_POINT ( 'NONE',  ( -13.89961937509977652, 13.97604488694528158, 65.62390960531436690 ) ) ;
#180717 = CARTESIAN_POINT ( 'NONE',  ( -12.06949235617756955, 12.14591786802309770, 105.6239096053143669 ) ) ;
#180718 = CIRCLE ( 'NONE', #22488, 61.99999999999998579 ) ;
#180719 = CARTESIAN_POINT ( 'NONE',  ( 19.02544592524334988, 5.153800228976608722, 66.45942372801899012 ) ) ;
#180720 = CARTESIAN_POINT ( 'NONE',  ( -10.72451020669898014, 18.67979575497178502, 70.41557627198102409 ) ) ;
#180721 = CARTESIAN_POINT ( 'NONE',  ( -19.02544592524334988, -5.153800228976617603, 38.95942372801900433 ) ) ;
#180722 = CARTESIAN_POINT ( 'NONE',  ( 18.56101223717332971, 5.500000000000004441, 98.94978406935679516 ) ) ;
#180723 = CARTESIAN_POINT ( 'NONE',  ( -0.05219959533907301413, -21.53943276465977519, 87.49890960531436690 ) ) ;
#180724 = CARTESIAN_POINT ( 'NONE',  ( -30.73962218707678318, 22.33364281372846705, -7.947842220587803652 ) ) ;
#180725 = CARTESIAN_POINT ( 'NONE',  ( -13.89961937509957401, -13.97604488694547875, 99.37609039468567573 ) ) ;
#180726 = CARTESIAN_POINT ( 'NONE',  ( -18.56453257813359770, 5.500000000000041744, 60.99000423690687711 ) ) ;
#180727 = CARTESIAN_POINT ( 'NONE',  ( 0.05219959533934541429, -16.53943276465976808, 30.00109039468568284 ) ) ;
#180728 = CARTESIAN_POINT ( 'NONE',  ( -5.153800228976328057, -19.02544592524343514, 47.29057627198102409 ) ) ;
#180729 = CARTESIAN_POINT ( 'NONE',  ( -13.97604488694527625, -13.89961937509977652, 111.8739096053143243 ) ) ;
#180730 = CARTESIAN_POINT ( 'NONE',  ( -10.72451020669898014, 18.67979575497178502, 95.41557627198102409 ) ) ;
#180731 = CARTESIAN_POINT ( 'NONE',  ( 10.72451020669871369, 18.67979575497193778, 57.08442372801901854 ) ) ;
#180733 = CARTESIAN_POINT ( 'NONE',  ( 9.474510206698729675, 16.51473224551082808, 22.08442372801899722 ) ) ;
#180732 = CARTESIAN_POINT ( 'NONE',  ( -9.564922557961040184, 16.46253265017147172, 102.9177570613523329 ) ) ;
#180734 = CARTESIAN_POINT ( 'NONE',  ( -4.483927247898539470, -16.52544592524342804, 32.29057627198102409 ) ) ;
#180735 = CARTESIAN_POINT ( 'NONE',  ( -18.62759615963270932, 10.81492255796079327, 95.83224293864770971 ) ) ;
#180736 = CARTESIAN_POINT ( 'NONE',  ( 12.06949235617757843, -12.14591786802309237, 48.12390960531436690 ) ) ;
#180737 = CARTESIAN_POINT ( 'NONE',  ( 13.97604488694548053, -13.89961937509957401, 90.62609039468567573 ) ) ;
#180738 = CARTESIAN_POINT ( 'NONE',  ( 16.46253265017146816, 9.564922557961045513, 56.66775706135233293 ) ) ;
#180739 = CARTESIAN_POINT ( 'NONE',  ( 21.55341960407619695, -5.719274019375665929, 71.04275706135234714 ) ) ;
#180740 = CARTESIAN_POINT ( 'NONE',  ( 5.049401038297881783, 19.05341960407617563, 42.29275706135234003 ) ) ;
#180741 = CARTESIAN_POINT ( 'NONE',  ( 8.314922557960818139, 14.29746914071049879, 114.5822429386477097 ) ) ;
#180742 = CARTESIAN_POINT ( 'NONE',  ( -18.62759615963270932, 10.81492255796079327, 50.83224293864770971 ) ) ;
#180743 = CARTESIAN_POINT ( 'NONE',  ( -16.55341960407611168, -4.379528057220339221, 41.45724293864769550 ) ) ;
#180744 = CARTESIAN_POINT ( 'NONE',  ( 5.719274019375673035, 21.55341960407619339, 107.2927570613523471 ) ) ;
#180745 = CARTESIAN_POINT ( 'NONE',  ( -8.224510206698735004, -14.34966873604973081, 69.58442372801900433 ) ) ;
#180746 = CARTESIAN_POINT ( 'NONE',  ( -16.52544592524342804, 4.483927247898546575, 36.04057627198102409 ) ) ;
#180747 = CARTESIAN_POINT ( 'NONE',  ( 21.53943276465977519, 0.05219959533937863772, 71.25109039468568994 ) ) ;
#180748 = CARTESIAN_POINT ( 'NONE',  ( -5.823673210054431948, 21.52544592524334988, 67.70942372801901854 ) ) ;
#180749 = CARTESIAN_POINT ( 'NONE',  ( -5.823673210054116645, -21.52544592524344225, 72.29057627198102409 ) ) ;
#180750 = CARTESIAN_POINT ( 'NONE',  ( 19.05341960407611168, 5.049401038298154454, 33.95724293864769550 ) ) ;
#180751 = CARTESIAN_POINT ( 'NONE',  ( -10.81492255796105439, 18.62759615963255655, 37.91775706135235424 ) ) ;
#180752 = CARTESIAN_POINT ( 'NONE',  ( 16.53943276465976808, -0.05219959533910856209, 113.7489096053143527 ) ) ;
#180753 = CARTESIAN_POINT ( 'NONE',  ( 19.03943276465977164, -0.05219959533909143690, 38.74890960531436690 ) ) ;
#180754 = CARTESIAN_POINT ( 'NONE',  ( -16.53943276465976808, 0.05219959533911058130, 96.24890960531435269 ) ) ;
#180755 = CARTESIAN_POINT ( 'NONE',  ( -13.89961937509977652, 13.97604488694528158, 90.62390960531432427 ) ) ;
#180756 = CARTESIAN_POINT ( 'NONE',  ( 0.05219959533910956823, 16.53943276465976808, 44.99890960531435979 ) ) ;
#180757 = CARTESIAN_POINT ( 'NONE',  ( 12.14591786802309770, 12.06949235617756955, 94.37390960531436690 ) ) ;
#180758 = CARTESIAN_POINT ( 'NONE',  ( 5.823673210054125526, 21.52544592524343514, 69.79057627198102409 ) ) ;
#180759 = CARTESIAN_POINT ( 'NONE',  ( -21.55341960407610458, -5.719274019375992779, 101.4572429386476955 ) ) ;
#180760 = CARTESIAN_POINT ( 'NONE',  ( 13.97604488694527802, 13.89961937509977652, 109.3739096053143669 ) ) ;
#180762 = CARTESIAN_POINT ( 'NONE',  ( -8.314922557961024197, 14.29746914071037800, 27.91775706135234358 ) ) ;
#180761 = CARTESIAN_POINT ( 'NONE',  ( 13.89961937509977652, -13.97604488694527269, 63.12390960531435979 ) ) ;
#180763 = CARTESIAN_POINT ( 'NONE',  ( 18.62759615963271287, -10.81492255796078972, 58.33224293864768839 ) ) ;
#180764 = CARTESIAN_POINT ( 'NONE',  ( -10.72451020669870658, -18.67979575497194134, 89.58442372801901854 ) ) ;
#180765 = CARTESIAN_POINT ( 'NONE',  ( 5.153800228976335163, 19.02544592524342804, 79.79057627198102409 ) ) ;
#180766 = CARTESIAN_POINT ( 'NONE',  ( 15.80617190586746368, 15.72974639402197994, 114.3739096053143527 ) ) ;
#180767 = ADVANCED_FACE ( 'NONE', ( #12178 ), #28345, .F. ) ;
#180768 = CARTESIAN_POINT ( 'NONE',  ( 16.51473224551069308, 9.474510206698969483, 109.1655762719810383 ) ) ;
#180769 = CARTESIAN_POINT ( 'NONE',  ( 14.29746914071037800, 8.314922557961029526, 91.66775706135234714 ) ) ;
#180770 = CARTESIAN_POINT ( 'NONE',  ( 5.719274019375673035, 21.55341960407619339, 72.29275706135236135 ) ) ;
#180771 = CARTESIAN_POINT ( 'NONE',  ( 21.53943276465977519, 0.05219959533937863772, 96.25109039468568994 ) ) ;
#180772 = CARTESIAN_POINT ( 'NONE',  ( 16.55341960407618274, -4.379528057220086978, 56.04275706135235424 ) ) ;
#180773 = CARTESIAN_POINT ( 'NONE',  ( -10.72451020669870658, -18.67979575497194134, 19.58442372801901143 ) ) ;
#180774 = CARTESIAN_POINT ( 'NONE',  ( -9.474510206698964154, 16.51473224551069663, 25.41557627198103120 ) ) ;
#180775 = CARTESIAN_POINT ( 'NONE',  ( 15.72974639402176855, 15.80617190586768217, 91.87609039468568994 ) ) ;
#180776 = CARTESIAN_POINT ( 'NONE',  ( -5.823673210054116645, -21.52544592524344225, 92.29057627198103830 ) ) ;
#180777 = CARTESIAN_POINT ( 'NONE',  ( -9.474510206698720793, -16.51473224551083518, 49.58442372801899722 ) ) ;
#180778 = CARTESIAN_POINT ( 'NONE',  ( 15.80617190586746368, 15.72974639402197994, 54.37390960531435979 ) ) ;
#180780 = CARTESIAN_POINT ( 'NONE',  ( 8.224510206698953496, -14.34966873604960469, 42.91557627198103120 ) ) ;
#180779 = CARTESIAN_POINT ( 'NONE',  ( 19.05341960407611168, 5.049401038298154454, 98.95724293864766707 ) ) ;
#180781 = CARTESIAN_POINT ( 'NONE',  ( -36.91746825000000598, 2.428612866367529932E-14, -10.62499999726881406 ) ) ;
#180782 = CARTESIAN_POINT ( 'NONE',  ( 26.46959431505284499, -27.26463967846488146, -10.00000000000000000 ) ) ;
#180783 = CARTESIAN_POINT ( 'NONE',  ( -5.153800228976607833, 19.02544592524334988, 102.7094237280189759 ) ) ;
#180784 = CARTESIAN_POINT ( 'NONE',  ( -21.53943276465977519, 0.05219959533907696930, 86.24890960531436690 ) ) ;
#180785 = CARTESIAN_POINT ( 'NONE',  ( 0.05219959533910956823, 16.53943276465976808, 49.99890960531437401 ) ) ;
#180786 = CARTESIAN_POINT ( 'NONE',  ( 8.224510206698742110, 14.34966873604972548, 27.08442372801901854 ) ) ;
#180787 = CARTESIAN_POINT ( 'NONE',  ( 13.97604488694527802, 13.89961937509977652, 39.37390960531435269 ) ) ;
#180789 = CARTESIAN_POINT ( 'NONE',  ( 19.02544592524334988, 5.153800228976608722, 86.45942372801900433 ) ) ;
#180788 = CARTESIAN_POINT ( 'NONE',  ( 18.67979575497178502, 10.72451020669898547, 114.1655762719810383 ) ) ;
#180790 = CARTESIAN_POINT ( 'NONE',  ( -5.049401038298153566, 19.05341960407611168, 85.20724293864766707 ) ) ;
#180791 = CARTESIAN_POINT ( 'NONE',  ( -19.03943276465977164, 0.05219959533909376836, 76.24890960531435269 ) ) ;
#180792 = CARTESIAN_POINT ( 'NONE',  ( -15.80617190586745835, -15.72974639402198527, 76.87390960531439532 ) ) ;
#180793 = CARTESIAN_POINT ( 'NONE',  ( 0.05219959533909260263, 19.03943276465977164, 44.99890960531435979 ) ) ;
#180794 = FACE_OUTER_BOUND ( 'NONE', #31630, .T. ) ;
#180795 = CARTESIAN_POINT ( 'NONE',  ( 16.53943276465976808, -0.05219959533910856209, 58.74890960531436690 ) ) ;
#180796 = CARTESIAN_POINT ( 'NONE',  ( -9.564922557960796823, -16.46253265017161027, 87.08224293864769550 ) ) ;
#180797 = DIRECTION ( 'NONE',  ( 1.000000000000000000, 0.000000000000000000, 0.000000000000000000 ) ) ;
#180798 = CARTESIAN_POINT ( 'NONE',  ( 19.03943276465977164, 0.05219959533936151252, 61.25109039468566863 ) ) ;
#180799 = CARTESIAN_POINT ( 'NONE',  ( 10.81492255796078972, 18.62759615963270932, 79.58224293864769550 ) ) ;
#180800 = CARTESIAN_POINT ( 'NONE',  ( 19.02544592524334988, 5.153800228976608722, 31.45942372801900433 ) ) ;
#180801 = CARTESIAN_POINT ( 'NONE',  ( -13.97604488694527625, -13.89961937509977652, 96.87390960531433848 ) ) ;
#180802 = CARTESIAN_POINT ( 'NONE',  ( -17.50000000000000000, 3.345213924137367734, 114.5876862309434898 ) ) ;
#180803 = CARTESIAN_POINT ( 'NONE',  ( -15.72974639402197994, 15.80617190586746368, 35.62390960531437401 ) ) ;
#180804 = CARTESIAN_POINT ( 'NONE',  ( -16.46253265017160317, 9.564922557960807481, 75.83224293864769550 ) ) ;
#180805 = CARTESIAN_POINT ( 'NONE',  ( -15.72974639402176322, -15.80617190586768395, 69.37609039468567573 ) ) ;
#180806 = CARTESIAN_POINT ( 'NONE',  ( -19.02544592524342804, 5.153800228976336051, 31.04057627198102409 ) ) ;
#180808 = EDGE_LOOP ( 'NONE', ( #85773, #16373, #186475, #166337 ) ) ;
#180807 = CARTESIAN_POINT ( 'NONE',  ( 21.55341960407619695, -5.719274019375665929, 21.04275706135234714 ) ) ;
#180809 = CARTESIAN_POINT ( 'NONE',  ( 21.53943276465977519, 0.05219959533937863772, 51.25109039468568994 ) ) ;
#180810 = ORIENTED_EDGE ( 'NONE', *, *, #158766, .F. ) ;
#180811 = CARTESIAN_POINT ( 'NONE',  ( -9.474510206698964154, 16.51473224551069663, 100.4155762719810241 ) ) ;
#180812 = CARTESIAN_POINT ( 'NONE',  ( -18.22780087662122028, 5.500000000000031086, 88.51540105326107266 ) ) ;
#180813 = CARTESIAN_POINT ( 'NONE',  ( -0.05219959533907301413, -21.53943276465977519, 102.4989096053143811 ) ) ;
#180814 = CARTESIAN_POINT ( 'NONE',  ( -13.97604488694527625, -13.89961937509977652, 56.87390960531434558 ) ) ;
#180815 = CARTESIAN_POINT ( 'NONE',  ( 0.05219959533934541429, -16.53943276465976808, 40.00109039468567573 ) ) ;
#180816 = CARTESIAN_POINT ( 'NONE',  ( -6.020228577223754586E-15, 39.95556452105416412, -8.249999994537628112 ) ) ;
#180817 = CARTESIAN_POINT ( 'NONE',  ( 21.53943276465977519, 0.05219959533937863772, 106.2510903946856757 ) ) ;
#180818 = CARTESIAN_POINT ( 'NONE',  ( 0.05219959533909260263, 19.03943276465977164, 44.99890960531435979 ) ) ;
#180819 = CARTESIAN_POINT ( 'NONE',  ( 18.62759615963255655, 10.81492255796105972, 101.6677570613523613 ) ) ;
#180821 = CARTESIAN_POINT ( 'NONE',  ( 21.53943276465977519, 0.05219959533937863772, 66.25109039468567573 ) ) ;
#180820 = CARTESIAN_POINT ( 'NONE',  ( 16.46253265017160672, -9.564922557960803928, 93.33224293864769550 ) ) ;
#180822 = VECTOR ( 'NONE', #55191, 1000.000000000000000 ) ;
#180823 = CARTESIAN_POINT ( 'NONE',  ( 5.381136069153227730, -3.845012989623188382, -62.42122758075691280 ) ) ;
#180824 = CARTESIAN_POINT ( 'NONE',  ( 19.02544592524343514, -5.153800228976328945, 108.5405762719810383 ) ) ;
#180825 = LINE ( 'NONE', #135311, #4878 ) ;
#180827 = CARTESIAN_POINT ( 'NONE',  ( -15.72974639402176322, -15.80617190586768395, 64.37609039468568994 ) ) ;
#180826 = CARTESIAN_POINT ( 'NONE',  ( -14.34966873604972548, 8.224510206698743886, 58.33442372801901143 ) ) ;
#180828 = CARTESIAN_POINT ( 'NONE',  ( 5.823673210054444382, -21.52544592524334988, 95.20942372801903275 ) ) ;
#180829 = DIRECTION ( 'NONE',  ( -1.000000000000000000, 0.000000000000000000, -6.982962677686266711E-15 ) ) ;
#180830 =( BOUNDED_CURVE ( )  B_SPLINE_CURVE ( 2, ( #13090, #41434, #56603, #167756, #90886, #75729, #199085, #73773, #118277, #25285, #148610 ),
 .UNSPECIFIED., .F., .T. ) 
 B_SPLINE_CURVE_WITH_KNOTS ( ( 3, 2, 2, 2, 2, 3 ),
 ( 0.2000000000000001776, 0.2199999999999996403, 0.2399999999999991029, 0.2599999999999985656, 0.2799999999999980282, 0.2999999999999974909 ),
 .UNSPECIFIED. ) 
 CURVE ( )  GEOMETRIC_REPRESENTATION_ITEM ( )  RATIONAL_B_SPLINE_CURVE ( ( 0.9999999999999994449, 0.9510565162951540863, 1.000000000000000000, 0.9510565162951535312, 1.000000000000000000, 0.9510565162951535312, 1.000000000000000000, 0.9510565162951535312, 1.000000000000000000, 0.9510565162951597484, 0.9999999999999937828 ) ) 
 REPRESENTATION_ITEM ( '' )  );
#180831 = CARTESIAN_POINT ( 'NONE',  ( -0.05219959533934338120, 16.53943276465976808, 22.50109039468567573 ) ) ;
#180832 = CARTESIAN_POINT ( 'NONE',  ( 5.049401038298161559, -19.05341960407611168, 67.70724293864769550 ) ) ;
#180833 = CARTESIAN_POINT ( 'NONE',  ( -16.51473224551069308, -9.474510206698971260, 106.6655762719810383 ) ) ;
#180834 = CARTESIAN_POINT ( 'NONE',  ( 16.36317988757058828, 7.306389748694951614, 43.40210391636777132 ) ) ;
#180835 = CARTESIAN_POINT ( 'NONE',  ( -9.474510206698964154, 16.51473224551069663, 25.41557627198103120 ) ) ;
#180836 = CARTESIAN_POINT ( 'NONE',  ( -21.53943276465977519, 0.05219959533907696930, 41.24890960531435269 ) ) ;
#180837 = CARTESIAN_POINT ( 'NONE',  ( -12.06949235617739369, -12.14591786802326823, 99.37609039468568994 ) ) ;
#180839 = CARTESIAN_POINT ( 'NONE',  ( 5.049401038298161559, -19.05341960407611168, 62.70724293864769550 ) ) ;
#180838 = CARTESIAN_POINT ( 'NONE',  ( 12.14591786802309770, 12.06949235617756955, 79.37390960531436690 ) ) ;
#180840 = CARTESIAN_POINT ( 'NONE',  ( 0.05219959533937995610, -21.53943276465977519, 95.00109039468568994 ) ) ;
#180841 = CARTESIAN_POINT ( 'NONE',  ( -23.66491666289338980, 1.240847218223332327, -57.22545927231451657 ) ) ;
#180842 = CARTESIAN_POINT ( 'NONE',  ( -12.14591786802326823, 12.06949235617739902, 28.12609039468568284 ) ) ;
#180843 = CARTESIAN_POINT ( 'NONE',  ( 16.53943276465976808, -0.05219959533910856209, 93.74890960531436690 ) ) ;
#180844 = CARTESIAN_POINT ( 'NONE',  ( 21.52544592524334988, 5.823673210054432836, 46.45942372801901854 ) ) ;
#180845 = CARTESIAN_POINT ( 'NONE',  ( -10.72451020669898014, 18.67979575497178502, 70.41557627198102409 ) ) ;
#180846 = CARTESIAN_POINT ( 'NONE',  ( 19.02544592524334988, 5.153800228976608722, 36.45942372801900433 ) ) ;
#180847 = CARTESIAN_POINT ( 'NONE',  ( -34.37196153507748164, 7.030587757552860140, 47.62314794725694611 ) ) ;
#180848 = CARTESIAN_POINT ( 'NONE',  ( 13.89961937509977652, -13.97604488694527269, 78.12390960531433848 ) ) ;
#180849 = CARTESIAN_POINT ( 'NONE',  ( 0.05219959533910956823, 16.53943276465976808, 64.99890960531435269 ) ) ;
#180850 = CIRCLE ( 'NONE', #158147, 5.000000000000000000 ) ;
#180851 = CARTESIAN_POINT ( 'NONE',  ( -14.29746914071049879, 8.314922557960819915, 30.83224293864770260 ) ) ;
#180852 = CARTESIAN_POINT ( 'NONE',  ( -16.53943276465976808, -0.05219959533934237506, 113.7510903946856757 ) ) ;
#180853 = CARTESIAN_POINT ( 'NONE',  ( -19.05341960407617563, 5.049401038297882671, 68.54275706135230450 ) ) ;
#180854 = CARTESIAN_POINT ( 'NONE',  ( 18.22780087662122739, 5.500000000000000888, 76.48236817873106475 ) ) ;
#180855 = CARTESIAN_POINT ( 'NONE',  ( -18.67979575497178146, -10.72451020669898902, 21.66557627198102409 ) ) ;
#180856 = ADVANCED_FACE ( 'NONE', ( #106138 ), #74821, .T. ) ;
#180857 = CARTESIAN_POINT ( 'NONE',  ( 16.55341960407611168, 4.379528057220329451, 83.95724293864770971 ) ) ;
#180858 = CARTESIAN_POINT ( 'NONE',  ( 5.000000000000000888, -140.0000000000000000, -13.00000000000000000 ) ) ;
#180860 = CARTESIAN_POINT ( 'NONE',  ( 18.67979575497178502, 10.72451020669898547, 49.16557627198102409 ) ) ;
#180859 = CARTESIAN_POINT ( 'NONE',  ( -9.474510206698964154, 16.51473224551069663, 40.41557627198103120 ) ) ;
#180861 = CARTESIAN_POINT ( 'NONE',  ( 15.72974639402199770, -15.80617190586745480, 68.12390960531436690 ) ) ;
#180862 = CARTESIAN_POINT ( 'NONE',  ( 14.29746914071049879, -8.314922557960816363, 108.3322429386477097 ) ) ;
#180864 = CARTESIAN_POINT ( 'NONE',  ( -0.05219959533909027116, -19.03943276465977164, 47.49890960531435979 ) ) ;
#180863 = CARTESIAN_POINT ( 'NONE',  ( -16.52544592524335698, -4.483927247898792601, 58.95942372801902565 ) ) ;
#180865 = CARTESIAN_POINT ( 'NONE',  ( 5.719274019375673035, 21.55341960407619339, 57.29275706135234714 ) ) ;
#180866 = CARTESIAN_POINT ( 'NONE',  ( -14.34966873604960291, -8.224510206698953496, 106.6655762719810383 ) ) ;
#180867 = CARTESIAN_POINT ( 'NONE',  ( 5.153800228976615827, -19.02544592524334988, 95.20942372801897591 ) ) ;
#180868 = CARTESIAN_POINT ( 'NONE',  ( -29.86685920354755552, 21.69954338932564397, -3.324999997268813345 ) ) ;
#180870 = CARTESIAN_POINT ( 'NONE',  ( 21.55341960407610458, 5.719274019375980345, 28.95724293864769905 ) ) ;
#180869 = FACE_OUTER_BOUND ( 'NONE', #108427, .T. ) ;
#180871 = CARTESIAN_POINT ( 'NONE',  ( -19.02544592524342804, 5.153800228976336051, 26.04057627198103120 ) ) ;
#180872 = CARTESIAN_POINT ( 'NONE',  ( -21.52544592524334988, -5.823673210054445271, 68.95942372801901854 ) ) ;
#180874 = CARTESIAN_POINT ( 'NONE',  ( 16.55341960407611168, 4.379528057220329451, 43.95724293864769550 ) ) ;
#180873 = CARTESIAN_POINT ( 'NONE',  ( -0.05219959533934338120, 16.53943276465976808, 62.50109039468568284 ) ) ;
#180875 = CARTESIAN_POINT ( 'NONE',  ( 21.53943276465977519, -0.05219959533907433946, 63.74890960531435979 ) ) ;
#180877 = CARTESIAN_POINT ( 'NONE',  ( 10.81492255796078972, 18.62759615963270932, 74.58224293864768129 ) ) ;
#180876 = PRODUCT_DEFINITION ( 'UNKNOWN', '', #108208, #94919 ) ;
#180878 = CARTESIAN_POINT ( 'NONE',  ( 28.47622644277404191, -25.16156846422445881, -16.68312038616162241 ) ) ;
#180880 = CARTESIAN_POINT ( 'NONE',  ( 9.474510206698971260, -16.51473224551069308, 112.9155762719810383 ) ) ;
#180879 = CARTESIAN_POINT ( 'NONE',  ( -19.02544592524334988, -5.153800228976617603, 88.95942372801897591 ) ) ;
#180881 = CARTESIAN_POINT ( 'NONE',  ( 19.03943276465977164, -0.05219959533909143690, 48.74890960531435979 ) ) ;
#180882 = CARTESIAN_POINT ( 'NONE',  ( -4.379528057220328563, 16.55341960407611168, 110.2072429386477239 ) ) ;
#180883 = FACE_BOUND ( 'NONE', #113801, .T. ) ;
#180884 = ORIENTED_EDGE ( 'NONE', *, *, #75190, .T. ) ;
#180885 = CARTESIAN_POINT ( 'NONE',  ( -16.52544592524335698, -4.483927247898792601, 63.95942372801901854 ) ) ;
#180886 = CARTESIAN_POINT ( 'NONE',  ( -10.72451020669898014, 18.67979575497178502, 100.4155762719810241 ) ) ;
#180887 = CARTESIAN_POINT ( 'NONE',  ( 13.97604488694527802, 13.89961937509977652, 64.37390960531436690 ) ) ;
#180888 = CARTESIAN_POINT ( 'NONE',  ( 18.62759615963255655, 10.81492255796105972, 36.66775706135234714 ) ) ;
#180889 = CARTESIAN_POINT ( 'NONE',  ( -19.02544592524342804, 5.153800228976336051, 91.04057627198100988 ) ) ;
#180890 = CARTESIAN_POINT ( 'NONE',  ( -28.61471831746303707, -27.54183658529284529, -20.22090314798039401 ) ) ;
#180891 = ORIENTED_EDGE ( 'NONE', *, *, #90570, .T. ) ;
#180892 = CARTESIAN_POINT ( 'NONE',  ( -18.62759615963255300, -10.81492255796106328, 29.16775706135234003 ) ) ;
#180894 = CARTESIAN_POINT ( 'NONE',  ( 0.05219959533936267826, -19.03943276465977164, 85.00109039468567573 ) ) ;
#180893 = CARTESIAN_POINT ( 'NONE',  ( 19.05341960407611168, 5.049401038298154454, 28.95724293864769550 ) ) ;
#180895 = CARTESIAN_POINT ( 'NONE',  ( 5.153800228976615827, -19.02544592524334988, 45.20942372801901143 ) ) ;
#180896 = CARTESIAN_POINT ( 'NONE',  ( 21.52544592524344225, -5.823673210054117533, 113.5405762719810383 ) ) ;
#180897 = CARTESIAN_POINT ( 'NONE',  ( -5.153800228976607833, 19.02544592524334988, 37.70942372801899722 ) ) ;
#180898 = CARTESIAN_POINT ( 'NONE',  ( -16.51473224551082808, 9.474510206698731452, 53.33442372801900433 ) ) ;
#180899 = CARTESIAN_POINT ( 'NONE',  ( 16.55341960407618274, -4.379528057220086978, 91.04275706135236135 ) ) ;
#180900 = ORIENTED_EDGE ( 'NONE', *, *, #184834, .T. ) ;
#180901 = CARTESIAN_POINT ( 'NONE',  ( 19.05341960407611168, 5.049401038298154454, 73.95724293864768129 ) ) ;
#180902 = CARTESIAN_POINT ( 'NONE',  ( -10.81492255796105439, 18.62759615963255655, 72.91775706135234714 ) ) ;
#180903 = CARTESIAN_POINT ( 'NONE',  ( -18.62759615963255300, -10.81492255796106328, 99.16775706135234714 ) ) ;
#180904 = CARTESIAN_POINT ( 'NONE',  ( 21.39623730026196924, -0.5392447798056823061, -56.39940532337662660 ) ) ;
#180905 = CARTESIAN_POINT ( 'NONE',  ( 16.46253265017160672, -9.564922557960803928, 83.33224293864768129 ) ) ;
#180906 = CARTESIAN_POINT ( 'NONE',  ( -0.05219959533937732626, 21.53943276465977519, 57.50109039468568994 ) ) ;
#180907 = CARTESIAN_POINT ( 'NONE',  ( -5.153800228976607833, 19.02544592524334988, 97.70942372801900433 ) ) ;
#180908 = CARTESIAN_POINT ( 'NONE',  ( -19.03943276465977164, 0.05219959533909376836, 66.24890960531436690 ) ) ;
#180909 = CARTESIAN_POINT ( 'NONE',  ( 19.03943276465977164, -0.05219959533909143690, 113.7489096053143669 ) ) ;
#180910 = CARTESIAN_POINT ( 'NONE',  ( 13.89961937509977652, -13.97604488694527269, 73.12390960531436690 ) ) ;
#180911 = CARTESIAN_POINT ( 'NONE',  ( -17.49999999999999645, 5.499999999999992895, 43.71769037696436300 ) ) ;
#180912 = CARTESIAN_POINT ( 'NONE',  ( 9.564922557960805705, 16.46253265017160317, 64.58224293864769550 ) ) ;
#180913 = CARTESIAN_POINT ( 'NONE',  ( -13.97604488694527625, -13.89961937509977652, 46.87390960531435979 ) ) ;
#180914 = CARTESIAN_POINT ( 'NONE',  ( 15.72974639402176855, 15.80617190586768217, 21.87609039468567573 ) ) ;
#180915 = CARTESIAN_POINT ( 'NONE',  ( 12.06949235617739724, 12.14591786802326823, 86.87609039468568994 ) ) ;
#180916 = DIRECTION ( 'NONE',  ( -0.000000000000000000, -0.000000000000000000, 1.000000000000000000 ) ) ;
#180917 = CARTESIAN_POINT ( 'NONE',  ( -21.46320343559624533, 20.96320343559661481, 4.646446609406719830 ) ) ;
#180918 = CARTESIAN_POINT ( 'NONE',  ( 9.474510206698729675, 16.51473224551082808, 62.08442372801899722 ) ) ;
#180919 = CARTESIAN_POINT ( 'NONE',  ( 9.564922557960805705, 16.46253265017160317, 74.58224293864769550 ) ) ;
#180920 = CARTESIAN_POINT ( 'NONE',  ( -16.53943276465976808, 0.05219959533911058130, 71.24890960531435269 ) ) ;
#180921 = CARTESIAN_POINT ( 'NONE',  ( -4.483927247898539470, -16.52544592524342804, 112.2905762719810241 ) ) ;
#180922 = CARTESIAN_POINT ( 'NONE',  ( -9.474510206698964154, 16.51473224551069663, 115.4155762719810241 ) ) ;
#180923 = CARTESIAN_POINT ( 'NONE',  ( -5.049401038298153566, 19.05341960407611168, 100.2072429386476955 ) ) ;
#180924 = CARTESIAN_POINT ( 'NONE',  ( -0.05219959533910754901, -16.53943276465976808, 87.49890960531436690 ) ) ;
#180925 = LINE ( 'NONE', #12078, #156513 ) ;
#180926 = CARTESIAN_POINT ( 'NONE',  ( -9.474510206698720793, -16.51473224551083518, 29.58442372801900433 ) ) ;
#180927 = CARTESIAN_POINT ( 'NONE',  ( 16.52544592524335698, 4.483927247898782831, 111.4594237280190328 ) ) ;
#180928 = CARTESIAN_POINT ( 'NONE',  ( -19.05341960407611168, -5.049401038298163336, 86.45724293864769550 ) ) ;
#180929 = CARTESIAN_POINT ( 'NONE',  ( 21.55341960407619695, -5.719274019375665929, 56.04275706135235424 ) ) ;
#180930 = CARTESIAN_POINT ( 'NONE',  ( 18.62759615963271287, -10.81492255796078972, 38.33224293864768839 ) ) ;
#180931 = CARTESIAN_POINT ( 'NONE',  ( 5.719274019375673035, 21.55341960407619339, 22.29275706135235069 ) ) ;
#180932 = CARTESIAN_POINT ( 'NONE',  ( -15.72974639402197994, 15.80617190586746368, 65.62390960531436690 ) ) ;
#180933 = CARTESIAN_POINT ( 'NONE',  ( 8.314922557960818139, 14.29746914071049879, 89.58224293864768129 ) ) ;
#180934 = CARTESIAN_POINT ( 'NONE',  ( 19.02544592524334988, 5.153800228976608722, 51.45942372801900433 ) ) ;
#180935 = CARTESIAN_POINT ( 'NONE',  ( -5.153800228976328057, -19.02544592524343514, 27.29057627198103120 ) ) ;
#180936 = CARTESIAN_POINT ( 'NONE',  ( 5.153800228976335163, 19.02544592524342804, 89.79057627198102409 ) ) ;
#180937 = CARTESIAN_POINT ( 'NONE',  ( 19.03943276465977164, -0.05219959533909143690, 98.74890960531436690 ) ) ;
#180938 = CARTESIAN_POINT ( 'NONE',  ( 0.05219959533910956823, 16.53943276465976808, 114.9989096053143669 ) ) ;
#180939 = CARTESIAN_POINT ( 'NONE',  ( 4.483927247898545687, 16.52544592524342804, 24.79057627198103120 ) ) ;
#180940 = CARTESIAN_POINT ( 'NONE',  ( 12.06949235617739724, 12.14591786802326823, 46.87609039468568994 ) ) ;
#180941 = CARTESIAN_POINT ( 'NONE',  ( -5.823673210054431948, 21.52544592524334988, 107.7094237280190328 ) ) ;
#180942 = CARTESIAN_POINT ( 'NONE',  ( 13.89961937509977652, -13.97604488694527269, 98.12390960531433848 ) ) ;
#180943 = CARTESIAN_POINT ( 'NONE',  ( 21.55341960407619695, -5.719274019375665929, 31.04275706135234714 ) ) ;
#180944 = CARTESIAN_POINT ( 'NONE',  ( 9.474510206698971260, -16.51473224551069308, 47.91557627198102409 ) ) ;
#180945 = CARTESIAN_POINT ( 'NONE',  ( 12.14591786802327356, -12.06949235617739191, 50.62609039468568994 ) ) ;
#180946 = CARTESIAN_POINT ( 'NONE',  ( -16.55341960407617563, 4.379528057220093196, 88.54275706135236135 ) ) ;
#180947 = CARTESIAN_POINT ( 'NONE',  ( 19.02544592524334988, 5.153800228976608722, 111.4594237280190043 ) ) ;
#180948 = CARTESIAN_POINT ( 'NONE',  ( 19.02544592524343514, -5.153800228976328945, 28.54057627198102409 ) ) ;
#180949 = CARTESIAN_POINT ( 'NONE',  ( 8.224510206698953496, -14.34966873604960469, 97.91557627198103830 ) ) ;
#180950 = CARTESIAN_POINT ( 'NONE',  ( -18.62759615963270932, 10.81492255796079327, 105.8322429386476955 ) ) ;
#180951 = CARTESIAN_POINT ( 'NONE',  ( 9.474510206698971260, -16.51473224551069308, 27.91557627198103120 ) ) ;
#180952 = CARTESIAN_POINT ( 'NONE',  ( 16.51473224551069308, 9.474510206698969483, 109.1655762719810383 ) ) ;
#180953 = CARTESIAN_POINT ( 'NONE',  ( -21.53943276465977519, -0.05219959533937600094, 28.75109039468567929 ) ) ;
#180954 = CARTESIAN_POINT ( 'NONE',  ( -21.30000000000002913, 2.244099063931684814E-13, -58.85720012050612837 ) ) ;
#180955 = CARTESIAN_POINT ( 'NONE',  ( -9.474510206698964154, 16.51473224551069663, 100.4155762719810241 ) ) ;
#180956 = CARTESIAN_POINT ( 'NONE',  ( 17.50000000000000000, -5.500000000000000000, 111.2176903769643559 ) ) ;
#180957 = CARTESIAN_POINT ( 'NONE',  ( -0.05219959533909027116, -19.03943276465977164, 82.49890960531436690 ) ) ;
#180959 = CARTESIAN_POINT ( 'NONE',  ( -14.34966873604960291, -8.224510206698953496, 91.66557627198103830 ) ) ;
#180958 = CARTESIAN_POINT ( 'NONE',  ( 18.62759615963255655, 10.81492255796105972, 26.66775706135235424 ) ) ;
#180960 = CARTESIAN_POINT ( 'NONE',  ( -9.564922557960796823, -16.46253265017161027, 92.08224293864769550 ) ) ;
#180961 = CARTESIAN_POINT ( 'NONE',  ( -9.564922557961040184, 16.46253265017147172, 22.91775706135233648 ) ) ;
#180962 = CARTESIAN_POINT ( 'NONE',  ( -14.34966873604972548, 8.224510206698743886, 63.33442372801900433 ) ) ;
#180963 = CARTESIAN_POINT ( 'NONE',  ( -10.81492255796105439, 18.62759615963255655, 72.91775706135234714 ) ) ;
#180964 = CARTESIAN_POINT ( 'NONE',  ( 0.05219959533934541429, -16.53943276465976808, 45.00109039468568284 ) ) ;
#180965 = CARTESIAN_POINT ( 'NONE',  ( 13.89961937509977652, -13.97604488694527269, 83.12390960531436690 ) ) ;
#180966 = CARTESIAN_POINT ( 'NONE',  ( 13.89961937509957401, 13.97604488694547697, 101.8760903946856331 ) ) ;
#180967 = CARTESIAN_POINT ( 'NONE',  ( -8.224510206698735004, -14.34966873604973081, 69.58442372801900433 ) ) ;
#180968 = CARTESIAN_POINT ( 'NONE',  ( -18.62759615963255300, -10.81492255796106328, 109.1677570613523613 ) ) ;
#180969 = CARTESIAN_POINT ( 'NONE',  ( 16.51473224551083163, -9.474510206698727899, 80.83442372801899012 ) ) ;
#180970 = CARTESIAN_POINT ( 'NONE',  ( 0.05219959533909260263, 19.03943276465977164, 59.99890960531436690 ) ) ;
#180971 = CARTESIAN_POINT ( 'NONE',  ( 21.53943276465977519, -0.05219959533907433946, 83.74890960531435269 ) ) ;
#180973 = CARTESIAN_POINT ( 'NONE',  ( -19.05341960407617563, 5.049401038297882671, 88.54275706135230450 ) ) ;
#180972 = CARTESIAN_POINT ( 'NONE',  ( 0.05219959533910956823, 16.53943276465976808, 74.99890960531435269 ) ) ;
#180974 = CARTESIAN_POINT ( 'NONE',  ( 4.379528057220092307, 16.55341960407617563, 62.29275706135236845 ) ) ;
#180975 = CARTESIAN_POINT ( 'NONE',  ( -19.02130022317636815, 5.499999999999800160, 80.78188669246576126 ) ) ;
#180976 = CARTESIAN_POINT ( 'NONE',  ( 0.05219959533936267826, -19.03943276465977164, 55.00109039468566863 ) ) ;
#180977 = CARTESIAN_POINT ( 'NONE',  ( -4.483927247898782831, 16.52544592524335698, 107.7094237280190328 ) ) ;
#180978 = CARTESIAN_POINT ( 'NONE',  ( -14.34966873604960291, -8.224510206698953496, 76.66557627198103830 ) ) ;
#180980 = CARTESIAN_POINT ( 'NONE',  ( -18.56453257813363678, 5.500000000000055067, 90.99000423690687001 ) ) ;
#180979 = CARTESIAN_POINT ( 'NONE',  ( 21.52544592524334988, 5.823673210054432836, 111.4594237280190328 ) ) ;
#180981 = CARTESIAN_POINT ( 'NONE',  ( 18.62759615963271287, -10.81492255796078972, 113.3322429386476955 ) ) ;
#180982 = CARTESIAN_POINT ( 'NONE',  ( -19.03943276465977164, 0.05219959533909376836, 106.2489096053143669 ) ) ;
#180983 = CARTESIAN_POINT ( 'NONE',  ( 16.46253265017160672, -9.564922557960803928, 78.33224293864769550 ) ) ;
#180984 = CARTESIAN_POINT ( 'NONE',  ( 18.67979575497194134, -10.72451020669871369, 85.83442372801901854 ) ) ;
#180985 = CARTESIAN_POINT ( 'NONE',  ( 9.474510206698971260, -16.51473224551069308, 57.91557627198103120 ) ) ;
#180986 = ORIENTED_EDGE ( 'NONE', *, *, #124720, .F. ) ;
#180987 = CARTESIAN_POINT ( 'NONE',  ( -10.81492255796078084, -18.62759615963271287, 27.08224293864769550 ) ) ;
#180988 = CARTESIAN_POINT ( 'NONE',  ( 4.379528057220339221, -16.55341960407611168, 82.70724293864770971 ) ) ;
#180989 = CARTESIAN_POINT ( 'NONE',  ( -9.564922557960796823, -16.46253265017161027, 37.08224293864768839 ) ) ;
#180990 = CARTESIAN_POINT ( 'NONE',  ( -8.314922557960811034, -14.29746914071050412, 97.08224293864770971 ) ) ;
#180991 = CARTESIAN_POINT ( 'NONE',  ( 21.53943276465977519, -0.05219959533907433946, 103.7489096053143669 ) ) ;
#180992 = CIRCLE ( 'NONE', #67934, 4.250000000000000000 ) ;
#180993 = CARTESIAN_POINT ( 'NONE',  ( 10.72451020669871369, 18.67979575497193778, 47.08442372801901854 ) ) ;
#180994 = CARTESIAN_POINT ( 'NONE',  ( -19.02544592524342804, 5.153800228976336051, 31.04057627198102409 ) ) ;
#180995 = CARTESIAN_POINT ( 'NONE',  ( 12.06949235617739724, 12.14591786802326823, 66.87609039468568994 ) ) ;
#180996 = B_SPLINE_CURVE_WITH_KNOTS ( 'NONE', 3,
 ( #119338, #55655, #85989, #40491, #197180, #26342, #104162, #149670, #118340, #148678, #87982, #181024 ),
 .UNSPECIFIED., .F., .F.,
 ( 4, 2, 2, 2, 2, 4 ),
 ( 1.969502665979568066E-07, 0.0004083572201530094635, 0.0008165174900394210449, 0.001632838029812235317, 0.002449158569585050023, 0.003265479109357864295 ),
 .UNSPECIFIED. ) ;
#180997 = CARTESIAN_POINT ( 'NONE',  ( 10.72451020669898902, -18.67979575497178502, 97.91557627198103830 ) ) ;
#180998 = CARTESIAN_POINT ( 'NONE',  ( -21.55341960407610458, -5.719274019375992779, 96.45724293864770971 ) ) ;
#181000 = CARTESIAN_POINT ( 'NONE',  ( 13.89961937509977652, -13.97604488694527269, 53.12390960531434558 ) ) ;
#180999 = CARTESIAN_POINT ( 'NONE',  ( -5.049401038297874678, -19.05341960407617918, 34.79275706135233293 ) ) ;
#181001 = CARTESIAN_POINT ( 'NONE',  ( 5.153800228976335163, 19.02544592524342804, 114.7905762719810241 ) ) ;
#181002 = CARTESIAN_POINT ( 'NONE',  ( 10.72451020669871369, 18.67979575497193778, 57.08442372801901854 ) ) ;
#181003 = EDGE_CURVE ( 'NONE', #71610, #66950, #44589, .T. ) ;
#181004 = CARTESIAN_POINT ( 'NONE',  ( -21.55341960407610458, -5.719274019375992779, 61.45724293864770260 ) ) ;
#181005 = CARTESIAN_POINT ( 'NONE',  ( -16.52544592524342804, 4.483927247898546575, 31.04057627198102409 ) ) ;
#181007 = CARTESIAN_POINT ( 'NONE',  ( 0.05219959533937995610, -21.53943276465977519, 110.0010903946856757 ) ) ;
#181006 = CARTESIAN_POINT ( 'NONE',  ( 10.72451020669871369, 18.67979575497193778, 82.08442372801901854 ) ) ;
#181008 = CARTESIAN_POINT ( 'NONE',  ( 12.14591786802309770, 12.06949235617756955, 59.37390960531436690 ) ) ;
#181009 = CARTESIAN_POINT ( 'NONE',  ( -16.55341960407611168, -4.379528057220339221, 101.4572429386476955 ) ) ;
#181010 = CARTESIAN_POINT ( 'NONE',  ( 13.97604488694548053, -13.89961937509957401, 45.62609039468566863 ) ) ;
#181011 = CARTESIAN_POINT ( 'NONE',  ( 12.06949235617739724, 12.14591786802326823, 106.8760903946856899 ) ) ;
#181012 = CARTESIAN_POINT ( 'NONE',  ( -18.67979575497193778, 10.72451020669871902, 73.33442372801901854 ) ) ;
#181013 = CARTESIAN_POINT ( 'NONE',  ( -19.03943276465977164, 0.05219959533909376836, 61.24890960531436690 ) ) ;
#181014 = CARTESIAN_POINT ( 'NONE',  ( 5.153800228976615827, -19.02544592524334988, 30.20942372801900433 ) ) ;
#181015 = CARTESIAN_POINT ( 'NONE',  ( 0.05219959533907565091, 21.53943276465977519, 39.99890960531436690 ) ) ;
#181016 = CARTESIAN_POINT ( 'NONE',  ( -5.719274019375665041, -21.55341960407619695, 34.79275706135235424 ) ) ;
#181017 = CARTESIAN_POINT ( 'NONE',  ( 21.52544592524344225, -5.823673210054117533, 88.54057627198103830 ) ) ;
#181018 = CARTESIAN_POINT ( 'NONE',  ( -9.564922557961040184, 16.46253265017147172, 82.91775706135233293 ) ) ;
#181019 = CARTESIAN_POINT ( 'NONE',  ( -12.06949235617739369, -12.14591786802326823, 49.37609039468569705 ) ) ;
#181021 = CARTESIAN_POINT ( 'NONE',  ( -0.05219959533907301413, -21.53943276465977519, 92.49890960531436690 ) ) ;
#181020 = DIRECTION ( 'NONE',  ( 0.000000000000000000, 0.000000000000000000, -1.000000000000000000 ) ) ;
#181023 = CARTESIAN_POINT ( 'NONE',  ( -16.52544592524342804, 4.483927247898546575, 71.04057627198103830 ) ) ;
#181022 = CARTESIAN_POINT ( 'NONE',  ( 12.14591786802327356, -12.06949235617739191, 75.62609039468567573 ) ) ;
#181024 = CARTESIAN_POINT ( 'NONE',  ( 1.500000000000003553, 30.40000000000004476, -47.75060438757614634 ) ) ;
#181025 = CARTESIAN_POINT ( 'NONE',  ( 5.153800228976615827, -19.02544592524334988, 105.2094237280190185 ) ) ;
#181026 = CARTESIAN_POINT ( 'NONE',  ( 5.719274019375991003, -21.55341960407610458, 32.70724293864770260 ) ) ;
#181027 = CARTESIAN_POINT ( 'NONE',  ( -16.46253265017160317, 9.564922557960807481, 95.83224293864769550 ) ) ;
#181028 = CARTESIAN_POINT ( 'NONE',  ( -14.34966873604972548, 8.224510206698743886, 58.33442372801901143 ) ) ;
#181029 = CARTESIAN_POINT ( 'NONE',  ( 18.62759615963255655, 10.81492255796105972, 26.66775706135235424 ) ) ;
#181030 = CARTESIAN_POINT ( 'NONE',  ( 15.72974639402199770, -15.80617190586745480, 43.12390960531435269 ) ) ;
#181031 = CARTESIAN_POINT ( 'NONE',  ( -12.06949235617739369, -12.14591786802326823, 64.37609039468568994 ) ) ;
#181032 = CARTESIAN_POINT ( 'NONE',  ( 19.02544592524343514, -5.153800228976328945, 83.54057627198100988 ) ) ;
#181034 = CARTESIAN_POINT ( 'NONE',  ( -9.564922557960796823, -16.46253265017161027, 27.08224293864769550 ) ) ;
#181033 = CARTESIAN_POINT ( 'NONE',  ( -21.55341960407619339, 5.719274019375674811, 58.54275706135235424 ) ) ;
#181035 = CARTESIAN_POINT ( 'NONE',  ( -15.72974639402197994, 15.80617190586746368, 40.62390960531435269 ) ) ;
#181036 = ORIENTED_EDGE ( 'NONE', *, *, #132905, .F. ) ;
#181037 = CARTESIAN_POINT ( 'NONE',  ( -0.05219959533936034679, 19.03943276465977164, 37.50109039468567573 ) ) ;
#181038 = CARTESIAN_POINT ( 'NONE',  ( -12.06949235617739369, -12.14591786802326823, 49.37609039468569705 ) ) ;
#181039 = CARTESIAN_POINT ( 'NONE',  ( -21.53943276465977519, 0.05219959533907696930, 21.24890960531436690 ) ) ;
#181040 = EDGE_LOOP ( 'NONE', ( #180136, #104411, #80129 ) ) ;
#181041 = CARTESIAN_POINT ( 'NONE',  ( -13.89961937509977652, 13.97604488694528158, 80.62390960531436690 ) ) ;
#181042 = CARTESIAN_POINT ( 'NONE',  ( 4.483927247898790824, -16.52544592524335698, 105.2094237280190328 ) ) ;
#181043 = CARTESIAN_POINT ( 'NONE',  ( -5.427562675786936573E-15, 30.27659582821221207, 141.7656553485623760 ) ) ;
#181044 = CARTESIAN_POINT ( 'NONE',  ( -12.06949235617756955, 12.14591786802309770, 100.6239096053143811 ) ) ;
#181045 = CARTESIAN_POINT ( 'NONE',  ( -10.72451020669898014, 18.67979575497178502, 30.41557627198101699 ) ) ;
#181046 = CARTESIAN_POINT ( 'NONE',  ( -16.46253265017160317, 9.564922557960807481, 25.83224293864769194 ) ) ;
#181047 = CARTESIAN_POINT ( 'NONE',  ( -16.52544592524335698, -4.483927247898792601, 78.95942372801901854 ) ) ;
#181048 = CARTESIAN_POINT ( 'NONE',  ( -18.67979575497178146, -10.72451020669898902, 111.6655762719810525 ) ) ;
#181049 = CARTESIAN_POINT ( 'NONE',  ( 16.46253265017146816, 9.564922557961045513, 71.66775706135233293 ) ) ;
#181050 = CARTESIAN_POINT ( 'NONE',  ( 13.97604488694527802, 13.89961937509977652, 44.37390960531435269 ) ) ;
#181051 = CARTESIAN_POINT ( 'NONE',  ( -13.89961937509977652, 13.97604488694528158, 115.6239096053143669 ) ) ;
#181052 = CARTESIAN_POINT ( 'NONE',  ( 15.80617190586769283, -15.72974639402175789, 100.6260903946857184 ) ) ;
#181053 = CARTESIAN_POINT ( 'NONE',  ( -5.153800228976328057, -19.02544592524343514, 62.29057627198100988 ) ) ;
#181054 = CARTESIAN_POINT ( 'NONE',  ( -14.29746914071037622, -8.314922557961029526, 54.16775706135235424 ) ) ;
#181055 = CARTESIAN_POINT ( 'NONE',  ( 10.81492255796106328, -18.62759615963255655, 90.41775706135236135 ) ) ;
#181056 = CARTESIAN_POINT ( 'NONE',  ( 19.02544592524334988, 5.153800228976608722, 51.45942372801900433 ) ) ;
#181057 = CARTESIAN_POINT ( 'NONE',  ( 5.153800228976615827, -19.02544592524334988, 50.20942372801897591 ) ) ;
#181058 = EDGE_LOOP ( 'NONE', ( #57163, #53193, #104077 ) ) ;
#181059 = CARTESIAN_POINT ( 'NONE',  ( 21.55341960407619695, -5.719274019375665929, 46.04275706135234714 ) ) ;
#181060 = CIRCLE ( 'NONE', #16348, 35.99626262588765258 ) ;
#181061 = DIRECTION ( 'NONE',  ( 0.000000000000000000, 0.000000000000000000, 1.000000000000000000 ) ) ;
#181062 = CARTESIAN_POINT ( 'NONE',  ( -19.02544592524334988, -5.153800228976617603, 48.95942372801900433 ) ) ;
#181063 = CARTESIAN_POINT ( 'NONE',  ( 5.153800228976335163, 19.02544592524342804, 94.79057627198103830 ) ) ;
#181064 = CARTESIAN_POINT ( 'NONE',  ( 19.03943276465977164, -0.05219959533909143690, 88.74890960531436690 ) ) ;
#181065 = CARTESIAN_POINT ( 'NONE',  ( 4.379528057220339221, -16.55341960407611168, 42.70724293864770260 ) ) ;
#181066 = CARTESIAN_POINT ( 'NONE',  ( 5.823673210054125526, 21.52544592524343514, 34.79057627198103120 ) ) ;
#181067 = CARTESIAN_POINT ( 'NONE',  ( -22.81625015709510507, 31.40387420917330275, -3.424999997268813434 ) ) ;
#181068 = DIRECTION ( 'NONE',  ( -1.000000000000000000, 0.000000000000000000, 0.000000000000000000 ) ) ;
#181069 = CARTESIAN_POINT ( 'NONE',  ( -21.53943276465977519, -0.05219959533937600094, 108.7510903946857042 ) ) ;
#181070 = CARTESIAN_POINT ( 'NONE',  ( 12.55500000000001748, 0.000000000000000000, 0.000000000000000000 ) ) ;
#181071 = CARTESIAN_POINT ( 'NONE',  ( -13.97604488694527625, -13.89961937509977652, 41.87390960531435979 ) ) ;
#181072 = CARTESIAN_POINT ( 'NONE',  ( -16.46253265017160317, 9.564922557960807481, 25.83224293864769194 ) ) ;
#181073 = CARTESIAN_POINT ( 'NONE',  ( -19.24578484527059175, -180.9428398739491684, -15.00000000000000000 ) ) ;
#181074 = CARTESIAN_POINT ( 'NONE',  ( -35.81018071281594217, -12.25470802944819937, -7.999999999999998224 ) ) ;
#181075 = CARTESIAN_POINT ( 'NONE',  ( -14.29746914071037622, -8.314922557961029526, 59.16775706135234714 ) ) ;
#181076 = CARTESIAN_POINT ( 'NONE',  ( 18.62759615963271287, -10.81492255796078972, 88.33224293864769550 ) ) ;
#181077 = CARTESIAN_POINT ( 'NONE',  ( 0.05219959533910956823, 16.53943276465976808, 44.99890960531435979 ) ) ;
#181079 = CARTESIAN_POINT ( 'NONE',  ( 9.564922557960805705, 16.46253265017160317, 114.5822429386476955 ) ) ;
#181078 = CARTESIAN_POINT ( 'NONE',  ( -19.02544592524342804, 5.153800228976336051, 31.04057627198102409 ) ) ;
#181080 = CARTESIAN_POINT ( 'NONE',  ( 10.81492255796106328, -18.62759615963255655, 30.41775706135234358 ) ) ;
#181081 = CARTESIAN_POINT ( 'NONE',  ( 5.153800228976615827, -19.02544592524334988, 30.20942372801900433 ) ) ;
#181082 = CARTESIAN_POINT ( 'NONE',  ( 19.03943276465977164, -0.05219959533909143690, 33.74890960531435979 ) ) ;
#181083 = CARTESIAN_POINT ( 'NONE',  ( -5.823673210054431948, 21.52544592524334988, 77.70942372801900433 ) ) ;
#181084 = DIRECTION ( 'NONE',  ( -1.000000000000000000, -0.000000000000000000, -0.000000000000000000 ) ) ;
#181085 = CARTESIAN_POINT ( 'NONE',  ( -14.29746914071049879, 8.314922557960819915, 25.83224293864769194 ) ) ;
#181086 = CARTESIAN_POINT ( 'NONE',  ( 17.50000000000147793, 3.202012800152207905, 112.5717758397275077 ) ) ;
#181087 = CARTESIAN_POINT ( 'NONE',  ( 15.80617190586746368, 15.72974639402197994, 29.37390960531435269 ) ) ;
#181088 = CARTESIAN_POINT ( 'NONE',  ( 8.314922557960818139, 14.29746914071049879, 99.58224293864770971 ) ) ;
#181089 = CARTESIAN_POINT ( 'NONE',  ( -5.945206945974415014, -6.768871089493145199, -63.97253992123162902 ) ) ;
#181090 = CARTESIAN_POINT ( 'NONE',  ( -16.46253265017160317, 9.564922557960807481, 95.83224293864769550 ) ) ;
#181091 = CARTESIAN_POINT ( 'NONE',  ( -0.05219959533910754901, -16.53943276465976808, 77.49890960531433848 ) ) ;
#181092 = CARTESIAN_POINT ( 'NONE',  ( 0.05219959533936267826, -19.03943276465977164, 105.0010903946856615 ) ) ;
#181093 = CARTESIAN_POINT ( 'NONE',  ( -5.823673210054116645, -21.52544592524344225, 57.29057627198103120 ) ) ;
#181094 = ORIENTED_EDGE ( 'NONE', *, *, #15986, .F. ) ;
#181095 = EDGE_CURVE ( 'NONE', #92863, #102442, #143556, .T. ) ;
#181096 = CARTESIAN_POINT ( 'NONE',  ( 13.89961937509977652, -13.97604488694527269, 38.12390960531436690 ) ) ;
#181098 = CARTESIAN_POINT ( 'NONE',  ( 15.80617190586746368, 15.72974639402197994, 89.37390960531435269 ) ) ;
#181097 = CARTESIAN_POINT ( 'NONE',  ( -19.02544592524342804, 5.153800228976336051, 86.04057627198103830 ) ) ;
#181100 = CARTESIAN_POINT ( 'NONE',  ( -19.05341960407611168, -5.049401038298163336, 91.45724293864766707 ) ) ;
#181099 = CARTESIAN_POINT ( 'NONE',  ( 16.52544592524335698, 4.483927247898782831, 101.4594237280190185 ) ) ;
#181101 = CARTESIAN_POINT ( 'NONE',  ( -19.02544592524334988, -5.153800228976617603, 83.95942372801901854 ) ) ;
#181102 = CARTESIAN_POINT ( 'NONE',  ( -21.55341960407619339, 5.719274019375674811, 98.54275706135234714 ) ) ;
#181103 = CARTESIAN_POINT ( 'NONE',  ( 15.72974639402199770, -15.80617190586745480, 78.12390960531436690 ) ) ;
#181104 = CARTESIAN_POINT ( 'NONE',  ( -5.823673210054116645, -21.52544592524344225, 32.29057627198102409 ) ) ;
#181105 = CARTESIAN_POINT ( 'NONE',  ( 19.02544592524343514, -5.153800228976328945, 48.54057627198103120 ) ) ;
#181106 = CARTESIAN_POINT ( 'NONE',  ( -8.224510206698948167, 14.34966873604960824, 25.41557627198103120 ) ) ;
#181107 = CARTESIAN_POINT ( 'NONE',  ( 19.05341960407611168, 5.049401038298154454, 58.95724293864768129 ) ) ;
#181108 = CARTESIAN_POINT ( 'NONE',  ( -31.99650548583506193, -5.647492055662677757, 90.04056618753070040 ) ) ;
#181109 = CARTESIAN_POINT ( 'NONE',  ( -13.97604488694547697, 13.89961937509957934, 28.12609039468565797 ) ) ;
#181110 = CARTESIAN_POINT ( 'NONE',  ( -8.224510206698948167, 14.34966873604960824, 75.41557627198102409 ) ) ;
#181111 = CARTESIAN_POINT ( 'NONE',  ( 10.81492255796078972, 18.62759615963270932, 109.5822429386476955 ) ) ;
#181112 = CARTESIAN_POINT ( 'NONE',  ( 10.72451020669898902, -18.67979575497178502, 112.9155762719810383 ) ) ;
#181113 = CARTESIAN_POINT ( 'NONE',  ( -6.837149423127150349, 5.759383325533883990, -63.98874707071205847 ) ) ;
#181114 = CARTESIAN_POINT ( 'NONE',  ( 15.72974639402199770, -15.80617190586745480, 53.12390960531436690 ) ) ;
#181115 = CARTESIAN_POINT ( 'NONE',  ( 4.483927247898790824, -16.52544592524335698, 100.2094237280190043 ) ) ;
#181116 = CARTESIAN_POINT ( 'NONE',  ( -16.55341960407611168, -4.379528057220339221, 101.4572429386476955 ) ) ;
#181117 = CARTESIAN_POINT ( 'NONE',  ( 19.03943276465977164, -0.05219959533909143690, 63.74890960531435979 ) ) ;
#181118 = CARTESIAN_POINT ( 'NONE',  ( -16.55341960407611168, -4.379528057220339221, 26.45724293864768839 ) ) ;
#181119 = ADVANCED_FACE ( 'NONE', ( #149674 ), #199152, .T. ) ;
#181120 = CARTESIAN_POINT ( 'NONE',  ( 10.81492255796106328, -18.62759615963255655, 40.41775706135234714 ) ) ;
#181121 = CARTESIAN_POINT ( 'NONE',  ( -19.03943276465977164, 0.05219959533909376836, 106.2489096053143669 ) ) ;
#181122 = CARTESIAN_POINT ( 'NONE',  ( -21.53943276465977519, -0.05219959533937600094, 78.75109039468568994 ) ) ;
#181123 = CARTESIAN_POINT ( 'NONE',  ( 13.89961937509977652, -13.97604488694527269, 28.12390960531435624 ) ) ;
#181124 = CARTESIAN_POINT ( 'NONE',  ( -13.97604488694527625, -13.89961937509977652, 41.87390960531435979 ) ) ;
#181125 = ORIENTED_EDGE ( 'NONE', *, *, #126300, .F. ) ;
#181126 = CARTESIAN_POINT ( 'NONE',  ( 18.67979575497194134, -10.72451020669871369, 85.83442372801901854 ) ) ;
#181127 = CARTESIAN_POINT ( 'NONE',  ( 14.29746914071037800, 8.314922557961029526, 51.66775706135234714 ) ) ;
#181128 = CARTESIAN_POINT ( 'NONE',  ( -21.53943276465977519, -0.05219959533937600094, 68.75109039468568994 ) ) ;
#181129 = CARTESIAN_POINT ( 'NONE',  ( 13.97604488694527802, 13.89961937509977652, 104.3739096053143385 ) ) ;
#181130 = CARTESIAN_POINT ( 'NONE',  ( 16.46253265017146816, 9.564922557961045513, 81.66775706135233293 ) ) ;
#181131 = CARTESIAN_POINT ( 'NONE',  ( 21.52544592524334988, 5.823673210054432836, 61.45942372801901854 ) ) ;
#181132 = CARTESIAN_POINT ( 'NONE',  ( 16.53943276465976808, 0.05219959533934440121, 26.25109039468567573 ) ) ;
#181133 = CARTESIAN_POINT ( 'NONE',  ( -19.05341960407617563, 5.049401038297882671, 78.54275706135233293 ) ) ;
#181134 = CARTESIAN_POINT ( 'NONE',  ( 9.564922557960805705, 16.46253265017160317, 54.58224293864769550 ) ) ;
#181135 = CARTESIAN_POINT ( 'NONE',  ( 13.97604488694548053, -13.89961937509957401, 80.62609039468567573 ) ) ;
#181136 = CARTESIAN_POINT ( 'NONE',  ( -8.224510206698948167, 14.34966873604960824, 25.41557627198103120 ) ) ;
#181137 = CARTESIAN_POINT ( 'NONE',  ( -9.474510206698720793, -16.51473224551083518, 94.58442372801900433 ) ) ;
#181138 = CARTESIAN_POINT ( 'NONE',  ( 8.314922557960818139, 14.29746914071049879, 34.58224293864770260 ) ) ;
#181139 = CARTESIAN_POINT ( 'NONE',  ( -19.02544592524334988, -5.153800228976617603, 68.95942372801896170 ) ) ;
#181140 = CARTESIAN_POINT ( 'NONE',  ( -14.29746914071037622, -8.314922557961029526, 49.16775706135234003 ) ) ;
#181141 = CARTESIAN_POINT ( 'NONE',  ( 13.97604488694548053, -13.89961937509957401, 20.62609039468567573 ) ) ;
#181142 = CARTESIAN_POINT ( 'NONE',  ( 9.474510206698971260, -16.51473224551069308, 42.91557627198103120 ) ) ;
#181143 = CARTESIAN_POINT ( 'NONE',  ( -8.224510206698735004, -14.34966873604973081, 49.58442372801901143 ) ) ;
#181144 = DIRECTION ( 'NONE',  ( 1.000000000000000000, 0.000000000000000000, 0.000000000000000000 ) ) ;
#181145 = CARTESIAN_POINT ( 'NONE',  ( -27.73933785331498925, -9.013057229001049109, 140.9750000027311501 ) ) ;
#181146 = CARTESIAN_POINT ( 'NONE',  ( -16.46253265017160317, 9.564922557960807481, 85.83224293864769550 ) ) ;
#181147 = DIRECTION ( 'NONE',  ( 0.000000000000000000, 0.000000000000000000, -1.000000000000000000 ) ) ;
#181148 = EDGE_LOOP ( 'NONE', ( #176645, #3944, #86268, #172125, #118444 ) ) ;
#181149 = CARTESIAN_POINT ( 'NONE',  ( 16.46253265017146816, 9.564922557961045513, 91.66775706135234714 ) ) ;
#181150 = CARTESIAN_POINT ( 'NONE',  ( 13.97604488694527802, 13.89961937509977652, 114.3739096053143669 ) ) ;
#181152 = CARTESIAN_POINT ( 'NONE',  ( -9.564922557961040184, 16.46253265017147172, 107.9177570613523471 ) ) ;
#181151 = CARTESIAN_POINT ( 'NONE',  ( -21.55341960407619339, 5.719274019375674811, 113.5427570613523756 ) ) ;
#181153 = CARTESIAN_POINT ( 'NONE',  ( -16.53943276465976808, 0.05219959533911058130, 116.2489096053143669 ) ) ;
#181154 = CARTESIAN_POINT ( 'NONE',  ( 19.05341960407611168, 5.049401038298154454, 38.95724293864767418 ) ) ;
#181155 = CARTESIAN_POINT ( 'NONE',  ( 15.80617190586746368, 15.72974639402197994, 69.37390960531436690 ) ) ;
#181156 = CARTESIAN_POINT ( 'NONE',  ( -19.05341960407611168, -5.049401038298163336, 41.45724293864769550 ) ) ;
#181157 = CARTESIAN_POINT ( 'NONE',  ( -9.564922557961040184, 16.46253265017147172, 47.91775706135233293 ) ) ;
#181158 = CARTESIAN_POINT ( 'NONE',  ( 19.02544592524334988, 5.153800228976608722, 66.45942372801899012 ) ) ;
#181159 = CARTESIAN_POINT ( 'NONE',  ( 0.05219959533910956823, 16.53943276465976808, 49.99890960531437401 ) ) ;
#181160 = CARTESIAN_POINT ( 'NONE',  ( 15.80617190586746368, 15.72974639402197994, 34.37390960531435979 ) ) ;
#181161 = CARTESIAN_POINT ( 'NONE',  ( -15.80617190586768217, 15.72974639402176855, 88.12609039468570415 ) ) ;
#181162 = CARTESIAN_POINT ( 'NONE',  ( -18.67979575497178146, -10.72451020669898902, 81.66557627198103830 ) ) ;
#181163 = CARTESIAN_POINT ( 'NONE',  ( -21.52544592524334988, -5.823673210054445271, 53.95942372801900433 ) ) ;
#181164 = CARTESIAN_POINT ( 'NONE',  ( -15.80617190586768217, 15.72974639402176855, 68.12609039468567573 ) ) ;
#181165 = CARTESIAN_POINT ( 'NONE',  ( -9.564922557960796823, -16.46253265017161027, 97.08224293864769550 ) ) ;
#181167 = CARTESIAN_POINT ( 'NONE',  ( -5.719274019375665041, -21.55341960407619695, 64.79275706135234714 ) ) ;
#181166 = CARTESIAN_POINT ( 'NONE',  ( -16.55341960407617563, 4.379528057220093196, 98.54275706135234714 ) ) ;
#181168 = CARTESIAN_POINT ( 'NONE',  ( 19.02544592524343514, -5.153800228976328945, 58.54057627198102409 ) ) ;
#181169 = CARTESIAN_POINT ( 'NONE',  ( -5.153800228976328057, -19.02544592524343514, 27.29057627198103120 ) ) ;
#181170 = CARTESIAN_POINT ( 'NONE',  ( -9.564922557960796823, -16.46253265017161027, 72.08224293864770971 ) ) ;
#181171 = CARTESIAN_POINT ( 'NONE',  ( -16.52544592524342804, 4.483927247898546575, 71.04057627198103830 ) ) ;
#181172 = CARTESIAN_POINT ( 'NONE',  ( 12.06949235617757843, -12.14591786802309237, 38.12390960531436690 ) ) ;
#181173 = CARTESIAN_POINT ( 'NONE',  ( -21.53943276465977519, 0.05219959533907696930, 46.24890960531435979 ) ) ;
#181174 = CARTESIAN_POINT ( 'NONE',  ( -19.05341960407611168, -5.049401038298163336, 41.45724293864769550 ) ) ;
#181175 = CARTESIAN_POINT ( 'NONE',  ( 21.53943276465977519, -0.05219959533907433946, 63.74890960531435979 ) ) ;
#181176 = CARTESIAN_POINT ( 'NONE',  ( 13.97604488694548053, -13.89961937509957401, 50.62609039468566152 ) ) ;
#181178 = CARTESIAN_POINT ( 'NONE',  ( -16.53943276465976808, 0.05219959533911058130, 66.24890960531436690 ) ) ;
#181177 = DIRECTION ( 'NONE',  ( 1.000000000000000000, 0.000000000000000000, 3.469446951953612217E-15 ) ) ;
#181179 = CARTESIAN_POINT ( 'NONE',  ( -15.80617190586745835, -15.72974639402198527, 41.87390960531435979 ) ) ;
#181180 = ORIENTED_EDGE ( 'NONE', *, *, #183592, .F. ) ;
#181181 = ORIENTED_EDGE ( 'NONE', *, *, #75553, .F. ) ;
#181182 = CARTESIAN_POINT ( 'NONE',  ( 28.82186960331498327, 2.781578969918950771E-14, 141.2500000054623683 ) ) ;
#181183 = CARTESIAN_POINT ( 'NONE',  ( -4.483927247898782831, 16.52544592524335698, 82.70942372801900433 ) ) ;
#181184 = CARTESIAN_POINT ( 'NONE',  ( -16.51473224551082808, 9.474510206698731452, 78.33442372801900433 ) ) ;
#181185 = CARTESIAN_POINT ( 'NONE',  ( -8.224510206698948167, 14.34966873604960824, 60.41557627198102409 ) ) ;
#181186 = DIRECTION ( 'NONE',  ( -1.000000000000000000, -0.000000000000000000, -0.000000000000000000 ) ) ;
#181187 = CARTESIAN_POINT ( 'NONE',  ( 19.05341960407611168, 5.049401038298154454, 53.95724293864770260 ) ) ;
#181188 = CARTESIAN_POINT ( 'NONE',  ( -16.52544592524342804, 4.483927247898546575, 41.04057627198103120 ) ) ;
#181189 = CARTESIAN_POINT ( 'NONE',  ( -16.51473224551069308, -9.474510206698971260, 51.66557627198102409 ) ) ;
#181190 = CARTESIAN_POINT ( 'NONE',  ( -19.05341960407611168, -5.049401038298163336, 76.45724293864769550 ) ) ;
#181191 = CARTESIAN_POINT ( 'NONE',  ( -13.97604488694527625, -13.89961937509977652, 36.87390960531436690 ) ) ;
#181192 = CARTESIAN_POINT ( 'NONE',  ( 21.52544592524334988, 5.823673210054432836, 41.45942372801901143 ) ) ;
#181193 = CARTESIAN_POINT ( 'NONE',  ( -9.564922557960796823, -16.46253265017161027, 67.08224293864769550 ) ) ;
#181194 = CARTESIAN_POINT ( 'NONE',  ( -13.89961937509977652, 13.97604488694528158, 30.62390960531435269 ) ) ;
#181195 = CARTESIAN_POINT ( 'NONE',  ( -19.02544592524342804, 5.153800228976336051, 66.04057627198103830 ) ) ;
#181196 = EDGE_CURVE ( 'NONE', #182074, #117961, #119342, .T. ) ;
#181197 = CARTESIAN_POINT ( 'NONE',  ( -10.81492255796078084, -18.62759615963271287, 47.08224293864770260 ) ) ;
#181198 = CARTESIAN_POINT ( 'NONE',  ( -16.51473224551069308, -9.474510206698971260, 36.66557627198102409 ) ) ;
#181199 = CARTESIAN_POINT ( 'NONE',  ( -5.719274019375978568, 21.55341960407610458, 45.20724293864769550 ) ) ;
#181200 = CARTESIAN_POINT ( 'NONE',  ( -16.55341960407617563, 4.379528057220093196, 98.54275706135234714 ) ) ;
#181201 = CARTESIAN_POINT ( 'NONE',  ( -19.03943276465977164, -0.05219959533935918106, 23.75109039468566152 ) ) ;
#181203 = CARTESIAN_POINT ( 'NONE',  ( -8.224510206698735004, -14.34966873604973081, 79.58442372801903275 ) ) ;
#181202 = CARTESIAN_POINT ( 'NONE',  ( 4.483927247898790824, -16.52544592524335698, 50.20942372801901854 ) ) ;
#181204 = FACE_OUTER_BOUND ( 'NONE', #76473, .T. ) ;
#181205 = ADVANCED_FACE ( 'NONE', ( #44483 ), #169799, .F. ) ;
#181206 = CARTESIAN_POINT ( 'NONE',  ( -0.05219959533934338120, 16.53943276465976808, 72.50109039468568994 ) ) ;
#181207 = CARTESIAN_POINT ( 'NONE',  ( 12.14591786802327356, -12.06949235617739191, 45.62609039468567573 ) ) ;
#181208 = CARTESIAN_POINT ( 'NONE',  ( -5.153800228976328057, -19.02544592524343514, 102.2905762719810383 ) ) ;
#181209 = CARTESIAN_POINT ( 'NONE',  ( -4.483927247898782831, 16.52544592524335698, 37.70942372801900433 ) ) ;
#181210 = CARTESIAN_POINT ( 'NONE',  ( -16.51473224551069308, -9.474510206698971260, 31.66557627198102054 ) ) ;
#181211 = CARTESIAN_POINT ( 'NONE',  ( -21.53943276465977519, -0.05219959533937600094, 23.75109039468567929 ) ) ;
#181212 = CARTESIAN_POINT ( 'NONE',  ( 4.379528057220092307, 16.55341960407617563, 37.29275706135235424 ) ) ;
#181213 = CARTESIAN_POINT ( 'NONE',  ( -12.06949235617739369, -12.14591786802326823, 99.37609039468568994 ) ) ;
#181214 = DIRECTION ( 'NONE',  ( -0.3041824702427698979, 0.9526137857479317628, -0.000000000000000000 ) ) ;
#181215 = CARTESIAN_POINT ( 'NONE',  ( 5.823673210054444382, -21.52544592524334988, 100.2094237280190043 ) ) ;
#181216 = CARTESIAN_POINT ( 'NONE',  ( 0.05219959533936267826, -19.03943276465977164, 95.00109039468567573 ) ) ;
#181217 = CARTESIAN_POINT ( 'NONE',  ( 4.379528057220339221, -16.55341960407611168, 57.70724293864770260 ) ) ;
#181218 = CARTESIAN_POINT ( 'NONE',  ( -19.03943276465977164, 0.05219959533909376836, 21.24890960531436335 ) ) ;
#181220 = CARTESIAN_POINT ( 'NONE',  ( 16.20579543436695502, -7.371946100355079246, 56.93479165828049560 ) ) ;
#181219 = CARTESIAN_POINT ( 'NONE',  ( -13.97604488694547697, 13.89961937509957934, 63.12609039468566152 ) ) ;
#181221 = CARTESIAN_POINT ( 'NONE',  ( -5.719274019375665041, -21.55341960407619695, 59.79275706135234714 ) ) ;
#181222 = CARTESIAN_POINT ( 'NONE',  ( -12.06949235617739369, -12.14591786802326823, 29.37609039468568284 ) ) ;
#181223 = CARTESIAN_POINT ( 'NONE',  ( -2.500000000000000000, 3.061616997868383141E-16, -64.92179855667829713 ) ) ;
#181224 = CARTESIAN_POINT ( 'NONE',  ( -15.80617190586745835, -15.72974639402198527, 26.87390960531435979 ) ) ;
#181225 = CARTESIAN_POINT ( 'NONE',  ( 18.67979575497178502, 10.72451020669898547, 74.16557627198102409 ) ) ;
#181226 = CARTESIAN_POINT ( 'NONE',  ( 19.02544592524334988, 5.153800228976608722, 106.4594237280190185 ) ) ;
#181227 = CARTESIAN_POINT ( 'NONE',  ( 19.03943276465977164, -0.05219959533909143690, 98.74890960531436690 ) ) ;
#181228 = CARTESIAN_POINT ( 'NONE',  ( 5.281959635518922447, -27.36706763425078748, 140.0000000000000000 ) ) ;
#181229 = CARTESIAN_POINT ( 'NONE',  ( 0.05219959533909260263, 19.03943276465977164, 24.99890960531435269 ) ) ;
#181230 = CARTESIAN_POINT ( 'NONE',  ( -18.67979575497193778, 10.72451020669871902, 108.3344237280190185 ) ) ;
#181231 = CARTESIAN_POINT ( 'NONE',  ( 19.05341960407611168, 5.049401038298154454, 43.95724293864769550 ) ) ;
#181232 = CARTESIAN_POINT ( 'NONE',  ( -18.67979575497193778, 10.72451020669871902, 53.33442372801901854 ) ) ;
#181233 = CARTESIAN_POINT ( 'NONE',  ( 21.55341960407619695, -5.719274019375665929, 96.04275706135236135 ) ) ;
#181234 = CARTESIAN_POINT ( 'NONE',  ( -0.05219959533934338120, 16.53943276465976808, 102.5010903946856899 ) ) ;
#181235 = CARTESIAN_POINT ( 'NONE',  ( 9.564922557960805705, 16.46253265017160317, 84.58224293864769550 ) ) ;
#181236 = CARTESIAN_POINT ( 'NONE',  ( -21.53943276465977519, -0.05219959533937600094, 43.75109039468568284 ) ) ;
#181237 = CARTESIAN_POINT ( 'NONE',  ( -10.72451020669870658, -18.67979575497194134, 59.58442372801901854 ) ) ;
#181239 = CARTESIAN_POINT ( 'NONE',  ( -5.153800228976328057, -19.02544592524343514, 87.29057627198103830 ) ) ;
#181238 = CARTESIAN_POINT ( 'NONE',  ( 16.51473224551083163, -9.474510206698727899, 80.83442372801899012 ) ) ;
#181240 = CARTESIAN_POINT ( 'NONE',  ( 12.06949235617757843, -12.14591786802309237, 108.1239096053143811 ) ) ;
#181241 = CARTESIAN_POINT ( 'NONE',  ( -10.81492255796078084, -18.62759615963271287, 97.08224293864770971 ) ) ;
#181242 = CARTESIAN_POINT ( 'NONE',  ( -5.153800228976607833, 19.02544592524334988, 27.70942372801899722 ) ) ;
#181243 = CARTESIAN_POINT ( 'NONE',  ( -14.34966873604960291, -8.224510206698953496, 101.6655762719810383 ) ) ;
#181244 = CARTESIAN_POINT ( 'NONE',  ( 16.46253265017160672, -9.564922557960803928, 48.33224293864769550 ) ) ;
#181245 = CARTESIAN_POINT ( 'NONE',  ( -16.51473224551082808, 9.474510206698731452, 88.33442372801900433 ) ) ;
#181246 = CARTESIAN_POINT ( 'NONE',  ( 8.314922557960818139, 14.29746914071049879, 54.58224293864769550 ) ) ;
#181247 = CARTESIAN_POINT ( 'NONE',  ( -15.80617190586768217, 15.72974639402176855, 113.1260903946856899 ) ) ;
#181248 = CARTESIAN_POINT ( 'NONE',  ( 5.153800228976335163, 19.02544592524342804, 104.7905762719809957 ) ) ;
#181249 = CARTESIAN_POINT ( 'NONE',  ( -13.89961937509957401, -13.97604488694547875, 69.37609039468564731 ) ) ;
#181250 = CARTESIAN_POINT ( 'NONE',  ( -15.80617190586745835, -15.72974639402198527, 71.87390960531438111 ) ) ;
#181251 = CARTESIAN_POINT ( 'NONE',  ( 15.80617190586769283, -15.72974639402175789, 30.62609039468567929 ) ) ;
#181252 = CARTESIAN_POINT ( 'NONE',  ( -14.34966873604972548, 8.224510206698743886, 28.33442372801902209 ) ) ;
#181253 = CARTESIAN_POINT ( 'NONE',  ( -14.29746914071037622, -8.314922557961029526, 99.16775706135234714 ) ) ;
#181255 = CARTESIAN_POINT ( 'NONE',  ( 21.53943276465977519, 0.05219959533937863772, 36.25109039468567573 ) ) ;
#181254 = CARTESIAN_POINT ( 'NONE',  ( 17.44279575226822843, 5.990770900252482711, 61.66442432485680314 ) ) ;
#181256 = CARTESIAN_POINT ( 'NONE',  ( -18.62759615963270932, 10.81492255796079327, 40.83224293864769550 ) ) ;
#181257 = CARTESIAN_POINT ( 'NONE',  ( 0.05219959533909260263, 19.03943276465977164, 24.99890960531435269 ) ) ;
#181258 = CARTESIAN_POINT ( 'NONE',  ( -36.91746825000000598, 2.428612866367529932E-14, -1.124999997268813390 ) ) ;
#181259 = CARTESIAN_POINT ( 'NONE',  ( 16.52544592524335698, 4.483927247898782831, 56.45942372801902565 ) ) ;
#181260 = CARTESIAN_POINT ( 'NONE',  ( 12.06949235617757843, -12.14591786802309237, 93.12390960531436690 ) ) ;
#181261 = CARTESIAN_POINT ( 'NONE',  ( 5.719274019375991003, -21.55341960407610458, 77.70724293864770971 ) ) ;
#181262 = CARTESIAN_POINT ( 'NONE',  ( -14.29746914071049879, 8.314922557960819915, 25.83224293864769194 ) ) ;
#181263 = CARTESIAN_POINT ( 'NONE',  ( -4.483927247898782831, 16.52544592524335698, 42.70942372801901854 ) ) ;
#181264 = CARTESIAN_POINT ( 'NONE',  ( 19.05341960407611168, 5.049401038298154454, 43.95724293864769550 ) ) ;
#181265 = CARTESIAN_POINT ( 'NONE',  ( -16.55341960407617563, 4.379528057220093196, 98.54275706135234714 ) ) ;
#181266 = CARTESIAN_POINT ( 'NONE',  ( 19.03943276465977164, 0.05219959533936151252, 81.25109039468567573 ) ) ;
#181267 = CARTESIAN_POINT ( 'NONE',  ( -15.72974639402197994, 15.80617190586746368, 85.62390960531436690 ) ) ;
#181268 = CARTESIAN_POINT ( 'NONE',  ( 4.483927247898790824, -16.52544592524335698, 105.2094237280190328 ) ) ;
#181269 = EDGE_LOOP ( 'NONE', ( #92438, #1856, #173824, #70454, #110214 ) ) ;
#181270 = CARTESIAN_POINT ( 'NONE',  ( 19.05341960407611168, 5.049401038298154454, 113.9572429386477097 ) ) ;
#181271 = CARTESIAN_POINT ( 'NONE',  ( -5.719274019375978568, 21.55341960407610458, 65.20724293864768129 ) ) ;
#181272 = CARTESIAN_POINT ( 'NONE',  ( 4.379528057220092307, 16.55341960407617563, 97.29275706135234714 ) ) ;
#181273 = EDGE_LOOP ( 'NONE', ( #53281, #21832, #39551, #85416 ) ) ;
#181274 = CARTESIAN_POINT ( 'NONE',  ( 18.62759615963271287, -10.81492255796078972, 28.33224293864769550 ) ) ;
#181275 = CARTESIAN_POINT ( 'NONE',  ( -19.25663599770061651, 5.499999999999451994, 73.99419308057201761 ) ) ;
#181276 = CARTESIAN_POINT ( 'NONE',  ( -10.72451020669898014, 18.67979575497178502, 75.41557627198102409 ) ) ;
#181277 = CARTESIAN_POINT ( 'NONE',  ( 8.314922557960818139, 14.29746914071049879, 29.58224293864769905 ) ) ;
#181278 = CARTESIAN_POINT ( 'NONE',  ( 0.05219959533934541429, -16.53943276465976808, 20.00109039468568639 ) ) ;
#181279 = CARTESIAN_POINT ( 'NONE',  ( -19.02544592524342804, 5.153800228976336051, 41.04057627198103120 ) ) ;
#181280 = CARTESIAN_POINT ( 'NONE',  ( -16.52544592524335698, -4.483927247898792601, 28.95942372801902209 ) ) ;
#181281 = CARTESIAN_POINT ( 'NONE',  ( 16.51473224551069308, 9.474510206698969483, 49.16557627198102409 ) ) ;
#181282 = CARTESIAN_POINT ( 'NONE',  ( -8.906447517083053711, -27.41122689804191026, 148.4000000000000057 ) ) ;
#181283 = CARTESIAN_POINT ( 'NONE',  ( 9.564922557960805705, 16.46253265017160317, 109.5822429386476955 ) ) ;
#181284 = CARTESIAN_POINT ( 'NONE',  ( -5.153800228976328057, -19.02544592524343514, 107.2905762719810383 ) ) ;
#181285 = CARTESIAN_POINT ( 'NONE',  ( -12.06949235617739369, -12.14591786802326823, 84.37609039468570415 ) ) ;
#181286 = CARTESIAN_POINT ( 'NONE',  ( -5.153800228976607833, 19.02544592524334988, 97.70942372801900433 ) ) ;
#181287 = CARTESIAN_POINT ( 'NONE',  ( -19.03943276465977164, -0.05219959533935918106, 38.75109039468566152 ) ) ;
#181288 = CARTESIAN_POINT ( 'NONE',  ( -21.53943276465977519, 0.05219959533907696930, 71.24890960531435269 ) ) ;
#181289 = CARTESIAN_POINT ( 'NONE',  ( -0.05219959533934338120, 16.53943276465976808, 97.50109039468567573 ) ) ;
#181290 = CARTESIAN_POINT ( 'NONE',  ( 21.55341960407610458, 5.719274019375980345, 38.95724293864768839 ) ) ;
#181291 = CARTESIAN_POINT ( 'NONE',  ( 19.05341960407617918, -5.049401038297876454, 91.04275706135234714 ) ) ;
#181292 = CARTESIAN_POINT ( 'NONE',  ( 19.03943276465977164, -0.05219959533909143690, 48.74890960531435979 ) ) ;
#181293 = CARTESIAN_POINT ( 'NONE',  ( -13.89961937509977652, 13.97604488694528158, 90.62390960531432427 ) ) ;
#181294 = CARTESIAN_POINT ( 'NONE',  ( 5.823673210054444382, -21.52544592524334988, 60.20942372801902565 ) ) ;
#181295 = CARTESIAN_POINT ( 'NONE',  ( 19.05341960407611168, 5.049401038298154454, 58.95724293864768129 ) ) ;
#181296 = CARTESIAN_POINT ( 'NONE',  ( 16.55341960407611168, 4.379528057220329451, 98.95724293864770971 ) ) ;
#181297 = CARTESIAN_POINT ( 'NONE',  ( 19.49401214000073779, -12.39993551617566503, 169.9999999999999716 ) ) ;
#181298 = CARTESIAN_POINT ( 'NONE',  ( 8.314922557960818139, 14.29746914071049879, 74.58224293864768129 ) ) ;
#181299 = CARTESIAN_POINT ( 'NONE',  ( 18.62759615963271287, -10.81492255796078972, 68.33224293864769550 ) ) ;
#181300 = CARTESIAN_POINT ( 'NONE',  ( 0.05219959533936267826, -19.03943276465977164, 85.00109039468567573 ) ) ;
#181301 = CARTESIAN_POINT ( 'NONE',  ( 17.50000000000000000, -5.499999999999992895, 81.21769037696435589 ) ) ;
#181302 = CARTESIAN_POINT ( 'NONE',  ( 9.564922557960805705, 16.46253265017160317, 59.58224293864769550 ) ) ;
#181303 = DIRECTION ( 'NONE',  ( -4.336808689942017120E-17, -1.000000000000000000, 0.000000000000000000 ) ) ;
#181305 = CARTESIAN_POINT ( 'NONE',  ( -5.153800228976328057, -19.02544592524343514, 82.29057627198103830 ) ) ;
#181304 = CARTESIAN_POINT ( 'NONE',  ( -19.02544592524342804, 5.153800228976336051, 71.04057627198099567 ) ) ;
#181306 = CARTESIAN_POINT ( 'NONE',  ( -0.05219959533934338120, 16.53943276465976808, 67.50109039468568994 ) ) ;
#181307 = CARTESIAN_POINT ( 'NONE',  ( -16.52216118717205973, -7.221426719304517405, 51.07599021046991083 ) ) ;
#181308 = CARTESIAN_POINT ( 'NONE',  ( -5.049401038297874678, -19.05341960407617918, 49.79275706135231871 ) ) ;
#181309 = CARTESIAN_POINT ( 'NONE',  ( 17.47980958864297918, 5.499999999999998224, 21.71653220162190934 ) ) ;
#181310 = CARTESIAN_POINT ( 'NONE',  ( 9.474510206698971260, -16.51473224551069308, 112.9155762719810383 ) ) ;
#181311 = CARTESIAN_POINT ( 'NONE',  ( -12.14591786802326823, 12.06949235617739902, 108.1260903946856757 ) ) ;
#181312 = CARTESIAN_POINT ( 'NONE',  ( 5.153800228976617603, -19.02544592524335343, 75.20942372801899012 ) ) ;
#181313 = CARTESIAN_POINT ( 'NONE',  ( 14.29746914071037800, 8.314922557961029526, 76.66775706135234714 ) ) ;
#181314 = CARTESIAN_POINT ( 'NONE',  ( -17.40805194822031154, 6.112264579159340627, 30.83371272510612826 ) ) ;
#181315 = CARTESIAN_POINT ( 'NONE',  ( -12.14591786802326823, 12.06949235617739902, 63.12609039468568994 ) ) ;
#181316 = CARTESIAN_POINT ( 'NONE',  ( -19.99999999999998224, -188.0000000000000000, -25.00000000000000000 ) ) ;
#181317 = CARTESIAN_POINT ( 'NONE',  ( -21.53943276465977519, -0.05219959533937600094, 63.75109039468568284 ) ) ;
#181318 = CARTESIAN_POINT ( 'NONE',  ( 9.474510206698729675, 16.51473224551082808, 77.08442372801900433 ) ) ;
#181319 = CARTESIAN_POINT ( 'NONE',  ( 19.02544592524334988, 5.153800228976608722, 26.45942372801899722 ) ) ;
#181320 = CARTESIAN_POINT ( 'NONE',  ( 9.564922557960805705, 16.46253265017160317, 59.58224293864769550 ) ) ;
#181321 = CARTESIAN_POINT ( 'NONE',  ( 13.97604488694527802, 13.89961937509977652, 49.37390960531434558 ) ) ;
#181322 = CARTESIAN_POINT ( 'NONE',  ( -19.73163076381609216, -34.79465882235955121, -6.355234051081566804 ) ) ;
#181323 = CARTESIAN_POINT ( 'NONE',  ( -21.53943276465977519, 0.05219959533907696930, 81.24890960531436690 ) ) ;
#181324 = CARTESIAN_POINT ( 'NONE',  ( 5.823673210054125526, 21.52544592524343514, 34.79057627198103120 ) ) ;
#181325 = CARTESIAN_POINT ( 'NONE',  ( 8.314922557960818139, 14.29746914071049879, 114.5822429386477097 ) ) ;
#181326 = CARTESIAN_POINT ( 'NONE',  ( -8.314922557961024197, 14.29746914071037800, 47.91775706135234714 ) ) ;
#181327 = ORIENTED_EDGE ( 'NONE', *, *, #53259, .F. ) ;
#181328 = CARTESIAN_POINT ( 'NONE',  ( 10.81492255796106328, -18.62759615963255655, 30.41775706135234358 ) ) ;
#181330 = CARTESIAN_POINT ( 'NONE',  ( 30.74264578624799782, 22.33583958711400541, -4.800000000000000711 ) ) ;
#181329 = CARTESIAN_POINT ( 'NONE',  ( 8.314922557960818139, 14.29746914071049879, 49.58224293864769550 ) ) ;
#181331 = CARTESIAN_POINT ( 'NONE',  ( -16.52544592524335698, -4.483927247898792601, 23.95942372801901143 ) ) ;
#181332 = CARTESIAN_POINT ( 'NONE',  ( 0.05219959533936267826, -19.03943276465977164, 35.00109039468566863 ) ) ;
#181333 = CARTESIAN_POINT ( 'NONE',  ( 12.06949235617757843, -12.14591786802309237, 48.12390960531436690 ) ) ;
#181334 = CARTESIAN_POINT ( 'NONE',  ( -18.62759615963255300, -10.81492255796106328, 19.16775706135234714 ) ) ;
#181336 = CARTESIAN_POINT ( 'NONE',  ( 10.72451020669898902, -18.67979575497178502, 82.91557627198103830 ) ) ;
#181335 = CARTESIAN_POINT ( 'NONE',  ( 1.315892071381018269, 15.92644080175540466, -59.47647726036166915 ) ) ;
#181337 = CARTESIAN_POINT ( 'NONE',  ( -5.049401038298153566, 19.05341960407611168, 95.20724293864770971 ) ) ;
#181338 = CARTESIAN_POINT ( 'NONE',  ( -16.55341960407611168, -4.379528057220339221, 61.45724293864770260 ) ) ;
#181339 = CARTESIAN_POINT ( 'NONE',  ( 9.474510206698971260, -16.51473224551069308, 97.91557627198102409 ) ) ;
#181340 = DIRECTION ( 'NONE',  ( 0.000000000000000000, 0.000000000000000000, 1.000000000000000000 ) ) ;
#181341 = CARTESIAN_POINT ( 'NONE',  ( 9.564922557961047289, -16.46253265017146816, 70.41775706135233293 ) ) ;
#181342 = CARTESIAN_POINT ( 'NONE',  ( -15.72974639402197994, 15.80617190586746368, 110.6239096053143669 ) ) ;
#181343 = CARTESIAN_POINT ( 'NONE',  ( 16.51473224551069308, 9.474510206698969483, 54.16557627198103120 ) ) ;
#181344 = CARTESIAN_POINT ( 'NONE',  ( -12.14591786802309592, -12.06949235617757132, 106.8739096053143811 ) ) ;
#181345 = CARTESIAN_POINT ( 'NONE',  ( -21.53943276465977519, -0.05219959533937600094, 48.75109039468568284 ) ) ;
#181346 = DIRECTION ( 'NONE',  ( 0.000000000000000000, 0.000000000000000000, -1.000000000000000000 ) ) ;
#181347 = CARTESIAN_POINT ( 'NONE',  ( -16.52544592524342804, 4.483927247898546575, 36.04057627198102409 ) ) ;
#181348 = CARTESIAN_POINT ( 'NONE',  ( 19.03943276465977164, -0.05219959533909143690, 48.74890960531435979 ) ) ;
#181349 = CARTESIAN_POINT ( 'NONE',  ( -19.05341960407611168, -5.049401038298163336, 101.4572429386476955 ) ) ;
#181350 = CARTESIAN_POINT ( 'NONE',  ( -18.67979575497178146, -10.72451020669898902, 76.66557627198103830 ) ) ;
#181351 = CARTESIAN_POINT ( 'NONE',  ( 22.44159573604009239, 16.30477369853692693, 146.0750000027311728 ) ) ;
#181352 = CARTESIAN_POINT ( 'NONE',  ( -13.89961937509977652, 13.97604488694528158, 50.62390960531435979 ) ) ;
#181353 = CARTESIAN_POINT ( 'NONE',  ( -5.719274019375978568, 21.55341960407610458, 65.20724293864768129 ) ) ;
#181354 = EDGE_CURVE ( 'NONE', #73091, #53519, #25268, .T. ) ;
#181355 = CARTESIAN_POINT ( 'NONE',  ( 18.62759615963255655, 10.81492255796105972, 86.66775706135234714 ) ) ;
#181358 = CARTESIAN_POINT ( 'NONE',  ( 16.55341960407611168, 4.379528057220329451, 83.95724293864770971 ) ) ;
#181357 = CARTESIAN_POINT ( 'NONE',  ( -12.14591786802326823, 12.06949235617739902, 83.12609039468568994 ) ) ;
#181356 = CARTESIAN_POINT ( 'NONE',  ( 28.79475375365586132, 2.781246896534039337E-14, 155.0000000000000000 ) ) ;
#181359 = CARTESIAN_POINT ( 'NONE',  ( 19.05341960407611168, 5.049401038298154454, 68.95724293864769550 ) ) ;
#181360 = ORIENTED_EDGE ( 'NONE', *, *, #9668, .T. ) ;
#181361 = CARTESIAN_POINT ( 'NONE',  ( 13.89961937509957401, 13.97604488694547697, 36.87609039468565442 ) ) ;
#181362 = CARTESIAN_POINT ( 'NONE',  ( 16.53943276465976808, 0.05219959533934440121, 91.25109039468568994 ) ) ;
#181363 = CARTESIAN_POINT ( 'NONE',  ( 18.67979575497194134, -10.72451020669871369, 110.8344237280190043 ) ) ;
#181364 = CARTESIAN_POINT ( 'NONE',  ( 0.05219959533909260263, 19.03943276465977164, 94.99890960531436690 ) ) ;
#181365 = CARTESIAN_POINT ( 'NONE',  ( 18.67979575497178502, 10.72451020669898547, 44.16557627198103120 ) ) ;
#181366 = CARTESIAN_POINT ( 'NONE',  ( 21.52544592524334988, 5.823673210054432836, 96.45942372801901854 ) ) ;
#181367 = CARTESIAN_POINT ( 'NONE',  ( -16.55341960407617563, 4.379528057220093196, 63.54275706135234003 ) ) ;
#181368 = CARTESIAN_POINT ( 'NONE',  ( 5.719274019375991003, -21.55341960407610458, 107.7072429386476955 ) ) ;
#181369 = CARTESIAN_POINT ( 'NONE',  ( -12.14591786802326823, 12.06949235617739902, 28.12609039468568284 ) ) ;
#181371 = EDGE_CURVE ( 'NONE', #142224, #14026, #168793, .T. ) ;
#181370 = CARTESIAN_POINT ( 'NONE',  ( -5.153800228976328057, -19.02544592524343514, 87.29057627198103830 ) ) ;
#181372 = CARTESIAN_POINT ( 'NONE',  ( -12.06949235617739369, -12.14591786802326823, 29.37609039468568284 ) ) ;
#181373 = CARTESIAN_POINT ( 'NONE',  ( -13.97604488694527625, -13.89961937509977652, 56.87390960531434558 ) ) ;
#181374 = CARTESIAN_POINT ( 'NONE',  ( 12.06949235617739724, 12.14591786802326823, 31.87609039468567929 ) ) ;
#181375 = CARTESIAN_POINT ( 'NONE',  ( -16.52544592524342804, 4.483927247898546575, 81.04057627198102409 ) ) ;
#181376 = CARTESIAN_POINT ( 'NONE',  ( 16.52544592524335698, 4.483927247898782831, 91.45942372801901854 ) ) ;
#181378 = CARTESIAN_POINT ( 'NONE',  ( -16.51473224551069308, -9.474510206698971260, 66.66557627198102409 ) ) ;
#181377 = CARTESIAN_POINT ( 'NONE',  ( 5.823673210054444382, -21.52544592524334988, 40.20942372801901854 ) ) ;
#181379 = CARTESIAN_POINT ( 'NONE',  ( -13.97604488694527625, -13.89961937509977652, 86.87390960531436690 ) ) ;
#181380 = CARTESIAN_POINT ( 'NONE',  ( -12.06949235617756955, 12.14591786802309770, 35.62390960531437401 ) ) ;
#181381 = CARTESIAN_POINT ( 'NONE',  ( 0.05219959533934541429, -16.53943276465976808, 80.00109039468568994 ) ) ;
#181382 = ORIENTED_EDGE ( 'NONE', *, *, #187343, .F. ) ;
#181383 = CARTESIAN_POINT ( 'NONE',  ( 5.153800228976615827, -19.02544592524334988, 25.20942372801900433 ) ) ;
#181384 = CARTESIAN_POINT ( 'NONE',  ( -19.03943276465977164, 0.05219959533909376836, 96.24890960531436690 ) ) ;
#181385 = CARTESIAN_POINT ( 'NONE',  ( -19.02544592524342804, 5.153800228976336051, 46.04057627198101699 ) ) ;
#181386 = CARTESIAN_POINT ( 'NONE',  ( -5.950531402560715689E-15, 38.81732327939063509, -5.124999997268813168 ) ) ;
#181387 = CARTESIAN_POINT ( 'NONE',  ( 8.224510206698742110, 14.34966873604972548, 47.08442372801901854 ) ) ;
#181389 = CARTESIAN_POINT ( 'NONE',  ( -8.314922557961024197, 14.29746914071037800, 57.91775706135234714 ) ) ;
#181388 = CARTESIAN_POINT ( 'NONE',  ( 19.03943276465977164, 0.05219959533936151252, 71.25109039468566152 ) ) ;
#181390 = CARTESIAN_POINT ( 'NONE',  ( 9.474510206698971260, -16.51473224551069308, 112.9155762719810383 ) ) ;
#181391 =( BOUNDED_SURFACE ( )  B_SPLINE_SURFACE ( 1, 2, ( 
 ( #59456, #74645, #155454, #170627, #1764, #107940, #121130, #186815, #109940, #106951, #91765, #140271, #105965, #90783, #139283, #60447, #167650, #93773, #171622, #185803, #29146, #198980, #151490, #154461, #184798, #199976, #138295, #152467, #30124, #122122, #12981, #760, #16944, #13953, #197986, #78598, #153460, #63441, #136311, #31123, #123113, #76617, #137299, #92771, #62431, #124103, #47290, #32116, #125117, #48285, #128078, #94766, #174607, #188789, #50272, #145245, #6726, #126106, #176609, #189781, #52241, #111930, #20907, #34103, #95760, #82566, #144247, #110929, #51253, #191756, #21914, #175596, #130056, #129065, #37072, #159412, #156448, #112913, #127081, #98732, #97722, #173616, #36073, #35086, #5731, #83566, #65420, #68404, #187802, #190766, #67410, #141270, #17948, #157445, #113898, #160425, #53239, #18940, #158428, #114916, #96739 ),
 ( #79601, #2760, #19916, #64436, #4727, #49271, #81558, #172615, #80585, #142259, #3743, #143244, #66417, #74164, #26673, #166177, #122624, #150002, #146239, #161423, #44806, #59963, #91269, #135836, #10499, #76121, #199483, #134850, #181351, #29636, #133835, #180365, #105479, #11508, #72160, #183325, #60949, #75136, #195526, #88314, #38083, #43816, #197505, #89318, #27678, #41833, #196528, #73179, #99739, #167166, #106461, #56999, #84561, #168140, #42830, #152960, #22915, #58972, #151011, #104495, #118674, #103501, #165178, #57999, #12502, #120640, #119669, #14458, #182338, #28665, #90300, #151985, #13473, #137799, #136806, #198490, #121629, #79099, #141765, #1258, #110436, #123605, #185300, #172117, #33603, #268, #140772, #81079, #111434, #64931, #19432, #18446, #126590, #48782, #65918, #2261, #16452, #188292, #187311, #78101, #63944 ) ),
 .UNSPECIFIED., .F., .F., .T. ) 
 B_SPLINE_SURFACE_WITH_KNOTS ( ( 2, 2 ),
 ( 3, 2, 2, 2, 2, 2, 2, 2, 2, 2, 2, 2, 2, 2, 2, 2, 2, 2, 2, 2, 2, 2, 2, 2, 2, 2, 2, 2, 2, 2, 2, 2, 2, 2, 2, 2, 2, 2, 2, 2, 2, 2, 2, 2, 2, 2, 2, 2, 2, 2, 3 ),
 ( 0.000000000000000000, 1.000000000000000000 ),
 ( 0.000000000000000000, 0.02000000000000000042, 0.04000000000000000083, 0.05999999999999999778, 0.08000000000000000167, 0.1000000000000000056, 0.1199999999999999956, 0.1400000000000000133, 0.1600000000000000033, 0.1799999999999999933, 0.2000000000000000111, 0.2200000000000000011, 0.2399999999999999911, 0.2600000000000000089, 0.2800000000000000266, 0.2999999999999999889, 0.3200000000000000067, 0.3400000000000000244, 0.3599999999999999867, 0.3800000000000000044, 0.4000000000000000222, 0.4199999999999999845, 0.4400000000000000022, 0.4600000000000000200, 0.4799999999999999822, 0.5000000000000000000, 0.5200000000000000178, 0.5400000000000000355, 0.5600000000000000533, 0.5799999999999999600, 0.5999999999999999778, 0.6199999999999999956, 0.6400000000000000133, 0.6600000000000000311, 0.6800000000000000488, 0.6999999999999999556, 0.7199999999999999734, 0.7399999999999999911, 0.7600000000000000089, 0.7800000000000000266, 0.8000000000000000444, 0.8199999999999999512, 0.8399999999999999689, 0.8599999999999999867, 0.8800000000000000044, 0.9000000000000000222, 0.9200000000000000400, 0.9399999999999999467, 0.9599999999999999645, 0.9799999999999999822, 1.000000000000000000 ),
 .UNSPECIFIED. ) 
 GEOMETRIC_REPRESENTATION_ITEM ( )  RATIONAL_B_SPLINE_SURFACE ( (
 ( 1.000000000000000000, 0.9510565162951535312, 1.000000000000000000, 0.9510565162951535312, 1.000000000000000000, 0.9510565162951535312, 1.000000000000000000, 0.9510565162951535312, 1.000000000000000000, 0.9510565162951535312, 1.000000000000000000, 0.9510565162951535312, 1.000000000000000000, 0.9510565162951535312, 1.000000000000000000, 0.9510565162951535312, 1.000000000000000000, 0.9510565162951535312, 1.000000000000000000, 0.9510565162951535312, 1.000000000000000000, 0.9510565162951535312, 1.000000000000000000, 0.9510565162951535312, 1.000000000000000000, 0.9510565162951535312, 1.000000000000000000, 0.9510565162951535312, 1.000000000000000000, 0.9510565162951535312, 1.000000000000000000, 0.9510565162951535312, 1.000000000000000000, 0.9510565162951535312, 1.000000000000000000, 0.9510565162951535312, 1.000000000000000000, 0.9510565162951535312, 1.000000000000000000, 0.9510565162951535312, 1.000000000000000000, 0.9510565162951535312, 1.000000000000000000, 0.9510565162951535312, 1.000000000000000000, 0.9510565162951535312, 1.000000000000000000, 0.9510565162951535312, 1.000000000000000000, 0.9510565162951535312, 1.000000000000000000, 0.9510565162951535312, 1.000000000000000000, 0.9510565162951535312, 1.000000000000000000, 0.9510565162951535312, 1.000000000000000000, 0.9510565162951535312, 1.000000000000000000, 0.9510565162951535312, 1.000000000000000000, 0.9510565162951535312, 1.000000000000000000, 0.9510565162951535312, 1.000000000000000000, 0.9510565162951535312, 1.000000000000000000, 0.9510565162951535312, 1.000000000000000000, 0.9510565162951535312, 1.000000000000000000, 0.9510565162951535312, 1.000000000000000000, 0.9510565162951535312, 1.000000000000000000, 0.9510565162951535312, 1.000000000000000000, 0.9510565162951535312, 1.000000000000000000, 0.9510565162951535312, 1.000000000000000000, 0.9510565162951535312, 1.000000000000000000, 0.9510565162951535312, 1.000000000000000000, 0.9510565162951535312, 1.000000000000000000, 0.9510565162951535312, 1.000000000000000000, 0.9510565162951535312, 1.000000000000000000, 0.9510565162951535312, 1.000000000000000000, 0.9510565162951535312, 1.000000000000000000, 0.9510565162951535312, 1.000000000000000000, 0.9510565162951535312, 1.000000000000000000, 0.9510565162951535312, 1.000000000000000000),
 ( 1.000000000000000000, 0.9510565162951535312, 1.000000000000000000, 0.9510565162951535312, 1.000000000000000000, 0.9510565162951535312, 1.000000000000000000, 0.9510565162951535312, 1.000000000000000000, 0.9510565162951535312, 1.000000000000000000, 0.9510565162951535312, 1.000000000000000000, 0.9510565162951535312, 1.000000000000000000, 0.9510565162951535312, 1.000000000000000000, 0.9510565162951535312, 1.000000000000000000, 0.9510565162951535312, 1.000000000000000000, 0.9510565162951535312, 1.000000000000000000, 0.9510565162951535312, 1.000000000000000000, 0.9510565162951535312, 1.000000000000000000, 0.9510565162951535312, 1.000000000000000000, 0.9510565162951535312, 1.000000000000000000, 0.9510565162951535312, 1.000000000000000000, 0.9510565162951535312, 1.000000000000000000, 0.9510565162951535312, 1.000000000000000000, 0.9510565162951535312, 1.000000000000000000, 0.9510565162951535312, 1.000000000000000000, 0.9510565162951535312, 1.000000000000000000, 0.9510565162951535312, 1.000000000000000000, 0.9510565162951535312, 1.000000000000000000, 0.9510565162951535312, 1.000000000000000000, 0.9510565162951535312, 1.000000000000000000, 0.9510565162951535312, 1.000000000000000000, 0.9510565162951535312, 1.000000000000000000, 0.9510565162951535312, 1.000000000000000000, 0.9510565162951535312, 1.000000000000000000, 0.9510565162951535312, 1.000000000000000000, 0.9510565162951535312, 1.000000000000000000, 0.9510565162951535312, 1.000000000000000000, 0.9510565162951535312, 1.000000000000000000, 0.9510565162951535312, 1.000000000000000000, 0.9510565162951535312, 1.000000000000000000, 0.9510565162951535312, 1.000000000000000000, 0.9510565162951535312, 1.000000000000000000, 0.9510565162951535312, 1.000000000000000000, 0.9510565162951535312, 1.000000000000000000, 0.9510565162951535312, 1.000000000000000000, 0.9510565162951535312, 1.000000000000000000, 0.9510565162951535312, 1.000000000000000000, 0.9510565162951535312, 1.000000000000000000, 0.9510565162951535312, 1.000000000000000000, 0.9510565162951535312, 1.000000000000000000, 0.9510565162951535312, 1.000000000000000000, 0.9510565162951535312, 1.000000000000000000, 0.9510565162951535312, 1.000000000000000000, 0.9510565162951535312, 1.000000000000000000, 0.9510565162951535312, 1.000000000000000000) ) ) 
 REPRESENTATION_ITEM ( '' )  SURFACE ( )  );
#181392 = CARTESIAN_POINT ( 'NONE',  ( -13.97604488694527625, -13.89961937509977652, 71.87390960531433848 ) ) ;
#181393 = CARTESIAN_POINT ( 'NONE',  ( -21.53943276465977519, -0.05219959533937600094, 18.75109039468568639 ) ) ;
#181394 = CARTESIAN_POINT ( 'NONE',  ( -13.97604488694547697, 13.89961937509957934, 68.12609039468563310 ) ) ;
#181396 = CARTESIAN_POINT ( 'NONE',  ( 13.97604488694527802, 13.89961937509977652, 24.37390960531435624 ) ) ;
#181395 = CARTESIAN_POINT ( 'NONE',  ( -19.03943276465977164, 0.05219959533909376836, 106.2489096053143669 ) ) ;
#181397 = CARTESIAN_POINT ( 'NONE',  ( 5.049401038298161559, -19.05341960407611168, 72.70724293864768129 ) ) ;
#181399 = CARTESIAN_POINT ( 'NONE',  ( -4.500000000000000000, 5.510910596163088569E-16, 0.000000000000000000 ) ) ;
#181398 = CARTESIAN_POINT ( 'NONE',  ( -16.53943276465976808, 0.05219959533911058130, 41.24890960531435269 ) ) ;
#181400 = CARTESIAN_POINT ( 'NONE',  ( 5.049401038297881783, 19.05341960407617563, 32.29275706135233293 ) ) ;
#181401 = CARTESIAN_POINT ( 'NONE',  ( -14.29746914071049879, 8.314922557960819915, 70.83224293864770971 ) ) ;
#181402 = CARTESIAN_POINT ( 'NONE',  ( -5.823673210054431948, 21.52544592524334988, 107.7094237280190328 ) ) ;
#181403 = CARTESIAN_POINT ( 'NONE',  ( -5.153800228976328057, -19.02544592524343514, 57.29057627198103120 ) ) ;
#181405 = CARTESIAN_POINT ( 'NONE',  ( 21.52544592524334988, 5.823673210054432836, 101.4594237280190185 ) ) ;
#181404 = CARTESIAN_POINT ( 'NONE',  ( 0.05219959533910956823, 16.53943276465976808, 39.99890960531436690 ) ) ;
#181406 = CARTESIAN_POINT ( 'NONE',  ( 19.02544592524343514, -5.153800228976328945, 88.54057627198102409 ) ) ;
#181407 = CARTESIAN_POINT ( 'NONE',  ( -16.46253265017160317, 9.564922557960807481, 110.8322429386476955 ) ) ;
#181408 = CARTESIAN_POINT ( 'NONE',  ( -0.05219959533909027116, -19.03943276465977164, 37.49890960531436690 ) ) ;
#181409 = CARTESIAN_POINT ( 'NONE',  ( 8.224510206698953496, -14.34966873604960469, 102.9155762719810383 ) ) ;
#181410 = CARTESIAN_POINT ( 'NONE',  ( -8.314922557960811034, -14.29746914071050412, 87.08224293864769550 ) ) ;
#181411 = CARTESIAN_POINT ( 'NONE',  ( 18.67979575497178502, 10.72451020669898547, 79.16557627198103830 ) ) ;
#181412 = CARTESIAN_POINT ( 'NONE',  ( -19.05341960407611168, -5.049401038298163336, 86.45724293864769550 ) ) ;
#181413 = CARTESIAN_POINT ( 'NONE',  ( -5.719274019375978568, 21.55341960407610458, 95.20724293864769550 ) ) ;
#181414 = CARTESIAN_POINT ( 'NONE',  ( 5.153800228976335163, 19.02544592524342804, 89.79057627198102409 ) ) ;
#181416 = CARTESIAN_POINT ( 'NONE',  ( -14.34966873604960291, -8.224510206698953496, 106.6655762719810383 ) ) ;
#181415 = CARTESIAN_POINT ( 'NONE',  ( 11.30153831258470731, -180.0000000000000000, -4.999999999999999112 ) ) ;
#181417 = CARTESIAN_POINT ( 'NONE',  ( 5.153800228976335163, 19.02544592524342804, 69.79057627198103830 ) ) ;
#181418 = CARTESIAN_POINT ( 'NONE',  ( -21.53943276465977519, 0.05219959533907696930, 81.24890960531436690 ) ) ;
#181419 = CARTESIAN_POINT ( 'NONE',  ( -4.000000000000000888, -105.0000000000000000, -23.00000000000000000 ) ) ;
#181421 = CARTESIAN_POINT ( 'NONE',  ( 6.677994727576218814, -3.424326230466335996, 1.353258418600855606 ) ) ;
#181420 = CARTESIAN_POINT ( 'NONE',  ( -18.67979575497178146, -10.72451020669898902, 31.66557627198102054 ) ) ;
#181422 = CARTESIAN_POINT ( 'NONE',  ( -16.55341960407617563, 4.379528057220093196, 38.54275706135234714 ) ) ;
#181423 = CARTESIAN_POINT ( 'NONE',  ( 8.224510206698953496, -14.34966873604960469, 92.91557627198103830 ) ) ;
#181424 = DIRECTION ( 'NONE',  ( 1.000000000000000000, -5.392603844284257652E-33, 0.000000000000000000 ) ) ;
#181425 = CARTESIAN_POINT ( 'NONE',  ( 13.97604488694527802, 13.89961937509977652, 94.37390960531436690 ) ) ;
#181426 = CARTESIAN_POINT ( 'NONE',  ( -19.05341960407611168, -5.049401038298163336, 51.45724293864770260 ) ) ;
#181427 = CARTESIAN_POINT ( 'NONE',  ( -16.52544592524342804, 4.483927247898546575, 81.04057627198102409 ) ) ;
#181428 = CARTESIAN_POINT ( 'NONE',  ( -15.72974639402197994, 15.80617190586746368, 25.62390960531435624 ) ) ;
#181429 = CARTESIAN_POINT ( 'NONE',  ( 12.06949235617757843, -12.14591786802309237, 53.12390960531436690 ) ) ;
#181430 = CARTESIAN_POINT ( 'NONE',  ( -5.049401038297874678, -19.05341960407617918, 99.79275706135234714 ) ) ;
#181431 = CARTESIAN_POINT ( 'NONE',  ( 15.80617190586769283, -15.72974639402175789, 55.62609039468568284 ) ) ;
#181432 = CARTESIAN_POINT ( 'NONE',  ( -27.73933785331498925, 2.428612866367529932E-14, 148.8750000027311842 ) ) ;
#181433 = CARTESIAN_POINT ( 'NONE',  ( -9.564922557960796823, -16.46253265017161027, 97.08224293864769550 ) ) ;
#181434 = CARTESIAN_POINT ( 'NONE',  ( 12.06949235617739724, 12.14591786802326823, 86.87609039468568994 ) ) ;
#181435 = CARTESIAN_POINT ( 'NONE',  ( -16.51473224551069308, -9.474510206698971260, 26.66557627198103120 ) ) ;
#181436 = CARTESIAN_POINT ( 'NONE',  ( 13.89961937509977652, -13.97604488694527269, 73.12390960531436690 ) ) ;
#181437 = CARTESIAN_POINT ( 'NONE',  ( 18.67979575497178502, 10.72451020669898547, 84.16557627198103830 ) ) ;
#181438 = CARTESIAN_POINT ( 'NONE',  ( 5.153800228976615827, -19.02544592524334988, 105.2094237280190185 ) ) ;
#181440 = CARTESIAN_POINT ( 'NONE',  ( 18.67979575497194134, -10.72451020669871369, 55.83442372801901854 ) ) ;
#181439 = CARTESIAN_POINT ( 'NONE',  ( 8.224510206698953496, -14.34966873604960469, 52.91557627198103830 ) ) ;
#181441 = B_SPLINE_CURVE_WITH_KNOTS ( 'NONE', 3,
 ( #64385, #49220, #66366, #3690, #142207, #36020, #126053, #160372, #37018, #95706, #129016, #87275 ),
 .UNSPECIFIED., .F., .F.,
 ( 4, 2, 2, 2, 2, 4 ),
 ( 0.002654191900342570219, 0.003314442422523698230, 0.003974692944704825807, 0.004634943466885954252, 0.004965068727976518909, 0.005295193989067083565 ),
 .UNSPECIFIED. ) ;
#181443 = CARTESIAN_POINT ( 'NONE',  ( 5.153800228976335163, 19.02544592524342804, 114.7905762719810241 ) ) ;
#181442 = CARTESIAN_POINT ( 'NONE',  ( 14.29746914071037800, 8.314922557961029526, 81.66775706135236135 ) ) ;
#181444 = CARTESIAN_POINT ( 'NONE',  ( -16.51473224551069308, -9.474510206698971260, 111.6655762719810383 ) ) ;
#181445 = CARTESIAN_POINT ( 'NONE',  ( -4.500000000000001776, -125.9646863569935107, 7.891563605355330857 ) ) ;
#181446 = CARTESIAN_POINT ( 'NONE',  ( 16.52544592524335698, 4.483927247898782831, 106.4594237280190328 ) ) ;
#181447 = CARTESIAN_POINT ( 'NONE',  ( 16.53943276465976808, 0.05219959533934440121, 66.25109039468567573 ) ) ;
#181448 = CARTESIAN_POINT ( 'NONE',  ( -0.05219959533909027116, -19.03943276465977164, 72.49890960531435269 ) ) ;
#181449 = CARTESIAN_POINT ( 'NONE',  ( -0.05219959533909027116, -19.03943276465977164, 77.49890960531435269 ) ) ;
#181450 = CARTESIAN_POINT ( 'NONE',  ( -18.67979575497193778, 10.72451020669871902, 78.33442372801901854 ) ) ;
#181451 = CARTESIAN_POINT ( 'NONE',  ( 8.314922557961029526, -14.29746914071037800, 80.41775706135234714 ) ) ;
#181452 = CARTESIAN_POINT ( 'NONE',  ( -12.14591786802309592, -12.06949235617757132, 46.87390960531435979 ) ) ;
#181453 = CARTESIAN_POINT ( 'NONE',  ( 19.02544592524343514, -5.153800228976328945, 53.54057627198102409 ) ) ;
#181454 = CARTESIAN_POINT ( 'NONE',  ( 5.049401038298161559, -19.05341960407611168, 52.70724293864767418 ) ) ;
#181456 = ORIENTED_EDGE ( 'NONE', *, *, #163492, .T. ) ;
#181455 = CARTESIAN_POINT ( 'NONE',  ( -12.14591786802326823, 12.06949235617739902, 38.12609039468567573 ) ) ;
#181457 = CARTESIAN_POINT ( 'NONE',  ( -9.474510206698720793, -16.51473224551083518, 94.58442372801900433 ) ) ;
#181458 = CARTESIAN_POINT ( 'NONE',  ( 14.34966873604960469, 8.224510206698951720, 94.16557627198103830 ) ) ;
#181459 = CARTESIAN_POINT ( 'NONE',  ( 5.049401038298161559, -19.05341960407611168, 67.70724293864769550 ) ) ;
#181461 = CARTESIAN_POINT ( 'NONE',  ( -6.020228577223754586E-15, 39.95556452105416412, -2.500000000000000444 ) ) ;
#181460 = CARTESIAN_POINT ( 'NONE',  ( 9.474510206698729675, 16.51473224551082808, 107.0844237280190043 ) ) ;
#181462 = CARTESIAN_POINT ( 'NONE',  ( 21.55341960407619695, -5.719274019375665929, 101.0427570613523756 ) ) ;
#181463 = CARTESIAN_POINT ( 'NONE',  ( 14.34966873604972726, -8.224510206698740333, 70.83442372801901854 ) ) ;
#181464 = LINE ( 'NONE', #29749, #53430 ) ;
#181465 = CARTESIAN_POINT ( 'NONE',  ( -10.81492255796078084, -18.62759615963271287, 67.08224293864770971 ) ) ;
#181466 = CARTESIAN_POINT ( 'NONE',  ( 8.314922557961029526, -14.29746914071037800, 55.41775706135234714 ) ) ;
#181467 = CARTESIAN_POINT ( 'NONE',  ( 31.79999999999936477, 1.011767027235951731E-12, 92.30000000000021032 ) ) ;
#181468 = CARTESIAN_POINT ( 'NONE',  ( 16.51473224551083163, -9.474510206698727899, 45.83442372801900433 ) ) ;
#181469 = CARTESIAN_POINT ( 'NONE',  ( 19.05341960407611168, 5.049401038298154454, 83.95724293864766707 ) ) ;
#181470 = CARTESIAN_POINT ( 'NONE',  ( 13.89961937509977652, -13.97604488694527269, 23.12390960531436335 ) ) ;
#181471 = CARTESIAN_POINT ( 'NONE',  ( -16.46253265017160317, 9.564922557960807481, 60.83224293864769550 ) ) ;
#181472 = CARTESIAN_POINT ( 'NONE',  ( 18.67979575497194134, -10.72451020669871369, 70.83442372801901854 ) ) ;
#181473 = CARTESIAN_POINT ( 'NONE',  ( 13.97604488694548053, -13.89961937509957401, 45.62609039468566863 ) ) ;
#181474 = CARTESIAN_POINT ( 'NONE',  ( -16.51473224551082808, 9.474510206698731452, 28.33442372801900433 ) ) ;
#181475 = CARTESIAN_POINT ( 'NONE',  ( -0.05219959533909027116, -19.03943276465977164, 62.49890960531435979 ) ) ;
#181476 = CARTESIAN_POINT ( 'NONE',  ( -19.02544592524342804, 5.153800228976336051, 116.0405762719810383 ) ) ;
#181477 = CARTESIAN_POINT ( 'NONE',  ( -10.81492255796105439, 18.62759615963255655, 82.91775706135234714 ) ) ;
#181478 = CARTESIAN_POINT ( 'NONE',  ( -16.46253265017160317, 9.564922557960807481, 70.83224293864770971 ) ) ;
#181479 = CARTESIAN_POINT ( 'NONE',  ( -21.55341960407619339, 5.719274019375674811, 88.54275706135236135 ) ) ;
#181480 = CARTESIAN_POINT ( 'NONE',  ( 21.52544592524344225, -5.823673210054117533, 38.54057627198103120 ) ) ;
#181481 = AXIS2_PLACEMENT_3D ( 'NONE', #74938, #151782, #90100 ) ;
#181482 = CARTESIAN_POINT ( 'NONE',  ( 19.02544592524343514, -5.153800228976328945, 88.54057627198102409 ) ) ;
#181483 = CARTESIAN_POINT ( 'NONE',  ( 21.52544592524334988, 5.823673210054432836, 41.45942372801901143 ) ) ;
#181484 = CARTESIAN_POINT ( 'NONE',  ( 19.02544592524334988, 5.153800228976608722, 61.45942372801900433 ) ) ;
#181485 = CARTESIAN_POINT ( 'NONE',  ( 13.89961937509977652, -13.97604488694527269, 48.12390960531435979 ) ) ;
#181486 = CARTESIAN_POINT ( 'NONE',  ( 5.153800228976335163, 19.02544592524342804, 89.79057627198102409 ) ) ;
#181487 = CARTESIAN_POINT ( 'NONE',  ( 16.52544592524335698, 4.483927247898782831, 26.45942372801901854 ) ) ;
#181488 = CARTESIAN_POINT ( 'NONE',  ( 16.52544592524342804, -4.483927247898539470, 88.54057627198103830 ) ) ;
#181489 = CARTESIAN_POINT ( 'NONE',  ( -13.89961937509977652, 13.97604488694528158, 65.62390960531436690 ) ) ;
#181490 = CARTESIAN_POINT ( 'NONE',  ( -5.823673210054116645, -21.52544592524344225, 52.29057627198102409 ) ) ;
#181491 = CARTESIAN_POINT ( 'NONE',  ( -16.55341960407617563, 4.379528057220093196, 23.54275706135235424 ) ) ;
#181492 = CARTESIAN_POINT ( 'NONE',  ( -5.823673210054116645, -21.52544592524344225, 112.2905762719810241 ) ) ;
#181493 = CARTESIAN_POINT ( 'NONE',  ( -15.72974639402176322, -15.80617190586768395, 69.37609039468567573 ) ) ;
#181494 = CARTESIAN_POINT ( 'NONE',  ( 4.483927247898790824, -16.52544592524335698, 75.20942372801901854 ) ) ;
#181495 = CARTESIAN_POINT ( 'NONE',  ( -0.05219959533934338120, 16.53943276465976808, 67.50109039468568994 ) ) ;
#181496 = CARTESIAN_POINT ( 'NONE',  ( -16.51473224551069308, -9.474510206698971260, 66.66557627198102409 ) ) ;
#181497 = CARTESIAN_POINT ( 'NONE',  ( 8.224510206698742110, 14.34966873604972548, 97.08442372801904696 ) ) ;
#181498 = CARTESIAN_POINT ( 'NONE',  ( 19.03943276465977164, 0.05219959533936151252, 36.25109039468567573 ) ) ;
#181499 = CARTESIAN_POINT ( 'NONE',  ( 21.52544592524334988, 5.823673210054432836, 26.45942372801901854 ) ) ;
#181500 = CARTESIAN_POINT ( 'NONE',  ( -8.314922557960811034, -14.29746914071050412, 72.08224293864769550 ) ) ;
#181501 = CARTESIAN_POINT ( 'NONE',  ( -19.05341960407611168, -5.049401038298163336, 101.4572429386476955 ) ) ;
#181502 = CARTESIAN_POINT ( 'NONE',  ( 16.55341960407618274, -4.379528057220086978, 86.04275706135236135 ) ) ;
#181503 = CARTESIAN_POINT ( 'NONE',  ( 0.05219959533937995610, -21.53943276465977519, 55.00109039468568284 ) ) ;
#181504 = CARTESIAN_POINT ( 'NONE',  ( 8.314922557961029526, -14.29746914071037800, 25.41775706135235779 ) ) ;
#181505 = CARTESIAN_POINT ( 'NONE',  ( 5.719274019375673035, 21.55341960407619339, 22.29275706135235069 ) ) ;
#181506 = CARTESIAN_POINT ( 'NONE',  ( -0.05219959533910754901, -16.53943276465976808, 52.49890960531435979 ) ) ;
#181507 = ORIENTED_EDGE ( 'NONE', *, *, #143157, .F. ) ;
#181508 = CARTESIAN_POINT ( 'NONE',  ( -18.62759615963270932, 10.81492255796079327, 100.8322429386477097 ) ) ;
#181509 = CARTESIAN_POINT ( 'NONE',  ( -16.53943276465976808, 0.05219959533911058130, 36.24890960531435979 ) ) ;
#181510 = ORIENTED_EDGE ( 'NONE', *, *, #183088, .T. ) ;
#181511 = CARTESIAN_POINT ( 'NONE',  ( 34.37196153507746743, 7.030587757552861916, 47.62314794725693901 ) ) ;
#181512 = CARTESIAN_POINT ( 'NONE',  ( -15.72974639402197994, 15.80617190586746368, 30.62390960531436335 ) ) ;
#181513 = CARTESIAN_POINT ( 'NONE',  ( 18.62759615963255655, 10.81492255796105972, 41.66775706135235424 ) ) ;
#181514 = CARTESIAN_POINT ( 'NONE',  ( -16.55341960407611168, -4.379528057220339221, 66.45724293864768129 ) ) ;
#181515 = CARTESIAN_POINT ( 'NONE',  ( 0.05219959533907565091, 21.53943276465977519, 59.99890960531436690 ) ) ;
#181516 = CARTESIAN_POINT ( 'NONE',  ( -13.97604488694527625, -13.89961937509977652, 76.87390960531433848 ) ) ;
#181518 = CARTESIAN_POINT ( 'NONE',  ( -9.564922557961040184, 16.46253265017147172, 72.91775706135233293 ) ) ;
#181517 = CARTESIAN_POINT ( 'NONE',  ( -5.153800228976328057, -19.02544592524343514, 27.29057627198103120 ) ) ;
#181519 = CARTESIAN_POINT ( 'NONE',  ( 5.719274019375991003, -21.55341960407610458, 42.70724293864770260 ) ) ;
#181520 = CARTESIAN_POINT ( 'NONE',  ( 19.03943276465977164, -0.05219959533909143690, 63.74890960531435979 ) ) ;
#181521 = ORIENTED_EDGE ( 'NONE', *, *, #145209, .F. ) ;
#181522 = CARTESIAN_POINT ( 'NONE',  ( 16.55341960407618274, -4.379528057220086978, 41.04275706135236135 ) ) ;
#181523 = CARTESIAN_POINT ( 'NONE',  ( -21.53943276465977519, 0.05219959533907696930, 111.2489096053143669 ) ) ;
#181524 = CARTESIAN_POINT ( 'NONE',  ( 4.379528057220339221, -16.55341960407611168, 47.70724293864770260 ) ) ;
#181525 = CARTESIAN_POINT ( 'NONE',  ( -19.05341960407611168, -5.049401038298163336, 101.4572429386476955 ) ) ;
#181526 = CARTESIAN_POINT ( 'NONE',  ( 10.72451020669898902, -18.67979575497178502, 72.91557627198103830 ) ) ;
#181528 = CARTESIAN_POINT ( 'NONE',  ( -4.483927247898782831, 16.52544592524335698, 42.70942372801901854 ) ) ;
#181527 = CARTESIAN_POINT ( 'NONE',  ( -5.719274019375978568, 21.55341960407610458, 110.2072429386477239 ) ) ;
#181529 = CARTESIAN_POINT ( 'NONE',  ( -21.53943276465977519, 0.05219959533907696930, 51.24890960531436690 ) ) ;
#181530 = CARTESIAN_POINT ( 'NONE',  ( 21.53943276465977519, 0.05219959533937863772, 106.2510903946856757 ) ) ;
#181531 = CARTESIAN_POINT ( 'NONE',  ( 19.02544592524343514, -5.153800228976328945, 43.54057627198103120 ) ) ;
#181532 = CARTESIAN_POINT ( 'NONE',  ( 16.51473224551069308, 9.474510206698969483, 99.16557627198102409 ) ) ;
#181533 = CARTESIAN_POINT ( 'NONE',  ( 16.51473224551069308, 9.474510206698969483, 79.16557627198103830 ) ) ;
#181534 = CARTESIAN_POINT ( 'NONE',  ( 16.38665767534995155, -7.295008042176409191, 87.76400864214471653 ) ) ;
#181535 = CARTESIAN_POINT ( 'NONE',  ( 5.153800228976615827, -19.02544592524334988, 55.20942372801899722 ) ) ;
#181537 = CARTESIAN_POINT ( 'NONE',  ( -0.05219959533907301413, -21.53943276465977519, 27.49890960531435269 ) ) ;
#181536 = CARTESIAN_POINT ( 'NONE',  ( -10.81492255796105439, 18.62759615963255655, 107.9177570613523471 ) ) ;
#181538 = CARTESIAN_POINT ( 'NONE',  ( 14.34966873604972726, -8.224510206698740333, 105.8344237280190328 ) ) ;
#181539 = CARTESIAN_POINT ( 'NONE',  ( -0.05219959533936034679, 19.03943276465977164, 82.50109039468567573 ) ) ;
#181540 = CARTESIAN_POINT ( 'NONE',  ( -17.05587630539785593, 6.762274262135693270, 60.74180309037313208 ) ) ;
#181541 = CARTESIAN_POINT ( 'NONE',  ( 13.97604488694548053, -13.89961937509957401, 80.62609039468567573 ) ) ;
#181542 = CARTESIAN_POINT ( 'NONE',  ( 16.46253265017146816, 9.564922557961045513, 46.66775706135233293 ) ) ;
#181543 = B_SPLINE_CURVE_WITH_KNOTS ( 'NONE', 3,
 ( #87013, #6162, #70852, #131514, #36497, #144677 ),
 .UNSPECIFIED., .F., .F.,
 ( 4, 2, 4 ),
 ( 0.003989672132298103559, 0.004372778065220524202, 0.004755883998142945712 ),
 .UNSPECIFIED. ) ;
#181544 = CARTESIAN_POINT ( 'NONE',  ( -16.62475595723695321, -7.163666690055258357, 44.47286648189535185 ) ) ;
#181545 = CARTESIAN_POINT ( 'NONE',  ( -5.153800228976328057, -19.02544592524343514, 42.29057627198101699 ) ) ;
#181546 = CARTESIAN_POINT ( 'NONE',  ( -16.53943276465976808, 0.05219959533911058130, 56.24890960531436690 ) ) ;
#181547 = CARTESIAN_POINT ( 'NONE',  ( -5.153800228976328057, -19.02544592524343514, 32.29057627198102409 ) ) ;
#181548 = CARTESIAN_POINT ( 'NONE',  ( -16.55341960407611168, -4.379528057220339221, 36.45724293864768839 ) ) ;
#181549 = CARTESIAN_POINT ( 'NONE',  ( 10.20000000000000107, 0.000000000000000000, 0.000000000000000000 ) ) ;
#181550 = CARTESIAN_POINT ( 'NONE',  ( -4.379528057220086978, -16.55341960407618274, 109.7927570613523613 ) ) ;
#181551 = CARTESIAN_POINT ( 'NONE',  ( 19.05341960407611168, 5.049401038298154454, 48.95724293864768129 ) ) ;
#181552 = CARTESIAN_POINT ( 'NONE',  ( 18.62759615963255655, 10.81492255796105972, 106.6677570613523756 ) ) ;
#181553 = CARTESIAN_POINT ( 'NONE',  ( 0.05219959533934541429, -16.53943276465976808, 25.00109039468567218 ) ) ;
#181554 = CARTESIAN_POINT ( 'NONE',  ( -10.81492255796078084, -18.62759615963271287, 37.08224293864768129 ) ) ;
#181556 = VERTEX_POINT ( 'NONE', #150680 ) ;
#181555 = CARTESIAN_POINT ( 'NONE',  ( -5.719274019375665041, -21.55341960407619695, 94.79275706135234714 ) ) ;
#181557 = CARTESIAN_POINT ( 'NONE',  ( 9.474510206698971260, -16.51473224551069308, 107.9155762719810383 ) ) ;
#181558 = CARTESIAN_POINT ( 'NONE',  ( -9.474510206698964154, 16.51473224551069663, 80.41557627198103830 ) ) ;
#181559 = CARTESIAN_POINT ( 'NONE',  ( -29.86685920354755552, 21.69954338932564397, -8.824999997268815122 ) ) ;
#181560 = CARTESIAN_POINT ( 'NONE',  ( 15.80617190586746368, 15.72974639402197994, 109.3739096053143811 ) ) ;
#181561 = CARTESIAN_POINT ( 'NONE',  ( 0.05219959533910956823, 16.53943276465976808, 84.99890960531436690 ) ) ;
#181562 = CARTESIAN_POINT ( 'NONE',  ( 5.823673210054125526, 21.52544592524343514, 74.79057627198105251 ) ) ;
#181563 = CARTESIAN_POINT ( 'NONE',  ( 19.03943276465977164, -0.05219959533909143690, 68.74890960531436690 ) ) ;
#181564 = CARTESIAN_POINT ( 'NONE',  ( -10.72451020669898014, 18.67979575497178502, 100.4155762719810241 ) ) ;
#181565 = ORIENTED_EDGE ( 'NONE', *, *, #221, .F. ) ;
#181566 = CARTESIAN_POINT ( 'NONE',  ( -5.153800228976328057, -19.02544592524343514, 62.29057627198100988 ) ) ;
#181568 = CARTESIAN_POINT ( 'NONE',  ( 20.61108013404306405, -10.97331748574078780, 168.1441487092657781 ) ) ;
#181567 = CARTESIAN_POINT ( 'NONE',  ( 8.224510206698953496, -14.34966873604960469, 92.91557627198103830 ) ) ;
#181569 = CARTESIAN_POINT ( 'NONE',  ( 19.03943276465977164, -0.05219959533909143690, 63.74890960531435979 ) ) ;
#181570 = CARTESIAN_POINT ( 'NONE',  ( -16.46253265017146816, -9.564922557961047289, 84.16775706135233293 ) ) ;
#181571 = CARTESIAN_POINT ( 'NONE',  ( -16.53943276465976808, 0.05219959533911058130, 91.24890960531436690 ) ) ;
#181572 = CARTESIAN_POINT ( 'NONE',  ( 10.81492255796106328, -18.62759615963255655, 65.41775706135234714 ) ) ;
#181574 = CARTESIAN_POINT ( 'NONE',  ( -15.80617190586768217, 15.72974639402176855, 23.12609039468567573 ) ) ;
#181573 = CARTESIAN_POINT ( 'NONE',  ( -5.049401038298153566, 19.05341960407611168, 55.20724293864769550 ) ) ;
#181575 = CARTESIAN_POINT ( 'NONE',  ( -8.314922557960811034, -14.29746914071050412, 97.08224293864770971 ) ) ;
#181576 = CARTESIAN_POINT ( 'NONE',  ( -5.429308488886486681E-15, 30.30510711980690175, 147.7500000054623683 ) ) ;
#181577 = CARTESIAN_POINT ( 'NONE',  ( -16.46253265017160317, 9.564922557960807481, 65.83224293864769550 ) ) ;
#181578 = CYLINDRICAL_SURFACE ( 'NONE', #160240, 1.499999999999997780 ) ;
#181580 = CARTESIAN_POINT ( 'NONE',  ( -19.02544592524342804, 5.153800228976336051, 116.0405762719810383 ) ) ;
#181579 = CARTESIAN_POINT ( 'NONE',  ( -5.049401038297874678, -19.05341960407617918, 104.7927570613523471 ) ) ;
#181581 = CARTESIAN_POINT ( 'NONE',  ( -10.81492255796105439, 18.62759615963255655, 52.91775706135235424 ) ) ;
#181582 = CARTESIAN_POINT ( 'NONE',  ( 0.05219959533909260263, 19.03943276465977164, 99.99890960531436690 ) ) ;
#181583 = CARTESIAN_POINT ( 'NONE',  ( -16.51473224551082808, 9.474510206698731452, 88.33442372801900433 ) ) ;
#181584 = CARTESIAN_POINT ( 'NONE',  ( 0.05219959533909260263, 19.03943276465977164, 54.99890960531435979 ) ) ;
#181585 = CARTESIAN_POINT ( 'NONE',  ( 16.52544592524342804, -4.483927247898539470, 83.54057627198102409 ) ) ;
#181586 = CARTESIAN_POINT ( 'NONE',  ( -5.153800228976328057, -19.02544592524343514, 92.29057627198099567 ) ) ;
#181587 = CARTESIAN_POINT ( 'NONE',  ( 4.483927247898545687, 16.52544592524342804, 84.79057627198102409 ) ) ;
#181588 = CARTESIAN_POINT ( 'NONE',  ( 16.46253265017160672, -9.564922557960803928, 83.33224293864768129 ) ) ;
#181589 = EDGE_CURVE ( 'NONE', #165759, #179372, #146944, .T. ) ;
#181590 = CARTESIAN_POINT ( 'NONE',  ( -13.97604488694547697, 13.89961937509957934, 28.12609039468565797 ) ) ;
#181593 = CARTESIAN_POINT ( 'NONE',  ( -16.46253265017160317, 9.564922557960807481, 25.83224293864769194 ) ) ;
#181592 = CARTESIAN_POINT ( 'NONE',  ( 16.55341960407611168, 4.379528057220329451, 43.95724293864769550 ) ) ;
#181591 = CARTESIAN_POINT ( 'NONE',  ( 16.51473224551069308, 9.474510206698969483, 49.16557627198102409 ) ) ;
#181594 = VERTEX_POINT ( 'NONE', #77780 ) ;
#181595 = CARTESIAN_POINT ( 'NONE',  ( 21.53943276465977519, 0.05219959533937863772, 41.25109039468568284 ) ) ;
#181596 = CARTESIAN_POINT ( 'NONE',  ( -19.03943276465977164, -0.05219959533935918106, 78.75109039468567573 ) ) ;
#181597 = CARTESIAN_POINT ( 'NONE',  ( 12.14591786802309770, 12.06949235617756955, 29.37390960531435269 ) ) ;
#181598 = CARTESIAN_POINT ( 'NONE',  ( 10.72451020669898902, -18.67979575497178502, 82.91557627198103830 ) ) ;
#181599 = CARTESIAN_POINT ( 'NONE',  ( -5.719274019375978568, 21.55341960407610458, 35.20724293864768839 ) ) ;
#181600 = CARTESIAN_POINT ( 'NONE',  ( 8.314922557960818139, 14.29746914071049879, 69.58224293864769550 ) ) ;
#181601 = CARTESIAN_POINT ( 'NONE',  ( -9.474510206698964154, 16.51473224551069663, 45.41557627198103120 ) ) ;
#181602 = CARTESIAN_POINT ( 'NONE',  ( 14.29746914071037800, 8.314922557961029526, 96.66775706135234714 ) ) ;
#181603 = CARTESIAN_POINT ( 'NONE',  ( -14.34966873604972548, 8.224510206698743886, 68.33442372801900433 ) ) ;
#181604 = CARTESIAN_POINT ( 'NONE',  ( 9.474510206698729675, 16.51473224551082808, 22.08442372801899722 ) ) ;
#181605 = CARTESIAN_POINT ( 'NONE',  ( 13.97604488694527802, 13.89961937509977652, 89.37390960531436690 ) ) ;
#181606 = CARTESIAN_POINT ( 'NONE',  ( -0.05219959533909027116, -19.03943276465977164, 77.49890960531435269 ) ) ;
#181607 = CARTESIAN_POINT ( 'NONE',  ( 14.29746914071037800, 8.314922557961029526, 76.66775706135234714 ) ) ;
#181608 = CARTESIAN_POINT ( 'NONE',  ( 9.564922557960805705, 16.46253265017160317, 29.58224293864769550 ) ) ;
#181609 = CARTESIAN_POINT ( 'NONE',  ( -8.224510206698948167, 14.34966873604960824, 40.41557627198103120 ) ) ;
#181611 = CARTESIAN_POINT ( 'NONE',  ( -16.51473224551069308, -9.474510206698971260, 96.66557627198102409 ) ) ;
#181610 = CARTESIAN_POINT ( 'NONE',  ( 16.51473224551069308, 9.474510206698969483, 99.16557627198102409 ) ) ;
#181612 = CARTESIAN_POINT ( 'NONE',  ( 21.55341960407610458, 5.719274019375980345, 28.95724293864769905 ) ) ;
#181613 = CARTESIAN_POINT ( 'NONE',  ( 0.05219959533910956823, 16.53943276465976808, 74.99890960531435269 ) ) ;
#181614 = CARTESIAN_POINT ( 'NONE',  ( 14.29746914071049879, -8.314922557960816363, 63.33224293864770260 ) ) ;
#181616 = CARTESIAN_POINT ( 'NONE',  ( -18.22780087662126647, -5.499999999999827693, 58.98236817873108606 ) ) ;
#181615 = CARTESIAN_POINT ( 'NONE',  ( -16.55341960407617563, 4.379528057220093196, 58.54275706135235424 ) ) ;
#181617 = CARTESIAN_POINT ( 'NONE',  ( 19.03943276465977164, 0.05219959533936151252, 56.25109039468566863 ) ) ;
#181618 = CARTESIAN_POINT ( 'NONE',  ( -16.51473224551069308, -9.474510206698971260, 91.66557627198103830 ) ) ;
#181619 = CARTESIAN_POINT ( 'NONE',  ( 19.03943276465977164, 0.05219959533936151252, 61.25109039468566863 ) ) ;
#181620 = CARTESIAN_POINT ( 'NONE',  ( 8.571926809382597767, 26.38167802310806209, 142.7750000027311899 ) ) ;
#181622 = CARTESIAN_POINT ( 'NONE',  ( -14.34966873604972548, 8.224510206698743886, 93.33442372801901854 ) ) ;
#181621 = CARTESIAN_POINT ( 'NONE',  ( 9.564922557961047289, -16.46253265017146816, 110.4177570613523471 ) ) ;
#181623 = CARTESIAN_POINT ( 'NONE',  ( -19.03943276465977164, 0.05219959533909376836, 41.24890960531435269 ) ) ;
#181624 = CARTESIAN_POINT ( 'NONE',  ( 9.564922557960805705, 16.46253265017160317, 114.5822429386476955 ) ) ;
#181625 = CARTESIAN_POINT ( 'NONE',  ( -21.55341960407619339, 5.719274019375674811, 58.54275706135235424 ) ) ;
#181626 = CARTESIAN_POINT ( 'NONE',  ( -5.049401038297874678, -19.05341960407617918, 104.7927570613523471 ) ) ;
#181628 = CARTESIAN_POINT ( 'NONE',  ( -0.05219959533909027116, -19.03943276465977164, 72.49890960531435269 ) ) ;
#181627 = CARTESIAN_POINT ( 'NONE',  ( -13.89961937509957401, -13.97604488694547697, 54.37609039468566152 ) ) ;
#181629 = CARTESIAN_POINT ( 'NONE',  ( 37.99626262588765258, 2.893932880411085066E-14, -1.002157773949823083 ) ) ;
#181631 = CARTESIAN_POINT ( 'NONE',  ( -16.51473224551069308, -9.474510206698971260, 61.66557627198103120 ) ) ;
#181630 = CARTESIAN_POINT ( 'NONE',  ( -14.34966873604960291, -8.224510206698953496, 71.66557627198100988 ) ) ;
#181632 = CARTESIAN_POINT ( 'NONE',  ( 16.46253265017160672, -9.564922557960803928, 78.33224293864769550 ) ) ;
#181633 = CARTESIAN_POINT ( 'NONE',  ( -16.51473224551082808, 9.474510206698731452, 73.33442372801900433 ) ) ;
#181634 = CARTESIAN_POINT ( 'NONE',  ( 15.80617190586746368, 15.72974639402197994, 69.37390960531436690 ) ) ;
#181635 = CARTESIAN_POINT ( 'NONE',  ( -14.29746914071049879, 8.314922557960819915, 115.8322429386477097 ) ) ;
#181636 = CARTESIAN_POINT ( 'NONE',  ( -19.03943276465977164, -0.05219959533935918106, 53.75109039468566863 ) ) ;
#181637 = CARTESIAN_POINT ( 'NONE',  ( -19.05341960407611168, -5.049401038298163336, 51.45724293864770260 ) ) ;
#181638 = CARTESIAN_POINT ( 'NONE',  ( -9.474510206698964154, 16.51473224551069663, 90.41557627198103830 ) ) ;
#181639 =( BOUNDED_SURFACE ( )  B_SPLINE_SURFACE ( 3, 2, ( 
 ( #81295, #141003, #12968, #66146, #172341, #2491, #110661, #28153, #142979, #125837, #33830, #18670, #141989, #4457, #65154, #140000, #126813, #1489, #173348, #188519, #127809, #49996, #89794, #151477, #121116, #111661, #44293, #105952, #63167, #192498, #174339, #144975, #36796, #145974, #7456, #116648, #9486, #101465, #52963, #178338, #193500, #21646, #176338, #68137, #190502, #38815, #53982, #35809, #114640, #115655, #84295, #51976, #39800, #20638, #98461, #147997, #177344, #97455, #113634, #100473, #129788, #130807, #163156, #112647, #162152, #82291, #23648, #160155, #175329, #71150, #159141, #85296, #8475, #83299, #146988, #6456, #37810, #143982, #5463, #131820, #24659, #191485, #161151, #99471, #70150, #86308, #22648, #189514, #69140, #54978, #67145, #50987, #128803, #152945, #88299, #119655, #120626, #73164, #149987, #14444, #89304, #181337, #197491, #42816, #164169, #166163, #182323, #132816, #25667, #136790, #183310, #44792, #117652, #179349, #104479, #167151, #118659, #74149, #11493, #180350, #12488, #28650, #27664, #150996, #106445, #133821, #135821, #58958, #194502, #43802, #105465, #56985, #55975, #168126, #90286, #151970, #165164, #29622, #134834, #196513, #13458, #75122, #41818, #72145, #40812, #103486, #198476, #59948, #57983, #91254, #195512, #26657, #121615, #102482, #87312, #148996, #10485, #30612, #96241, #171110, #153949, #94254, #49753, #47777, #64917, #34584, #141753, #126578, #187296, #125599, #78088, #139756, #173107, #63930, #170113, #156937, #18434, #17429, #45781, #95252, #172103, #108437, #188279, #48768, #110422, #111421, #253, #107433, #186297, #61922, #123592, #33589, #3243, #109430, #80084, #169105, #92265, #1243, #46778, #155934, #60935, #122609, #157929, #32601, #31607, #15445, #79086, #76107, #137783, #199468, #184299, #77103, #140759, #138772, #62922, #185286, #93257, #154942, #16439, #2247, #124602, #8235, #19419, #98212, #65904, #127577, #192262, #143742, #142745, #174104, #193263, #191255, #69913, #178098, #85058, #131579, #130565, #68905, #21404, #83062, #116409, #7220, #113399, #100234, #161916, #160917, #189278, #38578, #115418, #51737, #54737, #53744, #177107, #39568, #5221, #50754, #129555, #66902, #128565, #23410, #146740, #52730, #101226, #112412, #35573, #144736, #190260, #99230, #4225, #97221, #81067, #114396, #175089, #158907, #176097, #20398, #82047, #36557, #159915, #6223, #84061, #67902, #37567, #22410, #145739, #41585, #135588, #119421, #133579, #151741, #162915, #103249, #9248, #70915, #197260, #87074, #86072, #117412, #27422, #149751, #194271, #196282, #12256, #44560, #55738, #166921, #13234, #74897, #147762, #132583, #11254, #58722, #148759, #104242, #180117, #10248, #42579, #120391, #134596, #72927, #136560, #163936, #165925, #57751, #24423, #181105, #73918, #71907, #179110, #198241, #89067, #150758, #195269, #59713, #164931, #26424, #182085, #43568, #56753, #102248, #40578, #118424, #105233, #28422, #88064, #121385, #25433, #90059, #183077, #171871, #137550, #123359, #60698, #122374, #126353, #1010, #184063, #124366, #62684, #61690, #3015, #168871, #153713, #17197, #33360, #199233, #185052, #45546, #107201, #188050, #186061, #30376, #47544, #79859, #77860, #95019, #64692, #156708, #18201, #78851, #155702, #108200, #169881, #106215, #94021, #16, #187069, #48539, #109198, #75874, #125373, #2019, #138538, #141527, #140530, #63698, #167899, #92021, #15209, #16205, #76868, #46540, #110193, #29399, #139527, #91029, #31374, #93024, #154712, #170877, #32368, #152715, #14206, #83818, #159668, #4983, #3994, #5985, #161675, #6978, #68659, #192010, #53495, #114153, #189048, #36321, #98986, #158677, #128332, #22167, #67665, #20166, #38334, #49520, #190031, #96015, #157700, #145498, #173873, #172873, #65674, #175855, #97975, #80839, #82820, #160675, #131335, #142516, #115172, #99990, #23171, #34354, #19190, #21164, #130314, #35343, #191018 ),
 ( #96994, #111183, #84814, #129322, #52493, #81811, #146494, #51505, #113167, #144501, #176865, #143499, #50523, #127336, #66669, #37327, #7985, #112185, #69668, #174855, #177862, #148518, #40330, #149508, #11005, #120158, #13000, #104995, #56503, #181849, #197025, #25190, #179872, #71668, #194035, #42342, #57513, #39331, #118180, #119181, #87822, #55499, #43328, #24181, #102006, #151507, #180866, #100990, #117168, #104004, #133335, #134354, #166683, #116172, #165682, #85831, #27180, #163688, #178864, #74663, #162674, #88827, #12019, #86832, #150520, #10008, #41340, #147521, #9009, #135353, #28185, #195026, #164687, #103002, #196037, #89827, #26182, #193023, #72678, #73680, #70677, #58492, #132343, #54500, #91783, #123130, #124121, #76633, #153477, #156463, #92788, #184815, #17962, #198997, #107957, #186832, #170643, #1780, #198004, #31140, #136330, #90801, #60464, #122139, #108963, #59474, #106966, #137316, #121148, #139298, #63458, #14973, #78614, #169644, #32131, #183826, #182841, #16961, #48300, #61459, #105982, #44324, #62446, #46301, #77629, #167667, #109957, #138311, #199992, #154476, #776, #171636, #15969, #168641, #185820, #47307, #125134, #93789, #33126, #155469, #29164, #94782, #152484, #140288, #13971, #75638, #45317, #30140, #110944, #189797, #65435, #3758, #37088, #6741, #51268, #52256, #172629, #49286, #4743, #50288, #159427, #64452, #126122, #113914, #112929, #35103, #34117, #36088, #191772, #98747, #160440, #21930, #83581, #144262, #18955, #66432, #129081, #188805, #158444, #175612, #97739, #111945, #68421, #79618, #19932, #187817, #95775, #145260, #127096, #2776, #157462, #5749, #128093, #80600, #174623, #190782, #161439, #142277, #130073, #53254, #114932, #173633, #96754, #20923, #176625, #81574, #82581, #143259, #67425, #38100, #99755, #141286, #71434, #73445, #23934, #25948, #56259, #84577, #41103, #72436, #147275, #104761, #58260, #102767, #164454, #55259, #135118, #24947, #101762, #9770, #103770, #8765, #162433, #146257, #70434, #87591, #179633, #178621, #119929, #85588, #132100, #134113, #88587, #54265, #40083, #177627, #39095, #43093, #117943, #100751, #149277, #196792, #194787, #11781, #181614, #150286, #22931, #195801, #57274, #86594, #148277, #7741, #10772, #116928, #165449, #26946, #118948, #192782, #42108, #180633, #163449, #69427, #133098, #193791, #131094, #115937, #12764, #538, #76398, #121902, #120906, #122893, #78372, #123876, #185574, #108726, #170403, #30904, #105748, #153234, #15730, #75406, #45080, #139059, #184581, #137077, #155234, #166450, #106737, #74428, #136095, #62210, #90571, #89588, #182604, #92551, #14737, #197770, #199755, #77390, #48065, #59236, #31895, #16724, #140048, #151274, #44090, #138074, #47066, #152252, #107717, #183595, #13737, #46063, #93548, #61222, #169397, #1537, #167434, #154240, #63214, #27946, #124894, #186593, #198766, #28930, #60232, #168412, #29907, #91546, #21693, #111710, #188568, #96521, #190549, #33879, #49054, #171405, #157226, #51034, #66195, #65202, #6504, #172391, #18718, #20685, #175375, #141052, #126861, #64220, #125885, #129836, #4505, #187585, #127858, #83347, #81343, #98508, #68184, #36844, #160203, #82339, #159189, #173396, #34867, #191535, #97503, #3526, #52022, #113681, #112696, #79383, #128849, #5511, #142038, #145023, #144029, #67192, #109721, #95538, #2538, #19701, #80365, #50047, #32891, #94543, #143027, #156224, #110709, #158211, #189562, #17724, #174387, #35857, #14236, #121416, #106246, #166949, #105263, #57781, #119451, #152746, #43598, #149782, #136589, #198269, #197289, #22696, #74926, #151770, #88096, #167928, #28452, #90088, #91059, #180148, #84343, #165956, #41616, #103281, #13263, #183108, #27457, #59746, #148791, #10281, #181136, #26454, #135618, #37860, #99519, #44590, #89098, #11285, #71939, #12285, #29428, #75908, #137582, #53012, #114691, #120421, #195303, #42610, #176386, #164961, #134627 ),
 ( #161201, #133609, #72958, #104274, #196312, #56784, #118456, #182112, #150789, #73949, #58752, #94053, #61723, #49553, #30409, #108233, #157733, #125403, #184096, #123391, #187100, #77891, #140560, #126385, #122406, #63728, #92056, #48570, #169913, #185083, #19222, #45579, #110223, #18234, #31405, #171904, #46572, #186093, #153745, #107232, #141558, #172908, #93056, #170906, #154743, #2049, #96046, #1043, #111216, #62716, #16239, #168903, #139559, #15240, #80872, #124399, #47575, #33392, #109227, #199265, #155731, #32398, #60733, #17229, #78881, #34386, #95051, #64723, #76899, #156740, #138570, #48, #79888, #3047, #188082, #4026, #128364, #158707, #65704, #175889, #115205, #51536, #192046, #6019, #7010, #5018, #146526, #130347, #100023, #159701, #50555, #8017, #99018, #144533, #114185, #127370, #38368, #36354, #98006, #67698, #37360, #161710, #21198, #190060, #160709, #113199, #176897, #82854, #23206, #22200, #142548, #189082, #173905, #129356, #84849, #112215, #68692, #53527, #20196, #191051, #52524, #83849, #145531, #35374, #97026, #81842, #143530, #66700, #174888, #155394, #109877, #1703, #124039, #172557, #187743, #107877, #48223, #49214, #17888, #185738, #173559, #154398, #32055, #81500, #110872, #169565, #47227, #34043, #63379, #64379, #50215, #46224, #95700, #15893, #157388, #93712, #108886, #143187, #31062, #18881, #142201, #16884, #80527, #170565, #171561, #77551, #92710, #65362, #96683, #78535, #94706, #140209, #126047, #19860, #125056, #35028, #186753, #33051, #139223, #156383, #698, #4667, #79542, #141212, #3684, #2702, #184739, #127023, #188730, #111869, #123053, #158371, #62370, #78687, #81648, #174697, #111020, #126194, #93861, #47379, #143332, #113003, #110032, #172706, #125208, #142351, #36161, #141362, #189869, #2849, #171710, #62521, #156539, #32204, #159502, #94858, #187890, #127171, #79692, #18038, #20998, #95851, #49357, #139367, #1851, #34190, #51343, #173710, #4819, #848, #157535, #124194, #155539, #63533, #186904, #112021, #185894, #33200, #140364, #109034, #3831, #66507, #64527, #128169, #19029, #35178, #48375, #170713, #20005, #97813, #80675, #17033, #65510, #188881, #50362, #96833, #158517, #133172, #23008, #84654, #54339, #85665, #56335, #146331, #53329, #24009, #38176, #9845, #7820, #71504, #132176, #82653, #194862, #144337, #161516, #117003, #164527, #147352, #8840, #67501, #99832, #130151, #39167, #100825, #118017, #102841, #179706, #69504, #41178, #86666, #115008, #131170, #192860, #83658, #193867, #70508, #129158, #116010, #55333, #177700, #145336, #5825, #113989, #191848, #190855, #178698, #52332, #6818, #40160, #162508, #101836, #175687, #37162, #163523, #176702, #98821, #25022, #160515, #22006, #148349, #68496, #13814, #166526, #43169, #46138, #182680, #12840, #107791, #88666, #197847, #76474, #60306, #91624, #87664, #120982, #26020, #180708, #150362, #11858, #198842, #149349, #196868, #27021, #10846, #29007, #153312, #181688, #168487, #59313, #121981, #73523, #72515, #106813, #138151, #151351, #195877, #134190, #152328, #136172, #167511, #57350, #14813, #90646, #44165, #135194, #104836, #42184, #105824, #199832, #183672, #45157, #29985, #61299, #75480, #165525, #74506, #137153, #58334, #28023, #122969, #184656, #120002, #119025, #103844, #89665, #15804, #77465, #142111, #93623, #92624, #123950, #33953, #156297, #612, #2614, #18793, #51106, #62282, #173469, #19772, #81413, #154315, #139135, #17798, #3596, #155308, #110785, #186665, #16797, #49127, #65275, #141124, #79455, #143099, #170477, #172466, #64291, #30977, #187656, #80438, #78447, #169476, #4578, #95611, #157296, #1612, #126934, #111781, #188642, #125958, #50121, #140121, #108798, #185648, #63288, #34942, #96594, #124968, #66271, #31967, #48135, #127930, #94618, #47140, #189632, #158283, #109792, #171475, #32964, #39926, #99593, #21767, #55098, #115776, #86432, #53087, #83418 ),
 ( #177465, #97574, #68257, #160276, #69263, #130929, #101595, #132939, #24784, #176459, #163283, #116768, #145095, #161273, #191608, #113753, #162273, #38934, #159262, #37932, #100591, #7577, #175449, #148118, #144102, #6578, #71274, #23773, #20758, #36919, #85423, #114765, #54102, #9609, #35928, #147114, #5582, #8601, #129908, #98582, #194627, #82413, #70274, #52096, #178459, #112766, #84416, #22768, #67262, #128920, #174459, #190621, #146093, #192620, #131942, #193626, #153066, #58103, #106569, #119773, #26781, #179472, #73286, #149119, #76226, #11618, #42935, #43921, #196634, #134956, #137906, #12606, #104599, #56097, #118786, #27783, #168246, #90406, #121736, #117778, #151114, #40937, #10610, #180475, #41946, #28768, #102609, #88423, #57112, #164295, #59075, #183428, #181457, #198600, #89425, #152091, #103612, #25788, #136913, #165288, #195639, #87434, #150117, #197610, #74270, #166287, #14568, #135940, #120742, #167269, #44913, #72271, #182441, #133948, #105583, #13575, #75242, #60068, #29742, #91377, #171230, #188394, #158043, #65034, #49872, #110539, #48884, #1363, #63042, #96355, #187416, #93376, #80197, #141868, #140877, #169229, #18549, #95367, #31728, #111537, #172220, #33705, #34698, #123708, #30736, #109549, #185405, #46896, #157052, #126690, #32719, #3359, #92383, #154070, #124721, #170234, #79208, #173222, #2367, #156051, #108556, #155062, #15564, #17548, #19533, #81178, #199588, #61055, #122727, #64047, #138891, #186419, #184418, #16557, #78204, #45898, #125717, #139874, #107551, #77222, #47895, #371, #62043, #94371, #67022, #66024, #97336, #7333, #129668, #174220, #176213, #192377, #24538, #35689, #146861, #193378, #54854, #127691, #189391, #191365, #177222, #128681, #84171, #160031, #190378, #22524, #38695, #114512, #52842, #116528, #143859, #145851, #37682, #4339, #161030, #53860, #51853, #142860, #178216, #69018, #130683, #175207, #115534, #85172, #100351, #99347, #23526, #21518, #159022, #20515, #163031, #162030, #82163, #8353, #39680, #70028, #131697, #101342, #50868, #112526, #5338, #113513, #144853, #6336, #36672, #98332, #83179, #68016, #31236, #30238, #55852, #108057, #184914, #121246, #139392, #76730, #138405, #124225, #10364, #117526, #199092, #72021, #133694, #46398, #16068, #60559, #61554, #179224, #40690, #14068, #59571, #168734, #77726, #91881, #45410, #198105, #44423, #102360, #107063, #874, #169741, #92885, #154572, #62549, #153572, #25548, #75735, #200086, #182940, #167763, #123223, #15069, #106076, #185921, #86188, #29261, #132696, #194385, #47406, #90892, #9364, #164049, #109062, #137411, #87192, #122234, #170740, #147878, #148873, #71029, #152578, #183925, #17060, #78715, #80703, #66535, #18066, #173738, #49386, #79721, #112050, #128199, #3859, #142381, #82681, #33227, #35207, #65538, #93888, #50390, #81676, #156571, #114016, #67528, #96860, #158544, #64557, #20034, #174724, #143359, #19056, #113032, #141390, #171739, #155566, #2878, #4851, #188912, #187917, #129185, #94887, #126221, #189896, #97841, #63560, #144365, #140391, #111049, #51371, #32230, #36187, #159529, #1879, #172737, #34217, #21028, #5852, #190883, #52359, #125234, #95880, #186932, #48402, #157563, #127198, #110059, #176729, #25049, #40186, #160544, #100851, #101866, #70534, #38202, #26044, #6845, #84680, #134217, #163549, #22033, #99858, #86692, #54365, #117029, #102866, #98849, #148376, #68524, #9871, #146359, #161542, #195903, #83685, #71531, #115036, #118045, #10870, #147378, #162533, #130178, #145363, #179735, #149374, #7846, #8867, #23035, #178724, #72540, #177726, #87689, #39195, #69533, #191875, #192887, #53359, #57378, #131197, #24037, #133197, #116037, #85692, #175713, #132203, #193894, #37192, #55359, #194888, #56362, #41205, #164551, #180733, #13840, #642, #73548, #43194, #104862, #91652, #42209, #89691, #120027, #103869, #122009, #184685, #74532, #61328, #90673, #14842 ),
 ( #183700, #75507, #28050, #136197, #135221, #137180, #31005, #76505, #138181, #122999, #46168, #45187, #58360, #105851, #92654, #165550, #197872, #153341, #119051, #106841, #168516, #27047, #59339, #166551, #198868, #60335, #107822, #139165, #154343, #182707, #169506, #15836, #151376, #167538, #121009, #181712, #30014, #199863, #88693, #44192, #77495, #150389, #12867, #11885, #196893, #29033, #152355, #188675, #47170, #125002, #50155, #141158, #3628, #189666, #185680, #126966, #155341, #111814, #32997, #48168, #82447, #108829, #173502, #1646, #4611, #97607, #33987, #49159, #16830, #170508, #66303, #35960, #94651, #95643, #109825, #65307, #159295, #64324, #112800, #125991, #156331, #31999, #79489, #78481, #144135, #17831, #110817, #34975, #2647, #187689, #62312, #18826, #172500, #123982, #186697, #157331, #174493, #96628, #127963, #93656, #80471, #140154, #63324, #171508, #142144, #158316, #19804, #81445, #143131, #51139, #20792, #71311, #161310, #148153, #177501, #101632, #53123, #25824, #86468, #117815, #130964, #175483, #87469, #131977, #115811, #147148, #128955, #132974, #192654, #114801, #9645, #8636, #179508, #146128, #176494, #70308, #22804, #194664, #54137, #56133, #55133, #5617, #84450, #67296, #162308, #38970, #190655, #68293, #100626, #40976, #39961, #102645, #52131, #23808, #113788, #160311, #129944, #191643, #178495, #36955, #37970, #6614, #98617, #193662, #164330, #7613, #21801, #85459, #163322, #99628, #83453, #145131, #69298, #116803, #24819, #169267, #75280, #59112, #90445, #72307, #76263, #135975, #58140, #91416, #152130, #122765, #89462, #119808, #13612, #104634, #137941, #74308, #199625, #198639, #149156, #61092, #10646, #27820, #183466, #30773, #136950, #60105, #133985, #166323, #196671, #105621, #167309, #184454, #195676, #45934, #12641, #107589, #153103, #181493, #197646, #151150, #150154, #121773, #44952, #57147, #120777, #106608, #43959, #11655, #118824, #180509, #42971, #41982, #168283, #103648, #73321, #29780, #182478, #14607, #165326, #26818, #88458, #134992, #28805, #63081, #78240, #112562, #15600, #80232, #31763, #34733, #127727, #64082, #79246, #46933, #407, #96391, #66060, #124760, #125752, #139911, #95403, #189429, #94408, #142894, #156089, #186456, #77258, #109586, #185443, #174257, #47932, #140917, #141903, #32757, #171269, #158078, #187452, #188430, #1401, #92420, #173258, #4376, #17586, #62079, #154106, #18585, #2404, #33743, #138927, #19569, #48920, #110574, #81213, #157089, #50904, #172255, #3394, #65069, #126726, #123744, #49908, #108592, #111574, #170269, #93412, #155098, #16592, #70065, #117561, #38730, #100388, #20552, #191402, #83215, #192414, #53896, #163068, #55888, #147912, #99383, #24573, #39714, #68052, #22561, #114551, #36708, #85210, #162066, #82202, #161066, #23562, #130722, #98370, #86222, #67059, #144890, #194418, #146900, #143894, #160068, #8390, #176250, #177258, #9398, #159058, #131733, #128717, #193415, #6372, #21555, #35725, #5375, #54890, #175243, #178253, #71064, #7370, #84207, #190414, #51890, #101377, #132730, #129706, #69055, #52879, #116564, #97372, #37721, #113549, #145887, #115571, #102395, #196426, #72055, #199382, #134744, #166073, #167063, #119568, #57896, #60846, #135734, #27576, #179261, #41733, #150907, #29540, #13374, #44705, #40726, #74063, #164083, #133729, #103397, #165075, #151884, #25582, #149896, #180263, #87226, #182230, #106359, #89214, #181251, #26569, #28564, #43715, #148908, #104390, #105376, #197405, #88212, #91173, #10398, #11403, #137697, #90201, #195422, #73072, #75038, #42728, #120537, #168043, #56899, #136704, #118573, #198385, #12401, #58871, #59862, #121529, #183224, #152862, #14357, #76022, #94167, #109342, #77013, #30522, #64836, #96159, #93171, #155846, #108349, #125516, #19340, #124516, #173022, #186211, #154856, #45693, #139669, #15357, #142662, #78002, #171024, #110336, #62832, #1157, #4141, #78999 ),
 ( #95165, #107344, #16354, #123504, #169017, #187213, #188196, #47692, #126498, #17343, #18348, #170028, #122521, #3163, #34501, #32515, #92174, #184211, #48684, #140673, #63844, #153859, #49668, #2165, #31518, #111332, #172017, #157848, #33506, #156853, #80003, #141672, #80987, #138685, #166, #61834, #185197, #46688, #127489, #144654, #100147, #147672, #68816, #130475, #50669, #21320, #113315, #22322, #83972, #193174, #85983, #178010, #129474, #54647, #69820, #98128, #53653, #159825, #146649, #8143, #7133, #35490, #84967, #161828, #82978, #116321, #115330, #177021, #101138, #190176, #97140, #176013, #51651, #175007, #23323, #39477, #37482, #38491, #158823, #20311, #191173, #36471, #145652, #162824, #192172, #131487, #6137, #67819, #81959, #24333, #65820, #189194, #112329, #174019, #143651, #5135, #66817, #52647, #128480, #114311, #99144, #160833, #165836, #180027, #198153, #9160, #87976, #55649, #117321, #181997, #133488, #132495, #163843, #73832, #196192, #40485, #42491, #58638, #90941, #102157, #13148, #59623, #121297, #194184, #179017, #57664, #43480, #195180, #150669, #26336, #56661, #88979, #105147, #181017, #119331, #182989, #10160, #12167, #104155, #70827, #27333, #120304, #118334, #25344, #44473, #135503, #197173, #41496, #166833, #151654, #28334, #89973, #74811, #103160, #148672, #86985, #164840, #136473, #106128, #149664, #167812, #71820, #11162, #29311, #72836, #134506, #169790, #107113, #168784, #172786, #47454, #30286, #170789, #126268, #124274, #141439, #111096, #18114, #2926, #63608, #1929, #154622, #16116, #49435, #79769, #108106, #94934, #185970, #48452, #200133, #34267, #33275, #64605, #77773, #122284, #152628, #78762, #62596, #93936, #75785, #187965, #139440, #61602, #156619, #155615, #14118, #92934, #123271, #17111, #31283, #137463, #922, #199143, #125284, #60609, #183973, #45459, #109110, #186981, #91931, #140439, #110109, #153623, #32281, #184962, #171787, #15119, #76781, #138452, #46446, #162335, #87494, #102670, #130991, #85485, #177528, #99655, #148179, #163349, #80752, #23836, #24845, #193691, #161339, #149183, #127248, #7641, #57174, #86494, #142429, #22831, #9672, #38997, #39987, #25851, #19102, #71337, #188961, #132999, #69325, #84478, #118851, #3908, #194690, #38000, #41003, #134010, #70336, #147174, #53151, #65588, #164355, #72335, #192683, #132003, #146155, #101658, #195702, #100653, #10671, #8663, #54166, #114830, #115839, #176524, #180534, #55159, #116829, #56160, #178520, #117842, #95926, #179534, #157611, #123772, #104665, #13638, #92448, #76292, #107615, #103673, #136976, #42008, #196696, #166350, #27848, #14633, #165351, #12668, #42998, #26845, #44977, #106637, #88486, #197672, #89489, #198665, #60132, #169293, #62109, #154136, #105646, #30799, #45961, #74335, #28832, #120805, #151180, #91442, #168310, #150181, #167335, #29806, #121800, #136001, #15628, #73348, #59137, #434, #153130, #11682, #182505, #137970, #43985, #183493, #77285, #135021, #199652, #58167, #61118, #90473, #152155, #119834, #181519, #122792, #75305, #184482, #138955, #157117, #172283, #139941, #93440, #127754, #159085, #156117, #18613, #171298, #188458, #82232, #187481, #35753, #48948, #17616, #108620, #2433, #78268, #5403, #140945, #33773, #173289, #125779, #64114, #67087, #141930, #95433, #185471, #47962, #80260, #97398, #19598, #50933, #46961, #3421, #170298, #1431, #109614, #32784, #158106, #31791, #79275, #186486, #155127, #49939, #112591, #110601, #189455, #65097, #81240, #94436, #16620, #66088, #20580, #126755, #63109, #124787, #111604, #34763, #96420, #142921, #174283, #4403, #143922, #71092, #131763, #102426, #69084, #99413, #70094, #84238, #55917, #53925, #117591, #178282, #128746, #40757, #190443, #7400, #163101, #10430, #193445, #164113, #113577, #175271, #177289, #24604, #114583, #54921, #145917, #176280, #8422, #86251, #100417, #38759, #179293, #129733, #116593, #162098 ),
 ( #83242, #36737, #132759, #25611, #161095, #23594, #37752, #39745, #87255, #130751, #148940, #192443, #22590, #51918, #115600, #21584, #98401, #85241, #146932, #101408, #147941, #9427, #160097, #194446, #144918, #6400, #191430, #68081, #52907, #89248, #74096, #72088, #181283, #133762, #41764, #26601, #88244, #150940, #56932, #149929, #165108, #118606, #166106, #197437, #73107, #135766, #42760, #12434, #11436, #195457, #120569, #180296, #27608, #134777, #103429, #196459, #182263, #57929, #104423, #119600, #58903, #161749, #195098, #55570, #26254, #193094, #23244, #194107, #8061, #179945, #177934, #41412, #102077, #52564, #164759, #114224, #131407, #86905, #134426, #117244, #178936, #37400, #69738, #100064, #9077, #70747, #103078, #72755, #87895, #116242, #149581, #56580, #84888, #39401, #54570, #53567, #163762, #40406, #11079, #101061, #175929, #25262, #99059, #160747, #22239, #162746, #148588, #83888, #10080, #71738, #145571, #24254, #146567, #132415, #133409, #7048, #68730, #130388, #85904, #192085, #118254, #147592, #115245, #176937, #38407, #45384, #60532, #180936, #121220, #122208, #90866, #58562, #46370, #27250, #105069, #154546, #183899, #42411, #120228, #107037, #74735, #137384, #123198, #119252, #168709, #88900, #30211, #166754, #181918, #16041, #104074, #91854, #135424, #138380, #31208, #167735, #182910, #150590, #165756, #200061, #169715, #28257, #29233, #43399, #199063, #92859, #198075, #108029, #59542, #89896, #12089, #13068, #73752, #77700, #151579, #44395, #153546, #136398, #106049, #196112, #152551, #14039, #57582, #75705, #15043, #197095, #76704, #61529, #184888, #26681, #195534, #167173, #29645, #28672, #57008, #106469, #183332, #119676, #137807, #75144, #136815, #122631, #11517, #118681, #197512, #73187, #134858, #44814, #14467, #58980, #59970, #180373, #41843, #12509, #58006, #90307, #76129, #151993, #43823, #196536, #42838, #103510, #105487, #199491, #168148, #91277, #74173, #181359, #152968, #13479, #60957, #27685, #104503, #198499, #166184, #184321, #135843, #45802, #121637, #87333, #107454, #149019, #89326, #169129, #10507, #72169, #133844, #165186, #151018, #120647, #88321, #150011, #182345, #50773, #142764, #94274, #19438, #34602, #62941, #17449, #109448, #31627, #80103, #95272, #15468, #155952, #156955, #125619, #93277, #81086, #61944, #139776, #189296, #18452, #77125, #154962, #141771, #171131, #172123, #157947, #153971, #3264, #123611, #64937, #1264, #16458, #112433, #138794, #126596, #170133, #173127, #65924, #2267, #79105, #185306, #275, #96261, #4244, #124621, #63950, #78107, #33609, #127597, #32620, #30634, #140778, #186316, #46797, #47798, #108456, #92287, #187317, #48788, #188298, #110442, #49775, #111440, #130585, #160935, #55756, #36575, #145756, #24441, #8253, #39586, #84077, #177126, #147781, #192280, #98230, #159933, #146759, #97239, #144756, #175106, #158927, #38597, #101245, #129573, #116430, #7238, #69933, #21420, #194290, #54756, #86090, #99248, #143759, #174122, #100253, #68923, #115435, #20416, #162934, #22427, #9267, #23429, #35593, #70933, #82066, #52745, #131597, #5240, #161934, #85076, #66920, #191270, #83080, #53761, #193282, #132600, #128584, #190278, #37586, #51754, #178118, #6241, #113415, #114414, #67920, #176115, #182101, #102267, #42597, #43586, #12272, #180134, #167917, #148778, #26441, #75895, #105252, #163955, #41603, #166938, #196298, #58740, #44578, #40596, #28441, #10267, #90076, #88083, #103268, #137570, #25453, #151759, #56769, #59734, #152735, #89085, #104260, #71926, #87093, #121403, #91048, #149769, #150777, #164948, #120409, #14225, #119438, #29417, #181123, #11271, #133596, #134614, #195288, #199253, #72944, #165943, #13252, #57768, #27443, #117430, #73937, #135606, #179128, #197277, #74915, #118441, #136578, #183097, #198258, #106234, #34375, #78869, #185071, #46559, #33380, #184083, #31394, #61709, #45567, #63717, #126374, #16227 ) ),
 .UNSPECIFIED., .T., .F., .F. ) 
 B_SPLINE_SURFACE_WITH_KNOTS ( ( 4, 3, 4 ),
 ( 3, 2, 2, 2, 2, 2, 2, 2, 2, 2, 2, 2, 2, 2, 2, 2, 2, 2, 2, 2, 2, 2, 2, 2, 2, 2, 2, 2, 2, 2, 2, 2, 2, 2, 2, 2, 2, 2, 2, 2, 2, 2, 2, 2, 2, 2, 2, 2, 2, 2, 2, 2, 2, 2, 2, 2, 2, 2, 2, 2, 2, 2, 2, 2, 2, 2, 2, 2, 2, 2, 2, 2, 2, 2, 2, 2, 2, 2, 2, 2, 2, 2, 2, 2, 2, 2, 2, 2, 2, 2, 2, 2, 2, 2, 2, 2, 2, 2, 2, 2, 2, 2, 2, 2, 2, 2, 2, 2, 2, 2, 2, 2, 2, 2, 2, 2, 2, 2, 2, 2, 2, 2, 2, 2, 2, 2, 2, 2, 2, 2, 2, 2, 2, 2, 2, 2, 2, 2, 2, 2, 2, 2, 2, 2, 2, 2, 2, 2, 2, 2, 2, 2, 2, 2, 2, 2, 2, 2, 2, 2, 2, 2, 2, 2, 2, 2, 2, 2, 2, 2, 2, 2, 2, 2, 2, 2, 2, 2, 2, 2, 2, 2, 2, 2, 2, 2, 2, 2, 2, 2, 2, 2, 2, 2, 2, 2, 2, 2, 2, 2, 2, 2, 2, 2, 2, 2, 2, 2, 2, 2, 2, 2, 2, 2, 2, 2, 2, 2, 2, 2, 2, 2, 2, 2, 2, 2, 2, 2, 3 ),
 ( 0.000000000000000000, 0.5000000000000000000, 1.000000000000000000 ),
 ( 0.000000000000000000, 0.004385964912280701511, 0.008771929824561403022, 0.01315789473684210453, 0.01754385964912280604, 0.02192982456140350755, 0.02631578947368420907, 0.03070175438596491058, 0.03508771929824561209, 0.03947368421052631360, 0.04385964912280701511, 0.04824561403508771662, 0.05263157894736841813, 0.05701754385964911964, 0.06140350877192982115, 0.06578947368421052266, 0.07017543859649122417, 0.07456140350877192569, 0.07894736842105262720, 0.08333333333333332871, 0.08771929824561403022, 0.09210526315789473173, 0.09649122807017543324, 0.1008771929824561348, 0.1052631578947368363, 0.1096491228070175378, 0.1140350877192982393, 0.1184210526315789408, 0.1228070175438596423, 0.1271929824561403577, 0.1315789473684210453, 0.1359649122807017607, 0.1403508771929824483, 0.1447368421052631637, 0.1491228070175438514, 0.1535087719298245668, 0.1578947368421052544, 0.1622807017543859698, 0.1666666666666666574, 0.1710526315789473728, 0.1754385964912280604, 0.1798245614035087758, 0.1842105263157894635, 0.1885964912280701788, 0.1929824561403508665, 0.1973684210526315819, 0.2017543859649122695, 0.2061403508771929849, 0.2105263157894736725, 0.2149122807017543879, 0.2192982456140350755, 0.2236842105263157909, 0.2280701754385964786, 0.2324561403508771940, 0.2368421052631578816, 0.2412280701754385970, 0.2456140350877192846, 0.2500000000000000000, 0.2543859649122807154, 0.2587719298245614308, 0.2631578947368420907, 0.2675438596491228060, 0.2719298245614035214, 0.2763157894736842368, 0.2807017543859648967, 0.2850877192982456121, 0.2894736842105263275, 0.2938596491228070429, 0.2982456140350877027, 0.3026315789473684181, 0.3070175438596491335, 0.3114035087719298489, 0.3157894736842105088, 0.3201754385964912242, 0.3245614035087719396, 0.3289473684210526550, 0.3333333333333333148, 0.3377192982456140302, 0.3421052631578947456, 0.3464912280701754610, 0.3508771929824561209, 0.3552631578947368363, 0.3596491228070175517, 0.3640350877192982670, 0.3684210526315789269, 0.3728070175438596423, 0.3771929824561403577, 0.3815789473684210731, 0.3859649122807017330, 0.3903508771929824483, 0.3947368421052631637, 0.3991228070175438791, 0.4035087719298245390, 0.4078947368421052544, 0.4122807017543859698, 0.4166666666666666852, 0.4210526315789473450, 0.4254385964912280604, 0.4298245614035087758, 0.4342105263157894912, 0.4385964912280701511, 0.4429824561403508665, 0.4473684210526315819, 0.4517543859649122973, 0.4561403508771929571, 0.4605263157894736725, 0.4649122807017543879, 0.4692982456140351033, 0.4736842105263157632, 0.4780701754385964786, 0.4824561403508771940, 0.4868421052631579093, 0.4912280701754385692, 0.4956140350877192846, 0.5000000000000000000, 0.5043859649122807154, 0.5087719298245614308, 0.5131578947368421462, 0.5175438596491228616, 0.5219298245614034659, 0.5263157894736841813, 0.5307017543859648967, 0.5350877192982456121, 0.5394736842105263275, 0.5438596491228070429, 0.5482456140350877583, 0.5526315789473684736, 0.5570175438596490780, 0.5614035087719297934, 0.5657894736842105088, 0.5701754385964912242, 0.5745614035087719396, 0.5789473684210526550, 0.5833333333333333703, 0.5877192982456140857, 0.5921052631578946901, 0.5964912280701754055, 0.6008771929824561209, 0.6052631578947368363, 0.6096491228070175517, 0.6140350877192982670, 0.6184210526315789824, 0.6228070175438596978, 0.6271929824561403022, 0.6315789473684210176, 0.6359649122807017330, 0.6403508771929824483, 0.6447368421052631637, 0.6491228070175438791, 0.6535087719298245945, 0.6578947368421053099, 0.6622807017543859143, 0.6666666666666666297, 0.6710526315789473450, 0.6754385964912280604, 0.6798245614035087758, 0.6842105263157894912, 0.6885964912280702066, 0.6929824561403509220, 0.6973684210526315264, 0.7017543859649122417, 0.7061403508771929571, 0.7105263157894736725, 0.7149122807017543879, 0.7192982456140351033, 0.7236842105263158187, 0.7280701754385965341, 0.7324561403508771384, 0.7368421052631578538, 0.7412280701754385692, 0.7456140350877192846, 0.7500000000000000000, 0.7543859649122807154, 0.7587719298245614308, 0.7631578947368421462, 0.7675438596491228616, 0.7719298245614034659, 0.7763157894736841813, 0.7807017543859648967, 0.7850877192982456121, 0.7894736842105263275, 0.7938596491228070429, 0.7982456140350877583, 0.8026315789473684736, 0.8070175438596490780, 0.8114035087719297934, 0.8157894736842105088, 0.8201754385964912242, 0.8245614035087719396, 0.8289473684210526550, 0.8333333333333333703, 0.8377192982456140857, 0.8421052631578946901, 0.8464912280701754055, 0.8508771929824561209, 0.8552631578947368363, 0.8596491228070175517, 0.8640350877192982670, 0.8684210526315789824, 0.8728070175438596978, 0.8771929824561403022, 0.8815789473684210176, 0.8859649122807017330, 0.8903508771929824483, 0.8947368421052631637, 0.8991228070175438791, 0.9035087719298245945, 0.9078947368421053099, 0.9122807017543859143, 0.9166666666666666297, 0.9210526315789473450, 0.9254385964912280604, 0.9298245614035087758, 0.9342105263157894912, 0.9385964912280702066, 0.9429824561403509220, 0.9473684210526315264, 0.9517543859649122417, 0.9561403508771929571, 0.9605263157894736725, 0.9649122807017543879, 0.9692982456140351033, 0.9736842105263158187, 0.9780701754385965341, 0.9824561403508771384, 0.9868421052631578538, 0.9912280701754385692, 0.9956140350877192846, 1.000000000000000000 ),
 .UNSPECIFIED. ) 
 GEOMETRIC_REPRESENTATION_ITEM ( )  RATIONAL_B_SPLINE_SURFACE ( (
 ( 1.000000000000000000, 0.9659258262890683122, 1.000000000000000000, 0.9659258262890683122, 1.000000000000000000, 0.9659258262890683122, 1.000000000000000000, 0.9659258262890683122, 1.000000000000000000, 0.9659258262890683122, 1.000000000000000000, 0.9659258262890683122, 1.000000000000000000, 0.9659258262890683122, 1.000000000000000000, 0.9659258262890683122, 1.000000000000000000, 0.9659258262890683122, 1.000000000000000000, 0.9659258262890683122, 1.000000000000000000, 0.9659258262890683122, 1.000000000000000000, 0.9659258262890683122, 1.000000000000000000, 0.9659258262890683122, 1.000000000000000000, 0.9659258262890683122, 1.000000000000000000, 0.9659258262890683122, 1.000000000000000000, 0.9659258262890683122, 1.000000000000000000, 0.9659258262890683122, 1.000000000000000000, 0.9659258262890683122, 1.000000000000000000, 0.9659258262890683122, 1.000000000000000000, 0.9659258262890683122, 1.000000000000000000, 0.9659258262890683122, 1.000000000000000000, 0.9659258262890683122, 1.000000000000000000, 0.9659258262890683122, 1.000000000000000000, 0.9659258262890683122, 1.000000000000000000, 0.9659258262890683122, 1.000000000000000000, 0.9659258262890683122, 1.000000000000000000, 0.9659258262890683122, 1.000000000000000000, 0.9659258262890683122, 1.000000000000000000, 0.9659258262890683122, 1.000000000000000000, 0.9659258262890683122, 1.000000000000000000, 0.9659258262890683122, 1.000000000000000000, 0.9659258262890683122, 1.000000000000000000, 0.9659258262890683122, 1.000000000000000000, 0.9659258262890683122, 1.000000000000000000, 0.9659258262890683122, 1.000000000000000000, 0.9659258262890683122, 1.000000000000000000, 0.9659258262890683122, 1.000000000000000000, 0.9659258262890683122, 1.000000000000000000, 0.9659258262890683122, 1.000000000000000000, 0.9659258262890683122, 1.000000000000000000, 0.9659258262890683122, 1.000000000000000000, 0.9659258262890683122, 1.000000000000000000, 0.9659258262890683122, 1.000000000000000000, 0.9659258262890683122, 1.000000000000000000, 0.9659258262890683122, 1.000000000000000000, 0.9659258262890683122, 1.000000000000000000, 0.9659258262890683122, 1.000000000000000000, 0.9659258262890683122, 1.000000000000000000, 0.9659258262890683122, 1.000000000000000000, 0.9659258262890683122, 1.000000000000000000, 0.9659258262890683122, 1.000000000000000000, 0.9659258262890683122, 1.000000000000000000, 0.9659258262890683122, 1.000000000000000000, 0.9659258262890683122, 1.000000000000000000, 0.9659258262890683122, 1.000000000000000000, 0.9659258262890683122, 1.000000000000000000, 0.9659258262890683122, 1.000000000000000000, 0.9659258262890683122, 1.000000000000000000, 0.9659258262890683122, 1.000000000000000000, 0.9659258262890683122, 1.000000000000000000, 0.9659258262890683122, 1.000000000000000000, 0.9659258262890683122, 1.000000000000000000, 0.9659258262890683122, 1.000000000000000000, 0.9659258262890683122, 1.000000000000000000, 0.9659258262890683122, 1.000000000000000000, 0.9659258262890683122, 1.000000000000000000, 0.9659258262890683122, 1.000000000000000000, 0.9659258262890683122, 1.000000000000000000, 0.9659258262890683122, 1.000000000000000000, 0.9659258262890683122, 1.000000000000000000, 0.9659258262890683122, 1.000000000000000000, 0.9659258262890683122, 1.000000000000000000, 0.9659258262890683122, 1.000000000000000000, 0.9659258262890683122, 1.000000000000000000, 0.9659258262890683122, 1.000000000000000000, 0.9659258262890683122, 1.000000000000000000, 0.9659258262890683122, 1.000000000000000000, 0.9659258262890683122, 1.000000000000000000, 0.9659258262890683122, 1.000000000000000000, 0.9659258262890683122, 1.000000000000000000, 0.9659258262890683122, 1.000000000000000000, 0.9659258262890683122, 1.000000000000000000, 0.9659258262890683122, 1.000000000000000000, 0.9659258262890683122, 1.000000000000000000, 0.9659258262890683122, 1.000000000000000000, 0.9659258262890683122, 1.000000000000000000, 0.9659258262890683122, 1.000000000000000000, 0.9659258262890683122, 1.000000000000000000, 0.9659258262890683122, 1.000000000000000000, 0.9659258262890683122, 1.000000000000000000, 0.9659258262890683122, 1.000000000000000000, 0.9659258262890683122, 1.000000000000000000, 0.9659258262890683122, 1.000000000000000000, 0.9659258262890683122, 1.000000000000000000, 0.9659258262890683122, 1.000000000000000000, 0.9659258262890683122, 1.000000000000000000, 0.9659258262890683122, 1.000000000000000000, 0.9659258262890683122, 1.000000000000000000, 0.9659258262890683122, 1.000000000000000000, 0.9659258262890683122, 1.000000000000000000, 0.9659258262890683122, 1.000000000000000000, 0.9659258262890683122, 1.000000000000000000, 0.9659258262890683122, 1.000000000000000000, 0.9659258262890683122, 1.000000000000000000, 0.9659258262890683122, 1.000000000000000000, 0.9659258262890683122, 1.000000000000000000, 0.9659258262890683122, 1.000000000000000000, 0.9659258262890683122, 1.000000000000000000, 0.9659258262890683122, 1.000000000000000000, 0.9659258262890683122, 1.000000000000000000, 0.9659258262890683122, 1.000000000000000000, 0.9659258262890683122, 1.000000000000000000, 0.9659258262890683122, 1.000000000000000000, 0.9659258262890683122, 1.000000000000000000, 0.9659258262890683122, 1.000000000000000000, 0.9659258262890683122, 1.000000000000000000, 0.9659258262890683122, 1.000000000000000000, 0.9659258262890683122, 1.000000000000000000, 0.9659258262890683122, 1.000000000000000000, 0.9659258262890683122, 1.000000000000000000, 0.9659258262890683122, 1.000000000000000000, 0.9659258262890683122, 1.000000000000000000, 0.9659258262890683122, 1.000000000000000000, 0.9659258262890683122, 1.000000000000000000, 0.9659258262890683122, 1.000000000000000000, 0.9659258262890683122, 1.000000000000000000, 0.9659258262890683122, 1.000000000000000000, 0.9659258262890683122, 1.000000000000000000, 0.9659258262890683122, 1.000000000000000000, 0.9659258262890683122, 1.000000000000000000, 0.9659258262890683122, 1.000000000000000000, 0.9659258262890683122, 1.000000000000000000, 0.9659258262890683122, 1.000000000000000000, 0.9659258262890683122, 1.000000000000000000, 0.9659258262890683122, 1.000000000000000000, 0.9659258262890683122, 1.000000000000000000, 0.9659258262890683122, 1.000000000000000000, 0.9659258262890683122, 1.000000000000000000, 0.9659258262890683122, 1.000000000000000000, 0.9659258262890683122, 1.000000000000000000, 0.9659258262890683122, 1.000000000000000000, 0.9659258262890683122, 1.000000000000000000, 0.9659258262890683122, 1.000000000000000000, 0.9659258262890683122, 1.000000000000000000, 0.9659258262890683122, 1.000000000000000000, 0.9659258262890683122, 1.000000000000000000, 0.9659258262890683122, 1.000000000000000000, 0.9659258262890683122, 1.000000000000000000, 0.9659258262890683122, 1.000000000000000000, 0.9659258262890683122, 1.000000000000000000, 0.9659258262890683122, 1.000000000000000000, 0.9659258262890683122, 1.000000000000000000, 0.9659258262890683122, 1.000000000000000000, 0.9659258262890683122, 1.000000000000000000, 0.9659258262890683122, 1.000000000000000000, 0.9659258262890683122, 1.000000000000000000, 0.9659258262890683122, 1.000000000000000000, 0.9659258262890683122, 1.000000000000000000, 0.9659258262890683122, 1.000000000000000000, 0.9659258262890683122, 1.000000000000000000, 0.9659258262890683122, 1.000000000000000000, 0.9659258262890683122, 1.000000000000000000, 0.9659258262890683122, 1.000000000000000000, 0.9659258262890683122, 1.000000000000000000, 0.9659258262890683122, 1.000000000000000000, 0.9659258262890683122, 1.000000000000000000, 0.9659258262890683122, 1.000000000000000000, 0.9659258262890683122, 1.000000000000000000, 0.9659258262890683122, 1.000000000000000000, 0.9659258262890683122, 1.000000000000000000, 0.9659258262890683122, 1.000000000000000000, 0.9659258262890683122, 1.000000000000000000, 0.9659258262890683122, 1.000000000000000000, 0.9659258262890683122, 1.000000000000000000, 0.9659258262890683122, 1.000000000000000000, 0.9659258262890683122, 1.000000000000000000, 0.9659258262890683122, 1.000000000000000000, 0.9659258262890683122, 1.000000000000000000, 0.9659258262890683122, 1.000000000000000000, 0.9659258262890683122, 1.000000000000000000, 0.9659258262890683122, 1.000000000000000000, 0.9659258262890683122, 1.000000000000000000, 0.9659258262890683122, 1.000000000000000000, 0.9659258262890683122, 1.000000000000000000, 0.9659258262890683122, 1.000000000000000000, 0.9659258262890683122, 1.000000000000000000, 0.9659258262890683122, 1.000000000000000000, 0.9659258262890683122, 1.000000000000000000, 0.9659258262890683122, 1.000000000000000000, 0.9659258262890683122, 1.000000000000000000, 0.9659258262890683122, 1.000000000000000000, 0.9659258262890683122, 1.000000000000000000, 0.9659258262890683122, 1.000000000000000000, 0.9659258262890683122, 1.000000000000000000, 0.9659258262890683122, 1.000000000000000000, 0.9659258262890683122, 1.000000000000000000, 0.9659258262890683122, 1.000000000000000000, 0.9659258262890683122, 1.000000000000000000, 0.9659258262890683122, 1.000000000000000000, 0.9659258262890683122, 1.000000000000000000, 0.9659258262890683122, 1.000000000000000000, 0.9659258262890683122, 1.000000000000000000, 0.9659258262890683122, 1.000000000000000000, 0.9659258262890683122, 1.000000000000000000, 0.9659258262890683122, 1.000000000000000000, 0.9659258262890683122, 1.000000000000000000, 0.9659258262890683122, 1.000000000000000000, 0.9659258262890683122, 1.000000000000000000, 0.9659258262890683122, 1.000000000000000000, 0.9659258262890683122, 1.000000000000000000, 0.9659258262890683122, 1.000000000000000000, 0.9659258262890683122, 1.000000000000000000, 0.9659258262890683122, 1.000000000000000000, 0.9659258262890683122, 1.000000000000000000, 0.9659258262890683122, 1.000000000000000000, 0.9659258262890683122, 1.000000000000000000, 0.9659258262890683122, 1.000000000000000000, 0.9659258262890683122, 1.000000000000000000, 0.9659258262890683122, 1.000000000000000000, 0.9659258262890683122, 1.000000000000000000, 0.9659258262890683122, 1.000000000000000000, 0.9659258262890683122, 1.000000000000000000, 0.9659258262890683122, 1.000000000000000000, 0.9659258262890683122, 1.000000000000000000, 0.9659258262890683122, 1.000000000000000000, 0.9659258262890683122, 1.000000000000000000, 0.9659258262890683122, 1.000000000000000000, 0.9659258262890683122, 1.000000000000000000),
 ( 0.3333333333333333703, 0.3219752754296894559, 0.3333333333333333703, 0.3219752754296894559, 0.3333333333333333703, 0.3219752754296894559, 0.3333333333333333703, 0.3219752754296894559, 0.3333333333333333703, 0.3219752754296894559, 0.3333333333333333703, 0.3219752754296894559, 0.3333333333333333703, 0.3219752754296894559, 0.3333333333333333703, 0.3219752754296894559, 0.3333333333333333703, 0.3219752754296894559, 0.3333333333333333703, 0.3219752754296894559, 0.3333333333333333703, 0.3219752754296894559, 0.3333333333333333703, 0.3219752754296894559, 0.3333333333333333703, 0.3219752754296894559, 0.3333333333333333703, 0.3219752754296894559, 0.3333333333333333703, 0.3219752754296894559, 0.3333333333333333703, 0.3219752754296894559, 0.3333333333333333703, 0.3219752754296894559, 0.3333333333333333703, 0.3219752754296894559, 0.3333333333333333703, 0.3219752754296894559, 0.3333333333333333703, 0.3219752754296894559, 0.3333333333333333703, 0.3219752754296894559, 0.3333333333333333703, 0.3219752754296894559, 0.3333333333333333703, 0.3219752754296894559, 0.3333333333333333703, 0.3219752754296894559, 0.3333333333333333703, 0.3219752754296894559, 0.3333333333333333703, 0.3219752754296894559, 0.3333333333333333703, 0.3219752754296894559, 0.3333333333333333703, 0.3219752754296894559, 0.3333333333333333703, 0.3219752754296894559, 0.3333333333333333703, 0.3219752754296894559, 0.3333333333333333703, 0.3219752754296894559, 0.3333333333333333703, 0.3219752754296894559, 0.3333333333333333703, 0.3219752754296894559, 0.3333333333333333703, 0.3219752754296894559, 0.3333333333333333703, 0.3219752754296894559, 0.3333333333333333703, 0.3219752754296894559, 0.3333333333333333703, 0.3219752754296894559, 0.3333333333333333703, 0.3219752754296894559, 0.3333333333333333703, 0.3219752754296894559, 0.3333333333333333703, 0.3219752754296894559, 0.3333333333333333703, 0.3219752754296894559, 0.3333333333333333703, 0.3219752754296894559, 0.3333333333333333703, 0.3219752754296894559, 0.3333333333333333703, 0.3219752754296894559, 0.3333333333333333703, 0.3219752754296894559, 0.3333333333333333703, 0.3219752754296894559, 0.3333333333333333703, 0.3219752754296894559, 0.3333333333333333703, 0.3219752754296894559, 0.3333333333333333703, 0.3219752754296894559, 0.3333333333333333703, 0.3219752754296894559, 0.3333333333333333703, 0.3219752754296894559, 0.3333333333333333703, 0.3219752754296894559, 0.3333333333333333703, 0.3219752754296894559, 0.3333333333333333703, 0.3219752754296894559, 0.3333333333333333703, 0.3219752754296894559, 0.3333333333333333703, 0.3219752754296894559, 0.3333333333333333703, 0.3219752754296894559, 0.3333333333333333703, 0.3219752754296894559, 0.3333333333333333703, 0.3219752754296894559, 0.3333333333333333703, 0.3219752754296894559, 0.3333333333333333703, 0.3219752754296894559, 0.3333333333333333703, 0.3219752754296894559, 0.3333333333333333703, 0.3219752754296894559, 0.3333333333333333703, 0.3219752754296894559, 0.3333333333333333703, 0.3219752754296894559, 0.3333333333333333703, 0.3219752754296894559, 0.3333333333333333703, 0.3219752754296894559, 0.3333333333333333703, 0.3219752754296894559, 0.3333333333333333703, 0.3219752754296894559, 0.3333333333333333703, 0.3219752754296894559, 0.3333333333333333703, 0.3219752754296894559, 0.3333333333333333703, 0.3219752754296894559, 0.3333333333333333703, 0.3219752754296894559, 0.3333333333333333703, 0.3219752754296894559, 0.3333333333333333703, 0.3219752754296894559, 0.3333333333333333703, 0.3219752754296894559, 0.3333333333333333703, 0.3219752754296894559, 0.3333333333333333703, 0.3219752754296894559, 0.3333333333333333703, 0.3219752754296894559, 0.3333333333333333703, 0.3219752754296894559, 0.3333333333333333703, 0.3219752754296894559, 0.3333333333333333703, 0.3219752754296894559, 0.3333333333333333703, 0.3219752754296894559, 0.3333333333333333703, 0.3219752754296894559, 0.3333333333333333703, 0.3219752754296894559, 0.3333333333333333703, 0.3219752754296894559, 0.3333333333333333703, 0.3219752754296894559, 0.3333333333333333703, 0.3219752754296894559, 0.3333333333333333703, 0.3219752754296894559, 0.3333333333333333703, 0.3219752754296894559, 0.3333333333333333703, 0.3219752754296894559, 0.3333333333333333703, 0.3219752754296894559, 0.3333333333333333703, 0.3219752754296894559, 0.3333333333333333703, 0.3219752754296894559, 0.3333333333333333703, 0.3219752754296894559, 0.3333333333333333703, 0.3219752754296894559, 0.3333333333333333703, 0.3219752754296894559, 0.3333333333333333703, 0.3219752754296894559, 0.3333333333333333703, 0.3219752754296894559, 0.3333333333333333703, 0.3219752754296894559, 0.3333333333333333703, 0.3219752754296894559, 0.3333333333333333703, 0.3219752754296894559, 0.3333333333333333703, 0.3219752754296894559, 0.3333333333333333703, 0.3219752754296894559, 0.3333333333333333703, 0.3219752754296894559, 0.3333333333333333703, 0.3219752754296894559, 0.3333333333333333703, 0.3219752754296894559, 0.3333333333333333703, 0.3219752754296894559, 0.3333333333333333703, 0.3219752754296894559, 0.3333333333333333703, 0.3219752754296894559, 0.3333333333333333703, 0.3219752754296894559, 0.3333333333333333703, 0.3219752754296894559, 0.3333333333333333703, 0.3219752754296894559, 0.3333333333333333703, 0.3219752754296894559, 0.3333333333333333703, 0.3219752754296894559, 0.3333333333333333703, 0.3219752754296894559, 0.3333333333333333703, 0.3219752754296894559, 0.3333333333333333703, 0.3219752754296894559, 0.3333333333333333703, 0.3219752754296894559, 0.3333333333333333703, 0.3219752754296894559, 0.3333333333333333703, 0.3219752754296894559, 0.3333333333333333703, 0.3219752754296894559, 0.3333333333333333703, 0.3219752754296894559, 0.3333333333333333703, 0.3219752754296894559, 0.3333333333333333703, 0.3219752754296894559, 0.3333333333333333703, 0.3219752754296894559, 0.3333333333333333703, 0.3219752754296894559, 0.3333333333333333703, 0.3219752754296894559, 0.3333333333333333703, 0.3219752754296894559, 0.3333333333333333703, 0.3219752754296894559, 0.3333333333333333703, 0.3219752754296894559, 0.3333333333333333703, 0.3219752754296894559, 0.3333333333333333703, 0.3219752754296894559, 0.3333333333333333703, 0.3219752754296894559, 0.3333333333333333703, 0.3219752754296894559, 0.3333333333333333703, 0.3219752754296894559, 0.3333333333333333703, 0.3219752754296894559, 0.3333333333333333703, 0.3219752754296894559, 0.3333333333333333703, 0.3219752754296894559, 0.3333333333333333703, 0.3219752754296894559, 0.3333333333333333703, 0.3219752754296894559, 0.3333333333333333703, 0.3219752754296894559, 0.3333333333333333703, 0.3219752754296894559, 0.3333333333333333703, 0.3219752754296894559, 0.3333333333333333703, 0.3219752754296894559, 0.3333333333333333703, 0.3219752754296894559, 0.3333333333333333703, 0.3219752754296894559, 0.3333333333333333703, 0.3219752754296894559, 0.3333333333333333703, 0.3219752754296894559, 0.3333333333333333703, 0.3219752754296894559, 0.3333333333333333703, 0.3219752754296894559, 0.3333333333333333703, 0.3219752754296894559, 0.3333333333333333703, 0.3219752754296894559, 0.3333333333333333703, 0.3219752754296894559, 0.3333333333333333703, 0.3219752754296894559, 0.3333333333333333703, 0.3219752754296894559, 0.3333333333333333703, 0.3219752754296894559, 0.3333333333333333703, 0.3219752754296894559, 0.3333333333333333703, 0.3219752754296894559, 0.3333333333333333703, 0.3219752754296894559, 0.3333333333333333703, 0.3219752754296894559, 0.3333333333333333703, 0.3219752754296894559, 0.3333333333333333703, 0.3219752754296894559, 0.3333333333333333703, 0.3219752754296894559, 0.3333333333333333703, 0.3219752754296894559, 0.3333333333333333703, 0.3219752754296894559, 0.3333333333333333703, 0.3219752754296894559, 0.3333333333333333703, 0.3219752754296894559, 0.3333333333333333703, 0.3219752754296894559, 0.3333333333333333703, 0.3219752754296894559, 0.3333333333333333703, 0.3219752754296894559, 0.3333333333333333703, 0.3219752754296894559, 0.3333333333333333703, 0.3219752754296894559, 0.3333333333333333703, 0.3219752754296894559, 0.3333333333333333703, 0.3219752754296894559, 0.3333333333333333703, 0.3219752754296894559, 0.3333333333333333703, 0.3219752754296894559, 0.3333333333333333703, 0.3219752754296894559, 0.3333333333333333703, 0.3219752754296894559, 0.3333333333333333703, 0.3219752754296894559, 0.3333333333333333703, 0.3219752754296894559, 0.3333333333333333703, 0.3219752754296894559, 0.3333333333333333703, 0.3219752754296894559, 0.3333333333333333703, 0.3219752754296894559, 0.3333333333333333703, 0.3219752754296894559, 0.3333333333333333703, 0.3219752754296894559, 0.3333333333333333703, 0.3219752754296894559, 0.3333333333333333703, 0.3219752754296894559, 0.3333333333333333703, 0.3219752754296894559, 0.3333333333333333703, 0.3219752754296894559, 0.3333333333333333703, 0.3219752754296894559, 0.3333333333333333703, 0.3219752754296894559, 0.3333333333333333703, 0.3219752754296894559, 0.3333333333333333703, 0.3219752754296894559, 0.3333333333333333703, 0.3219752754296894559, 0.3333333333333333703, 0.3219752754296894559, 0.3333333333333333703, 0.3219752754296894559, 0.3333333333333333703, 0.3219752754296894559, 0.3333333333333333703, 0.3219752754296894559, 0.3333333333333333703, 0.3219752754296894559, 0.3333333333333333703, 0.3219752754296894559, 0.3333333333333333703, 0.3219752754296894559, 0.3333333333333333703, 0.3219752754296894559, 0.3333333333333333703, 0.3219752754296894559, 0.3333333333333333703, 0.3219752754296894559, 0.3333333333333333703, 0.3219752754296894559, 0.3333333333333333703, 0.3219752754296894559, 0.3333333333333333703, 0.3219752754296894559, 0.3333333333333333703, 0.3219752754296894559, 0.3333333333333333703, 0.3219752754296894559, 0.3333333333333333703, 0.3219752754296894559, 0.3333333333333333703, 0.3219752754296894559, 0.3333333333333333703, 0.3219752754296894559, 0.3333333333333333703, 0.3219752754296894559, 0.3333333333333333703, 0.3219752754296894559, 0.3333333333333333703, 0.3219752754296894559, 0.3333333333333333703, 0.3219752754296894559, 0.3333333333333333703, 0.3219752754296894559, 0.3333333333333333703, 0.3219752754296894559, 0.3333333333333333703, 0.3219752754296894559, 0.3333333333333333703, 0.3219752754296894559, 0.3333333333333333703, 0.3219752754296894559, 0.3333333333333333703, 0.3219752754296894559, 0.3333333333333333703, 0.3219752754296894559, 0.3333333333333333703, 0.3219752754296894559, 0.3333333333333333703, 0.3219752754296894559, 0.3333333333333333703, 0.3219752754296894559, 0.3333333333333333703, 0.3219752754296894559, 0.3333333333333333703),
 ( 0.3333333333333333703, 0.3219752754296894559, 0.3333333333333333703, 0.3219752754296894559, 0.3333333333333333703, 0.3219752754296894559, 0.3333333333333333703, 0.3219752754296894559, 0.3333333333333333703, 0.3219752754296894559, 0.3333333333333333703, 0.3219752754296894559, 0.3333333333333333703, 0.3219752754296894559, 0.3333333333333333703, 0.3219752754296894559, 0.3333333333333333703, 0.3219752754296894559, 0.3333333333333333703, 0.3219752754296894559, 0.3333333333333333703, 0.3219752754296894559, 0.3333333333333333703, 0.3219752754296894559, 0.3333333333333333703, 0.3219752754296894559, 0.3333333333333333703, 0.3219752754296894559, 0.3333333333333333703, 0.3219752754296894559, 0.3333333333333333703, 0.3219752754296894559, 0.3333333333333333703, 0.3219752754296894559, 0.3333333333333333703, 0.3219752754296894559, 0.3333333333333333703, 0.3219752754296894559, 0.3333333333333333703, 0.3219752754296894559, 0.3333333333333333703, 0.3219752754296894559, 0.3333333333333333703, 0.3219752754296894559, 0.3333333333333333703, 0.3219752754296894559, 0.3333333333333333703, 0.3219752754296894559, 0.3333333333333333703, 0.3219752754296894559, 0.3333333333333333703, 0.3219752754296894559, 0.3333333333333333703, 0.3219752754296894559, 0.3333333333333333703, 0.3219752754296894559, 0.3333333333333333703, 0.3219752754296894559, 0.3333333333333333703, 0.3219752754296894559, 0.3333333333333333703, 0.3219752754296894559, 0.3333333333333333703, 0.3219752754296894559, 0.3333333333333333703, 0.3219752754296894559, 0.3333333333333333703, 0.3219752754296894559, 0.3333333333333333703, 0.3219752754296894559, 0.3333333333333333703, 0.3219752754296894559, 0.3333333333333333703, 0.3219752754296894559, 0.3333333333333333703, 0.3219752754296894559, 0.3333333333333333703, 0.3219752754296894559, 0.3333333333333333703, 0.3219752754296894559, 0.3333333333333333703, 0.3219752754296894559, 0.3333333333333333703, 0.3219752754296894559, 0.3333333333333333703, 0.3219752754296894559, 0.3333333333333333703, 0.3219752754296894559, 0.3333333333333333703, 0.3219752754296894559, 0.3333333333333333703, 0.3219752754296894559, 0.3333333333333333703, 0.3219752754296894559, 0.3333333333333333703, 0.3219752754296894559, 0.3333333333333333703, 0.3219752754296894559, 0.3333333333333333703, 0.3219752754296894559, 0.3333333333333333703, 0.3219752754296894559, 0.3333333333333333703, 0.3219752754296894559, 0.3333333333333333703, 0.3219752754296894559, 0.3333333333333333703, 0.3219752754296894559, 0.3333333333333333703, 0.3219752754296894559, 0.3333333333333333703, 0.3219752754296894559, 0.3333333333333333703, 0.3219752754296894559, 0.3333333333333333703, 0.3219752754296894559, 0.3333333333333333703, 0.3219752754296894559, 0.3333333333333333703, 0.3219752754296894559, 0.3333333333333333703, 0.3219752754296894559, 0.3333333333333333703, 0.3219752754296894559, 0.3333333333333333703, 0.3219752754296894559, 0.3333333333333333703, 0.3219752754296894559, 0.3333333333333333703, 0.3219752754296894559, 0.3333333333333333703, 0.3219752754296894559, 0.3333333333333333703, 0.3219752754296894559, 0.3333333333333333703, 0.3219752754296894559, 0.3333333333333333703, 0.3219752754296894559, 0.3333333333333333703, 0.3219752754296894559, 0.3333333333333333703, 0.3219752754296894559, 0.3333333333333333703, 0.3219752754296894559, 0.3333333333333333703, 0.3219752754296894559, 0.3333333333333333703, 0.3219752754296894559, 0.3333333333333333703, 0.3219752754296894559, 0.3333333333333333703, 0.3219752754296894559, 0.3333333333333333703, 0.3219752754296894559, 0.3333333333333333703, 0.3219752754296894559, 0.3333333333333333703, 0.3219752754296894559, 0.3333333333333333703, 0.3219752754296894559, 0.3333333333333333703, 0.3219752754296894559, 0.3333333333333333703, 0.3219752754296894559, 0.3333333333333333703, 0.3219752754296894559, 0.3333333333333333703, 0.3219752754296894559, 0.3333333333333333703, 0.3219752754296894559, 0.3333333333333333703, 0.3219752754296894559, 0.3333333333333333703, 0.3219752754296894559, 0.3333333333333333703, 0.3219752754296894559, 0.3333333333333333703, 0.3219752754296894559, 0.3333333333333333703, 0.3219752754296894559, 0.3333333333333333703, 0.3219752754296894559, 0.3333333333333333703, 0.3219752754296894559, 0.3333333333333333703, 0.3219752754296894559, 0.3333333333333333703, 0.3219752754296894559, 0.3333333333333333703, 0.3219752754296894559, 0.3333333333333333703, 0.3219752754296894559, 0.3333333333333333703, 0.3219752754296894559, 0.3333333333333333703, 0.3219752754296894559, 0.3333333333333333703, 0.3219752754296894559, 0.3333333333333333703, 0.3219752754296894559, 0.3333333333333333703, 0.3219752754296894559, 0.3333333333333333703, 0.3219752754296894559, 0.3333333333333333703, 0.3219752754296894559, 0.3333333333333333703, 0.3219752754296894559, 0.3333333333333333703, 0.3219752754296894559, 0.3333333333333333703, 0.3219752754296894559, 0.3333333333333333703, 0.3219752754296894559, 0.3333333333333333703, 0.3219752754296894559, 0.3333333333333333703, 0.3219752754296894559, 0.3333333333333333703, 0.3219752754296894559, 0.3333333333333333703, 0.3219752754296894559, 0.3333333333333333703, 0.3219752754296894559, 0.3333333333333333703, 0.3219752754296894559, 0.3333333333333333703, 0.3219752754296894559, 0.3333333333333333703, 0.3219752754296894559, 0.3333333333333333703, 0.3219752754296894559, 0.3333333333333333703, 0.3219752754296894559, 0.3333333333333333703, 0.3219752754296894559, 0.3333333333333333703, 0.3219752754296894559, 0.3333333333333333703, 0.3219752754296894559, 0.3333333333333333703, 0.3219752754296894559, 0.3333333333333333703, 0.3219752754296894559, 0.3333333333333333703, 0.3219752754296894559, 0.3333333333333333703, 0.3219752754296894559, 0.3333333333333333703, 0.3219752754296894559, 0.3333333333333333703, 0.3219752754296894559, 0.3333333333333333703, 0.3219752754296894559, 0.3333333333333333703, 0.3219752754296894559, 0.3333333333333333703, 0.3219752754296894559, 0.3333333333333333703, 0.3219752754296894559, 0.3333333333333333703, 0.3219752754296894559, 0.3333333333333333703, 0.3219752754296894559, 0.3333333333333333703, 0.3219752754296894559, 0.3333333333333333703, 0.3219752754296894559, 0.3333333333333333703, 0.3219752754296894559, 0.3333333333333333703, 0.3219752754296894559, 0.3333333333333333703, 0.3219752754296894559, 0.3333333333333333703, 0.3219752754296894559, 0.3333333333333333703, 0.3219752754296894559, 0.3333333333333333703, 0.3219752754296894559, 0.3333333333333333703, 0.3219752754296894559, 0.3333333333333333703, 0.3219752754296894559, 0.3333333333333333703, 0.3219752754296894559, 0.3333333333333333703, 0.3219752754296894559, 0.3333333333333333703, 0.3219752754296894559, 0.3333333333333333703, 0.3219752754296894559, 0.3333333333333333703, 0.3219752754296894559, 0.3333333333333333703, 0.3219752754296894559, 0.3333333333333333703, 0.3219752754296894559, 0.3333333333333333703, 0.3219752754296894559, 0.3333333333333333703, 0.3219752754296894559, 0.3333333333333333703, 0.3219752754296894559, 0.3333333333333333703, 0.3219752754296894559, 0.3333333333333333703, 0.3219752754296894559, 0.3333333333333333703, 0.3219752754296894559, 0.3333333333333333703, 0.3219752754296894559, 0.3333333333333333703, 0.3219752754296894559, 0.3333333333333333703, 0.3219752754296894559, 0.3333333333333333703, 0.3219752754296894559, 0.3333333333333333703, 0.3219752754296894559, 0.3333333333333333703, 0.3219752754296894559, 0.3333333333333333703, 0.3219752754296894559, 0.3333333333333333703, 0.3219752754296894559, 0.3333333333333333703, 0.3219752754296894559, 0.3333333333333333703, 0.3219752754296894559, 0.3333333333333333703, 0.3219752754296894559, 0.3333333333333333703, 0.3219752754296894559, 0.3333333333333333703, 0.3219752754296894559, 0.3333333333333333703, 0.3219752754296894559, 0.3333333333333333703, 0.3219752754296894559, 0.3333333333333333703, 0.3219752754296894559, 0.3333333333333333703, 0.3219752754296894559, 0.3333333333333333703, 0.3219752754296894559, 0.3333333333333333703, 0.3219752754296894559, 0.3333333333333333703, 0.3219752754296894559, 0.3333333333333333703, 0.3219752754296894559, 0.3333333333333333703, 0.3219752754296894559, 0.3333333333333333703, 0.3219752754296894559, 0.3333333333333333703, 0.3219752754296894559, 0.3333333333333333703, 0.3219752754296894559, 0.3333333333333333703, 0.3219752754296894559, 0.3333333333333333703, 0.3219752754296894559, 0.3333333333333333703, 0.3219752754296894559, 0.3333333333333333703, 0.3219752754296894559, 0.3333333333333333703, 0.3219752754296894559, 0.3333333333333333703, 0.3219752754296894559, 0.3333333333333333703, 0.3219752754296894559, 0.3333333333333333703, 0.3219752754296894559, 0.3333333333333333703, 0.3219752754296894559, 0.3333333333333333703, 0.3219752754296894559, 0.3333333333333333703, 0.3219752754296894559, 0.3333333333333333703, 0.3219752754296894559, 0.3333333333333333703, 0.3219752754296894559, 0.3333333333333333703, 0.3219752754296894559, 0.3333333333333333703, 0.3219752754296894559, 0.3333333333333333703, 0.3219752754296894559, 0.3333333333333333703, 0.3219752754296894559, 0.3333333333333333703, 0.3219752754296894559, 0.3333333333333333703, 0.3219752754296894559, 0.3333333333333333703, 0.3219752754296894559, 0.3333333333333333703, 0.3219752754296894559, 0.3333333333333333703, 0.3219752754296894559, 0.3333333333333333703, 0.3219752754296894559, 0.3333333333333333703, 0.3219752754296894559, 0.3333333333333333703, 0.3219752754296894559, 0.3333333333333333703, 0.3219752754296894559, 0.3333333333333333703, 0.3219752754296894559, 0.3333333333333333703, 0.3219752754296894559, 0.3333333333333333703, 0.3219752754296894559, 0.3333333333333333703, 0.3219752754296894559, 0.3333333333333333703, 0.3219752754296894559, 0.3333333333333333703, 0.3219752754296894559, 0.3333333333333333703, 0.3219752754296894559, 0.3333333333333333703, 0.3219752754296894559, 0.3333333333333333703, 0.3219752754296894559, 0.3333333333333333703, 0.3219752754296894559, 0.3333333333333333703, 0.3219752754296894559, 0.3333333333333333703, 0.3219752754296894559, 0.3333333333333333703, 0.3219752754296894559, 0.3333333333333333703, 0.3219752754296894559, 0.3333333333333333703, 0.3219752754296894559, 0.3333333333333333703, 0.3219752754296894559, 0.3333333333333333703, 0.3219752754296894559, 0.3333333333333333703, 0.3219752754296894559, 0.3333333333333333703, 0.3219752754296894559, 0.3333333333333333703, 0.3219752754296894559, 0.3333333333333333703, 0.3219752754296894559, 0.3333333333333333703, 0.3219752754296894559, 0.3333333333333333703),
 ( 1.000000000000000000, 0.9659258262890683122, 1.000000000000000000, 0.9659258262890683122, 1.000000000000000000, 0.9659258262890683122, 1.000000000000000000, 0.9659258262890683122, 1.000000000000000000, 0.9659258262890683122, 1.000000000000000000, 0.9659258262890683122, 1.000000000000000000, 0.9659258262890683122, 1.000000000000000000, 0.9659258262890683122, 1.000000000000000000, 0.9659258262890683122, 1.000000000000000000, 0.9659258262890683122, 1.000000000000000000, 0.9659258262890683122, 1.000000000000000000, 0.9659258262890683122, 1.000000000000000000, 0.9659258262890683122, 1.000000000000000000, 0.9659258262890683122, 1.000000000000000000, 0.9659258262890683122, 1.000000000000000000, 0.9659258262890683122, 1.000000000000000000, 0.9659258262890683122, 1.000000000000000000, 0.9659258262890683122, 1.000000000000000000, 0.9659258262890683122, 1.000000000000000000, 0.9659258262890683122, 1.000000000000000000, 0.9659258262890683122, 1.000000000000000000, 0.9659258262890683122, 1.000000000000000000, 0.9659258262890683122, 1.000000000000000000, 0.9659258262890683122, 1.000000000000000000, 0.9659258262890683122, 1.000000000000000000, 0.9659258262890683122, 1.000000000000000000, 0.9659258262890683122, 1.000000000000000000, 0.9659258262890683122, 1.000000000000000000, 0.9659258262890683122, 1.000000000000000000, 0.9659258262890683122, 1.000000000000000000, 0.9659258262890683122, 1.000000000000000000, 0.9659258262890683122, 1.000000000000000000, 0.9659258262890683122, 1.000000000000000000, 0.9659258262890683122, 1.000000000000000000, 0.9659258262890683122, 1.000000000000000000, 0.9659258262890683122, 1.000000000000000000, 0.9659258262890683122, 1.000000000000000000, 0.9659258262890683122, 1.000000000000000000, 0.9659258262890683122, 1.000000000000000000, 0.9659258262890683122, 1.000000000000000000, 0.9659258262890683122, 1.000000000000000000, 0.9659258262890683122, 1.000000000000000000, 0.9659258262890683122, 1.000000000000000000, 0.9659258262890683122, 1.000000000000000000, 0.9659258262890683122, 1.000000000000000000, 0.9659258262890683122, 1.000000000000000000, 0.9659258262890683122, 1.000000000000000000, 0.9659258262890683122, 1.000000000000000000, 0.9659258262890683122, 1.000000000000000000, 0.9659258262890683122, 1.000000000000000000, 0.9659258262890683122, 1.000000000000000000, 0.9659258262890683122, 1.000000000000000000, 0.9659258262890683122, 1.000000000000000000, 0.9659258262890683122, 1.000000000000000000, 0.9659258262890683122, 1.000000000000000000, 0.9659258262890683122, 1.000000000000000000, 0.9659258262890683122, 1.000000000000000000, 0.9659258262890683122, 1.000000000000000000, 0.9659258262890683122, 1.000000000000000000, 0.9659258262890683122, 1.000000000000000000, 0.9659258262890683122, 1.000000000000000000, 0.9659258262890683122, 1.000000000000000000, 0.9659258262890683122, 1.000000000000000000, 0.9659258262890683122, 1.000000000000000000, 0.9659258262890683122, 1.000000000000000000, 0.9659258262890683122, 1.000000000000000000, 0.9659258262890683122, 1.000000000000000000, 0.9659258262890683122, 1.000000000000000000, 0.9659258262890683122, 1.000000000000000000, 0.9659258262890683122, 1.000000000000000000, 0.9659258262890683122, 1.000000000000000000, 0.9659258262890683122, 1.000000000000000000, 0.9659258262890683122, 1.000000000000000000, 0.9659258262890683122, 1.000000000000000000, 0.9659258262890683122, 1.000000000000000000, 0.9659258262890683122, 1.000000000000000000, 0.9659258262890683122, 1.000000000000000000, 0.9659258262890683122, 1.000000000000000000, 0.9659258262890683122, 1.000000000000000000, 0.9659258262890683122, 1.000000000000000000, 0.9659258262890683122, 1.000000000000000000, 0.9659258262890683122, 1.000000000000000000, 0.9659258262890683122, 1.000000000000000000, 0.9659258262890683122, 1.000000000000000000, 0.9659258262890683122, 1.000000000000000000, 0.9659258262890683122, 1.000000000000000000, 0.9659258262890683122, 1.000000000000000000, 0.9659258262890683122, 1.000000000000000000, 0.9659258262890683122, 1.000000000000000000, 0.9659258262890683122, 1.000000000000000000, 0.9659258262890683122, 1.000000000000000000, 0.9659258262890683122, 1.000000000000000000, 0.9659258262890683122, 1.000000000000000000, 0.9659258262890683122, 1.000000000000000000, 0.9659258262890683122, 1.000000000000000000, 0.9659258262890683122, 1.000000000000000000, 0.9659258262890683122, 1.000000000000000000, 0.9659258262890683122, 1.000000000000000000, 0.9659258262890683122, 1.000000000000000000, 0.9659258262890683122, 1.000000000000000000, 0.9659258262890683122, 1.000000000000000000, 0.9659258262890683122, 1.000000000000000000, 0.9659258262890683122, 1.000000000000000000, 0.9659258262890683122, 1.000000000000000000, 0.9659258262890683122, 1.000000000000000000, 0.9659258262890683122, 1.000000000000000000, 0.9659258262890683122, 1.000000000000000000, 0.9659258262890683122, 1.000000000000000000, 0.9659258262890683122, 1.000000000000000000, 0.9659258262890683122, 1.000000000000000000, 0.9659258262890683122, 1.000000000000000000, 0.9659258262890683122, 1.000000000000000000, 0.9659258262890683122, 1.000000000000000000, 0.9659258262890683122, 1.000000000000000000, 0.9659258262890683122, 1.000000000000000000, 0.9659258262890683122, 1.000000000000000000, 0.9659258262890683122, 1.000000000000000000, 0.9659258262890683122, 1.000000000000000000, 0.9659258262890683122, 1.000000000000000000, 0.9659258262890683122, 1.000000000000000000, 0.9659258262890683122, 1.000000000000000000, 0.9659258262890683122, 1.000000000000000000, 0.9659258262890683122, 1.000000000000000000, 0.9659258262890683122, 1.000000000000000000, 0.9659258262890683122, 1.000000000000000000, 0.9659258262890683122, 1.000000000000000000, 0.9659258262890683122, 1.000000000000000000, 0.9659258262890683122, 1.000000000000000000, 0.9659258262890683122, 1.000000000000000000, 0.9659258262890683122, 1.000000000000000000, 0.9659258262890683122, 1.000000000000000000, 0.9659258262890683122, 1.000000000000000000, 0.9659258262890683122, 1.000000000000000000, 0.9659258262890683122, 1.000000000000000000, 0.9659258262890683122, 1.000000000000000000, 0.9659258262890683122, 1.000000000000000000, 0.9659258262890683122, 1.000000000000000000, 0.9659258262890683122, 1.000000000000000000, 0.9659258262890683122, 1.000000000000000000, 0.9659258262890683122, 1.000000000000000000, 0.9659258262890683122, 1.000000000000000000, 0.9659258262890683122, 1.000000000000000000, 0.9659258262890683122, 1.000000000000000000, 0.9659258262890683122, 1.000000000000000000, 0.9659258262890683122, 1.000000000000000000, 0.9659258262890683122, 1.000000000000000000, 0.9659258262890683122, 1.000000000000000000, 0.9659258262890683122, 1.000000000000000000, 0.9659258262890683122, 1.000000000000000000, 0.9659258262890683122, 1.000000000000000000, 0.9659258262890683122, 1.000000000000000000, 0.9659258262890683122, 1.000000000000000000, 0.9659258262890683122, 1.000000000000000000, 0.9659258262890683122, 1.000000000000000000, 0.9659258262890683122, 1.000000000000000000, 0.9659258262890683122, 1.000000000000000000, 0.9659258262890683122, 1.000000000000000000, 0.9659258262890683122, 1.000000000000000000, 0.9659258262890683122, 1.000000000000000000, 0.9659258262890683122, 1.000000000000000000, 0.9659258262890683122, 1.000000000000000000, 0.9659258262890683122, 1.000000000000000000, 0.9659258262890683122, 1.000000000000000000, 0.9659258262890683122, 1.000000000000000000, 0.9659258262890683122, 1.000000000000000000, 0.9659258262890683122, 1.000000000000000000, 0.9659258262890683122, 1.000000000000000000, 0.9659258262890683122, 1.000000000000000000, 0.9659258262890683122, 1.000000000000000000, 0.9659258262890683122, 1.000000000000000000, 0.9659258262890683122, 1.000000000000000000, 0.9659258262890683122, 1.000000000000000000, 0.9659258262890683122, 1.000000000000000000, 0.9659258262890683122, 1.000000000000000000, 0.9659258262890683122, 1.000000000000000000, 0.9659258262890683122, 1.000000000000000000, 0.9659258262890683122, 1.000000000000000000, 0.9659258262890683122, 1.000000000000000000, 0.9659258262890683122, 1.000000000000000000, 0.9659258262890683122, 1.000000000000000000, 0.9659258262890683122, 1.000000000000000000, 0.9659258262890683122, 1.000000000000000000, 0.9659258262890683122, 1.000000000000000000, 0.9659258262890683122, 1.000000000000000000, 0.9659258262890683122, 1.000000000000000000, 0.9659258262890683122, 1.000000000000000000, 0.9659258262890683122, 1.000000000000000000, 0.9659258262890683122, 1.000000000000000000, 0.9659258262890683122, 1.000000000000000000, 0.9659258262890683122, 1.000000000000000000, 0.9659258262890683122, 1.000000000000000000, 0.9659258262890683122, 1.000000000000000000, 0.9659258262890683122, 1.000000000000000000, 0.9659258262890683122, 1.000000000000000000, 0.9659258262890683122, 1.000000000000000000, 0.9659258262890683122, 1.000000000000000000, 0.9659258262890683122, 1.000000000000000000, 0.9659258262890683122, 1.000000000000000000, 0.9659258262890683122, 1.000000000000000000, 0.9659258262890683122, 1.000000000000000000, 0.9659258262890683122, 1.000000000000000000, 0.9659258262890683122, 1.000000000000000000, 0.9659258262890683122, 1.000000000000000000, 0.9659258262890683122, 1.000000000000000000, 0.9659258262890683122, 1.000000000000000000, 0.9659258262890683122, 1.000000000000000000, 0.9659258262890683122, 1.000000000000000000, 0.9659258262890683122, 1.000000000000000000, 0.9659258262890683122, 1.000000000000000000, 0.9659258262890683122, 1.000000000000000000, 0.9659258262890683122, 1.000000000000000000, 0.9659258262890683122, 1.000000000000000000, 0.9659258262890683122, 1.000000000000000000, 0.9659258262890683122, 1.000000000000000000, 0.9659258262890683122, 1.000000000000000000, 0.9659258262890683122, 1.000000000000000000, 0.9659258262890683122, 1.000000000000000000, 0.9659258262890683122, 1.000000000000000000, 0.9659258262890683122, 1.000000000000000000, 0.9659258262890683122, 1.000000000000000000, 0.9659258262890683122, 1.000000000000000000, 0.9659258262890683122, 1.000000000000000000, 0.9659258262890683122, 1.000000000000000000, 0.9659258262890683122, 1.000000000000000000, 0.9659258262890683122, 1.000000000000000000, 0.9659258262890683122, 1.000000000000000000, 0.9659258262890683122, 1.000000000000000000, 0.9659258262890683122, 1.000000000000000000),
 ( 0.3333333333333333703, 0.3219752754296894559, 0.3333333333333333703, 0.3219752754296894559, 0.3333333333333333703, 0.3219752754296894559, 0.3333333333333333703, 0.3219752754296894559, 0.3333333333333333703, 0.3219752754296894559, 0.3333333333333333703, 0.3219752754296894559, 0.3333333333333333703, 0.3219752754296894559, 0.3333333333333333703, 0.3219752754296894559, 0.3333333333333333703, 0.3219752754296894559, 0.3333333333333333703, 0.3219752754296894559, 0.3333333333333333703, 0.3219752754296894559, 0.3333333333333333703, 0.3219752754296894559, 0.3333333333333333703, 0.3219752754296894559, 0.3333333333333333703, 0.3219752754296894559, 0.3333333333333333703, 0.3219752754296894559, 0.3333333333333333703, 0.3219752754296894559, 0.3333333333333333703, 0.3219752754296894559, 0.3333333333333333703, 0.3219752754296894559, 0.3333333333333333703, 0.3219752754296894559, 0.3333333333333333703, 0.3219752754296894559, 0.3333333333333333703, 0.3219752754296894559, 0.3333333333333333703, 0.3219752754296894559, 0.3333333333333333703, 0.3219752754296894559, 0.3333333333333333703, 0.3219752754296894559, 0.3333333333333333703, 0.3219752754296894559, 0.3333333333333333703, 0.3219752754296894559, 0.3333333333333333703, 0.3219752754296894559, 0.3333333333333333703, 0.3219752754296894559, 0.3333333333333333703, 0.3219752754296894559, 0.3333333333333333703, 0.3219752754296894559, 0.3333333333333333703, 0.3219752754296894559, 0.3333333333333333703, 0.3219752754296894559, 0.3333333333333333703, 0.3219752754296894559, 0.3333333333333333703, 0.3219752754296894559, 0.3333333333333333703, 0.3219752754296894559, 0.3333333333333333703, 0.3219752754296894559, 0.3333333333333333703, 0.3219752754296894559, 0.3333333333333333703, 0.3219752754296894559, 0.3333333333333333703, 0.3219752754296894559, 0.3333333333333333703, 0.3219752754296894559, 0.3333333333333333703, 0.3219752754296894559, 0.3333333333333333703, 0.3219752754296894559, 0.3333333333333333703, 0.3219752754296894559, 0.3333333333333333703, 0.3219752754296894559, 0.3333333333333333703, 0.3219752754296894559, 0.3333333333333333703, 0.3219752754296894559, 0.3333333333333333703, 0.3219752754296894559, 0.3333333333333333703, 0.3219752754296894559, 0.3333333333333333703, 0.3219752754296894559, 0.3333333333333333703, 0.3219752754296894559, 0.3333333333333333703, 0.3219752754296894559, 0.3333333333333333703, 0.3219752754296894559, 0.3333333333333333703, 0.3219752754296894559, 0.3333333333333333703, 0.3219752754296894559, 0.3333333333333333703, 0.3219752754296894559, 0.3333333333333333703, 0.3219752754296894559, 0.3333333333333333703, 0.3219752754296894559, 0.3333333333333333703, 0.3219752754296894559, 0.3333333333333333703, 0.3219752754296894559, 0.3333333333333333703, 0.3219752754296894559, 0.3333333333333333703, 0.3219752754296894559, 0.3333333333333333703, 0.3219752754296894559, 0.3333333333333333703, 0.3219752754296894559, 0.3333333333333333703, 0.3219752754296894559, 0.3333333333333333703, 0.3219752754296894559, 0.3333333333333333703, 0.3219752754296894559, 0.3333333333333333703, 0.3219752754296894559, 0.3333333333333333703, 0.3219752754296894559, 0.3333333333333333703, 0.3219752754296894559, 0.3333333333333333703, 0.3219752754296894559, 0.3333333333333333703, 0.3219752754296894559, 0.3333333333333333703, 0.3219752754296894559, 0.3333333333333333703, 0.3219752754296894559, 0.3333333333333333703, 0.3219752754296894559, 0.3333333333333333703, 0.3219752754296894559, 0.3333333333333333703, 0.3219752754296894559, 0.3333333333333333703, 0.3219752754296894559, 0.3333333333333333703, 0.3219752754296894559, 0.3333333333333333703, 0.3219752754296894559, 0.3333333333333333703, 0.3219752754296894559, 0.3333333333333333703, 0.3219752754296894559, 0.3333333333333333703, 0.3219752754296894559, 0.3333333333333333703, 0.3219752754296894559, 0.3333333333333333703, 0.3219752754296894559, 0.3333333333333333703, 0.3219752754296894559, 0.3333333333333333703, 0.3219752754296894559, 0.3333333333333333703, 0.3219752754296894559, 0.3333333333333333703, 0.3219752754296894559, 0.3333333333333333703, 0.3219752754296894559, 0.3333333333333333703, 0.3219752754296894559, 0.3333333333333333703, 0.3219752754296894559, 0.3333333333333333703, 0.3219752754296894559, 0.3333333333333333703, 0.3219752754296894559, 0.3333333333333333703, 0.3219752754296894559, 0.3333333333333333703, 0.3219752754296894559, 0.3333333333333333703, 0.3219752754296894559, 0.3333333333333333703, 0.3219752754296894559, 0.3333333333333333703, 0.3219752754296894559, 0.3333333333333333703, 0.3219752754296894559, 0.3333333333333333703, 0.3219752754296894559, 0.3333333333333333703, 0.3219752754296894559, 0.3333333333333333703, 0.3219752754296894559, 0.3333333333333333703, 0.3219752754296894559, 0.3333333333333333703, 0.3219752754296894559, 0.3333333333333333703, 0.3219752754296894559, 0.3333333333333333703, 0.3219752754296894559, 0.3333333333333333703, 0.3219752754296894559, 0.3333333333333333703, 0.3219752754296894559, 0.3333333333333333703, 0.3219752754296894559, 0.3333333333333333703, 0.3219752754296894559, 0.3333333333333333703, 0.3219752754296894559, 0.3333333333333333703, 0.3219752754296894559, 0.3333333333333333703, 0.3219752754296894559, 0.3333333333333333703, 0.3219752754296894559, 0.3333333333333333703, 0.3219752754296894559, 0.3333333333333333703, 0.3219752754296894559, 0.3333333333333333703, 0.3219752754296894559, 0.3333333333333333703, 0.3219752754296894559, 0.3333333333333333703, 0.3219752754296894559, 0.3333333333333333703, 0.3219752754296894559, 0.3333333333333333703, 0.3219752754296894559, 0.3333333333333333703, 0.3219752754296894559, 0.3333333333333333703, 0.3219752754296894559, 0.3333333333333333703, 0.3219752754296894559, 0.3333333333333333703, 0.3219752754296894559, 0.3333333333333333703, 0.3219752754296894559, 0.3333333333333333703, 0.3219752754296894559, 0.3333333333333333703, 0.3219752754296894559, 0.3333333333333333703, 0.3219752754296894559, 0.3333333333333333703, 0.3219752754296894559, 0.3333333333333333703, 0.3219752754296894559, 0.3333333333333333703, 0.3219752754296894559, 0.3333333333333333703, 0.3219752754296894559, 0.3333333333333333703, 0.3219752754296894559, 0.3333333333333333703, 0.3219752754296894559, 0.3333333333333333703, 0.3219752754296894559, 0.3333333333333333703, 0.3219752754296894559, 0.3333333333333333703, 0.3219752754296894559, 0.3333333333333333703, 0.3219752754296894559, 0.3333333333333333703, 0.3219752754296894559, 0.3333333333333333703, 0.3219752754296894559, 0.3333333333333333703, 0.3219752754296894559, 0.3333333333333333703, 0.3219752754296894559, 0.3333333333333333703, 0.3219752754296894559, 0.3333333333333333703, 0.3219752754296894559, 0.3333333333333333703, 0.3219752754296894559, 0.3333333333333333703, 0.3219752754296894559, 0.3333333333333333703, 0.3219752754296894559, 0.3333333333333333703, 0.3219752754296894559, 0.3333333333333333703, 0.3219752754296894559, 0.3333333333333333703, 0.3219752754296894559, 0.3333333333333333703, 0.3219752754296894559, 0.3333333333333333703, 0.3219752754296894559, 0.3333333333333333703, 0.3219752754296894559, 0.3333333333333333703, 0.3219752754296894559, 0.3333333333333333703, 0.3219752754296894559, 0.3333333333333333703, 0.3219752754296894559, 0.3333333333333333703, 0.3219752754296894559, 0.3333333333333333703, 0.3219752754296894559, 0.3333333333333333703, 0.3219752754296894559, 0.3333333333333333703, 0.3219752754296894559, 0.3333333333333333703, 0.3219752754296894559, 0.3333333333333333703, 0.3219752754296894559, 0.3333333333333333703, 0.3219752754296894559, 0.3333333333333333703, 0.3219752754296894559, 0.3333333333333333703, 0.3219752754296894559, 0.3333333333333333703, 0.3219752754296894559, 0.3333333333333333703, 0.3219752754296894559, 0.3333333333333333703, 0.3219752754296894559, 0.3333333333333333703, 0.3219752754296894559, 0.3333333333333333703, 0.3219752754296894559, 0.3333333333333333703, 0.3219752754296894559, 0.3333333333333333703, 0.3219752754296894559, 0.3333333333333333703, 0.3219752754296894559, 0.3333333333333333703, 0.3219752754296894559, 0.3333333333333333703, 0.3219752754296894559, 0.3333333333333333703, 0.3219752754296894559, 0.3333333333333333703, 0.3219752754296894559, 0.3333333333333333703, 0.3219752754296894559, 0.3333333333333333703, 0.3219752754296894559, 0.3333333333333333703, 0.3219752754296894559, 0.3333333333333333703, 0.3219752754296894559, 0.3333333333333333703, 0.3219752754296894559, 0.3333333333333333703, 0.3219752754296894559, 0.3333333333333333703, 0.3219752754296894559, 0.3333333333333333703, 0.3219752754296894559, 0.3333333333333333703, 0.3219752754296894559, 0.3333333333333333703, 0.3219752754296894559, 0.3333333333333333703, 0.3219752754296894559, 0.3333333333333333703, 0.3219752754296894559, 0.3333333333333333703, 0.3219752754296894559, 0.3333333333333333703, 0.3219752754296894559, 0.3333333333333333703, 0.3219752754296894559, 0.3333333333333333703, 0.3219752754296894559, 0.3333333333333333703, 0.3219752754296894559, 0.3333333333333333703, 0.3219752754296894559, 0.3333333333333333703, 0.3219752754296894559, 0.3333333333333333703, 0.3219752754296894559, 0.3333333333333333703, 0.3219752754296894559, 0.3333333333333333703, 0.3219752754296894559, 0.3333333333333333703, 0.3219752754296894559, 0.3333333333333333703, 0.3219752754296894559, 0.3333333333333333703, 0.3219752754296894559, 0.3333333333333333703, 0.3219752754296894559, 0.3333333333333333703, 0.3219752754296894559, 0.3333333333333333703, 0.3219752754296894559, 0.3333333333333333703, 0.3219752754296894559, 0.3333333333333333703, 0.3219752754296894559, 0.3333333333333333703, 0.3219752754296894559, 0.3333333333333333703, 0.3219752754296894559, 0.3333333333333333703, 0.3219752754296894559, 0.3333333333333333703, 0.3219752754296894559, 0.3333333333333333703, 0.3219752754296894559, 0.3333333333333333703, 0.3219752754296894559, 0.3333333333333333703, 0.3219752754296894559, 0.3333333333333333703, 0.3219752754296894559, 0.3333333333333333703, 0.3219752754296894559, 0.3333333333333333703, 0.3219752754296894559, 0.3333333333333333703, 0.3219752754296894559, 0.3333333333333333703, 0.3219752754296894559, 0.3333333333333333703, 0.3219752754296894559, 0.3333333333333333703, 0.3219752754296894559, 0.3333333333333333703, 0.3219752754296894559, 0.3333333333333333703, 0.3219752754296894559, 0.3333333333333333703, 0.3219752754296894559, 0.3333333333333333703, 0.3219752754296894559, 0.3333333333333333703, 0.3219752754296894559, 0.3333333333333333703, 0.3219752754296894559, 0.3333333333333333703),
 ( 0.3333333333333333703, 0.3219752754296894559, 0.3333333333333333703, 0.3219752754296894559, 0.3333333333333333703, 0.3219752754296894559, 0.3333333333333333703, 0.3219752754296894559, 0.3333333333333333703, 0.3219752754296894559, 0.3333333333333333703, 0.3219752754296894559, 0.3333333333333333703, 0.3219752754296894559, 0.3333333333333333703, 0.3219752754296894559, 0.3333333333333333703, 0.3219752754296894559, 0.3333333333333333703, 0.3219752754296894559, 0.3333333333333333703, 0.3219752754296894559, 0.3333333333333333703, 0.3219752754296894559, 0.3333333333333333703, 0.3219752754296894559, 0.3333333333333333703, 0.3219752754296894559, 0.3333333333333333703, 0.3219752754296894559, 0.3333333333333333703, 0.3219752754296894559, 0.3333333333333333703, 0.3219752754296894559, 0.3333333333333333703, 0.3219752754296894559, 0.3333333333333333703, 0.3219752754296894559, 0.3333333333333333703, 0.3219752754296894559, 0.3333333333333333703, 0.3219752754296894559, 0.3333333333333333703, 0.3219752754296894559, 0.3333333333333333703, 0.3219752754296894559, 0.3333333333333333703, 0.3219752754296894559, 0.3333333333333333703, 0.3219752754296894559, 0.3333333333333333703, 0.3219752754296894559, 0.3333333333333333703, 0.3219752754296894559, 0.3333333333333333703, 0.3219752754296894559, 0.3333333333333333703, 0.3219752754296894559, 0.3333333333333333703, 0.3219752754296894559, 0.3333333333333333703, 0.3219752754296894559, 0.3333333333333333703, 0.3219752754296894559, 0.3333333333333333703, 0.3219752754296894559, 0.3333333333333333703, 0.3219752754296894559, 0.3333333333333333703, 0.3219752754296894559, 0.3333333333333333703, 0.3219752754296894559, 0.3333333333333333703, 0.3219752754296894559, 0.3333333333333333703, 0.3219752754296894559, 0.3333333333333333703, 0.3219752754296894559, 0.3333333333333333703, 0.3219752754296894559, 0.3333333333333333703, 0.3219752754296894559, 0.3333333333333333703, 0.3219752754296894559, 0.3333333333333333703, 0.3219752754296894559, 0.3333333333333333703, 0.3219752754296894559, 0.3333333333333333703, 0.3219752754296894559, 0.3333333333333333703, 0.3219752754296894559, 0.3333333333333333703, 0.3219752754296894559, 0.3333333333333333703, 0.3219752754296894559, 0.3333333333333333703, 0.3219752754296894559, 0.3333333333333333703, 0.3219752754296894559, 0.3333333333333333703, 0.3219752754296894559, 0.3333333333333333703, 0.3219752754296894559, 0.3333333333333333703, 0.3219752754296894559, 0.3333333333333333703, 0.3219752754296894559, 0.3333333333333333703, 0.3219752754296894559, 0.3333333333333333703, 0.3219752754296894559, 0.3333333333333333703, 0.3219752754296894559, 0.3333333333333333703, 0.3219752754296894559, 0.3333333333333333703, 0.3219752754296894559, 0.3333333333333333703, 0.3219752754296894559, 0.3333333333333333703, 0.3219752754296894559, 0.3333333333333333703, 0.3219752754296894559, 0.3333333333333333703, 0.3219752754296894559, 0.3333333333333333703, 0.3219752754296894559, 0.3333333333333333703, 0.3219752754296894559, 0.3333333333333333703, 0.3219752754296894559, 0.3333333333333333703, 0.3219752754296894559, 0.3333333333333333703, 0.3219752754296894559, 0.3333333333333333703, 0.3219752754296894559, 0.3333333333333333703, 0.3219752754296894559, 0.3333333333333333703, 0.3219752754296894559, 0.3333333333333333703, 0.3219752754296894559, 0.3333333333333333703, 0.3219752754296894559, 0.3333333333333333703, 0.3219752754296894559, 0.3333333333333333703, 0.3219752754296894559, 0.3333333333333333703, 0.3219752754296894559, 0.3333333333333333703, 0.3219752754296894559, 0.3333333333333333703, 0.3219752754296894559, 0.3333333333333333703, 0.3219752754296894559, 0.3333333333333333703, 0.3219752754296894559, 0.3333333333333333703, 0.3219752754296894559, 0.3333333333333333703, 0.3219752754296894559, 0.3333333333333333703, 0.3219752754296894559, 0.3333333333333333703, 0.3219752754296894559, 0.3333333333333333703, 0.3219752754296894559, 0.3333333333333333703, 0.3219752754296894559, 0.3333333333333333703, 0.3219752754296894559, 0.3333333333333333703, 0.3219752754296894559, 0.3333333333333333703, 0.3219752754296894559, 0.3333333333333333703, 0.3219752754296894559, 0.3333333333333333703, 0.3219752754296894559, 0.3333333333333333703, 0.3219752754296894559, 0.3333333333333333703, 0.3219752754296894559, 0.3333333333333333703, 0.3219752754296894559, 0.3333333333333333703, 0.3219752754296894559, 0.3333333333333333703, 0.3219752754296894559, 0.3333333333333333703, 0.3219752754296894559, 0.3333333333333333703, 0.3219752754296894559, 0.3333333333333333703, 0.3219752754296894559, 0.3333333333333333703, 0.3219752754296894559, 0.3333333333333333703, 0.3219752754296894559, 0.3333333333333333703, 0.3219752754296894559, 0.3333333333333333703, 0.3219752754296894559, 0.3333333333333333703, 0.3219752754296894559, 0.3333333333333333703, 0.3219752754296894559, 0.3333333333333333703, 0.3219752754296894559, 0.3333333333333333703, 0.3219752754296894559, 0.3333333333333333703, 0.3219752754296894559, 0.3333333333333333703, 0.3219752754296894559, 0.3333333333333333703, 0.3219752754296894559, 0.3333333333333333703, 0.3219752754296894559, 0.3333333333333333703, 0.3219752754296894559, 0.3333333333333333703, 0.3219752754296894559, 0.3333333333333333703, 0.3219752754296894559, 0.3333333333333333703, 0.3219752754296894559, 0.3333333333333333703, 0.3219752754296894559, 0.3333333333333333703, 0.3219752754296894559, 0.3333333333333333703, 0.3219752754296894559, 0.3333333333333333703, 0.3219752754296894559, 0.3333333333333333703, 0.3219752754296894559, 0.3333333333333333703, 0.3219752754296894559, 0.3333333333333333703, 0.3219752754296894559, 0.3333333333333333703, 0.3219752754296894559, 0.3333333333333333703, 0.3219752754296894559, 0.3333333333333333703, 0.3219752754296894559, 0.3333333333333333703, 0.3219752754296894559, 0.3333333333333333703, 0.3219752754296894559, 0.3333333333333333703, 0.3219752754296894559, 0.3333333333333333703, 0.3219752754296894559, 0.3333333333333333703, 0.3219752754296894559, 0.3333333333333333703, 0.3219752754296894559, 0.3333333333333333703, 0.3219752754296894559, 0.3333333333333333703, 0.3219752754296894559, 0.3333333333333333703, 0.3219752754296894559, 0.3333333333333333703, 0.3219752754296894559, 0.3333333333333333703, 0.3219752754296894559, 0.3333333333333333703, 0.3219752754296894559, 0.3333333333333333703, 0.3219752754296894559, 0.3333333333333333703, 0.3219752754296894559, 0.3333333333333333703, 0.3219752754296894559, 0.3333333333333333703, 0.3219752754296894559, 0.3333333333333333703, 0.3219752754296894559, 0.3333333333333333703, 0.3219752754296894559, 0.3333333333333333703, 0.3219752754296894559, 0.3333333333333333703, 0.3219752754296894559, 0.3333333333333333703, 0.3219752754296894559, 0.3333333333333333703, 0.3219752754296894559, 0.3333333333333333703, 0.3219752754296894559, 0.3333333333333333703, 0.3219752754296894559, 0.3333333333333333703, 0.3219752754296894559, 0.3333333333333333703, 0.3219752754296894559, 0.3333333333333333703, 0.3219752754296894559, 0.3333333333333333703, 0.3219752754296894559, 0.3333333333333333703, 0.3219752754296894559, 0.3333333333333333703, 0.3219752754296894559, 0.3333333333333333703, 0.3219752754296894559, 0.3333333333333333703, 0.3219752754296894559, 0.3333333333333333703, 0.3219752754296894559, 0.3333333333333333703, 0.3219752754296894559, 0.3333333333333333703, 0.3219752754296894559, 0.3333333333333333703, 0.3219752754296894559, 0.3333333333333333703, 0.3219752754296894559, 0.3333333333333333703, 0.3219752754296894559, 0.3333333333333333703, 0.3219752754296894559, 0.3333333333333333703, 0.3219752754296894559, 0.3333333333333333703, 0.3219752754296894559, 0.3333333333333333703, 0.3219752754296894559, 0.3333333333333333703, 0.3219752754296894559, 0.3333333333333333703, 0.3219752754296894559, 0.3333333333333333703, 0.3219752754296894559, 0.3333333333333333703, 0.3219752754296894559, 0.3333333333333333703, 0.3219752754296894559, 0.3333333333333333703, 0.3219752754296894559, 0.3333333333333333703, 0.3219752754296894559, 0.3333333333333333703, 0.3219752754296894559, 0.3333333333333333703, 0.3219752754296894559, 0.3333333333333333703, 0.3219752754296894559, 0.3333333333333333703, 0.3219752754296894559, 0.3333333333333333703, 0.3219752754296894559, 0.3333333333333333703, 0.3219752754296894559, 0.3333333333333333703, 0.3219752754296894559, 0.3333333333333333703, 0.3219752754296894559, 0.3333333333333333703, 0.3219752754296894559, 0.3333333333333333703, 0.3219752754296894559, 0.3333333333333333703, 0.3219752754296894559, 0.3333333333333333703, 0.3219752754296894559, 0.3333333333333333703, 0.3219752754296894559, 0.3333333333333333703, 0.3219752754296894559, 0.3333333333333333703, 0.3219752754296894559, 0.3333333333333333703, 0.3219752754296894559, 0.3333333333333333703, 0.3219752754296894559, 0.3333333333333333703, 0.3219752754296894559, 0.3333333333333333703, 0.3219752754296894559, 0.3333333333333333703, 0.3219752754296894559, 0.3333333333333333703, 0.3219752754296894559, 0.3333333333333333703, 0.3219752754296894559, 0.3333333333333333703, 0.3219752754296894559, 0.3333333333333333703, 0.3219752754296894559, 0.3333333333333333703, 0.3219752754296894559, 0.3333333333333333703, 0.3219752754296894559, 0.3333333333333333703, 0.3219752754296894559, 0.3333333333333333703, 0.3219752754296894559, 0.3333333333333333703, 0.3219752754296894559, 0.3333333333333333703, 0.3219752754296894559, 0.3333333333333333703, 0.3219752754296894559, 0.3333333333333333703, 0.3219752754296894559, 0.3333333333333333703, 0.3219752754296894559, 0.3333333333333333703, 0.3219752754296894559, 0.3333333333333333703, 0.3219752754296894559, 0.3333333333333333703, 0.3219752754296894559, 0.3333333333333333703, 0.3219752754296894559, 0.3333333333333333703, 0.3219752754296894559, 0.3333333333333333703, 0.3219752754296894559, 0.3333333333333333703, 0.3219752754296894559, 0.3333333333333333703, 0.3219752754296894559, 0.3333333333333333703, 0.3219752754296894559, 0.3333333333333333703, 0.3219752754296894559, 0.3333333333333333703, 0.3219752754296894559, 0.3333333333333333703, 0.3219752754296894559, 0.3333333333333333703, 0.3219752754296894559, 0.3333333333333333703, 0.3219752754296894559, 0.3333333333333333703, 0.3219752754296894559, 0.3333333333333333703, 0.3219752754296894559, 0.3333333333333333703, 0.3219752754296894559, 0.3333333333333333703, 0.3219752754296894559, 0.3333333333333333703, 0.3219752754296894559, 0.3333333333333333703, 0.3219752754296894559, 0.3333333333333333703, 0.3219752754296894559, 0.3333333333333333703),
 ( 1.000000000000000000, 0.9659258262890683122, 1.000000000000000000, 0.9659258262890683122, 1.000000000000000000, 0.9659258262890683122, 1.000000000000000000, 0.9659258262890683122, 1.000000000000000000, 0.9659258262890683122, 1.000000000000000000, 0.9659258262890683122, 1.000000000000000000, 0.9659258262890683122, 1.000000000000000000, 0.9659258262890683122, 1.000000000000000000, 0.9659258262890683122, 1.000000000000000000, 0.9659258262890683122, 1.000000000000000000, 0.9659258262890683122, 1.000000000000000000, 0.9659258262890683122, 1.000000000000000000, 0.9659258262890683122, 1.000000000000000000, 0.9659258262890683122, 1.000000000000000000, 0.9659258262890683122, 1.000000000000000000, 0.9659258262890683122, 1.000000000000000000, 0.9659258262890683122, 1.000000000000000000, 0.9659258262890683122, 1.000000000000000000, 0.9659258262890683122, 1.000000000000000000, 0.9659258262890683122, 1.000000000000000000, 0.9659258262890683122, 1.000000000000000000, 0.9659258262890683122, 1.000000000000000000, 0.9659258262890683122, 1.000000000000000000, 0.9659258262890683122, 1.000000000000000000, 0.9659258262890683122, 1.000000000000000000, 0.9659258262890683122, 1.000000000000000000, 0.9659258262890683122, 1.000000000000000000, 0.9659258262890683122, 1.000000000000000000, 0.9659258262890683122, 1.000000000000000000, 0.9659258262890683122, 1.000000000000000000, 0.9659258262890683122, 1.000000000000000000, 0.9659258262890683122, 1.000000000000000000, 0.9659258262890683122, 1.000000000000000000, 0.9659258262890683122, 1.000000000000000000, 0.9659258262890683122, 1.000000000000000000, 0.9659258262890683122, 1.000000000000000000, 0.9659258262890683122, 1.000000000000000000, 0.9659258262890683122, 1.000000000000000000, 0.9659258262890683122, 1.000000000000000000, 0.9659258262890683122, 1.000000000000000000, 0.9659258262890683122, 1.000000000000000000, 0.9659258262890683122, 1.000000000000000000, 0.9659258262890683122, 1.000000000000000000, 0.9659258262890683122, 1.000000000000000000, 0.9659258262890683122, 1.000000000000000000, 0.9659258262890683122, 1.000000000000000000, 0.9659258262890683122, 1.000000000000000000, 0.9659258262890683122, 1.000000000000000000, 0.9659258262890683122, 1.000000000000000000, 0.9659258262890683122, 1.000000000000000000, 0.9659258262890683122, 1.000000000000000000, 0.9659258262890683122, 1.000000000000000000, 0.9659258262890683122, 1.000000000000000000, 0.9659258262890683122, 1.000000000000000000, 0.9659258262890683122, 1.000000000000000000, 0.9659258262890683122, 1.000000000000000000, 0.9659258262890683122, 1.000000000000000000, 0.9659258262890683122, 1.000000000000000000, 0.9659258262890683122, 1.000000000000000000, 0.9659258262890683122, 1.000000000000000000, 0.9659258262890683122, 1.000000000000000000, 0.9659258262890683122, 1.000000000000000000, 0.9659258262890683122, 1.000000000000000000, 0.9659258262890683122, 1.000000000000000000, 0.9659258262890683122, 1.000000000000000000, 0.9659258262890683122, 1.000000000000000000, 0.9659258262890683122, 1.000000000000000000, 0.9659258262890683122, 1.000000000000000000, 0.9659258262890683122, 1.000000000000000000, 0.9659258262890683122, 1.000000000000000000, 0.9659258262890683122, 1.000000000000000000, 0.9659258262890683122, 1.000000000000000000, 0.9659258262890683122, 1.000000000000000000, 0.9659258262890683122, 1.000000000000000000, 0.9659258262890683122, 1.000000000000000000, 0.9659258262890683122, 1.000000000000000000, 0.9659258262890683122, 1.000000000000000000, 0.9659258262890683122, 1.000000000000000000, 0.9659258262890683122, 1.000000000000000000, 0.9659258262890683122, 1.000000000000000000, 0.9659258262890683122, 1.000000000000000000, 0.9659258262890683122, 1.000000000000000000, 0.9659258262890683122, 1.000000000000000000, 0.9659258262890683122, 1.000000000000000000, 0.9659258262890683122, 1.000000000000000000, 0.9659258262890683122, 1.000000000000000000, 0.9659258262890683122, 1.000000000000000000, 0.9659258262890683122, 1.000000000000000000, 0.9659258262890683122, 1.000000000000000000, 0.9659258262890683122, 1.000000000000000000, 0.9659258262890683122, 1.000000000000000000, 0.9659258262890683122, 1.000000000000000000, 0.9659258262890683122, 1.000000000000000000, 0.9659258262890683122, 1.000000000000000000, 0.9659258262890683122, 1.000000000000000000, 0.9659258262890683122, 1.000000000000000000, 0.9659258262890683122, 1.000000000000000000, 0.9659258262890683122, 1.000000000000000000, 0.9659258262890683122, 1.000000000000000000, 0.9659258262890683122, 1.000000000000000000, 0.9659258262890683122, 1.000000000000000000, 0.9659258262890683122, 1.000000000000000000, 0.9659258262890683122, 1.000000000000000000, 0.9659258262890683122, 1.000000000000000000, 0.9659258262890683122, 1.000000000000000000, 0.9659258262890683122, 1.000000000000000000, 0.9659258262890683122, 1.000000000000000000, 0.9659258262890683122, 1.000000000000000000, 0.9659258262890683122, 1.000000000000000000, 0.9659258262890683122, 1.000000000000000000, 0.9659258262890683122, 1.000000000000000000, 0.9659258262890683122, 1.000000000000000000, 0.9659258262890683122, 1.000000000000000000, 0.9659258262890683122, 1.000000000000000000, 0.9659258262890683122, 1.000000000000000000, 0.9659258262890683122, 1.000000000000000000, 0.9659258262890683122, 1.000000000000000000, 0.9659258262890683122, 1.000000000000000000, 0.9659258262890683122, 1.000000000000000000, 0.9659258262890683122, 1.000000000000000000, 0.9659258262890683122, 1.000000000000000000, 0.9659258262890683122, 1.000000000000000000, 0.9659258262890683122, 1.000000000000000000, 0.9659258262890683122, 1.000000000000000000, 0.9659258262890683122, 1.000000000000000000, 0.9659258262890683122, 1.000000000000000000, 0.9659258262890683122, 1.000000000000000000, 0.9659258262890683122, 1.000000000000000000, 0.9659258262890683122, 1.000000000000000000, 0.9659258262890683122, 1.000000000000000000, 0.9659258262890683122, 1.000000000000000000, 0.9659258262890683122, 1.000000000000000000, 0.9659258262890683122, 1.000000000000000000, 0.9659258262890683122, 1.000000000000000000, 0.9659258262890683122, 1.000000000000000000, 0.9659258262890683122, 1.000000000000000000, 0.9659258262890683122, 1.000000000000000000, 0.9659258262890683122, 1.000000000000000000, 0.9659258262890683122, 1.000000000000000000, 0.9659258262890683122, 1.000000000000000000, 0.9659258262890683122, 1.000000000000000000, 0.9659258262890683122, 1.000000000000000000, 0.9659258262890683122, 1.000000000000000000, 0.9659258262890683122, 1.000000000000000000, 0.9659258262890683122, 1.000000000000000000, 0.9659258262890683122, 1.000000000000000000, 0.9659258262890683122, 1.000000000000000000, 0.9659258262890683122, 1.000000000000000000, 0.9659258262890683122, 1.000000000000000000, 0.9659258262890683122, 1.000000000000000000, 0.9659258262890683122, 1.000000000000000000, 0.9659258262890683122, 1.000000000000000000, 0.9659258262890683122, 1.000000000000000000, 0.9659258262890683122, 1.000000000000000000, 0.9659258262890683122, 1.000000000000000000, 0.9659258262890683122, 1.000000000000000000, 0.9659258262890683122, 1.000000000000000000, 0.9659258262890683122, 1.000000000000000000, 0.9659258262890683122, 1.000000000000000000, 0.9659258262890683122, 1.000000000000000000, 0.9659258262890683122, 1.000000000000000000, 0.9659258262890683122, 1.000000000000000000, 0.9659258262890683122, 1.000000000000000000, 0.9659258262890683122, 1.000000000000000000, 0.9659258262890683122, 1.000000000000000000, 0.9659258262890683122, 1.000000000000000000, 0.9659258262890683122, 1.000000000000000000, 0.9659258262890683122, 1.000000000000000000, 0.9659258262890683122, 1.000000000000000000, 0.9659258262890683122, 1.000000000000000000, 0.9659258262890683122, 1.000000000000000000, 0.9659258262890683122, 1.000000000000000000, 0.9659258262890683122, 1.000000000000000000, 0.9659258262890683122, 1.000000000000000000, 0.9659258262890683122, 1.000000000000000000, 0.9659258262890683122, 1.000000000000000000, 0.9659258262890683122, 1.000000000000000000, 0.9659258262890683122, 1.000000000000000000, 0.9659258262890683122, 1.000000000000000000, 0.9659258262890683122, 1.000000000000000000, 0.9659258262890683122, 1.000000000000000000, 0.9659258262890683122, 1.000000000000000000, 0.9659258262890683122, 1.000000000000000000, 0.9659258262890683122, 1.000000000000000000, 0.9659258262890683122, 1.000000000000000000, 0.9659258262890683122, 1.000000000000000000, 0.9659258262890683122, 1.000000000000000000, 0.9659258262890683122, 1.000000000000000000, 0.9659258262890683122, 1.000000000000000000, 0.9659258262890683122, 1.000000000000000000, 0.9659258262890683122, 1.000000000000000000, 0.9659258262890683122, 1.000000000000000000, 0.9659258262890683122, 1.000000000000000000, 0.9659258262890683122, 1.000000000000000000, 0.9659258262890683122, 1.000000000000000000, 0.9659258262890683122, 1.000000000000000000, 0.9659258262890683122, 1.000000000000000000, 0.9659258262890683122, 1.000000000000000000, 0.9659258262890683122, 1.000000000000000000, 0.9659258262890683122, 1.000000000000000000, 0.9659258262890683122, 1.000000000000000000, 0.9659258262890683122, 1.000000000000000000, 0.9659258262890683122, 1.000000000000000000, 0.9659258262890683122, 1.000000000000000000, 0.9659258262890683122, 1.000000000000000000, 0.9659258262890683122, 1.000000000000000000, 0.9659258262890683122, 1.000000000000000000, 0.9659258262890683122, 1.000000000000000000, 0.9659258262890683122, 1.000000000000000000, 0.9659258262890683122, 1.000000000000000000, 0.9659258262890683122, 1.000000000000000000, 0.9659258262890683122, 1.000000000000000000, 0.9659258262890683122, 1.000000000000000000, 0.9659258262890683122, 1.000000000000000000, 0.9659258262890683122, 1.000000000000000000, 0.9659258262890683122, 1.000000000000000000, 0.9659258262890683122, 1.000000000000000000, 0.9659258262890683122, 1.000000000000000000, 0.9659258262890683122, 1.000000000000000000, 0.9659258262890683122, 1.000000000000000000, 0.9659258262890683122, 1.000000000000000000, 0.9659258262890683122, 1.000000000000000000, 0.9659258262890683122, 1.000000000000000000, 0.9659258262890683122, 1.000000000000000000, 0.9659258262890683122, 1.000000000000000000, 0.9659258262890683122, 1.000000000000000000, 0.9659258262890683122, 1.000000000000000000, 0.9659258262890683122, 1.000000000000000000) ) ) 
 REPRESENTATION_ITEM ( '' )  SURFACE ( )  );
#181640 = CARTESIAN_POINT ( 'NONE',  ( 0.05219959533907565091, 21.53943276465977519, 89.99890960531438111 ) ) ;
#181642 = CARTESIAN_POINT ( 'NONE',  ( -9.474510206698720793, -16.51473224551083518, 54.58442372801899722 ) ) ;
#181641 = CARTESIAN_POINT ( 'NONE',  ( 4.379528057220339221, -16.55341960407611168, 77.70724293864770971 ) ) ;
#181643 = CARTESIAN_POINT ( 'NONE',  ( -5.719274019375978568, 21.55341960407610458, 75.20724293864769550 ) ) ;
#181644 = CARTESIAN_POINT ( 'NONE',  ( 21.53943276465977519, -0.05219959533907433946, 53.74890960531437401 ) ) ;
#181645 = CARTESIAN_POINT ( 'NONE',  ( 12.14591786802309770, 12.06949235617756955, 34.37390960531435979 ) ) ;
#181646 = CARTESIAN_POINT ( 'NONE',  ( 0.05219959533937995610, -21.53943276465977519, 100.0010903946857042 ) ) ;
#181647 = CARTESIAN_POINT ( 'NONE',  ( -19.02544592524342804, 5.153800228976336051, 76.04057627198102409 ) ) ;
#181648 = CARTESIAN_POINT ( 'NONE',  ( -5.049401038298153566, 19.05341960407611168, 35.20724293864768839 ) ) ;
#181649 = CARTESIAN_POINT ( 'NONE',  ( -21.55341960407619339, 5.719274019375674811, 43.54275706135235424 ) ) ;
#181650 = CARTESIAN_POINT ( 'NONE',  ( -5.823673210054431948, 21.52544592524334988, 42.70942372801901854 ) ) ;
#181651 = CARTESIAN_POINT ( 'NONE',  ( -13.89961937509977652, 13.97604488694528158, 45.62390960531433848 ) ) ;
#181652 = CARTESIAN_POINT ( 'NONE',  ( -21.53943276465977519, 0.05219959533907696930, 116.2489096053143669 ) ) ;
#181653 = CARTESIAN_POINT ( 'NONE',  ( -19.02544592524334988, -5.153800228976617603, 63.95942372801899012 ) ) ;
#181654 = CARTESIAN_POINT ( 'NONE',  ( -0.05219959533909027116, -19.03943276465977164, 32.49890960531435979 ) ) ;
#181655 = CARTESIAN_POINT ( 'NONE',  ( -4.483927247898782831, 16.52544592524335698, 27.70942372801901854 ) ) ;
#181656 = CARTESIAN_POINT ( 'NONE',  ( 19.05341960407611168, 5.049401038298154454, 23.95724293864769194 ) ) ;
#181657 = CARTESIAN_POINT ( 'NONE',  ( 14.34966873604972726, -8.224510206698740333, 70.83442372801901854 ) ) ;
#181658 = CARTESIAN_POINT ( 'NONE',  ( 19.03943276465977164, -0.05219959533909143690, 38.74890960531436690 ) ) ;
#181659 = DIRECTION ( 'NONE',  ( -1.000000000000000000, 0.000000000000000000, 0.000000000000000000 ) ) ;
#181660 = CARTESIAN_POINT ( 'NONE',  ( 9.474510206698971260, -16.51473224551069308, 87.91557627198102409 ) ) ;
#181661 = CARTESIAN_POINT ( 'NONE',  ( -5.153800228976328057, -19.02544592524343514, 22.29057627198102765 ) ) ;
#181662 = CARTESIAN_POINT ( 'NONE',  ( -18.62759615963270932, 10.81492255796079327, 75.83224293864769550 ) ) ;
#181663 = CARTESIAN_POINT ( 'NONE',  ( -14.34966873604972548, 8.224510206698743886, 43.33442372801901143 ) ) ;
#181664 = CARTESIAN_POINT ( 'NONE',  ( -15.72974639402176322, -15.80617190586768395, 104.3760903946856899 ) ) ;
#181665 = CARTESIAN_POINT ( 'NONE',  ( 19.05341960407611168, 5.049401038298154454, 43.95724293864769550 ) ) ;
#181666 = CARTESIAN_POINT ( 'NONE',  ( 8.314922557960818139, 14.29746914071049879, 34.58224293864770260 ) ) ;
#181667 = CARTESIAN_POINT ( 'NONE',  ( -12.06949235617756955, 12.14591786802309770, 70.62390960531436690 ) ) ;
#181668 = CARTESIAN_POINT ( 'NONE',  ( -9.474510206698964154, 16.51473224551069663, 60.41557627198102409 ) ) ;
#181669 = CARTESIAN_POINT ( 'NONE',  ( -5.823673210054431948, 21.52544592524334988, 112.7094237280190328 ) ) ;
#181670 = CARTESIAN_POINT ( 'NONE',  ( -0.05219959533937732626, 21.53943276465977519, 22.50109039468567573 ) ) ;
#181671 = CARTESIAN_POINT ( 'NONE',  ( -13.89961937509977652, 13.97604488694528158, 85.62390960531433848 ) ) ;
#181672 = CARTESIAN_POINT ( 'NONE',  ( 5.719274019375673035, 21.55341960407619339, 92.29275706135236135 ) ) ;
#181673 = CARTESIAN_POINT ( 'NONE',  ( -4.483927247898782831, 16.52544592524335698, 57.70942372801901143 ) ) ;
#181674 = CARTESIAN_POINT ( 'NONE',  ( -16.53943276465976808, -0.05219959533934237506, 28.75109039468567929 ) ) ;
#181676 = CARTESIAN_POINT ( 'NONE',  ( 18.62759615963255655, 10.81492255796105972, 101.6677570613523613 ) ) ;
#181675 = CARTESIAN_POINT ( 'NONE',  ( -14.29746914071049879, 8.314922557960819915, 90.83224293864769550 ) ) ;
#181677 = CARTESIAN_POINT ( 'NONE',  ( -0.05219959533910754901, -16.53943276465976808, 37.49890960531436690 ) ) ;
#181678 = CARTESIAN_POINT ( 'NONE',  ( -16.46253265017160317, 9.564922557960807481, 30.83224293864769550 ) ) ;
#181679 = CARTESIAN_POINT ( 'NONE',  ( -16.53943276465976808, -0.05219959533934237506, 58.75109039468568994 ) ) ;
#181680 = CARTESIAN_POINT ( 'NONE',  ( 14.29746914071049879, -8.314922557960816363, 48.33224293864770260 ) ) ;
#181681 = CARTESIAN_POINT ( 'NONE',  ( -14.34966873604972548, 8.224510206698743886, 98.33442372801901854 ) ) ;
#181682 = CARTESIAN_POINT ( 'NONE',  ( 5.049401038298161559, -19.05341960407611168, 112.7072429386476813 ) ) ;
#181683 = CARTESIAN_POINT ( 'NONE',  ( 10.72451020669898902, -18.67979575497178502, 32.91557627198102409 ) ) ;
#181684 = CARTESIAN_POINT ( 'NONE',  ( -0.05219959533937732626, 21.53943276465977519, 112.5010903946857042 ) ) ;
#181685 = CARTESIAN_POINT ( 'NONE',  ( -14.34966873604960291, -8.224510206698953496, 81.66557627198103830 ) ) ;
#181686 = CARTESIAN_POINT ( 'NONE',  ( 19.03943276465977164, -0.05219959533909143690, 98.74890960531436690 ) ) ;
#181687 = EDGE_LOOP ( 'NONE', ( #121638, #103041, #56743 ) ) ;
#181688 = CARTESIAN_POINT ( 'NONE',  ( 14.29746914071037800, 8.314922557961029526, 41.66775706135235424 ) ) ;
#181689 = CARTESIAN_POINT ( 'NONE',  ( 13.97604488694527802, 13.89961937509977652, 39.37390960531435269 ) ) ;
#181690 = CARTESIAN_POINT ( 'NONE',  ( 16.52544592524335698, 4.483927247898782831, 51.45942372801901854 ) ) ;
#181691 = CARTESIAN_POINT ( 'NONE',  ( 16.51473224551083163, -9.474510206698727899, 45.83442372801900433 ) ) ;
#181692 = CARTESIAN_POINT ( 'NONE',  ( -0.05219959533909027116, -19.03943276465977164, 47.49890960531435979 ) ) ;
#181693 = CARTESIAN_POINT ( 'NONE',  ( -14.29746914071037622, -8.314922557961029526, 84.16775706135234714 ) ) ;
#181694 = CARTESIAN_POINT ( 'NONE',  ( 5.049401038297881783, 19.05341960407617563, 77.29275706135231871 ) ) ;
#181695 = CARTESIAN_POINT ( 'NONE',  ( -5.049401038297874678, -19.05341960407617918, 24.79275706135233648 ) ) ;
#181696 = CARTESIAN_POINT ( 'NONE',  ( -13.89961937509977652, 13.97604488694528158, 55.62390960531434558 ) ) ;
#181697 = CARTESIAN_POINT ( 'NONE',  ( 4.379528057220339221, -16.55341960407611168, 92.70724293864770971 ) ) ;
#181698 = CARTESIAN_POINT ( 'NONE',  ( -19.03943276465977164, -0.05219959533935918106, 63.75109039468566863 ) ) ;
#181699 = CARTESIAN_POINT ( 'NONE',  ( -5.719274019375978568, 21.55341960407610458, 60.20724293864768839 ) ) ;
#181700 = CARTESIAN_POINT ( 'NONE',  ( -19.05341960407617563, 5.049401038297882671, 38.54275706135233293 ) ) ;
#181701 = CARTESIAN_POINT ( 'NONE',  ( 19.05341960407611168, 5.049401038298154454, 108.9572429386477097 ) ) ;
#181702 = CARTESIAN_POINT ( 'NONE',  ( 21.52544592524344225, -5.823673210054117533, 73.54057627198102409 ) ) ;
#181703 = CARTESIAN_POINT ( 'NONE',  ( -16.52216118717208104, 7.221426719304498754, 83.92400978953007495 ) ) ;
#181704 = CARTESIAN_POINT ( 'NONE',  ( -16.51473224551082808, 9.474510206698731452, 103.3344237280190043 ) ) ;
#181705 = CARTESIAN_POINT ( 'NONE',  ( 37.58407650405589351, 2.428612866815129610E-14, 39.49999999999996447 ) ) ;
#181706 = CARTESIAN_POINT ( 'NONE',  ( -8.314922557961024197, 14.29746914071037800, 27.91775706135234358 ) ) ;
#181707 = CARTESIAN_POINT ( 'NONE',  ( -19.03943276465977164, 0.05219959533909376836, 31.24890960531435979 ) ) ;
#181708 = CARTESIAN_POINT ( 'NONE',  ( -18.67979575497178146, -10.72451020669898902, 21.66557627198102409 ) ) ;
#181709 = CARTESIAN_POINT ( 'NONE',  ( -18.62759615963270932, 10.81492255796079327, 85.83224293864768129 ) ) ;
#181710 = CARTESIAN_POINT ( 'NONE',  ( 15.80617190586769283, -15.72974639402175789, 55.62609039468568284 ) ) ;
#181712 = CARTESIAN_POINT ( 'NONE',  ( 21.52544592524334988, 5.823673210054432836, 106.4594237280190328 ) ) ;
#181711 = CARTESIAN_POINT ( 'NONE',  ( -16.51473224551082808, 9.474510206698731452, 103.3344237280190043 ) ) ;
#181713 = CARTESIAN_POINT ( 'NONE',  ( 4.379528057220339221, -16.55341960407611168, 22.70724293864769194 ) ) ;
#181714 = CARTESIAN_POINT ( 'NONE',  ( 21.55341960407610458, 5.719274019375980345, 93.95724293864770971 ) ) ;
#181715 = CARTESIAN_POINT ( 'NONE',  ( 4.379528057220339221, -16.55341960407611168, 52.70724293864769550 ) ) ;
#181716 = CARTESIAN_POINT ( 'NONE',  ( -16.51473224551082808, 9.474510206698731452, 78.33442372801900433 ) ) ;
#181717 = ADVANCED_FACE ( 'NONE', ( #3915 ), #113083, .T. ) ;
#181718 = CARTESIAN_POINT ( 'NONE',  ( -19.02544592524334988, -5.153800228976617603, 53.95942372801898301 ) ) ;
#181719 = CARTESIAN_POINT ( 'NONE',  ( -0.05219959533937732626, 21.53943276465977519, 72.50109039468568994 ) ) ;
#181720 = CARTESIAN_POINT ( 'NONE',  ( 5.049401038297881783, 19.05341960407617563, 37.29275706135232582 ) ) ;
#181721 = CARTESIAN_POINT ( 'NONE',  ( 14.29746914071049879, -8.314922557960816363, 103.3322429386476955 ) ) ;
#181722 = CARTESIAN_POINT ( 'NONE',  ( -0.05219959533907301413, -21.53943276465977519, 42.49890960531435979 ) ) ;
#181724 = ADVANCED_FACE ( 'NONE', ( #35260 ), #80759, .T. ) ;
#181723 = CARTESIAN_POINT ( 'NONE',  ( -8.224510206698948167, 14.34966873604960824, 30.41557627198101699 ) ) ;
#181725 = CARTESIAN_POINT ( 'NONE',  ( 15.80617190586769283, -15.72974639402175789, 105.6260903946856899 ) ) ;
#181726 = CARTESIAN_POINT ( 'NONE',  ( -4.483927247898782831, 16.52544592524335698, 67.70942372801901854 ) ) ;
#181727 = CARTESIAN_POINT ( 'NONE',  ( 4.379528057220339221, -16.55341960407611168, 27.70724293864769905 ) ) ;
#181728 = CARTESIAN_POINT ( 'NONE',  ( -21.53943276465977519, -0.05219959533937600094, 68.75109039468568994 ) ) ;
#181729 = CARTESIAN_POINT ( 'NONE',  ( -10.72451020669870658, -18.67979575497194134, 69.58442372801900433 ) ) ;
#181730 = CARTESIAN_POINT ( 'NONE',  ( 18.62759615963271287, -10.81492255796078972, 68.33224293864769550 ) ) ;
#181731 = ORIENTED_EDGE ( 'NONE', *, *, #1190, .T. ) ;
#181732 = CARTESIAN_POINT ( 'NONE',  ( -19.05341960407611168, -5.049401038298163336, 26.45724293864769550 ) ) ;
#181733 = CARTESIAN_POINT ( 'NONE',  ( -21.53943276465977519, -0.05219959533937600094, 43.75109039468568284 ) ) ;
#181734 = CARTESIAN_POINT ( 'NONE',  ( -5.153800228976328057, -19.02544592524343514, 22.29057627198102765 ) ) ;
#181735 = CARTESIAN_POINT ( 'NONE',  ( -9.564922557960796823, -16.46253265017161027, 37.08224293864768839 ) ) ;
#181736 = CARTESIAN_POINT ( 'NONE',  ( 12.06949235617757843, -12.14591786802309237, 83.12390960531436690 ) ) ;
#181737 = CARTESIAN_POINT ( 'NONE',  ( -5.049401038298153566, 19.05341960407611168, 90.20724293864766707 ) ) ;
#181738 = CARTESIAN_POINT ( 'NONE',  ( -8.314922557960811034, -14.29746914071050412, 22.08224293864769194 ) ) ;
#181739 = CARTESIAN_POINT ( 'NONE',  ( 4.379528057220339221, -16.55341960407611168, 102.7072429386476955 ) ) ;
#181740 = CARTESIAN_POINT ( 'NONE',  ( -5.719274019375978568, 21.55341960407610458, 70.20724293864769550 ) ) ;
#181741 = CARTESIAN_POINT ( 'NONE',  ( -10.81492255796078084, -18.62759615963271287, 107.0822429386476955 ) ) ;
#181742 = CARTESIAN_POINT ( 'NONE',  ( 16.46253265017160672, -9.564922557960803928, 113.3322429386476955 ) ) ;
#181744 = CARTESIAN_POINT ( 'NONE',  ( -4.483927247898782831, 16.52544592524335698, 22.70942372801901499 ) ) ;
#181743 = CARTESIAN_POINT ( 'NONE',  ( 9.564922557960805705, 16.46253265017160317, 69.58224293864770971 ) ) ;
#181745 = CARTESIAN_POINT ( 'NONE',  ( -5.823673210054116645, -21.52544592524344225, 57.29057627198103120 ) ) ;
#181746 = CARTESIAN_POINT ( 'NONE',  ( -15.72974639402176322, -15.80617190586768395, 84.37609039468570415 ) ) ;
#181747 = B_SPLINE_CURVE_WITH_KNOTS ( 'NONE', 3,
 ( #86038, #120354, #41549, #9212, #43532, #54701, #102211, #72890, #118386, #134558, #146702, #196246, #12220, #39530, #119385, #103212, #42543, #180080, #23376, #178062, #104206, #88027 ),
 .UNSPECIFIED., .F., .F.,
 ( 4, 2, 2, 2, 2, 2, 2, 2, 2, 2, 4 ),
 ( 2.778238173776314926E-07, 0.0007557225233028428031, 0.001511167222788308093, 0.002266611922273773384, 0.003022056621759238240, 0.003777501321244703530, 0.004532946020730169688, 0.004910668370472905803, 0.005288390720215642785, 0.005666113069958378899, 0.006043835419701115881 ),
 .UNSPECIFIED. ) ;
#181748 = CARTESIAN_POINT ( 'NONE',  ( -13.89961937509977652, 13.97604488694528158, 85.62390960531433848 ) ) ;
#181749 = CARTESIAN_POINT ( 'NONE',  ( -19.05341960407611168, -5.049401038298163336, 111.4572429386476671 ) ) ;
#181750 = CARTESIAN_POINT ( 'NONE',  ( 16.52544592524335698, 4.483927247898782831, 81.45942372801900433 ) ) ;
#181751 = CARTESIAN_POINT ( 'NONE',  ( -15.80617190586768217, 15.72974639402176855, 53.12609039468568284 ) ) ;
#181752 = CARTESIAN_POINT ( 'NONE',  ( -15.72974639402176322, -15.80617190586768395, 99.37609039468568994 ) ) ;
#181753 = CARTESIAN_POINT ( 'NONE',  ( 8.314922557961029526, -14.29746914071037800, 60.41775706135235424 ) ) ;
#181754 = CARTESIAN_POINT ( 'NONE',  ( -10.81492255796078084, -18.62759615963271287, 112.0822429386477097 ) ) ;
#181755 = CARTESIAN_POINT ( 'NONE',  ( 0.05219959533909260263, 19.03943276465977164, 114.9989096053143669 ) ) ;
#181756 = CARTESIAN_POINT ( 'NONE',  ( 0.05219959533907565091, 21.53943276465977519, 89.99890960531438111 ) ) ;
#181757 = CARTESIAN_POINT ( 'NONE',  ( -0.05219959533936034679, 19.03943276465977164, 42.50109039468566152 ) ) ;
#181758 = CARTESIAN_POINT ( 'NONE',  ( -10.72451020669898014, 18.67979575497178502, 45.41557627198103830 ) ) ;
#181760 = CARTESIAN_POINT ( 'NONE',  ( -16.53943276465976808, 0.05219959533911058130, 41.24890960531435269 ) ) ;
#181759 = CARTESIAN_POINT ( 'NONE',  ( 19.03943276465977164, -0.05219959533909143690, 93.74890960531435269 ) ) ;
#181761 = DIRECTION ( 'NONE',  ( 1.000000000000000000, 0.000000000000000000, 0.000000000000000000 ) ) ;
#181762 = AXIS2_PLACEMENT_3D ( 'NONE', #107961, #169648, #121152 ) ;
#181763 = CARTESIAN_POINT ( 'NONE',  ( -19.49190055781012276, -5.499999999999968026, 80.56116087098781975 ) ) ;
#181764 = CARTESIAN_POINT ( 'NONE',  ( 0.05219959533936267826, -19.03943276465977164, 100.0010903946856757 ) ) ;
#181765 = CARTESIAN_POINT ( 'NONE',  ( -21.55341960407610458, -5.719274019375992779, 71.45724293864769550 ) ) ;
#181766 = CARTESIAN_POINT ( 'NONE',  ( 8.224510206698953496, -14.34966873604960469, 52.91557627198103830 ) ) ;
#181767 = CARTESIAN_POINT ( 'NONE',  ( 8.314922557961029526, -14.29746914071037800, 30.41775706135234358 ) ) ;
#181768 = CARTESIAN_POINT ( 'NONE',  ( -13.89961937509977652, 13.97604488694528158, 45.62390960531433848 ) ) ;
#181770 = CARTESIAN_POINT ( 'NONE',  ( 5.153800228976615827, -19.02544592524334988, 80.20942372801901854 ) ) ;
#181769 = CARTESIAN_POINT ( 'NONE',  ( 10.81492255796106328, -18.62759615963255655, 20.41775706135234714 ) ) ;
#181771 = CARTESIAN_POINT ( 'NONE',  ( 13.89961937509977652, -13.97604488694527269, 78.12390960531433848 ) ) ;
#181772 = CARTESIAN_POINT ( 'NONE',  ( -16.46253265017160317, 9.564922557960807481, 70.83224293864770971 ) ) ;
#181773 = CARTESIAN_POINT ( 'NONE',  ( 0.05219959533907565091, 21.53943276465977519, 79.99890960531435269 ) ) ;
#181774 = CARTESIAN_POINT ( 'NONE',  ( 19.03943276465977164, -0.05219959533909143690, 28.74890960531435624 ) ) ;
#181775 = LINE ( 'NONE', #101932, #115496 ) ;
#181776 = CARTESIAN_POINT ( 'NONE',  ( -8.224510206698948167, 14.34966873604960824, 60.41557627198102409 ) ) ;
#181777 = CARTESIAN_POINT ( 'NONE',  ( -5.153800228976328057, -19.02544592524343514, 92.29057627198099567 ) ) ;
#181778 = CARTESIAN_POINT ( 'NONE',  ( -17.49999999999999645, -5.500000000000000888, 120.0000000000000142 ) ) ;
#181779 = CARTESIAN_POINT ( 'NONE',  ( 9.564922557961047289, -16.46253265017146816, 50.41775706135233293 ) ) ;
#181780 = CARTESIAN_POINT ( 'NONE',  ( -0.05219959533907301413, -21.53943276465977519, 77.49890960531433848 ) ) ;
#181781 = CARTESIAN_POINT ( 'NONE',  ( -13.89961937509957401, -13.97604488694547875, 39.37609039468566152 ) ) ;
#181782 = CARTESIAN_POINT ( 'NONE',  ( -0.05219959533909027116, -19.03943276465977164, 87.49890960531436690 ) ) ;
#181783 = CARTESIAN_POINT ( 'NONE',  ( -17.72560187377286667, -5.499999999999973355, 74.07814504131320632 ) ) ;
#181784 = CARTESIAN_POINT ( 'NONE',  ( 5.719274019375991003, -21.55341960407610458, 27.70724293864769905 ) ) ;
#181785 = CARTESIAN_POINT ( 'NONE',  ( -16.51473224551069308, -9.474510206698971260, 76.66557627198103830 ) ) ;
#181786 = CARTESIAN_POINT ( 'NONE',  ( -18.67979575497193778, 10.72451020669871902, 58.33442372801901143 ) ) ;
#181787 = CARTESIAN_POINT ( 'NONE',  ( -19.05341960407611168, -5.049401038298163336, 21.45724293864768839 ) ) ;
#181788 = EDGE_CURVE ( 'NONE', #26617, #108481, #157322, .T. ) ;
#181791 = ORIENTED_EDGE ( 'NONE', *, *, #105844, .F. ) ;
#181790 = CARTESIAN_POINT ( 'NONE',  ( -5.153800228976328057, -19.02544592524343514, 97.29057627198099567 ) ) ;
#181789 = CARTESIAN_POINT ( 'NONE',  ( -21.52544592524343514, 5.823673210054127303, 111.0405762719810525 ) ) ;
#181792 = CARTESIAN_POINT ( 'NONE',  ( 15.80617190586769283, -15.72974639402175789, 35.62609039468568994 ) ) ;
#181793 = ORIENTED_EDGE ( 'NONE', *, *, #47633, .T. ) ;
#181794 = CARTESIAN_POINT ( 'NONE',  ( 16.51473224551069308, 9.474510206698969483, 94.16557627198103830 ) ) ;
#181795 = VECTOR ( 'NONE', #55576, 1000.000000000000000 ) ;
#181796 = DIRECTION ( 'NONE',  ( 0.000000000000000000, 0.000000000000000000, 1.000000000000000000 ) ) ;
#181797 = CARTESIAN_POINT ( 'NONE',  ( -21.53943276465977519, 0.05219959533907696930, 101.2489096053143669 ) ) ;
#181798 = CARTESIAN_POINT ( 'NONE',  ( -5.049401038298153566, 19.05341960407611168, 65.20724293864765286 ) ) ;
#181799 = CARTESIAN_POINT ( 'NONE',  ( -16.51473224551082808, 9.474510206698731452, 113.3344237280190043 ) ) ;
#181800 = CARTESIAN_POINT ( 'NONE',  ( -29.86685920354755197, -21.69954338932560134, -2.924999997268813878 ) ) ;
#181801 = CARTESIAN_POINT ( 'NONE',  ( 10.81492255796106328, -18.62759615963255655, 105.4177570613523613 ) ) ;
#181802 = CARTESIAN_POINT ( 'NONE',  ( 16.51473224551069308, 9.474510206698969483, 49.16557627198102409 ) ) ;
#181803 = CARTESIAN_POINT ( 'NONE',  ( 5.823673210054444382, -21.52544592524334988, 105.2094237280190328 ) ) ;
#181804 = EDGE_CURVE ( 'NONE', #123761, #118127, #168782, .T. ) ;
#181806 = CARTESIAN_POINT ( 'NONE',  ( -10.72451020669870658, -18.67979575497194134, 64.58442372801900433 ) ) ;
#181805 = CARTESIAN_POINT ( 'NONE',  ( -16.46253265017160317, 9.564922557960807481, 85.83224293864769550 ) ) ;
#181807 = CARTESIAN_POINT ( 'NONE',  ( -22.44159573604010305, 16.30477369853692338, 145.1750000027311671 ) ) ;
#181808 = CARTESIAN_POINT ( 'NONE',  ( 13.97604488694527802, 13.89961937509977652, 104.3739096053143385 ) ) ;
#181809 = DIRECTION ( 'NONE',  ( -1.000000000000000000, -0.000000000000000000, -0.000000000000000000 ) ) ;
#181812 = CARTESIAN_POINT ( 'NONE',  ( -21.52544592524334988, -5.823673210054445271, 58.95942372801902565 ) ) ;
#181811 = CARTESIAN_POINT ( 'NONE',  ( 8.224510206698742110, 14.34966873604972548, 67.08442372801901854 ) ) ;
#181810 = CARTESIAN_POINT ( 'NONE',  ( 16.55341960407618274, -4.379528057220086978, 51.04275706135234714 ) ) ;
#181813 = CARTESIAN_POINT ( 'NONE',  ( -15.72974639402176322, -15.80617190586768395, 89.37609039468568994 ) ) ;
#181814 = CARTESIAN_POINT ( 'NONE',  ( -11.95556478057400973, 11.66180171105670027, -59.13370768023891344 ) ) ;
#181815 = CARTESIAN_POINT ( 'NONE',  ( -12.14591786802326823, 12.06949235617739902, 23.12609039468567573 ) ) ;
#181816 = CARTESIAN_POINT ( 'NONE',  ( 9.474510206698971260, -16.51473224551069308, 77.91557627198103830 ) ) ;
#181817 = CARTESIAN_POINT ( 'NONE',  ( -16.51473224551069308, -9.474510206698971260, 91.66557627198103830 ) ) ;
#181818 = CARTESIAN_POINT ( 'NONE',  ( -1.282731051913078346, -29.61737564226529074, -51.85482277101433368 ) ) ;
#181819 = CARTESIAN_POINT ( 'NONE',  ( 16.46253265017160672, -9.564922557960803928, 28.33224293864769550 ) ) ;
#181820 = CARTESIAN_POINT ( 'NONE',  ( 5.823673210054125526, 21.52544592524343514, 24.79057627198103120 ) ) ;
#181821 = CARTESIAN_POINT ( 'NONE',  ( -14.34966873604972548, 8.224510206698743886, 88.33442372801901854 ) ) ;
#181823 = CARTESIAN_POINT ( 'NONE',  ( 19.05341960407611168, 5.049401038298154454, 73.95724293864768129 ) ) ;
#181822 = CARTESIAN_POINT ( 'NONE',  ( -8.314922557960811034, -14.29746914071050412, 87.08224293864769550 ) ) ;
#181824 = CARTESIAN_POINT ( 'NONE',  ( -18.67979575497193778, 10.72451020669871902, 93.33442372801901854 ) ) ;
#181825 = CARTESIAN_POINT ( 'NONE',  ( -21.94104750614014065, 1.245073757423197369, -58.42286556281733567 ) ) ;
#181826 = CARTESIAN_POINT ( 'NONE',  ( -16.53943276465976808, -0.05219959533934237506, 23.75109039468567929 ) ) ;
#181827 = CARTESIAN_POINT ( 'NONE',  ( -16.53943276465976808, 0.05219959533911058130, 71.24890960531435269 ) ) ;
#181828 = CARTESIAN_POINT ( 'NONE',  ( -15.80617190586768217, 15.72974639402176855, 48.12609039468568284 ) ) ;
#181829 = CARTESIAN_POINT ( 'NONE',  ( -5.719274019375978568, 21.55341960407610458, 80.20724293864769550 ) ) ;
#181830 = CARTESIAN_POINT ( 'NONE',  ( -9.564922557961040184, 16.46253265017147172, 42.91775706135234003 ) ) ;
#181831 = CARTESIAN_POINT ( 'NONE',  ( -34.36935609104192224, 7.254501760396899535, 46.91913033384989262 ) ) ;
#181832 = CARTESIAN_POINT ( 'NONE',  ( -5.049401038298153566, 19.05341960407611168, 85.20724293864766707 ) ) ;
#181833 = CARTESIAN_POINT ( 'NONE',  ( -4.483927247898539470, -16.52544592524342804, 47.29057627198103120 ) ) ;
#181834 = CARTESIAN_POINT ( 'NONE',  ( -14.34966873604960291, -8.224510206698953496, 31.66557627198102054 ) ) ;
#181835 = CARTESIAN_POINT ( 'NONE',  ( -8.314922557961024197, 14.29746914071037800, 107.9177570613523471 ) ) ;
#181836 = CARTESIAN_POINT ( 'NONE',  ( 19.02544592524334988, 5.153800228976608722, 61.45942372801900433 ) ) ;
#181837 = DIRECTION ( 'NONE',  ( 0.000000000000000000, 0.000000000000000000, 1.000000000000000000 ) ) ;
#181838 = CARTESIAN_POINT ( 'NONE',  ( -21.55341960407610458, -5.719274019375992779, 21.45724293864769550 ) ) ;
#181839 = CARTESIAN_POINT ( 'NONE',  ( -14.29746914071049879, 8.314922557960819915, 85.83224293864768129 ) ) ;
#181840 = CARTESIAN_POINT ( 'NONE',  ( -0.3535533905929588716, 30.00000000000000711, 4.646446609406719830 ) ) ;
#181842 = CARTESIAN_POINT ( 'NONE',  ( -10.72451020669898014, 18.67979575497178502, 40.41557627198103120 ) ) ;
#181841 = CARTESIAN_POINT ( 'NONE',  ( 13.89961937509977652, -13.97604488694527269, 28.12390960531435624 ) ) ;
#181843 = CARTESIAN_POINT ( 'NONE',  ( 21.55341960407610458, 5.719274019375980345, 73.95724293864769550 ) ) ;
#181844 = CARTESIAN_POINT ( 'NONE',  ( 12.06949235617757843, -12.14591786802309237, 113.1239096053143953 ) ) ;
#181846 = CARTESIAN_POINT ( 'NONE',  ( 16.51473224551069308, 9.474510206698969483, 44.16557627198103120 ) ) ;
#181845 = CARTESIAN_POINT ( 'NONE',  ( -16.53943276465976808, -0.05219959533934237506, 63.75109039468568284 ) ) ;
#181847 = CARTESIAN_POINT ( 'NONE',  ( 0.05219959533937995610, -21.53943276465977519, 55.00109039468568284 ) ) ;
#181848 = ORIENTED_EDGE ( 'NONE', *, *, #132933, .F. ) ;
#181849 = CARTESIAN_POINT ( 'NONE',  ( -4.379528057220328563, 16.55341960407611168, 110.2072429386477239 ) ) ;
#181850 = CARTESIAN_POINT ( 'NONE',  ( -5.049401038297874678, -19.05341960407617918, 89.79275706135230450 ) ) ;
#181851 = CARTESIAN_POINT ( 'NONE',  ( 11.40812507854754365, 35.11059874428196537, -3.724999997268813701 ) ) ;
#181853 = CARTESIAN_POINT ( 'NONE',  ( 15.72974639402199770, -15.80617190586745480, 38.12390960531436690 ) ) ;
#181852 = CARTESIAN_POINT ( 'NONE',  ( -0.9841389949900990475, -21.65131445265850019, -58.61993113718296655 ) ) ;
#181854 = DIRECTION ( 'NONE',  ( 1.000000000000000000, 0.000000000000000000, 0.000000000000000000 ) ) ;
#181855 = CARTESIAN_POINT ( 'NONE',  ( 15.80617190586769283, -15.72974639402175789, 75.62609039468567573 ) ) ;
#181857 = CARTESIAN_POINT ( 'NONE',  ( -12.14591786802309592, -12.06949235617757132, 46.87390960531435979 ) ) ;
#181856 = CARTESIAN_POINT ( 'NONE',  ( -8.314922557961024197, 14.29746914071037800, 57.91775706135234714 ) ) ;
#181858 = CARTESIAN_POINT ( 'NONE',  ( 10.81492255796078972, 18.62759615963270932, 64.58224293864769550 ) ) ;
#181859 = CARTESIAN_POINT ( 'NONE',  ( -21.53943276465977519, 0.05219959533907696930, 61.24890960531435979 ) ) ;
#181860 = CARTESIAN_POINT ( 'NONE',  ( -21.91636330721479808, -8.102911641865347292, 172.4379571683061556 ) ) ;
#181862 = CARTESIAN_POINT ( 'NONE',  ( -5.823673210054116645, -21.52544592524344225, 22.29057627198102765 ) ) ;
#181861 = CARTESIAN_POINT ( 'NONE',  ( 19.05341960407617918, -5.049401038297876454, 81.04275706135231871 ) ) ;
#181863 = CARTESIAN_POINT ( 'NONE',  ( 5.049401038298161559, -19.05341960407611168, 52.70724293864767418 ) ) ;
#181864 = CARTESIAN_POINT ( 'NONE',  ( -14.34966873604960291, -8.224510206698953496, 111.6655762719810525 ) ) ;
#181865 = CARTESIAN_POINT ( 'NONE',  ( 16.46253265017160672, -9.564922557960803928, 108.3322429386476955 ) ) ;
#181866 = VERTEX_POINT ( 'NONE', #127255 ) ;
#181867 = CARTESIAN_POINT ( 'NONE',  ( 14.34966873604972726, -8.224510206698740333, 65.83442372801900433 ) ) ;
#181868 = CARTESIAN_POINT ( 'NONE',  ( -18.67979575497178146, -10.72451020669898902, 101.6655762719810383 ) ) ;
#181869 = CARTESIAN_POINT ( 'NONE',  ( 19.05341960407611168, 5.049401038298154454, 73.95724293864768129 ) ) ;
#181870 = CARTESIAN_POINT ( 'NONE',  ( -15.80617190586768217, 15.72974639402176855, 43.12609039468568284 ) ) ;
#181871 = CARTESIAN_POINT ( 'NONE',  ( -9.564922557960796823, -16.46253265017161027, 97.08224293864769550 ) ) ;
#181872 = CARTESIAN_POINT ( 'NONE',  ( -23.17010908001108405, -32.51358278116562417, -22.50838357034306014 ) ) ;
#181873 = ORIENTED_EDGE ( 'NONE', *, *, #55568, .T. ) ;
#181874 = CARTESIAN_POINT ( 'NONE',  ( -5.719274019375665041, -21.55341960407619695, 29.79275706135234358 ) ) ;
#181876 = CARTESIAN_POINT ( 'NONE',  ( 19.05341960407617918, -5.049401038297876454, 86.04275706135233293 ) ) ;
#181875 = CARTESIAN_POINT ( 'NONE',  ( -9.564922557960796823, -16.46253265017161027, 102.0822429386477097 ) ) ;
#181877 = CARTESIAN_POINT ( 'NONE',  ( 16.51473224551083163, -9.474510206698727899, 45.83442372801900433 ) ) ;
#181878 = CARTESIAN_POINT ( 'NONE',  ( 10.81492255796078972, 18.62759615963270932, 94.58224293864769550 ) ) ;
#181879 = CARTESIAN_POINT ( 'NONE',  ( 9.474510206698729675, 16.51473224551082808, 32.08442372801900433 ) ) ;
#181880 = CARTESIAN_POINT ( 'NONE',  ( 16.46253265017146816, 9.564922557961045513, 51.66775706135233293 ) ) ;
#181881 = CARTESIAN_POINT ( 'NONE',  ( 12.06949235617739724, 12.14591786802326823, 86.87609039468568994 ) ) ;
#181883 = EDGE_LOOP ( 'NONE', ( #175134, #56448, #87766, #132369, #117189 ) ) ;
#181882 = CARTESIAN_POINT ( 'NONE',  ( 23.42531737588076979, -11.30614151570997272, 165.8025732123263936 ) ) ;
#181884 = CARTESIAN_POINT ( 'NONE',  ( 5.049401038298161559, -19.05341960407611168, 77.70724293864765286 ) ) ;
#181885 = CARTESIAN_POINT ( 'NONE',  ( 10.81492255796106328, -18.62759615963255655, 80.41775706135234714 ) ) ;
#181886 = CARTESIAN_POINT ( 'NONE',  ( 15.80617190586769283, -15.72974639402175789, 80.62609039468567573 ) ) ;
#181887 = CARTESIAN_POINT ( 'NONE',  ( 24.11542121825894114, -0.7284999611695349708, -54.35861002160293509 ) ) ;
#181888 = CARTESIAN_POINT ( 'NONE',  ( 13.89961937509977652, -13.97604488694527269, 93.12390960531436690 ) ) ;
#181889 = CARTESIAN_POINT ( 'NONE',  ( -21.55341960407619339, 5.719274019375674811, 63.54275706135234003 ) ) ;
#181890 = CARTESIAN_POINT ( 'NONE',  ( 19.05341960407617918, -5.049401038297876454, 101.0427570613523045 ) ) ;
#181891 = CARTESIAN_POINT ( 'NONE',  ( 5.049401038298161559, -19.05341960407611168, 72.70724293864768129 ) ) ;
#181892 = CARTESIAN_POINT ( 'NONE',  ( 16.51473224551069308, 9.474510206698969483, 109.1655762719810383 ) ) ;
#181893 = CARTESIAN_POINT ( 'NONE',  ( -16.51473224551069308, -9.474510206698971260, 81.66557627198103830 ) ) ;
#181894 = CARTESIAN_POINT ( 'NONE',  ( -3.573655867281984216E-15, 2.428612866367529932E-14, -13.00000000000000000 ) ) ;
#181895 = CARTESIAN_POINT ( 'NONE',  ( 13.97604488694527802, 13.89961937509977652, 69.37390960531436690 ) ) ;
#181896 = CARTESIAN_POINT ( 'NONE',  ( -19.05341960407611168, -5.049401038298163336, 56.45724293864768129 ) ) ;
#181897 = CARTESIAN_POINT ( 'NONE',  ( -18.67979575497178146, -10.72451020669898902, 111.6655762719810525 ) ) ;
#181898 = CARTESIAN_POINT ( 'NONE',  ( 12.06949235617739724, 12.14591786802326823, 91.87609039468568994 ) ) ;
#181899 = CARTESIAN_POINT ( 'NONE',  ( 7.794767548047360606, -1.499903966022425816, -64.20498622968423774 ) ) ;
#181900 = CARTESIAN_POINT ( 'NONE',  ( -16.51473224551082808, 9.474510206698731452, 48.33442372801900433 ) ) ;
#181901 = CARTESIAN_POINT ( 'NONE',  ( 9.564922557960805705, 16.46253265017160317, 84.58224293864769550 ) ) ;
#181902 = CARTESIAN_POINT ( 'NONE',  ( 8.224510206698953496, -14.34966873604960469, 72.91557627198103830 ) ) ;
#181903 = CARTESIAN_POINT ( 'NONE',  ( -4.379528057220328563, 16.55341960407611168, 110.2072429386477239 ) ) ;
#181904 = CARTESIAN_POINT ( 'NONE',  ( -5.719274019375978568, 21.55341960407610458, 25.20724293864769550 ) ) ;
#181905 = CARTESIAN_POINT ( 'NONE',  ( 0.05219959533909260263, 19.03943276465977164, 104.9989096053143669 ) ) ;
#181906 = CARTESIAN_POINT ( 'NONE',  ( 14.34966873604960469, 8.224510206698951720, 84.16557627198103830 ) ) ;
#181907 = CARTESIAN_POINT ( 'NONE',  ( 23.48298174826590667, -32.32155151706770368, -3.302157773949822683 ) ) ;
#181908 = CARTESIAN_POINT ( 'NONE',  ( 9.474510206698729675, 16.51473224551082808, 27.08442372801900433 ) ) ;
#181909 = CARTESIAN_POINT ( 'NONE',  ( -0.05219959533934338120, 16.53943276465976808, 107.5010903946856899 ) ) ;
#181910 = CARTESIAN_POINT ( 'NONE',  ( -5.153800228976328057, -19.02544592524343514, 87.29057627198103830 ) ) ;
#181911 = CARTESIAN_POINT ( 'NONE',  ( -21.53943276465977519, -0.05219959533937600094, 58.75109039468568994 ) ) ;
#181912 = CARTESIAN_POINT ( 'NONE',  ( -15.80617190586745835, -15.72974639402198527, 46.87390960531435979 ) ) ;
#181913 = CARTESIAN_POINT ( 'NONE',  ( 21.55341960407619695, -5.719274019375665929, 21.04275706135234714 ) ) ;
#181914 = CARTESIAN_POINT ( 'NONE',  ( -21.52544592524343514, 5.823673210054127303, 71.04057627198103830 ) ) ;
#181915 = CARTESIAN_POINT ( 'NONE',  ( -16.55341960407611168, -4.379528057220339221, 91.45724293864769550 ) ) ;
#181916 = CARTESIAN_POINT ( 'NONE',  ( -13.89961937509957401, -13.97604488694547875, 54.37609039468565442 ) ) ;
#181917 = CARTESIAN_POINT ( 'NONE',  ( 0.05219959533909260263, 19.03943276465977164, 24.99890960531435269 ) ) ;
#181918 = CARTESIAN_POINT ( 'NONE',  ( -9.474510206698964154, 16.51473224551069663, 85.41557627198102409 ) ) ;
#181919 = CARTESIAN_POINT ( 'NONE',  ( -13.97604488694527625, -13.89961937509977652, 81.87390960531436690 ) ) ;
#181920 = CARTESIAN_POINT ( 'NONE',  ( 4.483927247898545687, 16.52544592524342804, 104.7905762719810241 ) ) ;
#181921 = VERTEX_POINT ( 'NONE', #143417 ) ;
#181922 = CARTESIAN_POINT ( 'NONE',  ( -12.06949235617756955, 12.14591786802309770, 25.62390960531435624 ) ) ;
#181923 = CARTESIAN_POINT ( 'NONE',  ( -14.34966873604972548, 8.224510206698743886, 38.33442372801900433 ) ) ;
#181924 = CARTESIAN_POINT ( 'NONE',  ( 15.72974639402176855, 15.80617190586768217, 106.8760903946856899 ) ) ;
#181925 = CARTESIAN_POINT ( 'NONE',  ( -5.049401038298153566, 19.05341960407611168, 95.20724293864770971 ) ) ;
#181926 = CARTESIAN_POINT ( 'NONE',  ( -5.719274019375665041, -21.55341960407619695, 39.79275706135235424 ) ) ;
#181927 = CARTESIAN_POINT ( 'NONE',  ( 19.05341960407611168, 5.049401038298154454, 48.95724293864768129 ) ) ;
#181928 = CARTESIAN_POINT ( 'NONE',  ( -16.55341960407617563, 4.379528057220093196, 38.54275706135234714 ) ) ;
#181929 = CARTESIAN_POINT ( 'NONE',  ( -16.51473224551082808, 9.474510206698731452, 103.3344237280190043 ) ) ;
#181930 = CARTESIAN_POINT ( 'NONE',  ( -19.03943276465977164, 0.05219959533909376836, 36.24890960531436690 ) ) ;
#181931 = AXIS2_PLACEMENT_3D ( 'NONE', #129876, #50088, #189599 ) ;
#181932 = CARTESIAN_POINT ( 'NONE',  ( -12.06949235617756955, 12.14591786802309770, 90.62390960531436690 ) ) ;
#181933 = CARTESIAN_POINT ( 'NONE',  ( 21.53943276465977519, -0.05219959533907433946, 108.7489096053143669 ) ) ;
#181934 = CARTESIAN_POINT ( 'NONE',  ( 16.51473224551083163, -9.474510206698727899, 85.83442372801900433 ) ) ;
#181935 = CARTESIAN_POINT ( 'NONE',  ( -9.564922557960796823, -16.46253265017161027, 92.08224293864769550 ) ) ;
#181936 = CARTESIAN_POINT ( 'NONE',  ( 18.62759615963255655, 10.81492255796105972, 26.66775706135235424 ) ) ;
#181937 = CARTESIAN_POINT ( 'NONE',  ( 16.51473224551069308, 9.474510206698969483, 24.16557627198102765 ) ) ;
#181938 = CARTESIAN_POINT ( 'NONE',  ( -19.05341960407611168, -5.049401038298163336, 96.45724293864769550 ) ) ;
#181939 = DIRECTION ( 'NONE',  ( 1.000000000000000000, -4.336808689942018352E-17, 0.000000000000000000 ) ) ;
#181940 = CARTESIAN_POINT ( 'NONE',  ( 16.51473224551069308, 9.474510206698969483, 84.16557627198102409 ) ) ;
#181942 = CARTESIAN_POINT ( 'NONE',  ( 8.314922557960818139, 14.29746914071049879, 84.58224293864769550 ) ) ;
#181941 = CARTESIAN_POINT ( 'NONE',  ( -21.52544592524334988, -5.823673210054445271, 33.95942372801901143 ) ) ;
#181943 = CARTESIAN_POINT ( 'NONE',  ( 19.03943276465977164, -0.05219959533909143690, 98.74890960531436690 ) ) ;
#181944 = CARTESIAN_POINT ( 'NONE',  ( 19.03943276465977164, 0.05219959533936151252, 31.25109039468566863 ) ) ;
#181945 = CARTESIAN_POINT ( 'NONE',  ( -12.06949235617739369, -12.14591786802326823, 49.37609039468569705 ) ) ;
#181946 = CARTESIAN_POINT ( 'NONE',  ( -0.05219959533937732626, 21.53943276465977519, 77.50109039468567573 ) ) ;
#181947 = CARTESIAN_POINT ( 'NONE',  ( 8.314922557961029526, -14.29746914071037800, 30.41775706135234358 ) ) ;
#181949 = EDGE_CURVE ( 'NONE', #89587, #10420, #34274, .T. ) ;
#181948 = CARTESIAN_POINT ( 'NONE',  ( 16.51473224551069308, 9.474510206698969483, 74.16557627198103830 ) ) ;
#181950 = CARTESIAN_POINT ( 'NONE',  ( 0.05219959533936267826, -19.03943276465977164, 100.0010903946856757 ) ) ;
#181951 = CARTESIAN_POINT ( 'NONE',  ( -12.14591786802326823, 12.06949235617739902, 73.12609039468567573 ) ) ;
#181952 = CARTESIAN_POINT ( 'NONE',  ( 18.67979575497194134, -10.72451020669871369, 110.8344237280190043 ) ) ;
#181953 = CARTESIAN_POINT ( 'NONE',  ( -16.51473224551082808, 9.474510206698731452, 83.33442372801899012 ) ) ;
#181954 = CARTESIAN_POINT ( 'NONE',  ( -13.89961937509977652, 13.97604488694528158, 60.62390960531436690 ) ) ;
#181955 = CARTESIAN_POINT ( 'NONE',  ( -15.72974639402197994, 15.80617190586746368, 90.62390960531436690 ) ) ;
#181957 = CARTESIAN_POINT ( 'NONE',  ( -5.049401038297874678, -19.05341960407617918, 74.79275706135231871 ) ) ;
#181956 = CARTESIAN_POINT ( 'NONE',  ( -8.224510206698948167, 14.34966873604960824, 80.41557627198103830 ) ) ;
#181958 = CARTESIAN_POINT ( 'NONE',  ( -18.56399227203342761, -5.499999999999928058, 68.97830131249901342 ) ) ;
#181959 = CARTESIAN_POINT ( 'NONE',  ( -0.05219959533936034679, 19.03943276465977164, 52.50109039468566863 ) ) ;
#181960 = CARTESIAN_POINT ( 'NONE',  ( 14.34966873604972726, -8.224510206698740333, 110.8344237280190043 ) ) ;
#181961 = CARTESIAN_POINT ( 'NONE',  ( 4.483927247898545687, 16.52544592524342804, 84.79057627198102409 ) ) ;
#181963 = CARTESIAN_POINT ( 'NONE',  ( -27.73933785331498925, 2.428612866367529932E-14, 146.8750000027311842 ) ) ;
#181962 = CARTESIAN_POINT ( 'NONE',  ( -10.81492255796105439, 18.62759615963255655, 107.9177570613523471 ) ) ;
#181964 = CARTESIAN_POINT ( 'NONE',  ( -0.05219959533907301413, -21.53943276465977519, 102.4989096053143811 ) ) ;
#181965 = CARTESIAN_POINT ( 'NONE',  ( -9.564922557960796823, -16.46253265017161027, 97.08224293864769550 ) ) ;
#181966 = CARTESIAN_POINT ( 'NONE',  ( 13.89961937509977652, -13.97604488694527269, 63.12390960531435979 ) ) ;
#181967 = CARTESIAN_POINT ( 'NONE',  ( -15.80617190586768217, 15.72974639402176855, 83.12609039468568994 ) ) ;
#181968 = CARTESIAN_POINT ( 'NONE',  ( 13.89961937509977652, -13.97604488694527269, 58.12390960531436690 ) ) ;
#181969 = EDGE_LOOP ( 'NONE', ( #106986, #44912 ) ) ;
#181970 = CARTESIAN_POINT ( 'NONE',  ( 0.05219959533909260263, 19.03943276465977164, 34.99890960531435979 ) ) ;
#181971 = CARTESIAN_POINT ( 'NONE',  ( 5.719274019375991003, -21.55341960407610458, 32.70724293864770260 ) ) ;
#181972 = CARTESIAN_POINT ( 'NONE',  ( 4.379528057220339221, -16.55341960407611168, 72.70724293864769550 ) ) ;
#181973 = CARTESIAN_POINT ( 'NONE',  ( 0.05219959533909260263, 19.03943276465977164, 44.99890960531435979 ) ) ;
#181974 = CARTESIAN_POINT ( 'NONE',  ( 8.224510206698953496, -14.34966873604960469, 97.91557627198103830 ) ) ;
#181975 = CARTESIAN_POINT ( 'NONE',  ( -18.67979575497178146, -10.72451020669898902, 111.6655762719810525 ) ) ;
#181976 = CARTESIAN_POINT ( 'NONE',  ( -18.62759615963255300, -10.81492255796106328, 44.16775706135234714 ) ) ;
#181977 = CARTESIAN_POINT ( 'NONE',  ( -16.51473224551069308, -9.474510206698971260, 31.66557627198102054 ) ) ;
#181978 = CARTESIAN_POINT ( 'NONE',  ( -0.05219959533934338120, 16.53943276465976808, 67.50109039468568994 ) ) ;
#181979 = EDGE_CURVE ( 'NONE', #79638, #195827, #188968, .T. ) ;
#181980 = CARTESIAN_POINT ( 'NONE',  ( -0.05219959533907301413, -21.53943276465977519, 107.4989096053143669 ) ) ;
#181981 = CARTESIAN_POINT ( 'NONE',  ( -5.823673210054116645, -21.52544592524344225, 97.29057627198105251 ) ) ;
#181983 = CARTESIAN_POINT ( 'NONE',  ( -19.02544592524342804, 5.153800228976336051, 46.04057627198101699 ) ) ;
#181982 = CARTESIAN_POINT ( 'NONE',  ( -16.46253265017146816, -9.564922557961047289, 29.16775706135232937 ) ) ;
#181984 = DIRECTION ( 'NONE',  ( 0.000000000000000000, 0.000000000000000000, -1.000000000000000000 ) ) ;
#181985 = CARTESIAN_POINT ( 'NONE',  ( 5.823673210054444382, -21.52544592524334988, 60.20942372801902565 ) ) ;
#181986 = CARTESIAN_POINT ( 'NONE',  ( 5.719274019375991003, -21.55341960407610458, 62.70724293864769550 ) ) ;
#181987 = CARTESIAN_POINT ( 'NONE',  ( 8.314922557960818139, 14.29746914071049879, 29.58224293864769905 ) ) ;
#181989 = CARTESIAN_POINT ( 'NONE',  ( -13.89961937509957401, -13.97604488694547875, 19.37609039468566507 ) ) ;
#181988 = CARTESIAN_POINT ( 'NONE',  ( 10.72451020669871369, 18.67979575497193778, 77.08442372801901854 ) ) ;
#181990 = CARTESIAN_POINT ( 'NONE',  ( 16.51473224551083163, -9.474510206698727899, 50.83442372801899722 ) ) ;
#181991 = CARTESIAN_POINT ( 'NONE',  ( 12.06949235617739724, 12.14591786802326823, 96.87609039468568994 ) ) ;
#181992 = CARTESIAN_POINT ( 'NONE',  ( 18.67979575497194134, -10.72451020669871369, 60.83442372801901854 ) ) ;
#181993 = CARTESIAN_POINT ( 'NONE',  ( 19.03943276465977164, -0.05219959533909143690, 58.74890960531435979 ) ) ;
#181994 = CARTESIAN_POINT ( 'NONE',  ( 19.03943276465977164, 0.05219959533936151252, 36.25109039468567573 ) ) ;
#181995 = CARTESIAN_POINT ( 'NONE',  ( -15.72974639402197994, 15.80617190586746368, 40.62390960531435269 ) ) ;
#181996 = CARTESIAN_POINT ( 'NONE',  ( -18.62759615963255300, -10.81492255796106328, 34.16775706135234714 ) ) ;
#181997 = CARTESIAN_POINT ( 'NONE',  ( 21.52544592524344225, -5.823673210054117533, 93.54057627198103830 ) ) ;
#181998 = CARTESIAN_POINT ( 'NONE',  ( 9.474510206698729675, 16.51473224551082808, 87.08442372801900433 ) ) ;
#181999 = CARTESIAN_POINT ( 'NONE',  ( -14.29746914071037622, -8.314922557961029526, 49.16775706135234003 ) ) ;
#182001 = CARTESIAN_POINT ( 'NONE',  ( 15.80617190586746368, 15.72974639402197994, 89.37390960531435269 ) ) ;
#182000 = CARTESIAN_POINT ( 'NONE',  ( -5.773958127069001911, 3.915344532211590067, -62.35465819465156301 ) ) ;
#182003 = CARTESIAN_POINT ( 'NONE',  ( -14.34966873604960291, -8.224510206698953496, 81.66557627198103830 ) ) ;
#182002 = CARTESIAN_POINT ( 'NONE',  ( -16.55341960407617563, 4.379528057220093196, 83.54275706135234714 ) ) ;
#182004 = CARTESIAN_POINT ( 'NONE',  ( -25.05471026796672618, -28.22563722313813983, -20.55515279800755479 ) ) ;
#182005 = CARTESIAN_POINT ( 'NONE',  ( -19.03943276465977164, -0.05219959533935918106, 103.7510903946856757 ) ) ;
#182006 = AXIS2_PLACEMENT_3D ( 'NONE', #18158, #53448, #111139 ) ;
#182007 = CARTESIAN_POINT ( 'NONE',  ( -18.67979575497178146, -10.72451020669898902, 36.66557627198103120 ) ) ;
#182008 = CARTESIAN_POINT ( 'NONE',  ( -9.687362902255795660, -9.687362902255630459, -60.44446360152740993 ) ) ;
#182009 = CARTESIAN_POINT ( 'NONE',  ( -16.53943276465976808, -0.05219959533934237506, 48.75109039468568284 ) ) ;
#182010 = CARTESIAN_POINT ( 'NONE',  ( -18.67979575497193778, 10.72451020669871902, 23.33442372801901499 ) ) ;
#182011 = CARTESIAN_POINT ( 'NONE',  ( 21.53943276465977519, -0.05219959533907433946, 28.74890960531435624 ) ) ;
#182012 = CARTESIAN_POINT ( 'NONE',  ( -12.14591786802326823, 12.06949235617739902, 73.12609039468567573 ) ) ;
#182013 = CARTESIAN_POINT ( 'NONE',  ( -13.89961937509977652, 13.97604488694528158, 80.62390960531436690 ) ) ;
#182015 = CARTESIAN_POINT ( 'NONE',  ( -19.02544592524342804, 5.153800228976336051, 26.04057627198103120 ) ) ;
#182014 = CARTESIAN_POINT ( 'NONE',  ( -5.719274019375665041, -21.55341960407619695, 54.79275706135235424 ) ) ;
#182016 = CARTESIAN_POINT ( 'NONE',  ( -0.05219959533907301413, -21.53943276465977519, 32.49890960531435979 ) ) ;
#182017 = ORIENTED_EDGE ( 'NONE', *, *, #135020, .F. ) ;
#182018 = CARTESIAN_POINT ( 'NONE',  ( 5.153800228976615827, -19.02544592524334988, 45.20942372801901143 ) ) ;
#182019 = CARTESIAN_POINT ( 'NONE',  ( 4.483927247898790824, -16.52544592524335698, 50.20942372801901854 ) ) ;
#182020 = CARTESIAN_POINT ( 'NONE',  ( 13.97604488694527802, 13.89961937509977652, 114.3739096053143669 ) ) ;
#182021 = CARTESIAN_POINT ( 'NONE',  ( -5.049401038298153566, 19.05341960407611168, 70.20724293864769550 ) ) ;
#182022 = CARTESIAN_POINT ( 'NONE',  ( 8.314922557961029526, -14.29746914071037800, 105.4177570613523613 ) ) ;
#182023 = CARTESIAN_POINT ( 'NONE',  ( -5.049401038298153566, 19.05341960407611168, 115.2072429386477097 ) ) ;
#182024 = CARTESIAN_POINT ( 'NONE',  ( -16.55341960407611168, -4.379528057220339221, 96.45724293864770971 ) ) ;
#182025 = CARTESIAN_POINT ( 'NONE',  ( 10.81492255796078972, 18.62759615963270932, 29.58224293864769905 ) ) ;
#182026 = CARTESIAN_POINT ( 'NONE',  ( 5.049401038298161559, -19.05341960407611168, 27.70724293864769550 ) ) ;
#182027 = CARTESIAN_POINT ( 'NONE',  ( 8.314922557961029526, -14.29746914071037800, 70.41775706135236135 ) ) ;
#182028 = CARTESIAN_POINT ( 'NONE',  ( -10.72451020669870658, -18.67979575497194134, 19.58442372801901143 ) ) ;
#182029 = CARTESIAN_POINT ( 'NONE',  ( 5.049401038297881783, 19.05341960407617563, 77.29275706135231871 ) ) ;
#182030 = CARTESIAN_POINT ( 'NONE',  ( 19.03943276465977164, -0.05219959533909143690, 38.74890960531436690 ) ) ;
#182031 = CARTESIAN_POINT ( 'NONE',  ( -18.67979575497178146, -10.72451020669898902, 71.66557627198100988 ) ) ;
#182032 = CARTESIAN_POINT ( 'NONE',  ( 7.052343178074679031, 2.552343178074557350, 1.110912703473986074 ) ) ;
#182033 = CARTESIAN_POINT ( 'NONE',  ( 0.05219959533937995610, -21.53943276465977519, 90.00109039468567573 ) ) ;
#182034 = CARTESIAN_POINT ( 'NONE',  ( 13.97604488694527802, 13.89961937509977652, 69.37390960531436690 ) ) ;
#182035 = EDGE_CURVE ( 'NONE', #7157, #98258, #176680, .T. ) ;
#182036 = CARTESIAN_POINT ( 'NONE',  ( 4.483927247898790824, -16.52544592524335698, 55.20942372801902565 ) ) ;
#182037 = CARTESIAN_POINT ( 'NONE',  ( 21.52544592524334988, 5.823673210054432836, 76.45942372801901854 ) ) ;
#182038 = CARTESIAN_POINT ( 'NONE',  ( 13.97604488694548053, -13.89961937509957401, 45.62609039468566863 ) ) ;
#182039 = CARTESIAN_POINT ( 'NONE',  ( 16.46253265017146816, 9.564922557961045513, 56.66775706135233293 ) ) ;
#182040 = ORIENTED_EDGE ( 'NONE', *, *, #58394, .T. ) ;
#182041 = CARTESIAN_POINT ( 'NONE',  ( -21.52544592524334988, -5.823673210054445271, 48.95942372801902565 ) ) ;
#182042 = LINE ( 'NONE', #26381, #185145 ) ;
#182043 = CARTESIAN_POINT ( 'NONE',  ( -9.564922557961040184, 16.46253265017147172, 47.91775706135233293 ) ) ;
#182044 = CARTESIAN_POINT ( 'NONE',  ( 9.474510206698971260, -16.51473224551069308, 102.9155762719810241 ) ) ;
#182045 = CARTESIAN_POINT ( 'NONE',  ( 19.03943276465977164, -0.05219959533909143690, 83.74890960531436690 ) ) ;
#182046 = CARTESIAN_POINT ( 'NONE',  ( 8.314922557960818139, 14.29746914071049879, 39.58224293864769550 ) ) ;
#182047 = CARTESIAN_POINT ( 'NONE',  ( 0.05219959533907565091, 21.53943276465977519, 29.99890960531435979 ) ) ;
#182048 = CARTESIAN_POINT ( 'NONE',  ( -11.40812507854755609, 35.11059874428196537, -9.524999997268816188 ) ) ;
#182049 = CARTESIAN_POINT ( 'NONE',  ( -28.79475375365586842, 2.428612866367529932E-14, 141.9843446568999923 ) ) ;
#182050 = CARTESIAN_POINT ( 'NONE',  ( -5.823673210054431948, 21.52544592524334988, 92.70942372801901854 ) ) ;
#182051 = CARTESIAN_POINT ( 'NONE',  ( -7.656827144875921753, -71.74905178543390605, -15.00000000000000178 ) ) ;
#182052 = CARTESIAN_POINT ( 'NONE',  ( 9.474510206698971260, -16.51473224551069308, 37.91557627198102409 ) ) ;
#182053 = CARTESIAN_POINT ( 'NONE',  ( 5.153800228976335163, 19.02544592524342804, 114.7905762719810241 ) ) ;
#182054 = CARTESIAN_POINT ( 'NONE',  ( -29.87996255909766319, -22.90263037402382551, -8.000000000000003553 ) ) ;
#182055 = CARTESIAN_POINT ( 'NONE',  ( 16.55341960407618274, -4.379528057220086978, 56.04275706135235424 ) ) ;
#182056 = CARTESIAN_POINT ( 'NONE',  ( -21.52544592524343514, 5.823673210054127303, 86.04057627198102409 ) ) ;
#182057 = CARTESIAN_POINT ( 'NONE',  ( 4.483927247898545687, 16.52544592524342804, 34.79057627198103120 ) ) ;
#182059 = CARTESIAN_POINT ( 'NONE',  ( -13.89961937509977652, 13.97604488694528158, 105.6239096053143527 ) ) ;
#182058 = CARTESIAN_POINT ( 'NONE',  ( 16.46253265017160672, -9.564922557960803928, 28.33224293864769550 ) ) ;
#182060 = CARTESIAN_POINT ( 'NONE',  ( 21.52544592524334988, 5.823673210054432836, 26.45942372801901854 ) ) ;
#182061 = CARTESIAN_POINT ( 'NONE',  ( -16.46253265017146816, -9.564922557961047289, 29.16775706135232937 ) ) ;
#182062 = CARTESIAN_POINT ( 'NONE',  ( -16.52544592524342804, 4.483927247898546575, 116.0405762719810383 ) ) ;
#182063 = CARTESIAN_POINT ( 'NONE',  ( -21.52544592524334988, -5.823673210054445271, 78.95942372801901854 ) ) ;
#182064 = CARTESIAN_POINT ( 'NONE',  ( 16.21995358207306737, -7.366697692864086378, 32.43551001512160781 ) ) ;
#182065 = CARTESIAN_POINT ( 'NONE',  ( -16.53943276465976808, 0.05219959533911058130, 21.24890960531436690 ) ) ;
#182066 = CARTESIAN_POINT ( 'NONE',  ( 17.50000000000000000, 5.499999999999995559, 113.7823096230356583 ) ) ;
#182067 = CARTESIAN_POINT ( 'NONE',  ( -15.80617190586745835, -15.72974639402198527, 21.87390960531436690 ) ) ;
#182068 = CARTESIAN_POINT ( 'NONE',  ( -8.224510206698948167, 14.34966873604960824, 90.41557627198103830 ) ) ;
#182069 = CARTESIAN_POINT ( 'NONE',  ( 7.776400214313169634, -46.08030136692364920, -22.42299576004354833 ) ) ;
#182070 = CARTESIAN_POINT ( 'NONE',  ( 0.05219959533909260263, 19.03943276465977164, 74.99890960531435269 ) ) ;
#182071 = CARTESIAN_POINT ( 'NONE',  ( -14.34966873604960291, -8.224510206698953496, 71.66557627198100988 ) ) ;
#182072 = CARTESIAN_POINT ( 'NONE',  ( 19.03943276465977164, 0.05219959533936151252, 106.2510903946856615 ) ) ;
#182073 = CARTESIAN_POINT ( 'NONE',  ( 5.823673210054125526, 21.52544592524343514, 64.79057627198103830 ) ) ;
#182074 = VERTEX_POINT ( 'NONE', #128251 ) ;
#182075 = CARTESIAN_POINT ( 'NONE',  ( 19.02544592524343514, -5.153800228976328945, 38.54057627198103120 ) ) ;
#182077 = CARTESIAN_POINT ( 'NONE',  ( 21.55341960407610458, 5.719274019375980345, 73.95724293864769550 ) ) ;
#182076 = CARTESIAN_POINT ( 'NONE',  ( -5.049401038298153566, 19.05341960407611168, 90.20724293864766707 ) ) ;
#182078 = CIRCLE ( 'NONE', #7693, 3.799999999999999378 ) ;
#182080 = CARTESIAN_POINT ( 'NONE',  ( 19.02544592524343514, -5.153800228976328945, 93.54057627198102409 ) ) ;
#182079 = CARTESIAN_POINT ( 'NONE',  ( -16.52544592524335698, -4.483927247898792601, 108.9594237280190185 ) ) ;
#182081 = CARTESIAN_POINT ( 'NONE',  ( 16.46253265017146816, 9.564922557961045513, 61.66775706135234003 ) ) ;
#182082 = CARTESIAN_POINT ( 'NONE',  ( 5.823673210054444382, -21.52544592524334988, 90.20942372801903275 ) ) ;
#182083 = CARTESIAN_POINT ( 'NONE',  ( -5.823673210054116645, -21.52544592524344225, 72.29057627198102409 ) ) ;
#182084 = CARTESIAN_POINT ( 'NONE',  ( -13.89961937509977652, 13.97604488694528158, 115.6239096053143669 ) ) ;
#182085 = CARTESIAN_POINT ( 'NONE',  ( -19.03943276465977164, 0.05219959533909376836, 46.24890960531435979 ) ) ;
#182086 = CARTESIAN_POINT ( 'NONE',  ( -16.53943276465976808, 0.05219959533911058130, 21.24890960531436690 ) ) ;
#182087 = CARTESIAN_POINT ( 'NONE',  ( 5.049401038298161559, -19.05341960407611168, 57.70724293864769550 ) ) ;
#182088 = DIRECTION ( 'NONE',  ( 1.000000000000000000, 0.000000000000000000, 0.000000000000000000 ) ) ;
#182089 = CARTESIAN_POINT ( 'NONE',  ( -5.719274019375665041, -21.55341960407619695, 104.7927570613523898 ) ) ;
#182090 = CARTESIAN_POINT ( 'NONE',  ( -16.52544592524342804, 4.483927247898546575, 71.04057627198103830 ) ) ;
#182091 = CARTESIAN_POINT ( 'NONE',  ( 15.80617190586746368, 15.72974639402197994, 104.3739096053143669 ) ) ;
#182092 = CARTESIAN_POINT ( 'NONE',  ( 21.55341960407610458, 5.719274019375980345, 103.9572429386476813 ) ) ;
#182093 = CARTESIAN_POINT ( 'NONE',  ( -28.28060372831499336, 2.428612866367529932E-14, 148.5625000040967620 ) ) ;
#182094 = CARTESIAN_POINT ( 'NONE',  ( -15.72974639402197994, 15.80617190586746368, 65.62390960531436690 ) ) ;
#182095 = CARTESIAN_POINT ( 'NONE',  ( 16.53943276465976808, 0.05219959533934440121, 81.25109039468568994 ) ) ;
#182096 = CARTESIAN_POINT ( 'NONE',  ( 16.53943276465976808, -0.05219959533910856209, 108.7489096053143669 ) ) ;
#182097 = CARTESIAN_POINT ( 'NONE',  ( 19.02544592524343514, -5.153800228976328945, 53.54057627198102409 ) ) ;
#182098 = CARTESIAN_POINT ( 'NONE',  ( -16.53943276465976808, -0.05219959533934237506, 103.7510903946857042 ) ) ;
#182099 = CARTESIAN_POINT ( 'NONE',  ( -15.72974639402176322, -15.80617190586768395, 44.37609039468567573 ) ) ;
#182100 = CARTESIAN_POINT ( 'NONE',  ( 18.67979575497194134, -10.72451020669871369, 80.83442372801901854 ) ) ;
#182101 = CARTESIAN_POINT ( 'NONE',  ( -13.97604488694527625, -13.89961937509977652, 36.87390960531436690 ) ) ;
#182102 = CARTESIAN_POINT ( 'NONE',  ( -19.05341960407611168, -5.049401038298163336, 36.45724293864766707 ) ) ;
#182103 = ORIENTED_EDGE ( 'NONE', *, *, #15442, .F. ) ;
#182104 = CARTESIAN_POINT ( 'NONE',  ( -15.72974639402176322, -15.80617190586768395, 69.37609039468567573 ) ) ;
#182105 = CARTESIAN_POINT ( 'NONE',  ( 5.049401038298161559, -19.05341960407611168, 97.70724293864766707 ) ) ;
#182106 = CARTESIAN_POINT ( 'NONE',  ( 9.564922557961047289, -16.46253265017146816, 80.41775706135234714 ) ) ;
#182107 = CARTESIAN_POINT ( 'NONE',  ( 0.05219959533937995610, -21.53943276465977519, 55.00109039468568284 ) ) ;
#182108 = CARTESIAN_POINT ( 'NONE',  ( -16.55341960407617563, 4.379528057220093196, 23.54275706135235424 ) ) ;
#182109 = CARTESIAN_POINT ( 'NONE',  ( 16.51473224551083163, -9.474510206698727899, 75.83442372801900433 ) ) ;
#182110 = CARTESIAN_POINT ( 'NONE',  ( 9.474510206698971260, -16.51473224551069308, 47.91557627198102409 ) ) ;
#182111 = CARTESIAN_POINT ( 'NONE',  ( 13.89961937509957401, 13.97604488694547697, 86.87609039468567573 ) ) ;
#182112 = CARTESIAN_POINT ( 'NONE',  ( 4.379528057220092307, 16.55341960407617563, 112.2927570613523471 ) ) ;
#182113 = CARTESIAN_POINT ( 'NONE',  ( 9.474510206698729675, 16.51473224551082808, 87.08442372801900433 ) ) ;
#182114 = CARTESIAN_POINT ( 'NONE',  ( -12.14591786802309592, -12.06949235617757132, 41.87390960531435979 ) ) ;
#182115 = CARTESIAN_POINT ( 'NONE',  ( -9.564922557961040184, 16.46253265017147172, 57.91775706135233293 ) ) ;
#182116 = CARTESIAN_POINT ( 'NONE',  ( -8.314922557961024197, 14.29746914071037800, 52.91775706135235424 ) ) ;
#182117 = CARTESIAN_POINT ( 'NONE',  ( -9.564922557961040184, 16.46253265017147172, 22.91775706135233648 ) ) ;
#182118 = CARTESIAN_POINT ( 'NONE',  ( 5.049401038298161559, -19.05341960407611168, 47.70724293864770260 ) ) ;
#182119 = CARTESIAN_POINT ( 'NONE',  ( -17.31728774477271671, -6.344390552232408886, 64.18093348310682700 ) ) ;
#182120 = CARTESIAN_POINT ( 'NONE',  ( -12.06949235617739369, -12.14591786802326823, 39.37609039468567573 ) ) ;
#182121 = B_SPLINE_CURVE_WITH_KNOTS ( 'NONE', 3,
 ( #93772, #155453, #141269, #16943, #78597, #140270, #1763, #2759, #174606, #39078, #191754, #161421, #129064, #112912, #38081, #176607, #134848, #22913, #103499, #37071 ),
 .UNSPECIFIED., .F., .F.,
 ( 4, 2, 2, 2, 2, 2, 2, 2, 2, 4 ),
 ( 3.469446951953614189E-18, 0.0004987090165372363819, 0.0009974180330744692943, 0.001246772541343085751, 0.001496127049611702207, 0.001994836066148977186, 0.002493545082686252166, 0.002742899590954890089, 0.002992254099223527579, 0.003989672132298154733 ),
 .UNSPECIFIED. ) ;
#182122 = CARTESIAN_POINT ( 'NONE',  ( 28.82186960331498327, 2.781578969918950771E-14, 139.2500000054623683 ) ) ;
#182123 = EDGE_CURVE ( 'NONE', #120381, #27708, #91413, .T. ) ;
#182124 = CARTESIAN_POINT ( 'NONE',  ( -27.73933785331498925, 2.428612866367529932E-14, 146.8750000027311842 ) ) ;
#182125 = CARTESIAN_POINT ( 'NONE',  ( 16.46253265017160672, -9.564922557960803928, 93.33224293864769550 ) ) ;
#182126 = CARTESIAN_POINT ( 'NONE',  ( 17.50000000000000355, 3.242565516147348337, 102.5000000000000142 ) ) ;
#182127 = VERTEX_POINT ( 'NONE', #17119 ) ;
#182128 = CARTESIAN_POINT ( 'NONE',  ( -19.05341960407617563, 5.049401038297882671, 103.5427570613523329 ) ) ;
#182129 = CARTESIAN_POINT ( 'NONE',  ( -5.049401038298153566, 19.05341960407611168, 115.2072429386477097 ) ) ;
#182131 = CARTESIAN_POINT ( 'NONE',  ( 5.049401038297881783, 19.05341960407617563, 97.29275706135233293 ) ) ;
#182130 = CARTESIAN_POINT ( 'NONE',  ( 5.719274019375673035, 21.55341960407619339, 107.2927570613523471 ) ) ;
#182132 = CARTESIAN_POINT ( 'NONE',  ( 8.314922557960818139, 14.29746914071049879, 114.5822429386477097 ) ) ;
#182133 = CARTESIAN_POINT ( 'NONE',  ( 0.05219959533909260263, 19.03943276465977164, 34.99890960531435979 ) ) ;
#182134 = CARTESIAN_POINT ( 'NONE',  ( 0.05219959533907565091, 21.53943276465977519, 64.99890960531435269 ) ) ;
#182135 = VECTOR ( 'NONE', #48898, 1000.000000000000000 ) ;
#182136 = CARTESIAN_POINT ( 'NONE',  ( 4.379528057220339221, -16.55341960407611168, 112.7072429386476955 ) ) ;
#182137 = CARTESIAN_POINT ( 'NONE',  ( 17.62203461105334767, -16.12203461105336189, -54.55577602037946150 ) ) ;
#182138 = CARTESIAN_POINT ( 'NONE',  ( 16.46253265017146816, 9.564922557961045513, 76.66775706135234714 ) ) ;
#182139 = CARTESIAN_POINT ( 'NONE',  ( -12.14591786802309592, -12.06949235617757132, 46.87390960531435979 ) ) ;
#182140 = CARTESIAN_POINT ( 'NONE',  ( 15.80617190586746368, 15.72974639402197994, 29.37390960531435269 ) ) ;
#182141 = CARTESIAN_POINT ( 'NONE',  ( -21.55341960407619339, 5.719274019375674811, 88.54275706135236135 ) ) ;
#182142 = CARTESIAN_POINT ( 'NONE',  ( -21.53943276465977519, 0.05219959533907696930, 81.24890960531436690 ) ) ;
#182143 = CARTESIAN_POINT ( 'NONE',  ( -10.72451020669870658, -18.67979575497194134, 59.58442372801901854 ) ) ;
#182144 = CARTESIAN_POINT ( 'NONE',  ( -5.719274019375665041, -21.55341960407619695, 64.79275706135234714 ) ) ;
#182145 = CARTESIAN_POINT ( 'NONE',  ( 5.153800228976335163, 19.02544592524342804, 89.79057627198102409 ) ) ;
#182147 = CARTESIAN_POINT ( 'NONE',  ( 0.05219959533937995610, -21.53943276465977519, 60.00109039468568284 ) ) ;
#182146 = CARTESIAN_POINT ( 'NONE',  ( -16.53943276465976808, -0.05219959533934237506, 88.75109039468567573 ) ) ;
#182148 = CARTESIAN_POINT ( 'NONE',  ( -16.53943276465976808, 0.05219959533911058130, 116.2489096053143669 ) ) ;
#182149 = CARTESIAN_POINT ( 'NONE',  ( -0.05219959533910754901, -16.53943276465976808, 62.49890960531436690 ) ) ;
#182150 = CARTESIAN_POINT ( 'NONE',  ( 14.34966873604960469, 8.224510206698951720, 39.16557627198102409 ) ) ;
#182151 = CARTESIAN_POINT ( 'NONE',  ( 5.823673210054125526, 21.52544592524343514, 39.79057627198103830 ) ) ;
#182152 = CARTESIAN_POINT ( 'NONE',  ( 0.05219959533909260263, 19.03943276465977164, 49.99890960531435979 ) ) ;
#182153 = CARTESIAN_POINT ( 'NONE',  ( -21.52544592524343514, 5.823673210054127303, 56.04057627198102409 ) ) ;
#182155 = VECTOR ( 'NONE', #74905, 1000.000000000000114 ) ;
#182154 = CARTESIAN_POINT ( 'NONE',  ( 16.51473224551083163, -9.474510206698727899, 45.83442372801900433 ) ) ;
#182157 = CARTESIAN_POINT ( 'NONE',  ( 8.314922557960818139, 14.29746914071049879, 44.58224293864769550 ) ) ;
#182156 = CARTESIAN_POINT ( 'NONE',  ( -16.31925111598457079, -7.325300261831483084, 39.83575461032750553 ) ) ;
#182158 = CARTESIAN_POINT ( 'NONE',  ( -10.81492255796078084, -18.62759615963271287, 22.08224293864769194 ) ) ;
#182159 = ORIENTED_EDGE ( 'NONE', *, *, #43648, .T. ) ;
#182160 = VERTEX_POINT ( 'NONE', #78771 ) ;
#182161 = DIRECTION ( 'NONE',  ( 0.000000000000000000, 0.000000000000000000, -1.000000000000000000 ) ) ;
#182162 = CARTESIAN_POINT ( 'NONE',  ( -16.55341960407617563, 4.379528057220093196, 78.54275706135236135 ) ) ;
#182163 = CARTESIAN_POINT ( 'NONE',  ( -5.153800228976607833, 19.02544592524334988, 77.70942372801900433 ) ) ;
#182164 = CARTESIAN_POINT ( 'NONE',  ( 4.379528057220339221, -16.55341960407611168, 52.70724293864769550 ) ) ;
#182165 = CARTESIAN_POINT ( 'NONE',  ( 17.13100169013303287, -6.664070546373075388, 53.26789835699850784 ) ) ;
#182166 = CARTESIAN_POINT ( 'NONE',  ( -4.483927247898539470, -16.52544592524342804, 22.29057627198102765 ) ) ;
#182167 = CARTESIAN_POINT ( 'NONE',  ( -5.049401038298153566, 19.05341960407611168, 50.20724293864770260 ) ) ;
#182168 = CARTESIAN_POINT ( 'NONE',  ( -19.03943276465977164, 0.05219959533909376836, 76.24890960531435269 ) ) ;
#182169 = CARTESIAN_POINT ( 'NONE',  ( 19.02544592524343514, -5.153800228976328945, 33.54057627198102409 ) ) ;
#182170 = CARTESIAN_POINT ( 'NONE',  ( -0.05219959533937732626, 21.53943276465977519, 47.50109039468568994 ) ) ;
#182171 = CARTESIAN_POINT ( 'NONE',  ( -16.51473224551069308, -9.474510206698971260, 66.66557627198102409 ) ) ;
#182172 = LINE ( 'NONE', #45637, #93639 ) ;
#182173 = CARTESIAN_POINT ( 'NONE',  ( -9.474510206698964154, 16.51473224551069663, 65.41557627198102409 ) ) ;
#182174 = CARTESIAN_POINT ( 'NONE',  ( 21.53943276465977519, -0.05219959533907433946, 33.74890960531436690 ) ) ;
#182175 = CARTESIAN_POINT ( 'NONE',  ( -13.97604488694527625, -13.89961937509977652, 31.87390960531435979 ) ) ;
#182176 = CARTESIAN_POINT ( 'NONE',  ( -21.52544592524343514, 5.823673210054127303, 36.04057627198102409 ) ) ;
#182177 = CARTESIAN_POINT ( 'NONE',  ( 16.53943276465976808, 0.05219959533934440121, 91.25109039468568994 ) ) ;
#182178 = CARTESIAN_POINT ( 'NONE',  ( -19.05341960407617563, 5.049401038297882671, 23.54275706135233648 ) ) ;
#182180 = CARTESIAN_POINT ( 'NONE',  ( -16.53943276465976808, -0.05219959533934237506, 73.75109039468567573 ) ) ;
#182179 = CARTESIAN_POINT ( 'NONE',  ( -16.53943276465976808, -0.05219959533934237506, 43.75109039468568284 ) ) ;
#182181 = CARTESIAN_POINT ( 'NONE',  ( -19.05341960407611168, -5.049401038298163336, 106.4572429386476955 ) ) ;
#182182 = CARTESIAN_POINT ( 'NONE',  ( -8.314922557961024197, 14.29746914071037800, 72.91775706135234714 ) ) ;
#182183 = CARTESIAN_POINT ( 'NONE',  ( 8.314922557961029526, -14.29746914071037800, 35.41775706135234003 ) ) ;
#182184 = CARTESIAN_POINT ( 'NONE',  ( 9.474510206698971260, -16.51473224551069308, 107.9155762719810383 ) ) ;
#182185 = CARTESIAN_POINT ( 'NONE',  ( 16.53943276465976808, 0.05219959533934440121, 21.25109039468567218 ) ) ;
#182186 = CARTESIAN_POINT ( 'NONE',  ( 0.05219959533909260263, 19.03943276465977164, 34.99890960531435979 ) ) ;
#182187 = CARTESIAN_POINT ( 'NONE',  ( 18.62759615963255655, 10.81492255796105972, 31.66775706135234358 ) ) ;
#182188 = CARTESIAN_POINT ( 'NONE',  ( 5.049401038297881783, 19.05341960407617563, 112.2927570613523471 ) ) ;
#182189 = CARTESIAN_POINT ( 'NONE',  ( -14.34966873604972548, 8.224510206698743886, 93.33442372801901854 ) ) ;
#182190 = DIRECTION ( 'NONE',  ( -1.000000000000000000, -0.000000000000000000, 0.000000000000000000 ) ) ;
#182191 = CARTESIAN_POINT ( 'NONE',  ( 15.72974639402176855, 15.80617190586768217, 96.87609039468568994 ) ) ;
#182192 = CARTESIAN_POINT ( 'NONE',  ( 9.474510206698729675, 16.51473224551082808, 97.08442372801900433 ) ) ;
#182193 = CARTESIAN_POINT ( 'NONE',  ( -8.314922557960811034, -14.29746914071050412, 57.08224293864769550 ) ) ;
#182194 = CARTESIAN_POINT ( 'NONE',  ( 9.564922557960805705, 16.46253265017160317, 24.58224293864769194 ) ) ;
#182196 = CARTESIAN_POINT ( 'NONE',  ( -9.090093023806474548, 0.1983487321477290510, -63.95305636720455311 ) ) ;
#182195 = CARTESIAN_POINT ( 'NONE',  ( -13.89961937509957401, -13.97604488694547875, 64.37609039468567573 ) ) ;
#182197 = CARTESIAN_POINT ( 'NONE',  ( 10.81492255796106328, -18.62759615963255655, 50.41775706135235424 ) ) ;
#182198 = CARTESIAN_POINT ( 'NONE',  ( -8.314922557961024197, 14.29746914071037800, 32.91775706135234714 ) ) ;
#182199 = CARTESIAN_POINT ( 'NONE',  ( 16.36317988757058473, 7.306389748694940067, 83.40210391636773579 ) ) ;
#182200 = CARTESIAN_POINT ( 'NONE',  ( -5.153800228976328057, -19.02544592524343514, 112.2905762719810099 ) ) ;
#182201 = CARTESIAN_POINT ( 'NONE',  ( 5.719274019375991003, -21.55341960407610458, 72.70724293864769550 ) ) ;
#182202 = CARTESIAN_POINT ( 'NONE',  ( 5.049401038297881783, 19.05341960407617563, 112.2927570613523471 ) ) ;
#182203 = EDGE_CURVE ( 'NONE', #193478, #142350, #186344, .T. ) ;
#182204 = CARTESIAN_POINT ( 'NONE',  ( -13.97604488694527625, -13.89961937509977652, 96.87390960531433848 ) ) ;
#182205 = CARTESIAN_POINT ( 'NONE',  ( -14.34215988523096286, -24.36250104427641006, 140.0000000000000000 ) ) ;
#182206 = CARTESIAN_POINT ( 'NONE',  ( 16.46253265017160672, -9.564922557960803928, 23.33224293864769194 ) ) ;
#182207 = CARTESIAN_POINT ( 'NONE',  ( 21.53943276465977519, 0.05219959533937863772, 96.25109039468568994 ) ) ;
#182208 = CARTESIAN_POINT ( 'NONE',  ( 19.05341960407611168, 5.049401038298154454, 38.95724293864767418 ) ) ;
#182209 = CARTESIAN_POINT ( 'NONE',  ( 21.52544592524334988, 5.823673210054432836, 46.45942372801901854 ) ) ;
#182210 = CARTESIAN_POINT ( 'NONE',  ( -21.53943276465977519, -0.05219959533937600094, 88.75109039468567573 ) ) ;
#182211 = CARTESIAN_POINT ( 'NONE',  ( 16.55341960407618274, -4.379528057220086978, 101.0427570613523756 ) ) ;
#182212 = EDGE_CURVE ( 'NONE', #165860, #138761, #118518, .T. ) ;
#182213 = CARTESIAN_POINT ( 'NONE',  ( 5.049401038298161559, -19.05341960407611168, 77.70724293864765286 ) ) ;
#182214 = CARTESIAN_POINT ( 'NONE',  ( 18.67979575497194134, -10.72451020669871369, 45.83442372801901854 ) ) ;
#182215 = CARTESIAN_POINT ( 'NONE',  ( 18.62759615963255655, 10.81492255796105972, 36.66775706135234714 ) ) ;
#182217 = CARTESIAN_POINT ( 'NONE',  ( -16.51473224551069308, -9.474510206698971260, 86.66557627198102409 ) ) ;
#182216 = CARTESIAN_POINT ( 'NONE',  ( 13.97604488694548053, -13.89961937509957401, 75.62609039468564731 ) ) ;
#182218 = CARTESIAN_POINT ( 'NONE',  ( -8.224510206698948167, 14.34966873604960824, 100.4155762719810241 ) ) ;
#182219 = CARTESIAN_POINT ( 'NONE',  ( 21.55341960407610458, 5.719274019375980345, 98.95724293864770971 ) ) ;
#182220 = CARTESIAN_POINT ( 'NONE',  ( -12.06949235617756955, 12.14591786802309770, 80.62390960531438111 ) ) ;
#182221 = CARTESIAN_POINT ( 'NONE',  ( 19.03943276465977164, 0.05219959533936151252, 21.25109039468565797 ) ) ;
#182222 = CARTESIAN_POINT ( 'NONE',  ( -4.483927247898539470, -16.52544592524342804, 102.2905762719810383 ) ) ;
#182223 = CARTESIAN_POINT ( 'NONE',  ( -9.474510206698964154, 16.51473224551069663, 35.41557627198102409 ) ) ;
#182224 = CARTESIAN_POINT ( 'NONE',  ( 0.05219959533936267826, -19.03943276465977164, 85.00109039468567573 ) ) ;
#182225 = CARTESIAN_POINT ( 'NONE',  ( 8.224510206698953496, -14.34966873604960469, 42.91557627198103120 ) ) ;
#182226 = CARTESIAN_POINT ( 'NONE',  ( -15.72974639402176322, -15.80617190586768395, 94.37609039468568994 ) ) ;
#182227 = CARTESIAN_POINT ( 'NONE',  ( -19.05341960407611168, -5.049401038298163336, 111.4572429386476671 ) ) ;
#182228 = CARTESIAN_POINT ( 'NONE',  ( 5.153800228976615827, -19.02544592524334988, 70.20942372801899012 ) ) ;
#182229 = CARTESIAN_POINT ( 'NONE',  ( 10.81492255796078972, 18.62759615963270932, 79.58224293864769550 ) ) ;
#182230 = CARTESIAN_POINT ( 'NONE',  ( 21.53943276465977519, 0.05219959533937863772, 31.25109039468568639 ) ) ;
#182231 = CARTESIAN_POINT ( 'NONE',  ( -16.55341960407617563, 4.379528057220093196, 28.54275706135234358 ) ) ;
#182232 = CARTESIAN_POINT ( 'NONE',  ( 0.05219959533934541429, -16.53943276465976808, 95.00109039468568994 ) ) ;
#182234 = CARTESIAN_POINT ( 'NONE',  ( 21.52544592524334988, 5.823673210054432836, 41.45942372801901143 ) ) ;
#182233 = CARTESIAN_POINT ( 'NONE',  ( 16.46253265017160672, -9.564922557960803928, 23.33224293864769194 ) ) ;
#182235 = CARTESIAN_POINT ( 'NONE',  ( 5.153800228976335163, 19.02544592524342804, 24.79057627198102765 ) ) ;
#182236 = CARTESIAN_POINT ( 'NONE',  ( -36.91746825000000598, 2.428612866367529932E-14, -3.124999997268813168 ) ) ;
#182237 = CARTESIAN_POINT ( 'NONE',  ( -16.52544592524335698, -4.483927247898792601, 48.95942372801902565 ) ) ;
#182238 = CARTESIAN_POINT ( 'NONE',  ( 8.314922557960818139, 14.29746914071049879, 79.58224293864769550 ) ) ;
#182239 = CARTESIAN_POINT ( 'NONE',  ( -18.62759615963270932, 10.81492255796079327, 70.83224293864770971 ) ) ;
#182240 = CARTESIAN_POINT ( 'NONE',  ( 12.06949235617739724, 12.14591786802326823, 111.8760903946856615 ) ) ;
#182241 = CARTESIAN_POINT ( 'NONE',  ( -4.379528057220086978, -16.55341960407618274, 54.79275706135235424 ) ) ;
#182242 = CARTESIAN_POINT ( 'NONE',  ( 19.02544592524343514, -5.153800228976328945, 43.54057627198103120 ) ) ;
#182243 = CARTESIAN_POINT ( 'NONE',  ( 14.34966873604972726, -8.224510206698740333, 95.83442372801903275 ) ) ;
#182244 = CARTESIAN_POINT ( 'NONE',  ( -19.03943276465977164, -0.05219959533935918106, 88.75109039468567573 ) ) ;
#182245 = CARTESIAN_POINT ( 'NONE',  ( 18.67979575497178502, 10.72451020669898547, 89.16557627198102409 ) ) ;
#182246 = CARTESIAN_POINT ( 'NONE',  ( 14.29746914071037800, 8.314922557961029526, 111.6677570613523613 ) ) ;
#182247 = EDGE_LOOP ( 'NONE', ( #189215, #64449, #55097, #28582 ) ) ;
#182248 = CARTESIAN_POINT ( 'NONE',  ( 25.80209238092448487, 7.370998251475543661, 174.5109820657625619 ) ) ;
#182249 = AXIS2_PLACEMENT_3D ( 'NONE', #47460, #125289, #44479 ) ;
#182250 = CARTESIAN_POINT ( 'NONE',  ( -15.72974639402197994, 15.80617190586746368, 60.62390960531437401 ) ) ;
#182251 = ORIENTED_EDGE ( 'NONE', *, *, #120148, .T. ) ;
#182252 = CARTESIAN_POINT ( 'NONE',  ( 14.34966873604972726, -8.224510206698740333, 85.83442372801901854 ) ) ;
#182253 = ORIENTED_EDGE ( 'NONE', *, *, #29688, .F. ) ;
#182254 = CARTESIAN_POINT ( 'NONE',  ( 19.03943276465977164, -0.05219959533909143690, 108.7489096053143527 ) ) ;
#182255 = CARTESIAN_POINT ( 'NONE',  ( -18.87580814761074777, 5.500000000000058620, 75.87172394265758157 ) ) ;
#182256 = CARTESIAN_POINT ( 'NONE',  ( 15.72974639402199770, -15.80617190586745480, 73.12390960531436690 ) ) ;
#182257 = CARTESIAN_POINT ( 'NONE',  ( -14.34966873604972548, 8.224510206698743886, 113.3344237280190328 ) ) ;
#182258 = CARTESIAN_POINT ( 'NONE',  ( 8.224510206698742110, 14.34966873604972548, 27.08442372801901854 ) ) ;
#182259 = CARTESIAN_POINT ( 'NONE',  ( 8.224510206698953496, -14.34966873604960469, 112.9155762719810383 ) ) ;
#182260 = CARTESIAN_POINT ( 'NONE',  ( -14.29746914071037622, -8.314922557961029526, 29.16775706135234003 ) ) ;
#182261 = CARTESIAN_POINT ( 'NONE',  ( -9.474510206698964154, 16.51473224551069663, 55.41557627198103120 ) ) ;
#182262 = CARTESIAN_POINT ( 'NONE',  ( 17.81289503416610742, 24.51734667627700404, 149.2999999999999545 ) ) ;
#182263 = CARTESIAN_POINT ( 'NONE',  ( 9.564922557960805705, 16.46253265017160317, 104.5822429386476955 ) ) ;
#182264 = CARTESIAN_POINT ( 'NONE',  ( -13.89961937509977652, 13.97604488694528158, 100.6239096053143669 ) ) ;
#182265 = AXIS2_PLACEMENT_3D ( 'NONE', #74935, #133619, #181144 ) ;
#182266 = CARTESIAN_POINT ( 'NONE',  ( -16.55341960407617563, 4.379528057220093196, 88.54275706135236135 ) ) ;
#182267 = CARTESIAN_POINT ( 'NONE',  ( -9.564922557961040184, 16.46253265017147172, 97.91775706135233293 ) ) ;
#182268 = CARTESIAN_POINT ( 'NONE',  ( -19.05341960407617563, 5.049401038297882671, 43.54275706135232582 ) ) ;
#182269 = CARTESIAN_POINT ( 'NONE',  ( 5.823673210054125526, 21.52544592524343514, 74.79057627198105251 ) ) ;
#182270 = CARTESIAN_POINT ( 'NONE',  ( 4.483927247898790824, -16.52544592524335698, 95.20942372801903275 ) ) ;
#182271 = CARTESIAN_POINT ( 'NONE',  ( 18.62759615963271287, -10.81492255796078972, 38.33224293864768839 ) ) ;
#182272 = CARTESIAN_POINT ( 'NONE',  ( -13.89961937509957401, -13.97604488694547875, 99.37609039468567573 ) ) ;
#182273 = CARTESIAN_POINT ( 'NONE',  ( 13.97604488694527802, 13.89961937509977652, 44.37390960531435269 ) ) ;
#182275 = CIRCLE ( 'NONE', #66055, 2.500000000000002220 ) ;
#182274 = CARTESIAN_POINT ( 'NONE',  ( -16.46253265017160317, 9.564922557960807481, 85.83224293864769550 ) ) ;
#182276 = CARTESIAN_POINT ( 'NONE',  ( -15.80617190586768217, 15.72974639402176855, 58.12609039468568994 ) ) ;
#182277 = CARTESIAN_POINT ( 'NONE',  ( 0.05219959533909260263, 19.03943276465977164, 64.99890960531436690 ) ) ;
#182278 = CARTESIAN_POINT ( 'NONE',  ( 12.14591786802309770, 12.06949235617756955, 89.37390960531435269 ) ) ;
#182279 = CARTESIAN_POINT ( 'NONE',  ( -17.50000000000001066, -5.499999999999943157, 86.28230962303568674 ) ) ;
#182280 = CARTESIAN_POINT ( 'NONE',  ( -12.06949235617756955, 12.14591786802309770, 80.62390960531438111 ) ) ;
#182281 = CARTESIAN_POINT ( 'NONE',  ( -5.719274019375978568, 21.55341960407610458, 70.20724293864769550 ) ) ;
#182282 = CARTESIAN_POINT ( 'NONE',  ( 13.89961937509957401, 13.97604488694547697, 96.87609039468566152 ) ) ;
#182283 = COLOUR_RGB ( '', 0.31764706, 0.68627451, 0.89019608) ;
#182284 = DIRECTION ( 'NONE',  ( 0.000000000000000000, 0.000000000000000000, -1.000000000000000000 ) ) ;
#182285 = CARTESIAN_POINT ( 'NONE',  ( 9.564922557961047289, -16.46253265017146816, 45.41775706135232582 ) ) ;
#182286 = CARTESIAN_POINT ( 'NONE',  ( 17.31747979337956878, -6.344076630960847396, 71.12055131934816643 ) ) ;
#182288 = CARTESIAN_POINT ( 'NONE',  ( 9.564922557960805705, 16.46253265017160317, 84.58224293864769550 ) ) ;
#182287 = CARTESIAN_POINT ( 'NONE',  ( -13.97604488694527625, -13.89961937509977652, 81.87390960531436690 ) ) ;
#182289 = CARTESIAN_POINT ( 'NONE',  ( 0.05219959533934541429, -16.53943276465976808, 65.00109039468568994 ) ) ;
#182290 = CARTESIAN_POINT ( 'NONE',  ( -21.98831087263039308, 5.509728484239381885, 173.5901369092266577 ) ) ;
#182291 = CARTESIAN_POINT ( 'NONE',  ( -0.05219959533936034679, 19.03943276465977164, 47.50109039468566863 ) ) ;
#182292 = CARTESIAN_POINT ( 'NONE',  ( 9.809999999999998721, 2.449293598294705921E-16, -1.999999999999999556 ) ) ;
#182293 = CARTESIAN_POINT ( 'NONE',  ( -13.97604488694527625, -13.89961937509977652, 106.8739096053143669 ) ) ;
#182294 = CARTESIAN_POINT ( 'NONE',  ( 14.29746914071037800, 8.314922557961029526, 101.6677570613523613 ) ) ;
#182295 = CARTESIAN_POINT ( 'NONE',  ( 13.90528855463211677, -0.7844626028950130170, -60.35633530387646317 ) ) ;
#182296 = CARTESIAN_POINT ( 'NONE',  ( 12.06949235617739724, 12.14591786802326823, 76.87609039468567573 ) ) ;
#182297 = CARTESIAN_POINT ( 'NONE',  ( -17.05587630539785593, 6.762274262135690606, 30.74180309037313563 ) ) ;
#182298 = CARTESIAN_POINT ( 'NONE',  ( 0.05219959533934541429, -16.53943276465976808, 60.00109039468568284 ) ) ;
#182299 = LINE ( 'NONE', #88277, #101872 ) ;
#182300 = CARTESIAN_POINT ( 'NONE',  ( 5.719274019375673035, 21.55341960407619339, 72.29275706135236135 ) ) ;
#182301 = CARTESIAN_POINT ( 'NONE',  ( -5.049401038297874678, -19.05341960407617918, 69.79275706135233293 ) ) ;
#182302 = CARTESIAN_POINT ( 'NONE',  ( 13.97604488694548053, -13.89961937509957401, 25.62609039468566507 ) ) ;
#182303 = CARTESIAN_POINT ( 'NONE',  ( 13.89961937509977652, -13.97604488694527269, 58.12390960531436690 ) ) ;
#182304 = CARTESIAN_POINT ( 'NONE',  ( 16.51473224551069308, 9.474510206698969483, 44.16557627198103120 ) ) ;
#182305 = LINE ( 'NONE', #75107, #49618 ) ;
#182306 = CARTESIAN_POINT ( 'NONE',  ( -15.72974639402197994, 15.80617190586746368, 70.62390960531436690 ) ) ;
#182307 = AXIS2_PLACEMENT_3D ( 'NONE', #13010, #73693, #165693 ) ;
#182308 = B_SPLINE_CURVE_WITH_KNOTS ( 'NONE', 3,
 ( #156711, #128336, #190035, #126357, #157704, #19194, #48542, #125376, #96019, #94024, #188054, #80843, #81815, #36325, #159672, #189052, #82824, #158681, #96998, #32371 ),
 .UNSPECIFIED., .F., .F.,
 ( 4, 2, 2, 2, 2, 2, 2, 2, 2, 4 ),
 ( 0.000000000000000000, 0.0004987090165372654385, 0.0009974180330745308770, 0.001246772541343163596, 0.001496127049611796532, 0.001994836066149057851, 0.002493545082686318953, 0.002742899590954949503, 0.002992254099223580488, 0.003989672132298186825 ),
 .UNSPECIFIED. ) ;
#182309 = CARTESIAN_POINT ( 'NONE',  ( -5.823673210054116645, -21.52544592524344225, 37.29057627198102409 ) ) ;
#182310 = CARTESIAN_POINT ( 'NONE',  ( -16.53943276465976808, 0.05219959533911058130, 111.2489096053143669 ) ) ;
#182311 = CARTESIAN_POINT ( 'NONE',  ( 4.483927247898790824, -16.52544592524335698, 50.20942372801901854 ) ) ;
#182312 = ORIENTED_EDGE ( 'NONE', *, *, #7758, .T. ) ;
#182313 = CARTESIAN_POINT ( 'NONE',  ( -21.52544592524334988, -5.823673210054445271, 28.95942372801902209 ) ) ;
#182315 = CARTESIAN_POINT ( 'NONE',  ( -11.74264578624800670, 36.14014761921585972, -4.400000000000000355 ) ) ;
#182314 = CARTESIAN_POINT ( 'NONE',  ( 14.34966873604960469, 8.224510206698951720, 54.16557627198103120 ) ) ;
#182316 = CARTESIAN_POINT ( 'NONE',  ( 19.05341960407617918, -5.049401038297876454, 101.0427570613523045 ) ) ;
#182317 = CARTESIAN_POINT ( 'NONE',  ( 19.02544592524334988, 5.153800228976608722, 41.45942372801900433 ) ) ;
#182318 = CARTESIAN_POINT ( 'NONE',  ( 14.29746914071049879, -8.314922557960816363, 43.33224293864769550 ) ) ;
#182320 = EDGE_CURVE ( 'NONE', #139989, #161460, #18478, .T. ) ;
#182319 = CARTESIAN_POINT ( 'NONE',  ( -5.823673210054431948, 21.52544592524334988, 22.70942372801901499 ) ) ;
#182322 = CARTESIAN_POINT ( 'NONE',  ( -15.80617190586745835, -15.72974639402198527, 81.87390960531435269 ) ) ;
#182321 = FACE_OUTER_BOUND ( 'NONE', #61858, .T. ) ;
#182323 = CARTESIAN_POINT ( 'NONE',  ( 16.51473224551069308, 9.474510206698969483, 94.16557627198103830 ) ) ;
#182324 = CARTESIAN_POINT ( 'NONE',  ( 16.53943276465976808, -0.05219959533910856209, 58.74890960531436690 ) ) ;
#182325 = CARTESIAN_POINT ( 'NONE',  ( -0.05219959533909027116, -19.03943276465977164, 102.4989096053143669 ) ) ;
#182326 = DIRECTION ( 'NONE',  ( -0.000000000000000000, -0.000000000000000000, 1.000000000000000000 ) ) ;
#182327 = CARTESIAN_POINT ( 'NONE',  ( 5.153800228976615827, -19.02544592524334988, 50.20942372801897591 ) ) ;
#182328 = CARTESIAN_POINT ( 'NONE',  ( 15.72974639402199770, -15.80617190586745480, 108.1239096053143811 ) ) ;
#182329 = CARTESIAN_POINT ( 'NONE',  ( 19.02544592524343514, -5.153800228976328945, 48.54057627198103120 ) ) ;
#182330 = CARTESIAN_POINT ( 'NONE',  ( 8.224510206698953496, -14.34966873604960469, 107.9155762719810241 ) ) ;
#182331 = CARTESIAN_POINT ( 'NONE',  ( -5.719274019375665041, -21.55341960407619695, 49.79275706135234714 ) ) ;
#182332 = CARTESIAN_POINT ( 'NONE',  ( -27.73933785331498925, 2.428612866367529932E-14, 146.8750000027311842 ) ) ;
#182333 = EDGE_CURVE ( 'NONE', #114833, #113576, #195318, .T. ) ;
#182334 = CARTESIAN_POINT ( 'NONE',  ( 12.14591786802309770, 12.06949235617756955, 34.37390960531435979 ) ) ;
#182335 = CARTESIAN_POINT ( 'NONE',  ( -9.564922557960796823, -16.46253265017161027, 52.08224293864768839 ) ) ;
#182336 = CARTESIAN_POINT ( 'NONE',  ( 13.97604488694527802, 13.89961937509977652, 99.37390960531436690 ) ) ;
#182337 = CARTESIAN_POINT ( 'NONE',  ( -10.72451020669898014, 18.67979575497178502, 75.41557627198102409 ) ) ;
#182338 = CARTESIAN_POINT ( 'NONE',  ( 22.44159573604009239, 16.30477369853692693, 142.0750000027311728 ) ) ;
#182339 = CARTESIAN_POINT ( 'NONE',  ( 9.564922557960805705, 16.46253265017160317, 44.58224293864769550 ) ) ;
#182340 = CARTESIAN_POINT ( 'NONE',  ( -15.80617190586745835, -15.72974639402198527, 56.87390960531436690 ) ) ;
#182341 = CARTESIAN_POINT ( 'NONE',  ( 18.67979575497194134, -10.72451020669871369, 85.83442372801901854 ) ) ;
#182344 = CARTESIAN_POINT ( 'NONE',  ( -12.06949235617756955, 12.14591786802309770, 65.62390960531436690 ) ) ;
#182343 = CARTESIAN_POINT ( 'NONE',  ( -12.14591786802326823, 12.06949235617739902, 78.12609039468570415 ) ) ;
#182342 = DIRECTION ( 'NONE',  ( 1.000000000000000000, -0.000000000000000000, -0.000000000000000000 ) ) ;
#182345 = CARTESIAN_POINT ( 'NONE',  ( 19.03943276465977164, -0.05219959533909143690, 63.74890960531435979 ) ) ;
#182346 = VERTEX_POINT ( 'NONE', #114071 ) ;
#182347 = CARTESIAN_POINT ( 'NONE',  ( -19.05341960407617563, 5.049401038297882671, 23.54275706135233648 ) ) ;
#182348 = CARTESIAN_POINT ( 'NONE',  ( 12.06949235617739724, 12.14591786802326823, 86.87609039468568994 ) ) ;
#182349 = CARTESIAN_POINT ( 'NONE',  ( 21.55341960407619695, -5.719274019375665929, 111.0427570613523613 ) ) ;
#182350 = CARTESIAN_POINT ( 'NONE',  ( -9.474510206698964154, 16.51473224551069663, 80.41557627198103830 ) ) ;
#182351 = CARTESIAN_POINT ( 'NONE',  ( 10.72451020669898902, -18.67979575497178502, 52.91557627198103830 ) ) ;
#182352 = CARTESIAN_POINT ( 'NONE',  ( -8.224510206698735004, -14.34966873604973081, 19.58442372801901143 ) ) ;
#182353 = CARTESIAN_POINT ( 'NONE',  ( 10.81492255796106328, -18.62759615963255655, 100.4177570613523471 ) ) ;
#182354 = CARTESIAN_POINT ( 'NONE',  ( 14.29746914071037800, 8.314922557961029526, 66.66775706135234714 ) ) ;
#182355 = CARTESIAN_POINT ( 'NONE',  ( -10.72451020669898014, 18.67979575497178502, 115.4155762719810241 ) ) ;
#182356 = CARTESIAN_POINT ( 'NONE',  ( -19.05341960407617563, 5.049401038297882671, 113.5427570613523471 ) ) ;
#182357 = CARTESIAN_POINT ( 'NONE',  ( -16.46253265017160317, 9.564922557960807481, 85.83224293864769550 ) ) ;
#182358 = CARTESIAN_POINT ( 'NONE',  ( -12.14591786802326823, 12.06949235617739902, 23.12609039468567573 ) ) ;
#182359 = CARTESIAN_POINT ( 'NONE',  ( 16.46253265017160672, -9.564922557960803928, 53.33224293864768839 ) ) ;
#182360 = CARTESIAN_POINT ( 'NONE',  ( 16.52544592524335698, 4.483927247898782831, 36.45942372801901143 ) ) ;
#182361 = CARTESIAN_POINT ( 'NONE',  ( 14.29746914071049879, -8.314922557960816363, 73.33224293864769550 ) ) ;
#182362 = CARTESIAN_POINT ( 'NONE',  ( 8.224510206698742110, 14.34966873604972548, 82.08442372801901854 ) ) ;
#182364 = CARTESIAN_POINT ( 'NONE',  ( 19.02544592524343514, -5.153800228976328945, 58.54057627198102409 ) ) ;
#182363 = CARTESIAN_POINT ( 'NONE',  ( -21.52544592524334988, -5.823673210054445271, 48.95942372801902565 ) ) ;
#182365 = CARTESIAN_POINT ( 'NONE',  ( -0.05219959533909027116, -19.03943276465977164, 82.49890960531436690 ) ) ;
#182366 = CARTESIAN_POINT ( 'NONE',  ( -12.14591786802326823, 12.06949235617739902, 83.12609039468568994 ) ) ;
#182367 = EDGE_CURVE ( 'NONE', #187814, #39277, #132257, .T. ) ;
#182368 = CIRCLE ( 'NONE', #198521, 23.10356920737165254 ) ;
#182369 = CARTESIAN_POINT ( 'NONE',  ( -24.02130208662955013, -8.352503713167614308, 169.2769999910357512 ) ) ;
#182370 = ORIENTED_EDGE ( 'NONE', *, *, #35450, .T. ) ;
#182371 = CARTESIAN_POINT ( 'NONE',  ( 5.153800228976615827, -19.02544592524334988, 35.20942372801899722 ) ) ;
#182372 = CARTESIAN_POINT ( 'NONE',  ( -19.02544592524342804, 5.153800228976336051, 96.04057627198103830 ) ) ;
#182373 = CARTESIAN_POINT ( 'NONE',  ( 9.474510206698971260, -16.51473224551069308, 52.91557627198102409 ) ) ;
#182374 = CARTESIAN_POINT ( 'NONE',  ( 13.89961937509977652, -13.97604488694527269, 108.1239096053143669 ) ) ;
#182375 = CARTESIAN_POINT ( 'NONE',  ( -16.55341960407617563, 4.379528057220093196, 38.54275706135234714 ) ) ;
#182377 = CARTESIAN_POINT ( 'NONE',  ( -14.34966873604972548, 8.224510206698743886, 58.33442372801901143 ) ) ;
#182376 = CARTESIAN_POINT ( 'NONE',  ( 9.564922557961047289, -16.46253265017146816, 60.41775706135233293 ) ) ;
#182378 = CARTESIAN_POINT ( 'NONE',  ( 19.03943276465977164, -0.05219959533909143690, 108.7489096053143527 ) ) ;
#182379 = CARTESIAN_POINT ( 'NONE',  ( -5.153800228976328057, -19.02544592524343514, 77.29057627198099567 ) ) ;
#182380 = CARTESIAN_POINT ( 'NONE',  ( 18.62759615963271287, -10.81492255796078972, 98.33224293864769550 ) ) ;
#182381 = CARTESIAN_POINT ( 'NONE',  ( 13.97604488694548053, -13.89961937509957401, 60.62609039468564731 ) ) ;
#182383 = CARTESIAN_POINT ( 'NONE',  ( 19.03943276465977164, -0.05219959533909143690, 23.74890960531435269 ) ) ;
#182382 = CARTESIAN_POINT ( 'NONE',  ( -13.97604488694527625, -13.89961937509977652, 96.87390960531433848 ) ) ;
#182384 = CARTESIAN_POINT ( 'NONE',  ( 16.46253265017160672, -9.564922557960803928, 83.33224293864768129 ) ) ;
#182386 = CARTESIAN_POINT ( 'NONE',  ( 16.51473224551069308, 9.474510206698969483, 24.16557627198102765 ) ) ;
#182385 = CARTESIAN_POINT ( 'NONE',  ( 14.34966873604960469, 8.224510206698951720, 34.16557627198102409 ) ) ;
#182387 = CARTESIAN_POINT ( 'NONE',  ( 5.049401038297881783, 19.05341960407617563, 42.29275706135234003 ) ) ;
#182388 = CARTESIAN_POINT ( 'NONE',  ( 4.483927247898545687, 16.52544592524342804, 74.79057627198105251 ) ) ;
#182389 = CARTESIAN_POINT ( 'NONE',  ( 18.62759615963255655, 10.81492255796105972, 101.6677570613523613 ) ) ;
#182390 = CARTESIAN_POINT ( 'NONE',  ( -19.02544592524342804, 5.153800228976336051, 36.04057627198100988 ) ) ;
#182392 = CARTESIAN_POINT ( 'NONE',  ( 5.823673210054444382, -21.52544592524334988, 110.2094237280190185 ) ) ;
#182391 = CARTESIAN_POINT ( 'NONE',  ( -14.34966873604960291, -8.224510206698953496, 36.66557627198103120 ) ) ;
#182393 = CARTESIAN_POINT ( 'NONE',  ( -9.564922557960796823, -16.46253265017161027, 92.08224293864769550 ) ) ;
#182394 = CARTESIAN_POINT ( 'NONE',  ( 16.51473224551069308, 9.474510206698969483, 89.16557627198103830 ) ) ;
#182395 = CARTESIAN_POINT ( 'NONE',  ( -19.05341960407611168, -5.049401038298163336, 26.45724293864769550 ) ) ;
#182396 = CARTESIAN_POINT ( 'NONE',  ( -16.52544592524342804, 4.483927247898546575, 101.0405762719810383 ) ) ;
#182397 = CARTESIAN_POINT ( 'NONE',  ( 4.483927247898545687, 16.52544592524342804, 69.79057627198102409 ) ) ;
#182398 = CARTESIAN_POINT ( 'NONE',  ( 15.80617190586746368, 15.72974639402197994, 79.37390960531436690 ) ) ;
#182399 = CARTESIAN_POINT ( 'NONE',  ( 13.97604488694527802, 13.89961937509977652, 94.37390960531436690 ) ) ;
#182400 = CARTESIAN_POINT ( 'NONE',  ( -21.53943276465977519, 0.05219959533907696930, 101.2489096053143669 ) ) ;
#182401 = CARTESIAN_POINT ( 'NONE',  ( 13.97604488694527802, 13.89961937509977652, 84.37390960531433848 ) ) ;
#182403 = CARTESIAN_POINT ( 'NONE',  ( 12.14591786802309770, 12.06949235617756955, 89.37390960531435269 ) ) ;
#182402 = CARTESIAN_POINT ( 'NONE',  ( -18.87255363501902750, -5.500000000000064837, 91.32513748171830059 ) ) ;
#182404 = CARTESIAN_POINT ( 'NONE',  ( -13.89961937509977652, 13.97604488694528158, 65.62390960531436690 ) ) ;
#182405 = CARTESIAN_POINT ( 'NONE',  ( -21.55341960407610458, -5.719274019375992779, 61.45724293864770260 ) ) ;
#182406 = LINE ( 'NONE', #55063, #20390 ) ;
#182408 = DIRECTION ( 'NONE',  ( 0.000000000000000000, 0.000000000000000000, -1.000000000000000000 ) ) ;
#182407 = CARTESIAN_POINT ( 'NONE',  ( -0.05219959533907301413, -21.53943276465977519, 27.49890960531435269 ) ) ;
#182409 = CARTESIAN_POINT ( 'NONE',  ( -4.379528057220086978, -16.55341960407618274, 24.79275706135235779 ) ) ;
#182410 = CARTESIAN_POINT ( 'NONE',  ( 12.14591786802309770, 12.06949235617756955, 94.37390960531436690 ) ) ;
#182411 = CARTESIAN_POINT ( 'NONE',  ( -17.60779699588840330, -5.500000000000024869, 46.34981316670106111 ) ) ;
#182412 = CARTESIAN_POINT ( 'NONE',  ( -13.97604488694527625, -13.89961937509977652, 86.87390960531436690 ) ) ;
#182413 = CARTESIAN_POINT ( 'NONE',  ( -16.51473224551069308, -9.474510206698971260, 46.66557627198102409 ) ) ;
#182414 = CARTESIAN_POINT ( 'NONE',  ( -8.224510206698948167, 14.34966873604960824, 85.41557627198102409 ) ) ;
#182415 = CARTESIAN_POINT ( 'NONE',  ( 19.05341960407611168, 5.049401038298154454, 113.9572429386477097 ) ) ;
#182416 = CARTESIAN_POINT ( 'NONE',  ( -5.153800228976607833, 19.02544592524334988, 107.7094237280189759 ) ) ;
#182417 = CARTESIAN_POINT ( 'NONE',  ( 21.52544592524334988, 5.823673210054432836, 61.45942372801901854 ) ) ;
#182418 = VECTOR ( 'NONE', #95371, 999.9999999999997726 ) ;
#182419 = CARTESIAN_POINT ( 'NONE',  ( 13.89961937509977652, -13.97604488694527269, 103.1239096053143527 ) ) ;
#182420 = CARTESIAN_POINT ( 'NONE',  ( -21.53943276465977519, 0.05219959533907696930, 86.24890960531436690 ) ) ;
#182421 = CARTESIAN_POINT ( 'NONE',  ( 16.55341960407618274, -4.379528057220086978, 86.04275706135236135 ) ) ;
#182422 = VECTOR ( 'NONE', #87282, 1000.000000000000000 ) ;
#182423 = CARTESIAN_POINT ( 'NONE',  ( 5.049401038298161559, -19.05341960407611168, 22.70724293864769194 ) ) ;
#182424 = CARTESIAN_POINT ( 'NONE',  ( -13.97604488694527625, -13.89961937509977652, 71.87390960531433848 ) ) ;
#182425 = CARTESIAN_POINT ( 'NONE',  ( 10.72451020669898902, -18.67979575497178502, 77.91557627198102409 ) ) ;
#182426 = CARTESIAN_POINT ( 'NONE',  ( -16.51473224551082808, 9.474510206698731452, 108.3344237280190043 ) ) ;
#182428 = CARTESIAN_POINT ( 'NONE',  ( 15.72974639402176855, 15.80617190586768217, 56.87609039468568994 ) ) ;
#182427 = CARTESIAN_POINT ( 'NONE',  ( 4.483927247898545687, 16.52544592524342804, 39.79057627198103830 ) ) ;
#182430 = CARTESIAN_POINT ( 'NONE',  ( 5.719274019375991003, -21.55341960407610458, 27.70724293864769905 ) ) ;
#182429 = CARTESIAN_POINT ( 'NONE',  ( -12.14591786802326823, 12.06949235617739902, 83.12609039468568994 ) ) ;
#182431 = DIRECTION ( 'NONE',  ( 1.000000000000000000, 0.000000000000000000, 0.000000000000000000 ) ) ;
#182432 = CARTESIAN_POINT ( 'NONE',  ( 12.06949235617739724, 12.14591786802326823, 101.8760903946857042 ) ) ;
#182433 = CARTESIAN_POINT ( 'NONE',  ( -4.379528057220086978, -16.55341960407618274, 49.79275706135234714 ) ) ;
#182434 = CARTESIAN_POINT ( 'NONE',  ( 5.153800228976335163, 19.02544592524342804, 64.79057627198100988 ) ) ;
#182435 = CARTESIAN_POINT ( 'NONE',  ( -13.97604488694527625, -13.89961937509977652, 71.87390960531433848 ) ) ;
#182436 = CARTESIAN_POINT ( 'NONE',  ( 4.379528057220092307, 16.55341960407617563, 72.29275706135236135 ) ) ;
#182437 = CARTESIAN_POINT ( 'NONE',  ( -4.483927247898539470, -16.52544592524342804, 52.29057627198102409 ) ) ;
#182438 = CARTESIAN_POINT ( 'NONE',  ( 13.89961937509977652, -13.97604488694527269, 58.12390960531436690 ) ) ;
#182439 = CARTESIAN_POINT ( 'NONE',  ( 19.02544592524343514, -5.153800228976328945, 48.54057627198103120 ) ) ;
#182440 = CARTESIAN_POINT ( 'NONE',  ( 0.05219959533934541429, -16.53943276465976808, 40.00109039468567573 ) ) ;
#182441 = CARTESIAN_POINT ( 'NONE',  ( 9.564922557961047289, -16.46253265017146816, 90.41775706135234714 ) ) ;
#182442 = CARTESIAN_POINT ( 'NONE',  ( 16.52544592524342804, -4.483927247898539470, 103.5405762719810383 ) ) ;
#182443 = CARTESIAN_POINT ( 'NONE',  ( -19.05341960407611168, -5.049401038298163336, 66.45724293864769550 ) ) ;
#182445 = CARTESIAN_POINT ( 'NONE',  ( 11.74264578624799427, 36.14014761921585972, -6.599999999999999645 ) ) ;
#182444 = CARTESIAN_POINT ( 'NONE',  ( 19.02544592524334988, 5.153800228976608722, 101.4594237280189759 ) ) ;
#182446 = CARTESIAN_POINT ( 'NONE',  ( -15.80617190586768217, 15.72974639402176855, 93.12609039468568994 ) ) ;
#182447 = CARTESIAN_POINT ( 'NONE',  ( 4.379528057220092307, 16.55341960407617563, 67.29275706135234714 ) ) ;
#182448 = CARTESIAN_POINT ( 'NONE',  ( 37.99626262588765258, 2.893932880411085066E-14, -6.747842220587804363 ) ) ;
#182449 = CARTESIAN_POINT ( 'NONE',  ( 10.72451020669898902, -18.67979575497178502, 67.91557627198102409 ) ) ;
#182450 = CARTESIAN_POINT ( 'NONE',  ( 16.53943276465976808, 0.05219959533934440121, 51.25109039468568994 ) ) ;
#182451 = CARTESIAN_POINT ( 'NONE',  ( -18.22780087662123805, 5.499999999999981348, 71.01763182126894947 ) ) ;
#182452 = CARTESIAN_POINT ( 'NONE',  ( 19.05341960407617918, -5.049401038297876454, 41.04275706135233293 ) ) ;
#182453 = CARTESIAN_POINT ( 'NONE',  ( -13.89961937509977652, 13.97604488694528158, 90.62390960531432427 ) ) ;
#182454 = CARTESIAN_POINT ( 'NONE',  ( 12.06949235617757843, -12.14591786802309237, 113.1239096053143953 ) ) ;
#182455 = CARTESIAN_POINT ( 'NONE',  ( -9.474510206698964154, 16.51473224551069663, 70.41557627198102409 ) ) ;
#182456 = AXIS2_PLACEMENT_3D ( 'NONE', #181894, #44370, #137361 ) ;
#182457 = CARTESIAN_POINT ( 'NONE',  ( 17.02389920581777716, 17.34149035984847131, -54.21489346206828230 ) ) ;
#182458 = CARTESIAN_POINT ( 'NONE',  ( -10.81492255796105439, 18.62759615963255655, 77.91775706135231871 ) ) ;
#182459 = CARTESIAN_POINT ( 'NONE',  ( 13.97604488694548053, -13.89961937509957401, 35.62609039468567573 ) ) ;
#182460 = CARTESIAN_POINT ( 'NONE',  ( -5.153800228976607833, 19.02544592524334988, 22.70942372801899012 ) ) ;
#182461 = CARTESIAN_POINT ( 'NONE',  ( 13.89961937509977652, -13.97604488694527269, 53.12390960531434558 ) ) ;
#182462 = CARTESIAN_POINT ( 'NONE',  ( -21.53943276465977519, 0.05219959533907696930, 26.24890960531435624 ) ) ;
#182463 = CARTESIAN_POINT ( 'NONE',  ( 15.72974639402176855, 15.80617190586768217, 86.87609039468568994 ) ) ;
#182464 = CARTESIAN_POINT ( 'NONE',  ( -5.153800228976328057, -19.02544592524343514, 67.29057627198102409 ) ) ;
#182465 = CARTESIAN_POINT ( 'NONE',  ( -10.72451020669870658, -18.67979575497194134, 84.58442372801903275 ) ) ;
#182466 = CARTESIAN_POINT ( 'NONE',  ( 5.719274019375991003, -21.55341960407610458, 37.70724293864769550 ) ) ;
#182467 = CARTESIAN_POINT ( 'NONE',  ( -19.03943276465977164, 0.05219959533909376836, 66.24890960531436690 ) ) ;
#182468 = CARTESIAN_POINT ( 'NONE',  ( -15.72974639402176322, -15.80617190586768395, 39.37609039468567573 ) ) ;
#182469 = CARTESIAN_POINT ( 'NONE',  ( -9.564922557961040184, 16.46253265017147172, 67.91775706135233293 ) ) ;
#182470 = CARTESIAN_POINT ( 'NONE',  ( 16.46253265017160672, -9.564922557960803928, 43.33224293864769550 ) ) ;
#182471 = CARTESIAN_POINT ( 'NONE',  ( -19.03943276465977164, 0.05219959533909376836, 96.24890960531436690 ) ) ;
#182472 = CARTESIAN_POINT ( 'NONE',  ( 8.224510206698742110, 14.34966873604972548, 27.08442372801901854 ) ) ;
#182473 = CARTESIAN_POINT ( 'NONE',  ( -12.14591786802309592, -12.06949235617757132, 86.87390960531438111 ) ) ;
#182474 = CARTESIAN_POINT ( 'NONE',  ( 19.02544592524343514, -5.153800228976328945, 53.54057627198102409 ) ) ;
#182475 = CARTESIAN_POINT ( 'NONE',  ( -21.53943276465977519, 0.05219959533907696930, 46.24890960531435979 ) ) ;
#182476 = CARTESIAN_POINT ( 'NONE',  ( -13.97604488694547697, 13.89961937509957934, 113.1260903946856757 ) ) ;
#182477 = CARTESIAN_POINT ( 'NONE',  ( -10.72451020669870658, -18.67979575497194134, 19.58442372801901143 ) ) ;
#182478 = CARTESIAN_POINT ( 'NONE',  ( 10.81492255796106328, -18.62759615963255655, 65.41775706135234714 ) ) ;
#182479 = CARTESIAN_POINT ( 'NONE',  ( 14.29746914071037800, 8.314922557961029526, 66.66775706135234714 ) ) ;
#182480 = CARTESIAN_POINT ( 'NONE',  ( -12.06949235617739369, -12.14591786802326823, 69.37609039468567573 ) ) ;
#182481 = CARTESIAN_POINT ( 'NONE',  ( 5.049401038298161559, -19.05341960407611168, 57.70724293864769550 ) ) ;
#182482 = CARTESIAN_POINT ( 'NONE',  ( 12.14591786802327356, -12.06949235617739191, 95.62609039468568994 ) ) ;
#182483 = CARTESIAN_POINT ( 'NONE',  ( 19.02544592524334988, 5.153800228976608722, 41.45942372801900433 ) ) ;
#182484 = CARTESIAN_POINT ( 'NONE',  ( 5.823673210054125526, 21.52544592524343514, 109.7905762719810383 ) ) ;
#182485 = CARTESIAN_POINT ( 'NONE',  ( 16.52544592524342804, -4.483927247898539470, 63.54057627198103830 ) ) ;
#182486 = CARTESIAN_POINT ( 'NONE',  ( -19.02544592524342804, 5.153800228976336051, 86.04057627198103830 ) ) ;
#182487 = CARTESIAN_POINT ( 'NONE',  ( -4.379528057220086978, -16.55341960407618274, 89.79275706135236135 ) ) ;
#182488 = CARTESIAN_POINT ( 'NONE',  ( -0.05219959533937732626, 21.53943276465977519, 52.50109039468567573 ) ) ;
#182489 = CARTESIAN_POINT ( 'NONE',  ( -14.34966873604972548, 8.224510206698743886, 38.33442372801900433 ) ) ;
#182490 = CARTESIAN_POINT ( 'NONE',  ( -15.80617190586768217, 15.72974639402176855, 33.12609039468569705 ) ) ;
#182491 = CARTESIAN_POINT ( 'NONE',  ( 16.55341960407611168, 4.379528057220329451, 53.95724293864770260 ) ) ;
#182492 = EDGE_CURVE ( 'NONE', #196503, #144904, #9440, .T. ) ;
#182493 = ORIENTED_EDGE ( 'NONE', *, *, #48581, .F. ) ;
#182494 = CARTESIAN_POINT ( 'NONE',  ( 18.62759615963271287, -10.81492255796078972, 98.33224293864769550 ) ) ;
#182495 = CARTESIAN_POINT ( 'NONE',  ( 4.379528057220339221, -16.55341960407611168, 37.70724293864769550 ) ) ;
#182496 = VERTEX_POINT ( 'NONE', #119101 ) ;
#182497 = DIRECTION ( 'NONE',  ( -1.000000000000000000, 0.000000000000000000, -0.000000000000000000 ) ) ;
#182498 = TOROIDAL_SURFACE ( 'NONE', #8114, 206.0437394197456911, 10.00000000000000000 ) ;
#182499 = CARTESIAN_POINT ( 'NONE',  ( -0.05219959533907301413, -21.53943276465977519, 27.49890960531435269 ) ) ;
#182500 = CARTESIAN_POINT ( 'NONE',  ( -21.55341960407619339, 5.719274019375674811, 33.54275706135234714 ) ) ;
#182501 = CARTESIAN_POINT ( 'NONE',  ( 14.29746914071049879, -8.314922557960816363, 68.33224293864769550 ) ) ;
#182502 = CARTESIAN_POINT ( 'NONE',  ( 19.03943276465977164, -0.05219959533909143690, 78.74890960531436690 ) ) ;
#182504 = CARTESIAN_POINT ( 'NONE',  ( -16.51473224551082808, 9.474510206698731452, 68.33442372801900433 ) ) ;
#182503 = CARTESIAN_POINT ( 'NONE',  ( -16.46253265017160317, 9.564922557960807481, 30.83224293864769550 ) ) ;
#182505 = CARTESIAN_POINT ( 'NONE',  ( -5.719274019375978568, 21.55341960407610458, 45.20724293864769550 ) ) ;
#182506 = CARTESIAN_POINT ( 'NONE',  ( -23.38845648566745794, -29.41134498177912704, -18.89001425235596088 ) ) ;
#182507 = CARTESIAN_POINT ( 'NONE',  ( -16.51473224551069308, -9.474510206698971260, 61.66557627198103120 ) ) ;
#182508 = CARTESIAN_POINT ( 'NONE',  ( 16.52544592524335698, 4.483927247898782831, 41.45942372801901143 ) ) ;
#182509 = CARTESIAN_POINT ( 'NONE',  ( 21.55341960407619695, -5.719274019375665929, 21.04275706135234714 ) ) ;
#182510 = CARTESIAN_POINT ( 'NONE',  ( -4.483927247898539470, -16.52544592524342804, 42.29057627198103120 ) ) ;
#182511 = VECTOR ( 'NONE', #155004, 1000.000000000000000 ) ;
#182512 = ORIENTED_EDGE ( 'NONE', *, *, #5788, .F. ) ;
#182513 = CARTESIAN_POINT ( 'NONE',  ( 9.474510206698971260, -16.51473224551069308, 87.91557627198102409 ) ) ;
#182514 = CARTESIAN_POINT ( 'NONE',  ( -10.72451020669898014, 18.67979575497178502, 70.41557627198102409 ) ) ;
#182516 = CARTESIAN_POINT ( 'NONE',  ( 14.34966873604972726, -8.224510206698740333, 35.83442372801901143 ) ) ;
#182515 = CARTESIAN_POINT ( 'NONE',  ( 5.719274019375991003, -21.55341960407610458, 112.7072429386476955 ) ) ;
#182517 = CARTESIAN_POINT ( 'NONE',  ( -21.53943276465977519, 0.05219959533907696930, 36.24890960531435979 ) ) ;
#182518 = CARTESIAN_POINT ( 'NONE',  ( -15.80617190586768217, 15.72974639402176855, 103.1260903946856757 ) ) ;
#182519 = CARTESIAN_POINT ( 'NONE',  ( 13.97604488694527802, 13.89961937509977652, 94.37390960531436690 ) ) ;
#182520 = CARTESIAN_POINT ( 'NONE',  ( 9.474510206698971260, -16.51473224551069308, 37.91557627198102409 ) ) ;
#182521 = CARTESIAN_POINT ( 'NONE',  ( 16.46253265017160672, -9.564922557960803928, 93.33224293864769550 ) ) ;
#182522 = CARTESIAN_POINT ( 'NONE',  ( -5.049401038298153566, 19.05341960407611168, 75.20724293864769550 ) ) ;
#182523 = CARTESIAN_POINT ( 'NONE',  ( -20.28159948851298822, -33.49867931359609941, -17.64937754809734827 ) ) ;
#182524 = CARTESIAN_POINT ( 'NONE',  ( 16.51473224551083163, -9.474510206698727899, 50.83442372801899722 ) ) ;
#182526 = CARTESIAN_POINT ( 'NONE',  ( -10.72451020669898014, 18.67979575497178502, 25.41557627198103120 ) ) ;
#182525 = CARTESIAN_POINT ( 'NONE',  ( 18.67979575497194134, -10.72451020669871369, 110.8344237280190043 ) ) ;
#182527 = CARTESIAN_POINT ( 'NONE',  ( 4.483927247898790824, -16.52544592524335698, 110.2094237280190185 ) ) ;
#182528 = CARTESIAN_POINT ( 'NONE',  ( -13.89961937509957401, -13.97604488694547875, 84.37609039468567573 ) ) ;
#182529 = CARTESIAN_POINT ( 'NONE',  ( -17.44270441346513323, 5.991230190323084237, 58.63664920735774189 ) ) ;
#182530 = CARTESIAN_POINT ( 'NONE',  ( -13.97604488694547697, 13.89961937509957934, 83.12609039468564731 ) ) ;
#182531 = CARTESIAN_POINT ( 'NONE',  ( 16.51473224551083163, -9.474510206698727899, 40.83442372801900433 ) ) ;
#182532 = DIRECTION ( 'NONE',  ( 1.000000000000000000, 0.000000000000000000, 0.000000000000000000 ) ) ;
#182533 = CARTESIAN_POINT ( 'NONE',  ( -9.564922557960796823, -16.46253265017161027, 42.08224293864769550 ) ) ;
#182534 = CARTESIAN_POINT ( 'NONE',  ( -14.29746914071049879, 8.314922557960819915, 45.83224293864769550 ) ) ;
#182535 = CARTESIAN_POINT ( 'NONE',  ( -17.40861289039001392, -6.110651285853327508, 111.3723247082743626 ) ) ;
#182536 = CARTESIAN_POINT ( 'NONE',  ( -8.224510206698948167, 14.34966873604960824, 25.41557627198103120 ) ) ;
#182537 = CARTESIAN_POINT ( 'NONE',  ( -3.573655867282028392E-15, 2.428612866367529932E-14, -25.00000000000000000 ) ) ;
#182538 = CARTESIAN_POINT ( 'NONE',  ( -14.29746914071037622, -8.314922557961029526, 99.16775706135234714 ) ) ;
#182539 = CARTESIAN_POINT ( 'NONE',  ( -19.03943276465977164, 0.05219959533909376836, 46.24890960531435979 ) ) ;
#182540 = CARTESIAN_POINT ( 'NONE',  ( 10.72451020669871369, 18.67979575497193778, 102.0844237280190185 ) ) ;
#182541 = CARTESIAN_POINT ( 'NONE',  ( 5.049401038297881783, 19.05341960407617563, 112.2927570613523471 ) ) ;
#182543 = VERTEX_POINT ( 'NONE', #180782 ) ;
#182542 = CARTESIAN_POINT ( 'NONE',  ( 10.72451020669871369, 18.67979575497193778, 97.08442372801904696 ) ) ;
#182544 = CARTESIAN_POINT ( 'NONE',  ( -13.97604488694527625, -13.89961937509977652, 96.87390960531433848 ) ) ;
#182545 = CARTESIAN_POINT ( 'NONE',  ( -16.51473224551069308, -9.474510206698971260, 81.66557627198103830 ) ) ;
#182546 = CARTESIAN_POINT ( 'NONE',  ( -36.91746825000000598, 2.428612866367529932E-14, -6.624999997268814056 ) ) ;
#182547 = CARTESIAN_POINT ( 'NONE',  ( -0.05219959533907301413, -21.53943276465977519, 107.4989096053143669 ) ) ;
#182548 = AXIS2_PLACEMENT_3D ( 'NONE', #98688, #157403, #83522 ) ;
#182549 = CARTESIAN_POINT ( 'NONE',  ( -16.53943276465976808, 0.05219959533911058130, 76.24890960531435269 ) ) ;
#182550 = CARTESIAN_POINT ( 'NONE',  ( 18.62759615963271287, -10.81492255796078972, 73.33224293864769550 ) ) ;
#182551 = CARTESIAN_POINT ( 'NONE',  ( 19.03943276465977164, -0.05219959533909143690, 63.74890960531435979 ) ) ;
#182553 = CARTESIAN_POINT ( 'NONE',  ( 12.14591786802327356, -12.06949235617739191, 95.62609039468568994 ) ) ;
#182552 = CARTESIAN_POINT ( 'NONE',  ( -5.719274019375978568, 21.55341960407610458, 100.2072429386476955 ) ) ;
#182554 = ORIENTED_EDGE ( 'NONE', *, *, #151864, .F. ) ;
#182555 = CARTESIAN_POINT ( 'NONE',  ( -19.03943276465977164, 0.05219959533909376836, 61.24890960531436690 ) ) ;
#182557 = LINE ( 'NONE', #62159, #152722 ) ;
#182556 = CARTESIAN_POINT ( 'NONE',  ( 4.379528057220339221, -16.55341960407611168, 97.70724293864772392 ) ) ;
#182558 = CARTESIAN_POINT ( 'NONE',  ( -19.05341960407611168, -5.049401038298163336, 66.45724293864769550 ) ) ;
#182559 = CARTESIAN_POINT ( 'NONE',  ( 0.05219959533936267826, -19.03943276465977164, 75.00109039468566152 ) ) ;
#182560 = CARTESIAN_POINT ( 'NONE',  ( 4.379528057220339221, -16.55341960407611168, 82.70724293864770971 ) ) ;
#182561 = CARTESIAN_POINT ( 'NONE',  ( 5.823673210054444382, -21.52544592524334988, 60.20942372801902565 ) ) ;
#182563 = CARTESIAN_POINT ( 'NONE',  ( -21.53943276465977519, -0.05219959533937600094, 18.75109039468568639 ) ) ;
#182562 = CARTESIAN_POINT ( 'NONE',  ( -19.02544592524342804, 5.153800228976336051, 46.04057627198101699 ) ) ;
#182564 = CARTESIAN_POINT ( 'NONE',  ( -14.29746914071049879, 8.314922557960819915, 100.8322429386477097 ) ) ;
#182565 = CARTESIAN_POINT ( 'NONE',  ( 7.587788125977466436, -46.88744275388935989, -24.49805083758646873 ) ) ;
#182566 = CARTESIAN_POINT ( 'NONE',  ( 13.89961937509977652, -13.97604488694527269, 63.12390960531435979 ) ) ;
#182567 = CARTESIAN_POINT ( 'NONE',  ( 28.82186960331477010, -9.364793116373819615, 139.1500000054623740 ) ) ;
#182569 = CARTESIAN_POINT ( 'NONE',  ( -21.55341960407610458, -5.719274019375992779, 21.45724293864769550 ) ) ;
#182568 = CARTESIAN_POINT ( 'NONE',  ( 9.564922557961047289, -16.46253265017146816, 110.4177570613523471 ) ) ;
#182570 = CARTESIAN_POINT ( 'NONE',  ( -5.823673210054431948, 21.52544592524334988, 47.70942372801902565 ) ) ;
#182571 = CARTESIAN_POINT ( 'NONE',  ( 5.153800228976335163, 19.02544592524342804, 99.79057627198102409 ) ) ;
#182572 = CARTESIAN_POINT ( 'NONE',  ( 13.89961937509957401, 13.97604488694547697, 81.87609039468564731 ) ) ;
#182573 = CARTESIAN_POINT ( 'NONE',  ( 5.049401038298161559, -19.05341960407611168, 62.70724293864769550 ) ) ;
#182574 = CARTESIAN_POINT ( 'NONE',  ( 4.483927247898545687, 16.52544592524342804, 69.79057627198102409 ) ) ;
#182575 = CARTESIAN_POINT ( 'NONE',  ( -14.29746914071049879, 8.314922557960819915, 75.83224293864769550 ) ) ;
#182576 = CARTESIAN_POINT ( 'NONE',  ( -19.05341960407611168, -5.049401038298163336, 86.45724293864769550 ) ) ;
#182577 = CARTESIAN_POINT ( 'NONE',  ( 0.05219959533910956823, 16.53943276465976808, 79.99890960531435269 ) ) ;
#182578 = CARTESIAN_POINT ( 'NONE',  ( 19.05341960407611168, 5.049401038298154454, 88.95724293864769550 ) ) ;
#182579 = CARTESIAN_POINT ( 'NONE',  ( 9.474510206698729675, 16.51473224551082808, 37.08442372801899722 ) ) ;
#182582 = CARTESIAN_POINT ( 'NONE',  ( 16.46253265017160672, -9.564922557960803928, 23.33224293864769194 ) ) ;
#182581 = CARTESIAN_POINT ( 'NONE',  ( 4.483927247898545687, 16.52544592524342804, 24.79057627198103120 ) ) ;
#182580 = CARTESIAN_POINT ( 'NONE',  ( -13.89961937509977652, 13.97604488694528158, 50.62390960531435979 ) ) ;
#182583 = ORIENTED_EDGE ( 'NONE', *, *, #127855, .F. ) ;
#182584 = CARTESIAN_POINT ( 'NONE',  ( 0.05219959533937995610, -21.53943276465977519, 50.00109039468568994 ) ) ;
#182585 = CARTESIAN_POINT ( 'NONE',  ( 0.05219959533936267826, -19.03943276465977164, 65.00109039468567573 ) ) ;
#182586 = CARTESIAN_POINT ( 'NONE',  ( -8.314922557960811034, -14.29746914071050412, 37.08224293864768129 ) ) ;
#182587 = CARTESIAN_POINT ( 'NONE',  ( 21.52544592524344225, -5.823673210054117533, 83.54057627198102409 ) ) ;
#182588 = CARTESIAN_POINT ( 'NONE',  ( 21.53943276465977519, -0.05219959533907433946, 28.74890960531435624 ) ) ;
#182589 = CARTESIAN_POINT ( 'NONE',  ( -8.224510206698948167, 14.34966873604960824, 70.41557627198102409 ) ) ;
#182590 = CARTESIAN_POINT ( 'NONE',  ( 0.05219959533909260263, 19.03943276465977164, 39.99890960531436690 ) ) ;
#182591 = CARTESIAN_POINT ( 'NONE',  ( -13.97604488694547697, 13.89961937509957934, 38.12609039468566152 ) ) ;
#182592 = CARTESIAN_POINT ( 'NONE',  ( -4.483927247898782831, 16.52544592524335698, 107.7094237280190328 ) ) ;
#182593 = CARTESIAN_POINT ( 'NONE',  ( 8.314922557961029526, -14.29746914071037800, 55.41775706135234714 ) ) ;
#182594 = CARTESIAN_POINT ( 'NONE',  ( 18.67979575497178502, 10.72451020669898547, 39.16557627198102409 ) ) ;
#182595 = CARTESIAN_POINT ( 'NONE',  ( -15.80617190586768217, 15.72974639402176855, 113.1260903946856899 ) ) ;
#182596 = CARTESIAN_POINT ( 'NONE',  ( -13.97604488694527625, -13.89961937509977652, 86.87390960531436690 ) ) ;
#182597 = CARTESIAN_POINT ( 'NONE',  ( -14.29746914071037622, -8.314922557961029526, 79.16775706135234714 ) ) ;
#182598 = CARTESIAN_POINT ( 'NONE',  ( 16.53943276465976808, -0.05219959533910856209, 113.7489096053143527 ) ) ;
#182599 = CARTESIAN_POINT ( 'NONE',  ( -4.379528057220328563, 16.55341960407611168, 30.20724293864769550 ) ) ;
#182601 = CARTESIAN_POINT ( 'NONE',  ( -5.153800228976328057, -19.02544592524343514, 92.29057627198099567 ) ) ;
#182600 = CARTESIAN_POINT ( 'NONE',  ( 13.97604488694527802, 13.89961937509977652, 99.37390960531436690 ) ) ;
#182602 = CARTESIAN_POINT ( 'NONE',  ( 15.72974639402199770, -15.80617190586745480, 28.12390960531435979 ) ) ;
#182603 = CARTESIAN_POINT ( 'NONE',  ( -12.14591786802309592, -12.06949235617757132, 76.87390960531439532 ) ) ;
#182604 = CARTESIAN_POINT ( 'NONE',  ( 8.224510206698953496, -14.34966873604960469, 52.91557627198103830 ) ) ;
#182605 = ORIENTED_EDGE ( 'NONE', *, *, #147752, .T. ) ;
#182607 = DIRECTION ( 'NONE',  ( 1.000000000000000000, 0.000000000000000000, 0.000000000000000000 ) ) ;
#182606 = CARTESIAN_POINT ( 'NONE',  ( 4.483927247898790824, -16.52544592524335698, 55.20942372801902565 ) ) ;
#182608 = CARTESIAN_POINT ( 'NONE',  ( 9.474510206698729675, 16.51473224551082808, 57.08442372801900433 ) ) ;
#182609 = CARTESIAN_POINT ( 'NONE',  ( 13.89961937509977652, -13.97604488694527269, 83.12390960531436690 ) ) ;
#182610 = CARTESIAN_POINT ( 'NONE',  ( 16.51473224551083163, -9.474510206698727899, 70.83442372801900433 ) ) ;
#182611 = CARTESIAN_POINT ( 'NONE',  ( -17.14385361876520264, -23.59649016807271593, 143.6750000027311671 ) ) ;
#182612 = CARTESIAN_POINT ( 'NONE',  ( 19.03943276465977164, 0.05219959533936151252, 61.25109039468566863 ) ) ;
#182614 = CARTESIAN_POINT ( 'NONE',  ( 4.483927247898790824, -16.52544592524335698, 95.20942372801903275 ) ) ;
#182613 = CARTESIAN_POINT ( 'NONE',  ( 16.51473224551083163, -9.474510206698727899, 95.83442372801900433 ) ) ;
#182615 = CARTESIAN_POINT ( 'NONE',  ( 22.44159573604009239, 16.30477369853692693, 144.5750000027311728 ) ) ;
#182616 = CARTESIAN_POINT ( 'NONE',  ( -5.049401038298153566, 19.05341960407611168, 45.20724293864769550 ) ) ;
#182617 = CARTESIAN_POINT ( 'NONE',  ( -19.03943276465977164, 0.05219959533909376836, 111.2489096053143669 ) ) ;
#182618 = CARTESIAN_POINT ( 'NONE',  ( 5.719274019375673035, 21.55341960407619339, 57.29275706135234714 ) ) ;
#182619 = CARTESIAN_POINT ( 'NONE',  ( 16.51473224551083163, -9.474510206698727899, 100.8344237280190043 ) ) ;
#182621 = CARTESIAN_POINT ( 'NONE',  ( -16.51473224551069308, -9.474510206698971260, 61.66557627198103120 ) ) ;
#182620 = DIRECTION ( 'NONE',  ( 0.000000000000000000, 0.000000000000000000, 1.000000000000000000 ) ) ;
#182622 = CARTESIAN_POINT ( 'NONE',  ( -9.474510206698964154, 16.51473224551069663, 110.4155762719810383 ) ) ;
#182624 = CARTESIAN_POINT ( 'NONE',  ( 5.153800228976335163, 19.02544592524342804, 69.79057627198103830 ) ) ;
#182623 = CARTESIAN_POINT ( 'NONE',  ( -8.224510206698948167, 14.34966873604960824, 75.41557627198102409 ) ) ;
#182625 = CARTESIAN_POINT ( 'NONE',  ( -9.564922557960796823, -16.46253265017161027, 77.08224293864769550 ) ) ;
#182626 = CARTESIAN_POINT ( 'NONE',  ( 19.02544592524334988, 5.153800228976608722, 71.45942372801900433 ) ) ;
#182627 = CARTESIAN_POINT ( 'NONE',  ( -21.55341960407610458, -5.719274019375992779, 66.45724293864768129 ) ) ;
#182628 = CARTESIAN_POINT ( 'NONE',  ( -19.03943276465977164, 0.05219959533909376836, 21.24890960531436335 ) ) ;
#182629 = CARTESIAN_POINT ( 'NONE',  ( 9.474510206698729675, 16.51473224551082808, 42.08442372801900433 ) ) ;
#182630 = CARTESIAN_POINT ( 'NONE',  ( 19.03943276465977164, -0.05219959533909143690, 48.74890960531435979 ) ) ;
#182631 = CARTESIAN_POINT ( 'NONE',  ( -5.153800228976328057, -19.02544592524343514, 82.29057627198103830 ) ) ;
#182632 = CARTESIAN_POINT ( 'NONE',  ( 15.80617190586746368, 15.72974639402197994, 89.37390960531435269 ) ) ;
#182634 = CARTESIAN_POINT ( 'NONE',  ( -13.89961937509957401, -13.97604488694547875, 54.37609039468565442 ) ) ;
#182633 = CARTESIAN_POINT ( 'NONE',  ( -4.379528057220328563, 16.55341960407611168, 80.20724293864769550 ) ) ;
#182636 = B_SPLINE_CURVE_WITH_KNOTS ( 'NONE', 3,
 ( #130074, #82582, #172630, #114933, #33127, #19933, #187818, #4744, #49287, #34118, #36089, #66433, #95777, #142278, #128094, #20924, #189798, #159428, #51270, #174624 ),
 .UNSPECIFIED., .F., .F.,
 ( 4, 2, 2, 2, 2, 2, 2, 2, 2, 4 ),
 ( 0.004000878361811908805, 0.004499404418915909157, 0.004997930476019910376, 0.005496456533123911595, 0.005994982590227911946, 0.006244245618779911688, 0.006493508647331912298, 0.006992034704435916986, 0.007490560761539923409, 0.007989086818643928098 ),
 .UNSPECIFIED. ) ;
#182635 = CARTESIAN_POINT ( 'NONE',  ( 15.72974639402199770, -15.80617190586745480, 78.12390960531436690 ) ) ;
#182637 = CARTESIAN_POINT ( 'NONE',  ( 15.72974639402199770, -15.80617190586745480, 63.12390960531435979 ) ) ;
#182638 = CARTESIAN_POINT ( 'NONE',  ( -5.823673210054116645, -21.52544592524344225, 42.29057627198103120 ) ) ;
#182639 = CARTESIAN_POINT ( 'NONE',  ( -21.53943276465977519, -0.05219959533937600094, 88.75109039468567573 ) ) ;
#182640 = CARTESIAN_POINT ( 'NONE',  ( -5.153800228976328057, -19.02544592524343514, 77.29057627198099567 ) ) ;
#182641 = CARTESIAN_POINT ( 'NONE',  ( -16.53943276465976808, 0.05219959533911058130, 116.2489096053143669 ) ) ;
#182642 = CARTESIAN_POINT ( 'NONE',  ( 21.52544592524334988, 5.823673210054432836, 31.45942372801901854 ) ) ;
#182643 = CARTESIAN_POINT ( 'NONE',  ( -21.55341960407619339, 5.719274019375674811, 38.54275706135234714 ) ) ;
#182644 = CARTESIAN_POINT ( 'NONE',  ( -19.05341960407611168, -5.049401038298163336, 51.45724293864770260 ) ) ;
#182645 = CARTESIAN_POINT ( 'NONE',  ( 15.80617190586769283, -15.72974639402175789, 25.62609039468567929 ) ) ;
#182646 = CARTESIAN_POINT ( 'NONE',  ( 5.153800228976615827, -19.02544592524334988, 60.20942372801899012 ) ) ;
#182647 = CARTESIAN_POINT ( 'NONE',  ( 5.153800228976335163, 19.02544592524342804, 39.79057627198100988 ) ) ;
#182648 = CARTESIAN_POINT ( 'NONE',  ( -14.29746914071037622, -8.314922557961029526, 24.16775706135235424 ) ) ;
#182649 = CARTESIAN_POINT ( 'NONE',  ( -19.02544592524342804, 5.153800228976336051, 31.04057627198102409 ) ) ;
#182650 = CARTESIAN_POINT ( 'NONE',  ( -16.55341960407617563, 4.379528057220093196, 58.54275706135235424 ) ) ;
#182651 = CARTESIAN_POINT ( 'NONE',  ( 0.05219959533909260263, 19.03943276465977164, 44.99890960531435979 ) ) ;
#182652 = CARTESIAN_POINT ( 'NONE',  ( -26.77313074627600997, -4.631999166350019514, 170.7390164845734546 ) ) ;
#182653 = CARTESIAN_POINT ( 'NONE',  ( 0.05219959533909260263, 19.03943276465977164, 84.99890960531436690 ) ) ;
#182654 = CARTESIAN_POINT ( 'NONE',  ( -16.46253265017160317, 9.564922557960807481, 25.83224293864769194 ) ) ;
#182655 = CARTESIAN_POINT ( 'NONE',  ( -10.81492255796078084, -18.62759615963271287, 57.08224293864769550 ) ) ;
#182656 = CARTESIAN_POINT ( 'NONE',  ( 8.314922557961029526, -14.29746914071037800, 50.41775706135235424 ) ) ;
#182657 = CARTESIAN_POINT ( 'NONE',  ( -21.55341960407619339, 5.719274019375674811, 93.54275706135234714 ) ) ;
#182658 = CARTESIAN_POINT ( 'NONE',  ( 16.46253265017160672, -9.564922557960803928, 38.33224293864768839 ) ) ;
#182659 = CARTESIAN_POINT ( 'NONE',  ( -16.53943276465976808, 0.05219959533911058130, 36.24890960531435979 ) ) ;
#182660 = CARTESIAN_POINT ( 'NONE',  ( 16.52544592524342804, -4.483927247898539470, 73.54057627198102409 ) ) ;
#182661 = CARTESIAN_POINT ( 'NONE',  ( -5.153800228976328057, -19.02544592524343514, 62.29057627198100988 ) ) ;
#182662 = CARTESIAN_POINT ( 'NONE',  ( 10.81492255796106328, -18.62759615963255655, 110.4177570613523756 ) ) ;
#182663 = CARTESIAN_POINT ( 'NONE',  ( -15.72974639402176322, -15.80617190586768395, 19.37609039468568639 ) ) ;
#182664 = CARTESIAN_POINT ( 'NONE',  ( -10.81492255796105439, 18.62759615963255655, 87.91775706135234714 ) ) ;
#182665 = CARTESIAN_POINT ( 'NONE',  ( -16.53943276465976808, -0.05219959533934237506, 48.75109039468568284 ) ) ;
#182666 = CARTESIAN_POINT ( 'NONE',  ( -16.55341960407617563, 4.379528057220093196, 28.54275706135234358 ) ) ;
#182668 = CARTESIAN_POINT ( 'NONE',  ( 5.823673210054444382, -21.52544592524334988, 95.20942372801903275 ) ) ;
#182667 = CARTESIAN_POINT ( 'NONE',  ( 4.379528057220339221, -16.55341960407611168, 92.70724293864770971 ) ) ;
#182669 = CARTESIAN_POINT ( 'NONE',  ( -8.314922557960811034, -14.29746914071050412, 32.08224293864769550 ) ) ;
#182670 = CARTESIAN_POINT ( 'NONE',  ( 5.049401038298161559, -19.05341960407611168, 32.70724293864768129 ) ) ;
#182671 = CARTESIAN_POINT ( 'NONE',  ( 8.224510206698742110, 14.34966873604972548, 47.08442372801901854 ) ) ;
#182672 = CARTESIAN_POINT ( 'NONE',  ( -16.52544592524342804, 4.483927247898546575, 56.04057627198102409 ) ) ;
#182673 = CARTESIAN_POINT ( 'NONE',  ( 8.224510206698742110, 14.34966873604972548, 102.0844237280190185 ) ) ;
#182674 = CARTESIAN_POINT ( 'NONE',  ( 19.02544592524343514, -5.153800228976328945, 113.5405762719810241 ) ) ;
#182675 = CARTESIAN_POINT ( 'NONE',  ( -0.05219959533909027116, -19.03943276465977164, 107.4989096053143527 ) ) ;
#182676 = CARTESIAN_POINT ( 'NONE',  ( -21.55341960407619339, 5.719274019375674811, 113.5427570613523756 ) ) ;
#182677 = CARTESIAN_POINT ( 'NONE',  ( -8.224510206698948167, 14.34966873604960824, 85.41557627198102409 ) ) ;
#182678 = CARTESIAN_POINT ( 'NONE',  ( 16.46253265017160672, -9.564922557960803928, 93.33224293864769550 ) ) ;
#182679 = EDGE_LOOP ( 'NONE', ( #161111, #4160, #91481, #82958 ) ) ;
#182680 = CARTESIAN_POINT ( 'NONE',  ( 16.55341960407618274, -4.379528057220086978, 46.04275706135234714 ) ) ;
#182681 = CARTESIAN_POINT ( 'NONE',  ( -0.05219959533909027116, -19.03943276465977164, 47.49890960531435979 ) ) ;
#182682 = CARTESIAN_POINT ( 'NONE',  ( 13.97604488694527802, 13.89961937509977652, 104.3739096053143385 ) ) ;
#182684 = CARTESIAN_POINT ( 'NONE',  ( 18.22780087662123805, 5.499999999999960032, 101.4823681787310647 ) ) ;
#182683 = CARTESIAN_POINT ( 'NONE',  ( -14.29746914071037622, -8.314922557961029526, 49.16775706135234003 ) ) ;
#182685 = CARTESIAN_POINT ( 'NONE',  ( -5.049401038297874678, -19.05341960407617918, 54.79275706135234003 ) ) ;
#182686 = CARTESIAN_POINT ( 'NONE',  ( -13.97604488694527625, -13.89961937509977652, 41.87390960531435979 ) ) ;
#182687 = CARTESIAN_POINT ( 'NONE',  ( -8.224510206698735004, -14.34966873604973081, 79.58442372801903275 ) ) ;
#182688 = CARTESIAN_POINT ( 'NONE',  ( -13.97604488694547697, 13.89961937509957934, 78.12609039468567573 ) ) ;
#182689 = CARTESIAN_POINT ( 'NONE',  ( -19.05341960407617563, 5.049401038297882671, 33.54275706135231871 ) ) ;
#182690 = CARTESIAN_POINT ( 'NONE',  ( -19.03943276465977164, 0.05219959533909376836, 56.24890960531435979 ) ) ;
#182691 = CARTESIAN_POINT ( 'NONE',  ( 8.314922557960818139, 14.29746914071049879, 99.58224293864770971 ) ) ;
#182692 = EDGE_CURVE ( 'NONE', #44348, #47952, #138227, .T. ) ;
#182693 = CARTESIAN_POINT ( 'NONE',  ( -16.51473224551082808, 9.474510206698731452, 73.33442372801900433 ) ) ;
#182694 = CARTESIAN_POINT ( 'NONE',  ( -10.72451020669898014, 18.67979575497178502, 60.41557627198102409 ) ) ;
#182695 = CARTESIAN_POINT ( 'NONE',  ( -9.564922557961040184, 16.46253265017147172, 32.91775706135233293 ) ) ;
#182696 = CARTESIAN_POINT ( 'NONE',  ( 5.049401038298161559, -19.05341960407611168, 97.70724293864766707 ) ) ;
#182697 = CARTESIAN_POINT ( 'NONE',  ( 10.72451020669898902, -18.67979575497178502, 72.91557627198103830 ) ) ;
#182698 = CARTESIAN_POINT ( 'NONE',  ( -17.40861289039003168, 6.110651285853254677, 83.62767529172566583 ) ) ;
#182699 = CARTESIAN_POINT ( 'NONE',  ( 19.03943276465977164, 0.05219959533936151252, 96.25109039468567573 ) ) ;
#182700 = CARTESIAN_POINT ( 'NONE',  ( -17.49999999999999645, -5.500000000000000888, 120.0000000000000142 ) ) ;
#182701 = CARTESIAN_POINT ( 'NONE',  ( -8.224510206698735004, -14.34966873604973081, 29.58442372801901854 ) ) ;
#182702 = CARTESIAN_POINT ( 'NONE',  ( -5.153800228976328057, -19.02544592524343514, 27.29057627198103120 ) ) ;
#182703 = CARTESIAN_POINT ( 'NONE',  ( 13.97604488694527802, 13.89961937509977652, 114.3739096053143669 ) ) ;
#182704 = CARTESIAN_POINT ( 'NONE',  ( -21.53943276465977519, 0.05219959533907696930, 86.24890960531436690 ) ) ;
#182705 = CARTESIAN_POINT ( 'NONE',  ( 0.05219959533937995610, -21.53943276465977519, 65.00109039468568994 ) ) ;
#182707 = CARTESIAN_POINT ( 'NONE',  ( -5.823673210054431948, 21.52544592524334988, 107.7094237280190328 ) ) ;
#182706 = CARTESIAN_POINT ( 'NONE',  ( 13.89961937509957401, 13.97604488694547697, 111.8760903946856757 ) ) ;
#182708 = CARTESIAN_POINT ( 'NONE',  ( 12.06949235617739724, 12.14591786802326823, 106.8760903946856899 ) ) ;
#182709 = CARTESIAN_POINT ( 'NONE',  ( -18.67979575497178146, -10.72451020669898902, 96.66557627198102409 ) ) ;
#182710 = CARTESIAN_POINT ( 'NONE',  ( -4.379528057220328563, 16.55341960407611168, 55.20724293864770260 ) ) ;
#182711 = CARTESIAN_POINT ( 'NONE',  ( 19.02544592524334988, 5.153800228976608722, 81.45942372801897591 ) ) ;
#182712 = CARTESIAN_POINT ( 'NONE',  ( -16.46253265017146816, -9.564922557961047289, 59.16775706135233293 ) ) ;
#182713 = CARTESIAN_POINT ( 'NONE',  ( -18.67979575497193778, 10.72451020669871902, 63.33442372801900433 ) ) ;
#182714 = CARTESIAN_POINT ( 'NONE',  ( -16.51473224551082808, 9.474510206698731452, 43.33442372801900433 ) ) ;
#182715 = CARTESIAN_POINT ( 'NONE',  ( -12.06949235617756955, 12.14591786802309770, 110.6239096053143669 ) ) ;
#182716 = CARTESIAN_POINT ( 'NONE',  ( 15.80617190586746368, 15.72974639402197994, 24.37390960531435979 ) ) ;
#182717 = CARTESIAN_POINT ( 'NONE',  ( 8.314922557960818139, 14.29746914071049879, 34.58224293864770260 ) ) ;
#182718 = CARTESIAN_POINT ( 'NONE',  ( -5.719274019375665041, -21.55341960407619695, 94.79275706135234714 ) ) ;
#182719 = CARTESIAN_POINT ( 'NONE',  ( -4.483927247898782831, 16.52544592524335698, 77.70942372801900433 ) ) ;
#182720 = CARTESIAN_POINT ( 'NONE',  ( -4.483927247898539470, -16.52544592524342804, 32.29057627198102409 ) ) ;
#182721 = CARTESIAN_POINT ( 'NONE',  ( 18.62759615963255655, 10.81492255796105972, 61.66775706135235424 ) ) ;
#182722 = CARTESIAN_POINT ( 'NONE',  ( -21.52544592524334988, -5.823673210054445271, 63.95942372801901854 ) ) ;
#182723 = CARTESIAN_POINT ( 'NONE',  ( -15.80617190586745835, -15.72974639402198527, 71.87390960531438111 ) ) ;
#182724 = ADVANCED_FACE ( 'NONE', ( #87740 ), #12911, .F. ) ;
#182725 = ORIENTED_EDGE ( 'NONE', *, *, #101956, .F. ) ;
#182726 = CARTESIAN_POINT ( 'NONE',  ( -19.03943276465977164, 0.05219959533909376836, 31.24890960531435979 ) ) ;
#182727 = CARTESIAN_POINT ( 'NONE',  ( -5.719274019375665041, -21.55341960407619695, 49.79275706135234714 ) ) ;
#182728 = CARTESIAN_POINT ( 'NONE',  ( -19.02544592524342804, 5.153800228976336051, 26.04057627198103120 ) ) ;
#182729 = CARTESIAN_POINT ( 'NONE',  ( -13.97604488694527625, -13.89961937509977652, 36.87390960531436690 ) ) ;
#182730 = CARTESIAN_POINT ( 'NONE',  ( -12.06949235617756955, 12.14591786802309770, 75.62390960531439532 ) ) ;
#182731 = CARTESIAN_POINT ( 'NONE',  ( -0.05219959533909027116, -19.03943276465977164, 87.49890960531436690 ) ) ;
#182732 = CARTESIAN_POINT ( 'NONE',  ( 14.29746914071049879, -8.314922557960816363, 23.33224293864769194 ) ) ;
#182733 = CARTESIAN_POINT ( 'NONE',  ( -16.55341960407611168, -4.379528057220339221, 96.45724293864770971 ) ) ;
#182734 = CARTESIAN_POINT ( 'NONE',  ( -21.55341960407610458, -5.719274019375992779, 66.45724293864768129 ) ) ;
#182735 = AXIS2_PLACEMENT_3D ( 'NONE', #176814, #40279, #8956 ) ;
#182736 = CARTESIAN_POINT ( 'NONE',  ( 21.55341960407610458, 5.719274019375980345, 108.9572429386476955 ) ) ;
#182737 = CARTESIAN_POINT ( 'NONE',  ( 19.03943276465977164, -0.05219959533909143690, 113.7489096053143669 ) ) ;
#182739 = CARTESIAN_POINT ( 'NONE',  ( -9.564922557961040184, 16.46253265017147172, 107.9177570613523471 ) ) ;
#182738 = CARTESIAN_POINT ( 'NONE',  ( 19.03943276465977164, -0.05219959533909143690, 63.74890960531435979 ) ) ;
#182740 = CARTESIAN_POINT ( 'NONE',  ( 21.53943276465977519, -0.05219959533907433946, 63.74890960531435979 ) ) ;
#182741 = CARTESIAN_POINT ( 'NONE',  ( -21.53943276465977519, -0.05219959533937600094, 83.75109039468568994 ) ) ;
#182742 = CARTESIAN_POINT ( 'NONE',  ( 13.89961937509977652, -13.97604488694527269, 73.12390960531436690 ) ) ;
#182743 = CARTESIAN_POINT ( 'NONE',  ( 19.05341960407611168, 5.049401038298154454, 93.95724293864769550 ) ) ;
#182744 = CARTESIAN_POINT ( 'NONE',  ( 8.314922557961029526, -14.29746914071037800, 75.41775706135233293 ) ) ;
#182745 = CARTESIAN_POINT ( 'NONE',  ( -10.72451020669870658, -18.67979575497194134, 59.58442372801901854 ) ) ;
#182746 = CARTESIAN_POINT ( 'NONE',  ( -10.72451020669870658, -18.67979575497194134, 104.5844237280190185 ) ) ;
#182747 = CARTESIAN_POINT ( 'NONE',  ( -5.823673210054116645, -21.52544592524344225, 112.2905762719810241 ) ) ;
#182749 = CARTESIAN_POINT ( 'NONE',  ( 10.72451020669898902, -18.67979575497178502, 72.91557627198103830 ) ) ;
#182748 = B_SPLINE_CURVE_WITH_KNOTS ( 'NONE', 3,
 ( #63655, #14161, #137507, #199188, #94978, #159622, #68611, #97929, #189983, #65629, #2968, #35294, #95971, #64648, #130267, #19144, #83770, #113119, #156663, #36274 ),
 .UNSPECIFIED., .F., .F.,
 ( 4, 2, 2, 2, 2, 2, 2, 2, 2, 4 ),
 ( 0.000000000000000000, 0.0004987090165372679322, 0.0009974180330745358643, 0.001246772541343169668, 0.001496127049611803905, 0.001994836066149056984, 0.002493545082686310279, 0.002742899590954944733, 0.002992254099223578320, 0.003989672132298099222 ),
 .UNSPECIFIED. ) ;
#182750 = CARTESIAN_POINT ( 'NONE',  ( -19.02544592524334988, -5.153800228976617603, 43.95942372801899012 ) ) ;
#182751 = CARTESIAN_POINT ( 'NONE',  ( 5.719274019375991003, -21.55341960407610458, 37.70724293864769550 ) ) ;
#182753 = CARTESIAN_POINT ( 'NONE',  ( -0.05219959533910754901, -16.53943276465976808, 37.49890960531436690 ) ) ;
#182752 = CARTESIAN_POINT ( 'NONE',  ( -19.03943276465977164, 0.05219959533909376836, 76.24890960531435269 ) ) ;
#182754 = CARTESIAN_POINT ( 'NONE',  ( -17.44279575226823198, 5.990770900252463171, 65.83557567514320397 ) ) ;
#182755 = DIRECTION ( 'NONE',  ( 1.000000000000000000, 0.000000000000000000, 0.000000000000000000 ) ) ;
#182756 = CARTESIAN_POINT ( 'NONE',  ( -13.89961937509957401, -13.97604488694547875, 94.37609039468566152 ) ) ;
#182757 = CARTESIAN_POINT ( 'NONE',  ( -15.72974639402197994, 15.80617190586746368, 75.62390960531439532 ) ) ;
#182758 = CARTESIAN_POINT ( 'NONE',  ( -14.34966873604960291, -8.224510206698953496, 56.66557627198103830 ) ) ;
#182759 = CARTESIAN_POINT ( 'NONE',  ( -14.29746914071037622, -8.314922557961029526, 29.16775706135234003 ) ) ;
#182760 = CARTESIAN_POINT ( 'NONE',  ( 5.153800228976335163, 19.02544592524342804, 49.79057627198100988 ) ) ;
#182762 = CARTESIAN_POINT ( 'NONE',  ( 9.474510206698729675, 16.51473224551082808, 87.08442372801900433 ) ) ;
#182761 = CARTESIAN_POINT ( 'NONE',  ( -0.05219959533907301413, -21.53943276465977519, 107.4989096053143669 ) ) ;
#182763 = CARTESIAN_POINT ( 'NONE',  ( -5.049401038298153566, 19.05341960407611168, 75.20724293864769550 ) ) ;
#182764 = CARTESIAN_POINT ( 'NONE',  ( -4.483927247898539470, -16.52544592524342804, 87.29057627198103830 ) ) ;
#182765 = CARTESIAN_POINT ( 'NONE',  ( 16.51473224551069308, 9.474510206698969483, 59.16557627198102409 ) ) ;
#182766 = CARTESIAN_POINT ( 'NONE',  ( -16.55341960407611168, -4.379528057220339221, 61.45724293864770260 ) ) ;
#182767 = CARTESIAN_POINT ( 'NONE',  ( -19.05341960407611168, -5.049401038298163336, 26.45724293864769550 ) ) ;
#182768 = CARTESIAN_POINT ( 'NONE',  ( -17.28531771875952572, -5.454187267896333680, 21.09794194731993500 ) ) ;
#182769 = CARTESIAN_POINT ( 'NONE',  ( 8.224510206698953496, -14.34966873604960469, 37.91557627198102409 ) ) ;
#182770 = CARTESIAN_POINT ( 'NONE',  ( -16.46253265017160317, 9.564922557960807481, 90.83224293864769550 ) ) ;
#182771 = CARTESIAN_POINT ( 'NONE',  ( -28.82186960331499037, 2.428612866367529932E-14, 144.0000000000000000 ) ) ;
#182772 = CARTESIAN_POINT ( 'NONE',  ( 9.474510206698729675, 16.51473224551082808, 47.08442372801900433 ) ) ;
#182773 = CARTESIAN_POINT ( 'NONE',  ( -4.379528057220086978, -16.55341960407618274, 59.79275706135234714 ) ) ;
#182774 = VECTOR ( 'NONE', #157174, 1000.000000000000114 ) ;
#182775 = CARTESIAN_POINT ( 'NONE',  ( 21.55341960407610458, 5.719274019375980345, 83.95724293864770971 ) ) ;
#182776 = CARTESIAN_POINT ( 'NONE',  ( -19.05341960407617563, 5.049401038297882671, 38.54275706135233293 ) ) ;
#182777 = CARTESIAN_POINT ( 'NONE',  ( 9.564922557960805705, 16.46253265017160317, 89.58224293864769550 ) ) ;
#182778 = CARTESIAN_POINT ( 'NONE',  ( -17.49999999999999645, 3.471454075611698276, 114.4833258114436489 ) ) ;
#182779 = CARTESIAN_POINT ( 'NONE',  ( 18.67979575497178502, 10.72451020669898547, 34.16557627198102409 ) ) ;
#182780 = CARTESIAN_POINT ( 'NONE',  ( -13.97604488694527625, -13.89961937509977652, 76.87390960531433848 ) ) ;
#182781 = CARTESIAN_POINT ( 'NONE',  ( 21.52544592524334988, 5.823673210054432836, 51.45942372801901854 ) ) ;
#182782 = CARTESIAN_POINT ( 'NONE',  ( 4.483927247898545687, 16.52544592524342804, 114.7905762719810383 ) ) ;
#182785 = ORIENTED_EDGE ( 'NONE', *, *, #8030, .T. ) ;
#182784 = CARTESIAN_POINT ( 'NONE',  ( -13.89961937509977652, 13.97604488694528158, 90.62390960531432427 ) ) ;
#182783 = CARTESIAN_POINT ( 'NONE',  ( -18.67979575497178146, -10.72451020669898902, 111.6655762719810525 ) ) ;
#182786 = CARTESIAN_POINT ( 'NONE',  ( -21.55341960407619339, 5.719274019375674811, 33.54275706135234714 ) ) ;
#182787 = EDGE_LOOP ( 'NONE', ( #100776, #166004, #191191 ) ) ;
#182788 = CARTESIAN_POINT ( 'NONE',  ( -19.05341960407611168, -5.049401038298163336, 101.4572429386476955 ) ) ;
#182789 = DIRECTION ( 'NONE',  ( 0.8164965809277243691, 0.000000000000000000, -0.5773502691896280625 ) ) ;
#182790 = CARTESIAN_POINT ( 'NONE',  ( -10.81492255796078084, -18.62759615963271287, 112.0822429386477097 ) ) ;
#182791 = CARTESIAN_POINT ( 'NONE',  ( -19.02544592524342804, 5.153800228976336051, 46.04057627198101699 ) ) ;
#182792 = CARTESIAN_POINT ( 'NONE',  ( -8.224510206698735004, -14.34966873604973081, 24.58442372801901499 ) ) ;
#182793 = CARTESIAN_POINT ( 'NONE',  ( 11.40812507854754365, 35.11059874428196537, -5.724999997268812812 ) ) ;
#182794 = CARTESIAN_POINT ( 'NONE',  ( 18.62759615963255655, 10.81492255796105972, 106.6677570613523756 ) ) ;
#182795 = CARTESIAN_POINT ( 'NONE',  ( 9.564922557960805705, 16.46253265017160317, 34.58224293864770260 ) ) ;
#182796 = CARTESIAN_POINT ( 'NONE',  ( -5.823673210054431948, 21.52544592524334988, 102.7094237280190185 ) ) ;
#182798 = CARTESIAN_POINT ( 'NONE',  ( 21.53943276465977519, 0.05219959533937863772, 61.25109039468567573 ) ) ;
#182797 = CARTESIAN_POINT ( 'NONE',  ( 16.51473224551069308, 9.474510206698969483, 84.16557627198102409 ) ) ;
#182799 = CARTESIAN_POINT ( 'NONE',  ( -22.44159573604010305, 16.30477369853692338, 141.1750000027311671 ) ) ;
#182800 = CARTESIAN_POINT ( 'NONE',  ( 19.03943276465977164, -0.05219959533909143690, 98.74890960531436690 ) ) ;
#182801 = CARTESIAN_POINT ( 'NONE',  ( -17.49999999999999289, 3.850315288878727316, 29.26629130603453177 ) ) ;
#182804 = CARTESIAN_POINT ( 'NONE',  ( 10.81492255796106328, -18.62759615963255655, 60.41775706135235424 ) ) ;
#182803 = CARTESIAN_POINT ( 'NONE',  ( 12.06949235617739724, 12.14591786802326823, 61.87609039468568284 ) ) ;
#182802 = CARTESIAN_POINT ( 'NONE',  ( -8.224510206698735004, -14.34966873604973081, 59.58442372801901854 ) ) ;
#182805 = CARTESIAN_POINT ( 'NONE',  ( 21.55341960407619695, -5.719274019375665929, 96.04275706135236135 ) ) ;
#182806 = CARTESIAN_POINT ( 'NONE',  ( -10.97788116290294447, 9.262594875851808851, -60.18097545586277874 ) ) ;
#182807 = CARTESIAN_POINT ( 'NONE',  ( -4.483927247898782831, 16.52544592524335698, 27.70942372801901854 ) ) ;
#182808 = CARTESIAN_POINT ( 'NONE',  ( 19.03943276465977164, -0.05219959533909143690, 68.74890960531436690 ) ) ;
#182809 = CARTESIAN_POINT ( 'NONE',  ( -0.05219959533909027116, -19.03943276465977164, 97.49890960531436690 ) ) ;
#182810 = CARTESIAN_POINT ( 'NONE',  ( 0.000000000000000000, 0.000000000000000000, -25.00000000000000000 ) ) ;
#182811 = CARTESIAN_POINT ( 'NONE',  ( -16.46253265017160317, 9.564922557960807481, 25.83224293864769194 ) ) ;
#182812 = CARTESIAN_POINT ( 'NONE',  ( 21.55341960407610458, 5.719274019375980345, 23.95724293864769550 ) ) ;
#182813 = CARTESIAN_POINT ( 'NONE',  ( 16.52544592524335698, 4.483927247898782831, 86.45942372801901854 ) ) ;
#182816 = CARTESIAN_POINT ( 'NONE',  ( 13.97604488694527802, 13.89961937509977652, 74.37390960531436690 ) ) ;
#182815 =( BOUNDED_CURVE ( )  B_SPLINE_CURVE ( 2, ( #195312, #56793, #180157, #120430, #41626, #103290, #75917, #104282, #182122 ),
 .UNSPECIFIED., .F., .T. ) 
 B_SPLINE_CURVE_WITH_KNOTS ( ( 3, 2, 2, 2, 3 ),
 ( 0.8250928956683720727, 0.8400000000000000799, 0.8600000000000003197, 0.8800000000000005596, 0.9000000000000007994 ),
 .UNSPECIFIED. ) 
 CURVE ( )  GEOMETRIC_REPRESENTATION_ITEM ( )  RATIONAL_B_SPLINE_CURVE ( ( 0.9814209735438295112, 0.9635197191029262198, 1.000000000000000000, 0.9510565162951535312, 1.000000000000000000, 0.9510565162951535312, 1.000000000000000000, 0.9510565162951516438, 1.000000000000001998 ) ) 
 REPRESENTATION_ITEM ( '' )  );
#182814 = CARTESIAN_POINT ( 'NONE',  ( -14.34966873604960291, -8.224510206698953496, 66.66557627198102409 ) ) ;
#182817 = CARTESIAN_POINT ( 'NONE',  ( -15.80617190586768217, 15.72974639402176855, 93.12609039468568994 ) ) ;
#182818 = CARTESIAN_POINT ( 'NONE',  ( -24.20670376297026749, 0.5310992180249298755, -56.83968087238906719 ) ) ;
#182819 = CARTESIAN_POINT ( 'NONE',  ( 16.52544592524335698, 4.483927247898782831, 21.45942372801901499 ) ) ;
#182820 = CARTESIAN_POINT ( 'NONE',  ( 14.34966873604960469, 8.224510206698951720, 74.16557627198102409 ) ) ;
#182821 = CARTESIAN_POINT ( 'NONE',  ( -10.81492255796105439, 18.62759615963255655, 32.91775706135234714 ) ) ;
#182822 = CARTESIAN_POINT ( 'NONE',  ( 15.80617190586746368, 15.72974639402197994, 74.37390960531436690 ) ) ;
#182823 = CARTESIAN_POINT ( 'NONE',  ( -13.97604488694547697, 13.89961937509957934, 38.12609039468566152 ) ) ;
#182824 = CARTESIAN_POINT ( 'NONE',  ( -35.67631076299765169, 1.230297745838609957, 37.59750771353017740 ) ) ;
#182825 = CARTESIAN_POINT ( 'NONE',  ( 13.89961937509977652, -13.97604488694527269, 83.12390960531436690 ) ) ;
#182826 = CARTESIAN_POINT ( 'NONE',  ( 16.55341960407611168, 4.379528057220329451, 53.95724293864770260 ) ) ;
#182827 = CARTESIAN_POINT ( 'NONE',  ( 16.55341960407611168, 4.379528057220329451, 38.95724293864768839 ) ) ;
#182828 = CARTESIAN_POINT ( 'NONE',  ( -12.14591786802326823, 12.06949235617739902, 108.1260903946856757 ) ) ;
#182829 = CARTESIAN_POINT ( 'NONE',  ( -0.05219959533936034679, 19.03943276465977164, 62.50109039468566863 ) ) ;
#182830 = CYLINDRICAL_SURFACE ( 'NONE', #173089, 2.000000000000001776 ) ;
#182831 = CARTESIAN_POINT ( 'NONE',  ( 5.049401038298161559, -19.05341960407611168, 102.7072429386476955 ) ) ;
#182832 = CARTESIAN_POINT ( 'NONE',  ( -12.14591786802309592, -12.06949235617757132, 76.87390960531439532 ) ) ;
#182833 = CARTESIAN_POINT ( 'NONE',  ( 0.000000000000000000, 0.000000000000000000, -49.13275782002545355 ) ) ;
#182835 = CARTESIAN_POINT ( 'NONE',  ( -15.80617190586745835, -15.72974639402198527, 31.87390960531435979 ) ) ;
#182834 = CARTESIAN_POINT ( 'NONE',  ( -19.05341960407611168, -5.049401038298163336, 26.45724293864769550 ) ) ;
#182836 = CARTESIAN_POINT ( 'NONE',  ( 21.53943276465977519, -0.05219959533907433946, 68.74890960531435269 ) ) ;
#182837 = CARTESIAN_POINT ( 'NONE',  ( -0.05219959533910754901, -16.53943276465976808, 112.4989096053143669 ) ) ;
#182839 = CARTESIAN_POINT ( 'NONE',  ( 13.97604488694527802, 13.89961937509977652, 49.37390960531434558 ) ) ;
#182838 = CARTESIAN_POINT ( 'NONE',  ( -4.483927247898782831, 16.52544592524335698, 62.70942372801902565 ) ) ;
#182840 = CARTESIAN_POINT ( 'NONE',  ( -21.53943276465977519, -0.05219959533937600094, 58.75109039468568994 ) ) ;
#182841 = CARTESIAN_POINT ( 'NONE',  ( -8.314922557960811034, -14.29746914071050412, 92.08224293864769550 ) ) ;
#182842 = CARTESIAN_POINT ( 'NONE',  ( 17.12812012977025233, -6.668231424566041454, 36.14051240676857191 ) ) ;
#182843 = CARTESIAN_POINT ( 'NONE',  ( -36.91746825000000598, -11.99521256947794789, -9.024999997268812635 ) ) ;
#182844 = CARTESIAN_POINT ( 'NONE',  ( -10.72451020669898014, 18.67979575497178502, 30.41557627198101699 ) ) ;
#182845 = CARTESIAN_POINT ( 'NONE',  ( 17.97161686093727084, -5.499999999999964473, 78.49637206859165417 ) ) ;
#182847 = CARTESIAN_POINT ( 'NONE',  ( -18.10062525802553424, 5.500000000000031086, 43.51383468041920821 ) ) ;
#182846 = CARTESIAN_POINT ( 'NONE',  ( 5.823673210054444382, -21.52544592524334988, 70.20942372801904696 ) ) ;
#182849 = CARTESIAN_POINT ( 'NONE',  ( -16.55341960407611168, -4.379528057220339221, 41.45724293864769550 ) ) ;
#182848 = CARTESIAN_POINT ( 'NONE',  ( -4.379528057220086978, -16.55341960407618274, 59.79275706135234714 ) ) ;
#182850 = CARTESIAN_POINT ( 'NONE',  ( 18.67979575497178502, 10.72451020669898547, 69.16557627198102409 ) ) ;
#182851 = CARTESIAN_POINT ( 'NONE',  ( -18.67979575497178146, -10.72451020669898902, 56.66557627198103830 ) ) ;
#182852 = FACE_OUTER_BOUND ( 'NONE', #148254, .T. ) ;
#182855 = EDGE_CURVE ( 'NONE', #26587, #183244, #74575, .T. ) ;
#182854 = CARTESIAN_POINT ( 'NONE',  ( -19.03943276465977164, 0.05219959533909376836, 96.24890960531436690 ) ) ;
#182853 = CARTESIAN_POINT ( 'NONE',  ( 9.474510206698729675, 16.51473224551082808, 82.08442372801899012 ) ) ;
#182856 = CARTESIAN_POINT ( 'NONE',  ( 0.05219959533909260263, 19.03943276465977164, 44.99890960531435979 ) ) ;
#182857 = CARTESIAN_POINT ( 'NONE',  ( 16.55341960407611168, 4.379528057220329451, 108.9572429386476955 ) ) ;
#182858 =( NAMED_UNIT ( * ) PLANE_ANGLE_UNIT ( ) SI_UNIT ( $, .RADIAN. ) );
#182859 = DIRECTION ( 'NONE',  ( 0.000000000000000000, 0.000000000000000000, -1.000000000000000000 ) ) ;
#182860 = ORIENTED_EDGE ( 'NONE', *, *, #40254, .F. ) ;
#182861 = CARTESIAN_POINT ( 'NONE',  ( -12.14591786802326823, 12.06949235617739902, 63.12609039468568994 ) ) ;
#182862 = CARTESIAN_POINT ( 'NONE',  ( 10.72451020669898902, -18.67979575497178502, 107.9155762719810241 ) ) ;
#182863 = CARTESIAN_POINT ( 'NONE',  ( -13.97604488694527625, -13.89961937509977652, 56.87390960531434558 ) ) ;
#182864 = CARTESIAN_POINT ( 'NONE',  ( 10.81492255796106328, -18.62759615963255655, 45.41775706135234003 ) ) ;
#182865 = CARTESIAN_POINT ( 'NONE',  ( -9.564922557960796823, -16.46253265017161027, 92.08224293864769550 ) ) ;
#182866 = CARTESIAN_POINT ( 'NONE',  ( -27.73791293435188621, -28.12602025316166632, -18.50562026185692943 ) ) ;
#182867 = ORIENTED_EDGE ( 'NONE', *, *, #48487, .F. ) ;
#182868 = CARTESIAN_POINT ( 'NONE',  ( 21.53943276465977519, 0.05219959533937863772, 36.25109039468567573 ) ) ;
#182870 = CARTESIAN_POINT ( 'NONE',  ( -16.46253265017146816, -9.564922557961047289, 94.16775706135233293 ) ) ;
#182869 = CARTESIAN_POINT ( 'NONE',  ( -5.153800228976328057, -19.02544592524343514, 112.2905762719810099 ) ) ;
#182871 = CARTESIAN_POINT ( 'NONE',  ( 13.97604488694548053, -13.89961937509957401, 35.62609039468567573 ) ) ;
#182872 = CARTESIAN_POINT ( 'NONE',  ( 21.55341960407610458, 5.719274019375980345, 93.95724293864770971 ) ) ;
#182873 = CARTESIAN_POINT ( 'NONE',  ( 13.89961937509957401, 13.97604488694547697, 36.87609039468565442 ) ) ;
#182874 = CARTESIAN_POINT ( 'NONE',  ( -5.049401038297874678, -19.05341960407617918, 34.79275706135233293 ) ) ;
#182875 = CARTESIAN_POINT ( 'NONE',  ( -16.55341960407617563, 4.379528057220093196, 88.54275706135236135 ) ) ;
#182876 = CARTESIAN_POINT ( 'NONE',  ( -9.474510206698964154, 16.51473224551069663, 115.4155762719810241 ) ) ;
#182877 = CARTESIAN_POINT ( 'NONE',  ( -19.03943276465977164, 0.05219959533909376836, 56.24890960531435979 ) ) ;
#182878 = CARTESIAN_POINT ( 'NONE',  ( 15.72974639402176855, 15.80617190586768217, 66.87609039468568994 ) ) ;
#182879 = CARTESIAN_POINT ( 'NONE',  ( -0.05219959533937732626, 21.53943276465977519, 82.50109039468568994 ) ) ;
#182880 = DIRECTION ( 'NONE',  ( -1.000000000000000000, 0.000000000000000000, 0.000000000000000000 ) ) ;
#182881 = CARTESIAN_POINT ( 'NONE',  ( 19.02544592524343514, -5.153800228976328945, 93.54057627198102409 ) ) ;
#182882 = CARTESIAN_POINT ( 'NONE',  ( 21.55341960407619695, -5.719274019375665929, 66.04275706135236135 ) ) ;
#182883 = CARTESIAN_POINT ( 'NONE',  ( -19.02544592524334988, -5.153800228976617603, 103.9594237280190043 ) ) ;
#182884 = CARTESIAN_POINT ( 'NONE',  ( 5.153800228976335163, 19.02544592524342804, 64.79057627198100988 ) ) ;
#182885 = CARTESIAN_POINT ( 'NONE',  ( -19.05341960407611168, -5.049401038298163336, 111.4572429386476671 ) ) ;
#182886 = CARTESIAN_POINT ( 'NONE',  ( -13.97604488694527625, -13.89961937509977652, 81.87390960531436690 ) ) ;
#182887 = CARTESIAN_POINT ( 'NONE',  ( -5.000000000000003553, -4.999999999999996447, -18.00000000000000000 ) ) ;
#182888 = CARTESIAN_POINT ( 'NONE',  ( 0.05219959533909260263, 19.03943276465977164, 69.99890960531435269 ) ) ;
#182889 = CARTESIAN_POINT ( 'NONE',  ( 16.46253265017160672, -9.564922557960803928, 58.33224293864769550 ) ) ;
#182890 = CARTESIAN_POINT ( 'NONE',  ( 10.81492255796078972, 18.62759615963270932, 94.58224293864769550 ) ) ;
#182891 = CARTESIAN_POINT ( 'NONE',  ( -16.52544592524335698, -4.483927247898792601, 93.95942372801903275 ) ) ;
#182892 = CARTESIAN_POINT ( 'NONE',  ( -13.89961937509957401, -13.97604488694547875, 39.37609039468566152 ) ) ;
#182893 = CARTESIAN_POINT ( 'NONE',  ( 0.05219959533909260263, 19.03943276465977164, 74.99890960531435269 ) ) ;
#182894 = CARTESIAN_POINT ( 'NONE',  ( -8.224510206698948167, 14.34966873604960824, 75.41557627198102409 ) ) ;
#182895 = CARTESIAN_POINT ( 'NONE',  ( -16.53943276465976808, 0.05219959533911058130, 111.2489096053143669 ) ) ;
#182896 = CARTESIAN_POINT ( 'NONE',  ( -19.02544592524342804, 5.153800228976336051, 116.0405762719810383 ) ) ;
#182897 = CARTESIAN_POINT ( 'NONE',  ( 9.474510206698971260, -16.51473224551069308, 107.9155762719810383 ) ) ;
#182898 = CARTESIAN_POINT ( 'NONE',  ( -4.379528057220328563, 16.55341960407611168, 75.20724293864769550 ) ) ;
#182899 = CARTESIAN_POINT ( 'NONE',  ( 17.58332526062529411, -7.635886036038496805, 83.42334959558465357 ) ) ;
#182900 = CARTESIAN_POINT ( 'NONE',  ( -19.03943276465977164, -0.05219959533935918106, 33.75109039468566863 ) ) ;
#182901 = CARTESIAN_POINT ( 'NONE',  ( -4.483927247898782831, 16.52544592524335698, 97.70942372801904696 ) ) ;
#182902 = CARTESIAN_POINT ( 'NONE',  ( 0.05219959533909260263, 19.03943276465977164, 79.99890960531436690 ) ) ;
#182903 = CARTESIAN_POINT ( 'NONE',  ( 0.05219959533937995610, -21.53943276465977519, 50.00109039468568994 ) ) ;
#182904 = CARTESIAN_POINT ( 'NONE',  ( 21.55341960407610458, 5.719274019375980345, 38.95724293864768839 ) ) ;
#182905 = CARTESIAN_POINT ( 'NONE',  ( 10.72451020669871369, 18.67979575497193778, 22.08442372801901143 ) ) ;
#182906 = CARTESIAN_POINT ( 'NONE',  ( -21.55341960407610458, -5.719274019375992779, 76.45724293864769550 ) ) ;
#182907 = CARTESIAN_POINT ( 'NONE',  ( -8.224510206698948167, 14.34966873604960824, 100.4155762719810241 ) ) ;
#182908 = CARTESIAN_POINT ( 'NONE',  ( 19.02544592524334988, 5.153800228976608722, 61.45942372801900433 ) ) ;
#182909 = CARTESIAN_POINT ( 'NONE',  ( -5.049401038298153566, 19.05341960407611168, 35.20724293864768839 ) ) ;
#182910 = CARTESIAN_POINT ( 'NONE',  ( 19.03943276465977164, -0.05219959533909143690, 83.74890960531436690 ) ) ;
#182911 = CARTESIAN_POINT ( 'NONE',  ( 19.02544592524343514, -5.153800228976328945, 83.54057627198100988 ) ) ;
#182912 = CARTESIAN_POINT ( 'NONE',  ( 16.55341960407611168, 4.379528057220329451, 103.9572429386476813 ) ) ;
#182913 = VERTEX_POINT ( 'NONE', #105896 ) ;
#182914 = AXIS2_PLACEMENT_3D ( 'NONE', #187808, #61449, #49277 ) ;
#182915 = CARTESIAN_POINT ( 'NONE',  ( 12.06949235617757843, -12.14591786802309237, 23.12390960531436335 ) ) ;
#182916 = CARTESIAN_POINT ( 'NONE',  ( 14.34966873604972726, -8.224510206698740333, 30.83442372801902209 ) ) ;
#182917 = CARTESIAN_POINT ( 'NONE',  ( 21.53943276465977519, 0.05219959533937863772, 96.25109039468568994 ) ) ;
#182918 = CARTESIAN_POINT ( 'NONE',  ( 19.05341960407611168, 5.049401038298154454, 98.95724293864766707 ) ) ;
#182919 = CARTESIAN_POINT ( 'NONE',  ( 18.67979575497194134, -10.72451020669871369, 20.83442372801901143 ) ) ;
#182920 = CARTESIAN_POINT ( 'NONE',  ( -19.05341960407611168, -5.049401038298163336, 41.45724293864769550 ) ) ;
#182921 = AXIS2_PLACEMENT_3D ( 'NONE', #101230, #194275, #56756 ) ;
#182922 = EDGE_CURVE ( 'NONE', #72646, #1176, #45594, .T. ) ;
#182923 = CARTESIAN_POINT ( 'NONE',  ( 12.14591786802327356, -12.06949235617739191, 45.62609039468567573 ) ) ;
#182924 = CARTESIAN_POINT ( 'NONE',  ( -16.51473224551082808, 9.474510206698731452, 113.3344237280190043 ) ) ;
#182925 = CARTESIAN_POINT ( 'NONE',  ( 5.049401038298161559, -19.05341960407611168, 32.70724293864768129 ) ) ;
#182926 = CARTESIAN_POINT ( 'NONE',  ( 14.29746914071049879, -8.314922557960816363, 93.33224293864769550 ) ) ;
#182927 = CARTESIAN_POINT ( 'NONE',  ( 21.55341960407610458, 5.719274019375980345, 98.95724293864770971 ) ) ;
#182928 = CARTESIAN_POINT ( 'NONE',  ( -19.03943276465977164, -0.05219959533935918106, 63.75109039468566863 ) ) ;
#182929 = FILL_AREA_STYLE_COLOUR ( '', #160782 ) ;
#182930 = CARTESIAN_POINT ( 'NONE',  ( 15.80617190586769283, -15.72974639402175789, 20.62609039468568639 ) ) ;
#182931 = CARTESIAN_POINT ( 'NONE',  ( -9.474510206698964154, 16.51473224551069663, 25.41557627198103120 ) ) ;
#182932 = CARTESIAN_POINT ( 'NONE',  ( -13.89961937509977652, 13.97604488694528158, 95.62390960531436690 ) ) ;
#182933 = CARTESIAN_POINT ( 'NONE',  ( 17.12812012977027010, -6.668231424565989940, 111.1405124067685648 ) ) ;
#182934 = CARTESIAN_POINT ( 'NONE',  ( 16.51473224551069308, 9.474510206698969483, 89.16557627198103830 ) ) ;
#182936 = CARTESIAN_POINT ( 'NONE',  ( 16.53943276465976808, -0.05219959533910856209, 83.74890960531435269 ) ) ;
#182935 = CARTESIAN_POINT ( 'NONE',  ( -5.719274019375665041, -21.55341960407619695, 29.79275706135234358 ) ) ;
#182937 = CARTESIAN_POINT ( 'NONE',  ( 5.049401038298161559, -19.05341960407611168, 77.70724293864765286 ) ) ;
#182938 = CARTESIAN_POINT ( 'NONE',  ( 13.97604488694548053, -13.89961937509957401, 20.62609039468567573 ) ) ;
#182940 = CARTESIAN_POINT ( 'NONE',  ( -19.03943276465977164, -0.05219959533935918106, 53.75109039468566863 ) ) ;
#182939 = CARTESIAN_POINT ( 'NONE',  ( -8.314922557961024197, 14.29746914071037800, 47.91775706135234714 ) ) ;
#182941 = CARTESIAN_POINT ( 'NONE',  ( -10.81492255796105439, 18.62759615963255655, 62.91775706135236135 ) ) ;
#182942 = CARTESIAN_POINT ( 'NONE',  ( -16.52544592524335698, -4.483927247898792601, 28.95942372801902209 ) ) ;
#182943 = CARTESIAN_POINT ( 'NONE',  ( 16.46253265017160672, -9.564922557960803928, 63.33224293864769550 ) ) ;
#182944 = CARTESIAN_POINT ( 'NONE',  ( -16.51473224551082808, 9.474510206698731452, 98.33442372801900433 ) ) ;
#182945 = CARTESIAN_POINT ( 'NONE',  ( -16.52544592524335698, -4.483927247898792601, 63.95942372801901854 ) ) ;
#182946 = CARTESIAN_POINT ( 'NONE',  ( 5.719274019375673035, 21.55341960407619339, 97.29275706135234714 ) ) ;
#182947 = CARTESIAN_POINT ( 'NONE',  ( 19.05341960407617918, -5.049401038297876454, 86.04275706135233293 ) ) ;
#182948 = CARTESIAN_POINT ( 'NONE',  ( -16.46253265017160317, 9.564922557960807481, 55.83224293864769550 ) ) ;
#182949 = CARTESIAN_POINT ( 'NONE',  ( -10.72451020669898014, 18.67979575497178502, 80.41557627198103830 ) ) ;
#182951 = CARTESIAN_POINT ( 'NONE',  ( 9.474510206698729675, 16.51473224551082808, 72.08442372801900433 ) ) ;
#182950 = CARTESIAN_POINT ( 'NONE',  ( -4.483927247898539470, -16.52544592524342804, 82.29057627198103830 ) ) ;
#182952 = CARTESIAN_POINT ( 'NONE',  ( -11.30153831258471442, -180.0000000000000000, -15.00000000000000000 ) ) ;
#182953 = CARTESIAN_POINT ( 'NONE',  ( -19.02544592524334988, -5.153800228976617603, 43.95942372801899012 ) ) ;
#182954 = CARTESIAN_POINT ( 'NONE',  ( -16.55341960407617563, 4.379528057220093196, 113.5427570613523756 ) ) ;
#182955 = CARTESIAN_POINT ( 'NONE',  ( -14.29746914071049879, 8.314922557960819915, 70.83224293864770971 ) ) ;
#182957 = CARTESIAN_POINT ( 'NONE',  ( 22.44159573604009239, 16.30477369853692693, 148.0750000027312012 ) ) ;
#182956 = CARTESIAN_POINT ( 'NONE',  ( -18.62759615963255300, -10.81492255796106328, 104.1677570613523471 ) ) ;
#182958 = CARTESIAN_POINT ( 'NONE',  ( 21.55341960407610458, 5.719274019375980345, 113.9572429386477239 ) ) ;
#182959 = CARTESIAN_POINT ( 'NONE',  ( -9.564922557960796823, -16.46253265017161027, 62.08224293864769550 ) ) ;
#182960 = CARTESIAN_POINT ( 'NONE',  ( 15.80617190586769283, -15.72974639402175789, 80.62609039468567573 ) ) ;
#182961 = CARTESIAN_POINT ( 'NONE',  ( -19.03943276465977164, 0.05219959533909376836, 61.24890960531436690 ) ) ;
#182962 = ORIENTED_EDGE ( 'NONE', *, *, #164879, .F. ) ;
#182963 = CARTESIAN_POINT ( 'NONE',  ( -14.29746914071049879, 8.314922557960819915, 115.8322429386477097 ) ) ;
#182964 = CARTESIAN_POINT ( 'NONE',  ( 18.67979575497178502, 10.72451020669898547, 34.16557627198102409 ) ) ;
#182965 = CARTESIAN_POINT ( 'NONE',  ( 8.224510206698953496, -14.34966873604960469, 62.91557627198102409 ) ) ;
#182966 = CARTESIAN_POINT ( 'NONE',  ( -5.153800228976328057, -19.02544592524343514, 47.29057627198102409 ) ) ;
#182967 = CARTESIAN_POINT ( 'NONE',  ( 16.52544592524342804, -4.483927247898539470, 103.5405762719810383 ) ) ;
#182968 = CARTESIAN_POINT ( 'NONE',  ( 0.05219959533907565091, 21.53943276465977519, 114.9989096053143669 ) ) ;
#182969 = CARTESIAN_POINT ( 'NONE',  ( 21.53943276465977519, 0.05219959533937863772, 51.25109039468568994 ) ) ;
#182970 = CARTESIAN_POINT ( 'NONE',  ( 5.153800228976335163, 19.02544592524342804, 29.79057627198102409 ) ) ;
#182971 = CARTESIAN_POINT ( 'NONE',  ( 8.314922557961029526, -14.29746914071037800, 60.41775706135235424 ) ) ;
#182972 = CARTESIAN_POINT ( 'NONE',  ( 21.52544592524344225, -5.823673210054117533, 103.5405762719810383 ) ) ;
#182973 = CARTESIAN_POINT ( 'NONE',  ( -10.72451020669898014, 18.67979575497178502, 100.4155762719810241 ) ) ;
#182975 = CARTESIAN_POINT ( 'NONE',  ( 16.51473224551069308, 9.474510206698969483, 54.16557627198103120 ) ) ;
#182974 = CARTESIAN_POINT ( 'NONE',  ( 5.153800228976615827, -19.02544592524334988, 20.20942372801899722 ) ) ;
#182976 = CARTESIAN_POINT ( 'NONE',  ( -9.564922557960796823, -16.46253265017161027, 102.0822429386477097 ) ) ;
#182977 = CARTESIAN_POINT ( 'NONE',  ( -21.52544592524334988, -5.823673210054445271, 63.95942372801901854 ) ) ;
#182978 = CARTESIAN_POINT ( 'NONE',  ( -15.80617190586745835, -15.72974639402198527, 46.87390960531435979 ) ) ;
#182979 = CARTESIAN_POINT ( 'NONE',  ( 12.14591786802309770, 12.06949235617756955, 24.37390960531435979 ) ) ;
#182981 = CARTESIAN_POINT ( 'NONE',  ( 15.80617190586769283, -15.72974639402175789, 95.62609039468568994 ) ) ;
#182980 = CARTESIAN_POINT ( 'NONE',  ( -15.80617190586768217, 15.72974639402176855, 58.12609039468568994 ) ) ;
#182982 = CARTESIAN_POINT ( 'NONE',  ( 5.049401038297881783, 19.05341960407617563, 42.29275706135234003 ) ) ;
#182983 = CARTESIAN_POINT ( 'NONE',  ( 16.55341960407618274, -4.379528057220086978, 106.0427570613523471 ) ) ;
#182984 = CARTESIAN_POINT ( 'NONE',  ( -15.72974639402176322, -15.80617190586768395, 49.37609039468569705 ) ) ;
#182985 = CARTESIAN_POINT ( 'NONE',  ( -5.049401038298153566, 19.05341960407611168, 60.20724293864768129 ) ) ;
#182986 = CARTESIAN_POINT ( 'NONE',  ( 16.46253265017146816, 9.564922557961045513, 26.66775706135234003 ) ) ;
#182987 = CARTESIAN_POINT ( 'NONE',  ( -21.53943276465977519, 0.05219959533907696930, 21.24890960531436690 ) ) ;
#182988 = CARTESIAN_POINT ( 'NONE',  ( 21.53943276465977519, 0.05219959533937863772, 26.25109039468567573 ) ) ;
#182989 = CARTESIAN_POINT ( 'NONE',  ( 15.72974639402199770, -15.80617190586745480, 88.12390960531436690 ) ) ;
#182990 = CARTESIAN_POINT ( 'NONE',  ( -19.03943276465977164, -0.05219959533935918106, 88.75109039468567573 ) ) ;
#182991 = CARTESIAN_POINT ( 'NONE',  ( 16.55341960407618274, -4.379528057220086978, 41.04275706135236135 ) ) ;
#182993 = CARTESIAN_POINT ( 'NONE',  ( -21.55341960407610458, -5.719274019375992779, 76.45724293864769550 ) ) ;
#182992 = CARTESIAN_POINT ( 'NONE',  ( 17.50000000000001066, -3.203707223489874689, 37.27319652649031667 ) ) ;
#182995 = CARTESIAN_POINT ( 'NONE',  ( 14.29746914071049879, -8.314922557960816363, 78.33224293864770971 ) ) ;
#182994 = CARTESIAN_POINT ( 'NONE',  ( -8.314922557961024197, 14.29746914071037800, 62.91775706135236135 ) ) ;
#182996 = CARTESIAN_POINT ( 'NONE',  ( 1.398757915179067002, 29.85213727369407266, -48.47147718930269633 ) ) ;
#182997 = CARTESIAN_POINT ( 'NONE',  ( -5.049401038297874678, -19.05341960407617918, 109.7927570613523187 ) ) ;
#182998 = CARTESIAN_POINT ( 'NONE',  ( 5.823673210054125526, 21.52544592524343514, 34.79057627198103120 ) ) ;
#182999 = CARTESIAN_POINT ( 'NONE',  ( 13.97604488694527802, 13.89961937509977830, 94.37390960531436690 ) ) ;
#183000 = CARTESIAN_POINT ( 'NONE',  ( 12.06949235617739724, 12.14591786802326823, 36.87609039468568994 ) ) ;
#183001 = CARTESIAN_POINT ( 'NONE',  ( -15.80617190586745835, -15.72974639402198527, 106.8739096053143811 ) ) ;
#183002 = CARTESIAN_POINT ( 'NONE',  ( -10.81492255796078084, -18.62759615963271287, 27.08224293864769550 ) ) ;
#183003 = CARTESIAN_POINT ( 'NONE',  ( 8.314922557961029526, -14.29746914071037800, 65.41775706135234714 ) ) ;
#183004 = CARTESIAN_POINT ( 'NONE',  ( -19.02544592524342804, 5.153800228976336051, 81.04057627198103830 ) ) ;
#183006 = CARTESIAN_POINT ( 'NONE',  ( 5.153800228976335163, 19.02544592524342804, 29.79057627198102409 ) ) ;
#183005 = CARTESIAN_POINT ( 'NONE',  ( -5.719274019375665041, -21.55341960407619695, 59.79275706135234714 ) ) ;
#183007 = CARTESIAN_POINT ( 'NONE',  ( -16.46253265017160317, 9.564922557960807481, 115.8322429386477097 ) ) ;
#183008 = ORIENTED_EDGE ( 'NONE', *, *, #172144, .F. ) ;
#183009 = CARTESIAN_POINT ( 'NONE',  ( 0.05219959533936267826, -19.03943276465977164, 40.00109039468566152 ) ) ;
#183010 = CARTESIAN_POINT ( 'NONE',  ( -16.52544592524335698, -4.483927247898792601, 53.95942372801900433 ) ) ;
#183011 = CARTESIAN_POINT ( 'NONE',  ( -5.049401038298153566, 19.05341960407611168, 110.2072429386476671 ) ) ;
#183012 = CARTESIAN_POINT ( 'NONE',  ( -5.153800228976328057, -19.02544592524343514, 72.29057627198102409 ) ) ;
#183013 = CARTESIAN_POINT ( 'NONE',  ( -12.06949235617739369, -12.14591786802326823, 94.37609039468568994 ) ) ;
#183014 = CARTESIAN_POINT ( 'NONE',  ( 23.29544513554940011, 16.92513159979228021, 141.4656553485623931 ) ) ;
#183015 = CARTESIAN_POINT ( 'NONE',  ( -12.14591786802309592, -12.06949235617757132, 91.87390960531436690 ) ) ;
#183016 = CARTESIAN_POINT ( 'NONE',  ( 21.53943276465977519, -0.05219959533907433946, 38.74890960531435979 ) ) ;
#183017 = CARTESIAN_POINT ( 'NONE',  ( -13.89961937509977652, 13.97604488694528158, 35.62390960531435269 ) ) ;
#183018 = CARTESIAN_POINT ( 'NONE',  ( 14.29746914071037800, 8.314922557961029526, 61.66775706135235424 ) ) ;
#183019 = CARTESIAN_POINT ( 'NONE',  ( 21.55341960407619695, -5.719274019375665929, 21.04275706135234714 ) ) ;
#183020 = CARTESIAN_POINT ( 'NONE',  ( -19.03943276465977164, -0.05219959533935918106, 73.75109039468566152 ) ) ;
#183021 = CARTESIAN_POINT ( 'NONE',  ( 19.02544592524343514, -5.153800228976328945, 38.54057627198103120 ) ) ;
#183022 = CARTESIAN_POINT ( 'NONE',  ( -21.53943276465977519, 0.05219959533907696930, 66.24890960531436690 ) ) ;
#183023 = CIRCLE ( 'NONE', #95816, 40.49999999999999289 ) ;
#183024 = CARTESIAN_POINT ( 'NONE',  ( 19.03943276465977164, -0.05219959533909143690, 113.7489096053143669 ) ) ;
#183025 = CARTESIAN_POINT ( 'NONE',  ( 21.53943276465977519, 0.05219959533937863772, 91.25109039468568994 ) ) ;
#183026 = CARTESIAN_POINT ( 'NONE',  ( -9.474510206698964154, 16.51473224551069663, 65.41557627198102409 ) ) ;
#183027 = CARTESIAN_POINT ( 'NONE',  ( -0.05219959533934338120, 16.53943276465976808, 47.50109039468568994 ) ) ;
#183028 = CARTESIAN_POINT ( 'NONE',  ( 19.05341960407611168, 5.049401038298154454, 63.95724293864769550 ) ) ;
#183029 = CARTESIAN_POINT ( 'NONE',  ( -15.80617190586768217, 15.72974639402176855, 78.12609039468570415 ) ) ;
#183030 = CARTESIAN_POINT ( 'NONE',  ( -5.049401038297874678, -19.05341960407617918, 34.79275706135233293 ) ) ;
#183031 = CARTESIAN_POINT ( 'NONE',  ( 9.474510206698729675, 16.51473224551082808, 57.08442372801900433 ) ) ;
#183032 = CARTESIAN_POINT ( 'NONE',  ( 21.53943276465977519, 0.05219959533937863772, 46.25109039468567573 ) ) ;
#183033 = CARTESIAN_POINT ( 'NONE',  ( -6.691772886347780336, 1.197744245042939859, -62.38710104649955923 ) ) ;
#183034 = CARTESIAN_POINT ( 'NONE',  ( 16.46253265017146816, 9.564922557961045513, 46.66775706135233293 ) ) ;
#183035 = CARTESIAN_POINT ( 'NONE',  ( -9.474510206698964154, 16.51473224551069663, 100.4155762719810241 ) ) ;
#183036 = CARTESIAN_POINT ( 'NONE',  ( -9.474510206698964154, 16.51473224551069663, 85.41557627198102409 ) ) ;
#183037 = CARTESIAN_POINT ( 'NONE',  ( 16.53943276465976808, -0.05219959533910856209, 33.74890960531436690 ) ) ;
#183039 = CARTESIAN_POINT ( 'NONE',  ( -15.80617190586768217, 15.72974639402176855, 103.1260903946856757 ) ) ;
#183038 = CARTESIAN_POINT ( 'NONE',  ( -21.52544592524343514, 5.823673210054127303, 31.04057627198102409 ) ) ;
#183040 = CARTESIAN_POINT ( 'NONE',  ( 22.81625015709509441, 31.40387420917330275, -1.324999997268813123 ) ) ;
#183041 = CARTESIAN_POINT ( 'NONE',  ( 16.29526858892878849, 7.335722546919997811, 58.29670597800210174 ) ) ;
#183042 = CARTESIAN_POINT ( 'NONE',  ( 5.719274019375673035, 21.55341960407619339, 92.29275706135236135 ) ) ;
#183043 = CARTESIAN_POINT ( 'NONE',  ( -27.60788766665604399, 7.718175339870851026, 162.2452582881568617 ) ) ;
#183044 = CARTESIAN_POINT ( 'NONE',  ( -19.03943276465977164, 0.05219959533909376836, 41.24890960531435269 ) ) ;
#183045 = CARTESIAN_POINT ( 'NONE',  ( -5.153800228976328057, -19.02544592524343514, 107.2905762719810383 ) ) ;
#183046 = CARTESIAN_POINT ( 'NONE',  ( 33.75669036400348944, 3.362847000060356972, 99.36731340788949751 ) ) ;
#183047 = CARTESIAN_POINT ( 'NONE',  ( 16.55341960407618274, -4.379528057220086978, 51.04275706135234714 ) ) ;
#183048 = CARTESIAN_POINT ( 'NONE',  ( -0.05219959533907301413, -21.53943276465977519, 67.49890960531436690 ) ) ;
#183049 = CARTESIAN_POINT ( 'NONE',  ( -16.52544592524342804, 4.483927247898546575, 46.04057627198103830 ) ) ;
#183051 = CARTESIAN_POINT ( 'NONE',  ( 9.474510206698971260, -16.51473224551069308, 102.9155762719810241 ) ) ;
#183050 = CARTESIAN_POINT ( 'NONE',  ( -13.89961937509977652, 13.97604488694528158, 25.62390960531434558 ) ) ;
#183052 = CARTESIAN_POINT ( 'NONE',  ( -15.80617190586768217, 15.72974639402176855, 23.12609039468567573 ) ) ;
#183053 = CARTESIAN_POINT ( 'NONE',  ( 5.049401038297881783, 19.05341960407617563, 32.29275706135233293 ) ) ;
#183054 = CARTESIAN_POINT ( 'NONE',  ( 14.34966873604960469, 8.224510206698951720, 109.1655762719810383 ) ) ;
#183055 = CARTESIAN_POINT ( 'NONE',  ( 10.72451020669871369, 18.67979575497193778, 62.08442372801901143 ) ) ;
#183056 = CARTESIAN_POINT ( 'NONE',  ( 30.00000000000000000, -5.499999999999992895, 102.5000000000000142 ) ) ;
#183057 = CARTESIAN_POINT ( 'NONE',  ( -4.483927247898539470, -16.52544592524342804, 27.29057627198103120 ) ) ;
#183058 = CARTESIAN_POINT ( 'NONE',  ( -22.81625015709510507, 31.40387420917330275, -5.424999997268812990 ) ) ;
#183059 = CARTESIAN_POINT ( 'NONE',  ( 21.55341960407610458, 5.719274019375980345, 23.95724293864769550 ) ) ;
#183060 = CARTESIAN_POINT ( 'NONE',  ( -14.29746914071049879, 8.314922557960819915, 85.83224293864768129 ) ) ;
#183061 = CARTESIAN_POINT ( 'NONE',  ( 9.444085519387883210, -44.71325174467972374, -21.93802053968663657 ) ) ;
#183062 = AXIS2_PLACEMENT_3D ( 'NONE', #102009, #115175, #72682 ) ;
#183063 = CARTESIAN_POINT ( 'NONE',  ( -0.05219959533909027116, -19.03943276465977164, 72.49890960531435269 ) ) ;
#183064 = CARTESIAN_POINT ( 'NONE',  ( -16.55341960407611168, -4.379528057220339221, 71.45724293864769550 ) ) ;
#183065 = CARTESIAN_POINT ( 'NONE',  ( -19.03943276465977164, -0.05219959533935918106, 103.7510903946856757 ) ) ;
#183066 = CARTESIAN_POINT ( 'NONE',  ( 21.55341960407610458, 5.719274019375980345, 53.95724293864770260 ) ) ;
#183067 = ORIENTED_EDGE ( 'NONE', *, *, #127999, .F. ) ;
#183068 = CARTESIAN_POINT ( 'NONE',  ( -16.52544592524342804, 4.483927247898546575, 116.0405762719810383 ) ) ;
#183070 = CARTESIAN_POINT ( 'NONE',  ( 21.52544592524344225, -5.823673210054117533, 73.54057627198102409 ) ) ;
#183069 = CARTESIAN_POINT ( 'NONE',  ( -13.97604488694527625, -13.89961937509977652, 76.87390960531433848 ) ) ;
#183072 = CARTESIAN_POINT ( 'NONE',  ( -13.97604488694527625, -13.89961937509977652, 91.87390960531432427 ) ) ;
#183071 = CARTESIAN_POINT ( 'NONE',  ( 14.34966873604972726, -8.224510206698740333, 100.8344237280190185 ) ) ;
#183073 = CARTESIAN_POINT ( 'NONE',  ( 13.97604488694548053, -13.89961937509957401, 60.62609039468564731 ) ) ;
#183074 = CARTESIAN_POINT ( 'NONE',  ( 10.72451020669871369, 18.67979575497193778, 97.08442372801904696 ) ) ;
#183075 = CARTESIAN_POINT ( 'NONE',  ( 15.72974639402199770, -15.80617190586745480, 68.12390960531436690 ) ) ;
#183076 = CARTESIAN_POINT ( 'NONE',  ( 19.03943276465977164, -0.05219959533909143690, 113.7489096053143669 ) ) ;
#183077 = CARTESIAN_POINT ( 'NONE',  ( 19.03943276465977164, -0.05219959533909143690, 43.74890960531435979 ) ) ;
#183078 = CARTESIAN_POINT ( 'NONE',  ( 4.379528057220092307, 16.55341960407617563, 102.2927570613523613 ) ) ;
#183079 = CARTESIAN_POINT ( 'NONE',  ( -0.05219959533909027116, -19.03943276465977164, 62.49890960531435979 ) ) ;
#183080 = CARTESIAN_POINT ( 'NONE',  ( 8.314922557961029526, -14.29746914071037800, 25.41775706135235779 ) ) ;
#183081 = CARTESIAN_POINT ( 'NONE',  ( 16.81555441253550853, 7.025013491695498047, 51.86314554665744936 ) ) ;
#183082 = CARTESIAN_POINT ( 'NONE',  ( -15.80617190586768217, 15.72974639402176855, 113.1260903946856899 ) ) ;
#183083 = CARTESIAN_POINT ( 'NONE',  ( 16.55341960407611168, 4.379528057220329451, 68.95724293864769550 ) ) ;
#183084 = CARTESIAN_POINT ( 'NONE',  ( 5.719274019375991003, -21.55341960407610458, 107.7072429386476955 ) ) ;
#183085 = CARTESIAN_POINT ( 'NONE',  ( 21.52544592524344225, -5.823673210054117533, 108.5405762719810241 ) ) ;
#183086 = CARTESIAN_POINT ( 'NONE',  ( 27.73933785331498925, -9.013057229001033122, 140.2750000027311330 ) ) ;
#183088 = EDGE_CURVE ( 'NONE', #125361, #59792, #199187, .T. ) ;
#183087 = CARTESIAN_POINT ( 'NONE',  ( -21.55341960407610458, -5.719274019375992779, 56.45724293864768839 ) ) ;
#183089 = CARTESIAN_POINT ( 'NONE',  ( -4.483927247898782831, 16.52544592524335698, 77.70942372801900433 ) ) ;
#183090 = CARTESIAN_POINT ( 'NONE',  ( 16.55341960407611168, 4.379528057220329451, 108.9572429386476955 ) ) ;
#183091 = CARTESIAN_POINT ( 'NONE',  ( 9.474510206698971260, -16.51473224551069308, 62.91557627198102409 ) ) ;
#183092 =( LENGTH_UNIT ( ) NAMED_UNIT ( * ) SI_UNIT ( .MILLI., .METRE. ) );
#183093 = CARTESIAN_POINT ( 'NONE',  ( -14.34966873604972548, 8.224510206698743886, 108.3344237280190185 ) ) ;
#183094 = CARTESIAN_POINT ( 'NONE',  ( 21.55341960407619695, -5.719274019375665929, 46.04275706135234714 ) ) ;
#183095 = CARTESIAN_POINT ( 'NONE',  ( -19.02544592524342804, 5.153800228976336051, 96.04057627198103830 ) ) ;
#183096 = CARTESIAN_POINT ( 'NONE',  ( -18.62759615963255300, -10.81492255796106328, 84.16775706135234714 ) ) ;
#183097 = CARTESIAN_POINT ( 'NONE',  ( 16.51473224551069308, 9.474510206698969483, 24.16557627198102765 ) ) ;
#183098 = CARTESIAN_POINT ( 'NONE',  ( -0.05219959533909027116, -19.03943276465977164, 42.49890960531435269 ) ) ;
#183099 = ORIENTED_EDGE ( 'NONE', *, *, #196970, .F. ) ;
#183100 = CARTESIAN_POINT ( 'NONE',  ( 21.52544592524334988, 5.823673210054432836, 71.45942372801901854 ) ) ;
#183101 = CARTESIAN_POINT ( 'NONE',  ( -19.03943276465977164, 0.05219959533909376836, 106.2489096053143669 ) ) ;
#183102 = CARTESIAN_POINT ( 'NONE',  ( 9.474510206698729675, 16.51473224551082808, 82.08442372801899012 ) ) ;
#183103 = CARTESIAN_POINT ( 'NONE',  ( -21.55341960407619339, 5.719274019375674811, 38.54275706135234714 ) ) ;
#183104 = CARTESIAN_POINT ( 'NONE',  ( -19.03943276465977164, -0.05219959533935918106, 113.7510903946856757 ) ) ;
#183105 = CARTESIAN_POINT ( 'NONE',  ( 9.564922557961047289, -16.46253265017146816, 75.41775706135234714 ) ) ;
#183106 = CARTESIAN_POINT ( 'NONE',  ( 16.51473224551069308, 9.474510206698969483, 54.16557627198103120 ) ) ;
#183107 = CARTESIAN_POINT ( 'NONE',  ( 13.97604488694548053, -13.89961937509957401, 85.62609039468568994 ) ) ;
#183108 = CARTESIAN_POINT ( 'NONE',  ( -16.55341960407611168, -4.379528057220339221, 26.45724293864768839 ) ) ;
#183109 = CARTESIAN_POINT ( 'NONE',  ( 16.51473224551083163, -9.474510206698727899, 95.83442372801900433 ) ) ;
#183110 = CARTESIAN_POINT ( 'NONE',  ( -14.29746914071049879, 8.314922557960819915, 35.83224293864768839 ) ) ;
#183111 = CARTESIAN_POINT ( 'NONE',  ( 5.049401038297881783, 19.05341960407617563, 57.29275706135231871 ) ) ;
#183112 = CARTESIAN_POINT ( 'NONE',  ( 4.483927247898790824, -16.52544592524335698, 50.20942372801901854 ) ) ;
#183113 = CARTESIAN_POINT ( 'NONE',  ( -21.53943276465977519, -0.05219959533937600094, 113.7510903946856757 ) ) ;
#183114 = CARTESIAN_POINT ( 'NONE',  ( -5.049401038298153566, 19.05341960407611168, 30.20724293864768839 ) ) ;
#183115 = CARTESIAN_POINT ( 'NONE',  ( -17.48853670773242186, -5.747243402303177540, 66.33328700250008580 ) ) ;
#183116 = CARTESIAN_POINT ( 'NONE',  ( 8.314922557961029526, -14.29746914071037800, 50.41775706135235424 ) ) ;
#183117 = CARTESIAN_POINT ( 'NONE',  ( -40.00200000000003087, -1.163414459189985801E-14, 87.50000000000000000 ) ) ;
#183118 = CARTESIAN_POINT ( 'NONE',  ( 8.571926809382603096, -26.38167802310801235, 141.4750000027312069 ) ) ;
#183119 = CARTESIAN_POINT ( 'NONE',  ( 5.153800228976335163, 19.02544592524342804, 89.79057627198102409 ) ) ;
#183120 = CARTESIAN_POINT ( 'NONE',  ( 17.50000000000000355, 3.242565516147348337, 102.5000000000000142 ) ) ;
#183121 = ORIENTED_EDGE ( 'NONE', *, *, #135435, .F. ) ;
#183122 = CARTESIAN_POINT ( 'NONE',  ( 9.564922557961047289, -16.46253265017146816, 80.41775706135234714 ) ) ;
#183123 = CARTESIAN_POINT ( 'NONE',  ( 15.72974639402199770, -15.80617190586745480, 23.12390960531436335 ) ) ;
#183125 = CARTESIAN_POINT ( 'NONE',  ( 5.153800228976615827, -19.02544592524334988, 100.2094237280190043 ) ) ;
#183124 = CARTESIAN_POINT ( 'NONE',  ( 5.719274019375673035, 21.55341960407619339, 112.2927570613523471 ) ) ;
#183126 = CARTESIAN_POINT ( 'NONE',  ( 12.14591786802309770, 12.06949235617756955, 109.3739096053143811 ) ) ;
#183127 = CARTESIAN_POINT ( 'NONE',  ( 16.46253265017160672, -9.564922557960803928, 33.33224293864770260 ) ) ;
#183128 = CARTESIAN_POINT ( 'NONE',  ( -0.05219959533907301413, -21.53943276465977519, 62.49890960531436690 ) ) ;
#183129 = CARTESIAN_POINT ( 'NONE',  ( 16.46253265017160672, -9.564922557960803928, 28.33224293864769550 ) ) ;
#183130 = DIRECTION ( 'NONE',  ( 1.000000000000000000, 0.000000000000000000, 0.000000000000000000 ) ) ;
#183131 = CARTESIAN_POINT ( 'NONE',  ( 13.89961937509957401, 13.97604488694547697, 66.87609039468567573 ) ) ;
#183132 = CARTESIAN_POINT ( 'NONE',  ( -12.06949235617756955, 12.14591786802309770, 35.62390960531437401 ) ) ;
#183133 = CARTESIAN_POINT ( 'NONE',  ( 9.564922557960805705, 16.46253265017160317, 109.5822429386476955 ) ) ;
#183134 = CARTESIAN_POINT ( 'NONE',  ( -10.72451020669870658, -18.67979575497194134, 99.58442372801900433 ) ) ;
#183135 = CARTESIAN_POINT ( 'NONE',  ( -15.72974639402197994, 15.80617190586746368, 90.62390960531436690 ) ) ;
#183136 = CARTESIAN_POINT ( 'NONE',  ( 15.80617190586769283, -15.72974639402175789, 55.62609039468568284 ) ) ;
#183137 = CARTESIAN_POINT ( 'NONE',  ( 10.72451020669871369, 18.67979575497193778, 62.08442372801901143 ) ) ;
#183138 = CARTESIAN_POINT ( 'NONE',  ( 13.89961937509977652, -13.97604488694527269, 93.12390960531436690 ) ) ;
#183140 = CARTESIAN_POINT ( 'NONE',  ( 10.72451020669871369, 18.67979575497193778, 52.08442372801901854 ) ) ;
#183139 = CARTESIAN_POINT ( 'NONE',  ( -14.34966873604972548, 8.224510206698743886, 93.33442372801901854 ) ) ;
#183141 = CARTESIAN_POINT ( 'NONE',  ( 14.29746914071049879, -8.314922557960816363, 113.3322429386476955 ) ) ;
#183142 = CARTESIAN_POINT ( 'NONE',  ( 16.55341960407611168, 4.379528057220329451, 73.95724293864769550 ) ) ;
#183143 = CARTESIAN_POINT ( 'NONE',  ( -14.29746914071049879, 8.314922557960819915, 40.83224293864769550 ) ) ;
#183144 = CARTESIAN_POINT ( 'NONE',  ( -18.67979575497178146, -10.72451020669898902, 46.66557627198102409 ) ) ;
#183145 = CARTESIAN_POINT ( 'NONE',  ( 0.05219959533909260263, 19.03943276465977164, 69.99890960531435269 ) ) ;
#183146 = CARTESIAN_POINT ( 'NONE',  ( 5.049401038298161559, -19.05341960407611168, 47.70724293864770260 ) ) ;
#183147 = CARTESIAN_POINT ( 'NONE',  ( 21.52544592524344225, -5.823673210054117533, 63.54057627198103830 ) ) ;
#183148 = CARTESIAN_POINT ( 'NONE',  ( -19.02544592524334988, -5.153800228976617603, 43.95942372801899012 ) ) ;
#183150 = CARTESIAN_POINT ( 'NONE',  ( -14.29746914071049879, 8.314922557960819915, 50.83224293864770971 ) ) ;
#183149 = CARTESIAN_POINT ( 'NONE',  ( -17.48847506799968343, -5.747544572773810145, 39.17302562156721990 ) ) ;
#183151 = CARTESIAN_POINT ( 'NONE',  ( 18.67979575497178502, 10.72451020669898547, 29.16557627198103120 ) ) ;
#183152 = ORIENTED_EDGE ( 'NONE', *, *, #141448, .F. ) ;
#183153 = ORIENTED_EDGE ( 'NONE', *, *, #26840, .T. ) ;
#183154 = LINE ( 'NONE', #153791, #103296 ) ;
#183155 = CARTESIAN_POINT ( 'NONE',  ( 12.06949235617739724, 12.14591786802326823, 71.87609039468568994 ) ) ;
#183156 = EDGE_CURVE ( 'NONE', #42832, #85800, #88744, .T. ) ;
#183157 = CARTESIAN_POINT ( 'NONE',  ( 5.153800228976615827, -19.02544592524334988, 80.20942372801901854 ) ) ;
#183158 = CARTESIAN_POINT ( 'NONE',  ( -16.53943276465976808, 0.05219959533911058130, 41.24890960531435269 ) ) ;
#183159 = CARTESIAN_POINT ( 'NONE',  ( -18.89770734986050016, -5.499999999999909406, 59.10214472496638649 ) ) ;
#183160 = CARTESIAN_POINT ( 'NONE',  ( 12.14591786802309770, 12.06949235617756955, 29.37390960531435269 ) ) ;
#183161 = CARTESIAN_POINT ( 'NONE',  ( -13.89961937509977652, 13.97604488694528158, 45.62390960531433848 ) ) ;
#183162 = CARTESIAN_POINT ( 'NONE',  ( -16.46253265017160317, 9.564922557960807481, 80.83224293864769550 ) ) ;
#183163 = CARTESIAN_POINT ( 'NONE',  ( 9.474510206698971260, -16.51473224551069308, 32.91557627198102409 ) ) ;
#183164 = CARTESIAN_POINT ( 'NONE',  ( 18.67979575497194134, -10.72451020669871369, 45.83442372801901854 ) ) ;
#183165 = CARTESIAN_POINT ( 'NONE',  ( 5.049401038298161559, -19.05341960407611168, 52.70724293864767418 ) ) ;
#183166 = CARTESIAN_POINT ( 'NONE',  ( 17.72696623605158806, -5.500000000000042633, 81.09811031808415294 ) ) ;
#183167 = VECTOR ( 'NONE', #44239, 999.9999999999998863 ) ;
#183168 = CARTESIAN_POINT ( 'NONE',  ( 5.153800228976335163, 19.02544592524342804, 54.79057627198103120 ) ) ;
#183169 = CARTESIAN_POINT ( 'NONE',  ( -15.80617190586745835, -15.72974639402198527, 31.87390960531435979 ) ) ;
#183170 = CARTESIAN_POINT ( 'NONE',  ( -16.53943276465976808, 0.05219959533911058130, 116.2489096053143669 ) ) ;
#183171 = CARTESIAN_POINT ( 'NONE',  ( -10.72451020669898014, 18.67979575497178502, 45.41557627198103830 ) ) ;
#183172 = CARTESIAN_POINT ( 'NONE',  ( 16.53943276465976808, 0.05219959533934440121, 86.25109039468568994 ) ) ;
#183173 = CARTESIAN_POINT ( 'NONE',  ( 5.719274019375673035, 21.55341960407619339, 107.2927570613523471 ) ) ;
#183174 = AXIS2_PLACEMENT_3D ( 'NONE', #45746, #107398, #27629 ) ;
#183175 = CARTESIAN_POINT ( 'NONE',  ( 0.05219959533934541429, -16.53943276465976808, 65.00109039468568994 ) ) ;
#183176 = CARTESIAN_POINT ( 'NONE',  ( 16.51473224551069308, 9.474510206698969483, 109.1655762719810383 ) ) ;
#183177 = CARTESIAN_POINT ( 'NONE',  ( 16.55341960407618274, -4.379528057220086978, 51.04275706135234714 ) ) ;
#183178 = CARTESIAN_POINT ( 'NONE',  ( -12.06949235617739369, -12.14591786802326823, 34.37609039468568284 ) ) ;
#183179 = CARTESIAN_POINT ( 'NONE',  ( 13.89961937509977652, -13.97604488694527269, 113.1239096053143527 ) ) ;
#183180 = CARTESIAN_POINT ( 'NONE',  ( -16.52544592524335698, -4.483927247898792601, 18.95942372801901143 ) ) ;
#183181 = CARTESIAN_POINT ( 'NONE',  ( -9.564922557960796823, -16.46253265017161027, 37.08224293864768839 ) ) ;
#183182 = CARTESIAN_POINT ( 'NONE',  ( 21.53943276465977519, 0.05219959533937863772, 21.25109039468567218 ) ) ;
#183183 = CARTESIAN_POINT ( 'NONE',  ( 4.483927247898790824, -16.52544592524335698, 25.20942372801901854 ) ) ;
#183184 = CARTESIAN_POINT ( 'NONE',  ( -16.52544592524335698, -4.483927247898792601, 83.95942372801900433 ) ) ;
#183185 = LINE ( 'NONE', #153821, #108663 ) ;
#183186 = CARTESIAN_POINT ( 'NONE',  ( -15.80617190586768217, 15.72974639402176855, 83.12609039468568994 ) ) ;
#183187 = CARTESIAN_POINT ( 'NONE',  ( -16.51473224551082808, 9.474510206698731452, 93.33442372801900433 ) ) ;
#183188 = CARTESIAN_POINT ( 'NONE',  ( -0.05219959533910754901, -16.53943276465976808, 57.49890960531435979 ) ) ;
#183189 = CARTESIAN_POINT ( 'NONE',  ( 8.224510206698953496, -14.34966873604960469, 112.9155762719810383 ) ) ;
#183191 = CARTESIAN_POINT ( 'NONE',  ( -9.051314012904519757, 0.3916721525566201900, -63.96062167512634034 ) ) ;
#183190 = CARTESIAN_POINT ( 'NONE',  ( -19.05341960407617563, 5.049401038297882671, 43.54275706135232582 ) ) ;
#183192 = CARTESIAN_POINT ( 'NONE',  ( -10.81492255796105439, 18.62759615963255655, 52.91775706135235424 ) ) ;
#183193 = CARTESIAN_POINT ( 'NONE',  ( -16.53943276465976808, -0.05219959533934237506, 18.75109039468568639 ) ) ;
#183194 = CARTESIAN_POINT ( 'NONE',  ( -5.000000000000000000, -130.0000000000000000, -13.00000000000000000 ) ) ;
#183195 = CARTESIAN_POINT ( 'NONE',  ( 9.474510206698971260, -16.51473224551069308, 102.9155762719810241 ) ) ;
#183196 = CARTESIAN_POINT ( 'NONE',  ( -21.52544592524343514, 5.823673210054127303, 66.04057627198103830 ) ) ;
#183197 = CARTESIAN_POINT ( 'NONE',  ( -5.049401038297874678, -19.05341960407617918, 99.79275706135234714 ) ) ;
#183198 = CARTESIAN_POINT ( 'NONE',  ( 16.46253265017160672, -9.564922557960803928, 98.33224293864769550 ) ) ;
#183199 = CARTESIAN_POINT ( 'NONE',  ( -21.81230582904512261, 7.807068725604178638, 172.9985625539982550 ) ) ;
#183200 = CARTESIAN_POINT ( 'NONE',  ( 4.379528057220339221, -16.55341960407611168, 107.7072429386476955 ) ) ;
#183201 = CARTESIAN_POINT ( 'NONE',  ( -15.80617190586768217, 15.72974639402176855, 93.12609039468568994 ) ) ;
#183202 = CARTESIAN_POINT ( 'NONE',  ( 19.03943276465977164, -0.05219959533909143690, 48.74890960531435979 ) ) ;
#183204 = CARTESIAN_POINT ( 'NONE',  ( -5.823673210054431948, 21.52544592524334988, 57.70942372801901143 ) ) ;
#183203 = AXIS2_PLACEMENT_3D ( 'NONE', #79790, #138476, #200157 ) ;
#183205 = CARTESIAN_POINT ( 'NONE',  ( -15.80617190586768217, 15.72974639402176855, 83.12609039468568994 ) ) ;
#183206 = CARTESIAN_POINT ( 'NONE',  ( 14.34966873604972726, -8.224510206698740333, 100.8344237280190185 ) ) ;
#183207 = CARTESIAN_POINT ( 'NONE',  ( 13.89961937509977652, -13.97604488694527269, 63.12390960531435979 ) ) ;
#183208 = CARTESIAN_POINT ( 'NONE',  ( -5.719274019375665041, -21.55341960407619695, 49.79275706135234714 ) ) ;
#183209 = CARTESIAN_POINT ( 'NONE',  ( 18.62759615963255655, 10.81492255796105972, 41.66775706135235424 ) ) ;
#183211 = CARTESIAN_POINT ( 'NONE',  ( 9.564922557960805705, 16.46253265017160317, 94.58224293864769550 ) ) ;
#183210 = CARTESIAN_POINT ( 'NONE',  ( 16.46253265017146816, 9.564922557961045513, 71.66775706135233293 ) ) ;
#183212 = CARTESIAN_POINT ( 'NONE',  ( -4.483927247898539470, -16.52544592524342804, 102.2905762719810383 ) ) ;
#183213 = CARTESIAN_POINT ( 'NONE',  ( -15.80617190586745835, -15.72974639402198527, 101.8739096053143811 ) ) ;
#183214 = CARTESIAN_POINT ( 'NONE',  ( 16.55341960407611168, 4.379528057220329451, 63.95724293864770260 ) ) ;
#183215 = CARTESIAN_POINT ( 'NONE',  ( -19.03943276465977164, -0.05219959533935918106, 23.75109039468566152 ) ) ;
#183216 = CARTESIAN_POINT ( 'NONE',  ( 4.483927247898545687, 16.52544592524342804, 84.79057627198102409 ) ) ;
#183217 = CARTESIAN_POINT ( 'NONE',  ( 5.049401038298161559, -19.05341960407611168, 37.70724293864768839 ) ) ;
#183218 = CARTESIAN_POINT ( 'NONE',  ( 19.05341960407617918, -5.049401038297876454, 86.04275706135233293 ) ) ;
#183219 = CARTESIAN_POINT ( 'NONE',  ( 16.55341960407611168, 4.379528057220329451, 53.95724293864770260 ) ) ;
#183220 = CARTESIAN_POINT ( 'NONE',  ( 18.62759615963255655, 10.81492255796105972, 101.6677570613523613 ) ) ;
#183221 = CARTESIAN_POINT ( 'NONE',  ( -19.03943276465977164, 0.05219959533909376836, 86.24890960531436690 ) ) ;
#183222 = CARTESIAN_POINT ( 'NONE',  ( -13.97604488694547697, 13.89961937509957934, 68.12609039468563310 ) ) ;
#183223 = CARTESIAN_POINT ( 'NONE',  ( -15.80617190586745835, -15.72974639402198527, 81.87390960531435269 ) ) ;
#183224 = CARTESIAN_POINT ( 'NONE',  ( -5.719274019375665041, -21.55341960407619695, 24.79275706135235779 ) ) ;
#183225 = CARTESIAN_POINT ( 'NONE',  ( -12.14591786802326823, 12.06949235617739902, 33.12609039468569705 ) ) ;
#183226 = CARTESIAN_POINT ( 'NONE',  ( 12.14591786802327356, -12.06949235617739191, 95.62609039468568994 ) ) ;
#183228 = CARTESIAN_POINT ( 'NONE',  ( -0.05219959533937732626, 21.53943276465977519, 27.50109039468567929 ) ) ;
#183227 = CARTESIAN_POINT ( 'NONE',  ( 9.474510206698971260, -16.51473224551069308, 22.91557627198102765 ) ) ;
#183229 = CARTESIAN_POINT ( 'NONE',  ( 9.474510206698971260, -16.51473224551069308, 22.91557627198102765 ) ) ;
#183230 = CARTESIAN_POINT ( 'NONE',  ( -11.40812507854754720, -35.11059874428192273, -8.724999997268813701 ) ) ;
#183231 = CARTESIAN_POINT ( 'NONE',  ( 14.34966873604972726, -8.224510206698740333, 45.83442372801901854 ) ) ;
#183232 = CARTESIAN_POINT ( 'NONE',  ( 16.52544592524342804, -4.483927247898539470, 78.54057627198103830 ) ) ;
#183233 = CARTESIAN_POINT ( 'NONE',  ( -10.81492255796078084, -18.62759615963271287, 82.08224293864768129 ) ) ;
#183234 = CARTESIAN_POINT ( 'NONE',  ( 4.483927247898545687, 16.52544592524342804, 29.79057627198102409 ) ) ;
#183235 = CARTESIAN_POINT ( 'NONE',  ( 16.53943276465976808, 0.05219959533934440121, 46.25109039468567573 ) ) ;
#183236 = CARTESIAN_POINT ( 'NONE',  ( 19.03943276465977164, -0.05219959533909143690, 48.74890960531435979 ) ) ;
#183237 = CARTESIAN_POINT ( 'NONE',  ( 16.53943276465976808, 0.05219959533934440121, 86.25109039468568994 ) ) ;
#183238 = CARTESIAN_POINT ( 'NONE',  ( -9.474510206698720793, -16.51473224551083518, 69.58442372801901854 ) ) ;
#183239 = CARTESIAN_POINT ( 'NONE',  ( 15.80617190586746368, 15.72974639402197994, 69.37390960531436690 ) ) ;
#183240 = CARTESIAN_POINT ( 'NONE',  ( -0.05219959533910754901, -16.53943276465976808, 22.49890960531436335 ) ) ;
#183241 = ORIENTED_EDGE ( 'NONE', *, *, #124318, .F. ) ;
#183242 = CARTESIAN_POINT ( 'NONE',  ( 21.97054992548844865, 8.562709642470919036, 171.7904333278019351 ) ) ;
#183243 = CARTESIAN_POINT ( 'NONE',  ( 15.80617190586746368, 15.72974639402197994, 64.37390960531435269 ) ) ;
#183244 = VERTEX_POINT ( 'NONE', #167582 ) ;
#183245 = VERTEX_POINT ( 'NONE', #11933 ) ;
#183246 = CARTESIAN_POINT ( 'NONE',  ( -16.53943276465976808, -0.05219959533934237506, 93.75109039468567573 ) ) ;
#183247 = VERTEX_POINT ( 'NONE', #135268 ) ;
#183248 = CARTESIAN_POINT ( 'NONE',  ( 16.51473224551069308, 9.474510206698969483, 114.1655762719810241 ) ) ;
#183249 = CARTESIAN_POINT ( 'NONE',  ( -19.02130022317636815, 5.499999999999801048, 75.78188669246573284 ) ) ;
#183250 = CARTESIAN_POINT ( 'NONE',  ( 21.55341960407610458, 5.719274019375980345, 68.95724293864769550 ) ) ;
#183251 = CARTESIAN_POINT ( 'NONE',  ( -4.379528057220086978, -16.55341960407618274, 104.7927570613523898 ) ) ;
#183252 = CARTESIAN_POINT ( 'NONE',  ( 5.049401038297881783, 19.05341960407617563, 112.2927570613523471 ) ) ;
#183253 = CARTESIAN_POINT ( 'NONE',  ( -5.049401038298153566, 19.05341960407611168, 25.20724293864768484 ) ) ;
#183254 = CARTESIAN_POINT ( 'NONE',  ( 4.483927247898790824, -16.52544592524335698, 25.20942372801901854 ) ) ;
#183255 = CARTESIAN_POINT ( 'NONE',  ( 5.049401038298161559, -19.05341960407611168, 57.70724293864769550 ) ) ;
#183256 = CARTESIAN_POINT ( 'NONE',  ( 28.82186960331498327, 2.781578969918950771E-14, 141.0000000000000000 ) ) ;
#183257 = CARTESIAN_POINT ( 'NONE',  ( -13.89961937509977652, 13.97604488694528158, 110.6239096053143243 ) ) ;
#183258 = CARTESIAN_POINT ( 'NONE',  ( -4.379528057220086978, -16.55341960407618274, 89.79275706135236135 ) ) ;
#183259 = CARTESIAN_POINT ( 'NONE',  ( 16.46253265017146816, 9.564922557961045513, 86.66775706135233293 ) ) ;
#183260 = CARTESIAN_POINT ( 'NONE',  ( 16.51473224551083163, -9.474510206698727899, 30.83442372801900433 ) ) ;
#183261 = CARTESIAN_POINT ( 'NONE',  ( -10.72451020669898014, 18.67979575497178502, 75.41557627198102409 ) ) ;
#183262 = EDGE_CURVE ( 'NONE', #125394, #120381, #29077, .T. ) ;
#183263 = CARTESIAN_POINT ( 'NONE',  ( -12.14591786802326823, 12.06949235617739902, 103.1260903946856757 ) ) ;
#183264 = CARTESIAN_POINT ( 'NONE',  ( -5.049401038297874678, -19.05341960407617918, 99.79275706135234714 ) ) ;
#183265 = CARTESIAN_POINT ( 'NONE',  ( 16.51473224551069308, 9.474510206698969483, 49.16557627198102409 ) ) ;
#183266 = CARTESIAN_POINT ( 'NONE',  ( -19.05341960407611168, -5.049401038298163336, 91.45724293864766707 ) ) ;
#183267 = CARTESIAN_POINT ( 'NONE',  ( 18.67979575497194134, -10.72451020669871369, 55.83442372801901854 ) ) ;
#183268 = CARTESIAN_POINT ( 'NONE',  ( 19.05341960407611168, 5.049401038298154454, 48.95724293864768129 ) ) ;
#183269 = CARTESIAN_POINT ( 'NONE',  ( -17.05116617787827593, -6.768360034955819948, 86.34324446740804149 ) ) ;
#183270 = CARTESIAN_POINT ( 'NONE',  ( -16.55341960407611168, -4.379528057220339221, 81.45724293864769550 ) ) ;
#183271 = CARTESIAN_POINT ( 'NONE',  ( 15.80617190586746368, 15.72974639402197994, 79.37390960531436690 ) ) ;
#183272 = CARTESIAN_POINT ( 'NONE',  ( 20.02699684519808798, 3.713461942911795433, 102.5000000000000284 ) ) ;
#183273 = CARTESIAN_POINT ( 'NONE',  ( 5.000000000000000000, -140.0000000000000000, 22.27940468532398910 ) ) ;
#183274 = CARTESIAN_POINT ( 'NONE',  ( -19.05341960407617563, 5.049401038297882671, 48.54275706135233293 ) ) ;
#183275 = CARTESIAN_POINT ( 'NONE',  ( 17.50000000000000000, -5.624438216177559902, 73.31670344914644488 ) ) ;
#183277 = CARTESIAN_POINT ( 'NONE',  ( -5.049401038298153566, 19.05341960407611168, 90.20724293864766707 ) ) ;
#183276 = CARTESIAN_POINT ( 'NONE',  ( -13.97604488694527625, -13.89961937509977652, 71.87390960531433848 ) ) ;
#183278 = CARTESIAN_POINT ( 'NONE',  ( 0.05219959533934541429, -16.53943276465976808, 60.00109039468568284 ) ) ;
#183279 = CARTESIAN_POINT ( 'NONE',  ( 21.71309667856398917, -34.72214947970702781, -18.33762378602110843 ) ) ;
#183280 = CARTESIAN_POINT ( 'NONE',  ( -9.474510206698720793, -16.51473224551083518, 34.58442372801899722 ) ) ;
#183281 = CARTESIAN_POINT ( 'NONE',  ( -28.82186960331499037, 2.428612866367529932E-14, 142.0000000000000000 ) ) ;
#183282 = CARTESIAN_POINT ( 'NONE',  ( 16.51473224551069308, 9.474510206698969483, 114.1655762719810241 ) ) ;
#183283 = CARTESIAN_POINT ( 'NONE',  ( -4.379528057220086978, -16.55341960407618274, 84.79275706135234714 ) ) ;
#183284 = CARTESIAN_POINT ( 'NONE',  ( -0.8180345313831235421, -24.06132300323554674, -54.40060964255545173 ) ) ;
#183285 = CARTESIAN_POINT ( 'NONE',  ( -16.55341960407617563, 4.379528057220093196, 73.54275706135234714 ) ) ;
#183286 = CARTESIAN_POINT ( 'NONE',  ( -16.21995358207306737, 7.366697692864089930, 29.93551001512158294 ) ) ;
#183287 = CARTESIAN_POINT ( 'NONE',  ( 14.34966873604972726, -8.224510206698740333, 60.83442372801901854 ) ) ;
#183288 = CARTESIAN_POINT ( 'NONE',  ( -17.72560187377285246, -5.500000000000056843, 59.07814504131317790 ) ) ;
#183289 = CARTESIAN_POINT ( 'NONE',  ( -15.72974639402176322, -15.80617190586768395, 69.37609039468567573 ) ) ;
#183290 = CARTESIAN_POINT ( 'NONE',  ( 9.474510206698729675, 16.51473224551082808, 82.08442372801899012 ) ) ;
#183291 = CARTESIAN_POINT ( 'NONE',  ( -5.049401038297874678, -19.05341960407617918, 24.79275706135233648 ) ) ;
#183292 = CARTESIAN_POINT ( 'NONE',  ( 9.564922557960805705, 16.46253265017160317, 54.58224293864769550 ) ) ;
#183293 = CARTESIAN_POINT ( 'NONE',  ( 16.51473224551069308, 9.474510206698969483, 39.16557627198103120 ) ) ;
#183294 = CARTESIAN_POINT ( 'NONE',  ( -19.96598992073551671, -34.66064120484043087, -5.351514793237743817 ) ) ;
#183295 = CARTESIAN_POINT ( 'NONE',  ( -21.53943276465977519, 0.05219959533907696930, 61.24890960531435979 ) ) ;
#183296 = CIRCLE ( 'NONE', #189784, 61.99999999999998579 ) ;
#183297 = CARTESIAN_POINT ( 'NONE',  ( -21.53943276465977519, 0.05219959533907696930, 26.24890960531435624 ) ) ;
#183298 = CARTESIAN_POINT ( 'NONE',  ( 0.05219959533909260263, 19.03943276465977164, 24.99890960531435269 ) ) ;
#183299 = CARTESIAN_POINT ( 'NONE',  ( 16.55341960407618274, -4.379528057220086978, 51.04275706135234714 ) ) ;
#183300 = ORIENTED_EDGE ( 'NONE', *, *, #66112, .T. ) ;
#183301 = CARTESIAN_POINT ( 'NONE',  ( -21.52544592524334988, -5.823673210054445271, 23.95942372801901143 ) ) ;
#183303 = CARTESIAN_POINT ( 'NONE',  ( -23.48529157249600985, 32.32473071737754111, -4.299999999999999822 ) ) ;
#183302 = CARTESIAN_POINT ( 'NONE',  ( 8.224510206698953496, -14.34966873604960469, 52.91557627198103830 ) ) ;
#183304 = CARTESIAN_POINT ( 'NONE',  ( -19.03943276465977164, -0.05219959533935918106, 108.7510903946856615 ) ) ;
#183305 = CARTESIAN_POINT ( 'NONE',  ( -5.049401038297874678, -19.05341960407617918, 34.79275706135233293 ) ) ;
#183306 = CARTESIAN_POINT ( 'NONE',  ( -12.06949235617756955, 12.14591786802309770, 40.62390960531435269 ) ) ;
#183307 = CARTESIAN_POINT ( 'NONE',  ( 15.80617190586769283, -15.72974639402175789, 20.62609039468568639 ) ) ;
#183309 = CARTESIAN_POINT ( 'NONE',  ( 10.81492255796078972, 18.62759615963270932, 59.58224293864770260 ) ) ;
#183308 = CARTESIAN_POINT ( 'NONE',  ( 11.30153831258470731, -180.0000000000000000, -15.00000000000000000 ) ) ;
#183310 = CARTESIAN_POINT ( 'NONE',  ( 16.46253265017160672, -9.564922557960803928, 93.33224293864769550 ) ) ;
#183311 = CARTESIAN_POINT ( 'NONE',  ( -14.29746914071049879, 8.314922557960819915, 45.83224293864769550 ) ) ;
#183312 = CARTESIAN_POINT ( 'NONE',  ( 9.474510206698971260, -16.51473224551069308, 102.9155762719810241 ) ) ;
#183313 = CARTESIAN_POINT ( 'NONE',  ( -36.77885060843721021, 5.319724886534321406, 46.40826345025692490 ) ) ;
#183314 = CARTESIAN_POINT ( 'NONE',  ( -16.51473224551082808, 9.474510206698731452, 48.33442372801900433 ) ) ;
#183315 = CARTESIAN_POINT ( 'NONE',  ( 21.52544592524344225, -5.823673210054117533, 98.54057627198105251 ) ) ;
#183316 = CARTESIAN_POINT ( 'NONE',  ( 0.05219959533909260263, 19.03943276465977164, 44.99890960531435979 ) ) ;
#183317 = CARTESIAN_POINT ( 'NONE',  ( 16.53943276465976808, -0.05219959533910856209, 108.7489096053143669 ) ) ;
#183318 = CARTESIAN_POINT ( 'NONE',  ( -10.72451020669870658, -18.67979575497194134, 44.58442372801901854 ) ) ;
#183319 = TOROIDAL_SURFACE ( 'NONE', #57338, 4.000000000000000000, 0.2500000000000000000 ) ;
#183320 = CARTESIAN_POINT ( 'NONE',  ( -8.571926809382601320, -26.38167802310801591, 143.2750000027311899 ) ) ;
#183321 = CARTESIAN_POINT ( 'NONE',  ( 14.29746914071049879, -8.314922557960816363, 23.33224293864769194 ) ) ;
#183322 = CARTESIAN_POINT ( 'NONE',  ( 5.153800228976335163, 19.02544592524342804, 49.79057627198100988 ) ) ;
#183323 = CARTESIAN_POINT ( 'NONE',  ( 13.89961937509977652, -13.97604488694527269, 93.12390960531436690 ) ) ;
#183324 = CARTESIAN_POINT ( 'NONE',  ( 10.81492255796078972, 18.62759615963270932, 69.58224293864769550 ) ) ;
#183325 = CARTESIAN_POINT ( 'NONE',  ( 1.784210473542230573E-15, -29.16686587814331588, 145.3750000027311842 ) ) ;
#183326 = CARTESIAN_POINT ( 'NONE',  ( 16.51473224551069308, 9.474510206698969483, 44.16557627198103120 ) ) ;
#183327 = CARTESIAN_POINT ( 'NONE',  ( -18.67979575497178146, -10.72451020669898902, 51.66557627198102409 ) ) ;
#183328 = CARTESIAN_POINT ( 'NONE',  ( -5.719274019375665041, -21.55341960407619695, 89.79275706135236135 ) ) ;
#183331 = CARTESIAN_POINT ( 'NONE',  ( 16.52544592524342804, -4.483927247898539470, 63.54057627198103830 ) ) ;
#183330 = CARTESIAN_POINT ( 'NONE',  ( 8.314922557961029526, -14.29746914071037800, 80.41775706135234714 ) ) ;
#183329 = CARTESIAN_POINT ( 'NONE',  ( 18.37348032456297275, -33.26197007282152640, -21.07589179612142161 ) ) ;
#183332 = CARTESIAN_POINT ( 'NONE',  ( -9.474510206698964154, 16.51473224551069663, 75.41557627198103830 ) ) ;
#183333 = ORIENTED_EDGE ( 'NONE', *, *, #61495, .T. ) ;
#183334 = CARTESIAN_POINT ( 'NONE',  ( 19.05341960407617918, -5.049401038297876454, 21.04275706135232582 ) ) ;
#183335 = CARTESIAN_POINT ( 'NONE',  ( 0.05219959533934541429, -16.53943276465976808, 85.00109039468568994 ) ) ;
#183336 = CARTESIAN_POINT ( 'NONE',  ( -19.03943276465977164, -0.05219959533935918106, 18.75109039468567218 ) ) ;
#183337 = CARTESIAN_POINT ( 'NONE',  ( 16.51473224551069308, 9.474510206698969483, 69.16557627198102409 ) ) ;
#183338 = CARTESIAN_POINT ( 'NONE',  ( -15.80617190586745835, -15.72974639402198527, 51.87390960531437401 ) ) ;
#183339 = CARTESIAN_POINT ( 'NONE',  ( 0.05219959533934541429, -16.53943276465976808, 25.00109039468567218 ) ) ;
#183340 = CARTESIAN_POINT ( 'NONE',  ( -18.67979575497193778, 10.72451020669871902, 78.33442372801901854 ) ) ;
#183341 = CARTESIAN_POINT ( 'NONE',  ( 16.55341960407618274, -4.379528057220086978, 61.04275706135234714 ) ) ;
#183342 = CARTESIAN_POINT ( 'NONE',  ( -21.55341960407610458, -5.719274019375992779, 111.4572429386476813 ) ) ;
#183343 = CARTESIAN_POINT ( 'NONE',  ( -0.05219959533936034679, 19.03943276465977164, 107.5010903946856615 ) ) ;
#183344 = CARTESIAN_POINT ( 'NONE',  ( 5.049401038298161559, -19.05341960407611168, 92.70724293864769550 ) ) ;
#183345 = CARTESIAN_POINT ( 'NONE',  ( -4.483927247898782831, 16.52544592524335698, 27.70942372801901854 ) ) ;
#183346 = CARTESIAN_POINT ( 'NONE',  ( 5.153800228976335163, 19.02544592524342804, 44.79057627198103830 ) ) ;
#183347 = CARTESIAN_POINT ( 'NONE',  ( -12.14591786802326823, 12.06949235617739902, 38.12609039468567573 ) ) ;
#183348 = CARTESIAN_POINT ( 'NONE',  ( 0.05219959533910956823, 16.53943276465976808, 79.99890960531435269 ) ) ;
#183349 = CARTESIAN_POINT ( 'NONE',  ( -16.52544592524335698, -4.483927247898792601, 88.95942372801901854 ) ) ;
#183351 = CARTESIAN_POINT ( 'NONE',  ( 16.46253265017160672, -9.564922557960803928, 63.33224293864769550 ) ) ;
#183350 = CARTESIAN_POINT ( 'NONE',  ( -10.72451020669870658, -18.67979575497194134, 34.58442372801900433 ) ) ;
#183353 = EDGE_CURVE ( 'NONE', #114628, #120796, #130078, .T. ) ;
#183352 = CARTESIAN_POINT ( 'NONE',  ( -9.564922557960796823, -16.46253265017161027, 87.08224293864769550 ) ) ;
#183354 = CARTESIAN_POINT ( 'NONE',  ( -4.483927247898782831, 16.52544592524335698, 82.70942372801900433 ) ) ;
#183356 = ORIENTED_EDGE ( 'NONE', *, *, #10604, .T. ) ;
#183355 = CARTESIAN_POINT ( 'NONE',  ( -23.97133246043718557, -5.390759101651049434, 174.7603932261090733 ) ) ;
#183357 = ORIENTED_EDGE ( 'NONE', *, *, #194116, .F. ) ;
#183358 = CARTESIAN_POINT ( 'NONE',  ( -9.564922557961040184, 16.46253265017147172, 32.91775706135233293 ) ) ;
#183359 = CARTESIAN_POINT ( 'NONE',  ( 5.049401038298161559, -19.05341960407611168, 97.70724293864766707 ) ) ;
#183360 = CARTESIAN_POINT ( 'NONE',  ( -16.46253265017160317, 9.564922557960807481, 45.83224293864769550 ) ) ;
#183362 = ORIENTED_EDGE ( 'NONE', *, *, #119482, .F. ) ;
#183361 = CARTESIAN_POINT ( 'NONE',  ( -0.05219959533909027116, -19.03943276465977164, 112.4989096053143669 ) ) ;
#183363 = CARTESIAN_POINT ( 'NONE',  ( 8.314922557961029526, -14.29746914071037800, 25.41775706135235779 ) ) ;
#183365 = CARTESIAN_POINT ( 'NONE',  ( 16.52544592524335698, 4.483927247898782831, 46.45942372801901854 ) ) ;
#183364 = CARTESIAN_POINT ( 'NONE',  ( -19.05341960407617563, 5.049401038297882671, 53.54275706135231871 ) ) ;
#183366 = CARTESIAN_POINT ( 'NONE',  ( 5.049401038298161559, -19.05341960407611168, 107.7072429386476955 ) ) ;
#183367 = CARTESIAN_POINT ( 'NONE',  ( -19.03943276465977164, 0.05219959533909376836, 71.24890960531435269 ) ) ;
#183368 = CARTESIAN_POINT ( 'NONE',  ( -5.719274019375978568, 21.55341960407610458, 95.20724293864769550 ) ) ;
#183369 = CARTESIAN_POINT ( 'NONE',  ( 0.05219959533936267826, -19.03943276465977164, 60.00109039468566863 ) ) ;
#183371 = CARTESIAN_POINT ( 'NONE',  ( -19.05341960407611168, -5.049401038298163336, 26.45724293864769550 ) ) ;
#183370 = CARTESIAN_POINT ( 'NONE',  ( 13.89961937509977652, -13.97604488694527269, 93.12390960531436690 ) ) ;
#183372 = PRODUCT_DEFINITION ( 'UNKNOWN', '', #75881, #64589 ) ;
#183373 = CARTESIAN_POINT ( 'NONE',  ( -5.153800228976328057, -19.02544592524343514, 67.29057627198102409 ) ) ;
#183375 = CARTESIAN_POINT ( 'NONE',  ( -0.05219959533909027116, -19.03943276465977164, 27.49890960531435624 ) ) ;
#183374 = CARTESIAN_POINT ( 'NONE',  ( 4.483927247898545687, 16.52544592524342804, 29.79057627198102409 ) ) ;
#183376 = CARTESIAN_POINT ( 'NONE',  ( -13.97604488694547697, 13.89961937509957934, 38.12609039468566152 ) ) ;
#183377 = CARTESIAN_POINT ( 'NONE',  ( 14.34966873604960469, 8.224510206698951720, 74.16557627198102409 ) ) ;
#183378 = CARTESIAN_POINT ( 'NONE',  ( -21.52544592524334988, -5.823673210054445271, 98.95942372801903275 ) ) ;
#183379 = CARTESIAN_POINT ( 'NONE',  ( 16.46253265017160672, -9.564922557960803928, 43.33224293864769550 ) ) ;
#183380 = CARTESIAN_POINT ( 'NONE',  ( 12.06949235617739724, 12.14591786802326823, 56.87609039468568994 ) ) ;
#183382 = CARTESIAN_POINT ( 'NONE',  ( 10.72451020669871369, 18.67979575497193778, 87.08442372801901854 ) ) ;
#183381 = CARTESIAN_POINT ( 'NONE',  ( 12.06949235617757843, -12.14591786802309237, 43.12390960531435269 ) ) ;
#183383 = CARTESIAN_POINT ( 'NONE',  ( 9.564922557960805705, 16.46253265017160317, 89.58224293864769550 ) ) ;
#183384 = CARTESIAN_POINT ( 'NONE',  ( -19.05341960407611168, -5.049401038298163336, 101.4572429386476955 ) ) ;
#183385 = CARTESIAN_POINT ( 'NONE',  ( -14.34966873604960291, -8.224510206698953496, 101.6655762719810383 ) ) ;
#183386 = CARTESIAN_POINT ( 'NONE',  ( 16.53943276465976808, -0.05219959533910856209, 68.74890960531435269 ) ) ;
#183387 = CARTESIAN_POINT ( 'NONE',  ( 18.62759615963271287, -10.81492255796078972, 78.33224293864770971 ) ) ;
#183388 = CARTESIAN_POINT ( 'NONE',  ( 16.51473224551069308, 9.474510206698969483, 84.16557627198102409 ) ) ;
#183389 = CARTESIAN_POINT ( 'NONE',  ( -18.62759615963270932, 10.81492255796079327, 95.83224293864770971 ) ) ;
#183390 = CARTESIAN_POINT ( 'NONE',  ( 19.05341960407611168, 5.049401038298154454, 88.95724293864769550 ) ) ;
#183392 = CARTESIAN_POINT ( 'NONE',  ( 16.52544592524342804, -4.483927247898539470, 83.54057627198102409 ) ) ;
#183391 = FACE_OUTER_BOUND ( 'NONE', #191155, .T. ) ;
#183393 = CARTESIAN_POINT ( 'NONE',  ( -19.05341960407611168, -5.049401038298163336, 56.45724293864768129 ) ) ;
#183394 = CARTESIAN_POINT ( 'NONE',  ( -15.80617190586745835, -15.72974639402198527, 61.87390960531436690 ) ) ;
#183395 = CARTESIAN_POINT ( 'NONE',  ( 16.52216118717208460, -7.221426719304491648, 26.42400978953008561 ) ) ;
#183396 = CARTESIAN_POINT ( 'NONE',  ( -16.53943276465976808, -0.05219959533934237506, 113.7510903946856757 ) ) ;
#183397 = CARTESIAN_POINT ( 'NONE',  ( 19.02544592524334988, 5.153800228976608722, 111.4594237280190043 ) ) ;
#183398 = CARTESIAN_POINT ( 'NONE',  ( -4.379528057220328563, 16.55341960407611168, 85.20724293864770971 ) ) ;
#183399 = CARTESIAN_POINT ( 'NONE',  ( -16.62475595723696742, -7.163666690055314312, 94.47286648189535185 ) ) ;
#183400 = CARTESIAN_POINT ( 'NONE',  ( 19.05341960407611168, 5.049401038298154454, 73.95724293864768129 ) ) ;
#183401 = CARTESIAN_POINT ( 'NONE',  ( 9.564922557960805705, 16.46253265017160317, 44.58224293864769550 ) ) ;
#183402 = CARTESIAN_POINT ( 'NONE',  ( -14.29746914071049879, 8.314922557960819915, 60.83224293864769550 ) ) ;
#183403 = CARTESIAN_POINT ( 'NONE',  ( 10.72451020669898902, -18.67979575497178502, 22.91557627198102765 ) ) ;
#183404 = CARTESIAN_POINT ( 'NONE',  ( -16.51473224551082808, 9.474510206698731452, 103.3344237280190043 ) ) ;
#183405 = CARTESIAN_POINT ( 'NONE',  ( 13.97604488694527802, 13.89961937509977652, 99.37390960531436690 ) ) ;
#183406 = CARTESIAN_POINT ( 'NONE',  ( 18.62759615963271287, -10.81492255796078972, 73.33224293864769550 ) ) ;
#183407 = CARTESIAN_POINT ( 'NONE',  ( 16.53943276465976808, 0.05219959533934440121, 76.25109039468568994 ) ) ;
#183408 = CARTESIAN_POINT ( 'NONE',  ( -16.81555441253469851, 7.025013491696157075, 95.63685445334218116 ) ) ;
#183409 = CARTESIAN_POINT ( 'NONE',  ( -9.474510206698964154, 16.51473224551069663, 80.41557627198103830 ) ) ;
#183410 = CARTESIAN_POINT ( 'NONE',  ( -10.81492255796078084, -18.62759615963271287, 77.08224293864769550 ) ) ;
#183411 = CARTESIAN_POINT ( 'NONE',  ( 16.51473224551083163, -9.474510206698727899, 110.8344237280190043 ) ) ;
#183413 = CARTESIAN_POINT ( 'NONE',  ( -10.81492255796105439, 18.62759615963255655, 62.91775706135236135 ) ) ;
#183412 = CARTESIAN_POINT ( 'NONE',  ( 14.34966873604960469, 8.224510206698951720, 39.16557627198102409 ) ) ;
#183415 = CARTESIAN_POINT ( 'NONE',  ( -19.05341960407611168, -5.049401038298163336, 111.4572429386476671 ) ) ;
#183414 = CARTESIAN_POINT ( 'NONE',  ( 0.05219959533934541429, -16.53943276465976808, 90.00109039468567573 ) ) ;
#183416 = CARTESIAN_POINT ( 'NONE',  ( -18.22780087662122028, -5.500000000000014211, 101.4845989467389273 ) ) ;
#183417 = DIRECTION ( 'NONE',  ( 0.000000000000000000, 0.000000000000000000, 1.000000000000000000 ) ) ;
#183418 = CARTESIAN_POINT ( 'NONE',  ( 14.34966873604972726, -8.224510206698740333, 95.83442372801903275 ) ) ;
#183419 = CARTESIAN_POINT ( 'NONE',  ( 8.314922557961029526, -14.29746914071037800, 50.41775706135235424 ) ) ;
#183420 = CARTESIAN_POINT ( 'NONE',  ( -0.05219959533909027116, -19.03943276465977164, 62.49890960531435979 ) ) ;
#183421 = CARTESIAN_POINT ( 'NONE',  ( -5.153800228976328057, -19.02544592524343514, 77.29057627198099567 ) ) ;
#183422 = CARTESIAN_POINT ( 'NONE',  ( 10.72451020669871369, 18.67979575497193778, 67.08442372801901854 ) ) ;
#183423 = CARTESIAN_POINT ( 'NONE',  ( -8.224510206698735004, -14.34966873604973081, 59.58442372801901854 ) ) ;
#183424 = CARTESIAN_POINT ( 'NONE',  ( 8.314922557960818139, 14.29746914071049879, 39.58224293864769550 ) ) ;
#183425 = CARTESIAN_POINT ( 'NONE',  ( 13.97604488694527802, 13.89961937509977652, 44.37390960531435269 ) ) ;
#183426 = CARTESIAN_POINT ( 'NONE',  ( 9.564922557960805705, 16.46253265017160317, 44.58224293864769550 ) ) ;
#183427 = CARTESIAN_POINT ( 'NONE',  ( 12.14591786802327356, -12.06949235617739191, 35.62609039468568994 ) ) ;
#183428 = CARTESIAN_POINT ( 'NONE',  ( -5.049401038297874678, -19.05341960407617918, 94.79275706135230450 ) ) ;
#183429 = CARTESIAN_POINT ( 'NONE',  ( -14.29746914071049879, 8.314922557960819915, 95.83224293864770971 ) ) ;
#183430 = CARTESIAN_POINT ( 'NONE',  ( -5.049401038298153566, 19.05341960407611168, 70.20724293864769550 ) ) ;
#183432 = DIRECTION ( 'NONE',  ( 0.7071067811865483499, 0.000000000000000000, -0.7071067811865465735 ) ) ;
#183431 = CARTESIAN_POINT ( 'NONE',  ( 16.51473224551083163, -9.474510206698727899, 85.83442372801900433 ) ) ;
#183433 = CARTESIAN_POINT ( 'NONE',  ( -21.52544592524334988, -5.823673210054445271, 88.95942372801901854 ) ) ;
#183434 = CARTESIAN_POINT ( 'NONE',  ( -12.06949235617739369, -12.14591786802326823, 69.37609039468567573 ) ) ;
#183435 = DIRECTION ( 'NONE',  ( -1.000000000000000000, -0.000000000000000000, -0.000000000000000000 ) ) ;
#183436 = CARTESIAN_POINT ( 'NONE',  ( 21.53943276465977519, -0.05219959533907433946, 43.74890960531435979 ) ) ;
#183437 = CARTESIAN_POINT ( 'NONE',  ( 14.34966873604972726, -8.224510206698740333, 35.83442372801901143 ) ) ;
#183438 = CARTESIAN_POINT ( 'NONE',  ( -18.87075004821565472, 5.500000000000079048, 68.67408112101045958 ) ) ;
#183439 = CARTESIAN_POINT ( 'NONE',  ( -13.89961937509957401, -13.97604488694547875, 44.37609039468566863 ) ) ;
#183440 = CARTESIAN_POINT ( 'NONE',  ( -16.51473224551069308, -9.474510206698971260, 96.66557627198102409 ) ) ;
#183441 = CARTESIAN_POINT ( 'NONE',  ( -5.153800228976328057, -19.02544592524343514, 22.29057627198102765 ) ) ;
#183442 = CARTESIAN_POINT ( 'NONE',  ( 9.474510206698971260, -16.51473224551069308, 52.91557627198102409 ) ) ;
#183443 = VECTOR ( 'NONE', #122293, 1000.000000000000000 ) ;
#183444 = CARTESIAN_POINT ( 'NONE',  ( -20.67563680669853099, -22.75846771606805063, -50.58532599174672129 ) ) ;
#183445 = CARTESIAN_POINT ( 'NONE',  ( 10.81492255796106328, -18.62759615963255655, 75.41775706135233293 ) ) ;
#183446 = DIRECTION ( 'NONE',  ( -0.000000000000000000, 0.000000000000000000, 1.000000000000000000 ) ) ;
#183447 = CARTESIAN_POINT ( 'NONE',  ( -19.03943276465977164, -0.05219959533935918106, 28.75109039468566507 ) ) ;
#183448 = CARTESIAN_POINT ( 'NONE',  ( 21.53943276465977519, 0.05219959533937863772, 111.2510903946856899 ) ) ;
#183449 = CARTESIAN_POINT ( 'NONE',  ( 12.14591786802309770, 12.06949235617756955, 49.37390960531436690 ) ) ;
#183450 = CARTESIAN_POINT ( 'NONE',  ( -19.03943276465977164, 0.05219959533909376836, 51.24890960531436690 ) ) ;
#183451 = CARTESIAN_POINT ( 'NONE',  ( 9.474510206698971260, -16.51473224551069308, 102.9155762719810241 ) ) ;
#183452 = CARTESIAN_POINT ( 'NONE',  ( 0.05219959533937995610, -21.53943276465977519, 85.00109039468568994 ) ) ;
#183453 = CARTESIAN_POINT ( 'NONE',  ( -16.46253265017160317, 9.564922557960807481, 60.83224293864769550 ) ) ;
#183454 = CARTESIAN_POINT ( 'NONE',  ( -18.62759615963255300, -10.81492255796106328, 74.16775706135231871 ) ) ;
#183455 = CARTESIAN_POINT ( 'NONE',  ( 0.05219959533907565091, 21.53943276465977519, 39.99890960531436690 ) ) ;
#183456 = CARTESIAN_POINT ( 'NONE',  ( 0.05219959533937995610, -21.53943276465977519, 35.00109039468568284 ) ) ;
#183457 = CARTESIAN_POINT ( 'NONE',  ( 13.97604488694548053, -13.89961937509957401, 65.62609039468567573 ) ) ;
#183458 = CARTESIAN_POINT ( 'NONE',  ( -16.46253265017160317, 9.564922557960807481, 30.83224293864769550 ) ) ;
#183459 = CARTESIAN_POINT ( 'NONE',  ( 13.89961937509977652, -13.97604488694527269, 73.12390960531436690 ) ) ;
#183460 = CARTESIAN_POINT ( 'NONE',  ( -14.29746914071037622, -8.314922557961029526, 29.16775706135234003 ) ) ;
#183461 = CARTESIAN_POINT ( 'NONE',  ( 16.55341960407611168, 4.379528057220329451, 93.95724293864770971 ) ) ;
#183462 = CARTESIAN_POINT ( 'NONE',  ( -0.05219959533909027116, -19.03943276465977164, 62.49890960531435979 ) ) ;
#183463 = CARTESIAN_POINT ( 'NONE',  ( 5.719274019375991003, -21.55341960407610458, 37.70724293864769550 ) ) ;
#183464 = CARTESIAN_POINT ( 'NONE',  ( 19.05341960407617918, -5.049401038297876454, 111.0427570613523329 ) ) ;
#183465 = CARTESIAN_POINT ( 'NONE',  ( -21.53943276465977519, -0.05219959533937600094, 23.75109039468567929 ) ) ;
#183466 = CARTESIAN_POINT ( 'NONE',  ( -0.05219959533937732626, 21.53943276465977519, 72.50109039468568994 ) ) ;
#183467 = CARTESIAN_POINT ( 'NONE',  ( 16.52544592524335698, 4.483927247898782831, 66.45942372801903275 ) ) ;
#183468 = CARTESIAN_POINT ( 'NONE',  ( 16.53943276465976808, 0.05219959533934440121, 71.25109039468568994 ) ) ;
#183469 = ORIENTED_EDGE ( 'NONE', *, *, #17615, .T. ) ;
#183470 = CARTESIAN_POINT ( 'NONE',  ( 13.97604488694527802, 13.89961937509977652, 64.37390960531436690 ) ) ;
#183471 = CARTESIAN_POINT ( 'NONE',  ( 16.55341960407618274, -4.379528057220086978, 86.04275706135236135 ) ) ;
#183472 = CARTESIAN_POINT ( 'NONE',  ( 16.46253265017146816, 9.564922557961045513, 36.66775706135233293 ) ) ;
#183473 = VECTOR ( 'NONE', #185910, 1000.000000000000000 ) ;
#183474 = CARTESIAN_POINT ( 'NONE',  ( 21.53943276465977519, 0.05219959533937863772, 21.25109039468567218 ) ) ;
#183475 = CARTESIAN_POINT ( 'NONE',  ( 12.14591786802309770, 12.06949235617756955, 59.37390960531436690 ) ) ;
#183476 = CARTESIAN_POINT ( 'NONE',  ( 16.46253265017160672, -9.564922557960803928, 83.33224293864768129 ) ) ;
#183477 = CARTESIAN_POINT ( 'NONE',  ( 4.379528057220092307, 16.55341960407617563, 87.29275706135236135 ) ) ;
#183478 = CARTESIAN_POINT ( 'NONE',  ( -18.62759615963255300, -10.81492255796106328, 54.16775706135235424 ) ) ;
#183479 = CARTESIAN_POINT ( 'NONE',  ( -16.53943276465976808, -0.05219959533934237506, 28.75109039468567929 ) ) ;
#183480 = CARTESIAN_POINT ( 'NONE',  ( 10.81492255796078972, 18.62759615963270932, 109.5822429386476955 ) ) ;
#183481 = CARTESIAN_POINT ( 'NONE',  ( 4.379528057220339221, -16.55341960407611168, 57.70724293864770260 ) ) ;
#183482 = ORIENTED_EDGE ( 'NONE', *, *, #63651, .F. ) ;
#183483 = CARTESIAN_POINT ( 'NONE',  ( -21.55341960407610458, -5.719274019375992779, 96.45724293864770971 ) ) ;
#183484 = CARTESIAN_POINT ( 'NONE',  ( -8.224510206698948167, 14.34966873604960824, 35.41557627198102409 ) ) ;
#183485 = ORIENTED_EDGE ( 'NONE', *, *, #101956, .T. ) ;
#183486 = CARTESIAN_POINT ( 'NONE',  ( 34.91303292417840964, 6.360705039060885468, 41.01876028008884845 ) ) ;
#183487 = CARTESIAN_POINT ( 'NONE',  ( -19.02544592524342804, 5.153800228976336051, 106.0405762719810241 ) ) ;
#183488 = CARTESIAN_POINT ( 'NONE',  ( 0.05219959533937995610, -21.53943276465977519, 35.00109039468568284 ) ) ;
#183489 = CARTESIAN_POINT ( 'NONE',  ( 4.483927247898545687, 16.52544592524342804, 54.79057627198104541 ) ) ;
#183490 = CARTESIAN_POINT ( 'NONE',  ( -5.049401038298153566, 19.05341960407611168, 60.20724293864768129 ) ) ;
#183491 = CARTESIAN_POINT ( 'NONE',  ( -13.89961937509957401, -13.97604488694547875, 69.37609039468564731 ) ) ;
#183492 = CARTESIAN_POINT ( 'NONE',  ( -5.153800228976328057, -19.02544592524343514, 92.29057627198099567 ) ) ;
#183493 = CARTESIAN_POINT ( 'NONE',  ( 10.81492255796078972, 18.62759615963270932, 44.58224293864769550 ) ) ;
#183494 = CARTESIAN_POINT ( 'NONE',  ( -9.554919064904160209, -36.23455639189580069, -31.31948065624796840 ) ) ;
#183495 = CARTESIAN_POINT ( 'NONE',  ( 19.05341960407611168, 5.049401038298154454, 53.95724293864770260 ) ) ;
#183496 = CARTESIAN_POINT ( 'NONE',  ( -0.05219959533934338120, 16.53943276465976808, 32.50109039468568284 ) ) ;
#183497 = CARTESIAN_POINT ( 'NONE',  ( 19.03943276465977164, 0.05219959533936151252, 61.25109039468566863 ) ) ;
#183498 = CARTESIAN_POINT ( 'NONE',  ( 21.55341960407610458, 5.719274019375980345, 108.9572429386476955 ) ) ;
#183499 = EDGE_CURVE ( 'NONE', #99831, #41082, #91698, .T. ) ;
#183500 = CARTESIAN_POINT ( 'NONE',  ( -16.53943276465976808, 0.05219959533911058130, 51.24890960531436690 ) ) ;
#183501 = ORIENTED_EDGE ( 'NONE', *, *, #181003, .T. ) ;
#183502 = CARTESIAN_POINT ( 'NONE',  ( -9.564922557960796823, -16.46253265017161027, 92.08224293864769550 ) ) ;
#183503 = CARTESIAN_POINT ( 'NONE',  ( -15.80617190586745835, -15.72974639402198527, 66.87390960531436690 ) ) ;
#183505 = CARTESIAN_POINT ( 'NONE',  ( -16.52544592524335698, -4.483927247898792601, 38.95942372801901854 ) ) ;
#183504 = CARTESIAN_POINT ( 'NONE',  ( -18.67979575497178146, -10.72451020669898902, 111.6655762719810525 ) ) ;
#183506 = CARTESIAN_POINT ( 'NONE',  ( 21.55341960407610458, 5.719274019375980345, 33.95724293864769550 ) ) ;
#183507 = CARTESIAN_POINT ( 'NONE',  ( 0.05219959533937995610, -21.53943276465977519, 100.0010903946857042 ) ) ;
#183508 = CARTESIAN_POINT ( 'NONE',  ( -0.05219959533909027116, -19.03943276465977164, 102.4989096053143669 ) ) ;
#183509 = B_SPLINE_CURVE_WITH_KNOTS ( 'NONE', 3,
 ( #56003, #24689, #139541, #109211, #25695, #199248, #77874, #194532, #108216, #47558, #86338, #168885, #102513, #123374, #122389, #124381, #184077, #1026, #30391, #169896, #31389, #73194, #93039, #62698, #164197, #60715 ),
 .UNSPECIFIED., .F., .F.,
 ( 4, 2, 2, 2, 2, 2, 2, 2, 2, 2, 2, 2, 4 ),
 ( 4.906538933386797396E-18, 0.002279955776188823027, 0.004559911552377641716, 0.006839867328566459105, 0.009119823104755278229, 0.01367973465713291821, 0.01823964620951055646, 0.02279955776188819991, 0.02735946931426583642, 0.02963942509045465468, 0.03191938086664347640, 0.03419933664283229119, 0.03647929241902110598 ),
 .UNSPECIFIED. ) ;
#183510 = CARTESIAN_POINT ( 'NONE',  ( -19.03943276465977164, 0.05219959533909376836, 46.24890960531435979 ) ) ;
#183511 = CARTESIAN_POINT ( 'NONE',  ( -9.564922557960796823, -16.46253265017161027, 92.08224293864769550 ) ) ;
#183512 = CARTESIAN_POINT ( 'NONE',  ( 9.474510206698971260, -16.51473224551069308, 77.91557627198103830 ) ) ;
#183513 = CARTESIAN_POINT ( 'NONE',  ( 17.13100169013223706, -6.664070546374243342, 88.26789835699827336 ) ) ;
#183514 = CARTESIAN_POINT ( 'NONE',  ( -16.51473224551082808, 9.474510206698731452, 58.33442372801900433 ) ) ;
#183516 = CARTESIAN_POINT ( 'NONE',  ( 0.05219959533907565091, 21.53943276465977519, 34.99890960531435979 ) ) ;
#183515 = CARTESIAN_POINT ( 'NONE',  ( 18.62759615963255655, 10.81492255796105972, 111.6677570613523613 ) ) ;
#183517 = CARTESIAN_POINT ( 'NONE',  ( 14.29746914071037800, 8.314922557961029526, 101.6677570613523613 ) ) ;
#183518 = CARTESIAN_POINT ( 'NONE',  ( -17.26058549869091152, 6.457015423128609655, 58.62254162523934298 ) ) ;
#183519 = CARTESIAN_POINT ( 'NONE',  ( 19.05341960407617918, -5.049401038297876454, 86.04275706135233293 ) ) ;
#183520 = CARTESIAN_POINT ( 'NONE',  ( 0.05219959533936267826, -19.03943276465977164, 30.00109039468566863 ) ) ;
#183521 = CARTESIAN_POINT ( 'NONE',  ( 17.72560187377285246, 5.500000000000046185, 71.57814504131319211 ) ) ;
#183522 = CARTESIAN_POINT ( 'NONE',  ( -19.05341960407611168, -5.049401038298163336, 36.45724293864766707 ) ) ;
#183523 = CARTESIAN_POINT ( 'NONE',  ( 12.14591786802309770, 12.06949235617756955, 39.37390960531436690 ) ) ;
#183524 = CARTESIAN_POINT ( 'NONE',  ( -17.48847506799969409, -5.747544572773738203, 109.1730256215671631 ) ) ;
#183525 = CARTESIAN_POINT ( 'NONE',  ( 0.05219959533910956823, 16.53943276465976808, 29.99890960531435979 ) ) ;
#183526 = DIRECTION ( 'NONE',  ( 0.000000000000000000, 0.000000000000000000, 1.000000000000000000 ) ) ;
#183527 = CARTESIAN_POINT ( 'NONE',  ( 16.53943276465976808, 0.05219959533934440121, 91.25109039468568994 ) ) ;
#183528 = CARTESIAN_POINT ( 'NONE',  ( 13.89961937509977652, -13.97604488694527269, 53.12390960531434558 ) ) ;
#183529 = CARTESIAN_POINT ( 'NONE',  ( -15.80617190586768217, 15.72974639402176855, 103.1260903946856757 ) ) ;
#183530 = CARTESIAN_POINT ( 'NONE',  ( -16.46253265017146816, -9.564922557961047289, 109.1677570613523471 ) ) ;
#183531 = CARTESIAN_POINT ( 'NONE',  ( -15.80617190586768217, 15.72974639402176855, 88.12609039468570415 ) ) ;
#183532 = CARTESIAN_POINT ( 'NONE',  ( 13.89961937509957401, 13.97604488694547697, 71.87609039468567573 ) ) ;
#183533 = CARTESIAN_POINT ( 'NONE',  ( 5.049401038298161559, -19.05341960407611168, 87.70724293864769550 ) ) ;
#183534 = CARTESIAN_POINT ( 'NONE',  ( -5.153800228976328057, -19.02544592524343514, 87.29057627198103830 ) ) ;
#183535 = CARTESIAN_POINT ( 'NONE',  ( 3.556970738554034288E-15, -38.81732327939057114, -8.124999997268814056 ) ) ;
#183536 = CARTESIAN_POINT ( 'NONE',  ( 5.823673210054125526, 21.52544592524343514, 109.7905762719810383 ) ) ;
#183537 = CARTESIAN_POINT ( 'NONE',  ( -16.53943276465976808, 0.05219959533911058130, 81.24890960531436690 ) ) ;
#183538 = CARTESIAN_POINT ( 'NONE',  ( 21.52544592524344225, -5.823673210054117533, 58.54057627198103120 ) ) ;
#183539 = CARTESIAN_POINT ( 'NONE',  ( -19.02544592524342804, 5.153800228976336051, 61.04057627198103120 ) ) ;
#183541 = CARTESIAN_POINT ( 'NONE',  ( -4.379528057220086978, -16.55341960407618274, 84.79275706135234714 ) ) ;
#183540 = CARTESIAN_POINT ( 'NONE',  ( 21.53943276465977519, -0.05219959533907433946, 93.74890960531436690 ) ) ;
#183542 = VERTEX_POINT ( 'NONE', #57428 ) ;
#183543 = CARTESIAN_POINT ( 'NONE',  ( -5.049401038298153566, 19.05341960407611168, 60.20724293864768129 ) ) ;
#183545 = DIRECTION ( 'NONE',  ( 1.000000000000000000, 0.000000000000000000, 0.000000000000000000 ) ) ;
#183544 = CARTESIAN_POINT ( 'NONE',  ( 14.34966873604960469, 8.224510206698951720, 99.16557627198100988 ) ) ;
#183546 = CARTESIAN_POINT ( 'NONE',  ( -13.89961937509977652, 13.97604488694528158, 55.62390960531434558 ) ) ;
#183547 = CARTESIAN_POINT ( 'NONE',  ( 19.02544592524334988, 5.153800228976608722, 86.45942372801900433 ) ) ;
#183548 = CARTESIAN_POINT ( 'NONE',  ( 16.55341960407611168, 4.379528057220329451, 83.95724293864770971 ) ) ;
#183549 = CARTESIAN_POINT ( 'NONE',  ( 15.72974639402176855, 15.80617190586768217, 56.87609039468568994 ) ) ;
#183551 = CARTESIAN_POINT ( 'NONE',  ( 21.52544592524344225, -5.823673210054117533, 98.54057627198105251 ) ) ;
#183550 = CARTESIAN_POINT ( 'NONE',  ( -13.89961937509977652, 13.97604488694528158, 30.62390960531435269 ) ) ;
#183552 = CARTESIAN_POINT ( 'NONE',  ( 14.29746914071049879, -8.314922557960816363, 98.33224293864769550 ) ) ;
#183553 = LINE ( 'NONE', #169353, #91684 ) ;
#183554 = CARTESIAN_POINT ( 'NONE',  ( -0.05219959533909027116, -19.03943276465977164, 57.49890960531435979 ) ) ;
#183555 = CARTESIAN_POINT ( 'NONE',  ( -9.248023074035629065, -10.74802307403544077, -62.40259441833023857 ) ) ;
#183557 = CARTESIAN_POINT ( 'NONE',  ( -9.474510206698964154, 16.51473224551069663, 115.4155762719810241 ) ) ;
#183556 = CARTESIAN_POINT ( 'NONE',  ( 19.03943276465977164, 0.05219959533936151252, 101.2510903946856757 ) ) ;
#183558 = CARTESIAN_POINT ( 'NONE',  ( -21.55341960407619339, 5.719274019375674811, 48.54275706135234714 ) ) ;
#183559 = CARTESIAN_POINT ( 'NONE',  ( 0.05219959533909260263, 19.03943276465977164, 89.99890960531436690 ) ) ;
#183560 = CARTESIAN_POINT ( 'NONE',  ( -0.05219959533936034679, 19.03943276465977164, 67.50109039468566152 ) ) ;
#183561 = CARTESIAN_POINT ( 'NONE',  ( -19.05341960407611168, -5.049401038298163336, 56.45724293864768129 ) ) ;
#183562 = APPLICATION_CONTEXT ( 'automotive_design' ) ;
#183563 = CARTESIAN_POINT ( 'NONE',  ( -8.224510206698948167, 14.34966873604960824, 80.41557627198103830 ) ) ;
#183564 = CARTESIAN_POINT ( 'NONE',  ( -0.05219959533910754901, -16.53943276465976808, 72.49890960531435269 ) ) ;
#183565 = CARTESIAN_POINT ( 'NONE',  ( 5.153800228976335163, 19.02544592524342804, 94.79057627198103830 ) ) ;
#183566 = CARTESIAN_POINT ( 'NONE',  ( 12.06949235617757843, -12.14591786802309237, 78.12390960531436690 ) ) ;
#183567 = CARTESIAN_POINT ( 'NONE',  ( 5.153800228976335163, 19.02544592524342804, 79.79057627198102409 ) ) ;
#183568 = CARTESIAN_POINT ( 'NONE',  ( 16.46253265017146816, 9.564922557961045513, 26.66775706135234003 ) ) ;
#183571 = CARTESIAN_POINT ( 'NONE',  ( -4.379528057220328563, 16.55341960407611168, 115.2072429386476955 ) ) ;
#183570 = CARTESIAN_POINT ( 'NONE',  ( -8.314922557960811034, -14.29746914071050412, 32.08224293864769550 ) ) ;
#183569 = CARTESIAN_POINT ( 'NONE',  ( -19.02544592524342804, 5.153800228976336051, 46.04057627198101699 ) ) ;
#183572 = ORIENTED_EDGE ( 'NONE', *, *, #147777, .T. ) ;
#183573 = CARTESIAN_POINT ( 'NONE',  ( -18.62759615963255300, -10.81492255796106328, 49.16775706135234003 ) ) ;
#183574 = CARTESIAN_POINT ( 'NONE',  ( -16.51473224551082808, 9.474510206698731452, 68.33442372801900433 ) ) ;
#183575 = CARTESIAN_POINT ( 'NONE',  ( 16.55341960407611168, 4.379528057220329451, 33.95724293864769550 ) ) ;
#183576 = CARTESIAN_POINT ( 'NONE',  ( 5.823673210054125526, 21.52544592524343514, 84.79057627198102409 ) ) ;
#183577 = CARTESIAN_POINT ( 'NONE',  ( 19.02544592524343514, -5.153800228976328945, 113.5405762719810241 ) ) ;
#183578 = CARTESIAN_POINT ( 'NONE',  ( -16.52544592524342804, 4.483927247898546575, 71.04057627198103830 ) ) ;
#183579 = CARTESIAN_POINT ( 'NONE',  ( -16.51473224551069308, -9.474510206698971260, 46.66557627198102409 ) ) ;
#183580 = CARTESIAN_POINT ( 'NONE',  ( -0.05219959533936034679, 19.03943276465977164, 42.50109039468566152 ) ) ;
#183581 = CARTESIAN_POINT ( 'NONE',  ( 12.06949235617739724, 12.14591786802326823, 101.8760903946857042 ) ) ;
#183582 = CARTESIAN_POINT ( 'NONE',  ( 16.52544592524335698, 4.483927247898782831, 61.45942372801901854 ) ) ;
#183583 = CARTESIAN_POINT ( 'NONE',  ( -18.62759615963270932, 10.81492255796079327, 35.83224293864768839 ) ) ;
#183584 = CARTESIAN_POINT ( 'NONE',  ( -10.81492255796105439, 18.62759615963255655, 102.9177570613523756 ) ) ;
#183585 = CARTESIAN_POINT ( 'NONE',  ( 5.153800228976335163, 19.02544592524342804, 94.79057627198103830 ) ) ;
#183586 = CARTESIAN_POINT ( 'NONE',  ( 8.314922557961029526, -14.29746914071037800, 75.41775706135233293 ) ) ;
#183587 = CARTESIAN_POINT ( 'NONE',  ( 16.46253265017160672, -9.564922557960803928, 23.33224293864769194 ) ) ;
#183588 = CARTESIAN_POINT ( 'NONE',  ( -12.14591786802309592, -12.06949235617757132, 31.87390960531435979 ) ) ;
#183590 = CARTESIAN_POINT ( 'NONE',  ( -19.02544592524342804, 5.153800228976336051, 91.04057627198100988 ) ) ;
#183589 = CARTESIAN_POINT ( 'NONE',  ( 0.05219959533909260263, 19.03943276465977164, 109.9989096053143669 ) ) ;
#183592 = EDGE_CURVE ( 'NONE', #123077, #1850, #2250, .T. ) ;
#183591 = CARTESIAN_POINT ( 'NONE',  ( 21.52544592524344225, -5.823673210054117533, 28.54057627198103120 ) ) ;
#183593 = CARTESIAN_POINT ( 'NONE',  ( -16.53943276465976808, 0.05219959533911058130, 56.24890960531436690 ) ) ;
#183594 = CARTESIAN_POINT ( 'NONE',  ( -4.483927247898539470, -16.52544592524342804, 37.29057627198102409 ) ) ;
#183595 = CARTESIAN_POINT ( 'NONE',  ( 12.14591786802309770, 12.06949235617756955, 49.37390960531436690 ) ) ;
#183596 = ORIENTED_EDGE ( 'NONE', *, *, #15852, .F. ) ;
#183598 = DIRECTION ( 'NONE',  ( 0.000000000000000000, -0.000000000000000000, 1.000000000000000000 ) ) ;
#183597 = CARTESIAN_POINT ( 'NONE',  ( 12.14591786802327356, -12.06949235617739191, 50.62609039468568994 ) ) ;
#183599 = CARTESIAN_POINT ( 'NONE',  ( -19.05341960407617563, 5.049401038297882671, 48.54275706135233293 ) ) ;
#183600 = CARTESIAN_POINT ( 'NONE',  ( 16.51473224551069308, 9.474510206698969483, 89.16557627198103830 ) ) ;
#183601 = CARTESIAN_POINT ( 'NONE',  ( 19.05341960407617918, -5.049401038297876454, 66.04275706135233293 ) ) ;
#183602 = CARTESIAN_POINT ( 'NONE',  ( 27.73933785331498214, 9.013057229001095294, 144.4750000027311501 ) ) ;
#183603 = CARTESIAN_POINT ( 'NONE',  ( -19.05341960407617563, 5.049401038297882671, 58.54275706135234003 ) ) ;
#183605 = CARTESIAN_POINT ( 'NONE',  ( -4.483927247898782831, 16.52544592524335698, 77.70942372801900433 ) ) ;
#183604 = CARTESIAN_POINT ( 'NONE',  ( -16.51473224551082808, 9.474510206698731452, 93.33442372801900433 ) ) ;
#183606 = CARTESIAN_POINT ( 'NONE',  ( 8.571926809382597767, 26.38167802310806209, 142.7750000027311899 ) ) ;
#183607 = CARTESIAN_POINT ( 'NONE',  ( 5.153800228976335163, 19.02544592524342804, 29.79057627198102409 ) ) ;
#183608 = CARTESIAN_POINT ( 'NONE',  ( -10.81492255796078084, -18.62759615963271287, 22.08224293864769194 ) ) ;
#183609 = CARTESIAN_POINT ( 'NONE',  ( -5.719274019375665041, -21.55341960407619695, 39.79275706135235424 ) ) ;
#183610 = CARTESIAN_POINT ( 'NONE',  ( -5.153800228976607833, 19.02544592524334988, 102.7094237280189759 ) ) ;
#183612 = CARTESIAN_POINT ( 'NONE',  ( -9.564922557960796823, -16.46253265017161027, 67.08224293864769550 ) ) ;
#183611 = FACE_OUTER_BOUND ( 'NONE', #56530, .T. ) ;
#183613 = CIRCLE ( 'NONE', #18926, 216.0437394197456342 ) ;
#183614 = CARTESIAN_POINT ( 'NONE',  ( 13.89961937509977652, -13.97604488694527269, 108.1239096053143669 ) ) ;
#183616 = CARTESIAN_POINT ( 'NONE',  ( -9.474510206698964154, 16.51473224551069663, 60.41557627198102409 ) ) ;
#183615 = CARTESIAN_POINT ( 'NONE',  ( 16.53943276465976808, -0.05219959533910856209, 78.74890960531436690 ) ) ;
#183617 = CARTESIAN_POINT ( 'NONE',  ( 9.564922557960805705, 16.46253265017160317, 74.58224293864769550 ) ) ;
#183618 = CARTESIAN_POINT ( 'NONE',  ( -16.51473224551082808, 9.474510206698731452, 83.33442372801899012 ) ) ;
#183619 = CARTESIAN_POINT ( 'NONE',  ( -15.72974639402197994, 15.80617190586746368, 55.62390960531436690 ) ) ;
#183620 = CARTESIAN_POINT ( 'NONE',  ( 13.89961937509977652, -13.97604488694527269, 23.12390960531436335 ) ) ;
#183621 = CARTESIAN_POINT ( 'NONE',  ( -19.05341960407617563, 5.049401038297882671, 38.54275706135233293 ) ) ;
#183623 = EDGE_CURVE ( 'NONE', #112207, #42860, #15164, .T. ) ;
#183622 = CARTESIAN_POINT ( 'NONE',  ( -16.51473224551069308, -9.474510206698971260, 76.66557627198103830 ) ) ;
#183624 = CARTESIAN_POINT ( 'NONE',  ( 5.823673210054125526, 21.52544592524343514, 79.79057627198102409 ) ) ;
#183626 = CARTESIAN_POINT ( 'NONE',  ( -5.049401038297874678, -19.05341960407617918, 49.79275706135231871 ) ) ;
#183625 = CARTESIAN_POINT ( 'NONE',  ( 0.05219959533910956823, 16.53943276465976808, 84.99890960531436690 ) ) ;
#183627 = CARTESIAN_POINT ( 'NONE',  ( -10.72451020669898014, 18.67979575497178502, 75.41557627198102409 ) ) ;
#183628 = CARTESIAN_POINT ( 'NONE',  ( -21.53943276465977519, 0.05219959533907696930, 66.24890960531436690 ) ) ;
#183629 = CARTESIAN_POINT ( 'NONE',  ( -21.53943276465977519, 0.05219959533907696930, 36.24890960531435979 ) ) ;
#183630 = CARTESIAN_POINT ( 'NONE',  ( 21.53943276465977519, 0.05219959533937863772, 86.25109039468568994 ) ) ;
#183631 = CARTESIAN_POINT ( 'NONE',  ( -5.049401038298153566, 19.05341960407611168, 65.20724293864765286 ) ) ;
#183632 = CARTESIAN_POINT ( 'NONE',  ( -16.52544592524342804, 4.483927247898546575, 116.0405762719810383 ) ) ;
#183633 = CARTESIAN_POINT ( 'NONE',  ( 5.823673210054444382, -21.52544592524334988, 30.20942372801902565 ) ) ;
#183634 = CARTESIAN_POINT ( 'NONE',  ( 18.67979575497194134, -10.72451020669871369, 45.83442372801901854 ) ) ;
#183635 = CARTESIAN_POINT ( 'NONE',  ( 16.46253265017160672, -9.564922557960803928, 28.33224293864769550 ) ) ;
#183636 = CARTESIAN_POINT ( 'NONE',  ( 5.823673210054125526, 21.52544592524343514, 109.7905762719810383 ) ) ;
#183637 = CARTESIAN_POINT ( 'NONE',  ( 9.474510206698729675, 16.51473224551082808, 47.08442372801900433 ) ) ;
#183638 = CARTESIAN_POINT ( 'NONE',  ( -0.05219959533909027116, -19.03943276465977164, 37.49890960531436690 ) ) ;
#183639 = CARTESIAN_POINT ( 'NONE',  ( 5.049401038298161559, -19.05341960407611168, 22.70724293864769194 ) ) ;
#183640 = DIRECTION ( 'NONE',  ( 0.000000000000000000, 0.000000000000000000, -1.000000000000000000 ) ) ;
#183641 = CARTESIAN_POINT ( 'NONE',  ( 12.14591786802327356, -12.06949235617739191, 60.62609039468567573 ) ) ;
#183642 = CARTESIAN_POINT ( 'NONE',  ( 0.05219959533909260263, 19.03943276465977164, 29.99890960531435979 ) ) ;
#183643 = CARTESIAN_POINT ( 'NONE',  ( -20.14845677604829888, -11.85354687992341205, 170.0217845860067598 ) ) ;
#183644 = CARTESIAN_POINT ( 'NONE',  ( -13.97604488694527625, -13.89961937509977652, 81.87390960531436690 ) ) ;
#183645 = CARTESIAN_POINT ( 'NONE',  ( 4.379528057220339221, -16.55341960407611168, 102.7072429386476955 ) ) ;
#183646 = CARTESIAN_POINT ( 'NONE',  ( -0.05219959533907301413, -21.53943276465977519, 57.49890960531435979 ) ) ;
#183647 = CARTESIAN_POINT ( 'NONE',  ( 4.379528057220092307, 16.55341960407617563, 47.29275706135234003 ) ) ;
#183648 = CARTESIAN_POINT ( 'NONE',  ( -18.62759615963255300, -10.81492255796106328, 104.1677570613523471 ) ) ;
#183649 = CARTESIAN_POINT ( 'NONE',  ( -9.474510206698964154, 16.51473224551069663, 35.41557627198102409 ) ) ;
#183650 = CARTESIAN_POINT ( 'NONE',  ( 16.55341960407618274, -4.379528057220086978, 111.0427570613523613 ) ) ;
#183651 = CARTESIAN_POINT ( 'NONE',  ( 12.06949235617757843, -12.14591786802309237, 58.12390960531435979 ) ) ;
#183652 = CARTESIAN_POINT ( 'NONE',  ( 9.474510206698971260, -16.51473224551069308, 62.91557627198102409 ) ) ;
#183653 = CARTESIAN_POINT ( 'NONE',  ( -21.52544592524334988, -5.823673210054445271, 103.9594237280190185 ) ) ;
#183654 = CARTESIAN_POINT ( 'NONE',  ( -21.52544592524334988, -5.823673210054445271, 23.95942372801901143 ) ) ;
#183655 = CARTESIAN_POINT ( 'NONE',  ( -21.52544592524334988, -5.823673210054445271, 68.95942372801901854 ) ) ;
#183656 = CARTESIAN_POINT ( 'NONE',  ( 8.224510206698742110, 14.34966873604972548, 52.08442372801901854 ) ) ;
#183657 = CARTESIAN_POINT ( 'NONE',  ( -8.314922557961024197, 14.29746914071037800, 27.91775706135234358 ) ) ;
#183659 = CARTESIAN_POINT ( 'NONE',  ( -18.67979575497193778, 10.72451020669871902, 93.33442372801901854 ) ) ;
#183658 = CARTESIAN_POINT ( 'NONE',  ( -16.53943276465976808, 0.05219959533911058130, 76.24890960531435269 ) ) ;
#183660 = CARTESIAN_POINT ( 'NONE',  ( -12.14591786802309592, -12.06949235617757132, 31.87390960531435979 ) ) ;
#183661 = CARTESIAN_POINT ( 'NONE',  ( -17.40805194822031510, 6.112264579159310429, 115.8337127251061531 ) ) ;
#183662 = CARTESIAN_POINT ( 'NONE',  ( -14.34966873604972548, 8.224510206698743886, 38.33442372801900433 ) ) ;
#183663 = CARTESIAN_POINT ( 'NONE',  ( -4.483927247898539470, -16.52544592524342804, 47.29057627198103120 ) ) ;
#183664 = CARTESIAN_POINT ( 'NONE',  ( -8.224510206698735004, -14.34966873604973081, 84.58442372801903275 ) ) ;
#183665 = CARTESIAN_POINT ( 'NONE',  ( -16.51473224551069308, -9.474510206698971260, 101.6655762719810241 ) ) ;
#183666 = CARTESIAN_POINT ( 'NONE',  ( 10.81492255796078972, 18.62759615963270932, 24.58224293864768839 ) ) ;
#183667 = CARTESIAN_POINT ( 'NONE',  ( -5.719274019375665041, -21.55341960407619695, 104.7927570613523898 ) ) ;
#183668 = CARTESIAN_POINT ( 'NONE',  ( 16.52544592524335698, 4.483927247898782831, 106.4594237280190328 ) ) ;
#183669 = CARTESIAN_POINT ( 'NONE',  ( 4.379528057220339221, -16.55341960407611168, 92.70724293864770971 ) ) ;
#183670 = CARTESIAN_POINT ( 'NONE',  ( 13.89961937509977652, -13.97604488694527269, 88.12390960531438111 ) ) ;
#183671 = ORIENTED_EDGE ( 'NONE', *, *, #175152, .F. ) ;
#183672 = CARTESIAN_POINT ( 'NONE',  ( 12.06949235617739724, 12.14591786802326823, 36.87609039468568994 ) ) ;
#183673 = CARTESIAN_POINT ( 'NONE',  ( -16.51473224551069308, -9.474510206698971260, 41.66557627198103120 ) ) ;
#183674 = CARTESIAN_POINT ( 'NONE',  ( -19.03943276465977164, 0.05219959533909376836, 101.2489096053143669 ) ) ;
#183676 = CARTESIAN_POINT ( 'NONE',  ( 36.91746824999999177, 2.880721459617395097E-14, -1.624999997268813390 ) ) ;
#183675 = CARTESIAN_POINT ( 'NONE',  ( 16.53943276465976808, 0.05219959533934440121, 51.25109039468568994 ) ) ;
#183677 = CARTESIAN_POINT ( 'NONE',  ( -5.049401038297874678, -19.05341960407617918, 29.79275706135232227 ) ) ;
#183678 = CARTESIAN_POINT ( 'NONE',  ( -8.224510206698735004, -14.34966873604973081, 104.5844237280190185 ) ) ;
#183679 = CARTESIAN_POINT ( 'NONE',  ( -19.05341960407611168, -5.049401038298163336, 46.45724293864768129 ) ) ;
#183680 = CARTESIAN_POINT ( 'NONE',  ( -14.34966873604972548, 8.224510206698743886, 83.33442372801903275 ) ) ;
#183681 = CARTESIAN_POINT ( 'NONE',  ( 13.97604488694548053, -13.89961937509957401, 85.62609039468568994 ) ) ;
#183682 = CARTESIAN_POINT ( 'NONE',  ( -9.564922557961040184, 16.46253265017147172, 22.91775706135233648 ) ) ;
#183683 = CARTESIAN_POINT ( 'NONE',  ( -16.46253265017160317, 9.564922557960807481, 65.83224293864769550 ) ) ;
#183684 = CARTESIAN_POINT ( 'NONE',  ( -14.29746914071049879, 8.314922557960819915, 95.83224293864770971 ) ) ;
#183685 = CARTESIAN_POINT ( 'NONE',  ( -13.97604488694547697, 13.89961937509957934, 63.12609039468566152 ) ) ;
#183686 = CARTESIAN_POINT ( 'NONE',  ( 15.72974639402199770, -15.80617190586745480, 58.12390960531435979 ) ) ;
#183687 = CARTESIAN_POINT ( 'NONE',  ( 9.474510206698729675, 16.51473224551082808, 27.08442372801900433 ) ) ;
#183688 = CARTESIAN_POINT ( 'NONE',  ( 16.46253265017160672, -9.564922557960803928, 103.3322429386476955 ) ) ;
#183689 = CARTESIAN_POINT ( 'NONE',  ( -21.53943276465977519, 0.05219959533907696930, 71.24890960531435269 ) ) ;
#183690 = CARTESIAN_POINT ( 'NONE',  ( -0.05219959533909027116, -19.03943276465977164, 112.4989096053143669 ) ) ;
#183691 = CARTESIAN_POINT ( 'NONE',  ( 13.97604488694548053, -13.89961937509957401, 95.62609039468563310 ) ) ;
#183692 = CARTESIAN_POINT ( 'NONE',  ( 19.03943276465977164, -0.05219959533909143690, 113.7489096053143669 ) ) ;
#183693 = EDGE_CURVE ( 'NONE', #58678, #93013, #8817, .T. ) ;
#183694 = CARTESIAN_POINT ( 'NONE',  ( -14.34966873604972548, 8.224510206698743886, 23.33442372801901499 ) ) ;
#183695 = CARTESIAN_POINT ( 'NONE',  ( 16.51473224551069308, 9.474510206698969483, 29.16557627198103475 ) ) ;
#183696 = CARTESIAN_POINT ( 'NONE',  ( -9.474510206698964154, 16.51473224551069663, 95.41557627198102409 ) ) ;
#183697 = CARTESIAN_POINT ( 'NONE',  ( -21.55341960407610458, -5.719274019375992779, 86.45724293864770971 ) ) ;
#183698 = CARTESIAN_POINT ( 'NONE',  ( 21.53943276465977519, 0.05219959533937863772, 61.25109039468567573 ) ) ;
#183700 = CARTESIAN_POINT ( 'NONE',  ( -21.53943276465977519, -0.05219959533937600094, 113.7510903946856757 ) ) ;
#183699 = CARTESIAN_POINT ( 'NONE',  ( 13.89961937509957401, 13.97604488694547697, 101.8760903946856331 ) ) ;
#183701 = CARTESIAN_POINT ( 'NONE',  ( 12.14591786802327356, -12.06949235617739191, 110.6260903946857042 ) ) ;
#183702 = CARTESIAN_POINT ( 'NONE',  ( -5.719274019375978568, 21.55341960407610458, 95.20724293864769550 ) ) ;
#183703 = CARTESIAN_POINT ( 'NONE',  ( -8.314922557960811034, -14.29746914071050412, 42.08224293864769550 ) ) ;
#183704 = CARTESIAN_POINT ( 'NONE',  ( -9.564922557961040184, 16.46253265017147172, 77.91775706135234714 ) ) ;
#183705 = CARTESIAN_POINT ( 'NONE',  ( -5.153800228976607833, 19.02544592524334988, 57.70942372801899012 ) ) ;
#183706 = CARTESIAN_POINT ( 'NONE',  ( 18.67979575497194134, -10.72451020669871369, 60.83442372801901854 ) ) ;
#183707 = CARTESIAN_POINT ( 'NONE',  ( -5.153800228976607833, 19.02544592524334988, 42.70942372801901143 ) ) ;
#183708 = CARTESIAN_POINT ( 'NONE',  ( -8.314922557960811034, -14.29746914071050412, 112.0822429386477097 ) ) ;
#183709 = CARTESIAN_POINT ( 'NONE',  ( 5.719274019375991003, -21.55341960407610458, 32.70724293864770260 ) ) ;
#183710 = CARTESIAN_POINT ( 'NONE',  ( -12.06949235617756955, 12.14591786802309770, 40.62390960531435269 ) ) ;
#183711 = CARTESIAN_POINT ( 'NONE',  ( -0.05219959533937732626, 21.53943276465977519, 92.50109039468567573 ) ) ;
#183712 = CARTESIAN_POINT ( 'NONE',  ( -16.52544592524335698, -4.483927247898792601, 73.95942372801901854 ) ) ;
#183713 = CARTESIAN_POINT ( 'NONE',  ( -8.224510206698948167, 14.34966873604960824, 30.41557627198101699 ) ) ;
#183714 = CARTESIAN_POINT ( 'NONE',  ( -21.55341960407619339, 5.719274019375674811, 68.54275706135234714 ) ) ;
#183715 = CARTESIAN_POINT ( 'NONE',  ( -18.67979575497193778, 10.72451020669871902, 73.33442372801901854 ) ) ;
#183716 = ORIENTED_EDGE ( 'NONE', *, *, #74445, .T. ) ;
#183717 = CARTESIAN_POINT ( 'NONE',  ( 13.97604488694527802, 13.89961937509977652, 24.37390960531435624 ) ) ;
#183718 = CARTESIAN_POINT ( 'NONE',  ( 18.67979575497194134, -10.72451020669871369, 40.83442372801901854 ) ) ;
#183719 = CARTESIAN_POINT ( 'NONE',  ( -19.05341960407611168, -5.049401038298163336, 26.45724293864769550 ) ) ;
#183720 = CARTESIAN_POINT ( 'NONE',  ( -13.97604488694527625, -13.89961937509977652, 41.87390960531435979 ) ) ;
#183721 = CARTESIAN_POINT ( 'NONE',  ( 0.05219959533910956823, 16.53943276465976808, 84.99890960531436690 ) ) ;
#183722 = CARTESIAN_POINT ( 'NONE',  ( -19.03943276465977164, 0.05219959533909376836, 91.24890960531436690 ) ) ;
#183723 = CARTESIAN_POINT ( 'NONE',  ( 8.224510206698953496, -14.34966873604960469, 32.91557627198102409 ) ) ;
#183724 = CARTESIAN_POINT ( 'NONE',  ( -18.67979575497178146, -10.72451020669898902, 61.66557627198103120 ) ) ;
#183725 = CARTESIAN_POINT ( 'NONE',  ( -5.719274019375978568, 21.55341960407610458, 105.2072429386477097 ) ) ;
#183726 = CARTESIAN_POINT ( 'NONE',  ( 9.474510206698971260, -16.51473224551069308, 102.9155762719810241 ) ) ;
#183728 = CARTESIAN_POINT ( 'NONE',  ( 9.564922557961047289, -16.46253265017146816, 100.4177570613523329 ) ) ;
#183727 = CARTESIAN_POINT ( 'NONE',  ( -19.03943276465977164, 0.05219959533909376836, 71.24890960531435269 ) ) ;
#183729 = CARTESIAN_POINT ( 'NONE',  ( 0.05219959533907565091, 21.53943276465977519, 54.99890960531435269 ) ) ;
#183730 = CARTESIAN_POINT ( 'NONE',  ( -18.62759615963255300, -10.81492255796106328, 79.16775706135234714 ) ) ;
#183731 = CARTESIAN_POINT ( 'NONE',  ( 19.05341960407611168, 5.049401038298154454, 68.95724293864769550 ) ) ;
#183732 = CARTESIAN_POINT ( 'NONE',  ( 0.05219959533909260263, 19.03943276465977164, 104.9989096053143669 ) ) ;
#183733 = CARTESIAN_POINT ( 'NONE',  ( -16.53943276465976808, -0.05219959533934237506, 78.75109039468568994 ) ) ;
#183734 = CARTESIAN_POINT ( 'NONE',  ( -18.67979575497193778, 10.72451020669871902, 58.33442372801901143 ) ) ;
#183735 = CARTESIAN_POINT ( 'NONE',  ( 21.53943276465977519, 0.05219959533937863772, 86.25109039468568994 ) ) ;
#183736 = CARTESIAN_POINT ( 'NONE',  ( -18.62759615963255300, -10.81492255796106328, 19.16775706135234714 ) ) ;
#183737 = CARTESIAN_POINT ( 'NONE',  ( -14.29746914071037622, -8.314922557961029526, 74.16775706135231871 ) ) ;
#183738 = CARTESIAN_POINT ( 'NONE',  ( -21.52544592524343514, 5.823673210054127303, 71.04057627198103830 ) ) ;
#183739 = CARTESIAN_POINT ( 'NONE',  ( 9.474510206698729675, 16.51473224551082808, 47.08442372801900433 ) ) ;
#183740 = CARTESIAN_POINT ( 'NONE',  ( -10.81492255796078084, -18.62759615963271287, 42.08224293864769550 ) ) ;
#183742 = CARTESIAN_POINT ( 'NONE',  ( 12.06949235617757843, -12.14591786802309237, 43.12390960531435269 ) ) ;
#183741 = CARTESIAN_POINT ( 'NONE',  ( 5.049401038298161559, -19.05341960407611168, 77.70724293864765286 ) ) ;
#183743 = CYLINDRICAL_SURFACE ( 'NONE', #59540, 40.00000000000000000 ) ;
#183744 =( BOUNDED_SURFACE ( )  B_SPLINE_SURFACE ( 3, 2, ( 
 ( #22282, #37442, #64800 ),
 ( #83933, #49632, #35448 ),
 ( #99102, #110300, #126461 ),
 ( #127450, #80948, #158784 ),
 ( #128439, #156818, #174967 ),
 ( #18310, #143611, #159784 ),
 ( #98086, #113275, #191133 ),
 ( #111295, #145614, #21279 ),
 ( #67778, #114269, #5095 ),
 ( #160794, #7093, #187177 ),
 ( #172984, #175973, #171982 ),
 ( #96121, #157809, #19300 ),
 ( #142623, #4102, #189156 ),
 ( #50629, #147632, #23285 ),
 ( #133451, #177972, #131448 ),
 ( #11122, #88941, #165797 ),
 ( #119292, #130432, #149624 ),
 ( #53612, #118296, #195141 ),
 ( #41455, #104115, #42451 ),
 ( #179987, #84929, #148631 ),
 ( #100106, #163803, #72797 ),
 ( #9120, #10121, #86947 ),
 ( #193135, #71781, #70787 ),
 ( #115288, #56622, #39440 ) ),
 .UNSPECIFIED., .F., .F., .T. ) 
 B_SPLINE_SURFACE_WITH_KNOTS ( ( 4, 2, 2, 2, 2, 2, 2, 2, 2, 2, 2, 4 ),
 ( 3, 3 ),
 ( -8.673617379884035472E-19, 0.001899702839891689908, 0.002849554259837535405, 0.003799405679783380684, 0.005699108519675071677, 0.006648959939620916956, 0.007598811359566762236, 0.008548662779512607515, 0.009498514199458452795, 0.01139821703935014335, 0.01329791987924183391, 0.01519762271913352621 ),
 ( 0.000000000000000000, 1.000000000000000000 ),
 .UNSPECIFIED. ) 
 GEOMETRIC_REPRESENTATION_ITEM ( )  RATIONAL_B_SPLINE_SURFACE ( (
 ( 1.000000000000000000, 0.7660444431189795678, 1.000000000000000000),
 ( 1.000000000000000000, 0.7753720600382404404, 1.000000000000000000),
 ( 1.000000000000000000, 0.7832595754285938128, 1.000000000000000000),
 ( 1.000000000000000000, 0.7928595458705487431, 1.000000000000000000),
 ( 1.000000000000000000, 0.7956872332516284896, 1.000000000000000000),
 ( 1.000000000000000000, 0.8005750596157428234, 1.000000000000000000),
 ( 1.000000000000000000, 0.8026302056541881891, 1.000000000000000000),
 ( 1.000000000000000000, 0.8075080643848097095, 1.000000000000000000),
 ( 1.000000000000000000, 0.8091143015810103867, 1.000000000000000000),
 ( 1.000000000000000000, 0.8093067629632916260, 1.000000000000000000),
 ( 1.000000000000000000, 0.8089952915732693262, 1.000000000000000000),
 ( 1.000000000000000000, 0.8076919994861299079, 1.000000000000000000),
 ( 1.000000000000000000, 0.8067078407648542449, 1.000000000000000000),
 ( 1.000000000000000000, 0.8041786842467808505, 1.000000000000000000),
 ( 1.000000000000000000, 0.8026334674876917097, 1.000000000000000000),
 ( 1.000000000000000000, 0.7990747329469513049, 1.000000000000000000),
 ( 1.000000000000000000, 0.7970509760942319222, 1.000000000000000000),
 ( 1.000000000000000000, 0.7904793850862328330, 1.000000000000000000),
 ( 1.000000000000000000, 0.7855040224315206210, 1.000000000000000000),
 ( 1.000000000000000000, 0.7751942650506107313, 1.000000000000000000),
 ( 1.000000000000000000, 0.7698260778212773214, 1.000000000000000000),
 ( 1.000000000000000000, 0.7598259884959708277, 1.000000000000000000),
 ( 1.000000000000000000, 0.7551428682221226207, 1.000000000000000000),
 ( 1.000000000000000000, 0.7510191126010858920, 1.000000000000000000) ) ) 
 REPRESENTATION_ITEM ( '' )  SURFACE ( )  );
#183745 = CARTESIAN_POINT ( 'NONE',  ( -13.89961937509977652, 13.97604488694528158, 115.6239096053143669 ) ) ;
#183746 = CARTESIAN_POINT ( 'NONE',  ( -19.49671883438226772, -5.500000000000084377, 79.89279849105686537 ) ) ;
#183747 = CARTESIAN_POINT ( 'NONE',  ( -19.03943276465977164, -0.05219959533935918106, 98.75109039468567573 ) ) ;
#183748 = CARTESIAN_POINT ( 'NONE',  ( -18.67979575497178146, -10.72451020669898902, 76.66557627198103830 ) ) ;
#183749 = CARTESIAN_POINT ( 'NONE',  ( 16.52544592524342804, -4.483927247898539470, 53.54057627198103120 ) ) ;
#183750 = CARTESIAN_POINT ( 'NONE',  ( 4.483927247898790824, -16.52544592524335698, 20.20942372801900788 ) ) ;
#183751 = CARTESIAN_POINT ( 'NONE',  ( -9.474510206698964154, 16.51473224551069663, 40.41557627198103120 ) ) ;
#183753 = CARTESIAN_POINT ( 'NONE',  ( 13.97604488694548053, -13.89961937509957401, 65.62609039468567573 ) ) ;
#183752 = CARTESIAN_POINT ( 'NONE',  ( 10.72451020669898902, -18.67979575497178502, 102.9155762719810383 ) ) ;
#183754 = CARTESIAN_POINT ( 'NONE',  ( 16.51473224551069308, 9.474510206698969483, 84.16557627198102409 ) ) ;
#183755 = CARTESIAN_POINT ( 'NONE',  ( 14.34966873604960469, 8.224510206698951720, 84.16557627198103830 ) ) ;
#183756 = CARTESIAN_POINT ( 'NONE',  ( 5.153800228976335163, 19.02544592524342804, 59.79057627198100988 ) ) ;
#183757 = CARTESIAN_POINT ( 'NONE',  ( 4.483927247898545687, 16.52544592524342804, 64.79057627198103830 ) ) ;
#183758 = CARTESIAN_POINT ( 'NONE',  ( 19.02544592524343514, -5.153800228976328945, 28.54057627198102409 ) ) ;
#183759 = CARTESIAN_POINT ( 'NONE',  ( -36.84749596837620089, -2.912325675875796716, 49.66910675224617222 ) ) ;
#183760 = CARTESIAN_POINT ( 'NONE',  ( -12.14591786802309592, -12.06949235617757132, 41.87390960531435979 ) ) ;
#183761 = CARTESIAN_POINT ( 'NONE',  ( -9.474510206698964154, 16.51473224551069663, 95.41557627198102409 ) ) ;
#183762 = CARTESIAN_POINT ( 'NONE',  ( -1.500078752102835811, -15.01195240492206651, -59.87740586969341905 ) ) ;
#183763 = CARTESIAN_POINT ( 'NONE',  ( -9.474510206698720793, -16.51473224551083518, 49.58442372801899722 ) ) ;
#183764 = CARTESIAN_POINT ( 'NONE',  ( -12.06949235617739369, -12.14591786802326823, 54.37609039468568994 ) ) ;
#183765 = CARTESIAN_POINT ( 'NONE',  ( 5.823673210054125526, 21.52544592524343514, 79.79057627198102409 ) ) ;
#183766 = CARTESIAN_POINT ( 'NONE',  ( -19.05341960407617563, 5.049401038297882671, 33.54275706135231871 ) ) ;
#183767 = CARTESIAN_POINT ( 'NONE',  ( 5.049401038298161559, -19.05341960407611168, 92.70724293864769550 ) ) ;
#183768 = LINE ( 'NONE', #186768, #53338 ) ;
#183769 = CARTESIAN_POINT ( 'NONE',  ( 5.823673210054125526, 21.52544592524343514, 34.79057627198103120 ) ) ;
#183770 = CARTESIAN_POINT ( 'NONE',  ( -5.153800228976328057, -19.02544592524343514, 62.29057627198100988 ) ) ;
#183771 = CARTESIAN_POINT ( 'NONE',  ( -0.05219959533937732626, 21.53943276465977519, 52.50109039468567573 ) ) ;
#183772 = CARTESIAN_POINT ( 'NONE',  ( 0.05219959533909260263, 19.03943276465977164, 29.99890960531435979 ) ) ;
#183775 = ORIENTED_EDGE ( 'NONE', *, *, #188269, .T. ) ;
#183774 = CARTESIAN_POINT ( 'NONE',  ( -19.02544592524342804, 5.153800228976336051, 91.04057627198100988 ) ) ;
#183773 = CARTESIAN_POINT ( 'NONE',  ( -15.72974639402197994, 15.80617190586746368, 110.6239096053143669 ) ) ;
#183776 = CARTESIAN_POINT ( 'NONE',  ( -10.72451020669870658, -18.67979575497194134, 34.58442372801900433 ) ) ;
#183777 = ORIENTED_EDGE ( 'NONE', *, *, #186584, .T. ) ;
#183778 = CARTESIAN_POINT ( 'NONE',  ( 9.564922557960805705, 16.46253265017160317, 104.5822429386476955 ) ) ;
#183779 = CARTESIAN_POINT ( 'NONE',  ( -16.46253265017160317, 9.564922557960807481, 90.83224293864769550 ) ) ;
#183780 = CARTESIAN_POINT ( 'NONE',  ( 5.719274019375991003, -21.55341960407610458, 107.7072429386476955 ) ) ;
#183781 = CARTESIAN_POINT ( 'NONE',  ( 16.46253265017160672, -9.564922557960803928, 48.33224293864769550 ) ) ;
#183782 = CARTESIAN_POINT ( 'NONE',  ( -4.379528057220086978, -16.55341960407618274, 29.79275706135234358 ) ) ;
#183783 = CARTESIAN_POINT ( 'NONE',  ( -36.91746825000001309, -11.99521256947794789, -3.024999997268812635 ) ) ;
#183784 = CARTESIAN_POINT ( 'NONE',  ( 16.46253265017160672, -9.564922557960803928, 33.33224293864770260 ) ) ;
#183785 = CARTESIAN_POINT ( 'NONE',  ( 10.81492255796106328, -18.62759615963255655, 100.4177570613523471 ) ) ;
#183787 = CARTESIAN_POINT ( 'NONE',  ( -18.62759615963255300, -10.81492255796106328, 54.16775706135235424 ) ) ;
#183786 = CARTESIAN_POINT ( 'NONE',  ( -5.049401038298153566, 19.05341960407611168, 70.20724293864769550 ) ) ;
#183788 = CARTESIAN_POINT ( 'NONE',  ( -22.44159573604010305, 16.30477369853692338, 143.1750000027311671 ) ) ;
#183789 = CARTESIAN_POINT ( 'NONE',  ( 19.02544592524343514, -5.153800228976328945, 93.54057627198102409 ) ) ;
#183790 = CARTESIAN_POINT ( 'NONE',  ( 14.30785154961629857, 24.18559174397515577, 140.0000000000000853 ) ) ;
#183793 = CARTESIAN_POINT ( 'NONE',  ( -21.52544592524334988, -5.823673210054445271, 63.95942372801901854 ) ) ;
#183792 = CARTESIAN_POINT ( 'NONE',  ( 16.53943276465976808, 0.05219959533934440121, 71.25109039468568994 ) ) ;
#183791 = CARTESIAN_POINT ( 'NONE',  ( 16.52544592524335698, 4.483927247898782831, 41.45942372801901143 ) ) ;
#183794 = CARTESIAN_POINT ( 'NONE',  ( -15.80617190586768217, 15.72974639402176855, 93.12609039468568994 ) ) ;
#183795 = CARTESIAN_POINT ( 'NONE',  ( 4.704316316549549626, 6.719756334737494896, -62.10423353180173933 ) ) ;
#183796 = CARTESIAN_POINT ( 'NONE',  ( 9.564922557961047289, -16.46253265017146816, 105.4177570613523471 ) ) ;
#183797 = CARTESIAN_POINT ( 'NONE',  ( -5.049401038298153566, 19.05341960407611168, 80.20724293864769550 ) ) ;
#183798 = CARTESIAN_POINT ( 'NONE',  ( -9.474510206698964154, 16.51473224551069663, 100.4155762719810241 ) ) ;
#183799 = CARTESIAN_POINT ( 'NONE',  ( -16.51473224551069308, -9.474510206698971260, 31.66557627198102054 ) ) ;
#183800 = CARTESIAN_POINT ( 'NONE',  ( -10.81492255796078084, -18.62759615963271287, 32.08224293864769550 ) ) ;
#183801 = CARTESIAN_POINT ( 'NONE',  ( -16.53943276465976808, -0.05219959533934237506, 93.75109039468567573 ) ) ;
#183803 = CARTESIAN_POINT ( 'NONE',  ( 13.97604488694527802, 13.89961937509977652, 54.37390960531435979 ) ) ;
#183802 = CARTESIAN_POINT ( 'NONE',  ( 16.53943276465976808, -0.05219959533910856209, 63.74890960531435979 ) ) ;
#183804 = CARTESIAN_POINT ( 'NONE',  ( 18.62759615963255655, 10.81492255796105972, 96.66775706135234714 ) ) ;
#183805 = CARTESIAN_POINT ( 'NONE',  ( 17.49700485646017256, 4.621336975095707622, 21.88126978150424762 ) ) ;
#183806 = CARTESIAN_POINT ( 'NONE',  ( 9.564922557961047289, -16.46253265017146816, 105.4177570613523471 ) ) ;
#183807 = CARTESIAN_POINT ( 'NONE',  ( -16.53943276465976808, 0.05219959533911058130, 81.24890960531436690 ) ) ;
#183808 = CARTESIAN_POINT ( 'NONE',  ( -0.05219959533937732626, 21.53943276465977519, 27.50109039468567929 ) ) ;
#183809 = CARTESIAN_POINT ( 'NONE',  ( 15.72974639402199770, -15.80617190586745480, 58.12390960531435979 ) ) ;
#183810 = CARTESIAN_POINT ( 'NONE',  ( 16.51473224551083163, -9.474510206698727899, 40.83442372801900433 ) ) ;
#183811 = CARTESIAN_POINT ( 'NONE',  ( 9.564922557960805705, 16.46253265017160317, 89.58224293864769550 ) ) ;
#183812 = CARTESIAN_POINT ( 'NONE',  ( 8.314922557960818139, 14.29746914071049879, 49.58224293864769550 ) ) ;
#183813 = CARTESIAN_POINT ( 'NONE',  ( -12.14591786802309592, -12.06949235617757132, 36.87390960531435979 ) ) ;
#183814 = CARTESIAN_POINT ( 'NONE',  ( 14.34966873604972726, -8.224510206698740333, 100.8344237280190185 ) ) ;
#183815 = CARTESIAN_POINT ( 'NONE',  ( -16.51473224551082808, 9.474510206698731452, 48.33442372801900433 ) ) ;
#183816 = CARTESIAN_POINT ( 'NONE',  ( -9.564922557961040184, 16.46253265017147172, 77.91775706135234714 ) ) ;
#183817 = CARTESIAN_POINT ( 'NONE',  ( 13.89961937509977652, -13.97604488694527269, 103.1239096053143527 ) ) ;
#183818 = CARTESIAN_POINT ( 'NONE',  ( -12.06949235617756955, 12.14591786802309770, 70.62390960531436690 ) ) ;
#183819 = CARTESIAN_POINT ( 'NONE',  ( -9.564922557961040184, 16.46253265017147172, 47.91775706135233293 ) ) ;
#183821 = CARTESIAN_POINT ( 'NONE',  ( -21.52544592524343514, 5.823673210054127303, 36.04057627198102409 ) ) ;
#183820 = CARTESIAN_POINT ( 'NONE',  ( 16.51473224551069308, 9.474510206698969483, 34.16557627198102409 ) ) ;
#183822 = CARTESIAN_POINT ( 'NONE',  ( -18.67979575497178146, -10.72451020669898902, 71.66557627198100988 ) ) ;
#183823 = CARTESIAN_POINT ( 'NONE',  ( 4.483927247898545687, 16.52544592524342804, 114.7905762719810383 ) ) ;
#183824 = CARTESIAN_POINT ( 'NONE',  ( 8.224510206698742110, 14.34966873604972548, 52.08442372801901854 ) ) ;
#183825 = CARTESIAN_POINT ( 'NONE',  ( -18.62759615963255300, -10.81492255796106328, 39.16775706135235424 ) ) ;
#183826 = CARTESIAN_POINT ( 'NONE',  ( -4.483927247898539470, -16.52544592524342804, 92.29057627198103830 ) ) ;
#183827 = EDGE_CURVE ( 'NONE', #49235, #17604, #95970, .T. ) ;
#183828 = CARTESIAN_POINT ( 'NONE',  ( 17.31747979337950838, -6.344076630960994834, 36.12055131934817354 ) ) ;
#183829 = CARTESIAN_POINT ( 'NONE',  ( -22.81625015709509441, -31.40387420917324590, -8.824999997268811569 ) ) ;
#183830 = CARTESIAN_POINT ( 'NONE',  ( 10.81492255796078972, 18.62759615963270932, 34.58224293864770260 ) ) ;
#183831 = CARTESIAN_POINT ( 'NONE',  ( 17.48853670773243252, -5.747243402303153559, 66.16671299749991420 ) ) ;
#183832 = CARTESIAN_POINT ( 'NONE',  ( -11.74149087413294623, -36.13659316521243881, -7.347842220587803119 ) ) ;
#183833 = AXIS2_PLACEMENT_3D ( 'NONE', #147725, #8199, #162879 ) ;
#183835 = CARTESIAN_POINT ( 'NONE',  ( -14.34966873604960291, -8.224510206698953496, 41.66557627198103120 ) ) ;
#183834 = CARTESIAN_POINT ( 'NONE',  ( 16.53943276465976808, 0.05219959533934440121, 41.25109039468568284 ) ) ;
#183836 = CARTESIAN_POINT ( 'NONE',  ( 5.719274019375991003, -21.55341960407610458, 67.70724293864769550 ) ) ;
#183837 = CARTESIAN_POINT ( 'NONE',  ( 5.049401038297881783, 19.05341960407617563, 82.29275706135229029 ) ) ;
#183838 = CARTESIAN_POINT ( 'NONE',  ( 10.72451020669898902, -18.67979575497178502, 67.91557627198102409 ) ) ;
#183839 = CARTESIAN_POINT ( 'NONE',  ( 30.11859102234670615, -23.17191052982427735, -18.99406613714113234 ) ) ;
#183841 = CARTESIAN_POINT ( 'NONE',  ( 5.049401038298161559, -19.05341960407611168, 102.7072429386476955 ) ) ;
#183840 = CARTESIAN_POINT ( 'NONE',  ( 13.89961937509977652, -13.97604488694527269, 38.12390960531436690 ) ) ;
#183842 = CARTESIAN_POINT ( 'NONE',  ( 9.474510206698971260, -16.51473224551069308, 52.91557627198102409 ) ) ;
#183843 = CARTESIAN_POINT ( 'NONE',  ( 4.379528057220339221, -16.55341960407611168, 112.7072429386476955 ) ) ;
#183844 = DIRECTION ( 'NONE',  ( 0.000000000000000000, 0.000000000000000000, 1.000000000000000000 ) ) ;
#183845 = FACE_BOUND ( 'NONE', #25927, .T. ) ;
#183846 = ORIENTED_EDGE ( 'NONE', *, *, #39485, .F. ) ;
#183847 = CARTESIAN_POINT ( 'NONE',  ( 8.224510206698742110, 14.34966873604972548, 67.08442372801901854 ) ) ;
#183848 = CARTESIAN_POINT ( 'NONE',  ( 5.719274019375991003, -21.55341960407610458, 97.70724293864772392 ) ) ;
#183849 = CARTESIAN_POINT ( 'NONE',  ( -0.05219959533909027116, -19.03943276465977164, 57.49890960531435979 ) ) ;
#183850 = CARTESIAN_POINT ( 'NONE',  ( 15.72974639402176855, 15.80617190586768217, 26.87609039468567218 ) ) ;
#183851 = CARTESIAN_POINT ( 'NONE',  ( 16.46253265017160672, -9.564922557960803928, 88.33224293864769550 ) ) ;
#183853 = ADVANCED_FACE ( 'NONE', ( #126038, #93703 ), #78526, .T. ) ;
#183852 = CARTESIAN_POINT ( 'NONE',  ( -34.63261191445433695, -20.08610687336648581, -21.92908410841864608 ) ) ;
#183854 = ORIENTED_EDGE ( 'NONE', *, *, #116186, .F. ) ;
#183855 = CARTESIAN_POINT ( 'NONE',  ( 15.72974639402176855, 15.80617190586768217, 36.87609039468568994 ) ) ;
#183858 = CARTESIAN_POINT ( 'NONE',  ( 13.97604488694548053, -13.89961937509957401, 90.62609039468567573 ) ) ;
#183857 = CARTESIAN_POINT ( 'NONE',  ( 16.51473224551069308, 9.474510206698969483, 104.1655762719810241 ) ) ;
#183856 = CARTESIAN_POINT ( 'NONE',  ( -16.46253265017160317, 9.564922557960807481, 30.83224293864769550 ) ) ;
#183859 = CARTESIAN_POINT ( 'NONE',  ( -5.049401038297874678, -19.05341960407617918, 44.79275706135232582 ) ) ;
#183860 = CARTESIAN_POINT ( 'NONE',  ( 0.05219959533907565091, 21.53943276465977519, 99.99890960531436690 ) ) ;
#183861 = CARTESIAN_POINT ( 'NONE',  ( -19.03943276465977164, -0.05219959533935918106, 38.75109039468566152 ) ) ;
#183862 = CARTESIAN_POINT ( 'NONE',  ( -13.97604488694547697, 13.89961937509957934, 33.12609039468566863 ) ) ;
#183863 = CARTESIAN_POINT ( 'NONE',  ( 16.53943276465976808, 0.05219959533934440121, 86.25109039468568994 ) ) ;
#183865 = EDGE_LOOP ( 'NONE', ( #159617, #90276 ) ) ;
#183864 = CARTESIAN_POINT ( 'NONE',  ( -19.03943276465977164, 0.05219959533909376836, 111.2489096053143669 ) ) ;
#183866 = CARTESIAN_POINT ( 'NONE',  ( 13.97604488694527802, 13.89961937509977652, 54.37390960531435979 ) ) ;
#183867 = AXIS2_PLACEMENT_3D ( 'NONE', #95927, #35254, #156620 ) ;
#183868 = CARTESIAN_POINT ( 'NONE',  ( 10.72451020669871369, 18.67979575497193778, 62.08442372801901143 ) ) ;
#183869 = CARTESIAN_POINT ( 'NONE',  ( 5.719274019375673035, 21.55341960407619339, 77.29275706135234714 ) ) ;
#183870 = CARTESIAN_POINT ( 'NONE',  ( 0.05219959533909260263, 19.03943276465977164, 114.9989096053143669 ) ) ;
#183871 = CARTESIAN_POINT ( 'NONE',  ( 16.51473224551069308, 9.474510206698969483, 79.16557627198103830 ) ) ;
#183872 = CARTESIAN_POINT ( 'NONE',  ( 10.72451020669871369, 18.67979575497193778, 52.08442372801901854 ) ) ;
#183873 = CARTESIAN_POINT ( 'NONE',  ( -16.51473224551082808, 9.474510206698731452, 98.33442372801900433 ) ) ;
#183874 = CARTESIAN_POINT ( 'NONE',  ( -16.51473224551069308, -9.474510206698971260, 51.66557627198102409 ) ) ;
#183875 = CARTESIAN_POINT ( 'NONE',  ( -9.474510206698964154, 16.51473224551069663, 105.4155762719810383 ) ) ;
#183876 = CARTESIAN_POINT ( 'NONE',  ( -9.474510206698964154, 16.51473224551069663, 80.41557627198103830 ) ) ;
#183877 = CARTESIAN_POINT ( 'NONE',  ( 9.474510206698971260, -16.51473224551069308, 77.91557627198103830 ) ) ;
#183878 = CARTESIAN_POINT ( 'NONE',  ( -5.153800228976328057, -19.02544592524343514, 62.29057627198100988 ) ) ;
#183879 = CARTESIAN_POINT ( 'NONE',  ( 0.05219959533907565091, 21.53943276465977519, 94.99890960531436690 ) ) ;
#183880 = CARTESIAN_POINT ( 'NONE',  ( -12.14591786802326823, 12.06949235617739902, 83.12609039468568994 ) ) ;
#183881 = CARTESIAN_POINT ( 'NONE',  ( -6.856101608890819192E-16, -67.16067257189654072, -12.99988689144064402 ) ) ;
#183882 = CARTESIAN_POINT ( 'NONE',  ( -5.049401038297874678, -19.05341960407617918, 39.79275706135232582 ) ) ;
#183883 = CARTESIAN_POINT ( 'NONE',  ( -5.153800228976328057, -19.02544592524343514, 82.29057627198103830 ) ) ;
#183884 = CARTESIAN_POINT ( 'NONE',  ( -8.314922557960811034, -14.29746914071050412, 57.08224293864769550 ) ) ;
#183885 = CARTESIAN_POINT ( 'NONE',  ( -16.55341960407611168, -4.379528057220339221, 96.45724293864770971 ) ) ;
#183886 = CARTESIAN_POINT ( 'NONE',  ( 0.05219959533907565091, 21.53943276465977519, 24.99890960531435624 ) ) ;
#183887 = CARTESIAN_POINT ( 'NONE',  ( 0.05219959533909260263, 19.03943276465977164, 99.99890960531436690 ) ) ;
#183888 = CARTESIAN_POINT ( 'NONE',  ( 0.05219959533909260263, 19.03943276465977164, 114.9989096053143669 ) ) ;
#183889 = CARTESIAN_POINT ( 'NONE',  ( 19.05341960407617918, -5.049401038297876454, 36.04275706135234003 ) ) ;
#183890 = CARTESIAN_POINT ( 'NONE',  ( -16.52544592524335698, -4.483927247898792601, 98.95942372801903275 ) ) ;
#183891 = CARTESIAN_POINT ( 'NONE',  ( 19.03943276465977164, -0.05219959533909143690, 78.74890960531436690 ) ) ;
#183892 = CARTESIAN_POINT ( 'NONE',  ( -18.62759615963255300, -10.81492255796106328, 39.16775706135235424 ) ) ;
#183893 = CARTESIAN_POINT ( 'NONE',  ( 15.80617190586746368, 15.72974639402197994, 34.37390960531435979 ) ) ;
#183894 = CARTESIAN_POINT ( 'NONE',  ( 15.80617190586746368, 15.72974639402197994, 114.3739096053143527 ) ) ;
#183895 = CARTESIAN_POINT ( 'NONE',  ( 5.719274019375991003, -21.55341960407610458, 72.70724293864769550 ) ) ;
#183896 = CARTESIAN_POINT ( 'NONE',  ( 12.14591786802309770, 12.06949235617756955, 89.37390960531435269 ) ) ;
#183897 = CARTESIAN_POINT ( 'NONE',  ( 16.51473224551083163, -9.474510206698727899, 55.83442372801899722 ) ) ;
#183898 = CARTESIAN_POINT ( 'NONE',  ( 9.474510206698971260, -16.51473224551069308, 32.91557627198102409 ) ) ;
#183899 = CARTESIAN_POINT ( 'NONE',  ( 9.474510206698971260, -16.51473224551069308, 87.91557627198102409 ) ) ;
#183900 = CARTESIAN_POINT ( 'NONE',  ( -16.51473224551069308, -9.474510206698971260, 86.66557627198102409 ) ) ;
#183901 = CARTESIAN_POINT ( 'NONE',  ( 1.350817277425566232, 6.940587957980362432, -64.37020913546857059 ) ) ;
#183902 = CARTESIAN_POINT ( 'NONE',  ( 12.14591786802309770, 12.06949235617756955, 104.3739096053143669 ) ) ;
#183903 = ORIENTED_EDGE ( 'NONE', *, *, #27433, .T. ) ;
#183904 = CARTESIAN_POINT ( 'NONE',  ( -14.34966873604960291, -8.224510206698953496, 31.66557627198102054 ) ) ;
#183905 = CARTESIAN_POINT ( 'NONE',  ( 16.53943276465976808, 0.05219959533934440121, 21.25109039468567218 ) ) ;
#183906 = CARTESIAN_POINT ( 'NONE',  ( 21.53943276465977519, 0.05219959533937863772, 91.25109039468568994 ) ) ;
#183907 = CARTESIAN_POINT ( 'NONE',  ( 9.474510206698971260, -16.51473224551069308, 102.9155762719810241 ) ) ;
#183908 = CARTESIAN_POINT ( 'NONE',  ( -15.80617190586745835, -15.72974639402198527, 111.8739096053143669 ) ) ;
#183909 = CARTESIAN_POINT ( 'NONE',  ( 9.474510206698971260, -16.51473224551069308, 42.91557627198103120 ) ) ;
#183910 = CARTESIAN_POINT ( 'NONE',  ( 16.55341960407618274, -4.379528057220086978, 46.04275706135234714 ) ) ;
#183911 = CARTESIAN_POINT ( 'NONE',  ( -12.06949235617739369, -12.14591786802326823, 19.37609039468568639 ) ) ;
#183912 = CARTESIAN_POINT ( 'NONE',  ( -16.52544592524342804, 4.483927247898546575, 91.04057627198103830 ) ) ;
#183913 = CARTESIAN_POINT ( 'NONE',  ( -5.823673210054116645, -21.52544592524344225, 107.2905762719810525 ) ) ;
#183914 = CARTESIAN_POINT ( 'NONE',  ( -9.564922557961040184, 16.46253265017147172, 72.91775706135233293 ) ) ;
#183915 = DIRECTION ( 'NONE',  ( 1.000000000000000000, 0.000000000000000000, 0.000000000000000000 ) ) ;
#183916 = CARTESIAN_POINT ( 'NONE',  ( 5.719274019375673035, 21.55341960407619339, 22.29275706135235069 ) ) ;
#183917 = CARTESIAN_POINT ( 'NONE',  ( -5.429308488886486681E-15, 30.30510711980690175, 141.7500000054623683 ) ) ;
#183918 = CARTESIAN_POINT ( 'NONE',  ( 16.46253265017160672, -9.564922557960803928, 93.33224293864769550 ) ) ;
#183919 = CARTESIAN_POINT ( 'NONE',  ( 17.50000000000000000, -5.500000000000000888, 113.2969038253417153 ) ) ;
#183920 = CARTESIAN_POINT ( 'NONE',  ( 0.05219959533909260263, 19.03943276465977164, 89.99890960531436690 ) ) ;
#183922 = CARTESIAN_POINT ( 'NONE',  ( -4.483927247898539470, -16.52544592524342804, 82.29057627198103830 ) ) ;
#183921 = CARTESIAN_POINT ( 'NONE',  ( 15.80617190586769283, -15.72974639402175789, 30.62609039468567929 ) ) ;
#183923 = CARTESIAN_POINT ( 'NONE',  ( 5.049401038298161559, -19.05341960407611168, 87.70724293864769550 ) ) ;
#183925 = CARTESIAN_POINT ( 'NONE',  ( -19.02544592524334988, -5.153800228976617603, 48.95942372801900433 ) ) ;
#183924 = CARTESIAN_POINT ( 'NONE',  ( 14.29746914071037800, 8.314922557961029526, 51.66775706135234714 ) ) ;
#183926 = CARTESIAN_POINT ( 'NONE',  ( -15.72974639402176322, -15.80617190586768395, 59.37609039468568284 ) ) ;
#183927 = CARTESIAN_POINT ( 'NONE',  ( 16.52544592524335698, 4.483927247898782831, 31.45942372801901854 ) ) ;
#183928 = CARTESIAN_POINT ( 'NONE',  ( 19.05341960407611168, 5.049401038298154454, 63.95724293864769550 ) ) ;
#183929 = CARTESIAN_POINT ( 'NONE',  ( 9.474510206698729675, 16.51473224551082808, 102.0844237280190043 ) ) ;
#183930 = CARTESIAN_POINT ( 'NONE',  ( 16.53943276465976808, 0.05219959533934440121, 61.25109039468567573 ) ) ;
#183931 = CARTESIAN_POINT ( 'NONE',  ( 0.05219959533937995610, -21.53943276465977519, 95.00109039468568994 ) ) ;
#183932 = CARTESIAN_POINT ( 'NONE',  ( -0.05219959533936034679, 19.03943276465977164, 77.50109039468566152 ) ) ;
#183933 = CARTESIAN_POINT ( 'NONE',  ( -13.89961937509977652, 13.97604488694528158, 45.62390960531433848 ) ) ;
#183934 = CARTESIAN_POINT ( 'NONE',  ( -21.55341960407610458, -5.719274019375992779, 71.45724293864769550 ) ) ;
#183936 = CARTESIAN_POINT ( 'NONE',  ( -9.564922557961040184, 16.46253265017147172, 77.91775706135234714 ) ) ;
#183935 = CARTESIAN_POINT ( 'NONE',  ( 8.224510206698953496, -14.34966873604960469, 82.91557627198103830 ) ) ;
#183937 = CARTESIAN_POINT ( 'NONE',  ( -18.89770734986048950, -5.500000000000011546, 69.10214472496642202 ) ) ;
#183938 = CARTESIAN_POINT ( 'NONE',  ( -0.05219959533936034679, 19.03943276465977164, 37.50109039468567573 ) ) ;
#183939 = CARTESIAN_POINT ( 'NONE',  ( 8.224510206698953496, -14.34966873604960469, 22.91557627198102765 ) ) ;
#183940 = CARTESIAN_POINT ( 'NONE',  ( 14.34966873604960469, 8.224510206698951720, 64.16557627198102409 ) ) ;
#183942 = CARTESIAN_POINT ( 'NONE',  ( 27.73933785331498214, 9.013057229001095294, 143.9750000027312069 ) ) ;
#183941 = CARTESIAN_POINT ( 'NONE',  ( -18.62759615963255300, -10.81492255796106328, 109.1677570613523613 ) ) ;
#183943 = CARTESIAN_POINT ( 'NONE',  ( 5.719274019375991003, -21.55341960407610458, 107.7072429386476955 ) ) ;
#183944 = CARTESIAN_POINT ( 'NONE',  ( 9.564922557960805705, 16.46253265017160317, 64.58224293864769550 ) ) ;
#183945 = CARTESIAN_POINT ( 'NONE',  ( -5.719274019375665041, -21.55341960407619695, 89.79275706135236135 ) ) ;
#183946 = CARTESIAN_POINT ( 'NONE',  ( 19.02544592524343514, -5.153800228976328945, 63.54057627198103830 ) ) ;
#183947 = CARTESIAN_POINT ( 'NONE',  ( 4.483927247898545687, 16.52544592524342804, 114.7905762719810383 ) ) ;
#183948 = CARTESIAN_POINT ( 'NONE',  ( -5.823673210054116645, -21.52544592524344225, 27.29057627198103120 ) ) ;
#183949 = CARTESIAN_POINT ( 'NONE',  ( 8.224510206698953496, -14.34966873604960469, 72.91557627198103830 ) ) ;
#183950 = CARTESIAN_POINT ( 'NONE',  ( -5.153800228976328057, -19.02544592524343514, 42.29057627198101699 ) ) ;
#183951 = CARTESIAN_POINT ( 'NONE',  ( 16.53943276465976808, -0.05219959533910856209, 83.74890960531435269 ) ) ;
#183952 = CARTESIAN_POINT ( 'NONE',  ( -0.05219959533907301413, -21.53943276465977519, 112.4989096053143669 ) ) ;
#183953 = CARTESIAN_POINT ( 'NONE',  ( 10.81492255796106328, -18.62759615963255655, 50.41775706135235424 ) ) ;
#183954 = CARTESIAN_POINT ( 'NONE',  ( -19.03943276465977164, 0.05219959533909376836, 36.24890960531436690 ) ) ;
#183955 = CARTESIAN_POINT ( 'NONE',  ( -8.224510206698735004, -14.34966873604973081, 54.58442372801901143 ) ) ;
#183956 = CARTESIAN_POINT ( 'NONE',  ( 5.719274019375991003, -21.55341960407610458, 97.70724293864772392 ) ) ;
#183958 = CARTESIAN_POINT ( 'NONE',  ( -19.03943276465977164, 0.05219959533909376836, 51.24890960531436690 ) ) ;
#183957 = CARTESIAN_POINT ( 'NONE',  ( 13.97604488694548053, -13.89961937509957401, 25.62609039468566507 ) ) ;
#183959 = CARTESIAN_POINT ( 'NONE',  ( 5.049401038298161559, -19.05341960407611168, 102.7072429386476955 ) ) ;
#183960 = CARTESIAN_POINT ( 'NONE',  ( 21.53943276465977519, 0.05219959533937863772, 56.25109039468568284 ) ) ;
#183961 = CARTESIAN_POINT ( 'NONE',  ( 18.67979575497178502, 10.72451020669898547, 49.16557627198102409 ) ) ;
#183962 = CARTESIAN_POINT ( 'NONE',  ( 14.34966873604972726, -8.224510206698740333, 110.8344237280190043 ) ) ;
#183964 = CARTESIAN_POINT ( 'NONE',  ( -15.80617190586768217, 15.72974639402176855, 103.1260903946856757 ) ) ;
#183963 = CARTESIAN_POINT ( 'NONE',  ( -18.62759615963255300, -10.81492255796106328, 64.16775706135234714 ) ) ;
#183965 = CARTESIAN_POINT ( 'NONE',  ( -0.05219959533936034679, 19.03943276465977164, 32.50109039468566863 ) ) ;
#183966 = CARTESIAN_POINT ( 'NONE',  ( -4.379528057220086978, -16.55341960407618274, 99.79275706135234714 ) ) ;
#183967 = CARTESIAN_POINT ( 'NONE',  ( -0.05219959533937732626, 21.53943276465977519, 57.50109039468568994 ) ) ;
#183968 = CARTESIAN_POINT ( 'NONE',  ( 19.03943276465977164, -0.05219959533909143690, 48.74890960531435979 ) ) ;
#183969 = CARTESIAN_POINT ( 'NONE',  ( -9.564922557961040184, 16.46253265017147172, 27.91775706135232582 ) ) ;
#183970 = CARTESIAN_POINT ( 'NONE',  ( 0.05219959533909260263, 19.03943276465977164, 114.9989096053143669 ) ) ;
#183971 = CARTESIAN_POINT ( 'NONE',  ( 18.62759615963255655, 10.81492255796105972, 21.66775706135235069 ) ) ;
#183972 = CIRCLE ( 'NONE', #96760, 9.100000000000001421 ) ;
#183973 = CARTESIAN_POINT ( 'NONE',  ( -21.55341960407610458, -5.719274019375992779, 71.45724293864769550 ) ) ;
#183974 = CARTESIAN_POINT ( 'NONE',  ( -16.55341960407617563, 4.379528057220093196, 38.54275706135234714 ) ) ;
#183976 = CARTESIAN_POINT ( 'NONE',  ( 15.80617190586746368, 15.72974639402197994, 79.37390960531436690 ) ) ;
#183975 = CARTESIAN_POINT ( 'NONE',  ( -6.687054376293257718, 6.125853549498580186, -61.90253133708612410 ) ) ;
#183978 = CARTESIAN_POINT ( 'NONE',  ( 0.05219959533910956823, 16.53943276465976808, 74.99890960531435269 ) ) ;
#183977 = CARTESIAN_POINT ( 'NONE',  ( 4.379528057220092307, 16.55341960407617563, 62.29275706135236845 ) ) ;
#183979 = CARTESIAN_POINT ( 'NONE',  ( -27.39399371936811534, -5.109217719441272010, 166.7881433183803210 ) ) ;
#183980 = CARTESIAN_POINT ( 'NONE',  ( -16.51473224551082808, 9.474510206698731452, 103.3344237280190043 ) ) ;
#183981 = EDGE_CURVE ( 'NONE', #60353, #25387, #57185, .T. ) ;
#183982 = CARTESIAN_POINT ( 'NONE',  ( -15.72974639402197994, 15.80617190586746368, 30.62390960531436335 ) ) ;
#183983 = DIRECTION ( 'NONE',  ( 0.000000000000000000, 0.000000000000000000, 1.000000000000000000 ) ) ;
#183984 = CARTESIAN_POINT ( 'NONE',  ( -14.29746914071037622, -8.314922557961029526, 44.16775706135234714 ) ) ;
#183985 = CARTESIAN_POINT ( 'NONE',  ( 10.81492255796078972, 18.62759615963270932, 114.5822429386477097 ) ) ;
#183986 = CARTESIAN_POINT ( 'NONE',  ( 21.55341960407610458, 5.719274019375980345, 28.95724293864769905 ) ) ;
#183987 = CARTESIAN_POINT ( 'NONE',  ( -4.483927247898782831, 16.52544592524335698, 72.70942372801901854 ) ) ;
#183988 = CARTESIAN_POINT ( 'NONE',  ( 5.049401038298161559, -19.05341960407611168, 87.70724293864769550 ) ) ;
#183990 = CARTESIAN_POINT ( 'NONE',  ( -16.52544592524335698, -4.483927247898792601, 18.95942372801901143 ) ) ;
#183989 = CARTESIAN_POINT ( 'NONE',  ( -5.719274019375665041, -21.55341960407619695, 44.79275706135234714 ) ) ;
#183991 = CARTESIAN_POINT ( 'NONE',  ( -5.823673210054116645, -21.52544592524344225, 32.29057627198102409 ) ) ;
#183992 = ORIENTED_EDGE ( 'NONE', *, *, #35192, .T. ) ;
#183993 = CARTESIAN_POINT ( 'NONE',  ( -13.97604488694547697, 13.89961937509957934, 23.12609039468565442 ) ) ;
#183994 =( BOUNDED_SURFACE ( )  B_SPLINE_SURFACE ( 3, 2, ( 
 ( #139749, #158901, #187290, #174098, #141747, #80078, #173101, #34578, #109423, #82039, #95246, #1236, #190254, #96235, #3237, #157923, #93249, #20392, #156931, #79080, #143736, #5215, #51731, #64911, #31600, #4219, #110415, #170106, #65897, #154935, #127571, #124595, #47770, #171102, #189272, #50748, #32595, #94247, #155928, #17423, #33583, #2241, #63924, #69908, #40573, #71902, #192257, #115413, #129550, #10243, #179104, #161911, #159910, #102243, #68900, #55733, #85053, #23405, #54732, #178093, #52725, #25428, #38573, #83057, #133574, #39563, #146734, #116404, #36552, #163931, #100229, #22405, #117407, #87069, #195264, #8230, #175084, #101221, #130559, #148754, #131574, #113394, #162910, #98206, #21399, #144731, #70910, #24418, #6218, #86067, #147757, #67897, #53739, #160912, #193258, #9243, #191250, #114390, #176092, #132578, #84056, #177102, #194266, #37562, #99225, #145734, #7215, #197255, #88059, #182080, #121380, #151736, #119416, #72922, #150753, #60693, #76863, #183072, #41580, #181100, #44555, #137545, #11248, #199228, #168866, #106210, #149746, #167894, #27416, #103244, #28417, #138533, #15204, #196277, #122369, #92015, #90054, #43563, #134591, #164926, #184058, #30371, #89062, #13229, #42574, #59707, #153708, #58717, #107195, #12251, #29394, #91024, #57746, #152710, #56748, #73913, #74892, #14201, #120386, #45541, #104237, #136555, #105228, #118419, #165920, #198236, #180112, #75869, #26419, #135583, #166916, #158672, #157694, #155697, #3009, #34349, #93019, #64686, #96990, #94016, #18196, #96010, #2014, #3989, #62679, #156702, #187064, #81807, #124360, #171866, #50518, #19185, #65669, #186055, #47539, #20162, #80834, #11, #78846, #63693, #16200, #61685, #127331, #48534, #46535, #189043, #17192, #142511, #33355, #110188, #141522, #126348, #139522, #112181, #125368, #169876, #123354, #188045, #95014, #49515, #185047, #173869, #79853, #109193, #35337, #108194, #31369, #111178, #154707, #172868, #140524, #77855, #1005, #170872, #32363, #143494, #55494, #4979, #100986, #54496, #102002, #146489, #7980, #128328, #98981, #191013, #99986, #161671, #70672, #147515, #85827, #69664, #114149, #83814, #23167, #116168, #115168, #113161, #130310, #145494, #174851, #68654, #131331, #38330, #5980, #159663, #37323, #9005, #163684, #193019, #190027, #67660, #177858, #24176, #97971, #132339, #117164, #39327, #36317, #162670, #175850, #51501, #176861, #25187, #66665, #82815, #194031, #178860, #84810, #192005, #21160, #144497, #40326, #129317, #160671, #52489, #22163, #6974, #53491, #88825, #137314, #136327, #150518, #12016, #73677, #135349, #124876, #28182, #43326, #133332, #197023, #148515, #121145, #71665, #57510, #72675, #198002, #186575, #11003, #118177, #119179, #182839, #167665, #59472, #13969, #58489, #44321, #179868, #56499, #120156, #180864, #166681, #75636, #89824, #104993, #196034, #152482, #42340, #104001, #105980, #29161, #90798, #198995, #63196, #151505, #26179, #181846, #48048, #12997, #109704, #171386, #86829, #165679, #10005, #195023, #27178, #41338, #102999, #164685, #134352, #87820, #149506, #74660, #79362, #3507, #110689, #144010, #66176, #36825, #175357, #187567, #18699, #17705, #141033, #81325, #67174, #98491, #174369, #52994, #19683, #112677, #128831, #4486, #143008, #2520, #127838, #173378, #64200, #94523, #51016, #82320, #157205, #189544, #125867, #35839, #97485, #65183, #159171, #160184, #5491, #20666, #113663, #80346, #172369, #156205, #142018, #190530, #52004, #188548, #129818, #95519, #126842, #49034, #68166, #21674, #83328, #145005, #6486, #191517, #32873, #114672, #33859, #50026, #111691, #34848, #96503, #158193, #72178, #56004, #7487, #194533, #162182, #99501, #39831, #41851, #118689, #192529, #25696, #57016, #101497, #116677, #69171, #22678, #87341, #195542, #23680, #163186, #177374, #9515, #180381, #70182, #133852, #85328, #71181, #117682, #130838, #132845 ),
 ( #179379, #149027, #115686, #38846, #176368, #102514, #37841, #193533, #55007, #54012, #161182, #84325, #86339, #100503, #146004, #40841, #147020, #8504, #131850, #178367, #24690, #164198, #148026, #10515, #64130, #169309, #15644, #171314, #16637, #125795, #173304, #48963, #2448, #155144, #111619, #78284, #139957, #157133, #3436, #65112, #188474, #49955, #110617, #185487, #32801, #95448, #172299, #18628, #141946, #81255, #1447, #34779, #45977, #124804, #92464, #154152, #80275, #170314, #77303, #138972, #63125, #450, #186502, #123788, #126770, #79292, #96435, #158122, #62125, #31807, #30815, #46977, #94453, #19613, #142937, #187497, #66104, #156133, #33788, #4418, #17632, #140961, #108636, #127770, #47978, #93457, #107631, #109631, #143938, #131778, #101424, #53940, #82247, #38776, #160112, #174299, #161110, #71109, #147957, #128761, #193460, #24619, #22606, #176294, #5419, #97414, #54937, #163116, #21600, #84252, #175287, #192457, #86267, #191445, #39761, #144933, #115615, #23610, #67102, #177304, #9444, #83258, #7415, #85256, #52921, #116609, #51933, #145933, #37766, #189470, #113593, #69098, #50948, #146948, #178297, #36752, #98416, #112607, #8437, #35768, #68096, #114597, #190460, #159101, #20595, #99428, #6415, #129748, #130765, #100432, #162113, #70109, #74111, #197452, #72104, #73123, #180310, #120586, #56946, #58918, #42776, #135781, #55933, #59907, #119615, #41778, #75083, #183270, #91216, #104438, #194462, #182280, #88258, #121575, #57944, #44750, #43761, #132775, #106406, #117608, #90247, #105425, #152907, #167108, #28609, #179308, #149945, #103444, #89263, #150955, #168088, #136750, #198434, #151930, #165123, #134792, #12449, #13419, #166122, #102441, #181298, #196473, #164128, #27624, #29585, #14404, #195470, #148955, #26615, #40772, #25626, #87271, #10444, #118620, #133777, #11451, #199428, #45742, #1206, #46739, #155895, #3208, #79049, #32562, #185248, #141718, #108400, #170077, #187262, #33554, #95216, #18398, #80049, #140723, #15405, #62883, #125565, #2213, #48731, #172067, #111382, #31568, #64882, #76068, #154904, #122570, #184260, #110385, #214, #107394, #169067, #93219, #30573, #16403, #153910, #156902, #109392, #126543, #188242, #92224, #61883, #60894, #77062, #124564, #49717, #173070, #17393, #96206, #186261, #63894, #34547, #47739, #171072, #138734, #94216, #78049, #123553, #137744, #157895, #139718, #143702, #67866, #65867, #22373, #37531, #51701, #99194, #161880, #68868, #6186, #100198, #5184, #158871, #81033, #66865, #160882, #176064, #175056, #116372, #82008, #128528, #174069, #54699, #129521, #84024, #114359, #191221, #177071, #19384, #52695, #130527, #53706, #178060, #8197, #39528, #85019, #69872, #192224, #115383, #21368, #83026, #144700, #145702, #101188, #7184, #38542, #127539, #23374, #142709, #146700, #4188, #190222, #113364, #131541, #189241, #36520, #50719, #98175, #193225, #112377, #35538, #97185, #159877, #20360, #198202, #87036, #194233, #133537, #197222, #43529, #12217, #164891, #26385, #181065, #86036, #132544, #88024, #195229, #42540, #90020, #165884, #119382, #71869, #28382, #56710, #118383, #73880, #120351, #182046, #105194, #166881, #27381, #102209, #149712, #135550, #89027, #58684, #151703, #59672, #180077, #13196, #162877, #41546, #9210, #70877, #74859, #148721, #55699, #117372, #103209, #179069, #11211, #40538, #136521, #196243, #121344, #183037, #163898, #10209, #147723, #25394, #72886, #44520, #24385, #104203, #134555, #57712, #150718, #140491, #77819, #154669, #14165, #970, #46496, #75833, #167859, #124323, #155663, #30337, #16165, #152676, #109159, #186021, #138499, #47503, #48500, #17159, #92984, #187029, #91978, #45506, #29359, #153672, #170838, #62646, #61650, #2971, #168832, #15169, #60659, #141488, #139488, #32330, #93983, #78812, #63659, #106176, #1979, #125332, #110154, #64651, #94981, #126313, #171832, #156666, #33320, #18161 ),
 ( #137511, #79817, #199192, #188010, #123318, #90989, #122332, #184024, #107161, #76828, #200181, #108157, #185011, #169839, #31333, #175812, #159626, #190975, #172833, #176820, #36278, #158634, #191966, #99946, #7942, #21121, #111143, #52452, #4941, #38292, #174813, #161632, #98942, #49480, #23126, #34312, #6936, #160633, #69625, #114109, #37285, #95975, #66625, #96954, #5943, #67619, #84771, #53452, #115127, #22124, #20125, #189987, #129280, #83774, #82777, #19148, #97933, #51461, #80798, #144458, #145454, #68615, #112141, #65633, #143456, #146449, #131291, #130271, #157659, #173833, #142476, #3954, #127293, #189006, #50481, #35298, #81769, #128289, #113123, #177817, #167382, #77335, #154185, #132298, #138019, #30849, #28879, #182553, #147473, #100944, #199702, #169340, #163642, #90519, #178817, #198712, #92496, #194980, #46008, #148471, #60179, #29854, #85787, #121848, #15675, #86786, #13685, #91491, #59184, #61168, #55452, #152201, #44035, #192979, #117123, #75352, #107663, #153178, #122839, #40287, #101961, #54458, #14681, #116128, #71624, #120853, #8963, #39287, #184528, #70631, #9964, #162628, #25144, #193990, #106685, #137022, #24135, #133290, #105696, #183541, #45026, #168358, #76343, #173335, #142967, #80305, #159129, #125825, #189499, #174328, #34808, #19642, #93489, #81284, #50975, #3466, #31838, #188506, #109663, #123819, #110648, #20627, #97444, #78314, #4445, #35797, #172329, #187528, #155175, #47009, #66133, #112635, #171343, #33818, #124834, #141978, #139002, #140991, #481, #94482, #65143, #96463, #16666, #126800, #62155, #32831, #157165, #158151, #2479, #127798, #1476, #95478, #48993, #185517, #63155, #18659, #108668, #170346, #139987, #186534, #48007, #156163, #17661, #79321, #64160, #49985, #111649, #179338, #147986, #130794, #128790, #9475, #37795, #24648, #53969, #192487, #23636, #146976, #21631, #22635, #129776, #70138, #6443, #8464, #115643, #85285, #5449, #71139, #69128, #191472, #86297, #132804, #40801, #177332, #143969, #131809, #99458, #194491, #7443, #55963, #193488, #82276, #117640, #67132, #39789, #54966, #102471, #116637, #178326, #190491, #161138, #52951, #38804, #100460, #164158, #51962, #113622, #114626, #176326, #101454, #163145, #175316, #36783, #98448, #160142, #83287, #162140, #144961, #68124, #84281, #145962, #60923, #196502, #14432, #25656, #104467, #72134, #133809, #198465, #149976, #56974, #118648, #42805, #195500, #57972, #103475, #136779, #58947, #29611, #168115, #180339, #11481, #10473, #41807, #74138, #59936, #91243, #167139, #45768, #12477, #120615, #183299, #165153, #119644, #26644, #182311, #166151, #88287, #87301, #43790, #75111, #73152, #135810, #134823, #28638, #105454, #181326, #90275, #152933, #121603, #197480, #106433, #27653, #89292, #148984, #150984, #151959, #13447, #44780, #122597, #76095, #137770, #199455, #184286, #107420, #110409, #63919, #155922, #126567, #169093, #17417, #80073, #3232, #4213, #157918, #127566, #34573, #19408, #141742, #18423, #171097, #32589, #94242, #79075, #65891, #172091, #125588, #15432, #140748, #30600, #64906, #153937, #139742, #154929, #188266, #189267, #93244, #241, #1231, #49741, #111410, #173095, #2236, #187285, #48756, #92253, #138759, #33578, #62910, #95240, #96230, #156926, #81057, #78074, #142734, #50742, #77090, #61908, #31595, #123579, #185274, #46766, #16427, #108425, #170101, #124590, #186285, #47765, #109418, #70903, #69900, #132570, #191244, #114382, #128551, #9236, #178086, #160906, #158896, #39555, #67891, #54724, #84049, #22399, #53732, #177095, #51725, #52718, #159904, #100223, #36544, #38567, #145728, #115407, #35562, #101213, #99218, #21392, #116397, #162902, #194259, #7209, #174093, #161904, #129544, #24411, #37556, #86060, #23398, #112401, #147749, #97210, #131567, #85045, #20386, #146726, #8223, #82033, #176086, #83051, #68893, #130553, #143730, #5209, #66890, #193251, #144725 ),
 ( #6211, #190248, #113388, #98200, #175078, #192250, #151729, #136547, #10235, #198228, #167887, #120379, #148747, #105221, #26412, #40566, #27409, #137538, #14192, #195256, #59700, #91017, #89055, #42567, #71895, #163924, #121372, #29386, #88051, #150745, #41573, #58709, #152703, #57739, #106203, #11240, #182072, #90047, #133566, #43555, #75862, #149739, #181092, #166909, #12244, #118412, #56741, #72914, #183065, #55726, #180105, #117398, #179097, #13222, #44548, #103236, #102236, #25420, #28408, #164918, #74885, #134584, #87062, #73906, #196270, #119409, #104230, #165911, #135576, #197248, #186047, #153700, #107187, #141514, #172859, #169867, #170864, #185039, #2006, #96001, #997, #49506, #154697, #63685, #33347, #92006, #125359, #157685, #93011, #17184, #95006, #62671, #3000, #61677, #155689, #47530, #80824, #123346, #32355, #111169, #156694, #64677, #46526, #108186, #19176, #18188, #199220, #77847, #124352, #15195, #60686, #126339, #109185, #45533, #188036, #16192, #34340, #94008, #78838, #140516, #187056, #138525, #139514, #31361, #48526, #110180, #171859, #79845, #122361, #184050, #168858, #30363, #76854, #3, #193010, #100977, #114139, #3980, #83805, #97962, #69654, #67651, #131321, #191995, #142502, #54487, #65660, #99977, #53481, #162661, #145485, #6965, #127322, #159654, #190017, #98972, #160663, #116159, #146480, #84801, #68645, #113152, #82806, #22154, #115159, #175840, #112172, #129308, #144488, #173860, #130301, #176852, #51491, #7971, #174842, #36307, #38322, #161661, #23158, #177849, #39317, #24167, #81797, #191004, #189034, #50508, #35327, #96980, #158661, #21151, #20152, #143484, #5971, #4969, #66655, #128317, #52480, #37314, #178850, #102988, #132330, #56489, #163674, #197013, #119169, #89814, #28172, #40316, #71655, #70663, #194021, #134341, #120145, #151495, #27168, #105970, #72665, #180853, #43316, #101993, #118167, #55484, #42329, #26169, #117154, #147505, #103990, #135339, #9995, #196025, #25176, #88815, #165669, #179858, #150508, #12987, #58478, #57500, #166670, #133322, #86818, #8995, #195012, #12006, #73667, #41328, #182829, #148505, #164674, #87810, #121135, #181836, #104983, #74650, #136316, #197991, #85818, #59462, #44311, #167655, #149496, #10993, #187807, #94771, #79606, #140277, #78603, #31128, #92777, #154466, #15958, #64441, #170632, #185809, #75625, #77618, #90788, #63447, #13958, #199981, #14962, #1769, #126112, #153465, #60453, #61447, #125123, #109946, #186820, #139288, #765, #47295, #152472, #198985, #62436, #123118, #108952, #156454, #124109, #32121, #93778, #155459, #48290, #29151, #16949, #171627, #33115, #49276, #17953, #110934, #141276, #2765, #137304, #122127, #183815, #45305, #106956, #168629, #30129, #91771, #76622, #138300, #184803, #46289, #107946, #169632, #143249, #158434, #21920, #7730, #96744, #3748, #4733, #6731, #53244, #83571, #174613, #36078, #190771, #95765, #142265, #97727, #66422, #52246, #99744, #175601, #129070, #81563, #38089, #128083, #189787, #145250, #130062, #191761, #114921, #176614, #37078, #111935, #159417, #68409, #98737, #161428, #22920, #69416, #51258, #84566, #172621, #112918, #18945, #80590, #146244, #19921, #65425, #127086, #20913, #188795, #82571, #50277, #131082, #5738, #192771, #54255, #173622, #144252, #157451, #35091, #67415, #34108, #113903, #160430, #136085, #102757, #149268, #73435, #8754, #86582, #23923, #10760, #56250, #85578, #177616, #134102, #165439, #40073, #164444, #162421, #118938, #195792, #148265, #57264, #58250, #26934, #25938, #196782, #101751, #55249, #39084, #163439, #180623, #72424, #71422, #12754, #178610, #24936, #70425, #151264, #132091, #74419, #87581, #42095, #103760, #88576, #135106, #115926, #150274, #11770, #119918, #197759, #104749, #100740, #181604, #166440, #43082, #27935, #117932, #179621, #41093, #89578, #147264, #193780, #116917, #9758, #133086, #194776, #93536, #44079, #29896 ),
 ( #185561, #169385, #527, #182595, #186580, #46051, #168401, #1523, #109709, #17711, #30893, #120895, #62199, #14726, #48053, #184570, #171392, #108712, #59226, #32879, #105738, #16710, #170391, #79368, #123863, #47055, #167425, #76386, #106727, #15719, #77379, #94529, #63201, #124881, #31882, #91534, #199744, #139047, #155221, #92540, #28921, #107706, #61210, #90561, #154229, #78360, #140034, #121891, #75394, #153221, #156211, #141039, #183584, #152243, #13728, #137066, #198756, #60221, #45069, #138063, #122882, #95526, #54755, #176114, #187573, #177125, #87092, #163954, #142025, #147780, #40595, #38596, #192279, #157212, #110696, #9266, #179127, #37585, #100252, #188555, #8252, #102266, #7237, #55755, #160934, #80353, #116429, #161933, #70932, #132599, #18706, #50033, #49041, #172376, #53760, #39585, #194289, #146758, #25452, #115434, #23428, #162933, #3514, #99247, #33866, #85075, #145755, #65190, #64206, #69932, #178117, #126849, #131596, #114413, #193281, #101244, #22426, #24440, #117429, #86089, #2526, #125873, #84076, #68922, #130584, #196297, #90075, #105251, #104259, #45566, #11270, #57767, #103267, #184082, #135605, #151758, #43585, #197276, #106233, #148777, #58739, #59733, #183096, #107219, #137569, #168890, #14224, #199252, #121402, #198257, #150776, #12271, #73936, #120408, #30395, #13251, #166937, #195287, #182100, #10266, #44577, #133595, #119437, #134613, #167916, #71925, #72943, #180133, #181122, #29416, #91047, #152734, #28440, #74914, #136577, #56768, #118440, #75894, #42596, #60719, #122393, #41602, #164947, #165942, #26440, #27442, #89084, #88082, #149768, #49541, #34374, #96034, #156728, #31393, #78868, #141546, #95037, #3035, #188070, #127358, #62702, #80860, #92042, #170894, #138557, #35, #64711, #16226, #123378, #185070, #109215, #61708, #124385, #189071, #154730, #139545, #46558, #50543, #140548, #33379, #187088, #2036, #111203, #153731, #63716, #126373, #172895, #112204, #142536, #173894, #157721, #4015, #19210, #65693, #94041, #155719, #17216, #125391, #15227, #18221, #48558, #108220, #110211, #76886, #169900, #93043, #186080, #77878, #1030, #47562, #32386, #171892, #79877, #100012, #174877, #175877, #82843, #23195, #159689, #161698, #145519, #176886, #158696, #162697, #22189, #144522, #177885, #85852, #194059, #6999, #97015, #38357, #191040, #24203, #160698, #147541, #84838, #35363, #9029, #20185, #193046, #146517, #55520, #8007, #69690, #81831, #52513, #6007, #192034, #53516, #70698, #39354, #101013, #131357, #67687, #37349, #115194, #54523, #68681, #5007, #83837, #99007, #66690, #130336, #116196, #132366, #97996, #51525, #129345, #117193, #143518, #21187, #128352, #190050, #113188, #36343, #114174, #121170, #90821, #43349, #71691, #28207, #149532, #163711, #150540, #60486, #137337, #118205, #182864, #13993, #12040, #165705, #133358, #86856, #44345, #152504, #11027, #73704, #164710, #181870, #120180, #134375, #106003, #104026, #167690, #89848, #178886, #75660, #40354, #136351, #151531, #199017, #105020, #166704, #25214, #196061, #26205, #135376, #197046, #29187, #102029, #148540, #13020, #72702, #119203, #58514, #74685, #198027, #10031, #27202, #180888, #195048, #88848, #59495, #56527, #41362, #179896, #57534, #103028, #87844, #42363, #172654, #157487, #17989, #2800, #76656, #64478, #34142, #186857, #14996, #171661, #92813, #106990, #93813, #3783, #80626, #61482, #126145, #18980, #155493, #108987, #138335, #30163, #187841, #95801, #154500, #16985, #107980, #125158, #142303, #124146, #122161, #77653, #48326, #156487, #200015, #109981, #183850, #15995, #140314, #79642, #185845, #49310, #184841, #78639, #170668, #45338, #46326, #1804, #168663, #141311, #110970, #169668, #31163, #91807, #153499, #123153, #801, #47332, #139321, #62474, #32156, #63482, #33150, #94808, #128118, #81599, #98770, #67449, #37111, #160464, #143283, #159451, #189821, #21955, #4769, #83605 ),
 ( #174647, #51293, #52280, #113938, #38126, #176650, #114957, #145284, #112954, #20947, #175637, #6767, #129107, #173661, #144285, #82604, #35128, #5774, #68446, #130100, #66456, #158469, #36112, #99780, #69452, #97764, #161465, #146282, #191797, #53278, #19957, #22955, #84603, #7769, #96780, #131119, #190806, #188829, #65460, #127123, #50313, #111969, #111675, #78341, #187552, #124861, #18683, #62180, #77361, #199726, #185542, #79347, #94508, #93516, #34832, #508, #47036, #92521, #173362, #186560, #141018, #32858, #48032, #95503, #138045, #109689, #49019, #172354, #96487, #126826, #158177, #3490, #188532, #110674, #33843, #140015, #1503, #63181, #171370, #19667, #2505, #156190, #184552, #17689, #61192, #157189, #122864, #108693, #123844, #169366, #64185, #80330, #46033, #170371, #142002, #65167, #50010, #125851, #107688, #30875, #154211, #15700, #139029, #31863, #155202, #16691, #84308, #37824, #190514, #147002, #51988, #175341, #192511, #38828, #100486, #23662, #85311, #145987, #20650, #68150, #130820, #7470, #53995, #177358, #116660, #113647, #21658, #115669, #129801, #162165, #5475, #82304, #142992, #128815, #22661, #99484, #36808, #178351, #143994, #98475, #35823, #39814, #191500, #69154, #176351, #52976, #8488, #81308, #114654, #70164, #131833, #101480, #193515, #163169, #54991, #4470, #66160, #127822, #83311, #144988, #6469, #161165, #189528, #51000, #112661, #174352, #97469, #159154, #67158, #160168, #195525, #10498, #55989, #134849, #167165, #86323, #56998, #58971, #105478, #74163, #26672, #88313, #42829, #148010, #194515, #150001, #118673, #104494, #151984, #27677, #181350, #133834, #90299, #180364, #41832, #135835, #182337, #43815, #28664, #13472, #89317, #164182, #11507, #197504, #151010, #120639, #75135, #59962, #103500, #136805, #24673, #165177, #71164, #132829, #198489, #149010, #117666, #179362, #73178, #40825, #196527, #102497, #121628, #57998, #183324, #44805, #25680, #72159, #9500, #87325, #119668, #106460, #166176, #12501, #191023, #154955, #1257, #125611, #60948, #138786, #76120, #62934, #108449, #137798, #29635, #186309, #17442, #92278, #16451, #14457, #171124, #47790, #109441, #144506, #79098, #124614, #174860, #110435, #122623, #153962, #152959, #199482, #78100, #2260, #36326, #32613, #52498, #139769, #94267, #187310, #184313, #267, #45794, #155946, #170125, #107446, #91268, #140771, #63943, #15460, #48781, #169120, #97980, #159673, #21169, #5990, #31620, #82825, #67670, #129328, #77116, #30625, #61935, #123604, #168139, #185299, #46790, #93270, #176869, #161679, #68663, #149512, #100994, #55503, #9013, #162679, #71672, #114158, #24185, #25194, #148522, #11009, #103006, #72683, #179876, #164691, #86836, #163692, #116176, #177866, #39335, #85835, #134358, #117173, #70681, #160680, #147525, #175860, #10012, #98991, #84819, #99994, #145502, #132347, #56507, #37332, #146498, #133339, #195030, #118185, #194039, #178868, #40335, #22172, #83822, #102010, #7989, #41344, #26186, #87826, #196042, #23175, #6983, #69672, #131339, #130318, #192015, #53499, #115176, #38338, #193027, #54504, #44327, #106970, #60467, #168644, #153480, #92791, #28189, #46304, #57517, #136333, #104008, #165686, #30143, #181853, #88831, #150524, #74666, #27184, #89831, #135357, #199995, #31143, #151511, #29168, #43332, #122142, #154479, #59477, #107960, #13003, #183830, #91786, #12023, #45320, #15972, #198007, #75641, #14976, #121151, #61462, #120162, #13974, #105986, #139301, #105000, #90804, #169647, #76636, #123133, #166687, #182844, #77632, #138314, #119185, #167670, #152487, #73685, #180870, #184819, #137319, #197029, #199000, #42346, #58496, #3761, #110947, #142280, #65438, #140292, #141289, #48303, #188808, #125137, #127099, #172632, #50291, #124124, #128096, #187820, #109960, #143262, #51272, #159430, #34120, #62450, #111948, #156466, #189800, #126125, #112932, #173637, #779, #174626, #185823, #158447 ),
 ( #171639, #2779, #157465, #35106, #95779, #170646, #49289, #64455, #32134, #18958, #96757, #80603, #63461, #16964, #94785, #4746, #20926, #186835, #36091, #97742, #19935, #81577, #155472, #66435, #82584, #47310, #93792, #108965, #33129, #78617, #1783, #17966, #79621, #162436, #71437, #68424, #132103, #131097, #98750, #52259, #113917, #5752, #23937, #193794, #130076, #192785, #190785, #147278, #85591, #8768, #117946, #84580, #55262, #54268, #24950, #191775, #83584, #67428, #53257, #70437, #100754, #99758, #41106, #6745, #114935, #160443, #179636, #115940, #116931, #39098, #177630, #101765, #144265, #178624, #40087, #163452, #102770, #133101, #164457, #9773, #194790, #86597, #148280, #146260, #7744, #69430, #56263, #25951, #129085, #175615, #37091, #21933, #145263, #176628, #38103, #161442, #22934, #118951, #197775, #29911, #149280, #58264, #121907, #168416, #137082, #89592, #151279, #105752, #10775, #57277, #12768, #119933, #167438, #14741, #90576, #44094, #196796, #153238, #181618, #43097, #198770, #45084, #106741, #91551, #76402, #152257, #26950, #74432, #60236, #13742, #183600, #138078, #122897, #104766, #199759, #87594, #166454, #134116, #195805, #61226, #11785, #180637, #42112, #27951, #103774, #136099, #165453, #184586, #120910, #46067, #107721, #88592, #73449, #72440, #150290, #59241, #169402, #135122, #28935, #182609, #75410, #64224, #188571, #123881, #1542, #139064, #125889, #171409, #142041, #65205, #66198, #19704, #189565, #96524, #81346, #3529, #80368, #32895, #94547, #156228, #17729, #127861, #172395, #187589, #77394, #79387, #92556, #126864, #15735, #63218, #16728, #62213, #141056, #173399, #154244, #124898, #50051, #111713, #34870, #2542, #49058, #110713, #542, #185579, #33884, #186597, #95541, #158214, #157229, #18721, #140052, #143030, #48069, #109725, #4508, #51037, #112699, #30908, #47070, #108730, #170407, #31899, #93552, #155238, #78376, #70203, #9535, #145027, #163207, #174391, #53016, #20688, #82343, #147041, #98513, #5514, #67194, #191539, #144032, #6508, #52025, #85348, #7508, #178387, #116697, #128852, #160207, #159193, #190552, #22700, #8525, #39851, #115707, #194554, #161205, #69192, #131870, #113683, #68188, #175378, #130859, #114696, #36847, #35861, #192550, #23700, #21697, #84347, #83351, #177395, #54033, #38867, #148045, #176390, #193555, #146025, #55027, #129840, #37864, #97507, #99523, #100523, #162202, #101517, #71202, #24711, #86360, #132865, #56024, #104529, #59007, #12534, #166210, #75171, #117702, #27711, #41872, #168175, #152994, #13506, #198528, #72199, #59998, #29671, #182373, #10535, #167201, #88348, #102536, #89354, #199517, #76156, #135868, #44842, #103539, #105516, #151044, #133873, #25716, #121665, #91303, #150041, #74199, #165214, #120674, #14494, #119702, #137836, #73214, #43850, #152020, #195563, #28699, #179398, #11546, #197539, #136843, #181385, #183360, #180400, #90335, #106498, #40862, #26709, #164219, #87362, #149047, #57037, #134885, #196561, #118710, #58032, #42864, #139803, #126622, #125646, #95297, #45829, #31656, #46824, #92315, #171160, #3291, #122659, #93305, #156981, #141797, #110467, #62969, #124649, #79133, #184347, #30662, #186345, #154990, #140805, #188323, #63976, #17476, #170163, #49802, #16486, #78135, #172149, #18479, #80128, #64963, #111467, #187344, #303, #47825, #33635, #48814, #173152, #34627, #96286, #1291, #157972, #60984, #109476, #107480, #169158, #19465, #185334, #154000, #15496, #32646, #77152, #94301, #138823, #81110, #155979, #142790, #61971, #123637, #108484, #2295, #50798, #52771, #38622, #8280, #145781, #24466, #174147, #191295, #144783, #35619, #129599, #68947, #99273, #66949, #20442, #98257, #69958, #86116, #128611, #54782, #39611, #100279, #85101, #158952, #146787, #116457, #130610, #97264, #53786, #175133, #189321, #176142, #4271, #162960, #22453, #131624, #190303, #192306, #114440, #82093 ) ),
 .UNSPECIFIED., .T., .F., .F. ) 
 B_SPLINE_SURFACE_WITH_KNOTS ( ( 4, 3, 4 ),
 ( 3, 2, 2, 2, 2, 2, 2, 2, 2, 2, 2, 2, 2, 2, 2, 2, 2, 2, 2, 2, 2, 2, 2, 2, 2, 2, 2, 2, 2, 2, 2, 2, 2, 2, 2, 2, 2, 2, 2, 2, 2, 2, 2, 2, 2, 2, 2, 2, 2, 2, 2, 2, 2, 2, 2, 2, 2, 2, 2, 2, 2, 2, 2, 2, 2, 2, 2, 2, 2, 2, 2, 2, 2, 2, 2, 2, 2, 2, 2, 2, 2, 2, 2, 2, 2, 2, 2, 2, 2, 2, 2, 2, 2, 2, 2, 2, 2, 2, 2, 2, 2, 2, 2, 2, 2, 2, 2, 2, 2, 2, 2, 2, 2, 2, 2, 2, 2, 2, 2, 2, 2, 2, 2, 2, 2, 2, 2, 2, 2, 2, 2, 2, 2, 2, 2, 2, 2, 2, 2, 2, 2, 2, 2, 2, 2, 2, 2, 2, 2, 2, 2, 2, 2, 2, 2, 2, 2, 2, 2, 2, 2, 2, 2, 2, 2, 2, 2, 2, 2, 2, 2, 2, 2, 2, 2, 2, 2, 2, 2, 2, 2, 2, 2, 2, 2, 2, 2, 2, 2, 2, 2, 2, 2, 2, 2, 2, 2, 2, 2, 2, 2, 2, 2, 2, 2, 2, 2, 2, 2, 2, 2, 2, 2, 2, 2, 2, 2, 2, 2, 2, 2, 2, 2, 2, 2, 2, 2, 2, 3 ),
 ( 0.000000000000000000, 0.5000000000000000000, 1.000000000000000000 ),
 ( 0.000000000000000000, 0.004385964912280701511, 0.008771929824561403022, 0.01315789473684210453, 0.01754385964912280604, 0.02192982456140350755, 0.02631578947368420907, 0.03070175438596491058, 0.03508771929824561209, 0.03947368421052631360, 0.04385964912280701511, 0.04824561403508771662, 0.05263157894736841813, 0.05701754385964911964, 0.06140350877192982115, 0.06578947368421052266, 0.07017543859649122417, 0.07456140350877192569, 0.07894736842105262720, 0.08333333333333332871, 0.08771929824561403022, 0.09210526315789473173, 0.09649122807017543324, 0.1008771929824561348, 0.1052631578947368363, 0.1096491228070175378, 0.1140350877192982393, 0.1184210526315789408, 0.1228070175438596423, 0.1271929824561403577, 0.1315789473684210453, 0.1359649122807017607, 0.1403508771929824483, 0.1447368421052631637, 0.1491228070175438514, 0.1535087719298245668, 0.1578947368421052544, 0.1622807017543859698, 0.1666666666666666574, 0.1710526315789473728, 0.1754385964912280604, 0.1798245614035087758, 0.1842105263157894635, 0.1885964912280701788, 0.1929824561403508665, 0.1973684210526315819, 0.2017543859649122695, 0.2061403508771929849, 0.2105263157894736725, 0.2149122807017543879, 0.2192982456140350755, 0.2236842105263157909, 0.2280701754385964786, 0.2324561403508771940, 0.2368421052631578816, 0.2412280701754385970, 0.2456140350877192846, 0.2500000000000000000, 0.2543859649122807154, 0.2587719298245614308, 0.2631578947368420907, 0.2675438596491228060, 0.2719298245614035214, 0.2763157894736842368, 0.2807017543859648967, 0.2850877192982456121, 0.2894736842105263275, 0.2938596491228070429, 0.2982456140350877027, 0.3026315789473684181, 0.3070175438596491335, 0.3114035087719298489, 0.3157894736842105088, 0.3201754385964912242, 0.3245614035087719396, 0.3289473684210526550, 0.3333333333333333148, 0.3377192982456140302, 0.3421052631578947456, 0.3464912280701754610, 0.3508771929824561209, 0.3552631578947368363, 0.3596491228070175517, 0.3640350877192982670, 0.3684210526315789269, 0.3728070175438596423, 0.3771929824561403577, 0.3815789473684210731, 0.3859649122807017330, 0.3903508771929824483, 0.3947368421052631637, 0.3991228070175438791, 0.4035087719298245390, 0.4078947368421052544, 0.4122807017543859698, 0.4166666666666666852, 0.4210526315789473450, 0.4254385964912280604, 0.4298245614035087758, 0.4342105263157894912, 0.4385964912280701511, 0.4429824561403508665, 0.4473684210526315819, 0.4517543859649122973, 0.4561403508771929571, 0.4605263157894736725, 0.4649122807017543879, 0.4692982456140351033, 0.4736842105263157632, 0.4780701754385964786, 0.4824561403508771940, 0.4868421052631579093, 0.4912280701754385692, 0.4956140350877192846, 0.5000000000000000000, 0.5043859649122807154, 0.5087719298245614308, 0.5131578947368421462, 0.5175438596491228616, 0.5219298245614034659, 0.5263157894736841813, 0.5307017543859648967, 0.5350877192982456121, 0.5394736842105263275, 0.5438596491228070429, 0.5482456140350877583, 0.5526315789473684736, 0.5570175438596490780, 0.5614035087719297934, 0.5657894736842105088, 0.5701754385964912242, 0.5745614035087719396, 0.5789473684210526550, 0.5833333333333333703, 0.5877192982456140857, 0.5921052631578946901, 0.5964912280701754055, 0.6008771929824561209, 0.6052631578947368363, 0.6096491228070175517, 0.6140350877192982670, 0.6184210526315789824, 0.6228070175438596978, 0.6271929824561403022, 0.6315789473684210176, 0.6359649122807017330, 0.6403508771929824483, 0.6447368421052631637, 0.6491228070175438791, 0.6535087719298245945, 0.6578947368421053099, 0.6622807017543859143, 0.6666666666666666297, 0.6710526315789473450, 0.6754385964912280604, 0.6798245614035087758, 0.6842105263157894912, 0.6885964912280702066, 0.6929824561403509220, 0.6973684210526315264, 0.7017543859649122417, 0.7061403508771929571, 0.7105263157894736725, 0.7149122807017543879, 0.7192982456140351033, 0.7236842105263158187, 0.7280701754385965341, 0.7324561403508771384, 0.7368421052631578538, 0.7412280701754385692, 0.7456140350877192846, 0.7500000000000000000, 0.7543859649122807154, 0.7587719298245614308, 0.7631578947368421462, 0.7675438596491228616, 0.7719298245614034659, 0.7763157894736841813, 0.7807017543859648967, 0.7850877192982456121, 0.7894736842105263275, 0.7938596491228070429, 0.7982456140350877583, 0.8026315789473684736, 0.8070175438596490780, 0.8114035087719297934, 0.8157894736842105088, 0.8201754385964912242, 0.8245614035087719396, 0.8289473684210526550, 0.8333333333333333703, 0.8377192982456140857, 0.8421052631578946901, 0.8464912280701754055, 0.8508771929824561209, 0.8552631578947368363, 0.8596491228070175517, 0.8640350877192982670, 0.8684210526315789824, 0.8728070175438596978, 0.8771929824561403022, 0.8815789473684210176, 0.8859649122807017330, 0.8903508771929824483, 0.8947368421052631637, 0.8991228070175438791, 0.9035087719298245945, 0.9078947368421053099, 0.9122807017543859143, 0.9166666666666666297, 0.9210526315789473450, 0.9254385964912280604, 0.9298245614035087758, 0.9342105263157894912, 0.9385964912280702066, 0.9429824561403509220, 0.9473684210526315264, 0.9517543859649122417, 0.9561403508771929571, 0.9605263157894736725, 0.9649122807017543879, 0.9692982456140351033, 0.9736842105263158187, 0.9780701754385965341, 0.9824561403508771384, 0.9868421052631578538, 0.9912280701754385692, 0.9956140350877192846, 1.000000000000000000 ),
 .UNSPECIFIED. ) 
 GEOMETRIC_REPRESENTATION_ITEM ( )  RATIONAL_B_SPLINE_SURFACE ( (
 ( 1.000000000000000000, 0.9659258262890683122, 1.000000000000000000, 0.9659258262890683122, 1.000000000000000000, 0.9659258262890683122, 1.000000000000000000, 0.9659258262890683122, 1.000000000000000000, 0.9659258262890683122, 1.000000000000000000, 0.9659258262890683122, 1.000000000000000000, 0.9659258262890683122, 1.000000000000000000, 0.9659258262890683122, 1.000000000000000000, 0.9659258262890683122, 1.000000000000000000, 0.9659258262890683122, 1.000000000000000000, 0.9659258262890683122, 1.000000000000000000, 0.9659258262890683122, 1.000000000000000000, 0.9659258262890683122, 1.000000000000000000, 0.9659258262890683122, 1.000000000000000000, 0.9659258262890683122, 1.000000000000000000, 0.9659258262890683122, 1.000000000000000000, 0.9659258262890683122, 1.000000000000000000, 0.9659258262890683122, 1.000000000000000000, 0.9659258262890683122, 1.000000000000000000, 0.9659258262890683122, 1.000000000000000000, 0.9659258262890683122, 1.000000000000000000, 0.9659258262890683122, 1.000000000000000000, 0.9659258262890683122, 1.000000000000000000, 0.9659258262890683122, 1.000000000000000000, 0.9659258262890683122, 1.000000000000000000, 0.9659258262890683122, 1.000000000000000000, 0.9659258262890683122, 1.000000000000000000, 0.9659258262890683122, 1.000000000000000000, 0.9659258262890683122, 1.000000000000000000, 0.9659258262890683122, 1.000000000000000000, 0.9659258262890683122, 1.000000000000000000, 0.9659258262890683122, 1.000000000000000000, 0.9659258262890683122, 1.000000000000000000, 0.9659258262890683122, 1.000000000000000000, 0.9659258262890683122, 1.000000000000000000, 0.9659258262890683122, 1.000000000000000000, 0.9659258262890683122, 1.000000000000000000, 0.9659258262890683122, 1.000000000000000000, 0.9659258262890683122, 1.000000000000000000, 0.9659258262890683122, 1.000000000000000000, 0.9659258262890683122, 1.000000000000000000, 0.9659258262890683122, 1.000000000000000000, 0.9659258262890683122, 1.000000000000000000, 0.9659258262890683122, 1.000000000000000000, 0.9659258262890683122, 1.000000000000000000, 0.9659258262890683122, 1.000000000000000000, 0.9659258262890683122, 1.000000000000000000, 0.9659258262890683122, 1.000000000000000000, 0.9659258262890683122, 1.000000000000000000, 0.9659258262890683122, 1.000000000000000000, 0.9659258262890683122, 1.000000000000000000, 0.9659258262890683122, 1.000000000000000000, 0.9659258262890683122, 1.000000000000000000, 0.9659258262890683122, 1.000000000000000000, 0.9659258262890683122, 1.000000000000000000, 0.9659258262890683122, 1.000000000000000000, 0.9659258262890683122, 1.000000000000000000, 0.9659258262890683122, 1.000000000000000000, 0.9659258262890683122, 1.000000000000000000, 0.9659258262890683122, 1.000000000000000000, 0.9659258262890683122, 1.000000000000000000, 0.9659258262890683122, 1.000000000000000000, 0.9659258262890683122, 1.000000000000000000, 0.9659258262890683122, 1.000000000000000000, 0.9659258262890683122, 1.000000000000000000, 0.9659258262890683122, 1.000000000000000000, 0.9659258262890683122, 1.000000000000000000, 0.9659258262890683122, 1.000000000000000000, 0.9659258262890683122, 1.000000000000000000, 0.9659258262890683122, 1.000000000000000000, 0.9659258262890683122, 1.000000000000000000, 0.9659258262890683122, 1.000000000000000000, 0.9659258262890683122, 1.000000000000000000, 0.9659258262890683122, 1.000000000000000000, 0.9659258262890683122, 1.000000000000000000, 0.9659258262890683122, 1.000000000000000000, 0.9659258262890683122, 1.000000000000000000, 0.9659258262890683122, 1.000000000000000000, 0.9659258262890683122, 1.000000000000000000, 0.9659258262890683122, 1.000000000000000000, 0.9659258262890683122, 1.000000000000000000, 0.9659258262890683122, 1.000000000000000000, 0.9659258262890683122, 1.000000000000000000, 0.9659258262890683122, 1.000000000000000000, 0.9659258262890683122, 1.000000000000000000, 0.9659258262890683122, 1.000000000000000000, 0.9659258262890683122, 1.000000000000000000, 0.9659258262890683122, 1.000000000000000000, 0.9659258262890683122, 1.000000000000000000, 0.9659258262890683122, 1.000000000000000000, 0.9659258262890683122, 1.000000000000000000, 0.9659258262890683122, 1.000000000000000000, 0.9659258262890683122, 1.000000000000000000, 0.9659258262890683122, 1.000000000000000000, 0.9659258262890683122, 1.000000000000000000, 0.9659258262890683122, 1.000000000000000000, 0.9659258262890683122, 1.000000000000000000, 0.9659258262890683122, 1.000000000000000000, 0.9659258262890683122, 1.000000000000000000, 0.9659258262890683122, 1.000000000000000000, 0.9659258262890683122, 1.000000000000000000, 0.9659258262890683122, 1.000000000000000000, 0.9659258262890683122, 1.000000000000000000, 0.9659258262890683122, 1.000000000000000000, 0.9659258262890683122, 1.000000000000000000, 0.9659258262890683122, 1.000000000000000000, 0.9659258262890683122, 1.000000000000000000, 0.9659258262890683122, 1.000000000000000000, 0.9659258262890683122, 1.000000000000000000, 0.9659258262890683122, 1.000000000000000000, 0.9659258262890683122, 1.000000000000000000, 0.9659258262890683122, 1.000000000000000000, 0.9659258262890683122, 1.000000000000000000, 0.9659258262890683122, 1.000000000000000000, 0.9659258262890683122, 1.000000000000000000, 0.9659258262890683122, 1.000000000000000000, 0.9659258262890683122, 1.000000000000000000, 0.9659258262890683122, 1.000000000000000000, 0.9659258262890683122, 1.000000000000000000, 0.9659258262890683122, 1.000000000000000000, 0.9659258262890683122, 1.000000000000000000, 0.9659258262890683122, 1.000000000000000000, 0.9659258262890683122, 1.000000000000000000, 0.9659258262890683122, 1.000000000000000000, 0.9659258262890683122, 1.000000000000000000, 0.9659258262890683122, 1.000000000000000000, 0.9659258262890683122, 1.000000000000000000, 0.9659258262890683122, 1.000000000000000000, 0.9659258262890683122, 1.000000000000000000, 0.9659258262890683122, 1.000000000000000000, 0.9659258262890683122, 1.000000000000000000, 0.9659258262890683122, 1.000000000000000000, 0.9659258262890683122, 1.000000000000000000, 0.9659258262890683122, 1.000000000000000000, 0.9659258262890683122, 1.000000000000000000, 0.9659258262890683122, 1.000000000000000000, 0.9659258262890683122, 1.000000000000000000, 0.9659258262890683122, 1.000000000000000000, 0.9659258262890683122, 1.000000000000000000, 0.9659258262890683122, 1.000000000000000000, 0.9659258262890683122, 1.000000000000000000, 0.9659258262890683122, 1.000000000000000000, 0.9659258262890683122, 1.000000000000000000, 0.9659258262890683122, 1.000000000000000000, 0.9659258262890683122, 1.000000000000000000, 0.9659258262890683122, 1.000000000000000000, 0.9659258262890683122, 1.000000000000000000, 0.9659258262890683122, 1.000000000000000000, 0.9659258262890683122, 1.000000000000000000, 0.9659258262890683122, 1.000000000000000000, 0.9659258262890683122, 1.000000000000000000, 0.9659258262890683122, 1.000000000000000000, 0.9659258262890683122, 1.000000000000000000, 0.9659258262890683122, 1.000000000000000000, 0.9659258262890683122, 1.000000000000000000, 0.9659258262890683122, 1.000000000000000000, 0.9659258262890683122, 1.000000000000000000, 0.9659258262890683122, 1.000000000000000000, 0.9659258262890683122, 1.000000000000000000, 0.9659258262890683122, 1.000000000000000000, 0.9659258262890683122, 1.000000000000000000, 0.9659258262890683122, 1.000000000000000000, 0.9659258262890683122, 1.000000000000000000, 0.9659258262890683122, 1.000000000000000000, 0.9659258262890683122, 1.000000000000000000, 0.9659258262890683122, 1.000000000000000000, 0.9659258262890683122, 1.000000000000000000, 0.9659258262890683122, 1.000000000000000000, 0.9659258262890683122, 1.000000000000000000, 0.9659258262890683122, 1.000000000000000000, 0.9659258262890683122, 1.000000000000000000, 0.9659258262890683122, 1.000000000000000000, 0.9659258262890683122, 1.000000000000000000, 0.9659258262890683122, 1.000000000000000000, 0.9659258262890683122, 1.000000000000000000, 0.9659258262890683122, 1.000000000000000000, 0.9659258262890683122, 1.000000000000000000, 0.9659258262890683122, 1.000000000000000000, 0.9659258262890683122, 1.000000000000000000, 0.9659258262890683122, 1.000000000000000000, 0.9659258262890683122, 1.000000000000000000, 0.9659258262890683122, 1.000000000000000000, 0.9659258262890683122, 1.000000000000000000, 0.9659258262890683122, 1.000000000000000000, 0.9659258262890683122, 1.000000000000000000, 0.9659258262890683122, 1.000000000000000000, 0.9659258262890683122, 1.000000000000000000, 0.9659258262890683122, 1.000000000000000000, 0.9659258262890683122, 1.000000000000000000, 0.9659258262890683122, 1.000000000000000000, 0.9659258262890683122, 1.000000000000000000, 0.9659258262890683122, 1.000000000000000000, 0.9659258262890683122, 1.000000000000000000, 0.9659258262890683122, 1.000000000000000000, 0.9659258262890683122, 1.000000000000000000, 0.9659258262890683122, 1.000000000000000000, 0.9659258262890683122, 1.000000000000000000, 0.9659258262890683122, 1.000000000000000000, 0.9659258262890683122, 1.000000000000000000, 0.9659258262890683122, 1.000000000000000000, 0.9659258262890683122, 1.000000000000000000, 0.9659258262890683122, 1.000000000000000000, 0.9659258262890683122, 1.000000000000000000, 0.9659258262890683122, 1.000000000000000000, 0.9659258262890683122, 1.000000000000000000, 0.9659258262890683122, 1.000000000000000000, 0.9659258262890683122, 1.000000000000000000, 0.9659258262890683122, 1.000000000000000000, 0.9659258262890683122, 1.000000000000000000, 0.9659258262890683122, 1.000000000000000000, 0.9659258262890683122, 1.000000000000000000, 0.9659258262890683122, 1.000000000000000000, 0.9659258262890683122, 1.000000000000000000, 0.9659258262890683122, 1.000000000000000000, 0.9659258262890683122, 1.000000000000000000, 0.9659258262890683122, 1.000000000000000000, 0.9659258262890683122, 1.000000000000000000, 0.9659258262890683122, 1.000000000000000000, 0.9659258262890683122, 1.000000000000000000, 0.9659258262890683122, 1.000000000000000000, 0.9659258262890683122, 1.000000000000000000, 0.9659258262890683122, 1.000000000000000000, 0.9659258262890683122, 1.000000000000000000, 0.9659258262890683122, 1.000000000000000000, 0.9659258262890683122, 1.000000000000000000, 0.9659258262890683122, 1.000000000000000000, 0.9659258262890683122, 1.000000000000000000, 0.9659258262890683122, 1.000000000000000000),
 ( 0.3333333333333333703, 0.3219752754296894559, 0.3333333333333333703, 0.3219752754296894559, 0.3333333333333333703, 0.3219752754296894559, 0.3333333333333333703, 0.3219752754296894559, 0.3333333333333333703, 0.3219752754296894559, 0.3333333333333333703, 0.3219752754296894559, 0.3333333333333333703, 0.3219752754296894559, 0.3333333333333333703, 0.3219752754296894559, 0.3333333333333333703, 0.3219752754296894559, 0.3333333333333333703, 0.3219752754296894559, 0.3333333333333333703, 0.3219752754296894559, 0.3333333333333333703, 0.3219752754296894559, 0.3333333333333333703, 0.3219752754296894559, 0.3333333333333333703, 0.3219752754296894559, 0.3333333333333333703, 0.3219752754296894559, 0.3333333333333333703, 0.3219752754296894559, 0.3333333333333333703, 0.3219752754296894559, 0.3333333333333333703, 0.3219752754296894559, 0.3333333333333333703, 0.3219752754296894559, 0.3333333333333333703, 0.3219752754296894559, 0.3333333333333333703, 0.3219752754296894559, 0.3333333333333333703, 0.3219752754296894559, 0.3333333333333333703, 0.3219752754296894559, 0.3333333333333333703, 0.3219752754296894559, 0.3333333333333333703, 0.3219752754296894559, 0.3333333333333333703, 0.3219752754296894559, 0.3333333333333333703, 0.3219752754296894559, 0.3333333333333333703, 0.3219752754296894559, 0.3333333333333333703, 0.3219752754296894559, 0.3333333333333333703, 0.3219752754296894559, 0.3333333333333333703, 0.3219752754296894559, 0.3333333333333333703, 0.3219752754296894559, 0.3333333333333333703, 0.3219752754296894559, 0.3333333333333333703, 0.3219752754296894559, 0.3333333333333333703, 0.3219752754296894559, 0.3333333333333333703, 0.3219752754296894559, 0.3333333333333333703, 0.3219752754296894559, 0.3333333333333333703, 0.3219752754296894559, 0.3333333333333333703, 0.3219752754296894559, 0.3333333333333333703, 0.3219752754296894559, 0.3333333333333333703, 0.3219752754296894559, 0.3333333333333333703, 0.3219752754296894559, 0.3333333333333333703, 0.3219752754296894559, 0.3333333333333333703, 0.3219752754296894559, 0.3333333333333333703, 0.3219752754296894559, 0.3333333333333333703, 0.3219752754296894559, 0.3333333333333333703, 0.3219752754296894559, 0.3333333333333333703, 0.3219752754296894559, 0.3333333333333333703, 0.3219752754296894559, 0.3333333333333333703, 0.3219752754296894559, 0.3333333333333333703, 0.3219752754296894559, 0.3333333333333333703, 0.3219752754296894559, 0.3333333333333333703, 0.3219752754296894559, 0.3333333333333333703, 0.3219752754296894559, 0.3333333333333333703, 0.3219752754296894559, 0.3333333333333333703, 0.3219752754296894559, 0.3333333333333333703, 0.3219752754296894559, 0.3333333333333333703, 0.3219752754296894559, 0.3333333333333333703, 0.3219752754296894559, 0.3333333333333333703, 0.3219752754296894559, 0.3333333333333333703, 0.3219752754296894559, 0.3333333333333333703, 0.3219752754296894559, 0.3333333333333333703, 0.3219752754296894559, 0.3333333333333333703, 0.3219752754296894559, 0.3333333333333333703, 0.3219752754296894559, 0.3333333333333333703, 0.3219752754296894559, 0.3333333333333333703, 0.3219752754296894559, 0.3333333333333333703, 0.3219752754296894559, 0.3333333333333333703, 0.3219752754296894559, 0.3333333333333333703, 0.3219752754296894559, 0.3333333333333333703, 0.3219752754296894559, 0.3333333333333333703, 0.3219752754296894559, 0.3333333333333333703, 0.3219752754296894559, 0.3333333333333333703, 0.3219752754296894559, 0.3333333333333333703, 0.3219752754296894559, 0.3333333333333333703, 0.3219752754296894559, 0.3333333333333333703, 0.3219752754296894559, 0.3333333333333333703, 0.3219752754296894559, 0.3333333333333333703, 0.3219752754296894559, 0.3333333333333333703, 0.3219752754296894559, 0.3333333333333333703, 0.3219752754296894559, 0.3333333333333333703, 0.3219752754296894559, 0.3333333333333333703, 0.3219752754296894559, 0.3333333333333333703, 0.3219752754296894559, 0.3333333333333333703, 0.3219752754296894559, 0.3333333333333333703, 0.3219752754296894559, 0.3333333333333333703, 0.3219752754296894559, 0.3333333333333333703, 0.3219752754296894559, 0.3333333333333333703, 0.3219752754296894559, 0.3333333333333333703, 0.3219752754296894559, 0.3333333333333333703, 0.3219752754296894559, 0.3333333333333333703, 0.3219752754296894559, 0.3333333333333333703, 0.3219752754296894559, 0.3333333333333333703, 0.3219752754296894559, 0.3333333333333333703, 0.3219752754296894559, 0.3333333333333333703, 0.3219752754296894559, 0.3333333333333333703, 0.3219752754296894559, 0.3333333333333333703, 0.3219752754296894559, 0.3333333333333333703, 0.3219752754296894559, 0.3333333333333333703, 0.3219752754296894559, 0.3333333333333333703, 0.3219752754296894559, 0.3333333333333333703, 0.3219752754296894559, 0.3333333333333333703, 0.3219752754296894559, 0.3333333333333333703, 0.3219752754296894559, 0.3333333333333333703, 0.3219752754296894559, 0.3333333333333333703, 0.3219752754296894559, 0.3333333333333333703, 0.3219752754296894559, 0.3333333333333333703, 0.3219752754296894559, 0.3333333333333333703, 0.3219752754296894559, 0.3333333333333333703, 0.3219752754296894559, 0.3333333333333333703, 0.3219752754296894559, 0.3333333333333333703, 0.3219752754296894559, 0.3333333333333333703, 0.3219752754296894559, 0.3333333333333333703, 0.3219752754296894559, 0.3333333333333333703, 0.3219752754296894559, 0.3333333333333333703, 0.3219752754296894559, 0.3333333333333333703, 0.3219752754296894559, 0.3333333333333333703, 0.3219752754296894559, 0.3333333333333333703, 0.3219752754296894559, 0.3333333333333333703, 0.3219752754296894559, 0.3333333333333333703, 0.3219752754296894559, 0.3333333333333333703, 0.3219752754296894559, 0.3333333333333333703, 0.3219752754296894559, 0.3333333333333333703, 0.3219752754296894559, 0.3333333333333333703, 0.3219752754296894559, 0.3333333333333333703, 0.3219752754296894559, 0.3333333333333333703, 0.3219752754296894559, 0.3333333333333333703, 0.3219752754296894559, 0.3333333333333333703, 0.3219752754296894559, 0.3333333333333333703, 0.3219752754296894559, 0.3333333333333333703, 0.3219752754296894559, 0.3333333333333333703, 0.3219752754296894559, 0.3333333333333333703, 0.3219752754296894559, 0.3333333333333333703, 0.3219752754296894559, 0.3333333333333333703, 0.3219752754296894559, 0.3333333333333333703, 0.3219752754296894559, 0.3333333333333333703, 0.3219752754296894559, 0.3333333333333333703, 0.3219752754296894559, 0.3333333333333333703, 0.3219752754296894559, 0.3333333333333333703, 0.3219752754296894559, 0.3333333333333333703, 0.3219752754296894559, 0.3333333333333333703, 0.3219752754296894559, 0.3333333333333333703, 0.3219752754296894559, 0.3333333333333333703, 0.3219752754296894559, 0.3333333333333333703, 0.3219752754296894559, 0.3333333333333333703, 0.3219752754296894559, 0.3333333333333333703, 0.3219752754296894559, 0.3333333333333333703, 0.3219752754296894559, 0.3333333333333333703, 0.3219752754296894559, 0.3333333333333333703, 0.3219752754296894559, 0.3333333333333333703, 0.3219752754296894559, 0.3333333333333333703, 0.3219752754296894559, 0.3333333333333333703, 0.3219752754296894559, 0.3333333333333333703, 0.3219752754296894559, 0.3333333333333333703, 0.3219752754296894559, 0.3333333333333333703, 0.3219752754296894559, 0.3333333333333333703, 0.3219752754296894559, 0.3333333333333333703, 0.3219752754296894559, 0.3333333333333333703, 0.3219752754296894559, 0.3333333333333333703, 0.3219752754296894559, 0.3333333333333333703, 0.3219752754296894559, 0.3333333333333333703, 0.3219752754296894559, 0.3333333333333333703, 0.3219752754296894559, 0.3333333333333333703, 0.3219752754296894559, 0.3333333333333333703, 0.3219752754296894559, 0.3333333333333333703, 0.3219752754296894559, 0.3333333333333333703, 0.3219752754296894559, 0.3333333333333333703, 0.3219752754296894559, 0.3333333333333333703, 0.3219752754296894559, 0.3333333333333333703, 0.3219752754296894559, 0.3333333333333333703, 0.3219752754296894559, 0.3333333333333333703, 0.3219752754296894559, 0.3333333333333333703, 0.3219752754296894559, 0.3333333333333333703, 0.3219752754296894559, 0.3333333333333333703, 0.3219752754296894559, 0.3333333333333333703, 0.3219752754296894559, 0.3333333333333333703, 0.3219752754296894559, 0.3333333333333333703, 0.3219752754296894559, 0.3333333333333333703, 0.3219752754296894559, 0.3333333333333333703, 0.3219752754296894559, 0.3333333333333333703, 0.3219752754296894559, 0.3333333333333333703, 0.3219752754296894559, 0.3333333333333333703, 0.3219752754296894559, 0.3333333333333333703, 0.3219752754296894559, 0.3333333333333333703, 0.3219752754296894559, 0.3333333333333333703, 0.3219752754296894559, 0.3333333333333333703, 0.3219752754296894559, 0.3333333333333333703, 0.3219752754296894559, 0.3333333333333333703, 0.3219752754296894559, 0.3333333333333333703, 0.3219752754296894559, 0.3333333333333333703, 0.3219752754296894559, 0.3333333333333333703, 0.3219752754296894559, 0.3333333333333333703, 0.3219752754296894559, 0.3333333333333333703, 0.3219752754296894559, 0.3333333333333333703, 0.3219752754296894559, 0.3333333333333333703, 0.3219752754296894559, 0.3333333333333333703, 0.3219752754296894559, 0.3333333333333333703, 0.3219752754296894559, 0.3333333333333333703, 0.3219752754296894559, 0.3333333333333333703, 0.3219752754296894559, 0.3333333333333333703, 0.3219752754296894559, 0.3333333333333333703, 0.3219752754296894559, 0.3333333333333333703, 0.3219752754296894559, 0.3333333333333333703, 0.3219752754296894559, 0.3333333333333333703, 0.3219752754296894559, 0.3333333333333333703, 0.3219752754296894559, 0.3333333333333333703, 0.3219752754296894559, 0.3333333333333333703, 0.3219752754296894559, 0.3333333333333333703, 0.3219752754296894559, 0.3333333333333333703, 0.3219752754296894559, 0.3333333333333333703, 0.3219752754296894559, 0.3333333333333333703, 0.3219752754296894559, 0.3333333333333333703, 0.3219752754296894559, 0.3333333333333333703, 0.3219752754296894559, 0.3333333333333333703, 0.3219752754296894559, 0.3333333333333333703, 0.3219752754296894559, 0.3333333333333333703, 0.3219752754296894559, 0.3333333333333333703, 0.3219752754296894559, 0.3333333333333333703, 0.3219752754296894559, 0.3333333333333333703, 0.3219752754296894559, 0.3333333333333333703, 0.3219752754296894559, 0.3333333333333333703, 0.3219752754296894559, 0.3333333333333333703, 0.3219752754296894559, 0.3333333333333333703, 0.3219752754296894559, 0.3333333333333333703, 0.3219752754296894559, 0.3333333333333333703, 0.3219752754296894559, 0.3333333333333333703, 0.3219752754296894559, 0.3333333333333333703, 0.3219752754296894559, 0.3333333333333333703),
 ( 0.3333333333333333703, 0.3219752754296894559, 0.3333333333333333703, 0.3219752754296894559, 0.3333333333333333703, 0.3219752754296894559, 0.3333333333333333703, 0.3219752754296894559, 0.3333333333333333703, 0.3219752754296894559, 0.3333333333333333703, 0.3219752754296894559, 0.3333333333333333703, 0.3219752754296894559, 0.3333333333333333703, 0.3219752754296894559, 0.3333333333333333703, 0.3219752754296894559, 0.3333333333333333703, 0.3219752754296894559, 0.3333333333333333703, 0.3219752754296894559, 0.3333333333333333703, 0.3219752754296894559, 0.3333333333333333703, 0.3219752754296894559, 0.3333333333333333703, 0.3219752754296894559, 0.3333333333333333703, 0.3219752754296894559, 0.3333333333333333703, 0.3219752754296894559, 0.3333333333333333703, 0.3219752754296894559, 0.3333333333333333703, 0.3219752754296894559, 0.3333333333333333703, 0.3219752754296894559, 0.3333333333333333703, 0.3219752754296894559, 0.3333333333333333703, 0.3219752754296894559, 0.3333333333333333703, 0.3219752754296894559, 0.3333333333333333703, 0.3219752754296894559, 0.3333333333333333703, 0.3219752754296894559, 0.3333333333333333703, 0.3219752754296894559, 0.3333333333333333703, 0.3219752754296894559, 0.3333333333333333703, 0.3219752754296894559, 0.3333333333333333703, 0.3219752754296894559, 0.3333333333333333703, 0.3219752754296894559, 0.3333333333333333703, 0.3219752754296894559, 0.3333333333333333703, 0.3219752754296894559, 0.3333333333333333703, 0.3219752754296894559, 0.3333333333333333703, 0.3219752754296894559, 0.3333333333333333703, 0.3219752754296894559, 0.3333333333333333703, 0.3219752754296894559, 0.3333333333333333703, 0.3219752754296894559, 0.3333333333333333703, 0.3219752754296894559, 0.3333333333333333703, 0.3219752754296894559, 0.3333333333333333703, 0.3219752754296894559, 0.3333333333333333703, 0.3219752754296894559, 0.3333333333333333703, 0.3219752754296894559, 0.3333333333333333703, 0.3219752754296894559, 0.3333333333333333703, 0.3219752754296894559, 0.3333333333333333703, 0.3219752754296894559, 0.3333333333333333703, 0.3219752754296894559, 0.3333333333333333703, 0.3219752754296894559, 0.3333333333333333703, 0.3219752754296894559, 0.3333333333333333703, 0.3219752754296894559, 0.3333333333333333703, 0.3219752754296894559, 0.3333333333333333703, 0.3219752754296894559, 0.3333333333333333703, 0.3219752754296894559, 0.3333333333333333703, 0.3219752754296894559, 0.3333333333333333703, 0.3219752754296894559, 0.3333333333333333703, 0.3219752754296894559, 0.3333333333333333703, 0.3219752754296894559, 0.3333333333333333703, 0.3219752754296894559, 0.3333333333333333703, 0.3219752754296894559, 0.3333333333333333703, 0.3219752754296894559, 0.3333333333333333703, 0.3219752754296894559, 0.3333333333333333703, 0.3219752754296894559, 0.3333333333333333703, 0.3219752754296894559, 0.3333333333333333703, 0.3219752754296894559, 0.3333333333333333703, 0.3219752754296894559, 0.3333333333333333703, 0.3219752754296894559, 0.3333333333333333703, 0.3219752754296894559, 0.3333333333333333703, 0.3219752754296894559, 0.3333333333333333703, 0.3219752754296894559, 0.3333333333333333703, 0.3219752754296894559, 0.3333333333333333703, 0.3219752754296894559, 0.3333333333333333703, 0.3219752754296894559, 0.3333333333333333703, 0.3219752754296894559, 0.3333333333333333703, 0.3219752754296894559, 0.3333333333333333703, 0.3219752754296894559, 0.3333333333333333703, 0.3219752754296894559, 0.3333333333333333703, 0.3219752754296894559, 0.3333333333333333703, 0.3219752754296894559, 0.3333333333333333703, 0.3219752754296894559, 0.3333333333333333703, 0.3219752754296894559, 0.3333333333333333703, 0.3219752754296894559, 0.3333333333333333703, 0.3219752754296894559, 0.3333333333333333703, 0.3219752754296894559, 0.3333333333333333703, 0.3219752754296894559, 0.3333333333333333703, 0.3219752754296894559, 0.3333333333333333703, 0.3219752754296894559, 0.3333333333333333703, 0.3219752754296894559, 0.3333333333333333703, 0.3219752754296894559, 0.3333333333333333703, 0.3219752754296894559, 0.3333333333333333703, 0.3219752754296894559, 0.3333333333333333703, 0.3219752754296894559, 0.3333333333333333703, 0.3219752754296894559, 0.3333333333333333703, 0.3219752754296894559, 0.3333333333333333703, 0.3219752754296894559, 0.3333333333333333703, 0.3219752754296894559, 0.3333333333333333703, 0.3219752754296894559, 0.3333333333333333703, 0.3219752754296894559, 0.3333333333333333703, 0.3219752754296894559, 0.3333333333333333703, 0.3219752754296894559, 0.3333333333333333703, 0.3219752754296894559, 0.3333333333333333703, 0.3219752754296894559, 0.3333333333333333703, 0.3219752754296894559, 0.3333333333333333703, 0.3219752754296894559, 0.3333333333333333703, 0.3219752754296894559, 0.3333333333333333703, 0.3219752754296894559, 0.3333333333333333703, 0.3219752754296894559, 0.3333333333333333703, 0.3219752754296894559, 0.3333333333333333703, 0.3219752754296894559, 0.3333333333333333703, 0.3219752754296894559, 0.3333333333333333703, 0.3219752754296894559, 0.3333333333333333703, 0.3219752754296894559, 0.3333333333333333703, 0.3219752754296894559, 0.3333333333333333703, 0.3219752754296894559, 0.3333333333333333703, 0.3219752754296894559, 0.3333333333333333703, 0.3219752754296894559, 0.3333333333333333703, 0.3219752754296894559, 0.3333333333333333703, 0.3219752754296894559, 0.3333333333333333703, 0.3219752754296894559, 0.3333333333333333703, 0.3219752754296894559, 0.3333333333333333703, 0.3219752754296894559, 0.3333333333333333703, 0.3219752754296894559, 0.3333333333333333703, 0.3219752754296894559, 0.3333333333333333703, 0.3219752754296894559, 0.3333333333333333703, 0.3219752754296894559, 0.3333333333333333703, 0.3219752754296894559, 0.3333333333333333703, 0.3219752754296894559, 0.3333333333333333703, 0.3219752754296894559, 0.3333333333333333703, 0.3219752754296894559, 0.3333333333333333703, 0.3219752754296894559, 0.3333333333333333703, 0.3219752754296894559, 0.3333333333333333703, 0.3219752754296894559, 0.3333333333333333703, 0.3219752754296894559, 0.3333333333333333703, 0.3219752754296894559, 0.3333333333333333703, 0.3219752754296894559, 0.3333333333333333703, 0.3219752754296894559, 0.3333333333333333703, 0.3219752754296894559, 0.3333333333333333703, 0.3219752754296894559, 0.3333333333333333703, 0.3219752754296894559, 0.3333333333333333703, 0.3219752754296894559, 0.3333333333333333703, 0.3219752754296894559, 0.3333333333333333703, 0.3219752754296894559, 0.3333333333333333703, 0.3219752754296894559, 0.3333333333333333703, 0.3219752754296894559, 0.3333333333333333703, 0.3219752754296894559, 0.3333333333333333703, 0.3219752754296894559, 0.3333333333333333703, 0.3219752754296894559, 0.3333333333333333703, 0.3219752754296894559, 0.3333333333333333703, 0.3219752754296894559, 0.3333333333333333703, 0.3219752754296894559, 0.3333333333333333703, 0.3219752754296894559, 0.3333333333333333703, 0.3219752754296894559, 0.3333333333333333703, 0.3219752754296894559, 0.3333333333333333703, 0.3219752754296894559, 0.3333333333333333703, 0.3219752754296894559, 0.3333333333333333703, 0.3219752754296894559, 0.3333333333333333703, 0.3219752754296894559, 0.3333333333333333703, 0.3219752754296894559, 0.3333333333333333703, 0.3219752754296894559, 0.3333333333333333703, 0.3219752754296894559, 0.3333333333333333703, 0.3219752754296894559, 0.3333333333333333703, 0.3219752754296894559, 0.3333333333333333703, 0.3219752754296894559, 0.3333333333333333703, 0.3219752754296894559, 0.3333333333333333703, 0.3219752754296894559, 0.3333333333333333703, 0.3219752754296894559, 0.3333333333333333703, 0.3219752754296894559, 0.3333333333333333703, 0.3219752754296894559, 0.3333333333333333703, 0.3219752754296894559, 0.3333333333333333703, 0.3219752754296894559, 0.3333333333333333703, 0.3219752754296894559, 0.3333333333333333703, 0.3219752754296894559, 0.3333333333333333703, 0.3219752754296894559, 0.3333333333333333703, 0.3219752754296894559, 0.3333333333333333703, 0.3219752754296894559, 0.3333333333333333703, 0.3219752754296894559, 0.3333333333333333703, 0.3219752754296894559, 0.3333333333333333703, 0.3219752754296894559, 0.3333333333333333703, 0.3219752754296894559, 0.3333333333333333703, 0.3219752754296894559, 0.3333333333333333703, 0.3219752754296894559, 0.3333333333333333703, 0.3219752754296894559, 0.3333333333333333703, 0.3219752754296894559, 0.3333333333333333703, 0.3219752754296894559, 0.3333333333333333703, 0.3219752754296894559, 0.3333333333333333703, 0.3219752754296894559, 0.3333333333333333703, 0.3219752754296894559, 0.3333333333333333703, 0.3219752754296894559, 0.3333333333333333703, 0.3219752754296894559, 0.3333333333333333703, 0.3219752754296894559, 0.3333333333333333703, 0.3219752754296894559, 0.3333333333333333703, 0.3219752754296894559, 0.3333333333333333703, 0.3219752754296894559, 0.3333333333333333703, 0.3219752754296894559, 0.3333333333333333703, 0.3219752754296894559, 0.3333333333333333703, 0.3219752754296894559, 0.3333333333333333703, 0.3219752754296894559, 0.3333333333333333703, 0.3219752754296894559, 0.3333333333333333703, 0.3219752754296894559, 0.3333333333333333703, 0.3219752754296894559, 0.3333333333333333703, 0.3219752754296894559, 0.3333333333333333703, 0.3219752754296894559, 0.3333333333333333703, 0.3219752754296894559, 0.3333333333333333703, 0.3219752754296894559, 0.3333333333333333703, 0.3219752754296894559, 0.3333333333333333703, 0.3219752754296894559, 0.3333333333333333703, 0.3219752754296894559, 0.3333333333333333703, 0.3219752754296894559, 0.3333333333333333703, 0.3219752754296894559, 0.3333333333333333703, 0.3219752754296894559, 0.3333333333333333703, 0.3219752754296894559, 0.3333333333333333703, 0.3219752754296894559, 0.3333333333333333703, 0.3219752754296894559, 0.3333333333333333703, 0.3219752754296894559, 0.3333333333333333703, 0.3219752754296894559, 0.3333333333333333703, 0.3219752754296894559, 0.3333333333333333703, 0.3219752754296894559, 0.3333333333333333703, 0.3219752754296894559, 0.3333333333333333703, 0.3219752754296894559, 0.3333333333333333703, 0.3219752754296894559, 0.3333333333333333703, 0.3219752754296894559, 0.3333333333333333703, 0.3219752754296894559, 0.3333333333333333703, 0.3219752754296894559, 0.3333333333333333703, 0.3219752754296894559, 0.3333333333333333703, 0.3219752754296894559, 0.3333333333333333703, 0.3219752754296894559, 0.3333333333333333703, 0.3219752754296894559, 0.3333333333333333703, 0.3219752754296894559, 0.3333333333333333703, 0.3219752754296894559, 0.3333333333333333703, 0.3219752754296894559, 0.3333333333333333703, 0.3219752754296894559, 0.3333333333333333703),
 ( 1.000000000000000000, 0.9659258262890683122, 1.000000000000000000, 0.9659258262890683122, 1.000000000000000000, 0.9659258262890683122, 1.000000000000000000, 0.9659258262890683122, 1.000000000000000000, 0.9659258262890683122, 1.000000000000000000, 0.9659258262890683122, 1.000000000000000000, 0.9659258262890683122, 1.000000000000000000, 0.9659258262890683122, 1.000000000000000000, 0.9659258262890683122, 1.000000000000000000, 0.9659258262890683122, 1.000000000000000000, 0.9659258262890683122, 1.000000000000000000, 0.9659258262890683122, 1.000000000000000000, 0.9659258262890683122, 1.000000000000000000, 0.9659258262890683122, 1.000000000000000000, 0.9659258262890683122, 1.000000000000000000, 0.9659258262890683122, 1.000000000000000000, 0.9659258262890683122, 1.000000000000000000, 0.9659258262890683122, 1.000000000000000000, 0.9659258262890683122, 1.000000000000000000, 0.9659258262890683122, 1.000000000000000000, 0.9659258262890683122, 1.000000000000000000, 0.9659258262890683122, 1.000000000000000000, 0.9659258262890683122, 1.000000000000000000, 0.9659258262890683122, 1.000000000000000000, 0.9659258262890683122, 1.000000000000000000, 0.9659258262890683122, 1.000000000000000000, 0.9659258262890683122, 1.000000000000000000, 0.9659258262890683122, 1.000000000000000000, 0.9659258262890683122, 1.000000000000000000, 0.9659258262890683122, 1.000000000000000000, 0.9659258262890683122, 1.000000000000000000, 0.9659258262890683122, 1.000000000000000000, 0.9659258262890683122, 1.000000000000000000, 0.9659258262890683122, 1.000000000000000000, 0.9659258262890683122, 1.000000000000000000, 0.9659258262890683122, 1.000000000000000000, 0.9659258262890683122, 1.000000000000000000, 0.9659258262890683122, 1.000000000000000000, 0.9659258262890683122, 1.000000000000000000, 0.9659258262890683122, 1.000000000000000000, 0.9659258262890683122, 1.000000000000000000, 0.9659258262890683122, 1.000000000000000000, 0.9659258262890683122, 1.000000000000000000, 0.9659258262890683122, 1.000000000000000000, 0.9659258262890683122, 1.000000000000000000, 0.9659258262890683122, 1.000000000000000000, 0.9659258262890683122, 1.000000000000000000, 0.9659258262890683122, 1.000000000000000000, 0.9659258262890683122, 1.000000000000000000, 0.9659258262890683122, 1.000000000000000000, 0.9659258262890683122, 1.000000000000000000, 0.9659258262890683122, 1.000000000000000000, 0.9659258262890683122, 1.000000000000000000, 0.9659258262890683122, 1.000000000000000000, 0.9659258262890683122, 1.000000000000000000, 0.9659258262890683122, 1.000000000000000000, 0.9659258262890683122, 1.000000000000000000, 0.9659258262890683122, 1.000000000000000000, 0.9659258262890683122, 1.000000000000000000, 0.9659258262890683122, 1.000000000000000000, 0.9659258262890683122, 1.000000000000000000, 0.9659258262890683122, 1.000000000000000000, 0.9659258262890683122, 1.000000000000000000, 0.9659258262890683122, 1.000000000000000000, 0.9659258262890683122, 1.000000000000000000, 0.9659258262890683122, 1.000000000000000000, 0.9659258262890683122, 1.000000000000000000, 0.9659258262890683122, 1.000000000000000000, 0.9659258262890683122, 1.000000000000000000, 0.9659258262890683122, 1.000000000000000000, 0.9659258262890683122, 1.000000000000000000, 0.9659258262890683122, 1.000000000000000000, 0.9659258262890683122, 1.000000000000000000, 0.9659258262890683122, 1.000000000000000000, 0.9659258262890683122, 1.000000000000000000, 0.9659258262890683122, 1.000000000000000000, 0.9659258262890683122, 1.000000000000000000, 0.9659258262890683122, 1.000000000000000000, 0.9659258262890683122, 1.000000000000000000, 0.9659258262890683122, 1.000000000000000000, 0.9659258262890683122, 1.000000000000000000, 0.9659258262890683122, 1.000000000000000000, 0.9659258262890683122, 1.000000000000000000, 0.9659258262890683122, 1.000000000000000000, 0.9659258262890683122, 1.000000000000000000, 0.9659258262890683122, 1.000000000000000000, 0.9659258262890683122, 1.000000000000000000, 0.9659258262890683122, 1.000000000000000000, 0.9659258262890683122, 1.000000000000000000, 0.9659258262890683122, 1.000000000000000000, 0.9659258262890683122, 1.000000000000000000, 0.9659258262890683122, 1.000000000000000000, 0.9659258262890683122, 1.000000000000000000, 0.9659258262890683122, 1.000000000000000000, 0.9659258262890683122, 1.000000000000000000, 0.9659258262890683122, 1.000000000000000000, 0.9659258262890683122, 1.000000000000000000, 0.9659258262890683122, 1.000000000000000000, 0.9659258262890683122, 1.000000000000000000, 0.9659258262890683122, 1.000000000000000000, 0.9659258262890683122, 1.000000000000000000, 0.9659258262890683122, 1.000000000000000000, 0.9659258262890683122, 1.000000000000000000, 0.9659258262890683122, 1.000000000000000000, 0.9659258262890683122, 1.000000000000000000, 0.9659258262890683122, 1.000000000000000000, 0.9659258262890683122, 1.000000000000000000, 0.9659258262890683122, 1.000000000000000000, 0.9659258262890683122, 1.000000000000000000, 0.9659258262890683122, 1.000000000000000000, 0.9659258262890683122, 1.000000000000000000, 0.9659258262890683122, 1.000000000000000000, 0.9659258262890683122, 1.000000000000000000, 0.9659258262890683122, 1.000000000000000000, 0.9659258262890683122, 1.000000000000000000, 0.9659258262890683122, 1.000000000000000000, 0.9659258262890683122, 1.000000000000000000, 0.9659258262890683122, 1.000000000000000000, 0.9659258262890683122, 1.000000000000000000, 0.9659258262890683122, 1.000000000000000000, 0.9659258262890683122, 1.000000000000000000, 0.9659258262890683122, 1.000000000000000000, 0.9659258262890683122, 1.000000000000000000, 0.9659258262890683122, 1.000000000000000000, 0.9659258262890683122, 1.000000000000000000, 0.9659258262890683122, 1.000000000000000000, 0.9659258262890683122, 1.000000000000000000, 0.9659258262890683122, 1.000000000000000000, 0.9659258262890683122, 1.000000000000000000, 0.9659258262890683122, 1.000000000000000000, 0.9659258262890683122, 1.000000000000000000, 0.9659258262890683122, 1.000000000000000000, 0.9659258262890683122, 1.000000000000000000, 0.9659258262890683122, 1.000000000000000000, 0.9659258262890683122, 1.000000000000000000, 0.9659258262890683122, 1.000000000000000000, 0.9659258262890683122, 1.000000000000000000, 0.9659258262890683122, 1.000000000000000000, 0.9659258262890683122, 1.000000000000000000, 0.9659258262890683122, 1.000000000000000000, 0.9659258262890683122, 1.000000000000000000, 0.9659258262890683122, 1.000000000000000000, 0.9659258262890683122, 1.000000000000000000, 0.9659258262890683122, 1.000000000000000000, 0.9659258262890683122, 1.000000000000000000, 0.9659258262890683122, 1.000000000000000000, 0.9659258262890683122, 1.000000000000000000, 0.9659258262890683122, 1.000000000000000000, 0.9659258262890683122, 1.000000000000000000, 0.9659258262890683122, 1.000000000000000000, 0.9659258262890683122, 1.000000000000000000, 0.9659258262890683122, 1.000000000000000000, 0.9659258262890683122, 1.000000000000000000, 0.9659258262890683122, 1.000000000000000000, 0.9659258262890683122, 1.000000000000000000, 0.9659258262890683122, 1.000000000000000000, 0.9659258262890683122, 1.000000000000000000, 0.9659258262890683122, 1.000000000000000000, 0.9659258262890683122, 1.000000000000000000, 0.9659258262890683122, 1.000000000000000000, 0.9659258262890683122, 1.000000000000000000, 0.9659258262890683122, 1.000000000000000000, 0.9659258262890683122, 1.000000000000000000, 0.9659258262890683122, 1.000000000000000000, 0.9659258262890683122, 1.000000000000000000, 0.9659258262890683122, 1.000000000000000000, 0.9659258262890683122, 1.000000000000000000, 0.9659258262890683122, 1.000000000000000000, 0.9659258262890683122, 1.000000000000000000, 0.9659258262890683122, 1.000000000000000000, 0.9659258262890683122, 1.000000000000000000, 0.9659258262890683122, 1.000000000000000000, 0.9659258262890683122, 1.000000000000000000, 0.9659258262890683122, 1.000000000000000000, 0.9659258262890683122, 1.000000000000000000, 0.9659258262890683122, 1.000000000000000000, 0.9659258262890683122, 1.000000000000000000, 0.9659258262890683122, 1.000000000000000000, 0.9659258262890683122, 1.000000000000000000, 0.9659258262890683122, 1.000000000000000000, 0.9659258262890683122, 1.000000000000000000, 0.9659258262890683122, 1.000000000000000000, 0.9659258262890683122, 1.000000000000000000, 0.9659258262890683122, 1.000000000000000000, 0.9659258262890683122, 1.000000000000000000, 0.9659258262890683122, 1.000000000000000000, 0.9659258262890683122, 1.000000000000000000, 0.9659258262890683122, 1.000000000000000000, 0.9659258262890683122, 1.000000000000000000, 0.9659258262890683122, 1.000000000000000000, 0.9659258262890683122, 1.000000000000000000, 0.9659258262890683122, 1.000000000000000000, 0.9659258262890683122, 1.000000000000000000, 0.9659258262890683122, 1.000000000000000000, 0.9659258262890683122, 1.000000000000000000, 0.9659258262890683122, 1.000000000000000000, 0.9659258262890683122, 1.000000000000000000, 0.9659258262890683122, 1.000000000000000000, 0.9659258262890683122, 1.000000000000000000, 0.9659258262890683122, 1.000000000000000000, 0.9659258262890683122, 1.000000000000000000, 0.9659258262890683122, 1.000000000000000000, 0.9659258262890683122, 1.000000000000000000, 0.9659258262890683122, 1.000000000000000000, 0.9659258262890683122, 1.000000000000000000, 0.9659258262890683122, 1.000000000000000000, 0.9659258262890683122, 1.000000000000000000, 0.9659258262890683122, 1.000000000000000000, 0.9659258262890683122, 1.000000000000000000, 0.9659258262890683122, 1.000000000000000000, 0.9659258262890683122, 1.000000000000000000, 0.9659258262890683122, 1.000000000000000000, 0.9659258262890683122, 1.000000000000000000, 0.9659258262890683122, 1.000000000000000000, 0.9659258262890683122, 1.000000000000000000, 0.9659258262890683122, 1.000000000000000000, 0.9659258262890683122, 1.000000000000000000, 0.9659258262890683122, 1.000000000000000000, 0.9659258262890683122, 1.000000000000000000, 0.9659258262890683122, 1.000000000000000000, 0.9659258262890683122, 1.000000000000000000, 0.9659258262890683122, 1.000000000000000000, 0.9659258262890683122, 1.000000000000000000, 0.9659258262890683122, 1.000000000000000000, 0.9659258262890683122, 1.000000000000000000, 0.9659258262890683122, 1.000000000000000000, 0.9659258262890683122, 1.000000000000000000, 0.9659258262890683122, 1.000000000000000000),
 ( 0.3333333333333333703, 0.3219752754296894559, 0.3333333333333333703, 0.3219752754296894559, 0.3333333333333333703, 0.3219752754296894559, 0.3333333333333333703, 0.3219752754296894559, 0.3333333333333333703, 0.3219752754296894559, 0.3333333333333333703, 0.3219752754296894559, 0.3333333333333333703, 0.3219752754296894559, 0.3333333333333333703, 0.3219752754296894559, 0.3333333333333333703, 0.3219752754296894559, 0.3333333333333333703, 0.3219752754296894559, 0.3333333333333333703, 0.3219752754296894559, 0.3333333333333333703, 0.3219752754296894559, 0.3333333333333333703, 0.3219752754296894559, 0.3333333333333333703, 0.3219752754296894559, 0.3333333333333333703, 0.3219752754296894559, 0.3333333333333333703, 0.3219752754296894559, 0.3333333333333333703, 0.3219752754296894559, 0.3333333333333333703, 0.3219752754296894559, 0.3333333333333333703, 0.3219752754296894559, 0.3333333333333333703, 0.3219752754296894559, 0.3333333333333333703, 0.3219752754296894559, 0.3333333333333333703, 0.3219752754296894559, 0.3333333333333333703, 0.3219752754296894559, 0.3333333333333333703, 0.3219752754296894559, 0.3333333333333333703, 0.3219752754296894559, 0.3333333333333333703, 0.3219752754296894559, 0.3333333333333333703, 0.3219752754296894559, 0.3333333333333333703, 0.3219752754296894559, 0.3333333333333333703, 0.3219752754296894559, 0.3333333333333333703, 0.3219752754296894559, 0.3333333333333333703, 0.3219752754296894559, 0.3333333333333333703, 0.3219752754296894559, 0.3333333333333333703, 0.3219752754296894559, 0.3333333333333333703, 0.3219752754296894559, 0.3333333333333333703, 0.3219752754296894559, 0.3333333333333333703, 0.3219752754296894559, 0.3333333333333333703, 0.3219752754296894559, 0.3333333333333333703, 0.3219752754296894559, 0.3333333333333333703, 0.3219752754296894559, 0.3333333333333333703, 0.3219752754296894559, 0.3333333333333333703, 0.3219752754296894559, 0.3333333333333333703, 0.3219752754296894559, 0.3333333333333333703, 0.3219752754296894559, 0.3333333333333333703, 0.3219752754296894559, 0.3333333333333333703, 0.3219752754296894559, 0.3333333333333333703, 0.3219752754296894559, 0.3333333333333333703, 0.3219752754296894559, 0.3333333333333333703, 0.3219752754296894559, 0.3333333333333333703, 0.3219752754296894559, 0.3333333333333333703, 0.3219752754296894559, 0.3333333333333333703, 0.3219752754296894559, 0.3333333333333333703, 0.3219752754296894559, 0.3333333333333333703, 0.3219752754296894559, 0.3333333333333333703, 0.3219752754296894559, 0.3333333333333333703, 0.3219752754296894559, 0.3333333333333333703, 0.3219752754296894559, 0.3333333333333333703, 0.3219752754296894559, 0.3333333333333333703, 0.3219752754296894559, 0.3333333333333333703, 0.3219752754296894559, 0.3333333333333333703, 0.3219752754296894559, 0.3333333333333333703, 0.3219752754296894559, 0.3333333333333333703, 0.3219752754296894559, 0.3333333333333333703, 0.3219752754296894559, 0.3333333333333333703, 0.3219752754296894559, 0.3333333333333333703, 0.3219752754296894559, 0.3333333333333333703, 0.3219752754296894559, 0.3333333333333333703, 0.3219752754296894559, 0.3333333333333333703, 0.3219752754296894559, 0.3333333333333333703, 0.3219752754296894559, 0.3333333333333333703, 0.3219752754296894559, 0.3333333333333333703, 0.3219752754296894559, 0.3333333333333333703, 0.3219752754296894559, 0.3333333333333333703, 0.3219752754296894559, 0.3333333333333333703, 0.3219752754296894559, 0.3333333333333333703, 0.3219752754296894559, 0.3333333333333333703, 0.3219752754296894559, 0.3333333333333333703, 0.3219752754296894559, 0.3333333333333333703, 0.3219752754296894559, 0.3333333333333333703, 0.3219752754296894559, 0.3333333333333333703, 0.3219752754296894559, 0.3333333333333333703, 0.3219752754296894559, 0.3333333333333333703, 0.3219752754296894559, 0.3333333333333333703, 0.3219752754296894559, 0.3333333333333333703, 0.3219752754296894559, 0.3333333333333333703, 0.3219752754296894559, 0.3333333333333333703, 0.3219752754296894559, 0.3333333333333333703, 0.3219752754296894559, 0.3333333333333333703, 0.3219752754296894559, 0.3333333333333333703, 0.3219752754296894559, 0.3333333333333333703, 0.3219752754296894559, 0.3333333333333333703, 0.3219752754296894559, 0.3333333333333333703, 0.3219752754296894559, 0.3333333333333333703, 0.3219752754296894559, 0.3333333333333333703, 0.3219752754296894559, 0.3333333333333333703, 0.3219752754296894559, 0.3333333333333333703, 0.3219752754296894559, 0.3333333333333333703, 0.3219752754296894559, 0.3333333333333333703, 0.3219752754296894559, 0.3333333333333333703, 0.3219752754296894559, 0.3333333333333333703, 0.3219752754296894559, 0.3333333333333333703, 0.3219752754296894559, 0.3333333333333333703, 0.3219752754296894559, 0.3333333333333333703, 0.3219752754296894559, 0.3333333333333333703, 0.3219752754296894559, 0.3333333333333333703, 0.3219752754296894559, 0.3333333333333333703, 0.3219752754296894559, 0.3333333333333333703, 0.3219752754296894559, 0.3333333333333333703, 0.3219752754296894559, 0.3333333333333333703, 0.3219752754296894559, 0.3333333333333333703, 0.3219752754296894559, 0.3333333333333333703, 0.3219752754296894559, 0.3333333333333333703, 0.3219752754296894559, 0.3333333333333333703, 0.3219752754296894559, 0.3333333333333333703, 0.3219752754296894559, 0.3333333333333333703, 0.3219752754296894559, 0.3333333333333333703, 0.3219752754296894559, 0.3333333333333333703, 0.3219752754296894559, 0.3333333333333333703, 0.3219752754296894559, 0.3333333333333333703, 0.3219752754296894559, 0.3333333333333333703, 0.3219752754296894559, 0.3333333333333333703, 0.3219752754296894559, 0.3333333333333333703, 0.3219752754296894559, 0.3333333333333333703, 0.3219752754296894559, 0.3333333333333333703, 0.3219752754296894559, 0.3333333333333333703, 0.3219752754296894559, 0.3333333333333333703, 0.3219752754296894559, 0.3333333333333333703, 0.3219752754296894559, 0.3333333333333333703, 0.3219752754296894559, 0.3333333333333333703, 0.3219752754296894559, 0.3333333333333333703, 0.3219752754296894559, 0.3333333333333333703, 0.3219752754296894559, 0.3333333333333333703, 0.3219752754296894559, 0.3333333333333333703, 0.3219752754296894559, 0.3333333333333333703, 0.3219752754296894559, 0.3333333333333333703, 0.3219752754296894559, 0.3333333333333333703, 0.3219752754296894559, 0.3333333333333333703, 0.3219752754296894559, 0.3333333333333333703, 0.3219752754296894559, 0.3333333333333333703, 0.3219752754296894559, 0.3333333333333333703, 0.3219752754296894559, 0.3333333333333333703, 0.3219752754296894559, 0.3333333333333333703, 0.3219752754296894559, 0.3333333333333333703, 0.3219752754296894559, 0.3333333333333333703, 0.3219752754296894559, 0.3333333333333333703, 0.3219752754296894559, 0.3333333333333333703, 0.3219752754296894559, 0.3333333333333333703, 0.3219752754296894559, 0.3333333333333333703, 0.3219752754296894559, 0.3333333333333333703, 0.3219752754296894559, 0.3333333333333333703, 0.3219752754296894559, 0.3333333333333333703, 0.3219752754296894559, 0.3333333333333333703, 0.3219752754296894559, 0.3333333333333333703, 0.3219752754296894559, 0.3333333333333333703, 0.3219752754296894559, 0.3333333333333333703, 0.3219752754296894559, 0.3333333333333333703, 0.3219752754296894559, 0.3333333333333333703, 0.3219752754296894559, 0.3333333333333333703, 0.3219752754296894559, 0.3333333333333333703, 0.3219752754296894559, 0.3333333333333333703, 0.3219752754296894559, 0.3333333333333333703, 0.3219752754296894559, 0.3333333333333333703, 0.3219752754296894559, 0.3333333333333333703, 0.3219752754296894559, 0.3333333333333333703, 0.3219752754296894559, 0.3333333333333333703, 0.3219752754296894559, 0.3333333333333333703, 0.3219752754296894559, 0.3333333333333333703, 0.3219752754296894559, 0.3333333333333333703, 0.3219752754296894559, 0.3333333333333333703, 0.3219752754296894559, 0.3333333333333333703, 0.3219752754296894559, 0.3333333333333333703, 0.3219752754296894559, 0.3333333333333333703, 0.3219752754296894559, 0.3333333333333333703, 0.3219752754296894559, 0.3333333333333333703, 0.3219752754296894559, 0.3333333333333333703, 0.3219752754296894559, 0.3333333333333333703, 0.3219752754296894559, 0.3333333333333333703, 0.3219752754296894559, 0.3333333333333333703, 0.3219752754296894559, 0.3333333333333333703, 0.3219752754296894559, 0.3333333333333333703, 0.3219752754296894559, 0.3333333333333333703, 0.3219752754296894559, 0.3333333333333333703, 0.3219752754296894559, 0.3333333333333333703, 0.3219752754296894559, 0.3333333333333333703, 0.3219752754296894559, 0.3333333333333333703, 0.3219752754296894559, 0.3333333333333333703, 0.3219752754296894559, 0.3333333333333333703, 0.3219752754296894559, 0.3333333333333333703, 0.3219752754296894559, 0.3333333333333333703, 0.3219752754296894559, 0.3333333333333333703, 0.3219752754296894559, 0.3333333333333333703, 0.3219752754296894559, 0.3333333333333333703, 0.3219752754296894559, 0.3333333333333333703, 0.3219752754296894559, 0.3333333333333333703, 0.3219752754296894559, 0.3333333333333333703, 0.3219752754296894559, 0.3333333333333333703, 0.3219752754296894559, 0.3333333333333333703, 0.3219752754296894559, 0.3333333333333333703, 0.3219752754296894559, 0.3333333333333333703, 0.3219752754296894559, 0.3333333333333333703, 0.3219752754296894559, 0.3333333333333333703, 0.3219752754296894559, 0.3333333333333333703, 0.3219752754296894559, 0.3333333333333333703, 0.3219752754296894559, 0.3333333333333333703, 0.3219752754296894559, 0.3333333333333333703, 0.3219752754296894559, 0.3333333333333333703, 0.3219752754296894559, 0.3333333333333333703, 0.3219752754296894559, 0.3333333333333333703, 0.3219752754296894559, 0.3333333333333333703, 0.3219752754296894559, 0.3333333333333333703, 0.3219752754296894559, 0.3333333333333333703, 0.3219752754296894559, 0.3333333333333333703, 0.3219752754296894559, 0.3333333333333333703, 0.3219752754296894559, 0.3333333333333333703, 0.3219752754296894559, 0.3333333333333333703, 0.3219752754296894559, 0.3333333333333333703, 0.3219752754296894559, 0.3333333333333333703, 0.3219752754296894559, 0.3333333333333333703, 0.3219752754296894559, 0.3333333333333333703, 0.3219752754296894559, 0.3333333333333333703, 0.3219752754296894559, 0.3333333333333333703, 0.3219752754296894559, 0.3333333333333333703, 0.3219752754296894559, 0.3333333333333333703, 0.3219752754296894559, 0.3333333333333333703, 0.3219752754296894559, 0.3333333333333333703, 0.3219752754296894559, 0.3333333333333333703, 0.3219752754296894559, 0.3333333333333333703, 0.3219752754296894559, 0.3333333333333333703, 0.3219752754296894559, 0.3333333333333333703),
 ( 0.3333333333333333703, 0.3219752754296894559, 0.3333333333333333703, 0.3219752754296894559, 0.3333333333333333703, 0.3219752754296894559, 0.3333333333333333703, 0.3219752754296894559, 0.3333333333333333703, 0.3219752754296894559, 0.3333333333333333703, 0.3219752754296894559, 0.3333333333333333703, 0.3219752754296894559, 0.3333333333333333703, 0.3219752754296894559, 0.3333333333333333703, 0.3219752754296894559, 0.3333333333333333703, 0.3219752754296894559, 0.3333333333333333703, 0.3219752754296894559, 0.3333333333333333703, 0.3219752754296894559, 0.3333333333333333703, 0.3219752754296894559, 0.3333333333333333703, 0.3219752754296894559, 0.3333333333333333703, 0.3219752754296894559, 0.3333333333333333703, 0.3219752754296894559, 0.3333333333333333703, 0.3219752754296894559, 0.3333333333333333703, 0.3219752754296894559, 0.3333333333333333703, 0.3219752754296894559, 0.3333333333333333703, 0.3219752754296894559, 0.3333333333333333703, 0.3219752754296894559, 0.3333333333333333703, 0.3219752754296894559, 0.3333333333333333703, 0.3219752754296894559, 0.3333333333333333703, 0.3219752754296894559, 0.3333333333333333703, 0.3219752754296894559, 0.3333333333333333703, 0.3219752754296894559, 0.3333333333333333703, 0.3219752754296894559, 0.3333333333333333703, 0.3219752754296894559, 0.3333333333333333703, 0.3219752754296894559, 0.3333333333333333703, 0.3219752754296894559, 0.3333333333333333703, 0.3219752754296894559, 0.3333333333333333703, 0.3219752754296894559, 0.3333333333333333703, 0.3219752754296894559, 0.3333333333333333703, 0.3219752754296894559, 0.3333333333333333703, 0.3219752754296894559, 0.3333333333333333703, 0.3219752754296894559, 0.3333333333333333703, 0.3219752754296894559, 0.3333333333333333703, 0.3219752754296894559, 0.3333333333333333703, 0.3219752754296894559, 0.3333333333333333703, 0.3219752754296894559, 0.3333333333333333703, 0.3219752754296894559, 0.3333333333333333703, 0.3219752754296894559, 0.3333333333333333703, 0.3219752754296894559, 0.3333333333333333703, 0.3219752754296894559, 0.3333333333333333703, 0.3219752754296894559, 0.3333333333333333703, 0.3219752754296894559, 0.3333333333333333703, 0.3219752754296894559, 0.3333333333333333703, 0.3219752754296894559, 0.3333333333333333703, 0.3219752754296894559, 0.3333333333333333703, 0.3219752754296894559, 0.3333333333333333703, 0.3219752754296894559, 0.3333333333333333703, 0.3219752754296894559, 0.3333333333333333703, 0.3219752754296894559, 0.3333333333333333703, 0.3219752754296894559, 0.3333333333333333703, 0.3219752754296894559, 0.3333333333333333703, 0.3219752754296894559, 0.3333333333333333703, 0.3219752754296894559, 0.3333333333333333703, 0.3219752754296894559, 0.3333333333333333703, 0.3219752754296894559, 0.3333333333333333703, 0.3219752754296894559, 0.3333333333333333703, 0.3219752754296894559, 0.3333333333333333703, 0.3219752754296894559, 0.3333333333333333703, 0.3219752754296894559, 0.3333333333333333703, 0.3219752754296894559, 0.3333333333333333703, 0.3219752754296894559, 0.3333333333333333703, 0.3219752754296894559, 0.3333333333333333703, 0.3219752754296894559, 0.3333333333333333703, 0.3219752754296894559, 0.3333333333333333703, 0.3219752754296894559, 0.3333333333333333703, 0.3219752754296894559, 0.3333333333333333703, 0.3219752754296894559, 0.3333333333333333703, 0.3219752754296894559, 0.3333333333333333703, 0.3219752754296894559, 0.3333333333333333703, 0.3219752754296894559, 0.3333333333333333703, 0.3219752754296894559, 0.3333333333333333703, 0.3219752754296894559, 0.3333333333333333703, 0.3219752754296894559, 0.3333333333333333703, 0.3219752754296894559, 0.3333333333333333703, 0.3219752754296894559, 0.3333333333333333703, 0.3219752754296894559, 0.3333333333333333703, 0.3219752754296894559, 0.3333333333333333703, 0.3219752754296894559, 0.3333333333333333703, 0.3219752754296894559, 0.3333333333333333703, 0.3219752754296894559, 0.3333333333333333703, 0.3219752754296894559, 0.3333333333333333703, 0.3219752754296894559, 0.3333333333333333703, 0.3219752754296894559, 0.3333333333333333703, 0.3219752754296894559, 0.3333333333333333703, 0.3219752754296894559, 0.3333333333333333703, 0.3219752754296894559, 0.3333333333333333703, 0.3219752754296894559, 0.3333333333333333703, 0.3219752754296894559, 0.3333333333333333703, 0.3219752754296894559, 0.3333333333333333703, 0.3219752754296894559, 0.3333333333333333703, 0.3219752754296894559, 0.3333333333333333703, 0.3219752754296894559, 0.3333333333333333703, 0.3219752754296894559, 0.3333333333333333703, 0.3219752754296894559, 0.3333333333333333703, 0.3219752754296894559, 0.3333333333333333703, 0.3219752754296894559, 0.3333333333333333703, 0.3219752754296894559, 0.3333333333333333703, 0.3219752754296894559, 0.3333333333333333703, 0.3219752754296894559, 0.3333333333333333703, 0.3219752754296894559, 0.3333333333333333703, 0.3219752754296894559, 0.3333333333333333703, 0.3219752754296894559, 0.3333333333333333703, 0.3219752754296894559, 0.3333333333333333703, 0.3219752754296894559, 0.3333333333333333703, 0.3219752754296894559, 0.3333333333333333703, 0.3219752754296894559, 0.3333333333333333703, 0.3219752754296894559, 0.3333333333333333703, 0.3219752754296894559, 0.3333333333333333703, 0.3219752754296894559, 0.3333333333333333703, 0.3219752754296894559, 0.3333333333333333703, 0.3219752754296894559, 0.3333333333333333703, 0.3219752754296894559, 0.3333333333333333703, 0.3219752754296894559, 0.3333333333333333703, 0.3219752754296894559, 0.3333333333333333703, 0.3219752754296894559, 0.3333333333333333703, 0.3219752754296894559, 0.3333333333333333703, 0.3219752754296894559, 0.3333333333333333703, 0.3219752754296894559, 0.3333333333333333703, 0.3219752754296894559, 0.3333333333333333703, 0.3219752754296894559, 0.3333333333333333703, 0.3219752754296894559, 0.3333333333333333703, 0.3219752754296894559, 0.3333333333333333703, 0.3219752754296894559, 0.3333333333333333703, 0.3219752754296894559, 0.3333333333333333703, 0.3219752754296894559, 0.3333333333333333703, 0.3219752754296894559, 0.3333333333333333703, 0.3219752754296894559, 0.3333333333333333703, 0.3219752754296894559, 0.3333333333333333703, 0.3219752754296894559, 0.3333333333333333703, 0.3219752754296894559, 0.3333333333333333703, 0.3219752754296894559, 0.3333333333333333703, 0.3219752754296894559, 0.3333333333333333703, 0.3219752754296894559, 0.3333333333333333703, 0.3219752754296894559, 0.3333333333333333703, 0.3219752754296894559, 0.3333333333333333703, 0.3219752754296894559, 0.3333333333333333703, 0.3219752754296894559, 0.3333333333333333703, 0.3219752754296894559, 0.3333333333333333703, 0.3219752754296894559, 0.3333333333333333703, 0.3219752754296894559, 0.3333333333333333703, 0.3219752754296894559, 0.3333333333333333703, 0.3219752754296894559, 0.3333333333333333703, 0.3219752754296894559, 0.3333333333333333703, 0.3219752754296894559, 0.3333333333333333703, 0.3219752754296894559, 0.3333333333333333703, 0.3219752754296894559, 0.3333333333333333703, 0.3219752754296894559, 0.3333333333333333703, 0.3219752754296894559, 0.3333333333333333703, 0.3219752754296894559, 0.3333333333333333703, 0.3219752754296894559, 0.3333333333333333703, 0.3219752754296894559, 0.3333333333333333703, 0.3219752754296894559, 0.3333333333333333703, 0.3219752754296894559, 0.3333333333333333703, 0.3219752754296894559, 0.3333333333333333703, 0.3219752754296894559, 0.3333333333333333703, 0.3219752754296894559, 0.3333333333333333703, 0.3219752754296894559, 0.3333333333333333703, 0.3219752754296894559, 0.3333333333333333703, 0.3219752754296894559, 0.3333333333333333703, 0.3219752754296894559, 0.3333333333333333703, 0.3219752754296894559, 0.3333333333333333703, 0.3219752754296894559, 0.3333333333333333703, 0.3219752754296894559, 0.3333333333333333703, 0.3219752754296894559, 0.3333333333333333703, 0.3219752754296894559, 0.3333333333333333703, 0.3219752754296894559, 0.3333333333333333703, 0.3219752754296894559, 0.3333333333333333703, 0.3219752754296894559, 0.3333333333333333703, 0.3219752754296894559, 0.3333333333333333703, 0.3219752754296894559, 0.3333333333333333703, 0.3219752754296894559, 0.3333333333333333703, 0.3219752754296894559, 0.3333333333333333703, 0.3219752754296894559, 0.3333333333333333703, 0.3219752754296894559, 0.3333333333333333703, 0.3219752754296894559, 0.3333333333333333703, 0.3219752754296894559, 0.3333333333333333703, 0.3219752754296894559, 0.3333333333333333703, 0.3219752754296894559, 0.3333333333333333703, 0.3219752754296894559, 0.3333333333333333703, 0.3219752754296894559, 0.3333333333333333703, 0.3219752754296894559, 0.3333333333333333703, 0.3219752754296894559, 0.3333333333333333703, 0.3219752754296894559, 0.3333333333333333703, 0.3219752754296894559, 0.3333333333333333703, 0.3219752754296894559, 0.3333333333333333703, 0.3219752754296894559, 0.3333333333333333703, 0.3219752754296894559, 0.3333333333333333703, 0.3219752754296894559, 0.3333333333333333703, 0.3219752754296894559, 0.3333333333333333703, 0.3219752754296894559, 0.3333333333333333703, 0.3219752754296894559, 0.3333333333333333703, 0.3219752754296894559, 0.3333333333333333703, 0.3219752754296894559, 0.3333333333333333703, 0.3219752754296894559, 0.3333333333333333703, 0.3219752754296894559, 0.3333333333333333703, 0.3219752754296894559, 0.3333333333333333703, 0.3219752754296894559, 0.3333333333333333703, 0.3219752754296894559, 0.3333333333333333703, 0.3219752754296894559, 0.3333333333333333703, 0.3219752754296894559, 0.3333333333333333703, 0.3219752754296894559, 0.3333333333333333703, 0.3219752754296894559, 0.3333333333333333703, 0.3219752754296894559, 0.3333333333333333703, 0.3219752754296894559, 0.3333333333333333703, 0.3219752754296894559, 0.3333333333333333703, 0.3219752754296894559, 0.3333333333333333703, 0.3219752754296894559, 0.3333333333333333703, 0.3219752754296894559, 0.3333333333333333703, 0.3219752754296894559, 0.3333333333333333703, 0.3219752754296894559, 0.3333333333333333703, 0.3219752754296894559, 0.3333333333333333703, 0.3219752754296894559, 0.3333333333333333703, 0.3219752754296894559, 0.3333333333333333703, 0.3219752754296894559, 0.3333333333333333703, 0.3219752754296894559, 0.3333333333333333703, 0.3219752754296894559, 0.3333333333333333703, 0.3219752754296894559, 0.3333333333333333703, 0.3219752754296894559, 0.3333333333333333703, 0.3219752754296894559, 0.3333333333333333703, 0.3219752754296894559, 0.3333333333333333703, 0.3219752754296894559, 0.3333333333333333703, 0.3219752754296894559, 0.3333333333333333703, 0.3219752754296894559, 0.3333333333333333703, 0.3219752754296894559, 0.3333333333333333703),
 ( 1.000000000000000000, 0.9659258262890683122, 1.000000000000000000, 0.9659258262890683122, 1.000000000000000000, 0.9659258262890683122, 1.000000000000000000, 0.9659258262890683122, 1.000000000000000000, 0.9659258262890683122, 1.000000000000000000, 0.9659258262890683122, 1.000000000000000000, 0.9659258262890683122, 1.000000000000000000, 0.9659258262890683122, 1.000000000000000000, 0.9659258262890683122, 1.000000000000000000, 0.9659258262890683122, 1.000000000000000000, 0.9659258262890683122, 1.000000000000000000, 0.9659258262890683122, 1.000000000000000000, 0.9659258262890683122, 1.000000000000000000, 0.9659258262890683122, 1.000000000000000000, 0.9659258262890683122, 1.000000000000000000, 0.9659258262890683122, 1.000000000000000000, 0.9659258262890683122, 1.000000000000000000, 0.9659258262890683122, 1.000000000000000000, 0.9659258262890683122, 1.000000000000000000, 0.9659258262890683122, 1.000000000000000000, 0.9659258262890683122, 1.000000000000000000, 0.9659258262890683122, 1.000000000000000000, 0.9659258262890683122, 1.000000000000000000, 0.9659258262890683122, 1.000000000000000000, 0.9659258262890683122, 1.000000000000000000, 0.9659258262890683122, 1.000000000000000000, 0.9659258262890683122, 1.000000000000000000, 0.9659258262890683122, 1.000000000000000000, 0.9659258262890683122, 1.000000000000000000, 0.9659258262890683122, 1.000000000000000000, 0.9659258262890683122, 1.000000000000000000, 0.9659258262890683122, 1.000000000000000000, 0.9659258262890683122, 1.000000000000000000, 0.9659258262890683122, 1.000000000000000000, 0.9659258262890683122, 1.000000000000000000, 0.9659258262890683122, 1.000000000000000000, 0.9659258262890683122, 1.000000000000000000, 0.9659258262890683122, 1.000000000000000000, 0.9659258262890683122, 1.000000000000000000, 0.9659258262890683122, 1.000000000000000000, 0.9659258262890683122, 1.000000000000000000, 0.9659258262890683122, 1.000000000000000000, 0.9659258262890683122, 1.000000000000000000, 0.9659258262890683122, 1.000000000000000000, 0.9659258262890683122, 1.000000000000000000, 0.9659258262890683122, 1.000000000000000000, 0.9659258262890683122, 1.000000000000000000, 0.9659258262890683122, 1.000000000000000000, 0.9659258262890683122, 1.000000000000000000, 0.9659258262890683122, 1.000000000000000000, 0.9659258262890683122, 1.000000000000000000, 0.9659258262890683122, 1.000000000000000000, 0.9659258262890683122, 1.000000000000000000, 0.9659258262890683122, 1.000000000000000000, 0.9659258262890683122, 1.000000000000000000, 0.9659258262890683122, 1.000000000000000000, 0.9659258262890683122, 1.000000000000000000, 0.9659258262890683122, 1.000000000000000000, 0.9659258262890683122, 1.000000000000000000, 0.9659258262890683122, 1.000000000000000000, 0.9659258262890683122, 1.000000000000000000, 0.9659258262890683122, 1.000000000000000000, 0.9659258262890683122, 1.000000000000000000, 0.9659258262890683122, 1.000000000000000000, 0.9659258262890683122, 1.000000000000000000, 0.9659258262890683122, 1.000000000000000000, 0.9659258262890683122, 1.000000000000000000, 0.9659258262890683122, 1.000000000000000000, 0.9659258262890683122, 1.000000000000000000, 0.9659258262890683122, 1.000000000000000000, 0.9659258262890683122, 1.000000000000000000, 0.9659258262890683122, 1.000000000000000000, 0.9659258262890683122, 1.000000000000000000, 0.9659258262890683122, 1.000000000000000000, 0.9659258262890683122, 1.000000000000000000, 0.9659258262890683122, 1.000000000000000000, 0.9659258262890683122, 1.000000000000000000, 0.9659258262890683122, 1.000000000000000000, 0.9659258262890683122, 1.000000000000000000, 0.9659258262890683122, 1.000000000000000000, 0.9659258262890683122, 1.000000000000000000, 0.9659258262890683122, 1.000000000000000000, 0.9659258262890683122, 1.000000000000000000, 0.9659258262890683122, 1.000000000000000000, 0.9659258262890683122, 1.000000000000000000, 0.9659258262890683122, 1.000000000000000000, 0.9659258262890683122, 1.000000000000000000, 0.9659258262890683122, 1.000000000000000000, 0.9659258262890683122, 1.000000000000000000, 0.9659258262890683122, 1.000000000000000000, 0.9659258262890683122, 1.000000000000000000, 0.9659258262890683122, 1.000000000000000000, 0.9659258262890683122, 1.000000000000000000, 0.9659258262890683122, 1.000000000000000000, 0.9659258262890683122, 1.000000000000000000, 0.9659258262890683122, 1.000000000000000000, 0.9659258262890683122, 1.000000000000000000, 0.9659258262890683122, 1.000000000000000000, 0.9659258262890683122, 1.000000000000000000, 0.9659258262890683122, 1.000000000000000000, 0.9659258262890683122, 1.000000000000000000, 0.9659258262890683122, 1.000000000000000000, 0.9659258262890683122, 1.000000000000000000, 0.9659258262890683122, 1.000000000000000000, 0.9659258262890683122, 1.000000000000000000, 0.9659258262890683122, 1.000000000000000000, 0.9659258262890683122, 1.000000000000000000, 0.9659258262890683122, 1.000000000000000000, 0.9659258262890683122, 1.000000000000000000, 0.9659258262890683122, 1.000000000000000000, 0.9659258262890683122, 1.000000000000000000, 0.9659258262890683122, 1.000000000000000000, 0.9659258262890683122, 1.000000000000000000, 0.9659258262890683122, 1.000000000000000000, 0.9659258262890683122, 1.000000000000000000, 0.9659258262890683122, 1.000000000000000000, 0.9659258262890683122, 1.000000000000000000, 0.9659258262890683122, 1.000000000000000000, 0.9659258262890683122, 1.000000000000000000, 0.9659258262890683122, 1.000000000000000000, 0.9659258262890683122, 1.000000000000000000, 0.9659258262890683122, 1.000000000000000000, 0.9659258262890683122, 1.000000000000000000, 0.9659258262890683122, 1.000000000000000000, 0.9659258262890683122, 1.000000000000000000, 0.9659258262890683122, 1.000000000000000000, 0.9659258262890683122, 1.000000000000000000, 0.9659258262890683122, 1.000000000000000000, 0.9659258262890683122, 1.000000000000000000, 0.9659258262890683122, 1.000000000000000000, 0.9659258262890683122, 1.000000000000000000, 0.9659258262890683122, 1.000000000000000000, 0.9659258262890683122, 1.000000000000000000, 0.9659258262890683122, 1.000000000000000000, 0.9659258262890683122, 1.000000000000000000, 0.9659258262890683122, 1.000000000000000000, 0.9659258262890683122, 1.000000000000000000, 0.9659258262890683122, 1.000000000000000000, 0.9659258262890683122, 1.000000000000000000, 0.9659258262890683122, 1.000000000000000000, 0.9659258262890683122, 1.000000000000000000, 0.9659258262890683122, 1.000000000000000000, 0.9659258262890683122, 1.000000000000000000, 0.9659258262890683122, 1.000000000000000000, 0.9659258262890683122, 1.000000000000000000, 0.9659258262890683122, 1.000000000000000000, 0.9659258262890683122, 1.000000000000000000, 0.9659258262890683122, 1.000000000000000000, 0.9659258262890683122, 1.000000000000000000, 0.9659258262890683122, 1.000000000000000000, 0.9659258262890683122, 1.000000000000000000, 0.9659258262890683122, 1.000000000000000000, 0.9659258262890683122, 1.000000000000000000, 0.9659258262890683122, 1.000000000000000000, 0.9659258262890683122, 1.000000000000000000, 0.9659258262890683122, 1.000000000000000000, 0.9659258262890683122, 1.000000000000000000, 0.9659258262890683122, 1.000000000000000000, 0.9659258262890683122, 1.000000000000000000, 0.9659258262890683122, 1.000000000000000000, 0.9659258262890683122, 1.000000000000000000, 0.9659258262890683122, 1.000000000000000000, 0.9659258262890683122, 1.000000000000000000, 0.9659258262890683122, 1.000000000000000000, 0.9659258262890683122, 1.000000000000000000, 0.9659258262890683122, 1.000000000000000000, 0.9659258262890683122, 1.000000000000000000, 0.9659258262890683122, 1.000000000000000000, 0.9659258262890683122, 1.000000000000000000, 0.9659258262890683122, 1.000000000000000000, 0.9659258262890683122, 1.000000000000000000, 0.9659258262890683122, 1.000000000000000000, 0.9659258262890683122, 1.000000000000000000, 0.9659258262890683122, 1.000000000000000000, 0.9659258262890683122, 1.000000000000000000, 0.9659258262890683122, 1.000000000000000000, 0.9659258262890683122, 1.000000000000000000, 0.9659258262890683122, 1.000000000000000000, 0.9659258262890683122, 1.000000000000000000, 0.9659258262890683122, 1.000000000000000000, 0.9659258262890683122, 1.000000000000000000, 0.9659258262890683122, 1.000000000000000000, 0.9659258262890683122, 1.000000000000000000, 0.9659258262890683122, 1.000000000000000000, 0.9659258262890683122, 1.000000000000000000, 0.9659258262890683122, 1.000000000000000000, 0.9659258262890683122, 1.000000000000000000, 0.9659258262890683122, 1.000000000000000000, 0.9659258262890683122, 1.000000000000000000, 0.9659258262890683122, 1.000000000000000000, 0.9659258262890683122, 1.000000000000000000, 0.9659258262890683122, 1.000000000000000000, 0.9659258262890683122, 1.000000000000000000, 0.9659258262890683122, 1.000000000000000000, 0.9659258262890683122, 1.000000000000000000, 0.9659258262890683122, 1.000000000000000000, 0.9659258262890683122, 1.000000000000000000, 0.9659258262890683122, 1.000000000000000000, 0.9659258262890683122, 1.000000000000000000, 0.9659258262890683122, 1.000000000000000000, 0.9659258262890683122, 1.000000000000000000, 0.9659258262890683122, 1.000000000000000000, 0.9659258262890683122, 1.000000000000000000, 0.9659258262890683122, 1.000000000000000000, 0.9659258262890683122, 1.000000000000000000, 0.9659258262890683122, 1.000000000000000000, 0.9659258262890683122, 1.000000000000000000, 0.9659258262890683122, 1.000000000000000000, 0.9659258262890683122, 1.000000000000000000, 0.9659258262890683122, 1.000000000000000000, 0.9659258262890683122, 1.000000000000000000, 0.9659258262890683122, 1.000000000000000000, 0.9659258262890683122, 1.000000000000000000, 0.9659258262890683122, 1.000000000000000000, 0.9659258262890683122, 1.000000000000000000, 0.9659258262890683122, 1.000000000000000000, 0.9659258262890683122, 1.000000000000000000, 0.9659258262890683122, 1.000000000000000000, 0.9659258262890683122, 1.000000000000000000, 0.9659258262890683122, 1.000000000000000000, 0.9659258262890683122, 1.000000000000000000, 0.9659258262890683122, 1.000000000000000000, 0.9659258262890683122, 1.000000000000000000, 0.9659258262890683122, 1.000000000000000000, 0.9659258262890683122, 1.000000000000000000, 0.9659258262890683122, 1.000000000000000000, 0.9659258262890683122, 1.000000000000000000, 0.9659258262890683122, 1.000000000000000000) ) ) 
 REPRESENTATION_ITEM ( '' )  SURFACE ( )  );
#183995 = CARTESIAN_POINT ( 'NONE',  ( -14.29746914071037622, -8.314922557961029526, 49.16775706135234003 ) ) ;
#183996 = CARTESIAN_POINT ( 'NONE',  ( -9.564922557960796823, -16.46253265017161027, 97.08224293864769550 ) ) ;
#183997 = CARTESIAN_POINT ( 'NONE',  ( 21.53943276465977519, -0.05219959533907433946, 103.7489096053143669 ) ) ;
#183998 = CARTESIAN_POINT ( 'NONE',  ( 13.97604488694527802, 13.89961937509977652, 74.37390960531436690 ) ) ;
#183999 = FACE_OUTER_BOUND ( 'NONE', #193431, .T. ) ;
#184000 = FACE_BOUND ( 'NONE', #116432, .T. ) ;
#184001 = CARTESIAN_POINT ( 'NONE',  ( 4.379528057220339221, -16.55341960407611168, 87.70724293864769550 ) ) ;
#184002 = CARTESIAN_POINT ( 'NONE',  ( -10.81492255796078084, -18.62759615963271287, 37.08224293864768129 ) ) ;
#184003 = CARTESIAN_POINT ( 'NONE',  ( 19.02544592524343514, -5.153800228976328945, 23.54057627198102054 ) ) ;
#184004 = CARTESIAN_POINT ( 'NONE',  ( 16.53943276465976808, 0.05219959533934440121, 61.25109039468567573 ) ) ;
#184005 = CARTESIAN_POINT ( 'NONE',  ( 0.05219959533907565091, 21.53943276465977519, 114.9989096053143669 ) ) ;
#184006 = CARTESIAN_POINT ( 'NONE',  ( 13.97604488694548053, -13.89961937509957401, 75.62609039468564731 ) ) ;
#184007 = CARTESIAN_POINT ( 'NONE',  ( -19.02544592524342804, 5.153800228976336051, 26.04057627198103120 ) ) ;
#184008 = CARTESIAN_POINT ( 'NONE',  ( 10.72451020669898902, -18.67979575497178502, 62.91557627198102409 ) ) ;
#184009 = VECTOR ( 'NONE', #150512, 1000.000000000000000 ) ;
#184010 = CARTESIAN_POINT ( 'NONE',  ( 13.89961937509977652, -13.97604488694527269, 103.1239096053143527 ) ) ;
#184011 = CARTESIAN_POINT ( 'NONE',  ( 0.05219959533937995610, -21.53943276465977519, 95.00109039468568994 ) ) ;
#184012 = CARTESIAN_POINT ( 'NONE',  ( 0.05219959533909260263, 19.03943276465977164, 64.99890960531436690 ) ) ;
#184013 = CARTESIAN_POINT ( 'NONE',  ( -0.05219959533934338120, 16.53943276465976808, 52.50109039468567573 ) ) ;
#184014 = CARTESIAN_POINT ( 'NONE',  ( -16.51473224551069308, -9.474510206698971260, 56.66557627198103120 ) ) ;
#184015 = CARTESIAN_POINT ( 'NONE',  ( 18.62759615963255655, 10.81492255796105972, 81.66775706135236135 ) ) ;
#184016 = ORIENTED_EDGE ( 'NONE', *, *, #76288, .F. ) ;
#184017 = CARTESIAN_POINT ( 'NONE',  ( -5.153800228976607833, 19.02544592524334988, 42.70942372801901143 ) ) ;
#184018 = CARTESIAN_POINT ( 'NONE',  ( -5.049401038297874678, -19.05341960407617918, 59.79275706135231871 ) ) ;
#184019 = CARTESIAN_POINT ( 'NONE',  ( -15.72974639402176322, -15.80617190586768395, 54.37609039468568994 ) ) ;
#184020 = FACE_OUTER_BOUND ( 'NONE', #62328, .T. ) ;
#184021 = CARTESIAN_POINT ( 'NONE',  ( -13.97604488694547697, 13.89961937509957934, 43.12609039468566152 ) ) ;
#184022 = CARTESIAN_POINT ( 'NONE',  ( -19.05341960407611168, -5.049401038298163336, 101.4572429386476955 ) ) ;
#184023 = CARTESIAN_POINT ( 'NONE',  ( 9.474510206698971260, -16.51473224551069308, 72.91557627198102409 ) ) ;
#184024 = CARTESIAN_POINT ( 'NONE',  ( 4.379528057220092307, 16.55341960407617563, 112.2927570613523471 ) ) ;
#184026 = CARTESIAN_POINT ( 'NONE',  ( 18.62759615963255655, 10.81492255796105972, 96.66775706135234714 ) ) ;
#184025 = CARTESIAN_POINT ( 'NONE',  ( -10.81492255796078084, -18.62759615963271287, 37.08224293864768129 ) ) ;
#184027 = CARTESIAN_POINT ( 'NONE',  ( -36.91746825000000598, 2.428612866367529932E-14, -2.624999997268813168 ) ) ;
#184028 = CARTESIAN_POINT ( 'NONE',  ( 17.44279575226823198, 5.990770900252482711, 56.66442432485683156 ) ) ;
#184029 = CARTESIAN_POINT ( 'NONE',  ( -21.53943276465977519, -0.05219959533937600094, 103.7510903946857042 ) ) ;
#184030 = CARTESIAN_POINT ( 'NONE',  ( 17.31728774477273447, -6.344390552232384906, 43.31906651689319432 ) ) ;
#184031 = CARTESIAN_POINT ( 'NONE',  ( -19.03943276465977164, 0.05219959533909376836, 26.24890960531435624 ) ) ;
#184032 = CARTESIAN_POINT ( 'NONE',  ( -5.153800228976328057, -19.02544592524343514, 112.2905762719810099 ) ) ;
#184033 = CARTESIAN_POINT ( 'NONE',  ( 33.98302989258738194, 4.936846515367096622, 92.54907045995906856 ) ) ;
#184034 = CARTESIAN_POINT ( 'NONE',  ( -16.52544592524335698, -4.483927247898792601, 48.95942372801902565 ) ) ;
#184035 = CARTESIAN_POINT ( 'NONE',  ( -15.72974639402197994, 15.80617190586746368, 70.62390960531436690 ) ) ;
#184036 = CARTESIAN_POINT ( 'NONE',  ( -8.224510206698948167, 14.34966873604960824, 40.41557627198103120 ) ) ;
#184038 = CARTESIAN_POINT ( 'NONE',  ( 19.02544592524343514, -5.153800228976328945, 108.5405762719810383 ) ) ;
#184037 = CARTESIAN_POINT ( 'NONE',  ( -16.53943276465976808, 0.05219959533911058130, 106.2489096053143811 ) ) ;
#184039 = CARTESIAN_POINT ( 'NONE',  ( -13.89961937509957401, -13.97604488694547875, 39.37609039468566152 ) ) ;
#184040 = CARTESIAN_POINT ( 'NONE',  ( 19.05341960407611168, 5.049401038298154454, 23.95724293864769194 ) ) ;
#184041 = CARTESIAN_POINT ( 'NONE',  ( -21.53943276465977519, -0.05219959533937600094, 63.75109039468568284 ) ) ;
#184042 = CARTESIAN_POINT ( 'NONE',  ( -18.22780087662122028, 5.500000000000031086, 78.51540105326107266 ) ) ;
#184043 = CARTESIAN_POINT ( 'NONE',  ( 14.34966873604972726, -8.224510206698740333, 105.8344237280190328 ) ) ;
#184044 = CARTESIAN_POINT ( 'NONE',  ( -5.153800228976607833, 19.02544592524335343, 67.70942372801900433 ) ) ;
#184045 = CARTESIAN_POINT ( 'NONE',  ( -5.719274019375978568, 21.55341960407610458, 25.20724293864769550 ) ) ;
#184046 = CARTESIAN_POINT ( 'NONE',  ( 16.55341960407611168, 4.379528057220329451, 88.95724293864769550 ) ) ;
#184047 = CARTESIAN_POINT ( 'NONE',  ( -13.97604488694547697, 13.89961937509957934, 58.12609039468566863 ) ) ;
#184048 = CARTESIAN_POINT ( 'NONE',  ( -13.97604488694527625, -13.89961937509977652, 71.87390960531433848 ) ) ;
#184049 = CARTESIAN_POINT ( 'NONE',  ( -16.55341960407611168, -4.379528057220339221, 81.45724293864769550 ) ) ;
#184050 = CARTESIAN_POINT ( 'NONE',  ( 13.89961937509957401, 13.97604488694547697, 86.87609039468567573 ) ) ;
#184051 = CARTESIAN_POINT ( 'NONE',  ( 15.80617190586746368, 15.72974639402197994, 44.37390960531435979 ) ) ;
#184052 = ORIENTED_EDGE ( 'NONE', *, *, #121704, .T. ) ;
#184053 = CARTESIAN_POINT ( 'NONE',  ( 16.52544592524342804, -4.483927247898539470, 108.5405762719810241 ) ) ;
#184054 = CARTESIAN_POINT ( 'NONE',  ( -16.31925111598457789, -7.325300261831485749, 29.83575461032750553 ) ) ;
#184056 = CARTESIAN_POINT ( 'NONE',  ( 0.05219959533907565091, 21.53943276465977519, 69.99890960531435269 ) ) ;
#184055 = CARTESIAN_POINT ( 'NONE',  ( 9.474510206698971260, -16.51473224551069308, 67.91557627198102409 ) ) ;
#184058 = CARTESIAN_POINT ( 'NONE',  ( -9.564922557960796823, -16.46253265017161027, 87.08224293864769550 ) ) ;
#184057 = CARTESIAN_POINT ( 'NONE',  ( 14.34966873604972726, -8.224510206698740333, 85.83442372801901854 ) ) ;
#184059 = CARTESIAN_POINT ( 'NONE',  ( -16.46253265017146816, -9.564922557961047289, 69.16775706135233293 ) ) ;
#184060 = CARTESIAN_POINT ( 'NONE',  ( -5.719274019375665041, -21.55341960407619695, 79.79275706135236135 ) ) ;
#184061 = CARTESIAN_POINT ( 'NONE',  ( -21.52544592524343514, 5.823673210054127303, 66.04057627198103830 ) ) ;
#184062 = CARTESIAN_POINT ( 'NONE',  ( -0.05219959533907301413, -21.53943276465977519, 22.49890960531436335 ) ) ;
#184063 = CARTESIAN_POINT ( 'NONE',  ( -9.564922557960796823, -16.46253265017161027, 42.08224293864769550 ) ) ;
#184064 = CARTESIAN_POINT ( 'NONE',  ( 14.29746914071037800, 8.314922557961029526, 106.6677570613523756 ) ) ;
#184065 = CARTESIAN_POINT ( 'NONE',  ( -13.89961937509977652, 13.97604488694528158, 60.62390960531436690 ) ) ;
#184066 = CARTESIAN_POINT ( 'NONE',  ( -4.483927247898782831, 16.52544592524335698, 27.70942372801901854 ) ) ;
#184067 = CARTESIAN_POINT ( 'NONE',  ( -31.65994483839897100, -2.419126180341527821, 102.1034561864646122 ) ) ;
#184068 = CARTESIAN_POINT ( 'NONE',  ( -5.823673210054431948, 21.52544592524334988, 107.7094237280190328 ) ) ;
#184069 = CARTESIAN_POINT ( 'NONE',  ( 8.314922557960818139, 14.29746914071049879, 79.58224293864769550 ) ) ;
#184070 = CARTESIAN_POINT ( 'NONE',  ( -5.719274019375978568, 21.55341960407610458, 110.2072429386477239 ) ) ;
#184071 = CARTESIAN_POINT ( 'NONE',  ( -21.55341960407610458, -5.719274019375992779, 101.4572429386476955 ) ) ;
#184072 = CARTESIAN_POINT ( 'NONE',  ( 8.571926809382597767, 26.38167802310806209, 140.7750000027311899 ) ) ;
#184073 = CARTESIAN_POINT ( 'NONE',  ( 18.67979575497178502, 10.72451020669898547, 49.16557627198102409 ) ) ;
#184074 = CARTESIAN_POINT ( 'NONE',  ( 16.55341960407618274, -4.379528057220086978, 76.04275706135237556 ) ) ;
#184075 = CARTESIAN_POINT ( 'NONE',  ( 4.379528057220339221, -16.55341960407611168, 107.7072429386476955 ) ) ;
#184076 = CARTESIAN_POINT ( 'NONE',  ( -16.51473224551069308, -9.474510206698971260, 61.66557627198103120 ) ) ;
#184077 = CARTESIAN_POINT ( 'NONE',  ( -12.39597446193840291, -43.61540881465732156, -22.87833536075119767 ) ) ;
#184078 = CARTESIAN_POINT ( 'NONE',  ( -16.55341960407617563, 4.379528057220093196, 108.5427570613523756 ) ) ;
#184079 = ORIENTED_EDGE ( 'NONE', *, *, #13320, .F. ) ;
#184080 = CARTESIAN_POINT ( 'NONE',  ( 18.67979575497194134, -10.72451020669871369, 50.83442372801901143 ) ) ;
#184081 = CARTESIAN_POINT ( 'NONE',  ( 5.049401038298161559, -19.05341960407611168, 92.70724293864769550 ) ) ;
#184082 = CARTESIAN_POINT ( 'NONE',  ( 21.55341960407619695, -5.719274019375665929, 86.04275706135236135 ) ) ;
#184083 = CARTESIAN_POINT ( 'NONE',  ( -0.05219959533909027116, -19.03943276465977164, 22.49890960531436690 ) ) ;
#184085 = EDGE_CURVE ( 'NONE', #20570, #89709, #107532, .T. ) ;
#184084 = CARTESIAN_POINT ( 'NONE',  ( 19.02544592524343514, -5.153800228976328945, 23.54057627198102054 ) ) ;
#184086 = VERTEX_POINT ( 'NONE', #127014 ) ;
#184087 = CARTESIAN_POINT ( 'NONE',  ( 15.72974639402176855, 15.80617190586768217, 66.87609039468568994 ) ) ;
#184088 = CARTESIAN_POINT ( 'NONE',  ( -16.51473224551069308, -9.474510206698971260, 56.66557627198103120 ) ) ;
#184089 = CARTESIAN_POINT ( 'NONE',  ( 19.02544592524343514, -5.153800228976328945, 108.5405762719810383 ) ) ;
#184090 = CARTESIAN_POINT ( 'NONE',  ( 19.02544592524334988, 5.153800228976608722, 86.45942372801900433 ) ) ;
#184091 = CARTESIAN_POINT ( 'NONE',  ( -10.72451020669870658, -18.67979575497194134, 44.58442372801901854 ) ) ;
#184092 = CARTESIAN_POINT ( 'NONE',  ( -19.03943276465977164, -0.05219959533935918106, 108.7510903946856615 ) ) ;
#184093 = CARTESIAN_POINT ( 'NONE',  ( -13.97604488694547697, 13.89961937509957934, 73.12609039468568994 ) ) ;
#184094 = CARTESIAN_POINT ( 'NONE',  ( 13.97604488694527802, 13.89961937509977652, 44.37390960531435269 ) ) ;
#184095 = CARTESIAN_POINT ( 'NONE',  ( -13.89961937509957401, -13.97604488694547875, 89.37609039468563310 ) ) ;
#184096 = CARTESIAN_POINT ( 'NONE',  ( 0.05219959533934541429, -16.53943276465976808, 110.0010903946856757 ) ) ;
#184097 = CARTESIAN_POINT ( 'NONE',  ( 9.474510206698729675, 16.51473224551082808, 77.08442372801900433 ) ) ;
#184098 = CARTESIAN_POINT ( 'NONE',  ( 4.379528057220339221, -16.55341960407611168, 32.70724293864770260 ) ) ;
#184099 = CARTESIAN_POINT ( 'NONE',  ( -5.049401038297874678, -19.05341960407617918, 64.79275706135233293 ) ) ;
#184100 = CARTESIAN_POINT ( 'NONE',  ( -10.81492255796105439, 18.62759615963255655, 102.9177570613523756 ) ) ;
#184101 = PRODUCT ( 'Mica Insulated Heating Coil Unit', 'Mica Insulated Heating Coil Unit', '', ( #113931 ) ) ;
#184102 = CARTESIAN_POINT ( 'NONE',  ( 19.02544592524334988, 5.153800228976608722, 31.45942372801900433 ) ) ;
#184103 = CARTESIAN_POINT ( 'NONE',  ( -16.46253265017160317, 9.564922557960807481, 35.83224293864768839 ) ) ;
#184104 = DIRECTION ( 'NONE',  ( -4.336808689942018352E-17, 1.000000000000000000, 0.000000000000000000 ) ) ;
#184105 = CARTESIAN_POINT ( 'NONE',  ( -16.53943276465976808, -0.05219959533934237506, 43.75109039468568284 ) ) ;
#184106 = DIRECTION ( 'NONE',  ( -1.000000000000000000, 0.000000000000000000, 0.000000000000000000 ) ) ;
#184107 = B_SPLINE_CURVE_WITH_KNOTS ( 'NONE', 3,
 ( #176823, #85790, #119142, #42301, #117126, #180823, #161635, #101964, #134311, #150478, #40290, #179829, #147476, #193993, #163645, #133293 ),
 .UNSPECIFIED., .F., .F.,
 ( 4, 2, 2, 2, 2, 2, 2, 4 ),
 ( 2.788259402197439630E-07, 0.0004455515445239860992, 0.0008908242631077525116, 0.001781369700275286854, 0.002226642418859052074, 0.002671915137442817077, 0.003117187856026582514, 0.003562460574610347517 ),
 .UNSPECIFIED. ) ;
#184108 = CARTESIAN_POINT ( 'NONE',  ( 8.571926809382603096, -26.38167802310801235, 143.4750000027312069 ) ) ;
#184109 = CARTESIAN_POINT ( 'NONE',  ( 5.153800228976335163, 19.02544592524342804, 94.79057627198103830 ) ) ;
#184110 = CARTESIAN_POINT ( 'NONE',  ( -35.00000000000000000, -0.3535533905932759513, 4.646446609406721606 ) ) ;
#184111 = CARTESIAN_POINT ( 'NONE',  ( -9.474510206698720793, -16.51473224551083518, 79.58442372801899012 ) ) ;
#184113 = CARTESIAN_POINT ( 'NONE',  ( -0.05219959533907301413, -21.53943276465977519, 27.49890960531435269 ) ) ;
#184112 = CIRCLE ( 'NONE', #151785, 1.250000000000006439 ) ;
#184115 = CARTESIAN_POINT ( 'NONE',  ( 13.97604488694548053, -13.89961937509957401, 95.62609039468563310 ) ) ;
#184114 = CARTESIAN_POINT ( 'NONE',  ( -16.51473224551082808, 9.474510206698731452, 23.33442372801900078 ) ) ;
#184116 = CARTESIAN_POINT ( 'NONE',  ( 16.52544592524342804, -4.483927247898539470, 113.5405762719810383 ) ) ;
#184117 = CARTESIAN_POINT ( 'NONE',  ( -16.46253265017160317, 9.564922557960807481, 25.83224293864769194 ) ) ;
#184118 = CARTESIAN_POINT ( 'NONE',  ( 5.823673210054125526, 21.52544592524343514, 64.79057627198103830 ) ) ;
#184119 = CARTESIAN_POINT ( 'NONE',  ( -15.80617190586745835, -15.72974639402198527, 51.87390960531437401 ) ) ;
#184120 = CARTESIAN_POINT ( 'NONE',  ( 5.153800228976335163, 19.02544592524342804, 29.79057627198102409 ) ) ;
#184121 = CYLINDRICAL_SURFACE ( 'NONE', #1479, 28.79475375365586487 ) ;
#184122 = CARTESIAN_POINT ( 'NONE',  ( 9.474510206698729675, 16.51473224551082808, 77.08442372801900433 ) ) ;
#184123 = CARTESIAN_POINT ( 'NONE',  ( 16.52544592524342804, -4.483927247898539470, 43.54057627198103830 ) ) ;
#184124 = CARTESIAN_POINT ( 'NONE',  ( -19.05341960407611168, -5.049401038298163336, 111.4572429386476671 ) ) ;
#184125 = CARTESIAN_POINT ( 'NONE',  ( 5.823673210054444382, -21.52544592524334988, 90.20942372801903275 ) ) ;
#184126 = CARTESIAN_POINT ( 'NONE',  ( -10.81492255796078084, -18.62759615963271287, 67.08224293864770971 ) ) ;
#184127 = CARTESIAN_POINT ( 'NONE',  ( -5.823673210054431948, 21.52544592524334988, 52.70942372801902565 ) ) ;
#184128 = CARTESIAN_POINT ( 'NONE',  ( 10.72451020669871369, 18.67979575497193778, 47.08442372801901854 ) ) ;
#184129 = CARTESIAN_POINT ( 'NONE',  ( -16.46253265017160317, 9.564922557960807481, 100.8322429386477097 ) ) ;
#184131 = CARTESIAN_POINT ( 'NONE',  ( 15.80617190586769283, -15.72974639402175789, 45.62609039468567573 ) ) ;
#184130 = CARTESIAN_POINT ( 'NONE',  ( -12.06949235617739369, -12.14591786802326823, 94.37609039468568994 ) ) ;
#184132 = CARTESIAN_POINT ( 'NONE',  ( 5.153800228976335163, 19.02544592524342804, 24.79057627198102765 ) ) ;
#184133 = CARTESIAN_POINT ( 'NONE',  ( 4.500000000000000888, -139.6710100716628631, 12.88025745871188654 ) ) ;
#184134 = CARTESIAN_POINT ( 'NONE',  ( 8.314922557960818139, 14.29746914071049879, 69.58224293864769550 ) ) ;
#184135 = CARTESIAN_POINT ( 'NONE',  ( 4.379528057220339221, -16.55341960407611168, 27.70724293864769905 ) ) ;
#184136 = CARTESIAN_POINT ( 'NONE',  ( -5.153800228976328057, -19.02544592524343514, 67.29057627198102409 ) ) ;
#184137 = CARTESIAN_POINT ( 'NONE',  ( -5.049401038298153566, 19.05341960407611168, 40.20724293864768839 ) ) ;
#184138 = CARTESIAN_POINT ( 'NONE',  ( -5.823673210054116645, -21.52544592524344225, 57.29057627198103120 ) ) ;
#184139 = CARTESIAN_POINT ( 'NONE',  ( 0.05219959533936267826, -19.03943276465977164, 40.00109039468566152 ) ) ;
#184141 = CARTESIAN_POINT ( 'NONE',  ( -4.483927247898539470, -16.52544592524342804, 47.29057627198103120 ) ) ;
#184140 = CARTESIAN_POINT ( 'NONE',  ( 22.96887126817271607, -21.84138762001119716, -49.40150514669699078 ) ) ;
#184143 = AXIS2_PLACEMENT_3D ( 'NONE', #51508, #145500, #130316 ) ;
#184142 = CARTESIAN_POINT ( 'NONE',  ( 15.72974639402199770, -15.80617190586745480, 28.12390960531435979 ) ) ;
#184144 = EDGE_LOOP ( 'NONE', ( #149977, #191957, #148457, #92289 ) ) ;
#184145 = CARTESIAN_POINT ( 'NONE',  ( -8.898068258721467672, -27.38543819252872069, 140.3843446568999696 ) ) ;
#184146 = CARTESIAN_POINT ( 'NONE',  ( -14.34966873604972548, 8.224510206698743886, 78.33442372801901854 ) ) ;
#184147 = CARTESIAN_POINT ( 'NONE',  ( -13.97604488694547697, 13.89961937509957934, 73.12609039468568994 ) ) ;
#184148 = CARTESIAN_POINT ( 'NONE',  ( -14.34966873604960291, -8.224510206698953496, 41.66557627198103120 ) ) ;
#184149 = CARTESIAN_POINT ( 'NONE',  ( 16.62475595723704558, -7.163666690055165098, 53.02713351810471210 ) ) ;
#184150 = CARTESIAN_POINT ( 'NONE',  ( -12.06949235617756955, 12.14591786802309770, 30.62390960531436335 ) ) ;
#184151 = CARTESIAN_POINT ( 'NONE',  ( 19.05341960407611168, 5.049401038298154454, 53.95724293864770260 ) ) ;
#184152 = CARTESIAN_POINT ( 'NONE',  ( -19.02544592524342804, 5.153800228976336051, 81.04057627198103830 ) ) ;
#184153 = CARTESIAN_POINT ( 'NONE',  ( 16.46253265017160672, -9.564922557960803928, 38.33224293864768839 ) ) ;
#184154 = CARTESIAN_POINT ( 'NONE',  ( -18.67979575497193778, 10.72451020669871902, 43.33442372801901143 ) ) ;
#184155 = CARTESIAN_POINT ( 'NONE',  ( 19.03943276465977164, -0.05219959533909143690, 63.74890960531435979 ) ) ;
#184156 = DIRECTION ( 'NONE',  ( 1.000000000000000000, 0.000000000000000000, 0.000000000000000000 ) ) ;
#184157 = CARTESIAN_POINT ( 'NONE',  ( -19.05341960407611168, -5.049401038298163336, 61.45724293864769550 ) ) ;
#184158 = CARTESIAN_POINT ( 'NONE',  ( -18.62759615963270932, 10.81492255796079327, 35.83224293864768839 ) ) ;
#184159 = CARTESIAN_POINT ( 'NONE',  ( -0.05219959533909027116, -19.03943276465977164, 22.49890960531436690 ) ) ;
#184160 = CARTESIAN_POINT ( 'NONE',  ( -21.55341960407610458, -5.719274019375992779, 26.45724293864768839 ) ) ;
#184161 = CARTESIAN_POINT ( 'NONE',  ( 14.29746914071037800, 8.314922557961029526, 91.66775706135234714 ) ) ;
#184162 = CARTESIAN_POINT ( 'NONE',  ( 10.72451020669871369, 18.67979575497193778, 102.0844237280190185 ) ) ;
#184163 = CARTESIAN_POINT ( 'NONE',  ( -16.52544592524335698, -4.483927247898792601, 63.95942372801901854 ) ) ;
#184164 = CARTESIAN_POINT ( 'NONE',  ( -5.049401038298153566, 19.05341960407611168, 110.2072429386476671 ) ) ;
#184165 = CARTESIAN_POINT ( 'NONE',  ( -8.224510206698735004, -14.34966873604973081, 59.58442372801901854 ) ) ;
#184166 = CARTESIAN_POINT ( 'NONE',  ( -0.05219959533934338120, 16.53943276465976808, 42.50109039468567573 ) ) ;
#184167 = CARTESIAN_POINT ( 'NONE',  ( -8.314922557961024197, 14.29746914071037800, 92.91775706135236135 ) ) ;
#184168 = CARTESIAN_POINT ( 'NONE',  ( -16.55341960407617563, 4.379528057220093196, 23.54275706135235424 ) ) ;
#184169 = CARTESIAN_POINT ( 'NONE',  ( 19.03943276465977164, -0.05219959533909143690, 38.74890960531436690 ) ) ;
#184170 = CARTESIAN_POINT ( 'NONE',  ( 0.05219959533907565091, 21.53943276465977519, 109.9989096053143527 ) ) ;
#184171 = CARTESIAN_POINT ( 'NONE',  ( -8.314922557961024197, 14.29746914071037800, 22.91775706135235069 ) ) ;
#184172 = CARTESIAN_POINT ( 'NONE',  ( -16.52544592524335698, -4.483927247898792601, 88.95942372801901854 ) ) ;
#184173 = CARTESIAN_POINT ( 'NONE',  ( 18.22780087662121673, 5.500000000000056843, 43.98459894673892734 ) ) ;
#184174 = CARTESIAN_POINT ( 'NONE',  ( -0.05219959533937732626, 21.53943276465977519, 82.50109039468568994 ) ) ;
#184175 = CARTESIAN_POINT ( 'NONE',  ( 19.05341960407617918, -5.049401038297876454, 81.04275706135231871 ) ) ;
#184176 = CARTESIAN_POINT ( 'NONE',  ( -4.483927247898539470, -16.52544592524342804, 62.29057627198102409 ) ) ;
#184177 = CARTESIAN_POINT ( 'NONE',  ( 4.483927247898545687, 16.52544592524342804, 49.79057627198102409 ) ) ;
#184178 = CARTESIAN_POINT ( 'NONE',  ( -14.34966873604960291, -8.224510206698953496, 101.6655762719810383 ) ) ;
#184180 = CARTESIAN_POINT ( 'NONE',  ( 17.60728821186572546, -5.499999999999887201, 53.36690927743005375 ) ) ;
#184179 = CARTESIAN_POINT ( 'NONE',  ( 13.89961937509957401, 13.97604488694547697, 41.87609039468566152 ) ) ;
#184181 = CARTESIAN_POINT ( 'NONE',  ( 15.80617190586769283, -15.72974639402175789, 45.62609039468567573 ) ) ;
#184182 = CARTESIAN_POINT ( 'NONE',  ( -19.02544592524334988, -5.153800228976617603, 108.9594237280189759 ) ) ;
#184183 = PLANE ( 'NONE',  #11630 ) ;
#184184 = CARTESIAN_POINT ( 'NONE',  ( -0.05219959533909027116, -19.03943276465977164, 107.4989096053143527 ) ) ;
#184185 = CARTESIAN_POINT ( 'NONE',  ( 21.55341960407610458, 5.719274019375980345, 68.95724293864769550 ) ) ;
#184186 = CARTESIAN_POINT ( 'NONE',  ( 19.05341960407617918, -5.049401038297876454, 101.0427570613523045 ) ) ;
#184187 = CARTESIAN_POINT ( 'NONE',  ( -19.05341960407611168, -5.049401038298163336, 101.4572429386476955 ) ) ;
#184188 = CARTESIAN_POINT ( 'NONE',  ( -9.474510206698720793, -16.51473224551083518, 49.58442372801899722 ) ) ;
#184189 = CARTESIAN_POINT ( 'NONE',  ( -0.05219959533910754901, -16.53943276465976808, 112.4989096053143669 ) ) ;
#184190 = CARTESIAN_POINT ( 'NONE',  ( -21.52544592524334988, -5.823673210054445271, 93.95942372801903275 ) ) ;
#184191 = CARTESIAN_POINT ( 'NONE',  ( 5.049401038298161559, -19.05341960407611168, 42.70724293864767418 ) ) ;
#184192 = CARTESIAN_POINT ( 'NONE',  ( 15.72974639402176855, 15.80617190586768217, 51.87609039468568284 ) ) ;
#184193 = CARTESIAN_POINT ( 'NONE',  ( 18.67979575497194134, -10.72451020669871369, 90.83442372801901854 ) ) ;
#184194 = CARTESIAN_POINT ( 'NONE',  ( -12.06949235617739369, -12.14591786802326823, 89.37609039468568994 ) ) ;
#184195 = CARTESIAN_POINT ( 'NONE',  ( 5.719274019375673035, 21.55341960407619339, 37.29275706135235424 ) ) ;
#184196 = CARTESIAN_POINT ( 'NONE',  ( -18.62759615963255300, -10.81492255796106328, 39.16775706135235424 ) ) ;
#184198 = CARTESIAN_POINT ( 'NONE',  ( 13.89961937509977652, -13.97604488694527269, 93.12390960531436690 ) ) ;
#184197 = CARTESIAN_POINT ( 'NONE',  ( 0.05219959533936267826, -19.03943276465977164, 65.00109039468567573 ) ) ;
#184199 = CARTESIAN_POINT ( 'NONE',  ( -12.14591786802309592, -12.06949235617757132, 106.8739096053143811 ) ) ;
#184200 = CARTESIAN_POINT ( 'NONE',  ( -10.72451020669898014, 18.67979575497178502, 85.41557627198102409 ) ) ;
#184201 = CARTESIAN_POINT ( 'NONE',  ( -12.14591786802309592, -12.06949235617757132, 61.87390960531436690 ) ) ;
#184202 = CARTESIAN_POINT ( 'NONE',  ( 21.53943276465977519, 0.05219959533937863772, 101.2510903946856757 ) ) ;
#184203 = CARTESIAN_POINT ( 'NONE',  ( -12.14591786802309592, -12.06949235617757132, 81.87390960531435269 ) ) ;
#184204 = CARTESIAN_POINT ( 'NONE',  ( -16.51473224551069308, -9.474510206698971260, 41.66557627198103120 ) ) ;
#184205 = CARTESIAN_POINT ( 'NONE',  ( 9.474510206698729675, 16.51473224551082808, 82.08442372801899012 ) ) ;
#184206 = CARTESIAN_POINT ( 'NONE',  ( 16.53943276465976808, -0.05219959533910856209, 48.74890960531435979 ) ) ;
#184207 = CARTESIAN_POINT ( 'NONE',  ( -5.719274019375665041, -21.55341960407619695, 99.79275706135234714 ) ) ;
#184208 = CARTESIAN_POINT ( 'NONE',  ( -13.89961937509977652, 13.97604488694528158, 95.62390960531436690 ) ) ;
#184209 = CARTESIAN_POINT ( 'NONE',  ( -0.05219959533936034679, 19.03943276465977164, 57.50109039468566863 ) ) ;
#184210 = CARTESIAN_POINT ( 'NONE',  ( 21.52544592524344225, -5.823673210054117533, 68.54057627198103830 ) ) ;
#184211 = CARTESIAN_POINT ( 'NONE',  ( 5.719274019375991003, -21.55341960407610458, 112.7072429386476955 ) ) ;
#184212 = CARTESIAN_POINT ( 'NONE',  ( 4.483927247898790824, -16.52544592524335698, 25.20942372801901854 ) ) ;
#184213 = CARTESIAN_POINT ( 'NONE',  ( 0.05219959533934541429, -16.53943276465976808, 85.00109039468568994 ) ) ;
#184215 = CARTESIAN_POINT ( 'NONE',  ( 10.72451020669871369, 18.67979575497193778, 22.08442372801901143 ) ) ;
#184214 = LINE ( 'NONE', #180266, #177382 ) ;
#184216 = CARTESIAN_POINT ( 'NONE',  ( 16.46253265017160672, -9.564922557960803928, 23.33224293864769194 ) ) ;
#184217 = CARTESIAN_POINT ( 'NONE',  ( 36.91746824999999177, 2.880721459617395097E-14, -4.124999997268813168 ) ) ;
#184218 = CARTESIAN_POINT ( 'NONE',  ( 12.14591786802327356, -12.06949235617739191, 45.62609039468567573 ) ) ;
#184219 = EDGE_CURVE ( 'NONE', #22576, #96464, #95691, .T. ) ;
#184220 = CARTESIAN_POINT ( 'NONE',  ( 4.483927247898545687, 16.52544592524342804, 79.79057627198102409 ) ) ;
#184221 = CARTESIAN_POINT ( 'NONE',  ( -5.823673210054116645, -21.52544592524344225, 77.29057627198102409 ) ) ;
#184222 = CARTESIAN_POINT ( 'NONE',  ( -16.55341960407611168, -4.379528057220339221, 31.45724293864769550 ) ) ;
#184223 = CARTESIAN_POINT ( 'NONE',  ( -12.06949235617739369, -12.14591786802326823, 34.37609039468568284 ) ) ;
#184224 = CARTESIAN_POINT ( 'NONE',  ( 0.05219959533909260263, 19.03943276465977164, 49.99890960531435979 ) ) ;
#184225 = CARTESIAN_POINT ( 'NONE',  ( 14.34966873604972726, -8.224510206698740333, 75.83442372801900433 ) ) ;
#184226 = CARTESIAN_POINT ( 'NONE',  ( -16.51473224551082808, 9.474510206698731452, 68.33442372801900433 ) ) ;
#184227 = CARTESIAN_POINT ( 'NONE',  ( -5.823673210054116645, -21.52544592524344225, 77.29057627198102409 ) ) ;
#184228 = CARTESIAN_POINT ( 'NONE',  ( 16.52544592524335698, 4.483927247898782831, 111.4594237280190328 ) ) ;
#184229 = ORIENTED_EDGE ( 'NONE', *, *, #31655, .T. ) ;
#184230 = DIRECTION ( 'NONE',  ( 1.000000000000000000, -1.776356839400250465E-15, 0.000000000000000000 ) ) ;
#184231 = CARTESIAN_POINT ( 'NONE',  ( -10.81492255796078084, -18.62759615963271287, 47.08224293864770260 ) ) ;
#184232 = ORIENTED_EDGE ( 'NONE', *, *, #95409, .F. ) ;
#184233 = CARTESIAN_POINT ( 'NONE',  ( 16.52544592524335698, 4.483927247898782831, 96.45942372801901854 ) ) ;
#184234 = CARTESIAN_POINT ( 'NONE',  ( -10.72451020669898014, 18.67979575497178502, 50.41557627198103120 ) ) ;
#184235 = ORIENTED_EDGE ( 'NONE', *, *, #92250, .T. ) ;
#184236 = CARTESIAN_POINT ( 'NONE',  ( -16.51473224551069308, -9.474510206698971260, 111.6655762719810383 ) ) ;
#184237 = CARTESIAN_POINT ( 'NONE',  ( 17.49999999999998934, 3.305555262949649187, 107.8748284784340541 ) ) ;
#184238 = CARTESIAN_POINT ( 'NONE',  ( -16.52544592524342804, 4.483927247898546575, 116.0405762719810383 ) ) ;
#184239 = CARTESIAN_POINT ( 'NONE',  ( 0.05219959533907565091, 21.53943276465977519, 69.99890960531435269 ) ) ;
#184240 = CARTESIAN_POINT ( 'NONE',  ( -0.05219959533934338120, 16.53943276465976808, 102.5010903946856899 ) ) ;
#184241 = CARTESIAN_POINT ( 'NONE',  ( -18.67979575497193778, 10.72451020669871902, 63.33442372801900433 ) ) ;
#184242 = CARTESIAN_POINT ( 'NONE',  ( 12.06949235617739724, 12.14591786802326823, 21.87609039468567573 ) ) ;
#184243 = CARTESIAN_POINT ( 'NONE',  ( 0.05219959533910956823, 16.53943276465976808, 109.9989096053143527 ) ) ;
#184244 = CARTESIAN_POINT ( 'NONE',  ( 8.314922557961029526, -14.29746914071037800, 35.41775706135234003 ) ) ;
#184245 = CARTESIAN_POINT ( 'NONE',  ( -5.153800228976328057, -19.02544592524343514, 52.29057627198100988 ) ) ;
#184246 = CARTESIAN_POINT ( 'NONE',  ( 16.49741402511621757, -0.7792920370541633890, -61.43171317168471290 ) ) ;
#184247 = CARTESIAN_POINT ( 'NONE',  ( 0.05219959533909260263, 19.03943276465977164, 109.9989096053143669 ) ) ;
#184248 = CARTESIAN_POINT ( 'NONE',  ( 14.34966873604972726, -8.224510206698740333, 85.83442372801901854 ) ) ;
#184249 = CARTESIAN_POINT ( 'NONE',  ( -16.46253265017146816, -9.564922557961047289, 94.16775706135233293 ) ) ;
#184250 = CARTESIAN_POINT ( 'NONE',  ( -18.67979575497193778, 10.72451020669871902, 113.3344237280190328 ) ) ;
#184251 = CARTESIAN_POINT ( 'NONE',  ( 21.52544592524344225, -5.823673210054117533, 78.54057627198103830 ) ) ;
#184252 = CARTESIAN_POINT ( 'NONE',  ( 8.224510206698742110, 14.34966873604972548, 102.0844237280190185 ) ) ;
#184253 = CARTESIAN_POINT ( 'NONE',  ( -9.564922557961040184, 16.46253265017147172, 97.91775706135233293 ) ) ;
#184254 = CARTESIAN_POINT ( 'NONE',  ( -9.474510206698964154, 16.51473224551069663, 50.41557627198102409 ) ) ;
#184255 = CARTESIAN_POINT ( 'NONE',  ( 9.474510206698971260, -16.51473224551069308, 97.91557627198102409 ) ) ;
#184256 = CARTESIAN_POINT ( 'NONE',  ( 10.81492255796106328, -18.62759615963255655, 50.41775706135235424 ) ) ;
#184257 = CARTESIAN_POINT ( 'NONE',  ( 16.46253265017160672, -9.564922557960803928, 43.33224293864769550 ) ) ;
#184258 = CARTESIAN_POINT ( 'NONE',  ( -16.61371651742603461, -7.165104196376156587, 86.14584930007006847 ) ) ;
#184259 = CARTESIAN_POINT ( 'NONE',  ( -5.153800228976328057, -19.02544592524343514, 112.2905762719810099 ) ) ;
#184260 = CARTESIAN_POINT ( 'NONE',  ( 0.05219959533910956823, 16.53943276465976808, 64.99890960531435269 ) ) ;
#184261 = CARTESIAN_POINT ( 'NONE',  ( -18.62759615963270932, 10.81492255796079327, 70.83224293864770971 ) ) ;
#184262 = DIRECTION ( 'NONE',  ( 0.000000000000000000, 0.000000000000000000, 1.000000000000000000 ) ) ;
#184263 = CARTESIAN_POINT ( 'NONE',  ( 16.46253265017146816, 9.564922557961045513, 36.66775706135233293 ) ) ;
#184264 = CARTESIAN_POINT ( 'NONE',  ( 17.50000000000001776, -3.242565516147306592, 37.50000000000000000 ) ) ;
#184266 = CARTESIAN_POINT ( 'NONE',  ( -19.05341960407611168, -5.049401038298163336, 81.45724293864769550 ) ) ;
#184265 = CARTESIAN_POINT ( 'NONE',  ( 9.564922557960805705, 16.46253265017160317, 64.58224293864769550 ) ) ;
#184267 = CARTESIAN_POINT ( 'NONE',  ( 14.34966873604972726, -8.224510206698740333, 55.83442372801901854 ) ) ;
#184268 = CARTESIAN_POINT ( 'NONE',  ( 24.78074900657736990, -31.51706519598950607, -17.29086010071286950 ) ) ;
#184269 = CARTESIAN_POINT ( 'NONE',  ( -16.46253265017146816, -9.564922557961047289, 34.16775706135233293 ) ) ;
#184270 = CARTESIAN_POINT ( 'NONE',  ( 14.29746914071037800, 8.314922557961029526, 91.66775706135234714 ) ) ;
#184271 = CARTESIAN_POINT ( 'NONE',  ( -1.344113590474603992, -22.10945809693575725, -55.87741762761908149 ) ) ;
#184272 = CARTESIAN_POINT ( 'NONE',  ( 4.483927247898790824, -16.52544592524335698, 85.20942372801901854 ) ) ;
#184273 = CARTESIAN_POINT ( 'NONE',  ( -14.34966873604972548, 8.224510206698743886, 58.33442372801901143 ) ) ;
#184274 = CARTESIAN_POINT ( 'NONE',  ( -19.05341960407617563, 5.049401038297882671, 23.54275706135233648 ) ) ;
#184276 = LINE ( 'NONE', #166140, #59872 ) ;
#184275 = CARTESIAN_POINT ( 'NONE',  ( 5.153800228976335163, 19.02544592524342804, 59.79057627198100988 ) ) ;
#184277 = CARTESIAN_POINT ( 'NONE',  ( 21.55341960407619695, -5.719274019375665929, 61.04275706135234714 ) ) ;
#184278 = CARTESIAN_POINT ( 'NONE',  ( 13.89961937509957401, 13.97604488694547697, 76.87609039468566152 ) ) ;
#184279 = CARTESIAN_POINT ( 'NONE',  ( 5.823673210054444382, -21.52544592524334988, 110.2094237280190185 ) ) ;
#184280 = CARTESIAN_POINT ( 'NONE',  ( 5.153800228976335163, 19.02544592524342804, 49.79057627198100988 ) ) ;
#184281 = CARTESIAN_POINT ( 'NONE',  ( 17.33830594066689912, 6.305085581112166437, 23.88102644207486946 ) ) ;
#184282 = CARTESIAN_POINT ( 'NONE',  ( 21.53943276465977519, -0.05219959533907433946, 68.74890960531435269 ) ) ;
#184283 = AXIS2_PLACEMENT_3D ( 'NONE', #141384, #34211, #157557 ) ;
#184284 = CARTESIAN_POINT ( 'NONE',  ( 15.80617190586746368, 15.72974639402197994, 24.37390960531435979 ) ) ;
#184285 = CARTESIAN_POINT ( 'NONE',  ( -12.06949235617756955, 12.14591786802309770, 115.6239096053143669 ) ) ;
#184286 = CARTESIAN_POINT ( 'NONE',  ( -12.06949235617739369, -12.14591786802326823, 44.37609039468567573 ) ) ;
#184287 = ADVANCED_FACE ( 'NONE', ( #65353 ), #153998, .F. ) ;
#184288 = CARTESIAN_POINT ( 'NONE',  ( -4.379528057220328563, 16.55341960407611168, 30.20724293864769550 ) ) ;
#184289 = ORIENTED_EDGE ( 'NONE', *, *, #175843, .F. ) ;
#184290 = CARTESIAN_POINT ( 'NONE',  ( 18.62759615963255655, 10.81492255796105972, 21.66775706135235069 ) ) ;
#184292 = CARTESIAN_POINT ( 'NONE',  ( 11.74264578624800315, -36.14014761921581709, -5.400000000000000355 ) ) ;
#184291 = CARTESIAN_POINT ( 'NONE',  ( -14.34966873604960291, -8.224510206698953496, 46.66557627198102409 ) ) ;
#184293 = CARTESIAN_POINT ( 'NONE',  ( -9.564922557961040184, 16.46253265017147172, 107.9177570613523471 ) ) ;
#184294 = CARTESIAN_POINT ( 'NONE',  ( 0.05219959533936267826, -19.03943276465977164, 45.00109039468566863 ) ) ;
#184295 = CARTESIAN_POINT ( 'NONE',  ( -8.314922557960811034, -14.29746914071050412, 47.08224293864770260 ) ) ;
#184296 = CARTESIAN_POINT ( 'NONE',  ( -18.67979575497178146, -10.72451020669898902, 101.6655762719810383 ) ) ;
#184298 = CARTESIAN_POINT ( 'NONE',  ( -5.823673210054116645, -21.52544592524344225, 67.29057627198103830 ) ) ;
#184297 = CARTESIAN_POINT ( 'NONE',  ( 20.96320343559639454, -21.46320343559646560, 5.353553390593268624 ) ) ;
#184299 = CARTESIAN_POINT ( 'NONE',  ( -0.05219959533909027116, -19.03943276465977164, 72.49890960531435269 ) ) ;
#184300 = CARTESIAN_POINT ( 'NONE',  ( -12.06949235617756955, 12.14591786802309770, 45.62390960531436690 ) ) ;
#184301 = CARTESIAN_POINT ( 'NONE',  ( -5.049401038298153566, 19.05341960407611168, 100.2072429386476955 ) ) ;
#184302 = ADVANCED_FACE ( 'NONE', ( #32046 ), #66811, .T. ) ;
#184303 = CARTESIAN_POINT ( 'NONE',  ( -36.78370799935940738, 4.380135692641567324, 48.34576877258191274 ) ) ;
#184304 = CARTESIAN_POINT ( 'NONE',  ( 19.05341960407617918, -5.049401038297876454, 61.04275706135232582 ) ) ;
#184305 = CARTESIAN_POINT ( 'NONE',  ( -15.72974639402197994, 15.80617190586746368, 100.6239096053143811 ) ) ;
#184306 = CARTESIAN_POINT ( 'NONE',  ( 19.03943276465977164, -0.05219959533909143690, 43.74890960531435979 ) ) ;
#184307 = CARTESIAN_POINT ( 'NONE',  ( 9.564922557960805705, 16.46253265017160317, 24.58224293864769194 ) ) ;
#184308 = CARTESIAN_POINT ( 'NONE',  ( -21.55341960407619339, 5.719274019375674811, 53.54275706135234714 ) ) ;
#184309 = CARTESIAN_POINT ( 'NONE',  ( 1.784210473542230573E-15, -29.16686587814331588, 143.3750000027311557 ) ) ;
#184310 = CARTESIAN_POINT ( 'NONE',  ( -16.53943276465976808, -0.05219959533934237506, 113.7510903946856757 ) ) ;
#184311 = CARTESIAN_POINT ( 'NONE',  ( -5.153800228976328057, -19.02544592524343514, 47.29057627198102409 ) ) ;
#184312 = CARTESIAN_POINT ( 'NONE',  ( -5.049401038298153566, 19.05341960407611168, 100.2072429386476955 ) ) ;
#184313 = CARTESIAN_POINT ( 'NONE',  ( 0.05219959533907565091, 21.53943276465977519, 59.99890960531436690 ) ) ;
#184314 = CARTESIAN_POINT ( 'NONE',  ( -19.25663599770061651, 5.499999999999455547, 43.99419308057201761 ) ) ;
#184315 = CARTESIAN_POINT ( 'NONE',  ( 13.97604488694527802, 13.89961937509977652, 49.37390960531434558 ) ) ;
#184316 = CARTESIAN_POINT ( 'NONE',  ( -10.81492255796078084, -18.62759615963271287, 52.08224293864768839 ) ) ;
#184317 = CARTESIAN_POINT ( 'NONE',  ( 10.72451020669871369, 18.67979575497193778, 87.08442372801901854 ) ) ;
#184319 = CARTESIAN_POINT ( 'NONE',  ( -14.34966873604972548, 8.224510206698743886, 78.33442372801901854 ) ) ;
#184318 = CARTESIAN_POINT ( 'NONE',  ( 20.47606263882783040, -31.78721852328014918, -20.08103504831379027 ) ) ;
#184320 = CARTESIAN_POINT ( 'NONE',  ( -16.53943276465976808, -0.05219959533934237506, 93.75109039468567573 ) ) ;
#184321 = CARTESIAN_POINT ( 'NONE',  ( -5.153800228976328057, -19.02544592524343514, 67.29057627198102409 ) ) ;
#184322 = ORIENTED_EDGE ( 'NONE', *, *, #163889, .F. ) ;
#184323 = CARTESIAN_POINT ( 'NONE',  ( 9.564922557961047289, -16.46253265017146816, 30.41775706135232937 ) ) ;
#184324 = CARTESIAN_POINT ( 'NONE',  ( -16.55341960407617563, 4.379528057220093196, 83.54275706135234714 ) ) ;
#184325 = CARTESIAN_POINT ( 'NONE',  ( 18.62759615963255655, 10.81492255796105972, 111.6677570613523613 ) ) ;
#184326 = CARTESIAN_POINT ( 'NONE',  ( -13.89961937509977652, 13.97604488694528158, 75.62390960531438111 ) ) ;
#184327 = CARTESIAN_POINT ( 'NONE',  ( 18.67979575497178502, 10.72451020669898547, 49.16557627198102409 ) ) ;
#184328 = CARTESIAN_POINT ( 'NONE',  ( -4.483927247898782831, 16.52544592524335698, 22.70942372801901499 ) ) ;
#184329 = CARTESIAN_POINT ( 'NONE',  ( 18.67979575497194134, -10.72451020669871369, 80.83442372801901854 ) ) ;
#184330 = CARTESIAN_POINT ( 'NONE',  ( -16.53943276465976808, -0.05219959533934237506, 63.75109039468568284 ) ) ;
#184331 = CARTESIAN_POINT ( 'NONE',  ( -15.72974639402197994, 15.80617190586746368, 115.6239096053143669 ) ) ;
#184332 = CARTESIAN_POINT ( 'NONE',  ( 19.05341960407617918, -5.049401038297876454, 111.0427570613523329 ) ) ;
#184333 = CARTESIAN_POINT ( 'NONE',  ( 0.05219959533909260263, 19.03943276465977164, 94.99890960531436690 ) ) ;
#184334 = CARTESIAN_POINT ( 'NONE',  ( 12.14591786802327356, -12.06949235617739191, 25.62609039468567929 ) ) ;
#184335 = CARTESIAN_POINT ( 'NONE',  ( -19.02544592524342804, 5.153800228976336051, 41.04057627198103120 ) ) ;
#184336 = CARTESIAN_POINT ( 'NONE',  ( 14.29746914071037800, 8.314922557961029526, 21.66775706135235069 ) ) ;
#184337 = CARTESIAN_POINT ( 'NONE',  ( 12.14591786802309770, 12.06949235617756955, 79.37390960531436690 ) ) ;
#184338 = CARTESIAN_POINT ( 'NONE',  ( -14.34966873604972548, 8.224510206698743886, 88.33442372801901854 ) ) ;
#184340 = CARTESIAN_POINT ( 'NONE',  ( -13.89961937509977652, 13.97604488694528158, 60.62390960531436690 ) ) ;
#184339 = CARTESIAN_POINT ( 'NONE',  ( -18.62759615963255300, -10.81492255796106328, 29.16775706135234003 ) ) ;
#184341 = CARTESIAN_POINT ( 'NONE',  ( 19.03943276465977164, -0.05219959533909143690, 63.74890960531435979 ) ) ;
#184342 = CARTESIAN_POINT ( 'NONE',  ( 16.55341960407618274, -4.379528057220086978, 86.04275706135236135 ) ) ;
#184344 = ORIENTED_EDGE ( 'NONE', *, *, #7609, .T. ) ;
#184343 = CARTESIAN_POINT ( 'NONE',  ( -24.20757866959952764, -5.698759791480821235, 172.9004493943157001 ) ) ;
#184345 = ORIENTED_EDGE ( 'NONE', *, *, #147079, .F. ) ;
#184346 = CARTESIAN_POINT ( 'NONE',  ( 5.049401038297881783, 19.05341960407617563, 27.29275706135232937 ) ) ;
#184347 = CARTESIAN_POINT ( 'NONE',  ( 19.05341960407611168, 5.049401038298154454, 38.95724293864767418 ) ) ;
#184349 = VERTEX_POINT ( 'NONE', #140200 ) ;
#184348 = CARTESIAN_POINT ( 'NONE',  ( 1.218433102416749181, 14.30315789272851390, -62.33600599370836193 ) ) ;
#184350 = CARTESIAN_POINT ( 'NONE',  ( 16.53943276465976808, 0.05219959533934440121, 31.25109039468568639 ) ) ;
#184352 = CARTESIAN_POINT ( 'NONE',  ( -4.483927247898782831, 16.52544592524335698, 42.70942372801901854 ) ) ;
#184351 = CARTESIAN_POINT ( 'NONE',  ( 19.05341960407617918, -5.049401038297876454, 61.04275706135232582 ) ) ;
#184353 = CARTESIAN_POINT ( 'NONE',  ( 16.51473224551069308, 9.474510206698969483, 109.1655762719810383 ) ) ;
#184354 = CARTESIAN_POINT ( 'NONE',  ( -9.474510206698964154, 16.51473224551069663, 80.41557627198103830 ) ) ;
#184355 = CARTESIAN_POINT ( 'NONE',  ( -10.72451020669898014, 18.67979575497178502, 100.4155762719810241 ) ) ;
#184356 = CARTESIAN_POINT ( 'NONE',  ( -16.46253265017146816, -9.564922557961047289, 64.16775706135233293 ) ) ;
#184358 = CARTESIAN_POINT ( 'NONE',  ( -3.573655867282028392E-15, 2.428612866367529932E-14, 139.9999999999999716 ) ) ;
#184357 = CARTESIAN_POINT ( 'NONE',  ( 9.474510206698971260, -16.51473224551069308, 97.91557627198102409 ) ) ;
#184359 = CARTESIAN_POINT ( 'NONE',  ( 9.564922557960805705, 16.46253265017160317, 64.58224293864769550 ) ) ;
#184361 = CARTESIAN_POINT ( 'NONE',  ( 0.05219959533909260263, 19.03943276465977164, 69.99890960531435269 ) ) ;
#184360 = CARTESIAN_POINT ( 'NONE',  ( -16.55341960407617563, 4.379528057220093196, 113.5427570613523756 ) ) ;
#184362 = CARTESIAN_POINT ( 'NONE',  ( -5.049401038297874678, -19.05341960407617918, 34.79275706135233293 ) ) ;
#184363 = CARTESIAN_POINT ( 'NONE',  ( 4.379528057220339221, -16.55341960407611168, 72.70724293864769550 ) ) ;
#184364 = CARTESIAN_POINT ( 'NONE',  ( 21.55341960407619695, -5.719274019375665929, 96.04275706135236135 ) ) ;
#184365 = CARTESIAN_POINT ( 'NONE',  ( -19.03943276465977164, 0.05219959533909376836, 41.24890960531435269 ) ) ;
#184366 = CARTESIAN_POINT ( 'NONE',  ( 16.55341960407618274, -4.379528057220086978, 51.04275706135234714 ) ) ;
#184368 = CARTESIAN_POINT ( 'NONE',  ( 18.62759615963255655, 10.81492255796105972, 86.66775706135234714 ) ) ;
#184367 = CARTESIAN_POINT ( 'NONE',  ( -16.52544592524342804, 4.483927247898546575, 41.04057627198103120 ) ) ;
#184369 = CARTESIAN_POINT ( 'NONE',  ( 16.46253265017160672, -9.564922557960803928, 73.33224293864769550 ) ) ;
#184370 = CARTESIAN_POINT ( 'NONE',  ( -19.03943276465977164, 0.05219959533909376836, 101.2489096053143669 ) ) ;
#184371 = CARTESIAN_POINT ( 'NONE',  ( 16.55341960407611168, 4.379528057220329451, 103.9572429386476813 ) ) ;
#184372 = CARTESIAN_POINT ( 'NONE',  ( 12.06949235617757843, -12.14591786802309237, 73.12390960531436690 ) ) ;
#184373 = CARTESIAN_POINT ( 'NONE',  ( 15.80617190586746368, 15.72974639402197994, 89.37390960531435269 ) ) ;
#184374 = CARTESIAN_POINT ( 'NONE',  ( -16.51473224551069308, -9.474510206698971260, 86.66557627198102409 ) ) ;
#184375 = CARTESIAN_POINT ( 'NONE',  ( -5.823673210054116645, -21.52544592524344225, 97.29057627198105251 ) ) ;
#184376 = CARTESIAN_POINT ( 'NONE',  ( -19.03943276465977164, -0.05219959533935918106, 73.75109039468566152 ) ) ;
#184378 = CARTESIAN_POINT ( 'NONE',  ( 8.224510206698953496, -14.34966873604960469, 87.91557627198103830 ) ) ;
#184377 = CARTESIAN_POINT ( 'NONE',  ( 19.52837319214028611, -5.499999999999893419, 47.10471352585541638 ) ) ;
#184379 = CARTESIAN_POINT ( 'NONE',  ( -5.153800228976328057, -19.02544592524343514, 52.29057627198100988 ) ) ;
#184380 = CARTESIAN_POINT ( 'NONE',  ( 0.05219959533907565091, 21.53943276465977519, 59.99890960531436690 ) ) ;
#184381 = CARTESIAN_POINT ( 'NONE',  ( 16.29526858892873875, -7.335722546920261600, 26.70329402199794444 ) ) ;
#184383 = CARTESIAN_POINT ( 'NONE',  ( 8.571926809382597767, 26.38167802310806209, 148.7750000027311899 ) ) ;
#184382 = CARTESIAN_POINT ( 'NONE',  ( 16.55341960407618274, -4.379528057220086978, 106.0427570613523471 ) ) ;
#184384 = CARTESIAN_POINT ( 'NONE',  ( 8.224510206698742110, 14.34966873604972548, 22.08442372801901143 ) ) ;
#184385 = CARTESIAN_POINT ( 'NONE',  ( 4.379528057220339221, -16.55341960407611168, 82.70724293864770971 ) ) ;
#184386 = CARTESIAN_POINT ( 'NONE',  ( 18.87580814761078329, -5.499999999999872102, 53.37172394265758868 ) ) ;
#184387 = CARTESIAN_POINT ( 'NONE',  ( 19.02544592524343514, -5.153800228976328945, 73.54057627198103830 ) ) ;
#184388 = CARTESIAN_POINT ( 'NONE',  ( 13.97604488694527802, 13.89961937509977652, 29.37390960531435979 ) ) ;
#184390 = EDGE_CURVE ( 'NONE', #153137, #72946, #196036, .T. ) ;
#184389 = CARTESIAN_POINT ( 'NONE',  ( 14.29746914071049879, -8.314922557960816363, 73.33224293864769550 ) ) ;
#184391 = CARTESIAN_POINT ( 'NONE',  ( 16.51473224551069308, 9.474510206698969483, 114.1655762719810241 ) ) ;
#184392 = CARTESIAN_POINT ( 'NONE',  ( -9.564922557961040184, 16.46253265017147172, 82.91775706135233293 ) ) ;
#184393 = CARTESIAN_POINT ( 'NONE',  ( 9.564922557960805705, 16.46253265017160317, 99.58224293864770971 ) ) ;
#184394 = CARTESIAN_POINT ( 'NONE',  ( -0.05219959533907301413, -21.53943276465977519, 72.49890960531435269 ) ) ;
#184395 = CARTESIAN_POINT ( 'NONE',  ( 16.52544592524335698, 4.483927247898782831, 66.45942372801903275 ) ) ;
#184396 = CARTESIAN_POINT ( 'NONE',  ( 19.03943276465977164, 0.05219959533936151252, 106.2510903946856615 ) ) ;
#184397 = CARTESIAN_POINT ( 'NONE',  ( 5.049401038298161559, -19.05341960407611168, 67.70724293864769550 ) ) ;
#184398 = CARTESIAN_POINT ( 'NONE',  ( 15.80617190586746368, 15.72974639402197994, 69.37390960531436690 ) ) ;
#184399 = CARTESIAN_POINT ( 'NONE',  ( 9.474510206698729675, 16.51473224551082808, 102.0844237280190043 ) ) ;
#184401 = CARTESIAN_POINT ( 'NONE',  ( 10.81492255796106328, -18.62759615963255655, 60.41775706135235424 ) ) ;
#184400 = CARTESIAN_POINT ( 'NONE',  ( 4.379528057220339221, -16.55341960407611168, 37.70724293864769550 ) ) ;
#184402 = CARTESIAN_POINT ( 'NONE',  ( 16.46253265017146816, 9.564922557961045513, 71.66775706135233293 ) ) ;
#184404 = CARTESIAN_POINT ( 'NONE',  ( -13.89961937509977652, 13.97604488694528158, 110.6239096053143243 ) ) ;
#184403 = CARTESIAN_POINT ( 'NONE',  ( 4.483927247898790824, -16.52544592524335698, 75.20942372801901854 ) ) ;
#184405 = CARTESIAN_POINT ( 'NONE',  ( -26.79475375365586842, 2.428612866367529932E-14, 155.0000000000000000 ) ) ;
#184406 = CARTESIAN_POINT ( 'NONE',  ( -1.221313414957698099E-14, 31.90000000000003411, -49.13275782002545355 ) ) ;
#184407 = CARTESIAN_POINT ( 'NONE',  ( -8.314922557961024197, 14.29746914071037800, 92.91775706135236135 ) ) ;
#184408 = CARTESIAN_POINT ( 'NONE',  ( -12.14591786802326823, 12.06949235617739902, 48.12609039468568284 ) ) ;
#184409 = CARTESIAN_POINT ( 'NONE',  ( 5.049401038298161559, -19.05341960407611168, 62.70724293864769550 ) ) ;
#184410 = CARTESIAN_POINT ( 'NONE',  ( 19.05341960407611168, 5.049401038298154454, 78.95724293864769550 ) ) ;
#184411 = CARTESIAN_POINT ( 'NONE',  ( -10.72451020669870658, -18.67979575497194134, 69.58442372801900433 ) ) ;
#184412 = CARTESIAN_POINT ( 'NONE',  ( 4.379528057220092307, 16.55341960407617563, 57.29275706135234714 ) ) ;
#184413 = CARTESIAN_POINT ( 'NONE',  ( 14.34966873604960469, 8.224510206698951720, 29.16557627198103120 ) ) ;
#184414 = CARTESIAN_POINT ( 'NONE',  ( 5.049401038298161559, -19.05341960407611168, 37.70724293864768839 ) ) ;
#184415 = CARTESIAN_POINT ( 'NONE',  ( -19.02544592524342804, 5.153800228976336051, 36.04057627198100988 ) ) ;
#184417 = ORIENTED_EDGE ( 'NONE', *, *, #114488, .T. ) ;
#184416 = CARTESIAN_POINT ( 'NONE',  ( -16.55341960407617563, 4.379528057220093196, 28.54275706135234358 ) ) ;
#184418 = CARTESIAN_POINT ( 'NONE',  ( -9.564922557961040184, 16.46253265017147172, 77.91775706135234714 ) ) ;
#184419 = CARTESIAN_POINT ( 'NONE',  ( -14.34966873604960291, -8.224510206698953496, 96.66557627198102409 ) ) ;
#184420 = CARTESIAN_POINT ( 'NONE',  ( 16.51473224551069308, 9.474510206698969483, 49.16557627198102409 ) ) ;
#184422 = CARTESIAN_POINT ( 'NONE',  ( -8.898068258721467672, -27.38543819252872069, 148.3843446568999980 ) ) ;
#184421 = CARTESIAN_POINT ( 'NONE',  ( -0.05219959533936034679, 19.03943276465977164, 82.50109039468567573 ) ) ;
#184423 = CARTESIAN_POINT ( 'NONE',  ( 0.05219959533937995610, -21.53943276465977519, 85.00109039468568994 ) ) ;
#184424 = CARTESIAN_POINT ( 'NONE',  ( 12.06949235617739724, 12.14591786802326823, 51.87609039468568284 ) ) ;
#184425 = CYLINDRICAL_SURFACE ( 'NONE', #79266, 10.00000000000000000 ) ;
#184426 = CARTESIAN_POINT ( 'NONE',  ( 18.62759615963271287, -10.81492255796078972, 53.33224293864769550 ) ) ;
#184427 = CARTESIAN_POINT ( 'NONE',  ( -16.52544592524335698, -4.483927247898792601, 33.95942372801901143 ) ) ;
#184428 = CARTESIAN_POINT ( 'NONE',  ( 16.51473224551069308, 9.474510206698969483, 34.16557627198102409 ) ) ;
#184429 = CARTESIAN_POINT ( 'NONE',  ( -19.05341960407617563, 5.049401038297882671, 43.54275706135232582 ) ) ;
#184430 = CARTESIAN_POINT ( 'NONE',  ( -5.153800228976328057, -19.02544592524343514, 92.29057627198099567 ) ) ;
#184431 = CARTESIAN_POINT ( 'NONE',  ( -19.05341960407611168, -5.049401038298163336, 51.45724293864770260 ) ) ;
#184432 = CARTESIAN_POINT ( 'NONE',  ( 15.66972982126930702, 17.56366054824405865, -54.83331888096113005 ) ) ;
#184433 = CARTESIAN_POINT ( 'NONE',  ( 21.52544592524334988, 5.823673210054432836, 76.45942372801901854 ) ) ;
#184434 = CARTESIAN_POINT ( 'NONE',  ( -18.96320343559621691, 23.46320343559659705, 1.110912703473986074 ) ) ;
#184435 = CARTESIAN_POINT ( 'NONE',  ( 9.564922557961047289, -16.46253265017146816, 35.41775706135233293 ) ) ;
#184436 = CARTESIAN_POINT ( 'NONE',  ( 18.67979575497194134, -10.72451020669871369, 105.8344237280190328 ) ) ;
#184437 = CARTESIAN_POINT ( 'NONE',  ( 4.483927247898545687, 16.52544592524342804, 34.79057627198103120 ) ) ;
#184438 = CARTESIAN_POINT ( 'NONE',  ( -16.51473224551069308, -9.474510206698971260, 61.66557627198103120 ) ) ;
#184439 = CARTESIAN_POINT ( 'NONE',  ( 16.51473224551069308, 9.474510206698969483, 109.1655762719810383 ) ) ;
#184440 = CARTESIAN_POINT ( 'NONE',  ( 21.53943276465977519, 0.05219959533937863772, 86.25109039468568994 ) ) ;
#184441 = CARTESIAN_POINT ( 'NONE',  ( -16.51473224551069308, -9.474510206698971260, 66.66557627198102409 ) ) ;
#184442 = CARTESIAN_POINT ( 'NONE',  ( -21.52544592524334988, -5.823673210054445271, 83.95942372801900433 ) ) ;
#184443 = CARTESIAN_POINT ( 'NONE',  ( 18.67979575497178502, 10.72451020669898547, 34.16557627198102409 ) ) ;
#184444 = CARTESIAN_POINT ( 'NONE',  ( 21.52544592524334988, 5.823673210054432836, 26.45942372801901854 ) ) ;
#184445 = CARTESIAN_POINT ( 'NONE',  ( -19.02544592524334988, -5.153800228976617603, 43.95942372801899012 ) ) ;
#184446 = CARTESIAN_POINT ( 'NONE',  ( -0.05219959533909027116, -19.03943276465977164, 32.49890960531435979 ) ) ;
#184447 = CARTESIAN_POINT ( 'NONE',  ( -13.89961937509977652, 13.97604488694528158, 70.62390960531432427 ) ) ;
#184448 = CARTESIAN_POINT ( 'NONE',  ( 12.06949235617739724, 12.14591786802326823, 26.87609039468567218 ) ) ;
#184449 = CARTESIAN_POINT ( 'NONE',  ( -12.14591786802309592, -12.06949235617757132, 91.87390960531436690 ) ) ;
#184450 = CARTESIAN_POINT ( 'NONE',  ( 19.05341960407611168, 5.049401038298154454, 63.95724293864769550 ) ) ;
#184451 = CARTESIAN_POINT ( 'NONE',  ( 18.62759615963271287, -10.81492255796078972, 33.33224293864769550 ) ) ;
#184452 = CARTESIAN_POINT ( 'NONE',  ( 19.02544592524334988, 5.153800228976608722, 101.4594237280189759 ) ) ;
#184453 = CARTESIAN_POINT ( 'NONE',  ( -15.80617190586745835, -15.72974639402198527, 106.8739096053143811 ) ) ;
#184454 = CARTESIAN_POINT ( 'NONE',  ( 15.80617190586769283, -15.72974639402175789, 70.62609039468567573 ) ) ;
#184455 = CARTESIAN_POINT ( 'NONE',  ( 4.379528057220092307, 16.55341960407617563, 72.29275706135236135 ) ) ;
#184456 = CARTESIAN_POINT ( 'NONE',  ( 12.14591786802327356, -12.06949235617739191, 65.62609039468568994 ) ) ;
#184457 = CARTESIAN_POINT ( 'NONE',  ( 9.474510206698971260, -16.51473224551069308, 67.91557627198102409 ) ) ;
#184458 = CARTESIAN_POINT ( 'NONE',  ( -14.34966873604972548, 8.224510206698743886, 88.33442372801901854 ) ) ;
#184459 = CARTESIAN_POINT ( 'NONE',  ( -19.03943276465977164, -0.05219959533935918106, 43.75109039468566863 ) ) ;
#184460 = ADVANCED_FACE ( 'NONE', ( #124030 ), #48214, .F. ) ;
#184461 = CARTESIAN_POINT ( 'NONE',  ( -18.62759615963255300, -10.81492255796106328, 19.16775706135234714 ) ) ;
#184462 = CARTESIAN_POINT ( 'NONE',  ( -8.314922557960811034, -14.29746914071050412, 67.08224293864770971 ) ) ;
#184463 = CARTESIAN_POINT ( 'NONE',  ( -13.89961937509977652, 13.97604488694528158, 85.62390960531433848 ) ) ;
#184464 = CARTESIAN_POINT ( 'NONE',  ( 12.06949235617739724, 12.14591786802326823, 71.87609039468568994 ) ) ;
#184465 = CARTESIAN_POINT ( 'NONE',  ( -21.52544592524334988, -5.823673210054445271, 63.95942372801901854 ) ) ;
#184466 = CARTESIAN_POINT ( 'NONE',  ( 16.55341960407618274, -4.379528057220086978, 21.04275706135234714 ) ) ;
#184467 = CARTESIAN_POINT ( 'NONE',  ( -10.72451020669870658, -18.67979575497194134, 19.58442372801901143 ) ) ;
#184468 = CARTESIAN_POINT ( 'NONE',  ( -16.55341960407611168, -4.379528057220339221, 61.45724293864770260 ) ) ;
#184469 = ORIENTED_EDGE ( 'NONE', *, *, #51668, .F. ) ;
#184470 = CARTESIAN_POINT ( 'NONE',  ( -10.81492255796078084, -18.62759615963271287, 92.08224293864769550 ) ) ;
#184471 = CARTESIAN_POINT ( 'NONE',  ( -14.34966873604960291, -8.224510206698953496, 41.66557627198103120 ) ) ;
#184472 = VERTEX_POINT ( 'NONE', #3675 ) ;
#184473 = CARTESIAN_POINT ( 'NONE',  ( 34.77165353390492442, 6.824181688848570460, 41.87898302971509423 ) ) ;
#184474 = CARTESIAN_POINT ( 'NONE',  ( -5.823673210054116645, -21.52544592524344225, 112.2905762719810241 ) ) ;
#184475 = CARTESIAN_POINT ( 'NONE',  ( -16.51473224551069308, -9.474510206698971260, 106.6655762719810383 ) ) ;
#184476 = CARTESIAN_POINT ( 'NONE',  ( 10.81492255796106328, -18.62759615963255655, 30.41775706135234358 ) ) ;
#184477 = CARTESIAN_POINT ( 'NONE',  ( -8.314922557960811034, -14.29746914071050412, 57.08224293864769550 ) ) ;
#184478 = CARTESIAN_POINT ( 'NONE',  ( -0.05219959533909027116, -19.03943276465977164, 67.49890960531436690 ) ) ;
#184479 = CARTESIAN_POINT ( 'NONE',  ( 9.564922557961047289, -16.46253265017146816, 70.41775706135233293 ) ) ;
#184480 = CARTESIAN_POINT ( 'NONE',  ( -16.46253265017160317, 9.564922557960807481, 95.83224293864769550 ) ) ;
#184481 = ADVANCED_FACE ( 'NONE', ( #4658 ), #96674, .F. ) ;
#184482 = CARTESIAN_POINT ( 'NONE',  ( -10.81492255796078084, -18.62759615963271287, 42.08224293864769550 ) ) ;
#184483 = CARTESIAN_POINT ( 'NONE',  ( -10.65591991698828700, -43.63381331855018885, -21.52219975116658190 ) ) ;
#184484 = CARTESIAN_POINT ( 'NONE',  ( 13.89961937509977652, -13.97604488694527269, 58.12390960531436690 ) ) ;
#184485 = CARTESIAN_POINT ( 'NONE',  ( 16.52544592524335698, 4.483927247898782831, 36.45942372801901143 ) ) ;
#184486 = CARTESIAN_POINT ( 'NONE',  ( -19.02544592524334988, -5.153800228976617603, 58.95942372801900433 ) ) ;
#184487 = CARTESIAN_POINT ( 'NONE',  ( -0.05219959533937732626, 21.53943276465977519, 22.50109039468567573 ) ) ;
#184488 = CARTESIAN_POINT ( 'NONE',  ( 14.29746914071049879, -8.314922557960816363, 48.33224293864770260 ) ) ;
#184489 = CARTESIAN_POINT ( 'NONE',  ( 5.049401038298161559, -19.05341960407611168, 87.70724293864769550 ) ) ;
#184490 = CARTESIAN_POINT ( 'NONE',  ( -21.53943276465977519, 0.05219959533907696930, 66.24890960531436690 ) ) ;
#184492 = CARTESIAN_POINT ( 'NONE',  ( -16.52544592524335698, -4.483927247898792601, 43.95942372801902565 ) ) ;
#184491 = CARTESIAN_POINT ( 'NONE',  ( 5.719274019375991003, -21.55341960407610458, 107.7072429386476955 ) ) ;
#184493 = CARTESIAN_POINT ( 'NONE',  ( 18.67979575497178502, 10.72451020669898547, 39.16557627198102409 ) ) ;
#184494 = CARTESIAN_POINT ( 'NONE',  ( 5.719274019375673035, 21.55341960407619339, 102.2927570613523613 ) ) ;
#184495 = CARTESIAN_POINT ( 'NONE',  ( -19.03943276465977164, 0.05219959533909376836, 91.24890960531436690 ) ) ;
#184496 = CARTESIAN_POINT ( 'NONE',  ( -0.05219959533909027116, -19.03943276465977164, 42.49890960531435269 ) ) ;
#184497 = CARTESIAN_POINT ( 'NONE',  ( 5.153800228976335163, 19.02544592524342804, 99.79057627198102409 ) ) ;
#184498 = CARTESIAN_POINT ( 'NONE',  ( -19.02544592524342804, 5.153800228976336051, 71.04057627198099567 ) ) ;
#184499 = CARTESIAN_POINT ( 'NONE',  ( -16.53943276465976808, -0.05219959533934237506, 28.75109039468567929 ) ) ;
#184500 = CARTESIAN_POINT ( 'NONE',  ( -3.573655867282028392E-15, 2.428612866367529932E-14, 0.000000000000000000 ) ) ;
#184501 = CARTESIAN_POINT ( 'NONE',  ( 9.474510206698729675, 16.51473224551082808, 52.08442372801900433 ) ) ;
#184503 = CARTESIAN_POINT ( 'NONE',  ( -21.52544592524343514, 5.823673210054127303, 31.04057627198102409 ) ) ;
#184502 = CARTESIAN_POINT ( 'NONE',  ( -21.55341960407619339, 5.719274019375674811, 113.5427570613523756 ) ) ;
#184504 = CARTESIAN_POINT ( 'NONE',  ( -16.52544592524335698, -4.483927247898792601, 93.95942372801903275 ) ) ;
#184505 = CARTESIAN_POINT ( 'NONE',  ( 22.64533781646232669, -20.52407392197266489, -47.58305834096859854 ) ) ;
#184506 = CARTESIAN_POINT ( 'NONE',  ( 9.564922557961047289, -16.46253265017146816, 65.41775706135233293 ) ) ;
#184507 = CARTESIAN_POINT ( 'NONE',  ( 0.05219959533936267826, -19.03943276465977164, 25.00109039468566152 ) ) ;
#184508 = CARTESIAN_POINT ( 'NONE',  ( 37.99999999999999289, 2.428612866367529932E-14, -25.00000000000000000 ) ) ;
#184509 = CARTESIAN_POINT ( 'NONE',  ( -5.049401038298153566, 19.05341960407611168, 35.20724293864768839 ) ) ;
#184510 = CARTESIAN_POINT ( 'NONE',  ( -14.29746914071049879, 8.314922557960819915, 30.83224293864770260 ) ) ;
#184511 = CARTESIAN_POINT ( 'NONE',  ( -19.05341960407611168, -5.049401038298163336, 26.45724293864769550 ) ) ;
#184512 = CARTESIAN_POINT ( 'NONE',  ( 4.483927247898545687, 16.52544592524342804, 29.79057627198102409 ) ) ;
#184513 = LINE ( 'NONE', #169325, #64604 ) ;
#184514 = CARTESIAN_POINT ( 'NONE',  ( 4.379528057220092307, 16.55341960407617563, 92.29275706135236135 ) ) ;
#184515 = CARTESIAN_POINT ( 'NONE',  ( 19.03943276465977164, -0.05219959533909143690, 33.74890960531435979 ) ) ;
#184516 = CARTESIAN_POINT ( 'NONE',  ( -21.52544592524334988, -5.823673210054445271, 103.9594237280190185 ) ) ;
#184517 = CARTESIAN_POINT ( 'NONE',  ( 16.53943276465976808, 0.05219959533934440121, 21.25109039468567218 ) ) ;
#184518 = CARTESIAN_POINT ( 'NONE',  ( -15.80617190586768217, 15.72974639402176855, 73.12609039468567573 ) ) ;
#184519 = CARTESIAN_POINT ( 'NONE',  ( -5.153800228976607833, 19.02544592524334988, 57.70942372801899012 ) ) ;
#184520 = CARTESIAN_POINT ( 'NONE',  ( 16.46253265017160672, -9.564922557960803928, 93.33224293864769550 ) ) ;
#184521 = CARTESIAN_POINT ( 'NONE',  ( -13.89961937509977652, 13.97604488694528158, 80.62390960531436690 ) ) ;
#184522 = CARTESIAN_POINT ( 'NONE',  ( 16.38665767535054485, 7.295008042176069019, 72.23599135785453029 ) ) ;
#184523 = CARTESIAN_POINT ( 'NONE',  ( 5.823673210054125526, 21.52544592524343514, 104.7905762719810241 ) ) ;
#184524 = CARTESIAN_POINT ( 'NONE',  ( 16.52544592524342804, -4.483927247898539470, 68.54057627198103830 ) ) ;
#184525 = CARTESIAN_POINT ( 'NONE',  ( -21.52544592524343514, 5.823673210054127303, 56.04057627198102409 ) ) ;
#184526 = CARTESIAN_POINT ( 'NONE',  ( -13.97604488694527625, -13.89961937509977652, 61.87390960531435979 ) ) ;
#184528 = CARTESIAN_POINT ( 'NONE',  ( 8.224510206698742110, 14.34966873604972548, 87.08442372801901854 ) ) ;
#184527 = CARTESIAN_POINT ( 'NONE',  ( -18.67979575497178146, -10.72451020669898902, 91.66557627198103830 ) ) ;
#184529 = ORIENTED_EDGE ( 'NONE', *, *, #21229, .F. ) ;
#184530 = CARTESIAN_POINT ( 'NONE',  ( -19.05341960407611168, -5.049401038298163336, 56.45724293864768129 ) ) ;
#184532 = DIRECTION ( 'NONE',  ( 0.000000000000000000, 0.000000000000000000, 1.000000000000000000 ) ) ;
#184531 = CARTESIAN_POINT ( 'NONE',  ( 12.06949235617757843, -12.14591786802309237, 98.12390960531436690 ) ) ;
#184533 = CARTESIAN_POINT ( 'NONE',  ( 19.03943276465977164, -0.05219959533909143690, 53.74890960531436690 ) ) ;
#184534 = CARTESIAN_POINT ( 'NONE',  ( -19.02544592524334988, -5.153800228976617603, 78.95942372801900433 ) ) ;
#184535 = CARTESIAN_POINT ( 'NONE',  ( 16.55341960407611168, 4.379528057220329451, 88.95724293864769550 ) ) ;
#184536 = CARTESIAN_POINT ( 'NONE',  ( 15.72974639402176855, 15.80617190586768217, 41.87609039468568284 ) ) ;
#184538 = CARTESIAN_POINT ( 'NONE',  ( 15.72974639402199770, -15.80617190586745480, 98.12390960531436690 ) ) ;
#184537 = CARTESIAN_POINT ( 'NONE',  ( -0.05219959533909027116, -19.03943276465977164, 42.49890960531435269 ) ) ;
#184539 = CARTESIAN_POINT ( 'NONE',  ( -4.379528057220328563, 16.55341960407611168, 90.20724293864770971 ) ) ;
#184540 = CARTESIAN_POINT ( 'NONE',  ( 6.767138868728925338, -40.03474714072476814, -25.59093536067049612 ) ) ;
#184541 = CARTESIAN_POINT ( 'NONE',  ( -9.474510206698964154, 16.51473224551069663, 65.41557627198102409 ) ) ;
#184542 = CARTESIAN_POINT ( 'NONE',  ( 18.89770734986051792, 5.499999999999905853, 46.60214472496640781 ) ) ;
#184544 = CARTESIAN_POINT ( 'NONE',  ( -13.89961937509977652, 13.97604488694528158, 110.6239096053143243 ) ) ;
#184543 = CARTESIAN_POINT ( 'NONE',  ( -13.97604488694547697, 13.89961937509957934, 98.12609039468566152 ) ) ;
#184545 = CARTESIAN_POINT ( 'NONE',  ( -0.05219959533937732626, 21.53943276465977519, 32.50109039468568284 ) ) ;
#184546 = CARTESIAN_POINT ( 'NONE',  ( -9.564922557960796823, -16.46253265017161027, 82.08224293864768129 ) ) ;
#184547 = CARTESIAN_POINT ( 'NONE',  ( 0.05219959533936267826, -19.03943276465977164, 65.00109039468567573 ) ) ;
#184548 = CARTESIAN_POINT ( 'NONE',  ( -16.46253265017160317, 9.564922557960807481, 55.83224293864769550 ) ) ;
#184549 = CARTESIAN_POINT ( 'NONE',  ( -16.53943276465976808, 0.05219959533911058130, 81.24890960531436690 ) ) ;
#184550 = CARTESIAN_POINT ( 'NONE',  ( 4.379528057220339221, -16.55341960407611168, 62.70724293864769550 ) ) ;
#184551 = CARTESIAN_POINT ( 'NONE',  ( -19.03943276465977164, 0.05219959533909376836, 86.24890960531436690 ) ) ;
#184552 = CARTESIAN_POINT ( 'NONE',  ( 18.67979575497178502, 10.72451020669898547, 99.16557627198100988 ) ) ;
#184553 = CARTESIAN_POINT ( 'NONE',  ( 9.474510206698971260, -16.51473224551069308, 87.91557627198102409 ) ) ;
#184554 = CARTESIAN_POINT ( 'NONE',  ( -5.049401038297874678, -19.05341960407617918, 29.79275706135232227 ) ) ;
#184557 = CARTESIAN_POINT ( 'NONE',  ( 12.06949235617757843, -12.14591786802309237, 113.1239096053143953 ) ) ;
#184556 = CARTESIAN_POINT ( 'NONE',  ( -8.224510206698948167, 14.34966873604960824, 35.41557627198102409 ) ) ;
#184555 = CARTESIAN_POINT ( 'NONE',  ( -9.474510206698964154, 16.51473224551069663, 40.41557627198103120 ) ) ;
#184558 = ORIENTED_EDGE ( 'NONE', *, *, #87010, .T. ) ;
#184559 = CARTESIAN_POINT ( 'NONE',  ( 18.67979575497194134, -10.72451020669871369, 35.83442372801901143 ) ) ;
#184560 = CARTESIAN_POINT ( 'NONE',  ( 19.03943276465977164, 0.05219959533936151252, 66.25109039468567573 ) ) ;
#184561 = CARTESIAN_POINT ( 'NONE',  ( -0.05219959533910754901, -16.53943276465976808, 37.49890960531436690 ) ) ;
#184562 = CARTESIAN_POINT ( 'NONE',  ( -0.05219959533907301413, -21.53943276465977519, 92.49890960531436690 ) ) ;
#184563 = CARTESIAN_POINT ( 'NONE',  ( -18.67979575497178146, -10.72451020669898902, 21.66557627198102409 ) ) ;
#184564 = CARTESIAN_POINT ( 'NONE',  ( 8.224510206698953496, -14.34966873604960469, 67.91557627198102409 ) ) ;
#184565 = CARTESIAN_POINT ( 'NONE',  ( -5.049401038298153566, 19.05341960407611168, 30.20724293864768839 ) ) ;
#184566 = CARTESIAN_POINT ( 'NONE',  ( -9.564922557961040184, 16.46253265017147172, 22.91775706135233648 ) ) ;
#184567 = CARTESIAN_POINT ( 'NONE',  ( -16.55341960407617563, 4.379528057220093196, 103.5427570613523613 ) ) ;
#184568 = CARTESIAN_POINT ( 'NONE',  ( 12.06949235617739724, 12.14591786802326823, 56.87609039468568994 ) ) ;
#184569 = CARTESIAN_POINT ( 'NONE',  ( -21.55341960407610458, -5.719274019375992779, 36.45724293864768839 ) ) ;
#184570 = CARTESIAN_POINT ( 'NONE',  ( 15.80617190586769283, -15.72974639402175789, 110.6260903946857042 ) ) ;
#184571 = CARTESIAN_POINT ( 'NONE',  ( 13.97604488694527802, 13.89961937509977652, 74.37390960531436690 ) ) ;
#184572 = CARTESIAN_POINT ( 'NONE',  ( 16.53943276465976808, 0.05219959533934440121, 76.25109039468568994 ) ) ;
#184573 = CARTESIAN_POINT ( 'NONE',  ( -16.52544592524342804, 4.483927247898546575, 116.0405762719810383 ) ) ;
#184574 = CARTESIAN_POINT ( 'NONE',  ( -4.483927247898539470, -16.52544592524342804, 32.29057627198102409 ) ) ;
#184576 = CARTESIAN_POINT ( 'NONE',  ( 16.46253265017160672, -9.564922557960803928, 93.33224293864769550 ) ) ;
#184575 = CARTESIAN_POINT ( 'NONE',  ( -19.05341960407611168, -5.049401038298163336, 111.4572429386476671 ) ) ;
#184577 = CARTESIAN_POINT ( 'NONE',  ( 19.03943276465977164, -0.05219959533909143690, 113.7489096053143669 ) ) ;
#184578 = CARTESIAN_POINT ( 'NONE',  ( 0.05219959533910956823, 16.53943276465976808, 59.99890960531436690 ) ) ;
#184579 = CARTESIAN_POINT ( 'NONE',  ( 16.52544592524342804, -4.483927247898539470, 28.54057627198103120 ) ) ;
#184580 = B_SPLINE_CURVE_WITH_KNOTS ( 'NONE', 3,
 ( #16413, #78060, #153923, #139728, #15417, #77075, #28624, #59921, #13433, #75097 ),
 .UNSPECIFIED., .F., .F.,
 ( 4, 2, 2, 2, 4 ),
 ( 2.788292365864085830E-07, 0.0002942923369301741164, 0.0005883058446237618942, 0.0008823193523173495636, 0.001176332860010937233 ),
 .UNSPECIFIED. ) ;
#184581 = CARTESIAN_POINT ( 'NONE',  ( 0.05219959533910956823, 16.53943276465976808, 54.99890960531435269 ) ) ;
#184582 = VERTEX_POINT ( 'NONE', #123044 ) ;
#184584 = CARTESIAN_POINT ( 'NONE',  ( 17.49999999999999289, -3.850315288878723763, 31.76629130603453888 ) ) ;
#184583 = CARTESIAN_POINT ( 'NONE',  ( 4.379528057220092307, 16.55341960407617563, 42.29275706135235424 ) ) ;
#184585 = CARTESIAN_POINT ( 'NONE',  ( -16.51473224551082808, 9.474510206698731452, 53.33442372801900433 ) ) ;
#184586 = CARTESIAN_POINT ( 'NONE',  ( -13.89961937509977652, 13.97604488694528158, 85.62390960531433848 ) ) ;
#184587 = CARTESIAN_POINT ( 'NONE',  ( -19.05341960407617563, 5.049401038297882671, 63.54275706135234003 ) ) ;
#184588 = CARTESIAN_POINT ( 'NONE',  ( 27.73933785331498214, 9.013057229001095294, 146.4750000027311501 ) ) ;
#184589 = CARTESIAN_POINT ( 'NONE',  ( -5.153800228976607833, 19.02544592524334988, 62.70942372801899722 ) ) ;
#184591 = CARTESIAN_POINT ( 'NONE',  ( -14.29746914071037622, -8.314922557961029526, 89.16775706135236135 ) ) ;
#184590 = CARTESIAN_POINT ( 'NONE',  ( -9.564922557961040184, 16.46253265017147172, 97.91775706135233293 ) ) ;
#184592 = CARTESIAN_POINT ( 'NONE',  ( 8.571926809382603096, -26.38167802310801235, 143.9750000027312069 ) ) ;
#184593 = CARTESIAN_POINT ( 'NONE',  ( 16.46253265017160672, -9.564922557960803928, 23.33224293864769194 ) ) ;
#184594 = CARTESIAN_POINT ( 'NONE',  ( -10.72451020669898014, 18.67979575497178502, 25.41557627198103120 ) ) ;
#184595 = CARTESIAN_POINT ( 'NONE',  ( 15.80617190586769283, -15.72974639402175789, 40.62609039468567573 ) ) ;
#184596 = CARTESIAN_POINT ( 'NONE',  ( 0.05219959533936267826, -19.03943276465977164, 105.0010903946856615 ) ) ;
#184598 = CARTESIAN_POINT ( 'NONE',  ( -5.153800228976328057, -19.02544592524343514, 62.29057627198100988 ) ) ;
#184597 = CARTESIAN_POINT ( 'NONE',  ( 17.50000000000002132, -4.658240926743160593, 106.4447041781680383 ) ) ;
#184599 = CARTESIAN_POINT ( 'NONE',  ( 5.049401038298161559, -19.05341960407611168, 97.70724293864766707 ) ) ;
#184601 = CARTESIAN_POINT ( 'NONE',  ( -9.564922557960796823, -16.46253265017161027, 67.08224293864769550 ) ) ;
#184600 = CARTESIAN_POINT ( 'NONE',  ( -8.314922557960811034, -14.29746914071050412, 67.08224293864770971 ) ) ;
#184602 = CARTESIAN_POINT ( 'NONE',  ( 13.89961937509977652, -13.97604488694527269, 68.12390960531436690 ) ) ;
#184603 = CARTESIAN_POINT ( 'NONE',  ( -5.049401038297874678, -19.05341960407617918, 79.79275706135233293 ) ) ;
#184604 = CARTESIAN_POINT ( 'NONE',  ( 21.52544592524344225, -5.823673210054117533, 53.54057627198103120 ) ) ;
#184605 = CARTESIAN_POINT ( 'NONE',  ( 5.049401038298161559, -19.05341960407611168, 22.70724293864769194 ) ) ;
#184606 = CARTESIAN_POINT ( 'NONE',  ( -5.049401038297874678, -19.05341960407617918, 44.79275706135232582 ) ) ;
#184607 = CARTESIAN_POINT ( 'NONE',  ( 0.05219959533909260263, 19.03943276465977164, 84.99890960531436690 ) ) ;
#184608 = CARTESIAN_POINT ( 'NONE',  ( -5.719274019375978568, 21.55341960407610458, 70.20724293864769550 ) ) ;
#184610 = CARTESIAN_POINT ( 'NONE',  ( 19.05341960407617918, -5.049401038297876454, 36.04275706135234003 ) ) ;
#184609 = CARTESIAN_POINT ( 'NONE',  ( -14.29746914071049879, 8.314922557960819915, 75.83224293864769550 ) ) ;
#184611 = CARTESIAN_POINT ( 'NONE',  ( 18.62759615963271287, -10.81492255796078972, 63.33224293864770260 ) ) ;
#184612 = CARTESIAN_POINT ( 'NONE',  ( -10.72451020669898014, 18.67979575497178502, 45.41557627198103830 ) ) ;
#184613 = CARTESIAN_POINT ( 'NONE',  ( 21.55341960407619695, -5.719274019375665929, 96.04275706135236135 ) ) ;
#184614 = CARTESIAN_POINT ( 'NONE',  ( -5.153800228976328057, -19.02544592524343514, 67.29057627198102409 ) ) ;
#184615 = CARTESIAN_POINT ( 'NONE',  ( 5.049401038298161559, -19.05341960407611168, 22.70724293864769194 ) ) ;
#184616 = CARTESIAN_POINT ( 'NONE',  ( -21.53943276465977519, -0.05219959533937600094, 28.75109039468567929 ) ) ;
#184617 = CARTESIAN_POINT ( 'NONE',  ( 21.52544592524334988, 5.823673210054432836, 41.45942372801901143 ) ) ;
#184618 = CARTESIAN_POINT ( 'NONE',  ( 19.02544592524343514, -5.153800228976328945, 38.54057627198103120 ) ) ;
#184619 = CARTESIAN_POINT ( 'NONE',  ( 15.80617190586746368, 15.72974639402197994, 109.3739096053143811 ) ) ;
#184620 = CARTESIAN_POINT ( 'NONE',  ( -9.564922557961040184, 16.46253265017147172, 47.91775706135233293 ) ) ;
#184621 = CARTESIAN_POINT ( 'NONE',  ( 17.50000000000000000, -5.499999999999992895, 76.21769037696435589 ) ) ;
#184622 = CARTESIAN_POINT ( 'NONE',  ( 16.46253265017160672, -9.564922557960803928, 28.33224293864769550 ) ) ;
#184623 = PRESENTATION_STYLE_ASSIGNMENT (( #61266 ) ) ;
#184624 = CARTESIAN_POINT ( 'NONE',  ( -12.06949235617739369, -12.14591786802326823, 59.37609039468568284 ) ) ;
#184625 = CARTESIAN_POINT ( 'NONE',  ( 13.89961937509977652, -13.97604488694527269, 23.12390960531436335 ) ) ;
#184626 = CARTESIAN_POINT ( 'NONE',  ( -25.73063820182027328, -8.702599028573553497, 171.6270364942855053 ) ) ;
#184627 = CARTESIAN_POINT ( 'NONE',  ( -5.049401038298153566, 19.05341960407611168, 70.20724293864769550 ) ) ;
#184629 = ADVANCED_FACE ( 'NONE', ( #109868 ), #17879, .F. ) ;
#184628 = CARTESIAN_POINT ( 'NONE',  ( 4.379528057220339221, -16.55341960407611168, 112.7072429386476955 ) ) ;
#184630 = VECTOR ( 'NONE', #29440, 1000.000000000000000 ) ;
#184631 = CARTESIAN_POINT ( 'NONE',  ( 10.81492255796078972, 18.62759615963270932, 59.58224293864770260 ) ) ;
#184632 = CARTESIAN_POINT ( 'NONE',  ( -16.53943276465976808, -0.05219959533934237506, 43.75109039468568284 ) ) ;
#184633 = CARTESIAN_POINT ( 'NONE',  ( -21.52544592524334988, -5.823673210054445271, 93.95942372801903275 ) ) ;
#184634 = CARTESIAN_POINT ( 'NONE',  ( 13.97604488694527802, 13.89961937509977652, 24.37390960531435624 ) ) ;
#184635 = CARTESIAN_POINT ( 'NONE',  ( 4.379528057220092307, 16.55341960407617563, 112.2927570613523471 ) ) ;
#184636 = CARTESIAN_POINT ( 'NONE',  ( -14.29746914071049879, 8.314922557960819915, 50.83224293864770971 ) ) ;
#184637 = CARTESIAN_POINT ( 'NONE',  ( -19.05341960407611168, -5.049401038298163336, 51.45724293864770260 ) ) ;
#184638 = CARTESIAN_POINT ( 'NONE',  ( -15.72974639402176322, -15.80617190586768395, 94.37609039468568994 ) ) ;
#184639 = CARTESIAN_POINT ( 'NONE',  ( 10.81492255796106328, -18.62759615963255655, 20.41775706135234714 ) ) ;
#184640 = CARTESIAN_POINT ( 'NONE',  ( -21.53943276465977519, -0.05219959533937600094, 68.75109039468568994 ) ) ;
#184641 = CARTESIAN_POINT ( 'NONE',  ( 0.05219959533934541429, -16.53943276465976808, 55.00109039468568284 ) ) ;
#184643 = CARTESIAN_POINT ( 'NONE',  ( 0.05219959533937995610, -21.53943276465977519, 95.00109039468568994 ) ) ;
#184642 = CARTESIAN_POINT ( 'NONE',  ( -14.29746914071049879, 8.314922557960819915, 80.83224293864769550 ) ) ;
#184644 = CARTESIAN_POINT ( 'NONE',  ( 16.53943276465976808, -0.05219959533910856209, 23.74890960531435269 ) ) ;
#184645 = DIRECTION ( 'NONE',  ( -0.8164965809277229258, 0.000000000000000000, -0.5773502691896299499 ) ) ;
#184646 = CARTESIAN_POINT ( 'NONE',  ( -14.29746914071037622, -8.314922557961029526, 34.16775706135234714 ) ) ;
#184647 = CARTESIAN_POINT ( 'NONE',  ( 8.224510206698953496, -14.34966873604960469, 42.91557627198103120 ) ) ;
#184648 = CARTESIAN_POINT ( 'NONE',  ( 12.06949235617739724, 12.14591786802326823, 86.87609039468568994 ) ) ;
#184649 = CARTESIAN_POINT ( 'NONE',  ( 13.89961937509977652, -13.97604488694527269, 98.12390960531433848 ) ) ;
#184650 = CARTESIAN_POINT ( 'NONE',  ( -16.51473224551069308, -9.474510206698971260, 111.6655762719810383 ) ) ;
#184651 = CARTESIAN_POINT ( 'NONE',  ( -21.53943276465977519, -0.05219959533937600094, 93.75109039468567573 ) ) ;
#184652 = CARTESIAN_POINT ( 'NONE',  ( 4.379528057220092307, 16.55341960407617563, 97.29275706135234714 ) ) ;
#184653 = CARTESIAN_POINT ( 'NONE',  ( 16.55341960407611168, 4.379528057220329451, 68.95724293864769550 ) ) ;
#184654 = CARTESIAN_POINT ( 'NONE',  ( 5.153800228976335163, 19.02544592524342804, 79.79057627198102409 ) ) ;
#184655 = VERTEX_POINT ( 'NONE', #46215 ) ;
#184656 = CARTESIAN_POINT ( 'NONE',  ( -8.224510206698735004, -14.34966873604973081, 34.58442372801900433 ) ) ;
#184657 = CARTESIAN_POINT ( 'NONE',  ( 19.02544592524343514, -5.153800228976328945, 43.54057627198103120 ) ) ;
#184658 = CARTESIAN_POINT ( 'NONE',  ( -16.46253265017160317, 9.564922557960807481, 95.83224293864769550 ) ) ;
#184660 = CARTESIAN_POINT ( 'NONE',  ( -36.91746825000000598, 2.428612866367529932E-14, -0.6249999972688132788 ) ) ;
#184659 = CARTESIAN_POINT ( 'NONE',  ( 16.53943276465976808, 0.05219959533934440121, 31.25109039468568639 ) ) ;
#184661 = CARTESIAN_POINT ( 'NONE',  ( -9.474510206698720793, -16.51473224551083518, 29.58442372801900433 ) ) ;
#184662 = CARTESIAN_POINT ( 'NONE',  ( 8.224510206698742110, 14.34966873604972548, 97.08442372801904696 ) ) ;
#184663 = CARTESIAN_POINT ( 'NONE',  ( 19.03943276465977164, -0.05219959533909143690, 33.74890960531435979 ) ) ;
#184664 = CARTESIAN_POINT ( 'NONE',  ( 12.14591786802327356, -12.06949235617739191, 85.62609039468568994 ) ) ;
#184665 = CARTESIAN_POINT ( 'NONE',  ( -12.06949235617739369, -12.14591786802326823, 69.37609039468567573 ) ) ;
#184666 = CARTESIAN_POINT ( 'NONE',  ( 9.474510206698729675, 16.51473224551082808, 87.08442372801900433 ) ) ;
#184667 = CARTESIAN_POINT ( 'NONE',  ( 0.05219959533936267826, -19.03943276465977164, 25.00109039468566152 ) ) ;
#184668 = CARTESIAN_POINT ( 'NONE',  ( -16.46253265017160317, 9.564922557960807481, 45.83224293864769550 ) ) ;
#184669 = CARTESIAN_POINT ( 'NONE',  ( 8.314922557960818139, 14.29746914071049879, 79.58224293864769550 ) ) ;
#184670 = CARTESIAN_POINT ( 'NONE',  ( 19.05341960407617918, -5.049401038297876454, 56.04275706135234714 ) ) ;
#184671 = CARTESIAN_POINT ( 'NONE',  ( -18.67979575497178146, -10.72451020669898902, 56.66557627198103830 ) ) ;
#184672 = CARTESIAN_POINT ( 'NONE',  ( -16.51473224551082808, 9.474510206698731452, 33.33442372801899722 ) ) ;
#184673 = CARTESIAN_POINT ( 'NONE',  ( -5.153800228976328057, -19.02544592524343514, 102.2905762719810383 ) ) ;
#184674 = CARTESIAN_POINT ( 'NONE',  ( 15.72974639402199770, -15.80617190586745480, 83.12390960531436690 ) ) ;
#184675 = CARTESIAN_POINT ( 'NONE',  ( 16.51473224551069308, 9.474510206698969483, 114.1655762719810241 ) ) ;
#184676 = CARTESIAN_POINT ( 'NONE',  ( -5.153800228976607833, 19.02544592524334988, 107.7094237280189759 ) ) ;
#184677 = CARTESIAN_POINT ( 'NONE',  ( 13.89961937509977652, -13.97604488694527269, 113.1239096053143527 ) ) ;
#184678 = CARTESIAN_POINT ( 'NONE',  ( 16.51473224551083163, -9.474510206698727899, 110.8344237280190043 ) ) ;
#184679 = CARTESIAN_POINT ( 'NONE',  ( -19.05341960407611168, -5.049401038298163336, 36.45724293864766707 ) ) ;
#184680 = CARTESIAN_POINT ( 'NONE',  ( -19.05341960407611168, -5.049401038298163336, 96.45724293864769550 ) ) ;
#184681 = CARTESIAN_POINT ( 'NONE',  ( -18.67979575497178146, -10.72451020669898902, 76.66557627198103830 ) ) ;
#184682 = CARTESIAN_POINT ( 'NONE',  ( 16.55341960407618274, -4.379528057220086978, 51.04275706135234714 ) ) ;
#184683 = CARTESIAN_POINT ( 'NONE',  ( -10.72451020669870658, -18.67979575497194134, 64.58442372801900433 ) ) ;
#184685 = CARTESIAN_POINT ( 'NONE',  ( -9.474510206698720793, -16.51473224551083518, 19.58442372801899722 ) ) ;
#184684 = CARTESIAN_POINT ( 'NONE',  ( 13.97604488694548053, -13.89961937509957401, 105.6260903946856757 ) ) ;
#184686 = CARTESIAN_POINT ( 'NONE',  ( -4.483927247898782831, 16.52544592524335698, 112.7094237280190328 ) ) ;
#184687 = CARTESIAN_POINT ( 'NONE',  ( -18.67979575497178146, -10.72451020669898902, 106.6655762719810383 ) ) ;
#184688 = CARTESIAN_POINT ( 'NONE',  ( 4.483927247898545687, 16.52544592524342804, 34.79057627198103120 ) ) ;
#184689 = CARTESIAN_POINT ( 'NONE',  ( 5.153800228976615827, -19.02544592524334988, 85.20942372801900433 ) ) ;
#184690 = CARTESIAN_POINT ( 'NONE',  ( -18.67979575497193778, 10.72451020669871902, 58.33442372801901143 ) ) ;
#184691 = CARTESIAN_POINT ( 'NONE',  ( 9.564922557961047289, -16.46253265017146816, 45.41775706135232582 ) ) ;
#184692 = CARTESIAN_POINT ( 'NONE',  ( -16.52544592524342804, 4.483927247898546575, 101.0405762719810383 ) ) ;
#184693 = CARTESIAN_POINT ( 'NONE',  ( 0.05219959533907565091, 21.53943276465977519, 24.99890960531435624 ) ) ;
#184694 = CARTESIAN_POINT ( 'NONE',  ( 12.06949235617757843, -12.14591786802309237, 33.12390960531435979 ) ) ;
#184695 = CARTESIAN_POINT ( 'NONE',  ( -15.80617190586768217, 15.72974639402176855, 103.1260903946856757 ) ) ;
#184696 = CARTESIAN_POINT ( 'NONE',  ( -4.483927247898782831, 16.52544592524335698, 57.70942372801901143 ) ) ;
#184697 = CARTESIAN_POINT ( 'NONE',  ( 12.06949235617757843, -12.14591786802309237, 23.12390960531436335 ) ) ;
#184698 = CARTESIAN_POINT ( 'NONE',  ( 10.81492255796106328, -18.62759615963255655, 65.41775706135234714 ) ) ;
#184699 = CARTESIAN_POINT ( 'NONE',  ( 0.05219959533937995610, -21.53943276465977519, 60.00109039468568284 ) ) ;
#184700 = CARTESIAN_POINT ( 'NONE',  ( -16.51473224551069308, -9.474510206698971260, 21.66557627198102765 ) ) ;
#184701 = CARTESIAN_POINT ( 'NONE',  ( 21.55341960407619695, -5.719274019375665929, 26.04275706135235779 ) ) ;
#184702 = CARTESIAN_POINT ( 'NONE',  ( -0.05219959533910754901, -16.53943276465976808, 107.4989096053143669 ) ) ;
#184703 = CARTESIAN_POINT ( 'NONE',  ( -5.049401038298153566, 19.05341960407611168, 35.20724293864768839 ) ) ;
#184704 = CARTESIAN_POINT ( 'NONE',  ( -14.34966873604960291, -8.224510206698953496, 76.66557627198103830 ) ) ;
#184705 = CARTESIAN_POINT ( 'NONE',  ( 0.05219959533909260263, 19.03943276465977164, 74.99890960531435269 ) ) ;
#184706 = CARTESIAN_POINT ( 'NONE',  ( 4.379528057220339221, -16.55341960407611168, 27.70724293864769905 ) ) ;
#184707 = CARTESIAN_POINT ( 'NONE',  ( -15.72974639402197994, 15.80617190586746368, 55.62390960531436690 ) ) ;
#184708 = CARTESIAN_POINT ( 'NONE',  ( 8.314922557960818139, 14.29746914071049879, 89.58224293864768129 ) ) ;
#184709 = CARTESIAN_POINT ( 'NONE',  ( -5.823673210054116645, -21.52544592524344225, 112.2905762719810241 ) ) ;
#184710 = CARTESIAN_POINT ( 'NONE',  ( -5.153800228976328057, -19.02544592524343514, 97.29057627198099567 ) ) ;
#184712 = CARTESIAN_POINT ( 'NONE',  ( -19.02544592524334988, -5.153800228976617603, 103.9594237280190043 ) ) ;
#184711 = CARTESIAN_POINT ( 'NONE',  ( 19.02544592524343514, -5.153800228976328945, 48.54057627198103120 ) ) ;
#184713 = EDGE_CURVE ( 'NONE', #181594, #145515, #101082, .T. ) ;
#184714 = CARTESIAN_POINT ( 'NONE',  ( -0.05219959533907301413, -21.53943276465977519, 62.49890960531436690 ) ) ;
#184715 = CARTESIAN_POINT ( 'NONE',  ( 15.72974639402176855, 15.80617190586768217, 86.87609039468568994 ) ) ;
#184716 = CARTESIAN_POINT ( 'NONE',  ( 5.049401038298161559, -19.05341960407611168, 67.70724293864769550 ) ) ;
#184717 = CARTESIAN_POINT ( 'NONE',  ( 0.05219959533909260263, 19.03943276465977164, 99.99890960531436690 ) ) ;
#184718 = CARTESIAN_POINT ( 'NONE',  ( -0.05219959533934338120, 16.53943276465976808, 82.50109039468568994 ) ) ;
#184719 = CARTESIAN_POINT ( 'NONE',  ( 18.62759615963255655, 10.81492255796105972, 61.66775706135235424 ) ) ;
#184720 = CARTESIAN_POINT ( 'NONE',  ( 18.62759615963255655, 10.81492255796105972, 86.66775706135234714 ) ) ;
#184721 = CARTESIAN_POINT ( 'NONE',  ( -21.52544592524343514, 5.823673210054127303, 116.0405762719810383 ) ) ;
#184722 = CARTESIAN_POINT ( 'NONE',  ( -8.314922557961024197, 14.29746914071037800, 77.91775706135231871 ) ) ;
#184723 = CARTESIAN_POINT ( 'NONE',  ( 15.72974639402199770, -15.80617190586745480, 78.12390960531436690 ) ) ;
#184724 = CARTESIAN_POINT ( 'NONE',  ( 19.02544592524334988, 5.153800228976608722, 41.45942372801900433 ) ) ;
#184725 = CARTESIAN_POINT ( 'NONE',  ( -0.05219959533907301413, -21.53943276465977519, 37.49890960531436690 ) ) ;
#184727 = CARTESIAN_POINT ( 'NONE',  ( 4.483927247898545687, 16.52544592524342804, 24.79057627198103120 ) ) ;
#184726 = CARTESIAN_POINT ( 'NONE',  ( -13.97604488694527625, -13.89961937509977652, 81.87390960531436690 ) ) ;
#184728 = CARTESIAN_POINT ( 'NONE',  ( -16.52216118717209170, 7.221426719304499642, 63.92400978953008206 ) ) ;
#184729 = CARTESIAN_POINT ( 'NONE',  ( 15.80617190586746368, 15.72974639402197994, 24.37390960531435979 ) ) ;
#184730 = DIRECTION ( 'NONE',  ( 1.000000000000000000, 0.000000000000000000, 0.000000000000000000 ) ) ;
#184731 = CARTESIAN_POINT ( 'NONE',  ( 19.03943276465977164, 0.05219959533936151252, 101.2510903946856757 ) ) ;
#184732 = CARTESIAN_POINT ( 'NONE',  ( -5.823673210054116645, -21.52544592524344225, 72.29057627198102409 ) ) ;
#184733 = CARTESIAN_POINT ( 'NONE',  ( 4.379528057220339221, -16.55341960407611168, 47.70724293864770260 ) ) ;
#184734 = CARTESIAN_POINT ( 'NONE',  ( 16.46253265017146816, 9.564922557961045513, 111.6677570613523329 ) ) ;
#184735 = CARTESIAN_POINT ( 'NONE',  ( -9.474510206698964154, 16.51473224551069663, 35.41557627198102409 ) ) ;
#184736 = CARTESIAN_POINT ( 'NONE',  ( 0.05219959533934541429, -16.53943276465976808, 20.00109039468568639 ) ) ;
#184738 = CARTESIAN_POINT ( 'NONE',  ( 16.46253265017146816, 9.564922557961045513, 71.66775706135233293 ) ) ;
#184737 = CARTESIAN_POINT ( 'NONE',  ( -10.72451020669898014, 18.67979575497178502, 100.4155762719810241 ) ) ;
#184739 = CARTESIAN_POINT ( 'NONE',  ( 0.05219959533934541429, -16.53943276465976808, 75.00109039468568994 ) ) ;
#184740 = CARTESIAN_POINT ( 'NONE',  ( -13.97604488694527625, -13.89961937509977652, 81.87390960531436690 ) ) ;
#184741 = CARTESIAN_POINT ( 'NONE',  ( -14.34966873604960291, -8.224510206698953496, 71.66557627198100988 ) ) ;
#184742 = CARTESIAN_POINT ( 'NONE',  ( 9.564922557960805705, 16.46253265017160317, 64.58224293864769550 ) ) ;
#184743 = CARTESIAN_POINT ( 'NONE',  ( 16.52544592524342804, -4.483927247898539470, 68.54057627198103830 ) ) ;
#184744 = CARTESIAN_POINT ( 'NONE',  ( -16.51473224551069308, -9.474510206698971260, 36.66557627198102409 ) ) ;
#184745 = CARTESIAN_POINT ( 'NONE',  ( -37.43820758241025715, -2.754439498815796750, 40.23603015349058154 ) ) ;
#184746 = CARTESIAN_POINT ( 'NONE',  ( 4.379528057220339221, -16.55341960407611168, 42.70724293864770260 ) ) ;
#184747 = CARTESIAN_POINT ( 'NONE',  ( -5.049401038298153566, 19.05341960407611168, 75.20724293864769550 ) ) ;
#184748 = CARTESIAN_POINT ( 'NONE',  ( -30.00000000000000000, 5.499999999999992895, 102.5000000000000142 ) ) ;
#184749 = CARTESIAN_POINT ( 'NONE',  ( 13.89961937509957401, 13.97604488694547697, 56.87609039468564731 ) ) ;
#184750 = CARTESIAN_POINT ( 'NONE',  ( 4.483927247898790824, -16.52544592524335698, 60.20942372801902565 ) ) ;
#184751 = CARTESIAN_POINT ( 'NONE',  ( 18.62759615963271287, -10.81492255796078972, 58.33224293864768839 ) ) ;
#184752 = CARTESIAN_POINT ( 'NONE',  ( -16.51473224551082808, 9.474510206698731452, 28.33442372801900433 ) ) ;
#184753 = CARTESIAN_POINT ( 'NONE',  ( 16.51473224551069308, 9.474510206698969483, 94.16557627198103830 ) ) ;
#184754 = CYLINDRICAL_SURFACE ( 'NONE', #124348, 1.499999999999997780 ) ;
#184755 = CARTESIAN_POINT ( 'NONE',  ( -10.81492255796078084, -18.62759615963271287, 32.08224293864769550 ) ) ;
#184756 = CARTESIAN_POINT ( 'NONE',  ( -13.89961937509977652, 13.97604488694528158, 65.62390960531436690 ) ) ;
#184757 = CARTESIAN_POINT ( 'NONE',  ( 21.52544592524334988, 5.823673210054432836, 56.45942372801902565 ) ) ;
#184758 = CARTESIAN_POINT ( 'NONE',  ( 16.55341960407611168, 4.379528057220329451, 108.9572429386476955 ) ) ;
#184761 = VERTEX_POINT ( 'NONE', #99672 ) ;
#184760 = CARTESIAN_POINT ( 'NONE',  ( 9.564922557960805705, 16.46253265017160317, 99.58224293864770971 ) ) ;
#184759 = CARTESIAN_POINT ( 'NONE',  ( -18.67979575497178146, -10.72451020669898902, 106.6655762719810383 ) ) ;
#184762 = CARTESIAN_POINT ( 'NONE',  ( -10.81492255796105439, 18.62759615963255655, 42.91775706135235424 ) ) ;
#184763 = ORIENTED_EDGE ( 'NONE', *, *, #56725, .F. ) ;
#184764 = CARTESIAN_POINT ( 'NONE',  ( -19.02544592524342804, 5.153800228976336051, 101.0405762719810241 ) ) ;
#184765 = DIRECTION ( 'NONE',  ( 1.000000000000000000, 0.000000000000000000, 3.709348145883536076E-20 ) ) ;
#184766 = CARTESIAN_POINT ( 'NONE',  ( -0.05219959533907301413, -21.53943276465977519, 97.49890960531436690 ) ) ;
#184767 = CARTESIAN_POINT ( 'NONE',  ( 5.049401038298161559, -19.05341960407611168, 42.70724293864767418 ) ) ;
#184768 = CARTESIAN_POINT ( 'NONE',  ( -12.06949235617739369, -12.14591786802326823, 19.37609039468568639 ) ) ;
#184769 = CARTESIAN_POINT ( 'NONE',  ( 11.40812507854754365, 35.11059874428196537, -1.724999997268813479 ) ) ;
#184770 = CARTESIAN_POINT ( 'NONE',  ( -0.05219959533909027116, -19.03943276465977164, 27.49890960531435624 ) ) ;
#184771 = CARTESIAN_POINT ( 'NONE',  ( -21.52544592524334988, -5.823673210054445271, 103.9594237280190185 ) ) ;
#184773 = CARTESIAN_POINT ( 'NONE',  ( 18.67979575497194134, -10.72451020669871369, 45.83442372801901854 ) ) ;
#184772 = CARTESIAN_POINT ( 'NONE',  ( -9.474510206698964154, 16.51473224551069663, 75.41557627198103830 ) ) ;
#184774 = CARTESIAN_POINT ( 'NONE',  ( -21.52544592524334988, -5.823673210054445271, 28.95942372801902209 ) ) ;
#184775 = CARTESIAN_POINT ( 'NONE',  ( -22.44159573604009950, -16.30477369853688430, 143.5750000027311728 ) ) ;
#184776 = CARTESIAN_POINT ( 'NONE',  ( -13.97604488694527625, -13.89961937509977652, 101.8739096053143811 ) ) ;
#184777 = CARTESIAN_POINT ( 'NONE',  ( 1.542446121169174900, 28.32207039655730085, 140.0000000000000568 ) ) ;
#184780 = CARTESIAN_POINT ( 'NONE',  ( -0.05219959533937732626, 21.53943276465977519, 52.50109039468567573 ) ) ;
#184779 = CARTESIAN_POINT ( 'NONE',  ( -0.05219959533934338120, 16.53943276465976808, 72.50109039468568994 ) ) ;
#184778 = CARTESIAN_POINT ( 'NONE',  ( -16.52544592524335698, -4.483927247898792601, 43.95942372801902565 ) ) ;
#184781 = CARTESIAN_POINT ( 'NONE',  ( -18.67979575497193778, 10.72451020669871902, 78.33442372801901854 ) ) ;
#184782 = CARTESIAN_POINT ( 'NONE',  ( 2.500000000000000000, 0.000000000000000000, -65.00100000000003320 ) ) ;
#184783 = CARTESIAN_POINT ( 'NONE',  ( -19.05341960407617563, 5.049401038297882671, 103.5427570613523329 ) ) ;
#184784 = CARTESIAN_POINT ( 'NONE',  ( 16.46253265017160672, -9.564922557960803928, 73.33224293864769550 ) ) ;
#184785 = CARTESIAN_POINT ( 'NONE',  ( 19.02544592524343514, -5.153800228976328945, 98.54057627198100988 ) ) ;
#184786 = CARTESIAN_POINT ( 'NONE',  ( 12.06949235617757843, -12.14591786802309237, 108.1239096053143811 ) ) ;
#184787 = CARTESIAN_POINT ( 'NONE',  ( -18.62759615963270932, 10.81492255796079327, 35.83224293864768839 ) ) ;
#184788 = CARTESIAN_POINT ( 'NONE',  ( -4.483927247898782831, 16.52544592524335698, 87.70942372801901854 ) ) ;
#184790 = CARTESIAN_POINT ( 'NONE',  ( -19.03943276465977164, 0.05219959533909376836, 56.24890960531435979 ) ) ;
#184789 = CARTESIAN_POINT ( 'NONE',  ( 4.379528057220339221, -16.55341960407611168, 72.70724293864769550 ) ) ;
#184791 = CARTESIAN_POINT ( 'NONE',  ( -21.55341960407619339, 5.719274019375674811, 78.54275706135236135 ) ) ;
#184792 = CARTESIAN_POINT ( 'NONE',  ( -23.88070017481512508, 1.044764468832944493, -57.07230391339724207 ) ) ;
#184793 = CARTESIAN_POINT ( 'NONE',  ( -16.51473224551082808, 9.474510206698731452, 108.3344237280190043 ) ) ;
#184794 = CARTESIAN_POINT ( 'NONE',  ( 8.314922557960818139, 14.29746914071049879, 74.58224293864768129 ) ) ;
#184795 = CARTESIAN_POINT ( 'NONE',  ( 15.80617190586769283, -15.72974639402175789, 25.62609039468567929 ) ) ;
#184796 = CARTESIAN_POINT ( 'NONE',  ( -10.72451020669898014, 18.67979575497178502, 60.41557627198102409 ) ) ;
#184797 = FACE_OUTER_BOUND ( 'NONE', #192721, .T. ) ;
#184798 = CARTESIAN_POINT ( 'NONE',  ( -8.906447517083060816, 27.41122689804195645, 145.8500000054623627 ) ) ;
#184799 = CARTESIAN_POINT ( 'NONE',  ( -9.474510206698964154, 16.51473224551069663, 85.41557627198102409 ) ) ;
#184800 = CARTESIAN_POINT ( 'NONE',  ( -16.53943276465976808, 0.05219959533911058130, 56.24890960531436690 ) ) ;
#184801 = CARTESIAN_POINT ( 'NONE',  ( -12.14591786802326823, 12.06949235617739902, 108.1260903946856757 ) ) ;
#184802 = CARTESIAN_POINT ( 'NONE',  ( -14.34966873604972548, 8.224510206698743886, 93.33442372801901854 ) ) ;
#184803 = CARTESIAN_POINT ( 'NONE',  ( 16.46253265017146816, 9.564922557961045513, 46.66775706135233293 ) ) ;
#184804 = CARTESIAN_POINT ( 'NONE',  ( -22.77340731150486874, -12.66915506687109527, 165.5704399981227937 ) ) ;
#184805 = CARTESIAN_POINT ( 'NONE',  ( 16.46253265017160672, -9.564922557960803928, 103.3322429386476955 ) ) ;
#184806 = CARTESIAN_POINT ( 'NONE',  ( -14.29746914071049879, 8.314922557960819915, 75.83224293864769550 ) ) ;
#184807 = CARTESIAN_POINT ( 'NONE',  ( 5.049401038297881783, 19.05341960407617563, 37.29275706135232582 ) ) ;
#184809 = CARTESIAN_POINT ( 'NONE',  ( 5.719274019375991003, -21.55341960407610458, 32.70724293864770260 ) ) ;
#184808 = CARTESIAN_POINT ( 'NONE',  ( -19.05341960407611168, -5.049401038298163336, 31.45724293864769550 ) ) ;
#184811 = ORIENTED_EDGE ( 'NONE', *, *, #40219, .T. ) ;
#184810 = CARTESIAN_POINT ( 'NONE',  ( 18.67979575497178502, 10.72451020669898547, 69.16557627198102409 ) ) ;
#184812 = CARTESIAN_POINT ( 'NONE',  ( 16.53943276465976808, -0.05219959533910856209, 98.74890960531438111 ) ) ;
#184813 = CARTESIAN_POINT ( 'NONE',  ( -14.29746914071037622, -8.314922557961029526, 49.16775706135234003 ) ) ;
#184814 = CARTESIAN_POINT ( 'NONE',  ( 21.52544592524334988, 5.823673210054432836, 41.45942372801901143 ) ) ;
#184815 = CARTESIAN_POINT ( 'NONE',  ( -4.483927247898539470, -16.52544592524342804, 97.29057627198105251 ) ) ;
#184816 = EDGE_CURVE ( 'NONE', #26208, #99459, #81723, .T. ) ;
#184817 = DIRECTION ( 'NONE',  ( -1.000000000000000000, 0.000000000000000000, 0.000000000000000000 ) ) ;
#184818 = CARTESIAN_POINT ( 'NONE',  ( -17.48853670773243252, 5.747243402303158000, 48.66671299749990709 ) ) ;
#184819 = CARTESIAN_POINT ( 'NONE',  ( 21.53943276465977519, -0.05219959533907433946, 28.74890960531435624 ) ) ;
#184820 = CARTESIAN_POINT ( 'NONE',  ( -17.49999999999999645, -5.500000000000000888, 120.0000000000000142 ) ) ;
#184821 = CARTESIAN_POINT ( 'NONE',  ( 0.7567881333757656703, 8.898838318008483128, -63.99035486850526411 ) ) ;
#184823 = CARTESIAN_POINT ( 'NONE',  ( -0.05219959533910754901, -16.53943276465976808, 27.49890960531435269 ) ) ;
#184822 = CARTESIAN_POINT ( 'NONE',  ( 4.379528057220092307, 16.55341960407617563, 37.29275706135235424 ) ) ;
#184824 = CARTESIAN_POINT ( 'NONE',  ( 15.72974639402199770, -15.80617190586745480, 58.12390960531435979 ) ) ;
#184825 = CARTESIAN_POINT ( 'NONE',  ( 5.153800228976615827, -19.02544592524334988, 80.20942372801901854 ) ) ;
#184826 = CARTESIAN_POINT ( 'NONE',  ( 21.55341960407610458, 5.719274019375980345, 63.95724293864770260 ) ) ;
#184827 = CARTESIAN_POINT ( 'NONE',  ( -5.823673210054431948, 21.52544592524334988, 77.70942372801900433 ) ) ;
#184828 = CYLINDRICAL_SURFACE ( 'NONE', #53104, 2.000000000000000000 ) ;
#184829 = CARTESIAN_POINT ( 'NONE',  ( 8.314922557961029526, -14.29746914071037800, 45.41775706135234003 ) ) ;
#184831 = CARTESIAN_POINT ( 'NONE',  ( -9.474510206698964154, 16.51473224551069663, 100.4155762719810241 ) ) ;
#184830 = CARTESIAN_POINT ( 'NONE',  ( -13.89961937509977652, 13.97604488694528158, 40.62390960531435979 ) ) ;
#184832 = CARTESIAN_POINT ( 'NONE',  ( 19.03943276465977164, -0.05219959533909143690, 33.74890960531435979 ) ) ;
#184834 = EDGE_CURVE ( 'NONE', #23884, #14621, #88071, .T. ) ;
#184833 = CARTESIAN_POINT ( 'NONE',  ( 16.55341960407611168, 4.379528057220329451, 103.9572429386476813 ) ) ;
#184835 = DIRECTION ( 'NONE',  ( 1.000000000000000000, 0.000000000000000000, 0.000000000000000000 ) ) ;
#184836 = CARTESIAN_POINT ( 'NONE',  ( 9.564922557960805705, 16.46253265017160317, 109.5822429386476955 ) ) ;
#184837 = ORIENTED_EDGE ( 'NONE', *, *, #77338, .F. ) ;
#184838 = CARTESIAN_POINT ( 'NONE',  ( 8.314922557961029526, -14.29746914071037800, 70.41775706135236135 ) ) ;
#184839 = CARTESIAN_POINT ( 'NONE',  ( 5.719274019375991003, -21.55341960407610458, 87.70724293864769550 ) ) ;
#184840 = CARTESIAN_POINT ( 'NONE',  ( 13.97604488694527802, 13.89961937509977652, 54.37390960531435979 ) ) ;
#184841 = CARTESIAN_POINT ( 'NONE',  ( 15.80617190586769283, -15.72974639402175789, 25.62609039468567929 ) ) ;
#184842 = CARTESIAN_POINT ( 'NONE',  ( 13.97604488694527802, 13.89961937509977652, 79.37390960531435269 ) ) ;
#184843 = CARTESIAN_POINT ( 'NONE',  ( 1.784589286804354247, 7.284589286804251884, 8.181980515339454030 ) ) ;
#184844 = ORIENTED_EDGE ( 'NONE', *, *, #103523, .T. ) ;
#184845 = CARTESIAN_POINT ( 'NONE',  ( -21.53943276465977519, 0.05219959533907696930, 116.2489096053143669 ) ) ;
#184848 = CARTESIAN_POINT ( 'NONE',  ( -19.02544592524334988, -5.153800228976617603, 73.95942372801900433 ) ) ;
#184847 = CARTESIAN_POINT ( 'NONE',  ( -13.97604488694527625, -13.89961937509977652, 111.8739096053143243 ) ) ;
#184846 = CARTESIAN_POINT ( 'NONE',  ( -13.97604488694527625, -13.89961937509977652, 26.87390960531434558 ) ) ;
#184849 = CARTESIAN_POINT ( 'NONE',  ( 19.03943276465977164, 0.05219959533936151252, 26.25109039468566507 ) ) ;
#184850 = CARTESIAN_POINT ( 'NONE',  ( -15.80617190586745835, -15.72974639402198527, 96.87390960531436690 ) ) ;
#184851 = CARTESIAN_POINT ( 'NONE',  ( -13.97604488694547697, 13.89961937509957934, 38.12609039468566152 ) ) ;
#184852 = CARTESIAN_POINT ( 'NONE',  ( -12.06949235617739369, -12.14591786802326823, 79.37609039468567573 ) ) ;
#184853 = CARTESIAN_POINT ( 'NONE',  ( -9.564922557960796823, -16.46253265017161027, 107.0822429386476955 ) ) ;
#184854 = CARTESIAN_POINT ( 'NONE',  ( 13.89961937509977652, -13.97604488694527269, 53.12390960531434558 ) ) ;
#184855 = CARTESIAN_POINT ( 'NONE',  ( 15.80617190586769283, -15.72974639402175789, 65.62609039468568994 ) ) ;
#184856 = CARTESIAN_POINT ( 'NONE',  ( -18.62759615963255300, -10.81492255796106328, 84.16775706135234714 ) ) ;
#184857 = FACE_OUTER_BOUND ( 'NONE', #156409, .T. ) ;
#184858 = CARTESIAN_POINT ( 'NONE',  ( 9.564922557960805705, 16.46253265017160317, 69.58224293864770971 ) ) ;
#184859 = CARTESIAN_POINT ( 'NONE',  ( -18.67979575497193778, 10.72451020669871902, 43.33442372801901143 ) ) ;
#184860 = CARTESIAN_POINT ( 'NONE',  ( 19.03943276465977164, 0.05219959533936151252, 86.25109039468567573 ) ) ;
#184861 = CARTESIAN_POINT ( 'NONE',  ( 9.474510206698971260, -16.51473224551069308, 57.91557627198103120 ) ) ;
#184862 = CARTESIAN_POINT ( 'NONE',  ( 13.97604488694527802, 13.89961937509977652, 99.37390960531436690 ) ) ;
#184863 = CARTESIAN_POINT ( 'NONE',  ( 16.46253265017160672, -9.564922557960803928, 68.33224293864770971 ) ) ;
#184864 = CARTESIAN_POINT ( 'NONE',  ( 17.50000000000008882, -3.296979923273363866, 22.57062549986184052 ) ) ;
#184866 = EDGE_CURVE ( 'NONE', #19226, #723, #173343, .T. ) ;
#184865 = CARTESIAN_POINT ( 'NONE',  ( 16.46253265017160672, -9.564922557960803928, 58.33224293864769550 ) ) ;
#184867 = CARTESIAN_POINT ( 'NONE',  ( 15.72974639402199770, -15.80617190586745480, 103.1239096053143811 ) ) ;
#184868 = CARTESIAN_POINT ( 'NONE',  ( 16.52544592524335698, 4.483927247898782831, 91.45942372801901854 ) ) ;
#184869 = CARTESIAN_POINT ( 'NONE',  ( -24.14511064691435749, 7.743397529680777325, 169.7652520481140641 ) ) ;
#184870 = CARTESIAN_POINT ( 'NONE',  ( 9.474510206698729675, 16.51473224551082808, 47.08442372801900433 ) ) ;
#184871 = CARTESIAN_POINT ( 'NONE',  ( 0.05219959533909260263, 19.03943276465977164, 59.99890960531436690 ) ) ;
#184872 = CARTESIAN_POINT ( 'NONE',  ( 0.05219959533910956823, 16.53943276465976808, 64.99890960531435269 ) ) ;
#184873 = CARTESIAN_POINT ( 'NONE',  ( -16.52544592524342804, 4.483927247898546575, 91.04057627198103830 ) ) ;
#184874 = CARTESIAN_POINT ( 'NONE',  ( 10.81492255796078972, 18.62759615963270932, 24.58224293864768839 ) ) ;
#184875 = CARTESIAN_POINT ( 'NONE',  ( -9.474510206698964154, 16.51473224551069663, 95.41557627198102409 ) ) ;
#184876 = CARTESIAN_POINT ( 'NONE',  ( 5.049401038298161559, -19.05341960407611168, 102.7072429386476955 ) ) ;
#184877 = CARTESIAN_POINT ( 'NONE',  ( -16.46253265017146816, -9.564922557961047289, 24.16775706135233648 ) ) ;
#184878 = CARTESIAN_POINT ( 'NONE',  ( -8.314922557961024197, 14.29746914071037800, 87.91775706135234714 ) ) ;
#184879 = CARTESIAN_POINT ( 'NONE',  ( -19.03943276465977164, 0.05219959533909376836, 71.24890960531435269 ) ) ;
#184880 = CARTESIAN_POINT ( 'NONE',  ( -10.72451020669870658, -18.67979575497194134, 34.58442372801900433 ) ) ;
#184881 = CARTESIAN_POINT ( 'NONE',  ( -18.67979575497178146, -10.72451020669898902, 26.66557627198103475 ) ) ;
#184882 = CARTESIAN_POINT ( 'NONE',  ( 18.67979575497194134, -10.72451020669871369, 20.83442372801901143 ) ) ;
#184883 = CARTESIAN_POINT ( 'NONE',  ( -21.53943276465977519, 0.05219959533907696930, 71.24890960531435269 ) ) ;
#184884 = CARTESIAN_POINT ( 'NONE',  ( -19.02544592524342804, 5.153800228976336051, 56.04057627198100988 ) ) ;
#184885 = CARTESIAN_POINT ( 'NONE',  ( 8.224510206698953496, -14.34966873604960469, 82.91557627198103830 ) ) ;
#184886 = CARTESIAN_POINT ( 'NONE',  ( 5.049401038297881783, 19.05341960407617563, 37.29275706135232582 ) ) ;
#184887 = CARTESIAN_POINT ( 'NONE',  ( 14.29746914071049879, -8.314922557960816363, 113.3322429386476955 ) ) ;
#184888 = CARTESIAN_POINT ( 'NONE',  ( -9.564922557960796823, -16.46253265017161027, 77.08224293864769550 ) ) ;
#184889 = CARTESIAN_POINT ( 'NONE',  ( -13.89961937509977652, 13.97604488694528158, 75.62390960531438111 ) ) ;
#184890 = CARTESIAN_POINT ( 'NONE',  ( 8.571926809382597767, 26.38167802310806209, 146.2750000027311899 ) ) ;
#184891 = CARTESIAN_POINT ( 'NONE',  ( 16.52544592524342804, -4.483927247898539470, 98.54057627198105251 ) ) ;
#184892 = ORIENTED_EDGE ( 'NONE', *, *, #189014, .T. ) ;
#184893 = CARTESIAN_POINT ( 'NONE',  ( -16.55341960407617563, 4.379528057220093196, 108.5427570613523756 ) ) ;
#184894 = CARTESIAN_POINT ( 'NONE',  ( -0.05219959533934338120, 16.53943276465976808, 22.50109039468567573 ) ) ;
#184895 = CARTESIAN_POINT ( 'NONE',  ( 15.72974639402176855, 15.80617190586768217, 86.87609039468568994 ) ) ;
#184896 = CARTESIAN_POINT ( 'NONE',  ( 16.51473224551069308, 9.474510206698969483, 99.16557627198102409 ) ) ;
#184897 = CARTESIAN_POINT ( 'NONE',  ( -10.81492255796105439, 18.62759615963255655, 22.91775706135235069 ) ) ;
#184898 = CARTESIAN_POINT ( 'NONE',  ( 5.153800228976335163, 19.02544592524342804, 34.79057627198102409 ) ) ;
#184899 = CARTESIAN_POINT ( 'NONE',  ( -16.52544592524335698, -4.483927247898792601, 33.95942372801901143 ) ) ;
#184900 = CARTESIAN_POINT ( 'NONE',  ( -13.97604488694547697, 13.89961937509957934, 98.12609039468566152 ) ) ;
#184901 = CARTESIAN_POINT ( 'NONE',  ( -18.67979575497178146, -10.72451020669898902, 91.66557627198103830 ) ) ;
#184902 = CARTESIAN_POINT ( 'NONE',  ( -13.89961937509957401, -13.97604488694547875, 64.37609039468567573 ) ) ;
#184903 = CARTESIAN_POINT ( 'NONE',  ( -19.05341960407611168, -5.049401038298163336, 21.45724293864768839 ) ) ;
#184904 = CARTESIAN_POINT ( 'NONE',  ( -21.55341960407619339, 5.719274019375674811, 23.54275706135235424 ) ) ;
#184905 = LINE ( 'NONE', #84669, #175732 ) ;
#184906 = CARTESIAN_POINT ( 'NONE',  ( 19.03943276465977164, -0.05219959533909143690, 88.74890960531436690 ) ) ;
#184907 = CARTESIAN_POINT ( 'NONE',  ( 12.99999999999999822, 2.789133085058097101E-16, -2.055000000000000160 ) ) ;
#184908 = CARTESIAN_POINT ( 'NONE',  ( 13.97604488694527802, 13.89961937509977652, 89.37390960531436690 ) ) ;
#184910 = CARTESIAN_POINT ( 'NONE',  ( -4.483927247898539470, -16.52544592524342804, 77.29057627198102409 ) ) ;
#184909 = CARTESIAN_POINT ( 'NONE',  ( 10.72451020669898902, -18.67979575497178502, 112.9155762719810383 ) ) ;
#184911 = CARTESIAN_POINT ( 'NONE',  ( -19.03943276465977164, 0.05219959533909376836, 86.24890960531436690 ) ) ;
#184914 = CARTESIAN_POINT ( 'NONE',  ( 19.03943276465977164, 0.05219959533936151252, 61.25109039468566863 ) ) ;
#184913 =( BOUNDED_CURVE ( )  B_SPLINE_CURVE ( 3, ( #32158, #77655, #187843, #184843 ),
 .UNSPECIFIED., .F., .F. ) 
 B_SPLINE_CURVE_WITH_KNOTS ( ( 4, 4 ),
 ( 5.150538010968860547, 5.257537365396775186 ),
 .UNSPECIFIED. ) 
 CURVE ( )  GEOMETRIC_REPRESENTATION_ITEM ( )  RATIONAL_B_SPLINE_CURVE ( ( 1.000000000000000000, 0.9990461557208837329, 0.9990461557208837329, 1.000000000000000000 ) ) 
 REPRESENTATION_ITEM ( '' )  );
#184912 = CARTESIAN_POINT ( 'NONE',  ( 0.05219959533934541429, -16.53943276465976808, 50.00109039468568994 ) ) ;
#184915 = CARTESIAN_POINT ( 'NONE',  ( 21.53943276465977519, 0.05219959533937863772, 61.25109039468567573 ) ) ;
#184916 = CARTESIAN_POINT ( 'NONE',  ( 16.53943276465976808, 0.05219959533934440121, 21.25109039468567218 ) ) ;
#184917 = CARTESIAN_POINT ( 'NONE',  ( -16.51473224551069308, -9.474510206698971260, 71.66557627198102409 ) ) ;
#184918 = CARTESIAN_POINT ( 'NONE',  ( -9.474510206698720793, -16.51473224551083518, 89.58442372801900433 ) ) ;
#184919 = CARTESIAN_POINT ( 'NONE',  ( 16.55341960407618274, -4.379528057220086978, 56.04275706135235424 ) ) ;
#184920 = CARTESIAN_POINT ( 'NONE',  ( 21.53943276465977519, 0.05219959533937863772, 91.25109039468568994 ) ) ;
#184921 = CARTESIAN_POINT ( 'NONE',  ( 9.564922557961047289, -16.46253265017146816, 75.41775706135234714 ) ) ;
#184922 = CARTESIAN_POINT ( 'NONE',  ( 5.153800228976335163, 19.02544592524342804, 44.79057627198103830 ) ) ;
#184923 = CARTESIAN_POINT ( 'NONE',  ( 18.62759615963271287, -10.81492255796078972, 68.33224293864769550 ) ) ;
#184925 = CARTESIAN_POINT ( 'NONE',  ( -13.97604488694547697, 13.89961937509957934, 78.12609039468567573 ) ) ;
#184924 = CARTESIAN_POINT ( 'NONE',  ( -16.53943276465976808, 0.05219959533911058130, 71.24890960531435269 ) ) ;
#184926 = CARTESIAN_POINT ( 'NONE',  ( 16.18388926212235646, -7.379444403734614077, 62.06046848633851454 ) ) ;
#184927 = CARTESIAN_POINT ( 'NONE',  ( -13.97604488694547697, 13.89961937509957934, 48.12609039468566863 ) ) ;
#184928 = CARTESIAN_POINT ( 'NONE',  ( -16.53943276465976808, -0.05219959533934237506, 108.7510903946857042 ) ) ;
#184929 = CARTESIAN_POINT ( 'NONE',  ( 4.483927247898545687, 16.52544592524342804, 64.79057627198103830 ) ) ;
#184931 = CARTESIAN_POINT ( 'NONE',  ( 27.73933785331498925, -9.013057229001033122, 145.7750000027311899 ) ) ;
#184930 = CARTESIAN_POINT ( 'NONE',  ( 21.52544592524334988, 5.823673210054432836, 101.4594237280190185 ) ) ;
#184932 = CARTESIAN_POINT ( 'NONE',  ( -15.80617190586745835, -15.72974639402198527, 106.8739096053143811 ) ) ;
#184933 = CARTESIAN_POINT ( 'NONE',  ( -19.05341960407611168, -5.049401038298163336, 61.45724293864769550 ) ) ;
#184934 = CARTESIAN_POINT ( 'NONE',  ( 0.05219959533937995610, -21.53943276465977519, 90.00109039468567573 ) ) ;
#184935 = CARTESIAN_POINT ( 'NONE',  ( 19.02544592524343514, -5.153800228976328945, 58.54057627198102409 ) ) ;
#184936 = ORIENTED_EDGE ( 'NONE', *, *, #36648, .T. ) ;
#184937 = CARTESIAN_POINT ( 'NONE',  ( 13.97604488694527802, 13.89961937509977652, 24.37390960531435624 ) ) ;
#184938 = CARTESIAN_POINT ( 'NONE',  ( -19.02544592524342804, 5.153800228976336051, 116.0405762719810383 ) ) ;
#184939 = CARTESIAN_POINT ( 'NONE',  ( -16.52544592524342804, 4.483927247898546575, 71.04057627198103830 ) ) ;
#184940 = CARTESIAN_POINT ( 'NONE',  ( 5.049401038298161559, -19.05341960407611168, 27.70724293864769550 ) ) ;
#184941 = CARTESIAN_POINT ( 'NONE',  ( -4.483927247898539470, -16.52544592524342804, 82.29057627198103830 ) ) ;
#184942 = CARTESIAN_POINT ( 'NONE',  ( -10.72451020669898014, 18.67979575497178502, 95.41557627198102409 ) ) ;
#184943 = CARTESIAN_POINT ( 'NONE',  ( 15.80617190586769283, -15.72974639402175789, 50.62609039468568994 ) ) ;
#184944 = CARTESIAN_POINT ( 'NONE',  ( 27.89965394715913405, -6.788920637341042230, 161.9771076211712000 ) ) ;
#184945 = CARTESIAN_POINT ( 'NONE',  ( -12.06949235617739369, -12.14591786802326823, 54.37609039468568994 ) ) ;
#184946 = CARTESIAN_POINT ( 'NONE',  ( 15.72974639402199770, -15.80617190586745480, 93.12390960531436690 ) ) ;
#184947 = CARTESIAN_POINT ( 'NONE',  ( -19.05341960407617563, 5.049401038297882671, 28.54275706135232937 ) ) ;
#184948 = CARTESIAN_POINT ( 'NONE',  ( -13.89961937509977652, 13.97604488694528158, 110.6239096053143243 ) ) ;
#184949 = CARTESIAN_POINT ( 'NONE',  ( -15.80617190586768217, 15.72974639402176855, 43.12609039468568284 ) ) ;
#184950 = VECTOR ( 'NONE', #143580, 1000.000000000000000 ) ;
#184951 = CARTESIAN_POINT ( 'NONE',  ( 0.05219959533907565091, 21.53943276465977519, 44.99890960531435979 ) ) ;
#184952 = CARTESIAN_POINT ( 'NONE',  ( -16.53943276465976808, -0.05219959533934237506, 113.7510903946856757 ) ) ;
#184954 = CARTESIAN_POINT ( 'NONE',  ( 21.53943276465977519, 0.05219959533937863772, 91.25109039468568994 ) ) ;
#184953 = CARTESIAN_POINT ( 'NONE',  ( 21.55341960407619695, -5.719274019375665929, 61.04275706135234714 ) ) ;
#184955 = CARTESIAN_POINT ( 'NONE',  ( 19.05341960407617918, -5.049401038297876454, 36.04275706135234003 ) ) ;
#184956 = CARTESIAN_POINT ( 'NONE',  ( -4.379528057220086978, -16.55341960407618274, 84.79275706135234714 ) ) ;
#184957 = CARTESIAN_POINT ( 'NONE',  ( 5.823673210054444382, -21.52544592524334988, 60.20942372801902565 ) ) ;
#184958 = CARTESIAN_POINT ( 'NONE',  ( -9.564922557960796823, -16.46253265017161027, 42.08224293864769550 ) ) ;
#184959 = CARTESIAN_POINT ( 'NONE',  ( 19.05341960407617918, -5.049401038297876454, 26.04275706135233293 ) ) ;
#184960 = CARTESIAN_POINT ( 'NONE',  ( 0.05219959533907565091, 21.53943276465977519, 29.99890960531435979 ) ) ;
#184961 = CARTESIAN_POINT ( 'NONE',  ( 5.823673210054125526, 21.52544592524343514, 114.7905762719810383 ) ) ;
#184962 = CARTESIAN_POINT ( 'NONE',  ( 10.81492255796078972, 18.62759615963270932, 69.58224293864769550 ) ) ;
#184963 = CARTESIAN_POINT ( 'NONE',  ( 8.314922557961029526, -14.29746914071037800, 45.41775706135234003 ) ) ;
#184965 = CARTESIAN_POINT ( 'NONE',  ( 18.67979575497178502, 10.72451020669898547, 84.16557627198103830 ) ) ;
#184964 = CARTESIAN_POINT ( 'NONE',  ( -6.791538853603066528, -3.181980515339470905, 8.889087296526001936 ) ) ;
#184967 = CARTESIAN_POINT ( 'NONE',  ( 8.314922557960818139, 14.29746914071049879, 59.58224293864770260 ) ) ;
#184966 = CARTESIAN_POINT ( 'NONE',  ( 12.06949235617739724, 12.14591786802326823, 71.87609039468568994 ) ) ;
#184968 = CARTESIAN_POINT ( 'NONE',  ( -27.05641397906351742, -3.631740835637518927, 169.9999999999999716 ) ) ;
#184969 = CARTESIAN_POINT ( 'NONE',  ( -16.46253265017146816, -9.564922557961047289, 99.16775706135233293 ) ) ;
#184970 = CARTESIAN_POINT ( 'NONE',  ( -5.823673210054116645, -21.52544592524344225, 37.29057627198102409 ) ) ;
#184971 = DIRECTION ( 'NONE',  ( 0.000000000000000000, 0.000000000000000000, -1.000000000000000000 ) ) ;
#184972 = CARTESIAN_POINT ( 'NONE',  ( -16.52544592524335698, -4.483927247898792601, 38.95942372801901854 ) ) ;
#184973 = CARTESIAN_POINT ( 'NONE',  ( -21.53943276465977519, -0.05219959533937600094, 18.75109039468568639 ) ) ;
#184974 = CARTESIAN_POINT ( 'NONE',  ( -15.80617190586745835, -15.72974639402198527, 26.87390960531435979 ) ) ;
#184975 = CARTESIAN_POINT ( 'NONE',  ( 8.224510206698742110, 14.34966873604972548, 52.08442372801901854 ) ) ;
#184976 = CARTESIAN_POINT ( 'NONE',  ( 5.153800228976335163, 19.02544592524342804, 84.79057627198099567 ) ) ;
#184978 = CARTESIAN_POINT ( 'NONE',  ( 9.474510206698729675, 16.51473224551082808, 112.0844237280190043 ) ) ;
#184977 = CARTESIAN_POINT ( 'NONE',  ( 21.52544592524334988, 5.823673210054432836, 36.45942372801901143 ) ) ;
#184979 = EDGE_CURVE ( 'NONE', #89057, #13627, #40003, .T. ) ;
#184980 = CARTESIAN_POINT ( 'NONE',  ( -5.823673210054116645, -21.52544592524344225, 27.29057627198103120 ) ) ;
#184981 = ORIENTED_EDGE ( 'NONE', *, *, #136550, .F. ) ;
#184982 = CARTESIAN_POINT ( 'NONE',  ( 5.049401038297881783, 19.05341960407617563, 22.29275706135233648 ) ) ;
#184983 = CARTESIAN_POINT ( 'NONE',  ( 8.314922557961029526, -14.29746914071037800, 45.41775706135234003 ) ) ;
#184984 = CARTESIAN_POINT ( 'NONE',  ( -9.474510206698964154, 16.51473224551069663, 95.41557627198102409 ) ) ;
#184985 = CARTESIAN_POINT ( 'NONE',  ( -18.67979575497178146, -10.72451020669898902, 101.6655762719810383 ) ) ;
#184986 = CARTESIAN_POINT ( 'NONE',  ( -0.05219959533909027116, -19.03943276465977164, 77.49890960531435269 ) ) ;
#184987 = DIRECTION ( 'NONE',  ( 0.000000000000000000, 0.000000000000000000, 1.000000000000000000 ) ) ;
#184988 = CARTESIAN_POINT ( 'NONE',  ( -12.14591786802309592, -12.06949235617757132, 86.87390960531438111 ) ) ;
#184989 = CARTESIAN_POINT ( 'NONE',  ( -10.72451020669898014, 18.67979575497178502, 35.41557627198102409 ) ) ;
#184990 = FACE_OUTER_BOUND ( 'NONE', #15966, .T. ) ;
#184991 = CARTESIAN_POINT ( 'NONE',  ( 14.34966873604972726, -8.224510206698740333, 60.83442372801901854 ) ) ;
#184992 = CARTESIAN_POINT ( 'NONE',  ( 18.62759615963271287, -10.81492255796078972, 98.33224293864769550 ) ) ;
#184993 = CARTESIAN_POINT ( 'NONE',  ( 19.03943276465977164, 0.05219959533936151252, 81.25109039468567573 ) ) ;
#184994 = ADVANCED_FACE ( 'NONE', ( #68337 ), #53168, .F. ) ;
#184995 = CARTESIAN_POINT ( 'NONE',  ( 13.89961937509977652, -13.97604488694527269, 23.12390960531436335 ) ) ;
#184996 = CARTESIAN_POINT ( 'NONE',  ( 0.05219959533907565091, 21.53943276465977519, 69.99890960531435269 ) ) ;
#184997 = CARTESIAN_POINT ( 'NONE',  ( 9.564922557960805705, 16.46253265017160317, 94.58224293864769550 ) ) ;
#184998 = CARTESIAN_POINT ( 'NONE',  ( 18.67979575497194134, -10.72451020669871369, 85.83442372801901854 ) ) ;
#184999 = CARTESIAN_POINT ( 'NONE',  ( -0.05219959533909027116, -19.03943276465977164, 62.49890960531435979 ) ) ;
#185000 = CARTESIAN_POINT ( 'NONE',  ( 14.34966873604972726, -8.224510206698740333, 45.83442372801901854 ) ) ;
#185001 = CARTESIAN_POINT ( 'NONE',  ( 9.564922557960805705, 16.46253265017160317, 54.58224293864769550 ) ) ;
#185002 = CARTESIAN_POINT ( 'NONE',  ( 10.81492255796106328, -18.62759615963255655, 75.41775706135233293 ) ) ;
#185003 = VERTEX_POINT ( 'NONE', #84494 ) ;
#185004 = CARTESIAN_POINT ( 'NONE',  ( 19.05341960407617918, -5.049401038297876454, 41.04275706135233293 ) ) ;
#185005 = CARTESIAN_POINT ( 'NONE',  ( -9.474510206698720793, -16.51473224551083518, 44.58442372801900433 ) ) ;
#185006 = CARTESIAN_POINT ( 'NONE',  ( 18.67979575497194134, -10.72451020669871369, 35.83442372801901143 ) ) ;
#185007 = CARTESIAN_POINT ( 'NONE',  ( -8.898068258721474777, 27.38543819252877043, 143.5843446569000150 ) ) ;
#185008 = CARTESIAN_POINT ( 'NONE',  ( -13.89961937509957401, -13.97604488694547875, 34.37609039468566863 ) ) ;
#185009 = CARTESIAN_POINT ( 'NONE',  ( 9.564922557960805705, 16.46253265017160317, 84.58224293864769550 ) ) ;
#185010 = CARTESIAN_POINT ( 'NONE',  ( -19.05341960407611168, -5.049401038298163336, 71.45724293864766707 ) ) ;
#185011 = CARTESIAN_POINT ( 'NONE',  ( 16.53943276465976808, 0.05219959533934440121, 111.2510903946856899 ) ) ;
#185013 = CARTESIAN_POINT ( 'NONE',  ( -15.80617190586768217, 15.72974639402176855, 88.12609039468570415 ) ) ;
#185012 = CARTESIAN_POINT ( 'NONE',  ( -18.62759615963270932, 10.81492255796079327, 25.83224293864769194 ) ) ;
#185014 = CARTESIAN_POINT ( 'NONE',  ( 3.556970738554033499E-15, -38.81732327939057825, -10.62499999726881050 ) ) ;
#185015 = CARTESIAN_POINT ( 'NONE',  ( 17.12812012977024878, 6.668231424566068100, 58.85948759323144941 ) ) ;
#185016 = CARTESIAN_POINT ( 'NONE',  ( 0.05219959533937995610, -21.53943276465977519, 95.00109039468568994 ) ) ;
#185017 =( REPRESENTATION_RELATIONSHIP ('NONE','NONE', #154205, #71529 ) REPRESENTATION_RELATIONSHIP_WITH_TRANSFORMATION ( #116946 )SHAPE_REPRESENTATION_RELATIONSHIP( ) );
#185018 = CARTESIAN_POINT ( 'NONE',  ( -37.99626262588765968, -12.34573411038913626, -3.647842220587803386 ) ) ;
#185019 = CARTESIAN_POINT ( 'NONE',  ( -5.049401038298153566, 19.05341960407611168, 25.20724293864768484 ) ) ;
#185020 = CARTESIAN_POINT ( 'NONE',  ( -5.049401038298153566, 19.05341960407611168, 110.2072429386476671 ) ) ;
#185021 = CARTESIAN_POINT ( 'NONE',  ( 35.00000000000000000, 0.3535533905932759513, 4.646446609406721606 ) ) ;
#185022 = CARTESIAN_POINT ( 'NONE',  ( 14.29746914071037800, 8.314922557961029526, 51.66775706135234714 ) ) ;
#185023 = CARTESIAN_POINT ( 'NONE',  ( 21.52544592524344225, -5.823673210054117533, 63.54057627198103830 ) ) ;
#185024 = CARTESIAN_POINT ( 'NONE',  ( 0.05219959533910956823, 16.53943276465976808, 39.99890960531436690 ) ) ;
#185026 = CARTESIAN_POINT ( 'NONE',  ( -19.02544592524342804, 5.153800228976336051, 96.04057627198103830 ) ) ;
#185025 = CARTESIAN_POINT ( 'NONE',  ( 12.14591786802309770, 12.06949235617756955, 104.3739096053143669 ) ) ;
#185027 = CARTESIAN_POINT ( 'NONE',  ( 19.05341960407617918, -5.049401038297876454, 26.04275706135233293 ) ) ;
#185028 = CARTESIAN_POINT ( 'NONE',  ( 5.049401038298161559, -19.05341960407611168, 22.70724293864769194 ) ) ;
#185029 = CARTESIAN_POINT ( 'NONE',  ( -21.55341960407619339, 5.719274019375674811, 68.54275706135234714 ) ) ;
#185030 = DIRECTION ( 'NONE',  ( 1.000000000000000000, 0.000000000000000000, 0.000000000000000000 ) ) ;
#185031 = CARTESIAN_POINT ( 'NONE',  ( 8.224510206698742110, 14.34966873604972548, 102.0844237280190185 ) ) ;
#185032 = CARTESIAN_POINT ( 'NONE',  ( -0.05219959533936034679, 19.03943276465977164, 62.50109039468566863 ) ) ;
#185033 = CARTESIAN_POINT ( 'NONE',  ( -5.950531402560715689E-15, 38.81732327939063509, -5.624999997268813168 ) ) ;
#185034 = CARTESIAN_POINT ( 'NONE',  ( 15.80617190586746368, 15.72974639402197994, 34.37390960531435979 ) ) ;
#185035 = CARTESIAN_POINT ( 'NONE',  ( -0.05219959533910754901, -16.53943276465976808, 87.49890960531436690 ) ) ;
#185036 = CARTESIAN_POINT ( 'NONE',  ( -13.97604488694547697, 13.89961937509957934, 53.12609039468565442 ) ) ;
#185037 = CARTESIAN_POINT ( 'NONE',  ( -19.05341960407611168, -5.049401038298163336, 76.45724293864769550 ) ) ;
#185038 = CARTESIAN_POINT ( 'NONE',  ( 16.55341960407611168, 4.379528057220329451, 68.95724293864769550 ) ) ;
#185039 = CARTESIAN_POINT ( 'NONE',  ( -5.153800228976607833, 19.02544592524334988, 97.70942372801900433 ) ) ;
#185040 = CARTESIAN_POINT ( 'NONE',  ( 18.62759615963271287, -10.81492255796078972, 43.33224293864769550 ) ) ;
#185041 = ORIENTED_EDGE ( 'NONE', *, *, #47644, .T. ) ;
#185042 = CARTESIAN_POINT ( 'NONE',  ( 19.05341960407611168, 5.049401038298154454, 23.95724293864769194 ) ) ;
#185043 = PLANE ( 'NONE',  #32314 ) ;
#185045 = CARTESIAN_POINT ( 'NONE',  ( 5.719274019375991003, -21.55341960407610458, 77.70724293864770971 ) ) ;
#185044 = CARTESIAN_POINT ( 'NONE',  ( 16.51473224551069308, 9.474510206698969483, 74.16557627198103830 ) ) ;
#185047 = CARTESIAN_POINT ( 'NONE',  ( -9.474510206698964154, 16.51473224551069663, 70.41557627198102409 ) ) ;
#185046 = CARTESIAN_POINT ( 'NONE',  ( -14.34966873604972548, 8.224510206698743886, 93.33442372801901854 ) ) ;
#185048 = CARTESIAN_POINT ( 'NONE',  ( 9.564922557961047289, -16.46253265017146816, 65.41775706135233293 ) ) ;
#185049 = CARTESIAN_POINT ( 'NONE',  ( 21.53943276465977519, 0.05219959533937863772, 86.25109039468568994 ) ) ;
#185050 = CARTESIAN_POINT ( 'NONE',  ( 21.55341960407610458, 5.719274019375980345, 63.95724293864770260 ) ) ;
#185051 = CARTESIAN_POINT ( 'NONE',  ( -18.67979575497178146, -10.72451020669898902, 21.66557627198102409 ) ) ;
#185052 = CARTESIAN_POINT ( 'NONE',  ( 0.05219959533909260263, 19.03943276465977164, 39.99890960531436690 ) ) ;
#185053 = CARTESIAN_POINT ( 'NONE',  ( -4.379528057220086978, -16.55341960407618274, 99.79275706135234714 ) ) ;
#185054 = CARTESIAN_POINT ( 'NONE',  ( -16.46253265017160317, 9.564922557960807481, 55.83224293864769550 ) ) ;
#185055 = CARTESIAN_POINT ( 'NONE',  ( 19.05341960407617918, -5.049401038297876454, 111.0427570613523329 ) ) ;
#185056 = CARTESIAN_POINT ( 'NONE',  ( 17.26172910966777962, 6.454744622555866229, 51.69353091350778584 ) ) ;
#185057 = CARTESIAN_POINT ( 'NONE',  ( 10.72451020669871369, 18.67979575497193778, 107.0844237280190043 ) ) ;
#185058 = CARTESIAN_POINT ( 'NONE',  ( -12.06949235617756955, 12.14591786802309770, 65.62390960531436690 ) ) ;
#185059 = CARTESIAN_POINT ( 'NONE',  ( -10.81492255796078084, -18.62759615963271287, 102.0822429386476955 ) ) ;
#185060 = CARTESIAN_POINT ( 'NONE',  ( 21.53943276465977519, -0.05219959533907433946, 108.7489096053143669 ) ) ;
#185061 = CARTESIAN_POINT ( 'NONE',  ( -4.896406352259377925, 3.948644494436257979, -64.50244604205114740 ) ) ;
#185062 = CARTESIAN_POINT ( 'NONE',  ( 15.80617190586746368, 15.72974639402197994, 44.37390960531435979 ) ) ;
#185063 = CARTESIAN_POINT ( 'NONE',  ( 14.29746914071037800, 8.314922557961029526, 81.66775706135236135 ) ) ;
#185064 = CARTESIAN_POINT ( 'NONE',  ( -0.05219959533910754901, -16.53943276465976808, 97.49890960531436690 ) ) ;
#185065 = CARTESIAN_POINT ( 'NONE',  ( -16.46253265017160317, 9.564922557960807481, 60.83224293864769550 ) ) ;
#185066 = CARTESIAN_POINT ( 'NONE',  ( -18.87580814761073356, 5.500000000000047962, 50.87172394265760289 ) ) ;
#185067 = CARTESIAN_POINT ( 'NONE',  ( 4.483927247898790824, -16.52544592524335698, 105.2094237280190328 ) ) ;
#185068 = CARTESIAN_POINT ( 'NONE',  ( 5.719274019375673035, 21.55341960407619339, 32.29275706135235424 ) ) ;
#185069 = CARTESIAN_POINT ( 'NONE',  ( -19.02544592524342804, 5.153800228976336051, 101.0405762719810241 ) ) ;
#185070 = CARTESIAN_POINT ( 'NONE',  ( 5.823673210054444382, -21.52544592524334988, 70.20942372801904696 ) ) ;
#185071 = CARTESIAN_POINT ( 'NONE',  ( 13.89961937509977652, -13.97604488694527269, 23.12390960531436335 ) ) ;
#185072 = CARTESIAN_POINT ( 'NONE',  ( 13.97604488694527802, 13.89961937509977652, 29.37390960531435979 ) ) ;
#185073 = VERTEX_POINT ( 'NONE', #194707 ) ;
#185074 = CARTESIAN_POINT ( 'NONE',  ( -21.53943276465977519, -0.05219959533937600094, 63.75109039468568284 ) ) ;
#185075 = CARTESIAN_POINT ( 'NONE',  ( -9.474510206698964154, 16.51473224551069663, 50.41557627198102409 ) ) ;
#185076 = CARTESIAN_POINT ( 'NONE',  ( -19.02544592524342804, 5.153800228976336051, 96.04057627198103830 ) ) ;
#185077 = CARTESIAN_POINT ( 'NONE',  ( -9.564922557961040184, 16.46253265017147172, 72.91775706135233293 ) ) ;
#185078 = CARTESIAN_POINT ( 'NONE',  ( 21.53943276465977519, 0.05219959533937863772, 46.25109039468567573 ) ) ;
#185079 = CARTESIAN_POINT ( 'NONE',  ( -9.474510206698720793, -16.51473224551083518, 99.58442372801900433 ) ) ;
#185080 = CARTESIAN_POINT ( 'NONE',  ( 16.51473224551083163, -9.474510206698727899, 70.83442372801900433 ) ) ;
#185081 = CARTESIAN_POINT ( 'NONE',  ( -16.46253265017160317, 9.564922557960807481, 35.83224293864768839 ) ) ;
#185082 = CARTESIAN_POINT ( 'NONE',  ( -9.474510206698720793, -16.51473224551083518, 79.58442372801899012 ) ) ;
#185083 = CARTESIAN_POINT ( 'NONE',  ( -4.483927247898782831, 16.52544592524335698, 107.7094237280190328 ) ) ;
#185084 = CARTESIAN_POINT ( 'NONE',  ( -9.474510206698720793, -16.51473224551083518, 79.58442372801899012 ) ) ;
#185085 = CARTESIAN_POINT ( 'NONE',  ( 14.34966873604960469, 8.224510206698951720, 24.16557627198103120 ) ) ;
#185086 = CARTESIAN_POINT ( 'NONE',  ( -13.89961937509957401, -13.97604488694547875, 49.37609039468567573 ) ) ;
#185087 = CARTESIAN_POINT ( 'NONE',  ( 21.53943276465977519, 0.05219959533937863772, 111.2510903946856899 ) ) ;
#185088 = CARTESIAN_POINT ( 'NONE',  ( 13.97604488694548053, -13.89961937509957401, 20.62609039468567573 ) ) ;
#185089 = CARTESIAN_POINT ( 'NONE',  ( 5.153800228976335163, 19.02544592524342804, 24.79057627198102765 ) ) ;
#185090 = CARTESIAN_POINT ( 'NONE',  ( -21.53943276465977519, -0.05219959533937600094, 93.75109039468567573 ) ) ;
#185091 = CARTESIAN_POINT ( 'NONE',  ( -14.34966873604972548, 8.224510206698743886, 28.33442372801902209 ) ) ;
#185092 = CARTESIAN_POINT ( 'NONE',  ( 16.46253265017160672, -9.564922557960803928, 88.33224293864769550 ) ) ;
#185093 = VECTOR ( 'NONE', #113475, 999.9999999999998863 ) ;
#185094 = CARTESIAN_POINT ( 'NONE',  ( 17.14385361876520264, 23.59649016807275856, 146.1750000027311387 ) ) ;
#185095 = CARTESIAN_POINT ( 'NONE',  ( 13.97604488694527802, 13.89961937509977652, 74.37390960531436690 ) ) ;
#185096 = CARTESIAN_POINT ( 'NONE',  ( -17.50000000001354294, 5.500000000000027534, 95.79690382535056870 ) ) ;
#185097 = CARTESIAN_POINT ( 'NONE',  ( 16.46253265017146816, 9.564922557961045513, 86.66775706135233293 ) ) ;
#185098 = CARTESIAN_POINT ( 'NONE',  ( 16.51473224551069308, 9.474510206698969483, 114.1655762719810241 ) ) ;
#185100 = CARTESIAN_POINT ( 'NONE',  ( 19.03943276465977164, 0.05219959533936151252, 101.2510903946856757 ) ) ;
#185099 = CARTESIAN_POINT ( 'NONE',  ( -13.89961937509957401, -13.97604488694547875, 24.37609039468565442 ) ) ;
#185101 = CARTESIAN_POINT ( 'NONE',  ( -8.224510206698948167, 14.34966873604960824, 95.41557627198102409 ) ) ;
#185102 = CARTESIAN_POINT ( 'NONE',  ( 19.02544592524343514, -5.153800228976328945, 28.54057627198102409 ) ) ;
#185103 = CARTESIAN_POINT ( 'NONE',  ( -18.62759615963270932, 10.81492255796079327, 60.83224293864769550 ) ) ;
#185104 = CARTESIAN_POINT ( 'NONE',  ( 15.80617190586746368, 15.72974639402197994, 54.37390960531435979 ) ) ;
#185105 = CARTESIAN_POINT ( 'NONE',  ( -13.89961937509977652, 13.97604488694528158, 25.62390960531434558 ) ) ;
#185106 = DIRECTION ( 'NONE',  ( 0.000000000000000000, 0.000000000000000000, -1.000000000000000000 ) ) ;
#185107 = CARTESIAN_POINT ( 'NONE',  ( 13.89961937509957401, 13.97604488694547697, 51.87609039468566863 ) ) ;
#185108 = CARTESIAN_POINT ( 'NONE',  ( 16.52544592524342804, -4.483927247898539470, 33.54057627198102409 ) ) ;
#185109 = CARTESIAN_POINT ( 'NONE',  ( -13.97604488694527625, -13.89961937509977652, 111.8739096053143243 ) ) ;
#185110 = CARTESIAN_POINT ( 'NONE',  ( -10.81492255796105439, 18.62759615963255655, 77.91775706135231871 ) ) ;
#185111 = CARTESIAN_POINT ( 'NONE',  ( 5.823673210054125526, 21.52544592524343514, 64.79057627198103830 ) ) ;
#185112 = CARTESIAN_POINT ( 'NONE',  ( 21.53943276465977519, 0.05219959533937863772, 56.25109039468568284 ) ) ;
#185113 = CARTESIAN_POINT ( 'NONE',  ( -10.72451020669870658, -18.67979575497194134, 44.58442372801901854 ) ) ;
#185114 = CARTESIAN_POINT ( 'NONE',  ( -5.153800228976328057, -19.02544592524343514, 77.29057627198099567 ) ) ;
#185115 = CARTESIAN_POINT ( 'NONE',  ( 12.14591786802327356, -12.06949235617739191, 80.62609039468567573 ) ) ;
#185116 = CARTESIAN_POINT ( 'NONE',  ( 5.049401038298161559, -19.05341960407611168, 22.70724293864769194 ) ) ;
#185117 = CARTESIAN_POINT ( 'NONE',  ( -31.25082632804102190, 7.456723613865049671, 95.94516017006300501 ) ) ;
#185118 = CARTESIAN_POINT ( 'NONE',  ( -16.52544592524342804, 4.483927247898546575, 66.04057627198103830 ) ) ;
#185119 = CARTESIAN_POINT ( 'NONE',  ( 8.314922557960818139, 14.29746914071049879, 29.58224293864769905 ) ) ;
#185120 = CARTESIAN_POINT ( 'NONE',  ( 0.05219959533909260263, 19.03943276465977164, 59.99890960531436690 ) ) ;
#185121 = CARTESIAN_POINT ( 'NONE',  ( 19.03943276465977164, -0.05219959533909143690, 28.74890960531435624 ) ) ;
#185122 = CARTESIAN_POINT ( 'NONE',  ( -10.72451020669898014, 18.67979575497178502, 40.41557627198103120 ) ) ;
#185123 = CARTESIAN_POINT ( 'NONE',  ( 5.049401038297881783, 19.05341960407617563, 32.29275706135233293 ) ) ;
#185125 = CARTESIAN_POINT ( 'NONE',  ( 0.05219959533910956823, 16.53943276465976808, 44.99890960531435979 ) ) ;
#185124 = CARTESIAN_POINT ( 'NONE',  ( 4.500000000000000888, -120.9970989573719038, 14.58956564881030005 ) ) ;
#185126 = CARTESIAN_POINT ( 'NONE',  ( 15.80617190586746368, 15.72974639402197994, 24.37390960531435979 ) ) ;
#185127 = CARTESIAN_POINT ( 'NONE',  ( 17.76566638676855803, 1.079584607093802662, 37.49999999999999289 ) ) ;
#185128 = CARTESIAN_POINT ( 'NONE',  ( 0.05219959533934541429, -16.53943276465976808, 75.00109039468568994 ) ) ;
#185129 = CARTESIAN_POINT ( 'NONE',  ( -9.474510206698720793, -16.51473224551083518, 74.58442372801900433 ) ) ;
#185130 = CARTESIAN_POINT ( 'NONE',  ( 16.52544592524342804, -4.483927247898539470, 43.54057627198103830 ) ) ;
#185131 = EDGE_LOOP ( 'NONE', ( #33592, #146822, #16667, #61157 ) ) ;
#185132 = CARTESIAN_POINT ( 'NONE',  ( -19.53091890409953635, -5.499999999999947597, 75.06097431831420863 ) ) ;
#185133 = CARTESIAN_POINT ( 'NONE',  ( 16.52544592524342804, -4.483927247898539470, 28.54057627198103120 ) ) ;
#185134 = CARTESIAN_POINT ( 'NONE',  ( -0.05219959533909027116, -19.03943276465977164, 47.49890960531435979 ) ) ;
#185135 = CARTESIAN_POINT ( 'NONE',  ( 9.564922557960805705, 16.46253265017160317, 79.58224293864769550 ) ) ;
#185136 = CARTESIAN_POINT ( 'NONE',  ( -13.97604488694527625, -13.89961937509977652, 41.87390960531435979 ) ) ;
#185137 = CARTESIAN_POINT ( 'NONE',  ( -0.05219959533937732626, 21.53943276465977519, 52.50109039468567573 ) ) ;
#185138 = CARTESIAN_POINT ( 'NONE',  ( -5.049401038298153566, 19.05341960407611168, 60.20724293864768129 ) ) ;
#185139 = CARTESIAN_POINT ( 'NONE',  ( 17.50000000000000355, 5.499999999999989342, 103.7823096230356867 ) ) ;
#185140 = CARTESIAN_POINT ( 'NONE',  ( -0.05219959533909027116, -19.03943276465977164, 42.49890960531435269 ) ) ;
#185141 = CARTESIAN_POINT ( 'NONE',  ( -21.53943276465977519, 0.05219959533907696930, 31.24890960531435979 ) ) ;
#185143 = CARTESIAN_POINT ( 'NONE',  ( 4.483927247898545687, 16.52544592524342804, 114.7905762719810383 ) ) ;
#185142 = CARTESIAN_POINT ( 'NONE',  ( -21.53943276465977519, -0.05219959533937600094, 78.75109039468568994 ) ) ;
#185144 = CARTESIAN_POINT ( 'NONE',  ( 10.81492255796078972, 18.62759615963270932, 24.58224293864768839 ) ) ;
#185145 = VECTOR ( 'NONE', #132541, 1000.000000000000000 ) ;
#185146 = CARTESIAN_POINT ( 'NONE',  ( -12.14591786802326823, 12.06949235617739902, 93.12609039468568994 ) ) ;
#185147 = CARTESIAN_POINT ( 'NONE',  ( 18.62759615963255655, 10.81492255796105972, 111.6677570613523613 ) ) ;
#185148 = CARTESIAN_POINT ( 'NONE',  ( -0.05219959533934338120, 16.53943276465976808, 72.50109039468568994 ) ) ;
#185149 = CARTESIAN_POINT ( 'NONE',  ( 19.05341960407611168, 5.049401038298154454, 103.9572429386476671 ) ) ;
#185150 = CARTESIAN_POINT ( 'NONE',  ( -8.224510206698735004, -14.34966873604973081, 54.58442372801901143 ) ) ;
#185151 = CARTESIAN_POINT ( 'NONE',  ( 8.224510206698742110, 14.34966873604972548, 37.08442372801901143 ) ) ;
#185152 = CARTESIAN_POINT ( 'NONE',  ( 16.55341960407618274, -4.379528057220086978, 91.04275706135236135 ) ) ;
#185153 = CARTESIAN_POINT ( 'NONE',  ( 10.72451020669871369, 18.67979575497193778, 57.08442372801901854 ) ) ;
#185154 = CARTESIAN_POINT ( 'NONE',  ( -8.224510206698735004, -14.34966873604973081, 19.58442372801901143 ) ) ;
#185155 = CARTESIAN_POINT ( 'NONE',  ( 10.81492255796078972, 18.62759615963270932, 109.5822429386476955 ) ) ;
#185156 = CARTESIAN_POINT ( 'NONE',  ( -4.379528057220086978, -16.55341960407618274, 19.79275706135235069 ) ) ;
#185157 = CARTESIAN_POINT ( 'NONE',  ( 16.55341960407618274, -4.379528057220086978, 81.04275706135236135 ) ) ;
#185158 = DIRECTION ( 'NONE',  ( 0.000000000000000000, 0.000000000000000000, 1.000000000000000000 ) ) ;
#185159 = CARTESIAN_POINT ( 'NONE',  ( 18.62759615963255655, 10.81492255796105972, 91.66775706135234714 ) ) ;
#185160 = CARTESIAN_POINT ( 'NONE',  ( 19.03943276465977164, 0.05219959533936151252, 86.25109039468567573 ) ) ;
#185161 = CARTESIAN_POINT ( 'NONE',  ( 8.314922557960818139, 14.29746914071049879, 54.58224293864769550 ) ) ;
#185162 = CARTESIAN_POINT ( 'NONE',  ( 12.06949235617757843, -12.14591786802309237, 48.12390960531436690 ) ) ;
#185163 = CARTESIAN_POINT ( 'NONE',  ( -8.224510206698948167, 14.34966873604960824, 100.4155762719810241 ) ) ;
#185165 = LINE ( 'NONE', #113281, #7879 ) ;
#185164 = CARTESIAN_POINT ( 'NONE',  ( 13.89961937509957401, 13.97604488694547697, 51.87609039468566863 ) ) ;
#185166 = CARTESIAN_POINT ( 'NONE',  ( -18.62759615963255300, -10.81492255796106328, 44.16775706135234714 ) ) ;
#185167 = CARTESIAN_POINT ( 'NONE',  ( 16.46253265017146816, 9.564922557961045513, 111.6677570613523329 ) ) ;
#185168 = CARTESIAN_POINT ( 'NONE',  ( -8.636255518948912524, -38.40306468563544939, -32.12764100183819949 ) ) ;
#185169 = CARTESIAN_POINT ( 'NONE',  ( 0.05219959533909260263, 19.03943276465977164, 109.9989096053143669 ) ) ;
#185170 = CARTESIAN_POINT ( 'NONE',  ( -21.53943276465977519, 0.05219959533907696930, 71.24890960531435269 ) ) ;
#185171 = CARTESIAN_POINT ( 'NONE',  ( 19.03943276465977164, 0.05219959533936151252, 96.25109039468567573 ) ) ;
#185172 = CARTESIAN_POINT ( 'NONE',  ( -9.474510206698964154, 16.51473224551069663, 100.4155762719810241 ) ) ;
#185173 = CARTESIAN_POINT ( 'NONE',  ( 16.51473224551083163, -9.474510206698727899, 50.83442372801899722 ) ) ;
#185174 = CARTESIAN_POINT ( 'NONE',  ( -16.53943276465976808, 0.05219959533911058130, 106.2489096053143811 ) ) ;
#185175 = CARTESIAN_POINT ( 'NONE',  ( 21.52544592524334988, 5.823673210054432836, 91.45942372801901854 ) ) ;
#185176 = CARTESIAN_POINT ( 'NONE',  ( -0.05219959533909027116, -19.03943276465977164, 27.49890960531435624 ) ) ;
#185177 = CARTESIAN_POINT ( 'NONE',  ( -10.72451020669870658, -18.67979575497194134, 44.58442372801901854 ) ) ;
#185178 = ADVANCED_FACE ( 'NONE', ( #89505, #198682 ), #151195, .F. ) ;
#185179 = CARTESIAN_POINT ( 'NONE',  ( 0.05219959533937995610, -21.53943276465977519, 90.00109039468567573 ) ) ;
#185180 = CARTESIAN_POINT ( 'NONE',  ( 12.14591786802327356, -12.06949235617739191, 90.62609039468567573 ) ) ;
#185181 = CARTESIAN_POINT ( 'NONE',  ( -5.823673210054431948, 21.52544592524334988, 47.70942372801902565 ) ) ;
#185182 = CARTESIAN_POINT ( 'NONE',  ( 15.72974639402176855, 15.80617190586768217, 36.87609039468568994 ) ) ;
#185184 = CARTESIAN_POINT ( 'NONE',  ( -0.05219959533909027116, -19.03943276465977164, 77.49890960531435269 ) ) ;
#185183 = CARTESIAN_POINT ( 'NONE',  ( 19.03943276465977164, 0.05219959533936151252, 71.25109039468566152 ) ) ;
#185185 = CARTESIAN_POINT ( 'NONE',  ( 8.314922557960818139, 14.29746914071049879, 99.58224293864770971 ) ) ;
#185186 = CARTESIAN_POINT ( 'NONE',  ( -0.05219959533907301413, -21.53943276465977519, 77.49890960531433848 ) ) ;
#185187 = CARTESIAN_POINT ( 'NONE',  ( -4.379528057220328563, 16.55341960407611168, 60.20724293864768839 ) ) ;
#185188 = CARTESIAN_POINT ( 'NONE',  ( 15.72974639402176855, 15.80617190586768217, 101.8760903946857042 ) ) ;
#185189 = CARTESIAN_POINT ( 'NONE',  ( 14.29746914071049879, -8.314922557960816363, 83.33224293864769550 ) ) ;
#185190 = CARTESIAN_POINT ( 'NONE',  ( -13.97604488694527625, -13.89961937509977652, 36.87390960531436690 ) ) ;
#185191 = CARTESIAN_POINT ( 'NONE',  ( 9.564922557961047289, -16.46253265017146816, 65.41775706135233293 ) ) ;
#185192 = CARTESIAN_POINT ( 'NONE',  ( -16.53943276465976808, 0.05219959533911058130, 31.24890960531435979 ) ) ;
#185193 = CARTESIAN_POINT ( 'NONE',  ( 21.52544592524334988, 5.823673210054432836, 96.45942372801901854 ) ) ;
#185194 = CARTESIAN_POINT ( 'NONE',  ( -13.97604488694527625, -13.89961937509977652, 86.87390960531436690 ) ) ;
#185195 = CARTESIAN_POINT ( 'NONE',  ( 19.03943276465977164, 0.05219959533936151252, 56.25109039468566863 ) ) ;
#185196 = CARTESIAN_POINT ( 'NONE',  ( 15.80617190586746368, 15.72974639402197994, 69.37390960531436690 ) ) ;
#185197 = CARTESIAN_POINT ( 'NONE',  ( 21.53943276465977519, -0.05219959533907433946, 108.7489096053143669 ) ) ;
#185198 = CARTESIAN_POINT ( 'NONE',  ( 0.05219959533936267826, -19.03943276465977164, 110.0010903946856757 ) ) ;
#185199 = CARTESIAN_POINT ( 'NONE',  ( 0.05219959533934541429, -16.53943276465976808, 75.00109039468568994 ) ) ;
#185201 = CARTESIAN_POINT ( 'NONE',  ( 0.05219959533937995610, -21.53943276465977519, 20.00109039468568639 ) ) ;
#185200 = CARTESIAN_POINT ( 'NONE',  ( -0.3535533905933764265, -30.00000000000000355, 5.353553390593269512 ) ) ;
#185202 = CARTESIAN_POINT ( 'NONE',  ( 8.314922557960818139, 14.29746914071049879, 109.5822429386476955 ) ) ;
#185203 = CARTESIAN_POINT ( 'NONE',  ( -29.86685920354755552, 21.69954338932564397, -9.324999997268813345 ) ) ;
#185204 = CARTESIAN_POINT ( 'NONE',  ( -4.483927247898782831, 16.52544592524335698, 47.70942372801902565 ) ) ;
#185205 = CARTESIAN_POINT ( 'NONE',  ( -4.483927247898539470, -16.52544592524342804, 77.29057627198102409 ) ) ;
#185206 = CARTESIAN_POINT ( 'NONE',  ( -21.52544592524343514, 5.823673210054127303, 81.04057627198102409 ) ) ;
#185207 = CARTESIAN_POINT ( 'NONE',  ( 16.55341960407618274, -4.379528057220086978, 101.0427570613523756 ) ) ;
#185208 = CARTESIAN_POINT ( 'NONE',  ( -14.34966873604972548, 8.224510206698743886, 38.33442372801900433 ) ) ;
#185209 = CARTESIAN_POINT ( 'NONE',  ( -13.89961937509977652, 13.97604488694528158, 45.62390960531433848 ) ) ;
#185210 = CARTESIAN_POINT ( 'NONE',  ( 8.314922557961029526, -14.29746914071037800, 75.41775706135233293 ) ) ;
#185211 = CARTESIAN_POINT ( 'NONE',  ( -16.51473224551082808, 9.474510206698731452, 73.33442372801900433 ) ) ;
#185212 = CARTESIAN_POINT ( 'NONE',  ( -0.05219959533907301413, -21.53943276465977519, 77.49890960531433848 ) ) ;
#185213 = CARTESIAN_POINT ( 'NONE',  ( -16.55341960407617563, 4.379528057220093196, 103.5427570613523613 ) ) ;
#185214 = CARTESIAN_POINT ( 'NONE',  ( -18.67979575497193778, 10.72451020669871902, 83.33442372801903275 ) ) ;
#185215 = EDGE_CURVE ( 'NONE', #4972, #12274, #111998, .T. ) ;
#185216 = CARTESIAN_POINT ( 'NONE',  ( 18.62759615963271287, -10.81492255796078972, 63.33224293864770260 ) ) ;
#185217 = CARTESIAN_POINT ( 'NONE',  ( -21.55341960407610458, -5.719274019375992779, 41.45724293864769550 ) ) ;
#185218 = ORIENTED_EDGE ( 'NONE', *, *, #191742, .F. ) ;
#185219 = CARTESIAN_POINT ( 'NONE',  ( -12.06949235617739369, -12.14591786802326823, 84.37609039468570415 ) ) ;
#185220 = CARTESIAN_POINT ( 'NONE',  ( 10.72451020669898902, -18.67979575497178502, 47.91557627198102409 ) ) ;
#185221 = EDGE_LOOP ( 'NONE', ( #166340, #103843, #86007, #48374, #15915, #196326, #81059, #63098, #20704, #149020, #13738, #19588, #22401, #89851 ) ) ;
#185222 = CARTESIAN_POINT ( 'NONE',  ( 5.049401038298161559, -19.05341960407611168, 112.7072429386476813 ) ) ;
#185223 = CARTESIAN_POINT ( 'NONE',  ( 30.74264578624799782, 22.33583958711400541, -8.549999994537627046 ) ) ;
#185224 = CARTESIAN_POINT ( 'NONE',  ( 19.02544592524343514, -5.153800228976328945, 23.54057627198102054 ) ) ;
#185225 = CARTESIAN_POINT ( 'NONE',  ( 5.719274019375991003, -21.55341960407610458, 77.70724293864770971 ) ) ;
#185226 = CARTESIAN_POINT ( 'NONE',  ( 4.483927247898790824, -16.52544592524335698, 100.2094237280190043 ) ) ;
#185227 = CARTESIAN_POINT ( 'NONE',  ( -15.72974639402176322, -15.80617190586768395, 64.37609039468568994 ) ) ;
#185228 = CARTESIAN_POINT ( 'NONE',  ( 12.14591786802327356, -12.06949235617739191, 20.62609039468568639 ) ) ;
#185229 = CARTESIAN_POINT ( 'NONE',  ( -13.89961937509977652, 13.97604488694528158, 25.62390960531434558 ) ) ;
#185230 = CARTESIAN_POINT ( 'NONE',  ( -0.05219959533936034679, 19.03943276465977164, 112.5010903946856757 ) ) ;
#185231 = CARTESIAN_POINT ( 'NONE',  ( 9.564922557960805705, 16.46253265017160317, 34.58224293864770260 ) ) ;
#185232 = CARTESIAN_POINT ( 'NONE',  ( -23.31738231874055245, -16.94106989632524574, 142.1999999999999886 ) ) ;
#185233 = CARTESIAN_POINT ( 'NONE',  ( -9.564922557960796823, -16.46253265017161027, 102.0822429386477097 ) ) ;
#185234 = CARTESIAN_POINT ( 'NONE',  ( -12.14591786802326823, 12.06949235617739902, 83.12609039468568994 ) ) ;
#185235 = CARTESIAN_POINT ( 'NONE',  ( -5.153800228976607833, 19.02544592524334988, 82.70942372801897591 ) ) ;
#185236 = CARTESIAN_POINT ( 'NONE',  ( 13.89961937509957401, 13.97604488694547697, 26.87609039468566507 ) ) ;
#185237 = CARTESIAN_POINT ( 'NONE',  ( 18.67979575497178502, 10.72451020669898547, 59.16557627198103120 ) ) ;
#185238 = CARTESIAN_POINT ( 'NONE',  ( -16.53943276465976808, -0.05219959533934237506, 88.75109039468567573 ) ) ;
#185239 = AXIS2_PLACEMENT_3D ( 'NONE', #136055, #120865, #58222 ) ;
#185240 = CARTESIAN_POINT ( 'NONE',  ( -16.51473224551082808, 9.474510206698731452, 88.33442372801900433 ) ) ;
#185241 = CARTESIAN_POINT ( 'NONE',  ( -16.51473224551069308, -9.474510206698971260, 46.66557627198102409 ) ) ;
#185242 = CARTESIAN_POINT ( 'NONE',  ( 16.51473224551069308, 9.474510206698969483, 94.16557627198103830 ) ) ;
#185243 = CARTESIAN_POINT ( 'NONE',  ( -15.80617190586768217, 15.72974639402176855, 53.12609039468568284 ) ) ;
#185244 = CARTESIAN_POINT ( 'NONE',  ( 5.049401038298161559, -19.05341960407611168, 42.70724293864767418 ) ) ;
#185245 = B_SPLINE_CURVE_WITH_KNOTS ( 'NONE', 3,
 ( #94976, #96948, #156661, #64646, #173827, #82771, #35291, #20119, #81763, #36272, #66619, #128283, #174807, #10952, #70624, #6930, #25136, #24127, #26129, #133282, #71616, #56451, #160627, #163634 ),
 .UNSPECIFIED., .F., .F.,
 ( 4, 2, 2, 2, 2, 2, 2, 2, 2, 2, 2, 4 ),
 ( 0.000000000000000000, 0.002690955612256999523, 0.005381911224513999045, 0.008072866836771004639, 0.009418344642899506569, 0.01009108354596376447, 0.01076382244902802238, 0.01210930025515653992, 0.01345477806128506093, 0.01614573367354209601, 0.01883668928579913110, 0.02152764489805616965 ),
 .UNSPECIFIED. ) ;
#185246 = CARTESIAN_POINT ( 'NONE',  ( 0.000000000000000000, 0.000000000000000000, -56.46919128290398504 ) ) ;
#185247 = CARTESIAN_POINT ( 'NONE',  ( 5.153800228976335163, 19.02544592524342804, 104.7905762719809957 ) ) ;
#185248 = CARTESIAN_POINT ( 'NONE',  ( 8.314922557960818139, 14.29746914071049879, 69.58224293864769550 ) ) ;
#185249 = CARTESIAN_POINT ( 'NONE',  ( -10.81492255796078084, -18.62759615963271287, 57.08224293864769550 ) ) ;
#185250 = CARTESIAN_POINT ( 'NONE',  ( 28.79475375365586132, 2.781246896534039337E-14, 143.2656553485623760 ) ) ;
#185251 = CARTESIAN_POINT ( 'NONE',  ( 16.51473224551083163, -9.474510206698727899, 45.83442372801900433 ) ) ;
#185252 =( NAMED_UNIT ( * ) SI_UNIT ( $, .STERADIAN. ) SOLID_ANGLE_UNIT ( ) );
#185254 = CARTESIAN_POINT ( 'NONE',  ( -5.153800228976328057, -19.02544592524343514, 72.29057627198102409 ) ) ;
#185253 = CARTESIAN_POINT ( 'NONE',  ( 13.97604488694527802, 13.89961937509977652, 64.37390960531436690 ) ) ;
#185255 = CARTESIAN_POINT ( 'NONE',  ( -0.05219959533934338120, 16.53943276465976808, 57.50109039468568994 ) ) ;
#185256 = CARTESIAN_POINT ( 'NONE',  ( 0.05219959533936267826, -19.03943276465977164, 80.00109039468567573 ) ) ;
#185257 = B_SPLINE_CURVE_WITH_KNOTS ( 'NONE', 3,
 ( #157668, #79826, #159636, #22136, #173842, #98954, #189997, #52462, #3962, #176834, #37295, #68627, #81779, #126321, #38305, #82787, #66635, #21132, #141496, #6947, #96962, #114120, #51472, #158642 ),
 .UNSPECIFIED., .F., .F.,
 ( 4, 2, 2, 2, 2, 2, 2, 2, 2, 2, 2, 4 ),
 ( 0.000000000000000000, 0.002556407831644171621, 0.005112815663288348446, 0.007669223494932524837, 0.008947427410754611732, 0.009586529368665658649, 0.01022563132657670557, 0.01150383524239879246, 0.01278203915822087589, 0.01533844698986504620, 0.01789485482150921652, 0.02045126265315338338 ),
 .UNSPECIFIED. ) ;
#185258 = DIRECTION ( 'NONE',  ( 0.000000000000000000, -0.8164965809277232589, -0.5773502691896295058 ) ) ;
#185259 = CARTESIAN_POINT ( 'NONE',  ( 16.52544592524335698, 4.483927247898782831, 86.45942372801901854 ) ) ;
#185260 = DIRECTION ( 'NONE',  ( -1.000000000000000000, 0.000000000000000000, 0.000000000000000000 ) ) ;
#185261 = CARTESIAN_POINT ( 'NONE',  ( -0.05219959533934338120, 16.53943276465976808, 82.50109039468568994 ) ) ;
#185262 = CARTESIAN_POINT ( 'NONE',  ( 16.52544592524335698, 4.483927247898782831, 51.45942372801901854 ) ) ;
#185263 = CARTESIAN_POINT ( 'NONE',  ( 16.46253265017146816, 9.564922557961045513, 21.66775706135233648 ) ) ;
#185265 = CARTESIAN_POINT ( 'NONE',  ( 17.62203461105333702, -16.12203461105326951, -57.08650645001478097 ) ) ;
#185264 = CARTESIAN_POINT ( 'NONE',  ( 9.474510206698971260, -16.51473224551069308, 52.91557627198102409 ) ) ;
#185266 = CARTESIAN_POINT ( 'NONE',  ( -5.719274019375665041, -21.55341960407619695, 54.79275706135235424 ) ) ;
#185267 = CARTESIAN_POINT ( 'NONE',  ( 5.049401038297881783, 19.05341960407617563, 72.29275706135234714 ) ) ;
#185268 = CARTESIAN_POINT ( 'NONE',  ( -5.823673210054431948, 21.52544592524334988, 112.7094237280190328 ) ) ;
#185269 = CARTESIAN_POINT ( 'NONE',  ( -16.51473224551069308, -9.474510206698971260, 36.66557627198102409 ) ) ;
#185270 = CARTESIAN_POINT ( 'NONE',  ( 16.86294246435915767, 6.972627225432042941, 23.78307040723333543 ) ) ;
#185271 = CARTESIAN_POINT ( 'NONE',  ( 21.55341960407610458, 5.719274019375980345, 68.95724293864769550 ) ) ;
#185272 = CARTESIAN_POINT ( 'NONE',  ( -16.46253265017160317, 9.564922557960807481, 115.8322429386477097 ) ) ;
#185273 = CARTESIAN_POINT ( 'NONE',  ( -12.14591786802309592, -12.06949235617757132, 111.8739096053143669 ) ) ;
#185274 = CARTESIAN_POINT ( 'NONE',  ( -0.05219959533934338120, 16.53943276465976808, 32.50109039468568284 ) ) ;
#185275 = CARTESIAN_POINT ( 'NONE',  ( 12.14591786802309770, 12.06949235617756955, 24.37390960531435979 ) ) ;
#185276 = ORIENTED_EDGE ( 'NONE', *, *, #46382, .F. ) ;
#185277 = CARTESIAN_POINT ( 'NONE',  ( -18.62759615963255300, -10.81492255796106328, 19.16775706135234714 ) ) ;
#185279 = CARTESIAN_POINT ( 'NONE',  ( -23.48529157249600985, 32.32473071737754111, -6.300000000000000711 ) ) ;
#185278 = CARTESIAN_POINT ( 'NONE',  ( 8.314922557960818139, 14.29746914071049879, 44.58224293864769550 ) ) ;
#185280 = CARTESIAN_POINT ( 'NONE',  ( 13.97604488694548053, -13.89961937509957401, 105.6260903946856757 ) ) ;
#185281 = CARTESIAN_POINT ( 'NONE',  ( 19.05341960407617918, -5.049401038297876454, 21.04275706135232582 ) ) ;
#185282 = CARTESIAN_POINT ( 'NONE',  ( 14.34966873604960469, 8.224510206698951720, 39.16557627198102409 ) ) ;
#185283 = CARTESIAN_POINT ( 'NONE',  ( 21.55341960407610458, 5.719274019375980345, 108.9572429386476955 ) ) ;
#185285 = CARTESIAN_POINT ( 'NONE',  ( 18.67979575497178502, 10.72451020669898547, 69.16557627198102409 ) ) ;
#185284 = DIRECTION ( 'NONE',  ( 1.000000000000000000, 0.000000000000000000, 0.000000000000000000 ) ) ;
#185286 = CARTESIAN_POINT ( 'NONE',  ( -19.05341960407611168, -5.049401038298163336, 71.45724293864766707 ) ) ;
#185287 = CARTESIAN_POINT ( 'NONE',  ( 12.06949235617757843, -12.14591786802309237, 43.12390960531435269 ) ) ;
#185288 = CARTESIAN_POINT ( 'NONE',  ( -0.05219959533909027116, -19.03943276465977164, 92.49890960531436690 ) ) ;
#185289 = DIRECTION ( 'NONE',  ( 1.000000000000000000, -0.000000000000000000, -0.000000000000000000 ) ) ;
#185290 = CARTESIAN_POINT ( 'NONE',  ( 19.02544592524334988, 5.153800228976608722, 61.45942372801900433 ) ) ;
#185291 = CARTESIAN_POINT ( 'NONE',  ( 15.72974639402199770, -15.80617190586745480, 88.12390960531436690 ) ) ;
#185292 = CARTESIAN_POINT ( 'NONE',  ( 8.314922557960818139, 14.29746914071049879, 99.58224293864770971 ) ) ;
#185293 = AXIS2_PLACEMENT_3D ( 'NONE', #157159, #18654, #188501 ) ;
#185294 = CARTESIAN_POINT ( 'NONE',  ( 18.62759615963255655, 10.81492255796105972, 46.66775706135234714 ) ) ;
#185295 = CARTESIAN_POINT ( 'NONE',  ( -27.73933785331498925, 2.428612866367529932E-14, 144.8750000027311842 ) ) ;
#185296 = CARTESIAN_POINT ( 'NONE',  ( 12.06949235617757843, -12.14591786802309237, 33.12390960531435979 ) ) ;
#185297 = CARTESIAN_POINT ( 'NONE',  ( -19.02544592524342804, 5.153800228976336051, 41.04057627198103120 ) ) ;
#185298 = CARTESIAN_POINT ( 'NONE',  ( -5.049401038298153566, 19.05341960407611168, 95.20724293864770971 ) ) ;
#185299 = CARTESIAN_POINT ( 'NONE',  ( 5.823673210054125526, 21.52544592524343514, 54.79057627198104541 ) ) ;
#185300 = CARTESIAN_POINT ( 'NONE',  ( -22.44159573604010305, 16.30477369853692338, 140.6750000027311671 ) ) ;
#185301 = CARTESIAN_POINT ( 'NONE',  ( 5.049401038298161559, -19.05341960407611168, 37.70724293864768839 ) ) ;
#185302 = CARTESIAN_POINT ( 'NONE',  ( 15.80617190586746368, 15.72974639402197994, 59.37390960531436690 ) ) ;
#185303 = CARTESIAN_POINT ( 'NONE',  ( -18.62759615963255300, -10.81492255796106328, 69.16775706135234714 ) ) ;
#185305 = CARTESIAN_POINT ( 'NONE',  ( 8.224510206698742110, 14.34966873604972548, 87.08442372801901854 ) ) ;
#185304 = CARTESIAN_POINT ( 'NONE',  ( 15.59283147534792136, -34.52683219100885026, -28.07673947522060232 ) ) ;
#185306 = CARTESIAN_POINT ( 'NONE',  ( 0.05219959533909260263, 19.03943276465977164, 54.99890960531435979 ) ) ;
#185307 = CARTESIAN_POINT ( 'NONE',  ( 16.51473224551069308, 9.474510206698969483, 69.16557627198102409 ) ) ;
#185308 = ORIENTED_EDGE ( 'NONE', *, *, #179989, .T. ) ;
#185309 = CARTESIAN_POINT ( 'NONE',  ( 16.46253265017146816, 9.564922557961045513, 31.66775706135232937 ) ) ;
#185310 = CARTESIAN_POINT ( 'NONE',  ( 16.53943276465976808, 0.05219959533934440121, 76.25109039468568994 ) ) ;
#185311 = CARTESIAN_POINT ( 'NONE',  ( -5.719274019375665041, -21.55341960407619695, 94.79275706135234714 ) ) ;
#185312 = CARTESIAN_POINT ( 'NONE',  ( -19.02544592524342804, 5.153800228976336051, 81.04057627198103830 ) ) ;
#185313 = CARTESIAN_POINT ( 'NONE',  ( 5.823673210054125526, 21.52544592524343514, 34.79057627198103120 ) ) ;
#185314 = CARTESIAN_POINT ( 'NONE',  ( -12.14591786802326823, 12.06949235617739902, 28.12609039468568284 ) ) ;
#185315 = CARTESIAN_POINT ( 'NONE',  ( -15.72974639402176322, -15.80617190586768395, 84.37609039468570415 ) ) ;
#185316 = CARTESIAN_POINT ( 'NONE',  ( -14.29746914071037622, -8.314922557961029526, 54.16775706135235424 ) ) ;
#185317 = CARTESIAN_POINT ( 'NONE',  ( -5.719274019375978568, 21.55341960407610458, 105.2072429386477097 ) ) ;
#185318 = CARTESIAN_POINT ( 'NONE',  ( 9.564922557961047289, -16.46253265017146816, 110.4177570613523471 ) ) ;
#185319 = CARTESIAN_POINT ( 'NONE',  ( 5.153800228976335163, 19.02544592524342804, 79.79057627198102409 ) ) ;
#185320 = CARTESIAN_POINT ( 'NONE',  ( 8.224510206698742110, 14.34966873604972548, 27.08442372801901854 ) ) ;
#185321 = CARTESIAN_POINT ( 'NONE',  ( -13.97604488694527625, -13.89961937509977652, 36.87390960531436690 ) ) ;
#185322 = CIRCLE ( 'NONE', #17465, 24.30000000000003268 ) ;
#185323 = CARTESIAN_POINT ( 'NONE',  ( 19.05341960407617918, -5.049401038297876454, 111.0427570613523329 ) ) ;
#185324 = CARTESIAN_POINT ( 'NONE',  ( 16.52544592524342804, -4.483927247898539470, 78.54057627198103830 ) ) ;
#185325 = CARTESIAN_POINT ( 'NONE',  ( 4.483927247898790824, -16.52544592524335698, 85.20942372801901854 ) ) ;
#185327 = CARTESIAN_POINT ( 'NONE',  ( -19.03943276465977164, 0.05219959533909376836, 46.24890960531435979 ) ) ;
#185326 = CARTESIAN_POINT ( 'NONE',  ( -21.53943276465977519, -0.05219959533937600094, 33.75109039468568284 ) ) ;
#185328 = CARTESIAN_POINT ( 'NONE',  ( -9.474510206698964154, 16.51473224551069663, 65.41557627198102409 ) ) ;
#185329 = CARTESIAN_POINT ( 'NONE',  ( 16.53943276465976808, 0.05219959533934440121, 86.25109039468568994 ) ) ;
#185331 = ORIENTED_EDGE ( 'NONE', *, *, #77828, .F. ) ;
#185330 = CARTESIAN_POINT ( 'NONE',  ( -24.24385185424069533, -7.025880200331405590, 170.5073520790474788 ) ) ;
#185332 = ORIENTED_EDGE ( 'NONE', *, *, #26831, .T. ) ;
#185333 = CARTESIAN_POINT ( 'NONE',  ( -19.03943276465977164, -0.05219959533935918106, 18.75109039468567218 ) ) ;
#185334 = CARTESIAN_POINT ( 'NONE',  ( -5.153800228976328057, -19.02544592524343514, 32.29057627198102409 ) ) ;
#185336 = ORIENTED_EDGE ( 'NONE', *, *, #133615, .T. ) ;
#185335 = CARTESIAN_POINT ( 'NONE',  ( -19.03943276465977164, 0.05219959533909376836, 116.2489096053143669 ) ) ;
#185337 = CARTESIAN_POINT ( 'NONE',  ( 14.29746914071037800, 8.314922557961029526, 26.66775706135235424 ) ) ;
#185339 = CARTESIAN_POINT ( 'NONE',  ( 12.06949235617739724, 12.14591786802326823, 46.87609039468568994 ) ) ;
#185338 = CARTESIAN_POINT ( 'NONE',  ( 16.46253265017146816, 9.564922557961045513, 51.66775706135233293 ) ) ;
#185340 = CARTESIAN_POINT ( 'NONE',  ( -13.97604488694527625, -13.89961937509977652, 106.8739096053143669 ) ) ;
#185341 = CARTESIAN_POINT ( 'NONE',  ( 5.049401038298161559, -19.05341960407611168, 62.70724293864769550 ) ) ;
#185342 = CARTESIAN_POINT ( 'NONE',  ( 0.05219959533907565091, 21.53943276465977519, 94.99890960531436690 ) ) ;
#185344 = DIRECTION ( 'NONE',  ( -3.875508829633682909E-46, 1.000000000000000000, 7.149051953565419487E-31 ) ) ;
#185343 = CARTESIAN_POINT ( 'NONE',  ( 5.153800228976335163, 19.02544592524342804, 89.79057627198102409 ) ) ;
#185345 = ADVANCED_FACE ( 'NONE', ( #73365 ), #56176, .T. ) ;
#185346 = CARTESIAN_POINT ( 'NONE',  ( 16.46253265017160672, -9.564922557960803928, 68.33224293864770971 ) ) ;
#185348 = CARTESIAN_POINT ( 'NONE',  ( 16.51473224551069308, 9.474510206698969483, 69.16557627198102409 ) ) ;
#185347 = CARTESIAN_POINT ( 'NONE',  ( 0.05219959533934541429, -16.53943276465976808, 110.0010903946856757 ) ) ;
#185349 = CARTESIAN_POINT ( 'NONE',  ( -19.02544592524334988, -5.153800228976617603, 18.95942372801899722 ) ) ;
#185350 = CARTESIAN_POINT ( 'NONE',  ( -16.52544592524342804, 4.483927247898546575, 66.04057627198103830 ) ) ;
#185351 = CARTESIAN_POINT ( 'NONE',  ( -5.823673210054431948, 21.52544592524334988, 102.7094237280190185 ) ) ;
#185352 = CARTESIAN_POINT ( 'NONE',  ( -9.564922557960796823, -16.46253265017161027, 42.08224293864769550 ) ) ;
#185354 = CARTESIAN_POINT ( 'NONE',  ( 21.52544592524334988, 5.823673210054432836, 96.45942372801901854 ) ) ;
#185353 = CARTESIAN_POINT ( 'NONE',  ( 4.379528057220339221, -16.55341960407611168, 37.70724293864769550 ) ) ;
#185355 = CARTESIAN_POINT ( 'NONE',  ( 5.049401038298161559, -19.05341960407611168, 82.70724293864770971 ) ) ;
#185356 = CARTESIAN_POINT ( 'NONE',  ( -16.46253265017160317, 9.564922557960807481, 100.8322429386477097 ) ) ;
#185357 = CARTESIAN_POINT ( 'NONE',  ( -12.14591786802309592, -12.06949235617757132, 106.8739096053143811 ) ) ;
#185358 = CARTESIAN_POINT ( 'NONE',  ( 12.14591786802309770, 12.06949235617756955, 74.37390960531436690 ) ) ;
#185359 = CARTESIAN_POINT ( 'NONE',  ( 21.53943276465977519, -0.05219959533907433946, 83.74890960531435269 ) ) ;
#185360 = CARTESIAN_POINT ( 'NONE',  ( -9.474510206698964154, 16.51473224551069663, 70.41557627198102409 ) ) ;
#185361 = CARTESIAN_POINT ( 'NONE',  ( 21.55341960407610458, 5.719274019375980345, 83.95724293864770971 ) ) ;
#185362 = CARTESIAN_POINT ( 'NONE',  ( -19.03943276465977164, -0.05219959533935918106, 83.75109039468567573 ) ) ;
#185364 = CARTESIAN_POINT ( 'NONE',  ( -16.53943276465976808, 0.05219959533911058130, 91.24890960531436690 ) ) ;
#185363 = CARTESIAN_POINT ( 'NONE',  ( 18.56453257813361191, -5.500000000000031974, 48.49000423690687001 ) ) ;
#185365 = CARTESIAN_POINT ( 'NONE',  ( -16.51473224551069308, -9.474510206698971260, 61.66557627198103120 ) ) ;
#185366 = CARTESIAN_POINT ( 'NONE',  ( -18.62759615963270932, 10.81492255796079327, 70.83224293864770971 ) ) ;
#185367 = CARTESIAN_POINT ( 'NONE',  ( -17.72560187377285956, -5.499999999999973355, 84.07814504131316369 ) ) ;
#185369 = CARTESIAN_POINT ( 'NONE',  ( -27.73933785331498925, 9.013057229001088189, 149.2750000027311614 ) ) ;
#185368 = CARTESIAN_POINT ( 'NONE',  ( 4.483927247898790824, -16.52544592524335698, 110.2094237280190185 ) ) ;
#185370 = CARTESIAN_POINT ( 'NONE',  ( 9.564922557961047289, -16.46253265017146816, 110.4177570613523471 ) ) ;
#185371 = CARTESIAN_POINT ( 'NONE',  ( -8.224510206698948167, 14.34966873604960824, 75.41557627198102409 ) ) ;
#185372 = CARTESIAN_POINT ( 'NONE',  ( -18.87255363501902750, -5.500000000000005329, 96.32513748171830059 ) ) ;
#185373 = CARTESIAN_POINT ( 'NONE',  ( 19.05341960407611168, 5.049401038298154454, 68.95724293864769550 ) ) ;
#185374 = CARTESIAN_POINT ( 'NONE',  ( 5.049401038298161559, -19.05341960407611168, 37.70724293864768839 ) ) ;
#185375 = CARTESIAN_POINT ( 'NONE',  ( 16.55341960407611168, 4.379528057220329451, 68.95724293864769550 ) ) ;
#185376 = AXIS2_PLACEMENT_3D ( 'NONE', #150571, #56559, #152533 ) ;
#185377 = CARTESIAN_POINT ( 'NONE',  ( 5.153800228976335163, 19.02544592524342804, 114.7905762719810241 ) ) ;
#185379 = CARTESIAN_POINT ( 'NONE',  ( -5.153800228976328057, -19.02544592524343514, 77.29057627198099567 ) ) ;
#185378 = CARTESIAN_POINT ( 'NONE',  ( -9.474510206698720793, -16.51473224551083518, 89.58442372801900433 ) ) ;
#185380 = CARTESIAN_POINT ( 'NONE',  ( -0.05219959533909027116, -19.03943276465977164, 92.49890960531436690 ) ) ;
#185381 = CARTESIAN_POINT ( 'NONE',  ( 5.823673210054125526, 21.52544592524343514, 69.79057627198102409 ) ) ;
#185382 = CARTESIAN_POINT ( 'NONE',  ( 12.14591786802327356, -12.06949235617739191, 75.62609039468567573 ) ) ;
#185383 = CARTESIAN_POINT ( 'NONE',  ( -17.50000000000000355, 5.622605283950836252, 93.68792689403892382 ) ) ;
#185384 = CARTESIAN_POINT ( 'NONE',  ( 16.46253265017160672, -9.564922557960803928, 68.33224293864770971 ) ) ;
#185385 = CARTESIAN_POINT ( 'NONE',  ( -21.55341960407610458, -5.719274019375992779, 61.45724293864770260 ) ) ;
#185386 = CARTESIAN_POINT ( 'NONE',  ( -5.153800228976607833, 19.02544592524334988, 112.7094237280190043 ) ) ;
#185388 = CARTESIAN_POINT ( 'NONE',  ( 15.80617190586769283, -15.72974639402175789, 40.62609039468567573 ) ) ;
#185387 = CARTESIAN_POINT ( 'NONE',  ( 16.53943276465976808, -0.05219959533910856209, 38.74890960531435979 ) ) ;
#185389 = CARTESIAN_POINT ( 'NONE',  ( -4.313351365237978463, -4.313351365237916291, -62.50719930893269805 ) ) ;
#185391 = CARTESIAN_POINT ( 'NONE',  ( 19.03943276465977164, -0.05219959533909143690, 108.7489096053143527 ) ) ;
#185390 = CARTESIAN_POINT ( 'NONE',  ( -16.55341960407617563, 4.379528057220093196, 73.54275706135234714 ) ) ;
#185392 = CARTESIAN_POINT ( 'NONE',  ( 13.89961937509978007, -13.97604488694527269, 108.1239096053143669 ) ) ;
#185393 = DIRECTION ( 'NONE',  ( -6.948002486793210646E-15, 0.9991276842514723588, -0.04175967627138119781 ) ) ;
#185394 = CARTESIAN_POINT ( 'NONE',  ( 8.314922557961029526, -14.29746914071037800, 90.41775706135236135 ) ) ;
#185395 = CARTESIAN_POINT ( 'NONE',  ( 16.53943276465976808, 0.05219959533934440121, 51.25109039468568994 ) ) ;
#185396 = CARTESIAN_POINT ( 'NONE',  ( -5.153800228976328057, -19.02544592524343514, 57.29057627198103120 ) ) ;
#185397 = CARTESIAN_POINT ( 'NONE',  ( 13.89961937509977652, -13.97604488694527269, 78.12390960531433848 ) ) ;
#185398 = CARTESIAN_POINT ( 'NONE',  ( 10.81492255796106328, -18.62759615963255655, 50.41775706135235424 ) ) ;
#185399 = CARTESIAN_POINT ( 'NONE',  ( -16.53943276465976808, -0.05219959533934237506, 63.75109039468568284 ) ) ;
#185400 = CARTESIAN_POINT ( 'NONE',  ( -8.314922557960811034, -14.29746914071050412, 27.08224293864769550 ) ) ;
#185401 = CARTESIAN_POINT ( 'NONE',  ( -9.474510206698964154, 16.51473224551069663, 35.41557627198102409 ) ) ;
#185402 = CARTESIAN_POINT ( 'NONE',  ( 0.05219959533909260263, 19.03943276465977164, 29.99890960531435979 ) ) ;
#185403 = CARTESIAN_POINT ( 'NONE',  ( -8.314922557961024197, 14.29746914071037800, 22.91775706135235069 ) ) ;
#185404 = CONICAL_SURFACE ( 'NONE', #36867, 2.500000000000002220, 1.029744258676656754 ) ;
#185405 = CARTESIAN_POINT ( 'NONE',  ( -16.51473224551082808, 9.474510206698731452, 83.33442372801899012 ) ) ;
#185406 = CARTESIAN_POINT ( 'NONE',  ( 4.483927247898545687, 16.52544592524342804, 79.79057627198102409 ) ) ;
#185407 = CARTESIAN_POINT ( 'NONE',  ( -13.89961937509977652, 13.97604488694528158, 45.62390960531433848 ) ) ;
#185409 = CARTESIAN_POINT ( 'NONE',  ( -11.74264578624800670, 36.14014761921585972, -8.400000000000000355 ) ) ;
#185408 = CARTESIAN_POINT ( 'NONE',  ( 5.049401038297881783, 19.05341960407617563, 92.29275706135234714 ) ) ;
#185410 = CARTESIAN_POINT ( 'NONE',  ( -5.719274019375665041, -21.55341960407619695, 94.79275706135234714 ) ) ;
#185411 = CARTESIAN_POINT ( 'NONE',  ( 16.53943276465976808, 0.05219959533934440121, 51.25109039468568994 ) ) ;
#185412 = CARTESIAN_POINT ( 'NONE',  ( 17.05587630539785238, 6.762274262135711922, 36.75819690962688924 ) ) ;
#185413 = CARTESIAN_POINT ( 'NONE',  ( 0.05219959533907565091, 21.53943276465977519, 44.99890960531435979 ) ) ;
#185414 = CARTESIAN_POINT ( 'NONE',  ( -12.14591786802326823, 12.06949235617739902, 43.12609039468568284 ) ) ;
#185415 = CYLINDRICAL_SURFACE ( 'NONE', #34478, 2.000000000000001776 ) ;
#185416 = CARTESIAN_POINT ( 'NONE',  ( 13.97604488694548053, -13.89961937509957401, 45.62609039468566863 ) ) ;
#185417 = CARTESIAN_POINT ( 'NONE',  ( 9.564922557960805705, 16.46253265017160317, 74.58224293864769550 ) ) ;
#185418 = CARTESIAN_POINT ( 'NONE',  ( -13.97604488694527625, -13.89961937509977652, 56.87390960531434558 ) ) ;
#185419 = LINE ( 'NONE', #28782, #49486 ) ;
#185420 = CARTESIAN_POINT ( 'NONE',  ( -19.02544592524342804, 5.153800228976336051, 66.04057627198103830 ) ) ;
#185421 = DIRECTION ( 'NONE',  ( 0.1736481776669307198, 0.000000000000000000, -0.9848077530122080203 ) ) ;
#185422 = EDGE_CURVE ( 'NONE', #29006, #197049, #106126, .T. ) ;
#185423 = CARTESIAN_POINT ( 'NONE',  ( 0.05219959533936267826, -19.03943276465977164, 30.00109039468566863 ) ) ;
#185424 = CARTESIAN_POINT ( 'NONE',  ( 0.05219959533937995610, -21.53943276465977519, 110.0010903946856757 ) ) ;
#185425 = CARTESIAN_POINT ( 'NONE',  ( -12.06949235617756955, 12.14591786802309770, 40.62390960531435269 ) ) ;
#185426 = CARTESIAN_POINT ( 'NONE',  ( -0.05219959533909027116, -19.03943276465977164, 37.49890960531436690 ) ) ;
#185427 = CIRCLE ( 'NONE', #43410, 7.500000000000007105 ) ;
#185428 = CARTESIAN_POINT ( 'NONE',  ( -13.97604488694527625, -13.89961937509977652, 111.8739096053143243 ) ) ;
#185429 = CARTESIAN_POINT ( 'NONE',  ( 15.72974639402176855, 15.80617190586768217, 81.87609039468568994 ) ) ;
#185430 = CARTESIAN_POINT ( 'NONE',  ( 19.02544592524343514, -5.153800228976328945, 53.54057627198102409 ) ) ;
#185431 = CARTESIAN_POINT ( 'NONE',  ( -5.823673210054431948, 21.52544592524334988, 82.70942372801900433 ) ) ;
#185432 = CARTESIAN_POINT ( 'NONE',  ( -18.62759615963270932, 10.81492255796079327, 35.83224293864768839 ) ) ;
#185433 = CARTESIAN_POINT ( 'NONE',  ( 15.80617190586769283, -15.72974639402175789, 20.62609039468568639 ) ) ;
#185434 = CARTESIAN_POINT ( 'NONE',  ( -0.05219959533936034679, 19.03943276465977164, 47.50109039468566863 ) ) ;
#185435 = CARTESIAN_POINT ( 'NONE',  ( 9.474510206698971260, -16.51473224551069308, 32.91557627198102409 ) ) ;
#185436 = CARTESIAN_POINT ( 'NONE',  ( 19.03943276465977164, -0.05219959533909143690, 78.74890960531436690 ) ) ;
#185437 = CARTESIAN_POINT ( 'NONE',  ( 19.03943276465977164, 0.05219959533936151252, 111.2510903946856757 ) ) ;
#185438 = CARTESIAN_POINT ( 'NONE',  ( 4.379528057220339221, -16.55341960407611168, 92.70724293864770971 ) ) ;
#185439 = CARTESIAN_POINT ( 'NONE',  ( -9.564922557960796823, -16.46253265017161027, 52.08224293864768839 ) ) ;
#185440 = CARTESIAN_POINT ( 'NONE',  ( -0.05219959533907301413, -21.53943276465977519, 32.49890960531435979 ) ) ;
#185441 = CARTESIAN_POINT ( 'NONE',  ( 5.153800228976615827, -19.02544592524334988, 105.2094237280190185 ) ) ;
#185442 = CARTESIAN_POINT ( 'NONE',  ( -18.62759615963270932, 10.81492255796079327, 100.8322429386477097 ) ) ;
#185443 = CARTESIAN_POINT ( 'NONE',  ( -21.53943276465977519, -0.05219959533937600094, 58.75109039468568994 ) ) ;
#185444 = CARTESIAN_POINT ( 'NONE',  ( 4.379528057220092307, 16.55341960407617563, 57.29275706135234714 ) ) ;
#185445 = CARTESIAN_POINT ( 'NONE',  ( -16.55341960407617563, 4.379528057220093196, 68.54275706135234714 ) ) ;
#185446 = CARTESIAN_POINT ( 'NONE',  ( 16.51473224551069308, 9.474510206698969483, 64.16557627198102409 ) ) ;
#185447 = CARTESIAN_POINT ( 'NONE',  ( -8.224510206698735004, -14.34966873604973081, 89.58442372801901854 ) ) ;
#185448 = CARTESIAN_POINT ( 'NONE',  ( 18.62759615963255655, 10.81492255796105972, 21.66775706135235069 ) ) ;
#185449 = CARTESIAN_POINT ( 'NONE',  ( -4.379528057220328563, 16.55341960407611168, 70.20724293864769550 ) ) ;
#185450 = CARTESIAN_POINT ( 'NONE',  ( -0.05219959533909027116, -19.03943276465977164, 92.49890960531436690 ) ) ;
#185451 = CARTESIAN_POINT ( 'NONE',  ( 16.55341960407618274, -4.379528057220086978, 71.04275706135234714 ) ) ;
#185452 = CARTESIAN_POINT ( 'NONE',  ( -10.81492255796105439, 18.62759615963255655, 62.91775706135236135 ) ) ;
#185453 = CARTESIAN_POINT ( 'NONE',  ( 5.153800228976615827, -19.02544592524334988, 110.2094237280189901 ) ) ;
#185454 = CARTESIAN_POINT ( 'NONE',  ( -15.80617190586745835, -15.72974639402198527, 111.8739096053143669 ) ) ;
#185455 = CARTESIAN_POINT ( 'NONE',  ( 12.06949235617757843, -12.14591786802309237, 53.12390960531436690 ) ) ;
#185456 = VERTEX_POINT ( 'NONE', #71353 ) ;
#185457 = CARTESIAN_POINT ( 'NONE',  ( 19.25663599770062007, -5.499999999999442224, 91.49419308057203182 ) ) ;
#185458 = CARTESIAN_POINT ( 'NONE',  ( 5.823673210054125526, 21.52544592524343514, 84.79057627198102409 ) ) ;
#185459 = CARTESIAN_POINT ( 'NONE',  ( 4.483927247898545687, 16.52544592524342804, 44.79057627198103120 ) ) ;
#185460 = ORIENTED_EDGE ( 'NONE', *, *, #26227, .T. ) ;
#185461 = CARTESIAN_POINT ( 'NONE',  ( 35.63758492646879006, 1.954004632199990432, 37.74231687961066228 ) ) ;
#185462 = CARTESIAN_POINT ( 'NONE',  ( 0.05219959533937995610, -21.53943276465977519, 20.00109039468568639 ) ) ;
#185463 = CARTESIAN_POINT ( 'NONE',  ( -10.81492255796078084, -18.62759615963271287, 22.08224293864769194 ) ) ;
#185464 = CARTESIAN_POINT ( 'NONE',  ( -15.72974639402176322, -15.80617190586768395, 24.37609039468567573 ) ) ;
#185465 = CARTESIAN_POINT ( 'NONE',  ( 12.14591786802309770, 12.06949235617756955, 49.37390960531436690 ) ) ;
#185467 = CARTESIAN_POINT ( 'NONE',  ( -0.05219959533934338120, 16.53943276465976808, 67.50109039468568994 ) ) ;
#185466 = AXIS2_PLACEMENT_3D ( 'NONE', #96057, #80884, #190074 ) ;
#185468 = CARTESIAN_POINT ( 'NONE',  ( -19.05341960407611168, -5.049401038298163336, 61.45724293864769550 ) ) ;
#185469 = CARTESIAN_POINT ( 'NONE',  ( 19.02544592524334988, 5.153800228976608722, 66.45942372801899012 ) ) ;
#185470 = CARTESIAN_POINT ( 'NONE',  ( -5.049401038298153566, 19.05341960407611168, 75.20724293864769550 ) ) ;
#185471 = CARTESIAN_POINT ( 'NONE',  ( -21.52544592524343514, 5.823673210054127303, 36.04057627198102409 ) ) ;
#185472 = CARTESIAN_POINT ( 'NONE',  ( -19.06840828309120184, -32.80151167437442439, -20.74459427421103896 ) ) ;
#185473 = CARTESIAN_POINT ( 'NONE',  ( 9.564922557960805705, 16.46253265017160317, 59.58224293864769550 ) ) ;
#185474 = CARTESIAN_POINT ( 'NONE',  ( -16.52544592524335698, -4.483927247898792601, 28.95942372801902209 ) ) ;
#185475 = CARTESIAN_POINT ( 'NONE',  ( 19.05341960407617918, -5.049401038297876454, 61.04275706135232582 ) ) ;
#185476 = CARTESIAN_POINT ( 'NONE',  ( -21.53943276465977519, -0.05219959533937600094, 18.75109039468568639 ) ) ;
#185477 = CARTESIAN_POINT ( 'NONE',  ( -14.29746914071049879, 8.314922557960819915, 50.83224293864770971 ) ) ;
#185478 = CARTESIAN_POINT ( 'NONE',  ( 9.564922557960805705, 16.46253265017160317, 89.58224293864769550 ) ) ;
#185479 = CARTESIAN_POINT ( 'NONE',  ( -21.55341960407610458, -5.719274019375992779, 56.45724293864768839 ) ) ;
#185481 = CARTESIAN_POINT ( 'NONE',  ( 8.224510206698742110, 14.34966873604972548, 37.08442372801901143 ) ) ;
#185480 = CARTESIAN_POINT ( 'NONE',  ( 21.52544592524344225, -5.823673210054117533, 98.54057627198105251 ) ) ;
#185482 = CARTESIAN_POINT ( 'NONE',  ( -0.05219959533907301413, -21.53943276465977519, 42.49890960531435979 ) ) ;
#185483 = CARTESIAN_POINT ( 'NONE',  ( 21.52544592524334988, 5.823673210054432836, 86.45942372801901854 ) ) ;
#185484 = CARTESIAN_POINT ( 'NONE',  ( 5.049401038298161559, -19.05341960407611168, 87.70724293864769550 ) ) ;
#185485 = CARTESIAN_POINT ( 'NONE',  ( -16.51473224551069308, -9.474510206698971260, 36.66557627198102409 ) ) ;
#185486 = CARTESIAN_POINT ( 'NONE',  ( -19.02544592524342804, 5.153800228976336051, 91.04057627198100988 ) ) ;
#185487 = CARTESIAN_POINT ( 'NONE',  ( -4.483927247898539470, -16.52544592524342804, 107.2905762719810525 ) ) ;
#185488 = CARTESIAN_POINT ( 'NONE',  ( 9.564922557960805705, 16.46253265017160317, 59.58224293864769550 ) ) ;
#185489 = CARTESIAN_POINT ( 'NONE',  ( -9.564922557961040184, 16.46253265017147172, 112.9177570613523329 ) ) ;
#185490 = LINE ( 'NONE', #173307, #89193 ) ;
#185492 = CARTESIAN_POINT ( 'NONE',  ( -5.823673210054116645, -21.52544592524344225, 32.29057627198102409 ) ) ;
#185491 = CARTESIAN_POINT ( 'NONE',  ( -10.81492255796105439, 18.62759615963255655, 92.91775706135236135 ) ) ;
#185493 = CARTESIAN_POINT ( 'NONE',  ( 16.52544592524335698, 4.483927247898782831, 86.45942372801901854 ) ) ;
#185494 = CARTESIAN_POINT ( 'NONE',  ( -17.49999999999999645, -5.500000000000000888, 120.0000000000000142 ) ) ;
#185495 = CARTESIAN_POINT ( 'NONE',  ( -5.049401038297874678, -19.05341960407617918, 69.79275706135233293 ) ) ;
#185496 = CARTESIAN_POINT ( 'NONE',  ( 9.474510206698729675, 16.51473224551082808, 32.08442372801900433 ) ) ;
#185497 = CARTESIAN_POINT ( 'NONE',  ( 4.313351365237949153, 4.313351365237946489, -64.53213882399992940 ) ) ;
#185498 = CARTESIAN_POINT ( 'NONE',  ( 9.564922557960805705, 16.46253265017160317, 29.58224293864769550 ) ) ;
#185499 = CARTESIAN_POINT ( 'NONE',  ( 8.314922557960818139, 14.29746914071049879, 34.58224293864770260 ) ) ;
#185500 = CARTESIAN_POINT ( 'NONE',  ( -17.05116617787823685, -6.768360034955810178, 111.3432444674080841 ) ) ;
#185501 = CARTESIAN_POINT ( 'NONE',  ( -16.53943276465976808, 0.05219959533911058130, 21.24890960531436690 ) ) ;
#185502 = CARTESIAN_POINT ( 'NONE',  ( 17.48847506799968698, 5.747544572773809257, 66.67302562156720569 ) ) ;
#185503 = CARTESIAN_POINT ( 'NONE',  ( -16.52544592524335698, -4.483927247898792601, 98.95942372801903275 ) ) ;
#185504 = CARTESIAN_POINT ( 'NONE',  ( -9.564922557960796823, -16.46253265017161027, 42.08224293864769550 ) ) ;
#185505 = CARTESIAN_POINT ( 'NONE',  ( 18.62759615963255655, 10.81492255796105972, 111.6677570613523613 ) ) ;
#185506 = CARTESIAN_POINT ( 'NONE',  ( -16.52544592524335698, -4.483927247898792601, 23.95942372801901143 ) ) ;
#185507 = CARTESIAN_POINT ( 'NONE',  ( -0.05219959533937732626, 21.53943276465977519, 72.50109039468568994 ) ) ;
#185508 = CARTESIAN_POINT ( 'NONE',  ( 0.05219959533936267826, -19.03943276465977164, 50.00109039468566863 ) ) ;
#185509 = CARTESIAN_POINT ( 'NONE',  ( 13.89961937509977652, -13.97604488694527269, 88.12390960531438111 ) ) ;
#185510 = CARTESIAN_POINT ( 'NONE',  ( 9.564922557960805705, 16.46253265017160317, 69.58224293864770971 ) ) ;
#185511 = CARTESIAN_POINT ( 'NONE',  ( -19.53037848336981241, 5.499999999999901412, 39.85532783611445495 ) ) ;
#185512 = CARTESIAN_POINT ( 'NONE',  ( -21.53943276465977519, 0.05219959533907696930, 96.24890960531435269 ) ) ;
#185513 = CARTESIAN_POINT ( 'NONE',  ( -12.06949235617756955, 12.14591786802309770, 60.62390960531437401 ) ) ;
#185514 = CARTESIAN_POINT ( 'NONE',  ( 15.72974639402199770, -15.80617190586745480, 63.12390960531435979 ) ) ;
#185515 = CARTESIAN_POINT ( 'NONE',  ( -5.153800228976328057, -19.02544592524343514, 62.29057627198100988 ) ) ;
#185517 = CARTESIAN_POINT ( 'NONE',  ( -16.55341960407617563, 4.379528057220093196, 73.54275706135234714 ) ) ;
#185516 = CARTESIAN_POINT ( 'NONE',  ( 5.823673210054125526, 21.52544592524343514, 89.79057627198103830 ) ) ;
#185518 = ORIENTED_EDGE ( 'NONE', *, *, #2128, .F. ) ;
#185519 = CARTESIAN_POINT ( 'NONE',  ( -19.05341960407611168, -5.049401038298163336, 41.45724293864769550 ) ) ;
#185521 = CARTESIAN_POINT ( 'NONE',  ( 21.85375568585899586, -8.111533062293291962, 169.4628294566284126 ) ) ;
#185520 = CARTESIAN_POINT ( 'NONE',  ( 4.483927247898545687, 16.52544592524342804, 74.79057627198105251 ) ) ;
#185522 = CARTESIAN_POINT ( 'NONE',  ( 19.05341960407611168, 5.049401038298154454, 53.95724293864770260 ) ) ;
#185523 = CARTESIAN_POINT ( 'NONE',  ( 16.52544592524342804, -4.483927247898539470, 113.5405762719810383 ) ) ;
#185524 = CARTESIAN_POINT ( 'NONE',  ( 19.03943276465977164, 0.05219959533936151252, 61.25109039468566863 ) ) ;
#185525 = CARTESIAN_POINT ( 'NONE',  ( 0.05219959533910956823, 16.53943276465976808, 84.99890960531436690 ) ) ;
#185526 = CARTESIAN_POINT ( 'NONE',  ( -18.62759615963255300, -10.81492255796106328, 44.16775706135234714 ) ) ;
#185528 = CARTESIAN_POINT ( 'NONE',  ( 15.80617190586746368, 15.72974639402197994, 99.37390960531436690 ) ) ;
#185527 = CARTESIAN_POINT ( 'NONE',  ( 13.97604488694527802, 13.89961937509977652, 29.37390960531435979 ) ) ;
#185529 = CARTESIAN_POINT ( 'NONE',  ( 16.52544592524342804, -4.483927247898539470, 83.54057627198102409 ) ) ;
#185530 = CARTESIAN_POINT ( 'NONE',  ( 17.43506102071334496, -39.09281690108636553, -20.41854293743994120 ) ) ;
#185531 = CARTESIAN_POINT ( 'NONE',  ( -5.153800228976328057, -19.02544592524343514, 57.29057627198103120 ) ) ;
#185532 = CARTESIAN_POINT ( 'NONE',  ( -9.889834268056119981, -11.98662851468406920, -61.85832361008505842 ) ) ;
#185534 = CARTESIAN_POINT ( 'NONE',  ( 9.564922557960805705, 16.46253265017160317, 99.58224293864770971 ) ) ;
#185533 = CARTESIAN_POINT ( 'NONE',  ( 13.97604488694548053, -13.89961937509957401, 95.62609039468563310 ) ) ;
#185535 = CARTESIAN_POINT ( 'NONE',  ( -21.55341960407619339, 5.719274019375674811, 33.54275706135234714 ) ) ;
#185536 = CARTESIAN_POINT ( 'NONE',  ( 19.05341960407611168, 5.049401038298154454, 88.95724293864769550 ) ) ;
#185537 = CARTESIAN_POINT ( 'NONE',  ( 16.46253265017146816, 9.564922557961045513, 66.66775706135233293 ) ) ;
#185538 = CARTESIAN_POINT ( 'NONE',  ( 9.564922557960805705, 16.46253265017160317, 54.58224293864769550 ) ) ;
#185539 = CARTESIAN_POINT ( 'NONE',  ( 4.483927247898545687, 16.52544592524342804, 74.79057627198105251 ) ) ;
#185540 = CARTESIAN_POINT ( 'NONE',  ( 16.53943276465976808, -0.05219959533910856209, 63.74890960531435979 ) ) ;
#185541 = CARTESIAN_POINT ( 'NONE',  ( 19.02544592524343514, -5.153800228976328945, 83.54057627198100988 ) ) ;
#185542 = CARTESIAN_POINT ( 'NONE',  ( -18.62759615963270932, 10.81492255796079327, 105.8322429386476955 ) ) ;
#185543 = CARTESIAN_POINT ( 'NONE',  ( 19.05341960407611168, 5.049401038298154454, 78.95724293864769550 ) ) ;
#185544 = CARTESIAN_POINT ( 'NONE',  ( -9.564922557961040184, 16.46253265017147172, 27.91775706135232582 ) ) ;
#185547 = CARTESIAN_POINT ( 'NONE',  ( 14.29746914071049879, -8.314922557960816363, 103.3322429386476955 ) ) ;
#185546 = CARTESIAN_POINT ( 'NONE',  ( 8.224510206698953496, -14.34966873604960469, 27.91557627198103830 ) ) ;
#185545 = CARTESIAN_POINT ( 'NONE',  ( 0.05219959533909260263, 19.03943276465977164, 29.99890960531435979 ) ) ;
#185548 = CARTESIAN_POINT ( 'NONE',  ( -0.05219959533936034679, 19.03943276465977164, 102.5010903946856757 ) ) ;
#185549 = ORIENTED_EDGE ( 'NONE', *, *, #111459, .T. ) ;
#185550 = CARTESIAN_POINT ( 'NONE',  ( -15.72974639402176322, -15.80617190586768395, 29.37609039468568284 ) ) ;
#185551 = CARTESIAN_POINT ( 'NONE',  ( 16.51473224551083163, -9.474510206698727899, 70.83442372801900433 ) ) ;
#185552 = CARTESIAN_POINT ( 'NONE',  ( -0.05219959533910754901, -16.53943276465976808, 22.49890960531436335 ) ) ;
#185553 = CARTESIAN_POINT ( 'NONE',  ( 21.53943276465977519, -0.05219959533907433946, 88.74890960531436690 ) ) ;
#185554 = CARTESIAN_POINT ( 'NONE',  ( 19.05341960407611168, 5.049401038298154454, 113.9572429386477097 ) ) ;
#185555 = CARTESIAN_POINT ( 'NONE',  ( -0.05219959533910754901, -16.53943276465976808, 72.49890960531435269 ) ) ;
#185556 = CARTESIAN_POINT ( 'NONE',  ( 16.46253265017160672, -9.564922557960803928, 23.33224293864769194 ) ) ;
#185557 = CARTESIAN_POINT ( 'NONE',  ( 0.05219959533936267826, -19.03943276465977164, 25.00109039468566152 ) ) ;
#185558 = CARTESIAN_POINT ( 'NONE',  ( 8.314922557961029526, -14.29746914071037800, 85.41775706135236135 ) ) ;
#185559 = CARTESIAN_POINT ( 'NONE',  ( -12.14591786802326823, 12.06949235617739902, 58.12609039468568994 ) ) ;
#185560 = CARTESIAN_POINT ( 'NONE',  ( 15.72974639402199770, -15.80617190586745480, 28.12390960531435979 ) ) ;
#185561 = CARTESIAN_POINT ( 'NONE',  ( -21.53943276465977519, -0.05219959533937600094, 113.7510903946856757 ) ) ;
#185562 = CARTESIAN_POINT ( 'NONE',  ( 13.89961937509977652, -13.97604488694527269, 73.12390960531436690 ) ) ;
#185563 = CARTESIAN_POINT ( 'NONE',  ( 12.06949235617739724, 12.14591786802326823, 61.87609039468568284 ) ) ;
#185564 = CARTESIAN_POINT ( 'NONE',  ( 16.46253265017160672, -9.564922557960803928, 28.33224293864769550 ) ) ;
#185565 = CARTESIAN_POINT ( 'NONE',  ( 14.34966873604960469, 8.224510206698951720, 39.16557627198102409 ) ) ;
#185566 = CARTESIAN_POINT ( 'NONE',  ( -3.573655867282028392E-15, 2.428612866367529932E-14, 155.0000000000000000 ) ) ;
#185568 = CARTESIAN_POINT ( 'NONE',  ( 13.97604488694527802, 13.89961937509977652, 74.37390960531436690 ) ) ;
#185567 = CARTESIAN_POINT ( 'NONE',  ( -5.153800228976328057, -19.02544592524343514, 102.2905762719810383 ) ) ;
#185569 = CARTESIAN_POINT ( 'NONE',  ( -9.564922557960796823, -16.46253265017161027, 112.0822429386476955 ) ) ;
#185570 = AXIS2_PLACEMENT_3D ( 'NONE', #43607, #164970, #26463 ) ;
#185571 = CARTESIAN_POINT ( 'NONE',  ( 16.53943276465976808, -0.05219959533910856209, 58.74890960531436690 ) ) ;
#185572 = CARTESIAN_POINT ( 'NONE',  ( 12.06949235617757843, -12.14591786802309237, 33.12390960531435979 ) ) ;
#185573 = ORIENTED_EDGE ( 'NONE', *, *, #146110, .F. ) ;
#185574 = CARTESIAN_POINT ( 'NONE',  ( -8.314922557960811034, -14.29746914071050412, 57.08224293864769550 ) ) ;
#185577 = VECTOR ( 'NONE', #58068, 1000.000000000000000 ) ;
#185576 = CARTESIAN_POINT ( 'NONE',  ( 16.51473224551083163, -9.474510206698727899, 60.83442372801900433 ) ) ;
#185575 = CARTESIAN_POINT ( 'NONE',  ( 16.53943276465976808, 0.05219959533934440121, 46.25109039468567573 ) ) ;
#185578 = CARTESIAN_POINT ( 'NONE',  ( 19.02544592524334988, 5.153800228976608722, 56.45942372801898301 ) ) ;
#185579 = CARTESIAN_POINT ( 'NONE',  ( 19.05341960407611168, 5.049401038298154454, 73.95724293864768129 ) ) ;
#185580 = CARTESIAN_POINT ( 'NONE',  ( -13.97604488694547697, 13.89961937509957934, 53.12609039468565442 ) ) ;
#185581 = CARTESIAN_POINT ( 'NONE',  ( -27.73933785331498925, 2.428612866367529932E-14, 145.3750000027311842 ) ) ;
#185582 = CARTESIAN_POINT ( 'NONE',  ( -9.564922557961040184, 16.46253265017147172, 52.91775706135233293 ) ) ;
#185584 = CARTESIAN_POINT ( 'NONE',  ( -4.379528057220086978, -16.55341960407618274, 84.79275706135234714 ) ) ;
#185583 = CARTESIAN_POINT ( 'NONE',  ( -5.049401038297874678, -19.05341960407617918, 94.79275706135230450 ) ) ;
#185585 = CARTESIAN_POINT ( 'NONE',  ( -27.73933785331498925, 2.428612866367529932E-14, 143.3750000027311842 ) ) ;
#185586 = CARTESIAN_POINT ( 'NONE',  ( 13.89961937509977652, -13.97604488694527269, 23.12390960531436335 ) ) ;
#185587 = CARTESIAN_POINT ( 'NONE',  ( -0.05219959533909027116, -19.03943276465977164, 97.49890960531436690 ) ) ;
#185588 = CARTESIAN_POINT ( 'NONE',  ( -5.823673210054431948, 21.52544592524334988, 47.70942372801902565 ) ) ;
#185589 = CARTESIAN_POINT ( 'NONE',  ( 9.564922557961047289, -16.46253265017146816, 105.4177570613523471 ) ) ;
#185591 = CARTESIAN_POINT ( 'NONE',  ( -19.05341960407611168, -5.049401038298163336, 56.45724293864768129 ) ) ;
#185590 = CARTESIAN_POINT ( 'NONE',  ( 17.50000000000000000, -5.500000000000001776, 106.2176903769643417 ) ) ;
#185592 = EDGE_CURVE ( 'NONE', #109472, #65144, #178492, .T. ) ;
#185593 = CARTESIAN_POINT ( 'NONE',  ( -16.51473224551069308, -9.474510206698971260, 101.6655762719810241 ) ) ;
#185595 = CARTESIAN_POINT ( 'NONE',  ( 19.05341960407611168, 5.049401038298154454, 63.95724293864769550 ) ) ;
#185594 = CARTESIAN_POINT ( 'NONE',  ( -12.06949235617756955, 12.14591786802309770, 60.62390960531437401 ) ) ;
#185596 = CARTESIAN_POINT ( 'NONE',  ( -19.05341960407611168, -5.049401038298163336, 66.45724293864769550 ) ) ;
#185597 = CARTESIAN_POINT ( 'NONE',  ( 16.51473224551083163, -9.474510206698727899, 80.83442372801899012 ) ) ;
#185598 = CARTESIAN_POINT ( 'NONE',  ( 0.05219959533907565091, 21.53943276465977519, 54.99890960531435269 ) ) ;
#185599 = CARTESIAN_POINT ( 'NONE',  ( 13.89961937509957401, 13.97604488694547697, 41.87609039468566152 ) ) ;
#185600 = CARTESIAN_POINT ( 'NONE',  ( 0.05219959533909260263, 19.03943276465977164, 74.99890960531435269 ) ) ;
#185601 = CARTESIAN_POINT ( 'NONE',  ( 21.53943276465977519, -0.05219959533907433946, 78.74890960531436690 ) ) ;
#185603 = CARTESIAN_POINT ( 'NONE',  ( 13.89961937509957401, 13.97604488694547697, 31.87609039468566863 ) ) ;
#185602 = CARTESIAN_POINT ( 'NONE',  ( 4.483927247898545687, 16.52544592524342804, 74.79057627198105251 ) ) ;
#185604 = CARTESIAN_POINT ( 'NONE',  ( -5.823673210054116645, -21.52544592524344225, 57.29057627198103120 ) ) ;
#185605 = CARTESIAN_POINT ( 'NONE',  ( 21.53943276465977519, -0.05219959533907433946, 43.74890960531435979 ) ) ;
#185606 = CARTESIAN_POINT ( 'NONE',  ( -19.02544592524342804, 5.153800228976336051, 61.04057627198103120 ) ) ;
#185607 = CARTESIAN_POINT ( 'NONE',  ( 12.06949235617757843, -12.14591786802309237, 108.1239096053143811 ) ) ;
#185608 = CIRCLE ( 'NONE', #98395, 61.99999999999998579 ) ;
#185609 = CARTESIAN_POINT ( 'NONE',  ( 10.72451020669871369, 18.67979575497193778, 32.08442372801901854 ) ) ;
#185610 = CARTESIAN_POINT ( 'NONE',  ( 9.474510206698971260, -16.51473224551069308, 112.9155762719810383 ) ) ;
#185611 = CARTESIAN_POINT ( 'NONE',  ( 21.55341960407619695, -5.719274019375665929, 46.04275706135234714 ) ) ;
#185612 = CARTESIAN_POINT ( 'NONE',  ( -16.46253265017160317, 9.564922557960807481, 35.83224293864768839 ) ) ;
#185613 = CARTESIAN_POINT ( 'NONE',  ( 5.719274019375991003, -21.55341960407610458, 102.7072429386476955 ) ) ;
#185614 = CARTESIAN_POINT ( 'NONE',  ( -19.02544592524334988, -5.153800228976617603, 48.95942372801900433 ) ) ;
#185615 = CARTESIAN_POINT ( 'NONE',  ( -13.97604488694527625, -13.89961937509977652, 26.87390960531434558 ) ) ;
#185616 = CARTESIAN_POINT ( 'NONE',  ( 19.02544592524343514, -5.153800228976328945, 28.54057627198102409 ) ) ;
#185617 = CARTESIAN_POINT ( 'NONE',  ( 16.58166387080255433, -7.087407987291991063, 21.43250955971513250 ) ) ;
#185618 = CARTESIAN_POINT ( 'NONE',  ( 8.224510206698742110, 14.34966873604972548, 57.08442372801901854 ) ) ;
#185619 = CARTESIAN_POINT ( 'NONE',  ( -5.153800228976328057, -19.02544592524343514, 22.29057627198102765 ) ) ;
#185620 = CARTESIAN_POINT ( 'NONE',  ( -21.92083080610932200, -8.096106818373623781, 172.4353877980944674 ) ) ;
#185621 = CARTESIAN_POINT ( 'NONE',  ( -5.153800228976328057, -19.02544592524343514, 67.29057627198102409 ) ) ;
#185622 = CARTESIAN_POINT ( 'NONE',  ( -12.06949235617756955, 12.14591786802309770, 100.6239096053143811 ) ) ;
#185623 = CARTESIAN_POINT ( 'NONE',  ( 15.80617190586746368, 15.72974639402197994, 59.37390960531436690 ) ) ;
#185624 = CARTESIAN_POINT ( 'NONE',  ( -4.483927247898782831, 16.52544592524335698, 32.70942372801900433 ) ) ;
#185625 = CARTESIAN_POINT ( 'NONE',  ( -5.719274019375665041, -21.55341960407619695, 104.7927570613523898 ) ) ;
#185626 = CARTESIAN_POINT ( 'NONE',  ( 9.474510206698971260, -16.51473224551069308, 27.91557627198103120 ) ) ;
#185627 = CARTESIAN_POINT ( 'NONE',  ( -8.314922557961024197, 14.29746914071037800, 107.9177570613523471 ) ) ;
#185628 = CARTESIAN_POINT ( 'NONE',  ( -4.483927247898539470, -16.52544592524342804, 57.29057627198103120 ) ) ;
#185629 = CARTESIAN_POINT ( 'NONE',  ( -0.05219959533909027116, -19.03943276465977164, 57.49890960531435979 ) ) ;
#185630 = CARTESIAN_POINT ( 'NONE',  ( 18.62759615963255655, 10.81492255796105972, 91.66775706135234714 ) ) ;
#185631 = CARTESIAN_POINT ( 'NONE',  ( -18.67979575497178146, -10.72451020669898902, 106.6655762719810383 ) ) ;
#185632 = CARTESIAN_POINT ( 'NONE',  ( -21.53943276465977519, -0.05219959533937600094, 73.75109039468567573 ) ) ;
#185633 = CARTESIAN_POINT ( 'NONE',  ( -8.224510206698735004, -14.34966873604973081, 49.58442372801901143 ) ) ;
#185635 = CARTESIAN_POINT ( 'NONE',  ( 15.72974639402176855, 15.80617190586768217, 96.87609039468568994 ) ) ;
#185634 = CARTESIAN_POINT ( 'NONE',  ( -12.06949235617756955, 12.14591786802309770, 80.62390960531438111 ) ) ;
#185636 = CARTESIAN_POINT ( 'NONE',  ( -8.224510206698735004, -14.34966873604973081, 109.5844237280190328 ) ) ;
#185637 = CARTESIAN_POINT ( 'NONE',  ( -17.50000000000000000, 5.622605283950884214, 113.6879268940389665 ) ) ;
#185638 = CARTESIAN_POINT ( 'NONE',  ( -12.14591786802326823, 12.06949235617739902, 33.12609039468569705 ) ) ;
#185639 = CARTESIAN_POINT ( 'NONE',  ( 8.224510206698953496, -14.34966873604960469, 37.91557627198102409 ) ) ;
#185640 = CARTESIAN_POINT ( 'NONE',  ( 16.53943276465976808, 0.05219959533934440121, 86.25109039468568994 ) ) ;
#185641 = CARTESIAN_POINT ( 'NONE',  ( 13.89961937509977652, -13.97604488694527269, 93.12390960531436690 ) ) ;
#185642 = CARTESIAN_POINT ( 'NONE',  ( 19.03943276465977164, -0.05219959533909143690, 108.7489096053143527 ) ) ;
#185643 = CARTESIAN_POINT ( 'NONE',  ( -21.55341960407619339, 5.719274019375674811, 93.54275706135234714 ) ) ;
#185644 = CARTESIAN_POINT ( 'NONE',  ( -4.483927247898782831, 16.52544592524335698, 102.7094237280190185 ) ) ;
#185645 = CARTESIAN_POINT ( 'NONE',  ( -14.34966873604960291, -8.224510206698953496, 76.66557627198103830 ) ) ;
#185646 = CARTESIAN_POINT ( 'NONE',  ( -19.02544592524342804, 5.153800228976336051, 76.04057627198102409 ) ) ;
#185647 = ORIENTED_EDGE ( 'NONE', *, *, #189654, .T. ) ;
#185648 = CARTESIAN_POINT ( 'NONE',  ( -16.55341960407617563, 4.379528057220093196, 23.54275706135235424 ) ) ;
#185649 = CARTESIAN_POINT ( 'NONE',  ( -5.049401038298153566, 19.05341960407611168, 25.20724293864768484 ) ) ;
#185650 = CARTESIAN_POINT ( 'NONE',  ( -19.03943276465977164, 0.05219959533909376836, 86.24890960531436690 ) ) ;
#185652 = CARTESIAN_POINT ( 'NONE',  ( -22.81625015709510507, 31.40387420917330275, -4.924999997268813878 ) ) ;
#185651 = CARTESIAN_POINT ( 'NONE',  ( -16.53943276465976808, -0.05219959533934237506, 38.75109039468567573 ) ) ;
#185653 = CARTESIAN_POINT ( 'NONE',  ( -13.89961937509957401, -13.97604488694547875, 39.37609039468566152 ) ) ;
#185654 = CARTESIAN_POINT ( 'NONE',  ( -14.34966873604972548, 8.224510206698743886, 88.33442372801901854 ) ) ;
#185655 = CARTESIAN_POINT ( 'NONE',  ( 5.153800228976335163, 19.02544592524342804, 34.79057627198102409 ) ) ;
#185656 = CARTESIAN_POINT ( 'NONE',  ( -16.55341960407617563, 4.379528057220093196, 73.54275706135234714 ) ) ;
#185657 = CARTESIAN_POINT ( 'NONE',  ( 12.14591786802327356, -12.06949235617739191, 65.62609039468568994 ) ) ;
#185658 = CARTESIAN_POINT ( 'NONE',  ( 5.153800228976615827, -19.02544592524334988, 80.20942372801901854 ) ) ;
#185659 = CARTESIAN_POINT ( 'NONE',  ( 19.05341960407617918, -5.049401038297876454, 31.04275706135232227 ) ) ;
#185660 = CARTESIAN_POINT ( 'NONE',  ( -13.97604488694527625, -13.89961937509977652, 46.87390960531435979 ) ) ;
#185661 = CARTESIAN_POINT ( 'NONE',  ( -9.564922557960796823, -16.46253265017161027, 97.08224293864769550 ) ) ;
#185662 = CARTESIAN_POINT ( 'NONE',  ( -16.53943276465976808, 0.05219959533911058130, 81.24890960531436690 ) ) ;
#185663 = EDGE_CURVE ( 'NONE', #128521, #13391, #151285, .T. ) ;
#185664 = CARTESIAN_POINT ( 'NONE',  ( -0.05219959533936034679, 19.03943276465977164, 52.50109039468566863 ) ) ;
#185665 = CARTESIAN_POINT ( 'NONE',  ( -18.67979575497178146, -10.72451020669898902, 51.66557627198102409 ) ) ;
#185666 = CARTESIAN_POINT ( 'NONE',  ( 19.02544592524334988, 5.153800228976608722, 31.45942372801900433 ) ) ;
#185667 = CARTESIAN_POINT ( 'NONE',  ( -16.46253265017160317, 9.564922557960807481, 100.8322429386477097 ) ) ;
#185668 = CARTESIAN_POINT ( 'NONE',  ( 21.53943276465977519, -0.05219959533907433946, 83.74890960531435269 ) ) ;
#185669 = CARTESIAN_POINT ( 'NONE',  ( 13.89961937509977652, -13.97604488694527269, 113.1239096053143527 ) ) ;
#185670 = CARTESIAN_POINT ( 'NONE',  ( -19.02544592524334988, -5.153800228976617603, 83.95942372801901854 ) ) ;
#185671 = CARTESIAN_POINT ( 'NONE',  ( -17.50000000000000711, 4.640572885337571840, 110.6378816454884486 ) ) ;
#185672 = CARTESIAN_POINT ( 'NONE',  ( -19.03943276465977164, -0.05219959533935918106, 113.7510903946856757 ) ) ;
#185673 = EDGE_CURVE ( 'NONE', #64689, #157949, #64133, .T. ) ;
#185674 = CARTESIAN_POINT ( 'NONE',  ( -13.89961937509977652, 13.97604488694528158, 30.62390960531435269 ) ) ;
#185675 = CARTESIAN_POINT ( 'NONE',  ( 13.97604488694527802, 13.89961937509977652, 99.37390960531436690 ) ) ;
#185676 = CARTESIAN_POINT ( 'NONE',  ( -18.62759615963270932, 10.81492255796079327, 70.83224293864770971 ) ) ;
#185677 = CARTESIAN_POINT ( 'NONE',  ( 14.29746914071037800, 8.314922557961029526, 51.66775706135234714 ) ) ;
#185678 = CARTESIAN_POINT ( 'NONE',  ( 5.719274019375673035, 21.55341960407619339, 52.29275706135236135 ) ) ;
#185680 = CARTESIAN_POINT ( 'NONE',  ( -0.05219959533937732626, 21.53943276465977519, 102.5010903946856899 ) ) ;
#185679 = CARTESIAN_POINT ( 'NONE',  ( -13.97604488694547697, 13.89961937509957934, 98.12609039468566152 ) ) ;
#185681 = CARTESIAN_POINT ( 'NONE',  ( -12.14591786802326823, 12.06949235617739902, 113.1260903946856899 ) ) ;
#185682 = CARTESIAN_POINT ( 'NONE',  ( -19.02544592524342804, 5.153800228976336051, 96.04057627198103830 ) ) ;
#185683 = CARTESIAN_POINT ( 'NONE',  ( 4.483927247898545687, 16.52544592524342804, 94.79057627198105251 ) ) ;
#185684 = CARTESIAN_POINT ( 'NONE',  ( 4.379528057220339221, -16.55341960407611168, 37.70724293864769550 ) ) ;
#185685 = CARTESIAN_POINT ( 'NONE',  ( 9.564922557961047289, -16.46253265017146816, 70.41775706135233293 ) ) ;
#185686 = CARTESIAN_POINT ( 'NONE',  ( 10.72451020669871369, 18.67979575497193778, 62.08442372801901143 ) ) ;
#185687 = CARTESIAN_POINT ( 'NONE',  ( -16.46253265017146816, -9.564922557961047289, 29.16775706135232937 ) ) ;
#185688 = CARTESIAN_POINT ( 'NONE',  ( 8.224510206698953496, -14.34966873604960469, 102.9155762719810383 ) ) ;
#185689 = CARTESIAN_POINT ( 'NONE',  ( -18.62759615963270932, 10.81492255796079327, 35.83224293864768839 ) ) ;
#185690 = CARTESIAN_POINT ( 'NONE',  ( -16.53943276465976808, -0.05219959533934237506, 113.7510903946856757 ) ) ;
#185691 = CARTESIAN_POINT ( 'NONE',  ( -10.81492255796105439, 18.62759615963255655, 97.91775706135236135 ) ) ;
#185692 = CARTESIAN_POINT ( 'NONE',  ( 16.55341960407618274, -4.379528057220086978, 56.04275706135235424 ) ) ;
#185693 = CARTESIAN_POINT ( 'NONE',  ( -14.34966873604960291, -8.224510206698953496, 26.66557627198103475 ) ) ;
#185694 = CARTESIAN_POINT ( 'NONE',  ( 18.62759615963255655, 10.81492255796105972, 66.66775706135234714 ) ) ;
#185695 = CARTESIAN_POINT ( 'NONE',  ( 18.62759615963255655, 10.81492255796105972, 51.66775706135234714 ) ) ;
#185696 = ORIENTED_EDGE ( 'NONE', *, *, #468, .T. ) ;
#185697 = CARTESIAN_POINT ( 'NONE',  ( 16.46253265017160672, -9.564922557960803928, 23.33224293864769194 ) ) ;
#185698 = CARTESIAN_POINT ( 'NONE',  ( -5.719274019375665041, -21.55341960407619695, 24.79275706135235779 ) ) ;
#185699 = CARTESIAN_POINT ( 'NONE',  ( -12.06949235617756955, 12.14591786802309770, 100.6239096053143811 ) ) ;
#185700 = CARTESIAN_POINT ( 'NONE',  ( -9.564922557960796823, -16.46253265017161027, 32.08224293864769550 ) ) ;
#185701 = CARTESIAN_POINT ( 'NONE',  ( 14.29746914071049879, -8.314922557960816363, 83.33224293864769550 ) ) ;
#185702 = CARTESIAN_POINT ( 'NONE',  ( 9.564922557960805705, 16.46253265017160317, 69.58224293864770971 ) ) ;
#185703 = CARTESIAN_POINT ( 'NONE',  ( 12.06949235617757843, -12.14591786802309237, 23.12390960531436335 ) ) ;
#185704 = CARTESIAN_POINT ( 'NONE',  ( -0.05219959533907301413, -21.53943276465977519, 57.49890960531435979 ) ) ;
#185705 = CARTESIAN_POINT ( 'NONE',  ( 8.224510206698953496, -14.34966873604960469, 87.91557627198103830 ) ) ;
#185706 = CARTESIAN_POINT ( 'NONE',  ( -10.72451020669898014, 18.67979575497178502, 90.41557627198103830 ) ) ;
#185707 = CARTESIAN_POINT ( 'NONE',  ( -13.89961937509977652, 13.97604488694528158, 100.6239096053143669 ) ) ;
#185709 = CARTESIAN_POINT ( 'NONE',  ( -0.05219959533936034679, 19.03943276465977164, 102.5010903946856757 ) ) ;
#185708 = CARTESIAN_POINT ( 'NONE',  ( -16.46253265017160317, 9.564922557960807481, 45.83224293864769550 ) ) ;
#185710 = CARTESIAN_POINT ( 'NONE',  ( 18.62759615963271287, -10.81492255796078972, 43.33224293864769550 ) ) ;
#185711 = CARTESIAN_POINT ( 'NONE',  ( 21.52544592524334988, 5.823673210054432836, 81.45942372801900433 ) ) ;
#185712 = CARTESIAN_POINT ( 'NONE',  ( 16.46253265017160672, -9.564922557960803928, 63.33224293864769550 ) ) ;
#185713 = CARTESIAN_POINT ( 'NONE',  ( -19.03943276465977164, 0.05219959533909376836, 96.24890960531436690 ) ) ;
#185714 = CARTESIAN_POINT ( 'NONE',  ( -16.52544592524335698, -4.483927247898792601, 78.95942372801901854 ) ) ;
#185715 = CARTESIAN_POINT ( 'NONE',  ( -5.823673210054431948, 21.52544592524334988, 57.70942372801901143 ) ) ;
#185716 = CARTESIAN_POINT ( 'NONE',  ( 0.05219959533937995610, -21.53943276465977519, 80.00109039468568994 ) ) ;
#185717 = CARTESIAN_POINT ( 'NONE',  ( -5.823673210054116645, -21.52544592524344225, 97.29057627198105251 ) ) ;
#185718 = CIRCLE ( 'NONE', #50049, 206.0437394197456911 ) ;
#185720 = CARTESIAN_POINT ( 'NONE',  ( 4.483927247898790824, -16.52544592524335698, 75.20942372801901854 ) ) ;
#185719 = CARTESIAN_POINT ( 'NONE',  ( -21.55341960407619339, 5.719274019375674811, 38.54275706135234714 ) ) ;
#185721 = CARTESIAN_POINT ( 'NONE',  ( -10.81492255796078084, -18.62759615963271287, 77.08224293864769550 ) ) ;
#185722 = CARTESIAN_POINT ( 'NONE',  ( 5.153800228976615827, -19.02544592524334988, 35.20942372801899722 ) ) ;
#185723 = CARTESIAN_POINT ( 'NONE',  ( 5.823673210054125526, 21.52544592524343514, 44.79057627198103120 ) ) ;
#185724 = CIRCLE ( 'NONE', #40390, 59.99999999999998579 ) ;
#185726 = CARTESIAN_POINT ( 'NONE',  ( 8.314922557960818139, 14.29746914071049879, 24.58224293864768839 ) ) ;
#185725 = CARTESIAN_POINT ( 'NONE',  ( -19.03943276465977164, 0.05219959533909376836, 86.24890960531436690 ) ) ;
#185727 = DIRECTION ( 'NONE',  ( 0.000000000000000000, 0.000000000000000000, -1.000000000000000000 ) ) ;
#185728 = CARTESIAN_POINT ( 'NONE',  ( -13.97604488694527625, -13.89961937509977652, 101.8739096053143811 ) ) ;
#185729 = DIRECTION ( 'NONE',  ( -1.000000000000000000, -0.000000000000000000, -0.000000000000000000 ) ) ;
#185730 = CARTESIAN_POINT ( 'NONE',  ( 16.51473224551083163, -9.474510206698727899, 100.8344237280190043 ) ) ;
#185731 = CARTESIAN_POINT ( 'NONE',  ( 5.719274019375991003, -21.55341960407610458, 77.70724293864770971 ) ) ;
#185732 = CARTESIAN_POINT ( 'NONE',  ( 14.29746914071049879, -8.314922557960816363, 43.33224293864769550 ) ) ;
#185733 = CARTESIAN_POINT ( 'NONE',  ( 13.97604488694548053, -13.89961937509957401, 110.6260903946856615 ) ) ;
#185734 = CARTESIAN_POINT ( 'NONE',  ( -19.03943276465977164, 0.05219959533909376836, 26.24890960531435624 ) ) ;
#185735 = CARTESIAN_POINT ( 'NONE',  ( 9.474510206698729675, 16.51473224551082808, 107.0844237280190043 ) ) ;
#185737 = CARTESIAN_POINT ( 'NONE',  ( 19.05341960407617918, -5.049401038297876454, 71.04275706135234714 ) ) ;
#185736 = CARTESIAN_POINT ( 'NONE',  ( -5.719274019375978568, 21.55341960407610458, 105.2072429386477097 ) ) ;
#185738 = CARTESIAN_POINT ( 'NONE',  ( -4.379528057220086978, -16.55341960407618274, 84.79275706135234714 ) ) ;
#185739 = CARTESIAN_POINT ( 'NONE',  ( -19.03943276465977164, 0.05219959533909376836, 66.24890960531436690 ) ) ;
#185740 = CARTESIAN_POINT ( 'NONE',  ( 14.34966873604960469, 8.224510206698951720, 79.16557627198103830 ) ) ;
#185741 =( BOUNDED_CURVE ( )  B_SPLINE_CURVE ( 2, ( #52411, #113081, #33280, #187970, #5903, #142434, #111101, #127253, #37244, #128249, #190934 ),
 .UNSPECIFIED., .F., .F. ) 
 B_SPLINE_CURVE_WITH_KNOTS ( ( 3, 2, 2, 2, 2, 3 ),
 ( 0.1000000000000000888, 0.1200000000000006478, 0.1400000000000012346, 0.1600000000000018074, 0.1800000000000023526, 0.2000000000000029532 ),
 .UNSPECIFIED. ) 
 CURVE ( )  GEOMETRIC_REPRESENTATION_ITEM ( )  RATIONAL_B_SPLINE_CURVE ( ( 0.9999999999999997780, 0.9510565162951537532, 1.000000000000000000, 0.9510565162951535312, 1.000000000000000000, 0.9510565162951535312, 1.000000000000000000, 0.9510565162951535312, 1.000000000000000000, 0.9510565162951463147, 1.000000000000007105 ) ) 
 REPRESENTATION_ITEM ( '' )  );
#185742 = CARTESIAN_POINT ( 'NONE',  ( -19.02544592524342804, 5.153800228976336051, 56.04057627198100988 ) ) ;
#185743 = CARTESIAN_POINT ( 'NONE',  ( 16.55341960407611168, 4.379528057220329451, 63.95724293864770260 ) ) ;
#185744 = CARTESIAN_POINT ( 'NONE',  ( 0.05219959533909260263, 19.03943276465977164, 24.99890960531435269 ) ) ;
#185745 = CARTESIAN_POINT ( 'NONE',  ( 17.44323487119282134, -16.85911479061552143, -54.24972394154876554 ) ) ;
#185746 = CARTESIAN_POINT ( 'NONE',  ( 8.314922557960818139, 14.29746914071049879, 39.58224293864769550 ) ) ;
#185747 = CARTESIAN_POINT ( 'NONE',  ( -5.153800228976328057, -19.02544592524343514, 72.29057627198102409 ) ) ;
#185748 = CARTESIAN_POINT ( 'NONE',  ( -1.151164073136592192, -16.16661445520355755, -59.37042179516132023 ) ) ;
#185749 = CARTESIAN_POINT ( 'NONE',  ( 16.51473224551083163, -9.474510206698727899, 45.83442372801900433 ) ) ;
#185750 = CARTESIAN_POINT ( 'NONE',  ( -16.53943276465976808, -0.05219959533934237506, 58.75109039468568994 ) ) ;
#185751 = CARTESIAN_POINT ( 'NONE',  ( -0.05219959533907301413, -21.53943276465977519, 67.49890960531436690 ) ) ;
#185752 = CARTESIAN_POINT ( 'NONE',  ( 5.153800228976615827, -19.02544592524334988, 20.20942372801899722 ) ) ;
#185753 = CARTESIAN_POINT ( 'NONE',  ( 5.049401038298161559, -19.05341960407611168, 82.70724293864770971 ) ) ;
#185754 = CARTESIAN_POINT ( 'NONE',  ( -21.27150294653347729, -22.98525001747979601, -46.52314187507937504 ) ) ;
#185755 = CARTESIAN_POINT ( 'NONE',  ( 21.53943276465977519, -0.05219959533907433946, 33.74890960531436690 ) ) ;
#185756 = AXIS2_PLACEMENT_3D ( 'NONE', #82546, #23898, #85551 ) ;
#185757 = CARTESIAN_POINT ( 'NONE',  ( -13.89961937509977652, 13.97604488694528158, 60.62390960531436690 ) ) ;
#185758 = CARTESIAN_POINT ( 'NONE',  ( -0.05219959533937732626, 21.53943276465977519, 57.50109039468568994 ) ) ;
#185760 = CARTESIAN_POINT ( 'NONE',  ( -4.379528057220328563, 16.55341960407611168, 105.2072429386477097 ) ) ;
#185759 = PRODUCT_DEFINITION_SHAPE ( 'NONE', 'NONE',  #115338 ) ;
#185763 = VERTEX_POINT ( 'NONE', #1450 ) ;
#185762 = CARTESIAN_POINT ( 'NONE',  ( -19.03943276465977164, 0.05219959533909376836, 96.24890960531436690 ) ) ;
#185761 = CARTESIAN_POINT ( 'NONE',  ( -0.05219959533907301413, -21.53943276465977519, 107.4989096053143669 ) ) ;
#185764 = CARTESIAN_POINT ( 'NONE',  ( 10.72451020669871369, 18.67979575497193778, 37.08442372801901143 ) ) ;
#185765 = VERTEX_POINT ( 'NONE', #76311 ) ;
#185766 = CARTESIAN_POINT ( 'NONE',  ( -13.97604488694527625, -13.89961937509977652, 91.87390960531432427 ) ) ;
#185767 = ADVANCED_FACE ( 'NONE', ( #32804 ), #28184, .T. ) ;
#185768 = CARTESIAN_POINT ( 'NONE',  ( -18.22780087662122028, 5.500000000000031086, 63.51540105326107266 ) ) ;
#185769 = CARTESIAN_POINT ( 'NONE',  ( 18.62759615963271287, -10.81492255796078972, 93.33224293864769550 ) ) ;
#185770 = CARTESIAN_POINT ( 'NONE',  ( 5.049401038298161559, -19.05341960407611168, 52.70724293864767418 ) ) ;
#185771 = CARTESIAN_POINT ( 'NONE',  ( 4.483927247898790824, -16.52544592524335698, 30.20942372801902565 ) ) ;
#185772 = CARTESIAN_POINT ( 'NONE',  ( 36.91746824999999177, 2.880721459617395097E-14, -2.124999997268813168 ) ) ;
#185773 = CARTESIAN_POINT ( 'NONE',  ( 16.51473224551069308, 9.474510206698969483, 34.16557627198102409 ) ) ;
#185774 = CARTESIAN_POINT ( 'NONE',  ( 5.719274019375673035, 21.55341960407619339, 82.29275706135234714 ) ) ;
#185776 = CARTESIAN_POINT ( 'NONE',  ( -5.823673210054431948, 21.52544592524334988, 42.70942372801901854 ) ) ;
#185775 = CARTESIAN_POINT ( 'NONE',  ( 13.97604488694527802, 13.89961937509977652, 69.37390960531436690 ) ) ;
#185777 = CARTESIAN_POINT ( 'NONE',  ( -18.67979575497193778, 10.72451020669871902, 23.33442372801901499 ) ) ;
#185778 = CARTESIAN_POINT ( 'NONE',  ( 27.73933785331498214, 9.013057229001095294, 142.4750000027311785 ) ) ;
#185779 = CARTESIAN_POINT ( 'NONE',  ( -19.02544592524342804, 5.153800228976336051, 106.0405762719810241 ) ) ;
#185780 = DIRECTION ( 'NONE',  ( 1.000000000000000000, 0.000000000000000000, 0.000000000000000000 ) ) ;
#185783 = CARTESIAN_POINT ( 'NONE',  ( -5.823673210054431948, 21.52544592524334988, 42.70942372801901854 ) ) ;
#185782 = CARTESIAN_POINT ( 'NONE',  ( 14.29746914071037800, 8.314922557961029526, 71.66775706135234714 ) ) ;
#185781 = CARTESIAN_POINT ( 'NONE',  ( 4.379528057220092307, 16.55341960407617563, 37.29275706135235424 ) ) ;
#185784 = CARTESIAN_POINT ( 'NONE',  ( 10.72451020669871369, 18.67979575497193778, 72.08442372801899012 ) ) ;
#185785 = CARTESIAN_POINT ( 'NONE',  ( 11.80868324581538253, -11.80868324581533457, -59.13370768023891344 ) ) ;
#185786 = CARTESIAN_POINT ( 'NONE',  ( -12.06949235617739369, -12.14591786802326823, 19.37609039468568639 ) ) ;
#185787 = CARTESIAN_POINT ( 'NONE',  ( 16.51473224551069308, 9.474510206698969483, 59.16557627198102409 ) ) ;
#185788 = CARTESIAN_POINT ( 'NONE',  ( 5.153800228976335163, 19.02544592524342804, 94.79057627198103830 ) ) ;
#185789 = CARTESIAN_POINT ( 'NONE',  ( -16.52544592524342804, 4.483927247898546575, 111.0405762719810525 ) ) ;
#185790 = CARTESIAN_POINT ( 'NONE',  ( 16.53943276465976808, -0.05219959533910856209, 98.74890960531438111 ) ) ;
#185791 = CARTESIAN_POINT ( 'NONE',  ( 15.80617190586746368, 15.72974639402197994, 34.37390960531435979 ) ) ;
#185792 = CARTESIAN_POINT ( 'NONE',  ( 12.06949235617739724, 12.14591786802326823, 81.87609039468568994 ) ) ;
#185794 = CARTESIAN_POINT ( 'NONE',  ( 13.97604488694527802, 13.89961937509977652, 49.37390960531434558 ) ) ;
#185793 = CARTESIAN_POINT ( 'NONE',  ( -4.483927247898539470, -16.52544592524342804, 67.29057627198103830 ) ) ;
#185795 = CARTESIAN_POINT ( 'NONE',  ( 5.719274019375673035, 21.55341960407619339, 72.29275706135236135 ) ) ;
#185796 = CARTESIAN_POINT ( 'NONE',  ( -18.67979575497193778, 10.72451020669871902, 68.33442372801900433 ) ) ;
#185797 = CARTESIAN_POINT ( 'NONE',  ( 19.02544592524334988, 5.153800228976608722, 106.4594237280190185 ) ) ;
#185798 = CARTESIAN_POINT ( 'NONE',  ( 16.53943276465976808, -0.05219959533910856209, 73.74890960531433848 ) ) ;
#185799 = CARTESIAN_POINT ( 'NONE',  ( 21.53943276465977519, 0.05219959533937863772, 31.25109039468568639 ) ) ;
#185800 = CARTESIAN_POINT ( 'NONE',  ( 21.53943276465977519, -0.05219959533907433946, 63.74890960531435979 ) ) ;
#185802 = CARTESIAN_POINT ( 'NONE',  ( -17.50000000000001421, -5.622605283950884214, 106.3120731059611899 ) ) ;
#185801 = CIRCLE ( 'NONE', #63101, 0.1999999999999987899 ) ;
#185803 = CARTESIAN_POINT ( 'NONE',  ( -28.82186960331499392, -9.364793116373526516, 146.3500000054623627 ) ) ;
#185804 = CARTESIAN_POINT ( 'NONE',  ( 9.474510206698971260, -16.51473224551069308, 67.91557627198102409 ) ) ;
#185805 = CARTESIAN_POINT ( 'NONE',  ( -12.14591786802309592, -12.06949235617757132, 46.87390960531435979 ) ) ;
#185806 = EDGE_CURVE ( 'NONE', #36039, #2296, #167008, .T. ) ;
#185807 = CARTESIAN_POINT ( 'NONE',  ( 12.06949235617757843, -12.14591786802309237, 23.12390960531436335 ) ) ;
#185808 = CARTESIAN_POINT ( 'NONE',  ( 0.05219959533934541429, -16.53943276465976808, 100.0010903946857042 ) ) ;
#185809 = CARTESIAN_POINT ( 'NONE',  ( 13.89961937509957401, 13.97604488694547697, 56.87609039468564731 ) ) ;
#185810 = CARTESIAN_POINT ( 'NONE',  ( 16.31925111598458145, 7.325300261831479531, 47.33575461032752685 ) ) ;
#185811 = CARTESIAN_POINT ( 'NONE',  ( 5.049401038298161559, -19.05341960407611168, 107.7072429386476955 ) ) ;
#185812 = CARTESIAN_POINT ( 'NONE',  ( -14.29746914071049879, 8.314922557960819915, 70.83224293864770971 ) ) ;
#185813 = CARTESIAN_POINT ( 'NONE',  ( 5.153800228976615827, -19.02544592524334988, 45.20942372801901143 ) ) ;
#185815 = CARTESIAN_POINT ( 'NONE',  ( -18.67979575497178146, -10.72451020669898902, 36.66557627198103120 ) ) ;
#185814 = CARTESIAN_POINT ( 'NONE',  ( 0.05219959533909260263, 19.03943276465977164, 29.99890960531435979 ) ) ;
#185817 = ORIENTED_EDGE ( 'NONE', *, *, #154620, .T. ) ;
#185816 = CARTESIAN_POINT ( 'NONE',  ( -21.53943276465977519, 0.05219959533907696930, 51.24890960531436690 ) ) ;
#185818 = CARTESIAN_POINT ( 'NONE',  ( 12.06949235617757843, -12.14591786802309237, 98.12390960531436690 ) ) ;
#185819 = CARTESIAN_POINT ( 'NONE',  ( 14.34966873604972726, -8.224510206698740333, 55.83442372801901854 ) ) ;
#185820 = CARTESIAN_POINT ( 'NONE',  ( 14.29746914071049879, -8.314922557960816363, 88.33224293864769550 ) ) ;
#185821 = CARTESIAN_POINT ( 'NONE',  ( 16.88567814943165502, -6.947325034625567497, 36.20998877347415856 ) ) ;
#185822 = CARTESIAN_POINT ( 'NONE',  ( -22.81625015709509441, -31.40387420917324590, -10.82499999726881335 ) ) ;
#185823 = CARTESIAN_POINT ( 'NONE',  ( -21.55341960407610458, -5.719274019375992779, 21.45724293864769550 ) ) ;
#185824 = CARTESIAN_POINT ( 'NONE',  ( 6.100000000000006750, 0.000000000000000000, -62.50719930893269805 ) ) ;
#185825 = CARTESIAN_POINT ( 'NONE',  ( 1.314058473856374532, 8.348982836029733789, -64.09739989910906388 ) ) ;
#185826 = VERTEX_POINT ( 'NONE', #186505 ) ;
#185828 = CARTESIAN_POINT ( 'NONE',  ( 8.314922557960818139, 14.29746914071049879, 34.58224293864770260 ) ) ;
#185827 = CARTESIAN_POINT ( 'NONE',  ( -8.314922557961024197, 14.29746914071037800, 47.91775706135234714 ) ) ;
#185829 = CARTESIAN_POINT ( 'NONE',  ( -15.80617190586745835, -15.72974639402198527, 51.87390960531437401 ) ) ;
#185830 = CARTESIAN_POINT ( 'NONE',  ( 9.564922557961047289, -16.46253265017146816, 85.41775706135233293 ) ) ;
#185831 = CARTESIAN_POINT ( 'NONE',  ( -10.81492255796078084, -18.62759615963271287, 52.08224293864768839 ) ) ;
#185832 = CARTESIAN_POINT ( 'NONE',  ( 10.72451020669871369, 18.67979575497193778, 82.08442372801901854 ) ) ;
#185833 = CARTESIAN_POINT ( 'NONE',  ( -11.80868324581538253, 11.80868324581533457, -61.34707691135562868 ) ) ;
#185834 = CARTESIAN_POINT ( 'NONE',  ( 12.06949235617739724, 12.14591786802326823, 41.87609039468568284 ) ) ;
#185836 = CARTESIAN_POINT ( 'NONE',  ( 13.89961937509977652, -13.97604488694527269, 98.12390960531433848 ) ) ;
#185835 = CARTESIAN_POINT ( 'NONE',  ( -19.05341960407611168, -5.049401038298163336, 31.45724293864769550 ) ) ;
#185837 = CARTESIAN_POINT ( 'NONE',  ( -19.02544592524342804, 5.153800228976336051, 36.04057627198100988 ) ) ;
#185838 = CARTESIAN_POINT ( 'NONE',  ( -12.06949235617756955, 12.14591786802309770, 100.6239096053143811 ) ) ;
#185839 = CARTESIAN_POINT ( 'NONE',  ( -37.00000000000000711, -5.510910596163089556E-15, 45.00000000000000000 ) ) ;
#185840 = CARTESIAN_POINT ( 'NONE',  ( 5.153800228976335163, 19.02544592524342804, 99.79057627198102409 ) ) ;
#185841 = ORIENTED_EDGE ( 'NONE', *, *, #45518, .F. ) ;
#185842 = CARTESIAN_POINT ( 'NONE',  ( -8.314922557961024197, 14.29746914071037800, 57.91775706135234714 ) ) ;
#185843 = CARTESIAN_POINT ( 'NONE',  ( 10.81492255796078972, 18.62759615963270932, 84.58224293864769550 ) ) ;
#185844 = CARTESIAN_POINT ( 'NONE',  ( 16.46253265017160672, -9.564922557960803928, 58.33224293864769550 ) ) ;
#185845 = CARTESIAN_POINT ( 'NONE',  ( 21.55341960407619695, -5.719274019375665929, 26.04275706135235779 ) ) ;
#185846 = CARTESIAN_POINT ( 'NONE',  ( 5.153800228976335163, 19.02544592524342804, 84.79057627198099567 ) ) ;
#185847 = LINE ( 'NONE', #79644, #180003 ) ;
#185848 = ORIENTED_EDGE ( 'NONE', *, *, #199458, .F. ) ;
#185849 = CARTESIAN_POINT ( 'NONE',  ( 15.80617190586769283, -15.72974639402175789, 20.62609039468568639 ) ) ;
#185852 = CARTESIAN_POINT ( 'NONE',  ( 9.474510206698729675, 16.51473224551082808, 72.08442372801900433 ) ) ;
#185851 = CARTESIAN_POINT ( 'NONE',  ( -9.474510206698964154, 16.51473224551069663, 110.4155762719810383 ) ) ;
#185850 = CARTESIAN_POINT ( 'NONE',  ( 13.97604488694527802, 13.89961937509977652, 29.37390960531435979 ) ) ;
#185853 = EDGE_CURVE ( 'NONE', #23611, #90645, #185490, .T. ) ;
#185854 = CARTESIAN_POINT ( 'NONE',  ( -19.02544592524334988, -5.153800228976617603, 23.95942372801900078 ) ) ;
#185855 = CARTESIAN_POINT ( 'NONE',  ( -21.52544592524343514, 5.823673210054127303, 106.0405762719810525 ) ) ;
#185856 = CARTESIAN_POINT ( 'NONE',  ( -5.049401038297874678, -19.05341960407617918, 39.79275706135232582 ) ) ;
#185857 = CARTESIAN_POINT ( 'NONE',  ( -12.14591786802326823, 12.06949235617739902, 73.12609039468567573 ) ) ;
#185858 = CARTESIAN_POINT ( 'NONE',  ( -13.97604488694527625, -13.89961937509977652, 101.8739096053143811 ) ) ;
#185859 = CARTESIAN_POINT ( 'NONE',  ( 5.049401038298161559, -19.05341960407611168, 52.70724293864767418 ) ) ;
#185860 = CIRCLE ( 'NONE', #47004, 206.0437394197456911 ) ;
#185861 = CARTESIAN_POINT ( 'NONE',  ( 10.81492255796106328, -18.62759615963255655, 70.41775706135236135 ) ) ;
#185862 = CARTESIAN_POINT ( 'NONE',  ( -10.81492255796105439, 18.62759615963255655, 77.91775706135231871 ) ) ;
#185863 = CARTESIAN_POINT ( 'NONE',  ( -9.474510206698964154, 16.51473224551069663, 75.41557627198103830 ) ) ;
#185864 = CARTESIAN_POINT ( 'NONE',  ( -18.62759615963255300, -10.81492255796106328, 44.16775706135234714 ) ) ;
#185865 = CARTESIAN_POINT ( 'NONE',  ( -9.474510206698720793, -16.51473224551083518, 84.58442372801900433 ) ) ;
#185866 = ADVANCED_FACE ( 'NONE', ( #95451 ), #141949, .T. ) ;
#185867 = CARTESIAN_POINT ( 'NONE',  ( -0.05219959533909027116, -19.03943276465977164, 52.49890960531436690 ) ) ;
#185868 = CARTESIAN_POINT ( 'NONE',  ( -13.89961937509977652, 13.97604488694528158, 100.6239096053143669 ) ) ;
#185869 = CARTESIAN_POINT ( 'NONE',  ( -5.049401038298153566, 19.05341960407611168, 70.20724293864769550 ) ) ;
#185870 = CARTESIAN_POINT ( 'NONE',  ( 19.03943276465977164, -0.05219959533909143690, 108.7489096053143527 ) ) ;
#185871 = CARTESIAN_POINT ( 'NONE',  ( 0.05219959533909260263, 19.03943276465977164, 54.99890960531435979 ) ) ;
#185872 = CARTESIAN_POINT ( 'NONE',  ( 15.80617190586746368, 15.72974639402197994, 104.3739096053143669 ) ) ;
#185873 = CARTESIAN_POINT ( 'NONE',  ( -12.06949235617739369, -12.14591786802326823, 79.37609039468567573 ) ) ;
#185874 = CARTESIAN_POINT ( 'NONE',  ( -24.73536985823982803, 3.645104810711965460, 171.5180696409406380 ) ) ;
#185875 = CARTESIAN_POINT ( 'NONE',  ( -9.474510206698720793, -16.51473224551083518, 39.58442372801899722 ) ) ;
#185876 = CARTESIAN_POINT ( 'NONE',  ( 5.153800228976335163, 19.02544592524342804, 64.79057627198100988 ) ) ;
#185877 = CARTESIAN_POINT ( 'NONE',  ( -0.05219959533910754901, -16.53943276465976808, 52.49890960531435979 ) ) ;
#185878 = CARTESIAN_POINT ( 'NONE',  ( -0.05219959533910754901, -16.53943276465976808, 92.49890960531436690 ) ) ;
#185879 = AXIS2_PLACEMENT_3D ( 'NONE', #109675, #124846, #32844 ) ;
#185880 = CARTESIAN_POINT ( 'NONE',  ( -5.049401038298153566, 19.05341960407611168, 95.20724293864770971 ) ) ;
#185881 = CARTESIAN_POINT ( 'NONE',  ( -13.89961937509977652, 13.97604488694528158, 85.62390960531433848 ) ) ;
#185882 = CARTESIAN_POINT ( 'NONE',  ( 0.05219959533909260263, 19.03943276465977164, 104.9989096053143669 ) ) ;
#185883 = CARTESIAN_POINT ( 'NONE',  ( 18.62759615963255655, 10.81492255796105972, 106.6677570613523756 ) ) ;
#185884 = CARTESIAN_POINT ( 'NONE',  ( 12.06949235617739724, 12.14591786802326823, 86.87609039468568994 ) ) ;
#185885 = CARTESIAN_POINT ( 'NONE',  ( 19.03943276465977164, -0.05219959533909143690, 73.74890960531435269 ) ) ;
#185886 = CARTESIAN_POINT ( 'NONE',  ( -5.823673210054431948, 21.52544592524334988, 37.70942372801900433 ) ) ;
#185887 = CARTESIAN_POINT ( 'NONE',  ( 5.823673210054125526, 21.52544592524343514, 29.79057627198102409 ) ) ;
#185888 = CARTESIAN_POINT ( 'NONE',  ( -15.80617190586745835, -15.72974639402198527, 106.8739096053143811 ) ) ;
#185889 = CARTESIAN_POINT ( 'NONE',  ( -16.55341960407611168, -4.379528057220339221, 56.45724293864768839 ) ) ;
#185890 = CARTESIAN_POINT ( 'NONE',  ( 16.46253265017160672, -9.564922557960803928, 48.33224293864769550 ) ) ;
#185891 = CARTESIAN_POINT ( 'NONE',  ( -14.34966873604960291, -8.224510206698953496, 81.66557627198103830 ) ) ;
#185892 = CARTESIAN_POINT ( 'NONE',  ( 9.564922557961047289, -16.46253265017146816, 50.41775706135233293 ) ) ;
#185893 = CARTESIAN_POINT ( 'NONE',  ( -4.483927247898539470, -16.52544592524342804, 107.2905762719810525 ) ) ;
#185894 = CARTESIAN_POINT ( 'NONE',  ( -8.224510206698735004, -14.34966873604973081, 64.58442372801900433 ) ) ;
#185895 = CARTESIAN_POINT ( 'NONE',  ( -9.474510206698964154, 16.51473224551069663, 80.41557627198103830 ) ) ;
#185896 = CARTESIAN_POINT ( 'NONE',  ( -8.571926809382601320, -26.38167802310801591, 145.2750000027311899 ) ) ;
#185897 = CARTESIAN_POINT ( 'NONE',  ( -8.224510206698948167, 14.34966873604960824, 105.4155762719810383 ) ) ;
#185898 = CARTESIAN_POINT ( 'NONE',  ( -0.05219959533907301413, -21.53943276465977519, 37.49890960531436690 ) ) ;
#185899 = ORIENTED_EDGE ( 'NONE', *, *, #128937, .T. ) ;
#185900 = CARTESIAN_POINT ( 'NONE',  ( 14.34966873604972726, -8.224510206698740333, 100.8344237280190185 ) ) ;
#185901 = CARTESIAN_POINT ( 'NONE',  ( 12.14591786802327356, -12.06949235617739191, 25.62609039468567929 ) ) ;
#185902 = CARTESIAN_POINT ( 'NONE',  ( -0.05219959533937732626, 21.53943276465977519, 87.50109039468568994 ) ) ;
#185903 = CARTESIAN_POINT ( 'NONE',  ( -5.049401038298153566, 19.05341960407611168, 85.20724293864766707 ) ) ;
#185904 = CARTESIAN_POINT ( 'NONE',  ( -15.72974639402197994, 15.80617190586746368, 115.6239096053143669 ) ) ;
#185905 = CARTESIAN_POINT ( 'NONE',  ( -5.049401038298153566, 19.05341960407611168, 25.20724293864768484 ) ) ;
#185906 = CARTESIAN_POINT ( 'NONE',  ( 14.34966873604972726, -8.224510206698740333, 35.83442372801901143 ) ) ;
#185907 = CARTESIAN_POINT ( 'NONE',  ( 13.97604488694548053, -13.89961937509957401, 90.62609039468567573 ) ) ;
#185908 = CARTESIAN_POINT ( 'NONE',  ( 0.05219959533907565091, 21.53943276465977519, 84.99890960531436690 ) ) ;
#185909 = CARTESIAN_POINT ( 'NONE',  ( 19.03943276465977164, 0.05219959533936151252, 66.25109039468567573 ) ) ;
#185910 = DIRECTION ( 'NONE',  ( 0.000000000000000000, 0.000000000000000000, 1.000000000000000000 ) ) ;
#185911 = CARTESIAN_POINT ( 'NONE',  ( -18.62759615963255300, -10.81492255796106328, 24.16775706135235424 ) ) ;
#185912 = CARTESIAN_POINT ( 'NONE',  ( 5.049401038298163336, -19.05341960407611168, 72.70724293864769550 ) ) ;
#185913 = CARTESIAN_POINT ( 'NONE',  ( -13.89961937509977652, 13.97604488694528158, 90.62390960531432427 ) ) ;
#185914 = CARTESIAN_POINT ( 'NONE',  ( 16.53943276465976808, 0.05219959533934440121, 31.25109039468568639 ) ) ;
#185915 = CARTESIAN_POINT ( 'NONE',  ( 19.97888994334925172, -34.65319547504297049, -5.351457953959465108 ) ) ;
#185916 = CARTESIAN_POINT ( 'NONE',  ( -5.153800228976607833, 19.02544592524334988, 57.70942372801899012 ) ) ;
#185918 = CARTESIAN_POINT ( 'NONE',  ( -16.55341960407611168, -4.379528057220339221, 76.45724293864769550 ) ) ;
#185917 = CARTESIAN_POINT ( 'NONE',  ( 10.81492255796078972, 18.62759615963270932, 114.5822429386477097 ) ) ;
#185919 = CARTESIAN_POINT ( 'NONE',  ( -13.89961937509977652, 13.97604488694528158, 85.62390960531433848 ) ) ;
#185921 = CARTESIAN_POINT ( 'NONE',  ( -5.153800228976607833, 19.02544592524334988, 52.70942372801900433 ) ) ;
#185920 = CARTESIAN_POINT ( 'NONE',  ( 14.29746914071037800, 8.314922557961029526, 36.66775706135234714 ) ) ;
#185922 = CARTESIAN_POINT ( 'NONE',  ( 5.823673210054444382, -21.52544592524334988, 70.20942372801904696 ) ) ;
#185923 = CARTESIAN_POINT ( 'NONE',  ( -4.379528057220086978, -16.55341960407618274, 24.79275706135235779 ) ) ;
#185924 = CARTESIAN_POINT ( 'NONE',  ( 19.02544592524343514, -5.153800228976328945, 68.54057627198103830 ) ) ;
#185925 = CARTESIAN_POINT ( 'NONE',  ( 16.51473224551083163, -9.474510206698727899, 80.83442372801899012 ) ) ;
#185926 = CARTESIAN_POINT ( 'NONE',  ( 4.379528057220092307, 16.55341960407617563, 62.29275706135236845 ) ) ;
#185927 = CARTESIAN_POINT ( 'NONE',  ( 21.52544592524334988, 5.823673210054432836, 101.4594237280190185 ) ) ;
#185928 = CARTESIAN_POINT ( 'NONE',  ( 19.05341960407617918, -5.049401038297876454, 71.04275706135234714 ) ) ;
#185929 = CARTESIAN_POINT ( 'NONE',  ( -19.05341960407611168, -5.049401038298163336, 51.45724293864770260 ) ) ;
#185930 = CARTESIAN_POINT ( 'NONE',  ( 18.67979575497178502, 10.72451020669898547, 69.16557627198102409 ) ) ;
#185932 = CARTESIAN_POINT ( 'NONE',  ( 5.049401038297881783, 19.05341960407617563, 77.29275706135231871 ) ) ;
#185931 = CARTESIAN_POINT ( 'NONE',  ( 4.379528057220339221, -16.55341960407611168, 67.70724293864769550 ) ) ;
#185933 = LINE ( 'NONE', #106089, #86019 ) ;
#185934 = CARTESIAN_POINT ( 'NONE',  ( 16.46253265017146816, 9.564922557961045513, 46.66775706135233293 ) ) ;
#185935 = CARTESIAN_POINT ( 'NONE',  ( -16.52544592524335698, -4.483927247898792601, 103.9594237280190185 ) ) ;
#185936 = CARTESIAN_POINT ( 'NONE',  ( -4.379528057220328563, 16.55341960407611168, 70.20724293864769550 ) ) ;
#185938 = CARTESIAN_POINT ( 'NONE',  ( 22.44159573604009239, 16.30477369853692693, 146.0750000027311728 ) ) ;
#185937 = CARTESIAN_POINT ( 'NONE',  ( -21.52544592524334988, -5.823673210054445271, 98.95942372801903275 ) ) ;
#185939 = CARTESIAN_POINT ( 'NONE',  ( 10.81492255796078972, 18.62759615963270932, 94.58224293864769550 ) ) ;
#185940 = CARTESIAN_POINT ( 'NONE',  ( -5.049401038298153566, 19.05341960407611168, 70.20724293864769550 ) ) ;
#185941 = CARTESIAN_POINT ( 'NONE',  ( -18.67979575497193778, 10.72451020669871902, 73.33442372801901854 ) ) ;
#185942 = CARTESIAN_POINT ( 'NONE',  ( -13.97604488694527625, -13.89961937509977652, 51.87390960531436690 ) ) ;
#185943 = EDGE_LOOP ( 'NONE', ( #77748, #37588, #3021, #139800, #143921 ) ) ;
#185944 = CARTESIAN_POINT ( 'NONE',  ( 13.89961937509977652, -13.97604488694527269, 23.12390960531436335 ) ) ;
#185945 = CARTESIAN_POINT ( 'NONE',  ( 9.564922557960805705, 16.46253265017160317, 109.5822429386476955 ) ) ;
#185946 = CIRCLE ( 'NONE', #76088, 214.0437394197456342 ) ;
#185947 = CARTESIAN_POINT ( 'NONE',  ( 16.53943276465976808, -0.05219959533910856209, 63.74890960531435979 ) ) ;
#185948 = CARTESIAN_POINT ( 'NONE',  ( 19.03943276465977164, -0.05219959533909143690, 28.74890960531435624 ) ) ;
#185949 = CARTESIAN_POINT ( 'NONE',  ( 12.14591786802309770, 12.06949235617756955, 79.37390960531436690 ) ) ;
#185950 = CARTESIAN_POINT ( 'NONE',  ( -21.52544592524343514, 5.823673210054127303, 96.04057627198102409 ) ) ;
#185951 = CARTESIAN_POINT ( 'NONE',  ( 0.05219959533937995610, -21.53943276465977519, 35.00109039468568284 ) ) ;
#185952 = CARTESIAN_POINT ( 'NONE',  ( 1.351073136246558226, 6.941121712480402550, -62.33638022162458725 ) ) ;
#185953 = CARTESIAN_POINT ( 'NONE',  ( -4.483927247898782831, 16.52544592524335698, 52.70942372801902565 ) ) ;
#185954 = CARTESIAN_POINT ( 'NONE',  ( 10.81492255796078972, 18.62759615963270932, 89.58224293864768129 ) ) ;
#185955 = CARTESIAN_POINT ( 'NONE',  ( 9.474510206698729675, 16.51473224551082808, 22.08442372801899722 ) ) ;
#185956 = CARTESIAN_POINT ( 'NONE',  ( 19.05341960407611168, 5.049401038298154454, 103.9572429386476671 ) ) ;
#185957 = CARTESIAN_POINT ( 'NONE',  ( -5.719274019375665041, -21.55341960407619695, 39.79275706135235424 ) ) ;
#185958 = CARTESIAN_POINT ( 'NONE',  ( 10.72451020669898902, -18.67979575497178502, 42.91557627198103120 ) ) ;
#185959 = CARTESIAN_POINT ( 'NONE',  ( -0.05219959533910754901, -16.53943276465976808, 22.49890960531436335 ) ) ;
#185961 = CARTESIAN_POINT ( 'NONE',  ( 0.05219959533937995610, -21.53943276465977519, 95.00109039468568994 ) ) ;
#185960 = CARTESIAN_POINT ( 'NONE',  ( 21.53943276465977519, 0.05219959533937863772, 66.25109039468567573 ) ) ;
#185962 = CARTESIAN_POINT ( 'NONE',  ( -5.049401038297874678, -19.05341960407617918, 24.79275706135233648 ) ) ;
#185963 = CARTESIAN_POINT ( 'NONE',  ( 14.34966873604972726, -8.224510206698740333, 85.83442372801901854 ) ) ;
#185965 = EDGE_CURVE ( 'NONE', #95725, #24895, #40973, .T. ) ;
#185964 = CARTESIAN_POINT ( 'NONE',  ( 21.55341960407619695, -5.719274019375665929, 56.04275706135235424 ) ) ;
#185966 = CARTESIAN_POINT ( 'NONE',  ( 13.89961937509977652, -13.97604488694527269, 48.12390960531435979 ) ) ;
#185967 = CARTESIAN_POINT ( 'NONE',  ( 18.62759615963255655, 10.81492255796105972, 111.6677570613523613 ) ) ;
#185968 = CARTESIAN_POINT ( 'NONE',  ( -18.67979575497178146, -10.72451020669898902, 26.66557627198103475 ) ) ;
#185969 = CARTESIAN_POINT ( 'NONE',  ( -18.62759615963270932, 10.81492255796079327, 115.8322429386477097 ) ) ;
#185970 = CARTESIAN_POINT ( 'NONE',  ( -5.823673210054116645, -21.52544592524344225, 77.29057627198102409 ) ) ;
#185971 = CARTESIAN_POINT ( 'NONE',  ( -8.224510206698735004, -14.34966873604973081, 44.58442372801901854 ) ) ;
#185973 = CARTESIAN_POINT ( 'NONE',  ( 21.53943276465977519, -0.05219959533907433946, 73.74890960531433848 ) ) ;
#185972 = DIRECTION ( 'NONE',  ( 1.000000000000000000, 0.000000000000000000, 0.000000000000000000 ) ) ;
#185975 = CARTESIAN_POINT ( 'NONE',  ( -16.53943276465976808, 0.05219959533911058130, 61.24890960531435979 ) ) ;
#185974 = CARTESIAN_POINT ( 'NONE',  ( 4.483927247898790824, -16.52544592524335698, 65.20942372801901854 ) ) ;
#185976 = DIRECTION ( 'NONE',  ( 0.000000000000000000, 0.000000000000000000, -1.000000000000000000 ) ) ;
#185977 = CARTESIAN_POINT ( 'NONE',  ( 9.474510206698729675, 16.51473224551082808, 97.08442372801900433 ) ) ;
#185978 = CARTESIAN_POINT ( 'NONE',  ( -24.28759355007370857, 0.2213677808129483893, -54.22458008397516949 ) ) ;
#185979 = ADVANCED_FACE ( 'NONE', ( #96437 ), #113596, .F. ) ;
#185980 = CARTESIAN_POINT ( 'NONE',  ( 4.483927247898790824, -16.52544592524335698, 35.20942372801901854 ) ) ;
#185981 = CARTESIAN_POINT ( 'NONE',  ( 5.719274019375991003, -21.55341960407610458, 112.7072429386476955 ) ) ;
#185982 = CARTESIAN_POINT ( 'NONE',  ( 5.719274019375991003, -21.55341960407610458, 77.70724293864770971 ) ) ;
#185983 = CARTESIAN_POINT ( 'NONE',  ( -21.53943276465977519, 0.05219959533907696930, 36.24890960531435979 ) ) ;
#185984 = CARTESIAN_POINT ( 'NONE',  ( -0.05219959533934338120, 16.53943276465976808, 62.50109039468568284 ) ) ;
#185985 = CARTESIAN_POINT ( 'NONE',  ( 16.46253265017160672, -9.564922557960803928, 68.33224293864770971 ) ) ;
#185987 = CARTESIAN_POINT ( 'NONE',  ( 19.02544592524334988, 5.153800228976608722, 106.4594237280190185 ) ) ;
#185986 = CARTESIAN_POINT ( 'NONE',  ( -10.72451020669870658, -18.67979575497194134, 39.58442372801901143 ) ) ;
#185988 = CARTESIAN_POINT ( 'NONE',  ( -10.72451020669898014, 18.67979575497178502, 30.41557627198101699 ) ) ;
#185989 = CARTESIAN_POINT ( 'NONE',  ( -19.05341960407617563, 5.049401038297882671, 23.54275706135233648 ) ) ;
#185990 = CARTESIAN_POINT ( 'NONE',  ( -14.34966873604972548, 8.224510206698743886, 38.33442372801900433 ) ) ;
#185991 = CARTESIAN_POINT ( 'NONE',  ( -5.153800228976328057, -19.02544592524343514, 102.2905762719810383 ) ) ;
#185992 = CARTESIAN_POINT ( 'NONE',  ( -5.719274019375978568, 21.55341960407610458, 105.2072429386477097 ) ) ;
#185993 = CARTESIAN_POINT ( 'NONE',  ( -16.46253265017160317, 9.564922557960807481, 75.83224293864769550 ) ) ;
#185994 = CARTESIAN_POINT ( 'NONE',  ( -16.36317988757058828, 7.306389748694928521, 24.09789608363227487 ) ) ;
#185995 = CARTESIAN_POINT ( 'NONE',  ( -8.314922557960811034, -14.29746914071050412, 87.08224293864769550 ) ) ;
#185996 = CARTESIAN_POINT ( 'NONE',  ( -16.46253265017160317, 9.564922557960807481, 110.8322429386476955 ) ) ;
#185997 = LINE ( 'NONE', #187007, #128314 ) ;
#185998 = CARTESIAN_POINT ( 'NONE',  ( 12.06949235617739724, 12.14591786802326823, 66.87609039468568994 ) ) ;
#185999 = CARTESIAN_POINT ( 'NONE',  ( -10.72451020669898014, 18.67979575497178502, 105.4155762719810383 ) ) ;
#186000 = CARTESIAN_POINT ( 'NONE',  ( -5.049401038297874678, -19.05341960407617918, 64.79275706135233293 ) ) ;
#186001 = VECTOR ( 'NONE', #176426, 1000.000000000000000 ) ;
#186002 = CARTESIAN_POINT ( 'NONE',  ( 21.55341960407610458, 5.719274019375980345, 33.95724293864769550 ) ) ;
#186003 = CARTESIAN_POINT ( 'NONE',  ( -13.97604488694527625, -13.89961937509977652, 26.87390960531434558 ) ) ;
#186004 = CARTESIAN_POINT ( 'NONE',  ( -15.72974639402197994, 15.80617190586746368, 70.62390960531436690 ) ) ;
#186005 = CARTESIAN_POINT ( 'NONE',  ( 19.03943276465977164, -0.05219959533909143690, 93.74890960531435269 ) ) ;
#186006 = CARTESIAN_POINT ( 'NONE',  ( -15.80617190586768217, 15.72974639402176855, 93.12609039468568994 ) ) ;
#186007 = CARTESIAN_POINT ( 'NONE',  ( 5.049401038298161559, -19.05341960407611168, 47.70724293864770260 ) ) ;
#186008 = CARTESIAN_POINT ( 'NONE',  ( 0.05219959533910956823, 16.53943276465976808, 89.99890960531438111 ) ) ;
#186009 = CARTESIAN_POINT ( 'NONE',  ( 14.34966873604972726, -8.224510206698740333, 35.83442372801901143 ) ) ;
#186010 = CARTESIAN_POINT ( 'NONE',  ( 9.474510206698971260, -16.51473224551069308, 57.91557627198103120 ) ) ;
#186011 = CARTESIAN_POINT ( 'NONE',  ( -15.72974639402176322, -15.80617190586768395, 79.37609039468567573 ) ) ;
#186012 = EDGE_LOOP ( 'NONE', ( #179537, #63864 ) ) ;
#186013 = CARTESIAN_POINT ( 'NONE',  ( -19.02544592524334988, -5.153800228976617603, 28.95942372801900433 ) ) ;
#186014 = ADVANCED_FACE ( 'NONE', ( #23613 ), #21603, .F. ) ;
#186015 = CARTESIAN_POINT ( 'NONE',  ( 19.03943276465977164, 0.05219959533936151252, 36.25109039468567573 ) ) ;
#186016 = CARTESIAN_POINT ( 'NONE',  ( 21.53943276465977519, 0.05219959533937863772, 31.25109039468568639 ) ) ;
#186017 = CARTESIAN_POINT ( 'NONE',  ( 9.564922557960805705, 16.46253265017160317, 54.58224293864769550 ) ) ;
#186018 = CARTESIAN_POINT ( 'NONE',  ( 16.46253265017146816, 9.564922557961045513, 31.66775706135232937 ) ) ;
#186019 = CARTESIAN_POINT ( 'NONE',  ( -19.05341960407611168, -5.049401038298163336, 81.45724293864769550 ) ) ;
#186020 = CARTESIAN_POINT ( 'NONE',  ( -16.46253265017160317, 9.564922557960807481, 75.83224293864769550 ) ) ;
#186021 = CARTESIAN_POINT ( 'NONE',  ( 14.29746914071049879, -8.314922557960816363, 28.33224293864769550 ) ) ;
#186023 = CARTESIAN_POINT ( 'NONE',  ( -10.81492255796105439, 18.62759615963255655, 87.91775706135234714 ) ) ;
#186022 = CARTESIAN_POINT ( 'NONE',  ( 19.02544592524343514, -5.153800228976328945, 113.5405762719810241 ) ) ;
#186024 = CARTESIAN_POINT ( 'NONE',  ( -36.91746825000001309, 11.99521256947798342, -2.724999997268813701 ) ) ;
#186025 = CARTESIAN_POINT ( 'NONE',  ( 16.61371651742604172, 7.165104196376048229, 58.64584930007005426 ) ) ;
#186026 = CARTESIAN_POINT ( 'NONE',  ( -21.53943276465977519, -0.05219959533937600094, 93.75109039468567573 ) ) ;
#186027 = CARTESIAN_POINT ( 'NONE',  ( 22.62413958104535183, -1.500431131851388766, -57.95367621771160316 ) ) ;
#186028 = CARTESIAN_POINT ( 'NONE',  ( 9.564922557960805705, 16.46253265017160317, 109.5822429386476955 ) ) ;
#186029 = CARTESIAN_POINT ( 'NONE',  ( 34.11680238834244250, 4.370175642590067078, 91.64155955192001102 ) ) ;
#186030 = CARTESIAN_POINT ( 'NONE',  ( 14.34966873604972726, -8.224510206698740333, 45.83442372801901854 ) ) ;
#186031 = CARTESIAN_POINT ( 'NONE',  ( 21.53943276465977519, -0.05219959533907433946, 68.74890960531435269 ) ) ;
#186032 = CARTESIAN_POINT ( 'NONE',  ( 16.55341960407611168, 4.379528057220329451, 23.95724293864769550 ) ) ;
#186034 = CARTESIAN_POINT ( 'NONE',  ( 0.05219959533909260263, 19.03943276465977164, 99.99890960531436690 ) ) ;
#186033 = CARTESIAN_POINT ( 'NONE',  ( -16.52544592524342804, 4.483927247898546575, 116.0405762719810383 ) ) ;
#186035 = CARTESIAN_POINT ( 'NONE',  ( -21.53943276465977519, -0.05219959533937600094, 113.7510903946856757 ) ) ;
#186036 = CARTESIAN_POINT ( 'NONE',  ( -8.314922557960811034, -14.29746914071050412, 112.0822429386477097 ) ) ;
#186037 = CARTESIAN_POINT ( 'NONE',  ( 21.55341960407619695, -5.719274019375665929, 71.04275706135234714 ) ) ;
#186038 = CARTESIAN_POINT ( 'NONE',  ( -16.55341960407617563, 4.379528057220093196, 108.5427570613523756 ) ) ;
#186039 = CARTESIAN_POINT ( 'NONE',  ( 19.03943276465977164, 0.05219959533936151252, 61.25109039468566863 ) ) ;
#186040 = CARTESIAN_POINT ( 'NONE',  ( 36.91746824999999177, 2.880721459617395097E-14, -4.124999997268813168 ) ) ;
#186041 = CARTESIAN_POINT ( 'NONE',  ( 19.02544592524343514, -5.153800228976328945, 108.5405762719810383 ) ) ;
#186042 = CARTESIAN_POINT ( 'NONE',  ( -4.483927247898539470, -16.52544592524342804, 92.29057627198103830 ) ) ;
#186044 = CARTESIAN_POINT ( 'NONE',  ( -16.51473224551082808, 9.474510206698731452, 58.33442372801900433 ) ) ;
#186043 = AXIS2_PLACEMENT_3D ( 'NONE', #171317, #80278, #14651 ) ;
#186045 = CARTESIAN_POINT ( 'NONE',  ( -5.049401038298153566, 19.05341960407611168, 75.20724293864769550 ) ) ;
#186046 = CARTESIAN_POINT ( 'NONE',  ( 14.29746914071049879, -8.314922557960816363, 58.33224293864768839 ) ) ;
#186047 = CARTESIAN_POINT ( 'NONE',  ( -16.46253265017146816, -9.564922557961047289, 99.16775706135233293 ) ) ;
#186048 = CARTESIAN_POINT ( 'NONE',  ( -0.05219959533907301413, -21.53943276465977519, 52.49890960531435979 ) ) ;
#186049 = ORIENTED_EDGE ( 'NONE', *, *, #179839, .F. ) ;
#186050 = CARTESIAN_POINT ( 'NONE',  ( -0.05219959533910754901, -16.53943276465976808, 112.4989096053143669 ) ) ;
#186051 = DIRECTION ( 'NONE',  ( 1.000000000000000000, 0.000000000000000000, -0.000000000000000000 ) ) ;
#186053 = CARTESIAN_POINT ( 'NONE',  ( -15.80617190586745835, -15.72974639402198527, 71.87390960531438111 ) ) ;
#186052 = CARTESIAN_POINT ( 'NONE',  ( 19.03943276465977164, -0.05219959533909143690, 73.74890960531435269 ) ) ;
#186055 = CARTESIAN_POINT ( 'NONE',  ( -19.02544592524342804, 5.153800228976336051, 76.04057627198102409 ) ) ;
#186054 = CARTESIAN_POINT ( 'NONE',  ( -0.05219959533934338120, 16.53943276465976808, 87.50109039468568994 ) ) ;
#186056 = CARTESIAN_POINT ( 'NONE',  ( -13.97604488694547697, 13.89961937509957934, 63.12609039468566152 ) ) ;
#186057 = CARTESIAN_POINT ( 'NONE',  ( -21.53943276465977519, -0.05219959533937600094, 83.75109039468568994 ) ) ;
#186058 = VERTEX_POINT ( 'NONE', #158124 ) ;
#186059 = CARTESIAN_POINT ( 'NONE',  ( 0.05219959533907565091, 21.53943276465977519, 64.99890960531435269 ) ) ;
#186060 = CARTESIAN_POINT ( 'NONE',  ( 18.62759615963271287, -10.81492255796078972, 28.33224293864769550 ) ) ;
#186061 = CARTESIAN_POINT ( 'NONE',  ( 16.51473224551069308, 9.474510206698969483, 39.16557627198103120 ) ) ;
#186062 = CARTESIAN_POINT ( 'NONE',  ( -8.314922557961024197, 14.29746914071037800, 102.9177570613523756 ) ) ;
#186063 = CARTESIAN_POINT ( 'NONE',  ( -16.46253265017160317, 9.564922557960807481, 50.83224293864770260 ) ) ;
#186064 = CARTESIAN_POINT ( 'NONE',  ( -16.55341960407617563, 4.379528057220093196, 28.54275706135234358 ) ) ;
#186065 = CARTESIAN_POINT ( 'NONE',  ( 9.474510206698729675, 16.51473224551082808, 82.08442372801899012 ) ) ;
#186066 = CARTESIAN_POINT ( 'NONE',  ( -5.823673210054431948, 21.52544592524334988, 112.7094237280190328 ) ) ;
#186067 = CARTESIAN_POINT ( 'NONE',  ( 12.14591786802309770, 12.06949235617756955, 54.37390960531435979 ) ) ;
#186068 = CARTESIAN_POINT ( 'NONE',  ( -21.53943276465977519, 0.05219959533907696930, 101.2489096053143669 ) ) ;
#186069 = CARTESIAN_POINT ( 'NONE',  ( 18.62759615963271287, -10.81492255796078972, 98.33224293864769550 ) ) ;
#186070 = CARTESIAN_POINT ( 'NONE',  ( 16.31925111598454592, -7.325300261831587001, 97.66424538967254421 ) ) ;
#186071 = CARTESIAN_POINT ( 'NONE',  ( -15.72974639402197994, 15.80617190586746368, 50.62390960531435979 ) ) ;
#186072 = CARTESIAN_POINT ( 'NONE',  ( 4.379528057220092307, 16.55341960407617563, 77.29275706135234714 ) ) ;
#186073 = CARTESIAN_POINT ( 'NONE',  ( -16.52544592524342804, 4.483927247898546575, 96.04057627198102409 ) ) ;
#186074 = CARTESIAN_POINT ( 'NONE',  ( 16.51473224551069308, 9.474510206698969483, 44.16557627198103120 ) ) ;
#186075 = SURFACE_STYLE_USAGE ( .BOTH. , #122388 ) ;
#186076 = CARTESIAN_POINT ( 'NONE',  ( -19.36337904590692460, 5.499999999999952927, 50.41494137495620009 ) ) ;
#186077 = CARTESIAN_POINT ( 'NONE',  ( -16.52544592524335698, -4.483927247898792601, 103.9594237280190185 ) ) ;
#186078 = CARTESIAN_POINT ( 'NONE',  ( 15.72974639402176855, 15.80617190586768217, 26.87609039468567218 ) ) ;
#186079 = CARTESIAN_POINT ( 'NONE',  ( -19.03943276465977164, 0.05219959533909376836, 91.24890960531436690 ) ) ;
#186080 = CARTESIAN_POINT ( 'NONE',  ( -0.05219959533937732626, 21.53943276465977519, 62.50109039468568284 ) ) ;
#186081 = DIRECTION ( 'NONE',  ( -0.8660254037844410391, 0.000000000000000000, 0.4999999999999958367 ) ) ;
#186082 = CARTESIAN_POINT ( 'NONE',  ( 13.97604488694527802, 13.89961937509977652, 24.37390960531435624 ) ) ;
#186083 = ORIENTED_EDGE ( 'NONE', *, *, #116452, .T. ) ;
#186084 = CARTESIAN_POINT ( 'NONE',  ( -18.62759615963255300, -10.81492255796106328, 54.16775706135235424 ) ) ;
#186086 = CARTESIAN_POINT ( 'NONE',  ( -9.474510206698964154, 16.51473224551069663, 110.4155762719810383 ) ) ;
#186085 = CARTESIAN_POINT ( 'NONE',  ( -5.153800228976328057, -19.02544592524343514, 52.29057627198100988 ) ) ;
#186087 = CARTESIAN_POINT ( 'NONE',  ( 13.89961937509977652, -13.97604488694527269, 93.12390960531436690 ) ) ;
#186088 = CARTESIAN_POINT ( 'NONE',  ( -19.03943276465977164, -0.05219959533935918106, 68.75109039468566152 ) ) ;
#186089 = CARTESIAN_POINT ( 'NONE',  ( 21.52544592524334988, 5.823673210054432836, 46.45942372801901854 ) ) ;
#186090 = CARTESIAN_POINT ( 'NONE',  ( 16.51473224551083163, -9.474510206698727899, 100.8344237280190043 ) ) ;
#186091 = CARTESIAN_POINT ( 'NONE',  ( -5.049401038297874678, -19.05341960407617918, 59.79275706135231871 ) ) ;
#186092 = CARTESIAN_POINT ( 'NONE',  ( 5.049401038298161559, -19.05341960407611168, 37.70724293864768839 ) ) ;
#186093 = CARTESIAN_POINT ( 'NONE',  ( 16.55341960407618274, -4.379528057220086978, 106.0427570613523471 ) ) ;
#186094 = CARTESIAN_POINT ( 'NONE',  ( 16.46253265017146816, 9.564922557961045513, 76.66775706135234714 ) ) ;
#186095 = CARTESIAN_POINT ( 'NONE',  ( 4.379528057220339221, -16.55341960407611168, 27.70724293864769905 ) ) ;
#186096 = CARTESIAN_POINT ( 'NONE',  ( -5.049401038297874678, -19.05341960407617918, 44.79275706135232582 ) ) ;
#186097 = CARTESIAN_POINT ( 'NONE',  ( -10.72451020669870658, -18.67979575497194134, 104.5844237280190185 ) ) ;
#186098 = CARTESIAN_POINT ( 'NONE',  ( -19.03943276465977164, -0.05219959533935918106, 23.75109039468566152 ) ) ;
#186099 = CARTESIAN_POINT ( 'NONE',  ( 19.05341960407611168, 5.049401038298154454, 23.95724293864769194 ) ) ;
#186100 = CARTESIAN_POINT ( 'NONE',  ( -18.67979575497193778, 10.72451020669871902, 93.33442372801901854 ) ) ;
#186101 = CARTESIAN_POINT ( 'NONE',  ( -0.05219959533934338120, 16.53943276465976808, 32.50109039468568284 ) ) ;
#186102 = ADVANCED_FACE ( 'NONE', ( #100435 ), #38779, .T. ) ;
#186103 = CARTESIAN_POINT ( 'NONE',  ( -13.97604488694527625, -13.89961937509977652, 86.87390960531436690 ) ) ;
#186104 = DIRECTION ( 'NONE',  ( 0.000000000000000000, 0.000000000000000000, 1.000000000000000000 ) ) ;
#186105 = CARTESIAN_POINT ( 'NONE',  ( 5.049401038298161559, -19.05341960407611168, 82.70724293864770971 ) ) ;
#186106 = CARTESIAN_POINT ( 'NONE',  ( -17.72517630441457470, 5.499999999999976907, 95.92175719257602395 ) ) ;
#186107 = CARTESIAN_POINT ( 'NONE',  ( 9.564922557961047289, -16.46253265017146816, 85.41775706135233293 ) ) ;
#186108 = CARTESIAN_POINT ( 'NONE',  ( -16.46253265017160317, 9.564922557960807481, 105.8322429386476955 ) ) ;
#186109 = CARTESIAN_POINT ( 'NONE',  ( -10.81492255796105439, 18.62759615963255655, 97.91775706135236135 ) ) ;
#186110 = CARTESIAN_POINT ( 'NONE',  ( -12.14591786802309592, -12.06949235617757132, 96.87390960531436690 ) ) ;
#186111 = CARTESIAN_POINT ( 'NONE',  ( 23.62199046085592613, -10.84149981712626065, 165.9137635136254403 ) ) ;
#186112 = CARTESIAN_POINT ( 'NONE',  ( 10.81492255796078972, 18.62759615963270932, 59.58224293864770260 ) ) ;
#186113 =( BOUNDED_SURFACE ( )  B_SPLINE_SURFACE ( 1, 2, ( 
 ( #89029, #118385, #150720, #26387, #128774, #99443, #180079, #97428, #72889, #114609, #84266, #149714, #134557, #192470, #68109, #56713, #41548, #27383, #160126, #103211, #52935, #104205, #57714, #181067, #35781, #176307, #5432, #119384, #145947, #37779, #164893, #11213, #129761, #113606, #196245, #42542, #135552, #165886, #12219, #161123, #7428, #159114, #73882, #20608, #130778, #143952, #197224, #58686, #175300, #67116, #82260, #190473, #51946, #36766, #21614, #83272, #144946, #6427, #191457, #168835, #90022, #199195, #32333, #155666, #30340, #93986, #74861, #15172, #47506, #63662, #153675, #92987, #60663, #122336, #76831, #123321, #75836, #109162, #78815, #45509, #16168, #138503, #200184, #14168, #182048, #61653, #91981, #17162, #28384, #151705, #107164, #140494, #13198, #169842, #1982, #185014, #198204, #46500, #154673, #43531, #105196 ),
 ( #108160, #136523, #31336, #166883, #59675, #121347, #77822, #183040, #170842, #44523, #62649, #139491, #106179, #90992, #167862, #973, #124326, #29362, #152679, #137514, #184027, #186024, #66628, #94984, #128292, #114112, #189009, #156669, #19152, #3957, #141491, #36281, #98946, #160636, #158637, #65636, #189990, #110157, #126316, #172836, #145457, #21124, #50484, #33323, #82780, #187033, #20128, #159629, #2975, #51465, #144461, #5946, #112144, #49483, #18164, #34315, #48503, #113126, #127296, #22127, #175815, #64654, #80801, #142479, #171836, #79820, #37288, #81772, #143459, #67623, #173836, #35302, #97936, #129283, #4944, #157662, #174816, #190978, #83778, #188013, #52455, #96957, #6939, #125335, #111146, #95978, #8966, #38295, #149467, #55455, #70635, #25147, #194983, #162631, #146452, #71627, #9967, #165640, #56461, #72636, #132301 ) ),
 .UNSPECIFIED., .F., .F., .F. ) 
 B_SPLINE_SURFACE_WITH_KNOTS ( ( 2, 2 ),
 ( 3, 2, 2, 2, 2, 2, 2, 2, 2, 2, 2, 2, 2, 2, 2, 2, 2, 2, 2, 2, 2, 2, 2, 2, 2, 2, 2, 2, 2, 2, 2, 2, 2, 2, 2, 2, 2, 2, 2, 2, 2, 2, 2, 2, 2, 2, 2, 2, 2, 2, 3 ),
 ( 0.000000000000000000, 1.000000000000000000 ),
 ( 0.000000000000000000, 0.02000000000000000042, 0.04000000000000000083, 0.05999999999999999778, 0.08000000000000000167, 0.1000000000000000056, 0.1199999999999999956, 0.1400000000000000133, 0.1600000000000000033, 0.1799999999999999933, 0.2000000000000000111, 0.2200000000000000011, 0.2399999999999999911, 0.2600000000000000089, 0.2800000000000000266, 0.2999999999999999889, 0.3200000000000000067, 0.3400000000000000244, 0.3599999999999999867, 0.3800000000000000044, 0.4000000000000000222, 0.4199999999999999845, 0.4400000000000000022, 0.4600000000000000200, 0.4799999999999999822, 0.5000000000000000000, 0.5200000000000000178, 0.5400000000000000355, 0.5600000000000000533, 0.5799999999999999600, 0.5999999999999999778, 0.6199999999999999956, 0.6400000000000000133, 0.6600000000000000311, 0.6800000000000000488, 0.6999999999999999556, 0.7199999999999999734, 0.7399999999999999911, 0.7600000000000000089, 0.7800000000000000266, 0.8000000000000000444, 0.8199999999999999512, 0.8399999999999999689, 0.8599999999999999867, 0.8800000000000000044, 0.9000000000000000222, 0.9200000000000000400, 0.9399999999999999467, 0.9599999999999999645, 0.9799999999999999822, 1.000000000000000000 ),
 .UNSPECIFIED. ) 
 GEOMETRIC_REPRESENTATION_ITEM ( )  RATIONAL_B_SPLINE_SURFACE ( (
 ( 1.000000000000000000, 0.9510565162951535312, 1.000000000000000000, 0.9510565162951535312, 1.000000000000000000, 0.9510565162951535312, 1.000000000000000000, 0.9510565162951535312, 1.000000000000000000, 0.9510565162951535312, 1.000000000000000000, 0.9510565162951535312, 1.000000000000000000, 0.9510565162951535312, 1.000000000000000000, 0.9510565162951535312, 1.000000000000000000, 0.9510565162951535312, 1.000000000000000000, 0.9510565162951535312, 1.000000000000000000, 0.9510565162951535312, 1.000000000000000000, 0.9510565162951535312, 1.000000000000000000, 0.9510565162951535312, 1.000000000000000000, 0.9510565162951535312, 1.000000000000000000, 0.9510565162951535312, 1.000000000000000000, 0.9510565162951535312, 1.000000000000000000, 0.9510565162951535312, 1.000000000000000000, 0.9510565162951535312, 1.000000000000000000, 0.9510565162951535312, 1.000000000000000000, 0.9510565162951535312, 1.000000000000000000, 0.9510565162951535312, 1.000000000000000000, 0.9510565162951535312, 1.000000000000000000, 0.9510565162951535312, 1.000000000000000000, 0.9510565162951535312, 1.000000000000000000, 0.9510565162951535312, 1.000000000000000000, 0.9510565162951535312, 1.000000000000000000, 0.9510565162951535312, 1.000000000000000000, 0.9510565162951535312, 1.000000000000000000, 0.9510565162951535312, 1.000000000000000000, 0.9510565162951535312, 1.000000000000000000, 0.9510565162951535312, 1.000000000000000000, 0.9510565162951535312, 1.000000000000000000, 0.9510565162951535312, 1.000000000000000000, 0.9510565162951535312, 1.000000000000000000, 0.9510565162951535312, 1.000000000000000000, 0.9510565162951535312, 1.000000000000000000, 0.9510565162951535312, 1.000000000000000000, 0.9510565162951535312, 1.000000000000000000, 0.9510565162951535312, 1.000000000000000000, 0.9510565162951535312, 1.000000000000000000, 0.9510565162951535312, 1.000000000000000000, 0.9510565162951535312, 1.000000000000000000, 0.9510565162951535312, 1.000000000000000000, 0.9510565162951535312, 1.000000000000000000, 0.9510565162951535312, 1.000000000000000000, 0.9510565162951535312, 1.000000000000000000, 0.9510565162951535312, 1.000000000000000000, 0.9510565162951535312, 1.000000000000000000, 0.9510565162951535312, 1.000000000000000000, 0.9510565162951535312, 1.000000000000000000),
 ( 1.000000000000000000, 0.9510565162951535312, 1.000000000000000000, 0.9510565162951535312, 1.000000000000000000, 0.9510565162951535312, 1.000000000000000000, 0.9510565162951535312, 1.000000000000000000, 0.9510565162951535312, 1.000000000000000000, 0.9510565162951535312, 1.000000000000000000, 0.9510565162951535312, 1.000000000000000000, 0.9510565162951535312, 1.000000000000000000, 0.9510565162951535312, 1.000000000000000000, 0.9510565162951535312, 1.000000000000000000, 0.9510565162951535312, 1.000000000000000000, 0.9510565162951535312, 1.000000000000000000, 0.9510565162951535312, 1.000000000000000000, 0.9510565162951535312, 1.000000000000000000, 0.9510565162951535312, 1.000000000000000000, 0.9510565162951535312, 1.000000000000000000, 0.9510565162951535312, 1.000000000000000000, 0.9510565162951535312, 1.000000000000000000, 0.9510565162951535312, 1.000000000000000000, 0.9510565162951535312, 1.000000000000000000, 0.9510565162951535312, 1.000000000000000000, 0.9510565162951535312, 1.000000000000000000, 0.9510565162951535312, 1.000000000000000000, 0.9510565162951535312, 1.000000000000000000, 0.9510565162951535312, 1.000000000000000000, 0.9510565162951535312, 1.000000000000000000, 0.9510565162951535312, 1.000000000000000000, 0.9510565162951535312, 1.000000000000000000, 0.9510565162951535312, 1.000000000000000000, 0.9510565162951535312, 1.000000000000000000, 0.9510565162951535312, 1.000000000000000000, 0.9510565162951535312, 1.000000000000000000, 0.9510565162951535312, 1.000000000000000000, 0.9510565162951535312, 1.000000000000000000, 0.9510565162951535312, 1.000000000000000000, 0.9510565162951535312, 1.000000000000000000, 0.9510565162951535312, 1.000000000000000000, 0.9510565162951535312, 1.000000000000000000, 0.9510565162951535312, 1.000000000000000000, 0.9510565162951535312, 1.000000000000000000, 0.9510565162951535312, 1.000000000000000000, 0.9510565162951535312, 1.000000000000000000, 0.9510565162951535312, 1.000000000000000000, 0.9510565162951535312, 1.000000000000000000, 0.9510565162951535312, 1.000000000000000000, 0.9510565162951535312, 1.000000000000000000, 0.9510565162951535312, 1.000000000000000000, 0.9510565162951535312, 1.000000000000000000, 0.9510565162951535312, 1.000000000000000000, 0.9510565162951535312, 1.000000000000000000) ) ) 
 REPRESENTATION_ITEM ( '' )  SURFACE ( )  );
#186114 = CARTESIAN_POINT ( 'NONE',  ( -0.05219959533907301413, -21.53943276465977519, 37.49890960531436690 ) ) ;
#186115 = CARTESIAN_POINT ( 'NONE',  ( 8.224510206698953496, -14.34966873604960469, 112.9155762719810383 ) ) ;
#186116 = CYLINDRICAL_SURFACE ( 'NONE', #108006, 38.00000000000000000 ) ;
#186117 = CARTESIAN_POINT ( 'NONE',  ( 19.05341960407617918, -5.049401038297876454, 51.04275706135231871 ) ) ;
#186118 = CARTESIAN_POINT ( 'NONE',  ( 0.05219959533910956823, 16.53943276465976808, 44.99890960531435979 ) ) ;
#186119 = CARTESIAN_POINT ( 'NONE',  ( 15.72974639402199770, -15.80617190586745480, 23.12390960531436335 ) ) ;
#186120 = CARTESIAN_POINT ( 'NONE',  ( -18.62759615963255300, -10.81492255796106328, 74.16775706135231871 ) ) ;
#186121 = CARTESIAN_POINT ( 'NONE',  ( -0.05219959533907301413, -21.53943276465977519, 67.49890960531436690 ) ) ;
#186122 = CARTESIAN_POINT ( 'NONE',  ( -5.823673210054431948, 21.52544592524334988, 47.70942372801902565 ) ) ;
#186123 = CARTESIAN_POINT ( 'NONE',  ( -21.52544592524343514, 5.823673210054127303, 96.04057627198102409 ) ) ;
#186124 = CARTESIAN_POINT ( 'NONE',  ( 21.55341960407619695, -5.719274019375665929, 51.04275706135234714 ) ) ;
#186125 = CARTESIAN_POINT ( 'NONE',  ( -19.03943276465977164, 0.05219959533909376836, 26.24890960531435624 ) ) ;
#186126 = EDGE_CURVE ( 'NONE', #146762, #1415, #85260, .T. ) ;
#186127 = CARTESIAN_POINT ( 'NONE',  ( -13.97604488694527625, -13.89961937509977652, 81.87390960531436690 ) ) ;
#186128 = CARTESIAN_POINT ( 'NONE',  ( -14.34966873604972548, 8.224510206698743886, 78.33442372801901854 ) ) ;
#186129 = CARTESIAN_POINT ( 'NONE',  ( 14.29746914071049879, -8.314922557960816363, 103.3322429386476955 ) ) ;
#186130 = CARTESIAN_POINT ( 'NONE',  ( 2.973862142520697471, -93.04182470242776049, -4.999999999999999112 ) ) ;
#186131 = CARTESIAN_POINT ( 'NONE',  ( 4.379528057220339221, -16.55341960407611168, 52.70724293864769550 ) ) ;
#186132 = CARTESIAN_POINT ( 'NONE',  ( 12.14591786802327356, -12.06949235617739191, 110.6260903946857042 ) ) ;
#186133 = CARTESIAN_POINT ( 'NONE',  ( 16.51473224551069308, 9.474510206698969483, 69.16557627198102409 ) ) ;
#186134 = CARTESIAN_POINT ( 'NONE',  ( -5.049401038298153566, 19.05341960407611168, 35.20724293864768839 ) ) ;
#186135 = CARTESIAN_POINT ( 'NONE',  ( -5.719274019375978568, 21.55341960407610458, 50.20724293864769550 ) ) ;
#186136 = CARTESIAN_POINT ( 'NONE',  ( 16.46253265017146816, 9.564922557961045513, 41.66775706135234003 ) ) ;
#186138 = CARTESIAN_POINT ( 'NONE',  ( 4.483927247898545687, 16.52544592524342804, 54.79057627198104541 ) ) ;
#186137 = DIRECTION ( 'NONE',  ( 0.000000000000000000, 0.000000000000000000, 1.000000000000000000 ) ) ;
#186139 = CARTESIAN_POINT ( 'NONE',  ( 21.55341960407610458, 5.719274019375980345, 28.95724293864769905 ) ) ;
#186140 = CARTESIAN_POINT ( 'NONE',  ( -18.62759615963255300, -10.81492255796106328, 59.16775706135234714 ) ) ;
#186141 = CARTESIAN_POINT ( 'NONE',  ( 2.500000000000000000, -2.357898499370432610, 3.252606517456513302E-15 ) ) ;
#186142 = CARTESIAN_POINT ( 'NONE',  ( 12.06949235617739724, 12.14591786802326823, 66.87609039468568994 ) ) ;
#186143 = CARTESIAN_POINT ( 'NONE',  ( -5.153800228976607833, 19.02544592524334988, 57.70942372801899012 ) ) ;
#186144 = CARTESIAN_POINT ( 'NONE',  ( -8.314922557960811034, -14.29746914071050412, 42.08224293864769550 ) ) ;
#186145 = CARTESIAN_POINT ( 'NONE',  ( 17.05116617787822264, -6.768360034955866134, 51.15675553259197983 ) ) ;
#186146 = CARTESIAN_POINT ( 'NONE',  ( 4.379528057220339221, -16.55341960407611168, 32.70724293864770260 ) ) ;
#186147 = CARTESIAN_POINT ( 'NONE',  ( 19.05341960407611168, 5.049401038298154454, 38.95724293864767418 ) ) ;
#186148 = CARTESIAN_POINT ( 'NONE',  ( 19.03943276465977164, -0.05219959533909143690, 63.74890960531435979 ) ) ;
#186149 = CARTESIAN_POINT ( 'NONE',  ( -12.06949235617756955, 12.14591786802309770, 115.6239096053143669 ) ) ;
#186150 = CARTESIAN_POINT ( 'NONE',  ( -21.55341960407619339, 5.719274019375674811, 33.54275706135234714 ) ) ;
#186151 = CARTESIAN_POINT ( 'NONE',  ( -13.97604488694527625, -13.89961937509977652, 56.87390960531434558 ) ) ;
#186152 = DIRECTION ( 'NONE',  ( -0.000000000000000000, 0.000000000000000000, 1.000000000000000000 ) ) ;
#186153 = CARTESIAN_POINT ( 'NONE',  ( 5.049401038298161559, -19.05341960407611168, 47.70724293864770260 ) ) ;
#186154 = CARTESIAN_POINT ( 'NONE',  ( 21.53943276465977519, -0.05219959533907433946, 38.74890960531435979 ) ) ;
#186155 = B_SPLINE_CURVE_WITH_KNOTS ( 'NONE', 3,
 ( #10126, #162791, #38456, #72802, #165802, #147637, #25310, #103125, #55615, #23290, #84934, #196157, #27299, #24300, #86952, #193140, #71786, #88946, #9126, #57630, #70792, #119297, #146615, #132460, #8107, #69785, #7098, #148636, #131453, #133456, #116287, #195146 ),
 .UNSPECIFIED., .F., .F.,
 ( 4, 2, 2, 2, 2, 2, 2, 2, 2, 2, 2, 2, 2, 2, 2, 4 ),
 ( 1.644325935668032048E-15, 0.0003712461730052168583, 0.0007424923460087894155, 0.001113738519012361919, 0.001484984692015934530, 0.002227477038023092330, 0.002598723211026664724, 0.002969969384030237119, 0.003341215557033808646, 0.003712461730037381041, 0.004083707903040952568, 0.004454954076044524529, 0.004826200249048096490, 0.005197446422051668451, 0.005568692595055240412, 0.005939938768058812373 ),
 .UNSPECIFIED. ) ;
#186157 = CARTESIAN_POINT ( 'NONE',  ( -16.52544592524342804, 4.483927247898546575, 116.0405762719810383 ) ) ;
#186156 = CARTESIAN_POINT ( 'NONE',  ( 10.81492255796106328, -18.62759615963255655, 55.41775706135234714 ) ) ;
#186158 = CARTESIAN_POINT ( 'NONE',  ( -18.67979575497178146, -10.72451020669898902, 21.66557627198102409 ) ) ;
#186159 = CARTESIAN_POINT ( 'NONE',  ( -14.29746914071037622, -8.314922557961029526, 89.16775706135236135 ) ) ;
#186160 = CARTESIAN_POINT ( 'NONE',  ( -5.719274019375665041, -21.55341960407619695, 99.79275706135234714 ) ) ;
#186161 = CARTESIAN_POINT ( 'NONE',  ( 16.53943276465976808, 0.05219959533934440121, 61.25109039468567573 ) ) ;
#186162 = CARTESIAN_POINT ( 'NONE',  ( -13.97604488694527625, -13.89961937509977652, 106.8739096053143669 ) ) ;
#186163 = CARTESIAN_POINT ( 'NONE',  ( 16.52544592524335698, 4.483927247898782831, 56.45942372801902565 ) ) ;
#186164 = CARTESIAN_POINT ( 'NONE',  ( 16.52544592524335698, 4.483927247898782831, 31.45942372801901854 ) ) ;
#186165 = CARTESIAN_POINT ( 'NONE',  ( 12.14591786802327356, -12.06949235617739191, 100.6260903946857184 ) ) ;
#186166 = CARTESIAN_POINT ( 'NONE',  ( 21.55341960407619695, -5.719274019375665929, 51.04275706135234714 ) ) ;
#186167 = CARTESIAN_POINT ( 'NONE',  ( 4.379528057220092307, 16.55341960407617563, 27.29275706135234358 ) ) ;
#186168 = CARTESIAN_POINT ( 'NONE',  ( -5.823673210054116645, -21.52544592524344225, 112.2905762719810241 ) ) ;
#186169 = CARTESIAN_POINT ( 'NONE',  ( -16.52544592524335698, -4.483927247898792601, 23.95942372801901143 ) ) ;
#186170 = CARTESIAN_POINT ( 'NONE',  ( 14.29746914071037800, 8.314922557961029526, 81.66775706135236135 ) ) ;
#186171 = CARTESIAN_POINT ( 'NONE',  ( 11.74264578624799427, 36.14014761921585972, -4.349999994537626868 ) ) ;
#186172 = CARTESIAN_POINT ( 'NONE',  ( 21.52544592524334988, 5.823673210054432836, 86.45942372801901854 ) ) ;
#186173 = CARTESIAN_POINT ( 'NONE',  ( -9.474510206698720793, -16.51473224551083518, 84.58442372801900433 ) ) ;
#186174 = CARTESIAN_POINT ( 'NONE',  ( 14.29746914071049879, -8.314922557960816363, 48.33224293864770260 ) ) ;
#186175 = CARTESIAN_POINT ( 'NONE',  ( 4.379528057220339221, -16.55341960407611168, 47.70724293864770260 ) ) ;
#186176 = CARTESIAN_POINT ( 'NONE',  ( -0.05219959533910754901, -16.53943276465976808, 102.4989096053143811 ) ) ;
#186178 = CARTESIAN_POINT ( 'NONE',  ( 17.26058549869107850, -6.457015423128172671, 56.12254162523934298 ) ) ;
#186177 = CARTESIAN_POINT ( 'NONE',  ( -9.474510206698720793, -16.51473224551083518, 49.58442372801899722 ) ) ;
#186179 = CARTESIAN_POINT ( 'NONE',  ( -21.53943276465977519, -0.05219959533937600094, 48.75109039468568284 ) ) ;
#186180 = CARTESIAN_POINT ( 'NONE',  ( 16.51473224551083163, -9.474510206698727899, 105.8344237280190043 ) ) ;
#186181 = FACE_OUTER_BOUND ( 'NONE', #60520, .T. ) ;
#186182 = CARTESIAN_POINT ( 'NONE',  ( -9.474510206698964154, 16.51473224551069663, 100.4155762719810241 ) ) ;
#186183 = CARTESIAN_POINT ( 'NONE',  ( 0.05219959533907565091, 21.53943276465977519, 54.99890960531435269 ) ) ;
#186184 = CARTESIAN_POINT ( 'NONE',  ( -5.153800228976607833, 19.02544592524334988, 92.70942372801901854 ) ) ;
#186185 = CARTESIAN_POINT ( 'NONE',  ( -13.97604488694527625, -13.89961937509977652, 86.87390960531436690 ) ) ;
#186186 = CARTESIAN_POINT ( 'NONE',  ( -5.719274019375978568, 21.55341960407610458, 60.20724293864768839 ) ) ;
#186187 = CARTESIAN_POINT ( 'NONE',  ( 4.483927247898545687, 16.52544592524342804, 109.7905762719810383 ) ) ;
#186188 = CARTESIAN_POINT ( 'NONE',  ( 5.153800228976335163, 19.02544592524342804, 64.79057627198100988 ) ) ;
#186189 = CARTESIAN_POINT ( 'NONE',  ( -13.97604488694527625, -13.89961937509977652, 26.87390960531434558 ) ) ;
#186190 = VECTOR ( 'NONE', #198117, 1000.000000000000000 ) ;
#186191 = CARTESIAN_POINT ( 'NONE',  ( -18.62759615963255300, -10.81492255796106328, 34.16775706135234714 ) ) ;
#186192 = CARTESIAN_POINT ( 'NONE',  ( -15.80617190586768217, 15.72974639402176855, 93.12609039468568994 ) ) ;
#186193 = CARTESIAN_POINT ( 'NONE',  ( 8.224510206698742110, 14.34966873604972548, 92.08442372801901854 ) ) ;
#186194 = CARTESIAN_POINT ( 'NONE',  ( -18.62759615963255300, -10.81492255796106328, 29.16775706135234003 ) ) ;
#186195 = CARTESIAN_POINT ( 'NONE',  ( 18.67979575497194134, -10.72451020669871369, 45.83442372801901854 ) ) ;
#186197 = CARTESIAN_POINT ( 'NONE',  ( -9.564922557960796823, -16.46253265017161027, 82.08224293864768129 ) ) ;
#186196 = CARTESIAN_POINT ( 'NONE',  ( 9.474510206698729675, 16.51473224551082808, 67.08442372801900433 ) ) ;
#186198 = CARTESIAN_POINT ( 'NONE',  ( 10.81492255796106328, -18.62759615963255655, 90.41775706135236135 ) ) ;
#186199 = CARTESIAN_POINT ( 'NONE',  ( -18.67979575497178146, -10.72451020669898902, 81.66557627198103830 ) ) ;
#186200 = CARTESIAN_POINT ( 'NONE',  ( 16.55341960407611168, 4.379528057220329451, 58.95724293864770971 ) ) ;
#186201 = CARTESIAN_POINT ( 'NONE',  ( 5.719274019375673035, 21.55341960407619339, 107.2927570613523471 ) ) ;
#186202 = CARTESIAN_POINT ( 'NONE',  ( 12.06949235617757843, -12.14591786802309237, 83.12390960531436690 ) ) ;
#186203 = CARTESIAN_POINT ( 'NONE',  ( -16.51473224551069308, -9.474510206698971260, 31.66557627198102054 ) ) ;
#186204 = CARTESIAN_POINT ( 'NONE',  ( 13.97604488694548053, -13.89961937509957401, 75.62609039468564731 ) ) ;
#186205 = CARTESIAN_POINT ( 'NONE',  ( 12.06949235617757843, -12.14591786802309237, 33.12390960531435979 ) ) ;
#186207 = EDGE_CURVE ( 'NONE', #16981, #191214, #174302, .T. ) ;
#186206 = CARTESIAN_POINT ( 'NONE',  ( 18.62759615963255655, 10.81492255796105972, 91.66775706135234714 ) ) ;
#186208 = CARTESIAN_POINT ( 'NONE',  ( -5.153800228976328057, -19.02544592524343514, 92.29057627198099567 ) ) ;
#186209 = CARTESIAN_POINT ( 'NONE',  ( -19.05341960407617563, 5.049401038297882671, 63.54275706135234003 ) ) ;
#186210 = CARTESIAN_POINT ( 'NONE',  ( 10.81492255796078972, 18.62759615963270932, 69.58224293864769550 ) ) ;
#186211 = CARTESIAN_POINT ( 'NONE',  ( 21.53943276465977519, 0.05219959533937863772, 21.25109039468567218 ) ) ;
#186212 = CARTESIAN_POINT ( 'NONE',  ( 9.564922557961047289, -16.46253265017146816, 105.4177570613523471 ) ) ;
#186213 = CARTESIAN_POINT ( 'NONE',  ( -0.05219959533934338120, 16.53943276465976808, 82.50109039468568994 ) ) ;
#186215 = CARTESIAN_POINT ( 'NONE',  ( -21.55341960407619339, 5.719274019375674811, 23.54275706135235424 ) ) ;
#186214 = DIRECTION ( 'NONE',  ( -1.000000000000000000, -0.000000000000000000, -0.000000000000000000 ) ) ;
#186216 = CARTESIAN_POINT ( 'NONE',  ( 12.06949235617757843, -12.14591786802309237, 103.1239096053143811 ) ) ;
#186217 = CARTESIAN_POINT ( 'NONE',  ( -22.81625015709510507, 31.40387420917330275, -7.424999997268812990 ) ) ;
#186218 = CARTESIAN_POINT ( 'NONE',  ( 4.379528057220092307, 16.55341960407617563, 52.29275706135236135 ) ) ;
#186219 = CARTESIAN_POINT ( 'NONE',  ( -18.62759615963270932, 10.81492255796079327, 65.83224293864769550 ) ) ;
#186220 = CARTESIAN_POINT ( 'NONE',  ( 12.06949235617739724, 12.14591786802326823, 101.8760903946857042 ) ) ;
#186221 = CARTESIAN_POINT ( 'NONE',  ( -8.224510206698735004, -14.34966873604973081, 34.58442372801900433 ) ) ;
#186222 = CARTESIAN_POINT ( 'NONE',  ( 19.02544592524343514, -5.153800228976328945, 28.54057627198102409 ) ) ;
#186223 = CARTESIAN_POINT ( 'NONE',  ( -16.52544592524335698, -4.483927247898792601, 78.95942372801901854 ) ) ;
#186224 = CARTESIAN_POINT ( 'NONE',  ( 9.564922557961047289, -16.46253265017146816, 75.41775706135234714 ) ) ;
#186225 = CARTESIAN_POINT ( 'NONE',  ( -21.55341960407610458, -5.719274019375992779, 76.45724293864769550 ) ) ;
#186226 = CARTESIAN_POINT ( 'NONE',  ( 16.55341960407618274, -4.379528057220086978, 91.04275706135236135 ) ) ;
#186227 = EDGE_CURVE ( 'NONE', #111780, #177280, #50374, .T. ) ;
#186228 = CARTESIAN_POINT ( 'NONE',  ( -15.72974639402176322, -15.80617190586768395, 79.37609039468567573 ) ) ;
#186229 = CARTESIAN_POINT ( 'NONE',  ( 5.719274019375991003, -21.55341960407610458, 67.70724293864769550 ) ) ;
#186230 = CARTESIAN_POINT ( 'NONE',  ( -10.72451020669898014, 18.67979575497178502, 50.41557627198103120 ) ) ;
#186231 = EDGE_LOOP ( 'NONE', ( #30660, #70711, #159906, #101206 ) ) ;
#186232 = ORIENTED_EDGE ( 'NONE', *, *, #96707, .T. ) ;
#186233 = CARTESIAN_POINT ( 'NONE',  ( 16.52544592524335698, 4.483927247898782831, 76.45942372801901854 ) ) ;
#186234 = CARTESIAN_POINT ( 'NONE',  ( 10.72451020669898902, -18.67979575497178502, 42.91557627198103120 ) ) ;
#186235 = ORIENTED_EDGE ( 'NONE', *, *, #109644, .F. ) ;
#186236 = CARTESIAN_POINT ( 'NONE',  ( 19.03943276465977164, -0.05219959533909143690, 113.7489096053143669 ) ) ;
#186237 = CARTESIAN_POINT ( 'NONE',  ( -23.88378066561469382, -7.642901331109204222, 172.4262957903898155 ) ) ;
#186238 = CARTESIAN_POINT ( 'NONE',  ( 19.05341960407611168, 5.049401038298154454, 23.95724293864769194 ) ) ;
#186239 = CARTESIAN_POINT ( 'NONE',  ( 18.62759615963271287, -10.81492255796078972, 68.33224293864769550 ) ) ;
#186240 = CARTESIAN_POINT ( 'NONE',  ( -14.34966873604972548, 8.224510206698743886, 103.3344237280190043 ) ) ;
#186241 = CARTESIAN_POINT ( 'NONE',  ( 0.05219959533937995610, -21.53943276465977519, 45.00109039468568284 ) ) ;
#186242 = CARTESIAN_POINT ( 'NONE',  ( -16.46253265017146816, -9.564922557961047289, 99.16775706135233293 ) ) ;
#186243 = CARTESIAN_POINT ( 'NONE',  ( 9.474510206698971260, -16.51473224551069308, 27.91557627198103120 ) ) ;
#186244 = CARTESIAN_POINT ( 'NONE',  ( -14.29746914071037622, -8.314922557961029526, 19.16775706135234714 ) ) ;
#186245 = CARTESIAN_POINT ( 'NONE',  ( 19.05341960407611168, 5.049401038298154454, 43.95724293864769550 ) ) ;
#186246 = CARTESIAN_POINT ( 'NONE',  ( 1.993301997531345292E-15, -30.30510711980685912, 142.4999999999999716 ) ) ;
#186247 = CARTESIAN_POINT ( 'NONE',  ( -0.05219959533909027116, -19.03943276465977164, 92.49890960531436690 ) ) ;
#186248 = CARTESIAN_POINT ( 'NONE',  ( 14.29746914071037800, 8.314922557961029526, 76.66775706135234714 ) ) ;
#186249 = CARTESIAN_POINT ( 'NONE',  ( -19.05341960407617563, 5.049401038297882671, 73.54275706135233293 ) ) ;
#186250 = CARTESIAN_POINT ( 'NONE',  ( -19.05341960407617563, 5.049401038297882671, 23.54275706135233648 ) ) ;
#186251 = CARTESIAN_POINT ( 'NONE',  ( -15.72974639402197994, 15.80617190586746368, 65.62390960531436690 ) ) ;
#186252 = CARTESIAN_POINT ( 'NONE',  ( 16.52544592524335698, 4.483927247898782831, 81.45942372801900433 ) ) ;
#186253 = CARTESIAN_POINT ( 'NONE',  ( -0.05219959533936034679, 19.03943276465977164, 82.50109039468567573 ) ) ;
#186254 = CARTESIAN_POINT ( 'NONE',  ( -19.03943276465977164, 0.05219959533909376836, 41.24890960531435269 ) ) ;
#186255 = CARTESIAN_POINT ( 'NONE',  ( -19.02544592524342804, 5.153800228976336051, 81.04057627198103830 ) ) ;
#186256 = CARTESIAN_POINT ( 'NONE',  ( -21.53943276465977519, -0.05219959533937600094, 53.75109039468568994 ) ) ;
#186257 = CARTESIAN_POINT ( 'NONE',  ( -16.51473224551069308, -9.474510206698971260, 51.66557627198102409 ) ) ;
#186258 = CARTESIAN_POINT ( 'NONE',  ( 13.97604488694548053, -13.89961937509957401, 75.62609039468564731 ) ) ;
#186259 = CARTESIAN_POINT ( 'NONE',  ( 26.38458505201419513, -8.641005086744103281, 167.3773361139121789 ) ) ;
#186260 = CARTESIAN_POINT ( 'NONE',  ( 9.564922557960805705, 16.46253265017160317, 104.5822429386476955 ) ) ;
#186261 = CARTESIAN_POINT ( 'NONE',  ( -8.224510206698948167, 14.34966873604960824, 60.41557627198102409 ) ) ;
#186262 = CARTESIAN_POINT ( 'NONE',  ( 15.80617190586746368, 15.72974639402197994, 54.37390960531435979 ) ) ;
#186263 = CARTESIAN_POINT ( 'NONE',  ( 19.50973618000807619, 5.499999999999992895, 102.5000000000000142 ) ) ;
#186264 = CARTESIAN_POINT ( 'NONE',  ( -9.474510206698720793, -16.51473224551083518, 39.58442372801899722 ) ) ;
#186266 = CARTESIAN_POINT ( 'NONE',  ( -0.05219959533909027116, -19.03943276465977164, 67.49890960531436690 ) ) ;
#186265 = CARTESIAN_POINT ( 'NONE',  ( -19.02544592524342804, 5.153800228976336051, 66.04057627198103830 ) ) ;
#186267 = CARTESIAN_POINT ( 'NONE',  ( 4.483927247898790824, -16.52544592524335698, 45.20942372801901854 ) ) ;
#186268 = CARTESIAN_POINT ( 'NONE',  ( 8.906447517083050158, 27.41122689804195645, 143.4000000000000057 ) ) ;
#186269 = CARTESIAN_POINT ( 'NONE',  ( 17.60728821186567217, -5.500000000000025757, 93.36690927743009638 ) ) ;
#186270 = CARTESIAN_POINT ( 'NONE',  ( -12.14591786802326823, 12.06949235617739902, 83.12609039468568994 ) ) ;
#186271 = CARTESIAN_POINT ( 'NONE',  ( 21.38418241377623019, 5.438282248597753110, 174.2683007571264113 ) ) ;
#186272 = CARTESIAN_POINT ( 'NONE',  ( 14.34966873604972726, -8.224510206698740333, 70.83442372801901854 ) ) ;
#186273 = CARTESIAN_POINT ( 'NONE',  ( -14.34966873604972548, 8.224510206698743886, 38.33442372801900433 ) ) ;
#186274 = CARTESIAN_POINT ( 'NONE',  ( 16.46253265017146816, 9.564922557961045513, 26.66775706135234003 ) ) ;
#186276 = DIRECTION ( 'NONE',  ( -1.000000000000000000, 0.000000000000000000, 0.000000000000000000 ) ) ;
#186275 = CARTESIAN_POINT ( 'NONE',  ( 9.564922557960805705, 16.46253265017160317, 54.58224293864769550 ) ) ;
#186277 = CARTESIAN_POINT ( 'NONE',  ( -0.05219959533937732626, 21.53943276465977519, 57.50109039468568994 ) ) ;
#186278 = CARTESIAN_POINT ( 'NONE',  ( -19.03943276465977164, -0.05219959533935918106, 63.75109039468566863 ) ) ;
#186279 = CARTESIAN_POINT ( 'NONE',  ( -15.80617190586768217, 15.72974639402176855, 113.1260903946856899 ) ) ;
#186280 = CARTESIAN_POINT ( 'NONE',  ( -19.03943276465977164, 0.05219959533909376836, 26.24890960531435624 ) ) ;
#186281 = CARTESIAN_POINT ( 'NONE',  ( 16.22749556775600865, 7.364991527249977743, 23.15813903950547825 ) ) ;
#186282 = CARTESIAN_POINT ( 'NONE',  ( -0.05219959533907301413, -21.53943276465977519, 72.49890960531435269 ) ) ;
#186283 = CARTESIAN_POINT ( 'NONE',  ( 21.52544592524344225, -5.823673210054117533, 23.54057627198102765 ) ) ;
#186284 = CARTESIAN_POINT ( 'NONE',  ( 8.224510206698953496, -14.34966873604960469, 97.91557627198103830 ) ) ;
#186285 = CARTESIAN_POINT ( 'NONE',  ( 16.53943276465976808, 0.05219959533934440121, 31.25109039468568639 ) ) ;
#186286 = CARTESIAN_POINT ( 'NONE',  ( 16.52544592524342804, -4.483927247898539470, 28.54057627198103120 ) ) ;
#186287 = VERTEX_POINT ( 'NONE', #70112 ) ;
#186288 = CARTESIAN_POINT ( 'NONE',  ( -10.81492255796078084, -18.62759615963271287, 112.0822429386477097 ) ) ;
#186290 = CARTESIAN_POINT ( 'NONE',  ( 23.48529157249600630, -32.32473071737749137, -9.300000000000002487 ) ) ;
#186289 = CARTESIAN_POINT ( 'NONE',  ( -16.55341960407611168, -4.379528057220339221, 36.45724293864768839 ) ) ;
#186291 = CARTESIAN_POINT ( 'NONE',  ( 19.05341960407617918, -5.049401038297876454, 111.0427570613523329 ) ) ;
#186292 = CARTESIAN_POINT ( 'NONE',  ( 5.153800228976615827, -19.02544592524334988, 20.20942372801899722 ) ) ;
#186293 = CARTESIAN_POINT ( 'NONE',  ( -12.06949235617756955, 12.14591786802309770, 25.62390960531435624 ) ) ;
#186294 = CARTESIAN_POINT ( 'NONE',  ( -5.719274019375978568, 21.55341960407610458, 100.2072429386476955 ) ) ;
#186296 = CARTESIAN_POINT ( 'NONE',  ( -15.72974639402197994, 15.80617190586746368, 65.62390960531436690 ) ) ;
#186295 = CARTESIAN_POINT ( 'NONE',  ( 17.48847506799968343, 5.747544572773804816, 31.67302562156722345 ) ) ;
#186297 = CARTESIAN_POINT ( 'NONE',  ( -9.564922557960796823, -16.46253265017161027, 77.08224293864769550 ) ) ;
#186298 = CARTESIAN_POINT ( 'NONE',  ( -14.34966873604960291, -8.224510206698953496, 51.66557627198102409 ) ) ;
#186299 = CARTESIAN_POINT ( 'NONE',  ( 13.97604488694527802, 13.89961937509977652, 84.37390960531433848 ) ) ;
#186300 = DIRECTION ( 'NONE',  ( -1.000000000000000000, 0.000000000000000000, 0.000000000000000000 ) ) ;
#186301 = CARTESIAN_POINT ( 'NONE',  ( -16.51473224551082808, 9.474510206698731452, 58.33442372801900433 ) ) ;
#186302 = CARTESIAN_POINT ( 'NONE',  ( 21.53943276465977519, -0.05219959533907433946, 93.74890960531436690 ) ) ;
#186303 = CARTESIAN_POINT ( 'NONE',  ( -8.224510206698948167, 14.34966873604960824, 100.4155762719810241 ) ) ;
#186304 = CARTESIAN_POINT ( 'NONE',  ( -21.55341960407619339, 5.719274019375674811, 33.54275706135234714 ) ) ;
#186305 = CARTESIAN_POINT ( 'NONE',  ( 27.73933785331498214, 9.013057229001095294, 141.9750000027311501 ) ) ;
#186306 = CARTESIAN_POINT ( 'NONE',  ( 12.06949235617757843, -12.14591786802309237, 28.12390960531435979 ) ) ;
#186307 = CARTESIAN_POINT ( 'NONE',  ( 19.05341960407611168, 5.049401038298154454, 33.95724293864769550 ) ) ;
#186308 = CARTESIAN_POINT ( 'NONE',  ( -13.89961937509977652, 13.97604488694528158, 80.62390960531436690 ) ) ;
#186309 = CARTESIAN_POINT ( 'NONE',  ( -5.719274019375978568, 21.55341960407610458, 65.20724293864768129 ) ) ;
#186310 = CARTESIAN_POINT ( 'NONE',  ( -18.22780087662122028, 5.500000000000031086, 83.51540105326107266 ) ) ;
#186311 = CARTESIAN_POINT ( 'NONE',  ( -16.51473224551069308, -9.474510206698971260, 26.66557627198103120 ) ) ;
#186312 = CARTESIAN_POINT ( 'NONE',  ( -21.55341960407610458, -5.719274019375992779, 51.45724293864770260 ) ) ;
#186313 = CARTESIAN_POINT ( 'NONE',  ( -10.72451020669870658, -18.67979575497194134, 74.58442372801901854 ) ) ;
#186315 = CARTESIAN_POINT ( 'NONE',  ( -8.224510206698735004, -14.34966873604973081, 64.58442372801900433 ) ) ;
#186314 = CARTESIAN_POINT ( 'NONE',  ( 22.83040865997484303, -30.22555755525017673, -21.93998231254684583 ) ) ;
#186316 = CARTESIAN_POINT ( 'NONE',  ( -0.05219959533909027116, -19.03943276465977164, 52.49890960531436690 ) ) ;
#186317 = CARTESIAN_POINT ( 'NONE',  ( -16.46253265017160317, 9.564922557960807481, 60.83224293864769550 ) ) ;
#186318 = ORIENTED_EDGE ( 'NONE', *, *, #100439, .T. ) ;
#186319 = CARTESIAN_POINT ( 'NONE',  ( -19.02544592524334988, -5.153800228976617603, 28.95942372801900433 ) ) ;
#186320 = CARTESIAN_POINT ( 'NONE',  ( 14.34966873604972726, -8.224510206698740333, 70.83442372801901854 ) ) ;
#186321 = CARTESIAN_POINT ( 'NONE',  ( -18.67979575497193778, 10.72451020669871902, 93.33442372801901854 ) ) ;
#186322 = CARTESIAN_POINT ( 'NONE',  ( 5.153800228976335163, 19.02544592524342804, 74.79057627198103830 ) ) ;
#186323 = CARTESIAN_POINT ( 'NONE',  ( 10.72451020669898902, -18.67979575497178502, 37.91557627198102409 ) ) ;
#186324 = CARTESIAN_POINT ( 'NONE',  ( -19.03943276465977164, -0.05219959533935918106, 113.7510903946856757 ) ) ;
#186325 = CARTESIAN_POINT ( 'NONE',  ( -5.823673210054431948, 21.52544592524334988, 87.70942372801901854 ) ) ;
#186326 = CARTESIAN_POINT ( 'NONE',  ( -16.55341960407617563, 4.379528057220093196, 43.54275706135235424 ) ) ;
#186327 = CARTESIAN_POINT ( 'NONE',  ( -10.81492255796078084, -18.62759615963271287, 102.0822429386476955 ) ) ;
#186328 = CARTESIAN_POINT ( 'NONE',  ( -5.049401038297874678, -19.05341960407617918, 109.7927570613523187 ) ) ;
#186329 = CARTESIAN_POINT ( 'NONE',  ( -9.474510206698964154, 16.51473224551069663, 75.41557627198103830 ) ) ;
#186330 = CARTESIAN_POINT ( 'NONE',  ( -19.05341960407617563, 5.049401038297882671, 113.5427570613523471 ) ) ;
#186331 = CARTESIAN_POINT ( 'NONE',  ( 9.474510206698971260, -16.51473224551069308, 42.91557627198103120 ) ) ;
#186332 = AXIS2_PLACEMENT_3D ( 'NONE', #43466, #102142, #25328 ) ;
#186333 = CARTESIAN_POINT ( 'NONE',  ( -8.314922557961024197, 14.29746914071037800, 22.91775706135235069 ) ) ;
#186334 = CARTESIAN_POINT ( 'NONE',  ( -4.483927247898539470, -16.52544592524342804, 67.29057627198103830 ) ) ;
#186335 = CARTESIAN_POINT ( 'NONE',  ( 12.14591786802327356, -12.06949235617739191, 70.62609039468567573 ) ) ;
#186337 = CARTESIAN_POINT ( 'NONE',  ( 16.51473224551069308, 9.474510206698969483, 54.16557627198103120 ) ) ;
#186336 = CARTESIAN_POINT ( 'NONE',  ( -15.72974639402176322, -15.80617190586768395, 29.37609039468568284 ) ) ;
#186338 = CARTESIAN_POINT ( 'NONE',  ( -16.51473224551069308, -9.474510206698971260, 66.66557627198102409 ) ) ;
#186339 = CARTESIAN_POINT ( 'NONE',  ( 16.53943276465976808, 0.05219959533934440121, 76.25109039468568994 ) ) ;
#186341 = ORIENTED_EDGE ( 'NONE', *, *, #121605, .T. ) ;
#186340 = CARTESIAN_POINT ( 'NONE',  ( -21.81230582904511550, -5.969922009378025862, 172.1979875755928049 ) ) ;
#186342 = ORIENTED_EDGE ( 'NONE', *, *, #86135, .T. ) ;
#186343 = CARTESIAN_POINT ( 'NONE',  ( -16.46253265017146816, -9.564922557961047289, 24.16775706135233648 ) ) ;
#186344 = CIRCLE ( 'NONE', #163687, 214.0437394197456342 ) ;
#186345 = CARTESIAN_POINT ( 'NONE',  ( 19.02544592524343514, -5.153800228976328945, 38.54057627198103120 ) ) ;
#186347 = VERTEX_POINT ( 'NONE', #98419 ) ;
#186346 = CARTESIAN_POINT ( 'NONE',  ( 16.46253265017160672, -9.564922557960803928, 98.33224293864769550 ) ) ;
#186348 = CARTESIAN_POINT ( 'NONE',  ( 8.224510206698742110, 14.34966873604972548, 27.08442372801901854 ) ) ;
#186350 = CARTESIAN_POINT ( 'NONE',  ( -4.483927247898782831, 16.52544592524335698, 37.70942372801900433 ) ) ;
#186349 = CARTESIAN_POINT ( 'NONE',  ( -5.153800228976607833, 19.02544592524334988, 62.70942372801899722 ) ) ;
#186351 = CARTESIAN_POINT ( 'NONE',  ( -9.564922557960796823, -16.46253265017161027, 37.08224293864768839 ) ) ;
#186352 = CARTESIAN_POINT ( 'NONE',  ( -5.049401038298153566, 19.05341960407611168, 105.2072429386476671 ) ) ;
#186353 = CARTESIAN_POINT ( 'NONE',  ( 19.02544592524343514, -5.153800228976328945, 58.54057627198102409 ) ) ;
#186354 = CARTESIAN_POINT ( 'NONE',  ( 21.52544592524344225, -5.823673210054117533, 103.5405762719810383 ) ) ;
#186356 = CARTESIAN_POINT ( 'NONE',  ( -16.51473224551069308, -9.474510206698971260, 111.6655762719810383 ) ) ;
#186355 = CARTESIAN_POINT ( 'NONE',  ( -16.46253265017160317, 9.564922557960807481, 90.83224293864769550 ) ) ;
#186357 = CARTESIAN_POINT ( 'NONE',  ( -19.02544592524342804, 5.153800228976336051, 61.04057627198103120 ) ) ;
#186359 = CARTESIAN_POINT ( 'NONE',  ( -22.00000000000000000, -1.163414459189985801E-14, 95.00000000000000000 ) ) ;
#186358 = CARTESIAN_POINT ( 'NONE',  ( 12.14591786802327356, -12.06949235617739191, 110.6260903946857042 ) ) ;
#186360 = CARTESIAN_POINT ( 'NONE',  ( -19.05341960407617563, 5.049401038297882671, 103.5427570613523329 ) ) ;
#186361 = CARTESIAN_POINT ( 'NONE',  ( 16.46253265017146816, 9.564922557961045513, 21.66775706135233648 ) ) ;
#186362 = CARTESIAN_POINT ( 'NONE',  ( 0.05219959533910956823, 16.53943276465976808, 54.99890960531435269 ) ) ;
#186363 = CARTESIAN_POINT ( 'NONE',  ( 18.67979575497194134, -10.72451020669871369, 100.8344237280190185 ) ) ;
#186364 = CARTESIAN_POINT ( 'NONE',  ( 19.02544592524343514, -5.153800228976328945, 43.54057627198103120 ) ) ;
#186365 = EDGE_CURVE ( 'NONE', #184655, #36039, #144936, .T. ) ;
#186367 = CARTESIAN_POINT ( 'NONE',  ( -21.53943276465977519, -0.05219959533937600094, 83.75109039468568994 ) ) ;
#186366 = CARTESIAN_POINT ( 'NONE',  ( 16.55341960407611168, 4.379528057220329451, 23.95724293864769550 ) ) ;
#186368 = CARTESIAN_POINT ( 'NONE',  ( 16.46253265017160672, -9.564922557960803928, 78.33224293864769550 ) ) ;
#186369 = CARTESIAN_POINT ( 'NONE',  ( -13.97604488694527625, -13.89961937509977652, 91.87390960531432427 ) ) ;
#186370 = CARTESIAN_POINT ( 'NONE',  ( -12.14591786802309592, -12.06949235617757132, 96.87390960531436690 ) ) ;
#186371 = CARTESIAN_POINT ( 'NONE',  ( 12.14591786802309770, 12.06949235617756955, 54.37390960531435979 ) ) ;
#186372 = CARTESIAN_POINT ( 'NONE',  ( -18.62759615963270932, 10.81492255796079327, 70.83224293864770971 ) ) ;
#186373 = CARTESIAN_POINT ( 'NONE',  ( 0.05219959533909260263, 19.03943276465977164, 69.99890960531435269 ) ) ;
#186374 = CARTESIAN_POINT ( 'NONE',  ( -18.62759615963270932, 10.81492255796079327, 85.83224293864768129 ) ) ;
#186375 = CARTESIAN_POINT ( 'NONE',  ( 19.05341960407617918, -5.049401038297876454, 81.04275706135231871 ) ) ;
#186377 = CARTESIAN_POINT ( 'NONE',  ( 0.05219959533910956823, 16.53943276465976808, 89.99890960531438111 ) ) ;
#186376 = CARTESIAN_POINT ( 'NONE',  ( 18.56197773271732387, -5.499999999999896971, 46.05066217314453070 ) ) ;
#186379 = CARTESIAN_POINT ( 'NONE',  ( -16.51473224551069308, -9.474510206698971260, 56.66557627198103120 ) ) ;
#186378 = VECTOR ( 'NONE', #28188, 1000.000000000000000 ) ;
#186380 = CARTESIAN_POINT ( 'NONE',  ( -0.05219959533907301413, -21.53943276465977519, 72.49890960531435269 ) ) ;
#186381 = CARTESIAN_POINT ( 'NONE',  ( 17.48847506799967633, -5.747544572773779059, 28.32697437843280497 ) ) ;
#186383 = DIRECTION ( 'NONE',  ( -0.1736481776669307198, -2.126576849575776229E-17, -0.9848077530122080203 ) ) ;
#186382 = CARTESIAN_POINT ( 'NONE',  ( 0.05219959533910956823, 16.53943276465976808, 24.99890960531435624 ) ) ;
#186384 = CARTESIAN_POINT ( 'NONE',  ( -9.474510206698720793, -16.51473224551083518, 109.5844237280190043 ) ) ;
#186385 = CARTESIAN_POINT ( 'NONE',  ( 16.55341960407611168, 4.379528057220329451, 83.95724293864770971 ) ) ;
#186386 = B_SPLINE_CURVE_WITH_KNOTS ( 'NONE', 3,
 ( #4190, #160884, #115385, #65869, #177073, #130529 ),
 .UNSPECIFIED., .F., .F.,
 ( 4, 2, 4 ),
 ( 0.003239945802372268171, 0.003620412082092120364, 0.004000878361811972990 ),
 .UNSPECIFIED. ) ;
#186387 = CARTESIAN_POINT ( 'NONE',  ( -19.34837522270366250, -5.499999999999798383, 95.86337684832578532 ) ) ;
#186388 = CARTESIAN_POINT ( 'NONE',  ( 19.03943276465977164, -0.05219959533909143690, 73.74890960531435269 ) ) ;
#186389 = CARTESIAN_POINT ( 'NONE',  ( 16.51473224551069308, 9.474510206698969483, 34.16557627198102409 ) ) ;
#186390 = CARTESIAN_POINT ( 'NONE',  ( -16.52544592524342804, 4.483927247898546575, 66.04057627198103830 ) ) ;
#186391 = CARTESIAN_POINT ( 'NONE',  ( 5.153800228976335163, 19.02544592524342804, 99.79057627198102409 ) ) ;
#186393 = CARTESIAN_POINT ( 'NONE',  ( -5.153800228976328057, -19.02544592524343514, 72.29057627198102409 ) ) ;
#186392 = CARTESIAN_POINT ( 'NONE',  ( -19.02544592524334988, -5.153800228976617603, 83.95942372801901854 ) ) ;
#186394 = CARTESIAN_POINT ( 'NONE',  ( -16.51473224551069308, -9.474510206698971260, 91.66557627198103830 ) ) ;
#186395 = CARTESIAN_POINT ( 'NONE',  ( -10.72451020669898014, 18.67979575497178502, 75.41557627198102409 ) ) ;
#186396 = CARTESIAN_POINT ( 'NONE',  ( 4.379528057220092307, 16.55341960407617563, 77.29275706135234714 ) ) ;
#186397 = CARTESIAN_POINT ( 'NONE',  ( 9.564922557961047289, -16.46253265017146816, 110.4177570613523471 ) ) ;
#186398 = CARTESIAN_POINT ( 'NONE',  ( -19.02544592524342804, 5.153800228976336051, 61.04057627198103120 ) ) ;
#186399 = CARTESIAN_POINT ( 'NONE',  ( -21.52544592524343514, 5.823673210054127303, 66.04057627198103830 ) ) ;
#186400 = CARTESIAN_POINT ( 'NONE',  ( 13.97604488694548053, -13.89961937509957401, 95.62609039468563310 ) ) ;
#186402 = CARTESIAN_POINT ( 'NONE',  ( -10.72451020669870658, -18.67979575497194134, 39.58442372801901143 ) ) ;
#186401 = CARTESIAN_POINT ( 'NONE',  ( 4.483927247898545687, 16.52544592524342804, 44.79057627198103120 ) ) ;
#186403 = CARTESIAN_POINT ( 'NONE',  ( 23.31738231874054890, -16.94106989632523508, 145.0500000054623513 ) ) ;
#186405 = CARTESIAN_POINT ( 'NONE',  ( -5.153800228976328057, -19.02544592524343514, 112.2905762719810099 ) ) ;
#186404 = CARTESIAN_POINT ( 'NONE',  ( 4.483927247898790824, -16.52544592524335698, 70.20942372801904696 ) ) ;
#186406 = DIRECTION ( 'NONE',  ( -0.000000000000000000, -0.000000000000000000, -1.000000000000000000 ) ) ;
#186407 = CYLINDRICAL_SURFACE ( 'NONE', #116444, 5.000000000000004441 ) ;
#186408 = CARTESIAN_POINT ( 'NONE',  ( -12.14591786802326823, 12.06949235617739902, 88.12609039468570415 ) ) ;
#186409 = CARTESIAN_POINT ( 'NONE',  ( 16.53943276465976808, 0.05219959533934440121, 46.25109039468567573 ) ) ;
#186410 = CARTESIAN_POINT ( 'NONE',  ( -16.46253265017160317, 9.564922557960807481, 55.83224293864769550 ) ) ;
#186411 = CARTESIAN_POINT ( 'NONE',  ( 13.97604488694527802, 13.89961937509977652, 59.37390960531434558 ) ) ;
#186412 = CARTESIAN_POINT ( 'NONE',  ( -18.67979575497193778, 10.72451020669871902, 53.33442372801901854 ) ) ;
#186413 = CARTESIAN_POINT ( 'NONE',  ( 14.29746914071037800, 8.314922557961029526, 66.66775706135234714 ) ) ;
#186414 = CARTESIAN_POINT ( 'NONE',  ( 14.34966873604960469, 8.224510206698951720, 39.16557627198102409 ) ) ;
#186415 = CARTESIAN_POINT ( 'NONE',  ( 9.564922557960805705, 16.46253265017160317, 44.58224293864769550 ) ) ;
#186416 = CARTESIAN_POINT ( 'NONE',  ( -5.049401038298153566, 19.05341960407611168, 35.20724293864768839 ) ) ;
#186418 = VERTEX_POINT ( 'NONE', #128764 ) ;
#186417 = CARTESIAN_POINT ( 'NONE',  ( -8.314922557961024197, 14.29746914071037800, 32.91775706135234714 ) ) ;
#186419 = CARTESIAN_POINT ( 'NONE',  ( -13.97604488694547697, 13.89961937509957934, 78.12609039468567573 ) ) ;
#186420 = CARTESIAN_POINT ( 'NONE',  ( 0.05219959533910956823, 16.53943276465976808, 89.99890960531438111 ) ) ;
#186421 = CARTESIAN_POINT ( 'NONE',  ( 19.05341960407611168, 5.049401038298154454, 53.95724293864770260 ) ) ;
#186423 = CARTESIAN_POINT ( 'NONE',  ( -38.00000000000001421, -12.34694845685042708, -9.899999999999998579 ) ) ;
#186422 = CARTESIAN_POINT ( 'NONE',  ( 16.46253265017146816, 9.564922557961045513, 91.66775706135234714 ) ) ;
#186424 = CARTESIAN_POINT ( 'NONE',  ( 15.72974639402176855, 15.80617190586768217, 86.87609039468568994 ) ) ;
#186425 = CARTESIAN_POINT ( 'NONE',  ( 14.34966873604972726, -8.224510206698740333, 55.83442372801901854 ) ) ;
#186426 = CARTESIAN_POINT ( 'NONE',  ( 16.20579543436681291, 7.371946100354972664, 38.06520834171877965 ) ) ;
#186427 = CARTESIAN_POINT ( 'NONE',  ( -15.72974639402197994, 15.80617190586746368, 45.62390960531436690 ) ) ;
#186428 = CARTESIAN_POINT ( 'NONE',  ( -16.52544592524335698, -4.483927247898792601, 43.95942372801902565 ) ) ;
#186429 = CARTESIAN_POINT ( 'NONE',  ( -5.153800228976328057, -19.02544592524343514, 32.29057627198102409 ) ) ;
#186430 = CARTESIAN_POINT ( 'NONE',  ( 9.564922557961047289, -16.46253265017146816, 30.41775706135232937 ) ) ;
#186431 = CARTESIAN_POINT ( 'NONE',  ( -13.97604488694527625, -13.89961937509977652, 71.87390960531433848 ) ) ;
#186432 = FACE_OUTER_BOUND ( 'NONE', #29005, .T. ) ;
#186433 = CARTESIAN_POINT ( 'NONE',  ( 0.05219959533909260263, 19.03943276465977164, 54.99890960531435979 ) ) ;
#186434 = CARTESIAN_POINT ( 'NONE',  ( 14.91361452257043929, 15.22666363356478492, -56.46021433273639900 ) ) ;
#186435 = CARTESIAN_POINT ( 'NONE',  ( -5.153800228976328057, -19.02544592524343514, 67.29057627198102409 ) ) ;
#186436 = CARTESIAN_POINT ( 'NONE',  ( -19.39720447994795904, -5.499999999999977796, 54.66317477297177874 ) ) ;
#186437 = CARTESIAN_POINT ( 'NONE',  ( 19.02544592524334988, 5.153800228976608722, 36.45942372801900433 ) ) ;
#186438 = CARTESIAN_POINT ( 'NONE',  ( -0.05219959533937732626, 21.53943276465977519, 112.5010903946857042 ) ) ;
#186439 = CARTESIAN_POINT ( 'NONE',  ( -16.53943276465976808, 0.05219959533911058130, 41.24890960531435269 ) ) ;
#186440 = CARTESIAN_POINT ( 'NONE',  ( -9.564922557960796823, -16.46253265017161027, 42.08224293864769550 ) ) ;
#186441 = CARTESIAN_POINT ( 'NONE',  ( 9.564922557960805705, 16.46253265017160317, 104.5822429386476955 ) ) ;
#186442 = CARTESIAN_POINT ( 'NONE',  ( 15.72974639402176855, 15.80617190586768217, 71.87609039468568994 ) ) ;
#186443 = CARTESIAN_POINT ( 'NONE',  ( 16.51473224551069308, 9.474510206698969483, 54.16557627198103120 ) ) ;
#186444 = CARTESIAN_POINT ( 'NONE',  ( 10.72451020669871369, 18.67979575497193778, 82.08442372801901854 ) ) ;
#186445 = CARTESIAN_POINT ( 'NONE',  ( -15.72974639402197994, 15.80617190586746368, 25.62390960531435624 ) ) ;
#186446 = CARTESIAN_POINT ( 'NONE',  ( 13.89961937509977652, -13.97604488694527269, 33.12390960531434558 ) ) ;
#186447 = CARTESIAN_POINT ( 'NONE',  ( 18.67979575497194134, -10.72451020669871369, 20.83442372801901143 ) ) ;
#186448 = CARTESIAN_POINT ( 'NONE',  ( 5.049401038297881783, 19.05341960407617563, 47.29275706135231161 ) ) ;
#186449 = CARTESIAN_POINT ( 'NONE',  ( -0.05219959533909027116, -19.03943276465977164, 27.49890960531435624 ) ) ;
#186450 = CARTESIAN_POINT ( 'NONE',  ( 0.05219959533909260263, 19.03943276465977164, 74.99890960531435269 ) ) ;
#186451 = CARTESIAN_POINT ( 'NONE',  ( -16.51473224551082808, 9.474510206698731452, 108.3344237280190043 ) ) ;
#186452 = CARTESIAN_POINT ( 'NONE',  ( 14.34966873604960469, 8.224510206698951720, 79.16557627198103830 ) ) ;
#186453 = CARTESIAN_POINT ( 'NONE',  ( 15.72974639402199770, -15.80617190586745480, 38.12390960531436690 ) ) ;
#186454 = CARTESIAN_POINT ( 'NONE',  ( 5.049401038297881783, 19.05341960407617563, 102.2927570613523045 ) ) ;
#186455 = CARTESIAN_POINT ( 'NONE',  ( -21.55341960407610458, -5.719274019375992779, 111.4572429386476813 ) ) ;
#186456 = CARTESIAN_POINT ( 'NONE',  ( -15.72974639402176322, -15.80617190586768395, 59.37609039468568284 ) ) ;
#186457 = CARTESIAN_POINT ( 'NONE',  ( 14.34966873604972726, -8.224510206698740333, 55.83442372801901854 ) ) ;
#186458 = CARTESIAN_POINT ( 'NONE',  ( -8.224510206698735004, -14.34966873604973081, 54.58442372801901143 ) ) ;
#186459 = CARTESIAN_POINT ( 'NONE',  ( 10.72451020669898902, -18.67979575497178502, 72.91557627198103830 ) ) ;
#186460 = CARTESIAN_POINT ( 'NONE',  ( -13.97604488694527625, -13.89961937509977652, 46.87390960531435979 ) ) ;
#186461 = CARTESIAN_POINT ( 'NONE',  ( -8.224510206698735004, -14.34966873604973081, 94.58442372801901854 ) ) ;
#186462 = B_SPLINE_CURVE_WITH_KNOTS ( 'NONE', 3,
 ( #156390, #182768, #17894, #121074, #13900, #75566, #137242, #122067, #45245, #106899 ),
 .UNSPECIFIED., .F., .F.,
 ( 4, 2, 2, 2, 4 ),
 ( 2.459394992999530923E-17, 0.0001682128350528851516, 0.0003364256701057457459, 0.0005046385051586063132, 0.0006728513402114668805 ),
 .UNSPECIFIED. ) ;
#186463 = CARTESIAN_POINT ( 'NONE',  ( -15.72974639402197994, 15.80617190586746368, 100.6239096053143811 ) ) ;
#186464 = CARTESIAN_POINT ( 'NONE',  ( -14.29746914071049879, 8.314922557960819915, 50.83224293864770971 ) ) ;
#186465 = CARTESIAN_POINT ( 'NONE',  ( -5.153800228976328057, -19.02544592524343514, 82.29057627198103830 ) ) ;
#186466 = CARTESIAN_POINT ( 'NONE',  ( 8.224510206698742110, 14.34966873604972548, 82.08442372801901854 ) ) ;
#186467 = CARTESIAN_POINT ( 'NONE',  ( 15.72974639402176855, 15.80617190586768217, 51.87609039468568284 ) ) ;
#186468 = CARTESIAN_POINT ( 'NONE',  ( -8.224510206698735004, -14.34966873604973081, 24.58442372801901499 ) ) ;
#186469 = CARTESIAN_POINT ( 'NONE',  ( 21.55341960407610458, 5.719274019375980345, 113.9572429386477239 ) ) ;
#186470 = CARTESIAN_POINT ( 'NONE',  ( -4.379528057220328563, 16.55341960407611168, 50.20724293864769550 ) ) ;
#186471 = ORIENTED_EDGE ( 'NONE', *, *, #65570, .T. ) ;
#186472 = CARTESIAN_POINT ( 'NONE',  ( 18.56197773271728835, -5.499999999999983125, 91.05066217314453070 ) ) ;
#186473 = CARTESIAN_POINT ( 'NONE',  ( 15.72974639402199770, -15.80617190586745480, 93.12390960531436690 ) ) ;
#186474 = CARTESIAN_POINT ( 'NONE',  ( 4.379528057220092307, 16.55341960407617563, 112.2927570613523471 ) ) ;
#186475 = ORIENTED_EDGE ( 'NONE', *, *, #179869, .F. ) ;
#186476 = CARTESIAN_POINT ( 'NONE',  ( 2.200000000000000178, 0.000000000000000000, 0.000000000000000000 ) ) ;
#186477 = CARTESIAN_POINT ( 'NONE',  ( -21.52544592524343514, 5.823673210054127303, 111.0405762719810525 ) ) ;
#186478 = CARTESIAN_POINT ( 'NONE',  ( -16.51473224551069308, -9.474510206698971260, 111.6655762719810383 ) ) ;
#186479 = CARTESIAN_POINT ( 'NONE',  ( -21.52544592524334988, -5.823673210054445271, 18.95942372801901143 ) ) ;
#186480 = CARTESIAN_POINT ( 'NONE',  ( 8.224510206698953496, -14.34966873604960469, 57.91557627198103120 ) ) ;
#186481 = CARTESIAN_POINT ( 'NONE',  ( 14.29746914071037800, 8.314922557961029526, 66.66775706135234714 ) ) ;
#186482 = AXIS2_PLACEMENT_3D ( 'NONE', #39526, #148719, #178058 ) ;
#186483 = CARTESIAN_POINT ( 'NONE',  ( 0.05219959533909260263, 19.03943276465977164, 64.99890960531436690 ) ) ;
#186484 = CARTESIAN_POINT ( 'NONE',  ( 0.05219959533936267826, -19.03943276465977164, 70.00109039468566152 ) ) ;
#186485 = CARTESIAN_POINT ( 'NONE',  ( 19.03943276465977164, -0.05219959533909143690, 78.74890960531436690 ) ) ;
#186486 = CARTESIAN_POINT ( 'NONE',  ( 10.72451020669898902, -18.67979575497178502, 32.91557627198102409 ) ) ;
#186487 = CARTESIAN_POINT ( 'NONE',  ( -33.23029939923285525, -20.96646023091586386, -17.75854212242423102 ) ) ;
#186488 = CARTESIAN_POINT ( 'NONE',  ( 16.51473224551069308, 9.474510206698969483, 44.16557627198103120 ) ) ;
#186489 = CARTESIAN_POINT ( 'NONE',  ( -16.53943276465976808, -0.05219959533934237506, 23.75109039468567929 ) ) ;
#186490 = CARTESIAN_POINT ( 'NONE',  ( 0.05219959533936267826, -19.03943276465977164, 65.00109039468567573 ) ) ;
#186491 = CARTESIAN_POINT ( 'NONE',  ( 21.52544592524344225, -5.823673210054117533, 98.54057627198105251 ) ) ;
#186492 = CARTESIAN_POINT ( 'NONE',  ( -4.483927247898539470, -16.52544592524342804, 32.29057627198102409 ) ) ;
#186493 = CARTESIAN_POINT ( 'NONE',  ( 5.153800228976335163, 19.02544592524342804, 94.79057627198103830 ) ) ;
#186494 = CARTESIAN_POINT ( 'NONE',  ( 21.52544592524344225, -5.823673210054117533, 53.54057627198103120 ) ) ;
#186496 = CARTESIAN_POINT ( 'NONE',  ( 16.52544592524335698, 4.483927247898782831, 26.45942372801901854 ) ) ;
#186495 = CARTESIAN_POINT ( 'NONE',  ( -15.72974639402197994, 15.80617190586746368, 100.6239096053143811 ) ) ;
#186497 = CARTESIAN_POINT ( 'NONE',  ( -5.719274019375978568, 21.55341960407610458, 30.20724293864769550 ) ) ;
#186498 = CARTESIAN_POINT ( 'NONE',  ( 15.72974639402176855, 15.80617190586768217, 86.87609039468568994 ) ) ;
#186499 = CARTESIAN_POINT ( 'NONE',  ( -19.03943276465977164, 0.05219959533909376836, 86.24890960531436690 ) ) ;
#186500 = CARTESIAN_POINT ( 'NONE',  ( -16.51473224551069308, -9.474510206698971260, 21.66557627198102765 ) ) ;
#186501 = CARTESIAN_POINT ( 'NONE',  ( 16.46253265017160672, -9.564922557960803928, 88.33224293864769550 ) ) ;
#186502 = CARTESIAN_POINT ( 'NONE',  ( 14.29746914071049879, -8.314922557960816363, 103.3322429386476955 ) ) ;
#186503 = CARTESIAN_POINT ( 'NONE',  ( -0.05219959533909027116, -19.03943276465977164, 67.49890960531436690 ) ) ;
#186504 = CARTESIAN_POINT ( 'NONE',  ( -4.483927247898782831, 16.52544592524335698, 22.70942372801901499 ) ) ;
#186505 = CARTESIAN_POINT ( 'NONE',  ( 1.500000000000008438, 22.80000000000002913, -57.83153971412246364 ) ) ;
#186506 = EDGE_CURVE ( 'NONE', #84987, #3247, #6418, .T. ) ;
#186507 = AXIS2_PLACEMENT_3D ( 'NONE', #61887, #32567, #65871 ) ;
#186509 = CARTESIAN_POINT ( 'NONE',  ( 0.05219959533909260263, 19.03943276465977164, 114.9989096053143669 ) ) ;
#186508 = CARTESIAN_POINT ( 'NONE',  ( -5.823673210054431948, 21.52544592524334988, 92.70942372801901854 ) ) ;
#186510 = CARTESIAN_POINT ( 'NONE',  ( 8.224510206698742110, 14.34966873604972548, 87.08442372801901854 ) ) ;
#186511 = CARTESIAN_POINT ( 'NONE',  ( 193.3062444957835453, -155.7167183371837496, -13.00000000000000000 ) ) ;
#186512 = CARTESIAN_POINT ( 'NONE',  ( 0.05219959533936267826, -19.03943276465977164, 75.00109039468566152 ) ) ;
#186513 = CARTESIAN_POINT ( 'NONE',  ( 16.51473224551083163, -9.474510206698727899, 35.83442372801899722 ) ) ;
#186514 = CARTESIAN_POINT ( 'NONE',  ( -17.12812012977024523, -6.668231424566069876, 46.35948759323146362 ) ) ;
#186515 = CARTESIAN_POINT ( 'NONE',  ( -9.564922557960796823, -16.46253265017161027, 32.08224293864769550 ) ) ;
#186516 = CARTESIAN_POINT ( 'NONE',  ( -16.55341960407611168, -4.379528057220339221, 36.45724293864768839 ) ) ;
#186517 = CARTESIAN_POINT ( 'NONE',  ( 13.89961937509977652, -13.97604488694527269, 23.12390960531436335 ) ) ;
#186518 = CARTESIAN_POINT ( 'NONE',  ( 16.52544592524342804, -4.483927247898539470, 33.54057627198102409 ) ) ;
#186519 = CARTESIAN_POINT ( 'NONE',  ( 22.34691611882956863, -20.25371774921029200, -51.27624273403993982 ) ) ;
#186520 = CARTESIAN_POINT ( 'NONE',  ( 16.55341960407618274, -4.379528057220086978, 96.04275706135236135 ) ) ;
#186521 = CARTESIAN_POINT ( 'NONE',  ( 9.474510206698971260, -16.51473224551069308, 42.91557627198103120 ) ) ;
#186522 = CARTESIAN_POINT ( 'NONE',  ( 5.719274019375673035, 21.55341960407619339, 97.29275706135234714 ) ) ;
#186523 = CARTESIAN_POINT ( 'NONE',  ( -13.89961937509957401, -13.97604488694547875, 104.3760903946856757 ) ) ;
#186524 = CARTESIAN_POINT ( 'NONE',  ( -18.67979575497193778, 10.72451020669871902, 83.33442372801903275 ) ) ;
#186525 = CARTESIAN_POINT ( 'NONE',  ( -0.05219959533936034679, 19.03943276465977164, 52.50109039468566863 ) ) ;
#186526 = CARTESIAN_POINT ( 'NONE',  ( -16.46253265017160317, 9.564922557960807481, 95.83224293864769550 ) ) ;
#186527 = CARTESIAN_POINT ( 'NONE',  ( 5.049401038298161559, -19.05341960407611168, 67.70724293864769550 ) ) ;
#186528 = CARTESIAN_POINT ( 'NONE',  ( 17.13100169013299023, 6.664070546373165094, 71.73210164300154190 ) ) ;
#186529 = CIRCLE ( 'NONE', #102523, 37.99626262588765968 ) ;
#186530 = CARTESIAN_POINT ( 'NONE',  ( 14.34966873604960469, 8.224510206698951720, 69.16557627198102409 ) ) ;
#186531 = CARTESIAN_POINT ( 'NONE',  ( 21.55341960407610458, 5.719274019375980345, 63.95724293864770260 ) ) ;
#186532 = CARTESIAN_POINT ( 'NONE',  ( -16.51473224551069308, -9.474510206698971260, 66.66557627198102409 ) ) ;
#186534 = CARTESIAN_POINT ( 'NONE',  ( 4.379528057220092307, 16.55341960407617563, 72.29275706135236135 ) ) ;
#186533 = CARTESIAN_POINT ( 'NONE',  ( -21.53943276465977519, 0.05219959533907696930, 81.24890960531436690 ) ) ;
#186535 = ORIENTED_EDGE ( 'NONE', *, *, #47794, .F. ) ;
#186536 = CARTESIAN_POINT ( 'NONE',  ( -5.153800228976328057, -19.02544592524343514, 52.29057627198100988 ) ) ;
#186538 = CARTESIAN_POINT ( 'NONE',  ( 36.91746824999999177, 2.880721459617395097E-14, -5.624999997268813168 ) ) ;
#186537 = CARTESIAN_POINT ( 'NONE',  ( 8.314922557960818139, 14.29746914071049879, 74.58224293864768129 ) ) ;
#186539 = CARTESIAN_POINT ( 'NONE',  ( -16.51473224551069308, -9.474510206698971260, 46.66557627198102409 ) ) ;
#186540 = CARTESIAN_POINT ( 'NONE',  ( -16.53943276465976808, 0.05219959533911058130, 111.2489096053143669 ) ) ;
#186541 = CARTESIAN_POINT ( 'NONE',  ( -16.51473224551082808, 9.474510206698731452, 68.33442372801900433 ) ) ;
#186542 = CARTESIAN_POINT ( 'NONE',  ( -8.224510206698948167, 14.34966873604960824, 85.41557627198102409 ) ) ;
#186543 = CARTESIAN_POINT ( 'NONE',  ( -5.719274019375665041, -21.55341960407619695, 39.79275706135235424 ) ) ;
#186545 = CARTESIAN_POINT ( 'NONE',  ( 15.72974639402199770, -15.80617190586745480, 108.1239096053143811 ) ) ;
#186544 = CARTESIAN_POINT ( 'NONE',  ( -5.153800228976328057, -19.02544592524343514, 32.29057627198102409 ) ) ;
#186546 = CARTESIAN_POINT ( 'NONE',  ( -3.573655867282028392E-15, 2.428612866367529932E-14, -15.00000000000000000 ) ) ;
#186547 = CARTESIAN_POINT ( 'NONE',  ( 12.14591786802309770, 12.06949235617756955, 94.37390960531436690 ) ) ;
#186548 = CARTESIAN_POINT ( 'NONE',  ( 26.72240360495968758, -29.37940146934077035, -20.20861161914950799 ) ) ;
#186549 = CARTESIAN_POINT ( 'NONE',  ( 13.89961937509977652, -13.97604488694527269, 43.12390960531434558 ) ) ;
#186550 = CARTESIAN_POINT ( 'NONE',  ( -10.85841070881430959, -12.25138988246575167, -61.49687578711335334 ) ) ;
#186552 = CARTESIAN_POINT ( 'NONE',  ( 19.03943276465977164, -0.05219959533909143690, 98.74890960531436690 ) ) ;
#186551 = CARTESIAN_POINT ( 'NONE',  ( 9.564922557961047289, -16.46253265017146816, 100.4177570613523329 ) ) ;
#186553 = CARTESIAN_POINT ( 'NONE',  ( 0.05219959533937995610, -21.53943276465977519, 35.00109039468568284 ) ) ;
#186554 = CARTESIAN_POINT ( 'NONE',  ( 16.46253265017160672, -9.564922557960803928, 83.33224293864768129 ) ) ;
#186555 = CARTESIAN_POINT ( 'NONE',  ( 19.03943276465977164, 0.05219959533936151252, 71.25109039468566152 ) ) ;
#186556 = CARTESIAN_POINT ( 'NONE',  ( 13.89961937509977652, -13.97604488694527269, 43.12390960531434558 ) ) ;
#186557 = CARTESIAN_POINT ( 'NONE',  ( 14.34966873604960469, 8.224510206698951720, 79.16557627198103830 ) ) ;
#186558 = CARTESIAN_POINT ( 'NONE',  ( 8.314922557960818139, 14.29746914071049879, 69.58224293864769550 ) ) ;
#186559 = CARTESIAN_POINT ( 'NONE',  ( -0.05219959533909027116, -19.03943276465977164, 77.49890960531435269 ) ) ;
#186560 = CARTESIAN_POINT ( 'NONE',  ( 21.55341960407610458, 5.719274019375980345, 103.9572429386476813 ) ) ;
#186561 = CARTESIAN_POINT ( 'NONE',  ( -16.46253265017160317, 9.564922557960807481, 65.83224293864769550 ) ) ;
#186562 = CARTESIAN_POINT ( 'NONE',  ( -21.53943276465977519, -0.05219959533937600094, 113.7510903946856757 ) ) ;
#186565 = CARTESIAN_POINT ( 'NONE',  ( 8.314922557960818139, 14.29746914071049879, 114.5822429386477097 ) ) ;
#186564 = CARTESIAN_POINT ( 'NONE',  ( 12.14591786802309770, 12.06949235617756955, 29.37390960531435269 ) ) ;
#186563 = CARTESIAN_POINT ( 'NONE',  ( 13.89961937509977652, -13.97604488694527269, 43.12390960531434558 ) ) ;
#186566 = CARTESIAN_POINT ( 'NONE',  ( 16.46253265017146816, 9.564922557961045513, 101.6677570613523329 ) ) ;
#186567 = VERTEX_POINT ( 'NONE', #160116 ) ;
#186568 = CARTESIAN_POINT ( 'NONE',  ( 5.823673210054444382, -21.52544592524334988, 25.20942372801901854 ) ) ;
#186569 = CARTESIAN_POINT ( 'NONE',  ( 19.05341960407617918, -5.049401038297876454, 61.04275706135232582 ) ) ;
#186570 = CARTESIAN_POINT ( 'NONE',  ( 16.52544592524342804, -4.483927247898539470, 28.54057627198103120 ) ) ;
#186571 = CARTESIAN_POINT ( 'NONE',  ( 21.55341960407610458, 5.719274019375980345, 68.95724293864769550 ) ) ;
#186572 = CARTESIAN_POINT ( 'NONE',  ( 5.823673210054125526, 21.52544592524343514, 24.79057627198103120 ) ) ;
#186573 = CARTESIAN_POINT ( 'NONE',  ( -8.314922557960811034, -14.29746914071050412, 52.08224293864768839 ) ) ;
#186574 = CARTESIAN_POINT ( 'NONE',  ( -16.46253265017160317, 9.564922557960807481, 25.83224293864769194 ) ) ;
#186575 = CARTESIAN_POINT ( 'NONE',  ( -5.049401038298153566, 19.05341960407611168, 50.20724293864770260 ) ) ;
#186576 = CARTESIAN_POINT ( 'NONE',  ( -9.564922557961040184, 16.46253265017147172, 27.91775706135232582 ) ) ;
#186577 = CARTESIAN_POINT ( 'NONE',  ( -4.483927247898782831, 16.52544592524335698, 87.70942372801901854 ) ) ;
#186578 = CARTESIAN_POINT ( 'NONE',  ( -8.224510206698735004, -14.34966873604973081, 59.58442372801901854 ) ) ;
#186579 = CARTESIAN_POINT ( 'NONE',  ( -15.80617190586745835, -15.72974639402198527, 26.87390960531435979 ) ) ;
#186580 = CARTESIAN_POINT ( 'NONE',  ( -10.81492255796105439, 18.62759615963255655, 112.9177570613523329 ) ) ;
#186581 = CARTESIAN_POINT ( 'NONE',  ( -5.153800228976328057, -19.02544592524343514, 77.29057627198099567 ) ) ;
#186582 = CARTESIAN_POINT ( 'NONE',  ( 12.06949235617739724, 12.14591786802326823, 66.87609039468568994 ) ) ;
#186583 = CARTESIAN_POINT ( 'NONE',  ( -8.224510206698948167, 14.34966873604960824, 105.4155762719810383 ) ) ;
#186584 = EDGE_CURVE ( 'NONE', #151987, #15377, #76186, .T. ) ;
#186585 = CARTESIAN_POINT ( 'NONE',  ( -16.52544592524335698, -4.483927247898792601, 108.9594237280190185 ) ) ;
#186586 = FACE_OUTER_BOUND ( 'NONE', #12187, .T. ) ;
#186589 = CARTESIAN_POINT ( 'NONE',  ( 9.474510206698971260, -16.51473224551069308, 72.91557627198102409 ) ) ;
#186588 = CARTESIAN_POINT ( 'NONE',  ( 5.049401038298161559, -19.05341960407611168, 97.70724293864766707 ) ) ;
#186587 = CARTESIAN_POINT ( 'NONE',  ( 21.55341960407619695, -5.719274019375665929, 66.04275706135236135 ) ) ;
#186590 = CARTESIAN_POINT ( 'NONE',  ( -0.05219959533909027116, -19.03943276465977164, 107.4989096053143527 ) ) ;
#186591 = CARTESIAN_POINT ( 'NONE',  ( -12.06949235617756955, 12.14591786802309770, 55.62390960531436690 ) ) ;
#186592 = CARTESIAN_POINT ( 'NONE',  ( 16.52544592524335698, 4.483927247898782831, 111.4594237280190328 ) ) ;
#186593 = CARTESIAN_POINT ( 'NONE',  ( -12.14591786802309592, -12.06949235617757132, 46.87390960531435979 ) ) ;
#186595 = DIRECTION ( 'NONE',  ( -1.000000000000000000, 0.000000000000000000, 0.000000000000000000 ) ) ;
#186594 = CARTESIAN_POINT ( 'NONE',  ( 12.06949235617739724, 12.14591786802326823, 46.87609039468568994 ) ) ;
#186596 = CARTESIAN_POINT ( 'NONE',  ( 5.153800228976615827, -19.02544592524334988, 35.20942372801899722 ) ) ;
#186597 = CARTESIAN_POINT ( 'NONE',  ( 19.02544592524343514, -5.153800228976328945, 73.54057627198103830 ) ) ;
#186598 = CARTESIAN_POINT ( 'NONE',  ( -19.05341960407617563, 5.049401038297882671, 48.54275706135233293 ) ) ;
#186599 = CARTESIAN_POINT ( 'NONE',  ( -19.02544592524334988, -5.153800228976617603, 58.95942372801900433 ) ) ;
#186601 = CARTESIAN_POINT ( 'NONE',  ( 8.314922557961029526, -14.29746914071037800, 85.41775706135236135 ) ) ;
#186600 = CARTESIAN_POINT ( 'NONE',  ( -19.02544592524334988, -5.153800228976617603, 103.9594237280190043 ) ) ;
#186602 = CARTESIAN_POINT ( 'NONE',  ( -5.153800228976328057, -19.02544592524343514, 27.29057627198103120 ) ) ;
#186603 = CARTESIAN_POINT ( 'NONE',  ( -19.05341960407611168, -5.049401038298163336, 106.4572429386476955 ) ) ;
#186604 = CARTESIAN_POINT ( 'NONE',  ( 18.67979575497194134, -10.72451020669871369, 35.83442372801901143 ) ) ;
#186605 = CARTESIAN_POINT ( 'NONE',  ( 13.97604488694548053, -13.89961937509957401, 95.62609039468563310 ) ) ;
#186607 = CARTESIAN_POINT ( 'NONE',  ( -19.03943276465977164, 0.05219959533909376836, 66.24890960531436690 ) ) ;
#186606 = CARTESIAN_POINT ( 'NONE',  ( 17.50000000000000355, -3.805241302050290209, 107.8735247278259521 ) ) ;
#186608 = CARTESIAN_POINT ( 'NONE',  ( -5.049401038298153566, 19.05341960407611168, 100.2072429386476955 ) ) ;
#186610 = CARTESIAN_POINT ( 'NONE',  ( -19.03943276465977164, 0.05219959533909376836, 51.24890960531436690 ) ) ;
#186609 = CARTESIAN_POINT ( 'NONE',  ( 4.379528057220339221, -16.55341960407611168, 62.70724293864769550 ) ) ;
#186611 = CARTESIAN_POINT ( 'NONE',  ( -19.02544592524342804, 5.153800228976336051, 66.04057627198103830 ) ) ;
#186612 = CARTESIAN_POINT ( 'NONE',  ( -19.05341960407617563, 5.049401038297882671, 68.54275706135230450 ) ) ;
#186613 = CARTESIAN_POINT ( 'NONE',  ( -5.049401038297874678, -19.05341960407617918, 49.79275706135231871 ) ) ;
#186614 = CARTESIAN_POINT ( 'NONE',  ( -9.474510206698964154, 16.51473224551069663, 75.41557627198103830 ) ) ;
#186615 = CARTESIAN_POINT ( 'NONE',  ( 10.72451020669898902, -18.67979575497178502, 77.91557627198102409 ) ) ;
#186617 = CARTESIAN_POINT ( 'NONE',  ( 16.51473224551083163, -9.474510206698727899, 40.83442372801900433 ) ) ;
#186616 = CARTESIAN_POINT ( 'NONE',  ( -8.224510206698948167, 14.34966873604960824, 60.41557627198102409 ) ) ;
#186618 = CARTESIAN_POINT ( 'NONE',  ( -5.823673210054116645, -21.52544592524344225, 42.29057627198103120 ) ) ;
#186619 = CARTESIAN_POINT ( 'NONE',  ( 5.823673210054125526, 21.52544592524343514, 34.79057627198103120 ) ) ;
#186620 = CARTESIAN_POINT ( 'NONE',  ( -19.03943276465977164, 0.05219959533909376836, 71.24890960531435269 ) ) ;
#186621 = CARTESIAN_POINT ( 'NONE',  ( 19.05341960407611168, 5.049401038298154454, 58.95724293864768129 ) ) ;
#186622 = CARTESIAN_POINT ( 'NONE',  ( 14.29746914071049879, -8.314922557960816363, 108.3322429386477097 ) ) ;
#186623 = AXIS2_PLACEMENT_3D ( 'NONE', #27682, #102503, #135840 ) ;
#186624 = CARTESIAN_POINT ( 'NONE',  ( 10.81492255796106328, -18.62759615963255655, 20.41775706135234714 ) ) ;
#186625 = CARTESIAN_POINT ( 'NONE',  ( 0.05219959533909260263, 19.03943276465977164, 109.9989096053143669 ) ) ;
#186626 = CARTESIAN_POINT ( 'NONE',  ( 5.823673210054444382, -21.52544592524334988, 25.20942372801901854 ) ) ;
#186627 = CARTESIAN_POINT ( 'NONE',  ( -0.05219959533909027116, -19.03943276465977164, 32.49890960531435979 ) ) ;
#186628 = CARTESIAN_POINT ( 'NONE',  ( -21.53943276465977519, 0.05219959533907696930, 101.2489096053143669 ) ) ;
#186629 = CARTESIAN_POINT ( 'NONE',  ( 16.46253265017146816, 9.564922557961045513, 46.66775706135233293 ) ) ;
#186630 = CARTESIAN_POINT ( 'NONE',  ( -28.82186960331499037, 2.428612866367529932E-14, 146.0000000000000000 ) ) ;
#186631 = CARTESIAN_POINT ( 'NONE',  ( -13.89961937509977652, 13.97604488694528158, 25.62390960531434558 ) ) ;
#186632 = DIRECTION ( 'NONE',  ( 0.000000000000000000, 0.000000000000000000, -1.000000000000000000 ) ) ;
#186633 = CARTESIAN_POINT ( 'NONE',  ( 0.05219959533934541429, -16.53943276465976808, 60.00109039468568284 ) ) ;
#186634 = CARTESIAN_POINT ( 'NONE',  ( -14.29746914071049879, 8.314922557960819915, 115.8322429386477097 ) ) ;
#186635 = CARTESIAN_POINT ( 'NONE',  ( 33.72427247603957312, -5.492275790717719985, 95.34298344322786534 ) ) ;
#186636 = CARTESIAN_POINT ( 'NONE',  ( -13.97604488694527625, -13.89961937509977652, 71.87390960531433848 ) ) ;
#186637 = CARTESIAN_POINT ( 'NONE',  ( 8.224510206698953496, -14.34966873604960469, 107.9155762719810241 ) ) ;
#186638 = CARTESIAN_POINT ( 'NONE',  ( 21.55341960407610458, 5.719274019375980345, 48.95724293864770971 ) ) ;
#186639 = CARTESIAN_POINT ( 'NONE',  ( -14.34966873604960291, -8.224510206698953496, 76.66557627198103830 ) ) ;
#186640 = CARTESIAN_POINT ( 'NONE',  ( -8.314922557961024197, 14.29746914071037800, 27.91775706135234358 ) ) ;
#186641 = CARTESIAN_POINT ( 'NONE',  ( 10.81492255796106328, -18.62759615963255655, 85.41775706135236135 ) ) ;
#186642 = CARTESIAN_POINT ( 'NONE',  ( 16.51473224551069308, 9.474510206698969483, 24.16557627198102765 ) ) ;
#186643 = CARTESIAN_POINT ( 'NONE',  ( -8.314922557961024197, 14.29746914071037800, 112.9177570613523329 ) ) ;
#186644 = CARTESIAN_POINT ( 'NONE',  ( 0.05219959533910956823, 16.53943276465976808, 59.99890960531436690 ) ) ;
#186645 = CARTESIAN_POINT ( 'NONE',  ( -5.049401038298153566, 19.05341960407611168, 50.20724293864770260 ) ) ;
#186646 = CARTESIAN_POINT ( 'NONE',  ( 21.53943276465977519, 0.05219959533937863772, 101.2510903946856757 ) ) ;
#186647 = CARTESIAN_POINT ( 'NONE',  ( -15.72974639402197994, 15.80617190586746368, 110.6239096053143669 ) ) ;
#186648 = CARTESIAN_POINT ( 'NONE',  ( -5.823673210054431948, 21.52544592524334988, 72.70942372801901854 ) ) ;
#186649 = CARTESIAN_POINT ( 'NONE',  ( -0.05219959533934338120, 16.53943276465976808, 42.50109039468567573 ) ) ;
#186651 = CARTESIAN_POINT ( 'NONE',  ( -5.823673210054431948, 21.52544592524334988, 82.70942372801900433 ) ) ;
#186650 = CARTESIAN_POINT ( 'NONE',  ( 12.06949235617757843, -12.14591786802309237, 73.12390960531436690 ) ) ;
#186652 = CIRCLE ( 'NONE', #125292, 2.000000000000001776 ) ;
#186653 = CARTESIAN_POINT ( 'NONE',  ( -12.06949235617756955, 12.14591786802309770, 25.62390960531435624 ) ) ;
#186654 = CARTESIAN_POINT ( 'NONE',  ( 17.60769864724393940, -5.499999999999833022, 61.15024842019166584 ) ) ;
#186655 = CARTESIAN_POINT ( 'NONE',  ( -0.05219959533934338120, 16.53943276465976808, 42.50109039468567573 ) ) ;
#186656 = CARTESIAN_POINT ( 'NONE',  ( -16.52544592524342804, 4.483927247898546575, 46.04057627198103830 ) ) ;
#186657 = CARTESIAN_POINT ( 'NONE',  ( -16.55341960407617563, 4.379528057220093196, 88.54275706135236135 ) ) ;
#186658 = CARTESIAN_POINT ( 'NONE',  ( 9.474510206698971260, -16.51473224551069308, 97.91557627198102409 ) ) ;
#186659 = CARTESIAN_POINT ( 'NONE',  ( -5.823673210054116645, -21.52544592524344225, 22.29057627198102765 ) ) ;
#186660 = CARTESIAN_POINT ( 'NONE',  ( 18.67979575497194134, -10.72451020669871369, 100.8344237280190185 ) ) ;
#186661 = CARTESIAN_POINT ( 'NONE',  ( -0.05219959533934338120, 16.53943276465976808, 102.5010903946856899 ) ) ;
#186662 = CARTESIAN_POINT ( 'NONE',  ( 14.34966873604960469, 8.224510206698951720, 69.16557627198102409 ) ) ;
#186663 = CARTESIAN_POINT ( 'NONE',  ( -5.049401038298153566, 19.05341960407611168, 80.20724293864769550 ) ) ;
#186664 = ORIENTED_EDGE ( 'NONE', *, *, #42100, .T. ) ;
#186665 = CARTESIAN_POINT ( 'NONE',  ( -16.52544592524335698, -4.483927247898792601, 28.95942372801902209 ) ) ;
#186666 = CARTESIAN_POINT ( 'NONE',  ( 5.049401038298161559, -19.05341960407611168, 32.70724293864768129 ) ) ;
#186667 = CARTESIAN_POINT ( 'NONE',  ( -13.97604488694527625, -13.89961937509977652, 86.87390960531436690 ) ) ;
#186669 = LINE ( 'NONE', #140125, #82342 ) ;
#186668 = CARTESIAN_POINT ( 'NONE',  ( -14.34966873604972548, 8.224510206698743886, 33.33442372801900433 ) ) ;
#186670 = CARTESIAN_POINT ( 'NONE',  ( 13.89961937509957401, 13.97604488694547697, 36.87609039468565442 ) ) ;
#186671 = CARTESIAN_POINT ( 'NONE',  ( 8.224510206698742110, 14.34966873604972548, 92.08442372801901854 ) ) ;
#186672 = CARTESIAN_POINT ( 'NONE',  ( -5.049401038297874678, -19.05341960407617918, 109.7927570613523187 ) ) ;
#186673 = CARTESIAN_POINT ( 'NONE',  ( -0.05219959533909027116, -19.03943276465977164, 27.49890960531435624 ) ) ;
#186674 = CARTESIAN_POINT ( 'NONE',  ( -14.29746914071037622, -8.314922557961029526, 74.16775706135231871 ) ) ;
#186675 = CARTESIAN_POINT ( 'NONE',  ( -16.55341960407617563, 4.379528057220093196, 68.54275706135234714 ) ) ;
#186676 = CARTESIAN_POINT ( 'NONE',  ( 13.97604488694527802, 13.89961937509977652, 34.37390960531436690 ) ) ;
#186677 = CARTESIAN_POINT ( 'NONE',  ( -16.51473224551082808, 9.474510206698731452, 73.33442372801900433 ) ) ;
#186678 = CARTESIAN_POINT ( 'NONE',  ( -16.46253265017146816, -9.564922557961047289, 19.16775706135233293 ) ) ;
#186679 = CARTESIAN_POINT ( 'NONE',  ( -5.153800228976328057, -19.02544592524343514, 47.29057627198102409 ) ) ;
#186680 = CARTESIAN_POINT ( 'NONE',  ( 13.89961937509977652, -13.97604488694527269, 98.12390960531433848 ) ) ;
#186681 = CARTESIAN_POINT ( 'NONE',  ( -4.483927247898539470, -16.52544592524342804, 87.29057627198103830 ) ) ;
#186682 = CARTESIAN_POINT ( 'NONE',  ( -19.02544592524334988, -5.153800228976617603, 48.95942372801900433 ) ) ;
#186683 = CARTESIAN_POINT ( 'NONE',  ( 18.62759615963271287, -10.81492255796078972, 53.33224293864769550 ) ) ;
#186684 = CARTESIAN_POINT ( 'NONE',  ( -13.89961937509957401, -13.97604488694547875, 34.37609039468566863 ) ) ;
#186685 = CARTESIAN_POINT ( 'NONE',  ( 0.05219959533909260263, 19.03943276465977164, 84.99890960531436690 ) ) ;
#186686 = CARTESIAN_POINT ( 'NONE',  ( 0.05219959533936267826, -19.03943276465977164, 20.00109039468567218 ) ) ;
#186687 = CARTESIAN_POINT ( 'NONE',  ( -5.823673210054116645, -21.52544592524344225, 62.29057627198102409 ) ) ;
#186688 = CARTESIAN_POINT ( 'NONE',  ( -19.03943276465977164, 0.05219959533909376836, 106.2489096053143669 ) ) ;
#186689 = CARTESIAN_POINT ( 'NONE',  ( 5.153800228976615827, -19.02544592524334988, 90.20942372801900433 ) ) ;
#186690 = CARTESIAN_POINT ( 'NONE',  ( 5.153800228976335163, 19.02544592524342804, 109.7905762719810099 ) ) ;
#186691 = CARTESIAN_POINT ( 'NONE',  ( -13.97604488694547697, 13.89961937509957934, 113.1260903946856757 ) ) ;
#186692 = CARTESIAN_POINT ( 'NONE',  ( -4.379528057220328563, 16.55341960407611168, 115.2072429386476955 ) ) ;
#186693 = CARTESIAN_POINT ( 'NONE',  ( -9.474510206698964154, 16.51473224551069663, 100.4155762719810241 ) ) ;
#186694 = CARTESIAN_POINT ( 'NONE',  ( 21.53943276465977519, -0.05219959533907433946, 73.74890960531433848 ) ) ;
#186695 = CARTESIAN_POINT ( 'NONE',  ( 16.55341960407618274, -4.379528057220086978, 46.04275706135234714 ) ) ;
#186696 = CARTESIAN_POINT ( 'NONE',  ( -21.53943276465977519, -0.05219959533937600094, 43.75109039468568284 ) ) ;
#186697 = CARTESIAN_POINT ( 'NONE',  ( -18.62759615963255300, -10.81492255796106328, 94.16775706135237556 ) ) ;
#186698 = CARTESIAN_POINT ( 'NONE',  ( -14.29746914071037622, -8.314922557961029526, 94.16775706135237556 ) ) ;
#186699 = CARTESIAN_POINT ( 'NONE',  ( -0.05219959533909027116, -19.03943276465977164, 87.49890960531436690 ) ) ;
#186700 = CARTESIAN_POINT ( 'NONE',  ( 14.29746914071049879, -8.314922557960816363, 93.33224293864769550 ) ) ;
#186701 = CARTESIAN_POINT ( 'NONE',  ( -12.14591786802309592, -12.06949235617757132, 31.87390960531435979 ) ) ;
#186702 = CARTESIAN_POINT ( 'NONE',  ( 19.03943276465977164, 0.05219959533936151252, 66.25109039468567573 ) ) ;
#186703 = ADVANCED_FACE ( 'NONE', ( #112610 ), #97417, .T. ) ;
#186704 = CARTESIAN_POINT ( 'NONE',  ( -0.05219959533937732626, 21.53943276465977519, 57.50109039468568994 ) ) ;
#186705 = CARTESIAN_POINT ( 'NONE',  ( 19.03943276465977164, 0.05219959533936151252, 21.25109039468565797 ) ) ;
#186706 = CARTESIAN_POINT ( 'NONE',  ( -8.224510206698948167, 14.34966873604960824, 90.41557627198103830 ) ) ;
#186707 = CARTESIAN_POINT ( 'NONE',  ( 5.823673210054125526, 21.52544592524343514, 24.79057627198103120 ) ) ;
#186708 = CARTESIAN_POINT ( 'NONE',  ( 16.55341960407618274, -4.379528057220086978, 111.0427570613523613 ) ) ;
#186709 = CARTESIAN_POINT ( 'NONE',  ( 10.72451020669871369, 18.67979575497193778, 97.08442372801904696 ) ) ;
#186710 = CARTESIAN_POINT ( 'NONE',  ( -8.224510206698735004, -14.34966873604973081, 54.58442372801901143 ) ) ;
#186711 = CARTESIAN_POINT ( 'NONE',  ( 14.34966873604972726, -8.224510206698740333, 105.8344237280190328 ) ) ;
#186712 = CARTESIAN_POINT ( 'NONE',  ( -18.67979575497193778, 10.72451020669871902, 48.33442372801902565 ) ) ;
#186713 = CARTESIAN_POINT ( 'NONE',  ( -10.72451020669870658, -18.67979575497194134, 59.58442372801901854 ) ) ;
#186714 = ORIENTED_EDGE ( 'NONE', *, *, #69759, .T. ) ;
#186715 = CARTESIAN_POINT ( 'NONE',  ( 5.719274019375673035, 21.55341960407619339, 27.29275706135234358 ) ) ;
#186716 = CARTESIAN_POINT ( 'NONE',  ( 16.52544592524342804, -4.483927247898539470, 103.5405762719810383 ) ) ;
#186717 = CARTESIAN_POINT ( 'NONE',  ( -19.05341960407611168, -5.049401038298163336, 26.45724293864769550 ) ) ;
#186718 = CARTESIAN_POINT ( 'NONE',  ( -16.55341960407611168, -4.379528057220339221, 66.45724293864768129 ) ) ;
#186719 = CARTESIAN_POINT ( 'NONE',  ( -13.89961937509977652, 13.97604488694528158, 65.62390960531436690 ) ) ;
#186720 = CARTESIAN_POINT ( 'NONE',  ( -0.05219959533934338120, 16.53943276465976808, 107.5010903946856899 ) ) ;
#186721 = CARTESIAN_POINT ( 'NONE',  ( 0.05219959533907565091, 21.53943276465977519, 59.99890960531436690 ) ) ;
#186722 = CARTESIAN_POINT ( 'NONE',  ( -14.29746914071049879, 8.314922557960819915, 85.83224293864768129 ) ) ;
#186723 = CARTESIAN_POINT ( 'NONE',  ( -21.55341960407610458, -5.719274019375992779, 91.45724293864769550 ) ) ;
#186724 = CARTESIAN_POINT ( 'NONE',  ( -16.46253265017160317, 9.564922557960807481, 100.8322429386477097 ) ) ;
#186726 = CARTESIAN_POINT ( 'NONE',  ( -5.153800228976607833, 19.02544592524334988, 102.7094237280189759 ) ) ;
#186725 = CARTESIAN_POINT ( 'NONE',  ( 19.03943276465977164, -0.05219959533909143690, 53.74890960531436690 ) ) ;
#186727 = CARTESIAN_POINT ( 'NONE',  ( -15.80617190586745835, -15.72974639402198527, 46.87390960531435979 ) ) ;
#186728 = CARTESIAN_POINT ( 'NONE',  ( -10.72451020669870658, -18.67979575497194134, 74.58442372801901854 ) ) ;
#186729 = CARTESIAN_POINT ( 'NONE',  ( 0.05219959533909260263, 19.03943276465977164, 64.99890960531436690 ) ) ;
#186730 = CARTESIAN_POINT ( 'NONE',  ( 9.474510206698971260, -16.51473224551069308, 97.91557627198102409 ) ) ;
#186731 = CARTESIAN_POINT ( 'NONE',  ( -16.53943276465976808, -0.05219959533934237506, 58.75109039468568994 ) ) ;
#186732 = CARTESIAN_POINT ( 'NONE',  ( 15.72974639402176855, 15.80617190586768217, 46.87609039468568994 ) ) ;
#186733 = CARTESIAN_POINT ( 'NONE',  ( -5.719274019375665041, -21.55341960407619695, 89.79275706135236135 ) ) ;
#186734 = CARTESIAN_POINT ( 'NONE',  ( 15.80617190586746368, 15.72974639402197994, 99.37390960531436690 ) ) ;
#186736 = CARTESIAN_POINT ( 'NONE',  ( 16.53943276465976808, 0.05219959533934440121, 81.25109039468568994 ) ) ;
#186735 = CARTESIAN_POINT ( 'NONE',  ( 15.72974639402176855, 15.80617190586768217, 41.87609039468568284 ) ) ;
#186737 = CARTESIAN_POINT ( 'NONE',  ( -21.55341960407610458, -5.719274019375992779, 81.45724293864769550 ) ) ;
#186738 = CARTESIAN_POINT ( 'NONE',  ( -9.474510206698720793, -16.51473224551083518, 34.58442372801899722 ) ) ;
#186740 = CARTESIAN_POINT ( 'NONE',  ( -4.379528057220328563, 16.55341960407611168, 25.20724293864769550 ) ) ;
#186739 = CARTESIAN_POINT ( 'NONE',  ( 5.153800228976335163, 19.02544592524342804, 79.79057627198102409 ) ) ;
#186741 = CARTESIAN_POINT ( 'NONE',  ( 18.09805431107249518, -5.499999999999974243, 83.51606229291887473 ) ) ;
#186742 = CARTESIAN_POINT ( 'NONE',  ( -0.05219959533909027116, -19.03943276465977164, 97.49890960531436690 ) ) ;
#186743 = DIRECTION ( 'NONE',  ( 1.000000000000000000, 0.000000000000000000, 0.000000000000000000 ) ) ;
#186744 = EDGE_CURVE ( 'NONE', #61486, #147783, #76724, .T. ) ;
#186745 = CARTESIAN_POINT ( 'NONE',  ( -9.564922557961040184, 16.46253265017147172, 82.91775706135233293 ) ) ;
#186746 = CARTESIAN_POINT ( 'NONE',  ( 21.55341960407610458, 5.719274019375980345, 63.95724293864770260 ) ) ;
#186747 = CARTESIAN_POINT ( 'NONE',  ( -0.05219959533910754901, -16.53943276465976808, 42.49890960531435979 ) ) ;
#186748 = CARTESIAN_POINT ( 'NONE',  ( 14.29746914071037800, 8.314922557961029526, 21.66775706135235069 ) ) ;
#186749 = CARTESIAN_POINT ( 'NONE',  ( -13.89961937509977652, 13.97604488694528158, 30.62390960531435269 ) ) ;
#186750 = CARTESIAN_POINT ( 'NONE',  ( -12.06949235617739369, -12.14591786802326823, 19.37609039468568639 ) ) ;
#186752 = CARTESIAN_POINT ( 'NONE',  ( -5.153800228976607833, 19.02544592524334988, 72.70942372801900433 ) ) ;
#186751 = CARTESIAN_POINT ( 'NONE',  ( -15.80617190586745835, -15.72974639402198527, 96.87390960531436690 ) ) ;
#186753 = CARTESIAN_POINT ( 'NONE',  ( 8.224510206698742110, 14.34966873604972548, 77.08442372801901854 ) ) ;
#186754 = CARTESIAN_POINT ( 'NONE',  ( 19.02544592524343514, -5.153800228976328945, 73.54057627198103830 ) ) ;
#186755 = CARTESIAN_POINT ( 'NONE',  ( -16.55341960407611168, -4.379528057220339221, 71.45724293864769550 ) ) ;
#186756 = CARTESIAN_POINT ( 'NONE',  ( 19.03943276465977164, -0.05219959533909143690, 58.74890960531435979 ) ) ;
#186757 = CARTESIAN_POINT ( 'NONE',  ( -8.224510206698948167, 14.34966873604960824, 65.41557627198102409 ) ) ;
#186758 = CARTESIAN_POINT ( 'NONE',  ( 1.300000000000000044, -1.443375672974063884, -3.691112476943992763E-18 ) ) ;
#186759 = CARTESIAN_POINT ( 'NONE',  ( -28.28060372831499336, 2.428612866367529932E-14, 138.5625000040967620 ) ) ;
#186760 = CARTESIAN_POINT ( 'NONE',  ( 12.06949235617757843, -12.14591786802309237, 48.12390960531436690 ) ) ;
#186761 = CARTESIAN_POINT ( 'NONE',  ( -19.03943276465977164, 0.05219959533909376836, 76.24890960531435269 ) ) ;
#186762 = DIRECTION ( 'NONE',  ( -0.000000000000000000, -0.000000000000000000, 1.000000000000000000 ) ) ;
#186763 = CARTESIAN_POINT ( 'NONE',  ( 9.564922557961047289, -16.46253265017146816, 35.41775706135233293 ) ) ;
#186764 = CARTESIAN_POINT ( 'NONE',  ( 16.53943276465976808, 0.05219959533934440121, 61.25109039468567573 ) ) ;
#186765 = CARTESIAN_POINT ( 'NONE',  ( 18.62759615963271287, -10.81492255796078972, 68.33224293864769550 ) ) ;
#186766 = CARTESIAN_POINT ( 'NONE',  ( 19.05341960407617918, -5.049401038297876454, 26.04275706135233293 ) ) ;
#186767 = CARTESIAN_POINT ( 'NONE',  ( -16.46253265017160317, 9.564922557960807481, 70.83224293864770971 ) ) ;
#186768 = CARTESIAN_POINT ( 'NONE',  ( 5.000000000000000000, -139.5000000000000000, 54.87277500418469600 ) ) ;
#186769 = CARTESIAN_POINT ( 'NONE',  ( 13.97604488694527802, 13.89961937509977652, 109.3739096053143669 ) ) ;
#186770 = CARTESIAN_POINT ( 'NONE',  ( -19.05341960407611168, -5.049401038298163336, 56.45724293864768129 ) ) ;
#186771 = CARTESIAN_POINT ( 'NONE',  ( -0.05219959533937732626, 21.53943276465977519, 42.50109039468567573 ) ) ;
#186772 = CARTESIAN_POINT ( 'NONE',  ( 8.314922557960818139, 14.29746914071049879, 109.5822429386476955 ) ) ;
#186775 = ORIENTED_EDGE ( 'NONE', *, *, #8138, .T. ) ;
#186774 = CARTESIAN_POINT ( 'NONE',  ( 0.05219959533909260263, 19.03943276465977164, 84.99890960531436690 ) ) ;
#186773 = CARTESIAN_POINT ( 'NONE',  ( -5.823673210054116645, -21.52544592524344225, 97.29057627198105251 ) ) ;
#186776 = CARTESIAN_POINT ( 'NONE',  ( 18.62759615963255655, 10.81492255796105972, 26.66775706135235424 ) ) ;
#186778 = EDGE_LOOP ( 'NONE', ( #64679, #77127, #164358, #118414 ) ) ;
#186777 = B_SPLINE_CURVE_WITH_KNOTS ( 'NONE', 3,
 ( #16652, #81271, #93473, #1462, #158137, #189486 ),
 .UNSPECIFIED., .F., .F.,
 ( 4, 2, 4 ),
 ( 0.003557987005820478950, 0.004145727928114205374, 0.004733468850407931798 ),
 .UNSPECIFIED. ) ;
#186779 = CARTESIAN_POINT ( 'NONE',  ( -9.564922557960796823, -16.46253265017161027, 82.08224293864768129 ) ) ;
#186780 = DIRECTION ( 'NONE',  ( 0.000000000000000000, 0.000000000000000000, 1.000000000000000000 ) ) ;
#186781 = CARTESIAN_POINT ( 'NONE',  ( -15.80617190586745835, -15.72974639402198527, 96.87390960531436690 ) ) ;
#186782 = CARTESIAN_POINT ( 'NONE',  ( -16.46253265017160317, 9.564922557960807481, 40.83224293864769550 ) ) ;
#186783 = CARTESIAN_POINT ( 'NONE',  ( 19.02544592524334988, 5.153800228976608722, 101.4594237280189759 ) ) ;
#186784 = CARTESIAN_POINT ( 'NONE',  ( -11.40812507854754720, -35.11059874428192273, -10.72499999726881548 ) ) ;
#186785 = CARTESIAN_POINT ( 'NONE',  ( -19.03943276465977164, 0.05219959533909376836, 31.24890960531435979 ) ) ;
#186786 = CARTESIAN_POINT ( 'NONE',  ( 10.81492255796106328, -18.62759615963255655, 90.41775706135236135 ) ) ;
#186788 = CARTESIAN_POINT ( 'NONE',  ( -5.719274019375665041, -21.55341960407619695, 49.79275706135234714 ) ) ;
#186787 = CARTESIAN_POINT ( 'NONE',  ( -16.51473224551069308, -9.474510206698971260, 81.66557627198103830 ) ) ;
#186789 = CARTESIAN_POINT ( 'NONE',  ( -15.72974639402176322, -15.80617190586768395, 29.37609039468568284 ) ) ;
#186790 = CARTESIAN_POINT ( 'NONE',  ( -23.31738231874055245, -16.94106989632524574, 146.1999999999999886 ) ) ;
#186791 = CARTESIAN_POINT ( 'NONE',  ( 19.03943276465977164, -0.05219959533909143690, 88.74890960531436690 ) ) ;
#186792 = CARTESIAN_POINT ( 'NONE',  ( -9.572641798195965279, 26.93160034404219161, 140.0000000000000000 ) ) ;
#186795 = CARTESIAN_POINT ( 'NONE',  ( 5.823673210054444382, -21.52544592524334988, 50.20942372801901854 ) ) ;
#186794 = CARTESIAN_POINT ( 'NONE',  ( -5.823673210054116645, -21.52544592524344225, 47.29057627198103120 ) ) ;
#186793 = CARTESIAN_POINT ( 'NONE',  ( 8.314922557961029526, -14.29746914071037800, 35.41775706135234003 ) ) ;
#186796 = CARTESIAN_POINT ( 'NONE',  ( 18.62759615963255655, 10.81492255796105972, 71.66775706135234714 ) ) ;
#186797 = CARTESIAN_POINT ( 'NONE',  ( 17.72566875460847768, -5.500000000000063061, 38.42186708195907130 ) ) ;
#186798 = CARTESIAN_POINT ( 'NONE',  ( -0.05219959533936034679, 19.03943276465977164, 107.5010903946856615 ) ) ;
#186799 = CARTESIAN_POINT ( 'NONE',  ( 13.97604488694527802, 13.89961937509977652, 59.37390960531434558 ) ) ;
#186800 = CARTESIAN_POINT ( 'NONE',  ( 13.89961937509977652, -13.97604488694527269, 83.12390960531436690 ) ) ;
#186801 = CIRCLE ( 'NONE', #157759, 2.500000000000000444 ) ;
#186802 = CARTESIAN_POINT ( 'NONE',  ( 12.06949235617757843, -12.14591786802309237, 103.1239096053143811 ) ) ;
#186803 = CARTESIAN_POINT ( 'NONE',  ( 12.14591786802309770, 12.06949235617756955, 99.37390960531436690 ) ) ;
#186804 = CARTESIAN_POINT ( 'NONE',  ( 0.05219959533909260263, 19.03943276465977164, 109.9989096053143669 ) ) ;
#186805 = CARTESIAN_POINT ( 'NONE',  ( -4.379528057220086978, -16.55341960407618274, 79.79275706135236135 ) ) ;
#186807 = CARTESIAN_POINT ( 'NONE',  ( 0.05219959533909260263, 19.03943276465977164, 54.99890960531435979 ) ) ;
#186806 = CARTESIAN_POINT ( 'NONE',  ( -8.314922557960811034, -14.29746914071050412, 72.08224293864769550 ) ) ;
#186808 = CARTESIAN_POINT ( 'NONE',  ( -21.55341960407619339, 5.719274019375674811, 83.54275706135234714 ) ) ;
#186809 = CARTESIAN_POINT ( 'NONE',  ( 10.81492255796106328, -18.62759615963255655, 70.41775706135236135 ) ) ;
#186810 = CARTESIAN_POINT ( 'NONE',  ( -9.564922557961040184, 16.46253265017147172, 102.9177570613523329 ) ) ;
#186811 = CARTESIAN_POINT ( 'NONE',  ( -16.52544592524342804, 4.483927247898546575, 56.04057627198102409 ) ) ;
#186812 = CARTESIAN_POINT ( 'NONE',  ( -5.823673210054431948, 21.52544592524334988, 22.70942372801901499 ) ) ;
#186813 = CARTESIAN_POINT ( 'NONE',  ( -15.80617190586745835, -15.72974639402198527, 61.87390960531436690 ) ) ;
#186814 = CARTESIAN_POINT ( 'NONE',  ( 17.50000000000000000, 5.499999999999997335, 120.0000000000000142 ) ) ;
#186815 = CARTESIAN_POINT ( 'NONE',  ( 17.81289503416610742, 24.51734667627700404, 147.5500000054623229 ) ) ;
#186816 = CARTESIAN_POINT ( 'NONE',  ( 19.02544592524343514, -5.153800228976328945, 73.54057627198103830 ) ) ;
#186817 = CARTESIAN_POINT ( 'NONE',  ( -12.06949235617756955, 12.14591786802309770, 35.62390960531437401 ) ) ;
#186818 = CARTESIAN_POINT ( 'NONE',  ( 14.29746914071049879, -8.314922557960816363, 23.33224293864769194 ) ) ;
#186819 = CARTESIAN_POINT ( 'NONE',  ( 4.483927247898790824, -16.52544592524335698, 100.2094237280190043 ) ) ;
#186820 = CARTESIAN_POINT ( 'NONE',  ( -19.03943276465977164, -0.05219959533935918106, 53.75109039468566863 ) ) ;
#186821 = LINE ( 'NONE', #48291, #18231 ) ;
#186822 = CARTESIAN_POINT ( 'NONE',  ( -13.97604488694527625, -13.89961937509977652, 101.8739096053143811 ) ) ;
#186823 = ADVANCED_FACE ( 'NONE', ( #59910 ), #189226, .T. ) ;
#186824 = CARTESIAN_POINT ( 'NONE',  ( -0.05219959533910754901, -16.53943276465976808, 72.49890960531435269 ) ) ;
#186825 = CARTESIAN_POINT ( 'NONE',  ( -13.89961937509957401, -13.97604488694547875, 49.37609039468567573 ) ) ;
#186827 = CARTESIAN_POINT ( 'NONE',  ( 13.89961937509977652, -13.97604488694527269, 113.1239096053143527 ) ) ;
#186826 = CARTESIAN_POINT ( 'NONE',  ( 17.05587630539786659, -6.762274262135694158, 103.2418030903731250 ) ) ;
#186829 = ORIENTED_EDGE ( 'NONE', *, *, #70721, .F. ) ;
#186828 = CARTESIAN_POINT ( 'NONE',  ( -18.67979575497178146, -10.72451020669898902, 51.66557627198102409 ) ) ;
#186830 = CARTESIAN_POINT ( 'NONE',  ( 16.52544592524342804, -4.483927247898539470, 103.5405762719810383 ) ) ;
#186831 = CARTESIAN_POINT ( 'NONE',  ( 16.53943276465976808, 0.05219959533934440121, 46.25109039468567573 ) ) ;
#186832 = CARTESIAN_POINT ( 'NONE',  ( -16.55341960407611168, -4.379528057220339221, 96.45724293864770971 ) ) ;
#186833 = CARTESIAN_POINT ( 'NONE',  ( 16.20579543436675607, -7.371946100355228459, 36.93479165828124167 ) ) ;
#186834 = CARTESIAN_POINT ( 'NONE',  ( -16.88567814943165146, 6.947325034625571050, 48.70998877347415856 ) ) ;
#186835 = CARTESIAN_POINT ( 'NONE',  ( 5.049401038298161559, -19.05341960407611168, 112.7072429386476813 ) ) ;
#186837 = ADVANCED_FACE ( 'NONE', ( #57947 ), #85868, .F. ) ;
#186836 = CARTESIAN_POINT ( 'NONE',  ( -36.91746825000000598, 2.428612866367529932E-14, -7.124999997268813168 ) ) ;
#186838 = CARTESIAN_POINT ( 'NONE',  ( -18.22780087662122028, 5.500000000000031086, 43.51540105326107977 ) ) ;
#186840 = CARTESIAN_POINT ( 'NONE',  ( -4.483927247898539470, -16.52544592524342804, 27.29057627198103120 ) ) ;
#186839 = CARTESIAN_POINT ( 'NONE',  ( -16.53943276465976808, -0.05219959533934237506, 48.75109039468568284 ) ) ;
#186841 = CARTESIAN_POINT ( 'NONE',  ( 18.67979575497178502, 10.72451020669898547, 54.16557627198103120 ) ) ;
#186842 = CARTESIAN_POINT ( 'NONE',  ( 9.474510206698729675, 16.51473224551082808, 82.08442372801899012 ) ) ;
#186843 = CARTESIAN_POINT ( 'NONE',  ( 0.05219959533907565091, 21.53943276465977519, 54.99890960531435269 ) ) ;
#186844 = CARTESIAN_POINT ( 'NONE',  ( 0.05219959533937995610, -21.53943276465977519, 85.00109039468568994 ) ) ;
#186845 = CARTESIAN_POINT ( 'NONE',  ( 10.46900522708367198, -36.04764466666197364, -30.96889465344744607 ) ) ;
#186846 = CARTESIAN_POINT ( 'NONE',  ( 16.52544592524335698, 4.483927247898782831, 31.45942372801901854 ) ) ;
#186848 = CARTESIAN_POINT ( 'NONE',  ( -16.51473224551069308, -9.474510206698971260, 96.66557627198102409 ) ) ;
#186847 = CARTESIAN_POINT ( 'NONE',  ( -5.153800228976328057, -19.02544592524343514, 42.29057627198101699 ) ) ;
#186849 = CARTESIAN_POINT ( 'NONE',  ( 19.05341960407611168, 5.049401038298154454, 33.95724293864769550 ) ) ;
#186850 = CARTESIAN_POINT ( 'NONE',  ( 12.06949235617757843, -12.14591786802309237, 98.12390960531436690 ) ) ;
#186851 = CARTESIAN_POINT ( 'NONE',  ( 0.000000000000000000, 0.000000000000000000, 0.000000000000000000 ) ) ;
#186852 = CARTESIAN_POINT ( 'NONE',  ( 5.153800228976335163, 19.02544592524342804, 94.79057627198103830 ) ) ;
#186853 = ORIENTED_EDGE ( 'NONE', *, *, #39357, .F. ) ;
#186854 = CARTESIAN_POINT ( 'NONE',  ( 12.14591786802327356, -12.06949235617739191, 50.62609039468568994 ) ) ;
#186855 = CARTESIAN_POINT ( 'NONE',  ( -21.53943276465977519, 0.05219959533907696930, 91.24890960531436690 ) ) ;
#186856 = CARTESIAN_POINT ( 'NONE',  ( -19.03943276465977164, 0.05219959533909376836, 46.24890960531435979 ) ) ;
#186857 = CARTESIAN_POINT ( 'NONE',  ( -10.81492255796105439, 18.62759615963255655, 32.91775706135234714 ) ) ;
#186858 = CARTESIAN_POINT ( 'NONE',  ( -13.89961937509977652, 13.97604488694528158, 85.62390960531433848 ) ) ;
#186859 = CARTESIAN_POINT ( 'NONE',  ( 28.79475375365586132, 2.781246896534039337E-14, 144.9843446568999923 ) ) ;
#186860 = ORIENTED_EDGE ( 'NONE', *, *, #193126, .T. ) ;
#186861 = CARTESIAN_POINT ( 'NONE',  ( 14.34966873604972726, -8.224510206698740333, 40.83442372801901854 ) ) ;
#186862 = CARTESIAN_POINT ( 'NONE',  ( 10.72451020669871369, 18.67979575497193778, 22.08442372801901143 ) ) ;
#186865 = CARTESIAN_POINT ( 'NONE',  ( -16.46253265017146816, -9.564922557961047289, 79.16775706135234714 ) ) ;
#186864 = CARTESIAN_POINT ( 'NONE',  ( 19.03943276465977164, -0.05219959533909143690, 93.74890960531435269 ) ) ;
#186863 = CARTESIAN_POINT ( 'NONE',  ( -19.02544592524342804, 5.153800228976336051, 31.04057627198102409 ) ) ;
#186866 = CARTESIAN_POINT ( 'NONE',  ( -16.51473224551082808, 9.474510206698731452, 23.33442372801900078 ) ) ;
#186867 = CARTESIAN_POINT ( 'NONE',  ( -5.719274019375978568, 21.55341960407610458, 85.20724293864770971 ) ) ;
#186868 = CARTESIAN_POINT ( 'NONE',  ( -5.153800228976607833, 19.02544592524334988, 37.70942372801899722 ) ) ;
#186869 = CARTESIAN_POINT ( 'NONE',  ( -4.379528057220086978, -16.55341960407618274, 79.79275706135236135 ) ) ;
#186870 = CARTESIAN_POINT ( 'NONE',  ( 9.474510206698971260, -16.51473224551069308, 112.9155762719810383 ) ) ;
#186871 = CARTESIAN_POINT ( 'NONE',  ( -13.89961937509977652, 13.97604488694528158, 65.62390960531436690 ) ) ;
#186872 = CARTESIAN_POINT ( 'NONE',  ( 15.72974639402176855, 15.80617190586768217, 71.87609039468568994 ) ) ;
#186873 = CARTESIAN_POINT ( 'NONE',  ( -0.05219959533937732626, 21.53943276465977519, 62.50109039468568284 ) ) ;
#186874 = CARTESIAN_POINT ( 'NONE',  ( -9.564922557960796823, -16.46253265017161027, 77.08224293864769550 ) ) ;
#186875 = CARTESIAN_POINT ( 'NONE',  ( 21.55341960407619695, -5.719274019375665929, 46.04275706135234714 ) ) ;
#186876 = CARTESIAN_POINT ( 'NONE',  ( -5.153800228976607833, 19.02544592524334988, 87.70942372801897591 ) ) ;
#186877 = CARTESIAN_POINT ( 'NONE',  ( -19.02544592524342804, 5.153800228976336051, 56.04057627198100988 ) ) ;
#186878 = CARTESIAN_POINT ( 'NONE',  ( -16.51473224551069308, -9.474510206698971260, 101.6655762719810241 ) ) ;
#186879 = CARTESIAN_POINT ( 'NONE',  ( -0.05219959533909027116, -19.03943276465977164, 72.49890960531435269 ) ) ;
#186880 = CARTESIAN_POINT ( 'NONE',  ( -16.46253265017160317, 9.564922557960807481, 110.8322429386476955 ) ) ;
#186881 = CARTESIAN_POINT ( 'NONE',  ( -19.02544592524342804, 5.153800228976336051, 56.04057627198100988 ) ) ;
#186882 = CARTESIAN_POINT ( 'NONE',  ( -21.55341960407610458, -5.719274019375992779, 96.45724293864770971 ) ) ;
#186883 = CARTESIAN_POINT ( 'NONE',  ( 14.34966873604972726, -8.224510206698740333, 75.83442372801900433 ) ) ;
#186884 = CARTESIAN_POINT ( 'NONE',  ( -21.97054992548900998, 7.027819292989580191, 170.5066066589220100 ) ) ;
#186885 = CARTESIAN_POINT ( 'NONE',  ( -16.46253265017146816, -9.564922557961047289, 29.16775706135232937 ) ) ;
#186886 = CARTESIAN_POINT ( 'NONE',  ( -9.474510206698964154, 16.51473224551069663, 60.41557627198102409 ) ) ;
#186887 = CARTESIAN_POINT ( 'NONE',  ( -16.55341960407611168, -4.379528057220339221, 61.45724293864770260 ) ) ;
#186888 = CARTESIAN_POINT ( 'NONE',  ( 12.14591786802309770, 12.06949235617756955, 99.37390960531436690 ) ) ;
#186889 = CARTESIAN_POINT ( 'NONE',  ( -19.03943276465977164, 0.05219959533909376836, 106.2489096053143669 ) ) ;
#186890 = CARTESIAN_POINT ( 'NONE',  ( -16.51473224551069308, -9.474510206698971260, 96.66557627198102409 ) ) ;
#186891 = CARTESIAN_POINT ( 'NONE',  ( 5.153800228976335163, 19.02544592524342804, 109.7905762719810099 ) ) ;
#186892 = CARTESIAN_POINT ( 'NONE',  ( 21.55341960407619695, -5.719274019375665929, 111.0427570613523613 ) ) ;
#186893 = CARTESIAN_POINT ( 'NONE',  ( 4.379528057220092307, 16.55341960407617563, 77.29275706135234714 ) ) ;
#186894 = CARTESIAN_POINT ( 'NONE',  ( 18.67979575497194134, -10.72451020669871369, 35.83442372801901143 ) ) ;
#186895 = CARTESIAN_POINT ( 'NONE',  ( 15.80617190586746368, 15.72974639402197994, 29.37390960531435269 ) ) ;
#186896 = CARTESIAN_POINT ( 'NONE',  ( -10.72451020669898014, 18.67979575497178502, 100.4155762719810241 ) ) ;
#186897 = CARTESIAN_POINT ( 'NONE',  ( 8.314922557960818139, 14.29746914071049879, 59.58224293864770260 ) ) ;
#186898 = CARTESIAN_POINT ( 'NONE',  ( 9.474510206698971260, -16.51473224551069308, 57.91557627198103120 ) ) ;
#186899 = CARTESIAN_POINT ( 'NONE',  ( -0.05219959533910754901, -16.53943276465976808, 82.49890960531436690 ) ) ;
#186900 = CARTESIAN_POINT ( 'NONE',  ( -18.67979575497178146, -10.72451020669898902, 41.66557627198103120 ) ) ;
#186901 = CARTESIAN_POINT ( 'NONE',  ( -9.474510206698720793, -16.51473224551083518, 44.58442372801900433 ) ) ;
#186902 = CARTESIAN_POINT ( 'NONE',  ( 16.55341960407611168, 4.379528057220329451, 113.9572429386477239 ) ) ;
#186903 = EDGE_LOOP ( 'NONE', ( #188038, #134060, #97262, #43557 ) ) ;
#186904 = CARTESIAN_POINT ( 'NONE',  ( 0.05219959533934541429, -16.53943276465976808, 65.00109039468568994 ) ) ;
#186905 = CARTESIAN_POINT ( 'NONE',  ( 13.89961937509977652, -13.97604488694527269, 68.12390960531436690 ) ) ;
#186906 = CARTESIAN_POINT ( 'NONE',  ( 8.571926809382597767, 26.38167802310806209, 144.2750000027311899 ) ) ;
#186907 = CARTESIAN_POINT ( 'NONE',  ( -16.53943276465976808, 0.05219959533911058130, 91.24890960531436690 ) ) ;
#186908 = CARTESIAN_POINT ( 'NONE',  ( 21.55341960407610458, 5.719274019375980345, 33.95724293864769550 ) ) ;
#186909 = CARTESIAN_POINT ( 'NONE',  ( 0.05219959533934541429, -16.53943276465976808, 105.0010903946856757 ) ) ;
#186910 = CARTESIAN_POINT ( 'NONE',  ( 8.224510206698742110, 14.34966873604972548, 22.08442372801901143 ) ) ;
#186911 = CARTESIAN_POINT ( 'NONE',  ( 15.80617190586769283, -15.72974639402175789, 90.62609039468567573 ) ) ;
#186912 = CARTESIAN_POINT ( 'NONE',  ( -13.97604488694527625, -13.89961937509977652, 91.87390960531432427 ) ) ;
#186913 = CARTESIAN_POINT ( 'NONE',  ( 5.823673210054444382, -21.52544592524334988, 25.20942372801901854 ) ) ;
#186914 = CARTESIAN_POINT ( 'NONE',  ( -8.314922557961024197, 14.29746914071037800, 52.91775706135235424 ) ) ;
#186915 = CARTESIAN_POINT ( 'NONE',  ( 9.564922557960805705, 16.46253265017160317, 29.58224293864769550 ) ) ;
#186916 = CARTESIAN_POINT ( 'NONE',  ( 8.314922557961029526, -14.29746914071037800, 30.41775706135234358 ) ) ;
#186917 = CARTESIAN_POINT ( 'NONE',  ( -19.02544592524334988, -5.153800228976617603, 88.95942372801897591 ) ) ;
#186918 = EDGE_CURVE ( 'NONE', #120796, #111025, #18051, .T. ) ;
#186919 = CARTESIAN_POINT ( 'NONE',  ( -10.72451020669898014, 18.67979575497178502, 95.41557627198102409 ) ) ;
#186920 = CARTESIAN_POINT ( 'NONE',  ( 0.05219959533936267826, -19.03943276465977164, 65.00109039468567573 ) ) ;
#186921 = CARTESIAN_POINT ( 'NONE',  ( 0.000000000000000000, 0.000000000000000000, -65.00100000000003320 ) ) ;
#186922 = CARTESIAN_POINT ( 'NONE',  ( -5.823673210054431948, 21.52544592524334988, 22.70942372801901499 ) ) ;
#186923 = CARTESIAN_POINT ( 'NONE',  ( 9.474510206698971260, -16.51473224551069308, 72.91557627198102409 ) ) ;
#186924 = CARTESIAN_POINT ( 'NONE',  ( -16.46253265017160317, 9.564922557960807481, 75.83224293864769550 ) ) ;
#186925 = CARTESIAN_POINT ( 'NONE',  ( 12.06949235617739724, 12.14591786802326823, 26.87609039468567218 ) ) ;
#186926 = CARTESIAN_POINT ( 'NONE',  ( 19.29714446218642721, -35.03787052511701461, -7.260590851364162823 ) ) ;
#186927 = CARTESIAN_POINT ( 'NONE',  ( 9.474510206698729675, 16.51473224551082808, 57.08442372801900433 ) ) ;
#186929 = CARTESIAN_POINT ( 'NONE',  ( -16.55341960407611168, -4.379528057220339221, 81.45724293864769550 ) ) ;
#186928 = CARTESIAN_POINT ( 'NONE',  ( -0.05219959533907301413, -21.53943276465977519, 112.4989096053143669 ) ) ;
#186930 = CARTESIAN_POINT ( 'NONE',  ( 16.46253265017160672, -9.564922557960803928, 78.33224293864769550 ) ) ;
#186932 = CARTESIAN_POINT ( 'NONE',  ( 19.02544592524334988, 5.153800228976608722, 36.45942372801900433 ) ) ;
#186931 = CARTESIAN_POINT ( 'NONE',  ( -14.34966873604972548, 8.224510206698743886, 33.33442372801900433 ) ) ;
#186933 = CARTESIAN_POINT ( 'NONE',  ( -15.72974639402176322, -15.80617190586768395, 64.37609039468568994 ) ) ;
#186934 = CARTESIAN_POINT ( 'NONE',  ( -4.379528057220086978, -16.55341960407618274, 19.79275706135235069 ) ) ;
#186935 = CARTESIAN_POINT ( 'NONE',  ( 19.03943276465977164, -0.05219959533909143690, 53.74890960531436690 ) ) ;
#186936 = CARTESIAN_POINT ( 'NONE',  ( -0.05219959533936034679, 19.03943276465977164, 82.50109039468567573 ) ) ;
#186937 = CARTESIAN_POINT ( 'NONE',  ( 14.29746914071037800, 8.314922557961029526, 61.66775706135235424 ) ) ;
#186938 = CARTESIAN_POINT ( 'NONE',  ( 18.67979575497194134, -10.72451020669871369, 95.83442372801903275 ) ) ;
#186939 = CARTESIAN_POINT ( 'NONE',  ( 13.97604488694548053, -13.89961937509957401, 70.62609039468567573 ) ) ;
#186940 = CARTESIAN_POINT ( 'NONE',  ( -9.474510206698964154, 16.51473224551069663, 45.41557627198103120 ) ) ;
#186941 = CARTESIAN_POINT ( 'NONE',  ( 15.72974639402199770, -15.80617190586745480, 73.12390960531436690 ) ) ;
#186943 = CARTESIAN_POINT ( 'NONE',  ( 13.89961937509957401, 13.97604488694547697, 66.87609039468567573 ) ) ;
#186942 = CARTESIAN_POINT ( 'NONE',  ( -4.483927247898539470, -16.52544592524342804, 67.29057627198103830 ) ) ;
#186944 = DIRECTION ( 'NONE',  ( 1.000000000000000000, 0.000000000000000000, 0.000000000000000000 ) ) ;
#186945 = CARTESIAN_POINT ( 'NONE',  ( -13.89961937509957401, -13.97604488694547875, 39.37609039468566152 ) ) ;
#186946 = CARTESIAN_POINT ( 'NONE',  ( -8.224510206698735004, -14.34966873604973081, 104.5844237280190185 ) ) ;
#186947 = CARTESIAN_POINT ( 'NONE',  ( -16.53943276465976808, 0.05219959533911058130, 61.24890960531435979 ) ) ;
#186949 = CARTESIAN_POINT ( 'NONE',  ( -22.44159573604009950, -16.30477369853688430, 141.0750000027311728 ) ) ;
#186948 = CARTESIAN_POINT ( 'NONE',  ( -21.52544592524334988, -5.823673210054445271, 88.95942372801901854 ) ) ;
#186950 = CARTESIAN_POINT ( 'NONE',  ( 5.823673210054125526, 21.52544592524343514, 99.79057627198103830 ) ) ;
#186951 =( BOUNDED_CURVE ( )  B_SPLINE_CURVE ( 2, ( #87556, #149243, #197732, #103734, #147237, #88550, #59198, #8729, #118912, #26907, #44050 ),
 .UNSPECIFIED., .F., .T. ) 
 B_SPLINE_CURVE_WITH_KNOTS ( ( 3, 2, 2, 2, 2, 3 ),
 ( 0.4000000000000003553, 0.4200000000000003175, 0.4400000000000003908, 0.4600000000000004086, 0.4800000000000004263, 0.5000000000000004441 ),
 .UNSPECIFIED. ) 
 CURVE ( )  GEOMETRIC_REPRESENTATION_ITEM ( )  RATIONAL_B_SPLINE_CURVE ( ( 0.9999999999999992228, 0.9510565162951543083, 1.000000000000000000, 0.9510565162951535312, 1.000000000000000000, 0.9510565162951535312, 1.000000000000000000, 0.9510565162951535312, 1.000000000000000000, 0.9510565162951524210, 1.000000000000001110 ) ) 
 REPRESENTATION_ITEM ( '' )  );
#186952 = CARTESIAN_POINT ( 'NONE',  ( -5.049401038298153566, 19.05341960407611168, 55.20724293864769550 ) ) ;
#186953 = CARTESIAN_POINT ( 'NONE',  ( -21.55341960407619339, 5.719274019375674811, 68.54275706135234714 ) ) ;
#186954 = CARTESIAN_POINT ( 'NONE',  ( 19.05341960407611168, 5.049401038298154454, 43.95724293864769550 ) ) ;
#186955 = CARTESIAN_POINT ( 'NONE',  ( -5.049401038298153566, 19.05341960407611168, 60.20724293864768129 ) ) ;
#186956 = CARTESIAN_POINT ( 'NONE',  ( 19.02544592524343514, -5.153800228976328945, 23.54057627198102054 ) ) ;
#186957 = CARTESIAN_POINT ( 'NONE',  ( 5.719274019375991003, -21.55341960407610458, 22.70724293864769194 ) ) ;
#186958 = CARTESIAN_POINT ( 'NONE',  ( -16.52544592524342804, 4.483927247898546575, 56.04057627198102409 ) ) ;
#186959 = CARTESIAN_POINT ( 'NONE',  ( 0.05219959533909260263, 19.03943276465977164, 24.99890960531435269 ) ) ;
#186960 = CARTESIAN_POINT ( 'NONE',  ( 14.34966873604960469, 8.224510206698951720, 84.16557627198103830 ) ) ;
#186961 = EDGE_CURVE ( 'NONE', #139778, #89587, #42779, .T. ) ;
#186962 = CARTESIAN_POINT ( 'NONE',  ( -18.67979575497178146, -10.72451020669898902, 101.6655762719810383 ) ) ;
#186963 = CARTESIAN_POINT ( 'NONE',  ( 18.67979575497194134, -10.72451020669871369, 30.83442372801902209 ) ) ;
#186964 = DIRECTION ( 'NONE',  ( -0.5000000000000002220, -0.4999999999999985012, 0.7071067811865483499 ) ) ;
#186965 = CARTESIAN_POINT ( 'NONE',  ( 0.05219959533934541429, -16.53943276465976808, 45.00109039468568284 ) ) ;
#186966 = CARTESIAN_POINT ( 'NONE',  ( 18.67979575497178502, 10.72451020669898547, 89.16557627198102409 ) ) ;
#186967 = CARTESIAN_POINT ( 'NONE',  ( -5.719274019375665041, -21.55341960407619695, 104.7927570613523898 ) ) ;
#186968 = CARTESIAN_POINT ( 'NONE',  ( -19.05341960407611168, -5.049401038298163336, 106.4572429386476955 ) ) ;
#186969 = CARTESIAN_POINT ( 'NONE',  ( -10.81492255796105439, 18.62759615963255655, 47.91775706135234714 ) ) ;
#186970 = CARTESIAN_POINT ( 'NONE',  ( 15.80617190586746368, 15.72974639402197994, 44.37390960531435979 ) ) ;
#186971 = CARTESIAN_POINT ( 'NONE',  ( -14.34966873604972548, 8.224510206698743886, 98.33442372801901854 ) ) ;
#186973 = CARTESIAN_POINT ( 'NONE',  ( -5.823673210054431948, 21.52544592524334988, 102.7094237280190185 ) ) ;
#186972 = CARTESIAN_POINT ( 'NONE',  ( -21.52544592524334988, -5.823673210054445271, 58.95942372801902565 ) ) ;
#186974 = CARTESIAN_POINT ( 'NONE',  ( 16.51473224551083163, -9.474510206698727899, 30.83442372801900433 ) ) ;
#186975 = CARTESIAN_POINT ( 'NONE',  ( 16.55341960407618274, -4.379528057220086978, 91.04275706135236135 ) ) ;
#186976 = CARTESIAN_POINT ( 'NONE',  ( 21.52544592524334988, 5.823673210054432836, 46.45942372801901854 ) ) ;
#186977 = CARTESIAN_POINT ( 'NONE',  ( -19.02544592524342804, 5.153800228976336051, 51.04057627198103120 ) ) ;
#186978 = CARTESIAN_POINT ( 'NONE',  ( 15.72974639402176855, 15.80617190586768217, 111.8760903946856615 ) ) ;
#186979 = CARTESIAN_POINT ( 'NONE',  ( -15.80617190586745835, -15.72974639402198527, 21.87390960531436690 ) ) ;
#186980 = CARTESIAN_POINT ( 'NONE',  ( 21.52544592524334988, 5.823673210054432836, 21.45942372801901499 ) ) ;
#186981 = CARTESIAN_POINT ( 'NONE',  ( -18.62759615963270932, 10.81492255796079327, 70.83224293864770971 ) ) ;
#186983 = CARTESIAN_POINT ( 'NONE',  ( 0.05219959533907565091, 21.53943276465977519, 79.99890960531435269 ) ) ;
#186982 = DIRECTION ( 'NONE',  ( 0.000000000000000000, -0.8164965809277233699, -0.5773502691896295058 ) ) ;
#186985 = CARTESIAN_POINT ( 'NONE',  ( -0.05219959533910754901, -16.53943276465976808, 67.49890960531436690 ) ) ;
#186984 = CARTESIAN_POINT ( 'NONE',  ( 12.14591786802327356, -12.06949235617739191, 65.62609039468568994 ) ) ;
#186986 = CARTESIAN_POINT ( 'NONE',  ( 1.065438805247536314, 29.32802529041667228, -49.14125557145903400 ) ) ;
#186987 = CARTESIAN_POINT ( 'NONE',  ( -9.474510206698720793, -16.51473224551083518, 94.58442372801900433 ) ) ;
#186988 = CARTESIAN_POINT ( 'NONE',  ( -9.396639952208071023, -10.08966692039653523, -60.41061585848335369 ) ) ;
#186989 = EDGE_CURVE ( 'NONE', #102442, #93070, #64551, .T. ) ;
#186990 = CARTESIAN_POINT ( 'NONE',  ( -16.53943276465976808, -0.05219959533934237506, 43.75109039468568284 ) ) ;
#186991 = CARTESIAN_POINT ( 'NONE',  ( -15.80617190586745835, -15.72974639402198527, 96.87390960531436690 ) ) ;
#186992 = CARTESIAN_POINT ( 'NONE',  ( 15.72974639402199770, -15.80617190586745480, 73.12390960531436690 ) ) ;
#186993 = CARTESIAN_POINT ( 'NONE',  ( -13.97604488694527625, -13.89961937509977652, 111.8739096053143243 ) ) ;
#186994 = CARTESIAN_POINT ( 'NONE',  ( 16.52544592524335698, 4.483927247898782831, 56.45942372801902565 ) ) ;
#186995 = CARTESIAN_POINT ( 'NONE',  ( -16.46253265017160317, 9.564922557960807481, 70.83224293864770971 ) ) ;
#186997 = CARTESIAN_POINT ( 'NONE',  ( -19.03943276465977164, -0.05219959533935918106, 113.7510903946856757 ) ) ;
#186996 = CARTESIAN_POINT ( 'NONE',  ( 21.55341960407619695, -5.719274019375665929, 41.04275706135236135 ) ) ;
#186998 = CARTESIAN_POINT ( 'NONE',  ( -5.049401038298153566, 19.05341960407611168, 105.2072429386476671 ) ) ;
#186999 = CARTESIAN_POINT ( 'NONE',  ( 13.97604488694548053, -13.89961937509957401, 25.62609039468566507 ) ) ;
#187000 = CARTESIAN_POINT ( 'NONE',  ( 14.34966873604972726, -8.224510206698740333, 40.83442372801901854 ) ) ;
#187001 = CARTESIAN_POINT ( 'NONE',  ( 5.153800228976335163, 19.02544592524342804, 99.79057627198102409 ) ) ;
#187002 = CARTESIAN_POINT ( 'NONE',  ( 21.52544592524344225, -5.823673210054117533, 98.54057627198105251 ) ) ;
#187003 = CARTESIAN_POINT ( 'NONE',  ( -9.474510206698964154, 16.51473224551069663, 55.41557627198103120 ) ) ;
#187004 = CARTESIAN_POINT ( 'NONE',  ( -17.44270441346515099, 5.991230190323086013, 23.63664920735773123 ) ) ;
#187005 = CARTESIAN_POINT ( 'NONE',  ( -4.483927247898539470, -16.52544592524342804, 77.29057627198102409 ) ) ;
#187006 = CARTESIAN_POINT ( 'NONE',  ( -9.474510206698964154, 16.51473224551069663, 115.4155762719810241 ) ) ;
#187007 = CARTESIAN_POINT ( 'NONE',  ( -35.00000000000000000, 0.3535533905932703447, 5.353553390593268624 ) ) ;
#187008 = CARTESIAN_POINT ( 'NONE',  ( -21.52544592524343514, 5.823673210054127303, 101.0405762719810383 ) ) ;
#187009 = CARTESIAN_POINT ( 'NONE',  ( 5.049401038297881783, 19.05341960407617563, 57.29275706135231871 ) ) ;
#187010 = CARTESIAN_POINT ( 'NONE',  ( -9.474510206698964154, 16.51473224551069663, 115.4155762719810241 ) ) ;
#187011 = CARTESIAN_POINT ( 'NONE',  ( 13.89961937509977652, -13.97604488694527269, 33.12390960531434558 ) ) ;
#187012 = CARTESIAN_POINT ( 'NONE',  ( 5.823673210054125526, 21.52544592524343514, 54.79057627198104541 ) ) ;
#187013 = CARTESIAN_POINT ( 'NONE',  ( -19.02544592524342804, 5.153800228976336051, 106.0405762719810241 ) ) ;
#187014 = CARTESIAN_POINT ( 'NONE',  ( 21.52544592524334988, 5.823673210054432836, 76.45942372801901854 ) ) ;
#187015 = CARTESIAN_POINT ( 'NONE',  ( -16.51473224551069308, -9.474510206698971260, 46.66557627198102409 ) ) ;
#187016 = EDGE_CURVE ( 'NONE', #93013, #152327, #127846, .T. ) ;
#187017 = CARTESIAN_POINT ( 'NONE',  ( -16.52544592524342804, 4.483927247898546575, 91.04057627198103830 ) ) ;
#187018 = CARTESIAN_POINT ( 'NONE',  ( -8.224510206698735004, -14.34966873604973081, 29.58442372801901854 ) ) ;
#187019 = CARTESIAN_POINT ( 'NONE',  ( -0.05219959533909027116, -19.03943276465977164, 62.49890960531435979 ) ) ;
#187020 = CARTESIAN_POINT ( 'NONE',  ( -21.55341960407619339, 5.719274019375674811, 63.54275706135234003 ) ) ;
#187021 = ORIENTED_EDGE ( 'NONE', *, *, #59945, .T. ) ;
#187022 = CARTESIAN_POINT ( 'NONE',  ( 5.049401038297881783, 19.05341960407617563, 22.29275706135233648 ) ) ;
#187023 = CARTESIAN_POINT ( 'NONE',  ( -19.05341960407617563, 5.049401038297882671, 43.54275706135232582 ) ) ;
#187024 = CARTESIAN_POINT ( 'NONE',  ( -38.00000000000000711, 2.428612866367529932E-14, -5.749999994537626336 ) ) ;
#187025 = CARTESIAN_POINT ( 'NONE',  ( -10.81492255796105439, 18.62759615963255655, 37.91775706135235424 ) ) ;
#187026 = CARTESIAN_POINT ( 'NONE',  ( 0.05219959533909260263, 19.03943276465977164, 54.99890960531435979 ) ) ;
#187027 = CARTESIAN_POINT ( 'NONE',  ( 9.564922557961047289, -16.46253265017146816, 35.41775706135233293 ) ) ;
#187028 = CARTESIAN_POINT ( 'NONE',  ( 19.03943276465977164, -0.05219959533909143690, 63.74890960531435979 ) ) ;
#187029 = CARTESIAN_POINT ( 'NONE',  ( -8.314922557960811034, -14.29746914071050412, 27.08224293864769550 ) ) ;
#187031 = CARTESIAN_POINT ( 'NONE',  ( -10.81492255796105439, 18.62759615963255655, 92.91775706135236135 ) ) ;
#187030 = CARTESIAN_POINT ( 'NONE',  ( -21.53943276465977519, 0.05219959533907696930, 26.24890960531435624 ) ) ;
#187032 = AXIS2_PLACEMENT_3D ( 'NONE', #198452, #57960, #119631 ) ;
#187033 = CARTESIAN_POINT ( 'NONE',  ( -5.950531402560715689E-15, 38.81732327939063509, -5.124999997268813168 ) ) ;
#187034 = CARTESIAN_POINT ( 'NONE',  ( 17.13100169013299379, 6.664070546373164206, 56.73210164300152059 ) ) ;
#187035 = CARTESIAN_POINT ( 'NONE',  ( -21.55341960407619339, 5.719274019375674811, 88.54275706135236135 ) ) ;
#187036 = CARTESIAN_POINT ( 'NONE',  ( 3.765340386950246872E-15, -39.95163481335715971, -3.247842220587803030 ) ) ;
#187037 = CARTESIAN_POINT ( 'NONE',  ( -16.51473224551069308, -9.474510206698971260, 96.66557627198102409 ) ) ;
#187038 = CARTESIAN_POINT ( 'NONE',  ( -23.64874990377911956, -15.04272038711346582, 165.8682408883346397 ) ) ;
#187039 = CARTESIAN_POINT ( 'NONE',  ( -0.05219959533909027116, -19.03943276465977164, 47.49890960531435979 ) ) ;
#187040 = CARTESIAN_POINT ( 'NONE',  ( 21.52544592524344225, -5.823673210054117533, 73.54057627198102409 ) ) ;
#187041 = CARTESIAN_POINT ( 'NONE',  ( 12.06949235617757843, -12.14591786802309237, 33.12390960531435979 ) ) ;
#187043 = CARTESIAN_POINT ( 'NONE',  ( 5.153800228976335163, 19.02544592524342804, 99.79057627198102409 ) ) ;
#187042 = CARTESIAN_POINT ( 'NONE',  ( -8.224510206698948167, 14.34966873604960824, 115.4155762719810241 ) ) ;
#187044 = CARTESIAN_POINT ( 'NONE',  ( 21.55341960407619695, -5.719274019375665929, 111.0427570613523613 ) ) ;
#187045 = CARTESIAN_POINT ( 'NONE',  ( 16.52544592524342804, -4.483927247898539470, 103.5405762719810383 ) ) ;
#187046 = CARTESIAN_POINT ( 'NONE',  ( 21.53943276465977519, 0.05219959533937863772, 66.25109039468567573 ) ) ;
#187047 = CARTESIAN_POINT ( 'NONE',  ( 13.89961937509978007, -13.97604488694527269, 98.12390960531435269 ) ) ;
#187048 = CARTESIAN_POINT ( 'NONE',  ( 4.379528057220092307, 16.55341960407617563, 112.2927570613523471 ) ) ;
#187049 = CARTESIAN_POINT ( 'NONE',  ( 13.89961937509957401, 13.97604488694547697, 61.87609039468566863 ) ) ;
#187050 = CARTESIAN_POINT ( 'NONE',  ( -29.86685920354755552, 21.69954338932564397, -7.324999997268814234 ) ) ;
#187051 = CARTESIAN_POINT ( 'NONE',  ( -9.564922557960796823, -16.46253265017161027, 112.0822429386476955 ) ) ;
#187052 = CARTESIAN_POINT ( 'NONE',  ( -16.53943276465976808, 0.05219959533911058130, 71.24890960531435269 ) ) ;
#187053 = CARTESIAN_POINT ( 'NONE',  ( 5.153800228976615827, -19.02544592524334988, 60.20942372801899012 ) ) ;
#187054 = CARTESIAN_POINT ( 'NONE',  ( 9.564922557960805705, 16.46253265017160317, 59.58224293864769550 ) ) ;
#187055 = CARTESIAN_POINT ( 'NONE',  ( 16.55341960407611168, 4.379528057220329451, 58.95724293864770971 ) ) ;
#187056 = CARTESIAN_POINT ( 'NONE',  ( -19.03943276465977164, -0.05219959533935918106, 88.75109039468567573 ) ) ;
#187057 = CARTESIAN_POINT ( 'NONE',  ( -5.719274019375978568, 21.55341960407610458, 50.20724293864769550 ) ) ;
#187058 = ORIENTED_EDGE ( 'NONE', *, *, #98810, .F. ) ;
#187059 = CARTESIAN_POINT ( 'NONE',  ( 8.224510206698953496, -14.34966873604960469, 112.9155762719810383 ) ) ;
#187060 = CARTESIAN_POINT ( 'NONE',  ( -17.44279575226822843, -5.990770900252486264, 29.16442432485682801 ) ) ;
#187062 = CARTESIAN_POINT ( 'NONE',  ( 21.55341960407610458, 5.719274019375980345, 63.95724293864770260 ) ) ;
#187061 = CARTESIAN_POINT ( 'NONE',  ( -19.02544592524342804, 5.153800228976336051, 76.04057627198102409 ) ) ;
#187064 = CARTESIAN_POINT ( 'NONE',  ( -0.05219959533909027116, -19.03943276465977164, 77.49890960531435269 ) ) ;
#187063 = CARTESIAN_POINT ( 'NONE',  ( 12.06949235617739724, 12.14591786802326823, 91.87609039468568994 ) ) ;
#187065 = CARTESIAN_POINT ( 'NONE',  ( 9.474510206698729675, 16.51473224551082808, 57.08442372801900433 ) ) ;
#187066 = CARTESIAN_POINT ( 'NONE',  ( -0.05219959533937732626, 21.53943276465977519, 87.50109039468568994 ) ) ;
#187067 = CARTESIAN_POINT ( 'NONE',  ( 18.67979575497178502, 10.72451020669898547, 64.16557627198102409 ) ) ;
#187068 = CARTESIAN_POINT ( 'NONE',  ( -19.05341960407611168, -5.049401038298163336, 106.4572429386476955 ) ) ;
#187069 = CARTESIAN_POINT ( 'NONE',  ( -16.46253265017160317, 9.564922557960807481, 35.83224293864768839 ) ) ;
#187070 = CARTESIAN_POINT ( 'NONE',  ( 4.379528057220092307, 16.55341960407617563, 97.29275706135234714 ) ) ;
#187071 = CARTESIAN_POINT ( 'NONE',  ( -16.53943276465976808, -0.05219959533934237506, 18.75109039468568639 ) ) ;
#187072 = CARTESIAN_POINT ( 'NONE',  ( -3.573655867282028392E-15, 2.428612866367529932E-14, 1.984260520772446048E-44 ) ) ;
#187073 = CARTESIAN_POINT ( 'NONE',  ( 10.81492255796106328, -18.62759615963255655, 95.41775706135234714 ) ) ;
#187074 = ORIENTED_EDGE ( 'NONE', *, *, #199705, .F. ) ;
#187075 = CARTESIAN_POINT ( 'NONE',  ( 4.483927247898545687, 16.52544592524342804, 59.79057627198103120 ) ) ;
#187076 = CARTESIAN_POINT ( 'NONE',  ( 14.34966873604960469, 8.224510206698951720, 69.16557627198102409 ) ) ;
#187077 = CARTESIAN_POINT ( 'NONE',  ( 18.62759615963271287, -10.81492255796078972, 93.33224293864769550 ) ) ;
#187078 = CARTESIAN_POINT ( 'NONE',  ( -18.62759615963270932, 10.81492255796079327, 85.83224293864768129 ) ) ;
#187079 = CARTESIAN_POINT ( 'NONE',  ( 17.31747979337947640, -6.344076630961051677, 96.12055131934815222 ) ) ;
#187080 = CARTESIAN_POINT ( 'NONE',  ( -10.81492255796078084, -18.62759615963271287, 52.08224293864768839 ) ) ;
#187081 = CARTESIAN_POINT ( 'NONE',  ( -12.14591786802326823, 12.06949235617739902, 73.12609039468567573 ) ) ;
#187082 = CARTESIAN_POINT ( 'NONE',  ( 16.53943276465976808, -0.05219959533910856209, 88.74890960531436690 ) ) ;
#187083 = CARTESIAN_POINT ( 'NONE',  ( -9.564922557960796823, -16.46253265017161027, 42.08224293864769550 ) ) ;
#187084 = DIRECTION ( 'NONE',  ( 1.000000000000000000, 0.000000000000000000, 3.709348145883536076E-20 ) ) ;
#187085 = CARTESIAN_POINT ( 'NONE',  ( 12.06949235617739724, 12.14591786802326823, 101.8760903946857042 ) ) ;
#187086 = CARTESIAN_POINT ( 'NONE',  ( 18.67979575497194134, -10.72451020669871369, 30.83442372801902209 ) ) ;
#187087 = CARTESIAN_POINT ( 'NONE',  ( 9.564922557960805705, 16.46253265017160317, 94.58224293864769550 ) ) ;
#187088 = CARTESIAN_POINT ( 'NONE',  ( -10.81492255796105439, 18.62759615963255655, 67.91775706135234714 ) ) ;
#187089 = CARTESIAN_POINT ( 'NONE',  ( -28.28060372831499336, 2.428612866367529932E-14, 149.6875000013656063 ) ) ;
#187090 = CARTESIAN_POINT ( 'NONE',  ( 5.049401038298161559, -19.05341960407611168, 22.70724293864769194 ) ) ;
#187091 = ORIENTED_EDGE ( 'NONE', *, *, #184390, .T. ) ;
#187092 = CARTESIAN_POINT ( 'NONE',  ( -18.67979575497193778, 10.72451020669871902, 58.33442372801901143 ) ) ;
#187094 = CARTESIAN_POINT ( 'NONE',  ( 18.22780087662119897, -5.500000000000096811, 58.51763182126894947 ) ) ;
#187093 = CARTESIAN_POINT ( 'NONE',  ( 19.03943276465977164, -0.05219959533909143690, 53.74890960531436690 ) ) ;
#187095 = CARTESIAN_POINT ( 'NONE',  ( 19.02544592524343514, -5.153800228976328945, 88.54057627198102409 ) ) ;
#187096 = CARTESIAN_POINT ( 'NONE',  ( 19.05341960407617918, -5.049401038297876454, 61.04275706135232582 ) ) ;
#187097 = CARTESIAN_POINT ( 'NONE',  ( -21.55341960407619339, 5.719274019375674811, 48.54275706135234714 ) ) ;
#187098 = CARTESIAN_POINT ( 'NONE',  ( 16.51473224551083163, -9.474510206698727899, 55.83442372801899722 ) ) ;
#187099 = CARTESIAN_POINT ( 'NONE',  ( 5.153800228976335163, 19.02544592524342804, 39.79057627198100988 ) ) ;
#187100 = CARTESIAN_POINT ( 'NONE',  ( -8.224510206698735004, -14.34966873604973081, 109.5844237280190328 ) ) ;
#187101 = CARTESIAN_POINT ( 'NONE',  ( 5.049401038297881783, 19.05341960407617563, 77.29275706135231871 ) ) ;
#187102 = CARTESIAN_POINT ( 'NONE',  ( -8.314922557961024197, 14.29746914071037800, 112.9177570613523329 ) ) ;
#187103 = CARTESIAN_POINT ( 'NONE',  ( 13.89961937509957401, 13.97604488694547697, 46.87609039468565442 ) ) ;
#187104 = CARTESIAN_POINT ( 'NONE',  ( 5.049401038298161559, -19.05341960407611168, 102.7072429386476955 ) ) ;
#187105 = CARTESIAN_POINT ( 'NONE',  ( -10.72451020669870658, -18.67979575497194134, 109.5844237280190328 ) ) ;
#187106 = CARTESIAN_POINT ( 'NONE',  ( 13.97604488694548053, -13.89961937509957401, 30.62609039468566863 ) ) ;
#187107 = CARTESIAN_POINT ( 'NONE',  ( -5.153800228976328057, -19.02544592524343514, 32.29057627198102409 ) ) ;
#187108 = CARTESIAN_POINT ( 'NONE',  ( -21.52544592524334988, -5.823673210054445271, 88.95942372801901854 ) ) ;
#187109 = CARTESIAN_POINT ( 'NONE',  ( 16.52544592524335698, 4.483927247898782831, 36.45942372801901143 ) ) ;
#187110 = CARTESIAN_POINT ( 'NONE',  ( -19.02544592524342804, 5.153800228976336051, 96.04057627198103830 ) ) ;
#187111 = CARTESIAN_POINT ( 'NONE',  ( -27.73933785331498925, 2.428612866367529932E-14, 138.8750000027311842 ) ) ;
#187112 = CARTESIAN_POINT ( 'NONE',  ( 9.474510206698971260, -16.51473224551069308, 72.91557627198102409 ) ) ;
#187113 = CARTESIAN_POINT ( 'NONE',  ( 0.05219959533936267826, -19.03943276465977164, 75.00109039468566152 ) ) ;
#187114 = CARTESIAN_POINT ( 'NONE',  ( -19.05341960407611168, -5.049401038298163336, 101.4572429386476955 ) ) ;
#187115 = CARTESIAN_POINT ( 'NONE',  ( -10.72451020669870658, -18.67979575497194134, 99.58442372801900433 ) ) ;
#187116 = CARTESIAN_POINT ( 'NONE',  ( 4.483927247898545687, 16.52544592524342804, 94.79057627198105251 ) ) ;
#187117 = CARTESIAN_POINT ( 'NONE',  ( 9.564922557960805705, 16.46253265017160317, 29.58224293864769550 ) ) ;
#187118 = CARTESIAN_POINT ( 'NONE',  ( 5.823673210054125526, 21.52544592524343514, 44.79057627198103120 ) ) ;
#187119 = CARTESIAN_POINT ( 'NONE',  ( 21.55341960407610458, 5.719274019375980345, 38.95724293864768839 ) ) ;
#187120 = CARTESIAN_POINT ( 'NONE',  ( 16.55341960407611168, 4.379528057220329451, 103.9572429386476813 ) ) ;
#187121 = CARTESIAN_POINT ( 'NONE',  ( -0.9205664139720410866, -8.788389965099099754, -61.95844424577440179 ) ) ;
#187122 = CARTESIAN_POINT ( 'NONE',  ( -16.46253265017146816, -9.564922557961047289, 59.16775706135233293 ) ) ;
#187123 = CARTESIAN_POINT ( 'NONE',  ( -4.483927247898539470, -16.52544592524342804, 37.29057627198102409 ) ) ;
#187124 = CARTESIAN_POINT ( 'NONE',  ( -13.89961937509977652, 13.97604488694528158, 115.6239096053143669 ) ) ;
#187125 = CARTESIAN_POINT ( 'NONE',  ( -21.53943276465977519, -0.05219959533937600094, 78.75109039468568994 ) ) ;
#187126 = CARTESIAN_POINT ( 'NONE',  ( -10.72451020669898014, 18.67979575497178502, 75.41557627198102409 ) ) ;
#187127 = CARTESIAN_POINT ( 'NONE',  ( -15.80617190586768217, 15.72974639402176855, 43.12609039468568284 ) ) ;
#187128 = CARTESIAN_POINT ( 'NONE',  ( -18.67979575497178146, -10.72451020669898902, 91.66557627198103830 ) ) ;
#187129 = CARTESIAN_POINT ( 'NONE',  ( 15.80617190586769283, -15.72974639402175789, 50.62609039468568994 ) ) ;
#187130 = CARTESIAN_POINT ( 'NONE',  ( -13.89961937509977652, 13.97604488694528158, 30.62390960531435269 ) ) ;
#187131 = CARTESIAN_POINT ( 'NONE',  ( -9.474510206698964154, 16.51473224551069663, 85.41557627198102409 ) ) ;
#187132 = CARTESIAN_POINT ( 'NONE',  ( 4.483927247898790824, -16.52544592524335698, 75.20942372801901854 ) ) ;
#187133 = CARTESIAN_POINT ( 'NONE',  ( -14.29746914071049879, 8.314922557960819915, 100.8322429386477097 ) ) ;
#187134 = CARTESIAN_POINT ( 'NONE',  ( -13.97604488694527625, -13.89961937509977652, 106.8739096053143669 ) ) ;
#187135 = CARTESIAN_POINT ( 'NONE',  ( 14.34966873604960469, 8.224510206698951720, 54.16557627198103120 ) ) ;
#187136 = CARTESIAN_POINT ( 'NONE',  ( 12.06949235617757843, -12.14591786802309237, 23.12390960531436335 ) ) ;
#187137 = CARTESIAN_POINT ( 'NONE',  ( -13.97604488694527625, -13.89961937509977652, 71.87390960531433848 ) ) ;
#187138 = CARTESIAN_POINT ( 'NONE',  ( 19.05341960407611168, 5.049401038298154454, 28.95724293864769550 ) ) ;
#187139 = CARTESIAN_POINT ( 'NONE',  ( -21.55341960407610458, -5.719274019375992779, 51.45724293864770260 ) ) ;
#187140 = CARTESIAN_POINT ( 'NONE',  ( -19.03943276465977164, -0.05219959533935918106, 38.75109039468566152 ) ) ;
#187142 = CARTESIAN_POINT ( 'NONE',  ( -16.53943276465976808, 0.05219959533911058130, 31.24890960531435979 ) ) ;
#187141 = CARTESIAN_POINT ( 'NONE',  ( -17.05116617787826527, -6.768360034955709814, 41.34324446740802017 ) ) ;
#187143 = CARTESIAN_POINT ( 'NONE',  ( -5.049401038298153566, 19.05341960407611168, 110.2072429386476671 ) ) ;
#187144 = CARTESIAN_POINT ( 'NONE',  ( -15.72974639402176322, -15.80617190586768395, 59.37609039468568284 ) ) ;
#187145 = CARTESIAN_POINT ( 'NONE',  ( 13.97604488694527802, 13.89961937509977652, 114.3739096053143669 ) ) ;
#187146 = CARTESIAN_POINT ( 'NONE',  ( -4.379528057220086978, -16.55341960407618274, 64.79275706135234714 ) ) ;
#187147 = CARTESIAN_POINT ( 'NONE',  ( -0.05219959533936034679, 19.03943276465977164, 57.50109039468566863 ) ) ;
#187148 = CARTESIAN_POINT ( 'NONE',  ( 12.14591786802309770, 12.06949235617756955, 29.37390960531435269 ) ) ;
#187149 = CARTESIAN_POINT ( 'NONE',  ( 16.36317988757059538, -7.306389748694852138, 51.59789608363229974 ) ) ;
#187150 = CARTESIAN_POINT ( 'NONE',  ( 14.34966873604972726, -8.224510206698740333, 100.8344237280190185 ) ) ;
#187151 = CARTESIAN_POINT ( 'NONE',  ( -19.05341960407611168, -5.049401038298163336, 36.45724293864766707 ) ) ;
#187152 = ADVANCED_FACE ( 'NONE', ( #43764 ), #153696, .T. ) ;
#187153 = CARTESIAN_POINT ( 'NONE',  ( -9.474510206698964154, 16.51473224551069663, 55.41557627198103120 ) ) ;
#187154 = CARTESIAN_POINT ( 'NONE',  ( 5.153800228976335163, 19.02544592524342804, 29.79057627198102409 ) ) ;
#187155 = CARTESIAN_POINT ( 'NONE',  ( -21.53943276465977519, -0.05219959533937600094, 33.75109039468568284 ) ) ;
#187156 = CARTESIAN_POINT ( 'NONE',  ( 5.153800228976335163, 19.02544592524342804, 59.79057627198100988 ) ) ;
#187157 = FACE_OUTER_BOUND ( 'NONE', #28130, .T. ) ;
#187158 = CARTESIAN_POINT ( 'NONE',  ( -9.564922557960796823, -16.46253265017161027, 42.08224293864769550 ) ) ;
#187159 = CARTESIAN_POINT ( 'NONE',  ( 15.80617190586746368, 15.72974639402197994, 29.37390960531435269 ) ) ;
#187160 = AXIS2_PLACEMENT_3D ( 'NONE', #128649, #176182, #116499 ) ;
#187162 = CARTESIAN_POINT ( 'NONE',  ( 16.46253265017160672, -9.564922557960803928, 28.33224293864769550 ) ) ;
#187161 = CARTESIAN_POINT ( 'NONE',  ( -21.55341960407619339, 5.719274019375674811, 53.54275706135234714 ) ) ;
#187163 = CARTESIAN_POINT ( 'NONE',  ( -15.72974639402197994, 15.80617190586746368, 25.62390960531435624 ) ) ;
#187164 = CARTESIAN_POINT ( 'NONE',  ( 0.05219959533934541429, -16.53943276465976808, 75.00109039468568994 ) ) ;
#187165 = CARTESIAN_POINT ( 'NONE',  ( 21.55341960407619695, -5.719274019375665929, 106.0427570613523471 ) ) ;
#187166 = CARTESIAN_POINT ( 'NONE',  ( -16.52544592524335698, -4.483927247898792601, 53.95942372801900433 ) ) ;
#187167 = CARTESIAN_POINT ( 'NONE',  ( -9.474510206698964154, 16.51473224551069663, 90.41557627198103830 ) ) ;
#187168 = CARTESIAN_POINT ( 'NONE',  ( 8.224510206698742110, 14.34966873604972548, 37.08442372801901143 ) ) ;
#187169 = CARTESIAN_POINT ( 'NONE',  ( 16.53943276465976808, 0.05219959533934440121, 21.25109039468567218 ) ) ;
#187170 = CARTESIAN_POINT ( 'NONE',  ( -4.379528057220086978, -16.55341960407618274, 94.79275706135234714 ) ) ;
#187171 = CARTESIAN_POINT ( 'NONE',  ( 5.823673210054444382, -21.52544592524334988, 60.20942372801902565 ) ) ;
#187172 = CARTESIAN_POINT ( 'NONE',  ( -16.51473224551082808, 9.474510206698731452, 103.3344237280190043 ) ) ;
#187173 = CARTESIAN_POINT ( 'NONE',  ( 15.80617190586746368, 15.72974639402197994, 114.3739096053143527 ) ) ;
#187175 = CARTESIAN_POINT ( 'NONE',  ( 0.05219959533936267826, -19.03943276465977164, 110.0010903946856757 ) ) ;
#187174 = CARTESIAN_POINT ( 'NONE',  ( 14.29746914071049879, -8.314922557960816363, 98.33224293864769550 ) ) ;
#187176 = CARTESIAN_POINT ( 'NONE',  ( 16.52544592524335698, 4.483927247898782831, 86.45942372801901854 ) ) ;
#187177 = CARTESIAN_POINT ( 'NONE',  ( 24.51266705573306481, 8.027923408435615471, 167.0300397585818644 ) ) ;
#187178 = CARTESIAN_POINT ( 'NONE',  ( 16.51473224551083163, -9.474510206698727899, 80.83442372801899012 ) ) ;
#187179 = CARTESIAN_POINT ( 'NONE',  ( -0.05219959533910754901, -16.53943276465976808, 47.49890960531435979 ) ) ;
#187180 = CARTESIAN_POINT ( 'NONE',  ( 8.314922557960818139, 14.29746914071049879, 44.58224293864769550 ) ) ;
#187181 = CARTESIAN_POINT ( 'NONE',  ( -12.14591786802309592, -12.06949235617757132, 106.8739096053143811 ) ) ;
#187183 = CARTESIAN_POINT ( 'NONE',  ( -17.49999999999998934, 5.624438216177589211, 90.81670344914643067 ) ) ;
#187182 = CARTESIAN_POINT ( 'NONE',  ( 16.46253265017146816, 9.564922557961045513, 51.66775706135233293 ) ) ;
#187184 = CARTESIAN_POINT ( 'NONE',  ( 18.67979575497194134, -10.72451020669871369, 30.83442372801902209 ) ) ;
#187185 = CARTESIAN_POINT ( 'NONE',  ( 0.05219959533936267826, -19.03943276465977164, 110.0010903946856757 ) ) ;
#187186 = CARTESIAN_POINT ( 'NONE',  ( -0.8613000766923508689, 7.878827036337495926, 6.568406857878970939 ) ) ;
#187187 = CARTESIAN_POINT ( 'NONE',  ( -9.564922557960796823, -16.46253265017161027, 107.0822429386476955 ) ) ;
#187188 = CARTESIAN_POINT ( 'NONE',  ( 19.03943276465977164, -0.05219959533909143690, 83.74890960531436690 ) ) ;
#187189 = CARTESIAN_POINT ( 'NONE',  ( -18.67979575497178146, -10.72451020669898902, 56.66557627198103830 ) ) ;
#187190 = CARTESIAN_POINT ( 'NONE',  ( 8.224510206698953496, -14.34966873604960469, 112.9155762719810383 ) ) ;
#187191 = CARTESIAN_POINT ( 'NONE',  ( -13.89961937509977652, 13.97604488694528158, 75.62390960531438111 ) ) ;
#187192 = CARTESIAN_POINT ( 'NONE',  ( 5.153800228976335163, 19.02544592524342804, 29.79057627198102409 ) ) ;
#187193 = CARTESIAN_POINT ( 'NONE',  ( -18.67979575497193778, 10.72451020669871902, 33.33442372801900433 ) ) ;
#187194 = AXIS2_PLACEMENT_3D ( 'NONE', #56664, #118337, #30288 ) ;
#187195 = CARTESIAN_POINT ( 'NONE',  ( -18.62759615963255300, -10.81492255796106328, 74.16775706135231871 ) ) ;
#187196 = CARTESIAN_POINT ( 'NONE',  ( -16.52544592524335698, -4.483927247898792601, 88.95942372801901854 ) ) ;
#187197 = CARTESIAN_POINT ( 'NONE',  ( -21.52544592524334988, -5.823673210054445271, 23.95942372801901143 ) ) ;
#187198 = CARTESIAN_POINT ( 'NONE',  ( 5.719274019375673035, 21.55341960407619339, 22.29275706135235069 ) ) ;
#187200 = CARTESIAN_POINT ( 'NONE',  ( 9.474510206698971260, -16.51473224551069308, 82.91557627198103830 ) ) ;
#187199 = CARTESIAN_POINT ( 'NONE',  ( -0.05219959533936034679, 19.03943276465977164, 67.50109039468566152 ) ) ;
#187201 = CARTESIAN_POINT ( 'NONE',  ( 15.80617190586769283, -15.72974639402175789, 90.62609039468567573 ) ) ;
#187202 = CARTESIAN_POINT ( 'NONE',  ( -18.67979575497178146, -10.72451020669898902, 86.66557627198102409 ) ) ;
#187203 = CARTESIAN_POINT ( 'NONE',  ( -14.29746914071049879, 8.314922557960819915, 70.83224293864770971 ) ) ;
#187204 = CARTESIAN_POINT ( 'NONE',  ( -10.81492255796105439, 18.62759615963255655, 97.91775706135236135 ) ) ;
#187205 = CARTESIAN_POINT ( 'NONE',  ( 12.14591786802309770, 12.06949235617756955, 79.37390960531436690 ) ) ;
#187206 = CARTESIAN_POINT ( 'NONE',  ( -5.153800228976328057, -19.02544592524343514, 22.29057627198102765 ) ) ;
#187207 = CARTESIAN_POINT ( 'NONE',  ( -19.02544592524334988, -5.153800228976617603, 73.95942372801900433 ) ) ;
#187208 = CARTESIAN_POINT ( 'NONE',  ( -8.314922557960811034, -14.29746914071050412, 42.08224293864769550 ) ) ;
#187209 = CARTESIAN_POINT ( 'NONE',  ( 18.62759615963255655, 10.81492255796105972, 81.66775706135236135 ) ) ;
#187210 = CARTESIAN_POINT ( 'NONE',  ( 13.89961937509977652, -13.97604488694527269, 93.12390960531436690 ) ) ;
#187211 = CARTESIAN_POINT ( 'NONE',  ( 19.03943276465977164, 0.05219959533936151252, 61.25109039468566863 ) ) ;
#187212 = CARTESIAN_POINT ( 'NONE',  ( -5.823673210054116645, -21.52544592524344225, 62.29057627198102409 ) ) ;
#187213 = CARTESIAN_POINT ( 'NONE',  ( -5.719274019375978568, 21.55341960407610458, 115.2072429386476955 ) ) ;
#187214 = CARTESIAN_POINT ( 'NONE',  ( -0.05219959533934338120, 16.53943276465976808, 22.50109039468567573 ) ) ;
#187215 = CARTESIAN_POINT ( 'NONE',  ( 4.483927247898790824, -16.52544592524335698, 80.20942372801901854 ) ) ;
#187217 = CARTESIAN_POINT ( 'NONE',  ( -15.72974639402176322, -15.80617190586768395, 19.37609039468568639 ) ) ;
#187216 = CARTESIAN_POINT ( 'NONE',  ( -4.911121358187451425E-30, -78.67194367458512261, -13.00000000000000000 ) ) ;
#187218 = CARTESIAN_POINT ( 'NONE',  ( -8.224510206698948167, 14.34966873604960824, 100.4155762719810241 ) ) ;
#187219 = CARTESIAN_POINT ( 'NONE',  ( 29.86685920354754842, -21.69954338932559068, -8.324999997268813345 ) ) ;
#187220 = CARTESIAN_POINT ( 'NONE',  ( 16.53943276465976808, 0.05219959533934440121, 31.25109039468568639 ) ) ;
#187221 = CARTESIAN_POINT ( 'NONE',  ( 10.72451020669898902, -18.67979575497178502, 67.91557627198102409 ) ) ;
#187222 = CARTESIAN_POINT ( 'NONE',  ( -14.34966873604972548, 8.224510206698743886, 103.3344237280190043 ) ) ;
#187223 = CARTESIAN_POINT ( 'NONE',  ( -4.483927247898782831, 16.52544592524335698, 37.70942372801900433 ) ) ;
#187224 = CARTESIAN_POINT ( 'NONE',  ( 16.46253265017160672, -9.564922557960803928, 28.33224293864769550 ) ) ;
#187225 = CARTESIAN_POINT ( 'NONE',  ( -12.14591786802326823, 12.06949235617739902, 83.12609039468568994 ) ) ;
#187226 = CARTESIAN_POINT ( 'NONE',  ( -9.564922557961040184, 16.46253265017147172, 72.91775706135233293 ) ) ;
#187227 = CARTESIAN_POINT ( 'NONE',  ( 0.05219959533907565091, 21.53943276465977519, 69.99890960531435269 ) ) ;
#187228 = CARTESIAN_POINT ( 'NONE',  ( 4.379528057220092307, 16.55341960407617563, 102.2927570613523613 ) ) ;
#187229 = CARTESIAN_POINT ( 'NONE',  ( -15.80617190586768217, 15.72974639402176855, 78.12609039468570415 ) ) ;
#187230 = CARTESIAN_POINT ( 'NONE',  ( -18.67979575497178146, -10.72451020669898902, 56.66557627198103830 ) ) ;
#187231 = CARTESIAN_POINT ( 'NONE',  ( -5.719274019375978568, 21.55341960407610458, 50.20724293864769550 ) ) ;
#187232 = ORIENTED_EDGE ( 'NONE', *, *, #36811, .F. ) ;
#187233 = CARTESIAN_POINT ( 'NONE',  ( 8.314922557961029526, -14.29746914071037800, 85.41775706135236135 ) ) ;
#187234 = CARTESIAN_POINT ( 'NONE',  ( -18.62759615963270932, 10.81492255796079327, 40.83224293864769550 ) ) ;
#187235 = ORIENTED_EDGE ( 'NONE', *, *, #17219, .F. ) ;
#187236 = CARTESIAN_POINT ( 'NONE',  ( 5.153800228976335163, 19.02544592524342804, 94.79057627198103830 ) ) ;
#187237 = FACE_OUTER_BOUND ( 'NONE', #199640, .T. ) ;
#187238 = CARTESIAN_POINT ( 'NONE',  ( -5.153800228976328057, -19.02544592524343514, 27.29057627198103120 ) ) ;
#187239 = CARTESIAN_POINT ( 'NONE',  ( 21.53943276465977519, -0.05219959533907433946, 63.74890960531435979 ) ) ;
#187240 = CARTESIAN_POINT ( 'NONE',  ( -12.14591786802326823, 12.06949235617739902, 98.12609039468570415 ) ) ;
#187241 = CARTESIAN_POINT ( 'NONE',  ( 21.53943276465977519, 0.05219959533937863772, 51.25109039468568994 ) ) ;
#187242 = CARTESIAN_POINT ( 'NONE',  ( 9.474510206698729675, 16.51473224551082808, 107.0844237280190043 ) ) ;
#187243 = CARTESIAN_POINT ( 'NONE',  ( 8.224510206698953496, -14.34966873604960469, 107.9155762719810241 ) ) ;
#187244 = CARTESIAN_POINT ( 'NONE',  ( -16.46253265017146816, -9.564922557961047289, 109.1677570613523471 ) ) ;
#187245 = CARTESIAN_POINT ( 'NONE',  ( -16.51473224551069308, -9.474510206698971260, 41.66557627198103120 ) ) ;
#187246 = CARTESIAN_POINT ( 'NONE',  ( -3.573655867282028392E-15, 2.428612866367529932E-14, 2.000000000000000000 ) ) ;
#187247 = CARTESIAN_POINT ( 'NONE',  ( -0.05219959533909027116, -19.03943276465977164, 97.49890960531436690 ) ) ;
#187248 = EDGE_CURVE ( 'NONE', #83417, #189747, #47195, .T. ) ;
#187249 = CARTESIAN_POINT ( 'NONE',  ( 16.53943276465976808, 0.05219959533934440121, 81.25109039468568994 ) ) ;
#187250 = CARTESIAN_POINT ( 'NONE',  ( 5.153800228976615827, -19.02544592524334988, 75.20942372801896170 ) ) ;
#187251 = CARTESIAN_POINT ( 'NONE',  ( -21.52544592524334988, -5.823673210054445271, 103.9594237280190185 ) ) ;
#187252 = CARTESIAN_POINT ( 'NONE',  ( 15.80617190586746368, 15.72974639402197994, 64.37390960531435269 ) ) ;
#187253 = CARTESIAN_POINT ( 'NONE',  ( -12.14591786802326823, 12.06949235617739902, 93.12609039468568994 ) ) ;
#187254 = CARTESIAN_POINT ( 'NONE',  ( -19.05341960407617563, 5.049401038297882671, 83.54275706135233293 ) ) ;
#187255 = CARTESIAN_POINT ( 'NONE',  ( 13.97604488694527802, 13.89961937509977652, 39.37390960531435269 ) ) ;
#187256 = CARTESIAN_POINT ( 'NONE',  ( 9.474510206698971260, -16.51473224551069308, 72.91557627198102409 ) ) ;
#187257 = CARTESIAN_POINT ( 'NONE',  ( -21.52544592524334988, -5.823673210054445271, 48.95942372801902565 ) ) ;
#187258 = CARTESIAN_POINT ( 'NONE',  ( 19.03943276465977164, -0.05219959533909143690, 43.74890960531435979 ) ) ;
#187259 = CARTESIAN_POINT ( 'NONE',  ( -19.03943276465977164, -0.05219959533935918106, 73.75109039468566152 ) ) ;
#187260 = CARTESIAN_POINT ( 'NONE',  ( 25.85231681326417785, -7.957828899752770191, 172.6576833274880300 ) ) ;
#187261 = CARTESIAN_POINT ( 'NONE',  ( 16.51473224551069308, 9.474510206698969483, 109.1655762719810383 ) ) ;
#187262 = CARTESIAN_POINT ( 'NONE',  ( 16.53943276465976808, -0.05219959533910856209, 68.74890960531435269 ) ) ;
#187263 = CARTESIAN_POINT ( 'NONE',  ( -0.05219959533907301413, -21.53943276465977519, 57.49890960531435979 ) ) ;
#187264 = CARTESIAN_POINT ( 'NONE',  ( -8.898068258721474777, 27.38543819252877398, 143.8656553485623704 ) ) ;
#187265 = CARTESIAN_POINT ( 'NONE',  ( -13.89961937509957401, -13.97604488694547875, 24.37609039468565442 ) ) ;
#187266 = FACE_OUTER_BOUND ( 'NONE', #77849, .T. ) ;
#187268 = CARTESIAN_POINT ( 'NONE',  ( 16.46253265017160672, -9.564922557960803928, 68.33224293864770971 ) ) ;
#187267 = CARTESIAN_POINT ( 'NONE',  ( -5.049401038298153566, 19.05341960407611168, 65.20724293864765286 ) ) ;
#187269 = CARTESIAN_POINT ( 'NONE',  ( 12.06949235617739724, 12.14591786802326823, 51.87609039468568284 ) ) ;
#187270 = CARTESIAN_POINT ( 'NONE',  ( 13.97604488694548053, -13.89961937509957401, 80.62609039468567573 ) ) ;
#187271 = DIRECTION ( 'NONE',  ( -1.000000000000000000, 0.000000000000000000, 0.000000000000000000 ) ) ;
#187272 = CARTESIAN_POINT ( 'NONE',  ( 4.379528057220092307, 16.55341960407617563, 92.29275706135236135 ) ) ;
#187273 = CARTESIAN_POINT ( 'NONE',  ( 22.55670631985092456, -22.55670631985084995, -45.64921306006598201 ) ) ;
#187274 = CARTESIAN_POINT ( 'NONE',  ( -16.55341960407617563, 4.379528057220093196, 63.54275706135234003 ) ) ;
#187275 = CARTESIAN_POINT ( 'NONE',  ( 4.379528057220092307, 16.55341960407617563, 37.29275706135235424 ) ) ;
#187277 = DIRECTION ( 'NONE',  ( -1.000000000000000000, 0.000000000000000000, -6.982962677686266711E-15 ) ) ;
#187276 = CARTESIAN_POINT ( 'NONE',  ( 19.03943276465977164, -0.05219959533909143690, 58.74890960531435979 ) ) ;
#187278 = CARTESIAN_POINT ( 'NONE',  ( -18.62759615963255300, -10.81492255796106328, 49.16775706135234003 ) ) ;
#187279 = CARTESIAN_POINT ( 'NONE',  ( -5.153800228976607833, 19.02544592524334988, 67.70942372801900433 ) ) ;
#187280 = CARTESIAN_POINT ( 'NONE',  ( 15.80617190586769283, -15.72974639402175789, 110.6260903946857042 ) ) ;
#187281 = CARTESIAN_POINT ( 'NONE',  ( 19.05341960407611168, 5.049401038298154454, 23.95724293864769194 ) ) ;
#187282 = CARTESIAN_POINT ( 'NONE',  ( 21.55341960407610458, 5.719274019375980345, 48.95724293864770971 ) ) ;
#187283 = CARTESIAN_POINT ( 'NONE',  ( -21.52544592524343514, 5.823673210054127303, 26.04057627198103475 ) ) ;
#187284 = CARTESIAN_POINT ( 'NONE',  ( 8.224510206698953496, -14.34966873604960469, 102.9155762719810383 ) ) ;
#187285 = CARTESIAN_POINT ( 'NONE',  ( 16.55341960407618274, -4.379528057220086978, 36.04275706135234714 ) ) ;
#187286 = CARTESIAN_POINT ( 'NONE',  ( -12.14591786802309592, -12.06949235617757132, 31.87390960531435979 ) ) ;
#187287 = ORIENTED_EDGE ( 'NONE', *, *, #172657, .F. ) ;
#187288 = CARTESIAN_POINT ( 'NONE',  ( 15.80617190586769283, -15.72974639402175789, 20.62609039468568639 ) ) ;
#187290 = CARTESIAN_POINT ( 'NONE',  ( -16.46253265017160317, 9.564922557960807481, 115.8322429386477097 ) ) ;
#187289 = CARTESIAN_POINT ( 'NONE',  ( 8.224510206698953496, -14.34966873604960469, 37.91557627198102409 ) ) ;
#187291 = CARTESIAN_POINT ( 'NONE',  ( -5.049401038297874678, -19.05341960407617918, 94.79275706135230450 ) ) ;
#187292 = CARTESIAN_POINT ( 'NONE',  ( 5.153800228976615827, -19.02544592524334988, 25.20942372801900433 ) ) ;
#187293 = CARTESIAN_POINT ( 'NONE',  ( 14.34966873604960469, 8.224510206698951720, 34.16557627198102409 ) ) ;
#187294 = CARTESIAN_POINT ( 'NONE',  ( 21.55341960407610458, 5.719274019375980345, 98.95724293864770971 ) ) ;
#187295 = CARTESIAN_POINT ( 'NONE',  ( 5.823673210054125526, 21.52544592524343514, 64.79057627198103830 ) ) ;
#187296 = CARTESIAN_POINT ( 'NONE',  ( -19.03943276465977164, 0.05219959533909376836, 81.24890960531436690 ) ) ;
#187297 = CARTESIAN_POINT ( 'NONE',  ( 16.55341960407611168, 4.379528057220329451, 53.95724293864770260 ) ) ;
#187298 = CARTESIAN_POINT ( 'NONE',  ( -9.564922557960796823, -16.46253265017161027, 97.08224293864769550 ) ) ;
#187299 = VECTOR ( 'NONE', #137629, 1000.000000000000000 ) ;
#187300 = CARTESIAN_POINT ( 'NONE',  ( 38.00373040315627549, 2.428612866367529932E-14, -0.1220970790697140096 ) ) ;
#187301 = CARTESIAN_POINT ( 'NONE',  ( 19.05341960407617918, -5.049401038297876454, 36.04275706135234003 ) ) ;
#187302 = CARTESIAN_POINT ( 'NONE',  ( 10.81492255796078972, 18.62759615963270932, 94.58224293864769550 ) ) ;
#187303 = CARTESIAN_POINT ( 'NONE',  ( 12.14591786802309770, 12.06949235617756955, 99.37390960531436690 ) ) ;
#187304 =( BOUNDED_CURVE ( )  B_SPLINE_CURVE ( 2, ( #135214, #136190, #117022, #75499, #196886, #193887, #178717, #150381, #120020, #87682, #194881, #58353, #43186 ),
 .UNSPECIFIED., .F., .T. ) 
 B_SPLINE_CURVE_WITH_KNOTS ( ( 3, 2, 2, 2, 2, 2, 3 ),
 ( 0.1603708530912406061, 0.1622807017543859698, 0.1666666666666666574, 0.1710526315789473728, 0.1754385964912280604, 0.1798245614035087758, 0.1817800898887444450 ),
 .UNSPECIFIED. ) 
 CURVE ( )  GEOMETRIC_REPRESENTATION_ITEM ( )  RATIONAL_B_SPLINE_CURVE ( ( 0.9832469066685285419, 0.9851625545550100060, 1.000000000000000000, 0.9659258262890683122, 1.000000000000000000, 0.9659258262890683122, 1.000000000000000000, 0.9659258262890683122, 1.000000000000000000, 0.9659258262890683122, 1.000000000000000000, 0.9848076720550082985, 0.9831626618144004848 ) ) 
 REPRESENTATION_ITEM ( '' )  );
#187305 = CARTESIAN_POINT ( 'NONE',  ( -21.53943276465977519, -0.05219959533937600094, 33.75109039468568284 ) ) ;
#187306 = CARTESIAN_POINT ( 'NONE',  ( 8.571926809382597767, 26.38167802310806209, 140.2750000027311899 ) ) ;
#187307 = CARTESIAN_POINT ( 'NONE',  ( 16.53943276465976808, -0.05219959533910856209, 23.74890960531435269 ) ) ;
#187308 = CARTESIAN_POINT ( 'NONE',  ( -13.89961937509977652, 13.97604488694528158, 35.62390960531435269 ) ) ;
#187309 = CARTESIAN_POINT ( 'NONE',  ( -16.51473224551069308, -9.474510206698971260, 91.66557627198103830 ) ) ;
#187310 = CARTESIAN_POINT ( 'NONE',  ( -5.719274019375978568, 21.55341960407610458, 60.20724293864768839 ) ) ;
#187311 = CARTESIAN_POINT ( 'NONE',  ( -22.44159573604009950, -16.30477369853688430, 139.0750000027311728 ) ) ;
#187312 = CARTESIAN_POINT ( 'NONE',  ( 13.97604488694527802, 13.89961937509977652, 29.37390960531435979 ) ) ;
#187313 = CARTESIAN_POINT ( 'NONE',  ( -16.55341960407611168, -4.379528057220339221, 41.45724293864769550 ) ) ;
#187314 = CARTESIAN_POINT ( 'NONE',  ( -5.719274019375665041, -21.55341960407619695, 74.79275706135234714 ) ) ;
#187316 = CARTESIAN_POINT ( 'NONE',  ( -14.34966873604972548, 8.224510206698743886, 63.33442372801900433 ) ) ;
#187315 = CARTESIAN_POINT ( 'NONE',  ( 24.21728366753059802, -29.00647930567947341, -20.95994360447972582 ) ) ;
#187317 = CARTESIAN_POINT ( 'NONE',  ( -19.05341960407611168, -5.049401038298163336, 51.45724293864770260 ) ) ;
#187318 = CARTESIAN_POINT ( 'NONE',  ( 19.03943276465977164, -0.05219959533909143690, 68.74890960531436690 ) ) ;
#187319 = ORIENTED_EDGE ( 'NONE', *, *, #168190, .T. ) ;
#187320 = CARTESIAN_POINT ( 'NONE',  ( -0.05219959533937732626, 21.53943276465977519, 107.5010903946856899 ) ) ;
#187321 = CARTESIAN_POINT ( 'NONE',  ( 12.06949235617739724, 12.14591786802326823, 71.87609039468568994 ) ) ;
#187322 = CARTESIAN_POINT ( 'NONE',  ( -21.53943276465977519, -0.05219959533937600094, 98.75109039468568994 ) ) ;
#187323 = CARTESIAN_POINT ( 'NONE',  ( 19.03943276465977164, -0.05219959533909143690, 58.74890960531435979 ) ) ;
#187324 = CARTESIAN_POINT ( 'NONE',  ( 0.05219959533907565091, 21.53943276465977519, 39.99890960531436690 ) ) ;
#187325 = CARTESIAN_POINT ( 'NONE',  ( 13.89961937509957401, 13.97604488694547697, 101.8760903946856331 ) ) ;
#187326 = CARTESIAN_POINT ( 'NONE',  ( -15.80617190586768217, 15.72974639402176855, 83.12609039468568994 ) ) ;
#187327 = CARTESIAN_POINT ( 'NONE',  ( 16.52544592524335698, 4.483927247898782831, 51.45942372801901854 ) ) ;
#187328 = CARTESIAN_POINT ( 'NONE',  ( 21.52544592524344225, -5.823673210054117533, 103.5405762719810383 ) ) ;
#187329 = CARTESIAN_POINT ( 'NONE',  ( 5.049401038297881783, 19.05341960407617563, 102.2927570613523045 ) ) ;
#187330 = CARTESIAN_POINT ( 'NONE',  ( 19.03943276465977164, -0.05219959533909143690, 83.74890960531436690 ) ) ;
#187331 = CARTESIAN_POINT ( 'NONE',  ( 16.51473224551083163, -9.474510206698727899, 105.8344237280190043 ) ) ;
#187332 = AXIS2_PLACEMENT_3D ( 'NONE', #143410, #4898, #55405 ) ;
#187333 = CARTESIAN_POINT ( 'NONE',  ( -16.52544592524335698, -4.483927247898792601, 18.95942372801901143 ) ) ;
#187334 = CARTESIAN_POINT ( 'NONE',  ( -14.34966873604960291, -8.224510206698953496, 61.66557627198103120 ) ) ;
#187335 = CARTESIAN_POINT ( 'NONE',  ( -16.53943276465976808, -0.05219959533934237506, 68.75109039468568994 ) ) ;
#187337 = CARTESIAN_POINT ( 'NONE',  ( 19.03943276465977164, -0.05219959533909143690, 48.74890960531435979 ) ) ;
#187336 = CARTESIAN_POINT ( 'NONE',  ( 18.67979575497194134, -10.72451020669871369, 25.83442372801901499 ) ) ;
#187338 = CARTESIAN_POINT ( 'NONE',  ( -16.51473224551069308, -9.474510206698971260, 71.66557627198102409 ) ) ;
#187339 = CARTESIAN_POINT ( 'NONE',  ( 0.05219959533934541429, -16.53943276465976808, 70.00109039468568994 ) ) ;
#187340 = CARTESIAN_POINT ( 'NONE',  ( 8.906447517083057264, -27.41122689804191026, 146.8500000054623627 ) ) ;
#187341 = ORIENTED_EDGE ( 'NONE', *, *, #130602, .F. ) ;
#187342 = CARTESIAN_POINT ( 'NONE',  ( 10.72451020669871369, 18.67979575497193778, 107.0844237280190043 ) ) ;
#187343 = EDGE_CURVE ( 'NONE', #87616, #71610, #92344, .T. ) ;
#187344 = CARTESIAN_POINT ( 'NONE',  ( -9.474510206698964154, 16.51473224551069663, 35.41557627198102409 ) ) ;
#187345 = ORIENTED_EDGE ( 'NONE', *, *, #84741, .F. ) ;
#187346 = CARTESIAN_POINT ( 'NONE',  ( -16.55341960407617563, 4.379528057220093196, 33.54275706135234714 ) ) ;
#187348 = CARTESIAN_POINT ( 'NONE',  ( -14.29746914071037622, -8.314922557961029526, 49.16775706135234003 ) ) ;
#187347 = CARTESIAN_POINT ( 'NONE',  ( 5.153800228976615827, -19.02544592524334988, 45.20942372801901143 ) ) ;
#187349 = CARTESIAN_POINT ( 'NONE',  ( -16.46253265017160317, 9.564922557960807481, 45.83224293864769550 ) ) ;
#187350 = CARTESIAN_POINT ( 'NONE',  ( 13.97604488694527802, 13.89961937509977652, 69.37390960531436690 ) ) ;
#187351 = CARTESIAN_POINT ( 'NONE',  ( 21.52544592524344225, -5.823673210054117533, 83.54057627198102409 ) ) ;
#187353 = CARTESIAN_POINT ( 'NONE',  ( 5.049401038298161559, -19.05341960407611168, 107.7072429386476955 ) ) ;
#187352 = CARTESIAN_POINT ( 'NONE',  ( -16.46253265017160317, 9.564922557960807481, 80.83224293864769550 ) ) ;
#187354 = CARTESIAN_POINT ( 'NONE',  ( -0.05219959533909027116, -19.03943276465977164, 67.49890960531436690 ) ) ;
#187355 = CARTESIAN_POINT ( 'NONE',  ( 37.99999999999999289, 2.893978650043524126E-14, -10.74999999453762811 ) ) ;
#187356 = CARTESIAN_POINT ( 'NONE',  ( 19.02544592524334988, 5.153800228976608722, 101.4594237280189759 ) ) ;
#187357 = CARTESIAN_POINT ( 'NONE',  ( -21.52544592524343514, 5.823673210054127303, 81.04057627198102409 ) ) ;
#187358 = CARTESIAN_POINT ( 'NONE',  ( -13.97604488694547697, 13.89961937509957934, 23.12609039468565442 ) ) ;
#187359 = EDGE_CURVE ( 'NONE', #168893, #92733, #173055, .T. ) ;
#187360 = CARTESIAN_POINT ( 'NONE',  ( -16.55341960407611168, -4.379528057220339221, 66.45724293864768129 ) ) ;
#187361 = CARTESIAN_POINT ( 'NONE',  ( -5.719274019375665041, -21.55341960407619695, 89.79275706135236135 ) ) ;
#187362 = CARTESIAN_POINT ( 'NONE',  ( -19.03943276465977164, 0.05219959533909376836, 31.24890960531435979 ) ) ;
#187364 = CARTESIAN_POINT ( 'NONE',  ( -15.80617190586768217, 15.72974639402176855, 88.12609039468570415 ) ) ;
#187363 = CARTESIAN_POINT ( 'NONE',  ( 8.224510206698953496, -14.34966873604960469, 27.91557627198103830 ) ) ;
#187365 = CARTESIAN_POINT ( 'NONE',  ( 19.02544592524343514, -5.153800228976328945, 83.54057627198100988 ) ) ;
#187366 = CARTESIAN_POINT ( 'NONE',  ( -5.823673210054431948, 21.52544592524334988, 42.70942372801901854 ) ) ;
#187367 = CARTESIAN_POINT ( 'NONE',  ( -13.97604488694527625, -13.89961937509977652, 76.87390960531433848 ) ) ;
#187368 = CARTESIAN_POINT ( 'NONE',  ( -0.05219959533910754901, -16.53943276465976808, 97.49890960531436690 ) ) ;
#187369 = CARTESIAN_POINT ( 'NONE',  ( -4.379528057220328563, 16.55341960407611168, 60.20724293864768839 ) ) ;
#187370 = CARTESIAN_POINT ( 'NONE',  ( -21.52544592524343514, 5.823673210054127303, 71.04057627198103830 ) ) ;
#187371 = CARTESIAN_POINT ( 'NONE',  ( 19.03943276465977164, -0.05219959533909143690, 73.74890960531435269 ) ) ;
#187372 = CARTESIAN_POINT ( 'NONE',  ( -15.80617190586745835, -15.72974639402198527, 91.87390960531436690 ) ) ;
#187373 = CARTESIAN_POINT ( 'NONE',  ( -5.153800228976607833, 19.02544592524334988, 82.70942372801897591 ) ) ;
#187375 = CARTESIAN_POINT ( 'NONE',  ( 8.224510206698953496, -14.34966873604960469, 82.91557627198103830 ) ) ;
#187374 = CARTESIAN_POINT ( 'NONE',  ( 5.153800228976617603, -19.02544592524335343, 35.20942372801899722 ) ) ;
#187376 = CARTESIAN_POINT ( 'NONE',  ( -18.62759615963270932, 10.81492255796079327, 55.83224293864770260 ) ) ;
#187377 = CARTESIAN_POINT ( 'NONE',  ( 16.31925111598458500, -7.325300261831447557, 27.66424538967253355 ) ) ;
#187379 = CARTESIAN_POINT ( 'NONE',  ( -5.359611314223446995E-15, 29.16686587814335851, 142.8750000027311842 ) ) ;
#187378 = CARTESIAN_POINT ( 'NONE',  ( -16.53943276465976808, -0.05219959533934237506, 108.7510903946857042 ) ) ;
#187380 = CARTESIAN_POINT ( 'NONE',  ( 5.153800228976615827, -19.02544592524334988, 105.2094237280190185 ) ) ;
#187381 = CARTESIAN_POINT ( 'NONE',  ( -4.379528057220328563, 16.55341960407611168, 80.20724293864769550 ) ) ;
#187382 = CARTESIAN_POINT ( 'NONE',  ( -17.50000000000014566, 3.417042746626901994, 35.17380396232475448 ) ) ;
#187383 = CARTESIAN_POINT ( 'NONE',  ( -13.97604488694527625, -13.89961937509977652, 71.87390960531433848 ) ) ;
#187384 = CARTESIAN_POINT ( 'NONE',  ( 16.51473224551069308, 9.474510206698969483, 29.16557627198103475 ) ) ;
#187385 = CARTESIAN_POINT ( 'NONE',  ( -12.14591786802309592, -12.06949235617757132, 61.87390960531436690 ) ) ;
#187386 = ADVANCED_FACE ( 'NONE', ( #143450 ), #17153, .F. ) ;
#187387 = CARTESIAN_POINT ( 'NONE',  ( -13.89961937509977652, 13.97604488694528158, 95.62390960531436690 ) ) ;
#187389 = CARTESIAN_POINT ( 'NONE',  ( -13.89961937509977652, 13.97604488694528158, 60.62390960531436690 ) ) ;
#187388 = CARTESIAN_POINT ( 'NONE',  ( -5.153800228976607833, 19.02544592524334988, 87.70942372801897591 ) ) ;
#187390 = CARTESIAN_POINT ( 'NONE',  ( -8.224510206698735004, -14.34966873604973081, 24.58442372801901499 ) ) ;
#187391 = CARTESIAN_POINT ( 'NONE',  ( -9.564922557960796823, -16.46253265017161027, 82.08224293864768129 ) ) ;
#187392 = CARTESIAN_POINT ( 'NONE',  ( -21.53943276465977519, 0.05219959533907696930, 61.24890960531435979 ) ) ;
#187393 = CARTESIAN_POINT ( 'NONE',  ( -4.379528057220086978, -16.55341960407618274, 59.79275706135234714 ) ) ;
#187394 = CARTESIAN_POINT ( 'NONE',  ( -13.97604488694547520, 13.89961937509957934, 113.1260903946856757 ) ) ;
#187395 = CARTESIAN_POINT ( 'NONE',  ( 19.05341960407611168, 5.049401038298154454, 58.95724293864768129 ) ) ;
#187396 = CARTESIAN_POINT ( 'NONE',  ( 0.05219959533907565091, 21.53943276465977519, 69.99890960531435269 ) ) ;
#187397 = CARTESIAN_POINT ( 'NONE',  ( -19.05341960407617563, 5.049401038297882671, 98.54275706135233293 ) ) ;
#187399 = CARTESIAN_POINT ( 'NONE',  ( 21.55341960407619695, -5.719274019375665929, 51.04275706135234714 ) ) ;
#187398 = CARTESIAN_POINT ( 'NONE',  ( -12.06949235617756955, 12.14591786802309770, 30.62390960531436335 ) ) ;
#187400 = CARTESIAN_POINT ( 'NONE',  ( -4.500000000000001776, -130.0000000000000000, 13.99999999999999822 ) ) ;
#187402 = CARTESIAN_POINT ( 'NONE',  ( 0.05219959533909260263, 19.03943276465977164, 104.9989096053143669 ) ) ;
#187401 = CARTESIAN_POINT ( 'NONE',  ( -12.06949235617739369, -12.14591786802326823, 69.37609039468567573 ) ) ;
#187403 = CARTESIAN_POINT ( 'NONE',  ( -0.05219959533909027116, -19.03943276465977164, 102.4989096053143669 ) ) ;
#187404 = CYLINDRICAL_SURFACE ( 'NONE', #32444, 1.499999999999997780 ) ;
#187405 = CARTESIAN_POINT ( 'NONE',  ( 8.224510206698742110, 14.34966873604972548, 92.08442372801901854 ) ) ;
#187406 = CARTESIAN_POINT ( 'NONE',  ( 12.06949235617739724, 12.14591786802326823, 31.87609039468567929 ) ) ;
#187407 = CARTESIAN_POINT ( 'NONE',  ( 5.049401038298161559, -19.05341960407611168, 47.70724293864770260 ) ) ;
#187408 = CARTESIAN_POINT ( 'NONE',  ( 16.46253265017160672, -9.564922557960803928, 48.33224293864769550 ) ) ;
#187409 = CARTESIAN_POINT ( 'NONE',  ( 5.153800228976335163, 19.02544592524342804, 54.79057627198103120 ) ) ;
#187410 = CARTESIAN_POINT ( 'NONE',  ( -10.81492255796105439, 18.62759615963255655, 47.91775706135234714 ) ) ;
#187411 = CARTESIAN_POINT ( 'NONE',  ( -14.34966873604972548, 8.224510206698743886, 58.33442372801901143 ) ) ;
#187412 = CARTESIAN_POINT ( 'NONE',  ( -12.14591786802309592, -12.06949235617757132, 36.87390960531435979 ) ) ;
#187413 = CARTESIAN_POINT ( 'NONE',  ( -19.03943276465977164, 0.05219959533909376836, 41.24890960531435269 ) ) ;
#187414 = CARTESIAN_POINT ( 'NONE',  ( 9.474510206698971260, -16.51473224551069308, 37.91557627198102409 ) ) ;
#187415 = CARTESIAN_POINT ( 'NONE',  ( -16.53943276465976808, -0.05219959533934237506, 28.75109039468567929 ) ) ;
#187416 = CARTESIAN_POINT ( 'NONE',  ( 16.46253265017146816, 9.564922557961045513, 86.66775706135233293 ) ) ;
#187417 = CARTESIAN_POINT ( 'NONE',  ( -16.55341960407611168, -4.379528057220339221, 86.45724293864770971 ) ) ;
#187418 = CARTESIAN_POINT ( 'NONE',  ( -13.89961937509977652, 13.97604488694528158, 50.62390960531435979 ) ) ;
#187420 = CARTESIAN_POINT ( 'NONE',  ( -11.74264578624799782, -36.14014761921581709, -7.599999999999999645 ) ) ;
#187419 = CARTESIAN_POINT ( 'NONE',  ( 9.474510206698729675, 16.51473224551082808, 92.08442372801900433 ) ) ;
#187421 = CARTESIAN_POINT ( 'NONE',  ( 18.62759615963255655, 10.81492255796105972, 71.66775706135234714 ) ) ;
#187422 = CARTESIAN_POINT ( 'NONE',  ( -4.379528057220086978, -16.55341960407618274, 49.79275706135234714 ) ) ;
#187423 = DIRECTION ( 'NONE',  ( 0.000000000000000000, -1.287488025362403787E-15, -1.000000000000000000 ) ) ;
#187424 = CARTESIAN_POINT ( 'NONE',  ( 5.719274019375991003, -21.55341960407610458, 47.70724293864770260 ) ) ;
#187425 = CARTESIAN_POINT ( 'NONE',  ( -14.34966873604972548, 8.224510206698743886, 38.33442372801900433 ) ) ;
#187426 = CARTESIAN_POINT ( 'NONE',  ( 19.02544592524343514, -5.153800228976328945, 23.54057627198102409 ) ) ;
#187427 = CARTESIAN_POINT ( 'NONE',  ( -16.51473224551082808, 9.474510206698731452, 28.33442372801900433 ) ) ;
#187428 = CARTESIAN_POINT ( 'NONE',  ( 10.51869806896810822, 12.24338688535743280, -59.40202214942378589 ) ) ;
#187429 = CARTESIAN_POINT ( 'NONE',  ( -9.474510206698964154, 16.51473224551069663, 50.41557627198102409 ) ) ;
#187430 = CARTESIAN_POINT ( 'NONE',  ( -28.79475375365683831, -9.355982642737862065, 142.3656553485623704 ) ) ;
#187431 = CARTESIAN_POINT ( 'NONE',  ( -16.51473224551069308, -9.474510206698971260, 66.66557627198102409 ) ) ;
#187432 = CARTESIAN_POINT ( 'NONE',  ( 17.50000000000000711, -3.565345528327973135, 111.9249448680647276 ) ) ;
#187433 = PRODUCT_DEFINITION_SHAPE ( 'NONE', 'NONE',  #117858 ) ;
#187434 = CARTESIAN_POINT ( 'NONE',  ( -0.05219959533937732626, 21.53943276465977519, 112.5010903946857042 ) ) ;
#187435 = CARTESIAN_POINT ( 'NONE',  ( 12.06949235617757843, -12.14591786802309237, 33.12390960531435979 ) ) ;
#187436 = CARTESIAN_POINT ( 'NONE',  ( -5.153800228976328057, -19.02544592524343514, 47.29057627198102409 ) ) ;
#187437 = CARTESIAN_POINT ( 'NONE',  ( -5.049401038298153566, 19.05341960407611168, 100.2072429386476955 ) ) ;
#187438 = CARTESIAN_POINT ( 'NONE',  ( 18.67979575497194134, -10.72451020669871369, 70.83442372801901854 ) ) ;
#187439 = CARTESIAN_POINT ( 'NONE',  ( -5.153800228976328057, -19.02544592524343514, 52.29057627198100988 ) ) ;
#187440 = CARTESIAN_POINT ( 'NONE',  ( 21.52544592524334988, 5.823673210054432836, 71.45942372801901854 ) ) ;
#187441 = CARTESIAN_POINT ( 'NONE',  ( -0.05219959533907301413, -21.53943276465977519, 22.49890960531436335 ) ) ;
#187442 = CARTESIAN_POINT ( 'NONE',  ( -9.474510206698964154, 16.51473224551069663, 35.41557627198102409 ) ) ;
#187443 = CARTESIAN_POINT ( 'NONE',  ( 18.67979575497194134, -10.72451020669871369, 25.83442372801901499 ) ) ;
#187444 = CARTESIAN_POINT ( 'NONE',  ( 19.03943276465977164, 0.05219959533936151252, 51.25109039468567573 ) ) ;
#187445 = CARTESIAN_POINT ( 'NONE',  ( -13.89961937509977652, 13.97604488694528158, 25.62390960531434558 ) ) ;
#187446 = CARTESIAN_POINT ( 'NONE',  ( -16.51473224551069308, -9.474510206698971260, 81.66557627198103830 ) ) ;
#187447 = CARTESIAN_POINT ( 'NONE',  ( 13.89961937509957401, 13.97604488694547697, 106.8760903946856757 ) ) ;
#187448 = CARTESIAN_POINT ( 'NONE',  ( -16.55341960407611168, -4.379528057220339221, 71.45724293864769550 ) ) ;
#187449 = CARTESIAN_POINT ( 'NONE',  ( -21.55341960407610458, -5.719274019375992779, 36.45724293864768839 ) ) ;
#187450 = CARTESIAN_POINT ( 'NONE',  ( 16.51473224551083163, -9.474510206698727899, 100.8344237280190043 ) ) ;
#187451 = CARTESIAN_POINT ( 'NONE',  ( -0.05219959533907301413, -21.53943276465977519, 107.4989096053143669 ) ) ;
#187452 = CARTESIAN_POINT ( 'NONE',  ( 10.72451020669871369, 18.67979575497193778, 57.08442372801901854 ) ) ;
#187453 = CARTESIAN_POINT ( 'NONE',  ( 8.314922557961029526, -14.29746914071037800, 55.41775706135234714 ) ) ;
#187454 = CARTESIAN_POINT ( 'NONE',  ( -14.34966873604972548, 8.224510206698743886, 53.33442372801901854 ) ) ;
#187455 = CARTESIAN_POINT ( 'NONE',  ( 10.72451020669898902, -18.67979575497178502, 62.91557627198102409 ) ) ;
#187456 = CARTESIAN_POINT ( 'NONE',  ( 13.89961937509977652, -13.97604488694527269, 48.12390960531435979 ) ) ;
#187457 = CARTESIAN_POINT ( 'NONE',  ( -4.483927247898782831, 16.52544592524335698, 77.70942372801900433 ) ) ;
#187458 = CARTESIAN_POINT ( 'NONE',  ( 0.05219959533907565091, 21.53943276465977519, 104.9989096053143669 ) ) ;
#187459 = CARTESIAN_POINT ( 'NONE',  ( -16.55341960407611168, -4.379528057220339221, 51.45724293864770260 ) ) ;
#187460 = CARTESIAN_POINT ( 'NONE',  ( -19.05341960407611168, -5.049401038298163336, 76.45724293864769550 ) ) ;
#187461 = CARTESIAN_POINT ( 'NONE',  ( -0.05219959533934338120, 16.53943276465976808, 82.50109039468568994 ) ) ;
#187462 = CARTESIAN_POINT ( 'NONE',  ( -16.52544592524335698, -4.483927247898792601, 18.95942372801901143 ) ) ;
#187463 = CARTESIAN_POINT ( 'NONE',  ( -5.719274019375978568, 21.55341960407610458, 110.2072429386477239 ) ) ;
#187464 = CARTESIAN_POINT ( 'NONE',  ( 16.55341960407611168, 4.379528057220329451, 38.95724293864768839 ) ) ;
#187465 = VERTEX_POINT ( 'NONE', #95968 ) ;
#187466 = CARTESIAN_POINT ( 'NONE',  ( -17.48847506799968343, 5.747544572773787941, 75.82697437843280852 ) ) ;
#187467 = CARTESIAN_POINT ( 'NONE',  ( 18.62759615963271287, -10.81492255796078972, 93.33224293864769550 ) ) ;
#187468 = CARTESIAN_POINT ( 'NONE',  ( 0.05219959533910956823, 16.53943276465976808, 24.99890960531435624 ) ) ;
#187469 = ORIENTED_EDGE ( 'NONE', *, *, #89537, .T. ) ;
#187470 = CARTESIAN_POINT ( 'NONE',  ( -16.79531203550650176, -7.028104445595493743, 56.25244988220440945 ) ) ;
#187471 = CARTESIAN_POINT ( 'NONE',  ( -10.81492255796078084, -18.62759615963271287, 102.0822429386476955 ) ) ;
#187472 = CARTESIAN_POINT ( 'NONE',  ( 0.05219959533909260263, 19.03943276465977164, 104.9989096053143669 ) ) ;
#187473 = CARTESIAN_POINT ( 'NONE',  ( 15.80617190586769283, -15.72974639402175789, 20.62609039468568639 ) ) ;
#187474 = CARTESIAN_POINT ( 'NONE',  ( 14.29746914071049879, -8.314922557960816363, 48.33224293864770260 ) ) ;
#187475 = CARTESIAN_POINT ( 'NONE',  ( 16.55341960407618274, -4.379528057220086978, 51.04275706135234714 ) ) ;
#187476 = CIRCLE ( 'NONE', #155123, 40.00000000000002132 ) ;
#187478 = EDGE_CURVE ( 'NONE', #42359, #140931, #127287, .T. ) ;
#187477 = CARTESIAN_POINT ( 'NONE',  ( 0.05219959533909260263, 19.03943276465977164, 54.99890960531435979 ) ) ;
#187479 = CARTESIAN_POINT ( 'NONE',  ( -19.05341960407617563, 5.049401038297882671, 53.54275706135231871 ) ) ;
#187480 = CARTESIAN_POINT ( 'NONE',  ( 16.51473224551069308, 9.474510206698969483, 79.16557627198103830 ) ) ;
#187481 = CARTESIAN_POINT ( 'NONE',  ( 15.80617190586746368, 15.72974639402197994, 39.37390960531436690 ) ) ;
#187482 = CARTESIAN_POINT ( 'NONE',  ( -5.049401038298153566, 19.05341960407611168, 65.20724293864766707 ) ) ;
#187483 = CARTESIAN_POINT ( 'NONE',  ( -5.049401038298153566, 19.05341960407611168, 45.20724293864769550 ) ) ;
#187484 = CARTESIAN_POINT ( 'NONE',  ( -16.51473224551082808, 9.474510206698731452, 113.3344237280190043 ) ) ;
#187485 = CARTESIAN_POINT ( 'NONE',  ( 5.153800228976615827, -19.02544592524334988, 70.20942372801899012 ) ) ;
#187486 = CARTESIAN_POINT ( 'NONE',  ( 21.52544592524344225, -5.823673210054117533, 103.5405762719810383 ) ) ;
#187487 = CARTESIAN_POINT ( 'NONE',  ( -12.06949235617756955, 12.14591786802309770, 40.62390960531435269 ) ) ;
#187488 = CARTESIAN_POINT ( 'NONE',  ( 19.05341960407611168, 5.049401038298154454, 83.95724293864766707 ) ) ;
#187489 = CARTESIAN_POINT ( 'NONE',  ( -0.05219959533907301413, -21.53943276465977519, 57.49890960531435979 ) ) ;
#187491 = CARTESIAN_POINT ( 'NONE',  ( 8.224510206698742110, 14.34966873604972548, 27.08442372801901854 ) ) ;
#187490 = CARTESIAN_POINT ( 'NONE',  ( 21.55341960407610458, 5.719274019375980345, 98.95724293864770971 ) ) ;
#187492 = CARTESIAN_POINT ( 'NONE',  ( -15.80617190586745835, -15.72974639402198527, 21.87390960531436690 ) ) ;
#187493 = CARTESIAN_POINT ( 'NONE',  ( -18.62759615963255300, -10.81492255796106328, 84.16775706135234714 ) ) ;
#187494 = CARTESIAN_POINT ( 'NONE',  ( 19.02544592524343514, -5.153800228976328945, 83.54057627198100988 ) ) ;
#187495 = CARTESIAN_POINT ( 'NONE',  ( 19.02544592524343514, -5.153800228976328945, 33.54057627198102409 ) ) ;
#187496 = CARTESIAN_POINT ( 'NONE',  ( 19.02544592524343514, -5.153800228976328945, 78.54057627198099567 ) ) ;
#187497 = CARTESIAN_POINT ( 'NONE',  ( -12.06949235617756955, 12.14591786802309770, 100.6239096053143811 ) ) ;
#187498 = CARTESIAN_POINT ( 'NONE',  ( 16.46253265017160672, -9.564922557960803928, 68.33224293864770971 ) ) ;
#187499 = CARTESIAN_POINT ( 'NONE',  ( -0.05219959533936034679, 19.03943276465977164, 112.5010903946856757 ) ) ;
#187500 = CARTESIAN_POINT ( 'NONE',  ( 9.474510206698729675, 16.51473224551082808, 42.08442372801900433 ) ) ;
#187502 = CARTESIAN_POINT ( 'NONE',  ( -9.564922557960796823, -16.46253265017161027, 107.0822429386476955 ) ) ;
#187501 = CARTESIAN_POINT ( 'NONE',  ( -21.53943276465977519, -0.05219959533937600094, 98.75109039468568994 ) ) ;
#187503 = CARTESIAN_POINT ( 'NONE',  ( 4.483927247898790824, -16.52544592524335698, 85.20942372801901854 ) ) ;
#187504 = CARTESIAN_POINT ( 'NONE',  ( -30.74264578624800492, -22.33583958711396278, -9.799999999999998934 ) ) ;
#187505 = CARTESIAN_POINT ( 'NONE',  ( 16.51473224551083163, -9.474510206698727899, 70.83442372801900433 ) ) ;
#187506 = CARTESIAN_POINT ( 'NONE',  ( 15.72974639402176855, 15.80617190586768217, 106.8760903946856899 ) ) ;
#187507 = CARTESIAN_POINT ( 'NONE',  ( 27.69393237830212939, -1.826213041496827616, 140.0000000000000000 ) ) ;
#187508 = CARTESIAN_POINT ( 'NONE',  ( 5.049401038298161559, -19.05341960407611168, 32.70724293864768129 ) ) ;
#187509 = CARTESIAN_POINT ( 'NONE',  ( -12.06949235617756955, 12.14591786802309770, 40.62390960531435269 ) ) ;
#187510 = EDGE_CURVE ( 'NONE', #56919, #116695, #111137, .T. ) ;
#187511 = DIRECTION ( 'NONE',  ( -1.000000000000000000, 0.000000000000000000, 0.000000000000000000 ) ) ;
#187512 = CARTESIAN_POINT ( 'NONE',  ( -8.224510206698735004, -14.34966873604973081, 109.5844237280190328 ) ) ;
#187513 = CARTESIAN_POINT ( 'NONE',  ( -19.25918095147779852, -5.499999999999484857, 84.45284276293931214 ) ) ;
#187514 = CARTESIAN_POINT ( 'NONE',  ( 16.53943276465976808, 0.05219959533934440121, 76.25109039468568994 ) ) ;
#187515 = CARTESIAN_POINT ( 'NONE',  ( -16.46253265017160317, 9.564922557960807481, 35.83224293864768839 ) ) ;
#187516 = CARTESIAN_POINT ( 'NONE',  ( 21.52544592524334988, 5.823673210054432836, 96.45942372801901854 ) ) ;
#187517 = CARTESIAN_POINT ( 'NONE',  ( 13.89961937509957401, 13.97604488694547697, 96.87609039468566152 ) ) ;
#187518 = CARTESIAN_POINT ( 'NONE',  ( 15.72974639402176855, 15.80617190586768217, 76.87609039468567573 ) ) ;
#187519 = CARTESIAN_POINT ( 'NONE',  ( 9.474510206698729675, 16.51473224551082808, 57.08442372801900433 ) ) ;
#187520 = CARTESIAN_POINT ( 'NONE',  ( 13.89961937509977652, -13.97604488694527269, 78.12390960531433848 ) ) ;
#187521 = CARTESIAN_POINT ( 'NONE',  ( -19.03943276465977164, 0.05219959533909376836, 66.24890960531436690 ) ) ;
#187522 = EDGE_CURVE ( 'NONE', #11857, #11672, #172827, .T. ) ;
#187523 = CARTESIAN_POINT ( 'NONE',  ( 17.26058549869091507, 6.457015423128499521, 73.87745837476064992 ) ) ;
#187524 = CARTESIAN_POINT ( 'NONE',  ( 4.483927247898545687, 16.52544592524342804, 69.79057627198102409 ) ) ;
#187525 = CARTESIAN_POINT ( 'NONE',  ( -21.53943276465977519, 0.05219959533907696930, 66.24890960531436690 ) ) ;
#187526 = CARTESIAN_POINT ( 'NONE',  ( -13.89961937509977652, 13.97604488694528158, 45.62390960531433848 ) ) ;
#187528 = CARTESIAN_POINT ( 'NONE',  ( -16.52544592524335698, -4.483927247898792601, 78.95942372801901854 ) ) ;
#187527 = CARTESIAN_POINT ( 'NONE',  ( 0.05219959533907565091, 21.53943276465977519, 84.99890960531436690 ) ) ;
#187529 = EDGE_LOOP ( 'NONE', ( #23578, #88422, #118854, #125154, #62443 ) ) ;
#187530 = CARTESIAN_POINT ( 'NONE',  ( -13.97604488694527625, -13.89961937509977652, 51.87390960531436690 ) ) ;
#187532 = CARTESIAN_POINT ( 'NONE',  ( 11.40812507854755253, -35.11059874428192273, -2.024999997268813079 ) ) ;
#187531 = CARTESIAN_POINT ( 'NONE',  ( 12.06949235617757843, -12.14591786802309237, 78.12390960531436690 ) ) ;
#187533 = CARTESIAN_POINT ( 'NONE',  ( -9.474510206698964154, 16.51473224551069663, 45.41557627198103120 ) ) ;
#187534 = CARTESIAN_POINT ( 'NONE',  ( -13.97604488694527625, -13.89961937509977652, 21.87390960531435979 ) ) ;
#187535 = CARTESIAN_POINT ( 'NONE',  ( 16.51473224551083163, -9.474510206698727899, 65.83442372801900433 ) ) ;
#187536 = CARTESIAN_POINT ( 'NONE',  ( 8.314922557960818139, 14.29746914071049879, 69.58224293864769550 ) ) ;
#187537 = CARTESIAN_POINT ( 'NONE',  ( -15.80617190586768217, 15.72974639402176855, 43.12609039468568284 ) ) ;
#187539 = CARTESIAN_POINT ( 'NONE',  ( -21.52544592524343514, 5.823673210054127303, 101.0405762719810383 ) ) ;
#187538 = CARTESIAN_POINT ( 'NONE',  ( -19.02544592524342804, 5.153800228976336051, 36.04057627198100988 ) ) ;
#187540 = CARTESIAN_POINT ( 'NONE',  ( -14.29746914071049879, 8.314922557960819915, 85.83224293864768129 ) ) ;
#187541 = CARTESIAN_POINT ( 'NONE',  ( 27.67003201002207291, -28.46598819372293931, -20.09023003179317257 ) ) ;
#187542 = CARTESIAN_POINT ( 'NONE',  ( -19.05341960407611168, -5.049401038298163336, 51.45724293864770260 ) ) ;
#187543 = CARTESIAN_POINT ( 'NONE',  ( -36.91746825000000598, 2.428612866367529932E-14, -0.6249999972688132788 ) ) ;
#187544 = CARTESIAN_POINT ( 'NONE',  ( 13.97604488694548053, -13.89961937509957401, 85.62609039468568994 ) ) ;
#187545 = CARTESIAN_POINT ( 'NONE',  ( 10.72451020669871369, 18.67979575497193778, 32.08442372801901854 ) ) ;
#187546 = CARTESIAN_POINT ( 'NONE',  ( 13.97604488694527802, 13.89961937509977652, 64.37390960531436690 ) ) ;
#187547 = CARTESIAN_POINT ( 'NONE',  ( 13.89961937509957401, 13.97604488694547697, 71.87609039468567573 ) ) ;
#187548 = CARTESIAN_POINT ( 'NONE',  ( 13.89961937509977652, -13.97604488694527269, 38.12390960531436690 ) ) ;
#187549 = CARTESIAN_POINT ( 'NONE',  ( -8.314922557960811034, -14.29746914071050412, 67.08224293864770971 ) ) ;
#187550 = CARTESIAN_POINT ( 'NONE',  ( 12.14591786802309770, 12.06949235617756955, 69.37390960531436690 ) ) ;
#187551 = CARTESIAN_POINT ( 'NONE',  ( -5.049401038298153566, 19.05341960407611168, 70.20724293864769550 ) ) ;
#187552 = CARTESIAN_POINT ( 'NONE',  ( -10.81492255796078084, -18.62759615963271287, 107.0822429386476955 ) ) ;
#187553 = CARTESIAN_POINT ( 'NONE',  ( -19.05341960407611168, -5.049401038298163336, 71.45724293864766707 ) ) ;
#187554 = CARTESIAN_POINT ( 'NONE',  ( -5.049401038297874678, -19.05341960407617918, 24.79275706135233648 ) ) ;
#187557 = CARTESIAN_POINT ( 'NONE',  ( -8.314922557960811034, -14.29746914071050412, 112.0822429386477097 ) ) ;
#187556 = CARTESIAN_POINT ( 'NONE',  ( -8.314922557961024197, 14.29746914071037800, 107.9177570613523471 ) ) ;
#187555 = CARTESIAN_POINT ( 'NONE',  ( -13.97604488694527625, -13.89961937509977652, 31.87390960531435979 ) ) ;
#187558 = CARTESIAN_POINT ( 'NONE',  ( -9.564922557961040184, 16.46253265017147172, 107.9177570613523471 ) ) ;
#187559 = EDGE_LOOP ( 'NONE', ( #67073, #10415, #117401 ) ) ;
#187560 = CARTESIAN_POINT ( 'NONE',  ( 21.52544592524334988, 5.823673210054432836, 31.45942372801901854 ) ) ;
#187561 = CARTESIAN_POINT ( 'NONE',  ( -19.03943276465977164, -0.05219959533935918106, 48.75109039468566863 ) ) ;
#187562 = CARTESIAN_POINT ( 'NONE',  ( -14.29746914071037622, -8.314922557961029526, 109.1677570613523613 ) ) ;
#187563 = CARTESIAN_POINT ( 'NONE',  ( 18.62759615963271287, -10.81492255796078972, 73.33224293864769550 ) ) ;
#187564 = CARTESIAN_POINT ( 'NONE',  ( 19.03943276465977164, -0.05219959533909143690, 108.7489096053143527 ) ) ;
#187565 = CARTESIAN_POINT ( 'NONE',  ( 12.06949235617757843, -12.14591786802309237, 53.12390960531436690 ) ) ;
#187566 = CARTESIAN_POINT ( 'NONE',  ( -19.03943276465977164, 0.05219959533909376836, 36.24890960531436690 ) ) ;
#187567 = CARTESIAN_POINT ( 'NONE',  ( 16.51473224551069308, 9.474510206698969483, 39.16557627198103120 ) ) ;
#187568 = CARTESIAN_POINT ( 'NONE',  ( 16.46253265017146816, 9.564922557961045513, 31.66775706135232937 ) ) ;
#187569 = CARTESIAN_POINT ( 'NONE',  ( -4.379528057220086978, -16.55341960407618274, 89.79275706135236135 ) ) ;
#187570 = CARTESIAN_POINT ( 'NONE',  ( -16.55341960407617563, 4.379528057220093196, 43.54275706135235424 ) ) ;
#187571 = CARTESIAN_POINT ( 'NONE',  ( -15.72974639402197994, 15.80617190586746368, 25.62390960531435624 ) ) ;
#187573 = CARTESIAN_POINT ( 'NONE',  ( 10.81492255796106328, -18.62759615963255655, 100.4177570613523471 ) ) ;
#187572 = CARTESIAN_POINT ( 'NONE',  ( -5.153800228976328057, -19.02544592524343514, 57.29057627198103120 ) ) ;
#187574 = CARTESIAN_POINT ( 'NONE',  ( 16.51473224551069308, 9.474510206698969483, 84.16557627198102409 ) ) ;
#187575 = CARTESIAN_POINT ( 'NONE',  ( -12.06949235617739369, -12.14591786802326823, 64.37609039468568994 ) ) ;
#187576 = CARTESIAN_POINT ( 'NONE',  ( -4.379528057220328563, 16.55341960407611168, 105.2072429386477097 ) ) ;
#187577 = CARTESIAN_POINT ( 'NONE',  ( 12.06949235617757843, -12.14591786802309237, 23.12390960531436335 ) ) ;
#187578 = LINE ( 'NONE', #94534, #108855 ) ;
#187581 = CARTESIAN_POINT ( 'NONE',  ( -19.03943276465977164, 0.05219959533909376836, 71.24890960531435269 ) ) ;
#187580 = CARTESIAN_POINT ( 'NONE',  ( -13.89961937509977652, 13.97604488694528158, 85.62390960531433848 ) ) ;
#187579 = CARTESIAN_POINT ( 'NONE',  ( 18.67979575497194134, -10.72451020669871369, 70.83442372801901854 ) ) ;
#187582 = CARTESIAN_POINT ( 'NONE',  ( -13.89961937509977652, 13.97604488694528158, 110.6239096053143243 ) ) ;
#187583 = CARTESIAN_POINT ( 'NONE',  ( 12.14591786802309770, 12.06949235617756955, 59.37390960531436690 ) ) ;
#187584 = CARTESIAN_POINT ( 'NONE',  ( -4.379528057220086978, -16.55341960407618274, 109.7927570613523613 ) ) ;
#187585 = CARTESIAN_POINT ( 'NONE',  ( -12.06949235617756955, 12.14591786802309770, 40.62390960531435269 ) ) ;
#187587 = DIRECTION ( 'NONE',  ( 0.000000000000000000, 0.000000000000000000, 1.000000000000000000 ) ) ;
#187586 = CARTESIAN_POINT ( 'NONE',  ( 14.34966873604972726, -8.224510206698740333, 40.83442372801901854 ) ) ;
#187588 = CARTESIAN_POINT ( 'NONE',  ( 9.474510206698729675, 16.51473224551082808, 42.08442372801900433 ) ) ;
#187589 = CARTESIAN_POINT ( 'NONE',  ( 13.89961937509977652, -13.97604488694527269, 78.12390960531433848 ) ) ;
#187590 = CARTESIAN_POINT ( 'NONE',  ( -5.153800228976607833, 19.02544592524334988, 57.70942372801899012 ) ) ;
#187591 = CARTESIAN_POINT ( 'NONE',  ( -29.86685920354755552, 21.69954338932564397, -2.824999997268813345 ) ) ;
#187592 = CARTESIAN_POINT ( 'NONE',  ( 18.09918380851992481, 5.500000000000036415, 58.98618307335610211 ) ) ;
#187594 = CARTESIAN_POINT ( 'NONE',  ( -4.379528057220086978, -16.55341960407618274, 79.79275706135236135 ) ) ;
#187593 = CARTESIAN_POINT ( 'NONE',  ( 19.03943276465977164, 0.05219959533936151252, 81.25109039468567573 ) ) ;
#187595 = DIRECTION ( 'NONE',  ( -0.000000000000000000, -0.000000000000000000, 1.000000000000000000 ) ) ;
#187596 = CARTESIAN_POINT ( 'NONE',  ( 19.02544592524343514, -5.153800228976328945, 108.5405762719810383 ) ) ;
#187597 = CARTESIAN_POINT ( 'NONE',  ( -5.823673210054431948, 21.52544592524334988, 42.70942372801901854 ) ) ;
#187598 = CARTESIAN_POINT ( 'NONE',  ( -19.03943276465977164, -0.05219959533935918106, 93.75109039468566152 ) ) ;
#187600 = CARTESIAN_POINT ( 'NONE',  ( -16.46253265017160317, 9.564922557960807481, 50.83224293864770260 ) ) ;
#187599 = CARTESIAN_POINT ( 'NONE',  ( 17.31728774477272736, 6.344390552232407110, 86.68093348310682700 ) ) ;
#187601 = CARTESIAN_POINT ( 'NONE',  ( 13.97604488694527802, 13.89961937509977652, 109.3739096053143669 ) ) ;
#187603 = CARTESIAN_POINT ( 'NONE',  ( -16.51473224551069308, -9.474510206698971260, 56.66557627198103120 ) ) ;
#187602 = CARTESIAN_POINT ( 'NONE',  ( -14.29746914071049879, 8.314922557960819915, 65.83224293864769550 ) ) ;
#187604 = CARTESIAN_POINT ( 'NONE',  ( -5.153800228976328057, -19.02544592524343514, 62.29057627198100988 ) ) ;
#187605 = CARTESIAN_POINT ( 'NONE',  ( -19.05341960407617563, 5.049401038297882671, 63.54275706135234003 ) ) ;
#187606 = CARTESIAN_POINT ( 'NONE',  ( 0.05219959533936267826, -19.03943276465977164, 30.00109039468566863 ) ) ;
#187607 = CARTESIAN_POINT ( 'NONE',  ( -16.51473224551069308, -9.474510206698971260, 61.66557627198103120 ) ) ;
#187608 = CARTESIAN_POINT ( 'NONE',  ( -15.72974639402197994, 15.80617190586746368, 75.62390960531439532 ) ) ;
#187610 = CARTESIAN_POINT ( 'NONE',  ( 16.51473224551083163, -9.474510206698727899, 30.83442372801900433 ) ) ;
#187609 = CARTESIAN_POINT ( 'NONE',  ( -0.05219959533910754901, -16.53943276465976808, 67.49890960531436690 ) ) ;
#187611 = CARTESIAN_POINT ( 'NONE',  ( 21.55341960407610458, 5.719274019375980345, 43.95724293864769550 ) ) ;
#187612 = CARTESIAN_POINT ( 'NONE',  ( -5.823673210054116645, -21.52544592524344225, 32.29057627198102409 ) ) ;
#187613 = CARTESIAN_POINT ( 'NONE',  ( 5.049401038298161559, -19.05341960407611168, 72.70724293864768129 ) ) ;
#187614 = CARTESIAN_POINT ( 'NONE',  ( -5.153800228976328057, -19.02544592524343514, 42.29057627198101699 ) ) ;
#187615 = CARTESIAN_POINT ( 'NONE',  ( 12.14591786802309770, 12.06949235617756955, 94.37390960531436690 ) ) ;
#187616 = CARTESIAN_POINT ( 'NONE',  ( 10.81492255796078972, 18.62759615963270932, 114.5822429386477097 ) ) ;
#187617 = CARTESIAN_POINT ( 'NONE',  ( 3.503282210674363295, -48.86437366581479580, -23.00000000000000000 ) ) ;
#187618 = CARTESIAN_POINT ( 'NONE',  ( -21.52544592524334988, -5.823673210054445271, 28.95942372801902209 ) ) ;
#187619 = CARTESIAN_POINT ( 'NONE',  ( 5.049401038298161559, -19.05341960407611168, 37.70724293864768839 ) ) ;
#187620 = CARTESIAN_POINT ( 'NONE',  ( -10.72451020669898014, 18.67979575497178502, 105.4155762719810383 ) ) ;
#187621 = CARTESIAN_POINT ( 'NONE',  ( 5.049401038297881783, 19.05341960407617563, 47.29275706135231161 ) ) ;
#187622 = CARTESIAN_POINT ( 'NONE',  ( 9.474510206698971260, -16.51473224551069308, 22.91557627198102765 ) ) ;
#187623 = CARTESIAN_POINT ( 'NONE',  ( 19.01533133064923931, -5.499999999999436895, 76.26586590595739779 ) ) ;
#187624 = CARTESIAN_POINT ( 'NONE',  ( -37.45873412500000654, 2.428612866367529932E-14, -0.3124999986344065839 ) ) ;
#187625 = CARTESIAN_POINT ( 'NONE',  ( 16.52544592524335698, 4.483927247898782831, 46.45942372801901854 ) ) ;
#187626 = CARTESIAN_POINT ( 'NONE',  ( -13.97604488694527625, -13.89961937509977652, 21.87390960531435979 ) ) ;
#187627 = CARTESIAN_POINT ( 'NONE',  ( 34.48725679702496905, -1.430676605895442766, 89.67714645826993092 ) ) ;
#187628 = CARTESIAN_POINT ( 'NONE',  ( 19.05341960407611168, 5.049401038298154454, 68.95724293864769550 ) ) ;
#187629 = CARTESIAN_POINT ( 'NONE',  ( 0.05219959533910956823, 16.53943276465976808, 104.9989096053143669 ) ) ;
#187630 = CARTESIAN_POINT ( 'NONE',  ( -15.72974639402197994, 15.80617190586746368, 40.62390960531435269 ) ) ;
#187631 = CARTESIAN_POINT ( 'NONE',  ( -16.55341960407611168, -4.379528057220339221, 76.45724293864769550 ) ) ;
#187632 = CARTESIAN_POINT ( 'NONE',  ( 8.314922557961029526, -14.29746914071037800, 40.41775706135234714 ) ) ;
#187633 = CARTESIAN_POINT ( 'NONE',  ( 10.81492255796106328, -18.62759615963255655, 80.41775706135234714 ) ) ;
#187634 = CARTESIAN_POINT ( 'NONE',  ( -13.89961937509977652, 13.97604488694528158, 25.62390960531434558 ) ) ;
#187635 = CARTESIAN_POINT ( 'NONE',  ( 14.29746914071037800, 8.314922557961029526, 106.6677570613523756 ) ) ;
#187636 = CARTESIAN_POINT ( 'NONE',  ( -16.53943276465976808, 0.05219959533911058130, 61.24890960531435979 ) ) ;
#187637 = CARTESIAN_POINT ( 'NONE',  ( 16.51473224551069308, 9.474510206698969483, 54.16557627198103120 ) ) ;
#187638 = CARTESIAN_POINT ( 'NONE',  ( 21.52544592524334988, 5.823673210054432836, 91.45942372801901854 ) ) ;
#187639 = CARTESIAN_POINT ( 'NONE',  ( -10.72451020669898014, 18.67979575497178502, 110.4155762719810383 ) ) ;
#187640 = CARTESIAN_POINT ( 'NONE',  ( 10.72451020669871369, 18.67979575497193778, 77.08442372801901854 ) ) ;
#187641 = CARTESIAN_POINT ( 'NONE',  ( -0.05219959533934338120, 16.53943276465976808, 37.50109039468568284 ) ) ;
#187643 = CARTESIAN_POINT ( 'NONE',  ( 15.72974639402176855, 15.80617190586768217, 91.87609039468568994 ) ) ;
#187642 = CARTESIAN_POINT ( 'NONE',  ( -14.34966873604960291, -8.224510206698953496, 81.66557627198103830 ) ) ;
#187644 = CARTESIAN_POINT ( 'NONE',  ( -4.483927247898539470, -16.52544592524342804, 22.29057627198102765 ) ) ;
#187645 = CARTESIAN_POINT ( 'NONE',  ( 24.95432927374997334, 3.806786798636384805, 190.0000000000000000 ) ) ;
#187646 = DIRECTION ( 'NONE',  ( -0.4999999999999967248, 0.5000000000000019984, 0.7071067811865484609 ) ) ;
#187647 = CARTESIAN_POINT ( 'NONE',  ( -8.224510206698948167, 14.34966873604960824, 35.41557627198102409 ) ) ;
#187648 = CARTESIAN_POINT ( 'NONE',  ( 4.379528057220092307, 16.55341960407617563, 87.29275706135236135 ) ) ;
#187649 = CARTESIAN_POINT ( 'NONE',  ( -16.51473224551069308, -9.474510206698971260, 91.66557627198103830 ) ) ;
#187650 = CARTESIAN_POINT ( 'NONE',  ( 9.474510206698971260, -16.51473224551069308, 97.91557627198102409 ) ) ;
#187651 = CARTESIAN_POINT ( 'NONE',  ( 21.52544592524334988, 5.823673210054432836, 96.45942372801901854 ) ) ;
#187652 = CARTESIAN_POINT ( 'NONE',  ( -16.55341960407617563, 4.379528057220093196, 108.5427570613523756 ) ) ;
#187653 = CARTESIAN_POINT ( 'NONE',  ( 8.224510206698953496, -14.34966873604960469, 67.91557627198102409 ) ) ;
#187654 = CARTESIAN_POINT ( 'NONE',  ( -16.51473224551069308, -9.474510206698971260, 81.66557627198103830 ) ) ;
#187655 = ORIENTED_EDGE ( 'NONE', *, *, #129609, .T. ) ;
#187656 = CARTESIAN_POINT ( 'NONE',  ( 14.29746914071037800, 8.314922557961029526, 26.66775706135235424 ) ) ;
#187657 = CARTESIAN_POINT ( 'NONE',  ( -19.05341960407611168, -5.049401038298163336, 26.45724293864769550 ) ) ;
#187658 = CARTESIAN_POINT ( 'NONE',  ( -5.153800228976328057, -19.02544592524343514, 87.29057627198103830 ) ) ;
#187660 = CARTESIAN_POINT ( 'NONE',  ( 11.40812507854754365, 35.11059874428196537, -1.224999997268813479 ) ) ;
#187659 = CARTESIAN_POINT ( 'NONE',  ( -16.55341960407617563, 4.379528057220093196, 28.54275706135234358 ) ) ;
#187661 = CARTESIAN_POINT ( 'NONE',  ( 16.46253265017146816, 9.564922557961045513, 41.66775706135234003 ) ) ;
#187662 = CARTESIAN_POINT ( 'NONE',  ( -12.06949235617739369, -12.14591786802326823, 94.37609039468568994 ) ) ;
#187663 = CARTESIAN_POINT ( 'NONE',  ( 19.03943276465977164, 0.05219959533936151252, 101.2510903946856757 ) ) ;
#187665 = B_SPLINE_CURVE_WITH_KNOTS ( 'NONE', 3,
 ( #19371, #144687, #67852, #176049, #36507, #49702 ),
 .UNSPECIFIED., .F., .F.,
 ( 4, 2, 4 ),
 ( 0.000000000000000000, 0.0003837532665635066433, 0.0007675065331270132865 ),
 .UNSPECIFIED. ) ;
#187664 = CARTESIAN_POINT ( 'NONE',  ( -5.153800228976328057, -19.02544592524343514, 27.29057627198103120 ) ) ;
#187666 = CARTESIAN_POINT ( 'NONE',  ( 12.14591786802327356, -12.06949235617739191, 75.62609039468567573 ) ) ;
#187667 = CARTESIAN_POINT ( 'NONE',  ( 14.29746914071037800, 8.314922557961029526, 61.66775706135235424 ) ) ;
#187668 = CARTESIAN_POINT ( 'NONE',  ( -37.99626262588766679, 2.428612866367529932E-14, -4.002157773949823749 ) ) ;
#187669 = CARTESIAN_POINT ( 'NONE',  ( -16.51473224551082808, 9.474510206698731452, 63.33442372801900433 ) ) ;
#187670 = CARTESIAN_POINT ( 'NONE',  ( 21.53943276465977519, 0.05219959533937863772, 106.2510903946856757 ) ) ;
#187671 = CARTESIAN_POINT ( 'NONE',  ( 0.05219959533909260263, 19.03943276465977164, 44.99890960531435979 ) ) ;
#187672 = CARTESIAN_POINT ( 'NONE',  ( -16.46253265017160317, 9.564922557960807481, 90.83224293864769550 ) ) ;
#187673 = CARTESIAN_POINT ( 'NONE',  ( -4.379528057220328563, 16.55341960407611168, 80.20724293864769550 ) ) ;
#187674 = CARTESIAN_POINT ( 'NONE',  ( 9.474510206698729675, 16.51473224551082808, 57.08442372801900433 ) ) ;
#187675 = CARTESIAN_POINT ( 'NONE',  ( 15.72974639402199770, -15.80617190586745480, 48.12390960531436690 ) ) ;
#187676 = CARTESIAN_POINT ( 'NONE',  ( 10.81492255796106328, -18.62759615963255655, 105.4177570613523613 ) ) ;
#187677 = CARTESIAN_POINT ( 'NONE',  ( -9.474510206698964154, 16.51473224551069663, 95.41557627198102409 ) ) ;
#187678 = CARTESIAN_POINT ( 'NONE',  ( 5.049401038297881783, 19.05341960407617563, 22.29275706135233648 ) ) ;
#187679 = CARTESIAN_POINT ( 'NONE',  ( 10.81492255796078972, 18.62759615963270932, 59.58224293864770260 ) ) ;
#187680 = CARTESIAN_POINT ( 'NONE',  ( -9.474510206698964154, 16.51473224551069663, 115.4155762719810241 ) ) ;
#187681 = CARTESIAN_POINT ( 'NONE',  ( -5.049401038297874678, -19.05341960407617918, 84.79275706135233293 ) ) ;
#187682 = CARTESIAN_POINT ( 'NONE',  ( -17.49999999999999645, 3.512728167236898624, 110.2280999518112310 ) ) ;
#187683 = CARTESIAN_POINT ( 'NONE',  ( -19.03943276465977164, -0.05219959533935918106, 103.7510903946856757 ) ) ;
#187684 = CARTESIAN_POINT ( 'NONE',  ( -19.05341960407611168, -5.049401038298163336, 26.45724293864769550 ) ) ;
#187685 = CARTESIAN_POINT ( 'NONE',  ( 0.05219959533909260263, 19.03943276465977164, 94.99890960531436690 ) ) ;
#187686 = CARTESIAN_POINT ( 'NONE',  ( -5.719274019375978568, 21.55341960407610458, 75.20724293864769550 ) ) ;
#187687 = CARTESIAN_POINT ( 'NONE',  ( -12.06949235617739369, -12.14591786802326823, 49.37609039468569705 ) ) ;
#187688 = CARTESIAN_POINT ( 'NONE',  ( -21.53943276465977519, -0.05219959533937600094, 53.75109039468568994 ) ) ;
#187689 = CARTESIAN_POINT ( 'NONE',  ( 5.823673210054444382, -21.52544592524334988, 95.20942372801903275 ) ) ;
#187690 = CARTESIAN_POINT ( 'NONE',  ( -4.483927247898782831, 16.52544592524335698, 92.70942372801901854 ) ) ;
#187691 = CARTESIAN_POINT ( 'NONE',  ( 9.474510206698971260, -16.51473224551069308, 82.91557627198103830 ) ) ;
#187692 = CARTESIAN_POINT ( 'NONE',  ( -14.29746914071049879, 8.314922557960819915, 95.83224293864770971 ) ) ;
#187693 = CARTESIAN_POINT ( 'NONE',  ( -16.53943276465976808, 0.05219959533911058130, 31.24890960531435979 ) ) ;
#187694 = CARTESIAN_POINT ( 'NONE',  ( -9.564922557961040184, 16.46253265017147172, 72.91775706135233293 ) ) ;
#187695 = CARTESIAN_POINT ( 'NONE',  ( -0.05219959533937732626, 21.53943276465977519, 47.50109039468568994 ) ) ;
#187696 = CARTESIAN_POINT ( 'NONE',  ( 19.03943276465977164, 0.05219959533936151252, 31.25109039468566863 ) ) ;
#187697 = CARTESIAN_POINT ( 'NONE',  ( 12.06949235617757843, -12.14591786802309237, 88.12390960531436690 ) ) ;
#187698 = CARTESIAN_POINT ( 'NONE',  ( -16.46253265017160317, 9.564922557960807481, 115.8322429386477097 ) ) ;
#187699 = CARTESIAN_POINT ( 'NONE',  ( 12.14591786802327356, -12.06949235617739191, 110.6260903946857042 ) ) ;
#187700 = CARTESIAN_POINT ( 'NONE',  ( -18.67979575497193778, 10.72451020669871902, 83.33442372801903275 ) ) ;
#187701 = CARTESIAN_POINT ( 'NONE',  ( 12.14591786802327356, -12.06949235617739191, 55.62609039468568284 ) ) ;
#187702 = CARTESIAN_POINT ( 'NONE',  ( 12.06949235617739724, 12.14591786802326823, 101.8760903946857042 ) ) ;
#187703 = CARTESIAN_POINT ( 'NONE',  ( -10.81492255796105439, 18.62759615963255655, 57.91775706135234714 ) ) ;
#187704 = CARTESIAN_POINT ( 'NONE',  ( 0.05219959533937995610, -21.53943276465977519, 30.00109039468568284 ) ) ;
#187705 = CARTESIAN_POINT ( 'NONE',  ( -8.224510206698948167, 14.34966873604960824, 110.4155762719810383 ) ) ;
#187706 = CARTESIAN_POINT ( 'NONE',  ( 20.28939339942064635, 0.9295024462022883904, 37.50000000000002842 ) ) ;
#187707 = CARTESIAN_POINT ( 'NONE',  ( -4.483927247898539470, -16.52544592524342804, 72.29057627198102409 ) ) ;
#187708 = CARTESIAN_POINT ( 'NONE',  ( -13.97604488694527625, -13.89961937509977652, 76.87390960531433848 ) ) ;
#187709 = CARTESIAN_POINT ( 'NONE',  ( -4.483927247898782831, 16.52544592524335698, 112.7094237280190328 ) ) ;
#187710 = CARTESIAN_POINT ( 'NONE',  ( 16.51473224551069308, 9.474510206698969483, 39.16557627198103120 ) ) ;
#187711 = CARTESIAN_POINT ( 'NONE',  ( -21.52544592524343514, 5.823673210054127303, 51.04057627198103120 ) ) ;
#187712 = CARTESIAN_POINT ( 'NONE',  ( -12.06949235617756955, 12.14591786802309770, 95.62390960531436690 ) ) ;
#187713 = CARTESIAN_POINT ( 'NONE',  ( -21.53943276465977519, 0.05219959533907696930, 91.24890960531436690 ) ) ;
#187715 = ADVANCED_FACE ( 'NONE', ( #19142 ), #18156, .T. ) ;
#187714 = CARTESIAN_POINT ( 'NONE',  ( -5.153800228976328057, -19.02544592524343514, 107.2905762719810383 ) ) ;
#187717 = CARTESIAN_POINT ( 'NONE',  ( 13.89961937509957401, 13.97604488694547697, 86.87609039468567573 ) ) ;
#187716 = CARTESIAN_POINT ( 'NONE',  ( 9.564922557960805705, 16.46253265017160317, 54.58224293864769550 ) ) ;
#187718 = CARTESIAN_POINT ( 'NONE',  ( -21.53943276465977519, 0.05219959533907696930, 41.24890960531435269 ) ) ;
#187719 = CARTESIAN_POINT ( 'NONE',  ( 15.72974639402176855, 15.80617190586768217, 61.87609039468568284 ) ) ;
#187720 = CARTESIAN_POINT ( 'NONE',  ( 0.05219959533909260263, 19.03943276465977164, 54.99890960531435979 ) ) ;
#187721 = CARTESIAN_POINT ( 'NONE',  ( -19.02544592524342804, 5.153800228976336051, 86.04057627198103830 ) ) ;
#187722 = CARTESIAN_POINT ( 'NONE',  ( 14.29746914071037800, 8.314922557961029526, 66.66775706135234714 ) ) ;
#187723 = CARTESIAN_POINT ( 'NONE',  ( -21.53943276465977519, -0.05219959533937600094, 43.75109039468568284 ) ) ;
#187724 = CARTESIAN_POINT ( 'NONE',  ( 10.81492255796106328, -18.62759615963255655, 85.41775706135236135 ) ) ;
#187725 = CARTESIAN_POINT ( 'NONE',  ( -21.55341960407610458, -5.719274019375992779, 96.45724293864770971 ) ) ;
#187727 = CARTESIAN_POINT ( 'NONE',  ( 16.52544592524335698, 4.483927247898782831, 61.45942372801901854 ) ) ;
#187726 = CARTESIAN_POINT ( 'NONE',  ( 21.55341960407619695, -5.719274019375665929, 31.04275706135234714 ) ) ;
#187728 = CARTESIAN_POINT ( 'NONE',  ( 0.05219959533907565091, 21.53943276465977519, 64.99890960531435269 ) ) ;
#187729 = CARTESIAN_POINT ( 'NONE',  ( 13.97604488694548053, -13.89961937509957401, 35.62609039468567573 ) ) ;
#187731 = CARTESIAN_POINT ( 'NONE',  ( 12.06949235617757843, -12.14591786802309237, 23.12390960531436335 ) ) ;
#187730 = CARTESIAN_POINT ( 'NONE',  ( -9.474510206698964154, 16.51473224551069663, 70.41557627198102409 ) ) ;
#187732 = CARTESIAN_POINT ( 'NONE',  ( 30.00000000000000000, -5.499999999999992895, 102.5000000000000142 ) ) ;
#187733 = CARTESIAN_POINT ( 'NONE',  ( 9.474510206698971260, -16.51473224551069308, 107.9155762719810383 ) ) ;
#187734 = DIRECTION ( 'NONE',  ( 1.000000000000000000, 0.000000000000000000, 0.000000000000000000 ) ) ;
#187735 = CARTESIAN_POINT ( 'NONE',  ( -5.049401038297874678, -19.05341960407617918, 79.79275706135233293 ) ) ;
#187736 = CARTESIAN_POINT ( 'NONE',  ( 21.52544592524344225, -5.823673210054117533, 63.54057627198103830 ) ) ;
#187737 = CARTESIAN_POINT ( 'NONE',  ( -12.14591786802309592, -12.06949235617757132, 41.87390960531435979 ) ) ;
#187738 = CARTESIAN_POINT ( 'NONE',  ( 8.314922557961029526, -14.29746914071037800, 20.41775706135234714 ) ) ;
#187739 = CARTESIAN_POINT ( 'NONE',  ( -13.97604488694527625, -13.89961937509977652, 36.87390960531436690 ) ) ;
#187740 = CARTESIAN_POINT ( 'NONE',  ( -13.89961937509957401, -13.97604488694547875, 109.3760903946856331 ) ) ;
#187742 = CARTESIAN_POINT ( 'NONE',  ( 19.02544592524334988, 5.153800228976608722, 76.45942372801897591 ) ) ;
#187741 = CARTESIAN_POINT ( 'NONE',  ( -18.67979575497178146, -10.72451020669898902, 101.6655762719810383 ) ) ;
#187743 = CARTESIAN_POINT ( 'NONE',  ( 14.34966873604972726, -8.224510206698740333, 85.83442372801901854 ) ) ;
#187744 = CARTESIAN_POINT ( 'NONE',  ( -16.51473224551069308, -9.474510206698971260, 71.66557627198102409 ) ) ;
#187745 = CARTESIAN_POINT ( 'NONE',  ( 0.05219959533910956823, 16.53943276465976808, 69.99890960531435269 ) ) ;
#187746 = EDGE_CURVE ( 'NONE', #156506, #74887, #78806, .T. ) ;
#187747 = CARTESIAN_POINT ( 'NONE',  ( -16.46253265017160317, 9.564922557960807481, 45.83224293864769550 ) ) ;
#187748 = CARTESIAN_POINT ( 'NONE',  ( -14.34966873604960291, -8.224510206698953496, 56.66557627198103830 ) ) ;
#187749 = CARTESIAN_POINT ( 'NONE',  ( 2.500000000000000000, 2.357898499370431722, -2.818925648462311528E-15 ) ) ;
#187750 = CARTESIAN_POINT ( 'NONE',  ( 32.64453336272026718, -0.4913453444576664220, 87.50000000000002842 ) ) ;
#187751 = CARTESIAN_POINT ( 'NONE',  ( 8.314922557960818139, 14.29746914071049879, 24.58224293864768839 ) ) ;
#187752 = CARTESIAN_POINT ( 'NONE',  ( 0.05219959533909260263, 19.03943276465977164, 79.99890960531436690 ) ) ;
#187753 = DIRECTION ( 'NONE',  ( 0.000000000000000000, 0.000000000000000000, -1.000000000000000000 ) ) ;
#187754 = CARTESIAN_POINT ( 'NONE',  ( -16.51473224551082808, 9.474510206698731452, 38.33442372801899722 ) ) ;
#187755 = CARTESIAN_POINT ( 'NONE',  ( 14.34966873604972726, -8.224510206698740333, 45.83442372801901854 ) ) ;
#187756 = CARTESIAN_POINT ( 'NONE',  ( 0.05219959533907565091, 21.53943276465977519, 59.99890960531436690 ) ) ;
#187757 = CARTESIAN_POINT ( 'NONE',  ( -5.153800228976607833, 19.02544592524334988, 22.70942372801899012 ) ) ;
#187758 = CARTESIAN_POINT ( 'NONE',  ( 16.51473224551069308, 9.474510206698969483, 69.16557627198102409 ) ) ;
#187759 = CARTESIAN_POINT ( 'NONE',  ( 0.1103826470145124194, 21.30000000000002558, -58.85720012050614258 ) ) ;
#187760 = CARTESIAN_POINT ( 'NONE',  ( -19.03943276465977164, 0.05219959533909376836, 116.2489096053143669 ) ) ;
#187761 = CARTESIAN_POINT ( 'NONE',  ( -10.81492255796105439, 18.62759615963255655, 37.91775706135235424 ) ) ;
#187762 = CARTESIAN_POINT ( 'NONE',  ( -14.34966873604960291, -8.224510206698953496, 111.6655762719810525 ) ) ;
#187765 = ORIENTED_EDGE ( 'NONE', *, *, #294, .T. ) ;
#187764 = CARTESIAN_POINT ( 'NONE',  ( -0.05219959533909027116, -19.03943276465977164, 77.49890960531435269 ) ) ;
#187763 = CARTESIAN_POINT ( 'NONE',  ( -5.719274019375978568, 21.55341960407610458, 95.20724293864769550 ) ) ;
#187766 = CARTESIAN_POINT ( 'NONE',  ( -5.719274019375665041, -21.55341960407619695, 24.79275706135235779 ) ) ;
#187767 = ORIENTED_EDGE ( 'NONE', *, *, #52301, .F. ) ;
#187768 = CARTESIAN_POINT ( 'NONE',  ( 5.049401038298161559, -19.05341960407611168, 87.70724293864769550 ) ) ;
#187769 = CARTESIAN_POINT ( 'NONE',  ( 5.199999999999996625, 0.000000000000000000, 0.000000000000000000 ) ) ;
#187770 = CARTESIAN_POINT ( 'NONE',  ( 5.049401038298161559, -19.05341960407611168, 27.70724293864769550 ) ) ;
#187771 = CARTESIAN_POINT ( 'NONE',  ( 0.05219959533936267826, -19.03943276465977164, 100.0010903946856757 ) ) ;
#187772 = CARTESIAN_POINT ( 'NONE',  ( -36.91746825000000598, 2.428612866367529932E-14, -7.124999997268813168 ) ) ;
#187773 = CARTESIAN_POINT ( 'NONE',  ( -12.06949235617756955, 12.14591786802309770, 115.6239096053143669 ) ) ;
#187774 = CARTESIAN_POINT ( 'NONE',  ( -5.823673210054431948, 21.52544592524334988, 82.70942372801900433 ) ) ;
#187776 = CARTESIAN_POINT ( 'NONE',  ( 18.62759615963255655, 10.81492255796105972, 51.66775706135234714 ) ) ;
#187775 = CARTESIAN_POINT ( 'NONE',  ( -9.474510206698964154, 16.51473224551069663, 80.41557627198103830 ) ) ;
#187777 = CARTESIAN_POINT ( 'NONE',  ( -21.52544592524334988, -5.823673210054445271, 23.95942372801901143 ) ) ;
#187778 = CARTESIAN_POINT ( 'NONE',  ( -27.73933785331498925, -9.013057229001049109, 139.4750000027311785 ) ) ;
#187779 = CARTESIAN_POINT ( 'NONE',  ( -5.049401038298153566, 19.05341960407611168, 85.20724293864766707 ) ) ;
#187780 = CARTESIAN_POINT ( 'NONE',  ( 10.31603103613401373, 26.32579789674820958, 139.9999999999999716 ) ) ;
#187782 = CARTESIAN_POINT ( 'NONE',  ( -5.719274019375978568, 21.55341960407610458, 45.20724293864769550 ) ) ;
#187781 = CARTESIAN_POINT ( 'NONE',  ( 16.55341960407618274, -4.379528057220086978, 36.04275706135234714 ) ) ;
#187783 = CARTESIAN_POINT ( 'NONE',  ( -10.81492255796105439, 18.62759615963255655, 82.91775706135234714 ) ) ;
#187784 = CARTESIAN_POINT ( 'NONE',  ( -3.573655867282013404E-15, -180.0000000000000000, -15.00000000000000000 ) ) ;
#187785 = CARTESIAN_POINT ( 'NONE',  ( 12.14591786802327356, -12.06949235617739191, 20.62609039468568639 ) ) ;
#187786 = CARTESIAN_POINT ( 'NONE',  ( 5.153800228976335163, 19.02544592524342804, 54.79057627198103120 ) ) ;
#187787 = CARTESIAN_POINT ( 'NONE',  ( -19.02544592524342804, 5.153800228976336051, 86.04057627198103830 ) ) ;
#187788 = B_SPLINE_CURVE_WITH_KNOTS ( 'NONE', 3,
 ( #187038, #48508, #110162, #171841, #91987, #978, #153682, #62654, #15178, #76837, #33329, #200191, #61659, #4950 ),
 .UNSPECIFIED., .F., .F.,
 ( 4, 2, 2, 2, 2, 2, 4 ),
 ( 0.000000000000000000, 0.002096066633256099630, 0.003144099949884144891, 0.004192133266512189718, 0.006288199899768280240, 0.007336233216396328104, 0.008384266533024375967 ),
 .UNSPECIFIED. ) ;
#187789 = CARTESIAN_POINT ( 'NONE',  ( -12.06949235617756955, 12.14591786802309770, 110.6239096053143669 ) ) ;
#187790 = CARTESIAN_POINT ( 'NONE',  ( -8.224510206698948167, 14.34966873604960824, 110.4155762719810383 ) ) ;
#187791 = CARTESIAN_POINT ( 'NONE',  ( -5.049401038298153566, 19.05341960407611168, 110.2072429386476671 ) ) ;
#187792 = CARTESIAN_POINT ( 'NONE',  ( 12.06949235617739724, 12.14591786802326823, 76.87609039468567573 ) ) ;
#187794 = CARTESIAN_POINT ( 'NONE',  ( 5.153800228976335163, 19.02544592524342804, 59.79057627198100988 ) ) ;
#187793 = CARTESIAN_POINT ( 'NONE',  ( -16.53943276465976808, 0.05219959533911058130, 61.24890960531435979 ) ) ;
#187795 = CARTESIAN_POINT ( 'NONE',  ( -18.67979575497193778, 10.72451020669871902, 78.33442372801901854 ) ) ;
#187796 = CARTESIAN_POINT ( 'NONE',  ( -10.72451020669870658, -18.67979575497194134, 64.58442372801900433 ) ) ;
#187797 = CARTESIAN_POINT ( 'NONE',  ( -19.02544592524334988, -5.153800228976617603, 108.9594237280189759 ) ) ;
#187798 = CARTESIAN_POINT ( 'NONE',  ( -12.06949235617756955, 12.14591786802309770, 65.62390960531436690 ) ) ;
#187799 = CARTESIAN_POINT ( 'NONE',  ( 5.823673210054444382, -21.52544592524334988, 20.20942372801900788 ) ) ;
#187800 = CARTESIAN_POINT ( 'NONE',  ( 21.52544592524344225, -5.823673210054117533, 63.54057627198103830 ) ) ;
#187801 = CARTESIAN_POINT ( 'NONE',  ( -16.38665767535054130, -7.295008042176104546, 104.7359913578545587 ) ) ;
#187802 = CARTESIAN_POINT ( 'NONE',  ( 23.31738231874054534, 16.94106989632529192, 139.4500000054623570 ) ) ;
#187803 = CARTESIAN_POINT ( 'NONE',  ( 19.03943276465977164, -0.05219959533909143690, 73.74890960531435269 ) ) ;
#187804 = CARTESIAN_POINT ( 'NONE',  ( 14.29746914071049879, -8.314922557960816363, 33.33224293864769550 ) ) ;
#187805 = CARTESIAN_POINT ( 'NONE',  ( 4.379528057220092307, 16.55341960407617563, 112.2927570613523471 ) ) ;
#187806 = CARTESIAN_POINT ( 'NONE',  ( 16.52544592524335698, 4.483927247898782831, 96.45942372801901854 ) ) ;
#187807 = CARTESIAN_POINT ( 'NONE',  ( -16.46253265017146816, -9.564922557961047289, 59.16775706135233293 ) ) ;
#187808 = CARTESIAN_POINT ( 'NONE',  ( -11.30153831258470731, -180.0000000000000568, -4.999999999999999112 ) ) ;
#187809 = CARTESIAN_POINT ( 'NONE',  ( -19.02544592524342804, 5.153800228976336051, 86.04057627198103830 ) ) ;
#187810 = CARTESIAN_POINT ( 'NONE',  ( -12.06949235617756955, 12.14591786802309770, 65.62390960531436690 ) ) ;
#187812 = CARTESIAN_POINT ( 'NONE',  ( -5.719274019375978568, 21.55341960407610458, 25.20724293864769550 ) ) ;
#187811 = CARTESIAN_POINT ( 'NONE',  ( 17.50000000000000711, -5.622605283950869115, 101.1879268940388812 ) ) ;
#187814 = VERTEX_POINT ( 'NONE', #1972 ) ;
#187813 = CARTESIAN_POINT ( 'NONE',  ( 15.72974639402199770, -15.80617190586745480, 48.12390960531436690 ) ) ;
#187815 = CARTESIAN_POINT ( 'NONE',  ( 8.224510206698953496, -14.34966873604960469, 92.91557627198103830 ) ) ;
#187816 = CARTESIAN_POINT ( 'NONE',  ( 4.483927247898790824, -16.52544592524335698, 50.20942372801901854 ) ) ;
#187817 = CARTESIAN_POINT ( 'NONE',  ( 4.379528057220339221, -16.55341960407611168, 77.70724293864770971 ) ) ;
#187818 = CARTESIAN_POINT ( 'NONE',  ( -19.35633801406906329, 5.499999999999777955, 64.13373818172762242 ) ) ;
#187819 = CARTESIAN_POINT ( 'NONE',  ( 16.46253265017146816, 9.564922557961045513, 76.66775706135234714 ) ) ;
#187820 = CARTESIAN_POINT ( 'NONE',  ( 10.81492255796078972, 18.62759615963270932, 24.58224293864768839 ) ) ;
#187821 = CARTESIAN_POINT ( 'NONE',  ( -29.86685920354755197, -21.69954338932560134, -2.924999997268813878 ) ) ;
#187822 = CARTESIAN_POINT ( 'NONE',  ( -9.564922557960796823, -16.46253265017161027, 42.08224293864769550 ) ) ;
#187824 = CARTESIAN_POINT ( 'NONE',  ( -16.52544592524342804, 4.483927247898546575, 26.04057627198103475 ) ) ;
#187823 = CARTESIAN_POINT ( 'NONE',  ( 4.379528057220092307, 16.55341960407617563, 42.29275706135235424 ) ) ;
#187825 = CARTESIAN_POINT ( 'NONE',  ( 21.55341960407610458, 5.719274019375980345, 58.95724293864770971 ) ) ;
#187826 = CARTESIAN_POINT ( 'NONE',  ( 16.51473224551083163, -9.474510206698727899, 85.83442372801900433 ) ) ;
#187827 = CARTESIAN_POINT ( 'NONE',  ( 10.72451020669898902, -18.67979575497178502, 42.91557627198103120 ) ) ;
#187828 = CARTESIAN_POINT ( 'NONE',  ( -15.72974639402176322, -15.80617190586768395, 79.37609039468567573 ) ) ;
#187829 = CARTESIAN_POINT ( 'NONE',  ( -11.16688150046374339, 9.295088167215947550, -62.26853652665834460 ) ) ;
#187830 = CARTESIAN_POINT ( 'NONE',  ( 4.483927247898790824, -16.52544592524335698, 30.20942372801902565 ) ) ;
#187832 = CARTESIAN_POINT ( 'NONE',  ( 19.02544592524343514, -5.153800228976328945, 83.54057627198100988 ) ) ;
#187831 = CARTESIAN_POINT ( 'NONE',  ( -5.049401038298153566, 19.05341960407611168, 40.20724293864768839 ) ) ;
#187833 = CARTESIAN_POINT ( 'NONE',  ( -16.46253265017160317, 9.564922557960807481, 30.83224293864769550 ) ) ;
#187834 = CARTESIAN_POINT ( 'NONE',  ( 16.52544592524342804, -4.483927247898539470, 103.5405762719810383 ) ) ;
#187835 = CONTEXT_DEPENDENT_SHAPE_REPRESENTATION ( #191494, #82525 ) ;
#187836 = CARTESIAN_POINT ( 'NONE',  ( 13.97604488694527802, 13.89961937509977652, 104.3739096053143385 ) ) ;
#187837 = ORIENTED_EDGE ( 'NONE', *, *, #171883, .T. ) ;
#187838 = CARTESIAN_POINT ( 'NONE',  ( -8.224510206698735004, -14.34966873604973081, 49.58442372801901143 ) ) ;
#187839 = CARTESIAN_POINT ( 'NONE',  ( -21.53943276465977519, 0.05219959533907696930, 96.24890960531435269 ) ) ;
#187840 = CARTESIAN_POINT ( 'NONE',  ( -13.97604488694527625, -13.89961937509977652, 41.87390960531435979 ) ) ;
#187841 = CARTESIAN_POINT ( 'NONE',  ( -5.719274019375665041, -21.55341960407619695, 29.79275706135234358 ) ) ;
#187842 = CARTESIAN_POINT ( 'NONE',  ( 5.153800228976335163, 19.02544592524342804, 79.79057627198102409 ) ) ;
#187843 = CARTESIAN_POINT ( 'NONE',  ( 2.044528755335782044, 7.220908937439987518, 8.410814283099853128 ) ) ;
#187844 = ORIENTED_EDGE ( 'NONE', *, *, #162564, .F. ) ;
#187845 = CARTESIAN_POINT ( 'NONE',  ( 16.53943276465976808, 0.05219959533934440121, 31.25109039468568639 ) ) ;
#187846 = CARTESIAN_POINT ( 'NONE',  ( 18.62759615963271287, -10.81492255796078972, 113.3322429386476955 ) ) ;
#187849 = CARTESIAN_POINT ( 'NONE',  ( 13.89961937509957401, 13.97604488694547697, 71.87609039468567573 ) ) ;
#187848 = CARTESIAN_POINT ( 'NONE',  ( 5.049401038298161559, -19.05341960407611168, 92.70724293864769550 ) ) ;
#187847 = CARTESIAN_POINT ( 'NONE',  ( 8.314922557960818139, 14.29746914071049879, 109.5822429386476955 ) ) ;
#187850 = CARTESIAN_POINT ( 'NONE',  ( 13.97604488694548053, -13.89961937509957401, 25.62609039468566507 ) ) ;
#187851 = CARTESIAN_POINT ( 'NONE',  ( -21.52544592524343514, 5.823673210054127303, 81.04057627198102409 ) ) ;
#187852 = CARTESIAN_POINT ( 'NONE',  ( -16.51473224551082808, 9.474510206698731452, 28.33442372801900433 ) ) ;
#187853 = CARTESIAN_POINT ( 'NONE',  ( 16.55341960407618274, -4.379528057220086978, 81.04275706135236135 ) ) ;
#187854 = CARTESIAN_POINT ( 'NONE',  ( 0.05219959533909260263, 19.03943276465977164, 104.9989096053143669 ) ) ;
#187855 = CARTESIAN_POINT ( 'NONE',  ( 9.564922557960805705, 16.46253265017160317, 49.58224293864770260 ) ) ;
#187856 = CARTESIAN_POINT ( 'NONE',  ( -21.53943276465977519, -0.05219959533937600094, 58.75109039468568994 ) ) ;
#187857 = CARTESIAN_POINT ( 'NONE',  ( -10.72451020669870658, -18.67979575497194134, 69.58442372801900433 ) ) ;
#187858 = CARTESIAN_POINT ( 'NONE',  ( -19.02544592524342804, 5.153800228976336051, 76.04057627198102409 ) ) ;
#187859 = CARTESIAN_POINT ( 'NONE',  ( -21.55341960407619339, 5.719274019375674811, 43.54275706135235424 ) ) ;
#187860 = CARTESIAN_POINT ( 'NONE',  ( 5.049401038297881783, 19.05341960407617563, 92.29275706135234714 ) ) ;
#187861 = CARTESIAN_POINT ( 'NONE',  ( -5.049401038298153566, 19.05341960407611168, 55.20724293864769550 ) ) ;
#187862 = CARTESIAN_POINT ( 'NONE',  ( -16.46253265017160317, 9.564922557960807481, 95.83224293864769550 ) ) ;
#187863 = CARTESIAN_POINT ( 'NONE',  ( 5.153800228976335163, 19.02544592524342804, 69.79057627198103830 ) ) ;
#187864 = CARTESIAN_POINT ( 'NONE',  ( 0.05219959533909260263, 19.03943276465977164, 109.9989096053143669 ) ) ;
#187865 = CARTESIAN_POINT ( 'NONE',  ( 9.474510206698971260, -16.51473224551069308, 52.91557627198102409 ) ) ;
#187866 = CARTESIAN_POINT ( 'NONE',  ( -21.53943276465977519, 0.05219959533907696930, 91.24890960531436690 ) ) ;
#187867 = CARTESIAN_POINT ( 'NONE',  ( -4.483927247898782831, 16.52544592524335698, 72.70942372801901854 ) ) ;
#187868 = CARTESIAN_POINT ( 'NONE',  ( -24.85114155361848276, 5.582993631601033790, 168.8590791472286412 ) ) ;
#187869 = CARTESIAN_POINT ( 'NONE',  ( 19.05341960407617918, -5.049401038297876454, 26.04275706135233293 ) ) ;
#187870 = CARTESIAN_POINT ( 'NONE',  ( -0.05219959533909027116, -19.03943276465977164, 62.49890960531435979 ) ) ;
#187871 = CARTESIAN_POINT ( 'NONE',  ( 12.14591786802309770, 12.06949235617756955, 59.37390960531436690 ) ) ;
#187872 = CARTESIAN_POINT ( 'NONE',  ( -8.224510206698948167, 14.34966873604960824, 100.4155762719810241 ) ) ;
#187873 = CARTESIAN_POINT ( 'NONE',  ( -5.153800228976328057, -19.02544592524343514, 97.29057627198099567 ) ) ;
#187874 = CARTESIAN_POINT ( 'NONE',  ( 0.05219959533909260263, 19.03943276465977164, 89.99890960531436690 ) ) ;
#187875 = CARTESIAN_POINT ( 'NONE',  ( 21.53943276465977519, 0.05219959533937863772, 56.25109039468568284 ) ) ;
#187876 = CARTESIAN_POINT ( 'NONE',  ( -16.46253265017160317, 9.564922557960807481, 100.8322429386477097 ) ) ;
#187877 = CARTESIAN_POINT ( 'NONE',  ( -9.474510206698720793, -16.51473224551083518, 19.58442372801899722 ) ) ;
#187878 = CARTESIAN_POINT ( 'NONE',  ( -14.29746914071037622, -8.314922557961029526, 74.16775706135231871 ) ) ;
#187879 = ADVANCED_FACE ( 'NONE', ( #51455 ), #60028, .F. ) ;
#187880 = CARTESIAN_POINT ( 'NONE',  ( 15.80617190586769283, -15.72974639402175789, 45.62609039468567573 ) ) ;
#187881 = CARTESIAN_POINT ( 'NONE',  ( 15.80617190586746368, 15.72974639402197994, 24.37390960531435979 ) ) ;
#187882 = CARTESIAN_POINT ( 'NONE',  ( 21.52544592524344225, -5.823673210054117533, 98.54057627198105251 ) ) ;
#187883 = CARTESIAN_POINT ( 'NONE',  ( -8.224510206698948167, 14.34966873604960824, 60.41557627198102409 ) ) ;
#187884 = CARTESIAN_POINT ( 'NONE',  ( -0.05219959533909027116, -19.03943276465977164, 52.49890960531436690 ) ) ;
#187885 = CARTESIAN_POINT ( 'NONE',  ( 16.52544592524342804, -4.483927247898539470, 83.54057627198102409 ) ) ;
#187886 = CARTESIAN_POINT ( 'NONE',  ( 10.72451020669898902, -18.67979575497178502, 37.91557627198102409 ) ) ;
#187887 = CARTESIAN_POINT ( 'NONE',  ( 5.153800228976615827, -19.02544592524334988, 40.20942372801898301 ) ) ;
#187888 = CARTESIAN_POINT ( 'NONE',  ( 4.379528057220339221, -16.55341960407611168, 112.7072429386476955 ) ) ;
#187889 = ORIENTED_EDGE ( 'NONE', *, *, #39120, .T. ) ;
#187890 = CARTESIAN_POINT ( 'NONE',  ( -16.53943276465976808, -0.05219959533934237506, 68.75109039468568994 ) ) ;
#187891 = CARTESIAN_POINT ( 'NONE',  ( 16.46253265017160672, -9.564922557960803928, 68.33224293864770971 ) ) ;
#187892 = CARTESIAN_POINT ( 'NONE',  ( -27.73933785331498925, -9.013057229001049109, 146.9750000027311785 ) ) ;
#187893 = CARTESIAN_POINT ( 'NONE',  ( 16.53943276465976808, -0.05219959533910856209, 88.74890960531436690 ) ) ;
#187894 = CARTESIAN_POINT ( 'NONE',  ( 18.67979575497178502, 10.72451020669898547, 44.16557627198103120 ) ) ;
#187895 = CARTESIAN_POINT ( 'NONE',  ( -16.55341960407617563, 4.379528057220093196, 113.5427570613523756 ) ) ;
#187896 = CARTESIAN_POINT ( 'NONE',  ( -16.46253265017146816, -9.564922557961047289, 104.1677570613523329 ) ) ;
#187897 = CARTESIAN_POINT ( 'NONE',  ( -10.81492255796105439, 18.62759615963255655, 82.91775706135234714 ) ) ;
#187898 = CARTESIAN_POINT ( 'NONE',  ( -16.46253265017160317, 9.564922557960807481, 85.83224293864769550 ) ) ;
#187899 = CARTESIAN_POINT ( 'NONE',  ( 5.719274019375991003, -21.55341960407610458, 102.7072429386476955 ) ) ;
#187900 = CARTESIAN_POINT ( 'NONE',  ( -16.52544592524335698, -4.483927247898792601, 53.95942372801900433 ) ) ;
#187901 = CARTESIAN_POINT ( 'NONE',  ( -16.51473224551069308, -9.474510206698971260, 26.66557627198103120 ) ) ;
#187902 = CARTESIAN_POINT ( 'NONE',  ( 8.224510206698742110, 14.34966873604972548, 32.08442372801901854 ) ) ;
#187903 = CARTESIAN_POINT ( 'NONE',  ( 0.05219959533936267826, -19.03943276465977164, 95.00109039468567573 ) ) ;
#187904 = CARTESIAN_POINT ( 'NONE',  ( 10.72451020669898902, -18.67979575497178502, 92.91557627198103830 ) ) ;
#187905 = CARTESIAN_POINT ( 'NONE',  ( -5.049401038297874678, -19.05341960407617918, 59.79275706135231871 ) ) ;
#187906 = DIRECTION ( 'NONE',  ( 0.000000000000000000, -0.6427876096865403621, -0.7660444431189770143 ) ) ;
#187907 = CARTESIAN_POINT ( 'NONE',  ( -18.67979575497178146, -10.72451020669898902, 101.6655762719810383 ) ) ;
#187908 = CARTESIAN_POINT ( 'NONE',  ( 22.55670631985092811, 22.55670631985084640, -64.92279855667830191 ) ) ;
#187909 = CARTESIAN_POINT ( 'NONE',  ( 19.02544592524343514, -5.153800228976328945, 73.54057627198103830 ) ) ;
#187910 = CARTESIAN_POINT ( 'NONE',  ( -16.55341960407617563, 4.379528057220093196, 38.54275706135234714 ) ) ;
#187911 = DIRECTION ( 'NONE',  ( -1.000000000000000000, 5.392603844284257652E-33, 0.000000000000000000 ) ) ;
#187912 = CARTESIAN_POINT ( 'NONE',  ( 19.03943276465977164, 0.05219959533936151252, 66.25109039468567573 ) ) ;
#187914 = CARTESIAN_POINT ( 'NONE',  ( -16.53943276465976808, 0.05219959533911058130, 66.24890960531436690 ) ) ;
#187913 = CARTESIAN_POINT ( 'NONE',  ( -21.53943276465977519, 0.05219959533907696930, 116.2489096053143669 ) ) ;
#187915 = CARTESIAN_POINT ( 'NONE',  ( -5.049401038298153566, 19.05341960407611168, 70.20724293864769550 ) ) ;
#187917 = CARTESIAN_POINT ( 'NONE',  ( 19.03943276465977164, 0.05219959533936151252, 41.25109039468566152 ) ) ;
#187916 = CARTESIAN_POINT ( 'NONE',  ( 12.06949235617739724, 12.14591786802326823, 41.87609039468568284 ) ) ;
#187918 = CARTESIAN_POINT ( 'NONE',  ( 10.72451020669871369, 18.67979575497193778, 47.08442372801901854 ) ) ;
#187919 = CARTESIAN_POINT ( 'NONE',  ( -16.51473224551082808, 9.474510206698731452, 103.3344237280190043 ) ) ;
#187920 = CARTESIAN_POINT ( 'NONE',  ( 5.153800228976335163, 19.02544592524342804, 49.79057627198100988 ) ) ;
#187921 = CARTESIAN_POINT ( 'NONE',  ( 5.049401038297881783, 19.05341960407617563, 82.29275706135229029 ) ) ;
#187922 = CARTESIAN_POINT ( 'NONE',  ( 15.80617190586769283, -15.72974639402175789, 90.62609039468567573 ) ) ;
#187923 = CARTESIAN_POINT ( 'NONE',  ( 19.03943276465977164, 0.05219959533936151252, 71.25109039468566152 ) ) ;
#187924 = CARTESIAN_POINT ( 'NONE',  ( 19.05341960407611168, 5.049401038298154454, 33.95724293864769550 ) ) ;
#187925 = CARTESIAN_POINT ( 'NONE',  ( 5.823673210054125526, 21.52544592524343514, 74.79057627198105251 ) ) ;
#187927 = CARTESIAN_POINT ( 'NONE',  ( -0.05219959533936034679, 19.03943276465977164, 67.50109039468566152 ) ) ;
#187926 = CARTESIAN_POINT ( 'NONE',  ( 16.52544592524342804, -4.483927247898539470, 58.54057627198103120 ) ) ;
#187928 = CARTESIAN_POINT ( 'NONE',  ( -16.38665767535055195, -7.295008042175997964, 24.73599135785456937 ) ) ;
#187929 = CARTESIAN_POINT ( 'NONE',  ( 9.474510206698729675, 16.51473224551082808, 32.08442372801900433 ) ) ;
#187930 = CARTESIAN_POINT ( 'NONE',  ( -16.53943276465976808, -0.05219959533934237506, 93.75109039468567573 ) ) ;
#187931 = CARTESIAN_POINT ( 'NONE',  ( 14.34966873604960469, 8.224510206698951720, 49.16557627198102409 ) ) ;
#187933 = CARTESIAN_POINT ( 'NONE',  ( 27.73933785331498925, -9.013057229001033122, 141.7750000027311899 ) ) ;
#187932 = CARTESIAN_POINT ( 'NONE',  ( 15.80617190586769283, -15.72974639402175789, 95.62609039468568994 ) ) ;
#187934 = CARTESIAN_POINT ( 'NONE',  ( 21.52544592524344225, -5.823673210054117533, 93.54057627198103830 ) ) ;
#187935 = CARTESIAN_POINT ( 'NONE',  ( -19.05341960407611168, -5.049401038298163336, 46.45724293864768129 ) ) ;
#187936 = CARTESIAN_POINT ( 'NONE',  ( 0.05219959533937995610, -21.53943276465977519, 65.00109039468568994 ) ) ;
#187937 = CARTESIAN_POINT ( 'NONE',  ( 0.05219959533909260263, 19.03943276465977164, 49.99890960531435979 ) ) ;
#187938 = VERTEX_POINT ( 'NONE', #79810 ) ;
#187939 = CARTESIAN_POINT ( 'NONE',  ( 16.51473224551069308, 9.474510206698969483, 69.16557627198102409 ) ) ;
#187940 = CARTESIAN_POINT ( 'NONE',  ( -16.55341960407611168, -4.379528057220339221, 106.4572429386477097 ) ) ;
#187941 = CARTESIAN_POINT ( 'NONE',  ( 16.46253265017160672, -9.564922557960803928, 108.3322429386476955 ) ) ;
#187942 = CARTESIAN_POINT ( 'NONE',  ( 8.224510206698953496, -14.34966873604960469, 57.91557627198103120 ) ) ;
#187943 = CARTESIAN_POINT ( 'NONE',  ( -9.474510206698964154, 16.51473224551069663, 30.41557627198102054 ) ) ;
#187944 = CARTESIAN_POINT ( 'NONE',  ( -8.224510206698948167, 14.34966873604960824, 90.41557627198103830 ) ) ;
#187945 = CARTESIAN_POINT ( 'NONE',  ( -5.719274019375978568, 21.55341960407610458, 90.20724293864770971 ) ) ;
#187946 = CARTESIAN_POINT ( 'NONE',  ( 15.80617190586769283, -15.72974639402175789, 40.62609039468567573 ) ) ;
#187947 = CARTESIAN_POINT ( 'NONE',  ( 11.30153831258470731, -180.0000000000000000, 0.000000000000000000 ) ) ;
#187948 = EDGE_CURVE ( 'NONE', #127622, #63455, #43099, .T. ) ;
#187949 = CARTESIAN_POINT ( 'NONE',  ( -16.53943276465976808, -0.05219959533934237506, 38.75109039468567573 ) ) ;
#187950 = CARTESIAN_POINT ( 'NONE',  ( 18.67979575497178502, 10.72451020669898547, 79.16557627198103830 ) ) ;
#187951 = CARTESIAN_POINT ( 'NONE',  ( 21.55341960407619695, -5.719274019375665929, 111.0427570613523613 ) ) ;
#187952 = CARTESIAN_POINT ( 'NONE',  ( 16.51473224551069308, 9.474510206698969483, 89.16557627198103830 ) ) ;
#187953 = CARTESIAN_POINT ( 'NONE',  ( 18.67979575497194134, -10.72451020669871369, 45.83442372801901854 ) ) ;
#187954 = CARTESIAN_POINT ( 'NONE',  ( -15.72974639402197994, 15.80617190586746368, 30.62390960531436335 ) ) ;
#187955 = CARTESIAN_POINT ( 'NONE',  ( -16.55341960407617563, 4.379528057220093196, 108.5427570613523756 ) ) ;
#187957 = CARTESIAN_POINT ( 'NONE',  ( 0.05219959533937995610, -21.53943276465977519, 85.00109039468568994 ) ) ;
#187956 = CARTESIAN_POINT ( 'NONE',  ( 0.05219959533937995610, -21.53943276465977519, 50.00109039468568994 ) ) ;
#187958 = CARTESIAN_POINT ( 'NONE',  ( 13.89961937509957401, 13.97604488694547697, 31.87609039468566863 ) ) ;
#187959 = CARTESIAN_POINT ( 'NONE',  ( -16.55341960407617563, 4.379528057220093196, 88.54275706135236135 ) ) ;
#187960 = CARTESIAN_POINT ( 'NONE',  ( -0.05219959533937732626, 21.53943276465977519, 42.50109039468567573 ) ) ;
#187961 = CARTESIAN_POINT ( 'NONE',  ( -13.97604488694527625, -13.89961937509977652, 41.87390960531435979 ) ) ;
#187962 = CARTESIAN_POINT ( 'NONE',  ( -0.05219959533937732626, 21.53943276465977519, 102.5010903946856899 ) ) ;
#187963 = CARTESIAN_POINT ( 'NONE',  ( -19.05341960407611168, -5.049401038298163336, 101.4572429386476955 ) ) ;
#187964 = CARTESIAN_POINT ( 'NONE',  ( 21.52544592524344225, -5.823673210054117533, 113.5405762719810383 ) ) ;
#187965 = CARTESIAN_POINT ( 'NONE',  ( 10.81492255796078972, 18.62759615963270932, 74.58224293864768129 ) ) ;
#187967 = CARTESIAN_POINT ( 'NONE',  ( 5.719274019375991003, -21.55341960407610458, 67.70724293864769550 ) ) ;
#187966 = CARTESIAN_POINT ( 'NONE',  ( -17.60779699588839975, -5.500000000000020428, 61.34981316670106821 ) ) ;
#187969 = CARTESIAN_POINT ( 'NONE',  ( -8.314922557960811034, -14.29746914071050412, 57.08224293864769550 ) ) ;
#187968 = CARTESIAN_POINT ( 'NONE',  ( -14.29746914071037622, -8.314922557961029526, 49.16775706135234003 ) ) ;
#187970 = CARTESIAN_POINT ( 'NONE',  ( 17.79613651744294245, -24.49428055684527550, 146.9656553485623931 ) ) ;
#187971 = CARTESIAN_POINT ( 'NONE',  ( -13.89961937509957401, -13.97604488694547875, 84.37609039468567573 ) ) ;
#187972 = CARTESIAN_POINT ( 'NONE',  ( -21.94965239947789826, 1.250870343808954788, -55.99511580764671237 ) ) ;
#187973 = CARTESIAN_POINT ( 'NONE',  ( 16.53943276465976808, 0.05219959533934440121, 31.25109039468568639 ) ) ;
#187974 = CARTESIAN_POINT ( 'NONE',  ( 10.72451020669898902, -18.67979575497178502, 92.91557627198103830 ) ) ;
#187975 = CARTESIAN_POINT ( 'NONE',  ( 21.53943276465977519, -0.05219959533907433946, 68.74890960531435269 ) ) ;
#187976 = CARTESIAN_POINT ( 'NONE',  ( 19.03943276465977164, -0.05219959533909143690, 108.7489096053143527 ) ) ;
#187977 = CARTESIAN_POINT ( 'NONE',  ( -14.34966873604972548, 8.224510206698743886, 53.33442372801901854 ) ) ;
#187978 = CARTESIAN_POINT ( 'NONE',  ( -13.89961937509977652, 13.97604488694528158, 70.62390960531432427 ) ) ;
#187980 = CARTESIAN_POINT ( 'NONE',  ( -16.51473224551082808, 9.474510206698731452, 113.3344237280190043 ) ) ;
#187979 = CARTESIAN_POINT ( 'NONE',  ( -21.53943276465977519, -0.05219959533937600094, 48.75109039468568284 ) ) ;
#187981 = CARTESIAN_POINT ( 'NONE',  ( 16.46253265017160672, -9.564922557960803928, 108.3322429386476955 ) ) ;
#187982 = CARTESIAN_POINT ( 'NONE',  ( -9.474510206698964154, 16.51473224551069663, 100.4155762719810241 ) ) ;
#187983 = CARTESIAN_POINT ( 'NONE',  ( 15.72974639402199770, -15.80617190586745480, 98.12390960531436690 ) ) ;
#187984 = CARTESIAN_POINT ( 'NONE',  ( 19.03943276465977164, -0.05219959533909143690, 53.74890960531436690 ) ) ;
#187985 = CARTESIAN_POINT ( 'NONE',  ( -17.50000000000000000, 5.499999999999992895, 23.71769037696436300 ) ) ;
#187986 = CARTESIAN_POINT ( 'NONE',  ( -16.53943276465976808, 0.05219959533911058130, 76.24890960531435269 ) ) ;
#187987 = CARTESIAN_POINT ( 'NONE',  ( 21.53943276465977519, -0.05219959533907433946, 23.74890960531435269 ) ) ;
#187988 = DIRECTION ( 'NONE',  ( -0.7071067811865312525, 8.659560562355131306E-17, -0.7071067811865637820 ) ) ;
#187989 = CARTESIAN_POINT ( 'NONE',  ( -21.55341960407610458, -5.719274019375992779, 101.4572429386476955 ) ) ;
#187990 = CARTESIAN_POINT ( 'NONE',  ( 19.05341960407617918, -5.049401038297876454, 61.04275706135232582 ) ) ;
#187991 = CARTESIAN_POINT ( 'NONE',  ( 10.81492255796078972, 18.62759615963270932, 24.58224293864768839 ) ) ;
#187992 = CARTESIAN_POINT ( 'NONE',  ( 19.03943276465977164, -0.05219959533909143690, 28.74890960531435624 ) ) ;
#187993 = CARTESIAN_POINT ( 'NONE',  ( 10.81492255796078972, 18.62759615963270932, 49.58224293864769550 ) ) ;
#187994 = CARTESIAN_POINT ( 'NONE',  ( -13.97604488694527625, -13.89961937509977652, 101.8739096053143811 ) ) ;
#187995 = CARTESIAN_POINT ( 'NONE',  ( -15.72974639402176322, -15.80617190586768395, 79.37609039468567573 ) ) ;
#187996 = CARTESIAN_POINT ( 'NONE',  ( -9.474510206698964154, 16.51473224551069663, 45.41557627198103120 ) ) ;
#187997 = CARTESIAN_POINT ( 'NONE',  ( -8.314922557960811034, -14.29746914071050412, 92.08224293864769550 ) ) ;
#187998 = CARTESIAN_POINT ( 'NONE',  ( -8.224510206698735004, -14.34966873604973081, 39.58442372801901143 ) ) ;
#187999 = CARTESIAN_POINT ( 'NONE',  ( -5.719274019375665041, -21.55341960407619695, 69.79275706135234714 ) ) ;
#188000 = ORIENTED_EDGE ( 'NONE', *, *, #165982, .T. ) ;
#188001 = CARTESIAN_POINT ( 'NONE',  ( 13.89961937509957401, 13.97604488694547697, 26.87609039468566507 ) ) ;
#188002 = CARTESIAN_POINT ( 'NONE',  ( 9.564922557961047289, -16.46253265017146816, 85.41775706135233293 ) ) ;
#188003 = CARTESIAN_POINT ( 'NONE',  ( 16.46253265017146816, 9.564922557961045513, 36.66775706135233293 ) ) ;
#188004 = DIRECTION ( 'NONE',  ( 0.000000000000000000, 0.000000000000000000, -1.000000000000000000 ) ) ;
#188005 = CARTESIAN_POINT ( 'NONE',  ( -21.55341960407619339, 5.719274019375674811, 33.54275706135234714 ) ) ;
#188006 = CARTESIAN_POINT ( 'NONE',  ( -11.74264578624800670, 36.14014761921585972, -2.149999994537626691 ) ) ;
#188007 = CARTESIAN_POINT ( 'NONE',  ( 13.89961937509957401, 13.97604488694547697, 36.87609039468565442 ) ) ;
#188008 = CARTESIAN_POINT ( 'NONE',  ( 9.564922557960805705, 16.46253265017160317, 74.58224293864769550 ) ) ;
#188009 = CARTESIAN_POINT ( 'NONE',  ( 13.97604488694548053, -13.89961937509957401, 25.62609039468566507 ) ) ;
#188010 = CARTESIAN_POINT ( 'NONE',  ( -12.14591786802326823, 12.06949235617739902, 113.1260903946856899 ) ) ;
#188012 = CARTESIAN_POINT ( 'NONE',  ( 21.53943276465977519, 0.05219959533937863772, 81.25109039468568994 ) ) ;
#188011 = CARTESIAN_POINT ( 'NONE',  ( 21.52544592524344225, -5.823673210054117533, 23.54057627198102765 ) ) ;
#188013 = CARTESIAN_POINT ( 'NONE',  ( -36.91746825000001309, -11.99521256947794789, -8.524999997268812635 ) ) ;
#188014 = CARTESIAN_POINT ( 'NONE',  ( -33.76801240946108607, 5.498839508946046450, 94.61983786177950151 ) ) ;
#188015 = CARTESIAN_POINT ( 'NONE',  ( -15.72974639402176322, -15.80617190586768395, 79.37609039468567573 ) ) ;
#188016 = CARTESIAN_POINT ( 'NONE',  ( 16.38665767535054485, -7.295008042176021945, 42.76400864214548392 ) ) ;
#188017 = CARTESIAN_POINT ( 'NONE',  ( -9.474510206698964154, 16.51473224551069663, 100.4155762719810241 ) ) ;
#188018 = FACE_OUTER_BOUND ( 'NONE', #173150, .T. ) ;
#188019 = CARTESIAN_POINT ( 'NONE',  ( -16.51473224551069308, -9.474510206698971260, 46.66557627198102409 ) ) ;
#188020 = CARTESIAN_POINT ( 'NONE',  ( 10.72451020669898902, -18.67979575497178502, 62.91557627198102409 ) ) ;
#188021 = CARTESIAN_POINT ( 'NONE',  ( 12.06949235617757843, -12.14591786802309237, 23.12390960531436335 ) ) ;
#188023 = CARTESIAN_POINT ( 'NONE',  ( 16.46253265017160672, -9.564922557960803928, 98.33224293864769550 ) ) ;
#188022 = CARTESIAN_POINT ( 'NONE',  ( 12.06949235617757843, -12.14591786802309237, 103.1239096053143811 ) ) ;
#188024 = CARTESIAN_POINT ( 'NONE',  ( 5.049401038297881783, 19.05341960407617563, 22.29275706135233648 ) ) ;
#188025 = CARTESIAN_POINT ( 'NONE',  ( -14.29746914071049879, 8.314922557960819915, 95.83224293864770971 ) ) ;
#188026 = CARTESIAN_POINT ( 'NONE',  ( 21.52544592524334988, 5.823673210054432836, 61.45942372801901854 ) ) ;
#188027 = CARTESIAN_POINT ( 'NONE',  ( 69.65682714487590488, -71.74905178543389184, -15.00000000000000000 ) ) ;
#188028 = CARTESIAN_POINT ( 'NONE',  ( 14.29746914071037800, 8.314922557961029526, 111.6677570613523613 ) ) ;
#188029 = CARTESIAN_POINT ( 'NONE',  ( 9.564922557961047289, -16.46253265017146816, 70.41775706135233293 ) ) ;
#188030 = CARTESIAN_POINT ( 'NONE',  ( -27.86273085795037474, -28.69962071417356242, -4.999999999999999112 ) ) ;
#188031 = CARTESIAN_POINT ( 'NONE',  ( -13.89961937509977652, 13.97604488694528158, 115.6239096053143669 ) ) ;
#188032 = CARTESIAN_POINT ( 'NONE',  ( -8.224510206698948167, 14.34966873604960824, 80.41557627198103830 ) ) ;
#188033 = CARTESIAN_POINT ( 'NONE',  ( 13.89961937509957401, 13.97604488694547697, 61.87609039468566863 ) ) ;
#188034 = CARTESIAN_POINT ( 'NONE',  ( -5.153800228976328057, -19.02544592524343514, 57.29057627198103120 ) ) ;
#188035 = CARTESIAN_POINT ( 'NONE',  ( -8.224510206698948167, 14.34966873604960824, 55.41557627198102409 ) ) ;
#188036 = CARTESIAN_POINT ( 'NONE',  ( 0.05219959533936267826, -19.03943276465977164, 90.00109039468567573 ) ) ;
#188037 = CARTESIAN_POINT ( 'NONE',  ( 0.05219959533907565091, 21.53943276465977519, 34.99890960531435979 ) ) ;
#188038 = ORIENTED_EDGE ( 'NONE', *, *, #49302, .F. ) ;
#188039 = CARTESIAN_POINT ( 'NONE',  ( -4.483927247898539470, -16.52544592524342804, 97.29057627198105251 ) ) ;
#188040 = CARTESIAN_POINT ( 'NONE',  ( -3.573655867282028392E-15, 2.428612866367529932E-14, 169.9999999999999716 ) ) ;
#188042 = CARTESIAN_POINT ( 'NONE',  ( -10.81492255796078084, -18.62759615963271287, 57.08224293864769550 ) ) ;
#188041 = CARTESIAN_POINT ( 'NONE',  ( 13.89961937509977652, -13.97604488694527269, 63.12390960531435979 ) ) ;
#188043 = CARTESIAN_POINT ( 'NONE',  ( -19.02544592524342804, 5.153800228976336051, 41.04057627198103120 ) ) ;
#188045 = CARTESIAN_POINT ( 'NONE',  ( -19.02544592524342804, 5.153800228976336051, 71.04057627198099567 ) ) ;
#188044 = CARTESIAN_POINT ( 'NONE',  ( -8.314922557961024197, 14.29746914071037800, 92.91775706135236135 ) ) ;
#188046 = CARTESIAN_POINT ( 'NONE',  ( -19.05341960407617563, 5.049401038297882671, 53.54275706135231871 ) ) ;
#188047 = CARTESIAN_POINT ( 'NONE',  ( 18.62759615963255655, 10.81492255796105972, 81.66775706135236135 ) ) ;
#188048 = CARTESIAN_POINT ( 'NONE',  ( 10.72451020669898902, -18.67979575497178502, 47.91557627198102409 ) ) ;
#188049 = CARTESIAN_POINT ( 'NONE',  ( -19.03943276465977164, 0.05219959533909376836, 106.2489096053143669 ) ) ;
#188050 = CARTESIAN_POINT ( 'NONE',  ( 13.97604488694527802, 13.89961937509977652, 39.37390960531435269 ) ) ;
#188051 = CARTESIAN_POINT ( 'NONE',  ( 8.314922557961029526, -14.29746914071037800, 85.41775706135236135 ) ) ;
#188052 = CARTESIAN_POINT ( 'NONE',  ( 16.51473224551083163, -9.474510206698727899, 105.8344237280190043 ) ) ;
#188053 = CARTESIAN_POINT ( 'NONE',  ( -5.153800228976328057, -19.02544592524343514, 22.29057627198102765 ) ) ;
#188054 = CARTESIAN_POINT ( 'NONE',  ( 19.52851543214743302, 5.500000000000029310, 77.89357721762580411 ) ) ;
#188055 = CARTESIAN_POINT ( 'NONE',  ( 21.55341960407619695, -5.719274019375665929, 96.04275706135236135 ) ) ;
#188056 = CARTESIAN_POINT ( 'NONE',  ( 16.53943276465976808, -0.05219959533910856209, 58.74890960531436690 ) ) ;
#188057 = CARTESIAN_POINT ( 'NONE',  ( -16.53943276465976808, 0.05219959533911058130, 76.24890960531435269 ) ) ;
#188058 = CARTESIAN_POINT ( 'NONE',  ( 5.823673210054125526, 21.52544592524343514, 94.79057627198105251 ) ) ;
#188059 = CARTESIAN_POINT ( 'NONE',  ( 21.52544592524344225, -5.823673210054117533, 83.54057627198102409 ) ) ;
#188060 = CARTESIAN_POINT ( 'NONE',  ( -28.79475375365586842, 2.428612866367529932E-14, 145.9843446568999923 ) ) ;
#188061 = CARTESIAN_POINT ( 'NONE',  ( 21.55341960407610458, 5.719274019375980345, 43.95724293864769550 ) ) ;
#188062 = CARTESIAN_POINT ( 'NONE',  ( 12.14591786802327356, -12.06949235617739191, 60.62609039468567573 ) ) ;
#188063 = CARTESIAN_POINT ( 'NONE',  ( 12.06949235617757843, -12.14591786802309237, 88.12390960531436690 ) ) ;
#188064 = CARTESIAN_POINT ( 'NONE',  ( 13.97604488694527802, 13.89961937509977652, 49.37390960531434558 ) ) ;
#188065 =( NAMED_UNIT ( * ) PLANE_ANGLE_UNIT ( ) SI_UNIT ( $, .RADIAN. ) );
#188066 = CARTESIAN_POINT ( 'NONE',  ( 35.50125023021172410, -3.320518091344034417, 38.27062242752713672 ) ) ;
#188067 = CARTESIAN_POINT ( 'NONE',  ( 4.379528057220092307, 16.55341960407617563, 97.29275706135234714 ) ) ;
#188068 = CARTESIAN_POINT ( 'NONE',  ( -18.62759615963255300, -10.81492255796106328, 29.16775706135234003 ) ) ;
#188069 = CARTESIAN_POINT ( 'NONE',  ( 5.153800228976335163, 19.02544592524342804, 84.79057627198099567 ) ) ;
#188070 = CARTESIAN_POINT ( 'NONE',  ( -0.05219959533937732626, 21.53943276465977519, 72.50109039468568994 ) ) ;
#188071 = DIRECTION ( 'NONE',  ( -0.1045284632676537068, 0.000000000000000000, 0.9945218953682734009 ) ) ;
#188072 = CARTESIAN_POINT ( 'NONE',  ( 9.564922557960805705, 16.46253265017160317, 24.58224293864769194 ) ) ;
#188073 = ORIENTED_EDGE ( 'NONE', *, *, #178304, .F. ) ;
#188074 = CARTESIAN_POINT ( 'NONE',  ( 21.52544592524334988, 5.823673210054432836, 61.45942372801901854 ) ) ;
#188076 = CARTESIAN_POINT ( 'NONE',  ( -5.153800228976328057, -19.02544592524343514, 112.2905762719810099 ) ) ;
#188075 = CARTESIAN_POINT ( 'NONE',  ( -9.564922557960796823, -16.46253265017161027, 32.08224293864769550 ) ) ;
#188077 = CARTESIAN_POINT ( 'NONE',  ( 19.03943276465977164, -0.05219959533909143690, 93.74890960531435269 ) ) ;
#188078 = CARTESIAN_POINT ( 'NONE',  ( 5.049401038297881783, 19.05341960407617563, 72.29275706135234714 ) ) ;
#188079 = CARTESIAN_POINT ( 'NONE',  ( 21.52544592524334988, 5.823673210054432836, 26.45942372801901854 ) ) ;
#188080 = CARTESIAN_POINT ( 'NONE',  ( -0.05219959533936034679, 19.03943276465977164, 62.50109039468566863 ) ) ;
#188081 = CARTESIAN_POINT ( 'NONE',  ( -9.474510206698964154, 16.51473224551069663, 40.41557627198103120 ) ) ;
#188082 = CARTESIAN_POINT ( 'NONE',  ( -14.34966873604972548, 8.224510206698743886, 98.33442372801901854 ) ) ;
#188083 = CARTESIAN_POINT ( 'NONE',  ( 13.97604488694548053, -13.89961937509957401, 75.62609039468564731 ) ) ;
#188084 = CARTESIAN_POINT ( 'NONE',  ( 0.05219959533910956823, 16.53943276465976808, 24.99890960531435624 ) ) ;
#188085 = CARTESIAN_POINT ( 'NONE',  ( 5.153800228976615827, -19.02544592524334988, 55.20942372801899722 ) ) ;
#188086 = CARTESIAN_POINT ( 'NONE',  ( -0.05219959533909027116, -19.03943276465977164, 97.49890960531436690 ) ) ;
#188087 = CARTESIAN_POINT ( 'NONE',  ( 10.81492255796106328, -18.62759615963255655, 110.4177570613523756 ) ) ;
#188088 = CARTESIAN_POINT ( 'NONE',  ( 21.55341960407619695, -5.719274019375665929, 111.0427570613523613 ) ) ;
#188089 = CARTESIAN_POINT ( 'NONE',  ( -3.573655867282028392E-15, 2.428612866367529932E-14, -25.00000000000000000 ) ) ;
#188090 = CARTESIAN_POINT ( 'NONE',  ( 10.81492255796106328, -18.62759615963255655, 85.41775706135236135 ) ) ;
#188091 = CARTESIAN_POINT ( 'NONE',  ( 4.379528057220092307, 16.55341960407617563, 27.29275706135234358 ) ) ;
#188092 = CARTESIAN_POINT ( 'NONE',  ( -16.51473224551069308, -9.474510206698971260, 91.66557627198103830 ) ) ;
#188093 = CARTESIAN_POINT ( 'NONE',  ( -38.00000000000000711, -12.34694845685042708, -9.649999994537626691 ) ) ;
#188094 = CARTESIAN_POINT ( 'NONE',  ( 5.049401038298161559, -19.05341960407611168, 77.70724293864765286 ) ) ;
#188095 = CARTESIAN_POINT ( 'NONE',  ( 31.99364916731008179, -5.510910596142776387E-15, 42.35000000000022169 ) ) ;
#188096 = CARTESIAN_POINT ( 'NONE',  ( 9.564922557961047289, -16.46253265017146816, 75.41775706135234714 ) ) ;
#188097 = CARTESIAN_POINT ( 'NONE',  ( -19.02544592524342804, 5.153800228976336051, 106.0405762719810241 ) ) ;
#188098 = CARTESIAN_POINT ( 'NONE',  ( 15.80617190586769283, -15.72974639402175789, 95.62609039468568994 ) ) ;
#188099 = CARTESIAN_POINT ( 'NONE',  ( 12.06949235617757843, -12.14591786802309237, 98.12390960531436690 ) ) ;
#188100 = CARTESIAN_POINT ( 'NONE',  ( -5.823673210054116645, -21.52544592524344225, 42.29057627198103120 ) ) ;
#188101 = CARTESIAN_POINT ( 'NONE',  ( -15.80617190586745835, -15.72974639402198527, 36.87390960531435979 ) ) ;
#188102 = CARTESIAN_POINT ( 'NONE',  ( -12.14591786802309592, -12.06949235617757132, 101.8739096053143811 ) ) ;
#188103 = CARTESIAN_POINT ( 'NONE',  ( -3.181980515339104532, 35.00000000000003553, 8.889087296526001936 ) ) ;
#188104 = CARTESIAN_POINT ( 'NONE',  ( -19.05341960407617563, 5.049401038297882671, 53.54275706135231871 ) ) ;
#188105 = CARTESIAN_POINT ( 'NONE',  ( 0.05219959533910956823, 16.53943276465976808, 24.99890960531435624 ) ) ;
#188107 = EDGE_CURVE ( 'NONE', #92192, #38777, #108737, .T. ) ;
#188106 = CARTESIAN_POINT ( 'NONE',  ( 16.46253265017160672, -9.564922557960803928, 98.33224293864769550 ) ) ;
#188108 = CARTESIAN_POINT ( 'NONE',  ( 5.719274019375673035, 21.55341960407619339, 82.29275706135234714 ) ) ;
#188109 = CARTESIAN_POINT ( 'NONE',  ( 21.53943276465977519, -0.05219959533907433946, 68.74890960531435269 ) ) ;
#188110 = CARTESIAN_POINT ( 'NONE',  ( 21.52544592524334988, 5.823673210054432836, 46.45942372801901854 ) ) ;
#188111 = CARTESIAN_POINT ( 'NONE',  ( -18.62759615963270932, 10.81492255796079327, 100.8322429386477097 ) ) ;
#188112 = CARTESIAN_POINT ( 'NONE',  ( -18.67979575497193778, 10.72451020669871902, 48.33442372801902565 ) ) ;
#188113 = CARTESIAN_POINT ( 'NONE',  ( -5.049401038298153566, 19.05341960407611168, 25.20724293864768484 ) ) ;
#188114 = CARTESIAN_POINT ( 'NONE',  ( -16.46253265017160317, 9.564922557960807481, 80.83224293864769550 ) ) ;
#188115 = CARTESIAN_POINT ( 'NONE',  ( -16.52544592524335698, -4.483927247898792601, 78.95942372801901854 ) ) ;
#188116 =( BOUNDED_SURFACE ( )  B_SPLINE_SURFACE ( 3, 2, ( 
 ( #170942, #94088, #102572, #133909, #195600, #57073, #140595, #190098, #52565, #128401, #99060, #35409, #129394, #3082, #33428, #4063, #65741, #51573, #113237, #114225, #110258, #112250, #173942, #97061, #50591, #98045, #21239, #191090, #142584, #127409, #175930, #158743, #78918, #143572, #37401, #2085, #20232, #81880, #17265, #63765, #48606, #189118, #159743, #125438, #66740, #187134, #171939, #5054, #95087, #174928, #36391, #156775, #18269, #79922, #82894, #144572, #141595, #64758, #6058, #67736, #126420, #188118, #49589, #111252, #172943, #34422, #96081, #157770, #19261, #80907, #117245, #133410, #132416, #41413, #193095, #192086, #195099, #85905, #25263, #55571, #23245, #176938, #54571, #164760, #180937, #84889, #11080, #196113, #56581, #119253, #145572, #70748, #9078, #86906, #53568, #10081, #131408, #26255, #7049, #68731, #147593, #42412, #102078, #160748, #22240, #87896, #8062, #149582, #194108, #163763, #148589, #57583, #71739, #118255, #116243, #103079, #39402, #179946, #83889, #72756, #134427, #177935, #178937, #130389, #115246, #38408, #162747, #100065, #146568, #161750, #40407, #69739, #101062, #24255, #74736, #89897, #28258, #166755, #151580, #62522, #61530, #169716, #183900, #120229, #31209, #73753, #92860, #60533, #106050, #167736, #13069, #43400, #107038, #90867, #154547, #849, #135425, #182911, #104075, #75706, #59543, #136399, #137385, #44396, #45385, #181919, #124195, #27251, #29234, #16042, #152552, #30212, #185895, #165757, #88901, #108030, #150591, #168710, #122209, #14040, #91855, #123199, #12090, #197096, #46371, #153547, #199064, #58563, #105070, #15044, #198076, #76705, #138381, #200062, #121221, #184889, #77701, #139368, #82654, #172707, #113004, #65511, #36162, #173711, #93862, #174698, #19030, #2850, #18039, #79693, #64528, #141363, #125209, #158518, #80676, #126195, #48376, #97814, #155540, #32205, #17034, #95852, #81649, #51344, #188882, #67502, #34191, #142352, #4820, #140365, #187891, #186905, #110033, #109035, #143333, #170714, #127172, #96834, #171711, #33201, #66508, #128170, #49358, #157536, #3832, #94859, #63534, #1852, #50363, #111021, #189870, #20006, #159503, #20999, #112022, #5826, #156540, #78688, #144338, #129159, #47380, #35179, #8841, #102842, #176703, #6819, #177701, #39168, #101837, #25023, #26021, #83659, #85666, #147353, #70509, #24010, #71505, #194863, #164528, #116011, #100826, #87665, #132177, #52333, #117004, #149350, #113990, #193868, #55334, #72516, #175688, #22007, #162509, #133173, #37163, #40161, #10847, #145337, #98822, #56336, #192861, #178699, #190856, #69505, #160516, #163524, #86667, #68497, #130152, #191849, #148350, #53330, #9846, #118018, #115009, #38177, #99833, #179707, #41179, #161517, #23009, #84655, #146332, #7821, #131171, #54340, #121983, #90647, #30978, #195878, #182681, #58335, #74507, #152329, #106814, #105825, #14814, #166527, #165526, #168488, #59314, #198843, #29008, #196869, #150363, #28024, #138152, #154316, #120003, #184657, #169477, #29986, #92625, #119026, #44166, #167512, #60307, #27022, #183673, #104837, #199833, #180709, #42185, #120983, #15805, #75481, #134191, #57351, #61300, #181689, #122970, #13815, #137154, #45158, #103845, #91625, #153313, #89666, #76475, #12841, #46139, #88667, #107793, #11859, #151352, #73524, #135195, #43170, #136173, #197848, #81414, #140122, #158284, #64292, #189633, #159263, #157297, #48136, #63289, #1613, #124969, #186666, #35929, #34943, #143100, #18794, #93624, #4579, #47141, #66272, #33954, #79456, #141125, #109793, #16798, #80439, #125959, #127931, #174460, #108799, #156298, #77466, #49128, #32965, #171476, #110786, #17799, #142112, #155309, #97575, #613, #187657, #19773, #139136, #126935, #62283, #170478, #185649, #51108, #2615, #172467, #123951, #112767, #31968, #3597, #95612, #65276, #188643, #96595, #78448, #94619, #50122, #111782, #173470, #20759, #175450, #161274 ),
 ( #9610, #71275, #8602, #177466, #117779, #82414, #69264, #145096, #22769, #38935, #193627, #192621, #101596, #53088, #52097, #55099, #146094, #85424, #115777, #83419, #36921, #114766, #24785, #40938, #6579, #132940, #56098, #116769, #179473, #5583, #130930, #54103, #147115, #113754, #70275, #191609, #86433, #67263, #128921, #7578, #102610, #162274, #144103, #190622, #148119, #68258, #194628, #100592, #23774, #131943, #98583, #178460, #39927, #176460, #163284, #99594, #160277, #21768, #129909, #37933, #84417, #182442, #167270, #133949, #60069, #166288, #168247, #26782, #44914, #151115, #76227, #45899, #43922, #134957, #150118, #88424, #11619, #73287, #122728, #121737, #29743, #105584, #180476, #91378, #195640, #153067, #120743, #27784, #89426, #59076, #196635, #41947, #58104, #14569, #184419, #119774, #137907, #199589, #183429, #164296, #149120, #74271, #12607, #28769, #57113, #13576, #181458, #61056, #10611, #72272, #135941, #25789, #90407, #87435, #118787, #103613, #42936, #165289, #197611, #152092, #75243, #104600, #136914, #198601, #106570, #188395, #186420, #48885, #107552, #126691, #19534, #139875, #125718, #110540, #77223, #3360, #109550, #111538, #170235, #49873, #94372, #81179, #189392, #187417, #78205, #93377, #31729, #155063, #16558, #66025, #65035, #173223, #172221, #123709, #34699, #138892, #96356, #64048, #171231, #32720, #1364, #46897, #33706, #156052, #158044, #4340, #372, #47896, #169230, #79209, #63043, #124722, #140878, #17549, #95368, #185406, #127692, #30737, #2368, #142861, #157053, #18550, #92384, #154071, #15565, #80198, #108557, #141869, #62044, #190379, #9365, #50869, #8354, #162031, #71030, #147879, #161031, #178217, #37683, #39681, #101343, #38696, #7334, #132697, #112527, #99348, #175208, #191366, #69019, #23527, #22525, #131698, #83180, #82164, #85173, #176214, #115535, #20516, #146862, #52843, #54855, #113514, #193379, #84172, #163032, #174221, #130684, #21519, #36673, #98333, #160032, #144854, #35690, #70029, #116529, #192378, #67023, #24539, #143860, #86189, #53861, #114513, #145852, #6337, #51854, #177223, #100352, #97337, #159023, #5339, #129669, #128682, #68017, #149863, #41699, #27538, #134710, #135699, #72022, #152828, #117527, #73038, #106323, #42693, #120502, #14322, #55853, #75987, #58835, #133695, #74028, #119534, #195387, #194386, #179225, #151848, #105340, #40691, #91139, #104354, #121494, #181217, #183188, #44670, #182193, #150871, #102361, #164050, #166038, #118540, #196393, #12365, #167027, #89179, #75003, #26535, #25549, #28529, #197370, #43678, #90165, #56865, #10365, #88179, #198350, #87193, #180230, #168009, #29505, #13339, #148874, #103364, #136668, #59824, #165042, #11368, #57862, #108312, #141638, #184177, #122486, #124479, #19303, #78965, #137660, #199347, #3128, #185162, #64803, #186175, #140640, #2130, #34465, #125484, #110303, #93135, #18313, #16318, #63811, #60812, #156821, #49635, #169992, #155812, #187180, #15320, #48651, #170987, #31483, #138650, #126464, #45659, #107310, #168983, #47657, #171985, #188162, #33473, #157813, #109308, #32480, #95131, #30487, #154820, #76979, #131, #92138, #79970, #153825, #17310, #111298, #61800, #123470, #172987, #96124, #77968, #94133, #46653, #139635, #1123, #62797, #163550, #162534, #179736, #56363, #10871, #134218, #25050, #42210, #81921, #4105, #118046, #119052, #194889, #165551, #101867, #195904, #69534, #97103, #70535, #132204, #41206, #102867, #180734, #173983, #178725, #40187, #86693, #117030, #164552, #87690, #57379, #8868, #193895, #103870, #148377, #142626, #9872, #80951, #65784, #71532, #133198, #127453, #189159, #112293, #55360, #26045, #50632, #149375, #35452, #158787, #20275, #72541, #85693, #146360, #7847, #131198, #192888, #54366, #116038, #177727, #39196, #100852, #24038, #147379, #169507, #153342, #75508, #27048, #181713, #167539, #135222, #168517, #138182, #198869, #88694, #30015 ),
 ( #197873, #44193, #59340, #185681, #150390, #184686, #199865, #47171, #123983, #137181, #154344, #13841, #15837, #77496, #14843, #183701, #108830, #11886, #60336, #151377, #29034, #45188, #61329, #122010, #107823, #121010, #58361, #123000, #152356, #91653, #106842, #89692, #43195, #182708, #31006, #73549, #12868, #139166, #62313, #46169, #196894, #120028, #76506, #92655, #643, #104863, #166552, #105852, #28051, #74533, #136198, #90674, #52132, #111815, #170509, #32000, #174494, #17832, #35961, #18827, #173503, #34976, #67297, #158317, #143132, #125992, #51140, #49160, #96629, #93657, #189667, #82448, #2648, #188676, #19805, #140155, #66304, #172501, #97608, #32998, #112801, #157332, #144136, #155342, #50156, #141159, #156332, #94652, #79490, #64325, #128956, #127964, #159296, #81446, #186698, #20793, #1647, #5618, #126967, #33988, #95644, #187690, #109826, #4612, #16831, #190656, #78482, #63325, #125003, #80472, #65308, #48169, #171509, #110818, #142145, #3629, #38971, #178496, #71312, #36956, #160312, #56134, #39962, #162309, #113789, #68294, #54138, #21802, #55134, #24820, #85460, #117816, #101633, #23809, #175484, #129945, #115812, #83454, #116804, #86469, #147149, #98618, #163324, #148154, #9646, #149157, #100628, #179509, #131978, #102646, #132975, #145132, #40977, #8637, #69299, #84451, #146129, #130965, #7614, #191644, #194665, #70309, #192655, #114802, #164331, #6615, #53124, #176495, #193663, #25825, #87470, #10647, #133986, #72308, #195677, #37971, #99629, #177502, #161311, #22805, #118825, #91417, #180510, #75281, #106609, #181494, #42972, #76264, #137942, #12642, #105622, #167310, #196672, #73322, #150155, #136951, #135976, #153104, #29781, #184455, #107590, #198640, #15601, #58141, #41983, #14608, #92421, #168284, #138928, #60106, #169268, #104635, #134993, #43960, #28806, #199626, #61093, #154107, #11656, #152131, #13614, #121774, #90446, #122766, #45935, #30774, #182479, #183467, #77259, #44953, #103649, #57148, #165327, #26819, #88459, #119809, #166324, #27821, #89463, #151152, #74309, #197647, #59113, #120778, #173259, #170270, #66061, #2405, #95404, #159059, #4377, #62080, #3395, #157090, #125753, #65070, #158079, #123745, #46934, #139912, #16593, #93413, #80233, #79247, #96392, #34734, #127728, #50905, #141904, #20553, #1403, #185444, #19570, #35726, #111575, #82203, #18586, #112563, #186457, #78241, #187453, #48921, #81214, #142895, #97373, #155099, #126728, #188431, #49909, #33744, #189430, #174258, #408, #110575, #172256, #108593, #31764, #63082, #124761, #47933, #109587, #171270, #32758, #94409, #156090, #17587, #140918, #64084, #5376, #67060, #39715, #116565, #113550, #9399, #145888, #38731, #102397, #147913, #128718, #146901, #100389, #69056, #8391, #101378, #190415, #51891, #86223, #70066, #192415, #143895, #98371, #84208, #175244, #85211, #54891, #115572, #36709, #131734, #193416, #163069, #179262, #130723, #71065, #162067, #132731, #178254, #160069, #194419, #177259, #99384, #114553, #176251, #161067, #37722, #21556, #24574, #23563, #22562, #144891, #55889, #83216, #6373, #68053, #53897, #117562, #40727, #164084, #25583, #129707, #191403, #52880, #7371, #57897, #165076, #26570, #148909, #121530, #10399, #105377, #136705, #11404, #73073, #106360, #168044, #42729, #135735, #197406, #183225, #91174, #28565, #107345, #74064, #120538, #44706, #180264, #119569, #88213, #149897, #72056, #29541, #133730, #167064, #198386, #134745, #196427, #152863, #14358, #104391, #58872, #182231, #181252, #103398, #41734, #90202, #166074, #76023, #59863, #137698, #199383, #151885, #45694, #27577, #195423, #60847, #122522, #184212, #169018, #13375, #87227, #89215, #150908, #43716, #75039, #56900, #118574, #12402, #123505, #125517, #187214, #48685, #63845, #111333, #34502, #4142, #155847, #17344, #65821, #172018, #92175, #156854, #127490, #153860, #110337, #95166, #112330, #15358, #61835 ),
 ( #171025, #33507, #108350, #189195, #77014, #109343, #142663, #79000, #18349, #50670, #138686, #30523, #80004, #170029, #141673, #140674, #31519, #167, #185198, #188197, #3164, #46689, #93172, #2166, #157849, #64837, #19341, #80988, #126499, #49669, #154857, #16355, #173023, #78003, #32516, #96160, #139670, #1158, #62833, #124517, #186212, #47693, #94168, #38492, #68817, #70828, #83973, #101139, #160834, #162825, #24334, #161829, #130476, #132496, #35491, #22323, #98129, #114312, #192173, #146650, #145653, #54648, #6138, #5136, #8144, #99145, #100148, #53654, #36472, #190177, #67820, #178011, #194185, #159826, #85984, #9161, #69821, #55650, #158824, #7134, #115331, #23324, #66818, #84968, #144655, #39478, #20312, #81960, #177022, #174020, #131488, #97141, #143652, #147673, #21321, #128481, #193175, #116322, #51652, #113316, #175008, #82979, #129475, #191174, #52648, #176014, #37483, #43481, #74812, #103161, #27334, #150670, #25345, #120305, #72837, #28335, #56662, #105148, #57665, #136474, #182990, #88980, #164841, #118335, #180028, #41497, #26337, #121298, #181998, #89974, #12168, #10161, #151655, #86986, #13149, #104156, #134507, #196193, #87977, #133489, #73833, #59624, #149665, #119332, #165837, #11163, #117322, #42492, #181018, #135504, #197174, #58639, #166834, #195181, #179018, #102158, #198154, #40486, #163844, #148673, #71821, #159473, #179675, #162476, #175658, #177670, #22975, #37132, #56303, #97784, #55301, #8809, #117985, #147321, #193837, #133139, #84624, #163493, #115981, #86635, #23978, #144306, #24991, #69474, #53299, #68467, #130122, #114978, #191819, #98792, #70478, #131140, #176671, #160486, #148318, #5796, #82624, #67469, #146302, #132144, #101805, #39138, #20967, #7791, #192828, #116973, #190826, #38147, #21976, #83628, #129128, #178664, #52302, #100793, #40127, #145305, #6788, #9813, #71474, #99801, #54309, #85634, #161487, #113959, #194830, #140386, #124219, #49381, #187912, #146111, #34212, #19051, #1874, #129927, #125229, #111044, #46393, #68276, #161291, #78710, #64552, #172731, #16063, #142375, #48397, #53106, #109057, #191626, #33222, #22786, #130947, #126216, #17055, #32225, #170734, #93883, #155561, #7595, #6597, #114784, #95875, #62544, #176477, #77721, #37953, #2873, #110054, #171734, #63555, #185916, #157558, #69281, #186927, #94882, #80698, #156563, #108051, #18061, #79716, #141385, #99611, #84433, #169736, #47401, #31231, #92880, #154567, #139387, #869, #118805, #151130, #54120, #74287, #57129, #70291, #72288, #117797, #131959, #12622, #192637, #150135, #104615, #24801, #10627, #195658, #162291, #88440, #194644, #196651, #55116, #73303, #179490, #166304, #115793, #133966, #163303, #178476, #116785, #39943, #101614, #177483, #11636, #58120, #180491, #8619, #119789, #23791, #181473, #149137, #56114, #40955, #86450, #193644, #41963, #89441, #148135, #102627, #103629, #71293, #38952, #164312, #9626, #132956, #25805, #87451, #165305, #26799, #100608, #85441, #134974, #27800, #42951, #147131, #94389, #197626, #17566, #387, #13593, #15581, #61072, #75260, #156068, #135956, #93393, #46914, #59092, #32737, #45915, #63062, #122744, #124741, #186437, #123725, #92401, #120758, #182459, #184435, #60086, #76244, #154087, #108574, #107569, #16574, #168264, #167288, #170251, #169246, #62060, #30754, #198620, #152110, #29761, #139892, #43940, #121754, #47913, #171249, #31745, #105601, #28785, #77239, #138907, #185423, #90424, #155080, #106588, #1381, #136931, #183447, #78221, #44931, #109567, #91395, #153084, #14588, #137922, #199606, #157071, #82180, #20532, #176230, #67039, #51871, #34715, #160048, #158060, #143875, #79227, #98349, #96373, #127708, #189409, #18567, #95385, #66041, #64064, #19551, #50885, #113530, #6353, #129685, #159039, #37700, #80214, #2385, #175224, #114529, #190395, #161046, #97353, #191382, #65051, #141885, #112543, #174238, #36689, #21536 ),
 ( #140898, #5356, #99363, #125734, #35706, #128698, #187434, #48901, #110556, #83196, #144870, #172237, #33722, #68033, #52858, #3376, #126707, #81195, #188411, #49888, #111555, #173240, #142876, #4356, #147894, #87208, #180245, #145867, #69034, #165057, #148889, #71045, #22540, #177238, #163048, #130699, #164065, #133710, #194400, #84187, #25564, #72037, #118555, #57878, #9380, #88194, #40708, #11384, #10380, #192394, #149878, #55868, #178232, #193394, #54870, #39696, #116544, #100367, #195403, #117542, #101358, #23542, #73054, #53876, #7350, #115550, #132712, #56881, #26550, #41714, #42709, #179241, #102377, #103379, #38710, #24555, #162046, #85189, #146878, #134726, #8370, #196408, #119550, #70045, #131713, #181233, #104370, #86204, #199364, #59842, #167044, #154837, #12382, #150888, #74044, #14338, #147, #170009, #107326, #186192, #152844, #60828, #123486, #58851, #136684, #43695, #105357, #27555, #61816, #89195, #184193, #15338, #90182, #151865, #185179, #46669, #121510, #76004, #137678, #28545, #182210, #122503, #135715, #44686, #45675, #138667, #93152, #16335, #168999, #124497, #13355, #197386, #108329, #1139, #76995, #47673, #30503, #77984, #75019, #198366, #92154, #153841, #31500, #139651, #62813, #120518, #166054, #183205, #106340, #168025, #29521, #91155, #82954, #34480, #96138, #144631, #50646, #171005, #35468, #6114, #32496, #65798, #173997, #191151, #94149, #140655, #19318, #51629, #155828, #17325, #5112, #81936, #78980, #174984, #111312, #4119, #67797, #113293, #2147, #112307, #127467, #157827, #97117, #66794, #63825, #125497, #36448, #158800, #80965, #109324, #187195, #49649, #48665, #20289, #143627, #142641, #110317, #128457, #190153, #98105, #129452, #189173, #159801, #21296, #171999, #33487, #95145, #156834, #18329, #79984, #141652, #3143, #173001, #64817, #126478, #188176, #101116, #162802, #192148, #68792, #39455, #37459, #131465, #24311, #25321, #180005, #103136, #132472, #11140, #53629, #175990, #86963, #87953, #163820, #134483, #70803, #164818, #38467, #130450, #85960, #147649, #148649, #10137, #149642, #145630, #9137, #194162, #55626, #117299, #133467, #56639, #26313, #177988, #178995, #72814, #40463, #114288, #102135, #52625, #99120, #71798, #195158, #160811, #22299, #83950, #118312, #41472, #7110, #115305, #176997, #100124, #161806, #23301, #54623, #84945, #146627, #8119, #69797, #193151, #116299, #121275, #60589, #153604, #119308, #42470, #138434, #122264, #44453, #196170, #150649, #136452, #104132, #137442, #107093, #167791, #57642, #199121, #45440, #91911, #31265, #182969, #61584, #14097, #184943, #183953, #88959, #29291, #58617, #151633, #166813, #28314, #13128, #89953, #73812, #168763, #90921, #74790, #197152, #46428, #165814, #180993, #27312, #106106, #30266, #200115, #15100, #16097, #152607, #75765, #76760, #12147, #198133, #135482, #120284, #181976, #123252, #43458, #108087, #169771, #105127, #59602, #92916, #154601, #77755, #50420, #21056, #157593, #51399, #125265, #155596, #126250, #187946, #112079, #173769, #174751, #32260, #34248, #95908, #19084, #172768, #20061, #143388, #113059, #64585, #49416, #36215, #80732, #903, #65568, #97868, #62578, #142411, #3889, #139421, #124256, #170771, #111078, #81705, #185951, #47435, #35235, #96889, #109092, #4880, #141420, #127228, #159558, #66562, #93918, #188943, #158572, #128227, #189924, #17091, #78744, #140421, #1911, #63590, #186963, #48433, #110089, #79750, #171768, #33257, #94915, #156601, #18095, #2907, #132230, #178751, #118072, #7875, #148404, #100879, #71559, #85721, #175743, #54393, #145390, #38230, #53387, #115066, #99885, #176757, #160572, #193923, #116066, #161570, #83712, #133224, #129213, #67556, #190911, #131227, #117056, #86719, #24066, #102893, #69561, #177754, #40215, #37221, #23063, #22061, #6872, #144394, #101894, #5879, #162561, #55386, #68551, #130207, #163576, #25076, #84708, #192916, #39223 ),
 ( #147408, #9898, #8895, #194915, #146387, #114045, #56390, #70563, #179763, #41232, #191902, #98877, #164578, #82711, #52388, #150417, #76531, #61353, #122035, #184709, #10896, #136224, #74557, #90698, #119077, #75533, #196920, #30037, #72569, #134244, #12894, #107847, #167565, #26072, #87715, #182736, #152381, #120054, #103896, #29058, #13866, #123024, #137208, #198895, #181741, #106865, #104890, #60363, #149401, #45211, #138207, #58387, #44220, #183725, #195930, #168539, #28079, #91676, #88721, #153368, #197899, #199889, #57405, #105878, #43222, #11912, #73575, #135248, #166579, #46194, #14870, #180759, #42235, #165576, #27075, #89719, #151404, #59368, #121038, #171533, #16855, #108856, #172527, #66327, #63350, #17857, #126018, #48194, #169532, #141183, #125027, #78506, #2672, #109848, #110843, #47196, #127988, #92681, #33021, #81469, #79513, #95670, #189691, #31032, #51163, #34013, #170535, #49185, #94676, #32025, #154369, #15863, #126992, #80497, #77521, #139193, #64349, #96652, #156355, #186723, #187713, #668, #62338, #124008, #185706, #157357, #93683, #18851, #142170, #50181, #173527, #143155, #3654, #65332, #4636, #188699, #155366, #111838, #140179, #1672, #34997, #158339, #19828, #97630, #144156, #22825, #55154, #174516, #35983, #8658, #85480, #82471, #178515, #114824, #7636, #71332, #116824, #159319, #115834, #69320, #37994, #177523, #70331, #20814, #5641, #39981, #38992, #161333, #112824, #67318, #53145, #128979, #54161, #23830, #84471, #190677, #100648, #162329, #131998, #148174, #99649, #101652, #130986, #163344, #147169, #52153, #146149, #175505, #68315, #83476, #145154, #129966, #6637, #113810, #193686, #192678, #191666, #36979, #24840, #98640, #160335, #21824, #86489, #9666, #132994, #194685, #176517, #42994, #89485, #16371, #149179, #26841, #134006, #195697, #117836, #93189, #179529, #74331, #108369, #180530, #42004, #78019, #139688, #11678, #104661, #166346, #57169, #72331, #27844, #40999, #135016, #151175, #31536, #186229, #109359, #135997, #17361, #118847, #102666, #154874, #94184, #170046, #140692, #197668, #171041, #103669, #165347, #12663, #61853, #1174, #62851, #155863, #10667, #123522, #185216, #46707, #124533, #79016, #47709, #164351, #32532, #56155, #25847, #87490, #88481, #150177, #73343, #196693, #58163, #119830, #181515, #63862, #98144, #175025, #172035, #67835, #4158, #97157, #160850, #6155, #125533, #5152, #158840, #127507, #66834, #159843, #187230, #48701, #144670, #128498, #50689, #2182, #156871, #142679, #110353, #143671, #113332, #174037, #33523, #190193, #51669, #21336, #37498, #189211, #129492, #20328, #191189, #36488, #95185, #35507, #64853, #157866, #173040, #34518, #19356, #96177, #80020, #82994, #81977, #81005, #3180, #52665, #18368, #141689, #126515, #112346, #114327, #176030, #99160, #22339, #83990, #188213, #49685, #111350, #65837, #23340, #84985, #7151, #180046, #68834, #163863, #195199, #69837, #131504, #164858, #26354, #101155, #194201, #55666, #146666, #161846, #132512, #130493, #24350, #117340, #118353, #72855, #196212, #25362, #104173, #8161, #192189, #41515, #181035, #56679, #27351, #87003, #57683, #193191, #54664, #179036, #40504, #103178, #87994, #42509, #38508, #102175, #148690, #10178, #71838, #149682, #11180, #119351, #70844, #165855, #133507, #145669, #116338, #53670, #134525, #115348, #177038, #100164, #178027, #39495, #162843, #86001, #147690, #9177, #200150, #123288, #124291, #182016, #183991, #45476, #107131, #122301, #169807, #92952, #62613, #14135, #75802, #185988, #30305, #150688, #15136, #47471, #12186, #168801, #153641, #170806, #73851, #120322, #199160, #31300, #135521, #197192, #184980, #61620, #58656, #154638, #90958, #91948, #109128, #16133, #43499, #76798, #138469, #137480, #46464, #108124, #105165, #166851, #77788, #139457, #60627, #88997, #28353, #29330, #89991, #938, #151673, #13166, #74830, #136491, #198171, #59641 ),
 ( #152645, #121315, #183007, #44491, #106147, #167829, #63626, #4913, #157628, #96924, #127264, #94951, #48468, #126284, #36250, #52422, #156635, #82748, #67591, #128260, #190945, #17128, #142446, #80768, #158606, #125302, #81740, #2942, #97903, #78780, #140457, #19118, #114080, #173804, #32298, #93954, #188977, #20096, #187981, #110125, #35269, #143426, #129250, #66596, #50453, #3924, #189958, #51433, #155632, #1946, #174784, #113092, #65604, #186998, #171803, #172802, #33291, #159594, #21091, #112112, #18131, #144428, #5914, #79785, #141457, #64622, #49450, #111113, #34283, #95943, #68585, #147442, #38263, #131261, #146419, #7910, #192949, #69594, #53421, #86755, #8930, #54428, #176790, #164611, #22095, #160605, #83745, #24101, #9933, #179795, #117091, #195964, #162597, #70598, #133258, #130241, #116098, #115098, #99917, #37255, #71592, #98912, #193957, #25111, #161602, #23096, #194949, #56425, #177786, #85755, #132266, #84742, #191937, #55420, #145424, #39256, #178786, #148438, #102926, #26105, #40255, #134276, #100912, #6907, #118106, #10929, #41264, #57436, #101928, #87748, #163610, #149433, #72602, #175781, #30065, #153400, #154399, #11941, #13894, #75561, #137237, #152407, #199918, #123054, #92711, #44247, #105904, #15894, #60390, #180790, #45240, #77552, #42267, #198921, #183754, #699, #103927, #150445, #29085, #61382, #165607, #27106, #14898, #91706, #88752, #184740, #121069, #122062, #139224, #46225, #73605, #106894, #59395, #168567, #196948, #119109, #135276, #197927, #31063, #167590, #76559, #58416, #120083, #181771, #138235, #43252, #107878, #90724, #104920, #166607, #28107, #169566, #89746, #151432, #12919, #74583, #136251, #182763, #17889, #110873, #159353, #170566, #20849, #124040, #172558, #186754, #2703, #18882, #35029, #34044, #143188, #94707, #93713, #96684, #187744, #127024, #157389, #125057, #78536, #156384, #66360, #82507, #48224, #112857, #97664, #158372, #144189, #47228, #95701, #80528, #188731, #155395, #111870, #33052, #128021, #108887, #32056, #49215, #62371, #3685, #185739, #16885, #142202, #50216, #79543, #140210, #65363, #173560, #1704, #19861, #81501, #141213, #4668, #64380, #189723, #63380, #51196, #174548, #126048, #36015, #109878, #171562, #101686, #7668, #9698, #68347, #86521, #192710, #117870, #87521, #85513, #176551, #191698, #129998, #53181, #114857, #164384, #163375, #71363, #147201, #21857, #133027, #175538, #194717, #162361, #69352, #131021, #38027, #145185, #8692, #102696, #99683, #54193, #23862, #84505, #5675, #177555, #161367, #22858, #83508, #115866, #190711, #146183, #39024, #178547, #56187, #179560, #70362, #25877, #6669, #100679, #132029, #67351, #24872, #41030, #193719, #55187, #116856, #37012, #148205, #40013, #129011, #52184, #113842, #98673, #160367, #30828, #28860, #119860, #135048, #73376, #11709, #196724, #107644, #106665, #14660, #90500, #165379, #76320, #118878, #137998, #105676, #151205, #12693, #58192, #88516, #152182, #45989, #43023, #197699, #167362, #27874, #149209, #120833, #104690, #181545, #182533, #89515, #13666, #26873, #169321, #72363, #74359, #61147, #59165, #75333, #10700, #134037, #195730, #137003, #150212, #198692, #136025, #166378, #57203, #180562, #168338, #60159, #42036, #103700, #44015, #199682, #121828, #183522, #45005, #29834, #91471, #153159, #122819, #184509, #16648, #32813, #48975, #65124, #64142, #173316, #124815, #123800, #126782, #17643, #157146, #187508, #155156, #108648, #186515, #96446, #112619, #78295, #142948, #127782, #188488, #50960, #77315, #2460, #140972, #18641, #185498, #141959, #63136, #158133, #138983, #461, #79303, #174311, #33800, #92476, #95460, #170326, #154164, #15656, #171325, #4429, #125806, #80287, #62136, #46989, #31818, #3448, #93469, #172311, #110630, #139969, #1458, #47989, #49967, #111631, #109642, #189482, #34791, #19625, #81267, #94464, #66117, #156145, #143951, #132788, #97427 ) ),
 .UNSPECIFIED., .T., .F., .T. ) 
 B_SPLINE_SURFACE_WITH_KNOTS ( ( 4, 3, 4 ),
 ( 3, 2, 2, 2, 2, 2, 2, 2, 2, 2, 2, 2, 2, 2, 2, 2, 2, 2, 2, 2, 2, 2, 2, 2, 2, 2, 2, 2, 2, 2, 2, 2, 2, 2, 2, 2, 2, 2, 2, 2, 2, 2, 2, 2, 2, 2, 2, 2, 2, 2, 2, 2, 2, 2, 2, 2, 2, 2, 2, 2, 2, 2, 2, 2, 2, 2, 2, 2, 2, 2, 2, 2, 2, 2, 2, 2, 2, 2, 2, 2, 2, 2, 2, 2, 2, 2, 2, 2, 2, 2, 2, 2, 2, 2, 2, 2, 2, 2, 2, 2, 2, 2, 2, 2, 2, 2, 2, 2, 2, 2, 2, 2, 2, 2, 2, 2, 2, 2, 2, 2, 2, 2, 2, 2, 2, 2, 2, 2, 2, 2, 2, 2, 2, 2, 2, 2, 2, 2, 2, 2, 2, 2, 2, 2, 2, 2, 2, 2, 2, 2, 2, 2, 2, 2, 2, 2, 2, 2, 2, 2, 2, 2, 2, 2, 2, 2, 2, 2, 2, 2, 2, 2, 2, 2, 2, 2, 2, 2, 2, 2, 2, 2, 2, 2, 2, 2, 2, 2, 2, 2, 2, 2, 2, 2, 2, 2, 2, 2, 2, 2, 2, 2, 2, 2, 2, 2, 2, 2, 2, 2, 2, 2, 2, 2, 2, 2, 2, 2, 2, 2, 2, 2, 2, 2, 2, 2, 2, 2, 3 ),
 ( 0.000000000000000000, 0.5000000000000000000, 1.000000000000000000 ),
 ( 0.000000000000000000, 0.004385964912280701511, 0.008771929824561403022, 0.01315789473684210453, 0.01754385964912280604, 0.02192982456140350755, 0.02631578947368420907, 0.03070175438596491058, 0.03508771929824561209, 0.03947368421052631360, 0.04385964912280701511, 0.04824561403508771662, 0.05263157894736841813, 0.05701754385964911964, 0.06140350877192982115, 0.06578947368421052266, 0.07017543859649122417, 0.07456140350877192569, 0.07894736842105262720, 0.08333333333333332871, 0.08771929824561403022, 0.09210526315789473173, 0.09649122807017543324, 0.1008771929824561348, 0.1052631578947368363, 0.1096491228070175378, 0.1140350877192982393, 0.1184210526315789408, 0.1228070175438596423, 0.1271929824561403577, 0.1315789473684210453, 0.1359649122807017607, 0.1403508771929824483, 0.1447368421052631637, 0.1491228070175438514, 0.1535087719298245668, 0.1578947368421052544, 0.1622807017543859698, 0.1666666666666666574, 0.1710526315789473728, 0.1754385964912280604, 0.1798245614035087758, 0.1842105263157894635, 0.1885964912280701788, 0.1929824561403508665, 0.1973684210526315819, 0.2017543859649122695, 0.2061403508771929849, 0.2105263157894736725, 0.2149122807017543879, 0.2192982456140350755, 0.2236842105263157909, 0.2280701754385964786, 0.2324561403508771940, 0.2368421052631578816, 0.2412280701754385970, 0.2456140350877192846, 0.2500000000000000000, 0.2543859649122807154, 0.2587719298245614308, 0.2631578947368420907, 0.2675438596491228060, 0.2719298245614035214, 0.2763157894736842368, 0.2807017543859648967, 0.2850877192982456121, 0.2894736842105263275, 0.2938596491228070429, 0.2982456140350877027, 0.3026315789473684181, 0.3070175438596491335, 0.3114035087719298489, 0.3157894736842105088, 0.3201754385964912242, 0.3245614035087719396, 0.3289473684210526550, 0.3333333333333333148, 0.3377192982456140302, 0.3421052631578947456, 0.3464912280701754610, 0.3508771929824561209, 0.3552631578947368363, 0.3596491228070175517, 0.3640350877192982670, 0.3684210526315789269, 0.3728070175438596423, 0.3771929824561403577, 0.3815789473684210731, 0.3859649122807017330, 0.3903508771929824483, 0.3947368421052631637, 0.3991228070175438791, 0.4035087719298245390, 0.4078947368421052544, 0.4122807017543859698, 0.4166666666666666852, 0.4210526315789473450, 0.4254385964912280604, 0.4298245614035087758, 0.4342105263157894912, 0.4385964912280701511, 0.4429824561403508665, 0.4473684210526315819, 0.4517543859649122973, 0.4561403508771929571, 0.4605263157894736725, 0.4649122807017543879, 0.4692982456140351033, 0.4736842105263157632, 0.4780701754385964786, 0.4824561403508771940, 0.4868421052631579093, 0.4912280701754385692, 0.4956140350877192846, 0.5000000000000000000, 0.5043859649122807154, 0.5087719298245614308, 0.5131578947368421462, 0.5175438596491228616, 0.5219298245614034659, 0.5263157894736841813, 0.5307017543859648967, 0.5350877192982456121, 0.5394736842105263275, 0.5438596491228070429, 0.5482456140350877583, 0.5526315789473684736, 0.5570175438596490780, 0.5614035087719297934, 0.5657894736842105088, 0.5701754385964912242, 0.5745614035087719396, 0.5789473684210526550, 0.5833333333333333703, 0.5877192982456140857, 0.5921052631578946901, 0.5964912280701754055, 0.6008771929824561209, 0.6052631578947368363, 0.6096491228070175517, 0.6140350877192982670, 0.6184210526315789824, 0.6228070175438596978, 0.6271929824561403022, 0.6315789473684210176, 0.6359649122807017330, 0.6403508771929824483, 0.6447368421052631637, 0.6491228070175438791, 0.6535087719298245945, 0.6578947368421053099, 0.6622807017543859143, 0.6666666666666666297, 0.6710526315789473450, 0.6754385964912280604, 0.6798245614035087758, 0.6842105263157894912, 0.6885964912280702066, 0.6929824561403509220, 0.6973684210526315264, 0.7017543859649122417, 0.7061403508771929571, 0.7105263157894736725, 0.7149122807017543879, 0.7192982456140351033, 0.7236842105263158187, 0.7280701754385965341, 0.7324561403508771384, 0.7368421052631578538, 0.7412280701754385692, 0.7456140350877192846, 0.7500000000000000000, 0.7543859649122807154, 0.7587719298245614308, 0.7631578947368421462, 0.7675438596491228616, 0.7719298245614034659, 0.7763157894736841813, 0.7807017543859648967, 0.7850877192982456121, 0.7894736842105263275, 0.7938596491228070429, 0.7982456140350877583, 0.8026315789473684736, 0.8070175438596490780, 0.8114035087719297934, 0.8157894736842105088, 0.8201754385964912242, 0.8245614035087719396, 0.8289473684210526550, 0.8333333333333333703, 0.8377192982456140857, 0.8421052631578946901, 0.8464912280701754055, 0.8508771929824561209, 0.8552631578947368363, 0.8596491228070175517, 0.8640350877192982670, 0.8684210526315789824, 0.8728070175438596978, 0.8771929824561403022, 0.8815789473684210176, 0.8859649122807017330, 0.8903508771929824483, 0.8947368421052631637, 0.8991228070175438791, 0.9035087719298245945, 0.9078947368421053099, 0.9122807017543859143, 0.9166666666666666297, 0.9210526315789473450, 0.9254385964912280604, 0.9298245614035087758, 0.9342105263157894912, 0.9385964912280702066, 0.9429824561403509220, 0.9473684210526315264, 0.9517543859649122417, 0.9561403508771929571, 0.9605263157894736725, 0.9649122807017543879, 0.9692982456140351033, 0.9736842105263158187, 0.9780701754385965341, 0.9824561403508771384, 0.9868421052631578538, 0.9912280701754385692, 0.9956140350877192846, 1.000000000000000000 ),
 .UNSPECIFIED. ) 
 GEOMETRIC_REPRESENTATION_ITEM ( )  RATIONAL_B_SPLINE_SURFACE ( (
 ( 1.000000000000000000, 0.9659258262890683122, 1.000000000000000000, 0.9659258262890683122, 1.000000000000000000, 0.9659258262890683122, 1.000000000000000000, 0.9659258262890683122, 1.000000000000000000, 0.9659258262890683122, 1.000000000000000000, 0.9659258262890683122, 1.000000000000000000, 0.9659258262890683122, 1.000000000000000000, 0.9659258262890683122, 1.000000000000000000, 0.9659258262890683122, 1.000000000000000000, 0.9659258262890683122, 1.000000000000000000, 0.9659258262890683122, 1.000000000000000000, 0.9659258262890683122, 1.000000000000000000, 0.9659258262890683122, 1.000000000000000000, 0.9659258262890683122, 1.000000000000000000, 0.9659258262890683122, 1.000000000000000000, 0.9659258262890683122, 1.000000000000000000, 0.9659258262890683122, 1.000000000000000000, 0.9659258262890683122, 1.000000000000000000, 0.9659258262890683122, 1.000000000000000000, 0.9659258262890683122, 1.000000000000000000, 0.9659258262890683122, 1.000000000000000000, 0.9659258262890683122, 1.000000000000000000, 0.9659258262890683122, 1.000000000000000000, 0.9659258262890683122, 1.000000000000000000, 0.9659258262890683122, 1.000000000000000000, 0.9659258262890683122, 1.000000000000000000, 0.9659258262890683122, 1.000000000000000000, 0.9659258262890683122, 1.000000000000000000, 0.9659258262890683122, 1.000000000000000000, 0.9659258262890683122, 1.000000000000000000, 0.9659258262890683122, 1.000000000000000000, 0.9659258262890683122, 1.000000000000000000, 0.9659258262890683122, 1.000000000000000000, 0.9659258262890683122, 1.000000000000000000, 0.9659258262890683122, 1.000000000000000000, 0.9659258262890683122, 1.000000000000000000, 0.9659258262890683122, 1.000000000000000000, 0.9659258262890683122, 1.000000000000000000, 0.9659258262890683122, 1.000000000000000000, 0.9659258262890683122, 1.000000000000000000, 0.9659258262890683122, 1.000000000000000000, 0.9659258262890683122, 1.000000000000000000, 0.9659258262890683122, 1.000000000000000000, 0.9659258262890683122, 1.000000000000000000, 0.9659258262890683122, 1.000000000000000000, 0.9659258262890683122, 1.000000000000000000, 0.9659258262890683122, 1.000000000000000000, 0.9659258262890683122, 1.000000000000000000, 0.9659258262890683122, 1.000000000000000000, 0.9659258262890683122, 1.000000000000000000, 0.9659258262890683122, 1.000000000000000000, 0.9659258262890683122, 1.000000000000000000, 0.9659258262890683122, 1.000000000000000000, 0.9659258262890683122, 1.000000000000000000, 0.9659258262890683122, 1.000000000000000000, 0.9659258262890683122, 1.000000000000000000, 0.9659258262890683122, 1.000000000000000000, 0.9659258262890683122, 1.000000000000000000, 0.9659258262890683122, 1.000000000000000000, 0.9659258262890683122, 1.000000000000000000, 0.9659258262890683122, 1.000000000000000000, 0.9659258262890683122, 1.000000000000000000, 0.9659258262890683122, 1.000000000000000000, 0.9659258262890683122, 1.000000000000000000, 0.9659258262890683122, 1.000000000000000000, 0.9659258262890683122, 1.000000000000000000, 0.9659258262890683122, 1.000000000000000000, 0.9659258262890683122, 1.000000000000000000, 0.9659258262890683122, 1.000000000000000000, 0.9659258262890683122, 1.000000000000000000, 0.9659258262890683122, 1.000000000000000000, 0.9659258262890683122, 1.000000000000000000, 0.9659258262890683122, 1.000000000000000000, 0.9659258262890683122, 1.000000000000000000, 0.9659258262890683122, 1.000000000000000000, 0.9659258262890683122, 1.000000000000000000, 0.9659258262890683122, 1.000000000000000000, 0.9659258262890683122, 1.000000000000000000, 0.9659258262890683122, 1.000000000000000000, 0.9659258262890683122, 1.000000000000000000, 0.9659258262890683122, 1.000000000000000000, 0.9659258262890683122, 1.000000000000000000, 0.9659258262890683122, 1.000000000000000000, 0.9659258262890683122, 1.000000000000000000, 0.9659258262890683122, 1.000000000000000000, 0.9659258262890683122, 1.000000000000000000, 0.9659258262890683122, 1.000000000000000000, 0.9659258262890683122, 1.000000000000000000, 0.9659258262890683122, 1.000000000000000000, 0.9659258262890683122, 1.000000000000000000, 0.9659258262890683122, 1.000000000000000000, 0.9659258262890683122, 1.000000000000000000, 0.9659258262890683122, 1.000000000000000000, 0.9659258262890683122, 1.000000000000000000, 0.9659258262890683122, 1.000000000000000000, 0.9659258262890683122, 1.000000000000000000, 0.9659258262890683122, 1.000000000000000000, 0.9659258262890683122, 1.000000000000000000, 0.9659258262890683122, 1.000000000000000000, 0.9659258262890683122, 1.000000000000000000, 0.9659258262890683122, 1.000000000000000000, 0.9659258262890683122, 1.000000000000000000, 0.9659258262890683122, 1.000000000000000000, 0.9659258262890683122, 1.000000000000000000, 0.9659258262890683122, 1.000000000000000000, 0.9659258262890683122, 1.000000000000000000, 0.9659258262890683122, 1.000000000000000000, 0.9659258262890683122, 1.000000000000000000, 0.9659258262890683122, 1.000000000000000000, 0.9659258262890683122, 1.000000000000000000, 0.9659258262890683122, 1.000000000000000000, 0.9659258262890683122, 1.000000000000000000, 0.9659258262890683122, 1.000000000000000000, 0.9659258262890683122, 1.000000000000000000, 0.9659258262890683122, 1.000000000000000000, 0.9659258262890683122, 1.000000000000000000, 0.9659258262890683122, 1.000000000000000000, 0.9659258262890683122, 1.000000000000000000, 0.9659258262890683122, 1.000000000000000000, 0.9659258262890683122, 1.000000000000000000, 0.9659258262890683122, 1.000000000000000000, 0.9659258262890683122, 1.000000000000000000, 0.9659258262890683122, 1.000000000000000000, 0.9659258262890683122, 1.000000000000000000, 0.9659258262890683122, 1.000000000000000000, 0.9659258262890683122, 1.000000000000000000, 0.9659258262890683122, 1.000000000000000000, 0.9659258262890683122, 1.000000000000000000, 0.9659258262890683122, 1.000000000000000000, 0.9659258262890683122, 1.000000000000000000, 0.9659258262890683122, 1.000000000000000000, 0.9659258262890683122, 1.000000000000000000, 0.9659258262890683122, 1.000000000000000000, 0.9659258262890683122, 1.000000000000000000, 0.9659258262890683122, 1.000000000000000000, 0.9659258262890683122, 1.000000000000000000, 0.9659258262890683122, 1.000000000000000000, 0.9659258262890683122, 1.000000000000000000, 0.9659258262890683122, 1.000000000000000000, 0.9659258262890683122, 1.000000000000000000, 0.9659258262890683122, 1.000000000000000000, 0.9659258262890683122, 1.000000000000000000, 0.9659258262890683122, 1.000000000000000000, 0.9659258262890683122, 1.000000000000000000, 0.9659258262890683122, 1.000000000000000000, 0.9659258262890683122, 1.000000000000000000, 0.9659258262890683122, 1.000000000000000000, 0.9659258262890683122, 1.000000000000000000, 0.9659258262890683122, 1.000000000000000000, 0.9659258262890683122, 1.000000000000000000, 0.9659258262890683122, 1.000000000000000000, 0.9659258262890683122, 1.000000000000000000, 0.9659258262890683122, 1.000000000000000000, 0.9659258262890683122, 1.000000000000000000, 0.9659258262890683122, 1.000000000000000000, 0.9659258262890683122, 1.000000000000000000, 0.9659258262890683122, 1.000000000000000000, 0.9659258262890683122, 1.000000000000000000, 0.9659258262890683122, 1.000000000000000000, 0.9659258262890683122, 1.000000000000000000, 0.9659258262890683122, 1.000000000000000000, 0.9659258262890683122, 1.000000000000000000, 0.9659258262890683122, 1.000000000000000000, 0.9659258262890683122, 1.000000000000000000, 0.9659258262890683122, 1.000000000000000000, 0.9659258262890683122, 1.000000000000000000, 0.9659258262890683122, 1.000000000000000000, 0.9659258262890683122, 1.000000000000000000, 0.9659258262890683122, 1.000000000000000000, 0.9659258262890683122, 1.000000000000000000, 0.9659258262890683122, 1.000000000000000000, 0.9659258262890683122, 1.000000000000000000, 0.9659258262890683122, 1.000000000000000000, 0.9659258262890683122, 1.000000000000000000, 0.9659258262890683122, 1.000000000000000000, 0.9659258262890683122, 1.000000000000000000, 0.9659258262890683122, 1.000000000000000000, 0.9659258262890683122, 1.000000000000000000, 0.9659258262890683122, 1.000000000000000000, 0.9659258262890683122, 1.000000000000000000, 0.9659258262890683122, 1.000000000000000000, 0.9659258262890683122, 1.000000000000000000, 0.9659258262890683122, 1.000000000000000000, 0.9659258262890683122, 1.000000000000000000, 0.9659258262890683122, 1.000000000000000000, 0.9659258262890683122, 1.000000000000000000, 0.9659258262890683122, 1.000000000000000000, 0.9659258262890683122, 1.000000000000000000, 0.9659258262890683122, 1.000000000000000000, 0.9659258262890683122, 1.000000000000000000, 0.9659258262890683122, 1.000000000000000000, 0.9659258262890683122, 1.000000000000000000, 0.9659258262890683122, 1.000000000000000000, 0.9659258262890683122, 1.000000000000000000, 0.9659258262890683122, 1.000000000000000000, 0.9659258262890683122, 1.000000000000000000, 0.9659258262890683122, 1.000000000000000000, 0.9659258262890683122, 1.000000000000000000, 0.9659258262890683122, 1.000000000000000000, 0.9659258262890683122, 1.000000000000000000, 0.9659258262890683122, 1.000000000000000000, 0.9659258262890683122, 1.000000000000000000, 0.9659258262890683122, 1.000000000000000000, 0.9659258262890683122, 1.000000000000000000, 0.9659258262890683122, 1.000000000000000000, 0.9659258262890683122, 1.000000000000000000, 0.9659258262890683122, 1.000000000000000000, 0.9659258262890683122, 1.000000000000000000, 0.9659258262890683122, 1.000000000000000000, 0.9659258262890683122, 1.000000000000000000, 0.9659258262890683122, 1.000000000000000000, 0.9659258262890683122, 1.000000000000000000, 0.9659258262890683122, 1.000000000000000000, 0.9659258262890683122, 1.000000000000000000, 0.9659258262890683122, 1.000000000000000000, 0.9659258262890683122, 1.000000000000000000, 0.9659258262890683122, 1.000000000000000000, 0.9659258262890683122, 1.000000000000000000, 0.9659258262890683122, 1.000000000000000000, 0.9659258262890683122, 1.000000000000000000, 0.9659258262890683122, 1.000000000000000000, 0.9659258262890683122, 1.000000000000000000, 0.9659258262890683122, 1.000000000000000000, 0.9659258262890683122, 1.000000000000000000, 0.9659258262890683122, 1.000000000000000000, 0.9659258262890683122, 1.000000000000000000, 0.9659258262890683122, 1.000000000000000000, 0.9659258262890683122, 1.000000000000000000),
 ( 0.3333333333333333703, 0.3219752754296894559, 0.3333333333333333703, 0.3219752754296894559, 0.3333333333333333703, 0.3219752754296894559, 0.3333333333333333703, 0.3219752754296894559, 0.3333333333333333703, 0.3219752754296894559, 0.3333333333333333703, 0.3219752754296894559, 0.3333333333333333703, 0.3219752754296894559, 0.3333333333333333703, 0.3219752754296894559, 0.3333333333333333703, 0.3219752754296894559, 0.3333333333333333703, 0.3219752754296894559, 0.3333333333333333703, 0.3219752754296894559, 0.3333333333333333703, 0.3219752754296894559, 0.3333333333333333703, 0.3219752754296894559, 0.3333333333333333703, 0.3219752754296894559, 0.3333333333333333703, 0.3219752754296894559, 0.3333333333333333703, 0.3219752754296894559, 0.3333333333333333703, 0.3219752754296894559, 0.3333333333333333703, 0.3219752754296894559, 0.3333333333333333703, 0.3219752754296894559, 0.3333333333333333703, 0.3219752754296894559, 0.3333333333333333703, 0.3219752754296894559, 0.3333333333333333703, 0.3219752754296894559, 0.3333333333333333703, 0.3219752754296894559, 0.3333333333333333703, 0.3219752754296894559, 0.3333333333333333703, 0.3219752754296894559, 0.3333333333333333703, 0.3219752754296894559, 0.3333333333333333703, 0.3219752754296894559, 0.3333333333333333703, 0.3219752754296894559, 0.3333333333333333703, 0.3219752754296894559, 0.3333333333333333703, 0.3219752754296894559, 0.3333333333333333703, 0.3219752754296894559, 0.3333333333333333703, 0.3219752754296894559, 0.3333333333333333703, 0.3219752754296894559, 0.3333333333333333703, 0.3219752754296894559, 0.3333333333333333703, 0.3219752754296894559, 0.3333333333333333703, 0.3219752754296894559, 0.3333333333333333703, 0.3219752754296894559, 0.3333333333333333703, 0.3219752754296894559, 0.3333333333333333703, 0.3219752754296894559, 0.3333333333333333703, 0.3219752754296894559, 0.3333333333333333703, 0.3219752754296894559, 0.3333333333333333703, 0.3219752754296894559, 0.3333333333333333703, 0.3219752754296894559, 0.3333333333333333703, 0.3219752754296894559, 0.3333333333333333703, 0.3219752754296894559, 0.3333333333333333703, 0.3219752754296894559, 0.3333333333333333703, 0.3219752754296894559, 0.3333333333333333703, 0.3219752754296894559, 0.3333333333333333703, 0.3219752754296894559, 0.3333333333333333703, 0.3219752754296894559, 0.3333333333333333703, 0.3219752754296894559, 0.3333333333333333703, 0.3219752754296894559, 0.3333333333333333703, 0.3219752754296894559, 0.3333333333333333703, 0.3219752754296894559, 0.3333333333333333703, 0.3219752754296894559, 0.3333333333333333703, 0.3219752754296894559, 0.3333333333333333703, 0.3219752754296894559, 0.3333333333333333703, 0.3219752754296894559, 0.3333333333333333703, 0.3219752754296894559, 0.3333333333333333703, 0.3219752754296894559, 0.3333333333333333703, 0.3219752754296894559, 0.3333333333333333703, 0.3219752754296894559, 0.3333333333333333703, 0.3219752754296894559, 0.3333333333333333703, 0.3219752754296894559, 0.3333333333333333703, 0.3219752754296894559, 0.3333333333333333703, 0.3219752754296894559, 0.3333333333333333703, 0.3219752754296894559, 0.3333333333333333703, 0.3219752754296894559, 0.3333333333333333703, 0.3219752754296894559, 0.3333333333333333703, 0.3219752754296894559, 0.3333333333333333703, 0.3219752754296894559, 0.3333333333333333703, 0.3219752754296894559, 0.3333333333333333703, 0.3219752754296894559, 0.3333333333333333703, 0.3219752754296894559, 0.3333333333333333703, 0.3219752754296894559, 0.3333333333333333703, 0.3219752754296894559, 0.3333333333333333703, 0.3219752754296894559, 0.3333333333333333703, 0.3219752754296894559, 0.3333333333333333703, 0.3219752754296894559, 0.3333333333333333703, 0.3219752754296894559, 0.3333333333333333703, 0.3219752754296894559, 0.3333333333333333703, 0.3219752754296894559, 0.3333333333333333703, 0.3219752754296894559, 0.3333333333333333703, 0.3219752754296894559, 0.3333333333333333703, 0.3219752754296894559, 0.3333333333333333703, 0.3219752754296894559, 0.3333333333333333703, 0.3219752754296894559, 0.3333333333333333703, 0.3219752754296894559, 0.3333333333333333703, 0.3219752754296894559, 0.3333333333333333703, 0.3219752754296894559, 0.3333333333333333703, 0.3219752754296894559, 0.3333333333333333703, 0.3219752754296894559, 0.3333333333333333703, 0.3219752754296894559, 0.3333333333333333703, 0.3219752754296894559, 0.3333333333333333703, 0.3219752754296894559, 0.3333333333333333703, 0.3219752754296894559, 0.3333333333333333703, 0.3219752754296894559, 0.3333333333333333703, 0.3219752754296894559, 0.3333333333333333703, 0.3219752754296894559, 0.3333333333333333703, 0.3219752754296894559, 0.3333333333333333703, 0.3219752754296894559, 0.3333333333333333703, 0.3219752754296894559, 0.3333333333333333703, 0.3219752754296894559, 0.3333333333333333703, 0.3219752754296894559, 0.3333333333333333703, 0.3219752754296894559, 0.3333333333333333703, 0.3219752754296894559, 0.3333333333333333703, 0.3219752754296894559, 0.3333333333333333703, 0.3219752754296894559, 0.3333333333333333703, 0.3219752754296894559, 0.3333333333333333703, 0.3219752754296894559, 0.3333333333333333703, 0.3219752754296894559, 0.3333333333333333703, 0.3219752754296894559, 0.3333333333333333703, 0.3219752754296894559, 0.3333333333333333703, 0.3219752754296894559, 0.3333333333333333703, 0.3219752754296894559, 0.3333333333333333703, 0.3219752754296894559, 0.3333333333333333703, 0.3219752754296894559, 0.3333333333333333703, 0.3219752754296894559, 0.3333333333333333703, 0.3219752754296894559, 0.3333333333333333703, 0.3219752754296894559, 0.3333333333333333703, 0.3219752754296894559, 0.3333333333333333703, 0.3219752754296894559, 0.3333333333333333703, 0.3219752754296894559, 0.3333333333333333703, 0.3219752754296894559, 0.3333333333333333703, 0.3219752754296894559, 0.3333333333333333703, 0.3219752754296894559, 0.3333333333333333703, 0.3219752754296894559, 0.3333333333333333703, 0.3219752754296894559, 0.3333333333333333703, 0.3219752754296894559, 0.3333333333333333703, 0.3219752754296894559, 0.3333333333333333703, 0.3219752754296894559, 0.3333333333333333703, 0.3219752754296894559, 0.3333333333333333703, 0.3219752754296894559, 0.3333333333333333703, 0.3219752754296894559, 0.3333333333333333703, 0.3219752754296894559, 0.3333333333333333703, 0.3219752754296894559, 0.3333333333333333703, 0.3219752754296894559, 0.3333333333333333703, 0.3219752754296894559, 0.3333333333333333703, 0.3219752754296894559, 0.3333333333333333703, 0.3219752754296894559, 0.3333333333333333703, 0.3219752754296894559, 0.3333333333333333703, 0.3219752754296894559, 0.3333333333333333703, 0.3219752754296894559, 0.3333333333333333703, 0.3219752754296894559, 0.3333333333333333703, 0.3219752754296894559, 0.3333333333333333703, 0.3219752754296894559, 0.3333333333333333703, 0.3219752754296894559, 0.3333333333333333703, 0.3219752754296894559, 0.3333333333333333703, 0.3219752754296894559, 0.3333333333333333703, 0.3219752754296894559, 0.3333333333333333703, 0.3219752754296894559, 0.3333333333333333703, 0.3219752754296894559, 0.3333333333333333703, 0.3219752754296894559, 0.3333333333333333703, 0.3219752754296894559, 0.3333333333333333703, 0.3219752754296894559, 0.3333333333333333703, 0.3219752754296894559, 0.3333333333333333703, 0.3219752754296894559, 0.3333333333333333703, 0.3219752754296894559, 0.3333333333333333703, 0.3219752754296894559, 0.3333333333333333703, 0.3219752754296894559, 0.3333333333333333703, 0.3219752754296894559, 0.3333333333333333703, 0.3219752754296894559, 0.3333333333333333703, 0.3219752754296894559, 0.3333333333333333703, 0.3219752754296894559, 0.3333333333333333703, 0.3219752754296894559, 0.3333333333333333703, 0.3219752754296894559, 0.3333333333333333703, 0.3219752754296894559, 0.3333333333333333703, 0.3219752754296894559, 0.3333333333333333703, 0.3219752754296894559, 0.3333333333333333703, 0.3219752754296894559, 0.3333333333333333703, 0.3219752754296894559, 0.3333333333333333703, 0.3219752754296894559, 0.3333333333333333703, 0.3219752754296894559, 0.3333333333333333703, 0.3219752754296894559, 0.3333333333333333703, 0.3219752754296894559, 0.3333333333333333703, 0.3219752754296894559, 0.3333333333333333703, 0.3219752754296894559, 0.3333333333333333703, 0.3219752754296894559, 0.3333333333333333703, 0.3219752754296894559, 0.3333333333333333703, 0.3219752754296894559, 0.3333333333333333703, 0.3219752754296894559, 0.3333333333333333703, 0.3219752754296894559, 0.3333333333333333703, 0.3219752754296894559, 0.3333333333333333703, 0.3219752754296894559, 0.3333333333333333703, 0.3219752754296894559, 0.3333333333333333703, 0.3219752754296894559, 0.3333333333333333703, 0.3219752754296894559, 0.3333333333333333703, 0.3219752754296894559, 0.3333333333333333703, 0.3219752754296894559, 0.3333333333333333703, 0.3219752754296894559, 0.3333333333333333703, 0.3219752754296894559, 0.3333333333333333703, 0.3219752754296894559, 0.3333333333333333703, 0.3219752754296894559, 0.3333333333333333703, 0.3219752754296894559, 0.3333333333333333703, 0.3219752754296894559, 0.3333333333333333703, 0.3219752754296894559, 0.3333333333333333703, 0.3219752754296894559, 0.3333333333333333703, 0.3219752754296894559, 0.3333333333333333703, 0.3219752754296894559, 0.3333333333333333703, 0.3219752754296894559, 0.3333333333333333703, 0.3219752754296894559, 0.3333333333333333703, 0.3219752754296894559, 0.3333333333333333703, 0.3219752754296894559, 0.3333333333333333703, 0.3219752754296894559, 0.3333333333333333703, 0.3219752754296894559, 0.3333333333333333703, 0.3219752754296894559, 0.3333333333333333703, 0.3219752754296894559, 0.3333333333333333703, 0.3219752754296894559, 0.3333333333333333703, 0.3219752754296894559, 0.3333333333333333703, 0.3219752754296894559, 0.3333333333333333703, 0.3219752754296894559, 0.3333333333333333703, 0.3219752754296894559, 0.3333333333333333703, 0.3219752754296894559, 0.3333333333333333703, 0.3219752754296894559, 0.3333333333333333703, 0.3219752754296894559, 0.3333333333333333703, 0.3219752754296894559, 0.3333333333333333703, 0.3219752754296894559, 0.3333333333333333703, 0.3219752754296894559, 0.3333333333333333703, 0.3219752754296894559, 0.3333333333333333703, 0.3219752754296894559, 0.3333333333333333703, 0.3219752754296894559, 0.3333333333333333703, 0.3219752754296894559, 0.3333333333333333703, 0.3219752754296894559, 0.3333333333333333703, 0.3219752754296894559, 0.3333333333333333703, 0.3219752754296894559, 0.3333333333333333703, 0.3219752754296894559, 0.3333333333333333703, 0.3219752754296894559, 0.3333333333333333703, 0.3219752754296894559, 0.3333333333333333703),
 ( 0.3333333333333333703, 0.3219752754296894559, 0.3333333333333333703, 0.3219752754296894559, 0.3333333333333333703, 0.3219752754296894559, 0.3333333333333333703, 0.3219752754296894559, 0.3333333333333333703, 0.3219752754296894559, 0.3333333333333333703, 0.3219752754296894559, 0.3333333333333333703, 0.3219752754296894559, 0.3333333333333333703, 0.3219752754296894559, 0.3333333333333333703, 0.3219752754296894559, 0.3333333333333333703, 0.3219752754296894559, 0.3333333333333333703, 0.3219752754296894559, 0.3333333333333333703, 0.3219752754296894559, 0.3333333333333333703, 0.3219752754296894559, 0.3333333333333333703, 0.3219752754296894559, 0.3333333333333333703, 0.3219752754296894559, 0.3333333333333333703, 0.3219752754296894559, 0.3333333333333333703, 0.3219752754296894559, 0.3333333333333333703, 0.3219752754296894559, 0.3333333333333333703, 0.3219752754296894559, 0.3333333333333333703, 0.3219752754296894559, 0.3333333333333333703, 0.3219752754296894559, 0.3333333333333333703, 0.3219752754296894559, 0.3333333333333333703, 0.3219752754296894559, 0.3333333333333333703, 0.3219752754296894559, 0.3333333333333333703, 0.3219752754296894559, 0.3333333333333333703, 0.3219752754296894559, 0.3333333333333333703, 0.3219752754296894559, 0.3333333333333333703, 0.3219752754296894559, 0.3333333333333333703, 0.3219752754296894559, 0.3333333333333333703, 0.3219752754296894559, 0.3333333333333333703, 0.3219752754296894559, 0.3333333333333333703, 0.3219752754296894559, 0.3333333333333333703, 0.3219752754296894559, 0.3333333333333333703, 0.3219752754296894559, 0.3333333333333333703, 0.3219752754296894559, 0.3333333333333333703, 0.3219752754296894559, 0.3333333333333333703, 0.3219752754296894559, 0.3333333333333333703, 0.3219752754296894559, 0.3333333333333333703, 0.3219752754296894559, 0.3333333333333333703, 0.3219752754296894559, 0.3333333333333333703, 0.3219752754296894559, 0.3333333333333333703, 0.3219752754296894559, 0.3333333333333333703, 0.3219752754296894559, 0.3333333333333333703, 0.3219752754296894559, 0.3333333333333333703, 0.3219752754296894559, 0.3333333333333333703, 0.3219752754296894559, 0.3333333333333333703, 0.3219752754296894559, 0.3333333333333333703, 0.3219752754296894559, 0.3333333333333333703, 0.3219752754296894559, 0.3333333333333333703, 0.3219752754296894559, 0.3333333333333333703, 0.3219752754296894559, 0.3333333333333333703, 0.3219752754296894559, 0.3333333333333333703, 0.3219752754296894559, 0.3333333333333333703, 0.3219752754296894559, 0.3333333333333333703, 0.3219752754296894559, 0.3333333333333333703, 0.3219752754296894559, 0.3333333333333333703, 0.3219752754296894559, 0.3333333333333333703, 0.3219752754296894559, 0.3333333333333333703, 0.3219752754296894559, 0.3333333333333333703, 0.3219752754296894559, 0.3333333333333333703, 0.3219752754296894559, 0.3333333333333333703, 0.3219752754296894559, 0.3333333333333333703, 0.3219752754296894559, 0.3333333333333333703, 0.3219752754296894559, 0.3333333333333333703, 0.3219752754296894559, 0.3333333333333333703, 0.3219752754296894559, 0.3333333333333333703, 0.3219752754296894559, 0.3333333333333333703, 0.3219752754296894559, 0.3333333333333333703, 0.3219752754296894559, 0.3333333333333333703, 0.3219752754296894559, 0.3333333333333333703, 0.3219752754296894559, 0.3333333333333333703, 0.3219752754296894559, 0.3333333333333333703, 0.3219752754296894559, 0.3333333333333333703, 0.3219752754296894559, 0.3333333333333333703, 0.3219752754296894559, 0.3333333333333333703, 0.3219752754296894559, 0.3333333333333333703, 0.3219752754296894559, 0.3333333333333333703, 0.3219752754296894559, 0.3333333333333333703, 0.3219752754296894559, 0.3333333333333333703, 0.3219752754296894559, 0.3333333333333333703, 0.3219752754296894559, 0.3333333333333333703, 0.3219752754296894559, 0.3333333333333333703, 0.3219752754296894559, 0.3333333333333333703, 0.3219752754296894559, 0.3333333333333333703, 0.3219752754296894559, 0.3333333333333333703, 0.3219752754296894559, 0.3333333333333333703, 0.3219752754296894559, 0.3333333333333333703, 0.3219752754296894559, 0.3333333333333333703, 0.3219752754296894559, 0.3333333333333333703, 0.3219752754296894559, 0.3333333333333333703, 0.3219752754296894559, 0.3333333333333333703, 0.3219752754296894559, 0.3333333333333333703, 0.3219752754296894559, 0.3333333333333333703, 0.3219752754296894559, 0.3333333333333333703, 0.3219752754296894559, 0.3333333333333333703, 0.3219752754296894559, 0.3333333333333333703, 0.3219752754296894559, 0.3333333333333333703, 0.3219752754296894559, 0.3333333333333333703, 0.3219752754296894559, 0.3333333333333333703, 0.3219752754296894559, 0.3333333333333333703, 0.3219752754296894559, 0.3333333333333333703, 0.3219752754296894559, 0.3333333333333333703, 0.3219752754296894559, 0.3333333333333333703, 0.3219752754296894559, 0.3333333333333333703, 0.3219752754296894559, 0.3333333333333333703, 0.3219752754296894559, 0.3333333333333333703, 0.3219752754296894559, 0.3333333333333333703, 0.3219752754296894559, 0.3333333333333333703, 0.3219752754296894559, 0.3333333333333333703, 0.3219752754296894559, 0.3333333333333333703, 0.3219752754296894559, 0.3333333333333333703, 0.3219752754296894559, 0.3333333333333333703, 0.3219752754296894559, 0.3333333333333333703, 0.3219752754296894559, 0.3333333333333333703, 0.3219752754296894559, 0.3333333333333333703, 0.3219752754296894559, 0.3333333333333333703, 0.3219752754296894559, 0.3333333333333333703, 0.3219752754296894559, 0.3333333333333333703, 0.3219752754296894559, 0.3333333333333333703, 0.3219752754296894559, 0.3333333333333333703, 0.3219752754296894559, 0.3333333333333333703, 0.3219752754296894559, 0.3333333333333333703, 0.3219752754296894559, 0.3333333333333333703, 0.3219752754296894559, 0.3333333333333333703, 0.3219752754296894559, 0.3333333333333333703, 0.3219752754296894559, 0.3333333333333333703, 0.3219752754296894559, 0.3333333333333333703, 0.3219752754296894559, 0.3333333333333333703, 0.3219752754296894559, 0.3333333333333333703, 0.3219752754296894559, 0.3333333333333333703, 0.3219752754296894559, 0.3333333333333333703, 0.3219752754296894559, 0.3333333333333333703, 0.3219752754296894559, 0.3333333333333333703, 0.3219752754296894559, 0.3333333333333333703, 0.3219752754296894559, 0.3333333333333333703, 0.3219752754296894559, 0.3333333333333333703, 0.3219752754296894559, 0.3333333333333333703, 0.3219752754296894559, 0.3333333333333333703, 0.3219752754296894559, 0.3333333333333333703, 0.3219752754296894559, 0.3333333333333333703, 0.3219752754296894559, 0.3333333333333333703, 0.3219752754296894559, 0.3333333333333333703, 0.3219752754296894559, 0.3333333333333333703, 0.3219752754296894559, 0.3333333333333333703, 0.3219752754296894559, 0.3333333333333333703, 0.3219752754296894559, 0.3333333333333333703, 0.3219752754296894559, 0.3333333333333333703, 0.3219752754296894559, 0.3333333333333333703, 0.3219752754296894559, 0.3333333333333333703, 0.3219752754296894559, 0.3333333333333333703, 0.3219752754296894559, 0.3333333333333333703, 0.3219752754296894559, 0.3333333333333333703, 0.3219752754296894559, 0.3333333333333333703, 0.3219752754296894559, 0.3333333333333333703, 0.3219752754296894559, 0.3333333333333333703, 0.3219752754296894559, 0.3333333333333333703, 0.3219752754296894559, 0.3333333333333333703, 0.3219752754296894559, 0.3333333333333333703, 0.3219752754296894559, 0.3333333333333333703, 0.3219752754296894559, 0.3333333333333333703, 0.3219752754296894559, 0.3333333333333333703, 0.3219752754296894559, 0.3333333333333333703, 0.3219752754296894559, 0.3333333333333333703, 0.3219752754296894559, 0.3333333333333333703, 0.3219752754296894559, 0.3333333333333333703, 0.3219752754296894559, 0.3333333333333333703, 0.3219752754296894559, 0.3333333333333333703, 0.3219752754296894559, 0.3333333333333333703, 0.3219752754296894559, 0.3333333333333333703, 0.3219752754296894559, 0.3333333333333333703, 0.3219752754296894559, 0.3333333333333333703, 0.3219752754296894559, 0.3333333333333333703, 0.3219752754296894559, 0.3333333333333333703, 0.3219752754296894559, 0.3333333333333333703, 0.3219752754296894559, 0.3333333333333333703, 0.3219752754296894559, 0.3333333333333333703, 0.3219752754296894559, 0.3333333333333333703, 0.3219752754296894559, 0.3333333333333333703, 0.3219752754296894559, 0.3333333333333333703, 0.3219752754296894559, 0.3333333333333333703, 0.3219752754296894559, 0.3333333333333333703, 0.3219752754296894559, 0.3333333333333333703, 0.3219752754296894559, 0.3333333333333333703, 0.3219752754296894559, 0.3333333333333333703, 0.3219752754296894559, 0.3333333333333333703, 0.3219752754296894559, 0.3333333333333333703, 0.3219752754296894559, 0.3333333333333333703, 0.3219752754296894559, 0.3333333333333333703, 0.3219752754296894559, 0.3333333333333333703, 0.3219752754296894559, 0.3333333333333333703, 0.3219752754296894559, 0.3333333333333333703, 0.3219752754296894559, 0.3333333333333333703, 0.3219752754296894559, 0.3333333333333333703, 0.3219752754296894559, 0.3333333333333333703, 0.3219752754296894559, 0.3333333333333333703, 0.3219752754296894559, 0.3333333333333333703, 0.3219752754296894559, 0.3333333333333333703, 0.3219752754296894559, 0.3333333333333333703, 0.3219752754296894559, 0.3333333333333333703, 0.3219752754296894559, 0.3333333333333333703, 0.3219752754296894559, 0.3333333333333333703, 0.3219752754296894559, 0.3333333333333333703, 0.3219752754296894559, 0.3333333333333333703, 0.3219752754296894559, 0.3333333333333333703, 0.3219752754296894559, 0.3333333333333333703, 0.3219752754296894559, 0.3333333333333333703, 0.3219752754296894559, 0.3333333333333333703, 0.3219752754296894559, 0.3333333333333333703, 0.3219752754296894559, 0.3333333333333333703, 0.3219752754296894559, 0.3333333333333333703, 0.3219752754296894559, 0.3333333333333333703, 0.3219752754296894559, 0.3333333333333333703, 0.3219752754296894559, 0.3333333333333333703, 0.3219752754296894559, 0.3333333333333333703, 0.3219752754296894559, 0.3333333333333333703, 0.3219752754296894559, 0.3333333333333333703, 0.3219752754296894559, 0.3333333333333333703, 0.3219752754296894559, 0.3333333333333333703, 0.3219752754296894559, 0.3333333333333333703, 0.3219752754296894559, 0.3333333333333333703, 0.3219752754296894559, 0.3333333333333333703, 0.3219752754296894559, 0.3333333333333333703, 0.3219752754296894559, 0.3333333333333333703, 0.3219752754296894559, 0.3333333333333333703, 0.3219752754296894559, 0.3333333333333333703, 0.3219752754296894559, 0.3333333333333333703, 0.3219752754296894559, 0.3333333333333333703, 0.3219752754296894559, 0.3333333333333333703),
 ( 1.000000000000000000, 0.9659258262890683122, 1.000000000000000000, 0.9659258262890683122, 1.000000000000000000, 0.9659258262890683122, 1.000000000000000000, 0.9659258262890683122, 1.000000000000000000, 0.9659258262890683122, 1.000000000000000000, 0.9659258262890683122, 1.000000000000000000, 0.9659258262890683122, 1.000000000000000000, 0.9659258262890683122, 1.000000000000000000, 0.9659258262890683122, 1.000000000000000000, 0.9659258262890683122, 1.000000000000000000, 0.9659258262890683122, 1.000000000000000000, 0.9659258262890683122, 1.000000000000000000, 0.9659258262890683122, 1.000000000000000000, 0.9659258262890683122, 1.000000000000000000, 0.9659258262890683122, 1.000000000000000000, 0.9659258262890683122, 1.000000000000000000, 0.9659258262890683122, 1.000000000000000000, 0.9659258262890683122, 1.000000000000000000, 0.9659258262890683122, 1.000000000000000000, 0.9659258262890683122, 1.000000000000000000, 0.9659258262890683122, 1.000000000000000000, 0.9659258262890683122, 1.000000000000000000, 0.9659258262890683122, 1.000000000000000000, 0.9659258262890683122, 1.000000000000000000, 0.9659258262890683122, 1.000000000000000000, 0.9659258262890683122, 1.000000000000000000, 0.9659258262890683122, 1.000000000000000000, 0.9659258262890683122, 1.000000000000000000, 0.9659258262890683122, 1.000000000000000000, 0.9659258262890683122, 1.000000000000000000, 0.9659258262890683122, 1.000000000000000000, 0.9659258262890683122, 1.000000000000000000, 0.9659258262890683122, 1.000000000000000000, 0.9659258262890683122, 1.000000000000000000, 0.9659258262890683122, 1.000000000000000000, 0.9659258262890683122, 1.000000000000000000, 0.9659258262890683122, 1.000000000000000000, 0.9659258262890683122, 1.000000000000000000, 0.9659258262890683122, 1.000000000000000000, 0.9659258262890683122, 1.000000000000000000, 0.9659258262890683122, 1.000000000000000000, 0.9659258262890683122, 1.000000000000000000, 0.9659258262890683122, 1.000000000000000000, 0.9659258262890683122, 1.000000000000000000, 0.9659258262890683122, 1.000000000000000000, 0.9659258262890683122, 1.000000000000000000, 0.9659258262890683122, 1.000000000000000000, 0.9659258262890683122, 1.000000000000000000, 0.9659258262890683122, 1.000000000000000000, 0.9659258262890683122, 1.000000000000000000, 0.9659258262890683122, 1.000000000000000000, 0.9659258262890683122, 1.000000000000000000, 0.9659258262890683122, 1.000000000000000000, 0.9659258262890683122, 1.000000000000000000, 0.9659258262890683122, 1.000000000000000000, 0.9659258262890683122, 1.000000000000000000, 0.9659258262890683122, 1.000000000000000000, 0.9659258262890683122, 1.000000000000000000, 0.9659258262890683122, 1.000000000000000000, 0.9659258262890683122, 1.000000000000000000, 0.9659258262890683122, 1.000000000000000000, 0.9659258262890683122, 1.000000000000000000, 0.9659258262890683122, 1.000000000000000000, 0.9659258262890683122, 1.000000000000000000, 0.9659258262890683122, 1.000000000000000000, 0.9659258262890683122, 1.000000000000000000, 0.9659258262890683122, 1.000000000000000000, 0.9659258262890683122, 1.000000000000000000, 0.9659258262890683122, 1.000000000000000000, 0.9659258262890683122, 1.000000000000000000, 0.9659258262890683122, 1.000000000000000000, 0.9659258262890683122, 1.000000000000000000, 0.9659258262890683122, 1.000000000000000000, 0.9659258262890683122, 1.000000000000000000, 0.9659258262890683122, 1.000000000000000000, 0.9659258262890683122, 1.000000000000000000, 0.9659258262890683122, 1.000000000000000000, 0.9659258262890683122, 1.000000000000000000, 0.9659258262890683122, 1.000000000000000000, 0.9659258262890683122, 1.000000000000000000, 0.9659258262890683122, 1.000000000000000000, 0.9659258262890683122, 1.000000000000000000, 0.9659258262890683122, 1.000000000000000000, 0.9659258262890683122, 1.000000000000000000, 0.9659258262890683122, 1.000000000000000000, 0.9659258262890683122, 1.000000000000000000, 0.9659258262890683122, 1.000000000000000000, 0.9659258262890683122, 1.000000000000000000, 0.9659258262890683122, 1.000000000000000000, 0.9659258262890683122, 1.000000000000000000, 0.9659258262890683122, 1.000000000000000000, 0.9659258262890683122, 1.000000000000000000, 0.9659258262890683122, 1.000000000000000000, 0.9659258262890683122, 1.000000000000000000, 0.9659258262890683122, 1.000000000000000000, 0.9659258262890683122, 1.000000000000000000, 0.9659258262890683122, 1.000000000000000000, 0.9659258262890683122, 1.000000000000000000, 0.9659258262890683122, 1.000000000000000000, 0.9659258262890683122, 1.000000000000000000, 0.9659258262890683122, 1.000000000000000000, 0.9659258262890683122, 1.000000000000000000, 0.9659258262890683122, 1.000000000000000000, 0.9659258262890683122, 1.000000000000000000, 0.9659258262890683122, 1.000000000000000000, 0.9659258262890683122, 1.000000000000000000, 0.9659258262890683122, 1.000000000000000000, 0.9659258262890683122, 1.000000000000000000, 0.9659258262890683122, 1.000000000000000000, 0.9659258262890683122, 1.000000000000000000, 0.9659258262890683122, 1.000000000000000000, 0.9659258262890683122, 1.000000000000000000, 0.9659258262890683122, 1.000000000000000000, 0.9659258262890683122, 1.000000000000000000, 0.9659258262890683122, 1.000000000000000000, 0.9659258262890683122, 1.000000000000000000, 0.9659258262890683122, 1.000000000000000000, 0.9659258262890683122, 1.000000000000000000, 0.9659258262890683122, 1.000000000000000000, 0.9659258262890683122, 1.000000000000000000, 0.9659258262890683122, 1.000000000000000000, 0.9659258262890683122, 1.000000000000000000, 0.9659258262890683122, 1.000000000000000000, 0.9659258262890683122, 1.000000000000000000, 0.9659258262890683122, 1.000000000000000000, 0.9659258262890683122, 1.000000000000000000, 0.9659258262890683122, 1.000000000000000000, 0.9659258262890683122, 1.000000000000000000, 0.9659258262890683122, 1.000000000000000000, 0.9659258262890683122, 1.000000000000000000, 0.9659258262890683122, 1.000000000000000000, 0.9659258262890683122, 1.000000000000000000, 0.9659258262890683122, 1.000000000000000000, 0.9659258262890683122, 1.000000000000000000, 0.9659258262890683122, 1.000000000000000000, 0.9659258262890683122, 1.000000000000000000, 0.9659258262890683122, 1.000000000000000000, 0.9659258262890683122, 1.000000000000000000, 0.9659258262890683122, 1.000000000000000000, 0.9659258262890683122, 1.000000000000000000, 0.9659258262890683122, 1.000000000000000000, 0.9659258262890683122, 1.000000000000000000, 0.9659258262890683122, 1.000000000000000000, 0.9659258262890683122, 1.000000000000000000, 0.9659258262890683122, 1.000000000000000000, 0.9659258262890683122, 1.000000000000000000, 0.9659258262890683122, 1.000000000000000000, 0.9659258262890683122, 1.000000000000000000, 0.9659258262890683122, 1.000000000000000000, 0.9659258262890683122, 1.000000000000000000, 0.9659258262890683122, 1.000000000000000000, 0.9659258262890683122, 1.000000000000000000, 0.9659258262890683122, 1.000000000000000000, 0.9659258262890683122, 1.000000000000000000, 0.9659258262890683122, 1.000000000000000000, 0.9659258262890683122, 1.000000000000000000, 0.9659258262890683122, 1.000000000000000000, 0.9659258262890683122, 1.000000000000000000, 0.9659258262890683122, 1.000000000000000000, 0.9659258262890683122, 1.000000000000000000, 0.9659258262890683122, 1.000000000000000000, 0.9659258262890683122, 1.000000000000000000, 0.9659258262890683122, 1.000000000000000000, 0.9659258262890683122, 1.000000000000000000, 0.9659258262890683122, 1.000000000000000000, 0.9659258262890683122, 1.000000000000000000, 0.9659258262890683122, 1.000000000000000000, 0.9659258262890683122, 1.000000000000000000, 0.9659258262890683122, 1.000000000000000000, 0.9659258262890683122, 1.000000000000000000, 0.9659258262890683122, 1.000000000000000000, 0.9659258262890683122, 1.000000000000000000, 0.9659258262890683122, 1.000000000000000000, 0.9659258262890683122, 1.000000000000000000, 0.9659258262890683122, 1.000000000000000000, 0.9659258262890683122, 1.000000000000000000, 0.9659258262890683122, 1.000000000000000000, 0.9659258262890683122, 1.000000000000000000, 0.9659258262890683122, 1.000000000000000000, 0.9659258262890683122, 1.000000000000000000, 0.9659258262890683122, 1.000000000000000000, 0.9659258262890683122, 1.000000000000000000, 0.9659258262890683122, 1.000000000000000000, 0.9659258262890683122, 1.000000000000000000, 0.9659258262890683122, 1.000000000000000000, 0.9659258262890683122, 1.000000000000000000, 0.9659258262890683122, 1.000000000000000000, 0.9659258262890683122, 1.000000000000000000, 0.9659258262890683122, 1.000000000000000000, 0.9659258262890683122, 1.000000000000000000, 0.9659258262890683122, 1.000000000000000000, 0.9659258262890683122, 1.000000000000000000, 0.9659258262890683122, 1.000000000000000000, 0.9659258262890683122, 1.000000000000000000, 0.9659258262890683122, 1.000000000000000000, 0.9659258262890683122, 1.000000000000000000, 0.9659258262890683122, 1.000000000000000000, 0.9659258262890683122, 1.000000000000000000, 0.9659258262890683122, 1.000000000000000000, 0.9659258262890683122, 1.000000000000000000, 0.9659258262890683122, 1.000000000000000000, 0.9659258262890683122, 1.000000000000000000, 0.9659258262890683122, 1.000000000000000000, 0.9659258262890683122, 1.000000000000000000, 0.9659258262890683122, 1.000000000000000000, 0.9659258262890683122, 1.000000000000000000, 0.9659258262890683122, 1.000000000000000000, 0.9659258262890683122, 1.000000000000000000, 0.9659258262890683122, 1.000000000000000000, 0.9659258262890683122, 1.000000000000000000, 0.9659258262890683122, 1.000000000000000000, 0.9659258262890683122, 1.000000000000000000, 0.9659258262890683122, 1.000000000000000000, 0.9659258262890683122, 1.000000000000000000, 0.9659258262890683122, 1.000000000000000000, 0.9659258262890683122, 1.000000000000000000, 0.9659258262890683122, 1.000000000000000000, 0.9659258262890683122, 1.000000000000000000, 0.9659258262890683122, 1.000000000000000000, 0.9659258262890683122, 1.000000000000000000, 0.9659258262890683122, 1.000000000000000000, 0.9659258262890683122, 1.000000000000000000, 0.9659258262890683122, 1.000000000000000000, 0.9659258262890683122, 1.000000000000000000, 0.9659258262890683122, 1.000000000000000000, 0.9659258262890683122, 1.000000000000000000, 0.9659258262890683122, 1.000000000000000000, 0.9659258262890683122, 1.000000000000000000),
 ( 0.3333333333333333703, 0.3219752754296894559, 0.3333333333333333703, 0.3219752754296894559, 0.3333333333333333703, 0.3219752754296894559, 0.3333333333333333703, 0.3219752754296894559, 0.3333333333333333703, 0.3219752754296894559, 0.3333333333333333703, 0.3219752754296894559, 0.3333333333333333703, 0.3219752754296894559, 0.3333333333333333703, 0.3219752754296894559, 0.3333333333333333703, 0.3219752754296894559, 0.3333333333333333703, 0.3219752754296894559, 0.3333333333333333703, 0.3219752754296894559, 0.3333333333333333703, 0.3219752754296894559, 0.3333333333333333703, 0.3219752754296894559, 0.3333333333333333703, 0.3219752754296894559, 0.3333333333333333703, 0.3219752754296894559, 0.3333333333333333703, 0.3219752754296894559, 0.3333333333333333703, 0.3219752754296894559, 0.3333333333333333703, 0.3219752754296894559, 0.3333333333333333703, 0.3219752754296894559, 0.3333333333333333703, 0.3219752754296894559, 0.3333333333333333703, 0.3219752754296894559, 0.3333333333333333703, 0.3219752754296894559, 0.3333333333333333703, 0.3219752754296894559, 0.3333333333333333703, 0.3219752754296894559, 0.3333333333333333703, 0.3219752754296894559, 0.3333333333333333703, 0.3219752754296894559, 0.3333333333333333703, 0.3219752754296894559, 0.3333333333333333703, 0.3219752754296894559, 0.3333333333333333703, 0.3219752754296894559, 0.3333333333333333703, 0.3219752754296894559, 0.3333333333333333703, 0.3219752754296894559, 0.3333333333333333703, 0.3219752754296894559, 0.3333333333333333703, 0.3219752754296894559, 0.3333333333333333703, 0.3219752754296894559, 0.3333333333333333703, 0.3219752754296894559, 0.3333333333333333703, 0.3219752754296894559, 0.3333333333333333703, 0.3219752754296894559, 0.3333333333333333703, 0.3219752754296894559, 0.3333333333333333703, 0.3219752754296894559, 0.3333333333333333703, 0.3219752754296894559, 0.3333333333333333703, 0.3219752754296894559, 0.3333333333333333703, 0.3219752754296894559, 0.3333333333333333703, 0.3219752754296894559, 0.3333333333333333703, 0.3219752754296894559, 0.3333333333333333703, 0.3219752754296894559, 0.3333333333333333703, 0.3219752754296894559, 0.3333333333333333703, 0.3219752754296894559, 0.3333333333333333703, 0.3219752754296894559, 0.3333333333333333703, 0.3219752754296894559, 0.3333333333333333703, 0.3219752754296894559, 0.3333333333333333703, 0.3219752754296894559, 0.3333333333333333703, 0.3219752754296894559, 0.3333333333333333703, 0.3219752754296894559, 0.3333333333333333703, 0.3219752754296894559, 0.3333333333333333703, 0.3219752754296894559, 0.3333333333333333703, 0.3219752754296894559, 0.3333333333333333703, 0.3219752754296894559, 0.3333333333333333703, 0.3219752754296894559, 0.3333333333333333703, 0.3219752754296894559, 0.3333333333333333703, 0.3219752754296894559, 0.3333333333333333703, 0.3219752754296894559, 0.3333333333333333703, 0.3219752754296894559, 0.3333333333333333703, 0.3219752754296894559, 0.3333333333333333703, 0.3219752754296894559, 0.3333333333333333703, 0.3219752754296894559, 0.3333333333333333703, 0.3219752754296894559, 0.3333333333333333703, 0.3219752754296894559, 0.3333333333333333703, 0.3219752754296894559, 0.3333333333333333703, 0.3219752754296894559, 0.3333333333333333703, 0.3219752754296894559, 0.3333333333333333703, 0.3219752754296894559, 0.3333333333333333703, 0.3219752754296894559, 0.3333333333333333703, 0.3219752754296894559, 0.3333333333333333703, 0.3219752754296894559, 0.3333333333333333703, 0.3219752754296894559, 0.3333333333333333703, 0.3219752754296894559, 0.3333333333333333703, 0.3219752754296894559, 0.3333333333333333703, 0.3219752754296894559, 0.3333333333333333703, 0.3219752754296894559, 0.3333333333333333703, 0.3219752754296894559, 0.3333333333333333703, 0.3219752754296894559, 0.3333333333333333703, 0.3219752754296894559, 0.3333333333333333703, 0.3219752754296894559, 0.3333333333333333703, 0.3219752754296894559, 0.3333333333333333703, 0.3219752754296894559, 0.3333333333333333703, 0.3219752754296894559, 0.3333333333333333703, 0.3219752754296894559, 0.3333333333333333703, 0.3219752754296894559, 0.3333333333333333703, 0.3219752754296894559, 0.3333333333333333703, 0.3219752754296894559, 0.3333333333333333703, 0.3219752754296894559, 0.3333333333333333703, 0.3219752754296894559, 0.3333333333333333703, 0.3219752754296894559, 0.3333333333333333703, 0.3219752754296894559, 0.3333333333333333703, 0.3219752754296894559, 0.3333333333333333703, 0.3219752754296894559, 0.3333333333333333703, 0.3219752754296894559, 0.3333333333333333703, 0.3219752754296894559, 0.3333333333333333703, 0.3219752754296894559, 0.3333333333333333703, 0.3219752754296894559, 0.3333333333333333703, 0.3219752754296894559, 0.3333333333333333703, 0.3219752754296894559, 0.3333333333333333703, 0.3219752754296894559, 0.3333333333333333703, 0.3219752754296894559, 0.3333333333333333703, 0.3219752754296894559, 0.3333333333333333703, 0.3219752754296894559, 0.3333333333333333703, 0.3219752754296894559, 0.3333333333333333703, 0.3219752754296894559, 0.3333333333333333703, 0.3219752754296894559, 0.3333333333333333703, 0.3219752754296894559, 0.3333333333333333703, 0.3219752754296894559, 0.3333333333333333703, 0.3219752754296894559, 0.3333333333333333703, 0.3219752754296894559, 0.3333333333333333703, 0.3219752754296894559, 0.3333333333333333703, 0.3219752754296894559, 0.3333333333333333703, 0.3219752754296894559, 0.3333333333333333703, 0.3219752754296894559, 0.3333333333333333703, 0.3219752754296894559, 0.3333333333333333703, 0.3219752754296894559, 0.3333333333333333703, 0.3219752754296894559, 0.3333333333333333703, 0.3219752754296894559, 0.3333333333333333703, 0.3219752754296894559, 0.3333333333333333703, 0.3219752754296894559, 0.3333333333333333703, 0.3219752754296894559, 0.3333333333333333703, 0.3219752754296894559, 0.3333333333333333703, 0.3219752754296894559, 0.3333333333333333703, 0.3219752754296894559, 0.3333333333333333703, 0.3219752754296894559, 0.3333333333333333703, 0.3219752754296894559, 0.3333333333333333703, 0.3219752754296894559, 0.3333333333333333703, 0.3219752754296894559, 0.3333333333333333703, 0.3219752754296894559, 0.3333333333333333703, 0.3219752754296894559, 0.3333333333333333703, 0.3219752754296894559, 0.3333333333333333703, 0.3219752754296894559, 0.3333333333333333703, 0.3219752754296894559, 0.3333333333333333703, 0.3219752754296894559, 0.3333333333333333703, 0.3219752754296894559, 0.3333333333333333703, 0.3219752754296894559, 0.3333333333333333703, 0.3219752754296894559, 0.3333333333333333703, 0.3219752754296894559, 0.3333333333333333703, 0.3219752754296894559, 0.3333333333333333703, 0.3219752754296894559, 0.3333333333333333703, 0.3219752754296894559, 0.3333333333333333703, 0.3219752754296894559, 0.3333333333333333703, 0.3219752754296894559, 0.3333333333333333703, 0.3219752754296894559, 0.3333333333333333703, 0.3219752754296894559, 0.3333333333333333703, 0.3219752754296894559, 0.3333333333333333703, 0.3219752754296894559, 0.3333333333333333703, 0.3219752754296894559, 0.3333333333333333703, 0.3219752754296894559, 0.3333333333333333703, 0.3219752754296894559, 0.3333333333333333703, 0.3219752754296894559, 0.3333333333333333703, 0.3219752754296894559, 0.3333333333333333703, 0.3219752754296894559, 0.3333333333333333703, 0.3219752754296894559, 0.3333333333333333703, 0.3219752754296894559, 0.3333333333333333703, 0.3219752754296894559, 0.3333333333333333703, 0.3219752754296894559, 0.3333333333333333703, 0.3219752754296894559, 0.3333333333333333703, 0.3219752754296894559, 0.3333333333333333703, 0.3219752754296894559, 0.3333333333333333703, 0.3219752754296894559, 0.3333333333333333703, 0.3219752754296894559, 0.3333333333333333703, 0.3219752754296894559, 0.3333333333333333703, 0.3219752754296894559, 0.3333333333333333703, 0.3219752754296894559, 0.3333333333333333703, 0.3219752754296894559, 0.3333333333333333703, 0.3219752754296894559, 0.3333333333333333703, 0.3219752754296894559, 0.3333333333333333703, 0.3219752754296894559, 0.3333333333333333703, 0.3219752754296894559, 0.3333333333333333703, 0.3219752754296894559, 0.3333333333333333703, 0.3219752754296894559, 0.3333333333333333703, 0.3219752754296894559, 0.3333333333333333703, 0.3219752754296894559, 0.3333333333333333703, 0.3219752754296894559, 0.3333333333333333703, 0.3219752754296894559, 0.3333333333333333703, 0.3219752754296894559, 0.3333333333333333703, 0.3219752754296894559, 0.3333333333333333703, 0.3219752754296894559, 0.3333333333333333703, 0.3219752754296894559, 0.3333333333333333703, 0.3219752754296894559, 0.3333333333333333703, 0.3219752754296894559, 0.3333333333333333703, 0.3219752754296894559, 0.3333333333333333703, 0.3219752754296894559, 0.3333333333333333703, 0.3219752754296894559, 0.3333333333333333703, 0.3219752754296894559, 0.3333333333333333703, 0.3219752754296894559, 0.3333333333333333703, 0.3219752754296894559, 0.3333333333333333703, 0.3219752754296894559, 0.3333333333333333703, 0.3219752754296894559, 0.3333333333333333703, 0.3219752754296894559, 0.3333333333333333703, 0.3219752754296894559, 0.3333333333333333703, 0.3219752754296894559, 0.3333333333333333703, 0.3219752754296894559, 0.3333333333333333703, 0.3219752754296894559, 0.3333333333333333703, 0.3219752754296894559, 0.3333333333333333703, 0.3219752754296894559, 0.3333333333333333703, 0.3219752754296894559, 0.3333333333333333703, 0.3219752754296894559, 0.3333333333333333703, 0.3219752754296894559, 0.3333333333333333703, 0.3219752754296894559, 0.3333333333333333703, 0.3219752754296894559, 0.3333333333333333703, 0.3219752754296894559, 0.3333333333333333703, 0.3219752754296894559, 0.3333333333333333703, 0.3219752754296894559, 0.3333333333333333703, 0.3219752754296894559, 0.3333333333333333703, 0.3219752754296894559, 0.3333333333333333703, 0.3219752754296894559, 0.3333333333333333703, 0.3219752754296894559, 0.3333333333333333703, 0.3219752754296894559, 0.3333333333333333703, 0.3219752754296894559, 0.3333333333333333703, 0.3219752754296894559, 0.3333333333333333703, 0.3219752754296894559, 0.3333333333333333703, 0.3219752754296894559, 0.3333333333333333703, 0.3219752754296894559, 0.3333333333333333703, 0.3219752754296894559, 0.3333333333333333703, 0.3219752754296894559, 0.3333333333333333703, 0.3219752754296894559, 0.3333333333333333703, 0.3219752754296894559, 0.3333333333333333703, 0.3219752754296894559, 0.3333333333333333703, 0.3219752754296894559, 0.3333333333333333703, 0.3219752754296894559, 0.3333333333333333703, 0.3219752754296894559, 0.3333333333333333703, 0.3219752754296894559, 0.3333333333333333703, 0.3219752754296894559, 0.3333333333333333703),
 ( 0.3333333333333333703, 0.3219752754296894559, 0.3333333333333333703, 0.3219752754296894559, 0.3333333333333333703, 0.3219752754296894559, 0.3333333333333333703, 0.3219752754296894559, 0.3333333333333333703, 0.3219752754296894559, 0.3333333333333333703, 0.3219752754296894559, 0.3333333333333333703, 0.3219752754296894559, 0.3333333333333333703, 0.3219752754296894559, 0.3333333333333333703, 0.3219752754296894559, 0.3333333333333333703, 0.3219752754296894559, 0.3333333333333333703, 0.3219752754296894559, 0.3333333333333333703, 0.3219752754296894559, 0.3333333333333333703, 0.3219752754296894559, 0.3333333333333333703, 0.3219752754296894559, 0.3333333333333333703, 0.3219752754296894559, 0.3333333333333333703, 0.3219752754296894559, 0.3333333333333333703, 0.3219752754296894559, 0.3333333333333333703, 0.3219752754296894559, 0.3333333333333333703, 0.3219752754296894559, 0.3333333333333333703, 0.3219752754296894559, 0.3333333333333333703, 0.3219752754296894559, 0.3333333333333333703, 0.3219752754296894559, 0.3333333333333333703, 0.3219752754296894559, 0.3333333333333333703, 0.3219752754296894559, 0.3333333333333333703, 0.3219752754296894559, 0.3333333333333333703, 0.3219752754296894559, 0.3333333333333333703, 0.3219752754296894559, 0.3333333333333333703, 0.3219752754296894559, 0.3333333333333333703, 0.3219752754296894559, 0.3333333333333333703, 0.3219752754296894559, 0.3333333333333333703, 0.3219752754296894559, 0.3333333333333333703, 0.3219752754296894559, 0.3333333333333333703, 0.3219752754296894559, 0.3333333333333333703, 0.3219752754296894559, 0.3333333333333333703, 0.3219752754296894559, 0.3333333333333333703, 0.3219752754296894559, 0.3333333333333333703, 0.3219752754296894559, 0.3333333333333333703, 0.3219752754296894559, 0.3333333333333333703, 0.3219752754296894559, 0.3333333333333333703, 0.3219752754296894559, 0.3333333333333333703, 0.3219752754296894559, 0.3333333333333333703, 0.3219752754296894559, 0.3333333333333333703, 0.3219752754296894559, 0.3333333333333333703, 0.3219752754296894559, 0.3333333333333333703, 0.3219752754296894559, 0.3333333333333333703, 0.3219752754296894559, 0.3333333333333333703, 0.3219752754296894559, 0.3333333333333333703, 0.3219752754296894559, 0.3333333333333333703, 0.3219752754296894559, 0.3333333333333333703, 0.3219752754296894559, 0.3333333333333333703, 0.3219752754296894559, 0.3333333333333333703, 0.3219752754296894559, 0.3333333333333333703, 0.3219752754296894559, 0.3333333333333333703, 0.3219752754296894559, 0.3333333333333333703, 0.3219752754296894559, 0.3333333333333333703, 0.3219752754296894559, 0.3333333333333333703, 0.3219752754296894559, 0.3333333333333333703, 0.3219752754296894559, 0.3333333333333333703, 0.3219752754296894559, 0.3333333333333333703, 0.3219752754296894559, 0.3333333333333333703, 0.3219752754296894559, 0.3333333333333333703, 0.3219752754296894559, 0.3333333333333333703, 0.3219752754296894559, 0.3333333333333333703, 0.3219752754296894559, 0.3333333333333333703, 0.3219752754296894559, 0.3333333333333333703, 0.3219752754296894559, 0.3333333333333333703, 0.3219752754296894559, 0.3333333333333333703, 0.3219752754296894559, 0.3333333333333333703, 0.3219752754296894559, 0.3333333333333333703, 0.3219752754296894559, 0.3333333333333333703, 0.3219752754296894559, 0.3333333333333333703, 0.3219752754296894559, 0.3333333333333333703, 0.3219752754296894559, 0.3333333333333333703, 0.3219752754296894559, 0.3333333333333333703, 0.3219752754296894559, 0.3333333333333333703, 0.3219752754296894559, 0.3333333333333333703, 0.3219752754296894559, 0.3333333333333333703, 0.3219752754296894559, 0.3333333333333333703, 0.3219752754296894559, 0.3333333333333333703, 0.3219752754296894559, 0.3333333333333333703, 0.3219752754296894559, 0.3333333333333333703, 0.3219752754296894559, 0.3333333333333333703, 0.3219752754296894559, 0.3333333333333333703, 0.3219752754296894559, 0.3333333333333333703, 0.3219752754296894559, 0.3333333333333333703, 0.3219752754296894559, 0.3333333333333333703, 0.3219752754296894559, 0.3333333333333333703, 0.3219752754296894559, 0.3333333333333333703, 0.3219752754296894559, 0.3333333333333333703, 0.3219752754296894559, 0.3333333333333333703, 0.3219752754296894559, 0.3333333333333333703, 0.3219752754296894559, 0.3333333333333333703, 0.3219752754296894559, 0.3333333333333333703, 0.3219752754296894559, 0.3333333333333333703, 0.3219752754296894559, 0.3333333333333333703, 0.3219752754296894559, 0.3333333333333333703, 0.3219752754296894559, 0.3333333333333333703, 0.3219752754296894559, 0.3333333333333333703, 0.3219752754296894559, 0.3333333333333333703, 0.3219752754296894559, 0.3333333333333333703, 0.3219752754296894559, 0.3333333333333333703, 0.3219752754296894559, 0.3333333333333333703, 0.3219752754296894559, 0.3333333333333333703, 0.3219752754296894559, 0.3333333333333333703, 0.3219752754296894559, 0.3333333333333333703, 0.3219752754296894559, 0.3333333333333333703, 0.3219752754296894559, 0.3333333333333333703, 0.3219752754296894559, 0.3333333333333333703, 0.3219752754296894559, 0.3333333333333333703, 0.3219752754296894559, 0.3333333333333333703, 0.3219752754296894559, 0.3333333333333333703, 0.3219752754296894559, 0.3333333333333333703, 0.3219752754296894559, 0.3333333333333333703, 0.3219752754296894559, 0.3333333333333333703, 0.3219752754296894559, 0.3333333333333333703, 0.3219752754296894559, 0.3333333333333333703, 0.3219752754296894559, 0.3333333333333333703, 0.3219752754296894559, 0.3333333333333333703, 0.3219752754296894559, 0.3333333333333333703, 0.3219752754296894559, 0.3333333333333333703, 0.3219752754296894559, 0.3333333333333333703, 0.3219752754296894559, 0.3333333333333333703, 0.3219752754296894559, 0.3333333333333333703, 0.3219752754296894559, 0.3333333333333333703, 0.3219752754296894559, 0.3333333333333333703, 0.3219752754296894559, 0.3333333333333333703, 0.3219752754296894559, 0.3333333333333333703, 0.3219752754296894559, 0.3333333333333333703, 0.3219752754296894559, 0.3333333333333333703, 0.3219752754296894559, 0.3333333333333333703, 0.3219752754296894559, 0.3333333333333333703, 0.3219752754296894559, 0.3333333333333333703, 0.3219752754296894559, 0.3333333333333333703, 0.3219752754296894559, 0.3333333333333333703, 0.3219752754296894559, 0.3333333333333333703, 0.3219752754296894559, 0.3333333333333333703, 0.3219752754296894559, 0.3333333333333333703, 0.3219752754296894559, 0.3333333333333333703, 0.3219752754296894559, 0.3333333333333333703, 0.3219752754296894559, 0.3333333333333333703, 0.3219752754296894559, 0.3333333333333333703, 0.3219752754296894559, 0.3333333333333333703, 0.3219752754296894559, 0.3333333333333333703, 0.3219752754296894559, 0.3333333333333333703, 0.3219752754296894559, 0.3333333333333333703, 0.3219752754296894559, 0.3333333333333333703, 0.3219752754296894559, 0.3333333333333333703, 0.3219752754296894559, 0.3333333333333333703, 0.3219752754296894559, 0.3333333333333333703, 0.3219752754296894559, 0.3333333333333333703, 0.3219752754296894559, 0.3333333333333333703, 0.3219752754296894559, 0.3333333333333333703, 0.3219752754296894559, 0.3333333333333333703, 0.3219752754296894559, 0.3333333333333333703, 0.3219752754296894559, 0.3333333333333333703, 0.3219752754296894559, 0.3333333333333333703, 0.3219752754296894559, 0.3333333333333333703, 0.3219752754296894559, 0.3333333333333333703, 0.3219752754296894559, 0.3333333333333333703, 0.3219752754296894559, 0.3333333333333333703, 0.3219752754296894559, 0.3333333333333333703, 0.3219752754296894559, 0.3333333333333333703, 0.3219752754296894559, 0.3333333333333333703, 0.3219752754296894559, 0.3333333333333333703, 0.3219752754296894559, 0.3333333333333333703, 0.3219752754296894559, 0.3333333333333333703, 0.3219752754296894559, 0.3333333333333333703, 0.3219752754296894559, 0.3333333333333333703, 0.3219752754296894559, 0.3333333333333333703, 0.3219752754296894559, 0.3333333333333333703, 0.3219752754296894559, 0.3333333333333333703, 0.3219752754296894559, 0.3333333333333333703, 0.3219752754296894559, 0.3333333333333333703, 0.3219752754296894559, 0.3333333333333333703, 0.3219752754296894559, 0.3333333333333333703, 0.3219752754296894559, 0.3333333333333333703, 0.3219752754296894559, 0.3333333333333333703, 0.3219752754296894559, 0.3333333333333333703, 0.3219752754296894559, 0.3333333333333333703, 0.3219752754296894559, 0.3333333333333333703, 0.3219752754296894559, 0.3333333333333333703, 0.3219752754296894559, 0.3333333333333333703, 0.3219752754296894559, 0.3333333333333333703, 0.3219752754296894559, 0.3333333333333333703, 0.3219752754296894559, 0.3333333333333333703, 0.3219752754296894559, 0.3333333333333333703, 0.3219752754296894559, 0.3333333333333333703, 0.3219752754296894559, 0.3333333333333333703, 0.3219752754296894559, 0.3333333333333333703, 0.3219752754296894559, 0.3333333333333333703, 0.3219752754296894559, 0.3333333333333333703, 0.3219752754296894559, 0.3333333333333333703, 0.3219752754296894559, 0.3333333333333333703, 0.3219752754296894559, 0.3333333333333333703, 0.3219752754296894559, 0.3333333333333333703, 0.3219752754296894559, 0.3333333333333333703, 0.3219752754296894559, 0.3333333333333333703, 0.3219752754296894559, 0.3333333333333333703, 0.3219752754296894559, 0.3333333333333333703, 0.3219752754296894559, 0.3333333333333333703, 0.3219752754296894559, 0.3333333333333333703, 0.3219752754296894559, 0.3333333333333333703, 0.3219752754296894559, 0.3333333333333333703, 0.3219752754296894559, 0.3333333333333333703, 0.3219752754296894559, 0.3333333333333333703, 0.3219752754296894559, 0.3333333333333333703, 0.3219752754296894559, 0.3333333333333333703, 0.3219752754296894559, 0.3333333333333333703, 0.3219752754296894559, 0.3333333333333333703, 0.3219752754296894559, 0.3333333333333333703, 0.3219752754296894559, 0.3333333333333333703, 0.3219752754296894559, 0.3333333333333333703, 0.3219752754296894559, 0.3333333333333333703, 0.3219752754296894559, 0.3333333333333333703, 0.3219752754296894559, 0.3333333333333333703, 0.3219752754296894559, 0.3333333333333333703, 0.3219752754296894559, 0.3333333333333333703, 0.3219752754296894559, 0.3333333333333333703, 0.3219752754296894559, 0.3333333333333333703, 0.3219752754296894559, 0.3333333333333333703, 0.3219752754296894559, 0.3333333333333333703, 0.3219752754296894559, 0.3333333333333333703, 0.3219752754296894559, 0.3333333333333333703, 0.3219752754296894559, 0.3333333333333333703, 0.3219752754296894559, 0.3333333333333333703, 0.3219752754296894559, 0.3333333333333333703, 0.3219752754296894559, 0.3333333333333333703, 0.3219752754296894559, 0.3333333333333333703),
 ( 1.000000000000000000, 0.9659258262890683122, 1.000000000000000000, 0.9659258262890683122, 1.000000000000000000, 0.9659258262890683122, 1.000000000000000000, 0.9659258262890683122, 1.000000000000000000, 0.9659258262890683122, 1.000000000000000000, 0.9659258262890683122, 1.000000000000000000, 0.9659258262890683122, 1.000000000000000000, 0.9659258262890683122, 1.000000000000000000, 0.9659258262890683122, 1.000000000000000000, 0.9659258262890683122, 1.000000000000000000, 0.9659258262890683122, 1.000000000000000000, 0.9659258262890683122, 1.000000000000000000, 0.9659258262890683122, 1.000000000000000000, 0.9659258262890683122, 1.000000000000000000, 0.9659258262890683122, 1.000000000000000000, 0.9659258262890683122, 1.000000000000000000, 0.9659258262890683122, 1.000000000000000000, 0.9659258262890683122, 1.000000000000000000, 0.9659258262890683122, 1.000000000000000000, 0.9659258262890683122, 1.000000000000000000, 0.9659258262890683122, 1.000000000000000000, 0.9659258262890683122, 1.000000000000000000, 0.9659258262890683122, 1.000000000000000000, 0.9659258262890683122, 1.000000000000000000, 0.9659258262890683122, 1.000000000000000000, 0.9659258262890683122, 1.000000000000000000, 0.9659258262890683122, 1.000000000000000000, 0.9659258262890683122, 1.000000000000000000, 0.9659258262890683122, 1.000000000000000000, 0.9659258262890683122, 1.000000000000000000, 0.9659258262890683122, 1.000000000000000000, 0.9659258262890683122, 1.000000000000000000, 0.9659258262890683122, 1.000000000000000000, 0.9659258262890683122, 1.000000000000000000, 0.9659258262890683122, 1.000000000000000000, 0.9659258262890683122, 1.000000000000000000, 0.9659258262890683122, 1.000000000000000000, 0.9659258262890683122, 1.000000000000000000, 0.9659258262890683122, 1.000000000000000000, 0.9659258262890683122, 1.000000000000000000, 0.9659258262890683122, 1.000000000000000000, 0.9659258262890683122, 1.000000000000000000, 0.9659258262890683122, 1.000000000000000000, 0.9659258262890683122, 1.000000000000000000, 0.9659258262890683122, 1.000000000000000000, 0.9659258262890683122, 1.000000000000000000, 0.9659258262890683122, 1.000000000000000000, 0.9659258262890683122, 1.000000000000000000, 0.9659258262890683122, 1.000000000000000000, 0.9659258262890683122, 1.000000000000000000, 0.9659258262890683122, 1.000000000000000000, 0.9659258262890683122, 1.000000000000000000, 0.9659258262890683122, 1.000000000000000000, 0.9659258262890683122, 1.000000000000000000, 0.9659258262890683122, 1.000000000000000000, 0.9659258262890683122, 1.000000000000000000, 0.9659258262890683122, 1.000000000000000000, 0.9659258262890683122, 1.000000000000000000, 0.9659258262890683122, 1.000000000000000000, 0.9659258262890683122, 1.000000000000000000, 0.9659258262890683122, 1.000000000000000000, 0.9659258262890683122, 1.000000000000000000, 0.9659258262890683122, 1.000000000000000000, 0.9659258262890683122, 1.000000000000000000, 0.9659258262890683122, 1.000000000000000000, 0.9659258262890683122, 1.000000000000000000, 0.9659258262890683122, 1.000000000000000000, 0.9659258262890683122, 1.000000000000000000, 0.9659258262890683122, 1.000000000000000000, 0.9659258262890683122, 1.000000000000000000, 0.9659258262890683122, 1.000000000000000000, 0.9659258262890683122, 1.000000000000000000, 0.9659258262890683122, 1.000000000000000000, 0.9659258262890683122, 1.000000000000000000, 0.9659258262890683122, 1.000000000000000000, 0.9659258262890683122, 1.000000000000000000, 0.9659258262890683122, 1.000000000000000000, 0.9659258262890683122, 1.000000000000000000, 0.9659258262890683122, 1.000000000000000000, 0.9659258262890683122, 1.000000000000000000, 0.9659258262890683122, 1.000000000000000000, 0.9659258262890683122, 1.000000000000000000, 0.9659258262890683122, 1.000000000000000000, 0.9659258262890683122, 1.000000000000000000, 0.9659258262890683122, 1.000000000000000000, 0.9659258262890683122, 1.000000000000000000, 0.9659258262890683122, 1.000000000000000000, 0.9659258262890683122, 1.000000000000000000, 0.9659258262890683122, 1.000000000000000000, 0.9659258262890683122, 1.000000000000000000, 0.9659258262890683122, 1.000000000000000000, 0.9659258262890683122, 1.000000000000000000, 0.9659258262890683122, 1.000000000000000000, 0.9659258262890683122, 1.000000000000000000, 0.9659258262890683122, 1.000000000000000000, 0.9659258262890683122, 1.000000000000000000, 0.9659258262890683122, 1.000000000000000000, 0.9659258262890683122, 1.000000000000000000, 0.9659258262890683122, 1.000000000000000000, 0.9659258262890683122, 1.000000000000000000, 0.9659258262890683122, 1.000000000000000000, 0.9659258262890683122, 1.000000000000000000, 0.9659258262890683122, 1.000000000000000000, 0.9659258262890683122, 1.000000000000000000, 0.9659258262890683122, 1.000000000000000000, 0.9659258262890683122, 1.000000000000000000, 0.9659258262890683122, 1.000000000000000000, 0.9659258262890683122, 1.000000000000000000, 0.9659258262890683122, 1.000000000000000000, 0.9659258262890683122, 1.000000000000000000, 0.9659258262890683122, 1.000000000000000000, 0.9659258262890683122, 1.000000000000000000, 0.9659258262890683122, 1.000000000000000000, 0.9659258262890683122, 1.000000000000000000, 0.9659258262890683122, 1.000000000000000000, 0.9659258262890683122, 1.000000000000000000, 0.9659258262890683122, 1.000000000000000000, 0.9659258262890683122, 1.000000000000000000, 0.9659258262890683122, 1.000000000000000000, 0.9659258262890683122, 1.000000000000000000, 0.9659258262890683122, 1.000000000000000000, 0.9659258262890683122, 1.000000000000000000, 0.9659258262890683122, 1.000000000000000000, 0.9659258262890683122, 1.000000000000000000, 0.9659258262890683122, 1.000000000000000000, 0.9659258262890683122, 1.000000000000000000, 0.9659258262890683122, 1.000000000000000000, 0.9659258262890683122, 1.000000000000000000, 0.9659258262890683122, 1.000000000000000000, 0.9659258262890683122, 1.000000000000000000, 0.9659258262890683122, 1.000000000000000000, 0.9659258262890683122, 1.000000000000000000, 0.9659258262890683122, 1.000000000000000000, 0.9659258262890683122, 1.000000000000000000, 0.9659258262890683122, 1.000000000000000000, 0.9659258262890683122, 1.000000000000000000, 0.9659258262890683122, 1.000000000000000000, 0.9659258262890683122, 1.000000000000000000, 0.9659258262890683122, 1.000000000000000000, 0.9659258262890683122, 1.000000000000000000, 0.9659258262890683122, 1.000000000000000000, 0.9659258262890683122, 1.000000000000000000, 0.9659258262890683122, 1.000000000000000000, 0.9659258262890683122, 1.000000000000000000, 0.9659258262890683122, 1.000000000000000000, 0.9659258262890683122, 1.000000000000000000, 0.9659258262890683122, 1.000000000000000000, 0.9659258262890683122, 1.000000000000000000, 0.9659258262890683122, 1.000000000000000000, 0.9659258262890683122, 1.000000000000000000, 0.9659258262890683122, 1.000000000000000000, 0.9659258262890683122, 1.000000000000000000, 0.9659258262890683122, 1.000000000000000000, 0.9659258262890683122, 1.000000000000000000, 0.9659258262890683122, 1.000000000000000000, 0.9659258262890683122, 1.000000000000000000, 0.9659258262890683122, 1.000000000000000000, 0.9659258262890683122, 1.000000000000000000, 0.9659258262890683122, 1.000000000000000000, 0.9659258262890683122, 1.000000000000000000, 0.9659258262890683122, 1.000000000000000000, 0.9659258262890683122, 1.000000000000000000, 0.9659258262890683122, 1.000000000000000000, 0.9659258262890683122, 1.000000000000000000, 0.9659258262890683122, 1.000000000000000000, 0.9659258262890683122, 1.000000000000000000, 0.9659258262890683122, 1.000000000000000000, 0.9659258262890683122, 1.000000000000000000, 0.9659258262890683122, 1.000000000000000000, 0.9659258262890683122, 1.000000000000000000, 0.9659258262890683122, 1.000000000000000000, 0.9659258262890683122, 1.000000000000000000, 0.9659258262890683122, 1.000000000000000000, 0.9659258262890683122, 1.000000000000000000, 0.9659258262890683122, 1.000000000000000000, 0.9659258262890683122, 1.000000000000000000, 0.9659258262890683122, 1.000000000000000000, 0.9659258262890683122, 1.000000000000000000, 0.9659258262890683122, 1.000000000000000000, 0.9659258262890683122, 1.000000000000000000, 0.9659258262890683122, 1.000000000000000000, 0.9659258262890683122, 1.000000000000000000, 0.9659258262890683122, 1.000000000000000000, 0.9659258262890683122, 1.000000000000000000, 0.9659258262890683122, 1.000000000000000000, 0.9659258262890683122, 1.000000000000000000, 0.9659258262890683122, 1.000000000000000000, 0.9659258262890683122, 1.000000000000000000, 0.9659258262890683122, 1.000000000000000000, 0.9659258262890683122, 1.000000000000000000, 0.9659258262890683122, 1.000000000000000000, 0.9659258262890683122, 1.000000000000000000, 0.9659258262890683122, 1.000000000000000000, 0.9659258262890683122, 1.000000000000000000, 0.9659258262890683122, 1.000000000000000000, 0.9659258262890683122, 1.000000000000000000, 0.9659258262890683122, 1.000000000000000000, 0.9659258262890683122, 1.000000000000000000, 0.9659258262890683122, 1.000000000000000000, 0.9659258262890683122, 1.000000000000000000, 0.9659258262890683122, 1.000000000000000000, 0.9659258262890683122, 1.000000000000000000, 0.9659258262890683122, 1.000000000000000000, 0.9659258262890683122, 1.000000000000000000, 0.9659258262890683122, 1.000000000000000000, 0.9659258262890683122, 1.000000000000000000, 0.9659258262890683122, 1.000000000000000000, 0.9659258262890683122, 1.000000000000000000, 0.9659258262890683122, 1.000000000000000000, 0.9659258262890683122, 1.000000000000000000, 0.9659258262890683122, 1.000000000000000000, 0.9659258262890683122, 1.000000000000000000, 0.9659258262890683122, 1.000000000000000000, 0.9659258262890683122, 1.000000000000000000, 0.9659258262890683122, 1.000000000000000000, 0.9659258262890683122, 1.000000000000000000, 0.9659258262890683122, 1.000000000000000000, 0.9659258262890683122, 1.000000000000000000, 0.9659258262890683122, 1.000000000000000000, 0.9659258262890683122, 1.000000000000000000, 0.9659258262890683122, 1.000000000000000000, 0.9659258262890683122, 1.000000000000000000, 0.9659258262890683122, 1.000000000000000000, 0.9659258262890683122, 1.000000000000000000, 0.9659258262890683122, 1.000000000000000000, 0.9659258262890683122, 1.000000000000000000, 0.9659258262890683122, 1.000000000000000000, 0.9659258262890683122, 1.000000000000000000) ) ) 
 REPRESENTATION_ITEM ( '' )  SURFACE ( )  );
#188117 = CARTESIAN_POINT ( 'NONE',  ( 4.483927247898545687, 16.52544592524342804, 99.79057627198103830 ) ) ;
#188118 = CARTESIAN_POINT ( 'NONE',  ( 19.02544592524343514, -5.153800228976328945, 103.5405762719809957 ) ) ;
#188119 = CARTESIAN_POINT ( 'NONE',  ( -14.29746914071049879, 8.314922557960819915, 55.83224293864770260 ) ) ;
#188120 = CARTESIAN_POINT ( 'NONE',  ( -16.53943276465976808, -0.05219959533934237506, 108.7510903946857042 ) ) ;
#188121 = CARTESIAN_POINT ( 'NONE',  ( 19.02544592524343514, -5.153800228976328945, 53.54057627198102409 ) ) ;
#188122 = CARTESIAN_POINT ( 'NONE',  ( -5.153800228976328057, -19.02544592524343514, 37.29057627198102409 ) ) ;
#188123 = CARTESIAN_POINT ( 'NONE',  ( 18.62759615963271287, -10.81492255796078972, 43.33224293864769550 ) ) ;
#188124 = CARTESIAN_POINT ( 'NONE',  ( -0.05219959533936034679, 19.03943276465977164, 27.50109039468566507 ) ) ;
#188126 = CARTESIAN_POINT ( 'NONE',  ( 8.224510206698953496, -14.34966873604960469, 37.91557627198102409 ) ) ;
#188125 = DIRECTION ( 'NONE',  ( -0.1178549842436473205, -0.9930308165857339997, 6.133374237849951452E-17 ) ) ;
#188127 = CARTESIAN_POINT ( 'NONE',  ( 10.72451020669871369, 18.67979575497193778, 42.08442372801901854 ) ) ;
#188128 = CARTESIAN_POINT ( 'NONE',  ( 24.74823625077140932, -6.005039613785480235, 168.8763313249075395 ) ) ;
#188129 = CARTESIAN_POINT ( 'NONE',  ( -0.05219959533934338120, 16.53943276465976808, 52.50109039468567573 ) ) ;
#188130 = CARTESIAN_POINT ( 'NONE',  ( -19.03943276465977164, -0.05219959533935918106, 58.75109039468566863 ) ) ;
#188131 = EDGE_CURVE ( 'NONE', #51008, #88773, #185245, .T. ) ;
#188132 = CARTESIAN_POINT ( 'NONE',  ( 14.29746914071049879, -8.314922557960816363, 23.33224293864769194 ) ) ;
#188133 = CARTESIAN_POINT ( 'NONE',  ( -19.34837522270364474, -5.499999999999852562, 75.86337684832575690 ) ) ;
#188134 = CARTESIAN_POINT ( 'NONE',  ( 12.14591786802327356, -12.06949235617739191, 110.6260903946857042 ) ) ;
#188135 = CARTESIAN_POINT ( 'NONE',  ( 0.05219959533909260263, 19.03943276465977164, 39.99890960531436690 ) ) ;
#188136 = CARTESIAN_POINT ( 'NONE',  ( -9.474510206698964154, 16.51473224551069663, 65.41557627198102409 ) ) ;
#188137 = CARTESIAN_POINT ( 'NONE',  ( 9.564922557960805705, 16.46253265017160317, 24.58224293864769194 ) ) ;
#188138 = CARTESIAN_POINT ( 'NONE',  ( -21.55341960407619339, 5.719274019375674811, 38.54275706135234714 ) ) ;
#188139 = CARTESIAN_POINT ( 'NONE',  ( 19.03943276465977164, -0.05219959533909143690, 43.74890960531435979 ) ) ;
#188140 = CARTESIAN_POINT ( 'NONE',  ( 17.49999999999999645, 5.500000000000009770, 58.78230962303567253 ) ) ;
#188141 = CARTESIAN_POINT ( 'NONE',  ( -16.46253265017160317, 9.564922557960807481, 50.83224293864770260 ) ) ;
#188142 = CARTESIAN_POINT ( 'NONE',  ( 10.72451020669898902, -18.67979575497178502, 27.91557627198103830 ) ) ;
#188144 = CARTESIAN_POINT ( 'NONE',  ( 12.14591786802309770, 12.06949235617756955, 99.37390960531436690 ) ) ;
#188143 = CARTESIAN_POINT ( 'NONE',  ( -0.05219959533937732626, 21.53943276465977519, 62.50109039468568284 ) ) ;
#188145 = CARTESIAN_POINT ( 'NONE',  ( 21.55341960407610458, 5.719274019375980345, 23.95724293864769550 ) ) ;
#188146 = CARTESIAN_POINT ( 'NONE',  ( 16.53943276465976808, 0.05219959533934440121, 71.25109039468568994 ) ) ;
#188147 = CARTESIAN_POINT ( 'NONE',  ( -5.823673210054431948, 21.52544592524334988, 92.70942372801901854 ) ) ;
#188148 = CARTESIAN_POINT ( 'NONE',  ( -16.53943276465976808, -0.05219959533934237506, 48.75109039468568284 ) ) ;
#188149 = CARTESIAN_POINT ( 'NONE',  ( 16.51473224551069308, 9.474510206698969483, 89.16557627198103830 ) ) ;
#188150 = CARTESIAN_POINT ( 'NONE',  ( -8.314922557961024197, 14.29746914071037800, 37.91775706135235424 ) ) ;
#188151 = CARTESIAN_POINT ( 'NONE',  ( -12.14591786802326823, 12.06949235617739902, 23.12609039468567573 ) ) ;
#188152 = CARTESIAN_POINT ( 'NONE',  ( 16.52544592524335698, 4.483927247898782831, 96.45942372801901854 ) ) ;
#188153 = CARTESIAN_POINT ( 'NONE',  ( 21.52544592524334988, 5.823673210054432836, 51.45942372801901854 ) ) ;
#188154 = CARTESIAN_POINT ( 'NONE',  ( 13.97604488694548053, -13.89961937509957401, 100.6260903946856615 ) ) ;
#188155 = CARTESIAN_POINT ( 'NONE',  ( 0.05219959533907565091, 21.53943276465977519, 114.9989096053143669 ) ) ;
#188157 = CARTESIAN_POINT ( 'NONE',  ( -13.97604488694547697, 13.89961937509957934, 103.1260903946856473 ) ) ;
#188156 = CARTESIAN_POINT ( 'NONE',  ( -12.14591786802309592, -12.06949235617757132, 106.8739096053143811 ) ) ;
#188158 = CARTESIAN_POINT ( 'NONE',  ( 12.14591786802327356, -12.06949235617739191, 75.62609039468567573 ) ) ;
#188159 = CARTESIAN_POINT ( 'NONE',  ( -17.50000000000000711, 5.622605283950838029, 43.68792689403891671 ) ) ;
#188160 = CARTESIAN_POINT ( 'NONE',  ( 5.153800228976615827, -19.02544592524334988, 90.20942372801900433 ) ) ;
#188161 = CARTESIAN_POINT ( 'NONE',  ( 0.05219959533910956823, 16.53943276465976808, 39.99890960531436690 ) ) ;
#188162 = CARTESIAN_POINT ( 'NONE',  ( -8.314922557960811034, -14.29746914071050412, 42.08224293864769550 ) ) ;
#188163 = CARTESIAN_POINT ( 'NONE',  ( -8.224510206698948167, 14.34966873604960824, 95.41557627198102409 ) ) ;
#188165 = CARTESIAN_POINT ( 'NONE',  ( -16.81555441253553695, 7.025013491695484724, 90.63685445334257906 ) ) ;
#188164 = CARTESIAN_POINT ( 'NONE',  ( -13.89961937509957401, -13.97604488694547875, 29.37609039468565797 ) ) ;
#188166 = CARTESIAN_POINT ( 'NONE',  ( -21.52544592524334988, -5.823673210054445271, 33.95942372801901143 ) ) ;
#188167 = CARTESIAN_POINT ( 'NONE',  ( -5.049401038297874678, -19.05341960407617918, 99.79275706135234714 ) ) ;
#188168 = PLANE ( 'NONE',  #130941 ) ;
#188169 = CARTESIAN_POINT ( 'NONE',  ( -19.05341960407611168, -5.049401038298163336, 86.45724293864769550 ) ) ;
#188170 = CARTESIAN_POINT ( 'NONE',  ( 5.153800228976335163, 19.02544592524342804, 94.79057627198103830 ) ) ;
#188171 = CARTESIAN_POINT ( 'NONE',  ( -5.823673210054116645, -21.52544592524344225, 52.29057627198102409 ) ) ;
#188172 = CARTESIAN_POINT ( 'NONE',  ( -0.05219959533910754901, -16.53943276465976808, 92.49890960531436690 ) ) ;
#188173 = CARTESIAN_POINT ( 'NONE',  ( 19.03943276465977164, -0.05219959533909143690, 73.74890960531435269 ) ) ;
#188174 = CARTESIAN_POINT ( 'NONE',  ( -16.46253265017160317, 9.564922557960807481, 30.83224293864769550 ) ) ;
#188175 = CARTESIAN_POINT ( 'NONE',  ( -18.67979575497193778, 10.72451020669871902, 38.33442372801900433 ) ) ;
#188176 = CARTESIAN_POINT ( 'NONE',  ( -21.52544592524334988, -5.823673210054445271, 68.95942372801901854 ) ) ;
#188177 = EDGE_CURVE ( 'NONE', #132572, #157648, #169863, .T. ) ;
#188178 = CARTESIAN_POINT ( 'NONE',  ( 12.06949235617739724, 12.14591786802326823, 86.87609039468568994 ) ) ;
#188179 = CARTESIAN_POINT ( 'NONE',  ( 21.55341960407619695, -5.719274019375665929, 36.04275706135234714 ) ) ;
#188180 = CARTESIAN_POINT ( 'NONE',  ( -10.81492255796105439, 18.62759615963255655, 32.91775706135234714 ) ) ;
#188182 = CARTESIAN_POINT ( 'NONE',  ( -9.564922557960796823, -16.46253265017161027, 77.08224293864769550 ) ) ;
#188181 = CARTESIAN_POINT ( 'NONE',  ( 19.05341960407617918, -5.049401038297876454, 51.04275706135231871 ) ) ;
#188183 = CARTESIAN_POINT ( 'NONE',  ( 10.81492255796106328, -18.62759615963255655, 80.41775706135234714 ) ) ;
#188184 = CARTESIAN_POINT ( 'NONE',  ( 21.53943276465977519, -0.05219959533907433946, 78.74890960531436690 ) ) ;
#188185 = CARTESIAN_POINT ( 'NONE',  ( 4.379528057220339221, -16.55341960407611168, 47.70724293864770260 ) ) ;
#188187 = CARTESIAN_POINT ( 'NONE',  ( -19.02544592524334988, -5.153800228976617603, 28.95942372801900433 ) ) ;
#188186 = CARTESIAN_POINT ( 'NONE',  ( -0.05219959533937732626, 21.53943276465977519, 107.5010903946856899 ) ) ;
#188188 = CARTESIAN_POINT ( 'NONE',  ( -4.379528057220328563, 16.55341960407611168, 70.20724293864769550 ) ) ;
#188189 = CARTESIAN_POINT ( 'NONE',  ( -4.483927247898539470, -16.52544592524342804, 112.2905762719810241 ) ) ;
#188190 = CARTESIAN_POINT ( 'NONE',  ( 9.564922557961047289, -16.46253265017146816, 70.41775706135233293 ) ) ;
#188191 = CARTESIAN_POINT ( 'NONE',  ( -16.52544592524342804, 4.483927247898546575, 36.04057627198102409 ) ) ;
#188192 = CARTESIAN_POINT ( 'NONE',  ( -0.05219959533937732626, 21.53943276465977519, 77.50109039468567573 ) ) ;
#188193 = CARTESIAN_POINT ( 'NONE',  ( -19.05341960407611168, -5.049401038298163336, 81.45724293864769550 ) ) ;
#188194 = CARTESIAN_POINT ( 'NONE',  ( 9.474510206698729675, 16.51473224551082808, 42.08442372801900433 ) ) ;
#188195 = CARTESIAN_POINT ( 'NONE',  ( 15.80617190586746368, 15.72974639402197994, 64.37390960531435269 ) ) ;
#188196 = CARTESIAN_POINT ( 'NONE',  ( 0.05219959533907565091, 21.53943276465977519, 114.9989096053143669 ) ) ;
#188197 = CARTESIAN_POINT ( 'NONE',  ( -5.049401038297874678, -19.05341960407617918, 109.7927570613523187 ) ) ;
#188198 = CARTESIAN_POINT ( 'NONE',  ( 14.29746914071037800, 8.314922557961029526, 76.66775706135234714 ) ) ;
#188200 = CARTESIAN_POINT ( 'NONE',  ( 15.72974639402199770, -15.80617190586745480, 113.1239096053143953 ) ) ;
#188199 = CARTESIAN_POINT ( 'NONE',  ( 16.18388926212241685, 7.379444403734408908, 62.93953151366150678 ) ) ;
#188201 = CARTESIAN_POINT ( 'NONE',  ( 16.52544592524342804, -4.483927247898539470, 98.54057627198105251 ) ) ;
#188202 = CARTESIAN_POINT ( 'NONE',  ( 3.556970738554033499E-15, -38.81732327939057825, -10.62499999726881050 ) ) ;
#188203 = CARTESIAN_POINT ( 'NONE',  ( 4.483927247898790824, -16.52544592524335698, 40.20942372801901854 ) ) ;
#188204 = CARTESIAN_POINT ( 'NONE',  ( 18.62759615963271287, -10.81492255796078972, 63.33224293864770260 ) ) ;
#188205 = CARTESIAN_POINT ( 'NONE',  ( 14.34966873604972726, -8.224510206698740333, 100.8344237280190185 ) ) ;
#188206 = CARTESIAN_POINT ( 'NONE',  ( -19.03943276465977164, 0.05219959533909376836, 36.24890960531436690 ) ) ;
#188207 = CARTESIAN_POINT ( 'NONE',  ( 12.14591786802327356, -12.06949235617739191, 70.62609039468567573 ) ) ;
#188208 = CARTESIAN_POINT ( 'NONE',  ( 13.89961937509957401, 13.97604488694547697, 66.87609039468567573 ) ) ;
#188209 = CARTESIAN_POINT ( 'NONE',  ( 21.53943276465977519, 0.05219959533937863772, 46.25109039468567573 ) ) ;
#188210 = CARTESIAN_POINT ( 'NONE',  ( -21.53943276465977519, 0.05219959533907696930, 56.24890960531436690 ) ) ;
#188211 = CARTESIAN_POINT ( 'NONE',  ( -16.52544592524335698, -4.483927247898792601, 98.95942372801903275 ) ) ;
#188212 = CARTESIAN_POINT ( 'NONE',  ( -21.52544592524334988, -5.823673210054445271, 83.95942372801900433 ) ) ;
#188213 = CARTESIAN_POINT ( 'NONE',  ( -5.823673210054116645, -21.52544592524344225, 47.29057627198103120 ) ) ;
#188214 = CARTESIAN_POINT ( 'NONE',  ( -15.80617190586745835, -15.72974639402198527, 31.87390960531435979 ) ) ;
#188215 = ORIENTED_EDGE ( 'NONE', *, *, #153559, .T. ) ;
#188216 = CARTESIAN_POINT ( 'NONE',  ( 16.52544592524335698, 4.483927247898782831, 81.45942372801900433 ) ) ;
#188217 = CARTESIAN_POINT ( 'NONE',  ( -10.81492255796078084, -18.62759615963271287, 42.08224293864769550 ) ) ;
#188218 = ORIENTED_EDGE ( 'NONE', *, *, #84003, .F. ) ;
#188219 = CARTESIAN_POINT ( 'NONE',  ( 13.89961937509977652, -13.97604488694527269, 98.12390960531433848 ) ) ;
#188220 = DIRECTION ( 'NONE',  ( -0.8164965809277260345, 0.000000000000000000, -0.5773502691896258421 ) ) ;
#188221 = CARTESIAN_POINT ( 'NONE',  ( -9.474510206698964154, 16.51473224551069663, 30.41557627198102054 ) ) ;
#188222 = CARTESIAN_POINT ( 'NONE',  ( 15.80617190586746368, 15.72974639402197994, 59.37390960531436690 ) ) ;
#188223 = CARTESIAN_POINT ( 'NONE',  ( 4.379528057220092307, 16.55341960407617563, 97.29275706135234714 ) ) ;
#188224 = CARTESIAN_POINT ( 'NONE',  ( -10.81492255796105439, 18.62759615963255655, 47.91775706135234714 ) ) ;
#188225 = CARTESIAN_POINT ( 'NONE',  ( -13.97604488694547697, 13.89961937509957934, 108.1260903946856331 ) ) ;
#188226 = CARTESIAN_POINT ( 'NONE',  ( -0.05219959533910754901, -16.53943276465976808, 97.49890960531436690 ) ) ;
#188227 = CARTESIAN_POINT ( 'NONE',  ( -16.52544592524335698, -4.483927247898792601, 18.95942372801901143 ) ) ;
#188228 = CARTESIAN_POINT ( 'NONE',  ( -0.05219959533909027116, -19.03943276465977164, 37.49890960531436690 ) ) ;
#188229 = CARTESIAN_POINT ( 'NONE',  ( 1.053409450988196827, 23.87225889828500058, -54.54687963008630192 ) ) ;
#188230 = CARTESIAN_POINT ( 'NONE',  ( 9.564922557960805705, 16.46253265017160317, 94.58224293864769550 ) ) ;
#188231 = CARTESIAN_POINT ( 'NONE',  ( 4.379528057220092307, 16.55341960407617563, 82.29275706135234714 ) ) ;
#188232 = CARTESIAN_POINT ( 'NONE',  ( 15.80617190586769283, -15.72974639402175789, 100.6260903946857184 ) ) ;
#188233 = CARTESIAN_POINT ( 'NONE',  ( 5.719274019375991003, -21.55341960407610458, 67.70724293864769550 ) ) ;
#188234 = CARTESIAN_POINT ( 'NONE',  ( -16.52544592524335698, -4.483927247898792601, 88.95942372801901854 ) ) ;
#188235 = CARTESIAN_POINT ( 'NONE',  ( -0.05219959533936034679, 19.03943276465977164, 77.50109039468566152 ) ) ;
#188236 = CARTESIAN_POINT ( 'NONE',  ( 9.564922557960805705, 16.46253265017160317, 39.58224293864768839 ) ) ;
#188237 = CARTESIAN_POINT ( 'NONE',  ( 13.97604488694527802, 13.89961937509977652, 84.37390960531433848 ) ) ;
#188238 = CARTESIAN_POINT ( 'NONE',  ( 19.05341960407611168, 5.049401038298154454, 28.95724293864769550 ) ) ;
#188239 = CARTESIAN_POINT ( 'NONE',  ( -19.02544592524334988, -5.153800228976617603, 73.95942372801900433 ) ) ;
#188240 = CARTESIAN_POINT ( 'NONE',  ( 21.92083080610931489, -8.096106818373623781, 172.4353877980944674 ) ) ;
#188241 = CARTESIAN_POINT ( 'NONE',  ( 9.564922557960805705, 16.46253265017160317, 109.5822429386476955 ) ) ;
#188242 = CARTESIAN_POINT ( 'NONE',  ( -0.05219959533910754901, -16.53943276465976808, 62.49890960531436690 ) ) ;
#188243 = CARTESIAN_POINT ( 'NONE',  ( 21.52544592524344225, -5.823673210054117533, 58.54057627198103120 ) ) ;
#188244 = PLANE ( 'NONE',  #164368 ) ;
#188245 = CIRCLE ( 'NONE', #165314, 5.000000000000000000 ) ;
#188246 = CARTESIAN_POINT ( 'NONE',  ( 19.02544592524334988, 5.153800228976608722, 26.45942372801899722 ) ) ;
#188247 = SURFACE_STYLE_USAGE ( .BOTH. , #142713 ) ;
#188249 = CARTESIAN_POINT ( 'NONE',  ( 5.153800228976335163, 19.02544592524342804, 74.79057627198103830 ) ) ;
#188248 = CARTESIAN_POINT ( 'NONE',  ( -13.89961937509977652, 13.97604488694528158, 65.62390960531436690 ) ) ;
#188250 = CARTESIAN_POINT ( 'NONE',  ( -8.224510206698735004, -14.34966873604973081, 49.58442372801901143 ) ) ;
#188251 = FACE_OUTER_BOUND ( 'NONE', #176100, .T. ) ;
#188252 = DIRECTION ( 'NONE',  ( 0.000000000000000000, 0.000000000000000000, 1.000000000000000000 ) ) ;
#188253 = CARTESIAN_POINT ( 'NONE',  ( 4.379528057220092307, 16.55341960407617563, 72.29275706135236135 ) ) ;
#188254 = DIRECTION ( 'NONE',  ( 0.000000000000000000, -0.000000000000000000, -1.000000000000000000 ) ) ;
#188255 = CARTESIAN_POINT ( 'NONE',  ( 8.224510206698742110, 14.34966873604972548, 72.08442372801899012 ) ) ;
#188256 = CARTESIAN_POINT ( 'NONE',  ( 4.483927247898790824, -16.52544592524335698, 35.20942372801901854 ) ) ;
#188258 = FACE_OUTER_BOUND ( 'NONE', #136044, .T. ) ;
#188257 = CARTESIAN_POINT ( 'NONE',  ( -16.46253265017160317, 9.564922557960807481, 55.83224293864769550 ) ) ;
#188259 = CARTESIAN_POINT ( 'NONE',  ( 21.53943276465977519, 0.05219959533937863772, 56.25109039468568284 ) ) ;
#188260 = CARTESIAN_POINT ( 'NONE',  ( -16.46253265017146816, -9.564922557961047289, 64.16775706135233293 ) ) ;
#188261 = CARTESIAN_POINT ( 'NONE',  ( 21.52544592524334988, 5.823673210054432836, 111.4594237280190328 ) ) ;
#188262 = CARTESIAN_POINT ( 'NONE',  ( -19.05341960407611168, -5.049401038298163336, 36.45724293864766707 ) ) ;
#188263 = CARTESIAN_POINT ( 'NONE',  ( 15.72974639402199770, -15.80617190586745480, 58.12390960531435979 ) ) ;
#188264 = CARTESIAN_POINT ( 'NONE',  ( 19.05341960407611168, 5.049401038298154454, 108.9572429386477097 ) ) ;
#188265 = CARTESIAN_POINT ( 'NONE',  ( -16.53943276465976808, 0.05219959533911058130, 101.2489096053143669 ) ) ;
#188266 = CARTESIAN_POINT ( 'NONE',  ( -8.314922557961024197, 14.29746914071037800, 37.91775706135235424 ) ) ;
#188267 = CARTESIAN_POINT ( 'NONE',  ( 8.314922557960818139, 14.29746914071049879, 24.58224293864768839 ) ) ;
#188268 = ORIENTED_EDGE ( 'NONE', *, *, #10280, .F. ) ;
#188269 = EDGE_CURVE ( 'NONE', #106915, #59419, #82664, .T. ) ;
#188270 = CARTESIAN_POINT ( 'NONE',  ( -21.55341960407610458, -5.719274019375992779, 96.45724293864770971 ) ) ;
#188271 = AXIS2_PLACEMENT_3D ( 'NONE', #51579, #127417, #94095 ) ;
#188273 = CARTESIAN_POINT ( 'NONE',  ( 38.00000000000000000, 12.34694845685046616, -8.899999999999996803 ) ) ;
#188272 = CARTESIAN_POINT ( 'NONE',  ( -16.53943276465976808, 0.05219959533911058130, 41.24890960531435269 ) ) ;
#188274 = CARTESIAN_POINT ( 'NONE',  ( -9.474510206698720793, -16.51473224551083518, 89.58442372801900433 ) ) ;
#188275 = CARTESIAN_POINT ( 'NONE',  ( 19.02544592524334988, 5.153800228976608722, 21.45942372801899012 ) ) ;
#188276 = CARTESIAN_POINT ( 'NONE',  ( -14.29746914071049879, 8.314922557960819915, 25.83224293864769194 ) ) ;
#188277 = CARTESIAN_POINT ( 'NONE',  ( 18.67979575497178502, 10.72451020669898547, 109.1655762719810383 ) ) ;
#188278 = CARTESIAN_POINT ( 'NONE',  ( 5.719274019375991003, -21.55341960407610458, 52.70724293864769550 ) ) ;
#188279 = CARTESIAN_POINT ( 'NONE',  ( 16.46253265017160672, -9.564922557960803928, 78.33224293864769550 ) ) ;
#188280 = CARTESIAN_POINT ( 'NONE',  ( -0.05219959533910754901, -16.53943276465976808, 37.49890960531436690 ) ) ;
#188281 = CARTESIAN_POINT ( 'NONE',  ( -19.03943276465977164, 0.05219959533909376836, 91.24890960531436690 ) ) ;
#188282 = ORIENTED_EDGE ( 'NONE', *, *, #105202, .F. ) ;
#188283 = CARTESIAN_POINT ( 'NONE',  ( 5.153800228976335163, 19.02544592524342804, 79.79057627198102409 ) ) ;
#188284 = CARTESIAN_POINT ( 'NONE',  ( -13.97604488694547697, 13.89961937509957934, 38.12609039468566152 ) ) ;
#188285 = CARTESIAN_POINT ( 'NONE',  ( -5.823673210054116645, -21.52544592524344225, 77.29057627198102409 ) ) ;
#188286 = CARTESIAN_POINT ( 'NONE',  ( -14.34966873604960291, -8.224510206698953496, 96.66557627198102409 ) ) ;
#188287 = CARTESIAN_POINT ( 'NONE',  ( -5.823673210054431948, 21.52544592524334988, 42.70942372801901854 ) ) ;
#188288 = CARTESIAN_POINT ( 'NONE',  ( -8.571926809382601320, -26.38167802310801591, 141.2750000027311899 ) ) ;
#188289 = CARTESIAN_POINT ( 'NONE',  ( 16.52544592524335698, 4.483927247898782831, 106.4594237280190328 ) ) ;
#188290 = CARTESIAN_POINT ( 'NONE',  ( -19.02544592524342804, 5.153800228976336051, 36.04057627198100988 ) ) ;
#188291 = CARTESIAN_POINT ( 'NONE',  ( -16.46253265017160317, 9.564922557960807481, 80.83224293864769550 ) ) ;
#188292 = CARTESIAN_POINT ( 'NONE',  ( -17.14385361876520264, -23.59649016807271593, 139.1750000027311955 ) ) ;
#188293 = CARTESIAN_POINT ( 'NONE',  ( 13.89961937509977652, -13.97604488694527269, 33.12390960531434558 ) ) ;
#188294 = CARTESIAN_POINT ( 'NONE',  ( 0.05219959533910956823, 16.53943276465976808, 49.99890960531437401 ) ) ;
#188295 = CARTESIAN_POINT ( 'NONE',  ( 5.719274019375673035, 21.55341960407619339, 72.29275706135236135 ) ) ;
#188297 = CARTESIAN_POINT ( 'NONE',  ( -14.29746914071037622, -8.314922557961029526, 74.16775706135231871 ) ) ;
#188296 = CARTESIAN_POINT ( 'NONE',  ( 28.03958666231585184, -24.95204343637638900, -18.68191426762921736 ) ) ;
#188298 = CARTESIAN_POINT ( 'NONE',  ( -19.02544592524342804, 5.153800228976336051, 51.04057627198103120 ) ) ;
#188299 = CARTESIAN_POINT ( 'NONE',  ( -19.03943276465977164, 0.05219959533909376836, 61.24890960531436690 ) ) ;
#188300 = EDGE_LOOP ( 'NONE', ( #105928, #46009, #133624, #17992, #91194, #12423, #50758, #177274 ) ) ;
#188301 = CARTESIAN_POINT ( 'NONE',  ( -0.05219959533937732626, 21.53943276465977519, 112.5010903946857042 ) ) ;
#188302 = CARTESIAN_POINT ( 'NONE',  ( -12.06949235617739369, -12.14591786802326823, 79.37609039468567573 ) ) ;
#188303 = CARTESIAN_POINT ( 'NONE',  ( -18.62759615963255300, -10.81492255796106328, 99.16775706135234714 ) ) ;
#188304 = CARTESIAN_POINT ( 'NONE',  ( 16.46253265017160672, -9.564922557960803928, 58.33224293864769550 ) ) ;
#188305 = CARTESIAN_POINT ( 'NONE',  ( 21.53943276465977519, -0.05219959533907433946, 28.74890960531435624 ) ) ;
#188306 = CARTESIAN_POINT ( 'NONE',  ( 13.97604488694548053, -13.89961937509957401, 110.6260903946856615 ) ) ;
#188307 = CARTESIAN_POINT ( 'NONE',  ( -21.53943276465977519, -0.05219959533937600094, 63.75109039468568284 ) ) ;
#188308 = CARTESIAN_POINT ( 'NONE',  ( 16.55341960407618274, -4.379528057220086978, 46.04275706135234714 ) ) ;
#188309 = CARTESIAN_POINT ( 'NONE',  ( 21.53943276465977519, -0.05219959533907433946, 103.7489096053143669 ) ) ;
#188310 = CARTESIAN_POINT ( 'NONE',  ( -19.02544592524334988, -5.153800228976617603, 98.95942372801900433 ) ) ;
#188311 = CARTESIAN_POINT ( 'NONE',  ( -16.51473224551069308, -9.474510206698971260, 76.66557627198103830 ) ) ;
#188312 = CARTESIAN_POINT ( 'NONE',  ( -13.89961937509957401, -13.97604488694547875, 104.3760903946856757 ) ) ;
#188313 = CARTESIAN_POINT ( 'NONE',  ( 0.05219959533934541429, -16.53943276465976808, 25.00109039468567218 ) ) ;
#188314 = CARTESIAN_POINT ( 'NONE',  ( 12.14591786802309770, 12.06949235617756955, 59.37390960531436690 ) ) ;
#188315 = CARTESIAN_POINT ( 'NONE',  ( -4.483927247898782831, 16.52544592524335698, 77.70942372801900433 ) ) ;
#188317 = CARTESIAN_POINT ( 'NONE',  ( 19.05341960407611168, 5.049401038298154454, 53.95724293864770260 ) ) ;
#188316 = CARTESIAN_POINT ( 'NONE',  ( 5.719274019375991003, -21.55341960407610458, 112.7072429386476955 ) ) ;
#188318 = CARTESIAN_POINT ( 'NONE',  ( -13.89961937509977652, 13.97604488694528158, 65.62390960531436690 ) ) ;
#188319 = CARTESIAN_POINT ( 'NONE',  ( 16.53943276465976808, 0.05219959533934440121, 66.25109039468567573 ) ) ;
#188320 = CARTESIAN_POINT ( 'NONE',  ( 17.81289503416610742, 24.51734667627700404, 147.5500000054623229 ) ) ;
#188321 = VERTEX_POINT ( 'NONE', #86778 ) ;
#188322 = CARTESIAN_POINT ( 'NONE',  ( 0.05219959533936267826, -19.03943276465977164, 20.00109039468567218 ) ) ;
#188323 = CARTESIAN_POINT ( 'NONE',  ( 9.474510206698971260, -16.51473224551069308, 37.91557627198102409 ) ) ;
#188324 = VERTEX_POINT ( 'NONE', #83768 ) ;
#188325 = CARTESIAN_POINT ( 'NONE',  ( 19.05341960407617918, -5.049401038297876454, 106.0427570613523471 ) ) ;
#188327 = CARTESIAN_POINT ( 'NONE',  ( -12.14591786802326823, 12.06949235617739902, 23.12609039468567573 ) ) ;
#188326 = CARTESIAN_POINT ( 'NONE',  ( -9.474510206698720793, -16.51473224551083518, 39.58442372801899722 ) ) ;
#188328 = CARTESIAN_POINT ( 'NONE',  ( 5.049401038298161559, -19.05341960407611168, 47.70724293864770260 ) ) ;
#188329 = CARTESIAN_POINT ( 'NONE',  ( -9.474510206698964154, 16.51473224551069663, 65.41557627198102409 ) ) ;
#188330 = CARTESIAN_POINT ( 'NONE',  ( 5.719274019375991003, -21.55341960407610458, 82.70724293864770971 ) ) ;
#188331 = CARTESIAN_POINT ( 'NONE',  ( -5.049401038298153566, 19.05341960407611168, 110.2072429386476671 ) ) ;
#188332 = VECTOR ( 'NONE', #97690, 1000.000000000000000 ) ;
#188333 = CARTESIAN_POINT ( 'NONE',  ( -5.049401038298153566, 19.05341960407611168, 45.20724293864769550 ) ) ;
#188334 = CARTESIAN_POINT ( 'NONE',  ( -17.97182807773872781, 5.499999999999960920, 93.53038844047289047 ) ) ;
#188335 = CARTESIAN_POINT ( 'NONE',  ( -9.564922557961040184, 16.46253265017147172, 97.91775706135233293 ) ) ;
#188336 = CARTESIAN_POINT ( 'NONE',  ( -8.314922557960811034, -14.29746914071050412, 72.08224293864769550 ) ) ;
#188337 = CARTESIAN_POINT ( 'NONE',  ( 19.05341960407617918, -5.049401038297876454, 26.04275706135233293 ) ) ;
#188338 = CARTESIAN_POINT ( 'NONE',  ( -8.224510206698948167, 14.34966873604960824, 65.41557627198102409 ) ) ;
#188339 = CARTESIAN_POINT ( 'NONE',  ( -0.05219959533937732626, 21.53943276465977519, 87.50109039468568994 ) ) ;
#188340 = CARTESIAN_POINT ( 'NONE',  ( -0.05219959533909027116, -19.03943276465977164, 32.49890960531435979 ) ) ;
#188341 = CARTESIAN_POINT ( 'NONE',  ( 15.80617190586769283, -15.72974639402175789, 85.62609039468568994 ) ) ;
#188343 = CARTESIAN_POINT ( 'NONE',  ( 15.72974639402176855, 15.80617190586768217, 76.87609039468567573 ) ) ;
#188342 = CARTESIAN_POINT ( 'NONE',  ( -16.53943276465976808, 0.05219959533911058130, 26.24890960531435624 ) ) ;
#188344 = CARTESIAN_POINT ( 'NONE',  ( -9.474510206698964154, 16.51473224551069663, 75.41557627198103830 ) ) ;
#188345 = ADVANCED_FACE ( 'NONE', ( #149457 ), #161626, .T. ) ;
#188346 = CARTESIAN_POINT ( 'NONE',  ( 21.52544592524334988, 5.823673210054432836, 41.45942372801901143 ) ) ;
#188347 = CARTESIAN_POINT ( 'NONE',  ( 16.51473224551069308, 9.474510206698969483, 79.16557627198103830 ) ) ;
#188348 = CARTESIAN_POINT ( 'NONE',  ( -12.06949235617756955, 12.14591786802309770, 100.6239096053143811 ) ) ;
#188349 = CARTESIAN_POINT ( 'NONE',  ( -14.29746914071049879, 8.314922557960819915, 60.83224293864769550 ) ) ;
#188350 = CARTESIAN_POINT ( 'NONE',  ( 21.53943276465977519, -0.05219959533907433946, 73.74890960531433848 ) ) ;
#188351 = CARTESIAN_POINT ( 'NONE',  ( -19.03943276465977164, 0.05219959533909376836, 81.24890960531436690 ) ) ;
#188352 = CARTESIAN_POINT ( 'NONE',  ( -0.05219959533907301413, -21.53943276465977519, 87.49890960531436690 ) ) ;
#188353 = CARTESIAN_POINT ( 'NONE',  ( 5.153800228976615827, -19.02544592524334988, 80.20942372801901854 ) ) ;
#188355 = CARTESIAN_POINT ( 'NONE',  ( 8.224510206698953496, -14.34966873604960469, 77.91557627198102409 ) ) ;
#188354 = CARTESIAN_POINT ( 'NONE',  ( -0.05219959533936034679, 19.03943276465977164, 27.50109039468566507 ) ) ;
#188356 = CARTESIAN_POINT ( 'NONE',  ( -10.72451020669898014, 18.67979575497178502, 50.41557627198103120 ) ) ;
#188357 = CARTESIAN_POINT ( 'NONE',  ( -24.49873734152929572, -24.99873734152903282, 4.646446609406721606 ) ) ;
#188359 = CARTESIAN_POINT ( 'NONE',  ( 22.44159573604009594, -16.30477369853687364, 148.1750000027311671 ) ) ;
#188358 = CARTESIAN_POINT ( 'NONE',  ( 14.29746914071037800, 8.314922557961029526, 96.66775706135234714 ) ) ;
#188360 = CARTESIAN_POINT ( 'NONE',  ( -9.474510206698720793, -16.51473224551083518, 104.5844237280190043 ) ) ;
#188361 = EDGE_CURVE ( 'NONE', #63287, #153996, #73052, .T. ) ;
#188362 = CARTESIAN_POINT ( 'NONE',  ( -8.314922557960811034, -14.29746914071050412, 67.08224293864770971 ) ) ;
#188363 = CARTESIAN_POINT ( 'NONE',  ( 6.691772886347784777, -1.197744245042889011, -62.38710104649955213 ) ) ;
#188364 = CARTESIAN_POINT ( 'NONE',  ( 5.049401038298161559, -19.05341960407611168, 67.70724293864769550 ) ) ;
#188365 = CARTESIAN_POINT ( 'NONE',  ( -8.224510206698948167, 14.34966873604960824, 50.41557627198103120 ) ) ;
#188366 = CARTESIAN_POINT ( 'NONE',  ( -9.474510206698964154, 16.51473224551069663, 95.41557627198102409 ) ) ;
#188368 = CARTESIAN_POINT ( 'NONE',  ( -5.049401038298153566, 19.05341960407611168, 65.20724293864765286 ) ) ;
#188367 = CARTESIAN_POINT ( 'NONE',  ( -16.46253265017146816, -9.564922557961047289, 89.16775706135234714 ) ) ;
#188369 = CARTESIAN_POINT ( 'NONE',  ( 13.97604488694527802, 13.89961937509977652, 84.37390960531433848 ) ) ;
#188370 = CARTESIAN_POINT ( 'NONE',  ( 5.153800228976335163, 19.02544592524342804, 89.79057627198102409 ) ) ;
#188371 = CARTESIAN_POINT ( 'NONE',  ( 21.55341960407610458, 5.719274019375980345, 58.95724293864770971 ) ) ;
#188372 = CARTESIAN_POINT ( 'NONE',  ( -8.314922557961024197, 14.29746914071037800, 52.91775706135235424 ) ) ;
#188373 = CARTESIAN_POINT ( 'NONE',  ( -5.049401038297874678, -19.05341960407618274, 104.7927570613523471 ) ) ;
#188374 = CARTESIAN_POINT ( 'NONE',  ( 9.474510206698971260, -16.51473224551069308, 67.91557627198102409 ) ) ;
#188375 = CARTESIAN_POINT ( 'NONE',  ( 21.53943276465977519, -0.05219959533907433946, 63.74890960531435979 ) ) ;
#188376 = CARTESIAN_POINT ( 'NONE',  ( 19.05341960407617918, -5.049401038297876454, 96.04275706135231871 ) ) ;
#188378 = CARTESIAN_POINT ( 'NONE',  ( 21.52544592524334988, 5.823673210054432836, 51.45942372801901854 ) ) ;
#188377 = CARTESIAN_POINT ( 'NONE',  ( -4.379528057220328563, 16.55341960407611168, 25.20724293864769550 ) ) ;
#188379 = CARTESIAN_POINT ( 'NONE',  ( -5.153800228976607833, 19.02544592524334988, 42.70942372801901143 ) ) ;
#188381 = CARTESIAN_POINT ( 'NONE',  ( -14.29746914071037622, -8.314922557961029526, 99.16775706135234714 ) ) ;
#188380 = CARTESIAN_POINT ( 'NONE',  ( -8.224510206698735004, -14.34966873604973081, 74.58442372801901854 ) ) ;
#188382 = CARTESIAN_POINT ( 'NONE',  ( 28.79475375365586132, 2.781246896534039337E-14, 147.2656553485624045 ) ) ;
#188383 = CARTESIAN_POINT ( 'NONE',  ( 4.483927247898790824, -16.52544592524335698, 85.20942372801901854 ) ) ;
#188384 = CARTESIAN_POINT ( 'NONE',  ( 16.53943276465976808, 0.05219959533934440121, 36.25109039468567573 ) ) ;
#188385 = CARTESIAN_POINT ( 'NONE',  ( 16.51473224551069308, 9.474510206698969483, 44.16557627198103120 ) ) ;
#188386 = CARTESIAN_POINT ( 'NONE',  ( -13.97604488694527625, -13.89961937509977652, 46.87390960531435979 ) ) ;
#188387 = CARTESIAN_POINT ( 'NONE',  ( -9.474510206698964154, 16.51473224551069663, 55.41557627198103120 ) ) ;
#188388 = CARTESIAN_POINT ( 'NONE',  ( 18.67979575497194134, -10.72451020669871369, 50.83442372801901143 ) ) ;
#188389 = CARTESIAN_POINT ( 'NONE',  ( 14.34966873604972726, -8.224510206698740333, 50.83442372801901143 ) ) ;
#188390 = CARTESIAN_POINT ( 'NONE',  ( 4.483927247898545687, 16.52544592524342804, 24.79057627198103120 ) ) ;
#188391 = CARTESIAN_POINT ( 'NONE',  ( 13.89961937509977652, -13.97604488694527269, 28.12390960531435624 ) ) ;
#188392 = CARTESIAN_POINT ( 'NONE',  ( 16.51473224551069308, 9.474510206698969483, 39.16557627198103120 ) ) ;
#188393 = CARTESIAN_POINT ( 'NONE',  ( 4.483927247898790824, -16.52544592524335698, 25.20942372801901854 ) ) ;
#188394 = CARTESIAN_POINT ( 'NONE',  ( -19.05341960407617563, 5.049401038297882671, 88.54275706135230450 ) ) ;
#188395 = CARTESIAN_POINT ( 'NONE',  ( -4.379528057220328563, 16.55341960407611168, 90.20724293864770971 ) ) ;
#188396 = CARTESIAN_POINT ( 'NONE',  ( 19.02544592524343514, -5.153800228976328945, 38.54057627198103120 ) ) ;
#188398 = CARTESIAN_POINT ( 'NONE',  ( 17.50000000000000000, 5.499999999999997335, 120.0000000000000142 ) ) ;
#188397 = CARTESIAN_POINT ( 'NONE',  ( 16.46253265017146816, 9.564922557961045513, 71.66775706135233293 ) ) ;
#188399 = CARTESIAN_POINT ( 'NONE',  ( -21.53943276465977519, -0.05219959533937600094, 73.75109039468567573 ) ) ;
#188400 = CARTESIAN_POINT ( 'NONE',  ( 8.314922557961029526, -14.29746914071037800, 50.41775706135235424 ) ) ;
#188401 = CARTESIAN_POINT ( 'NONE',  ( 2.500000000000000000, 1.178949249685212974, -2.042000000000001148 ) ) ;
#188402 = CARTESIAN_POINT ( 'NONE',  ( -15.72974639402197994, 15.80617190586746368, 35.62390960531437401 ) ) ;
#188403 = CARTESIAN_POINT ( 'NONE',  ( 12.06949235617739724, 12.14591786802326823, 26.87609039468567218 ) ) ;
#188404 = CARTESIAN_POINT ( 'NONE',  ( -5.049401038298153566, 19.05341960407611168, 30.20724293864769194 ) ) ;
#188405 = CARTESIAN_POINT ( 'NONE',  ( -19.03943276465977164, -0.05219959533935918106, 28.75109039468566507 ) ) ;
#188406 = CARTESIAN_POINT ( 'NONE',  ( 11.10918730048722836, 12.21811429388709946, -59.22494048452016102 ) ) ;
#188407 = CARTESIAN_POINT ( 'NONE',  ( -16.51473224551069308, -9.474510206698971260, 36.66557627198102409 ) ) ;
#188408 = DIRECTION ( 'NONE',  ( -1.000000000000000000, 0.000000000000000000, 0.000000000000000000 ) ) ;
#188409 = CARTESIAN_POINT ( 'NONE',  ( -9.474510206698964154, 16.51473224551069663, 70.41557627198102409 ) ) ;
#188410 = CARTESIAN_POINT ( 'NONE',  ( 17.49999999999999645, -3.189878218039153168, 112.3705143742875237 ) ) ;
#188411 = CARTESIAN_POINT ( 'NONE',  ( 0.05219959533937995610, -21.53943276465977519, 110.0010903946856757 ) ) ;
#188412 = CARTESIAN_POINT ( 'NONE',  ( -0.05219959533910754901, -16.53943276465976808, 37.49890960531436690 ) ) ;
#188413 = CARTESIAN_POINT ( 'NONE',  ( 19.02544592524343514, -5.153800228976328945, 38.54057627198103120 ) ) ;
#188414 = CARTESIAN_POINT ( 'NONE',  ( 5.153800228976335163, 19.02544592524342804, 94.79057627198103830 ) ) ;
#188415 = CARTESIAN_POINT ( 'NONE',  ( 15.80617190586769283, -15.72974639402175789, 65.62609039468568994 ) ) ;
#188416 = CARTESIAN_POINT ( 'NONE',  ( -9.564922557960796823, -16.46253265017161027, 47.08224293864769550 ) ) ;
#188417 = AXIS2_PLACEMENT_3D ( 'NONE', #159994, #3323, #96319 ) ;
#188418 = CARTESIAN_POINT ( 'NONE',  ( 18.62759615963255655, 10.81492255796105972, 61.66775706135235424 ) ) ;
#188419 = CARTESIAN_POINT ( 'NONE',  ( 18.62759615963271287, -10.81492255796078972, 28.33224293864769550 ) ) ;
#188420 = CARTESIAN_POINT ( 'NONE',  ( 0.05219959533909260263, 19.03943276465977164, 29.99890960531435979 ) ) ;
#188421 = CARTESIAN_POINT ( 'NONE',  ( 21.55341960407619695, -5.719274019375665929, 26.04275706135235779 ) ) ;
#188422 = CARTESIAN_POINT ( 'NONE',  ( 5.049401038297881783, 19.05341960407617563, 52.29275706135234003 ) ) ;
#188423 = CARTESIAN_POINT ( 'NONE',  ( 12.06949235617757843, -12.14591786802309237, 113.1239096053143953 ) ) ;
#188424 = CARTESIAN_POINT ( 'NONE',  ( 16.46253265017160672, -9.564922557960803928, 63.33224293864769550 ) ) ;
#188425 = CARTESIAN_POINT ( 'NONE',  ( 0.05219959533934541429, -16.53943276465976808, 20.00109039468568639 ) ) ;
#188426 = CARTESIAN_POINT ( 'NONE',  ( -14.29746914071049879, 8.314922557960819915, 70.83224293864770971 ) ) ;
#188427 = CARTESIAN_POINT ( 'NONE',  ( -19.03943276465977164, 0.05219959533909376836, 116.2489096053143669 ) ) ;
#188428 = CARTESIAN_POINT ( 'NONE',  ( 9.564922557961047289, -16.46253265017146816, 100.4177570613523329 ) ) ;
#188429 = CARTESIAN_POINT ( 'NONE',  ( -10.81492255796078084, -18.62759615963271287, 107.0822429386476955 ) ) ;
#188430 = CARTESIAN_POINT ( 'NONE',  ( 15.72974639402176855, 15.80617190586768217, 56.87609039468568994 ) ) ;
#188431 = CARTESIAN_POINT ( 'NONE',  ( -16.52544592524335698, -4.483927247898792601, 53.95942372801900433 ) ) ;
#188432 = CARTESIAN_POINT ( 'NONE',  ( -16.55341960407617563, 4.379528057220093196, 58.54275706135235424 ) ) ;
#188433 = CARTESIAN_POINT ( 'NONE',  ( 10.81492255796078972, 18.62759615963270932, 59.58224293864770260 ) ) ;
#188434 = CARTESIAN_POINT ( 'NONE',  ( -13.89961937509977652, 13.97604488694528158, 50.62390960531435979 ) ) ;
#188435 = CARTESIAN_POINT ( 'NONE',  ( -8.224510206698735004, -14.34966873604973081, 74.58442372801901854 ) ) ;
#188436 = CARTESIAN_POINT ( 'NONE',  ( -15.72974639402197994, 15.80617190586746368, 95.62390960531436690 ) ) ;
#188437 = CARTESIAN_POINT ( 'NONE',  ( 14.29746914071049879, -8.314922557960816363, 48.33224293864770260 ) ) ;
#188438 = CARTESIAN_POINT ( 'NONE',  ( -5.153800228976328057, -19.02544592524343514, 72.29057627198102409 ) ) ;
#188439 = CARTESIAN_POINT ( 'NONE',  ( 16.55341960407618274, -4.379528057220086978, 81.04275706135236135 ) ) ;
#188440 = CARTESIAN_POINT ( 'NONE',  ( -4.379528057220086978, -16.55341960407618274, 24.79275706135235779 ) ) ;
#188441 = CARTESIAN_POINT ( 'NONE',  ( -21.52544592524343514, 5.823673210054127303, 101.0405762719810383 ) ) ;
#188442 = CARTESIAN_POINT ( 'NONE',  ( 16.53943276465976808, -0.05219959533910856209, 38.74890960531435979 ) ) ;
#188443 = VERTEX_POINT ( 'NONE', #22118 ) ;
#188444 = CARTESIAN_POINT ( 'NONE',  ( 19.53037848336980531, -5.499999999999989342, 92.35532783611446916 ) ) ;
#188445 = CARTESIAN_POINT ( 'NONE',  ( 10.72451020669898902, -18.67979575497178502, 82.91557627198103830 ) ) ;
#188446 = CARTESIAN_POINT ( 'NONE',  ( -16.55341960407611168, -4.379528057220339221, 26.45724293864768839 ) ) ;
#188447 = VERTEX_POINT ( 'NONE', #131284 ) ;
#188448 = CARTESIAN_POINT ( 'NONE',  ( -16.18388926212241330, -7.379444403734409796, 55.43953151366151388 ) ) ;
#188449 = CARTESIAN_POINT ( 'NONE',  ( 21.53943276465977519, -0.05219959533907433946, 98.74890960531438111 ) ) ;
#188450 = CARTESIAN_POINT ( 'NONE',  ( 16.46253265017160672, -9.564922557960803928, 98.33224293864769550 ) ) ;
#188451 = CARTESIAN_POINT ( 'NONE',  ( -10.72451020669898014, 18.67979575497178502, 115.4155762719810241 ) ) ;
#188452 = CARTESIAN_POINT ( 'NONE',  ( -4.379528057220328563, 16.55341960407611168, 40.20724293864769550 ) ) ;
#188453 = CARTESIAN_POINT ( 'NONE',  ( -16.52544592524335698, -4.483927247898792601, 48.95942372801902565 ) ) ;
#188454 = CARTESIAN_POINT ( 'NONE',  ( 9.564922557960805705, 16.46253265017160317, 54.58224293864769550 ) ) ;
#188455 = CARTESIAN_POINT ( 'NONE',  ( -9.564922557961040184, 16.46253265017147172, 57.91775706135233293 ) ) ;
#188456 = CARTESIAN_POINT ( 'NONE',  ( 13.89961937509977652, -13.97604488694527269, 78.12390960531433848 ) ) ;
#188457 = VERTEX_POINT ( 'NONE', #146442 ) ;
#188458 = CARTESIAN_POINT ( 'NONE',  ( 5.823673210054125526, 21.52544592524343514, 39.79057627198103830 ) ) ;
#188459 = CARTESIAN_POINT ( 'NONE',  ( -28.03958666231389074, -24.95204343637547240, -18.68191426763402063 ) ) ;
#188460 = CARTESIAN_POINT ( 'NONE',  ( 5.049401038297881783, 19.05341960407617563, 112.2927570613523471 ) ) ;
#188461 = CARTESIAN_POINT ( 'NONE',  ( -5.049401038297874678, -19.05341960407617918, 44.79275706135232582 ) ) ;
#188462 = CARTESIAN_POINT ( 'NONE',  ( -21.55341960407610458, -5.719274019375992779, 96.45724293864770971 ) ) ;
#188463 = CARTESIAN_POINT ( 'NONE',  ( -16.53943276465976808, 0.05219959533911058130, 31.24890960531435979 ) ) ;
#188464 = CARTESIAN_POINT ( 'NONE',  ( -19.03943276465977164, 0.05219959533909376836, 81.24890960531436690 ) ) ;
#188465 = CARTESIAN_POINT ( 'NONE',  ( -10.72451020669898014, 18.67979575497178502, 55.41557627198102409 ) ) ;
#188467 = CARTESIAN_POINT ( 'NONE',  ( 8.314922557961029526, -14.29746914071037800, 30.41775706135234358 ) ) ;
#188466 = CARTESIAN_POINT ( 'NONE',  ( -15.80617190586745835, -15.72974639402198527, 96.87390960531436690 ) ) ;
#188468 = ADVANCED_FACE ( 'NONE', ( #116121 ), #192972, .T. ) ;
#188469 = CARTESIAN_POINT ( 'NONE',  ( -18.67979575497178146, -10.72451020669898902, 26.66557627198103475 ) ) ;
#188470 = CARTESIAN_POINT ( 'NONE',  ( 5.823673210054444382, -21.52544592524334988, 85.20942372801901854 ) ) ;
#188471 = CARTESIAN_POINT ( 'NONE',  ( -0.05219959533909027116, -19.03943276465977164, 82.49890960531436690 ) ) ;
#188472 = CARTESIAN_POINT ( 'NONE',  ( 16.51473224551069308, 9.474510206698969483, 29.16557627198103475 ) ) ;
#188473 = CARTESIAN_POINT ( 'NONE',  ( 5.153800228976335163, 19.02544592524342804, 84.79057627198099567 ) ) ;
#188474 = CARTESIAN_POINT ( 'NONE',  ( 8.224510206698953496, -14.34966873604960469, 107.9155762719810241 ) ) ;
#188475 = CARTESIAN_POINT ( 'NONE',  ( -13.89961937509977652, 13.97604488694528158, 60.62390960531436690 ) ) ;
#188476 = CARTESIAN_POINT ( 'NONE',  ( -0.05219959533936034679, 19.03943276465977164, 102.5010903946856757 ) ) ;
#188477 = AXIS2_PLACEMENT_3D ( 'NONE', #197476, #58942, #102466 ) ;
#188478 = CARTESIAN_POINT ( 'NONE',  ( 17.50000000000000355, 3.237210098469580632, 32.78763012620459705 ) ) ;
#188479 = CARTESIAN_POINT ( 'NONE',  ( -19.02544592524342804, 5.153800228976336051, 76.04057627198102409 ) ) ;
#188481 = CARTESIAN_POINT ( 'NONE',  ( -9.474510206698964154, 16.51473224551069663, 115.4155762719810241 ) ) ;
#188480 = CARTESIAN_POINT ( 'NONE',  ( 21.53943276465977519, 0.05219959533937863772, 101.2510903946856757 ) ) ;
#188483 = EDGE_CURVE ( 'NONE', #4972, #65926, #192392, .T. ) ;
#188482 = CARTESIAN_POINT ( 'NONE',  ( 14.29746914071037800, 8.314922557961029526, 91.66775706135234714 ) ) ;
#188484 = CARTESIAN_POINT ( 'NONE',  ( 20.59158986795031865, -20.29504437421338636, -49.65986060686195458 ) ) ;
#188485 = CARTESIAN_POINT ( 'NONE',  ( 16.51473224551083163, -9.474510206698727899, 75.83442372801900433 ) ) ;
#188486 = CARTESIAN_POINT ( 'NONE',  ( -5.049401038297874678, -19.05341960407617918, 19.79275706135233293 ) ) ;
#188487 = CARTESIAN_POINT ( 'NONE',  ( 13.91092067181850922, -24.01619779967536417, 139.9999999999999716 ) ) ;
#188488 = CARTESIAN_POINT ( 'NONE',  ( -16.46253265017160317, 9.564922557960807481, 30.83224293864769550 ) ) ;
#188489 = CARTESIAN_POINT ( 'NONE',  ( 4.483927247898545687, 16.52544592524342804, 24.79057627198103120 ) ) ;
#188490 = CARTESIAN_POINT ( 'NONE',  ( -35.52771690032648166, -3.099362195827484179, 38.16599597228981366 ) ) ;
#188491 = CARTESIAN_POINT ( 'NONE',  ( -12.06949235617739369, -12.14591786802326823, 104.3760903946856899 ) ) ;
#188492 = CARTESIAN_POINT ( 'NONE',  ( -19.53091890409953635, -5.499999999999944933, 85.06097431831423705 ) ) ;
#188493 = CARTESIAN_POINT ( 'NONE',  ( 14.34966873604972726, -8.224510206698740333, 75.83442372801900433 ) ) ;
#188494 = CARTESIAN_POINT ( 'NONE',  ( -0.05219959533909027116, -19.03943276465977164, 42.49890960531435269 ) ) ;
#188495 = CARTESIAN_POINT ( 'NONE',  ( -0.05219959533937732626, 21.53943276465977519, 92.50109039468567573 ) ) ;
#188496 = CARTESIAN_POINT ( 'NONE',  ( 13.89961937509957401, 13.97604488694547697, 106.8760903946856757 ) ) ;
#188497 = CARTESIAN_POINT ( 'NONE',  ( 18.67979575497194134, -10.72451020669871369, 75.83442372801900433 ) ) ;
#188498 = CARTESIAN_POINT ( 'NONE',  ( -19.03943276465977164, -0.05219959533935918106, 53.75109039468566863 ) ) ;
#188499 = CARTESIAN_POINT ( 'NONE',  ( -16.46253265017160317, 9.564922557960807481, 75.83224293864769550 ) ) ;
#188500 = CARTESIAN_POINT ( 'NONE',  ( -19.05341960407611168, -5.049401038298163336, 66.45724293864769550 ) ) ;
#188501 = DIRECTION ( 'NONE',  ( 0.000000000000000000, 0.000000000000000000, -1.000000000000000000 ) ) ;
#188502 = CARTESIAN_POINT ( 'NONE',  ( -0.05219959533910754901, -16.53943276465976808, 62.49890960531436690 ) ) ;
#188503 = CARTESIAN_POINT ( 'NONE',  ( 18.67979575497178502, 10.72451020669898547, 44.16557627198103120 ) ) ;
#188504 = CARTESIAN_POINT ( 'NONE',  ( -13.97604488694527625, -13.89961937509977652, 41.87390960531435979 ) ) ;
#188506 = CARTESIAN_POINT ( 'NONE',  ( 16.55341960407618274, -4.379528057220086978, 81.04275706135236135 ) ) ;
#188505 = CARTESIAN_POINT ( 'NONE',  ( 15.72974639402199770, -15.80617190586745480, 88.12390960531436690 ) ) ;
#188508 = ORIENTED_EDGE ( 'NONE', *, *, #146334, .F. ) ;
#188507 = B_SPLINE_CURVE_WITH_KNOTS ( 'NONE', 3,
 ( #28502, #134678, #166010, #27510, #57832, #60785, #122456, #182165, #43650, #167000, #184149, #45630, #87162, #76950, #110274, #141609, #64773, #78934, #187149, #126435, #17280, #2100, #153795, #186145, #109278, #108283, #111267, #140610, #31453, #34436, #138620, #63781 ),
 .UNSPECIFIED., .F., .F.,
 ( 4, 2, 2, 2, 2, 2, 2, 2, 2, 2, 2, 2, 2, 2, 2, 4 ),
 ( 8.044049492208757700E-17, 0.0003712461730037431022, 0.0007424923460074057567, 0.001113738519011068248, 0.001484984692014731066, 0.002227477038022061904, 0.002598723211025727540, 0.002969969384029393176, 0.003341215557033058812, 0.003712461730036724014, 0.004083707903040389650, 0.004454954076044054419, 0.004826200249047720055, 0.005197446422051385691, 0.005568692595055050459, 0.005939938768058716095 ),
 .UNSPECIFIED. ) ;
#188509 = EDGE_CURVE ( 'NONE', #168893, #184086, #117115, .T. ) ;
#188511 = CARTESIAN_POINT ( 'NONE',  ( 36.91746824999999177, 2.880721459617395097E-14, -3.624999997268813168 ) ) ;
#188510 = CARTESIAN_POINT ( 'NONE',  ( 8.224510206698953496, -14.34966873604960469, 82.91557627198103830 ) ) ;
#188512 = CARTESIAN_POINT ( 'NONE',  ( 4.379528057220092307, 16.55341960407617563, 37.29275706135235424 ) ) ;
#188513 = CARTESIAN_POINT ( 'NONE',  ( 16.55341960407611168, 4.379528057220329451, 113.9572429386477239 ) ) ;
#188514 = CARTESIAN_POINT ( 'NONE',  ( -19.03943276465977164, -0.05219959533935918106, 63.75109039468566863 ) ) ;
#188515 = CARTESIAN_POINT ( 'NONE',  ( -8.224510206698948167, 14.34966873604960824, 65.41557627198102409 ) ) ;
#188516 = CARTESIAN_POINT ( 'NONE',  ( -21.53943276465977519, -0.05219959533937600094, 48.75109039468568284 ) ) ;
#188518 = CARTESIAN_POINT ( 'NONE',  ( -15.80617190586745835, -15.72974639402198527, 91.87390960531436690 ) ) ;
#188517 = CARTESIAN_POINT ( 'NONE',  ( 19.03943276465977164, -0.05219959533909143690, 28.74890960531435624 ) ) ;
#188519 = CARTESIAN_POINT ( 'NONE',  ( -5.153800228976328057, -19.02544592524343514, 112.2905762719810099 ) ) ;
#188520 = CARTESIAN_POINT ( 'NONE',  ( -4.483927247898539470, -16.52544592524342804, 92.29057627198103830 ) ) ;
#188521 = CARTESIAN_POINT ( 'NONE',  ( 26.35186391108388548, -29.45501048290770640, -18.59600737859850739 ) ) ;
#188522 = CARTESIAN_POINT ( 'NONE',  ( 5.153800228976335163, 19.02544592524342804, 49.79057627198100988 ) ) ;
#188523 = CARTESIAN_POINT ( 'NONE',  ( -29.86685920354755197, -21.69954338932560134, -2.424999997268813434 ) ) ;
#188524 = CARTESIAN_POINT ( 'NONE',  ( 19.03943276465977164, 0.05219959533936151252, 76.25109039468566152 ) ) ;
#188525 = CARTESIAN_POINT ( 'NONE',  ( -10.81492255796105439, 18.62759615963255655, 37.91775706135235424 ) ) ;
#188526 = CARTESIAN_POINT ( 'NONE',  ( -16.46253265017160317, 9.564922557960807481, 70.83224293864770971 ) ) ;
#188527 = CARTESIAN_POINT ( 'NONE',  ( -16.51473224551082808, 9.474510206698731452, 53.33442372801900433 ) ) ;
#188528 = CARTESIAN_POINT ( 'NONE',  ( -5.049401038298153566, 19.05341960407611168, 45.20724293864769550 ) ) ;
#188529 = CARTESIAN_POINT ( 'NONE',  ( -12.14591786802309592, -12.06949235617757132, 56.87390960531436690 ) ) ;
#188530 = CARTESIAN_POINT ( 'NONE',  ( 4.483927247898545687, 16.52544592524342804, 54.79057627198104541 ) ) ;
#188531 = CARTESIAN_POINT ( 'NONE',  ( 19.02544592524343514, -5.153800228976328945, 73.54057627198103830 ) ) ;
#188532 = CARTESIAN_POINT ( 'NONE',  ( -21.53943276465977519, 0.05219959533907696930, 101.2489096053143669 ) ) ;
#188533 = CARTESIAN_POINT ( 'NONE',  ( 19.05341960407611168, 5.049401038298154454, 73.95724293864768129 ) ) ;
#188534 = CARTESIAN_POINT ( 'NONE',  ( -21.52544592524343514, 5.823673210054127303, 76.04057627198102409 ) ) ;
#188535 = CARTESIAN_POINT ( 'NONE',  ( -10.81492255796105439, 18.62759615963255655, 107.9177570613523471 ) ) ;
#188538 = CARTESIAN_POINT ( 'NONE',  ( -8.224510206698948167, 14.34966873604960824, 90.41557627198103830 ) ) ;
#188537 = CARTESIAN_POINT ( 'NONE',  ( -16.53943276465976808, -0.05219959533934237506, 103.7510903946857042 ) ) ;
#188536 = CARTESIAN_POINT ( 'NONE',  ( -13.97604488694527625, -13.89961937509977652, 41.87390960531435979 ) ) ;
#188539 = CARTESIAN_POINT ( 'NONE',  ( 19.02544592524334988, 5.153800228976608722, 101.4594237280189759 ) ) ;
#188540 = ORIENTED_EDGE ( 'NONE', *, *, #76322, .T. ) ;
#188541 = CARTESIAN_POINT ( 'NONE',  ( -18.62759615963255300, -10.81492255796106328, 29.16775706135234003 ) ) ;
#188542 = CARTESIAN_POINT ( 'NONE',  ( -9.474510206698720793, -16.51473224551083518, 54.58442372801899722 ) ) ;
#188543 = CARTESIAN_POINT ( 'NONE',  ( 0.05219959533934541429, -16.53943276465976808, 110.0010903946856757 ) ) ;
#188544 = CARTESIAN_POINT ( 'NONE',  ( -10.81492255796078084, -18.62759615963271287, 77.08224293864769550 ) ) ;
#188545 = CARTESIAN_POINT ( 'NONE',  ( -19.02544592524342804, 5.153800228976336051, 96.04057627198103830 ) ) ;
#188546 = CARTESIAN_POINT ( 'NONE',  ( -16.53943276465976808, 0.05219959533911058130, 61.24890960531435979 ) ) ;
#188547 = CARTESIAN_POINT ( 'NONE',  ( -5.049401038298153566, 19.05341960407611168, 35.20724293864768839 ) ) ;
#188548 = CARTESIAN_POINT ( 'NONE',  ( -19.03943276465977164, 0.05219959533909376836, 31.24890960531435979 ) ) ;
#188549 = CARTESIAN_POINT ( 'NONE',  ( -18.67979575497193778, 10.72451020669871902, 108.3344237280190185 ) ) ;
#188550 = CARTESIAN_POINT ( 'NONE',  ( -8.224510206698735004, -14.34966873604973081, 89.58442372801901854 ) ) ;
#188551 = CARTESIAN_POINT ( 'NONE',  ( 18.67979575497194134, -10.72451020669871369, 35.83442372801901143 ) ) ;
#188552 = CARTESIAN_POINT ( 'NONE',  ( 16.53943276465976808, 0.05219959533934440121, 41.25109039468568284 ) ) ;
#188553 = CARTESIAN_POINT ( 'NONE',  ( -19.03943276465977164, 0.05219959533909376836, 116.2489096053143669 ) ) ;
#188555 = CARTESIAN_POINT ( 'NONE',  ( 5.719274019375673035, 21.55341960407619339, 97.29275706135234714 ) ) ;
#188554 = CARTESIAN_POINT ( 'NONE',  ( 5.049401038298161559, -19.05341960407611168, 52.70724293864767418 ) ) ;
#188556 = CARTESIAN_POINT ( 'NONE',  ( 9.564922557960805705, 16.46253265017160317, 74.58224293864769550 ) ) ;
#188557 = CARTESIAN_POINT ( 'NONE',  ( -14.29746914071037622, -8.314922557961029526, 59.16775706135234714 ) ) ;
#188558 = CARTESIAN_POINT ( 'NONE',  ( 8.314922557960818139, 14.29746914071049879, 104.5822429386477097 ) ) ;
#188559 = CARTESIAN_POINT ( 'NONE',  ( 4.379528057220092307, 16.55341960407617563, 112.2927570613523471 ) ) ;
#188560 = CARTESIAN_POINT ( 'NONE',  ( 13.97604488694527802, 13.89961937509977830, 49.37390960531435269 ) ) ;
#188563 = CARTESIAN_POINT ( 'NONE',  ( 13.97604488694527802, 13.89961937509977652, 79.37390960531435269 ) ) ;
#188562 = CARTESIAN_POINT ( 'NONE',  ( 16.51473224551069308, 9.474510206698969483, 94.16557627198103830 ) ) ;
#188561 = CARTESIAN_POINT ( 'NONE',  ( 21.53943276465977519, 0.05219959533937863772, 51.25109039468568994 ) ) ;
#188564 = CARTESIAN_POINT ( 'NONE',  ( 5.049401038298161559, -19.05341960407611168, 112.7072429386476813 ) ) ;
#188565 = CARTESIAN_POINT ( 'NONE',  ( 14.34966873604960469, 8.224510206698951720, 44.16557627198103120 ) ) ;
#188566 = CARTESIAN_POINT ( 'NONE',  ( -16.55341960407611168, -4.379528057220339221, 26.45724293864768839 ) ) ;
#188567 = AXIS2_PLACEMENT_3D ( 'NONE', #159199, #81352, #6515 ) ;
#188568 = CARTESIAN_POINT ( 'NONE',  ( 0.05219959533910956823, 16.53943276465976808, 44.99890960531435979 ) ) ;
#188569 = CARTESIAN_POINT ( 'NONE',  ( 1.300000000000000044, 1.443375672974065216, 7.017607234860990640E-28 ) ) ;
#188570 = CARTESIAN_POINT ( 'NONE',  ( 13.89961937509957401, 13.97604488694547697, 31.87609039468566863 ) ) ;
#188571 = CARTESIAN_POINT ( 'NONE',  ( -0.05219959533909027116, -19.03943276465977164, 82.49890960531436690 ) ) ;
#188572 = CARTESIAN_POINT ( 'NONE',  ( -13.89961937509957401, -13.97604488694547875, 54.37609039468565442 ) ) ;
#188573 = CARTESIAN_POINT ( 'NONE',  ( -22.81625015709509441, -31.40387420917324590, -10.82499999726881157 ) ) ;
#188574 = CARTESIAN_POINT ( 'NONE',  ( -13.97604488694527625, -13.89961937509977830, 66.87390960531436690 ) ) ;
#188576 = CARTESIAN_POINT ( 'NONE',  ( -0.05219959533934338120, 16.53943276465976808, 72.50109039468568994 ) ) ;
#188575 = CARTESIAN_POINT ( 'NONE',  ( 16.46253265017146816, 9.564922557961045513, 86.66775706135233293 ) ) ;
#188577 = CARTESIAN_POINT ( 'NONE',  ( 17.44279575226823908, 5.990770900252462283, 91.66442432485682446 ) ) ;
#188578 = CARTESIAN_POINT ( 'NONE',  ( 19.03943276465977164, -0.05219959533909143690, 108.7489096053143527 ) ) ;
#188579 = CARTESIAN_POINT ( 'NONE',  ( 10.81492255796106328, -18.62759615963255655, 30.41775706135234358 ) ) ;
#188580 = CARTESIAN_POINT ( 'NONE',  ( 0.05219959533936267826, -19.03943276465977164, 85.00109039468567573 ) ) ;
#188582 = CARTESIAN_POINT ( 'NONE',  ( 16.51473224551069308, 9.474510206698969483, 44.16557627198103120 ) ) ;
#188581 = CARTESIAN_POINT ( 'NONE',  ( 16.36317988757060604, 7.306389748694960495, 88.40210391636782106 ) ) ;
#188583 = CARTESIAN_POINT ( 'NONE',  ( 19.02544592524343514, -5.153800228976328945, 88.54057627198102409 ) ) ;
#188585 = CARTESIAN_POINT ( 'NONE',  ( 19.03943276465977164, -0.05219959533909143690, 48.74890960531435979 ) ) ;
#188584 = CARTESIAN_POINT ( 'NONE',  ( 14.34966873604960469, 8.224510206698951720, 64.16557627198102409 ) ) ;
#188586 = CARTESIAN_POINT ( 'NONE',  ( 19.05341960407611168, 5.049401038298154454, 58.95724293864768129 ) ) ;
#188587 = CARTESIAN_POINT ( 'NONE',  ( -16.46253265017146816, -9.564922557961047289, 64.16775706135233293 ) ) ;
#188588 = CARTESIAN_POINT ( 'NONE',  ( 9.564922557961047289, -16.46253265017146816, 30.41775706135232937 ) ) ;
#188589 = CARTESIAN_POINT ( 'NONE',  ( -9.474510206698964154, 16.51473224551069663, 70.41557627198102409 ) ) ;
#188590 = CARTESIAN_POINT ( 'NONE',  ( -18.62759615963270932, 10.81492255796079327, 65.83224293864769550 ) ) ;
#188592 = CARTESIAN_POINT ( 'NONE',  ( 9.564922557961047289, -16.46253265017146816, 40.41775706135234003 ) ) ;
#188591 = CARTESIAN_POINT ( 'NONE',  ( 12.06949235617757843, -12.14591786802309237, 68.12390960531436690 ) ) ;
#188593 = DIRECTION ( 'NONE',  ( -0.000000000000000000, -0.000000000000000000, -1.000000000000000000 ) ) ;
#188594 = CARTESIAN_POINT ( 'NONE',  ( 18.67979575497178502, 10.72451020669898547, 44.16557627198103120 ) ) ;
#188595 = CARTESIAN_POINT ( 'NONE',  ( 15.80617190586746368, 15.72974639402197994, 24.37390960531435979 ) ) ;
#188596 = CARTESIAN_POINT ( 'NONE',  ( -16.51473224551069308, -9.474510206698971260, 51.66557627198102409 ) ) ;
#188597 = CARTESIAN_POINT ( 'NONE',  ( 9.474510206698971260, -16.51473224551069308, 42.91557627198103120 ) ) ;
#188598 = CARTESIAN_POINT ( 'NONE',  ( -8.224510206698948167, 14.34966873604960824, 100.4155762719810241 ) ) ;
#188599 = CARTESIAN_POINT ( 'NONE',  ( -21.53943276465977519, 0.05219959533907696930, 116.2489096053143669 ) ) ;
#188600 = CARTESIAN_POINT ( 'NONE',  ( 25.38323934330066578, -4.814940836774085575, 166.7856488131975539 ) ) ;
#188601 = CARTESIAN_POINT ( 'NONE',  ( -15.80617190586768217, 15.72974639402176855, 28.12609039468568284 ) ) ;
#188602 = CARTESIAN_POINT ( 'NONE',  ( -16.52544592524342804, 4.483927247898546575, 111.0405762719810525 ) ) ;
#188603 = CARTESIAN_POINT ( 'NONE',  ( -15.80617190586768217, 15.72974639402176855, 83.12609039468568994 ) ) ;
#188604 = CARTESIAN_POINT ( 'NONE',  ( 18.67979575497178502, 10.72451020669898547, 89.16557627198102409 ) ) ;
#188605 = CARTESIAN_POINT ( 'NONE',  ( -0.05219959533936034679, 19.03943276465977164, 37.50109039468567573 ) ) ;
#188606 = CARTESIAN_POINT ( 'NONE',  ( -0.05219959533909027116, -19.03943276465977164, 22.49890960531436690 ) ) ;
#188607 = CARTESIAN_POINT ( 'NONE',  ( 5.049401038298163336, -19.05341960407611168, 52.70724293864768129 ) ) ;
#188608 = CARTESIAN_POINT ( 'NONE',  ( 11.74264578624800315, -36.14014761921581709, -1.399999999999999689 ) ) ;
#188609 = CARTESIAN_POINT ( 'NONE',  ( 8.314922557961029526, -14.29746914071037800, 45.41775706135234003 ) ) ;
#188610 = CARTESIAN_POINT ( 'NONE',  ( -12.06949235617756955, 12.14591786802309770, 105.6239096053143669 ) ) ;
#188611 = CARTESIAN_POINT ( 'NONE',  ( 33.86249154851669374, -5.319940558880595916, 93.55791698674948975 ) ) ;
#188612 = CARTESIAN_POINT ( 'NONE',  ( 13.97604488694527802, 13.89961937509977652, 74.37390960531436690 ) ) ;
#188613 = CARTESIAN_POINT ( 'NONE',  ( 8.314922557960818139, 14.29746914071049879, 94.58224293864769550 ) ) ;
#188614 = CARTESIAN_POINT ( 'NONE',  ( -15.80617190586745835, -15.72974639402198527, 46.87390960531435979 ) ) ;
#188615 = CARTESIAN_POINT ( 'NONE',  ( -4.483927247898539470, -16.52544592524342804, 82.29057627198103830 ) ) ;
#188616 = CARTESIAN_POINT ( 'NONE',  ( -8.224510206698735004, -14.34966873604973081, 29.58442372801901854 ) ) ;
#188617 = CARTESIAN_POINT ( 'NONE',  ( -15.80617190586768217, 15.72974639402176855, 93.12609039468568994 ) ) ;
#188618 = CARTESIAN_POINT ( 'NONE',  ( 19.02544592524343514, -5.153800228976328945, 28.54057627198102409 ) ) ;
#188619 = CARTESIAN_POINT ( 'NONE',  ( 4.379528057220092307, 16.55341960407617563, 102.2927570613523613 ) ) ;
#188620 = CARTESIAN_POINT ( 'NONE',  ( -4.483927247898539470, -16.52544592524342804, 42.29057627198103120 ) ) ;
#188621 = CARTESIAN_POINT ( 'NONE',  ( -0.05219959533909027116, -19.03943276465977164, 47.49890960531435979 ) ) ;
#188622 = CARTESIAN_POINT ( 'NONE',  ( 18.62759615963255655, 10.81492255796105972, 101.6677570613523613 ) ) ;
#188623 = CARTESIAN_POINT ( 'NONE',  ( 21.55341960407610458, 5.719274019375980345, 108.9572429386476955 ) ) ;
#188624 =( GEOMETRIC_REPRESENTATION_CONTEXT ( 3 ) GLOBAL_UNCERTAINTY_ASSIGNED_CONTEXT ( ( #189501 ) ) GLOBAL_UNIT_ASSIGNED_CONTEXT ( ( #34369, #169895, #111198 ) ) REPRESENTATION_CONTEXT ( 'NONE', 'WORKASPACE' ) );
#188625 = CARTESIAN_POINT ( 'NONE',  ( -15.80617190586768217, 15.72974639402176855, 53.12609039468568284 ) ) ;
#188626 = CARTESIAN_POINT ( 'NONE',  ( -16.55341960407617563, 4.379528057220093196, 33.54275706135234714 ) ) ;
#188628 = CARTESIAN_POINT ( 'NONE',  ( -21.52544592524334988, -5.823673210054445271, 83.95942372801900433 ) ) ;
#188627 = CARTESIAN_POINT ( 'NONE',  ( 4.483927247898545687, 16.52544592524342804, 64.79057627198103830 ) ) ;
#188629 = CARTESIAN_POINT ( 'NONE',  ( -0.05219959533934338120, 16.53943276465976808, 107.5010903946856899 ) ) ;
#188630 = DIRECTION ( 'NONE',  ( 0.000000000000000000, 1.000000000000000000, 0.000000000000000000 ) ) ;
#188631 = CARTESIAN_POINT ( 'NONE',  ( -19.19724070472091171, -5.500000000000165201, 66.06193348274382515 ) ) ;
#188632 = CARTESIAN_POINT ( 'NONE',  ( -14.34966873604960291, -8.224510206698953496, 26.66557627198103475 ) ) ;
#188633 = CARTESIAN_POINT ( 'NONE',  ( -12.14591786802326823, 12.06949235617739902, 78.12609039468570415 ) ) ;
#188634 = CARTESIAN_POINT ( 'NONE',  ( 13.89961937509977652, -13.97604488694527269, 88.12390960531438111 ) ) ;
#188635 = CARTESIAN_POINT ( 'NONE',  ( -13.97604488694527625, -13.89961937509977652, 101.8739096053143811 ) ) ;
#188636 = CARTESIAN_POINT ( 'NONE',  ( 18.62759615963255655, 10.81492255796105972, 81.66775706135236135 ) ) ;
#188637 = EDGE_CURVE ( 'NONE', #194003, #45948, #148463, .T. ) ;
#188638 = CARTESIAN_POINT ( 'NONE',  ( -14.29746914071037622, -8.314922557961029526, 84.16775706135234714 ) ) ;
#188639 = CARTESIAN_POINT ( 'NONE',  ( -12.14591786802309592, -12.06949235617757132, 76.87390960531439532 ) ) ;
#188640 = CARTESIAN_POINT ( 'NONE',  ( 13.97604488694527802, 13.89961937509977652, 69.37390960531436690 ) ) ;
#188641 = VERTEX_POINT ( 'NONE', #52446 ) ;
#188642 = CARTESIAN_POINT ( 'NONE',  ( -8.224510206698735004, -14.34966873604973081, 24.58442372801901499 ) ) ;
#188643 = CARTESIAN_POINT ( 'NONE',  ( 13.89961937509977652, -13.97604488694527269, 23.12390960531436335 ) ) ;
#188644 = CARTESIAN_POINT ( 'NONE',  ( 0.05219959533909260263, 19.03943276465977164, 94.99890960531436690 ) ) ;
#188646 = CARTESIAN_POINT ( 'NONE',  ( 3.556970738554033499E-15, -38.81732327939057825, -10.12499999726881228 ) ) ;
#188645 = CARTESIAN_POINT ( 'NONE',  ( 12.14591786802327356, -12.06949235617739191, 35.62609039468568994 ) ) ;
#188647 = CARTESIAN_POINT ( 'NONE',  ( 19.05341960407617918, -5.049401038297876454, 26.04275706135233293 ) ) ;
#188648 = CARTESIAN_POINT ( 'NONE',  ( -16.52544592524335698, -4.483927247898792601, 88.95942372801901854 ) ) ;
#188649 = CARTESIAN_POINT ( 'NONE',  ( 5.153800228976615827, -19.02544592524334988, 105.2094237280190185 ) ) ;
#188650 = CARTESIAN_POINT ( 'NONE',  ( -19.03943276465977164, 0.05219959533909376836, 21.24890960531436335 ) ) ;
#188651 = CARTESIAN_POINT ( 'NONE',  ( -0.05219959533934338120, 16.53943276465976808, 82.50109039468568994 ) ) ;
#188652 = CARTESIAN_POINT ( 'NONE',  ( 12.14591786802327356, -12.06949235617739191, 60.62609039468567573 ) ) ;
#188653 = CARTESIAN_POINT ( 'NONE',  ( 19.03943276465977164, -0.05219959533909143690, 23.74890960531435269 ) ) ;
#188654 = CARTESIAN_POINT ( 'NONE',  ( -19.05341960407617563, 5.049401038297882671, 73.54275706135233293 ) ) ;
#188655 = CARTESIAN_POINT ( 'NONE',  ( -18.62759615963255300, -10.81492255796106328, 104.1677570613523471 ) ) ;
#188656 = CARTESIAN_POINT ( 'NONE',  ( 19.05341960407611168, 5.049401038298154454, 53.95724293864770260 ) ) ;
#188657 = CARTESIAN_POINT ( 'NONE',  ( 9.564922557960805705, 16.46253265017160317, 94.58224293864769550 ) ) ;
#188658 = CARTESIAN_POINT ( 'NONE',  ( 0.05219959533910956823, 16.53943276465976808, 79.99890960531435269 ) ) ;
#188659 = CIRCLE ( 'NONE', #36779, 12.50000000000000000 ) ;
#188660 = CARTESIAN_POINT ( 'NONE',  ( 19.05341960407617918, -5.049401038297876454, 51.04275706135231871 ) ) ;
#188661 = CARTESIAN_POINT ( 'NONE',  ( -5.719274019375978568, 21.55341960407610458, 50.20724293864769550 ) ) ;
#188662 = CARTESIAN_POINT ( 'NONE',  ( 18.67979575497194134, -10.72451020669871369, 110.8344237280190043 ) ) ;
#188663 = CARTESIAN_POINT ( 'NONE',  ( 5.153800228976335163, 19.02544592524342804, 94.79057627198103830 ) ) ;
#188664 = CARTESIAN_POINT ( 'NONE',  ( -15.80617190586768217, 15.72974639402176855, 108.1260903946856757 ) ) ;
#188665 = CARTESIAN_POINT ( 'NONE',  ( 18.62759615963271287, -10.81492255796078972, 58.33224293864768839 ) ) ;
#188666 = CARTESIAN_POINT ( 'NONE',  ( -16.51473224551069308, -9.474510206698971260, 101.6655762719810241 ) ) ;
#188667 = CARTESIAN_POINT ( 'NONE',  ( -9.474510206698720793, -16.51473224551083518, 89.58442372801900433 ) ) ;
#188668 = CARTESIAN_POINT ( 'NONE',  ( 19.03943276465977164, -0.05219959533909143690, 108.7489096053143527 ) ) ;
#188669 = CARTESIAN_POINT ( 'NONE',  ( -9.474510206698720793, -16.51473224551083518, 109.5844237280190043 ) ) ;
#188670 = CARTESIAN_POINT ( 'NONE',  ( 14.34966873604960469, 8.224510206698951720, 109.1655762719810383 ) ) ;
#188671 = CARTESIAN_POINT ( 'NONE',  ( 19.05341960407611168, 5.049401038298154454, 83.95724293864766707 ) ) ;
#188672 = CARTESIAN_POINT ( 'NONE',  ( -10.81492255796078084, -18.62759615963271287, 82.08224293864768129 ) ) ;
#188673 = CARTESIAN_POINT ( 'NONE',  ( -16.55341960407617563, 4.379528057220093196, 43.54275706135235424 ) ) ;
#188674 = CARTESIAN_POINT ( 'NONE',  ( -0.05219959533937732626, 21.53943276465977519, 42.50109039468567573 ) ) ;
#188675 = CARTESIAN_POINT ( 'NONE',  ( -21.52544592524334988, -5.823673210054445271, 103.9594237280190185 ) ) ;
#188676 = CARTESIAN_POINT ( 'NONE',  ( -16.55341960407617563, 4.379528057220093196, 98.54275706135234714 ) ) ;
#188677 = CARTESIAN_POINT ( 'NONE',  ( -19.02544592524342804, 5.153800228976336051, 86.04057627198103830 ) ) ;
#188678 = CARTESIAN_POINT ( 'NONE',  ( -16.55341960407611168, -4.379528057220339221, 86.45724293864770971 ) ) ;
#188679 = CARTESIAN_POINT ( 'NONE',  ( 16.52544592524342804, -4.483927247898539470, 23.54057627198102765 ) ) ;
#188680 = CARTESIAN_POINT ( 'NONE',  ( -0.05219959533936034679, 19.03943276465977164, 72.50109039468566152 ) ) ;
#188681 = CARTESIAN_POINT ( 'NONE',  ( 10.81492255796106328, -18.62759615963255655, 45.41775706135234003 ) ) ;
#188683 = CARTESIAN_POINT ( 'NONE',  ( 14.29746914071049879, -8.314922557960816363, 93.33224293864769550 ) ) ;
#188682 = AXIS2_PLACEMENT_3D ( 'NONE', #8687, #174543, #36010 ) ;
#188684 = CARTESIAN_POINT ( 'NONE',  ( 9.474510206698971260, -16.51473224551069308, 107.9155762719810383 ) ) ;
#188685 = CARTESIAN_POINT ( 'NONE',  ( 16.52544592524342804, -4.483927247898539470, 28.54057627198103120 ) ) ;
#188686 = CARTESIAN_POINT ( 'NONE',  ( 15.80617190586769283, -15.72974639402175789, 90.62609039468567573 ) ) ;
#188687 = CARTESIAN_POINT ( 'NONE',  ( -12.06949235617739369, -12.14591786802326823, 64.37609039468568994 ) ) ;
#188688 = CARTESIAN_POINT ( 'NONE',  ( -4.379528057220086978, -16.55341960407618274, 99.79275706135234714 ) ) ;
#188689 = CARTESIAN_POINT ( 'NONE',  ( 5.823673210054444382, -21.52544592524334988, 45.20942372801901854 ) ) ;
#188690 = CARTESIAN_POINT ( 'NONE',  ( -15.72974639402176322, -15.80617190586768395, 24.37609039468567573 ) ) ;
#188691 = CARTESIAN_POINT ( 'NONE',  ( -16.55341960407611168, -4.379528057220339221, 111.4572429386476813 ) ) ;
#188692 = CARTESIAN_POINT ( 'NONE',  ( -9.474510206698964154, 16.51473224551069663, 30.41557627198102054 ) ) ;
#188693 = CARTESIAN_POINT ( 'NONE',  ( 16.52544592524342804, -4.483927247898539470, 68.54057627198103830 ) ) ;
#188694 = CARTESIAN_POINT ( 'NONE',  ( 13.89961937509977652, -13.97604488694527269, 78.12390960531433848 ) ) ;
#188695 = CARTESIAN_POINT ( 'NONE',  ( 4.483927247898790824, -16.52544592524335698, 100.2094237280190043 ) ) ;
#188696 = CARTESIAN_POINT ( 'NONE',  ( 19.02544592524343514, -5.153800228976328945, 43.54057627198103120 ) ) ;
#188697 = CARTESIAN_POINT ( 'NONE',  ( 21.53943276465977519, -0.05219959533907433946, 48.74890960531435979 ) ) ;
#188698 = CARTESIAN_POINT ( 'NONE',  ( 14.29746914071049879, -8.314922557960816363, 93.33224293864769550 ) ) ;
#188699 = CARTESIAN_POINT ( 'NONE',  ( 15.72974639402199770, -15.80617190586745480, 88.12390960531436690 ) ) ;
#188700 = CARTESIAN_POINT ( 'NONE',  ( -16.46253265017160317, 9.564922557960807481, 90.83224293864769550 ) ) ;
#188702 = CARTESIAN_POINT ( 'NONE',  ( 16.51473224551083163, -9.474510206698727899, 85.83442372801900433 ) ) ;
#188701 = CARTESIAN_POINT ( 'NONE',  ( 13.97604488694527802, 13.89961937509977652, 49.37390960531434558 ) ) ;
#188703 = CARTESIAN_POINT ( 'NONE',  ( 10.72451020669898902, -18.67979575497178502, 37.91557627198102409 ) ) ;
#188704 = CARTESIAN_POINT ( 'NONE',  ( -5.823673210054431948, 21.52544592524334988, 72.70942372801901854 ) ) ;
#188705 = CARTESIAN_POINT ( 'NONE',  ( -13.89961937509977652, 13.97604488694528158, 55.62390960531434558 ) ) ;
#188706 = CARTESIAN_POINT ( 'NONE',  ( 13.97604488694527802, 13.89961937509977652, 79.37390960531435269 ) ) ;
#188707 = VERTEX_POINT ( 'NONE', #178809 ) ;
#188708 = CARTESIAN_POINT ( 'NONE',  ( 4.483927247898790824, -16.52544592524335698, 60.20942372801902565 ) ) ;
#188709 = CARTESIAN_POINT ( 'NONE',  ( -10.72451020669870658, -18.67979575497194134, 49.58442372801901143 ) ) ;
#188710 = CARTESIAN_POINT ( 'NONE',  ( -5.719274019375665041, -21.55341960407619695, 69.79275706135234714 ) ) ;
#188711 = CARTESIAN_POINT ( 'NONE',  ( -5.153800228976328057, -19.02544592524343514, 112.2905762719810099 ) ) ;
#188712 = CARTESIAN_POINT ( 'NONE',  ( -21.52544592524343514, 5.823673210054127303, 96.04057627198102409 ) ) ;
#188714 = CARTESIAN_POINT ( 'NONE',  ( -16.52544592524335698, -4.483927247898792601, 68.95942372801901854 ) ) ;
#188713 = CARTESIAN_POINT ( 'NONE',  ( 10.72451020669871369, 18.67979575497193778, 37.08442372801901143 ) ) ;
#188715 = CARTESIAN_POINT ( 'NONE',  ( -5.823673210054116645, -21.52544592524344225, 62.29057627198102409 ) ) ;
#188716 = CARTESIAN_POINT ( 'NONE',  ( -5.049401038297874678, -19.05341960407617918, 34.79275706135233293 ) ) ;
#188718 = CARTESIAN_POINT ( 'NONE',  ( 16.52544592524335698, 4.483927247898782831, 96.45942372801901854 ) ) ;
#188717 = CARTESIAN_POINT ( 'NONE',  ( 13.97604488694527802, 13.89961937509977652, 69.37390960531436690 ) ) ;
#188719 = DIRECTION ( 'NONE',  ( 1.000000000000000000, -0.000000000000000000, -0.000000000000000000 ) ) ;
#188720 = CARTESIAN_POINT ( 'NONE',  ( 19.05341960407611168, 5.049401038298154454, 108.9572429386477097 ) ) ;
#188721 = DIRECTION ( 'NONE',  ( 0.000000000000000000, 0.000000000000000000, 1.000000000000000000 ) ) ;
#188722 = CARTESIAN_POINT ( 'NONE',  ( 0.05219959533936267826, -19.03943276465977164, 80.00109039468567573 ) ) ;
#188723 = CARTESIAN_POINT ( 'NONE',  ( 10.81492255796078972, 18.62759615963270932, 64.58224293864769550 ) ) ;
#188724 = CARTESIAN_POINT ( 'NONE',  ( -4.379528057220328563, 16.55341960407611168, 40.20724293864769550 ) ) ;
#188725 = CARTESIAN_POINT ( 'NONE',  ( -13.97604488694547697, 13.89961937509957934, 98.12609039468566152 ) ) ;
#188726 = CARTESIAN_POINT ( 'NONE',  ( 19.02544592524343514, -5.153800228976328945, 28.54057627198102409 ) ) ;
#188727 = CARTESIAN_POINT ( 'NONE',  ( 19.05341960407617918, -5.049401038297876454, 106.0427570613523471 ) ) ;
#188729 = CARTESIAN_POINT ( 'NONE',  ( -16.51473224551082808, 9.474510206698731452, 58.33442372801900433 ) ) ;
#188728 = CARTESIAN_POINT ( 'NONE',  ( -10.72451020669898014, 18.67979575497178502, 85.41557627198102409 ) ) ;
#188730 = CARTESIAN_POINT ( 'NONE',  ( -8.224510206698735004, -14.34966873604973081, 74.58442372801901854 ) ) ;
#188731 = CARTESIAN_POINT ( 'NONE',  ( 16.46253265017160672, -9.564922557960803928, 68.33224293864770971 ) ) ;
#188732 = CARTESIAN_POINT ( 'NONE',  ( 4.483927247898545687, 16.52544592524342804, 74.79057627198105251 ) ) ;
#188733 = CARTESIAN_POINT ( 'NONE',  ( 16.46253265017160672, -9.564922557960803928, 48.33224293864769550 ) ) ;
#188734 = CARTESIAN_POINT ( 'NONE',  ( 0.05219959533910956823, 16.53943276465976808, 49.99890960531437401 ) ) ;
#188735 = DIRECTION ( 'NONE',  ( 1.000000000000000000, 0.000000000000000000, 0.000000000000000000 ) ) ;
#188736 = CARTESIAN_POINT ( 'NONE',  ( 0.6709015534586495466, 8.945245563437705272, -61.92617404244804646 ) ) ;
#188737 = CARTESIAN_POINT ( 'NONE',  ( -0.05219959533910754901, -16.53943276465976808, 22.49890960531436335 ) ) ;
#188738 = CARTESIAN_POINT ( 'NONE',  ( 13.97604488694527802, 13.89961937509977652, 79.37390960531435269 ) ) ;
#188739 = CARTESIAN_POINT ( 'NONE',  ( -1.697796032038645597, 7.741785448087978416, 5.990689250852168968 ) ) ;
#188740 = CARTESIAN_POINT ( 'NONE',  ( -5.153800228976607833, 19.02544592524334988, 32.70942372801899722 ) ) ;
#188741 = CARTESIAN_POINT ( 'NONE',  ( 0.05219959533934541429, -16.53943276465976808, 45.00109039468568284 ) ) ;
#188742 = CARTESIAN_POINT ( 'NONE',  ( -10.81492255796078084, -18.62759615963271287, 67.08224293864770971 ) ) ;
#188743 = CARTESIAN_POINT ( 'NONE',  ( -15.80617190586768217, 15.72974639402176855, 113.1260903946856899 ) ) ;
#188744 = CARTESIAN_POINT ( 'NONE',  ( 19.03943276465977164, -0.05219959533909143690, 73.74890960531435269 ) ) ;
#188745 = CARTESIAN_POINT ( 'NONE',  ( -13.89961937509977652, 13.97604488694528158, 115.6239096053143669 ) ) ;
#188746 = CARTESIAN_POINT ( 'NONE',  ( 13.89961937509977652, -13.97604488694527269, 108.1239096053143669 ) ) ;
#188747 = CARTESIAN_POINT ( 'NONE',  ( 21.52544592524334988, 5.823673210054432836, 36.45942372801901143 ) ) ;
#188748 = CARTESIAN_POINT ( 'NONE',  ( 8.224510206698953496, -14.34966873604960469, 102.9155762719810383 ) ) ;
#188751 = VERTEX_POINT ( 'NONE', #147466 ) ;
#188750 = CARTESIAN_POINT ( 'NONE',  ( -5.049401038298153566, 19.05341960407611168, 75.20724293864769550 ) ) ;
#188749 = CARTESIAN_POINT ( 'NONE',  ( -10.72451020669898014, 18.67979575497178502, 105.4155762719810383 ) ) ;
#188752 = CARTESIAN_POINT ( 'NONE',  ( 15.80617190586769283, -15.72974639402175789, 25.62609039468567929 ) ) ;
#188753 = ORIENTED_EDGE ( 'NONE', *, *, #52659, .T. ) ;
#188754 = CARTESIAN_POINT ( 'NONE',  ( -19.02544592524342804, 5.153800228976336051, 81.04057627198103830 ) ) ;
#188755 = CARTESIAN_POINT ( 'NONE',  ( 19.25663599770060586, -5.499999999999437783, 81.49419308057203182 ) ) ;
#188757 = CARTESIAN_POINT ( 'NONE',  ( -9.564922557960796823, -16.46253265017161027, 27.08224293864769550 ) ) ;
#188756 = CARTESIAN_POINT ( 'NONE',  ( 19.03943276465977164, -0.05219959533909143690, 23.74890960531435269 ) ) ;
#188758 = CARTESIAN_POINT ( 'NONE',  ( -13.89961937509957401, -13.97604488694547875, 109.3760903946856331 ) ) ;
#188759 = CARTESIAN_POINT ( 'NONE',  ( -22.81625015709510507, 31.40387420917330275, -9.424999997268812990 ) ) ;
#188760 = AXIS2_PLACEMENT_3D ( 'NONE', #52706, #144713, #143718 ) ;
#188761 = CARTESIAN_POINT ( 'NONE',  ( -4.483927247898539470, -16.52544592524342804, 112.2905762719810241 ) ) ;
#188762 = CARTESIAN_POINT ( 'NONE',  ( 10.72451020669871369, 18.67979575497193778, 82.08442372801901854 ) ) ;
#188764 = CARTESIAN_POINT ( 'NONE',  ( 0.05219959533937995610, -21.53943276465977519, 40.00109039468567573 ) ) ;
#188763 = CARTESIAN_POINT ( 'NONE',  ( 19.02544592524343514, -5.153800228976328945, 58.54057627198102409 ) ) ;
#188765 = CARTESIAN_POINT ( 'NONE',  ( -0.05219959533937732626, 21.53943276465977519, 32.50109039468568284 ) ) ;
#188766 = CARTESIAN_POINT ( 'NONE',  ( 27.73933785331498569, 2.768321779492822058E-14, 140.3750000027311842 ) ) ;
#188767 = CARTESIAN_POINT ( 'NONE',  ( -9.564922557960796823, -16.46253265017161027, 82.08224293864768129 ) ) ;
#188768 = CARTESIAN_POINT ( 'NONE',  ( 26.70615770596319649, 7.662262839729889308, 167.2520072419550559 ) ) ;
#188770 = CARTESIAN_POINT ( 'NONE',  ( 10.72451020669898902, -18.67979575497178502, 42.91557627198103120 ) ) ;
#188769 = CARTESIAN_POINT ( 'NONE',  ( -8.224510206698735004, -14.34966873604973081, 24.58442372801901499 ) ) ;
#188771 = CARTESIAN_POINT ( 'NONE',  ( -15.72974639402176322, -15.80617190586768395, 74.37609039468568994 ) ) ;
#188772 = AXIS2_PLACEMENT_3D ( 'NONE', #200010, #106984, #15989 ) ;
#188773 = CARTESIAN_POINT ( 'NONE',  ( -9.564922557960796823, -16.46253265017161027, 107.0822429386476955 ) ) ;
#188774 = CARTESIAN_POINT ( 'NONE',  ( 9.474510206698729675, 16.51473224551082808, 97.08442372801900433 ) ) ;
#188775 = CARTESIAN_POINT ( 'NONE',  ( -5.049401038298153566, 19.05341960407611168, 65.20724293864765286 ) ) ;
#188776 = CARTESIAN_POINT ( 'NONE',  ( 16.46253265017160672, -9.564922557960803928, 88.33224293864769550 ) ) ;
#188777 = CARTESIAN_POINT ( 'NONE',  ( -8.224510206698948167, 14.34966873604960824, 100.4155762719810241 ) ) ;
#188778 = CARTESIAN_POINT ( 'NONE',  ( 14.34966873604960469, 8.224510206698951720, 109.1655762719810383 ) ) ;
#188779 = CARTESIAN_POINT ( 'NONE',  ( -13.89961937509977652, 13.97604488694528158, 110.6239096053143243 ) ) ;
#188780 = CARTESIAN_POINT ( 'NONE',  ( 16.55341960407618274, -4.379528057220086978, 76.04275706135237556 ) ) ;
#188782 = CARTESIAN_POINT ( 'NONE',  ( 5.153800228976335163, 19.02544592524342804, 44.79057627198103830 ) ) ;
#188781 = CARTESIAN_POINT ( 'NONE',  ( -4.379528057220328563, 16.55341960407611168, 60.20724293864768839 ) ) ;
#188783 = CARTESIAN_POINT ( 'NONE',  ( 15.72974639402176855, 15.80617190586768217, 66.87609039468568994 ) ) ;
#188784 = CARTESIAN_POINT ( 'NONE',  ( -13.97604488694547697, 13.89961937509957934, 98.12609039468566152 ) ) ;
#188785 = CARTESIAN_POINT ( 'NONE',  ( -0.05219959533910754901, -16.53943276465976808, 62.49890960531436690 ) ) ;
#188786 = CARTESIAN_POINT ( 'NONE',  ( 10.72451020669898902, -18.67979575497178502, 112.9155762719810383 ) ) ;
#188787 = CARTESIAN_POINT ( 'NONE',  ( 18.67979575497178502, 10.72451020669898547, 44.16557627198103120 ) ) ;
#188788 = CARTESIAN_POINT ( 'NONE',  ( -23.31738231874055245, -16.94106989632524574, 140.1999999999999886 ) ) ;
#188789 = CARTESIAN_POINT ( 'NONE',  ( 17.81289503416611453, -24.51734667627695785, 142.9500000054623854 ) ) ;
#188790 = CARTESIAN_POINT ( 'NONE',  ( 5.049401038298161559, -19.05341960407611168, 72.70724293864768129 ) ) ;
#188791 = CARTESIAN_POINT ( 'NONE',  ( -0.05219959533910754901, -16.53943276465976808, 37.49890960531436690 ) ) ;
#188792 = VECTOR ( 'NONE', #145509, 1000.000000000000000 ) ;
#188793 = CARTESIAN_POINT ( 'NONE',  ( 8.224510206698742110, 14.34966873604972548, 112.0844237280190185 ) ) ;
#188794 = CARTESIAN_POINT ( 'NONE',  ( 16.53943276465976808, 0.05219959533934440121, 81.25109039468568994 ) ) ;
#188795 = CARTESIAN_POINT ( 'NONE',  ( 13.97604488694548053, -13.89961937509957401, 35.62609039468567573 ) ) ;
#188796 = CARTESIAN_POINT ( 'NONE',  ( 16.52216118717208460, 7.221426719304526287, 48.57599021046995347 ) ) ;
#188797 = CARTESIAN_POINT ( 'NONE',  ( -0.05219959533909027116, -19.03943276465977164, 97.49890960531436690 ) ) ;
#188798 = CARTESIAN_POINT ( 'NONE',  ( -8.224510206698948167, 14.34966873604960824, 55.41557627198102409 ) ) ;
#188800 = CARTESIAN_POINT ( 'NONE',  ( -15.80617190586745835, -15.72974639402198527, 21.87390960531436690 ) ) ;
#188799 = CARTESIAN_POINT ( 'NONE',  ( 16.81555441253553695, -7.025013491695479395, 103.1368544533426075 ) ) ;
#188802 = ORIENTED_EDGE ( 'NONE', *, *, #164988, .T. ) ;
#188801 = CARTESIAN_POINT ( 'NONE',  ( 5.823673210054125526, 21.52544592524343514, 54.79057627198104541 ) ) ;
#188803 = CARTESIAN_POINT ( 'NONE',  ( 4.483927247898545687, 16.52544592524342804, 104.7905762719810241 ) ) ;
#188804 = CARTESIAN_POINT ( 'NONE',  ( -12.06949235617739369, -12.14591786802326823, 34.37609039468568284 ) ) ;
#188805 = CARTESIAN_POINT ( 'NONE',  ( 12.14591786802309770, 12.06949235617756955, 79.37390960531436690 ) ) ;
#188806 = LINE ( 'NONE', #50289, #51093 ) ;
#188807 = CARTESIAN_POINT ( 'NONE',  ( 19.02544592524334988, 5.153800228976608722, 81.45942372801897591 ) ) ;
#188808 = CARTESIAN_POINT ( 'NONE',  ( -21.52544592524343514, 5.823673210054127303, 26.04057627198103475 ) ) ;
#188809 = CARTESIAN_POINT ( 'NONE',  ( -29.86685920354755197, -21.69954338932560134, -6.924999997268813878 ) ) ;
#188811 = CARTESIAN_POINT ( 'NONE',  ( -16.55341960407611168, -4.379528057220339221, 36.45724293864768839 ) ) ;
#188810 = CARTESIAN_POINT ( 'NONE',  ( -16.53943276465976808, -0.05219959533934237506, 28.75109039468567929 ) ) ;
#188812 = CARTESIAN_POINT ( 'NONE',  ( -18.62759615963270932, 10.81492255796079327, 60.83224293864769550 ) ) ;
#188813 = CARTESIAN_POINT ( 'NONE',  ( -16.46253265017146816, -9.564922557961047289, 74.16775706135234714 ) ) ;
#188814 = CARTESIAN_POINT ( 'NONE',  ( -5.719274019375978568, 21.55341960407610458, 55.20724293864770260 ) ) ;
#188815 = CARTESIAN_POINT ( 'NONE',  ( -5.719274019375665041, -21.55341960407619695, 74.79275706135234714 ) ) ;
#188816 = CARTESIAN_POINT ( 'NONE',  ( -9.839468975293884867, 9.550175731184090466, -62.57644703671204667 ) ) ;
#188817 = CARTESIAN_POINT ( 'NONE',  ( 0.05219959533934541429, -16.53943276465976808, 40.00109039468567573 ) ) ;
#188819 = CARTESIAN_POINT ( 'NONE',  ( -0.05219959533909027116, -19.03943276465977164, 87.49890960531436690 ) ) ;
#188818 = CARTESIAN_POINT ( 'NONE',  ( 19.05341960407611168, 5.049401038298154454, 28.95724293864769550 ) ) ;
#188820 = CARTESIAN_POINT ( 'NONE',  ( -13.89961937509977652, 13.97604488694528158, 30.62390960531435269 ) ) ;
#188821 = CARTESIAN_POINT ( 'NONE',  ( -4.379528057220328563, 16.55341960407611168, 100.2072429386476955 ) ) ;
#188822 = APPLICATION_PROTOCOL_DEFINITION ( 'draft international standard', 'automotive_design', 1998, #173204 ) ;
#188823 = CARTESIAN_POINT ( 'NONE',  ( -0.05219959533909027116, -19.03943276465977164, 97.49890960531436690 ) ) ;
#188824 = ORIENTED_EDGE ( 'NONE', *, *, #132574, .F. ) ;
#188825 = CARTESIAN_POINT ( 'NONE',  ( -4.379528057220086978, -16.55341960407618274, 54.79275706135235424 ) ) ;
#188826 = CARTESIAN_POINT ( 'NONE',  ( -15.72974639402197994, 15.80617190586746368, 75.62390960531439532 ) ) ;
#188827 = CARTESIAN_POINT ( 'NONE',  ( -5.153800228976328057, -19.02544592524343514, 37.29057627198102409 ) ) ;
#188829 = CARTESIAN_POINT ( 'NONE',  ( 21.52544592524344225, -5.823673210054117533, 108.5405762719810241 ) ) ;
#188828 = CARTESIAN_POINT ( 'NONE',  ( 19.03943276465977164, 0.05219959533936151252, 76.25109039468566152 ) ) ;
#188830 = CARTESIAN_POINT ( 'NONE',  ( 5.049401038298161559, -19.05341960407611168, 67.70724293864769550 ) ) ;
#188831 = CARTESIAN_POINT ( 'NONE',  ( -16.46253265017160317, 9.564922557960807481, 110.8322429386476955 ) ) ;
#188832 = ORIENTED_EDGE ( 'NONE', *, *, #137445, .T. ) ;
#188833 = CARTESIAN_POINT ( 'NONE',  ( 14.29746914071037800, 8.314922557961029526, 36.66775706135234714 ) ) ;
#188834 = CARTESIAN_POINT ( 'NONE',  ( 21.52544592524344225, -5.823673210054117533, 98.54057627198105251 ) ) ;
#188837 = CARTESIAN_POINT ( 'NONE',  ( 5.153800228976615827, -19.02544592524334988, 80.20942372801901854 ) ) ;
#188836 = CARTESIAN_POINT ( 'NONE',  ( 19.05341960407611168, 5.049401038298154454, 88.95724293864769550 ) ) ;
#188835 = CARTESIAN_POINT ( 'NONE',  ( 12.06949235617757843, -12.14591786802309237, 103.1239096053143811 ) ) ;
#188838 = CARTESIAN_POINT ( 'NONE',  ( -18.62759615963270932, 10.81492255796079327, 80.83224293864769550 ) ) ;
#188839 = CARTESIAN_POINT ( 'NONE',  ( -8.314922557960811034, -14.29746914071050412, 52.08224293864768839 ) ) ;
#188840 = CARTESIAN_POINT ( 'NONE',  ( 19.02544592524334988, 5.153800228976608722, 26.45942372801899722 ) ) ;
#188841 = CARTESIAN_POINT ( 'NONE',  ( -14.34966873604972548, 8.224510206698743886, 78.33442372801901854 ) ) ;
#188843 = VERTEX_POINT ( 'NONE', #118130 ) ;
#188842 = CARTESIAN_POINT ( 'NONE',  ( 13.97604488694527802, 13.89961937509977652, 89.37390960531436690 ) ) ;
#188844 = CARTESIAN_POINT ( 'NONE',  ( 19.03943276465977164, -0.05219959533909143690, 43.74890960531435979 ) ) ;
#188845 = CARTESIAN_POINT ( 'NONE',  ( -5.823673210054431948, 21.52544592524334988, 57.70942372801901143 ) ) ;
#188846 = CARTESIAN_POINT ( 'NONE',  ( 5.719274019375673035, 21.55341960407619339, 72.29275706135236135 ) ) ;
#188847 = CARTESIAN_POINT ( 'NONE',  ( -9.564922557960796823, -16.46253265017161027, 62.08224293864769550 ) ) ;
#188848 = CARTESIAN_POINT ( 'NONE',  ( -10.72451020669870658, -18.67979575497194134, 34.58442372801900433 ) ) ;
#188849 = CARTESIAN_POINT ( 'NONE',  ( 0.05219959533936267826, -19.03943276465977164, 90.00109039468567573 ) ) ;
#188850 = CARTESIAN_POINT ( 'NONE',  ( -19.05341960407611168, -5.049401038298163336, 36.45724293864766707 ) ) ;
#188851 = CARTESIAN_POINT ( 'NONE',  ( 4.483927247898790824, -16.52544592524335698, 85.20942372801901854 ) ) ;
#188852 = CARTESIAN_POINT ( 'NONE',  ( -5.153800228976328057, -19.02544592524343514, 67.29057627198102409 ) ) ;
#188853 = CARTESIAN_POINT ( 'NONE',  ( 13.97604488694527802, 13.89961937509977652, 109.3739096053143669 ) ) ;
#188854 = CARTESIAN_POINT ( 'NONE',  ( 5.049401038298161559, -19.05341960407611168, 47.70724293864770260 ) ) ;
#188855 = VECTOR ( 'NONE', #171174, 1000.000000000000000 ) ;
#188856 = CARTESIAN_POINT ( 'NONE',  ( 15.80617190586746368, 15.72974639402197994, 89.37390960531435269 ) ) ;
#188857 = CARTESIAN_POINT ( 'NONE',  ( -4.379528057220086978, -16.55341960407618274, 74.79275706135234714 ) ) ;
#188858 = CARTESIAN_POINT ( 'NONE',  ( -24.50238749460114462, 2.981321037229033521, 173.3223451563238200 ) ) ;
#188859 = CARTESIAN_POINT ( 'NONE',  ( -19.03943276465977164, -0.05219959533935918106, 33.75109039468566863 ) ) ;
#188860 = CARTESIAN_POINT ( 'NONE',  ( -19.02544592524342804, 5.153800228976336051, 61.04057627198103120 ) ) ;
#188861 = CARTESIAN_POINT ( 'NONE',  ( 0.05219959533910956823, 16.53943276465976808, 49.99890960531437401 ) ) ;
#188862 = CARTESIAN_POINT ( 'NONE',  ( 16.52544592524342804, -4.483927247898539470, 83.54057627198102409 ) ) ;
#188863 = CARTESIAN_POINT ( 'NONE',  ( 0.05219959533909260263, 19.03943276465977164, 104.9989096053143669 ) ) ;
#188864 = CARTESIAN_POINT ( 'NONE',  ( 16.51473224551069308, 9.474510206698969483, 94.16557627198103830 ) ) ;
#188865 = CARTESIAN_POINT ( 'NONE',  ( 21.55341960407619695, -5.719274019375665929, 56.04275706135235424 ) ) ;
#188866 = CARTESIAN_POINT ( 'NONE',  ( -19.02544592524342804, 5.153800228976336051, 101.0405762719810241 ) ) ;
#188867 = CARTESIAN_POINT ( 'NONE',  ( -18.62759615963255300, -10.81492255796106328, 109.1677570613523613 ) ) ;
#188868 = CARTESIAN_POINT ( 'NONE',  ( -8.224510206698735004, -14.34966873604973081, 79.58442372801903275 ) ) ;
#188869 = CARTESIAN_POINT ( 'NONE',  ( 10.81492255796106328, -18.62759615963255655, 30.41775706135234358 ) ) ;
#188870 = CARTESIAN_POINT ( 'NONE',  ( -19.03943276465977164, 0.05219959533909376836, 111.2489096053143669 ) ) ;
#188871 = CARTESIAN_POINT ( 'NONE',  ( 18.62759615963271287, -10.81492255796078972, 108.3322429386477097 ) ) ;
#188872 = CARTESIAN_POINT ( 'NONE',  ( 16.55341960407611168, 4.379528057220329451, 53.95724293864770260 ) ) ;
#188874 = CARTESIAN_POINT ( 'NONE',  ( -19.02544592524342804, 5.153800228976336051, 41.04057627198103120 ) ) ;
#188873 = CONICAL_SURFACE ( 'NONE', #50009, 2.500000000000000000, 1.029744258676656976 ) ;
#188875 = CARTESIAN_POINT ( 'NONE',  ( 16.55341960407611168, 4.379528057220329451, 78.95724293864769550 ) ) ;
#188876 = CARTESIAN_POINT ( 'NONE',  ( 18.62759615963271287, -10.81492255796078972, 33.33224293864769550 ) ) ;
#188877 = CARTESIAN_POINT ( 'NONE',  ( 0.05219959533936267826, -19.03943276465977164, 50.00109039468566863 ) ) ;
#188878 = ADVANCED_FACE ( 'NONE', ( #84765 ), #175806, .F. ) ;
#188879 = CARTESIAN_POINT ( 'NONE',  ( 4.483927247898545687, 16.52544592524342804, 114.7905762719810383 ) ) ;
#188880 = ORIENTED_EDGE ( 'NONE', *, *, #154932, .F. ) ;
#188881 = CARTESIAN_POINT ( 'NONE',  ( 16.55341960407618274, -4.379528057220086978, 61.04275706135234714 ) ) ;
#188882 = CARTESIAN_POINT ( 'NONE',  ( 9.564922557960805705, 16.46253265017160317, 69.58224293864770971 ) ) ;
#188883 = CARTESIAN_POINT ( 'NONE',  ( -8.571926809382608425, 26.38167802310805854, 142.4750000027312069 ) ) ;
#188884 = CARTESIAN_POINT ( 'NONE',  ( -14.34966873604960291, -8.224510206698953496, 86.66557627198102409 ) ) ;
#188885 = CARTESIAN_POINT ( 'NONE',  ( 18.62759615963271287, -10.81492255796078972, 38.33224293864768839 ) ) ;
#188886 = CARTESIAN_POINT ( 'NONE',  ( 12.14591786802327356, -12.06949235617739191, 105.6260903946856899 ) ) ;
#188887 = CARTESIAN_POINT ( 'NONE',  ( -5.153800228976607833, 19.02544592524334988, 102.7094237280189759 ) ) ;
#188888 = CARTESIAN_POINT ( 'NONE',  ( 15.72974639402176855, 15.80617190586768217, 81.87609039468568994 ) ) ;
#188889 = CARTESIAN_POINT ( 'NONE',  ( 5.153800228976335163, 19.02544592524342804, 89.79057627198102409 ) ) ;
#188890 = CARTESIAN_POINT ( 'NONE',  ( 21.52544592524344225, -5.823673210054117533, 98.54057627198105251 ) ) ;
#188891 = CARTESIAN_POINT ( 'NONE',  ( -8.314922557961024197, 14.29746914071037800, 57.91775706135234714 ) ) ;
#188893 = CARTESIAN_POINT ( 'NONE',  ( -19.05341960407611168, -5.049401038298163336, 36.45724293864766707 ) ) ;
#188892 = VECTOR ( 'NONE', #175552, 1000.000000000000000 ) ;
#188894 = CARTESIAN_POINT ( 'NONE',  ( -4.483927247898782831, 16.52544592524335698, 37.70942372801900433 ) ) ;
#188895 = CARTESIAN_POINT ( 'NONE',  ( 5.153800228976615827, -19.02544592524334988, 100.2094237280190043 ) ) ;
#188896 = CARTESIAN_POINT ( 'NONE',  ( 15.80617190586746368, 15.72974639402197994, 89.37390960531435269 ) ) ;
#188897 = CARTESIAN_POINT ( 'NONE',  ( -5.153800228976607833, 19.02544592524334988, 52.70942372801900433 ) ) ;
#188898 = CARTESIAN_POINT ( 'NONE',  ( 5.000000000000000000, -120.0000000000000142, 14.99999999999998757 ) ) ;
#188899 = CARTESIAN_POINT ( 'NONE',  ( -18.62759615963270932, 10.81492255796079327, 100.8322429386477097 ) ) ;
#188900 = CARTESIAN_POINT ( 'NONE',  ( 17.50000000000002842, 3.512728167236816912, 27.27190004818877966 ) ) ;
#188901 = CARTESIAN_POINT ( 'NONE',  ( 5.153800228976335163, 19.02544592524342804, 74.79057627198103830 ) ) ;
#188902 = TOROIDAL_SURFACE ( 'NONE', #95210, 206.0437394197456342, 10.00000000000000000 ) ;
#188903 = LINE ( 'NONE', #23026, #1280 ) ;
#188904 = CARTESIAN_POINT ( 'NONE',  ( -0.05219959533934338120, 16.53943276465976808, 32.50109039468568284 ) ) ;
#188905 = CARTESIAN_POINT ( 'NONE',  ( 19.92827645216230437, -34.68249012782280261, -5.691795689800142277 ) ) ;
#188907 = CARTESIAN_POINT ( 'NONE',  ( 12.14591786802309770, 12.06949235617756955, 64.37390960531435269 ) ) ;
#188906 = CARTESIAN_POINT ( 'NONE',  ( -18.67979575497178146, -10.72451020669898902, 111.6655762719810525 ) ) ;
#188908 = CARTESIAN_POINT ( 'NONE',  ( -13.89961937509977652, 13.97604488694528158, 65.62390960531436690 ) ) ;
#188909 = AXIS2_PLACEMENT_3D ( 'NONE', #160124, #128772, #84264 ) ;
#188910 = PRODUCT_DEFINITION_FORMATION_WITH_SPECIFIED_SOURCE ( 'ANY', '', #92061, .NOT_KNOWN. ) ;
#188912 = CARTESIAN_POINT ( 'NONE',  ( 19.02544592524334988, 5.153800228976608722, 41.45942372801900433 ) ) ;
#188911 = CARTESIAN_POINT ( 'NONE',  ( -14.29746914071037622, -8.314922557961029526, 39.16775706135235424 ) ) ;
#188913 = CARTESIAN_POINT ( 'NONE',  ( -21.53943276465977519, -0.05219959533937600094, 53.75109039468568994 ) ) ;
#188914 = CARTESIAN_POINT ( 'NONE',  ( 9.474510206698729675, 16.51473224551082808, 112.0844237280190043 ) ) ;
#188915 = CARTESIAN_POINT ( 'NONE',  ( -13.97604488694527625, -13.89961937509977652, 56.87390960531434558 ) ) ;
#188916 = CARTESIAN_POINT ( 'NONE',  ( -16.46253265017146816, -9.564922557961047289, 79.16775706135234714 ) ) ;
#188917 = CARTESIAN_POINT ( 'NONE',  ( -21.52544592524334988, -5.823673210054445271, 83.95942372801900433 ) ) ;
#188918 = CARTESIAN_POINT ( 'NONE',  ( 9.474510206698729675, 16.51473224551082808, 62.08442372801899722 ) ) ;
#188919 = CARTESIAN_POINT ( 'NONE',  ( 9.474510206698971260, -16.51473224551069308, 37.91557627198102409 ) ) ;
#188920 = CARTESIAN_POINT ( 'NONE',  ( -21.53943276465977519, 0.05219959533907696930, 61.24890960531435979 ) ) ;
#188922 = CARTESIAN_POINT ( 'NONE',  ( 19.02544592524334988, 5.153800228976608722, 66.45942372801899012 ) ) ;
#188921 = CARTESIAN_POINT ( 'NONE',  ( -16.52544592524342804, 4.483927247898546575, 61.04057627198103120 ) ) ;
#188923 = CARTESIAN_POINT ( 'NONE',  ( -17.72662750342726667, -5.499999999999957367, 101.4017949228374391 ) ) ;
#188924 = CARTESIAN_POINT ( 'NONE',  ( -19.03943276465977164, -0.05219959533935918106, 23.75109039468566152 ) ) ;
#188925 = CARTESIAN_POINT ( 'NONE',  ( -14.29746914071037622, -8.314922557961029526, 99.16775706135234714 ) ) ;
#188926 = CARTESIAN_POINT ( 'NONE',  ( 12.14591786802309770, 12.06949235617756955, 54.37390960531435979 ) ) ;
#188928 = CARTESIAN_POINT ( 'NONE',  ( 8.571926809382603096, -26.38167802310801235, 141.4750000027312069 ) ) ;
#188927 = CARTESIAN_POINT ( 'NONE',  ( 10.72451020669871369, 18.67979575497193778, 92.08442372801901854 ) ) ;
#188929 = CARTESIAN_POINT ( 'NONE',  ( -15.72974639402176322, -15.80617190586768395, 89.37609039468568994 ) ) ;
#188930 = CARTESIAN_POINT ( 'NONE',  ( -21.53943276465977519, 0.05219959533907696930, 96.24890960531435269 ) ) ;
#188931 = CARTESIAN_POINT ( 'NONE',  ( -16.46253265017160317, 9.564922557960807481, 50.83224293864770260 ) ) ;
#188932 = CARTESIAN_POINT ( 'NONE',  ( -21.52544592524334988, -5.823673210054445271, 73.95942372801901854 ) ) ;
#188933 = CARTESIAN_POINT ( 'NONE',  ( -16.46253265017160317, 9.564922557960807481, 50.83224293864770260 ) ) ;
#188934 = VERTEX_POINT ( 'NONE', #99940 ) ;
#188935 = CARTESIAN_POINT ( 'NONE',  ( -19.03943276465977164, 0.05219959533909376836, 66.24890960531436690 ) ) ;
#188936 = CARTESIAN_POINT ( 'NONE',  ( -12.14591786802309592, -12.06949235617757132, 111.8739096053143669 ) ) ;
#188937 = CARTESIAN_POINT ( 'NONE',  ( 19.03943276465977164, -0.05219959533909143690, 108.7489096053143527 ) ) ;
#188938 = CARTESIAN_POINT ( 'NONE',  ( 12.14591786802309770, 12.06949235617756955, 49.37390960531436690 ) ) ;
#188939 = CARTESIAN_POINT ( 'NONE',  ( 13.97604488694527802, 13.89961937509977652, 29.37390960531435979 ) ) ;
#188940 = CARTESIAN_POINT ( 'NONE',  ( 12.14591786802309770, 12.06949235617756955, 74.37390960531436690 ) ) ;
#188941 = VECTOR ( 'NONE', #58450, 1000.000000000000000 ) ;
#188942 = CARTESIAN_POINT ( 'NONE',  ( 21.52544592524344225, -5.823673210054117533, 93.54057627198103830 ) ) ;
#188943 = CARTESIAN_POINT ( 'NONE',  ( -5.823673210054431948, 21.52544592524334988, 32.70942372801900433 ) ) ;
#188944 = CARTESIAN_POINT ( 'NONE',  ( 0.3967178197656787142, 6.139882670400419684, -62.49912032061806855 ) ) ;
#188945 = CARTESIAN_POINT ( 'NONE',  ( -12.06949235617739369, -12.14591786802326823, 34.37609039468568284 ) ) ;
#188946 = CARTESIAN_POINT ( 'NONE',  ( 5.719274019375991003, -21.55341960407610458, 82.70724293864770971 ) ) ;
#188947 = CARTESIAN_POINT ( 'NONE',  ( -15.72974639402176322, -15.80617190586768395, 104.3760903946856899 ) ) ;
#188948 = CARTESIAN_POINT ( 'NONE',  ( -19.02544592524342804, 5.153800228976336051, 91.04057627198100988 ) ) ;
#188949 = CARTESIAN_POINT ( 'NONE',  ( -15.80617190586768217, 15.72974639402176855, 48.12609039468568284 ) ) ;
#188950 = CARTESIAN_POINT ( 'NONE',  ( 10.81492255796078972, 18.62759615963270932, 24.58224293864768839 ) ) ;
#188951 = CARTESIAN_POINT ( 'NONE',  ( 4.379528057220092307, 16.55341960407617563, 97.29275706135234714 ) ) ;
#188953 = CARTESIAN_POINT ( 'NONE',  ( -15.80617190586768217, 15.72974639402176855, 88.12609039468570415 ) ) ;
#188952 = CARTESIAN_POINT ( 'NONE',  ( 15.72974639402176855, 15.80617190586768217, 46.87609039468568994 ) ) ;
#188954 = CARTESIAN_POINT ( 'NONE',  ( 21.53943276465977519, 0.05219959533937863772, 111.2510903946856899 ) ) ;
#188955 = CARTESIAN_POINT ( 'NONE',  ( 8.314922557961029526, -14.29746914071037800, 85.41775706135236135 ) ) ;
#188956 = CARTESIAN_POINT ( 'NONE',  ( 21.55341960407619695, -5.719274019375665929, 41.04275706135236135 ) ) ;
#188957 = CARTESIAN_POINT ( 'NONE',  ( -16.51473224551069308, -9.474510206698971260, 26.66557627198103120 ) ) ;
#188958 = CARTESIAN_POINT ( 'NONE',  ( -10.81492255796105439, 18.62759615963255655, 97.91775706135236135 ) ) ;
#188959 = CARTESIAN_POINT ( 'NONE',  ( 13.97604488694527802, 13.89961937509977652, 104.3739096053143385 ) ) ;
#188960 = CARTESIAN_POINT ( 'NONE',  ( -5.719274019375978568, 21.55341960407610458, 105.2072429386477097 ) ) ;
#188961 = CARTESIAN_POINT ( 'NONE',  ( 5.719274019375991003, -21.55341960407610458, 62.70724293864769550 ) ) ;
#188963 = CARTESIAN_POINT ( 'NONE',  ( -21.55341960407610458, -5.719274019375992779, 71.45724293864769550 ) ) ;
#188962 = FACE_OUTER_BOUND ( 'NONE', #186778, .T. ) ;
#188965 = CARTESIAN_POINT ( 'NONE',  ( 12.14591786802309770, 12.06949235617756955, 59.37390960531436690 ) ) ;
#188964 = CARTESIAN_POINT ( 'NONE',  ( -8.314922557961024197, 14.29746914071037800, 57.91775706135234714 ) ) ;
#188966 = LINE ( 'NONE', #2931, #95041 ) ;
#188967 = CARTESIAN_POINT ( 'NONE',  ( -19.05341960407617563, 5.049401038297882671, 88.54275706135230450 ) ) ;
#188968 = LINE ( 'NONE', #50444, #73359 ) ;
#188969 = CARTESIAN_POINT ( 'NONE',  ( 14.29746914071037800, 8.314922557961029526, 31.66775706135234358 ) ) ;
#188970 = CARTESIAN_POINT ( 'NONE',  ( -15.80617190586745835, -15.72974639402198527, 101.8739096053143811 ) ) ;
#188971 = CARTESIAN_POINT ( 'NONE',  ( -21.55341960407610458, -5.719274019375992779, 76.45724293864769550 ) ) ;
#188972 = CARTESIAN_POINT ( 'NONE',  ( 18.62759615963271287, -10.81492255796078972, 23.33224293864769194 ) ) ;
#188973 = CARTESIAN_POINT ( 'NONE',  ( -16.55341960407617563, 4.379528057220093196, 53.54275706135234714 ) ) ;
#188974 = CARTESIAN_POINT ( 'NONE',  ( 0.05219959533909260263, 19.03943276465977164, 69.99890960531435269 ) ) ;
#188976 = CARTESIAN_POINT ( 'NONE',  ( -16.46253265017146816, -9.564922557961047289, 104.1677570613523329 ) ) ;
#188975 = CARTESIAN_POINT ( 'NONE',  ( -10.72451020669870658, -18.67979575497194134, 24.58442372801901499 ) ) ;
#188977 = CARTESIAN_POINT ( 'NONE',  ( 19.03943276465977164, -0.05219959533909143690, 108.7489096053143527 ) ) ;
#188978 = CARTESIAN_POINT ( 'NONE',  ( 19.02544592524343514, -5.153800228976328945, 88.54057627198102409 ) ) ;
#188979 = CARTESIAN_POINT ( 'NONE',  ( 10.81492255796078972, 18.62759615963270932, 84.58224293864769550 ) ) ;
#188980 = CARTESIAN_POINT ( 'NONE',  ( -16.46253265017160317, 9.564922557960807481, 60.83224293864769550 ) ) ;
#188981 = CARTESIAN_POINT ( 'NONE',  ( -17.49999999999999645, -5.499999999999992895, 59.20309617465829177 ) ) ;
#188982 = CARTESIAN_POINT ( 'NONE',  ( 8.314922557960818139, 14.29746914071049879, 74.58224293864768129 ) ) ;
#188983 = CARTESIAN_POINT ( 'NONE',  ( 18.62759615963271287, -10.81492255796078972, 28.33224293864769550 ) ) ;
#188984 = CARTESIAN_POINT ( 'NONE',  ( -30.58708291193883255, 1.497147075633844526, -50.73425184351846440 ) ) ;
#188985 = VECTOR ( 'NONE', #64859, 1000.000000000000000 ) ;
#188986 = CARTESIAN_POINT ( 'NONE',  ( 5.719274019375991003, -21.55341960407610458, 107.7072429386476955 ) ) ;
#188987 = CARTESIAN_POINT ( 'NONE',  ( -16.51473224551082808, 9.474510206698731452, 68.33442372801900433 ) ) ;
#188988 = CARTESIAN_POINT ( 'NONE',  ( -19.03943276465977164, 0.05219959533909376836, 116.2489096053143669 ) ) ;
#188989 = CARTESIAN_POINT ( 'NONE',  ( -10.81492255796078084, -18.62759615963271287, 57.08224293864769550 ) ) ;
#188990 = CARTESIAN_POINT ( 'NONE',  ( -19.03943276465977164, 0.05219959533909376836, 91.24890960531436690 ) ) ;
#188991 = CARTESIAN_POINT ( 'NONE',  ( 18.62759615963255655, 10.81492255796105972, 81.66775706135236135 ) ) ;
#188992 = CARTESIAN_POINT ( 'NONE',  ( 13.97604488694527802, 13.89961937509977652, 49.37390960531434558 ) ) ;
#188993 = CARTESIAN_POINT ( 'NONE',  ( 4.483927247898545687, 16.52544592524342804, 89.79057627198103830 ) ) ;
#188994 = CARTESIAN_POINT ( 'NONE',  ( -8.224510206698735004, -14.34966873604973081, 34.58442372801900433 ) ) ;
#188995 = CARTESIAN_POINT ( 'NONE',  ( -21.52544592524334988, -5.823673210054445271, 63.95942372801901854 ) ) ;
#188996 = ORIENTED_EDGE ( 'NONE', *, *, #5508, .F. ) ;
#188997 = CARTESIAN_POINT ( 'NONE',  ( 9.474510206698729675, 16.51473224551082808, 32.08442372801900433 ) ) ;
#188998 = CARTESIAN_POINT ( 'NONE',  ( 13.97604488694548053, -13.89961937509957401, 80.62609039468567573 ) ) ;
#188999 = CARTESIAN_POINT ( 'NONE',  ( 13.89961937509957401, 13.97604488694547697, 41.87609039468566152 ) ) ;
#189000 = DIRECTION ( 'NONE',  ( 0.000000000000000000, 0.000000000000000000, 1.000000000000000000 ) ) ;
#189001 = CARTESIAN_POINT ( 'NONE',  ( -10.72451020669870658, -18.67979575497194134, 39.58442372801901143 ) ) ;
#189002 = CARTESIAN_POINT ( 'NONE',  ( -38.00000000000001421, 12.34694845685046438, -3.849999994537626868 ) ) ;
#189003 = CARTESIAN_POINT ( 'NONE',  ( -5.049401038297874678, -19.05341960407617918, 34.79275706135233293 ) ) ;
#189004 = CARTESIAN_POINT ( 'NONE',  ( 9.564922557960805705, 16.46253265017160317, 59.58224293864769550 ) ) ;
#189005 = CARTESIAN_POINT ( 'NONE',  ( 19.02544592524334988, 5.153800228976608722, 26.45942372801899722 ) ) ;
#189006 = CARTESIAN_POINT ( 'NONE',  ( -16.55341960407617563, 4.379528057220093196, 98.54275706135234714 ) ) ;
#189008 = CARTESIAN_POINT ( 'NONE',  ( -10.72451020669870658, -18.67979575497194134, 84.58442372801903275 ) ) ;
#189007 = CARTESIAN_POINT ( 'NONE',  ( -5.823673210054116645, -21.52544592524344225, 27.29057627198103120 ) ) ;
#189009 = CARTESIAN_POINT ( 'NONE',  ( 11.40812507854754365, 35.11059874428196537, -3.224999997268813701 ) ) ;
#189010 = CARTESIAN_POINT ( 'NONE',  ( -17.50000000000000355, -3.209263204892690791, 35.23803174393751192 ) ) ;
#189011 = CARTESIAN_POINT ( 'NONE',  ( 10.81492255796106328, -18.62759615963255655, 85.41775706135236135 ) ) ;
#189012 = CARTESIAN_POINT ( 'NONE',  ( -19.24578484527059175, -180.9428398739491684, -25.00000000000000000 ) ) ;
#189013 = CARTESIAN_POINT ( 'NONE',  ( -13.97604488694527625, -13.89961937509977652, 106.8739096053143669 ) ) ;
#189014 = EDGE_CURVE ( 'NONE', #119499, #103252, #132248, .T. ) ;
#189015 = CARTESIAN_POINT ( 'NONE',  ( -0.7913989229878302112, -31.67901979315911021, -49.40962234820035093 ) ) ;
#189016 = CARTESIAN_POINT ( 'NONE',  ( 19.05341960407611168, 5.049401038298154454, 58.95724293864768129 ) ) ;
#189017 = CARTESIAN_POINT ( 'NONE',  ( 15.80617190586746368, 15.72974639402197994, 59.37390960531436690 ) ) ;
#189018 = CARTESIAN_POINT ( 'NONE',  ( -12.14591786802309592, -12.06949235617757132, 21.87390960531436690 ) ) ;
#189020 = CARTESIAN_POINT ( 'NONE',  ( -19.05341960407611168, -5.049401038298163336, 86.45724293864769550 ) ) ;
#189019 = CARTESIAN_POINT ( 'NONE',  ( 14.34966873604960469, 8.224510206698951720, 94.16557627198103830 ) ) ;
#189021 = CARTESIAN_POINT ( 'NONE',  ( 0.05219959533936267826, -19.03943276465977164, 25.00109039468566152 ) ) ;
#189022 = CARTESIAN_POINT ( 'NONE',  ( 16.46253265017160672, -9.564922557960803928, 33.33224293864770260 ) ) ;
#189023 = CARTESIAN_POINT ( 'NONE',  ( -16.55341960407611168, -4.379528057220339221, 106.4572429386477097 ) ) ;
#189024 = CARTESIAN_POINT ( 'NONE',  ( 5.823673210054444382, -21.52544592524334988, 50.20942372801901854 ) ) ;
#189025 = CARTESIAN_POINT ( 'NONE',  ( -21.52544592524343514, 5.823673210054127303, 86.04057627198102409 ) ) ;
#189026 = CARTESIAN_POINT ( 'NONE',  ( 5.153800228976615827, -19.02544592524334988, 70.20942372801899012 ) ) ;
#189027 = DIRECTION ( 'NONE',  ( -1.000000000000000000, 0.000000000000000000, 0.000000000000000000 ) ) ;
#189028 = CARTESIAN_POINT ( 'NONE',  ( -0.05219959533909027116, -19.03943276465977164, 107.4989096053143527 ) ) ;
#189029 = CARTESIAN_POINT ( 'NONE',  ( 0.05219959533910956823, 16.53943276465976808, 74.99890960531435269 ) ) ;
#189030 = AXIS2_PLACEMENT_3D ( 'NONE', #1092, #124449, #136305 ) ;
#189031 = CARTESIAN_POINT ( 'NONE',  ( 0.05219959533936267826, -19.03943276465977164, 45.00109039468566863 ) ) ;
#189032 = CARTESIAN_POINT ( 'NONE',  ( -13.89961937509977652, 13.97604488694528158, 65.62390960531436690 ) ) ;
#189033 = CARTESIAN_POINT ( 'NONE',  ( -0.05219959533910754901, -16.53943276465976808, 67.49890960531436690 ) ) ;
#189034 = CARTESIAN_POINT ( 'NONE',  ( 9.564922557961047289, -16.46253265017146816, 75.41775706135234714 ) ) ;
#189035 = CARTESIAN_POINT ( 'NONE',  ( 21.55341960407610458, 5.719274019375980345, 38.95724293864768839 ) ) ;
#189036 = ORIENTED_EDGE ( 'NONE', *, *, #80402, .T. ) ;
#189037 = CARTESIAN_POINT ( 'NONE',  ( -4.483927247898539470, -16.52544592524342804, 107.2905762719810525 ) ) ;
#189038 = CARTESIAN_POINT ( 'NONE',  ( -28.79475375365586842, 2.428612866367529932E-14, 140.2656553485623760 ) ) ;
#189040 = CARTESIAN_POINT ( 'NONE',  ( 18.62759615963271287, -10.81492255796078972, 68.33224293864769550 ) ) ;
#189039 = CARTESIAN_POINT ( 'NONE',  ( 19.02544592524343514, -5.153800228976328945, 53.54057627198102409 ) ) ;
#189041 = CARTESIAN_POINT ( 'NONE',  ( -16.51473224551069308, -9.474510206698971260, 41.66557627198103120 ) ) ;
#189043 = CARTESIAN_POINT ( 'NONE',  ( 19.02544592524343514, -5.153800228976328945, 73.54057627198103830 ) ) ;
#189042 = CARTESIAN_POINT ( 'NONE',  ( -12.14591786802326823, 12.06949235617739902, 78.12609039468570415 ) ) ;
#189044 = CARTESIAN_POINT ( 'NONE',  ( -16.51473224551082808, 9.474510206698731452, 58.33442372801900433 ) ) ;
#189045 = CARTESIAN_POINT ( 'NONE',  ( 15.80617190586769283, -15.72974639402175789, 65.62609039468568994 ) ) ;
#189046 = CARTESIAN_POINT ( 'NONE',  ( -5.719274019375978568, 21.55341960407610458, 50.20724293864769550 ) ) ;
#189047 = CARTESIAN_POINT ( 'NONE',  ( -0.05219959533909027116, -19.03943276465977164, 107.4989096053143527 ) ) ;
#189048 = CARTESIAN_POINT ( 'NONE',  ( 9.474510206698971260, -16.51473224551069308, 27.91557627198103120 ) ) ;
#189049 = CARTESIAN_POINT ( 'NONE',  ( -16.55341960407617563, 4.379528057220093196, 83.54275706135234714 ) ) ;
#189050 = CARTESIAN_POINT ( 'NONE',  ( -0.05219959533936034679, 19.03943276465977164, 107.5010903946856615 ) ) ;
#189051 = PLANE ( 'NONE',  #51768 ) ;
#189052 = CARTESIAN_POINT ( 'NONE',  ( 19.25918095147779496, 5.499999999999574563, 76.95284276293931214 ) ) ;
#189053 = CARTESIAN_POINT ( 'NONE',  ( -10.72451020669870658, -18.67979575497194134, 99.58442372801900433 ) ) ;
#189055 = VERTEX_POINT ( 'NONE', #166630 ) ;
#189054 = AXIS2_PLACEMENT_3D ( 'NONE', #11984, #101976, #163656 ) ;
#189056 = CARTESIAN_POINT ( 'NONE',  ( -12.06949235617756955, 12.14591786802309770, 60.62390960531437401 ) ) ;
#189058 = CARTESIAN_POINT ( 'NONE',  ( -12.06949235617756955, 12.14591786802309770, 70.62390960531436690 ) ) ;
#189057 =( BOUNDED_CURVE ( )  B_SPLINE_CURVE ( 2, ( #68120, #176322, #85280, #99454, #161134, #84277, #145958, #83283, #69123, #82272, #130790, #100456, #101449 ),
 .UNSPECIFIED., .F., .T. ) 
 B_SPLINE_CURVE_WITH_KNOTS ( ( 3, 2, 2, 2, 2, 2, 3 ),
 ( 0.2919041206375714848, 0.2938596491228070429, 0.2982456140350877027, 0.3026315789473684181, 0.3070175438596491335, 0.3114035087719298489, 0.3133133574350753237 ),
 .UNSPECIFIED. ) 
 CURVE ( )  GEOMETRIC_REPRESENTATION_ITEM ( )  RATIONAL_B_SPLINE_CURVE ( ( 0.9831626618144004848, 0.9848076720550091867, 1.000000000000000000, 0.9659258262890683122, 1.000000000000000000, 0.9659258262890683122, 1.000000000000000000, 0.9659258262890683122, 1.000000000000000000, 0.9659258262890683122, 1.000000000000000000, 0.9851625545550088958, 0.9832469066685279868 ) ) 
 REPRESENTATION_ITEM ( '' )  );
#189059 = CARTESIAN_POINT ( 'NONE',  ( -5.823673210054116645, -21.52544592524344225, 97.29057627198105251 ) ) ;
#189060 = CARTESIAN_POINT ( 'NONE',  ( -0.05219959533907301413, -21.53943276465977519, 82.49890960531436690 ) ) ;
#189061 = CARTESIAN_POINT ( 'NONE',  ( 17.31728774477274158, -6.344390552232389346, 98.31906651689324406 ) ) ;
#189062 = CARTESIAN_POINT ( 'NONE',  ( -5.719274019375978568, 21.55341960407610458, 35.20724293864768839 ) ) ;
#189064 = AXIS2_PLACEMENT_3D ( 'NONE', #95231, #156917, #81048 ) ;
#189063 = CARTESIAN_POINT ( 'NONE',  ( -16.52544592524335698, -4.483927247898792601, 68.95942372801901854 ) ) ;
#189065 = CARTESIAN_POINT ( 'NONE',  ( 4.379528057220339221, -16.55341960407611168, 97.70724293864772392 ) ) ;
#189066 = CARTESIAN_POINT ( 'NONE',  ( 0.05219959533909260263, 19.03943276465977164, 44.99890960531435979 ) ) ;
#189067 = CARTESIAN_POINT ( 'NONE',  ( 34.77074502975525405, -6.826893893699448768, 41.88499232265944272 ) ) ;
#189068 = CARTESIAN_POINT ( 'NONE',  ( -8.314922557961024197, 14.29746914071037800, 97.91775706135236135 ) ) ;
#189069 = CARTESIAN_POINT ( 'NONE',  ( 10.72451020669871369, 18.67979575497193778, 32.08442372801901854 ) ) ;
#189070 = CARTESIAN_POINT ( 'NONE',  ( -5.153800228976328057, -19.02544592524343514, 87.29057627198103830 ) ) ;
#189071 = CARTESIAN_POINT ( 'NONE',  ( -15.72974639402176322, -15.80617190586768395, 69.37609039468567573 ) ) ;
#189072 = CARTESIAN_POINT ( 'NONE',  ( 5.049401038298161559, -19.05341960407611168, 112.7072429386476813 ) ) ;
#189073 = CARTESIAN_POINT ( 'NONE',  ( -6.300487686722341607, -38.77208804323718283, -32.75369354553867396 ) ) ;
#189074 = EDGE_LOOP ( 'NONE', ( #102658, #162142, #170882, #115826 ) ) ;
#189075 = CARTESIAN_POINT ( 'NONE',  ( 21.53943276465977519, 0.05219959533937863772, 56.25109039468568284 ) ) ;
#189077 = CARTESIAN_POINT ( 'NONE',  ( -19.02544592524342804, 5.153800228976336051, 111.0405762719810099 ) ) ;
#189076 = CARTESIAN_POINT ( 'NONE',  ( 0.05219959533909260263, 19.03943276465977164, 34.99890960531435979 ) ) ;
#189078 = CARTESIAN_POINT ( 'NONE',  ( -5.049401038297874678, -19.05341960407617918, 64.79275706135233293 ) ) ;
#189079 = CARTESIAN_POINT ( 'NONE',  ( 10.81492255796106328, -18.62759615963255655, 30.41775706135234358 ) ) ;
#189080 = CARTESIAN_POINT ( 'NONE',  ( 16.46253265017146816, 9.564922557961045513, 61.66775706135234003 ) ) ;
#189081 = CARTESIAN_POINT ( 'NONE',  ( -19.03943276465977164, 0.05219959533909376836, 26.24890960531435624 ) ) ;
#189082 = CARTESIAN_POINT ( 'NONE',  ( 12.14591786802327356, -12.06949235617739191, 90.62609039468567573 ) ) ;
#189083 = CARTESIAN_POINT ( 'NONE',  ( 16.51473224551083163, -9.474510206698727899, 60.83442372801900433 ) ) ;
#189084 = CARTESIAN_POINT ( 'NONE',  ( 16.53943276465976808, -0.05219959533910856209, 28.74890960531435624 ) ) ;
#189085 = CARTESIAN_POINT ( 'NONE',  ( 5.153800228976615827, -19.02544592524334988, 50.20942372801897591 ) ) ;
#189086 = CARTESIAN_POINT ( 'NONE',  ( -19.03943276465977164, 0.05219959533909376836, 86.24890960531436690 ) ) ;
#189087 = CARTESIAN_POINT ( 'NONE',  ( -18.67979575497193778, 10.72451020669871902, 98.33442372801901854 ) ) ;
#189089 = EDGE_CURVE ( 'NONE', #49235, #152202, #138261, .T. ) ;
#189088 = CARTESIAN_POINT ( 'NONE',  ( 21.55341960407619695, -5.719274019375665929, 106.0427570613523471 ) ) ;
#189090 = DIRECTION ( 'NONE',  ( -1.000000000000000000, -0.000000000000000000, -0.000000000000000000 ) ) ;
#189091 = CARTESIAN_POINT ( 'NONE',  ( -15.80617190586768217, 15.72974639402176855, 88.12609039468570415 ) ) ;
#189092 = CARTESIAN_POINT ( 'NONE',  ( -16.53943276465976808, -0.05219959533934237506, 38.75109039468567573 ) ) ;
#189093 = CARTESIAN_POINT ( 'NONE',  ( 19.03943276465977164, -0.05219959533909143690, 98.74890960531436690 ) ) ;
#189094 = CARTESIAN_POINT ( 'NONE',  ( -0.05219959533907301413, -21.53943276465977519, 27.49890960531435269 ) ) ;
#189095 = CARTESIAN_POINT ( 'NONE',  ( 0.000000000000000000, 0.000000000000000000, -15.00000000000000000 ) ) ;
#189096 = CARTESIAN_POINT ( 'NONE',  ( 9.474510206698971260, -16.51473224551069308, 77.91557627198103830 ) ) ;
#189097 = CARTESIAN_POINT ( 'NONE',  ( -18.56101223717331905, -5.499999999999949374, 41.44978406935677384 ) ) ;
#189098 = CARTESIAN_POINT ( 'NONE',  ( 13.89961937509957401, 13.97604488694547697, 76.87609039468566152 ) ) ;
#189099 = CARTESIAN_POINT ( 'NONE',  ( -5.153800228976328057, -19.02544592524343514, 112.2905762719810099 ) ) ;
#189100 = CARTESIAN_POINT ( 'NONE',  ( -15.80617190586768217, 15.72974639402176855, 103.1260903946856757 ) ) ;
#189101 = CARTESIAN_POINT ( 'NONE',  ( 16.53943276465976808, -0.05219959533910856209, 98.74890960531438111 ) ) ;
#189102 = CARTESIAN_POINT ( 'NONE',  ( -5.719274019375978568, 21.55341960407610458, 45.20724293864769550 ) ) ;
#189103 = CARTESIAN_POINT ( 'NONE',  ( 15.80617190586746368, 15.72974639402197994, 34.37390960531435979 ) ) ;
#189104 = CARTESIAN_POINT ( 'NONE',  ( 8.314922557960818139, 14.29746914071049879, 99.58224293864770971 ) ) ;
#189105 = CARTESIAN_POINT ( 'NONE',  ( -40.00000000000000711, 2.918471586026471156E-14, -25.00000000000000000 ) ) ;
#189106 = CARTESIAN_POINT ( 'NONE',  ( -5.153800228976607833, 19.02544592524334988, 52.70942372801900433 ) ) ;
#189107 = CARTESIAN_POINT ( 'NONE',  ( 14.29746914071049879, -8.314922557960816363, 28.33224293864769550 ) ) ;
#189108 = CARTESIAN_POINT ( 'NONE',  ( -16.46253265017160317, 9.564922557960807481, 95.83224293864769550 ) ) ;
#189109 = CARTESIAN_POINT ( 'NONE',  ( -18.62759615963255300, -10.81492255796106328, 79.16775706135234714 ) ) ;
#189110 = CARTESIAN_POINT ( 'NONE',  ( 5.719274019375991003, -21.55341960407610458, 57.70724293864770260 ) ) ;
#189111 = CARTESIAN_POINT ( 'NONE',  ( 21.53943276465977519, 0.05219959533937863772, 51.25109039468568994 ) ) ;
#189112 = CARTESIAN_POINT ( 'NONE',  ( -0.05219959533907301413, -21.53943276465977519, 92.49890960531436690 ) ) ;
#189113 = CARTESIAN_POINT ( 'NONE',  ( -21.55341960407619339, 5.719274019375674811, 33.54275706135234714 ) ) ;
#189114 = CARTESIAN_POINT ( 'NONE',  ( -9.474510206698964154, 16.51473224551069663, 25.41557627198103120 ) ) ;
#189115 = CARTESIAN_POINT ( 'NONE',  ( 19.03943276465977164, -0.05219959533909143690, 78.74890960531436690 ) ) ;
#189116 = CARTESIAN_POINT ( 'NONE',  ( -14.29746914071037622, -8.314922557961029526, 84.16775706135234714 ) ) ;
#189117 = CARTESIAN_POINT ( 'NONE',  ( -8.224510206698948167, 14.34966873604960824, 105.4155762719810383 ) ) ;
#189118 = CARTESIAN_POINT ( 'NONE',  ( 5.049401038298161559, -19.05341960407611168, 107.7072429386476955 ) ) ;
#189119 = CONICAL_SURFACE ( 'NONE', #101937, 2.041999999999999815, 1.047197551196591858 ) ;
#189120 = CARTESIAN_POINT ( 'NONE',  ( 14.34966873604960469, 8.224510206698951720, 59.16557627198103120 ) ) ;
#189121 = CARTESIAN_POINT ( 'NONE',  ( -12.14591786802309592, -12.06949235617757132, 26.87390960531435979 ) ) ;
#189122 = CARTESIAN_POINT ( 'NONE',  ( 5.049401038298161559, -19.05341960407611168, 47.70724293864770260 ) ) ;
#189123 = CARTESIAN_POINT ( 'NONE',  ( 13.97604488694527802, 13.89961937509977652, 24.37390960531435624 ) ) ;
#189124 = CARTESIAN_POINT ( 'NONE',  ( -10.72451020669898014, 18.67979575497178502, 50.41557627198103120 ) ) ;
#189125 = CARTESIAN_POINT ( 'NONE',  ( 19.05341960407617918, -5.049401038297876454, 31.04275706135232227 ) ) ;
#189127 = CARTESIAN_POINT ( 'NONE',  ( 8.314922557960818139, 14.29746914071049879, 34.58224293864770260 ) ) ;
#189126 = CARTESIAN_POINT ( 'NONE',  ( -17.50000000000001066, -5.499999999999943157, 86.28230962303568674 ) ) ;
#189128 = CARTESIAN_POINT ( 'NONE',  ( -15.72974639402176322, -15.80617190586768395, 49.37609039468569705 ) ) ;
#189129 = CARTESIAN_POINT ( 'NONE',  ( 24.62642639703176073, -5.957135776930575943, 169.3344962860537350 ) ) ;
#189130 = CARTESIAN_POINT ( 'NONE',  ( -8.224510206698735004, -14.34966873604973081, 54.58442372801901143 ) ) ;
#189131 = CARTESIAN_POINT ( 'NONE',  ( -5.049401038297874678, -19.05341960407617918, 64.79275706135233293 ) ) ;
#189132 = CARTESIAN_POINT ( 'NONE',  ( 14.34966873604960469, 8.224510206698951720, 24.16557627198103120 ) ) ;
#189133 = CARTESIAN_POINT ( 'NONE',  ( 0.05219959533934541429, -16.53943276465976808, 100.0010903946857042 ) ) ;
#189134 = CARTESIAN_POINT ( 'NONE',  ( 13.97604488694527802, 13.89961937509977652, 39.37390960531435269 ) ) ;
#189135 = CARTESIAN_POINT ( 'NONE',  ( -13.89961937509977652, 13.97604488694528158, 60.62390960531436690 ) ) ;
#189136 = CARTESIAN_POINT ( 'NONE',  ( -5.153800228976328057, -19.02544592524343514, 22.29057627198102765 ) ) ;
#189137 = CARTESIAN_POINT ( 'NONE',  ( -0.05219959533937732626, 21.53943276465977519, 37.50109039468568284 ) ) ;
#189138 = CARTESIAN_POINT ( 'NONE',  ( 13.97604488694527802, 13.89961937509977652, 44.37390960531435269 ) ) ;
#189139 = CARTESIAN_POINT ( 'NONE',  ( 5.153800228976335163, 19.02544592524342804, 39.79057627198100988 ) ) ;
#189140 = CARTESIAN_POINT ( 'NONE',  ( -10.72451020669898014, 18.67979575497178502, 25.41557627198103120 ) ) ;
#189142 = CARTESIAN_POINT ( 'NONE',  ( -14.29746914071049879, 8.314922557960819915, 100.8322429386477097 ) ) ;
#189141 = CARTESIAN_POINT ( 'NONE',  ( -21.53943276465977519, -0.05219959533937600094, 63.75109039468568284 ) ) ;
#189143 = CARTESIAN_POINT ( 'NONE',  ( -5.049401038298153566, 19.05341960407611168, 115.2072429386477097 ) ) ;
#189144 = CARTESIAN_POINT ( 'NONE',  ( 0.05219959533934541429, -16.53943276465976808, 80.00109039468568994 ) ) ;
#189145 = CARTESIAN_POINT ( 'NONE',  ( 21.53943276465977519, 0.05219959533937863772, 86.25109039468568994 ) ) ;
#189146 = CARTESIAN_POINT ( 'NONE',  ( -14.29746914071037622, -8.314922557961029526, 59.16775706135234714 ) ) ;
#189147 = CARTESIAN_POINT ( 'NONE',  ( 19.02544592524343514, -5.153800228976328945, 98.54057627198100988 ) ) ;
#189148 = CARTESIAN_POINT ( 'NONE',  ( -8.224510206698735004, -14.34966873604973081, 34.58442372801900433 ) ) ;
#189149 = CARTESIAN_POINT ( 'NONE',  ( 4.379528057220092307, 16.55341960407617563, 22.29275706135235069 ) ) ;
#189150 = CARTESIAN_POINT ( 'NONE',  ( -16.55341960407617563, 4.379528057220093196, 83.54275706135234714 ) ) ;
#189151 = CARTESIAN_POINT ( 'NONE',  ( -19.03943276465977164, -0.05219959533935918106, 108.7510903946856615 ) ) ;
#189152 = CARTESIAN_POINT ( 'NONE',  ( -21.52544592524343514, 5.823673210054127303, 96.04057627198102409 ) ) ;
#189154 = CARTESIAN_POINT ( 'NONE',  ( 19.05341960407617918, -5.049401038297876454, 106.0427570613523471 ) ) ;
#189153 = CARTESIAN_POINT ( 'NONE',  ( 14.29746914071049879, -8.314922557960816363, 108.3322429386477097 ) ) ;
#189155 = CARTESIAN_POINT ( 'NONE',  ( 8.224510206698742110, 14.34966873604972548, 67.08442372801901854 ) ) ;
#189156 = CARTESIAN_POINT ( 'NONE',  ( 24.72709851008551496, 6.869189314501217503, 167.7661538690258567 ) ) ;
#189157 = CARTESIAN_POINT ( 'NONE',  ( -5.049401038297874678, -19.05341960407617918, 64.79275706135233293 ) ) ;
#189158 = CARTESIAN_POINT ( 'NONE',  ( -16.52544592524342804, 4.483927247898546575, 51.04057627198103120 ) ) ;
#189159 = CARTESIAN_POINT ( 'NONE',  ( 12.06949235617757843, -12.14591786802309237, 28.12390960531435979 ) ) ;
#189160 = CARTESIAN_POINT ( 'NONE',  ( 12.14591786802309770, 12.06949235617756955, 89.37390960531435269 ) ) ;
#189162 = CARTESIAN_POINT ( 'NONE',  ( -19.01533133064924641, 5.499999999999447553, 88.76586590595742621 ) ) ;
#189161 = CARTESIAN_POINT ( 'NONE',  ( -13.97604488694547697, 13.89961937509957934, 28.12609039468565797 ) ) ;
#189163 = CARTESIAN_POINT ( 'NONE',  ( 18.67979575497194134, -10.72451020669871369, 35.83442372801901143 ) ) ;
#189164 = CARTESIAN_POINT ( 'NONE',  ( 13.89961937509957401, 13.97604488694547697, 91.87609039468567573 ) ) ;
#189165 = CARTESIAN_POINT ( 'NONE',  ( -13.99740082693642229, -37.19577201402449163, -29.83961662117135560 ) ) ;
#189166 = CARTESIAN_POINT ( 'NONE',  ( 5.049401038298161559, -19.05341960407611168, 97.70724293864766707 ) ) ;
#189167 = CARTESIAN_POINT ( 'NONE',  ( -16.51473224551069308, -9.474510206698971260, 91.66557627198103830 ) ) ;
#189168 = CARTESIAN_POINT ( 'NONE',  ( -10.72451020669898014, 18.67979575497178502, 50.41557627198103120 ) ) ;
#189169 = CARTESIAN_POINT ( 'NONE',  ( 16.55341960407611168, 4.379528057220329451, 98.95724293864770971 ) ) ;
#189170 = CARTESIAN_POINT ( 'NONE',  ( -5.153800228976328057, -19.02544592524343514, 72.29057627198102409 ) ) ;
#189171 = CARTESIAN_POINT ( 'NONE',  ( -5.049401038298153566, 19.05341960407611168, 25.20724293864768484 ) ) ;
#189172 = CARTESIAN_POINT ( 'NONE',  ( 21.55341960407619695, -5.719274019375665929, 36.04275706135234714 ) ) ;
#189173 = CARTESIAN_POINT ( 'NONE',  ( 15.72974639402176855, 15.80617190586768217, 71.87609039468568994 ) ) ;
#189174 = CARTESIAN_POINT ( 'NONE',  ( -16.46253265017160317, 9.564922557960807481, 55.83224293864769550 ) ) ;
#189175 = CARTESIAN_POINT ( 'NONE',  ( 12.06949235617739724, 12.14591786802326823, 76.87609039468567573 ) ) ;
#189176 = CARTESIAN_POINT ( 'NONE',  ( -5.823673210054431948, 21.52544592524334988, 27.70942372801901854 ) ) ;
#189177 = CARTESIAN_POINT ( 'NONE',  ( -15.72974639402176322, -15.80617190586768395, 29.37609039468568284 ) ) ;
#189179 = CARTESIAN_POINT ( 'NONE',  ( -19.02544592524342804, 5.153800228976336051, 76.04057627198102409 ) ) ;
#189178 = CARTESIAN_POINT ( 'NONE',  ( 9.474510206698729675, 16.51473224551082808, 47.08442372801900433 ) ) ;
#189180 = CARTESIAN_POINT ( 'NONE',  ( 19.02544592524334988, 5.153800228976608722, 31.45942372801900433 ) ) ;
#189181 = CARTESIAN_POINT ( 'NONE',  ( -5.719274019375665041, -21.55341960407619695, 79.79275706135236135 ) ) ;
#189182 = CARTESIAN_POINT ( 'NONE',  ( 21.52544592524344225, -5.823673210054117533, 73.54057627198102409 ) ) ;
#189183 = CARTESIAN_POINT ( 'NONE',  ( 8.224510206698953496, -14.34966873604960469, 52.91557627198103830 ) ) ;
#189185 = CARTESIAN_POINT ( 'NONE',  ( -5.049401038297874678, -19.05341960407617918, 24.79275706135233648 ) ) ;
#189184 = CARTESIAN_POINT ( 'NONE',  ( -21.52544592524334988, -5.823673210054445271, 88.95942372801901854 ) ) ;
#189186 = CARTESIAN_POINT ( 'NONE',  ( -4.483927247898539470, -16.52544592524342804, 67.29057627198103830 ) ) ;
#189187 = CARTESIAN_POINT ( 'NONE',  ( -0.05219959533909027116, -19.03943276465977164, 22.49890960531436690 ) ) ;
#189188 = CARTESIAN_POINT ( 'NONE',  ( -0.05219959533936034679, 19.03943276465977164, 72.50109039468566152 ) ) ;
#189189 = CARTESIAN_POINT ( 'NONE',  ( 16.55341960407611168, 4.379528057220329451, 33.95724293864769550 ) ) ;
#189190 = CARTESIAN_POINT ( 'NONE',  ( 5.823673210054444382, -21.52544592524334988, 80.20942372801901854 ) ) ;
#189191 = CARTESIAN_POINT ( 'NONE',  ( -9.564922557960796823, -16.46253265017161027, 82.08224293864768129 ) ) ;
#189192 = CARTESIAN_POINT ( 'NONE',  ( 13.97604488694548053, -13.89961937509957401, 50.62609039468566152 ) ) ;
#189193 = CARTESIAN_POINT ( 'NONE',  ( -21.52544592524343514, 5.823673210054127303, 56.04057627198102409 ) ) ;
#189194 = CARTESIAN_POINT ( 'NONE',  ( -5.823673210054116645, -21.52544592524344225, 97.29057627198105251 ) ) ;
#189195 = CARTESIAN_POINT ( 'NONE',  ( -13.97604488694547697, 13.89961937509957934, 113.1260903946856757 ) ) ;
#189196 = CARTESIAN_POINT ( 'NONE',  ( 16.52544592524335698, 4.483927247898782831, 66.45942372801903275 ) ) ;
#189198 = CARTESIAN_POINT ( 'NONE',  ( 18.62759615963271287, -10.81492255796078972, 108.3322429386477097 ) ) ;
#189197 = CARTESIAN_POINT ( 'NONE',  ( 16.29526858892878849, 7.335722546919996034, 63.29670597800208043 ) ) ;
#189199 = CARTESIAN_POINT ( 'NONE',  ( 14.34966873604960469, 8.224510206698951720, 99.16557627198100988 ) ) ;
#189200 = CARTESIAN_POINT ( 'NONE',  ( -17.49999999999998579, -3.345213924137320216, 30.41231376905646044 ) ) ;
#189201 = CARTESIAN_POINT ( 'NONE',  ( 16.53943276465976808, 0.05219959533934440121, 36.25109039468567573 ) ) ;
#189202 = CARTESIAN_POINT ( 'NONE',  ( 21.52544592524344225, -5.823673210054117533, 58.54057627198103120 ) ) ;
#189203 = CARTESIAN_POINT ( 'NONE',  ( -4.379528057220086978, -16.55341960407618274, 104.7927570613523898 ) ) ;
#189204 = CARTESIAN_POINT ( 'NONE',  ( 9.474510206698971260, -16.51473224551069308, 32.91557627198102409 ) ) ;
#189205 = CARTESIAN_POINT ( 'NONE',  ( -16.52544592524335698, -4.483927247898792601, 63.95942372801901854 ) ) ;
#189206 = CARTESIAN_POINT ( 'NONE',  ( 9.564922557961047289, -16.46253265017146816, 60.41775706135233293 ) ) ;
#189207 = CARTESIAN_POINT ( 'NONE',  ( -21.53943276465977519, -0.05219959533937600094, 38.75109039468567573 ) ) ;
#189208 = CARTESIAN_POINT ( 'NONE',  ( -21.52544592524343514, 5.823673210054127303, 56.04057627198102409 ) ) ;
#189209 = CARTESIAN_POINT ( 'NONE',  ( -12.14591786802326823, 12.06949235617739902, 93.12609039468568994 ) ) ;
#189210 = CARTESIAN_POINT ( 'NONE',  ( 15.72974639402176855, 15.80617190586768217, 81.87609039468568994 ) ) ;
#189211 = CARTESIAN_POINT ( 'NONE',  ( 15.72974639402199770, -15.80617190586745480, 53.12390960531436690 ) ) ;
#189212 = CARTESIAN_POINT ( 'NONE',  ( 21.53943276465977519, -0.05219959533907433946, 28.74890960531435624 ) ) ;
#189213 = CARTESIAN_POINT ( 'NONE',  ( -8.224510206698735004, -14.34966873604973081, 84.58442372801903275 ) ) ;
#189214 = CARTESIAN_POINT ( 'NONE',  ( -18.67979575497178146, -10.72451020669898902, 36.66557627198103120 ) ) ;
#189215 = ORIENTED_EDGE ( 'NONE', *, *, #199664, .F. ) ;
#189216 = CARTESIAN_POINT ( 'NONE',  ( 9.564922557960805705, 16.46253265017160317, 99.58224293864770971 ) ) ;
#189217 = CARTESIAN_POINT ( 'NONE',  ( -14.34966873604960291, -8.224510206698953496, 21.66557627198102409 ) ) ;
#189218 = CYLINDRICAL_SURFACE ( 'NONE', #1762, 1.500000000000001332 ) ;
#189219 = CARTESIAN_POINT ( 'NONE',  ( -14.34966873604960291, -8.224510206698953496, 106.6655762719810383 ) ) ;
#189220 = CARTESIAN_POINT ( 'NONE',  ( 5.719274019375991003, -21.55341960407610458, 57.70724293864770260 ) ) ;
#189221 = CARTESIAN_POINT ( 'NONE',  ( 4.483927247898790824, -16.52544592524335698, 85.20942372801901854 ) ) ;
#189222 = CARTESIAN_POINT ( 'NONE',  ( 15.80617190586769283, -15.72974639402175789, 40.62609039468567573 ) ) ;
#189223 = CARTESIAN_POINT ( 'NONE',  ( -19.03943276465977164, -0.05219959533935918106, 103.7510903946856757 ) ) ;
#189224 = CARTESIAN_POINT ( 'NONE',  ( -4.379528057220328563, 16.55341960407611168, 105.2072429386477097 ) ) ;
#189225 = CARTESIAN_POINT ( 'NONE',  ( 9.474510206698729675, 16.51473224551082808, 107.0844237280190043 ) ) ;
#189226 = CONICAL_SURFACE ( 'NONE', #147218, 1.610000000000000098, 0.7853981633974458365 ) ;
#189227 = CARTESIAN_POINT ( 'NONE',  ( 16.46253265017160672, -9.564922557960803928, 23.33224293864769194 ) ) ;
#189228 = FACE_OUTER_BOUND ( 'NONE', #180522, .T. ) ;
#189229 = CARTESIAN_POINT ( 'NONE',  ( 19.03943276465977164, -0.05219959533909143690, 93.74890960531435269 ) ) ;
#189230 = CARTESIAN_POINT ( 'NONE',  ( -14.29746914071037622, -8.314922557961029526, 74.16775706135231871 ) ) ;
#189231 = CARTESIAN_POINT ( 'NONE',  ( 18.67979575497194134, -10.72451020669871369, 100.8344237280190185 ) ) ;
#189232 = CARTESIAN_POINT ( 'NONE',  ( 21.53943276465977519, -0.05219959533907433946, 63.74890960531435979 ) ) ;
#189233 = CARTESIAN_POINT ( 'NONE',  ( -8.224510206698735004, -14.34966873604973081, 84.58442372801903275 ) ) ;
#189234 = CARTESIAN_POINT ( 'NONE',  ( 13.97604488694548053, -13.89961937509957401, 85.62609039468568994 ) ) ;
#189235 = CARTESIAN_POINT ( 'NONE',  ( -13.89961937509977652, 13.97604488694528158, 30.62390960531435269 ) ) ;
#189236 = CARTESIAN_POINT ( 'NONE',  ( 13.97604488694527802, 13.89961937509977652, 79.37390960531435269 ) ) ;
#189237 = CARTESIAN_POINT ( 'NONE',  ( -0.05219959533909027116, -19.03943276465977164, 27.49890960531435624 ) ) ;
#189238 = CARTESIAN_POINT ( 'NONE',  ( 13.89961937509957401, 13.97604488694547697, 66.87609039468567573 ) ) ;
#189239 = CARTESIAN_POINT ( 'NONE',  ( 21.96844466259035400, -8.667631922777625064, 171.6690673070883690 ) ) ;
#189240 = CARTESIAN_POINT ( 'NONE',  ( -19.05341960407611168, -5.049401038298163336, 96.45724293864769550 ) ) ;
#189241 = CARTESIAN_POINT ( 'NONE',  ( -14.34966873604960291, -8.224510206698953496, 46.66557627198102409 ) ) ;
#189242 = CARTESIAN_POINT ( 'NONE',  ( -21.55341960407610458, -5.719274019375992779, 66.45724293864768129 ) ) ;
#189243 = CARTESIAN_POINT ( 'NONE',  ( -17.50000000000000000, 3.237210098469633923, 104.7123698737954385 ) ) ;
#189244 = CARTESIAN_POINT ( 'NONE',  ( -5.153800228976607833, 19.02544592524334988, 32.70942372801899722 ) ) ;
#189245 = DIRECTION ( 'NONE',  ( 0.000000000000000000, 0.000000000000000000, -1.000000000000000000 ) ) ;
#189247 = CARTESIAN_POINT ( 'NONE',  ( -9.474510206698964154, 16.51473224551069663, 75.41557627198103830 ) ) ;
#189246 = CARTESIAN_POINT ( 'NONE',  ( -9.474510206698964154, 16.51473224551069663, 50.41557627198102409 ) ) ;
#189248 = ADVANCED_FACE ( 'NONE', ( #197952 ), #89772, .F. ) ;
#189249 = CARTESIAN_POINT ( 'NONE',  ( 14.29746914071037800, 8.314922557961029526, 41.66775706135235424 ) ) ;
#189250 = DIRECTION ( 'NONE',  ( 0.000000000000000000, 0.000000000000000000, 1.000000000000000000 ) ) ;
#189251 = CARTESIAN_POINT ( 'NONE',  ( 2.366582413085430048, -37.03054742343285710, -7.999999999999996447 ) ) ;
#189252 = CARTESIAN_POINT ( 'NONE',  ( 16.53943276465976808, 0.05219959533934440121, 71.25109039468568994 ) ) ;
#189254 = CARTESIAN_POINT ( 'NONE',  ( -21.55341960407610458, -5.719274019375992779, 91.45724293864769550 ) ) ;
#189253 = CARTESIAN_POINT ( 'NONE',  ( 14.34966873604972726, -8.224510206698740333, 65.83442372801900433 ) ) ;
#189255 = CARTESIAN_POINT ( 'NONE',  ( 4.379528057220092307, 16.55341960407617563, 42.29275706135235424 ) ) ;
#189257 = DIRECTION ( 'NONE',  ( 1.000000000000000000, 0.000000000000000000, 3.469446951953612217E-15 ) ) ;
#189256 = CARTESIAN_POINT ( 'NONE',  ( -19.02544592524342804, 5.153800228976336051, 46.04057627198101699 ) ) ;
#189258 = CARTESIAN_POINT ( 'NONE',  ( -10.81492255796105439, 18.62759615963255655, 52.91775706135235424 ) ) ;
#189259 = CARTESIAN_POINT ( 'NONE',  ( -13.97604488694547697, 13.89961937509957934, 63.12609039468566152 ) ) ;
#189260 = CARTESIAN_POINT ( 'NONE',  ( 15.72974639402176855, 15.80617190586768217, 91.87609039468568994 ) ) ;
#189261 = AXIS2_PLACEMENT_3D ( 'NONE', #55485, #83806, #191996 ) ;
#189262 = CARTESIAN_POINT ( 'NONE',  ( -13.89961937509977652, 13.97604488694528158, 25.62390960531434558 ) ) ;
#189263 = CARTESIAN_POINT ( 'NONE',  ( -16.08916976210838001, 1.211883243535291088, -59.40465844715060229 ) ) ;
#189264 = CARTESIAN_POINT ( 'NONE',  ( -10.81492255796078084, -18.62759615963271287, 52.08224293864768839 ) ) ;
#189265 = CARTESIAN_POINT ( 'NONE',  ( 9.564922557960805705, 16.46253265017160317, 99.58224293864770971 ) ) ;
#189266 = CARTESIAN_POINT ( 'NONE',  ( 0.05219959533910956823, 16.53943276465976808, 104.9989096053143669 ) ) ;
#189267 = CARTESIAN_POINT ( 'NONE',  ( -4.483927247898782831, 16.52544592524335698, 37.70942372801900433 ) ) ;
#189268 = CARTESIAN_POINT ( 'NONE',  ( 12.06949235617739724, 12.14591786802326823, 106.8760903946856899 ) ) ;
#189269 = ORIENTED_EDGE ( 'NONE', *, *, #157283, .F. ) ;
#189270 = CARTESIAN_POINT ( 'NONE',  ( -5.823673210054116645, -21.52544592524344225, 97.29057627198105251 ) ) ;
#189272 = CARTESIAN_POINT ( 'NONE',  ( 16.51473224551069308, 9.474510206698969483, 109.1655762719810383 ) ) ;
#189271 = CARTESIAN_POINT ( 'NONE',  ( 16.55341960407611168, 4.379528057220329451, 33.95724293864769550 ) ) ;
#189273 = CARTESIAN_POINT ( 'NONE',  ( 19.02544592524334988, 5.153800228976608722, 96.45942372801897591 ) ) ;
#189274 = CARTESIAN_POINT ( 'NONE',  ( 5.049401038297881783, 19.05341960407617563, 22.29275706135233648 ) ) ;
#189275 = CARTESIAN_POINT ( 'NONE',  ( 16.53943276465976808, -0.05219959533910856209, 33.74890960531436690 ) ) ;
#189276 = CARTESIAN_POINT ( 'NONE',  ( -21.55341960407610458, -5.719274019375992779, 91.45724293864769550 ) ) ;
#189277 = CARTESIAN_POINT ( 'NONE',  ( -5.823673210054116645, -21.52544592524344225, 57.29057627198103120 ) ) ;
#189278 = CARTESIAN_POINT ( 'NONE',  ( 0.05219959533909260263, 19.03943276465977164, 64.99890960531436690 ) ) ;
#189279 = CARTESIAN_POINT ( 'NONE',  ( 14.34966873604960469, 8.224510206698951720, 34.16557627198102409 ) ) ;
#189280 = CARTESIAN_POINT ( 'NONE',  ( -19.02544592524342804, 5.153800228976336051, 91.04057627198100988 ) ) ;
#189281 = CARTESIAN_POINT ( 'NONE',  ( -5.049401038298153566, 19.05341960407611168, 80.20724293864769550 ) ) ;
#189282 = CARTESIAN_POINT ( 'NONE',  ( -16.46253265017146816, -9.564922557961047289, 39.16775706135234003 ) ) ;
#189283 = CARTESIAN_POINT ( 'NONE',  ( 0.05219959533907565091, 21.53943276465977519, 74.99890960531435269 ) ) ;
#189284 = CARTESIAN_POINT ( 'NONE',  ( 4.483927247898545687, 16.52544592524342804, 99.79057627198103830 ) ) ;
#189285 = CARTESIAN_POINT ( 'NONE',  ( 18.62759615963255655, 10.81492255796105972, 41.66775706135235424 ) ) ;
#189286 = CARTESIAN_POINT ( 'NONE',  ( 22.44159573604009239, 16.30477369853692693, 140.0750000027311728 ) ) ;
#189287 = CARTESIAN_POINT ( 'NONE',  ( -16.53943276465976808, -0.05219959533934237506, 103.7510903946857042 ) ) ;
#189288 = CARTESIAN_POINT ( 'NONE',  ( -5.049401038298153566, 19.05341960407611168, 35.20724293864768839 ) ) ;
#189289 = CARTESIAN_POINT ( 'NONE',  ( -13.97604488694527625, -13.89961937509977652, 91.87390960531432427 ) ) ;
#189290 =( NAMED_UNIT ( * ) PLANE_ANGLE_UNIT ( ) SI_UNIT ( $, .RADIAN. ) );
#189291 = CARTESIAN_POINT ( 'NONE',  ( -16.51473224551069308, -9.474510206698971260, 31.66557627198102054 ) ) ;
#189292 = CARTESIAN_POINT ( 'NONE',  ( -16.53943276465976808, 0.05219959533911058130, 46.24890960531435979 ) ) ;
#189293 = CARTESIAN_POINT ( 'NONE',  ( 5.719274019375673035, 21.55341960407619339, 77.29275706135234714 ) ) ;
#189295 = CARTESIAN_POINT ( 'NONE',  ( -8.224510206698735004, -14.34966873604973081, 74.58442372801901854 ) ) ;
#189294 = CARTESIAN_POINT ( 'NONE',  ( 29.42957871419392291, -23.46871120496999552, -19.15262919804625241 ) ) ;
#189296 = CARTESIAN_POINT ( 'NONE',  ( 9.564922557960805705, 16.46253265017160317, 59.58224293864769550 ) ) ;
#189297 = CARTESIAN_POINT ( 'NONE',  ( 19.05341960407611168, 5.049401038298154454, 53.95724293864770260 ) ) ;
#189298 = EDGE_LOOP ( 'NONE', ( #140803, #129720 ) ) ;
#189299 = CARTESIAN_POINT ( 'NONE',  ( 15.80617190586769283, -15.72974639402175789, 110.6260903946857042 ) ) ;
#189300 = CARTESIAN_POINT ( 'NONE',  ( 12.14591786802327356, -12.06949235617739191, 75.62609039468567573 ) ) ;
#189301 = CARTESIAN_POINT ( 'NONE',  ( 15.80617190586769283, -15.72974639402175789, 95.62609039468568994 ) ) ;
#189302 = CARTESIAN_POINT ( 'NONE',  ( 0.05219959533907565091, 21.53943276465977519, 34.99890960531435979 ) ) ;
#189303 = CARTESIAN_POINT ( 'NONE',  ( 16.46253265017146816, 9.564922557961045513, 106.6677570613523471 ) ) ;
#189304 = CARTESIAN_POINT ( 'NONE',  ( -15.72974639402176322, -15.80617190586768395, 74.37609039468568994 ) ) ;
#189305 = CARTESIAN_POINT ( 'NONE',  ( 16.53943276465976808, 0.05219959533934440121, 51.25109039468568994 ) ) ;
#189306 = CARTESIAN_POINT ( 'NONE',  ( -15.80617190586745835, -15.72974639402198527, 96.87390960531436690 ) ) ;
#189307 = CARTESIAN_POINT ( 'NONE',  ( -9.474510206698720793, -16.51473224551083518, 104.5844237280190043 ) ) ;
#189308 = CARTESIAN_POINT ( 'NONE',  ( 16.46253265017160672, -9.564922557960803928, 63.33224293864769550 ) ) ;
#189309 = CARTESIAN_POINT ( 'NONE',  ( -5.049401038297874678, -19.05341960407617918, 109.7927570613523187 ) ) ;
#189310 = CARTESIAN_POINT ( 'NONE',  ( -9.564922557961040184, 16.46253265017147172, 102.9177570613523329 ) ) ;
#189311 = CARTESIAN_POINT ( 'NONE',  ( 0.05219959533910956823, 16.53943276465976808, 69.99890960531435269 ) ) ;
#189312 = CARTESIAN_POINT ( 'NONE',  ( 16.52544592524335698, 4.483927247898782831, 76.45942372801901854 ) ) ;
#189313 = EDGE_CURVE ( 'NONE', #38864, #27838, #8368, .T. ) ;
#189315 = CARTESIAN_POINT ( 'NONE',  ( -5.153800228976328057, -19.02544592524343514, 52.29057627198100988 ) ) ;
#189314 = CARTESIAN_POINT ( 'NONE',  ( -10.72451020669870658, -18.67979575497194134, 19.58442372801901143 ) ) ;
#189316 = CARTESIAN_POINT ( 'NONE',  ( -19.02544592524342804, 5.153800228976336051, 56.04057627198100988 ) ) ;
#189317 = CARTESIAN_POINT ( 'NONE',  ( -12.14591786802326823, 12.06949235617739902, 68.12609039468567573 ) ) ;
#189318 = CARTESIAN_POINT ( 'NONE',  ( 17.14385361876520264, -23.59649016807271238, 148.0750000027311728 ) ) ;
#189319 = CARTESIAN_POINT ( 'NONE',  ( -17.81289503416611808, 24.51734667627700404, 143.9500000054623854 ) ) ;
#189320 = CARTESIAN_POINT ( 'NONE',  ( -16.46253265017146816, -9.564922557961047289, 19.16775706135233293 ) ) ;
#189321 = CARTESIAN_POINT ( 'NONE',  ( 13.89961937509977652, -13.97604488694527269, 23.12390960531436335 ) ) ;
#189322 = VERTEX_POINT ( 'NONE', #180812 ) ;
#189323 = CARTESIAN_POINT ( 'NONE',  ( 13.97604488694548053, -13.89961937509957401, 105.6260903946856757 ) ) ;
#189324 = CARTESIAN_POINT ( 'NONE',  ( 15.80617190586746368, 15.72974639402197994, 54.37390960531435979 ) ) ;
#189326 = CARTESIAN_POINT ( 'NONE',  ( 8.314922557961029526, -14.29746914071037800, 30.41775706135234358 ) ) ;
#189325 = CARTESIAN_POINT ( 'NONE',  ( -13.97604488694547697, 13.89961937509957934, 48.12609039468566863 ) ) ;
#189327 = CARTESIAN_POINT ( 'NONE',  ( -13.97604488694527625, -13.89961937509977652, 41.87390960531435979 ) ) ;
#189328 = CARTESIAN_POINT ( 'NONE',  ( 13.97604488694527802, 13.89961937509977652, 49.37390960531434558 ) ) ;
#189329 = CARTESIAN_POINT ( 'NONE',  ( 18.62759615963271287, -10.81492255796078972, 83.33224293864769550 ) ) ;
#189330 = CARTESIAN_POINT ( 'NONE',  ( -19.05341960407611168, -5.049401038298163336, 111.4572429386476671 ) ) ;
#189331 = CARTESIAN_POINT ( 'NONE',  ( -9.564922557960796823, -16.46253265017161027, 47.08224293864769550 ) ) ;
#189332 = CARTESIAN_POINT ( 'NONE',  ( -17.49999999999999645, -5.500000000000000888, 118.0000000000000142 ) ) ;
#189333 = CARTESIAN_POINT ( 'NONE',  ( 13.89961937509957401, 13.97604488694547697, 96.87609039468566152 ) ) ;
#189334 = CARTESIAN_POINT ( 'NONE',  ( -12.06949235617756955, 12.14591786802309770, 65.62390960531436690 ) ) ;
#189335 = CARTESIAN_POINT ( 'NONE',  ( -19.05341960407617563, 5.049401038297882671, 28.54275706135232937 ) ) ;
#189336 = CARTESIAN_POINT ( 'NONE',  ( -4.483927247898539470, -16.52544592524342804, 57.29057627198103120 ) ) ;
#189337 = CARTESIAN_POINT ( 'NONE',  ( 21.55341960407619695, -5.719274019375665929, 81.04275706135236135 ) ) ;
#189338 = CARTESIAN_POINT ( 'NONE',  ( -9.564922557960796823, -16.46253265017161027, 32.08224293864769550 ) ) ;
#189339 = CARTESIAN_POINT ( 'NONE',  ( 10.81492255796106328, -18.62759615963255655, 95.41775706135234714 ) ) ;
#189341 = CARTESIAN_POINT ( 'NONE',  ( -5.823673210054431948, 21.52544592524334988, 82.70942372801900433 ) ) ;
#189340 = CARTESIAN_POINT ( 'NONE',  ( 12.06949235617757843, -12.14591786802309237, 23.12390960531436335 ) ) ;
#189342 = CARTESIAN_POINT ( 'NONE',  ( -19.03943276465977164, 0.05219959533909376836, 71.24890960531435269 ) ) ;
#189343 = CARTESIAN_POINT ( 'NONE',  ( 21.53943276465977519, 0.05219959533937863772, 46.25109039468567573 ) ) ;
#189344 = CARTESIAN_POINT ( 'NONE',  ( -5.153800228976328057, -19.02544592524343514, 77.29057627198099567 ) ) ;
#189345 = CARTESIAN_POINT ( 'NONE',  ( 16.52544592524342804, -4.483927247898539470, 93.54057627198103830 ) ) ;
#189346 = CARTESIAN_POINT ( 'NONE',  ( 16.52544592524342804, -4.483927247898539470, 58.54057627198103120 ) ) ;
#189347 = CARTESIAN_POINT ( 'NONE',  ( -21.52544592524343514, 5.823673210054127303, 76.04057627198102409 ) ) ;
#189348 = CARTESIAN_POINT ( 'NONE',  ( -13.97604488694527625, -13.89961937509977652, 71.87390960531433848 ) ) ;
#189349 = CARTESIAN_POINT ( 'NONE',  ( 5.823673210054125526, 21.52544592524343514, 79.79057627198102409 ) ) ;
#189350 = CARTESIAN_POINT ( 'NONE',  ( -19.05341960407617563, 5.049401038297882671, 68.54275706135230450 ) ) ;
#189353 = CARTESIAN_POINT ( 'NONE',  ( -4.379528057220328563, 16.55341960407611168, 75.20724293864769550 ) ) ;
#189352 = CARTESIAN_POINT ( 'NONE',  ( -5.049401038297874678, -19.05341960407618274, 29.79275706135232582 ) ) ;
#189351 = CIRCLE ( 'NONE', #15010, 28.79475375365586487 ) ;
#189354 = CARTESIAN_POINT ( 'NONE',  ( -0.05219959533907301413, -21.53943276465977519, 52.49890960531435979 ) ) ;
#189355 = DIRECTION ( 'NONE',  ( 0.000000000000000000, 0.000000000000000000, -1.000000000000000000 ) ) ;
#189357 = CARTESIAN_POINT ( 'NONE',  ( -27.73933785331498925, -9.013057229001049109, 147.4750000027311785 ) ) ;
#189356 = CARTESIAN_POINT ( 'NONE',  ( -16.52544592524335698, -4.483927247898792601, 98.95942372801903275 ) ) ;
#189358 = CARTESIAN_POINT ( 'NONE',  ( 19.03943276465977164, 0.05219959533936151252, 106.2510903946856615 ) ) ;
#189359 = CARTESIAN_POINT ( 'NONE',  ( 16.55341960407611168, 4.379528057220329451, 68.95724293864769550 ) ) ;
#189360 = CARTESIAN_POINT ( 'NONE',  ( 6.615873399348748407, -1.136345303629790804, -62.40252569733545585 ) ) ;
#189361 = CARTESIAN_POINT ( 'NONE',  ( -9.564922557960796823, -16.46253265017161027, 67.08224293864769550 ) ) ;
#189362 = CARTESIAN_POINT ( 'NONE',  ( 14.29746914071049879, -8.314922557960816363, 48.33224293864770260 ) ) ;
#189363 = CARTESIAN_POINT ( 'NONE',  ( 19.05341960407611168, 5.049401038298154454, 98.95724293864766707 ) ) ;
#189365 = CARTESIAN_POINT ( 'NONE',  ( 13.97604488694527802, 13.89961937509977652, 64.37390960531436690 ) ) ;
#189364 = CARTESIAN_POINT ( 'NONE',  ( 16.46253265017146816, 9.564922557961045513, 76.66775706135234714 ) ) ;
#189366 = CARTESIAN_POINT ( 'NONE',  ( -9.564922557960796823, -16.46253265017161027, 92.08224293864769550 ) ) ;
#189367 = CARTESIAN_POINT ( 'NONE',  ( -9.474510206698964154, 16.51473224551069663, 80.41557627198103830 ) ) ;
#189368 = CARTESIAN_POINT ( 'NONE',  ( -18.62759615963270932, 10.81492255796079327, 65.83224293864769550 ) ) ;
#189369 = CARTESIAN_POINT ( 'NONE',  ( -12.14591786802326823, 12.06949235617739902, 53.12609039468568284 ) ) ;
#189370 = FACE_OUTER_BOUND ( 'NONE', #107900, .T. ) ;
#189371 = CARTESIAN_POINT ( 'NONE',  ( 19.05341960407611168, 5.049401038298154454, 48.95724293864768129 ) ) ;
#189372 = CARTESIAN_POINT ( 'NONE',  ( 21.52544592524344225, -5.823673210054117533, 58.54057627198103120 ) ) ;
#189373 = CARTESIAN_POINT ( 'NONE',  ( 16.46253265017146816, 9.564922557961045513, 96.66775706135233293 ) ) ;
#189375 = CARTESIAN_POINT ( 'NONE',  ( -21.52544592524334988, -5.823673210054445271, 48.95942372801902565 ) ) ;
#189374 = CARTESIAN_POINT ( 'NONE',  ( 0.05219959533910956823, 16.53943276465976808, 24.99890960531435624 ) ) ;
#189376 = CARTESIAN_POINT ( 'NONE',  ( -0.05219959533936034679, 19.03943276465977164, 37.50109039468567573 ) ) ;
#189378 = CARTESIAN_POINT ( 'NONE',  ( 12.14591786802327356, -12.06949235617739191, 90.62609039468567573 ) ) ;
#189377 = CARTESIAN_POINT ( 'NONE',  ( -14.29746914071037622, -8.314922557961029526, 64.16775706135234714 ) ) ;
#189379 = CARTESIAN_POINT ( 'NONE',  ( -17.60769864724391098, 5.499999999999986677, 53.65024842019163032 ) ) ;
#189380 = CARTESIAN_POINT ( 'NONE',  ( -16.52544592524335698, -4.483927247898792601, 83.95942372801900433 ) ) ;
#189381 = CARTESIAN_POINT ( 'NONE',  ( -16.53943276465976808, -0.05219959533934237506, 38.75109039468567573 ) ) ;
#189382 = CARTESIAN_POINT ( 'NONE',  ( 0.05219959533909260263, 19.03943276465977164, 49.99890960531435979 ) ) ;
#189383 = CARTESIAN_POINT ( 'NONE',  ( 0.05219959533909260263, 19.03943276465977164, 49.99890960531435979 ) ) ;
#189384 = CARTESIAN_POINT ( 'NONE',  ( -13.97604488694527625, -13.89961937509977652, 61.87390960531435979 ) ) ;
#189385 = CARTESIAN_POINT ( 'NONE',  ( -10.72451020669870658, -18.67979575497194134, 39.58442372801901143 ) ) ;
#189386 = CARTESIAN_POINT ( 'NONE',  ( -0.05219959533934338120, 16.53943276465976808, 47.50109039468568994 ) ) ;
#189387 = CARTESIAN_POINT ( 'NONE',  ( -12.06949235617739369, -12.14591786802326823, 109.3760903946857042 ) ) ;
#189388 = CARTESIAN_POINT ( 'NONE',  ( 16.46253265017160672, -9.564922557960803928, 33.33224293864770260 ) ) ;
#189389 = CARTESIAN_POINT ( 'NONE',  ( -21.52544592524334988, -5.823673210054445271, 108.9594237280190185 ) ) ;
#189390 = CARTESIAN_POINT ( 'NONE',  ( 19.03943276465977164, 0.05219959533936151252, 106.2510903946856615 ) ) ;
#189391 = CARTESIAN_POINT ( 'NONE',  ( -0.05219959533936034679, 19.03943276465977164, 72.50109039468566152 ) ) ;
#189392 = CARTESIAN_POINT ( 'NONE',  ( -14.34966873604960291, -8.224510206698953496, 86.66557627198102409 ) ) ;
#189393 = CARTESIAN_POINT ( 'NONE',  ( 13.97604488694527802, 13.89961937509977652, 34.37390960531436690 ) ) ;
#189395 = CARTESIAN_POINT ( 'NONE',  ( 16.62475595723696387, -7.163666690055295660, 93.02713351810467657 ) ) ;
#189394 = CARTESIAN_POINT ( 'NONE',  ( 0.05219959533936267826, -19.03943276465977164, 70.00109039468566152 ) ) ;
#189396 = CARTESIAN_POINT ( 'NONE',  ( 21.52544592524334988, 5.823673210054432836, 76.45942372801901854 ) ) ;
#189397 = CARTESIAN_POINT ( 'NONE',  ( 4.379528057220092307, 16.55341960407617563, 47.29275706135234003 ) ) ;
#189398 = CARTESIAN_POINT ( 'NONE',  ( 16.81555441253551209, 7.025013491695498047, 36.86314554665744936 ) ) ;
#189399 = CARTESIAN_POINT ( 'NONE',  ( -15.80617190586745835, -15.72974639402198527, 41.87390960531435979 ) ) ;
#189400 = CARTESIAN_POINT ( 'NONE',  ( -0.05219959533934338120, 16.53943276465976808, 22.50109039468567573 ) ) ;
#189401 = CARTESIAN_POINT ( 'NONE',  ( 5.049401038298163336, -19.05341960407611168, 22.70724293864768839 ) ) ;
#189402 = CARTESIAN_POINT ( 'NONE',  ( 16.51473224551083163, -9.474510206698727899, 35.83442372801899722 ) ) ;
#189403 = DIRECTION ( 'NONE',  ( -0.000000000000000000, -0.000000000000000000, 1.000000000000000000 ) ) ;
#189404 = CARTESIAN_POINT ( 'NONE',  ( 16.51473224551069308, 9.474510206698969483, 34.16557627198102409 ) ) ;
#189405 = CARTESIAN_POINT ( 'NONE',  ( 17.79613651744294245, -24.49428055684527550, 142.9656553485623931 ) ) ;
#189406 = CARTESIAN_POINT ( 'NONE',  ( 9.564922557960805705, 16.46253265017160317, 74.58224293864769550 ) ) ;
#189408 = CARTESIAN_POINT ( 'NONE',  ( -17.97161686093721045, 5.500000000000142997, 65.99637206859163996 ) ) ;
#189407 = CIRCLE ( 'NONE', #95719, 26.79475375365586487 ) ;
#189409 = CARTESIAN_POINT ( 'NONE',  ( -19.02544592524334988, -5.153800228976617603, 23.95942372801900078 ) ) ;
#189410 = CARTESIAN_POINT ( 'NONE',  ( 4.483927247898545687, 16.52544592524342804, 29.79057627198102409 ) ) ;
#189411 = CARTESIAN_POINT ( 'NONE',  ( -0.05219959533909027116, -19.03943276465977164, 47.49890960531435979 ) ) ;
#189412 = CARTESIAN_POINT ( 'NONE',  ( -19.05341960407611168, -5.049401038298163336, 96.45724293864769550 ) ) ;
#189413 = CARTESIAN_POINT ( 'NONE',  ( 18.67979575497194134, -10.72451020669871369, 65.83442372801900433 ) ) ;
#189414 = CARTESIAN_POINT ( 'NONE',  ( 13.89961937509977652, -13.97604488694527269, 48.12390960531435979 ) ) ;
#189415 = EDGE_CURVE ( 'NONE', #192521, #187465, #129378, .T. ) ;
#189416 = CARTESIAN_POINT ( 'NONE',  ( 18.67979575497194134, -10.72451020669871369, 70.83442372801901854 ) ) ;
#189418 = CARTESIAN_POINT ( 'NONE',  ( -10.72451020669898014, 18.67979575497178502, 30.41557627198101699 ) ) ;
#189417 = CARTESIAN_POINT ( 'NONE',  ( 5.153800228976615827, -19.02544592524334988, 95.20942372801897591 ) ) ;
#189419 = CARTESIAN_POINT ( 'NONE',  ( -19.02544592524342804, 5.153800228976336051, 36.04057627198100988 ) ) ;
#189420 = CARTESIAN_POINT ( 'NONE',  ( 5.823673210054125526, 21.52544592524343514, 109.7905762719810383 ) ) ;
#189421 = CARTESIAN_POINT ( 'NONE',  ( -19.02544592524334988, -5.153800228976617603, 28.95942372801900433 ) ) ;
#189422 = CARTESIAN_POINT ( 'NONE',  ( -12.06949235617756955, 12.14591786802309770, 105.6239096053143669 ) ) ;
#189423 = CARTESIAN_POINT ( 'NONE',  ( 16.46253265017160672, -9.564922557960803928, 68.33224293864770971 ) ) ;
#189424 = CARTESIAN_POINT ( 'NONE',  ( -4.483927247898782831, 16.52544592524335698, 22.70942372801901499 ) ) ;
#189425 = CARTESIAN_POINT ( 'NONE',  ( 16.52544592524342804, -4.483927247898539470, 73.54057627198102409 ) ) ;
#189426 = CARTESIAN_POINT ( 'NONE',  ( 15.72974639402199770, -15.80617190586745480, 23.12390960531436335 ) ) ;
#189427 = CARTESIAN_POINT ( 'NONE',  ( 19.03943276465977164, 0.05219959533936151252, 86.25109039468567573 ) ) ;
#189428 = CARTESIAN_POINT ( 'NONE',  ( 5.719274019375991003, -21.55341960407610458, 97.70724293864772392 ) ) ;
#189429 = CARTESIAN_POINT ( 'NONE',  ( 5.823673210054444382, -21.52544592524334988, 60.20942372801902565 ) ) ;
#189430 = CARTESIAN_POINT ( 'NONE',  ( -14.34966873604972548, 8.224510206698743886, 53.33442372801901854 ) ) ;
#189431 = CARTESIAN_POINT ( 'NONE',  ( -0.05219959533934338120, 16.53943276465976808, 57.50109039468568994 ) ) ;
#189432 = CARTESIAN_POINT ( 'NONE',  ( 21.53943276465977519, -0.05219959533907433946, 53.74890960531437401 ) ) ;
#189433 = CARTESIAN_POINT ( 'NONE',  ( -5.153800228976328057, -19.02544592524343514, 42.29057627198101699 ) ) ;
#189434 = CARTESIAN_POINT ( 'NONE',  ( -6.020228577223754586E-15, 39.95556452105416412, -4.249999994537627224 ) ) ;
#189435 = CARTESIAN_POINT ( 'NONE',  ( 8.314922557961029526, -14.29746914071037800, 75.41775706135233293 ) ) ;
#189436 = CARTESIAN_POINT ( 'NONE',  ( -18.67979575497178146, -10.72451020669898902, 106.6655762719810383 ) ) ;
#189437 = CARTESIAN_POINT ( 'NONE',  ( 8.224510206698953496, -14.34966873604960469, 47.91557627198102409 ) ) ;
#189438 = CARTESIAN_POINT ( 'NONE',  ( 8.314922557961029526, -14.29746914071037800, 65.41775706135234714 ) ) ;
#189439 = CARTESIAN_POINT ( 'NONE',  ( 13.97604488694548053, -13.89961937509957401, 100.6260903946856615 ) ) ;
#189440 = CARTESIAN_POINT ( 'NONE',  ( 15.72974639402199770, -15.80617190586745480, 93.12390960531436690 ) ) ;
#189441 = CARTESIAN_POINT ( 'NONE',  ( -4.379528057220328563, 16.55341960407611168, 40.20724293864769550 ) ) ;
#189442 = ORIENTED_EDGE ( 'NONE', *, *, #167527, .F. ) ;
#189443 = CARTESIAN_POINT ( 'NONE',  ( -16.79531203550646978, 7.028104445595605654, 73.74755011779562608 ) ) ;
#189444 = CARTESIAN_POINT ( 'NONE',  ( 15.72974639402199770, -15.80617190586745480, 78.12390960531436690 ) ) ;
#189445 = CARTESIAN_POINT ( 'NONE',  ( -4.483927247898539470, -16.52544592524342804, 22.29057627198102765 ) ) ;
#189446 = EDGE_LOOP ( 'NONE', ( #17038, #88665, #82278, #189036 ) ) ;
#189447 = CARTESIAN_POINT ( 'NONE',  ( -37.99533089065118219, -0.2660902954431525469, -7.999999999999996447 ) ) ;
#189448 = CARTESIAN_POINT ( 'NONE',  ( 5.719274019375991003, -21.55341960407610458, 97.70724293864772392 ) ) ;
#189449 = CARTESIAN_POINT ( 'NONE',  ( 18.62759615963255655, 10.81492255796105972, 26.66775706135235424 ) ) ;
#189450 = CARTESIAN_POINT ( 'NONE',  ( 16.55341960407611168, 4.379528057220329451, 43.95724293864769550 ) ) ;
#189451 = CARTESIAN_POINT ( 'NONE',  ( 8.224510206698742110, 14.34966873604972548, 47.08442372801901854 ) ) ;
#189452 = CARTESIAN_POINT ( 'NONE',  ( 9.474510206698971260, -16.51473224551069308, 52.91557627198102409 ) ) ;
#189453 = CARTESIAN_POINT ( 'NONE',  ( 19.02544592524343514, -5.153800228976328945, 83.54057627198100988 ) ) ;
#189454 = ORIENTED_EDGE ( 'NONE', *, *, #95776, .T. ) ;
#189455 = CARTESIAN_POINT ( 'NONE',  ( -15.80617190586745835, -15.72974639402198527, 31.87390960531435979 ) ) ;
#189456 = CARTESIAN_POINT ( 'NONE',  ( 0.05219959533909260263, 19.03943276465977164, 64.99890960531436690 ) ) ;
#189457 = CARTESIAN_POINT ( 'NONE',  ( 14.29746914071037800, 8.314922557961029526, 21.66775706135235069 ) ) ;
#189458 = CARTESIAN_POINT ( 'NONE',  ( -16.46253265017146816, -9.564922557961047289, 49.16775706135233293 ) ) ;
#189459 = CARTESIAN_POINT ( 'NONE',  ( -21.52544592524343514, 5.823673210054127303, 96.04057627198102409 ) ) ;
#189460 = CARTESIAN_POINT ( 'NONE',  ( -0.05219959533910754901, -16.53943276465976808, 37.49890960531436690 ) ) ;
#189461 = CARTESIAN_POINT ( 'NONE',  ( -9.564922557960796823, -16.46253265017161027, 77.08224293864769550 ) ) ;
#189462 = CARTESIAN_POINT ( 'NONE',  ( -15.72974639402197994, 15.80617190586746368, 65.62390960531436690 ) ) ;
#189464 = CARTESIAN_POINT ( 'NONE',  ( -19.03943276465977164, -0.05219959533935918106, 113.7510903946856757 ) ) ;
#189463 = CARTESIAN_POINT ( 'NONE',  ( 15.72974639402199770, -15.80617190586745480, 83.12390960531436690 ) ) ;
#189465 = CARTESIAN_POINT ( 'NONE',  ( 5.823673210054125526, 21.52544592524343514, 24.79057627198103120 ) ) ;
#189466 = CARTESIAN_POINT ( 'NONE',  ( 10.72451020669871369, 18.67979575497193778, 77.08442372801901854 ) ) ;
#189467 = CARTESIAN_POINT ( 'NONE',  ( -5.049401038298153566, 19.05341960407611168, 70.20724293864769550 ) ) ;
#189468 = CARTESIAN_POINT ( 'NONE',  ( 9.564922557960805705, 16.46253265017160317, 29.58224293864769550 ) ) ;
#189469 = CARTESIAN_POINT ( 'NONE',  ( -16.51473224551069308, -9.474510206698971260, 81.66557627198103830 ) ) ;
#189470 = CARTESIAN_POINT ( 'NONE',  ( 12.14591786802309770, 12.06949235617756955, 89.37390960531435269 ) ) ;
#189471 = ORIENTED_EDGE ( 'NONE', *, *, #170510, .T. ) ;
#189472 = CARTESIAN_POINT ( 'NONE',  ( -16.46253265017146816, -9.564922557961047289, 104.1677570613523329 ) ) ;
#189473 = CARTESIAN_POINT ( 'NONE',  ( 40.00000000000001421, 2.428612866367529932E-14, 0.000000000000000000 ) ) ;
#189474 = CARTESIAN_POINT ( 'NONE',  ( -9.564922557960796823, -16.46253265017161027, 72.08224293864770971 ) ) ;
#189476 = CARTESIAN_POINT ( 'NONE',  ( -19.02544592524342804, 5.153800228976336051, 116.0405762719810383 ) ) ;
#189475 = CARTESIAN_POINT ( 'NONE',  ( -21.52544592524334988, -5.823673210054445271, 103.9594237280190185 ) ) ;
#189477 = CARTESIAN_POINT ( 'NONE',  ( -16.53943276465976808, -0.05219959533934237506, 73.75109039468567573 ) ) ;
#189478 = CARTESIAN_POINT ( 'NONE',  ( -29.20736712825161163, 0.9155518048966417854, -49.29216761470104302 ) ) ;
#189479 = CARTESIAN_POINT ( 'NONE',  ( -19.05341960407617563, 5.049401038297882671, 58.54275706135234003 ) ) ;
#189480 = CARTESIAN_POINT ( 'NONE',  ( -15.80617190586768217, 15.72974639402176855, 113.1260903946856899 ) ) ;
#189481 = CARTESIAN_POINT ( 'NONE',  ( 6.126184129041763349, 6.686840650406337794, -63.95889547717843726 ) ) ;
#189482 = CARTESIAN_POINT ( 'NONE',  ( 13.89961937509977652, -13.97604488694527269, 23.12390960531436335 ) ) ;
#189483 = CARTESIAN_POINT ( 'NONE',  ( 16.52544592524342804, -4.483927247898539470, 23.54057627198102765 ) ) ;
#189484 = FACE_OUTER_BOUND ( 'NONE', #108223, .T. ) ;
#189485 = CARTESIAN_POINT ( 'NONE',  ( 12.14591786802327356, -12.06949235617739191, 110.6260903946857042 ) ) ;
#189486 = CARTESIAN_POINT ( 'NONE',  ( 6.434671708797603529, -6.434671708797564449, -63.95112321872120731 ) ) ;
#189487 = CARTESIAN_POINT ( 'NONE',  ( 4.483927247898790824, -16.52544592524335698, 85.20942372801901854 ) ) ;
#189488 = CARTESIAN_POINT ( 'NONE',  ( -5.153800228976328057, -19.02544592524343514, 22.29057627198102765 ) ) ;
#189489 = CARTESIAN_POINT ( 'NONE',  ( -21.55341960407619339, 5.719274019375674811, 88.54275706135236135 ) ) ;
#189490 = CARTESIAN_POINT ( 'NONE',  ( 9.564922557961047289, -16.46253265017146816, 105.4177570613523471 ) ) ;
#189491 = CARTESIAN_POINT ( 'NONE',  ( -15.72974639402176322, -15.80617190586768395, 64.37609039468568994 ) ) ;
#189492 = CARTESIAN_POINT ( 'NONE',  ( -13.97604488694547697, 13.89961937509957934, 43.12609039468566152 ) ) ;
#189493 = CARTESIAN_POINT ( 'NONE',  ( -5.153800228976328057, -19.02544592524343514, 82.29057627198103830 ) ) ;
#189494 = CARTESIAN_POINT ( 'NONE',  ( 16.51473224551069308, 9.474510206698969483, 64.16557627198102409 ) ) ;
#189495 = CARTESIAN_POINT ( 'NONE',  ( -1.022580077288041090E-15, -16.70000000000002061, -61.34707691135562868 ) ) ;
#189496 = AXIS2_PLACEMENT_3D ( 'NONE', #192630, #71284, #195649 ) ;
#189497 = CARTESIAN_POINT ( 'NONE',  ( -21.55341960407610458, -5.719274019375992779, 41.45724293864769550 ) ) ;
#189498 = CARTESIAN_POINT ( 'NONE',  ( -5.049401038298153566, 19.05341960407611168, 45.20724293864769550 ) ) ;
#189499 = CARTESIAN_POINT ( 'NONE',  ( -8.314922557961024197, 14.29746914071037800, 82.91775706135234714 ) ) ;
#189500 = EDGE_CURVE ( 'NONE', #159190, #37612, #162493, .T. ) ;
#189501 = UNCERTAINTY_MEASURE_WITH_UNIT (LENGTH_MEASURE( 1.000000000000000082E-05 ), #34369, 'distance_accuracy_value', 'NONE');
#189502 = ORIENTED_EDGE ( 'NONE', *, *, #46506, .T. ) ;
#189504 = CARTESIAN_POINT ( 'NONE',  ( -22.81625015709510507, 31.40387420917330275, -0.9249999972688132122 ) ) ;
#189503 = CARTESIAN_POINT ( 'NONE',  ( -16.53943276465976808, 0.05219959533911058130, 81.24890960531436690 ) ) ;
#189505 = CARTESIAN_POINT ( 'NONE',  ( 14.29746914071037800, 8.314922557961029526, 36.66775706135234714 ) ) ;
#189506 = CARTESIAN_POINT ( 'NONE',  ( 8.314922557960818139, 14.29746914071049879, 114.5822429386477097 ) ) ;
#189507 = CARTESIAN_POINT ( 'NONE',  ( 9.474510206698729675, 16.51473224551082808, 62.08442372801899722 ) ) ;
#189508 = AXIS2_PLACEMENT_3D ( 'NONE', #102918, #103919, #182755 ) ;
#189509 = CARTESIAN_POINT ( 'NONE',  ( -4.483927247898539470, -16.52544592524342804, 67.29057627198103830 ) ) ;
#189510 = CARTESIAN_POINT ( 'NONE',  ( 5.823673210054444382, -21.52544592524334988, 35.20942372801901854 ) ) ;
#189512 = CARTESIAN_POINT ( 'NONE',  ( 21.53943276465977519, -0.05219959533907433946, 93.74890960531436690 ) ) ;
#189511 = CARTESIAN_POINT ( 'NONE',  ( -4.500000000000001776, -130.0000000000000000, 15.00000000000000000 ) ) ;
#189513 = ADVANCED_BREP_SHAPE_REPRESENTATION ( '', ( #7058, #82054 ), #50057 ) ;
#189514 = CARTESIAN_POINT ( 'NONE',  ( 13.89961937509977652, -13.97604488694527269, 98.12390960531433848 ) ) ;
#189515 = CARTESIAN_POINT ( 'NONE',  ( 12.14591786802309770, 12.06949235617756955, 74.37390960531436690 ) ) ;
#189516 = CARTESIAN_POINT ( 'NONE',  ( 27.14096102835587132, -28.70429377953545469, -18.51261060099296785 ) ) ;
#189517 = CARTESIAN_POINT ( 'NONE',  ( -13.97604488694527625, -13.89961937509977652, 46.87390960531435979 ) ) ;
#189518 = CARTESIAN_POINT ( 'NONE',  ( -5.950531402560715689E-15, 38.81732327939063509, -7.124999997268814056 ) ) ;
#189519 = CARTESIAN_POINT ( 'NONE',  ( 0.05219959533936267826, -19.03943276465977164, 75.00109039468566152 ) ) ;
#189520 = CARTESIAN_POINT ( 'NONE',  ( 10.81492255796106328, -18.62759615963255655, 20.41775706135234714 ) ) ;
#189521 = CARTESIAN_POINT ( 'NONE',  ( -13.97604488694527625, -13.89961937509977652, 66.87390960531436690 ) ) ;
#189522 = CARTESIAN_POINT ( 'NONE',  ( 16.46253265017146816, 9.564922557961045513, 56.66775706135233293 ) ) ;
#189523 = CARTESIAN_POINT ( 'NONE',  ( -5.049401038298153566, 19.05341960407611168, 50.20724293864770260 ) ) ;
#189524 = PRODUCT_DEFINITION ( 'UNKNOWN', '', #143706, #5884 ) ;
#189525 = CARTESIAN_POINT ( 'NONE',  ( -16.55341960407611168, -4.379528057220339221, 66.45724293864768129 ) ) ;
#189526 = CARTESIAN_POINT ( 'NONE',  ( -4.379528057220328563, 16.55341960407611168, 50.20724293864769550 ) ) ;
#189527 = CARTESIAN_POINT ( 'NONE',  ( -19.05341960407611168, -5.049401038298163336, 81.45724293864769550 ) ) ;
#189528 = CARTESIAN_POINT ( 'NONE',  ( -0.05219959533907301413, -21.53943276465977519, 82.49890960531436690 ) ) ;
#189529 = CARTESIAN_POINT ( 'NONE',  ( -9.474510206698964154, 16.51473224551069663, 75.41557627198103830 ) ) ;
#189530 = CARTESIAN_POINT ( 'NONE',  ( 0.05219959533907565091, 21.53943276465977519, 84.99890960531436690 ) ) ;
#189531 = CARTESIAN_POINT ( 'NONE',  ( -16.51473224551082808, 9.474510206698731452, 23.33442372801900078 ) ) ;
#189534 = CARTESIAN_POINT ( 'NONE',  ( 16.52544592524342804, -4.483927247898539470, 93.54057627198103830 ) ) ;
#189533 = CARTESIAN_POINT ( 'NONE',  ( -16.55341960407617563, 4.379528057220093196, 113.5427570613523756 ) ) ;
#189532 = CARTESIAN_POINT ( 'NONE',  ( -13.97604488694527625, -13.89961937509977652, 21.87390960531435979 ) ) ;
#189535 = CARTESIAN_POINT ( 'NONE',  ( 19.02544592524334988, 5.153800228976608722, 106.4594237280190185 ) ) ;
#189536 = VERTEX_POINT ( 'NONE', #61408 ) ;
#189537 = CARTESIAN_POINT ( 'NONE',  ( -5.719274019375978568, 21.55341960407610458, 115.2072429386476955 ) ) ;
#189538 = CARTESIAN_POINT ( 'NONE',  ( 13.89961937509957401, 13.97604488694547697, 51.87609039468566863 ) ) ;
#189539 = CARTESIAN_POINT ( 'NONE',  ( 14.29746914071037800, 8.314922557961029526, 111.6677570613523613 ) ) ;
#189540 = CARTESIAN_POINT ( 'NONE',  ( 0.05219959533907565091, 21.53943276465977519, 69.99890960531435269 ) ) ;
#189541 = CARTESIAN_POINT ( 'NONE',  ( 16.51473224551069308, 9.474510206698969483, 99.16557627198102409 ) ) ;
#189542 = CARTESIAN_POINT ( 'NONE',  ( -14.34966873604960291, -8.224510206698953496, 56.66557627198103830 ) ) ;
#189543 = CARTESIAN_POINT ( 'NONE',  ( -0.05219959533909027116, -19.03943276465977164, 22.49890960531436690 ) ) ;
#189544 = CARTESIAN_POINT ( 'NONE',  ( 9.564922557960805705, 16.46253265017160317, 34.58224293864770260 ) ) ;
#189545 = CARTESIAN_POINT ( 'NONE',  ( -18.67979575497193778, 10.72451020669871902, 103.3344237280190043 ) ) ;
#189546 = CARTESIAN_POINT ( 'NONE',  ( 12.06949235617739724, 12.14591786802326823, 91.87609039468568994 ) ) ;
#189547 = CARTESIAN_POINT ( 'NONE',  ( 18.67979575497194134, -10.72451020669871369, 45.83442372801901854 ) ) ;
#189548 = CARTESIAN_POINT ( 'NONE',  ( 0.05219959533934541429, -16.53943276465976808, 45.00109039468568284 ) ) ;
#189549 = CARTESIAN_POINT ( 'NONE',  ( -0.05219959533907301413, -21.53943276465977519, 27.49890960531435269 ) ) ;
#189550 = CARTESIAN_POINT ( 'NONE',  ( -9.564922557960796823, -16.46253265017161027, 47.08224293864769550 ) ) ;
#189551 = CARTESIAN_POINT ( 'NONE',  ( 13.89961937509977652, -13.97604488694527269, 63.12390960531435979 ) ) ;
#189552 = CARTESIAN_POINT ( 'NONE',  ( -14.29746914071037622, -8.314922557961029526, 49.16775706135234003 ) ) ;
#189553 = CARTESIAN_POINT ( 'NONE',  ( 4.379528057220339221, -16.55341960407611168, 107.7072429386476955 ) ) ;
#189554 = CARTESIAN_POINT ( 'NONE',  ( -14.29746914071037622, -8.314922557961029526, 109.1677570613523613 ) ) ;
#189555 = CARTESIAN_POINT ( 'NONE',  ( 22.00000000000000000, -1.132798289211302014E-14, 97.50000000000000000 ) ) ;
#189558 = CARTESIAN_POINT ( 'NONE',  ( -19.05341960407611168, -5.049401038298163336, 76.45724293864769550 ) ) ;
#189557 = CARTESIAN_POINT ( 'NONE',  ( -19.03943276465977164, 0.05219959533909376836, 96.24890960531436690 ) ) ;
#189556 = CARTESIAN_POINT ( 'NONE',  ( 5.823673210054444382, -21.52544592524334988, 50.20942372801901854 ) ) ;
#189559 = CARTESIAN_POINT ( 'NONE',  ( -0.05219959533909027116, -19.03943276465977164, 97.49890960531436690 ) ) ;
#189560 = CARTESIAN_POINT ( 'NONE',  ( -14.34966873604960291, -8.224510206698953496, 41.66557627198103120 ) ) ;
#189561 = CARTESIAN_POINT ( 'NONE',  ( 14.29746914071049879, -8.314922557960816363, 23.33224293864769194 ) ) ;
#189562 = CARTESIAN_POINT ( 'NONE',  ( 8.224510206698953496, -14.34966873604960469, 32.91557627198102409 ) ) ;
#189563 = CARTESIAN_POINT ( 'NONE',  ( 17.50000000000000000, 5.499999999999997335, 120.0000000000000142 ) ) ;
#189564 = CARTESIAN_POINT ( 'NONE',  ( -5.049401038297874678, -19.05341960407617918, 39.79275706135232582 ) ) ;
#189565 = CARTESIAN_POINT ( 'NONE',  ( -9.474510206698964154, 16.51473224551069663, 80.41557627198103830 ) ) ;
#189566 = CARTESIAN_POINT ( 'NONE',  ( -9.474510206698720793, -16.51473224551083518, 49.58442372801899722 ) ) ;
#189567 = CARTESIAN_POINT ( 'NONE',  ( 29.86685920354754487, 21.69954338932564752, -7.924999997268814766 ) ) ;
#189568 = CARTESIAN_POINT ( 'NONE',  ( 17.18269478283314911, 17.18269478283310647, -64.92279855667830191 ) ) ;
#189570 = CARTESIAN_POINT ( 'NONE',  ( -12.14591786802326823, 12.06949235617739902, 68.12609039468567573 ) ) ;
#189569 = CARTESIAN_POINT ( 'NONE',  ( -19.02544592524334988, -5.153800228976617603, 78.95942372801900433 ) ) ;
#189571 = CARTESIAN_POINT ( 'NONE',  ( 16.52216118717206683, 7.221426719304505859, 93.57599021046993926 ) ) ;
#189572 = CARTESIAN_POINT ( 'NONE',  ( 16.51473224551069308, 9.474510206698969483, 109.1655762719810383 ) ) ;
#189573 = CARTESIAN_POINT ( 'NONE',  ( 10.72451020669871369, 18.67979575497193778, 22.08442372801901143 ) ) ;
#189574 = CARTESIAN_POINT ( 'NONE',  ( -13.89961937509957401, -13.97604488694547875, 89.37609039468563310 ) ) ;
#189576 = CARTESIAN_POINT ( 'NONE',  ( 13.89961937509977652, -13.97604488694527269, 53.12390960531434558 ) ) ;
#189575 = CARTESIAN_POINT ( 'NONE',  ( 17.50000000000000000, 5.499999999999992895, 86.70309617465828467 ) ) ;
#189577 = CARTESIAN_POINT ( 'NONE',  ( 16.46253265017160672, -9.564922557960803928, 93.33224293864769550 ) ) ;
#189579 = CARTESIAN_POINT ( 'NONE',  ( -13.97604488694527625, -13.89961937509977652, 51.87390960531436690 ) ) ;
#189578 = CARTESIAN_POINT ( 'NONE',  ( 16.52544592524342804, -4.483927247898539470, 43.54057627198103830 ) ) ;
#189580 = CARTESIAN_POINT ( 'NONE',  ( 19.05341960407617918, -5.049401038297876454, 61.04275706135232582 ) ) ;
#189581 = CARTESIAN_POINT ( 'NONE',  ( 13.97604488694548053, -13.89961937509957401, 30.62609039468566863 ) ) ;
#189582 = CARTESIAN_POINT ( 'NONE',  ( -19.02544592524342804, 5.153800228976336051, 66.04057627198103830 ) ) ;
#189583 = CARTESIAN_POINT ( 'NONE',  ( 15.72974639402199770, -15.80617190586745480, 63.12390960531435979 ) ) ;
#189585 = CARTESIAN_POINT ( 'NONE',  ( -18.67979575497193778, 10.72451020669871902, 113.3344237280190328 ) ) ;
#189584 = CARTESIAN_POINT ( 'NONE',  ( 14.29746914071049879, -8.314922557960816363, 68.33224293864769550 ) ) ;
#189586 = PLANE ( 'NONE',  #124495 ) ;
#189587 = CARTESIAN_POINT ( 'NONE',  ( -5.049401038298153566, 19.05341960407611168, 115.2072429386477097 ) ) ;
#189588 = CARTESIAN_POINT ( 'NONE',  ( -19.05341960407611168, -5.049401038298163336, 56.45724293864768129 ) ) ;
#189589 = CARTESIAN_POINT ( 'NONE',  ( -16.51473224551069308, -9.474510206698971260, 36.66557627198102409 ) ) ;
#189590 = CARTESIAN_POINT ( 'NONE',  ( -12.14591786802309592, -12.06949235617757132, 96.87390960531436690 ) ) ;
#189591 = CARTESIAN_POINT ( 'NONE',  ( -5.823673210054116645, -21.52544592524344225, 112.2905762719810241 ) ) ;
#189592 = CARTESIAN_POINT ( 'NONE',  ( 19.03943276465977164, -0.05219959533909143690, 113.7489096053143669 ) ) ;
#189593 = CARTESIAN_POINT ( 'NONE',  ( -18.67979575497193778, 10.72451020669871902, 33.33442372801900433 ) ) ;
#189594 = CARTESIAN_POINT ( 'NONE',  ( 0.05219959533909260263, 19.03943276465977164, 99.99890960531436690 ) ) ;
#189595 = CARTESIAN_POINT ( 'NONE',  ( -13.97604488694527625, -13.89961937509977652, 26.87390960531434558 ) ) ;
#189596 = CARTESIAN_POINT ( 'NONE',  ( -15.80617190586768217, 15.72974639402176855, 73.12609039468567573 ) ) ;
#189597 = CARTESIAN_POINT ( 'NONE',  ( -18.67979575497178146, -10.72451020669898902, 96.66557627198102409 ) ) ;
#189598 = CARTESIAN_POINT ( 'NONE',  ( 17.40805194822030799, -6.112264579159321087, 108.3337127251061247 ) ) ;
#189599 = DIRECTION ( 'NONE',  ( -0.7071067811865483499, 0.000000000000000000, -0.7071067811865466846 ) ) ;
#189600 = CARTESIAN_POINT ( 'NONE',  ( 28.90000000000003411, -0.1280799071098031872, -52.65483682830183199 ) ) ;
#189601 = CARTESIAN_POINT ( 'NONE',  ( 4.483927247898790824, -16.52544592524335698, 45.20942372801901854 ) ) ;
#189602 = CARTESIAN_POINT ( 'NONE',  ( 14.34966873604960469, 8.224510206698951720, 114.1655762719810383 ) ) ;
#189603 = CARTESIAN_POINT ( 'NONE',  ( -17.18269478283327345, -17.18269478283298568, -56.77278709839600879 ) ) ;
#189604 = CARTESIAN_POINT ( 'NONE',  ( 16.46253265017160672, -9.564922557960803928, 63.33224293864769550 ) ) ;
#189605 = CARTESIAN_POINT ( 'NONE',  ( 16.55341960407611168, 4.379528057220329451, 93.95724293864770971 ) ) ;
#189606 = CARTESIAN_POINT ( 'NONE',  ( 21.53943276465977519, -0.05219959533907433946, 48.74890960531435979 ) ) ;
#189607 = CARTESIAN_POINT ( 'NONE',  ( 8.314922557960818139, 14.29746914071049879, 64.58224293864769550 ) ) ;
#189608 = CARTESIAN_POINT ( 'NONE',  ( -12.14591786802326823, 12.06949235617739902, 33.12609039468569705 ) ) ;
#189609 = CARTESIAN_POINT ( 'NONE',  ( 15.72974639402176855, 15.80617190586768217, 91.87609039468568994 ) ) ;
#189610 = CARTESIAN_POINT ( 'NONE',  ( 16.31925111598455302, -7.325300261831589665, 77.66424538967254421 ) ) ;
#189611 = CARTESIAN_POINT ( 'NONE',  ( 16.52544592524335698, 4.483927247898782831, 96.45942372801901854 ) ) ;
#189612 = CARTESIAN_POINT ( 'NONE',  ( 12.14591786802309770, 12.06949235617756955, 39.37390960531436690 ) ) ;
#189613 = CARTESIAN_POINT ( 'NONE',  ( -16.51473224551069308, -9.474510206698971260, 41.66557627198103120 ) ) ;
#189614 = CARTESIAN_POINT ( 'NONE',  ( 13.97604488694527802, 13.89961937509977652, 94.37390960531436690 ) ) ;
#189615 = CARTESIAN_POINT ( 'NONE',  ( -10.72451020669898014, 18.67979575497178502, 95.41557627198102409 ) ) ;
#189616 = CARTESIAN_POINT ( 'NONE',  ( -18.67979575497193778, 10.72451020669871902, 53.33442372801901854 ) ) ;
#189617 = CARTESIAN_POINT ( 'NONE',  ( -8.224510206698735004, -14.34966873604973081, 34.58442372801900433 ) ) ;
#189619 = CARTESIAN_POINT ( 'NONE',  ( 10.81492255796106328, -18.62759615963255655, 80.41775706135234714 ) ) ;
#189618 = CARTESIAN_POINT ( 'NONE',  ( 16.52544592524342804, -4.483927247898539470, 68.54057627198103830 ) ) ;
#189620 = CARTESIAN_POINT ( 'NONE',  ( -8.224510206698735004, -14.34966873604973081, 99.58442372801900433 ) ) ;
#189621 = CARTESIAN_POINT ( 'NONE',  ( 16.19135201231351218, -7.376712067592055888, 47.31319145947882276 ) ) ;
#189622 = CARTESIAN_POINT ( 'NONE',  ( -23.46320343559626664, 18.96320343559662902, 8.889087296526001936 ) ) ;
#189623 = CARTESIAN_POINT ( 'NONE',  ( -8.314922557960811034, -14.29746914071050412, 27.08224293864769550 ) ) ;
#189624 = CARTESIAN_POINT ( 'NONE',  ( -12.14591786802326823, 12.06949235617739902, 73.12609039468567573 ) ) ;
#189625 = CARTESIAN_POINT ( 'NONE',  ( 13.97604488694527802, 13.89961937509977652, 79.37390960531435269 ) ) ;
#189626 = CARTESIAN_POINT ( 'NONE',  ( 19.02544592524343514, -5.153800228976328945, 103.5405762719809957 ) ) ;
#189627 = CARTESIAN_POINT ( 'NONE',  ( -18.62759615963255300, -10.81492255796106328, 79.16775706135234714 ) ) ;
#189628 = CARTESIAN_POINT ( 'NONE',  ( -14.29746914071037622, -8.314922557961029526, 89.16775706135236135 ) ) ;
#189629 = CARTESIAN_POINT ( 'NONE',  ( -16.53943276465976808, 0.05219959533911058130, 56.24890960531436690 ) ) ;
#189630 = CARTESIAN_POINT ( 'NONE',  ( 0.05219959533909260263, 19.03943276465977164, 64.99890960531436690 ) ) ;
#189631 = ORIENTED_EDGE ( 'NONE', *, *, #167871, .F. ) ;
#189632 = CARTESIAN_POINT ( 'NONE',  ( 16.53943276465976808, 0.05219959533934440121, 21.25109039468567218 ) ) ;
#189633 = CARTESIAN_POINT ( 'NONE',  ( 16.51473224551069308, 9.474510206698969483, 34.16557627198102409 ) ) ;
#189634 = CARTESIAN_POINT ( 'NONE',  ( 5.049401038298161559, -19.05341960407611168, 72.70724293864768129 ) ) ;
#189636 = CARTESIAN_POINT ( 'NONE',  ( -6.020228577223754586E-15, 39.95556452105416412, -0.4999999999999999445 ) ) ;
#189635 = CARTESIAN_POINT ( 'NONE',  ( 13.89961937509957401, 13.97604488694547697, 111.8760903946856757 ) ) ;
#189637 = CARTESIAN_POINT ( 'NONE',  ( 19.03943276465977164, 0.05219959533936151252, 21.25109039468565797 ) ) ;
#189638 = CARTESIAN_POINT ( 'NONE',  ( -12.14591786802326823, 12.06949235617739902, 78.12609039468570415 ) ) ;
#189639 = CARTESIAN_POINT ( 'NONE',  ( -9.474510206698720793, -16.51473224551083518, 109.5844237280190043 ) ) ;
#189640 = CARTESIAN_POINT ( 'NONE',  ( 14.34966873604960469, 8.224510206698951720, 114.1655762719810383 ) ) ;
#189641 = CARTESIAN_POINT ( 'NONE',  ( 14.29746914071037800, 8.314922557961029526, 61.66775706135235424 ) ) ;
#189642 = CARTESIAN_POINT ( 'NONE',  ( -4.483927247898782831, 16.52544592524335698, 52.70942372801902565 ) ) ;
#189643 = CARTESIAN_POINT ( 'NONE',  ( 13.89961937509977652, -13.97604488694527269, 28.12390960531435624 ) ) ;
#189644 = CARTESIAN_POINT ( 'NONE',  ( 9.564922557961047289, -16.46253265017146816, 75.41775706135234714 ) ) ;
#189645 = CARTESIAN_POINT ( 'NONE',  ( 21.52544592524334988, 5.823673210054432836, 106.4594237280190328 ) ) ;
#189646 = CARTESIAN_POINT ( 'NONE',  ( 5.153800228976335163, 19.02544592524342804, 34.79057627198102409 ) ) ;
#189647 = CARTESIAN_POINT ( 'NONE',  ( -13.97604488694527625, -13.89961937509977652, 76.87390960531433848 ) ) ;
#189648 = CARTESIAN_POINT ( 'NONE',  ( -16.53943276465976808, 0.05219959533911058130, 71.24890960531435269 ) ) ;
#189649 = CIRCLE ( 'NONE', #170294, 2.649999999999999911 ) ;
#189650 = CARTESIAN_POINT ( 'NONE',  ( -13.97604488694547697, 13.89961937509957934, 43.12609039468566152 ) ) ;
#189651 = CARTESIAN_POINT ( 'NONE',  ( 15.80617190586746368, 15.72974639402197994, 39.37390960531436690 ) ) ;
#189652 = CARTESIAN_POINT ( 'NONE',  ( 21.52544592524334988, 5.823673210054432836, 111.4594237280190328 ) ) ;
#189653 = CARTESIAN_POINT ( 'NONE',  ( -9.564922557960796823, -16.46253265017161027, 97.08224293864769550 ) ) ;
#189654 = EDGE_CURVE ( 'NONE', #70174, #91244, #44272, .T. ) ;
#189655 = CARTESIAN_POINT ( 'NONE',  ( 10.81492255796106328, -18.62759615963255655, 105.4177570613523613 ) ) ;
#189656 = CARTESIAN_POINT ( 'NONE',  ( -0.05219959533907301413, -21.53943276465977519, 57.49890960531435979 ) ) ;
#189657 = CARTESIAN_POINT ( 'NONE',  ( -9.474510206698964154, 16.51473224551069663, 95.41557627198102409 ) ) ;
#189658 = CARTESIAN_POINT ( 'NONE',  ( 0.05219959533936267826, -19.03943276465977164, 90.00109039468567573 ) ) ;
#189659 = CARTESIAN_POINT ( 'NONE',  ( 13.97604488694527802, 13.89961937509977652, 99.37390960531436690 ) ) ;
#189660 = CARTESIAN_POINT ( 'NONE',  ( 5.153800228976615827, -19.02544592524334988, 95.20942372801897591 ) ) ;
#189661 = CARTESIAN_POINT ( 'NONE',  ( -0.05219959533910754901, -16.53943276465976808, 112.4989096053143669 ) ) ;
#189662 = CARTESIAN_POINT ( 'NONE',  ( -13.89961937509977652, 13.97604488694528158, 85.62390960531433848 ) ) ;
#189663 = CARTESIAN_POINT ( 'NONE',  ( 18.62759615963271287, -10.81492255796078972, 63.33224293864770260 ) ) ;
#189664 = CARTESIAN_POINT ( 'NONE',  ( 16.53943276465976808, 0.05219959533934440121, 36.25109039468567573 ) ) ;
#189665 = CARTESIAN_POINT ( 'NONE',  ( -18.67979575497193778, 10.72451020669871902, 43.33442372801901143 ) ) ;
#189666 = CARTESIAN_POINT ( 'NONE',  ( -5.823673210054431948, 21.52544592524334988, 102.7094237280190185 ) ) ;
#189667 = CARTESIAN_POINT ( 'NONE',  ( -14.29746914071037622, -8.314922557961029526, 99.16775706135234714 ) ) ;
#189668 = CARTESIAN_POINT ( 'NONE',  ( -5.153800228976328057, -19.02544592524343514, 87.29057627198103830 ) ) ;
#189669 = CARTESIAN_POINT ( 'NONE',  ( 14.34966873604960469, 8.224510206698951720, 89.16557627198102409 ) ) ;
#189670 = CARTESIAN_POINT ( 'NONE',  ( 16.55341960407618274, -4.379528057220086978, 111.0427570613523613 ) ) ;
#189671 = CARTESIAN_POINT ( 'NONE',  ( -5.153800228976607833, 19.02544592524334988, 62.70942372801899722 ) ) ;
#189672 =( GEOMETRIC_REPRESENTATION_CONTEXT ( 3 ) GLOBAL_UNCERTAINTY_ASSIGNED_CONTEXT ( ( #23637 ) ) GLOBAL_UNIT_ASSIGNED_CONTEXT ( ( #54703, #22377, #53710 ) ) REPRESENTATION_CONTEXT ( 'NONE', 'WORKASPACE' ) );
#189673 = CARTESIAN_POINT ( 'NONE',  ( -5.823673210054431948, 21.52544592524334988, 47.70942372801902565 ) ) ;
#189674 = CARTESIAN_POINT ( 'NONE',  ( -16.55341960407611168, -4.379528057220339221, 91.45724293864769550 ) ) ;
#189675 = CARTESIAN_POINT ( 'NONE',  ( -19.05341960407611168, -5.049401038298163336, 106.4572429386476955 ) ) ;
#189676 = CARTESIAN_POINT ( 'NONE',  ( 8.314922557960818139, 14.29746914071049879, 29.58224293864769905 ) ) ;
#189677 = CARTESIAN_POINT ( 'NONE',  ( 5.823673210054444382, -21.52544592524334988, 90.20942372801903275 ) ) ;
#189678 = CARTESIAN_POINT ( 'NONE',  ( -0.05219959533934338120, 16.53943276465976808, 42.50109039468567573 ) ) ;
#189679 = CARTESIAN_POINT ( 'NONE',  ( 5.823673210054444382, -21.52544592524334988, 40.20942372801901854 ) ) ;
#189680 = ORIENTED_EDGE ( 'NONE', *, *, #74286, .F. ) ;
#189681 = CARTESIAN_POINT ( 'NONE',  ( 0.05219959533937995610, -21.53943276465977519, 20.00109039468568639 ) ) ;
#189682 = CARTESIAN_POINT ( 'NONE',  ( 14.34966873604960469, 8.224510206698951720, 89.16557627198102409 ) ) ;
#189683 = CARTESIAN_POINT ( 'NONE',  ( -19.25176906914649066, -5.499999999999738876, 50.99927264242279534 ) ) ;
#189684 = CARTESIAN_POINT ( 'NONE',  ( 14.34966873604960469, 8.224510206698951720, 64.16557627198102409 ) ) ;
#189685 = CARTESIAN_POINT ( 'NONE',  ( 9.564922557960805705, 16.46253265017160317, 54.58224293864769550 ) ) ;
#189686 = CARTESIAN_POINT ( 'NONE',  ( -12.06949235617739369, -12.14591786802326823, 109.3760903946857042 ) ) ;
#189687 = CARTESIAN_POINT ( 'NONE',  ( 9.564922557960805705, 16.46253265017160317, 44.58224293864769550 ) ) ;
#189688 = CARTESIAN_POINT ( 'NONE',  ( -10.81492255796078084, -18.62759615963271287, 42.08224293864769550 ) ) ;
#189689 = CARTESIAN_POINT ( 'NONE',  ( 14.34966873604960469, 8.224510206698951720, 74.16557627198102409 ) ) ;
#189690 = VECTOR ( 'NONE', #92719, 1000.000000000000000 ) ;
#189691 = CARTESIAN_POINT ( 'NONE',  ( 0.05219959533907565091, 21.53943276465977519, 94.99890960531436690 ) ) ;
#189692 = CARTESIAN_POINT ( 'NONE',  ( 5.049401038298161559, -19.05341960407611168, 87.70724293864769550 ) ) ;
#189694 = CARTESIAN_POINT ( 'NONE',  ( -16.46253265017146816, -9.564922557961047289, 94.16775706135233293 ) ) ;
#189693 = CARTESIAN_POINT ( 'NONE',  ( 16.51473224551069308, 9.474510206698969483, 39.16557627198103120 ) ) ;
#189695 = CARTESIAN_POINT ( 'NONE',  ( -15.80617190586745835, -15.72974639402198527, 41.87390960531435979 ) ) ;
#189696 = CARTESIAN_POINT ( 'NONE',  ( -10.81492255796105439, 18.62759615963255655, 72.91775706135234714 ) ) ;
#189697 = CARTESIAN_POINT ( 'NONE',  ( -16.51473224551069308, -9.474510206698971260, 51.66557627198102409 ) ) ;
#189698 = CARTESIAN_POINT ( 'NONE',  ( 9.564922557960805705, 16.46253265017160317, 79.58224293864769550 ) ) ;
#189699 = ORIENTED_EDGE ( 'NONE', *, *, #114623, .T. ) ;
#189700 = CARTESIAN_POINT ( 'NONE',  ( -8.314922557961024197, 14.29746914071037800, 57.91775706135234714 ) ) ;
#189701 = CARTESIAN_POINT ( 'NONE',  ( -21.52544592524334988, -5.823673210054445271, 43.95942372801902565 ) ) ;
#189702 = CARTESIAN_POINT ( 'NONE',  ( -0.05219959533937732626, 21.53943276465977519, 77.50109039468567573 ) ) ;
#189703 = CARTESIAN_POINT ( 'NONE',  ( -5.049401038298153566, 19.05341960407611168, 115.2072429386477097 ) ) ;
#189704 = CARTESIAN_POINT ( 'NONE',  ( -21.53943276465977519, 0.05219959533907696930, 101.2489096053143669 ) ) ;
#189706 = CARTESIAN_POINT ( 'NONE',  ( -4.483927247898782831, 16.52544592524335698, 67.70942372801901854 ) ) ;
#189705 = CARTESIAN_POINT ( 'NONE',  ( -10.81492255796105439, 18.62759615963255655, 42.91775706135235424 ) ) ;
#189707 = CARTESIAN_POINT ( 'NONE',  ( -0.05219959533907301413, -21.53943276465977519, 62.49890960531436690 ) ) ;
#189708 = CARTESIAN_POINT ( 'NONE',  ( -19.05341960407617563, 5.049401038297882671, 33.54275706135231871 ) ) ;
#189710 = CARTESIAN_POINT ( 'NONE',  ( 16.52544592524335698, 4.483927247898782831, 101.4594237280190185 ) ) ;
#189709 = CARTESIAN_POINT ( 'NONE',  ( 13.89961937509977652, -13.97604488694527269, 68.12390960531436690 ) ) ;
#189711 = CARTESIAN_POINT ( 'NONE',  ( -19.99999999999998224, -188.0000000000000000, 0.000000000000000000 ) ) ;
#189712 = CARTESIAN_POINT ( 'NONE',  ( 5.153800228976335163, 19.02544592524342804, 99.79057627198102409 ) ) ;
#189713 = CARTESIAN_POINT ( 'NONE',  ( -9.564922557961040184, 16.46253265017147172, 52.91775706135233293 ) ) ;
#189714 = CARTESIAN_POINT ( 'NONE',  ( 13.97604488694548053, -13.89961937509957401, 80.62609039468567573 ) ) ;
#189715 = CARTESIAN_POINT ( 'NONE',  ( 15.80617190586746368, 15.72974639402197994, 64.37390960531435269 ) ) ;
#189716 = CARTESIAN_POINT ( 'NONE',  ( -4.379528057220328563, 16.55341960407611168, 45.20724293864769550 ) ) ;
#189717 = CARTESIAN_POINT ( 'NONE',  ( -9.564922557961040184, 16.46253265017147172, 92.91775706135233293 ) ) ;
#189718 = CARTESIAN_POINT ( 'NONE',  ( 193.3062444957835453, -155.7167183371837496, 0.000000000000000000 ) ) ;
#189719 = CARTESIAN_POINT ( 'NONE',  ( -0.05219959533936034679, 19.03943276465977164, 102.5010903946856757 ) ) ;
#189721 = CARTESIAN_POINT ( 'NONE',  ( 13.97604488694548053, -13.89961937509957401, 55.62609039468566863 ) ) ;
#189720 = CARTESIAN_POINT ( 'NONE',  ( -21.52544592524343514, 5.823673210054127303, 81.04057627198102409 ) ) ;
#189722 = CARTESIAN_POINT ( 'NONE',  ( 26.33854305698156395, -8.833284547248206664, 167.2806188263833747 ) ) ;
#189723 = CARTESIAN_POINT ( 'NONE',  ( 16.46253265017160672, -9.564922557960803928, 63.33224293864769550 ) ) ;
#189724 = CARTESIAN_POINT ( 'NONE',  ( -16.53943276465976808, 0.05219959533911058130, 66.24890960531436690 ) ) ;
#189725 = CARTESIAN_POINT ( 'NONE',  ( -5.049401038298153566, 19.05341960407611168, 45.20724293864769550 ) ) ;
#189726 = CARTESIAN_POINT ( 'NONE',  ( -4.379528057220328563, 16.55341960407611168, 60.20724293864768839 ) ) ;
#189727 = CARTESIAN_POINT ( 'NONE',  ( -5.049401038298153566, 19.05341960407611168, 25.20724293864768484 ) ) ;
#189728 = CARTESIAN_POINT ( 'NONE',  ( 31.37893600750392409, -5.659358439387617068, 99.94586368981259739 ) ) ;
#189729 = CARTESIAN_POINT ( 'NONE',  ( -16.53943276465976808, 0.05219959533911058130, 31.24890960531435979 ) ) ;
#189730 = CARTESIAN_POINT ( 'NONE',  ( -5.049401038298153566, 19.05341960407611168, 65.20724293864765286 ) ) ;
#189731 = DIRECTION ( 'NONE',  ( -0.000000000000000000, -0.000000000000000000, 1.000000000000000000 ) ) ;
#189732 = CARTESIAN_POINT ( 'NONE',  ( 13.97604488694548053, -13.89961937509957401, 35.62609039468567573 ) ) ;
#189733 = CARTESIAN_POINT ( 'NONE',  ( 14.29746914071037800, 8.314922557961029526, 46.66775706135234714 ) ) ;
#189734 = CARTESIAN_POINT ( 'NONE',  ( 5.823673210054125526, 21.52544592524343514, 49.79057627198102409 ) ) ;
#189735 = CARTESIAN_POINT ( 'NONE',  ( 21.52544592524334988, 5.823673210054432836, 111.4594237280190328 ) ) ;
#189736 = CARTESIAN_POINT ( 'NONE',  ( -5.049401038298153566, 19.05341960407611168, 75.20724293864769550 ) ) ;
#189737 = CARTESIAN_POINT ( 'NONE',  ( -6.586805632895485375E-13, -76.33425854457905757, -24.99989890116611946 ) ) ;
#189738 = CARTESIAN_POINT ( 'NONE',  ( 0.05219959533909260263, 19.03943276465977164, 104.9989096053143669 ) ) ;
#189739 = CARTESIAN_POINT ( 'NONE',  ( 5.823673210054444382, -21.52544592524334988, 40.20942372801901854 ) ) ;
#189740 = CARTESIAN_POINT ( 'NONE',  ( 16.52544592524342804, -4.483927247898539470, 98.54057627198105251 ) ) ;
#189743 = VERTEX_POINT ( 'NONE', #30092 ) ;
#189742 = CARTESIAN_POINT ( 'NONE',  ( -16.51473224551069308, -9.474510206698971260, 81.66557627198103830 ) ) ;
#189741 = CARTESIAN_POINT ( 'NONE',  ( 21.53943276465977519, -0.05219959533907433946, 88.74890960531436690 ) ) ;
#189744 = CARTESIAN_POINT ( 'NONE',  ( 19.05341960407611168, 5.049401038298154454, 83.95724293864766707 ) ) ;
#189745 = CARTESIAN_POINT ( 'NONE',  ( 18.67979575497194134, -10.72451020669871369, 20.83442372801901143 ) ) ;
#189746 = EDGE_CURVE ( 'NONE', #59237, #126834, #123079, .T. ) ;
#189747 = VERTEX_POINT ( 'NONE', #75586 ) ;
#189748 = CARTESIAN_POINT ( 'NONE',  ( -13.97604488694527625, -13.89961937509977652, 81.87390960531436690 ) ) ;
#189749 = FACE_OUTER_BOUND ( 'NONE', #182679, .T. ) ;
#189751 = CARTESIAN_POINT ( 'NONE',  ( 13.89961937509977652, -13.97604488694527269, 33.12390960531434558 ) ) ;
#189750 = CARTESIAN_POINT ( 'NONE',  ( 13.89961937509977652, -13.97604488694527269, 23.12390960531436335 ) ) ;
#189752 = CARTESIAN_POINT ( 'NONE',  ( 9.474510206698729675, 16.51473224551082808, 107.0844237280190043 ) ) ;
#189753 = CARTESIAN_POINT ( 'NONE',  ( 36.91746824999999887, 11.99521256947799053, -10.02499999726881086 ) ) ;
#189754 = CARTESIAN_POINT ( 'NONE',  ( -12.06949235617756955, 12.14591786802309770, 105.6239096053143669 ) ) ;
#189755 = CARTESIAN_POINT ( 'NONE',  ( -15.80617190586768217, 15.72974639402176855, 88.12609039468570415 ) ) ;
#189757 = CARTESIAN_POINT ( 'NONE',  ( -15.80617190586768217, 15.72974639402176855, 33.12609039468569705 ) ) ;
#189756 = CARTESIAN_POINT ( 'NONE',  ( 13.89961937509977652, -13.97604488694527269, 63.12390960531435979 ) ) ;
#189758 = CARTESIAN_POINT ( 'NONE',  ( -18.67979575497178146, -10.72451020669898902, 106.6655762719810383 ) ) ;
#189759 = CARTESIAN_POINT ( 'NONE',  ( -8.571926809382601320, -26.38167802310801591, 139.7750000027311899 ) ) ;
#189760 = CARTESIAN_POINT ( 'NONE',  ( 16.51473224551069308, 9.474510206698969483, 84.16557627198102409 ) ) ;
#189761 = CARTESIAN_POINT ( 'NONE',  ( 27.77709992218785828, 7.633332386730715236, 161.4489275245684041 ) ) ;
#189763 = CARTESIAN_POINT ( 'NONE',  ( -18.67979575497178146, -10.72451020669898902, 41.66557627198103120 ) ) ;
#189762 = CARTESIAN_POINT ( 'NONE',  ( 14.34966873604972726, -8.224510206698740333, 25.83442372801901499 ) ) ;
#189764 = CARTESIAN_POINT ( 'NONE',  ( 18.67979575497194134, -10.72451020669871369, 60.83442372801901854 ) ) ;
#189765 = CARTESIAN_POINT ( 'NONE',  ( 9.474510206698971260, -16.51473224551069308, 112.9155762719810383 ) ) ;
#189766 = CARTESIAN_POINT ( 'NONE',  ( 13.97604488694548053, -13.89961937509957401, 95.62609039468563310 ) ) ;
#189767 = CARTESIAN_POINT ( 'NONE',  ( 9.474510206698971260, -16.51473224551069308, 62.91557627198102409 ) ) ;
#189768 = CARTESIAN_POINT ( 'NONE',  ( 13.89961937509977652, -13.97604488694527269, 88.12390960531438111 ) ) ;
#189769 = CARTESIAN_POINT ( 'NONE',  ( 14.34966873604960469, 8.224510206698951720, 94.16557627198103830 ) ) ;
#189770 = CARTESIAN_POINT ( 'NONE',  ( -4.379528057220328563, 16.55341960407611168, 100.2072429386476955 ) ) ;
#189772 = ADVANCED_FACE ( 'NONE', ( #90749, #195987 ), #153427, .T. ) ;
#189771 = CARTESIAN_POINT ( 'NONE',  ( -16.51473224551069308, -9.474510206698971260, 111.6655762719810383 ) ) ;
#189774 = CARTESIAN_POINT ( 'NONE',  ( -13.97604488694527625, -13.89961937509977652, 46.87390960531435979 ) ) ;
#189773 = CARTESIAN_POINT ( 'NONE',  ( -14.29746914071049879, 8.314922557960819915, 50.83224293864770971 ) ) ;
#189775 = CARTESIAN_POINT ( 'NONE',  ( 10.72451020669871369, 18.67979575497193778, 67.08442372801901854 ) ) ;
#189776 = CARTESIAN_POINT ( 'NONE',  ( -19.03943276465977164, -0.05219959533935918106, 88.75109039468567573 ) ) ;
#189777 = CARTESIAN_POINT ( 'NONE',  ( 16.52544592524342804, -4.483927247898539470, 63.54057627198103830 ) ) ;
#189778 = CARTESIAN_POINT ( 'NONE',  ( -21.52544592524334988, -5.823673210054445271, 18.95942372801901143 ) ) ;
#189779 = CARTESIAN_POINT ( 'NONE',  ( -21.55341960407610458, -5.719274019375992779, 41.45724293864769550 ) ) ;
#189780 = CARTESIAN_POINT ( 'NONE',  ( -9.564922557960796823, -16.46253265017161027, 107.0822429386476955 ) ) ;
#189781 = CARTESIAN_POINT ( 'NONE',  ( -28.82186960331499392, -9.364793116373526516, 142.3500000054623342 ) ) ;
#189782 = CARTESIAN_POINT ( 'NONE',  ( -0.05219959533909027116, -19.03943276465977164, 67.49890960531436690 ) ) ;
#189783 = CARTESIAN_POINT ( 'NONE',  ( -16.55341960407611168, -4.379528057220339221, 41.45724293864769550 ) ) ;
#189784 = AXIS2_PLACEMENT_3D ( 'NONE', #158181, #23668, #147008 ) ;
#189785 = CARTESIAN_POINT ( 'NONE',  ( -12.14591786802326823, 12.06949235617739902, 103.1260903946856757 ) ) ;
#189786 = CARTESIAN_POINT ( 'NONE',  ( 4.483927247898790824, -16.52544592524335698, 80.20942372801901854 ) ) ;
#189787 = CARTESIAN_POINT ( 'NONE',  ( 16.51473224551083163, -9.474510206698727899, 40.83442372801900433 ) ) ;
#189788 = CARTESIAN_POINT ( 'NONE',  ( -17.50000000001358202, 5.499999999999951150, 100.7969038253505687 ) ) ;
#189789 = CARTESIAN_POINT ( 'NONE',  ( 5.049401038298161559, -19.05341960407611168, 97.70724293864766707 ) ) ;
#189790 = CARTESIAN_POINT ( 'NONE',  ( 19.03943276465977164, -0.05219959533909143690, 48.74890960531435979 ) ) ;
#189791 = CARTESIAN_POINT ( 'NONE',  ( 14.29746914071049879, -8.314922557960816363, 63.33224293864770260 ) ) ;
#189793 = CARTESIAN_POINT ( 'NONE',  ( 21.52544592524344225, -5.823673210054117533, 23.54057627198102765 ) ) ;
#189792 = CARTESIAN_POINT ( 'NONE',  ( 17.31747979337947996, -6.344076630961053453, 101.1205513193481664 ) ) ;
#189794 = CARTESIAN_POINT ( 'NONE',  ( 5.823673210054125526, 21.52544592524343514, 49.79057627198102409 ) ) ;
#189795 = CARTESIAN_POINT ( 'NONE',  ( -8.224510206698948167, 14.34966873604960824, 90.41557627198103830 ) ) ;
#189796 = CARTESIAN_POINT ( 'NONE',  ( 4.379528057220092307, 16.55341960407617563, 37.29275706135235424 ) ) ;
#189797 = CARTESIAN_POINT ( 'NONE',  ( -4.379528057220328563, 16.55341960407611168, 85.20724293864770971 ) ) ;
#189798 = CARTESIAN_POINT ( 'NONE',  ( -18.87580814761070513, 5.500000000000040856, 65.87172394265761000 ) ) ;
#189799 = CARTESIAN_POINT ( 'NONE',  ( -19.05341960407617563, 5.049401038297882671, 73.54275706135233293 ) ) ;
#189800 = CARTESIAN_POINT ( 'NONE',  ( 5.719274019375991003, -21.55341960407610458, 22.70724293864769194 ) ) ;
#189801 = CARTESIAN_POINT ( 'NONE',  ( 36.91746825000000598, -11.99521256947793546, -6.224999997268814589 ) ) ;
#189802 = CARTESIAN_POINT ( 'NONE',  ( 19.42893418801160621, 5.499999999999992895, 102.2141673858846076 ) ) ;
#189804 = CARTESIAN_POINT ( 'NONE',  ( 14.34966873604972726, -8.224510206698740333, 110.8344237280190043 ) ) ;
#189803 = CARTESIAN_POINT ( 'NONE',  ( 8.314922557961029526, -14.29746914071037800, 25.41775706135235779 ) ) ;
#189805 = CARTESIAN_POINT ( 'NONE',  ( -16.51473224551082808, 9.474510206698731452, 68.33442372801900433 ) ) ;
#189806 = CARTESIAN_POINT ( 'NONE',  ( 15.80617190586746368, 15.72974639402197994, 54.37390960531435979 ) ) ;
#189807 = CARTESIAN_POINT ( 'NONE',  ( 5.719274019375673035, 21.55341960407619339, 62.29275706135236845 ) ) ;
#189808 = CARTESIAN_POINT ( 'NONE',  ( 18.59930490233253408, 5.500000000000118128, 38.94150099494206785 ) ) ;
#189809 = CARTESIAN_POINT ( 'NONE',  ( -12.06949235617739369, -12.14591786802326823, 34.37609039468568284 ) ) ;
#189811 = CARTESIAN_POINT ( 'NONE',  ( -13.97604488694527625, -13.89961937509977652, 81.87390960531436690 ) ) ;
#189810 = CARTESIAN_POINT ( 'NONE',  ( 5.153800228976335163, 19.02544592524342804, 24.79057627198102765 ) ) ;
#189812 = MECHANICAL_DESIGN_GEOMETRIC_PRESENTATION_REPRESENTATION (  '', ( #121967 ), #54280 ) ;
#189813 = CARTESIAN_POINT ( 'NONE',  ( 5.153800228976335163, 19.02544592524342804, 24.79057627198102765 ) ) ;
#189814 = CARTESIAN_POINT ( 'NONE',  ( -8.314922557960811034, -14.29746914071050412, 87.08224293864769550 ) ) ;
#189815 = CARTESIAN_POINT ( 'NONE',  ( -13.97604488694527625, -13.89961937509977652, 96.87390960531433848 ) ) ;
#189816 = VERTEX_POINT ( 'NONE', #196971 ) ;
#189817 = CARTESIAN_POINT ( 'NONE',  ( 19.03943276465977164, 0.05219959533936151252, 101.2510903946856757 ) ) ;
#189818 = CARTESIAN_POINT ( 'NONE',  ( -15.80617190586745835, -15.72974639402198527, 76.87390960531439532 ) ) ;
#189819 = CARTESIAN_POINT ( 'NONE',  ( 19.03943276465977164, -0.05219959533909143690, 48.74890960531435979 ) ) ;
#189821 = CARTESIAN_POINT ( 'NONE',  ( -15.72974639402176322, -15.80617190586768395, 19.37609039468568639 ) ) ;
#189820 = CARTESIAN_POINT ( 'NONE',  ( 0.05219959533936267826, -19.03943276465977164, 65.00109039468567573 ) ) ;
#189822 = CARTESIAN_POINT ( 'NONE',  ( 13.97604488694527802, 13.89961937509977652, 64.37390960531436690 ) ) ;
#189823 = CARTESIAN_POINT ( 'NONE',  ( -16.46253265017160317, 9.564922557960807481, 105.8322429386476955 ) ) ;
#189824 = ORIENTED_EDGE ( 'NONE', *, *, #187510, .F. ) ;
#189825 = CARTESIAN_POINT ( 'NONE',  ( 14.34966873604972726, -8.224510206698740333, 35.83442372801901143 ) ) ;
#189826 = CARTESIAN_POINT ( 'NONE',  ( 15.72974639402199770, -15.80617190586745480, 98.12390960531436690 ) ) ;
#189829 = CARTESIAN_POINT ( 'NONE',  ( 5.049401038297881783, 19.05341960407617563, 67.29275706135234714 ) ) ;
#189828 = CARTESIAN_POINT ( 'NONE',  ( -13.97604488694527625, -13.89961937509977652, 91.87390960531432427 ) ) ;
#189827 = CARTESIAN_POINT ( 'NONE',  ( -4.379528057220328563, 16.55341960407611168, 110.2072429386477239 ) ) ;
#189830 = CARTESIAN_POINT ( 'NONE',  ( 18.62759615963271287, -10.81492255796078972, 93.33224293864769550 ) ) ;
#189831 = CARTESIAN_POINT ( 'NONE',  ( -12.06949235617756955, 12.14591786802309770, 50.62390960531435979 ) ) ;
#189832 = CARTESIAN_POINT ( 'NONE',  ( 5.153800228976615827, -19.02544592524334988, 20.20942372801899722 ) ) ;
#189833 = CARTESIAN_POINT ( 'NONE',  ( -16.52544592524335698, -4.483927247898792601, 63.95942372801901854 ) ) ;
#189834 = CARTESIAN_POINT ( 'NONE',  ( -13.89961937509977652, 13.97604488694528158, 90.62390960531432427 ) ) ;
#189835 = CARTESIAN_POINT ( 'NONE',  ( -16.46253265017160317, 9.564922557960807481, 45.83224293864769550 ) ) ;
#189836 = CARTESIAN_POINT ( 'NONE',  ( 15.80617190586769283, -15.72974639402175789, 50.62609039468568994 ) ) ;
#189837 = CARTESIAN_POINT ( 'NONE',  ( 15.80617190586769283, -15.72974639402175789, 70.62609039468567573 ) ) ;
#189838 = CARTESIAN_POINT ( 'NONE',  ( 9.564922557960805705, 16.46253265017160317, 59.58224293864769550 ) ) ;
#189839 = CARTESIAN_POINT ( 'NONE',  ( -5.719274019375665041, -21.55341960407619695, 29.79275706135234358 ) ) ;
#189840 = CARTESIAN_POINT ( 'NONE',  ( -13.97604488694547697, 13.89961937509957934, 78.12609039468567573 ) ) ;
#189841 = CARTESIAN_POINT ( 'NONE',  ( 19.02544592524343514, -5.153800228976328945, 38.54057627198103120 ) ) ;
#189842 = CARTESIAN_POINT ( 'NONE',  ( 14.29746914071037800, 8.314922557961029526, 81.66775706135236135 ) ) ;
#189843 = CARTESIAN_POINT ( 'NONE',  ( -16.51473224551069308, -9.474510206698971260, 56.66557627198103120 ) ) ;
#189844 = CARTESIAN_POINT ( 'NONE',  ( 11.74149087413294268, 36.13659316521247433, -2.347842220587804452 ) ) ;
#189845 = CARTESIAN_POINT ( 'NONE',  ( -13.97604488694527625, -13.89961937509977652, 36.87390960531436690 ) ) ;
#189846 = CARTESIAN_POINT ( 'NONE',  ( 10.81492255796078972, 18.62759615963270932, 89.58224293864768129 ) ) ;
#189847 = CARTESIAN_POINT ( 'NONE',  ( 8.314922557961029526, -14.29746914071037800, 75.41775706135233293 ) ) ;
#189848 = DIRECTION ( 'NONE',  ( 0.000000000000000000, 0.000000000000000000, 1.000000000000000000 ) ) ;
#189849 = CARTESIAN_POINT ( 'NONE',  ( -19.03943276465977164, -0.05219959533935918106, 28.75109039468566507 ) ) ;
#189850 = ADVANCED_FACE ( 'NONE', ( #58438 ), #46251, .T. ) ;
#189851 = CARTESIAN_POINT ( 'NONE',  ( 19.03943276465977164, -0.05219959533909143690, 58.74890960531435979 ) ) ;
#189852 = CARTESIAN_POINT ( 'NONE',  ( -8.224510206698948167, 14.34966873604960824, 45.41557627198103830 ) ) ;
#189853 = CARTESIAN_POINT ( 'NONE',  ( -16.53943276465976808, 0.05219959533911058130, 76.24890960531435269 ) ) ;
#189854 = CARTESIAN_POINT ( 'NONE',  ( -13.97604488694527625, -13.89961937509977652, 101.8739096053143811 ) ) ;
#189855 = CARTESIAN_POINT ( 'NONE',  ( 16.51473224551069308, 9.474510206698969483, 84.16557627198102409 ) ) ;
#189856 = CARTESIAN_POINT ( 'NONE',  ( 21.52544592524334988, 5.823673210054432836, 51.45942372801901854 ) ) ;
#189857 = CARTESIAN_POINT ( 'NONE',  ( 0.05219959533909260263, 19.03943276465977164, 94.99890960531436690 ) ) ;
#189858 = CARTESIAN_POINT ( 'NONE',  ( -21.53943276465977519, -0.05219959533937600094, 98.75109039468568994 ) ) ;
#189859 = CARTESIAN_POINT ( 'NONE',  ( -4.379528057220086978, -16.55341960407618274, 84.79275706135234714 ) ) ;
#189860 = CARTESIAN_POINT ( 'NONE',  ( -18.67979575497193778, 10.72451020669871902, 23.33442372801901499 ) ) ;
#189861 = CARTESIAN_POINT ( 'NONE',  ( -18.62759615963270932, 10.81492255796079327, 105.8322429386476955 ) ) ;
#189862 = CARTESIAN_POINT ( 'NONE',  ( -14.34966873604960291, -8.224510206698953496, 66.66557627198102409 ) ) ;
#189863 = CARTESIAN_POINT ( 'NONE',  ( -13.97604488694527625, -13.89961937509977652, 36.87390960531436690 ) ) ;
#189864 = CARTESIAN_POINT ( 'NONE',  ( -14.29746914071049879, 8.314922557960819915, 70.83224293864770971 ) ) ;
#189865 = CARTESIAN_POINT ( 'NONE',  ( 21.52544592524344225, -5.823673210054117533, 28.54057627198103120 ) ) ;
#189866 = CARTESIAN_POINT ( 'NONE',  ( -19.05341960407617563, 5.049401038297882671, 33.54275706135231871 ) ) ;
#189867 = CARTESIAN_POINT ( 'NONE',  ( -12.06949235617756955, 12.14591786802309770, 105.6239096053143669 ) ) ;
#189868 = ORIENTED_EDGE ( 'NONE', *, *, #132933, .T. ) ;
#189869 = CARTESIAN_POINT ( 'NONE',  ( 8.314922557961029526, -14.29746914071037800, 70.41775706135236135 ) ) ;
#189870 = CARTESIAN_POINT ( 'NONE',  ( 16.51473224551069308, 9.474510206698969483, 64.16557627198102409 ) ) ;
#189871 = CARTESIAN_POINT ( 'NONE',  ( -12.14591786802309592, -12.06949235617757132, 86.87390960531438111 ) ) ;
#189872 = CARTESIAN_POINT ( 'NONE',  ( -15.72974639402197994, 15.80617190586746368, 40.62390960531435269 ) ) ;
#189873 = CARTESIAN_POINT ( 'NONE',  ( 16.55341960407618274, -4.379528057220086978, 96.04275706135236135 ) ) ;
#189874 = CARTESIAN_POINT ( 'NONE',  ( -16.52544592524335698, -4.483927247898792601, 18.95942372801901143 ) ) ;
#189875 = CARTESIAN_POINT ( 'NONE',  ( 18.62759615963255655, 10.81492255796105972, 81.66775706135236135 ) ) ;
#189876 = CARTESIAN_POINT ( 'NONE',  ( -13.97604488694527625, -13.89961937509977652, 81.87390960531436690 ) ) ;
#189877 = CARTESIAN_POINT ( 'NONE',  ( -5.823673210054116645, -21.52544592524344225, 102.2905762719810383 ) ) ;
#189878 = CARTESIAN_POINT ( 'NONE',  ( 4.379528057220092307, 16.55341960407617563, 52.29275706135236135 ) ) ;
#189879 = CARTESIAN_POINT ( 'NONE',  ( -19.05341960407611168, -5.049401038298163336, 21.45724293864768839 ) ) ;
#189880 = CARTESIAN_POINT ( 'NONE',  ( -5.153800228976607833, 19.02544592524334988, 112.7094237280190043 ) ) ;
#189881 = CARTESIAN_POINT ( 'NONE',  ( -16.51473224551082808, 9.474510206698731452, 83.33442372801899012 ) ) ;
#189882 = CARTESIAN_POINT ( 'NONE',  ( 15.80617190586746368, 15.72974639402197994, 79.37390960531436690 ) ) ;
#189883 = CARTESIAN_POINT ( 'NONE',  ( 0.05219959533936267826, -19.03943276465977164, 50.00109039468566863 ) ) ;
#189884 = DIRECTION ( 'NONE',  ( -0.000000000000000000, -0.000000000000000000, -1.000000000000000000 ) ) ;
#189885 = CARTESIAN_POINT ( 'NONE',  ( 0.05219959533907565091, 21.53943276465977519, 104.9989096053143669 ) ) ;
#189886 = CARTESIAN_POINT ( 'NONE',  ( -17.81289503416611097, -24.51734667627696496, 148.2999999999999545 ) ) ;
#189887 = CARTESIAN_POINT ( 'NONE',  ( -5.153800228976328057, -19.02544592524343514, 77.29057627198099567 ) ) ;
#189888 = DIRECTION ( 'NONE',  ( 1.000000000000000000, -3.552713678800500929E-15, 0.000000000000000000 ) ) ;
#189889 = CARTESIAN_POINT ( 'NONE',  ( -16.53943276465976808, -0.05219959533934237506, 28.75109039468567929 ) ) ;
#189890 = CARTESIAN_POINT ( 'NONE',  ( 36.77739090780051612, -5.326908766905467552, 46.41547615974452867 ) ) ;
#189892 = CARTESIAN_POINT ( 'NONE',  ( 8.314922557960818139, 14.29746914071049879, 69.58224293864769550 ) ) ;
#189891 = CARTESIAN_POINT ( 'NONE',  ( 15.72974639402199770, -15.80617190586745480, 98.12390960531436690 ) ) ;
#189893 = CARTESIAN_POINT ( 'NONE',  ( -19.03943276465977164, 0.05219959533909376836, 66.24890960531436690 ) ) ;
#189894 = CARTESIAN_POINT ( 'NONE',  ( -0.05219959533937732626, 21.53943276465977519, 87.50109039468568994 ) ) ;
#189896 = CARTESIAN_POINT ( 'NONE',  ( 9.564922557961047289, -16.46253265017146816, 40.41775706135234003 ) ) ;
#189895 = CARTESIAN_POINT ( 'NONE',  ( 16.52544592524335698, 4.483927247898782831, 36.45942372801901143 ) ) ;
#189897 = CARTESIAN_POINT ( 'NONE',  ( -18.62759615963255300, -10.81492255796106328, 54.16775706135235424 ) ) ;
#189898 = CARTESIAN_POINT ( 'NONE',  ( -10.72451020669898014, 18.67979575497178502, 55.41557627198102409 ) ) ;
#189899 = CARTESIAN_POINT ( 'NONE',  ( 16.51473224551083163, -9.474510206698727899, 105.8344237280190043 ) ) ;
#189900 = CARTESIAN_POINT ( 'NONE',  ( -13.89961937509977652, 13.97604488694528158, 55.62390960531434558 ) ) ;
#189901 = CARTESIAN_POINT ( 'NONE',  ( 19.03943276465977164, 0.05219959533936151252, 86.25109039468567573 ) ) ;
#189902 = CARTESIAN_POINT ( 'NONE',  ( -18.62759615963255300, -10.81492255796106328, 84.16775706135234714 ) ) ;
#189903 = CARTESIAN_POINT ( 'NONE',  ( -5.049401038297874678, -19.05341960407617918, 69.79275706135233293 ) ) ;
#189904 = CARTESIAN_POINT ( 'NONE',  ( 16.46253265017160672, -9.564922557960803928, 33.33224293864770260 ) ) ;
#189905 = CARTESIAN_POINT ( 'NONE',  ( -15.80617190586745835, -15.72974639402198527, 56.87390960531436690 ) ) ;
#189906 = CARTESIAN_POINT ( 'NONE',  ( 8.224510206698953496, -14.34966873604960469, 57.91557627198103120 ) ) ;
#189907 = CARTESIAN_POINT ( 'NONE',  ( 21.92716348790884240, 9.076607822308496054, 171.2490935175191282 ) ) ;
#189908 = CARTESIAN_POINT ( 'NONE',  ( 19.02544592524334988, 5.153800228976608722, 36.45942372801900433 ) ) ;
#189909 = CARTESIAN_POINT ( 'NONE',  ( -8.224510206698735004, -14.34966873604973081, 94.58442372801901854 ) ) ;
#189910 = CARTESIAN_POINT ( 'NONE',  ( -14.29746914071049879, 8.314922557960819915, 55.83224293864770260 ) ) ;
#189911 = CARTESIAN_POINT ( 'NONE',  ( 10.81492255796106328, -18.62759615963255655, 85.41775706135236135 ) ) ;
#189912 = CARTESIAN_POINT ( 'NONE',  ( 10.72451020669871369, 18.67979575497193778, 82.08442372801901854 ) ) ;
#189913 = CARTESIAN_POINT ( 'NONE',  ( 5.719274019375991003, -21.55341960407610458, 97.70724293864772392 ) ) ;
#189914 = CARTESIAN_POINT ( 'NONE',  ( -0.05219959533909027116, -19.03943276465977164, 52.49890960531436690 ) ) ;
#189915 = CARTESIAN_POINT ( 'NONE',  ( -21.53943276465977519, -0.05219959533937600094, 63.75109039468568284 ) ) ;
#189916 = CARTESIAN_POINT ( 'NONE',  ( 19.05341960407611168, 5.049401038298154454, 48.95724293864768129 ) ) ;
#189917 = ORIENTED_EDGE ( 'NONE', *, *, #150856, .T. ) ;
#189918 = CARTESIAN_POINT ( 'NONE',  ( -16.46253265017160317, 9.564922557960807481, 60.83224293864769550 ) ) ;
#189919 = CARTESIAN_POINT ( 'NONE',  ( -4.379528057220328563, 16.55341960407611168, 110.2072429386477239 ) ) ;
#189920 = CARTESIAN_POINT ( 'NONE',  ( 0.05219959533909260263, 19.03943276465977164, 94.99890960531436690 ) ) ;
#189921 = CARTESIAN_POINT ( 'NONE',  ( -16.53943276465976808, 0.05219959533911058130, 56.24890960531436690 ) ) ;
#189922 = CARTESIAN_POINT ( 'NONE',  ( 13.89961937509977652, -13.97604488694527269, 23.12390960531436335 ) ) ;
#189923 = CARTESIAN_POINT ( 'NONE',  ( -10.72451020669898014, 18.67979575497178502, 80.41557627198103830 ) ) ;
#189924 = CARTESIAN_POINT ( 'NONE',  ( 10.72451020669871369, 18.67979575497193778, 32.08442372801901854 ) ) ;
#189925 = DIRECTION ( 'NONE',  ( -0.000000000000000000, -0.000000000000000000, -1.000000000000000000 ) ) ;
#189926 = CARTESIAN_POINT ( 'NONE',  ( 8.314922557961029526, -14.29746914071037800, 35.41775706135234003 ) ) ;
#189927 = CARTESIAN_POINT ( 'NONE',  ( -0.05219959533907301413, -21.53943276465977519, 82.49890960531436690 ) ) ;
#189928 = CARTESIAN_POINT ( 'NONE',  ( 5.719274019375673035, 21.55341960407619339, 112.2927570613523471 ) ) ;
#189929 = CARTESIAN_POINT ( 'NONE',  ( 16.46253265017160672, -9.564922557960803928, 93.33224293864769550 ) ) ;
#189930 = CARTESIAN_POINT ( 'NONE',  ( 21.55341960407619695, -5.719274019375665929, 31.04275706135234714 ) ) ;
#189931 = CARTESIAN_POINT ( 'NONE',  ( -21.53943276465977519, 0.05219959533907696930, 31.24890960531435979 ) ) ;
#189932 = CARTESIAN_POINT ( 'NONE',  ( -14.34966873604972548, 8.224510206698743886, 108.3344237280190185 ) ) ;
#189934 = CARTESIAN_POINT ( 'NONE',  ( -10.72451020669870658, -18.67979575497194134, 79.58442372801903275 ) ) ;
#189933 = CARTESIAN_POINT ( 'NONE',  ( -21.55341960407619339, 5.719274019375674811, 48.54275706135234714 ) ) ;
#189935 = CARTESIAN_POINT ( 'NONE',  ( 0.05219959533937995610, -21.53943276465977519, 110.0010903946856757 ) ) ;
#189936 = CARTESIAN_POINT ( 'NONE',  ( -12.06949235617739369, -12.14591786802326823, 69.37609039468567573 ) ) ;
#189937 = CARTESIAN_POINT ( 'NONE',  ( -10.81492255796105439, 18.62759615963255655, 47.91775706135234714 ) ) ;
#189938 = CARTESIAN_POINT ( 'NONE',  ( 19.02544592524343514, -5.153800228976328945, 38.54057627198103120 ) ) ;
#189939 = CARTESIAN_POINT ( 'NONE',  ( -21.55341960407619339, 5.719274019375674811, 103.5427570613523613 ) ) ;
#189940 = CARTESIAN_POINT ( 'NONE',  ( -16.46253265017160317, 9.564922557960807481, 105.8322429386476955 ) ) ;
#189941 = CARTESIAN_POINT ( 'NONE',  ( 10.81492255796078972, 18.62759615963270932, 104.5822429386477097 ) ) ;
#189943 = CARTESIAN_POINT ( 'NONE',  ( 15.72974639402199770, -15.80617190586745480, 68.12390960531436690 ) ) ;
#189942 = DIRECTION ( 'NONE',  ( -1.000000000000000000, 0.000000000000000000, 0.000000000000000000 ) ) ;
#189945 = CARTESIAN_POINT ( 'NONE',  ( -4.379528057220328563, 16.55341960407611168, 50.20724293864769550 ) ) ;
#189944 = CARTESIAN_POINT ( 'NONE',  ( 12.14591786802327356, -12.06949235617739191, 45.62609039468567573 ) ) ;
#189946 = DIRECTION ( 'NONE',  ( -0.000000000000000000, -0.000000000000000000, 1.000000000000000000 ) ) ;
#189947 = CARTESIAN_POINT ( 'NONE',  ( 13.97604488694548053, -13.89961937509957401, 85.62609039468568994 ) ) ;
#189948 = CIRCLE ( 'NONE', #60759, 1.000000000000000888 ) ;
#189949 = CARTESIAN_POINT ( 'NONE',  ( 3.181980515339348337, -35.00000000000001421, 8.889087296526001936 ) ) ;
#189950 = CARTESIAN_POINT ( 'NONE',  ( -12.06949235617739369, -12.14591786802326823, 29.37609039468568284 ) ) ;
#189951 = CARTESIAN_POINT ( 'NONE',  ( 21.52544592524344225, -5.823673210054117533, 103.5405762719810383 ) ) ;
#189952 = CARTESIAN_POINT ( 'NONE',  ( -5.719274019375978568, 21.55341960407610458, 70.20724293864769550 ) ) ;
#189953 = CARTESIAN_POINT ( 'NONE',  ( 19.05341960407611168, 5.049401038298154454, 108.9572429386477097 ) ) ;
#189954 = CARTESIAN_POINT ( 'NONE',  ( -12.06949235617739369, -12.14591786802326823, 44.37609039468567573 ) ) ;
#189955 = CARTESIAN_POINT ( 'NONE',  ( 19.03943276465977164, -0.05219959533909143690, 63.74890960531435979 ) ) ;
#189957 = CARTESIAN_POINT ( 'NONE',  ( 16.51473224551083163, -9.474510206698727899, 95.83442372801900433 ) ) ;
#189956 = CARTESIAN_POINT ( 'NONE',  ( 10.81492255796106328, -18.62759615963255655, 30.41775706135234358 ) ) ;
#189958 = CARTESIAN_POINT ( 'NONE',  ( -16.51473224551069308, -9.474510206698971260, 106.6655762719810383 ) ) ;
#189959 = CARTESIAN_POINT ( 'NONE',  ( -9.564922557960796823, -16.46253265017161027, 82.08224293864768129 ) ) ;
#189960 = CARTESIAN_POINT ( 'NONE',  ( -21.55341960407610458, -5.719274019375992779, 91.45724293864769550 ) ) ;
#189961 = CARTESIAN_POINT ( 'NONE',  ( 16.51473224551069308, 9.474510206698969483, 54.16557627198103120 ) ) ;
#189962 = CARTESIAN_POINT ( 'NONE',  ( -16.19135201231369336, -7.376712067591814304, 60.18680854052035301 ) ) ;
#189963 = CARTESIAN_POINT ( 'NONE',  ( 8.224510206698953496, -14.34966873604960469, 72.91557627198103830 ) ) ;
#189964 = CARTESIAN_POINT ( 'NONE',  ( -13.89961937509977652, 13.97604488694528158, 115.6239096053143669 ) ) ;
#189965 = CARTESIAN_POINT ( 'NONE',  ( -3.573655867282028392E-15, 2.428612866367529932E-14, 155.0000000000000000 ) ) ;
#189966 = CARTESIAN_POINT ( 'NONE',  ( 21.55341960407610458, 5.719274019375980345, 88.95724293864769550 ) ) ;
#189967 = CARTESIAN_POINT ( 'NONE',  ( -9.474510206698720793, -16.51473224551083518, 69.58442372801901854 ) ) ;
#189968 = CARTESIAN_POINT ( 'NONE',  ( -21.52544592524343514, 5.823673210054127303, 26.04057627198103475 ) ) ;
#189969 = CARTESIAN_POINT ( 'NONE',  ( -3.573655867282028392E-15, -180.0000000000000000, -25.00000000000000000 ) ) ;
#189970 = CARTESIAN_POINT ( 'NONE',  ( 10.81492255796078972, 18.62759615963270932, 54.58224293864769550 ) ) ;
#189971 = CARTESIAN_POINT ( 'NONE',  ( -19.02544592524342804, 5.153800228976336051, 81.04057627198103830 ) ) ;
#189972 = CARTESIAN_POINT ( 'NONE',  ( 21.52544592524334988, 5.823673210054432836, 81.45942372801900433 ) ) ;
#189973 = CARTESIAN_POINT ( 'NONE',  ( -9.564922557960796823, -16.46253265017161027, 37.08224293864768839 ) ) ;
#189974 = CARTESIAN_POINT ( 'NONE',  ( 8.314922557960818139, 14.29746914071049879, 74.58224293864768129 ) ) ;
#189975 = CARTESIAN_POINT ( 'NONE',  ( 16.55341960407618274, -4.379528057220086978, 41.04275706135236135 ) ) ;
#189976 = CARTESIAN_POINT ( 'NONE',  ( -0.05219959533937732626, 21.53943276465977519, 72.50109039468568994 ) ) ;
#189977 = ORIENTED_EDGE ( 'NONE', *, *, #167871, .T. ) ;
#189978 = CARTESIAN_POINT ( 'NONE',  ( -9.474510206698720793, -16.51473224551083518, 29.58442372801900433 ) ) ;
#189979 = CARTESIAN_POINT ( 'NONE',  ( -13.89961937509957401, -13.97604488694547875, 84.37609039468567573 ) ) ;
#189980 = CARTESIAN_POINT ( 'NONE',  ( 9.100000000000001421, -3.435030038190235346E-14, -64.92279855667830191 ) ) ;
#189981 = B_SPLINE_CURVE_WITH_KNOTS ( 'NONE', 3,
 ( #122383, #168880, #30385, #156718, #96025, #189061, #154721, #110202, #112195, #18210, #111193, #31384, #186070, #171881, #139536, #172884, #142527, #3026, #93033, #33370, #109206, #77869, #34364, #140539, #158687, #157711, #187079, #79868, #128342, #1020, #65684, #95028 ),
 .UNSPECIFIED., .F., .F.,
 ( 4, 2, 2, 2, 2, 2, 2, 2, 2, 2, 2, 2, 2, 2, 2, 4 ),
 ( 2.195984522899319715E-17, 0.0003712461730037024989, 0.0007424923460073830968, 0.001113738519011063478, 0.001484984692014744076, 0.002227477038022111777, 0.002598723211025781316, 0.002969969384029451289, 0.003341215557033120395, 0.003712461730036789934, 0.004083707903040459039, 0.004454954076044128145, 0.004826200249047797250, 0.005197446422051466355, 0.005568692595055136328, 0.005939938768058804566 ),
 .UNSPECIFIED. ) ;
#189982 = CARTESIAN_POINT ( 'NONE',  ( -15.72974639402176322, -15.80617190586768395, 29.37609039468568284 ) ) ;
#189983 = CARTESIAN_POINT ( 'NONE',  ( -19.39056639909672342, -5.500000000000052403, 45.78948781074343088 ) ) ;
#189984 = CARTESIAN_POINT ( 'NONE',  ( 15.72974639402176855, 15.80617190586768217, 111.8760903946856615 ) ) ;
#189985 = CARTESIAN_POINT ( 'NONE',  ( 0.05219959533909260263, 19.03943276465977164, 59.99890960531436690 ) ) ;
#189986 = CARTESIAN_POINT ( 'NONE',  ( 5.153800228976615827, -19.02544592524334988, 30.20942372801900433 ) ) ;
#189987 = CARTESIAN_POINT ( 'NONE',  ( -12.14591786802326823, 12.06949235617739902, 103.1260903946856757 ) ) ;
#189989 = CARTESIAN_POINT ( 'NONE',  ( 18.67979575497194134, -10.72451020669871369, 75.83442372801900433 ) ) ;
#189988 = CARTESIAN_POINT ( 'NONE',  ( 19.03943276465977164, -0.05219959533909143690, 108.7489096053143527 ) ) ;
#189990 = CARTESIAN_POINT ( 'NONE',  ( -11.40812507854754720, -35.11059874428192273, -4.224999997268813701 ) ) ;
#189991 = CARTESIAN_POINT ( 'NONE',  ( -17.49999999999996092, -3.345213924137635964, 35.41231376905670203 ) ) ;
#189992 = CARTESIAN_POINT ( 'NONE',  ( 10.72451020669871369, 18.67979575497193778, 82.08442372801901854 ) ) ;
#189993 = CARTESIAN_POINT ( 'NONE',  ( -10.72451020669870658, -18.67979575497194134, 109.5844237280190328 ) ) ;
#189994 = DIRECTION ( 'NONE',  ( 1.000000000000000000, 0.000000000000000000, 0.000000000000000000 ) ) ;
#189995 = CARTESIAN_POINT ( 'NONE',  ( 19.02544592524343514, -5.153800228976328945, 103.5405762719809957 ) ) ;
#189996 = CARTESIAN_POINT ( 'NONE',  ( -16.51473224551082808, 9.474510206698731452, 23.33442372801900078 ) ) ;
#189997 = CARTESIAN_POINT ( 'NONE',  ( 28.61453998622355144, -24.72048905145110709, -21.14736193440035095 ) ) ;
#189998 = CARTESIAN_POINT ( 'NONE',  ( 19.05341960407611168, 5.049401038298154454, 43.95724293864769550 ) ) ;
#190000 = ADVANCED_FACE ( 'NONE', ( #104944 ), #158396, .T. ) ;
#189999 = CARTESIAN_POINT ( 'NONE',  ( 18.62759615963271287, -10.81492255796078972, 58.33224293864768839 ) ) ;
#190001 = CARTESIAN_POINT ( 'NONE',  ( -12.06949235617756955, 12.14591786802309770, 30.62390960531436335 ) ) ;
#190003 = CARTESIAN_POINT ( 'NONE',  ( 16.46253265017160672, -9.564922557960803928, 78.33224293864769550 ) ) ;
#190002 = CARTESIAN_POINT ( 'NONE',  ( -16.53943276465976808, 0.05219959533911058130, 91.24890960531436690 ) ) ;
#190004 = CARTESIAN_POINT ( 'NONE',  ( -18.62759615963255300, -10.81492255796106328, 104.1677570613523471 ) ) ;
#190005 = CARTESIAN_POINT ( 'NONE',  ( -5.049401038298153566, 19.05341960407611168, 30.20724293864768839 ) ) ;
#190006 = CARTESIAN_POINT ( 'NONE',  ( 0.05219959533910956823, 16.53943276465976808, 99.99890960531436690 ) ) ;
#190007 = CARTESIAN_POINT ( 'NONE',  ( 15.80617190586769283, -15.72974639402175789, 55.62609039468568284 ) ) ;
#190008 = CARTESIAN_POINT ( 'NONE',  ( -18.62759615963270932, 10.81492255796079327, 85.83224293864768129 ) ) ;
#190009 = CARTESIAN_POINT ( 'NONE',  ( -13.89961937509957401, -13.97604488694547875, 49.37609039468567573 ) ) ;
#190010 = CARTESIAN_POINT ( 'NONE',  ( -19.99604614807107694, -21.41307096498895390, -49.20022480689105038 ) ) ;
#190011 = CARTESIAN_POINT ( 'NONE',  ( 9.564922557960805705, 16.46253265017160317, 104.5822429386476955 ) ) ;
#190012 = CARTESIAN_POINT ( 'NONE',  ( -12.06949235617756955, 12.14591786802309770, 80.62390960531438111 ) ) ;
#190013 = EDGE_CURVE ( 'NONE', #60746, #179813, #129703, .T. ) ;
#190014 = CARTESIAN_POINT ( 'NONE',  ( -19.03943276465977164, -0.05219959533935918106, 38.75109039468566152 ) ) ;
#190015 = CARTESIAN_POINT ( 'NONE',  ( -5.153800228976328057, -19.02544592524343514, 62.29057627198100988 ) ) ;
#190016 = CARTESIAN_POINT ( 'NONE',  ( -16.55341960407611168, -4.379528057220339221, 61.45724293864770260 ) ) ;
#190017 = CARTESIAN_POINT ( 'NONE',  ( 16.46253265017146816, 9.564922557961045513, 81.66775706135233293 ) ) ;
#190018 = CARTESIAN_POINT ( 'NONE',  ( 7.500000000000001776, 1.104226503365437706, 6.811333284551975176 ) ) ;
#190019 = CARTESIAN_POINT ( 'NONE',  ( 21.53943276465977519, -0.05219959533907433946, 33.74890960531436690 ) ) ;
#190020 = ORIENTED_EDGE ( 'NONE', *, *, #127529, .T. ) ;
#190021 = CARTESIAN_POINT ( 'NONE',  ( 4.483927247898545687, 16.52544592524342804, 99.79057627198103830 ) ) ;
#190022 = FACE_BOUND ( 'NONE', #6226, .T. ) ;
#190024 = CARTESIAN_POINT ( 'NONE',  ( 18.67979575497178502, 10.72451020669898547, 64.16557627198102409 ) ) ;
#190023 = CARTESIAN_POINT ( 'NONE',  ( 19.02544592524343514, -5.153800228976328945, 63.54057627198103830 ) ) ;
#190025 = CARTESIAN_POINT ( 'NONE',  ( -5.153800228976328057, -19.02544592524343514, 32.29057627198102409 ) ) ;
#190027 = CARTESIAN_POINT ( 'NONE',  ( 0.05219959533909260263, 19.03943276465977164, 59.99890960531436690 ) ) ;
#190026 = CARTESIAN_POINT ( 'NONE',  ( 4.379528057220092307, 16.55341960407617563, 77.29275706135234714 ) ) ;
#190028 = CARTESIAN_POINT ( 'NONE',  ( -5.049401038297874678, -19.05341960407617918, 49.79275706135231871 ) ) ;
#190029 = CARTESIAN_POINT ( 'NONE',  ( -0.05219959533937732626, 21.53943276465977519, 62.50109039468568284 ) ) ;
#190030 = CARTESIAN_POINT ( 'NONE',  ( 18.62759615963271287, -10.81492255796078972, 53.33224293864769550 ) ) ;
#190031 = CARTESIAN_POINT ( 'NONE',  ( -16.46253265017160317, 9.564922557960807481, 25.83224293864769194 ) ) ;
#190032 = CARTESIAN_POINT ( 'NONE',  ( -12.06949235617739369, -12.14591786802326823, 89.37609039468568994 ) ) ;
#190033 = CARTESIAN_POINT ( 'NONE',  ( 16.51473224551083163, -9.474510206698727899, 100.8344237280190043 ) ) ;
#190034 = CARTESIAN_POINT ( 'NONE',  ( 5.153800228976335163, 19.02544592524342804, 24.79057627198102765 ) ) ;
#190035 = CARTESIAN_POINT ( 'NONE',  ( 18.56101223717332616, 5.499999999999945821, 78.94978406935679516 ) ) ;
#190036 = CARTESIAN_POINT ( 'NONE',  ( 21.53943276465977519, 0.05219959533937863772, 101.2510903946856757 ) ) ;
#190037 = CARTESIAN_POINT ( 'NONE',  ( 16.52544592524342804, -4.483927247898539470, 43.54057627198103830 ) ) ;
#190038 = CARTESIAN_POINT ( 'NONE',  ( 12.06949235617757843, -12.14591786802309237, 53.12390960531436690 ) ) ;
#190039 = CARTESIAN_POINT ( 'NONE',  ( -15.80617190586745835, -15.72974639402198527, 91.87390960531436690 ) ) ;
#190040 = CARTESIAN_POINT ( 'NONE',  ( 10.72451020669898902, -18.67979575497178502, 92.91557627198103830 ) ) ;
#190041 = CARTESIAN_POINT ( 'NONE',  ( -1.503321482105500984, -30.27664185797782537, -47.91583118997741764 ) ) ;
#190042 = CARTESIAN_POINT ( 'NONE',  ( -21.53943276465977519, 0.05219959533907696930, 36.24890960531435979 ) ) ;
#190043 = CARTESIAN_POINT ( 'NONE',  ( 14.34966873604972726, -8.224510206698740333, 65.83442372801900433 ) ) ;
#190044 = CARTESIAN_POINT ( 'NONE',  ( 0.05219959533910956823, 16.53943276465976808, 79.99890960531435269 ) ) ;
#190045 = CARTESIAN_POINT ( 'NONE',  ( -9.474510206698964154, 16.51473224551069663, 50.41557627198102409 ) ) ;
#190046 = DIRECTION ( 'NONE',  ( 0.9974398506828145994, -0.07151044867601324961, 1.161577285759629397E-15 ) ) ;
#190047 = CARTESIAN_POINT ( 'NONE',  ( -16.53943276465976808, -0.05219959533934237506, 93.75109039468567573 ) ) ;
#190048 = CARTESIAN_POINT ( 'NONE',  ( -18.62759615963255300, -10.81492255796106328, 19.16775706135234714 ) ) ;
#190049 = CARTESIAN_POINT ( 'NONE',  ( -9.564922557960796823, -16.46253265017161027, 87.08224293864769550 ) ) ;
#190050 = CARTESIAN_POINT ( 'NONE',  ( -21.55341960407619339, 5.719274019375674811, 48.54275706135234714 ) ) ;
#190051 = CARTESIAN_POINT ( 'NONE',  ( 16.46253265017160672, -9.564922557960803928, 103.3322429386476955 ) ) ;
#190052 = VERTEX_POINT ( 'NONE', #185768 ) ;
#190053 = CARTESIAN_POINT ( 'NONE',  ( 5.823673210054444382, -21.52544592524334988, 50.20942372801901854 ) ) ;
#190055 = CARTESIAN_POINT ( 'NONE',  ( 19.02544592524343514, -5.153800228976328945, 113.5405762719810241 ) ) ;
#190054 = CARTESIAN_POINT ( 'NONE',  ( -5.049401038298153566, 19.05341960407611168, 40.20724293864768839 ) ) ;
#190056 = CARTESIAN_POINT ( 'NONE',  ( -5.153800228976607833, 19.02544592524334988, 57.70942372801899012 ) ) ;
#190057 = CARTESIAN_POINT ( 'NONE',  ( 15.80617190586769283, -15.72974639402175789, 35.62609039468568994 ) ) ;
#190058 = CARTESIAN_POINT ( 'NONE',  ( 9.474510206698729675, 16.51473224551082808, 62.08442372801899722 ) ) ;
#190059 = CARTESIAN_POINT ( 'NONE',  ( 9.474510206698971260, -16.51473224551069308, 27.91557627198103120 ) ) ;
#190060 = CARTESIAN_POINT ( 'NONE',  ( 4.379528057220092307, 16.55341960407617563, 92.29275706135236135 ) ) ;
#190061 = CARTESIAN_POINT ( 'NONE',  ( -16.46253265017146816, -9.564922557961047289, 64.16775706135233293 ) ) ;
#190062 = CARTESIAN_POINT ( 'NONE',  ( 8.224510206698742110, 14.34966873604972548, 102.0844237280190185 ) ) ;
#190063 = DIRECTION ( 'NONE',  ( 0.000000000000000000, -1.000000000000000000, 0.000000000000000000 ) ) ;
#190064 = CARTESIAN_POINT ( 'NONE',  ( 5.049401038298161559, -19.05341960407611168, 82.70724293864770971 ) ) ;
#190065 = CARTESIAN_POINT ( 'NONE',  ( -21.53943276465977519, -0.05219959533937600094, 98.75109039468568994 ) ) ;
#190066 = CARTESIAN_POINT ( 'NONE',  ( -10.81492255796105439, 18.62759615963255655, 102.9177570613523756 ) ) ;
#190067 = DIRECTION ( 'NONE',  ( 5.204170427930421283E-16, 7.149051953565419487E-31, -1.000000000000000000 ) ) ;
#190068 = CARTESIAN_POINT ( 'NONE',  ( -9.474510206698964154, 16.51473224551069663, 95.41557627198102409 ) ) ;
#190069 = CARTESIAN_POINT ( 'NONE',  ( 21.52544592524334988, 5.823673210054432836, 71.45942372801901854 ) ) ;
#190070 = CARTESIAN_POINT ( 'NONE',  ( 14.34966873604972726, -8.224510206698740333, 20.83442372801901143 ) ) ;
#190071 = CARTESIAN_POINT ( 'NONE',  ( -19.02544592524342804, 5.153800228976336051, 81.04057627198103830 ) ) ;
#190072 = CARTESIAN_POINT ( 'NONE',  ( 0.05219959533907565091, 21.53943276465977519, 29.99890960531435979 ) ) ;
#190073 = CARTESIAN_POINT ( 'NONE',  ( 5.153800228976335163, 19.02544592524342804, 94.79057627198103830 ) ) ;
#190074 = DIRECTION ( 'NONE',  ( 0.000000000000000000, -0.7071067811865485719, 0.7071067811865465735 ) ) ;
#190075 = CARTESIAN_POINT ( 'NONE',  ( 5.153800228976335163, 19.02544592524342804, 69.79057627198103830 ) ) ;
#190076 = CARTESIAN_POINT ( 'NONE',  ( -8.314922557961024197, 14.29746914071037800, 112.9177570613523329 ) ) ;
#190077 = CARTESIAN_POINT ( 'NONE',  ( -17.49999999999999645, 5.499999999999992895, 98.71769037696435589 ) ) ;
#190078 = CARTESIAN_POINT ( 'NONE',  ( 19.03943276465977164, 0.05219959533936151252, 76.25109039468566152 ) ) ;
#190079 = CARTESIAN_POINT ( 'NONE',  ( 13.97604488694527802, 13.89961937509977652, 94.37390960531436690 ) ) ;
#190080 = CARTESIAN_POINT ( 'NONE',  ( 0.05219959533910956823, 16.53943276465976808, 89.99890960531438111 ) ) ;
#190081 = CARTESIAN_POINT ( 'NONE',  ( 5.719274019375991003, -21.55341960407610458, 52.70724293864769550 ) ) ;
#190082 = CARTESIAN_POINT ( 'NONE',  ( -15.72974639402197994, 15.80617190586746368, 40.62390960531435269 ) ) ;
#190083 = CARTESIAN_POINT ( 'NONE',  ( -4.483927247898539470, -16.52544592524342804, 107.2905762719810525 ) ) ;
#190084 = CARTESIAN_POINT ( 'NONE',  ( -16.79531203550650176, 7.028104445595466210, 53.74755011779559766 ) ) ;
#190085 = CARTESIAN_POINT ( 'NONE',  ( -19.02544592524334988, -5.153800228976617603, 43.95942372801899012 ) ) ;
#190087 = VECTOR ( 'NONE', #174389, 1000.000000000000000 ) ;
#190086 = CARTESIAN_POINT ( 'NONE',  ( -12.14591786802309592, -12.06949235617757132, 31.87390960531435979 ) ) ;
#190088 = CARTESIAN_POINT ( 'NONE',  ( 5.049401038298161559, -19.05341960407611168, 97.70724293864766707 ) ) ;
#190089 = CARTESIAN_POINT ( 'NONE',  ( -21.55341960407619339, 5.719274019375674811, 68.54275706135234714 ) ) ;
#190090 = CARTESIAN_POINT ( 'NONE',  ( -15.80617190586745835, -15.72974639402198527, 56.87390960531436690 ) ) ;
#190091 = CARTESIAN_POINT ( 'NONE',  ( -21.55341960407619339, 5.719274019375674811, 48.54275706135234714 ) ) ;
#190092 = CARTESIAN_POINT ( 'NONE',  ( 18.62759615963271287, -10.81492255796078972, 93.33224293864769550 ) ) ;
#190093 = CARTESIAN_POINT ( 'NONE',  ( 15.72974639402176855, 15.80617190586768217, 41.87609039468568284 ) ) ;
#190094 = CARTESIAN_POINT ( 'NONE',  ( 14.34966873604960469, 8.224510206698951720, 104.1655762719810241 ) ) ;
#190095 = CARTESIAN_POINT ( 'NONE',  ( -13.89961937509957401, -13.97604488694547875, 69.37609039468564731 ) ) ;
#190096 = CARTESIAN_POINT ( 'NONE',  ( 0.05219959533909260263, 19.03943276465977164, 59.99890960531436690 ) ) ;
#190097 = CARTESIAN_POINT ( 'NONE',  ( -14.34966873604960291, -8.224510206698953496, 106.6655762719810383 ) ) ;
#190098 = CARTESIAN_POINT ( 'NONE',  ( 5.153800228976335163, 19.02544592524342804, 114.7905762719810241 ) ) ;
#190099 = CARTESIAN_POINT ( 'NONE',  ( 12.14591786802309770, 12.06949235617756955, 54.37390960531435979 ) ) ;
#190100 = CARTESIAN_POINT ( 'NONE',  ( 14.29746914071037800, 8.314922557961029526, 111.6677570613523613 ) ) ;
#190101 = CARTESIAN_POINT ( 'NONE',  ( 5.153800228976335163, 19.02544592524342804, 54.79057627198103120 ) ) ;
#190102 = CARTESIAN_POINT ( 'NONE',  ( -5.153800228976328057, -19.02544592524343514, 27.29057627198103120 ) ) ;
#190103 = CARTESIAN_POINT ( 'NONE',  ( 5.049401038297881783, 19.05341960407617563, 22.29275706135233648 ) ) ;
#190105 = CARTESIAN_POINT ( 'NONE',  ( -4.483927247898539470, -16.52544592524342804, 32.29057627198102409 ) ) ;
#190104 = CARTESIAN_POINT ( 'NONE',  ( 17.60691670004650788, 5.500000000000058620, 51.63333313366440080 ) ) ;
#190106 = CARTESIAN_POINT ( 'NONE',  ( 21.53943276465977519, 0.05219959533937863772, 46.25109039468567573 ) ) ;
#190107 = CARTESIAN_POINT ( 'NONE',  ( 21.38418241377623019, -5.438282248597753110, 174.2683007571264113 ) ) ;
#190108 = CARTESIAN_POINT ( 'NONE',  ( -12.06949235617739369, -12.14591786802326823, 64.37609039468568994 ) ) ;
#190109 = CARTESIAN_POINT ( 'NONE',  ( 16.52544592524342804, -4.483927247898539470, 28.54057627198103120 ) ) ;
#190110 = CARTESIAN_POINT ( 'NONE',  ( -0.05219959533934338120, 16.53943276465976808, 102.5010903946856899 ) ) ;
#190111 = CARTESIAN_POINT ( 'NONE',  ( 19.03943276465977164, -0.05219959533909143690, 43.74890960531435979 ) ) ;
#190112 = CARTESIAN_POINT ( 'NONE',  ( 13.97604488694527802, 13.89961937509977652, 44.37390960531435269 ) ) ;
#190113 = CARTESIAN_POINT ( 'NONE',  ( -0.05219959533909027116, -19.03943276465977164, 22.49890960531436690 ) ) ;
#190114 = CARTESIAN_POINT ( 'NONE',  ( -5.719274019375665041, -21.55341960407619695, 29.79275706135234358 ) ) ;
#190115 = CARTESIAN_POINT ( 'NONE',  ( -16.51473224551069308, -9.474510206698971260, 46.66557627198102409 ) ) ;
#190116 = CYLINDRICAL_SURFACE ( 'NONE', #151814, 10.00000000000000000 ) ;
#190117 = CARTESIAN_POINT ( 'NONE',  ( 19.03943276465977164, -0.05219959533909143690, 38.74890960531436690 ) ) ;
#190118 = CARTESIAN_POINT ( 'NONE',  ( 18.67979575497178502, 10.72451020669898547, 29.16557627198103120 ) ) ;
#190120 = CARTESIAN_POINT ( 'NONE',  ( -16.53943276465976808, 0.05219959533911058130, 106.2489096053143811 ) ) ;
#190119 = CARTESIAN_POINT ( 'NONE',  ( -21.55341960407619339, 5.719274019375674811, 58.54275706135235424 ) ) ;
#190121 = CARTESIAN_POINT ( 'NONE',  ( -9.564922557960796823, -16.46253265017161027, 107.0822429386476955 ) ) ;
#190122 = CARTESIAN_POINT ( 'NONE',  ( 14.34966873604972726, -8.224510206698740333, 75.83442372801900433 ) ) ;
#190123 = ADVANCED_FACE ( 'NONE', ( #64404 ), #126073, .T. ) ;
#190124 = CARTESIAN_POINT ( 'NONE',  ( 15.72974639402176855, 15.80617190586768217, 91.87609039468568994 ) ) ;
#190125 = CARTESIAN_POINT ( 'NONE',  ( 12.14591786802327356, -12.06949235617739191, 50.62609039468568994 ) ) ;
#190126 = CARTESIAN_POINT ( 'NONE',  ( 16.51473224551069308, 9.474510206698969483, 99.16557627198102409 ) ) ;
#190127 = CARTESIAN_POINT ( 'NONE',  ( -12.06949235617739369, -12.14591786802326823, 44.37609039468567573 ) ) ;
#190128 = CARTESIAN_POINT ( 'NONE',  ( -4.483927247898782831, 16.52544592524335698, 32.70942372801900433 ) ) ;
#190129 = CARTESIAN_POINT ( 'NONE',  ( -4.379528057220086978, -16.55341960407618274, 79.79275706135236135 ) ) ;
#190130 = CARTESIAN_POINT ( 'NONE',  ( -9.564922557961040184, 16.46253265017147172, 107.9177570613523471 ) ) ;
#190131 = CARTESIAN_POINT ( 'NONE',  ( 19.02544592524343514, -5.153800228976328945, 78.54057627198099567 ) ) ;
#190132 = CARTESIAN_POINT ( 'NONE',  ( 21.53943276465977519, -0.05219959533907433946, 98.74890960531438111 ) ) ;
#190134 = CARTESIAN_POINT ( 'NONE',  ( -9.474510206698720793, -16.51473224551083518, 109.5844237280190043 ) ) ;
#190133 = CARTESIAN_POINT ( 'NONE',  ( -12.14591786802309592, -12.06949235617757132, 101.8739096053143811 ) ) ;
#190135 = CARTESIAN_POINT ( 'NONE',  ( -0.05219959533934338120, 16.53943276465976808, 72.50109039468568994 ) ) ;
#190136 = FACE_OUTER_BOUND ( 'NONE', #66383, .T. ) ;
#190137 = CARTESIAN_POINT ( 'NONE',  ( 19.02544592524334988, 5.153800228976608722, 66.45942372801899012 ) ) ;
#190138 = CARTESIAN_POINT ( 'NONE',  ( -4.379528057220328563, 16.55341960407611168, 50.20724293864769550 ) ) ;
#190139 = CARTESIAN_POINT ( 'NONE',  ( -4.483927247898539470, -16.52544592524342804, 87.29057627198103830 ) ) ;
#190140 = CARTESIAN_POINT ( 'NONE',  ( 19.03943276465977164, 0.05219959533936151252, 36.25109039468567573 ) ) ;
#190141 = CARTESIAN_POINT ( 'NONE',  ( -18.67979575497193778, 10.72451020669871902, 38.33442372801900433 ) ) ;
#190142 = CARTESIAN_POINT ( 'NONE',  ( -9.474510206698720793, -16.51473224551083518, 94.58442372801900433 ) ) ;
#190143 = DIRECTION ( 'NONE',  ( 1.000000000000000000, 0.000000000000000000, 0.000000000000000000 ) ) ;
#190144 = CARTESIAN_POINT ( 'NONE',  ( -5.153800228976328057, -19.02544592524343514, 92.29057627198099567 ) ) ;
#190145 = B_SPLINE_CURVE_WITH_KNOTS ( 'NONE', 3,
 ( #33221, #2872, #64550, #170733, #31230, #138399 ),
 .UNSPECIFIED., .F., .F.,
 ( 4, 2, 4 ),
 ( 0.000000000000000000, 0.0003837532665554268434, 0.0007675065331108536868 ),
 .UNSPECIFIED. ) ;
#190146 = CARTESIAN_POINT ( 'NONE',  ( 10.72451020669871369, 18.67979575497193778, 112.0844237280190185 ) ) ;
#190147 = CARTESIAN_POINT ( 'NONE',  ( -16.46253265017160317, 9.564922557960807481, 90.83224293864769550 ) ) ;
#190148 = CARTESIAN_POINT ( 'NONE',  ( -10.72451020669898014, 18.67979575497178502, 60.41557627198102409 ) ) ;
#190149 = CARTESIAN_POINT ( 'NONE',  ( -14.34966873604960291, -8.224510206698953496, 96.66557627198102409 ) ) ;
#190150 = CARTESIAN_POINT ( 'NONE',  ( -5.049401038298153566, 19.05341960407611168, 55.20724293864769550 ) ) ;
#190151 = CARTESIAN_POINT ( 'NONE',  ( -5.153800228976328057, -19.02544592524343514, 22.29057627198102765 ) ) ;
#190152 = CARTESIAN_POINT ( 'NONE',  ( -15.72974639402176322, -15.80617190586768395, 29.37609039468568284 ) ) ;
#190153 = CARTESIAN_POINT ( 'NONE',  ( -0.05219959533937732626, 21.53943276465977519, 72.50109039468568994 ) ) ;
#190154 = CARTESIAN_POINT ( 'NONE',  ( -16.51473224551069308, -9.474510206698971260, 41.66557627198103120 ) ) ;
#190155 = CARTESIAN_POINT ( 'NONE',  ( 14.29746914071037800, 8.314922557961029526, 71.66775706135234714 ) ) ;
#190156 = CARTESIAN_POINT ( 'NONE',  ( -5.719274019375665041, -21.55341960407619695, 34.79275706135235424 ) ) ;
#190157 = CARTESIAN_POINT ( 'NONE',  ( 5.719274019375673035, 21.55341960407619339, 32.29275706135235424 ) ) ;
#190159 = CARTESIAN_POINT ( 'NONE',  ( 13.97604488694527802, 13.89961937509977652, 64.37390960531436690 ) ) ;
#190158 = CARTESIAN_POINT ( 'NONE',  ( -13.89961937509957401, -13.97604488694547875, 54.37609039468565442 ) ) ;
#190160 = CARTESIAN_POINT ( 'NONE',  ( 19.03943276465977164, 0.05219959533936151252, 26.25109039468566507 ) ) ;
#190161 = CARTESIAN_POINT ( 'NONE',  ( -5.719274019375665041, -21.55341960407619695, 89.79275706135236135 ) ) ;
#190162 = CARTESIAN_POINT ( 'NONE',  ( 10.81492255796078972, 18.62759615963270932, 64.58224293864769550 ) ) ;
#190163 = CARTESIAN_POINT ( 'NONE',  ( -16.55341960407611168, -4.379528057220339221, 51.45724293864770260 ) ) ;
#190165 = CARTESIAN_POINT ( 'NONE',  ( -13.97604488694547697, 13.89961937509957934, 28.12609039468565797 ) ) ;
#190164 = CARTESIAN_POINT ( 'NONE',  ( 5.719274019375673035, 21.55341960407619339, 87.29275706135236135 ) ) ;
#190166 = CARTESIAN_POINT ( 'NONE',  ( -4.483927247898539470, -16.52544592524342804, 72.29057627198102409 ) ) ;
#190167 = CARTESIAN_POINT ( 'NONE',  ( -13.97604488694527625, -13.89961937509977652, 26.87390960531434558 ) ) ;
#190168 = CARTESIAN_POINT ( 'NONE',  ( -5.153800228976607833, 19.02544592524334988, 62.70942372801899722 ) ) ;
#190169 = CARTESIAN_POINT ( 'NONE',  ( 14.34966873604960469, 8.224510206698951720, 24.16557627198103120 ) ) ;
#190170 = CARTESIAN_POINT ( 'NONE',  ( -15.80617190586768217, 15.72974639402176855, 78.12609039468570415 ) ) ;
#190171 = CARTESIAN_POINT ( 'NONE',  ( -9.564922557960796823, -16.46253265017161027, 72.08224293864770971 ) ) ;
#190172 = CARTESIAN_POINT ( 'NONE',  ( 16.51473224551083163, -9.474510206698727899, 45.83442372801900433 ) ) ;
#190173 = CARTESIAN_POINT ( 'NONE',  ( -21.52544592524343514, 5.823673210054127303, 46.04057627198103830 ) ) ;
#190174 = CARTESIAN_POINT ( 'NONE',  ( 21.55341960407619695, -5.719274019375665929, 51.04275706135234714 ) ) ;
#190175 = CIRCLE ( 'NONE', #103009, 6.100000000000006750 ) ;
#190176 = CARTESIAN_POINT ( 'NONE',  ( -15.80617190586745835, -15.72974639402198527, 101.8739096053143811 ) ) ;
#190177 = CARTESIAN_POINT ( 'NONE',  ( -13.89961937509957401, -13.97604488694547875, 99.37609039468567573 ) ) ;
#190178 = CARTESIAN_POINT ( 'NONE',  ( 16.53943276465976808, 0.05219959533934440121, 61.25109039468567573 ) ) ;
#190180 = CARTESIAN_POINT ( 'NONE',  ( -10.81492255796078084, -18.62759615963271287, 112.0822429386477097 ) ) ;
#190179 = CARTESIAN_POINT ( 'NONE',  ( -18.22780087662119541, 5.500000000000102141, 56.01763182126894947 ) ) ;
#190181 = CARTESIAN_POINT ( 'NONE',  ( 16.53943276465976808, -0.05219959533910856209, 88.74890960531436690 ) ) ;
#190182 = CARTESIAN_POINT ( 'NONE',  ( -36.91746825000000598, 2.428612866367529932E-14, -11.12499999726881228 ) ) ;
#190183 = CARTESIAN_POINT ( 'NONE',  ( -16.55341960407617563, 4.379528057220093196, 38.54275706135234714 ) ) ;
#190184 = CARTESIAN_POINT ( 'NONE',  ( 15.72974639402199770, -15.80617190586745480, 63.12390960531435979 ) ) ;
#190185 = CARTESIAN_POINT ( 'NONE',  ( 4.379528057220092307, 16.55341960407617563, 97.29275706135234714 ) ) ;
#190186 = CARTESIAN_POINT ( 'NONE',  ( -0.05219959533909027116, -19.03943276465977164, 27.49890960531435624 ) ) ;
#190187 = CARTESIAN_POINT ( 'NONE',  ( 12.14591786802327356, -12.06949235617739191, 60.62609039468567573 ) ) ;
#190188 = CARTESIAN_POINT ( 'NONE',  ( 19.05341960407617918, -5.049401038297876454, 66.04275706135233293 ) ) ;
#190189 = CARTESIAN_POINT ( 'NONE',  ( -5.719274019375665041, -21.55341960407619695, 44.79275706135234714 ) ) ;
#190190 = CARTESIAN_POINT ( 'NONE',  ( -10.72451020669898014, 18.67979575497178502, 60.41557627198102409 ) ) ;
#190191 = CARTESIAN_POINT ( 'NONE',  ( -12.14591786802326823, 12.06949235617739902, 83.12609039468568994 ) ) ;
#190192 = CARTESIAN_POINT ( 'NONE',  ( -21.53943276465977519, -0.05219959533937600094, 68.75109039468568994 ) ) ;
#190193 = CARTESIAN_POINT ( 'NONE',  ( 21.55341960407610458, 5.719274019375980345, 53.95724293864770260 ) ) ;
#190194 = CARTESIAN_POINT ( 'NONE',  ( -15.80617190586745835, -15.72974639402198527, 36.87390960531435979 ) ) ;
#190195 = CARTESIAN_POINT ( 'NONE',  ( -14.29746914071037622, -8.314922557961029526, 64.16775706135234714 ) ) ;
#190196 = CARTESIAN_POINT ( 'NONE',  ( -18.62759615963270932, 10.81492255796079327, 30.83224293864770260 ) ) ;
#190197 = ORIENTED_EDGE ( 'NONE', *, *, #133545, .F. ) ;
#190198 = CARTESIAN_POINT ( 'NONE',  ( 16.51473224551069308, 9.474510206698969483, 99.16557627198102409 ) ) ;
#190199 = CARTESIAN_POINT ( 'NONE',  ( -8.224510206698948167, 14.34966873604960824, 25.41557627198103120 ) ) ;
#190200 = CARTESIAN_POINT ( 'NONE',  ( -25.66098555633789857, 7.783268508282411346, 170.2231668181882753 ) ) ;
#190201 = CARTESIAN_POINT ( 'NONE',  ( -4.483927247898539470, -16.52544592524342804, 102.2905762719810383 ) ) ;
#190202 = CARTESIAN_POINT ( 'NONE',  ( 15.72974639402199770, -15.80617190586745480, 63.12390960531435979 ) ) ;
#190203 = CARTESIAN_POINT ( 'NONE',  ( 4.379528057220092307, 16.55341960407617563, 92.29275706135236135 ) ) ;
#190204 = CARTESIAN_POINT ( 'NONE',  ( 18.67979575497194134, -10.72451020669871369, 35.83442372801901143 ) ) ;
#190205 = CARTESIAN_POINT ( 'NONE',  ( 0.05219959533936267826, -19.03943276465977164, 105.0010903946856615 ) ) ;
#190206 = CARTESIAN_POINT ( 'NONE',  ( -12.14591786802309592, -12.06949235617757132, 101.8739096053143811 ) ) ;
#190207 = CARTESIAN_POINT ( 'NONE',  ( -19.03943276465977164, 0.05219959533909376836, 51.24890960531436690 ) ) ;
#190208 = CARTESIAN_POINT ( 'NONE',  ( 5.049401038298161559, -19.05341960407611168, 22.70724293864769194 ) ) ;
#190209 = CARTESIAN_POINT ( 'NONE',  ( 15.01118352434402858, -1.500065973499219218, -62.04667436142315040 ) ) ;
#190210 = CARTESIAN_POINT ( 'NONE',  ( -9.564922557960796823, -16.46253265017161027, 87.08224293864769550 ) ) ;
#190211 = CARTESIAN_POINT ( 'NONE',  ( -4.483927247898782831, 16.52544592524335698, 72.70942372801901854 ) ) ;
#190212 = CARTESIAN_POINT ( 'NONE',  ( -10.72451020669870658, -18.67979575497194134, 109.5844237280190328 ) ) ;
#190213 = CARTESIAN_POINT ( 'NONE',  ( -18.62759615963270932, 10.81492255796079327, 45.83224293864769550 ) ) ;
#190214 = CARTESIAN_POINT ( 'NONE',  ( -8.224510206698735004, -14.34966873604973081, 74.58442372801901854 ) ) ;
#190215 = CARTESIAN_POINT ( 'NONE',  ( 9.474510206698729675, 16.51473224551082808, 82.08442372801899012 ) ) ;
#190216 = CARTESIAN_POINT ( 'NONE',  ( 13.89961937509977652, -13.97604488694527269, 33.12390960531434558 ) ) ;
#190217 = CARTESIAN_POINT ( 'NONE',  ( -13.89961937509977652, 13.97604488694528158, 75.62390960531438111 ) ) ;
#190218 = CARTESIAN_POINT ( 'NONE',  ( -0.05219959533909027116, -19.03943276465977164, 37.49890960531436690 ) ) ;
#190219 = CARTESIAN_POINT ( 'NONE',  ( 19.03943276465977164, 0.05219959533936151252, 71.25109039468566152 ) ) ;
#190220 = CARTESIAN_POINT ( 'NONE',  ( 21.75836449082841284, -9.620754668593853864, 170.8405250346328046 ) ) ;
#190221 = CARTESIAN_POINT ( 'NONE',  ( -16.51473224551069308, -9.474510206698971260, 101.6655762719810241 ) ) ;
#190222 = CARTESIAN_POINT ( 'NONE',  ( -4.483927247898539470, -16.52544592524342804, 47.29057627198103120 ) ) ;
#190223 = CARTESIAN_POINT ( 'NONE',  ( -18.62759615963270932, 10.81492255796079327, 40.83224293864769550 ) ) ;
#190224 = CARTESIAN_POINT ( 'NONE',  ( -17.50000000000014921, 3.292511757969716513, 105.0652027021053954 ) ) ;
#190225 =( BOUNDED_CURVE ( )  B_SPLINE_CURVE ( 3, ( #23632, #66130, #174324, #115639 ),
 .UNSPECIFIED., .F., .T. ) 
 B_SPLINE_CURVE_WITH_KNOTS ( ( 4, 4 ),
 ( 5.150538010968860547, 5.257537365396776075 ),
 .UNSPECIFIED. ) 
 CURVE ( )  GEOMETRIC_REPRESENTATION_ITEM ( )  RATIONAL_B_SPLINE_CURVE ( ( 1.000000000000000000, 0.9990461557208837329, 0.9990461557208837329, 1.000000000000000000 ) ) 
 REPRESENTATION_ITEM ( '' )  );
#190226 = CARTESIAN_POINT ( 'NONE',  ( 19.05341960407617918, -5.049401038297876454, 26.04275706135233293 ) ) ;
#190227 = SURFACE_STYLE_USAGE ( .BOTH. , #24390 ) ;
#190228 = CARTESIAN_POINT ( 'NONE',  ( -16.46253265017160317, 9.564922557960807481, 50.83224293864770260 ) ) ;
#190229 = CARTESIAN_POINT ( 'NONE',  ( -0.05219959533934338120, 16.53943276465976808, 37.50109039468568284 ) ) ;
#190230 = LINE ( 'NONE', #192231, #172483 ) ;
#190231 = CARTESIAN_POINT ( 'NONE',  ( -17.49999999999999645, 5.500000000000000888, 108.7176903769643559 ) ) ;
#190232 = CARTESIAN_POINT ( 'NONE',  ( 4.379528057220092307, 16.55341960407617563, 77.29275706135234714 ) ) ;
#190234 = EDGE_CURVE ( 'NONE', #40506, #166185, #172582, .T. ) ;
#190233 = CARTESIAN_POINT ( 'NONE',  ( -21.53943276465977519, 0.05219959533907696930, 101.2489096053143669 ) ) ;
#190235 = CARTESIAN_POINT ( 'NONE',  ( -16.55341960407617563, 4.379528057220093196, 43.54275706135235424 ) ) ;
#190237 = DIRECTION ( 'NONE',  ( 1.000000000000000000, 0.000000000000000000, 0.000000000000000000 ) ) ;
#190236 = CARTESIAN_POINT ( 'NONE',  ( -0.05219959533909027116, -19.03943276465977164, 47.49890960531435979 ) ) ;
#190238 = CARTESIAN_POINT ( 'NONE',  ( -21.55341960407619339, 5.719274019375674811, 43.54275706135235424 ) ) ;
#190239 = CARTESIAN_POINT ( 'NONE',  ( 16.46253265017146816, 9.564922557961045513, 56.66775706135233293 ) ) ;
#190240 = CARTESIAN_POINT ( 'NONE',  ( 10.72451020669871369, 18.67979575497193778, 97.08442372801904696 ) ) ;
#190241 = CARTESIAN_POINT ( 'NONE',  ( -17.97182807773869584, 5.499999999999855227, 48.53038844047289757 ) ) ;
#190242 = CARTESIAN_POINT ( 'NONE',  ( -4.483927247898539470, -16.52544592524342804, 47.29057627198103120 ) ) ;
#190243 = CARTESIAN_POINT ( 'NONE',  ( 19.25176906914648711, 5.499999999999731770, 43.49927264242279534 ) ) ;
#190244 = CARTESIAN_POINT ( 'NONE',  ( -5.823673210054116645, -21.52544592524344225, 52.29057627198102409 ) ) ;
#190245 = CARTESIAN_POINT ( 'NONE',  ( 17.14385361876520264, 23.59649016807275856, 144.1750000027311671 ) ) ;
#190246 = CARTESIAN_POINT ( 'NONE',  ( -0.05219959533909027116, -19.03943276465977164, 97.49890960531436690 ) ) ;
#190247 = CARTESIAN_POINT ( 'NONE',  ( -8.314922557960811034, -14.29746914071050412, 107.0822429386476955 ) ) ;
#190248 = CARTESIAN_POINT ( 'NONE',  ( -19.05341960407617563, 5.049401038297882671, 113.5427570613523471 ) ) ;
#190249 = CARTESIAN_POINT ( 'NONE',  ( -14.34966873604960291, -8.224510206698953496, 21.66557627198102409 ) ) ;
#190250 = ORIENTED_EDGE ( 'NONE', *, *, #121940, .T. ) ;
#190252 = CARTESIAN_POINT ( 'NONE',  ( 21.52544592524344225, -5.823673210054117533, 108.5405762719810241 ) ) ;
#190251 = CARTESIAN_POINT ( 'NONE',  ( -13.97604488694527625, -13.89961937509977652, 96.87390960531433848 ) ) ;
#190254 = CARTESIAN_POINT ( 'NONE',  ( 19.03943276465977164, -0.05219959533909143690, 113.7489096053143669 ) ) ;
#190253 = CARTESIAN_POINT ( 'NONE',  ( -12.14591786802309592, -12.06949235617757132, 26.87390960531435979 ) ) ;
#190255 = CARTESIAN_POINT ( 'NONE',  ( -5.049401038297874678, -19.05341960407617918, 99.79275706135234714 ) ) ;
#190256 = CARTESIAN_POINT ( 'NONE',  ( 21.53943276465977519, 0.05219959533937863772, 106.2510903946856757 ) ) ;
#190257 = CARTESIAN_POINT ( 'NONE',  ( 16.52544592524342804, -4.483927247898539470, 33.54057627198102409 ) ) ;
#190258 = CARTESIAN_POINT ( 'NONE',  ( -21.52544592524343514, 5.823673210054127303, 86.04057627198102409 ) ) ;
#190259 = CARTESIAN_POINT ( 'NONE',  ( -5.823673210054116645, -21.52544592524344225, 47.29057627198103120 ) ) ;
#190260 = CARTESIAN_POINT ( 'NONE',  ( -16.46253265017160317, 9.564922557960807481, 60.83224293864769550 ) ) ;
#190261 = CARTESIAN_POINT ( 'NONE',  ( 12.06949235617757843, -12.14591786802309237, 28.12390960531435979 ) ) ;
#190262 = CARTESIAN_POINT ( 'NONE',  ( -5.049401038298153566, 19.05341960407611168, 80.20724293864769550 ) ) ;
#190263 = ORIENTED_EDGE ( 'NONE', *, *, #37032, .F. ) ;
#190264 = CARTESIAN_POINT ( 'NONE',  ( 19.39056639909671986, 5.500000000000041744, 58.28948781074345220 ) ) ;
#190265 = CARTESIAN_POINT ( 'NONE',  ( -16.51473224551082808, 9.474510206698731452, 38.33442372801899722 ) ) ;
#190266 = CARTESIAN_POINT ( 'NONE',  ( 0.05219959533907565091, 21.53943276465977519, 79.99890960531435269 ) ) ;
#190267 = CARTESIAN_POINT ( 'NONE',  ( -4.483927247898539470, -16.52544592524342804, 82.29057627198103830 ) ) ;
#190268 = CARTESIAN_POINT ( 'NONE',  ( 18.62759615963255655, 10.81492255796105972, 36.66775706135234714 ) ) ;
#190269 = CARTESIAN_POINT ( 'NONE',  ( 17.14385361876520264, 23.59649016807275856, 142.1750000027311671 ) ) ;
#190270 = CARTESIAN_POINT ( 'NONE',  ( 16.53943276465976808, 0.05219959533934440121, 101.2510903946856757 ) ) ;
#190271 = CARTESIAN_POINT ( 'NONE',  ( 19.02544592524343514, -5.153800228976328945, 28.54057627198102409 ) ) ;
#190272 = CARTESIAN_POINT ( 'NONE',  ( -5.049401038298153566, 19.05341960407611168, 80.20724293864769550 ) ) ;
#190273 =( LENGTH_UNIT ( ) NAMED_UNIT ( * ) SI_UNIT ( .MILLI., .METRE. ) );
#190274 = CARTESIAN_POINT ( 'NONE',  ( -11.74264578624800670, 36.14014761921585972, -10.14999999453762669 ) ) ;
#190275 = CARTESIAN_POINT ( 'NONE',  ( 8.224510206698953496, -14.34966873604960469, 42.91557627198103120 ) ) ;
#190276 = CARTESIAN_POINT ( 'NONE',  ( -18.62759615963255300, -10.81492255796106328, 64.16775706135234714 ) ) ;
#190277 = CARTESIAN_POINT ( 'NONE',  ( 33.23029939923979725, -20.96646023091231470, -17.75854212242024843 ) ) ;
#190278 = CARTESIAN_POINT ( 'NONE',  ( 19.03943276465977164, -0.05219959533909143690, 38.74890960531436690 ) ) ;
#190279 = CARTESIAN_POINT ( 'NONE',  ( 16.51473224551069308, 9.474510206698969483, 49.16557627198102409 ) ) ;
#190280 = ORIENTED_EDGE ( 'NONE', *, *, #18014, .T. ) ;
#190281 = CARTESIAN_POINT ( 'NONE',  ( -21.53943276465977519, -0.05219959533937600094, 103.7510903946857042 ) ) ;
#190282 = CARTESIAN_POINT ( 'NONE',  ( 16.55341960407618274, -4.379528057220086978, 61.04275706135234714 ) ) ;
#190283 = CARTESIAN_POINT ( 'NONE',  ( -5.719274019375665041, -21.55341960407619695, 84.79275706135234714 ) ) ;
#190284 = CARTESIAN_POINT ( 'NONE',  ( -19.05341960407611168, -5.049401038298163336, 111.4572429386476671 ) ) ;
#190285 = CARTESIAN_POINT ( 'NONE',  ( 0.05219959533936267826, -19.03943276465977164, 90.00109039468567573 ) ) ;
#190286 = CARTESIAN_POINT ( 'NONE',  ( 10.81492255796106328, -18.62759615963255655, 65.41775706135234714 ) ) ;
#190287 = CARTESIAN_POINT ( 'NONE',  ( 16.55341960407618274, -4.379528057220086978, 31.04275706135234714 ) ) ;
#190288 = CARTESIAN_POINT ( 'NONE',  ( -15.80617190586745835, -15.72974639402198527, 81.87390960531435269 ) ) ;
#190289 = CARTESIAN_POINT ( 'NONE',  ( 19.02544592524334988, 5.153800228976608722, 96.45942372801897591 ) ) ;
#190290 = CARTESIAN_POINT ( 'NONE',  ( 19.05341960407611168, 5.049401038298154454, 68.95724293864769550 ) ) ;
#190291 = CARTESIAN_POINT ( 'NONE',  ( -0.05219959533936034679, 19.03943276465977164, 107.5010903946856615 ) ) ;
#190292 = CARTESIAN_POINT ( 'NONE',  ( -19.02544592524334988, -5.153800228976617603, 98.95942372801900433 ) ) ;
#190293 = CARTESIAN_POINT ( 'NONE',  ( 8.314922557960818139, 14.29746914071049879, 59.58224293864770260 ) ) ;
#190294 = CARTESIAN_POINT ( 'NONE',  ( 19.03943276465977164, 0.05219959533936151252, 76.25109039468566152 ) ) ;
#190295 = CARTESIAN_POINT ( 'NONE',  ( -14.29746914071037622, -8.314922557961029526, 79.16775706135234714 ) ) ;
#190297 = CARTESIAN_POINT ( 'NONE',  ( 16.51473224551069308, 9.474510206698969483, 44.16557627198103120 ) ) ;
#190296 = CARTESIAN_POINT ( 'NONE',  ( 5.719274019375673035, 21.55341960407619339, 22.29275706135235069 ) ) ;
#190298 = CARTESIAN_POINT ( 'NONE',  ( -19.03943276465977164, 0.05219959533909376836, 51.24890960531436690 ) ) ;
#190299 = CARTESIAN_POINT ( 'NONE',  ( 12.06949235617739724, 12.14591786802326823, 76.87609039468567573 ) ) ;
#190300 = CARTESIAN_POINT ( 'NONE',  ( -17.72517630441458181, 5.499999999999974243, 45.92175719257601685 ) ) ;
#190301 = CARTESIAN_POINT ( 'NONE',  ( 28.82186960331498327, 9.364793116373570925, 143.3500000054623342 ) ) ;
#190302 = CARTESIAN_POINT ( 'NONE',  ( -13.89961937509977652, 13.97604488694528158, 100.6239096053143669 ) ) ;
#190303 = CARTESIAN_POINT ( 'NONE',  ( -13.97604488694527625, -13.89961937509977652, 21.87390960531435979 ) ) ;
#190304 = ORIENTED_EDGE ( 'NONE', *, *, #59958, .T. ) ;
#190305 = CARTESIAN_POINT ( 'NONE',  ( -14.29746914071037622, -8.314922557961029526, 19.16775706135234714 ) ) ;
#190307 = CARTESIAN_POINT ( 'NONE',  ( -21.55341960407610458, -5.719274019375992779, 56.45724293864768839 ) ) ;
#190306 = CIRCLE ( 'NONE', #128952, 1.899999999999999689 ) ;
#190309 = CARTESIAN_POINT ( 'NONE',  ( 12.14591786802327356, -12.06949235617739191, 30.62609039468567929 ) ) ;
#190308 = CARTESIAN_POINT ( 'NONE',  ( -19.03943276465977164, -0.05219959533935918106, 48.75109039468566863 ) ) ;
#190310 = CARTESIAN_POINT ( 'NONE',  ( 13.97604488694527802, 13.89961937509977652, 34.37390960531436690 ) ) ;
#190311 = CARTESIAN_POINT ( 'NONE',  ( -19.05341960407611168, -5.049401038298163336, 56.45724293864768129 ) ) ;
#190312 = CARTESIAN_POINT ( 'NONE',  ( 21.55341960407610458, 5.719274019375980345, 88.95724293864769550 ) ) ;
#190313 = CARTESIAN_POINT ( 'NONE',  ( -0.05219959533909027116, -19.03943276465977164, 107.4989096053143527 ) ) ;
#190314 = CARTESIAN_POINT ( 'NONE',  ( 9.474510206698971260, -16.51473224551069308, 52.91557627198102409 ) ) ;
#190315 = CARTESIAN_POINT ( 'NONE',  ( 27.73933785331498925, -9.013057229001034898, 148.2750000027311614 ) ) ;
#190316 = CARTESIAN_POINT ( 'NONE',  ( 19.05341960407617918, -5.049401038297876454, 91.04275706135234714 ) ) ;
#190317 = CARTESIAN_POINT ( 'NONE',  ( 16.55341960407611168, 4.379528057220329451, 68.95724293864769550 ) ) ;
#190318 = CARTESIAN_POINT ( 'NONE',  ( 21.53943276465977519, 0.05219959533937863772, 106.2510903946856757 ) ) ;
#190319 = CARTESIAN_POINT ( 'NONE',  ( 21.52544592524344225, -5.823673210054117533, 103.5405762719810383 ) ) ;
#190320 = CARTESIAN_POINT ( 'NONE',  ( -5.719274019375665041, -21.55341960407619695, 84.79275706135234714 ) ) ;
#190321 = CARTESIAN_POINT ( 'NONE',  ( 9.474510206698971260, -16.51473224551069308, 22.91557627198102765 ) ) ;
#190322 = CARTESIAN_POINT ( 'NONE',  ( -15.80617190586768217, 15.72974639402176855, 78.12609039468570415 ) ) ;
#190323 = CARTESIAN_POINT ( 'NONE',  ( 0.05219959533909260263, 19.03943276465977164, 109.9989096053143669 ) ) ;
#190325 = CARTESIAN_POINT ( 'NONE',  ( -10.81492255796105439, 18.62759615963255655, 72.91775706135234714 ) ) ;
#190324 = CARTESIAN_POINT ( 'NONE',  ( 8.224510206698953496, -14.34966873604960469, 32.91557627198102409 ) ) ;
#190326 = CARTESIAN_POINT ( 'NONE',  ( 19.05341960407611168, 5.049401038298154454, 63.95724293864769550 ) ) ;
#190327 = CARTESIAN_POINT ( 'NONE',  ( 18.67979575497194134, -10.72451020669871369, 40.83442372801901854 ) ) ;
#190328 = CARTESIAN_POINT ( 'NONE',  ( 9.474510206698971260, -16.51473224551069308, 77.91557627198103830 ) ) ;
#190329 = CARTESIAN_POINT ( 'NONE',  ( -4.483927247898539470, -16.52544592524342804, 92.29057627198103830 ) ) ;
#190330 = CARTESIAN_POINT ( 'NONE',  ( 16.52544592524342804, -4.483927247898539470, 63.54057627198103830 ) ) ;
#190331 = CARTESIAN_POINT ( 'NONE',  ( -10.72451020669898014, 18.67979575497178502, 65.41557627198102409 ) ) ;
#190332 = CARTESIAN_POINT ( 'NONE',  ( 13.89961937509977652, -13.97604488694527269, 63.12390960531435979 ) ) ;
#190333 = CARTESIAN_POINT ( 'NONE',  ( 21.52544592524344225, -5.823673210054117533, 68.54057627198103830 ) ) ;
#190334 = CARTESIAN_POINT ( 'NONE',  ( 5.153800228976615827, -19.02544592524334988, 60.20942372801899012 ) ) ;
#190336 = CARTESIAN_POINT ( 'NONE',  ( -8.224510206698948167, 14.34966873604960824, 80.41557627198103830 ) ) ;
#190335 = CARTESIAN_POINT ( 'NONE',  ( 19.02544592524335343, 5.153800228976608722, 31.45942372801900788 ) ) ;
#190338 = AXIS2_PLACEMENT_3D ( 'NONE', #158826, #123507, #5138 ) ;
#190337 = CARTESIAN_POINT ( 'NONE',  ( -10.72451020669898014, 18.67979575497178502, 55.41557627198102409 ) ) ;
#190339 = CARTESIAN_POINT ( 'NONE',  ( 17.31728774477274158, 6.344390552232390235, 101.6809334831068270 ) ) ;
#190341 = CARTESIAN_POINT ( 'NONE',  ( -5.359611314223446995E-15, 29.16686587814335851, 146.8750000027311557 ) ) ;
#190340 = CARTESIAN_POINT ( 'NONE',  ( -16.55341960407617563, 4.379528057220093196, 98.54275706135234714 ) ) ;
#190342 = CARTESIAN_POINT ( 'NONE',  ( -13.97604488694547697, 13.89961937509957934, 103.1260903946856473 ) ) ;
#190343 = CARTESIAN_POINT ( 'NONE',  ( -4.483927247898539470, -16.52544592524342804, 72.29057627198102409 ) ) ;
#190344 = CARTESIAN_POINT ( 'NONE',  ( -30.00000000000000000, -5.499999999999992895, 37.50000000000000000 ) ) ;
#190345 = CARTESIAN_POINT ( 'NONE',  ( -13.89961937509977652, 13.97604488694528158, 55.62390960531434558 ) ) ;
#190346 = CARTESIAN_POINT ( 'NONE',  ( -12.14591786802309592, -12.06949235617757132, 51.87390960531437401 ) ) ;
#190347 = CARTESIAN_POINT ( 'NONE',  ( -5.153800228976328057, -19.02544592524343514, 107.2905762719810383 ) ) ;
#190349 = CARTESIAN_POINT ( 'NONE',  ( 0.05219959533909260263, 19.03943276465977164, 69.99890960531435269 ) ) ;
#190348 = CARTESIAN_POINT ( 'NONE',  ( 9.474510206698729675, 16.51473224551082808, 72.08442372801900433 ) ) ;
#190350 = CARTESIAN_POINT ( 'NONE',  ( -5.049401038298153566, 19.05341960407611168, 85.20724293864766707 ) ) ;
#190351 = CARTESIAN_POINT ( 'NONE',  ( 16.46253265017160672, -9.564922557960803928, 68.33224293864770971 ) ) ;
#190352 = CARTESIAN_POINT ( 'NONE',  ( 5.823673210054125526, 21.52544592524343514, 64.79057627198103830 ) ) ;
#190353 = CARTESIAN_POINT ( 'NONE',  ( -14.29746914071037622, -8.314922557961029526, 64.16775706135234714 ) ) ;
#190354 = CARTESIAN_POINT ( 'NONE',  ( -6.856101608890801443E-16, -64.86648100006283357, -22.99999901186701123 ) ) ;
#190355 = CARTESIAN_POINT ( 'NONE',  ( 5.153800228976335163, 19.02544592524342804, 49.79057627198100988 ) ) ;
#190356 = CARTESIAN_POINT ( 'NONE',  ( 21.52544592524344225, -5.823673210054117533, 48.54057627198103120 ) ) ;
#190357 = CARTESIAN_POINT ( 'NONE',  ( 13.89961937509957401, 13.97604488694547697, 76.87609039468566152 ) ) ;
#190359 = CARTESIAN_POINT ( 'NONE',  ( -21.52544592524334988, -5.823673210054445271, 38.95942372801901854 ) ) ;
#190358 = CARTESIAN_POINT ( 'NONE',  ( -16.53943276465976808, 0.05219959533911058130, 21.24890960531436690 ) ) ;
#190360 = EDGE_CURVE ( 'NONE', #41053, #165860, #139960, .T. ) ;
#190361 = CARTESIAN_POINT ( 'NONE',  ( -5.153800228976607833, 19.02544592524334988, 37.70942372801899722 ) ) ;
#190363 = CARTESIAN_POINT ( 'NONE',  ( -8.224510206698735004, -14.34966873604973081, 89.58442372801901854 ) ) ;
#190362 = CARTESIAN_POINT ( 'NONE',  ( 16.53943276465976808, 0.05219959533934440121, 56.25109039468568284 ) ) ;
#190364 = CARTESIAN_POINT ( 'NONE',  ( 27.88129983271663903, -6.733757357602863536, 162.1517353552116560 ) ) ;
#190365 = CARTESIAN_POINT ( 'NONE',  ( -4.379528057220086978, -16.55341960407618274, 84.79275706135234714 ) ) ;
#190367 = CARTESIAN_POINT ( 'NONE',  ( -16.52544592524335698, -4.483927247898792601, 38.95942372801901854 ) ) ;
#190366 = CARTESIAN_POINT ( 'NONE',  ( 21.52544592524344225, -5.823673210054117533, 28.54057627198103120 ) ) ;
#190368 = EDGE_CURVE ( 'NONE', #67444, #167085, #96708, .T. ) ;
#190369 = CARTESIAN_POINT ( 'NONE',  ( -19.03943276465977164, 0.05219959533909376836, 46.24890960531435979 ) ) ;
#190370 = CARTESIAN_POINT ( 'NONE',  ( 16.51473224551069308, 9.474510206698969483, 49.16557627198102409 ) ) ;
#190371 = CARTESIAN_POINT ( 'NONE',  ( -19.05341960407611168, -5.049401038298163336, 66.45724293864769550 ) ) ;
#190372 = CARTESIAN_POINT ( 'NONE',  ( -0.05219959533937732626, 21.53943276465977519, 37.50109039468568284 ) ) ;
#190373 = CARTESIAN_POINT ( 'NONE',  ( -8.314922557961024197, 14.29746914071037800, 52.91775706135235424 ) ) ;
#190374 = CARTESIAN_POINT ( 'NONE',  ( -16.53943276465976808, 0.05219959533911058130, 26.24890960531435624 ) ) ;
#190375 = CARTESIAN_POINT ( 'NONE',  ( 5.153800228976335163, 19.02544592524342804, 34.79057627198102409 ) ) ;
#190376 = CARTESIAN_POINT ( 'NONE',  ( 18.62759615963255655, 10.81492255796105972, 111.6677570613523613 ) ) ;
#190377 = CARTESIAN_POINT ( 'NONE',  ( -16.51473224551082808, 9.474510206698731452, 113.3344237280190043 ) ) ;
#190378 = CARTESIAN_POINT ( 'NONE',  ( 19.03943276465977164, 0.05219959533936151252, 71.25109039468566152 ) ) ;
#190379 = CARTESIAN_POINT ( 'NONE',  ( -12.14591786802309592, -12.06949235617757132, 76.87390960531439532 ) ) ;
#190380 = CARTESIAN_POINT ( 'NONE',  ( 13.97604488694527802, 13.89961937509977652, 39.37390960531435269 ) ) ;
#190382 = CARTESIAN_POINT ( 'NONE',  ( 17.40805194822030799, 6.112264579159357503, 76.66628727489388950 ) ) ;
#190381 = CARTESIAN_POINT ( 'NONE',  ( -13.89961937509957401, -13.97604488694547875, 79.37609039468567573 ) ) ;
#190383 = CARTESIAN_POINT ( 'NONE',  ( -21.55341960407619339, 5.719274019375674811, 78.54275706135236135 ) ) ;
#190384 = CARTESIAN_POINT ( 'NONE',  ( 12.06949235617739724, 12.14591786802326823, 41.87609039468568284 ) ) ;
#190385 = FACE_OUTER_BOUND ( 'NONE', #36490, .T. ) ;
#190386 = CARTESIAN_POINT ( 'NONE',  ( 5.823673210054125526, 21.52544592524343514, 29.79057627198102409 ) ) ;
#190387 = CARTESIAN_POINT ( 'NONE',  ( -16.53943276465976808, -0.05219959533934237506, 23.75109039468567929 ) ) ;
#190388 = CARTESIAN_POINT ( 'NONE',  ( -19.02544592524342804, 5.153800228976336939, 31.04057627198102054 ) ) ;
#190389 = CARTESIAN_POINT ( 'NONE',  ( -19.02544592524334988, -5.153800228976617603, 33.95942372801897591 ) ) ;
#190390 = CARTESIAN_POINT ( 'NONE',  ( -29.40414617605185654, -24.07794639774997236, -17.69092940303636396 ) ) ;
#190391 = CARTESIAN_POINT ( 'NONE',  ( -16.46253265017160317, 9.564922557960807481, 40.83224293864769550 ) ) ;
#190392 = CARTESIAN_POINT ( 'NONE',  ( -20.06002596795686443, -21.05152699199194899, -52.46707657590843610 ) ) ;
#190393 = CARTESIAN_POINT ( 'NONE',  ( -19.03943276465977164, 0.05219959533909376836, 61.24890960531436690 ) ) ;
#190394 = CARTESIAN_POINT ( 'NONE',  ( 17.50000000000014566, -3.417042746626890892, 112.6738039623247545 ) ) ;
#190395 = CARTESIAN_POINT ( 'NONE',  ( 13.97604488694548053, -13.89961937509957401, 20.62609039468567573 ) ) ;
#190396 = CARTESIAN_POINT ( 'NONE',  ( -0.05219959533934338120, 16.53943276465976808, 112.5010903946857042 ) ) ;
#190397 = CARTESIAN_POINT ( 'NONE',  ( -9.564922557960796823, -16.46253265017161027, 32.08224293864769550 ) ) ;
#190398 = CARTESIAN_POINT ( 'NONE',  ( -13.97604488694527625, -13.89961937509977652, 91.87390960531432427 ) ) ;
#190399 = CARTESIAN_POINT ( 'NONE',  ( 5.823673210054444382, -21.52544592524334988, 65.20942372801901854 ) ) ;
#190400 = CARTESIAN_POINT ( 'NONE',  ( -0.05219959533909027116, -19.03943276465977164, 32.49890960531435979 ) ) ;
#190401 = CARTESIAN_POINT ( 'NONE',  ( 0.05219959533937995610, -21.53943276465977519, 65.00109039468568994 ) ) ;
#190403 = CARTESIAN_POINT ( 'NONE',  ( -13.89961937509977652, 13.97604488694528158, 115.6239096053143669 ) ) ;
#190402 = CARTESIAN_POINT ( 'NONE',  ( -19.05341960407617563, 5.049401038297882671, 98.54275706135233293 ) ) ;
#190404 = CARTESIAN_POINT ( 'NONE',  ( 0.05219959533909260263, 19.03943276465977164, 39.99890960531436690 ) ) ;
#190405 = CARTESIAN_POINT ( 'NONE',  ( 5.823673210054125526, 21.52544592524343514, 104.7905762719810241 ) ) ;
#190406 = CARTESIAN_POINT ( 'NONE',  ( -16.51473224551082808, 9.474510206698731452, 38.33442372801899722 ) ) ;
#190407 = CARTESIAN_POINT ( 'NONE',  ( 8.314922557960818139, 14.29746914071049879, 109.5822429386476955 ) ) ;
#190408 = CARTESIAN_POINT ( 'NONE',  ( 13.97604488694527802, 13.89961937509977652, 69.37390960531436690 ) ) ;
#190409 = CARTESIAN_POINT ( 'NONE',  ( -19.02544592524334988, -5.153800228976617603, 98.95942372801900433 ) ) ;
#190410 = CARTESIAN_POINT ( 'NONE',  ( -0.05219959533910754901, -16.53943276465976808, 72.49890960531435269 ) ) ;
#190411 = CARTESIAN_POINT ( 'NONE',  ( 13.89961937509977652, -13.97604488694527269, 113.1239096053143527 ) ) ;
#190412 = CARTESIAN_POINT ( 'NONE',  ( -0.05219959533936034679, 19.03943276465977164, 82.50109039468567573 ) ) ;
#190413 = CARTESIAN_POINT ( 'NONE',  ( 21.55341960407610458, 5.719274019375980345, 93.95724293864770971 ) ) ;
#190414 = CARTESIAN_POINT ( 'NONE',  ( 0.05219959533937995610, -21.53943276465977519, 40.00109039468567573 ) ) ;
#190415 = CARTESIAN_POINT ( 'NONE',  ( 16.53943276465976808, 0.05219959533934440121, 46.25109039468567573 ) ) ;
#190417 = CARTESIAN_POINT ( 'NONE',  ( 10.81492255796106328, -18.62759615963255655, 55.41775706135234714 ) ) ;
#190416 = CARTESIAN_POINT ( 'NONE',  ( -0.05219959533934338120, 16.53943276465976808, 52.50109039468567573 ) ) ;
#190418 = CARTESIAN_POINT ( 'NONE',  ( 18.67979575497178502, 10.72451020669898547, 59.16557627198103120 ) ) ;
#190419 = CARTESIAN_POINT ( 'NONE',  ( -19.03943276465977164, 0.05219959533909376836, 46.24890960531435979 ) ) ;
#190420 = CARTESIAN_POINT ( 'NONE',  ( 3.766062262543149401E-15, -39.95556452105413570, -5.249999994537625447 ) ) ;
#190421 = CARTESIAN_POINT ( 'NONE',  ( -16.52544592524335698, -4.483927247898792601, 73.95942372801901854 ) ) ;
#190422 = CARTESIAN_POINT ( 'NONE',  ( 10.72451020669898902, -18.67979575497178502, 97.91557627198103830 ) ) ;
#190423 = CARTESIAN_POINT ( 'NONE',  ( 14.29746914071049879, -8.314922557960816363, 53.33224293864769550 ) ) ;
#190424 = CARTESIAN_POINT ( 'NONE',  ( 0.05219959533934541429, -16.53943276465976808, 65.00109039468568994 ) ) ;
#190425 = CARTESIAN_POINT ( 'NONE',  ( 19.05341960407617918, -5.049401038297876454, 96.04275706135231871 ) ) ;
#190426 = CARTESIAN_POINT ( 'NONE',  ( -15.80617190586745835, -15.72974639402198527, 96.87390960531436690 ) ) ;
#190427 = CARTESIAN_POINT ( 'NONE',  ( -8.314922557960811034, -14.29746914071050412, 47.08224293864770260 ) ) ;
#190428 = ORIENTED_EDGE ( 'NONE', *, *, #176141, .F. ) ;
#190429 = CARTESIAN_POINT ( 'NONE',  ( 0.05219959533934541429, -16.53943276465976808, 75.00109039468568994 ) ) ;
#190430 = CARTESIAN_POINT ( 'NONE',  ( 20.69372460268669300, 11.29034304323151794, 170.1224388339879567 ) ) ;
#190431 = CARTESIAN_POINT ( 'NONE',  ( -21.53943276465977519, 0.05219959533907696930, 71.24890960531435269 ) ) ;
#190432 = CARTESIAN_POINT ( 'NONE',  ( -4.379528057220328563, 16.55341960407611168, 25.20724293864769550 ) ) ;
#190433 = ORIENTED_EDGE ( 'NONE', *, *, #18906, .F. ) ;
#190434 = DIRECTION ( 'NONE',  ( 0.000000000000000000, -0.7071067811865467956, 0.7071067811865483499 ) ) ;
#190435 = CARTESIAN_POINT ( 'NONE',  ( -18.62759615963270932, 10.81492255796079327, 100.8322429386477097 ) ) ;
#190436 = CARTESIAN_POINT ( 'NONE',  ( -15.80617190586745835, -15.72974639402198527, 111.8739096053143669 ) ) ;
#190437 = CARTESIAN_POINT ( 'NONE',  ( -8.224510206698948167, 14.34966873604960824, 40.41557627198103120 ) ) ;
#190438 = CARTESIAN_POINT ( 'NONE',  ( -0.05219959533934338120, 16.53943276465976808, 52.50109039468567573 ) ) ;
#190439 = CARTESIAN_POINT ( 'NONE',  ( 0.05219959533909260263, 19.03943276465977164, 44.99890960531435979 ) ) ;
#190440 = CARTESIAN_POINT ( 'NONE',  ( 19.02544592524343514, -5.153800228976328945, 63.54057627198103830 ) ) ;
#190441 = ORIENTED_EDGE ( 'NONE', *, *, #198923, .T. ) ;
#190442 = EDGE_CURVE ( 'NONE', #85848, #141234, #21219, .T. ) ;
#190443 = CARTESIAN_POINT ( 'NONE',  ( -15.72974639402197994, 15.80617190586746368, 25.62390960531435624 ) ) ;
#190444 = CARTESIAN_POINT ( 'NONE',  ( -35.57212018828867883, -18.96864681237437722, -18.54270186059685344 ) ) ;
#190445 = CARTESIAN_POINT ( 'NONE',  ( 16.51473224551083163, -9.474510206698727899, 100.8344237280190043 ) ) ;
#190446 = CARTESIAN_POINT ( 'NONE',  ( 19.02544592524334988, 5.153800228976608722, 56.45942372801898301 ) ) ;
#190447 = CARTESIAN_POINT ( 'NONE',  ( -10.81492255796078084, -18.62759615963271287, 102.0822429386476955 ) ) ;
#190448 = CARTESIAN_POINT ( 'NONE',  ( 16.52544592524335698, 4.483927247898782831, 111.4594237280190328 ) ) ;
#190449 = CARTESIAN_POINT ( 'NONE',  ( -19.02544592524342804, 5.153800228976336051, 76.04057627198102409 ) ) ;
#190450 = CARTESIAN_POINT ( 'NONE',  ( -0.05219959533907301413, -21.53943276465977519, 42.49890960531435979 ) ) ;
#190452 = CARTESIAN_POINT ( 'NONE',  ( 14.34966873604972726, -8.224510206698740333, 25.83442372801901499 ) ) ;
#190451 = CARTESIAN_POINT ( 'NONE',  ( 18.67979575497178502, 10.72451020669898547, 79.16557627198103830 ) ) ;
#190453 = CARTESIAN_POINT ( 'NONE',  ( 9.564922557960805705, 16.46253265017160317, 114.5822429386476955 ) ) ;
#190454 = CARTESIAN_POINT ( 'NONE',  ( -5.823673210054431948, 21.52544592524334988, 72.70942372801901854 ) ) ;
#190456 = ADVANCED_FACE ( 'NONE', ( #4694 ), #110897, .T. ) ;
#190455 = CARTESIAN_POINT ( 'NONE',  ( -5.049401038298153566, 19.05341960407611168, 80.20724293864769550 ) ) ;
#190457 = CIRCLE ( 'NONE', #109772, 26.79475375365586487 ) ;
#190458 = CARTESIAN_POINT ( 'NONE',  ( -13.97604488694527625, -13.89961937509977652, 31.87390960531435979 ) ) ;
#190459 = CARTESIAN_POINT ( 'NONE',  ( 9.564922557960805705, 16.46253265017160317, 79.58224293864769550 ) ) ;
#190460 = CARTESIAN_POINT ( 'NONE',  ( -14.34966873604960291, -8.224510206698953496, 86.66557627198102409 ) ) ;
#190461 = ORIENTED_EDGE ( 'NONE', *, *, #199705, .T. ) ;
#190462 = CARTESIAN_POINT ( 'NONE',  ( 0.05219959533936267826, -19.03943276465977164, 100.0010903946856757 ) ) ;
#190463 = CARTESIAN_POINT ( 'NONE',  ( -3.573655867282028392E-15, 2.428612866367529932E-14, 139.9999999999999716 ) ) ;
#190464 = CARTESIAN_POINT ( 'NONE',  ( 19.03943276465977164, -0.05219959533909143690, 68.74890960531436690 ) ) ;
#190466 = CARTESIAN_POINT ( 'NONE',  ( 19.05341960407611168, 5.049401038298154454, 98.95724293864766707 ) ) ;
#190465 = CARTESIAN_POINT ( 'NONE',  ( 21.55341960407619695, -5.719274019375665929, 81.04275706135236135 ) ) ;
#190467 = CARTESIAN_POINT ( 'NONE',  ( -4.483927247898782831, 16.52544592524335698, 72.70942372801901854 ) ) ;
#190468 = CARTESIAN_POINT ( 'NONE',  ( -31.61347055016709007, 0.9086318102908346184, -46.06737158113915598 ) ) ;
#190469 = CARTESIAN_POINT ( 'NONE',  ( 9.474510206698729675, 16.51473224551082808, 52.08442372801900433 ) ) ;
#190470 = CARTESIAN_POINT ( 'NONE',  ( 15.72974639402176855, 15.80617190586768217, 111.8760903946856615 ) ) ;
#190471 = CARTESIAN_POINT ( 'NONE',  ( 37.58407650405589351, 2.428612866815129610E-14, 39.49999999999996447 ) ) ;
#190472 = CARTESIAN_POINT ( 'NONE',  ( 3.766062262543149401E-15, -39.95556452105413570, -7.249999994537627224 ) ) ;
#190473 = CARTESIAN_POINT ( 'NONE',  ( 36.91746825000000598, -11.99521256947793546, -6.224999997268814589 ) ) ;
#190474 = CARTESIAN_POINT ( 'NONE',  ( -14.29746914071049879, 8.314922557960819915, 25.83224293864769194 ) ) ;
#190475 = DIRECTION ( 'NONE',  ( 1.000000000000000000, 0.000000000000000000, 0.000000000000000000 ) ) ;
#190476 = CARTESIAN_POINT ( 'NONE',  ( 0.05219959533934541429, -16.53943276465976808, 110.0010903946856757 ) ) ;
#190477 = CARTESIAN_POINT ( 'NONE',  ( -23.29544513554941076, 16.92513159979227666, 146.0656553485623590 ) ) ;
#190478 =( BOUNDED_CURVE ( )  B_SPLINE_CURVE ( 2, ( #74128, #199444, #136768, #76084, #168104, #42795, #28628, #58936, #153928, #134812, #43779, #122588, #106423 ),
 .UNSPECIFIED., .F., .T. ) 
 B_SPLINE_CURVE_WITH_KNOTS ( ( 3, 2, 2, 2, 2, 2, 3 ),
 ( 0.4234830680059925023, 0.4254385964912280604, 0.4298245614035087758, 0.4342105263157894912, 0.4385964912280701511, 0.4429824561403508665, 0.4448923048034963412 ),
 .UNSPECIFIED. ) 
 CURVE ( )  GEOMETRIC_REPRESENTATION_ITEM ( )  RATIONAL_B_SPLINE_CURVE ( ( 0.9831626618144004848, 0.9848076720550091867, 1.000000000000000000, 0.9659258262890683122, 1.000000000000000000, 0.9659258262890683122, 1.000000000000000000, 0.9659258262890683122, 1.000000000000000000, 0.9659258262890683122, 1.000000000000000000, 0.9851625545550091179, 0.9832469066685282089 ) ) 
 REPRESENTATION_ITEM ( '' )  );
#190479 = CARTESIAN_POINT ( 'NONE',  ( 16.52544592524335698, 4.483927247898782831, 81.45942372801900433 ) ) ;
#190480 = CARTESIAN_POINT ( 'NONE',  ( 18.62759615963255655, 10.81492255796105972, 96.66775706135234714 ) ) ;
#190481 = CARTESIAN_POINT ( 'NONE',  ( 9.564922557961047289, -16.46253265017146816, 100.4177570613523329 ) ) ;
#190482 = CARTESIAN_POINT ( 'NONE',  ( -21.53943276465977519, -0.05219959533937600094, 68.75109039468568994 ) ) ;
#190483 = CARTESIAN_POINT ( 'NONE',  ( -9.474510206698720793, -16.51473224551083518, 34.58442372801899722 ) ) ;
#190484 = CARTESIAN_POINT ( 'NONE',  ( 19.02544592524343514, -5.153800228976328945, 78.54057627198099567 ) ) ;
#190485 = CARTESIAN_POINT ( 'NONE',  ( -16.46253265017160317, 9.564922557960807481, 55.83224293864769550 ) ) ;
#190486 = CARTESIAN_POINT ( 'NONE',  ( -12.23824476834559150, -38.08322923102583957, -12.22663129986431052 ) ) ;
#190487 = CARTESIAN_POINT ( 'NONE',  ( 21.52544592524344225, -5.823673210054117533, 98.54057627198105251 ) ) ;
#190488 = AXIS2_PLACEMENT_3D ( 'NONE', #108290, #108, #16296 ) ;
#190489 = CARTESIAN_POINT ( 'NONE',  ( -15.72974639402197994, 15.80617190586746368, 50.62390960531435979 ) ) ;
#190490 = CARTESIAN_POINT ( 'NONE',  ( -5.153800228976328057, -19.02544592524343514, 52.29057627198100988 ) ) ;
#190491 = CARTESIAN_POINT ( 'NONE',  ( 12.06949235617739724, 12.14591786802326823, 61.87609039468568284 ) ) ;
#190492 = ORIENTED_EDGE ( 'NONE', *, *, #26831, .F. ) ;
#190493 = CARTESIAN_POINT ( 'NONE',  ( 15.80617190586769283, -15.72974639402175789, 45.62609039468567573 ) ) ;
#190494 = CARTESIAN_POINT ( 'NONE',  ( -14.29746914071049879, 8.314922557960819915, 60.83224293864769550 ) ) ;
#190495 = CARTESIAN_POINT ( 'NONE',  ( -16.53943276465976808, -0.05219959533934237506, 38.75109039468567573 ) ) ;
#190496 = CARTESIAN_POINT ( 'NONE',  ( 16.53943276465976808, -0.05219959533910856209, 103.7489096053143669 ) ) ;
#190497 = CARTESIAN_POINT ( 'NONE',  ( -19.03943276465977164, -0.05219959533935918106, 48.75109039468566863 ) ) ;
#190498 = CARTESIAN_POINT ( 'NONE',  ( -16.55341960407611168, -4.379528057220339221, 66.45724293864768129 ) ) ;
#190499 = CARTESIAN_POINT ( 'NONE',  ( -5.719274019375665041, -21.55341960407619695, 34.79275706135235424 ) ) ;
#190501 = CARTESIAN_POINT ( 'NONE',  ( 18.67979575497178502, 10.72451020669898547, 94.16557627198103830 ) ) ;
#190500 = CARTESIAN_POINT ( 'NONE',  ( -9.564922557960796823, -16.46253265017161027, 27.08224293864769550 ) ) ;
#190502 = CARTESIAN_POINT ( 'NONE',  ( -9.564922557960796823, -16.46253265017161027, 107.0822429386476955 ) ) ;
#190503 = CARTESIAN_POINT ( 'NONE',  ( -8.224510206698948167, 14.34966873604960824, 75.41557627198102409 ) ) ;
#190504 = CARTESIAN_POINT ( 'NONE',  ( 0.05219959533909260263, 19.03943276465977164, 114.9989096053143669 ) ) ;
#190505 = CARTESIAN_POINT ( 'NONE',  ( -11.40812507854755609, 35.11059874428196537, -3.024999997268813523 ) ) ;
#190506 = CARTESIAN_POINT ( 'NONE',  ( -16.46253265017146816, -9.564922557961047289, 84.16775706135233293 ) ) ;
#190507 = CARTESIAN_POINT ( 'NONE',  ( -21.52544592524334988, -5.823673210054445271, 28.95942372801902209 ) ) ;
#190508 = CARTESIAN_POINT ( 'NONE',  ( 19.02544592524343514, -5.153800228976328945, 68.54057627198103830 ) ) ;
#190509 = CARTESIAN_POINT ( 'NONE',  ( 19.03943276465977164, 0.05219959533936151252, 56.25109039468566863 ) ) ;
#190510 = CARTESIAN_POINT ( 'NONE',  ( 5.153800228976335163, 19.02544592524342804, 24.79057627198102765 ) ) ;
#190511 = CARTESIAN_POINT ( 'NONE',  ( 12.06949235617757843, -12.14591786802309237, 58.12390960531435979 ) ) ;
#190512 = CARTESIAN_POINT ( 'NONE',  ( -14.34966873604960291, -8.224510206698953496, 51.66557627198102409 ) ) ;
#190513 = CARTESIAN_POINT ( 'NONE',  ( 5.049401038298161559, -19.05341960407611168, 72.70724293864768129 ) ) ;
#190514 = CARTESIAN_POINT ( 'NONE',  ( 21.53943276465977519, -0.05219959533907433946, 93.74890960531436690 ) ) ;
#190515 = CARTESIAN_POINT ( 'NONE',  ( -5.049401038298153566, 19.05341960407611168, 70.20724293864769550 ) ) ;
#190516 = CARTESIAN_POINT ( 'NONE',  ( 10.81492255796078972, 18.62759615963270932, 79.58224293864769550 ) ) ;
#190517 = CARTESIAN_POINT ( 'NONE',  ( -13.89961937509957401, -13.97604488694547875, 24.37609039468565442 ) ) ;
#190520 = CARTESIAN_POINT ( 'NONE',  ( 16.53943276465976808, -0.05219959533910856209, 93.74890960531436690 ) ) ;
#190519 = CARTESIAN_POINT ( 'NONE',  ( 4.379528057220339221, -16.55341960407611168, 22.70724293864769194 ) ) ;
#190518 = CARTESIAN_POINT ( 'NONE',  ( -19.03943276465977164, 0.05219959533909376836, 26.24890960531435624 ) ) ;
#190521 = CARTESIAN_POINT ( 'NONE',  ( 0.05219959533936267826, -19.03943276465977164, 95.00109039468567573 ) ) ;
#190522 = VERTEX_POINT ( 'NONE', #66385 ) ;
#190523 = CARTESIAN_POINT ( 'NONE',  ( 5.719274019375673035, 21.55341960407619339, 22.29275706135235069 ) ) ;
#190524 = CARTESIAN_POINT ( 'NONE',  ( -13.89961937509957401, -13.97604488694547875, 49.37609039468567573 ) ) ;
#190525 = CARTESIAN_POINT ( 'NONE',  ( 4.379528057220092307, 16.55341960407617563, 107.2927570613523471 ) ) ;
#190526 = CARTESIAN_POINT ( 'NONE',  ( -16.46253265017146816, -9.564922557961047289, 39.16775706135234003 ) ) ;
#190527 = CARTESIAN_POINT ( 'NONE',  ( -13.89961937509977652, 13.97604488694528158, 100.6239096053143669 ) ) ;
#190528 = CARTESIAN_POINT ( 'NONE',  ( -8.224510206698948167, 14.34966873604960824, 55.41557627198102409 ) ) ;
#190529 = CARTESIAN_POINT ( 'NONE',  ( -18.56197773271724571, 5.499999999999873879, 48.55066217314450228 ) ) ;
#190530 = CARTESIAN_POINT ( 'NONE',  ( -16.51473224551069308, -9.474510206698971260, 31.66557627198102054 ) ) ;
#190531 = CARTESIAN_POINT ( 'NONE',  ( 10.81492255796106328, -18.62759615963255655, 110.4177570613523756 ) ) ;
#190532 = CARTESIAN_POINT ( 'NONE',  ( 4.379528057220092307, 16.55341960407617563, 77.29275706135234714 ) ) ;
#190533 = CARTESIAN_POINT ( 'NONE',  ( -15.80617190586768217, 15.72974639402176855, 38.12609039468567573 ) ) ;
#190534 = CARTESIAN_POINT ( 'NONE',  ( 8.314922557961029526, -14.29746914071037800, 50.41775706135235424 ) ) ;
#190535 = CARTESIAN_POINT ( 'NONE',  ( 0.05219959533909260263, 19.03943276465977164, 104.9989096053143669 ) ) ;
#190536 = CARTESIAN_POINT ( 'NONE',  ( 16.51473224551069308, 9.474510206698969483, 59.16557627198102409 ) ) ;
#190537 = CARTESIAN_POINT ( 'NONE',  ( -16.51473224551069308, -9.474510206698971260, 66.66557627198102409 ) ) ;
#190538 = CARTESIAN_POINT ( 'NONE',  ( -4.379528057220086978, -16.55341960407618274, 44.79275706135234714 ) ) ;
#190539 = CARTESIAN_POINT ( 'NONE',  ( 14.29746914071049879, -8.314922557960816363, 108.3322429386477097 ) ) ;
#190540 = CARTESIAN_POINT ( 'NONE',  ( 16.53943276465976808, -0.05219959533910856209, 23.74890960531435269 ) ) ;
#190541 = CARTESIAN_POINT ( 'NONE',  ( -5.000000000000000888, -130.0000000000000000, -13.99999999999999822 ) ) ;
#190544 = CARTESIAN_POINT ( 'NONE',  ( -16.51473224551069308, -9.474510206698971260, 61.66557627198103120 ) ) ;
#190543 = CARTESIAN_POINT ( 'NONE',  ( -5.049401038298153566, 19.05341960407611168, 95.20724293864770971 ) ) ;
#190542 = CARTESIAN_POINT ( 'NONE',  ( 0.05219959533937995610, -21.53943276465977519, 60.00109039468568284 ) ) ;
#190545 = CARTESIAN_POINT ( 'NONE',  ( 9.474510206698971260, -16.51473224551069308, 92.91557627198103830 ) ) ;
#190546 = CARTESIAN_POINT ( 'NONE',  ( 8.314922557960818139, 14.29746914071049879, 49.58224293864769550 ) ) ;
#190547 = ADVANCED_FACE ( 'NONE', ( #189749 ), #18907, .F. ) ;
#190548 = CARTESIAN_POINT ( 'NONE',  ( 14.29746914071037800, 8.314922557961029526, 111.6677570613523613 ) ) ;
#190549 = CARTESIAN_POINT ( 'NONE',  ( 8.314922557960818139, 14.29746914071049879, 44.58224293864769550 ) ) ;
#190550 = VERTEX_POINT ( 'NONE', #78563 ) ;
#190551 = CARTESIAN_POINT ( 'NONE',  ( -37.45873412500000654, 2.428612866367529932E-14, -10.31249999863440792 ) ) ;
#190552 = CARTESIAN_POINT ( 'NONE',  ( 9.564922557960805705, 16.46253265017160317, 64.58224293864769550 ) ) ;
#190553 = CARTESIAN_POINT ( 'NONE',  ( -16.46253265017146816, -9.564922557961047289, 39.16775706135234003 ) ) ;
#190554 = CARTESIAN_POINT ( 'NONE',  ( -11.40812507854754720, -35.11059874428192273, -8.724999997268813701 ) ) ;
#190555 = CYLINDRICAL_SURFACE ( 'NONE', #53819, 28.79475375365586487 ) ;
#190557 = CARTESIAN_POINT ( 'NONE',  ( -16.55341960407617563, 4.379528057220093196, 68.54275706135234714 ) ) ;
#190556 = CARTESIAN_POINT ( 'NONE',  ( 5.049401038297881783, 19.05341960407617563, 82.29275706135229029 ) ) ;
#190558 = CYLINDRICAL_SURFACE ( 'NONE', #49709, 5.000000000000000000 ) ;
#190559 = CARTESIAN_POINT ( 'NONE',  ( -13.97604488694527625, -13.89961937509977652, 96.87390960531433848 ) ) ;
#190560 = CARTESIAN_POINT ( 'NONE',  ( -15.80617190586768217, 15.72974639402176855, 33.12609039468569705 ) ) ;
#190561 = CARTESIAN_POINT ( 'NONE',  ( 13.97604488694548053, -13.89961937509957401, 90.62609039468567573 ) ) ;
#190563 = CARTESIAN_POINT ( 'NONE',  ( 16.51473224551069308, 9.474510206698969483, 49.16557627198102409 ) ) ;
#190562 = CARTESIAN_POINT ( 'NONE',  ( -9.564922557960796823, -16.46253265017161027, 112.0822429386476955 ) ) ;
#190564 = CARTESIAN_POINT ( 'NONE',  ( 0.05219959533909260263, 19.03943276465977164, 84.99890960531436690 ) ) ;
#190566 = CARTESIAN_POINT ( 'NONE',  ( -9.474510206698964154, 16.51473224551069663, 55.41557627198103120 ) ) ;
#190565 = CARTESIAN_POINT ( 'NONE',  ( -12.14591786802309592, -12.06949235617757132, 41.87390960531435979 ) ) ;
#190567 = CARTESIAN_POINT ( 'NONE',  ( 16.51473224551083163, -9.474510206698727899, 70.83442372801900433 ) ) ;
#190568 = CARTESIAN_POINT ( 'NONE',  ( 8.314922557960818139, 14.29746914071049879, 89.58224293864768129 ) ) ;
#190569 = CARTESIAN_POINT ( 'NONE',  ( -19.05341960407617563, 5.049401038297882671, 28.54275706135232937 ) ) ;
#190570 = CARTESIAN_POINT ( 'NONE',  ( -19.05341960407611168, -5.049401038298163336, 66.45724293864769550 ) ) ;
#190571 = CARTESIAN_POINT ( 'NONE',  ( -15.72974639402197994, 15.80617190586746368, 60.62390960531437401 ) ) ;
#190573 = CARTESIAN_POINT ( 'NONE',  ( 10.81492255796106328, -18.62759615963255655, 110.4177570613523756 ) ) ;
#190572 = CARTESIAN_POINT ( 'NONE',  ( -0.05219959533910754901, -16.53943276465976808, 62.49890960531436690 ) ) ;
#190574 = CARTESIAN_POINT ( 'NONE',  ( 13.97604488694527802, 13.89961937509977652, 104.3739096053143385 ) ) ;
#190575 = CARTESIAN_POINT ( 'NONE',  ( -5.823673210054116645, -21.52544592524344225, 27.29057627198103120 ) ) ;
#190576 = CARTESIAN_POINT ( 'NONE',  ( 19.05341960407611168, 5.049401038298154454, 53.95724293864770260 ) ) ;
#190577 = CARTESIAN_POINT ( 'NONE',  ( 0.05219959533909260263, 19.03943276465977164, 44.99890960531435979 ) ) ;
#190578 = CARTESIAN_POINT ( 'NONE',  ( 14.34966873604960469, 8.224510206698951720, 104.1655762719810241 ) ) ;
#190579 = CARTESIAN_POINT ( 'NONE',  ( -18.62759615963255300, -10.81492255796106328, 19.16775706135234714 ) ) ;
#190580 = CARTESIAN_POINT ( 'NONE',  ( -16.46253265017160317, 9.564922557960807481, 95.83224293864769550 ) ) ;
#190581 = CARTESIAN_POINT ( 'NONE',  ( -0.05219959533937732626, 21.53943276465977519, 32.50109039468568284 ) ) ;
#190582 = CARTESIAN_POINT ( 'NONE',  ( 19.02544592524343514, -5.153800228976328945, 108.5405762719810383 ) ) ;
#190583 = CARTESIAN_POINT ( 'NONE',  ( -19.05341960407611168, -5.049401038298163336, 26.45724293864769550 ) ) ;
#190584 = CARTESIAN_POINT ( 'NONE',  ( -0.05219959533937732626, 21.53943276465977519, 82.50109039468568994 ) ) ;
#190585 = CARTESIAN_POINT ( 'NONE',  ( 15.80617190586746368, 15.72974639402197994, 99.37390960531436690 ) ) ;
#190586 = CARTESIAN_POINT ( 'NONE',  ( 17.50000000000000000, -5.500000000000001776, 106.2176903769643417 ) ) ;
#190587 = CARTESIAN_POINT ( 'NONE',  ( 5.000000000000003553, -4.999999999999996447, -18.00000000000000000 ) ) ;
#190588 = CARTESIAN_POINT ( 'NONE',  ( -18.22780087662119897, 5.500000000000102141, 61.01763182126894947 ) ) ;
#190589 = CARTESIAN_POINT ( 'NONE',  ( 12.14591786802327356, -12.06949235617739191, 45.62609039468567573 ) ) ;
#190590 = CARTESIAN_POINT ( 'NONE',  ( -0.05219959533910754901, -16.53943276465976808, 107.4989096053143669 ) ) ;
#190591 = CARTESIAN_POINT ( 'NONE',  ( -26.36463166569307859, -3.076743934663885405, 174.2851114983685932 ) ) ;
#190592 = CARTESIAN_POINT ( 'NONE',  ( 13.89961937509977652, -13.97604488694527269, 63.12390960531435979 ) ) ;
#190593 = CARTESIAN_POINT ( 'NONE',  ( -12.06949235617756955, 12.14591786802309770, 95.62390960531436690 ) ) ;
#190594 = CARTESIAN_POINT ( 'NONE',  ( -0.05219959533907301413, -21.53943276465977519, 42.49890960531435979 ) ) ;
#190595 = CARTESIAN_POINT ( 'NONE',  ( -14.34966873604960291, -8.224510206698953496, 71.66557627198100988 ) ) ;
#190596 = CARTESIAN_POINT ( 'NONE',  ( 16.53943276465976808, 0.05219959533934440121, 21.25109039468567218 ) ) ;
#190597 = CARTESIAN_POINT ( 'NONE',  ( 18.67979575497194134, -10.72451020669871369, 75.83442372801900433 ) ) ;
#190598 = CARTESIAN_POINT ( 'NONE',  ( 17.50000000000001421, -5.622605283950867339, 76.18792689403886698 ) ) ;
#190599 = CARTESIAN_POINT ( 'NONE',  ( 16.53943276465976808, 0.05219959533934440121, 96.25109039468568994 ) ) ;
#190600 = CARTESIAN_POINT ( 'NONE',  ( -12.14591786802309592, -12.06949235617757132, 36.87390960531435979 ) ) ;
#190601 = AXIS2_PLACEMENT_3D ( 'NONE', #4433, #139973, #18645 ) ;
#190602 = CARTESIAN_POINT ( 'NONE',  ( -9.564922557960796823, -16.46253265017161027, 37.08224293864768839 ) ) ;
#190603 = CARTESIAN_POINT ( 'NONE',  ( 19.02544592524343514, -5.153800228976328945, 83.54057627198100988 ) ) ;
#190604 = CARTESIAN_POINT ( 'NONE',  ( 21.53943276465977519, -0.05219959533907433946, 88.74890960531436690 ) ) ;
#190605 = CARTESIAN_POINT ( 'NONE',  ( -16.55341960407617563, 4.379528057220093196, 38.54275706135234714 ) ) ;
#190607 = CARTESIAN_POINT ( 'NONE',  ( 0.05219959533937995610, -21.53943276465977519, 75.00109039468568994 ) ) ;
#190606 = CARTESIAN_POINT ( 'NONE',  ( -4.483927247898539470, -16.52544592524342804, 67.29057627198103830 ) ) ;
#190608 = ADVANCED_FACE ( 'NONE', ( #140236 ), #156411, .T. ) ;
#190609 = CARTESIAN_POINT ( 'NONE',  ( -4.379528057220086978, -16.55341960407618274, 99.79275706135234714 ) ) ;
#190610 = CARTESIAN_POINT ( 'NONE',  ( 17.26058549869101810, -6.457015423128417808, 46.12254162523932877 ) ) ;
#190611 = CARTESIAN_POINT ( 'NONE',  ( -19.35543954521081034, -5.499999999999585221, 64.58901960356450900 ) ) ;
#190612 = CARTESIAN_POINT ( 'NONE',  ( 14.29746914071049879, -8.314922557960816363, 23.33224293864769194 ) ) ;
#190613 = CARTESIAN_POINT ( 'NONE',  ( -8.314922557961024197, 14.29746914071037800, 67.91775706135234714 ) ) ;
#190614 = CARTESIAN_POINT ( 'NONE',  ( -9.474510206698964154, 16.51473224551069663, 90.41557627198103830 ) ) ;
#190615 = CARTESIAN_POINT ( 'NONE',  ( -19.02544592524342804, 5.153800228976336051, 106.0405762719810241 ) ) ;
#190616 = CARTESIAN_POINT ( 'NONE',  ( 18.67979575497194134, -10.72451020669871369, 85.83442372801901854 ) ) ;
#190617 = CARTESIAN_POINT ( 'NONE',  ( 14.34966873604972726, -8.224510206698740333, 85.83442372801901854 ) ) ;
#190618 = CARTESIAN_POINT ( 'NONE',  ( -12.14591786802309592, -12.06949235617757132, 56.87390960531436690 ) ) ;
#190619 = CARTESIAN_POINT ( 'NONE',  ( 16.46253265017160672, -9.564922557960803928, 68.33224293864770971 ) ) ;
#190620 = ORIENTED_EDGE ( 'NONE', *, *, #151672, .F. ) ;
#190621 = CARTESIAN_POINT ( 'NONE',  ( -13.97604488694547697, 13.89961937509957934, 103.1260903946856473 ) ) ;
#190622 = CARTESIAN_POINT ( 'NONE',  ( -4.483927247898539470, -16.52544592524342804, 107.2905762719810525 ) ) ;
#190623 = CARTESIAN_POINT ( 'NONE',  ( 13.97604488694527802, 13.89961937509977652, 79.37390960531435269 ) ) ;
#190625 = CARTESIAN_POINT ( 'NONE',  ( 36.91746825000000598, -11.99521256947793546, -9.724999997268813701 ) ) ;
#190624 = CARTESIAN_POINT ( 'NONE',  ( -13.89961937509957401, -13.97604488694547875, 109.3760903946856331 ) ) ;
#190626 = CARTESIAN_POINT ( 'NONE',  ( -19.02544592524334988, -5.153800228976617603, 18.95942372801899722 ) ) ;
#190627 = CARTESIAN_POINT ( 'NONE',  ( -14.29746914071037622, -8.314922557961029526, 74.16775706135231871 ) ) ;
#190628 = CARTESIAN_POINT ( 'NONE',  ( -19.03943276465977164, -0.05219959533935918106, 103.7510903946856757 ) ) ;
#190629 = CARTESIAN_POINT ( 'NONE',  ( -4.379528057220328563, 16.55341960407611168, 110.2072429386477239 ) ) ;
#190630 = CARTESIAN_POINT ( 'NONE',  ( -4.483927247898782831, 16.52544592524335698, 67.70942372801901854 ) ) ;
#190631 = CARTESIAN_POINT ( 'NONE',  ( -14.29746914071037622, -8.314922557961029526, 59.16775706135234714 ) ) ;
#190632 = CARTESIAN_POINT ( 'NONE',  ( -16.51473224551069308, -9.474510206698971260, 26.66557627198103120 ) ) ;
#190633 = CARTESIAN_POINT ( 'NONE',  ( 16.51473224551083163, -9.474510206698727899, 65.83442372801900433 ) ) ;
#190634 = CARTESIAN_POINT ( 'NONE',  ( -15.80617190586768217, 15.72974639402176855, 93.12609039468568994 ) ) ;
#190635 = CARTESIAN_POINT ( 'NONE',  ( -16.46253265017160317, 9.564922557960807481, 30.83224293864769550 ) ) ;
#190636 = CARTESIAN_POINT ( 'NONE',  ( 5.049401038298161559, -19.05341960407611168, 72.70724293864768129 ) ) ;
#190637 = CARTESIAN_POINT ( 'NONE',  ( 14.29746914071049879, -8.314922557960816363, 68.33224293864769550 ) ) ;
#190638 = EDGE_CURVE ( 'NONE', #110833, #22958, #48250, .T. ) ;
#190639 = CARTESIAN_POINT ( 'NONE',  ( -19.03943276465977164, -0.05219959533935918106, 43.75109039468566863 ) ) ;
#190640 = CARTESIAN_POINT ( 'NONE',  ( 10.81492255796078972, 18.62759615963270932, 39.58224293864769550 ) ) ;
#190641 = CARTESIAN_POINT ( 'NONE',  ( -15.80617190586768217, 15.72974639402176855, 113.1260903946856899 ) ) ;
#190642 = CARTESIAN_POINT ( 'NONE',  ( -16.46253265017160317, 9.564922557960807481, 85.83224293864769550 ) ) ;
#190643 = CARTESIAN_POINT ( 'NONE',  ( 21.53943276465977519, 0.05219959533937863772, 111.2510903946856899 ) ) ;
#190644 = CARTESIAN_POINT ( 'NONE',  ( -15.72974639402197994, 15.80617190586746368, 65.62390960531436690 ) ) ;
#190645 = CARTESIAN_POINT ( 'NONE',  ( -13.97604488694527625, -13.89961937509977652, 96.87390960531433848 ) ) ;
#190646 = CARTESIAN_POINT ( 'NONE',  ( -19.05341960407617563, 5.049401038297882671, 73.54275706135233293 ) ) ;
#190647 = CARTESIAN_POINT ( 'NONE',  ( 16.51473224551069308, 9.474510206698969483, 109.1655762719810383 ) ) ;
#190648 = CARTESIAN_POINT ( 'NONE',  ( -9.564922557961040184, 16.46253265017147172, 92.91775706135233293 ) ) ;
#190649 = CARTESIAN_POINT ( 'NONE',  ( 16.55341960407618274, -4.379528057220086978, 61.04275706135234714 ) ) ;
#190650 = CARTESIAN_POINT ( 'NONE',  ( 5.153800228976335163, 19.02544592524342804, 24.79057627198102765 ) ) ;
#190651 = CARTESIAN_POINT ( 'NONE',  ( -13.89961937509977652, 13.97604488694528158, 90.62390960531432427 ) ) ;
#190652 = CARTESIAN_POINT ( 'NONE',  ( 21.52544592524344225, -5.823673210054117533, 58.54057627198103120 ) ) ;
#190653 = CARTESIAN_POINT ( 'NONE',  ( -14.34966873604972548, 8.224510206698743886, 28.33442372801902209 ) ) ;
#190654 = CARTESIAN_POINT ( 'NONE',  ( -18.67979575497193778, 10.72451020669871902, 33.33442372801900433 ) ) ;
#190655 = CARTESIAN_POINT ( 'NONE',  ( -18.67979575497193778, 10.72451020669871902, 83.33442372801903275 ) ) ;
#190656 = CARTESIAN_POINT ( 'NONE',  ( 12.06949235617739724, 12.14591786802326823, 91.87609039468568994 ) ) ;
#190657 = CARTESIAN_POINT ( 'NONE',  ( -16.51473224551069308, -9.474510206698971260, 81.66557627198103830 ) ) ;
#190658 = CARTESIAN_POINT ( 'NONE',  ( -16.52544592524342804, 4.483927247898546575, 81.04057627198102409 ) ) ;
#190659 = CARTESIAN_POINT ( 'NONE',  ( -4.483927247898539470, -16.52544592524342804, 22.29057627198102765 ) ) ;
#190660 = CARTESIAN_POINT ( 'NONE',  ( 13.97604488694548053, -13.89961937509957401, 60.62609039468564731 ) ) ;
#190661 = CARTESIAN_POINT ( 'NONE',  ( 0.05219959533937995610, -21.53943276465977519, 45.00109039468568284 ) ) ;
#190662 = CARTESIAN_POINT ( 'NONE',  ( -16.53943276465976808, 0.05219959533911058130, 91.24890960531436690 ) ) ;
#190663 = CARTESIAN_POINT ( 'NONE',  ( -5.049401038298153566, 19.05341960407611168, 115.2072429386477097 ) ) ;
#190664 = CARTESIAN_POINT ( 'NONE',  ( -12.06949235617739369, -12.14591786802326823, 99.37609039468568994 ) ) ;
#190665 = CARTESIAN_POINT ( 'NONE',  ( 21.52544592524334988, 5.823673210054432836, 86.45942372801901854 ) ) ;
#190666 = CARTESIAN_POINT ( 'NONE',  ( 8.224510206698742110, 14.34966873604972548, 42.08442372801901854 ) ) ;
#190667 = CARTESIAN_POINT ( 'NONE',  ( -21.53943276465977519, -0.05219959533937600094, 38.75109039468567573 ) ) ;
#190668 = ORIENTED_EDGE ( 'NONE', *, *, #101580, .F. ) ;
#190669 = CARTESIAN_POINT ( 'NONE',  ( 15.72974639402199770, -15.80617190586745480, 108.1239096053143811 ) ) ;
#190670 = CARTESIAN_POINT ( 'NONE',  ( -8.314922557960811034, -14.29746914071050412, 87.08224293864769550 ) ) ;
#190671 = CARTESIAN_POINT ( 'NONE',  ( -19.39720447994795904, -5.499999999999981348, 49.66317477297177163 ) ) ;
#190672 = CARTESIAN_POINT ( 'NONE',  ( -16.52544592524342804, 4.483927247898546575, 61.04057627198103120 ) ) ;
#190673 = CARTESIAN_POINT ( 'NONE',  ( 12.06949235617739724, 12.14591786802326823, 111.8760903946856615 ) ) ;
#190674 = CARTESIAN_POINT ( 'NONE',  ( -13.97604488694527625, -13.89961937509977652, 36.87390960531436690 ) ) ;
#190675 = CARTESIAN_POINT ( 'NONE',  ( -21.55341960407610458, -5.719274019375992779, 36.45724293864768839 ) ) ;
#190676 = CARTESIAN_POINT ( 'NONE',  ( -14.34966873604960291, -8.224510206698953496, 81.66557627198103830 ) ) ;
#190677 = CARTESIAN_POINT ( 'NONE',  ( 5.823673210054125526, 21.52544592524343514, 79.79057627198102409 ) ) ;
#190678 = CARTESIAN_POINT ( 'NONE',  ( 16.51473224551069308, 9.474510206698969483, 89.16557627198103830 ) ) ;
#190680 = CARTESIAN_POINT ( 'NONE',  ( 19.03943276465977164, 0.05219959533936151252, 91.25109039468566152 ) ) ;
#190679 = CARTESIAN_POINT ( 'NONE',  ( -9.474510206698964154, 16.51473224551069663, 35.41557627198102409 ) ) ;
#190681 = EDGE_CURVE ( 'NONE', #169831, #132379, #170921, .T. ) ;
#190682 = CARTESIAN_POINT ( 'NONE',  ( -15.72974639402197994, 15.80617190586746368, 30.62390960531436335 ) ) ;
#190683 = CARTESIAN_POINT ( 'NONE',  ( -5.823673210054431948, 21.52544592524334988, 67.70942372801901854 ) ) ;
#190684 = CARTESIAN_POINT ( 'NONE',  ( 9.474510206698971260, -16.51473224551069308, 52.91557627198102409 ) ) ;
#190685 = CARTESIAN_POINT ( 'NONE',  ( -5.153800228976328057, -19.02544592524343514, 87.29057627198103830 ) ) ;
#190686 = ORIENTED_EDGE ( 'NONE', *, *, #164374, .F. ) ;
#190687 = CARTESIAN_POINT ( 'NONE',  ( -0.05219959533934338120, 16.53943276465976808, 62.50109039468568284 ) ) ;
#190688 = CARTESIAN_POINT ( 'NONE',  ( 15.80617190586769283, -15.72974639402175789, 45.62609039468567573 ) ) ;
#190689 = CARTESIAN_POINT ( 'NONE',  ( -15.80617190586768217, 15.72974639402176855, 73.12609039468567573 ) ) ;
#190690 = CARTESIAN_POINT ( 'NONE',  ( -15.80617190586745835, -15.72974639402198527, 21.87390960531436690 ) ) ;
#190691 = CARTESIAN_POINT ( 'NONE',  ( -15.72974639402197994, 15.80617190586746368, 85.62390960531436690 ) ) ;
#190693 = CARTESIAN_POINT ( 'NONE',  ( 4.379528057220092307, 16.55341960407617563, 62.29275706135236845 ) ) ;
#190692 = CARTESIAN_POINT ( 'NONE',  ( 18.62759615963255655, 10.81492255796105972, 26.66775706135235424 ) ) ;
#190694 = CARTESIAN_POINT ( 'NONE',  ( -10.72451020669898014, 18.67979575497178502, 60.41557627198102409 ) ) ;
#190695 = CARTESIAN_POINT ( 'NONE',  ( 5.153800228976615827, -19.02544592524334988, 20.20942372801899722 ) ) ;
#190697 = CARTESIAN_POINT ( 'NONE',  ( -4.483927247898782831, 16.52544592524335698, 107.7094237280190328 ) ) ;
#190696 = CARTESIAN_POINT ( 'NONE',  ( 9.474510206698971260, -16.51473224551069308, 62.91557627198102409 ) ) ;
#190698 = CARTESIAN_POINT ( 'NONE',  ( -17.50000000000001421, -4.049696124445921086, 105.8196032933405633 ) ) ;
#190699 = CARTESIAN_POINT ( 'NONE',  ( -13.89961937509977652, 13.97604488694528158, 85.62390960531433848 ) ) ;
#190701 = B_SPLINE_CURVE_WITH_KNOTS ( 'NONE', 3,
 ( #170609, #125099, #32099, #186797, #172598, #171605 ),
 .UNSPECIFIED., .F., .F.,
 ( 4, 2, 4 ),
 ( 0.001769412596444684812, 0.002152742221722617720, 0.002536071847000550411 ),
 .UNSPECIFIED. ) ;
#190700 = CARTESIAN_POINT ( 'NONE',  ( 17.50000000000051159, 4.380085919831660846, 103.4503187307105776 ) ) ;
#190702 = CARTESIAN_POINT ( 'NONE',  ( -13.97604488694547697, 13.89961937509957934, 88.12609039468563310 ) ) ;
#190703 = CARTESIAN_POINT ( 'NONE',  ( -21.52544592524343514, 5.823673210054127303, 56.04057627198102409 ) ) ;
#190704 = CARTESIAN_POINT ( 'NONE',  ( -16.53943276465976808, -0.05219959533934237506, 113.7510903946856757 ) ) ;
#190705 = CARTESIAN_POINT ( 'NONE',  ( -5.153800228976607833, 19.02544592524334988, 102.7094237280189759 ) ) ;
#190706 = CARTESIAN_POINT ( 'NONE',  ( -13.89961937509977830, 13.97604488694528158, 40.62390960531435269 ) ) ;
#190707 = CARTESIAN_POINT ( 'NONE',  ( 16.51473224551083163, -9.474510206698727899, 90.83442372801900433 ) ) ;
#190709 = CARTESIAN_POINT ( 'NONE',  ( 19.03943276465977164, 0.05219959533936151252, 56.25109039468566863 ) ) ;
#190708 = CARTESIAN_POINT ( 'NONE',  ( 21.55341960407610458, 5.719274019375980345, 93.95724293864770971 ) ) ;
#190710 = CARTESIAN_POINT ( 'NONE',  ( 0.000000000000000000, 0.000000000000000000, -32.60000000000000142 ) ) ;
#190711 = CARTESIAN_POINT ( 'NONE',  ( 19.02544592524343514, -5.153800228976328945, 53.54057627198102409 ) ) ;
#190712 = CARTESIAN_POINT ( 'NONE',  ( 4.379528057220339221, -16.55341960407611168, 57.70724293864770260 ) ) ;
#190713 = CARTESIAN_POINT ( 'NONE',  ( -16.51473224551069308, -9.474510206698971260, 51.66557627198102409 ) ) ;
#190714 = CARTESIAN_POINT ( 'NONE',  ( -16.53943276465976808, 0.05219959533911058130, 56.24890960531436690 ) ) ;
#190715 = CARTESIAN_POINT ( 'NONE',  ( -23.36741966814226146, -32.36690354120219837, -22.32433735814168330 ) ) ;
#190716 = CARTESIAN_POINT ( 'NONE',  ( 31.48242569098776755, -7.251655820954947096, 93.02470426148725835 ) ) ;
#190717 = CARTESIAN_POINT ( 'NONE',  ( 14.34966873604960469, 8.224510206698951720, 29.16557627198103120 ) ) ;
#190718 = CARTESIAN_POINT ( 'NONE',  ( 5.049401038298161559, -19.05341960407611168, 67.70724293864769550 ) ) ;
#190719 = CARTESIAN_POINT ( 'NONE',  ( -5.153800228976607833, 19.02544592524335343, 72.70942372801900433 ) ) ;
#190720 = CARTESIAN_POINT ( 'NONE',  ( -5.049401038297874678, -19.05341960407617918, 39.79275706135232582 ) ) ;
#190721 = CARTESIAN_POINT ( 'NONE',  ( 0.05219959533934541429, -16.53943276465976808, 50.00109039468568994 ) ) ;
#190722 = CARTESIAN_POINT ( 'NONE',  ( -10.72451020669898014, 18.67979575497178502, 50.41557627198103120 ) ) ;
#190723 = CARTESIAN_POINT ( 'NONE',  ( 15.72974639402176855, 15.80617190586768217, 111.8760903946856615 ) ) ;
#190724 = CARTESIAN_POINT ( 'NONE',  ( -9.564922557960796823, -16.46253265017161027, 77.08224293864769550 ) ) ;
#190725 = CARTESIAN_POINT ( 'NONE',  ( -0.05219959533909027116, -19.03943276465977164, 112.4989096053143669 ) ) ;
#190726 = CARTESIAN_POINT ( 'NONE',  ( 9.564922557960805705, 16.46253265017160317, 114.5822429386476955 ) ) ;
#190727 = DIRECTION ( 'NONE',  ( 0.000000000000000000, -0.1045284632676537068, 0.9945218953682734009 ) ) ;
#190728 = CARTESIAN_POINT ( 'NONE',  ( -21.53943276465977519, -0.05219959533937600094, 18.75109039468568639 ) ) ;
#190729 = CARTESIAN_POINT ( 'NONE',  ( 14.29746914071049879, -8.314922557960816363, 93.33224293864769550 ) ) ;
#190731 = CARTESIAN_POINT ( 'NONE',  ( 16.46253265017160672, -9.564922557960803928, 83.33224293864768129 ) ) ;
#190730 = CARTESIAN_POINT ( 'NONE',  ( 15.80617190586746368, 15.72974639402197994, 94.37390960531436690 ) ) ;
#190732 = CARTESIAN_POINT ( 'NONE',  ( 16.51473224551069308, 9.474510206698969483, 89.16557627198103830 ) ) ;
#190733 = CARTESIAN_POINT ( 'NONE',  ( -10.72451020669898014, 18.67979575497178502, 110.4155762719810383 ) ) ;
#190734 = VERTEX_POINT ( 'NONE', #7694 ) ;
#190735 = CARTESIAN_POINT ( 'NONE',  ( 16.51473224551069308, 9.474510206698969483, 74.16557627198103830 ) ) ;
#190736 = CARTESIAN_POINT ( 'NONE',  ( 18.87075004821569024, -5.499999999999984013, 96.17408112101044537 ) ) ;
#190738 = CARTESIAN_POINT ( 'NONE',  ( -5.049401038298153566, 19.05341960407611168, 40.20724293864768839 ) ) ;
#190737 = CARTESIAN_POINT ( 'NONE',  ( 16.51473224551069308, 9.474510206698969483, 29.16557627198103475 ) ) ;
#190739 = CARTESIAN_POINT ( 'NONE',  ( -9.474510206698720793, -16.51473224551083518, 99.58442372801900433 ) ) ;
#190740 = CARTESIAN_POINT ( 'NONE',  ( 0.05219959533910956823, 16.53943276465976808, 114.9989096053143669 ) ) ;
#190741 = CARTESIAN_POINT ( 'NONE',  ( 10.81492255796106328, -18.62759615963255655, 70.41775706135236135 ) ) ;
#190743 = CARTESIAN_POINT ( 'NONE',  ( -18.62759615963255300, -10.81492255796106328, 29.16775706135234003 ) ) ;
#190742 = CARTESIAN_POINT ( 'NONE',  ( 19.05341960407611168, 5.049401038298154454, 63.95724293864769550 ) ) ;
#190744 = CARTESIAN_POINT ( 'NONE',  ( 5.719274019375991003, -21.55341960407610458, 107.7072429386476955 ) ) ;
#190745 = CARTESIAN_POINT ( 'NONE',  ( -5.429308488886486681E-15, 30.30510711980690175, 149.5000000000000000 ) ) ;
#190746 = CARTESIAN_POINT ( 'NONE',  ( 5.153800228976335163, 19.02544592524342804, 84.79057627198099567 ) ) ;
#190747 = CARTESIAN_POINT ( 'NONE',  ( 27.67912082740223312, 7.698001346386336152, 161.8872396492157577 ) ) ;
#190749 = CARTESIAN_POINT ( 'NONE',  ( -5.719274019375978568, 21.55341960407610458, 50.20724293864769550 ) ) ;
#190748 = CARTESIAN_POINT ( 'NONE',  ( 12.14591786802327356, -12.06949235617739191, 30.62609039468567929 ) ) ;
#190750 = CARTESIAN_POINT ( 'NONE',  ( 18.62759615963255655, 10.81492255796105972, 61.66775706135235424 ) ) ;
#190751 = CARTESIAN_POINT ( 'NONE',  ( 19.05341960407611168, 5.049401038298154454, 113.9572429386477097 ) ) ;
#190752 = CARTESIAN_POINT ( 'NONE',  ( 5.153800228976615827, -19.02544592524334988, 90.20942372801900433 ) ) ;
#190753 = CARTESIAN_POINT ( 'NONE',  ( 5.049401038298161559, -19.05341960407611168, 47.70724293864770260 ) ) ;
#190754 = CARTESIAN_POINT ( 'NONE',  ( -5.153800228976328057, -19.02544592524343514, 87.29057627198103830 ) ) ;
#190755 = CARTESIAN_POINT ( 'NONE',  ( -8.314922557960811034, -14.29746914071050412, 97.08224293864770971 ) ) ;
#190756 = CARTESIAN_POINT ( 'NONE',  ( -16.52544592524342804, 4.483927247898546575, 86.04057627198102409 ) ) ;
#190757 = CARTESIAN_POINT ( 'NONE',  ( 5.049401038298161559, -19.05341960407611168, 107.7072429386476955 ) ) ;
#190759 = CARTESIAN_POINT ( 'NONE',  ( -16.46253265017160317, 9.564922557960807481, 45.83224293864769550 ) ) ;
#190758 = CARTESIAN_POINT ( 'NONE',  ( -16.52544592524342804, 4.483927247898546575, 61.04057627198103120 ) ) ;
#190760 = CARTESIAN_POINT ( 'NONE',  ( 10.72451020669871369, 18.67979575497193778, 62.08442372801901143 ) ) ;
#190761 = CARTESIAN_POINT ( 'NONE',  ( -19.02544592524334988, -5.153800228976617603, 93.95942372801900433 ) ) ;
#190762 = CARTESIAN_POINT ( 'NONE',  ( 8.224510206698953496, -14.34966873604960469, 67.91557627198102409 ) ) ;
#190763 = CARTESIAN_POINT ( 'NONE',  ( 21.55341960407619695, -5.719274019375665929, 21.04275706135234714 ) ) ;
#190764 = CARTESIAN_POINT ( 'NONE',  ( -21.52544592524343514, 5.823673210054127303, 51.04057627198103120 ) ) ;
#190765 = CARTESIAN_POINT ( 'NONE',  ( 16.51473224551069308, 9.474510206698969483, 109.1655762719810383 ) ) ;
#190766 = CARTESIAN_POINT ( 'NONE',  ( 28.82186960331498327, 9.364793116373570925, 139.3500000054623911 ) ) ;
#190767 = CARTESIAN_POINT ( 'NONE',  ( 13.89961937509977652, -13.97604488694527269, 53.12390960531434558 ) ) ;
#190768 = CARTESIAN_POINT ( 'NONE',  ( -14.34966873604960291, -8.224510206698953496, 31.66557627198102054 ) ) ;
#190769 = CARTESIAN_POINT ( 'NONE',  ( 16.53943276465976808, 0.05219959533934440121, 96.25109039468568994 ) ) ;
#190770 = CARTESIAN_POINT ( 'NONE',  ( -16.53943276465976808, -0.05219959533934237506, 78.75109039468568994 ) ) ;
#190771 = CARTESIAN_POINT ( 'NONE',  ( -16.51473224551082808, 9.474510206698731452, 43.33442372801900433 ) ) ;
#190772 = CARTESIAN_POINT ( 'NONE',  ( -17.44279575226823908, 5.990770900252465836, 70.83557567514318976 ) ) ;
#190773 = CARTESIAN_POINT ( 'NONE',  ( 19.03943276465977164, -0.05219959533909143690, 88.74890960531436690 ) ) ;
#190774 = CARTESIAN_POINT ( 'NONE',  ( -9.564922557960796823, -16.46253265017161027, 57.08224293864769550 ) ) ;
#190775 = CARTESIAN_POINT ( 'NONE',  ( -0.05219959533910754901, -16.53943276465976808, 67.49890960531436690 ) ) ;
#190777 = CARTESIAN_POINT ( 'NONE',  ( 15.72974639402199770, -15.80617190586745480, 23.12390960531436335 ) ) ;
#190776 = CARTESIAN_POINT ( 'NONE',  ( 5.153800228976335163, 19.02544592524342804, 24.79057627198102765 ) ) ;
#190778 = CARTESIAN_POINT ( 'NONE',  ( 5.719274019375991003, -21.55341960407610458, 42.70724293864770260 ) ) ;
#190779 = CARTESIAN_POINT ( 'NONE',  ( -8.224510206698948167, 14.34966873604960824, 85.41557627198102409 ) ) ;
#190780 = CARTESIAN_POINT ( 'NONE',  ( 16.53943276465976808, 0.05219959533934440121, 41.25109039468568284 ) ) ;
#190781 = EDGE_CURVE ( 'NONE', #49688, #4689, #116880, .T. ) ;
#190782 = CARTESIAN_POINT ( 'NONE',  ( -12.06949235617756955, 12.14591786802309770, 75.62390960531439532 ) ) ;
#190783 = CARTESIAN_POINT ( 'NONE',  ( -3.573655867282028392E-15, 2.428612866367529932E-14, 167.9999999999999716 ) ) ;
#190784 = CARTESIAN_POINT ( 'NONE',  ( -0.05219959533936034679, 19.03943276465977164, 77.50109039468566152 ) ) ;
#190785 = CARTESIAN_POINT ( 'NONE',  ( -16.51473224551069308, -9.474510206698971260, 106.6655762719810383 ) ) ;
#190786 = CARTESIAN_POINT ( 'NONE',  ( 29.86685920354754487, 21.69954338932564752, -5.924999997268813878 ) ) ;
#190787 = CARTESIAN_POINT ( 'NONE',  ( -22.99870628207715484, 21.53952979013931213, -49.63989001790915268 ) ) ;
#190789 = CARTESIAN_POINT ( 'NONE',  ( 14.29746914071037800, 8.314922557961029526, 111.6677570613523613 ) ) ;
#190788 = CARTESIAN_POINT ( 'NONE',  ( 12.14591786802327356, -12.06949235617739191, 35.62609039468568994 ) ) ;
#190790 = CARTESIAN_POINT ( 'NONE',  ( 13.89961937509957401, 13.97604488694547697, 66.87609039468567573 ) ) ;
#190791 = CARTESIAN_POINT ( 'NONE',  ( 21.55341960407610458, 5.719274019375980345, 33.95724293864769550 ) ) ;
#190792 = CARTESIAN_POINT ( 'NONE',  ( 10.72451020669871369, 18.67979575497193778, 67.08442372801901854 ) ) ;
#190793 = CARTESIAN_POINT ( 'NONE',  ( -22.72581825106521336, -12.75361973299659368, 165.5645137041830708 ) ) ;
#190794 = CARTESIAN_POINT ( 'NONE',  ( 0.05219959533934541429, -16.53943276465976808, 30.00109039468568284 ) ) ;
#190796 = CARTESIAN_POINT ( 'NONE',  ( 19.05341960407611168, 5.049401038298154454, 88.95724293864769550 ) ) ;
#190795 = CARTESIAN_POINT ( 'NONE',  ( 19.05341960407611168, 5.049401038298154454, 23.95724293864769194 ) ) ;
#190797 = CARTESIAN_POINT ( 'NONE',  ( -16.46253265017160317, 9.564922557960807481, 25.83224293864769194 ) ) ;
#190798 = CARTESIAN_POINT ( 'NONE',  ( 8.224510206698953496, -14.34966873604960469, 87.91557627198103830 ) ) ;
#190799 = ITEM_DEFINED_TRANSFORMATION ( 'NONE', 'NONE', #4711,  #82054 ) ;
#190800 = CARTESIAN_POINT ( 'NONE',  ( 5.049401038298161559, -19.05341960407611168, 82.70724293864770971 ) ) ;
#190801 = ORIENTED_EDGE ( 'NONE', *, *, #93266, .T. ) ;
#190802 = CARTESIAN_POINT ( 'NONE',  ( -5.049401038297874678, -19.05341960407617918, 99.79275706135234714 ) ) ;
#190803 = CARTESIAN_POINT ( 'NONE',  ( 15.80617190586746368, 15.72974639402197994, 84.37390960531438111 ) ) ;
#190804 = CARTESIAN_POINT ( 'NONE',  ( -19.02544592524342804, 5.153800228976336051, 41.04057627198103120 ) ) ;
#190806 = CARTESIAN_POINT ( 'NONE',  ( 21.53943276465977519, -0.05219959533907433946, 108.7489096053143669 ) ) ;
#190805 = CARTESIAN_POINT ( 'NONE',  ( -19.03943276465977164, -0.05219959533935918106, 63.75109039468566863 ) ) ;
#190807 = CARTESIAN_POINT ( 'NONE',  ( 19.02544592524343514, -5.153800228976328945, 63.54057627198103830 ) ) ;
#190808 = CARTESIAN_POINT ( 'NONE',  ( -16.51473224551069308, -9.474510206698971260, 106.6655762719810383 ) ) ;
#190809 = EDGE_LOOP ( 'NONE', ( #139690, #154931, #99937, #76397 ) ) ;
#190810 = CARTESIAN_POINT ( 'NONE',  ( -4.379528057220086978, -16.55341960407618274, 39.79275706135235424 ) ) ;
#190811 = CARTESIAN_POINT ( 'NONE',  ( 0.05219959533907565091, 21.53943276465977519, 109.9989096053143527 ) ) ;
#190814 = CARTESIAN_POINT ( 'NONE',  ( 9.474510206698729675, 16.51473224551082808, 62.08442372801899722 ) ) ;
#190813 = CARTESIAN_POINT ( 'NONE',  ( 16.46253265017160672, -9.564922557960803928, 88.33224293864769550 ) ) ;
#190812 = CARTESIAN_POINT ( 'NONE',  ( 4.483927247898545687, 16.52544592524342804, 109.7905762719810383 ) ) ;
#190815 = CARTESIAN_POINT ( 'NONE',  ( -5.823673210054116645, -21.52544592524344225, 82.29057627198103830 ) ) ;
#190816 = CARTESIAN_POINT ( 'NONE',  ( 12.06949235617757843, -12.14591786802309237, 48.12390960531436690 ) ) ;
#190817 = CARTESIAN_POINT ( 'NONE',  ( 10.72451020669871369, 18.67979575497193778, 112.0844237280190185 ) ) ;
#190818 = CARTESIAN_POINT ( 'NONE',  ( -16.52544592524335698, -4.483927247898792601, 68.95942372801901854 ) ) ;
#190819 = CARTESIAN_POINT ( 'NONE',  ( 16.51473224551069308, 9.474510206698969483, 89.16557627198103830 ) ) ;
#190820 = CARTESIAN_POINT ( 'NONE',  ( -13.89961937509977652, 13.97604488694528158, 50.62390960531435979 ) ) ;
#190821 = CARTESIAN_POINT ( 'NONE',  ( 18.67979575497194134, -10.72451020669871369, 55.83442372801901854 ) ) ;
#190822 = CARTESIAN_POINT ( 'NONE',  ( 0.05219959533937995610, -21.53943276465977519, 65.00109039468568994 ) ) ;
#190823 = CARTESIAN_POINT ( 'NONE',  ( -5.049401038298153566, 19.05341960407611168, 65.20724293864765286 ) ) ;
#190824 = CARTESIAN_POINT ( 'NONE',  ( 15.72974639402176855, 15.80617190586768217, 31.87609039468567929 ) ) ;
#190825 = CARTESIAN_POINT ( 'NONE',  ( -9.564922557961040184, 16.46253265017147172, 67.91775706135233293 ) ) ;
#190826 = CARTESIAN_POINT ( 'NONE',  ( 16.51473224551083163, -9.474510206698727899, 70.83442372801900433 ) ) ;
#190827 = CARTESIAN_POINT ( 'NONE',  ( 19.05341960407611168, 5.049401038298154454, 38.95724293864767418 ) ) ;
#190828 = CARTESIAN_POINT ( 'NONE',  ( 8.314922557961029526, -14.29746914071037800, 90.41775706135236135 ) ) ;
#190829 = CARTESIAN_POINT ( 'NONE',  ( -9.564922557960796823, -16.46253265017161027, 47.08224293864769550 ) ) ;
#190830 = CARTESIAN_POINT ( 'NONE',  ( -9.564922557960796823, -16.46253265017161027, 22.08224293864768839 ) ) ;
#190831 = CARTESIAN_POINT ( 'NONE',  ( 16.46253265017160672, -9.564922557960803928, 98.33224293864769550 ) ) ;
#190832 = CARTESIAN_POINT ( 'NONE',  ( -16.46253265017160317, 9.564922557960807481, 40.83224293864769550 ) ) ;
#190833 = CARTESIAN_POINT ( 'NONE',  ( 18.67979575497178502, 10.72451020669898547, 84.16557627198103830 ) ) ;
#190834 = CARTESIAN_POINT ( 'NONE',  ( 12.06949235617739724, 12.14591786802326823, 61.87609039468568284 ) ) ;
#190835 = CARTESIAN_POINT ( 'NONE',  ( -9.564922557961040184, 16.46253265017147172, 27.91775706135232582 ) ) ;
#190836 = CARTESIAN_POINT ( 'NONE',  ( 5.049401038298161559, -19.05341960407611168, 57.70724293864769550 ) ) ;
#190837 = CARTESIAN_POINT ( 'NONE',  ( -16.52544592524342804, 4.483927247898546575, 41.04057627198103120 ) ) ;
#190838 = CARTESIAN_POINT ( 'NONE',  ( 8.224510206698953496, -14.34966873604960469, 82.91557627198103830 ) ) ;
#190839 = CARTESIAN_POINT ( 'NONE',  ( 16.51473224551069308, 9.474510206698969483, 94.16557627198103830 ) ) ;
#190840 = CARTESIAN_POINT ( 'NONE',  ( -13.89961937509977652, 13.97604488694528158, 75.62390960531438111 ) ) ;
#190841 = CARTESIAN_POINT ( 'NONE',  ( 21.52544592524334988, 5.823673210054432836, 31.45942372801901854 ) ) ;
#190842 = CARTESIAN_POINT ( 'NONE',  ( 19.02544592524343514, -5.153800228976328945, 93.54057627198102409 ) ) ;
#190843 = CARTESIAN_POINT ( 'NONE',  ( 10.72451020669871369, 18.67979575497193778, 102.0844237280190185 ) ) ;
#190844 = CARTESIAN_POINT ( 'NONE',  ( -8.314922557961024197, 14.29746914071037800, 72.91775706135234714 ) ) ;
#190845 = CARTESIAN_POINT ( 'NONE',  ( 10.72451020669871369, 18.67979575497193778, 22.08442372801901143 ) ) ;
#190846 = CARTESIAN_POINT ( 'NONE',  ( 15.80617190586746368, 15.72974639402197994, 94.37390960531436690 ) ) ;
#190847 = CARTESIAN_POINT ( 'NONE',  ( 14.34966873604960469, 8.224510206698951720, 44.16557627198103120 ) ) ;
#190848 = CARTESIAN_POINT ( 'NONE',  ( 16.51473224551069308, 9.474510206698969483, 44.16557627198103120 ) ) ;
#190849 = CARTESIAN_POINT ( 'NONE',  ( 4.483927247898545687, 16.52544592524342804, 74.79057627198105251 ) ) ;
#190850 = CARTESIAN_POINT ( 'NONE',  ( -21.53943276465977519, 0.05219959533907696930, 31.24890960531435979 ) ) ;
#190851 = CARTESIAN_POINT ( 'NONE',  ( -5.153800228976607833, 19.02544592524334988, 27.70942372801899722 ) ) ;
#190852 = CARTESIAN_POINT ( 'NONE',  ( -16.55341960407611168, -4.379528057220339221, 101.4572429386476955 ) ) ;
#190853 = CARTESIAN_POINT ( 'NONE',  ( 5.153800228976335163, 19.02544592524342804, 109.7905762719810099 ) ) ;
#190854 = ORIENTED_EDGE ( 'NONE', *, *, #109281, .F. ) ;
#190855 = CARTESIAN_POINT ( 'NONE',  ( 8.314922557961029526, -14.29746914071037800, 50.41775706135235424 ) ) ;
#190856 = CARTESIAN_POINT ( 'NONE',  ( 16.46253265017160672, -9.564922557960803928, 53.33224293864768839 ) ) ;
#190857 = CARTESIAN_POINT ( 'NONE',  ( -17.08307644218149690, -6.499664160759800247, 21.28380661205804358 ) ) ;
#190858 = CARTESIAN_POINT ( 'NONE',  ( -13.89961937509977652, 13.97604488694528158, 115.6239096053143669 ) ) ;
#190859 = CARTESIAN_POINT ( 'NONE',  ( -16.53943276465976808, -0.05219959533934237506, 88.75109039468567573 ) ) ;
#190860 = CARTESIAN_POINT ( 'NONE',  ( 13.89961937509957401, 13.97604488694547697, 106.8760903946856757 ) ) ;
#190861 = CARTESIAN_POINT ( 'NONE',  ( 18.67979575497194134, -10.72451020669871369, 85.83442372801901854 ) ) ;
#190862 = CARTESIAN_POINT ( 'NONE',  ( 13.97604488694527802, 13.89961937509977652, 74.37390960531436690 ) ) ;
#190863 = CARTESIAN_POINT ( 'NONE',  ( 5.719274019375991003, -21.55341960407610458, 97.70724293864772392 ) ) ;
#190864 = CARTESIAN_POINT ( 'NONE',  ( 0.05219959533934541429, -16.53943276465976808, 55.00109039468568284 ) ) ;
#190865 = CARTESIAN_POINT ( 'NONE',  ( 19.02544592524343514, -5.153800228976328945, 23.54057627198102054 ) ) ;
#190866 = CARTESIAN_POINT ( 'NONE',  ( 16.55341960407618274, -4.379528057220086978, 21.04275706135234714 ) ) ;
#190867 = ADVANCED_FACE ( 'NONE', ( #55211 ), #70386, .F. ) ;
#190868 = CARTESIAN_POINT ( 'NONE',  ( -9.474510206698720793, -16.51473224551083518, 84.58442372801900433 ) ) ;
#190869 = CARTESIAN_POINT ( 'NONE',  ( 21.53943276465977519, -0.05219959533907433946, 73.74890960531433848 ) ) ;
#190870 = CARTESIAN_POINT ( 'NONE',  ( -9.474510206698720793, -16.51473224551083518, 59.58442372801900433 ) ) ;
#190871 = DIRECTION ( 'NONE',  ( -0.000000000000000000, -0.000000000000000000, 1.000000000000000000 ) ) ;
#190872 = CARTESIAN_POINT ( 'NONE',  ( -18.62759615963270932, 10.81492255796079327, 105.8322429386476955 ) ) ;
#190873 = CARTESIAN_POINT ( 'NONE',  ( -17.49999999999999645, 5.624438216177591876, 85.81670344914643067 ) ) ;
#190874 = CARTESIAN_POINT ( 'NONE',  ( 5.049401038298161559, -19.05341960407611168, 62.70724293864769550 ) ) ;
#190875 = FACE_OUTER_BOUND ( 'NONE', #51934, .T. ) ;
#190876 = CARTESIAN_POINT ( 'NONE',  ( -16.55341960407617563, 4.379528057220093196, 23.54275706135235424 ) ) ;
#190877 = CARTESIAN_POINT ( 'NONE',  ( 36.76911729423384401, -4.939512937650262003, 47.42567687524350362 ) ) ;
#190879 = CARTESIAN_POINT ( 'NONE',  ( -0.05219959533910754901, -16.53943276465976808, 67.49890960531436690 ) ) ;
#190878 = CARTESIAN_POINT ( 'NONE',  ( 5.823673210054125526, 21.52544592524343514, 109.7905762719810383 ) ) ;
#190880 = CARTESIAN_POINT ( 'NONE',  ( 19.02544592524343514, -5.153800228976328945, 73.54057627198103830 ) ) ;
#190881 = CARTESIAN_POINT ( 'NONE',  ( -18.62759615963255300, -10.81492255796106328, 69.16775706135234714 ) ) ;
#190883 = CARTESIAN_POINT ( 'NONE',  ( 5.049401038297881783, 19.05341960407617563, 37.29275706135232582 ) ) ;
#190882 = CARTESIAN_POINT ( 'NONE',  ( -4.483927247898782831, 16.52544592524335698, 27.70942372801901854 ) ) ;
#190884 = CARTESIAN_POINT ( 'NONE',  ( -10.72451020669870658, -18.67979575497194134, 54.58442372801901143 ) ) ;
#190885 = CARTESIAN_POINT ( 'NONE',  ( 21.53943276465977519, -0.05219959533907433946, 113.7489096053143527 ) ) ;
#190886 = CARTESIAN_POINT ( 'NONE',  ( -18.67979575497178146, -10.72451020669898902, 56.66557627198103830 ) ) ;
#190887 = CARTESIAN_POINT ( 'NONE',  ( 5.049401038297881783, 19.05341960407617563, 107.2927570613523187 ) ) ;
#190888 = CARTESIAN_POINT ( 'NONE',  ( -5.049401038298153566, 19.05341960407611168, 50.20724293864770260 ) ) ;
#190889 = CARTESIAN_POINT ( 'NONE',  ( -5.049401038297874678, -19.05341960407617918, 69.79275706135233293 ) ) ;
#190890 = CARTESIAN_POINT ( 'NONE',  ( -15.80617190586768217, 15.72974639402176855, 88.12609039468570415 ) ) ;
#190891 = CARTESIAN_POINT ( 'NONE',  ( -5.153800228976607833, 19.02544592524334988, 47.70942372801900433 ) ) ;
#190892 = CARTESIAN_POINT ( 'NONE',  ( 5.049401038298161559, -19.05341960407611168, 32.70724293864768129 ) ) ;
#190893 = CARTESIAN_POINT ( 'NONE',  ( 10.81492255796078972, 18.62759615963270932, 59.58224293864770260 ) ) ;
#190894 = CARTESIAN_POINT ( 'NONE',  ( -12.14591786802309592, -12.06949235617757132, 51.87390960531437401 ) ) ;
#190895 = DIRECTION ( 'NONE',  ( 0.000000000000000000, 0.000000000000000000, 1.000000000000000000 ) ) ;
#190896 = CARTESIAN_POINT ( 'NONE',  ( -9.474510206698720793, -16.51473224551083518, 29.58442372801900433 ) ) ;
#190897 = CARTESIAN_POINT ( 'NONE',  ( 0.05219959533934541429, -16.53943276465976808, 85.00109039468568994 ) ) ;
#190898 = CARTESIAN_POINT ( 'NONE',  ( 4.483927247898545687, 16.52544592524342804, 49.79057627198102409 ) ) ;
#190899 = CARTESIAN_POINT ( 'NONE',  ( -5.823673210054431948, 21.52544592524334988, 87.70942372801901854 ) ) ;
#190900 = CARTESIAN_POINT ( 'NONE',  ( 18.62759615963255655, 10.81492255796105972, 86.66775706135234714 ) ) ;
#190901 = CARTESIAN_POINT ( 'NONE',  ( -0.05219959533907301413, -21.53943276465977519, 82.49890960531436690 ) ) ;
#190902 = CARTESIAN_POINT ( 'NONE',  ( -13.97604488694527625, -13.89961937509977652, 46.87390960531435979 ) ) ;
#190903 = CARTESIAN_POINT ( 'NONE',  ( -21.53943276465977519, -0.05219959533937600094, 53.75109039468568994 ) ) ;
#190904 = CARTESIAN_POINT ( 'NONE',  ( 13.97604488694527802, 13.89961937509977652, 34.37390960531436690 ) ) ;
#190905 = CARTESIAN_POINT ( 'NONE',  ( 16.51473224551069308, 9.474510206698969483, 49.16557627198102409 ) ) ;
#190906 = CARTESIAN_POINT ( 'NONE',  ( -16.55341960407611168, -4.379528057220339221, 101.4572429386476955 ) ) ;
#190907 = CARTESIAN_POINT ( 'NONE',  ( -9.564922557960796823, -16.46253265017161027, 92.08224293864769550 ) ) ;
#190908 = CARTESIAN_POINT ( 'NONE',  ( -12.14591786802309592, -12.06949235617757132, 56.87390960531436690 ) ) ;
#190909 = CARTESIAN_POINT ( 'NONE',  ( 16.52544592524342804, -4.483927247898539470, 113.5405762719810383 ) ) ;
#190910 = CARTESIAN_POINT ( 'NONE',  ( 18.67979575497178502, 10.72451020669898547, 89.16557627198102409 ) ) ;
#190911 = CARTESIAN_POINT ( 'NONE',  ( -21.53943276465977519, -0.05219959533937600094, 23.75109039468567929 ) ) ;
#190912 = CARTESIAN_POINT ( 'NONE',  ( 19.97888994334924107, -34.65319547504298470, -5.000000000000000000 ) ) ;
#190913 = CARTESIAN_POINT ( 'NONE',  ( 8.224510206698742110, 14.34966873604972548, 37.08442372801901143 ) ) ;
#190914 = ORIENTED_EDGE ( 'NONE', *, *, #162246, .T. ) ;
#190915 = CARTESIAN_POINT ( 'NONE',  ( 15.80617190586746368, 15.72974639402197994, 74.37390960531436690 ) ) ;
#190916 = CARTESIAN_POINT ( 'NONE',  ( -15.72974639402176322, -15.80617190586768395, 109.3760903946857042 ) ) ;
#190917 = CARTESIAN_POINT ( 'NONE',  ( 13.89961937509977652, -13.97604488694527269, 93.12390960531436690 ) ) ;
#190918 = CARTESIAN_POINT ( 'NONE',  ( -15.80617190586768217, 15.72974639402176855, 33.12609039468569705 ) ) ;
#190919 = CARTESIAN_POINT ( 'NONE',  ( -21.53943276465977519, 0.05219959533907696930, 36.24890960531435979 ) ) ;
#190920 = CARTESIAN_POINT ( 'NONE',  ( -16.55341960407617563, 4.379528057220093196, 103.5427570613523613 ) ) ;
#190922 = CARTESIAN_POINT ( 'NONE',  ( -10.81492255796105439, 18.62759615963255655, 82.91775706135234714 ) ) ;
#190921 = CARTESIAN_POINT ( 'NONE',  ( 5.823673210054444382, -21.52544592524334988, 45.20942372801901854 ) ) ;
#190923 = CARTESIAN_POINT ( 'NONE',  ( 10.72451020669871369, 18.67979575497193778, 107.0844237280190043 ) ) ;
#190924 = CARTESIAN_POINT ( 'NONE',  ( 8.224510206698742110, 14.34966873604972548, 77.08442372801901854 ) ) ;
#190925 = CARTESIAN_POINT ( 'NONE',  ( 18.67979575497194134, -10.72451020669871369, 35.83442372801901143 ) ) ;
#190926 = CARTESIAN_POINT ( 'NONE',  ( -19.05341960407611168, -5.049401038298163336, 26.45724293864769550 ) ) ;
#190927 = CARTESIAN_POINT ( 'NONE',  ( 21.52544592524334988, 5.823673210054432836, 101.4594237280190185 ) ) ;
#190928 = CARTESIAN_POINT ( 'NONE',  ( 19.03943276465977164, -0.05219959533909143690, 108.7489096053143527 ) ) ;
#190929 = CARTESIAN_POINT ( 'NONE',  ( 10.81492255796078972, 18.62759615963270932, 109.5822429386476955 ) ) ;
#190931 = CARTESIAN_POINT ( 'NONE',  ( 10.81492255796078972, 18.62759615963270932, 64.58224293864769550 ) ) ;
#190930 = CARTESIAN_POINT ( 'NONE',  ( -7.005188342139613944, -46.65430082754587460, -22.59844067006689272 ) ) ;
#190933 = CARTESIAN_POINT ( 'NONE',  ( -14.29746914071049879, 8.314922557960819915, 55.83224293864770260 ) ) ;
#190932 = CARTESIAN_POINT ( 'NONE',  ( -8.224510206698735004, -14.34966873604973081, 49.58442372801901143 ) ) ;
#190934 = CARTESIAN_POINT ( 'NONE',  ( -28.79475375365586842, 2.428612866367529932E-14, 146.2656553485623760 ) ) ;
#190935 = CARTESIAN_POINT ( 'NONE',  ( -9.564922557961040184, 16.46253265017147172, 82.91775706135233293 ) ) ;
#190936 = CARTESIAN_POINT ( 'NONE',  ( -16.81555441253552985, 7.025013491695478507, 105.6368544533425791 ) ) ;
#190937 = CARTESIAN_POINT ( 'NONE',  ( -14.34966873604972548, 8.224510206698743886, 23.33442372801901499 ) ) ;
#190938 = CARTESIAN_POINT ( 'NONE',  ( 21.55341960407610458, 5.719274019375980345, 103.9572429386476813 ) ) ;
#190939 = CARTESIAN_POINT ( 'NONE',  ( -14.34966873604960291, -8.224510206698953496, 71.66557627198100988 ) ) ;
#190940 = CARTESIAN_POINT ( 'NONE',  ( -21.55341960407610458, -5.719274019375992779, 21.45724293864769550 ) ) ;
#190941 = CARTESIAN_POINT ( 'NONE',  ( -12.14591786802326823, 12.06949235617739902, 38.12609039468567573 ) ) ;
#190942 = CARTESIAN_POINT ( 'NONE',  ( -5.153800228976328057, -19.02544592524343514, 52.29057627198100988 ) ) ;
#190944 = CARTESIAN_POINT ( 'NONE',  ( 5.153800228976615827, -19.02544592524334988, 100.2094237280190043 ) ) ;
#190943 = CARTESIAN_POINT ( 'NONE',  ( 5.823673210054444382, -21.52544592524334988, 30.20942372801902565 ) ) ;
#190945 = CARTESIAN_POINT ( 'NONE',  ( -9.564922557960796823, -16.46253265017161027, 112.0822429386476955 ) ) ;
#190946 = CARTESIAN_POINT ( 'NONE',  ( 13.97604488694527802, 13.89961937509977652, 89.37390960531436690 ) ) ;
#190947 = CARTESIAN_POINT ( 'NONE',  ( 10.81492255796078972, 18.62759615963270932, 89.58224293864768129 ) ) ;
#190948 = CARTESIAN_POINT ( 'NONE',  ( 19.03943276465977164, -0.05219959533909143690, 58.74890960531435979 ) ) ;
#190949 = DIRECTION ( 'NONE',  ( 0.000000000000000000, 1.000000000000000000, 0.000000000000000000 ) ) ;
#190950 = CARTESIAN_POINT ( 'NONE',  ( -14.34966873604960291, -8.224510206698953496, 71.66557627198100988 ) ) ;
#190951 = CARTESIAN_POINT ( 'NONE',  ( 16.51473224551069308, 9.474510206698969483, 109.1655762719810383 ) ) ;
#190952 = CARTESIAN_POINT ( 'NONE',  ( -31.78116016545939715, 0.5954834035870623099, -49.28208245900471240 ) ) ;
#190953 = CARTESIAN_POINT ( 'NONE',  ( -16.51473224551082808, 9.474510206698731452, 78.33442372801900433 ) ) ;
#190954 = CARTESIAN_POINT ( 'NONE',  ( -21.52544592524343514, 5.823673210054127303, 96.04057627198102409 ) ) ;
#190955 = CARTESIAN_POINT ( 'NONE',  ( 0.05219959533936267826, -19.03943276465977164, 45.00109039468566863 ) ) ;
#190956 = CARTESIAN_POINT ( 'NONE',  ( -15.80617190586745835, -15.72974639402198527, 21.87390960531436690 ) ) ;
#190957 = CARTESIAN_POINT ( 'NONE',  ( 19.49190055781011210, 5.500000000000053291, 68.06116087098781975 ) ) ;
#190958 = CARTESIAN_POINT ( 'NONE',  ( -0.05219959533907301413, -21.53943276465977519, 52.49890960531435979 ) ) ;
#190959 = CARTESIAN_POINT ( 'NONE',  ( -0.05219959533909027116, -19.03943276465977164, 82.49890960531436690 ) ) ;
#190960 = CARTESIAN_POINT ( 'NONE',  ( 15.80617190586769283, -15.72974639402175789, 80.62609039468567573 ) ) ;
#190961 = CARTESIAN_POINT ( 'NONE',  ( 16.46253265017160672, -9.564922557960803928, 43.33224293864769550 ) ) ;
#190962 = CARTESIAN_POINT ( 'NONE',  ( 4.379528057220339221, -16.55341960407611168, 67.70724293864769550 ) ) ;
#190963 = CARTESIAN_POINT ( 'NONE',  ( -0.05219959533934338120, 16.53943276465976808, 22.50109039468567573 ) ) ;
#190964 = CARTESIAN_POINT ( 'NONE',  ( 0.05219959533937995610, -21.53943276465977519, 70.00109039468568994 ) ) ;
#190965 = VERTEX_POINT ( 'NONE', #178572 ) ;
#190966 = CARTESIAN_POINT ( 'NONE',  ( 9.474510206698971260, -16.51473224551069308, 112.9155762719810383 ) ) ;
#190967 = CARTESIAN_POINT ( 'NONE',  ( -19.02544592524334988, -5.153800228976617603, 73.95942372801900433 ) ) ;
#190968 = DIRECTION ( 'NONE',  ( -0.000000000000000000, -0.000000000000000000, 1.000000000000000000 ) ) ;
#190969 = CARTESIAN_POINT ( 'NONE',  ( -15.72974639402197994, 15.80617190586746368, 115.6239096053143669 ) ) ;
#190970 = EDGE_CURVE ( 'NONE', #177604, #181866, #170738, .T. ) ;
#190971 = CARTESIAN_POINT ( 'NONE',  ( -6.020228577223754586E-15, 39.95556452105416412, -2.249999994537625891 ) ) ;
#190972 = CARTESIAN_POINT ( 'NONE',  ( -15.72974639402176322, -15.80617190586768395, 109.3760903946857042 ) ) ;
#190973 = CARTESIAN_POINT ( 'NONE',  ( 5.153800228976335163, 19.02544592524342804, 49.79057627198100988 ) ) ;
#190974 = CARTESIAN_POINT ( 'NONE',  ( -5.823673210054431948, 21.52544592524334988, 107.7094237280190328 ) ) ;
#190975 = CARTESIAN_POINT ( 'NONE',  ( 4.483927247898790824, -16.52544592524335698, 110.2094237280190185 ) ) ;
#190977 = CARTESIAN_POINT ( 'NONE',  ( -21.53943276465977519, -0.05219959533937600094, 78.75109039468568994 ) ) ;
#190976 = CARTESIAN_POINT ( 'NONE',  ( -19.03943276465977164, 0.05219959533909376836, 96.24890960531436690 ) ) ;
#190978 = CARTESIAN_POINT ( 'NONE',  ( -22.81625015709509441, -31.40387420917324590, -8.324999997268815122 ) ) ;
#190979 = CARTESIAN_POINT ( 'NONE',  ( -17.50000000000001776, -3.512728167236664145, 34.77190004818887559 ) ) ;
#190980 = CARTESIAN_POINT ( 'NONE',  ( 5.823673210054444382, -21.52544592524334988, 80.20942372801901854 ) ) ;
#190981 = CARTESIAN_POINT ( 'NONE',  ( -10.72451020669870658, -18.67979575497194134, 99.58442372801900433 ) ) ;
#190982 = FACE_OUTER_BOUND ( 'NONE', #720, .T. ) ;
#190983 = CARTESIAN_POINT ( 'NONE',  ( 19.02544592524343514, -5.153800228976328945, 88.54057627198102409 ) ) ;
#190984 = CARTESIAN_POINT ( 'NONE',  ( -9.564922557961040184, 16.46253265017147172, 22.91775706135233648 ) ) ;
#190985 = EDGE_CURVE ( 'NONE', #139245, #110833, #159381, .T. ) ;
#190986 = CARTESIAN_POINT ( 'NONE',  ( -2.500000000000000000, -105.0000000000000000, 12.00000000000000355 ) ) ;
#190987 = CARTESIAN_POINT ( 'NONE',  ( 5.049401038298161559, -19.05341960407611168, 42.70724293864767418 ) ) ;
#190988 = CARTESIAN_POINT ( 'NONE',  ( -0.05219959533907301413, -21.53943276465977519, 57.49890960531435979 ) ) ;
#190989 = CARTESIAN_POINT ( 'NONE',  ( -4.379528057220086978, -16.55341960407618274, 109.7927570613523613 ) ) ;
#190991 = CARTESIAN_POINT ( 'NONE',  ( 0.05219959533909260263, 19.03943276465977164, 79.99890960531436690 ) ) ;
#190990 = CARTESIAN_POINT ( 'NONE',  ( -16.52544592524342804, 4.483927247898546575, 96.04057627198102409 ) ) ;
#190992 = CARTESIAN_POINT ( 'NONE',  ( -21.55341960407619339, 5.719274019375674811, 98.54275706135234714 ) ) ;
#190993 = CARTESIAN_POINT ( 'NONE',  ( 19.05341960407611168, 5.049401038298154454, 33.95724293864769550 ) ) ;
#190994 = CARTESIAN_POINT ( 'NONE',  ( -16.52544592524342804, 4.483927247898546575, 106.0405762719810525 ) ) ;
#190995 = CARTESIAN_POINT ( 'NONE',  ( 21.55341960407619695, -5.719274019375665929, 51.04275706135234714 ) ) ;
#190996 = CARTESIAN_POINT ( 'NONE',  ( -5.823673210054116645, -21.52544592524344225, 82.29057627198103830 ) ) ;
#190997 = CARTESIAN_POINT ( 'NONE',  ( -13.97604488694547697, 13.89961937509957934, 48.12609039468566863 ) ) ;
#190998 = DIRECTION ( 'NONE',  ( 0.000000000000000000, 0.000000000000000000, 1.000000000000000000 ) ) ;
#190999 = CARTESIAN_POINT ( 'NONE',  ( -5.153800228976328057, -19.02544592524343514, 97.29057627198099567 ) ) ;
#191000 = CARTESIAN_POINT ( 'NONE',  ( 16.52544592524342804, -4.483927247898539470, 73.54057627198102409 ) ) ;
#191001 = CARTESIAN_POINT ( 'NONE',  ( -19.03943276465977164, -0.05219959533935918106, 48.75109039468566863 ) ) ;
#191002 = CARTESIAN_POINT ( 'NONE',  ( -9.564922557960796823, -16.46253265017161027, 62.08224293864769550 ) ) ;
#191003 = CARTESIAN_POINT ( 'NONE',  ( -16.55341960407611168, -4.379528057220339221, 46.45724293864769550 ) ) ;
#191004 = CARTESIAN_POINT ( 'NONE',  ( 13.97604488694548053, -13.89961937509957401, 75.62609039468564731 ) ) ;
#191005 = CARTESIAN_POINT ( 'NONE',  ( 7.260022482700429158, 2.182060888568188251, 7.889167669754723278 ) ) ;
#191006 = CARTESIAN_POINT ( 'NONE',  ( 5.719274019375991003, -21.55341960407610458, 42.70724293864770260 ) ) ;
#191007 = CARTESIAN_POINT ( 'NONE',  ( -16.55341960407611168, -4.379528057220339221, 106.4572429386477097 ) ) ;
#191008 = CARTESIAN_POINT ( 'NONE',  ( 2.539210307071009592E-15, -74.04165629597449083, -14.99410988461187699 ) ) ;
#191010 = CARTESIAN_POINT ( 'NONE',  ( -21.55341960407610458, -5.719274019375992779, 66.45724293864768129 ) ) ;
#191009 = CARTESIAN_POINT ( 'NONE',  ( -0.05219959533909027116, -19.03943276465977164, 62.49890960531435979 ) ) ;
#191011 = CARTESIAN_POINT ( 'NONE',  ( -19.03943276465977164, 0.05219959533909376836, 26.24890960531435624 ) ) ;
#191013 = CARTESIAN_POINT ( 'NONE',  ( -5.049401038298153566, 19.05341960407611168, 65.20724293864765286 ) ) ;
#191012 = CARTESIAN_POINT ( 'NONE',  ( 14.29746914071037800, 8.314922557961029526, 81.66775706135236135 ) ) ;
#191015 = EDGE_CURVE ( 'NONE', #140310, #29006, #14062, .T. ) ;
#191014 = CARTESIAN_POINT ( 'NONE',  ( -9.564922557961040184, 16.46253265017147172, 57.91775706135233293 ) ) ;
#191016 = CARTESIAN_POINT ( 'NONE',  ( 5.719274019375673035, 21.55341960407619339, 62.29275706135236845 ) ) ;
#191017 = CARTESIAN_POINT ( 'NONE',  ( -15.72974639402197994, 15.80617190586746368, 50.62390960531435979 ) ) ;
#191018 = CARTESIAN_POINT ( 'NONE',  ( -19.03943276465977164, 0.05219959533909376836, 21.24890960531436335 ) ) ;
#191019 = CARTESIAN_POINT ( 'NONE',  ( 16.55341960407618274, -4.379528057220086978, 91.04275706135236135 ) ) ;
#191020 = CARTESIAN_POINT ( 'NONE',  ( -13.89961937509957401, -13.97604488694547875, 99.37609039468567573 ) ) ;
#191021 = CARTESIAN_POINT ( 'NONE',  ( 19.05341960407611168, 5.049401038298154454, 23.95724293864769194 ) ) ;
#191023 = CARTESIAN_POINT ( 'NONE',  ( -0.05219959533907301413, -21.53943276465977519, 67.49890960531436690 ) ) ;
#191022 = CARTESIAN_POINT ( 'NONE',  ( 16.88567814943165502, 6.947325034625595919, 53.79001122652586986 ) ) ;
#191024 = CARTESIAN_POINT ( 'NONE',  ( -21.55341960407619339, 5.719274019375674811, 88.54275706135236135 ) ) ;
#191025 = CARTESIAN_POINT ( 'NONE',  ( -8.314922557960811034, -14.29746914071050412, 47.08224293864770260 ) ) ;
#191026 = CARTESIAN_POINT ( 'NONE',  ( -8.224510206698948167, 14.34966873604960824, 50.41557627198103120 ) ) ;
#191027 = CARTESIAN_POINT ( 'NONE',  ( -21.55341960407610458, -5.719274019375992779, 81.45724293864769550 ) ) ;
#191028 = CARTESIAN_POINT ( 'NONE',  ( 5.823673210054125526, 21.52544592524343514, 94.79057627198105251 ) ) ;
#191029 = CARTESIAN_POINT ( 'NONE',  ( 5.000000000000000888, -140.0000000000000000, -13.00000000000000000 ) ) ;
#191030 = CARTESIAN_POINT ( 'NONE',  ( -5.823673210054116645, -21.52544592524344225, 37.29057627198102409 ) ) ;
#191031 = CARTESIAN_POINT ( 'NONE',  ( 16.53943276465976808, 0.05219959533934440121, 66.25109039468567573 ) ) ;
#191032 = CARTESIAN_POINT ( 'NONE',  ( 16.53943276465976808, -0.05219959533910856209, 83.74890960531435269 ) ) ;
#191033 = CARTESIAN_POINT ( 'NONE',  ( -9.474510206698964154, 16.51473224551069663, 35.41557627198102409 ) ) ;
#191034 = FILL_AREA_STYLE_COLOUR ( '', #159726 ) ;
#191035 = CARTESIAN_POINT ( 'NONE',  ( 35.70266437024449147, 2.428612576286966776E-14, 37.50000000000000000 ) ) ;
#191036 = ORIENTED_EDGE ( 'NONE', *, *, #89104, .F. ) ;
#191037 = CARTESIAN_POINT ( 'NONE',  ( 12.06949235617739724, 12.14591786802326823, 91.87609039468568994 ) ) ;
#191038 = CARTESIAN_POINT ( 'NONE',  ( -15.80617190586745835, -15.72974639402198527, 111.8739096053143669 ) ) ;
#191039 = CARTESIAN_POINT ( 'NONE',  ( -5.153800228976328057, -19.02544592524343514, 77.29057627198099567 ) ) ;
#191040 = CARTESIAN_POINT ( 'NONE',  ( 10.72451020669871369, 18.67979575497193778, 57.08442372801901854 ) ) ;
#191041 = CARTESIAN_POINT ( 'NONE',  ( -5.153800228976328057, -19.02544592524343514, 112.2905762719810099 ) ) ;
#191042 = CARTESIAN_POINT ( 'NONE',  ( -13.59403193627398387, -42.61206874334182970, -22.32444481402297498 ) ) ;
#191043 = ORIENTED_EDGE ( 'NONE', *, *, #23592, .F. ) ;
#191044 = CARTESIAN_POINT ( 'NONE',  ( -0.05219959533937732626, 21.53943276465977519, 47.50109039468568994 ) ) ;
#191046 = CARTESIAN_POINT ( 'NONE',  ( -19.02544592524342804, 5.153800228976336051, 101.0405762719810241 ) ) ;
#191045 = CARTESIAN_POINT ( 'NONE',  ( -0.05219959533909027116, -19.03943276465977164, 37.49890960531436690 ) ) ;
#191047 = CARTESIAN_POINT ( 'NONE',  ( 19.03943276465977164, 0.05219959533936151252, 51.25109039468567573 ) ) ;
#191048 = CARTESIAN_POINT ( 'NONE',  ( -21.52544592524334988, -5.823673210054445271, 33.95942372801901143 ) ) ;
#191049 = CARTESIAN_POINT ( 'NONE',  ( 9.564922557961047289, -16.46253265017146816, 50.41775706135233293 ) ) ;
#191050 = CARTESIAN_POINT ( 'NONE',  ( -9.474510206698964154, 16.51473224551069663, 30.41557627198102054 ) ) ;
#191051 = CARTESIAN_POINT ( 'NONE',  ( -16.52544592524335698, -4.483927247898792601, 88.95942372801901854 ) ) ;
#191052 = CARTESIAN_POINT ( 'NONE',  ( -5.153800228976607833, 19.02544592524334988, 57.70942372801899012 ) ) ;
#191053 = CARTESIAN_POINT ( 'NONE',  ( 16.52544592524335698, 4.483927247898782831, 101.4594237280190185 ) ) ;
#191055 = ORIENTED_EDGE ( 'NONE', *, *, #145315, .T. ) ;
#191054 = CARTESIAN_POINT ( 'NONE',  ( 17.50000000000000000, 5.499999999999992895, 86.70309617465828467 ) ) ;
#191056 = CARTESIAN_POINT ( 'NONE',  ( 9.564922557960805705, 16.46253265017160317, 79.58224293864769550 ) ) ;
#191057 = CARTESIAN_POINT ( 'NONE',  ( 21.52544592524334988, 5.823673210054432836, 96.45942372801901854 ) ) ;
#191058 = CARTESIAN_POINT ( 'NONE',  ( -0.05219959533937732626, 21.53943276465977519, 102.5010903946856899 ) ) ;
#191059 = CARTESIAN_POINT ( 'NONE',  ( 17.72560187377284535, 5.500000000000042633, 66.57814504131322053 ) ) ;
#191060 = CARTESIAN_POINT ( 'NONE',  ( 16.51473224551069308, 9.474510206698969483, 99.16557627198102409 ) ) ;
#191061 = CARTESIAN_POINT ( 'NONE',  ( 18.67979575497194134, -10.72451020669871369, 75.83442372801900433 ) ) ;
#191062 = CARTESIAN_POINT ( 'NONE',  ( 0.05219959533934541429, -16.53943276465976808, 20.00109039468568639 ) ) ;
#191063 = CARTESIAN_POINT ( 'NONE',  ( -9.564922557960796823, -16.46253265017161027, 82.08224293864768129 ) ) ;
#191064 = CARTESIAN_POINT ( 'NONE',  ( -21.53943276465977519, 0.05219959533907696930, 31.24890960531435979 ) ) ;
#191065 = CARTESIAN_POINT ( 'NONE',  ( -5.153800228976328057, -19.02544592524343514, 97.29057627198099567 ) ) ;
#191066 = CARTESIAN_POINT ( 'NONE',  ( -38.00000000000000711, 2.428612866367529932E-14, -9.749999994537626336 ) ) ;
#191067 = CARTESIAN_POINT ( 'NONE',  ( 5.049401038298161559, -19.05341960407611168, 82.70724293864770971 ) ) ;
#191068 = CARTESIAN_POINT ( 'NONE',  ( -9.564922557960796823, -16.46253265017161027, 72.08224293864770971 ) ) ;
#191069 = CARTESIAN_POINT ( 'NONE',  ( 4.379528057220092307, 16.55341960407617563, 102.2927570613523613 ) ) ;
#191070 = CARTESIAN_POINT ( 'NONE',  ( -17.50000000000001421, 5.622605283950837141, 98.68792689403895224 ) ) ;
#191071 = CARTESIAN_POINT ( 'NONE',  ( 16.51473224551083163, -9.474510206698727899, 70.83442372801900433 ) ) ;
#191072 = CARTESIAN_POINT ( 'NONE',  ( 13.97604488694527802, 13.89961937509977652, 89.37390960531436690 ) ) ;
#191073 = CARTESIAN_POINT ( 'NONE',  ( -4.483927247898539470, -16.52544592524342804, 82.29057627198103830 ) ) ;
#191074 = CARTESIAN_POINT ( 'NONE',  ( 5.823673210054125526, 21.52544592524343514, 49.79057627198102409 ) ) ;
#191075 = CARTESIAN_POINT ( 'NONE',  ( 15.72974639402199770, -15.80617190586745480, 23.12390960531436335 ) ) ;
#191076 = CARTESIAN_POINT ( 'NONE',  ( -8.224510206698948167, 14.34966873604960824, 105.4155762719810383 ) ) ;
#191077 = CARTESIAN_POINT ( 'NONE',  ( -0.7627558185761093013, -6.293264767923594682, -62.46802126132829613 ) ) ;
#191078 = CARTESIAN_POINT ( 'NONE',  ( -5.153800228976607833, 19.02544592524334988, 37.70942372801899722 ) ) ;
#191079 = CARTESIAN_POINT ( 'NONE',  ( 12.06949235617757843, -12.14591786802309237, 23.12390960531436335 ) ) ;
#191080 = CARTESIAN_POINT ( 'NONE',  ( 9.474510206698971260, -16.51473224551069308, 102.9155762719810241 ) ) ;
#191081 = CARTESIAN_POINT ( 'NONE',  ( -0.05219959533937732626, 21.53943276465977519, 62.50109039468568284 ) ) ;
#191082 = CARTESIAN_POINT ( 'NONE',  ( 18.67979575497178502, 10.72451020669898547, 54.16557627198103120 ) ) ;
#191083 = CARTESIAN_POINT ( 'NONE',  ( 21.55341960407619695, -5.719274019375665929, 31.04275706135234714 ) ) ;
#191084 = CARTESIAN_POINT ( 'NONE',  ( -0.05219959533907301413, -21.53943276465977519, 87.49890960531436690 ) ) ;
#191085 = CARTESIAN_POINT ( 'NONE',  ( 0.05219959533937995610, -21.53943276465977519, 40.00109039468567573 ) ) ;
#191086 = CARTESIAN_POINT ( 'NONE',  ( -8.314922557960811034, -14.29746914071050412, 112.0822429386477097 ) ) ;
#191087 = CARTESIAN_POINT ( 'NONE',  ( 5.153800228976615827, -19.02544592524334988, 65.20942372801900433 ) ) ;
#191088 = CARTESIAN_POINT ( 'NONE',  ( 19.05341960407611168, 5.049401038298154454, 43.95724293864769550 ) ) ;
#191089 = CARTESIAN_POINT ( 'NONE',  ( 4.379528057220339221, -16.55341960407611168, 97.70724293864772392 ) ) ;
#191090 = CARTESIAN_POINT ( 'NONE',  ( -13.89961937509977652, 13.97604488694528158, 110.6239096053143243 ) ) ;
#191091 = CARTESIAN_POINT ( 'NONE',  ( -19.02544592524342804, 5.153800228976336051, 26.04057627198103120 ) ) ;
#191092 = CARTESIAN_POINT ( 'NONE',  ( -8.314922557960811034, -14.29746914071050412, 47.08224293864770260 ) ) ;
#191093 = CARTESIAN_POINT ( 'NONE',  ( 12.06949235617739724, 12.14591786802326823, 106.8760903946856899 ) ) ;
#191094 = CARTESIAN_POINT ( 'NONE',  ( 19.03943276465977164, -0.05219959533909143690, 58.74890960531435979 ) ) ;
#191095 = CARTESIAN_POINT ( 'NONE',  ( 9.564922557960805705, 16.46253265017160317, 24.58224293864769194 ) ) ;
#191096 = CARTESIAN_POINT ( 'NONE',  ( 13.97604488694548053, -13.89961937509957401, 20.62609039468567573 ) ) ;
#191098 = CARTESIAN_POINT ( 'NONE',  ( -0.05219959533910754901, -16.53943276465976808, 37.49890960531436690 ) ) ;
#191097 = CARTESIAN_POINT ( 'NONE',  ( -19.05341960407611168, -5.049401038298163336, 111.4572429386476671 ) ) ;
#191099 = CARTESIAN_POINT ( 'NONE',  ( -18.62759615963255300, -10.81492255796106328, 44.16775706135234714 ) ) ;
#191100 = ADVANCED_FACE ( 'NONE', ( #110551, #186432 ), #66036, .T. ) ;
#191101 = CARTESIAN_POINT ( 'NONE',  ( -8.969129508634374304, -36.34711360786828749, -31.52745775292092034 ) ) ;
#191102 = CARTESIAN_POINT ( 'NONE',  ( -16.53943276465976808, -0.05219959533934237506, 53.75109039468568994 ) ) ;
#191103 = CARTESIAN_POINT ( 'NONE',  ( -0.05219959533910754901, -16.53943276465976808, 22.49890960531436335 ) ) ;
#191104 = CARTESIAN_POINT ( 'NONE',  ( 8.224510206698742110, 14.34966873604972548, 112.0844237280190185 ) ) ;
#191105 = CARTESIAN_POINT ( 'NONE',  ( -14.29746914071037622, -8.314922557961029526, 29.16775706135234003 ) ) ;
#191106 = CARTESIAN_POINT ( 'NONE',  ( -16.46253265017160317, 9.564922557960807481, 50.83224293864770260 ) ) ;
#191107 = CARTESIAN_POINT ( 'NONE',  ( 0.05219959533910956823, 16.53943276465976808, 104.9989096053143669 ) ) ;
#191108 = CARTESIAN_POINT ( 'NONE',  ( 5.823673210054444382, -21.52544592524334988, 25.20942372801901854 ) ) ;
#191109 = CARTESIAN_POINT ( 'NONE',  ( 9.564922557960805705, 16.46253265017160317, 39.58224293864768839 ) ) ;
#191110 = VECTOR ( 'NONE', #171917, 1000.000000000000000 ) ;
#191111 = DIRECTION ( 'NONE',  ( -0.000000000000000000, -0.000000000000000000, 1.000000000000000000 ) ) ;
#191112 = CARTESIAN_POINT ( 'NONE',  ( -0.05219959533909027116, -19.03943276465977164, 27.49890960531435624 ) ) ;
#191113 = CARTESIAN_POINT ( 'NONE',  ( -5.823673210054116645, -21.52544592524344225, 22.29057627198102765 ) ) ;
#191114 = CARTESIAN_POINT ( 'NONE',  ( 3.885274725274726393, -8.673617379884035472E-16, 0.000000000000000000 ) ) ;
#191115 = CARTESIAN_POINT ( 'NONE',  ( -19.03943276465977164, 0.05219959533909376836, 96.24890960531436690 ) ) ;
#191117 = CARTESIAN_POINT ( 'NONE',  ( 16.53943276465976808, -0.05219959533910856209, 98.74890960531438111 ) ) ;
#191116 = CARTESIAN_POINT ( 'NONE',  ( -18.67979575497193778, 10.72451020669871902, 48.33442372801902565 ) ) ;
#191118 = CARTESIAN_POINT ( 'NONE',  ( 19.03943276465977164, -0.05219959533909143690, 103.7489096053143669 ) ) ;
#191119 = CARTESIAN_POINT ( 'NONE',  ( -27.60805440473040662, -7.718125693464772397, 162.2444234560585130 ) ) ;
#191120 = CARTESIAN_POINT ( 'NONE',  ( -8.224510206698735004, -14.34966873604973081, 74.58442372801901854 ) ) ;
#191121 = CARTESIAN_POINT ( 'NONE',  ( 5.823673210054444382, -21.52544592524334988, 95.20942372801903275 ) ) ;
#191122 = CARTESIAN_POINT ( 'NONE',  ( 4.483927247898790824, -16.52544592524335698, 60.20942372801902565 ) ) ;
#191123 = CARTESIAN_POINT ( 'NONE',  ( 5.049401038298161559, -19.05341960407611168, 97.70724293864766707 ) ) ;
#191124 = CARTESIAN_POINT ( 'NONE',  ( -16.52544592524335698, -4.483927247898792601, 43.95942372801902565 ) ) ;
#191125 = CARTESIAN_POINT ( 'NONE',  ( 5.153800228976615827, -19.02544592524334988, 110.2094237280189901 ) ) ;
#191126 = CARTESIAN_POINT ( 'NONE',  ( -8.314922557961024197, 14.29746914071037800, 77.91775706135231871 ) ) ;
#191127 = CARTESIAN_POINT ( 'NONE',  ( 19.05341960407617918, -5.049401038297876454, 111.0427570613523329 ) ) ;
#191128 = CARTESIAN_POINT ( 'NONE',  ( 16.46253265017160672, -9.564922557960803928, 78.33224293864769550 ) ) ;
#191129 = CARTESIAN_POINT ( 'NONE',  ( -21.52544592524343514, 5.823673210054127303, 91.04057627198103830 ) ) ;
#191131 = CARTESIAN_POINT ( 'NONE',  ( 5.049401038297881783, 19.05341960407617563, 102.2927570613523045 ) ) ;
#191130 = CARTESIAN_POINT ( 'NONE',  ( -16.53943276465976808, 0.05219959533911058130, 106.2489096053143811 ) ) ;
#191132 = CARTESIAN_POINT ( 'NONE',  ( -8.224510206698735004, -14.34966873604973081, 74.58442372801901854 ) ) ;
#191133 = CARTESIAN_POINT ( 'NONE',  ( 23.75112013235324326, 10.51683317207912971, 166.0021274478077089 ) ) ;
#191135 = EDGE_CURVE ( 'NONE', #126569, #64219, #174863, .T. ) ;
#191134 = CARTESIAN_POINT ( 'NONE',  ( 9.474510206698729675, 16.51473224551082808, 67.08442372801900433 ) ) ;
#191136 = CARTESIAN_POINT ( 'NONE',  ( 14.29746914071049879, -8.314922557960816363, 38.33224293864768839 ) ) ;
#191137 = CARTESIAN_POINT ( 'NONE',  ( -4.483927247898539470, -16.52544592524342804, 92.29057627198103830 ) ) ;
#191139 = CARTESIAN_POINT ( 'NONE',  ( -17.44270441346519362, 5.991230190322972327, 88.63664920735774899 ) ) ;
#191138 = CARTESIAN_POINT ( 'NONE',  ( -19.02544592524334988, -5.153800228976617603, 33.95942372801897591 ) ) ;
#191140 = CARTESIAN_POINT ( 'NONE',  ( 10.72451020669871369, 18.67979575497193778, 32.08442372801901854 ) ) ;
#191141 = CARTESIAN_POINT ( 'NONE',  ( 13.97604488694548053, -13.89961937509957401, 95.62609039468563310 ) ) ;
#191142 = DIRECTION ( 'NONE',  ( 0.000000000000000000, 0.000000000000000000, -1.000000000000000000 ) ) ;
#191143 = CARTESIAN_POINT ( 'NONE',  ( -13.97604488694527625, -13.89961937509977652, 96.87390960531433848 ) ) ;
#191144 = CARTESIAN_POINT ( 'NONE',  ( -15.80617190586768217, 15.72974639402176855, 103.1260903946856757 ) ) ;
#191145 = CARTESIAN_POINT ( 'NONE',  ( -5.153800228976328057, -19.02544592524343514, 77.29057627198099567 ) ) ;
#191146 = CARTESIAN_POINT ( 'NONE',  ( 18.62759615963271287, -10.81492255796078972, 38.33224293864768839 ) ) ;
#191147 = CARTESIAN_POINT ( 'NONE',  ( -8.314922557960811034, -14.29746914071050412, 92.08224293864769550 ) ) ;
#191148 = CARTESIAN_POINT ( 'NONE',  ( -9.564922557960796823, -16.46253265017161027, 52.08224293864768839 ) ) ;
#191149 = CARTESIAN_POINT ( 'NONE',  ( 4.379528057220339221, -16.55341960407611168, 107.7072429386476955 ) ) ;
#191150 = CARTESIAN_POINT ( 'NONE',  ( 0.05219959533937995610, -21.53943276465977519, 20.00109039468568639 ) ) ;
#191151 = CARTESIAN_POINT ( 'NONE',  ( -5.719274019375665041, -21.55341960407619695, 79.79275706135236135 ) ) ;
#191152 = CARTESIAN_POINT ( 'NONE',  ( 0.05219959533909260263, 19.03943276465977164, 49.99890960531435979 ) ) ;
#191153 = CARTESIAN_POINT ( 'NONE',  ( -14.29746914071037622, -8.314922557961029526, 74.16775706135231871 ) ) ;
#191154 = CARTESIAN_POINT ( 'NONE',  ( -0.05219959533907301413, -21.53943276465977519, 112.4989096053143669 ) ) ;
#191155 = EDGE_LOOP ( 'NONE', ( #197771, #46137, #129514, #111989 ) ) ;
#191156 = CARTESIAN_POINT ( 'NONE',  ( -18.67979575497193778, 10.72451020669871902, 28.33442372801902209 ) ) ;
#191158 = CARTESIAN_POINT ( 'NONE',  ( 13.97604488694527802, 13.89961937509977652, 59.37390960531434558 ) ) ;
#191157 = CARTESIAN_POINT ( 'NONE',  ( -5.153800228976607833, 19.02544592524334988, 52.70942372801900433 ) ) ;
#191159 = CARTESIAN_POINT ( 'NONE',  ( 19.05341960407617918, -5.049401038297876454, 36.04275706135234003 ) ) ;
#191160 = CARTESIAN_POINT ( 'NONE',  ( -5.823673210054431948, 21.52544592524334988, 72.70942372801901854 ) ) ;
#191161 = CARTESIAN_POINT ( 'NONE',  ( -18.67979575497178146, -10.72451020669898902, 71.66557627198100988 ) ) ;
#191162 = CARTESIAN_POINT ( 'NONE',  ( -16.52544592524342804, 4.483927247898546575, 56.04057627198102409 ) ) ;
#191164 = CARTESIAN_POINT ( 'NONE',  ( -16.46253265017146816, -9.564922557961047289, 29.16775706135232937 ) ) ;
#191163 = CARTESIAN_POINT ( 'NONE',  ( 21.55341960407619695, -5.719274019375665929, 86.04275706135236135 ) ) ;
#191165 = CARTESIAN_POINT ( 'NONE',  ( -0.05219959533910754901, -16.53943276465976808, 67.49890960531436690 ) ) ;
#191166 = CARTESIAN_POINT ( 'NONE',  ( 0.05219959533909260263, 19.03943276465977164, 24.99890960531435269 ) ) ;
#191167 = CARTESIAN_POINT ( 'NONE',  ( -13.97604488694547697, 13.89961937509957934, 58.12609039468566863 ) ) ;
#191168 = CARTESIAN_POINT ( 'NONE',  ( 4.483927247898790824, -16.52544592524335698, 110.2094237280190185 ) ) ;
#191169 = CARTESIAN_POINT ( 'NONE',  ( 5.823673210054444382, -21.52544592524334988, 85.20942372801901854 ) ) ;
#191170 = CARTESIAN_POINT ( 'NONE',  ( -16.51473224551082808, 9.474510206698731452, 53.33442372801900433 ) ) ;
#191171 = CARTESIAN_POINT ( 'NONE',  ( -10.72451020669898014, 18.67979575497178502, 50.41557627198103120 ) ) ;
#191172 = CARTESIAN_POINT ( 'NONE',  ( -10.72451020669870658, -18.67979575497194134, 39.58442372801901143 ) ) ;
#191173 = CARTESIAN_POINT ( 'NONE',  ( 10.81492255796078972, 18.62759615963270932, 99.58224293864770971 ) ) ;
#191174 = CARTESIAN_POINT ( 'NONE',  ( 5.049401038297881783, 19.05341960407617563, 92.29275706135234714 ) ) ;
#191175 = CARTESIAN_POINT ( 'NONE',  ( 4.379528057220092307, 16.55341960407617563, 67.29275706135234714 ) ) ;
#191177 = CARTESIAN_POINT ( 'NONE',  ( -21.53943276465977519, 0.05219959533907696930, 106.2489096053143811 ) ) ;
#191176 = CARTESIAN_POINT ( 'NONE',  ( -14.62203461105352886, -16.42370670853598824, -58.41511589169243024 ) ) ;
#191178 = CARTESIAN_POINT ( 'NONE',  ( -8.224510206698948167, 14.34966873604960824, 90.41557627198103830 ) ) ;
#191179 = CARTESIAN_POINT ( 'NONE',  ( -17.40805194822030444, -6.112264579159341515, 99.16628727489390371 ) ) ;
#191180 = CARTESIAN_POINT ( 'NONE',  ( 8.314922557961029526, -14.29746914071037800, 40.41775706135234714 ) ) ;
#191181 = CARTESIAN_POINT ( 'NONE',  ( -5.823673210054116645, -21.52544592524344225, 52.29057627198102409 ) ) ;
#191182 = CARTESIAN_POINT ( 'NONE',  ( 8.224510206698742110, 14.34966873604972548, 92.08442372801901854 ) ) ;
#191183 = CARTESIAN_POINT ( 'NONE',  ( -19.05341960407611168, -5.049401038298163336, 21.45724293864768839 ) ) ;
#191184 = CARTESIAN_POINT ( 'NONE',  ( 12.14591786802327356, -12.06949235617739191, 65.62609039468568994 ) ) ;
#191185 = CARTESIAN_POINT ( 'NONE',  ( -15.80617190586768217, 15.72974639402176855, 43.12609039468568284 ) ) ;
#191186 = CARTESIAN_POINT ( 'NONE',  ( 21.52544592524344225, -5.823673210054117533, 58.54057627198103120 ) ) ;
#191187 = CARTESIAN_POINT ( 'NONE',  ( -16.55341960407617563, 4.379528057220093196, 78.54275706135236135 ) ) ;
#191188 = CARTESIAN_POINT ( 'NONE',  ( 21.55341960407619695, -5.719274019375665929, 71.04275706135234714 ) ) ;
#191189 = CARTESIAN_POINT ( 'NONE',  ( -0.05219959533907301413, -21.53943276465977519, 52.49890960531435979 ) ) ;
#191190 = CARTESIAN_POINT ( 'NONE',  ( -21.55341960407610458, -5.719274019375992779, 36.45724293864768839 ) ) ;
#191191 = ORIENTED_EDGE ( 'NONE', *, *, #193397, .F. ) ;
#191192 = CARTESIAN_POINT ( 'NONE',  ( 4.483927247898790824, -16.52544592524335698, 70.20942372801904696 ) ) ;
#191193 = CARTESIAN_POINT ( 'NONE',  ( 15.80617190586746368, 15.72974639402197994, 34.37390960531435979 ) ) ;
#191194 = ORIENTED_EDGE ( 'NONE', *, *, #82217, .F. ) ;
#191195 = CARTESIAN_POINT ( 'NONE',  ( -13.89961937509977652, 13.97604488694528158, 105.6239096053143527 ) ) ;
#191196 = CARTESIAN_POINT ( 'NONE',  ( 16.52544592524342804, -4.483927247898539470, 23.54057627198102765 ) ) ;
#191197 = DIRECTION ( 'NONE',  ( 1.000000000000000000, 0.000000000000000000, 0.000000000000000000 ) ) ;
#191198 = CARTESIAN_POINT ( 'NONE',  ( -14.29746914071049879, 8.314922557960819915, 110.8322429386476955 ) ) ;
#191199 = CARTESIAN_POINT ( 'NONE',  ( -21.53943276465977519, 0.05219959533907696930, 51.24890960531436690 ) ) ;
#191200 = CARTESIAN_POINT ( 'NONE',  ( -9.564922557960796823, -16.46253265017161027, 42.08224293864769550 ) ) ;
#191201 = CARTESIAN_POINT ( 'NONE',  ( 0.05219959533934541429, -16.53943276465976808, 95.00109039468568994 ) ) ;
#191202 = CARTESIAN_POINT ( 'NONE',  ( -15.72974639402176322, -15.80617190586768395, 39.37609039468567573 ) ) ;
#191203 = CARTESIAN_POINT ( 'NONE',  ( -5.049401038297874678, -19.05341960407617918, 84.79275706135233293 ) ) ;
#191204 = CARTESIAN_POINT ( 'NONE',  ( -14.29746914071049879, 8.314922557960819915, 100.8322429386477097 ) ) ;
#191205 = CARTESIAN_POINT ( 'NONE',  ( -9.564922557960796823, -16.46253265017161027, 57.08224293864769550 ) ) ;
#191206 = LINE ( 'NONE', #41532, #66792 ) ;
#191207 = PLANE ( 'NONE',  #96397 ) ;
#191208 = CARTESIAN_POINT ( 'NONE',  ( -5.049401038298153566, 19.05341960407611168, 75.20724293864769550 ) ) ;
#191209 = CARTESIAN_POINT ( 'NONE',  ( 8.314922557961029526, -14.29746914071037800, 60.41775706135235424 ) ) ;
#191210 = CARTESIAN_POINT ( 'NONE',  ( -18.62759615963255300, -10.81492255796106328, 104.1677570613523471 ) ) ;
#191211 = CARTESIAN_POINT ( 'NONE',  ( 0.05219959533907565091, 21.53943276465977519, 54.99890960531435269 ) ) ;
#191212 = CARTESIAN_POINT ( 'NONE',  ( 0.05219959533934541429, -16.53943276465976808, 70.00109039468568994 ) ) ;
#191213 = CARTESIAN_POINT ( 'NONE',  ( -13.97604488694547697, 13.89961937509957934, 63.12609039468566152 ) ) ;
#191214 = VERTEX_POINT ( 'NONE', #81190 ) ;
#191215 = CARTESIAN_POINT ( 'NONE',  ( -21.52544592524334988, -5.823673210054445271, 58.95942372801902565 ) ) ;
#191216 = CARTESIAN_POINT ( 'NONE',  ( -19.03943276465977164, 0.05219959533909376836, 71.24890960531435269 ) ) ;
#191217 = CARTESIAN_POINT ( 'NONE',  ( -9.474510206698964154, 16.51473224551069663, 40.41557627198103120 ) ) ;
#191218 = CARTESIAN_POINT ( 'NONE',  ( -9.474510206698720793, -16.51473224551083518, 59.58442372801900433 ) ) ;
#191219 = CARTESIAN_POINT ( 'NONE',  ( -17.49999999999999645, 5.499999999999997335, 120.0000000000000142 ) ) ;
#191220 = CARTESIAN_POINT ( 'NONE',  ( 5.049401038298161559, -19.05341960407611168, 92.70724293864769550 ) ) ;
#191221 = CARTESIAN_POINT ( 'NONE',  ( -0.05219959533910754901, -16.53943276465976808, 52.49890960531435979 ) ) ;
#191222 = CARTESIAN_POINT ( 'NONE',  ( 15.72974639402199770, -15.80617190586745480, 43.12390960531435269 ) ) ;
#191223 = CARTESIAN_POINT ( 'NONE',  ( -17.50000000000147793, 3.254303733634563933, 105.0239589307140307 ) ) ;
#191224 = CARTESIAN_POINT ( 'NONE',  ( -19.05341960407617563, 5.049401038297882671, 28.54275706135232937 ) ) ;
#191225 = FACE_OUTER_BOUND ( 'NONE', #111891, .T. ) ;
#191226 = CARTESIAN_POINT ( 'NONE',  ( -19.02544592524342804, 5.153800228976336051, 51.04057627198103120 ) ) ;
#191227 = CARTESIAN_POINT ( 'NONE',  ( -18.22780087662123805, -5.499999999999968026, 98.98236817873106475 ) ) ;
#191228 = DIRECTION ( 'NONE',  ( -1.000000000000000000, 0.000000000000000000, 0.000000000000000000 ) ) ;
#191229 = CARTESIAN_POINT ( 'NONE',  ( 8.224510206698742110, 14.34966873604972548, 77.08442372801901854 ) ) ;
#191230 = CARTESIAN_POINT ( 'NONE',  ( 18.62759615963271287, -10.81492255796078972, 93.33224293864769550 ) ) ;
#191232 = DIRECTION ( 'NONE',  ( -1.000000000000000000, -0.000000000000000000, 0.000000000000000000 ) ) ;
#191231 = CARTESIAN_POINT ( 'NONE',  ( -0.05219959533909027116, -19.03943276465977164, 42.49890960531435269 ) ) ;
#191233 = CARTESIAN_POINT ( 'NONE',  ( 21.53943276465977519, 0.05219959533937863772, 36.25109039468567573 ) ) ;
#191234 = CARTESIAN_POINT ( 'NONE',  ( 5.049401038297881783, 19.05341960407617563, 52.29275706135234003 ) ) ;
#191235 = CARTESIAN_POINT ( 'NONE',  ( 16.46253265017160672, -9.564922557960803928, 48.33224293864769550 ) ) ;
#191236 = CARTESIAN_POINT ( 'NONE',  ( -5.823673210054431948, 21.52544592524334988, 97.70942372801904696 ) ) ;
#191237 = CARTESIAN_POINT ( 'NONE',  ( 17.05116617787825106, 6.768360034955821725, 98.84324446740804149 ) ) ;
#191238 = CARTESIAN_POINT ( 'NONE',  ( -14.34966873604960291, -8.224510206698953496, 36.66557627198103120 ) ) ;
#191239 = CARTESIAN_POINT ( 'NONE',  ( -3.181980515339492221, -6.791538853603052317, 1.110912703473986074 ) ) ;
#191240 = CARTESIAN_POINT ( 'NONE',  ( -10.72451020669898014, 18.67979575497178502, 40.41557627198103120 ) ) ;
#191241 = CARTESIAN_POINT ( 'NONE',  ( 24.38138396336205815, 13.63488425290815620, 140.0383846261352403 ) ) ;
#191242 = CARTESIAN_POINT ( 'NONE',  ( 19.05341960407611168, 5.049401038298154454, 98.95724293864766707 ) ) ;
#191243 = CARTESIAN_POINT ( 'NONE',  ( -12.14591786802309592, -12.06949235617757132, 91.87390960531436690 ) ) ;
#191244 = CARTESIAN_POINT ( 'NONE',  ( 0.05219959533934541429, -16.53943276465976808, 30.00109039468568284 ) ) ;
#191245 = CARTESIAN_POINT ( 'NONE',  ( -14.34966873604972548, 8.224510206698743886, 103.3344237280190043 ) ) ;
#191246 = ORIENTED_EDGE ( 'NONE', *, *, #120835, .F. ) ;
#191248 = CARTESIAN_POINT ( 'NONE',  ( 15.80617190586746368, 15.72974639402197994, 99.37390960531436690 ) ) ;
#191247 = CARTESIAN_POINT ( 'NONE',  ( -19.03943276465977164, 0.05219959533909376836, 96.24890960531436690 ) ) ;
#191250 = CARTESIAN_POINT ( 'NONE',  ( -19.03943276465977164, 0.05219959533909376836, 96.24890960531436690 ) ) ;
#191249 = CARTESIAN_POINT ( 'NONE',  ( -16.53943276465976808, -0.05219959533934237506, 113.7510903946856757 ) ) ;
#191251 = CARTESIAN_POINT ( 'NONE',  ( -16.46253265017146816, -9.564922557961047289, 94.16775706135233293 ) ) ;
#191252 = CARTESIAN_POINT ( 'NONE',  ( 0.05219959533937995610, -21.53943276465977519, 105.0010903946856757 ) ) ;
#191253 = CARTESIAN_POINT ( 'NONE',  ( -18.62759615963270932, 10.81492255796079327, 95.83224293864770971 ) ) ;
#191254 = CARTESIAN_POINT ( 'NONE',  ( 5.823673210054125526, 21.52544592524343514, 49.79057627198102409 ) ) ;
#191255 = CARTESIAN_POINT ( 'NONE',  ( 13.89961937509977652, -13.97604488694527269, 68.12390960531436690 ) ) ;
#191256 = CARTESIAN_POINT ( 'NONE',  ( 0.05219959533910956823, 16.53943276465976808, 39.99890960531436690 ) ) ;
#191257 = CARTESIAN_POINT ( 'NONE',  ( -16.46253265017160317, 9.564922557960807481, 75.83224293864769550 ) ) ;
#191258 = CARTESIAN_POINT ( 'NONE',  ( 19.25176906914649066, 5.499999999999730882, 58.49927264242278824 ) ) ;
#191259 = CARTESIAN_POINT ( 'NONE',  ( -9.564922557961040184, 16.46253265017147172, 42.91775706135234003 ) ) ;
#191260 = CARTESIAN_POINT ( 'NONE',  ( 4.379528057220339221, -16.55341960407611168, 87.70724293864769550 ) ) ;
#191261 = CARTESIAN_POINT ( 'NONE',  ( -10.72451020669870658, -18.67979575497194134, 29.58442372801901854 ) ) ;
#191262 = CARTESIAN_POINT ( 'NONE',  ( -27.73933785331498925, -9.013057229001049109, 145.4750000027311501 ) ) ;
#191263 = CARTESIAN_POINT ( 'NONE',  ( 16.52544592524335698, 4.483927247898782831, 111.4594237280190328 ) ) ;
#191264 = CARTESIAN_POINT ( 'NONE',  ( -4.379528057220328563, 16.55341960407611168, 115.2072429386476955 ) ) ;
#191265 = CARTESIAN_POINT ( 'NONE',  ( -16.51473224551069308, -9.474510206698971260, 66.66557627198102409 ) ) ;
#191266 = CARTESIAN_POINT ( 'NONE',  ( -38.00000000000000711, 12.34694845685046438, -9.849999994537625980 ) ) ;
#191267 = CARTESIAN_POINT ( 'NONE',  ( 16.53943276465976808, -0.05219959533910856209, 38.74890960531435979 ) ) ;
#191268 = CARTESIAN_POINT ( 'NONE',  ( 21.52544592524334988, 5.823673210054432836, 61.45942372801901854 ) ) ;
#191269 = CARTESIAN_POINT ( 'NONE',  ( 26.89045226410947720, -26.45365283845879745, -20.38637362917750551 ) ) ;
#191270 = CARTESIAN_POINT ( 'NONE',  ( 0.05219959533909260263, 19.03943276465977164, 39.99890960531436690 ) ) ;
#191271 = CARTESIAN_POINT ( 'NONE',  ( -16.51473224551069308, -9.474510206698971260, 56.66557627198103120 ) ) ;
#191272 = ORIENTED_EDGE ( 'NONE', *, *, #130121, .F. ) ;
#191273 = CARTESIAN_POINT ( 'NONE',  ( -15.80617190586768217, 15.72974639402176855, 113.1260903946856899 ) ) ;
#191274 = CARTESIAN_POINT ( 'NONE',  ( 4.379528057220092307, 16.55341960407617563, 62.29275706135236845 ) ) ;
#191275 = CARTESIAN_POINT ( 'NONE',  ( 5.823673210054444382, -21.52544592524334988, 85.20942372801901854 ) ) ;
#191276 = CARTESIAN_POINT ( 'NONE',  ( -9.474510206698964154, 16.51473224551069663, 115.4155762719810241 ) ) ;
#191277 = CARTESIAN_POINT ( 'NONE',  ( -5.153800228976607833, 19.02544592524334988, 97.70942372801900433 ) ) ;
#191278 = CARTESIAN_POINT ( 'NONE',  ( 18.67979575497194134, -10.72451020669871369, 70.83442372801901854 ) ) ;
#191279 = CARTESIAN_POINT ( 'NONE',  ( -4.379528057220086978, -16.55341960407618274, 39.79275706135235424 ) ) ;
#191280 = CARTESIAN_POINT ( 'NONE',  ( 5.823673210054125526, 21.52544592524343514, 89.79057627198103830 ) ) ;
#191281 = CARTESIAN_POINT ( 'NONE',  ( 9.474510206698729675, 16.51473224551082808, 102.0844237280190043 ) ) ;
#191282 = CARTESIAN_POINT ( 'NONE',  ( -19.03943276465977164, 0.05219959533909376836, 61.24890960531436690 ) ) ;
#191283 = CARTESIAN_POINT ( 'NONE',  ( -16.46253265017146816, -9.564922557961047289, 94.16775706135233293 ) ) ;
#191284 = CARTESIAN_POINT ( 'NONE',  ( -0.05219959533936034679, 19.03943276465977164, 102.5010903946856757 ) ) ;
#191285 = CARTESIAN_POINT ( 'NONE',  ( -16.55341960407611168, -4.379528057220339221, 56.45724293864768839 ) ) ;
#191286 = CARTESIAN_POINT ( 'NONE',  ( 9.474510206698729675, 16.51473224551082808, 72.08442372801900433 ) ) ;
#191287 = CARTESIAN_POINT ( 'NONE',  ( 12.06949235617739724, 12.14591786802326823, 56.87609039468568994 ) ) ;
#191289 = CARTESIAN_POINT ( 'NONE',  ( -19.03943276465977164, 0.05219959533909376836, 41.24890960531435269 ) ) ;
#191288 = CARTESIAN_POINT ( 'NONE',  ( 0.05219959533937995610, -21.53943276465977519, 20.00109039468568639 ) ) ;
#191290 = CARTESIAN_POINT ( 'NONE',  ( 16.46253265017160672, -9.564922557960803928, 58.33224293864769550 ) ) ;
#191291 = CARTESIAN_POINT ( 'NONE',  ( -0.05219959533934338120, 16.53943276465976808, 62.50109039468568284 ) ) ;
#191292 = CARTESIAN_POINT ( 'NONE',  ( -17.18269478283327345, -17.18269478283298568, -64.92279855667830191 ) ) ;
#191293 = DIRECTION ( 'NONE',  ( -1.000000000000000000, 0.000000000000000000, 0.000000000000000000 ) ) ;
#191294 = CARTESIAN_POINT ( 'NONE',  ( 5.153800228976335163, 19.02544592524342804, 99.79057627198102409 ) ) ;
#191295 = CARTESIAN_POINT ( 'NONE',  ( 9.474510206698971260, -16.51473224551069308, 27.91557627198103120 ) ) ;
#191296 = ORIENTED_EDGE ( 'NONE', *, *, #197529, .T. ) ;
#191297 = CARTESIAN_POINT ( 'NONE',  ( -13.89961937509957401, -13.97604488694547875, 109.3760903946856331 ) ) ;
#191298 = CARTESIAN_POINT ( 'NONE',  ( 18.67979575497178502, 10.72451020669898547, 44.16557627198103120 ) ) ;
#191300 = CARTESIAN_POINT ( 'NONE',  ( 0.05219959533934541429, -16.53943276465976808, 25.00109039468567218 ) ) ;
#191299 = CARTESIAN_POINT ( 'NONE',  ( 5.049401038297881783, 19.05341960407617563, 47.29275706135231161 ) ) ;
#191301 = CARTESIAN_POINT ( 'NONE',  ( 0.05219959533909260263, 19.03943276465977164, 34.99890960531435979 ) ) ;
#191302 = CARTESIAN_POINT ( 'NONE',  ( 9.474510206698971260, -16.51473224551069308, 47.91557627198102409 ) ) ;
#191303 = CARTESIAN_POINT ( 'NONE',  ( 10.81492255796078972, 18.62759615963270932, 84.58224293864769550 ) ) ;
#191304 = CARTESIAN_POINT ( 'NONE',  ( -16.46253265017160317, 9.564922557960807481, 100.8322429386477097 ) ) ;
#191305 = CARTESIAN_POINT ( 'NONE',  ( 19.02544592524343514, -5.153800228976328945, 48.54057627198103120 ) ) ;
#191306 = CARTESIAN_POINT ( 'NONE',  ( -22.44159573604010305, 16.30477369853692338, 141.1750000027311671 ) ) ;
#191307 = CARTESIAN_POINT ( 'NONE',  ( 16.46253265017146816, 9.564922557961045513, 81.66775706135233293 ) ) ;
#191308 = CARTESIAN_POINT ( 'NONE',  ( -14.34966873604960291, -8.224510206698953496, 66.66557627198102409 ) ) ;
#191309 = CARTESIAN_POINT ( 'NONE',  ( 0.05219959533937995610, -21.53943276465977519, 100.0010903946857042 ) ) ;
#191310 = CARTESIAN_POINT ( 'NONE',  ( -21.53943276465977519, 0.05219959533907696930, 91.24890960531436690 ) ) ;
#191311 = CARTESIAN_POINT ( 'NONE',  ( -5.719274019375665041, -21.55341960407619695, 79.79275706135236135 ) ) ;
#191312 = CARTESIAN_POINT ( 'NONE',  ( -18.62759615963255300, -10.81492255796106328, 74.16775706135231871 ) ) ;
#191313 = CARTESIAN_POINT ( 'NONE',  ( 0.05219959533909260263, 19.03943276465977164, 114.9989096053143669 ) ) ;
#191315 = CARTESIAN_POINT ( 'NONE',  ( 5.823673210054444382, -21.52544592524334988, 75.20942372801901854 ) ) ;
#191314 = CARTESIAN_POINT ( 'NONE',  ( -14.29746914071037622, -8.314922557961029526, 109.1677570613523613 ) ) ;
#191316 = CARTESIAN_POINT ( 'NONE',  ( -16.46253265017160317, 9.564922557960807481, 65.83224293864769550 ) ) ;
#191317 = CARTESIAN_POINT ( 'NONE',  ( -5.823673210054431948, 21.52544592524334988, 47.70942372801902565 ) ) ;
#191318 = CARTESIAN_POINT ( 'NONE',  ( 9.564922557960805705, 16.46253265017160317, 79.58224293864769550 ) ) ;
#191319 = CARTESIAN_POINT ( 'NONE',  ( -12.06949235617756955, 12.14591786802309770, 75.62390960531439532 ) ) ;
#191320 = CARTESIAN_POINT ( 'NONE',  ( 4.483927247898545687, 16.52544592524342804, 49.79057627198102409 ) ) ;
#191321 = CARTESIAN_POINT ( 'NONE',  ( -21.52544592524343514, 5.823673210054127303, 61.04057627198103120 ) ) ;
#191322 = CARTESIAN_POINT ( 'NONE',  ( -13.89961937509977652, 13.97604488694528158, 65.62390960531436690 ) ) ;
#191323 = CARTESIAN_POINT ( 'NONE',  ( 5.719274019375991003, -21.55341960407610458, 67.70724293864769550 ) ) ;
#191324 = CARTESIAN_POINT ( 'NONE',  ( -13.89961937509957401, -13.97604488694547875, 69.37609039468564731 ) ) ;
#191326 = CARTESIAN_POINT ( 'NONE',  ( -14.34966873604960291, -8.224510206698953496, 71.66557627198100988 ) ) ;
#191325 = CARTESIAN_POINT ( 'NONE',  ( -19.02544592524335343, -5.153800228976618492, 28.95942372801900788 ) ) ;
#191327 = CARTESIAN_POINT ( 'NONE',  ( 21.55341960407610458, 5.719274019375980345, 48.95724293864770971 ) ) ;
#191328 = ADVANCED_FACE ( 'NONE', ( #127703 ), #141880, .T. ) ;
#191329 = CARTESIAN_POINT ( 'NONE',  ( 17.13100169013300089, 6.664070546373150883, 101.7321016430015277 ) ) ;
#191331 = CARTESIAN_POINT ( 'NONE',  ( -27.73933785331498925, -9.013057229001049109, 143.4750000027312069 ) ) ;
#191330 = CARTESIAN_POINT ( 'NONE',  ( -16.52544592524335698, -4.483927247898792601, 103.9594237280190185 ) ) ;
#191332 = CARTESIAN_POINT ( 'NONE',  ( 19.02544592524334988, 5.153800228976608722, 106.4594237280190185 ) ) ;
#191333 = CARTESIAN_POINT ( 'NONE',  ( 8.314922557960818139, 14.29746914071049879, 69.58224293864769550 ) ) ;
#191334 = DIRECTION ( 'NONE',  ( 0.000000000000000000, -0.8164965809277251463, 0.5773502691896268413 ) ) ;
#191335 = CARTESIAN_POINT ( 'NONE',  ( -13.89961937509977652, 13.97604488694528158, 60.62390960531436690 ) ) ;
#191336 = CARTESIAN_POINT ( 'NONE',  ( -4.483927247898539470, -16.52544592524342804, 52.29057627198102409 ) ) ;
#191337 = CARTESIAN_POINT ( 'NONE',  ( -13.89961937509977652, 13.97604488694528158, 85.62390960531433848 ) ) ;
#191339 = CARTESIAN_POINT ( 'NONE',  ( -9.564922557960796823, -16.46253265017161027, 52.08224293864768839 ) ) ;
#191338 = CARTESIAN_POINT ( 'NONE',  ( 5.153800228976615827, -19.02544592524334988, 80.20942372801901854 ) ) ;
#191340 = CARTESIAN_POINT ( 'NONE',  ( 19.02544592524343514, -5.153800228976328945, 88.54057627198102409 ) ) ;
#191341 = CARTESIAN_POINT ( 'NONE',  ( 13.97604488694527802, 13.89961937509977652, 79.37390960531435269 ) ) ;
#191342 = CARTESIAN_POINT ( 'NONE',  ( -18.67979575497178146, -10.72451020669898902, 61.66557627198103120 ) ) ;
#191343 = CARTESIAN_POINT ( 'NONE',  ( 8.224510206698742110, 14.34966873604972548, 62.08442372801901143 ) ) ;
#191344 = DIRECTION ( 'NONE',  ( 0.000000000000000000, -3.469446951953611033E-15, -1.000000000000000000 ) ) ;
#191345 = CARTESIAN_POINT ( 'NONE',  ( 19.03943276465977164, -0.05219959533909143690, 53.74890960531436690 ) ) ;
#191346 = CARTESIAN_POINT ( 'NONE',  ( 0.05219959533907565091, 21.53943276465977519, 59.99890960531436690 ) ) ;
#191347 = CARTESIAN_POINT ( 'NONE',  ( 19.05341960407617918, -5.049401038297876454, 81.04275706135231871 ) ) ;
#191348 = CARTESIAN_POINT ( 'NONE',  ( -12.14591786802326823, 12.06949235617739902, 113.1260903946856899 ) ) ;
#191349 = CARTESIAN_POINT ( 'NONE',  ( -19.05341960407617563, 5.049401038297882671, 38.54275706135233293 ) ) ;
#191351 = CARTESIAN_POINT ( 'NONE',  ( 14.29746914071037800, 8.314922557961029526, 91.66775706135234714 ) ) ;
#191350 = CARTESIAN_POINT ( 'NONE',  ( 8.314922557961029526, -14.29746914071037800, 60.41775706135235424 ) ) ;
#191352 = CARTESIAN_POINT ( 'NONE',  ( 19.52217212775657984, -5.500000000000107470, 42.43993709005258808 ) ) ;
#191353 = CARTESIAN_POINT ( 'NONE',  ( 14.29746914071037800, 8.314922557961029526, 86.66775706135234714 ) ) ;
#191354 = CARTESIAN_POINT ( 'NONE',  ( -18.67979575497178146, -10.72451020669898902, 21.66557627198102409 ) ) ;
#191355 = CARTESIAN_POINT ( 'NONE',  ( -16.46253265017160317, 9.564922557960807481, 40.83224293864769550 ) ) ;
#191356 = CARTESIAN_POINT ( 'NONE',  ( 0.05219959533909260263, 19.03943276465977164, 44.99890960531435979 ) ) ;
#191357 = CARTESIAN_POINT ( 'NONE',  ( 19.02544592524343514, -5.153800228976328945, 43.54057627198103120 ) ) ;
#191358 = CARTESIAN_POINT ( 'NONE',  ( 15.80617190586769283, -15.72974639402175789, 35.62609039468568994 ) ) ;
#191359 = CARTESIAN_POINT ( 'NONE',  ( 0.05219959533934541429, -16.53943276465976808, 55.00109039468568284 ) ) ;
#191360 = CARTESIAN_POINT ( 'NONE',  ( -4.379528057220328563, 16.55341960407611168, 25.20724293864769550 ) ) ;
#191361 = CARTESIAN_POINT ( 'NONE',  ( 0.05219959533909260263, 19.03943276465977164, 24.99890960531435269 ) ) ;
#191362 = CARTESIAN_POINT ( 'NONE',  ( 19.02544592524334988, 5.153800228976608722, 21.45942372801899012 ) ) ;
#191364 = ADVANCED_FACE ( 'NONE', ( #32732 ), #94384, .T. ) ;
#191363 = CARTESIAN_POINT ( 'NONE',  ( -19.03943276465977164, -0.05219959533935918106, 108.7510903946856615 ) ) ;
#191365 = CARTESIAN_POINT ( 'NONE',  ( 5.049401038297881783, 19.05341960407617563, 72.29275706135234714 ) ) ;
#191366 = CARTESIAN_POINT ( 'NONE',  ( 12.06949235617757843, -12.14591786802309237, 73.12390960531436690 ) ) ;
#191367 = CARTESIAN_POINT ( 'NONE',  ( -19.05341960407611168, -5.049401038298163336, 36.45724293864766707 ) ) ;
#191369 = DIRECTION ( 'NONE',  ( -1.000000000000000000, 0.000000000000000000, 0.000000000000000000 ) ) ;
#191368 = CARTESIAN_POINT ( 'NONE',  ( -19.05341960407617563, 5.049401038297882671, 73.54275706135233293 ) ) ;
#191370 = CARTESIAN_POINT ( 'NONE',  ( 18.62759615963255655, 10.81492255796105972, 81.66775706135236135 ) ) ;
#191371 = CARTESIAN_POINT ( 'NONE',  ( -14.34966873604972548, 8.224510206698743886, 43.33442372801901143 ) ) ;
#191372 = CARTESIAN_POINT ( 'NONE',  ( 18.09805431107524498, -5.499999999999975131, 73.51606229291890315 ) ) ;
#191373 = CARTESIAN_POINT ( 'NONE',  ( -21.55341960407610458, -5.719274019375992779, 36.45724293864768839 ) ) ;
#191374 = CARTESIAN_POINT ( 'NONE',  ( 4.483927247898790824, -16.52544592524335698, 25.20942372801901854 ) ) ;
#191375 = CARTESIAN_POINT ( 'NONE',  ( 5.153800228976335163, 19.02544592524342804, 29.79057627198102054 ) ) ;
#191376 = CARTESIAN_POINT ( 'NONE',  ( 0.05219959533937995610, -21.53943276465977519, 105.0010903946856757 ) ) ;
#191377 = PLANE ( 'NONE',  #168965 ) ;
#191378 = CARTESIAN_POINT ( 'NONE',  ( -19.05341960407611168, -5.049401038298163336, 41.45724293864769550 ) ) ;
#191379 = LINE ( 'NONE', #52855, #182135 ) ;
#191380 = CARTESIAN_POINT ( 'NONE',  ( -19.05341960407611168, -5.049401038298163336, 61.45724293864769550 ) ) ;
#191381 = CARTESIAN_POINT ( 'NONE',  ( 21.52544592524334988, 5.823673210054432836, 61.45942372801901854 ) ) ;
#191382 = CARTESIAN_POINT ( 'NONE',  ( 0.05219959533936267826, -19.03943276465977164, 20.00109039468567218 ) ) ;
#191383 = CARTESIAN_POINT ( 'NONE',  ( -16.52544592524342804, 4.483927247898546575, 26.04057627198103475 ) ) ;
#191384 = CARTESIAN_POINT ( 'NONE',  ( 9.474510206698971260, -16.51473224551069308, 32.91557627198102409 ) ) ;
#191385 = CARTESIAN_POINT ( 'NONE',  ( 13.89961937509977652, -13.97604488694527269, 88.12390960531438111 ) ) ;
#191386 = CARTESIAN_POINT ( 'NONE',  ( -10.72451020669870658, -18.67979575497194134, 54.58442372801901143 ) ) ;
#191387 = CARTESIAN_POINT ( 'NONE',  ( -5.049401038298153566, 19.05341960407611168, 35.20724293864768839 ) ) ;
#191388 = CARTESIAN_POINT ( 'NONE',  ( 5.823673210054444382, -21.52544592524334988, 70.20942372801904696 ) ) ;
#191390 = CARTESIAN_POINT ( 'NONE',  ( -16.46253265017160317, 9.564922557960807481, 105.8322429386476955 ) ) ;
#191389 = CARTESIAN_POINT ( 'NONE',  ( 5.153800228976615827, -19.02544592524334988, 90.20942372801900433 ) ) ;
#191391 = CARTESIAN_POINT ( 'NONE',  ( -16.53943276465976808, 0.05219959533911058130, 111.2489096053143669 ) ) ;
#191392 = CARTESIAN_POINT ( 'NONE',  ( 21.52544592524344225, -5.823673210054117533, 113.5405762719810383 ) ) ;
#191393 = CARTESIAN_POINT ( 'NONE',  ( 9.474510206698729675, 16.51473224551082808, 32.08442372801900433 ) ) ;
#191394 = CARTESIAN_POINT ( 'NONE',  ( 4.483927247898545687, 16.52544592524342804, 114.7905762719810383 ) ) ;
#191395 = CARTESIAN_POINT ( 'NONE',  ( -9.564922557960796823, -16.46253265017161027, 62.08224293864769550 ) ) ;
#191396 = CARTESIAN_POINT ( 'NONE',  ( -19.03943276465977164, -0.05219959533935918106, 93.75109039468566152 ) ) ;
#191397 = CARTESIAN_POINT ( 'NONE',  ( 14.29746914071049879, -8.314922557960816363, 63.33224293864770260 ) ) ;
#191398 = CARTESIAN_POINT ( 'NONE',  ( 9.564922557961047289, -16.46253265017146816, 30.41775706135232937 ) ) ;
#191399 = CARTESIAN_POINT ( 'NONE',  ( -5.823673210054116645, -21.52544592524344225, 22.29057627198102765 ) ) ;
#191400 = CARTESIAN_POINT ( 'NONE',  ( 19.05341960407617918, -5.049401038297876454, 86.04275706135233293 ) ) ;
#191401 = CARTESIAN_POINT ( 'NONE',  ( 5.823673210054125526, 21.52544592524343514, 94.79057627198105251 ) ) ;
#191402 = CARTESIAN_POINT ( 'NONE',  ( -10.72451020669870658, -18.67979575497194134, 49.58442372801901143 ) ) ;
#191403 = CARTESIAN_POINT ( 'NONE',  ( 12.06949235617739724, 12.14591786802326823, 36.87609039468568994 ) ) ;
#191405 = CARTESIAN_POINT ( 'NONE',  ( -15.72974639402176322, -15.80617190586768395, 49.37609039468569705 ) ) ;
#191404 = CARTESIAN_POINT ( 'NONE',  ( -12.14591786802326823, 12.06949235617739902, 38.12609039468567573 ) ) ;
#191406 = CARTESIAN_POINT ( 'NONE',  ( 21.53943276465977519, -0.05219959533907433946, 58.74890960531436690 ) ) ;
#191407 =( BOUNDED_CURVE ( )  B_SPLINE_CURVE ( 2, ( #100409, #191423, #72080, #39737, #6393, #86244, #162090, #68072, #195448, #85233, #133754 ),
 .UNSPECIFIED., .F., .T. ) 
 B_SPLINE_CURVE_WITH_KNOTS ( ( 3, 2, 2, 2, 2, 3 ),
 ( 0.3000000000000000444, 0.3200000000000000622, 0.3400000000000000799, 0.3599999999999999867, 0.3800000000000000044, 0.4000000000000000222 ),
 .UNSPECIFIED. ) 
 CURVE ( )  GEOMETRIC_REPRESENTATION_ITEM ( )  RATIONAL_B_SPLINE_CURVE ( ( 0.9999999999999998890, 0.9510565162951536422, 1.000000000000000000, 0.9510565162951535312, 1.000000000000000000, 0.9510565162951535312, 1.000000000000000000, 0.9510565162951535312, 1.000000000000000000, 0.9510565162951535312, 1.000000000000000000 ) ) 
 REPRESENTATION_ITEM ( '' )  );
#191408 = CARTESIAN_POINT ( 'NONE',  ( 13.89961937509977652, -13.97604488694527269, 33.12390960531434558 ) ) ;
#191409 = CARTESIAN_POINT ( 'NONE',  ( 30.74264578624800137, -22.33583958711395212, -6.949999994537627401 ) ) ;
#191410 = CARTESIAN_POINT ( 'NONE',  ( 16.53943276465976808, 0.05219959533934440121, 76.25109039468568994 ) ) ;
#191411 = CARTESIAN_POINT ( 'NONE',  ( 18.62759615963271287, -10.81492255796078972, 93.33224293864769550 ) ) ;
#191412 = CARTESIAN_POINT ( 'NONE',  ( 14.34966873604960469, 8.224510206698951720, 39.16557627198102409 ) ) ;
#191413 = CARTESIAN_POINT ( 'NONE',  ( -4.483927247898782831, 16.52544592524335698, 57.70942372801901143 ) ) ;
#191414 = CARTESIAN_POINT ( 'NONE',  ( -16.46253265017146816, -9.564922557961047289, 99.16775706135233293 ) ) ;
#191415 = CARTESIAN_POINT ( 'NONE',  ( -5.823673210054116645, -21.52544592524344225, 92.29057627198103830 ) ) ;
#191416 = CARTESIAN_POINT ( 'NONE',  ( 14.29746914071049879, -8.314922557960816363, 28.33224293864769550 ) ) ;
#191417 = VERTEX_POINT ( 'NONE', #67034 ) ;
#191418 = CARTESIAN_POINT ( 'NONE',  ( -4.483927247898782831, 16.52544592524335698, 72.70942372801901854 ) ) ;
#191419 = CARTESIAN_POINT ( 'NONE',  ( 24.06609220500514468, 14.38661408136930753, 165.8682408874382475 ) ) ;
#191420 = CARTESIAN_POINT ( 'NONE',  ( 0.05219959533907565091, 21.53943276465977519, 69.99890960531435269 ) ) ;
#191421 = CARTESIAN_POINT ( 'NONE',  ( 16.53943276465976808, 0.05219959533934440121, 106.2510903946856757 ) ) ;
#191422 = ORIENTED_EDGE ( 'NONE', *, *, #55329, .F. ) ;
#191423 = CARTESIAN_POINT ( 'NONE',  ( 37.99999999999998579, -12.34694845685043951, -3.100000000000000977 ) ) ;
#191424 = CARTESIAN_POINT ( 'NONE',  ( 15.72974639402199770, -15.80617190586745480, 108.1239096053143811 ) ) ;
#191425 = CARTESIAN_POINT ( 'NONE',  ( 5.823673210054125526, 21.52544592524343514, 109.7905762719810383 ) ) ;
#191426 = CARTESIAN_POINT ( 'NONE',  ( -4.483927247898539470, -16.52544592524342804, 42.29057627198103120 ) ) ;
#191427 = CARTESIAN_POINT ( 'NONE',  ( -16.55341960407617563, 4.379528057220093196, 33.54275706135234714 ) ) ;
#191428 = CARTESIAN_POINT ( 'NONE',  ( -9.564922557960796823, -16.46253265017161027, 47.08224293864769550 ) ) ;
#191429 = CARTESIAN_POINT ( 'NONE',  ( -16.51473224551069308, -9.474510206698971260, 61.66557627198103120 ) ) ;
#191430 = CARTESIAN_POINT ( 'NONE',  ( -16.46253265017160317, 9.564922557960807481, 110.8322429386476955 ) ) ;
#191431 = CARTESIAN_POINT ( 'NONE',  ( -9.553523354579670723, -9.835363051420090486, -62.57666384180342334 ) ) ;
#191432 = CARTESIAN_POINT ( 'NONE',  ( -13.89961937509957401, -13.97604488694547875, 104.3760903946856757 ) ) ;
#191433 = CARTESIAN_POINT ( 'NONE',  ( -0.05219959533936034679, 19.03943276465977164, 57.50109039468566863 ) ) ;
#191434 = CARTESIAN_POINT ( 'NONE',  ( -21.52544592524343514, 5.823673210054127303, 86.04057627198102409 ) ) ;
#191435 = CARTESIAN_POINT ( 'NONE',  ( -8.314922557960811034, -14.29746914071050412, 27.08224293864769550 ) ) ;
#191436 = AXIS2_PLACEMENT_3D ( 'NONE', #77182, #137866, #30694 ) ;
#191437 = CARTESIAN_POINT ( 'NONE',  ( -21.53943276465977519, 0.05219959533907696930, 46.24890960531435979 ) ) ;
#191439 = CARTESIAN_POINT ( 'NONE',  ( 9.474510206698729675, 16.51473224551082808, 107.0844237280190043 ) ) ;
#191438 = CARTESIAN_POINT ( 'NONE',  ( 5.719274019375991003, -21.55341960407610458, 77.70724293864770971 ) ) ;
#191440 = CARTESIAN_POINT ( 'NONE',  ( -13.89961937509977652, 13.97604488694528158, 115.6239096053143669 ) ) ;
#191441 = CARTESIAN_POINT ( 'NONE',  ( 21.55341960407619695, -5.719274019375665929, 71.04275706135234714 ) ) ;
#191442 = CARTESIAN_POINT ( 'NONE',  ( 16.46253265017160672, -9.564922557960803928, 73.33224293864769550 ) ) ;
#191443 = CARTESIAN_POINT ( 'NONE',  ( 31.64616484836359334, 2.655180720736611377, 102.0186121717492682 ) ) ;
#191444 = CARTESIAN_POINT ( 'NONE',  ( 13.89961937509977652, -13.97604488694527269, 73.12390960531436690 ) ) ;
#191445 = CARTESIAN_POINT ( 'NONE',  ( 4.379528057220339221, -16.55341960407611168, 92.70724293864770971 ) ) ;
#191446 = EDGE_LOOP ( 'NONE', ( #2420, #18691, #102472, #171584, #5530, #134616, #108033, #161324, #193042, #67077, #35927, #3234, #34390, #55209 ) ) ;
#191447 = CARTESIAN_POINT ( 'NONE',  ( -9.564922557961040184, 16.46253265017147172, 102.9177570613523329 ) ) ;
#191448 = DIRECTION ( 'NONE',  ( -1.000000000000000000, 0.000000000000000000, 0.000000000000000000 ) ) ;
#191449 = CARTESIAN_POINT ( 'NONE',  ( -16.51473224551069308, -9.474510206698971260, 76.66557627198103830 ) ) ;
#191451 = CARTESIAN_POINT ( 'NONE',  ( -16.46253265017160317, 9.564922557960807481, 95.83224293864769550 ) ) ;
#191450 = CARTESIAN_POINT ( 'NONE',  ( -18.62759615963255300, -10.81492255796106328, 79.16775706135234714 ) ) ;
#191452 = CARTESIAN_POINT ( 'NONE',  ( 12.06949235617739724, 12.14591786802326823, 71.87609039468568994 ) ) ;
#191453 = CARTESIAN_POINT ( 'NONE',  ( -17.49999999999999289, -5.624438216177582994, 74.18329655085356933 ) ) ;
#191454 = CARTESIAN_POINT ( 'NONE',  ( 19.05341960407617918, -5.049401038297876454, 61.04275706135232582 ) ) ;
#191455 = CARTESIAN_POINT ( 'NONE',  ( -18.62759615963255300, -10.81492255796106328, 109.1677570613523613 ) ) ;
#191456 = CARTESIAN_POINT ( 'NONE',  ( 37.54602941011386719, 1.427078192699139159, 39.68530545529165465 ) ) ;
#191457 = CARTESIAN_POINT ( 'NONE',  ( -29.86685920354755197, -21.69954338932560134, -6.924999997268813878 ) ) ;
#191458 = CARTESIAN_POINT ( 'NONE',  ( 12.14591786802309770, 12.06949235617756955, 24.37390960531435979 ) ) ;
#191459 = CARTESIAN_POINT ( 'NONE',  ( -35.70266437024450568, -5.510913496957479854E-15, 37.50000000000000000 ) ) ;
#191460 = CARTESIAN_POINT ( 'NONE',  ( -12.06949235617739369, -12.14591786802326823, 109.3760903946857042 ) ) ;
#191461 = CARTESIAN_POINT ( 'NONE',  ( 16.21995358207305671, 7.366697692864118352, 67.56448998487842061 ) ) ;
#191462 = CARTESIAN_POINT ( 'NONE',  ( -4.379528057220086978, -16.55341960407618274, 84.79275706135234714 ) ) ;
#191463 = CARTESIAN_POINT ( 'NONE',  ( 18.67979575497194134, -10.72451020669871369, 85.83442372801901854 ) ) ;
#191464 = CARTESIAN_POINT ( 'NONE',  ( 19.05341960407617918, -5.049401038297876454, 91.04275706135234714 ) ) ;
#191465 = CARTESIAN_POINT ( 'NONE',  ( 9.564922557961047289, -16.46253265017146816, 45.41775706135232582 ) ) ;
#191466 = CARTESIAN_POINT ( 'NONE',  ( -9.474510206698964154, 16.51473224551069663, 85.41557627198102409 ) ) ;
#191467 = CARTESIAN_POINT ( 'NONE',  ( -16.46253265017160317, 9.564922557960807481, 50.83224293864770260 ) ) ;
#191468 = CARTESIAN_POINT ( 'NONE',  ( -19.36337904590690684, 5.499999999999948486, 40.41494137495620720 ) ) ;
#191469 = CARTESIAN_POINT ( 'NONE',  ( 15.80617190586746368, 15.72974639402197994, 89.37390960531435269 ) ) ;
#191470 = CARTESIAN_POINT ( 'NONE',  ( 21.53943276465977519, -0.05219959533907433946, 43.74890960531435979 ) ) ;
#191471 = CARTESIAN_POINT ( 'NONE',  ( -16.51473224551069308, -9.474510206698971260, 46.66557627198102409 ) ) ;
#191472 = CARTESIAN_POINT ( 'NONE',  ( 16.55341960407618274, -4.379528057220086978, 66.04275706135236135 ) ) ;
#191473 = UNCERTAINTY_MEASURE_WITH_UNIT (LENGTH_MEASURE( 1.000000000000000082E-05 ), #167752, 'distance_accuracy_value', 'NONE');
#191474 = VERTEX_POINT ( 'NONE', #160043 ) ;
#191475 = CARTESIAN_POINT ( 'NONE',  ( 5.823673210054444382, -21.52544592524334988, 45.20942372801901854 ) ) ;
#191477 = CARTESIAN_POINT ( 'NONE',  ( -29.86685920354755197, -21.69954338932560134, -10.42499999726881299 ) ) ;
#191476 = CARTESIAN_POINT ( 'NONE',  ( 12.06949235617757843, -12.14591786802309237, 63.12390960531435979 ) ) ;
#191478 = CARTESIAN_POINT ( 'NONE',  ( 0.05219959533934541429, -16.53943276465976808, 35.00109039468568284 ) ) ;
#191479 = CARTESIAN_POINT ( 'NONE',  ( 14.29746914071049879, -8.314922557960816363, 103.3322429386476955 ) ) ;
#191480 = CARTESIAN_POINT ( 'NONE',  ( -13.89961937509957401, -13.97604488694547875, 54.37609039468565442 ) ) ;
#191481 = CARTESIAN_POINT ( 'NONE',  ( -4.379528057220328563, 16.55341960407611168, 70.20724293864769550 ) ) ;
#191482 = CARTESIAN_POINT ( 'NONE',  ( -0.05219959533937732626, 21.53943276465977519, 27.50109039468567929 ) ) ;
#191484 = CARTESIAN_POINT ( 'NONE',  ( -5.823673210054116645, -21.52544592524344225, 87.29057627198103830 ) ) ;
#191483 = CARTESIAN_POINT ( 'NONE',  ( -0.05219959533909027116, -19.03943276465977164, 22.49890960531436690 ) ) ;
#191485 = CARTESIAN_POINT ( 'NONE',  ( 13.97604488694527802, 13.89961937509977652, 99.37390960531436690 ) ) ;
#191486 = CARTESIAN_POINT ( 'NONE',  ( -16.53943276465976808, 0.05219959533911058130, 71.24890960531435269 ) ) ;
#191487 = CARTESIAN_POINT ( 'NONE',  ( -19.03943276465977164, 0.05219959533909376836, 116.2489096053143669 ) ) ;
#191488 = CARTESIAN_POINT ( 'NONE',  ( 36.91746824999999887, -11.99521256947793546, -1.724999997268813479 ) ) ;
#191489 = CARTESIAN_POINT ( 'NONE',  ( 13.89961937509957401, 13.97604488694547697, 81.87609039468564731 ) ) ;
#191490 = CARTESIAN_POINT ( 'NONE',  ( 18.62759615963255655, 10.81492255796105972, 21.66775706135235069 ) ) ;
#191491 = CARTESIAN_POINT ( 'NONE',  ( 9.564922557960805705, 16.46253265017160317, 64.58224293864769550 ) ) ;
#191492 = CARTESIAN_POINT ( 'NONE',  ( 9.474510206698729675, 16.51473224551082808, 52.08442372801900433 ) ) ;
#191493 = CARTESIAN_POINT ( 'NONE',  ( 9.474510206698971260, -16.51473224551069308, 32.91557627198102409 ) ) ;
#191494 =( REPRESENTATION_RELATIONSHIP ('NONE','NONE', #154205, #85690 ) REPRESENTATION_RELATIONSHIP_WITH_TRANSFORMATION ( #83598 )SHAPE_REPRESENTATION_RELATIONSHIP( ) );
#191495 = EDGE_CURVE ( 'NONE', #133171, #122538, #110382, .T. ) ;
#191496 = CARTESIAN_POINT ( 'NONE',  ( 15.80617190586769283, -15.72974639402175789, 75.62609039468567573 ) ) ;
#191497 = CARTESIAN_POINT ( 'NONE',  ( 8.224510206698953496, -14.34966873604960469, 62.91557627198102409 ) ) ;
#191498 = CARTESIAN_POINT ( 'NONE',  ( 14.29746914071049879, -8.314922557960816363, 58.33224293864768839 ) ) ;
#191499 = CARTESIAN_POINT ( 'NONE',  ( 13.89961937509977652, -13.97604488694527269, 68.12390960531436690 ) ) ;
#191500 = CARTESIAN_POINT ( 'NONE',  ( -18.67979575497178146, -10.72451020669898902, 86.66557627198102409 ) ) ;
#191501 = CARTESIAN_POINT ( 'NONE',  ( -13.97604488694527625, -13.89961937509977652, 56.87390960531434558 ) ) ;
#191502 = ORIENTED_EDGE ( 'NONE', *, *, #49707, .T. ) ;
#191503 = CARTESIAN_POINT ( 'NONE',  ( -10.72451020669898014, 18.67979575497178502, 80.41557627198103830 ) ) ;
#191504 = CARTESIAN_POINT ( 'NONE',  ( -0.05219959533937732626, 21.53943276465977519, 97.50109039468567573 ) ) ;
#191507 = CARTESIAN_POINT ( 'NONE',  ( -16.52544592524342804, 4.483927247898546575, 101.0405762719810383 ) ) ;
#191506 = CARTESIAN_POINT ( 'NONE',  ( 16.52544592524335698, 4.483927247898782831, 96.45942372801901854 ) ) ;
#191505 = DIRECTION ( 'NONE',  ( -0.000000000000000000, 0.000000000000000000, -1.000000000000000000 ) ) ;
#191508 = CARTESIAN_POINT ( 'NONE',  ( -13.89961937509957401, -13.97604488694547875, 94.37609039468566152 ) ) ;
#191509 = ORIENTED_EDGE ( 'NONE', *, *, #141668, .T. ) ;
#191510 = CARTESIAN_POINT ( 'NONE',  ( 15.80617190586746368, 15.72974639402197994, 109.3739096053143811 ) ) ;
#191511 = CARTESIAN_POINT ( 'NONE',  ( -5.153800228976607833, 19.02544592524334988, 57.70942372801899012 ) ) ;
#191512 = CARTESIAN_POINT ( 'NONE',  ( 8.314922557961029526, -14.29746914071037800, 105.4177570613523613 ) ) ;
#191513 = CARTESIAN_POINT ( 'NONE',  ( -13.97604488694547697, 13.89961937509957934, 28.12609039468565797 ) ) ;
#191514 = CARTESIAN_POINT ( 'NONE',  ( -9.564922557960796823, -16.46253265017161027, 97.08224293864769550 ) ) ;
#191515 = CARTESIAN_POINT ( 'NONE',  ( -15.80617190586745835, -15.72974639402198527, 66.87390960531436690 ) ) ;
#191516 = CARTESIAN_POINT ( 'NONE',  ( 1.300000000000000044, -0.7216878364870318308, -1.250000000000000000 ) ) ;
#191517 = CARTESIAN_POINT ( 'NONE',  ( 16.51473224551069308, 9.474510206698969483, 29.16557627198103475 ) ) ;
#191518 = CARTESIAN_POINT ( 'NONE',  ( -13.89961937509957401, -13.97604488694547875, 19.37609039468566507 ) ) ;
#191519 = CARTESIAN_POINT ( 'NONE',  ( 4.483927247898790824, -16.52544592524335698, 70.20942372801904696 ) ) ;
#191520 = CARTESIAN_POINT ( 'NONE',  ( -18.62759615963255300, -10.81492255796106328, 24.16775706135235424 ) ) ;
#191521 = CARTESIAN_POINT ( 'NONE',  ( 4.483927247898790824, -16.52544592524335698, 50.20942372801901854 ) ) ;
#191522 = CARTESIAN_POINT ( 'NONE',  ( -5.049401038298153566, 19.05341960407611168, 100.2072429386476955 ) ) ;
#191523 = CARTESIAN_POINT ( 'NONE',  ( 19.05341960407611168, 5.049401038298154454, 48.95724293864768129 ) ) ;
#191524 = CARTESIAN_POINT ( 'NONE',  ( -13.89961937509977652, 13.97604488694528158, 65.62390960531436690 ) ) ;
#191525 = CARTESIAN_POINT ( 'NONE',  ( 14.34966873604972726, -8.224510206698740333, 50.83442372801901143 ) ) ;
#191526 = CARTESIAN_POINT ( 'NONE',  ( -12.06949235617756955, 12.14591786802309770, 90.62390960531436690 ) ) ;
#191527 = CARTESIAN_POINT ( 'NONE',  ( -16.52544592524335698, -4.483927247898792601, 103.9594237280190185 ) ) ;
#191528 = FACE_OUTER_BOUND ( 'NONE', #185943, .T. ) ;
#191531 = CARTESIAN_POINT ( 'NONE',  ( -19.05341960407611168, -5.049401038298163336, 61.45724293864769550 ) ) ;
#191530 = CARTESIAN_POINT ( 'NONE',  ( -0.05219959533909027116, -19.03943276465977164, 82.49890960531436690 ) ) ;
#191529 = CARTESIAN_POINT ( 'NONE',  ( 10.81492255796106328, -18.62759615963255655, 60.41775706135235424 ) ) ;
#191532 = CARTESIAN_POINT ( 'NONE',  ( -9.474510206698964154, 16.51473224551069663, 90.41557627198103830 ) ) ;
#191533 = CARTESIAN_POINT ( 'NONE',  ( -14.29746914071049879, 8.314922557960819915, 40.83224293864769550 ) ) ;
#191534 = CARTESIAN_POINT ( 'NONE',  ( -14.29746914071037622, -8.314922557961029526, 94.16775706135237556 ) ) ;
#191535 = CARTESIAN_POINT ( 'NONE',  ( 12.06949235617757843, -12.14591786802309237, 38.12390960531436690 ) ) ;
#191536 = ORIENTED_EDGE ( 'NONE', *, *, #199845, .F. ) ;
#191537 = CARTESIAN_POINT ( 'NONE',  ( 16.51473224551083163, -9.474510206698727899, 45.83442372801900433 ) ) ;
#191538 = CARTESIAN_POINT ( 'NONE',  ( 16.46253265017160672, -9.564922557960803928, 113.3322429386476955 ) ) ;
#191539 = CARTESIAN_POINT ( 'NONE',  ( -13.97604488694527625, -13.89961937509977652, 66.87390960531436690 ) ) ;
#191540 = CARTESIAN_POINT ( 'NONE',  ( -9.474510206698720793, -16.51473224551083518, 39.58442372801899722 ) ) ;
#191541 = CARTESIAN_POINT ( 'NONE',  ( -36.91746825000000598, 2.428612866367529932E-14, -9.124999997268814056 ) ) ;
#191542 = DIRECTION ( 'NONE',  ( 0.5000000000000037748, 0.4999999999999949485, 0.7071067811865484609 ) ) ;
#191544 = CARTESIAN_POINT ( 'NONE',  ( 12.14591786802327356, -12.06949235617739191, 75.62609039468567573 ) ) ;
#191543 = CARTESIAN_POINT ( 'NONE',  ( 9.564922557961047289, -16.46253265017146816, 90.41775706135234714 ) ) ;
#191545 = CARTESIAN_POINT ( 'NONE',  ( 16.62475595723697808, 7.163666690055314312, 91.97286648189532343 ) ) ;
#191546 = CARTESIAN_POINT ( 'NONE',  ( 9.564922557960805705, 16.46253265017160317, 89.58224293864769550 ) ) ;
#191547 = CARTESIAN_POINT ( 'NONE',  ( 21.53943276465977519, 0.05219959533937863772, 26.25109039468567573 ) ) ;
#191548 = CARTESIAN_POINT ( 'NONE',  ( 19.03943276465977164, 0.05219959533936151252, 71.25109039468566152 ) ) ;
#191550 = CARTESIAN_POINT ( 'NONE',  ( -9.564922557960796823, -16.46253265017161027, 52.08224293864768839 ) ) ;
#191549 = CARTESIAN_POINT ( 'NONE',  ( 17.44279575226822132, 5.990770900252481823, 86.66442432485682446 ) ) ;
#191551 = CARTESIAN_POINT ( 'NONE',  ( -9.564922557960796823, -16.46253265017161027, 92.08224293864769550 ) ) ;
#191553 = CARTESIAN_POINT ( 'NONE',  ( 19.02544592524343514, -5.153800228976328945, 38.54057627198103120 ) ) ;
#191552 = CARTESIAN_POINT ( 'NONE',  ( 14.34966873604960469, 8.224510206698951720, 49.16557627198102409 ) ) ;
#191554 = CARTESIAN_POINT ( 'NONE',  ( -13.97604488694547697, 13.89961937509957934, 53.12609039468565442 ) ) ;
#191555 = CARTESIAN_POINT ( 'NONE',  ( 4.379528057220339221, -16.55341960407611168, 82.70724293864770971 ) ) ;
#191556 = CARTESIAN_POINT ( 'NONE',  ( -13.89961937509957401, -13.97604488694547875, 24.37609039468565442 ) ) ;
#191557 = CARTESIAN_POINT ( 'NONE',  ( 19.03943276465977164, -0.05219959533909143690, 68.74890960531436690 ) ) ;
#191558 = CARTESIAN_POINT ( 'NONE',  ( 15.80617190586746368, 15.72974639402197994, 64.37390960531435269 ) ) ;
#191560 = CARTESIAN_POINT ( 'NONE',  ( -5.153800228976607833, 19.02544592524334988, 22.70942372801899012 ) ) ;
#191559 = CARTESIAN_POINT ( 'NONE',  ( 8.314922557960818139, 14.29746914071049879, 49.58224293864769550 ) ) ;
#191561 = CARTESIAN_POINT ( 'NONE',  ( -5.153800228976328057, -19.02544592524343514, 102.2905762719810383 ) ) ;
#191562 = CARTESIAN_POINT ( 'NONE',  ( 10.81492255796078972, 18.62759615963270932, 29.58224293864769905 ) ) ;
#191563 = CARTESIAN_POINT ( 'NONE',  ( -9.474510206698964154, 16.51473224551069663, 55.41557627198103120 ) ) ;
#191564 = CARTESIAN_POINT ( 'NONE',  ( -5.049401038298153566, 19.05341960407611168, 25.20724293864768484 ) ) ;
#191565 = CARTESIAN_POINT ( 'NONE',  ( 14.29746914071049879, -8.314922557960816363, 98.33224293864769550 ) ) ;
#191566 = CARTESIAN_POINT ( 'NONE',  ( 15.72974639402199770, -15.80617190586745480, 108.1239096053143811 ) ) ;
#191567 = CARTESIAN_POINT ( 'NONE',  ( 13.97604488694527802, 13.89961937509977652, 104.3739096053143385 ) ) ;
#191568 = CARTESIAN_POINT ( 'NONE',  ( 5.719274019375991003, -21.55341960407610458, 107.7072429386476955 ) ) ;
#191569 = CARTESIAN_POINT ( 'NONE',  ( 16.51473224551069308, 9.474510206698969483, 109.1655762719810383 ) ) ;
#191570 = CARTESIAN_POINT ( 'NONE',  ( -4.483927247898539470, -16.52544592524342804, 112.2905762719810241 ) ) ;
#191571 = CARTESIAN_POINT ( 'NONE',  ( 10.81492255796106328, -18.62759615963255655, 80.41775706135234714 ) ) ;
#191572 = CARTESIAN_POINT ( 'NONE',  ( 0.05219959533907565091, 21.53943276465977519, 89.99890960531438111 ) ) ;
#191573 = EDGE_CURVE ( 'NONE', #124248, #145335, #178101, .T. ) ;
#191574 = CARTESIAN_POINT ( 'NONE',  ( 17.26058549869091507, -6.457015423128527942, 106.1225416252393501 ) ) ;
#191575 = CARTESIAN_POINT ( 'NONE',  ( 19.48894818550246555, -5.499999999999912070, 77.60307310435240424 ) ) ;
#191576 = CARTESIAN_POINT ( 'NONE',  ( 16.51473224551069308, 9.474510206698969483, 59.16557627198102409 ) ) ;
#191577 = CARTESIAN_POINT ( 'NONE',  ( 12.06949235617739724, 12.14591786802326823, 41.87609039468568284 ) ) ;
#191578 = CARTESIAN_POINT ( 'NONE',  ( -14.34966873604960291, -8.224510206698953496, 106.6655762719810383 ) ) ;
#191579 = CYLINDRICAL_SURFACE ( 'NONE', #70961, 61.99999999999998579 ) ;
#191580 = CARTESIAN_POINT ( 'NONE',  ( -13.89961937509977652, 13.97604488694528158, 60.62390960531436690 ) ) ;
#191581 = CARTESIAN_POINT ( 'NONE',  ( -12.14591786802309592, -12.06949235617757132, 91.87390960531436690 ) ) ;
#191582 = AXIS2_PLACEMENT_3D ( 'NONE', #4543, #130897, #83386 ) ;
#191583 = CARTESIAN_POINT ( 'NONE',  ( -18.62759615963270932, 10.81492255796079327, 30.83224293864770260 ) ) ;
#191584 = CARTESIAN_POINT ( 'NONE',  ( -12.06949235617756955, 12.14591786802309770, 65.62390960531436690 ) ) ;
#191585 = CARTESIAN_POINT ( 'NONE',  ( -9.564922557961040184, 16.46253265017147172, 112.9177570613523329 ) ) ;
#191586 = CARTESIAN_POINT ( 'NONE',  ( -0.05219959533937732626, 21.53943276465977519, 67.50109039468568994 ) ) ;
#191587 = CARTESIAN_POINT ( 'NONE',  ( 18.22780087662122739, 5.500000000000000888, 66.48236817873106475 ) ) ;
#191588 = CARTESIAN_POINT ( 'NONE',  ( -8.224510206698735004, -14.34966873604973081, 99.58442372801900433 ) ) ;
#191589 = CARTESIAN_POINT ( 'NONE',  ( -16.52544592524342804, 4.483927247898546575, 41.04057627198103120 ) ) ;
#191590 = CARTESIAN_POINT ( 'NONE',  ( -19.03943276465977164, 0.05219959533909376836, 36.24890960531436690 ) ) ;
#191591 = CARTESIAN_POINT ( 'NONE',  ( -13.89961937509977652, 13.97604488694528158, 90.62390960531432427 ) ) ;
#191592 = CARTESIAN_POINT ( 'NONE',  ( -5.719274019375978568, 21.55341960407610458, 95.20724293864769550 ) ) ;
#191593 = CARTESIAN_POINT ( 'NONE',  ( 12.14591786802327356, -12.06949235617739191, 20.62609039468568639 ) ) ;
#191595 = CARTESIAN_POINT ( 'NONE',  ( -18.62759615963255300, -10.81492255796106328, 69.16775706135234714 ) ) ;
#191594 = CARTESIAN_POINT ( 'NONE',  ( -16.55341960407611168, -4.379528057220339221, 61.45724293864770260 ) ) ;
#191596 = CARTESIAN_POINT ( 'NONE',  ( -0.05219959533934338120, 16.53943276465976808, 102.5010903946856899 ) ) ;
#191597 = CARTESIAN_POINT ( 'NONE',  ( 17.44279575226823553, 5.990770900252484488, 26.66442432485683156 ) ) ;
#191598 = PLANE ( 'NONE',  #142262 ) ;
#191599 = CARTESIAN_POINT ( 'NONE',  ( -4.379528057220328563, 16.55341960407611168, 30.20724293864769550 ) ) ;
#191600 = CARTESIAN_POINT ( 'NONE',  ( 16.53943276465976808, 0.05219959533934440121, 71.25109039468568994 ) ) ;
#191601 = CARTESIAN_POINT ( 'NONE',  ( 19.03943276465977164, -0.05219959533909143690, 83.74890960531436690 ) ) ;
#191602 = CARTESIAN_POINT ( 'NONE',  ( 9.474510206698971260, -16.51473224551069308, 82.91557627198103830 ) ) ;
#191603 = CARTESIAN_POINT ( 'NONE',  ( -10.72451020669870658, -18.67979575497194134, 84.58442372801903275 ) ) ;
#191604 = CARTESIAN_POINT ( 'NONE',  ( 0.05219959533934541429, -16.53943276465976808, 90.00109039468567573 ) ) ;
#191605 = CARTESIAN_POINT ( 'NONE',  ( -12.06949235617756955, 12.14591786802309770, 55.62390960531436690 ) ) ;
#191606 = CARTESIAN_POINT ( 'NONE',  ( 5.153800228976335163, 19.02544592524342804, 64.79057627198100988 ) ) ;
#191607 = ORIENTED_EDGE ( 'NONE', *, *, #98059, .F. ) ;
#191608 = CARTESIAN_POINT ( 'NONE',  ( 16.51473224551083163, -9.474510206698727899, 110.8344237280190043 ) ) ;
#191609 = CARTESIAN_POINT ( 'NONE',  ( 16.55341960407611168, 4.379528057220329451, 108.9572429386476955 ) ) ;
#191610 = CARTESIAN_POINT ( 'NONE',  ( 9.474510206698971260, -16.51473224551069308, 82.91557627198103830 ) ) ;
#191612 = CARTESIAN_POINT ( 'NONE',  ( -36.91746825000000598, 2.428612866367529932E-14, -10.62499999726881406 ) ) ;
#191611 = CARTESIAN_POINT ( 'NONE',  ( -16.53943276465976808, -0.05219959533934237506, 18.75109039468568639 ) ) ;
#191613 = CARTESIAN_POINT ( 'NONE',  ( 21.55341960407619695, -5.719274019375665929, 111.0427570613523613 ) ) ;
#191614 = CARTESIAN_POINT ( 'NONE',  ( 16.53943276465976808, 0.05219959533934440121, 76.25109039468568994 ) ) ;
#191615 = CARTESIAN_POINT ( 'NONE',  ( -19.05341960407617563, 5.049401038297882671, 98.54275706135233293 ) ) ;
#191616 = CARTESIAN_POINT ( 'NONE',  ( -16.51473224551069308, -9.474510206698971260, 21.66557627198102765 ) ) ;
#191617 = CARTESIAN_POINT ( 'NONE',  ( -4.483927247898782831, 16.52544592524335698, 72.70942372801901854 ) ) ;
#191618 = CARTESIAN_POINT ( 'NONE',  ( -16.52544592524335698, -4.483927247898792601, 58.95942372801902565 ) ) ;
#191619 = PLANE ( 'NONE',  #44177 ) ;
#191620 = CARTESIAN_POINT ( 'NONE',  ( 5.049401038297881783, 19.05341960407617563, 57.29275706135231871 ) ) ;
#191621 = CARTESIAN_POINT ( 'NONE',  ( 10.81492255796106328, -18.62759615963255655, 95.41775706135234714 ) ) ;
#191622 = CARTESIAN_POINT ( 'NONE',  ( 19.02544592524343514, -5.153800228976328945, 28.54057627198102409 ) ) ;
#191623 = CARTESIAN_POINT ( 'NONE',  ( 5.049401038298161559, -19.05341960407611168, 82.70724293864770971 ) ) ;
#191624 = CARTESIAN_POINT ( 'NONE',  ( -14.29746914071049879, 8.314922557960819915, 70.83224293864770971 ) ) ;
#191625 = CARTESIAN_POINT ( 'NONE',  ( -10.81492255796105439, 18.62759615963255655, 87.91775706135234714 ) ) ;
#191626 = CARTESIAN_POINT ( 'NONE',  ( 5.049401038297881783, 19.05341960407617563, 62.29275706135234003 ) ) ;
#191627 = CARTESIAN_POINT ( 'NONE',  ( 19.03943276465977164, 0.05219959533936151252, 41.25109039468566152 ) ) ;
#191628 = CARTESIAN_POINT ( 'NONE',  ( -5.823673210054116645, -21.52544592524344225, 37.29057627198102409 ) ) ;
#191629 = CARTESIAN_POINT ( 'NONE',  ( -18.67979575497193778, 10.72451020669871902, 108.3344237280190185 ) ) ;
#191630 = CARTESIAN_POINT ( 'NONE',  ( -16.46253265017160317, 9.564922557960807481, 80.83224293864769550 ) ) ;
#191631 = CARTESIAN_POINT ( 'NONE',  ( -5.823673210054431948, 21.52544592524334988, 107.7094237280190328 ) ) ;
#191632 = CARTESIAN_POINT ( 'NONE',  ( 15.80617190586746368, 15.72974639402197994, 44.37390960531435979 ) ) ;
#191633 = CARTESIAN_POINT ( 'NONE',  ( 19.02544592524343514, -5.153800228976328945, 98.54057627198100988 ) ) ;
#191634 = CARTESIAN_POINT ( 'NONE',  ( 13.97604488694548053, -13.89961937509957401, 80.62609039468567573 ) ) ;
#191635 = CARTESIAN_POINT ( 'NONE',  ( 5.049401038298161559, -19.05341960407611168, 102.7072429386476955 ) ) ;
#191636 = CARTESIAN_POINT ( 'NONE',  ( 9.564922557961047289, -16.46253265017146816, 95.41775706135233293 ) ) ;
#191637 = CARTESIAN_POINT ( 'NONE',  ( -4.483927247898782831, 16.52544592524335698, 42.70942372801901854 ) ) ;
#191638 = CARTESIAN_POINT ( 'NONE',  ( -16.55341960407611168, -4.379528057220339221, 96.45724293864770971 ) ) ;
#191639 = CARTESIAN_POINT ( 'NONE',  ( -9.474510206698964154, 16.51473224551069663, 80.41557627198103830 ) ) ;
#191640 = CARTESIAN_POINT ( 'NONE',  ( -5.823673210054116645, -21.52544592524344225, 62.29057627198102409 ) ) ;
#191641 = CARTESIAN_POINT ( 'NONE',  ( 16.53943276465976808, 0.05219959533934440121, 26.25109039468567573 ) ) ;
#191642 = CARTESIAN_POINT ( 'NONE',  ( 0.05219959533937995610, -21.53943276465977519, 40.00109039468567573 ) ) ;
#191643 = CARTESIAN_POINT ( 'NONE',  ( 21.55341960407619695, -5.719274019375665929, 81.04275706135236135 ) ) ;
#191644 = CARTESIAN_POINT ( 'NONE',  ( 12.14591786802327356, -12.06949235617739191, 80.62609039468567573 ) ) ;
#191645 = VECTOR ( 'NONE', #141485, 1000.000000000000000 ) ;
#191646 = CARTESIAN_POINT ( 'NONE',  ( 13.89961937509977652, -13.97604488694527269, 73.12390960531436690 ) ) ;
#191647 = CARTESIAN_POINT ( 'NONE',  ( 14.34966873604960469, 8.224510206698951720, 79.16557627198103830 ) ) ;
#191648 = CARTESIAN_POINT ( 'NONE',  ( -8.224510206698948167, 14.34966873604960824, 25.41557627198103120 ) ) ;
#191649 = CARTESIAN_POINT ( 'NONE',  ( -19.05341960407617563, 5.049401038297882671, 53.54275706135231871 ) ) ;
#191650 = CARTESIAN_POINT ( 'NONE',  ( -21.53943276465977519, -0.05219959533937600094, 38.75109039468567573 ) ) ;
#191651 = CARTESIAN_POINT ( 'NONE',  ( 8.314922557960818139, 14.29746914071049879, 74.58224293864768129 ) ) ;
#191652 = CARTESIAN_POINT ( 'NONE',  ( 5.049401038298161559, -19.05341960407611168, 107.7072429386476955 ) ) ;
#191653 = CARTESIAN_POINT ( 'NONE',  ( 8.314922557961029526, -14.29746914071037800, 100.4177570613523471 ) ) ;
#191654 = CARTESIAN_POINT ( 'NONE',  ( -21.55341960407619339, 5.719274019375674811, 88.54275706135236135 ) ) ;
#191655 = CARTESIAN_POINT ( 'NONE',  ( -16.52544592524335698, -4.483927247898792601, 43.95942372801902565 ) ) ;
#191656 = CARTESIAN_POINT ( 'NONE',  ( 5.719274019375673035, 21.55341960407619339, 47.29275706135234003 ) ) ;
#191657 = ORIENTED_EDGE ( 'NONE', *, *, #7758, .F. ) ;
#191658 = CARTESIAN_POINT ( 'NONE',  ( 18.67979575497194134, -10.72451020669871369, 20.83442372801901143 ) ) ;
#191659 = CARTESIAN_POINT ( 'NONE',  ( -16.52544592524342804, 4.483927247898546575, 86.04057627198102409 ) ) ;
#191660 = CARTESIAN_POINT ( 'NONE',  ( 17.50000000000015987, -3.417042746626905103, 27.67380396232477580 ) ) ;
#191661 = CARTESIAN_POINT ( 'NONE',  ( 4.483927247898545687, 16.52544592524342804, 54.79057627198104541 ) ) ;
#191662 = CARTESIAN_POINT ( 'NONE',  ( 12.06949235617739724, 12.14591786802326823, 96.87609039468568994 ) ) ;
#191663 = CARTESIAN_POINT ( 'NONE',  ( 5.049401038298161559, -19.05341960407611168, 32.70724293864768129 ) ) ;
#191664 = CARTESIAN_POINT ( 'NONE',  ( -5.719274019375978568, 21.55341960407610458, 40.20724293864769550 ) ) ;
#191665 = CARTESIAN_POINT ( 'NONE',  ( 16.52544592524342804, -4.483927247898539470, 83.54057627198102409 ) ) ;
#191666 = CARTESIAN_POINT ( 'NONE',  ( -10.72451020669898014, 18.67979575497178502, 75.41557627198102409 ) ) ;
#191667 = CARTESIAN_POINT ( 'NONE',  ( -5.153800228976328057, -19.02544592524343514, 82.29057627198103830 ) ) ;
#191669 = CARTESIAN_POINT ( 'NONE',  ( -19.03943276465977164, -0.05219959533935918106, 88.75109039468567573 ) ) ;
#191668 = CARTESIAN_POINT ( 'NONE',  ( -9.564922557960796823, -16.46253265017161027, 37.08224293864768839 ) ) ;
#191670 = CARTESIAN_POINT ( 'NONE',  ( 5.719274019375991003, -21.55341960407610458, 32.70724293864770260 ) ) ;
#191671 = CARTESIAN_POINT ( 'NONE',  ( -21.52544592524334988, -5.823673210054445271, 58.95942372801902565 ) ) ;
#191672 = CARTESIAN_POINT ( 'NONE',  ( -0.05219959533909027116, -19.03943276465977164, 47.49890960531435979 ) ) ;
#191673 = CARTESIAN_POINT ( 'NONE',  ( -19.02544592524342804, 5.153800228976336051, 81.04057627198103830 ) ) ;
#191674 = ORIENTED_EDGE ( 'NONE', *, *, #35293, .F. ) ;
#191675 = CARTESIAN_POINT ( 'NONE',  ( -12.14591786802326823, 12.06949235617739902, 48.12609039468568284 ) ) ;
#191676 = CARTESIAN_POINT ( 'NONE',  ( 0.05219959533937995610, -21.53943276465977519, 25.00109039468567218 ) ) ;
#191677 = CARTESIAN_POINT ( 'NONE',  ( 21.52544592524334988, 5.823673210054432836, 71.45942372801901854 ) ) ;
#191678 = CARTESIAN_POINT ( 'NONE',  ( -13.89961937509977652, 13.97604488694528158, 115.6239096053143669 ) ) ;
#191679 = CARTESIAN_POINT ( 'NONE',  ( 5.719274019375991003, -21.55341960407610458, 82.70724293864770971 ) ) ;
#191681 = CARTESIAN_POINT ( 'NONE',  ( -0.05219959533934338120, 16.53943276465976808, 62.50109039468568284 ) ) ;
#191680 = CARTESIAN_POINT ( 'NONE',  ( 0.05219959533937995610, -21.53943276465977519, 30.00109039468568284 ) ) ;
#191682 = CARTESIAN_POINT ( 'NONE',  ( 5.823673210054125526, 21.52544592524343514, 69.79057627198102409 ) ) ;
#191683 = CARTESIAN_POINT ( 'NONE',  ( 21.52544592524334988, 5.823673210054432836, 111.4594237280190328 ) ) ;
#191684 = CARTESIAN_POINT ( 'NONE',  ( 9.564922557960805705, 16.46253265017160317, 59.58224293864769550 ) ) ;
#191685 = CARTESIAN_POINT ( 'NONE',  ( -19.05341960407611168, -5.049401038298163336, 111.4572429386476671 ) ) ;
#191686 = CARTESIAN_POINT ( 'NONE',  ( 13.89961937509977652, -13.97604488694527269, 83.12390960531436690 ) ) ;
#191687 = CARTESIAN_POINT ( 'NONE',  ( 20.08580022215228666, 20.97218796591011625, -49.51012018364364309 ) ) ;
#191688 = CARTESIAN_POINT ( 'NONE',  ( 0.05219959533936267826, -19.03943276465977164, 75.00109039468566152 ) ) ;
#191689 = CARTESIAN_POINT ( 'NONE',  ( -21.53943276465977519, 0.05219959533907696930, 41.24890960531435269 ) ) ;
#191690 = CARTESIAN_POINT ( 'NONE',  ( 12.06949235617757843, -12.14591786802309237, 23.12390960531436335 ) ) ;
#191691 = CARTESIAN_POINT ( 'NONE',  ( -19.05341960407617563, 5.049401038297882671, 103.5427570613523329 ) ) ;
#191692 = CARTESIAN_POINT ( 'NONE',  ( 19.05341960407611168, 5.049401038298154454, 23.95724293864769194 ) ) ;
#191693 = CARTESIAN_POINT ( 'NONE',  ( -5.153800228976607833, 19.02544592524334988, 22.70942372801899012 ) ) ;
#191694 = CARTESIAN_POINT ( 'NONE',  ( 19.02544592524334988, 5.153800228976608722, 96.45942372801897591 ) ) ;
#191696 = CARTESIAN_POINT ( 'NONE',  ( 16.46253265017146816, 9.564922557961045513, 51.66775706135233293 ) ) ;
#191695 = CARTESIAN_POINT ( 'NONE',  ( 21.55341960407610458, 5.719274019375980345, 88.95724293864769550 ) ) ;
#191697 = DIRECTION ( 'NONE',  ( 0.000000000000000000, 0.000000000000000000, -1.000000000000000000 ) ) ;
#191698 = CARTESIAN_POINT ( 'NONE',  ( 9.564922557960805705, 16.46253265017160317, 59.58224293864769550 ) ) ;
#191699 = CARTESIAN_POINT ( 'NONE',  ( 8.224510206698953496, -14.34966873604960469, 67.91557627198102409 ) ) ;
#191700 = CARTESIAN_POINT ( 'NONE',  ( 13.97604488694527802, 13.89961937509977652, 49.37390960531434558 ) ) ;
#191701 = CARTESIAN_POINT ( 'NONE',  ( -8.314922557960811034, -14.29746914071050412, 52.08224293864768839 ) ) ;
#191702 = LINE ( 'NONE', #23866, #180822 ) ;
#191703 = CARTESIAN_POINT ( 'NONE',  ( -14.29746914071049879, 8.314922557960819915, 25.83224293864769194 ) ) ;
#191704 = CARTESIAN_POINT ( 'NONE',  ( -19.05341960407611168, -5.049401038298163336, 61.45724293864769550 ) ) ;
#191705 = CARTESIAN_POINT ( 'NONE',  ( 13.89961937509957401, 13.97604488694547697, 21.87609039468566152 ) ) ;
#191706 = CARTESIAN_POINT ( 'NONE',  ( -16.52544592524335698, -4.483927247898792601, 48.95942372801902565 ) ) ;
#191707 = CARTESIAN_POINT ( 'NONE',  ( 21.55341960407610458, 5.719274019375980345, 53.95724293864770260 ) ) ;
#191709 = ORIENTED_EDGE ( 'NONE', *, *, #145315, .F. ) ;
#191708 = CARTESIAN_POINT ( 'NONE',  ( -21.55341960407619339, 5.719274019375674811, 108.5427570613523756 ) ) ;
#191710 = CARTESIAN_POINT ( 'NONE',  ( 5.153800228976335163, 19.02544592524342804, 64.79057627198100988 ) ) ;
#191711 = CARTESIAN_POINT ( 'NONE',  ( 1.508955259217861487E-14, -71.74905152827281540, -24.99410988490251029 ) ) ;
#191712 = CARTESIAN_POINT ( 'NONE',  ( 19.05341960407611168, 5.049401038298154454, 93.95724293864769550 ) ) ;
#191713 = CARTESIAN_POINT ( 'NONE',  ( 29.86685920354754487, 21.69954338932564752, -1.424999997268813212 ) ) ;
#191714 = CARTESIAN_POINT ( 'NONE',  ( -10.81492255796105439, 18.62759615963255655, 27.91775706135234358 ) ) ;
#191715 = CARTESIAN_POINT ( 'NONE',  ( 12.14591786802309770, 12.06949235617756955, 94.37390960531436690 ) ) ;
#191717 = CARTESIAN_POINT ( 'NONE',  ( -5.153800228976328057, -19.02544592524343514, 67.29057627198102409 ) ) ;
#191716 = CARTESIAN_POINT ( 'NONE',  ( 0.05219959533907565091, 21.53943276465977519, 89.99890960531438111 ) ) ;
#191718 = CARTESIAN_POINT ( 'NONE',  ( 5.153800228976335163, 19.02544592524342804, 89.79057627198102409 ) ) ;
#191719 = CARTESIAN_POINT ( 'NONE',  ( 18.62759615963271287, -10.81492255796078972, 108.3322429386477097 ) ) ;
#191720 = ORIENTED_EDGE ( 'NONE', *, *, #125126, .F. ) ;
#191721 = CARTESIAN_POINT ( 'NONE',  ( -0.05219959533909027116, -19.03943276465977164, 67.49890960531436690 ) ) ;
#191722 = AXIS2_PLACEMENT_3D ( 'NONE', #104055, #120209, #133388 ) ;
#191723 = CARTESIAN_POINT ( 'NONE',  ( 18.87580814761077974, -5.499999999999959144, 98.37172394265762421 ) ) ;
#191725 = CARTESIAN_POINT ( 'NONE',  ( 19.03943276465977164, -0.05219959533909143690, 28.74890960531435624 ) ) ;
#191724 = CARTESIAN_POINT ( 'NONE',  ( -16.53943276465976808, 0.05219959533911058130, 106.2489096053143811 ) ) ;
#191726 = CARTESIAN_POINT ( 'NONE',  ( 19.02544592524334988, 5.153800228976608722, 91.45942372801900433 ) ) ;
#191727 = CARTESIAN_POINT ( 'NONE',  ( -14.29746914071049879, 8.314922557960819915, 105.8322429386476955 ) ) ;
#191728 = CARTESIAN_POINT ( 'NONE',  ( -15.80617190586768217, 15.72974639402176855, 78.12609039468570415 ) ) ;
#191730 = CARTESIAN_POINT ( 'NONE',  ( 5.823673210054444382, -21.52544592524334988, 35.20942372801901854 ) ) ;
#191729 = CARTESIAN_POINT ( 'NONE',  ( -9.564922557960796823, -16.46253265017161027, 57.08224293864769550 ) ) ;
#191731 = CARTESIAN_POINT ( 'NONE',  ( 18.62759615963271287, -10.81492255796078972, 108.3322429386477097 ) ) ;
#191732 = CARTESIAN_POINT ( 'NONE',  ( 23.31738231874054890, -16.94106989632523508, 144.7999999999999829 ) ) ;
#191733 = CARTESIAN_POINT ( 'NONE',  ( 16.51473224551069308, 9.474510206698969483, 79.16557627198103830 ) ) ;
#191734 = LINE ( 'NONE', #175575, #46910 ) ;
#191736 = CARTESIAN_POINT ( 'NONE',  ( -21.53943276465977519, 0.05219959533907696930, 26.24890960531435624 ) ) ;
#191735 = CARTESIAN_POINT ( 'NONE',  ( -12.14591786802326823, 12.06949235617739902, 23.12609039468567573 ) ) ;
#191737 = CARTESIAN_POINT ( 'NONE',  ( 10.72451020669871369, 18.67979575497193778, 62.08442372801901143 ) ) ;
#191738 = CARTESIAN_POINT ( 'NONE',  ( 16.51473224551069308, 9.474510206698969483, 114.1655762719810241 ) ) ;
#191739 = CARTESIAN_POINT ( 'NONE',  ( -13.89961937509957401, -13.97604488694547875, 99.37609039468567573 ) ) ;
#191740 = CARTESIAN_POINT ( 'NONE',  ( -13.97604488694527625, -13.89961937509977652, 46.87390960531435979 ) ) ;
#191741 = CARTESIAN_POINT ( 'NONE',  ( 19.03943276465977164, -0.05219959533909143690, 73.74890960531435269 ) ) ;
#191742 = EDGE_CURVE ( 'NONE', #119352, #76158, #152812, .T. ) ;
#191743 = CARTESIAN_POINT ( 'NONE',  ( 0.05219959533910956823, 16.53943276465976808, 89.99890960531438111 ) ) ;
#191744 = CARTESIAN_POINT ( 'NONE',  ( -19.02544592524342804, 5.153800228976336051, 101.0405762719810241 ) ) ;
#191745 = CARTESIAN_POINT ( 'NONE',  ( -0.05219959533910754901, -16.53943276465976808, 97.49890960531436690 ) ) ;
#191746 = CARTESIAN_POINT ( 'NONE',  ( 16.51473224551069308, 9.474510206698969483, 104.1655762719810241 ) ) ;
#191748 = CARTESIAN_POINT ( 'NONE',  ( 0.05219959533909260263, 19.03943276465977164, 34.99890960531435979 ) ) ;
#191747 = CARTESIAN_POINT ( 'NONE',  ( 12.14591786802309770, 12.06949235617756955, 59.37390960531436690 ) ) ;
#191749 = CARTESIAN_POINT ( 'NONE',  ( -10.72451020669870658, -18.67979575497194134, 54.58442372801901143 ) ) ;
#191750 = CARTESIAN_POINT ( 'NONE',  ( -16.46253265017146816, -9.564922557961047289, 94.16775706135233293 ) ) ;
#191751 = CARTESIAN_POINT ( 'NONE',  ( -12.06949235617756955, 12.14591786802309770, 50.62390960531435979 ) ) ;
#191752 = CARTESIAN_POINT ( 'NONE',  ( 15.72974639402199770, -15.80617190586745480, 108.1239096053143811 ) ) ;
#191753 = CARTESIAN_POINT ( 'NONE',  ( -5.823673210054116645, -21.52544592524344225, 52.29057627198102409 ) ) ;
#191755 = CARTESIAN_POINT ( 'NONE',  ( -8.224510206698948167, 14.34966873604960824, 85.41557627198102409 ) ) ;
#191754 = CARTESIAN_POINT ( 'NONE',  ( 19.52851543214744012, 5.500000000000032863, 72.89357721762576148 ) ) ;
#191756 = CARTESIAN_POINT ( 'NONE',  ( 28.82186960331498327, 9.364793116373570925, 141.3500000054623627 ) ) ;
#191757 = CARTESIAN_POINT ( 'NONE',  ( 0.05219959533909260263, 19.03943276465977164, 59.99890960531436690 ) ) ;
#191758 = CARTESIAN_POINT ( 'NONE',  ( 8.314922557961029526, -14.29746914071037800, 110.4177570613523756 ) ) ;
#191759 = CARTESIAN_POINT ( 'NONE',  ( 8.314922557961029526, -14.29746914071037800, 105.4177570613523613 ) ) ;
#191760 = CARTESIAN_POINT ( 'NONE',  ( -14.34966873604972548, 8.224510206698743886, 83.33442372801903275 ) ) ;
#191761 = CARTESIAN_POINT ( 'NONE',  ( 5.153800228976615827, -19.02544592524334988, 40.20942372801898301 ) ) ;
#191762 = CARTESIAN_POINT ( 'NONE',  ( -17.26172910966779028, 6.454744622555852018, 70.80646908649224258 ) ) ;
#191763 = CARTESIAN_POINT ( 'NONE',  ( -0.05219959533909027116, -19.03943276465977164, 92.49890960531436690 ) ) ;
#191764 = CARTESIAN_POINT ( 'NONE',  ( -13.97604488694527625, -13.89961937509977652, 41.87390960531435979 ) ) ;
#191765 = CARTESIAN_POINT ( 'NONE',  ( 4.483927247898545687, 16.52544592524342804, 59.79057627198103120 ) ) ;
#191767 = CARTESIAN_POINT ( 'NONE',  ( -9.474510206698964154, 16.51473224551069663, 105.4155762719810383 ) ) ;
#191766 = CARTESIAN_POINT ( 'NONE',  ( 5.000000000000000888, -130.0000000000000000, -13.99999999999999822 ) ) ;
#191768 = CARTESIAN_POINT ( 'NONE',  ( 18.67979575497178502, 10.72451020669898547, 39.16557627198102409 ) ) ;
#191769 = CARTESIAN_POINT ( 'NONE',  ( -16.52544592524342804, 4.483927247898546575, 81.04057627198102409 ) ) ;
#191770 = CARTESIAN_POINT ( 'NONE',  ( -16.53943276465976808, -0.05219959533934237506, 43.75109039468568284 ) ) ;
#191771 = ORIENTED_EDGE ( 'NONE', *, *, #1347, .T. ) ;
#191772 = CARTESIAN_POINT ( 'NONE',  ( -16.53943276465976808, 0.05219959533911058130, 81.24890960531436690 ) ) ;
#191773 = FACE_OUTER_BOUND ( 'NONE', #128919, .T. ) ;
#191774 = CARTESIAN_POINT ( 'NONE',  ( 19.02544592524334988, 5.153800228976608722, 71.45942372801900433 ) ) ;
#191775 = CARTESIAN_POINT ( 'NONE',  ( 5.153800228976335163, 19.02544592524342804, 104.7905762719809957 ) ) ;
#191776 = CARTESIAN_POINT ( 'NONE',  ( -13.97604488694547697, 13.89961937509957934, 73.12609039468568994 ) ) ;
#191777 = DIRECTION ( 'NONE',  ( -1.000000000000000000, 0.000000000000000000, 0.000000000000000000 ) ) ;
#191779 = CARTESIAN_POINT ( 'NONE',  ( -14.34966873604972548, 8.224510206698743886, 103.3344237280190043 ) ) ;
#191778 = CARTESIAN_POINT ( 'NONE',  ( 14.29746914071037800, 8.314922557961029526, 31.66775706135234358 ) ) ;
#191781 = CARTESIAN_POINT ( 'NONE',  ( -19.02544592524334988, -5.153800228976617603, 68.95942372801896170 ) ) ;
#191780 = CIRCLE ( 'NONE', #104637, 10.00000000000000000 ) ;
#191782 = CARTESIAN_POINT ( 'NONE',  ( 5.719274019375991003, -21.55341960407610458, 32.70724293864770260 ) ) ;
#191783 = CARTESIAN_POINT ( 'NONE',  ( -15.72974639402176322, -15.80617190586768395, 74.37609039468568994 ) ) ;
#191784 = CARTESIAN_POINT ( 'NONE',  ( 18.41295718396490955, 5.500000000000055955, 38.98231844820842440 ) ) ;
#191785 = CARTESIAN_POINT ( 'NONE',  ( 14.29746914071037800, 8.314922557961029526, 21.66775706135235069 ) ) ;
#191787 = CARTESIAN_POINT ( 'NONE',  ( -19.02544592524342804, 5.153800228976336051, 86.04057627198103830 ) ) ;
#191786 = CARTESIAN_POINT ( 'NONE',  ( 19.02544592524343514, -5.153800228976328945, 28.54057627198102409 ) ) ;
#191788 = CARTESIAN_POINT ( 'NONE',  ( 16.51473224551069308, 9.474510206698969483, 24.16557627198102765 ) ) ;
#191790 = CARTESIAN_POINT ( 'NONE',  ( 5.049401038298161559, -19.05341960407611168, 87.70724293864769550 ) ) ;
#191789 = CARTESIAN_POINT ( 'NONE',  ( -16.52544592524342804, 4.483927247898546575, 91.04057627198103830 ) ) ;
#191791 = CARTESIAN_POINT ( 'NONE',  ( -5.049401038298153566, 19.05341960407611168, 90.20724293864766707 ) ) ;
#191792 = ORIENTED_EDGE ( 'NONE', *, *, #148801, .T. ) ;
#191793 = CARTESIAN_POINT ( 'NONE',  ( 0.05219959533936267826, -19.03943276465977164, 85.00109039468567573 ) ) ;
#191794 = CARTESIAN_POINT ( 'NONE',  ( -5.823673210054116645, -21.52544592524344225, 77.29057627198102409 ) ) ;
#191795 = CARTESIAN_POINT ( 'NONE',  ( 16.51473224551069308, 9.474510206698969483, 29.16557627198103475 ) ) ;
#191797 = CARTESIAN_POINT ( 'NONE',  ( -10.72451020669898014, 18.67979575497178502, 110.4155762719810383 ) ) ;
#191796 = CARTESIAN_POINT ( 'NONE',  ( 13.97604488694548053, -13.89961937509957401, 70.62609039468567573 ) ) ;
#191798 = CARTESIAN_POINT ( 'NONE',  ( 19.03943276465977164, -0.05219959533909143690, 68.74890960531436690 ) ) ;
#191799 = CARTESIAN_POINT ( 'NONE',  ( 5.049401038298161559, -19.05341960407611168, 102.7072429386476955 ) ) ;
#191800 = VERTEX_POINT ( 'NONE', #116539 ) ;
#191801 = CARTESIAN_POINT ( 'NONE',  ( -0.05219959533907301413, -21.53943276465977519, 102.4989096053143811 ) ) ;
#191804 = CARTESIAN_POINT ( 'NONE',  ( 19.05341960407617918, -5.049401038297876454, 56.04275706135234714 ) ) ;
#191803 = CARTESIAN_POINT ( 'NONE',  ( 16.51473224551069308, 9.474510206698969483, 84.16557627198102409 ) ) ;
#191802 = CARTESIAN_POINT ( 'NONE',  ( -16.55341960407611168, -4.379528057220339221, 101.4572429386476955 ) ) ;
#191805 = CARTESIAN_POINT ( 'NONE',  ( 10.72451020669898902, -18.67979575497178502, 87.91557627198103830 ) ) ;
#191806 = CARTESIAN_POINT ( 'NONE',  ( -10.81492255796078084, -18.62759615963271287, 77.08224293864769550 ) ) ;
#191807 = CARTESIAN_POINT ( 'NONE',  ( -0.05219959533910754901, -16.53943276465976808, 42.49890960531435979 ) ) ;
#191808 = CARTESIAN_POINT ( 'NONE',  ( -16.46253265017146816, -9.564922557961047289, 29.16775706135232937 ) ) ;
#191809 = CARTESIAN_POINT ( 'NONE',  ( -0.05219959533934338120, 16.53943276465976808, 67.50109039468568994 ) ) ;
#191810 = CARTESIAN_POINT ( 'NONE',  ( -16.51473224551069308, -9.474510206698971260, 96.66557627198102409 ) ) ;
#191811 = CARTESIAN_POINT ( 'NONE',  ( -9.474510206698964154, 16.51473224551069663, 40.41557627198103120 ) ) ;
#191812 = AXIS2_PLACEMENT_3D ( 'NONE', #128190, #177717, #39185 ) ;
#191813 = CARTESIAN_POINT ( 'NONE',  ( -21.52544592524334988, -5.823673210054445271, 58.95942372801902565 ) ) ;
#191814 = CARTESIAN_POINT ( 'NONE',  ( -5.719274019375665041, -21.55341960407619695, 49.79275706135234714 ) ) ;
#191815 = CARTESIAN_POINT ( 'NONE',  ( 16.51473224551069308, 9.474510206698969483, 64.16557627198102409 ) ) ;
#191816 = CARTESIAN_POINT ( 'NONE',  ( 18.67979575497194134, -10.72451020669871369, 40.83442372801901854 ) ) ;
#191817 = ADVANCED_FACE ( 'NONE', ( #70039 ), #191377, .F. ) ;
#191818 = CARTESIAN_POINT ( 'NONE',  ( 5.153800228976615827, -19.02544592524334988, 80.20942372801901854 ) ) ;
#191819 = CARTESIAN_POINT ( 'NONE',  ( -9.474510206698720793, -16.51473224551083518, 74.58442372801900433 ) ) ;
#191820 = CARTESIAN_POINT ( 'NONE',  ( 13.89961937509977652, -13.97604488694527269, 43.12390960531434558 ) ) ;
#191821 = CARTESIAN_POINT ( 'NONE',  ( 8.224510206698742110, 14.34966873604972548, 82.08442372801901854 ) ) ;
#191822 = CARTESIAN_POINT ( 'NONE',  ( 16.46253265017160672, -9.564922557960803928, 48.33224293864769550 ) ) ;
#191823 = CARTESIAN_POINT ( 'NONE',  ( 24.22576942085219542, -7.195495839727257703, 170.3116806589272301 ) ) ;
#191824 = CARTESIAN_POINT ( 'NONE',  ( -13.89961937509977652, 13.97604488694528158, 100.6239096053143669 ) ) ;
#191825 = CARTESIAN_POINT ( 'NONE',  ( -5.153800228976328057, -19.02544592524343514, 42.29057627198101699 ) ) ;
#191826 = CARTESIAN_POINT ( 'NONE',  ( 0.05219959533907565091, 21.53943276465977519, 79.99890960531435269 ) ) ;
#191827 = CARTESIAN_POINT ( 'NONE',  ( 14.34966873604972726, -8.224510206698740333, 65.83442372801900433 ) ) ;
#191828 = CARTESIAN_POINT ( 'NONE',  ( 15.72974639402176855, 15.80617190586768217, 106.8760903946856899 ) ) ;
#191829 = CARTESIAN_POINT ( 'NONE',  ( 13.97604488694527802, 13.89961937509977652, 54.37390960531435979 ) ) ;
#191830 = CARTESIAN_POINT ( 'NONE',  ( -16.52544592524342804, 4.483927247898546575, 46.04057627198103830 ) ) ;
#191831 = CARTESIAN_POINT ( 'NONE',  ( 4.379528057220339221, -16.55341960407611168, 87.70724293864769550 ) ) ;
#191832 = CARTESIAN_POINT ( 'NONE',  ( 13.89961937509977652, -13.97604488694527269, 73.12390960531436690 ) ) ;
#191833 = CARTESIAN_POINT ( 'NONE',  ( 18.67979575497194134, -10.72451020669871369, 35.83442372801901143 ) ) ;
#191834 = CARTESIAN_POINT ( 'NONE',  ( 19.03943276465977164, -0.05219959533909143690, 93.74890960531435269 ) ) ;
#191835 = CARTESIAN_POINT ( 'NONE',  ( -5.823673210054431948, 21.52544592524334988, 102.7094237280190185 ) ) ;
#191836 = CARTESIAN_POINT ( 'NONE',  ( 16.55341960407618274, -4.379528057220086978, 61.04275706135234714 ) ) ;
#191837 = CARTESIAN_POINT ( 'NONE',  ( 15.72974639402176855, 15.80617190586768217, 26.87609039468567218 ) ) ;
#191838 = CARTESIAN_POINT ( 'NONE',  ( 19.02544592524343514, -5.153800228976328945, 113.5405762719810241 ) ) ;
#191839 = CARTESIAN_POINT ( 'NONE',  ( -21.52544592524343514, 5.823673210054127303, 96.04057627198102409 ) ) ;
#191840 = CARTESIAN_POINT ( 'NONE',  ( 16.52544592524342804, -4.483927247898539470, 48.54057627198103120 ) ) ;
#191841 = CARTESIAN_POINT ( 'NONE',  ( -0.05219959533909027116, -19.03943276465977164, 42.49890960531435269 ) ) ;
#191842 = CARTESIAN_POINT ( 'NONE',  ( 8.224510206698953496, -14.34966873604960469, 62.91557627198102409 ) ) ;
#191843 = CARTESIAN_POINT ( 'NONE',  ( -21.52544592524343514, 5.823673210054127303, 26.04057627198103475 ) ) ;
#191844 = CARTESIAN_POINT ( 'NONE',  ( 13.89961937509957401, 13.97604488694547697, 36.87609039468565442 ) ) ;
#191845 = CARTESIAN_POINT ( 'NONE',  ( 14.34966873604960469, 8.224510206698951720, 104.1655762719810241 ) ) ;
#191846 = CARTESIAN_POINT ( 'NONE',  ( 16.51473224551069308, 9.474510206698969483, 109.1655762719810383 ) ) ;
#191847 = VERTEX_POINT ( 'NONE', #101353 ) ;
#191848 = CARTESIAN_POINT ( 'NONE',  ( 12.14591786802327356, -12.06949235617739191, 50.62609039468568994 ) ) ;
#191849 = CARTESIAN_POINT ( 'NONE',  ( -13.97604488694527625, -13.89961937509977652, 51.87390960531436690 ) ) ;
#191850 = DIRECTION ( 'NONE',  ( -4.336808689942017120E-17, -1.000000000000000000, 0.000000000000000000 ) ) ;
#191851 = CARTESIAN_POINT ( 'NONE',  ( 4.483927247898790824, -16.52544592524335698, 90.20942372801903275 ) ) ;
#191852 = CARTESIAN_POINT ( 'NONE',  ( -19.02544592524334988, -5.153800228976617603, 103.9594237280190043 ) ) ;
#191853 = CARTESIAN_POINT ( 'NONE',  ( 15.80617190586769283, -15.72974639402175789, 75.62609039468567573 ) ) ;
#191854 = CARTESIAN_POINT ( 'NONE',  ( -16.46253265017160317, 9.564922557960807481, 75.83224293864769550 ) ) ;
#191855 = CARTESIAN_POINT ( 'NONE',  ( -21.52544592524343514, 5.823673210054127303, 106.0405762719810525 ) ) ;
#191856 = CARTESIAN_POINT ( 'NONE',  ( -4.379528057220086978, -16.55341960407618274, 39.79275706135235424 ) ) ;
#191857 = CARTESIAN_POINT ( 'NONE',  ( -0.05219959533910754901, -16.53943276465976808, 107.4989096053143669 ) ) ;
#191858 = CARTESIAN_POINT ( 'NONE',  ( -16.53943276465976808, -0.05219959533934237506, 23.75109039468567929 ) ) ;
#191859 = CARTESIAN_POINT ( 'NONE',  ( -9.564922557961040184, 16.46253265017147172, 77.91775706135234714 ) ) ;
#191860 = CARTESIAN_POINT ( 'NONE',  ( -10.81492255796078084, -18.62759615963271287, 77.08224293864769550 ) ) ;
#191861 = CARTESIAN_POINT ( 'NONE',  ( 13.97604488694548053, -13.89961937509957401, 55.62609039468566863 ) ) ;
#191862 = CARTESIAN_POINT ( 'NONE',  ( -19.05341960407611168, -5.049401038298163336, 111.4572429386476671 ) ) ;
#191863 = CARTESIAN_POINT ( 'NONE',  ( 5.719274019375991003, -21.55341960407610458, 107.7072429386476955 ) ) ;
#191864 = CARTESIAN_POINT ( 'NONE',  ( 17.49999999999999645, 5.068104630630399399, 26.77181594659973030 ) ) ;
#191865 = CARTESIAN_POINT ( 'NONE',  ( 5.153800228976335163, 19.02544592524342804, 64.79057627198100988 ) ) ;
#191866 = DIRECTION ( 'NONE',  ( -1.000000000000000000, -0.000000000000000000, -0.000000000000000000 ) ) ;
#191867 = CARTESIAN_POINT ( 'NONE',  ( -5.049401038297874678, -19.05341960407617918, 109.7927570613523187 ) ) ;
#191868 = CARTESIAN_POINT ( 'NONE',  ( 24.79445753310783829, 6.337991946471497329, 168.1742925226654108 ) ) ;
#191869 = CARTESIAN_POINT ( 'NONE',  ( -10.72451020669870658, -18.67979575497194134, 59.58442372801901854 ) ) ;
#191871 = CARTESIAN_POINT ( 'NONE',  ( 14.34966873604960469, 8.224510206698951720, 69.16557627198102409 ) ) ;
#191870 = CARTESIAN_POINT ( 'NONE',  ( 0.05219959533907565091, 21.53943276465977519, 109.9989096053143527 ) ) ;
#191872 = CARTESIAN_POINT ( 'NONE',  ( 5.153800228976335163, 19.02544592524342804, 69.79057627198103830 ) ) ;
#191873 = CARTESIAN_POINT ( 'NONE',  ( 0.05219959533937995610, -21.53943276465977519, 70.00109039468568994 ) ) ;
#191875 = CARTESIAN_POINT ( 'NONE',  ( 16.51473224551083163, -9.474510206698727899, 25.83442372801900078 ) ) ;
#191874 = CARTESIAN_POINT ( 'NONE',  ( -8.224510206698735004, -14.34966873604973081, 19.58442372801901143 ) ) ;
#191876 = CARTESIAN_POINT ( 'NONE',  ( 5.719274019375673035, 21.55341960407619339, 37.29275706135235424 ) ) ;
#191877 = CARTESIAN_POINT ( 'NONE',  ( -18.62759615963255300, -10.81492255796106328, 19.16775706135234714 ) ) ;
#191878 = CARTESIAN_POINT ( 'NONE',  ( 5.719274019375991003, -21.55341960407610458, 57.70724293864770260 ) ) ;
#191879 = CARTESIAN_POINT ( 'NONE',  ( 9.564922557961047289, -16.46253265017146816, 100.4177570613523329 ) ) ;
#191880 = CARTESIAN_POINT ( 'NONE',  ( 9.564922557961047289, -16.46253265017146816, 70.41775706135233293 ) ) ;
#191881 = CARTESIAN_POINT ( 'NONE',  ( -5.823673210054431948, 21.52544592524334988, 82.70942372801900433 ) ) ;
#191882 = CARTESIAN_POINT ( 'NONE',  ( 9.474510206698729675, 16.51473224551082808, 47.08442372801900433 ) ) ;
#191883 = CARTESIAN_POINT ( 'NONE',  ( -13.89961937509977652, 13.97604488694528158, 40.62390960531435979 ) ) ;
#191884 = CARTESIAN_POINT ( 'NONE',  ( -21.52544592524343514, 5.823673210054127303, 51.04057627198103120 ) ) ;
#191885 = CARTESIAN_POINT ( 'NONE',  ( 4.379528057220339221, -16.55341960407611168, 52.70724293864769550 ) ) ;
#191886 = DIRECTION ( 'NONE',  ( 0.000000000000000000, 0.000000000000000000, 1.000000000000000000 ) ) ;
#191887 = CARTESIAN_POINT ( 'NONE',  ( -13.97604488694547697, 13.89961937509957934, 28.12609039468565797 ) ) ;
#191888 = CARTESIAN_POINT ( 'NONE',  ( 14.34966873604972726, -8.224510206698740333, 90.83442372801901854 ) ) ;
#191889 = CARTESIAN_POINT ( 'NONE',  ( -14.34966873604960291, -8.224510206698953496, 36.66557627198103120 ) ) ;
#191890 = CARTESIAN_POINT ( 'NONE',  ( -15.72974639402176322, -15.80617190586768395, 79.37609039468567573 ) ) ;
#191891 = CARTESIAN_POINT ( 'NONE',  ( 21.52544592524334988, 5.823673210054432836, 86.45942372801901854 ) ) ;
#191892 = CARTESIAN_POINT ( 'NONE',  ( 21.53943276465977519, -0.05219959533907433946, 78.74890960531436690 ) ) ;
#191893 = CARTESIAN_POINT ( 'NONE',  ( -16.51473224551069308, -9.474510206698971260, 36.66557627198102409 ) ) ;
#191894 = CARTESIAN_POINT ( 'NONE',  ( -21.53943276465977519, -0.05219959533937600094, 58.75109039468568994 ) ) ;
#191895 = CARTESIAN_POINT ( 'NONE',  ( -16.51473224551069308, -9.474510206698971260, 41.66557627198103120 ) ) ;
#191896 = CARTESIAN_POINT ( 'NONE',  ( -0.05219959533909027116, -19.03943276465977164, 57.49890960531435979 ) ) ;
#191897 = CARTESIAN_POINT ( 'NONE',  ( -4.483927247898539470, -16.52544592524342804, 112.2905762719810241 ) ) ;
#191898 = CARTESIAN_POINT ( 'NONE',  ( 5.049401038298161559, -19.05341960407611168, 102.7072429386476955 ) ) ;
#191899 = CARTESIAN_POINT ( 'NONE',  ( 8.224510206698953496, -14.34966873604960469, 42.91557627198103120 ) ) ;
#191900 = CARTESIAN_POINT ( 'NONE',  ( -13.97604488694527625, -13.89961937509977652, 21.87390960531435979 ) ) ;
#191901 = CARTESIAN_POINT ( 'NONE',  ( -18.67979575497178146, -10.72451020669898902, 81.66557627198103830 ) ) ;
#191902 = CARTESIAN_POINT ( 'NONE',  ( 18.67979575497178502, 10.72451020669898547, 114.1655762719810383 ) ) ;
#191903 = CARTESIAN_POINT ( 'NONE',  ( 27.91261209101638840, -7.473227146837556845, 160.9450349587941957 ) ) ;
#191904 = CARTESIAN_POINT ( 'NONE',  ( 16.52544592524335698, 4.483927247898782831, 41.45942372801901143 ) ) ;
#191905 = ORIENTED_EDGE ( 'NONE', *, *, #41619, .F. ) ;
#191906 = CARTESIAN_POINT ( 'NONE',  ( -10.72451020669898014, 18.67979575497178502, 65.41557627198102409 ) ) ;
#191907 = CARTESIAN_POINT ( 'NONE',  ( -10.72451020669870658, -18.67979575497194134, 94.58442372801901854 ) ) ;
#191908 = CARTESIAN_POINT ( 'NONE',  ( -9.474510206698964154, 16.51473224551069663, 95.41557627198102409 ) ) ;
#191909 = CARTESIAN_POINT ( 'NONE',  ( 10.81492255796106328, -18.62759615963255655, 25.41775706135235779 ) ) ;
#191910 = ADVANCED_FACE ( 'NONE', ( #84182 ), #140009, .T. ) ;
#191911 = CARTESIAN_POINT ( 'NONE',  ( -15.72974639402197994, 15.80617190586746368, 25.62390960531435624 ) ) ;
#191912 = CARTESIAN_POINT ( 'NONE',  ( 0.05219959533934541429, -16.53943276465976808, 85.00109039468568994 ) ) ;
#191913 = CARTESIAN_POINT ( 'NONE',  ( -21.55341960407619339, 5.719274019375674811, 68.54275706135234714 ) ) ;
#191914 = CARTESIAN_POINT ( 'NONE',  ( -5.823673210054431948, 21.52544592524334988, 112.7094237280190328 ) ) ;
#191915 = CARTESIAN_POINT ( 'NONE',  ( -14.34966873604972548, 8.224510206698743886, 78.33442372801901854 ) ) ;
#191916 = CARTESIAN_POINT ( 'NONE',  ( 18.67979575497194134, -10.72451020669871369, 25.83442372801901499 ) ) ;
#191917 = CIRCLE ( 'NONE', #175909, 8.000000000000000000 ) ;
#191918 = CARTESIAN_POINT ( 'NONE',  ( 9.564922557960805705, 16.46253265017160317, 29.58224293864769550 ) ) ;
#191919 = CARTESIAN_POINT ( 'NONE',  ( -5.719274019375665041, -21.55341960407619695, 99.79275706135234714 ) ) ;
#191920 = CARTESIAN_POINT ( 'NONE',  ( -19.03943276465977164, 0.05219959533909376836, 111.2489096053143669 ) ) ;
#191921 = CARTESIAN_POINT ( 'NONE',  ( 5.719274019375991003, -21.55341960407610458, 97.70724293864772392 ) ) ;
#191922 = CARTESIAN_POINT ( 'NONE',  ( -15.72974639402197994, 15.80617190586746368, 60.62390960531437401 ) ) ;
#191924 = CARTESIAN_POINT ( 'NONE',  ( 8.314922557960818139, 14.29746914071049879, 49.58224293864769550 ) ) ;
#191923 = CARTESIAN_POINT ( 'NONE',  ( -0.05219959533934338120, 16.53943276465976808, 47.50109039468568994 ) ) ;
#191925 = LINE ( 'NONE', #53409, #195241 ) ;
#191926 = CARTESIAN_POINT ( 'NONE',  ( -19.03943276465977164, -0.05219959533935918106, 78.75109039468567573 ) ) ;
#191927 =( GEOMETRIC_REPRESENTATION_CONTEXT ( 3 ) GLOBAL_UNCERTAINTY_ASSIGNED_CONTEXT ( ( #112636 ) ) GLOBAL_UNIT_ASSIGNED_CONTEXT ( ( #14220, #75889, #48553 ) ) REPRESENTATION_CONTEXT ( 'NONE', 'WORKASPACE' ) );
#191928 = CARTESIAN_POINT ( 'NONE',  ( -17.48853670773245739, 5.747243402303086945, 103.6667129974999568 ) ) ;
#191929 = CARTESIAN_POINT ( 'NONE',  ( -14.29746914071037622, -8.314922557961029526, 29.16775706135234003 ) ) ;
#191930 = CARTESIAN_POINT ( 'NONE',  ( -0.05219959533907301413, -21.53943276465977519, 82.49890960531436690 ) ) ;
#191931 = CARTESIAN_POINT ( 'NONE',  ( 16.55341960407611168, 4.379528057220329451, 68.95724293864769550 ) ) ;
#191932 = CARTESIAN_POINT ( 'NONE',  ( -9.474510206698964154, 16.51473224551069663, 100.4155762719810241 ) ) ;
#191933 = CARTESIAN_POINT ( 'NONE',  ( -8.314922557961024197, 14.29746914071037800, 42.91775706135235424 ) ) ;
#191934 = CARTESIAN_POINT ( 'NONE',  ( 19.05341960407611168, 5.049401038298154454, 58.95724293864768129 ) ) ;
#191936 = CARTESIAN_POINT ( 'NONE',  ( 19.02544592524334988, 5.153800228976608722, 101.4594237280189759 ) ) ;
#191935 = CARTESIAN_POINT ( 'NONE',  ( -15.80617190586768217, 15.72974639402176855, 23.12609039468567573 ) ) ;
#191937 = CARTESIAN_POINT ( 'NONE',  ( 9.474510206698971260, -16.51473224551069308, 92.91557627198103830 ) ) ;
#191938 = CARTESIAN_POINT ( 'NONE',  ( 0.05219959533909260263, 19.03943276465977164, 84.99890960531436690 ) ) ;
#191939 = CARTESIAN_POINT ( 'NONE',  ( 21.53943276465977519, -0.05219959533907433946, 93.74890960531436690 ) ) ;
#191940 = CARTESIAN_POINT ( 'NONE',  ( -13.97604488694527625, -13.89961937509977652, 41.87390960531435979 ) ) ;
#191941 = CARTESIAN_POINT ( 'NONE',  ( -16.52544592524342804, 4.483927247898546575, 66.04057627198103830 ) ) ;
#191942 = CARTESIAN_POINT ( 'NONE',  ( 9.564922557960805705, 16.46253265017160317, 104.5822429386476955 ) ) ;
#191943 = LINE ( 'NONE', #175788, #37849 ) ;
#191944 = CARTESIAN_POINT ( 'NONE',  ( 16.51473224551083163, -9.474510206698727899, 75.83442372801900433 ) ) ;
#191945 = CARTESIAN_POINT ( 'NONE',  ( 0.05219959533907565091, 21.53943276465977519, 84.99890960531436690 ) ) ;
#191946 = CARTESIAN_POINT ( 'NONE',  ( -19.03943276465977164, -0.05219959533935918106, 43.75109039468566863 ) ) ;
#191947 = CARTESIAN_POINT ( 'NONE',  ( -19.02544592524342804, 5.153800228976336051, 106.0405762719810241 ) ) ;
#191948 = DIRECTION ( 'NONE',  ( 0.000000000000000000, 0.000000000000000000, -1.000000000000000000 ) ) ;
#191949 = CARTESIAN_POINT ( 'NONE',  ( -18.67979575497178146, -10.72451020669898902, 46.66557627198102409 ) ) ;
#191950 = VECTOR ( 'NONE', #136374, 1000.000000000000000 ) ;
#191951 = CARTESIAN_POINT ( 'NONE',  ( -13.89961937509977652, 13.97604488694528158, 80.62390960531436690 ) ) ;
#191952 = CARTESIAN_POINT ( 'NONE',  ( -5.719274019375665041, -21.55341960407619695, 69.79275706135234714 ) ) ;
#191953 = CARTESIAN_POINT ( 'NONE',  ( 5.049401038298161559, -19.05341960407611168, 42.70724293864767418 ) ) ;
#191954 = CARTESIAN_POINT ( 'NONE',  ( -16.52544592524342804, 4.483927247898546575, 71.04057627198103830 ) ) ;
#191955 = CARTESIAN_POINT ( 'NONE',  ( -4.483927247898782831, 16.52544592524335698, 22.70942372801901499 ) ) ;
#191956 = CARTESIAN_POINT ( 'NONE',  ( 0.05219959533937995610, -21.53943276465977519, 55.00109039468568284 ) ) ;
#191957 = ORIENTED_EDGE ( 'NONE', *, *, #44038, .T. ) ;
#191958 = CARTESIAN_POINT ( 'NONE',  ( -13.97604488694527625, -13.89961937509977652, 111.8739096053143243 ) ) ;
#191959 = CARTESIAN_POINT ( 'NONE',  ( -5.153800228976607833, 19.02544592524334988, 67.70942372801900433 ) ) ;
#191960 = CARTESIAN_POINT ( 'NONE',  ( -4.500000000000001776, -139.5000000000000000, 13.35010376910484275 ) ) ;
#191961 = CARTESIAN_POINT ( 'NONE',  ( -21.55341960407619339, 5.719274019375674811, 23.54275706135235424 ) ) ;
#191962 = CARTESIAN_POINT ( 'NONE',  ( 17.50000000000000000, 5.499999999999997335, 120.0000000000000142 ) ) ;
#191963 = CARTESIAN_POINT ( 'NONE',  ( 5.049401038297881783, 19.05341960407617563, 22.29275706135233648 ) ) ;
#191964 = CARTESIAN_POINT ( 'NONE',  ( -19.05341960407611168, -5.049401038298163336, 51.45724293864770260 ) ) ;
#191965 = CARTESIAN_POINT ( 'NONE',  ( -5.719274019375665041, -21.55341960407619695, 109.7927570613523613 ) ) ;
#191966 = CARTESIAN_POINT ( 'NONE',  ( -14.29746914071037622, -8.314922557961029526, 109.1677570613523613 ) ) ;
#191968 = CARTESIAN_POINT ( 'NONE',  ( 21.52544592524334988, 5.823673210054432836, 71.45942372801901854 ) ) ;
#191967 = CARTESIAN_POINT ( 'NONE',  ( 16.51473224551069308, 9.474510206698969483, 109.1655762719810383 ) ) ;
#191969 = CARTESIAN_POINT ( 'NONE',  ( 27.73933785331498925, -9.013057229001033122, 148.2750000027311330 ) ) ;
#191970 = CARTESIAN_POINT ( 'NONE',  ( 19.03943276465977164, -0.05219959533909143690, 113.7489096053143669 ) ) ;
#191971 = LINE ( 'NONE', #172078, #24260 ) ;
#191972 = CARTESIAN_POINT ( 'NONE',  ( -0.05219959533937732626, 21.53943276465977519, 77.50109039468567573 ) ) ;
#191973 = CARTESIAN_POINT ( 'NONE',  ( 18.62759615963255655, 10.81492255796105972, 96.66775706135234714 ) ) ;
#191974 = LINE ( 'NONE', #145462, #167160 ) ;
#191975 = CARTESIAN_POINT ( 'NONE',  ( -19.03943276465977164, 0.05219959533909376836, 86.24890960531436690 ) ) ;
#191976 = CARTESIAN_POINT ( 'NONE',  ( 2.500000000000000000, 3.004629197474319246E-15, 2.042000000000000259 ) ) ;
#191977 = LINE ( 'NONE', #111152, #195567 ) ;
#191978 = CARTESIAN_POINT ( 'NONE',  ( 19.03943276465977164, -0.05219959533909143690, 38.74890960531436690 ) ) ;
#191979 = CARTESIAN_POINT ( 'NONE',  ( 5.719274019375991003, -21.55341960407610458, 52.70724293864769550 ) ) ;
#191980 = CARTESIAN_POINT ( 'NONE',  ( -8.314922557961024197, 14.29746914071037800, 102.9177570613523756 ) ) ;
#191982 = CARTESIAN_POINT ( 'NONE',  ( -13.97604488694527625, -13.89961937509977652, 81.87390960531436690 ) ) ;
#191981 = CARTESIAN_POINT ( 'NONE',  ( -8.314922557960811034, -14.29746914071050412, 97.08224293864770971 ) ) ;
#191983 = CARTESIAN_POINT ( 'NONE',  ( 18.62759615963255655, 10.81492255796105972, 106.6677570613523756 ) ) ;
#191984 = CARTESIAN_POINT ( 'NONE',  ( -0.05219959533909027116, -19.03943276465977164, 37.49890960531436690 ) ) ;
#191985 = CARTESIAN_POINT ( 'NONE',  ( 8.224510206698953496, -14.34966873604960469, 87.91557627198103830 ) ) ;
#191986 = CARTESIAN_POINT ( 'NONE',  ( -21.52544592524334988, -5.823673210054445271, 48.95942372801902565 ) ) ;
#191987 = CARTESIAN_POINT ( 'NONE',  ( -15.72974639402197994, 15.80617190586746368, 90.62390960531436690 ) ) ;
#191988 = CARTESIAN_POINT ( 'NONE',  ( -19.03943276465977164, -0.05219959533935918106, 48.75109039468566863 ) ) ;
#191989 = CARTESIAN_POINT ( 'NONE',  ( -9.564922557960796823, -16.46253265017161027, 47.08224293864769550 ) ) ;
#191990 = CARTESIAN_POINT ( 'NONE',  ( -19.05341960407611168, -5.049401038298163336, 91.45724293864766707 ) ) ;
#191991 = CARTESIAN_POINT ( 'NONE',  ( -4.483927247898539470, -16.52544592524342804, 57.29057627198103120 ) ) ;
#191992 = CARTESIAN_POINT ( 'NONE',  ( 5.049401038297881783, 19.05341960407617563, 47.29275706135231161 ) ) ;
#191993 = CARTESIAN_POINT ( 'NONE',  ( -16.46253265017160317, 9.564922557960807481, 50.83224293864770260 ) ) ;
#191994 = CARTESIAN_POINT ( 'NONE',  ( -0.05219959533910754901, -16.53943276465976808, 47.49890960531435979 ) ) ;
#191995 = CARTESIAN_POINT ( 'NONE',  ( -19.02544592524334988, -5.153800228976617603, 83.95942372801901854 ) ) ;
#191996 = DIRECTION ( 'NONE',  ( 1.000000000000000000, 0.000000000000000000, 0.000000000000000000 ) ) ;
#191997 = CARTESIAN_POINT ( 'NONE',  ( -15.72974639402197994, 15.80617190586746368, 30.62390960531436335 ) ) ;
#191998 = EDGE_CURVE ( 'NONE', #141920, #170763, #72741, .T. ) ;
#191999 = CARTESIAN_POINT ( 'NONE',  ( 8.314922557960818139, 14.29746914071049879, 104.5822429386477097 ) ) ;
#192000 = CARTESIAN_POINT ( 'NONE',  ( 2.500000000000000000, 1.768423874527823791, 1.020999999999998575 ) ) ;
#192002 = CARTESIAN_POINT ( 'NONE',  ( 18.62759615963271287, -10.81492255796078972, 53.33224293864769550 ) ) ;
#192001 = CARTESIAN_POINT ( 'NONE',  ( 5.049401038298161559, -19.05341960407611168, 52.70724293864767418 ) ) ;
#192003 = CARTESIAN_POINT ( 'NONE',  ( 13.89961937509977652, -13.97604488694527269, 33.12390960531434558 ) ) ;
#192005 = CARTESIAN_POINT ( 'NONE',  ( -19.02544592524342804, 5.153800228976336051, 56.04057627198100988 ) ) ;
#192004 = CARTESIAN_POINT ( 'NONE',  ( 16.53943276465976808, 0.05219959533934440121, 76.25109039468568994 ) ) ;
#192006 = CARTESIAN_POINT ( 'NONE',  ( 13.97604488694548053, -13.89961937509957401, 45.62609039468566863 ) ) ;
#192007 = CIRCLE ( 'NONE', #133869, 28.90000000000004476 ) ;
#192008 = CARTESIAN_POINT ( 'NONE',  ( -5.823673210054431948, 21.52544592524334988, 72.70942372801901854 ) ) ;
#192009 = CARTESIAN_POINT ( 'NONE',  ( -21.53943276465977519, 0.05219959533907696930, 56.24890960531436690 ) ) ;
#192010 = CARTESIAN_POINT ( 'NONE',  ( 19.02544592524343514, -5.153800228976328945, 28.54057627198102409 ) ) ;
#192012 = CARTESIAN_POINT ( 'NONE',  ( -13.89961937509957401, -13.97604488694547875, 104.3760903946856757 ) ) ;
#192011 = B_SPLINE_CURVE_WITH_KNOTS ( 'NONE', 3,
 ( #142758, #154956, #94268, #34596 ),
 .UNSPECIFIED., .F., .F.,
 ( 4, 4 ),
 ( 0.000000000000000000, 0.007966019813518861181 ),
 .UNSPECIFIED. ) ;
#192013 = CARTESIAN_POINT ( 'NONE',  ( 27.05641397906351386, 3.631740835637567333, 169.9999999999999716 ) ) ;
#192015 = CARTESIAN_POINT ( 'NONE',  ( -10.81492255796078084, -18.62759615963271287, 42.08224293864769550 ) ) ;
#192014 = DIRECTION ( 'NONE',  ( -1.000000000000000000, 0.000000000000000000, 0.000000000000000000 ) ) ;
#192016 = CARTESIAN_POINT ( 'NONE',  ( 16.61371651742598843, -7.165104196376269385, 66.35415069992994574 ) ) ;
#192017 = CARTESIAN_POINT ( 'NONE',  ( -18.67979575497193778, 10.72451020669871902, 78.33442372801901854 ) ) ;
#192018 = CARTESIAN_POINT ( 'NONE',  ( 14.29746914071049879, -8.314922557960816363, 48.33224293864770260 ) ) ;
#192019 = CARTESIAN_POINT ( 'NONE',  ( 14.34966873604960469, 8.224510206698951720, 54.16557627198103120 ) ) ;
#192020 = CARTESIAN_POINT ( 'NONE',  ( 21.52544592524344225, -5.823673210054117533, 83.54057627198102409 ) ) ;
#192021 = CARTESIAN_POINT ( 'NONE',  ( -18.67979575497178146, -10.72451020669898902, 71.66557627198100988 ) ) ;
#192022 = DIRECTION ( 'NONE',  ( 0.000000000000000000, 0.000000000000000000, 1.000000000000000000 ) ) ;
#192023 = CARTESIAN_POINT ( 'NONE',  ( 15.80617190586746368, 15.72974639402197994, 34.37390960531435979 ) ) ;
#192024 = CARTESIAN_POINT ( 'NONE',  ( -12.06949235617739369, -12.14591786802326823, 54.37609039468568994 ) ) ;
#192025 = CARTESIAN_POINT ( 'NONE',  ( 16.53943276465976808, -0.05219959533910856209, 78.74890960531436690 ) ) ;
#192026 = CARTESIAN_POINT ( 'NONE',  ( -19.02544592524342804, 5.153800228976336051, 66.04057627198103830 ) ) ;
#192027 = CARTESIAN_POINT ( 'NONE',  ( 19.05341960407611168, 5.049401038298154454, 38.95724293864767418 ) ) ;
#192028 = SURFACE_STYLE_USAGE ( .BOTH. , #51520 ) ;
#192029 = DIRECTION ( 'NONE',  ( -0.000000000000000000, -0.000000000000000000, 1.000000000000000000 ) ) ;
#192030 = ORIENTED_EDGE ( 'NONE', *, *, #143190, .T. ) ;
#192031 = CARTESIAN_POINT ( 'NONE',  ( -14.34966873604972548, 8.224510206698743886, 78.33442372801901854 ) ) ;
#192032 = CARTESIAN_POINT ( 'NONE',  ( 21.53943276465977519, 0.05219959533937863772, 21.25109039468567218 ) ) ;
#192033 = CARTESIAN_POINT ( 'NONE',  ( 13.89961937509977652, -13.97604488694527269, 88.12390960531438111 ) ) ;
#192034 = CARTESIAN_POINT ( 'NONE',  ( -21.53943276465977519, -0.05219959533937600094, 53.75109039468568994 ) ) ;
#192035 = CARTESIAN_POINT ( 'NONE',  ( -16.46253265017160317, 9.564922557960807481, 110.8322429386476955 ) ) ;
#192036 = CARTESIAN_POINT ( 'NONE',  ( -18.37518290867432214, -35.61898371400481267, -22.28534798804468053 ) ) ;
#192037 = AXIS2_PLACEMENT_3D ( 'NONE', #66525, #85680, #97831 ) ;
#192038 = VERTEX_POINT ( 'NONE', #138661 ) ;
#192039 = CARTESIAN_POINT ( 'NONE',  ( 15.80617190586769283, -15.72974639402175789, 40.62609039468567573 ) ) ;
#192041 = CARTESIAN_POINT ( 'NONE',  ( 16.51473224551069308, 9.474510206698969483, 104.1655762719810241 ) ) ;
#192040 = CARTESIAN_POINT ( 'NONE',  ( -16.51473224551069308, -9.474510206698971260, 41.66557627198103120 ) ) ;
#192042 = CARTESIAN_POINT ( 'NONE',  ( -16.51473224551082808, 9.474510206698731452, 53.33442372801900433 ) ) ;
#192043 = CARTESIAN_POINT ( 'NONE',  ( -21.55341960407610458, -5.719274019375992779, 111.4572429386476813 ) ) ;
#192044 = CARTESIAN_POINT ( 'NONE',  ( 5.049401038297881783, 19.05341960407617563, 42.29275706135234003 ) ) ;
#192045 = CARTESIAN_POINT ( 'NONE',  ( -19.05341960407611168, -5.049401038298163336, 31.45724293864769550 ) ) ;
#192046 = CARTESIAN_POINT ( 'NONE',  ( 14.29746914071037800, 8.314922557961029526, 96.66775706135234714 ) ) ;
#192047 = CARTESIAN_POINT ( 'NONE',  ( 13.97604488694548053, -13.89961937509957401, 60.62609039468564731 ) ) ;
#192048 = CARTESIAN_POINT ( 'NONE',  ( 16.53943276465976808, 0.05219959533934440121, 106.2510903946856757 ) ) ;
#192049 = DIRECTION ( 'NONE',  ( 1.000000000000000000, 0.000000000000000000, 0.000000000000000000 ) ) ;
#192050 = CARTESIAN_POINT ( 'NONE',  ( 19.02544592524343514, -5.153800228976328945, 83.54057627198100988 ) ) ;
#192051 = CARTESIAN_POINT ( 'NONE',  ( 0.05219959533937995610, -21.53943276465977519, 95.00109039468568994 ) ) ;
#192052 = CARTESIAN_POINT ( 'NONE',  ( 15.72974639402176855, 15.80617190586768217, 106.8760903946856899 ) ) ;
#192053 = DIRECTION ( 'NONE',  ( -0.000000000000000000, -0.000000000000000000, -1.000000000000000000 ) ) ;
#192054 = CARTESIAN_POINT ( 'NONE',  ( 9.474510206698971260, -16.51473224551069308, 107.9155762719810383 ) ) ;
#192055 = CARTESIAN_POINT ( 'NONE',  ( 21.55341960407619695, -5.719274019375665929, 81.04275706135236135 ) ) ;
#192056 = CARTESIAN_POINT ( 'NONE',  ( 19.02544592524334988, 5.153800228976608722, 111.4594237280190043 ) ) ;
#192057 = CARTESIAN_POINT ( 'NONE',  ( -9.474510206698964154, 16.51473224551069663, 80.41557627198103830 ) ) ;
#192058 = CARTESIAN_POINT ( 'NONE',  ( 5.823673210054125526, 21.52544592524343514, 24.79057627198103120 ) ) ;
#192059 = CARTESIAN_POINT ( 'NONE',  ( -13.97604488694527625, -13.89961937509977652, 86.87390960531436690 ) ) ;
#192060 = CARTESIAN_POINT ( 'NONE',  ( -16.79531203550648755, -7.028104445595603877, 91.25244988220444498 ) ) ;
#192061 = CARTESIAN_POINT ( 'NONE',  ( 5.153800228976335163, 19.02544592524342804, 84.79057627198099567 ) ) ;
#192062 = CARTESIAN_POINT ( 'NONE',  ( 13.89961937509977652, -13.97604488694527269, 68.12390960531436690 ) ) ;
#192063 = CARTESIAN_POINT ( 'NONE',  ( -16.52544592524335698, -4.483927247898792601, 98.95942372801903275 ) ) ;
#192064 = DIRECTION ( 'NONE',  ( -0.000000000000000000, -0.000000000000000000, -1.000000000000000000 ) ) ;
#192065 = CARTESIAN_POINT ( 'NONE',  ( 19.02544592524334988, 5.153800228976608722, 61.45942372801900433 ) ) ;
#192066 = CARTESIAN_POINT ( 'NONE',  ( -9.564922557960796823, -16.46253265017161027, 87.08224293864769550 ) ) ;
#192067 = CARTESIAN_POINT ( 'NONE',  ( 12.14591786802309770, 12.06949235617756955, 79.37390960531436690 ) ) ;
#192068 = CARTESIAN_POINT ( 'NONE',  ( -0.05219959533907301413, -21.53943276465977519, 37.49890960531436690 ) ) ;
#192069 =( GEOMETRIC_REPRESENTATION_CONTEXT ( 3 ) GLOBAL_UNCERTAINTY_ASSIGNED_CONTEXT ( ( #35798 ) ) GLOBAL_UNIT_ASSIGNED_CONTEXT ( ( #127353, #116191, #21182 ) ) REPRESENTATION_CONTEXT ( 'NONE', 'WORKASPACE' ) );
#192070 = CARTESIAN_POINT ( 'NONE',  ( 19.02544592524343514, -5.153800228976328945, 113.5405762719810241 ) ) ;
#192071 = CARTESIAN_POINT ( 'NONE',  ( -14.34966873604960291, -8.224510206698953496, 86.66557627198102409 ) ) ;
#192072 = FACE_OUTER_BOUND ( 'NONE', #160937, .T. ) ;
#192073 = CARTESIAN_POINT ( 'NONE',  ( -9.564922557961040184, 16.46253265017147172, 47.91775706135233293 ) ) ;
#192074 = CARTESIAN_POINT ( 'NONE',  ( 16.52544592524342804, -4.483927247898539470, 28.54057627198103120 ) ) ;
#192075 = CARTESIAN_POINT ( 'NONE',  ( -13.89961937509977652, 13.97604488694528158, 100.6239096053143669 ) ) ;
#192076 = CARTESIAN_POINT ( 'NONE',  ( 21.53943276465977519, 0.05219959533937863772, 66.25109039468567573 ) ) ;
#192077 = CARTESIAN_POINT ( 'NONE',  ( -5.823673210054116645, -21.52544592524344225, 52.29057627198102409 ) ) ;
#192078 = CARTESIAN_POINT ( 'NONE',  ( 18.62759615963255655, 10.81492255796105972, 31.66775706135234358 ) ) ;
#192079 = CARTESIAN_POINT ( 'NONE',  ( 18.62759615963271287, -10.81492255796078972, 83.33224293864769550 ) ) ;
#192080 = CARTESIAN_POINT ( 'NONE',  ( -10.81492255796105439, 18.62759615963255655, 42.91775706135235424 ) ) ;
#192081 = CARTESIAN_POINT ( 'NONE',  ( 0.05219959533910956823, 16.53943276465976808, 109.9989096053143527 ) ) ;
#192082 = CARTESIAN_POINT ( 'NONE',  ( 13.97604488694548053, -13.89961937509957401, 70.62609039468567573 ) ) ;
#192083 = CARTESIAN_POINT ( 'NONE',  ( 13.89961937509977652, -13.97604488694527269, 48.12390960531435979 ) ) ;
#192085 = CARTESIAN_POINT ( 'NONE',  ( -19.05341960407611168, -5.049401038298163336, 91.45724293864766707 ) ) ;
#192084 = CARTESIAN_POINT ( 'NONE',  ( 14.29746914071049879, -8.314922557960816363, 98.33224293864769550 ) ) ;
#192086 = CARTESIAN_POINT ( 'NONE',  ( -13.89961937509977652, 13.97604488694528158, 100.6239096053143669 ) ) ;
#192087 = CARTESIAN_POINT ( 'NONE',  ( -4.483927247898539470, -16.52544592524342804, 112.2905762719810241 ) ) ;
#192088 = CARTESIAN_POINT ( 'NONE',  ( -16.52544592524342804, 4.483927247898546575, 36.04057627198102409 ) ) ;
#192089 = CARTESIAN_POINT ( 'NONE',  ( 12.14591786802327356, -12.06949235617739191, 105.6260903946856899 ) ) ;
#192090 = CARTESIAN_POINT ( 'NONE',  ( -0.05219959533909027116, -19.03943276465977164, 57.49890960531435979 ) ) ;
#192091 = CARTESIAN_POINT ( 'NONE',  ( -16.53943276465976808, 0.05219959533911058130, 116.2489096053143669 ) ) ;
#192093 = AXIS2_PLACEMENT_3D ( 'NONE', #43775, #107406, #92237 ) ;
#192092 = CARTESIAN_POINT ( 'NONE',  ( -21.55341960407619339, 5.719274019375674811, 113.5427570613523756 ) ) ;
#192095 = CARTESIAN_POINT ( 'NONE',  ( 12.06949235617757843, -12.14591786802309237, 28.12390960531435979 ) ) ;
#192094 = CARTESIAN_POINT ( 'NONE',  ( -15.49999999999999822, 5.499999999999998224, 118.0000000000000142 ) ) ;
#192096 = CARTESIAN_POINT ( 'NONE',  ( 18.67979575497194134, -10.72451020669871369, 50.83442372801901143 ) ) ;
#192097 = CARTESIAN_POINT ( 'NONE',  ( -5.153800228976328057, -19.02544592524343514, 102.2905762719810383 ) ) ;
#192098 = CARTESIAN_POINT ( 'NONE',  ( -4.379528057220086978, -16.55341960407618274, 44.79275706135234714 ) ) ;
#192099 = CARTESIAN_POINT ( 'NONE',  ( 8.224510206698742110, 14.34966873604972548, 102.0844237280190185 ) ) ;
#192100 = CARTESIAN_POINT ( 'NONE',  ( -16.46253265017160317, 9.564922557960807481, 45.83224293864769550 ) ) ;
#192101 = CARTESIAN_POINT ( 'NONE',  ( -12.14591786802326823, 12.06949235617739902, 88.12609039468570415 ) ) ;
#192102 = CARTESIAN_POINT ( 'NONE',  ( -4.483927247898782831, 16.52544592524335698, 32.70942372801900433 ) ) ;
#192103 = CARTESIAN_POINT ( 'NONE',  ( 19.02544592524343514, -5.153800228976328945, 53.54057627198102409 ) ) ;
#192104 = CARTESIAN_POINT ( 'NONE',  ( -12.14591786802309592, -12.06949235617757132, 111.8739096053143669 ) ) ;
#192105 = CARTESIAN_POINT ( 'NONE',  ( -21.52544592524343514, 5.823673210054127303, 111.0405762719810525 ) ) ;
#192106 = CARTESIAN_POINT ( 'NONE',  ( -19.03943276465977164, 0.05219959533909376836, 31.24890960531435979 ) ) ;
#192107 = CARTESIAN_POINT ( 'NONE',  ( 5.049401038298161559, -19.05341960407611168, 102.7072429386476955 ) ) ;
#192108 = CARTESIAN_POINT ( 'NONE',  ( -5.049401038298153566, 19.05341960407611168, 35.20724293864768839 ) ) ;
#192109 = EDGE_CURVE ( 'NONE', #144449, #82312, #158723, .T. ) ;
#192110 = CARTESIAN_POINT ( 'NONE',  ( -19.03943276465977164, 0.05219959533909376836, 106.2489096053143669 ) ) ;
#192111 = LINE ( 'NONE', #102099, #6595 ) ;
#192112 = CARTESIAN_POINT ( 'NONE',  ( -13.89961937509977652, 13.97604488694528158, 100.6239096053143669 ) ) ;
#192114 = CARTESIAN_POINT ( 'NONE',  ( -14.34966873604960291, -8.224510206698953496, 106.6655762719810383 ) ) ;
#192113 = CARTESIAN_POINT ( 'NONE',  ( -18.62759615963255300, -10.81492255796106328, 39.16775706135235424 ) ) ;
#192115 = CARTESIAN_POINT ( 'NONE',  ( -16.46253265017160317, 9.564922557960807481, 105.8322429386476955 ) ) ;
#192116 = CARTESIAN_POINT ( 'NONE',  ( -27.83962847747548608, -7.578403945695542987, 161.1890875224084709 ) ) ;
#192117 = CARTESIAN_POINT ( 'NONE',  ( -16.53943276465976808, -0.05219959533934237506, 58.75109039468568994 ) ) ;
#192118 = CARTESIAN_POINT ( 'NONE',  ( 10.72451020669871369, 18.67979575497193778, 87.08442372801901854 ) ) ;
#192119 = CARTESIAN_POINT ( 'NONE',  ( 16.52544592524335698, 4.483927247898782831, 36.45942372801901143 ) ) ;
#192120 = CARTESIAN_POINT ( 'NONE',  ( -5.049401038298153566, 19.05341960407611168, 85.20724293864766707 ) ) ;
#192121 = EDGE_CURVE ( 'NONE', #22413, #178146, #133496, .T. ) ;
#192122 = CARTESIAN_POINT ( 'NONE',  ( -14.34966873604972548, 8.224510206698743886, 33.33442372801900433 ) ) ;
#192123 = CARTESIAN_POINT ( 'NONE',  ( -13.97604488694547697, 13.89961937509957934, 108.1260903946856331 ) ) ;
#192124 = CARTESIAN_POINT ( 'NONE',  ( -12.06949235617739369, -12.14591786802326823, 84.37609039468570415 ) ) ;
#192125 = CARTESIAN_POINT ( 'NONE',  ( -5.049401038297874678, -19.05341960407617918, 94.79275706135230450 ) ) ;
#192126 = CARTESIAN_POINT ( 'NONE',  ( -19.02544592524342804, 5.153800228976336051, 76.04057627198102409 ) ) ;
#192127 = CARTESIAN_POINT ( 'NONE',  ( -18.62759615963270932, 10.81492255796079327, 100.8322429386477097 ) ) ;
#192129 = CARTESIAN_POINT ( 'NONE',  ( 9.474510206698729675, 16.51473224551082808, 87.08442372801900433 ) ) ;
#192128 = CARTESIAN_POINT ( 'NONE',  ( 12.14591786802309770, 12.06949235617756955, 84.37390960531438111 ) ) ;
#192130 = CARTESIAN_POINT ( 'NONE',  ( -12.06949235617739369, -12.14591786802326823, 69.37609039468567573 ) ) ;
#192131 = CARTESIAN_POINT ( 'NONE',  ( 22.00000000000000000, -5.204748896376250896E-15, 47.50000000000000000 ) ) ;
#192132 = CARTESIAN_POINT ( 'NONE',  ( -13.97604488694547697, 13.89961937509957934, 73.12609039468568994 ) ) ;
#192133 = CARTESIAN_POINT ( 'NONE',  ( -4.379528057220328563, 16.55341960407611168, 35.20724293864768839 ) ) ;
#192134 = CARTESIAN_POINT ( 'NONE',  ( 16.55341960407611168, 4.379528057220329451, 88.95724293864769550 ) ) ;
#192136 = CARTESIAN_POINT ( 'NONE',  ( -9.474510206698720793, -16.51473224551083518, 44.58442372801900433 ) ) ;
#192135 = CARTESIAN_POINT ( 'NONE',  ( -19.05341960407617563, 5.049401038297882671, 33.54275706135231871 ) ) ;
#192137 = CARTESIAN_POINT ( 'NONE',  ( -21.52544592524334988, -5.823673210054445271, 28.95942372801902209 ) ) ;
#192138 = CARTESIAN_POINT ( 'NONE',  ( 16.51473224551069308, 9.474510206698969483, 109.1655762719810383 ) ) ;
#192139 = CARTESIAN_POINT ( 'NONE',  ( -0.05219959533909027116, -19.03943276465977164, 72.49890960531435269 ) ) ;
#192140 = CARTESIAN_POINT ( 'NONE',  ( 10.72451020669871369, 18.67979575497193778, 102.0844237280190185 ) ) ;
#192141 = CARTESIAN_POINT ( 'NONE',  ( -19.05341960407611168, -5.049401038298163336, 81.45724293864769550 ) ) ;
#192142 = CARTESIAN_POINT ( 'NONE',  ( -5.719274019375978568, 21.55341960407610458, 40.20724293864769550 ) ) ;
#192143 = CONICAL_SURFACE ( 'NONE', #153458, 2.500000000000000000, 1.029744258676656976 ) ;
#192144 = CARTESIAN_POINT ( 'NONE',  ( 16.53943276465976808, -0.05219959533910856209, 93.74890960531436690 ) ) ;
#192145 = CARTESIAN_POINT ( 'NONE',  ( -9.474510206698964154, 16.51473224551069663, 55.41557627198103120 ) ) ;
#192146 = CARTESIAN_POINT ( 'NONE',  ( 16.52544592524342804, -4.483927247898539470, 108.5405762719810241 ) ) ;
#192147 = CARTESIAN_POINT ( 'NONE',  ( 10.72451020669871369, 18.67979575497193778, 27.08442372801901854 ) ) ;
#192148 = CARTESIAN_POINT ( 'NONE',  ( -18.67979575497193778, 10.72451020669871902, 68.33442372801900433 ) ) ;
#192149 = CARTESIAN_POINT ( 'NONE',  ( -5.049401038298153566, 19.05341960407611168, 45.20724293864769550 ) ) ;
#192150 = CARTESIAN_POINT ( 'NONE',  ( -8.224510206698735004, -14.34966873604973081, 79.58442372801903275 ) ) ;
#192151 = CARTESIAN_POINT ( 'NONE',  ( 10.81492255796078972, 18.62759615963270932, 109.5822429386476955 ) ) ;
#192152 = ORIENTED_EDGE ( 'NONE', *, *, #96611, .F. ) ;
#192153 = CARTESIAN_POINT ( 'NONE',  ( -10.72451020669898014, 18.67979575497178502, 105.4155762719810383 ) ) ;
#192155 = CARTESIAN_POINT ( 'NONE',  ( -5.049401038298153566, 19.05341960407611168, 60.20724293864768129 ) ) ;
#192154 = CARTESIAN_POINT ( 'NONE',  ( 13.89961937509957401, 13.97604488694547697, 36.87609039468565442 ) ) ;
#192156 = CARTESIAN_POINT ( 'NONE',  ( 16.46253265017146816, 9.564922557961045513, 36.66775706135233293 ) ) ;
#192157 = CARTESIAN_POINT ( 'NONE',  ( 21.53943276465977519, 0.05219959533937863772, 76.25109039468568994 ) ) ;
#192158 = EDGE_CURVE ( 'NONE', #179309, #127046, #52443, .T. ) ;
#192159 = CARTESIAN_POINT ( 'NONE',  ( -15.80617190586745835, -15.72974639402198527, 66.87390960531436690 ) ) ;
#192160 = CARTESIAN_POINT ( 'NONE',  ( -8.224510206698948167, 14.34966873604960824, 35.41557627198102409 ) ) ;
#192162 = CARTESIAN_POINT ( 'NONE',  ( 19.05341960407617918, -5.049401038297876454, 31.04275706135232227 ) ) ;
#192161 = CARTESIAN_POINT ( 'NONE',  ( 21.53943276465977519, 0.05219959533937863772, 91.25109039468568994 ) ) ;
#192163 = CARTESIAN_POINT ( 'NONE',  ( 8.314922557960818139, 14.29746914071049879, 74.58224293864768129 ) ) ;
#192164 = CARTESIAN_POINT ( 'NONE',  ( 14.29746914071049879, -8.314922557960816363, 103.3322429386476955 ) ) ;
#192165 = CARTESIAN_POINT ( 'NONE',  ( 5.153800228976615827, -19.02544592524334988, 60.20942372801899012 ) ) ;
#192166 = CARTESIAN_POINT ( 'NONE',  ( -16.55341960407617563, 4.379528057220093196, 113.5427570613523756 ) ) ;
#192167 = CARTESIAN_POINT ( 'NONE',  ( 15.72974639402176855, 15.80617190586768217, 66.87609039468568994 ) ) ;
#192168 = CARTESIAN_POINT ( 'NONE',  ( 9.474510206698971260, -16.51473224551069308, 77.91557627198103830 ) ) ;
#192169 = CARTESIAN_POINT ( 'NONE',  ( -16.46253265017146816, -9.564922557961047289, 49.16775706135233293 ) ) ;
#192170 = CARTESIAN_POINT ( 'NONE',  ( -18.67979575497178146, -10.72451020669898902, 56.66557627198103830 ) ) ;
#192171 = CARTESIAN_POINT ( 'NONE',  ( 10.72451020669871369, 18.67979575497193778, 42.08442372801901854 ) ) ;
#192172 = CARTESIAN_POINT ( 'NONE',  ( 21.53943276465977519, -0.05219959533907433946, 98.74890960531438111 ) ) ;
#192173 = CARTESIAN_POINT ( 'NONE',  ( 16.46253265017146816, 9.564922557961045513, 101.6677570613523329 ) ) ;
#192174 = CARTESIAN_POINT ( 'NONE',  ( -14.34966873604972548, 8.224510206698743886, 68.33442372801900433 ) ) ;
#192176 = CARTESIAN_POINT ( 'NONE',  ( -5.719274019375978568, 21.55341960407610458, 110.2072429386477239 ) ) ;
#192175 = CARTESIAN_POINT ( 'NONE',  ( -16.17338109997596973, -17.62895962574413389, -57.05728224822367878 ) ) ;
#192177 = CARTESIAN_POINT ( 'NONE',  ( 8.224510206698953496, -14.34966873604960469, 87.91557627198103830 ) ) ;
#192178 = CARTESIAN_POINT ( 'NONE',  ( -17.50000000000001776, -4.049696124445835821, 30.81960329334054549 ) ) ;
#192179 = CARTESIAN_POINT ( 'NONE',  ( -4.379528057220086978, -16.55341960407618274, 19.79275706135235069 ) ) ;
#192180 = CARTESIAN_POINT ( 'NONE',  ( 10.81492255796078972, 18.62759615963270932, 49.58224293864769550 ) ) ;
#192181 = CARTESIAN_POINT ( 'NONE',  ( 14.29746914071037800, 8.314922557961029526, 86.66775706135234714 ) ) ;
#192182 = CARTESIAN_POINT ( 'NONE',  ( 36.91631499011236883, -2.427738359554614700, -8.000000000000001776 ) ) ;
#192183 = CARTESIAN_POINT ( 'NONE',  ( 8.224510206698742110, 14.34966873604972548, 67.08442372801901854 ) ) ;
#192184 = CARTESIAN_POINT ( 'NONE',  ( 5.719274019375673035, 21.55341960407619339, 42.29275706135235424 ) ) ;
#192185 = CARTESIAN_POINT ( 'NONE',  ( 0.05219959533907565091, 21.53943276465977519, 44.99890960531435979 ) ) ;
#192186 = CARTESIAN_POINT ( 'NONE',  ( -8.224510206698735004, -14.34966873604973081, 79.58442372801903275 ) ) ;
#192187 = CARTESIAN_POINT ( 'NONE',  ( -19.03943276465977164, 0.05219959533909376836, 101.2489096053143669 ) ) ;
#192188 = CARTESIAN_POINT ( 'NONE',  ( -21.55341960407619339, 5.719274019375674811, 68.54275706135234714 ) ) ;
#192189 = CARTESIAN_POINT ( 'NONE',  ( -21.52544592524343514, 5.823673210054127303, 41.04057627198103120 ) ) ;
#192190 = CARTESIAN_POINT ( 'NONE',  ( -10.72451020669898014, 18.67979575497178502, 30.41557627198101699 ) ) ;
#192191 = ORIENTED_EDGE ( 'NONE', *, *, #145468, .F. ) ;
#192192 = CARTESIAN_POINT ( 'NONE',  ( -13.97604488694547697, 13.89961937509957934, 53.12609039468565442 ) ) ;
#192193 = CARTESIAN_POINT ( 'NONE',  ( -4.379528057220086978, -16.55341960407618274, 64.79275706135234714 ) ) ;
#192194 = CARTESIAN_POINT ( 'NONE',  ( -5.823673210054116645, -21.52544592524344225, 32.29057627198102409 ) ) ;
#192195 = ORIENTED_EDGE ( 'NONE', *, *, #16394, .F. ) ;
#192196 = CARTESIAN_POINT ( 'NONE',  ( 9.564922557960805705, 16.46253265017160317, 84.58224293864769550 ) ) ;
#192197 = CARTESIAN_POINT ( 'NONE',  ( -16.53943276465976808, 0.05219959533911058130, 21.24890960531436690 ) ) ;
#192198 = CARTESIAN_POINT ( 'NONE',  ( 2.552343178074615970, -7.052343178074640839, 1.110912703473986074 ) ) ;
#192199 = CARTESIAN_POINT ( 'NONE',  ( 12.14591786802309770, 12.06949235617756955, 114.3739096053143527 ) ) ;
#192200 = CARTESIAN_POINT ( 'NONE',  ( 5.823673210054125526, 21.52544592524343514, 44.79057627198103120 ) ) ;
#192201 = CARTESIAN_POINT ( 'NONE',  ( -19.03943276465977164, 0.05219959533909376836, 51.24890960531436690 ) ) ;
#192202 = CARTESIAN_POINT ( 'NONE',  ( -16.53943276465976808, -0.05219959533934237506, 93.75109039468567573 ) ) ;
#192203 = CARTESIAN_POINT ( 'NONE',  ( -5.823673210054431948, 21.52544592524334988, 27.70942372801901854 ) ) ;
#192204 = CARTESIAN_POINT ( 'NONE',  ( 5.153800228976615827, -19.02544592524334988, 95.20942372801897591 ) ) ;
#192205 = CARTESIAN_POINT ( 'NONE',  ( -16.52544592524342804, 4.483927247898546575, 91.04057627198103830 ) ) ;
#192206 = CARTESIAN_POINT ( 'NONE',  ( -5.049401038298153566, 19.05341960407611168, 55.20724293864769550 ) ) ;
#192207 = CARTESIAN_POINT ( 'NONE',  ( 16.51473224551069308, 9.474510206698969483, 29.16557627198103475 ) ) ;
#192208 = CARTESIAN_POINT ( 'NONE',  ( 21.52544592524334988, 5.823673210054432836, 111.4594237280190328 ) ) ;
#192209 = CARTESIAN_POINT ( 'NONE',  ( -13.89961937509977652, 13.97604488694528158, 80.62390960531436690 ) ) ;
#192210 = CARTESIAN_POINT ( 'NONE',  ( -4.483927247898782831, 16.52544592524335698, 67.70942372801901854 ) ) ;
#192211 = CARTESIAN_POINT ( 'NONE',  ( 21.52544592524334988, 5.823673210054432836, 91.45942372801901854 ) ) ;
#192212 = CARTESIAN_POINT ( 'NONE',  ( 21.52544592524344225, -5.823673210054117533, 48.54057627198103120 ) ) ;
#192213 = CARTESIAN_POINT ( 'NONE',  ( -4.379528057220086978, -16.55341960407618274, 74.79275706135234714 ) ) ;
#192214 = CARTESIAN_POINT ( 'NONE',  ( -19.02544592524334988, -5.153800228976617603, 48.95942372801900433 ) ) ;
#192215 = CARTESIAN_POINT ( 'NONE',  ( 19.05341960407617918, -5.049401038297876454, 71.04275706135234714 ) ) ;
#192216 = ORIENTED_EDGE ( 'NONE', *, *, #22880, .T. ) ;
#192217 = CARTESIAN_POINT ( 'NONE',  ( 18.62759615963255655, 10.81492255796105972, 61.66775706135235424 ) ) ;
#192219 = TOROIDAL_SURFACE ( 'NONE', #53348, 69.99999999999998579, 8.000000000000000000 ) ;
#192218 = CARTESIAN_POINT ( 'NONE',  ( -13.89961937509977652, 13.97604488694528158, 60.62390960531436690 ) ) ;
#192220 = CARTESIAN_POINT ( 'NONE',  ( -16.46253265017160317, 9.564922557960807481, 30.83224293864769550 ) ) ;
#192221 = CARTESIAN_POINT ( 'NONE',  ( 13.89961937509957401, 13.97604488694547697, 56.87609039468564731 ) ) ;
#192222 = CARTESIAN_POINT ( 'NONE',  ( 19.05341960407611168, 5.049401038298154454, 108.9572429386477097 ) ) ;
#192223 = CARTESIAN_POINT ( 'NONE',  ( -13.97604488694527625, -13.89961937509977652, 96.87390960531433848 ) ) ;
#192224 = CARTESIAN_POINT ( 'NONE',  ( -4.379528057220328563, 16.55341960407611168, 50.20724293864769550 ) ) ;
#192225 = CARTESIAN_POINT ( 'NONE',  ( -21.52544592524343514, 5.823673210054127303, 46.04057627198103830 ) ) ;
#192226 = AXIS2_PLACEMENT_3D ( 'NONE', #125573, #154913, #79059 ) ;
#192227 = CYLINDRICAL_SURFACE ( 'NONE', #112651, 1.499999999999997780 ) ;
#192228 = CARTESIAN_POINT ( 'NONE',  ( -5.049401038297874678, -19.05341960407617918, 19.79275706135233293 ) ) ;
#192229 = CARTESIAN_POINT ( 'NONE',  ( -16.61371651742599909, -7.165104196376135270, 81.14584930007002583 ) ) ;
#192230 = CARTESIAN_POINT ( 'NONE',  ( -5.049401038298153566, 19.05341960407611168, 55.20724293864769550 ) ) ;
#192231 = CARTESIAN_POINT ( 'NONE',  ( 28.82186960331498327, 2.428612866367529932E-14, 139.9999999999999716 ) ) ;
#192232 = CARTESIAN_POINT ( 'NONE',  ( -17.40861289039002813, 6.110651285853322179, 108.6276752917256943 ) ) ;
#192233 = CARTESIAN_POINT ( 'NONE',  ( -16.52544592524335698, -4.483927247898792601, 78.95942372801901854 ) ) ;
#192234 = CARTESIAN_POINT ( 'NONE',  ( 10.72451020669898902, -18.67979575497178502, 92.91557627198103830 ) ) ;
#192235 =( BOUNDED_CURVE ( )  B_SPLINE_CURVE ( 3, ( #41878, #194560, #42869, #196566 ),
 .UNSPECIFIED., .F., .T. ) 
 B_SPLINE_CURVE_WITH_KNOTS ( ( 4, 4 ),
 ( 1.570796326794896780, 2.115944711806982959 ),
 .UNSPECIFIED. ) 
 CURVE ( )  GEOMETRIC_REPRESENTATION_ITEM ( )  RATIONAL_B_SPLINE_CURVE ( ( 1.000000000000000000, 0.9753873905749756990, 0.9753873905749756990, 1.000000000000000000 ) ) 
 REPRESENTATION_ITEM ( '' )  );
#192236 = CARTESIAN_POINT ( 'NONE',  ( -14.29746914071049879, 8.314922557960819915, 50.83224293864770971 ) ) ;
#192238 = DIRECTION ( 'NONE',  ( 1.000000000000000000, 0.000000000000000000, 0.000000000000000000 ) ) ;
#192237 = CARTESIAN_POINT ( 'NONE',  ( -9.474510206698964154, 16.51473224551069663, 35.41557627198102409 ) ) ;
#192239 = CARTESIAN_POINT ( 'NONE',  ( 18.62759615963255655, 10.81492255796105972, 36.66775706135234714 ) ) ;
#192240 = CARTESIAN_POINT ( 'NONE',  ( 5.049401038297881783, 19.05341960407617563, 42.29275706135234003 ) ) ;
#192241 = CARTESIAN_POINT ( 'NONE',  ( 0.05219959533909260263, 19.03943276465977164, 39.99890960531436690 ) ) ;
#192242 = CARTESIAN_POINT ( 'NONE',  ( 18.62759615963255655, 10.81492255796105972, 101.6677570613523613 ) ) ;
#192243 = CARTESIAN_POINT ( 'NONE',  ( -19.05341960407611168, -5.049401038298163336, 21.45724293864768839 ) ) ;
#192244 = CARTESIAN_POINT ( 'NONE',  ( 16.53943276465976808, -0.05219959533910856209, 38.74890960531435979 ) ) ;
#192245 = CARTESIAN_POINT ( 'NONE',  ( 0.2500000000000002220, 4.898587196589412829E-16, -4.000000000000000000 ) ) ;
#192246 = CARTESIAN_POINT ( 'NONE',  ( 15.80617190586746368, 15.72974639402197994, 39.37390960531436690 ) ) ;
#192247 = CARTESIAN_POINT ( 'NONE',  ( 1.820000000000000062, 0.000000000000000000, 0.000000000000000000 ) ) ;
#192248 = CARTESIAN_POINT ( 'NONE',  ( -16.46253265017160317, 9.564922557960807481, 105.8322429386476955 ) ) ;
#192249 = CARTESIAN_POINT ( 'NONE',  ( 12.14591786802309770, 12.06949235617756955, 84.37390960531438111 ) ) ;
#192250 = CARTESIAN_POINT ( 'NONE',  ( -5.153800228976607833, 19.02544592524334988, 112.7094237280190043 ) ) ;
#192251 = CARTESIAN_POINT ( 'NONE',  ( -14.29746914071037622, -8.314922557961029526, 109.1677570613523613 ) ) ;
#192252 = ORIENTED_EDGE ( 'NONE', *, *, #195257, .T. ) ;
#192253 = ADVANCED_FACE ( 'NONE', ( #99938 ), #114014, .T. ) ;
#192255 = CARTESIAN_POINT ( 'NONE',  ( 18.62759615963271287, -10.81492255796078972, 98.33224293864769550 ) ) ;
#192254 = CARTESIAN_POINT ( 'NONE',  ( 13.89961937509977652, -13.97604488694527269, 93.12390960531436690 ) ) ;
#192257 = CARTESIAN_POINT ( 'NONE',  ( -16.51473224551069308, -9.474510206698971260, 106.6655762719810383 ) ) ;
#192256 = CARTESIAN_POINT ( 'NONE',  ( -16.52544592524342804, 4.483927247898546575, 31.04057627198102409 ) ) ;
#192258 = CARTESIAN_POINT ( 'NONE',  ( -19.03943276465977164, -0.05219959533935918106, 83.75109039468567573 ) ) ;
#192259 = CARTESIAN_POINT ( 'NONE',  ( -10.81492255796105439, 18.62759615963255655, 112.9177570613523329 ) ) ;
#192260 = CARTESIAN_POINT ( 'NONE',  ( -5.719274019375978568, 21.55341960407610458, 85.20724293864770971 ) ) ;
#192261 = CARTESIAN_POINT ( 'NONE',  ( 18.67979575497178502, 10.72451020669898547, 54.16557627198103120 ) ) ;
#192262 = CARTESIAN_POINT ( 'NONE',  ( 16.51473224551069308, 9.474510206698969483, 69.16557627198102409 ) ) ;
#192263 = CARTESIAN_POINT ( 'NONE',  ( -16.55341960407611168, -4.379528057220339221, 31.45724293864769550 ) ) ;
#192264 = CARTESIAN_POINT ( 'NONE',  ( -0.05219959533909027116, -19.03943276465977164, 77.49890960531435269 ) ) ;
#192265 = ORIENTED_EDGE ( 'NONE', *, *, #95479, .F. ) ;
#192266 = CARTESIAN_POINT ( 'NONE',  ( -31.68593437162162729, -6.718755962661541403, 91.65819149638744534 ) ) ;
#192267 = CARTESIAN_POINT ( 'NONE',  ( -19.03943276465977164, -0.05219959533935918106, 23.75109039468566152 ) ) ;
#192268 = CARTESIAN_POINT ( 'NONE',  ( -8.314922557960811034, -14.29746914071050412, 87.08224293864769550 ) ) ;
#192269 = CARTESIAN_POINT ( 'NONE',  ( -18.62759615963255300, -10.81492255796106328, 24.16775706135235424 ) ) ;
#192270 = CARTESIAN_POINT ( 'NONE',  ( -8.571926809382601320, -26.38167802310801591, 141.7750000027311899 ) ) ;
#192271 = CARTESIAN_POINT ( 'NONE',  ( -0.05219959533934338120, 16.53943276465976808, 97.50109039468567573 ) ) ;
#192272 = CARTESIAN_POINT ( 'NONE',  ( -4.483927247898539470, -16.52544592524342804, 112.2905762719810241 ) ) ;
#192273 = CARTESIAN_POINT ( 'NONE',  ( 0.05219959533909260263, 19.03943276465977164, 74.99890960531435269 ) ) ;
#192274 = CARTESIAN_POINT ( 'NONE',  ( 16.51473224551069308, 9.474510206698969483, 24.16557627198102765 ) ) ;
#192275 = CARTESIAN_POINT ( 'NONE',  ( 14.34966873604960469, 8.224510206698951720, 29.16557627198103120 ) ) ;
#192276 = EDGE_CURVE ( 'NONE', #90870, #160624, #37871, .T. ) ;
#192277 = CARTESIAN_POINT ( 'NONE',  ( -18.62759615963255300, -10.81492255796106328, 54.16775706135235424 ) ) ;
#192278 = CARTESIAN_POINT ( 'NONE',  ( 28.83006054357690573, -24.83490584245822674, -16.72457388842970261 ) ) ;
#192279 = CARTESIAN_POINT ( 'NONE',  ( -21.53943276465977519, -0.05219959533937600094, 98.75109039468568994 ) ) ;
#192280 = CARTESIAN_POINT ( 'NONE',  ( 9.474510206698971260, -16.51473224551069308, 47.91557627198102409 ) ) ;
#192281 = CARTESIAN_POINT ( 'NONE',  ( -5.049401038298153566, 19.05341960407611168, 50.20724293864770260 ) ) ;
#192282 = ORIENTED_EDGE ( 'NONE', *, *, #58626, .T. ) ;
#192283 = CARTESIAN_POINT ( 'NONE',  ( 5.823673210054444382, -21.52544592524334988, 95.20942372801903275 ) ) ;
#192284 = CARTESIAN_POINT ( 'NONE',  ( -8.314922557961024197, 14.29746914071037800, 57.91775706135234714 ) ) ;
#192285 = B_SPLINE_CURVE_WITH_KNOTS ( 'NONE', 3,
 ( #17377, #168075, #29572, #14389, #60879, #184246, #45728, #169052, #50706, #156888, #81020, #65853, #3195, #190209, #126530, #34534, #159862, #37517, #80035, #173057, #64868, #97172 ),
 .UNSPECIFIED., .F., .F.,
 ( 4, 2, 2, 2, 2, 2, 2, 2, 2, 2, 4 ),
 ( 1.970604704475788300E-07, 0.0003054521314109980793, 0.0006107072023515486498, 0.001221217344232650116, 0.001831727486113751691, 0.002136982557054302369, 0.002442237627994853482, 0.003052747769875962646, 0.003663257911757071810, 0.004273768053638180540, 0.004884278195519286235 ),
 .UNSPECIFIED. ) ;
#192286 = CARTESIAN_POINT ( 'NONE',  ( -5.823673210054431948, 21.52544592524334988, 87.70942372801901854 ) ) ;
#192287 = CARTESIAN_POINT ( 'NONE',  ( -10.81492255796078084, -18.62759615963271287, 22.08224293864769194 ) ) ;
#192288 = CARTESIAN_POINT ( 'NONE',  ( -9.564922557961040184, 16.46253265017147172, 87.91775706135233293 ) ) ;
#192289 = CARTESIAN_POINT ( 'NONE',  ( -10.72451020669870658, -18.67979575497194134, 69.58442372801900433 ) ) ;
#192290 = CARTESIAN_POINT ( 'NONE',  ( 14.34966873604972726, -8.224510206698740333, 35.83442372801901143 ) ) ;
#192292 = CARTESIAN_POINT ( 'NONE',  ( -15.72974639402197994, 15.80617190586746368, 90.62390960531436690 ) ) ;
#192291 = AXIS2_PLACEMENT_3D ( 'NONE', #135947, #42942, #104606 ) ;
#192293 = CARTESIAN_POINT ( 'NONE',  ( 19.02544592524334988, 5.153800228976608722, 91.45942372801900433 ) ) ;
#192294 = CARTESIAN_POINT ( 'NONE',  ( 5.153800228976335163, 19.02544592524342804, 59.79057627198100988 ) ) ;
#192295 = CARTESIAN_POINT ( 'NONE',  ( -19.03943276465977164, -0.05219959533935918106, 98.75109039468567573 ) ) ;
#192296 = CARTESIAN_POINT ( 'NONE',  ( -19.03943276465977164, -0.05219959533935918106, 103.7510903946856757 ) ) ;
#192297 = CARTESIAN_POINT ( 'NONE',  ( 0.05219959533910956823, 16.53943276465976808, 49.99890960531437401 ) ) ;
#192298 = CARTESIAN_POINT ( 'NONE',  ( -0.05219959533936034679, 19.03943276465977164, 77.50109039468566152 ) ) ;
#192299 = CARTESIAN_POINT ( 'NONE',  ( 4.483927247898790824, -16.52544592524335698, 60.20942372801902565 ) ) ;
#192300 = CARTESIAN_POINT ( 'NONE',  ( 16.51473224551069308, 9.474510206698969483, 34.16557627198102409 ) ) ;
#192301 = CARTESIAN_POINT ( 'NONE',  ( -16.46253265017160317, 9.564922557960807481, 55.83224293864769550 ) ) ;
#192302 = CARTESIAN_POINT ( 'NONE',  ( -16.53943276465976808, -0.05219959533934237506, 58.75109039468568994 ) ) ;
#192303 = CARTESIAN_POINT ( 'NONE',  ( -8.571926809382601320, -26.38167802310801591, 139.7750000027311899 ) ) ;
#192304 = CARTESIAN_POINT ( 'NONE',  ( 8.571926809382597767, 26.38167802310806209, 148.2750000027311899 ) ) ;
#192305 = CARTESIAN_POINT ( 'NONE',  ( 9.474510206698971260, -16.51473224551069308, 107.9155762719810383 ) ) ;
#192306 = CARTESIAN_POINT ( 'NONE',  ( -16.51473224551069308, -9.474510206698971260, 21.66557627198102765 ) ) ;
#192307 = ORIENTED_EDGE ( 'NONE', *, *, #170515, .T. ) ;
#192308 = CARTESIAN_POINT ( 'NONE',  ( 19.03943276465977164, 0.05219959533936151252, 106.2510903946856615 ) ) ;
#192309 = CARTESIAN_POINT ( 'NONE',  ( -21.53943276465977519, 0.05219959533907696930, 41.24890960531435269 ) ) ;
#192311 = CARTESIAN_POINT ( 'NONE',  ( 12.06949235617739724, 12.14591786802326823, 26.87609039468567218 ) ) ;
#192310 = CARTESIAN_POINT ( 'NONE',  ( 19.03943276465977164, 0.05219959533936151252, 31.25109039468566863 ) ) ;
#192312 = CARTESIAN_POINT ( 'NONE',  ( -19.05341960407611168, -5.049401038298163336, 31.45724293864769550 ) ) ;
#192313 = CARTESIAN_POINT ( 'NONE',  ( -16.51473224551069308, -9.474510206698971260, 56.66557627198103120 ) ) ;
#192314 = CARTESIAN_POINT ( 'NONE',  ( -10.72451020669898014, 18.67979575497178502, 75.41557627198102409 ) ) ;
#192315 = CARTESIAN_POINT ( 'NONE',  ( -19.05341960407611168, -5.049401038298163336, 96.45724293864769550 ) ) ;
#192316 = CARTESIAN_POINT ( 'NONE',  ( 0.05219959533909260263, 19.03943276465977164, 44.99890960531435979 ) ) ;
#192317 = CARTESIAN_POINT ( 'NONE',  ( -27.73933785331498925, 2.428612866367529932E-14, 145.3750000027311842 ) ) ;
#192318 = CARTESIAN_POINT ( 'NONE',  ( 0.05219959533936267826, -19.03943276465977164, 80.00109039468567573 ) ) ;
#192319 = CARTESIAN_POINT ( 'NONE',  ( 12.14591786802309770, 12.06949235617756955, 64.37390960531435269 ) ) ;
#192320 = CARTESIAN_POINT ( 'NONE',  ( 21.52544592524344225, -5.823673210054117533, 43.54057627198103830 ) ) ;
#192321 = CARTESIAN_POINT ( 'NONE',  ( 21.52544592524334988, 5.823673210054432836, 106.4594237280190328 ) ) ;
#192322 = CARTESIAN_POINT ( 'NONE',  ( -10.72451020669898014, 18.67979575497178502, 100.4155762719810241 ) ) ;
#192323 = CARTESIAN_POINT ( 'NONE',  ( 15.80617190586769283, -15.72974639402175789, 75.62609039468567573 ) ) ;
#192324 = CARTESIAN_POINT ( 'NONE',  ( -5.823673210054431948, 21.52544592524334988, 77.70942372801900433 ) ) ;
#192325 = CARTESIAN_POINT ( 'NONE',  ( -19.05341960407611168, -5.049401038298163336, 111.4572429386476671 ) ) ;
#192327 = CARTESIAN_POINT ( 'NONE',  ( 18.62759615963255655, 10.81492255796105972, 71.66775706135234714 ) ) ;
#192326 = CARTESIAN_POINT ( 'NONE',  ( 8.224510206698742110, 14.34966873604972548, 112.0844237280190185 ) ) ;
#192328 = CARTESIAN_POINT ( 'NONE',  ( 0.05219959533909260263, 19.03943276465977164, 64.99890960531436690 ) ) ;
#192329 = CARTESIAN_POINT ( 'NONE',  ( 16.46253265017146816, 9.564922557961045513, 31.66775706135232937 ) ) ;
#192330 = CARTESIAN_POINT ( 'NONE',  ( -10.81492255796105439, 18.62759615963255655, 32.91775706135234714 ) ) ;
#192331 = CARTESIAN_POINT ( 'NONE',  ( 9.474510206698971260, -16.51473224551069308, 67.91557627198102409 ) ) ;
#192332 = CARTESIAN_POINT ( 'NONE',  ( 12.06949235617757843, -12.14591786802309237, 78.12390960531436690 ) ) ;
#192333 = CARTESIAN_POINT ( 'NONE',  ( 8.224510206698953496, -14.34966873604960469, 42.91557627198103120 ) ) ;
#192334 = CARTESIAN_POINT ( 'NONE',  ( 10.72451020669898902, -18.67979575497178502, 52.91557627198103830 ) ) ;
#192335 = CARTESIAN_POINT ( 'NONE',  ( -19.03943276465977164, 0.05219959533909376836, 66.24890960531436690 ) ) ;
#192336 = CARTESIAN_POINT ( 'NONE',  ( -15.72974639402197994, 15.80617190586746368, 65.62390960531436690 ) ) ;
#192337 = CARTESIAN_POINT ( 'NONE',  ( -19.03943276465977164, -0.05219959533935918106, 68.75109039468566152 ) ) ;
#192339 = CARTESIAN_POINT ( 'NONE',  ( 14.34966873604960469, 8.224510206698951720, 59.16557627198103120 ) ) ;
#192338 = FACE_OUTER_BOUND ( 'NONE', #84516, .T. ) ;
#192340 = CARTESIAN_POINT ( 'NONE',  ( 10.81492255796078972, 18.62759615963270932, 44.58224293864769550 ) ) ;
#192341 = ORIENTED_EDGE ( 'NONE', *, *, #152270, .T. ) ;
#192342 = CARTESIAN_POINT ( 'NONE',  ( -17.49999999999999289, 5.500000000000036415, 65.79690382534171533 ) ) ;
#192344 = CARTESIAN_POINT ( 'NONE',  ( 27.73933785331498925, -9.013057229001034898, 140.2750000027311614 ) ) ;
#192343 = CARTESIAN_POINT ( 'NONE',  ( 8.314922557961029526, -14.29746914071037800, 85.41775706135236135 ) ) ;
#192345 = CARTESIAN_POINT ( 'NONE',  ( -13.89961937509957401, -13.97604488694547875, 94.37609039468566152 ) ) ;
#192346 = CARTESIAN_POINT ( 'NONE',  ( 16.52544592524342804, -4.483927247898539470, 73.54057627198102409 ) ) ;
#192347 = FACE_OUTER_BOUND ( 'NONE', #75058, .T. ) ;
#192348 = CARTESIAN_POINT ( 'NONE',  ( 5.049401038298161559, -19.05341960407611168, 62.70724293864769550 ) ) ;
#192349 = CARTESIAN_POINT ( 'NONE',  ( -12.06949235617756955, 12.14591786802309770, 50.62390960531435979 ) ) ;
#192350 = CARTESIAN_POINT ( 'NONE',  ( -9.564922557960796823, -16.46253265017161027, 82.08224293864768129 ) ) ;
#192352 = CARTESIAN_POINT ( 'NONE',  ( 5.153800228976335163, 19.02544592524342804, 49.79057627198100988 ) ) ;
#192351 = CARTESIAN_POINT ( 'NONE',  ( -19.05341960407617563, 5.049401038297882671, 73.54275706135233293 ) ) ;
#192353 = CARTESIAN_POINT ( 'NONE',  ( -5.049401038298153566, 19.05341960407611168, 80.20724293864769550 ) ) ;
#192354 = CARTESIAN_POINT ( 'NONE',  ( -19.05341960407611168, -5.049401038298163336, 31.45724293864769550 ) ) ;
#192355 = CARTESIAN_POINT ( 'NONE',  ( -19.03943276465977164, 0.05219959533909376836, 66.24890960531436690 ) ) ;
#192356 = EDGE_CURVE ( 'NONE', #199940, #148926, #78623, .T. ) ;
#192357 = CARTESIAN_POINT ( 'NONE',  ( -15.72974639402197994, 15.80617190586746368, 55.62390960531436690 ) ) ;
#192358 = CARTESIAN_POINT ( 'NONE',  ( -13.89961937509977652, 13.97604488694528158, 55.62390960531434558 ) ) ;
#192359 = CARTESIAN_POINT ( 'NONE',  ( -10.72451020669898014, 18.67979575497178502, 50.41557627198103120 ) ) ;
#192360 = CARTESIAN_POINT ( 'NONE',  ( -16.46253265017146816, -9.564922557961047289, 79.16775706135234714 ) ) ;
#192361 = CARTESIAN_POINT ( 'NONE',  ( -12.14591786802326823, 12.06949235617739902, 103.1260903946856757 ) ) ;
#192362 = CARTESIAN_POINT ( 'NONE',  ( -13.97604488694547697, 13.89961937509957934, 43.12609039468566152 ) ) ;
#192364 = CARTESIAN_POINT ( 'NONE',  ( 4.379528057220092307, 16.55341960407617563, 92.29275706135236135 ) ) ;
#192363 = CARTESIAN_POINT ( 'NONE',  ( -16.55341960407617563, 4.379528057220093196, 63.54275706135234003 ) ) ;
#192365 = CARTESIAN_POINT ( 'NONE',  ( -17.49999999999999645, -5.499999999999992895, 94.20309617465827046 ) ) ;
#192366 = CARTESIAN_POINT ( 'NONE',  ( 16.53943276465976808, 0.05219959533934440121, 81.25109039468568994 ) ) ;
#192367 = CARTESIAN_POINT ( 'NONE',  ( 10.72451020669898902, -18.67979575497178502, 27.91557627198103830 ) ) ;
#192368 = CARTESIAN_POINT ( 'NONE',  ( -9.474510206698964154, 16.51473224551069663, 35.41557627198102409 ) ) ;
#192369 = CARTESIAN_POINT ( 'NONE',  ( -4.483927247898782831, 16.52544592524335698, 32.70942372801900433 ) ) ;
#192370 = CARTESIAN_POINT ( 'NONE',  ( 5.049401038298161559, -19.05341960407611168, 52.70724293864767418 ) ) ;
#192371 = CARTESIAN_POINT ( 'NONE',  ( -5.823673210054431948, 21.52544592524334988, 37.70942372801900433 ) ) ;
#192372 = CARTESIAN_POINT ( 'NONE',  ( -16.53943276465976808, -0.05219959533934237506, 43.75109039468568284 ) ) ;
#192373 = CARTESIAN_POINT ( 'NONE',  ( 16.53943276465976808, 0.05219959533934440121, 111.2510903946856899 ) ) ;
#192374 = CARTESIAN_POINT ( 'NONE',  ( -19.05341960407611168, -5.049401038298163336, 31.45724293864769550 ) ) ;
#192375 = CARTESIAN_POINT ( 'NONE',  ( 9.474510206698729675, 16.51473224551082808, 22.08442372801899722 ) ) ;
#192376 = CARTESIAN_POINT ( 'NONE',  ( -0.05219959533936034679, 19.03943276465977164, 107.5010903946856615 ) ) ;
#192377 = CARTESIAN_POINT ( 'NONE',  ( -19.02544592524334988, -5.153800228976617603, 73.95942372801900433 ) ) ;
#192378 = CARTESIAN_POINT ( 'NONE',  ( -4.483927247898539470, -16.52544592524342804, 67.29057627198103830 ) ) ;
#192379 = CARTESIAN_POINT ( 'NONE',  ( -9.474510206698964154, 16.51473224551069663, 40.41557627198103120 ) ) ;
#192381 = CARTESIAN_POINT ( 'NONE',  ( 17.44270441346516876, -5.991230190323020288, 91.13664920735770636 ) ) ;
#192380 = CARTESIAN_POINT ( 'NONE',  ( 9.564922557961047289, -16.46253265017146816, 80.41775706135234714 ) ) ;
#192382 = CARTESIAN_POINT ( 'NONE',  ( 15.72974639402176855, 15.80617190586768217, 61.87609039468568284 ) ) ;
#192383 = CARTESIAN_POINT ( 'NONE',  ( 14.34966873604972726, -8.224510206698740333, 45.83442372801901854 ) ) ;
#192384 = CARTESIAN_POINT ( 'NONE',  ( 18.39635199886966888, -5.500000000000096811, 58.51967076359999709 ) ) ;
#192385 = CARTESIAN_POINT ( 'NONE',  ( 10.72451020669898902, -18.67979575497178502, 42.91557627198103120 ) ) ;
#192386 = CARTESIAN_POINT ( 'NONE',  ( 14.29746914071037800, 8.314922557961029526, 26.66775706135235424 ) ) ;
#192387 = DIRECTION ( 'NONE',  ( 1.000000000000000000, 0.000000000000000000, 0.000000000000000000 ) ) ;
#192388 = DIRECTION ( 'NONE',  ( 0.9930308165857338887, -0.1178549842436482226, 0.000000000000000000 ) ) ;
#192389 = CARTESIAN_POINT ( 'NONE',  ( 19.02544592524343514, -5.153800228976328945, 38.54057627198103120 ) ) ;
#192390 = CARTESIAN_POINT ( 'NONE',  ( 21.55341960407619695, -5.719274019375665929, 106.0427570613523471 ) ) ;
#192391 = CARTESIAN_POINT ( 'NONE',  ( -19.05341960407611168, -5.049401038298163336, 51.45724293864770260 ) ) ;
#192392 = CIRCLE ( 'NONE', #27740, 0.4999999999999995559 ) ;
#192393 = CARTESIAN_POINT ( 'NONE',  ( 15.72974639402176855, 15.80617190586768217, 71.87609039468568994 ) ) ;
#192394 = CARTESIAN_POINT ( 'NONE',  ( -21.55341960407619339, 5.719274019375674811, 103.5427570613523613 ) ) ;
#192395 = CARTESIAN_POINT ( 'NONE',  ( 8.224510206698742110, 14.34966873604972548, 112.0844237280190185 ) ) ;
#192396 = CARTESIAN_POINT ( 'NONE',  ( -13.89961937509977652, 13.97604488694528158, 30.62390960531435269 ) ) ;
#192397 = CARTESIAN_POINT ( 'NONE',  ( 0.05219959533909260263, 19.03943276465977164, 94.99890960531436690 ) ) ;
#192398 = CARTESIAN_POINT ( 'NONE',  ( 21.53943276465977519, 0.05219959533937863772, 61.25109039468567573 ) ) ;
#192399 = CARTESIAN_POINT ( 'NONE',  ( -9.564922557960796823, -16.46253265017161027, 37.08224293864768839 ) ) ;
#192400 = CARTESIAN_POINT ( 'NONE',  ( -5.823673210054431948, 21.52544592524334988, 47.70942372801902565 ) ) ;
#192402 = CARTESIAN_POINT ( 'NONE',  ( -19.03943276465977164, 0.05219959533909376836, 101.2489096053143669 ) ) ;
#192401 = CARTESIAN_POINT ( 'NONE',  ( -13.89961937509957401, -13.97604488694547875, 89.37609039468563310 ) ) ;
#192403 = CARTESIAN_POINT ( 'NONE',  ( -5.153800228976328057, -19.02544592524343514, 27.29057627198103120 ) ) ;
#192404 = CARTESIAN_POINT ( 'NONE',  ( 0.05219959533907565091, 21.53943276465977519, 109.9989096053143527 ) ) ;
#192405 = CARTESIAN_POINT ( 'NONE',  ( 5.153800228976615827, -19.02544592524334988, 30.20942372801900433 ) ) ;
#192406 = CARTESIAN_POINT ( 'NONE',  ( 8.224510206698953496, -14.34966873604960469, 112.9155762719810383 ) ) ;
#192407 = CARTESIAN_POINT ( 'NONE',  ( -16.46253265017160317, 9.564922557960807481, 65.83224293864769550 ) ) ;
#192408 = CARTESIAN_POINT ( 'NONE',  ( -19.05341960407617563, 5.049401038297882671, 103.5427570613523329 ) ) ;
#192409 = CARTESIAN_POINT ( 'NONE',  ( 12.06949235617757843, -12.14591786802309237, 68.12390960531436690 ) ) ;
#192410 = CARTESIAN_POINT ( 'NONE',  ( 13.97604488694548053, -13.89961937509957401, 20.62609039468567573 ) ) ;
#192411 = CARTESIAN_POINT ( 'NONE',  ( -21.55341960407610458, -5.719274019375992779, 26.45724293864768839 ) ) ;
#192412 = CARTESIAN_POINT ( 'NONE',  ( 19.05341960407617918, -5.049401038297876454, 91.04275706135234714 ) ) ;
#192413 = CARTESIAN_POINT ( 'NONE',  ( 15.80617190586746368, 15.72974639402197994, 94.37390960531436690 ) ) ;
#192414 = CARTESIAN_POINT ( 'NONE',  ( -18.62759615963255300, -10.81492255796106328, 49.16775706135234003 ) ) ;
#192415 = CARTESIAN_POINT ( 'NONE',  ( 8.314922557961029526, -14.29746914071037800, 45.41775706135234003 ) ) ;
#192416 = CARTESIAN_POINT ( 'NONE',  ( 4.379528057220092307, 16.55341960407617563, 102.2927570613523613 ) ) ;
#192418 = CARTESIAN_POINT ( 'NONE',  ( -21.55341960407619339, 5.719274019375674811, 43.54275706135235424 ) ) ;
#192417 = CARTESIAN_POINT ( 'NONE',  ( -8.224510206698735004, -14.34966873604973081, 44.58442372801901854 ) ) ;
#192419 = CARTESIAN_POINT ( 'NONE',  ( 10.72451020669898902, -18.67979575497178502, 52.91557627198103830 ) ) ;
#192420 = CARTESIAN_POINT ( 'NONE',  ( 9.474510206698971260, -16.51473224551069308, 37.91557627198102409 ) ) ;
#192421 = CARTESIAN_POINT ( 'NONE',  ( 11.74264578624799427, 36.14014761921585972, -2.349999994537626868 ) ) ;
#192422 = CARTESIAN_POINT ( 'NONE',  ( -16.52544592524335698, -4.483927247898792601, 63.95942372801901854 ) ) ;
#192423 = CARTESIAN_POINT ( 'NONE',  ( 5.719274019375991003, -21.55341960407610458, 87.70724293864769550 ) ) ;
#192424 = CARTESIAN_POINT ( 'NONE',  ( 14.29746914071049879, -8.314922557960816363, 33.33224293864769550 ) ) ;
#192425 = CARTESIAN_POINT ( 'NONE',  ( -8.314922557961024197, 14.29746914071037800, 57.91775706135234714 ) ) ;
#192426 = CARTESIAN_POINT ( 'NONE',  ( -16.51473224551082808, 9.474510206698731452, 103.3344237280190043 ) ) ;
#192427 = CARTESIAN_POINT ( 'NONE',  ( -15.72974639402197994, 15.80617190586746368, 95.62390960531436690 ) ) ;
#192428 = CARTESIAN_POINT ( 'NONE',  ( -4.483927247898539470, -16.52544592524342804, 32.29057627198102409 ) ) ;
#192429 = EDGE_LOOP ( 'NONE', ( #24595, #45804, #86543, #60779 ) ) ;
#192430 = CARTESIAN_POINT ( 'NONE',  ( -8.314922557961024197, 14.29746914071037800, 72.91775706135234714 ) ) ;
#192431 = CARTESIAN_POINT ( 'NONE',  ( 24.05407591190764194, 13.01182159662919346, 169.7785964492052244 ) ) ;
#192432 = CARTESIAN_POINT ( 'NONE',  ( -15.72974639402197994, 15.80617190586746368, 75.62390960531439532 ) ) ;
#192433 = CARTESIAN_POINT ( 'NONE',  ( -12.06949235617739369, -12.14591786802326823, 99.37609039468568994 ) ) ;
#192434 = ORIENTED_EDGE ( 'NONE', *, *, #29924, .F. ) ;
#192435 = CARTESIAN_POINT ( 'NONE',  ( 18.89770734986049305, 5.499999999999896083, 86.60214472496637939 ) ) ;
#192436 = CARTESIAN_POINT ( 'NONE',  ( -21.52544592524343514, 5.823673210054127303, 86.04057627198102409 ) ) ;
#192437 = AXIS2_PLACEMENT_3D ( 'NONE', #167149, #43800, #151968 ) ;
#192438 = CARTESIAN_POINT ( 'NONE',  ( 18.67979575497178502, 10.72451020669898547, 104.1655762719810241 ) ) ;
#192439 = CARTESIAN_POINT ( 'NONE',  ( -0.05219959533910754901, -16.53943276465976808, 37.49890960531436690 ) ) ;
#192440 = CARTESIAN_POINT ( 'NONE',  ( 12.06949235617739724, 12.14591786802326823, 36.87609039468568994 ) ) ;
#192441 = CARTESIAN_POINT ( 'NONE',  ( -9.474510206698964154, 16.51473224551069663, 50.41557627198102409 ) ) ;
#192442 = CARTESIAN_POINT ( 'NONE',  ( 5.049401038298161559, -19.05341960407611168, 72.70724293864768129 ) ) ;
#192443 = CARTESIAN_POINT ( 'NONE',  ( 19.05341960407611168, 5.049401038298154454, 113.9572429386477097 ) ) ;
#192444 = CARTESIAN_POINT ( 'NONE',  ( -9.564922557960796823, -16.46253265017161027, 112.0822429386476955 ) ) ;
#192445 = CARTESIAN_POINT ( 'NONE',  ( -9.474510206698720793, -16.51473224551083518, 109.5844237280190043 ) ) ;
#192446 = CARTESIAN_POINT ( 'NONE',  ( 19.02544592524334988, 5.153800228976608722, 46.45942372801899012 ) ) ;
#192447 = CARTESIAN_POINT ( 'NONE',  ( 18.67979575497178502, 10.72451020669898547, 89.16557627198102409 ) ) ;
#192448 = CARTESIAN_POINT ( 'NONE',  ( -4.483927247898539470, -16.52544592524342804, 27.29057627198103120 ) ) ;
#192449 = CARTESIAN_POINT ( 'NONE',  ( 0.05219959533907565091, 21.53943276465977519, 39.99890960531436690 ) ) ;
#192451 = CARTESIAN_POINT ( 'NONE',  ( -9.564922557961040184, 16.46253265017147172, 112.9177570613523329 ) ) ;
#192450 = CARTESIAN_POINT ( 'NONE',  ( -21.53943276465977519, 0.05219959533907696930, 86.24890960531436690 ) ) ;
#192452 = CARTESIAN_POINT ( 'NONE',  ( -5.049401038298153566, 19.05341960407611168, 100.2072429386476955 ) ) ;
#192453 = CARTESIAN_POINT ( 'NONE',  ( 21.52544592524334988, 5.823673210054432836, 81.45942372801900433 ) ) ;
#192454 = CARTESIAN_POINT ( 'NONE',  ( 9.474510206698971260, -16.51473224551069308, 67.91557627198102409 ) ) ;
#192455 = CARTESIAN_POINT ( 'NONE',  ( 0.000000000000000000, 1.178949249685212974, -2.042000000000001148 ) ) ;
#192456 = CARTESIAN_POINT ( 'NONE',  ( 13.97604488694527802, 13.89961937509977652, 69.37390960531436690 ) ) ;
#192457 = CARTESIAN_POINT ( 'NONE',  ( 12.06949235617757843, -12.14591786802309237, 93.12390960531436690 ) ) ;
#192458 = VERTEX_POINT ( 'NONE', #195225 ) ;
#192459 = CARTESIAN_POINT ( 'NONE',  ( -19.02544592524334988, -5.153800228976617603, 103.9594237280190043 ) ) ;
#192460 = CARTESIAN_POINT ( 'NONE',  ( 16.20579543436679160, -7.371946100355085463, 81.93479165828128430 ) ) ;
#192461 = CARTESIAN_POINT ( 'NONE',  ( -13.89961937509977652, 13.97604488694528158, 60.62390960531436690 ) ) ;
#192463 = CARTESIAN_POINT ( 'NONE',  ( -19.05341960407611168, -5.049401038298163336, 106.4572429386476955 ) ) ;
#192462 = CARTESIAN_POINT ( 'NONE',  ( 18.62759615963255655, 10.81492255796105972, 86.66775706135234714 ) ) ;
#192464 = CARTESIAN_POINT ( 'NONE',  ( -8.314922557961024197, 14.29746914071037800, 82.91775706135234714 ) ) ;
#192465 = CARTESIAN_POINT ( 'NONE',  ( -30.11448378070091891, 1.481880339025834381, -48.12989299794421072 ) ) ;
#192466 = CARTESIAN_POINT ( 'NONE',  ( -13.89961937509957401, -13.97604488694547875, 59.37609039468566863 ) ) ;
#192467 = CARTESIAN_POINT ( 'NONE',  ( -0.05219959533937732626, 21.53943276465977519, 97.50109039468567573 ) ) ;
#192468 = CARTESIAN_POINT ( 'NONE',  ( 37.58407650405589351, 0.3600258186295152152, 39.49999999999997868 ) ) ;
#192469 = PLANE ( 'NONE',  #143465 ) ;
#192470 = CARTESIAN_POINT ( 'NONE',  ( 22.81625015709510151, -31.40387420917324590, -2.424999997268812546 ) ) ;
#192471 = CARTESIAN_POINT ( 'NONE',  ( -8.224510206698735004, -14.34966873604973081, 109.5844237280190328 ) ) ;
#192472 = CARTESIAN_POINT ( 'NONE',  ( -5.049401038297874678, -19.05341960407618274, 74.79275706135231871 ) ) ;
#192473 = CARTESIAN_POINT ( 'NONE',  ( 16.55341960407618274, -4.379528057220086978, 91.04275706135236135 ) ) ;
#192474 = FACE_OUTER_BOUND ( 'NONE', #116927, .T. ) ;
#192475 = CARTESIAN_POINT ( 'NONE',  ( 4.379528057220092307, 16.55341960407617563, 72.29275706135236135 ) ) ;
#192476 = CARTESIAN_POINT ( 'NONE',  ( -10.81492255796105439, 18.62759615963255655, 82.91775706135234714 ) ) ;
#192477 = CARTESIAN_POINT ( 'NONE',  ( -16.46253265017146816, -9.564922557961047289, 89.16775706135234714 ) ) ;
#192478 = CARTESIAN_POINT ( 'NONE',  ( -5.153800228976607833, 19.02544592524334988, 37.70942372801899722 ) ) ;
#192479 = CARTESIAN_POINT ( 'NONE',  ( 13.89961937509977652, -13.97604488694527269, 63.12390960531435979 ) ) ;
#192480 = CARTESIAN_POINT ( 'NONE',  ( 9.474510206698971260, -16.51473224551069308, 52.91557627198102409 ) ) ;
#192481 = AXIS2_PLACEMENT_3D ( 'NONE', #99558, #8564, #160243 ) ;
#192482 = LINE ( 'NONE', #67128, #33597 ) ;
#192483 = CARTESIAN_POINT ( 'NONE',  ( 15.80617190586746368, 15.72974639402197994, 84.37390960531438111 ) ) ;
#192484 = EDGE_CURVE ( 'NONE', #123757, #84237, #97940, .T. ) ;
#192485 = CARTESIAN_POINT ( 'NONE',  ( 0.05219959533907565091, 21.53943276465977519, 44.99890960531435979 ) ) ;
#192486 = CARTESIAN_POINT ( 'NONE',  ( -13.97604488694527625, -13.89961937509977652, 26.87390960531434558 ) ) ;
#192487 = CARTESIAN_POINT ( 'NONE',  ( -16.52544592524335698, -4.483927247898792601, 68.95942372801901854 ) ) ;
#192488 = ORIENTED_EDGE ( 'NONE', *, *, #129099, .T. ) ;
#192489 = CARTESIAN_POINT ( 'NONE',  ( 10.81492255796106328, -18.62759615963255655, 45.41775706135234003 ) ) ;
#192491 = CARTESIAN_POINT ( 'NONE',  ( -11.40812507854754720, -35.11059874428192273, -8.224999997268813701 ) ) ;
#192490 = CARTESIAN_POINT ( 'NONE',  ( 4.483927247898545687, 16.52544592524342804, 59.79057627198103120 ) ) ;
#192492 = CARTESIAN_POINT ( 'NONE',  ( 12.14591786802327356, -12.06949235617739191, 35.62609039468568994 ) ) ;
#192493 = CARTESIAN_POINT ( 'NONE',  ( 9.564922557961047289, -16.46253265017146816, 55.41775706135234003 ) ) ;
#192494 = CARTESIAN_POINT ( 'NONE',  ( 12.06949235617757843, -12.14591786802309237, 53.12390960531436690 ) ) ;
#192495 = CARTESIAN_POINT ( 'NONE',  ( 10.81492255796106328, -18.62759615963255655, 30.41775706135234358 ) ) ;
#192497 = CARTESIAN_POINT ( 'NONE',  ( -10.72451020669898014, 18.67979575497178502, 90.41557627198103830 ) ) ;
#192496 = CARTESIAN_POINT ( 'NONE',  ( -19.03943276465977164, 0.05219959533909376836, 26.24890960531435624 ) ) ;
#192498 = CARTESIAN_POINT ( 'NONE',  ( -5.049401038298153566, 19.05341960407611168, 110.2072429386476671 ) ) ;
#192499 = CARTESIAN_POINT ( 'NONE',  ( 16.52544592524342804, -4.483927247898539470, 78.54057627198103830 ) ) ;
#192500 = CARTESIAN_POINT ( 'NONE',  ( 19.02544592524343514, -5.153800228976328945, 113.5405762719810241 ) ) ;
#192501 = CARTESIAN_POINT ( 'NONE',  ( -37.58407650405589351, 1.968340676919130544E-14, 39.49999999999996447 ) ) ;
#192502 = CARTESIAN_POINT ( 'NONE',  ( -13.89961937509957401, -13.97604488694547875, 64.37609039468567573 ) ) ;
#192503 = CARTESIAN_POINT ( 'NONE',  ( -21.53943276465977519, 0.05219959533907696930, 116.2489096053143669 ) ) ;
#192504 = CARTESIAN_POINT ( 'NONE',  ( -16.46253265017160317, 9.564922557960807481, 60.83224293864769550 ) ) ;
#192505 = CARTESIAN_POINT ( 'NONE',  ( 9.564922557961047289, -16.46253265017146816, 45.41775706135232582 ) ) ;
#192506 = CARTESIAN_POINT ( 'NONE',  ( 16.46253265017160672, -9.564922557960803928, 28.33224293864769550 ) ) ;
#192507 = CARTESIAN_POINT ( 'NONE',  ( -21.53943276465977519, -0.05219959533937600094, 68.75109039468568994 ) ) ;
#192508 = CARTESIAN_POINT ( 'NONE',  ( -3.573655867282028392E-15, 2.428612866367529932E-14, 155.0000000000000000 ) ) ;
#192509 = CARTESIAN_POINT ( 'NONE',  ( -16.55341960407611168, -4.379528057220339221, 51.45724293864770260 ) ) ;
#192510 = CARTESIAN_POINT ( 'NONE',  ( 19.03943276465977164, -0.05219959533909143690, 63.74890960531435979 ) ) ;
#192511 = CARTESIAN_POINT ( 'NONE',  ( 10.72451020669898902, -18.67979575497178502, 92.91557627198103830 ) ) ;
#192512 = CARTESIAN_POINT ( 'NONE',  ( -13.97604488694527625, -13.89961937509977652, 61.87390960531435979 ) ) ;
#192513 = ORIENTED_EDGE ( 'NONE', *, *, #31579, .F. ) ;
#192514 = CARTESIAN_POINT ( 'NONE',  ( -21.52544592524343514, 5.823673210054127303, 86.04057627198102409 ) ) ;
#192515 = EDGE_CURVE ( 'NONE', #44815, #68886, #172159, .T. ) ;
#192516 = CARTESIAN_POINT ( 'NONE',  ( 18.62759615963255655, 10.81492255796105972, 101.6677570613523613 ) ) ;
#192519 = CARTESIAN_POINT ( 'NONE',  ( 14.34966873604960469, 8.224510206698951720, 79.16557627198103830 ) ) ;
#192518 = CARTESIAN_POINT ( 'NONE',  ( -8.314922557961024197, 14.29746914071037800, 92.91775706135236135 ) ) ;
#192517 = LINE ( 'NONE', #97473, #173619 ) ;
#192520 = CARTESIAN_POINT ( 'NONE',  ( 16.46253265017146816, 9.564922557961045513, 96.66775706135233293 ) ) ;
#192521 = VERTEX_POINT ( 'NONE', #131537 ) ;
#192522 = CARTESIAN_POINT ( 'NONE',  ( -21.52544592524334988, -5.823673210054445271, 18.95942372801901143 ) ) ;
#192523 = CARTESIAN_POINT ( 'NONE',  ( 16.51473224551083163, -9.474510206698727899, 45.83442372801900433 ) ) ;
#192524 = CARTESIAN_POINT ( 'NONE',  ( 4.483927247898790824, -16.52544592524335698, 100.2094237280190043 ) ) ;
#192525 = CARTESIAN_POINT ( 'NONE',  ( 13.97604488694548053, -13.89961937509957401, 30.62609039468566863 ) ) ;
#192526 = CARTESIAN_POINT ( 'NONE',  ( -16.51473224551069308, -9.474510206698971260, 91.66557627198103830 ) ) ;
#192527 = CARTESIAN_POINT ( 'NONE',  ( 10.72451020669898902, -18.67979575497178502, 57.91557627198103120 ) ) ;
#192528 = DIRECTION ( 'NONE',  ( 0.000000000000000000, 0.000000000000000000, 1.000000000000000000 ) ) ;
#192529 = CARTESIAN_POINT ( 'NONE',  ( -9.474510206698964154, 16.51473224551069663, 25.41557627198103120 ) ) ;
#192530 = CARTESIAN_POINT ( 'NONE',  ( 10.72451020669871369, 18.67979575497193778, 112.0844237280190185 ) ) ;
#192531 = CARTESIAN_POINT ( 'NONE',  ( 16.55341960407618274, -4.379528057220086978, 76.04275706135237556 ) ) ;
#192532 = CARTESIAN_POINT ( 'NONE',  ( 5.719274019375673035, 21.55341960407619339, 22.29275706135235069 ) ) ;
#192533 = CARTESIAN_POINT ( 'NONE',  ( 12.06949235617739724, 12.14591786802326823, 31.87609039468567929 ) ) ;
#192534 = CARTESIAN_POINT ( 'NONE',  ( 16.51473224551069308, 9.474510206698969483, 104.1655762719810241 ) ) ;
#192535 = CARTESIAN_POINT ( 'NONE',  ( -16.51473224551069308, -9.474510206698971260, 46.66557627198102409 ) ) ;
#192536 = CARTESIAN_POINT ( 'NONE',  ( 5.153800228976335163, 19.02544592524342804, 64.79057627198100988 ) ) ;
#192537 = AXIS2_PLACEMENT_3D ( 'NONE', #62793, #123466, #1119 ) ;
#192538 = CARTESIAN_POINT ( 'NONE',  ( 0.05219959533934541429, -16.53943276465976808, 45.00109039468568284 ) ) ;
#192539 = CARTESIAN_POINT ( 'NONE',  ( 12.06949235617757843, -12.14591786802309237, 88.12390960531436690 ) ) ;
#192540 = CARTESIAN_POINT ( 'NONE',  ( 14.34966873604972726, -8.224510206698740333, 95.83442372801903275 ) ) ;
#192543 = CARTESIAN_POINT ( 'NONE',  ( -9.564922557960796823, -16.46253265017161027, 67.08224293864769550 ) ) ;
#192542 = CARTESIAN_POINT ( 'NONE',  ( -9.474510206698964154, 16.51473224551069663, 75.41557627198103830 ) ) ;
#192541 = CARTESIAN_POINT ( 'NONE',  ( -5.823673210054431948, 21.52544592524334988, 62.70942372801902565 ) ) ;
#192544 = CARTESIAN_POINT ( 'NONE',  ( -16.51473224551069308, -9.474510206698971260, 96.66557627198102409 ) ) ;
#192545 = CARTESIAN_POINT ( 'NONE',  ( -16.55341960407611168, -4.379528057220339221, 41.45724293864769550 ) ) ;
#192546 = CARTESIAN_POINT ( 'NONE',  ( -14.34966873604972548, 8.224510206698743886, 93.33442372801901854 ) ) ;
#192547 = ORIENTED_EDGE ( 'NONE', *, *, #197529, .F. ) ;
#192548 = CARTESIAN_POINT ( 'NONE',  ( -9.474510206698720793, -16.51473224551083518, 49.58442372801899722 ) ) ;
#192549 = LINE ( 'NONE', #25715, #22784 ) ;
#192550 = CARTESIAN_POINT ( 'NONE',  ( -19.03943276465977164, 0.05219959533909376836, 61.24890960531436690 ) ) ;
#192551 = CARTESIAN_POINT ( 'NONE',  ( -16.51473224551082808, 9.474510206698731452, 43.33442372801900433 ) ) ;
#192552 = CARTESIAN_POINT ( 'NONE',  ( -36.91746825000001309, 11.99521256947798342, -8.724999997268813701 ) ) ;
#192553 = DIRECTION ( 'NONE',  ( -1.000000000000000000, 0.000000000000000000, 0.000000000000000000 ) ) ;
#192554 = CARTESIAN_POINT ( 'NONE',  ( 14.34966873604972726, -8.224510206698740333, 55.83442372801901854 ) ) ;
#192556 = CARTESIAN_POINT ( 'NONE',  ( 16.52544592524335698, 4.483927247898782831, 71.45942372801901854 ) ) ;
#192555 = CARTESIAN_POINT ( 'NONE',  ( -19.03943276465977164, -0.05219959533935918106, 68.75109039468566152 ) ) ;
#192557 = CARTESIAN_POINT ( 'NONE',  ( 17.31747979337948351, 6.344076630961057006, 93.87944868065186199 ) ) ;
#192558 = CARTESIAN_POINT ( 'NONE',  ( 19.02544592524343514, -5.153800228976328945, 93.54057627198102409 ) ) ;
#192559 = CARTESIAN_POINT ( 'NONE',  ( 5.719274019375673035, 21.55341960407619339, 27.29275706135234358 ) ) ;
#192560 = CARTESIAN_POINT ( 'NONE',  ( 16.51473224551083163, -9.474510206698727899, 75.83442372801900433 ) ) ;
#192562 = CARTESIAN_POINT ( 'NONE',  ( 19.05341960407611168, 5.049401038298154454, 38.95724293864767418 ) ) ;
#192561 = CARTESIAN_POINT ( 'NONE',  ( -19.03943276465977164, 0.05219959533909376836, 111.2489096053143669 ) ) ;
#192563 = CARTESIAN_POINT ( 'NONE',  ( -13.97604488694527625, -13.89961937509977652, 96.87390960531433848 ) ) ;
#192565 = CARTESIAN_POINT ( 'NONE',  ( -9.564922557960796823, -16.46253265017161027, 37.08224293864768839 ) ) ;
#192564 = CARTESIAN_POINT ( 'NONE',  ( 4.379528057220339221, -16.55341960407611168, 42.70724293864770260 ) ) ;
#192566 = CARTESIAN_POINT ( 'NONE',  ( 5.049401038297881783, 19.05341960407617563, 57.29275706135231871 ) ) ;
#192567 = CARTESIAN_POINT ( 'NONE',  ( 12.06949235617757843, -12.14591786802309237, 93.12390960531436690 ) ) ;
#192568 = CARTESIAN_POINT ( 'NONE',  ( -9.564922557961040184, 16.46253265017147172, 22.91775706135233648 ) ) ;
#192569 = CARTESIAN_POINT ( 'NONE',  ( 5.153800228976335163, 19.02544592524342804, 54.79057627198103120 ) ) ;
#192570 = CARTESIAN_POINT ( 'NONE',  ( 21.52544592524344225, -5.823673210054117533, 68.54057627198103830 ) ) ;
#192572 = CARTESIAN_POINT ( 'NONE',  ( 0.05219959533936267826, -19.03943276465977164, 20.00109039468567218 ) ) ;
#192571 = CARTESIAN_POINT ( 'NONE',  ( 16.55341960407611168, 4.379528057220329451, 48.95724293864770971 ) ) ;
#192573 = CARTESIAN_POINT ( 'NONE',  ( -19.05341960407611168, -5.049401038298163336, 101.4572429386476955 ) ) ;
#192574 = VECTOR ( 'NONE', #21921, 1000.000000000000000 ) ;
#192575 = CARTESIAN_POINT ( 'NONE',  ( -13.97604488694527625, -13.89961937509977652, 111.8739096053143243 ) ) ;
#192576 = CARTESIAN_POINT ( 'NONE',  ( -13.89961937509977652, 13.97604488694528158, 55.62390960531434558 ) ) ;
#192577 = CARTESIAN_POINT ( 'NONE',  ( 5.153800228976335163, 19.02544592524342804, 24.79057627198102765 ) ) ;
#192578 = CARTESIAN_POINT ( 'NONE',  ( 12.14591786802309770, 12.06949235617756955, 89.37390960531435269 ) ) ;
#192579 = CARTESIAN_POINT ( 'NONE',  ( -0.05219959533907301413, -21.53943276465977519, 92.49890960531436690 ) ) ;
#192580 = CARTESIAN_POINT ( 'NONE',  ( -19.02544592524342804, 5.153800228976336051, 106.0405762719810241 ) ) ;
#192581 = CARTESIAN_POINT ( 'NONE',  ( 18.67979575497178502, 10.72451020669898547, 109.1655762719810383 ) ) ;
#192582 = CARTESIAN_POINT ( 'NONE',  ( -5.153800228976328057, -19.02544592524343514, 107.2905762719810383 ) ) ;
#192583 = CARTESIAN_POINT ( 'NONE',  ( 4.379528057220339221, -16.55341960407611168, 107.7072429386476955 ) ) ;
#192584 = CARTESIAN_POINT ( 'NONE',  ( 21.55341960407619695, -5.719274019375665929, 76.04275706135237556 ) ) ;
#192585 = CARTESIAN_POINT ( 'NONE',  ( 21.53943276465977519, -0.05219959533907433946, 88.74890960531436690 ) ) ;
#192586 = CARTESIAN_POINT ( 'NONE',  ( 17.31728774477274158, -6.344390552232372471, 108.3190665168931730 ) ) ;
#192587 = CARTESIAN_POINT ( 'NONE',  ( 19.46398650005391318, -5.499999999999944045, 77.68269651486370719 ) ) ;
#192588 = CARTESIAN_POINT ( 'NONE',  ( 29.18776880969887699, -0.8894290736107985929, -52.33677266386643367 ) ) ;
#192589 = CARTESIAN_POINT ( 'NONE',  ( 16.53943276465976808, 0.05219959533934440121, 31.25109039468568639 ) ) ;
#192590 = CARTESIAN_POINT ( 'NONE',  ( 14.29746914071049879, -8.314922557960816363, 113.3322429386476955 ) ) ;
#192591 = CARTESIAN_POINT ( 'NONE',  ( 18.22780087662125226, -5.499999999999864997, 51.01540105326108687 ) ) ;
#192592 = CARTESIAN_POINT ( 'NONE',  ( -5.049401038298153566, 19.05341960407611168, 55.20724293864769550 ) ) ;
#192593 = CARTESIAN_POINT ( 'NONE',  ( -4.483927247898539470, -16.52544592524342804, 97.29057627198105251 ) ) ;
#192594 = CARTESIAN_POINT ( 'NONE',  ( 21.53943276465977519, -0.05219959533907433946, 28.74890960531435624 ) ) ;
#192595 = CARTESIAN_POINT ( 'NONE',  ( 8.314922557960818139, 14.29746914071049879, 69.58224293864769550 ) ) ;
#192596 = CARTESIAN_POINT ( 'NONE',  ( 13.97604488694548053, -13.89961937509957401, 110.6260903946856615 ) ) ;
#192597 = CARTESIAN_POINT ( 'NONE',  ( -21.53943276465977519, -0.05219959533937600094, 68.75109039468568994 ) ) ;
#192598 = CARTESIAN_POINT ( 'NONE',  ( 16.52216118717207749, -7.221426719304491648, 76.42400978953006074 ) ) ;
#192599 = CARTESIAN_POINT ( 'NONE',  ( -13.97604488694527625, -13.89961937509977652, 106.8739096053143669 ) ) ;
#192600 = CARTESIAN_POINT ( 'NONE',  ( -8.314922557961024197, 14.29746914071037800, 97.91775706135236135 ) ) ;
#192601 = CARTESIAN_POINT ( 'NONE',  ( -19.02544592524342804, 5.153800228976336051, 41.04057627198103120 ) ) ;
#192602 = CARTESIAN_POINT ( 'NONE',  ( 13.89961937509977652, -13.97604488694527269, 93.12390960531436690 ) ) ;
#192603 = CARTESIAN_POINT ( 'NONE',  ( 10.81492255796078972, 18.62759615963270932, 99.58224293864770971 ) ) ;
#192604 =( BOUNDED_CURVE ( )  B_SPLINE_CURVE ( 3, ( #25665, #163154, #24657, #86306 ),
 .UNSPECIFIED., .F., .T. ) 
 B_SPLINE_CURVE_WITH_KNOTS ( ( 4, 4 ),
 ( 5.503250352303675541, 7.063120262055497811 ),
 .UNSPECIFIED. ) 
 CURVE ( )  GEOMETRIC_REPRESENTATION_ITEM ( )  RATIONAL_B_SPLINE_CURVE ( ( 1.000000000000000000, 0.8073061876036302653, 0.8073061876036302653, 1.000000000000000000 ) ) 
 REPRESENTATION_ITEM ( '' )  );
#192605 = CARTESIAN_POINT ( 'NONE',  ( 12.14591786802327356, -12.06949235617739191, 25.62609039468567929 ) ) ;
#192607 = CARTESIAN_POINT ( 'NONE',  ( 15.72974639402176855, 15.80617190586768217, 66.87609039468568994 ) ) ;
#192606 = CARTESIAN_POINT ( 'NONE',  ( 14.34966873604960469, 8.224510206698951720, 59.16557627198103120 ) ) ;
#192608 = CARTESIAN_POINT ( 'NONE',  ( 14.29746914071037800, 8.314922557961029526, 96.66775706135234714 ) ) ;
#192609 = CARTESIAN_POINT ( 'NONE',  ( 17.44279575226787671, -5.990770900253883369, 48.33557567514320397 ) ) ;
#192610 = CARTESIAN_POINT ( 'NONE',  ( 10.20000000000000107, 0.000000000000000000, 0.000000000000000000 ) ) ;
#192611 = CARTESIAN_POINT ( 'NONE',  ( 0.05219959533910956823, 16.53943276465976808, 24.99890960531435624 ) ) ;
#192612 = CARTESIAN_POINT ( 'NONE',  ( -8.314922557961024197, 14.29746914071037800, 62.91775706135236135 ) ) ;
#192613 = CARTESIAN_POINT ( 'NONE',  ( 0.05219959533909260263, 19.03943276465977164, 69.99890960531435269 ) ) ;
#192614 = CARTESIAN_POINT ( 'NONE',  ( 16.46253265017160672, -9.564922557960803928, 83.33224293864768129 ) ) ;
#192615 = CARTESIAN_POINT ( 'NONE',  ( 21.53943276465977519, 0.05219959533937863772, 81.25109039468568994 ) ) ;
#192616 = CARTESIAN_POINT ( 'NONE',  ( -8.224510206698735004, -14.34966873604973081, 94.58442372801901854 ) ) ;
#192617 = CARTESIAN_POINT ( 'NONE',  ( 14.29746914071049879, -8.314922557960816363, 58.33224293864768839 ) ) ;
#192618 = CARTESIAN_POINT ( 'NONE',  ( -16.51473224551069308, -9.474510206698971260, 66.66557627198102409 ) ) ;
#192619 = ORIENTED_EDGE ( 'NONE', *, *, #25423, .T. ) ;
#192620 = CARTESIAN_POINT ( 'NONE',  ( -5.153800228976607833, 19.02544592524334988, 102.7094237280189759 ) ) ;
#192621 = CARTESIAN_POINT ( 'NONE',  ( 16.55341960407611168, 4.379528057220329451, 113.9572429386477239 ) ) ;
#192622 = CARTESIAN_POINT ( 'NONE',  ( -0.05219959533909027116, -19.03943276465977164, 82.49890960531436690 ) ) ;
#192624 = CARTESIAN_POINT ( 'NONE',  ( 36.91746824999999177, 2.880721459617395097E-14, -9.624999997268814056 ) ) ;
#192623 = CARTESIAN_POINT ( 'NONE',  ( 0.05219959533934541429, -16.53943276465976808, 25.00109039468567218 ) ) ;
#192625 = CARTESIAN_POINT ( 'NONE',  ( 9.564922557961047289, -16.46253265017146816, 20.41775706135233293 ) ) ;
#192626 = CARTESIAN_POINT ( 'NONE',  ( -4.483927247898782831, 16.52544592524335698, 77.70942372801900433 ) ) ;
#192627 = CARTESIAN_POINT ( 'NONE',  ( -13.89961937509957401, -13.97604488694547875, 99.37609039468567573 ) ) ;
#192628 = CARTESIAN_POINT ( 'NONE',  ( -4.483927247898539470, -16.52544592524342804, 112.2905762719810241 ) ) ;
#192629 = CARTESIAN_POINT ( 'NONE',  ( 16.52544592524335698, 4.483927247898782831, 66.45942372801903275 ) ) ;
#192630 = CARTESIAN_POINT ( 'NONE',  ( 4.500000000000000888, -120.9970989573719038, 14.58956564881029294 ) ) ;
#192631 = CARTESIAN_POINT ( 'NONE',  ( 16.51473224551083163, -9.474510206698727899, 55.83442372801899722 ) ) ;
#192632 = CARTESIAN_POINT ( 'NONE',  ( 15.72974639402176855, 15.80617190586768217, 101.8760903946857042 ) ) ;
#192633 = CARTESIAN_POINT ( 'NONE',  ( 13.97604488694527802, 13.89961937509977652, 34.37390960531436690 ) ) ;
#192634 = CARTESIAN_POINT ( 'NONE',  ( -19.02544592524342804, 5.153800228976336051, 81.04057627198103830 ) ) ;
#192635 = CARTESIAN_POINT ( 'NONE',  ( 4.379528057220339221, -16.55341960407611168, 77.70724293864770971 ) ) ;
#192636 = CARTESIAN_POINT ( 'NONE',  ( 5.823673210054444382, -21.52544592524334988, 95.20942372801903275 ) ) ;
#192637 = CARTESIAN_POINT ( 'NONE',  ( 19.02544592524334988, 5.153800228976608722, 51.45942372801900433 ) ) ;
#192638 = CARTESIAN_POINT ( 'NONE',  ( 19.05341960407617918, -5.049401038297876454, 46.04275706135233293 ) ) ;
#192639 = CARTESIAN_POINT ( 'NONE',  ( 18.62759615963271287, -10.81492255796078972, 43.33224293864769550 ) ) ;
#192640 = CARTESIAN_POINT ( 'NONE',  ( -18.62759615963255300, -10.81492255796106328, 94.16775706135237556 ) ) ;
#192641 = CARTESIAN_POINT ( 'NONE',  ( 19.03943276465977164, -0.05219959533909143690, 73.74890960531435269 ) ) ;
#192642 = CARTESIAN_POINT ( 'NONE',  ( -15.80617190586768217, 15.72974639402176855, 113.1260903946856899 ) ) ;
#192643 = CARTESIAN_POINT ( 'NONE',  ( 10.72451020669898902, -18.67979575497178502, 52.91557627198103830 ) ) ;
#192644 = CARTESIAN_POINT ( 'NONE',  ( 9.564922557960805705, 16.46253265017160317, 94.58224293864769550 ) ) ;
#192645 = CARTESIAN_POINT ( 'NONE',  ( -13.89961937509957401, -13.97604488694547875, 74.37609039468566152 ) ) ;
#192646 = CARTESIAN_POINT ( 'NONE',  ( -5.049401038298153566, 19.05341960407611168, 100.2072429386476955 ) ) ;
#192647 = CARTESIAN_POINT ( 'NONE',  ( -19.03943276465977164, -0.05219959533935918106, 98.75109039468567573 ) ) ;
#192648 = CARTESIAN_POINT ( 'NONE',  ( -14.34966873604972548, 8.224510206698743886, 43.33442372801901143 ) ) ;
#192649 = CARTESIAN_POINT ( 'NONE',  ( 12.14591786802309770, 12.06949235617756955, 104.3739096053143669 ) ) ;
#192650 = CARTESIAN_POINT ( 'NONE',  ( -16.46253265017160317, 9.564922557960807481, 90.83224293864769550 ) ) ;
#192651 = CARTESIAN_POINT ( 'NONE',  ( -18.67979575497178146, -10.72451020669898902, 66.66557627198102409 ) ) ;
#192652 = CARTESIAN_POINT ( 'NONE',  ( -4.483927247898782831, 16.52544592524335698, 32.70942372801900433 ) ) ;
#192653 = CARTESIAN_POINT ( 'NONE',  ( 15.80617190586769283, -15.72974639402175789, 35.62609039468568994 ) ) ;
#192654 = CARTESIAN_POINT ( 'NONE',  ( 10.72451020669871369, 18.67979575497193778, 87.08442372801901854 ) ) ;
#192655 = CARTESIAN_POINT ( 'NONE',  ( 0.05219959533934541429, -16.53943276465976808, 80.00109039468568994 ) ) ;
#192656 = CARTESIAN_POINT ( 'NONE',  ( 19.02544592524343514, -5.153800228976328945, 73.54057627198103830 ) ) ;
#192657 = CARTESIAN_POINT ( 'NONE',  ( 0.05219959533910956823, 16.53943276465976808, 74.99890960531435269 ) ) ;
#192658 = CARTESIAN_POINT ( 'NONE',  ( -12.14591786802309592, -12.06949235617757132, 26.87390960531435979 ) ) ;
#192659 = CARTESIAN_POINT ( 'NONE',  ( -5.153800228976607833, 19.02544592524334988, 57.70942372801899012 ) ) ;
#192660 = EDGE_CURVE ( 'NONE', #5010, #196218, #182042, .T. ) ;
#192661 = CARTESIAN_POINT ( 'NONE',  ( -21.52544592524334988, -5.823673210054445271, 33.95942372801901143 ) ) ;
#192662 = CARTESIAN_POINT ( 'NONE',  ( -8.224510206698948167, 14.34966873604960824, 80.41557627198103830 ) ) ;
#192663 = CARTESIAN_POINT ( 'NONE',  ( -16.46253265017160317, 9.564922557960807481, 100.8322429386477097 ) ) ;
#192664 = CARTESIAN_POINT ( 'NONE',  ( -14.34966873604972548, 8.224510206698743886, 103.3344237280190043 ) ) ;
#192665 = CARTESIAN_POINT ( 'NONE',  ( 21.55341960407619695, -5.719274019375665929, 66.04275706135236135 ) ) ;
#192666 = CARTESIAN_POINT ( 'NONE',  ( -4.379528057220086978, -16.55341960407618274, 44.79275706135234714 ) ) ;
#192667 = CARTESIAN_POINT ( 'NONE',  ( -15.80617190586768217, 15.72974639402176855, 38.12609039468567573 ) ) ;
#192668 = CARTESIAN_POINT ( 'NONE',  ( -12.14591786802309592, -12.06949235617757132, 76.87390960531439532 ) ) ;
#192669 = EDGE_LOOP ( 'NONE', ( #81317, #22697, #59702, #59498, #111591 ) ) ;
#192670 = CARTESIAN_POINT ( 'NONE',  ( -0.05219959533937732626, 21.53943276465977519, 22.50109039468567573 ) ) ;
#192671 = CARTESIAN_POINT ( 'NONE',  ( -16.53943276465976808, 0.05219959533911058130, 86.24890960531436690 ) ) ;
#192672 = CARTESIAN_POINT ( 'NONE',  ( 17.50000000000005329, -4.658240926743120625, 26.44470417816803121 ) ) ;
#192673 = CARTESIAN_POINT ( 'NONE',  ( 16.55341960407611168, 4.379528057220329451, 53.95724293864770260 ) ) ;
#192674 = CARTESIAN_POINT ( 'NONE',  ( 19.03943276465977164, -0.05219959533909143690, 28.74890960531435624 ) ) ;
#192675 = CARTESIAN_POINT ( 'NONE',  ( 10.81492255796078972, 18.62759615963270932, 39.58224293864769550 ) ) ;
#192676 = CARTESIAN_POINT ( 'NONE',  ( 12.14591786802309770, 12.06949235617756955, 79.37390960531436690 ) ) ;
#192677 = AXIS2_PLACEMENT_3D ( 'NONE', #85433, #147124, #193636 ) ;
#192678 = CARTESIAN_POINT ( 'NONE',  ( -15.72974639402197994, 15.80617190586746368, 75.62390960531439532 ) ) ;
#192679 = CARTESIAN_POINT ( 'NONE',  ( -13.97604488694527625, -13.89961937509977652, 81.87390960531436690 ) ) ;
#192681 = CARTESIAN_POINT ( 'NONE',  ( 13.97604488694548053, -13.89961937509957401, 85.62609039468568994 ) ) ;
#192680 = CARTESIAN_POINT ( 'NONE',  ( -19.03943276465977164, 0.05219959533909376836, 41.24890960531435269 ) ) ;
#192683 = CARTESIAN_POINT ( 'NONE',  ( 15.80617190586746368, 15.72974639402197994, 59.37390960531436690 ) ) ;
#192682 = CARTESIAN_POINT ( 'NONE',  ( -10.72451020669870658, -18.67979575497194134, 59.58442372801901854 ) ) ;
#192684 = CARTESIAN_POINT ( 'NONE',  ( -5.049401038298153566, 19.05341960407611168, 35.20724293864768839 ) ) ;
#192685 = CARTESIAN_POINT ( 'NONE',  ( 16.46253265017160672, -9.564922557960803928, 73.33224293864769550 ) ) ;
#192686 = VERTEX_POINT ( 'NONE', #196239 ) ;
#192687 = CARTESIAN_POINT ( 'NONE',  ( -14.34966873604972548, 8.224510206698743886, 53.33442372801901854 ) ) ;
#192688 = CARTESIAN_POINT ( 'NONE',  ( 18.67979575497194134, -10.72451020669871369, 30.83442372801902209 ) ) ;
#192689 = CARTESIAN_POINT ( 'NONE',  ( -15.80617190586768217, 15.72974639402176855, 68.12609039468567573 ) ) ;
#192690 = CARTESIAN_POINT ( 'NONE',  ( 0.05219959533909260263, 19.03943276465977164, 104.9989096053143669 ) ) ;
#192691 = CARTESIAN_POINT ( 'NONE',  ( 15.72974639402199770, -15.80617190586745480, 88.12390960531436690 ) ) ;
#192693 = CARTESIAN_POINT ( 'NONE',  ( -0.05219959533934338120, 16.53943276465976808, 47.50109039468568994 ) ) ;
#192692 = CARTESIAN_POINT ( 'NONE',  ( -15.72974639402197994, 15.80617190586746368, 115.6239096053143669 ) ) ;
#192694 = CARTESIAN_POINT ( 'NONE',  ( 5.823673210054125526, 21.52544592524343514, 49.79057627198102409 ) ) ;
#192695 = CARTESIAN_POINT ( 'NONE',  ( 15.80617190586769283, -15.72974639402175789, 110.6260903946857042 ) ) ;
#192696 = CARTESIAN_POINT ( 'NONE',  ( -9.564922557960796823, -16.46253265017161027, 57.08224293864769550 ) ) ;
#192697 = CARTESIAN_POINT ( 'NONE',  ( -0.05219959533909027116, -19.03943276465977164, 107.4989096053143527 ) ) ;
#192698 = CARTESIAN_POINT ( 'NONE',  ( -16.46253265017160317, 9.564922557960807481, 95.83224293864769550 ) ) ;
#192699 = CARTESIAN_POINT ( 'NONE',  ( 22.35296335725861994, 22.73357338108561265, -45.67722784712128714 ) ) ;
#192700 = CARTESIAN_POINT ( 'NONE',  ( -5.153800228976607833, 19.02544592524334988, 62.70942372801899722 ) ) ;
#192701 = CARTESIAN_POINT ( 'NONE',  ( 5.823673210054125526, 21.52544592524343514, 49.79057627198102409 ) ) ;
#192702 = CARTESIAN_POINT ( 'NONE',  ( -14.34966873604960291, -8.224510206698953496, 31.66557627198102054 ) ) ;
#192703 = CARTESIAN_POINT ( 'NONE',  ( -5.049401038297874678, -19.05341960407617918, 94.79275706135230450 ) ) ;
#192704 = CARTESIAN_POINT ( 'NONE',  ( 18.10062525802556621, -5.499999999999864997, 51.01383468041923663 ) ) ;
#192705 = CARTESIAN_POINT ( 'NONE',  ( -0.05219959533936034679, 19.03943276465977164, 27.50109039468566507 ) ) ;
#192706 = CARTESIAN_POINT ( 'NONE',  ( 9.474510206698729675, 16.51473224551082808, 92.08442372801900433 ) ) ;
#192708 = CARTESIAN_POINT ( 'NONE',  ( 5.049401038297881783, 19.05341960407617563, 52.29275706135234003 ) ) ;
#192707 = CARTESIAN_POINT ( 'NONE',  ( -21.53943276465977519, 0.05219959533907696930, 81.24890960531436690 ) ) ;
#192709 = CARTESIAN_POINT ( 'NONE',  ( 16.31925111598457789, 7.325300261831552362, 107.3357546103274558 ) ) ;
#192710 = CARTESIAN_POINT ( 'NONE',  ( -13.89961937509977652, 13.97604488694528158, 60.62390960531436690 ) ) ;
#192711 = CARTESIAN_POINT ( 'NONE',  ( -14.34966873604960291, -8.224510206698953496, 66.66557627198102409 ) ) ;
#192712 = CARTESIAN_POINT ( 'NONE',  ( -5.049401038298153566, 19.05341960407611168, 35.20724293864768839 ) ) ;
#192713 = CARTESIAN_POINT ( 'NONE',  ( -12.06949235617756955, 12.14591786802309770, 35.62390960531437401 ) ) ;
#192714 = CARTESIAN_POINT ( 'NONE',  ( 18.10062525802553779, -5.500000000000022204, 56.01383468041922242 ) ) ;
#192715 = CARTESIAN_POINT ( 'NONE',  ( 12.14591786802327356, -12.06949235617739191, 105.6260903946856899 ) ) ;
#192716 = CARTESIAN_POINT ( 'NONE',  ( -5.049401038298153566, 19.05341960407611168, 70.20724293864769550 ) ) ;
#192717 = CARTESIAN_POINT ( 'NONE',  ( 16.46253265017146816, 9.564922557961045513, 31.66775706135232937 ) ) ;
#192718 = CARTESIAN_POINT ( 'NONE',  ( 14.34966873604972726, -8.224510206698740333, 35.83442372801901143 ) ) ;
#192719 = CARTESIAN_POINT ( 'NONE',  ( -15.80617190586745835, -15.72974639402198527, 51.87390960531437401 ) ) ;
#192721 = EDGE_LOOP ( 'NONE', ( #44399, #166449, #133750 ) ) ;
#192720 = CARTESIAN_POINT ( 'NONE',  ( -10.72451020669870658, -18.67979575497194134, 104.5844237280190185 ) ) ;
#192722 = CARTESIAN_POINT ( 'NONE',  ( -16.46253265017160317, 9.564922557960807481, 60.83224293864769550 ) ) ;
#192723 = LINE ( 'NONE', #51210, #117886 ) ;
#192724 = CARTESIAN_POINT ( 'NONE',  ( -13.97604488694527625, -13.89961937509977652, 91.87390960531432427 ) ) ;
#192725 = CARTESIAN_POINT ( 'NONE',  ( -36.91746825000000598, 11.99521256947798520, -0.7249999972688133676 ) ) ;
#192726 = CARTESIAN_POINT ( 'NONE',  ( -18.67979575497193778, 10.72451020669871902, 23.33442372801901499 ) ) ;
#192727 = AXIS2_PLACEMENT_3D ( 'NONE', #190541, #6497, #173389 ) ;
#192728 = CARTESIAN_POINT ( 'NONE',  ( 4.483927247898545687, 16.52544592524342804, 99.79057627198103830 ) ) ;
#192729 = EDGE_CURVE ( 'NONE', #10184, #107085, #30198, .T. ) ;
#192731 = CARTESIAN_POINT ( 'NONE',  ( 19.05341960407611168, 5.049401038298154454, 63.95724293864769550 ) ) ;
#192730 = CARTESIAN_POINT ( 'NONE',  ( 18.62759615963271287, -10.81492255796078972, 83.33224293864769550 ) ) ;
#192732 = CARTESIAN_POINT ( 'NONE',  ( 13.89961937509977652, -13.97604488694527269, 68.12390960531436690 ) ) ;
#192733 = CARTESIAN_POINT ( 'NONE',  ( 18.67979575497178502, 10.72451020669898547, 104.1655762719810241 ) ) ;
#192734 = VERTEX_POINT ( 'NONE', #92980 ) ;
#192735 = CARTESIAN_POINT ( 'NONE',  ( -19.05341960407611168, -5.049401038298163336, 71.45724293864766707 ) ) ;
#192736 = CARTESIAN_POINT ( 'NONE',  ( -23.29544513554941076, 16.92513159979227666, 147.7843446569000037 ) ) ;
#192738 = CARTESIAN_POINT ( 'NONE',  ( 19.05341960407611168, 5.049401038298154454, 23.95724293864769194 ) ) ;
#192737 = CARTESIAN_POINT ( 'NONE',  ( 0.05219959533910956823, 16.53943276465976808, 99.99890960531436690 ) ) ;
#192739 = CARTESIAN_POINT ( 'NONE',  ( -19.02544592524334988, -5.153800228976617603, 88.95942372801897591 ) ) ;
#192740 = CARTESIAN_POINT ( 'NONE',  ( -4.483927247898539470, -16.52544592524342804, 92.29057627198103830 ) ) ;
#192741 = CARTESIAN_POINT ( 'NONE',  ( -10.72451020669870658, -18.67979575497194134, 74.58442372801901854 ) ) ;
#192743 = CARTESIAN_POINT ( 'NONE',  ( 21.55341960407619695, -5.719274019375665929, 36.04275706135234714 ) ) ;
#192742 = CARTESIAN_POINT ( 'NONE',  ( -13.89961937509977652, 13.97604488694528158, 65.62390960531436690 ) ) ;
#192744 = CARTESIAN_POINT ( 'NONE',  ( 21.53943276465977519, -0.05219959533907433946, 108.7489096053143669 ) ) ;
#192745 = CARTESIAN_POINT ( 'NONE',  ( -5.049401038298153566, 19.05341960407611168, 75.20724293864769550 ) ) ;
#192746 = CARTESIAN_POINT ( 'NONE',  ( 27.96809023454798648, 7.159247544362251858, 161.0916313341443811 ) ) ;
#192748 = CARTESIAN_POINT ( 'NONE',  ( -10.72451020669898014, 18.67979575497178502, 30.41557627198101699 ) ) ;
#192747 = CARTESIAN_POINT ( 'NONE',  ( 4.483927247898790824, -16.52544592524335698, 30.20942372801902565 ) ) ;
#192749 = CARTESIAN_POINT ( 'NONE',  ( 5.823673210054444382, -21.52544592524334988, 60.20942372801902565 ) ) ;
#192750 = CARTESIAN_POINT ( 'NONE',  ( 13.97604488694527802, 13.89961937509977652, 104.3739096053143385 ) ) ;
#192751 = CARTESIAN_POINT ( 'NONE',  ( 19.03943276465977164, 0.05219959533936151252, 96.25109039468567573 ) ) ;
#192752 = CARTESIAN_POINT ( 'NONE',  ( 5.153800228976335163, 19.02544592524342804, 44.79057627198103830 ) ) ;
#192753 = CARTESIAN_POINT ( 'NONE',  ( -13.97604488694527625, -13.89961937509977652, 76.87390960531433848 ) ) ;
#192754 = CARTESIAN_POINT ( 'NONE',  ( 12.14591786802309770, 12.06949235617756955, 99.37390960531436690 ) ) ;
#192755 = CARTESIAN_POINT ( 'NONE',  ( 16.51473224551069308, 9.474510206698969483, 109.1655762719810383 ) ) ;
#192756 = CARTESIAN_POINT ( 'NONE',  ( -4.483927247898539470, -16.52544592524342804, 87.29057627198103830 ) ) ;
#192757 = CARTESIAN_POINT ( 'NONE',  ( -19.03943276465977164, 0.05219959533909376836, 101.2489096053143669 ) ) ;
#192759 = CARTESIAN_POINT ( 'NONE',  ( -16.46253265017160317, 9.564922557960807481, 40.83224293864769550 ) ) ;
#192758 = CARTESIAN_POINT ( 'NONE',  ( 4.379528057220339221, -16.55341960407611168, 47.70724293864770260 ) ) ;
#192760 = CARTESIAN_POINT ( 'NONE',  ( 18.62759615963255655, 10.81492255796105972, 51.66775706135234714 ) ) ;
#192761 = CARTESIAN_POINT ( 'NONE',  ( 9.474510206698729675, 16.51473224551082808, 77.08442372801900433 ) ) ;
#192762 = CARTESIAN_POINT ( 'NONE',  ( -16.53943276465976808, 0.05219959533911058130, 51.24890960531436690 ) ) ;
#192763 = CARTESIAN_POINT ( 'NONE',  ( -15.72974639402197994, 15.80617190586746368, 100.6239096053143811 ) ) ;
#192764 = CARTESIAN_POINT ( 'NONE',  ( -5.719274019375978568, 21.55341960407610458, 50.20724293864769550 ) ) ;
#192766 = CARTESIAN_POINT ( 'NONE',  ( -14.34966873604960291, -8.224510206698953496, 81.66557627198103830 ) ) ;
#192765 = CARTESIAN_POINT ( 'NONE',  ( 16.46253265017160672, -9.564922557960803928, 108.3322429386476955 ) ) ;
#192767 = CARTESIAN_POINT ( 'NONE',  ( -5.153800228976328057, -19.02544592524343514, 52.29057627198100988 ) ) ;
#192768 = CARTESIAN_POINT ( 'NONE',  ( 14.34966873604960469, 8.224510206698951720, 29.16557627198103120 ) ) ;
#192769 = CARTESIAN_POINT ( 'NONE',  ( -8.314922557961024197, 14.29746914071037800, 102.9177570613523756 ) ) ;
#192770 = CARTESIAN_POINT ( 'NONE',  ( -16.55341960407617563, 4.379528057220093196, 78.54275706135236135 ) ) ;
#192771 = CARTESIAN_POINT ( 'NONE',  ( -9.474510206698720793, -16.51473224551083518, 34.58442372801899722 ) ) ;
#192773 = CARTESIAN_POINT ( 'NONE',  ( 19.03943276465977164, -0.05219959533909143690, 103.7489096053143669 ) ) ;
#192772 = CARTESIAN_POINT ( 'NONE',  ( -24.75981654686067657, 6.635759577896799932, 167.9384007923203797 ) ) ;
#192774 = CARTESIAN_POINT ( 'NONE',  ( -19.02544592524342804, 5.153800228976336051, 81.04057627198103830 ) ) ;
#192775 = CARTESIAN_POINT ( 'NONE',  ( -13.97604488694527625, -13.89961937509977652, 31.87390960531435979 ) ) ;
#192776 = CARTESIAN_POINT ( 'NONE',  ( 16.55341960407611168, 4.379528057220329451, 48.95724293864770971 ) ) ;
#192778 = CARTESIAN_POINT ( 'NONE',  ( -16.51473224551069308, -9.474510206698971260, 106.6655762719810383 ) ) ;
#192777 = CARTESIAN_POINT ( 'NONE',  ( 5.049401038298161559, -19.05341960407611168, 112.7072429386476813 ) ) ;
#192779 = CARTESIAN_POINT ( 'NONE',  ( 5.823673210054125526, 21.52544592524343514, 44.79057627198103120 ) ) ;
#192780 = CARTESIAN_POINT ( 'NONE',  ( -16.53943276465976808, 0.05219959533911058130, 86.24890960531436690 ) ) ;
#192781 = CARTESIAN_POINT ( 'NONE',  ( 8.314922557961029526, -14.29746914071037800, 40.41775706135234714 ) ) ;
#192782 = CARTESIAN_POINT ( 'NONE',  ( -12.06949235617756955, 12.14591786802309770, 60.62390960531437401 ) ) ;
#192783 = CARTESIAN_POINT ( 'NONE',  ( 18.22780087662122384, -5.500000000000022204, 86.01540105326108687 ) ) ;
#192784 = CARTESIAN_POINT ( 'NONE',  ( 0.05219959533936267826, -19.03943276465977164, 65.00109039468567573 ) ) ;
#192785 = CARTESIAN_POINT ( 'NONE',  ( -13.97604488694527625, -13.89961937509977652, 106.8739096053143669 ) ) ;
#192786 = CARTESIAN_POINT ( 'NONE',  ( 0.05219959533936267826, -19.03943276465977164, 85.00109039468567573 ) ) ;
#192788 = CARTESIAN_POINT ( 'NONE',  ( -5.359611314223446995E-15, 29.16686587814335496, 148.8750000027311842 ) ) ;
#192787 = B_SPLINE_CURVE_WITH_KNOTS ( 'NONE', 3,
 ( #83983, #145662, #116331, #7143, #23333, #68826, #130485, #192182, #53663, #115341, #38501, #101148, #177031, #193184, #84977, #146659, #8153, #178020, #162834, #85993, #200142, #27343, #198163, #45468 ),
 .UNSPECIFIED., .F., .F.,
 ( 4, 2, 2, 2, 2, 2, 2, 2, 2, 2, 2, 4 ),
 ( 0.000000000000000000, 0.007239606870481569631, 0.01085941030572235705, 0.01447921374096314273, 0.02171882061144471757, 0.02895842748192629240, 0.03257823091716707808, 0.03619803435240785683, 0.03981783778764864251, 0.04343764122288943513, 0.05067724809337099262, 0.05791685496385254317 ),
 .UNSPECIFIED. ) ;
#192790 = CARTESIAN_POINT ( 'NONE',  ( -4.483927247898782831, 16.52544592524335698, 112.7094237280190328 ) ) ;
#192789 = CARTESIAN_POINT ( 'NONE',  ( 4.379528057220092307, 16.55341960407617563, 32.29275706135235424 ) ) ;
#192791 = CARTESIAN_POINT ( 'NONE',  ( 16.46253265017146816, 9.564922557961045513, 71.66775706135233293 ) ) ;
#192792 = CARTESIAN_POINT ( 'NONE',  ( -0.05219959533907301413, -21.53943276465977519, 37.49890960531436690 ) ) ;
#192793 = CARTESIAN_POINT ( 'NONE',  ( 18.62759615963255655, 10.81492255796105972, 66.66775706135234714 ) ) ;
#192794 = CARTESIAN_POINT ( 'NONE',  ( 19.50973618000806198, 5.499999999999992895, 37.50000000000000000 ) ) ;
#192795 = CARTESIAN_POINT ( 'NONE',  ( 13.97604488694548053, -13.89961937509957401, 110.6260903946856615 ) ) ;
#192797 = CARTESIAN_POINT ( 'NONE',  ( 16.46253265017160672, -9.564922557960803928, 78.33224293864769550 ) ) ;
#192796 = CARTESIAN_POINT ( 'NONE',  ( 17.50000000000000000, 7.499999999999999112, 22.00000000000000711 ) ) ;
#192798 = CARTESIAN_POINT ( 'NONE',  ( -9.564922557960796823, -16.46253265017161027, 27.08224293864769550 ) ) ;
#192800 = CARTESIAN_POINT ( 'NONE',  ( 16.46253265017160672, -9.564922557960803928, 83.33224293864768129 ) ) ;
#192799 = CARTESIAN_POINT ( 'NONE',  ( 14.29746914071049879, -8.314922557960816363, 88.33224293864769550 ) ) ;
#192801 = CARTESIAN_POINT ( 'NONE',  ( -13.97604488694527625, -13.89961937509977652, 81.87390960531436690 ) ) ;
#192802 = ORIENTED_EDGE ( 'NONE', *, *, #48191, .T. ) ;
#192803 = CARTESIAN_POINT ( 'NONE',  ( 16.46253265017146816, 9.564922557961045513, 96.66775706135233293 ) ) ;
#192804 = B_SPLINE_CURVE_WITH_KNOTS ( 'NONE', 3,
 ( #7190, #67873, #35546, #128535, #177077, #49725, #34555, #111393, #115389, #129527, #20368, #36528, #52701, #113371, #160888, #112385, #173078, #114364, #5191, #191227 ),
 .UNSPECIFIED., .F., .F.,
 ( 4, 2, 2, 2, 2, 2, 2, 2, 2, 4 ),
 ( 3.469446951953614189E-18, 0.0004987090165372534039, 0.0009974180330745033383, 0.001246772541343131938, 0.001496127049611760537, 0.001994836066149021855, 0.002493545082686283391, 0.002742899590954914375, 0.002992254099223544492, 0.003989672132298145192 ),
 .UNSPECIFIED. ) ;
#192805 = CARTESIAN_POINT ( 'NONE',  ( -21.53943276465977519, 0.05219959533907696930, 76.24890960531435269 ) ) ;
#192806 = CARTESIAN_POINT ( 'NONE',  ( -19.03943276465977164, 0.05219959533909376836, 26.24890960531435624 ) ) ;
#192807 = CARTESIAN_POINT ( 'NONE',  ( 16.51473224551083163, -9.474510206698727899, 65.83442372801900433 ) ) ;
#192808 = CARTESIAN_POINT ( 'NONE',  ( -19.05341960407611168, -5.049401038298163336, 76.45724293864769550 ) ) ;
#192809 = CARTESIAN_POINT ( 'NONE',  ( 16.51473224551069308, 9.474510206698969483, 99.16557627198102409 ) ) ;
#192810 = ORIENTED_EDGE ( 'NONE', *, *, #55941, .F. ) ;
#192811 = CARTESIAN_POINT ( 'NONE',  ( 18.62759615963271287, -10.81492255796078972, 98.33224293864769550 ) ) ;
#192814 = CARTESIAN_POINT ( 'NONE',  ( -5.049401038297874678, -19.05341960407617918, 64.79275706135233293 ) ) ;
#192813 = CARTESIAN_POINT ( 'NONE',  ( -16.51473224551069308, -9.474510206698971260, 81.66557627198103830 ) ) ;
#192812 = CARTESIAN_POINT ( 'NONE',  ( 12.06949235617757843, -12.14591786802309237, 88.12390960531436690 ) ) ;
#192815 = CARTESIAN_POINT ( 'NONE',  ( 15.72974639402199770, -15.80617190586745480, 83.12390960531436690 ) ) ;
#192816 = CARTESIAN_POINT ( 'NONE',  ( 10.81492255796078972, 18.62759615963270932, 79.58224293864769550 ) ) ;
#192817 = CARTESIAN_POINT ( 'NONE',  ( 4.483927247898545687, 16.52544592524342804, 39.79057627198103830 ) ) ;
#192818 = CARTESIAN_POINT ( 'NONE',  ( 10.81492255796106328, -18.62759615963255655, 105.4177570613523613 ) ) ;
#192819 = CARTESIAN_POINT ( 'NONE',  ( -4.379528057220086978, -16.55341960407618274, 69.79275706135234714 ) ) ;
#192820 = CARTESIAN_POINT ( 'NONE',  ( -5.049401038298153566, 19.05341960407611168, 90.20724293864766707 ) ) ;
#192821 = CARTESIAN_POINT ( 'NONE',  ( -9.564922557960796823, -16.46253265017161027, 32.08224293864769550 ) ) ;
#192822 = VECTOR ( 'NONE', #142538, 1000.000000000000000 ) ;
#192823 = CARTESIAN_POINT ( 'NONE',  ( 18.67979575497194134, -10.72451020669871369, 35.83442372801901143 ) ) ;
#192824 = CARTESIAN_POINT ( 'NONE',  ( -0.05219959533937732626, 21.53943276465977519, 52.50109039468567573 ) ) ;
#192825 = CARTESIAN_POINT ( 'NONE',  ( -9.474510206698964154, 16.51473224551069663, 65.41557627198102409 ) ) ;
#192826 = CARTESIAN_POINT ( 'NONE',  ( 10.81492255796106328, -18.62759615963255655, 35.41775706135234003 ) ) ;
#192827 = CARTESIAN_POINT ( 'NONE',  ( 16.51473224551083163, -9.474510206698727899, 75.83442372801900433 ) ) ;
#192828 = CARTESIAN_POINT ( 'NONE',  ( 19.03943276465977164, 0.05219959533936151252, 71.25109039468566152 ) ) ;
#192829 = CARTESIAN_POINT ( 'NONE',  ( -19.05341960407611168, -5.049401038298163336, 41.45724293864769550 ) ) ;
#192830 = CARTESIAN_POINT ( 'NONE',  ( 4.483927247898790824, -16.52544592524335698, 70.20942372801904696 ) ) ;
#192831 = CARTESIAN_POINT ( 'NONE',  ( 9.564922557960805705, 16.46253265017160317, 49.58224293864770260 ) ) ;
#192832 = CARTESIAN_POINT ( 'NONE',  ( 21.51693143705270828, -9.260949364272995865, 168.7281092719938442 ) ) ;
#192833 = CARTESIAN_POINT ( 'NONE',  ( 13.89961937509977652, -13.97604488694527269, 93.12390960531436690 ) ) ;
#192834 = CARTESIAN_POINT ( 'NONE',  ( 13.97604488694527802, 13.89961937509977652, 44.37390960531435269 ) ) ;
#192835 = CARTESIAN_POINT ( 'NONE',  ( 18.62759615963271287, -10.81492255796078972, 68.33224293864769550 ) ) ;
#192836 = CARTESIAN_POINT ( 'NONE',  ( -8.224510206698735004, -14.34966873604973081, 64.58442372801900433 ) ) ;
#192837 = VECTOR ( 'NONE', #150437, 1000.000000000000000 ) ;
#192838 = CARTESIAN_POINT ( 'NONE',  ( 16.46253265017146816, 9.564922557961045513, 21.66775706135233648 ) ) ;
#192839 = CARTESIAN_POINT ( 'NONE',  ( -19.02544592524342804, 5.153800228976336051, 56.04057627198100988 ) ) ;
#192840 = CARTESIAN_POINT ( 'NONE',  ( 4.483927247898545687, 16.52544592524342804, 44.79057627198103120 ) ) ;
#192841 = CARTESIAN_POINT ( 'NONE',  ( 16.53943276465976808, -0.05219959533910856209, 78.74890960531436690 ) ) ;
#192842 = CARTESIAN_POINT ( 'NONE',  ( -19.05341960407611168, -5.049401038298163336, 76.45724293864769550 ) ) ;
#192843 = CARTESIAN_POINT ( 'NONE',  ( 0.05219959533937995610, -21.53943276465977519, 40.00109039468567573 ) ) ;
#192844 = CARTESIAN_POINT ( 'NONE',  ( -5.153800228976328057, -19.02544592524343514, 97.29057627198099567 ) ) ;
#192845 = CARTESIAN_POINT ( 'NONE',  ( -5.719274019375665041, -21.55341960407619695, 99.79275706135234714 ) ) ;
#192846 = CARTESIAN_POINT ( 'NONE',  ( -16.55341960407617563, 4.379528057220093196, 68.54275706135234714 ) ) ;
#192847 = CARTESIAN_POINT ( 'NONE',  ( -21.55341960407619339, 5.719274019375674811, 28.54275706135234358 ) ) ;
#192848 = CARTESIAN_POINT ( 'NONE',  ( -16.46253265017160317, 9.564922557960807481, 110.8322429386476955 ) ) ;
#192849 = EDGE_CURVE ( 'NONE', #177366, #83996, #146502, .T. ) ;
#192850 = CARTESIAN_POINT ( 'NONE',  ( -10.81492255796078084, -18.62759615963271287, 92.08224293864769550 ) ) ;
#192851 = CARTESIAN_POINT ( 'NONE',  ( 12.14591786802309770, 12.06949235617756955, 44.37390960531435979 ) ) ;
#192852 = CARTESIAN_POINT ( 'NONE',  ( 0.05219959533909260263, 19.03943276465977164, 34.99890960531435979 ) ) ;
#192853 = CARTESIAN_POINT ( 'NONE',  ( -4.483927247898539470, -16.52544592524342804, 62.29057627198102409 ) ) ;
#192854 = CARTESIAN_POINT ( 'NONE',  ( -15.80617190586745835, -15.72974639402198527, 26.87390960531435979 ) ) ;
#192855 = CARTESIAN_POINT ( 'NONE',  ( -5.823673210054116645, -21.52544592524344225, 27.29057627198103120 ) ) ;
#192856 = CARTESIAN_POINT ( 'NONE',  ( 0.05219959533936267826, -19.03943276465977164, 35.00109039468566863 ) ) ;
#192857 = CARTESIAN_POINT ( 'NONE',  ( 4.379528057220339221, -16.55341960407611168, 97.70724293864772392 ) ) ;
#192858 = CARTESIAN_POINT ( 'NONE',  ( 5.153800228976335163, 19.02544592524342804, 104.7905762719809957 ) ) ;
#192859 = ORIENTED_EDGE ( 'NONE', *, *, #48777, .T. ) ;
#192860 = CARTESIAN_POINT ( 'NONE',  ( -8.314922557961024197, 14.29746914071037800, 52.91775706135235424 ) ) ;
#192861 = CARTESIAN_POINT ( 'NONE',  ( 19.03943276465977164, -0.05219959533909143690, 53.74890960531436690 ) ) ;
#192862 = CARTESIAN_POINT ( 'NONE',  ( -16.80344708052379232, -6.753205037831589763, 21.14260904372344285 ) ) ;
#192863 = CARTESIAN_POINT ( 'NONE',  ( -9.474510206698720793, -16.51473224551083518, 59.58442372801900433 ) ) ;
#192864 = CARTESIAN_POINT ( 'NONE',  ( 16.53943276465976808, 0.05219959533934440121, 96.25109039468568994 ) ) ;
#192865 = CARTESIAN_POINT ( 'NONE',  ( 9.474510206698729675, 16.51473224551082808, 102.0844237280190043 ) ) ;
#192866 = CARTESIAN_POINT ( 'NONE',  ( -5.719274019375665041, -21.55341960407619695, 64.79275706135234714 ) ) ;
#192867 = CARTESIAN_POINT ( 'NONE',  ( 16.46253265017160672, -9.564922557960803928, 78.33224293864769550 ) ) ;
#192868 = CARTESIAN_POINT ( 'NONE',  ( 5.823673210054125526, 21.52544592524343514, 94.79057627198105251 ) ) ;
#192869 = CARTESIAN_POINT ( 'NONE',  ( 4.483927247898545687, 16.52544592524342804, 109.7905762719810383 ) ) ;
#192870 = CIRCLE ( 'NONE', #25032, 8.000000000000000000 ) ;
#192871 = CARTESIAN_POINT ( 'NONE',  ( 19.03943276465977164, 0.05219959533936151252, 76.25109039468566152 ) ) ;
#192872 = CARTESIAN_POINT ( 'NONE',  ( -18.67979575497178146, -10.72451020669898902, 71.66557627198100988 ) ) ;
#192873 = CARTESIAN_POINT ( 'NONE',  ( 9.474510206698729675, 16.51473224551082808, 42.08442372801900433 ) ) ;
#192874 = CARTESIAN_POINT ( 'NONE',  ( 19.25918095147779141, 5.499999999999523936, 96.95284276293932635 ) ) ;
#192875 = CARTESIAN_POINT ( 'NONE',  ( 21.53943276465977519, -0.05219959533907433946, 93.74890960531436690 ) ) ;
#192876 = CARTESIAN_POINT ( 'NONE',  ( 17.50000000000003197, 3.565345528327901636, 28.07505513193531854 ) ) ;
#192877 = CARTESIAN_POINT ( 'NONE',  ( 13.97604488694527802, 13.89961937509977652, 64.37390960531436690 ) ) ;
#192878 = CARTESIAN_POINT ( 'NONE',  ( -17.50000000000000000, 5.499999999999992895, 33.71769037696435589 ) ) ;
#192879 = CARTESIAN_POINT ( 'NONE',  ( 5.049401038297881783, 19.05341960407617563, 112.2927570613523471 ) ) ;
#192880 = CARTESIAN_POINT ( 'NONE',  ( 24.20533859822809930, 9.236745700548663507, 166.4300890397317971 ) ) ;
#192881 = CARTESIAN_POINT ( 'NONE',  ( 19.02544592524343514, -5.153800228976328945, 43.54057627198103120 ) ) ;
#192883 = CARTESIAN_POINT ( 'NONE',  ( -8.314922557960811034, -14.29746914071050412, 57.08224293864769550 ) ) ;
#192882 = CARTESIAN_POINT ( 'NONE',  ( 21.55341960407610458, 5.719274019375980345, 103.9572429386476813 ) ) ;
#192884 = CARTESIAN_POINT ( 'NONE',  ( -13.89961937509977652, 13.97604488694528158, 60.62390960531436690 ) ) ;
#192885 = CARTESIAN_POINT ( 'NONE',  ( -0.05219959533937732626, 21.53943276465977519, 72.50109039468568994 ) ) ;
#192887 = CARTESIAN_POINT ( 'NONE',  ( 13.97604488694548053, -13.89961937509957401, 25.62609039468566507 ) ) ;
#192886 = CARTESIAN_POINT ( 'NONE',  ( -13.97604488694547697, 13.89961937509957934, 113.1260903946856757 ) ) ;
#192888 = CARTESIAN_POINT ( 'NONE',  ( -4.379528057220328563, 16.55341960407611168, 25.20724293864769550 ) ) ;
#192889 = CARTESIAN_POINT ( 'NONE',  ( -21.52544592524334988, -5.823673210054445271, 43.95942372801902565 ) ) ;
#192890 = CARTESIAN_POINT ( 'NONE',  ( 5.719274019375673035, 21.55341960407619339, 22.29275706135235069 ) ) ;
#192891 = CARTESIAN_POINT ( 'NONE',  ( -18.62759615963270932, 10.81492255796079327, 60.83224293864769550 ) ) ;
#192892 = CARTESIAN_POINT ( 'NONE',  ( 16.51473224551083163, -9.474510206698727899, 90.83442372801900433 ) ) ;
#192893 = ADVANCED_FACE ( 'NONE', ( #184020 ), #10829, .F. ) ;
#192894 = CARTESIAN_POINT ( 'NONE',  ( 16.46253265017146816, 9.564922557961045513, 71.66775706135233293 ) ) ;
#192895 = CARTESIAN_POINT ( 'NONE',  ( 0.05219959533937995610, -21.53943276465977519, 75.00109039468568994 ) ) ;
#192896 = CARTESIAN_POINT ( 'NONE',  ( -19.02544592524334988, -5.153800228976617603, 48.95942372801900433 ) ) ;
#192897 = CARTESIAN_POINT ( 'NONE',  ( 13.89961937509977652, -13.97604488694527269, 28.12390960531435624 ) ) ;
#192898 = CARTESIAN_POINT ( 'NONE',  ( -0.05219959533907301413, -21.53943276465977519, 47.49890960531435979 ) ) ;
#192899 = CARTESIAN_POINT ( 'NONE',  ( 8.224510206698953496, -14.34966873604960469, 52.91557627198103830 ) ) ;
#192900 = CARTESIAN_POINT ( 'NONE',  ( -19.49149378614659511, 5.499999999999677591, 94.43757513605362419 ) ) ;
#192901 = CARTESIAN_POINT ( 'NONE',  ( 15.72974639402176855, 15.80617190586768217, 111.8760903946856615 ) ) ;
#192902 = CARTESIAN_POINT ( 'NONE',  ( 4.379528057220092307, 16.55341960407617563, 82.29275706135234714 ) ) ;
#192903 = CARTESIAN_POINT ( 'NONE',  ( 12.14591786802309770, 12.06949235617756955, 44.37390960531435979 ) ) ;
#192904 = CARTESIAN_POINT ( 'NONE',  ( -18.67979575497193778, 10.72451020669871902, 73.33442372801901854 ) ) ;
#192905 = CARTESIAN_POINT ( 'NONE',  ( 0.05219959533937995610, -21.53943276465977519, 75.00109039468568994 ) ) ;
#192906 = CARTESIAN_POINT ( 'NONE',  ( 15.72974639402199770, -15.80617190586745480, 88.12390960531436690 ) ) ;
#192907 = CARTESIAN_POINT ( 'NONE',  ( 19.03943276465977164, -0.05219959533909143690, 33.74890960531435979 ) ) ;
#192908 = CARTESIAN_POINT ( 'NONE',  ( 18.67979575497194134, -10.72451020669871369, 55.83442372801901854 ) ) ;
#192909 = CARTESIAN_POINT ( 'NONE',  ( -19.05341960407611168, -5.049401038298163336, 31.45724293864769550 ) ) ;
#192910 = CARTESIAN_POINT ( 'NONE',  ( 9.474510206698971260, -16.51473224551069308, 57.91557627198103120 ) ) ;
#192911 = CARTESIAN_POINT ( 'NONE',  ( 14.34966873604960469, 8.224510206698951720, 89.16557627198102409 ) ) ;
#192912 = CARTESIAN_POINT ( 'NONE',  ( -19.02544592524342804, 5.153800228976336051, 101.0405762719810241 ) ) ;
#192913 = CARTESIAN_POINT ( 'NONE',  ( -8.224510206698948167, 14.34966873604960824, 40.41557627198103120 ) ) ;
#192914 = CARTESIAN_POINT ( 'NONE',  ( -0.05219959533910754901, -16.53943276465976808, 107.4989096053143669 ) ) ;
#192915 = CARTESIAN_POINT ( 'NONE',  ( 18.62759615963271287, -10.81492255796078972, 78.33224293864770971 ) ) ;
#192916 = CARTESIAN_POINT ( 'NONE',  ( -21.52544592524334988, -5.823673210054445271, 18.95942372801901143 ) ) ;
#192917 = LINE ( 'NONE', #115067, #117865 ) ;
#192918 = CARTESIAN_POINT ( 'NONE',  ( 16.53943276465976808, 0.05219959533934440121, 26.25109039468567573 ) ) ;
#192919 = CARTESIAN_POINT ( 'NONE',  ( 5.719274019375991003, -21.55341960407610458, 67.70724293864769550 ) ) ;
#192920 = CARTESIAN_POINT ( 'NONE',  ( 18.62759615963255655, 10.81492255796105972, 91.66775706135234714 ) ) ;
#192921 = CARTESIAN_POINT ( 'NONE',  ( 16.46253265017160672, -9.564922557960803928, 83.33224293864768129 ) ) ;
#192922 = CARTESIAN_POINT ( 'NONE',  ( -21.53943276465977519, -0.05219959533937600094, 33.75109039468568284 ) ) ;
#192923 = CARTESIAN_POINT ( 'NONE',  ( 10.72451020669898902, -18.67979575497178502, 22.91557627198102765 ) ) ;
#192924 = CARTESIAN_POINT ( 'NONE',  ( 4.379528057220092307, 16.55341960407617563, 87.29275706135236135 ) ) ;
#192925 = CARTESIAN_POINT ( 'NONE',  ( 18.67979575497194134, -10.72451020669871369, 65.83442372801900433 ) ) ;
#192926 = CARTESIAN_POINT ( 'NONE',  ( -19.05341960407617563, 5.049401038297882671, 23.54275706135233648 ) ) ;
#192927 = CARTESIAN_POINT ( 'NONE',  ( 4.483927247898790824, -16.52544592524335698, 75.20942372801901854 ) ) ;
#192928 = CARTESIAN_POINT ( 'NONE',  ( 10.72451020669871369, 18.67979575497193778, 27.08442372801901854 ) ) ;
#192929 = CARTESIAN_POINT ( 'NONE',  ( -9.474510206698964154, 16.51473224551069663, 30.41557627198102054 ) ) ;
#192930 = CARTESIAN_POINT ( 'NONE',  ( -15.80617190586768217, 15.72974639402176855, 88.12609039468570415 ) ) ;
#192931 = CARTESIAN_POINT ( 'NONE',  ( -19.02544592524342804, 5.153800228976336051, 91.04057627198100988 ) ) ;
#192932 = B_SPLINE_CURVE_WITH_KNOTS ( 'NONE', 3,
 ( #181309, #9457, #13430, #11464, #134805, #196485, #58929, #75094, #57955, #10456 ),
 .UNSPECIFIED., .F., .F.,
 ( 4, 2, 2, 2, 4 ),
 ( 9.540979117872437479E-18, 0.0004927478742826785652, 0.0009854957485653475895, 0.001478243622848016614, 0.001970991497130685638 ),
 .UNSPECIFIED. ) ;
#192933 = CARTESIAN_POINT ( 'NONE',  ( -5.823673210054116645, -21.52544592524344225, 102.2905762719810383 ) ) ;
#192935 = CARTESIAN_POINT ( 'NONE',  ( 21.52544592524344225, -5.823673210054117533, 53.54057627198103120 ) ) ;
#192934 = CARTESIAN_POINT ( 'NONE',  ( 19.49671883438228548, 5.499999999999966249, 82.39279849105678011 ) ) ;
#192937 = CARTESIAN_POINT ( 'NONE',  ( -14.29746914071049879, 8.314922557960819915, 45.83224293864769550 ) ) ;
#192936 = CARTESIAN_POINT ( 'NONE',  ( -13.89961937509977652, 13.97604488694528158, 95.62390960531436690 ) ) ;
#192938 = DIRECTION ( 'NONE',  ( 0.7071067811865483499, 0.000000000000000000, 0.7071067811865465735 ) ) ;
#192939 = CARTESIAN_POINT ( 'NONE',  ( 13.97604488694548053, -13.89961937509957401, 75.62609039468564731 ) ) ;
#192940 = CARTESIAN_POINT ( 'NONE',  ( -16.52216118717205262, 7.221426719304517405, 103.9240097895301318 ) ) ;
#192941 = CARTESIAN_POINT ( 'NONE',  ( 0.05219959533936267826, -19.03943276465977164, 110.0010903946856757 ) ) ;
#192942 = CARTESIAN_POINT ( 'NONE',  ( 21.53943276465977519, -0.05219959533907433946, 83.74890960531435269 ) ) ;
#192943 = CARTESIAN_POINT ( 'NONE',  ( 14.34966873604960469, 8.224510206698951720, 64.16557627198102409 ) ) ;
#192944 = CARTESIAN_POINT ( 'NONE',  ( -5.153800228976328057, -19.02544592524343514, 97.29057627198099567 ) ) ;
#192945 = CARTESIAN_POINT ( 'NONE',  ( -16.53943276465976808, -0.05219959533934237506, 38.75109039468567573 ) ) ;
#192946 = CARTESIAN_POINT ( 'NONE',  ( -0.05219959533909027116, -19.03943276465977164, 62.49890960531435979 ) ) ;
#192948 = CARTESIAN_POINT ( 'NONE',  ( 5.153800228976615827, -19.02544592524334988, 95.20942372801897591 ) ) ;
#192947 = CARTESIAN_POINT ( 'NONE',  ( 21.53943276465977519, 0.05219959533937863772, 26.25109039468567573 ) ) ;
#192949 = CARTESIAN_POINT ( 'NONE',  ( -9.474510206698964154, 16.51473224551069663, 100.4155762719810241 ) ) ;
#192950 = CARTESIAN_POINT ( 'NONE',  ( 13.97604488694527802, 13.89961937509977652, 84.37390960531433848 ) ) ;
#192951 = CARTESIAN_POINT ( 'NONE',  ( 0.05219959533907565091, 21.53943276465977519, 89.99890960531438111 ) ) ;
#192952 = CARTESIAN_POINT ( 'NONE',  ( 9.564922557960805705, 16.46253265017160317, 44.58224293864769550 ) ) ;
#192953 = CARTESIAN_POINT ( 'NONE',  ( -17.49999999999999645, -5.500000000000020428, 61.28230962303567964 ) ) ;
#192954 = CARTESIAN_POINT ( 'NONE',  ( 12.06949235617757843, -12.14591786802309237, 68.12390960531436690 ) ) ;
#192955 = CARTESIAN_POINT ( 'NONE',  ( -19.03943276465977164, 0.05219959533909376836, 101.2489096053143669 ) ) ;
#192956 = CARTESIAN_POINT ( 'NONE',  ( 17.24269848851061226, -15.08844724069277454, -55.31736789360020623 ) ) ;
#192957 = CARTESIAN_POINT ( 'NONE',  ( -16.46253265017146816, -9.564922557961047289, 64.16775706135233293 ) ) ;
#192958 = CARTESIAN_POINT ( 'NONE',  ( 5.719274019375991003, -21.55341960407610458, 87.70724293864769550 ) ) ;
#192959 = CARTESIAN_POINT ( 'NONE',  ( -5.153800228976607833, 19.02544592524334988, 47.70942372801900433 ) ) ;
#192960 = CARTESIAN_POINT ( 'NONE',  ( -16.51473224551069308, -9.474510206698971260, 96.66557627198102409 ) ) ;
#192961 = CARTESIAN_POINT ( 'NONE',  ( -5.719274019375978568, 21.55341960407610458, 40.20724293864769550 ) ) ;
#192962 = CARTESIAN_POINT ( 'NONE',  ( -19.03943276465977164, 0.05219959533909376836, 86.24890960531436690 ) ) ;
#192963 = CARTESIAN_POINT ( 'NONE',  ( 5.823673210054444382, -21.52544592524334988, 70.20942372801904696 ) ) ;
#192964 = CARTESIAN_POINT ( 'NONE',  ( -16.46253265017160317, 9.564922557960807481, 40.83224293864769550 ) ) ;
#192965 = EDGE_CURVE ( 'NONE', #45827, #9769, #9059, .T. ) ;
#192966 = CARTESIAN_POINT ( 'NONE',  ( 16.55341960407611168, 4.379528057220329451, 73.95724293864769550 ) ) ;
#192967 = CARTESIAN_POINT ( 'NONE',  ( -19.05341960407617563, 5.049401038297882671, 113.5427570613523471 ) ) ;
#192968 = CARTESIAN_POINT ( 'NONE',  ( -5.719274019375665041, -21.55341960407619695, 49.79275706135234714 ) ) ;
#192969 = ORIENTED_EDGE ( 'NONE', *, *, #160152, .F. ) ;
#192970 = CARTESIAN_POINT ( 'NONE',  ( 16.46253265017160672, -9.564922557960803928, 113.3322429386476955 ) ) ;
#192971 = CARTESIAN_POINT ( 'NONE',  ( 5.153800228976615827, -19.02544592524334988, 70.20942372801899012 ) ) ;
#192972 = CYLINDRICAL_SURFACE ( 'NONE', #140706, 21.30000000000002913 ) ;
#192973 = CARTESIAN_POINT ( 'NONE',  ( -15.72974639402176322, -15.80617190586768395, 19.37609039468568639 ) ) ;
#192974 = CARTESIAN_POINT ( 'NONE',  ( -19.05341960407611168, -5.049401038298163336, 61.45724293864769550 ) ) ;
#192975 = CARTESIAN_POINT ( 'NONE',  ( -38.00000000000000711, 2.428612866367529932E-14, -7.749999994537626336 ) ) ;
#192976 = CARTESIAN_POINT ( 'NONE',  ( -13.97604488694547697, 13.89961937509957934, 23.12609039468565442 ) ) ;
#192977 = CARTESIAN_POINT ( 'NONE',  ( -5.153800228976328057, -19.02544592524343514, 42.29057627198101699 ) ) ;
#192978 = CARTESIAN_POINT ( 'NONE',  ( -0.05219959533937732626, 21.53943276465977519, 107.5010903946856899 ) ) ;
#192979 = CARTESIAN_POINT ( 'NONE',  ( 4.483927247898790824, -16.52544592524335698, 90.20942372801903275 ) ) ;
#192980 = EDGE_CURVE ( 'NONE', #156405, #181594, #60655, .T. ) ;
#192982 = CARTESIAN_POINT ( 'NONE',  ( 21.53943276465977519, 0.05219959533937863772, 71.25109039468568994 ) ) ;
#192981 = CARTESIAN_POINT ( 'NONE',  ( 13.89961937509977652, -13.97604488694527269, 108.1239096053143669 ) ) ;
#192983 = CARTESIAN_POINT ( 'NONE',  ( 22.44159573604009239, 16.30477369853692693, 148.5750000027312012 ) ) ;
#192984 = CARTESIAN_POINT ( 'NONE',  ( 16.51473224551069308, 9.474510206698969483, 109.1655762719810383 ) ) ;
#192985 = CARTESIAN_POINT ( 'NONE',  ( 24.12203661075783501, 5.823883908176390456, 170.5995460337422571 ) ) ;
#192987 = CARTESIAN_POINT ( 'NONE',  ( 18.67979575497194134, -10.72451020669871369, 70.83442372801901854 ) ) ;
#192986 = CARTESIAN_POINT ( 'NONE',  ( -4.379528057220086978, -16.55341960407618274, 69.79275706135234714 ) ) ;
#192988 = CARTESIAN_POINT ( 'NONE',  ( 10.81492255796106328, -18.62759615963255655, 100.4177570613523471 ) ) ;
#192989 = FACE_OUTER_BOUND ( 'NONE', #116412, .T. ) ;
#192990 = CARTESIAN_POINT ( 'NONE',  ( -16.46253265017160317, 9.564922557960807481, 80.83224293864769550 ) ) ;
#192991 = CARTESIAN_POINT ( 'NONE',  ( 16.46253265017160672, -9.564922557960803928, 113.3322429386476955 ) ) ;
#192992 = ORIENTED_EDGE ( 'NONE', *, *, #93145, .F. ) ;
#192993 = CIRCLE ( 'NONE', #105812, 13.70000000000001528 ) ;
#192994 = DIRECTION ( 'NONE',  ( 1.000000000000000000, -0.000000000000000000, -0.000000000000000000 ) ) ;
#192995 = CARTESIAN_POINT ( 'NONE',  ( -13.97604488694527625, -13.89961937509977652, 36.87390960531436690 ) ) ;
#192996 = CARTESIAN_POINT ( 'NONE',  ( -21.53943276465977519, 0.05219959533907696930, 46.24890960531435979 ) ) ;
#192997 = CARTESIAN_POINT ( 'NONE',  ( -16.55341960407617563, 4.379528057220093196, 103.5427570613523613 ) ) ;
#192999 = CARTESIAN_POINT ( 'NONE',  ( 19.02544592524343514, -5.153800228976328945, 78.54057627198099567 ) ) ;
#192998 = CARTESIAN_POINT ( 'NONE',  ( 14.29746914071049879, -8.314922557960816363, 78.33224293864770971 ) ) ;
#193000 = CARTESIAN_POINT ( 'NONE',  ( -18.62759615963255300, -10.81492255796106328, 109.1677570613523613 ) ) ;
#193001 = CARTESIAN_POINT ( 'NONE',  ( -9.564922557960796823, -16.46253265017161027, 32.08224293864769550 ) ) ;
#193002 = CARTESIAN_POINT ( 'NONE',  ( -8.224510206698948167, 14.34966873604960824, 85.41557627198102409 ) ) ;
#193003 = CARTESIAN_POINT ( 'NONE',  ( -15.72974639402176322, -15.80617190586768395, 39.37609039468567573 ) ) ;
#193004 = CARTESIAN_POINT ( 'NONE',  ( 5.719274019375991003, -21.55341960407610458, 82.70724293864770971 ) ) ;
#193005 = CARTESIAN_POINT ( 'NONE',  ( 16.46253265017146816, 9.564922557961045513, 51.66775706135233293 ) ) ;
#193006 = CARTESIAN_POINT ( 'NONE',  ( -34.45218533337747147, 5.971079431359530787, 49.56529461667049219 ) ) ;
#193007 = CARTESIAN_POINT ( 'NONE',  ( 5.049401038298161559, -19.05341960407611168, 97.70724293864766707 ) ) ;
#193008 = CARTESIAN_POINT ( 'NONE',  ( -12.06949235617756955, 12.14591786802309770, 65.62390960531436690 ) ) ;
#193009 = CARTESIAN_POINT ( 'NONE',  ( -12.14591786802309592, -12.06949235617757132, 46.87390960531435979 ) ) ;
#193010 = CARTESIAN_POINT ( 'NONE',  ( 16.51473224551083163, -9.474510206698727899, 85.83442372801900433 ) ) ;
#193011 = CARTESIAN_POINT ( 'NONE',  ( 2.500000000000000000, 2.357898499370431722, -2.818925648462311528E-15 ) ) ;
#193012 = CARTESIAN_POINT ( 'NONE',  ( -21.53943276465977519, 0.05219959533907696930, 21.24890960531436690 ) ) ;
#193013 = CARTESIAN_POINT ( 'NONE',  ( 8.314922557960818139, 14.29746914071049879, 89.58224293864768129 ) ) ;
#193014 = DIRECTION ( 'NONE',  ( -1.000000000000000000, 0.000000000000000000, 0.000000000000000000 ) ) ;
#193016 = CARTESIAN_POINT ( 'NONE',  ( -18.62759615963270932, 10.81492255796079327, 50.83224293864770971 ) ) ;
#193015 = CARTESIAN_POINT ( 'NONE',  ( 16.46253265017160672, -9.564922557960803928, 48.33224293864769550 ) ) ;
#193017 = CARTESIAN_POINT ( 'NONE',  ( -19.05341960407611168, -5.049401038298163336, 36.45724293864766707 ) ) ;
#193019 = CARTESIAN_POINT ( 'NONE',  ( -5.049401038298153566, 19.05341960407611168, 60.20724293864768129 ) ) ;
#193018 = CARTESIAN_POINT ( 'NONE',  ( -4.379528057220086978, -16.55341960407618274, 84.79275706135234714 ) ) ;
#193020 = CARTESIAN_POINT ( 'NONE',  ( 9.564922557961047289, -16.46253265017146816, 40.41775706135234003 ) ) ;
#193021 = CARTESIAN_POINT ( 'NONE',  ( -18.67979575497193778, 10.72451020669871902, 73.33442372801901854 ) ) ;
#193022 = CARTESIAN_POINT ( 'NONE',  ( -0.05219959533907301413, -21.53943276465977519, 42.49890960531435979 ) ) ;
#193023 = CARTESIAN_POINT ( 'NONE',  ( -4.379528057220328563, 16.55341960407611168, 100.2072429386476955 ) ) ;
#193024 = CARTESIAN_POINT ( 'NONE',  ( 5.049401038297881783, 19.05341960407617563, 87.29275706135234714 ) ) ;
#193025 = CARTESIAN_POINT ( 'NONE',  ( 11.40812507854754365, 35.11059874428196537, -5.724999997268812812 ) ) ;
#193027 = CARTESIAN_POINT ( 'NONE',  ( -21.53943276465977519, 0.05219959533907696930, 41.24890960531435269 ) ) ;
#193026 = CARTESIAN_POINT ( 'NONE',  ( 0.000000000000000000, 0.000000000000000000, -56.77278709839600879 ) ) ;
#193028 = CARTESIAN_POINT ( 'NONE',  ( 17.05116617787826883, -6.768360034955673399, 66.15675553259198693 ) ) ;
#193029 = CARTESIAN_POINT ( 'NONE',  ( 15.72974639402176855, 15.80617190586768217, 76.87609039468567573 ) ) ;
#193030 = CARTESIAN_POINT ( 'NONE',  ( 4.483927247898545687, 16.52544592524342804, 44.79057627198103120 ) ) ;
#193032 = CARTESIAN_POINT ( 'NONE',  ( -4.483927247898539470, -16.52544592524342804, 52.29057627198102409 ) ) ;
#193031 = CARTESIAN_POINT ( 'NONE',  ( 8.224510206698742110, 14.34966873604972548, 72.08442372801899012 ) ) ;
#193033 = CARTESIAN_POINT ( 'NONE',  ( -0.05219959533907301413, -21.53943276465977519, 87.49890960531436690 ) ) ;
#193034 = CARTESIAN_POINT ( 'NONE',  ( 5.823673210054125526, 21.52544592524343514, 74.79057627198105251 ) ) ;
#193035 = LINE ( 'NONE', #133347, #162948 ) ;
#193036 = CARTESIAN_POINT ( 'NONE',  ( -18.67979575497178146, -10.72451020669898902, 26.66557627198103475 ) ) ;
#193037 = CARTESIAN_POINT ( 'NONE',  ( 12.14591786802327356, -12.06949235617739191, 55.62609039468568284 ) ) ;
#193038 = CARTESIAN_POINT ( 'NONE',  ( -12.06949235617756955, 12.14591786802309770, 75.62390960531439532 ) ) ;
#193039 = CARTESIAN_POINT ( 'NONE',  ( 0.05219959533909260263, 19.03943276465977164, 64.99890960531436690 ) ) ;
#193040 = CARTESIAN_POINT ( 'NONE',  ( 16.46253265017160672, -9.564922557960803928, 33.33224293864770260 ) ) ;
#193041 = LINE ( 'NONE', #175873, #125263 ) ;
#193042 = ORIENTED_EDGE ( 'NONE', *, *, #143824, .T. ) ;
#193043 = CARTESIAN_POINT ( 'NONE',  ( 12.14591786802327356, -12.06949235617739191, 80.62609039468567573 ) ) ;
#193044 = CARTESIAN_POINT ( 'NONE',  ( 21.52544592524344225, -5.823673210054117533, 113.5405762719810383 ) ) ;
#193045 = CARTESIAN_POINT ( 'NONE',  ( -19.03943276465977164, 0.05219959533909376836, 71.24890960531435269 ) ) ;
#193046 = CARTESIAN_POINT ( 'NONE',  ( 10.81492255796106328, -18.62759615963255655, 55.41775706135234714 ) ) ;
#193047 = CARTESIAN_POINT ( 'NONE',  ( -9.474510206698964154, 16.51473224551069663, 110.4155762719810383 ) ) ;
#193048 = CARTESIAN_POINT ( 'NONE',  ( -7.905529020988549149, -46.70198807553910569, -24.42054064165492733 ) ) ;
#193049 = ORIENTED_EDGE ( 'NONE', *, *, #58736, .T. ) ;
#193050 = CARTESIAN_POINT ( 'NONE',  ( 21.53943276465977519, 0.05219959533937863772, 51.25109039468568994 ) ) ;
#193052 = CARTESIAN_POINT ( 'NONE',  ( -16.51473224551069308, -9.474510206698971260, 101.6655762719810241 ) ) ;
#193051 = CARTESIAN_POINT ( 'NONE',  ( 0.05219959533909260263, 19.03943276465977164, 29.99890960531435979 ) ) ;
#193053 = CARTESIAN_POINT ( 'NONE',  ( 19.02544592524334988, 5.153800228976608722, 56.45942372801898301 ) ) ;
#193054 = CARTESIAN_POINT ( 'NONE',  ( 18.67979575497194134, -10.72451020669871369, 20.83442372801901143 ) ) ;
#193055 = CARTESIAN_POINT ( 'NONE',  ( 16.46253265017146816, 9.564922557961045513, 41.66775706135234003 ) ) ;
#193056 = CARTESIAN_POINT ( 'NONE',  ( -19.05341960407617563, 5.049401038297882671, 53.54275706135231871 ) ) ;
#193057 = CARTESIAN_POINT ( 'NONE',  ( 12.06949235617739724, 12.14591786802326823, 106.8760903946856899 ) ) ;
#193059 = ORIENTED_EDGE ( 'NONE', *, *, #75719, .T. ) ;
#193058 = CARTESIAN_POINT ( 'NONE',  ( 9.621741624713976648, 11.74323870453916996, -62.00714677346290671 ) ) ;
#193060 = CARTESIAN_POINT ( 'NONE',  ( 16.46253265017160672, -9.564922557960803928, 83.33224293864768129 ) ) ;
#193061 = CARTESIAN_POINT ( 'NONE',  ( 21.53943276465977519, 0.05219959533937863772, 96.25109039468568994 ) ) ;
#193062 = CARTESIAN_POINT ( 'NONE',  ( -5.719274019375665041, -21.55341960407619695, 89.79275706135236135 ) ) ;
#193063 = CARTESIAN_POINT ( 'NONE',  ( 23.15940025311444472, -1.498759781556224580, -55.09305739490147857 ) ) ;
#193064 = CARTESIAN_POINT ( 'NONE',  ( 5.049401038298161559, -19.05341960407611168, 102.7072429386476955 ) ) ;
#193065 = CARTESIAN_POINT ( 'NONE',  ( -5.719274019375665041, -21.55341960407619695, 74.79275706135234714 ) ) ;
#193066 = CARTESIAN_POINT ( 'NONE',  ( -16.55341960407617563, 4.379528057220093196, 23.54275706135235424 ) ) ;
#193067 = CARTESIAN_POINT ( 'NONE',  ( 16.46253265017160672, -9.564922557960803928, 83.33224293864768129 ) ) ;
#193069 = EDGE_CURVE ( 'NONE', #39277, #34377, #36610, .T. ) ;
#193068 = CARTESIAN_POINT ( 'NONE',  ( -15.72974639402197994, 15.80617190586746368, 25.62390960531435624 ) ) ;
#193070 = CARTESIAN_POINT ( 'NONE',  ( -19.02544592524342804, 5.153800228976336051, 96.04057627198103830 ) ) ;
#193071 = CARTESIAN_POINT ( 'NONE',  ( -18.22780087662123805, -5.499999999999968026, 98.98236817873106475 ) ) ;
#193072 = CARTESIAN_POINT ( 'NONE',  ( -5.153800228976328057, -19.02544592524343514, 77.29057627198099567 ) ) ;
#193073 = CARTESIAN_POINT ( 'NONE',  ( 19.05341960407611168, 5.049401038298154454, 68.95724293864769550 ) ) ;
#193074 = CARTESIAN_POINT ( 'NONE',  ( 21.55341960407610458, 5.719274019375980345, 108.9572429386476955 ) ) ;
#193075 = CARTESIAN_POINT ( 'NONE',  ( 8.224510206698742110, 14.34966873604972548, 107.0844237280190043 ) ) ;
#193076 = CARTESIAN_POINT ( 'NONE',  ( -16.36317988757099329, 7.306389748694731345, 99.09789608363170998 ) ) ;
#193077 = CARTESIAN_POINT ( 'NONE',  ( -19.02544592524334988, -5.153800228976617603, 53.95942372801898301 ) ) ;
#193078 = CARTESIAN_POINT ( 'NONE',  ( -13.97604488694527625, -13.89961937509977652, 91.87390960531432427 ) ) ;
#193079 = CARTESIAN_POINT ( 'NONE',  ( 14.29746914071049879, -8.314922557960816363, 83.33224293864769550 ) ) ;
#193080 = CARTESIAN_POINT ( 'NONE',  ( -15.80617190586745835, -15.72974639402198527, 26.87390960531435979 ) ) ;
#193081 = CARTESIAN_POINT ( 'NONE',  ( 21.55341960407610458, 5.719274019375980345, 28.95724293864769905 ) ) ;
#193082 = CARTESIAN_POINT ( 'NONE',  ( 14.29746914071049879, -8.314922557960816363, 98.33224293864769550 ) ) ;
#193083 = CARTESIAN_POINT ( 'NONE',  ( -17.12812012977024168, 6.668231424566045895, 53.64051240676857191 ) ) ;
#193084 = CARTESIAN_POINT ( 'NONE',  ( -9.474510206698720793, -16.51473224551083518, 49.58442372801899722 ) ) ;
#193085 = CARTESIAN_POINT ( 'NONE',  ( -12.14591786802326823, 12.06949235617739902, 108.1260903946856757 ) ) ;
#193086 = CARTESIAN_POINT ( 'NONE',  ( 9.564922557960805705, 16.46253265017160317, 94.58224293864769550 ) ) ;
#193087 = CARTESIAN_POINT ( 'NONE',  ( 5.823673210054444382, -21.52544592524334988, 65.20942372801901854 ) ) ;
#193088 = CARTESIAN_POINT ( 'NONE',  ( -21.52544592524343514, 5.823673210054127303, 51.04057627198103120 ) ) ;
#193089 = CARTESIAN_POINT ( 'NONE',  ( 21.52544592524334988, 5.823673210054432836, 26.45942372801901854 ) ) ;
#193090 = CARTESIAN_POINT ( 'NONE',  ( -5.823673210054116645, -21.52544592524344225, 87.29057627198103830 ) ) ;
#193091 = CARTESIAN_POINT ( 'NONE',  ( 8.224510206698953496, -14.34966873604960469, 112.9155762719810383 ) ) ;
#193092 = CARTESIAN_POINT ( 'NONE',  ( 9.564922557961047289, -16.46253265017146816, 70.41775706135233293 ) ) ;
#193093 = CARTESIAN_POINT ( 'NONE',  ( 19.03943276465977164, -0.05219959533909143690, 43.74890960531435979 ) ) ;
#193094 = CARTESIAN_POINT ( 'NONE',  ( 5.049401038298161559, -19.05341960407611168, 102.7072429386476955 ) ) ;
#193095 = CARTESIAN_POINT ( 'NONE',  ( -16.46253265017160317, 9.564922557960807481, 100.8322429386477097 ) ) ;
#193096 = CARTESIAN_POINT ( 'NONE',  ( -16.52544592524342804, 4.483927247898546575, 111.0405762719810525 ) ) ;
#193097 = CARTESIAN_POINT ( 'NONE',  ( -0.05219959533910754901, -16.53943276465976808, 42.49890960531435979 ) ) ;
#193098 = CARTESIAN_POINT ( 'NONE',  ( -14.34966873604972548, 8.224510206698743886, 43.33442372801901143 ) ) ;
#193099 = CARTESIAN_POINT ( 'NONE',  ( 8.314922557960818139, 14.29746914071049879, 114.5822429386477097 ) ) ;
#193100 = CARTESIAN_POINT ( 'NONE',  ( 0.05219959533937995610, -21.53943276465977519, 100.0010903946857042 ) ) ;
#193103 = CARTESIAN_POINT ( 'NONE',  ( 8.224510206698953496, -14.34966873604960469, 22.91557627198102765 ) ) ;
#193102 = CARTESIAN_POINT ( 'NONE',  ( 13.89961937509977652, -13.97604488694527269, 108.1239096053143669 ) ) ;
#193101 = VECTOR ( 'NONE', #70694, 1000.000000000000000 ) ;
#193104 = CARTESIAN_POINT ( 'NONE',  ( 15.80617190586769283, -15.72974639402175789, 35.62609039468568994 ) ) ;
#193105 = CARTESIAN_POINT ( 'NONE',  ( 19.05341960407611168, 5.049401038298154454, 103.9572429386476671 ) ) ;
#193106 = CARTESIAN_POINT ( 'NONE',  ( -0.05219959533934338120, 16.53943276465976808, 112.5010903946857042 ) ) ;
#193107 = CARTESIAN_POINT ( 'NONE',  ( 14.29746914071037800, 8.314922557961029526, 86.66775706135234714 ) ) ;
#193108 = CARTESIAN_POINT ( 'NONE',  ( -16.55341960407617563, 4.379528057220093196, 28.54275706135234358 ) ) ;
#193109 = CARTESIAN_POINT ( 'NONE',  ( 5.049401038298161559, -19.05341960407611168, 47.70724293864770260 ) ) ;
#193110 = CARTESIAN_POINT ( 'NONE',  ( -4.483927247898539470, -16.52544592524342804, 107.2905762719810525 ) ) ;
#193111 = CARTESIAN_POINT ( 'NONE',  ( 5.719274019375991003, -21.55341960407610458, 112.7072429386476955 ) ) ;
#193112 = CARTESIAN_POINT ( 'NONE',  ( -0.05219959533909027116, -19.03943276465977164, 27.49890960531435624 ) ) ;
#193113 = CARTESIAN_POINT ( 'NONE',  ( 19.05341960407611168, 5.049401038298154454, 98.95724293864766707 ) ) ;
#193114 = CARTESIAN_POINT ( 'NONE',  ( -19.02544592524342804, 5.153800228976336051, 31.04057627198102409 ) ) ;
#193115 = CARTESIAN_POINT ( 'NONE',  ( 16.51473224551069308, 9.474510206698969483, 99.16557627198102409 ) ) ;
#193116 = DIRECTION ( 'NONE',  ( 0.000000000000000000, 1.000000000000000000, 0.000000000000000000 ) ) ;
#193117 = CARTESIAN_POINT ( 'NONE',  ( 16.46253265017160672, -9.564922557960803928, 93.33224293864769550 ) ) ;
#193119 = CARTESIAN_POINT ( 'NONE',  ( 12.06949235617757843, -12.14591786802309237, 93.12390960531436690 ) ) ;
#193118 = CARTESIAN_POINT ( 'NONE',  ( -5.719274019375665041, -21.55341960407619695, 49.79275706135234714 ) ) ;
#193120 = CARTESIAN_POINT ( 'NONE',  ( 5.049401038298161559, -19.05341960407611168, 92.70724293864769550 ) ) ;
#193121 = CARTESIAN_POINT ( 'NONE',  ( -26.70615770596270622, -7.662262839729761410, 167.2520072419578980 ) ) ;
#193122 = CARTESIAN_POINT ( 'NONE',  ( -16.55341960407617563, 4.379528057220093196, 68.54275706135234714 ) ) ;
#193123 = CARTESIAN_POINT ( 'NONE',  ( -18.67979575497193778, 10.72451020669871902, 83.33442372801903275 ) ) ;
#193124 = CARTESIAN_POINT ( 'NONE',  ( -16.52544592524335698, -4.483927247898792601, 33.95942372801901143 ) ) ;
#193126 = EDGE_CURVE ( 'NONE', #188751, #111352, #1975, .T. ) ;
#193125 = CARTESIAN_POINT ( 'NONE',  ( 19.05341960407611168, 5.049401038298154454, 83.95724293864766707 ) ) ;
#193127 = CARTESIAN_POINT ( 'NONE',  ( -13.89961937509957401, -13.97604488694547875, 104.3760903946856757 ) ) ;
#193128 = CARTESIAN_POINT ( 'NONE',  ( 16.55341960407618274, -4.379528057220086978, 81.04275706135236135 ) ) ;
#193129 = CARTESIAN_POINT ( 'NONE',  ( -19.03943276465977164, -0.05219959533935918106, 93.75109039468566152 ) ) ;
#193130 = CARTESIAN_POINT ( 'NONE',  ( 5.049401038298161559, -19.05341960407611168, 57.70724293864769550 ) ) ;
#193131 = CARTESIAN_POINT ( 'NONE',  ( -15.80617190586745835, -15.72974639402198527, 91.87390960531436690 ) ) ;
#193133 = CARTESIAN_POINT ( 'NONE',  ( -16.46253265017146816, -9.564922557961047289, 89.16775706135234714 ) ) ;
#193132 = CARTESIAN_POINT ( 'NONE',  ( 16.52544592524342804, -4.483927247898539470, 93.54057627198103830 ) ) ;
#193134 = CARTESIAN_POINT ( 'NONE',  ( -16.53943276465976808, -0.05219959533934237506, 58.75109039468568994 ) ) ;
#193135 = CARTESIAN_POINT ( 'NONE',  ( 21.47377332591981514, 5.474134792251744486, 173.8918256800989468 ) ) ;
#193136 = CARTESIAN_POINT ( 'NONE',  ( -5.153800228976607833, 19.02544592524334988, 57.70942372801899012 ) ) ;
#193137 = CARTESIAN_POINT ( 'NONE',  ( -12.14591786802309592, -12.06949235617757132, 31.87390960531435979 ) ) ;
#193138 = CARTESIAN_POINT ( 'NONE',  ( 14.34966873604960469, 8.224510206698951720, 74.16557627198102409 ) ) ;
#193140 = CARTESIAN_POINT ( 'NONE',  ( -16.18388926212246304, 7.379444403734580327, 39.56046848633771873 ) ) ;
#193139 = CARTESIAN_POINT ( 'NONE',  ( -10.81492255796105439, 18.62759615963255655, 112.9177570613523329 ) ) ;
#193141 = CARTESIAN_POINT ( 'NONE',  ( -5.719274019375978568, 21.55341960407610458, 115.2072429386476955 ) ) ;
#193142 = CARTESIAN_POINT ( 'NONE',  ( 16.46253265017160672, -9.564922557960803928, 113.3322429386476955 ) ) ;
#193143 = CARTESIAN_POINT ( 'NONE',  ( 19.03943276465977164, -0.05219959533909143690, 78.74890960531436690 ) ) ;
#193144 = CARTESIAN_POINT ( 'NONE',  ( -18.62759615963255300, -10.81492255796106328, 94.16775706135237556 ) ) ;
#193145 = CARTESIAN_POINT ( 'NONE',  ( -0.05219959533909027116, -19.03943276465977164, 82.49890960531436690 ) ) ;
#193146 = CARTESIAN_POINT ( 'NONE',  ( 21.55341960407610458, 5.719274019375980345, 38.95724293864768839 ) ) ;
#193147 = CARTESIAN_POINT ( 'NONE',  ( 16.55341960407611168, 4.379528057220329451, 78.95724293864769550 ) ) ;
#193148 = CARTESIAN_POINT ( 'NONE',  ( -13.89961937509977652, 13.97604488694528158, 55.62390960531434558 ) ) ;
#193149 = CARTESIAN_POINT ( 'NONE',  ( -12.06949235617756955, 12.14591786802309770, 105.6239096053143669 ) ) ;
#193150 = CARTESIAN_POINT ( 'NONE',  ( -21.55341960407619339, 5.719274019375674811, 28.54275706135234358 ) ) ;
#193151 = CARTESIAN_POINT ( 'NONE',  ( 18.67979575497194134, -10.72451020669871369, 55.83442372801901854 ) ) ;
#193152 = CARTESIAN_POINT ( 'NONE',  ( 5.153800228976335163, 19.02544592524342804, 39.79057627198100988 ) ) ;
#193153 = CARTESIAN_POINT ( 'NONE',  ( 14.34966873604972726, -8.224510206698740333, 70.83442372801901854 ) ) ;
#193154 = EDGE_CURVE ( 'NONE', #178458, #66658, #182748, .T. ) ;
#193155 = CARTESIAN_POINT ( 'NONE',  ( 0.05219959533937995610, -21.53943276465977519, 20.00109039468568639 ) ) ;
#193156 = CARTESIAN_POINT ( 'NONE',  ( 5.719274019375991003, -21.55341960407610458, 107.7072429386476955 ) ) ;
#193158 = CARTESIAN_POINT ( 'NONE',  ( 9.564922557960805705, 16.46253265017160317, 59.58224293864769550 ) ) ;
#193157 = CARTESIAN_POINT ( 'NONE',  ( 19.03943276465977164, 0.05219959533936151252, 36.25109039468567573 ) ) ;
#193159 = CARTESIAN_POINT ( 'NONE',  ( -19.02544592524334988, -5.153800228976617603, 28.95942372801900433 ) ) ;
#193160 = CARTESIAN_POINT ( 'NONE',  ( -21.53943276465977519, -0.05219959533937600094, 73.75109039468567573 ) ) ;
#193161 = CARTESIAN_POINT ( 'NONE',  ( -21.55341960407610458, -5.719274019375992779, 76.45724293864769550 ) ) ;
#193162 = CARTESIAN_POINT ( 'NONE',  ( -4.483927247898539470, -16.52544592524342804, 32.29057627198102409 ) ) ;
#193164 = CARTESIAN_POINT ( 'NONE',  ( 18.67979575497194134, -10.72451020669871369, 110.8344237280190043 ) ) ;
#193163 = CARTESIAN_POINT ( 'NONE',  ( -5.719274019375665041, -21.55341960407619695, 94.79275706135234714 ) ) ;
#193165 = CARTESIAN_POINT ( 'NONE',  ( 14.29746914071049879, -8.314922557960816363, 58.33224293864768839 ) ) ;
#193166 = CARTESIAN_POINT ( 'NONE',  ( -14.29746914071049879, 8.314922557960819915, 100.8322429386477097 ) ) ;
#193167 = CARTESIAN_POINT ( 'NONE',  ( -13.89961937509957401, -13.97604488694547875, 64.37609039468567573 ) ) ;
#193168 = CARTESIAN_POINT ( 'NONE',  ( -8.314922557960811034, -14.29746914071050412, 22.08224293864769194 ) ) ;
#193169 = CARTESIAN_POINT ( 'NONE',  ( -5.719274019375665041, -21.55341960407619695, 74.79275706135234714 ) ) ;
#193170 = CARTESIAN_POINT ( 'NONE',  ( 0.05219959533909260263, 19.03943276465977164, 74.99890960531435269 ) ) ;
#193171 = CARTESIAN_POINT ( 'NONE',  ( 19.02544592524334988, 5.153800228976608722, 31.45942372801900433 ) ) ;
#193172 = CARTESIAN_POINT ( 'NONE',  ( 5.719274019375991003, -21.55341960407610458, 52.70724293864769550 ) ) ;
#193173 = CARTESIAN_POINT ( 'NONE',  ( -21.52544592524334988, -5.823673210054445271, 43.95942372801902565 ) ) ;
#193174 = CARTESIAN_POINT ( 'NONE',  ( -21.52544592524343514, 5.823673210054127303, 106.0405762719810525 ) ) ;
#193175 = CARTESIAN_POINT ( 'NONE',  ( -19.03943276465977164, -0.05219959533935918106, 93.75109039468566152 ) ) ;
#193176 = CARTESIAN_POINT ( 'NONE',  ( 16.55341960407618274, -4.379528057220086978, 66.04275706135236135 ) ) ;
#193178 = CARTESIAN_POINT ( 'NONE',  ( 18.67979575497178502, 10.72451020669898547, 99.16557627198100988 ) ) ;
#193177 = CARTESIAN_POINT ( 'NONE',  ( 3.765340386950246872E-15, -39.95163481335715971, -5.502157773949822861 ) ) ;
#193179 = CARTESIAN_POINT ( 'NONE',  ( -14.29746914071049879, 8.314922557960819915, 85.83224293864768129 ) ) ;
#193180 = CARTESIAN_POINT ( 'NONE',  ( -16.88567814943161949, -6.947325034625704276, 101.2900112265258343 ) ) ;
#193181 = CARTESIAN_POINT ( 'NONE',  ( -14.34966873604972548, 8.224510206698743886, 23.33442372801901499 ) ) ;
#193182 = CARTESIAN_POINT ( 'NONE',  ( -18.67979575497178146, -10.72451020669898902, 46.66557627198102409 ) ) ;
#193183 = CARTESIAN_POINT ( 'NONE',  ( -16.52544592524335698, -4.483927247898792601, 88.95942372801901854 ) ) ;
#193184 = CARTESIAN_POINT ( 'NONE',  ( 31.99765134899338648, -18.45278125975086070, -7.999999999999998224 ) ) ;
#193185 = CARTESIAN_POINT ( 'NONE',  ( 16.52544592524335698, 4.483927247898782831, 51.45942372801901854 ) ) ;
#193186 = CARTESIAN_POINT ( 'NONE',  ( 21.52544592524334988, 5.823673210054432836, 26.45942372801901854 ) ) ;
#193187 = CARTESIAN_POINT ( 'NONE',  ( 15.80617190586746368, 15.72974639402197994, 39.37390960531436690 ) ) ;
#193188 = CARTESIAN_POINT ( 'NONE',  ( 14.34966873604972726, -8.224510206698740333, 80.83442372801901854 ) ) ;
#193189 = CARTESIAN_POINT ( 'NONE',  ( -0.05219959533909027116, -19.03943276465977164, 92.49890960531436690 ) ) ;
#193190 = CARTESIAN_POINT ( 'NONE',  ( -0.05219959533937732626, 21.53943276465977519, 72.50109039468568994 ) ) ;
#193191 = CARTESIAN_POINT ( 'NONE',  ( 10.81492255796078972, 18.62759615963270932, 39.58224293864769550 ) ) ;
#193192 = CARTESIAN_POINT ( 'NONE',  ( -21.55341960407610458, -5.719274019375992779, 26.45724293864768839 ) ) ;
#193193 = EDGE_LOOP ( 'NONE', ( #136274, #167611, #130994, #93303 ) ) ;
#193194 = CARTESIAN_POINT ( 'NONE',  ( -16.46253265017146816, -9.564922557961047289, 49.16775706135233293 ) ) ;
#193195 = CARTESIAN_POINT ( 'NONE',  ( 16.53943276465976808, 0.05219959533934440121, 71.25109039468568994 ) ) ;
#193196 = CARTESIAN_POINT ( 'NONE',  ( -0.05219959533907301413, -21.53943276465977519, 32.49890960531435979 ) ) ;
#193197 = ORIENTED_EDGE ( 'NONE', *, *, #127302, .T. ) ;
#193198 = CARTESIAN_POINT ( 'NONE',  ( -9.474510206698964154, 16.51473224551069663, 85.41557627198102409 ) ) ;
#193199 = CARTESIAN_POINT ( 'NONE',  ( -8.224510206698735004, -14.34966873604973081, 109.5844237280190328 ) ) ;
#193200 = CARTESIAN_POINT ( 'NONE',  ( 8.636255518949004895, -38.40306468563544229, -32.12764100183819949 ) ) ;
#193201 = CARTESIAN_POINT ( 'NONE',  ( -4.379528057220328563, 16.55341960407611168, 115.2072429386476955 ) ) ;
#193202 = CARTESIAN_POINT ( 'NONE',  ( -15.80617190586745835, -15.72974639402198527, 41.87390960531435979 ) ) ;
#193203 = CARTESIAN_POINT ( 'NONE',  ( 16.46253265017160672, -9.564922557960803928, 43.33224293864769550 ) ) ;
#193204 = CARTESIAN_POINT ( 'NONE',  ( -8.314922557961024197, 14.29746914071037800, 82.91775706135234714 ) ) ;
#193205 = CARTESIAN_POINT ( 'NONE',  ( 18.62759615963255655, 10.81492255796105972, 26.66775706135235424 ) ) ;
#193206 = CARTESIAN_POINT ( 'NONE',  ( -5.049401038297874678, -19.05341960407617918, 94.79275706135230450 ) ) ;
#193207 = CARTESIAN_POINT ( 'NONE',  ( 12.14591786802309770, 12.06949235617756955, 84.37390960531438111 ) ) ;
#193208 = CARTESIAN_POINT ( 'NONE',  ( 9.474510206698971260, -16.51473224551069308, 47.91557627198102409 ) ) ;
#193209 = CARTESIAN_POINT ( 'NONE',  ( -5.153800228976328057, -19.02544592524343514, 27.29057627198103120 ) ) ;
#193210 = CARTESIAN_POINT ( 'NONE',  ( 18.67979575497194134, -10.72451020669871369, 100.8344237280190185 ) ) ;
#193211 = CARTESIAN_POINT ( 'NONE',  ( -0.05219959533909027116, -19.03943276465977164, 82.49890960531436690 ) ) ;
#193212 = CARTESIAN_POINT ( 'NONE',  ( 4.483927247898790824, -16.52544592524335698, 65.20942372801901854 ) ) ;
#193213 = CARTESIAN_POINT ( 'NONE',  ( 5.719274019375673035, 21.55341960407619339, 92.29275706135236135 ) ) ;
#193214 = CARTESIAN_POINT ( 'NONE',  ( 21.55341960407610458, 5.719274019375980345, 53.95724293864770260 ) ) ;
#193215 = CARTESIAN_POINT ( 'NONE',  ( 12.14591786802327356, -12.06949235617739191, 75.62609039468567573 ) ) ;
#193216 = CARTESIAN_POINT ( 'NONE',  ( 9.564922557961047289, -16.46253265017146816, 55.41775706135234003 ) ) ;
#193217 = CARTESIAN_POINT ( 'NONE',  ( 9.564922557961047289, -16.46253265017146816, 60.41775706135233293 ) ) ;
#193218 = EDGE_LOOP ( 'NONE', ( #73856, #30850, #45432, #70267 ) ) ;
#193219 = CARTESIAN_POINT ( 'NONE',  ( -15.72974639402176322, -15.80617190586768395, 64.37609039468568994 ) ) ;
#193220 = CARTESIAN_POINT ( 'NONE',  ( 13.89961937509977652, -13.97604488694527269, 68.12390960531436690 ) ) ;
#193221 = CARTESIAN_POINT ( 'NONE',  ( -19.02544592524342804, 5.153800228976336051, 26.04057627198103120 ) ) ;
#193222 = CARTESIAN_POINT ( 'NONE',  ( 19.05341960407617918, -5.049401038297876454, 61.04275706135232582 ) ) ;
#193223 = DIRECTION ( 'NONE',  ( -1.000000000000000000, -0.000000000000000000, -0.000000000000000000 ) ) ;
#193224 = CARTESIAN_POINT ( 'NONE',  ( -19.02544592524342804, 5.153800228976336051, 101.0405762719810241 ) ) ;
#193225 = CARTESIAN_POINT ( 'NONE',  ( -14.29746914071049879, 8.314922557960819915, 45.83224293864769550 ) ) ;
#193226 = CARTESIAN_POINT ( 'NONE',  ( -21.53943276465977519, 0.05219959533907696930, 41.24890960531435269 ) ) ;
#193227 = CARTESIAN_POINT ( 'NONE',  ( 28.79475375365583290, 9.355982642739277821, 141.0843446569000150 ) ) ;
#193228 = CARTESIAN_POINT ( 'NONE',  ( -13.89961937509957401, -13.97604488694547875, 19.37609039468566507 ) ) ;
#193229 = FACE_OUTER_BOUND ( 'NONE', #8010, .T. ) ;
#193230 = CARTESIAN_POINT ( 'NONE',  ( 13.89961937509977652, -13.97604488694527269, 53.12390960531434558 ) ) ;
#193232 = CARTESIAN_POINT ( 'NONE',  ( -16.51473224551069308, -9.474510206698971260, 26.66557627198103120 ) ) ;
#193231 = B_SPLINE_CURVE_WITH_KNOTS ( 'NONE', 3,
 ( #79054, #141722, #109396, #94220, #140727, #64886 ),
 .UNSPECIFIED., .F., .F.,
 ( 4, 2, 4 ),
 ( 0.003239945802372282482, 0.003620412082092132073, 0.004000878361811981664 ),
 .UNSPECIFIED. ) ;
#193233 = CARTESIAN_POINT ( 'NONE',  ( -34.02657648861389106, -4.769071838117368678, 92.23683055719308754 ) ) ;
#193234 = DIRECTION ( 'NONE',  ( 1.000000000000000000, 0.000000000000000000, 0.000000000000000000 ) ) ;
#193235 = CARTESIAN_POINT ( 'NONE',  ( 8.314922557961029526, -14.29746914071037800, 60.41775706135235424 ) ) ;
#193236 = CARTESIAN_POINT ( 'NONE',  ( 15.72974639402199770, -15.80617190586745480, 88.12390960531436690 ) ) ;
#193237 = CARTESIAN_POINT ( 'NONE',  ( 8.224510206698953496, -14.34966873604960469, 52.91557627198103830 ) ) ;
#193239 = PLANE ( 'NONE',  #169707 ) ;
#193238 = CARTESIAN_POINT ( 'NONE',  ( -9.564922557960796823, -16.46253265017161027, 37.08224293864768839 ) ) ;
#193240 = CARTESIAN_POINT ( 'NONE',  ( 18.62759615963255655, 10.81492255796105972, 46.66775706135234714 ) ) ;
#193241 = CARTESIAN_POINT ( 'NONE',  ( -16.51473224551082808, 9.474510206698731452, 53.33442372801900433 ) ) ;
#193242 = CARTESIAN_POINT ( 'NONE',  ( -9.564922557960796823, -16.46253265017161027, 32.08224293864769550 ) ) ;
#193243 = CARTESIAN_POINT ( 'NONE',  ( 5.719274019375673035, 21.55341960407619339, 97.29275706135234714 ) ) ;
#193244 = CARTESIAN_POINT ( 'NONE',  ( -18.10062525802547029, 5.499999999999999112, 48.51383468041923663 ) ) ;
#193245 = CARTESIAN_POINT ( 'NONE',  ( -4.379528057220328563, 16.55341960407611168, 40.20724293864769550 ) ) ;
#193246 = CARTESIAN_POINT ( 'NONE',  ( -16.61636759701969979, 0.5040881997805581882, -59.17093420172795248 ) ) ;
#193247 = CARTESIAN_POINT ( 'NONE',  ( 18.67979575497178502, 10.72451020669898547, 39.16557627198102409 ) ) ;
#193248 = CARTESIAN_POINT ( 'NONE',  ( -8.571926809382601320, -26.38167802310801591, 143.2750000027311899 ) ) ;
#193249 = CARTESIAN_POINT ( 'NONE',  ( 5.049401038298161559, -19.05341960407611168, 87.70724293864769550 ) ) ;
#193250 = CARTESIAN_POINT ( 'NONE',  ( -0.05219959533910754901, -16.53943276465976808, 82.49890960531436690 ) ) ;
#193251 = CARTESIAN_POINT ( 'NONE',  ( -16.52544592524335698, -4.483927247898792601, 18.95942372801901143 ) ) ;
#193252 = CARTESIAN_POINT ( 'NONE',  ( -14.34966873604972548, 8.224510206698743886, 108.3344237280190185 ) ) ;
#193253 = ORIENTED_EDGE ( 'NONE', *, *, #155903, .F. ) ;
#193254 = CARTESIAN_POINT ( 'NONE',  ( 13.97604488694527802, 13.89961937509977652, 49.37390960531434558 ) ) ;
#193256 = CARTESIAN_POINT ( 'NONE',  ( 18.67979575497178502, 10.72451020669898547, 84.16557627198103830 ) ) ;
#193255 = CARTESIAN_POINT ( 'NONE',  ( 19.02544592524343514, -5.153800228976328945, 83.54057627198100988 ) ) ;
#193258 = CARTESIAN_POINT ( 'NONE',  ( -16.51473224551069308, -9.474510206698971260, 96.66557627198102409 ) ) ;
#193257 = CARTESIAN_POINT ( 'NONE',  ( 12.06949235617757843, -12.14591786802309237, 23.12390960531436335 ) ) ;
#193259 = CARTESIAN_POINT ( 'NONE',  ( -9.474510206698720793, -16.51473224551083518, 74.58442372801900433 ) ) ;
#193260 = CARTESIAN_POINT ( 'NONE',  ( -15.72974639402176322, -15.80617190586768395, 104.3760903946856899 ) ) ;
#193261 = CARTESIAN_POINT ( 'NONE',  ( 18.62759615963271287, -10.81492255796078972, 93.33224293864769550 ) ) ;
#193262 = CARTESIAN_POINT ( 'NONE',  ( 18.67979575497178502, 10.72451020669898547, 34.16557627198102409 ) ) ;
#193263 = CARTESIAN_POINT ( 'NONE',  ( 16.46253265017160672, -9.564922557960803928, 68.33224293864770971 ) ) ;
#193264 = CARTESIAN_POINT ( 'NONE',  ( -12.14591786802326823, 12.06949235617739902, 108.1260903946856757 ) ) ;
#193265 = CARTESIAN_POINT ( 'NONE',  ( -16.51473224551069308, -9.474510206698971260, 81.66557627198103830 ) ) ;
#193266 = ORIENTED_EDGE ( 'NONE', *, *, #94659, .T. ) ;
#193267 = CARTESIAN_POINT ( 'NONE',  ( 17.71576930673726480, 5.500000000000005329, 38.91742649432649159 ) ) ;
#193268 = CARTESIAN_POINT ( 'NONE',  ( 5.049401038297881783, 19.05341960407617563, 27.29275706135232937 ) ) ;
#193269 = CARTESIAN_POINT ( 'NONE',  ( 16.53943276465976808, -0.05219959533910856209, 88.74890960531436690 ) ) ;
#193270 = CARTESIAN_POINT ( 'NONE',  ( -0.05219959533937732626, 21.53943276465977519, 27.50109039468567929 ) ) ;
#193271 = AXIS2_PLACEMENT_3D ( 'NONE', #39096, #85589, #58262 ) ;
#193272 = CARTESIAN_POINT ( 'NONE',  ( 22.44159573604009594, -16.30477369853687364, 144.1750000027311671 ) ) ;
#193273 = CARTESIAN_POINT ( 'NONE',  ( 21.53943276465977519, -0.05219959533907433946, 78.74890960531436690 ) ) ;
#193274 = CARTESIAN_POINT ( 'NONE',  ( 0.05219959533934541429, -16.53943276465976808, 95.00109039468568994 ) ) ;
#193275 = CARTESIAN_POINT ( 'NONE',  ( 5.153800228976335163, 19.02544592524342804, 24.79057627198102765 ) ) ;
#193276 = CARTESIAN_POINT ( 'NONE',  ( -13.89961937509977652, 13.97604488694528158, 75.62390960531438111 ) ) ;
#193277 = CARTESIAN_POINT ( 'NONE',  ( -17.49999999999999645, -5.500000000000000888, 120.0000000000000142 ) ) ;
#193278 = CARTESIAN_POINT ( 'NONE',  ( 8.224510206698953496, -14.34966873604960469, 27.91557627198103830 ) ) ;
#193279 = CARTESIAN_POINT ( 'NONE',  ( -18.67979575497193778, 10.72451020669871902, 63.33442372801900433 ) ) ;
#193280 = CARTESIAN_POINT ( 'NONE',  ( -16.51473224551069308, -9.474510206698971260, 106.6655762719810383 ) ) ;
#193281 = CARTESIAN_POINT ( 'NONE',  ( 0.05219959533937995610, -21.53943276465977519, 90.00109039468567573 ) ) ;
#193282 = CARTESIAN_POINT ( 'NONE',  ( 13.97604488694527802, 13.89961937509977652, 39.37390960531435269 ) ) ;
#193283 = CARTESIAN_POINT ( 'NONE',  ( -9.564922557960796823, -16.46253265017161027, 52.08224293864768839 ) ) ;
#193284 = EDGE_LOOP ( 'NONE', ( #32152, #18454, #168149, #199313 ) ) ;
#193285 = CARTESIAN_POINT ( 'NONE',  ( 18.62759615963255655, 10.81492255796105972, 96.66775706135234714 ) ) ;
#193286 = CARTESIAN_POINT ( 'NONE',  ( -16.55341960407617563, 4.379528057220093196, 58.54275706135235424 ) ) ;
#193287 = CARTESIAN_POINT ( 'NONE',  ( 0.05219959533937995610, -21.53943276465977519, 90.00109039468567573 ) ) ;
#193288 = CARTESIAN_POINT ( 'NONE',  ( 15.80617190586746368, 15.72974639402197994, 24.37390960531435979 ) ) ;
#193289 = CARTESIAN_POINT ( 'NONE',  ( -9.564922557961040184, 16.46253265017147172, 97.91775706135233293 ) ) ;
#193290 = CARTESIAN_POINT ( 'NONE',  ( 18.62759615963255655, 10.81492255796105972, 51.66775706135234714 ) ) ;
#193291 = CARTESIAN_POINT ( 'NONE',  ( -16.53943276465976808, -0.05219959533934237506, 33.75109039468568284 ) ) ;
#193292 = CARTESIAN_POINT ( 'NONE',  ( -5.823673210054116645, -21.52544592524344225, 92.29057627198103830 ) ) ;
#193293 = CARTESIAN_POINT ( 'NONE',  ( 9.474510206698729675, 16.51473224551082808, 87.08442372801900433 ) ) ;
#193294 = CARTESIAN_POINT ( 'NONE',  ( 9.564922557960805705, 16.46253265017160317, 59.58224293864769550 ) ) ;
#193295 = CARTESIAN_POINT ( 'NONE',  ( -19.02544592524334988, -5.153800228976617603, 93.95942372801900433 ) ) ;
#193296 = CARTESIAN_POINT ( 'NONE',  ( -19.03943276465977164, -0.05219959533935918106, 98.75109039468567573 ) ) ;
#193297 = CARTESIAN_POINT ( 'NONE',  ( 14.29746914071049879, -8.314922557960816363, 58.33224293864768839 ) ) ;
#193298 = CARTESIAN_POINT ( 'NONE',  ( 16.46253265017146816, 9.564922557961045513, 76.66775706135234714 ) ) ;
#193299 = CARTESIAN_POINT ( 'NONE',  ( 16.52544592524335698, 4.483927247898782831, 56.45942372801902565 ) ) ;
#193300 = CARTESIAN_POINT ( 'NONE',  ( -19.05341960407617563, 5.049401038297882671, 38.54275706135233293 ) ) ;
#193301 = CARTESIAN_POINT ( 'NONE',  ( 9.564922557960805705, 16.46253265017160317, 34.58224293864770260 ) ) ;
#193302 = CARTESIAN_POINT ( 'NONE',  ( 5.153800228976335163, 19.02544592524342804, 54.79057627198103120 ) ) ;
#193303 = CARTESIAN_POINT ( 'NONE',  ( -4.483927247898782831, 16.52544592524335698, 57.70942372801901143 ) ) ;
#193304 = DIRECTION ( 'NONE',  ( -1.000000000000000000, 0.000000000000000000, -6.982962677686266711E-15 ) ) ;
#193305 = EDGE_CURVE ( 'NONE', #102181, #27924, #175808, .T. ) ;
#193306 = CARTESIAN_POINT ( 'NONE',  ( -17.81289503416611097, -24.51734667627696496, 142.5500000054623513 ) ) ;
#193307 = CARTESIAN_POINT ( 'NONE',  ( -0.05219959533909027116, -19.03943276465977164, 107.4989096053143527 ) ) ;
#193308 = DIRECTION ( 'NONE',  ( 1.000000000000000000, 0.000000000000000000, 0.000000000000000000 ) ) ;
#193309 = EDGE_LOOP ( 'NONE', ( #70675, #47948, #138259, #171474, #194481 ) ) ;
#193310 = CARTESIAN_POINT ( 'NONE',  ( -9.474510206698720793, -16.51473224551083518, 104.5844237280190043 ) ) ;
#193311 = CARTESIAN_POINT ( 'NONE',  ( 15.80617190586746368, 15.72974639402197994, 44.37390960531435979 ) ) ;
#193313 = CARTESIAN_POINT ( 'NONE',  ( -5.049401038297874678, -19.05341960407617918, 109.7927570613523187 ) ) ;
#193312 = CARTESIAN_POINT ( 'NONE',  ( -13.89961937509957401, -13.97604488694547875, 29.37609039468565797 ) ) ;
#193314 = CARTESIAN_POINT ( 'NONE',  ( -16.46253265017160317, 9.564922557960807481, 30.83224293864769550 ) ) ;
#193315 = CARTESIAN_POINT ( 'NONE',  ( -16.46253265017160317, 9.564922557960807481, 55.83224293864769550 ) ) ;
#193316 = CARTESIAN_POINT ( 'NONE',  ( -10.72451020669898014, 18.67979575497178502, 70.41557627198102409 ) ) ;
#193317 = CARTESIAN_POINT ( 'NONE',  ( 0.05219959533909260263, 19.03943276465977164, 99.99890960531436690 ) ) ;
#193318 = CARTESIAN_POINT ( 'NONE',  ( 19.03943276465977164, -0.05219959533909143690, 33.74890960531435979 ) ) ;
#193319 = CARTESIAN_POINT ( 'NONE',  ( 17.14385361876520264, 23.59649016807275856, 144.6750000027311671 ) ) ;
#193320 = CARTESIAN_POINT ( 'NONE',  ( 19.05341960407617918, -5.049401038297876454, 86.04275706135233293 ) ) ;
#193321 = CARTESIAN_POINT ( 'NONE',  ( -8.314922557960811034, -14.29746914071050412, 57.08224293864769550 ) ) ;
#193322 = CARTESIAN_POINT ( 'NONE',  ( -0.05219959533907301413, -21.53943276465977519, 42.49890960531435979 ) ) ;
#193323 = CARTESIAN_POINT ( 'NONE',  ( -5.823673210054431948, 21.52544592524334988, 112.7094237280190328 ) ) ;
#193324 = CARTESIAN_POINT ( 'NONE',  ( 18.62759615963271287, -10.81492255796078972, 103.3322429386476955 ) ) ;
#193325 = CARTESIAN_POINT ( 'NONE',  ( 21.55341960407619695, -5.719274019375665929, 66.04275706135236135 ) ) ;
#193326 = CARTESIAN_POINT ( 'NONE',  ( -18.67979575497193778, 10.72451020669871902, 83.33442372801903275 ) ) ;
#193327 = CARTESIAN_POINT ( 'NONE',  ( -0.05219959533909027116, -19.03943276465977164, 107.4989096053143527 ) ) ;
#193329 = CARTESIAN_POINT ( 'NONE',  ( 0.05219959533937995610, -21.53943276465977519, 70.00109039468568994 ) ) ;
#193328 = CARTESIAN_POINT ( 'NONE',  ( -0.05219959533934338120, 16.53943276465976808, 102.5010903946856899 ) ) ;
#193330 = CARTESIAN_POINT ( 'NONE',  ( -9.474510206698964154, 16.51473224551069663, 65.41557627198102409 ) ) ;
#193331 = CARTESIAN_POINT ( 'NONE',  ( 9.564922557961047289, -16.46253265017146816, 30.41775706135232937 ) ) ;
#193332 = CARTESIAN_POINT ( 'NONE',  ( -15.80617190586768217, 15.72974639402176855, 28.12609039468568284 ) ) ;
#193333 = CARTESIAN_POINT ( 'NONE',  ( -9.474510206698964154, 16.51473224551069663, 70.41557627198102409 ) ) ;
#193334 = CARTESIAN_POINT ( 'NONE',  ( -14.29746914071049879, 8.314922557960819915, 85.83224293864768129 ) ) ;
#193335 = CARTESIAN_POINT ( 'NONE',  ( 16.52544592524342804, -4.483927247898539470, 48.54057627198103120 ) ) ;
#193336 = CARTESIAN_POINT ( 'NONE',  ( -15.80617190586745835, -15.72974639402198527, 51.87390960531437401 ) ) ;
#193337 = CARTESIAN_POINT ( 'NONE',  ( 13.97604488694527802, 13.89961937509977652, 64.37390960531436690 ) ) ;
#193338 = CARTESIAN_POINT ( 'NONE',  ( 5.719274019375991003, -21.55341960407610458, 77.70724293864770971 ) ) ;
#193339 = CARTESIAN_POINT ( 'NONE',  ( -19.05341960407617563, 5.049401038297882671, 63.54275706135234003 ) ) ;
#193341 = CARTESIAN_POINT ( 'NONE',  ( -8.314922557960811034, -14.29746914071050412, 67.08224293864770971 ) ) ;
#193340 = CARTESIAN_POINT ( 'NONE',  ( -16.46253265017146816, -9.564922557961047289, 24.16775706135233648 ) ) ;
#193342 = CARTESIAN_POINT ( 'NONE',  ( 18.62759615963271287, -10.81492255796078972, 33.33224293864769550 ) ) ;
#193343 = VERTEX_POINT ( 'NONE', #96950 ) ;
#193344 = DIRECTION ( 'NONE',  ( 1.000000000000000000, 0.000000000000000000, 0.000000000000000000 ) ) ;
#193346 = CARTESIAN_POINT ( 'NONE',  ( 27.73933785331498569, 2.768321779492822058E-14, 147.8750000027311842 ) ) ;
#193345 = CARTESIAN_POINT ( 'NONE',  ( 4.483927247898790824, -16.52544592524335698, 80.20942372801901854 ) ) ;
#193347 = CARTESIAN_POINT ( 'NONE',  ( 9.474510206698729675, 16.51473224551082808, 82.08442372801899012 ) ) ;
#193348 = CARTESIAN_POINT ( 'NONE',  ( -8.314922557960811034, -14.29746914071050412, 57.08224293864769550 ) ) ;
#193349 = DIRECTION ( 'NONE',  ( -1.000000000000000000, -0.000000000000000000, 0.000000000000000000 ) ) ;
#193350 = CARTESIAN_POINT ( 'NONE',  ( -5.049401038298153566, 19.05341960407611168, 50.20724293864770260 ) ) ;
#193351 = CARTESIAN_POINT ( 'NONE',  ( 4.483927247898545687, 16.52544592524342804, 39.79057627198103830 ) ) ;
#193352 = CARTESIAN_POINT ( 'NONE',  ( 9.564922557960805705, 16.46253265017160317, 84.58224293864769550 ) ) ;
#193353 = CARTESIAN_POINT ( 'NONE',  ( -16.51473224551069308, -9.474510206698971260, 46.66557627198102409 ) ) ;
#193354 = CARTESIAN_POINT ( 'NONE',  ( 15.80617190586769283, -15.72974639402175789, 60.62609039468567573 ) ) ;
#193355 = CARTESIAN_POINT ( 'NONE',  ( -13.97604488694527625, -13.89961937509977652, 76.87390960531433848 ) ) ;
#193356 = CARTESIAN_POINT ( 'NONE',  ( -16.51473224551069308, -9.474510206698971260, 26.66557627198103120 ) ) ;
#193357 = CARTESIAN_POINT ( 'NONE',  ( 19.03943276465977164, -0.05219959533909143690, 78.74890960531436690 ) ) ;
#193358 = CARTESIAN_POINT ( 'NONE',  ( -0.05219959533907301413, -21.53943276465977519, 52.49890960531435979 ) ) ;
#193359 = CARTESIAN_POINT ( 'NONE',  ( 9.474510206698971260, -16.51473224551069308, 42.91557627198103120 ) ) ;
#193360 = CARTESIAN_POINT ( 'NONE',  ( -21.53943276465977519, 0.05219959533907696930, 51.24890960531436690 ) ) ;
#193361 = CARTESIAN_POINT ( 'NONE',  ( -13.89961937509957401, -13.97604488694547875, 84.37609039468567573 ) ) ;
#193362 = CARTESIAN_POINT ( 'NONE',  ( 16.53943276465976808, 0.05219959533934440121, 101.2510903946856757 ) ) ;
#193363 = CARTESIAN_POINT ( 'NONE',  ( 5.153800228976615827, -19.02544592524334988, 30.20942372801900433 ) ) ;
#193365 = CARTESIAN_POINT ( 'NONE',  ( -8.314922557961024197, 14.29746914071037800, 77.91775706135231871 ) ) ;
#193364 = CARTESIAN_POINT ( 'NONE',  ( 16.52544592524335698, 4.483927247898782831, 61.45942372801901854 ) ) ;
#193366 = CARTESIAN_POINT ( 'NONE',  ( 27.86273085795037119, -28.69962071417355531, 0.000000000000000000 ) ) ;
#193367 = CARTESIAN_POINT ( 'NONE',  ( -12.14591786802326823, 12.06949235617739902, 73.12609039468567573 ) ) ;
#193368 = CARTESIAN_POINT ( 'NONE',  ( 5.823673210054125526, 21.52544592524343514, 29.79057627198102409 ) ) ;
#193369 = CARTESIAN_POINT ( 'NONE',  ( -19.03943276465977164, 0.05219959533909376836, 31.24890960531435979 ) ) ;
#193370 = CARTESIAN_POINT ( 'NONE',  ( -16.53943276465976808, -0.05219959533934237506, 43.75109039468568284 ) ) ;
#193371 = CARTESIAN_POINT ( 'NONE',  ( 9.564922557960805705, 16.46253265017160317, 49.58224293864770260 ) ) ;
#193372 = CARTESIAN_POINT ( 'NONE',  ( -21.53943276465977519, -0.05219959533937600094, 38.75109039468567573 ) ) ;
#193373 = CARTESIAN_POINT ( 'NONE',  ( -16.55341960407617563, 4.379528057220093196, 38.54275706135234714 ) ) ;
#193374 = CARTESIAN_POINT ( 'NONE',  ( -4.379528057220086978, -16.55341960407618274, 104.7927570613523898 ) ) ;
#193375 = DIRECTION ( 'NONE',  ( 0.000000000000000000, 0.000000000000000000, 1.000000000000000000 ) ) ;
#193376 = CARTESIAN_POINT ( 'NONE',  ( 5.153800228976615827, -19.02544592524334988, 25.20942372801900433 ) ) ;
#193377 = CARTESIAN_POINT ( 'NONE',  ( -5.049401038297874678, -19.05341960407617918, 104.7927570613523471 ) ) ;
#193378 = CARTESIAN_POINT ( 'NONE',  ( -13.97604488694547697, 13.89961937509957934, 73.12609039468568994 ) ) ;
#193379 = CARTESIAN_POINT ( 'NONE',  ( 0.05219959533910956823, 16.53943276465976808, 69.99890960531435269 ) ) ;
#193380 = CARTESIAN_POINT ( 'NONE',  ( -4.379528057220328563, 16.55341960407611168, 115.2072429386476955 ) ) ;
#193382 = CARTESIAN_POINT ( 'NONE',  ( 16.29526858892907626, -7.335722546920041331, 56.70329402199735824 ) ) ;
#193381 = CARTESIAN_POINT ( 'NONE',  ( -13.89961937509957401, -13.97604488694547875, 59.37609039468566863 ) ) ;
#193383 = CARTESIAN_POINT ( 'NONE',  ( -5.719274019375665041, -21.55341960407619695, 69.79275706135234714 ) ) ;
#193384 = CARTESIAN_POINT ( 'NONE',  ( 12.06949235617739724, 12.14591786802326823, 26.87609039468567218 ) ) ;
#193385 = DIRECTION ( 'NONE',  ( 1.000000000000000000, 0.000000000000000000, 0.000000000000000000 ) ) ;
#193386 = CARTESIAN_POINT ( 'NONE',  ( -18.67979575497178146, -10.72451020669898902, 26.66557627198103475 ) ) ;
#193387 = CARTESIAN_POINT ( 'NONE',  ( -0.05219959533936034679, 19.03943276465977164, 102.5010903946856757 ) ) ;
#193388 = CARTESIAN_POINT ( 'NONE',  ( 19.05341960407611168, 5.049401038298154454, 113.9572429386477097 ) ) ;
#193389 = CARTESIAN_POINT ( 'NONE',  ( -23.64729612845683349, 13.72274676820478412, 169.8070494178799663 ) ) ;
#193390 = CARTESIAN_POINT ( 'NONE',  ( -19.05341960407611168, -5.049401038298163336, 31.45724293864769550 ) ) ;
#193391 = CARTESIAN_POINT ( 'NONE',  ( -18.67979575497193778, 10.72451020669871902, 103.3344237280190043 ) ) ;
#193392 = CARTESIAN_POINT ( 'NONE',  ( -16.46253265017160317, 9.564922557960807481, 50.83224293864770260 ) ) ;
#193393 = CARTESIAN_POINT ( 'NONE',  ( 0.05219959533937995610, -21.53943276465977519, 70.00109039468568994 ) ) ;
#193394 = CARTESIAN_POINT ( 'NONE',  ( -5.823673210054431948, 21.52544592524334988, 102.7094237280190185 ) ) ;
#193395 = CARTESIAN_POINT ( 'NONE',  ( 16.52544592524342804, -4.483927247898539470, 28.54057627198103120 ) ) ;
#193396 = CARTESIAN_POINT ( 'NONE',  ( 0.05219959533909260263, 19.03943276465977164, 34.99890960531435979 ) ) ;
#193397 = EDGE_CURVE ( 'NONE', #98417, #179309, #59296, .T. ) ;
#193398 = CARTESIAN_POINT ( 'NONE',  ( 0.05219959533909260263, 19.03943276465977164, 74.99890960531435269 ) ) ;
#193399 = CARTESIAN_POINT ( 'NONE',  ( 18.62759615963255655, 10.81492255796105972, 56.66775706135235424 ) ) ;
#193400 = CARTESIAN_POINT ( 'NONE',  ( -19.05341960407611168, -5.049401038298163336, 31.45724293864769550 ) ) ;
#193401 = CARTESIAN_POINT ( 'NONE',  ( 21.55341960407619695, -5.719274019375665929, 56.04275706135235424 ) ) ;
#193403 = CARTESIAN_POINT ( 'NONE',  ( 19.05341960407611168, 5.049401038298154454, 108.9572429386477097 ) ) ;
#193402 = CARTESIAN_POINT ( 'NONE',  ( -19.02544592524334988, -5.153800228976617603, 83.95942372801901854 ) ) ;
#193404 = CARTESIAN_POINT ( 'NONE',  ( -13.97604488694527625, -13.89961937509977652, 21.87390960531435979 ) ) ;
#193405 = CARTESIAN_POINT ( 'NONE',  ( -21.53943276465977519, 0.05219959533907696930, 111.2489096053143669 ) ) ;
#193406 = CARTESIAN_POINT ( 'NONE',  ( 5.153800228976615827, -19.02544592524334988, 40.20942372801898301 ) ) ;
#193407 = CARTESIAN_POINT ( 'NONE',  ( -0.05219959533910754901, -16.53943276465976808, 92.49890960531436690 ) ) ;
#193408 = CARTESIAN_POINT ( 'NONE',  ( 5.049401038298161559, -19.05341960407611168, 52.70724293864767418 ) ) ;
#193409 = CARTESIAN_POINT ( 'NONE',  ( 19.02544592524334988, 5.153800228976608722, 101.4594237280189759 ) ) ;
#193410 = CARTESIAN_POINT ( 'NONE',  ( 14.29746914071049879, -8.314922557960816363, 58.33224293864768839 ) ) ;
#193411 = CARTESIAN_POINT ( 'NONE',  ( -15.80617190586768217, 15.72974639402176855, 108.1260903946856757 ) ) ;
#193412 = CARTESIAN_POINT ( 'NONE',  ( 16.51473224551069308, 9.474510206698969483, 104.1655762719810241 ) ) ;
#193413 = CARTESIAN_POINT ( 'NONE',  ( -9.564922557961040184, 16.46253265017147172, 92.91775706135233293 ) ) ;
#193414 = CARTESIAN_POINT ( 'NONE',  ( 15.80617190586746368, 15.72974639402197994, 89.37390960531435269 ) ) ;
#193415 = CARTESIAN_POINT ( 'NONE',  ( 5.719274019375673035, 21.55341960407619339, 42.29275706135235424 ) ) ;
#193416 = CARTESIAN_POINT ( 'NONE',  ( -14.34966873604972548, 8.224510206698743886, 43.33442372801901143 ) ) ;
#193417 = CARTESIAN_POINT ( 'NONE',  ( 4.379528057220092307, 16.55341960407617563, 107.2927570613523471 ) ) ;
#193419 = CARTESIAN_POINT ( 'NONE',  ( 10.72451020669871369, 18.67979575497193778, 47.08442372801901854 ) ) ;
#193418 = CARTESIAN_POINT ( 'NONE',  ( -14.29746914071037622, -8.314922557961029526, 44.16775706135234714 ) ) ;
#193420 = CARTESIAN_POINT ( 'NONE',  ( -0.05219959533907301413, -21.53943276465977519, 42.49890960531435979 ) ) ;
#193421 = CARTESIAN_POINT ( 'NONE',  ( -13.89961937509977652, 13.97604488694528158, 30.62390960531435269 ) ) ;
#193422 = CARTESIAN_POINT ( 'NONE',  ( 38.00000000000000711, -12.34694845685040754, -2.849999994537626424 ) ) ;
#193423 = CARTESIAN_POINT ( 'NONE',  ( -8.224510206698735004, -14.34966873604973081, 64.58442372801900433 ) ) ;
#193424 = CARTESIAN_POINT ( 'NONE',  ( 10.72451020669898902, -18.67979575497178502, 82.91557627198103830 ) ) ;
#193425 = CARTESIAN_POINT ( 'NONE',  ( 12.06949235617757843, -12.14591786802309237, 33.12390960531435979 ) ) ;
#193426 = CARTESIAN_POINT ( 'NONE',  ( 16.55341960407618274, -4.379528057220086978, 61.04275706135234714 ) ) ;
#193427 = CARTESIAN_POINT ( 'NONE',  ( 16.51473224551069308, 9.474510206698969483, 64.16557627198102409 ) ) ;
#193428 = CARTESIAN_POINT ( 'NONE',  ( 5.153800228976615827, -19.02544592524334988, 95.20942372801897591 ) ) ;
#193429 = CARTESIAN_POINT ( 'NONE',  ( 0.05219959533907565091, 21.53943276465977519, 84.99890960531436690 ) ) ;
#193430 = CARTESIAN_POINT ( 'NONE',  ( -4.483927247898539470, -16.52544592524342804, 37.29057627198102409 ) ) ;
#193431 = EDGE_LOOP ( 'NONE', ( #87156, #68908, #72384, #109791 ) ) ;
#193432 = CARTESIAN_POINT ( 'NONE',  ( 24.42783677680703391, 12.30119602009721014, 169.8172178118632587 ) ) ;
#193433 =( BOUNDED_CURVE ( )  B_SPLINE_CURVE ( 2, ( #60702, #28425, #124370, #166924, #46544, #92025, #90062, #16209, #186065, #61694, #47548, #150761, #137554 ),
 .UNSPECIFIED., .F., .F. ) 
 B_SPLINE_CURVE_WITH_KNOTS ( ( 3, 2, 2, 2, 2, 2, 3 ),
 ( 0.3182655899333458605, 0.3201754385964912242, 0.3245614035087719396, 0.3289473684210526550, 0.3333333333333333148, 0.3377192982456140302, 0.3396748267308496994 ),
 .UNSPECIFIED. ) 
 CURVE ( )  GEOMETRIC_REPRESENTATION_ITEM ( )  RATIONAL_B_SPLINE_CURVE ( ( 0.9832469066685285419, 0.9851625545550100060, 1.000000000000000000, 0.9659258262890683122, 1.000000000000000000, 0.9659258262890683122, 1.000000000000000000, 0.9659258262890683122, 1.000000000000000000, 0.9659258262890683122, 1.000000000000000000, 0.9848076720550082985, 0.9831626618144002627 ) ) 
 REPRESENTATION_ITEM ( '' )  );
#193434 = CARTESIAN_POINT ( 'NONE',  ( 21.52544592524344225, -5.823673210054117533, 68.54057627198103830 ) ) ;
#193435 = CARTESIAN_POINT ( 'NONE',  ( 12.06949235617739724, 12.14591786802326823, 106.8760903946856899 ) ) ;
#193436 = VERTEX_POINT ( 'NONE', #173829 ) ;
#193437 = DIRECTION ( 'NONE',  ( 1.000000000000000000, 0.000000000000000000, 0.000000000000000000 ) ) ;
#193438 = CARTESIAN_POINT ( 'NONE',  ( 21.52544592524344225, -5.823673210054117533, 93.54057627198103830 ) ) ;
#193439 = CARTESIAN_POINT ( 'NONE',  ( -21.55341960407610458, -5.719274019375992779, 106.4572429386477097 ) ) ;
#193440 = CARTESIAN_POINT ( 'NONE',  ( -16.53943276465976808, 0.05219959533911058130, 26.24890960531435624 ) ) ;
#193441 = CARTESIAN_POINT ( 'NONE',  ( -4.379528057220086978, -16.55341960407618274, 39.79275706135235424 ) ) ;
#193442 = CARTESIAN_POINT ( 'NONE',  ( -19.03943276465977164, 0.05219959533909376836, 36.24890960531436690 ) ) ;
#193443 = CARTESIAN_POINT ( 'NONE',  ( -19.05341960407611168, -5.049401038298163336, 66.45724293864769550 ) ) ;
#193444 = CARTESIAN_POINT ( 'NONE',  ( -28.82186960331499037, 2.428612866367529932E-14, 150.0000000000000000 ) ) ;
#193445 = CARTESIAN_POINT ( 'NONE',  ( 5.823673210054125526, 21.52544592524343514, 24.79057627198103120 ) ) ;
#193446 = CARTESIAN_POINT ( 'NONE',  ( 17.60779699588839264, 5.500000000000007105, 78.84981316670105400 ) ) ;
#193447 = CARTESIAN_POINT ( 'NONE',  ( 19.05341960407617918, -5.049401038297876454, 111.0427570613523329 ) ) ;
#193448 = CARTESIAN_POINT ( 'NONE',  ( -16.46253265017146816, -9.564922557961047289, 39.16775706135234003 ) ) ;
#193449 = CARTESIAN_POINT ( 'NONE',  ( -5.719274019375978568, 21.55341960407610458, 85.20724293864770971 ) ) ;
#193450 = CARTESIAN_POINT ( 'NONE',  ( -16.55341960407617563, 4.379528057220093196, 108.5427570613523756 ) ) ;
#193451 = CARTESIAN_POINT ( 'NONE',  ( 21.55341960407610458, 5.719274019375980345, 43.95724293864769550 ) ) ;
#193453 = CARTESIAN_POINT ( 'NONE',  ( -9.564922557961040184, 16.46253265017147172, 107.9177570613523471 ) ) ;
#193452 = CARTESIAN_POINT ( 'NONE',  ( -0.05219959533907301413, -21.53943276465977519, 82.49890960531436690 ) ) ;
#193454 = CARTESIAN_POINT ( 'NONE',  ( -9.564922557960796823, -16.46253265017161027, 102.0822429386477097 ) ) ;
#193455 = CARTESIAN_POINT ( 'NONE',  ( 21.52544592524334988, 5.823673210054432836, 76.45942372801901854 ) ) ;
#193456 = CARTESIAN_POINT ( 'NONE',  ( 9.564922557960805705, 16.46253265017160317, 79.58224293864769550 ) ) ;
#193457 = CARTESIAN_POINT ( 'NONE',  ( 8.224510206698953496, -14.34966873604960469, 102.9155762719810383 ) ) ;
#193458 = DIRECTION ( 'NONE',  ( 1.000000000000000000, 0.000000000000000000, 0.000000000000000000 ) ) ;
#193459 = CARTESIAN_POINT ( 'NONE',  ( 5.049401038298161559, -19.05341960407611168, 67.70724293864769550 ) ) ;
#193460 = CARTESIAN_POINT ( 'NONE',  ( -8.224510206698948167, 14.34966873604960824, 95.41557627198102409 ) ) ;
#193461 = VERTEX_POINT ( 'NONE', #22120 ) ;
#193462 = CARTESIAN_POINT ( 'NONE',  ( -13.97604488694547697, 13.89961937509957934, 88.12609039468563310 ) ) ;
#193463 = CARTESIAN_POINT ( 'NONE',  ( 17.13100169013300444, -6.664070546373146442, 83.26789835699850073 ) ) ;
#193464 = CARTESIAN_POINT ( 'NONE',  ( 5.049401038298161559, -19.05341960407611168, 57.70724293864769550 ) ) ;
#193466 = CARTESIAN_POINT ( 'NONE',  ( -5.153800228976328057, -19.02544592524343514, 102.2905762719810383 ) ) ;
#193465 = CARTESIAN_POINT ( 'NONE',  ( 18.62759615963255655, 10.81492255796105972, 81.66775706135236135 ) ) ;
#193467 = CARTESIAN_POINT ( 'NONE',  ( -8.224510206698735004, -14.34966873604973081, 84.58442372801903275 ) ) ;
#193468 = CARTESIAN_POINT ( 'NONE',  ( -2.973862142520655727, -93.04182470242767522, -4.999999999999999112 ) ) ;
#193469 = CARTESIAN_POINT ( 'NONE',  ( 0.05219959533936267826, -19.03943276465977164, 60.00109039468566863 ) ) ;
#193470 = CARTESIAN_POINT ( 'NONE',  ( -21.52544592524334988, -5.823673210054445271, 98.95942372801903275 ) ) ;
#193471 = CARTESIAN_POINT ( 'NONE',  ( 4.884805615686635960, 6.795352961392285174, -64.11485260110077888 ) ) ;
#193472 = CARTESIAN_POINT ( 'NONE',  ( 11.74264578624800315, -36.14014761921581709, -7.149999994537626691 ) ) ;
#193473 = CARTESIAN_POINT ( 'NONE',  ( 8.224510206698742110, 14.34966873604972548, 102.0844237280190185 ) ) ;
#193474 = CARTESIAN_POINT ( 'NONE',  ( 16.68934465457933669, -0.2055526423334347597, -59.13845350790284527 ) ) ;
#193475 = CARTESIAN_POINT ( 'NONE',  ( -16.53943276465976808, -0.05219959533934237506, 88.75109039468567573 ) ) ;
#193476 = PLANE ( 'NONE',  #87267 ) ;
#193477 = CARTESIAN_POINT ( 'NONE',  ( -16.55341960407617563, 4.379528057220093196, 63.54275706135234003 ) ) ;
#193478 = VERTEX_POINT ( 'NONE', #67615 ) ;
#193479 = CARTESIAN_POINT ( 'NONE',  ( 15.72974639402176855, 15.80617190586768217, 86.87609039468568994 ) ) ;
#193480 = CARTESIAN_POINT ( 'NONE',  ( -9.474510206698720793, -16.51473224551083518, 84.58442372801900433 ) ) ;
#193481 = CARTESIAN_POINT ( 'NONE',  ( -0.05219959533936034679, 19.03943276465977164, 37.50109039468567573 ) ) ;
#193482 = CARTESIAN_POINT ( 'NONE',  ( 19.03943276465977164, -0.05219959533909143690, 63.74890960531435979 ) ) ;
#193483 = CARTESIAN_POINT ( 'NONE',  ( 9.474510206698971260, -16.51473224551069308, 57.91557627198103120 ) ) ;
#193484 = DIRECTION ( 'NONE',  ( 1.000000000000000000, 0.000000000000000000, 0.000000000000000000 ) ) ;
#193485 = CARTESIAN_POINT ( 'NONE',  ( -18.62759615963270932, 10.81492255796079327, 75.83224293864769550 ) ) ;
#193486 = CARTESIAN_POINT ( 'NONE',  ( 15.80617190586746368, 15.72974639402197994, 39.37390960531436690 ) ) ;
#193487 = CARTESIAN_POINT ( 'NONE',  ( 19.02544592524343514, -5.153800228976328945, 38.54057627198103120 ) ) ;
#193488 = CARTESIAN_POINT ( 'NONE',  ( -16.53943276465976808, -0.05219959533934237506, 63.75109039468568284 ) ) ;
#193489 = ORIENTED_EDGE ( 'NONE', *, *, #17219, .T. ) ;
#193490 = CARTESIAN_POINT ( 'NONE',  ( -15.80617190586768217, 15.72974639402176855, 28.12609039468568284 ) ) ;
#193492 = CARTESIAN_POINT ( 'NONE',  ( -38.00000000000001421, -12.34694845685042708, -1.899999999999999911 ) ) ;
#193491 = CARTESIAN_POINT ( 'NONE',  ( -14.34966873604960291, -8.224510206698953496, 71.66557627198100988 ) ) ;
#193493 = CARTESIAN_POINT ( 'NONE',  ( -14.29746914071037622, -8.314922557961029526, 29.16775706135234003 ) ) ;
#193494 = CARTESIAN_POINT ( 'NONE',  ( -13.97604488694547697, 13.89961937509957934, 53.12609039468565442 ) ) ;
#193495 = CARTESIAN_POINT ( 'NONE',  ( 14.29746914071049879, -8.314922557960816363, 53.33224293864769550 ) ) ;
#193497 = EDGE_CURVE ( 'NONE', #42657, #50238, #21117, .T. ) ;
#193496 = CARTESIAN_POINT ( 'NONE',  ( -5.823673210054431948, 21.52544592524334988, 37.70942372801900433 ) ) ;
#193499 = CARTESIAN_POINT ( 'NONE',  ( -21.52544592524343514, 5.823673210054127303, 71.04057627198103830 ) ) ;
#193498 = CARTESIAN_POINT ( 'NONE',  ( 1.500000000000122347, 15.29436794386904097, -59.75403449828548474 ) ) ;
#193500 = CARTESIAN_POINT ( 'NONE',  ( 9.474510206698971260, -16.51473224551069308, 107.9155762719810383 ) ) ;
#193501 = CARTESIAN_POINT ( 'NONE',  ( 8.314922557960818139, 14.29746914071049879, 74.58224293864768129 ) ) ;
#193502 = CARTESIAN_POINT ( 'NONE',  ( 28.71047547314890025, -27.16362253576316377, -18.60589795199476271 ) ) ;
#193503 = CIRCLE ( 'NONE', #15832, 28.02760797243269408 ) ;
#193504 = CARTESIAN_POINT ( 'NONE',  ( 17.49999999999999289, 5.500000000000009770, 43.78230962303566542 ) ) ;
#193505 = CARTESIAN_POINT ( 'NONE',  ( -16.46253265017146816, -9.564922557961047289, 64.16775706135233293 ) ) ;
#193506 = CARTESIAN_POINT ( 'NONE',  ( 10.72451020669898902, -18.67979575497178502, 112.9155762719810383 ) ) ;
#193507 = CARTESIAN_POINT ( 'NONE',  ( -5.153800228976328057, -19.02544592524343514, 57.29057627198103120 ) ) ;
#193508 = CARTESIAN_POINT ( 'NONE',  ( 19.03943276465977164, 0.05219959533936151252, 41.25109039468566152 ) ) ;
#193509 = CARTESIAN_POINT ( 'NONE',  ( -13.89961937509977652, 13.97604488694528158, 30.62390960531435269 ) ) ;
#193510 = CARTESIAN_POINT ( 'NONE',  ( 10.81492255796106328, -18.62759615963255655, 70.41775706135236135 ) ) ;
#193511 = DIRECTION ( 'NONE',  ( -0.000000000000000000, -0.000000000000000000, -1.000000000000000000 ) ) ;
#193512 = EDGE_CURVE ( 'NONE', #68126, #20566, #51457, .T. ) ;
#193513 = CARTESIAN_POINT ( 'NONE',  ( -16.55341960407611168, -4.379528057220339221, 46.45724293864769550 ) ) ;
#193514 = CARTESIAN_POINT ( 'NONE',  ( 13.97604488694527802, 13.89961937509977652, 64.37390960531436690 ) ) ;
#193515 = CARTESIAN_POINT ( 'NONE',  ( 10.81492255796078972, 18.62759615963270932, 84.58224293864769550 ) ) ;
#193516 = CARTESIAN_POINT ( 'NONE',  ( 13.97604488694527802, 13.89961937509977652, 59.37390960531434558 ) ) ;
#193517 = VERTEX_POINT ( 'NONE', #158630 ) ;
#193518 = CARTESIAN_POINT ( 'NONE',  ( -15.80617190586745835, -15.72974639402198527, 61.87390960531436690 ) ) ;
#193519 = ORIENTED_EDGE ( 'NONE', *, *, #186989, .F. ) ;
#193520 = CARTESIAN_POINT ( 'NONE',  ( 5.719274019375673035, 21.55341960407619339, 102.2927570613523613 ) ) ;
#193523 = CARTESIAN_POINT ( 'NONE',  ( 14.34966873604960469, 8.224510206698951720, 84.16557627198103830 ) ) ;
#193522 = CARTESIAN_POINT ( 'NONE',  ( 14.34966873604972726, -8.224510206698740333, 90.83442372801901854 ) ) ;
#193521 = CARTESIAN_POINT ( 'NONE',  ( 19.03943276465977164, -0.05219959533909143690, 23.74890960531435269 ) ) ;
#193524 = CARTESIAN_POINT ( 'NONE',  ( -19.03943276465977164, -0.05219959533935918106, 98.75109039468567573 ) ) ;
#193525 = VERTEX_POINT ( 'NONE', #5939 ) ;
#193526 = CARTESIAN_POINT ( 'NONE',  ( 10.81492255796106328, -18.62759615963255655, 20.41775706135234714 ) ) ;
#193527 = CARTESIAN_POINT ( 'NONE',  ( -13.97604488694547697, 13.89961937509957934, 43.12609039468566152 ) ) ;
#193528 = CARTESIAN_POINT ( 'NONE',  ( 16.53943276465976808, 0.05219959533934440121, 96.25109039468568994 ) ) ;
#193529 = CARTESIAN_POINT ( 'NONE',  ( 13.89961937509957401, 13.97604488694547697, 31.87609039468566863 ) ) ;
#193530 = CARTESIAN_POINT ( 'NONE',  ( -13.89961937509977652, 13.97604488694528158, 85.62390960531433848 ) ) ;
#193531 = CARTESIAN_POINT ( 'NONE',  ( -15.72974639402197994, 15.80617190586746368, 60.62390960531437401 ) ) ;
#193532 = DIRECTION ( 'NONE',  ( 0.000000000000000000, 0.000000000000000000, -1.000000000000000000 ) ) ;
#193533 = CARTESIAN_POINT ( 'NONE',  ( 4.483927247898545687, 16.52544592524342804, 114.7905762719810383 ) ) ;
#193534 = CARTESIAN_POINT ( 'NONE',  ( -18.62759615963255300, -10.81492255796106328, 99.16775706135234714 ) ) ;
#193535 = CARTESIAN_POINT ( 'NONE',  ( -16.55341960407617563, 4.379528057220093196, 73.54275706135234714 ) ) ;
#193536 = CARTESIAN_POINT ( 'NONE',  ( -21.52544592524334988, -5.823673210054445271, 23.95942372801901143 ) ) ;
#193537 = CARTESIAN_POINT ( 'NONE',  ( 14.29746914071037800, 8.314922557961029526, 26.66775706135235424 ) ) ;
#193538 = CARTESIAN_POINT ( 'NONE',  ( 19.05341960407611168, 5.049401038298154454, 98.95724293864766707 ) ) ;
#193539 = CARTESIAN_POINT ( 'NONE',  ( -5.153800228976328057, -19.02544592524343514, 37.29057627198102409 ) ) ;
#193540 = CARTESIAN_POINT ( 'NONE',  ( 9.564922557960805705, 16.46253265017160317, 69.58224293864770971 ) ) ;
#193541 = AXIS2_PLACEMENT_3D ( 'NONE', #22325, #145655, #82981 ) ;
#193542 = CARTESIAN_POINT ( 'NONE',  ( 4.483927247898790824, -16.52544592524335698, 45.20942372801901854 ) ) ;
#193543 = CARTESIAN_POINT ( 'NONE',  ( -16.52544592524342804, 4.483927247898546575, 96.04057627198102409 ) ) ;
#193544 = CARTESIAN_POINT ( 'NONE',  ( -8.224510206698735004, -14.34966873604973081, 94.58442372801901854 ) ) ;
#193547 = CARTESIAN_POINT ( 'NONE',  ( 19.02544592524343514, -5.153800228976328945, 58.54057627198102409 ) ) ;
#193546 = CARTESIAN_POINT ( 'NONE',  ( -9.474510206698964154, 16.51473224551069663, 80.41557627198103830 ) ) ;
#193545 = CARTESIAN_POINT ( 'NONE',  ( 18.67979575497194134, -10.72451020669871369, 40.83442372801901854 ) ) ;
#193548 = CARTESIAN_POINT ( 'NONE',  ( -19.05341960407611168, -5.049401038298163336, 101.4572429386476955 ) ) ;
#193549 = CARTESIAN_POINT ( 'NONE',  ( -16.53943276465976808, 0.05219959533911058130, 31.24890960531435979 ) ) ;
#193550 = CARTESIAN_POINT ( 'NONE',  ( 8.314922557961029526, -14.29746914071037800, 100.4177570613523471 ) ) ;
#193551 = EDGE_CURVE ( 'NONE', #122026, #199732, #156136, .T. ) ;
#193552 = ORIENTED_EDGE ( 'NONE', *, *, #165816, .F. ) ;
#193553 = CARTESIAN_POINT ( 'NONE',  ( 5.049401038297881783, 19.05341960407617563, 47.29275706135231161 ) ) ;
#193554 = CARTESIAN_POINT ( 'NONE',  ( -13.89961937509977652, 13.97604488694528158, 115.6239096053143669 ) ) ;
#193555 = CARTESIAN_POINT ( 'NONE',  ( 16.51473224551069308, 9.474510206698969483, 59.16557627198102409 ) ) ;
#193556 = CARTESIAN_POINT ( 'NONE',  ( 19.02544592524334988, 5.153800228976608722, 41.45942372801900433 ) ) ;
#193557 = CARTESIAN_POINT ( 'NONE',  ( 11.40812507854755253, -35.11059874428192273, -8.024999997268814411 ) ) ;
#193558 = CARTESIAN_POINT ( 'NONE',  ( -17.31747979337949062, -6.344076630961018815, 66.37944868065184778 ) ) ;
#193559 = CARTESIAN_POINT ( 'NONE',  ( -14.29746914071037622, -8.314922557961029526, 39.16775706135235424 ) ) ;
#193561 = CARTESIAN_POINT ( 'NONE',  ( -4.483927247898782831, 16.52544592524335698, 52.70942372801902565 ) ) ;
#193560 = CARTESIAN_POINT ( 'NONE',  ( 13.89961937509957401, 13.97604488694547697, 66.87609039468567573 ) ) ;
#193562 = DIRECTION ( 'NONE',  ( -1.000000000000000000, 0.000000000000000000, 0.000000000000000000 ) ) ;
#193563 = CARTESIAN_POINT ( 'NONE',  ( 5.153800228976335163, 19.02544592524342804, 94.79057627198103830 ) ) ;
#193564 = CARTESIAN_POINT ( 'NONE',  ( -5.823673210054116645, -21.52544592524344225, 107.2905762719810525 ) ) ;
#193565 = CARTESIAN_POINT ( 'NONE',  ( -9.564922557961040184, 16.46253265017147172, 72.91775706135233293 ) ) ;
#193567 = CARTESIAN_POINT ( 'NONE',  ( 19.05341960407611168, 5.049401038298154454, 28.95724293864769550 ) ) ;
#193566 = CARTESIAN_POINT ( 'NONE',  ( -13.89961937509977652, 13.97604488694528158, 105.6239096053143527 ) ) ;
#193568 = CARTESIAN_POINT ( 'NONE',  ( 19.02544592524343514, -5.153800228976328945, 73.54057627198103830 ) ) ;
#193570 = CARTESIAN_POINT ( 'NONE',  ( 16.46253265017160672, -9.564922557960803928, 43.33224293864769550 ) ) ;
#193569 = CARTESIAN_POINT ( 'NONE',  ( -8.314922557960811034, -14.29746914071050412, 47.08224293864770260 ) ) ;
#193571 = CARTESIAN_POINT ( 'NONE',  ( 9.564922557961047289, -16.46253265017146816, 55.41775706135234003 ) ) ;
#193572 = CARTESIAN_POINT ( 'NONE',  ( 12.14591786802309770, 12.06949235617756955, 89.37390960531435269 ) ) ;
#193573 = CARTESIAN_POINT ( 'NONE',  ( 18.62759615963255655, 10.81492255796105972, 106.6677570613523756 ) ) ;
#193574 = CARTESIAN_POINT ( 'NONE',  ( 5.153800228976335163, 19.02544592524342804, 49.79057627198100988 ) ) ;
#193575 = CARTESIAN_POINT ( 'NONE',  ( -21.55341960407610458, -5.719274019375992779, 56.45724293864768839 ) ) ;
#193577 = CARTESIAN_POINT ( 'NONE',  ( 0.05219959533936267826, -19.03943276465977164, 25.00109039468566152 ) ) ;
#193576 = CARTESIAN_POINT ( 'NONE',  ( 16.53943276465976808, -0.05219959533910856209, 53.74890960531437401 ) ) ;
#193578 = CARTESIAN_POINT ( 'NONE',  ( 19.02544592524343514, -5.153800228976328945, 108.5405762719810383 ) ) ;
#193579 = CARTESIAN_POINT ( 'NONE',  ( 9.474510206698971260, -16.51473224551069308, 102.9155762719810241 ) ) ;
#193580 = CARTESIAN_POINT ( 'NONE',  ( -16.46253265017160317, 9.564922557960807481, 40.83224293864769550 ) ) ;
#193581 = CARTESIAN_POINT ( 'NONE',  ( 0.05219959533909260263, 19.03943276465977164, 29.99890960531435979 ) ) ;
#193582 = CARTESIAN_POINT ( 'NONE',  ( -4.483927247898539470, -16.52544592524342804, 87.29057627198103830 ) ) ;
#193583 = CARTESIAN_POINT ( 'NONE',  ( -21.55341960407610458, -5.719274019375992779, 91.45724293864769550 ) ) ;
#193584 = CARTESIAN_POINT ( 'NONE',  ( 5.049401038298161559, -19.05341960407611168, 102.7072429386476955 ) ) ;
#193585 = CARTESIAN_POINT ( 'NONE',  ( -21.53943276465977519, 0.05219959533907696930, 106.2489096053143811 ) ) ;
#193586 = CARTESIAN_POINT ( 'NONE',  ( 19.02544592524343514, -5.153800228976328945, 103.5405762719809957 ) ) ;
#193588 = CARTESIAN_POINT ( 'NONE',  ( -8.314922557960811034, -14.29746914071050412, 97.08224293864770971 ) ) ;
#193587 = DIRECTION ( 'NONE',  ( 0.000000000000000000, 0.000000000000000000, 1.000000000000000000 ) ) ;
#193589 = CARTESIAN_POINT ( 'NONE',  ( 19.05341960407611168, 5.049401038298154454, 73.95724293864768129 ) ) ;
#193590 = CARTESIAN_POINT ( 'NONE',  ( 18.62759615963271287, -10.81492255796078972, 83.33224293864769550 ) ) ;
#193591 = CARTESIAN_POINT ( 'NONE',  ( 16.62475595723699939, -7.163666690055295660, 108.0271335181047050 ) ) ;
#193592 = CARTESIAN_POINT ( 'NONE',  ( -31.99364916731038022, -5.510910596163089556E-15, 45.00000000000000000 ) ) ;
#193594 = CARTESIAN_POINT ( 'NONE',  ( -193.3062444957834884, -155.7167183371838064, 0.000000000000000000 ) ) ;
#193593 = CARTESIAN_POINT ( 'NONE',  ( 10.81492255796078972, 18.62759615963270932, 24.58224293864768839 ) ) ;
#193595 = CARTESIAN_POINT ( 'NONE',  ( 16.52544592524335698, 4.483927247898782831, 31.45942372801901854 ) ) ;
#193596 = CARTESIAN_POINT ( 'NONE',  ( -12.14591786802309592, -12.06949235617757132, 96.87390960531436690 ) ) ;
#193597 = CARTESIAN_POINT ( 'NONE',  ( 19.25663599770058454, -5.499999999999650946, 51.49419308057199629 ) ) ;
#193598 = CARTESIAN_POINT ( 'NONE',  ( -5.153800228976328057, -19.02544592524343514, 62.29057627198100988 ) ) ;
#193599 = CARTESIAN_POINT ( 'NONE',  ( -14.34966873604960291, -8.224510206698953496, 86.66557627198102409 ) ) ;
#193600 = CARTESIAN_POINT ( 'NONE',  ( 10.81492255796078972, 18.62759615963270932, 39.58224293864769550 ) ) ;
#193601 = CARTESIAN_POINT ( 'NONE',  ( -16.55341960407611168, -4.379528057220339221, 71.45724293864769550 ) ) ;
#193602 = CARTESIAN_POINT ( 'NONE',  ( 16.46253265017146816, 9.564922557961045513, 111.6677570613523329 ) ) ;
#193603 = CARTESIAN_POINT ( 'NONE',  ( -18.62759615963255300, -10.81492255796106328, 74.16775706135231871 ) ) ;
#193604 = CARTESIAN_POINT ( 'NONE',  ( -17.14385361876520264, -23.59649016807271238, 147.1750000027311671 ) ) ;
#193605 = CARTESIAN_POINT ( 'NONE',  ( 21.52544592524344225, -5.823673210054117533, 23.54057627198102765 ) ) ;
#193606 = CARTESIAN_POINT ( 'NONE',  ( -12.06949235617739369, -12.14591786802326823, 79.37609039468567573 ) ) ;
#193607 = CARTESIAN_POINT ( 'NONE',  ( 19.05341960407611168, 5.049401038298154454, 33.95724293864769550 ) ) ;
#193608 = CARTESIAN_POINT ( 'NONE',  ( 16.46253265017160672, -9.564922557960803928, 88.33224293864769550 ) ) ;
#193609 = CARTESIAN_POINT ( 'NONE',  ( 21.55341960407610458, 5.719274019375980345, 98.95724293864770971 ) ) ;
#193610 = CARTESIAN_POINT ( 'NONE',  ( -14.29746914071037622, -8.314922557961029526, 29.16775706135234003 ) ) ;
#193612 = CARTESIAN_POINT ( 'NONE',  ( 21.53943276465977519, 0.05219959533937863772, 76.25109039468568994 ) ) ;
#193611 = CARTESIAN_POINT ( 'NONE',  ( -12.14591786802309592, -12.06949235617757132, 56.87390960531436690 ) ) ;
#193613 = CARTESIAN_POINT ( 'NONE',  ( 0.05219959533934541429, -16.53943276465976808, 105.0010903946856757 ) ) ;
#193614 = CARTESIAN_POINT ( 'NONE',  ( 9.474510206698971260, -16.51473224551069308, 112.9155762719810383 ) ) ;
#193615 = CARTESIAN_POINT ( 'NONE',  ( -17.05587630539786659, 6.762274262135700376, 80.74180309037312497 ) ) ;
#193616 = CARTESIAN_POINT ( 'NONE',  ( 14.29746914071037800, 8.314922557961029526, 111.6677570613523613 ) ) ;
#193617 = CARTESIAN_POINT ( 'NONE',  ( 12.06949235617739724, 12.14591786802326823, 61.87609039468568284 ) ) ;
#193619 = VERTEX_POINT ( 'NONE', #129276 ) ;
#193618 = CARTESIAN_POINT ( 'NONE',  ( 5.049401038298161559, -19.05341960407611168, 67.70724293864769550 ) ) ;
#193620 = CARTESIAN_POINT ( 'NONE',  ( -5.153800228976328057, -19.02544592524343514, 92.29057627198099567 ) ) ;
#193621 = CARTESIAN_POINT ( 'NONE',  ( -21.55341960407619339, 5.719274019375674811, 73.54275706135234714 ) ) ;
#193622 = CARTESIAN_POINT ( 'NONE',  ( 14.29746914071037800, 8.314922557961029526, 81.66775706135236135 ) ) ;
#193623 = CARTESIAN_POINT ( 'NONE',  ( 16.52544592524342804, -4.483927247898539470, 63.54057627198103830 ) ) ;
#193624 = CARTESIAN_POINT ( 'NONE',  ( 9.474510206698971260, -16.51473224551069308, 57.91557627198103120 ) ) ;
#193625 = ORIENTED_EDGE ( 'NONE', *, *, #156164, .F. ) ;
#193626 = CARTESIAN_POINT ( 'NONE',  ( 5.049401038297881783, 19.05341960407617563, 102.2927570613523045 ) ) ;
#193627 = CARTESIAN_POINT ( 'NONE',  ( 14.34966873604960469, 8.224510206698951720, 114.1655762719810383 ) ) ;
#193628 = CARTESIAN_POINT ( 'NONE',  ( 9.564922557960805705, 16.46253265017160317, 79.58224293864769550 ) ) ;
#193630 = CARTESIAN_POINT ( 'NONE',  ( -30.74264578624800492, 22.33583958711400186, -6.200000000000001066 ) ) ;
#193629 = CARTESIAN_POINT ( 'NONE',  ( -8.224510206698735004, -14.34966873604973081, 19.58442372801901143 ) ) ;
#193631 = CARTESIAN_POINT ( 'NONE',  ( -21.52544592524334988, -5.823673210054445271, 98.95942372801903275 ) ) ;
#193632 = CARTESIAN_POINT ( 'NONE',  ( 0.05219959533934541429, -16.53943276465976808, 75.00109039468568994 ) ) ;
#193633 = CARTESIAN_POINT ( 'NONE',  ( 13.89961937509957401, 13.97604488694547697, 96.87609039468566152 ) ) ;
#193634 = CARTESIAN_POINT ( 'NONE',  ( -0.05219959533907301413, -21.53943276465977519, 57.49890960531435979 ) ) ;
#193635 = CARTESIAN_POINT ( 'NONE',  ( 14.29746914071037800, 8.314922557961029526, 71.66775706135234714 ) ) ;
#193636 = DIRECTION ( 'NONE',  ( 0.000000000000000000, 0.000000000000000000, 1.000000000000000000 ) ) ;
#193637 = CARTESIAN_POINT ( 'NONE',  ( -0.05219959533936034679, 19.03943276465977164, 52.50109039468566863 ) ) ;
#193638 = CARTESIAN_POINT ( 'NONE',  ( 5.719274019375673035, 21.55341960407619339, 102.2927570613523613 ) ) ;
#193639 = CARTESIAN_POINT ( 'NONE',  ( 9.474510206698971260, -16.51473224551069308, 37.91557627198102409 ) ) ;
#193640 = CARTESIAN_POINT ( 'NONE',  ( 5.153800228976335163, 19.02544592524342804, 59.79057627198100988 ) ) ;
#193641 = CARTESIAN_POINT ( 'NONE',  ( 8.224510206698953496, -14.34966873604960469, 67.91557627198102409 ) ) ;
#193642 = ADVANCED_FACE ( 'NONE', ( #126310 ), #90994, .F. ) ;
#193643 = CARTESIAN_POINT ( 'NONE',  ( -0.05219959533937732626, 21.53943276465977519, 92.50109039468567573 ) ) ;
#193644 = CARTESIAN_POINT ( 'NONE',  ( -9.474510206698720793, -16.51473224551083518, 44.58442372801900433 ) ) ;
#193645 = CARTESIAN_POINT ( 'NONE',  ( -5.153800228976607833, 19.02544592524334988, 47.70942372801900433 ) ) ;
#193646 = CARTESIAN_POINT ( 'NONE',  ( 18.67979575497178502, 10.72451020669898547, 34.16557627198102409 ) ) ;
#193647 = CARTESIAN_POINT ( 'NONE',  ( -15.80617190586768217, 15.72974639402176855, 98.12609039468570415 ) ) ;
#193648 = CARTESIAN_POINT ( 'NONE',  ( 5.153800228976335163, 19.02544592524342804, 79.79057627198102409 ) ) ;
#193649 = CARTESIAN_POINT ( 'NONE',  ( -18.67979575497193778, 10.72451020669871902, 88.33442372801901854 ) ) ;
#193650 = CARTESIAN_POINT ( 'NONE',  ( -21.55341960407610458, -5.719274019375992779, 56.45724293864768839 ) ) ;
#193651 = CARTESIAN_POINT ( 'NONE',  ( -19.02544592524342804, 5.153800228976336051, 81.04057627198103830 ) ) ;
#193652 = CARTESIAN_POINT ( 'NONE',  ( 13.97604488694548053, -13.89961937509957401, 75.62609039468564731 ) ) ;
#193653 = CARTESIAN_POINT ( 'NONE',  ( 19.02544592524343514, -5.153800228976328945, 88.54057627198102409 ) ) ;
#193654 = CARTESIAN_POINT ( 'NONE',  ( 9.564922557961047289, -16.46253265017146816, 90.41775706135234714 ) ) ;
#193655 = CARTESIAN_POINT ( 'NONE',  ( 12.06949235617739724, 12.14591786802326823, 41.87609039468568284 ) ) ;
#193656 = CARTESIAN_POINT ( 'NONE',  ( -12.06949235617756955, 12.14591786802309770, 95.62390960531436690 ) ) ;
#193657 = CARTESIAN_POINT ( 'NONE',  ( 5.153800228976335163, 19.02544592524342804, 64.79057627198100988 ) ) ;
#193658 = CARTESIAN_POINT ( 'NONE',  ( -21.52544592524343514, 5.823673210054127303, 61.04057627198103120 ) ) ;
#193659 = AXIS2_PLACEMENT_3D ( 'NONE', #105313, #74000, #42663 ) ;
#193660 = CARTESIAN_POINT ( 'NONE',  ( -14.29746914071037622, -8.314922557961029526, 29.16775706135234003 ) ) ;
#193661 = CARTESIAN_POINT ( 'NONE',  ( -0.05219959533937732626, 21.53943276465977519, 32.50109039468568284 ) ) ;
#193662 = CARTESIAN_POINT ( 'NONE',  ( -5.719274019375665041, -21.55341960407619695, 79.79275706135236135 ) ) ;
#193663 = CARTESIAN_POINT ( 'NONE',  ( -16.53943276465976808, -0.05219959533934237506, 78.75109039468568994 ) ) ;
#193664 = CARTESIAN_POINT ( 'NONE',  ( 0.05219959533909260263, 19.03943276465977164, 74.99890960531435269 ) ) ;
#193665 = CARTESIAN_POINT ( 'NONE',  ( 14.29746914071049879, -8.314922557960816363, 78.33224293864770971 ) ) ;
#193666 = CARTESIAN_POINT ( 'NONE',  ( 12.14591786802327356, -12.06949235617739191, 105.6260903946856899 ) ) ;
#193667 = CARTESIAN_POINT ( 'NONE',  ( 16.46253265017146816, 9.564922557961045513, 61.66775706135234003 ) ) ;
#193668 = CARTESIAN_POINT ( 'NONE',  ( 5.823673210054444382, -21.52544592524334988, 25.20942372801901854 ) ) ;
#193669 = CARTESIAN_POINT ( 'NONE',  ( -4.483927247898539470, -16.52544592524342804, 82.29057627198103830 ) ) ;
#193670 = CARTESIAN_POINT ( 'NONE',  ( 0.05219959533909260263, 19.03943276465977164, 94.99890960531436690 ) ) ;
#193671 = CARTESIAN_POINT ( 'NONE',  ( -16.52544592524335698, -4.483927247898792601, 108.9594237280190185 ) ) ;
#193672 = CARTESIAN_POINT ( 'NONE',  ( 10.72451020669871369, 18.67979575497193778, 77.08442372801901854 ) ) ;
#193673 = CARTESIAN_POINT ( 'NONE',  ( 4.483927247898790824, -16.52544592524335698, 40.20942372801901854 ) ) ;
#193674 = CARTESIAN_POINT ( 'NONE',  ( 21.55341960407619695, -5.719274019375665929, 26.04275706135235779 ) ) ;
#193675 = CARTESIAN_POINT ( 'NONE',  ( -8.314922557960811034, -14.29746914071050412, 67.08224293864770971 ) ) ;
#193676 = EDGE_CURVE ( 'NONE', #136214, #107664, #17917, .T. ) ;
#193677 = VERTEX_POINT ( 'NONE', #126076 ) ;
#193678 = CARTESIAN_POINT ( 'NONE',  ( -10.72451020669898014, 18.67979575497178502, 110.4155762719810383 ) ) ;
#193679 = CARTESIAN_POINT ( 'NONE',  ( 17.50000000000015987, -3.292511757969701414, 27.56520270210538825 ) ) ;
#193680 = CARTESIAN_POINT ( 'NONE',  ( 4.379528057220339221, -16.55341960407611168, 52.70724293864769550 ) ) ;
#193681 = CARTESIAN_POINT ( 'NONE',  ( -9.474510206698964154, 16.51473224551069663, 30.41557627198102054 ) ) ;
#193682 = CARTESIAN_POINT ( 'NONE',  ( -18.62759615963270932, 10.81492255796079327, 35.83224293864768839 ) ) ;
#193683 = CARTESIAN_POINT ( 'NONE',  ( 16.55341960407611168, 4.379528057220329451, 73.95724293864769550 ) ) ;
#193684 = EDGE_CURVE ( 'NONE', #66459, #52978, #33456, .T. ) ;
#193685 = CIRCLE ( 'NONE', #106484, 2.000000000000001776 ) ;
#193686 = CARTESIAN_POINT ( 'NONE',  ( -18.62759615963270932, 10.81492255796079327, 75.83224293864769550 ) ) ;
#193687 = CARTESIAN_POINT ( 'NONE',  ( -5.049401038298153566, 19.05341960407611168, 80.20724293864769550 ) ) ;
#193689 = CARTESIAN_POINT ( 'NONE',  ( -19.03943276465977164, -0.05219959533935918106, 78.75109039468567573 ) ) ;
#193688 = CARTESIAN_POINT ( 'NONE',  ( 16.51473224551069308, 9.474510206698969483, 34.16557627198102409 ) ) ;
#193691 = CARTESIAN_POINT ( 'NONE',  ( -18.62759615963270932, 10.81492255796079327, 65.83224293864769550 ) ) ;
#193690 = CARTESIAN_POINT ( 'NONE',  ( 21.55341960407619695, -5.719274019375665929, 51.04275706135234714 ) ) ;
#193692 = CARTESIAN_POINT ( 'NONE',  ( -16.51473224551069308, -9.474510206698971260, 46.66557627198102409 ) ) ;
#193693 = CARTESIAN_POINT ( 'NONE',  ( -19.02544592524342804, 5.153800228976336051, 71.04057627198099567 ) ) ;
#193694 = CARTESIAN_POINT ( 'NONE',  ( 12.06949235617739724, 12.14591786802326823, 51.87609039468568284 ) ) ;
#193695 = CARTESIAN_POINT ( 'NONE',  ( 18.62759615963255655, 10.81492255796105972, 36.66775706135234714 ) ) ;
#193696 = CARTESIAN_POINT ( 'NONE',  ( -15.80617190586768217, 15.72974639402176855, 58.12609039468568994 ) ) ;
#193697 = CARTESIAN_POINT ( 'NONE',  ( 5.049401038298161559, -19.05341960407611168, 102.7072429386476955 ) ) ;
#193698 = CARTESIAN_POINT ( 'NONE',  ( 5.823673210054125526, 21.52544592524343514, 84.79057627198102409 ) ) ;
#193700 = CARTESIAN_POINT ( 'NONE',  ( -16.53943276465976808, -0.05219959533934237506, 53.75109039468568994 ) ) ;
#193699 = CARTESIAN_POINT ( 'NONE',  ( 21.52544592524334988, 5.823673210054432836, 21.45942372801901499 ) ) ;
#193701 = CARTESIAN_POINT ( 'NONE',  ( 0.05219959533907565091, 21.53943276465977519, 44.99890960531435979 ) ) ;
#193702 = CARTESIAN_POINT ( 'NONE',  ( 16.51473224551083163, -9.474510206698727899, 25.83442372801900078 ) ) ;
#193703 = B_SPLINE_CURVE_WITH_KNOTS ( 'NONE', 3,
 ( #169084, #59925, #29601, #183288, #133798, #92242 ),
 .UNSPECIFIED., .F., .F.,
 ( 4, 2, 4 ),
 ( 0.003989672132298142590, 0.004372778065220579713, 0.004755883998143016836 ),
 .UNSPECIFIED. ) ;
#193704 = CARTESIAN_POINT ( 'NONE',  ( -5.049401038298153566, 19.05341960407611168, 55.20724293864769550 ) ) ;
#193705 = DIRECTION ( 'NONE',  ( 0.000000000000000000, 0.000000000000000000, -1.000000000000000000 ) ) ;
#193706 = CARTESIAN_POINT ( 'NONE',  ( -9.474510206698964154, 16.51473224551069663, 85.41557627198102409 ) ) ;
#193707 = ORIENTED_EDGE ( 'NONE', *, *, #37197, .T. ) ;
#193708 = CARTESIAN_POINT ( 'NONE',  ( 17.50000000000051159, 3.947464652946200747, 103.2758644658976124 ) ) ;
#193709 = CARTESIAN_POINT ( 'NONE',  ( 5.049401038297881783, 19.05341960407617563, 72.29275706135234714 ) ) ;
#193710 = CARTESIAN_POINT ( 'NONE',  ( 5.823673210054125526, 21.52544592524343514, 44.79057627198103120 ) ) ;
#193711 = CARTESIAN_POINT ( 'NONE',  ( -16.55341960407611168, -4.379528057220339221, 26.45724293864768839 ) ) ;
#193712 = CARTESIAN_POINT ( 'NONE',  ( -13.89961937509957401, -13.97604488694547875, 89.37609039468563310 ) ) ;
#193713 = CARTESIAN_POINT ( 'NONE',  ( 5.199999999999996625, 3.061616997868383634E-16, -2.500000000000000444 ) ) ;
#193714 = CARTESIAN_POINT ( 'NONE',  ( -9.474510206698720793, -16.51473224551083518, 19.58442372801899722 ) ) ;
#193715 = CARTESIAN_POINT ( 'NONE',  ( 19.03943276465977164, 0.05219959533936151252, 101.2510903946856757 ) ) ;
#193716 = CARTESIAN_POINT ( 'NONE',  ( 19.03943276465977164, 0.05219959533936151252, 46.25109039468566863 ) ) ;
#193717 = B_SPLINE_CURVE_WITH_KNOTS ( 'NONE', 3,
 ( #128505, #172042, #156877, #95191, #35515, #18374, #190200, #51678, #80026, #142686 ),
 .UNSPECIFIED., .F., .F.,
 ( 4, 2, 2, 2, 4 ),
 ( 0.000000000000000000, 0.0009193652485011039217, 0.001838730497002207843, 0.002758095745503311765, 0.003677460994004415687 ),
 .UNSPECIFIED. ) ;
#193718 = DIRECTION ( 'NONE',  ( -1.000000000000000000, -0.000000000000000000, -0.000000000000000000 ) ) ;
#193719 = CARTESIAN_POINT ( 'NONE',  ( -13.89961937509977652, 13.97604488694528158, 50.62390960531435979 ) ) ;
#193720 = CARTESIAN_POINT ( 'NONE',  ( -16.55341960407611168, -4.379528057220339221, 66.45724293864768129 ) ) ;
#193721 = CARTESIAN_POINT ( 'NONE',  ( -16.51473224551069308, -9.474510206698971260, 31.66557627198102054 ) ) ;
#193722 = CARTESIAN_POINT ( 'NONE',  ( 4.483927247898545687, 16.52544592524342804, 39.79057627198103830 ) ) ;
#193723 = CARTESIAN_POINT ( 'NONE',  ( -31.65755289763026781, -24.31906878930451654, -22.32084141216703088 ) ) ;
#193724 = CARTESIAN_POINT ( 'NONE',  ( 4.379528057220092307, 16.55341960407617563, 102.2927570613523613 ) ) ;
#193725 = CARTESIAN_POINT ( 'NONE',  ( 9.564922557960805705, 16.46253265017160317, 59.58224293864769550 ) ) ;
#193726 = CARTESIAN_POINT ( 'NONE',  ( 0.05219959533936267826, -19.03943276465977164, 20.00109039468567218 ) ) ;
#193727 = CARTESIAN_POINT ( 'NONE',  ( 4.379528057220092307, 16.55341960407617563, 27.29275706135234358 ) ) ;
#193728 = CARTESIAN_POINT ( 'NONE',  ( 21.52544592524344225, -5.823673210054117533, 43.54057627198103830 ) ) ;
#193730 = ORIENTED_EDGE ( 'NONE', *, *, #115114, .F. ) ;
#193729 = CARTESIAN_POINT ( 'NONE',  ( -21.53943276465977519, -0.05219959533937600094, 103.7510903946857042 ) ) ;
#193731 = CARTESIAN_POINT ( 'NONE',  ( -0.05219959533909027116, -19.03943276465977164, 67.49890960531436690 ) ) ;
#193732 = CARTESIAN_POINT ( 'NONE',  ( 9.564922557960805705, 16.46253265017160317, 104.5822429386476955 ) ) ;
#193733 = CARTESIAN_POINT ( 'NONE',  ( 19.03943276465977164, -0.05219959533909143690, 93.74890960531435269 ) ) ;
#193734 = CARTESIAN_POINT ( 'NONE',  ( 11.40812507854754365, 35.11059874428196537, -1.224999997268813479 ) ) ;
#193735 = CARTESIAN_POINT ( 'NONE',  ( 15.80617190586769283, -15.72974639402175789, 30.62609039468567929 ) ) ;
#193736 = CARTESIAN_POINT ( 'NONE',  ( 12.06949235617757843, -12.14591786802309237, 93.12390960531436690 ) ) ;
#193738 = CARTESIAN_POINT ( 'NONE',  ( -13.97604488694527625, -13.89961937509977652, 61.87390960531435979 ) ) ;
#193737 = CARTESIAN_POINT ( 'NONE',  ( 21.52544592524344225, -5.823673210054117533, 88.54057627198103830 ) ) ;
#193739 = CARTESIAN_POINT ( 'NONE',  ( -9.564922557960796823, -16.46253265017161027, 67.08224293864769550 ) ) ;
#193740 = CARTESIAN_POINT ( 'NONE',  ( 21.55341960407610458, 5.719274019375980345, 108.9572429386476955 ) ) ;
#193741 = VERTEX_POINT ( 'NONE', #124737 ) ;
#193742 = CARTESIAN_POINT ( 'NONE',  ( 13.89961937509977652, -13.97604488694527269, 68.12390960531436690 ) ) ;
#193743 = CARTESIAN_POINT ( 'NONE',  ( 18.56197773271729190, -5.499999999999983125, 96.05066217314450228 ) ) ;
#193745 = DIRECTION ( 'NONE',  ( 1.000000000000000000, 3.552713678800500929E-15, 0.000000000000000000 ) ) ;
#193744 = CARTESIAN_POINT ( 'NONE',  ( -8.224510206698948167, 14.34966873604960824, 105.4155762719810383 ) ) ;
#193746 = CARTESIAN_POINT ( 'NONE',  ( -9.564922557960796823, -16.46253265017161027, 62.08224293864769550 ) ) ;
#193747 = CARTESIAN_POINT ( 'NONE',  ( -9.564922557961040184, 16.46253265017147172, 92.91775706135233293 ) ) ;
#193748 = CARTESIAN_POINT ( 'NONE',  ( 8.224510206698953496, -14.34966873604960469, 102.9155762719810383 ) ) ;
#193749 = CARTESIAN_POINT ( 'NONE',  ( -0.05219959533937732626, 21.53943276465977519, 77.50109039468567573 ) ) ;
#193751 = CARTESIAN_POINT ( 'NONE',  ( -5.719274019375665041, -21.55341960407619695, 24.79275706135235779 ) ) ;
#193750 = CARTESIAN_POINT ( 'NONE',  ( -5.153800228976328057, -19.02544592524343514, 52.29057627198100988 ) ) ;
#193752 = CARTESIAN_POINT ( 'NONE',  ( 15.80617190586746368, 15.72974639402197994, 114.3739096053143527 ) ) ;
#193753 = CARTESIAN_POINT ( 'NONE',  ( -23.31738231874055600, 16.94106989632528837, 148.0500000054623797 ) ) ;
#193754 = CARTESIAN_POINT ( 'NONE',  ( -9.474510206698964154, 16.51473224551069663, 70.41557627198102409 ) ) ;
#193755 = CARTESIAN_POINT ( 'NONE',  ( -8.906447517083053711, -27.41122689804191026, 138.6500000054623740 ) ) ;
#193757 = CARTESIAN_POINT ( 'NONE',  ( 5.823673210054125526, 21.52544592524343514, 24.79057627198103120 ) ) ;
#193756 = CARTESIAN_POINT ( 'NONE',  ( -19.05341960407617563, 5.049401038297882671, 103.5427570613523329 ) ) ;
#193758 = CARTESIAN_POINT ( 'NONE',  ( -5.719274019375665041, -21.55341960407619695, 64.79275706135234714 ) ) ;
#193759 = CARTESIAN_POINT ( 'NONE',  ( 16.46253265017160672, -9.564922557960803928, 103.3322429386476955 ) ) ;
#193760 = CARTESIAN_POINT ( 'NONE',  ( 13.97604488694548053, -13.89961937509957401, 85.62609039468568994 ) ) ;
#193761 = CARTESIAN_POINT ( 'NONE',  ( -9.564922557960796823, -16.46253265017161027, 47.08224293864769550 ) ) ;
#193762 = CARTESIAN_POINT ( 'NONE',  ( -9.564922557960796823, -16.46253265017161027, 67.08224293864769550 ) ) ;
#193763 = CARTESIAN_POINT ( 'NONE',  ( -12.06949235617756955, 12.14591786802309770, 80.62390960531438111 ) ) ;
#193764 = CARTESIAN_POINT ( 'NONE',  ( 5.049401038298161559, -19.05341960407611168, 97.70724293864766707 ) ) ;
#193765 = CARTESIAN_POINT ( 'NONE',  ( 12.06949235617757843, -12.14591786802309237, 98.12390960531436690 ) ) ;
#193766 = CARTESIAN_POINT ( 'NONE',  ( 9.474510206698971260, -16.51473224551069308, 102.9155762719810241 ) ) ;
#193768 = CARTESIAN_POINT ( 'NONE',  ( -9.474510206698964154, 16.51473224551069663, 25.41557627198103120 ) ) ;
#193767 = CARTESIAN_POINT ( 'NONE',  ( 0.05219959533910956823, 16.53943276465976808, 44.99890960531435979 ) ) ;
#193769 = ORIENTED_EDGE ( 'NONE', *, *, #158649, .F. ) ;
#193770 = CARTESIAN_POINT ( 'NONE',  ( 15.80617190586769283, -15.72974639402175789, 55.62609039468568284 ) ) ;
#193771 = CARTESIAN_POINT ( 'NONE',  ( 0.05219959533936267826, -19.03943276465977164, 75.00109039468566152 ) ) ;
#193772 = CARTESIAN_POINT ( 'NONE',  ( -12.06949235617756955, 12.14591786802309770, 55.62390960531436690 ) ) ;
#193773 = CARTESIAN_POINT ( 'NONE',  ( 21.53943276465977519, -0.05219959533907433946, 98.74890960531438111 ) ) ;
#193774 = CARTESIAN_POINT ( 'NONE',  ( -0.05219959533907301413, -21.53943276465977519, 27.49890960531435269 ) ) ;
#193775 = CARTESIAN_POINT ( 'NONE',  ( -12.14591786802309592, -12.06949235617757132, 86.87390960531438111 ) ) ;
#193776 = CARTESIAN_POINT ( 'NONE',  ( -9.474510206698964154, 16.51473224551069663, 60.41557627198102409 ) ) ;
#193777 = CARTESIAN_POINT ( 'NONE',  ( -8.224510206698948167, 14.34966873604960824, 25.41557627198103120 ) ) ;
#193778 = CARTESIAN_POINT ( 'NONE',  ( -16.52544592524335698, -4.483927247898792601, 103.9594237280190185 ) ) ;
#193779 = CARTESIAN_POINT ( 'NONE',  ( 8.314922557961029526, -14.29746914071037800, 70.41775706135236135 ) ) ;
#193780 = CARTESIAN_POINT ( 'NONE',  ( 5.153800228976615827, -19.02544592524334988, 20.20942372801899722 ) ) ;
#193781 = CARTESIAN_POINT ( 'NONE',  ( -13.89961937509977652, 13.97604488694528158, 100.6239096053143669 ) ) ;
#193782 = CARTESIAN_POINT ( 'NONE',  ( 19.02544592524343514, -5.153800228976328945, 78.54057627198099567 ) ) ;
#193783 = CARTESIAN_POINT ( 'NONE',  ( -5.049401038298153566, 19.05341960407611168, 35.20724293864768839 ) ) ;
#193784 = CARTESIAN_POINT ( 'NONE',  ( -12.14591786802309592, -12.06949235617757132, 51.87390960531437401 ) ) ;
#193786 = CARTESIAN_POINT ( 'NONE',  ( -19.02544592524342804, 5.153800228976336051, 101.0405762719810241 ) ) ;
#193785 = LINE ( 'NONE', #25944, #17856 ) ;
#193787 = CARTESIAN_POINT ( 'NONE',  ( 10.81492255796078972, 18.62759615963270932, 44.58224293864769550 ) ) ;
#193788 = CARTESIAN_POINT ( 'NONE',  ( 8.314922557960818139, 14.29746914071049879, 69.58224293864769550 ) ) ;
#193789 = CARTESIAN_POINT ( 'NONE',  ( -16.53943276465976808, -0.05219959533934237506, 28.75109039468567929 ) ) ;
#193790 = B_SPLINE_CURVE_WITH_KNOTS ( 'NONE', 3,
 ( #113156, #191008, #128323, #84805, #68649, #115163, #146484 ),
 .UNSPECIFIED., .F., .F.,
 ( 4, 3, 4 ),
 ( 0.006877813788783073562, 0.01375562809188920002, 0.01380070845639014970 ),
 .UNSPECIFIED. ) ;
#193791 = CARTESIAN_POINT ( 'NONE',  ( 12.14591786802309770, 12.06949235617756955, 59.37390960531436690 ) ) ;
#193792 = PLANE ( 'NONE',  #193271 ) ;
#193793 = CARTESIAN_POINT ( 'NONE',  ( 5.153800228976615827, -19.02544592524334988, 70.20942372801899012 ) ) ;
#193794 = CARTESIAN_POINT ( 'NONE',  ( -5.153800228976328057, -19.02544592524343514, 107.2905762719810383 ) ) ;
#193795 = CARTESIAN_POINT ( 'NONE',  ( 13.97604488694548053, -13.89961937509957401, 85.62609039468568994 ) ) ;
#193796 = CARTESIAN_POINT ( 'NONE',  ( 27.73933785331498569, 2.768321779492822058E-14, 148.3750000027311842 ) ) ;
#193797 = AXIS2_PLACEMENT_3D ( 'NONE', #12697, #197703, #44019 ) ;
#193799 = CARTESIAN_POINT ( 'NONE',  ( 4.379528057220092307, 16.55341960407617563, 112.2927570613523471 ) ) ;
#193798 = CARTESIAN_POINT ( 'NONE',  ( -13.97604488694547697, 13.89961937509957934, 108.1260903946856331 ) ) ;
#193800 = CARTESIAN_POINT ( 'NONE',  ( 9.564922557960805705, 16.46253265017160317, 39.58224293864768839 ) ) ;
#193801 =( BOUNDED_CURVE ( )  B_SPLINE_CURVE ( 2, ( #168728, #156562, #47400, #80697, #868, #200080, #142374, #62543, #91874, #61548, #3854 ),
 .UNSPECIFIED., .F., .F. ) 
 B_SPLINE_CURVE_WITH_KNOTS ( ( 3, 2, 2, 2, 2, 3 ),
 ( 0.3000000000000000999, 0.3200000000000000067, 0.3400000000000000799, 0.3600000000000000977, 0.3800000000000001155, 0.4000000000000001332 ),
 .UNSPECIFIED. ) 
 CURVE ( )  GEOMETRIC_REPRESENTATION_ITEM ( )  RATIONAL_B_SPLINE_CURVE ( ( 0.9999999999999998890, 0.9510565162951536422, 1.000000000000000000, 0.9510565162951535312, 1.000000000000000000, 0.9510565162951535312, 1.000000000000000000, 0.9510565162951535312, 1.000000000000000000, 0.9510565162951533091, 1.000000000000000222 ) ) 
 REPRESENTATION_ITEM ( '' )  );
#193802 = CARTESIAN_POINT ( 'NONE',  ( -15.80617190586745835, -15.72974639402198527, 31.87390960531435979 ) ) ;
#193803 = CARTESIAN_POINT ( 'NONE',  ( 21.52544592524334988, 5.823673210054432836, 51.45942372801901854 ) ) ;
#193804 = CARTESIAN_POINT ( 'NONE',  ( 1.993301997531345686E-15, -30.30510711980685556, 146.7500000054623683 ) ) ;
#193805 = CARTESIAN_POINT ( 'NONE',  ( -12.06949235617739369, -12.14591786802326823, 24.37609039468567573 ) ) ;
#193807 = CARTESIAN_POINT ( 'NONE',  ( 9.564922557960805705, 16.46253265017160317, 69.58224293864770971 ) ) ;
#193806 = LINE ( 'NONE', #87603, #18467 ) ;
#193808 = FACE_OUTER_BOUND ( 'NONE', #177333, .T. ) ;
#193810 = CARTESIAN_POINT ( 'NONE',  ( 19.05341960407611168, 5.049401038298154454, 73.95724293864768129 ) ) ;
#193809 = CARTESIAN_POINT ( 'NONE',  ( 12.06949235617757843, -12.14591786802309237, 83.12390960531436690 ) ) ;
#193811 = CARTESIAN_POINT ( 'NONE',  ( -19.05341960407611168, -5.049401038298163336, 86.45724293864769550 ) ) ;
#193812 = VERTEX_POINT ( 'NONE', #31742 ) ;
#193813 = CARTESIAN_POINT ( 'NONE',  ( -0.05219959533936034679, 19.03943276465977164, 87.50109039468567573 ) ) ;
#193814 = CARTESIAN_POINT ( 'NONE',  ( 5.823673210054125526, 21.52544592524343514, 69.79057627198102409 ) ) ;
#193815 = CARTESIAN_POINT ( 'NONE',  ( -16.46253265017160317, 9.564922557960807481, 30.83224293864769550 ) ) ;
#193816 = CARTESIAN_POINT ( 'NONE',  ( 13.89961937509957401, 13.97604488694547697, 51.87609039468566863 ) ) ;
#193817 = CARTESIAN_POINT ( 'NONE',  ( -9.474510206698964154, 16.51473224551069663, 50.41557627198102409 ) ) ;
#193818 = CARTESIAN_POINT ( 'NONE',  ( 13.89961937509977652, -13.97604488694527269, 88.12390960531438111 ) ) ;
#193819 = EDGE_LOOP ( 'NONE', ( #197427, #98773, #45334, #33633 ) ) ;
#193820 = CARTESIAN_POINT ( 'NONE',  ( 5.823673210054125526, 21.52544592524343514, 94.79057627198105251 ) ) ;
#193823 = CARTESIAN_POINT ( 'NONE',  ( 19.02544592524334988, 5.153800228976608722, 66.45942372801899012 ) ) ;
#193822 = CARTESIAN_POINT ( 'NONE',  ( -13.89961937509977652, 13.97604488694528158, 85.62390960531433848 ) ) ;
#193821 = CARTESIAN_POINT ( 'NONE',  ( 8.224510206698953496, -14.34966873604960469, 92.91557627198103830 ) ) ;
#193824 = CARTESIAN_POINT ( 'NONE',  ( -18.62759615963270932, 10.81492255796079327, 95.83224293864770971 ) ) ;
#193825 = CARTESIAN_POINT ( 'NONE',  ( -10.72451020669898014, 18.67979575497178502, 70.41557627198102409 ) ) ;
#193826 = CARTESIAN_POINT ( 'NONE',  ( 16.52544592524342804, -4.483927247898539470, 33.54057627198102409 ) ) ;
#193827 = CARTESIAN_POINT ( 'NONE',  ( 21.52544592524334988, 5.823673210054432836, 106.4594237280190328 ) ) ;
#193828 = CARTESIAN_POINT ( 'NONE',  ( 14.34966873604972726, -8.224510206698740333, 65.83442372801900433 ) ) ;
#193829 = CARTESIAN_POINT ( 'NONE',  ( -19.03943276465977164, 0.05219959533909376836, 76.24890960531435269 ) ) ;
#193830 = CARTESIAN_POINT ( 'NONE',  ( -16.46253265017160317, 9.564922557960807481, 35.83224293864768839 ) ) ;
#193831 = VECTOR ( 'NONE', #42923, 1000.000000000000000 ) ;
#193832 = CARTESIAN_POINT ( 'NONE',  ( -18.67979575497193778, 10.72451020669871902, 33.33442372801900433 ) ) ;
#193833 = CARTESIAN_POINT ( 'NONE',  ( 21.52544592524334988, 5.823673210054432836, 56.45942372801902565 ) ) ;
#193834 = CARTESIAN_POINT ( 'NONE',  ( 5.049401038298161559, -19.05341960407611168, 42.70724293864767418 ) ) ;
#193835 = CARTESIAN_POINT ( 'NONE',  ( 10.72451020669871369, 18.67979575497193778, 22.08442372801901143 ) ) ;
#193836 = CARTESIAN_POINT ( 'NONE',  ( 5.153800228976615827, -19.02544592524334988, 70.20942372801899012 ) ) ;
#193837 = CARTESIAN_POINT ( 'NONE',  ( -0.05219959533936034679, 19.03943276465977164, 77.50109039468566152 ) ) ;
#193838 = CARTESIAN_POINT ( 'NONE',  ( 5.049401038298161559, -19.05341960407611168, 22.70724293864769194 ) ) ;
#193839 = CARTESIAN_POINT ( 'NONE',  ( -12.14591786802326823, 12.06949235617739902, 68.12609039468567573 ) ) ;
#193840 = CARTESIAN_POINT ( 'NONE',  ( -5.153800228976328057, -19.02544592524343514, 47.29057627198102409 ) ) ;
#193841 = CARTESIAN_POINT ( 'NONE',  ( 21.75836449082896706, -8.509082329561300284, 169.1767350484858810 ) ) ;
#193842 = CARTESIAN_POINT ( 'NONE',  ( 9.564922557960805705, 16.46253265017160317, 104.5822429386476955 ) ) ;
#193843 = CARTESIAN_POINT ( 'NONE',  ( 5.049401038298161559, -19.05341960407611168, 27.70724293864769550 ) ) ;
#193844 = CARTESIAN_POINT ( 'NONE',  ( -21.55341960407610458, -5.719274019375992779, 76.45724293864769550 ) ) ;
#193845 = CARTESIAN_POINT ( 'NONE',  ( -4.379528057220086978, -16.55341960407618274, 59.79275706135234714 ) ) ;
#193846 = CARTESIAN_POINT ( 'NONE',  ( -18.67979575497193778, 10.72451020669871902, 108.3344237280190185 ) ) ;
#193847 = CARTESIAN_POINT ( 'NONE',  ( -5.049401038298153566, 19.05341960407611168, 55.20724293864769550 ) ) ;
#193848 = CARTESIAN_POINT ( 'NONE',  ( -12.14591786802309592, -12.06949235617757132, 31.87390960531435979 ) ) ;
#193849 = CARTESIAN_POINT ( 'NONE',  ( 12.06949235617757843, -12.14591786802309237, 68.12390960531436690 ) ) ;
#193850 = CARTESIAN_POINT ( 'NONE',  ( 5.153800228976335163, 19.02544592524342804, 74.79057627198103830 ) ) ;
#193851 = CARTESIAN_POINT ( 'NONE',  ( -5.719274019375665041, -21.55341960407619695, 34.79275706135235424 ) ) ;
#193852 = CARTESIAN_POINT ( 'NONE',  ( -0.05219959533909027116, -19.03943276465977164, 87.49890960531436690 ) ) ;
#193853 = CARTESIAN_POINT ( 'NONE',  ( 21.53943276465977519, 0.05219959533937863772, 96.25109039468568994 ) ) ;
#193854 = CARTESIAN_POINT ( 'NONE',  ( -8.224510206698735004, -14.34966873604973081, 69.58442372801900433 ) ) ;
#193855 = CARTESIAN_POINT ( 'NONE',  ( 9.564922557960805705, 16.46253265017160317, 114.5822429386476955 ) ) ;
#193856 = CARTESIAN_POINT ( 'NONE',  ( -5.823673210054116645, -21.52544592524344225, 92.29057627198103830 ) ) ;
#193857 = CARTESIAN_POINT ( 'NONE',  ( -0.05219959533910754901, -16.53943276465976808, 52.49890960531435979 ) ) ;
#193858 = CARTESIAN_POINT ( 'NONE',  ( 9.564922557960805705, 16.46253265017160317, 29.58224293864769550 ) ) ;
#193859 = CARTESIAN_POINT ( 'NONE',  ( 14.29746914071037800, 8.314922557961029526, 56.66775706135235424 ) ) ;
#193860 = CARTESIAN_POINT ( 'NONE',  ( 16.55341960407611168, 4.379528057220329451, 73.95724293864769550 ) ) ;
#193861 = CARTESIAN_POINT ( 'NONE',  ( 13.89961937509977652, -13.97604488694527269, 108.1239096053143669 ) ) ;
#193862 = CARTESIAN_POINT ( 'NONE',  ( -15.80617190586745835, -15.72974639402198527, 31.87390960531435979 ) ) ;
#193863 = CARTESIAN_POINT ( 'NONE',  ( 19.03943276465977164, 0.05219959533936151252, 21.25109039468565797 ) ) ;
#193864 = CARTESIAN_POINT ( 'NONE',  ( -16.52544592524342804, 4.483927247898546575, 106.0405762719810525 ) ) ;
#193865 = CARTESIAN_POINT ( 'NONE',  ( -16.51473224551069308, -9.474510206698971260, 106.6655762719810383 ) ) ;
#193866 = ORIENTED_EDGE ( 'NONE', *, *, #14429, .T. ) ;
#193867 = CARTESIAN_POINT ( 'NONE',  ( -0.05219959533934338120, 16.53943276465976808, 52.50109039468567573 ) ) ;
#193868 = CARTESIAN_POINT ( 'NONE',  ( -19.05341960407611168, -5.049401038298163336, 56.45724293864768129 ) ) ;
#193869 = CARTESIAN_POINT ( 'NONE',  ( -8.388830574159379737E-16, -13.70000000000001528, -64.92279855667830191 ) ) ;
#193870 = CARTESIAN_POINT ( 'NONE',  ( -0.05219959533936034679, 19.03943276465977164, 47.50109039468566863 ) ) ;
#193871 = CARTESIAN_POINT ( 'NONE',  ( -16.53943276465976808, -0.05219959533934237506, 93.75109039468567573 ) ) ;
#193872 = CARTESIAN_POINT ( 'NONE',  ( -19.02544592524334988, -5.153800228976617603, 98.95942372801900433 ) ) ;
#193873 = CARTESIAN_POINT ( 'NONE',  ( 21.52544592524334988, 5.823673210054432836, 71.45942372801901854 ) ) ;
#193874 = CARTESIAN_POINT ( 'NONE',  ( 13.97604488694527802, 13.89961937509977652, 69.37390960531436690 ) ) ;
#193875 = CARTESIAN_POINT ( 'NONE',  ( 15.80617190586746368, 15.72974639402197994, 94.37390960531436690 ) ) ;
#193876 = CARTESIAN_POINT ( 'NONE',  ( -4.379528057220328563, 16.55341960407611168, 110.2072429386477239 ) ) ;
#193877 = EDGE_CURVE ( 'NONE', #107606, #45770, #185419, .T. ) ;
#193878 = CARTESIAN_POINT ( 'NONE',  ( 13.89961937509957401, 13.97604488694547697, 81.87609039468564731 ) ) ;
#193879 = CARTESIAN_POINT ( 'NONE',  ( -18.67979575497178146, -10.72451020669898902, 76.66557627198103830 ) ) ;
#193880 = CARTESIAN_POINT ( 'NONE',  ( -13.89961937509957401, -13.97604488694547875, 39.37609039468566152 ) ) ;
#193881 = FACE_BOUND ( 'NONE', #72559, .T. ) ;
#193882 = CARTESIAN_POINT ( 'NONE',  ( -21.55341960407610458, -5.719274019375992779, 96.45724293864770971 ) ) ;
#193883 = CARTESIAN_POINT ( 'NONE',  ( -17.40805194822029378, 6.112264579159334410, 85.83371272510608208 ) ) ;
#193884 = CARTESIAN_POINT ( 'NONE',  ( 19.03943276465977164, -0.05219959533909143690, 68.74890960531436690 ) ) ;
#193885 = CARTESIAN_POINT ( 'NONE',  ( -32.00000000000000711, -1.163414459189985801E-14, 92.30000000000001137 ) ) ;
#193886 = CARTESIAN_POINT ( 'NONE',  ( 13.97604488694548053, -13.89961937509957401, 110.6260903946856615 ) ) ;
#193887 = CARTESIAN_POINT ( 'NONE',  ( -5.153800228976607833, 19.02544592524335343, 97.70942372801899012 ) ) ;
#193888 = CARTESIAN_POINT ( 'NONE',  ( -5.049401038298153566, 19.05341960407611168, 45.20724293864769550 ) ) ;
#193889 = CARTESIAN_POINT ( 'NONE',  ( -19.05341960407611168, -5.049401038298163336, 106.4572429386476955 ) ) ;
#193891 = CARTESIAN_POINT ( 'NONE',  ( -8.224510206698948167, 14.34966873604960824, 45.41557627198103830 ) ) ;
#193890 = CARTESIAN_POINT ( 'NONE',  ( -5.719274019375978568, 21.55341960407610458, 105.2072429386477097 ) ) ;
#193892 = CARTESIAN_POINT ( 'NONE',  ( -18.67979575497193778, 10.72451020669871902, 73.33442372801901854 ) ) ;
#193894 = CARTESIAN_POINT ( 'NONE',  ( -19.05341960407617563, 5.049401038297882671, 23.54275706135233648 ) ) ;
#193893 = CARTESIAN_POINT ( 'NONE',  ( -16.55341960407617563, 4.379528057220093196, 28.54275706135234358 ) ) ;
#193895 = CARTESIAN_POINT ( 'NONE',  ( -4.379528057220328563, 16.55341960407611168, 30.20724293864769550 ) ) ;
#193896 = EDGE_CURVE ( 'NONE', #91244, #157973, #6510, .T. ) ;
#193897 = CARTESIAN_POINT ( 'NONE',  ( -5.823673210054116645, -21.52544592524344225, 112.2905762719810241 ) ) ;
#193898 = CARTESIAN_POINT ( 'NONE',  ( 8.314922557960818139, 14.29746914071049879, 54.58224293864769550 ) ) ;
#193899 = CARTESIAN_POINT ( 'NONE',  ( -13.89961937509957401, -13.97604488694547875, 94.37609039468566152 ) ) ;
#193900 = CARTESIAN_POINT ( 'NONE',  ( 5.049401038297881783, 19.05341960407617563, 72.29275706135234714 ) ) ;
#193901 = CARTESIAN_POINT ( 'NONE',  ( -10.81492255796105439, 18.62759615963255655, 72.91775706135234714 ) ) ;
#193902 = CARTESIAN_POINT ( 'NONE',  ( -19.03943276465977164, -0.05219959533935918106, 48.75109039468566863 ) ) ;
#193903 = CARTESIAN_POINT ( 'NONE',  ( 14.34966873604960469, 8.224510206698951720, 114.1655762719810383 ) ) ;
#193904 = CARTESIAN_POINT ( 'NONE',  ( -18.62759615963270932, 10.81492255796079327, 40.83224293864769550 ) ) ;
#193905 = CARTESIAN_POINT ( 'NONE',  ( 8.224510206698953496, -14.34966873604960469, 47.91557627198102409 ) ) ;
#193906 = CARTESIAN_POINT ( 'NONE',  ( -23.48529157249600985, 32.32473071737754111, -2.049999994537626158 ) ) ;
#193907 = CARTESIAN_POINT ( 'NONE',  ( -5.823673210054431948, 21.52544592524334988, 107.7094237280190328 ) ) ;
#193908 = CARTESIAN_POINT ( 'NONE',  ( 0.05219959533934541429, -16.53943276465976808, 80.00109039468568994 ) ) ;
#193909 = CARTESIAN_POINT ( 'NONE',  ( -0.05219959533910754901, -16.53943276465976808, 37.49890960531436690 ) ) ;
#193910 = CARTESIAN_POINT ( 'NONE',  ( -10.72451020669870658, -18.67979575497194134, 79.58442372801903275 ) ) ;
#193911 = CARTESIAN_POINT ( 'NONE',  ( -0.05219959533937732626, 21.53943276465977519, 87.50109039468568994 ) ) ;
#193912 = CARTESIAN_POINT ( 'NONE',  ( 5.719274019375991003, -21.55341960407610458, 87.70724293864769550 ) ) ;
#193913 = EDGE_CURVE ( 'NONE', #192686, #115197, #108571, .T. ) ;
#193914 = CARTESIAN_POINT ( 'NONE',  ( -13.97604488694527625, -13.89961937509977652, 41.87390960531435979 ) ) ;
#193915 = CARTESIAN_POINT ( 'NONE',  ( 10.72451020669871369, 18.67979575497193778, 57.08442372801901854 ) ) ;
#193916 = CARTESIAN_POINT ( 'NONE',  ( -16.46253265017160317, 9.564922557960807481, 40.83224293864769550 ) ) ;
#193917 = CARTESIAN_POINT ( 'NONE',  ( -19.05341960407611168, -5.049401038298163336, 51.45724293864770260 ) ) ;
#193918 = CARTESIAN_POINT ( 'NONE',  ( 14.29746914071049879, -8.314922557960816363, 98.33224293864769550 ) ) ;
#193919 = CARTESIAN_POINT ( 'NONE',  ( 13.97604488694527802, 13.89961937509977652, 94.37390960531436690 ) ) ;
#193920 = CARTESIAN_POINT ( 'NONE',  ( -14.29746914071049879, 8.314922557960819915, 35.83224293864768839 ) ) ;
#193921 = CARTESIAN_POINT ( 'NONE',  ( -16.52544592524342804, 4.483927247898546575, 111.0405762719810525 ) ) ;
#193922 = CARTESIAN_POINT ( 'NONE',  ( 15.80617190586746368, 15.72974639402197994, 89.37390960531435269 ) ) ;
#193923 = CARTESIAN_POINT ( 'NONE',  ( 5.823673210054444382, -21.52544592524334988, 25.20942372801901854 ) ) ;
#193924 = CARTESIAN_POINT ( 'NONE',  ( -15.51017872335181558, 14.74842737557647787, -56.39952970130666898 ) ) ;
#193926 = CARTESIAN_POINT ( 'NONE',  ( -16.52544592524335698, -4.483927247898792601, 18.95942372801901143 ) ) ;
#193925 = CARTESIAN_POINT ( 'NONE',  ( 16.46253265017160672, -9.564922557960803928, 83.33224293864768129 ) ) ;
#193927 = CARTESIAN_POINT ( 'NONE',  ( -15.72974639402197994, 15.80617190586746368, 75.62390960531439532 ) ) ;
#193928 = CARTESIAN_POINT ( 'NONE',  ( 0.05219959533937995610, -21.53943276465977519, 95.00109039468568994 ) ) ;
#193929 = CARTESIAN_POINT ( 'NONE',  ( -19.03943276465977164, 0.05219959533909376836, 81.24890960531436690 ) ) ;
#193930 = CARTESIAN_POINT ( 'NONE',  ( 15.72974639402176855, 15.80617190586768217, 31.87609039468567929 ) ) ;
#193931 = CARTESIAN_POINT ( 'NONE',  ( -13.89961937509977652, 13.97604488694528158, 115.6239096053143669 ) ) ;
#193932 = CARTESIAN_POINT ( 'NONE',  ( 8.224510206698742110, 14.34966873604972548, 92.08442372801901854 ) ) ;
#193933 = CARTESIAN_POINT ( 'NONE',  ( 21.55341960407619695, -5.719274019375665929, 71.04275706135234714 ) ) ;
#193934 = CARTESIAN_POINT ( 'NONE',  ( 5.719274019375673035, 21.55341960407619339, 102.2927570613523613 ) ) ;
#193935 = CARTESIAN_POINT ( 'NONE',  ( -16.55341960407617563, 4.379528057220093196, 78.54275706135236135 ) ) ;
#193936 = CARTESIAN_POINT ( 'NONE',  ( -5.719274019375665041, -21.55341960407619695, 29.79275706135234358 ) ) ;
#193937 = CARTESIAN_POINT ( 'NONE',  ( -9.474510206698964154, 16.51473224551069663, 115.4155762719810241 ) ) ;
#193938 = CARTESIAN_POINT ( 'NONE',  ( -15.72974639402176322, -15.80617190586768395, 94.37609039468568994 ) ) ;
#193939 = CARTESIAN_POINT ( 'NONE',  ( -5.153800228976328057, -19.02544592524343514, 87.29057627198103830 ) ) ;
#193940 = CARTESIAN_POINT ( 'NONE',  ( 21.55341960407610458, 5.719274019375980345, 88.95724293864769550 ) ) ;
#193941 = CARTESIAN_POINT ( 'NONE',  ( -19.03943276465977164, -0.05219959533935918106, 63.75109039468566863 ) ) ;
#193943 = CARTESIAN_POINT ( 'NONE',  ( -5.719274019375978568, 21.55341960407610458, 50.20724293864769550 ) ) ;
#193942 = CARTESIAN_POINT ( 'NONE',  ( -5.630366384182114103, -47.63986359793420888, -22.87684677290789637 ) ) ;
#193945 = CARTESIAN_POINT ( 'NONE',  ( -12.06949235617756955, 12.14591786802309770, 50.62390960531435979 ) ) ;
#193944 = CARTESIAN_POINT ( 'NONE',  ( -19.03943276465977164, 0.05219959533909376836, 96.24890960531436690 ) ) ;
#193946 = CARTESIAN_POINT ( 'NONE',  ( 21.82787714368445009, 6.011549001344959287, 172.1028946673681048 ) ) ;
#193947 = CARTESIAN_POINT ( 'NONE',  ( 0.05219959533936267826, -19.03943276465977164, 75.00109039468566152 ) ) ;
#193948 = CARTESIAN_POINT ( 'NONE',  ( -1.428615351859108040, -15.66706267174403422, -61.77652290643389676 ) ) ;
#193949 = CARTESIAN_POINT ( 'NONE',  ( -12.06949235617739369, -12.14591786802326823, 19.37609039468568639 ) ) ;
#193950 = CARTESIAN_POINT ( 'NONE',  ( 18.67979575497178502, 10.72451020669898547, 84.16557627198103830 ) ) ;
#193951 = CARTESIAN_POINT ( 'NONE',  ( -16.52544592524342804, 4.483927247898546575, 66.04057627198103830 ) ) ;
#193952 = CARTESIAN_POINT ( 'NONE',  ( -16.46253265017160317, 9.564922557960807481, 95.83224293864769550 ) ) ;
#193953 = CARTESIAN_POINT ( 'NONE',  ( -14.29746914071037622, -8.314922557961029526, 49.16775706135234003 ) ) ;
#193954 = CARTESIAN_POINT ( 'NONE',  ( 19.03943276465977164, -0.05219959533909143690, 58.74890960531435979 ) ) ;
#193956 = CARTESIAN_POINT ( 'NONE',  ( 0.05219959533936267826, -19.03943276465977164, 90.00109039468567573 ) ) ;
#193955 = CARTESIAN_POINT ( 'NONE',  ( 5.719274019375673035, 21.55341960407619339, 22.29275706135235069 ) ) ;
#193957 = CARTESIAN_POINT ( 'NONE',  ( 0.05219959533909260263, 19.03943276465977164, 94.99890960531436690 ) ) ;
#193958 = CARTESIAN_POINT ( 'NONE',  ( -5.153800228976328057, -19.02544592524343514, 72.29057627198102409 ) ) ;
#193959 = CARTESIAN_POINT ( 'NONE',  ( -10.81492255796078084, -18.62759615963271287, 77.08224293864769550 ) ) ;
#193960 = CARTESIAN_POINT ( 'NONE',  ( 9.564922557960805705, 16.46253265017160317, 39.58224293864768839 ) ) ;
#193961 = CARTESIAN_POINT ( 'NONE',  ( -7.963732510761932559, 36.86606204792785491, -8.000000000000001776 ) ) ;
#193962 = CARTESIAN_POINT ( 'NONE',  ( 16.55341960407611168, 4.379528057220329451, 58.95724293864770971 ) ) ;
#193963 = CARTESIAN_POINT ( 'NONE',  ( 9.474510206698971260, -16.51473224551069308, 107.9155762719810383 ) ) ;
#193964 = CARTESIAN_POINT ( 'NONE',  ( 36.91128768240056246, 2.428612879436746321E-14, 50.50000000000002842 ) ) ;
#193965 = CARTESIAN_POINT ( 'NONE',  ( 0.05219959533936267826, -19.03943276465977164, 65.00109039468567573 ) ) ;
#193966 = CARTESIAN_POINT ( 'NONE',  ( 15.80617190586746368, 15.72974639402197994, 94.37390960531436690 ) ) ;
#193967 = CARTESIAN_POINT ( 'NONE',  ( 0.05219959533936267826, -19.03943276465977164, 50.00109039468566863 ) ) ;
#193968 = CARTESIAN_POINT ( 'NONE',  ( -19.05341960407611168, -5.049401038298163336, 101.4572429386476955 ) ) ;
#193969 = FACE_BOUND ( 'NONE', #97688, .T. ) ;
#193970 = CARTESIAN_POINT ( 'NONE',  ( -21.55341960407610458, -5.719274019375992779, 41.45724293864769550 ) ) ;
#193971 = AXIS2_PLACEMENT_3D ( 'NONE', #172730, #78709, #18060 ) ;
#193972 = CARTESIAN_POINT ( 'NONE',  ( 16.51473224551069308, 9.474510206698969483, 69.16557627198102409 ) ) ;
#193973 = CARTESIAN_POINT ( 'NONE',  ( 5.823673210054444382, -21.52544592524334988, 65.20942372801901854 ) ) ;
#193974 = CARTESIAN_POINT ( 'NONE',  ( -13.89961937509977652, 13.97604488694528158, 35.62390960531435269 ) ) ;
#193976 = ORIENTED_EDGE ( 'NONE', *, *, #100974, .F. ) ;
#193975 = CARTESIAN_POINT ( 'NONE',  ( -16.55341960407611168, -4.379528057220339221, 71.45724293864769550 ) ) ;
#193977 = CARTESIAN_POINT ( 'NONE',  ( -16.53943276465976808, -0.05219959533934237506, 23.75109039468567929 ) ) ;
#193978 = CARTESIAN_POINT ( 'NONE',  ( 21.52544592524334988, 5.823673210054432836, 56.45942372801902565 ) ) ;
#193979 = ORIENTED_EDGE ( 'NONE', *, *, #23510, .T. ) ;
#193980 = CARTESIAN_POINT ( 'NONE',  ( 9.564922557960805705, 16.46253265017160317, 114.5822429386476955 ) ) ;
#193981 = CARTESIAN_POINT ( 'NONE',  ( 5.153800228976615827, -19.02544592524334988, 65.20942372801900433 ) ) ;
#193982 = CARTESIAN_POINT ( 'NONE',  ( -69.65682714487590488, -71.74905178543390605, -23.00000000000000000 ) ) ;
#193983 = CARTESIAN_POINT ( 'NONE',  ( -5.823673210054431948, 21.52544592524334988, 27.70942372801901854 ) ) ;
#193984 = CARTESIAN_POINT ( 'NONE',  ( 16.46253265017160672, -9.564922557960803928, 58.33224293864769550 ) ) ;
#193985 = CARTESIAN_POINT ( 'NONE',  ( 8.224510206698742110, 14.34966873604972548, 37.08442372801901143 ) ) ;
#193986 = CARTESIAN_POINT ( 'NONE',  ( 37.99999999999999289, 2.893978650043524126E-14, -8.749999994537628112 ) ) ;
#193987 = CARTESIAN_POINT ( 'NONE',  ( -5.823673210054431948, 21.52544592524334988, 112.7094237280190328 ) ) ;
#193988 = CARTESIAN_POINT ( 'NONE',  ( -13.97604488694527625, -13.89961937509977652, 46.87390960531435979 ) ) ;
#193989 = CARTESIAN_POINT ( 'NONE',  ( -5.049401038297874678, -19.05341960407617918, 19.79275706135233293 ) ) ;
#193990 = CARTESIAN_POINT ( 'NONE',  ( 16.55341960407618274, -4.379528057220086978, 86.04275706135236135 ) ) ;
#193992 = CARTESIAN_POINT ( 'NONE',  ( -18.67979575497193778, 10.72451020669871902, 68.33442372801900433 ) ) ;
#193991 = CARTESIAN_POINT ( 'NONE',  ( 19.05341960407611168, 5.049401038298154454, 98.95724293864766707 ) ) ;
#193993 = CARTESIAN_POINT ( 'NONE',  ( 6.852329227654482047, -5.080395570733999833, -62.03049426788788878 ) ) ;
#193994 = CARTESIAN_POINT ( 'NONE',  ( -5.049401038298153566, 19.05341960407611168, 110.2072429386476671 ) ) ;
#193995 = CARTESIAN_POINT ( 'NONE',  ( -17.49999999999999645, 5.499999999999997335, 30.79690382534172599 ) ) ;
#193997 = CARTESIAN_POINT ( 'NONE',  ( -5.823673210054431948, 21.52544592524334988, 67.70942372801901854 ) ) ;
#193996 = CARTESIAN_POINT ( 'NONE',  ( -12.06949235617739369, -12.14591786802326823, 59.37609039468568284 ) ) ;
#193998 = CARTESIAN_POINT ( 'NONE',  ( -21.55341960407619339, 5.719274019375674811, 98.54275706135234714 ) ) ;
#193999 = CARTESIAN_POINT ( 'NONE',  ( -12.05038478428680371, 9.979736640218501265, -59.62998087139816761 ) ) ;
#194000 = CARTESIAN_POINT ( 'NONE',  ( 12.06949235617739724, 12.14591786802326823, 31.87609039468567929 ) ) ;
#194001 = CARTESIAN_POINT ( 'NONE',  ( 5.049401038298161559, -19.05341960407611168, 82.70724293864770971 ) ) ;
#194002 = CARTESIAN_POINT ( 'NONE',  ( 13.89961937509977652, -13.97604488694527269, 108.1239096053143669 ) ) ;
#194003 = VERTEX_POINT ( 'NONE', #167285 ) ;
#194004 = CARTESIAN_POINT ( 'NONE',  ( 17.40861289039002813, 6.110651285853277770, 43.87232470827434128 ) ) ;
#194005 = CARTESIAN_POINT ( 'NONE',  ( -13.97604488694527625, -13.89961937509977652, 41.87390960531435979 ) ) ;
#194006 = CARTESIAN_POINT ( 'NONE',  ( -5.823673210054116645, -21.52544592524344225, 47.29057627198103120 ) ) ;
#194007 = CARTESIAN_POINT ( 'NONE',  ( -8.314922557961024197, 14.29746914071037800, 107.9177570613523471 ) ) ;
#194009 = CARTESIAN_POINT ( 'NONE',  ( -19.05341960407611168, -5.049401038298163336, 71.45724293864766707 ) ) ;
#194008 = CARTESIAN_POINT ( 'NONE',  ( -12.14591786802309592, -12.06949235617757132, 81.87390960531435269 ) ) ;
#194010 = CARTESIAN_POINT ( 'NONE',  ( -5.719274019375665041, -21.55341960407619695, 99.79275706135234714 ) ) ;
#194011 = CARTESIAN_POINT ( 'NONE',  ( 0.05219959533934541429, -16.53943276465976808, 20.00109039468568639 ) ) ;
#194012 = CARTESIAN_POINT ( 'NONE',  ( 16.53943276465976808, -0.05219959533910856209, 83.74890960531435269 ) ) ;
#194013 = CARTESIAN_POINT ( 'NONE',  ( 15.72974639402176855, 15.80617190586768217, 41.87609039468568284 ) ) ;
#194014 = CARTESIAN_POINT ( 'NONE',  ( -21.55341960407610458, -5.719274019375992779, 76.45724293864769550 ) ) ;
#194015 = CARTESIAN_POINT ( 'NONE',  ( -9.564922557961040184, 16.46253265017147172, 57.91775706135233293 ) ) ;
#194016 = CARTESIAN_POINT ( 'NONE',  ( -35.09778042078744420, 5.635567127521238007, 40.04523299337172659 ) ) ;
#194017 = CARTESIAN_POINT ( 'NONE',  ( 19.05341960407611168, 5.049401038298154454, 98.95724293864766707 ) ) ;
#194018 = CARTESIAN_POINT ( 'NONE',  ( -4.483927247898539470, -16.52544592524342804, 67.29057627198103830 ) ) ;
#194019 = CARTESIAN_POINT ( 'NONE',  ( -12.14591786802309592, -12.06949235617757132, 51.87390960531437401 ) ) ;
#194020 = CARTESIAN_POINT ( 'NONE',  ( 16.53943276465976808, -0.05219959533910856209, 23.74890960531435269 ) ) ;
#194021 = CARTESIAN_POINT ( 'NONE',  ( 0.05219959533936267826, -19.03943276465977164, 70.00109039468566152 ) ) ;
#194022 = DIRECTION ( 'NONE',  ( 0.000000000000000000, -0.4999999999999993894, 0.8660254037844389297 ) ) ;
#194023 = CARTESIAN_POINT ( 'NONE',  ( 9.474510206698971260, -16.51473224551069308, 112.9155762719810383 ) ) ;
#194024 = CARTESIAN_POINT ( 'NONE',  ( -16.52544592524342804, 4.483927247898546575, 86.04057627198102409 ) ) ;
#194025 = DIRECTION ( 'NONE',  ( -1.000000000000000000, 0.000000000000000000, 0.000000000000000000 ) ) ;
#194027 = CARTESIAN_POINT ( 'NONE',  ( -10.72451020669898014, 18.67979575497178502, 55.41557627198102409 ) ) ;
#194026 = CARTESIAN_POINT ( 'NONE',  ( -16.51473224551069308, -9.474510206698971260, 41.66557627198103120 ) ) ;
#194028 = CARTESIAN_POINT ( 'NONE',  ( -18.62759615963270932, 10.81492255796079327, 80.83224293864769550 ) ) ;
#194029 = CARTESIAN_POINT ( 'NONE',  ( 9.564922557960805705, 16.46253265017160317, 24.58224293864769194 ) ) ;
#194031 = CARTESIAN_POINT ( 'NONE',  ( -16.51473224551069308, -9.474510206698971260, 56.66557627198103120 ) ) ;
#194030 = CARTESIAN_POINT ( 'NONE',  ( 8.224510206698742110, 14.34966873604972548, 62.08442372801901143 ) ) ;
#194032 = CARTESIAN_POINT ( 'NONE',  ( 5.049401038297881783, 19.05341960407617563, 42.29275706135234003 ) ) ;
#194033 = CARTESIAN_POINT ( 'NONE',  ( -15.72974639402176322, -15.80617190586768395, 49.37609039468569705 ) ) ;
#194034 = CARTESIAN_POINT ( 'NONE',  ( -10.81492255796078084, -18.62759615963271287, 42.08224293864769550 ) ) ;
#194035 = CARTESIAN_POINT ( 'NONE',  ( 14.34966873604960469, 8.224510206698951720, 109.1655762719810383 ) ) ;
#194036 = CARTESIAN_POINT ( 'NONE',  ( -9.564922557961040184, 16.46253265017147172, 87.91775706135233293 ) ) ;
#194037 = CARTESIAN_POINT ( 'NONE',  ( -29.86685920354755197, -21.69954338932560134, -6.924999997268813878 ) ) ;
#194039 = CARTESIAN_POINT ( 'NONE',  ( -10.72451020669898014, 18.67979575497178502, 45.41557627198103830 ) ) ;
#194038 = CARTESIAN_POINT ( 'NONE',  ( -0.5310992180246781880, -24.20670376297026749, -56.83968087238905298 ) ) ;
#194040 = CARTESIAN_POINT ( 'NONE',  ( 17.13100169013300800, -6.664070546373151771, 68.26789835699850073 ) ) ;
#194041 = CARTESIAN_POINT ( 'NONE',  ( 10.72451020669871369, 18.67979575497193778, 87.08442372801901854 ) ) ;
#194042 = CARTESIAN_POINT ( 'NONE',  ( 12.14591786802309770, 12.06949235617756955, 29.37390960531435269 ) ) ;
#194044 = CARTESIAN_POINT ( 'NONE',  ( -8.314922557960811034, -14.29746914071050412, 62.08224293864769550 ) ) ;
#194043 = CARTESIAN_POINT ( 'NONE',  ( 0.05219959533934541429, -16.53943276465976808, 55.00109039468568284 ) ) ;
#194045 = CARTESIAN_POINT ( 'NONE',  ( 10.72451020669898902, -18.67979575497178502, 77.91557627198102409 ) ) ;
#194046 = CARTESIAN_POINT ( 'NONE',  ( -5.719274019375978568, 21.55341960407610458, 70.20724293864769550 ) ) ;
#194047 = CARTESIAN_POINT ( 'NONE',  ( 0.000000000000000000, 0.000000000000000000, -18.00000000000000000 ) ) ;
#194050 = ADVANCED_FACE ( 'NONE', ( #30750 ), #60083, .T. ) ;
#194049 = CARTESIAN_POINT ( 'NONE',  ( -10.72451020669898014, 18.67979575497178502, 25.41557627198103120 ) ) ;
#194048 = CARTESIAN_POINT ( 'NONE',  ( -5.049401038297874678, -19.05341960407617918, 79.79275706135233293 ) ) ;
#194051 = CARTESIAN_POINT ( 'NONE',  ( -19.03943276465977164, 0.05219959533909376836, 66.24890960531436690 ) ) ;
#194052 = CARTESIAN_POINT ( 'NONE',  ( 13.89961937509977652, -13.97604488694527269, 28.12390960531435624 ) ) ;
#194053 =( NAMED_UNIT ( * ) SI_UNIT ( $, .STERADIAN. ) SOLID_ANGLE_UNIT ( ) );
#194054 = CARTESIAN_POINT ( 'NONE',  ( 28.79475375365586132, 2.781246896534039337E-14, 146.9843446568999923 ) ) ;
#194055 = ORIENTED_EDGE ( 'NONE', *, *, #165915, .F. ) ;
#194056 = CARTESIAN_POINT ( 'NONE',  ( -14.34966873604972548, 8.224510206698743886, 88.33442372801901854 ) ) ;
#194057 = CARTESIAN_POINT ( 'NONE',  ( -5.823673210054431948, 21.52544592524334988, 22.70942372801901499 ) ) ;
#194058 = CARTESIAN_POINT ( 'NONE',  ( 0.05219959533909260263, 19.03943276465977164, 74.99890960531435269 ) ) ;
#194059 = CARTESIAN_POINT ( 'NONE',  ( -10.81492255796105439, 18.62759615963255655, 57.91775706135234714 ) ) ;
#194060 = CARTESIAN_POINT ( 'NONE',  ( -16.46253265017160317, 9.564922557960807481, 90.83224293864769550 ) ) ;
#194061 = CARTESIAN_POINT ( 'NONE',  ( -25.90378602754346815, -30.37248848106881027, -17.06839622125142952 ) ) ;
#194062 = VERTEX_POINT ( 'NONE', #107565 ) ;
#194063 = CARTESIAN_POINT ( 'NONE',  ( -15.72974639402176322, -15.80617190586768395, 49.37609039468569705 ) ) ;
#194065 = CARTESIAN_POINT ( 'NONE',  ( 5.153800228976335163, 19.02544592524342804, 99.79057627198102409 ) ) ;
#194064 = CARTESIAN_POINT ( 'NONE',  ( -5.049401038298153566, 19.05341960407611168, 30.20724293864768839 ) ) ;
#194066 = CARTESIAN_POINT ( 'NONE',  ( -19.02544592524334988, -5.153800228976617603, 53.95942372801898301 ) ) ;
#194067 = CARTESIAN_POINT ( 'NONE',  ( 0.05219959533937995610, -21.53943276465977519, 20.00109039468568639 ) ) ;
#194068 = CARTESIAN_POINT ( 'NONE',  ( 5.049401038297881783, 19.05341960407617563, 47.29275706135231161 ) ) ;
#194069 = CARTESIAN_POINT ( 'NONE',  ( -16.51473224551082808, 9.474510206698731452, 48.33442372801900433 ) ) ;
#194071 = VERTEX_POINT ( 'NONE', #138905 ) ;
#194070 = CARTESIAN_POINT ( 'NONE',  ( -0.05219959533934338120, 16.53943276465976808, 107.5010903946856899 ) ) ;
#194072 = CARTESIAN_POINT ( 'NONE',  ( 10.33258783678506987, 12.20200080651908792, -61.66593582935062301 ) ) ;
#194073 = CARTESIAN_POINT ( 'NONE',  ( -5.153800228976328057, -19.02544592524343514, 72.29057627198102409 ) ) ;
#194074 = CARTESIAN_POINT ( 'NONE',  ( 5.719274019375673035, 21.55341960407619339, 77.29275706135234714 ) ) ;
#194075 = CARTESIAN_POINT ( 'NONE',  ( -15.72974639402176322, -15.80617190586768395, 99.37609039468568994 ) ) ;
#194076 = CARTESIAN_POINT ( 'NONE',  ( 24.30000000000003268, 0.000000000000000000, -54.21489346206828230 ) ) ;
#194077 = CARTESIAN_POINT ( 'NONE',  ( -13.97604488694527625, -13.89961937509977652, 81.87390960531436690 ) ) ;
#194078 = CARTESIAN_POINT ( 'NONE',  ( -18.67979575497193778, 10.72451020669871902, 73.33442372801901854 ) ) ;
#194079 = CARTESIAN_POINT ( 'NONE',  ( 9.474510206698729675, 16.51473224551082808, 112.0844237280190043 ) ) ;
#194080 = CARTESIAN_POINT ( 'NONE',  ( 9.564922557960805705, 16.46253265017160317, 64.58224293864769550 ) ) ;
#194081 = CARTESIAN_POINT ( 'NONE',  ( -9.474510206698964154, 16.51473224551069663, 110.4155762719810383 ) ) ;
#194082 = CARTESIAN_POINT ( 'NONE',  ( -5.153800228976328057, -19.02544592524343514, 92.29057627198099567 ) ) ;
#194083 = CARTESIAN_POINT ( 'NONE',  ( 18.22780087662122739, 5.500000000000000888, 86.48236817873107896 ) ) ;
#194084 = CARTESIAN_POINT ( 'NONE',  ( 13.89961937509977652, -13.97604488694527269, 78.12390960531433848 ) ) ;
#194085 = CARTESIAN_POINT ( 'NONE',  ( 0.05219959533909260263, 19.03943276465977164, 59.99890960531436690 ) ) ;
#194086 = CARTESIAN_POINT ( 'NONE',  ( -21.55341960407610458, -5.719274019375992779, 106.4572429386477097 ) ) ;
#194087 = CARTESIAN_POINT ( 'NONE',  ( 12.06949235617739724, 12.14591786802326823, 101.8760903946857042 ) ) ;
#194088 = CARTESIAN_POINT ( 'NONE',  ( 1.216837300817233514, 16.09857462465207334, -61.59776990020974097 ) ) ;
#194089 = CARTESIAN_POINT ( 'NONE',  ( 9.564922557961047289, -16.46253265017146816, 55.41775706135234003 ) ) ;
#194090 = CARTESIAN_POINT ( 'NONE',  ( 9.474510206698971260, -16.51473224551069308, 92.91557627198103830 ) ) ;
#194091 = CARTESIAN_POINT ( 'NONE',  ( 14.34966873604960469, 8.224510206698951720, 84.16557627198103830 ) ) ;
#194092 = CARTESIAN_POINT ( 'NONE',  ( 16.46253265017160672, -9.564922557960803928, 28.33224293864769550 ) ) ;
#194093 = CARTESIAN_POINT ( 'NONE',  ( -0.05219959533907301413, -21.53943276465977519, 27.49890960531435269 ) ) ;
#194094 = CARTESIAN_POINT ( 'NONE',  ( -5.823673210054116645, -21.52544592524344225, 27.29057627198103120 ) ) ;
#194095 = CARTESIAN_POINT ( 'NONE',  ( 12.14591786802309770, 12.06949235617756955, 94.37390960531436690 ) ) ;
#194096 = CARTESIAN_POINT ( 'NONE',  ( -27.73933785331498925, 2.428612866367529932E-14, 149.3750000027311842 ) ) ;
#194097 = CARTESIAN_POINT ( 'NONE',  ( -5.153800228976607833, 19.02544592524334988, 47.70942372801900433 ) ) ;
#194098 = CARTESIAN_POINT ( 'NONE',  ( 12.06949235617739724, 12.14591786802326823, 101.8760903946857042 ) ) ;
#194099 = CARTESIAN_POINT ( 'NONE',  ( -9.564922557960796823, -16.46253265017161027, 82.08224293864768129 ) ) ;
#194100 = CARTESIAN_POINT ( 'NONE',  ( 18.67979575497194134, -10.72451020669871369, 65.83442372801900433 ) ) ;
#194101 = CARTESIAN_POINT ( 'NONE',  ( -10.72451020669898014, 18.67979575497178502, 45.41557627198103830 ) ) ;
#194102 = CARTESIAN_POINT ( 'NONE',  ( -18.67979575497193778, 10.72451020669871902, 33.33442372801900433 ) ) ;
#194103 = CARTESIAN_POINT ( 'NONE',  ( -10.81492255796078084, -18.62759615963271287, 87.08224293864769550 ) ) ;
#194104 = CARTESIAN_POINT ( 'NONE',  ( 14.29746914071049879, -8.314922557960816363, 113.3322429386476955 ) ) ;
#194105 = CARTESIAN_POINT ( 'NONE',  ( 5.153800228976615827, -19.02544592524334988, 75.20942372801896170 ) ) ;
#194106 = CARTESIAN_POINT ( 'NONE',  ( -19.02544592524342804, 5.153800228976336051, 41.04057627198103120 ) ) ;
#194107 = CARTESIAN_POINT ( 'NONE',  ( -5.153800228976328057, -19.02544592524343514, 102.2905762719810383 ) ) ;
#194108 = CARTESIAN_POINT ( 'NONE',  ( 19.03943276465977164, -0.05219959533909143690, 93.74890960531435269 ) ) ;
#194109 = CARTESIAN_POINT ( 'NONE',  ( -8.314922557960811034, -14.29746914071050412, 112.0822429386477097 ) ) ;
#194110 = CARTESIAN_POINT ( 'NONE',  ( -16.52544592524342804, 4.483927247898546575, 41.04057627198103120 ) ) ;
#194111 = CARTESIAN_POINT ( 'NONE',  ( -16.55341960407617563, 4.379528057220093196, 43.54275706135235424 ) ) ;
#194112 = CARTESIAN_POINT ( 'NONE',  ( 15.72974639402176855, 15.80617190586768217, 111.8760903946856615 ) ) ;
#194113 = CARTESIAN_POINT ( 'NONE',  ( -16.53943276465976808, -0.05219959533934237506, 113.7510903946856757 ) ) ;
#194114 = CARTESIAN_POINT ( 'NONE',  ( 5.719274019375673035, 21.55341960407619339, 37.29275706135235424 ) ) ;
#194115 = CARTESIAN_POINT ( 'NONE',  ( -0.05219959533909027116, -19.03943276465977164, 102.4989096053143669 ) ) ;
#194116 = EDGE_CURVE ( 'NONE', #163522, #134048, #93390, .T. ) ;
#194117 = CARTESIAN_POINT ( 'NONE',  ( -8.314922557961024197, 14.29746914071037800, 107.9177570613523471 ) ) ;
#194118 = CARTESIAN_POINT ( 'NONE',  ( -16.52544592524335698, -4.483927247898792601, 93.95942372801903275 ) ) ;
#194119 = CARTESIAN_POINT ( 'NONE',  ( -4.379528057220086978, -16.55341960407618274, 24.79275706135235779 ) ) ;
#194120 = CARTESIAN_POINT ( 'NONE',  ( 13.97604488694527802, 13.89961937509977652, 49.37390960531434558 ) ) ;
#194121 = CARTESIAN_POINT ( 'NONE',  ( 4.379528057220339221, -16.55341960407611168, 102.7072429386476955 ) ) ;
#194122 = CARTESIAN_POINT ( 'NONE',  ( 15.80617190586769283, -15.72974639402175789, 20.62609039468568639 ) ) ;
#194123 = CARTESIAN_POINT ( 'NONE',  ( -19.05341960407611168, -5.049401038298163336, 26.45724293864769550 ) ) ;
#194124 = CARTESIAN_POINT ( 'NONE',  ( 19.02544592524343514, -5.153800228976328945, 108.5405762719810383 ) ) ;
#194125 = CARTESIAN_POINT ( 'NONE',  ( -18.62759615963255300, -10.81492255796106328, 29.16775706135234003 ) ) ;
#194126 = CARTESIAN_POINT ( 'NONE',  ( 19.02544592524343514, -5.153800228976328945, 28.54057627198102409 ) ) ;
#194127 = CARTESIAN_POINT ( 'NONE',  ( 13.97604488694527802, 13.89961937509977652, 104.3739096053143385 ) ) ;
#194128 = CARTESIAN_POINT ( 'NONE',  ( -16.52216118717209170, -7.221426719304468556, 36.07599021046992505 ) ) ;
#194129 = CARTESIAN_POINT ( 'NONE',  ( -13.89961937509977652, 13.97604488694528158, 95.62390960531436690 ) ) ;
#194131 = CARTESIAN_POINT ( 'NONE',  ( -12.14591786802309592, -12.06949235617757132, 86.87390960531438111 ) ) ;
#194130 = CARTESIAN_POINT ( 'NONE',  ( 0.05219959533937995610, -21.53943276465977519, 50.00109039468568994 ) ) ;
#194132 = CARTESIAN_POINT ( 'NONE',  ( 9.474510206698971260, -16.51473224551069308, 97.91557627198102409 ) ) ;
#194133 = CARTESIAN_POINT ( 'NONE',  ( -27.91695578976807823, -6.846979738067211940, 161.8037495850383607 ) ) ;
#194134 = CARTESIAN_POINT ( 'NONE',  ( 8.314922557961029526, -14.29746914071037800, 70.41775706135236135 ) ) ;
#194135 = CARTESIAN_POINT ( 'NONE',  ( -5.823673210054431948, 21.52544592524334988, 77.70942372801900433 ) ) ;
#194136 = CARTESIAN_POINT ( 'NONE',  ( 4.483927247898790824, -16.52544592524335698, 35.20942372801901854 ) ) ;
#194137 = CARTESIAN_POINT ( 'NONE',  ( -9.474510206698964154, 16.51473224551069663, 85.41557627198102409 ) ) ;
#194138 = CARTESIAN_POINT ( 'NONE',  ( 16.51473224551083163, -9.474510206698727899, 105.8344237280190043 ) ) ;
#194139 = CARTESIAN_POINT ( 'NONE',  ( -16.52544592524335698, -4.483927247898792601, 73.95942372801901854 ) ) ;
#194140 = CARTESIAN_POINT ( 'NONE',  ( -16.51473224551082808, 9.474510206698731452, 93.33442372801900433 ) ) ;
#194141 = CARTESIAN_POINT ( 'NONE',  ( 19.03943276465977164, -0.05219959533909143690, 63.74890960531435979 ) ) ;
#194142 = CARTESIAN_POINT ( 'NONE',  ( -10.72451020669898014, 18.67979575497178502, 90.41557627198103830 ) ) ;
#194144 = CARTESIAN_POINT ( 'NONE',  ( 16.46253265017146816, 9.564922557961045513, 86.66775706135233293 ) ) ;
#194143 = CARTESIAN_POINT ( 'NONE',  ( -16.55341960407611168, -4.379528057220339221, 91.45724293864769550 ) ) ;
#194145 = CARTESIAN_POINT ( 'NONE',  ( -16.55341960407617563, 4.379528057220093196, 53.54275706135234714 ) ) ;
#194146 = CARTESIAN_POINT ( 'NONE',  ( 17.26172910966780805, -6.454744622555771194, 63.30646908649223548 ) ) ;
#194147 = CARTESIAN_POINT ( 'NONE',  ( -13.89961937509957401, -13.97604488694547875, 54.37609039468565442 ) ) ;
#194148 = CARTESIAN_POINT ( 'NONE',  ( 16.55341960407611168, 4.379528057220329451, 38.95724293864768839 ) ) ;
#194149 = CARTESIAN_POINT ( 'NONE',  ( 8.314922557960818139, 14.29746914071049879, 84.58224293864769550 ) ) ;
#194151 = CARTESIAN_POINT ( 'NONE',  ( -19.36337904590694237, 5.499999999999952927, 90.41494137495621430 ) ) ;
#194150 = CARTESIAN_POINT ( 'NONE',  ( 19.05341960407617918, -5.049401038297876454, 21.04275706135232582 ) ) ;
#194152 = CARTESIAN_POINT ( 'NONE',  ( 21.53943276465977519, 0.05219959533937863772, 26.25109039468567573 ) ) ;
#194153 = SPHERICAL_SURFACE ( 'NONE', #124733, 2.000000000000000000 ) ;
#194154 = CARTESIAN_POINT ( 'NONE',  ( 9.474510206698971260, -16.51473224551069308, 72.91557627198102409 ) ) ;
#194155 = CARTESIAN_POINT ( 'NONE',  ( 18.62759615963255655, 10.81492255796105972, 91.66775706135234714 ) ) ;
#194156 = CARTESIAN_POINT ( 'NONE',  ( 19.05341960407611168, 5.049401038298154454, 73.95724293864768129 ) ) ;
#194157 = CARTESIAN_POINT ( 'NONE',  ( -21.55341960407610458, -5.719274019375992779, 46.45724293864769550 ) ) ;
#194158 = CARTESIAN_POINT ( 'NONE',  ( -16.52544592524342804, 4.483927247898546575, 76.04057627198102409 ) ) ;
#194159 = CARTESIAN_POINT ( 'NONE',  ( -13.97604488694527625, -13.89961937509977652, 61.87390960531435979 ) ) ;
#194160 = CARTESIAN_POINT ( 'NONE',  ( 14.29746914071049879, -8.314922557960816363, 113.3322429386476955 ) ) ;
#194161 = CARTESIAN_POINT ( 'NONE',  ( 5.823673210054444382, -21.52544592524334988, 25.20942372801901854 ) ) ;
#194162 = CARTESIAN_POINT ( 'NONE',  ( -0.05219959533937732626, 21.53943276465977519, 62.50109039468568284 ) ) ;
#194163 = CARTESIAN_POINT ( 'NONE',  ( -19.03943276465977164, 0.05219959533909376836, 46.24890960531435979 ) ) ;
#194164 = CARTESIAN_POINT ( 'NONE',  ( 8.224510206698742110, 14.34966873604972548, 67.08442372801901854 ) ) ;
#194165 = CARTESIAN_POINT ( 'NONE',  ( -10.72451020669898014, 18.67979575497178502, 115.4155762719810241 ) ) ;
#194166 = CARTESIAN_POINT ( 'NONE',  ( 18.62759615963271287, -10.81492255796078972, 108.3322429386477097 ) ) ;
#194168 = CARTESIAN_POINT ( 'NONE',  ( 16.46253265017160672, -9.564922557960803928, 68.33224293864770971 ) ) ;
#194167 = CARTESIAN_POINT ( 'NONE',  ( 19.05341960407617918, -5.049401038297876454, 46.04275706135233293 ) ) ;
#194169 = CARTESIAN_POINT ( 'NONE',  ( -17.49999999999998934, -5.500000000000015987, 56.28230962303566542 ) ) ;
#194170 = CARTESIAN_POINT ( 'NONE',  ( -10.72451020669870658, -18.67979575497194134, 64.58442372801900433 ) ) ;
#194171 = CARTESIAN_POINT ( 'NONE',  ( 15.72974639402199770, -15.80617190586745480, 53.12390960531436690 ) ) ;
#194172 = CARTESIAN_POINT ( 'NONE',  ( -12.14591786802309592, -12.06949235617757132, 36.87390960531435979 ) ) ;
#194174 = CARTESIAN_POINT ( 'NONE',  ( 5.153800228976615827, -19.02544592524334988, 20.20942372801899722 ) ) ;
#194173 = CARTESIAN_POINT ( 'NONE',  ( -0.05219959533937732626, 21.53943276465977519, 77.50109039468567573 ) ) ;
#194175 = CARTESIAN_POINT ( 'NONE',  ( 8.224510206698953496, -14.34966873604960469, 57.91557627198103120 ) ) ;
#194176 = CARTESIAN_POINT ( 'NONE',  ( 14.34966873604960469, 8.224510206698951720, 99.16557627198100988 ) ) ;
#194177 = CARTESIAN_POINT ( 'NONE',  ( -0.05219959533936034679, 19.03943276465977164, 62.50109039468566863 ) ) ;
#194178 = CARTESIAN_POINT ( 'NONE',  ( -0.05219959533934338120, 16.53943276465976808, 112.5010903946857042 ) ) ;
#194179 = CARTESIAN_POINT ( 'NONE',  ( 18.62759615963255655, 10.81492255796105972, 71.66775706135234714 ) ) ;
#194180 = CARTESIAN_POINT ( 'NONE',  ( -0.05219959533909027116, -19.03943276465977164, 77.49890960531435269 ) ) ;
#194181 = CARTESIAN_POINT ( 'NONE',  ( 0.05219959533936267826, -19.03943276465977164, 40.00109039468566152 ) ) ;
#194182 = CARTESIAN_POINT ( 'NONE',  ( 15.72974639402199770, -15.80617190586745480, 38.12390960531436690 ) ) ;
#194183 = CARTESIAN_POINT ( 'NONE',  ( -21.53943276465977519, -0.05219959533937600094, 38.75109039468567573 ) ) ;
#194184 = CARTESIAN_POINT ( 'NONE',  ( -15.72974639402197994, 15.80617190586746368, 90.62390960531436690 ) ) ;
#194185 = CARTESIAN_POINT ( 'NONE',  ( -19.03943276465977164, -0.05219959533935918106, 98.75109039468567573 ) ) ;
#194186 = CARTESIAN_POINT ( 'NONE',  ( 0.05219959533934541429, -16.53943276465976808, 50.00109039468568994 ) ) ;
#194188 = CARTESIAN_POINT ( 'NONE',  ( -10.72451020669898014, 18.67979575497178502, 90.41557627198103830 ) ) ;
#194187 = CARTESIAN_POINT ( 'NONE',  ( -23.48529157249600985, 32.32473071737754111, -6.299999999999999822 ) ) ;
#194189 = CARTESIAN_POINT ( 'NONE',  ( 12.14591786802309770, 12.06949235617756955, 89.37390960531435269 ) ) ;
#194190 = CARTESIAN_POINT ( 'NONE',  ( 17.97058386085788939, 5.500000000000048850, 41.50390968646216550 ) ) ;
#194191 = CARTESIAN_POINT ( 'NONE',  ( -16.53943276465976808, -0.05219959533934237506, 23.75109039468567929 ) ) ;
#194192 = CARTESIAN_POINT ( 'NONE',  ( -5.719274019375978568, 21.55341960407610458, 50.20724293864769550 ) ) ;
#194193 = CARTESIAN_POINT ( 'NONE',  ( -8.314922557961024197, 14.29746914071037800, 92.91775706135236135 ) ) ;
#194194 = CARTESIAN_POINT ( 'NONE',  ( 19.02544592524343514, -5.153800228976328945, 23.54057627198102054 ) ) ;
#194195 = CARTESIAN_POINT ( 'NONE',  ( 8.224510206698742110, 14.34966873604972548, 47.08442372801901854 ) ) ;
#194196 = CARTESIAN_POINT ( 'NONE',  ( 18.67979575497194134, -10.72451020669871369, 25.83442372801901499 ) ) ;
#194197 = CARTESIAN_POINT ( 'NONE',  ( 10.81492255796078972, 18.62759615963270932, 49.58224293864769550 ) ) ;
#194198 = CARTESIAN_POINT ( 'NONE',  ( 16.55341960407618274, -4.379528057220086978, 86.04275706135236135 ) ) ;
#194199 = CARTESIAN_POINT ( 'NONE',  ( 5.153800228976335163, 19.02544592524342804, 94.79057627198103830 ) ) ;
#194200 = CARTESIAN_POINT ( 'NONE',  ( 5.823673210054444382, -21.52544592524334988, 50.20942372801901854 ) ) ;
#194201 = CARTESIAN_POINT ( 'NONE',  ( 21.55341960407610458, 5.719274019375980345, 43.95724293864769550 ) ) ;
#194202 = CARTESIAN_POINT ( 'NONE',  ( -16.51473224551069308, -9.474510206698971260, 111.6655762719810383 ) ) ;
#194203 = ORIENTED_EDGE ( 'NONE', *, *, #178675, .T. ) ;
#194204 = CARTESIAN_POINT ( 'NONE',  ( -19.03943276465977164, -0.05219959533935918106, 33.75109039468566863 ) ) ;
#194205 = CARTESIAN_POINT ( 'NONE',  ( 16.53943276465976808, 0.05219959533934440121, 61.25109039468567573 ) ) ;
#194206 = CARTESIAN_POINT ( 'NONE',  ( 18.67979575497178502, 10.72451020669898547, 24.16557627198103120 ) ) ;
#194207 = VERTEX_POINT ( 'NONE', #105598 ) ;
#194208 = CARTESIAN_POINT ( 'NONE',  ( 16.51473224551069308, 9.474510206698969483, 84.16557627198102409 ) ) ;
#194209 = CARTESIAN_POINT ( 'NONE',  ( -14.34966873604972548, 8.224510206698743886, 98.33442372801901854 ) ) ;
#194210 = CARTESIAN_POINT ( 'NONE',  ( 15.38714178908743690, -36.74766143018467801, -28.97229394964844928 ) ) ;
#194211 = CARTESIAN_POINT ( 'NONE',  ( -0.05219959533910754901, -16.53943276465976808, 97.49890960531436690 ) ) ;
#194212 = CARTESIAN_POINT ( 'NONE',  ( 21.53943276465977519, -0.05219959533907433946, 48.74890960531435979 ) ) ;
#194213 = CARTESIAN_POINT ( 'NONE',  ( 5.049401038298161559, -19.05341960407611168, 32.70724293864768129 ) ) ;
#194214 = CARTESIAN_POINT ( 'NONE',  ( -14.34966873604972548, 8.224510206698743886, 78.33442372801901854 ) ) ;
#194215 = CARTESIAN_POINT ( 'NONE',  ( 5.823673210054444382, -21.52544592524334988, 35.20942372801901854 ) ) ;
#194216 = CARTESIAN_POINT ( 'NONE',  ( 9.564922557961047289, -16.46253265017146816, 85.41775706135233293 ) ) ;
#194217 = CARTESIAN_POINT ( 'NONE',  ( 8.314922557960818139, 14.29746914071049879, 89.58224293864768129 ) ) ;
#194218 = CARTESIAN_POINT ( 'NONE',  ( 9.564922557960805705, 16.46253265017160317, 49.58224293864770260 ) ) ;
#194219 = CARTESIAN_POINT ( 'NONE',  ( 13.97604488694527802, 13.89961937509977652, 114.3739096053143669 ) ) ;
#194220 = CARTESIAN_POINT ( 'NONE',  ( -21.53943276465977519, -0.05219959533937600094, 108.7510903946857042 ) ) ;
#194221 = CARTESIAN_POINT ( 'NONE',  ( 13.97604488694527802, 13.89961937509977652, 74.37390960531436690 ) ) ;
#194222 = CARTESIAN_POINT ( 'NONE',  ( -16.52544592524335698, -4.483927247898792601, 58.95942372801902565 ) ) ;
#194223 = CARTESIAN_POINT ( 'NONE',  ( -21.55341960407619339, 5.719274019375674811, 98.54275706135234714 ) ) ;
#194224 = CARTESIAN_POINT ( 'NONE',  ( -16.55341960407617563, 4.379528057220093196, 68.54275706135234714 ) ) ;
#194225 = CARTESIAN_POINT ( 'NONE',  ( 5.049401038297881783, 19.05341960407617563, 57.29275706135231871 ) ) ;
#194226 = CARTESIAN_POINT ( 'NONE',  ( -9.564922557961040184, 16.46253265017147172, 62.91775706135233293 ) ) ;
#194227 = CARTESIAN_POINT ( 'NONE',  ( -15.80617190586768217, 15.72974639402176855, 68.12609039468567573 ) ) ;
#194228 = CARTESIAN_POINT ( 'NONE',  ( -5.153800228976328057, -19.02544592524343514, 67.29057627198102409 ) ) ;
#194229 = CARTESIAN_POINT ( 'NONE',  ( -19.03943276465977164, 0.05219959533909376836, 26.24890960531435624 ) ) ;
#194230 = CARTESIAN_POINT ( 'NONE',  ( -16.46253265017146816, -9.564922557961047289, 64.16775706135233293 ) ) ;
#194231 = CARTESIAN_POINT ( 'NONE',  ( 13.97604488694527802, 13.89961937509977652, 114.3739096053143669 ) ) ;
#194232 = CARTESIAN_POINT ( 'NONE',  ( -19.02544592524342804, 5.153800228976336051, 86.04057627198103830 ) ) ;
#194233 = CARTESIAN_POINT ( 'NONE',  ( 14.34966873604960469, 8.224510206698951720, 44.16557627198103120 ) ) ;
#194234 = CARTESIAN_POINT ( 'NONE',  ( -15.80617190586745835, -15.72974639402198527, 46.87390960531435979 ) ) ;
#194235 = CARTESIAN_POINT ( 'NONE',  ( -5.427562675786936573E-15, 30.27659582821221207, 141.4843446568999923 ) ) ;
#194236 = CARTESIAN_POINT ( 'NONE',  ( 9.564922557961047289, -16.46253265017146816, 20.41775706135233293 ) ) ;
#194237 = CARTESIAN_POINT ( 'NONE',  ( -17.48853670773246094, -5.747243402303008786, 81.33328700250011423 ) ) ;
#194238 = CARTESIAN_POINT ( 'NONE',  ( 19.03943276465977164, -0.05219959533909143690, 33.74890960531435979 ) ) ;
#194239 = CARTESIAN_POINT ( 'NONE',  ( 19.02544592524343514, -5.153800228976328945, 23.54057627198102054 ) ) ;
#194240 = CARTESIAN_POINT ( 'NONE',  ( -9.887582997646811478, -11.98499751262841073, -59.67881039541425281 ) ) ;
#194241 = CARTESIAN_POINT ( 'NONE',  ( 5.719274019375673035, 21.55341960407619339, 62.29275706135236845 ) ) ;
#194242 = CYLINDRICAL_SURFACE ( 'NONE', #114700, 2.649999999999999467 ) ;
#194243 = CARTESIAN_POINT ( 'NONE',  ( -4.483927247898782831, 16.52544592524335698, 67.70942372801901854 ) ) ;
#194244 = CARTESIAN_POINT ( 'NONE',  ( 10.72451020669898902, -18.67979575497178502, 87.91557627198103830 ) ) ;
#194245 = CARTESIAN_POINT ( 'NONE',  ( 14.34966873604960469, 8.224510206698951720, 59.16557627198103120 ) ) ;
#194247 = CARTESIAN_POINT ( 'NONE',  ( 0.000000000000000000, 0.000000000000000000, -62.58071313852362039 ) ) ;
#194246 = CARTESIAN_POINT ( 'NONE',  ( -13.97604488694527625, -13.89961937509977652, 31.87390960531435979 ) ) ;
#194248 = CARTESIAN_POINT ( 'NONE',  ( -21.53943276465977519, -0.05219959533937600094, 38.75109039468567573 ) ) ;
#194249 = CARTESIAN_POINT ( 'NONE',  ( 9.474510206698729675, 16.51473224551082808, 52.08442372801900433 ) ) ;
#194250 = CARTESIAN_POINT ( 'NONE',  ( -16.46253265017160317, 9.564922557960807481, 30.83224293864769550 ) ) ;
#194251 = CARTESIAN_POINT ( 'NONE',  ( -18.67979575497193778, 10.72451020669871902, 88.33442372801901854 ) ) ;
#194252 = CARTESIAN_POINT ( 'NONE',  ( 16.46253265017160672, -9.564922557960803928, 23.33224293864769194 ) ) ;
#194253 = CARTESIAN_POINT ( 'NONE',  ( -12.06949235617756955, 12.14591786802309770, 35.62390960531437401 ) ) ;
#194254 = CARTESIAN_POINT ( 'NONE',  ( 11.40812507854754365, 35.11059874428196537, -1.724999997268813479 ) ) ;
#194255 = CARTESIAN_POINT ( 'NONE',  ( -21.52544592524343514, 5.823673210054127303, 46.04057627198103830 ) ) ;
#194256 = CARTESIAN_POINT ( 'NONE',  ( 8.571926809382597767, 26.38167802310806209, 144.2750000027311899 ) ) ;
#194257 = CARTESIAN_POINT ( 'NONE',  ( 16.46253265017160672, -9.564922557960803928, 93.33224293864769550 ) ) ;
#194258 = CARTESIAN_POINT ( 'NONE',  ( -14.29746914071049879, 8.314922557960819915, 85.83224293864768129 ) ) ;
#194259 = CARTESIAN_POINT ( 'NONE',  ( -14.29746914071037622, -8.314922557961029526, 24.16775706135235424 ) ) ;
#194260 = CARTESIAN_POINT ( 'NONE',  ( -21.55341960407610458, -5.719274019375992779, 61.45724293864770260 ) ) ;
#194261 = EDGE_LOOP ( 'NONE', ( #127599, #65386, #41751, #78642 ) ) ;
#194262 = CARTESIAN_POINT ( 'NONE',  ( -19.02544592524342804, 5.153800228976336051, 31.04057627198102409 ) ) ;
#194264 = CARTESIAN_POINT ( 'NONE',  ( -5.719274019375978568, 21.55341960407610458, 90.20724293864770971 ) ) ;
#194263 = CARTESIAN_POINT ( 'NONE',  ( -19.05341960407611168, -5.049401038298163336, 81.45724293864769550 ) ) ;
#194266 = CARTESIAN_POINT ( 'NONE',  ( 0.05219959533909260263, 19.03943276465977164, 94.99890960531436690 ) ) ;
#194265 = CARTESIAN_POINT ( 'NONE',  ( -16.55341960407611168, -4.379528057220339221, 31.45724293864769550 ) ) ;
#194267 = CARTESIAN_POINT ( 'NONE',  ( 16.51473224551083163, -9.474510206698727899, 80.83442372801899012 ) ) ;
#194268 = CARTESIAN_POINT ( 'NONE',  ( 15.72974639402176855, 15.80617190586768217, 96.87609039468568994 ) ) ;
#194269 = CARTESIAN_POINT ( 'NONE',  ( 5.719274019375991003, -21.55341960407610458, 72.70724293864769550 ) ) ;
#194270 = CARTESIAN_POINT ( 'NONE',  ( -10.81492255796078084, -18.62759615963271287, 42.08224293864769550 ) ) ;
#194271 = CARTESIAN_POINT ( 'NONE',  ( 19.03943276465977164, -0.05219959533909143690, 53.74890960531436690 ) ) ;
#194272 = CARTESIAN_POINT ( 'NONE',  ( -4.379528057220328563, 16.55341960407611168, 25.20724293864769550 ) ) ;
#194273 = CARTESIAN_POINT ( 'NONE',  ( -19.05341960407611168, -5.049401038298163336, 71.45724293864766707 ) ) ;
#194274 = ORIENTED_EDGE ( 'NONE', *, *, #136776, .T. ) ;
#194275 = DIRECTION ( 'NONE',  ( 0.000000000000000000, 1.000000000000000000, 0.000000000000000000 ) ) ;
#194276 = CARTESIAN_POINT ( 'NONE',  ( 9.474510206698729675, 16.51473224551082808, 32.08442372801900433 ) ) ;
#194277 = CARTESIAN_POINT ( 'NONE',  ( 8.224510206698953496, -14.34966873604960469, 82.91557627198103830 ) ) ;
#194278 = CARTESIAN_POINT ( 'NONE',  ( 0.05219959533937995610, -21.53943276465977519, 25.00109039468567218 ) ) ;
#194279 = CARTESIAN_POINT ( 'NONE',  ( 22.44159573604009239, 16.30477369853692693, 142.5750000027311728 ) ) ;
#194281 = EDGE_CURVE ( 'NONE', #44348, #73091, #3996, .T. ) ;
#194280 = CARTESIAN_POINT ( 'NONE',  ( 5.719274019375991003, -21.55341960407610458, 62.70724293864769550 ) ) ;
#194282 = CARTESIAN_POINT ( 'NONE',  ( 12.06949235617739724, 12.14591786802326823, 96.87609039468568994 ) ) ;
#194283 = CARTESIAN_POINT ( 'NONE',  ( -0.05219959533909027116, -19.03943276465977164, 27.49890960531435624 ) ) ;
#194284 = CARTESIAN_POINT ( 'NONE',  ( 19.03943276465977164, -0.05219959533909143690, 73.74890960531435269 ) ) ;
#194285 = DIRECTION ( 'NONE',  ( 3.469446951953612217E-15, 0.000000000000000000, -1.000000000000000000 ) ) ;
#194286 = CARTESIAN_POINT ( 'NONE',  ( -12.06949235617756955, 12.14591786802309770, 30.62390960531436335 ) ) ;
#194287 = CARTESIAN_POINT ( 'NONE',  ( 21.55341960407619695, -5.719274019375665929, 66.04275706135236135 ) ) ;
#194288 = CARTESIAN_POINT ( 'NONE',  ( 9.564922557960805705, 16.46253265017160317, 104.5822429386476955 ) ) ;
#194289 = CARTESIAN_POINT ( 'NONE',  ( -21.53943276465977519, -0.05219959533937600094, 93.75109039468567573 ) ) ;
#194290 = CARTESIAN_POINT ( 'NONE',  ( 5.153800228976335163, 19.02544592524342804, 44.79057627198103830 ) ) ;
#194291 = CARTESIAN_POINT ( 'NONE',  ( -19.03943276465977164, 0.05219959533909376836, 41.24890960531435269 ) ) ;
#194292 = ORIENTED_EDGE ( 'NONE', *, *, #105079, .T. ) ;
#194293 = CARTESIAN_POINT ( 'NONE',  ( -21.55341960407619339, 5.719274019375674811, 93.54275706135234714 ) ) ;
#194294 = CARTESIAN_POINT ( 'NONE',  ( -8.314922557961024197, 14.29746914071037800, 67.91775706135234714 ) ) ;
#194295 = CARTESIAN_POINT ( 'NONE',  ( -15.72974639402176322, -15.80617190586768395, 79.37609039468567573 ) ) ;
#194296 = CARTESIAN_POINT ( 'NONE',  ( 5.049401038298161559, -19.05341960407611168, 112.7072429386476813 ) ) ;
#194297 = CARTESIAN_POINT ( 'NONE',  ( 9.474510206698729675, 16.51473224551082808, 97.08442372801900433 ) ) ;
#194298 = CARTESIAN_POINT ( 'NONE',  ( -0.05219959533937732626, 21.53943276465977519, 57.50109039468568994 ) ) ;
#194299 = CARTESIAN_POINT ( 'NONE',  ( -16.55341960407617563, 4.379528057220093196, 33.54275706135234714 ) ) ;
#194300 = CARTESIAN_POINT ( 'NONE',  ( -5.153800228976607833, 19.02544592524334988, 87.70942372801897591 ) ) ;
#194301 = CARTESIAN_POINT ( 'NONE',  ( 9.564922557960805705, 16.46253265017160317, 49.58224293864770260 ) ) ;
#194302 = CARTESIAN_POINT ( 'NONE',  ( 9.474510206698729675, 16.51473224551082808, 92.08442372801900433 ) ) ;
#194303 = CARTESIAN_POINT ( 'NONE',  ( 19.03943276465977164, 0.05219959533936151252, 86.25109039468567573 ) ) ;
#194304 = CARTESIAN_POINT ( 'NONE',  ( 0.05219959533910956823, 16.53943276465976808, 54.99890960531435269 ) ) ;
#194305 = CARTESIAN_POINT ( 'NONE',  ( -19.03943276465977164, -0.05219959533935918106, 78.75109039468567573 ) ) ;
#194306 = CARTESIAN_POINT ( 'NONE',  ( -14.34966873604972548, 8.224510206698743886, 63.33442372801900433 ) ) ;
#194307 = CARTESIAN_POINT ( 'NONE',  ( -0.05219959533936034679, 19.03943276465977164, 27.50109039468566507 ) ) ;
#194308 = CARTESIAN_POINT ( 'NONE',  ( 19.03943276465977164, -0.05219959533909143690, 33.74890960531435979 ) ) ;
#194310 = EDGE_CURVE ( 'NONE', #178697, #44348, #170549, .T. ) ;
#194309 = CARTESIAN_POINT ( 'NONE',  ( -0.05219959533909027116, -19.03943276465977164, 42.49890960531435269 ) ) ;
#194311 = CARTESIAN_POINT ( 'NONE',  ( -8.224510206698735004, -14.34966873604973081, 64.58442372801900433 ) ) ;
#194312 = CARTESIAN_POINT ( 'NONE',  ( -22.44159573604010305, 16.30477369853692338, 141.1750000027311671 ) ) ;
#194313 = CARTESIAN_POINT ( 'NONE',  ( 28.82186960331498327, 9.364793116373570925, 141.3500000054623627 ) ) ;
#194314 = CARTESIAN_POINT ( 'NONE',  ( -5.153800228976328057, -19.02544592524343514, 102.2905762719810383 ) ) ;
#194315 = LINE ( 'NONE', #133622, #97404 ) ;
#194316 = ORIENTED_EDGE ( 'NONE', *, *, #3105, .F. ) ;
#194317 = CARTESIAN_POINT ( 'NONE',  ( -19.03943276465977164, -0.05219959533935918106, 93.75109039468566152 ) ) ;
#194318 = CARTESIAN_POINT ( 'NONE',  ( -18.67979575497178146, -10.72451020669898902, 41.66557627198103120 ) ) ;
#194320 = CARTESIAN_POINT ( 'NONE',  ( -19.02544592524334988, -5.153800228976617603, 108.9594237280189759 ) ) ;
#194319 = CARTESIAN_POINT ( 'NONE',  ( 16.46253265017146816, 9.564922557961045513, 31.66775706135232937 ) ) ;
#194321 = CARTESIAN_POINT ( 'NONE',  ( 16.46253265017160672, -9.564922557960803928, 33.33224293864770260 ) ) ;
#194322 = CARTESIAN_POINT ( 'NONE',  ( -0.05219959533909027116, -19.03943276465977164, 42.49890960531435269 ) ) ;
#194323 = CARTESIAN_POINT ( 'NONE',  ( -18.62759615963270932, 10.81492255796079327, 75.83224293864769550 ) ) ;
#194324 = CARTESIAN_POINT ( 'NONE',  ( -5.049401038298153566, 19.05341960407611168, 100.2072429386476955 ) ) ;
#194325 = CARTESIAN_POINT ( 'NONE',  ( -19.02544592524342804, 5.153800228976336051, 41.04057627198103120 ) ) ;
#194326 = CARTESIAN_POINT ( 'NONE',  ( 17.14385361876520264, -23.59649016807270883, 144.0750000027311444 ) ) ;
#194327 = CARTESIAN_POINT ( 'NONE',  ( -19.02544592524334988, -5.153800228976617603, 88.95942372801897591 ) ) ;
#194328 = CARTESIAN_POINT ( 'NONE',  ( 8.224510206698953496, -14.34966873604960469, 47.91557627198102409 ) ) ;
#194329 = CARTESIAN_POINT ( 'NONE',  ( -10.72451020669898014, 18.67979575497178502, 35.41557627198102409 ) ) ;
#194330 = CARTESIAN_POINT ( 'NONE',  ( 15.80617190586769283, -15.72974639402175789, 110.6260903946857042 ) ) ;
#194331 = CARTESIAN_POINT ( 'NONE',  ( 0.05219959533907565091, 21.53943276465977519, 99.99890960531436690 ) ) ;
#194332 = CARTESIAN_POINT ( 'NONE',  ( 15.80617190586769283, -15.72974639402175789, 65.62609039468568994 ) ) ;
#194333 = CARTESIAN_POINT ( 'NONE',  ( -21.55341960407619339, 5.719274019375674811, 78.54275706135236135 ) ) ;
#194334 = CARTESIAN_POINT ( 'NONE',  ( -19.03943276465977164, 0.05219959533909376836, 106.2489096053143669 ) ) ;
#194336 = CARTESIAN_POINT ( 'NONE',  ( 15.72974639402176855, 15.80617190586768217, 66.87609039468568994 ) ) ;
#194335 = CARTESIAN_POINT ( 'NONE',  ( 4.483927247898790824, -16.52544592524335698, 105.2094237280190328 ) ) ;
#194337 = CARTESIAN_POINT ( 'NONE',  ( -19.03943276465977164, 0.05219959533909376836, 56.24890960531435979 ) ) ;
#194338 = CARTESIAN_POINT ( 'NONE',  ( 9.474510206698729675, 16.51473224551082808, 37.08442372801899722 ) ) ;
#194339 = CARTESIAN_POINT ( 'NONE',  ( -15.80617190586768217, 15.72974639402176855, 33.12609039468569705 ) ) ;
#194340 = CARTESIAN_POINT ( 'NONE',  ( -19.02544592524342804, 5.153800228976336051, 71.04057627198099567 ) ) ;
#194341 = CARTESIAN_POINT ( 'NONE',  ( 16.53943276465976808, -0.05219959533910856209, 83.74890960531435269 ) ) ;
#194342 = CARTESIAN_POINT ( 'NONE',  ( -16.52544592524342804, 4.483927247898546575, 51.04057627198103120 ) ) ;
#194343 = CARTESIAN_POINT ( 'NONE',  ( 18.67979575497178502, 10.72451020669898547, 59.16557627198103120 ) ) ;
#194344 = CARTESIAN_POINT ( 'NONE',  ( -19.02544592524342804, 5.153800228976336051, 56.04057627198100988 ) ) ;
#194345 = CARTESIAN_POINT ( 'NONE',  ( -0.05219959533907301413, -21.53943276465977519, 72.49890960531435269 ) ) ;
#194346 = CARTESIAN_POINT ( 'NONE',  ( 13.97604488694548053, -13.89961937509957401, 55.62609039468566863 ) ) ;
#194348 = CARTESIAN_POINT ( 'NONE',  ( -14.34966873604960291, -8.224510206698953496, 66.66557627198102409 ) ) ;
#194347 = CARTESIAN_POINT ( 'NONE',  ( 24.81835880841864039, -6.052260367207979996, 168.4265213779230521 ) ) ;
#194349 = CARTESIAN_POINT ( 'NONE',  ( -10.72451020669898014, 18.67979575497178502, 35.41557627198102409 ) ) ;
#194350 = ORIENTED_EDGE ( 'NONE', *, *, #179822, .F. ) ;
#194351 = CARTESIAN_POINT ( 'NONE',  ( 16.79531203550646978, 7.028104445595615424, 103.7524498822044450 ) ) ;
#194353 = CARTESIAN_POINT ( 'NONE',  ( 8.571926809382603096, -26.38167802310801235, 139.9750000027311785 ) ) ;
#194352 = CARTESIAN_POINT ( 'NONE',  ( -16.55341960407617563, 4.379528057220093196, 88.54275706135236135 ) ) ;
#194354 = ADVANCED_FACE ( 'NONE', ( #20529 ), #97350, .F. ) ;
#194355 = CARTESIAN_POINT ( 'NONE',  ( -5.049401038297874678, -19.05341960407617918, 89.79275706135230450 ) ) ;
#194356 = CARTESIAN_POINT ( 'NONE',  ( 12.14591786802309770, 12.06949235617756955, 59.37390960531436690 ) ) ;
#194357 = CYLINDRICAL_SURFACE ( 'NONE', #74152, 37.99626262588765968 ) ;
#194358 = CARTESIAN_POINT ( 'NONE',  ( -19.05341960407611168, -5.049401038298163336, 51.45724293864770260 ) ) ;
#194359 = CARTESIAN_POINT ( 'NONE',  ( -16.53943276465976808, 0.05219959533911058130, 41.24890960531435269 ) ) ;
#194360 = CARTESIAN_POINT ( 'NONE',  ( -0.05219959533909027116, -19.03943276465977164, 92.49890960531436690 ) ) ;
#194361 = CARTESIAN_POINT ( 'NONE',  ( -13.89961937509977652, 13.97604488694528158, 50.62390960531435979 ) ) ;
#194362 = CARTESIAN_POINT ( 'NONE',  ( -15.80617190586768217, 15.72974639402176855, 63.12609039468568994 ) ) ;
#194363 = CARTESIAN_POINT ( 'NONE',  ( -16.51473224551069308, -9.474510206698971260, 71.66557627198102409 ) ) ;
#194364 = CARTESIAN_POINT ( 'NONE',  ( -5.153800228976328057, -19.02544592524343514, 32.29057627198102409 ) ) ;
#194365 = CARTESIAN_POINT ( 'NONE',  ( -9.564922557960796823, -16.46253265017161027, 77.08224293864769550 ) ) ;
#194366 = CARTESIAN_POINT ( 'NONE',  ( 21.55341960407610458, 5.719274019375980345, 43.95724293864769550 ) ) ;
#194367 = CARTESIAN_POINT ( 'NONE',  ( 9.564922557960805705, 16.46253265017160317, 39.58224293864768839 ) ) ;
#194368 = CARTESIAN_POINT ( 'NONE',  ( 10.72451020669898902, -18.67979575497178502, 47.91557627198102409 ) ) ;
#194369 = CARTESIAN_POINT ( 'NONE',  ( 12.14591786802327356, -12.06949235617739191, 110.6260903946857042 ) ) ;
#194370 = CARTESIAN_POINT ( 'NONE',  ( 16.46253265017146816, 9.564922557961045513, 26.66775706135234003 ) ) ;
#194372 = CARTESIAN_POINT ( 'NONE',  ( 8.314922557961029526, -14.29746914071037800, 85.41775706135236135 ) ) ;
#194371 = CARTESIAN_POINT ( 'NONE',  ( -14.29746914071037622, -8.314922557961029526, 44.16775706135234714 ) ) ;
#194373 = CARTESIAN_POINT ( 'NONE',  ( -17.60769864724390388, 5.499999999999986677, 68.65024842019165874 ) ) ;
#194374 = CARTESIAN_POINT ( 'NONE',  ( 4.379528057220092307, 16.55341960407617563, 62.29275706135236845 ) ) ;
#194375 = CARTESIAN_POINT ( 'NONE',  ( -15.72974639402197994, 15.80617190586746368, 25.62390960531435624 ) ) ;
#194376 = CARTESIAN_POINT ( 'NONE',  ( 13.89961937509977652, -13.97604488694527269, 38.12390960531436690 ) ) ;
#194377 = CARTESIAN_POINT ( 'NONE',  ( -16.55341960407617563, 4.379528057220093196, 43.54275706135235424 ) ) ;
#194378 = CARTESIAN_POINT ( 'NONE',  ( -0.05219959533909027116, -19.03943276465977164, 47.49890960531435979 ) ) ;
#194379 = CARTESIAN_POINT ( 'NONE',  ( 5.823673210054444382, -21.52544592524334988, 20.20942372801900788 ) ) ;
#194380 = CARTESIAN_POINT ( 'NONE',  ( -0.05219959533934338120, 16.53943276465976808, 32.50109039468568284 ) ) ;
#194381 = CARTESIAN_POINT ( 'NONE',  ( 0.05219959533934541429, -16.53943276465976808, 100.0010903946857042 ) ) ;
#194382 = PLANE ( 'NONE',  #115018 ) ;
#194383 = CARTESIAN_POINT ( 'NONE',  ( 10.81492255796106328, -18.62759615963255655, 95.41775706135234714 ) ) ;
#194384 = CARTESIAN_POINT ( 'NONE',  ( 5.153800228976615827, -19.02544592524334988, 100.2094237280190043 ) ) ;
#194385 = CARTESIAN_POINT ( 'NONE',  ( 13.89961937509957401, 13.97604488694547697, 51.87609039468566863 ) ) ;
#194386 = CARTESIAN_POINT ( 'NONE',  ( 12.14591786802309770, 12.06949235617756955, 59.37390960531436690 ) ) ;
#194387 = CARTESIAN_POINT ( 'NONE',  ( 19.02544592524343514, -5.153800228976328945, 28.54057627198102409 ) ) ;
#194389 = CARTESIAN_POINT ( 'NONE',  ( 17.48847506799950224, -5.747544572775292515, 58.32697437843292221 ) ) ;
#194388 = CARTESIAN_POINT ( 'NONE',  ( -5.049401038297874678, -19.05341960407617918, 54.79275706135234003 ) ) ;
#194390 = CARTESIAN_POINT ( 'NONE',  ( 5.823673210054444382, -21.52544592524334988, 70.20942372801904696 ) ) ;
#194391 = CARTESIAN_POINT ( 'NONE',  ( 12.14591786802327356, -12.06949235617739191, 30.62609039468567929 ) ) ;
#194392 = CARTESIAN_POINT ( 'NONE',  ( -17.72517630440432868, 5.499999999999969802, 90.92175719257211597 ) ) ;
#194393 = CARTESIAN_POINT ( 'NONE',  ( 10.81492255796078972, 18.62759615963270932, 29.58224293864769905 ) ) ;
#194394 = CARTESIAN_POINT ( 'NONE',  ( -16.53943276465976808, -0.05219959533934237506, 18.75109039468568639 ) ) ;
#194395 = DIRECTION ( 'NONE',  ( 0.000000000000000000, 0.000000000000000000, -1.000000000000000000 ) ) ;
#194396 = CARTESIAN_POINT ( 'NONE',  ( -19.03943276465977164, 0.05219959533909376836, 31.24890960531435979 ) ) ;
#194397 = CARTESIAN_POINT ( 'NONE',  ( -21.52544592524334988, -5.823673210054445271, 108.9594237280190185 ) ) ;
#194398 = CARTESIAN_POINT ( 'NONE',  ( -19.05341960407611168, -5.049401038298163336, 56.45724293864768129 ) ) ;
#194399 = CARTESIAN_POINT ( 'NONE',  ( -5.823673210054431948, 21.52544592524334988, 62.70942372801902565 ) ) ;
#194400 = CARTESIAN_POINT ( 'NONE',  ( 18.67979575497194134, -10.72451020669871369, 105.8344237280190328 ) ) ;
#194401 = CARTESIAN_POINT ( 'NONE',  ( -12.14591786802326823, 12.06949235617739902, 98.12609039468570415 ) ) ;
#194402 = CARTESIAN_POINT ( 'NONE',  ( -16.51473224551069308, -9.474510206698971260, 81.66557627198103830 ) ) ;
#194403 = CARTESIAN_POINT ( 'NONE',  ( -15.80617190586768217, 15.72974639402176855, 53.12609039468568284 ) ) ;
#194404 = CARTESIAN_POINT ( 'NONE',  ( 5.719274019375673035, 21.55341960407619339, 47.29275706135234003 ) ) ;
#194406 = CARTESIAN_POINT ( 'NONE',  ( -13.89961937509977652, 13.97604488694528158, 105.6239096053143527 ) ) ;
#194405 = CARTESIAN_POINT ( 'NONE',  ( -13.89961937509957401, -13.97604488694547875, 74.37609039468566152 ) ) ;
#194407 = CARTESIAN_POINT ( 'NONE',  ( 8.314922557960818139, 14.29746914071049879, 114.5822429386477097 ) ) ;
#194408 = CARTESIAN_POINT ( 'NONE',  ( -5.823673210054116645, -21.52544592524344225, 102.2905762719810383 ) ) ;
#194409 = CARTESIAN_POINT ( 'NONE',  ( 16.51473224551083163, -9.474510206698727899, 25.83442372801900078 ) ) ;
#194410 = CARTESIAN_POINT ( 'NONE',  ( 16.55341960407611168, 4.379528057220329451, 98.95724293864770971 ) ) ;
#194411 = CARTESIAN_POINT ( 'NONE',  ( -0.05219959533909027116, -19.03943276465977164, 47.49890960531435979 ) ) ;
#194412 = CARTESIAN_POINT ( 'NONE',  ( -19.03943276465977164, -0.05219959533935918106, 98.75109039468567573 ) ) ;
#194413 = CARTESIAN_POINT ( 'NONE',  ( -12.06949235617756955, 12.14591786802309770, 65.62390960531436690 ) ) ;
#194414 = CARTESIAN_POINT ( 'NONE',  ( -5.719274019375665041, -21.55341960407619695, 109.7927570613523613 ) ) ;
#194415 = CARTESIAN_POINT ( 'NONE',  ( -16.51473224551069308, -9.474510206698971260, 106.6655762719810383 ) ) ;
#194416 = CARTESIAN_POINT ( 'NONE',  ( -5.153800228976607833, 19.02544592524334988, 77.70942372801900433 ) ) ;
#194417 = CARTESIAN_POINT ( 'NONE',  ( -15.80617190586745835, -15.72974639402198527, 76.87390960531439532 ) ) ;
#194418 = CARTESIAN_POINT ( 'NONE',  ( -10.72451020669870658, -18.67979575497194134, 44.58442372801901854 ) ) ;
#194419 = CARTESIAN_POINT ( 'NONE',  ( 16.52544592524335698, 4.483927247898782831, 41.45942372801901143 ) ) ;
#194420 = CARTESIAN_POINT ( 'NONE',  ( -8.314922557961024197, 14.29746914071037800, 87.91775706135234714 ) ) ;
#194422 = CARTESIAN_POINT ( 'NONE',  ( -15.80617190586768217, 15.72974639402176855, 38.12609039468567573 ) ) ;
#194421 = CARTESIAN_POINT ( 'NONE',  ( 14.29746914071037800, 8.314922557961029526, 36.66775706135234714 ) ) ;
#194423 = CARTESIAN_POINT ( 'NONE',  ( -5.719274019375978568, 21.55341960407610458, 45.20724293864769550 ) ) ;
#194424 = CARTESIAN_POINT ( 'NONE',  ( -19.03943276465977164, 0.05219959533909376836, 31.24890960531435979 ) ) ;
#194425 = CARTESIAN_POINT ( 'NONE',  ( -11.74264578624799782, -36.14014761921581709, -9.349999994537627757 ) ) ;
#194426 = CARTESIAN_POINT ( 'NONE',  ( 0.05219959533934541429, -16.53943276465976808, 65.00109039468568994 ) ) ;
#194427 = CARTESIAN_POINT ( 'NONE',  ( 21.55341960407610458, 5.719274019375980345, 93.95724293864770971 ) ) ;
#194428 = CARTESIAN_POINT ( 'NONE',  ( -14.29746914071049879, 8.314922557960819915, 40.83224293864769550 ) ) ;
#194429 = CARTESIAN_POINT ( 'NONE',  ( -12.06949235617739369, -12.14591786802326823, 44.37609039468567573 ) ) ;
#194430 = CARTESIAN_POINT ( 'NONE',  ( -0.05219959533909027116, -19.03943276465977164, 62.49890960531435979 ) ) ;
#194431 = CARTESIAN_POINT ( 'NONE',  ( -5.049401038297874678, -19.05341960407617918, 84.79275706135233293 ) ) ;
#194432 = CARTESIAN_POINT ( 'NONE',  ( 10.72451020669898902, -18.67979575497178502, 82.91557627198103830 ) ) ;
#194433 = CARTESIAN_POINT ( 'NONE',  ( 12.06949235617757843, -12.14591786802309237, 33.12390960531435979 ) ) ;
#194434 = ORIENTED_EDGE ( 'NONE', *, *, #47118, .T. ) ;
#194435 = CARTESIAN_POINT ( 'NONE',  ( 21.70479006154310397, 9.754118203517286645, 170.7545476126474284 ) ) ;
#194436 = CARTESIAN_POINT ( 'NONE',  ( -21.53943276465977519, 0.05219959533907696930, 56.24890960531436690 ) ) ;
#194437 = CARTESIAN_POINT ( 'NONE',  ( 4.483927247898790824, -16.52544592524335698, 105.2094237280190328 ) ) ;
#194438 = ORIENTED_EDGE ( 'NONE', *, *, #58231, .T. ) ;
#194439 = CARTESIAN_POINT ( 'NONE',  ( 18.56399227203341695, 5.500000000000000888, 86.47830131249902763 ) ) ;
#194440 = CARTESIAN_POINT ( 'NONE',  ( -5.823673210054116645, -21.52544592524344225, 92.29057627198103830 ) ) ;
#194441 = CARTESIAN_POINT ( 'NONE',  ( -8.224510206698948167, 14.34966873604960824, 25.41557627198103120 ) ) ;
#194442 = CARTESIAN_POINT ( 'NONE',  ( 16.53943276465976808, 0.05219959533934440121, 36.25109039468567573 ) ) ;
#194443 = CARTESIAN_POINT ( 'NONE',  ( 9.564922557960805705, 16.46253265017160317, 34.58224293864770260 ) ) ;
#194444 = CARTESIAN_POINT ( 'NONE',  ( -5.153800228976328057, -19.02544592524343514, 72.29057627198102409 ) ) ;
#194445 = CARTESIAN_POINT ( 'NONE',  ( -23.31738231874055600, 16.94106989632528837, 149.7999999999999829 ) ) ;
#194446 = CARTESIAN_POINT ( 'NONE',  ( -19.05341960407611168, -5.049401038298163336, 111.4572429386476671 ) ) ;
#194447 = CARTESIAN_POINT ( 'NONE',  ( -9.616242481452241364, -9.758483323059184755, -62.58071313852360618 ) ) ;
#194448 = CARTESIAN_POINT ( 'NONE',  ( -16.55341960407617563, 4.379528057220093196, 98.54275706135234714 ) ) ;
#194449 = CARTESIAN_POINT ( 'NONE',  ( 9.474510206698729675, 16.51473224551082808, 112.0844237280190043 ) ) ;
#194450 = CARTESIAN_POINT ( 'NONE',  ( 5.049401038297881783, 19.05341960407617563, 32.29275706135233293 ) ) ;
#194451 = CARTESIAN_POINT ( 'NONE',  ( 10.72451020669898902, -18.67979575497178502, 92.91557627198103830 ) ) ;
#194452 = EDGE_CURVE ( 'NONE', #65322, #94244, #133540, .T. ) ;
#194453 = CARTESIAN_POINT ( 'NONE',  ( -0.05219959533910754901, -16.53943276465976808, 22.49890960531436335 ) ) ;
#194454 = CARTESIAN_POINT ( 'NONE',  ( -21.55341960407610458, -5.719274019375992779, 51.45724293864770260 ) ) ;
#194455 = CARTESIAN_POINT ( 'NONE',  ( -19.05341960407617563, 5.049401038297882671, 108.5427570613523187 ) ) ;
#194456 = CARTESIAN_POINT ( 'NONE',  ( -19.02544592524342804, 5.153800228976336051, 111.0405762719810099 ) ) ;
#194457 = CARTESIAN_POINT ( 'NONE',  ( 18.62759615963255655, 10.81492255796105972, 61.66775706135235424 ) ) ;
#194458 = CARTESIAN_POINT ( 'NONE',  ( -19.03943276465977164, 0.05219959533909376836, 66.24890960531436690 ) ) ;
#194459 = CARTESIAN_POINT ( 'NONE',  ( 16.52544592524342804, -4.483927247898539470, 103.5405762719810383 ) ) ;
#194460 = CARTESIAN_POINT ( 'NONE',  ( 32.53418548917480990, 2.421649558188258666, 87.88477275112332165 ) ) ;
#194461 = CARTESIAN_POINT ( 'NONE',  ( 13.89961937509977652, -13.97604488694527269, 68.12390960531436690 ) ) ;
#194462 = CARTESIAN_POINT ( 'NONE',  ( -14.29746914071049879, 8.314922557960819915, 80.83224293864769550 ) ) ;
#194463 = ORIENTED_EDGE ( 'NONE', *, *, #162141, .F. ) ;
#194464 = CARTESIAN_POINT ( 'NONE',  ( 5.049401038297881783, 19.05341960407617563, 92.29275706135234714 ) ) ;
#194465 = DIRECTION ( 'NONE',  ( -1.000000000000000000, 0.000000000000000000, 0.000000000000000000 ) ) ;
#194466 = CARTESIAN_POINT ( 'NONE',  ( 16.46253265017160672, -9.564922557960803928, 58.33224293864769550 ) ) ;
#194467 = CARTESIAN_POINT ( 'NONE',  ( 1.461575671818346356, 7.989192496695419976, -62.12244103964774666 ) ) ;
#194469 = CARTESIAN_POINT ( 'NONE',  ( -19.03943276465977164, 0.05219959533909376836, 101.2489096053143669 ) ) ;
#194468 = CARTESIAN_POINT ( 'NONE',  ( -18.62759615963255300, -10.81492255796106328, 84.16775706135234714 ) ) ;
#194470 = CARTESIAN_POINT ( 'NONE',  ( 14.29746914071037800, 8.314922557961029526, 66.66775706135234714 ) ) ;
#194471 = CARTESIAN_POINT ( 'NONE',  ( -3.573655867282028392E-15, 2.428612866367529932E-14, -15.00000000000000000 ) ) ;
#194472 = CARTESIAN_POINT ( 'NONE',  ( -5.153800228976607833, 19.02544592524334988, 42.70942372801901143 ) ) ;
#194473 = CARTESIAN_POINT ( 'NONE',  ( -15.72974639402176322, -15.80617190586768395, 104.3760903946856899 ) ) ;
#194474 = CARTESIAN_POINT ( 'NONE',  ( 36.80083376053583066, 5.466397602639213815, 45.70522705241149453 ) ) ;
#194475 = CARTESIAN_POINT ( 'NONE',  ( -15.49999999999999822, -5.500000000000000888, 20.00000000000000000 ) ) ;
#194476 = CARTESIAN_POINT ( 'NONE',  ( 8.314922557961029526, -14.29746914071037800, 105.4177570613523613 ) ) ;
#194477 = CARTESIAN_POINT ( 'NONE',  ( -34.46950536905809770, -7.498137530812974738, 44.48224578455060652 ) ) ;
#194478 = CARTESIAN_POINT ( 'NONE',  ( 4.483927247898790824, -16.52544592524335698, 90.20942372801903275 ) ) ;
#194479 = CARTESIAN_POINT ( 'NONE',  ( 16.88567814943161238, 6.947325034625711382, 68.79001122652584854 ) ) ;
#194480 = CARTESIAN_POINT ( 'NONE',  ( -14.29746914071037622, -8.314922557961029526, 69.16775706135234714 ) ) ;
#194481 = ORIENTED_EDGE ( 'NONE', *, *, #955, .F. ) ;
#194482 = CARTESIAN_POINT ( 'NONE',  ( -15.72974639402176322, -15.80617190586768395, 79.37609039468567573 ) ) ;
#194483 = CARTESIAN_POINT ( 'NONE',  ( 9.474510206698729675, 16.51473224551082808, 92.08442372801900433 ) ) ;
#194484 = CARTESIAN_POINT ( 'NONE',  ( 9.474510206698729675, 16.51473224551082808, 27.08442372801900433 ) ) ;
#194485 = CARTESIAN_POINT ( 'NONE',  ( 19.02544592524343514, -5.153800228976328945, 68.54057627198103830 ) ) ;
#194486 = CARTESIAN_POINT ( 'NONE',  ( 19.05341960407611168, 5.049401038298154454, 58.95724293864768129 ) ) ;
#194487 = CARTESIAN_POINT ( 'NONE',  ( 17.50000000000000000, -5.500000000000000888, 23.29690382534171889 ) ) ;
#194488 = CARTESIAN_POINT ( 'NONE',  ( 10.81492255796078972, 18.62759615963270932, 79.58224293864769550 ) ) ;
#194489 = CARTESIAN_POINT ( 'NONE',  ( -15.72974639402197994, 15.80617190586746368, 30.62390960531436335 ) ) ;
#194490 = CARTESIAN_POINT ( 'NONE',  ( 13.89961937509977652, -13.97604488694527269, 38.12390960531436690 ) ) ;
#194491 = CARTESIAN_POINT ( 'NONE',  ( -12.06949235617739369, -12.14591786802326823, 64.37609039468568994 ) ) ;
#194492 = VERTEX_POINT ( 'NONE', #98346 ) ;
#194493 = CARTESIAN_POINT ( 'NONE',  ( -10.81492255796105439, 18.62759615963255655, 37.91775706135235424 ) ) ;
#194495 = CARTESIAN_POINT ( 'NONE',  ( -36.91746825000000598, 2.428612866367529932E-14, -8.624999997268814056 ) ) ;
#194494 = CARTESIAN_POINT ( 'NONE',  ( 4.379528057220339221, -16.55341960407611168, 62.70724293864769550 ) ) ;
#194496 = CARTESIAN_POINT ( 'NONE',  ( -14.34966873604972548, 8.224510206698743886, 28.33442372801902209 ) ) ;
#194497 = CARTESIAN_POINT ( 'NONE',  ( 5.049401038297881783, 19.05341960407617563, 52.29275706135234003 ) ) ;
#194498 = CARTESIAN_POINT ( 'NONE',  ( 16.55341960407611168, 4.379528057220329451, 58.95724293864770971 ) ) ;
#194499 = CARTESIAN_POINT ( 'NONE',  ( 5.823673210054444382, -21.52544592524334988, 25.20942372801901854 ) ) ;
#194501 = CARTESIAN_POINT ( 'NONE',  ( 0.05219959533907565091, 21.53943276465977519, 74.99890960531435269 ) ) ;
#194500 = CARTESIAN_POINT ( 'NONE',  ( -17.58332526062529411, 7.635886036038502134, 100.9233495955846678 ) ) ;
#194502 = CARTESIAN_POINT ( 'NONE',  ( 9.564922557960805705, 16.46253265017160317, 89.58224293864769550 ) ) ;
#194503 = CARTESIAN_POINT ( 'NONE',  ( -8.224510206698948167, 14.34966873604960824, 60.41557627198102409 ) ) ;
#194504 = CARTESIAN_POINT ( 'NONE',  ( 9.564922557960805705, 16.46253265017160317, 114.5822429386476955 ) ) ;
#194505 = CARTESIAN_POINT ( 'NONE',  ( -36.93866063236283281, 5.356020730800094221, 43.73704834337281966 ) ) ;
#194506 = CARTESIAN_POINT ( 'NONE',  ( -0.05219959533936034679, 19.03943276465977164, 72.50109039468566152 ) ) ;
#194507 = CARTESIAN_POINT ( 'NONE',  ( -21.55341960407610458, -5.719274019375992779, 111.4572429386476813 ) ) ;
#194508 = CARTESIAN_POINT ( 'NONE',  ( -16.51473224551069308, -9.474510206698971260, 61.66557627198103120 ) ) ;
#194509 = CARTESIAN_POINT ( 'NONE',  ( -9.474510206698720793, -16.51473224551083518, 39.58442372801899722 ) ) ;
#194510 = CARTESIAN_POINT ( 'NONE',  ( -19.03943276465977164, 0.05219959533909376836, 31.24890960531435979 ) ) ;
#194511 = CARTESIAN_POINT ( 'NONE',  ( -10.81492255796105439, 18.62759615963255655, 67.91775706135234714 ) ) ;
#194512 = DIRECTION ( 'NONE',  ( -1.000000000000000000, -0.000000000000000000, 0.000000000000000000 ) ) ;
#194513 = CARTESIAN_POINT ( 'NONE',  ( -16.53943276465976808, 0.05219959533911058130, 36.24890960531435979 ) ) ;
#194514 = CARTESIAN_POINT ( 'NONE',  ( -16.51473224551069308, -9.474510206698971260, 61.66557627198103120 ) ) ;
#194515 = CARTESIAN_POINT ( 'NONE',  ( 10.72451020669898902, -18.67979575497178502, 77.91557627198102409 ) ) ;
#194516 = CARTESIAN_POINT ( 'NONE',  ( 16.51473224551069308, 9.474510206698969483, 64.16557627198102409 ) ) ;
#194517 = ORIENTED_EDGE ( 'NONE', *, *, #157548, .T. ) ;
#194518 = CARTESIAN_POINT ( 'NONE',  ( 21.53943276465977519, -0.05219959533907433946, 63.74890960531435979 ) ) ;
#194519 = ORIENTED_EDGE ( 'NONE', *, *, #100961, .F. ) ;
#194520 = CARTESIAN_POINT ( 'NONE',  ( 18.62759615963255655, 10.81492255796105972, 96.66775706135234714 ) ) ;
#194523 = CARTESIAN_POINT ( 'NONE',  ( 4.379528057220339221, -16.55341960407611168, 82.70724293864770971 ) ) ;
#194522 = CARTESIAN_POINT ( 'NONE',  ( -16.53943276465976808, -0.05219959533934237506, 98.75109039468568994 ) ) ;
#194521 = CARTESIAN_POINT ( 'NONE',  ( 2.802625768539491524, -39.09149893265185227, -22.99999999999999289 ) ) ;
#194524 = CARTESIAN_POINT ( 'NONE',  ( 13.97604488694548053, -13.89961937509957401, 95.62609039468563310 ) ) ;
#194525 = VERTEX_POINT ( 'NONE', #34712 ) ;
#194526 = CARTESIAN_POINT ( 'NONE',  ( 13.89961937509957401, 13.97604488694547697, 41.87609039468566152 ) ) ;
#194527 = CARTESIAN_POINT ( 'NONE',  ( 14.34966873604972726, -8.224510206698740333, 100.8344237280190185 ) ) ;
#194528 = ADVANCED_FACE ( 'NONE', ( #145864 ), #65048, .T. ) ;
#194529 = CARTESIAN_POINT ( 'NONE',  ( 9.564922557961047289, -16.46253265017146816, 35.41775706135233293 ) ) ;
#194530 = CARTESIAN_POINT ( 'NONE',  ( 19.03943276465977164, -0.05219959533909143690, 93.74890960531435269 ) ) ;
#194531 = CARTESIAN_POINT ( 'NONE',  ( 15.80617190586746368, 15.72974639402197994, 59.37390960531436690 ) ) ;
#194532 = CARTESIAN_POINT ( 'NONE',  ( -24.78074900657737345, -31.51706519598950607, -17.29086010071288726 ) ) ;
#194533 = CARTESIAN_POINT ( 'NONE',  ( -16.51473224551069308, -9.474510206698971260, 26.66557627198103120 ) ) ;
#194534 = CARTESIAN_POINT ( 'NONE',  ( -5.719274019375665041, -21.55341960407619695, 99.79275706135234714 ) ) ;
#194535 = CARTESIAN_POINT ( 'NONE',  ( 16.53943276465976808, 0.05219959533934440121, 81.25109039468568994 ) ) ;
#194536 = CARTESIAN_POINT ( 'NONE',  ( -18.67979575497193778, 10.72451020669871902, 33.33442372801900433 ) ) ;
#194537 = CARTESIAN_POINT ( 'NONE',  ( 16.53943276465976808, 0.05219959533934440121, 36.25109039468567573 ) ) ;
#194538 = CARTESIAN_POINT ( 'NONE',  ( -0.05219959533909027116, -19.03943276465977164, 107.4989096053143527 ) ) ;
#194539 = CARTESIAN_POINT ( 'NONE',  ( -16.51473224551069308, -9.474510206698971260, 36.66557627198102409 ) ) ;
#194540 = CARTESIAN_POINT ( 'NONE',  ( -9.564922557960796823, -16.46253265017161027, 52.08224293864768839 ) ) ;
#194541 = CARTESIAN_POINT ( 'NONE',  ( -12.14591786802326823, 12.06949235617739902, 33.12609039468569705 ) ) ;
#194542 = CARTESIAN_POINT ( 'NONE',  ( -14.29746914071049879, 8.314922557960819915, 95.83224293864770971 ) ) ;
#194543 = CARTESIAN_POINT ( 'NONE',  ( 16.52544592524335698, 4.483927247898782831, 101.4594237280190185 ) ) ;
#194546 = CARTESIAN_POINT ( 'NONE',  ( -13.89961937509977652, 13.97604488694528158, 65.62390960531436690 ) ) ;
#194545 = CARTESIAN_POINT ( 'NONE',  ( 5.049401038298161559, -19.05341960407611168, 77.70724293864765286 ) ) ;
#194544 = CARTESIAN_POINT ( 'NONE',  ( -21.53943276465977519, -0.05219959533937600094, 38.75109039468567573 ) ) ;
#194548 = EDGE_CURVE ( 'NONE', #11425, #192734, #69101, .T. ) ;
#194547 = CARTESIAN_POINT ( 'NONE',  ( 13.89961937509977652, -13.97604488694527269, 88.12390960531438111 ) ) ;
#194549 = CARTESIAN_POINT ( 'NONE',  ( 14.29746914071049879, -8.314922557960816363, 28.33224293864769550 ) ) ;
#194550 = CARTESIAN_POINT ( 'NONE',  ( 4.379528057220092307, 16.55341960407617563, 97.29275706135234714 ) ) ;
#194551 = ORIENTED_EDGE ( 'NONE', *, *, #9460, .T. ) ;
#194552 = CARTESIAN_POINT ( 'NONE',  ( -19.05341960407617563, 5.049401038297882671, 38.54275706135233293 ) ) ;
#194553 = CARTESIAN_POINT ( 'NONE',  ( -13.97604488694527625, -13.89961937509977652, 106.8739096053143669 ) ) ;
#194554 = CARTESIAN_POINT ( 'NONE',  ( 19.02544592524343514, -5.153800228976328945, 63.54057627198103830 ) ) ;
#194555 = CARTESIAN_POINT ( 'NONE',  ( 0.05219959533936267826, -19.03943276465977164, 35.00109039468566863 ) ) ;
#194556 = CARTESIAN_POINT ( 'NONE',  ( -5.950531402560715689E-15, 38.81732327939063509, -9.124999997268815832 ) ) ;
#194557 = CARTESIAN_POINT ( 'NONE',  ( 12.06949235617739724, 12.14591786802326823, 41.87609039468568284 ) ) ;
#194559 = CARTESIAN_POINT ( 'NONE',  ( 16.52544592524335698, 4.483927247898782831, 51.45942372801901854 ) ) ;
#194558 = CARTESIAN_POINT ( 'NONE',  ( -19.05341960407617563, 5.049401038297882671, 73.54275706135233293 ) ) ;
#194560 = CARTESIAN_POINT ( 'NONE',  ( 7.500000000000000888, 1.380023386739106961, 5.672916605552548397 ) ) ;
#194561 = CARTESIAN_POINT ( 'NONE',  ( -5.153800228976328057, -19.02544592524343514, 97.29057627198099567 ) ) ;
#194562 = CARTESIAN_POINT ( 'NONE',  ( -21.55341960407610458, -5.719274019375992779, 106.4572429386477097 ) ) ;
#194563 = CARTESIAN_POINT ( 'NONE',  ( -9.474510206698720793, -16.51473224551083518, 74.58442372801900433 ) ) ;
#194565 = CARTESIAN_POINT ( 'NONE',  ( -9.564922557960796823, -16.46253265017161027, 37.08224293864768839 ) ) ;
#194564 = CARTESIAN_POINT ( 'NONE',  ( 9.474510206698971260, -16.51473224551069308, 102.9155762719810241 ) ) ;
#194566 = CARTESIAN_POINT ( 'NONE',  ( -16.46253265017160317, 9.564922557960807481, 80.83224293864769550 ) ) ;
#194568 = CARTESIAN_POINT ( 'NONE',  ( -16.46253265017160317, 9.564922557960807481, 35.83224293864768839 ) ) ;
#194567 = CARTESIAN_POINT ( 'NONE',  ( 0.05219959533910956823, 16.53943276465976808, 34.99890960531435979 ) ) ;
#194569 = CARTESIAN_POINT ( 'NONE',  ( -13.89961937509957401, -13.97604488694547875, 49.37609039468567573 ) ) ;
#194570 = CARTESIAN_POINT ( 'NONE',  ( -12.14591786802309592, -12.06949235617757132, 86.87390960531438111 ) ) ;
#194571 = CARTESIAN_POINT ( 'NONE',  ( 5.153800228976615827, -19.02544592524334988, 20.20942372801899722 ) ) ;
#194572 = CARTESIAN_POINT ( 'NONE',  ( -16.51473224551069308, -9.474510206698971260, 46.66557627198102409 ) ) ;
#194573 = CARTESIAN_POINT ( 'NONE',  ( 5.823673210054125526, 21.52544592524343514, 44.79057627198103120 ) ) ;
#194575 = CARTESIAN_POINT ( 'NONE',  ( -15.72974639402176322, -15.80617190586768395, 109.3760903946857042 ) ) ;
#194574 = CARTESIAN_POINT ( 'NONE',  ( 4.379528057220339221, -16.55341960407611168, 52.70724293864769550 ) ) ;
#194576 = CARTESIAN_POINT ( 'NONE',  ( 19.02544592524343514, -5.153800228976328945, 103.5405762719809957 ) ) ;
#194577 = CARTESIAN_POINT ( 'NONE',  ( 19.05341960407611168, 5.049401038298154454, 108.9572429386477097 ) ) ;
#194578 = CARTESIAN_POINT ( 'NONE',  ( 19.03943276465977164, -0.05219959533909143690, 33.74890960531435979 ) ) ;
#194579 = CARTESIAN_POINT ( 'NONE',  ( 5.049401038298161559, -19.05341960407611168, 22.70724293864769194 ) ) ;
#194580 = CARTESIAN_POINT ( 'NONE',  ( -16.55341960407611168, -4.379528057220339221, 81.45724293864769550 ) ) ;
#194581 = CARTESIAN_POINT ( 'NONE',  ( 21.55341960407610458, 5.719274019375980345, 93.95724293864770971 ) ) ;
#194582 = CARTESIAN_POINT ( 'NONE',  ( -16.46253265017160317, 9.564922557960807481, 100.8322429386477097 ) ) ;
#194583 = CARTESIAN_POINT ( 'NONE',  ( -5.719274019375665041, -21.55341960407619695, 19.79275706135235069 ) ) ;
#194584 = CARTESIAN_POINT ( 'NONE',  ( -9.564922557960796823, -16.46253265017161027, 92.08224293864769550 ) ) ;
#194586 = CARTESIAN_POINT ( 'NONE',  ( -8.224510206698948167, 14.34966873604960824, 105.4155762719810383 ) ) ;
#194585 = DIRECTION ( 'NONE',  ( -1.000000000000000000, 0.000000000000000000, 0.000000000000000000 ) ) ;
#194587 = CARTESIAN_POINT ( 'NONE',  ( -5.049401038298153566, 19.05341960407611168, 70.20724293864769550 ) ) ;
#194588 = CARTESIAN_POINT ( 'NONE',  ( 5.823673210054125526, 21.52544592524343514, 74.79057627198105251 ) ) ;
#194589 = CARTESIAN_POINT ( 'NONE',  ( -31.45250202946436247, 4.971043627493211048, 100.6372900316469412 ) ) ;
#194590 = CARTESIAN_POINT ( 'NONE',  ( -21.48956683882228091, -5.485153550827159386, 173.8223501052718802 ) ) ;
#194591 = CARTESIAN_POINT ( 'NONE',  ( 21.52544592524344225, -5.823673210054117533, 28.54057627198103120 ) ) ;
#194592 = CARTESIAN_POINT ( 'NONE',  ( 8.224510206698742110, 14.34966873604972548, 37.08442372801901143 ) ) ;
#194593 = CARTESIAN_POINT ( 'NONE',  ( 14.34966873604960469, 8.224510206698951720, 94.16557627198103830 ) ) ;
#194594 = CARTESIAN_POINT ( 'NONE',  ( 18.87075004821568669, -5.500000000000105693, 51.17408112101046669 ) ) ;
#194595 = CARTESIAN_POINT ( 'NONE',  ( 19.05341960407611168, 5.049401038298154454, 88.95724293864769550 ) ) ;
#194596 = CARTESIAN_POINT ( 'NONE',  ( -16.46253265017160317, 9.564922557960807481, 50.83224293864770260 ) ) ;
#194597 = CARTESIAN_POINT ( 'NONE',  ( -16.52544592524342804, 4.483927247898546575, 76.04057627198102409 ) ) ;
#194598 = CARTESIAN_POINT ( 'NONE',  ( -15.72974639402197994, 15.80617190586746368, 35.62390960531437401 ) ) ;
#194599 = CARTESIAN_POINT ( 'NONE',  ( 14.29746914071049879, -8.314922557960816363, 58.33224293864768839 ) ) ;
#194600 = CARTESIAN_POINT ( 'NONE',  ( 16.46253265017146816, 9.564922557961045513, 96.66775706135233293 ) ) ;
#194601 = CARTESIAN_POINT ( 'NONE',  ( -21.55341960407619339, 5.719274019375674811, 73.54275706135234714 ) ) ;
#194602 = CARTESIAN_POINT ( 'NONE',  ( -17.14385361876520264, -23.59649016807271238, 145.1750000027311387 ) ) ;
#194603 = CARTESIAN_POINT ( 'NONE',  ( -5.153800228976328057, -19.02544592524343514, 112.2905762719810099 ) ) ;
#194604 = CARTESIAN_POINT ( 'NONE',  ( 0.05219959533934541429, -16.53943276465976808, 80.00109039468568994 ) ) ;
#194605 = CARTESIAN_POINT ( 'NONE',  ( 19.03943276465977164, -0.05219959533909143690, 23.74890960531435269 ) ) ;
#194606 = CARTESIAN_POINT ( 'NONE',  ( -5.153800228976328057, -19.02544592524343514, 72.29057627198102409 ) ) ;
#194607 = CARTESIAN_POINT ( 'NONE',  ( 15.80617190586746368, 15.72974639402197994, 84.37390960531438111 ) ) ;
#194608 = CARTESIAN_POINT ( 'NONE',  ( 4.379528057220092307, 16.55341960407617563, 32.29275706135235424 ) ) ;
#194610 = CARTESIAN_POINT ( 'NONE',  ( 10.81492255796106328, -18.62759615963255655, 75.41775706135233293 ) ) ;
#194609 = CARTESIAN_POINT ( 'NONE',  ( 8.314922557960818139, 14.29746914071049879, 54.58224293864769550 ) ) ;
#194612 = CARTESIAN_POINT ( 'NONE',  ( -10.81492255796078084, -18.62759615963271287, 27.08224293864769550 ) ) ;
#194611 = CARTESIAN_POINT ( 'NONE',  ( 8.314922557961029526, -14.29746914071037800, 90.41775706135236135 ) ) ;
#194613 = CARTESIAN_POINT ( 'NONE',  ( 24.02723517065434322, 14.44770145514793214, 165.8682408883346966 ) ) ;
#194614 = FACE_OUTER_BOUND ( 'NONE', #137481, .T. ) ;
#194615 = CARTESIAN_POINT ( 'NONE',  ( 16.52544592524335698, 4.483927247898782831, 101.4594237280190185 ) ) ;
#194616 = CARTESIAN_POINT ( 'NONE',  ( -16.53943276465976808, -0.05219959533934237506, 58.75109039468568994 ) ) ;
#194618 = ORIENTED_EDGE ( 'NONE', *, *, #193305, .F. ) ;
#194617 = CARTESIAN_POINT ( 'NONE',  ( -19.02544592524342804, 5.153800228976336051, 66.04057627198103830 ) ) ;
#194619 = CARTESIAN_POINT ( 'NONE',  ( -19.03943276465977164, 0.05219959533909376836, 86.24890960531436690 ) ) ;
#194620 = CARTESIAN_POINT ( 'NONE',  ( -15.72974639402176322, -15.80617190586768395, 69.37609039468567573 ) ) ;
#194621 = CARTESIAN_POINT ( 'NONE',  ( 8.224510206698742110, 14.34966873604972548, 82.08442372801901854 ) ) ;
#194622 = CARTESIAN_POINT ( 'NONE',  ( 4.379528057220339221, -16.55341960407611168, 52.70724293864769550 ) ) ;
#194623 = CARTESIAN_POINT ( 'NONE',  ( 16.51473224551069308, 9.474510206698969483, 54.16557627198103120 ) ) ;
#194624 = CARTESIAN_POINT ( 'NONE',  ( 19.03943276465977164, -0.05219959533909143690, 43.74890960531435979 ) ) ;
#194625 = ORIENTED_EDGE ( 'NONE', *, *, #62627, .T. ) ;
#194627 = CARTESIAN_POINT ( 'NONE',  ( 9.564922557961047289, -16.46253265017146816, 105.4177570613523471 ) ) ;
#194626 =( BOUNDED_CURVE ( )  B_SPLINE_CURVE ( 2, ( #144184, #5670, #67346, #190706, #21852, #52179, #37007, #83503, #150206, #75329, #45001, #137000, #90496 ),
 .UNSPECIFIED., .F., .T. ) 
 B_SPLINE_CURVE_WITH_KNOTS ( ( 3, 2, 2, 2, 2, 2, 3 ),
 ( 0.7919041206375715403, 0.7938596491228070429, 0.7982456140350877583, 0.8026315789473684736, 0.8070175438596490780, 0.8114035087719297934, 0.8133133574350752681 ),
 .UNSPECIFIED. ) 
 CURVE ( )  GEOMETRIC_REPRESENTATION_ITEM ( )  RATIONAL_B_SPLINE_CURVE ( ( 0.9831626618144007068, 0.9848076720550096308, 1.000000000000000000, 0.9659258262890683122, 1.000000000000000000, 0.9659258262890683122, 1.000000000000000000, 0.9659258262890683122, 1.000000000000000000, 0.9659258262890683122, 1.000000000000000000, 0.9851625545550091179, 0.9832469066685282089 ) ) 
 REPRESENTATION_ITEM ( '' )  );
#194628 = CARTESIAN_POINT ( 'NONE',  ( -14.34966873604960291, -8.224510206698953496, 106.6655762719810383 ) ) ;
#194629 = CARTESIAN_POINT ( 'NONE',  ( -16.46253265017160317, 9.564922557960807481, 70.83224293864770971 ) ) ;
#194631 = CARTESIAN_POINT ( 'NONE',  ( -38.00000000000000711, 2.428612866367529932E-14, -2.000000000000000000 ) ) ;
#194630 = CARTESIAN_POINT ( 'NONE',  ( 0.05219959533936267826, -19.03943276465977164, 100.0010903946856757 ) ) ;
#194632 = CARTESIAN_POINT ( 'NONE',  ( 21.53943276465977519, 0.05219959533937863772, 101.2510903946856757 ) ) ;
#194633 = CARTESIAN_POINT ( 'NONE',  ( 16.53943276465976808, 0.05219959533934440121, 66.25109039468567573 ) ) ;
#194634 = CARTESIAN_POINT ( 'NONE',  ( 16.51473224551083163, -9.474510206698727899, 95.83442372801900433 ) ) ;
#194635 = CARTESIAN_POINT ( 'NONE',  ( 21.53943276465977519, -0.05219959533907433946, 63.74890960531435979 ) ) ;
#194636 = CARTESIAN_POINT ( 'NONE',  ( -16.55341960407617563, 4.379528057220093196, 48.54275706135234714 ) ) ;
#194637 = CARTESIAN_POINT ( 'NONE',  ( 6.180203150055914918, 4.962140900324359727, 3.431593142121018847 ) ) ;
#194638 = CARTESIAN_POINT ( 'NONE',  ( -0.05219959533936034679, 19.03943276465977164, 62.50109039468566863 ) ) ;
#194639 = CARTESIAN_POINT ( 'NONE',  ( -10.72451020669870658, -18.67979575497194134, 99.58442372801900433 ) ) ;
#194640 = CARTESIAN_POINT ( 'NONE',  ( 0.05219959533910956823, 16.53943276465976808, 114.9989096053143669 ) ) ;
#194641 = CARTESIAN_POINT ( 'NONE',  ( -16.51473224551069308, -9.474510206698971260, 71.66557627198102409 ) ) ;
#194642 = CARTESIAN_POINT ( 'NONE',  ( 14.29746914071049879, -8.314922557960816363, 58.33224293864768839 ) ) ;
#194643 = CARTESIAN_POINT ( 'NONE',  ( 18.67979575497194134, -10.72451020669871369, 90.83442372801901854 ) ) ;
#194644 = CARTESIAN_POINT ( 'NONE',  ( -5.049401038297874678, -19.05341960407617918, 49.79275706135231871 ) ) ;
#194645 = CARTESIAN_POINT ( 'NONE',  ( -5.049401038297874678, -19.05341960407617918, 29.79275706135232227 ) ) ;
#194646 = CARTESIAN_POINT ( 'NONE',  ( -15.72974639402197994, 15.80617190586746368, 25.62390960531435624 ) ) ;
#194647 = CARTESIAN_POINT ( 'NONE',  ( -10.72451020669870658, -18.67979575497194134, 94.58442372801901854 ) ) ;
#194648 = CARTESIAN_POINT ( 'NONE',  ( 5.153800228976335163, 19.02544592524342804, 74.79057627198103830 ) ) ;
#194649 = VECTOR ( 'NONE', #42654, 1000.000000000000000 ) ;
#194650 = CARTESIAN_POINT ( 'NONE',  ( -21.53943276465977519, -0.05219959533937600094, 98.75109039468568994 ) ) ;
#194651 = CARTESIAN_POINT ( 'NONE',  ( 10.81492255796078972, 18.62759615963270932, 49.58224293864769550 ) ) ;
#194652 = CARTESIAN_POINT ( 'NONE',  ( -13.97604488694527625, -13.89961937509977652, 86.87390960531436690 ) ) ;
#194653 = CARTESIAN_POINT ( 'NONE',  ( -5.049401038297874678, -19.05341960407617918, 74.79275706135231871 ) ) ;
#194654 = CARTESIAN_POINT ( 'NONE',  ( 13.89961937509977652, -13.97604488694527269, 38.12390960531436690 ) ) ;
#194655 = CARTESIAN_POINT ( 'NONE',  ( 19.02544592524343514, -5.153800228976328945, 83.54057627198100988 ) ) ;
#194656 = ADVANCED_FACE ( 'NONE', ( #4353 ), #66038, .T. ) ;
#194657 = CARTESIAN_POINT ( 'NONE',  ( 0.05219959533936267826, -19.03943276465977164, 85.00109039468567573 ) ) ;
#194658 = CARTESIAN_POINT ( 'NONE',  ( -8.224510206698735004, -14.34966873604973081, 44.58442372801901854 ) ) ;
#194659 = CARTESIAN_POINT ( 'NONE',  ( 12.06949235617757843, -12.14591786802309237, 103.1239096053143811 ) ) ;
#194660 = CARTESIAN_POINT ( 'NONE',  ( -5.153800228976328057, -19.02544592524343514, 77.29057627198099567 ) ) ;
#194661 = CARTESIAN_POINT ( 'NONE',  ( 18.67979575497178502, 10.72451020669898547, 44.16557627198103120 ) ) ;
#194662 = CARTESIAN_POINT ( 'NONE',  ( 8.314922557961029526, -14.29746914071037800, 25.41775706135235779 ) ) ;
#194663 = CARTESIAN_POINT ( 'NONE',  ( 5.823673210054444382, -21.52544592524334988, 30.20942372801902565 ) ) ;
#194664 = CARTESIAN_POINT ( 'NONE',  ( 5.823673210054444382, -21.52544592524334988, 85.20942372801901854 ) ) ;
#194665 = CARTESIAN_POINT ( 'NONE',  ( 8.314922557961029526, -14.29746914071037800, 80.41775706135234714 ) ) ;
#194666 = CARTESIAN_POINT ( 'NONE',  ( 5.049401038298161559, -19.05341960407611168, 72.70724293864768129 ) ) ;
#194667 = CARTESIAN_POINT ( 'NONE',  ( -8.314922557961024197, 14.29746914071037800, 102.9177570613523756 ) ) ;
#194668 = CARTESIAN_POINT ( 'NONE',  ( 19.02544592524334988, 5.153800228976608722, 51.45942372801900433 ) ) ;
#194669 = CARTESIAN_POINT ( 'NONE',  ( 15.80617190586769283, -15.72974639402175789, 25.62609039468567929 ) ) ;
#194670 = EDGE_CURVE ( 'NONE', #184349, #37352, #106364, .T. ) ;
#194671 = CARTESIAN_POINT ( 'NONE',  ( -14.34966873604960291, -8.224510206698953496, 76.66557627198103830 ) ) ;
#194672 = CARTESIAN_POINT ( 'NONE',  ( 5.049401038298161559, -19.05341960407611168, 97.70724293864766707 ) ) ;
#194673 = CARTESIAN_POINT ( 'NONE',  ( -12.06949235617739369, -12.14591786802326823, 104.3760903946856899 ) ) ;
#194674 = CARTESIAN_POINT ( 'NONE',  ( -15.80617190586768217, 15.72974639402176855, 73.12609039468567573 ) ) ;
#194675 = CARTESIAN_POINT ( 'NONE',  ( -14.29746914071037622, -8.314922557961029526, 34.16775706135234714 ) ) ;
#194676 = CARTESIAN_POINT ( 'NONE',  ( -5.719274019375665041, -21.55341960407619695, 24.79275706135235779 ) ) ;
#194677 = CARTESIAN_POINT ( 'NONE',  ( 8.224510206698953496, -14.34966873604960469, 67.91557627198102409 ) ) ;
#194678 = ORIENTED_EDGE ( 'NONE', *, *, #54770, .F. ) ;
#194679 = CARTESIAN_POINT ( 'NONE',  ( -18.67979575497178146, -10.72451020669898902, 101.6655762719810383 ) ) ;
#194680 = CARTESIAN_POINT ( 'NONE',  ( 8.224510206698953496, -14.34966873604960469, 52.91557627198103830 ) ) ;
#194681 = CARTESIAN_POINT ( 'NONE',  ( -16.51473224551069308, -9.474510206698971260, 31.66557627198102054 ) ) ;
#194682 = CARTESIAN_POINT ( 'NONE',  ( -18.67979575497178146, -10.72451020669898902, 26.66557627198103475 ) ) ;
#194683 = CARTESIAN_POINT ( 'NONE',  ( 10.81492255796106328, -18.62759615963255655, 50.41775706135235424 ) ) ;
#194684 = CARTESIAN_POINT ( 'NONE',  ( -8.314922557960811034, -14.29746914071050412, 62.08224293864769550 ) ) ;
#194685 = CARTESIAN_POINT ( 'NONE',  ( 21.52544592524344225, -5.823673210054117533, 73.54057627198102409 ) ) ;
#194686 = CARTESIAN_POINT ( 'NONE',  ( 5.153800228976335163, 19.02544592524342804, 79.79057627198102409 ) ) ;
#194688 = CARTESIAN_POINT ( 'NONE',  ( 0.05219959533936267826, -19.03943276465977164, 85.00109039468567573 ) ) ;
#194687 = CARTESIAN_POINT ( 'NONE',  ( 5.153800228976335163, 19.02544592524342804, 24.79057627198102765 ) ) ;
#194690 = CARTESIAN_POINT ( 'NONE',  ( -21.55341960407610458, -5.719274019375992779, 61.45724293864770260 ) ) ;
#194689 = CARTESIAN_POINT ( 'NONE',  ( 21.52544592524334988, 5.823673210054432836, 61.45942372801901854 ) ) ;
#194691 = CARTESIAN_POINT ( 'NONE',  ( 5.049401038298161559, -19.05341960407611168, 42.70724293864767418 ) ) ;
#194692 = CARTESIAN_POINT ( 'NONE',  ( 19.02544592524343514, -5.153800228976328945, 73.54057627198103830 ) ) ;
#194693 = VERTEX_POINT ( 'NONE', #144867 ) ;
#194694 = CARTESIAN_POINT ( 'NONE',  ( 16.52544592524335698, 4.483927247898782831, 56.45942372801902565 ) ) ;
#194695 = CARTESIAN_POINT ( 'NONE',  ( 10.81492255796106328, -18.62759615963255655, 30.41775706135234358 ) ) ;
#194696 = EDGE_CURVE ( 'NONE', #116638, #21815, #191379, .T. ) ;
#194697 = CARTESIAN_POINT ( 'NONE',  ( -21.53943276465977519, -0.05219959533937600094, 63.75109039468568284 ) ) ;
#194698 = CARTESIAN_POINT ( 'NONE',  ( 19.03943276465977164, -0.05219959533909143690, 98.74890960531436690 ) ) ;
#194699 = CARTESIAN_POINT ( 'NONE',  ( -15.80617190586745835, -15.72974639402198527, 81.87390960531435269 ) ) ;
#194701 = CARTESIAN_POINT ( 'NONE',  ( 0.05219959533934541429, -16.53943276465976808, 45.00109039468568284 ) ) ;
#194700 = CARTESIAN_POINT ( 'NONE',  ( 5.823673210054444382, -21.52544592524334988, 30.20942372801902565 ) ) ;
#194702 = CARTESIAN_POINT ( 'NONE',  ( -5.823673210054116645, -21.52544592524344225, 52.29057627198102409 ) ) ;
#194703 = CARTESIAN_POINT ( 'NONE',  ( 10.81492255796106328, -18.62759615963255655, 110.4177570613523756 ) ) ;
#194704 = CARTESIAN_POINT ( 'NONE',  ( -19.02544592524342804, 5.153800228976336051, 51.04057627198103120 ) ) ;
#194705 = CARTESIAN_POINT ( 'NONE',  ( -19.03943276465977164, 0.05219959533909376836, 111.2489096053143669 ) ) ;
#194706 = CARTESIAN_POINT ( 'NONE',  ( 19.02544592524343514, -5.153800228976328945, 88.54057627198102409 ) ) ;
#194707 = CARTESIAN_POINT ( 'NONE',  ( 1.304248841091933035E-15, 21.30000000000002913, -56.46919128290398504 ) ) ;
#194708 = CARTESIAN_POINT ( 'NONE',  ( 9.564922557961047289, -16.46253265017146816, 70.41775706135233293 ) ) ;
#194709 = CARTESIAN_POINT ( 'NONE',  ( 15.80617190586746368, 15.72974639402197994, 44.37390960531435979 ) ) ;
#194710 = CARTESIAN_POINT ( 'NONE',  ( -4.379528057220328563, 16.55341960407611168, 30.20724293864769550 ) ) ;
#194711 = CARTESIAN_POINT ( 'NONE',  ( 0.05219959533936267826, -19.03943276465977164, 90.00109039468567573 ) ) ;
#194712 = CARTESIAN_POINT ( 'NONE',  ( -16.62475595723695676, 7.163666690055236153, 60.52713351810466946 ) ) ;
#194713 = CARTESIAN_POINT ( 'NONE',  ( 0.05219959533937995610, -21.53943276465977519, 110.0010903946856757 ) ) ;
#194714 = CARTESIAN_POINT ( 'NONE',  ( -16.46253265017146816, -9.564922557961047289, 84.16775706135233293 ) ) ;
#194715 = CARTESIAN_POINT ( 'NONE',  ( 19.02544592524334988, 5.153800228976608722, 46.45942372801899012 ) ) ;
#194716 = CARTESIAN_POINT ( 'NONE',  ( -14.98799772565112498, -15.13475115289583961, -56.46919128290397794 ) ) ;
#194717 = CARTESIAN_POINT ( 'NONE',  ( -5.153800228976328057, -19.02544592524343514, 57.29057627198103120 ) ) ;
#194718 = CARTESIAN_POINT ( 'NONE',  ( 4.379528057220339221, -16.55341960407611168, 47.70724293864770260 ) ) ;
#194719 = CARTESIAN_POINT ( 'NONE',  ( 19.02544592524343514, -5.153800228976328945, 28.54057627198102409 ) ) ;
#194720 = CARTESIAN_POINT ( 'NONE',  ( 8.314922557960818139, 14.29746914071049879, 44.58224293864769550 ) ) ;
#194721 = CARTESIAN_POINT ( 'NONE',  ( -20.41037832431298682, -34.40082058117823749, -25.00000000000009592 ) ) ;
#194722 = CARTESIAN_POINT ( 'NONE',  ( 14.34966873604972726, -8.224510206698740333, 110.8344237280190043 ) ) ;
#194723 = CARTESIAN_POINT ( 'NONE',  ( -5.049401038298153566, 19.05341960407611168, 55.20724293864769550 ) ) ;
#194724 = CARTESIAN_POINT ( 'NONE',  ( 16.46253265017146816, 9.564922557961045513, 26.66775706135234003 ) ) ;
#194725 = CARTESIAN_POINT ( 'NONE',  ( -8.224510206698735004, -14.34966873604973081, 34.58442372801900433 ) ) ;
#194726 = CARTESIAN_POINT ( 'NONE',  ( 18.67979575497178502, 10.72451020669898547, 34.16557627198102409 ) ) ;
#194728 = ORIENTED_EDGE ( 'NONE', *, *, #58459, .T. ) ;
#194727 = CARTESIAN_POINT ( 'NONE',  ( 21.55341960407619695, -5.719274019375665929, 96.04275706135236135 ) ) ;
#194729 = CARTESIAN_POINT ( 'NONE',  ( 13.89961937509977652, -13.97604488694527269, 58.12390960531436690 ) ) ;
#194730 = CARTESIAN_POINT ( 'NONE',  ( -9.564922557960796823, -16.46253265017161027, 112.0822429386476955 ) ) ;
#194731 = CARTESIAN_POINT ( 'NONE',  ( 13.89961937509977652, -13.97604488694527269, 103.1239096053143527 ) ) ;
#194732 = CARTESIAN_POINT ( 'NONE',  ( -29.15849868437705439, 8.010956209263452976, 149.7909430734646890 ) ) ;
#194733 = CARTESIAN_POINT ( 'NONE',  ( 15.72974639402176855, 15.80617190586768217, 21.87609039468567573 ) ) ;
#194734 = CARTESIAN_POINT ( 'NONE',  ( -12.14591786802309592, -12.06949235617757132, 76.87390960531439532 ) ) ;
#194736 = CARTESIAN_POINT ( 'NONE',  ( 16.46253265017160672, -9.564922557960803928, 68.33224293864770971 ) ) ;
#194735 = CARTESIAN_POINT ( 'NONE',  ( -21.53943276465977519, 0.05219959533907696930, 71.24890960531435269 ) ) ;
#194737 = CARTESIAN_POINT ( 'NONE',  ( 5.049401038298161559, -19.05341960407611168, 77.70724293864765286 ) ) ;
#194738 = CARTESIAN_POINT ( 'NONE',  ( -18.62759615963255300, -10.81492255796106328, 19.16775706135234714 ) ) ;
#194739 = ORIENTED_EDGE ( 'NONE', *, *, #68626, .T. ) ;
#194740 = CARTESIAN_POINT ( 'NONE',  ( 9.474510206698971260, -16.51473224551069308, 67.91557627198102409 ) ) ;
#194742 = PLANE ( 'NONE',  #133395 ) ;
#194741 = CARTESIAN_POINT ( 'NONE',  ( -12.14591786802309592, -12.06949235617757132, 101.8739096053143811 ) ) ;
#194743 = CARTESIAN_POINT ( 'NONE',  ( -13.97604488694527625, -13.89961937509977652, 61.87390960531435979 ) ) ;
#194744 = CARTESIAN_POINT ( 'NONE',  ( 16.46253265017146816, 9.564922557961045513, 96.66775706135233293 ) ) ;
#194745 = CARTESIAN_POINT ( 'NONE',  ( 14.34966873604960469, 8.224510206698951720, 94.16557627198103830 ) ) ;
#194746 = CARTESIAN_POINT ( 'NONE',  ( -21.55341960407619339, 5.719274019375674811, 73.54275706135234714 ) ) ;
#194748 = CARTESIAN_POINT ( 'NONE',  ( 18.62759615963255655, 10.81492255796105972, 21.66775706135235069 ) ) ;
#194747 = CARTESIAN_POINT ( 'NONE',  ( 9.564922557960805705, 16.46253265017160317, 44.58224293864769550 ) ) ;
#194749 = CARTESIAN_POINT ( 'NONE',  ( -16.55341960407611168, -4.379528057220339221, 96.45724293864770971 ) ) ;
#194750 = CARTESIAN_POINT ( 'NONE',  ( 17.81289503416610742, 24.51734667627700404, 143.2999999999999829 ) ) ;
#194751 = CARTESIAN_POINT ( 'NONE',  ( 19.03943276465977164, -0.05219959533909143690, 73.74890960531435269 ) ) ;
#194752 = CARTESIAN_POINT ( 'NONE',  ( 16.52216118717204907, 7.221426719304526287, 113.5759902104699393 ) ) ;
#194754 = CARTESIAN_POINT ( 'NONE',  ( -21.52544592524343514, 5.823673210054127303, 36.04057627198102409 ) ) ;
#194753 = CARTESIAN_POINT ( 'NONE',  ( -19.03943276465977164, -0.05219959533935918106, 113.7510903946856757 ) ) ;
#194755 = CARTESIAN_POINT ( 'NONE',  ( -15.72974639402176322, -15.80617190586768395, 54.37609039468568994 ) ) ;
#194756 = CARTESIAN_POINT ( 'NONE',  ( 5.153800228976335163, 19.02544592524342804, 94.79057627198103830 ) ) ;
#194757 = CARTESIAN_POINT ( 'NONE',  ( 5.049401038297881783, 19.05341960407617563, 77.29275706135231871 ) ) ;
#194758 = CARTESIAN_POINT ( 'NONE',  ( -5.049401038298153566, 19.05341960407611168, 70.20724293864769550 ) ) ;
#194759 = CARTESIAN_POINT ( 'NONE',  ( -8.224510206698948167, 14.34966873604960824, 80.41557627198103830 ) ) ;
#194760 = CARTESIAN_POINT ( 'NONE',  ( 19.05341960407611168, 5.049401038298154454, 98.95724293864766707 ) ) ;
#194761 = CARTESIAN_POINT ( 'NONE',  ( 8.224510206698953496, -14.34966873604960469, 77.91557627198102409 ) ) ;
#194762 = CARTESIAN_POINT ( 'NONE',  ( -9.564922557960796823, -16.46253265017161027, 102.0822429386477097 ) ) ;
#194764 = CARTESIAN_POINT ( 'NONE',  ( 5.153800228976335163, 19.02544592524342804, 29.79057627198102409 ) ) ;
#194763 = CARTESIAN_POINT ( 'NONE',  ( 16.53943276465976808, -0.05219959533910856209, 48.74890960531435979 ) ) ;
#194765 = EDGE_LOOP ( 'NONE', ( #53086, #162089, #98581, #151019, #167942 ) ) ;
#194766 = CARTESIAN_POINT ( 'NONE',  ( -21.55341960407619339, 5.719274019375674811, 53.54275706135234714 ) ) ;
#194767 = CARTESIAN_POINT ( 'NONE',  ( -5.049401038297874678, -19.05341960407617918, 84.79275706135233293 ) ) ;
#194768 = CARTESIAN_POINT ( 'NONE',  ( 4.483927247898545687, 16.52544592524342804, 49.79057627198102409 ) ) ;
#194769 = CARTESIAN_POINT ( 'NONE',  ( 15.80617190586746368, 15.72974639402197994, 99.37390960531436690 ) ) ;
#194770 = CARTESIAN_POINT ( 'NONE',  ( 15.72974639402199770, -15.80617190586745480, 33.12390960531435979 ) ) ;
#194771 = CARTESIAN_POINT ( 'NONE',  ( -16.52544592524342804, 4.483927247898546575, 86.04057627198102409 ) ) ;
#194772 = CARTESIAN_POINT ( 'NONE',  ( -13.97604488694527625, -13.89961937509977652, 41.87390960531435979 ) ) ;
#194773 = CARTESIAN_POINT ( 'NONE',  ( -14.34966873604960291, -8.224510206698953496, 21.66557627198102409 ) ) ;
#194774 = CARTESIAN_POINT ( 'NONE',  ( -8.224510206698735004, -14.34966873604973081, 94.58442372801901854 ) ) ;
#194775 = CARTESIAN_POINT ( 'NONE',  ( 14.34966873604972726, -8.224510206698740333, 65.83442372801900433 ) ) ;
#194776 = CARTESIAN_POINT ( 'NONE',  ( -13.89961937509957401, -13.97604488694547875, 19.37609039468566507 ) ) ;
#194777 = CARTESIAN_POINT ( 'NONE',  ( 19.02544592524343514, -5.153800228976328945, 98.54057627198100988 ) ) ;
#194778 = CARTESIAN_POINT ( 'NONE',  ( -5.153800228976328057, -19.02544592524343514, 77.29057627198099567 ) ) ;
#194779 = CARTESIAN_POINT ( 'NONE',  ( -4.379528057220086978, -16.55341960407618274, 89.79275706135236135 ) ) ;
#194780 = CARTESIAN_POINT ( 'NONE',  ( 16.51473224551069308, 9.474510206698969483, 34.16557627198102409 ) ) ;
#194781 = CARTESIAN_POINT ( 'NONE',  ( 14.34966873604960469, 8.224510206698951720, 49.16557627198102409 ) ) ;
#194783 = CARTESIAN_POINT ( 'NONE',  ( -16.46253265017160317, 9.564922557960807481, 100.8322429386477097 ) ) ;
#194782 = LINE ( 'NONE', #85583, #127522 ) ;
#194784 = CARTESIAN_POINT ( 'NONE',  ( -10.81492255796078084, -18.62759615963271287, 47.08224293864770260 ) ) ;
#194785 = CARTESIAN_POINT ( 'NONE',  ( -16.53943276465976808, 0.05219959533911058130, 76.24890960531435269 ) ) ;
#194786 = AXIS2_PLACEMENT_3D ( 'NONE', #111748, #175416, #112733 ) ;
#194787 = CARTESIAN_POINT ( 'NONE',  ( 16.53943276465976808, -0.05219959533910856209, 63.74890960531435979 ) ) ;
#194788 = DIRECTION ( 'NONE',  ( -0.000000000000000000, 0.4999999999999998890, -0.8660254037844387076 ) ) ;
#194789 = CARTESIAN_POINT ( 'NONE',  ( -16.46253265017146816, -9.564922557961047289, 69.16775706135233293 ) ) ;
#194790 = CARTESIAN_POINT ( 'NONE',  ( 9.564922557960805705, 16.46253265017160317, 99.58224293864770971 ) ) ;
#194791 = CARTESIAN_POINT ( 'NONE',  ( -13.89961937509957401, -13.97604488694547875, 74.37609039468566152 ) ) ;
#194792 = CARTESIAN_POINT ( 'NONE',  ( -13.89961937509957401, -13.97604488694547697, 94.37609039468566152 ) ) ;
#194794 = CARTESIAN_POINT ( 'NONE',  ( -8.224510206698735004, -14.34966873604973081, 89.58442372801901854 ) ) ;
#194793 = CARTESIAN_POINT ( 'NONE',  ( 19.05341960407617918, -5.049401038297876454, 106.0427570613523471 ) ) ;
#194795 = CARTESIAN_POINT ( 'NONE',  ( 13.97604488694527802, 13.89961937509977652, 34.37390960531436690 ) ) ;
#194796 = CARTESIAN_POINT ( 'NONE',  ( -15.72974639402197994, 15.80617190586746368, 40.62390960531435269 ) ) ;
#194797 = CARTESIAN_POINT ( 'NONE',  ( 21.52544592524334988, 5.823673210054432836, 61.45942372801901854 ) ) ;
#194798 = CARTESIAN_POINT ( 'NONE',  ( -12.14591786802326823, 12.06949235617739902, 23.12609039468567573 ) ) ;
#194800 = CARTESIAN_POINT ( 'NONE',  ( -19.05341960407611168, -5.049401038298163336, 76.45724293864769550 ) ) ;
#194799 = CARTESIAN_POINT ( 'NONE',  ( -27.16945489364050559, -10.00000000000000000, 149.7909430734646890 ) ) ;
#194802 = CARTESIAN_POINT ( 'NONE',  ( -19.05341960407611168, -5.049401038298163336, 71.45724293864766707 ) ) ;
#194801 = CARTESIAN_POINT ( 'NONE',  ( 8.314922557960818139, 14.29746914071049879, 74.58224293864768129 ) ) ;
#194803 = CONTEXT_DEPENDENT_SHAPE_REPRESENTATION ( #174685, #153419 ) ;
#194804 = CARTESIAN_POINT ( 'NONE',  ( -19.03943276465977164, 0.05219959533909376836, 91.24890960531436690 ) ) ;
#194805 = EDGE_LOOP ( 'NONE', ( #33952, #21202, #21190, #26706, #107277 ) ) ;
#194806 = CARTESIAN_POINT ( 'NONE',  ( 5.049401038297881783, 19.05341960407617563, 92.29275706135234714 ) ) ;
#194807 = CARTESIAN_POINT ( 'NONE',  ( -15.72974639402197994, 15.80617190586746368, 70.62390960531436690 ) ) ;
#194808 = CARTESIAN_POINT ( 'NONE',  ( 16.51473224551069308, 9.474510206698969483, 34.16557627198102409 ) ) ;
#194809 = CARTESIAN_POINT ( 'NONE',  ( -13.89961937509957401, -13.97604488694547875, 59.37609039468566863 ) ) ;
#194810 = CARTESIAN_POINT ( 'NONE',  ( -19.05341960407611168, -5.049401038298163336, 61.45724293864769550 ) ) ;
#194812 = ADVANCED_FACE ( 'NONE', ( #110553 ), #141882, .T. ) ;
#194811 = CARTESIAN_POINT ( 'NONE',  ( -19.03943276465977164, 0.05219959533909376836, 86.24890960531436690 ) ) ;
#194813 = ORIENTED_EDGE ( 'NONE', *, *, #163970, .T. ) ;
#194814 = CARTESIAN_POINT ( 'NONE',  ( -21.53943276465977519, 0.05219959533907696930, 86.24890960531436690 ) ) ;
#194816 = CARTESIAN_POINT ( 'NONE',  ( -16.51473224551082808, 9.474510206698731452, 53.33442372801900433 ) ) ;
#194815 = CARTESIAN_POINT ( 'NONE',  ( 8.224510206698953496, -14.34966873604960469, 97.91557627198103830 ) ) ;
#194818 = B_SPLINE_CURVE_WITH_KNOTS ( 'NONE', 3,
 ( #147276, #163450, #180635, #161440, #103772, #24948, #84578, #164455, #165451, #25949, #87592, #26948, #88589, #150288, #11783, #107719, #78374, #184584, #29909, #152255, #154242, #15733 ),
 .UNSPECIFIED., .F., .F.,
 ( 4, 2, 2, 2, 2, 2, 2, 2, 2, 2, 4 ),
 ( 8.673617379884035472E-18, 0.001309639967555159719, 0.001964459951332734374, 0.002291869943221526255, 0.002455574939165928051, 0.002619279935110330280, 0.002782984931054732075, 0.002946689926999134304, 0.003274099918887952640, 0.003928919902665601455, 0.005238559870220891278 ),
 .UNSPECIFIED. ) ;
#194817 = CARTESIAN_POINT ( 'NONE',  ( -15.80617190586745835, -15.72974639402198527, 86.87390960531438111 ) ) ;
#194819 = CARTESIAN_POINT ( 'NONE',  ( -5.719274019375978568, 21.55341960407610458, 70.20724293864769550 ) ) ;
#194820 = CARTESIAN_POINT ( 'NONE',  ( -4.379528057220328563, 16.55341960407611168, 30.20724293864769550 ) ) ;
#194821 = CARTESIAN_POINT ( 'NONE',  ( 5.719274019375673035, 21.55341960407619339, 102.2927570613523613 ) ) ;
#194822 = CARTESIAN_POINT ( 'NONE',  ( -16.55341960407617563, 4.379528057220093196, 48.54275706135234714 ) ) ;
#194823 = CARTESIAN_POINT ( 'NONE',  ( -13.89961937509977652, 13.97604488694528158, 80.62390960531436690 ) ) ;
#194824 = CARTESIAN_POINT ( 'NONE',  ( -19.05341960407611168, -5.049401038298163336, 26.45724293864769550 ) ) ;
#194825 = CARTESIAN_POINT ( 'NONE',  ( -10.72451020669870658, -18.67979575497194134, 44.58442372801901854 ) ) ;
#194826 = CARTESIAN_POINT ( 'NONE',  ( 15.72974639402176855, 15.80617190586768217, 56.87609039468568994 ) ) ;
#194827 = CARTESIAN_POINT ( 'NONE',  ( -9.564922557960796823, -16.46253265017161027, 42.08224293864769550 ) ) ;
#194828 = CARTESIAN_POINT ( 'NONE',  ( 0.05219959533937995610, -21.53943276465977519, 20.00109039468568639 ) ) ;
#194829 = CARTESIAN_POINT ( 'NONE',  ( 19.05341960407617918, -5.049401038297876454, 66.04275706135233293 ) ) ;
#194830 = CARTESIAN_POINT ( 'NONE',  ( 9.474510206698729675, 16.51473224551082808, 67.08442372801900433 ) ) ;
#194831 = CARTESIAN_POINT ( 'NONE',  ( -12.14591786802326823, 12.06949235617739902, 28.12609039468568284 ) ) ;
#194832 = CARTESIAN_POINT ( 'NONE',  ( -0.05219959533909027116, -19.03943276465977164, 27.49890960531435624 ) ) ;
#194833 = CARTESIAN_POINT ( 'NONE',  ( 12.06949235617739724, 12.14591786802326823, 66.87609039468568994 ) ) ;
#194834 = CARTESIAN_POINT ( 'NONE',  ( 13.89961937509977652, -13.97604488694527269, 43.12390960531434558 ) ) ;
#194835 = CARTESIAN_POINT ( 'NONE',  ( 23.91168844458706033, -8.792376985857295324, 168.9858545422794123 ) ) ;
#194836 = CARTESIAN_POINT ( 'NONE',  ( 5.153800228976335163, 19.02544592524342804, 99.79057627198102409 ) ) ;
#194837 = CARTESIAN_POINT ( 'NONE',  ( 13.97604488694527802, 13.89961937509977652, 29.37390960531435979 ) ) ;
#194838 = CARTESIAN_POINT ( 'NONE',  ( 18.62759615963271287, -10.81492255796078972, 78.33224293864770971 ) ) ;
#194839 = CARTESIAN_POINT ( 'NONE',  ( -12.06949235617739369, -12.14591786802326823, 64.37609039468568994 ) ) ;
#194840 = CARTESIAN_POINT ( 'NONE',  ( -10.81492255796105439, 18.62759615963255655, 107.9177570613523471 ) ) ;
#194841 = CARTESIAN_POINT ( 'NONE',  ( -5.153800228976328057, -19.02544592524343514, 42.29057627198101699 ) ) ;
#194842 = CARTESIAN_POINT ( 'NONE',  ( 8.224510206698953496, -14.34966873604960469, 37.91557627198102409 ) ) ;
#194843 = CARTESIAN_POINT ( 'NONE',  ( -4.379528057220328563, 16.55341960407611168, 70.20724293864769550 ) ) ;
#194844 = B_SPLINE_CURVE_WITH_KNOTS ( 'NONE', 3,
 ( #136674, #41705, #118546, #105346, #198356, #152834 ),
 .UNSPECIFIED., .F., .F.,
 ( 4, 2, 4 ),
 ( 0.003239945802372208323, 0.003620412082092058781, 0.004000878361811908805 ),
 .UNSPECIFIED. ) ;
#194845 = CARTESIAN_POINT ( 'NONE',  ( -19.05341960407611168, -5.049401038298163336, 71.45724293864766707 ) ) ;
#194846 = CARTESIAN_POINT ( 'NONE',  ( 5.719274019375673035, 21.55341960407619339, 37.29275706135235424 ) ) ;
#194847 = CARTESIAN_POINT ( 'NONE',  ( -9.564922557960796823, -16.46253265017161027, 77.08224293864769550 ) ) ;
#194848 = AXIS2_PLACEMENT_3D ( 'NONE', #95727, #33076, #141237 ) ;
#194849 = CARTESIAN_POINT ( 'NONE',  ( 10.81492255796106328, -18.62759615963255655, 90.41775706135236135 ) ) ;
#194850 = CARTESIAN_POINT ( 'NONE',  ( 16.52544592524335698, 4.483927247898782831, 61.45942372801901854 ) ) ;
#194851 = CARTESIAN_POINT ( 'NONE',  ( 19.02544592524343514, -5.153800228976328945, 103.5405762719809957 ) ) ;
#194852 = CARTESIAN_POINT ( 'NONE',  ( 16.52544592524342804, -4.483927247898539470, 33.54057627198102409 ) ) ;
#194853 = CARTESIAN_POINT ( 'NONE',  ( 19.05341960407611168, 5.049401038298154454, 33.95724293864769550 ) ) ;
#194854 = CARTESIAN_POINT ( 'NONE',  ( -12.06949235617739369, -12.14591786802326823, 54.37609039468568994 ) ) ;
#194855 = CARTESIAN_POINT ( 'NONE',  ( 12.06949235617757843, -12.14591786802309237, 53.12390960531436690 ) ) ;
#194856 = CARTESIAN_POINT ( 'NONE',  ( 5.049401038298161559, -19.05341960407611168, 107.7072429386476955 ) ) ;
#194857 = CARTESIAN_POINT ( 'NONE',  ( -15.72974639402197994, 15.80617190586746368, 25.62390960531435624 ) ) ;
#194858 = CARTESIAN_POINT ( 'NONE',  ( -21.52544592524334988, -5.823673210054445271, 108.9594237280190185 ) ) ;
#194859 = CARTESIAN_POINT ( 'NONE',  ( 0.05219959533910956823, 16.53943276465976808, 89.99890960531438111 ) ) ;
#194860 = CARTESIAN_POINT ( 'NONE',  ( 13.89961937509977652, -13.97604488694527269, 98.12390960531433848 ) ) ;
#194861 = ORIENTED_EDGE ( 'NONE', *, *, #187746, .T. ) ;
#194862 = CARTESIAN_POINT ( 'NONE',  ( 8.224510206698742110, 14.34966873604972548, 57.08442372801901854 ) ) ;
#194863 = CARTESIAN_POINT ( 'NONE',  ( 19.02544592524343514, -5.153800228976328945, 58.54057627198102409 ) ) ;
#194864 = CARTESIAN_POINT ( 'NONE',  ( 17.50000000000000355, -5.499999999999992006, 26.21769037696436300 ) ) ;
#194865 = CARTESIAN_POINT ( 'NONE',  ( -19.02544592524334988, -5.153800228976617603, 53.95942372801898301 ) ) ;
#194866 = CARTESIAN_POINT ( 'NONE',  ( 14.34966873604972726, -8.224510206698740333, 75.83442372801900433 ) ) ;
#194867 = CARTESIAN_POINT ( 'NONE',  ( 5.049401038297881783, 19.05341960407617563, 97.29275706135233293 ) ) ;
#194868 = CARTESIAN_POINT ( 'NONE',  ( 0.05219959533937995610, -21.53943276465977519, 60.00109039468568284 ) ) ;
#194869 = CARTESIAN_POINT ( 'NONE',  ( 9.564922557960805705, 16.46253265017160317, 79.58224293864769550 ) ) ;
#194870 = CARTESIAN_POINT ( 'NONE',  ( 18.67979575497178502, 10.72451020669898547, 89.16557627198102409 ) ) ;
#194871 = CARTESIAN_POINT ( 'NONE',  ( 14.29746914071049879, -8.314922557960816363, 103.3322429386476955 ) ) ;
#194872 = CARTESIAN_POINT ( 'NONE',  ( 13.97604488694548053, -13.89961937509957401, 65.62609039468567573 ) ) ;
#194873 = CARTESIAN_POINT ( 'NONE',  ( 5.719274019375991003, -21.55341960407610458, 62.70724293864769550 ) ) ;
#194874 = CARTESIAN_POINT ( 'NONE',  ( 5.049401038297881783, 19.05341960407617563, 47.29275706135231161 ) ) ;
#194875 = CARTESIAN_POINT ( 'NONE',  ( -19.02544592524342804, 5.153800228976336051, 116.0405762719810383 ) ) ;
#194876 = CARTESIAN_POINT ( 'NONE',  ( -15.72974639402197994, 15.80617190586746368, 95.62390960531436690 ) ) ;
#194877 = CARTESIAN_POINT ( 'NONE',  ( -19.36337904590690684, 5.499999999999947597, 55.41494137495620009 ) ) ;
#194878 = CARTESIAN_POINT ( 'NONE',  ( 13.97604488694527802, 13.89961937509977652, 69.37390960531436690 ) ) ;
#194879 = DIRECTION ( 'NONE',  ( 1.000000000000000000, 0.000000000000000000, 0.000000000000000000 ) ) ;
#194880 = CARTESIAN_POINT ( 'NONE',  ( 8.224510206698742110, 14.34966873604972548, 22.08442372801901143 ) ) ;
#194881 = CARTESIAN_POINT ( 'NONE',  ( 16.46253265017146816, 9.564922557961045513, 96.66775706135233293 ) ) ;
#194882 = CARTESIAN_POINT ( 'NONE',  ( 16.46253265017160672, -9.564922557960803928, 53.33224293864768839 ) ) ;
#194883 = CARTESIAN_POINT ( 'NONE',  ( -19.03943276465977164, 0.05219959533909376836, 116.2489096053143669 ) ) ;
#194885 = CARTESIAN_POINT ( 'NONE',  ( 16.53943276465976808, -0.05219959533910856209, 53.74890960531437401 ) ) ;
#194884 = CARTESIAN_POINT ( 'NONE',  ( 0.05219959533907565091, 21.53943276465977519, 84.99890960531436690 ) ) ;
#194886 = CARTESIAN_POINT ( 'NONE',  ( -18.62759615963255300, -10.81492255796106328, 74.16775706135231871 ) ) ;
#194888 = CARTESIAN_POINT ( 'NONE',  ( -9.564922557961040184, 16.46253265017147172, 22.91775706135233648 ) ) ;
#194887 = CARTESIAN_POINT ( 'NONE',  ( 16.52544592524335698, 4.483927247898782831, 26.45942372801901854 ) ) ;
#194889 = CARTESIAN_POINT ( 'NONE',  ( 12.14591786802309770, 12.06949235617756955, 34.37390960531435979 ) ) ;
#194890 = CARTESIAN_POINT ( 'NONE',  ( -21.52544592524343514, 5.823673210054127303, 116.0405762719810383 ) ) ;
#194891 = CARTESIAN_POINT ( 'NONE',  ( -14.29746914071049879, 8.314922557960819915, 50.83224293864770971 ) ) ;
#194892 = CARTESIAN_POINT ( 'NONE',  ( 13.97604488694548053, -13.89961937509957401, 95.62609039468563310 ) ) ;
#194893 = CARTESIAN_POINT ( 'NONE',  ( 16.51473224551083163, -9.474510206698727899, 70.83442372801900433 ) ) ;
#194894 = CARTESIAN_POINT ( 'NONE',  ( -5.719274019375665041, -21.55341960407619695, 64.79275706135234714 ) ) ;
#194895 = CARTESIAN_POINT ( 'NONE',  ( -13.89961937509957401, -13.97604488694547875, 49.37609039468567573 ) ) ;
#194896 = CARTESIAN_POINT ( 'NONE',  ( -4.483927247898539470, -16.52544592524342804, 112.2905762719810241 ) ) ;
#194897 = CARTESIAN_POINT ( 'NONE',  ( 18.67979575497178502, 10.72451020669898547, 44.16557627198103120 ) ) ;
#194898 = CARTESIAN_POINT ( 'NONE',  ( -14.29746914071049879, 8.314922557960819915, 55.83224293864770260 ) ) ;
#194899 = CARTESIAN_POINT ( 'NONE',  ( -17.50000000000000711, -5.500000000000025757, 51.28230962303570095 ) ) ;
#194900 = CARTESIAN_POINT ( 'NONE',  ( 21.55341960407619695, -5.719274019375665929, 111.0427570613523613 ) ) ;
#194901 = CARTESIAN_POINT ( 'NONE',  ( 16.53943276465976808, 0.05219959533934440121, 91.25109039468568994 ) ) ;
#194902 = CARTESIAN_POINT ( 'NONE',  ( -12.06949235617756955, 12.14591786802309770, 35.62390960531437401 ) ) ;
#194903 = CARTESIAN_POINT ( 'NONE',  ( 0.05219959533937995610, -21.53943276465977519, 80.00109039468568994 ) ) ;
#194904 = CARTESIAN_POINT ( 'NONE',  ( -21.55341960407619339, 5.719274019375674811, 68.54275706135234714 ) ) ;
#194905 = CARTESIAN_POINT ( 'NONE',  ( -10.81492255796078084, -18.62759615963271287, 77.08224293864769550 ) ) ;
#194906 = CARTESIAN_POINT ( 'NONE',  ( 16.51473224551069308, 9.474510206698969483, 44.16557627198103120 ) ) ;
#194907 = CARTESIAN_POINT ( 'NONE',  ( -10.81492255796105439, 18.62759615963255655, 57.91775706135234714 ) ) ;
#194908 = CARTESIAN_POINT ( 'NONE',  ( -13.89961937509977652, 13.97604488694528158, 40.62390960531435979 ) ) ;
#194909 = CARTESIAN_POINT ( 'NONE',  ( 5.153800228976335163, 19.02544592524342804, 49.79057627198100988 ) ) ;
#194910 = CARTESIAN_POINT ( 'NONE',  ( -4.483927247898539470, -16.52544592524342804, 97.29057627198105251 ) ) ;
#194911 = CARTESIAN_POINT ( 'NONE',  ( 0.05219959533909260263, 19.03943276465977164, 79.99890960531436690 ) ) ;
#194912 = CARTESIAN_POINT ( 'NONE',  ( -8.224510206698948167, 14.34966873604960824, 45.41557627198103830 ) ) ;
#194913 = CARTESIAN_POINT ( 'NONE',  ( 16.55341960407611168, 4.379528057220329451, 103.9572429386476813 ) ) ;
#194914 = CARTESIAN_POINT ( 'NONE',  ( -21.52544592524343514, 5.823673210054127303, 66.04057627198103830 ) ) ;
#194915 = CARTESIAN_POINT ( 'NONE',  ( -15.72974639402197994, 15.80617190586746368, 115.6239096053143669 ) ) ;
#194916 = CARTESIAN_POINT ( 'NONE',  ( -13.89961937509977652, 13.97604488694528158, 115.6239096053143669 ) ) ;
#194918 = CARTESIAN_POINT ( 'NONE',  ( -0.05219959533936034679, 19.03943276465977164, 112.5010903946856757 ) ) ;
#194917 = CARTESIAN_POINT ( 'NONE',  ( 9.564922557960805705, 16.46253265017160317, 84.58224293864769550 ) ) ;
#194919 = CARTESIAN_POINT ( 'NONE',  ( 15.72974639402199770, -15.80617190586745480, 73.12390960531436690 ) ) ;
#194920 = CARTESIAN_POINT ( 'NONE',  ( 5.719274019375673035, 21.55341960407619339, 92.29275706135236135 ) ) ;
#194921 = CARTESIAN_POINT ( 'NONE',  ( -16.46253265017160317, 9.564922557960807481, 80.83224293864769550 ) ) ;
#194922 = CARTESIAN_POINT ( 'NONE',  ( -10.72451020669898014, 18.67979575497178502, 110.4155762719810383 ) ) ;
#194923 = VECTOR ( 'NONE', #73219, 1000.000000000000114 ) ;
#194924 = CARTESIAN_POINT ( 'NONE',  ( 16.51473224551069308, 9.474510206698969483, 114.1655762719810241 ) ) ;
#194925 = CARTESIAN_POINT ( 'NONE',  ( 16.55341960407618274, -4.379528057220086978, 91.04275706135236135 ) ) ;
#194926 = CARTESIAN_POINT ( 'NONE',  ( 21.53943276465977519, 0.05219959533937863772, 66.25109039468567573 ) ) ;
#194927 = CARTESIAN_POINT ( 'NONE',  ( -5.719274019375665041, -21.55341960407619695, 94.79275706135234714 ) ) ;
#194928 = CARTESIAN_POINT ( 'NONE',  ( 16.53943276465976808, 0.05219959533934440121, 61.25109039468567573 ) ) ;
#194929 = CARTESIAN_POINT ( 'NONE',  ( 18.67979575497194134, -10.72451020669871369, 30.83442372801902209 ) ) ;
#194930 = CARTESIAN_POINT ( 'NONE',  ( 16.46253265017160672, -9.564922557960803928, 113.3322429386476955 ) ) ;
#194931 = CARTESIAN_POINT ( 'NONE',  ( 10.81492255796106328, -18.62759615963255655, 95.41775706135234714 ) ) ;
#194932 = CARTESIAN_POINT ( 'NONE',  ( -5.153800228976328057, -19.02544592524343514, 97.29057627198099567 ) ) ;
#194933 = CARTESIAN_POINT ( 'NONE',  ( -15.72974639402197994, 15.80617190586746368, 90.62390960531436690 ) ) ;
#194934 = CARTESIAN_POINT ( 'NONE',  ( -9.564922557961040184, 16.46253265017147172, 57.91775706135233293 ) ) ;
#194936 = CARTESIAN_POINT ( 'NONE',  ( 21.52544592524344225, -5.823673210054117533, 58.54057627198103120 ) ) ;
#194935 = CARTESIAN_POINT ( 'NONE',  ( -17.93416671128591489, -36.08982269496700468, -18.53391066944203303 ) ) ;
#194938 = CARTESIAN_POINT ( 'NONE',  ( -14.34966873604960291, -8.224510206698953496, 36.66557627198103120 ) ) ;
#194937 = CARTESIAN_POINT ( 'NONE',  ( -16.46253265017160317, 9.564922557960807481, 90.83224293864769550 ) ) ;
#194939 = CARTESIAN_POINT ( 'NONE',  ( -17.81289503416611808, 24.51734667627700404, 145.6999999999999886 ) ) ;
#194940 = CARTESIAN_POINT ( 'NONE',  ( 16.46253265017146816, 9.564922557961045513, 76.66775706135234714 ) ) ;
#194941 = CARTESIAN_POINT ( 'NONE',  ( -1.216645939406758359, -16.09882439466101189, -61.59766612755958448 ) ) ;
#194942 = CARTESIAN_POINT ( 'NONE',  ( -9.564922557961040184, 16.46253265017147172, 112.9177570613523329 ) ) ;
#194943 = CARTESIAN_POINT ( 'NONE',  ( -21.52544592524343514, 5.823673210054127303, 91.04057627198103830 ) ) ;
#194944 = CARTESIAN_POINT ( 'NONE',  ( 14.34966873604960469, 8.224510206698951720, 69.16557627198102409 ) ) ;
#194945 = CARTESIAN_POINT ( 'NONE',  ( -8.224510206698735004, -14.34966873604973081, 24.58442372801901499 ) ) ;
#194946 = CARTESIAN_POINT ( 'NONE',  ( 16.51473224551069308, 9.474510206698969483, 49.16557627198102409 ) ) ;
#194948 = CARTESIAN_POINT ( 'NONE',  ( 13.97604488694548053, -13.89961937509957401, 85.62609039468568994 ) ) ;
#194947 = CARTESIAN_POINT ( 'NONE',  ( -5.719274019375978568, 21.55341960407610458, 110.2072429386477239 ) ) ;
#194949 = CARTESIAN_POINT ( 'NONE',  ( 16.51473224551069308, 9.474510206698969483, 94.16557627198103830 ) ) ;
#194950 = CARTESIAN_POINT ( 'NONE',  ( 9.564922557960805705, 16.46253265017160317, 69.58224293864770971 ) ) ;
#194951 = CARTESIAN_POINT ( 'NONE',  ( -15.72974639402197994, 15.80617190586746368, 70.62390960531436690 ) ) ;
#194952 = CARTESIAN_POINT ( 'NONE',  ( -16.51473224551069308, -9.474510206698971260, 41.66557627198103120 ) ) ;
#194953 = CARTESIAN_POINT ( 'NONE',  ( -15.89947302414459607, 34.30766951777760454, -8.000000000000000000 ) ) ;
#194954 = CARTESIAN_POINT ( 'NONE',  ( 8.314922557960818139, 14.29746914071049879, 49.58224293864769550 ) ) ;
#194955 = CARTESIAN_POINT ( 'NONE',  ( 19.03943276465977164, -0.05219959533909143690, 98.74890960531436690 ) ) ;
#194956 = CARTESIAN_POINT ( 'NONE',  ( 1.993301997531345686E-15, -30.30510711980685556, 144.4999999999999716 ) ) ;
#194957 = CARTESIAN_POINT ( 'NONE',  ( 5.153800228976615827, -19.02544592524334988, 70.20942372801899012 ) ) ;
#194958 = CARTESIAN_POINT ( 'NONE',  ( -15.72974639402197994, 15.80617190586746368, 75.62390960531439532 ) ) ;
#194959 = CARTESIAN_POINT ( 'NONE',  ( -16.46253265017146816, -9.564922557961047289, 34.16775706135233293 ) ) ;
#194960 = CARTESIAN_POINT ( 'NONE',  ( -5.153800228976328057, -19.02544592524343514, 102.2905762719810383 ) ) ;
#194961 = CARTESIAN_POINT ( 'NONE',  ( 12.08085585438963605, -10.04536149086137264, -59.60010879982917231 ) ) ;
#194962 = CARTESIAN_POINT ( 'NONE',  ( -10.72451020669898014, 18.67979575497178502, 45.41557627198103830 ) ) ;
#194963 = CARTESIAN_POINT ( 'NONE',  ( -5.153800228976328057, -19.02544592524343514, 67.29057627198102409 ) ) ;
#194964 = CARTESIAN_POINT ( 'NONE',  ( 21.52544592524334988, 5.823673210054432836, 71.45942372801901854 ) ) ;
#194965 = CARTESIAN_POINT ( 'NONE',  ( -5.153800228976328057, -19.02544592524343514, 22.29057627198102765 ) ) ;
#194967 = ORIENTED_EDGE ( 'NONE', *, *, #90799, .F. ) ;
#194966 = CARTESIAN_POINT ( 'NONE',  ( 10.72451020669898902, -18.67979575497178502, 112.9155762719810383 ) ) ;
#194968 = CARTESIAN_POINT ( 'NONE',  ( 15.72974639402176855, 15.80617190586768217, 51.87609039468568284 ) ) ;
#194969 = VERTEX_POINT ( 'NONE', #18563 ) ;
#194970 = CARTESIAN_POINT ( 'NONE',  ( 13.97604488694527802, 13.89961937509977652, 109.3739096053143669 ) ) ;
#194971 = CARTESIAN_POINT ( 'NONE',  ( 13.97604488694548053, -13.89961937509957401, 65.62609039468567573 ) ) ;
#194972 = CARTESIAN_POINT ( 'NONE',  ( -21.44820451018248875, 9.431764332217083435, 168.6453917704523633 ) ) ;
#194973 = CARTESIAN_POINT ( 'NONE',  ( -21.52544592524343514, 5.823673210054127303, 111.0405762719810525 ) ) ;
#194974 = CARTESIAN_POINT ( 'NONE',  ( -13.97604488694527625, -13.89961937509977652, 66.87390960531436690 ) ) ;
#194975 = CARTESIAN_POINT ( 'NONE',  ( -16.52544592524335698, -4.483927247898792601, 33.95942372801901143 ) ) ;
#194976 = CARTESIAN_POINT ( 'NONE',  ( 30.74264578624799782, 22.33583958711400541, -8.549999994537627046 ) ) ;
#194977 = CARTESIAN_POINT ( 'NONE',  ( -5.823673210054431948, 21.52544592524334988, 102.7094237280190185 ) ) ;
#194978 = CARTESIAN_POINT ( 'NONE',  ( -13.97604488694527625, -13.89961937509977652, 36.87390960531436690 ) ) ;
#194979 = CARTESIAN_POINT ( 'NONE',  ( 0.05219959533936267826, -19.03943276465977164, 20.00109039468567218 ) ) ;
#194980 = CARTESIAN_POINT ( 'NONE',  ( -16.55341960407617563, 4.379528057220093196, 93.54275706135234714 ) ) ;
#194982 = CARTESIAN_POINT ( 'NONE',  ( -10.81492255796105439, 18.62759615963255655, 62.91775706135236135 ) ) ;
#194981 = CARTESIAN_POINT ( 'NONE',  ( -13.97604488694527625, -13.89961937509977652, 91.87390960531432427 ) ) ;
#194983 = CARTESIAN_POINT ( 'NONE',  ( 29.86685920354754842, -21.69954338932559068, -9.824999997268813345 ) ) ;
#194984 = CARTESIAN_POINT ( 'NONE',  ( 13.97604488694527802, 13.89961937509977652, 114.3739096053143669 ) ) ;
#194985 = CARTESIAN_POINT ( 'NONE',  ( -17.50000000000001066, 3.209263204892529142, 29.76196825606282204 ) ) ;
#194987 = CARTESIAN_POINT ( 'NONE',  ( -15.80617190586768217, 15.72974639402176855, 78.12609039468570415 ) ) ;
#194986 = CARTESIAN_POINT ( 'NONE',  ( -14.34966873604972548, 8.224510206698743886, 48.33442372801902565 ) ) ;
#194988 = CARTESIAN_POINT ( 'NONE',  ( -21.52544592524334988, -5.823673210054445271, 83.95942372801900433 ) ) ;
#194989 = AXIS2_PLACEMENT_3D ( 'NONE', #150738, #10230, #118405 ) ;
#194990 = DIRECTION ( 'NONE',  ( -0.000000000000000000, -0.6427876096865545730, -0.7660444431189654679 ) ) ;
#194991 = CARTESIAN_POINT ( 'NONE',  ( 0.05219959533934541429, -16.53943276465976808, 25.00109039468567218 ) ) ;
#194992 = CARTESIAN_POINT ( 'NONE',  ( -16.46253265017160317, 9.564922557960807481, 90.83224293864769550 ) ) ;
#194993 = CARTESIAN_POINT ( 'NONE',  ( 19.02544592524343514, -5.153800228976328945, 108.5405762719810383 ) ) ;
#194994 = CARTESIAN_POINT ( 'NONE',  ( 17.49999999999999289, 5.500000000000009770, 43.78230962303566542 ) ) ;
#194995 = CARTESIAN_POINT ( 'NONE',  ( 0.05219959533909260263, 19.03943276465977164, 29.99890960531435979 ) ) ;
#194996 = CARTESIAN_POINT ( 'NONE',  ( -5.719274019375978568, 21.55341960407610458, 40.20724293864769550 ) ) ;
#194997 = CARTESIAN_POINT ( 'NONE',  ( 8.314922557961029526, -14.29746914071037800, 105.4177570613523613 ) ) ;
#194999 = CARTESIAN_POINT ( 'NONE',  ( 9.564922557960805705, 16.46253265017160317, 69.58224293864770971 ) ) ;
#194998 = CARTESIAN_POINT ( 'NONE',  ( -8.314922557960811034, -14.29746914071050412, 82.08224293864768129 ) ) ;
#195000 = CARTESIAN_POINT ( 'NONE',  ( 21.52544592524334988, 5.823673210054432836, 86.45942372801901854 ) ) ;
#195001 = CARTESIAN_POINT ( 'NONE',  ( -16.52544592524335698, -4.483927247898792601, 28.95942372801902209 ) ) ;
#195002 = CARTESIAN_POINT ( 'NONE',  ( -0.05219959533910754901, -16.53943276465976808, 82.49890960531436690 ) ) ;
#195003 = CARTESIAN_POINT ( 'NONE',  ( -18.62759615963255300, -10.81492255796106328, 44.16775706135234714 ) ) ;
#195004 = CARTESIAN_POINT ( 'NONE',  ( 15.72974639402199770, -15.80617190586745480, 73.12390960531436690 ) ) ;
#195005 = CARTESIAN_POINT ( 'NONE',  ( 16.46253265017146816, 9.564922557961045513, 31.66775706135232937 ) ) ;
#195006 = CARTESIAN_POINT ( 'NONE',  ( -34.64436006561231096, 3.766901597203496710, 51.50401746017936944 ) ) ;
#195007 = CARTESIAN_POINT ( 'NONE',  ( -5.049401038298153566, 19.05341960407611168, 95.20724293864770971 ) ) ;
#195008 = CARTESIAN_POINT ( 'NONE',  ( 12.06949235617757843, -12.14591786802309237, 63.12390960531435979 ) ) ;
#195009 = VECTOR ( 'NONE', #106586, 1000.000000000000000 ) ;
#195010 = CARTESIAN_POINT ( 'NONE',  ( 0.05219959533910956823, 16.53943276465976808, 49.99890960531437401 ) ) ;
#195011 = CARTESIAN_POINT ( 'NONE',  ( 16.53943276465976808, 0.05219959533934440121, 111.2510903946856899 ) ) ;
#195013 = ADVANCED_FACE ( 'NONE', ( #145202 ), #161382, .F. ) ;
#195012 = CARTESIAN_POINT ( 'NONE',  ( -16.51473224551082808, 9.474510206698731452, 63.33442372801900433 ) ) ;
#195014 = CARTESIAN_POINT ( 'NONE',  ( -16.51473224551082808, 9.474510206698731452, 78.33442372801900433 ) ) ;
#195015 = CARTESIAN_POINT ( 'NONE',  ( 18.67979575497178502, 10.72451020669898547, 24.16557627198103120 ) ) ;
#195016 = CARTESIAN_POINT ( 'NONE',  ( -4.483927247898539470, -16.52544592524342804, 82.29057627198103830 ) ) ;
#195017 = CARTESIAN_POINT ( 'NONE',  ( 18.82182630884599561, -5.500000000000063061, 38.42483672716981147 ) ) ;
#195019 = CARTESIAN_POINT ( 'NONE',  ( 21.55341960407610458, 5.719274019375980345, 53.95724293864770260 ) ) ;
#195018 = CARTESIAN_POINT ( 'NONE',  ( 5.153800228976335163, 19.02544592524342804, 44.79057627198103830 ) ) ;
#195020 = CARTESIAN_POINT ( 'NONE',  ( 21.55341960407610458, 5.719274019375980345, 83.95724293864770971 ) ) ;
#195021 = CARTESIAN_POINT ( 'NONE',  ( -16.51473224551069308, -9.474510206698971260, 21.66557627198102765 ) ) ;
#195023 = CARTESIAN_POINT ( 'NONE',  ( -0.05219959533909027116, -19.03943276465977164, 42.49890960531435269 ) ) ;
#195022 = CARTESIAN_POINT ( 'NONE',  ( 4.379528057220092307, 16.55341960407617563, 62.29275706135236845 ) ) ;
#195024 = CARTESIAN_POINT ( 'NONE',  ( -9.474510206698720793, -16.51473224551083518, 39.58442372801899722 ) ) ;
#195025 = CARTESIAN_POINT ( 'NONE',  ( 21.53943276465977519, 0.05219959533937863772, 61.25109039468567573 ) ) ;
#195026 = CARTESIAN_POINT ( 'NONE',  ( -16.55341960407611168, -4.379528057220339221, 101.4572429386476955 ) ) ;
#195027 = CARTESIAN_POINT ( 'NONE',  ( 5.153800228976615827, -19.02544592524334988, 90.20942372801900433 ) ) ;
#195028 = CARTESIAN_POINT ( 'NONE',  ( 29.86685920354754487, 21.69954338932564752, -3.924999997268812990 ) ) ;
#195030 = CARTESIAN_POINT ( 'NONE',  ( -18.62759615963270932, 10.81492255796079327, 45.83224293864769550 ) ) ;
#195029 = CARTESIAN_POINT ( 'NONE',  ( -0.9720251121415244278, -23.94686256013569192, -57.02522261278124205 ) ) ;
#195031 = CARTESIAN_POINT ( 'NONE',  ( 5.049401038298161559, -19.05341960407611168, 27.70724293864769550 ) ) ;
#195032 = CARTESIAN_POINT ( 'NONE',  ( -5.719274019375665041, -21.55341960407619695, 84.79275706135234714 ) ) ;
#195033 = CARTESIAN_POINT ( 'NONE',  ( -14.34966873604960291, -8.224510206698953496, 26.66557627198103475 ) ) ;
#195035 = CARTESIAN_POINT ( 'NONE',  ( 0.05219959533910956823, 16.53943276465976808, 44.99890960531435979 ) ) ;
#195034 = CARTESIAN_POINT ( 'NONE',  ( -16.55341960407617563, 4.379528057220093196, 53.54275706135234714 ) ) ;
#195036 = CARTESIAN_POINT ( 'NONE',  ( -10.72451020669898014, 18.67979575497178502, 85.41557627198102409 ) ) ;
#195037 = CARTESIAN_POINT ( 'NONE',  ( -5.823673210054116645, -21.52544592524344225, 77.29057627198102409 ) ) ;
#195038 = CARTESIAN_POINT ( 'NONE',  ( -22.00000000000000000, -5.510910596163089556E-15, 45.00000000000000000 ) ) ;
#195040 = CARTESIAN_POINT ( 'NONE',  ( 5.823673210054125526, 21.52544592524343514, 24.79057627198103120 ) ) ;
#195039 = CARTESIAN_POINT ( 'NONE',  ( -5.049401038297874678, -19.05341960407617918, 84.79275706135233293 ) ) ;
#195041 = CARTESIAN_POINT ( 'NONE',  ( 9.474510206698971260, -16.51473224551069308, 42.91557627198103120 ) ) ;
#195042 = CARTESIAN_POINT ( 'NONE',  ( -5.049401038298153566, 19.05341960407611168, 30.20724293864768839 ) ) ;
#195043 = CARTESIAN_POINT ( 'NONE',  ( -27.86473085795038429, -130.0000000000000000, -13.99999999999999822 ) ) ;
#195044 = ORIENTED_EDGE ( 'NONE', *, *, #6212, .T. ) ;
#195045 = CARTESIAN_POINT ( 'NONE',  ( -16.55341960407617563, 4.379528057220093196, 83.54275706135234714 ) ) ;
#195046 = CARTESIAN_POINT ( 'NONE',  ( -5.823673210054116645, -21.52544592524344225, 107.2905762719810525 ) ) ;
#195047 = CARTESIAN_POINT ( 'NONE',  ( 19.03943276465977164, -0.05219959533909143690, 73.74890960531435269 ) ) ;
#195048 = CARTESIAN_POINT ( 'NONE',  ( 21.52544592524334988, 5.823673210054432836, 36.45942372801901143 ) ) ;
#195049 = CARTESIAN_POINT ( 'NONE',  ( 9.474510206698971260, -16.51473224551069308, 97.91557627198102409 ) ) ;
#195051 = EDGE_CURVE ( 'NONE', #66658, #193741, #45224, .T. ) ;
#195050 = CARTESIAN_POINT ( 'NONE',  ( -25.79201298824010991, -30.25621121864696050, -20.58051720724199996 ) ) ;
#195052 = ORIENTED_EDGE ( 'NONE', *, *, #192980, .T. ) ;
#195053 = CARTESIAN_POINT ( 'NONE',  ( 5.823673210054444382, -21.52544592524334988, 30.20942372801902565 ) ) ;
#195055 = CARTESIAN_POINT ( 'NONE',  ( -13.89961937509977652, 13.97604488694528158, 100.6239096053143669 ) ) ;
#195054 = CARTESIAN_POINT ( 'NONE',  ( -13.89961937509977652, 13.97604488694528158, 30.62390960531435269 ) ) ;
#195056 = CARTESIAN_POINT ( 'NONE',  ( -19.02544592524334988, -5.153800228976617603, 38.95942372801900433 ) ) ;
#195057 = CARTESIAN_POINT ( 'NONE',  ( -10.72451020669898014, 18.67979575497178502, 115.4155762719810241 ) ) ;
#195058 = CARTESIAN_POINT ( 'NONE',  ( 13.97604488694548053, -13.89961937509957401, 40.62609039468564731 ) ) ;
#195059 = CARTESIAN_POINT ( 'NONE',  ( -16.51473224551082808, 9.474510206698731452, 43.33442372801900433 ) ) ;
#195060 = CARTESIAN_POINT ( 'NONE',  ( -12.14591786802326823, 12.06949235617739902, 98.12609039468570415 ) ) ;
#195061 = CARTESIAN_POINT ( 'NONE',  ( 11.80868324581537543, 11.80868324581533990, -61.34707691135562868 ) ) ;
#195062 = CARTESIAN_POINT ( 'NONE',  ( 0.05219959533909260263, 19.03943276465977164, 69.99890960531435269 ) ) ;
#195063 = CARTESIAN_POINT ( 'NONE',  ( -15.80617190586768217, 15.72974639402176855, 73.12609039468567573 ) ) ;
#195064 = CARTESIAN_POINT ( 'NONE',  ( 21.55341960407619695, -5.719274019375665929, 91.04275706135236135 ) ) ;
#195065 = CARTESIAN_POINT ( 'NONE',  ( -1.500047742438159526, -7.503727747132431958, -64.26135111332261829 ) ) ;
#195066 = CARTESIAN_POINT ( 'NONE',  ( -5.153800228976328057, -19.02544592524343514, 82.29057627198103830 ) ) ;
#195067 = CARTESIAN_POINT ( 'NONE',  ( -10.72451020669870658, -18.67979575497194134, 64.58442372801900433 ) ) ;
#195068 = CARTESIAN_POINT ( 'NONE',  ( 13.89961937509957401, 13.97604488694547697, 101.8760903946856331 ) ) ;
#195069 = CARTESIAN_POINT ( 'NONE',  ( 9.474510206698971260, -16.51473224551069308, 62.91557627198102409 ) ) ;
#195070 = CARTESIAN_POINT ( 'NONE',  ( 5.153800228976335163, 19.02544592524342804, 114.7905762719810241 ) ) ;
#195071 = AXIS2_PLACEMENT_3D ( 'NONE', #180917, #87874, #195079 ) ;
#195072 = CARTESIAN_POINT ( 'NONE',  ( 9.564922557960805705, 16.46253265017160317, 84.58224293864769550 ) ) ;
#195073 = CARTESIAN_POINT ( 'NONE',  ( -17.44279575226824619, -5.990770900252441855, 89.16442432485686709 ) ) ;
#195074 = CARTESIAN_POINT ( 'NONE',  ( -19.05341960407611168, -5.049401038298163336, 61.45724293864769550 ) ) ;
#195075 = CARTESIAN_POINT ( 'NONE',  ( -16.51473224551069308, -9.474510206698971260, 56.66557627198103120 ) ) ;
#195076 = CARTESIAN_POINT ( 'NONE',  ( -18.62759615963270932, 10.81492255796079327, 115.8322429386477097 ) ) ;
#195077 = CARTESIAN_POINT ( 'NONE',  ( -16.55341960407617563, 4.379528057220093196, 98.54275706135234714 ) ) ;
#195078 = CARTESIAN_POINT ( 'NONE',  ( 17.50000000000000000, 5.499999999999997335, 120.0000000000000142 ) ) ;
#195079 = DIRECTION ( 'NONE',  ( -0.8164965809277243691, 0.000000000000000000, 0.5773502691896281735 ) ) ;
#195080 = CARTESIAN_POINT ( 'NONE',  ( 16.51473224551083163, -9.474510206698727899, 60.83442372801900433 ) ) ;
#195081 = CARTESIAN_POINT ( 'NONE',  ( -9.564922557960796823, -16.46253265017161027, 77.08224293864769550 ) ) ;
#195082 = CARTESIAN_POINT ( 'NONE',  ( -16.55341960407611168, -4.379528057220339221, 66.45724293864768129 ) ) ;
#195083 = CARTESIAN_POINT ( 'NONE',  ( 16.55341960407611168, 4.379528057220329451, 108.9572429386476955 ) ) ;
#195084 = CARTESIAN_POINT ( 'NONE',  ( 18.62759615963271287, -10.81492255796078972, 33.33224293864769550 ) ) ;
#195085 = CARTESIAN_POINT ( 'NONE',  ( 19.03943276465977164, -0.05219959533909143690, 103.7489096053143669 ) ) ;
#195086 = CARTESIAN_POINT ( 'NONE',  ( 8.314922557960818139, 14.29746914071049879, 89.58224293864768129 ) ) ;
#195087 = CARTESIAN_POINT ( 'NONE',  ( -13.89961937509957401, -13.97604488694547875, 24.37609039468565442 ) ) ;
#195088 = CARTESIAN_POINT ( 'NONE',  ( 14.29746914071037800, 8.314922557961029526, 106.6677570613523756 ) ) ;
#195089 = CARTESIAN_POINT ( 'NONE',  ( 16.51473224551069308, 9.474510206698969483, 94.16557627198103830 ) ) ;
#195090 = CARTESIAN_POINT ( 'NONE',  ( -18.62759615963255300, -10.81492255796106328, 49.16775706135234003 ) ) ;
#195091 = CARTESIAN_POINT ( 'NONE',  ( 18.67979575497178502, 10.72451020669898547, 49.16557627198102409 ) ) ;
#195092 = CARTESIAN_POINT ( 'NONE',  ( -10.81492255796105439, 18.62759615963255655, 37.91775706135235424 ) ) ;
#195093 = CARTESIAN_POINT ( 'NONE',  ( 15.72974639402199770, -15.80617190586745480, 78.12390960531436690 ) ) ;
#195094 = CARTESIAN_POINT ( 'NONE',  ( -16.52544592524342804, 4.483927247898546575, 101.0405762719810383 ) ) ;
#195095 = CARTESIAN_POINT ( 'NONE',  ( -19.03943276465977164, -0.05219959533935918106, 58.75109039468566863 ) ) ;
#195096 = AXIS2_PLACEMENT_3D ( 'NONE', #152521, #51058, #33906 ) ;
#195097 = CARTESIAN_POINT ( 'NONE',  ( 0.05219959533909260263, 19.03943276465977164, 44.99890960531435979 ) ) ;
#195098 = CARTESIAN_POINT ( 'NONE',  ( 16.46253265017160672, -9.564922557960803928, 103.3322429386476955 ) ) ;
#195099 = CARTESIAN_POINT ( 'NONE',  ( -9.474510206698964154, 16.51473224551069663, 100.4155762719810241 ) ) ;
#195100 = CARTESIAN_POINT ( 'NONE',  ( 8.224510206698953496, -14.34966873604960469, 112.9155762719810383 ) ) ;
#195101 = CARTESIAN_POINT ( 'NONE',  ( -0.05219959533910754901, -16.53943276465976808, 27.49890960531435269 ) ) ;
#195102 = CARTESIAN_POINT ( 'NONE',  ( 14.34966873604972726, -8.224510206698740333, 35.83442372801901143 ) ) ;
#195103 = CARTESIAN_POINT ( 'NONE',  ( -0.05219959533937732626, 21.53943276465977519, 112.5010903946857042 ) ) ;
#195105 = CARTESIAN_POINT ( 'NONE',  ( 8.224510206698953496, -14.34966873604960469, 27.91557627198103830 ) ) ;
#195104 = CARTESIAN_POINT ( 'NONE',  ( 9.564922557960805705, 16.46253265017160317, 114.5822429386476955 ) ) ;
#195106 = CARTESIAN_POINT ( 'NONE',  ( -10.81492255796105439, 18.62759615963255655, 37.91775706135235424 ) ) ;
#195107 = CARTESIAN_POINT ( 'NONE',  ( -5.049401038298153566, 19.05341960407611168, 110.2072429386476671 ) ) ;
#195108 = CARTESIAN_POINT ( 'NONE',  ( 14.34966873604972726, -8.224510206698740333, 50.83442372801901143 ) ) ;
#195109 = CARTESIAN_POINT ( 'NONE',  ( 4.379528057220092307, 16.55341960407617563, 112.2927570613523471 ) ) ;
#195110 = CARTESIAN_POINT ( 'NONE',  ( -4.379528057220086978, -16.55341960407618274, 89.79275706135236135 ) ) ;
#195111 = CARTESIAN_POINT ( 'NONE',  ( -8.224510206698735004, -14.34966873604973081, 24.58442372801901499 ) ) ;
#195112 = CARTESIAN_POINT ( 'NONE',  ( 0.05219959533909260263, 19.03943276465977164, 34.99890960531435979 ) ) ;
#195113 = CARTESIAN_POINT ( 'NONE',  ( -4.483927247898539470, -16.52544592524342804, 112.2905762719810241 ) ) ;
#195114 = CARTESIAN_POINT ( 'NONE',  ( -10.72451020669870658, -18.67979575497194134, 19.58442372801901143 ) ) ;
#195115 = CARTESIAN_POINT ( 'NONE',  ( 9.564922557960805705, 16.46253265017160317, 34.58224293864770260 ) ) ;
#195116 = CARTESIAN_POINT ( 'NONE',  ( 9.564922557960805705, 16.46253265017160317, 109.5822429386476955 ) ) ;
#195117 = CARTESIAN_POINT ( 'NONE',  ( 5.823673210054444382, -21.52544592524334988, 30.20942372801902565 ) ) ;
#195118 = CARTESIAN_POINT ( 'NONE',  ( 19.02544592524343514, -5.153800228976328945, 23.54057627198102054 ) ) ;
#195119 = CARTESIAN_POINT ( 'NONE',  ( -13.97604488694527625, -13.89961937509977652, 101.8739096053143811 ) ) ;
#195120 = CLOSED_SHELL ( 'NONE', ( #7349, #181119, #153392, #99122, #34450, #39897, #171120, #134165, #109377, #85440, #38588, #157811, #73604, #12967, #64638, #161662, #96947, #59605, #40135, #89114, #149007, #72193, #119923, #33560, #70007, #78559, #121162, #198694, #121823, #104659, #179081, #2575, #165110, #137794, #181724, #149760, #101197, #11219, #162483, #28210, #63977, #114053, #159372, #64613, #113118, #104650, #167383, #105983, #41055, #159748, #108000, #19925, #102571, #179207, #8948, #194528, #113133 ) ) ;
#195121 = CARTESIAN_POINT ( 'NONE',  ( 16.52216118717205973, -7.221426719304538722, 111.4240097895301034 ) ) ;
#195122 = CARTESIAN_POINT ( 'NONE',  ( 19.05341960407611168, 5.049401038298154454, 93.95724293864769550 ) ) ;
#195124 = CARTESIAN_POINT ( 'NONE',  ( -14.29746914071049879, 8.314922557960819915, 90.83224293864769550 ) ) ;
#195123 = CARTESIAN_POINT ( 'NONE',  ( 10.72451020669871369, 18.67979575497193778, 52.08442372801901854 ) ) ;
#195125 = CARTESIAN_POINT ( 'NONE',  ( 5.049401038298161559, -19.05341960407611168, 102.7072429386476955 ) ) ;
#195126 = CARTESIAN_POINT ( 'NONE',  ( 26.99873734152944138, 22.49873734152883387, 1.110912703473986074 ) ) ;
#195127 = COLOUR_RGB ( '', 0.09019608, 0.27058824, 0.51372549) ;
#195128 = CARTESIAN_POINT ( 'NONE',  ( -4.483927247898782831, 16.52544592524335698, 67.70942372801901854 ) ) ;
#195129 = CARTESIAN_POINT ( 'NONE',  ( -10.81492255796105439, 18.62759615963255655, 82.91775706135234714 ) ) ;
#195130 = CARTESIAN_POINT ( 'NONE',  ( -4.379528057220086978, -16.55341960407618274, 44.79275706135234714 ) ) ;
#195131 = CARTESIAN_POINT ( 'NONE',  ( 13.89961937509977652, -13.97604488694527269, 88.12390960531438111 ) ) ;
#195132 = CARTESIAN_POINT ( 'NONE',  ( 9.474510206698729675, 16.51473224551082808, 112.0844237280190043 ) ) ;
#195133 = CARTESIAN_POINT ( 'NONE',  ( -14.29746914071037622, -8.314922557961029526, 64.16775706135234714 ) ) ;
#195134 = CARTESIAN_POINT ( 'NONE',  ( -21.53943276465977519, -0.05219959533937600094, 108.7510903946857042 ) ) ;
#195135 = CARTESIAN_POINT ( 'NONE',  ( -19.03943276465977164, -0.05219959533935918106, 98.75109039468567573 ) ) ;
#195136 = CARTESIAN_POINT ( 'NONE',  ( 9.564922557960805705, 16.46253265017160317, 69.58224293864770971 ) ) ;
#195137 = CARTESIAN_POINT ( 'NONE',  ( -0.05219959533907301413, -21.53943276465977519, 87.49890960531436690 ) ) ;
#195139 = CARTESIAN_POINT ( 'NONE',  ( -0.05219959533936034679, 19.03943276465977164, 92.50109039468566152 ) ) ;
#195138 = CARTESIAN_POINT ( 'NONE',  ( -12.14591786802309592, -12.06949235617757132, 86.87390960531438111 ) ) ;
#195140 = CARTESIAN_POINT ( 'NONE',  ( -16.55341960407617563, 4.379528057220093196, 63.54275706135234003 ) ) ;
#195141 = CARTESIAN_POINT ( 'NONE',  ( 24.86035471869053382, 4.680034064337423416, 169.8578160361099094 ) ) ;
#195142 = CARTESIAN_POINT ( 'NONE',  ( 19.05341960407617918, -5.049401038297876454, 56.04275706135234714 ) ) ;
#195143 = CARTESIAN_POINT ( 'NONE',  ( 12.06949235617757843, -12.14591786802309237, 28.12390960531435979 ) ) ;
#195144 = CARTESIAN_POINT ( 'NONE',  ( -12.14591786802309592, -12.06949235617757132, 86.87390960531438111 ) ) ;
#195146 = CARTESIAN_POINT ( 'NONE',  ( -17.49999999999999645, 5.499999999999985789, 38.71769037696434879 ) ) ;
#195145 = CARTESIAN_POINT ( 'NONE',  ( -10.72451020669870658, -18.67979575497194134, 109.5844237280190328 ) ) ;
#195147 = CARTESIAN_POINT ( 'NONE',  ( -5.719274019375665041, -21.55341960407619695, 19.79275706135235069 ) ) ;
#195148 = CARTESIAN_POINT ( 'NONE',  ( 13.97604488694527802, 13.89961937509977652, 104.3739096053143385 ) ) ;
#195149 = CARTESIAN_POINT ( 'NONE',  ( -13.97604488694527625, -13.89961937509977652, 76.87390960531433848 ) ) ;
#195150 = CARTESIAN_POINT ( 'NONE',  ( -18.67979575497193778, 10.72451020669871902, 103.3344237280190043 ) ) ;
#195151 = CARTESIAN_POINT ( 'NONE',  ( 19.03943276465977164, -0.05219959533909143690, 73.74890960531435269 ) ) ;
#195152 = CARTESIAN_POINT ( 'NONE',  ( 18.67979575497178502, 10.72451020669898547, 49.16557627198102409 ) ) ;
#195153 = CARTESIAN_POINT ( 'NONE',  ( 12.06949235617757843, -12.14591786802309237, 78.12390960531436690 ) ) ;
#195154 = CARTESIAN_POINT ( 'NONE',  ( 13.97604488694527802, 13.89961937509977652, 39.37390960531435269 ) ) ;
#195155 = CARTESIAN_POINT ( 'NONE',  ( 4.483927247898545687, 16.52544592524342804, 104.7905762719810241 ) ) ;
#195156 = VECTOR ( 'NONE', #112941, 1000.000000000000000 ) ;
#195157 = CARTESIAN_POINT ( 'NONE',  ( -15.72974639402197994, 15.80617190586746368, 115.6239096053143669 ) ) ;
#195158 = CARTESIAN_POINT ( 'NONE',  ( -15.72974639402176322, -15.80617190586768395, 59.37609039468568284 ) ) ;
#195159 = CARTESIAN_POINT ( 'NONE',  ( -5.153800228976328057, -19.02544592524343514, 27.29057627198103120 ) ) ;
#195160 = CARTESIAN_POINT ( 'NONE',  ( -4.483927247898782831, 16.52544592524335698, 67.70942372801901854 ) ) ;
#195161 = CARTESIAN_POINT ( 'NONE',  ( -10.72451020669870658, -18.67979575497194134, 19.58442372801901143 ) ) ;
#195162 = CARTESIAN_POINT ( 'NONE',  ( -18.67979575497178146, -10.72451020669898902, 106.6655762719810383 ) ) ;
#195164 = CARTESIAN_POINT ( 'NONE',  ( 9.474510206698971260, -16.51473224551069308, 47.91557627198102409 ) ) ;
#195163 = CARTESIAN_POINT ( 'NONE',  ( -9.564922557961040184, 16.46253265017147172, 37.91775706135233293 ) ) ;
#195165 = CARTESIAN_POINT ( 'NONE',  ( -19.03943276465977164, 0.05219959533909376836, 116.2489096053143669 ) ) ;
#195166 = CARTESIAN_POINT ( 'NONE',  ( -10.81492255796105439, 18.62759615963255655, 72.91775706135234714 ) ) ;
#195167 = CARTESIAN_POINT ( 'NONE',  ( 5.823673210054125526, 21.52544592524343514, 59.79057627198103120 ) ) ;
#195168 = CARTESIAN_POINT ( 'NONE',  ( -12.06949235617756955, 12.14591786802309770, 40.62390960531435269 ) ) ;
#195170 = CARTESIAN_POINT ( 'NONE',  ( -0.05219959533937732626, 21.53943276465977519, 112.5010903946857042 ) ) ;
#195169 = CARTESIAN_POINT ( 'NONE',  ( -10.72451020669870658, -18.67979575497194134, 79.58442372801903275 ) ) ;
#195171 = CARTESIAN_POINT ( 'NONE',  ( 4.379528057220339221, -16.55341960407611168, 57.70724293864770260 ) ) ;
#195172 = CARTESIAN_POINT ( 'NONE',  ( -16.52544592524342804, 4.483927247898546575, 106.0405762719810525 ) ) ;
#195173 = CARTESIAN_POINT ( 'NONE',  ( 16.51473224551083163, -9.474510206698727899, 45.83442372801900433 ) ) ;
#195174 = CARTESIAN_POINT ( 'NONE',  ( 0.05219959533934541429, -16.53943276465976808, 95.00109039468568994 ) ) ;
#195175 = CARTESIAN_POINT ( 'NONE',  ( 5.823673210054444382, -21.52544592524334988, 65.20942372801901854 ) ) ;
#195176 = CARTESIAN_POINT ( 'NONE',  ( 5.153800228976335163, 19.02544592524342804, 64.79057627198100988 ) ) ;
#195177 = CARTESIAN_POINT ( 'NONE',  ( 16.51473224551083163, -9.474510206698727899, 35.83442372801899722 ) ) ;
#195178 = CARTESIAN_POINT ( 'NONE',  ( -15.80617190586745835, -15.72974639402198527, 31.87390960531435979 ) ) ;
#195179 = CARTESIAN_POINT ( 'NONE',  ( 10.81492255796106328, -18.62759615963255655, 30.41775706135234358 ) ) ;
#195180 = CARTESIAN_POINT ( 'NONE',  ( 5.823673210054125526, 21.52544592524343514, 89.79057627198103830 ) ) ;
#195181 = CARTESIAN_POINT ( 'NONE',  ( 13.89961937509957401, 13.97604488694547697, 81.87609039468564731 ) ) ;
#195182 = CARTESIAN_POINT ( 'NONE',  ( 8.314922557961029526, -14.29746914071037800, 55.41775706135234714 ) ) ;
#195184 = CARTESIAN_POINT ( 'NONE',  ( 5.823673210054125526, 21.52544592524343514, 94.79057627198105251 ) ) ;
#195183 = CARTESIAN_POINT ( 'NONE',  ( -4.713873842512037449, 4.023452810412264213, -62.49134662286012087 ) ) ;
#195185 = CARTESIAN_POINT ( 'NONE',  ( 4.483927247898545687, 16.52544592524342804, 74.79057627198105251 ) ) ;
#195186 = CARTESIAN_POINT ( 'NONE',  ( -30.51643230682433838, -22.56685799121283509, -22.94790682118908620 ) ) ;
#195187 = CARTESIAN_POINT ( 'NONE',  ( 13.89961937509957401, 13.97604488694547697, 111.8760903946856757 ) ) ;
#195188 = EDGE_CURVE ( 'NONE', #142912, #53136, #4420, .T. ) ;
#195189 = CARTESIAN_POINT ( 'NONE',  ( 10.81492255796078972, 18.62759615963270932, 44.58224293864769550 ) ) ;
#195190 = CARTESIAN_POINT ( 'NONE',  ( 14.34966873604972726, -8.224510206698740333, 75.83442372801900433 ) ) ;
#195191 = CARTESIAN_POINT ( 'NONE',  ( 9.564922557960805705, 16.46253265017160317, 24.58224293864769194 ) ) ;
#195192 = CARTESIAN_POINT ( 'NONE',  ( 16.52544592524335698, 4.483927247898782831, 56.45942372801902565 ) ) ;
#195193 = CARTESIAN_POINT ( 'NONE',  ( 21.55341960407619695, -5.719274019375665929, 21.04275706135234714 ) ) ;
#195194 = CARTESIAN_POINT ( 'NONE',  ( 21.55341960407610458, 5.719274019375980345, 43.95724293864769550 ) ) ;
#195195 = CARTESIAN_POINT ( 'NONE',  ( 14.34966873604972726, -8.224510206698740333, 75.83442372801900433 ) ) ;
#195196 = CARTESIAN_POINT ( 'NONE',  ( 13.89961937509977652, -13.97604488694527269, 93.12390960531436690 ) ) ;
#195198 = CARTESIAN_POINT ( 'NONE',  ( 19.02544592524343514, -5.153800228976328945, 28.54057627198102409 ) ) ;
#195197 = CARTESIAN_POINT ( 'NONE',  ( 18.62759615963255655, 10.81492255796105972, 56.66775706135235424 ) ) ;
#195199 = CARTESIAN_POINT ( 'NONE',  ( -5.719274019375978568, 21.55341960407610458, 45.20724293864769550 ) ) ;
#195200 = CARTESIAN_POINT ( 'NONE',  ( -5.823673210054116645, -21.52544592524344225, 27.29057627198103120 ) ) ;
#195201 = ORIENTED_EDGE ( 'NONE', *, *, #195850, .F. ) ;
#195202 = CARTESIAN_POINT ( 'NONE',  ( -16.51473224551082808, 9.474510206698731452, 38.33442372801899722 ) ) ;
#195203 = CARTESIAN_POINT ( 'NONE',  ( 16.55341960407618274, -4.379528057220086978, 51.04275706135234714 ) ) ;
#195204 = CARTESIAN_POINT ( 'NONE',  ( -19.03943276465977164, 0.05219959533909376836, 111.2489096053143669 ) ) ;
#195205 = ORIENTED_EDGE ( 'NONE', *, *, #172657, .T. ) ;
#195206 = CARTESIAN_POINT ( 'NONE',  ( -13.97604488694527625, -13.89961937509977652, 81.87390960531436690 ) ) ;
#195207 = CARTESIAN_POINT ( 'NONE',  ( 16.53943276465976808, 0.05219959533934440121, 101.2510903946856757 ) ) ;
#195208 = DIRECTION ( 'NONE',  ( -0.000000000000000000, -0.000000000000000000, 1.000000000000000000 ) ) ;
#195209 = CARTESIAN_POINT ( 'NONE',  ( -0.05219959533910754901, -16.53943276465976808, 92.49890960531436690 ) ) ;
#195210 = CARTESIAN_POINT ( 'NONE',  ( -10.72451020669898014, 18.67979575497178502, 50.41557627198103120 ) ) ;
#195211 = CARTESIAN_POINT ( 'NONE',  ( 16.51473224551069308, 9.474510206698969483, 29.16557627198103475 ) ) ;
#195212 = CARTESIAN_POINT ( 'NONE',  ( 4.483927247898790824, -16.52544592524335698, 80.20942372801901854 ) ) ;
#195213 = CARTESIAN_POINT ( 'NONE',  ( -15.72974639402176322, -15.80617190586768395, 24.37609039468567573 ) ) ;
#195214 = CARTESIAN_POINT ( 'NONE',  ( -0.05219959533936034679, 19.03943276465977164, 92.50109039468566152 ) ) ;
#195215 = CARTESIAN_POINT ( 'NONE',  ( -9.564922557960796823, -16.46253265017161027, 47.08224293864769550 ) ) ;
#195216 = CARTESIAN_POINT ( 'NONE',  ( -13.97604488694527625, -13.89961937509977652, 106.8739096053143669 ) ) ;
#195217 = CARTESIAN_POINT ( 'NONE',  ( -18.62759615963255300, -10.81492255796106328, 104.1677570613523471 ) ) ;
#195218 = CARTESIAN_POINT ( 'NONE',  ( 5.153800228976335163, 19.02544592524342804, 79.79057627198102409 ) ) ;
#195219 = CARTESIAN_POINT ( 'NONE',  ( 16.53943276465976808, 0.05219959533934440121, 56.25109039468568284 ) ) ;
#195220 = CARTESIAN_POINT ( 'NONE',  ( 15.80617190586769283, -15.72974639402175789, 95.62609039468568994 ) ) ;
#195221 = CARTESIAN_POINT ( 'NONE',  ( -19.03943276465977164, -0.05219959533935918106, 48.75109039468566863 ) ) ;
#195222 = CARTESIAN_POINT ( 'NONE',  ( 19.03943276465977164, 0.05219959533936151252, 66.25109039468567573 ) ) ;
#195223 = EDGE_LOOP ( 'NONE', ( #94617, #8271, #52516, #20353, #158392 ) ) ;
#195224 = CARTESIAN_POINT ( 'NONE',  ( -21.55341960407619339, 5.719274019375674811, 63.54275706135234003 ) ) ;
#195225 = CARTESIAN_POINT ( 'NONE',  ( 17.50000000000000000, -5.499999999999992895, 61.21769037696436300 ) ) ;
#195226 = CARTESIAN_POINT ( 'NONE',  ( -19.05341960407617563, 5.049401038297882671, 53.54275706135231871 ) ) ;
#195227 = CARTESIAN_POINT ( 'NONE',  ( 19.03943276465977164, -0.05219959533909143690, 103.7489096053143669 ) ) ;
#195228 = CARTESIAN_POINT ( 'NONE',  ( -16.46253265017160317, 9.564922557960807481, 80.83224293864769550 ) ) ;
#195229 = CARTESIAN_POINT ( 'NONE',  ( -12.14591786802309592, -12.06949235617757132, 41.87390960531435979 ) ) ;
#195230 = CARTESIAN_POINT ( 'NONE',  ( -0.05219959533907301413, -21.53943276465977519, 37.49890960531436690 ) ) ;
#195231 = CARTESIAN_POINT ( 'NONE',  ( -17.49999999999999645, 5.500000000000001776, 103.7176903769643701 ) ) ;
#195232 = CARTESIAN_POINT ( 'NONE',  ( 5.153800228976615827, -19.02544592524334988, 20.20942372801899722 ) ) ;
#195233 = CARTESIAN_POINT ( 'NONE',  ( -27.93385843979426397, 7.419916809875860331, 160.9064084702653190 ) ) ;
#195234 = CARTESIAN_POINT ( 'NONE',  ( -5.049401038298153566, 19.05341960407611168, 40.20724293864768839 ) ) ;
#195235 = CARTESIAN_POINT ( 'NONE',  ( 13.89961937509977652, -13.97604488694527269, 23.12390960531436335 ) ) ;
#195236 = CARTESIAN_POINT ( 'NONE',  ( -38.00000000000000711, 12.34694845685046438, -4.100000000000000533 ) ) ;
#195237 = CARTESIAN_POINT ( 'NONE',  ( 10.81492255796106328, -18.62759615963255655, 65.41775706135234714 ) ) ;
#195238 = PLANE ( 'NONE',  #166413 ) ;
#195239 = CARTESIAN_POINT ( 'NONE',  ( 14.29746914071037800, 8.314922557961029526, 61.66775706135235424 ) ) ;
#195240 = CARTESIAN_POINT ( 'NONE',  ( 10.81492255796078972, 18.62759615963270932, 89.58224293864768129 ) ) ;
#195241 = VECTOR ( 'NONE', #66585, 1000.000000000000000 ) ;
#195242 = CARTESIAN_POINT ( 'NONE',  ( -14.34966873604960291, -8.224510206698953496, 51.66557627198102409 ) ) ;
#195244 = CARTESIAN_POINT ( 'NONE',  ( 5.049401038298161559, -19.05341960407611168, 102.7072429386476955 ) ) ;
#195243 = CARTESIAN_POINT ( 'NONE',  ( 0.05219959533909260263, 19.03943276465977164, 34.99890960531435979 ) ) ;
#195245 = CARTESIAN_POINT ( 'NONE',  ( 18.67979575497194134, -10.72451020669871369, 30.83442372801902209 ) ) ;
#195246 = CARTESIAN_POINT ( 'NONE',  ( -19.03943276465977164, -0.05219959533935918106, 48.75109039468566863 ) ) ;
#195247 = CARTESIAN_POINT ( 'NONE',  ( 19.05341960407611168, 5.049401038298154454, 28.95724293864769550 ) ) ;
#195248 = CARTESIAN_POINT ( 'NONE',  ( -21.55341960407619339, 5.719274019375674811, 83.54275706135234714 ) ) ;
#195249 = CARTESIAN_POINT ( 'NONE',  ( 1.304248841091933035E-15, 21.30000000000002913, -65.00100000000003320 ) ) ;
#195250 = CARTESIAN_POINT ( 'NONE',  ( 16.55341960407611168, 4.379528057220329451, 23.95724293864769550 ) ) ;
#195251 = CARTESIAN_POINT ( 'NONE',  ( -18.62759615963270932, 10.81492255796079327, 40.83224293864769550 ) ) ;
#195252 = CARTESIAN_POINT ( 'NONE',  ( 8.224510206698953496, -14.34966873604960469, 102.9155762719810383 ) ) ;
#195253 = CARTESIAN_POINT ( 'NONE',  ( 11.55487914182273457, -42.80721638308649801, -21.19679778042605278 ) ) ;
#195254 = CARTESIAN_POINT ( 'NONE',  ( 19.05341960407611168, 5.049401038298154454, 88.95724293864769550 ) ) ;
#195255 = CARTESIAN_POINT ( 'NONE',  ( 14.29746914071049879, -8.314922557960816363, 88.33224293864769550 ) ) ;
#195256 = CARTESIAN_POINT ( 'NONE',  ( -5.049401038297874678, -19.05341960407617918, 109.7927570613523187 ) ) ;
#195257 = EDGE_CURVE ( 'NONE', #141549, #137721, #43192, .T. ) ;
#195258 = CARTESIAN_POINT ( 'NONE',  ( -0.05219959533907301413, -21.53943276465977519, 57.49890960531435979 ) ) ;
#195259 = ORIENTED_EDGE ( 'NONE', *, *, #105010, .T. ) ;
#195260 = CARTESIAN_POINT ( 'NONE',  ( -0.05219959533909027116, -19.03943276465977164, 27.49890960531435624 ) ) ;
#195262 = CARTESIAN_POINT ( 'NONE',  ( -5.719274019375978568, 21.55341960407610458, 95.20724293864769550 ) ) ;
#195261 = CARTESIAN_POINT ( 'NONE',  ( 19.03943276465977164, -0.05219959533909143690, 83.74890960531436690 ) ) ;
#195264 = CARTESIAN_POINT ( 'NONE',  ( -16.46253265017160317, 9.564922557960807481, 100.8322429386477097 ) ) ;
#195263 = CARTESIAN_POINT ( 'NONE',  ( 16.55341960407618274, -4.379528057220086978, 106.0427570613523471 ) ) ;
#195265 = CARTESIAN_POINT ( 'NONE',  ( 9.564922557961047289, -16.46253265017146816, 80.41775706135234714 ) ) ;
#195266 = CARTESIAN_POINT ( 'NONE',  ( 21.55341960407619695, -5.719274019375665929, 91.04275706135236135 ) ) ;
#195267 = CARTESIAN_POINT ( 'NONE',  ( 10.72451020669898902, -18.67979575497178502, 72.91557627198103830 ) ) ;
#195268 = CARTESIAN_POINT ( 'NONE',  ( 21.53943276465977519, -0.05219959533907433946, 38.74890960531435979 ) ) ;
#195269 = CARTESIAN_POINT ( 'NONE',  ( -9.564922557960796823, -16.46253265017161027, 47.08224293864769550 ) ) ;
#195270 = CARTESIAN_POINT ( 'NONE',  ( -8.314922557961024197, 14.29746914071037800, 107.9177570613523471 ) ) ;
#195271 = CARTESIAN_POINT ( 'NONE',  ( 16.46253265017160672, -9.564922557960803928, 68.33224293864770971 ) ) ;
#195272 = ORIENTED_EDGE ( 'NONE', *, *, #108717, .T. ) ;
#195273 = CARTESIAN_POINT ( 'NONE',  ( 28.79475375365586132, 2.781246896534039337E-14, 144.9843446568999923 ) ) ;
#195274 = CARTESIAN_POINT ( 'NONE',  ( -9.474510206698720793, -16.51473224551083518, 24.58442372801900078 ) ) ;
#195275 = CARTESIAN_POINT ( 'NONE',  ( 12.14591786802309770, 12.06949235617756955, 69.37390960531436690 ) ) ;
#195276 = PRESENTATION_LAYER_ASSIGNMENT (  '', '', ( #82207 ) ) ;
#195277 = CARTESIAN_POINT ( 'NONE',  ( -18.62759615963270932, 10.81492255796079327, 115.8322429386477097 ) ) ;
#195278 = CARTESIAN_POINT ( 'NONE',  ( -17.14385361876520619, 23.59649016807275856, 147.0750000027311728 ) ) ;
#195279 = CARTESIAN_POINT ( 'NONE',  ( 0.05219959533907565091, 21.53943276465977519, 54.99890960531435269 ) ) ;
#195280 = CARTESIAN_POINT ( 'NONE',  ( 8.224510206698742110, 14.34966873604972548, 92.08442372801901854 ) ) ;
#195281 = CARTESIAN_POINT ( 'NONE',  ( -8.314922557960811034, -14.29746914071050412, 107.0822429386476955 ) ) ;
#195282 = CARTESIAN_POINT ( 'NONE',  ( -9.564922557960796823, -16.46253265017161027, 77.08224293864769550 ) ) ;
#195283 =( NAMED_UNIT ( * ) PLANE_ANGLE_UNIT ( ) SI_UNIT ( $, .RADIAN. ) );
#195284 = CARTESIAN_POINT ( 'NONE',  ( -16.53943276465976808, 0.05219959533911058130, 31.24890960531435979 ) ) ;
#195285 = CARTESIAN_POINT ( 'NONE',  ( -5.719274019375665041, -21.55341960407619695, 49.79275706135234714 ) ) ;
#195286 = CARTESIAN_POINT ( 'NONE',  ( -9.474510206698964154, 16.51473224551069663, 105.4155762719810383 ) ) ;
#195287 = CARTESIAN_POINT ( 'NONE',  ( 21.55341960407619695, -5.719274019375665929, 81.04275706135236135 ) ) ;
#195288 = CARTESIAN_POINT ( 'NONE',  ( -5.153800228976328057, -19.02544592524343514, 27.29057627198103120 ) ) ;
#195289 = CARTESIAN_POINT ( 'NONE',  ( -5.153800228976328057, -19.02544592524343514, 32.29057627198102409 ) ) ;
#195290 = ORIENTED_EDGE ( 'NONE', *, *, #50044, .T. ) ;
#195291 = CARTESIAN_POINT ( 'NONE',  ( 10.81492255796106328, -18.62759615963255655, 95.41775706135234714 ) ) ;
#195292 = CARTESIAN_POINT ( 'NONE',  ( -8.224510206698735004, -14.34966873604973081, 54.58442372801901143 ) ) ;
#195293 = CARTESIAN_POINT ( 'NONE',  ( -21.53943276465977519, -0.05219959533937600094, 78.75109039468568994 ) ) ;
#195294 = CARTESIAN_POINT ( 'NONE',  ( 0.05219959533909260263, 19.03943276465977164, 104.9989096053143669 ) ) ;
#195295 = ORIENTED_EDGE ( 'NONE', *, *, #193397, .T. ) ;
#195296 = CARTESIAN_POINT ( 'NONE',  ( 0.05219959533936267826, -19.03943276465977164, 75.00109039468566152 ) ) ;
#195297 = CARTESIAN_POINT ( 'NONE',  ( -21.53943276465977519, -0.05219959533937600094, 58.75109039468568994 ) ) ;
#195298 = CARTESIAN_POINT ( 'NONE',  ( -19.05341960407617563, 5.049401038297882671, 113.5427570613523471 ) ) ;
#195299 = CARTESIAN_POINT ( 'NONE',  ( 0.05219959533936267826, -19.03943276465977164, 85.00109039468567573 ) ) ;
#195300 = CARTESIAN_POINT ( 'NONE',  ( -16.46253265017160317, 9.564922557960807481, 55.83224293864769550 ) ) ;
#195301 = CARTESIAN_POINT ( 'NONE',  ( -16.51473224551082808, 9.474510206698731452, 98.33442372801900433 ) ) ;
#195302 = VECTOR ( 'NONE', #144948, 1000.000000000000000 ) ;
#195303 = CARTESIAN_POINT ( 'NONE',  ( -8.314922557960811034, -14.29746914071050412, 22.08224293864769194 ) ) ;
#195304 = CARTESIAN_POINT ( 'NONE',  ( -5.049401038297874678, -19.05341960407617918, 89.79275706135230450 ) ) ;
#195305 = CARTESIAN_POINT ( 'NONE',  ( -12.06949235617756955, 12.14591786802309770, 45.62390960531436690 ) ) ;
#195306 = CARTESIAN_POINT ( 'NONE',  ( -9.474510206698720793, -16.51473224551083518, 59.58442372801900433 ) ) ;
#195307 = CARTESIAN_POINT ( 'NONE',  ( 8.224510206698742110, 14.34966873604972548, 57.08442372801901854 ) ) ;
#195308 = CARTESIAN_POINT ( 'NONE',  ( -15.80617190586768217, 15.72974639402176855, 113.1260903946856899 ) ) ;
#195309 = CARTESIAN_POINT ( 'NONE',  ( 4.483927247898545687, 16.52544592524342804, 114.7905762719810383 ) ) ;
#195310 = CARTESIAN_POINT ( 'NONE',  ( 9.474510206698971260, -16.51473224551069308, 47.91557627198102409 ) ) ;
#195311 = CARTESIAN_POINT ( 'NONE',  ( -12.14591786802326823, 12.06949235617739902, 53.12609039468568284 ) ) ;
#195312 = CARTESIAN_POINT ( 'NONE',  ( -20.34036572606774484, 20.41983568886641365, 139.9999999999999716 ) ) ;
#195313 = CARTESIAN_POINT ( 'NONE',  ( -23.31738231874055600, 16.94106989632528837, 142.0500000054623513 ) ) ;
#195314 = CARTESIAN_POINT ( 'NONE',  ( -9.564922557960796823, -16.46253265017161027, 87.08224293864769550 ) ) ;
#195315 = DIRECTION ( 'NONE',  ( -0.000000000000000000, -0.000000000000000000, 1.000000000000000000 ) ) ;
#195316 = ORIENTED_EDGE ( 'NONE', *, *, #175002, .T. ) ;
#195317 = CARTESIAN_POINT ( 'NONE',  ( -19.02544592524334988, -5.153800228976617603, 98.95942372801900433 ) ) ;
#195318 = B_SPLINE_CURVE_WITH_KNOTS ( 'NONE', 3,
 ( #8920, #68576, #176781, #100903, #177777, #39247, #130232, #7901, #25102, #190936, #23087, #6897, #38254, #98902, #53411, #131251, #21082, #159585, #52413, #192940, #84732, #115089, #67582, #144419, #162587, #163601, #116089, #99908, #146410, #191928, #24092, #117082 ),
 .UNSPECIFIED., .F., .F.,
 ( 4, 2, 2, 2, 2, 2, 2, 2, 2, 2, 2, 2, 2, 2, 2, 4 ),
 ( 5.204170427930422054E-18, 0.0003712461730036898137, 0.0007424923460073744232, 0.001113738519011058924, 0.001484984692014743642, 0.002227477038022112645, 0.002598723211025780015, 0.002969969384029447820, 0.003341215557033114757, 0.003712461730036782127, 0.004083707903040450365, 0.004454954076044117736, 0.004826200249047785107, 0.005197446422051451610, 0.005568692595055119848, 0.005939938768058787219 ),
 .UNSPECIFIED. ) ;
#195319 = CARTESIAN_POINT ( 'NONE',  ( 0.05219959533907565091, 21.53943276465977519, 34.99890960531435979 ) ) ;
#195321 = CARTESIAN_POINT ( 'NONE',  ( -16.46253265017146816, -9.564922557961047289, 109.1677570613523471 ) ) ;
#195320 = CARTESIAN_POINT ( 'NONE',  ( -9.564922557961040184, 16.46253265017147172, 37.91775706135233293 ) ) ;
#195322 = CARTESIAN_POINT ( 'NONE',  ( -13.97604488694527625, -13.89961937509977652, 21.87390960531435979 ) ) ;
#195323 = CARTESIAN_POINT ( 'NONE',  ( 13.97604488694527802, 13.89961937509977652, 39.37390960531435269 ) ) ;
#195324 = CARTESIAN_POINT ( 'NONE',  ( 10.72451020669898902, -18.67979575497178502, 72.91557627198103830 ) ) ;
#195325 = CARTESIAN_POINT ( 'NONE',  ( 13.89961937509977652, -13.97604488694527269, 38.12390960531436690 ) ) ;
#195326 = CARTESIAN_POINT ( 'NONE',  ( -17.14385361876520975, 23.59649016807275856, 143.0750000027311444 ) ) ;
#195327 = CARTESIAN_POINT ( 'NONE',  ( -13.89961937509957401, -13.97604488694547875, 79.37609039468567573 ) ) ;
#195328 = CARTESIAN_POINT ( 'NONE',  ( 4.379528057220339221, -16.55341960407611168, 47.70724293864770260 ) ) ;
#195329 = CARTESIAN_POINT ( 'NONE',  ( -10.81492255796078084, -18.62759615963271287, 27.08224293864769550 ) ) ;
#195330 = CARTESIAN_POINT ( 'NONE',  ( 0.05219959533937995610, -21.53943276465977519, 90.00109039468567573 ) ) ;
#195331 = CARTESIAN_POINT ( 'NONE',  ( -10.81492255796078084, -18.62759615963271287, 82.08224293864768129 ) ) ;
#195332 = CARTESIAN_POINT ( 'NONE',  ( 21.55341960407619695, -5.719274019375665929, 76.04275706135237556 ) ) ;
#195333 = CARTESIAN_POINT ( 'NONE',  ( -5.719274019375665041, -21.55341960407619695, 59.79275706135234714 ) ) ;
#195334 = CARTESIAN_POINT ( 'NONE',  ( -5.153800228976328057, -19.02544592524343514, 97.29057627198099567 ) ) ;
#195336 = CARTESIAN_POINT ( 'NONE',  ( 18.67979575497194134, -10.72451020669871369, 60.83442372801901854 ) ) ;
#195335 = CARTESIAN_POINT ( 'NONE',  ( 4.483927247898790824, -16.52544592524335698, 100.2094237280190043 ) ) ;
#195337 = CARTESIAN_POINT ( 'NONE',  ( 19.02544592524343514, -5.153800228976328945, 53.54057627198102409 ) ) ;
#195338 = CARTESIAN_POINT ( 'NONE',  ( -21.53943276465977519, -0.05219959533937600094, 33.75109039468568284 ) ) ;
#195339 = CARTESIAN_POINT ( 'NONE',  ( 16.51473224551069308, 9.474510206698969483, 69.16557627198102409 ) ) ;
#195340 = CARTESIAN_POINT ( 'NONE',  ( 12.06949235617757843, -12.14591786802309237, 83.12390960531436690 ) ) ;
#195341 = CARTESIAN_POINT ( 'NONE',  ( -12.06949235617756955, 12.14591786802309770, 45.62390960531436690 ) ) ;
#195342 = CARTESIAN_POINT ( 'NONE',  ( 21.53943276465977519, -0.05219959533907433946, 58.74890960531436690 ) ) ;
#195343 = CARTESIAN_POINT ( 'NONE',  ( 16.46253265017160672, -9.564922557960803928, 43.33224293864769550 ) ) ;
#195344 = CARTESIAN_POINT ( 'NONE',  ( 18.67979575497178502, 10.72451020669898547, 54.16557627198103120 ) ) ;
#195345 = CARTESIAN_POINT ( 'NONE',  ( 9.474510206698729675, 16.51473224551082808, 47.08442372801900433 ) ) ;
#195347 = CARTESIAN_POINT ( 'NONE',  ( -12.14591786802309592, -12.06949235617757132, 61.87390960531436690 ) ) ;
#195346 = CARTESIAN_POINT ( 'NONE',  ( -6.180203150055883832, -4.962140900324400583, 3.431593142121015294 ) ) ;
#195348 = CARTESIAN_POINT ( 'NONE',  ( -5.719274019375978568, 21.55341960407610458, 40.20724293864769550 ) ) ;
#195349 = EDGE_LOOP ( 'NONE', ( #198524, #88018 ) ) ;
#195350 = CARTESIAN_POINT ( 'NONE',  ( 1.300000000000000044, 0.7216878364870328300, 1.249999999999999778 ) ) ;
#195352 = CARTESIAN_POINT ( 'NONE',  ( 1.135581650430530276, 6.614994358112536332, -64.43300989196958994 ) ) ;
#195351 = CARTESIAN_POINT ( 'NONE',  ( -16.53943276465976808, -0.05219959533934237506, 83.75109039468568994 ) ) ;
#195353 = CARTESIAN_POINT ( 'NONE',  ( 19.03943276465977164, 0.05219959533936151252, 86.25109039468567573 ) ) ;
#195354 = CARTESIAN_POINT ( 'NONE',  ( 12.06949235617757843, -12.14591786802309237, 58.12390960531435979 ) ) ;
#195355 = CARTESIAN_POINT ( 'NONE',  ( -19.52851543214742946, -5.500000000000036415, 60.39357721762581832 ) ) ;
#195356 = CARTESIAN_POINT ( 'NONE',  ( -16.46253265017160317, 9.564922557960807481, 50.83224293864770260 ) ) ;
#195357 = CARTESIAN_POINT ( 'NONE',  ( -8.314922557960811034, -14.29746914071050412, 42.08224293864769550 ) ) ;
#195358 = CARTESIAN_POINT ( 'NONE',  ( 13.89961937509977652, -13.97604488694527269, 83.12390960531436690 ) ) ;
#195359 = AXIS2_PLACEMENT_3D ( 'NONE', #89122, #73972, #91083 ) ;
#195360 = CARTESIAN_POINT ( 'NONE',  ( 16.46253265017160672, -9.564922557960803928, 58.33224293864769550 ) ) ;
#195361 = CARTESIAN_POINT ( 'NONE',  ( -18.67979575497193778, 10.72451020669871902, 58.33442372801901143 ) ) ;
#195362 = CARTESIAN_POINT ( 'NONE',  ( -19.05341960407611168, -5.049401038298163336, 76.45724293864769550 ) ) ;
#195363 = CARTESIAN_POINT ( 'NONE',  ( -19.05341960407611168, -5.049401038298163336, 26.45724293864769550 ) ) ;
#195364 = CARTESIAN_POINT ( 'NONE',  ( 19.05341960407611168, 5.049401038298154454, 58.95724293864768129 ) ) ;
#195365 = CARTESIAN_POINT ( 'NONE',  ( 15.80617190586746368, 15.72974639402197994, 54.37390960531435979 ) ) ;
#195366 = CARTESIAN_POINT ( 'NONE',  ( 0.05219959533909260263, 19.03943276465977164, 29.99890960531435979 ) ) ;
#195367 = CARTESIAN_POINT ( 'NONE',  ( -21.52544592524343514, 5.823673210054127303, 46.04057627198103830 ) ) ;
#195368 = CARTESIAN_POINT ( 'NONE',  ( -0.05219959533934338120, 16.53943276465976808, 107.5010903946856899 ) ) ;
#195369 = CARTESIAN_POINT ( 'NONE',  ( -9.474510206698720793, -16.51473224551083518, 19.58442372801899722 ) ) ;
#195370 = EDGE_CURVE ( 'NONE', #171664, #119464, #134408, .T. ) ;
#195372 = CARTESIAN_POINT ( 'NONE',  ( -14.29746914071037622, -8.314922557961029526, 84.16775706135234714 ) ) ;
#195371 = CARTESIAN_POINT ( 'NONE',  ( 16.53943276465976808, 0.05219959533934440121, 41.25109039468568284 ) ) ;
#195373 = DIRECTION ( 'NONE',  ( 0.000000000000000000, 0.000000000000000000, -1.000000000000000000 ) ) ;
#195374 = CARTESIAN_POINT ( 'NONE',  ( -16.53943276465976808, -0.05219959533934237506, 68.75109039468568994 ) ) ;
#195375 = CARTESIAN_POINT ( 'NONE',  ( 8.314922557961029526, -14.29746914071037800, 50.41775706135235424 ) ) ;
#195376 = CARTESIAN_POINT ( 'NONE',  ( 19.02544592524343514, -5.153800228976328945, 103.5405762719809957 ) ) ;
#195377 = CIRCLE ( 'NONE', #40350, 2.500000000000000000 ) ;
#195378 = CARTESIAN_POINT ( 'NONE',  ( -13.89961937509977652, 13.97604488694528158, 30.62390960531435269 ) ) ;
#195379 = CARTESIAN_POINT ( 'NONE',  ( -12.14591786802326823, 12.06949235617739902, 43.12609039468568284 ) ) ;
#195380 = CARTESIAN_POINT ( 'NONE',  ( 16.46253265017160672, -9.564922557960803928, 48.33224293864769550 ) ) ;
#195381 = CARTESIAN_POINT ( 'NONE',  ( 10.72451020669871369, 18.67979575497193778, 27.08442372801901854 ) ) ;
#195382 = CARTESIAN_POINT ( 'NONE',  ( 8.314922557961029526, -14.29746914071037800, 35.41775706135234003 ) ) ;
#195383 = CARTESIAN_POINT ( 'NONE',  ( -12.14591786802326823, 12.06949235617739902, 98.12609039468570415 ) ) ;
#195384 = DIRECTION ( 'NONE',  ( -0.000000000000000000, -0.000000000000000000, -1.000000000000000000 ) ) ;
#195385 = CARTESIAN_POINT ( 'NONE',  ( 18.62759615963255655, 10.81492255796105972, 106.6677570613523756 ) ) ;
#195386 = CARTESIAN_POINT ( 'NONE',  ( 13.97604488694548053, -13.89961937509957401, 95.62609039468563310 ) ) ;
#195387 = CARTESIAN_POINT ( 'NONE',  ( 8.314922557960818139, 14.29746914071049879, 59.58224293864770260 ) ) ;
#195388 = CARTESIAN_POINT ( 'NONE',  ( 13.89961937509977652, -13.97604488694527269, 28.12390960531435624 ) ) ;
#195390 = CARTESIAN_POINT ( 'NONE',  ( -38.00000000000000711, -12.34694845685042708, -3.649999994537626691 ) ) ;
#195389 = CARTESIAN_POINT ( 'NONE',  ( 9.474510206698729675, 16.51473224551082808, 62.08442372801899722 ) ) ;
#195391 = CARTESIAN_POINT ( 'NONE',  ( 18.62759615963255655, 10.81492255796105972, 61.66775706135235424 ) ) ;
#195392 = CARTESIAN_POINT ( 'NONE',  ( -14.34966873604972548, 8.224510206698743886, 28.33442372801902209 ) ) ;
#195393 = CARTESIAN_POINT ( 'NONE',  ( 17.26058549869093284, 6.457015423128505738, 83.87745837476067834 ) ) ;
#195394 = CARTESIAN_POINT ( 'NONE',  ( -21.52544592524343514, 5.823673210054127303, 26.04057627198103475 ) ) ;
#195395 = CARTESIAN_POINT ( 'NONE',  ( -16.52544592524335698, -4.483927247898792601, 18.95942372801901143 ) ) ;
#195396 = DIRECTION ( 'NONE',  ( -0.9945218953682734009, 0.000000000000000000, 0.1045284632676528741 ) ) ;
#195397 = CARTESIAN_POINT ( 'NONE',  ( -25.62062145120080814, 9.171473787276466894, 171.1688781158127028 ) ) ;
#195398 = CARTESIAN_POINT ( 'NONE',  ( -13.97604488694527625, -13.89961937509977652, 26.87390960531434558 ) ) ;
#195399 = CARTESIAN_POINT ( 'NONE',  ( -10.72451020669870658, -18.67979575497194134, 104.5844237280190185 ) ) ;
#195400 = CARTESIAN_POINT ( 'NONE',  ( -16.51473224551069308, -9.474510206698971260, 41.66557627198103120 ) ) ;
#195401 = CIRCLE ( 'NONE', #11382, 2.649999999999999911 ) ;
#195402 = CARTESIAN_POINT ( 'NONE',  ( -21.55341960407619339, 5.719274019375674811, 63.54275706135234003 ) ) ;
#195403 = CARTESIAN_POINT ( 'NONE',  ( 18.62759615963255655, 10.81492255796105972, 101.6677570613523613 ) ) ;
#195404 = CARTESIAN_POINT ( 'NONE',  ( 4.483927247898790824, -16.52544592524335698, 105.2094237280190328 ) ) ;
#195405 = CARTESIAN_POINT ( 'NONE',  ( 9.564922557960805705, 16.46253265017160317, 74.58224293864769550 ) ) ;
#195406 = CARTESIAN_POINT ( 'NONE',  ( 15.80617190586769283, -15.72974639402175789, 50.62609039468568994 ) ) ;
#195407 = CARTESIAN_POINT ( 'NONE',  ( -18.62759615963255300, -10.81492255796106328, 59.16775706135234714 ) ) ;
#195409 = CARTESIAN_POINT ( 'NONE',  ( 16.46253265017160672, -9.564922557960803928, 103.3322429386476955 ) ) ;
#195408 = CARTESIAN_POINT ( 'NONE',  ( 13.97604488694548053, -13.89961937509957401, 85.62609039468568994 ) ) ;
#195410 = CARTESIAN_POINT ( 'NONE',  ( -9.474510206698964154, 16.51473224551069663, 25.41557627198103120 ) ) ;
#195411 = CARTESIAN_POINT ( 'NONE',  ( 21.53943276465977519, -0.05219959533907433946, 93.74890960531436690 ) ) ;
#195412 = CARTESIAN_POINT ( 'NONE',  ( -21.55341960407619339, 5.719274019375674811, 113.5427570613523756 ) ) ;
#195413 = CARTESIAN_POINT ( 'NONE',  ( 16.55341960407611168, 4.379528057220329451, 93.95724293864770971 ) ) ;
#195414 = CARTESIAN_POINT ( 'NONE',  ( 9.474510206698971260, -16.51473224551069308, 52.91557627198102409 ) ) ;
#195415 = CARTESIAN_POINT ( 'NONE',  ( -13.89961937509957401, -13.97604488694547875, 79.37609039468567573 ) ) ;
#195416 = CARTESIAN_POINT ( 'NONE',  ( 8.314922557960818139, 14.29746914071049879, 59.58224293864770260 ) ) ;
#195417 = CARTESIAN_POINT ( 'NONE',  ( -10.81492255796105439, 18.62759615963255655, 112.9177570613523329 ) ) ;
#195418 = CARTESIAN_POINT ( 'NONE',  ( 19.02544592524343514, -5.153800228976328945, 103.5405762719809957 ) ) ;
#195419 = CARTESIAN_POINT ( 'NONE',  ( 19.03943276465977164, 0.05219959533936151252, 76.25109039468566152 ) ) ;
#195420 = CARTESIAN_POINT ( 'NONE',  ( 15.80617190586746368, 15.72974639402197994, 74.37390960531436690 ) ) ;
#195421 = AXIS2_PLACEMENT_3D ( 'NONE', #150966, #136761, #41790 ) ;
#195422 = CARTESIAN_POINT ( 'NONE',  ( -5.823673210054431948, 21.52544592524334988, 27.70942372801901854 ) ) ;
#195423 = CARTESIAN_POINT ( 'NONE',  ( 14.34966873604972726, -8.224510206698740333, 25.83442372801901499 ) ) ;
#195424 = CARTESIAN_POINT ( 'NONE',  ( 14.29746914071037800, 8.314922557961029526, 86.66775706135234714 ) ) ;
#195426 = CARTESIAN_POINT ( 'NONE',  ( 15.80617190586769283, -15.72974639402175789, 30.62609039468567929 ) ) ;
#195425 = CARTESIAN_POINT ( 'NONE',  ( 8.224510206698742110, 14.34966873604972548, 42.08442372801901854 ) ) ;
#195427 = CARTESIAN_POINT ( 'NONE',  ( 5.719274019375991003, -21.55341960407610458, 37.70724293864769550 ) ) ;
#195428 = CARTESIAN_POINT ( 'NONE',  ( -16.53943276465976808, -0.05219959533934237506, 53.75109039468568994 ) ) ;
#195429 = CARTESIAN_POINT ( 'NONE',  ( -13.89961937509977652, 13.97604488694528158, 40.62390960531435979 ) ) ;
#195430 = CARTESIAN_POINT ( 'NONE',  ( -29.86685920354755552, 21.69954338932564397, -1.324999997268813345 ) ) ;
#195431 = CARTESIAN_POINT ( 'NONE',  ( -12.14591786802326823, 12.06949235617739902, 58.12609039468568994 ) ) ;
#195432 = EDGE_CURVE ( 'NONE', #33580, #165125, #35535, .T. ) ;
#195433 = CARTESIAN_POINT ( 'NONE',  ( -10.72451020669898014, 18.67979575497178502, 85.41557627198102409 ) ) ;
#195434 = CARTESIAN_POINT ( 'NONE',  ( -8.224510206698948167, 14.34966873604960824, 40.41557627198103120 ) ) ;
#195435 = CARTESIAN_POINT ( 'NONE',  ( -16.55341960407617563, 4.379528057220093196, 43.54275706135235424 ) ) ;
#195436 = CARTESIAN_POINT ( 'NONE',  ( 19.05341960407611168, 5.049401038298154454, 53.95724293864770260 ) ) ;
#195437 = CARTESIAN_POINT ( 'NONE',  ( -12.06949235617739369, -12.14591786802326823, 89.37609039468568994 ) ) ;
#195438 = CARTESIAN_POINT ( 'NONE',  ( 13.97604488694548053, -13.89961937509957401, 90.62609039468567573 ) ) ;
#195439 = CARTESIAN_POINT ( 'NONE',  ( -10.81492255796078084, -18.62759615963271287, 87.08224293864769550 ) ) ;
#195440 = CARTESIAN_POINT ( 'NONE',  ( -16.53943276465976808, 0.05219959533911058130, 36.24890960531435979 ) ) ;
#195441 = ORIENTED_EDGE ( 'NONE', *, *, #147508, .F. ) ;
#195442 = CARTESIAN_POINT ( 'NONE',  ( 25.75939503182846479, 8.559839547494778600, 171.7912139782359304 ) ) ;
#195443 = CARTESIAN_POINT ( 'NONE',  ( 10.81492255796078972, 18.62759615963270932, 54.58224293864769550 ) ) ;
#195444 = ORIENTED_EDGE ( 'NONE', *, *, #56442, .F. ) ;
#195445 = CARTESIAN_POINT ( 'NONE',  ( 16.53943276465976808, 0.05219959533934440121, 101.2510903946856757 ) ) ;
#195446 = ORIENTED_EDGE ( 'NONE', *, *, #22002, .T. ) ;
#195447 = CARTESIAN_POINT ( 'NONE',  ( -0.05219959533907301413, -21.53943276465977519, 27.49890960531435269 ) ) ;
#195448 = CARTESIAN_POINT ( 'NONE',  ( -30.74264578624800492, -22.33583958711396278, -3.799999999999999822 ) ) ;
#195449 = CARTESIAN_POINT ( 'NONE',  ( -15.80617190586745835, -15.72974639402198527, 86.87390960531438111 ) ) ;
#195450 = CARTESIAN_POINT ( 'NONE',  ( 14.29746914071037800, 8.314922557961029526, 111.6677570613523613 ) ) ;
#195452 = CARTESIAN_POINT ( 'NONE',  ( -8.314922557961024197, 14.29746914071037800, 32.91775706135234714 ) ) ;
#195451 = AXIS2_PLACEMENT_3D ( 'NONE', #67389, #173596, #35065 ) ;
#195453 = CARTESIAN_POINT ( 'NONE',  ( -0.05219959533909027116, -19.03943276465977164, 32.49890960531435979 ) ) ;
#195454 = CARTESIAN_POINT ( 'NONE',  ( 0.05219959533934541429, -16.53943276465976808, 35.00109039468568284 ) ) ;
#195455 = CARTESIAN_POINT ( 'NONE',  ( 9.564922557960805705, 16.46253265017160317, 54.58224293864769550 ) ) ;
#195456 = CARTESIAN_POINT ( 'NONE',  ( -8.571926809382608425, 26.38167802310805854, 140.9750000027312069 ) ) ;
#195457 = CARTESIAN_POINT ( 'NONE',  ( -19.02544592524342804, 5.153800228976336051, 106.0405762719810241 ) ) ;
#195458 = CARTESIAN_POINT ( 'NONE',  ( 1.223485768069169977, 29.52714030619467422, -51.95675375490479553 ) ) ;
#195459 = CARTESIAN_POINT ( 'NONE',  ( 4.483927247898790824, -16.52544592524335698, 100.2094237280190043 ) ) ;
#195460 = CARTESIAN_POINT ( 'NONE',  ( 9.474510206698729675, 16.51473224551082808, 87.08442372801900433 ) ) ;
#195461 = CARTESIAN_POINT ( 'NONE',  ( 19.05341960407617918, -5.049401038297876454, 41.04275706135233293 ) ) ;
#195462 = CARTESIAN_POINT ( 'NONE',  ( 15.72974639402199770, -15.80617190586745480, 78.12390960531436690 ) ) ;
#195463 = CARTESIAN_POINT ( 'NONE',  ( -12.06949235617739369, -12.14591786802326823, 94.37609039468568994 ) ) ;
#195464 = CARTESIAN_POINT ( 'NONE',  ( 15.80617190586746368, 15.72974639402197994, 34.37390960531435979 ) ) ;
#195465 = CARTESIAN_POINT ( 'NONE',  ( -9.564922557961040184, 16.46253265017147172, 102.9177570613523329 ) ) ;
#195466 = CARTESIAN_POINT ( 'NONE',  ( 16.46253265017160672, -9.564922557960803928, 108.3322429386476955 ) ) ;
#195467 = CARTESIAN_POINT ( 'NONE',  ( 0.05219959533937995610, -21.53943276465977519, 60.00109039468568284 ) ) ;
#195468 = CARTESIAN_POINT ( 'NONE',  ( -19.05341960407611168, -5.049401038298163336, 56.45724293864768129 ) ) ;
#195469 = CARTESIAN_POINT ( 'NONE',  ( -8.314922557960811034, -14.29746914071050412, 107.0822429386476955 ) ) ;
#195470 = CARTESIAN_POINT ( 'NONE',  ( 14.29746914071049879, -8.314922557960816363, 73.33224293864769550 ) ) ;
#195471 = ORIENTED_EDGE ( 'NONE', *, *, #169970, .F. ) ;
#195472 = CARTESIAN_POINT ( 'NONE',  ( 0.05219959533936267826, -19.03943276465977164, 90.00109039468567573 ) ) ;
#195473 = CARTESIAN_POINT ( 'NONE',  ( 18.56101223717332971, 5.500000000000005329, 93.94978406935678095 ) ) ;
#195474 = CARTESIAN_POINT ( 'NONE',  ( -16.46253265017160317, 9.564922557960807481, 65.83224293864769550 ) ) ;
#195475 = CARTESIAN_POINT ( 'NONE',  ( 31.60163464511076015, -3.334671618079683597, 101.7358725107059598 ) ) ;
#195477 = CARTESIAN_POINT ( 'NONE',  ( -9.474510206698964154, 16.51473224551069663, 85.41557627198102409 ) ) ;
#195476 = CARTESIAN_POINT ( 'NONE',  ( 16.46253265017160672, -9.564922557960803928, 78.33224293864769550 ) ) ;
#195478 = CARTESIAN_POINT ( 'NONE',  ( 14.34966873604972726, -8.224510206698740333, 70.83442372801901854 ) ) ;
#195479 = LINE ( 'NONE', #24627, #96257 ) ;
#195480 = CARTESIAN_POINT ( 'NONE',  ( -16.46253265017146816, -9.564922557961047289, 39.16775706135234003 ) ) ;
#195481 = CARTESIAN_POINT ( 'NONE',  ( 0.05219959533937995610, -21.53943276465977519, 95.00109039468568994 ) ) ;
#195482 = CARTESIAN_POINT ( 'NONE',  ( 36.99206003604233217, 5.206627989871538631, 43.21856904651838960 ) ) ;
#195483 = CARTESIAN_POINT ( 'NONE',  ( -5.049401038298153566, 19.05341960407611168, 115.2072429386477097 ) ) ;
#195484 = CARTESIAN_POINT ( 'NONE',  ( -14.29746914071037622, -8.314922557961029526, 109.1677570613523613 ) ) ;
#195485 = CARTESIAN_POINT ( 'NONE',  ( -34.80541354469661997, -6.720605140086532536, 41.66184804092133476 ) ) ;
#195486 = CARTESIAN_POINT ( 'NONE',  ( -8.314922557961024197, 14.29746914071037800, 92.91775706135236135 ) ) ;
#195487 = CARTESIAN_POINT ( 'NONE',  ( -17.13100169013300444, 6.664070546373151771, 30.76789835699849718 ) ) ;
#195488 = CARTESIAN_POINT ( 'NONE',  ( 16.52544592524335698, 4.483927247898782831, 61.45942372801901854 ) ) ;
#195489 = DIRECTION ( 'NONE',  ( 0.000000000000000000, -0.8164965809277232589, -0.5773502691896295058 ) ) ;
#195490 = CARTESIAN_POINT ( 'NONE',  ( 21.55341960407619695, -5.719274019375665929, 86.04275706135236135 ) ) ;
#195491 = CARTESIAN_POINT ( 'NONE',  ( 13.89961937509957401, 13.97604488694547697, 91.87609039468567573 ) ) ;
#195492 = CARTESIAN_POINT ( 'NONE',  ( 5.049401038297881783, 19.05341960407617563, 27.29275706135232937 ) ) ;
#195493 = TOROIDAL_SURFACE ( 'NONE', #72809, 69.99999999999998579, 8.000000000000000000 ) ;
#195494 = CARTESIAN_POINT ( 'NONE',  ( -13.97604488694527625, -13.89961937509977652, 71.87390960531433848 ) ) ;
#195495 = CARTESIAN_POINT ( 'NONE',  ( -5.049401038298153566, 19.05341960407611168, 50.20724293864770260 ) ) ;
#195496 = CARTESIAN_POINT ( 'NONE',  ( 16.56723268710308616, 7.192918735248206907, 22.04583401990673863 ) ) ;
#195497 = CARTESIAN_POINT ( 'NONE',  ( -21.52544592524343514, 5.823673210054127303, 86.04057627198102409 ) ) ;
#195498 = CARTESIAN_POINT ( 'NONE',  ( 21.52544592524344225, -5.823673210054117533, 28.54057627198103120 ) ) ;
#195499 = CARTESIAN_POINT ( 'NONE',  ( 13.89961937509977652, -13.97604488694527269, 28.12390960531435624 ) ) ;
#195500 = CARTESIAN_POINT ( 'NONE',  ( -4.379528057220086978, -16.55341960407618274, 54.79275706135235424 ) ) ;
#195501 = EDGE_CURVE ( 'NONE', #145210, #152430, #152953, .T. ) ;
#195502 = EDGE_LOOP ( 'NONE', ( #153879, #142908 ) ) ;
#195503 = CARTESIAN_POINT ( 'NONE',  ( 0.05219959533937995610, -21.53943276465977519, 25.00109039468567218 ) ) ;
#195505 = CARTESIAN_POINT ( 'NONE',  ( 36.91746825000000598, -11.99521256947793546, -9.724999997268813701 ) ) ;
#195504 = CARTESIAN_POINT ( 'NONE',  ( -12.06949235617756955, 12.14591786802309770, 55.62390960531436690 ) ) ;
#195506 = CARTESIAN_POINT ( 'NONE',  ( -16.53943276465976808, -0.05219959533934237506, 18.75109039468568639 ) ) ;
#195507 = CARTESIAN_POINT ( 'NONE',  ( -19.03943276465977164, -0.05219959533935918106, 33.75109039468566863 ) ) ;
#195508 = CARTESIAN_POINT ( 'NONE',  ( -12.14591786802309592, -12.06949235617757132, 56.87390960531436690 ) ) ;
#195509 = CARTESIAN_POINT ( 'NONE',  ( 21.55341960407619695, -5.719274019375665929, 21.04275706135234714 ) ) ;
#195511 = CARTESIAN_POINT ( 'NONE',  ( 15.80617190586746368, 15.72974639402197994, 74.37390960531436690 ) ) ;
#195510 = CARTESIAN_POINT ( 'NONE',  ( -30.00000000000000355, -3.889087296526017479, 8.181980515339454030 ) ) ;
#195512 = CARTESIAN_POINT ( 'NONE',  ( 0.05219959533909260263, 19.03943276465977164, 84.99890960531436690 ) ) ;
#195513 = CARTESIAN_POINT ( 'NONE',  ( -16.53943276465976808, 0.05219959533911058130, 66.24890960531436690 ) ) ;
#195514 = CARTESIAN_POINT ( 'NONE',  ( 13.89961937509977652, -13.97604488694527269, 103.1239096053143527 ) ) ;
#195515 = CARTESIAN_POINT ( 'NONE',  ( 11.40812507854754365, 35.11059874428196537, -7.224999997268813701 ) ) ;
#195516 = CARTESIAN_POINT ( 'NONE',  ( 19.03943276465977164, 0.05219959533936151252, 71.25109039468566152 ) ) ;
#195517 = CARTESIAN_POINT ( 'NONE',  ( -21.53943276465977519, 0.05219959533907696930, 101.2489096053143669 ) ) ;
#195518 = CARTESIAN_POINT ( 'NONE',  ( 9.564922557960805705, 16.46253265017160317, 59.58224293864769550 ) ) ;
#195519 = CARTESIAN_POINT ( 'NONE',  ( -19.02544592524334988, -5.153800228976617603, 43.95942372801899012 ) ) ;
#195520 = CARTESIAN_POINT ( 'NONE',  ( 4.379528057220339221, -16.55341960407611168, 112.7072429386476955 ) ) ;
#195521 = CARTESIAN_POINT ( 'NONE',  ( 15.72974639402176855, 15.80617190586768217, 66.87609039468568994 ) ) ;
#195522 = CARTESIAN_POINT ( 'NONE',  ( -18.39635199886970085, 5.499999999999979572, 101.0196707636000184 ) ) ;
#195523 = CARTESIAN_POINT ( 'NONE',  ( 16.55341960407611168, 4.379528057220329451, 38.95724293864768839 ) ) ;
#195524 = CARTESIAN_POINT ( 'NONE',  ( 16.46253265017160672, -9.564922557960803928, 63.33224293864769550 ) ) ;
#195525 = CARTESIAN_POINT ( 'NONE',  ( -18.62759615963270932, 10.81492255796079327, 80.83224293864769550 ) ) ;
#195526 = CARTESIAN_POINT ( 'NONE',  ( -22.44159573604009950, -16.30477369853688430, 145.0750000027311728 ) ) ;
#195527 = CARTESIAN_POINT ( 'NONE',  ( 16.46253265017160672, -9.564922557960803928, 58.33224293864769550 ) ) ;
#195528 = CARTESIAN_POINT ( 'NONE',  ( -18.62759615963270932, 10.81492255796079327, 65.83224293864769550 ) ) ;
#195529 = ORIENTED_EDGE ( 'NONE', *, *, #199792, .F. ) ;
#195530 = CARTESIAN_POINT ( 'NONE',  ( 21.55341960407619695, -5.719274019375665929, 101.0427570613523756 ) ) ;
#195533 = CARTESIAN_POINT ( 'NONE',  ( 8.314922557960818139, 14.29746914071049879, 84.58224293864769550 ) ) ;
#195532 = CARTESIAN_POINT ( 'NONE',  ( -8.314922557961024197, 14.29746914071037800, 102.9177570613523756 ) ) ;
#195531 = CARTESIAN_POINT ( 'NONE',  ( -40.00200000000003087, -4.592425496802575156E-15, 52.50000000000000000 ) ) ;
#195534 = CARTESIAN_POINT ( 'NONE',  ( -16.51473224551069308, -9.474510206698971260, 76.66557627198103830 ) ) ;
#195535 = ORIENTED_EDGE ( 'NONE', *, *, #85538, .T. ) ;
#195536 = CARTESIAN_POINT ( 'NONE',  ( -9.474510206698720793, -16.51473224551083518, 44.58442372801900433 ) ) ;
#195537 = CARTESIAN_POINT ( 'NONE',  ( -8.314922557961024197, 14.29746914071037800, 82.91775706135234714 ) ) ;
#195538 = CARTESIAN_POINT ( 'NONE',  ( 5.153800228976615827, -19.02544592524334988, 30.20942372801900433 ) ) ;
#195539 = CARTESIAN_POINT ( 'NONE',  ( -16.46253265017160317, 9.564922557960807481, 90.83224293864769550 ) ) ;
#195540 = CARTESIAN_POINT ( 'NONE',  ( 0.05219959533907565091, 21.53943276465977519, 54.99890960531435269 ) ) ;
#195541 = DIRECTION ( 'NONE',  ( 0.000000000000000000, 0.000000000000000000, 1.000000000000000000 ) ) ;
#195542 = CARTESIAN_POINT ( 'NONE',  ( 19.03943276465977164, -0.05219959533909143690, 23.74890960531435269 ) ) ;
#195543 = CARTESIAN_POINT ( 'NONE',  ( 15.80617190586769283, -15.72974639402175789, 95.62609039468568994 ) ) ;
#195544 = CARTESIAN_POINT ( 'NONE',  ( 12.14591786802327356, -12.06949235617739191, 60.62609039468567573 ) ) ;
#195545 = CARTESIAN_POINT ( 'NONE',  ( 10.72451020669871369, 18.67979575497193778, 27.08442372801901854 ) ) ;
#195546 = CARTESIAN_POINT ( 'NONE',  ( 4.483927247898790824, -16.52544592524335698, 30.20942372801902565 ) ) ;
#195547 = CARTESIAN_POINT ( 'NONE',  ( -16.51473224551069308, -9.474510206698971260, 96.66557627198102409 ) ) ;
#195548 = CARTESIAN_POINT ( 'NONE',  ( -5.049401038298153566, 19.05341960407611168, 40.20724293864768839 ) ) ;
#195549 = CARTESIAN_POINT ( 'NONE',  ( 5.153800228976335163, 19.02544592524342804, 54.79057627198103120 ) ) ;
#195550 = CIRCLE ( 'NONE', #24368, 9.100000000000001421 ) ;
#195551 = CARTESIAN_POINT ( 'NONE',  ( -4.483927247898782831, 16.52544592524335698, 32.70942372801900433 ) ) ;
#195552 = CARTESIAN_POINT ( 'NONE',  ( 12.06949235617757843, -12.14591786802309237, 93.12390960531436690 ) ) ;
#195553 = CARTESIAN_POINT ( 'NONE',  ( 12.14591786802327356, -12.06949235617739191, 105.6260903946856899 ) ) ;
#195556 = CARTESIAN_POINT ( 'NONE',  ( -5.153800228976328057, -19.02544592524343514, 57.29057627198103120 ) ) ;
#195555 = CARTESIAN_POINT ( 'NONE',  ( 16.51473224551069308, 9.474510206698969483, 74.16557627198103830 ) ) ;
#195554 = CARTESIAN_POINT ( 'NONE',  ( -15.72974639402176322, -15.80617190586768395, 44.37609039468567573 ) ) ;
#195557 = CARTESIAN_POINT ( 'NONE',  ( 16.46253265017160672, -9.564922557960803928, 78.33224293864769550 ) ) ;
#195558 = CARTESIAN_POINT ( 'NONE',  ( 12.06949235617757843, -12.14591786802309237, 33.12390960531435979 ) ) ;
#195559 = CARTESIAN_POINT ( 'NONE',  ( 4.483927247898790824, -16.52544592524335698, 95.20942372801903275 ) ) ;
#195560 = ORIENTED_EDGE ( 'NONE', *, *, #749, .T. ) ;
#195561 = CARTESIAN_POINT ( 'NONE',  ( -19.03943276465977164, -0.05219959533935918106, 38.75109039468566152 ) ) ;
#195562 = CARTESIAN_POINT ( 'NONE',  ( -13.97604488694527625, -13.89961937509977652, 111.8739096053143243 ) ) ;
#195563 = CARTESIAN_POINT ( 'NONE',  ( -5.153800228976328057, -19.02544592524343514, 47.29057627198102409 ) ) ;
#195564 = CARTESIAN_POINT ( 'NONE',  ( -0.05219959533936034679, 19.03943276465977164, 22.50109039468566152 ) ) ;
#195565 = CARTESIAN_POINT ( 'NONE',  ( -29.86685920354755197, -21.69954338932560134, -4.424999997268812990 ) ) ;
#195566 = CARTESIAN_POINT ( 'NONE',  ( 16.53943276465976808, 0.05219959533934440121, 36.25109039468567573 ) ) ;
#195567 = VECTOR ( 'NONE', #127304, 1000.000000000000000 ) ;
#195569 = CARTESIAN_POINT ( 'NONE',  ( 4.483927247898790824, -16.52544592524335698, 50.20942372801901854 ) ) ;
#195568 = CARTESIAN_POINT ( 'NONE',  ( 9.564922557961047289, -16.46253265017146816, 70.41775706135233293 ) ) ;
#195570 = CARTESIAN_POINT ( 'NONE',  ( 19.05341960407611168, 5.049401038298154454, 113.9572429386477097 ) ) ;
#195571 = CARTESIAN_POINT ( 'NONE',  ( -19.02544592524342804, 5.153800228976336051, 81.04057627198103830 ) ) ;
#195572 = CARTESIAN_POINT ( 'NONE',  ( -15.80617190586745835, -15.72974639402198527, 111.8739096053143669 ) ) ;
#195573 = CARTESIAN_POINT ( 'NONE',  ( -19.02544592524334988, -5.153800228976617603, 78.95942372801900433 ) ) ;
#195575 = CARTESIAN_POINT ( 'NONE',  ( 5.153800228976335163, 19.02544592524342804, 34.79057627198102409 ) ) ;
#195574 = CARTESIAN_POINT ( 'NONE',  ( -5.049401038298153566, 19.05341960407611168, 110.2072429386476671 ) ) ;
#195576 = CARTESIAN_POINT ( 'NONE',  ( 5.049401038298161559, -19.05341960407611168, 77.70724293864765286 ) ) ;
#195578 = CARTESIAN_POINT ( 'NONE',  ( -9.474510206698964154, 16.51473224551069663, 30.41557627198102054 ) ) ;
#195577 = CARTESIAN_POINT ( 'NONE',  ( 16.52544592524342804, -4.483927247898539470, 38.54057627198103120 ) ) ;
#195579 = CLOSED_SHELL ( 'NONE', ( #129135, #70778, #71148, #194050, #174806, #184460, #97292, #11482, #61485, #187386, #44161, #79380, #109611, #17861, #123330, #7466, #161836, #172508, #163302, #53964, #17963, #76561, #33975, #61711, #180856, #146491, #171353, #79813, #79289, #84282, #106136, #138616, #63761, #184302, #161701 ) ) ;
#195580 = CARTESIAN_POINT ( 'NONE',  ( 0.05219959533936267826, -19.03943276465977164, 50.00109039468566863 ) ) ;
#195581 = CARTESIAN_POINT ( 'NONE',  ( 16.53943276465976808, -0.05219959533910856209, 73.74890960531433848 ) ) ;
#195582 = CARTESIAN_POINT ( 'NONE',  ( -19.03943276465977164, -0.05219959533935918106, 18.75109039468567218 ) ) ;
#195583 = CARTESIAN_POINT ( 'NONE',  ( 0.05219959533909260263, 19.03943276465977164, 54.99890960531435979 ) ) ;
#195584 = CARTESIAN_POINT ( 'NONE',  ( -18.67979575497178146, -10.72451020669898902, 56.66557627198103830 ) ) ;
#195586 = CARTESIAN_POINT ( 'NONE',  ( -21.53943276465977519, -0.05219959533937600094, 103.7510903946857042 ) ) ;
#195585 = CARTESIAN_POINT ( 'NONE',  ( -8.314922557960811034, -14.29746914071050412, 57.08224293864769550 ) ) ;
#195587 = CARTESIAN_POINT ( 'NONE',  ( -13.97604488694527625, -13.89961937509977652, 91.87390960531432427 ) ) ;
#195588 = CARTESIAN_POINT ( 'NONE',  ( -0.05219959533909027116, -19.03943276465977164, 112.4989096053143669 ) ) ;
#195589 = CARTESIAN_POINT ( 'NONE',  ( -16.46253265017160317, 9.564922557960807481, 35.83224293864768839 ) ) ;
#195590 = CARTESIAN_POINT ( 'NONE',  ( 8.314922557960818139, 14.29746914071049879, 114.5822429386477097 ) ) ;
#195591 = CARTESIAN_POINT ( 'NONE',  ( -8.224510206698948167, 14.34966873604960824, 90.41557627198103830 ) ) ;
#195592 = CARTESIAN_POINT ( 'NONE',  ( -10.72451020669898014, 18.67979575497178502, 100.4155762719810241 ) ) ;
#195593 = CARTESIAN_POINT ( 'NONE',  ( 16.51473224551069308, 9.474510206698969483, 89.16557627198103830 ) ) ;
#195594 = CARTESIAN_POINT ( 'NONE',  ( 10.72451020669898902, -18.67979575497178502, 112.9155762719810383 ) ) ;
#195595 = CARTESIAN_POINT ( 'NONE',  ( 0.05219959533909260263, 19.03943276465977164, 89.99890960531436690 ) ) ;
#195597 = CARTESIAN_POINT ( 'NONE',  ( 12.14591786802309770, 12.06949235617756955, 99.37390960531436690 ) ) ;
#195596 = LINE ( 'NONE', #132896, #46533 ) ;
#195598 = CARTESIAN_POINT ( 'NONE',  ( 13.89961937509977652, -13.97604488694527269, 78.12390960531433848 ) ) ;
#195599 = CARTESIAN_POINT ( 'NONE',  ( -15.72974639402197994, 15.80617190586746368, 85.62390960531436690 ) ) ;
#195600 = CARTESIAN_POINT ( 'NONE',  ( -9.474510206698964154, 16.51473224551069663, 115.4155762719810241 ) ) ;
#195601 = DIRECTION ( 'NONE',  ( 1.000000000000000000, 0.000000000000000000, 0.000000000000000000 ) ) ;
#195603 = CARTESIAN_POINT ( 'NONE',  ( 18.87580814761071579, -5.500000000000034639, 68.37172394265761000 ) ) ;
#195602 = CARTESIAN_POINT ( 'NONE',  ( 21.52544592524344225, -5.823673210054117533, 23.54057627198102765 ) ) ;
#195604 = CARTESIAN_POINT ( 'NONE',  ( 4.379528057220092307, 16.55341960407617563, 37.29275706135235424 ) ) ;
#195605 = CARTESIAN_POINT ( 'NONE',  ( 16.55341960407611168, 4.379528057220329451, 88.95724293864769550 ) ) ;
#195606 = CARTESIAN_POINT ( 'NONE',  ( -17.49999999999999645, -5.499999999999992895, 94.20309617465827046 ) ) ;
#195607 = CARTESIAN_POINT ( 'NONE',  ( 16.51473224551069308, 9.474510206698969483, 84.16557627198102409 ) ) ;
#195608 = CARTESIAN_POINT ( 'NONE',  ( -13.97604488694527625, -13.89961937509977652, 41.87390960531435979 ) ) ;
#195610 = EDGE_CURVE ( 'NONE', #150779, #190965, #125819, .T. ) ;
#195609 = CARTESIAN_POINT ( 'NONE',  ( 8.224510206698953496, -14.34966873604960469, 82.91557627198103830 ) ) ;
#195611 = CARTESIAN_POINT ( 'NONE',  ( 15.72974639402199770, -15.80617190586745480, 33.12390960531435979 ) ) ;
#195612 = CARTESIAN_POINT ( 'NONE',  ( -0.05219959533910754901, -16.53943276465976808, 52.49890960531435979 ) ) ;
#195613 = CARTESIAN_POINT ( 'NONE',  ( 0.05219959533936267826, -19.03943276465977164, 100.0010903946856757 ) ) ;
#195614 = CARTESIAN_POINT ( 'NONE',  ( -21.55341960407619339, 5.719274019375674811, 58.54275706135235424 ) ) ;
#195615 = CARTESIAN_POINT ( 'NONE',  ( 17.14385361876520264, 23.59649016807275856, 148.1750000027311671 ) ) ;
#195616 = CARTESIAN_POINT ( 'NONE',  ( 5.049401038298161559, -19.05341960407611168, 112.7072429386476813 ) ) ;
#195617 = CARTESIAN_POINT ( 'NONE',  ( -12.14591786802326823, 12.06949235617739902, 78.12609039468570415 ) ) ;
#195618 = CARTESIAN_POINT ( 'NONE',  ( -17.26172910966712948, 6.454744622557082145, 95.80646908649208626 ) ) ;
#195619 = CARTESIAN_POINT ( 'NONE',  ( -9.564922557960796823, -16.46253265017161027, 72.08224293864770971 ) ) ;
#195620 = CARTESIAN_POINT ( 'NONE',  ( -5.823673210054116645, -21.52544592524344225, 77.29057627198102409 ) ) ;
#195621 = CARTESIAN_POINT ( 'NONE',  ( 14.34966873604972726, -8.224510206698740333, 25.83442372801901499 ) ) ;
#195623 = CARTESIAN_POINT ( 'NONE',  ( 21.53943276465977519, 0.05219959533937863772, 61.25109039468567573 ) ) ;
#195622 = CARTESIAN_POINT ( 'NONE',  ( 16.52544592524342804, -4.483927247898539470, 48.54057627198103120 ) ) ;
#195625 = CARTESIAN_POINT ( 'NONE',  ( 21.52544592524344225, -5.823673210054117533, 28.54057627198103120 ) ) ;
#195624 = CARTESIAN_POINT ( 'NONE',  ( -8.224510206698735004, -14.34966873604973081, 84.58442372801903275 ) ) ;
#195626 = CARTESIAN_POINT ( 'NONE',  ( -9.564922557960796823, -16.46253265017161027, 112.0822429386476955 ) ) ;
#195627 = DIRECTION ( 'NONE',  ( 0.000000000000000000, 0.000000000000000000, -1.000000000000000000 ) ) ;
#195628 = CARTESIAN_POINT ( 'NONE',  ( -0.05219959533934338120, 16.53943276465976808, 112.5010903946857042 ) ) ;
#195629 = CARTESIAN_POINT ( 'NONE',  ( -14.29746914071037622, -8.314922557961029526, 64.16775706135234714 ) ) ;
#195630 = CARTESIAN_POINT ( 'NONE',  ( -13.89961937509977652, 13.97604488694528158, 75.62390960531438111 ) ) ;
#195631 = CARTESIAN_POINT ( 'NONE',  ( 16.51473224551069308, 9.474510206698969483, 84.16557627198102409 ) ) ;
#195632 = CARTESIAN_POINT ( 'NONE',  ( -5.719274019375665041, -21.55341960407619695, 74.79275706135234714 ) ) ;
#195633 = CARTESIAN_POINT ( 'NONE',  ( -16.53943276465976808, -0.05219959533934237506, 78.75109039468568994 ) ) ;
#195634 = CARTESIAN_POINT ( 'NONE',  ( -8.224510206698948167, 14.34966873604960824, 40.41557627198103120 ) ) ;
#195635 = CARTESIAN_POINT ( 'NONE',  ( 0.05219959533909260263, 19.03943276465977164, 54.99890960531435979 ) ) ;
#195636 = CARTESIAN_POINT ( 'NONE',  ( 13.89961937509977652, -13.97604488694527269, 48.12390960531435979 ) ) ;
#195638 = ORIENTED_EDGE ( 'NONE', *, *, #197184, .T. ) ;
#195637 = CARTESIAN_POINT ( 'NONE',  ( 4.379528057220092307, 16.55341960407617563, 37.29275706135235424 ) ) ;
#195639 = CARTESIAN_POINT ( 'NONE',  ( -9.564922557961040184, 16.46253265017147172, 92.91775706135233293 ) ) ;
#195640 = CARTESIAN_POINT ( 'NONE',  ( 16.53943276465976808, -0.05219959533910856209, 98.74890960531438111 ) ) ;
#195641 = CARTESIAN_POINT ( 'NONE',  ( 19.05341960407611168, 5.049401038298154454, 58.95724293864768129 ) ) ;
#195643 = CARTESIAN_POINT ( 'NONE',  ( 23.48529157249599919, 32.32473071737754111, -2.700000000000000622 ) ) ;
#195642 = CARTESIAN_POINT ( 'NONE',  ( -19.03943276465977164, -0.05219959533935918106, 98.75109039468567573 ) ) ;
#195644 = CARTESIAN_POINT ( 'NONE',  ( 21.53943276465977519, 0.05219959533937863772, 106.2510903946856757 ) ) ;
#195645 = CARTESIAN_POINT ( 'NONE',  ( -16.55341960407617563, 4.379528057220093196, 68.54275706135234714 ) ) ;
#195646 = CARTESIAN_POINT ( 'NONE',  ( -0.05219959533936034679, 19.03943276465977164, 87.50109039468567573 ) ) ;
#195647 = CARTESIAN_POINT ( 'NONE',  ( -0.05219959533907301413, -21.53943276465977519, 62.49890960531436690 ) ) ;
#195648 = CARTESIAN_POINT ( 'NONE',  ( 4.379528057220092307, 16.55341960407617563, 57.29275706135234714 ) ) ;
#195649 = DIRECTION ( 'NONE',  ( 0.000000000000000000, -0.7660444431189836756, 0.6427876096865327016 ) ) ;
#195650 = CARTESIAN_POINT ( 'NONE',  ( -5.049401038297874678, -19.05341960407617918, 54.79275706135234003 ) ) ;
#195651 = AXIS2_PLACEMENT_3D ( 'NONE', #14328, #44676, #106329 ) ;
#195652 = CARTESIAN_POINT ( 'NONE',  ( -16.46253265017160317, 9.564922557960807481, 95.83224293864769550 ) ) ;
#195653 = CARTESIAN_POINT ( 'NONE',  ( -14.29746914071049879, 8.314922557960819915, 110.8322429386476955 ) ) ;
#195654 = CARTESIAN_POINT ( 'NONE',  ( 9.474510206698971260, -16.51473224551069308, 67.91557627198102409 ) ) ;
#195656 = EDGE_CURVE ( 'NONE', #85313, #515, #85111, .T. ) ;
#195655 = CARTESIAN_POINT ( 'NONE',  ( 16.52544592524342804, -4.483927247898539470, 53.54057627198103120 ) ) ;
#195657 = CARTESIAN_POINT ( 'NONE',  ( 21.53943276465977519, 0.05219959533937863772, 76.25109039468568994 ) ) ;
#195658 = CARTESIAN_POINT ( 'NONE',  ( 9.564922557961047289, -16.46253265017146816, 50.41775706135233293 ) ) ;
#195659 = CARTESIAN_POINT ( 'NONE',  ( 19.03943276465977164, 0.05219959533936151252, 31.25109039468566863 ) ) ;
#195660 = CARTESIAN_POINT ( 'NONE',  ( -9.474510206698964154, 16.51473224551069663, 115.4155762719810241 ) ) ;
#195661 = CARTESIAN_POINT ( 'NONE',  ( 10.81492255796106328, -18.62759615963255655, 90.41775706135236135 ) ) ;
#195662 = CARTESIAN_POINT ( 'NONE',  ( 5.049401038298161559, -19.05341960407611168, 57.70724293864769550 ) ) ;
#195663 = CARTESIAN_POINT ( 'NONE',  ( -21.55341960407619339, 5.719274019375674811, 98.54275706135234714 ) ) ;
#195664 = CARTESIAN_POINT ( 'NONE',  ( 18.67979575497178502, 10.72451020669898547, 49.16557627198102409 ) ) ;
#195665 = CARTESIAN_POINT ( 'NONE',  ( -16.51473224551069308, -9.474510206698971260, 81.66557627198103830 ) ) ;
#195666 = CARTESIAN_POINT ( 'NONE',  ( 19.02544592524334988, 5.153800228976608722, 66.45942372801899012 ) ) ;
#195667 = CARTESIAN_POINT ( 'NONE',  ( -19.03943276465977164, 0.05219959533909376836, 41.24890960531435269 ) ) ;
#195668 = CARTESIAN_POINT ( 'NONE',  ( 19.05341960407611168, 5.049401038298154454, 88.95724293864769550 ) ) ;
#195669 = CARTESIAN_POINT ( 'NONE',  ( -19.02544592524334988, -5.153800228976617603, 83.95942372801901854 ) ) ;
#195670 = CARTESIAN_POINT ( 'NONE',  ( 14.34966873604972726, -8.224510206698740333, 45.83442372801901854 ) ) ;
#195671 = CARTESIAN_POINT ( 'NONE',  ( 16.52544592524342804, -4.483927247898539470, 98.54057627198105251 ) ) ;
#195672 = CARTESIAN_POINT ( 'NONE',  ( -9.474510206698964154, 16.51473224551069663, 70.41557627198102409 ) ) ;
#195673 = CARTESIAN_POINT ( 'NONE',  ( -15.72974639402197994, 15.80617190586746368, 55.62390960531436690 ) ) ;
#195674 = CARTESIAN_POINT ( 'NONE',  ( -19.03943276465977164, -0.05219959533935918106, 108.7510903946856615 ) ) ;
#195675 = CARTESIAN_POINT ( 'NONE',  ( -18.62759615963255300, -10.81492255796106328, 19.16775706135234714 ) ) ;
#195676 = CARTESIAN_POINT ( 'NONE',  ( 10.81492255796106328, -18.62759615963255655, 70.41775706135236135 ) ) ;
#195677 = CARTESIAN_POINT ( 'NONE',  ( -0.05219959533934338120, 16.53943276465976808, 77.50109039468567573 ) ) ;
#195678 = CARTESIAN_POINT ( 'NONE',  ( 16.46253265017160672, -9.564922557960803928, 78.33224293864769550 ) ) ;
#195679 = CARTESIAN_POINT ( 'NONE',  ( 16.55341960407618274, -4.379528057220086978, 101.0427570613523756 ) ) ;
#195680 = CARTESIAN_POINT ( 'NONE',  ( 13.89961937509957401, 13.97604488694547697, 46.87609039468565442 ) ) ;
#195681 = CARTESIAN_POINT ( 'NONE',  ( 15.80617190586769283, -15.72974639402175789, 30.62609039468567929 ) ) ;
#195682 = CARTESIAN_POINT ( 'NONE',  ( -14.34966873604960291, -8.224510206698953496, 81.66557627198103830 ) ) ;
#195683 = CARTESIAN_POINT ( 'NONE',  ( 13.97604488694527802, 13.89961937509977652, 99.37390960531436690 ) ) ;
#195684 = CARTESIAN_POINT ( 'NONE',  ( 16.53943276465976808, 0.05219959533934440121, 91.25109039468568994 ) ) ;
#195685 = CARTESIAN_POINT ( 'NONE',  ( -5.823673210054431948, 21.52544592524334988, 77.70942372801900433 ) ) ;
#195686 = CARTESIAN_POINT ( 'NONE',  ( -12.06949235617739369, -12.14591786802326823, 29.37609039468568284 ) ) ;
#195687 = CARTESIAN_POINT ( 'NONE',  ( -5.719274019375665041, -21.55341960407619695, 29.79275706135234358 ) ) ;
#195688 = CARTESIAN_POINT ( 'NONE',  ( -8.314922557960811034, -14.29746914071050412, 72.08224293864769550 ) ) ;
#195689 = ORIENTED_EDGE ( 'NONE', *, *, #96176, .F. ) ;
#195690 = CARTESIAN_POINT ( 'NONE',  ( -21.52544592524343514, 5.823673210054127303, 106.0405762719810525 ) ) ;
#195691 = CARTESIAN_POINT ( 'NONE',  ( -14.29746914071049879, 8.314922557960819915, 50.83224293864770971 ) ) ;
#195692 = ORIENTED_EDGE ( 'NONE', *, *, #85978, .T. ) ;
#195693 = CARTESIAN_POINT ( 'NONE',  ( -5.153800228976328057, -19.02544592524343514, 32.29057627198102409 ) ) ;
#195694 = CARTESIAN_POINT ( 'NONE',  ( 18.62759615963271287, -10.81492255796078972, 33.33224293864769550 ) ) ;
#195695 = CARTESIAN_POINT ( 'NONE',  ( 15.80617190586769283, -15.72974639402175789, 40.62609039468567573 ) ) ;
#195696 = CARTESIAN_POINT ( 'NONE',  ( -8.314922557960811034, -14.29746914071050412, 67.08224293864770971 ) ) ;
#195697 = CARTESIAN_POINT ( 'NONE',  ( -15.80617190586745835, -15.72974639402198527, 71.87390960531438111 ) ) ;
#195698 = CARTESIAN_POINT ( 'NONE',  ( -9.474510206698964154, 16.51473224551069663, 80.41557627198103830 ) ) ;
#195700 = CARTESIAN_POINT ( 'NONE',  ( 13.97604488694548053, -13.89961937509957401, 75.62609039468564731 ) ) ;
#195699 = CARTESIAN_POINT ( 'NONE',  ( 13.89961937509977652, -13.97604488694527269, 23.12390960531436335 ) ) ;
#195701 = EDGE_CURVE ( 'NONE', #93860, #194492, #32826, .T. ) ;
#195702 = CARTESIAN_POINT ( 'NONE',  ( 21.52544592524344225, -5.823673210054117533, 58.54057627198103120 ) ) ;
#195703 = CARTESIAN_POINT ( 'NONE',  ( -9.564922557960796823, -16.46253265017161027, 37.08224293864768839 ) ) ;
#195704 = CARTESIAN_POINT ( 'NONE',  ( 5.049401038298161559, -19.05341960407611168, 77.70724293864765286 ) ) ;
#195705 = ORIENTED_EDGE ( 'NONE', *, *, #154616, .F. ) ;
#195706 = CARTESIAN_POINT ( 'NONE',  ( -16.52544592524335698, -4.483927247898792601, 33.95942372801901143 ) ) ;
#195707 = CARTESIAN_POINT ( 'NONE',  ( -15.72974639402176322, -15.80617190586768395, 34.37609039468568284 ) ) ;
#195708 = CARTESIAN_POINT ( 'NONE',  ( -18.67979575497193778, 10.72451020669871902, 53.33442372801901854 ) ) ;
#195709 = CARTESIAN_POINT ( 'NONE',  ( 16.51473224551069308, 9.474510206698969483, 109.1655762719810383 ) ) ;
#195710 = CARTESIAN_POINT ( 'NONE',  ( 18.62759615963271287, -10.81492255796078972, 73.33224293864769550 ) ) ;
#195712 = CARTESIAN_POINT ( 'NONE',  ( -8.314922557961024197, 14.29746914071037800, 47.91775706135234714 ) ) ;
#195711 = CARTESIAN_POINT ( 'NONE',  ( 21.55341960407610458, 5.719274019375980345, 108.9572429386476955 ) ) ;
#195713 = CARTESIAN_POINT ( 'NONE',  ( 5.823673210054125526, 21.52544592524343514, 54.79057627198104541 ) ) ;
#195714 = CARTESIAN_POINT ( 'NONE',  ( 10.81492255796106328, -18.62759615963255655, 105.4177570613523613 ) ) ;
#195715 = CARTESIAN_POINT ( 'NONE',  ( -19.05341960407611168, -5.049401038298163336, 61.45724293864769550 ) ) ;
#195716 = CARTESIAN_POINT ( 'NONE',  ( 13.89961937509977652, -13.97604488694527269, 113.1239096053143527 ) ) ;
#195717 = CARTESIAN_POINT ( 'NONE',  ( -19.02544592524342804, 5.153800228976336051, 81.04057627198103830 ) ) ;
#195718 = PRODUCT_RELATED_PRODUCT_CATEGORY ( 'part', '', ( #92061 ) ) ;
#195719 = CARTESIAN_POINT ( 'NONE',  ( -8.343164238912773811, -45.63112023308526233, -22.26988597240830003 ) ) ;
#195720 = CARTESIAN_POINT ( 'NONE',  ( -13.89961937509957401, -13.97604488694547875, 64.37609039468567573 ) ) ;
#195722 = CARTESIAN_POINT ( 'NONE',  ( -21.53943276465977519, 0.05219959533907696930, 46.24890960531435979 ) ) ;
#195721 = CARTESIAN_POINT ( 'NONE',  ( 21.55341960407619695, -5.719274019375665929, 111.0427570613523613 ) ) ;
#195723 = CARTESIAN_POINT ( 'NONE',  ( -4.379528057220086978, -16.55341960407618274, 99.79275706135234714 ) ) ;
#195724 = CARTESIAN_POINT ( 'NONE',  ( 19.02544592524334988, 5.153800228976608722, 81.45942372801897591 ) ) ;
#195725 = CARTESIAN_POINT ( 'NONE',  ( -17.13100169013299734, 6.664070546373147330, 60.76789835699850784 ) ) ;
#195726 = CARTESIAN_POINT ( 'NONE',  ( 0.05219959533936267826, -19.03943276465977164, 25.00109039468566152 ) ) ;
#195727 = CARTESIAN_POINT ( 'NONE',  ( -0.05219959533936034679, 19.03943276465977164, 77.50109039468566152 ) ) ;
#195728 = CARTESIAN_POINT ( 'NONE',  ( 0.05219959533936267826, -19.03943276465977164, 45.00109039468566863 ) ) ;
#195729 = CARTESIAN_POINT ( 'NONE',  ( -17.40805194822028668, -6.112264579159356614, 44.16628727489390371 ) ) ;
#195730 = CARTESIAN_POINT ( 'NONE',  ( 9.564922557960805705, 16.46253265017160317, 39.58224293864768839 ) ) ;
#195731 = CARTESIAN_POINT ( 'NONE',  ( 8.224510206698953496, -14.34966873604960469, 52.91557627198103830 ) ) ;
#195732 = CARTESIAN_POINT ( 'NONE',  ( 19.05341960407611168, 5.049401038298154454, 38.95724293864767418 ) ) ;
#195733 = CARTESIAN_POINT ( 'NONE',  ( -14.34966873604960291, -8.224510206698953496, 41.66557627198103120 ) ) ;
#195734 = DIRECTION ( 'NONE',  ( 0.000000000000000000, 0.000000000000000000, 1.000000000000000000 ) ) ;
#195735 = CARTESIAN_POINT ( 'NONE',  ( 8.224510206698742110, 14.34966873604972548, 112.0844237280190185 ) ) ;
#195736 = CARTESIAN_POINT ( 'NONE',  ( -0.05219959533909027116, -19.03943276465977164, 47.49890960531435979 ) ) ;
#195737 = CARTESIAN_POINT ( 'NONE',  ( 9.474510206698729675, 16.51473224551082808, 27.08442372801900433 ) ) ;
#195738 = CARTESIAN_POINT ( 'NONE',  ( 14.29746914071037800, 8.314922557961029526, 31.66775706135234358 ) ) ;
#195739 = CARTESIAN_POINT ( 'NONE',  ( 21.53943276465977519, -0.05219959533907433946, 38.74890960531435979 ) ) ;
#195740 = CARTESIAN_POINT ( 'NONE',  ( 15.80617190586769283, -15.72974639402175789, 95.62609039468568994 ) ) ;
#195741 = CARTESIAN_POINT ( 'NONE',  ( 5.153800228976335163, 19.02544592524342804, 109.7905762719810099 ) ) ;
#195742 = CARTESIAN_POINT ( 'NONE',  ( -9.474510206698964154, 16.51473224551069663, 85.41557627198102409 ) ) ;
#195743 = CARTESIAN_POINT ( 'NONE',  ( -32.86500790357915491, -22.80501606679668924, -22.13190935960392025 ) ) ;
#195744 = CARTESIAN_POINT ( 'NONE',  ( 21.53943276465977519, -0.05219959533907433946, 113.7489096053143527 ) ) ;
#195745 = VECTOR ( 'NONE', #191448, 1000.000000000000000 ) ;
#195746 = CARTESIAN_POINT ( 'NONE',  ( -14.34966873604960291, -8.224510206698953496, 86.66557627198102409 ) ) ;
#195748 = CARTESIAN_POINT ( 'NONE',  ( -13.89961937509977652, 13.97604488694528158, 65.62390960531436690 ) ) ;
#195747 = CARTESIAN_POINT ( 'NONE',  ( -18.67979575497178146, -10.72451020669898902, 76.66557627198103830 ) ) ;
#195749 = CARTESIAN_POINT ( 'NONE',  ( 13.89961937509977652, -13.97604488694527269, 78.12390960531433848 ) ) ;
#195750 = CARTESIAN_POINT ( 'NONE',  ( 5.719274019375991003, -21.55341960407610458, 102.7072429386476955 ) ) ;
#195751 = ORIENTED_EDGE ( 'NONE', *, *, #106434, .F. ) ;
#195752 = CARTESIAN_POINT ( 'NONE',  ( -9.474510206698964154, 16.51473224551069663, 55.41557627198103120 ) ) ;
#195754 = CARTESIAN_POINT ( 'NONE',  ( -19.02544592524342804, 5.153800228976336051, 26.04057627198103120 ) ) ;
#195753 = CARTESIAN_POINT ( 'NONE',  ( -4.483927247898539470, -16.52544592524342804, 102.2905762719810383 ) ) ;
#195755 = CARTESIAN_POINT ( 'NONE',  ( -16.46253265017160317, 9.564922557960807481, 60.83224293864769550 ) ) ;
#195756 = CARTESIAN_POINT ( 'NONE',  ( 16.51473224551083163, -9.474510206698727899, 85.83442372801900433 ) ) ;
#195757 = CARTESIAN_POINT ( 'NONE',  ( 4.483927247898545687, 16.52544592524342804, 94.79057627198105251 ) ) ;
#195758 = CARTESIAN_POINT ( 'NONE',  ( -10.81492255796105439, 18.62759615963255655, 62.91775706135236135 ) ) ;
#195760 = CARTESIAN_POINT ( 'NONE',  ( -21.53943276465977519, -0.05219959533937600094, 23.75109039468567929 ) ) ;
#195759 = CARTESIAN_POINT ( 'NONE',  ( -9.564922557960796823, -16.46253265017161027, 47.08224293864769550 ) ) ;
#195761 = CARTESIAN_POINT ( 'NONE',  ( -4.379528057220328563, 16.55341960407611168, 95.20724293864769550 ) ) ;
#195762 = CARTESIAN_POINT ( 'NONE',  ( -23.31738231874055245, -16.94106989632524574, 140.1999999999999886 ) ) ;
#195763 = CARTESIAN_POINT ( 'NONE',  ( -16.46253265017160317, 9.564922557960807481, 75.83224293864769550 ) ) ;
#195764 = CARTESIAN_POINT ( 'NONE',  ( -23.31738231874055245, -16.94106989632524574, 138.4500000054623570 ) ) ;
#195766 = CARTESIAN_POINT ( 'NONE',  ( -5.049401038298153566, 19.05341960407611168, 110.2072429386476671 ) ) ;
#195765 = CARTESIAN_POINT ( 'NONE',  ( 9.474510206698729675, 16.51473224551082808, 112.0844237280190043 ) ) ;
#195767 = CARTESIAN_POINT ( 'NONE',  ( 10.72451020669871369, 18.67979575497193778, 47.08442372801901854 ) ) ;
#195768 = CARTESIAN_POINT ( 'NONE',  ( 19.03943276465977164, -0.05219959533909143690, 93.74890960531435269 ) ) ;
#195769 = CARTESIAN_POINT ( 'NONE',  ( 16.46253265017146816, 9.564922557961045513, 81.66775706135233293 ) ) ;
#195770 = CARTESIAN_POINT ( 'NONE',  ( -13.89961937509977652, 13.97604488694528158, 65.62390960531436690 ) ) ;
#195771 = B_SPLINE_CURVE_WITH_KNOTS ( 'NONE', 3,
 ( #48268, #198964, #123096, #45282, #78580, #124085, #106935, #110912, #93756, #14941, #742, #107923, #76601, #2742, #60431, #122105, #183795, #62414, #109922, #30108, #16927, #92754, #155437, #64419, #168608, #34084 ),
 .UNSPECIFIED., .F., .F.,
 ( 4, 2, 2, 2, 2, 2, 2, 2, 2, 2, 2, 2, 4 ),
 ( 2.788259459799404871E-07, 0.0002964138711649459907, 0.0005925489163839111695, 0.0008886839616028763484, 0.001184819006821841419, 0.001777089097259771776, 0.002369359187697702568, 0.002665494232916669048, 0.002961629278135635094, 0.003257764323354601574, 0.003553899368573567186, 0.004146169459011494508, 0.004738439549449421397 ),
 .UNSPECIFIED. ) ;
#195772 = CARTESIAN_POINT ( 'NONE',  ( 0.05219959533910956823, 16.53943276465976808, 79.99890960531435269 ) ) ;
#195773 = CARTESIAN_POINT ( 'NONE',  ( -19.05341960407611168, -5.049401038298163336, 96.45724293864769550 ) ) ;
#195774 = CARTESIAN_POINT ( 'NONE',  ( 14.34966873604960469, 8.224510206698951720, 74.16557627198102409 ) ) ;
#195775 = CARTESIAN_POINT ( 'NONE',  ( -9.564922557960796823, -16.46253265017161027, 92.08224293864769550 ) ) ;
#195776 = CARTESIAN_POINT ( 'NONE',  ( 13.97604488694548053, -13.89961937509957401, 40.62609039468564731 ) ) ;
#195779 = CARTESIAN_POINT ( 'NONE',  ( -16.51473224551069308, -9.474510206698971260, 26.66557627198103120 ) ) ;
#195778 = CARTESIAN_POINT ( 'NONE',  ( 16.55341960407611168, 4.379528057220329451, 38.95724293864768839 ) ) ;
#195777 = CARTESIAN_POINT ( 'NONE',  ( -13.89961937509977652, 13.97604488694528158, 45.62390960531433848 ) ) ;
#195780 = ORIENTED_EDGE ( 'NONE', *, *, #65731, .T. ) ;
#195781 = CARTESIAN_POINT ( 'NONE',  ( -21.53943276465977519, -0.05219959533937600094, 48.75109039468568284 ) ) ;
#195782 = CARTESIAN_POINT ( 'NONE',  ( 16.51473224551083163, -9.474510206698727899, 85.83442372801900433 ) ) ;
#195783 = CARTESIAN_POINT ( 'NONE',  ( -12.06949235617756955, 12.14591786802309770, 30.62390960531436335 ) ) ;
#195784 = CARTESIAN_POINT ( 'NONE',  ( -21.53943276465977519, 0.05219959533907696930, 101.2489096053143669 ) ) ;
#195785 = CARTESIAN_POINT ( 'NONE',  ( -15.72974639402197994, 15.80617190586746368, 35.62390960531437401 ) ) ;
#195787 = CARTESIAN_POINT ( 'NONE',  ( 8.314922557960818139, 14.29746914071049879, 79.58224293864769550 ) ) ;
#195786 = AXIS2_PLACEMENT_3D ( 'NONE', #50985, #81293, #142977 ) ;
#195788 = CARTESIAN_POINT ( 'NONE',  ( 5.049401038298161559, -19.05341960407611168, 37.70724293864768839 ) ) ;
#195789 = CARTESIAN_POINT ( 'NONE',  ( -12.06949235617756955, 12.14591786802309770, 25.62390960531435624 ) ) ;
#195790 = CARTESIAN_POINT ( 'NONE',  ( -4.483927247898782831, 16.52544592524335698, 92.70942372801901854 ) ) ;
#195791 = CARTESIAN_POINT ( 'NONE',  ( -12.06949235617739369, -12.14591786802326823, 74.37609039468568994 ) ) ;
#195792 = CARTESIAN_POINT ( 'NONE',  ( -19.02544592524334988, -5.153800228976617603, 28.95942372801900433 ) ) ;
#195793 = CARTESIAN_POINT ( 'NONE',  ( 13.89961937509977652, -13.97604488694527269, 88.12390960531438111 ) ) ;
#195794 = CARTESIAN_POINT ( 'NONE',  ( 13.97604488694527802, 13.89961937509977652, 74.37390960531436690 ) ) ;
#195795 = CARTESIAN_POINT ( 'NONE',  ( 12.06949235617739724, 12.14591786802326823, 71.87609039468568994 ) ) ;
#195796 = CARTESIAN_POINT ( 'NONE',  ( 5.153800228976335163, 19.02544592524342804, 34.79057627198102409 ) ) ;
#195797 = CARTESIAN_POINT ( 'NONE',  ( 8.314922557960818139, 14.29746914071049879, 54.58224293864769550 ) ) ;
#195798 = CARTESIAN_POINT ( 'NONE',  ( 16.46253265017160672, -9.564922557960803928, 98.33224293864769550 ) ) ;
#195799 = CARTESIAN_POINT ( 'NONE',  ( -21.53943276465977519, 0.05219959533907696930, 26.24890960531435624 ) ) ;
#195800 = CARTESIAN_POINT ( 'NONE',  ( -12.06949235617756955, 12.14591786802309770, 75.62390960531439532 ) ) ;
#195801 = CARTESIAN_POINT ( 'NONE',  ( 4.379528057220339221, -16.55341960407611168, 62.70724293864769550 ) ) ;
#195802 = ADVANCED_FACE ( 'NONE', ( #61161 ), #122833, .F. ) ;
#195803 = CARTESIAN_POINT ( 'NONE',  ( 17.72696623605159516, -5.500000000000041744, 86.09811031808419557 ) ) ;
#195804 = CARTESIAN_POINT ( 'NONE',  ( 13.89961937509957401, 13.97604488694547697, 66.87609039468567573 ) ) ;
#195805 = CARTESIAN_POINT ( 'NONE',  ( -0.05219959533909027116, -19.03943276465977164, 87.49890960531436690 ) ) ;
#195806 = CARTESIAN_POINT ( 'NONE',  ( -5.049401038297874678, -19.05341960407617918, 84.79275706135233293 ) ) ;
#195807 = CARTESIAN_POINT ( 'NONE',  ( -22.44159573604010305, 16.30477369853692338, 149.1750000027311671 ) ) ;
#195809 = CARTESIAN_POINT ( 'NONE',  ( 16.55341960407618274, -4.379528057220086978, 96.04275706135236135 ) ) ;
#195808 = CARTESIAN_POINT ( 'NONE',  ( -5.049401038297874678, -19.05341960407617918, 109.7927570613523187 ) ) ;
#195810 = CARTESIAN_POINT ( 'NONE',  ( 0.05219959533909260263, 19.03943276465977164, 39.99890960531436690 ) ) ;
#195811 = CARTESIAN_POINT ( 'NONE',  ( -19.03943276465977164, 0.05219959533909376836, 116.2489096053143669 ) ) ;
#195812 = CARTESIAN_POINT ( 'NONE',  ( 18.62759615963255655, 10.81492255796105972, 51.66775706135234714 ) ) ;
#195813 = CARTESIAN_POINT ( 'NONE',  ( 12.14591786802327356, -12.06949235617739191, 20.62609039468568639 ) ) ;
#195815 = CARTESIAN_POINT ( 'NONE',  ( 9.564922557960805705, 16.46253265017160317, 74.58224293864769550 ) ) ;
#195814 = CARTESIAN_POINT ( 'NONE',  ( 5.153800228976617603, -19.02544592524335343, 55.20942372801899722 ) ) ;
#195816 = CARTESIAN_POINT ( 'NONE',  ( 16.46253265017160672, -9.564922557960803928, 113.3322429386476955 ) ) ;
#195818 = CARTESIAN_POINT ( 'NONE',  ( 13.97604488694527802, 13.89961937509977652, 74.37390960531436690 ) ) ;
#195817 = CARTESIAN_POINT ( 'NONE',  ( 14.29746914071049879, -8.314922557960816363, 73.33224293864769550 ) ) ;
#195819 = CARTESIAN_POINT ( 'NONE',  ( -13.89961937509977652, 13.97604488694528158, 70.62390960531432427 ) ) ;
#195820 = ORIENTED_EDGE ( 'NONE', *, *, #72341, .T. ) ;
#195821 = CARTESIAN_POINT ( 'NONE',  ( 19.02544592524334988, 5.153800228976608722, 91.45942372801900433 ) ) ;
#195822 = CARTESIAN_POINT ( 'NONE',  ( 18.62759615963271287, -10.81492255796078972, 63.33224293864770260 ) ) ;
#195823 = CARTESIAN_POINT ( 'NONE',  ( -19.02544592524342804, 5.153800228976336051, 26.04057627198103120 ) ) ;
#195824 = CARTESIAN_POINT ( 'NONE',  ( -19.02544592524334988, -5.153800228976617603, 58.95942372801900433 ) ) ;
#195825 = CARTESIAN_POINT ( 'NONE',  ( -5.153800228976328057, -19.02544592524343514, 57.29057627198103120 ) ) ;
#195826 = CARTESIAN_POINT ( 'NONE',  ( -5.153800228976328057, -19.02544592524343514, 92.29057627198099567 ) ) ;
#195827 = VERTEX_POINT ( 'NONE', #49980 ) ;
#195828 = CARTESIAN_POINT ( 'NONE',  ( 18.62759615963271287, -10.81492255796078972, 93.33224293864769550 ) ) ;
#195830 = CARTESIAN_POINT ( 'NONE',  ( 13.97604488694548053, -13.89961937509957401, 45.62609039468566863 ) ) ;
#195829 = CARTESIAN_POINT ( 'NONE',  ( 8.314922557960818139, 14.29746914071049879, 94.58224293864769550 ) ) ;
#195831 = CARTESIAN_POINT ( 'NONE',  ( 18.67979575497178502, 10.72451020669898547, 84.16557627198103830 ) ) ;
#195832 = CARTESIAN_POINT ( 'NONE',  ( 0.05219959533907565091, 21.53943276465977519, 74.99890960531435269 ) ) ;
#195833 = CARTESIAN_POINT ( 'NONE',  ( 16.52544592524342804, -4.483927247898539470, 38.54057627198103120 ) ) ;
#195834 = CARTESIAN_POINT ( 'NONE',  ( 21.55341960407619695, -5.719274019375665929, 106.0427570613523471 ) ) ;
#195835 = CARTESIAN_POINT ( 'NONE',  ( 19.05341960407611168, 5.049401038298154454, 83.95724293864766707 ) ) ;
#195836 = CARTESIAN_POINT ( 'NONE',  ( 5.153800228976335163, 19.02544592524342804, 34.79057627198102409 ) ) ;
#195837 = CARTESIAN_POINT ( 'NONE',  ( 5.719274019375673035, 21.55341960407619339, 37.29275706135235424 ) ) ;
#195838 = CARTESIAN_POINT ( 'NONE',  ( -18.62759615963255300, -10.81492255796106328, 59.16775706135234714 ) ) ;
#195839 = CARTESIAN_POINT ( 'NONE',  ( 9.564922557960805705, 16.46253265017160317, 44.58224293864769550 ) ) ;
#195840 = CARTESIAN_POINT ( 'NONE',  ( -10.72451020669870658, -18.67979575497194134, 19.58442372801901143 ) ) ;
#195841 = CARTESIAN_POINT ( 'NONE',  ( 5.049401038297881783, 19.05341960407617563, 62.29275706135234003 ) ) ;
#195842 = CARTESIAN_POINT ( 'NONE',  ( -16.51473224551069308, -9.474510206698971260, 36.66557627198102409 ) ) ;
#195843 = CARTESIAN_POINT ( 'NONE',  ( -12.14591786802326823, 12.06949235617739902, 23.12609039468567573 ) ) ;
#195844 = CARTESIAN_POINT ( 'NONE',  ( -16.46253265017160317, 9.564922557960807481, 30.83224293864769550 ) ) ;
#195845 = CARTESIAN_POINT ( 'NONE',  ( -4.379528057220086978, -16.55341960407618274, 79.79275706135236135 ) ) ;
#195846 = CARTESIAN_POINT ( 'NONE',  ( -9.474510206698964154, 16.51473224551069663, 35.41557627198102409 ) ) ;
#195847 = CARTESIAN_POINT ( 'NONE',  ( 24.06756124613666614, -8.142616467493763110, 169.4332804344608974 ) ) ;
#195848 = CARTESIAN_POINT ( 'NONE',  ( 0.05219959533909260263, 19.03943276465977164, 79.99890960531436690 ) ) ;
#195850 = EDGE_CURVE ( 'NONE', #126008, #95725, #31832, .T. ) ;
#195849 = CARTESIAN_POINT ( 'NONE',  ( -13.97604488694527625, -13.89961937509977652, 21.87390960531435979 ) ) ;
#195851 = CARTESIAN_POINT ( 'NONE',  ( -15.72974639402197994, 15.80617190586746368, 75.62390960531439532 ) ) ;
#195852 = CARTESIAN_POINT ( 'NONE',  ( -14.34966873604972548, 8.224510206698743886, 53.33442372801901854 ) ) ;
#195853 = CARTESIAN_POINT ( 'NONE',  ( 9.474510206698729675, 16.51473224551082808, 22.08442372801899722 ) ) ;
#195854 = CARTESIAN_POINT ( 'NONE',  ( 16.46253265017160672, -9.564922557960803928, 33.33224293864770260 ) ) ;
#195855 = CARTESIAN_POINT ( 'NONE',  ( -4.379528057220328563, 16.55341960407611168, 25.20724293864769550 ) ) ;
#195856 = CARTESIAN_POINT ( 'NONE',  ( 16.53943276465976808, -0.05219959533910856209, 73.74890960531433848 ) ) ;
#195857 = CARTESIAN_POINT ( 'NONE',  ( 0.05219959533909260263, 19.03943276465977164, 59.99890960531436690 ) ) ;
#195858 = CARTESIAN_POINT ( 'NONE',  ( -18.67979575497193778, 10.72451020669871902, 108.3344237280190185 ) ) ;
#195859 = CARTESIAN_POINT ( 'NONE',  ( 21.53943276465977519, 0.05219959533937863772, 21.25109039468567218 ) ) ;
#195860 = CARTESIAN_POINT ( 'NONE',  ( -5.049401038298153566, 19.05341960407611168, 85.20724293864766707 ) ) ;
#195861 = CARTESIAN_POINT ( 'NONE',  ( -21.53943276465977519, -0.05219959533937600094, 88.75109039468567573 ) ) ;
#195862 = CARTESIAN_POINT ( 'NONE',  ( 4.483927247898790824, -16.52544592524335698, 65.20942372801901854 ) ) ;
#195863 = CARTESIAN_POINT ( 'NONE',  ( -12.06949235617739369, -12.14591786802326823, 29.37609039468568284 ) ) ;
#195865 = CARTESIAN_POINT ( 'NONE',  ( 19.05341960407611168, 5.049401038298154454, 108.9572429386477097 ) ) ;
#195864 = CARTESIAN_POINT ( 'NONE',  ( 8.224510206698953496, -14.34966873604960469, 87.91557627198103830 ) ) ;
#195866 = CARTESIAN_POINT ( 'NONE',  ( 8.224510206698953496, -14.34966873604960469, 27.91557627198103830 ) ) ;
#195867 = CARTESIAN_POINT ( 'NONE',  ( 13.97604488694527802, 13.89961937509977652, 24.37390960531435624 ) ) ;
#195868 = CARTESIAN_POINT ( 'NONE',  ( 8.314922557961029526, -14.29746914071037800, 50.41775706135235424 ) ) ;
#195869 = CARTESIAN_POINT ( 'NONE',  ( 12.14591786802309770, 12.06949235617756955, 49.37390960531436690 ) ) ;
#195870 = CARTESIAN_POINT ( 'NONE',  ( 12.06949235617739724, 12.14591786802326823, 96.87609039468568994 ) ) ;
#195871 = CARTESIAN_POINT ( 'NONE',  ( -13.89961937509977652, 13.97604488694528158, 115.6239096053143669 ) ) ;
#195872 = CARTESIAN_POINT ( 'NONE',  ( 0.05219959533907565091, 21.53943276465977519, 34.99890960531435979 ) ) ;
#195873 = CARTESIAN_POINT ( 'NONE',  ( 16.46253265017146816, 9.564922557961045513, 21.66775706135233648 ) ) ;
#195874 = CARTESIAN_POINT ( 'NONE',  ( -16.53943276465976808, 0.05219959533911058130, 81.24890960531436690 ) ) ;
#195875 = CARTESIAN_POINT ( 'NONE',  ( 5.153800228976335163, 19.02544592524342804, 89.79057627198102409 ) ) ;
#195876 = ORIENTED_EDGE ( 'NONE', *, *, #72094, .T. ) ;
#195877 = CARTESIAN_POINT ( 'NONE',  ( -4.379528057220086978, -16.55341960407618274, 39.79275706135235424 ) ) ;
#195878 = CARTESIAN_POINT ( 'NONE',  ( 5.049401038298161559, -19.05341960407611168, 47.70724293864770260 ) ) ;
#195880 = LINE ( 'NONE', #9847, #140384 ) ;
#195879 = CARTESIAN_POINT ( 'NONE',  ( -14.29746914071037622, -8.314922557961029526, 44.16775706135234714 ) ) ;
#195881 = CARTESIAN_POINT ( 'NONE',  ( -13.89961937509957401, -13.97604488694547875, 54.37609039468565442 ) ) ;
#195882 = CARTESIAN_POINT ( 'NONE',  ( -16.46253265017160317, 9.564922557960807481, 50.83224293864770260 ) ) ;
#195883 = CARTESIAN_POINT ( 'NONE',  ( 4.483927247898790824, -16.52544592524335698, 75.20942372801901854 ) ) ;
#195884 = CARTESIAN_POINT ( 'NONE',  ( 19.03943276465977164, 0.05219959533936151252, 91.25109039468566152 ) ) ;
#195885 = CARTESIAN_POINT ( 'NONE',  ( -5.153800228976328057, -19.02544592524343514, 62.29057627198100988 ) ) ;
#195886 = CARTESIAN_POINT ( 'NONE',  ( -21.52544592524343514, 5.823673210054127303, 96.04057627198102409 ) ) ;
#195887 = CARTESIAN_POINT ( 'NONE',  ( -12.06949235617756955, 12.14591786802309770, 95.62390960531436690 ) ) ;
#195888 = AXIS2_PLACEMENT_3D ( 'NONE', #10187, #195208, #7160 ) ;
#195889 = CARTESIAN_POINT ( 'NONE',  ( 16.51473224551083163, -9.474510206698727899, 70.83442372801900433 ) ) ;
#195890 = CARTESIAN_POINT ( 'NONE',  ( 5.719274019375991003, -21.55341960407610458, 57.70724293864770260 ) ) ;
#195891 = CARTESIAN_POINT ( 'NONE',  ( 13.97604488694548053, -13.89961937509957401, 45.62609039468566863 ) ) ;
#195892 = CARTESIAN_POINT ( 'NONE',  ( -0.05219959533909027116, -19.03943276465977164, 112.4989096053143669 ) ) ;
#195893 = CARTESIAN_POINT ( 'NONE',  ( -5.719274019375978568, 21.55341960407610458, 90.20724293864770971 ) ) ;
#195894 = CARTESIAN_POINT ( 'NONE',  ( -18.39635199886966177, 5.500000000000103029, 56.01967076360000419 ) ) ;
#195895 = CARTESIAN_POINT ( 'NONE',  ( -13.97604488694547697, 13.89961937509957934, 108.1260903946856331 ) ) ;
#195896 = CARTESIAN_POINT ( 'NONE',  ( 37.54768727782017379, -1.429952535790606882, 39.67699414429140603 ) ) ;
#195897 = CARTESIAN_POINT ( 'NONE',  ( 16.52544592524335698, 4.483927247898782831, 26.45942372801901854 ) ) ;
#195898 = CARTESIAN_POINT ( 'NONE',  ( -19.03943276465977164, 0.05219959533909376836, 51.24890960531436690 ) ) ;
#195899 = CARTESIAN_POINT ( 'NONE',  ( -19.03943276465977164, 0.05219959533909376836, 111.2489096053143669 ) ) ;
#195900 = CARTESIAN_POINT ( 'NONE',  ( 21.52544592524344225, -5.823673210054117533, 83.54057627198102409 ) ) ;
#195901 = CARTESIAN_POINT ( 'NONE',  ( 5.719274019375673035, 21.55341960407619339, 62.29275706135236845 ) ) ;
#195903 = CARTESIAN_POINT ( 'NONE',  ( 5.153800228976615827, -19.02544592524334988, 30.20942372801900433 ) ) ;
#195902 = CARTESIAN_POINT ( 'NONE',  ( -5.049401038297874678, -19.05341960407617918, 99.79275706135234714 ) ) ;
#195904 = CARTESIAN_POINT ( 'NONE',  ( 16.53943276465976808, -0.05219959533910856209, 33.74890960531436690 ) ) ;
#195905 = CARTESIAN_POINT ( 'NONE',  ( -15.72974639402197994, 15.80617190586746368, 105.6239096053143669 ) ) ;
#195906 = CARTESIAN_POINT ( 'NONE',  ( 14.29746914071049879, -8.314922557960816363, 53.33224293864769550 ) ) ;
#195907 = CARTESIAN_POINT ( 'NONE',  ( 19.02544592524334988, 5.153800228976608722, 91.45942372801900433 ) ) ;
#195908 = CARTESIAN_POINT ( 'NONE',  ( -5.049401038297874678, -19.05341960407617918, 54.79275706135234003 ) ) ;
#195909 = CARTESIAN_POINT ( 'NONE',  ( -18.62759615963255300, -10.81492255796106328, 74.16775706135231871 ) ) ;
#195910 = CARTESIAN_POINT ( 'NONE',  ( 16.51473224551083163, -9.474510206698727899, 40.83442372801900433 ) ) ;
#195911 = CARTESIAN_POINT ( 'NONE',  ( -16.53943276465976808, 0.05219959533911058130, 116.2489096053143669 ) ) ;
#195912 = CARTESIAN_POINT ( 'NONE',  ( 18.62759615963271287, -10.81492255796078972, 48.33224293864770260 ) ) ;
#195913 = CARTESIAN_POINT ( 'NONE',  ( 14.29746914071049879, -8.314922557960816363, 33.33224293864769550 ) ) ;
#195914 = CARTESIAN_POINT ( 'NONE',  ( -21.55341960407619339, 5.719274019375674811, 108.5427570613523756 ) ) ;
#195915 = CARTESIAN_POINT ( 'NONE',  ( 0.05219959533934541429, -16.53943276465976808, 70.00109039468568994 ) ) ;
#195916 = CARTESIAN_POINT ( 'NONE',  ( 16.52544592524342804, -4.483927247898539470, 38.54057627198103120 ) ) ;
#195917 = CARTESIAN_POINT ( 'NONE',  ( 21.55341960407619695, -5.719274019375665929, 71.04275706135234714 ) ) ;
#195918 = CARTESIAN_POINT ( 'NONE',  ( -18.62759615963255300, -10.81492255796106328, 74.16775706135231871 ) ) ;
#195919 = CARTESIAN_POINT ( 'NONE',  ( 0.05219959533907565091, 21.53943276465977519, 69.99890960531435269 ) ) ;
#195920 = CARTESIAN_POINT ( 'NONE',  ( 9.564922557960805705, 16.46253265017160317, 34.58224293864770260 ) ) ;
#195921 = CARTESIAN_POINT ( 'NONE',  ( 18.62759615963255655, 10.81492255796105972, 41.66775706135235424 ) ) ;
#195922 = CARTESIAN_POINT ( 'NONE',  ( -19.05341960407611168, -5.049401038298163336, 21.45724293864768839 ) ) ;
#195923 = CARTESIAN_POINT ( 'NONE',  ( 19.05341960407611168, 5.049401038298154454, 38.95724293864767418 ) ) ;
#195924 = CARTESIAN_POINT ( 'NONE',  ( 16.52544592524342804, -4.483927247898539470, 88.54057627198103830 ) ) ;
#195925 = CARTESIAN_POINT ( 'NONE',  ( -9.564922557960796823, -16.46253265017161027, 87.08224293864769550 ) ) ;
#195926 = CARTESIAN_POINT ( 'NONE',  ( 12.14591786802309770, 12.06949235617756955, 39.37390960531436690 ) ) ;
#195927 = CARTESIAN_POINT ( 'NONE',  ( 4.483927247898545687, 16.52544592524342804, 94.79057627198105251 ) ) ;
#195928 = CARTESIAN_POINT ( 'NONE',  ( 21.52544592524344225, -5.823673210054117533, 63.54057627198103830 ) ) ;
#195929 = AXIS2_PLACEMENT_3D ( 'NONE', #30615, #1246, #60938 ) ;
#195930 = CARTESIAN_POINT ( 'NONE',  ( 0.05219959533907565091, 21.53943276465977519, 104.9989096053143669 ) ) ;
#195931 = CARTESIAN_POINT ( 'NONE',  ( 19.02544592524343514, -5.153800228976328945, 113.5405762719810241 ) ) ;
#195933 = CARTESIAN_POINT ( 'NONE',  ( -0.05219959533934338120, 16.53943276465976808, 27.50109039468567929 ) ) ;
#195932 = CARTESIAN_POINT ( 'NONE',  ( 13.97604488694527802, 13.89961937509977652, 59.37390960531434558 ) ) ;
#195934 = EDGE_CURVE ( 'NONE', #125647, #68158, #25908, .T. ) ;
#195935 = CARTESIAN_POINT ( 'NONE',  ( 18.67979575497178502, 10.72451020669898547, 64.16557627198102409 ) ) ;
#195936 = CARTESIAN_POINT ( 'NONE',  ( -10.81492255796105439, 18.62759615963255655, 92.91775706135236135 ) ) ;
#195937 = CARTESIAN_POINT ( 'NONE',  ( 13.97604488694527802, 13.89961937509977652, 84.37390960531433848 ) ) ;
#195938 = CARTESIAN_POINT ( 'NONE',  ( 21.55341960407619695, -5.719274019375665929, 21.04275706135234714 ) ) ;
#195939 = CARTESIAN_POINT ( 'NONE',  ( -9.564922557960796823, -16.46253265017161027, 107.0822429386476955 ) ) ;
#195940 = CARTESIAN_POINT ( 'NONE',  ( 4.379528057220092307, 16.55341960407617563, 92.29275706135236135 ) ) ;
#195941 = CARTESIAN_POINT ( 'NONE',  ( 21.55341960407619695, -5.719274019375665929, 66.04275706135236135 ) ) ;
#195942 = CARTESIAN_POINT ( 'NONE',  ( -15.80617190586768217, 15.72974639402176855, 98.12609039468570415 ) ) ;
#195943 = CARTESIAN_POINT ( 'NONE',  ( -8.224510206698735004, -14.34966873604973081, 59.58442372801901854 ) ) ;
#195944 = CARTESIAN_POINT ( 'NONE',  ( 10.81492255796106328, -18.62759615963255655, 25.41775706135235779 ) ) ;
#195945 = CARTESIAN_POINT ( 'NONE',  ( -19.02544592524342804, 5.153800228976336051, 111.0405762719810099 ) ) ;
#195946 = CARTESIAN_POINT ( 'NONE',  ( -18.62759615963255300, -10.81492255796106328, 89.16775706135236135 ) ) ;
#195947 = CARTESIAN_POINT ( 'NONE',  ( 9.474510206698971260, -16.51473224551069308, 97.91557627198102409 ) ) ;
#195948 = CARTESIAN_POINT ( 'NONE',  ( -21.52544592524343514, 5.823673210054127303, 96.04057627198102409 ) ) ;
#195949 = CARTESIAN_POINT ( 'NONE',  ( 19.03943276465977164, 0.05219959533936151252, 46.25109039468566863 ) ) ;
#195950 = CARTESIAN_POINT ( 'NONE',  ( -5.719274019375978568, 21.55341960407610458, 60.20724293864768839 ) ) ;
#195952 = CARTESIAN_POINT ( 'NONE',  ( -12.14591786802309592, -12.06949235617757132, 41.87390960531435979 ) ) ;
#195951 = CARTESIAN_POINT ( 'NONE',  ( -5.153800228976328057, -19.02544592524343514, 97.29057627198099567 ) ) ;
#195953 = CARTESIAN_POINT ( 'NONE',  ( -20.49784845693389101, -1.163414459189985801E-14, 95.00000000000000000 ) ) ;
#195954 = CARTESIAN_POINT ( 'NONE',  ( 19.02544592524334988, 5.153800228976608722, 61.45942372801900433 ) ) ;
#195955 = CARTESIAN_POINT ( 'NONE',  ( -19.34837522270364829, -5.499999999999849010, 80.86337684832577111 ) ) ;
#195956 = CARTESIAN_POINT ( 'NONE',  ( -9.474510206698720793, -16.51473224551083518, 104.5844237280190043 ) ) ;
#195957 = CARTESIAN_POINT ( 'NONE',  ( 10.72451020669898902, -18.67979575497178502, 87.91557627198103830 ) ) ;
#195958 = CARTESIAN_POINT ( 'NONE',  ( 12.06949235617757843, -12.14591786802309237, 53.12390960531436690 ) ) ;
#195959 = CARTESIAN_POINT ( 'NONE',  ( -12.06949235617739369, -12.14591786802326823, 34.37609039468568284 ) ) ;
#195960 = CARTESIAN_POINT ( 'NONE',  ( 9.474510206698971260, -16.51473224551069308, 47.91557627198102409 ) ) ;
#195962 = CARTESIAN_POINT ( 'NONE',  ( -16.51473224551082808, 9.474510206698731452, 88.33442372801900433 ) ) ;
#195961 = CARTESIAN_POINT ( 'NONE',  ( 0.05219959533937995610, -21.53943276465977519, 20.00109039468568639 ) ) ;
#195963 = ADVANCED_FACE ( 'NONE', ( #21626 ), #54961, .T. ) ;
#195964 = CARTESIAN_POINT ( 'NONE',  ( -5.153800228976328057, -19.02544592524343514, 97.29057627198099567 ) ) ;
#195965 = CARTESIAN_POINT ( 'NONE',  ( -13.89961937509977652, 13.97604488694528158, 75.62390960531438111 ) ) ;
#195966 = CARTESIAN_POINT ( 'NONE',  ( -5.823673210054116645, -21.52544592524344225, 82.29057627198103830 ) ) ;
#195967 = CARTESIAN_POINT ( 'NONE',  ( 19.03943276465977164, -0.05219959533909143690, 48.74890960531435979 ) ) ;
#195968 = CARTESIAN_POINT ( 'NONE',  ( 25.79464582014989205, 26.76891920992428453, -8.000000000000003553 ) ) ;
#195969 = CARTESIAN_POINT ( 'NONE',  ( -16.52544592524342804, 4.483927247898546575, 56.04057627198102409 ) ) ;
#195970 = CARTESIAN_POINT ( 'NONE',  ( 5.049401038298161559, -19.05341960407611168, 92.70724293864769550 ) ) ;
#195971 = CARTESIAN_POINT ( 'NONE',  ( 1.499999999999985789, 30.40000000000003766, -65.00100000000003320 ) ) ;
#195972 = CARTESIAN_POINT ( 'NONE',  ( -0.05219959533936034679, 19.03943276465977164, 62.50109039468566863 ) ) ;
#195973 = CARTESIAN_POINT ( 'NONE',  ( -21.55341960407610458, -5.719274019375992779, 71.45724293864769550 ) ) ;
#195974 = CARTESIAN_POINT ( 'NONE',  ( -0.05219959533936034679, 19.03943276465977164, 32.50109039468566863 ) ) ;
#195975 = CARTESIAN_POINT ( 'NONE',  ( 19.02544592524343514, -5.153800228976328945, 98.54057627198100988 ) ) ;
#195976 = CARTESIAN_POINT ( 'NONE',  ( -17.50000000000000000, 3.305555262949615436, 114.6251715215659317 ) ) ;
#195977 = CARTESIAN_POINT ( 'NONE',  ( -21.55341960407610458, -5.719274019375992779, 36.45724293864768839 ) ) ;
#195978 = CARTESIAN_POINT ( 'NONE',  ( -19.02544592524342804, 5.153800228976336051, 71.04057627198099567 ) ) ;
#195979 = CARTESIAN_POINT ( 'NONE',  ( -18.62759615963255300, -10.81492255796106328, 59.16775706135234714 ) ) ;
#195980 = CARTESIAN_POINT ( 'NONE',  ( 5.049401038298161559, -19.05341960407611168, 22.70724293864769194 ) ) ;
#195982 = EDGE_LOOP ( 'NONE', ( #13857, #153311, #67166, #88345, #2238 ) ) ;
#195981 = CARTESIAN_POINT ( 'NONE',  ( 18.67979575497178502, 10.72451020669898547, 109.1655762719810383 ) ) ;
#195983 = CARTESIAN_POINT ( 'NONE',  ( -5.823673210054431948, 21.52544592524334988, 47.70942372801902565 ) ) ;
#195984 = ORIENTED_EDGE ( 'NONE', *, *, #66709, .F. ) ;
#195985 = CARTESIAN_POINT ( 'NONE',  ( -5.049401038298153566, 19.05341960407611168, 105.2072429386476671 ) ) ;
#195986 = CARTESIAN_POINT ( 'NONE',  ( -19.03943276465977164, -0.05219959533935918106, 63.75109039468566863 ) ) ;
#195987 = FACE_OUTER_BOUND ( 'NONE', #152737, .T. ) ;
#195988 = CARTESIAN_POINT ( 'NONE',  ( 15.72974639402199770, -15.80617190586745480, 103.1239096053143811 ) ) ;
#195989 = CARTESIAN_POINT ( 'NONE',  ( -19.02544592524342804, 5.153800228976336051, 56.04057627198100988 ) ) ;
#195990 = CARTESIAN_POINT ( 'NONE',  ( -12.06949235617739369, -12.14591786802326823, 39.37609039468567573 ) ) ;
#195991 = CARTESIAN_POINT ( 'NONE',  ( -6.020228577223754586E-15, 39.95556452105416412, -10.24999999453762456 ) ) ;
#195992 = CARTESIAN_POINT ( 'NONE',  ( 15.72974639402176855, 15.80617190586768217, 96.87609039468568994 ) ) ;
#195993 = CARTESIAN_POINT ( 'NONE',  ( 19.02544592524343514, -5.153800228976328945, 38.54057627198103120 ) ) ;
#195994 = CARTESIAN_POINT ( 'NONE',  ( -18.62759615963255300, -10.81492255796106328, 104.1677570613523471 ) ) ;
#195996 = CARTESIAN_POINT ( 'NONE',  ( 0.05219959533937995610, -21.53943276465977519, 65.00109039468568994 ) ) ;
#195995 = CARTESIAN_POINT ( 'NONE',  ( 5.049401038298161559, -19.05341960407611168, 92.70724293864769550 ) ) ;
#195997 = CARTESIAN_POINT ( 'NONE',  ( -26.63278688795740834, 27.10001173645601114, -8.000000000000000000 ) ) ;
#195998 = CARTESIAN_POINT ( 'NONE',  ( -13.89961937509977652, 13.97604488694528158, 110.6239096053143243 ) ) ;
#195999 = CARTESIAN_POINT ( 'NONE',  ( -32.00000000000000711, -5.510910596163089556E-15, 42.29999999999999716 ) ) ;
#196001 = CARTESIAN_POINT ( 'NONE',  ( 15.80617190586769283, -15.72974639402175789, 55.62609039468568284 ) ) ;
#196000 = CARTESIAN_POINT ( 'NONE',  ( -16.55341960407617563, 4.379528057220093196, 53.54275706135234714 ) ) ;
#196002 = CARTESIAN_POINT ( 'NONE',  ( -5.823673210054431948, 21.52544592524334988, 92.70942372801901854 ) ) ;
#196003 = DIRECTION ( 'NONE',  ( -1.000000000000000000, -0.000000000000000000, -1.908195823574487804E-15 ) ) ;
#196004 = CARTESIAN_POINT ( 'NONE',  ( -12.14591786802326823, 12.06949235617739902, 33.12609039468569705 ) ) ;
#196005 = CARTESIAN_POINT ( 'NONE',  ( 13.89961937509977652, -13.97604488694527269, 78.12390960531433848 ) ) ;
#196006 = CARTESIAN_POINT ( 'NONE',  ( -0.05219959533909027116, -19.03943276465977164, 112.4989096053143669 ) ) ;
#196007 = CARTESIAN_POINT ( 'NONE',  ( 17.49999999999999289, 5.624438216177599870, 41.68329655085356933 ) ) ;
#196008 = CARTESIAN_POINT ( 'NONE',  ( -16.51473224551069308, -9.474510206698971260, 26.66557627198103120 ) ) ;
#196009 = CARTESIAN_POINT ( 'NONE',  ( 21.55341960407610458, 5.719274019375980345, 43.95724293864769550 ) ) ;
#196010 = CARTESIAN_POINT ( 'NONE',  ( -12.14591786802326823, 12.06949235617739902, 98.12609039468570415 ) ) ;
#196012 = CARTESIAN_POINT ( 'NONE',  ( 13.89961937509977652, -13.97604488694527269, 63.12390960531435979 ) ) ;
#196011 = CARTESIAN_POINT ( 'NONE',  ( 0.05219959533910956823, 16.53943276465976808, 84.99890960531436690 ) ) ;
#196013 = CARTESIAN_POINT ( 'NONE',  ( -5.719274019375665041, -21.55341960407619695, 84.79275706135234714 ) ) ;
#196014 = CARTESIAN_POINT ( 'NONE',  ( 16.53943276465976808, 0.05219959533934440121, 31.25109039468568639 ) ) ;
#196015 = CARTESIAN_POINT ( 'NONE',  ( -0.05219959533910754901, -16.53943276465976808, 92.49890960531436690 ) ) ;
#196016 = CARTESIAN_POINT ( 'NONE',  ( -5.823673210054431948, 21.52544592524334988, 37.70942372801900433 ) ) ;
#196017 = CARTESIAN_POINT ( 'NONE',  ( 18.67979575497178502, 10.72451020669898547, 74.16557627198102409 ) ) ;
#196018 = CARTESIAN_POINT ( 'NONE',  ( -16.46253265017146816, -9.564922557961047289, 39.16775706135234003 ) ) ;
#196019 = CARTESIAN_POINT ( 'NONE',  ( -34.78522506798724123, 0.4969912795167322761, 52.50000000000002132 ) ) ;
#196020 = CARTESIAN_POINT ( 'NONE',  ( -19.03943276465977164, 0.05219959533909376836, 81.24890960531436690 ) ) ;
#196021 = CARTESIAN_POINT ( 'NONE',  ( 16.55341960407611168, 4.379528057220329451, 68.95724293864769550 ) ) ;
#196022 = CIRCLE ( 'NONE', #60318, 24.30000000000003268 ) ;
#196023 = CARTESIAN_POINT ( 'NONE',  ( 12.06949235617757843, -12.14591786802309237, 33.12390960531435979 ) ) ;
#196024 = CARTESIAN_POINT ( 'NONE',  ( 12.14591786802327356, -12.06949235617739191, 105.6260903946856899 ) ) ;
#196025 = CARTESIAN_POINT ( 'NONE',  ( 19.05341960407617918, -5.049401038297876454, 66.04275706135233293 ) ) ;
#196026 = DIRECTION ( 'NONE',  ( -1.000000000000000000, -0.000000000000000000, -0.000000000000000000 ) ) ;
#196027 = CARTESIAN_POINT ( 'NONE',  ( 5.823673210054125526, 21.52544592524343514, 29.79057627198102409 ) ) ;
#196028 = CARTESIAN_POINT ( 'NONE',  ( 12.14591786802309770, 12.06949235617756955, 84.37390960531438111 ) ) ;
#196030 = CARTESIAN_POINT ( 'NONE',  ( -21.53943276465977519, 0.05219959533907696930, 46.24890960531435979 ) ) ;
#196029 = CARTESIAN_POINT ( 'NONE',  ( -19.03943276465977164, 0.05219959533909376836, 41.24890960531435269 ) ) ;
#196031 = CARTESIAN_POINT ( 'NONE',  ( -15.80617190586745835, -15.72974639402198527, 71.87390960531438111 ) ) ;
#196032 = CARTESIAN_POINT ( 'NONE',  ( -14.34966873604960291, -8.224510206698953496, 106.6655762719810383 ) ) ;
#196034 = CARTESIAN_POINT ( 'NONE',  ( -19.05341960407611168, -5.049401038298163336, 46.45724293864768129 ) ) ;
#196033 = CARTESIAN_POINT ( 'NONE',  ( -12.06949235617739369, -12.14591786802326823, 59.37609039468568284 ) ) ;
#196035 = CARTESIAN_POINT ( 'NONE',  ( 21.55341960407619695, -5.719274019375665929, 61.04275706135234714 ) ) ;
#196036 = CIRCLE ( 'NONE', #141149, 28.82186960331498682 ) ;
#196037 = CARTESIAN_POINT ( 'NONE',  ( -14.29746914071049879, 8.314922557960819915, 100.8322429386477097 ) ) ;
#196038 = EDGE_CURVE ( 'NONE', #106494, #47253, #33035, .T. ) ;
#196039 = CARTESIAN_POINT ( 'NONE',  ( 16.51473224551083163, -9.474510206698727899, 90.83442372801900433 ) ) ;
#196040 = CARTESIAN_POINT ( 'NONE',  ( 3.556970738554034288E-15, -38.81732327939057114, -6.624999997268814056 ) ) ;
#196042 = CARTESIAN_POINT ( 'NONE',  ( 18.62759615963271287, -10.81492255796078972, 43.33224293864769550 ) ) ;
#196041 = CARTESIAN_POINT ( 'NONE',  ( -0.2211803504528828124, -21.31248648291599324, -58.84879416108401529 ) ) ;
#196043 = CARTESIAN_POINT ( 'NONE',  ( 16.46253265017160672, -9.564922557960803928, 23.33224293864769194 ) ) ;
#196044 = CARTESIAN_POINT ( 'NONE',  ( -10.72451020669870658, -18.67979575497194134, 69.58442372801900433 ) ) ;
#196046 = CARTESIAN_POINT ( 'NONE',  ( 14.34966873604960469, 8.224510206698951720, 49.16557627198102409 ) ) ;
#196045 = CARTESIAN_POINT ( 'NONE',  ( 12.14591786802327356, -12.06949235617739191, 50.62609039468568994 ) ) ;
#196047 = CARTESIAN_POINT ( 'NONE',  ( -5.823673210054116645, -21.52544592524344225, 67.29057627198103830 ) ) ;
#196048 = CARTESIAN_POINT ( 'NONE',  ( 18.67979575497178502, 10.72451020669898547, 69.16557627198102409 ) ) ;
#196049 = CARTESIAN_POINT ( 'NONE',  ( -21.38418241377623374, -7.427326039334300134, 174.4773576836617224 ) ) ;
#196051 = CARTESIAN_POINT ( 'NONE',  ( -9.564922557960796823, -16.46253265017161027, 112.0822429386476955 ) ) ;
#196050 = CARTESIAN_POINT ( 'NONE',  ( -19.02544592524334988, -5.153800228976617603, 83.95942372801901854 ) ) ;
#196052 = CARTESIAN_POINT ( 'NONE',  ( 16.51473224551069308, 9.474510206698969483, 49.16557627198102409 ) ) ;
#196054 = EDGE_CURVE ( 'NONE', #120648, #60482, #189057, .T. ) ;
#196053 = CARTESIAN_POINT ( 'NONE',  ( 12.06949235617757843, -12.14591786802309237, 113.1239096053143953 ) ) ;
#196055 =( NAMED_UNIT ( * ) SI_UNIT ( $, .STERADIAN. ) SOLID_ANGLE_UNIT ( ) );
#196056 = CARTESIAN_POINT ( 'NONE',  ( -18.22780087662123805, 5.499999999999981348, 76.01763182126894947 ) ) ;
#196057 = EDGE_LOOP ( 'NONE', ( #81653, #41041, #64339, #194618 ) ) ;
#196058 = CARTESIAN_POINT ( 'NONE',  ( 14.34966873604972726, -8.224510206698740333, 85.83442372801901854 ) ) ;
#196059 = CARTESIAN_POINT ( 'NONE',  ( 21.52544592524344225, -5.823673210054117533, 103.5405762719810383 ) ) ;
#196060 = CARTESIAN_POINT ( 'NONE',  ( -19.02544592524342804, 5.153800228976336051, 66.04057627198103830 ) ) ;
#196061 = CARTESIAN_POINT ( 'NONE',  ( -5.719274019375665041, -21.55341960407619695, 39.79275706135235424 ) ) ;
#196062 = CARTESIAN_POINT ( 'NONE',  ( 9.474510206698971260, -16.51473224551069308, 92.91557627198103830 ) ) ;
#196063 = CARTESIAN_POINT ( 'NONE',  ( -23.74378949184693965, -32.05510596162310577, -22.01707947879407357 ) ) ;
#196064 = ORIENTED_EDGE ( 'NONE', *, *, #11729, .F. ) ;
#196065 = CARTESIAN_POINT ( 'NONE',  ( 5.823673210054444382, -21.52544592524334988, 35.20942372801901854 ) ) ;
#196067 = CARTESIAN_POINT ( 'NONE',  ( -5.049401038297874678, -19.05341960407617918, 84.79275706135233293 ) ) ;
#196066 = CARTESIAN_POINT ( 'NONE',  ( 13.97604488694527802, 13.89961937509977652, 29.37390960531435979 ) ) ;
#196068 = CARTESIAN_POINT ( 'NONE',  ( 9.564922557961047289, -16.46253265017146816, 35.41775706135233293 ) ) ;
#196069 = CARTESIAN_POINT ( 'NONE',  ( -15.72974639402197994, 15.80617190586746368, 115.6239096053143669 ) ) ;
#196070 = CARTESIAN_POINT ( 'NONE',  ( 5.153800228976615827, -19.02544592524334988, 35.20942372801899722 ) ) ;
#196071 = CARTESIAN_POINT ( 'NONE',  ( -19.05341960407617563, 5.049401038297882671, 48.54275706135233293 ) ) ;
#196072 = CARTESIAN_POINT ( 'NONE',  ( 14.29746914071037800, 8.314922557961029526, 96.66775706135234714 ) ) ;
#196074 = ORIENTED_EDGE ( 'NONE', *, *, #151672, .T. ) ;
#196073 = CARTESIAN_POINT ( 'NONE',  ( 19.02544592524343514, -5.153800228976328945, 113.5405762719810241 ) ) ;
#196075 = CARTESIAN_POINT ( 'NONE',  ( 9.474510206698971260, -16.51473224551069308, 67.91557627198102409 ) ) ;
#196076 = CIRCLE ( 'NONE', #118553, 0.2000000000000057288 ) ;
#196077 = CARTESIAN_POINT ( 'NONE',  ( 18.62759615963255655, 10.81492255796105972, 76.66775706135234714 ) ) ;
#196078 = CARTESIAN_POINT ( 'NONE',  ( 15.72974639402176855, 15.80617190586768217, 91.87609039468568994 ) ) ;
#196079 = CARTESIAN_POINT ( 'NONE',  ( -0.1983487321476344600, -9.090093023806476324, -63.95305636720455311 ) ) ;
#196080 = CARTESIAN_POINT ( 'NONE',  ( 13.89961937509977652, -13.97604488694527269, 83.12390960531436690 ) ) ;
#196081 = CARTESIAN_POINT ( 'NONE',  ( -5.823673210054431948, 21.52544592524334988, 57.70942372801901143 ) ) ;
#196082 = CARTESIAN_POINT ( 'NONE',  ( -5.049401038297874678, -19.05341960407617918, 94.79275706135230450 ) ) ;
#196083 = B_SPLINE_CURVE_WITH_KNOTS ( 'NONE', 3,
 ( #56714, #133539, #139492, #184028, #140495, #92988, #200185, #187034, #151706, #199196, #154674, #16169, #124327, #137515, #14169, #17163, #61654, #183041, #1983, #60664, #186025, #107165, #76832, #121348, #185015, #105197, #166884, #28385, #77823, #32334, #155667, #46501 ),
 .UNSPECIFIED., .F., .F.,
 ( 4, 2, 2, 2, 2, 2, 2, 2, 2, 2, 2, 2, 2, 2, 2, 4 ),
 ( 2.625112965618923374E-17, 0.0003712461730036955600, 0.0007424923460073648823, 0.001113738519011033988, 0.001484984692014703527, 0.002227477038022048893, 0.002598723211025728841, 0.002969969384029408788, 0.003341215557033088302, 0.003712461730036768683, 0.004083707903040447763, 0.004454954076044127277, 0.004826200249047807658, 0.005197446422051487172, 0.005568692595055167553, 0.005939938768058847067 ),
 .UNSPECIFIED. ) ;
#196084 = CARTESIAN_POINT ( 'NONE',  ( -9.474510206698964154, 16.51473224551069663, 60.41557627198102409 ) ) ;
#196085 = CARTESIAN_POINT ( 'NONE',  ( -9.474510206698964154, 16.51473224551069663, 115.4155762719810241 ) ) ;
#196086 = CARTESIAN_POINT ( 'NONE',  ( 19.05341960407611168, 5.049401038298154454, 73.95724293864768129 ) ) ;
#196087 = CARTESIAN_POINT ( 'NONE',  ( -13.97604488694527625, -13.89961937509977830, 76.87390960531435269 ) ) ;
#196088 = CARTESIAN_POINT ( 'NONE',  ( -19.02544592524342804, 5.153800228976336051, 66.04057627198103830 ) ) ;
#196089 = CARTESIAN_POINT ( 'NONE',  ( 19.03943276465977164, -0.05219959533909143690, 58.74890960531435979 ) ) ;
#196090 = CARTESIAN_POINT ( 'NONE',  ( 15.80617190586746368, 15.72974639402197994, 114.3739096053143527 ) ) ;
#196091 = CARTESIAN_POINT ( 'NONE',  ( -16.55341960407617563, 4.379528057220093196, 83.54275706135234714 ) ) ;
#196092 = LINE ( 'NONE', #57562, #85641 ) ;
#196093 = DIRECTION ( 'NONE',  ( 0.000000000000000000, 0.000000000000000000, 1.000000000000000000 ) ) ;
#196094 = CARTESIAN_POINT ( 'NONE',  ( 13.89961937509957401, 13.97604488694547697, 56.87609039468564731 ) ) ;
#196095 = CARTESIAN_POINT ( 'NONE',  ( -19.02544592524342804, 5.153800228976336051, 76.04057627198102409 ) ) ;
#196096 = CARTESIAN_POINT ( 'NONE',  ( -12.06949235617756955, 12.14591786802309770, 75.62390960531439532 ) ) ;
#196097 = CARTESIAN_POINT ( 'NONE',  ( 8.314922557960818139, 14.29746914071049879, 109.5822429386476955 ) ) ;
#196098 = CARTESIAN_POINT ( 'NONE',  ( -18.62759615963270932, 10.81492255796079327, 30.83224293864770260 ) ) ;
#196099 = CARTESIAN_POINT ( 'NONE',  ( -16.51473224551069308, -9.474510206698971260, 101.6655762719810241 ) ) ;
#196100 = CARTESIAN_POINT ( 'NONE',  ( 16.53943276465976808, -0.05219959533910856209, 93.74890960531436690 ) ) ;
#196101 = CARTESIAN_POINT ( 'NONE',  ( -9.564922557960796823, -16.46253265017161027, 82.08224293864768129 ) ) ;
#196102 = CARTESIAN_POINT ( 'NONE',  ( 19.05341960407617918, -5.049401038297876454, 31.04275706135232227 ) ) ;
#196103 = CARTESIAN_POINT ( 'NONE',  ( 14.34966873604972726, -8.224510206698740333, 110.8344237280190043 ) ) ;
#196104 = CARTESIAN_POINT ( 'NONE',  ( 19.03943276465977164, -0.05219959533909143690, 88.74890960531436690 ) ) ;
#196105 = CARTESIAN_POINT ( 'NONE',  ( -10.81492255796105439, 18.62759615963255655, 52.91775706135235424 ) ) ;
#196106 = CARTESIAN_POINT ( 'NONE',  ( -18.67979575497178146, -10.72451020669898902, 46.66557627198102409 ) ) ;
#196107 = CARTESIAN_POINT ( 'NONE',  ( -5.823673210054431948, 21.52544592524334988, 22.70942372801901499 ) ) ;
#196108 = CARTESIAN_POINT ( 'NONE',  ( 15.80617190586746368, 15.72974639402197994, 74.37390960531436690 ) ) ;
#196109 = CARTESIAN_POINT ( 'NONE',  ( 12.06949235617757843, -12.14591786802309237, 98.12390960531436690 ) ) ;
#196110 = CARTESIAN_POINT ( 'NONE',  ( 13.89961937509957401, 13.97604488694547697, 56.87609039468564731 ) ) ;
#196111 = CARTESIAN_POINT ( 'NONE',  ( 13.97604488694527802, 13.89961937509977652, 29.37390960531435979 ) ) ;
#196112 = CARTESIAN_POINT ( 'NONE',  ( 19.05341960407611168, 5.049401038298154454, 78.95724293864769550 ) ) ;
#196113 = CARTESIAN_POINT ( 'NONE',  ( 13.89961937509977652, -13.97604488694527269, 98.12390960531433848 ) ) ;
#196114 = CARTESIAN_POINT ( 'NONE',  ( -8.224510206698948167, 14.34966873604960824, 115.4155762719810241 ) ) ;
#196115 = CARTESIAN_POINT ( 'NONE',  ( 0.05219959533910956823, 16.53943276465976808, 29.99890960531435979 ) ) ;
#196116 = CARTESIAN_POINT ( 'NONE',  ( -4.483927247898782831, 16.52544592524335698, 37.70942372801900433 ) ) ;
#196117 = CARTESIAN_POINT ( 'NONE',  ( 15.80617190586769283, -15.72974639402175789, 110.6260903946857042 ) ) ;
#196118 = CARTESIAN_POINT ( 'NONE',  ( -9.564922557960796823, -16.46253265017161027, 102.0822429386477097 ) ) ;
#196119 = CARTESIAN_POINT ( 'NONE',  ( 10.72451020669871369, 18.67979575497193778, 32.08442372801901854 ) ) ;
#196120 = CARTESIAN_POINT ( 'NONE',  ( 19.05341960407611168, 5.049401038298154454, 43.95724293864769550 ) ) ;
#196121 = CARTESIAN_POINT ( 'NONE',  ( -8.224510206698735004, -14.34966873604973081, 49.58442372801901143 ) ) ;
#196122 = CARTESIAN_POINT ( 'NONE',  ( 12.06949235617739724, 12.14591786802326823, 111.8760903946856615 ) ) ;
#196123 = CARTESIAN_POINT ( 'NONE',  ( -12.06949235617739369, -12.14591786802326823, 89.37609039468568994 ) ) ;
#196124 = CARTESIAN_POINT ( 'NONE',  ( -9.474510206698720793, -16.51473224551083518, 104.5844237280190043 ) ) ;
#196125 = CARTESIAN_POINT ( 'NONE',  ( -0.05219959533909027116, -19.03943276465977164, 37.49890960531436690 ) ) ;
#196126 = CARTESIAN_POINT ( 'NONE',  ( -12.06949235617756955, 12.14591786802309770, 100.6239096053143811 ) ) ;
#196127 = CARTESIAN_POINT ( 'NONE',  ( 18.67979575497178502, 10.72451020669898547, 104.1655762719810241 ) ) ;
#196128 = CARTESIAN_POINT ( 'NONE',  ( 5.153800228976335163, 19.02544592524342804, 29.79057627198102409 ) ) ;
#196129 = CARTESIAN_POINT ( 'NONE',  ( -19.02544592524342804, 5.153800228976336051, 101.0405762719810241 ) ) ;
#196130 = CARTESIAN_POINT ( 'NONE',  ( 5.719274019375673035, 21.55341960407619339, 37.29275706135235424 ) ) ;
#196131 = CARTESIAN_POINT ( 'NONE',  ( -19.24578484527059175, -180.9428398739491684, 0.000000000000000000 ) ) ;
#196132 = CARTESIAN_POINT ( 'NONE',  ( 16.46253265017160672, -9.564922557960803928, 103.3322429386476955 ) ) ;
#196133 = CARTESIAN_POINT ( 'NONE',  ( 17.44270441346516876, -5.991230190323036275, 111.1366492073577490 ) ) ;
#196134 = CARTESIAN_POINT ( 'NONE',  ( 16.51473224551069308, 9.474510206698969483, 79.16557627198103830 ) ) ;
#196136 = CARTESIAN_POINT ( 'NONE',  ( 4.483927247898545687, 16.52544592524342804, 94.79057627198105251 ) ) ;
#196135 = CARTESIAN_POINT ( 'NONE',  ( 21.52544592524334988, 5.823673210054432836, 26.45942372801901854 ) ) ;
#196137 = CARTESIAN_POINT ( 'NONE',  ( -0.05219959533909027116, -19.03943276465977164, 97.49890960531436690 ) ) ;
#196138 = CARTESIAN_POINT ( 'NONE',  ( -13.89961937509957401, -13.97604488694547875, 24.37609039468565442 ) ) ;
#196139 = CARTESIAN_POINT ( 'NONE',  ( 12.14591786802327356, -12.06949235617739191, 70.62609039468567573 ) ) ;
#196140 = CARTESIAN_POINT ( 'NONE',  ( -21.52544592524334988, -5.823673210054445271, 83.95942372801900433 ) ) ;
#196141 = CARTESIAN_POINT ( 'NONE',  ( 16.52544592524335698, 4.483927247898782831, 46.45942372801901854 ) ) ;
#196142 = CARTESIAN_POINT ( 'NONE',  ( -19.03943276465977164, 0.05219959533909376836, 81.24890960531436690 ) ) ;
#196143 = CARTESIAN_POINT ( 'NONE',  ( -19.02544592524334988, -5.153800228976617603, 88.95942372801897591 ) ) ;
#196144 = CARTESIAN_POINT ( 'NONE',  ( -14.34966873604972548, 8.224510206698743886, 73.33442372801901854 ) ) ;
#196145 = CARTESIAN_POINT ( 'NONE',  ( 13.97604488694548053, -13.89961937509957401, 20.62609039468567573 ) ) ;
#196146 = CARTESIAN_POINT ( 'NONE',  ( -5.153800228976607833, 19.02544592524334988, 77.70942372801900433 ) ) ;
#196147 = CARTESIAN_POINT ( 'NONE',  ( 16.46253265017160672, -9.564922557960803928, 63.33224293864769550 ) ) ;
#196148 = CARTESIAN_POINT ( 'NONE',  ( 0.05219959533907565091, 21.53943276465977519, 84.99890960531436690 ) ) ;
#196150 = CARTESIAN_POINT ( 'NONE',  ( 9.474510206698729675, 16.51473224551082808, 97.08442372801900433 ) ) ;
#196149 = CARTESIAN_POINT ( 'NONE',  ( 4.483927247898545687, 16.52544592524342804, 84.79057627198102409 ) ) ;
#196151 = CARTESIAN_POINT ( 'NONE',  ( -16.52544592524335698, -4.483927247898792601, 58.95942372801902565 ) ) ;
#196152 = CARTESIAN_POINT ( 'NONE',  ( 0.000000000000000000, -0.7216878364870318308, -1.250000000000000000 ) ) ;
#196153 = CARTESIAN_POINT ( 'NONE',  ( -19.05341960407617563, 5.049401038297882671, 63.54275706135234003 ) ) ;
#196154 = CARTESIAN_POINT ( 'NONE',  ( 12.06949235617739724, 12.14591786802326823, 106.8760903946856899 ) ) ;
#196155 = CARTESIAN_POINT ( 'NONE',  ( 8.314922557960818139, 14.29746914071049879, 79.58224293864769550 ) ) ;
#196157 = CARTESIAN_POINT ( 'NONE',  ( -16.38665767534995155, 7.295008042176406526, 40.26400864214470943 ) ) ;
#196156 = CARTESIAN_POINT ( 'NONE',  ( 19.03943276465977164, 0.05219959533936151252, 21.25109039468565797 ) ) ;
#196158 = CARTESIAN_POINT ( 'NONE',  ( -21.52544592524343514, 5.823673210054127303, 116.0405762719810383 ) ) ;
#196159 = CARTESIAN_POINT ( 'NONE',  ( -9.564922557960796823, -16.46253265017161027, 107.0822429386476955 ) ) ;
#196160 = CARTESIAN_POINT ( 'NONE',  ( -5.153800228976328057, -19.02544592524343514, 72.29057627198102409 ) ) ;
#196161 = CARTESIAN_POINT ( 'NONE',  ( 5.719274019375673035, 21.55341960407619339, 87.29275706135236135 ) ) ;
#196162 = CARTESIAN_POINT ( 'NONE',  ( -19.03943276465977164, 0.05219959533909376836, 66.24890960531436690 ) ) ;
#196163 = CARTESIAN_POINT ( 'NONE',  ( 15.72974639402199770, -15.80617190586745480, 28.12390960531435979 ) ) ;
#196164 = CARTESIAN_POINT ( 'NONE',  ( 12.14591786802309770, 12.06949235617756955, 84.37390960531438111 ) ) ;
#196165 = CARTESIAN_POINT ( 'NONE',  ( 5.049401038298161559, -19.05341960407611168, 37.70724293864768839 ) ) ;
#196166 = CARTESIAN_POINT ( 'NONE',  ( 16.52544592524342804, -4.483927247898539470, 93.54057627198103830 ) ) ;
#196167 = VECTOR ( 'NONE', #4756, 1000.000000000000000 ) ;
#196168 = CARTESIAN_POINT ( 'NONE',  ( -5.823673210054116645, -21.52544592524344225, 112.2905762719810241 ) ) ;
#196169 = EDGE_CURVE ( 'NONE', #152161, #37524, #192482, .T. ) ;
#196170 = CARTESIAN_POINT ( 'NONE',  ( -21.53943276465977519, -0.05219959533937600094, 53.75109039468568994 ) ) ;
#196171 = CARTESIAN_POINT ( 'NONE',  ( -19.02544592524342804, 5.153800228976336051, 26.04057627198103120 ) ) ;
#196172 = CARTESIAN_POINT ( 'NONE',  ( 14.34966873604972726, -8.224510206698740333, 60.83442372801901854 ) ) ;
#196173 = CARTESIAN_POINT ( 'NONE',  ( 5.823673210054125526, 21.52544592524343514, 99.79057627198103830 ) ) ;
#196174 = CARTESIAN_POINT ( 'NONE',  ( 15.72974639402199770, -15.80617190586745480, 108.1239096053143811 ) ) ;
#196176 = CARTESIAN_POINT ( 'NONE',  ( 19.05341960407611168, 5.049401038298154454, 58.95724293864768129 ) ) ;
#196175 = CARTESIAN_POINT ( 'NONE',  ( 13.89961937509957401, 13.97604488694547697, 41.87609039468566152 ) ) ;
#196177 = CARTESIAN_POINT ( 'NONE',  ( 17.50000000000000000, -5.500000000000000888, 120.0000000000000142 ) ) ;
#196178 = CARTESIAN_POINT ( 'NONE',  ( 21.52544592524334988, 5.823673210054432836, 51.45942372801901854 ) ) ;
#196179 = CARTESIAN_POINT ( 'NONE',  ( 10.72451020669898902, -18.67979575497178502, 62.91557627198102409 ) ) ;
#196180 = CARTESIAN_POINT ( 'NONE',  ( 0.05219959533910956823, 16.53943276465976808, 39.99890960531436690 ) ) ;
#196182 = CARTESIAN_POINT ( 'NONE',  ( -15.72974639402176322, -15.80617190586768395, 109.3760903946857042 ) ) ;
#196181 = CARTESIAN_POINT ( 'NONE',  ( 18.67979575497194134, -10.72451020669871369, 70.83442372801901854 ) ) ;
#196183 = CARTESIAN_POINT ( 'NONE',  ( 8.224510206698953496, -14.34966873604960469, 62.91557627198102409 ) ) ;
#196184 = CARTESIAN_POINT ( 'NONE',  ( 16.55341960407611168, 4.379528057220329451, 103.9572429386476813 ) ) ;
#196185 = CARTESIAN_POINT ( 'NONE',  ( -16.51473224551082808, 9.474510206698731452, 38.33442372801899722 ) ) ;
#196186 = CARTESIAN_POINT ( 'NONE',  ( 12.06949235617739724, 12.14591786802326823, 101.8760903946857042 ) ) ;
#196187 = CARTESIAN_POINT ( 'NONE',  ( -5.719274019375665041, -21.55341960407619695, 64.79275706135234714 ) ) ;
#196188 = CARTESIAN_POINT ( 'NONE',  ( -9.474510206698964154, 16.51473224551069663, 60.41557627198102409 ) ) ;
#196189 = CARTESIAN_POINT ( 'NONE',  ( 0.05219959533936267826, -19.03943276465977164, 35.00109039468566863 ) ) ;
#196190 = CARTESIAN_POINT ( 'NONE',  ( -0.05219959533907301413, -21.53943276465977519, 42.49890960531435979 ) ) ;
#196191 = CARTESIAN_POINT ( 'NONE',  ( -21.52544592524334988, -5.823673210054445271, 33.95942372801901143 ) ) ;
#196192 = CARTESIAN_POINT ( 'NONE',  ( -0.05219959533907301413, -21.53943276465977519, 92.49890960531436690 ) ) ;
#196193 = CARTESIAN_POINT ( 'NONE',  ( 5.153800228976615827, -19.02544592524334988, 85.20942372801900433 ) ) ;
#196194 = CARTESIAN_POINT ( 'NONE',  ( 12.06949235617739724, 12.14591786802326823, 56.87609039468568994 ) ) ;
#196196 = CARTESIAN_POINT ( 'NONE',  ( 18.67979575497178502, 10.72451020669898547, 94.16557627198103830 ) ) ;
#196195 = CARTESIAN_POINT ( 'NONE',  ( 17.50000000000002487, -3.438020150447669288, 37.00844184464188658 ) ) ;
#196198 = CARTESIAN_POINT ( 'NONE',  ( 8.224510206698953496, -14.34966873604960469, 72.91557627198103830 ) ) ;
#196197 = CARTESIAN_POINT ( 'NONE',  ( -16.53943276465976808, -0.05219959533934237506, 78.75109039468568994 ) ) ;
#196199 = DIRECTION ( 'NONE',  ( 0.8164965809277243691, 0.000000000000000000, -0.5773502691896280625 ) ) ;
#196200 = CARTESIAN_POINT ( 'NONE',  ( 8.224510206698742110, 14.34966873604972548, 27.08442372801901854 ) ) ;
#196201 = CARTESIAN_POINT ( 'NONE',  ( 10.72451020669898902, -18.67979575497178502, 37.91557627198102409 ) ) ;
#196202 = CARTESIAN_POINT ( 'NONE',  ( 4.379528057220092307, 16.55341960407617563, 77.29275706135234714 ) ) ;
#196203 = CYLINDRICAL_SURFACE ( 'NONE', #86579, 1.500000000000001332 ) ;
#196204 = CARTESIAN_POINT ( 'NONE',  ( 16.53943276465976808, 0.05219959533934440121, 51.25109039468568994 ) ) ;
#196205 = CARTESIAN_POINT ( 'NONE',  ( -10.72451020669870658, -18.67979575497194134, 29.58442372801901854 ) ) ;
#196206 = CARTESIAN_POINT ( 'NONE',  ( -21.53943276465977519, 0.05219959533907696930, 51.24890960531436690 ) ) ;
#196207 = CARTESIAN_POINT ( 'NONE',  ( -12.06949235617739369, -12.14591786802326823, 74.37609039468568994 ) ) ;
#196208 = CARTESIAN_POINT ( 'NONE',  ( -5.153800228976328057, -19.02544592524343514, 87.29057627198103830 ) ) ;
#196210 = CARTESIAN_POINT ( 'NONE',  ( -16.51473224551069308, -9.474510206698971260, 26.66557627198103120 ) ) ;
#196209 = CARTESIAN_POINT ( 'NONE',  ( 5.719274019375673035, 21.55341960407619339, 62.29275706135236845 ) ) ;
#196211 = EDGE_CURVE ( 'NONE', #18224, #36918, #190225, .T. ) ;
#196212 = CARTESIAN_POINT ( 'NONE',  ( -15.80617190586745835, -15.72974639402198527, 41.87390960531435979 ) ) ;
#196213 = CARTESIAN_POINT ( 'NONE',  ( -19.02544592524342804, 5.153800228976336051, 116.0405762719810383 ) ) ;
#196214 = ORIENTED_EDGE ( 'NONE', *, *, #137780, .T. ) ;
#196215 = CARTESIAN_POINT ( 'NONE',  ( -13.97604488694547697, 13.89961937509957934, 43.12609039468566152 ) ) ;
#196216 = CARTESIAN_POINT ( 'NONE',  ( 14.29746914071037800, 8.314922557961029526, 56.66775706135235424 ) ) ;
#196217 = CARTESIAN_POINT ( 'NONE',  ( 21.55341960407610458, 5.719274019375980345, 23.95724293864769550 ) ) ;
#196218 = VERTEX_POINT ( 'NONE', #8460 ) ;
#196219 = CARTESIAN_POINT ( 'NONE',  ( -19.03943276465977164, 0.05219959533909376836, 81.24890960531436690 ) ) ;
#196220 = CARTESIAN_POINT ( 'NONE',  ( 14.29746914071037800, 8.314922557961029526, 101.6677570613523613 ) ) ;
#196221 = CARTESIAN_POINT ( 'NONE',  ( 5.035744501201078851E-13, -76.33743099897125717, -22.99988689144064580 ) ) ;
#196222 = CARTESIAN_POINT ( 'NONE',  ( -12.06949235617756955, 12.14591786802309770, 95.62390960531436690 ) ) ;
#196223 = CARTESIAN_POINT ( 'NONE',  ( -21.53943276465977519, 0.05219959533907696930, 31.24890960531435979 ) ) ;
#196224 = CARTESIAN_POINT ( 'NONE',  ( 9.474510206698971260, -16.51473224551069308, 27.91557627198103120 ) ) ;
#196225 = CARTESIAN_POINT ( 'NONE',  ( -16.55341960407617563, 4.379528057220093196, 78.54275706135236135 ) ) ;
#196226 = CARTESIAN_POINT ( 'NONE',  ( 5.823673210054125526, 21.52544592524343514, 114.7905762719810383 ) ) ;
#196227 = CARTESIAN_POINT ( 'NONE',  ( -19.05341960407617563, 5.049401038297882671, 73.54275706135233293 ) ) ;
#196228 = CARTESIAN_POINT ( 'NONE',  ( 16.51473224551069308, 9.474510206698969483, 34.16557627198102409 ) ) ;
#196229 = CIRCLE ( 'NONE', #83140, 69.99999999999998579 ) ;
#196230 = CARTESIAN_POINT ( 'NONE',  ( -5.153800228976328057, -19.02544592524343514, 112.2905762719810099 ) ) ;
#196231 = CARTESIAN_POINT ( 'NONE',  ( 15.72974639402176855, 15.80617190586768217, 106.8760903946856899 ) ) ;
#196232 = CARTESIAN_POINT ( 'NONE',  ( -19.02544592524342804, 5.153800228976336051, 61.04057627198103120 ) ) ;
#196233 = CARTESIAN_POINT ( 'NONE',  ( 0.05219959533934541429, -16.53943276465976808, 55.00109039468568284 ) ) ;
#196234 = CARTESIAN_POINT ( 'NONE',  ( -18.62759615963255300, -10.81492255796106328, 99.16775706135234714 ) ) ;
#196235 = CARTESIAN_POINT ( 'NONE',  ( -0.05219959533936034679, 19.03943276465977164, 57.50109039468566863 ) ) ;
#196236 = CARTESIAN_POINT ( 'NONE',  ( -19.05341960407617563, 5.049401038297882671, 48.54275706135233293 ) ) ;
#196237 = VERTEX_POINT ( 'NONE', #177328 ) ;
#196238 = CARTESIAN_POINT ( 'NONE',  ( -5.719274019375665041, -21.55341960407619695, 49.79275706135234714 ) ) ;
#196239 = CARTESIAN_POINT ( 'NONE',  ( -17.49999999999999645, 5.499999999999997335, 118.0000000000000142 ) ) ;
#196240 = CARTESIAN_POINT ( 'NONE',  ( 0.05219959533936267826, -19.03943276465977164, 40.00109039468566152 ) ) ;
#196241 = CARTESIAN_POINT ( 'NONE',  ( 19.05341960407611168, 5.049401038298154454, 103.9572429386476671 ) ) ;
#196242 = CARTESIAN_POINT ( 'NONE',  ( 13.97604488694527802, 13.89961937509977652, 84.37390960531433848 ) ) ;
#196243 = CARTESIAN_POINT ( 'NONE',  ( 14.34966873604960469, 8.224510206698951720, 34.16557627198102409 ) ) ;
#196244 = CARTESIAN_POINT ( 'NONE',  ( 15.72974639402199770, -15.80617190586745480, 28.12390960531435979 ) ) ;
#196245 = CARTESIAN_POINT ( 'NONE',  ( 11.40812507854755253, -35.11059874428192273, -4.524999997268813523 ) ) ;
#196246 = CARTESIAN_POINT ( 'NONE',  ( 21.00373069265142689, 22.92260996908688142, -50.16862556671883056 ) ) ;
#196247 = CARTESIAN_POINT ( 'NONE',  ( -21.52544592524334988, -5.823673210054445271, 108.9594237280190185 ) ) ;
#196248 = CARTESIAN_POINT ( 'NONE',  ( 29.17999648465608686, -8.032454009542489004, 149.7954620931811291 ) ) ;
#196249 = CARTESIAN_POINT ( 'NONE',  ( -19.02544592524342804, 5.153800228976336051, 31.04057627198102409 ) ) ;
#196250 = CARTESIAN_POINT ( 'NONE',  ( 5.153800228976335163, 19.02544592524342804, 84.79057627198100988 ) ) ;
#196251 = CARTESIAN_POINT ( 'NONE',  ( -33.90027759800518936, -5.214635694306275049, 93.21535130585120044 ) ) ;
#196252 = CARTESIAN_POINT ( 'NONE',  ( -36.29667422526105725, -10.80772347165230052, -7.999999999999994671 ) ) ;
#196253 = CARTESIAN_POINT ( 'NONE',  ( 4.483927247898790824, -16.52544592524335698, 65.20942372801901854 ) ) ;
#196254 = CARTESIAN_POINT ( 'NONE',  ( 21.53943276465977519, -0.05219959533907433946, 78.74890960531436690 ) ) ;
#196255 = CARTESIAN_POINT ( 'NONE',  ( -14.29746914071049879, 8.314922557960819915, 35.83224293864768839 ) ) ;
#196257 = CARTESIAN_POINT ( 'NONE',  ( -13.89961937509977652, 13.97604488694528158, 110.6239096053143243 ) ) ;
#196256 = CARTESIAN_POINT ( 'NONE',  ( -13.97604488694527625, -13.89961937509977652, 26.87390960531434558 ) ) ;
#196258 = CARTESIAN_POINT ( 'NONE',  ( -21.55341960407619339, 5.719274019375674811, 28.54275706135234358 ) ) ;
#196259 = CARTESIAN_POINT ( 'NONE',  ( -5.153800228976607833, 19.02544592524334988, 32.70942372801899722 ) ) ;
#196260 = CARTESIAN_POINT ( 'NONE',  ( 13.89961937509977652, -13.97604488694527269, 38.12390960531436690 ) ) ;
#196261 = CARTESIAN_POINT ( 'NONE',  ( 5.719274019375673035, 21.55341960407619339, 87.29275706135236135 ) ) ;
#196262 = DIRECTION ( 'NONE',  ( -0.5367108174878558735, -0.8437662581494460579, 0.000000000000000000 ) ) ;
#196263 = CARTESIAN_POINT ( 'NONE',  ( 14.29746914071049879, -8.314922557960816363, 33.33224293864769550 ) ) ;
#196264 = CARTESIAN_POINT ( 'NONE',  ( 29.86685920354754487, 21.69954338932564752, -1.924999997268813212 ) ) ;
#196265 = CARTESIAN_POINT ( 'NONE',  ( -15.72974639402197994, 15.80617190586746368, 30.62390960531436335 ) ) ;
#196266 = CARTESIAN_POINT ( 'NONE',  ( 0.05219959533910956823, 16.53943276465976808, 99.99890960531436690 ) ) ;
#196267 = CARTESIAN_POINT ( 'NONE',  ( 24.24789025133660303, -29.25582059975608118, -16.65643465479911711 ) ) ;
#196268 = CARTESIAN_POINT ( 'NONE',  ( 9.564922557960805705, 16.46253265017160317, 84.58224293864769550 ) ) ;
#196269 = CARTESIAN_POINT ( 'NONE',  ( 16.55341960407611168, 4.379528057220329451, 78.95724293864769550 ) ) ;
#196270 = CARTESIAN_POINT ( 'NONE',  ( 9.564922557961047289, -16.46253265017146816, 100.4177570613523329 ) ) ;
#196271 = CARTESIAN_POINT ( 'NONE',  ( 0.05219959533907565091, 21.53943276465977519, 59.99890960531436690 ) ) ;
#196272 = ORIENTED_EDGE ( 'NONE', *, *, #17849, .T. ) ;
#196273 = CARTESIAN_POINT ( 'NONE',  ( -9.564922557960796823, -16.46253265017161027, 27.08224293864769550 ) ) ;
#196275 = CARTESIAN_POINT ( 'NONE',  ( 15.72974639402199770, -15.80617190586745480, 88.12390960531436690 ) ) ;
#196274 = CARTESIAN_POINT ( 'NONE',  ( 19.03943276465977164, -0.05219959533909143690, 88.74890960531436690 ) ) ;
#196277 = CARTESIAN_POINT ( 'NONE',  ( 19.02544592524343514, -5.153800228976328945, 88.54057627198102409 ) ) ;
#196276 = CARTESIAN_POINT ( 'NONE',  ( 16.53943276465976808, 0.05219959533934440121, 101.2510903946856757 ) ) ;
#196278 = CARTESIAN_POINT ( 'NONE',  ( -16.46253265017146816, -9.564922557961047289, 79.16775706135234714 ) ) ;
#196279 = CARTESIAN_POINT ( 'NONE',  ( 15.80617190586769283, -15.72974639402175789, 90.62609039468567573 ) ) ;
#196280 = CARTESIAN_POINT ( 'NONE',  ( -15.80617190586745835, -15.72974639402198527, 81.87390960531435269 ) ) ;
#196281 = CARTESIAN_POINT ( 'NONE',  ( 21.55341960407610458, 5.719274019375980345, 33.95724293864769550 ) ) ;
#196282 = CARTESIAN_POINT ( 'NONE',  ( 19.02544592524343514, -5.153800228976328945, 53.54057627198102409 ) ) ;
#196283 = CARTESIAN_POINT ( 'NONE',  ( 0.05219959533910956823, 16.53943276465976808, 24.99890960531435624 ) ) ;
#196284 = CARTESIAN_POINT ( 'NONE',  ( 0.05219959533909260263, 19.03943276465977164, 59.99890960531436690 ) ) ;
#196285 = DIRECTION ( 'NONE',  ( -1.000000000000000000, 0.000000000000000000, 0.000000000000000000 ) ) ;
#196286 = CARTESIAN_POINT ( 'NONE',  ( 16.46253265017146816, 9.564922557961045513, 31.66775706135232937 ) ) ;
#196287 = CARTESIAN_POINT ( 'NONE',  ( -14.29746914071049879, 8.314922557960819915, 70.83224293864770971 ) ) ;
#196288 = CARTESIAN_POINT ( 'NONE',  ( 18.67979575497178502, 10.72451020669898547, 109.1655762719810383 ) ) ;
#196289 = CARTESIAN_POINT ( 'NONE',  ( -6.673977169394459175, 4.619345608252460877, -64.16796455867367399 ) ) ;
#196290 = CARTESIAN_POINT ( 'NONE',  ( -0.05219959533907301413, -21.53943276465977519, 57.49890960531435979 ) ) ;
#196291 = CARTESIAN_POINT ( 'NONE',  ( 16.53943276465976808, 0.05219959533934440121, 91.25109039468568994 ) ) ;
#196292 = CARTESIAN_POINT ( 'NONE',  ( -4.379528057220328563, 16.55341960407611168, 105.2072429386477097 ) ) ;
#196293 = CARTESIAN_POINT ( 'NONE',  ( -5.153800228976328057, -19.02544592524343514, 62.29057627198100988 ) ) ;
#196294 = CARTESIAN_POINT ( 'NONE',  ( 4.483927247898545687, 16.52544592524342804, 34.79057627198103120 ) ) ;
#196295 = CARTESIAN_POINT ( 'NONE',  ( 18.67979575497194134, -10.72451020669871369, 40.83442372801901854 ) ) ;
#196296 = CARTESIAN_POINT ( 'NONE',  ( 0.05219959533909260263, 19.03943276465977164, 109.9989096053143669 ) ) ;
#196297 = CARTESIAN_POINT ( 'NONE',  ( -5.823673210054431948, 21.52544592524334988, 87.70942372801901854 ) ) ;
#196298 = CARTESIAN_POINT ( 'NONE',  ( 19.05341960407611168, 5.049401038298154454, 33.95724293864769550 ) ) ;
#196299 = CARTESIAN_POINT ( 'NONE',  ( 19.02544592524343514, -5.153800228976328945, 38.54057627198103120 ) ) ;
#196300 = EDGE_LOOP ( 'NONE', ( #151453, #138560, #196685, #168116 ) ) ;
#196301 = CARTESIAN_POINT ( 'NONE',  ( 5.719274019375673035, 21.55341960407619339, 82.29275706135234714 ) ) ;
#196302 = CARTESIAN_POINT ( 'NONE',  ( 16.53943276465976808, 0.05219959533934440121, 46.25109039468567573 ) ) ;
#196303 = CARTESIAN_POINT ( 'NONE',  ( 10.81492255796106328, -18.62759615963255655, 70.41775706135236135 ) ) ;
#196304 = CARTESIAN_POINT ( 'NONE',  ( 16.46253265017160672, -9.564922557960803928, 103.3322429386476955 ) ) ;
#196305 = CARTESIAN_POINT ( 'NONE',  ( 19.05341960407617918, -5.049401038297876454, 86.04275706135233293 ) ) ;
#196306 = CARTESIAN_POINT ( 'NONE',  ( -5.823673210054431948, 21.52544592524334988, 57.70942372801901143 ) ) ;
#196307 = CARTESIAN_POINT ( 'NONE',  ( -8.224510206698735004, -14.34966873604973081, 24.58442372801901499 ) ) ;
#196308 = CARTESIAN_POINT ( 'NONE',  ( 16.46253265017146816, 9.564922557961045513, 86.66775706135233293 ) ) ;
#196309 = CARTESIAN_POINT ( 'NONE',  ( -13.97604488694527625, -13.89961937509977652, 51.87390960531436690 ) ) ;
#196310 = CARTESIAN_POINT ( 'NONE',  ( -9.564922557961040184, 16.46253265017147172, 82.91775706135233293 ) ) ;
#196311 = VECTOR ( 'NONE', #114170, 999.9999999999998863 ) ;
#196312 = CARTESIAN_POINT ( 'NONE',  ( -8.314922557961024197, 14.29746914071037800, 112.9177570613523329 ) ) ;
#196313 = CARTESIAN_POINT ( 'NONE',  ( -5.153800228976607833, 19.02544592524334988, 92.70942372801901854 ) ) ;
#196314 = CARTESIAN_POINT ( 'NONE',  ( -16.52544592524342804, 4.483927247898546575, 36.04057627198102409 ) ) ;
#196315 = CARTESIAN_POINT ( 'NONE',  ( -19.05341960407617563, 5.049401038297882671, 63.54275706135234003 ) ) ;
#196316 = CARTESIAN_POINT ( 'NONE',  ( 4.483927247898790824, -16.52544592524335698, 45.20942372801901854 ) ) ;
#196317 = CARTESIAN_POINT ( 'NONE',  ( 0.05219959533936267826, -19.03943276465977164, 30.00109039468566863 ) ) ;
#196318 = CARTESIAN_POINT ( 'NONE',  ( 14.34966873604960469, 8.224510206698951720, 114.1655762719810383 ) ) ;
#196319 = CARTESIAN_POINT ( 'NONE',  ( -5.153800228976328057, -19.02544592524343514, 37.29057627198102409 ) ) ;
#196320 = CARTESIAN_POINT ( 'NONE',  ( 12.14591786802327356, -12.06949235617739191, 50.62609039468568994 ) ) ;
#196321 = DIRECTION ( 'NONE',  ( 1.000000000000000000, 0.000000000000000000, 0.000000000000000000 ) ) ;
#196322 = B_SPLINE_CURVE_WITH_KNOTS ( 'NONE', 3,
 ( #197730, #107676, #139016, #105708, #76356, #121861 ),
 .UNSPECIFIED., .F., .F.,
 ( 4, 2, 4 ),
 ( 0.007228050697041537957, 0.007608510107495020450, 0.007988969517948503810 ),
 .UNSPECIFIED. ) ;
#196323 = CARTESIAN_POINT ( 'NONE',  ( -28.82186960331499392, 9.364793116373565596, 142.1500000054623740 ) ) ;
#196324 = CARTESIAN_POINT ( 'NONE',  ( 19.03943276465977164, -0.05219959533909143690, 98.74890960531436690 ) ) ;
#196325 = DIRECTION ( 'NONE',  ( 1.000000000000000000, 0.000000000000000000, 0.000000000000000000 ) ) ;
#196326 = ORIENTED_EDGE ( 'NONE', *, *, #155138, .F. ) ;
#196327 = CARTESIAN_POINT ( 'NONE',  ( -9.564922557961040184, 16.46253265017147172, 92.91775706135233293 ) ) ;
#196328 = CARTESIAN_POINT ( 'NONE',  ( -15.72974639402197994, 15.80617190586746368, 30.62390960531436335 ) ) ;
#196330 = CARTESIAN_POINT ( 'NONE',  ( 9.564922557961047289, -16.46253265017146816, 110.4177570613523471 ) ) ;
#196329 = CARTESIAN_POINT ( 'NONE',  ( -16.51473224551082808, 9.474510206698731452, 33.33442372801899722 ) ) ;
#196331 = CARTESIAN_POINT ( 'NONE',  ( 8.224510206698953496, -14.34966873604960469, 112.9155762719810383 ) ) ;
#196332 = CARTESIAN_POINT ( 'NONE',  ( -0.05219959533909027116, -19.03943276465977164, 32.49890960531435979 ) ) ;
#196333 = CARTESIAN_POINT ( 'NONE',  ( 15.80617190586746368, 15.72974639402197994, 79.37390960531436690 ) ) ;
#196334 = CARTESIAN_POINT ( 'NONE',  ( 16.46253265017160672, -9.564922557960803928, 33.33224293864770260 ) ) ;
#196335 = CARTESIAN_POINT ( 'NONE',  ( -17.59860650958993844, 7.585241751806885979, 48.42337014262493966 ) ) ;
#196336 = CARTESIAN_POINT ( 'NONE',  ( -13.89961937509957401, -13.97604488694547875, 69.37609039468564731 ) ) ;
#196337 = CARTESIAN_POINT ( 'NONE',  ( 16.55341960407611168, 4.379528057220329451, 53.95724293864770260 ) ) ;
#196338 = CARTESIAN_POINT ( 'NONE',  ( 0.05219959533907565091, 21.53943276465977519, 34.99890960531435979 ) ) ;
#196339 = CARTESIAN_POINT ( 'NONE',  ( -21.52544592524334988, -5.823673210054445271, 88.95942372801901854 ) ) ;
#196340 = CARTESIAN_POINT ( 'NONE',  ( 5.823673210054125526, 21.52544592524343514, 89.79057627198103830 ) ) ;
#196341 = CARTESIAN_POINT ( 'NONE',  ( 10.72451020669871369, 18.67979575497193778, 72.08442372801899012 ) ) ;
#196342 = CARTESIAN_POINT ( 'NONE',  ( -18.67979575497193778, 10.72451020669871902, 68.33442372801900433 ) ) ;
#196343 = CARTESIAN_POINT ( 'NONE',  ( -0.05219959533909027116, -19.03943276465977164, 92.49890960531436690 ) ) ;
#196345 = CARTESIAN_POINT ( 'NONE',  ( 5.823673210054444382, -21.52544592524334988, 70.20942372801904696 ) ) ;
#196344 = CARTESIAN_POINT ( 'NONE',  ( 16.52544592524335698, 4.483927247898782831, 96.45942372801901854 ) ) ;
#196346 = CARTESIAN_POINT ( 'NONE',  ( 16.46253265017160672, -9.564922557960803928, 53.33224293864768839 ) ) ;
#196347 = CARTESIAN_POINT ( 'NONE',  ( 5.719274019375673035, 21.55341960407619339, 32.29275706135235424 ) ) ;
#196348 = CARTESIAN_POINT ( 'NONE',  ( 5.153800228976335163, 19.02544592524342804, 64.79057627198100988 ) ) ;
#196349 = CARTESIAN_POINT ( 'NONE',  ( 14.34966873604960469, 8.224510206698951720, 64.16557627198102409 ) ) ;
#196350 = CARTESIAN_POINT ( 'NONE',  ( 16.52544592524342804, -4.483927247898539470, 33.54057627198102409 ) ) ;
#196351 = CARTESIAN_POINT ( 'NONE',  ( -0.05219959533907301413, -21.53943276465977519, 47.49890960531435979 ) ) ;
#196352 = CARTESIAN_POINT ( 'NONE',  ( 19.03943276465977164, -0.05219959533909143690, 43.74890960531435979 ) ) ;
#196353 = CARTESIAN_POINT ( 'NONE',  ( -21.55341960407610458, -5.719274019375992779, 56.45724293864768839 ) ) ;
#196354 = CARTESIAN_POINT ( 'NONE',  ( -9.474510206698720793, -16.51473224551083518, 54.58442372801899722 ) ) ;
#196356 = CARTESIAN_POINT ( 'NONE',  ( 12.14591786802309770, 12.06949235617756955, 64.37390960531435269 ) ) ;
#196355 = CARTESIAN_POINT ( 'NONE',  ( -17.31728774477272736, -6.344390552232413327, 39.18093348310684831 ) ) ;
#196357 = CARTESIAN_POINT ( 'NONE',  ( -21.55341960407610458, -5.719274019375992779, 46.45724293864769550 ) ) ;
#196358 = ORIENTED_EDGE ( 'NONE', *, *, #72094, .F. ) ;
#196359 = VERTEX_POINT ( 'NONE', #97441 ) ;
#196360 = CARTESIAN_POINT ( 'NONE',  ( 16.20579543436678094, 7.371946100355097897, 103.0652083417187441 ) ) ;
#196361 = CARTESIAN_POINT ( 'NONE',  ( -4.379528057220086978, -16.55341960407618274, 79.79275706135236135 ) ) ;
#196362 = CARTESIAN_POINT ( 'NONE',  ( 19.02544592524334988, 5.153800228976608722, 71.45942372801900433 ) ) ;
#196363 = CARTESIAN_POINT ( 'NONE',  ( -8.314922557960811034, -14.29746914071050412, 52.08224293864768839 ) ) ;
#196364 = CARTESIAN_POINT ( 'NONE',  ( -38.00000000000000711, 2.428612866367529932E-14, -10.00000000000000000 ) ) ;
#196365 = CARTESIAN_POINT ( 'NONE',  ( -19.05341960407611168, -5.049401038298163336, 46.45724293864768129 ) ) ;
#196366 = CARTESIAN_POINT ( 'NONE',  ( -16.53943276465976808, 0.05219959533911058130, 46.24890960531435979 ) ) ;
#196367 = CARTESIAN_POINT ( 'NONE',  ( 0.05219959533909260263, 19.03943276465977164, 54.99890960531435979 ) ) ;
#196368 = CARTESIAN_POINT ( 'NONE',  ( 5.153800228976335163, 19.02544592524342804, 74.79057627198103830 ) ) ;
#196369 = CARTESIAN_POINT ( 'NONE',  ( -9.564922557960796823, -16.46253265017161027, 37.08224293864768839 ) ) ;
#196370 = CARTESIAN_POINT ( 'NONE',  ( -10.81492255796105439, 18.62759615963255655, 42.91775706135235424 ) ) ;
#196371 = CARTESIAN_POINT ( 'NONE',  ( -0.05219959533909027116, -19.03943276465977164, 77.49890960531435269 ) ) ;
#196372 = CARTESIAN_POINT ( 'NONE',  ( -19.02544592524342804, 5.153800228976336051, 26.04057627198103120 ) ) ;
#196373 = CARTESIAN_POINT ( 'NONE',  ( -9.474510206698964154, 16.51473224551069663, 55.41557627198103120 ) ) ;
#196374 = CARTESIAN_POINT ( 'NONE',  ( -10.72451020669898014, 18.67979575497178502, 45.41557627198103830 ) ) ;
#196375 = CARTESIAN_POINT ( 'NONE',  ( 0.05219959533909260263, 19.03943276465977164, 39.99890960531436690 ) ) ;
#196376 = CARTESIAN_POINT ( 'NONE',  ( 21.53943276465977519, -0.05219959533907433946, 43.74890960531435979 ) ) ;
#196377 = CARTESIAN_POINT ( 'NONE',  ( -12.06949235617739369, -12.14591786802326823, 99.37609039468568994 ) ) ;
#196378 = CARTESIAN_POINT ( 'NONE',  ( -19.03943276465977164, -0.05219959533935918106, 18.75109039468567218 ) ) ;
#196380 = CARTESIAN_POINT ( 'NONE',  ( -4.379528057220086978, -16.55341960407618274, 74.79275706135234714 ) ) ;
#196379 = CARTESIAN_POINT ( 'NONE',  ( 12.14591786802327356, -12.06949235617739191, 45.62609039468567573 ) ) ;
#196381 = DIRECTION ( 'NONE',  ( 1.000000000000000000, -0.000000000000000000, -0.000000000000000000 ) ) ;
#196382 = CARTESIAN_POINT ( 'NONE',  ( 16.53943276465976808, 0.05219959533934440121, 66.25109039468567573 ) ) ;
#196383 = CARTESIAN_POINT ( 'NONE',  ( -4.379528057220086978, -16.55341960407618274, 59.79275706135234714 ) ) ;
#196384 = CARTESIAN_POINT ( 'NONE',  ( 9.474510206698971260, -16.51473224551069308, 102.9155762719810241 ) ) ;
#196385 = CARTESIAN_POINT ( 'NONE',  ( -16.52544592524335698, -4.483927247898792601, 43.95942372801902565 ) ) ;
#196386 = CARTESIAN_POINT ( 'NONE',  ( -16.46253265017160317, 9.564922557960807481, 30.83224293864769550 ) ) ;
#196387 = CARTESIAN_POINT ( 'NONE',  ( -15.80617190586768217, 15.72974639402176855, 33.12609039468569705 ) ) ;
#196388 = CARTESIAN_POINT ( 'NONE',  ( -0.05219959533934338120, 16.53943276465976808, 42.50109039468567573 ) ) ;
#196389 = CARTESIAN_POINT ( 'NONE',  ( -8.314922557961024197, 14.29746914071037800, 97.91775706135236135 ) ) ;
#196390 = CARTESIAN_POINT ( 'NONE',  ( 2.200000000000000622, 0.000000000000000000, 2.199999999999999289 ) ) ;
#196391 = CARTESIAN_POINT ( 'NONE',  ( 21.53943276465977519, 0.05219959533937863772, 106.2510903946856757 ) ) ;
#196392 = CARTESIAN_POINT ( 'NONE',  ( -16.46253265017146816, -9.564922557961047289, 99.16775706135233293 ) ) ;
#196393 = CARTESIAN_POINT ( 'NONE',  ( -14.29746914071049879, 8.314922557960819915, 55.83224293864770260 ) ) ;
#196394 = CARTESIAN_POINT ( 'NONE',  ( -0.05219959533909027116, -19.03943276465977164, 22.49890960531436690 ) ) ;
#196396 = CARTESIAN_POINT ( 'NONE',  ( 16.81555441253466299, -7.025013491696266321, 58.13685445334211011 ) ) ;
#196395 = CARTESIAN_POINT ( 'NONE',  ( 9.474510206698729675, 16.51473224551082808, 67.08442372801900433 ) ) ;
#196397 = CARTESIAN_POINT ( 'NONE',  ( 5.719274019375673035, 21.55341960407619339, 62.29275706135236845 ) ) ;
#196398 = CARTESIAN_POINT ( 'NONE',  ( -16.53943276465976808, -0.05219959533934237506, 33.75109039468568284 ) ) ;
#196399 = CARTESIAN_POINT ( 'NONE',  ( 1.300000000000000044, -1.082531754730548412, -0.6249999999999997780 ) ) ;
#196400 = CARTESIAN_POINT ( 'NONE',  ( 21.55341960407610458, 5.719274019375980345, 23.95724293864769550 ) ) ;
#196401 = CARTESIAN_POINT ( 'NONE',  ( 5.153800228976615827, -19.02544592524334988, 105.2094237280190185 ) ) ;
#196402 = CARTESIAN_POINT ( 'NONE',  ( -19.02544592524342804, 5.153800228976336051, 101.0405762719810241 ) ) ;
#196403 = CARTESIAN_POINT ( 'NONE',  ( 9.611906137939470796, -26.05071838941950801, 139.9999999999999716 ) ) ;
#196404 = CARTESIAN_POINT ( 'NONE',  ( -13.89961937509977652, 13.97604488694528158, 30.62390960531435269 ) ) ;
#196405 = CARTESIAN_POINT ( 'NONE',  ( -15.80617190586768217, 15.72974639402176855, 113.1260903946856899 ) ) ;
#196406 = CARTESIAN_POINT ( 'NONE',  ( -16.46253265017160317, 9.564922557960807481, 40.83224293864769550 ) ) ;
#196407 = CARTESIAN_POINT ( 'NONE',  ( 10.72451020669871369, 18.67979575497193778, 47.08442372801901854 ) ) ;
#196408 = CARTESIAN_POINT ( 'NONE',  ( 15.72974639402176855, 15.80617190586768217, 96.87609039468568994 ) ) ;
#196409 = CARTESIAN_POINT ( 'NONE',  ( 4.379528057220092307, 16.55341960407617563, 97.29275706135234714 ) ) ;
#196410 = CARTESIAN_POINT ( 'NONE',  ( -9.564922557960796823, -16.46253265017161027, 82.08224293864768129 ) ) ;
#196411 = CARTESIAN_POINT ( 'NONE',  ( -10.81492255796105439, 18.62759615963255655, 47.91775706135234714 ) ) ;
#196412 = CARTESIAN_POINT ( 'NONE',  ( -21.52544592524334988, -5.823673210054445271, 48.95942372801902565 ) ) ;
#196414 = CARTESIAN_POINT ( 'NONE',  ( 16.46253265017160672, -9.564922557960803928, 88.33224293864769550 ) ) ;
#196413 = CARTESIAN_POINT ( 'NONE',  ( -9.474510206698720793, -16.51473224551083518, 84.58442372801900433 ) ) ;
#196415 = CARTESIAN_POINT ( 'NONE',  ( 14.29746914071049879, -8.314922557960816363, 98.33224293864769550 ) ) ;
#196416 = CARTESIAN_POINT ( 'NONE',  ( 15.72974639402199770, -15.80617190586745480, 103.1239096053143811 ) ) ;
#196417 = CARTESIAN_POINT ( 'NONE',  ( 9.564922557961047289, -16.46253265017146816, 20.41775706135233293 ) ) ;
#196418 = CARTESIAN_POINT ( 'NONE',  ( 16.53943276465976808, -0.05219959533910856209, 93.74890960531436690 ) ) ;
#196419 = CARTESIAN_POINT ( 'NONE',  ( -16.46253265017160317, 9.564922557960807481, 45.83224293864769550 ) ) ;
#196420 = CARTESIAN_POINT ( 'NONE',  ( 5.049401038297881783, 19.05341960407617563, 87.29275706135234714 ) ) ;
#196421 = CARTESIAN_POINT ( 'NONE',  ( 4.379528057220339221, -16.55341960407611168, 52.70724293864769550 ) ) ;
#196422 = CARTESIAN_POINT ( 'NONE',  ( -10.72451020669870658, -18.67979575497194134, 104.5844237280190185 ) ) ;
#196423 = CARTESIAN_POINT ( 'NONE',  ( -5.153800228976328057, -19.02544592524343514, 107.2905762719810383 ) ) ;
#196424 = CARTESIAN_POINT ( 'NONE',  ( 13.97604488694548053, -13.89961937509957401, 75.62609039468564731 ) ) ;
#196425 = CARTESIAN_POINT ( 'NONE',  ( 15.72974639402199770, -15.80617190586745480, 78.12390960531436690 ) ) ;
#196426 = CARTESIAN_POINT ( 'NONE',  ( 10.72451020669871369, 18.67979575497193778, 37.08442372801901143 ) ) ;
#196427 = CARTESIAN_POINT ( 'NONE',  ( -8.224510206698735004, -14.34966873604973081, 29.58442372801901854 ) ) ;
#196428 = CARTESIAN_POINT ( 'NONE',  ( -16.53943276465976808, -0.05219959533934237506, 88.75109039468567573 ) ) ;
#196430 = CARTESIAN_POINT ( 'NONE',  ( 10.72451020669871369, 18.67979575497193778, 42.08442372801901854 ) ) ;
#196429 = CARTESIAN_POINT ( 'NONE',  ( 13.97604488694527802, 13.89961937509977652, 24.37390960531435624 ) ) ;
#196431 = CARTESIAN_POINT ( 'NONE',  ( 5.823673210054125526, 21.52544592524343514, 39.79057627198103830 ) ) ;
#196432 = CARTESIAN_POINT ( 'NONE',  ( -13.89961937509977652, 13.97604488694528158, 25.62390960531434558 ) ) ;
#196433 = CARTESIAN_POINT ( 'NONE',  ( 38.00000000000000711, -12.34694845685040754, -10.84999999453762598 ) ) ;
#196434 = CARTESIAN_POINT ( 'NONE',  ( -12.06949235617739369, -12.14591786802326823, 64.37609039468568994 ) ) ;
#196435 = CARTESIAN_POINT ( 'NONE',  ( -0.05219959533910754901, -16.53943276465976808, 87.49890960531436690 ) ) ;
#196436 = CARTESIAN_POINT ( 'NONE',  ( 10.81492255796078972, 18.62759615963270932, 79.58224293864769550 ) ) ;
#196437 = CARTESIAN_POINT ( 'NONE',  ( 14.29746914071049879, -8.314922557960816363, 23.33224293864769194 ) ) ;
#196438 = CARTESIAN_POINT ( 'NONE',  ( -14.29746914071037622, -8.314922557961029526, 44.16775706135234714 ) ) ;
#196439 = CARTESIAN_POINT ( 'NONE',  ( 13.97604488694527802, 13.89961937509977652, 64.37390960531436690 ) ) ;
#196440 = CARTESIAN_POINT ( 'NONE',  ( 14.29746914071037800, 8.314922557961029526, 86.66775706135234714 ) ) ;
#196441 = CARTESIAN_POINT ( 'NONE',  ( -5.153800228976607833, 19.02544592524334988, 82.70942372801897591 ) ) ;
#196442 = CARTESIAN_POINT ( 'NONE',  ( 15.72974639402199770, -15.80617190586745480, 83.12390960531436690 ) ) ;
#196443 = CARTESIAN_POINT ( 'NONE',  ( -16.53943276465976808, 0.05219959533911058130, 21.24890960531436690 ) ) ;
#196444 = ORIENTED_EDGE ( 'NONE', *, *, #84390, .T. ) ;
#196445 = CARTESIAN_POINT ( 'NONE',  ( 16.51473224551069308, 9.474510206698969483, 114.1655762719810241 ) ) ;
#196446 = ADVANCED_FACE ( 'NONE', ( #38799 ), #162136, .F. ) ;
#196447 = CARTESIAN_POINT ( 'NONE',  ( 21.52544592524344225, -5.823673210054117533, 58.54057627198103120 ) ) ;
#196448 = CARTESIAN_POINT ( 'NONE',  ( 8.314922557961029526, -14.29746914071037800, 90.41775706135236135 ) ) ;
#196449 = VERTEX_POINT ( 'NONE', #178322 ) ;
#196450 = CARTESIAN_POINT ( 'NONE',  ( -10.72451020669898014, 18.67979575497178502, 30.41557627198101699 ) ) ;
#196451 = CARTESIAN_POINT ( 'NONE',  ( 17.49999999999999645, 4.013004640162574077, 107.0539427900559417 ) ) ;
#196452 = CARTESIAN_POINT ( 'NONE',  ( -10.81492255796078084, -18.62759615963271287, 87.08224293864769550 ) ) ;
#196453 = CARTESIAN_POINT ( 'NONE',  ( 16.55341960407611168, 4.379528057220329451, 28.95724293864769905 ) ) ;
#196454 = CARTESIAN_POINT ( 'NONE',  ( 19.03943276465977164, 0.05219959533936151252, 111.2510903946856757 ) ) ;
#196455 = CARTESIAN_POINT ( 'NONE',  ( 19.02544592524343514, -5.153800228976328945, 33.54057627198102409 ) ) ;
#196456 = CARTESIAN_POINT ( 'NONE',  ( -8.314922557961024197, 14.29746914071037800, 27.91775706135234358 ) ) ;
#196457 = CARTESIAN_POINT ( 'NONE',  ( 5.049401038298161559, -19.05341960407611168, 47.70724293864770260 ) ) ;
#196458 = CARTESIAN_POINT ( 'NONE',  ( 1.993301997531345292E-15, -30.30510711980685912, 146.5000000000000000 ) ) ;
#196459 = CARTESIAN_POINT ( 'NONE',  ( 5.153800228976335163, 19.02544592524342804, 104.7905762719809957 ) ) ;
#196460 = CARTESIAN_POINT ( 'NONE',  ( 16.51473224551069308, 9.474510206698969483, 109.1655762719810383 ) ) ;
#196461 = CARTESIAN_POINT ( 'NONE',  ( -8.314922557961024197, 14.29746914071037800, 92.91775706135236135 ) ) ;
#196462 = CARTESIAN_POINT ( 'NONE',  ( 16.46253265017146816, 9.564922557961045513, 91.66775706135234714 ) ) ;
#196463 = CARTESIAN_POINT ( 'NONE',  ( 9.474510206698729675, 16.51473224551082808, 42.08442372801900433 ) ) ;
#196464 = CARTESIAN_POINT ( 'NONE',  ( 21.52544592524344225, -5.823673210054117533, 73.54057627198102409 ) ) ;
#196465 = CARTESIAN_POINT ( 'NONE',  ( -12.06949235617739369, -12.14591786802326823, 99.37609039468568994 ) ) ;
#196466 = CARTESIAN_POINT ( 'NONE',  ( 18.62759615963271287, -10.81492255796078972, 28.33224293864769550 ) ) ;
#196467 = CARTESIAN_POINT ( 'NONE',  ( -9.564922557961040184, 16.46253265017147172, 87.91775706135233293 ) ) ;
#196468 = CARTESIAN_POINT ( 'NONE',  ( 13.89961937509977652, -13.97604488694527269, 48.12390960531435979 ) ) ;
#196469 = CARTESIAN_POINT ( 'NONE',  ( -0.05219959533909027116, -19.03943276465977164, 107.4989096053143527 ) ) ;
#196470 = CARTESIAN_POINT ( 'NONE',  ( -21.55341960407619339, 5.719274019375674811, 58.54275706135235424 ) ) ;
#196471 = CARTESIAN_POINT ( 'NONE',  ( 16.46253265017160672, -9.564922557960803928, 63.33224293864769550 ) ) ;
#196472 = CARTESIAN_POINT ( 'NONE',  ( -8.314922557960811034, -14.29746914071050412, 102.0822429386476955 ) ) ;
#196473 = CARTESIAN_POINT ( 'NONE',  ( 12.14591786802309770, 12.06949235617756955, 74.37390960531436690 ) ) ;
#196474 = CARTESIAN_POINT ( 'NONE',  ( 15.80617190586746368, 15.72974639402197994, 74.37390960531436690 ) ) ;
#196475 = ORIENTED_EDGE ( 'NONE', *, *, #58736, .F. ) ;
#196476 = CARTESIAN_POINT ( 'NONE',  ( -0.05219959533936034679, 19.03943276465977164, 97.50109039468567573 ) ) ;
#196477 = CARTESIAN_POINT ( 'NONE',  ( 17.31747979337951193, -6.344076630960994834, 81.12055131934819485 ) ) ;
#196478 = CARTESIAN_POINT ( 'NONE',  ( -5.153800228976328057, -19.02544592524343514, 57.29057627198103120 ) ) ;
#196479 = CARTESIAN_POINT ( 'NONE',  ( 30.00000000000000355, 0.3535533905932729537, 4.646446609406719830 ) ) ;
#196481 = CARTESIAN_POINT ( 'NONE',  ( 9.474510206698971260, -16.51473224551069308, 92.91557627198103830 ) ) ;
#196480 = CARTESIAN_POINT ( 'NONE',  ( 5.153800228976335163, 19.02544592524342804, 74.79057627198103830 ) ) ;
#196482 = CARTESIAN_POINT ( 'NONE',  ( 14.34966873604972726, -8.224510206698740333, 60.83442372801901854 ) ) ;
#196483 = CARTESIAN_POINT ( 'NONE',  ( -17.49999999999999645, -5.624438216177605199, 49.18329655085356933 ) ) ;
#196484 = CARTESIAN_POINT ( 'NONE',  ( -19.02544592524334988, -5.153800228976617603, 38.95942372801900433 ) ) ;
#196485 = CARTESIAN_POINT ( 'NONE',  ( 17.16083808118622400, 6.592936235069069895, 21.72768779978462206 ) ) ;
#196486 = CARTESIAN_POINT ( 'NONE',  ( -9.474510206698964154, 16.51473224551069663, 115.4155762719810241 ) ) ;
#196487 = CARTESIAN_POINT ( 'NONE',  ( 4.483927247898790824, -16.52544592524335698, 100.2094237280190043 ) ) ;
#196488 = CARTESIAN_POINT ( 'NONE',  ( 17.59860650958994555, -7.585241751806880650, 75.92337014262494677 ) ) ;
#196489 = CARTESIAN_POINT ( 'NONE',  ( -14.29746914071037622, -8.314922557961029526, 94.16775706135237556 ) ) ;
#196490 = FACE_OUTER_BOUND ( 'NONE', #167083, .T. ) ;
#196491 = CARTESIAN_POINT ( 'NONE',  ( -16.53943276465976808, -0.05219959533934237506, 68.75109039468568994 ) ) ;
#196492 = CARTESIAN_POINT ( 'NONE',  ( -17.49999999999998579, -5.500000000000015099, 41.28230962303565832 ) ) ;
#196493 = CARTESIAN_POINT ( 'NONE',  ( 18.67979575497194134, -10.72451020669871369, 70.83442372801901854 ) ) ;
#196494 = CARTESIAN_POINT ( 'NONE',  ( 19.02544592524334988, 5.153800228976608722, 71.45942372801900433 ) ) ;
#196495 = CARTESIAN_POINT ( 'NONE',  ( -16.51473224551082808, 9.474510206698731452, 28.33442372801900433 ) ) ;
#196496 = CARTESIAN_POINT ( 'NONE',  ( -9.564922557960796823, -16.46253265017161027, 62.08224293864769550 ) ) ;
#196497 = CARTESIAN_POINT ( 'NONE',  ( -5.049401038298153566, 19.05341960407611168, 45.20724293864769550 ) ) ;
#196498 = CARTESIAN_POINT ( 'NONE',  ( 17.49999999999999645, -5.632147345228470492, 23.31793006472933882 ) ) ;
#196499 = CARTESIAN_POINT ( 'NONE',  ( 18.62759615963271287, -10.81492255796078972, 78.33224293864770971 ) ) ;
#196500 = CARTESIAN_POINT ( 'NONE',  ( 21.53943276465977519, -0.05219959533907433946, 28.74890960531435624 ) ) ;
#196501 = CARTESIAN_POINT ( 'NONE',  ( 19.03943276465977164, -0.05219959533909143690, 28.74890960531435624 ) ) ;
#196502 = CARTESIAN_POINT ( 'NONE',  ( 8.224510206698742110, 14.34966873604972548, 57.08442372801901854 ) ) ;
#196503 = VERTEX_POINT ( 'NONE', #189495 ) ;
#196504 = CARTESIAN_POINT ( 'NONE',  ( -10.72451020669870658, -18.67979575497194134, 34.58442372801900433 ) ) ;
#196506 = CARTESIAN_POINT ( 'NONE',  ( -11.74264578624800670, 36.14014761921585972, -8.400000000000000355 ) ) ;
#196505 = CARTESIAN_POINT ( 'NONE',  ( -4.379528057220328563, 16.55341960407611168, 50.20724293864769550 ) ) ;
#196507 = CARTESIAN_POINT ( 'NONE',  ( 16.55341960407618274, -4.379528057220086978, 31.04275706135234714 ) ) ;
#196508 = CARTESIAN_POINT ( 'NONE',  ( -9.474510206698720793, -16.51473224551083518, 39.58442372801899722 ) ) ;
#196509 = CARTESIAN_POINT ( 'NONE',  ( 12.14591786802309770, 12.06949235617756955, 44.37390960531435979 ) ) ;
#196510 = CARTESIAN_POINT ( 'NONE',  ( -15.72974639402197994, 15.80617190586746368, 110.6239096053143669 ) ) ;
#196512 = CARTESIAN_POINT ( 'NONE',  ( -21.52544592524343514, 5.823673210054127303, 76.04057627198102409 ) ) ;
#196511 = CARTESIAN_POINT ( 'NONE',  ( 1.212108430020047534, 16.08886519554586414, -59.40479301947630120 ) ) ;
#196513 = CARTESIAN_POINT ( 'NONE',  ( -5.153800228976328057, -19.02544592524343514, 87.29057627198103830 ) ) ;
#196514 = CARTESIAN_POINT ( 'NONE',  ( 8.314922557960818139, 14.29746914071049879, 64.58224293864769550 ) ) ;
#196515 = CARTESIAN_POINT ( 'NONE',  ( 13.97604488694527802, 13.89961937509977652, 99.37390960531436690 ) ) ;
#196516 = CARTESIAN_POINT ( 'NONE',  ( -37.55508611250748885, 1.249935417488349021, 39.64085810587564396 ) ) ;
#196517 = CARTESIAN_POINT ( 'NONE',  ( -19.03943276465977164, -0.05219959533935918106, 68.75109039468566152 ) ) ;
#196518 = CARTESIAN_POINT ( 'NONE',  ( -21.53943276465977519, 0.05219959533907696930, 111.2489096053143669 ) ) ;
#196519 = CARTESIAN_POINT ( 'NONE',  ( -19.05341960407611168, -5.049401038298163336, 56.45724293864768129 ) ) ;
#196520 = CARTESIAN_POINT ( 'NONE',  ( -0.05219959533936034679, 19.03943276465977164, 47.50109039468566863 ) ) ;
#196521 = CARTESIAN_POINT ( 'NONE',  ( -8.314922557960811034, -14.29746914071050412, 107.0822429386476955 ) ) ;
#196522 = CARTESIAN_POINT ( 'NONE',  ( -18.67979575497193778, 10.72451020669871902, 58.33442372801901143 ) ) ;
#196523 = CARTESIAN_POINT ( 'NONE',  ( -18.87580814761076908, 5.499999999999960032, 100.8717239426576242 ) ) ;
#196524 = CARTESIAN_POINT ( 'NONE',  ( -16.52544592524342804, 4.483927247898546575, 41.04057627198103120 ) ) ;
#196525 = CARTESIAN_POINT ( 'NONE',  ( 9.564922557960805705, 16.46253265017160317, 49.58224293864770260 ) ) ;
#196526 = CARTESIAN_POINT ( 'NONE',  ( 19.05341960407611168, 5.049401038298154454, 113.9572429386477097 ) ) ;
#196527 = CARTESIAN_POINT ( 'NONE',  ( -10.72451020669898014, 18.67979575497178502, 70.41557627198102409 ) ) ;
#196528 = CARTESIAN_POINT ( 'NONE',  ( 8.571926809382597767, 26.38167802310806209, 144.2750000027311899 ) ) ;
#196529 = CARTESIAN_POINT ( 'NONE',  ( 19.02544592524343514, -5.153800228976328945, 43.54057627198103120 ) ) ;
#196530 = ORIENTED_EDGE ( 'NONE', *, *, #161905, .T. ) ;
#196531 = CARTESIAN_POINT ( 'NONE',  ( 0.05219959533907565091, 21.53943276465977519, 59.99890960531436690 ) ) ;
#196532 = CARTESIAN_POINT ( 'NONE',  ( -0.05219959533937732626, 21.53943276465977519, 92.50109039468567573 ) ) ;
#196535 = CARTESIAN_POINT ( 'NONE',  ( 12.14591786802309770, 12.06949235617756955, 79.37390960531436690 ) ) ;
#196534 = CARTESIAN_POINT ( 'NONE',  ( 12.14591786802327356, -12.06949235617739191, 85.62609039468568994 ) ) ;
#196533 = CARTESIAN_POINT ( 'NONE',  ( 17.50000000000000000, -5.500000000000000888, 108.2969038253417153 ) ) ;
#196536 = CARTESIAN_POINT ( 'NONE',  ( -13.89961937509977652, 13.97604488694528158, 70.62390960531432427 ) ) ;
#196537 = ORIENTED_EDGE ( 'NONE', *, *, #183693, .F. ) ;
#196538 = CARTESIAN_POINT ( 'NONE',  ( 16.46253265017146816, 9.564922557961045513, 41.66775706135234003 ) ) ;
#196539 = CARTESIAN_POINT ( 'NONE',  ( -4.483927247898782831, 16.52544592524335698, 87.70942372801901854 ) ) ;
#196540 = CARTESIAN_POINT ( 'NONE',  ( 9.564922557961047289, -16.46253265017146816, 20.41775706135233293 ) ) ;
#196541 = CARTESIAN_POINT ( 'NONE',  ( -0.05219959533909027116, -19.03943276465977164, 82.49890960531436690 ) ) ;
#196542 = CARTESIAN_POINT ( 'NONE',  ( 18.62759615963271287, -10.81492255796078972, 43.33224293864769550 ) ) ;
#196543 = CARTESIAN_POINT ( 'NONE',  ( -15.72974639402176322, -15.80617190586768395, 94.37609039468568994 ) ) ;
#196544 = CARTESIAN_POINT ( 'NONE',  ( 14.34966873604972726, -8.224510206698740333, 60.83442372801901854 ) ) ;
#196545 = CARTESIAN_POINT ( 'NONE',  ( -18.67979575497178146, -10.72451020669898902, 106.6655762719810383 ) ) ;
#196546 = CARTESIAN_POINT ( 'NONE',  ( 14.34966873604972726, -8.224510206698740333, 30.83442372801902209 ) ) ;
#196547 = CARTESIAN_POINT ( 'NONE',  ( 19.02544592524343514, -5.153800228976328945, 88.54057627198102409 ) ) ;
#196548 = CARTESIAN_POINT ( 'NONE',  ( -16.51473224551069308, -9.474510206698971260, 41.66557627198103120 ) ) ;
#196549 = CARTESIAN_POINT ( 'NONE',  ( 16.51473224551069308, 9.474510206698969483, 54.16557627198103120 ) ) ;
#196550 = CARTESIAN_POINT ( 'NONE',  ( -12.14591786802326823, 12.06949235617739902, 28.12609039468568284 ) ) ;
#196551 = CARTESIAN_POINT ( 'NONE',  ( -16.55341960407611168, -4.379528057220339221, 81.45724293864769550 ) ) ;
#196552 = CARTESIAN_POINT ( 'NONE',  ( -0.05219959533934338120, 16.53943276465976808, 92.50109039468567573 ) ) ;
#196554 = CARTESIAN_POINT ( 'NONE',  ( 19.05341960407611168, 5.049401038298154454, 68.95724293864769550 ) ) ;
#196553 = CARTESIAN_POINT ( 'NONE',  ( 21.52544592524334988, 5.823673210054432836, 41.45942372801901143 ) ) ;
#196555 = CARTESIAN_POINT ( 'NONE',  ( 0.05219959533909260263, 19.03943276465977164, 79.99890960531436690 ) ) ;
#196556 = CARTESIAN_POINT ( 'NONE',  ( -16.53943276465976808, 0.05219959533911058130, 36.24890960531435979 ) ) ;
#196557 = CARTESIAN_POINT ( 'NONE',  ( 8.224510206698742110, 14.34966873604972548, 87.08442372801901854 ) ) ;
#196558 = ORIENTED_EDGE ( 'NONE', *, *, #87165, .T. ) ;
#196559 = CARTESIAN_POINT ( 'NONE',  ( -19.02544592524334988, -5.153800228976617603, 33.95942372801897591 ) ) ;
#196560 = CARTESIAN_POINT ( 'NONE',  ( 5.153800228976335163, 19.02544592524342804, 94.79057627198103830 ) ) ;
#196561 = CARTESIAN_POINT ( 'NONE',  ( 19.02544592524343514, -5.153800228976328945, 43.54057627198103120 ) ) ;
#196562 = CARTESIAN_POINT ( 'NONE',  ( -22.81625015709509441, -31.40387420917324590, -8.324999997268815122 ) ) ;
#196563 = CARTESIAN_POINT ( 'NONE',  ( -14.29746914071037622, -8.314922557961029526, 49.16775706135234003 ) ) ;
#196565 = CARTESIAN_POINT ( 'NONE',  ( -0.05219959533934338120, 16.53943276465976808, 62.50109039468568284 ) ) ;
#196564 = CARTESIAN_POINT ( 'NONE',  ( 5.153800228976615827, -19.02544592524334988, 75.20942372801896170 ) ) ;
#196566 = CARTESIAN_POINT ( 'NONE',  ( 6.412877669190332419, 3.889087296526017479, 8.181980515339454030 ) ) ;
#196567 = CARTESIAN_POINT ( 'NONE',  ( -5.153800228976328057, -19.02544592524343514, 72.29057627198102409 ) ) ;
#196568 = CARTESIAN_POINT ( 'NONE',  ( 5.823673210054125526, 21.52544592524343514, 114.7905762719810383 ) ) ;
#196569 = CARTESIAN_POINT ( 'NONE',  ( 5.049401038297881783, 19.05341960407617563, 62.29275706135234003 ) ) ;
#196571 = CARTESIAN_POINT ( 'NONE',  ( 16.51473224551069308, 9.474510206698969483, 34.16557627198102409 ) ) ;
#196570 = CARTESIAN_POINT ( 'NONE',  ( -9.474510206698964154, 16.51473224551069663, 105.4155762719810383 ) ) ;
#196572 = EDGE_CURVE ( 'NONE', #135096, #155722, #39785, .T. ) ;
#196573 = CARTESIAN_POINT ( 'NONE',  ( 16.51473224551069308, 9.474510206698969483, 79.16557627198103830 ) ) ;
#196575 = CARTESIAN_POINT ( 'NONE',  ( -19.03943276465977164, 0.05219959533909376836, 21.24890960531436335 ) ) ;
#196574 = CARTESIAN_POINT ( 'NONE',  ( -16.55341960407611168, -4.379528057220339221, 36.45724293864768839 ) ) ;
#196576 = CARTESIAN_POINT ( 'NONE',  ( -19.02544592524334988, -5.153800228976617603, 33.95942372801897591 ) ) ;
#196577 = CARTESIAN_POINT ( 'NONE',  ( -16.53943276465976808, 0.05219959533911058130, 71.24890960531435269 ) ) ;
#196578 = CARTESIAN_POINT ( 'NONE',  ( 21.55341960407619695, -5.719274019375665929, 111.0427570613523613 ) ) ;
#196579 = CARTESIAN_POINT ( 'NONE',  ( 13.89961937509977652, -13.97604488694527269, 58.12390960531436690 ) ) ;
#196581 = CARTESIAN_POINT ( 'NONE',  ( 18.62759615963255655, 10.81492255796105972, 106.6677570613523756 ) ) ;
#196580 = CARTESIAN_POINT ( 'NONE',  ( -16.55341960407611168, -4.379528057220339221, 46.45724293864769550 ) ) ;
#196582 = CARTESIAN_POINT ( 'NONE',  ( 19.05341960407611168, 5.049401038298154454, 88.95724293864769550 ) ) ;
#196583 = CARTESIAN_POINT ( 'NONE',  ( -16.51473224551069308, -9.474510206698971260, 111.6655762719810383 ) ) ;
#196584 = CARTESIAN_POINT ( 'NONE',  ( 9.564922557960805705, 16.46253265017160317, 39.58224293864768839 ) ) ;
#196585 = CARTESIAN_POINT ( 'NONE',  ( -16.52544592524342804, 4.483927247898546575, 111.0405762719810525 ) ) ;
#196586 = CARTESIAN_POINT ( 'NONE',  ( -8.314922557960811034, -14.29746914071050412, 92.08224293864769550 ) ) ;
#196587 = CARTESIAN_POINT ( 'NONE',  ( 18.62759615963271287, -10.81492255796078972, 93.33224293864769550 ) ) ;
#196588 = CARTESIAN_POINT ( 'NONE',  ( 16.46253265017160672, -9.564922557960803928, 93.33224293864769550 ) ) ;
#196589 = CARTESIAN_POINT ( 'NONE',  ( -0.05219959533907301413, -21.53943276465977519, 97.49890960531436690 ) ) ;
#196590 = CARTESIAN_POINT ( 'NONE',  ( -19.02544592524342804, 5.153800228976336051, 91.04057627198100988 ) ) ;
#196592 = CARTESIAN_POINT ( 'NONE',  ( -8.224510206698948167, 14.34966873604960824, 100.4155762719810241 ) ) ;
#196591 = CARTESIAN_POINT ( 'NONE',  ( -24.30454888808800717, 2.781629622375083599, 174.5654150192188183 ) ) ;
#196593 = CARTESIAN_POINT ( 'NONE',  ( -9.474510206698964154, 16.51473224551069663, 75.41557627198103830 ) ) ;
#196594 = CARTESIAN_POINT ( 'NONE',  ( -10.72451020669898014, 18.67979575497178502, 80.41557627198103830 ) ) ;
#196595 = CYLINDRICAL_SURFACE ( 'NONE', #175423, 4.000000000000000888 ) ;
#196597 = CARTESIAN_POINT ( 'NONE',  ( 22.00000000000000000, -1.163414459189985801E-14, 95.00000000000000000 ) ) ;
#196596 = CARTESIAN_POINT ( 'NONE',  ( -0.05219959533907301413, -21.53943276465977519, 22.49890960531436335 ) ) ;
#196598 = CARTESIAN_POINT ( 'NONE',  ( -8.314922557961024197, 14.29746914071037800, 27.91775706135234358 ) ) ;
#196599 = CARTESIAN_POINT ( 'NONE',  ( -16.52544592524342804, 4.483927247898546575, 96.04057627198102409 ) ) ;
#196600 = DIRECTION ( 'NONE',  ( 0.000000000000000000, 0.000000000000000000, -1.000000000000000000 ) ) ;
#196601 = CARTESIAN_POINT ( 'NONE',  ( 16.46253265017160672, -9.564922557960803928, 88.33224293864769550 ) ) ;
#196602 = CARTESIAN_POINT ( 'NONE',  ( 16.46253265017160672, -9.564922557960803928, 48.33224293864769550 ) ) ;
#196603 = CARTESIAN_POINT ( 'NONE',  ( -16.55341960407611168, -4.379528057220339221, 86.45724293864770971 ) ) ;
#196604 = CARTESIAN_POINT ( 'NONE',  ( 15.80617190586746368, 15.72974639402197994, 24.37390960531435979 ) ) ;
#196605 = CARTESIAN_POINT ( 'NONE',  ( 14.34966873604960469, 8.224510206698951720, 54.16557627198103120 ) ) ;
#196606 = CARTESIAN_POINT ( 'NONE',  ( 5.049401038297881783, 19.05341960407617563, 107.2927570613523187 ) ) ;
#196607 = CARTESIAN_POINT ( 'NONE',  ( 21.52544592524334988, 5.823673210054432836, 56.45942372801902565 ) ) ;
#196608 = CARTESIAN_POINT ( 'NONE',  ( 22.44159573604009239, 16.30477369853692693, 148.0750000027312012 ) ) ;
#196609 = CARTESIAN_POINT ( 'NONE',  ( 9.474510206698971260, -16.51473224551069308, 97.91557627198102409 ) ) ;
#196610 = CARTESIAN_POINT ( 'NONE',  ( -0.05219959533934338120, 16.53943276465976808, 87.50109039468568994 ) ) ;
#196611 = B_SPLINE_CURVE_WITH_KNOTS ( 'NONE', 3,
 ( #29470, #14283, #184140, #75951, #137625, #30452 ),
 .UNSPECIFIED., .F., .F.,
 ( 4, 2, 4 ),
 ( 0.004725762209527889501, 0.005384798814614493584, 0.006043835419701097667 ),
 .UNSPECIFIED. ) ;
#196612 = CARTESIAN_POINT ( 'NONE',  ( -16.51473224551069308, -9.474510206698971260, 31.66557627198102054 ) ) ;
#196613 = CARTESIAN_POINT ( 'NONE',  ( 5.049401038298161559, -19.05341960407611168, 77.70724293864765286 ) ) ;
#196614 = CARTESIAN_POINT ( 'NONE',  ( -5.823673210054116645, -21.52544592524344225, 82.29057627198103830 ) ) ;
#196615 = CARTESIAN_POINT ( 'NONE',  ( -16.51473224551082808, 9.474510206698731452, 113.3344237280190043 ) ) ;
#196617 = CARTESIAN_POINT ( 'NONE',  ( 18.62759615963255655, 10.81492255796105972, 56.66775706135235424 ) ) ;
#196616 = CARTESIAN_POINT ( 'NONE',  ( 16.55341960407611168, 4.379528057220329451, 48.95724293864770971 ) ) ;
#196619 = CARTESIAN_POINT ( 'NONE',  ( 15.80617190586746368, 15.72974639402197994, 24.37390960531435979 ) ) ;
#196618 = CARTESIAN_POINT ( 'NONE',  ( 14.34966873604972726, -8.224510206698740333, 90.83442372801901854 ) ) ;
#196620 = CARTESIAN_POINT ( 'NONE',  ( -5.153800228976328057, -19.02544592524343514, 112.2905762719810241 ) ) ;
#196621 = CARTESIAN_POINT ( 'NONE',  ( -3.573655867282028392E-15, 2.428612866367529932E-14, 150.0000000000000000 ) ) ;
#196622 = CARTESIAN_POINT ( 'NONE',  ( 16.52544592524335698, 4.483927247898782831, 111.4594237280190328 ) ) ;
#196623 = CARTESIAN_POINT ( 'NONE',  ( -16.53943276465976808, -0.05219959533934237506, 63.75109039468568284 ) ) ;
#196625 = ORIENTED_EDGE ( 'NONE', *, *, #110504, .F. ) ;
#196624 = CARTESIAN_POINT ( 'NONE',  ( -16.51473224551069308, -9.474510206698971260, 71.66557627198102409 ) ) ;
#196626 = CARTESIAN_POINT ( 'NONE',  ( 13.97604488694527802, 13.89961937509977652, 74.37390960531436690 ) ) ;
#196627 = CARTESIAN_POINT ( 'NONE',  ( -10.72451020669870658, -18.67979575497194134, 74.58442372801901854 ) ) ;
#196628 = CARTESIAN_POINT ( 'NONE',  ( -12.14591786802326823, 12.06949235617739902, 73.12609039468567573 ) ) ;
#196629 = CARTESIAN_POINT ( 'NONE',  ( 14.34966873604960469, 8.224510206698951720, 44.16557627198103120 ) ) ;
#196630 = CARTESIAN_POINT ( 'NONE',  ( 9.564922557960805705, 16.46253265017160317, 54.58224293864769550 ) ) ;
#196631 = CARTESIAN_POINT ( 'NONE',  ( 5.153800228976335163, 19.02544592524342804, 49.79057627198100988 ) ) ;
#196633 = EDGE_LOOP ( 'NONE', ( #41780, #72073, #109450, #8406 ) ) ;
#196632 = CARTESIAN_POINT ( 'NONE',  ( 8.314922557961029526, -14.29746914071037800, 40.41775706135234714 ) ) ;
#196634 = CARTESIAN_POINT ( 'NONE',  ( -9.474510206698720793, -16.51473224551083518, 99.58442372801900433 ) ) ;
#196635 = CARTESIAN_POINT ( 'NONE',  ( -0.05219959533910754901, -16.53943276465976808, 97.49890960531436690 ) ) ;
#196636 = CARTESIAN_POINT ( 'NONE',  ( -16.51473224551069308, -9.474510206698971260, 71.66557627198102409 ) ) ;
#196638 = CARTESIAN_POINT ( 'NONE',  ( 11.74264578624800315, -36.14014761921581709, -3.400000000000000355 ) ) ;
#196637 = CARTESIAN_POINT ( 'NONE',  ( 16.46253265017146816, 9.564922557961045513, 106.6677570613523471 ) ) ;
#196639 = CARTESIAN_POINT ( 'NONE',  ( -10.81492255796105439, 18.62759615963255655, 102.9177570613523756 ) ) ;
#196640 = CARTESIAN_POINT ( 'NONE',  ( -4.483927247898782831, 16.52544592524335698, 72.70942372801901854 ) ) ;
#196641 = PLANE ( 'NONE',  #56780 ) ;
#196642 = CARTESIAN_POINT ( 'NONE',  ( 21.55341960407610458, 5.719274019375980345, 68.95724293864769550 ) ) ;
#196643 = CARTESIAN_POINT ( 'NONE',  ( 16.53943276465976808, 0.05219959533934440121, 56.25109039468568284 ) ) ;
#196644 = CARTESIAN_POINT ( 'NONE',  ( 16.46253265017146816, 9.564922557961045513, 46.66775706135233293 ) ) ;
#196645 = CARTESIAN_POINT ( 'NONE',  ( 19.05341960407611168, 5.049401038298154454, 88.95724293864769550 ) ) ;
#196646 = CARTESIAN_POINT ( 'NONE',  ( -16.52544592524342804, 4.483927247898546575, 116.0405762719810383 ) ) ;
#196647 = CARTESIAN_POINT ( 'NONE',  ( -9.564922557960796823, -16.46253265017161027, 67.08224293864769550 ) ) ;
#196648 = CARTESIAN_POINT ( 'NONE',  ( 12.06949235617757843, -12.14591786802309237, 63.12390960531435979 ) ) ;
#196649 = CARTESIAN_POINT ( 'NONE',  ( 15.72974639402176855, 15.80617190586768217, 71.87609039468568994 ) ) ;
#196650 = EDGE_CURVE ( 'NONE', #127511, #54470, #158355, .T. ) ;
#196651 = CARTESIAN_POINT ( 'NONE',  ( -9.474510206698720793, -16.51473224551083518, 49.58442372801899722 ) ) ;
#196652 = CARTESIAN_POINT ( 'NONE',  ( 5.049401038297881783, 19.05341960407617563, 27.29275706135232937 ) ) ;
#196653 = CARTESIAN_POINT ( 'NONE',  ( -9.474510206698964154, 16.51473224551069663, 50.41557627198102409 ) ) ;
#196654 = CARTESIAN_POINT ( 'NONE',  ( -0.05219959533907301413, -21.53943276465977519, 27.49890960531435269 ) ) ;
#196655 = CARTESIAN_POINT ( 'NONE',  ( 21.52544592524334988, 5.823673210054432836, 86.45942372801901854 ) ) ;
#196656 = CARTESIAN_POINT ( 'NONE',  ( -0.05219959533909027116, -19.03943276465977164, 67.49890960531436690 ) ) ;
#196657 = CARTESIAN_POINT ( 'NONE',  ( 10.72451020669871369, 18.67979575497193778, 92.08442372801901854 ) ) ;
#196658 = CARTESIAN_POINT ( 'NONE',  ( -21.55341960407610458, -5.719274019375992779, 41.45724293864769550 ) ) ;
#196659 = CARTESIAN_POINT ( 'NONE',  ( 16.46253265017160672, -9.564922557960803928, 78.33224293864769550 ) ) ;
#196660 = CARTESIAN_POINT ( 'NONE',  ( -5.823673210054431948, 21.52544592524334988, 32.70942372801900433 ) ) ;
#196661 = CARTESIAN_POINT ( 'NONE',  ( 5.153800228976615827, -19.02544592524334988, 60.20942372801899012 ) ) ;
#196662 = CARTESIAN_POINT ( 'NONE',  ( 19.02544592524343514, -5.153800228976328945, 48.54057627198103120 ) ) ;
#196663 = CARTESIAN_POINT ( 'NONE',  ( 13.89961937509977652, -13.97604488694527269, 88.12390960531438111 ) ) ;
#196664 = CARTESIAN_POINT ( 'NONE',  ( -14.34966873604972548, 8.224510206698743886, 28.33442372801902209 ) ) ;
#196665 = CARTESIAN_POINT ( 'NONE',  ( -14.29746914071049879, 8.314922557960819915, 90.83224293864769550 ) ) ;
#196666 = CARTESIAN_POINT ( 'NONE',  ( 16.51473224551069308, 9.474510206698969483, 69.16557627198102409 ) ) ;
#196667 = EDGE_CURVE ( 'NONE', #123381, #199940, #76354, .T. ) ;
#196668 = CARTESIAN_POINT ( 'NONE',  ( -21.55341960407610458, -5.719274019375992779, 56.45724293864768839 ) ) ;
#196669 = CARTESIAN_POINT ( 'NONE',  ( 16.55341960407618274, -4.379528057220086978, 26.04275706135235779 ) ) ;
#196670 = CARTESIAN_POINT ( 'NONE',  ( 10.72451020669898902, -18.67979575497178502, 112.9155762719810383 ) ) ;
#196671 = CARTESIAN_POINT ( 'NONE',  ( 21.53943276465977519, 0.05219959533937863772, 71.25109039468568994 ) ) ;
#196672 = CARTESIAN_POINT ( 'NONE',  ( -16.53943276465976808, -0.05219959533934237506, 73.75109039468567573 ) ) ;
#196673 = CARTESIAN_POINT ( 'NONE',  ( -14.34966873604972548, 8.224510206698743886, 68.33442372801900433 ) ) ;
#196674 = CARTESIAN_POINT ( 'NONE',  ( -19.05341960407611168, -5.049401038298163336, 61.45724293864769550 ) ) ;
#196675 = CARTESIAN_POINT ( 'NONE',  ( 12.06949235617739724, 12.14591786802326823, 106.8760903946856899 ) ) ;
#196676 = CARTESIAN_POINT ( 'NONE',  ( -0.05219959533936034679, 19.03943276465977164, 37.50109039468567573 ) ) ;
#196677 = CARTESIAN_POINT ( 'NONE',  ( -0.05219959533937732626, 21.53943276465977519, 37.50109039468568284 ) ) ;
#196678 = CARTESIAN_POINT ( 'NONE',  ( -14.34966873604960291, -8.224510206698953496, 61.66557627198103120 ) ) ;
#196679 = CARTESIAN_POINT ( 'NONE',  ( -16.46253265017160317, 9.564922557960807481, 95.83224293864769550 ) ) ;
#196680 = CARTESIAN_POINT ( 'NONE',  ( -12.14591786802326823, 12.06949235617739902, 88.12609039468570415 ) ) ;
#196681 = CARTESIAN_POINT ( 'NONE',  ( -21.53943276465977519, -0.05219959533937600094, 58.75109039468568994 ) ) ;
#196682 = CARTESIAN_POINT ( 'NONE',  ( 16.53943276465976808, 0.05219959533934440121, 26.25109039468567573 ) ) ;
#196683 = CARTESIAN_POINT ( 'NONE',  ( 21.55341960407619695, -5.719274019375665929, 31.04275706135234714 ) ) ;
#196684 = CARTESIAN_POINT ( 'NONE',  ( 4.379528057220339221, -16.55341960407611168, 62.70724293864769550 ) ) ;
#196685 = ORIENTED_EDGE ( 'NONE', *, *, #176309, .F. ) ;
#196686 = CARTESIAN_POINT ( 'NONE',  ( -10.81492255796078084, -18.62759615963271287, 102.0822429386476955 ) ) ;
#196687 = CARTESIAN_POINT ( 'NONE',  ( -14.34966873604960291, -8.224510206698953496, 36.66557627198103120 ) ) ;
#196688 = VERTEX_POINT ( 'NONE', #180335 ) ;
#196689 = CARTESIAN_POINT ( 'NONE',  ( -16.46253265017160317, 9.564922557960807481, 30.83224293864769550 ) ) ;
#196690 = CARTESIAN_POINT ( 'NONE',  ( -10.81492255796078084, -18.62759615963271287, 32.08224293864769550 ) ) ;
#196691 = CARTESIAN_POINT ( 'NONE',  ( -5.823673210054431948, 21.52544592524334988, 32.70942372801900433 ) ) ;
#196692 = CARTESIAN_POINT ( 'NONE',  ( 12.06949235617757843, -12.14591786802309237, 68.12390960531436690 ) ) ;
#196693 = CARTESIAN_POINT ( 'NONE',  ( -15.72974639402197994, 15.80617190586746368, 60.62390960531437401 ) ) ;
#196694 = CARTESIAN_POINT ( 'NONE',  ( 16.51473224551069308, 9.474510206698969483, 69.16557627198102409 ) ) ;
#196695 = CARTESIAN_POINT ( 'NONE',  ( 19.05341960407617918, -5.049401038297876454, 76.04275706135230450 ) ) ;
#196696 = CARTESIAN_POINT ( 'NONE',  ( 15.72974639402199770, -15.80617190586745480, 53.12390960531436690 ) ) ;
#196697 = CARTESIAN_POINT ( 'NONE',  ( 16.51473224551069308, 9.474510206698969483, 39.16557627198103120 ) ) ;
#196698 = CARTESIAN_POINT ( 'NONE',  ( -16.51473224551069308, -9.474510206698971260, 76.66557627198103830 ) ) ;
#196699 = VERTEX_POINT ( 'NONE', #106429 ) ;
#196700 = CARTESIAN_POINT ( 'NONE',  ( 16.52544592524335698, 4.483927247898782831, 31.45942372801901854 ) ) ;
#196701 = CARTESIAN_POINT ( 'NONE',  ( 10.72451020669871369, 18.67979575497193778, 22.08442372801901143 ) ) ;
#196702 = CARTESIAN_POINT ( 'NONE',  ( -12.06949235617756955, 12.14591786802309770, 50.62390960531435979 ) ) ;
#196703 = CARTESIAN_POINT ( 'NONE',  ( 9.474510206698971260, -16.51473224551069308, 102.9155762719810241 ) ) ;
#196704 = CARTESIAN_POINT ( 'NONE',  ( -15.72974639402197994, 15.80617190586746368, 75.62390960531439532 ) ) ;
#196706 = CARTESIAN_POINT ( 'NONE',  ( 4.379528057220092307, 16.55341960407617563, 57.29275706135234714 ) ) ;
#196705 = CARTESIAN_POINT ( 'NONE',  ( 5.719274019375991003, -21.55341960407610458, 102.7072429386476955 ) ) ;
#196707 = CARTESIAN_POINT ( 'NONE',  ( -10.81492255796078084, -18.62759615963271287, 47.08224293864770260 ) ) ;
#196708 = CARTESIAN_POINT ( 'NONE',  ( 21.55341960407619695, -5.719274019375665929, 106.0427570613523471 ) ) ;
#196709 = CIRCLE ( 'NONE', #64321, 2.500000000000002220 ) ;
#196710 = CARTESIAN_POINT ( 'NONE',  ( -19.03943276465977164, 0.05219959533909376836, 36.24890960531436690 ) ) ;
#196711 = CARTESIAN_POINT ( 'NONE',  ( 9.474510206698971260, -16.51473224551069308, 102.9155762719810241 ) ) ;
#196712 = CARTESIAN_POINT ( 'NONE',  ( 5.153800228976335163, 19.02544592524342804, 69.79057627198103830 ) ) ;
#196713 = CARTESIAN_POINT ( 'NONE',  ( -14.53388260107741736, -39.78846373132474667, -19.96647037889510656 ) ) ;
#196714 = CARTESIAN_POINT ( 'NONE',  ( -9.474510206698720793, -16.51473224551083518, 59.58442372801900433 ) ) ;
#196716 = CARTESIAN_POINT ( 'NONE',  ( 0.05219959533907565091, 21.53943276465977519, 29.99890960531435979 ) ) ;
#196715 = CARTESIAN_POINT ( 'NONE',  ( -21.53943276465977519, -0.05219959533937600094, 108.7510903946857042 ) ) ;
#196717 = CARTESIAN_POINT ( 'NONE',  ( -16.53943276465976808, -0.05219959533934237506, 108.7510903946857042 ) ) ;
#196718 = CARTESIAN_POINT ( 'NONE',  ( -19.02544592524334988, -5.153800228976617603, 83.95942372801901854 ) ) ;
#196719 = CYLINDRICAL_SURFACE ( 'NONE', #51827, 4.250000000000000000 ) ;
#196720 = CARTESIAN_POINT ( 'NONE',  ( 16.46253265017160672, -9.564922557960803928, 108.3322429386476955 ) ) ;
#196721 = CARTESIAN_POINT ( 'NONE',  ( 5.049401038297881783, 19.05341960407617563, 77.29275706135231871 ) ) ;
#196722 = CARTESIAN_POINT ( 'NONE',  ( -19.05341960407617563, 5.049401038297882671, 48.54275706135233293 ) ) ;
#196723 = LINE ( 'NONE', #121827, #37037 ) ;
#196724 = CARTESIAN_POINT ( 'NONE',  ( -9.564922557960796823, -16.46253265017161027, 47.08224293864769550 ) ) ;
#196725 = CARTESIAN_POINT ( 'NONE',  ( 16.53943276465976808, -0.05219959533910856209, 48.74890960531435979 ) ) ;
#196726 = CARTESIAN_POINT ( 'NONE',  ( -5.049401038298153566, 19.05341960407611168, 30.20724293864768839 ) ) ;
#196727 = CARTESIAN_POINT ( 'NONE',  ( -0.05219959533910754901, -16.53943276465976808, 42.49890960531435979 ) ) ;
#196728 = CARTESIAN_POINT ( 'NONE',  ( 17.50000000001358202, -5.500000000000038192, 58.29690382535058291 ) ) ;
#196729 = CARTESIAN_POINT ( 'NONE',  ( -8.314922557961024197, 14.29746914071037800, 112.9177570613523329 ) ) ;
#196730 = CARTESIAN_POINT ( 'NONE',  ( 9.474510206698971260, -16.51473224551069308, 52.91557627198102409 ) ) ;
#196731 = CARTESIAN_POINT ( 'NONE',  ( 21.52544592524334988, 5.823673210054432836, 106.4594237280190328 ) ) ;
#196732 = CARTESIAN_POINT ( 'NONE',  ( -16.52544592524335698, -4.483927247898792601, 18.95942372801901143 ) ) ;
#196733 = CARTESIAN_POINT ( 'NONE',  ( -15.72974639402197994, 15.80617190586746368, 40.62390960531435269 ) ) ;
#196735 = ORIENTED_EDGE ( 'NONE', *, *, #71748, .T. ) ;
#196734 = CARTESIAN_POINT ( 'NONE',  ( 18.62759615963255655, 10.81492255796105972, 96.66775706135234714 ) ) ;
#196736 = CARTESIAN_POINT ( 'NONE',  ( -5.049401038298153566, 19.05341960407611168, 110.2072429386476671 ) ) ;
#196737 = CARTESIAN_POINT ( 'NONE',  ( -19.05341960407611168, -5.049401038298163336, 81.45724293864769550 ) ) ;
#196738 = CARTESIAN_POINT ( 'NONE',  ( -22.81625015709509441, -31.40387420917324590, -8.324999997268813345 ) ) ;
#196739 = CARTESIAN_POINT ( 'NONE',  ( -10.81492255796078084, -18.62759615963271287, 107.0822429386476955 ) ) ;
#196740 = CARTESIAN_POINT ( 'NONE',  ( -16.52544592524342804, 4.483927247898546575, 81.04057627198102409 ) ) ;
#196741 = CARTESIAN_POINT ( 'NONE',  ( -15.72974639402197994, 15.80617190586746368, 75.62390960531439532 ) ) ;
#196742 = CARTESIAN_POINT ( 'NONE',  ( 5.153800228976335163, 19.02544592524342804, 69.79057627198103830 ) ) ;
#196743 = CARTESIAN_POINT ( 'NONE',  ( -18.62759615963270932, 10.81492255796079327, 90.83224293864769550 ) ) ;
#196744 = ORIENTED_EDGE ( 'NONE', *, *, #160152, .T. ) ;
#196745 = CARTESIAN_POINT ( 'NONE',  ( -13.89961937509977652, 13.97604488694528158, 65.62390960531436690 ) ) ;
#196747 = CARTESIAN_POINT ( 'NONE',  ( 20.96276500525451070, -10.40013546722648030, 168.2886347277376160 ) ) ;
#196746 = CARTESIAN_POINT ( 'NONE',  ( -4.483927247898539470, -16.52544592524342804, 97.29057627198105251 ) ) ;
#196748 = CARTESIAN_POINT ( 'NONE',  ( -5.153800228976328057, -19.02544592524343514, 67.29057627198102409 ) ) ;
#196749 = CARTESIAN_POINT ( 'NONE',  ( 5.153800228976615827, -19.02544592524334988, 80.20942372801901854 ) ) ;
#196750 = CARTESIAN_POINT ( 'NONE',  ( -16.53943276465976808, 0.05219959533911058130, 96.24890960531435269 ) ) ;
#196751 = CARTESIAN_POINT ( 'NONE',  ( -5.719274019375665041, -21.55341960407619695, 59.79275706135234714 ) ) ;
#196753 = CARTESIAN_POINT ( 'NONE',  ( -0.05219959533937732626, 21.53943276465977519, 22.50109039468567573 ) ) ;
#196752 = CARTESIAN_POINT ( 'NONE',  ( -16.51473224551069308, -9.474510206698971260, 51.66557627198102409 ) ) ;
#196754 = CARTESIAN_POINT ( 'NONE',  ( -12.14591786802309592, -12.06949235617757132, 96.87390960531436690 ) ) ;
#196755 = CARTESIAN_POINT ( 'NONE',  ( 10.05780954200632493, -38.14163830725774318, -31.65208490131638541 ) ) ;
#196756 = CARTESIAN_POINT ( 'NONE',  ( 5.049401038298161559, -19.05341960407611168, 62.70724293864769550 ) ) ;
#196757 = CARTESIAN_POINT ( 'NONE',  ( 17.81289503416611453, -24.51734667627695785, 138.9500000054623570 ) ) ;
#196759 = CARTESIAN_POINT ( 'NONE',  ( -19.03943276465977164, 0.05219959533909376836, 116.2489096053143669 ) ) ;
#196758 = CARTESIAN_POINT ( 'NONE',  ( 5.153800228976615827, -19.02544592524334988, 105.2094237280190185 ) ) ;
#196760 = CARTESIAN_POINT ( 'NONE',  ( 10.81492255796106328, -18.62759615963255655, 50.41775706135235424 ) ) ;
#196761 = CARTESIAN_POINT ( 'NONE',  ( -13.97604488694527625, -13.89961937509977652, 96.87390960531433848 ) ) ;
#196762 = CARTESIAN_POINT ( 'NONE',  ( -0.05219959533936034679, 19.03943276465977164, 82.50109039468567573 ) ) ;
#196763 = CARTESIAN_POINT ( 'NONE',  ( -0.05219959533909027116, -19.03943276465977164, 62.49890960531435979 ) ) ;
#196764 = CARTESIAN_POINT ( 'NONE',  ( -8.314922557960811034, -14.29746914071050412, 77.08224293864769550 ) ) ;
#196765 = CARTESIAN_POINT ( 'NONE',  ( 16.51473224551069308, 9.474510206698969483, 94.16557627198103830 ) ) ;
#196766 = CARTESIAN_POINT ( 'NONE',  ( -4.483927247898539470, -16.52544592524342804, 72.29057627198102409 ) ) ;
#196767 = CARTESIAN_POINT ( 'NONE',  ( -5.049401038298153566, 19.05341960407611168, 85.20724293864766707 ) ) ;
#196768 = CARTESIAN_POINT ( 'NONE',  ( 13.97604488694548053, -13.89961937509957401, 30.62609039468566863 ) ) ;
#196771 = CARTESIAN_POINT ( 'NONE',  ( -19.03943276465977164, 0.05219959533909376836, 26.24890960531435624 ) ) ;
#196770 = CARTESIAN_POINT ( 'NONE',  ( 12.06949235617757843, -12.14591786802309237, 43.12390960531435269 ) ) ;
#196769 = CARTESIAN_POINT ( 'NONE',  ( -19.02544592524342804, 5.153800228976336051, 51.04057627198103120 ) ) ;
#196772 = ORIENTED_EDGE ( 'NONE', *, *, #26374, .F. ) ;
#196773 = CARTESIAN_POINT ( 'NONE',  ( -15.72974639402176322, -15.80617190586768395, 44.37609039468567573 ) ) ;
#196774 = CARTESIAN_POINT ( 'NONE',  ( 0.05219959533936267826, -19.03943276465977164, 85.00109039468567573 ) ) ;
#196775 = CARTESIAN_POINT ( 'NONE',  ( 4.483927247898545687, 16.52544592524342804, 29.79057627198102409 ) ) ;
#196776 = CARTESIAN_POINT ( 'NONE',  ( -21.55341960407610458, -5.719274019375992779, 96.45724293864770971 ) ) ;
#196777 = CARTESIAN_POINT ( 'NONE',  ( -21.52544592524343514, 5.823673210054127303, 31.04057627198102409 ) ) ;
#196778 = CARTESIAN_POINT ( 'NONE',  ( -4.483927247898539470, -16.52544592524342804, 72.29057627198102409 ) ) ;
#196779 = CARTESIAN_POINT ( 'NONE',  ( 19.05341960407611168, 5.049401038298154454, 43.95724293864769550 ) ) ;
#196780 = CARTESIAN_POINT ( 'NONE',  ( 12.14591786802327356, -12.06949235617739191, 100.6260903946857184 ) ) ;
#196781 = CARTESIAN_POINT ( 'NONE',  ( -4.379528057220086978, -16.55341960407618274, 64.79275706135234714 ) ) ;
#196782 = CARTESIAN_POINT ( 'NONE',  ( -5.153800228976607833, 19.02544592524334988, 27.70942372801899722 ) ) ;
#196783 = CARTESIAN_POINT ( 'NONE',  ( 13.97604488694527802, 13.89961937509977652, 94.37390960531436690 ) ) ;
#196784 = CARTESIAN_POINT ( 'NONE',  ( -16.46253265017160317, 9.564922557960807481, 80.83224293864769550 ) ) ;
#196785 = CARTESIAN_POINT ( 'NONE',  ( 12.14591786802327356, -12.06949235617739191, 80.62609039468567573 ) ) ;
#196786 = CARTESIAN_POINT ( 'NONE',  ( -16.51473224551069308, -9.474510206698971260, 21.66557627198102765 ) ) ;
#196787 = CARTESIAN_POINT ( 'NONE',  ( -16.52544592524342804, 4.483927247898546575, 51.04057627198103120 ) ) ;
#196789 = CARTESIAN_POINT ( 'NONE',  ( -5.049401038298153566, 19.05341960407611168, 85.20724293864766707 ) ) ;
#196788 = CARTESIAN_POINT ( 'NONE',  ( -19.03943276465977164, 0.05219959533909376836, 106.2489096053143669 ) ) ;
#196790 = CARTESIAN_POINT ( 'NONE',  ( -0.05219959533907301413, -21.53943276465977519, 22.49890960531436335 ) ) ;
#196791 = CARTESIAN_POINT ( 'NONE',  ( 8.224510206698953496, -14.34966873604960469, 77.91557627198102409 ) ) ;
#196792 = CARTESIAN_POINT ( 'NONE',  ( 16.55341960407611168, 4.379528057220329451, 63.95724293864770260 ) ) ;
#196794 = CARTESIAN_POINT ( 'NONE',  ( 17.60769864724391098, -5.499999999999978684, 86.15024842019167295 ) ) ;
#196793 = CARTESIAN_POINT ( 'NONE',  ( 8.314922557961029526, -14.29746914071037800, 50.41775706135235424 ) ) ;
#196795 = CARTESIAN_POINT ( 'NONE',  ( 19.03943276465977164, 0.05219959533936151252, 61.25109039468566863 ) ) ;
#196796 = CARTESIAN_POINT ( 'NONE',  ( -9.564922557960796823, -16.46253265017161027, 92.08224293864769550 ) ) ;
#196797 = CARTESIAN_POINT ( 'NONE',  ( -9.474510206698720793, -16.51473224551083518, 59.58442372801900433 ) ) ;
#196798 = CARTESIAN_POINT ( 'NONE',  ( 18.22780087662114212, -5.499999999999987566, 41.01540105326107977 ) ) ;
#196800 = CARTESIAN_POINT ( 'NONE',  ( -16.52544592524335698, -4.483927247898792601, 93.95942372801903275 ) ) ;
#196799 = CARTESIAN_POINT ( 'NONE',  ( 19.05341960407617918, -5.049401038297876454, 111.0427570613523329 ) ) ;
#196801 = CARTESIAN_POINT ( 'NONE',  ( -19.03943276465977164, 0.05219959533909376836, 36.24890960531436690 ) ) ;
#196802 = CARTESIAN_POINT ( 'NONE',  ( 15.72974639402199770, -15.80617190586745480, 23.12390960531436335 ) ) ;
#196803 = CARTESIAN_POINT ( 'NONE',  ( 0.05219959533937995610, -21.53943276465977519, 60.00109039468568284 ) ) ;
#196804 = CARTESIAN_POINT ( 'NONE',  ( -9.564922557961040184, 16.46253265017147172, 107.9177570613523471 ) ) ;
#196806 = CARTESIAN_POINT ( 'NONE',  ( -5.049401038298153566, 19.05341960407611168, 80.20724293864769550 ) ) ;
#196805 = DIRECTION ( 'NONE',  ( -0.000000000000000000, 0.5000000000000001110, 0.8660254037844385966 ) ) ;
#196807 = ADVANCED_FACE ( 'NONE', ( #148980 ), #25651, .F. ) ;
#196808 = CARTESIAN_POINT ( 'NONE',  ( 19.03943276465977164, -0.05219959533909143690, 113.7489096053143669 ) ) ;
#196810 = CARTESIAN_POINT ( 'NONE',  ( 5.153800228976335163, 19.02544592524342804, 74.79057627198103830 ) ) ;
#196809 = CARTESIAN_POINT ( 'NONE',  ( 16.55341960407611168, 4.379528057220329451, 73.95724293864769550 ) ) ;
#196811 = CARTESIAN_POINT ( 'NONE',  ( -19.05341960407611168, -5.049401038298163336, 71.45724293864766707 ) ) ;
#196812 = CARTESIAN_POINT ( 'NONE',  ( -13.89961937509957401, -13.97604488694547875, 74.37609039468566152 ) ) ;
#196813 = CARTESIAN_POINT ( 'NONE',  ( -18.62759615963270932, 10.81492255796079327, 60.83224293864769550 ) ) ;
#196814 = CARTESIAN_POINT ( 'NONE',  ( -12.06949235617756955, 12.14591786802309770, 115.6239096053143669 ) ) ;
#196815 = CARTESIAN_POINT ( 'NONE',  ( -19.02544592524334988, -5.153800228976617603, 53.95942372801898301 ) ) ;
#196816 = CARTESIAN_POINT ( 'NONE',  ( -16.46253265017160317, 9.564922557960807481, 50.83224293864770260 ) ) ;
#196817 = CARTESIAN_POINT ( 'NONE',  ( -9.474510206698964154, 16.51473224551069663, 95.41557627198102409 ) ) ;
#196818 = CARTESIAN_POINT ( 'NONE',  ( -18.67979575497178146, -10.72451020669898902, 96.66557627198102409 ) ) ;
#196820 = CARTESIAN_POINT ( 'NONE',  ( 16.46253265017146816, 9.564922557961045513, 46.66775706135233293 ) ) ;
#196819 = CARTESIAN_POINT ( 'NONE',  ( 4.483927247898545687, 16.52544592524342804, 99.79057627198103830 ) ) ;
#196821 = CARTESIAN_POINT ( 'NONE',  ( -15.80617190586745835, -15.72974639402198527, 76.87390960531439532 ) ) ;
#196822 = CARTESIAN_POINT ( 'NONE',  ( -21.53943276465977519, 0.05219959533907696930, 56.24890960531436690 ) ) ;
#196823 = CARTESIAN_POINT ( 'NONE',  ( -16.52544592524342804, 4.483927247898546575, 31.04057627198102409 ) ) ;
#196824 = CARTESIAN_POINT ( 'NONE',  ( 10.81492255796106328, -18.62759615963255655, 100.4177570613523471 ) ) ;
#196825 = CARTESIAN_POINT ( 'NONE',  ( -16.46253265017160317, 9.564922557960807481, 80.83224293864769550 ) ) ;
#196826 = CARTESIAN_POINT ( 'NONE',  ( 19.05341960407611168, 5.049401038298154454, 38.95724293864767418 ) ) ;
#196827 = CARTESIAN_POINT ( 'NONE',  ( 10.72451020669871369, 18.67979575497193778, 37.08442372801901143 ) ) ;
#196828 = CARTESIAN_POINT ( 'NONE',  ( 15.80617190586769283, -15.72974639402175789, 35.62609039468568994 ) ) ;
#196829 = CARTESIAN_POINT ( 'NONE',  ( 19.02544592524343514, -5.153800228976328945, 53.54057627198102409 ) ) ;
#196830 = CARTESIAN_POINT ( 'NONE',  ( 10.72451020669871369, 18.67979575497193778, 27.08442372801901854 ) ) ;
#196831 = CARTESIAN_POINT ( 'NONE',  ( 19.03943276465977164, 0.05219959533936151252, 61.25109039468566863 ) ) ;
#196832 = ADVANCED_FACE ( 'NONE', ( #72130 ), #166146, .F. ) ;
#196833 = CARTESIAN_POINT ( 'NONE',  ( -16.46253265017160317, 9.564922557960807481, 30.83224293864769550 ) ) ;
#196834 = CARTESIAN_POINT ( 'NONE',  ( 12.14591786802327356, -12.06949235617739191, 30.62609039468567929 ) ) ;
#196835 = CARTESIAN_POINT ( 'NONE',  ( 13.89961937509977652, -13.97604488694527269, 28.12390960531435624 ) ) ;
#196836 = CARTESIAN_POINT ( 'NONE',  ( 12.06949235617739724, 12.14591786802326823, 71.87609039468568994 ) ) ;
#196837 = CARTESIAN_POINT ( 'NONE',  ( 5.153800228976335163, 19.02544592524342804, 44.79057627198103830 ) ) ;
#196838 = CARTESIAN_POINT ( 'NONE',  ( -23.03403192006591382, -14.65170476119024556, 170.0000000000000000 ) ) ;
#196839 = CARTESIAN_POINT ( 'NONE',  ( 9.564922557960805705, 16.46253265017160317, 89.58224293864769550 ) ) ;
#196840 = CARTESIAN_POINT ( 'NONE',  ( -5.049401038298153566, 19.05341960407611168, 25.20724293864768484 ) ) ;
#196841 = CARTESIAN_POINT ( 'NONE',  ( 21.52544592524344225, -5.823673210054117533, 78.54057627198103830 ) ) ;
#196842 = CARTESIAN_POINT ( 'NONE',  ( 8.224510206698742110, 14.34966873604972548, 47.08442372801901854 ) ) ;
#196843 = CARTESIAN_POINT ( 'NONE',  ( 21.53943276465977519, 0.05219959533937863772, 96.25109039468568994 ) ) ;
#196844 = CARTESIAN_POINT ( 'NONE',  ( -16.46253265017160317, 9.564922557960807481, 40.83224293864769550 ) ) ;
#196845 = CARTESIAN_POINT ( 'NONE',  ( -16.55341960407611168, -4.379528057220339221, 31.45724293864769550 ) ) ;
#196846 = CARTESIAN_POINT ( 'NONE',  ( 14.34966873604960469, 8.224510206698951720, 69.16557627198102409 ) ) ;
#196847 = CIRCLE ( 'NONE', #112797, 0.1999999999999987899 ) ;
#196848 = CARTESIAN_POINT ( 'NONE',  ( 19.02544592524343514, -5.153800228976328945, 63.54057627198103830 ) ) ;
#196849 = CARTESIAN_POINT ( 'NONE',  ( -10.72451020669870658, -18.67979575497194134, 104.5844237280190185 ) ) ;
#196850 = CARTESIAN_POINT ( 'NONE',  ( 15.72974639402176855, 15.80617190586768217, 21.87609039468567573 ) ) ;
#196851 = CARTESIAN_POINT ( 'NONE',  ( -9.474510206698964154, 16.51473224551069663, 85.41557627198102409 ) ) ;
#196852 = CARTESIAN_POINT ( 'NONE',  ( -21.55341960407619339, 5.719274019375674811, 88.54275706135236135 ) ) ;
#196853 = CARTESIAN_POINT ( 'NONE',  ( 8.224510206698742110, 14.34966873604972548, 47.08442372801901854 ) ) ;
#196854 = CARTESIAN_POINT ( 'NONE',  ( -14.34966873604972548, 8.224510206698743886, 23.33442372801901499 ) ) ;
#196856 = CARTESIAN_POINT ( 'NONE',  ( 0.05219959533937995610, -21.53943276465977519, 105.0010903946856757 ) ) ;
#196855 = CARTESIAN_POINT ( 'NONE',  ( -4.379528057220328563, 16.55341960407611168, 90.20724293864770971 ) ) ;
#196857 = CARTESIAN_POINT ( 'NONE',  ( -16.52544592524342804, 4.483927247898546575, 36.04057627198102409 ) ) ;
#196858 = CARTESIAN_POINT ( 'NONE',  ( 13.97604488694527802, 13.89961937509977652, 34.37390960531436690 ) ) ;
#196859 = CARTESIAN_POINT ( 'NONE',  ( 4.483927247898790824, -16.52544592524335698, 55.20942372801902565 ) ) ;
#196860 = CARTESIAN_POINT ( 'NONE',  ( -12.06949235617756955, 12.14591786802309770, 60.62390960531437401 ) ) ;
#196861 = CARTESIAN_POINT ( 'NONE',  ( -14.29746914071037622, -8.314922557961029526, 99.16775706135234714 ) ) ;
#196862 = CARTESIAN_POINT ( 'NONE',  ( -21.55341960407610458, -5.719274019375992779, 21.45724293864769550 ) ) ;
#196863 = CARTESIAN_POINT ( 'NONE',  ( 5.719274019375991003, -21.55341960407610458, 32.70724293864770260 ) ) ;
#196864 = CARTESIAN_POINT ( 'NONE',  ( 16.51473224551083163, -9.474510206698727899, 20.83442372801899722 ) ) ;
#196865 = CARTESIAN_POINT ( 'NONE',  ( 8.224510206698953496, -14.34966873604960469, 87.91557627198103830 ) ) ;
#196866 = CARTESIAN_POINT ( 'NONE',  ( -9.474510206698964154, 16.51473224551069663, 100.4155762719810241 ) ) ;
#196867 = VERTEX_POINT ( 'NONE', #56970 ) ;
#196868 = CARTESIAN_POINT ( 'NONE',  ( -4.483927247898782831, 16.52544592524335698, 42.70942372801901854 ) ) ;
#196869 = CARTESIAN_POINT ( 'NONE',  ( 5.153800228976335163, 19.02544592524342804, 44.79057627198103830 ) ) ;
#196870 = CARTESIAN_POINT ( 'NONE',  ( 4.379528057220092307, 16.55341960407617563, 42.29275706135235424 ) ) ;
#196871 = CARTESIAN_POINT ( 'NONE',  ( -19.03943276465977164, -0.05219959533935918106, 48.75109039468566863 ) ) ;
#196872 = CARTESIAN_POINT ( 'NONE',  ( 9.564922557960805705, 16.46253265017160317, 39.58224293864768839 ) ) ;
#196873 = CARTESIAN_POINT ( 'NONE',  ( 0.05219959533934541429, -16.53943276465976808, 75.00109039468568994 ) ) ;
#196874 = CARTESIAN_POINT ( 'NONE',  ( 5.153800228976615827, -19.02544592524334988, 95.20942372801897591 ) ) ;
#196875 = CARTESIAN_POINT ( 'NONE',  ( -19.02544592524334988, -5.153800228976617603, 28.95942372801900433 ) ) ;
#196876 = CARTESIAN_POINT ( 'NONE',  ( -5.153800228976328057, -19.02544592524343514, 57.29057627198103120 ) ) ;
#196877 = CARTESIAN_POINT ( 'NONE',  ( 12.06949235617757843, -12.14591786802309237, 93.12390960531436690 ) ) ;
#196878 = EDGE_CURVE ( 'NONE', #5010, #176889, #117464, .T. ) ;
#196879 = CARTESIAN_POINT ( 'NONE',  ( -13.89961937509957401, -13.97604488694547875, 64.37609039468567573 ) ) ;
#196880 = CARTESIAN_POINT ( 'NONE',  ( 18.67979575497178502, 10.72451020669898547, 64.16557627198102409 ) ) ;
#196881 = CARTESIAN_POINT ( 'NONE',  ( 9.564922557961047289, -16.46253265017146816, 40.41775706135234003 ) ) ;
#196882 = CARTESIAN_POINT ( 'NONE',  ( 5.153800228976335163, 19.02544592524342804, 99.79057627198102409 ) ) ;
#196883 = CARTESIAN_POINT ( 'NONE',  ( 0.05219959533907565091, 21.53943276465977519, 74.99890960531435269 ) ) ;
#196884 = CARTESIAN_POINT ( 'NONE',  ( -16.81555441253553695, 7.025013491695484724, 85.63685445334262170 ) ) ;
#196885 = CARTESIAN_POINT ( 'NONE',  ( 13.89961937509957401, 13.97604488694547697, 96.87609039468566152 ) ) ;
#196886 = CARTESIAN_POINT ( 'NONE',  ( -9.564922557961040184, 16.46253265017147172, 97.91775706135233293 ) ) ;
#196887 = CARTESIAN_POINT ( 'NONE',  ( 14.34966873604972726, -8.224510206698740333, 30.83442372801902209 ) ) ;
#196888 = CARTESIAN_POINT ( 'NONE',  ( 19.05341960407611168, 5.049401038298154454, 43.95724293864769550 ) ) ;
#196889 = CARTESIAN_POINT ( 'NONE',  ( -9.474510206698964154, 16.51473224551069663, 110.4155762719810383 ) ) ;
#196890 = CARTESIAN_POINT ( 'NONE',  ( -10.72451020669898014, 18.67979575497178502, 90.41557627198103830 ) ) ;
#196891 = CARTESIAN_POINT ( 'NONE',  ( 5.823673210054444382, -21.52544592524334988, 60.20942372801902565 ) ) ;
#196893 = CARTESIAN_POINT ( 'NONE',  ( -10.72451020669870658, -18.67979575497194134, 104.5844237280190185 ) ) ;
#196892 = CARTESIAN_POINT ( 'NONE',  ( 0.05219959533936267826, -19.03943276465977164, 105.0010903946856615 ) ) ;
#196894 = CARTESIAN_POINT ( 'NONE',  ( 8.314922557961029526, -14.29746914071037800, 105.4177570613523613 ) ) ;
#196895 = CARTESIAN_POINT ( 'NONE',  ( -18.62759615963270932, 10.81492255796079327, 100.8322429386477097 ) ) ;
#196896 = CARTESIAN_POINT ( 'NONE',  ( -0.05219959533910754901, -16.53943276465976808, 47.49890960531435979 ) ) ;
#196897 = CARTESIAN_POINT ( 'NONE',  ( 13.97604488694548053, -13.89961937509957401, 85.62609039468568994 ) ) ;
#196898 = CARTESIAN_POINT ( 'NONE',  ( 9.474510206698729675, 16.51473224551082808, 57.08442372801900433 ) ) ;
#196899 = CARTESIAN_POINT ( 'NONE',  ( 15.72974639402176855, 15.80617190586768217, 76.87609039468567573 ) ) ;
#196900 = CARTESIAN_POINT ( 'NONE',  ( 9.474510206698729675, 16.51473224551082808, 37.08442372801899722 ) ) ;
#196901 = CARTESIAN_POINT ( 'NONE',  ( -16.53943276465976808, 0.05219959533911058130, 101.2489096053143669 ) ) ;
#196902 = CARTESIAN_POINT ( 'NONE',  ( 10.81492255796078972, 18.62759615963270932, 44.58224293864769550 ) ) ;
#196903 = CARTESIAN_POINT ( 'NONE',  ( 8.314922557960818139, 14.29746914071049879, 39.58224293864769550 ) ) ;
#196904 = CARTESIAN_POINT ( 'NONE',  ( 21.55341960407619695, -5.719274019375665929, 106.0427570613523471 ) ) ;
#196905 = CARTESIAN_POINT ( 'NONE',  ( 8.224510206698742110, 14.34966873604972548, 67.08442372801901854 ) ) ;
#196906 = CARTESIAN_POINT ( 'NONE',  ( -4.379528057220328563, 16.55341960407611168, 25.20724293864769550 ) ) ;
#196907 = CARTESIAN_POINT ( 'NONE',  ( 15.80617190586769283, -15.72974639402175789, 60.62609039468567573 ) ) ;
#196908 = CARTESIAN_POINT ( 'NONE',  ( 0.05219959533937995610, -21.53943276465977519, 70.00109039468568994 ) ) ;
#196909 = CARTESIAN_POINT ( 'NONE',  ( 21.55341960407610458, 5.719274019375980345, 73.95724293864769550 ) ) ;
#196910 = ORIENTED_EDGE ( 'NONE', *, *, #110318, .T. ) ;
#196911 = CARTESIAN_POINT ( 'NONE',  ( -16.46253265017160317, 9.564922557960807481, 30.83224293864769550 ) ) ;
#196912 = CARTESIAN_POINT ( 'NONE',  ( -21.52544592524334988, -5.823673210054445271, 48.95942372801902565 ) ) ;
#196913 = CARTESIAN_POINT ( 'NONE',  ( 9.564922557960805705, 16.46253265017160317, 24.58224293864769194 ) ) ;
#196914 = CARTESIAN_POINT ( 'NONE',  ( 16.51473224551069308, 9.474510206698969483, 39.16557627198103120 ) ) ;
#196915 = CARTESIAN_POINT ( 'NONE',  ( 0.05219959533910956823, 16.53943276465976808, 89.99890960531438111 ) ) ;
#196916 = CARTESIAN_POINT ( 'NONE',  ( 13.89961937509977652, -13.97604488694527269, 88.12390960531438111 ) ) ;
#196917 = CARTESIAN_POINT ( 'NONE',  ( 16.53943276465976808, -0.05219959533910856209, 33.74890960531436690 ) ) ;
#196918 = CARTESIAN_POINT ( 'NONE',  ( 0.05219959533910956823, 16.53943276465976808, 99.99890960531436690 ) ) ;
#196919 = CARTESIAN_POINT ( 'NONE',  ( -10.72451020669898014, 18.67979575497178502, 70.41557627198102409 ) ) ;
#196920 = CARTESIAN_POINT ( 'NONE',  ( -18.62759615963270932, 10.81492255796079327, 110.8322429386476955 ) ) ;
#196921 = CARTESIAN_POINT ( 'NONE',  ( 0.05219959533909260263, 19.03943276465977164, 109.9989096053143669 ) ) ;
#196923 = CARTESIAN_POINT ( 'NONE',  ( -12.06949235617739369, -12.14591786802326823, 24.37609039468567573 ) ) ;
#196922 = CARTESIAN_POINT ( 'NONE',  ( -13.89961937509977652, 13.97604488694528158, 70.62390960531432427 ) ) ;
#196924 = CARTESIAN_POINT ( 'NONE',  ( -5.719274019375978568, 21.55341960407610458, 60.20724293864768839 ) ) ;
#196925 = CARTESIAN_POINT ( 'NONE',  ( -21.55341960407619339, 5.719274019375674811, 83.54275706135234714 ) ) ;
#196926 = CARTESIAN_POINT ( 'NONE',  ( -19.05341960407611168, -5.049401038298163336, 86.45724293864769550 ) ) ;
#196927 = CARTESIAN_POINT ( 'NONE',  ( 16.46253265017160672, -9.564922557960803928, 113.3322429386476955 ) ) ;
#196928 = CARTESIAN_POINT ( 'NONE',  ( 4.483927247898790824, -16.52544592524335698, 75.20942372801901854 ) ) ;
#196929 = CARTESIAN_POINT ( 'NONE',  ( -21.52544592524334988, -5.823673210054445271, 53.95942372801900433 ) ) ;
#196930 = CARTESIAN_POINT ( 'NONE',  ( 21.55341960407619695, -5.719274019375665929, 106.0427570613523471 ) ) ;
#196931 = CARTESIAN_POINT ( 'NONE',  ( -12.06949235617739369, -12.14591786802326823, 64.37609039468568994 ) ) ;
#196932 = CARTESIAN_POINT ( 'NONE',  ( 21.53943276465977519, 0.05219959533937863772, 21.25109039468567218 ) ) ;
#196933 = CARTESIAN_POINT ( 'NONE',  ( 15.50000000000000178, 5.499999999999998224, 20.00000000000000000 ) ) ;
#196934 = CARTESIAN_POINT ( 'NONE',  ( 10.72451020669898902, -18.67979575497178502, 92.91557627198103830 ) ) ;
#196935 = CARTESIAN_POINT ( 'NONE',  ( -16.51473224551082808, 9.474510206698731452, 43.33442372801900433 ) ) ;
#196936 = CARTESIAN_POINT ( 'NONE',  ( -21.52544592524343514, 5.823673210054127303, 56.04057627198102409 ) ) ;
#196938 = CARTESIAN_POINT ( 'NONE',  ( 8.314922557960818139, 14.29746914071049879, 39.58224293864769550 ) ) ;
#196937 = CARTESIAN_POINT ( 'NONE',  ( 5.153800228976335163, 19.02544592524342804, 99.79057627198102409 ) ) ;
#196939 = CARTESIAN_POINT ( 'NONE',  ( 10.78896075761529261, -9.218258452770006883, -62.39945043303440997 ) ) ;
#196940 = CARTESIAN_POINT ( 'NONE',  ( 1.220435812286612354, 14.30591040068875408, -60.18371924376236137 ) ) ;
#196941 = CARTESIAN_POINT ( 'NONE',  ( -13.89961937509957401, -13.97604488694547875, 109.3760903946856331 ) ) ;
#196942 = CARTESIAN_POINT ( 'NONE',  ( -21.53943276465977519, 0.05219959533907696930, 76.24890960531435269 ) ) ;
#196943 = CARTESIAN_POINT ( 'NONE',  ( 4.379528057220339221, -16.55341960407611168, 52.70724293864769550 ) ) ;
#196944 = CARTESIAN_POINT ( 'NONE',  ( -14.29746914071037622, -8.314922557961029526, 34.16775706135234714 ) ) ;
#196945 = CARTESIAN_POINT ( 'NONE',  ( 13.89961937509977652, -13.97604488694527269, 43.12390960531434558 ) ) ;
#196947 = CARTESIAN_POINT ( 'NONE',  ( -9.564922557961040184, 16.46253265017147172, 82.91775706135233293 ) ) ;
#196946 = CARTESIAN_POINT ( 'NONE',  ( 21.55341960407610458, 5.719274019375980345, 108.9572429386476955 ) ) ;
#196948 = CARTESIAN_POINT ( 'NONE',  ( 0.05219959533909260263, 19.03943276465977164, 79.99890960531436690 ) ) ;
#196949 = CARTESIAN_POINT ( 'NONE',  ( 0.05219959533909260263, 19.03943276465977164, 69.99890960531435269 ) ) ;
#196950 = CARTESIAN_POINT ( 'NONE',  ( 10.72451020669898902, -18.67979575497178502, 77.91557627198102409 ) ) ;
#196951 = CARTESIAN_POINT ( 'NONE',  ( -19.03943276465977164, 0.05219959533909376836, 36.24890960531436690 ) ) ;
#196952 = CARTESIAN_POINT ( 'NONE',  ( -11.30153831258471975, -180.0000000000000000, -15.00000000000000178 ) ) ;
#196953 = CARTESIAN_POINT ( 'NONE',  ( 8.224510206698953496, -14.34966873604960469, 52.91557627198103830 ) ) ;
#196954 = CARTESIAN_POINT ( 'NONE',  ( -13.89961937509977652, 13.97604488694528158, 95.62390960531436690 ) ) ;
#196955 = DIRECTION ( 'NONE',  ( -0.000000000000000000, -0.000000000000000000, 1.000000000000000000 ) ) ;
#196956 = CARTESIAN_POINT ( 'NONE',  ( -19.02544592524334988, -5.153800228976617603, 63.95942372801899012 ) ) ;
#196957 = CARTESIAN_POINT ( 'NONE',  ( -10.72451020669898014, 18.67979575497178502, 75.41557627198102409 ) ) ;
#196958 = CARTESIAN_POINT ( 'NONE',  ( -16.46253265017146816, -9.564922557961047289, 39.16775706135234003 ) ) ;
#196959 = CARTESIAN_POINT ( 'NONE',  ( -5.153800228976328057, -19.02544592524343514, 87.29057627198103830 ) ) ;
#196960 = CARTESIAN_POINT ( 'NONE',  ( -17.50000000000146017, 3.254303733634615892, 115.0239589307140307 ) ) ;
#196961 = CARTESIAN_POINT ( 'NONE',  ( 10.81492255796078972, 18.62759615963270932, 29.58224293864769905 ) ) ;
#196962 = CARTESIAN_POINT ( 'NONE',  ( 16.46253265017160672, -9.564922557960803928, 73.33224293864769550 ) ) ;
#196963 = CARTESIAN_POINT ( 'NONE',  ( -21.55341960407619339, 5.719274019375674811, 48.54275706135234714 ) ) ;
#196964 = CARTESIAN_POINT ( 'NONE',  ( -5.049401038298153566, 19.05341960407611168, 25.20724293864768484 ) ) ;
#196966 = VERTEX_POINT ( 'NONE', #120611 ) ;
#196965 = CARTESIAN_POINT ( 'NONE',  ( 21.55341960407610458, 5.719274019375980345, 113.9572429386477239 ) ) ;
#196967 = CARTESIAN_POINT ( 'NONE',  ( -0.05219959533937732626, 21.53943276465977519, 42.50109039468567573 ) ) ;
#196968 = ORIENTED_EDGE ( 'NONE', *, *, #73495, .T. ) ;
#196969 = CARTESIAN_POINT ( 'NONE',  ( 0.05219959533909260263, 19.03943276465977164, 94.99890960531436690 ) ) ;
#196970 = EDGE_CURVE ( 'NONE', #90049, #177604, #182305, .T. ) ;
#196971 = CARTESIAN_POINT ( 'NONE',  ( 4.999999999999996447, 37.66961640367475184, -15.00000000000000000 ) ) ;
#196972 = CARTESIAN_POINT ( 'NONE',  ( 18.62759615963271287, -10.81492255796078972, 113.3322429386476955 ) ) ;
#196973 = CARTESIAN_POINT ( 'NONE',  ( -13.89961937509977652, 13.97604488694528158, 65.62390960531436690 ) ) ;
#196974 = CARTESIAN_POINT ( 'NONE',  ( -16.53943276465976808, -0.05219959533934237506, 18.75109039468568639 ) ) ;
#196975 = CARTESIAN_POINT ( 'NONE',  ( -23.48529157249599919, -32.32473071737750558, -5.449999994537626513 ) ) ;
#196976 = CARTESIAN_POINT ( 'NONE',  ( -10.81492255796105439, 18.62759615963255655, 102.9177570613523756 ) ) ;
#196977 = CARTESIAN_POINT ( 'NONE',  ( -5.153800228976328057, -19.02544592524343514, 47.29057627198102409 ) ) ;
#196978 = CARTESIAN_POINT ( 'NONE',  ( 15.80617190586769283, -15.72974639402175789, 95.62609039468568994 ) ) ;
#196980 = CARTESIAN_POINT ( 'NONE',  ( -0.05219959533937732626, 21.53943276465977519, 62.50109039468568284 ) ) ;
#196979 = CARTESIAN_POINT ( 'NONE',  ( 13.89961937509977652, -13.97604488694527269, 88.12390960531438111 ) ) ;
#196981 = VECTOR ( 'NONE', #31122, 1000.000000000000114 ) ;
#196982 = CARTESIAN_POINT ( 'NONE',  ( -27.73933785331498925, -9.013057229001049109, 143.4750000027311785 ) ) ;
#196983 = CARTESIAN_POINT ( 'NONE',  ( 9.564922557960805705, 16.46253265017160317, 104.5822429386476955 ) ) ;
#196984 = CARTESIAN_POINT ( 'NONE',  ( -17.50000000000149569, 3.202012800152202576, 29.92822416027271970 ) ) ;
#196987 = CARTESIAN_POINT ( 'NONE',  ( 5.719274019375673035, 21.55341960407619339, 57.29275706135234714 ) ) ;
#196986 = CARTESIAN_POINT ( 'NONE',  ( -16.53943276465976808, -0.05219959533934237506, 63.75109039468568284 ) ) ;
#196985 = CARTESIAN_POINT ( 'NONE',  ( 12.14591786802327356, -12.06949235617739191, 55.62609039468568284 ) ) ;
#196988 = CARTESIAN_POINT ( 'NONE',  ( -21.53943276465977519, -0.05219959533937600094, 93.75109039468567573 ) ) ;
#196989 = CARTESIAN_POINT ( 'NONE',  ( -11.80868324581538253, 11.80868324581533457, -59.13370768023891344 ) ) ;
#196990 = CARTESIAN_POINT ( 'NONE',  ( -14.29746914071037622, -8.314922557961029526, 34.16775706135234714 ) ) ;
#196991 = CARTESIAN_POINT ( 'NONE',  ( -13.97604488694527625, -13.89961937509977652, 76.87390960531433848 ) ) ;
#196992 = CARTESIAN_POINT ( 'NONE',  ( -13.97604488694527625, -13.89961937509977652, 91.87390960531432427 ) ) ;
#196993 = CARTESIAN_POINT ( 'NONE',  ( 17.48853670773242186, 5.747243402303174875, 43.83328700250010002 ) ) ;
#196994 = CARTESIAN_POINT ( 'NONE',  ( 9.474510206698971260, -16.51473224551069308, 27.91557627198103120 ) ) ;
#196995 = CARTESIAN_POINT ( 'NONE',  ( -18.67979575497178146, -10.72451020669898902, 31.66557627198102054 ) ) ;
#196996 = CARTESIAN_POINT ( 'NONE',  ( 8.314922557961029526, -14.29746914071037800, 95.41775706135234714 ) ) ;
#196999 = CARTESIAN_POINT ( 'NONE',  ( 13.97604488694527802, 13.89961937509977652, 69.37390960531436690 ) ) ;
#196998 =( BOUNDED_CURVE ( )  B_SPLINE_CURVE ( 2, ( #129759, #67114, #96445, #6426, #36764, #50959, #114608, #8447, #53951, #115627, #38787 ),
 .UNSPECIFIED., .F., .T. ) 
 B_SPLINE_CURVE_WITH_KNOTS ( ( 3, 2, 2, 2, 2, 3 ),
 ( 0.4000000000000003553, 0.4200000000000003730, 0.4400000000000003353, 0.4600000000000003531, 0.4800000000000004263, 0.5000000000000004441 ),
 .UNSPECIFIED. ) 
 CURVE ( )  GEOMETRIC_REPRESENTATION_ITEM ( )  RATIONAL_B_SPLINE_CURVE ( ( 0.9999999999999992228, 0.9510565162951543083, 1.000000000000000000, 0.9510565162951535312, 1.000000000000000000, 0.9510565162951535312, 1.000000000000000000, 0.9510565162951535312, 1.000000000000000000, 0.9510565162951524210, 1.000000000000001110 ) ) 
 REPRESENTATION_ITEM ( '' )  );
#196997 = CARTESIAN_POINT ( 'NONE',  ( -0.05219959533910754901, -16.53943276465976808, 87.49890960531436690 ) ) ;
#197000 = CARTESIAN_POINT ( 'NONE',  ( 18.67979575497194134, -10.72451020669871369, 90.83442372801901854 ) ) ;
#197001 = CARTESIAN_POINT ( 'NONE',  ( -23.16108095314128690, 1.467328942211057585, -57.58004187413776265 ) ) ;
#197002 = CARTESIAN_POINT ( 'NONE',  ( -12.06949235617739369, -12.14591786802326823, 29.37609039468568284 ) ) ;
#197003 = CARTESIAN_POINT ( 'NONE',  ( 8.224510206698953496, -14.34966873604960469, 77.91557627198102409 ) ) ;
#197004 = CARTESIAN_POINT ( 'NONE',  ( 18.67979575497194134, -10.72451020669871369, 45.83442372801901854 ) ) ;
#197005 = CARTESIAN_POINT ( 'NONE',  ( 21.52544592524344225, -5.823673210054117533, 68.54057627198103830 ) ) ;
#197006 = CARTESIAN_POINT ( 'NONE',  ( -19.05341960407617563, 5.049401038297882671, 33.54275706135231871 ) ) ;
#197007 = CARTESIAN_POINT ( 'NONE',  ( -34.71410084532070073, 2.653616468751188506, 52.01918243487460103 ) ) ;
#197008 = CARTESIAN_POINT ( 'NONE',  ( -16.51473224551069308, -9.474510206698971260, 76.66557627198103830 ) ) ;
#197009 = CARTESIAN_POINT ( 'NONE',  ( -4.379528057220328563, 16.55341960407611168, 45.20724293864769550 ) ) ;
#197010 = AXIS2_PLACEMENT_3D ( 'NONE', #198328, #123446, #91118 ) ;
#197011 = CARTESIAN_POINT ( 'NONE',  ( 16.53943276465976808, -0.05219959533910856209, 28.74890960531435624 ) ) ;
#197012 = CARTESIAN_POINT ( 'NONE',  ( 16.52544592524342804, -4.483927247898539470, 23.54057627198102765 ) ) ;
#197013 = CARTESIAN_POINT ( 'NONE',  ( 19.02544592524334988, 5.153800228976608722, 71.45942372801900433 ) ) ;
#197014 = DIRECTION ( 'NONE',  ( -0.000000000000000000, -0.000000000000000000, 1.000000000000000000 ) ) ;
#197015 = CARTESIAN_POINT ( 'NONE',  ( 15.72974639402199770, -15.80617190586745480, 23.12390960531436335 ) ) ;
#197016 = CARTESIAN_POINT ( 'NONE',  ( 12.06949235617757843, -12.14591786802309237, 83.12390960531436690 ) ) ;
#197017 = CARTESIAN_POINT ( 'NONE',  ( -15.06137443927361019, -15.06137443927335440, -58.85720012050613548 ) ) ;
#197019 = CARTESIAN_POINT ( 'NONE',  ( -15.72974639402197994, 15.80617190586746368, 30.62390960531436335 ) ) ;
#197018 = CARTESIAN_POINT ( 'NONE',  ( 13.97604488694527802, 13.89961937509977652, 49.37390960531434558 ) ) ;
#197020 = CARTESIAN_POINT ( 'NONE',  ( 5.823673210054125526, 21.52544592524343514, 69.79057627198102409 ) ) ;
#197021 = CARTESIAN_POINT ( 'NONE',  ( -16.53943276465976808, 0.05219959533911058130, 116.2489096053143669 ) ) ;
#197023 = CARTESIAN_POINT ( 'NONE',  ( -16.51473224551069308, -9.474510206698971260, 51.66557627198102409 ) ) ;
#197022 = CARTESIAN_POINT ( 'NONE',  ( 0.05219959533934541429, -16.53943276465976808, 70.00109039468568994 ) ) ;
#197024 = CARTESIAN_POINT ( 'NONE',  ( 21.53943276465977519, 0.05219959533937863772, 51.25109039468568994 ) ) ;
#197025 = CARTESIAN_POINT ( 'NONE',  ( 0.05219959533910956823, 16.53943276465976808, 109.9989096053143527 ) ) ;
#197026 = CARTESIAN_POINT ( 'NONE',  ( 16.51473224551083163, -9.474510206698727899, 95.83442372801900433 ) ) ;
#197027 = CARTESIAN_POINT ( 'NONE',  ( -5.950531402560715689E-15, 38.81732327939063509, -7.624999997268814056 ) ) ;
#197029 = CARTESIAN_POINT ( 'NONE',  ( 18.62759615963271287, -10.81492255796078972, 28.33224293864769550 ) ) ;
#197028 = CARTESIAN_POINT ( 'NONE',  ( -0.8193109935766856866, -21.52594032250406642, -58.70475745007095014 ) ) ;
#197030 = CARTESIAN_POINT ( 'NONE',  ( 17.44270441346514389, -5.991230190323081573, 66.13664920735772057 ) ) ;
#197031 = CARTESIAN_POINT ( 'NONE',  ( 5.823673210054444382, -21.52544592524334988, 65.20942372801901854 ) ) ;
#197033 = CARTESIAN_POINT ( 'NONE',  ( -16.52544592524342804, 4.483927247898546575, 46.04057627198103830 ) ) ;
#197032 = CARTESIAN_POINT ( 'NONE',  ( -4.379528057220086978, -16.55341960407618274, 54.79275706135235424 ) ) ;
#197034 = CARTESIAN_POINT ( 'NONE',  ( -18.62759615963270932, 10.81492255796079327, 65.83224293864769550 ) ) ;
#197035 = CARTESIAN_POINT ( 'NONE',  ( -21.52544592524343514, 5.823673210054127303, 66.04057627198103830 ) ) ;
#197036 = CARTESIAN_POINT ( 'NONE',  ( -21.57728377622141380, -10.02787190051640742, 170.5958156194641617 ) ) ;
#197038 = CARTESIAN_POINT ( 'NONE',  ( 19.03943276465977164, -0.05219959533909143690, 113.7489096053143669 ) ) ;
#197037 = CARTESIAN_POINT ( 'NONE',  ( 5.153800228976615827, -19.02544592524334988, 85.20942372801900433 ) ) ;
#197039 = CARTESIAN_POINT ( 'NONE',  ( 16.46253265017160672, -9.564922557960803928, 53.33224293864768839 ) ) ;
#197040 = CARTESIAN_POINT ( 'NONE',  ( -8.224510206698948167, 14.34966873604960824, 115.4155762719810241 ) ) ;
#197041 = CARTESIAN_POINT ( 'NONE',  ( 5.049401038298161559, -19.05341960407611168, 112.7072429386476813 ) ) ;
#197042 = ORIENTED_EDGE ( 'NONE', *, *, #158579, .F. ) ;
#197043 = CARTESIAN_POINT ( 'NONE',  ( -14.29746914071037622, -8.314922557961029526, 69.16775706135234714 ) ) ;
#197044 = CARTESIAN_POINT ( 'NONE',  ( 5.719274019375991003, -21.55341960407610458, 107.7072429386476955 ) ) ;
#197045 = CARTESIAN_POINT ( 'NONE',  ( -16.46253265017160317, 9.564922557960807481, 65.83224293864769550 ) ) ;
#197046 = CARTESIAN_POINT ( 'NONE',  ( -18.62759615963255300, -10.81492255796106328, 39.16775706135235424 ) ) ;
#197047 = CARTESIAN_POINT ( 'NONE',  ( -9.474510206698964154, 16.51473224551069663, 100.4155762719810241 ) ) ;
#197048 = CARTESIAN_POINT ( 'NONE',  ( -20.09009762002150978, -36.41118502144959024, -19.08443133123632762 ) ) ;
#197049 = VERTEX_POINT ( 'NONE', #133804 ) ;
#197050 = CARTESIAN_POINT ( 'NONE',  ( 21.52544592524334988, 5.823673210054432836, 31.45942372801901854 ) ) ;
#197052 = CARTESIAN_POINT ( 'NONE',  ( -5.049401038297874678, -19.05341960407617918, 89.79275706135230450 ) ) ;
#197051 = CARTESIAN_POINT ( 'NONE',  ( 19.05341960407611168, 5.049401038298154454, 23.95724293864769194 ) ) ;
#197053 = CARTESIAN_POINT ( 'NONE',  ( 0.05219959533936267826, -19.03943276465977164, 40.00109039468566152 ) ) ;
#197054 = CARTESIAN_POINT ( 'NONE',  ( -5.823673210054116645, -21.52544592524344225, 102.2905762719810383 ) ) ;
#197055 = CARTESIAN_POINT ( 'NONE',  ( -13.97604488694547697, 13.89961937509957934, 33.12609039468566863 ) ) ;
#197056 = CARTESIAN_POINT ( 'NONE',  ( -0.05219959533936034679, 19.03943276465977164, 47.50109039468566863 ) ) ;
#197057 = CARTESIAN_POINT ( 'NONE',  ( -4.379528057220086978, -16.55341960407618274, 89.79275706135236135 ) ) ;
#197059 = ORIENTED_EDGE ( 'NONE', *, *, #149169, .F. ) ;
#197058 = CARTESIAN_POINT ( 'NONE',  ( 16.51473224551069308, 9.474510206698969483, 114.1655762719810241 ) ) ;
#197060 = CARTESIAN_POINT ( 'NONE',  ( 19.05341960407611168, 5.049401038298154454, 78.95724293864769550 ) ) ;
#197061 = CARTESIAN_POINT ( 'NONE',  ( 10.72451020669871369, 18.67979575497193778, 82.08442372801901854 ) ) ;
#197062 = CARTESIAN_POINT ( 'NONE',  ( 5.823673210054444382, -21.52544592524334988, 90.20942372801903275 ) ) ;
#197063 = CARTESIAN_POINT ( 'NONE',  ( -1.425084765988079205, -7.121805330552575697, -64.33521149768087355 ) ) ;
#197064 = CARTESIAN_POINT ( 'NONE',  ( -5.153800228976328057, -19.02544592524343514, 87.29057627198103830 ) ) ;
#197065 = CARTESIAN_POINT ( 'NONE',  ( 18.67979575497194134, -10.72451020669871369, 60.83442372801901854 ) ) ;
#197066 = CARTESIAN_POINT ( 'NONE',  ( 13.89961937509957401, 13.97604488694547697, 106.8760903946856757 ) ) ;
#197067 = EDGE_CURVE ( 'NONE', #40368, #16134, #30519, .T. ) ;
#197068 = CARTESIAN_POINT ( 'NONE',  ( 9.564922557960805705, 16.46253265017160317, 59.58224293864769550 ) ) ;
#197069 = CARTESIAN_POINT ( 'NONE',  ( -5.049401038298153566, 19.05341960407611168, 115.2072429386477097 ) ) ;
#197070 = CARTESIAN_POINT ( 'NONE',  ( -5.153800228976328057, -19.02544592524343514, 82.29057627198103830 ) ) ;
#197071 = LINE ( 'NONE', #14016, #104796 ) ;
#197072 = CARTESIAN_POINT ( 'NONE',  ( -5.153800228976328057, -19.02544592524343514, 67.29057627198102409 ) ) ;
#197073 = CARTESIAN_POINT ( 'NONE',  ( -16.46253265017160317, 9.564922557960807481, 45.83224293864769550 ) ) ;
#197074 = CARTESIAN_POINT ( 'NONE',  ( -15.72974639402176322, -15.80617190586768395, 19.37609039468568639 ) ) ;
#197075 = CARTESIAN_POINT ( 'NONE',  ( 4.379528057220092307, 16.55341960407617563, 82.29275706135234714 ) ) ;
#197076 = CARTESIAN_POINT ( 'NONE',  ( -6.856101608890819192E-16, -64.86648100006283357, -12.99999901186700946 ) ) ;
#197077 = CARTESIAN_POINT ( 'NONE',  ( -19.02544592524334988, -5.153800228976617603, 48.95942372801900433 ) ) ;
#197078 = CARTESIAN_POINT ( 'NONE',  ( -19.02544592524342804, 5.153800228976336051, 86.04057627198103830 ) ) ;
#197079 = CARTESIAN_POINT ( 'NONE',  ( -4.483927247898539470, -16.52544592524342804, 67.29057627198103830 ) ) ;
#197080 = CARTESIAN_POINT ( 'NONE',  ( 12.06949235617757843, -12.14591786802309237, 113.1239096053143953 ) ) ;
#197081 = CARTESIAN_POINT ( 'NONE',  ( 18.67979575497178502, 10.72451020669898547, 24.16557627198103120 ) ) ;
#197082 = CARTESIAN_POINT ( 'NONE',  ( 5.049401038298161559, -19.05341960407611168, 107.7072429386476955 ) ) ;
#197083 = CARTESIAN_POINT ( 'NONE',  ( 14.29746914071049879, -8.314922557960816363, 73.33224293864769550 ) ) ;
#197084 = CARTESIAN_POINT ( 'NONE',  ( 37.99626262588765258, 2.893932880411085066E-14, -3.002157773949822861 ) ) ;
#197085 = CARTESIAN_POINT ( 'NONE',  ( 13.97604488694548053, -13.89961937509957401, 30.62609039468566863 ) ) ;
#197086 = CARTESIAN_POINT ( 'NONE',  ( 8.314922557961029526, -14.29746914071037800, 100.4177570613523471 ) ) ;
#197087 = CARTESIAN_POINT ( 'NONE',  ( 13.97604488694527802, 13.89961937509977652, 84.37390960531433848 ) ) ;
#197088 = CARTESIAN_POINT ( 'NONE',  ( -15.72974639402176322, -15.80617190586768395, 59.37609039468568284 ) ) ;
#197089 = CARTESIAN_POINT ( 'NONE',  ( -0.05219959533907301413, -21.53943276465977519, 42.49890960531435979 ) ) ;
#197090 = CARTESIAN_POINT ( 'NONE',  ( -15.72974639402197994, 15.80617190586746368, 110.6239096053143669 ) ) ;
#197091 = CARTESIAN_POINT ( 'NONE',  ( 0.05219959533907565091, 21.53943276465977519, 64.99890960531435269 ) ) ;
#197092 = CARTESIAN_POINT ( 'NONE',  ( -16.53943276465976808, 0.05219959533911058130, 101.2489096053143669 ) ) ;
#197093 = CARTESIAN_POINT ( 'NONE',  ( 9.474510206698729675, 16.51473224551082808, 57.08442372801900433 ) ) ;
#197094 = CARTESIAN_POINT ( 'NONE',  ( -5.049401038298153566, 19.05341960407611168, 25.20724293864768484 ) ) ;
#197095 = CARTESIAN_POINT ( 'NONE',  ( 5.049401038298161559, -19.05341960407611168, 77.70724293864765286 ) ) ;
#197096 = CARTESIAN_POINT ( 'NONE',  ( 13.89961937509977652, -13.97604488694527269, 78.12390960531433848 ) ) ;
#197097 = CARTESIAN_POINT ( 'NONE',  ( 8.314922557960818139, 14.29746914071049879, 99.58224293864770971 ) ) ;
#197098 = ORIENTED_EDGE ( 'NONE', *, *, #162675, .T. ) ;
#197099 = CARTESIAN_POINT ( 'NONE',  ( -4.379528057220328563, 16.55341960407611168, 25.20724293864769550 ) ) ;
#197100 = CARTESIAN_POINT ( 'NONE',  ( -8.224510206698735004, -14.34966873604973081, 44.58442372801901854 ) ) ;
#197101 = CARTESIAN_POINT ( 'NONE',  ( -10.81492255796105439, 18.62759615963255655, 102.9177570613523756 ) ) ;
#197102 = CARTESIAN_POINT ( 'NONE',  ( -13.89961937509977652, 13.97604488694528158, 95.62390960531436690 ) ) ;
#197103 = CARTESIAN_POINT ( 'NONE',  ( -21.52544592524334988, -5.823673210054445271, 33.95942372801901143 ) ) ;
#197104 = CARTESIAN_POINT ( 'NONE',  ( 13.97604488694527802, 13.89961937509977652, 44.37390960531435269 ) ) ;
#197105 = CARTESIAN_POINT ( 'NONE',  ( 4.483927247898790824, -16.52544592524335698, 45.20942372801901854 ) ) ;
#197106 = CARTESIAN_POINT ( 'NONE',  ( 19.03943276465977164, 0.05219959533936151252, 111.2510903946856757 ) ) ;
#197107 = CARTESIAN_POINT ( 'NONE',  ( 9.564922557960805705, 16.46253265017160317, 34.58224293864770260 ) ) ;
#197108 = CARTESIAN_POINT ( 'NONE',  ( -16.53943276465976808, 0.05219959533911058130, 91.24890960531436690 ) ) ;
#197109 = CARTESIAN_POINT ( 'NONE',  ( 21.53943276465977519, -0.05219959533907433946, 103.7489096053143669 ) ) ;
#197110 = CARTESIAN_POINT ( 'NONE',  ( 13.97604488694548053, -13.89961937509957401, 75.62609039468564731 ) ) ;
#197111 = CARTESIAN_POINT ( 'NONE',  ( -13.97604488694527625, -13.89961937509977652, 86.87390960531436690 ) ) ;
#197112 = CARTESIAN_POINT ( 'NONE',  ( -21.52544592524334988, -5.823673210054445271, 33.95942372801901143 ) ) ;
#197113 = CARTESIAN_POINT ( 'NONE',  ( -19.05341960407611168, -5.049401038298163336, 21.45724293864768839 ) ) ;
#197114 = CARTESIAN_POINT ( 'NONE',  ( 5.049401038298161559, -19.05341960407611168, 92.70724293864769550 ) ) ;
#197115 = CARTESIAN_POINT ( 'NONE',  ( 4.000000000000000888, -165.0000000000000000, 12.00000000000000355 ) ) ;
#197116 = CARTESIAN_POINT ( 'NONE',  ( 5.153800228976335163, 19.02544592524342804, 84.79057627198099567 ) ) ;
#197118 = CARTESIAN_POINT ( 'NONE',  ( 0.05219959533910956823, 16.53943276465976808, 89.99890960531438111 ) ) ;
#197117 = CARTESIAN_POINT ( 'NONE',  ( -10.81492255796105439, 18.62759615963255655, 32.91775706135234714 ) ) ;
#197119 = CARTESIAN_POINT ( 'NONE',  ( -9.564922557960796823, -16.46253265017161027, 102.0822429386477097 ) ) ;
#197120 = CARTESIAN_POINT ( 'NONE',  ( -18.67979575497193778, 10.72451020669871902, 113.3344237280190328 ) ) ;
#197121 = CARTESIAN_POINT ( 'NONE',  ( 4.483927247898790824, -16.52544592524335698, 55.20942372801902565 ) ) ;
#197122 = CARTESIAN_POINT ( 'NONE',  ( -15.80617190586768217, 15.72974639402176855, 73.12609039468567573 ) ) ;
#197123 = CARTESIAN_POINT ( 'NONE',  ( 14.34966873604972726, -8.224510206698740333, 25.83442372801901499 ) ) ;
#197124 = CARTESIAN_POINT ( 'NONE',  ( -13.97604488694527625, -13.89961937509977652, 71.87390960531433848 ) ) ;
#197125 = CARTESIAN_POINT ( 'NONE',  ( 5.153800228976615827, -19.02544592524334988, 95.20942372801897591 ) ) ;
#197126 = CARTESIAN_POINT ( 'NONE',  ( -4.483927247898782831, 16.52544592524335698, 72.70942372801901854 ) ) ;
#197127 = CARTESIAN_POINT ( 'NONE',  ( -5.049401038297874678, -19.05341960407617918, 19.79275706135233293 ) ) ;
#197128 = CARTESIAN_POINT ( 'NONE',  ( -5.049401038297874678, -19.05341960407617918, 79.79275706135233293 ) ) ;
#197129 = CARTESIAN_POINT ( 'NONE',  ( -5.153800228976328057, -19.02544592524343514, 67.29057627198102409 ) ) ;
#197130 = CARTESIAN_POINT ( 'NONE',  ( 5.719274019375991003, -21.55341960407610458, 82.70724293864770971 ) ) ;
#197132 = CARTESIAN_POINT ( 'NONE',  ( 19.02544592524334988, 5.153800228976608722, 76.45942372801897591 ) ) ;
#197131 = CARTESIAN_POINT ( 'NONE',  ( 4.483927247898545687, 16.52544592524342804, 74.79057627198105251 ) ) ;
#197133 = CARTESIAN_POINT ( 'NONE',  ( 16.61371651742597777, -7.165104196376198331, 61.35415069993000259 ) ) ;
#197134 = CARTESIAN_POINT ( 'NONE',  ( 5.153800228976615827, -19.02544592524334988, 60.20942372801899012 ) ) ;
#197135 = CARTESIAN_POINT ( 'NONE',  ( -4.483927247898539470, -16.52544592524342804, 22.29057627198102765 ) ) ;
#197136 = CARTESIAN_POINT ( 'NONE',  ( -14.29746914071049879, 8.314922557960819915, 85.83224293864768129 ) ) ;
#197138 = CARTESIAN_POINT ( 'NONE',  ( -8.571926809382608425, 26.38167802310805854, 146.4750000027311785 ) ) ;
#197137 = CARTESIAN_POINT ( 'NONE',  ( -9.474510206698720793, -16.51473224551083518, 24.58442372801900078 ) ) ;
#197139 = CARTESIAN_POINT ( 'NONE',  ( 5.823673210054125526, 21.52544592524343514, 114.7905762719810383 ) ) ;
#197140 = CARTESIAN_POINT ( 'NONE',  ( -0.05219959533909027116, -19.03943276465977164, 107.4989096053143527 ) ) ;
#197141 = CARTESIAN_POINT ( 'NONE',  ( -16.46253265017160317, 9.564922557960807481, 70.83224293864770971 ) ) ;
#197142 = CARTESIAN_POINT ( 'NONE',  ( 10.72451020669871369, 18.67979575497193778, 87.08442372801901854 ) ) ;
#197143 = CARTESIAN_POINT ( 'NONE',  ( 0.05219959533909260263, 19.03943276465977164, 59.99890960531436690 ) ) ;
#197144 = ORIENTED_EDGE ( 'NONE', *, *, #78587, .F. ) ;
#197145 = CARTESIAN_POINT ( 'NONE',  ( -9.474510206698964154, 16.51473224551069663, 35.41557627198102409 ) ) ;
#197146 = CARTESIAN_POINT ( 'NONE',  ( 0.05219959533907565091, 21.53943276465977519, 24.99890960531435624 ) ) ;
#197147 = CARTESIAN_POINT ( 'NONE',  ( 16.55341960407611168, 4.379528057220329451, 63.95724293864770260 ) ) ;
#197148 = CARTESIAN_POINT ( 'NONE',  ( -19.03943276465977164, 0.05219959533909376836, 41.24890960531435269 ) ) ;
#197149 = CARTESIAN_POINT ( 'NONE',  ( 16.55341960407611168, 4.379528057220329451, 103.9572429386476813 ) ) ;
#197150 = CARTESIAN_POINT ( 'NONE',  ( -18.62759615963270932, 10.81492255796079327, 115.8322429386477097 ) ) ;
#197151 = VECTOR ( 'NONE', #176962, 1000.000000000000000 ) ;
#197152 = CARTESIAN_POINT ( 'NONE',  ( -5.823673210054431948, 21.52544592524334988, 47.70942372801902565 ) ) ;
#197153 = CARTESIAN_POINT ( 'NONE',  ( -19.02544592524342804, 5.153800228976336051, 36.04057627198100988 ) ) ;
#197154 = CARTESIAN_POINT ( 'NONE',  ( 16.52544592524335698, 4.483927247898782831, 61.45942372801901854 ) ) ;
#197155 = CARTESIAN_POINT ( 'NONE',  ( -21.52544592524343514, 5.823673210054127303, 106.0405762719810525 ) ) ;
#197156 = CARTESIAN_POINT ( 'NONE',  ( -10.72451020669898014, 18.67979575497178502, 95.41557627198102409 ) ) ;
#197158 = CARTESIAN_POINT ( 'NONE',  ( -19.03943276465977164, 0.05219959533909376836, 46.24890960531435979 ) ) ;
#197157 = CARTESIAN_POINT ( 'NONE',  ( 16.46253265017146816, 9.564922557961045513, 31.66775706135232937 ) ) ;
#197159 = DIRECTION ( 'NONE',  ( 0.000000000000000000, 0.000000000000000000, -1.000000000000000000 ) ) ;
#197160 = CARTESIAN_POINT ( 'NONE',  ( -18.67979575497193778, 10.72451020669871902, 63.33442372801900433 ) ) ;
#197161 = CARTESIAN_POINT ( 'NONE',  ( -18.67979575497178146, -10.72451020669898902, 56.66557627198103830 ) ) ;
#197162 = CARTESIAN_POINT ( 'NONE',  ( -8.224510206698948167, 14.34966873604960824, 30.41557627198101699 ) ) ;
#197164 = CARTESIAN_POINT ( 'NONE',  ( 21.53943276465977519, 0.05219959533937863772, 111.2510903946856899 ) ) ;
#197163 = CARTESIAN_POINT ( 'NONE',  ( -5.823673210054431948, 21.52544592524334988, 77.70942372801900433 ) ) ;
#197165 = CARTESIAN_POINT ( 'NONE',  ( -5.049401038297874678, -19.05341960407617918, 49.79275706135231871 ) ) ;
#197166 = CARTESIAN_POINT ( 'NONE',  ( -12.14591786802326823, 12.06949235617739902, 108.1260903946856757 ) ) ;
#197168 = EDGE_CURVE ( 'NONE', #157920, #97386, #167207, .T. ) ;
#197167 = CARTESIAN_POINT ( 'NONE',  ( -5.823673210054431948, 21.52544592524334988, 52.70942372801902565 ) ) ;
#197169 = CARTESIAN_POINT ( 'NONE',  ( 13.89961937509977652, -13.97604488694527269, 63.12390960531435979 ) ) ;
#197170 = CARTESIAN_POINT ( 'NONE',  ( 5.049401038297881783, 19.05341960407617563, 37.29275706135232582 ) ) ;
#197171 = CARTESIAN_POINT ( 'NONE',  ( 5.719274019375991003, -21.55341960407610458, 37.70724293864769550 ) ) ;
#197172 = CARTESIAN_POINT ( 'NONE',  ( -5.719274019375665041, -21.55341960407619695, 29.79275706135234358 ) ) ;
#197173 = CARTESIAN_POINT ( 'NONE',  ( -18.62759615963270932, 10.81492255796079327, 85.83224293864768129 ) ) ;
#197174 = CARTESIAN_POINT ( 'NONE',  ( -0.05219959533936034679, 19.03943276465977164, 82.50109039468567573 ) ) ;
#197175 = CARTESIAN_POINT ( 'NONE',  ( -16.52544592524335698, -4.483927247898792601, 48.95942372801902565 ) ) ;
#197177 = CARTESIAN_POINT ( 'NONE',  ( 10.81492255796078972, 18.62759615963270932, 94.58224293864769550 ) ) ;
#197176 = CARTESIAN_POINT ( 'NONE',  ( -6.795175062723227022, 4.884302457959417865, -62.06722337258344879 ) ) ;
#197179 = CARTESIAN_POINT ( 'NONE',  ( -12.14591786802309592, -12.06949235617757132, 81.87390960531435269 ) ) ;
#197178 = CARTESIAN_POINT ( 'NONE',  ( 16.53943276465976808, 0.05219959533934440121, 81.25109039468568994 ) ) ;
#197180 = CARTESIAN_POINT ( 'NONE',  ( 0.6293029420441302868, 31.76613490820970398, -45.84550579068238818 ) ) ;
#197181 = CARTESIAN_POINT ( 'NONE',  ( -5.049401038297874678, -19.05341960407617918, 99.79275706135234714 ) ) ;
#197182 = CARTESIAN_POINT ( 'NONE',  ( -18.62759615963270932, 10.81492255796079327, 35.83224293864768839 ) ) ;
#197183 = CARTESIAN_POINT ( 'NONE',  ( 0.000000000000000000, 0.000000000000000000, -49.13275782002545355 ) ) ;
#197184 = EDGE_CURVE ( 'NONE', #75168, #150285, #91239, .T. ) ;
#197185 = CARTESIAN_POINT ( 'NONE',  ( -16.52544592524335698, -4.483927247898792601, 58.95942372801902565 ) ) ;
#197186 = CARTESIAN_POINT ( 'NONE',  ( -21.55341960407619339, 5.719274019375674811, 28.54275706135234358 ) ) ;
#197187 = CARTESIAN_POINT ( 'NONE',  ( -21.55341960407610458, -5.719274019375992779, 31.45724293864769550 ) ) ;
#197188 = CARTESIAN_POINT ( 'NONE',  ( -8.224510206698735004, -14.34966873604973081, 74.58442372801901854 ) ) ;
#197189 = CARTESIAN_POINT ( 'NONE',  ( -16.46253265017160317, 9.564922557960807481, 85.83224293864769550 ) ) ;
#197191 = CARTESIAN_POINT ( 'NONE',  ( 9.474510206698971260, -16.51473224551069308, 27.91557627198103120 ) ) ;
#197190 = CARTESIAN_POINT ( 'NONE',  ( 10.81492255796106328, -18.62759615963255655, 55.41775706135234714 ) ) ;
#197192 = CARTESIAN_POINT ( 'NONE',  ( -0.05219959533907301413, -21.53943276465977519, 27.49890960531435269 ) ) ;
#197193 = VERTEX_POINT ( 'NONE', #153933 ) ;
#197194 = CARTESIAN_POINT ( 'NONE',  ( 16.46253265017146816, 9.564922557961045513, 36.66775706135233293 ) ) ;
#197195 = CARTESIAN_POINT ( 'NONE',  ( 12.06949235617739724, 12.14591786802326823, 51.87609039468568284 ) ) ;
#197196 = CARTESIAN_POINT ( 'NONE',  ( 5.719274019375991003, -21.55341960407610458, 22.70724293864769194 ) ) ;
#197197 = CARTESIAN_POINT ( 'NONE',  ( -0.05219959533909027116, -19.03943276465977164, 67.49890960531436690 ) ) ;
#197198 = CARTESIAN_POINT ( 'NONE',  ( -4.379528057220086978, -16.55341960407618274, 104.7927570613523898 ) ) ;
#197199 = CARTESIAN_POINT ( 'NONE',  ( -13.89961937509977652, 13.97604488694528158, 115.6239096053143669 ) ) ;
#197200 = CARTESIAN_POINT ( 'NONE',  ( -16.52544592524342804, 4.483927247898546575, 96.04057627198102409 ) ) ;
#197201 = CARTESIAN_POINT ( 'NONE',  ( 18.62759615963271287, -10.81492255796078972, 33.33224293864769550 ) ) ;
#197202 = CARTESIAN_POINT ( 'NONE',  ( 19.02544592524343514, -5.153800228976328945, 33.54057627198102409 ) ) ;
#197203 = CARTESIAN_POINT ( 'NONE',  ( 12.06949235617739724, 12.14591786802326823, 71.87609039468568994 ) ) ;
#197204 = CARTESIAN_POINT ( 'NONE',  ( -0.05219959533907301413, -21.53943276465977519, 112.4989096053143669 ) ) ;
#197205 = CARTESIAN_POINT ( 'NONE',  ( -5.153800228976607833, 19.02544592524334988, 72.70942372801900433 ) ) ;
#197206 = CARTESIAN_POINT ( 'NONE',  ( -9.564922557960796823, -16.46253265017161027, 42.08224293864769550 ) ) ;
#197207 = CARTESIAN_POINT ( 'NONE',  ( 21.55341960407610458, 5.719274019375980345, 68.95724293864769550 ) ) ;
#197208 = CARTESIAN_POINT ( 'NONE',  ( 2.500000000000000000, 1.178949249685217193, 2.041999999999998483 ) ) ;
#197209 = CARTESIAN_POINT ( 'NONE',  ( 18.67979575497194134, -10.72451020669871369, 95.83442372801903275 ) ) ;
#197210 = CARTESIAN_POINT ( 'NONE',  ( 16.46253265017160672, -9.564922557960803928, 58.33224293864769550 ) ) ;
#197211 = CARTESIAN_POINT ( 'NONE',  ( -12.14591786802326823, 12.06949235617739902, 48.12609039468568284 ) ) ;
#197212 = CARTESIAN_POINT ( 'NONE',  ( -10.81492255796105439, 18.62759615963255655, 82.91775706135234714 ) ) ;
#197213 = CARTESIAN_POINT ( 'NONE',  ( 5.153800228976615827, -19.02544592524334988, 45.20942372801901143 ) ) ;
#197214 = EDGE_CURVE ( 'NONE', #25387, #133509, #78474, .T. ) ;
#197215 = CARTESIAN_POINT ( 'NONE',  ( 13.97604488694548053, -13.89961937509957401, 55.62609039468566863 ) ) ;
#197216 = VERTEX_POINT ( 'NONE', #109414 ) ;
#197217 = CARTESIAN_POINT ( 'NONE',  ( 10.81492255796106328, -18.62759615963255655, 50.41775706135235424 ) ) ;
#197218 = CARTESIAN_POINT ( 'NONE',  ( -13.89961937509977830, 13.97604488694528158, 55.62390960531435269 ) ) ;
#197219 = CARTESIAN_POINT ( 'NONE',  ( 13.97604488694548053, -13.89961937509957401, 45.62609039468566863 ) ) ;
#197220 = CARTESIAN_POINT ( 'NONE',  ( -19.05341960407611168, -5.049401038298163336, 106.4572429386476955 ) ) ;
#197221 = CARTESIAN_POINT ( 'NONE',  ( 5.049401038298161559, -19.05341960407611168, 87.70724293864769550 ) ) ;
#197222 = CARTESIAN_POINT ( 'NONE',  ( 16.53943276465976808, -0.05219959533910856209, 43.74890960531435979 ) ) ;
#197223 = CARTESIAN_POINT ( 'NONE',  ( 5.823673210054125526, 21.52544592524343514, 39.79057627198103830 ) ) ;
#197224 = CARTESIAN_POINT ( 'NONE',  ( 11.40812507854754365, 35.11059874428196537, -5.724999997268812812 ) ) ;
#197225 = CARTESIAN_POINT ( 'NONE',  ( 17.79613651744293534, 24.49428055684532524, 141.2843446568999752 ) ) ;
#197226 = CARTESIAN_POINT ( 'NONE',  ( -18.62759615963255300, -10.81492255796106328, 94.16775706135237556 ) ) ;
#197227 = CARTESIAN_POINT ( 'NONE',  ( -27.20489923017578704, 7.754340368643402925, 164.3890803562166809 ) ) ;
#197228 = CARTESIAN_POINT ( 'NONE',  ( 13.89961937509977652, -13.97604488694527269, 38.12390960531436690 ) ) ;
#197229 = FACE_OUTER_BOUND ( 'NONE', #2269, .T. ) ;
#197230 = CARTESIAN_POINT ( 'NONE',  ( -28.41048423428186354, -24.65169963600693492, -8.000000000000001776 ) ) ;
#197231 = CARTESIAN_POINT ( 'NONE',  ( 14.29746914071037800, 8.314922557961029526, 56.66775706135235424 ) ) ;
#197232 = CARTESIAN_POINT ( 'NONE',  ( -15.80617190586745835, -15.72974639402198527, 76.87390960531439532 ) ) ;
#197233 = CARTESIAN_POINT ( 'NONE',  ( -12.06949235617756955, 12.14591786802309770, 35.62390960531437401 ) ) ;
#197235 = CARTESIAN_POINT ( 'NONE',  ( 13.97604488694527802, 13.89961937509977652, 114.3739096053143669 ) ) ;
#197234 = CARTESIAN_POINT ( 'NONE',  ( 9.564922557960805705, 16.46253265017160317, 29.58224293864769550 ) ) ;
#197236 = CARTESIAN_POINT ( 'NONE',  ( 10.81492255796106328, -18.62759615963255655, 25.41775706135235779 ) ) ;
#197237 = CARTESIAN_POINT ( 'NONE',  ( -19.05341960407617563, 5.049401038297882671, 38.54275706135233293 ) ) ;
#197238 = CARTESIAN_POINT ( 'NONE',  ( -16.46253265017160317, 9.564922557960807481, 25.83224293864769194 ) ) ;
#197239 = CARTESIAN_POINT ( 'NONE',  ( -10.81492255796105439, 18.62759615963255655, 77.91775706135231871 ) ) ;
#197240 = CARTESIAN_POINT ( 'NONE',  ( 17.48847506799968343, -5.747544572773782612, 33.32697437843281563 ) ) ;
#197241 = CARTESIAN_POINT ( 'NONE',  ( -8.224510206698948167, 14.34966873604960824, 25.41557627198103120 ) ) ;
#197242 = CARTESIAN_POINT ( 'NONE',  ( -29.86685920354755552, 21.69954338932564397, -1.324999997268813345 ) ) ;
#197243 = CARTESIAN_POINT ( 'NONE',  ( -18.67979575497178146, -10.72451020669898902, 31.66557627198102054 ) ) ;
#197244 = CARTESIAN_POINT ( 'NONE',  ( -12.06949235617756955, 12.14591786802309770, 85.62390960531436690 ) ) ;
#197245 = CARTESIAN_POINT ( 'NONE',  ( 28.47622644277404191, -25.16156846422445881, -16.68312038616162241 ) ) ;
#197246 = CARTESIAN_POINT ( 'NONE',  ( -0.05219959533909027116, -19.03943276465977164, 87.49890960531436690 ) ) ;
#197247 = CARTESIAN_POINT ( 'NONE',  ( -16.52544592524342804, 4.483927247898546575, 81.04057627198102409 ) ) ;
#197248 = CARTESIAN_POINT ( 'NONE',  ( -13.89961937509957401, -13.97604488694547875, 99.37609039468567573 ) ) ;
#197249 = CARTESIAN_POINT ( 'NONE',  ( 18.62759615963271287, -10.81492255796078972, 63.33224293864770260 ) ) ;
#197250 = ORIENTED_EDGE ( 'NONE', *, *, #153922, .T. ) ;
#197251 = CARTESIAN_POINT ( 'NONE',  ( 5.049401038298161559, -19.05341960407611168, 27.70724293864769550 ) ) ;
#197253 = CARTESIAN_POINT ( 'NONE',  ( -21.52544592524343514, 5.823673210054127303, 86.04057627198102409 ) ) ;
#197252 = CARTESIAN_POINT ( 'NONE',  ( -5.153800228976328057, -19.02544592524343514, 87.29057627198103830 ) ) ;
#197255 = CARTESIAN_POINT ( 'NONE',  ( 19.05341960407611168, 5.049401038298154454, 93.95724293864769550 ) ) ;
#197254 = CARTESIAN_POINT ( 'NONE',  ( -16.53943276465976808, -0.05219959533934237506, 98.75109039468568994 ) ) ;
#197256 = CARTESIAN_POINT ( 'NONE',  ( 5.049401038297881783, 19.05341960407617563, 62.29275706135234003 ) ) ;
#197257 = CARTESIAN_POINT ( 'NONE',  ( 21.53943276465977519, 0.05219959533937863772, 101.2510903946856757 ) ) ;
#197258 = CARTESIAN_POINT ( 'NONE',  ( -10.72451020669898014, 18.67979575497178502, 80.41557627198103830 ) ) ;
#197259 = CARTESIAN_POINT ( 'NONE',  ( -19.03943276465977164, 0.05219959533909376836, 116.2489096053143669 ) ) ;
#197260 = CARTESIAN_POINT ( 'NONE',  ( 0.05219959533909260263, 19.03943276465977164, 54.99890960531435979 ) ) ;
#197261 = CARTESIAN_POINT ( 'NONE',  ( 14.29746914071049879, -8.314922557960816363, 23.33224293864769194 ) ) ;
#197262 = CARTESIAN_POINT ( 'NONE',  ( 16.51473224551069308, 9.474510206698969483, 59.16557627198102409 ) ) ;
#197263 = CARTESIAN_POINT ( 'NONE',  ( -31.72709406046300629, -0.4963711039036964312, 102.5000000000000142 ) ) ;
#197264 = CARTESIAN_POINT ( 'NONE',  ( 10.81492255796106328, -18.62759615963255655, 105.4177570613523613 ) ) ;
#197265 = CARTESIAN_POINT ( 'NONE',  ( 16.52544592524342804, -4.483927247898539470, 73.54057627198102409 ) ) ;
#197266 = CARTESIAN_POINT ( 'NONE',  ( 10.72451020669898902, -18.67979575497178502, 107.9155762719810241 ) ) ;
#197267 = CARTESIAN_POINT ( 'NONE',  ( -10.81492255796078084, -18.62759615963271287, 107.0822429386476955 ) ) ;
#197268 = CARTESIAN_POINT ( 'NONE',  ( -6.576150211591581751, 6.293193206003589779, -63.95112321872120731 ) ) ;
#197269 = CARTESIAN_POINT ( 'NONE',  ( 15.72974639402199770, -15.80617190586745480, 63.12390960531435979 ) ) ;
#197270 = CARTESIAN_POINT ( 'NONE',  ( 14.34966873604972726, -8.224510206698740333, 80.83442372801901854 ) ) ;
#197271 = CARTESIAN_POINT ( 'NONE',  ( 4.483927247898545687, 16.52544592524342804, 99.79057627198103830 ) ) ;
#197272 = CARTESIAN_POINT ( 'NONE',  ( 9.564922557960805705, 16.46253265017160317, 54.58224293864769550 ) ) ;
#197273 = CARTESIAN_POINT ( 'NONE',  ( -14.34966873604972548, 8.224510206698743886, 113.3344237280190328 ) ) ;
#197274 = CARTESIAN_POINT ( 'NONE',  ( -21.55341960407619339, 5.719274019375674811, 48.54275706135234714 ) ) ;
#197275 = CARTESIAN_POINT ( 'NONE',  ( -13.89961937509977652, 13.97604488694528158, 115.6239096053143669 ) ) ;
#197276 = CARTESIAN_POINT ( 'NONE',  ( 5.823673210054444382, -21.52544592524334988, 85.20942372801901854 ) ) ;
#197277 = CARTESIAN_POINT ( 'NONE',  ( 0.05219959533909260263, 19.03943276465977164, 24.99890960531435269 ) ) ;
#197278 = CARTESIAN_POINT ( 'NONE',  ( -16.51473224551069308, -9.474510206698971260, 36.66557627198102409 ) ) ;
#197279 = EDGE_LOOP ( 'NONE', ( #177185, #7223, #61169, #4446 ) ) ;
#197280 = CARTESIAN_POINT ( 'NONE',  ( -0.05219959533937732626, 21.53943276465977519, 82.50109039468568994 ) ) ;
#197281 = CARTESIAN_POINT ( 'NONE',  ( 18.62759615963255655, 10.81492255796105972, 66.66775706135234714 ) ) ;
#197282 = CARTESIAN_POINT ( 'NONE',  ( -9.564922557960796823, -16.46253265017161027, 107.0822429386476955 ) ) ;
#197283 = CARTESIAN_POINT ( 'NONE',  ( -5.049401038297874678, -19.05341960407617918, 84.79275706135233293 ) ) ;
#197284 = CARTESIAN_POINT ( 'NONE',  ( -5.719274019375665041, -21.55341960407619695, 54.79275706135235424 ) ) ;
#197285 = CARTESIAN_POINT ( 'NONE',  ( 12.06949235617739724, 12.14591786802326823, 26.87609039468567218 ) ) ;
#197286 = CARTESIAN_POINT ( 'NONE',  ( -16.46253265017146816, -9.564922557961047289, 74.16775706135234714 ) ) ;
#197287 = CARTESIAN_POINT ( 'NONE',  ( 13.89961937509977652, -13.97604488694527269, 48.12390960531435979 ) ) ;
#197288 = CARTESIAN_POINT ( 'NONE',  ( -16.51473224551082808, 9.474510206698731452, 88.33442372801900433 ) ) ;
#197289 = CARTESIAN_POINT ( 'NONE',  ( 8.314922557960818139, 14.29746914071049879, 29.58224293864769905 ) ) ;
#197290 = CARTESIAN_POINT ( 'NONE',  ( -0.05219959533936034679, 19.03943276465977164, 87.50109039468567573 ) ) ;
#197291 = CARTESIAN_POINT ( 'NONE',  ( 16.55341960407611168, 4.379528057220329451, 33.95724293864769550 ) ) ;
#197292 = CARTESIAN_POINT ( 'NONE',  ( -13.97604488694547697, 13.89961937509957934, 63.12609039468566152 ) ) ;
#197293 = CARTESIAN_POINT ( 'NONE',  ( -0.05219959533934338120, 16.53943276465976808, 42.50109039468567573 ) ) ;
#197294 = CARTESIAN_POINT ( 'NONE',  ( 13.89961937509957401, 13.97604488694547697, 26.87609039468566507 ) ) ;
#197295 = CARTESIAN_POINT ( 'NONE',  ( -19.05341960407611168, -5.049401038298163336, 46.45724293864768129 ) ) ;
#197296 = CARTESIAN_POINT ( 'NONE',  ( -16.79531203550648755, -7.028104445595491967, 66.25244988220440234 ) ) ;
#197297 = CARTESIAN_POINT ( 'NONE',  ( -4.379528057220086978, -16.55341960407618274, 39.79275706135235424 ) ) ;
#197298 = CARTESIAN_POINT ( 'NONE',  ( -3.573655867282028392E-15, 2.428612866367529932E-14, 155.0000000000000000 ) ) ;
#197299 = CARTESIAN_POINT ( 'NONE',  ( 27.73933785331498569, 2.768321779492822058E-14, 143.8750000027311842 ) ) ;
#197300 = CARTESIAN_POINT ( 'NONE',  ( 19.02544592524343514, -5.153800228976328945, 93.54057627198102409 ) ) ;
#197301 = CARTESIAN_POINT ( 'NONE',  ( -18.09867054820432131, -5.499999999999928058, 68.98393025253585620 ) ) ;
#197302 = ORIENTED_EDGE ( 'NONE', *, *, #134775, .T. ) ;
#197303 = CARTESIAN_POINT ( 'NONE',  ( 19.05341960407617918, -5.049401038297876454, 96.04275706135231871 ) ) ;
#197304 = CARTESIAN_POINT ( 'NONE',  ( -21.53943276465977519, 0.05219959533907696930, 21.24890960531436690 ) ) ;
#197306 = CARTESIAN_POINT ( 'NONE',  ( 13.97604488694548053, -13.89961937509957401, 105.6260903946856757 ) ) ;
#197305 = CARTESIAN_POINT ( 'NONE',  ( 10.81492255796106328, -18.62759615963255655, 110.4177570613523756 ) ) ;
#197307 = CARTESIAN_POINT ( 'NONE',  ( 9.474510206698971260, -16.51473224551069308, 22.91557627198102765 ) ) ;
#197308 = CARTESIAN_POINT ( 'NONE',  ( 9.564922557960805705, 16.46253265017160317, 39.58224293864768839 ) ) ;
#197309 = CARTESIAN_POINT ( 'NONE',  ( 18.67979575497178502, 10.72451020669898547, 54.16557627198103120 ) ) ;
#197310 = CARTESIAN_POINT ( 'NONE',  ( 13.97604488694527802, 13.89961937509977652, 24.37390960531435624 ) ) ;
#197311 = DIRECTION ( 'NONE',  ( -1.000000000000000000, 0.000000000000000000, 0.000000000000000000 ) ) ;
#197312 = CARTESIAN_POINT ( 'NONE',  ( 16.46253265017146816, 9.564922557961045513, 71.66775706135233293 ) ) ;
#197313 = CARTESIAN_POINT ( 'NONE',  ( -14.29746914071049879, 8.314922557960819915, 55.83224293864770260 ) ) ;
#197314 = CARTESIAN_POINT ( 'NONE',  ( -15.80617190586745835, -15.72974639402198527, 36.87390960531435979 ) ) ;
#197315 = CARTESIAN_POINT ( 'NONE',  ( -21.53943276465977519, -0.05219959533937600094, 88.75109039468567573 ) ) ;
#197316 = CARTESIAN_POINT ( 'NONE',  ( 5.719274019375991003, -21.55341960407610458, 82.70724293864770971 ) ) ;
#197317 = CARTESIAN_POINT ( 'NONE',  ( -18.67979575497193778, 10.72451020669871902, 58.33442372801901143 ) ) ;
#197318 = CARTESIAN_POINT ( 'NONE',  ( 5.719274019375673035, 21.55341960407619339, 67.29275706135234714 ) ) ;
#197319 = ADVANCED_FACE ( 'NONE', ( #64902 ), #171093, .F. ) ;
#197320 = CARTESIAN_POINT ( 'NONE',  ( -5.049401038298153566, 19.05341960407611168, 90.20724293864766707 ) ) ;
#197322 = CARTESIAN_POINT ( 'NONE',  ( 15.72974639402176855, 15.80617190586768217, 61.87609039468568284 ) ) ;
#197321 = CARTESIAN_POINT ( 'NONE',  ( 12.06949235617739724, 12.14591786802326823, 86.87609039468568994 ) ) ;
#197323 = CARTESIAN_POINT ( 'NONE',  ( -19.05341960407611168, -5.049401038298163336, 51.45724293864770260 ) ) ;
#197324 = CARTESIAN_POINT ( 'NONE',  ( -13.97604488694527625, -13.89961937509977652, 26.87390960531434558 ) ) ;
#197325 = CARTESIAN_POINT ( 'NONE',  ( 19.05341960407611168, 5.049401038298154454, 48.95724293864768129 ) ) ;
#197326 = CARTESIAN_POINT ( 'NONE',  ( -4.483927247898539470, -16.52544592524342804, 72.29057627198102409 ) ) ;
#197327 = CARTESIAN_POINT ( 'NONE',  ( -12.06949235617756955, 12.14591786802309770, 40.62390960531435269 ) ) ;
#197328 = CARTESIAN_POINT ( 'NONE',  ( 18.67979575497178502, 10.72451020669898547, 49.16557627198102409 ) ) ;
#197329 = EDGE_CURVE ( 'NONE', #28306, #41517, #52032, .T. ) ;
#197330 = CARTESIAN_POINT ( 'NONE',  ( -19.03943276465977164, 0.05219959533909376836, 46.24890960531435979 ) ) ;
#197331 = CARTESIAN_POINT ( 'NONE',  ( 10.72451020669898902, -18.67979575497178502, 52.91557627198103830 ) ) ;
#197332 = CARTESIAN_POINT ( 'NONE',  ( -5.153800228976607833, 19.02544592524334988, 47.70942372801900433 ) ) ;
#197334 = CARTESIAN_POINT ( 'NONE',  ( -12.14591786802309592, -12.06949235617757132, 46.87390960531435979 ) ) ;
#197333 = DIRECTION ( 'NONE',  ( 0.000000000000000000, 0.000000000000000000, 1.000000000000000000 ) ) ;
#197335 = CARTESIAN_POINT ( 'NONE',  ( -5.719274019375978568, 21.55341960407610458, 25.20724293864769550 ) ) ;
#197336 = ORIENTED_EDGE ( 'NONE', *, *, #111151, .T. ) ;
#197337 = VERTEX_POINT ( 'NONE', #48752 ) ;
#197338 = DIRECTION ( 'NONE',  ( -0.000000000000000000, 0.000000000000000000, 1.000000000000000000 ) ) ;
#197339 = CARTESIAN_POINT ( 'NONE',  ( 16.53943276465976808, 0.05219959533934440121, 76.25109039468568994 ) ) ;
#197340 = CARTESIAN_POINT ( 'NONE',  ( -19.03943276465977164, -0.05219959533935918106, 68.75109039468566152 ) ) ;
#197341 = CARTESIAN_POINT ( 'NONE',  ( 16.55341960407611168, 4.379528057220329451, 53.95724293864770260 ) ) ;
#197342 = CARTESIAN_POINT ( 'NONE',  ( 0.000000000000000000, -105.0000000000000000, 12.00000000000000355 ) ) ;
#197343 = CARTESIAN_POINT ( 'NONE',  ( -16.52544592524342804, 4.483927247898546575, 26.04057627198103475 ) ) ;
#197344 = CARTESIAN_POINT ( 'NONE',  ( -9.564922557960796823, -16.46253265017161027, 47.08224293864769550 ) ) ;
#197345 = CARTESIAN_POINT ( 'NONE',  ( 13.89961937509977652, -13.97604488694527269, 73.12390960531436690 ) ) ;
#197346 = CARTESIAN_POINT ( 'NONE',  ( 0.05219959533909260263, 19.03943276465977164, 39.99890960531436690 ) ) ;
#197347 = CARTESIAN_POINT ( 'NONE',  ( 21.52544592524334988, 5.823673210054432836, 46.45942372801901854 ) ) ;
#197348 = CARTESIAN_POINT ( 'NONE',  ( -5.153800228976328057, -19.02544592524343514, 67.29057627198102409 ) ) ;
#197349 = PLANE ( 'NONE',  #164671 ) ;
#197350 = CARTESIAN_POINT ( 'NONE',  ( 19.02544592524343514, -5.153800228976328945, 53.54057627198102409 ) ) ;
#197351 = CARTESIAN_POINT ( 'NONE',  ( 21.52544592524344225, -5.823673210054117533, 38.54057627198103120 ) ) ;
#197352 = CARTESIAN_POINT ( 'NONE',  ( 5.049401038298161559, -19.05341960407611168, 37.70724293864768839 ) ) ;
#197353 = CARTESIAN_POINT ( 'NONE',  ( -0.05219959533907301413, -21.53943276465977519, 42.49890960531435979 ) ) ;
#197354 = CARTESIAN_POINT ( 'NONE',  ( -14.34966873604972548, 8.224510206698743886, 93.33442372801901854 ) ) ;
#197355 = CARTESIAN_POINT ( 'NONE',  ( 16.51473224551083163, -9.474510206698727899, 25.83442372801900078 ) ) ;
#197357 = CARTESIAN_POINT ( 'NONE',  ( -12.06949235617739369, -12.14591786802326823, 74.37609039468568994 ) ) ;
#197356 = CARTESIAN_POINT ( 'NONE',  ( 16.53943276465976808, 0.05219959533934440121, 46.25109039468567573 ) ) ;
#197358 = CARTESIAN_POINT ( 'NONE',  ( 13.97604488694527802, 13.89961937509977652, 104.3739096053143385 ) ) ;
#197359 = CARTESIAN_POINT ( 'NONE',  ( 12.06949235617739724, 12.14591786802326823, 66.87609039468568994 ) ) ;
#197360 = CARTESIAN_POINT ( 'NONE',  ( 16.55341960407618274, -4.379528057220086978, 36.04275706135234714 ) ) ;
#197361 = CARTESIAN_POINT ( 'NONE',  ( 16.51473224551069308, 9.474510206698969483, 109.1655762719810383 ) ) ;
#197362 = CARTESIAN_POINT ( 'NONE',  ( -0.05219959533934338120, 16.53943276465976808, 22.50109039468567573 ) ) ;
#197363 = CARTESIAN_POINT ( 'NONE',  ( -5.153800228976328057, -19.02544592524343514, 32.29057627198102409 ) ) ;
#197364 = CARTESIAN_POINT ( 'NONE',  ( 18.67979575497194134, -10.72451020669871369, 25.83442372801901499 ) ) ;
#197365 = CARTESIAN_POINT ( 'NONE',  ( 8.224510206698742110, 14.34966873604972548, 32.08442372801901854 ) ) ;
#197366 = CARTESIAN_POINT ( 'NONE',  ( -16.52544592524335698, -4.483927247898792601, 93.95942372801903275 ) ) ;
#197367 = LINE ( 'NONE', #70025, #40849 ) ;
#197368 = CARTESIAN_POINT ( 'NONE',  ( -0.05219959533937732626, 21.53943276465977519, 97.50109039468567573 ) ) ;
#197369 = CARTESIAN_POINT ( 'NONE',  ( -9.564922557961040184, 16.46253265017147172, 102.9177570613523329 ) ) ;
#197370 = CARTESIAN_POINT ( 'NONE',  ( 14.34966873604960469, 8.224510206698951720, 54.16557627198103120 ) ) ;
#197371 = CARTESIAN_POINT ( 'NONE',  ( -16.53943276465976808, 0.05219959533911058130, 116.2489096053143669 ) ) ;
#197373 = CARTESIAN_POINT ( 'NONE',  ( -30.74264578624800492, -22.33583958711396278, -3.549999994537626602 ) ) ;
#197372 = CARTESIAN_POINT ( 'NONE',  ( 0.05219959533936267826, -19.03943276465977164, 55.00109039468566863 ) ) ;
#197374 = CARTESIAN_POINT ( 'NONE',  ( -0.05219959533937732626, 21.53943276465977519, 47.50109039468568994 ) ) ;
#197375 = CARTESIAN_POINT ( 'NONE',  ( 8.314922557961029526, -14.29746914071037800, 30.41775706135234358 ) ) ;
#197376 = CARTESIAN_POINT ( 'NONE',  ( 17.40861289039002813, 6.110651285853272441, 83.87232470827430575 ) ) ;
#197377 = CARTESIAN_POINT ( 'NONE',  ( 9.474510206698971260, -16.51473224551069308, 112.9155762719810383 ) ) ;
#197378 = CARTESIAN_POINT ( 'NONE',  ( -10.72451020669898014, 18.67979575497178502, 75.41557627198102409 ) ) ;
#197379 = CARTESIAN_POINT ( 'NONE',  ( -13.89961937509957401, -13.97604488694547875, 109.3760903946856331 ) ) ;
#197380 = CARTESIAN_POINT ( 'NONE',  ( 16.46253265017160672, -9.564922557960803928, 103.3322429386476955 ) ) ;
#197381 = CARTESIAN_POINT ( 'NONE',  ( -21.92083080610932910, 8.096106818377439396, 172.4353877980870493 ) ) ;
#197382 = CARTESIAN_POINT ( 'NONE',  ( -13.89961937509977652, 13.97604488694528158, 25.62390960531434558 ) ) ;
#197383 = CARTESIAN_POINT ( 'NONE',  ( 15.72974639402176855, 15.80617190586768217, 96.87609039468568994 ) ) ;
#197384 = CARTESIAN_POINT ( 'NONE',  ( -19.05341960407611168, -5.049401038298163336, 41.45724293864769550 ) ) ;
#197385 = CARTESIAN_POINT ( 'NONE',  ( -10.81492255796105439, 18.62759615963255655, 47.91775706135234714 ) ) ;
#197386 = CARTESIAN_POINT ( 'NONE',  ( 21.52544592524334988, 5.823673210054432836, 86.45942372801901854 ) ) ;
#197387 = CARTESIAN_POINT ( 'NONE',  ( 16.52544592524335698, 4.483927247898782831, 101.4594237280190185 ) ) ;
#197388 = CARTESIAN_POINT ( 'NONE',  ( -19.02544592524342804, 5.153800228976336051, 81.04057627198103830 ) ) ;
#197389 = CARTESIAN_POINT ( 'NONE',  ( -21.53943276465977519, -0.05219959533937600094, 38.75109039468567573 ) ) ;
#197390 = CARTESIAN_POINT ( 'NONE',  ( 0.05219959533937995610, -21.53943276465977519, 35.00109039468568284 ) ) ;
#197392 = CARTESIAN_POINT ( 'NONE',  ( 5.049401038298161559, -19.05341960407611168, 87.70724293864769550 ) ) ;
#197391 = CARTESIAN_POINT ( 'NONE',  ( 16.46253265017146816, 9.564922557961045513, 81.66775706135233293 ) ) ;
#197393 = CARTESIAN_POINT ( 'NONE',  ( -16.55341960407611168, -4.379528057220339221, 106.4572429386477097 ) ) ;
#197394 = CARTESIAN_POINT ( 'NONE',  ( -0.05219959533907301413, -21.53943276465977519, 102.4989096053143811 ) ) ;
#197395 = CARTESIAN_POINT ( 'NONE',  ( 16.55341960407611168, 4.379528057220329451, 78.95724293864769550 ) ) ;
#197396 = CARTESIAN_POINT ( 'NONE',  ( -15.80617190586768217, 15.72974639402176855, 113.1260903946856899 ) ) ;
#197397 = CARTESIAN_POINT ( 'NONE',  ( -8.224510206698948167, 14.34966873604960824, 100.4155762719810241 ) ) ;
#197398 = CARTESIAN_POINT ( 'NONE',  ( -5.049401038298153566, 19.05341960407611168, 40.20724293864768839 ) ) ;
#197399 = CARTESIAN_POINT ( 'NONE',  ( 13.97604488694548053, -13.89961937509957401, 85.62609039468568994 ) ) ;
#197400 = CARTESIAN_POINT ( 'NONE',  ( 16.52544592524342804, -4.483927247898539470, 53.54057627198103120 ) ) ;
#197401 = CARTESIAN_POINT ( 'NONE',  ( 5.823673210054444382, -21.52544592524334988, 110.2094237280190185 ) ) ;
#197402 = CARTESIAN_POINT ( 'NONE',  ( 5.049401038298161559, -19.05341960407611168, 107.7072429386476955 ) ) ;
#197403 = CARTESIAN_POINT ( 'NONE',  ( -16.46253265017146816, -9.564922557961047289, 79.16775706135234714 ) ) ;
#197404 = CARTESIAN_POINT ( 'NONE',  ( 0.05219959533907565091, 21.53943276465977519, 84.99890960531436690 ) ) ;
#197405 = CARTESIAN_POINT ( 'NONE',  ( -18.62759615963255300, -10.81492255796106328, 29.16775706135234003 ) ) ;
#197406 = CARTESIAN_POINT ( 'NONE',  ( -14.34966873604972548, 8.224510206698743886, 33.33442372801900433 ) ) ;
#197407 = CARTESIAN_POINT ( 'NONE',  ( 4.379528057220092307, 16.55341960407617563, 97.29275706135234714 ) ) ;
#197409 = CARTESIAN_POINT ( 'NONE',  ( 15.80617190586769283, -15.72974639402175789, 35.62609039468568994 ) ) ;
#197408 = CARTESIAN_POINT ( 'NONE',  ( 19.02544592524343514, -5.153800228976328945, 28.54057627198102409 ) ) ;
#197410 = CARTESIAN_POINT ( 'NONE',  ( -0.05219959533909027116, -19.03943276465977164, 22.49890960531436690 ) ) ;
#197411 = CARTESIAN_POINT ( 'NONE',  ( 3.556970738554033499E-15, -38.81732327939057825, -2.624999997268812724 ) ) ;
#197412 = CARTESIAN_POINT ( 'NONE',  ( -14.29746914071037622, -8.314922557961029526, 49.16775706135234003 ) ) ;
#197413 = CARTESIAN_POINT ( 'NONE',  ( 14.29746914071049879, -8.314922557960816363, 83.33224293864769550 ) ) ;
#197414 = CARTESIAN_POINT ( 'NONE',  ( 21.53943276465977519, -0.05219959533907433946, 78.74890960531436690 ) ) ;
#197415 = CARTESIAN_POINT ( 'NONE',  ( 12.14591786802309770, 12.06949235617756955, 24.37390960531435979 ) ) ;
#197416 = CARTESIAN_POINT ( 'NONE',  ( -4.379528057220086978, -16.55341960407618274, 49.79275706135234714 ) ) ;
#197417 = CARTESIAN_POINT ( 'NONE',  ( 19.03943276465977164, -0.05219959533909143690, 43.74890960531435979 ) ) ;
#197418 = CARTESIAN_POINT ( 'NONE',  ( 4.379528057220092307, 16.55341960407617563, 92.29275706135236135 ) ) ;
#197419 = CARTESIAN_POINT ( 'NONE',  ( 19.02544592524334988, 5.153800228976608722, 81.45942372801897591 ) ) ;
#197420 = CARTESIAN_POINT ( 'NONE',  ( -21.52544592524343514, 5.823673210054127303, 81.04057627198102409 ) ) ;
#197421 = CARTESIAN_POINT ( 'NONE',  ( 14.34966873604972726, -8.224510206698740333, 105.8344237280190328 ) ) ;
#197422 = ORIENTED_EDGE ( 'NONE', *, *, #176321, .F. ) ;
#197423 = CARTESIAN_POINT ( 'NONE',  ( 26.61723430050332340, 3.645106422946821301, 172.4622069319858895 ) ) ;
#197424 = CARTESIAN_POINT ( 'NONE',  ( 5.823673210054125526, 21.52544592524343514, 64.79057627198103830 ) ) ;
#197425 = ORIENTED_EDGE ( 'NONE', *, *, #151324, .F. ) ;
#197426 = CARTESIAN_POINT ( 'NONE',  ( 14.29746914071037800, 8.314922557961029526, 86.66775706135234714 ) ) ;
#197427 = ORIENTED_EDGE ( 'NONE', *, *, #78948, .F. ) ;
#197428 = CARTESIAN_POINT ( 'NONE',  ( 15.72974639402199770, -15.80617190586745480, 33.12390960531435979 ) ) ;
#197429 = CARTESIAN_POINT ( 'NONE',  ( -19.36337904590692460, 5.499999999999953815, 75.41494137495618588 ) ) ;
#197430 = CARTESIAN_POINT ( 'NONE',  ( -10.81492255796078084, -18.62759615963271287, 77.08224293864769550 ) ) ;
#197431 = CARTESIAN_POINT ( 'NONE',  ( 12.14591786802309770, 12.06949235617756955, 24.37390960531435979 ) ) ;
#197432 = CARTESIAN_POINT ( 'NONE',  ( 19.02544592524334988, 5.153800228976608722, 111.4594237280190043 ) ) ;
#197433 = CARTESIAN_POINT ( 'NONE',  ( -16.46253265017160317, 9.564922557960807481, 40.83224293864769550 ) ) ;
#197434 = CARTESIAN_POINT ( 'NONE',  ( -12.14591786802326823, 12.06949235617739902, 28.12609039468568284 ) ) ;
#197435 = CARTESIAN_POINT ( 'NONE',  ( 9.564922557960805705, 16.46253265017160317, 59.58224293864769550 ) ) ;
#197436 = CARTESIAN_POINT ( 'NONE',  ( -8.571926809382601320, -26.38167802310801591, 139.7750000027311899 ) ) ;
#197437 = CARTESIAN_POINT ( 'NONE',  ( -5.153800228976328057, -19.02544592524343514, 107.2905762719810383 ) ) ;
#197438 = CARTESIAN_POINT ( 'NONE',  ( -19.05341960407611168, -5.049401038298163336, 101.4572429386476955 ) ) ;
#197439 = CARTESIAN_POINT ( 'NONE',  ( 16.55341960407618274, -4.379528057220086978, 86.04275706135236135 ) ) ;
#197440 = CARTESIAN_POINT ( 'NONE',  ( -9.474510206698720793, -16.51473224551083518, 94.58442372801900433 ) ) ;
#197441 = CARTESIAN_POINT ( 'NONE',  ( -13.97604488694547697, 13.89961937509957934, 33.12609039468566863 ) ) ;
#197442 = CARTESIAN_POINT ( 'NONE',  ( -15.72974639402197994, 15.80617190586746368, 80.62390960531438111 ) ) ;
#197443 = CARTESIAN_POINT ( 'NONE',  ( -16.52544592524335698, -4.483927247898792601, 98.95942372801903275 ) ) ;
#197444 = CARTESIAN_POINT ( 'NONE',  ( -10.72451020669898014, 18.67979575497178502, 30.41557627198101699 ) ) ;
#197445 = CARTESIAN_POINT ( 'NONE',  ( -16.51473224551082808, 9.474510206698731452, 98.33442372801900433 ) ) ;
#197446 = CARTESIAN_POINT ( 'NONE',  ( 0.05219959533909260263, 19.03943276465977164, 44.99890960531435979 ) ) ;
#197447 = CARTESIAN_POINT ( 'NONE',  ( 19.02544592524343514, -5.153800228976328945, 88.54057627198102409 ) ) ;
#197448 = CARTESIAN_POINT ( 'NONE',  ( 21.52544592524334988, 5.823673210054432836, 61.45942372801901854 ) ) ;
#197449 = CARTESIAN_POINT ( 'NONE',  ( -16.51473224551069308, -9.474510206698971260, 61.66557627198103120 ) ) ;
#197450 = CARTESIAN_POINT ( 'NONE',  ( -4.483927247898539470, -16.52544592524342804, 82.29057627198103830 ) ) ;
#197451 = CARTESIAN_POINT ( 'NONE',  ( -17.48847506799969054, -5.747544572773762184, 84.17302562156724832 ) ) ;
#197452 = CARTESIAN_POINT ( 'NONE',  ( 12.14591786802309770, 12.06949235617756955, 84.37390960531438111 ) ) ;
#197453 = CARTESIAN_POINT ( 'NONE',  ( 21.52544592524344225, -5.823673210054117533, 73.54057627198102409 ) ) ;
#197454 = CARTESIAN_POINT ( 'NONE',  ( 16.51473224551083163, -9.474510206698727899, 95.83442372801900433 ) ) ;
#197455 = CARTESIAN_POINT ( 'NONE',  ( 18.87255363501903105, 5.500000000000005329, 93.82513748171824375 ) ) ;
#197456 = CARTESIAN_POINT ( 'NONE',  ( -19.05341960407617563, 5.049401038297882671, 38.54275706135233293 ) ) ;
#197457 = CARTESIAN_POINT ( 'NONE',  ( 17.50000000000000711, -5.622605283950830923, 71.18792689403890961 ) ) ;
#197459 = CARTESIAN_POINT ( 'NONE',  ( -13.89961937509977652, 13.97604488694528158, 80.62390960531436690 ) ) ;
#197458 = CARTESIAN_POINT ( 'NONE',  ( -13.97604488694527625, -13.89961937509977652, 76.87390960531433848 ) ) ;
#197460 = CARTESIAN_POINT ( 'NONE',  ( 16.53943276465976808, 0.05219959533934440121, 66.25109039468567573 ) ) ;
#197461 = DIRECTION ( 'NONE',  ( -0.000000000000000000, -0.000000000000000000, 1.000000000000000000 ) ) ;
#197462 = CARTESIAN_POINT ( 'NONE',  ( -19.02544592524334988, -5.153800228976617603, 43.95942372801899012 ) ) ;
#197463 = CARTESIAN_POINT ( 'NONE',  ( 17.46008511430124344, -15.43033707490625162, -57.51273177586173091 ) ) ;
#197464 = CARTESIAN_POINT ( 'NONE',  ( -9.474510206698964154, 16.51473224551069663, 105.4155762719810383 ) ) ;
#197465 = CARTESIAN_POINT ( 'NONE',  ( 4.379528057220092307, 16.55341960407617563, 107.2927570613523471 ) ) ;
#197466 = FACE_OUTER_BOUND ( 'NONE', #106289, .T. ) ;
#197467 = CARTESIAN_POINT ( 'NONE',  ( -8.314922557961024197, 14.29746914071037800, 77.91775706135231871 ) ) ;
#197468 = CARTESIAN_POINT ( 'NONE',  ( -17.48847506799968698, 5.747544572773788829, 30.82697437843281207 ) ) ;
#197469 = CARTESIAN_POINT ( 'NONE',  ( 4.379528057220092307, 16.55341960407617563, 57.29275706135234714 ) ) ;
#197470 = LINE ( 'NONE', #14420, #56261 ) ;
#197471 = CARTESIAN_POINT ( 'NONE',  ( 0.05219959533937995610, -21.53943276465977519, 70.00109039468568994 ) ) ;
#197472 = CARTESIAN_POINT ( 'NONE',  ( -16.46253265017146816, -9.564922557961047289, 79.16775706135234714 ) ) ;
#197473 = CARTESIAN_POINT ( 'NONE',  ( 16.46253265017146816, 9.564922557961045513, 26.66775706135234003 ) ) ;
#197474 = CARTESIAN_POINT ( 'NONE',  ( 16.46253265017160672, -9.564922557960803928, 48.33224293864769550 ) ) ;
#197475 = CARTESIAN_POINT ( 'NONE',  ( 16.46253265017160672, -9.564922557960803928, 38.33224293864768839 ) ) ;
#197476 = CARTESIAN_POINT ( 'NONE',  ( -3.573655867282028392E-15, 2.428612866367529932E-14, -15.00000000000000000 ) ) ;
#197477 = CARTESIAN_POINT ( 'NONE',  ( 15.72974639402199770, -15.80617190586745480, 68.12390960531436690 ) ) ;
#197478 = CARTESIAN_POINT ( 'NONE',  ( -15.80617190586745835, -15.72974639402198527, 31.87390960531435979 ) ) ;
#197479 = CARTESIAN_POINT ( 'NONE',  ( -14.29746914071049879, 8.314922557960819915, 115.8322429386477097 ) ) ;
#197480 = CARTESIAN_POINT ( 'NONE',  ( 8.224510206698742110, 14.34966873604972548, 47.08442372801901854 ) ) ;
#197481 = ORIENTED_EDGE ( 'NONE', *, *, #108717, .F. ) ;
#197482 = CARTESIAN_POINT ( 'NONE',  ( 5.823673210054444382, -21.52544592524334988, 35.20942372801901854 ) ) ;
#197484 = CARTESIAN_POINT ( 'NONE',  ( -38.00000000000001421, -12.34694845685042708, -5.900000000000000355 ) ) ;
#197483 = CARTESIAN_POINT ( 'NONE',  ( -12.14591786802309592, -12.06949235617757132, 56.87390960531436690 ) ) ;
#197485 = CARTESIAN_POINT ( 'NONE',  ( -16.53943276465976808, -0.05219959533934237506, 28.75109039468567929 ) ) ;
#197486 = CARTESIAN_POINT ( 'NONE',  ( -13.89961937509957401, -13.97604488694547875, 39.37609039468566152 ) ) ;
#197487 = CARTESIAN_POINT ( 'NONE',  ( 16.55341960407611168, 4.379528057220329451, 48.95724293864770971 ) ) ;
#197488 = CARTESIAN_POINT ( 'NONE',  ( 21.52544592524344225, -5.823673210054117533, 113.5405762719810383 ) ) ;
#197490 = CARTESIAN_POINT ( 'NONE',  ( 5.823673210054125526, 21.52544592524343514, 79.79057627198102409 ) ) ;
#197489 = CARTESIAN_POINT ( 'NONE',  ( -13.89961937509977830, 13.97604488694528158, 100.6239096053143669 ) ) ;
#197491 = CARTESIAN_POINT ( 'NONE',  ( 0.05219959533909260263, 19.03943276465977164, 94.99890960531436690 ) ) ;
#197492 = CARTESIAN_POINT ( 'NONE',  ( 0.05219959533910956823, 16.53943276465976808, 64.99890960531435269 ) ) ;
#197493 = CARTESIAN_POINT ( 'NONE',  ( 16.46253265017160672, -9.564922557960803928, 103.3322429386476955 ) ) ;
#197494 = DIRECTION ( 'NONE',  ( -0.000000000000000000, 1.000000000000000000, -0.000000000000000000 ) ) ;
#197495 = CARTESIAN_POINT ( 'NONE',  ( 5.049401038297881783, 19.05341960407617563, 57.29275706135231871 ) ) ;
#197496 = CARTESIAN_POINT ( 'NONE',  ( -5.823673210054116645, -21.52544592524344225, 112.2905762719810241 ) ) ;
#197497 = CARTESIAN_POINT ( 'NONE',  ( 13.97604488694527802, 13.89961937509977652, 44.37390960531435269 ) ) ;
#197498 = CARTESIAN_POINT ( 'NONE',  ( 14.29746914071049879, -8.314922557960816363, 113.3322429386476955 ) ) ;
#197499 = CARTESIAN_POINT ( 'NONE',  ( 10.72451020669871369, 18.67979575497193778, 52.08442372801901854 ) ) ;
#197500 = CARTESIAN_POINT ( 'NONE',  ( -27.73933785331498925, -9.013057229001049109, 146.9750000027311785 ) ) ;
#197501 = CARTESIAN_POINT ( 'NONE',  ( 0.05219959533910956823, 16.53943276465976808, 34.99890960531435979 ) ) ;
#197502 = CARTESIAN_POINT ( 'NONE',  ( -9.474510206698964154, 16.51473224551069663, 45.41557627198103120 ) ) ;
#197503 = CARTESIAN_POINT ( 'NONE',  ( 5.049401038298161559, -19.05341960407611168, 97.70724293864766707 ) ) ;
#197504 = CARTESIAN_POINT ( 'NONE',  ( 21.55341960407610458, 5.719274019375980345, 73.95724293864769550 ) ) ;
#197505 = CARTESIAN_POINT ( 'NONE',  ( -22.44159573604010305, 16.30477369853692338, 144.6750000027311671 ) ) ;
#197506 = CARTESIAN_POINT ( 'NONE',  ( 19.02544592524343514, -5.153800228976328945, 48.54057627198103120 ) ) ;
#197507 = CARTESIAN_POINT ( 'NONE',  ( -18.62759615963270932, 10.81492255796079327, 70.83224293864770971 ) ) ;
#197508 = CARTESIAN_POINT ( 'NONE',  ( -18.67979575497193778, 10.72451020669871902, 88.33442372801901854 ) ) ;
#197511 = CARTESIAN_POINT ( 'NONE',  ( 14.34966873604960469, 8.224510206698951720, 74.16557627198102409 ) ) ;
#197510 = CARTESIAN_POINT ( 'NONE',  ( -4.379528057220086978, -16.55341960407618274, 79.79275706135236135 ) ) ;
#197509 = FACE_OUTER_BOUND ( 'NONE', #34625, .T. ) ;
#197512 = CARTESIAN_POINT ( 'NONE',  ( 19.03943276465977164, -0.05219959533909143690, 73.74890960531435269 ) ) ;
#197513 = VERTEX_POINT ( 'NONE', #127561 ) ;
#197514 = CARTESIAN_POINT ( 'NONE',  ( 16.51473224551083163, -9.474510206698727899, 30.83442372801900433 ) ) ;
#197515 = CARTESIAN_POINT ( 'NONE',  ( -16.52544592524335698, -4.483927247898792601, 88.95942372801901854 ) ) ;
#197516 = CARTESIAN_POINT ( 'NONE',  ( 21.55341960407619695, -5.719274019375665929, 106.0427570613523471 ) ) ;
#197517 = CARTESIAN_POINT ( 'NONE',  ( 9.474510206698971260, -16.51473224551069308, 77.91557627198103830 ) ) ;
#197518 = CARTESIAN_POINT ( 'NONE',  ( 5.719274019375991003, -21.55341960407610458, 42.70724293864770260 ) ) ;
#197519 = CARTESIAN_POINT ( 'NONE',  ( -12.06949235617739369, -12.14591786802326823, 19.37609039468568639 ) ) ;
#197520 = CARTESIAN_POINT ( 'NONE',  ( -18.67979575497193778, 10.72451020669871902, 93.33442372801901854 ) ) ;
#197521 = CARTESIAN_POINT ( 'NONE',  ( 16.52544592524335698, 4.483927247898782831, 56.45942372801902565 ) ) ;
#197522 = CARTESIAN_POINT ( 'NONE',  ( -21.52544592524343514, 5.823673210054127303, 111.0405762719810525 ) ) ;
#197523 = CARTESIAN_POINT ( 'NONE',  ( -4.483927247898782831, 16.52544592524335698, 22.70942372801901499 ) ) ;
#197524 = CARTESIAN_POINT ( 'NONE',  ( 9.474510206698971260, -16.51473224551069308, 87.91557627198102409 ) ) ;
#197525 = CARTESIAN_POINT ( 'NONE',  ( -4.483927247898782831, 16.52544592524335698, 32.70942372801900433 ) ) ;
#197526 = CARTESIAN_POINT ( 'NONE',  ( -19.05341960407611168, -5.049401038298163336, 56.45724293864768129 ) ) ;
#197527 = CARTESIAN_POINT ( 'NONE',  ( -16.52544592524335698, -4.483927247898792601, 33.95942372801901143 ) ) ;
#197528 = CARTESIAN_POINT ( 'NONE',  ( 16.55341960407611168, 4.379528057220329451, 78.95724293864769550 ) ) ;
#197529 = EDGE_CURVE ( 'NONE', #73471, #21583, #159435, .T. ) ;
#197530 = CARTESIAN_POINT ( 'NONE',  ( -16.52544592524335698, -4.483927247898792601, 83.95942372801900433 ) ) ;
#197532 = CARTESIAN_POINT ( 'NONE',  ( 19.05341960407611168, 5.049401038298154454, 58.95724293864768129 ) ) ;
#197531 = CARTESIAN_POINT ( 'NONE',  ( -18.67979575497193778, 10.72451020669871902, 38.33442372801900433 ) ) ;
#197533 = CARTESIAN_POINT ( 'NONE',  ( -0.05219959533909027116, -19.03943276465977164, 87.49890960531436690 ) ) ;
#197534 = CARTESIAN_POINT ( 'NONE',  ( -12.06949235617739369, -12.14591786802326823, 79.37609039468567573 ) ) ;
#197535 = CARTESIAN_POINT ( 'NONE',  ( -24.72709851008508508, -6.869189314505666388, 167.7661538690216787 ) ) ;
#197536 = VERTEX_POINT ( 'NONE', #159898 ) ;
#197537 = CARTESIAN_POINT ( 'NONE',  ( 19.05341960407617918, -5.049401038297876454, 36.04275706135234003 ) ) ;
#197538 = CARTESIAN_POINT ( 'NONE',  ( -9.474510206698964154, 16.51473224551069663, 95.41557627198102409 ) ) ;
#197539 = CARTESIAN_POINT ( 'NONE',  ( -19.05341960407611168, -5.049401038298163336, 46.45724293864768129 ) ) ;
#197540 = CARTESIAN_POINT ( 'NONE',  ( 19.03943276465977164, -0.05219959533909143690, 108.7489096053143527 ) ) ;
#197541 = CARTESIAN_POINT ( 'NONE',  ( 16.55341960407618274, -4.379528057220086978, 46.04275706135234714 ) ) ;
#197543 = CARTESIAN_POINT ( 'NONE',  ( -4.483927247898782831, 16.52544592524335698, 57.70942372801901143 ) ) ;
#197542 = CARTESIAN_POINT ( 'NONE',  ( -19.05341960407617563, 5.049401038297882671, 63.54275706135234003 ) ) ;
#197544 = PLANE ( 'NONE',  #153039 ) ;
#197545 = CARTESIAN_POINT ( 'NONE',  ( -13.97604488694527625, -13.89961937509977652, 81.87390960531436690 ) ) ;
#197546 = CARTESIAN_POINT ( 'NONE',  ( 15.72974639402199770, -15.80617190586745480, 108.1239096053143811 ) ) ;
#197547 = CARTESIAN_POINT ( 'NONE',  ( 19.02544592524334988, 5.153800228976608722, 61.45942372801900433 ) ) ;
#197549 = CARTESIAN_POINT ( 'NONE',  ( -19.03943276465977164, 0.05219959533909376836, 26.24890960531435624 ) ) ;
#197548 = CARTESIAN_POINT ( 'NONE',  ( 19.03943276465977164, -0.05219959533909143690, 88.74890960531436690 ) ) ;
#197550 = CARTESIAN_POINT ( 'NONE',  ( -9.564922557960796823, -16.46253265017161027, 82.08224293864768129 ) ) ;
#197552 = CARTESIAN_POINT ( 'NONE',  ( 19.05341960407611168, 5.049401038298154454, 23.95724293864769194 ) ) ;
#197551 = CARTESIAN_POINT ( 'NONE',  ( 8.314922557960818139, 14.29746914071049879, 29.58224293864769905 ) ) ;
#197553 = CARTESIAN_POINT ( 'NONE',  ( -9.564922557961040184, 16.46253265017147172, 42.91775706135234003 ) ) ;
#197554 = CARTESIAN_POINT ( 'NONE',  ( 14.29746914071049879, -8.314922557960816363, 73.33224293864769550 ) ) ;
#197555 = CARTESIAN_POINT ( 'NONE',  ( -18.62759615963255300, -10.81492255796106328, 99.16775706135234714 ) ) ;
#197556 = CARTESIAN_POINT ( 'NONE',  ( -5.153800228976328057, -19.02544592524343514, 37.29057627198102409 ) ) ;
#197557 = EDGE_CURVE ( 'NONE', #107603, #45261, #8674, .T. ) ;
#197559 = CARTESIAN_POINT ( 'NONE',  ( -21.55341960407619339, 5.719274019375674811, 108.5427570613523756 ) ) ;
#197558 = CARTESIAN_POINT ( 'NONE',  ( -4.379528057220328563, 16.55341960407611168, 35.20724293864768839 ) ) ;
#197560 = CARTESIAN_POINT ( 'NONE',  ( 19.03943276465977164, -0.05219959533909143690, 93.74890960531435269 ) ) ;
#197561 = CARTESIAN_POINT ( 'NONE',  ( 9.564922557960805705, 16.46253265017160317, 89.58224293864769550 ) ) ;
#197562 = CARTESIAN_POINT ( 'NONE',  ( 13.97604488694527802, 13.89961937509977652, 39.37390960531435269 ) ) ;
#197563 = CARTESIAN_POINT ( 'NONE',  ( 4.379528057220339221, -16.55341960407611168, 102.7072429386476955 ) ) ;
#197564 = CARTESIAN_POINT ( 'NONE',  ( -4.379528057220328563, 16.55341960407611168, 70.20724293864769550 ) ) ;
#197565 = CARTESIAN_POINT ( 'NONE',  ( -10.72451020669898014, 18.67979575497178502, 80.41557627198103830 ) ) ;
#197566 = CARTESIAN_POINT ( 'NONE',  ( -0.05219959533909027116, -19.03943276465977164, 87.49890960531436690 ) ) ;
#197567 = CARTESIAN_POINT ( 'NONE',  ( 21.53943276465977519, -0.05219959533907433946, 103.7489096053143669 ) ) ;
#197568 = CARTESIAN_POINT ( 'NONE',  ( 16.46253265017160672, -9.564922557960803928, 93.33224293864769550 ) ) ;
#197570 = CARTESIAN_POINT ( 'NONE',  ( 16.53943276465976808, -0.05219959533910856209, 83.74890960531435269 ) ) ;
#197569 = DIRECTION ( 'NONE',  ( -0.000000000000000000, -0.000000000000000000, 1.000000000000000000 ) ) ;
#197571 = CARTESIAN_POINT ( 'NONE',  ( 13.97604488694527802, 13.89961937509977652, 69.37390960531436690 ) ) ;
#197572 = CARTESIAN_POINT ( 'NONE',  ( 5.823673210054125526, 21.52544592524343514, 79.79057627198102409 ) ) ;
#197573 = LINE ( 'NONE', #120707, #152900 ) ;
#197575 = DIRECTION ( 'NONE',  ( -0.000000000000000000, -0.000000000000000000, 1.000000000000000000 ) ) ;
#197574 = CARTESIAN_POINT ( 'NONE',  ( 18.67979575497178502, 10.72451020669898547, 29.16557627198103120 ) ) ;
#197576 = CARTESIAN_POINT ( 'NONE',  ( -13.89961937509957401, -13.97604488694547875, 109.3760903946856331 ) ) ;
#197577 = CARTESIAN_POINT ( 'NONE',  ( 16.53943276465976808, -0.05219959533910856209, 98.74890960531438111 ) ) ;
#197578 = CARTESIAN_POINT ( 'NONE',  ( -17.12812012977028076, -6.668231424565931320, 96.35948759323143520 ) ) ;
#197579 = CARTESIAN_POINT ( 'NONE',  ( 19.02544592524343514, -5.153800228976328945, 88.54057627198102409 ) ) ;
#197580 = CARTESIAN_POINT ( 'NONE',  ( 13.89961937509977652, -13.97604488694527269, 48.12390960531435979 ) ) ;
#197581 = CARTESIAN_POINT ( 'NONE',  ( 12.14591786802309770, 12.06949235617756955, 79.37390960531436690 ) ) ;
#197582 = CARTESIAN_POINT ( 'NONE',  ( -9.474510206698964154, 16.51473224551069663, 110.4155762719810383 ) ) ;
#197583 = CARTESIAN_POINT ( 'NONE',  ( -8.314922557960811034, -14.29746914071050412, 57.08224293864769550 ) ) ;
#197584 = CARTESIAN_POINT ( 'NONE',  ( -16.51473224551082808, 9.474510206698731452, 108.3344237280190043 ) ) ;
#197585 = CARTESIAN_POINT ( 'NONE',  ( -15.72974639402176322, -15.80617190586768395, 54.37609039468568994 ) ) ;
#197586 = CARTESIAN_POINT ( 'NONE',  ( -22.44159573604010305, 16.30477369853692338, 146.6750000027311671 ) ) ;
#197587 = CARTESIAN_POINT ( 'NONE',  ( -16.46253265017160317, 9.564922557960807481, 95.83224293864769550 ) ) ;
#197588 = CARTESIAN_POINT ( 'NONE',  ( 21.52544592524344225, -5.823673210054117533, 88.54057627198103830 ) ) ;
#197589 = CARTESIAN_POINT ( 'NONE',  ( -0.05219959533934338120, 16.53943276465976808, 82.50109039468568994 ) ) ;
#197590 = CARTESIAN_POINT ( 'NONE',  ( 16.46253265017160672, -9.564922557960803928, 28.33224293864769550 ) ) ;
#197591 = CARTESIAN_POINT ( 'NONE',  ( 16.51473224551069308, 9.474510206698969483, 74.16557627198103830 ) ) ;
#197592 = CARTESIAN_POINT ( 'NONE',  ( -15.72974639402197994, 15.80617190586746368, 80.62390960531438111 ) ) ;
#197593 = CARTESIAN_POINT ( 'NONE',  ( -19.03943276465977164, -0.05219959533935918106, 103.7510903946856757 ) ) ;
#197595 = CARTESIAN_POINT ( 'NONE',  ( -15.72974639402176322, -15.80617190586768395, 54.37609039468568994 ) ) ;
#197594 = CARTESIAN_POINT ( 'NONE',  ( -8.314922557960811034, -14.29746914071050412, 47.08224293864770260 ) ) ;
#197597 = CARTESIAN_POINT ( 'NONE',  ( 19.02544592524343514, -5.153800228976328945, 113.5405762719810241 ) ) ;
#197596 = CARTESIAN_POINT ( 'NONE',  ( 4.483927247898790824, -16.52544592524335698, 80.20942372801901854 ) ) ;
#197598 = CARTESIAN_POINT ( 'NONE',  ( -0.05219959533909027116, -19.03943276465977164, 112.4989096053143669 ) ) ;
#197599 = CARTESIAN_POINT ( 'NONE',  ( 1.500000000002908562, 30.39999999999990266, -50.95361246531977173 ) ) ;
#197600 = CARTESIAN_POINT ( 'NONE',  ( -4.483927247898782831, 16.52544592524335698, 107.7094237280190328 ) ) ;
#197601 = CARTESIAN_POINT ( 'NONE',  ( -12.14591786802326823, 12.06949235617739902, 53.12609039468568284 ) ) ;
#197602 = CARTESIAN_POINT ( 'NONE',  ( 19.02544592524343514, -5.153800228976328945, 63.54057627198103830 ) ) ;
#197603 = CARTESIAN_POINT ( 'NONE',  ( 19.02544592524343514, -5.153800228976328945, 68.54057627198103830 ) ) ;
#197604 = CARTESIAN_POINT ( 'NONE',  ( -4.379528057220086978, -16.55341960407618274, 74.79275706135234714 ) ) ;
#197605 = CARTESIAN_POINT ( 'NONE',  ( 4.483927247898545687, 16.52544592524342804, 44.79057627198103120 ) ) ;
#197606 = CARTESIAN_POINT ( 'NONE',  ( -13.89961937509977652, 13.97604488694528158, 50.62390960531435979 ) ) ;
#197607 = CARTESIAN_POINT ( 'NONE',  ( 5.153800228976335163, 19.02544592524342804, 44.79057627198103830 ) ) ;
#197609 = EDGE_LOOP ( 'NONE', ( #147987, #180052, #183469, #23431 ) ) ;
#197608 = CARTESIAN_POINT ( 'NONE',  ( 14.29746914071037800, 8.314922557961029526, 46.66775706135234714 ) ) ;
#197610 = CARTESIAN_POINT ( 'NONE',  ( 5.049401038297881783, 19.05341960407617563, 92.29275706135234714 ) ) ;
#197611 = CARTESIAN_POINT ( 'NONE',  ( -14.34966873604960291, -8.224510206698953496, 91.66557627198103830 ) ) ;
#197612 = CARTESIAN_POINT ( 'NONE',  ( -19.02544592524342804, 5.153800228976336051, 71.04057627198099567 ) ) ;
#197614 = CARTESIAN_POINT ( 'NONE',  ( 11.74264578624800315, -36.14014761921581709, -1.399999999999999689 ) ) ;
#197613 = CARTESIAN_POINT ( 'NONE',  ( -13.89961937509957401, -13.97604488694547875, 94.37609039468566152 ) ) ;
#197615 = CARTESIAN_POINT ( 'NONE',  ( 18.62759615963255655, 10.81492255796105972, 106.6677570613523756 ) ) ;
#197616 = CARTESIAN_POINT ( 'NONE',  ( 16.52544592524335698, 4.483927247898782831, 71.45942372801901854 ) ) ;
#197617 = DIRECTION ( 'NONE',  ( 1.000000000000000000, 0.000000000000000000, 0.000000000000000000 ) ) ;
#197618 = CARTESIAN_POINT ( 'NONE',  ( 10.81492255796078972, 18.62759615963270932, 69.58224293864769550 ) ) ;
#197619 = CARTESIAN_POINT ( 'NONE',  ( 4.483927247898790824, -16.52544592524335698, 55.20942372801902565 ) ) ;
#197620 = CARTESIAN_POINT ( 'NONE',  ( 16.46253265017160672, -9.564922557960803928, 38.33224293864768839 ) ) ;
#197621 = CARTESIAN_POINT ( 'NONE',  ( -0.05219959533936034679, 19.03943276465977164, 37.50109039468567573 ) ) ;
#197622 = CARTESIAN_POINT ( 'NONE',  ( -9.564922557960796823, -16.46253265017161027, 92.08224293864769550 ) ) ;
#197623 = CARTESIAN_POINT ( 'NONE',  ( 9.474510206698971260, -16.51473224551069308, 22.91557627198102765 ) ) ;
#197624 = CARTESIAN_POINT ( 'NONE',  ( 0.05219959533909260263, 19.03943276465977164, 59.99890960531436690 ) ) ;
#197625 = CARTESIAN_POINT ( 'NONE',  ( 21.52544592524334988, 5.823673210054432836, 81.45942372801900433 ) ) ;
#197626 = CARTESIAN_POINT ( 'NONE',  ( 0.05219959533936267826, -19.03943276465977164, 40.00109039468566152 ) ) ;
#197627 = CARTESIAN_POINT ( 'NONE',  ( 0.05219959533936267826, -19.03943276465977164, 25.00109039468566152 ) ) ;
#197628 = CARTESIAN_POINT ( 'NONE',  ( -9.564922557960796823, -16.46253265017161027, 62.08224293864769550 ) ) ;
#197629 = CARTESIAN_POINT ( 'NONE',  ( -5.823673210054116645, -21.52544592524344225, 27.29057627198103120 ) ) ;
#197630 = CARTESIAN_POINT ( 'NONE',  ( -15.80617190586768217, 15.72974639402176855, 83.12609039468568994 ) ) ;
#197631 = CARTESIAN_POINT ( 'NONE',  ( 19.05341960407611168, 5.049401038298154454, 58.95724293864768129 ) ) ;
#197632 = CARTESIAN_POINT ( 'NONE',  ( -21.53943276465977519, -0.05219959533937600094, 88.75109039468567573 ) ) ;
#197633 = CARTESIAN_POINT ( 'NONE',  ( 10.72451020669898902, -18.67979575497178502, 37.91557627198102409 ) ) ;
#197634 = VECTOR ( 'NONE', #102291, 1000.000000000000000 ) ;
#197635 = CARTESIAN_POINT ( 'NONE',  ( -5.153800228976328057, -19.02544592524343514, 87.29057627198103830 ) ) ;
#197636 = CARTESIAN_POINT ( 'NONE',  ( 10.72451020669871369, 18.67979575497193778, 37.08442372801901143 ) ) ;
#197637 = CARTESIAN_POINT ( 'NONE',  ( 19.05341960407617918, -5.049401038297876454, 66.04275706135233293 ) ) ;
#197638 = CARTESIAN_POINT ( 'NONE',  ( -19.03943276465977164, 0.05219959533909376836, 46.24890960531435979 ) ) ;
#197639 = CARTESIAN_POINT ( 'NONE',  ( -5.049401038298153566, 19.05341960407611168, 85.20724293864766707 ) ) ;
#197640 = CARTESIAN_POINT ( 'NONE',  ( -12.14591786802326823, 12.06949235617739902, 28.12609039468568284 ) ) ;
#197641 = CARTESIAN_POINT ( 'NONE',  ( -4.483927247898539470, -16.52544592524342804, 92.29057627198103830 ) ) ;
#197642 = CARTESIAN_POINT ( 'NONE',  ( 16.51473224551069308, 9.474510206698969483, 64.16557627198102409 ) ) ;
#197643 = CARTESIAN_POINT ( 'NONE',  ( -21.52544592524343514, 5.823673210054127303, 46.04057627198103830 ) ) ;
#197644 = CARTESIAN_POINT ( 'NONE',  ( -4.379528057220086978, -16.55341960407618274, 24.79275706135235779 ) ) ;
#197645 = CARTESIAN_POINT ( 'NONE',  ( 15.72974639402176855, 15.80617190586768217, 26.87609039468567218 ) ) ;
#197646 = CARTESIAN_POINT ( 'NONE',  ( -18.62759615963255300, -10.81492255796106328, 69.16775706135234714 ) ) ;
#197647 = CARTESIAN_POINT ( 'NONE',  ( -16.55341960407617563, 4.379528057220093196, 63.54275706135234003 ) ) ;
#197648 = CARTESIAN_POINT ( 'NONE',  ( 8.224510206698742110, 14.34966873604972548, 62.08442372801901143 ) ) ;
#197649 = CARTESIAN_POINT ( 'NONE',  ( 0.05219959533909260263, 19.03943276465977164, 59.99890960531436690 ) ) ;
#197650 = CARTESIAN_POINT ( 'NONE',  ( -0.05219959533934338120, 16.53943276465976808, 97.50109039468567573 ) ) ;
#197651 = CARTESIAN_POINT ( 'NONE',  ( 16.46253265017146816, 9.564922557961045513, 41.66775706135234003 ) ) ;
#197652 = CARTESIAN_POINT ( 'NONE',  ( 0.05219959533907565091, 21.53943276465977519, 109.9989096053143527 ) ) ;
#197653 = CARTESIAN_POINT ( 'NONE',  ( 0.05219959533910956823, 16.53943276465976808, 59.99890960531436690 ) ) ;
#197654 = CARTESIAN_POINT ( 'NONE',  ( -5.153800228976328057, -19.02544592524343514, 92.29057627198099567 ) ) ;
#197655 = CARTESIAN_POINT ( 'NONE',  ( 12.06949235617739724, 12.14591786802326823, 91.87609039468568994 ) ) ;
#197656 = CARTESIAN_POINT ( 'NONE',  ( 21.53943276465977519, 0.05219959533937863772, 61.25109039468567573 ) ) ;
#197657 = CARTESIAN_POINT ( 'NONE',  ( -0.05219959533934338120, 16.53943276465976808, 37.50109039468568284 ) ) ;
#197658 = CARTESIAN_POINT ( 'NONE',  ( 5.719274019375673035, 21.55341960407619339, 27.29275706135234358 ) ) ;
#197659 = CARTESIAN_POINT ( 'NONE',  ( 16.55341960407611168, 4.379528057220329451, 58.95724293864770971 ) ) ;
#197660 = ORIENTED_EDGE ( 'NONE', *, *, #100613, .F. ) ;
#197661 = CARTESIAN_POINT ( 'NONE',  ( 0.05219959533907565091, 21.53943276465977519, 99.99890960531436690 ) ) ;
#197662 = CARTESIAN_POINT ( 'NONE',  ( -12.06949235617756955, 12.14591786802309770, 35.62390960531437401 ) ) ;
#197663 = ORIENTED_EDGE ( 'NONE', *, *, #45960, .T. ) ;
#197664 = CARTESIAN_POINT ( 'NONE',  ( 34.78522506798722702, 0.4969912795167628072, 52.50000000000000000 ) ) ;
#197665 = CARTESIAN_POINT ( 'NONE',  ( -5.823673210054116645, -21.52544592524344225, 32.29057627198102409 ) ) ;
#197666 = CARTESIAN_POINT ( 'NONE',  ( 15.72974639402176855, 15.80617190586768217, 41.87609039468568284 ) ) ;
#197667 = CARTESIAN_POINT ( 'NONE',  ( -14.29746914071049879, 8.314922557960819915, 60.83224293864769550 ) ) ;
#197668 = CARTESIAN_POINT ( 'NONE',  ( -15.72974639402197994, 15.80617190586746368, 65.62390960531436690 ) ) ;
#197669 = CARTESIAN_POINT ( 'NONE',  ( 9.564922557960805705, 16.46253265017160317, 69.58224293864770971 ) ) ;
#197671 = CARTESIAN_POINT ( 'NONE',  ( 13.97604488694548053, -13.89961937509957401, 70.62609039468567573 ) ) ;
#197670 = CARTESIAN_POINT ( 'NONE',  ( 9.474510206698971260, -16.51473224551069308, 22.91557627198102765 ) ) ;
#197672 = CARTESIAN_POINT ( 'NONE',  ( -18.62759615963270932, 10.81492255796079327, 50.83224293864770971 ) ) ;
#197673 = CARTESIAN_POINT ( 'NONE',  ( -13.97604488694527625, -13.89961937509977652, 56.87390960531434558 ) ) ;
#197674 = CARTESIAN_POINT ( 'NONE',  ( 4.483927247898790824, -16.52544592524335698, 35.20942372801901854 ) ) ;
#197675 = CARTESIAN_POINT ( 'NONE',  ( 21.53943276465977519, 0.05219959533937863772, 21.25109039468567218 ) ) ;
#197676 = CARTESIAN_POINT ( 'NONE',  ( -4.483927247898539470, -16.52544592524342804, 47.29057627198103120 ) ) ;
#197677 = ORIENTED_EDGE ( 'NONE', *, *, #190781, .F. ) ;
#197678 = CARTESIAN_POINT ( 'NONE',  ( 16.46253265017160672, -9.564922557960803928, 88.33224293864769550 ) ) ;
#197679 = CARTESIAN_POINT ( 'NONE',  ( 21.52544592524344225, -5.823673210054117533, 73.54057627198102409 ) ) ;
#197681 = CARTESIAN_POINT ( 'NONE',  ( 4.379528057220092307, 16.55341960407617563, 32.29275706135235424 ) ) ;
#197680 = CARTESIAN_POINT ( 'NONE',  ( -15.80617190586745835, -15.72974639402198527, 106.8739096053143811 ) ) ;
#197682 = CARTESIAN_POINT ( 'NONE',  ( -18.67979575497178146, -10.72451020669898902, 41.66557627198103120 ) ) ;
#197683 = CARTESIAN_POINT ( 'NONE',  ( 18.67979575497194134, -10.72451020669871369, 95.83442372801903275 ) ) ;
#197684 = CARTESIAN_POINT ( 'NONE',  ( 0.05219959533909260263, 19.03943276465977164, 94.99890960531436690 ) ) ;
#197685 = CARTESIAN_POINT ( 'NONE',  ( 0.05219959533909260263, 19.03943276465977164, 34.99890960531435979 ) ) ;
#197686 = CARTESIAN_POINT ( 'NONE',  ( 19.05341960407611168, 5.049401038298154454, 93.95724293864769550 ) ) ;
#197687 = CARTESIAN_POINT ( 'NONE',  ( 16.46253265017160672, -9.564922557960803928, 78.33224293864769550 ) ) ;
#197688 = CARTESIAN_POINT ( 'NONE',  ( -21.25171708481316912, -32.43382446246058493, -17.33145006470357075 ) ) ;
#197689 = ADVANCED_FACE ( 'NONE', ( #34569, #114377 ), #112397, .T. ) ;
#197690 = CARTESIAN_POINT ( 'NONE',  ( 16.51473224551083163, -9.474510206698727899, 60.83442372801900433 ) ) ;
#197692 = CARTESIAN_POINT ( 'NONE',  ( -18.67979575497178146, -10.72451020669898902, 26.66557627198103475 ) ) ;
#197691 = CARTESIAN_POINT ( 'NONE',  ( 21.55341960407619695, -5.719274019375665929, 106.0427570613523471 ) ) ;
#197693 = CARTESIAN_POINT ( 'NONE',  ( -16.52544592524335698, -4.483927247898792601, 103.9594237280190185 ) ) ;
#197694 = CARTESIAN_POINT ( 'NONE',  ( 16.46253265017146816, 9.564922557961045513, 86.66775706135233293 ) ) ;
#197695 = CARTESIAN_POINT ( 'NONE',  ( -16.79531203550651242, 7.028104445595463545, 58.74755011779561187 ) ) ;
#197696 = CARTESIAN_POINT ( 'NONE',  ( 16.51473224551083163, -9.474510206698727899, 85.83442372801900433 ) ) ;
#197697 = CARTESIAN_POINT ( 'NONE',  ( -16.46253265017146816, -9.564922557961047289, 39.16775706135234003 ) ) ;
#197698 = DIRECTION ( 'NONE',  ( -1.000000000000000000, 0.000000000000000000, 0.000000000000000000 ) ) ;
#197699 = CARTESIAN_POINT ( 'NONE',  ( 19.02544592524343514, -5.153800228976328945, 43.54057627198103120 ) ) ;
#197700 = CARTESIAN_POINT ( 'NONE',  ( 16.52544592524342804, -4.483927247898539470, 48.54057627198103120 ) ) ;
#197701 = CARTESIAN_POINT ( 'NONE',  ( -16.62475595723698873, -7.163666690055296549, 109.4728664818953519 ) ) ;
#197702 = CARTESIAN_POINT ( 'NONE',  ( -8.314922557960811034, -14.29746914071050412, 32.08224293864769550 ) ) ;
#197703 = DIRECTION ( 'NONE',  ( -1.000000000000000000, -0.000000000000000000, 0.000000000000000000 ) ) ;
#197704 = CARTESIAN_POINT ( 'NONE',  ( 0.05219959533934541429, -16.53943276465976808, 90.00109039468567573 ) ) ;
#197705 = CARTESIAN_POINT ( 'NONE',  ( 5.049401038298161559, -19.05341960407611168, 47.70724293864770260 ) ) ;
#197706 = CARTESIAN_POINT ( 'NONE',  ( -0.05219959533937732626, 21.53943276465977519, 102.5010903946856899 ) ) ;
#197707 = CARTESIAN_POINT ( 'NONE',  ( 4.483927247898790824, -16.52544592524335698, 25.20942372801901854 ) ) ;
#197708 = CARTESIAN_POINT ( 'NONE',  ( -0.05219959533907301413, -21.53943276465977519, 37.49890960531436690 ) ) ;
#197710 = ORIENTED_EDGE ( 'NONE', *, *, #171523, .F. ) ;
#197709 = CARTESIAN_POINT ( 'NONE',  ( 21.52544592524334988, 5.823673210054432836, 96.45942372801901854 ) ) ;
#197711 = CARTESIAN_POINT ( 'NONE',  ( 19.03943276465977164, -0.05219959533909143690, 103.7489096053143669 ) ) ;
#197712 = CARTESIAN_POINT ( 'NONE',  ( 0.05219959533909260263, 19.03943276465977164, 79.99890960531436690 ) ) ;
#197713 = CARTESIAN_POINT ( 'NONE',  ( -11.40812507854754720, -35.11059874428192273, -8.224999997268813701 ) ) ;
#197714 = CARTESIAN_POINT ( 'NONE',  ( -0.05219959533907301413, -21.53943276465977519, 112.4989096053143669 ) ) ;
#197715 = CARTESIAN_POINT ( 'NONE',  ( 14.29746914071049879, -8.314922557960816363, 78.33224293864770971 ) ) ;
#197716 = CARTESIAN_POINT ( 'NONE',  ( 10.81492255796078972, 18.62759615963270932, 74.58224293864768129 ) ) ;
#197717 = CARTESIAN_POINT ( 'NONE',  ( -13.89961937509977652, 13.97604488694528158, 65.62390960531436690 ) ) ;
#197718 = CARTESIAN_POINT ( 'NONE',  ( -10.72451020669898014, 18.67979575497178502, 95.41557627198102409 ) ) ;
#197719 = ORIENTED_EDGE ( 'NONE', *, *, #117749, .T. ) ;
#197720 = CARTESIAN_POINT ( 'NONE',  ( 9.564922557960805705, 16.46253265017160317, 59.58224293864769550 ) ) ;
#197722 = CARTESIAN_POINT ( 'NONE',  ( 21.44820451018246388, -9.431764332217083435, 168.6453917704523633 ) ) ;
#197721 = CARTESIAN_POINT ( 'NONE',  ( -4.483927247898539470, -16.52544592524342804, 87.29057627198103830 ) ) ;
#197723 = CARTESIAN_POINT ( 'NONE',  ( -13.89961937509977652, 13.97604488694528158, 70.62390960531432427 ) ) ;
#197724 = CARTESIAN_POINT ( 'NONE',  ( -19.05341960407617563, 5.049401038297882671, 73.54275706135233293 ) ) ;
#197725 = CARTESIAN_POINT ( 'NONE',  ( -14.29746914071049879, 8.314922557960819915, 85.83224293864768129 ) ) ;
#197726 = CARTESIAN_POINT ( 'NONE',  ( -21.55341960407619339, 5.719274019375674811, 63.54275706135234003 ) ) ;
#197728 = CARTESIAN_POINT ( 'NONE',  ( 15.72974639402199770, -15.80617190586745480, 113.1239096053143953 ) ) ;
#197727 = CARTESIAN_POINT ( 'NONE',  ( 19.02544592524343514, -5.153800228976328945, 48.54057627198103120 ) ) ;
#197729 = CARTESIAN_POINT ( 'NONE',  ( 4.483927247898545687, 16.52544592524342804, 104.7905762719810241 ) ) ;
#197730 = CARTESIAN_POINT ( 'NONE',  ( 17.50000000000000711, 5.499999999999976907, 93.78230962303565832 ) ) ;
#197731 = CARTESIAN_POINT ( 'NONE',  ( 5.049401038298161559, -19.05341960407611168, 57.70724293864769550 ) ) ;
#197732 = CARTESIAN_POINT ( 'NONE',  ( -23.31738231874055600, 16.94106989632528837, 144.0500000054623513 ) ) ;
#197734 = CARTESIAN_POINT ( 'NONE',  ( 19.03943276465977164, -0.05219959533909143690, 113.7489096053143669 ) ) ;
#197733 = CARTESIAN_POINT ( 'NONE',  ( -9.474510206698720793, -16.51473224551083518, 109.5844237280190043 ) ) ;
#197735 = CARTESIAN_POINT ( 'NONE',  ( 5.719274019375673035, 21.55341960407619339, 52.29275706135236135 ) ) ;
#197736 = CARTESIAN_POINT ( 'NONE',  ( -19.02544592524342804, 5.153800228976336051, 91.04057627198100988 ) ) ;
#197737 = CARTESIAN_POINT ( 'NONE',  ( -19.02544592524334988, -5.153800228976617603, 88.95942372801897591 ) ) ;
#197738 = CARTESIAN_POINT ( 'NONE',  ( 19.05341960407611168, 5.049401038298154454, 58.95724293864768129 ) ) ;
#197739 = CARTESIAN_POINT ( 'NONE',  ( 4.379528057220339221, -16.55341960407611168, 72.70724293864769550 ) ) ;
#197740 = CARTESIAN_POINT ( 'NONE',  ( -16.53943276465976808, 0.05219959533911058130, 76.24890960531435269 ) ) ;
#197741 = CARTESIAN_POINT ( 'NONE',  ( -9.564922557960796823, -16.46253265017161027, 87.08224293864769550 ) ) ;
#197742 = CARTESIAN_POINT ( 'NONE',  ( 14.34966873604960469, 8.224510206698951720, 79.16557627198103830 ) ) ;
#197743 = CARTESIAN_POINT ( 'NONE',  ( -16.51473224551069308, -9.474510206698971260, 81.66557627198103830 ) ) ;
#197744 = CARTESIAN_POINT ( 'NONE',  ( 5.153800228976615827, -19.02544592524334988, 25.20942372801900433 ) ) ;
#197747 = CARTESIAN_POINT ( 'NONE',  ( 5.153800228976335163, 19.02544592524342804, 24.79057627198102765 ) ) ;
#197746 = CARTESIAN_POINT ( 'NONE',  ( -12.06949235617756955, 12.14591786802309770, 35.62390960531437401 ) ) ;
#197745 = CARTESIAN_POINT ( 'NONE',  ( 9.474510206698971260, -16.51473224551069308, 52.91557627198102409 ) ) ;
#197748 = ORIENTED_EDGE ( 'NONE', *, *, #44009, .F. ) ;
#197749 = CARTESIAN_POINT ( 'NONE',  ( 0.05219959533937995610, -21.53943276465977519, 45.00109039468568284 ) ) ;
#197750 = CARTESIAN_POINT ( 'NONE',  ( 13.89961937509957401, 13.97604488694547697, 61.87609039468566863 ) ) ;
#197751 = CARTESIAN_POINT ( 'NONE',  ( -14.34966873604960291, -8.224510206698953496, 36.66557627198103120 ) ) ;
#197752 = CARTESIAN_POINT ( 'NONE',  ( -5.719274019375978568, 21.55341960407610458, 90.20724293864770971 ) ) ;
#197753 = CARTESIAN_POINT ( 'NONE',  ( 21.52544592524344225, -5.823673210054117533, 33.54057627198102409 ) ) ;
#197754 = CARTESIAN_POINT ( 'NONE',  ( -4.379528057220328563, 16.55341960407611168, 75.20724293864769550 ) ) ;
#197755 = CARTESIAN_POINT ( 'NONE',  ( 5.153800228976335163, 19.02544592524342804, 39.79057627198100988 ) ) ;
#197756 = CARTESIAN_POINT ( 'NONE',  ( -14.29746914071037622, -8.314922557961029526, 109.1677570613523613 ) ) ;
#197757 = CARTESIAN_POINT ( 'NONE',  ( 16.52544592524335698, 4.483927247898782831, 71.45942372801901854 ) ) ;
#197758 = CARTESIAN_POINT ( 'NONE',  ( 5.823673210054125526, 21.52544592524343514, 34.79057627198103120 ) ) ;
#197759 = CARTESIAN_POINT ( 'NONE',  ( -5.153800228976607833, 19.02544592524334988, 22.70942372801899012 ) ) ;
#197760 = CARTESIAN_POINT ( 'NONE',  ( -19.03943276465977164, 0.05219959533909376836, 96.24890960531436690 ) ) ;
#197761 = CARTESIAN_POINT ( 'NONE',  ( -0.05219959533934338120, 16.53943276465976808, 77.50109039468567573 ) ) ;
#197762 = CARTESIAN_POINT ( 'NONE',  ( -8.224510206698948167, 14.34966873604960824, 115.4155762719810241 ) ) ;
#197763 = EDGE_CURVE ( 'NONE', #163091, #13391, #139014, .T. ) ;
#197764 = CARTESIAN_POINT ( 'NONE',  ( -8.314922557960811034, -14.29746914071050412, 32.08224293864769550 ) ) ;
#197766 = CARTESIAN_POINT ( 'NONE',  ( -13.89961937509977652, 13.97604488694528158, 85.62390960531433848 ) ) ;
#197765 = CARTESIAN_POINT ( 'NONE',  ( -5.049401038298153566, 19.05341960407611168, 100.2072429386476955 ) ) ;
#197767 = CARTESIAN_POINT ( 'NONE',  ( 5.719274019375991003, -21.55341960407610458, 22.70724293864769194 ) ) ;
#197768 = CARTESIAN_POINT ( 'NONE',  ( 16.55341960407611168, 4.379528057220329451, 68.95724293864769550 ) ) ;
#197769 = ORIENTED_EDGE ( 'NONE', *, *, #87117, .T. ) ;
#197770 = CARTESIAN_POINT ( 'NONE',  ( -4.483927247898539470, -16.52544592524342804, 52.29057627198102409 ) ) ;
#197771 = ORIENTED_EDGE ( 'NONE', *, *, #92972, .F. ) ;
#197773 = CARTESIAN_POINT ( 'NONE',  ( 9.564922557961047289, -16.46253265017146816, 60.41775706135233293 ) ) ;
#197772 = CARTESIAN_POINT ( 'NONE',  ( -4.379528057220086978, -16.55341960407618274, 59.79275706135234714 ) ) ;
#197774 = CARTESIAN_POINT ( 'NONE',  ( -5.049401038297874678, -19.05341960407617918, 49.79275706135231871 ) ) ;
#197775 = CARTESIAN_POINT ( 'NONE',  ( -16.46253265017160317, 9.564922557960807481, 95.83224293864769550 ) ) ;
#197776 = CARTESIAN_POINT ( 'NONE',  ( -5.049401038297874678, -19.05341960407617918, 69.79275706135233293 ) ) ;
#197777 = CARTESIAN_POINT ( 'NONE',  ( 22.44159573604009594, -16.30477369853687364, 144.1750000027311671 ) ) ;
#197778 = CARTESIAN_POINT ( 'NONE',  ( 19.05341960407617918, -5.049401038297876454, 56.04275706135234714 ) ) ;
#197780 = CARTESIAN_POINT ( 'NONE',  ( -16.53943276465976808, -0.05219959533934237506, 98.75109039468568994 ) ) ;
#197779 = CARTESIAN_POINT ( 'NONE',  ( 5.049401038297881783, 19.05341960407617563, 102.2927570613523045 ) ) ;
#197781 = CARTESIAN_POINT ( 'NONE',  ( 17.14385361876520264, 23.59649016807275856, 146.6750000027311671 ) ) ;
#197782 = CARTESIAN_POINT ( 'NONE',  ( 0.05219959533909260263, 19.03943276465977164, 44.99890960531435979 ) ) ;
#197783 = CARTESIAN_POINT ( 'NONE',  ( -9.474510206698964154, 16.51473224551069663, 115.4155762719810241 ) ) ;
#197784 = CARTESIAN_POINT ( 'NONE',  ( -5.823673210054431948, 21.52544592524334988, 57.70942372801901143 ) ) ;
#197785 = CARTESIAN_POINT ( 'NONE',  ( -9.474510206698720793, -16.51473224551083518, 99.58442372801900433 ) ) ;
#197787 = CARTESIAN_POINT ( 'NONE',  ( 13.97604488694527802, 13.89961937509977652, 59.37390960531434558 ) ) ;
#197786 = CARTESIAN_POINT ( 'NONE',  ( 13.97604488694548053, -13.89961937509957401, 55.62609039468566863 ) ) ;
#197788 = CARTESIAN_POINT ( 'NONE',  ( -13.89961937509977652, 13.97604488694528158, 110.6239096053143243 ) ) ;
#197790 = CARTESIAN_POINT ( 'NONE',  ( -5.049401038298153566, 19.05341960407611168, 65.20724293864765286 ) ) ;
#197789 = CARTESIAN_POINT ( 'NONE',  ( -14.34966873604960291, -8.224510206698953496, 76.66557627198103830 ) ) ;
#197791 = CARTESIAN_POINT ( 'NONE',  ( 9.564922557960805705, 16.46253265017160317, 79.58224293864769550 ) ) ;
#197792 = CARTESIAN_POINT ( 'NONE',  ( 13.89961937509957401, 13.97604488694547697, 71.87609039468567573 ) ) ;
#197793 = CARTESIAN_POINT ( 'NONE',  ( -18.67979575497178146, -10.72451020669898902, 66.66557627198102409 ) ) ;
#197794 = CARTESIAN_POINT ( 'NONE',  ( 12.14591786802309770, 12.06949235617756955, 109.3739096053143811 ) ) ;
#197795 = CARTESIAN_POINT ( 'NONE',  ( 13.97604488694548053, -13.89961937509957401, 55.62609039468566863 ) ) ;
#197796 = CARTESIAN_POINT ( 'NONE',  ( -19.02544592524342804, 5.153800228976336051, 61.04057627198103120 ) ) ;
#197797 = CARTESIAN_POINT ( 'NONE',  ( 19.05341960407611168, 5.049401038298154454, 73.95724293864768129 ) ) ;
#197798 = CARTESIAN_POINT ( 'NONE',  ( -21.55341960407610458, -5.719274019375992779, 91.45724293864769550 ) ) ;
#197800 = CARTESIAN_POINT ( 'NONE',  ( 0.05219959533936267826, -19.03943276465977164, 50.00109039468566863 ) ) ;
#197799 = CARTESIAN_POINT ( 'NONE',  ( 12.06949235617757843, -12.14591786802309237, 83.12390960531436690 ) ) ;
#197801 = CARTESIAN_POINT ( 'NONE',  ( -21.55341960407610458, -5.719274019375992779, 81.45724293864769550 ) ) ;
#197802 = CARTESIAN_POINT ( 'NONE',  ( 21.52544592524344225, -5.823673210054117533, 53.54057627198103120 ) ) ;
#197803 = CARTESIAN_POINT ( 'NONE',  ( -16.52544592524342804, 4.483927247898546575, 36.04057627198102409 ) ) ;
#197804 = CARTESIAN_POINT ( 'NONE',  ( -15.72974639402176322, -15.80617190586768395, 89.37609039468568994 ) ) ;
#197805 = CARTESIAN_POINT ( 'NONE',  ( -5.153800228976328057, -19.02544592524343514, 82.29057627198103830 ) ) ;
#197806 = CARTESIAN_POINT ( 'NONE',  ( -14.34966873604960291, -8.224510206698953496, 111.6655762719810525 ) ) ;
#197807 = CARTESIAN_POINT ( 'NONE',  ( 21.53943276465977519, 0.05219959533937863772, 26.25109039468567573 ) ) ;
#197808 = CARTESIAN_POINT ( 'NONE',  ( 10.81492255796106328, -18.62759615963255655, 40.41775706135234714 ) ) ;
#197809 = CARTESIAN_POINT ( 'NONE',  ( 19.02544592524343514, -5.153800228976328945, 43.54057627198103120 ) ) ;
#197810 = CARTESIAN_POINT ( 'NONE',  ( 5.823673210054444382, -21.52544592524334988, 25.20942372801901854 ) ) ;
#197811 = CARTESIAN_POINT ( 'NONE',  ( 13.97604488694548053, -13.89961937509957401, 60.62609039468564731 ) ) ;
#197813 = CARTESIAN_POINT ( 'NONE',  ( -16.51473224551069308, -9.474510206698971260, 41.66557627198103120 ) ) ;
#197812 = B_SPLINE_CURVE_WITH_KNOTS ( 'NONE', 3,
 ( #94939, #39245, #7898, #25100, #85744, #196939, #118095, #116087, #99906, #69583, #10919, #119099, #179785, #103918, #23085, #26094 ),
 .UNSPECIFIED., .F., .F.,
 ( 4, 2, 2, 2, 2, 2, 2, 4 ),
 ( 2.787258272608875357E-07, 0.0004619591141080896354, 0.0009236395023889183058, 0.001847000278950579116, 0.002308680667231405130, 0.002770361055512230927, 0.003232041443793056291, 0.003693721832073882522 ),
 .UNSPECIFIED. ) ;
#197814 = CARTESIAN_POINT ( 'NONE',  ( -16.52544592524335698, -4.483927247898792601, 28.95942372801902209 ) ) ;
#197815 = CARTESIAN_POINT ( 'NONE',  ( 19.03943276465977164, -0.05219959533909143690, 28.74890960531435624 ) ) ;
#197816 = CARTESIAN_POINT ( 'NONE',  ( 14.29746914071037800, 8.314922557961029526, 66.66775706135234714 ) ) ;
#197817 = CARTESIAN_POINT ( 'NONE',  ( -13.97604488694527625, -13.89961937509977652, 36.87390960531436690 ) ) ;
#197818 = CARTESIAN_POINT ( 'NONE',  ( -21.70479006154309687, -9.754118203517077035, 170.7545476126475421 ) ) ;
#197819 = CARTESIAN_POINT ( 'NONE',  ( -5.153800228976328057, -19.02544592524343514, 92.29057627198099567 ) ) ;
#197820 = CARTESIAN_POINT ( 'NONE',  ( 19.05341960407611168, 5.049401038298154454, 23.95724293864769194 ) ) ;
#197821 = CARTESIAN_POINT ( 'NONE',  ( 15.72974639402199770, -15.80617190586745480, 63.12390960531435979 ) ) ;
#197822 = CARTESIAN_POINT ( 'NONE',  ( -16.55341960407617563, 4.379528057220093196, 53.54275706135234714 ) ) ;
#197823 = CARTESIAN_POINT ( 'NONE',  ( 5.719274019375673035, 21.55341960407619339, 97.29275706135234714 ) ) ;
#197824 = CARTESIAN_POINT ( 'NONE',  ( 16.51473224551069308, 9.474510206698969483, 39.16557627198103120 ) ) ;
#197825 = CARTESIAN_POINT ( 'NONE',  ( -14.34966873604960291, -8.224510206698953496, 36.66557627198103120 ) ) ;
#197826 = CARTESIAN_POINT ( 'NONE',  ( -0.05219959533910754901, -16.53943276465976808, 72.49890960531435269 ) ) ;
#197827 = CARTESIAN_POINT ( 'NONE',  ( -5.049401038298153566, 19.05341960407611168, 65.20724293864765286 ) ) ;
#197828 = CARTESIAN_POINT ( 'NONE',  ( -21.53943276465977519, -0.05219959533937600094, 113.7510903946856757 ) ) ;
#197829 = CARTESIAN_POINT ( 'NONE',  ( 0.05219959533937995610, -21.53943276465977519, 20.00109039468568639 ) ) ;
#197830 = CARTESIAN_POINT ( 'NONE',  ( 13.89961937509977652, -13.97604488694527269, 83.12390960531436690 ) ) ;
#197831 = CARTESIAN_POINT ( 'NONE',  ( 21.53943276465977519, 0.05219959533937863772, 91.25109039468568994 ) ) ;
#197832 = CARTESIAN_POINT ( 'NONE',  ( 16.52544592524335698, 4.483927247898782831, 51.45942372801901854 ) ) ;
#197833 = CARTESIAN_POINT ( 'NONE',  ( 16.53943276465976808, 0.05219959533934440121, 31.25109039468568639 ) ) ;
#197835 = CARTESIAN_POINT ( 'NONE',  ( 21.53943276465977519, 0.05219959533937863772, 101.2510903946856757 ) ) ;
#197834 = CARTESIAN_POINT ( 'NONE',  ( 16.53943276465976808, -0.05219959533910856209, 93.74890960531436690 ) ) ;
#197836 = CARTESIAN_POINT ( 'NONE',  ( -14.29746914071049879, 8.314922557960819915, 30.83224293864770260 ) ) ;
#197837 = CARTESIAN_POINT ( 'NONE',  ( 16.51473224551069308, 9.474510206698969483, 24.16557627198102765 ) ) ;
#197838 = CARTESIAN_POINT ( 'NONE',  ( -4.483927247898782831, 16.52544592524335698, 47.70942372801902565 ) ) ;
#197839 = CARTESIAN_POINT ( 'NONE',  ( -14.29746914071049879, 8.314922557960819915, 60.83224293864769550 ) ) ;
#197840 = CARTESIAN_POINT ( 'NONE',  ( -4.379528057220086978, -16.55341960407618274, 94.79275706135234714 ) ) ;
#197841 = CARTESIAN_POINT ( 'NONE',  ( -13.89961937509977652, 13.97604488694528158, 110.6239096053143243 ) ) ;
#197842 = CARTESIAN_POINT ( 'NONE',  ( 5.049401038298161559, -19.05341960407611168, 107.7072429386476955 ) ) ;
#197843 = CARTESIAN_POINT ( 'NONE',  ( -13.97604488694547697, 13.89961937509957934, 23.12609039468565442 ) ) ;
#197844 = CARTESIAN_POINT ( 'NONE',  ( -16.52544592524342804, 4.483927247898546575, 86.04057627198102409 ) ) ;
#197845 = CARTESIAN_POINT ( 'NONE',  ( 0.05219959533909260263, 19.03943276465977164, 94.99890960531436690 ) ) ;
#197846 = VERTEX_POINT ( 'NONE', #38562 ) ;
#197847 = CARTESIAN_POINT ( 'NONE',  ( 4.483927247898790824, -16.52544592524335698, 45.20942372801901854 ) ) ;
#197848 = CARTESIAN_POINT ( 'NONE',  ( -5.049401038298153566, 19.05341960407611168, 35.20724293864768839 ) ) ;
#197850 = DIRECTION ( 'NONE',  ( 4.336808689942017120E-17, 1.000000000000000000, 0.000000000000000000 ) ) ;
#197849 = CARTESIAN_POINT ( 'NONE',  ( 12.14591786802327356, -12.06949235617739191, 50.62609039468568994 ) ) ;
#197851 = CARTESIAN_POINT ( 'NONE',  ( 13.97604488694548053, -13.89961937509957401, 50.62609039468566152 ) ) ;
#197852 = CARTESIAN_POINT ( 'NONE',  ( -0.05219959533909027116, -19.03943276465977164, 42.49890960531435269 ) ) ;
#197853 = CARTESIAN_POINT ( 'NONE',  ( -12.14591786802326823, 12.06949235617739902, 83.12609039468568994 ) ) ;
#197854 = CARTESIAN_POINT ( 'NONE',  ( -9.474510206698720793, -16.51473224551083518, 84.58442372801900433 ) ) ;
#197855 = CARTESIAN_POINT ( 'NONE',  ( -13.97604488694547697, 13.89961937509957934, 28.12609039468565797 ) ) ;
#197856 = CARTESIAN_POINT ( 'NONE',  ( 13.97604488694527802, 13.89961937509977652, 64.37390960531436690 ) ) ;
#197857 = CARTESIAN_POINT ( 'NONE',  ( -4.379528057220328563, 16.55341960407611168, 100.2072429386476955 ) ) ;
#197858 = CARTESIAN_POINT ( 'NONE',  ( 13.89961937509957401, 13.97604488694547697, 61.87609039468566863 ) ) ;
#197859 = CARTESIAN_POINT ( 'NONE',  ( -0.05219959533907301413, -21.53943276465977519, 62.49890960531436690 ) ) ;
#197860 = CARTESIAN_POINT ( 'NONE',  ( -16.46253265017146816, -9.564922557961047289, 24.16775706135233648 ) ) ;
#197861 = CARTESIAN_POINT ( 'NONE',  ( 16.51473224551069308, 9.474510206698969483, 104.1655762719810241 ) ) ;
#197862 = CARTESIAN_POINT ( 'NONE',  ( -18.62759615963270932, 10.81492255796079327, 75.83224293864769550 ) ) ;
#197863 = CARTESIAN_POINT ( 'NONE',  ( -17.26058549869092573, 6.457015423128482645, 83.62254162523933587 ) ) ;
#197864 = CARTESIAN_POINT ( 'NONE',  ( -16.46253265017146816, -9.564922557961047289, 99.16775706135233293 ) ) ;
#197865 = CARTESIAN_POINT ( 'NONE',  ( -19.52837319214028255, 5.499999999999902300, 59.60471352585542348 ) ) ;
#197866 = CARTESIAN_POINT ( 'NONE',  ( 8.224510206698742110, 14.34966873604972548, 32.08442372801901854 ) ) ;
#197867 = CARTESIAN_POINT ( 'NONE',  ( -19.02544592524342804, 5.153800228976336051, 31.04057627198102409 ) ) ;
#197868 = CARTESIAN_POINT ( 'NONE',  ( 5.153800228976335163, 19.02544592524342804, 104.7905762719809957 ) ) ;
#197869 = CARTESIAN_POINT ( 'NONE',  ( 10.72451020669898902, -18.67979575497178502, 87.91557627198103830 ) ) ;
#197870 = CARTESIAN_POINT ( 'NONE',  ( -5.719274019375665041, -21.55341960407619695, 59.79275706135234714 ) ) ;
#197872 = CARTESIAN_POINT ( 'NONE',  ( 10.81492255796106328, -18.62759615963255655, 110.4177570613523756 ) ) ;
#197871 = CARTESIAN_POINT ( 'NONE',  ( -5.049401038297874678, -19.05341960407617918, 104.7927570613523471 ) ) ;
#197873 = CARTESIAN_POINT ( 'NONE',  ( -16.53943276465976808, -0.05219959533934237506, 113.7510903946856757 ) ) ;
#197874 = CARTESIAN_POINT ( 'NONE',  ( 15.80617190586746368, 15.72974639402197994, 99.37390960531436690 ) ) ;
#197875 = CARTESIAN_POINT ( 'NONE',  ( 16.52544592524342804, -4.483927247898539470, 48.54057627198103120 ) ) ;
#197876 = CARTESIAN_POINT ( 'NONE',  ( 9.474510206698729675, 16.51473224551082808, 82.08442372801899012 ) ) ;
#197877 = CARTESIAN_POINT ( 'NONE',  ( -19.03943276465977164, -0.05219959533935918106, 53.75109039468566863 ) ) ;
#197878 = CARTESIAN_POINT ( 'NONE',  ( 18.67979575497194134, -10.72451020669871369, 55.83442372801901854 ) ) ;
#197879 = CARTESIAN_POINT ( 'NONE',  ( 5.153800228976615827, -19.02544592524334988, 40.20942372801898301 ) ) ;
#197880 = CARTESIAN_POINT ( 'NONE',  ( 16.52544592524342804, -4.483927247898539470, 103.5405762719810383 ) ) ;
#197881 = CARTESIAN_POINT ( 'NONE',  ( 21.52544592524344225, -5.823673210054117533, 33.54057627198102409 ) ) ;
#197882 = CARTESIAN_POINT ( 'NONE',  ( 8.224510206698953496, -14.34966873604960469, 42.91557627198103120 ) ) ;
#197883 = CARTESIAN_POINT ( 'NONE',  ( 0.05219959533937995610, -21.53943276465977519, 95.00109039468568994 ) ) ;
#197884 = CARTESIAN_POINT ( 'NONE',  ( 14.34966873604972726, -8.224510206698740333, 65.83442372801900433 ) ) ;
#197885 = CARTESIAN_POINT ( 'NONE',  ( -16.55341960407611168, -4.379528057220339221, 31.45724293864769550 ) ) ;
#197886 = CARTESIAN_POINT ( 'NONE',  ( 5.823673210054444382, -21.52544592524334988, 60.20942372801902565 ) ) ;
#197887 = CARTESIAN_POINT ( 'NONE',  ( 5.719274019375673035, 21.55341960407619339, 62.29275706135236845 ) ) ;
#197888 = CARTESIAN_POINT ( 'NONE',  ( 5.823673210054125526, 21.52544592524343514, 64.79057627198103830 ) ) ;
#197889 = ORIENTED_EDGE ( 'NONE', *, *, #168410, .F. ) ;
#197890 = CARTESIAN_POINT ( 'NONE',  ( 19.02544592524343514, -5.153800228976328945, 23.54057627198102054 ) ) ;
#197891 = CARTESIAN_POINT ( 'NONE',  ( -21.55341960407619339, 5.719274019375674811, 48.54275706135234714 ) ) ;
#197892 = CARTESIAN_POINT ( 'NONE',  ( 14.34966873604960469, 8.224510206698951720, 114.1655762719810383 ) ) ;
#197893 = CARTESIAN_POINT ( 'NONE',  ( 19.05341960407611168, 5.049401038298154454, 43.95724293864769550 ) ) ;
#197894 = CARTESIAN_POINT ( 'NONE',  ( 0.05219959533910956823, 16.53943276465976808, 79.99890960531435269 ) ) ;
#197895 = CARTESIAN_POINT ( 'NONE',  ( -16.46253265017160317, 9.564922557960807481, 85.83224293864769550 ) ) ;
#197896 = CARTESIAN_POINT ( 'NONE',  ( 16.52544592524342804, -4.483927247898539470, 28.54057627198103120 ) ) ;
#197897 = CARTESIAN_POINT ( 'NONE',  ( 8.314922557960818139, 14.29746914071049879, 104.5822429386477097 ) ) ;
#197898 = CARTESIAN_POINT ( 'NONE',  ( 10.81492255796078972, 18.62759615963270932, 69.58224293864769550 ) ) ;
#197899 = CARTESIAN_POINT ( 'NONE',  ( 21.53943276465977519, -0.05219959533907433946, 103.7489096053143669 ) ) ;
#197900 = FACE_OUTER_BOUND ( 'NONE', #147518, .T. ) ;
#197902 = CARTESIAN_POINT ( 'NONE',  ( 5.153800228976615827, -19.02544592524334988, 100.2094237280190043 ) ) ;
#197901 = CARTESIAN_POINT ( 'NONE',  ( 19.02544592524343514, -5.153800228976328945, 68.54057627198103830 ) ) ;
#197903 = CARTESIAN_POINT ( 'NONE',  ( -21.52544592524343514, 5.823673210054127303, 51.04057627198103120 ) ) ;
#197904 = CARTESIAN_POINT ( 'NONE',  ( 21.52544592524334988, 5.823673210054432836, 76.45942372801901854 ) ) ;
#197905 = CARTESIAN_POINT ( 'NONE',  ( 19.02544592524343514, -5.153800228976328945, 63.54057627198103830 ) ) ;
#197906 = CARTESIAN_POINT ( 'NONE',  ( -16.46253265017160317, 9.564922557960807481, 95.83224293864769550 ) ) ;
#197907 = CARTESIAN_POINT ( 'NONE',  ( 12.06949235617739724, 12.14591786802326823, 71.87609039468568994 ) ) ;
#197908 = CARTESIAN_POINT ( 'NONE',  ( -21.53943276465977519, -0.05219959533937600094, 53.75109039468568994 ) ) ;
#197909 = CARTESIAN_POINT ( 'NONE',  ( 21.55341960407619695, -5.719274019375665929, 101.0427570613523756 ) ) ;
#197910 = CARTESIAN_POINT ( 'NONE',  ( 15.80617190586769283, -15.72974639402175789, 20.62609039468568639 ) ) ;
#197911 = CARTESIAN_POINT ( 'NONE',  ( -21.53943276465977519, 0.05219959533907696930, 96.24890960531435269 ) ) ;
#197912 = CARTESIAN_POINT ( 'NONE',  ( -19.02544592524334988, -5.153800228976617603, 48.95942372801900433 ) ) ;
#197913 = CARTESIAN_POINT ( 'NONE',  ( -18.62759615963270932, 10.81492255796079327, 45.83224293864769550 ) ) ;
#197915 = CARTESIAN_POINT ( 'NONE',  ( -16.52544592524342804, 4.483927247898546575, 36.04057627198102409 ) ) ;
#197914 = CARTESIAN_POINT ( 'NONE',  ( -19.02544592524342804, 5.153800228976336051, 81.04057627198103830 ) ) ;
#197916 = CARTESIAN_POINT ( 'NONE',  ( -17.49999999999999645, 5.499999999999997335, 120.0000000000000142 ) ) ;
#197917 =( BOUNDED_CURVE ( )  B_SPLINE_CURVE ( 2, ( #65208, #81349, #143033, #112702, #67197, #175381, #20691, #5517, #113686, #188574, #50054, #135625, #28459 ),
 .UNSPECIFIED., .F., .T. ) 
 B_SPLINE_CURVE_WITH_KNOTS ( ( 3, 2, 2, 2, 2, 2, 3 ),
 ( 0.5024304364270452128, 0.5043859649122807154, 0.5087719298245614308, 0.5131578947368421462, 0.5175438596491228616, 0.5219298245614034659, 0.5238396732245489407 ),
 .UNSPECIFIED. ) 
 CURVE ( )  GEOMETRIC_REPRESENTATION_ITEM ( )  RATIONAL_B_SPLINE_CURVE ( ( 0.9831626618144007068, 0.9848076720550096308, 1.000000000000000000, 0.9659258262890683122, 1.000000000000000000, 0.9659258262890683122, 1.000000000000000000, 0.9659258262890683122, 1.000000000000000000, 0.9659258262890683122, 1.000000000000000000, 0.9851625545550091179, 0.9832469066685282089 ) ) 
 REPRESENTATION_ITEM ( '' )  );
#197918 = CARTESIAN_POINT ( 'NONE',  ( -19.52851543214745078, -5.499999999999944933, 80.39357721762576148 ) ) ;
#197919 = EDGE_CURVE ( 'NONE', #16610, #98258, #107774, .T. ) ;
#197920 = CARTESIAN_POINT ( 'NONE',  ( 9.564922557961047289, -16.46253265017146816, 95.41775706135233293 ) ) ;
#197921 = CARTESIAN_POINT ( 'NONE',  ( -18.62759615963270932, 10.81492255796079327, 65.83224293864769550 ) ) ;
#197922 = CARTESIAN_POINT ( 'NONE',  ( -14.29746914071049879, 8.314922557960819915, 55.83224293864770260 ) ) ;
#197923 = CARTESIAN_POINT ( 'NONE',  ( -14.34966873604972548, 8.224510206698743886, 28.33442372801902209 ) ) ;
#197924 = CARTESIAN_POINT ( 'NONE',  ( 19.03943276465977164, -0.05219959533909143690, 48.74890960531435979 ) ) ;
#197926 = CARTESIAN_POINT ( 'NONE',  ( -13.89961937509957401, -13.97604488694547875, 84.37609039468567573 ) ) ;
#197925 = CARTESIAN_POINT ( 'NONE',  ( -5.719274019375665041, -21.55341960407619695, 19.79275706135235069 ) ) ;
#197927 = CARTESIAN_POINT ( 'NONE',  ( 13.97604488694527802, 13.89961937509977652, 79.37390960531435269 ) ) ;
#197928 = CARTESIAN_POINT ( 'NONE',  ( 16.55341960407611168, 4.379528057220329451, 88.95724293864769550 ) ) ;
#197929 = CARTESIAN_POINT ( 'NONE',  ( 19.05341960407611168, 5.049401038298154454, 78.95724293864769550 ) ) ;
#197930 = CARTESIAN_POINT ( 'NONE',  ( 18.67979575497178502, 10.72451020669898547, 74.16557627198102409 ) ) ;
#197931 = CARTESIAN_POINT ( 'NONE',  ( -0.05219959533909027116, -19.03943276465977164, 27.49890960531435624 ) ) ;
#197932 = CARTESIAN_POINT ( 'NONE',  ( 18.55831789572370383, 32.36956839859214341, -7.999999999999994671 ) ) ;
#197933 = CARTESIAN_POINT ( 'NONE',  ( 14.29746914071049879, -8.314922557960816363, 53.33224293864769550 ) ) ;
#197934 = CARTESIAN_POINT ( 'NONE',  ( 19.05341960407611168, 5.049401038298154454, 88.95724293864769550 ) ) ;
#197935 = CARTESIAN_POINT ( 'NONE',  ( -9.564922557961040184, 16.46253265017147172, 47.91775706135233293 ) ) ;
#197936 = CARTESIAN_POINT ( 'NONE',  ( -14.29746914071037622, -8.314922557961029526, 54.16775706135235424 ) ) ;
#197937 = CARTESIAN_POINT ( 'NONE',  ( -5.719274019375978568, 21.55341960407610458, 75.20724293864769550 ) ) ;
#197938 = CARTESIAN_POINT ( 'NONE',  ( -9.564922557961040184, 16.46253265017147172, 42.91775706135234003 ) ) ;
#197939 = CARTESIAN_POINT ( 'NONE',  ( 16.46253265017160672, -9.564922557960803928, 83.33224293864768129 ) ) ;
#197940 = CARTESIAN_POINT ( 'NONE',  ( -17.49999999999999645, 5.499999999999996447, 113.7176903769643417 ) ) ;
#197941 = CARTESIAN_POINT ( 'NONE',  ( 15.72974639402199770, -15.80617190586745480, 23.12390960531436335 ) ) ;
#197942 = CARTESIAN_POINT ( 'NONE',  ( -13.97604488694527625, -13.89961937509977652, 71.87390960531433848 ) ) ;
#197943 = CARTESIAN_POINT ( 'NONE',  ( 15.80617190586769283, -15.72974639402175789, 55.62609039468568284 ) ) ;
#197944 = CARTESIAN_POINT ( 'NONE',  ( -0.05219959533909027116, -19.03943276465977164, 27.49890960531435624 ) ) ;
#197947 = VERTEX_POINT ( 'NONE', #157914 ) ;
#197946 = CARTESIAN_POINT ( 'NONE',  ( -13.89961937509977652, 13.97604488694528158, 100.6239096053143669 ) ) ;
#197945 = CARTESIAN_POINT ( 'NONE',  ( 0.05219959533937995610, -21.53943276465977519, 20.00109039468568639 ) ) ;
#197948 = CARTESIAN_POINT ( 'NONE',  ( 21.55341960407619695, -5.719274019375665929, 41.04275706135236135 ) ) ;
#197949 = VERTEX_POINT ( 'NONE', #119403 ) ;
#197950 = CARTESIAN_POINT ( 'NONE',  ( 5.049401038298161559, -19.05341960407611168, 102.7072429386476955 ) ) ;
#197951 = AXIS2_PLACEMENT_3D ( 'NONE', #114470, #165004, #26498 ) ;
#197952 = FACE_OUTER_BOUND ( 'NONE', #21694, .T. ) ;
#197953 = CARTESIAN_POINT ( 'NONE',  ( -10.72451020669898014, 18.67979575497178502, 110.4155762719810383 ) ) ;
#197954 = CARTESIAN_POINT ( 'NONE',  ( 19.03943276465977164, -0.05219959533909143690, 48.74890960531435979 ) ) ;
#197955 = CARTESIAN_POINT ( 'NONE',  ( -12.14591786802326823, 12.06949235617739902, 28.12609039468568284 ) ) ;
#197956 = CARTESIAN_POINT ( 'NONE',  ( -11.40812507854755609, 35.11059874428196537, -1.524999997268813301 ) ) ;
#197957 = CARTESIAN_POINT ( 'NONE',  ( 15.80617190586769283, -15.72974639402175789, 105.6260903946856899 ) ) ;
#197958 = CARTESIAN_POINT ( 'NONE',  ( 13.89961937509977652, -13.97604488694527269, 23.12390960531436335 ) ) ;
#197959 = CARTESIAN_POINT ( 'NONE',  ( -0.05219959533937732626, 21.53943276465977519, 92.50109039468567573 ) ) ;
#197961 = CARTESIAN_POINT ( 'NONE',  ( -15.72974639402176322, -15.80617190586768395, 64.37609039468568994 ) ) ;
#197960 = CARTESIAN_POINT ( 'NONE',  ( 5.153800228976335163, 19.02544592524342804, 84.79057627198099567 ) ) ;
#197962 = CARTESIAN_POINT ( 'NONE',  ( -27.73933785331498925, -9.013057229001049109, 141.4750000027311785 ) ) ;
#197963 = CARTESIAN_POINT ( 'NONE',  ( 16.51473224551069308, 9.474510206698969483, 104.1655762719810241 ) ) ;
#197964 = PLANE ( 'NONE',  #82227 ) ;
#197967 = CARTESIAN_POINT ( 'NONE',  ( -18.67979575497193778, 10.72451020669871902, 58.33442372801901143 ) ) ;
#197966 = CARTESIAN_POINT ( 'NONE',  ( 14.34966873604972726, -8.224510206698740333, 70.83442372801901854 ) ) ;
#197965 = CARTESIAN_POINT ( 'NONE',  ( 8.314922557961029526, -14.29746914071037800, 50.41775706135235424 ) ) ;
#197968 = CARTESIAN_POINT ( 'NONE',  ( 15.80617190586769283, -15.72974639402175789, 90.62609039468567573 ) ) ;
#197969 = DIRECTION ( 'NONE',  ( 0.000000000000000000, 0.000000000000000000, -1.000000000000000000 ) ) ;
#197970 = CARTESIAN_POINT ( 'NONE',  ( 16.52544592524335698, 4.483927247898782831, 26.45942372801901854 ) ) ;
#197971 = CARTESIAN_POINT ( 'NONE',  ( -0.05219959533909027116, -19.03943276465977164, 72.49890960531435269 ) ) ;
#197972 = CARTESIAN_POINT ( 'NONE',  ( -19.03943276465977164, 0.05219959533909376836, 101.2489096053143669 ) ) ;
#197973 = CARTESIAN_POINT ( 'NONE',  ( -3.181980515339399851, 6.791538853603101167, 8.889087296526001936 ) ) ;
#197974 = CARTESIAN_POINT ( 'NONE',  ( -13.89961937509977652, 13.97604488694528158, 30.62390960531435269 ) ) ;
#197975 = CARTESIAN_POINT ( 'NONE',  ( 18.67979575497178502, 10.72451020669898547, 24.16557627198103120 ) ) ;
#197976 = CARTESIAN_POINT ( 'NONE',  ( -8.314922557961024197, 14.29746914071037800, 92.91775706135236135 ) ) ;
#197978 = CARTESIAN_POINT ( 'NONE',  ( -9.564922557960796823, -16.46253265017161027, 67.08224293864769550 ) ) ;
#197977 = CARTESIAN_POINT ( 'NONE',  ( 4.379528057220339221, -16.55341960407611168, 67.70724293864769550 ) ) ;
#197979 = CARTESIAN_POINT ( 'NONE',  ( 5.823673210054444382, -21.52544592524334988, 95.20942372801903275 ) ) ;
#197980 = CARTESIAN_POINT ( 'NONE',  ( -19.03943276465977164, 0.05219959533909376836, 116.2489096053143669 ) ) ;
#197981 = CARTESIAN_POINT ( 'NONE',  ( 12.14591786802327356, -12.06949235617739191, 25.62609039468567929 ) ) ;
#197982 = CARTESIAN_POINT ( 'NONE',  ( -4.483927247898539470, -16.52544592524342804, 77.29057627198102409 ) ) ;
#197983 = CARTESIAN_POINT ( 'NONE',  ( 10.81492255796106328, -18.62759615963255655, 30.41775706135234358 ) ) ;
#197984 = CARTESIAN_POINT ( 'NONE',  ( -21.52544592524343514, 5.823673210054127303, 76.04057627198102409 ) ) ;
#197985 = CARTESIAN_POINT ( 'NONE',  ( 9.564922557961047289, -16.46253265017146816, 35.41775706135233293 ) ) ;
#197986 = CARTESIAN_POINT ( 'NONE',  ( 8.906447517083057264, -27.41122689804191026, 144.8500000054623911 ) ) ;
#197987 = CARTESIAN_POINT ( 'NONE',  ( -0.05219959533909027116, -19.03943276465977164, 82.49890960531436690 ) ) ;
#197988 = CARTESIAN_POINT ( 'NONE',  ( 14.34966873604960469, 8.224510206698951720, 54.16557627198103120 ) ) ;
#197989 = CARTESIAN_POINT ( 'NONE',  ( 14.34966873604960469, 8.224510206698951720, 39.16557627198102409 ) ) ;
#197990 = CARTESIAN_POINT ( 'NONE',  ( -12.06949235617739369, -12.14591786802326823, 109.3760903946857042 ) ) ;
#197991 = CARTESIAN_POINT ( 'NONE',  ( 13.97604488694548053, -13.89961937509957401, 60.62609039468564731 ) ) ;
#197992 = CARTESIAN_POINT ( 'NONE',  ( 19.39720447994795904, 5.499999999999972466, 52.16317477297178584 ) ) ;
#197993 = CARTESIAN_POINT ( 'NONE',  ( 9.564922557960805705, 16.46253265017160317, 109.5822429386476955 ) ) ;
#197994 = ADVANCED_FACE ( 'NONE', ( #13216 ), #136541, .T. ) ;
#197995 = CARTESIAN_POINT ( 'NONE',  ( 8.314922557960818139, 14.29746914071049879, 74.58224293864768129 ) ) ;
#197996 = CARTESIAN_POINT ( 'NONE',  ( -193.3062444957834884, -155.7167183371838064, -4.999999999999999112 ) ) ;
#197998 = CARTESIAN_POINT ( 'NONE',  ( 21.53943276465977519, -0.05219959533907433946, 38.74890960531435979 ) ) ;
#197997 = CARTESIAN_POINT ( 'NONE',  ( -9.564922557960796823, -16.46253265017161027, 27.08224293864769550 ) ) ;
#197999 = CARTESIAN_POINT ( 'NONE',  ( -15.80617190586745835, -15.72974639402198527, 61.87390960531436690 ) ) ;
#198000 = CARTESIAN_POINT ( 'NONE',  ( -5.153800228976328057, -19.02544592524343514, 22.29057627198102765 ) ) ;
#198002 = CARTESIAN_POINT ( 'NONE',  ( -9.474510206698964154, 16.51473224551069663, 50.41557627198102409 ) ) ;
#198001 = CARTESIAN_POINT ( 'NONE',  ( 16.55341960407618274, -4.379528057220086978, 61.04275706135234714 ) ) ;
#198003 = CARTESIAN_POINT ( 'NONE',  ( 21.52544592524334988, 5.823673210054432836, 61.45942372801901854 ) ) ;
#198004 = CARTESIAN_POINT ( 'NONE',  ( -14.29746914071049879, 8.314922557960819915, 95.83224293864770971 ) ) ;
#198005 = CARTESIAN_POINT ( 'NONE',  ( -37.45873412500000654, 2.428612866367529932E-14, -0.3124999986344065839 ) ) ;
#198006 = CARTESIAN_POINT ( 'NONE',  ( -17.40805194822030799, 6.112264579159339739, 50.83371272510613892 ) ) ;
#198007 = CARTESIAN_POINT ( 'NONE',  ( 21.52544592524344225, -5.823673210054117533, 33.54057627198102409 ) ) ;
#198008 = CARTESIAN_POINT ( 'NONE',  ( -3.573655867282028392E-15, 2.428612866367529932E-14, 2.000000000000000000 ) ) ;
#198010 = CARTESIAN_POINT ( 'NONE',  ( 0.1984113195539776442, 9.090086778104248921, -63.95305758601499235 ) ) ;
#198009 = CARTESIAN_POINT ( 'NONE',  ( -21.55341960407619339, 5.719274019375674811, 68.54275706135234714 ) ) ;
#198012 = CARTESIAN_POINT ( 'NONE',  ( 4.379528057220339221, -16.55341960407611168, 37.70724293864769550 ) ) ;
#198011 = CARTESIAN_POINT ( 'NONE',  ( 12.06949235617739724, 12.14591786802326823, 56.87609039468568994 ) ) ;
#198013 = CARTESIAN_POINT ( 'NONE',  ( 21.53943276465977519, -0.05219959533907433946, 73.74890960531433848 ) ) ;
#198014 = AXIS2_PLACEMENT_3D ( 'NONE', #108912, #170592, #93739 ) ;
#198015 = CARTESIAN_POINT ( 'NONE',  ( -0.05219959533907301413, -21.53943276465977519, 57.49890960531435979 ) ) ;
#198016 = CARTESIAN_POINT ( 'NONE',  ( 30.43137438583966059, -22.75957854975411010, -19.69424960774841082 ) ) ;
#198018 = CARTESIAN_POINT ( 'NONE',  ( -9.474510206698964154, 16.51473224551069663, 110.4155762719810383 ) ) ;
#198017 = CARTESIAN_POINT ( 'NONE',  ( 19.03943276465977164, 0.05219959533936151252, 86.25109039468567573 ) ) ;
#198019 = CARTESIAN_POINT ( 'NONE',  ( 13.89961937509977652, -13.97604488694527269, 48.12390960531435979 ) ) ;
#198020 = CARTESIAN_POINT ( 'NONE',  ( 8.314922557960818139, 14.29746914071049879, 114.5822429386477097 ) ) ;
#198021 =( LENGTH_UNIT ( ) NAMED_UNIT ( * ) SI_UNIT ( .MILLI., .METRE. ) );
#198022 = CARTESIAN_POINT ( 'NONE',  ( -19.02544592524342804, 5.153800228976336051, 111.0405762719810099 ) ) ;
#198023 = ORIENTED_EDGE ( 'NONE', *, *, #12852, .F. ) ;
#198024 = CARTESIAN_POINT ( 'NONE',  ( -14.34966873604972548, 8.224510206698743886, 73.33442372801901854 ) ) ;
#198025 = CARTESIAN_POINT ( 'NONE',  ( -18.62759615963270932, 10.81492255796079327, 100.8322429386477097 ) ) ;
#198026 = CARTESIAN_POINT ( 'NONE',  ( -16.46253265017160317, 9.564922557960807481, 50.83224293864770260 ) ) ;
#198027 = CARTESIAN_POINT ( 'NONE',  ( 5.719274019375673035, 21.55341960407619339, 37.29275706135235424 ) ) ;
#198028 = CARTESIAN_POINT ( 'NONE',  ( 16.46253265017160672, -9.564922557960803928, 93.33224293864769550 ) ) ;
#198029 = CARTESIAN_POINT ( 'NONE',  ( -32.63354670694344151, -22.83594557639104750, -20.39123836177964222 ) ) ;
#198030 = ORIENTED_EDGE ( 'NONE', *, *, #160761, .T. ) ;
#198031 = CARTESIAN_POINT ( 'NONE',  ( 18.67979575497194134, -10.72451020669871369, 30.83442372801902209 ) ) ;
#198033 = CARTESIAN_POINT ( 'NONE',  ( 5.049401038297881783, 19.05341960407617563, 82.29275706135229029 ) ) ;
#198032 = CARTESIAN_POINT ( 'NONE',  ( -19.05341960407611168, -5.049401038298163336, 101.4572429386476955 ) ) ;
#198034 = CARTESIAN_POINT ( 'NONE',  ( 19.03943276465977164, 0.05219959533936151252, 46.25109039468566863 ) ) ;
#198035 = CARTESIAN_POINT ( 'NONE',  ( 18.62759615963271287, -10.81492255796078972, 103.3322429386476955 ) ) ;
#198036 = CARTESIAN_POINT ( 'NONE',  ( 16.46253265017146816, 9.564922557961045513, 31.66775706135232937 ) ) ;
#198037 = CARTESIAN_POINT ( 'NONE',  ( 9.564922557961047289, -16.46253265017146816, 35.41775706135233293 ) ) ;
#198038 = CARTESIAN_POINT ( 'NONE',  ( -8.314922557961024197, 14.29746914071037800, 97.91775706135236135 ) ) ;
#198040 = EDGE_LOOP ( 'NONE', ( #59883, #137944, #36601, #188996 ) ) ;
#198039 = CARTESIAN_POINT ( 'NONE',  ( 19.03943276465977164, -0.05219959533909143690, 113.7489096053143669 ) ) ;
#198041 = CARTESIAN_POINT ( 'NONE',  ( -16.51473224551069308, -9.474510206698971260, 76.66557627198103830 ) ) ;
#198042 = CARTESIAN_POINT ( 'NONE',  ( -21.52544592524334988, -5.823673210054445271, 83.95942372801900433 ) ) ;
#198043 = CARTESIAN_POINT ( 'NONE',  ( -5.719274019375665041, -21.55341960407619695, 74.79275706135234714 ) ) ;
#198044 = DIRECTION ( 'NONE',  ( 1.000000000000000000, 3.552713678800500929E-15, 0.000000000000000000 ) ) ;
#198045 = CARTESIAN_POINT ( 'NONE',  ( -0.05219959533909027116, -19.03943276465977164, 87.49890960531436690 ) ) ;
#198046 = CARTESIAN_POINT ( 'NONE',  ( 10.72451020669871369, 18.67979575497193778, 67.08442372801901854 ) ) ;
#198047 = CARTESIAN_POINT ( 'NONE',  ( -0.05219959533936034679, 19.03943276465977164, 97.50109039468567573 ) ) ;
#198048 = CARTESIAN_POINT ( 'NONE',  ( -13.97604488694527625, -13.89961937509977652, 66.87390960531436690 ) ) ;
#198049 = CARTESIAN_POINT ( 'NONE',  ( 19.02544592524343514, -5.153800228976328945, 113.5405762719810241 ) ) ;
#198050 = CARTESIAN_POINT ( 'NONE',  ( -16.46253265017160317, 9.564922557960807481, 85.83224293864769550 ) ) ;
#198051 = CARTESIAN_POINT ( 'NONE',  ( -17.12812012977030562, -6.668231424565920662, 91.35948759323146362 ) ) ;
#198052 = CARTESIAN_POINT ( 'NONE',  ( -19.03943276465977164, 0.05219959533909376836, 66.24890960531436690 ) ) ;
#198053 = CARTESIAN_POINT ( 'NONE',  ( 9.564922557960805705, 16.46253265017160317, 49.58224293864770260 ) ) ;
#198054 = CARTESIAN_POINT ( 'NONE',  ( 0.05219959533907565091, 21.53943276465977519, 99.99890960531436690 ) ) ;
#198055 = CARTESIAN_POINT ( 'NONE',  ( 14.34966873604972726, -8.224510206698740333, 85.83442372801901854 ) ) ;
#198056 = CARTESIAN_POINT ( 'NONE',  ( 7.990187535671190666, -1.461319442807313740, -64.16708268805474802 ) ) ;
#198057 = CARTESIAN_POINT ( 'NONE',  ( 5.153800228976615827, -19.02544592524334988, 40.20942372801898301 ) ) ;
#198058 = CARTESIAN_POINT ( 'NONE',  ( 5.153800228976335163, 19.02544592524342804, 84.79057627198099567 ) ) ;
#198059 = CARTESIAN_POINT ( 'NONE',  ( 14.29746914071049879, -8.314922557960816363, 68.33224293864769550 ) ) ;
#198060 = CARTESIAN_POINT ( 'NONE',  ( -16.52544592524342804, 4.483927247898546575, 111.0405762719810525 ) ) ;
#198061 = CARTESIAN_POINT ( 'NONE',  ( 9.564922557960805705, 16.46253265017160317, 109.5822429386476955 ) ) ;
#198062 = CARTESIAN_POINT ( 'NONE',  ( -16.46253265017160317, 9.564922557960807481, 100.8322429386477097 ) ) ;
#198063 = CARTESIAN_POINT ( 'NONE',  ( 12.06949235617757843, -12.14591786802309237, 78.12390960531436690 ) ) ;
#198064 = DIRECTION ( 'NONE',  ( 0.000000000000000000, 0.000000000000000000, -1.000000000000000000 ) ) ;
#198065 = CARTESIAN_POINT ( 'NONE',  ( 16.46253265017146816, 9.564922557961045513, 36.66775706135233293 ) ) ;
#198066 = CARTESIAN_POINT ( 'NONE',  ( 4.483927247898790824, -16.52544592524335698, 90.20942372801903275 ) ) ;
#198067 = CARTESIAN_POINT ( 'NONE',  ( 9.474510206698971260, -16.51473224551069308, 72.91557627198102409 ) ) ;
#198068 = CARTESIAN_POINT ( 'NONE',  ( 5.823673210054444382, -21.52544592524334988, 55.20942372801902565 ) ) ;
#198069 = CARTESIAN_POINT ( 'NONE',  ( 21.53943276465977519, -0.05219959533907433946, 48.74890960531435979 ) ) ;
#198070 = CARTESIAN_POINT ( 'NONE',  ( -10.72451020669870658, -18.67979575497194134, 19.58442372801901143 ) ) ;
#198071 = CARTESIAN_POINT ( 'NONE',  ( 15.80617190586746368, 15.72974639402197994, 69.37390960531436690 ) ) ;
#198072 = CARTESIAN_POINT ( 'NONE',  ( 14.34966873604960469, 8.224510206698951720, 99.16557627198100988 ) ) ;
#198073 = CARTESIAN_POINT ( 'NONE',  ( -16.51473224551082808, 9.474510206698731452, 63.33442372801900433 ) ) ;
#198074 = CARTESIAN_POINT ( 'NONE',  ( -19.05341960407611168, -5.049401038298163336, 31.45724293864769550 ) ) ;
#198075 = CARTESIAN_POINT ( 'NONE',  ( -16.51473224551069308, -9.474510206698971260, 81.66557627198103830 ) ) ;
#198076 = CARTESIAN_POINT ( 'NONE',  ( -16.51473224551069308, -9.474510206698971260, 76.66557627198103830 ) ) ;
#198077 = CARTESIAN_POINT ( 'NONE',  ( -14.34966873604960291, -8.224510206698953496, 96.66557627198102409 ) ) ;
#198078 = ORIENTED_EDGE ( 'NONE', *, *, #36572, .T. ) ;
#198079 = CARTESIAN_POINT ( 'NONE',  ( 8.314922557960818139, 14.29746914071049879, 24.58224293864768839 ) ) ;
#198080 = CARTESIAN_POINT ( 'NONE',  ( -8.314922557961024197, 14.29746914071037800, 27.91775706135234358 ) ) ;
#198081 = CARTESIAN_POINT ( 'NONE',  ( -15.72974639402176322, -15.80617190586768395, 99.37609039468568994 ) ) ;
#198082 = CARTESIAN_POINT ( 'NONE',  ( -0.05219959533909027116, -19.03943276465977164, 102.4989096053143669 ) ) ;
#198083 = CARTESIAN_POINT ( 'NONE',  ( 15.72974639402199770, -15.80617190586745480, 113.1239096053143953 ) ) ;
#198084 = CARTESIAN_POINT ( 'NONE',  ( 19.02544592524343514, -5.153800228976328945, 38.54057627198103120 ) ) ;
#198085 = CARTESIAN_POINT ( 'NONE',  ( -12.06949235617739369, -12.14591786802326823, 39.37609039468567573 ) ) ;
#198086 = CARTESIAN_POINT ( 'NONE',  ( -14.29746914071037622, -8.314922557961029526, 19.16775706135234714 ) ) ;
#198087 = EDGE_CURVE ( 'NONE', #184086, #139805, #56135, .T. ) ;
#198088 = CARTESIAN_POINT ( 'NONE',  ( -9.474510206698964154, 16.51473224551069663, 35.41557627198102409 ) ) ;
#198089 = AXIS2_PLACEMENT_3D ( 'NONE', #9572, #28733, #151076 ) ;
#198090 = CARTESIAN_POINT ( 'NONE',  ( 12.06949235617757843, -12.14591786802309237, 98.12390960531436690 ) ) ;
#198091 = CARTESIAN_POINT ( 'NONE',  ( 15.80617190586746368, 15.72974639402197994, 104.3739096053143669 ) ) ;
#198092 = CARTESIAN_POINT ( 'NONE',  ( -5.049401038297874678, -19.05341960407617918, 69.79275706135233293 ) ) ;
#198093 = DIRECTION ( 'NONE',  ( 1.000000000000000000, -0.000000000000000000, -0.000000000000000000 ) ) ;
#198094 = CARTESIAN_POINT ( 'NONE',  ( -19.03943276465977164, 0.05219959533909376836, 96.24890960531436690 ) ) ;
#198095 = CARTESIAN_POINT ( 'NONE',  ( 10.72451020669871369, 18.67979575497193778, 22.08442372801901143 ) ) ;
#198096 = CARTESIAN_POINT ( 'NONE',  ( 12.55500000000001748, 3.061616997868383634E-16, -2.500000000000000444 ) ) ;
#198097 = CARTESIAN_POINT ( 'NONE',  ( -19.03943276465977164, 0.05219959533909376836, 86.24890960531436690 ) ) ;
#198098 = CARTESIAN_POINT ( 'NONE',  ( 17.40861289039003879, -6.110651285853326620, 111.1276752917257227 ) ) ;
#198099 = CARTESIAN_POINT ( 'NONE',  ( -19.05341960407611168, -5.049401038298163336, 81.45724293864769550 ) ) ;
#198101 = CARTESIAN_POINT ( 'NONE',  ( -16.53943276465976808, 0.05219959533911058130, 71.24890960531435269 ) ) ;
#198100 = CARTESIAN_POINT ( 'NONE',  ( 5.823673210054444382, -21.52544592524334988, 35.20942372801901854 ) ) ;
#198102 = CARTESIAN_POINT ( 'NONE',  ( -13.97604488694527625, -13.89961937509977652, 81.87390960531436690 ) ) ;
#198103 = CARTESIAN_POINT ( 'NONE',  ( 19.02544592524334988, 5.153800228976608722, 26.45942372801899722 ) ) ;
#198105 = CARTESIAN_POINT ( 'NONE',  ( 19.02544592524334988, 5.153800228976608722, 56.45942372801898301 ) ) ;
#198104 = CARTESIAN_POINT ( 'NONE',  ( -4.483927247898782831, 16.52544592524335698, 47.70942372801902565 ) ) ;
#198106 = CARTESIAN_POINT ( 'NONE',  ( -5.719274019375665041, -21.55341960407619695, 69.79275706135234714 ) ) ;
#198107 = CARTESIAN_POINT ( 'NONE',  ( 14.34966873604972726, -8.224510206698740333, 20.83442372801901143 ) ) ;
#198108 = CARTESIAN_POINT ( 'NONE',  ( 13.97604488694527802, 13.89961937509977652, 64.37390960531436690 ) ) ;
#198109 = CARTESIAN_POINT ( 'NONE',  ( 16.51473224551083163, -9.474510206698727899, 100.8344237280190043 ) ) ;
#198110 = CARTESIAN_POINT ( 'NONE',  ( -14.29746914071037622, -8.314922557961029526, 69.16775706135234714 ) ) ;
#198111 = CARTESIAN_POINT ( 'NONE',  ( 5.823673210054444382, -21.52544592524334988, 105.2094237280190328 ) ) ;
#198112 = CARTESIAN_POINT ( 'NONE',  ( 13.97604488694548053, -13.89961937509957401, 75.62609039468564731 ) ) ;
#198113 = CARTESIAN_POINT ( 'NONE',  ( -19.02544592524342804, 5.153800228976336051, 56.04057627198100988 ) ) ;
#198114 = CARTESIAN_POINT ( 'NONE',  ( 10.72451020669898902, -18.67979575497178502, 82.91557627198103830 ) ) ;
#198116 = CARTESIAN_POINT ( 'NONE',  ( -5.153800228976607833, 19.02544592524334988, 72.70942372801900433 ) ) ;
#198115 = CARTESIAN_POINT ( 'NONE',  ( 8.224510206698953496, -14.34966873604960469, 72.91557627198103830 ) ) ;
#198117 = DIRECTION ( 'NONE',  ( -0.000000000000000000, -0.000000000000000000, 1.000000000000000000 ) ) ;
#198118 = CARTESIAN_POINT ( 'NONE',  ( 13.89961937509957401, 13.97604488694547697, 41.87609039468566152 ) ) ;
#198119 = CARTESIAN_POINT ( 'NONE',  ( 12.14591786802327356, -12.06949235617739191, 105.6260903946856899 ) ) ;
#198120 = CARTESIAN_POINT ( 'NONE',  ( 12.06949235617757843, -12.14591786802309237, 73.12390960531436690 ) ) ;
#198122 = CARTESIAN_POINT ( 'NONE',  ( -27.73933785331498925, -9.013057229001049109, 142.9750000027312069 ) ) ;
#198121 = CARTESIAN_POINT ( 'NONE',  ( 0.05219959533937995610, -21.53943276465977519, 105.0010903946856757 ) ) ;
#198123 = CARTESIAN_POINT ( 'NONE',  ( -5.719274019375978568, 21.55341960407610458, 110.2072429386477239 ) ) ;
#198124 = CARTESIAN_POINT ( 'NONE',  ( -19.02544592524342804, 5.153800228976336051, 66.04057627198103830 ) ) ;
#198125 = CARTESIAN_POINT ( 'NONE',  ( -0.05219959533937732626, 21.53943276465977519, 77.50109039468567573 ) ) ;
#198126 = CARTESIAN_POINT ( 'NONE',  ( -19.05341960407611168, -5.049401038298163336, 56.45724293864768129 ) ) ;
#198127 = CARTESIAN_POINT ( 'NONE',  ( 0.05219959533910956823, 16.53943276465976808, 114.9989096053143669 ) ) ;
#198128 = CARTESIAN_POINT ( 'NONE',  ( 10.81492255796078972, 18.62759615963270932, 29.58224293864769905 ) ) ;
#198129 = CARTESIAN_POINT ( 'NONE',  ( 8.314922557960818139, 14.29746914071049879, 64.58224293864769550 ) ) ;
#198130 = CARTESIAN_POINT ( 'NONE',  ( 13.89961937509977652, -13.97604488694527269, 38.12390960531436690 ) ) ;
#198131 = CARTESIAN_POINT ( 'NONE',  ( -8.224510206698948167, 14.34966873604960824, 100.4155762719810241 ) ) ;
#198132 = CARTESIAN_POINT ( 'NONE',  ( 21.53943276465977519, -0.05219959533907433946, 113.7489096053143527 ) ) ;
#198133 = CARTESIAN_POINT ( 'NONE',  ( -5.719274019375665041, -21.55341960407619695, 44.79275706135234714 ) ) ;
#198134 = CARTESIAN_POINT ( 'NONE',  ( -16.51473224551069308, -9.474510206698971260, 36.66557627198102409 ) ) ;
#198135 = CARTESIAN_POINT ( 'NONE',  ( 4.379528057220092307, 16.55341960407617563, 67.29275706135234714 ) ) ;
#198136 = CARTESIAN_POINT ( 'NONE',  ( 0.05219959533907565091, 21.53943276465977519, 104.9989096053143669 ) ) ;
#198137 = CARTESIAN_POINT ( 'NONE',  ( 10.72451020669898902, -18.67979575497178502, 92.91557627198103830 ) ) ;
#198139 = CARTESIAN_POINT ( 'NONE',  ( -9.564922557960796823, -16.46253265017161027, 52.08224293864768839 ) ) ;
#198138 = CARTESIAN_POINT ( 'NONE',  ( 16.51473224551083163, -9.474510206698727899, 20.83442372801899722 ) ) ;
#198140 = CARTESIAN_POINT ( 'NONE',  ( -17.72517630441458536, 5.499999999999976907, 40.92175719257603106 ) ) ;
#198141 = CARTESIAN_POINT ( 'NONE',  ( -18.67979575497193778, 10.72451020669871902, 53.33442372801901854 ) ) ;
#198142 = CARTESIAN_POINT ( 'NONE',  ( -15.80617190586745835, -15.72974639402198527, 36.87390960531435979 ) ) ;
#198143 = CARTESIAN_POINT ( 'NONE',  ( -8.314922557960811034, -14.29746914071050412, 22.08224293864769194 ) ) ;
#198145 = CARTESIAN_POINT ( 'NONE',  ( 5.719274019375673035, 21.55341960407619339, 97.29275706135234714 ) ) ;
#198144 = CARTESIAN_POINT ( 'NONE',  ( -21.52544592524334988, -5.823673210054445271, 73.95942372801901854 ) ) ;
#198146 = CARTESIAN_POINT ( 'NONE',  ( 5.153800228976615827, -19.02544592524334988, 40.20942372801898301 ) ) ;
#198147 = CARTESIAN_POINT ( 'NONE',  ( -14.29746914071037622, -8.314922557961029526, 104.1677570613523471 ) ) ;
#198148 = CARTESIAN_POINT ( 'NONE',  ( 5.823673210054444382, -21.52544592524334988, 50.20942372801901854 ) ) ;
#198149 = CARTESIAN_POINT ( 'NONE',  ( 16.46253265017160672, -9.564922557960803928, 53.33224293864768839 ) ) ;
#198150 = CARTESIAN_POINT ( 'NONE',  ( 18.67979575497194134, -10.72451020669871369, 110.8344237280190043 ) ) ;
#198151 = CARTESIAN_POINT ( 'NONE',  ( 10.72451020669898902, -18.67979575497178502, 42.91557627198103120 ) ) ;
#198152 = CARTESIAN_POINT ( 'NONE',  ( 18.62759615963255655, 10.81492255796105972, 26.66775706135235424 ) ) ;
#198153 = CARTESIAN_POINT ( 'NONE',  ( 10.81492255796078972, 18.62759615963270932, 94.58224293864769550 ) ) ;
#198154 = CARTESIAN_POINT ( 'NONE',  ( 19.03943276465977164, 0.05219959533936151252, 81.25109039468567573 ) ) ;
#198155 = CARTESIAN_POINT ( 'NONE',  ( 12.14591786802327356, -12.06949235617739191, 35.62609039468568994 ) ) ;
#198157 = CARTESIAN_POINT ( 'NONE',  ( 5.823673210054125526, 21.52544592524343514, 79.79057627198102409 ) ) ;
#198156 = CARTESIAN_POINT ( 'NONE',  ( 17.60779699588839975, 5.500000000000013323, 63.84981316670106111 ) ) ;
#198159 = CARTESIAN_POINT ( 'NONE',  ( -4.483927247898539470, -16.52544592524342804, 72.29057627198102409 ) ) ;
#198158 = CARTESIAN_POINT ( 'NONE',  ( -14.34966873604972548, 8.224510206698743886, 63.33442372801900433 ) ) ;
#198160 = CARTESIAN_POINT ( 'NONE',  ( -20.97218796591018020, 20.08580022215221206, -49.51012018364362888 ) ) ;
#198161 = CARTESIAN_POINT ( 'NONE',  ( -9.564922557961040184, 16.46253265017147172, 97.91775706135233293 ) ) ;
#198162 = CARTESIAN_POINT ( 'NONE',  ( -21.53943276465977519, 0.05219959533907696930, 36.24890960531435979 ) ) ;
#198163 = CARTESIAN_POINT ( 'NONE',  ( 16.41480162262169529, -33.15536704053023698, -8.000000000000000000 ) ) ;
#198164 = CARTESIAN_POINT ( 'NONE',  ( 16.52544592524335698, 4.483927247898782831, 41.45942372801901143 ) ) ;
#198165 = CARTESIAN_POINT ( 'NONE',  ( -15.72974639402176322, -15.80617190586768395, 19.37609039468568639 ) ) ;
#198166 = CARTESIAN_POINT ( 'NONE',  ( 21.52544592524344225, -5.823673210054117533, 28.54057627198103120 ) ) ;
#198167 = CARTESIAN_POINT ( 'NONE',  ( -14.29746914071037622, -8.314922557961029526, 69.16775706135234714 ) ) ;
#198168 = CARTESIAN_POINT ( 'NONE',  ( -19.05341960407611168, -5.049401038298163336, 86.45724293864769550 ) ) ;
#198170 = CARTESIAN_POINT ( 'NONE',  ( -19.05341960407611168, -5.049401038298163336, 31.45724293864769550 ) ) ;
#198169 = CARTESIAN_POINT ( 'NONE',  ( 18.67979575497194134, -10.72451020669871369, 60.83442372801901854 ) ) ;
#198171 = CARTESIAN_POINT ( 'NONE',  ( -21.55341960407610458, -5.719274019375992779, 21.45724293864769550 ) ) ;
#198172 = ORIENTED_EDGE ( 'NONE', *, *, #118181, .F. ) ;
#198173 = CARTESIAN_POINT ( 'NONE',  ( -13.89961937509957401, -13.97604488694547875, 34.37609039468566863 ) ) ;
#198174 = CARTESIAN_POINT ( 'NONE',  ( 12.06949235617739724, 12.14591786802326823, 46.87609039468568994 ) ) ;
#198175 = CARTESIAN_POINT ( 'NONE',  ( -0.05219959533909027116, -19.03943276465977164, 112.4989096053143669 ) ) ;
#198176 = CARTESIAN_POINT ( 'NONE',  ( -5.153800228976328057, -19.02544592524343514, 77.29057627198099567 ) ) ;
#198177 = CARTESIAN_POINT ( 'NONE',  ( 14.34966873604972726, -8.224510206698740333, 95.83442372801903275 ) ) ;
#198178 = DIRECTION ( 'NONE',  ( 0.000000000000000000, 0.000000000000000000, -1.000000000000000000 ) ) ;
#198179 = CARTESIAN_POINT ( 'NONE',  ( 12.14591786802309770, 12.06949235617756955, 99.37390960531436690 ) ) ;
#198180 = CARTESIAN_POINT ( 'NONE',  ( 21.55341960407610458, 5.719274019375980345, 28.95724293864769905 ) ) ;
#198181 = CARTESIAN_POINT ( 'NONE',  ( 19.02544592524343514, -5.153800228976328945, 28.54057627198102409 ) ) ;
#198182 = CARTESIAN_POINT ( 'NONE',  ( -12.14591786802326823, 12.06949235617739902, 63.12609039468568994 ) ) ;
#198183 = CARTESIAN_POINT ( 'NONE',  ( 5.823673210054444382, -21.52544592524334988, 25.20942372801901854 ) ) ;
#198184 = CARTESIAN_POINT ( 'NONE',  ( -5.049401038297874678, -19.05341960407617918, 79.79275706135233293 ) ) ;
#198185 = CARTESIAN_POINT ( 'NONE',  ( -19.05341960407611168, -5.049401038298163336, 46.45724293864768129 ) ) ;
#198186 = CARTESIAN_POINT ( 'NONE',  ( -18.67979575497178146, -10.72451020669898902, 66.66557627198102409 ) ) ;
#198187 = CARTESIAN_POINT ( 'NONE',  ( 19.02544592524343514, -5.153800228976328945, 108.5405762719810383 ) ) ;
#198188 = CARTESIAN_POINT ( 'NONE',  ( 15.72974639402176855, 15.80617190586768217, 86.87609039468568994 ) ) ;
#198189 = CARTESIAN_POINT ( 'NONE',  ( 5.153800228976335163, 19.02544592524342804, 69.79057627198103830 ) ) ;
#198190 = EDGE_CURVE ( 'NONE', #181556, #127301, #169113, .T. ) ;
#198191 = CARTESIAN_POINT ( 'NONE',  ( 12.06949235617739724, 12.14591786802326823, 46.87609039468568994 ) ) ;
#198192 = CARTESIAN_POINT ( 'NONE',  ( 13.97604488694527802, 13.89961937509977652, 64.37390960531436690 ) ) ;
#198193 = CARTESIAN_POINT ( 'NONE',  ( 5.719274019375673035, 21.55341960407619339, 77.29275706135234714 ) ) ;
#198194 = CARTESIAN_POINT ( 'NONE',  ( -13.89961937509957401, -13.97604488694547875, 39.37609039468566152 ) ) ;
#198195 = CARTESIAN_POINT ( 'NONE',  ( 9.564922557961047289, -16.46253265017146816, 50.41775706135233293 ) ) ;
#198196 = ORIENTED_EDGE ( 'NONE', *, *, #148562, .T. ) ;
#198197 = CARTESIAN_POINT ( 'NONE',  ( 5.823673210054444382, -21.52544592524334988, 45.20942372801901854 ) ) ;
#198198 = CARTESIAN_POINT ( 'NONE',  ( -5.049401038298153566, 19.05341960407611168, 55.20724293864768839 ) ) ;
#198199 = CARTESIAN_POINT ( 'NONE',  ( 5.049401038297881783, 19.05341960407617563, 42.29275706135234003 ) ) ;
#198200 = CARTESIAN_POINT ( 'NONE',  ( 9.474510206698971260, -16.51473224551069308, 97.91557627198102409 ) ) ;
#198201 = CARTESIAN_POINT ( 'NONE',  ( 9.474510206698971260, -16.51473224551069308, 87.91557627198102409 ) ) ;
#198202 = CARTESIAN_POINT ( 'NONE',  ( 8.314922557960818139, 14.29746914071049879, 44.58224293864769550 ) ) ;
#198203 = CARTESIAN_POINT ( 'NONE',  ( 18.62759615963271287, -10.81492255796078972, 38.33224293864768839 ) ) ;
#198204 = CARTESIAN_POINT ( 'NONE',  ( -11.40812507854754720, -35.11059874428192273, -10.72499999726881548 ) ) ;
#198205 = DIRECTION ( 'NONE',  ( 0.000000000000000000, 0.000000000000000000, 1.000000000000000000 ) ) ;
#198206 = CARTESIAN_POINT ( 'NONE',  ( -21.55341960407619339, 5.719274019375674811, 103.5427570613523613 ) ) ;
#198207 = CARTESIAN_POINT ( 'NONE',  ( -27.91261209101616458, 7.473227146837950308, 160.9450349587949063 ) ) ;
#198208 = CARTESIAN_POINT ( 'NONE',  ( -9.564922557960796823, -16.46253265017161027, 32.08224293864769550 ) ) ;
#198209 = CARTESIAN_POINT ( 'NONE',  ( 5.049401038298161559, -19.05341960407611168, 107.7072429386476955 ) ) ;
#198210 = CARTESIAN_POINT ( 'NONE',  ( 34.02686120844015960, 4.767814797156205486, 92.23495037107730354 ) ) ;
#198211 = CARTESIAN_POINT ( 'NONE',  ( -4.483927247898782831, 16.52544592524335698, 47.70942372801902565 ) ) ;
#198212 = CARTESIAN_POINT ( 'NONE',  ( 21.55341960407610458, 5.719274019375980345, 73.95724293864769550 ) ) ;
#198213 = CARTESIAN_POINT ( 'NONE',  ( -8.314922557960811034, -14.29746914071050412, 42.08224293864769550 ) ) ;
#198215 = CARTESIAN_POINT ( 'NONE',  ( 13.97604488694527802, 13.89961937509977652, 109.3739096053143669 ) ) ;
#198214 = CARTESIAN_POINT ( 'NONE',  ( -5.049401038298153566, 19.05341960407611168, 25.20724293864768484 ) ) ;
#198216 = CARTESIAN_POINT ( 'NONE',  ( 5.823673210054444382, -21.52544592524334988, 25.20942372801901854 ) ) ;
#198217 = CARTESIAN_POINT ( 'NONE',  ( -9.474510206698720793, -16.51473224551083518, 34.58442372801899722 ) ) ;
#198218 = CARTESIAN_POINT ( 'NONE',  ( -16.52544592524342804, 4.483927247898546575, 111.0405762719810525 ) ) ;
#198219 = CARTESIAN_POINT ( 'NONE',  ( -18.67979575497193778, 10.72451020669871902, 63.33442372801900433 ) ) ;
#198220 = CARTESIAN_POINT ( 'NONE',  ( 17.48853670773243252, -5.747243402303149118, 31.16671299749990709 ) ) ;
#198221 = CARTESIAN_POINT ( 'NONE',  ( -0.05219959533910754901, -16.53943276465976808, 27.49890960531435269 ) ) ;
#198222 = CARTESIAN_POINT ( 'NONE',  ( 17.49999999999999289, 3.512728167236827570, 112.2719000481888258 ) ) ;
#198223 = CARTESIAN_POINT ( 'NONE',  ( 10.81492255796078972, 18.62759615963270932, 24.58224293864768839 ) ) ;
#198224 = CARTESIAN_POINT ( 'NONE',  ( 0.05219959533910956823, 16.53943276465976808, 89.99890960531438111 ) ) ;
#198225 = CARTESIAN_POINT ( 'NONE',  ( 15.49673173449294694, -38.75597260389996990, -19.54956558032594316 ) ) ;
#198226 = CARTESIAN_POINT ( 'NONE',  ( -9.474510206698964154, 16.51473224551069663, 75.41557627198103830 ) ) ;
#198227 = CARTESIAN_POINT ( 'NONE',  ( -8.314922557960811034, -14.29746914071050412, 77.08224293864769550 ) ) ;
#198228 = CARTESIAN_POINT ( 'NONE',  ( 13.89961937509957401, 13.97604488694547697, 111.8760903946856757 ) ) ;
#198229 = CARTESIAN_POINT ( 'NONE',  ( 10.81492255796078972, 18.62759615963270932, 64.58224293864769550 ) ) ;
#198230 = ORIENTED_EDGE ( 'NONE', *, *, #66504, .F. ) ;
#198231 = CARTESIAN_POINT ( 'NONE',  ( 5.153800228976335163, 19.02544592524342804, 24.79057627198102765 ) ) ;
#198233 = CARTESIAN_POINT ( 'NONE',  ( -15.80617190586745835, -15.72974639402198527, 81.87390960531435269 ) ) ;
#198232 = CARTESIAN_POINT ( 'NONE',  ( 0.05219959533909260263, 19.03943276465977164, 69.99890960531435269 ) ) ;
#198234 = TOROIDAL_SURFACE ( 'NONE', #140046, 2.199999999999999289, 0.2000000000000000111 ) ;
#198236 = CARTESIAN_POINT ( 'NONE',  ( -13.97604488694527625, -13.89961937509977652, 81.87390960531436690 ) ) ;
#198235 = CARTESIAN_POINT ( 'NONE',  ( 16.53943276465976808, 0.05219959533934440121, 111.2510903946856899 ) ) ;
#198237 = CARTESIAN_POINT ( 'NONE',  ( -16.51473224551082808, 9.474510206698731452, 63.33442372801900433 ) ) ;
#198238 = CARTESIAN_POINT ( 'NONE',  ( -18.62759615963255300, -10.81492255796106328, 99.16775706135234714 ) ) ;
#198239 = CARTESIAN_POINT ( 'NONE',  ( 21.55341960407610458, 5.719274019375980345, 73.95724293864769550 ) ) ;
#198240 = CARTESIAN_POINT ( 'NONE',  ( -5.049401038298153566, 19.05341960407611168, 115.2072429386477097 ) ) ;
#198241 = CARTESIAN_POINT ( 'NONE',  ( 5.049401038298161559, -19.05341960407611168, 47.70724293864770260 ) ) ;
#198242 = CARTESIAN_POINT ( 'NONE',  ( -16.55341960407617563, 4.379528057220093196, 98.54275706135234714 ) ) ;
#198243 = CARTESIAN_POINT ( 'NONE',  ( 16.46253265017160672, -9.564922557960803928, 63.33224293864769550 ) ) ;
#198244 = CARTESIAN_POINT ( 'NONE',  ( 17.40805194822031865, 6.112264579159360167, 51.66628727489388950 ) ) ;
#198245 = CARTESIAN_POINT ( 'NONE',  ( -21.53943276465977519, -0.05219959533937600094, 113.7510903946856757 ) ) ;
#198246 = CARTESIAN_POINT ( 'NONE',  ( -14.34966873604960291, -8.224510206698953496, 66.66557627198102409 ) ) ;
#198247 = CARTESIAN_POINT ( 'NONE',  ( 21.52544592524344225, -5.823673210054117533, 103.5405762719810383 ) ) ;
#198248 = CARTESIAN_POINT ( 'NONE',  ( 5.719274019375991003, -21.55341960407610458, 97.70724293864772392 ) ) ;
#198249 = CARTESIAN_POINT ( 'NONE',  ( 1.784210473542230573E-15, -29.16686587814331588, 139.8750000027311842 ) ) ;
#198250 = CARTESIAN_POINT ( 'NONE',  ( 15.80617190586746368, 15.72974639402197994, 59.37390960531436690 ) ) ;
#198251 = CARTESIAN_POINT ( 'NONE',  ( -12.06949235617739369, -12.14591786802326823, 79.37609039468567573 ) ) ;
#198252 = CARTESIAN_POINT ( 'NONE',  ( 0.05219959533910956823, 16.53943276465976808, 99.99890960531436690 ) ) ;
#198253 = CARTESIAN_POINT ( 'NONE',  ( -13.89961937509977652, 13.97604488694528158, 65.62390960531436690 ) ) ;
#198254 = CARTESIAN_POINT ( 'NONE',  ( 14.34966873604972726, -8.224510206698740333, 110.8344237280190043 ) ) ;
#198255 = CARTESIAN_POINT ( 'NONE',  ( 10.72451020669871369, 18.67979575497193778, 52.08442372801901854 ) ) ;
#198256 = CARTESIAN_POINT ( 'NONE',  ( -16.46253265017160317, 9.564922557960807481, 95.83224293864769550 ) ) ;
#198257 = CARTESIAN_POINT ( 'NONE',  ( -5.823673210054431948, 21.52544592524334988, 82.70942372801900433 ) ) ;
#198258 = CARTESIAN_POINT ( 'NONE',  ( 19.05341960407611168, 5.049401038298154454, 23.95724293864769194 ) ) ;
#198259 = CARTESIAN_POINT ( 'NONE',  ( 16.51473224551069308, 9.474510206698969483, 34.16557627198102409 ) ) ;
#198260 = EDGE_LOOP ( 'NONE', ( #76299, #182785, #79107, #16377 ) ) ;
#198261 = CARTESIAN_POINT ( 'NONE',  ( 15.80617190586769283, -15.72974639402175789, 75.62609039468567573 ) ) ;
#198262 = CARTESIAN_POINT ( 'NONE',  ( -0.05219959533909027116, -19.03943276465977164, 102.4989096053143669 ) ) ;
#198263 = CARTESIAN_POINT ( 'NONE',  ( -19.02544592524334988, -5.153800228976617603, 83.95942372801901854 ) ) ;
#198264 = CARTESIAN_POINT ( 'NONE',  ( -21.52544592524334988, -5.823673210054445271, 38.95942372801901854 ) ) ;
#198265 = CARTESIAN_POINT ( 'NONE',  ( -16.52544592524335698, -4.483927247898792601, 18.95942372801901143 ) ) ;
#198266 = CARTESIAN_POINT ( 'NONE',  ( -9.564922557961040184, 16.46253265017147172, 67.91775706135233293 ) ) ;
#198267 = CARTESIAN_POINT ( 'NONE',  ( -19.05341960407611168, -5.049401038298163336, 46.45724293864768129 ) ) ;
#198268 = CARTESIAN_POINT ( 'NONE',  ( -19.03943276465977164, -0.05219959533935918106, 83.75109039468567573 ) ) ;
#198269 = CARTESIAN_POINT ( 'NONE',  ( 4.483927247898545687, 16.52544592524342804, 29.79057627198102409 ) ) ;
#198270 = CARTESIAN_POINT ( 'NONE',  ( 5.153800228976615827, -19.02544592524334988, 85.20942372801900433 ) ) ;
#198271 = CARTESIAN_POINT ( 'NONE',  ( 12.06949235617757843, -12.14591786802309237, 38.12390960531436690 ) ) ;
#198272 = CARTESIAN_POINT ( 'NONE',  ( -13.97604488694547697, 13.89961937509957934, 58.12609039468566863 ) ) ;
#198273 = CARTESIAN_POINT ( 'NONE',  ( -16.53943276465976808, -0.05219959533934237506, 48.75109039468568284 ) ) ;
#198274 = CARTESIAN_POINT ( 'NONE',  ( -5.153800228976607833, 19.02544592524334988, 27.70942372801899722 ) ) ;
#198275 = CARTESIAN_POINT ( 'NONE',  ( 13.89961937509977652, -13.97604488694527269, 48.12390960531435979 ) ) ;
#198276 = DIRECTION ( 'NONE',  ( 0.000000000000000000, 0.000000000000000000, -1.000000000000000000 ) ) ;
#198277 = CARTESIAN_POINT ( 'NONE',  ( 4.483927247898790824, -16.52544592524335698, 45.20942372801901854 ) ) ;
#198278 = DIRECTION ( 'NONE',  ( 0.000000000000000000, 0.000000000000000000, -1.000000000000000000 ) ) ;
#198279 = CARTESIAN_POINT ( 'NONE',  ( 27.73933785331498214, 9.013057229001095294, 141.9750000027311501 ) ) ;
#198280 = CARTESIAN_POINT ( 'NONE',  ( -13.97604488694527625, -13.89961937509977652, 96.87390960531433848 ) ) ;
#198281 = CARTESIAN_POINT ( 'NONE',  ( 17.50000000000000000, -5.500000000000000888, 120.0000000000000142 ) ) ;
#198282 = VERTEX_POINT ( 'NONE', #88045 ) ;
#198283 = CARTESIAN_POINT ( 'NONE',  ( 16.51473224551083163, -9.474510206698727899, 85.83442372801900433 ) ) ;
#198284 = CARTESIAN_POINT ( 'NONE',  ( 21.52544592524344225, -5.823673210054117533, 28.54057627198103120 ) ) ;
#198286 = CARTESIAN_POINT ( 'NONE',  ( 13.89961937509957401, 13.97604488694547697, 96.87609039468566152 ) ) ;
#198285 = CARTESIAN_POINT ( 'NONE',  ( -16.46253265017146816, -9.564922557961047289, 24.16775706135233648 ) ) ;
#198287 = CARTESIAN_POINT ( 'NONE',  ( 4.379528057220339221, -16.55341960407611168, 112.7072429386476955 ) ) ;
#198288 = CARTESIAN_POINT ( 'NONE',  ( -9.564922557960796823, -16.46253265017161027, 42.08224293864769550 ) ) ;
#198289 = CARTESIAN_POINT ( 'NONE',  ( 21.53943276465977519, -0.05219959533907433946, 63.74890960531435979 ) ) ;
#198290 = VECTOR ( 'NONE', #24644, 1000.000000000000000 ) ;
#198291 = CARTESIAN_POINT ( 'NONE',  ( -19.03943276465977164, 0.05219959533909376836, 21.24890960531436335 ) ) ;
#198292 = CARTESIAN_POINT ( 'NONE',  ( 23.31738231874054890, -16.94106989632523508, 143.0500000054623513 ) ) ;
#198293 = CARTESIAN_POINT ( 'NONE',  ( -16.46253265017146816, -9.564922557961047289, 69.16775706135233293 ) ) ;
#198294 = CARTESIAN_POINT ( 'NONE',  ( 14.29746914071049879, -8.314922557960816363, 43.33224293864769550 ) ) ;
#198295 = CARTESIAN_POINT ( 'NONE',  ( 5.153800228976335163, 19.02544592524342804, 109.7905762719810099 ) ) ;
#198296 = CARTESIAN_POINT ( 'NONE',  ( 21.52544592524334988, 5.823673210054432836, 91.45942372801901854 ) ) ;
#198297 = CARTESIAN_POINT ( 'NONE',  ( -18.67979575497178146, -10.72451020669898902, 86.66557627198102409 ) ) ;
#198298 = CARTESIAN_POINT ( 'NONE',  ( -21.52544592524334988, -5.823673210054445271, 58.95942372801902565 ) ) ;
#198299 = CARTESIAN_POINT ( 'NONE',  ( 0.05219959533937995610, -21.53943276465977519, 65.00109039468568994 ) ) ;
#198300 = CARTESIAN_POINT ( 'NONE',  ( 19.03943276465977164, -0.05219959533909143690, 98.74890960531436690 ) ) ;
#198302 = CARTESIAN_POINT ( 'NONE',  ( 0.05219959533937995610, -21.53943276465977519, 55.00109039468568284 ) ) ;
#198301 = CARTESIAN_POINT ( 'NONE',  ( 12.06949235617739724, 12.14591786802326823, 96.87609039468568994 ) ) ;
#198303 = CARTESIAN_POINT ( 'NONE',  ( 16.53943276465976808, -0.05219959533910856209, 113.7489096053143527 ) ) ;
#198304 = CARTESIAN_POINT ( 'NONE',  ( 4.483927247898545687, 16.52544592524342804, 69.79057627198102409 ) ) ;
#198305 = CARTESIAN_POINT ( 'NONE',  ( 12.06949235617757843, -12.14591786802309237, 33.12390960531435979 ) ) ;
#198306 = CARTESIAN_POINT ( 'NONE',  ( 21.53943276465977519, -0.05219959533907433946, 43.74890960531435979 ) ) ;
#198307 = CARTESIAN_POINT ( 'NONE',  ( 19.02544592524343514, -5.153800228976328945, 53.54057627198102409 ) ) ;
#198308 = CARTESIAN_POINT ( 'NONE',  ( 5.719274019375991003, -21.55341960407610458, 52.70724293864769550 ) ) ;
#198310 = VECTOR ( 'NONE', #116028, 1000.000000000000000 ) ;
#198309 = CARTESIAN_POINT ( 'NONE',  ( 16.46253265017146816, 9.564922557961045513, 46.66775706135233293 ) ) ;
#198312 = CARTESIAN_POINT ( 'NONE',  ( 4.379528057220339221, -16.55341960407611168, 47.70724293864770260 ) ) ;
#198311 = CARTESIAN_POINT ( 'NONE',  ( 25.51181203389338137, 5.285008086477808398, 165.5623613760384956 ) ) ;
#198313 = CARTESIAN_POINT ( 'NONE',  ( -18.67979575497178146, -10.72451020669898902, 21.66557627198102409 ) ) ;
#198314 = ORIENTED_EDGE ( 'NONE', *, *, #11076, .T. ) ;
#198315 = ORIENTED_EDGE ( 'NONE', *, *, #49797, .F. ) ;
#198316 = DIRECTION ( 'NONE',  ( 0.000000000000000000, 0.000000000000000000, 1.000000000000000000 ) ) ;
#198317 = CARTESIAN_POINT ( 'NONE',  ( 16.55341960407618274, -4.379528057220086978, 71.04275706135234714 ) ) ;
#198318 = CARTESIAN_POINT ( 'NONE',  ( 19.02544592524334988, 5.153800228976608722, 76.45942372801897591 ) ) ;
#198319 = CARTESIAN_POINT ( 'NONE',  ( -8.224510206698948167, 14.34966873604960824, 35.41557627198102409 ) ) ;
#198320 = DIRECTION ( 'NONE',  ( 1.000000000000000000, 0.000000000000000000, -0.000000000000000000 ) ) ;
#198321 = CARTESIAN_POINT ( 'NONE',  ( -8.224510206698948167, 14.34966873604960824, 25.41557627198103120 ) ) ;
#198322 = CARTESIAN_POINT ( 'NONE',  ( -19.03943276465977164, 0.05219959533909376836, 56.24890960531435979 ) ) ;
#198323 = EDGE_CURVE ( 'NONE', #188641, #13916, #104996, .T. ) ;
#198324 = CARTESIAN_POINT ( 'NONE',  ( 16.46253265017160672, -9.564922557960803928, 78.33224293864769550 ) ) ;
#198325 = CARTESIAN_POINT ( 'NONE',  ( -16.51473224551069308, -9.474510206698971260, 41.66557627198103120 ) ) ;
#198326 = CARTESIAN_POINT ( 'NONE',  ( -10.72451020669870658, -18.67979575497194134, 44.58442372801901854 ) ) ;
#198327 = CARTESIAN_POINT ( 'NONE',  ( 19.02544592524343514, -5.153800228976328945, 63.54057627198103830 ) ) ;
#198328 = CARTESIAN_POINT ( 'NONE',  ( 19.49401214000076976, 12.39993551617566681, 164.9999999999999716 ) ) ;
#198329 = CARTESIAN_POINT ( 'NONE',  ( -19.05341960407611168, -5.049401038298163336, 56.45724293864768129 ) ) ;
#198330 = CARTESIAN_POINT ( 'NONE',  ( 18.62759615963271287, -10.81492255796078972, 33.33224293864769550 ) ) ;
#198331 = CARTESIAN_POINT ( 'NONE',  ( -9.474510206698964154, 16.51473224551069663, 35.41557627198102409 ) ) ;
#198332 = CARTESIAN_POINT ( 'NONE',  ( -18.62759615963270932, 10.81492255796079327, 45.83224293864769550 ) ) ;
#198333 = CARTESIAN_POINT ( 'NONE',  ( 12.06949235617739724, 12.14591786802326823, 86.87609039468568994 ) ) ;
#198334 = CARTESIAN_POINT ( 'NONE',  ( -10.72451020669870658, -18.67979575497194134, 104.5844237280190185 ) ) ;
#198335 = CARTESIAN_POINT ( 'NONE',  ( 4.379528057220092307, 16.55341960407617563, 62.29275706135236845 ) ) ;
#198336 = CARTESIAN_POINT ( 'NONE',  ( -13.89961937509977652, 13.97604488694528158, 110.6239096053143243 ) ) ;
#198337 = CARTESIAN_POINT ( 'NONE',  ( -12.14591786802326823, 12.06949235617739902, 53.12609039468568284 ) ) ;
#198338 = CARTESIAN_POINT ( 'NONE',  ( 4.483927247898790824, -16.52544592524335698, 45.20942372801901854 ) ) ;
#198339 = CARTESIAN_POINT ( 'NONE',  ( 19.02544592524343514, -5.153800228976328945, 113.5405762719810241 ) ) ;
#198340 = VECTOR ( 'NONE', #116621, 1000.000000000000000 ) ;
#198341 = CARTESIAN_POINT ( 'NONE',  ( -4.483927247898782831, 16.52544592524335698, 22.70942372801901499 ) ) ;
#198342 = CARTESIAN_POINT ( 'NONE',  ( 19.05341960407611168, 5.049401038298154454, 38.95724293864767418 ) ) ;
#198343 = B_SPLINE_CURVE_WITH_KNOTS ( 'NONE', 3,
 ( #129843, #125892, #6512, #68191, #187592, #128855 ),
 .UNSPECIFIED., .F., .F.,
 ( 4, 2, 4 ),
 ( 0.007228050697041341933, 0.007608510107494807079, 0.007988969517948273091 ),
 .UNSPECIFIED. ) ;
#198344 = CARTESIAN_POINT ( 'NONE',  ( 10.72451020669871369, 18.67979575497193778, 32.08442372801901854 ) ) ;
#198345 = CARTESIAN_POINT ( 'NONE',  ( -8.314922557961024197, 14.29746914071037800, 27.91775706135234358 ) ) ;
#198346 = CARTESIAN_POINT ( 'NONE',  ( 4.379528057220092307, 16.55341960407617563, 82.29275706135234714 ) ) ;
#198347 = FACE_OUTER_BOUND ( 'NONE', #197609, .T. ) ;
#198348 = CARTESIAN_POINT ( 'NONE',  ( -0.05219959533937732626, 21.53943276465977519, 102.5010903946856899 ) ) ;
#198349 = CARTESIAN_POINT ( 'NONE',  ( 16.51473224551083163, -9.474510206698727899, 95.83442372801900433 ) ) ;
#198350 = CARTESIAN_POINT ( 'NONE',  ( 8.224510206698953496, -14.34966873604960469, 52.91557627198103830 ) ) ;
#198351 = CARTESIAN_POINT ( 'NONE',  ( 16.55341960407611168, 4.379528057220329451, 108.9572429386476955 ) ) ;
#198353 = CARTESIAN_POINT ( 'NONE',  ( -6.404328268737242702, 0.9271017399332003306, -64.47359807031669732 ) ) ;
#198352 = CARTESIAN_POINT ( 'NONE',  ( -5.049401038297874678, -19.05341960407617918, 44.79275706135232582 ) ) ;
#198354 = CARTESIAN_POINT ( 'NONE',  ( 18.62759615963255655, 10.81492255796105972, 56.66775706135235424 ) ) ;
#198355 = CARTESIAN_POINT ( 'NONE',  ( -5.049401038297874678, -19.05341960407617918, 104.7927570613523471 ) ) ;
#198356 = CARTESIAN_POINT ( 'NONE',  ( -18.10062525802553779, 5.500000000000031974, 63.51383468041922953 ) ) ;
#198357 = CARTESIAN_POINT ( 'NONE',  ( 19.02544592524343514, -5.153800228976328945, 103.5405762719809957 ) ) ;
#198358 = CARTESIAN_POINT ( 'NONE',  ( 10.72451020669898902, -18.67979575497178502, 67.91557627198102409 ) ) ;
#198359 = CARTESIAN_POINT ( 'NONE',  ( 16.46253265017146816, 9.564922557961045513, 91.66775706135234714 ) ) ;
#198360 = CARTESIAN_POINT ( 'NONE',  ( 16.51473224551069308, 9.474510206698969483, 104.1655762719810241 ) ) ;
#198361 = CARTESIAN_POINT ( 'NONE',  ( 10.13896110635529446, -25.83826727361345021, 139.9999999999999716 ) ) ;
#198362 = CARTESIAN_POINT ( 'NONE',  ( 14.34966873604960469, 8.224510206698951720, 109.1655762719810383 ) ) ;
#198363 = CARTESIAN_POINT ( 'NONE',  ( 18.62759615963255655, 10.81492255796105972, 91.66775706135234714 ) ) ;
#198364 = CARTESIAN_POINT ( 'NONE',  ( 9.564922557960805705, 16.46253265017160317, 39.58224293864768839 ) ) ;
#198365 = CARTESIAN_POINT ( 'NONE',  ( 21.55341960407619695, -5.719274019375665929, 51.04275706135234714 ) ) ;
#198366 = CARTESIAN_POINT ( 'NONE',  ( -5.719274019375665041, -21.55341960407619695, 84.79275706135234714 ) ) ;
#198367 = CARTESIAN_POINT ( 'NONE',  ( 16.53943276465976808, 0.05219959533934440121, 101.2510903946856757 ) ) ;
#198368 = CARTESIAN_POINT ( 'NONE',  ( -16.46253265017160317, 9.564922557960807481, 70.83224293864770971 ) ) ;
#198369 = CARTESIAN_POINT ( 'NONE',  ( -18.67979575497193778, 10.72451020669871902, 48.33442372801902565 ) ) ;
#198370 = CARTESIAN_POINT ( 'NONE',  ( -10.81492255796105439, 18.62759615963255655, 42.91775706135235424 ) ) ;
#198372 = CARTESIAN_POINT ( 'NONE',  ( 19.03943276465977164, -0.05219959533909143690, 88.74890960531436690 ) ) ;
#198371 = CARTESIAN_POINT ( 'NONE',  ( 13.97604488694548053, -13.89961937509957401, 70.62609039468567573 ) ) ;
#198373 = CARTESIAN_POINT ( 'NONE',  ( 14.29746914071049879, -8.314922557960816363, 108.3322429386477097 ) ) ;
#198374 = CARTESIAN_POINT ( 'NONE',  ( -21.55341960407610458, -5.719274019375992779, 91.45724293864769550 ) ) ;
#198375 = CARTESIAN_POINT ( 'NONE',  ( 0.05219959533910956823, 16.53943276465976808, 64.99890960531435269 ) ) ;
#198376 = CARTESIAN_POINT ( 'NONE',  ( 18.67979575497194134, -10.72451020669871369, 110.8344237280190043 ) ) ;
#198377 = CARTESIAN_POINT ( 'NONE',  ( -4.379528057220328563, 16.55341960407611168, 85.20724293864770971 ) ) ;
#198378 = CARTESIAN_POINT ( 'NONE',  ( -13.89961937509977652, 13.97604488694528158, 30.62390960531435269 ) ) ;
#198379 = CARTESIAN_POINT ( 'NONE',  ( -13.89961937509957401, -13.97604488694547875, 89.37609039468563310 ) ) ;
#198380 = CARTESIAN_POINT ( 'NONE',  ( 16.53943276465976808, -0.05219959533910856209, 53.74890960531437401 ) ) ;
#198381 = CARTESIAN_POINT ( 'NONE',  ( 10.72451020669871369, 18.67979575497193778, 92.08442372801901854 ) ) ;
#198382 = CARTESIAN_POINT ( 'NONE',  ( -16.51473224551069308, -9.474510206698971260, 91.66557627198103830 ) ) ;
#198383 = CARTESIAN_POINT ( 'NONE',  ( -16.51473224551082808, 9.474510206698731452, 68.33442372801900433 ) ) ;
#198384 = CARTESIAN_POINT ( 'NONE',  ( 18.67979575497178502, 10.72451020669898547, 79.16557627198103830 ) ) ;
#198385 = CARTESIAN_POINT ( 'NONE',  ( 18.67979575497194134, -10.72451020669871369, 25.83442372801901499 ) ) ;
#198386 = CARTESIAN_POINT ( 'NONE',  ( 0.05219959533934541429, -16.53943276465976808, 30.00109039468568284 ) ) ;
#198387 = CARTESIAN_POINT ( 'NONE',  ( 16.52544592524335698, 4.483927247898782831, 96.45942372801901854 ) ) ;
#198389 = CARTESIAN_POINT ( 'NONE',  ( -5.823673210054431948, 21.52544592524334988, 37.70942372801900433 ) ) ;
#198388 = CARTESIAN_POINT ( 'NONE',  ( 13.89961937509977652, -13.97604488694527269, 23.12390960531436335 ) ) ;
#198390 = CARTESIAN_POINT ( 'NONE',  ( 14.34966873604960469, 8.224510206698951720, 114.1655762719810383 ) ) ;
#198391 = CARTESIAN_POINT ( 'NONE',  ( 22.81625015709509441, 31.40387420917330275, -5.824999997268813345 ) ) ;
#198392 = CARTESIAN_POINT ( 'NONE',  ( 8.314922557961029526, -14.29746914071037800, 55.41775706135234714 ) ) ;
#198393 = CARTESIAN_POINT ( 'NONE',  ( -14.29746914071049879, 8.314922557960819915, 75.83224293864769550 ) ) ;
#198394 = CARTESIAN_POINT ( 'NONE',  ( 21.55341960407610458, 5.719274019375980345, 73.95724293864769550 ) ) ;
#198395 = CARTESIAN_POINT ( 'NONE',  ( 16.53943276465976808, -0.05219959533910856209, 28.74890960531435624 ) ) ;
#198396 = CARTESIAN_POINT ( 'NONE',  ( -16.52544592524335698, -4.483927247898792601, 48.95942372801902565 ) ) ;
#198397 = CARTESIAN_POINT ( 'NONE',  ( 19.05341960407611168, 5.049401038298154454, 48.95724293864768129 ) ) ;
#198398 = CARTESIAN_POINT ( 'NONE',  ( -12.14591786802326823, 12.06949235617739902, 98.12609039468570415 ) ) ;
#198399 = CARTESIAN_POINT ( 'NONE',  ( -0.05219959533936034679, 19.03943276465977164, 92.50109039468566152 ) ) ;
#198400 = CARTESIAN_POINT ( 'NONE',  ( 21.52544592524344225, -5.823673210054117533, 73.54057627198102409 ) ) ;
#198401 = CARTESIAN_POINT ( 'NONE',  ( 4.379528057220339221, -16.55341960407611168, 22.70724293864769194 ) ) ;
#198402 = ORIENTED_EDGE ( 'NONE', *, *, #19810, .F. ) ;
#198403 = CARTESIAN_POINT ( 'NONE',  ( -16.46253265017160317, 9.564922557960807481, 115.8322429386477097 ) ) ;
#198404 = AXIS2_PLACEMENT_3D ( 'NONE', #110861, #188719, #50203 ) ;
#198405 = CARTESIAN_POINT ( 'NONE',  ( -5.823673210054116645, -21.52544592524344225, 57.29057627198103120 ) ) ;
#198406 = ORIENTED_EDGE ( 'NONE', *, *, #4868, .T. ) ;
#198407 = CARTESIAN_POINT ( 'NONE',  ( 16.55341960407618274, -4.379528057220086978, 86.04275706135236135 ) ) ;
#198408 = ORIENTED_EDGE ( 'NONE', *, *, #36310, .T. ) ;
#198409 = CARTESIAN_POINT ( 'NONE',  ( -10.81492255796078084, -18.62759615963271287, 22.08224293864769194 ) ) ;
#198410 = CARTESIAN_POINT ( 'NONE',  ( 17.50000000000000000, 5.076555817581239083, 108.6795149204977804 ) ) ;
#198411 = CARTESIAN_POINT ( 'NONE',  ( -10.72451020669898014, 18.67979575497178502, 70.41557627198102409 ) ) ;
#198412 = CARTESIAN_POINT ( 'NONE',  ( -12.06949235617739369, -12.14591786802326823, 109.3760903946857042 ) ) ;
#198413 = CARTESIAN_POINT ( 'NONE',  ( 16.46253265017146816, 9.564922557961045513, 111.6677570613523329 ) ) ;
#198414 = CARTESIAN_POINT ( 'NONE',  ( 4.379528057220339221, -16.55341960407611168, 112.7072429386476955 ) ) ;
#198415 = CARTESIAN_POINT ( 'NONE',  ( 16.55341960407618274, -4.379528057220086978, 26.04275706135235779 ) ) ;
#198416 = CARTESIAN_POINT ( 'NONE',  ( 13.97604488694527802, 13.89961937509977652, 49.37390960531434558 ) ) ;
#198417 = CARTESIAN_POINT ( 'NONE',  ( 1.993301997531345292E-15, -30.30510711980685912, 144.4999999999999432 ) ) ;
#198418 = CARTESIAN_POINT ( 'NONE',  ( 16.51473224551069308, 9.474510206698969483, 99.16557627198102409 ) ) ;
#198419 = EDGE_CURVE ( 'NONE', #4689, #21447, #168377, .T. ) ;
#198420 = CIRCLE ( 'NONE', #137074, 69.99999999999998579 ) ;
#198421 = CARTESIAN_POINT ( 'NONE',  ( 14.29746914071037800, 8.314922557961029526, 91.66775706135234714 ) ) ;
#198422 = CARTESIAN_POINT ( 'NONE',  ( -19.05341960407617563, 5.049401038297882671, 93.54275706135234714 ) ) ;
#198423 = CARTESIAN_POINT ( 'NONE',  ( -16.46253265017146816, -9.564922557961047289, 19.16775706135233293 ) ) ;
#198424 = CARTESIAN_POINT ( 'NONE',  ( -5.719274019375978568, 21.55341960407610458, 80.20724293864769550 ) ) ;
#198426 = B_SPLINE_CURVE_WITH_KNOTS ( 'NONE', 3,
 ( #176281, #193446, #180297, #37753, #117592, #118607 ),
 .UNSPECIFIED., .F., .F.,
 ( 4, 2, 4 ),
 ( 0.007228050697041589999, 0.007608510107495062083, 0.007988969517948535035 ),
 .UNSPECIFIED. ) ;
#198425 = CARTESIAN_POINT ( 'NONE',  ( 4.483927247898790824, -16.52544592524335698, 105.2094237280190328 ) ) ;
#198427 = CARTESIAN_POINT ( 'NONE',  ( -0.05219959533936034679, 19.03943276465977164, 97.50109039468567573 ) ) ;
#198428 = CARTESIAN_POINT ( 'NONE',  ( 19.02544592524343514, -5.153800228976328945, 43.54057627198103120 ) ) ;
#198430 =( GEOMETRIC_REPRESENTATION_CONTEXT ( 3 ) GLOBAL_UNCERTAINTY_ASSIGNED_CONTEXT ( ( #7444 ) ) GLOBAL_UNIT_ASSIGNED_CONTEXT ( ( #170444, #64259, #47107 ) ) REPRESENTATION_CONTEXT ( 'NONE', 'WORKASPACE' ) );
#198429 = CARTESIAN_POINT ( 'NONE',  ( 19.03943276465977164, -0.05219959533909143690, 93.74890960531435269 ) ) ;
#198431 = CARTESIAN_POINT ( 'NONE',  ( -18.67979575497193778, 10.72451020669871902, 68.33442372801900433 ) ) ;
#198432 = CARTESIAN_POINT ( 'NONE',  ( -0.05219959533909027116, -19.03943276465977164, 47.49890960531435979 ) ) ;
#198433 = CARTESIAN_POINT ( 'NONE',  ( -16.62475595723694965, -7.163666690055376485, 84.47286648189530922 ) ) ;
#198434 = CARTESIAN_POINT ( 'NONE',  ( -16.53943276465976808, 0.05219959533911058130, 76.24890960531435269 ) ) ;
#198435 = CARTESIAN_POINT ( 'NONE',  ( 10.72451020669898902, -18.67979575497178502, 77.91557627198102409 ) ) ;
#198436 = CARTESIAN_POINT ( 'NONE',  ( -23.29544513554941076, 16.92513159979227666, 144.0656553485623874 ) ) ;
#198437 =( GEOMETRIC_REPRESENTATION_CONTEXT ( 3 ) GLOBAL_UNCERTAINTY_ASSIGNED_CONTEXT ( ( #53970 ) ) GLOBAL_UNIT_ASSIGNED_CONTEXT ( ( #172890, #188065, #171887 ) ) REPRESENTATION_CONTEXT ( 'NONE', 'WORKASPACE' ) );
#198438 = CARTESIAN_POINT ( 'NONE',  ( -21.46320343559653665, -20.96320343559631638, 5.353553390593267736 ) ) ;
#198439 = CARTESIAN_POINT ( 'NONE',  ( -9.474510206698720793, -16.51473224551083518, 44.58442372801900433 ) ) ;
#198440 = CARTESIAN_POINT ( 'NONE',  ( 17.13100169013224061, -6.664070546374246007, 73.26789835699825915 ) ) ;
#198442 = CARTESIAN_POINT ( 'NONE',  ( 16.46253265017160672, -9.564922557960803928, 93.33224293864769550 ) ) ;
#198441 = CARTESIAN_POINT ( 'NONE',  ( -16.46253265017160317, 9.564922557960807481, 80.83224293864769550 ) ) ;
#198443 = CARTESIAN_POINT ( 'NONE',  ( 16.53943276465976808, 0.05219959533934440121, 61.25109039468567573 ) ) ;
#198444 = DIRECTION ( 'NONE',  ( 1.000000000000000000, -0.000000000000000000, -0.000000000000000000 ) ) ;
#198445 = CARTESIAN_POINT ( 'NONE',  ( 13.97604488694548053, -13.89961937509957401, 45.62609039468566863 ) ) ;
#198446 = CARTESIAN_POINT ( 'NONE',  ( 15.18083716703543651, -14.94191171151153341, -58.85720012050614969 ) ) ;
#198447 = CARTESIAN_POINT ( 'NONE',  ( -0.05219959533909027116, -19.03943276465977164, 107.4989096053143527 ) ) ;
#198448 = CARTESIAN_POINT ( 'NONE',  ( 16.55341960407618274, -4.379528057220086978, 86.04275706135236135 ) ) ;
#198449 = EDGE_CURVE ( 'NONE', #49283, #106381, #127012, .T. ) ;
#198450 = PLANE ( 'NONE',  #192093 ) ;
#198451 = CARTESIAN_POINT ( 'NONE',  ( -16.52544592524335698, -4.483927247898792601, 73.95942372801901854 ) ) ;
#198452 = CARTESIAN_POINT ( 'NONE',  ( -16.12203461105344005, -16.12203461105316649, -64.92279855667830191 ) ) ;
#198453 = CARTESIAN_POINT ( 'NONE',  ( 12.06949235617739724, 12.14591786802326823, 51.87609039468568284 ) ) ;
#198454 = CARTESIAN_POINT ( 'NONE',  ( -40.00000000000000711, 2.918471586026471156E-14, -25.00000000000000000 ) ) ;
#198455 = CARTESIAN_POINT ( 'NONE',  ( 18.67979575497194134, -10.72451020669871369, 60.83442372801901854 ) ) ;
#198456 = CARTESIAN_POINT ( 'NONE',  ( -13.97604488694547697, 13.89961937509957934, 78.12609039468567573 ) ) ;
#198457 = CARTESIAN_POINT ( 'NONE',  ( 0.05219959533936267826, -19.03943276465977164, 20.00109039468567218 ) ) ;
#198458 = CARTESIAN_POINT ( 'NONE',  ( -5.153800228976328057, -19.02544592524343514, 47.29057627198102409 ) ) ;
#198459 = CARTESIAN_POINT ( 'NONE',  ( 5.153800228976335163, 19.02544592524342804, 39.79057627198100988 ) ) ;
#198460 = CARTESIAN_POINT ( 'NONE',  ( -19.97888994334923751, -34.65319547504295628, -4.999999999999999112 ) ) ;
#198461 = CARTESIAN_POINT ( 'NONE',  ( -10.81492255796078084, -18.62759615963271287, 62.08224293864769550 ) ) ;
#198462 = VECTOR ( 'NONE', #66717, 1000.000000000000000 ) ;
#198463 = CARTESIAN_POINT ( 'NONE',  ( -16.46253265017160317, 9.564922557960807481, 110.8322429386476955 ) ) ;
#198464 = CARTESIAN_POINT ( 'NONE',  ( -12.06949235617756955, 12.14591786802309770, 110.6239096053143669 ) ) ;
#198465 = CARTESIAN_POINT ( 'NONE',  ( 14.34966873604972726, -8.224510206698740333, 55.83442372801901854 ) ) ;
#198466 = ORIENTED_EDGE ( 'NONE', *, *, #126710, .T. ) ;
#198467 = CARTESIAN_POINT ( 'NONE',  ( 15.72974639402199770, -15.80617190586745480, 113.1239096053143953 ) ) ;
#198469 = CARTESIAN_POINT ( 'NONE',  ( 23.48529157249600630, -32.32473071737749137, -5.300000000000000711 ) ) ;
#198468 = CARTESIAN_POINT ( 'NONE',  ( -8.314922557960811034, -14.29746914071050412, 52.08224293864768839 ) ) ;
#198470 = CARTESIAN_POINT ( 'NONE',  ( 19.02544592524334988, 5.153800228976608722, 106.4594237280190185 ) ) ;
#198471 = CARTESIAN_POINT ( 'NONE',  ( 13.97604488694548053, -13.89961937509957401, 35.62609039468567573 ) ) ;
#198472 = CARTESIAN_POINT ( 'NONE',  ( -8.224510206698948167, 14.34966873604960824, 40.41557627198103120 ) ) ;
#198473 = CARTESIAN_POINT ( 'NONE',  ( -18.62759615963270932, 10.81492255796079327, 115.8322429386477097 ) ) ;
#198475 = CARTESIAN_POINT ( 'NONE',  ( -21.52544592524343514, 5.823673210054127303, 61.04057627198103120 ) ) ;
#198474 = LINE ( 'NONE', #44790, #150594 ) ;
#198476 = CARTESIAN_POINT ( 'NONE',  ( -16.46253265017160317, 9.564922557960807481, 85.83224293864769550 ) ) ;
#198477 = CARTESIAN_POINT ( 'NONE',  ( -12.06949235617756955, 12.14591786802309770, 55.62390960531436690 ) ) ;
#198478 = CARTESIAN_POINT ( 'NONE',  ( -5.049401038298153566, 19.05341960407611168, 105.2072429386476671 ) ) ;
#198479 = DIRECTION ( 'NONE',  ( -1.000000000000000000, 0.000000000000000000, 0.000000000000000000 ) ) ;
#198480 = CARTESIAN_POINT ( 'NONE',  ( 9.564922557961047289, -16.46253265017146816, 50.41775706135233293 ) ) ;
#198481 = CARTESIAN_POINT ( 'NONE',  ( -0.05219959533907301413, -21.53943276465977519, 97.49890960531436690 ) ) ;
#198482 = CARTESIAN_POINT ( 'NONE',  ( -19.02544592524342804, 5.153800228976336051, 46.04057627198101699 ) ) ;
#198483 = CARTESIAN_POINT ( 'NONE',  ( 0.05219959533910956823, 16.53943276465976808, 109.9989096053143527 ) ) ;
#198484 = CARTESIAN_POINT ( 'NONE',  ( -5.719274019375665041, -21.55341960407619695, 44.79275706135234714 ) ) ;
#198485 = CARTESIAN_POINT ( 'NONE',  ( -17.14385361876520264, -23.59649016807271593, 145.1750000027311387 ) ) ;
#198486 = CARTESIAN_POINT ( 'NONE',  ( -8.314922557960811034, -14.29746914071050412, 32.08224293864769550 ) ) ;
#198487 = CARTESIAN_POINT ( 'NONE',  ( -9.474510206698964154, 16.51473224551069663, 50.41557627198102409 ) ) ;
#198488 = CARTESIAN_POINT ( 'NONE',  ( 19.03943276465977164, -0.05219959533909143690, 93.74890960531435269 ) ) ;
#198489 = CARTESIAN_POINT ( 'NONE',  ( -18.67979575497178146, -10.72451020669898902, 71.66557627198100988 ) ) ;
#198490 = CARTESIAN_POINT ( 'NONE',  ( 1.784210473542230573E-15, -29.16686587814331588, 141.3750000027311557 ) ) ;
#198491 = CARTESIAN_POINT ( 'NONE',  ( 9.564922557960805705, 16.46253265017160317, 39.58224293864768839 ) ) ;
#198492 = EDGE_LOOP ( 'NONE', ( #130978, #60108, #170649, #28640 ) ) ;
#198493 = CARTESIAN_POINT ( 'NONE',  ( -21.55341960407610458, -5.719274019375992779, 46.45724293864769550 ) ) ;
#198494 = ORIENTED_EDGE ( 'NONE', *, *, #9184, .T. ) ;
#198495 = CARTESIAN_POINT ( 'NONE',  ( -15.80617190586768217, 15.72974639402176855, 93.12609039468568994 ) ) ;
#198498 = CARTESIAN_POINT ( 'NONE',  ( -4.483927247898539470, -16.52544592524342804, 67.29057627198103830 ) ) ;
#198497 = CARTESIAN_POINT ( 'NONE',  ( 16.52544592524335698, 4.483927247898782831, 76.45942372801901854 ) ) ;
#198496 = CARTESIAN_POINT ( 'NONE',  ( -12.73749492396214578, -155.7167183371837496, -15.00000000000000178 ) ) ;
#198499 = CARTESIAN_POINT ( 'NONE',  ( 5.049401038298161559, -19.05341960407611168, 67.70724293864769550 ) ) ;
#198500 = EDGE_LOOP ( 'NONE', ( #186775, #138073, #11040, #197769, #168301 ) ) ;
#198501 = CARTESIAN_POINT ( 'NONE',  ( 19.02544592524334988, 5.153800228976608722, 26.45942372801899722 ) ) ;
#198502 = CARTESIAN_POINT ( 'NONE',  ( 14.34966873604972726, -8.224510206698740333, 85.83442372801901854 ) ) ;
#198503 = CARTESIAN_POINT ( 'NONE',  ( -21.55341960407619339, 5.719274019375674811, 113.5427570613523756 ) ) ;
#198504 = CARTESIAN_POINT ( 'NONE',  ( 9.564922557960805705, 16.46253265017160317, 69.58224293864770971 ) ) ;
#198505 = CARTESIAN_POINT ( 'NONE',  ( -5.823673210054116645, -21.52544592524344225, 52.29057627198102409 ) ) ;
#198506 = CARTESIAN_POINT ( 'NONE',  ( -8.224510206698735004, -14.34966873604973081, 29.58442372801901854 ) ) ;
#198507 = CARTESIAN_POINT ( 'NONE',  ( -10.81492255796105439, 18.62759615963255655, 82.91775706135234714 ) ) ;
#198508 = CARTESIAN_POINT ( 'NONE',  ( -0.05219959533934338120, 16.53943276465976808, 62.50109039468568284 ) ) ;
#198509 = CARTESIAN_POINT ( 'NONE',  ( -21.52544592524343514, 5.823673210054127303, 116.0405762719810383 ) ) ;
#198510 = CARTESIAN_POINT ( 'NONE',  ( -9.564922557961040184, 16.46253265017147172, 107.9177570613523471 ) ) ;
#198511 = CARTESIAN_POINT ( 'NONE',  ( -5.049401038298153566, 19.05341960407611168, 85.20724293864766707 ) ) ;
#198512 = CARTESIAN_POINT ( 'NONE',  ( -16.52544592524335698, -4.483927247898792601, 28.95942372801902209 ) ) ;
#198513 = CARTESIAN_POINT ( 'NONE',  ( -5.049401038298153566, 19.05341960407611168, 55.20724293864769550 ) ) ;
#198514 = CARTESIAN_POINT ( 'NONE',  ( 8.314922557961029526, -14.29746914071037800, 30.41775706135234358 ) ) ;
#198515 = CARTESIAN_POINT ( 'NONE',  ( 16.55341960407611168, 4.379528057220329451, 83.95724293864770971 ) ) ;
#198516 = CARTESIAN_POINT ( 'NONE',  ( -12.14591786802326823, 12.06949235617739902, 83.12609039468568994 ) ) ;
#198518 = CARTESIAN_POINT ( 'NONE',  ( -9.474510206698964154, 16.51473224551069663, 65.41557627198102409 ) ) ;
#198517 = CARTESIAN_POINT ( 'NONE',  ( 18.67979575497194134, -10.72451020669871369, 35.83442372801901143 ) ) ;
#198519 = CARTESIAN_POINT ( 'NONE',  ( -16.51473224551069308, -9.474510206698971260, 76.66557627198103830 ) ) ;
#198520 = CARTESIAN_POINT ( 'NONE',  ( 4.379528057220092307, 16.55341960407617563, 87.29275706135236135 ) ) ;
#198521 = AXIS2_PLACEMENT_3D ( 'NONE', #39390, #99044, #83875 ) ;
#198523 = EDGE_LOOP ( 'NONE', ( #177888, #22581, #54692, #79453, #103001 ) ) ;
#198522 = CARTESIAN_POINT ( 'NONE',  ( -24.50238749460122989, -2.981321037228370052, 173.3223451563238200 ) ) ;
#198524 = ORIENTED_EDGE ( 'NONE', *, *, #5174, .F. ) ;
#198525 = CARTESIAN_POINT ( 'NONE',  ( -16.46253265017146816, -9.564922557961047289, 29.16775706135232937 ) ) ;
#198526 = CARTESIAN_POINT ( 'NONE',  ( -9.474510206698964154, 16.51473224551069663, 105.4155762719810383 ) ) ;
#198527 = ADVANCED_FACE ( 'NONE', ( #122355 ), #45527, .F. ) ;
#198528 = CARTESIAN_POINT ( 'NONE',  ( 19.03943276465977164, -0.05219959533909143690, 53.74890960531436690 ) ) ;
#198529 = CARTESIAN_POINT ( 'NONE',  ( -11.30153831258471442, -180.0000000000000000, -13.00000000000000000 ) ) ;
#198530 = CARTESIAN_POINT ( 'NONE',  ( 16.52544592524335698, 4.483927247898782831, 31.45942372801901854 ) ) ;
#198532 = CARTESIAN_POINT ( 'NONE',  ( -16.55341960407617563, 4.379528057220093196, 38.54275706135234714 ) ) ;
#198531 = CARTESIAN_POINT ( 'NONE',  ( -19.03943276465977164, -0.05219959533935918106, 53.75109039468566863 ) ) ;
#198533 = CARTESIAN_POINT ( 'NONE',  ( 13.89961937509977652, -13.97604488694527269, 103.1239096053143527 ) ) ;
#198534 = CARTESIAN_POINT ( 'NONE',  ( -19.03943276465977164, 0.05219959533909376836, 81.24890960531436690 ) ) ;
#198535 = CARTESIAN_POINT ( 'NONE',  ( -21.52544592524343514, 5.823673210054127303, 96.04057627198102409 ) ) ;
#198536 = CARTESIAN_POINT ( 'NONE',  ( 19.02544592524334988, 5.153800228976608722, 66.45942372801899012 ) ) ;
#198538 = CARTESIAN_POINT ( 'NONE',  ( -9.564922557960796823, -16.46253265017161027, 27.08224293864769550 ) ) ;
#198537 = CARTESIAN_POINT ( 'NONE',  ( -0.05219959533909027116, -19.03943276465977164, 97.49890960531436690 ) ) ;
#198539 = CARTESIAN_POINT ( 'NONE',  ( 16.46253265017160672, -9.564922557960803928, 58.33224293864769550 ) ) ;
#198541 = CARTESIAN_POINT ( 'NONE',  ( -19.05341960407611168, -5.049401038298163336, 21.45724293864768839 ) ) ;
#198540 = CARTESIAN_POINT ( 'NONE',  ( 16.52544592524342804, -4.483927247898539470, 33.54057627198102409 ) ) ;
#198542 = CARTESIAN_POINT ( 'NONE',  ( -19.02544592524334988, -5.153800228976617603, 38.95942372801900433 ) ) ;
#198543 = VECTOR ( 'NONE', #67009, 1000.000000000000000 ) ;
#198544 = CARTESIAN_POINT ( 'NONE',  ( 8.314922557960818139, 14.29746914071049879, 74.58224293864768129 ) ) ;
#198545 = CARTESIAN_POINT ( 'NONE',  ( -10.72451020669870658, -18.67979575497194134, 94.58442372801901854 ) ) ;
#198546 = CARTESIAN_POINT ( 'NONE',  ( 16.46253265017160672, -9.564922557960803928, 33.33224293864770260 ) ) ;
#198547 = CARTESIAN_POINT ( 'NONE',  ( -8.314922557961024197, 14.29746914071037800, 52.91775706135235424 ) ) ;
#198549 = CARTESIAN_POINT ( 'NONE',  ( -21.52544592524334988, -5.823673210054445271, 98.95942372801903275 ) ) ;
#198548 = CARTESIAN_POINT ( 'NONE',  ( 12.14591786802309770, 12.06949235617756955, 34.37390960531435979 ) ) ;
#198550 = CARTESIAN_POINT ( 'NONE',  ( 9.474510206698971260, -16.51473224551069308, 97.91557627198102409 ) ) ;
#198551 = CARTESIAN_POINT ( 'NONE',  ( -19.02544592524342804, 5.153800228976336051, 101.0405762719810241 ) ) ;
#198552 = CARTESIAN_POINT ( 'NONE',  ( 0.05219959533910956823, 16.53943276465976808, 109.9989096053143527 ) ) ;
#198553 = CARTESIAN_POINT ( 'NONE',  ( -16.52544592524342804, 4.483927247898546575, 76.04057627198102409 ) ) ;
#198554 = CARTESIAN_POINT ( 'NONE',  ( 21.53943276465977519, -0.05219959533907433946, 78.74890960531436690 ) ) ;
#198555 = CARTESIAN_POINT ( 'NONE',  ( 5.049401038298161559, -19.05341960407611168, 87.70724293864769550 ) ) ;
#198556 = CARTESIAN_POINT ( 'NONE',  ( 18.62759615963271287, -10.81492255796078972, 103.3322429386476955 ) ) ;
#198557 = CIRCLE ( 'NONE', #163046, 21.30000000000002913 ) ;
#198558 = CARTESIAN_POINT ( 'NONE',  ( -9.564922557960796823, -16.46253265017161027, 97.08224293864769550 ) ) ;
#198560 = CARTESIAN_POINT ( 'NONE',  ( -4.379528057220328563, 16.55341960407611168, 85.20724293864770971 ) ) ;
#198559 = CARTESIAN_POINT ( 'NONE',  ( 9.564922557961047289, -16.46253265017146816, 65.41775706135233293 ) ) ;
#198561 = CARTESIAN_POINT ( 'NONE',  ( -9.564922557960796823, -16.46253265017161027, 57.08224293864769550 ) ) ;
#198562 = CARTESIAN_POINT ( 'NONE',  ( 15.72974639402199770, -15.80617190586745480, 68.12390960531436690 ) ) ;
#198563 = CARTESIAN_POINT ( 'NONE',  ( -25.12471020271278732, -7.795852113654130555, 170.9710663016989258 ) ) ;
#198565 = CARTESIAN_POINT ( 'NONE',  ( -17.14385361876520975, 23.59649016807275856, 149.0750000027312012 ) ) ;
#198564 = CARTESIAN_POINT ( 'NONE',  ( -16.55341960407617563, 4.379528057220093196, 108.5427570613523756 ) ) ;
#198566 = CARTESIAN_POINT ( 'NONE',  ( 16.46253265017146816, 9.564922557961045513, 111.6677570613523329 ) ) ;
#198567 = CARTESIAN_POINT ( 'NONE',  ( -4.483927247898539470, -16.52544592524342804, 77.29057627198102409 ) ) ;
#198568 = CARTESIAN_POINT ( 'NONE',  ( -17.48853670773245028, -5.747243402303098492, 96.33328700250011423 ) ) ;
#198569 = CARTESIAN_POINT ( 'NONE',  ( -19.02544592524342804, 5.153800228976336051, 76.04057627198102409 ) ) ;
#198570 = CARTESIAN_POINT ( 'NONE',  ( 19.02544592524343514, -5.153800228976328945, 43.54057627198103120 ) ) ;
#198571 = CARTESIAN_POINT ( 'NONE',  ( -14.29746914071049879, 8.314922557960819915, 70.83224293864770971 ) ) ;
#198572 = CARTESIAN_POINT ( 'NONE',  ( -16.46253265017160317, 9.564922557960807481, 110.8322429386476955 ) ) ;
#198573 = CARTESIAN_POINT ( 'NONE',  ( -0.05219959533936034679, 19.03943276465977164, 107.5010903946856615 ) ) ;
#198574 = CARTESIAN_POINT ( 'NONE',  ( 10.72451020669871369, 18.67979575497193778, 57.08442372801901854 ) ) ;
#198575 = VECTOR ( 'NONE', #150365, 1000.000000000000000 ) ;
#198576 = CARTESIAN_POINT ( 'NONE',  ( -13.89961937509977652, 13.97604488694528158, 95.62390960531436690 ) ) ;
#198577 = CARTESIAN_POINT ( 'NONE',  ( 21.52544592524344225, -5.823673210054117533, 78.54057627198103830 ) ) ;
#198578 = CARTESIAN_POINT ( 'NONE',  ( -16.55341960407617563, 4.379528057220093196, 73.54275706135234714 ) ) ;
#198579 = VECTOR ( 'NONE', #174824, 1000.000000000000000 ) ;
#198580 = CARTESIAN_POINT ( 'NONE',  ( -19.02544592524335343, -5.153800228976618492, 108.9594237280189901 ) ) ;
#198581 = CARTESIAN_POINT ( 'NONE',  ( 9.564922557960805705, 16.46253265017160317, 69.58224293864770971 ) ) ;
#198582 = CARTESIAN_POINT ( 'NONE',  ( -18.67979575497178146, -10.72451020669898902, 81.66557627198103830 ) ) ;
#198583 = CARTESIAN_POINT ( 'NONE',  ( -16.46253265017146816, -9.564922557961047289, 109.1677570613523471 ) ) ;
#198585 = CARTESIAN_POINT ( 'NONE',  ( -0.05219959533937732626, 21.53943276465977519, 62.50109039468568284 ) ) ;
#198584 = CARTESIAN_POINT ( 'NONE',  ( 14.29746914071049879, -8.314922557960816363, 38.33224293864768839 ) ) ;
#198587 = CARTESIAN_POINT ( 'NONE',  ( -19.03943276465977164, 0.05219959533909376836, 111.2489096053143669 ) ) ;
#198586 = CARTESIAN_POINT ( 'NONE',  ( -8.314922557961024197, 14.29746914071037800, 82.91775706135234714 ) ) ;
#198588 = FACE_BOUND ( 'NONE', #153790, .T. ) ;
#198589 = CARTESIAN_POINT ( 'NONE',  ( 1.363652971230786992, 31.04735526335058537, -50.18466865107295405 ) ) ;
#198590 = CARTESIAN_POINT ( 'NONE',  ( 16.53943276465976808, 0.05219959533934440121, 91.25109039468568994 ) ) ;
#198591 = CARTESIAN_POINT ( 'NONE',  ( 14.29746914071037800, 8.314922557961029526, 41.66775706135235424 ) ) ;
#198592 = CARTESIAN_POINT ( 'NONE',  ( 13.97604488694527802, 13.89961937509977652, 64.37390960531436690 ) ) ;
#198593 = CARTESIAN_POINT ( 'NONE',  ( -5.153800228976328057, -19.02544592524343514, 67.29057627198102409 ) ) ;
#198594 = CARTESIAN_POINT ( 'NONE',  ( 15.80617190586769283, -15.72974639402175789, 60.62609039468567573 ) ) ;
#198595 = CARTESIAN_POINT ( 'NONE',  ( -4.379528057220086978, -16.55341960407618274, 64.79275706135234714 ) ) ;
#198596 = CARTESIAN_POINT ( 'NONE',  ( -8.314922557960811034, -14.29746914071050412, 52.08224293864768839 ) ) ;
#198597 = CARTESIAN_POINT ( 'NONE',  ( -13.97604488694527625, -13.89961937509977652, 41.87390960531435979 ) ) ;
#198598 = CARTESIAN_POINT ( 'NONE',  ( 5.153800228976335163, 19.02544592524342804, 54.79057627198103120 ) ) ;
#198599 = CARTESIAN_POINT ( 'NONE',  ( 4.379528057220092307, 16.55341960407617563, 42.29275706135235424 ) ) ;
#198600 = CARTESIAN_POINT ( 'NONE',  ( -13.89961937509957401, -13.97604488694547875, 94.37609039468566152 ) ) ;
#198601 = CARTESIAN_POINT ( 'NONE',  ( -12.06949235617756955, 12.14591786802309770, 90.62390960531436690 ) ) ;
#198602 = CARTESIAN_POINT ( 'NONE',  ( 16.46253265017160672, -9.564922557960803928, 68.33224293864770971 ) ) ;
#198604 = CARTESIAN_POINT ( 'NONE',  ( -28.79475375365568013, -9.355982642739451904, 148.0843446568999866 ) ) ;
#198603 = CARTESIAN_POINT ( 'NONE',  ( -19.03943276465977164, -0.05219959533935918106, 93.75109039468566152 ) ) ;
#198605 = CARTESIAN_POINT ( 'NONE',  ( 10.72451020669871369, 18.67979575497193778, 87.08442372801901854 ) ) ;
#198606 = CARTESIAN_POINT ( 'NONE',  ( 16.52544592524335698, 4.483927247898782831, 66.45942372801903275 ) ) ;
#198607 = DIRECTION ( 'NONE',  ( -6.938893903907222067E-15, 0.000000000000000000, 1.000000000000000000 ) ) ;
#198608 = CARTESIAN_POINT ( 'NONE',  ( 21.52544592524344225, -5.823673210054117533, 48.54057627198103120 ) ) ;
#198609 = CARTESIAN_POINT ( 'NONE',  ( 0.05219959533934541429, -16.53943276465976808, 50.00109039468568994 ) ) ;
#198610 = CARTESIAN_POINT ( 'NONE',  ( -18.87580814761075843, 5.500000000000059508, 70.87172394265761000 ) ) ;
#198611 = CARTESIAN_POINT ( 'NONE',  ( 9.564922557961047289, -16.46253265017146816, 40.41775706135234003 ) ) ;
#198612 = CARTESIAN_POINT ( 'NONE',  ( 9.474510206698971260, -16.51473224551069308, 92.91557627198103830 ) ) ;
#198613 = CARTESIAN_POINT ( 'NONE',  ( 16.51473224551069308, 9.474510206698969483, 24.16557627198102765 ) ) ;
#198614 = CARTESIAN_POINT ( 'NONE',  ( -16.46253265017160317, 9.564922557960807481, 45.83224293864769550 ) ) ;
#198615 = CIRCLE ( 'NONE', #111407, 38.00000000000000000 ) ;
#198616 = CARTESIAN_POINT ( 'NONE',  ( 15.19344129729077331, 17.31327599691201868, -55.22348155082431731 ) ) ;
#198617 = CARTESIAN_POINT ( 'NONE',  ( -21.53943276465977519, -0.05219959533937600094, 78.75109039468568994 ) ) ;
#198618 = CYLINDRICAL_SURFACE ( 'NONE', #111126, 28.90000000000004476 ) ;
#198619 = PRODUCT_DEFINITION_SHAPE ( 'NONE', 'NONE',  #200205 ) ;
#198620 = CARTESIAN_POINT ( 'NONE',  ( -5.153800228976607833, 19.02544592524334988, 32.70942372801899722 ) ) ;
#198621 = CARTESIAN_POINT ( 'NONE',  ( -16.51473224551082808, 9.474510206698731452, 33.33442372801899722 ) ) ;
#198622 = CARTESIAN_POINT ( 'NONE',  ( 14.34966873604960469, 8.224510206698951720, 49.16557627198102409 ) ) ;
#198623 = CARTESIAN_POINT ( 'NONE',  ( -0.05219959533909027116, -19.03943276465977164, 52.49890960531436690 ) ) ;
#198624 = CARTESIAN_POINT ( 'NONE',  ( 5.719274019375991003, -21.55341960407610458, 22.70724293864769194 ) ) ;
#198625 = CARTESIAN_POINT ( 'NONE',  ( 5.719274019375673035, 21.55341960407619339, 77.29275706135234714 ) ) ;
#198626 = CARTESIAN_POINT ( 'NONE',  ( -5.049401038298153566, 19.05341960407611168, 65.20724293864765286 ) ) ;
#198627 = CARTESIAN_POINT ( 'NONE',  ( -18.67979575497193778, 10.72451020669871902, 83.33442372801903275 ) ) ;
#198628 = CARTESIAN_POINT ( 'NONE',  ( -15.72974639402197994, 15.80617190586746368, 30.62390960531436335 ) ) ;
#198629 = CARTESIAN_POINT ( 'NONE',  ( -5.823673210054431948, 21.52544592524334988, 37.70942372801900433 ) ) ;
#198630 = CARTESIAN_POINT ( 'NONE',  ( 9.474510206698729675, 16.51473224551082808, 67.08442372801900433 ) ) ;
#198631 = CARTESIAN_POINT ( 'NONE',  ( 19.05341960407611168, 5.049401038298154454, 28.95724293864769550 ) ) ;
#198632 = CARTESIAN_POINT ( 'NONE',  ( 9.474510206698971260, -16.51473224551069308, 77.91557627198103830 ) ) ;
#198633 = CARTESIAN_POINT ( 'NONE',  ( -0.05219959533934338120, 16.53943276465976808, 27.50109039468567929 ) ) ;
#198634 = CARTESIAN_POINT ( 'NONE',  ( 8.314922557960818139, 14.29746914071049879, 94.58224293864769550 ) ) ;
#198635 = CARTESIAN_POINT ( 'NONE',  ( -19.03943276465977164, 0.05219959533909376836, 51.24890960531436690 ) ) ;
#198636 = CARTESIAN_POINT ( 'NONE',  ( -5.719274019375978568, 21.55341960407610458, 55.20724293864770260 ) ) ;
#198637 = CARTESIAN_POINT ( 'NONE',  ( -16.53943276465976808, -0.05219959533934237506, 18.75109039468568639 ) ) ;
#198638 = CARTESIAN_POINT ( 'NONE',  ( -5.823673210054431948, 21.52544592524334988, 22.70942372801901499 ) ) ;
#198639 = CARTESIAN_POINT ( 'NONE',  ( -21.55341960407619339, 5.719274019375674811, 73.54275706135234714 ) ) ;
#198640 = CARTESIAN_POINT ( 'NONE',  ( 12.06949235617739724, 12.14591786802326823, 71.87609039468568994 ) ) ;
#198641 = CARTESIAN_POINT ( 'NONE',  ( -12.06949235617739369, -12.14591786802326823, 74.37609039468568994 ) ) ;
#198642 = ORIENTED_EDGE ( 'NONE', *, *, #53412, .T. ) ;
#198643 = CARTESIAN_POINT ( 'NONE',  ( 5.153800228976335163, 19.02544592524342804, 54.79057627198103120 ) ) ;
#198644 = CARTESIAN_POINT ( 'NONE',  ( 0.05219959533934541429, -16.53943276465976808, 90.00109039468567573 ) ) ;
#198645 = CARTESIAN_POINT ( 'NONE',  ( 9.474510206698729675, 16.51473224551082808, 37.08442372801899722 ) ) ;
#198646 = CARTESIAN_POINT ( 'NONE',  ( -21.52544592524343514, 5.823673210054127303, 111.0405762719810525 ) ) ;
#198647 = CARTESIAN_POINT ( 'NONE',  ( -16.53943276465976808, 0.05219959533911058130, 71.24890960531435269 ) ) ;
#198648 = CARTESIAN_POINT ( 'NONE',  ( 13.97604488694527802, 13.89961937509977652, 89.37390960531436690 ) ) ;
#198649 = CARTESIAN_POINT ( 'NONE',  ( -8.224510206698735004, -14.34966873604973081, 89.58442372801901854 ) ) ;
#198650 = CARTESIAN_POINT ( 'NONE',  ( -0.05219959533937732626, 21.53943276465977519, 57.50109039468568994 ) ) ;
#198651 = CARTESIAN_POINT ( 'NONE',  ( 4.379528057220092307, 16.55341960407617563, 37.29275706135235424 ) ) ;
#198652 = CARTESIAN_POINT ( 'NONE',  ( 15.80617190586746368, 15.72974639402197994, 114.3739096053143527 ) ) ;
#198653 = CARTESIAN_POINT ( 'NONE',  ( 16.53943276465976808, -0.05219959533910856209, 63.74890960531435979 ) ) ;
#198654 = ORIENTED_EDGE ( 'NONE', *, *, #115666, .T. ) ;
#198655 = CARTESIAN_POINT ( 'NONE',  ( -10.72451020669898014, 18.67979575497178502, 95.41557627198102409 ) ) ;
#198656 = CARTESIAN_POINT ( 'NONE',  ( -4.483927247898539470, -16.52544592524342804, 37.29057627198102409 ) ) ;
#198657 = VERTEX_POINT ( 'NONE', #30357 ) ;
#198658 = CARTESIAN_POINT ( 'NONE',  ( 34.87691056670618650, 6.486286472422006177, 41.22672555304436770 ) ) ;
#198659 = CIRCLE ( 'NONE', #50134, 4.999999999999998224 ) ;
#198660 = CARTESIAN_POINT ( 'NONE',  ( 9.474510206698971260, -16.51473224551069308, 107.9155762719810383 ) ) ;
#198661 = CARTESIAN_POINT ( 'NONE',  ( -0.05219959533937732626, 21.53943276465977519, 37.50109039468568284 ) ) ;
#198662 = CARTESIAN_POINT ( 'NONE',  ( 8.314922557960818139, 14.29746914071049879, 64.58224293864769550 ) ) ;
#198663 = CARTESIAN_POINT ( 'NONE',  ( -19.05341960407611168, -5.049401038298163336, 66.45724293864769550 ) ) ;
#198664 = CARTESIAN_POINT ( 'NONE',  ( 19.02544592524334988, 5.153800228976608722, 61.45942372801900433 ) ) ;
#198665 = CARTESIAN_POINT ( 'NONE',  ( -10.72451020669898014, 18.67979575497178502, 50.41557627198103120 ) ) ;
#198666 = CARTESIAN_POINT ( 'NONE',  ( -10.75775780536858051, -37.01749054245972559, -23.73535027650243023 ) ) ;
#198667 = CARTESIAN_POINT ( 'NONE',  ( 9.564922557960805705, 16.46253265017160317, 54.58224293864769550 ) ) ;
#198668 = CARTESIAN_POINT ( 'NONE',  ( -14.34966873604972548, 8.224510206698743886, 33.33442372801900433 ) ) ;
#198669 = CARTESIAN_POINT ( 'NONE',  ( -15.72974639402176322, -15.80617190586768395, 19.37609039468568639 ) ) ;
#198670 = CARTESIAN_POINT ( 'NONE',  ( -14.29746914071049879, 8.314922557960819915, 45.83224293864769550 ) ) ;
#198671 = VERTEX_POINT ( 'NONE', #78832 ) ;
#198672 = CARTESIAN_POINT ( 'NONE',  ( -19.03943276465977164, 0.05219959533909376836, 91.24890960531436690 ) ) ;
#198673 = CARTESIAN_POINT ( 'NONE',  ( 5.719274019375991003, -21.55341960407610458, 67.70724293864769550 ) ) ;
#198675 = CARTESIAN_POINT ( 'NONE',  ( 8.224510206698742110, 14.34966873604972548, 42.08442372801901854 ) ) ;
#198674 = CARTESIAN_POINT ( 'NONE',  ( -21.52544592524343514, 5.823673210054127303, 111.0405762719810525 ) ) ;
#198676 = CARTESIAN_POINT ( 'NONE',  ( -15.80617190586745835, -15.72974639402198527, 31.87390960531435979 ) ) ;
#198677 = CARTESIAN_POINT ( 'NONE',  ( 21.53943276465977519, 0.05219959533937863772, 101.2510903946856757 ) ) ;
#198678 = CARTESIAN_POINT ( 'NONE',  ( 13.97604488694527802, 13.89961937509977652, 104.3739096053143385 ) ) ;
#198679 = CARTESIAN_POINT ( 'NONE',  ( 5.153800228976335163, 19.02544592524342804, 44.79057627198103830 ) ) ;
#198680 = CARTESIAN_POINT ( 'NONE',  ( 9.564922557960805705, 16.46253265017160317, 99.58224293864770971 ) ) ;
#198681 = CARTESIAN_POINT ( 'NONE',  ( 9.474510206698971260, -16.51473224551069308, 82.91557627198103830 ) ) ;
#198682 = FACE_OUTER_BOUND ( 'NONE', #22950, .T. ) ;
#198683 = CARTESIAN_POINT ( 'NONE',  ( 19.03943276465977164, 0.05219959533936151252, 61.25109039468566863 ) ) ;
#198685 = CARTESIAN_POINT ( 'NONE',  ( 15.72974639402199770, -15.80617190586745480, 33.12390960531435979 ) ) ;
#198684 = CARTESIAN_POINT ( 'NONE',  ( -0.05219959533937732626, 21.53943276465977519, 107.5010903946856899 ) ) ;
#198686 = CARTESIAN_POINT ( 'NONE',  ( -12.06949235617739369, -12.14591786802326823, 109.3760903946857042 ) ) ;
#198687 = CARTESIAN_POINT ( 'NONE',  ( 13.89961937509957401, 13.97604488694547697, 71.87609039468567573 ) ) ;
#198688 = CARTESIAN_POINT ( 'NONE',  ( -16.29526858892873165, 7.335722546920269593, 59.20329402199793378 ) ) ;
#198689 = CARTESIAN_POINT ( 'NONE',  ( 9.564922557961047289, -16.46253265017146816, 80.41775706135234714 ) ) ;
#198690 = CARTESIAN_POINT ( 'NONE',  ( -13.89961937509957401, -13.97604488694547875, 29.37609039468565797 ) ) ;
#198691 = CARTESIAN_POINT ( 'NONE',  ( 18.22780087662122739, 5.500000000000000888, 71.48236817873106475 ) ) ;
#198692 = CARTESIAN_POINT ( 'NONE',  ( 19.05341960407611168, 5.049401038298154454, 38.95724293864767418 ) ) ;
#198693 = CARTESIAN_POINT ( 'NONE',  ( 16.53943276465976808, -0.05219959533910856209, 43.74890960531435979 ) ) ;
#198694 = ADVANCED_FACE ( 'NONE', ( #34333 ), #3974, .T. ) ;
#198695 = CARTESIAN_POINT ( 'NONE',  ( -17.40805194822030444, -6.112264579159319311, 109.1662872748939321 ) ) ;
#198696 = CARTESIAN_POINT ( 'NONE',  ( 14.34966873604960469, 8.224510206698951720, 29.16557627198103120 ) ) ;
#198697 = LINE ( 'NONE', #89519, #174440 ) ;
#198698 = CARTESIAN_POINT ( 'NONE',  ( -8.224510206698735004, -14.34966873604973081, 99.58442372801900433 ) ) ;
#198699 = CARTESIAN_POINT ( 'NONE',  ( 13.97604488694527802, 13.89961937509977652, 49.37390960531434558 ) ) ;
#198700 = CARTESIAN_POINT ( 'NONE',  ( 10.81492255796106328, -18.62759615963255655, 105.4177570613523613 ) ) ;
#198701 = CARTESIAN_POINT ( 'NONE',  ( 0.05219959533936267826, -19.03943276465977164, 110.0010903946856757 ) ) ;
#198702 = CARTESIAN_POINT ( 'NONE',  ( -5.719274019375665041, -21.55341960407619695, 89.79275706135236135 ) ) ;
#198703 = CARTESIAN_POINT ( 'NONE',  ( -16.46253265017160317, 9.564922557960807481, 90.83224293864769550 ) ) ;
#198704 = CARTESIAN_POINT ( 'NONE',  ( 19.02544592524343514, -5.153800228976328945, 88.54057627198102409 ) ) ;
#198705 = CARTESIAN_POINT ( 'NONE',  ( 3.556970738554034288E-15, -38.81732327939057114, -10.12499999726881228 ) ) ;
#198706 = CARTESIAN_POINT ( 'NONE',  ( 0.05219959533907565091, 21.53943276465977519, 114.9989096053143669 ) ) ;
#198707 = AXIS2_PLACEMENT_3D ( 'NONE', #112223, #5025, #66710 ) ;
#198708 = CARTESIAN_POINT ( 'NONE',  ( 16.55341960407611168, 4.379528057220329451, 83.95724293864770971 ) ) ;
#198709 = CARTESIAN_POINT ( 'NONE',  ( -18.62759615963270932, 10.81492255796079327, 80.83224293864769550 ) ) ;
#198710 = CARTESIAN_POINT ( 'NONE',  ( 13.97604488694527802, 13.89961937509977652, 59.37390960531434558 ) ) ;
#198712 = CARTESIAN_POINT ( 'NONE',  ( -16.52544592524335698, -4.483927247898792601, 93.95942372801903275 ) ) ;
#198711 = CARTESIAN_POINT ( 'NONE',  ( -15.80617190586745835, -15.72974639402198527, 101.8739096053143811 ) ) ;
#198713 = VERTEX_POINT ( 'NONE', #84796 ) ;
#198714 = CARTESIAN_POINT ( 'NONE',  ( 9.474510206698971260, -16.51473224551069308, 57.91557627198103120 ) ) ;
#198716 = CARTESIAN_POINT ( 'NONE',  ( -27.19095269391954517, 10.02149780027903780, 149.7954620931811291 ) ) ;
#198715 = CARTESIAN_POINT ( 'NONE',  ( 0.05219959533910956823, 16.53943276465976808, 94.99890960531436690 ) ) ;
#198717 = CARTESIAN_POINT ( 'NONE',  ( -13.97604488694527625, -13.89961937509977652, 56.87390960531434558 ) ) ;
#198718 = CARTESIAN_POINT ( 'NONE',  ( -5.049401038297874678, -19.05341960407617918, 84.79275706135233293 ) ) ;
#198719 = CARTESIAN_POINT ( 'NONE',  ( 12.14591786802309770, 12.06949235617756955, 79.37390960531436690 ) ) ;
#198720 = CARTESIAN_POINT ( 'NONE',  ( -18.62759615963255300, -10.81492255796106328, 59.16775706135234714 ) ) ;
#198722 = CARTESIAN_POINT ( 'NONE',  ( -0.05219959533907301413, -21.53943276465977519, 102.4989096053143811 ) ) ;
#198721 = CARTESIAN_POINT ( 'NONE',  ( -5.049401038298153566, 19.05341960407611168, 40.20724293864768839 ) ) ;
#198723 = CARTESIAN_POINT ( 'NONE',  ( 16.53943276465976808, -0.05219959533910856209, 98.74890960531438111 ) ) ;
#198724 = CARTESIAN_POINT ( 'NONE',  ( -3.573655867282028392E-15, 2.428612866367529932E-14, 150.0000000000000000 ) ) ;
#198725 = CARTESIAN_POINT ( 'NONE',  ( -19.05341960407611168, -5.049401038298163336, 61.45724293864769550 ) ) ;
#198726 = AXIS2_PLACEMENT_3D ( 'NONE', #170895, #123379, #32387 ) ;
#198727 = CARTESIAN_POINT ( 'NONE',  ( 19.25176906914649422, 5.499999999999730882, 48.49927264242280955 ) ) ;
#198729 = CARTESIAN_POINT ( 'NONE',  ( -15.80617190586745835, -15.72974639402198527, 21.87390960531436690 ) ) ;
#198728 = CARTESIAN_POINT ( 'NONE',  ( -9.564922557961040184, 16.46253265017147172, 97.91775706135233293 ) ) ;
#198730 = CARTESIAN_POINT ( 'NONE',  ( -5.719274019375665041, -21.55341960407619695, 54.79275706135235424 ) ) ;
#198731 = CARTESIAN_POINT ( 'NONE',  ( 0.05219959533909260263, 19.03943276465977164, 79.99890960531436690 ) ) ;
#198732 = CARTESIAN_POINT ( 'NONE',  ( 19.02544592524334988, 5.153800228976608722, 71.45942372801900433 ) ) ;
#198733 = CARTESIAN_POINT ( 'NONE',  ( -5.153800228976328057, -19.02544592524343514, 62.29057627198100988 ) ) ;
#198734 = VECTOR ( 'NONE', #139733, 1000.000000000000000 ) ;
#198735 = CARTESIAN_POINT ( 'NONE',  ( 12.14591786802309770, 12.06949235617756955, 74.37390960531436690 ) ) ;
#198736 = CARTESIAN_POINT ( 'NONE',  ( -0.05219959533910754901, -16.53943276465976808, 62.49890960531436690 ) ) ;
#198737 = CARTESIAN_POINT ( 'NONE',  ( 16.51473224551069308, 9.474510206698969483, 84.16557627198102409 ) ) ;
#198738 = CARTESIAN_POINT ( 'NONE',  ( -4.379528057220328563, 16.55341960407611168, 80.20724293864769550 ) ) ;
#198739 = CARTESIAN_POINT ( 'NONE',  ( -5.049401038298153566, 19.05341960407611168, 80.20724293864769550 ) ) ;
#198740 = CARTESIAN_POINT ( 'NONE',  ( 0.05219959533936267826, -19.03943276465977164, 30.00109039468566863 ) ) ;
#198743 = CARTESIAN_POINT ( 'NONE',  ( -8.224510206698948167, 14.34966873604960824, 110.4155762719810383 ) ) ;
#198742 = CARTESIAN_POINT ( 'NONE',  ( 16.53943276465976808, -0.05219959533910856209, 33.74890960531436690 ) ) ;
#198741 = CARTESIAN_POINT ( 'NONE',  ( 19.05341960407611168, 5.049401038298154454, 53.95724293864770260 ) ) ;
#198744 = VERTEX_POINT ( 'NONE', #96974 ) ;
#198745 = CARTESIAN_POINT ( 'NONE',  ( -21.52544592524334988, -5.823673210054445271, 38.95942372801901854 ) ) ;
#198746 = CARTESIAN_POINT ( 'NONE',  ( -9.564922557961040184, 16.46253265017147172, 67.91775706135233293 ) ) ;
#198747 = CARTESIAN_POINT ( 'NONE',  ( 12.06949235617757843, -12.14591786802309237, 38.12390960531436690 ) ) ;
#198748 = CARTESIAN_POINT ( 'NONE',  ( 5.823673210054125526, 21.52544592524343514, 79.79057627198102409 ) ) ;
#198749 = CARTESIAN_POINT ( 'NONE',  ( -10.81492255796078084, -18.62759615963271287, 22.08224293864769194 ) ) ;
#198750 = CARTESIAN_POINT ( 'NONE',  ( 16.52544592524342804, -4.483927247898539470, 68.54057627198103830 ) ) ;
#198751 = CARTESIAN_POINT ( 'NONE',  ( -13.89961937509977652, 13.97604488694528158, 45.62390960531433848 ) ) ;
#198752 = CARTESIAN_POINT ( 'NONE',  ( 9.564922557961047289, -16.46253265017146816, 45.41775706135232582 ) ) ;
#198753 = CARTESIAN_POINT ( 'NONE',  ( -4.379528057220086978, -16.55341960407618274, 104.7927570613523898 ) ) ;
#198754 = CARTESIAN_POINT ( 'NONE',  ( 12.14591786802327356, -12.06949235617739191, 60.62609039468567573 ) ) ;
#198755 = CARTESIAN_POINT ( 'NONE',  ( 10.72451020669898902, -18.67979575497178502, 32.91557627198102409 ) ) ;
#198756 = CARTESIAN_POINT ( 'NONE',  ( 10.72451020669871369, 18.67979575497193778, 102.0844237280190185 ) ) ;
#198757 = CARTESIAN_POINT ( 'NONE',  ( 13.97604488694527802, 13.89961937509977652, 99.37390960531436690 ) ) ;
#198758 = CARTESIAN_POINT ( 'NONE',  ( 4.483927247898790824, -16.52544592524335698, 70.20942372801904696 ) ) ;
#198759 = CARTESIAN_POINT ( 'NONE',  ( 5.153800228976335163, 19.02544592524342804, 24.79057627198102765 ) ) ;
#198760 = CARTESIAN_POINT ( 'NONE',  ( 12.06949235617757843, -12.14591786802309237, 38.12390960531436690 ) ) ;
#198762 = CARTESIAN_POINT ( 'NONE',  ( -19.05341960407611168, -5.049401038298163336, 91.45724293864766707 ) ) ;
#198761 = CARTESIAN_POINT ( 'NONE',  ( 5.153800228976335163, 19.02544592524342804, 109.7905762719810099 ) ) ;
#198763 = CARTESIAN_POINT ( 'NONE',  ( -21.52544592524343514, 5.823673210054127303, 31.04057627198102409 ) ) ;
#198764 = CARTESIAN_POINT ( 'NONE',  ( 4.483927247898545687, 16.52544592524342804, 59.79057627198103120 ) ) ;
#198765 = CARTESIAN_POINT ( 'NONE',  ( 14.29746914071049879, -8.314922557960816363, 33.33224293864769550 ) ) ;
#198766 = CARTESIAN_POINT ( 'NONE',  ( -14.34966873604960291, -8.224510206698953496, 46.66557627198102409 ) ) ;
#198768 = DIRECTION ( 'NONE',  ( 0.000000000000000000, 0.000000000000000000, -1.000000000000000000 ) ) ;
#198767 = CARTESIAN_POINT ( 'NONE',  ( 8.224510206698742110, 14.34966873604972548, 52.08442372801901854 ) ) ;
#198769 = CARTESIAN_POINT ( 'NONE',  ( -19.03943276465977164, -0.05219959533935918106, 48.75109039468566863 ) ) ;
#198770 = CARTESIAN_POINT ( 'NONE',  ( -19.03943276465977164, 0.05219959533909376836, 91.24890960531436690 ) ) ;
#198771 = CARTESIAN_POINT ( 'NONE',  ( 0.05219959533936267826, -19.03943276465977164, 65.00109039468567573 ) ) ;
#198772 = CARTESIAN_POINT ( 'NONE',  ( -22.44159573604009950, -16.30477369853688430, 145.5750000027311728 ) ) ;
#198773 = CARTESIAN_POINT ( 'NONE',  ( 5.153800228976615827, -19.02544592524334988, 50.20942372801897591 ) ) ;
#198775 = CARTESIAN_POINT ( 'NONE',  ( -12.14591786802326823, 12.06949235617739902, 88.12609039468570415 ) ) ;
#198774 = CARTESIAN_POINT ( 'NONE',  ( 16.46253265017146816, 9.564922557961045513, 96.66775706135233293 ) ) ;
#198776 = CARTESIAN_POINT ( 'NONE',  ( -17.14385361876520619, 23.59649016807275856, 143.0750000027311444 ) ) ;
#198777 = CARTESIAN_POINT ( 'NONE',  ( -5.049401038298153566, 19.05341960407611168, 30.20724293864768839 ) ) ;
#198778 = CARTESIAN_POINT ( 'NONE',  ( -13.97604488694527625, -13.89961937509977652, 111.8739096053143243 ) ) ;
#198779 = CARTESIAN_POINT ( 'NONE',  ( 18.67979575497194134, -10.72451020669871369, 45.83442372801901854 ) ) ;
#198780 = CARTESIAN_POINT ( 'NONE',  ( -19.03943276465977164, -0.05219959533935918106, 103.7510903946856757 ) ) ;
#198782 = CARTESIAN_POINT ( 'NONE',  ( 5.153800228976335163, 19.02544592524342804, 54.79057627198103120 ) ) ;
#198781 = CARTESIAN_POINT ( 'NONE',  ( 17.50000000000013856, -3.417042746626944183, 107.6738039623247545 ) ) ;
#198783 = CARTESIAN_POINT ( 'NONE',  ( 5.153800228976335163, 19.02544592524342804, 99.79057627198102409 ) ) ;
#198785 = CARTESIAN_POINT ( 'NONE',  ( 13.89961937509977652, -13.97604488694527269, 58.12390960531436690 ) ) ;
#198784 = CARTESIAN_POINT ( 'NONE',  ( 8.224510206698953496, -14.34966873604960469, 72.91557627198103830 ) ) ;
#198786 = CARTESIAN_POINT ( 'NONE',  ( -13.89961937509977652, 13.97604488694528158, 75.62390960531438111 ) ) ;
#198787 = CARTESIAN_POINT ( 'NONE',  ( -19.03943276465977164, -0.05219959533935918106, 83.75109039468567573 ) ) ;
#198788 = CARTESIAN_POINT ( 'NONE',  ( 18.67979575497178502, 10.72451020669898547, 54.16557627198103120 ) ) ;
#198789 = CARTESIAN_POINT ( 'NONE',  ( -8.314922557960811034, -14.29746914071050412, 112.0822429386477097 ) ) ;
#198790 = CARTESIAN_POINT ( 'NONE',  ( -19.05341960407617563, 5.049401038297882671, 43.54275706135232582 ) ) ;
#198791 = CARTESIAN_POINT ( 'NONE',  ( 9.474510206698971260, -16.51473224551069308, 72.91557627198102409 ) ) ;
#198792 = CARTESIAN_POINT ( 'NONE',  ( -15.72974639402197994, 15.80617190586746368, 80.62390960531438111 ) ) ;
#198794 = CARTESIAN_POINT ( 'NONE',  ( -5.153800228976607833, 19.02544592524334988, 52.70942372801900433 ) ) ;
#198793 = CARTESIAN_POINT ( 'NONE',  ( -16.53943276465976808, 0.05219959533911058130, 76.24890960531435269 ) ) ;
#198795 = CARTESIAN_POINT ( 'NONE',  ( 18.62759615963271287, -10.81492255796078972, 73.33224293864769550 ) ) ;
#198796 = CARTESIAN_POINT ( 'NONE',  ( -18.67979575497178146, -10.72451020669898902, 56.66557627198103830 ) ) ;
#198797 = AXIS2_PLACEMENT_3D ( 'NONE', #84466, #131993, #23825 ) ;
#198798 = CARTESIAN_POINT ( 'NONE',  ( -10.81492255796078084, -18.62759615963271287, 42.08224293864769550 ) ) ;
#198799 = CARTESIAN_POINT ( 'NONE',  ( -5.823673210054431948, 21.52544592524334988, 87.70942372801901854 ) ) ;
#198800 = CARTESIAN_POINT ( 'NONE',  ( 19.05341960407611168, 5.049401038298154454, 68.95724293864769550 ) ) ;
#198801 = CARTESIAN_POINT ( 'NONE',  ( 16.55341960407611168, 4.379528057220329451, 113.9572429386477239 ) ) ;
#198802 = CARTESIAN_POINT ( 'NONE',  ( 15.80617190586769283, -15.72974639402175789, 20.62609039468568639 ) ) ;
#198803 = CARTESIAN_POINT ( 'NONE',  ( 10.72451020669871369, 18.67979575497193778, 47.08442372801901854 ) ) ;
#198804 = CARTESIAN_POINT ( 'NONE',  ( 19.05341960407611168, 5.049401038298154454, 28.95724293864769550 ) ) ;
#198805 = CARTESIAN_POINT ( 'NONE',  ( 21.52544592524344225, -5.823673210054117533, 103.5405762719810383 ) ) ;
#198806 = CARTESIAN_POINT ( 'NONE',  ( 13.97604488694548053, -13.89961937509957401, 55.62609039468566863 ) ) ;
#198807 = CARTESIAN_POINT ( 'NONE',  ( 13.97604488694527802, 13.89961937509977652, 34.37390960531436690 ) ) ;
#198808 = CARTESIAN_POINT ( 'NONE',  ( -8.224510206698735004, -14.34966873604973081, 29.58442372801901854 ) ) ;
#198809 = LINE ( 'NONE', #60274, #37044 ) ;
#198810 = CARTESIAN_POINT ( 'NONE',  ( -12.14591786802326823, 12.06949235617739902, 63.12609039468568994 ) ) ;
#198811 = CARTESIAN_POINT ( 'NONE',  ( 19.02544592524343514, -5.153800228976328945, 33.54057627198102409 ) ) ;
#198812 = CARTESIAN_POINT ( 'NONE',  ( -24.18299921989768109, -12.77492350451736947, 169.7822198539309966 ) ) ;
#198813 = CARTESIAN_POINT ( 'NONE',  ( 9.564922557960805705, 16.46253265017160317, 84.58224293864769550 ) ) ;
#198814 = CARTESIAN_POINT ( 'NONE',  ( 8.224510206698953496, -14.34966873604960469, 112.9155762719810383 ) ) ;
#198815 = CARTESIAN_POINT ( 'NONE',  ( 0.05219959533907565091, 21.53943276465977519, 54.99890960531435269 ) ) ;
#198816 = CARTESIAN_POINT ( 'NONE',  ( -16.53943276465976808, -0.05219959533934237506, 48.75109039468568284 ) ) ;
#198817 = CARTESIAN_POINT ( 'NONE',  ( -18.67979575497193778, 10.72451020669871902, 98.33442372801901854 ) ) ;
#198818 = CARTESIAN_POINT ( 'NONE',  ( -9.564922557960796823, -16.46253265017161027, 42.08224293864769550 ) ) ;
#198819 = CARTESIAN_POINT ( 'NONE',  ( 0.05219959533934541429, -16.53943276465976808, 105.0010903946856757 ) ) ;
#198820 = CARTESIAN_POINT ( 'NONE',  ( 16.53943276465976808, -0.05219959533910856209, 58.74890960531436690 ) ) ;
#198821 = CARTESIAN_POINT ( 'NONE',  ( 13.97604488694527802, 13.89961937509977652, 64.37390960531436690 ) ) ;
#198822 = CARTESIAN_POINT ( 'NONE',  ( 5.823673210054444382, -21.52544592524334988, 105.2094237280190328 ) ) ;
#198823 = CARTESIAN_POINT ( 'NONE',  ( -21.52544592524343514, 5.823673210054127303, 116.0405762719810383 ) ) ;
#198824 = CARTESIAN_POINT ( 'NONE',  ( 10.81492255796106328, -18.62759615963255655, 85.41775706135236135 ) ) ;
#198825 = CARTESIAN_POINT ( 'NONE',  ( 8.224510206698742110, 14.34966873604972548, 57.08442372801901854 ) ) ;
#198826 = CARTESIAN_POINT ( 'NONE',  ( -16.52544592524335698, -4.483927247898792601, 28.95942372801902209 ) ) ;
#198827 = EDGE_CURVE ( 'NONE', #1415, #143427, #75463, .T. ) ;
#198829 = CARTESIAN_POINT ( 'NONE',  ( -21.52544592524334988, -5.823673210054445271, 98.95942372801903275 ) ) ;
#198828 = CARTESIAN_POINT ( 'NONE',  ( 14.29746914071049879, -8.314922557960816363, 73.33224293864769550 ) ) ;
#198830 = CARTESIAN_POINT ( 'NONE',  ( 16.55341960407611168, 4.379528057220329451, 38.95724293864768839 ) ) ;
#198831 = CARTESIAN_POINT ( 'NONE',  ( -16.52216118717206328, 7.221426719304524511, 113.9240097895301318 ) ) ;
#198832 = CARTESIAN_POINT ( 'NONE',  ( 12.14591786802327356, -12.06949235617739191, 40.62609039468567573 ) ) ;
#198833 = CARTESIAN_POINT ( 'NONE',  ( -16.53943276465976808, 0.05219959533911058130, 61.24890960531435979 ) ) ;
#198834 = CARTESIAN_POINT ( 'NONE',  ( -8.224510206698735004, -14.34966873604973081, 89.58442372801901854 ) ) ;
#198835 = CARTESIAN_POINT ( 'NONE',  ( -16.51473224551069308, -9.474510206698971260, 96.66557627198102409 ) ) ;
#198836 = CARTESIAN_POINT ( 'NONE',  ( 9.474510206698971260, -16.51473224551069308, 112.9155762719810383 ) ) ;
#198837 = CARTESIAN_POINT ( 'NONE',  ( 15.72974639402176855, 15.80617190586768217, 101.8760903946857042 ) ) ;
#198838 = CARTESIAN_POINT ( 'NONE',  ( -12.14591786802326823, 12.06949235617739902, 108.1260903946856757 ) ) ;
#198839 = CARTESIAN_POINT ( 'NONE',  ( -12.14591786802309592, -12.06949235617757132, 81.87390960531435269 ) ) ;
#198840 = CARTESIAN_POINT ( 'NONE',  ( 5.049401038298161559, -19.05341960407611168, 97.70724293864766707 ) ) ;
#198841 = ORIENTED_EDGE ( 'NONE', *, *, #145481, .T. ) ;
#198842 = CARTESIAN_POINT ( 'NONE',  ( -12.14591786802326823, 12.06949235617739902, 43.12609039468568284 ) ) ;
#198843 = CARTESIAN_POINT ( 'NONE',  ( -5.049401038298153566, 19.05341960407611168, 45.20724293864769550 ) ) ;
#198844 = CARTESIAN_POINT ( 'NONE',  ( 0.05219959533909260263, 19.03943276465977164, 109.9989096053143669 ) ) ;
#198846 = CARTESIAN_POINT ( 'NONE',  ( 17.97035753253451063, 5.499999999999972466, 101.5039701314110800 ) ) ;
#198845 = CARTESIAN_POINT ( 'NONE',  ( 16.52544592524335698, 4.483927247898782831, 46.45942372801901854 ) ) ;
#198847 = CARTESIAN_POINT ( 'NONE',  ( 9.474510206698729675, 16.51473224551082808, 37.08442372801899722 ) ) ;
#198848 = CARTESIAN_POINT ( 'NONE',  ( -19.02544592524342804, 5.153800228976336051, 41.04057627198103120 ) ) ;
#198849 = CARTESIAN_POINT ( 'NONE',  ( 12.06949235617739724, 12.14591786802326823, 76.87609039468567573 ) ) ;
#198850 = CARTESIAN_POINT ( 'NONE',  ( 0.05219959533936267826, -19.03943276465977164, 80.00109039468567573 ) ) ;
#198851 = CARTESIAN_POINT ( 'NONE',  ( 9.474510206698729675, 16.51473224551082808, 27.08442372801900433 ) ) ;
#198852 = CARTESIAN_POINT ( 'NONE',  ( 0.05219959533909260263, 19.03943276465977164, 54.99890960531435979 ) ) ;
#198853 = CARTESIAN_POINT ( 'NONE',  ( 4.483927247898545687, 16.52544592524342804, 99.79057627198103830 ) ) ;
#198854 = CARTESIAN_POINT ( 'NONE',  ( -16.51473224551082808, 9.474510206698731452, 68.33442372801900433 ) ) ;
#198855 = CARTESIAN_POINT ( 'NONE',  ( 10.81492255796078972, 18.62759615963270932, 69.58224293864769550 ) ) ;
#198856 = CARTESIAN_POINT ( 'NONE',  ( -0.05219959533936034679, 19.03943276465977164, 27.50109039468566507 ) ) ;
#198857 = CARTESIAN_POINT ( 'NONE',  ( 0.05219959533909260263, 19.03943276465977164, 104.9989096053143669 ) ) ;
#198858 = CARTESIAN_POINT ( 'NONE',  ( -15.80617190586745835, -15.72974639402198527, 71.87390960531438111 ) ) ;
#198859 = CARTESIAN_POINT ( 'NONE',  ( -5.049401038298153566, 19.05341960407611168, 110.2072429386476671 ) ) ;
#198860 = CARTESIAN_POINT ( 'NONE',  ( 5.049401038297881783, 19.05341960407617563, 102.2927570613523045 ) ) ;
#198861 = CARTESIAN_POINT ( 'NONE',  ( -17.49999999999999645, 5.500000000000000888, 108.7176903769643559 ) ) ;
#198862 = CARTESIAN_POINT ( 'NONE',  ( 12.14591786802327356, -12.06949235617739191, 25.62609039468567929 ) ) ;
#198863 = CARTESIAN_POINT ( 'NONE',  ( 0.05219959533909260263, 19.03943276465977164, 39.99890960531436690 ) ) ;
#198864 = CARTESIAN_POINT ( 'NONE',  ( 13.89961937509977652, -13.97604488694527269, 93.12390960531436690 ) ) ;
#198865 = CARTESIAN_POINT ( 'NONE',  ( -10.81492255796078084, -18.62759615963271287, 87.08224293864769550 ) ) ;
#198866 = CARTESIAN_POINT ( 'NONE',  ( 5.719274019375673035, 21.55341960407619339, 67.29275706135234714 ) ) ;
#198868 = CARTESIAN_POINT ( 'NONE',  ( -21.53943276465977519, -0.05219959533937600094, 108.7510903946857042 ) ) ;
#198867 = CARTESIAN_POINT ( 'NONE',  ( -19.03943276465977164, -0.05219959533935918106, 108.7510903946856615 ) ) ;
#198869 = CARTESIAN_POINT ( 'NONE',  ( -14.34966873604960291, -8.224510206698953496, 21.66557627198102409 ) ) ;
#198870 = CARTESIAN_POINT ( 'NONE',  ( -21.52544592524343514, 5.823673210054127303, 96.04057627198102409 ) ) ;
#198871 = CARTESIAN_POINT ( 'NONE',  ( 16.53943276465976808, -0.05219959533910856209, 33.74890960531436690 ) ) ;
#198872 = CARTESIAN_POINT ( 'NONE',  ( 16.51473224551083163, -9.474510206698727899, 80.83442372801899012 ) ) ;
#198873 = CARTESIAN_POINT ( 'NONE',  ( 19.05341960407617918, -5.049401038297876454, 61.04275706135232582 ) ) ;
#198874 = CARTESIAN_POINT ( 'NONE',  ( 5.823673210054444382, -21.52544592524334988, 55.20942372801902565 ) ) ;
#198875 = CARTESIAN_POINT ( 'NONE',  ( 16.46253265017146816, 9.564922557961045513, 41.66775706135234003 ) ) ;
#198876 = CARTESIAN_POINT ( 'NONE',  ( 0.05219959533910956823, 16.53943276465976808, 109.9989096053143527 ) ) ;
#198877 = CARTESIAN_POINT ( 'NONE',  ( -10.72451020669898014, 18.67979575497178502, 30.41557627198101699 ) ) ;
#198878 = CARTESIAN_POINT ( 'NONE',  ( -8.314922557960811034, -14.29746914071050412, 42.08224293864769550 ) ) ;
#198879 = CARTESIAN_POINT ( 'NONE',  ( -5.719274019375665041, -21.55341960407619695, 104.7927570613523898 ) ) ;
#198880 = CARTESIAN_POINT ( 'NONE',  ( 16.53943276465976808, 0.05219959533934440121, 76.25109039468568994 ) ) ;
#198881 = CARTESIAN_POINT ( 'NONE',  ( -12.06949235617756955, 12.14591786802309770, 25.62390960531435624 ) ) ;
#198882 = CARTESIAN_POINT ( 'NONE',  ( -15.72974639402176322, -15.80617190586768395, 64.37609039468568994 ) ) ;
#198883 = CARTESIAN_POINT ( 'NONE',  ( 21.55341960407619695, -5.719274019375665929, 66.04275706135236135 ) ) ;
#198884 = CARTESIAN_POINT ( 'NONE',  ( -5.719274019375978568, 21.55341960407610458, 65.20724293864768129 ) ) ;
#198885 = ORIENTED_EDGE ( 'NONE', *, *, #29329, .T. ) ;
#198886 = CARTESIAN_POINT ( 'NONE',  ( 5.049401038298163336, -19.05341960407611168, 62.70724293864769550 ) ) ;
#198887 = CARTESIAN_POINT ( 'NONE',  ( 21.52544592524334988, 5.823673210054432836, 41.45942372801901143 ) ) ;
#198888 = CARTESIAN_POINT ( 'NONE',  ( -19.03943276465977164, 0.05219959533909376836, 21.24890960531436335 ) ) ;
#198889 = CARTESIAN_POINT ( 'NONE',  ( -9.474510206698964154, 16.51473224551069663, 45.41557627198103120 ) ) ;
#198890 = CARTESIAN_POINT ( 'NONE',  ( 12.14591786802309770, 12.06949235617756955, 84.37390960531438111 ) ) ;
#198891 = CARTESIAN_POINT ( 'NONE',  ( -16.46253265017160317, 9.564922557960807481, 80.83224293864769550 ) ) ;
#198892 = CARTESIAN_POINT ( 'NONE',  ( 8.314922557960818139, 14.29746914071049879, 29.58224293864769905 ) ) ;
#198893 = CARTESIAN_POINT ( 'NONE',  ( 15.80617190586746368, 15.72974639402197994, 69.37390960531436690 ) ) ;
#198894 = AXIS2_PLACEMENT_3D ( 'NONE', #98936, #87772, #145448 ) ;
#198895 = CARTESIAN_POINT ( 'NONE',  ( -5.823673210054116645, -21.52544592524344225, 107.2905762719810525 ) ) ;
#198896 = CARTESIAN_POINT ( 'NONE',  ( -9.474510206698964154, 16.51473224551069663, 110.4155762719810383 ) ) ;
#198898 = CARTESIAN_POINT ( 'NONE',  ( 16.46253265017146816, 9.564922557961045513, 106.6677570613523471 ) ) ;
#198897 = CARTESIAN_POINT ( 'NONE',  ( 19.05341960407611168, 5.049401038298154454, 63.95724293864769550 ) ) ;
#198899 = CARTESIAN_POINT ( 'NONE',  ( -18.67979575497178146, -10.72451020669898902, 56.66557627198103830 ) ) ;
#198900 = CARTESIAN_POINT ( 'NONE',  ( 18.67979575497194134, -10.72451020669871369, 75.83442372801900433 ) ) ;
#198901 = CARTESIAN_POINT ( 'NONE',  ( -9.474510206698964154, 16.51473224551069663, 60.41557627198102409 ) ) ;
#198902 = CARTESIAN_POINT ( 'NONE',  ( 5.049401038298161559, -19.05341960407611168, 92.70724293864769550 ) ) ;
#198903 = CARTESIAN_POINT ( 'NONE',  ( -12.06949235617739369, -12.14591786802326823, 79.37609039468567573 ) ) ;
#198904 = CARTESIAN_POINT ( 'NONE',  ( 18.62759615963255655, 10.81492255796105972, 51.66775706135234714 ) ) ;
#198905 = CARTESIAN_POINT ( 'NONE',  ( 18.62759615963255655, 10.81492255796105972, 91.66775706135234714 ) ) ;
#198906 = CARTESIAN_POINT ( 'NONE',  ( 5.823673210054444382, -21.52544592524334988, 20.20942372801900788 ) ) ;
#198907 = CARTESIAN_POINT ( 'NONE',  ( -18.67979575497178146, -10.72451020669898902, 81.66557627198103830 ) ) ;
#198908 = CARTESIAN_POINT ( 'NONE',  ( -13.97604488694547697, 13.89961937509957934, 48.12609039468566863 ) ) ;
#198909 = CARTESIAN_POINT ( 'NONE',  ( -21.52544592524343514, 5.823673210054127303, 46.04057627198103830 ) ) ;
#198911 = CARTESIAN_POINT ( 'NONE',  ( -8.224510206698948167, 14.34966873604960824, 30.41557627198101699 ) ) ;
#198910 = CARTESIAN_POINT ( 'NONE',  ( -9.474510206698964154, 16.51473224551069663, 80.41557627198103830 ) ) ;
#198912 = CARTESIAN_POINT ( 'NONE',  ( -16.61371651742604882, 7.165104196376021584, 63.85415069992997417 ) ) ;
#198913 = CARTESIAN_POINT ( 'NONE',  ( 0.9479838643943441223, 14.02093834921316429, -60.30661765432581944 ) ) ;
#198914 = CARTESIAN_POINT ( 'NONE',  ( 5.153800228976615827, -19.02544592524334988, 90.20942372801900433 ) ) ;
#198915 = CARTESIAN_POINT ( 'NONE',  ( -0.05219959533907301413, -21.53943276465977519, 77.49890960531433848 ) ) ;
#198916 = CARTESIAN_POINT ( 'NONE',  ( -4.483927247898539470, -16.52544592524342804, 57.29057627198103120 ) ) ;
#198917 = CARTESIAN_POINT ( 'NONE',  ( 16.52544592524335698, 4.483927247898782831, 26.45942372801901854 ) ) ;
#198918 = CARTESIAN_POINT ( 'NONE',  ( -13.89961937509977652, 13.97604488694528158, 40.62390960531435979 ) ) ;
#198920 = CARTESIAN_POINT ( 'NONE',  ( -19.02544592524334988, -5.153800228976617603, 68.95942372801896170 ) ) ;
#198919 = CARTESIAN_POINT ( 'NONE',  ( 18.67979575497178502, 10.72451020669898547, 99.16557627198100988 ) ) ;
#198921 = CARTESIAN_POINT ( 'NONE',  ( 13.97604488694527802, 13.89961937509977652, 84.37390960531433848 ) ) ;
#198922 = CARTESIAN_POINT ( 'NONE',  ( -16.53943276465976808, 0.05219959533911058130, 96.24890960531435269 ) ) ;
#198923 = EDGE_CURVE ( 'NONE', #166994, #197193, #126812, .T. ) ;
#198924 = CARTESIAN_POINT ( 'NONE',  ( 13.97604488694527802, 13.89961937509977652, 59.37390960531434558 ) ) ;
#198925 = CARTESIAN_POINT ( 'NONE',  ( 16.55341960407611168, 4.379528057220329451, 68.95724293864769550 ) ) ;
#198926 = CARTESIAN_POINT ( 'NONE',  ( 16.51473224551069308, 9.474510206698969483, 39.16557627198103120 ) ) ;
#198927 = CARTESIAN_POINT ( 'NONE',  ( 17.62203461105334767, -16.12203461105336189, -54.55577602037946150 ) ) ;
#198928 = CARTESIAN_POINT ( 'NONE',  ( -14.34966873604960291, -8.224510206698953496, 46.66557627198102409 ) ) ;
#198929 = CARTESIAN_POINT ( 'NONE',  ( -13.89961937509977652, 13.97604488694528158, 85.62390960531433848 ) ) ;
#198930 = CARTESIAN_POINT ( 'NONE',  ( -1.022580077288041090E-15, -16.70000000000002061, -59.13370768023891344 ) ) ;
#198931 = CARTESIAN_POINT ( 'NONE',  ( 0.05219959533936267826, -19.03943276465977164, 50.00109039468566863 ) ) ;
#198932 = CARTESIAN_POINT ( 'NONE',  ( 4.483927247898790824, -16.52544592524335698, 65.20942372801901854 ) ) ;
#198933 = CONICAL_SURFACE ( 'NONE', #24598, 1732.050807568856271, 1.047197551196592524 ) ;
#198934 = CARTESIAN_POINT ( 'NONE',  ( -10.72451020669898014, 18.67979575497178502, 80.41557627198103830 ) ) ;
#198935 = CARTESIAN_POINT ( 'NONE',  ( 19.03943276465977164, 0.05219959533936151252, 41.25109039468566152 ) ) ;
#198936 = CARTESIAN_POINT ( 'NONE',  ( -16.46253265017160317, 9.564922557960807481, 85.83224293864769550 ) ) ;
#198937 = CARTESIAN_POINT ( 'NONE',  ( -21.71908475311230546, -22.98719380919931510, -46.06929478400958544 ) ) ;
#198938 = CARTESIAN_POINT ( 'NONE',  ( -5.823673210054116645, -21.52544592524344225, 22.29057627198102765 ) ) ;
#198939 = CARTESIAN_POINT ( 'NONE',  ( -0.05219959533909027116, -19.03943276465977164, 62.49890960531435979 ) ) ;
#198940 = CARTESIAN_POINT ( 'NONE',  ( -5.719274019375665041, -21.55341960407619695, 49.79275706135234714 ) ) ;
#198941 = CARTESIAN_POINT ( 'NONE',  ( 16.53943276465976808, -0.05219959533910856209, 113.7489096053143527 ) ) ;
#198944 = VERTEX_POINT ( 'NONE', #174836 ) ;
#198943 = CARTESIAN_POINT ( 'NONE',  ( 19.03943276465977164, -0.05219959533909143690, 98.74890960531436690 ) ) ;
#198942 = CARTESIAN_POINT ( 'NONE',  ( -15.72974639402197994, 15.80617190586746368, 115.6239096053143669 ) ) ;
#198945 = CARTESIAN_POINT ( 'NONE',  ( 18.62759615963255655, 10.81492255796105972, 41.66775706135235424 ) ) ;
#198946 = ORIENTED_EDGE ( 'NONE', *, *, #147318, .F. ) ;
#198947 = CARTESIAN_POINT ( 'NONE',  ( 5.153800228976335163, 19.02544592524342804, 99.79057627198102409 ) ) ;
#198948 = CARTESIAN_POINT ( 'NONE',  ( -21.85375568585902428, 8.111533062293290186, 169.4628294566284410 ) ) ;
#198949 = CARTESIAN_POINT ( 'NONE',  ( 18.67979575497178502, 10.72451020669898547, 104.1655762719810241 ) ) ;
#198950 = CARTESIAN_POINT ( 'NONE',  ( 9.474510206698971260, -16.51473224551069308, 47.91557627198102409 ) ) ;
#198951 = CARTESIAN_POINT ( 'NONE',  ( -4.483927247898782831, 16.52544592524335698, 22.70942372801901499 ) ) ;
#198952 = CARTESIAN_POINT ( 'NONE',  ( 30.74264578624799782, 22.33583958711400541, -10.54999999453762705 ) ) ;
#198953 = CARTESIAN_POINT ( 'NONE',  ( -16.46253265017160317, 9.564922557960807481, 30.83224293864769550 ) ) ;
#198954 = CARTESIAN_POINT ( 'NONE',  ( -18.62759615963255300, -10.81492255796106328, 94.16775706135237556 ) ) ;
#198956 = CARTESIAN_POINT ( 'NONE',  ( 5.823673210054444382, -21.52544592524334988, 65.20942372801901854 ) ) ;
#198955 = CARTESIAN_POINT ( 'NONE',  ( -16.46253265017160317, 9.564922557960807481, 90.83224293864769550 ) ) ;
#198957 = CARTESIAN_POINT ( 'NONE',  ( 8.571926809382597767, 26.38167802310806209, 146.7750000027311899 ) ) ;
#198958 = CARTESIAN_POINT ( 'NONE',  ( 19.03943276465977164, -0.05219959533909143690, 103.7489096053143669 ) ) ;
#198959 = CARTESIAN_POINT ( 'NONE',  ( -14.71622889490178920, 24.64770729138309591, 139.9999999999999716 ) ) ;
#198962 = CARTESIAN_POINT ( 'NONE',  ( -21.53943276465977519, -0.05219959533937600094, 58.75109039468568994 ) ) ;
#198961 = CARTESIAN_POINT ( 'NONE',  ( -14.34966873604972548, 8.224510206698743886, 73.33442372801901854 ) ) ;
#198960 = CARTESIAN_POINT ( 'NONE',  ( -16.53943276465976808, -0.05219959533934237506, 38.75109039468567573 ) ) ;
#198963 = CARTESIAN_POINT ( 'NONE',  ( -10.81492255796105439, 18.62759615963255655, 92.91775706135236135 ) ) ;
#198964 = CARTESIAN_POINT ( 'NONE',  ( 4.242540618128931129, 4.384162112346963625, -62.50719930893271226 ) ) ;
#198965 = CARTESIAN_POINT ( 'NONE',  ( 8.314922557961029526, -14.29746914071037800, 20.41775706135234714 ) ) ;
#198966 = CARTESIAN_POINT ( 'NONE',  ( 16.46253265017160672, -9.564922557960803928, 68.33224293864770971 ) ) ;
#198967 = CARTESIAN_POINT ( 'NONE',  ( 16.51473224551069308, 9.474510206698969483, 94.16557627198103830 ) ) ;
#198968 = CARTESIAN_POINT ( 'NONE',  ( 9.474510206698971260, -16.51473224551069308, 22.91557627198102765 ) ) ;
#198969 = CARTESIAN_POINT ( 'NONE',  ( 18.62759615963271287, -10.81492255796078972, 23.33224293864769194 ) ) ;
#198970 = CARTESIAN_POINT ( 'NONE',  ( 14.29746914071037800, 8.314922557961029526, 96.66775706135234714 ) ) ;
#198972 = CARTESIAN_POINT ( 'NONE',  ( 19.03943276465977164, -0.05219959533909143690, 58.74890960531435979 ) ) ;
#198971 = CARTESIAN_POINT ( 'NONE',  ( -14.29746914071049879, 8.314922557960819915, 75.83224293864769550 ) ) ;
#198973 = CARTESIAN_POINT ( 'NONE',  ( -21.53943276465977519, -0.05219959533937600094, 88.75109039468567573 ) ) ;
#198974 = FACE_OUTER_BOUND ( 'NONE', #85422, .T. ) ;
#198975 = CARTESIAN_POINT ( 'NONE',  ( -9.474510206698720793, -16.51473224551083518, 109.5844237280190043 ) ) ;
#198976 = CARTESIAN_POINT ( 'NONE',  ( 16.53943276465976808, -0.05219959533910856209, 78.74890960531436690 ) ) ;
#198977 = CARTESIAN_POINT ( 'NONE',  ( 10.72451020669871369, 18.67979575497193778, 32.08442372801901854 ) ) ;
#198978 = CARTESIAN_POINT ( 'NONE',  ( 10.81492255796078972, 18.62759615963270932, 64.58224293864769550 ) ) ;
#198979 = CARTESIAN_POINT ( 'NONE',  ( -19.03943276465977164, -0.05219959533935918106, 38.75109039468566152 ) ) ;
#198980 = CARTESIAN_POINT ( 'NONE',  ( -28.82186960331499392, 9.364793116373565596, 146.1500000054623456 ) ) ;
#198981 = CARTESIAN_POINT ( 'NONE',  ( -16.46253265017160317, 9.564922557960807481, 80.83224293864769550 ) ) ;
#198982 = CARTESIAN_POINT ( 'NONE',  ( -16.52544592524342804, 4.483927247898546575, 51.04057627198103120 ) ) ;
#198983 = CARTESIAN_POINT ( 'NONE',  ( 12.14591786802309770, 12.06949235617756955, 39.37390960531436690 ) ) ;
#198984 = CARTESIAN_POINT ( 'NONE',  ( 12.14591786802327356, -12.06949235617739191, 100.6260903946857184 ) ) ;
#198985 = CARTESIAN_POINT ( 'NONE',  ( -5.153800228976607833, 19.02544592524334988, 52.70942372801900433 ) ) ;
#198986 = CARTESIAN_POINT ( 'NONE',  ( -17.59860650958993844, 7.585241751806885979, 78.42337014262493256 ) ) ;
#198987 = CARTESIAN_POINT ( 'NONE',  ( -5.153800228976328057, -19.02544592524343514, 107.2905762719810383 ) ) ;
#198988 = CARTESIAN_POINT ( 'NONE',  ( -4.483927247898539470, -16.52544592524342804, 77.29057627198102409 ) ) ;
#198989 = CARTESIAN_POINT ( 'NONE',  ( -16.51473224551082808, 9.474510206698731452, 43.33442372801900433 ) ) ;
#198991 = CARTESIAN_POINT ( 'NONE',  ( -15.80617190586745835, -15.72974639402198527, 41.87390960531435979 ) ) ;
#198990 = CARTESIAN_POINT ( 'NONE',  ( -19.03943276465977164, 0.05219959533909376836, 36.24890960531436690 ) ) ;
#198992 = CARTESIAN_POINT ( 'NONE',  ( 0.05219959533907565091, 21.53943276465977519, 64.99890960531435269 ) ) ;
#198993 = CARTESIAN_POINT ( 'NONE',  ( 16.52544592524342804, -4.483927247898539470, 108.5405762719810241 ) ) ;
#198995 = CARTESIAN_POINT ( 'NONE',  ( 0.05219959533909260263, 19.03943276465977164, 44.99890960531435979 ) ) ;
#198994 = CARTESIAN_POINT ( 'NONE',  ( -12.14591786802326823, 12.06949235617739902, 58.12609039468568994 ) ) ;
#198996 = CARTESIAN_POINT ( 'NONE',  ( 15.72974639402176855, 15.80617190586768217, 41.87609039468568284 ) ) ;
#198997 = CARTESIAN_POINT ( 'NONE',  ( -12.14591786802309592, -12.06949235617757132, 96.87390960531436690 ) ) ;
#198998 = CARTESIAN_POINT ( 'NONE',  ( 17.50000000000000355, 5.500000000000011546, 78.78230962303567253 ) ) ;
#198999 = CARTESIAN_POINT ( 'NONE',  ( 3.556970738554034288E-15, -38.81732327939057114, -10.62499999726880873 ) ) ;
#199000 = CARTESIAN_POINT ( 'NONE',  ( 15.72974639402199770, -15.80617190586745480, 28.12390960531435979 ) ) ;
#199001 = CARTESIAN_POINT ( 'NONE',  ( 0.000000000000000000, 0.000000000000000000, -64.92279855667830191 ) ) ;
#199002 = CARTESIAN_POINT ( 'NONE',  ( -17.49999999999999645, 5.499999999999992895, 43.71769037696436300 ) ) ;
#199004 = CARTESIAN_POINT ( 'NONE',  ( 4.379528057220339221, -16.55341960407611168, 42.70724293864770260 ) ) ;
#199003 = CARTESIAN_POINT ( 'NONE',  ( 16.55341960407618274, -4.379528057220086978, 46.04275706135234714 ) ) ;
#199005 = CARTESIAN_POINT ( 'NONE',  ( -15.72974639402197994, 15.80617190586746368, 70.62390960531436690 ) ) ;
#199006 = CARTESIAN_POINT ( 'NONE',  ( -18.62759615963270932, 10.81492255796079327, 55.83224293864770260 ) ) ;
#199007 = DIRECTION ( 'NONE',  ( 1.000000000000000000, 0.000000000000000000, 0.000000000000000000 ) ) ;
#199009 = CARTESIAN_POINT ( 'NONE',  ( 13.97604488694527802, 13.89961937509977652, 104.3739096053143385 ) ) ;
#199008 = CARTESIAN_POINT ( 'NONE',  ( -9.474510206698964154, 16.51473224551069663, 35.41557627198102409 ) ) ;
#199010 = CARTESIAN_POINT ( 'NONE',  ( -13.89961937509977652, 13.97604488694528158, 45.62390960531433848 ) ) ;
#199011 = CARTESIAN_POINT ( 'NONE',  ( -12.06949235617756955, 12.14591786802309770, 115.6239096053143669 ) ) ;
#199012 = CARTESIAN_POINT ( 'NONE',  ( -19.03943276465977164, 0.05219959533909376836, 116.2489096053143669 ) ) ;
#199013 = ORIENTED_EDGE ( 'NONE', *, *, #125179, .F. ) ;
#199014 = CARTESIAN_POINT ( 'NONE',  ( 0.05219959533934541429, -16.53943276465976808, 75.00109039468568994 ) ) ;
#199015 = CARTESIAN_POINT ( 'NONE',  ( 15.80617190586746368, 15.72974639402197994, 99.37390960531436690 ) ) ;
#199016 = CARTESIAN_POINT ( 'NONE',  ( -19.03943276465977164, 0.05219959533909376836, 61.24890960531436690 ) ) ;
#199017 = CARTESIAN_POINT ( 'NONE',  ( 15.80617190586769283, -15.72974639402175789, 40.62609039468567573 ) ) ;
#199018 = CARTESIAN_POINT ( 'NONE',  ( 0.05219959533909260263, 19.03943276465977164, 84.99890960531436690 ) ) ;
#199019 = DIRECTION ( 'NONE',  ( -1.000000000000000000, 0.000000000000000000, 0.000000000000000000 ) ) ;
#199020 = ORIENTED_EDGE ( 'NONE', *, *, #104192, .F. ) ;
#199021 = CARTESIAN_POINT ( 'NONE',  ( -15.72974639402176322, -15.80617190586768395, 34.37609039468568284 ) ) ;
#199023 = CARTESIAN_POINT ( 'NONE',  ( -13.97604488694547697, 13.89961937509957934, 83.12609039468564731 ) ) ;
#199022 = CARTESIAN_POINT ( 'NONE',  ( -16.46253265017160317, 9.564922557960807481, 105.8322429386476955 ) ) ;
#199024 = CARTESIAN_POINT ( 'NONE',  ( 13.97604488694548053, -13.89961937509957401, 40.62609039468564731 ) ) ;
#199025 = CARTESIAN_POINT ( 'NONE',  ( -18.67979575497178146, -10.72451020669898902, 96.66557627198102409 ) ) ;
#199026 = CARTESIAN_POINT ( 'NONE',  ( -13.97604488694547697, 13.89961937509957934, 28.12609039468565797 ) ) ;
#199027 = CARTESIAN_POINT ( 'NONE',  ( 9.474510206698729675, 16.51473224551082808, 32.08442372801900433 ) ) ;
#199028 = CARTESIAN_POINT ( 'NONE',  ( -8.224510206698735004, -14.34966873604973081, 89.58442372801901854 ) ) ;
#199029 = CARTESIAN_POINT ( 'NONE',  ( 23.27014359241642438, -11.64952062020058499, 165.7333947824558891 ) ) ;
#199030 = CARTESIAN_POINT ( 'NONE',  ( 5.153800228976335163, 19.02544592524342804, 64.79057627198100988 ) ) ;
#199031 = CIRCLE ( 'NONE', #160334, 8.000000000000000000 ) ;
#199032 = CARTESIAN_POINT ( 'NONE',  ( -21.53943276465977519, -0.05219959533937600094, 68.75109039468568994 ) ) ;
#199033 = CARTESIAN_POINT ( 'NONE',  ( 21.52544592524334988, 5.823673210054432836, 86.45942372801901854 ) ) ;
#199034 = CARTESIAN_POINT ( 'NONE',  ( 16.46253265017160672, -9.564922557960803928, 78.33224293864769550 ) ) ;
#199035 = CARTESIAN_POINT ( 'NONE',  ( -0.05219959533937732626, 21.53943276465977519, 62.50109039468568284 ) ) ;
#199036 = CARTESIAN_POINT ( 'NONE',  ( 16.51473224551083163, -9.474510206698727899, 95.83442372801900433 ) ) ;
#199037 = CARTESIAN_POINT ( 'NONE',  ( 16.51473224551069308, 9.474510206698969483, 54.16557627198103120 ) ) ;
#199038 = CARTESIAN_POINT ( 'NONE',  ( -19.03943276465977164, 0.05219959533909376836, 101.2489096053143669 ) ) ;
#199039 = CARTESIAN_POINT ( 'NONE',  ( 16.46253265017160672, -9.564922557960803928, 73.33224293864769550 ) ) ;
#199040 = CARTESIAN_POINT ( 'NONE',  ( -9.564922557960796823, -16.46253265017161027, 77.08224293864769550 ) ) ;
#199041 = CARTESIAN_POINT ( 'NONE',  ( -5.049401038298153566, 19.05341960407611168, 60.20724293864768129 ) ) ;
#199042 = CARTESIAN_POINT ( 'NONE',  ( -15.72974639402197994, 15.80617190586746368, 105.6239096053143669 ) ) ;
#199043 = CARTESIAN_POINT ( 'NONE',  ( 8.224510206698742110, 14.34966873604972548, 92.08442372801901854 ) ) ;
#199044 = CARTESIAN_POINT ( 'NONE',  ( 8.349412516403786455, -1.313804288003802112, -64.09731636040743297 ) ) ;
#199045 = CARTESIAN_POINT ( 'NONE',  ( 13.97604488694548053, -13.89961937509957401, 40.62609039468564731 ) ) ;
#199046 = CARTESIAN_POINT ( 'NONE',  ( -19.02544592524342804, 5.153800228976336051, 81.04057627198103830 ) ) ;
#199047 = CARTESIAN_POINT ( 'NONE',  ( -12.14591786802309592, -12.06949235617757132, 66.87390960531436690 ) ) ;
#199048 = CARTESIAN_POINT ( 'NONE',  ( -4.379528057220328563, 16.55341960407611168, 100.2072429386476955 ) ) ;
#199049 = CARTESIAN_POINT ( 'NONE',  ( -16.46253265017160317, 9.564922557960807481, 115.8322429386477097 ) ) ;
#199050 = CARTESIAN_POINT ( 'NONE',  ( -5.153800228976328057, -19.02544592524343514, 102.2905762719810383 ) ) ;
#199051 = CARTESIAN_POINT ( 'NONE',  ( -4.814824860968089633E-30, -78.67194367458512261, -15.00000000000000000 ) ) ;
#199052 = CARTESIAN_POINT ( 'NONE',  ( -9.474510206698720793, -16.51473224551083518, 24.58442372801900078 ) ) ;
#199053 = CARTESIAN_POINT ( 'NONE',  ( 4.379528057220092307, 16.55341960407617563, 92.29275706135236135 ) ) ;
#199055 = ADVANCED_FACE ( 'NONE', ( #20146 ), #172852, .T. ) ;
#199054 = CARTESIAN_POINT ( 'NONE',  ( -19.02544592524342804, 5.153800228976336051, 71.04057627198099567 ) ) ;
#199056 = CARTESIAN_POINT ( 'NONE',  ( 18.62759615963255655, 10.81492255796105972, 51.66775706135234714 ) ) ;
#199057 = CARTESIAN_POINT ( 'NONE',  ( 21.53943276465977519, -0.05219959533907433946, 28.74890960531435624 ) ) ;
#199058 = CARTESIAN_POINT ( 'NONE',  ( -21.52544592524334988, -5.823673210054445271, 23.95942372801901143 ) ) ;
#199059 = CARTESIAN_POINT ( 'NONE',  ( -21.52544592524343514, 5.823673210054127303, 76.04057627198102409 ) ) ;
#199060 = CARTESIAN_POINT ( 'NONE',  ( 4.483927247898545687, 16.52544592524342804, 89.79057627198103830 ) ) ;
#199061 = CARTESIAN_POINT ( 'NONE',  ( 13.89961937509957401, 13.97604488694547697, 51.87609039468566863 ) ) ;
#199062 = CARTESIAN_POINT ( 'NONE',  ( 5.049401038298161559, -19.05341960407611168, 37.70724293864768839 ) ) ;
#199063 = CARTESIAN_POINT ( 'NONE',  ( -9.564922557960796823, -16.46253265017161027, 82.08224293864768129 ) ) ;
#199064 = CARTESIAN_POINT ( 'NONE',  ( -0.05219959533909027116, -19.03943276465977164, 77.49890960531435269 ) ) ;
#199065 = CARTESIAN_POINT ( 'NONE',  ( -22.44159573604009950, -16.30477369853688430, 139.5750000027311728 ) ) ;
#199066 = CARTESIAN_POINT ( 'NONE',  ( 4.379528057220339221, -16.55341960407611168, 97.70724293864772392 ) ) ;
#199067 = VERTEX_POINT ( 'NONE', #99972 ) ;
#199068 = CARTESIAN_POINT ( 'NONE',  ( 16.52544592524342804, -4.483927247898539470, 23.54057627198102765 ) ) ;
#199069 = CARTESIAN_POINT ( 'NONE',  ( 4.379528057220092307, 16.55341960407617563, 22.29275706135235069 ) ) ;
#199070 = CARTESIAN_POINT ( 'NONE',  ( -21.55341960407619339, 5.719274019375674811, 88.54275706135236135 ) ) ;
#199071 = CARTESIAN_POINT ( 'NONE',  ( 5.153800228976335163, 19.02544592524342804, 104.7905762719809957 ) ) ;
#199072 = CARTESIAN_POINT ( 'NONE',  ( -0.05219959533907301413, -21.53943276465977519, 112.4989096053143669 ) ) ;
#199073 = CARTESIAN_POINT ( 'NONE',  ( 5.049401038298161559, -19.05341960407611168, 37.70724293864768839 ) ) ;
#199074 = AXIS2_PLACEMENT_3D ( 'NONE', #79862, #34358, #173877 ) ;
#199075 = CARTESIAN_POINT ( 'NONE',  ( -16.52544592524335698, -4.483927247898792601, 48.95942372801902565 ) ) ;
#199076 = CARTESIAN_POINT ( 'NONE',  ( -9.564922557961040184, 16.46253265017147172, 112.9177570613523329 ) ) ;
#199077 = CARTESIAN_POINT ( 'NONE',  ( -16.46253265017160317, 9.564922557960807481, 30.83224293864769550 ) ) ;
#199078 = CARTESIAN_POINT ( 'NONE',  ( -16.52544592524342804, 4.483927247898546575, 96.04057627198102409 ) ) ;
#199079 = CARTESIAN_POINT ( 'NONE',  ( -0.05219959533907301413, -21.53943276465977519, 107.4989096053143669 ) ) ;
#199080 = CARTESIAN_POINT ( 'NONE',  ( -19.05341960407617563, 5.049401038297882671, 73.54275706135233293 ) ) ;
#199081 = FACE_OUTER_BOUND ( 'NONE', #26835, .T. ) ;
#199082 = CARTESIAN_POINT ( 'NONE',  ( -5.719274019375978568, 21.55341960407610458, 115.2072429386476955 ) ) ;
#199083 = CARTESIAN_POINT ( 'NONE',  ( -11.74149087413295511, 36.13659316521247433, -2.402157773949822772 ) ) ;
#199084 = CARTESIAN_POINT ( 'NONE',  ( -9.474510206698964154, 16.51473224551069663, 85.41557627198102409 ) ) ;
#199085 = CARTESIAN_POINT ( 'NONE',  ( 8.898068258721473001, -27.38543819252872069, 142.5843446569000150 ) ) ;
#199086 = CARTESIAN_POINT ( 'NONE',  ( -16.46253265017160317, 9.564922557960807481, 90.83224293864769550 ) ) ;
#199088 = CARTESIAN_POINT ( 'NONE',  ( 4.379528057220339221, -16.55341960407611168, 72.70724293864769550 ) ) ;
#199087 = CARTESIAN_POINT ( 'NONE',  ( -18.67979575497193778, 10.72451020669871902, 33.33442372801900433 ) ) ;
#199089 = CARTESIAN_POINT ( 'NONE',  ( -16.46253265017160317, 9.564922557960807481, 85.83224293864769550 ) ) ;
#199092 = CARTESIAN_POINT ( 'NONE',  ( -9.474510206698720793, -16.51473224551083518, 59.58442372801900433 ) ) ;
#199091 =( BOUNDED_CURVE ( )  B_SPLINE_CURVE ( 2, ( #171730, #91871, #48393, #153564, #109053, #183917, #49377, #138397, #110050, #2869, #154563 ),
 .UNSPECIFIED., .F., .F. ) 
 B_SPLINE_CURVE_WITH_KNOTS ( ( 3, 2, 2, 2, 2, 3 ),
 ( 0.6000000000000005329, 0.6200000000000005507, 0.6400000000000005684, 0.6600000000000006972, 0.6800000000000007150, 0.7000000000000006217 ),
 .UNSPECIFIED. ) 
 CURVE ( )  GEOMETRIC_REPRESENTATION_ITEM ( )  RATIONAL_B_SPLINE_CURVE ( ( 0.9999999999999986677, 0.9510565162951548634, 1.000000000000000000, 0.9510565162951535312, 1.000000000000000000, 0.9510565162951535312, 1.000000000000000000, 0.9510565162951535312, 1.000000000000000000, 0.9510565162951518658, 1.000000000000001554 ) ) 
 REPRESENTATION_ITEM ( '' )  );
#199090 = CARTESIAN_POINT ( 'NONE',  ( 12.14591786802327356, -12.06949235617739191, 50.62609039468568994 ) ) ;
#199093 = CARTESIAN_POINT ( 'NONE',  ( -15.80617190586768217, 15.72974639402176855, 63.12609039468568994 ) ) ;
#199094 = CARTESIAN_POINT ( 'NONE',  ( -14.34966873604972548, 8.224510206698743886, 33.33442372801900433 ) ) ;
#199095 = CARTESIAN_POINT ( 'NONE',  ( 16.46253265017160672, -9.564922557960803928, 68.33224293864770971 ) ) ;
#199096 = CARTESIAN_POINT ( 'NONE',  ( 9.474510206698729675, 16.51473224551082808, 92.08442372801900433 ) ) ;
#199097 = CARTESIAN_POINT ( 'NONE',  ( -8.314922557961024197, 14.29746914071037800, 52.91775706135235424 ) ) ;
#199098 = CARTESIAN_POINT ( 'NONE',  ( -18.67979575497193778, 10.72451020669871902, 98.33442372801901854 ) ) ;
#199099 = CARTESIAN_POINT ( 'NONE',  ( 9.564922557961047289, -16.46253265017146816, 80.41775706135234714 ) ) ;
#199100 = CARTESIAN_POINT ( 'NONE',  ( 9.474510206698971260, -16.51473224551069308, 47.91557627198102409 ) ) ;
#199101 = CARTESIAN_POINT ( 'NONE',  ( 5.719274019375991003, -21.55341960407610458, 72.70724293864769550 ) ) ;
#199103 = CARTESIAN_POINT ( 'NONE',  ( 19.03943276465977164, 0.05219959533936151252, 71.25109039468566152 ) ) ;
#199102 = CARTESIAN_POINT ( 'NONE',  ( -4.379528057220328563, 16.55341960407611168, 70.20724293864769550 ) ) ;
#199104 = DIRECTION ( 'NONE',  ( 0.000000000000000000, 0.000000000000000000, 1.000000000000000000 ) ) ;
#199105 = CARTESIAN_POINT ( 'NONE',  ( 19.02544592524334988, 5.153800228976608722, 41.45942372801900433 ) ) ;
#199106 = CARTESIAN_POINT ( 'NONE',  ( 16.53943276465976808, -0.05219959533910856209, 23.74890960531435269 ) ) ;
#199107 = CARTESIAN_POINT ( 'NONE',  ( -0.05219959533910754901, -16.53943276465976808, 72.49890960531435269 ) ) ;
#199109 = CARTESIAN_POINT ( 'NONE',  ( -17.14385361876520619, 23.59649016807275856, 144.5750000027312012 ) ) ;
#199108 = CARTESIAN_POINT ( 'NONE',  ( 21.52544592524334988, 5.823673210054432836, 106.4594237280190328 ) ) ;
#199110 = CARTESIAN_POINT ( 'NONE',  ( -21.55341960407610458, -5.719274019375992779, 111.4572429386476813 ) ) ;
#199111 = CARTESIAN_POINT ( 'NONE',  ( -9.564922557960796823, -16.46253265017161027, 67.08224293864769550 ) ) ;
#199112 = CARTESIAN_POINT ( 'NONE',  ( 21.53943276465977519, 0.05219959533937863772, 86.25109039468568994 ) ) ;
#199113 = CARTESIAN_POINT ( 'NONE',  ( -5.153800228976328057, -19.02544592524343514, 67.29057627198102409 ) ) ;
#199114 = ORIENTED_EDGE ( 'NONE', *, *, #166361, .F. ) ;
#199115 = CARTESIAN_POINT ( 'NONE',  ( -16.51473224551069308, -9.474510206698971260, 26.66557627198103120 ) ) ;
#199116 = CARTESIAN_POINT ( 'NONE',  ( -5.719274019375978568, 21.55341960407610458, 30.20724293864769550 ) ) ;
#199117 = CARTESIAN_POINT ( 'NONE',  ( 12.14591786802309770, 12.06949235617756955, 69.37390960531436690 ) ) ;
#199118 = CARTESIAN_POINT ( 'NONE',  ( -16.51473224551069308, -9.474510206698971260, 46.66557627198102409 ) ) ;
#199119 = CARTESIAN_POINT ( 'NONE',  ( -14.29746914071049879, 8.314922557960819915, 90.83224293864769550 ) ) ;
#199120 = CARTESIAN_POINT ( 'NONE',  ( -10.72451020669898014, 18.67979575497178502, 105.4155762719810383 ) ) ;
#199121 = CARTESIAN_POINT ( 'NONE',  ( 10.72451020669871369, 18.67979575497193778, 52.08442372801901854 ) ) ;
#199122 = CARTESIAN_POINT ( 'NONE',  ( -5.049401038298153566, 19.05341960407611168, 30.20724293864768839 ) ) ;
#199123 = EDGE_CURVE ( 'NONE', #59792, #47952, #32647, .T. ) ;
#199124 = CARTESIAN_POINT ( 'NONE',  ( 4.483927247898790824, -16.52544592524335698, 55.20942372801902565 ) ) ;
#199125 = CARTESIAN_POINT ( 'NONE',  ( 21.55341960407610458, 5.719274019375980345, 98.95724293864770971 ) ) ;
#199126 = CARTESIAN_POINT ( 'NONE',  ( 21.55341960407610458, 5.719274019375980345, 93.95724293864770971 ) ) ;
#199128 = CARTESIAN_POINT ( 'NONE',  ( -5.049401038298153566, 19.05341960407611168, 55.20724293864769550 ) ) ;
#199127 = CARTESIAN_POINT ( 'NONE',  ( 19.03943276465977164, 0.05219959533936151252, 26.25109039468566507 ) ) ;
#199129 = CARTESIAN_POINT ( 'NONE',  ( 13.89961937509977652, -13.97604488694527269, 113.1239096053143527 ) ) ;
#199130 = CARTESIAN_POINT ( 'NONE',  ( 18.62759615963255655, 10.81492255796105972, 51.66775706135234714 ) ) ;
#199131 = CARTESIAN_POINT ( 'NONE',  ( -5.719274019375978568, 21.55341960407610458, 45.20724293864769550 ) ) ;
#199132 = CARTESIAN_POINT ( 'NONE',  ( 12.14591786802327356, -12.06949235617739191, 110.6260903946857042 ) ) ;
#199134 = CARTESIAN_POINT ( 'NONE',  ( -21.52544592524334988, -5.823673210054445271, 93.95942372801903275 ) ) ;
#199133 = CARTESIAN_POINT ( 'NONE',  ( -5.719274019375665041, -21.55341960407619695, 69.79275706135234714 ) ) ;
#199135 = CARTESIAN_POINT ( 'NONE',  ( 19.03943276465977164, 0.05219959533936151252, 51.25109039468567573 ) ) ;
#199136 = CARTESIAN_POINT ( 'NONE',  ( -0.05219959533934338120, 16.53943276465976808, 107.5010903946856899 ) ) ;
#199137 = CARTESIAN_POINT ( 'NONE',  ( 21.52544592524334988, 5.823673210054432836, 61.45942372801901854 ) ) ;
#199138 = CARTESIAN_POINT ( 'NONE',  ( -19.05341960407611168, -5.049401038298163336, 46.45724293864768129 ) ) ;
#199139 = CARTESIAN_POINT ( 'NONE',  ( 16.51473224551083163, -9.474510206698727899, 25.83442372801900078 ) ) ;
#199140 = CARTESIAN_POINT ( 'NONE',  ( -0.05219959533907301413, -21.53943276465977519, 22.49890960531436335 ) ) ;
#199141 = EDGE_CURVE ( 'NONE', #155416, #116956, #52924, .T. ) ;
#199142 = CARTESIAN_POINT ( 'NONE',  ( -15.72974639402176322, -15.80617190586768395, 19.37609039468568639 ) ) ;
#199143 = CARTESIAN_POINT ( 'NONE',  ( -10.81492255796078084, -18.62759615963271287, 72.08224293864769550 ) ) ;
#199144 = CARTESIAN_POINT ( 'NONE',  ( -12.14591786802326823, 12.06949235617739902, 43.12609039468568284 ) ) ;
#199146 = CARTESIAN_POINT ( 'NONE',  ( 18.67979575497178502, 10.72451020669898547, 79.16557627198103830 ) ) ;
#199145 = CARTESIAN_POINT ( 'NONE',  ( -6.719756334737514436, 4.704316316549534527, -62.10423353180174644 ) ) ;
#199148 = CARTESIAN_POINT ( 'NONE',  ( -4.483927247898539470, -16.52544592524342804, 82.29057627198103830 ) ) ;
#199147 = CARTESIAN_POINT ( 'NONE',  ( 8.224510206698742110, 14.34966873604972548, 67.08442372801901854 ) ) ;
#199149 = CARTESIAN_POINT ( 'NONE',  ( 0.5056555311937657171, 28.98228079209996366, -49.57211623589792282 ) ) ;
#199150 = CARTESIAN_POINT ( 'NONE',  ( 9.474510206698729675, 16.51473224551082808, 102.0844237280190043 ) ) ;
#199151 = CARTESIAN_POINT ( 'NONE',  ( 0.05219959533907565091, 21.53943276465977519, 34.99890960531435979 ) ) ;
#199152 = CYLINDRICAL_SURFACE ( 'NONE', #18750, 5.000000000000000000 ) ;
#199153 = CARTESIAN_POINT ( 'NONE',  ( -14.29746914071037622, -8.314922557961029526, 34.16775706135234714 ) ) ;
#199154 = CARTESIAN_POINT ( 'NONE',  ( 5.823673210054444382, -21.52544592524334988, 20.20942372801900788 ) ) ;
#199155 = CARTESIAN_POINT ( 'NONE',  ( 18.62759615963271287, -10.81492255796078972, 38.33224293864768839 ) ) ;
#199156 = CARTESIAN_POINT ( 'NONE',  ( -4.379528057220086978, -16.55341960407618274, 69.79275706135234714 ) ) ;
#199157 = CARTESIAN_POINT ( 'NONE',  ( 9.564922557960805705, 16.46253265017160317, 84.58224293864769550 ) ) ;
#199159 = CARTESIAN_POINT ( 'NONE',  ( -19.05341960407611168, -5.049401038298163336, 26.45724293864769550 ) ) ;
#199158 = CARTESIAN_POINT ( 'NONE',  ( 10.72451020669871369, 18.67979575497193778, 42.08442372801901854 ) ) ;
#199160 = CARTESIAN_POINT ( 'NONE',  ( 15.72974639402199770, -15.80617190586745480, 28.12390960531435979 ) ) ;
#199161 = ORIENTED_EDGE ( 'NONE', *, *, #164239, .F. ) ;
#199162 = CARTESIAN_POINT ( 'NONE',  ( 13.89961937509957401, 13.97604488694547697, 26.87609039468566507 ) ) ;
#199163 = CARTESIAN_POINT ( 'NONE',  ( 16.53943276465976808, 0.05219959533934440121, 51.25109039468568994 ) ) ;
#199164 = CARTESIAN_POINT ( 'NONE',  ( 19.03943276465977164, -0.05219959533909143690, 98.74890960531436690 ) ) ;
#199165 = CARTESIAN_POINT ( 'NONE',  ( -15.80617190586745835, -15.72974639402198527, 96.87390960531436690 ) ) ;
#199166 = CARTESIAN_POINT ( 'NONE',  ( -9.564922557960796823, -16.46253265017161027, 67.08224293864769550 ) ) ;
#199167 = CARTESIAN_POINT ( 'NONE',  ( -17.49999999999999289, 5.624438216177593652, 25.81670344914644488 ) ) ;
#199168 = CARTESIAN_POINT ( 'NONE',  ( -4.570733098192837459E-16, -74.04324336000735229, -22.99263613531268291 ) ) ;
#199169 = CARTESIAN_POINT ( 'NONE',  ( 4.483927247898545687, 16.52544592524342804, 79.79057627198102409 ) ) ;
#199170 = CARTESIAN_POINT ( 'NONE',  ( 21.55341960407610458, 5.719274019375980345, 33.95724293864769550 ) ) ;
#199171 = CARTESIAN_POINT ( 'NONE',  ( -17.50000000000000000, 5.499999999999992895, 33.71769037696435589 ) ) ;
#199172 = CARTESIAN_POINT ( 'NONE',  ( 12.14591786802327356, -12.06949235617739191, 65.62609039468568994 ) ) ;
#199173 = CARTESIAN_POINT ( 'NONE',  ( -15.80617190586768217, 15.72974639402176855, 23.12609039468567573 ) ) ;
#199174 = CARTESIAN_POINT ( 'NONE',  ( 9.474510206698729675, 16.51473224551082808, 72.08442372801900433 ) ) ;
#199175 = CARTESIAN_POINT ( 'NONE',  ( -13.97604488694527625, -13.89961937509977652, 36.87390960531436690 ) ) ;
#199176 = CARTESIAN_POINT ( 'NONE',  ( -18.62759615963270932, 10.81492255796079327, 65.83224293864769550 ) ) ;
#199177 = VECTOR ( 'NONE', #184104, 1000.000000000000000 ) ;
#199178 = CARTESIAN_POINT ( 'NONE',  ( -9.474510206698964154, 16.51473224551069663, 105.4155762719810383 ) ) ;
#199179 = CARTESIAN_POINT ( 'NONE',  ( 18.67979575497194134, -10.72451020669871369, 90.83442372801901854 ) ) ;
#199180 = CARTESIAN_POINT ( 'NONE',  ( 19.03943276465977164, -0.05219959533909143690, 68.74890960531436690 ) ) ;
#199181 = CARTESIAN_POINT ( 'NONE',  ( -14.34966873604972548, 8.224510206698743886, 53.33442372801901854 ) ) ;
#199182 = CARTESIAN_POINT ( 'NONE',  ( 9.564922557960805705, 16.46253265017160317, 59.58224293864769550 ) ) ;
#199183 = CARTESIAN_POINT ( 'NONE',  ( -21.53943276465977519, -0.05219959533937600094, 73.75109039468567573 ) ) ;
#199184 = CARTESIAN_POINT ( 'NONE',  ( -19.03943276465977164, -0.05219959533935918106, 43.75109039468566863 ) ) ;
#199185 = CARTESIAN_POINT ( 'NONE',  ( 9.474510206698729675, 16.51473224551082808, 52.08442372801900433 ) ) ;
#199186 = CARTESIAN_POINT ( 'NONE',  ( 18.62759615963255655, 10.81492255796105972, 51.66775706135234714 ) ) ;
#199187 = CIRCLE ( 'NONE', #189508, 28.90000000000004476 ) ;
#199188 = CARTESIAN_POINT ( 'NONE',  ( -18.87255363501903105, -5.499999999999950262, 46.32513748171830059 ) ) ;
#199189 = CARTESIAN_POINT ( 'NONE',  ( -9.474510206698720793, -16.51473224551083518, 49.58442372801899722 ) ) ;
#199190 = CARTESIAN_POINT ( 'NONE',  ( -19.02544592524342804, 5.153800228976336051, 101.0405762719810241 ) ) ;
#199191 = CARTESIAN_POINT ( 'NONE',  ( 19.03943276465977164, -0.05219959533909143690, 68.74890960531436690 ) ) ;
#199192 = CARTESIAN_POINT ( 'NONE',  ( -14.34966873604972548, 8.224510206698743886, 113.3344237280190328 ) ) ;
#199194 = CARTESIAN_POINT ( 'NONE',  ( -21.55341960407619339, 5.719274019375674811, 98.54275706135234714 ) ) ;
#199193 = CARTESIAN_POINT ( 'NONE',  ( 15.72974639402199770, -15.80617190586745480, 38.12390960531436690 ) ) ;
#199195 = CARTESIAN_POINT ( 'NONE',  ( -36.91746825000001309, 11.99521256947798342, -7.224999997268814589 ) ) ;
#199196 = CARTESIAN_POINT ( 'NONE',  ( 16.81555441253551564, 7.025013491695498935, 56.86314554665743515 ) ) ;
#199197 = CARTESIAN_POINT ( 'NONE',  ( -10.81492255796105439, 18.62759615963255655, 97.91775706135236135 ) ) ;
#199198 = DIRECTION ( 'NONE',  ( 0.000000000000000000, 0.000000000000000000, 1.000000000000000000 ) ) ;
#199199 = CARTESIAN_POINT ( 'NONE',  ( -5.153800228976328057, -19.02544592524343514, 27.29057627198103120 ) ) ;
#199200 = CARTESIAN_POINT ( 'NONE',  ( 16.46253265017160672, -9.564922557960803928, 108.3322429386476955 ) ) ;
#199201 = B_SPLINE_CURVE_WITH_KNOTS ( 'NONE', 3,
 ( #34637, #113451, #80138, #188334, #50809, #47839 ),
 .UNSPECIFIED., .F., .F.,
 ( 4, 2, 4 ),
 ( 0.003239945802372238247, 0.003620412082092087404, 0.004000878361811936561 ),
 .UNSPECIFIED. ) ;
#199202 = CARTESIAN_POINT ( 'NONE',  ( 34.16333257229420894, 4.138830072290155648, 91.36021987110629539 ) ) ;
#199203 = CARTESIAN_POINT ( 'NONE',  ( 16.53943276465976808, 0.05219959533934440121, 51.25109039468568994 ) ) ;
#199204 = CARTESIAN_POINT ( 'NONE',  ( 15.80617190586746368, 15.72974639402197994, 74.37390960531436690 ) ) ;
#199205 = CARTESIAN_POINT ( 'NONE',  ( -16.52544592524342804, 4.483927247898546575, 41.04057627198103120 ) ) ;
#199207 = CARTESIAN_POINT ( 'NONE',  ( -9.564922557960796823, -16.46253265017161027, 112.0822429386476955 ) ) ;
#199206 = CARTESIAN_POINT ( 'NONE',  ( 16.52544592524342804, -4.483927247898539470, 108.5405762719810241 ) ) ;
#199208 = CARTESIAN_POINT ( 'NONE',  ( 16.51473224551083163, -9.474510206698727899, 35.83442372801899722 ) ) ;
#199209 = CARTESIAN_POINT ( 'NONE',  ( -9.474510206698964154, 16.51473224551069663, 25.41557627198103120 ) ) ;
#199210 = CARTESIAN_POINT ( 'NONE',  ( -5.823673210054431948, 21.52544592524334988, 67.70942372801901854 ) ) ;
#199211 = CARTESIAN_POINT ( 'NONE',  ( -18.22780087662122384, -5.500000000000025757, 96.48459894673894155 ) ) ;
#199212 = CARTESIAN_POINT ( 'NONE',  ( 12.14591786802309770, 12.06949235617756955, 29.37390960531435269 ) ) ;
#199213 = CARTESIAN_POINT ( 'NONE',  ( 3.556970738554034288E-15, -38.81732327939057114, -6.624999997268814056 ) ) ;
#199214 = CARTESIAN_POINT ( 'NONE',  ( 10.72451020669898902, -18.67979575497178502, 27.91557627198103830 ) ) ;
#199215 = CARTESIAN_POINT ( 'NONE',  ( 16.52544592524342804, -4.483927247898539470, 83.54057627198102409 ) ) ;
#199216 = CARTESIAN_POINT ( 'NONE',  ( -6.206754193738958314, -6.630370177702000767, -63.95556908907604310 ) ) ;
#199217 = AXIS2_PLACEMENT_3D ( 'NONE', #101025, #23209, #69702 ) ;
#199218 = CARTESIAN_POINT ( 'NONE',  ( 19.03943276465977164, -0.05219959533909143690, 73.74890960531435269 ) ) ;
#199219 = CARTESIAN_POINT ( 'NONE',  ( 12.14591786802309770, 12.06949235617756955, 69.37390960531436690 ) ) ;
#199220 = CARTESIAN_POINT ( 'NONE',  ( 16.46253265017146816, 9.564922557961045513, 91.66775706135234714 ) ) ;
#199221 = CARTESIAN_POINT ( 'NONE',  ( -5.823673210054116645, -21.52544592524344225, 47.29057627198103120 ) ) ;
#199222 = EDGE_LOOP ( 'NONE', ( #132749, #162849, #128762, #25888 ) ) ;
#199223 = CARTESIAN_POINT ( 'NONE',  ( -4.379528057220328563, 16.55341960407611168, 115.2072429386476955 ) ) ;
#199224 = EDGE_CURVE ( 'NONE', #154217, #178458, #63849, .T. ) ;
#199226 = CARTESIAN_POINT ( 'NONE',  ( -18.67979575497178146, -10.72451020669898902, 76.66557627198103830 ) ) ;
#199225 = CARTESIAN_POINT ( 'NONE',  ( 16.46253265017160672, -9.564922557960803928, 68.33224293864770971 ) ) ;
#199228 = CARTESIAN_POINT ( 'NONE',  ( -13.89961937509977652, 13.97604488694528158, 90.62390960531432427 ) ) ;
#199227 = CARTESIAN_POINT ( 'NONE',  ( -8.314922557961024197, 14.29746914071037800, 102.9177570613523756 ) ) ;
#199229 = CARTESIAN_POINT ( 'NONE',  ( -9.474510206698720793, -16.51473224551083518, 64.58442372801900433 ) ) ;
#199230 = CARTESIAN_POINT ( 'NONE',  ( 21.52544592524334988, 5.823673210054432836, 86.45942372801901854 ) ) ;
#199231 = CARTESIAN_POINT ( 'NONE',  ( -5.719274019375978568, 21.55341960407610458, 60.20724293864768839 ) ) ;
#199232 = CARTESIAN_POINT ( 'NONE',  ( -21.52544592524343514, 5.823673210054127303, 26.04057627198103475 ) ) ;
#199233 = CARTESIAN_POINT ( 'NONE',  ( -5.049401038298153566, 19.05341960407611168, 40.20724293864768839 ) ) ;
#199234 = CARTESIAN_POINT ( 'NONE',  ( 12.14591786802327356, -12.06949235617739191, 95.62609039468568994 ) ) ;
#199235 = CARTESIAN_POINT ( 'NONE',  ( 13.89961937509977652, -13.97604488694527269, 58.12390960531436690 ) ) ;
#199236 = CARTESIAN_POINT ( 'NONE',  ( -14.29746914071037622, -8.314922557961029526, 19.16775706135234714 ) ) ;
#199237 = CARTESIAN_POINT ( 'NONE',  ( 16.21995358207306026, 7.366697692864119240, 52.56448998487845614 ) ) ;
#199238 = CARTESIAN_POINT ( 'NONE',  ( -5.049401038297874678, -19.05341960407617918, 19.79275706135233293 ) ) ;
#199239 = CARTESIAN_POINT ( 'NONE',  ( 16.52544592524342804, -4.483927247898539470, 68.54057627198103830 ) ) ;
#199240 = CARTESIAN_POINT ( 'NONE',  ( -18.67979575497178146, -10.72451020669898902, 106.6655762719810383 ) ) ;
#199241 = CARTESIAN_POINT ( 'NONE',  ( -5.719274019375978568, 21.55341960407610458, 100.2072429386476955 ) ) ;
#199242 = CARTESIAN_POINT ( 'NONE',  ( -6.795352961392306490, 4.884805615686619973, -64.11485260110077888 ) ) ;
#199243 = CARTESIAN_POINT ( 'NONE',  ( 15.72974639402199770, -15.80617190586745480, 48.12390960531436690 ) ) ;
#199244 = CARTESIAN_POINT ( 'NONE',  ( 0.05219959533934541429, -16.53943276465976808, 85.00109039468568994 ) ) ;
#199245 = CARTESIAN_POINT ( 'NONE',  ( 14.34966873604960469, 8.224510206698951720, 99.16557627198100988 ) ) ;
#199246 = CARTESIAN_POINT ( 'NONE',  ( -13.89961937509977652, 13.97604488694528158, 60.62390960531436690 ) ) ;
#199247 = PRESENTATION_STYLE_ASSIGNMENT (( #186075 ) ) ;
#199248 = CARTESIAN_POINT ( 'NONE',  ( -26.36902008128208408, -29.90370362120039616, -17.00062383490520901 ) ) ;
#199249 = CARTESIAN_POINT ( 'NONE',  ( -16.55341960407617563, 4.379528057220093196, 113.5427570613523756 ) ) ;
#199250 = CARTESIAN_POINT ( 'NONE',  ( 21.53943276465977519, 0.05219959533937863772, 41.25109039468568284 ) ) ;
#199251 = CARTESIAN_POINT ( 'NONE',  ( 19.02544592524343514, -5.153800228976328945, 93.54057627198102409 ) ) ;
#199252 = CARTESIAN_POINT ( 'NONE',  ( -15.80617190586768217, 15.72974639402176855, 83.12609039468568994 ) ) ;
#199253 = CARTESIAN_POINT ( 'NONE',  ( -9.564922557960796823, -16.46253265017161027, 27.08224293864769550 ) ) ;
#199254 = CARTESIAN_POINT ( 'NONE',  ( -16.51473224551069308, -9.474510206698971260, 31.66557627198102054 ) ) ;
#199255 = VERTEX_POINT ( 'NONE', #104978 ) ;
#199256 = CARTESIAN_POINT ( 'NONE',  ( 5.823673210054444382, -21.52544592524334988, 70.20942372801904696 ) ) ;
#199257 = CARTESIAN_POINT ( 'NONE',  ( 5.153800228976335163, 19.02544592524342804, 54.79057627198103120 ) ) ;
#199258 = CARTESIAN_POINT ( 'NONE',  ( -5.049401038298153566, 19.05341960407611168, 100.2072429386476955 ) ) ;
#199259 = CARTESIAN_POINT ( 'NONE',  ( 19.03943276465977164, 0.05219959533936151252, 86.25109039468567573 ) ) ;
#199260 = CARTESIAN_POINT ( 'NONE',  ( -10.81492255796105439, 18.62759615963255655, 42.91775706135235424 ) ) ;
#199261 = CARTESIAN_POINT ( 'NONE',  ( 8.314922557961029526, -14.29746914071037800, 20.41775706135234714 ) ) ;
#199262 = CARTESIAN_POINT ( 'NONE',  ( 19.03943276465977164, 0.05219959533936151252, 66.25109039468567573 ) ) ;
#199263 = CARTESIAN_POINT ( 'NONE',  ( -5.049401038298153566, 19.05341960407611168, 35.20724293864768839 ) ) ;
#199264 = CARTESIAN_POINT ( 'NONE',  ( -5.049401038297874678, -19.05341960407617918, 84.79275706135233293 ) ) ;
#199265 = CARTESIAN_POINT ( 'NONE',  ( 16.52544592524335698, 4.483927247898782831, 101.4594237280190185 ) ) ;
#199266 = CARTESIAN_POINT ( 'NONE',  ( -19.02544592524334988, -5.153800228976617603, 73.95942372801900433 ) ) ;
#199267 = CARTESIAN_POINT ( 'NONE',  ( 8.224510206698953496, -14.34966873604960469, 32.91557627198102409 ) ) ;
#199268 = CARTESIAN_POINT ( 'NONE',  ( -13.89961937509957401, -13.97604488694547875, 69.37609039468564731 ) ) ;
#199269 = CARTESIAN_POINT ( 'NONE',  ( 21.53943276465977519, 0.05219959533937863772, 106.2510903946856757 ) ) ;
#199270 = CARTESIAN_POINT ( 'NONE',  ( -9.474510206698720793, -16.51473224551083518, 29.58442372801900433 ) ) ;
#199271 = CARTESIAN_POINT ( 'NONE',  ( -16.51473224551069308, -9.474510206698971260, 26.66557627198103120 ) ) ;
#199272 = CARTESIAN_POINT ( 'NONE',  ( -16.31925111598458145, -7.325300261831487525, 64.83575461032752685 ) ) ;
#199273 = CARTESIAN_POINT ( 'NONE',  ( 16.53943276465976808, 0.05219959533934440121, 46.25109039468567573 ) ) ;
#199274 = DIRECTION ( 'NONE',  ( -1.000000000000000000, 0.000000000000000000, 0.000000000000000000 ) ) ;
#199275 = CARTESIAN_POINT ( 'NONE',  ( 27.73933785331498925, -9.013057229001033122, 143.7750000027311614 ) ) ;
#199276 = B_SPLINE_CURVE_WITH_KNOTS ( 'NONE', 3,
 ( #171648, #139310, #188816, #64467, #154488, #156475, #124134, #92800, #187829, #79630, #15982, #32144, #789, #172641, #141298, #78627, #62461, #50299, #107969, #46314, #169656, #185833 ),
 .UNSPECIFIED., .F., .F.,
 ( 4, 2, 2, 2, 2, 2, 2, 2, 2, 2, 4 ),
 ( 2.787258305036405189E-07, 0.0003055402697144848283, 0.0006108018135984659511, 0.001221324901366425053, 0.001831847989134390009, 0.002137109533018372379, 0.002442371076902354748, 0.003052894164670319488, 0.003663417252438284661, 0.004273940340206248967, 0.004884463427974213706 ),
 .UNSPECIFIED. ) ;
#199277 = CARTESIAN_POINT ( 'NONE',  ( 19.05341960407611168, 5.049401038298154454, 98.95724293864766707 ) ) ;
#199278 = CARTESIAN_POINT ( 'NONE',  ( -17.49999999999999645, 5.624438216177557237, 100.8167034491464307 ) ) ;
#199279 = ORIENTED_EDGE ( 'NONE', *, *, #144774, .T. ) ;
#199280 = CARTESIAN_POINT ( 'NONE',  ( 0.05219959533936267826, -19.03943276465977164, 85.00109039468567573 ) ) ;
#199281 = CARTESIAN_POINT ( 'NONE',  ( 19.02544592524343514, -5.153800228976328945, 113.5405762719810241 ) ) ;
#199283 = CARTESIAN_POINT ( 'NONE',  ( 16.46253265017146816, 9.564922557961045513, 96.66775706135233293 ) ) ;
#199282 = CARTESIAN_POINT ( 'NONE',  ( 13.89961937509957401, 13.97604488694547697, 21.87609039468566152 ) ) ;
#199284 = CARTESIAN_POINT ( 'NONE',  ( -16.55341960407611168, -4.379528057220339221, 106.4572429386477097 ) ) ;
#199285 = CARTESIAN_POINT ( 'NONE',  ( 16.51473224551069308, 9.474510206698969483, 29.16557627198103475 ) ) ;
#199286 = CARTESIAN_POINT ( 'NONE',  ( -21.52544592524343514, 5.823673210054127303, 66.04057627198103830 ) ) ;
#199287 = CARTESIAN_POINT ( 'NONE',  ( 21.55341960407610458, 5.719274019375980345, 53.95724293864770260 ) ) ;
#199288 = CARTESIAN_POINT ( 'NONE',  ( 5.049401038298161559, -19.05341960407611168, 27.70724293864769550 ) ) ;
#199289 = CARTESIAN_POINT ( 'NONE',  ( 30.00000000000000000, -5.510910596163089556E-15, 45.00000000000000000 ) ) ;
#199290 = CARTESIAN_POINT ( 'NONE',  ( -13.97604488694547697, 13.89961937509957934, 73.12609039468568994 ) ) ;
#199291 = CARTESIAN_POINT ( 'NONE',  ( 14.34966873604960469, 8.224510206698951720, 34.16557627198102409 ) ) ;
#199293 = ADVANCED_FACE ( 'NONE', ( #164668 ), #27162, .F. ) ;
#199292 = CARTESIAN_POINT ( 'NONE',  ( 19.05341960407611168, 5.049401038298154454, 113.9572429386477097 ) ) ;
#199294 = CARTESIAN_POINT ( 'NONE',  ( -0.05219959533937732626, 21.53943276465977519, 97.50109039468567573 ) ) ;
#199295 = CARTESIAN_POINT ( 'NONE',  ( -21.55341960407610458, -5.719274019375992779, 66.45724293864768129 ) ) ;
#199296 = CARTESIAN_POINT ( 'NONE',  ( -21.55341960407619339, 5.719274019375674811, 53.54275706135234714 ) ) ;
#199297 = CARTESIAN_POINT ( 'NONE',  ( 5.719274019375673035, 21.55341960407619339, 52.29275706135236135 ) ) ;
#199298 = CARTESIAN_POINT ( 'NONE',  ( -0.05219959533909027116, -19.03943276465977164, 97.49890960531436690 ) ) ;
#199300 = CARTESIAN_POINT ( 'NONE',  ( -10.72451020669870658, -18.67979575497194134, 49.58442372801901143 ) ) ;
#199299 = CARTESIAN_POINT ( 'NONE',  ( -16.52544592524335698, -4.483927247898792601, 98.95942372801903275 ) ) ;
#199301 = CARTESIAN_POINT ( 'NONE',  ( 0.05219959533909260263, 19.03943276465977164, 24.99890960531435269 ) ) ;
#199302 = DIRECTION ( 'NONE',  ( -0.000000000000000000, -0.5000000000000002220, 0.8660254037844384856 ) ) ;
#199303 = CARTESIAN_POINT ( 'NONE',  ( 16.53943276465976808, -0.05219959533910856209, 68.74890960531435269 ) ) ;
#199304 = CARTESIAN_POINT ( 'NONE',  ( 0.05219959533910956823, 16.53943276465976808, 29.99890960531435979 ) ) ;
#199305 = CARTESIAN_POINT ( 'NONE',  ( 19.05341960407611168, 5.049401038298154454, 68.95724293864769550 ) ) ;
#199306 = CARTESIAN_POINT ( 'NONE',  ( -9.564922557960796823, -16.46253265017161027, 52.08224293864768839 ) ) ;
#199307 = CARTESIAN_POINT ( 'NONE',  ( -15.72974639402197994, 15.80617190586746368, 60.62390960531437401 ) ) ;
#199308 = CARTESIAN_POINT ( 'NONE',  ( -13.89961937509957401, -13.97604488694547875, 44.37609039468566863 ) ) ;
#199311 = CARTESIAN_POINT ( 'NONE',  ( -16.52544592524342804, 4.483927247898546575, 46.04057627198103830 ) ) ;
#199310 = CARTESIAN_POINT ( 'NONE',  ( 67.00000000000000000, -1.163414459189985801E-14, 95.00000000000000000 ) ) ;
#199309 = CIRCLE ( 'NONE', #112125, 2.000000000000000000 ) ;
#199312 = CARTESIAN_POINT ( 'NONE',  ( -0.05219959533907301413, -21.53943276465977519, 22.49890960531436335 ) ) ;
#199313 = ORIENTED_EDGE ( 'NONE', *, *, #156518, .F. ) ;
#199314 = DIRECTION ( 'NONE',  ( 0.000000000000000000, -1.000000000000000000, -0.000000000000000000 ) ) ;
#199315 = CARTESIAN_POINT ( 'NONE',  ( 14.34966873604972726, -8.224510206698740333, 65.83442372801900433 ) ) ;
#199316 = CARTESIAN_POINT ( 'NONE',  ( 5.049401038297881783, 19.05341960407617563, 72.29275706135234714 ) ) ;
#199317 = EDGE_CURVE ( 'NONE', #59885, #163091, #23708, .T. ) ;
#199318 = CARTESIAN_POINT ( 'NONE',  ( 4.483927247898545687, 16.52544592524342804, 44.79057627198103120 ) ) ;
#199319 = ORIENTED_EDGE ( 'NONE', *, *, #106368, .F. ) ;
#199320 = CARTESIAN_POINT ( 'NONE',  ( 4.647474457565486646E-15, -28.90000000000004476, -64.92279855667830191 ) ) ;
#199321 = CARTESIAN_POINT ( 'NONE',  ( -14.34966873604972548, 8.224510206698743886, 113.3344237280190328 ) ) ;
#199322 = CARTESIAN_POINT ( 'NONE',  ( -5.153800228976328057, -19.02544592524343514, 52.29057627198100988 ) ) ;
#199323 = CARTESIAN_POINT ( 'NONE',  ( 19.03943276465977164, -0.05219959533909143690, 73.74890960531435269 ) ) ;
#199324 = CARTESIAN_POINT ( 'NONE',  ( 19.03943276465977164, -0.05219959533909143690, 43.74890960531435979 ) ) ;
#199325 = CARTESIAN_POINT ( 'NONE',  ( -21.52544592524334988, -5.823673210054445271, 43.95942372801902565 ) ) ;
#199326 = CARTESIAN_POINT ( 'NONE',  ( -19.05341960407611168, -5.049401038298163336, 56.45724293864768129 ) ) ;
#199327 = DIRECTION ( 'NONE',  ( 1.000000000000000000, -0.000000000000000000, -0.000000000000000000 ) ) ;
#199328 = CARTESIAN_POINT ( 'NONE',  ( 13.89961937509977652, -13.97604488694527269, 53.12390960531434558 ) ) ;
#199329 = CARTESIAN_POINT ( 'NONE',  ( 18.67979575497178502, 10.72451020669898547, 34.16557627198102409 ) ) ;
#199330 = CARTESIAN_POINT ( 'NONE',  ( 5.049401038298161559, -19.05341960407611168, 22.70724293864769194 ) ) ;
#199331 = CARTESIAN_POINT ( 'NONE',  ( -10.72451020669898014, 18.67979575497178502, 30.41557627198101699 ) ) ;
#199332 = CARTESIAN_POINT ( 'NONE',  ( 0.05219959533934541429, -16.53943276465976808, 85.00109039468568994 ) ) ;
#199333 = CARTESIAN_POINT ( 'NONE',  ( -21.53943276465977519, -0.05219959533937600094, 108.7510903946857042 ) ) ;
#199334 = CARTESIAN_POINT ( 'NONE',  ( 14.29746914071037800, 8.314922557961029526, 66.66775706135234714 ) ) ;
#199335 = CARTESIAN_POINT ( 'NONE',  ( -19.02544592524342804, 5.153800228976336051, 111.0405762719810099 ) ) ;
#199336 = CARTESIAN_POINT ( 'NONE',  ( -16.52544592524335698, -4.483927247898792601, 53.95942372801900433 ) ) ;
#199337 = CARTESIAN_POINT ( 'NONE',  ( -4.483927247898782831, 16.52544592524335698, 42.70942372801901854 ) ) ;
#199338 = CARTESIAN_POINT ( 'NONE',  ( -9.564922557960796823, -16.46253265017161027, 107.0822429386476955 ) ) ;
#199339 = CARTESIAN_POINT ( 'NONE',  ( 16.55341960407618274, -4.379528057220086978, 31.04275706135234714 ) ) ;
#199340 = CARTESIAN_POINT ( 'NONE',  ( 5.049401038298161559, -19.05341960407611168, 37.70724293864768839 ) ) ;
#199341 = CARTESIAN_POINT ( 'NONE',  ( -10.72451020669870658, -18.67979575497194134, 19.58442372801901143 ) ) ;
#199342 = CARTESIAN_POINT ( 'NONE',  ( -19.05341960407617563, 5.049401038297882671, 113.5427570613523471 ) ) ;
#199343 = CARTESIAN_POINT ( 'NONE',  ( -8.314922557961024197, 14.29746914071037800, 82.91775706135234714 ) ) ;
#199344 = CARTESIAN_POINT ( 'NONE',  ( -17.26172910966715435, 6.454744622556958689, 45.80646908649209337 ) ) ;
#199345 = CARTESIAN_POINT ( 'NONE',  ( 5.823673210054444382, -21.52544592524334988, 85.20942372801901854 ) ) ;
#199346 = CARTESIAN_POINT ( 'NONE',  ( 9.474510206698729675, 16.51473224551082808, 87.08442372801900433 ) ) ;
#199347 = CARTESIAN_POINT ( 'NONE',  ( 16.52544592524342804, -4.483927247898539470, 48.54057627198103120 ) ) ;
#199348 = CARTESIAN_POINT ( 'NONE',  ( 12.06949235617757843, -12.14591786802309237, 103.1239096053143811 ) ) ;
#199350 = DIRECTION ( 'NONE',  ( 0.000000000000000000, 0.000000000000000000, 1.000000000000000000 ) ) ;
#199349 = CARTESIAN_POINT ( 'NONE',  ( -9.474510206698720793, -16.51473224551083518, 44.58442372801900433 ) ) ;
#199351 = CARTESIAN_POINT ( 'NONE',  ( 10.72451020669871369, 18.67979575497193778, 57.08442372801901854 ) ) ;
#199352 = CARTESIAN_POINT ( 'NONE',  ( 19.05341960407617918, -5.049401038297876454, 106.0427570613523471 ) ) ;
#199353 = CARTESIAN_POINT ( 'NONE',  ( 17.40805194822030444, 6.112264579159360167, 81.66628727489390371 ) ) ;
#199354 = CARTESIAN_POINT ( 'NONE',  ( 0.05219959533909260263, 19.03943276465977164, 99.99890960531436690 ) ) ;
#199355 = CARTESIAN_POINT ( 'NONE',  ( -10.81492255796078084, -18.62759615963271287, 77.08224293864769550 ) ) ;
#199356 = CARTESIAN_POINT ( 'NONE',  ( -9.564922557961040184, 16.46253265017147172, 97.91775706135233293 ) ) ;
#199357 = CARTESIAN_POINT ( 'NONE',  ( -13.97604488694527625, -13.89961937509977652, 101.8739096053143811 ) ) ;
#199358 = CARTESIAN_POINT ( 'NONE',  ( -16.25332922912272693, -23.18555326879971190, 140.0000000000000284 ) ) ;
#199359 = CARTESIAN_POINT ( 'NONE',  ( -12.06949235617756955, 12.14591786802309770, 100.6239096053143811 ) ) ;
#199360 = CARTESIAN_POINT ( 'NONE',  ( 5.823673210054444382, -21.52544592524334988, 100.2094237280190043 ) ) ;
#199361 = CARTESIAN_POINT ( 'NONE',  ( 0.05219959533909260263, 19.03943276465977164, 39.99890960531436690 ) ) ;
#199363 = CARTESIAN_POINT ( 'NONE',  ( -10.72451020669870658, -18.67979575497194134, 49.58442372801901143 ) ) ;
#199362 = VECTOR ( 'NONE', #34290, 1000.000000000000000 ) ;
#199364 = CARTESIAN_POINT ( 'NONE',  ( 10.81492255796106328, -18.62759615963255655, 95.41775706135234714 ) ) ;
#199365 = CARTESIAN_POINT ( 'NONE',  ( -4.379528057220086978, -16.55341960407618274, 84.79275706135234714 ) ) ;
#199366 = CARTESIAN_POINT ( 'NONE',  ( -18.62759615963255300, -10.81492255796106328, 39.16775706135235424 ) ) ;
#199367 = CARTESIAN_POINT ( 'NONE',  ( -15.80617190586768217, 15.72974639402176855, 38.12609039468567573 ) ) ;
#199369 = CARTESIAN_POINT ( 'NONE',  ( -16.46253265017160317, 9.564922557960807481, 90.83224293864769550 ) ) ;
#199368 = CARTESIAN_POINT ( 'NONE',  ( 16.46253265017146816, 9.564922557961045513, 61.66775706135234003 ) ) ;
#199370 = CARTESIAN_POINT ( 'NONE',  ( 4.379528057220339221, -16.55341960407611168, 102.7072429386476955 ) ) ;
#199371 = CARTESIAN_POINT ( 'NONE',  ( -15.72974639402197994, 15.80617190586746368, 80.62390960531438111 ) ) ;
#199372 = CARTESIAN_POINT ( 'NONE',  ( -4.483927247898539470, -16.52544592524342804, 62.29057627198102409 ) ) ;
#199373 = CARTESIAN_POINT ( 'NONE',  ( -21.53943276465977519, -0.05219959533937600094, 103.7510903946857042 ) ) ;
#199374 = CARTESIAN_POINT ( 'NONE',  ( -14.34966873604960291, -8.224510206698953496, 86.66557627198102409 ) ) ;
#199375 = CARTESIAN_POINT ( 'NONE',  ( -19.03943276465977164, 0.05219959533909376836, 36.24890960531436690 ) ) ;
#199376 = CARTESIAN_POINT ( 'NONE',  ( 9.474510206698729675, 16.51473224551082808, 87.08442372801900433 ) ) ;
#199377 = CARTESIAN_POINT ( 'NONE',  ( -16.55341960407611168, -4.379528057220339221, 51.45724293864770260 ) ) ;
#199378 = CARTESIAN_POINT ( 'NONE',  ( 21.52544592524334988, 5.823673210054432836, 101.4594237280190185 ) ) ;
#199379 = CARTESIAN_POINT ( 'NONE',  ( -9.474510206698964154, 16.51473224551069663, 85.41557627198102409 ) ) ;
#199380 = CARTESIAN_POINT ( 'NONE',  ( -19.02544592524334988, -5.153800228976617603, 58.95942372801900433 ) ) ;
#199381 = CARTESIAN_POINT ( 'NONE',  ( 10.81492255796078972, 18.62759615963270932, 59.58224293864770260 ) ) ;
#199382 = CARTESIAN_POINT ( 'NONE',  ( 18.62759615963255655, 10.81492255796105972, 36.66775706135234714 ) ) ;
#199383 = CARTESIAN_POINT ( 'NONE',  ( 14.29746914071037800, 8.314922557961029526, 26.66775706135235424 ) ) ;
#199384 = CARTESIAN_POINT ( 'NONE',  ( 16.53943276465976808, 0.05219959533934440121, 86.25109039468568994 ) ) ;
#199386 = CARTESIAN_POINT ( 'NONE',  ( 5.823673210054125526, 21.52544592524343514, 114.7905762719810383 ) ) ;
#199385 = CARTESIAN_POINT ( 'NONE',  ( -9.564922557960796823, -16.46253265017161027, 27.08224293864769550 ) ) ;
#199387 = CARTESIAN_POINT ( 'NONE',  ( 8.314922557960818139, 14.29746914071049879, 114.5822429386477097 ) ) ;
#199388 = CARTESIAN_POINT ( 'NONE',  ( -29.86685920354755197, -21.69954338932560134, -8.924999997268812990 ) ) ;
#199389 = CARTESIAN_POINT ( 'NONE',  ( 16.53943276465976808, 0.05219959533934440121, 51.25109039468568994 ) ) ;
#199390 = CARTESIAN_POINT ( 'NONE',  ( -12.14591786802309592, -12.06949235617757132, 76.87390960531439532 ) ) ;
#199391 = CARTESIAN_POINT ( 'NONE',  ( 10.81492255796078972, 18.62759615963270932, 74.58224293864768129 ) ) ;
#199392 = CARTESIAN_POINT ( 'NONE',  ( -12.06949235617756955, 12.14591786802309770, 25.62390960531435624 ) ) ;
#199393 = CARTESIAN_POINT ( 'NONE',  ( 12.14591786802327356, -12.06949235617739191, 35.62609039468568994 ) ) ;
#199394 = CARTESIAN_POINT ( 'NONE',  ( -9.564922557960796823, -16.46253265017161027, 42.08224293864769550 ) ) ;
#199395 = CARTESIAN_POINT ( 'NONE',  ( 14.29746914071037800, 8.314922557961029526, 76.66775706135234714 ) ) ;
#199396 = CARTESIAN_POINT ( 'NONE',  ( 19.03943276465977164, 0.05219959533936151252, 71.25109039468566152 ) ) ;
#199397 = CARTESIAN_POINT ( 'NONE',  ( -15.80617190586745835, -15.72974639402198527, 76.87390960531439532 ) ) ;
#199398 = CARTESIAN_POINT ( 'NONE',  ( 8.224510206698953496, -14.34966873604960469, 22.91557627198102765 ) ) ;
#199399 = ORIENTED_EDGE ( 'NONE', *, *, #192729, .F. ) ;
#199400 = CARTESIAN_POINT ( 'NONE',  ( 25.76143648877207681, 7.343476467569183264, 174.8772314887149264 ) ) ;
#199401 = CARTESIAN_POINT ( 'NONE',  ( 15.80617190586746368, 15.72974639402197994, 54.37390960531435979 ) ) ;
#199402 = ORIENTED_EDGE ( 'NONE', *, *, #59756, .T. ) ;
#199403 = ORIENTED_EDGE ( 'NONE', *, *, #68983, .T. ) ;
#199404 = CARTESIAN_POINT ( 'NONE',  ( 14.34966873604972726, -8.224510206698740333, 95.83442372801903275 ) ) ;
#199405 = ORIENTED_EDGE ( 'NONE', *, *, #116835, .T. ) ;
#199406 = CARTESIAN_POINT ( 'NONE',  ( 13.89961937509977652, -13.97604488694527269, 113.1239096053143527 ) ) ;
#199407 = CARTESIAN_POINT ( 'NONE',  ( -11.74264578624800670, 36.14014761921585972, -8.149999994537626691 ) ) ;
#199408 = CARTESIAN_POINT ( 'NONE',  ( 15.80617190586746368, 15.72974639402197994, 74.37390960531436690 ) ) ;
#199409 = CARTESIAN_POINT ( 'NONE',  ( 12.14591786802327356, -12.06949235617739191, 105.6260903946856899 ) ) ;
#199410 = CARTESIAN_POINT ( 'NONE',  ( 10.81492255796106328, -18.62759615963255655, 60.41775706135235424 ) ) ;
#199411 = CARTESIAN_POINT ( 'NONE',  ( -0.05219959533934338120, 16.53943276465976808, 22.50109039468567573 ) ) ;
#199412 = CARTESIAN_POINT ( 'NONE',  ( -8.224510206698948167, 14.34966873604960824, 110.4155762719810383 ) ) ;
#199413 = CARTESIAN_POINT ( 'NONE',  ( -8.314922557961024197, 14.29746914071037800, 22.91775706135235069 ) ) ;
#199414 = CARTESIAN_POINT ( 'NONE',  ( 19.02544592524343514, -5.153800228976328945, 53.54057627198102409 ) ) ;
#199415 = CARTESIAN_POINT ( 'NONE',  ( 17.81289503416611453, -24.51734667627695785, 144.6999999999999886 ) ) ;
#199416 = CARTESIAN_POINT ( 'NONE',  ( -9.564922557960796823, -16.46253265017161027, 107.0822429386476955 ) ) ;
#199417 = CARTESIAN_POINT ( 'NONE',  ( -4.379528057220086978, -16.55341960407618274, 94.79275706135234714 ) ) ;
#199418 = CARTESIAN_POINT ( 'NONE',  ( -5.049401038297874678, -19.05341960407617918, 94.79275706135230450 ) ) ;
#199419 = CARTESIAN_POINT ( 'NONE',  ( -13.89961937509957401, -13.97604488694547875, 29.37609039468565797 ) ) ;
#199420 = CARTESIAN_POINT ( 'NONE',  ( 21.55341960407610458, 5.719274019375980345, 68.95724293864769550 ) ) ;
#199421 = CARTESIAN_POINT ( 'NONE',  ( 14.34966873604972726, -8.224510206698740333, 100.8344237280190185 ) ) ;
#199422 = CARTESIAN_POINT ( 'NONE',  ( 19.05341960407617918, -5.049401038297876454, 96.04275706135231871 ) ) ;
#199423 = CARTESIAN_POINT ( 'NONE',  ( 9.474510206698971260, -16.51473224551069308, 52.91557627198102409 ) ) ;
#199424 = CARTESIAN_POINT ( 'NONE',  ( -9.564922557960796823, -16.46253265017161027, 92.08224293864769550 ) ) ;
#199425 = CARTESIAN_POINT ( 'NONE',  ( 10.81492255796106328, -18.62759615963255655, 55.41775706135234714 ) ) ;
#199426 = CARTESIAN_POINT ( 'NONE',  ( 13.89961937509977652, -13.97604488694527269, 48.12390960531435979 ) ) ;
#199427 = CARTESIAN_POINT ( 'NONE',  ( -17.26058549869093994, -6.457015423128474652, 86.37745837476066413 ) ) ;
#199428 = CARTESIAN_POINT ( 'NONE',  ( -16.53943276465976808, 0.05219959533911058130, 71.24890960531435269 ) ) ;
#199429 = CARTESIAN_POINT ( 'NONE',  ( -21.53943276465977519, 0.05219959533907696930, 71.24890960531435269 ) ) ;
#199430 = DIRECTION ( 'NONE',  ( 0.000000000000000000, 0.000000000000000000, 1.000000000000000000 ) ) ;
#199431 = CARTESIAN_POINT ( 'NONE',  ( 13.89961937509957401, 13.97604488694547697, 36.87609039468565442 ) ) ;
#199432 = LINE ( 'NONE', #10449, #157478 ) ;
#199434 = CARTESIAN_POINT ( 'NONE',  ( -9.564922557960796823, -16.46253265017161027, 87.08224293864769550 ) ) ;
#199433 = CARTESIAN_POINT ( 'NONE',  ( -0.05219959533909027116, -19.03943276465977164, 82.49890960531436690 ) ) ;
#199435 = CARTESIAN_POINT ( 'NONE',  ( 14.29746914071037800, 8.314922557961029526, 46.66775706135234714 ) ) ;
#199436 = CARTESIAN_POINT ( 'NONE',  ( -13.89961937509957401, -13.97604488694547697, 79.37609039468567573 ) ) ;
#199437 = CARTESIAN_POINT ( 'NONE',  ( 16.51473224551083163, -9.474510206698727899, 35.83442372801899722 ) ) ;
#199438 = CARTESIAN_POINT ( 'NONE',  ( -11.45643923738959735, 5.000000000000007105, -18.00000000000000000 ) ) ;
#199439 = CARTESIAN_POINT ( 'NONE',  ( 16.52544592524335698, 4.483927247898782831, 91.45942372801901854 ) ) ;
#199440 = CARTESIAN_POINT ( 'NONE',  ( 14.82524568295233891, -1.464953661134022367, -59.95866808466630005 ) ) ;
#199441 = CARTESIAN_POINT ( 'NONE',  ( 14.34966873604972726, -8.224510206698740333, 80.83442372801901854 ) ) ;
#199442 = CARTESIAN_POINT ( 'NONE',  ( -16.52544592524335698, -4.483927247898792601, 58.95942372801902565 ) ) ;
#199444 = CARTESIAN_POINT ( 'NONE',  ( -17.58332526062529411, 7.635886036038502134, 75.92334959558466778 ) ) ;
#199443 = CARTESIAN_POINT ( 'NONE',  ( -19.03943276465977164, 0.05219959533909376836, 51.24890960531436690 ) ) ;
#199445 = CARTESIAN_POINT ( 'NONE',  ( 15.72974639402176855, 15.80617190586768217, 61.87609039468568284 ) ) ;
#199446 = CARTESIAN_POINT ( 'NONE',  ( -19.05341960407617563, 5.049401038297882671, 73.54275706135233293 ) ) ;
#199447 = CARTESIAN_POINT ( 'NONE',  ( 21.53943276465977519, 0.05219959533937863772, 111.2510903946856899 ) ) ;
#199448 = CARTESIAN_POINT ( 'NONE',  ( 9.564922557960805705, 16.46253265017160317, 49.58224293864770260 ) ) ;
#199449 = CARTESIAN_POINT ( 'NONE',  ( -19.03943276465977164, 0.05219959533909376836, 46.24890960531435979 ) ) ;
#199450 = CARTESIAN_POINT ( 'NONE',  ( 16.38539452495360393, 7.295416311890092764, 23.44248723764945552 ) ) ;
#199451 = CARTESIAN_POINT ( 'NONE',  ( -5.719274019375978568, 21.55341960407610458, 70.20724293864769550 ) ) ;
#199452 = CIRCLE ( 'NONE', #73619, 7.999999999999998224 ) ;
#199453 = CARTESIAN_POINT ( 'NONE',  ( 15.72974639402199770, -15.80617190586745480, 23.12390960531436335 ) ) ;
#199454 = CARTESIAN_POINT ( 'NONE',  ( -19.05341960407611168, -5.049401038298163336, 26.45724293864769550 ) ) ;
#199455 = CARTESIAN_POINT ( 'NONE',  ( -8.224510206698735004, -14.34966873604973081, 44.58442372801901854 ) ) ;
#199456 = CARTESIAN_POINT ( 'NONE',  ( 4.379528057220339221, -16.55341960407611168, 32.70724293864770260 ) ) ;
#199457 = ORIENTED_EDGE ( 'NONE', *, *, #56324, .F. ) ;
#199458 = EDGE_CURVE ( 'NONE', #74853, #171133, #42324, .T. ) ;
#199459 = CARTESIAN_POINT ( 'NONE',  ( -15.80617190586768217, 15.72974639402176855, 23.12609039468567573 ) ) ;
#199461 = CARTESIAN_POINT ( 'NONE',  ( -23.48529157249599919, -32.32473071737750558, -5.700000000000000178 ) ) ;
#199460 = CARTESIAN_POINT ( 'NONE',  ( 4.379528057220339221, -16.55341960407611168, 52.70724293864769550 ) ) ;
#199462 = CARTESIAN_POINT ( 'NONE',  ( -19.05341960407617563, 5.049401038297882671, 103.5427570613523329 ) ) ;
#199463 = CARTESIAN_POINT ( 'NONE',  ( -13.89961937509957401, -13.97604488694547875, 44.37609039468566863 ) ) ;
#199464 = CARTESIAN_POINT ( 'NONE',  ( 12.06949235617757843, -12.14591786802309237, 38.12390960531436690 ) ) ;
#199465 = CARTESIAN_POINT ( 'NONE',  ( -5.823673210054116645, -21.52544592524344225, 102.2905762719810383 ) ) ;
#199467 = CARTESIAN_POINT ( 'NONE',  ( 21.55341960407610458, 5.719274019375980345, 68.95724293864769550 ) ) ;
#199466 = DIRECTION ( 'NONE',  ( -1.000000000000000000, 0.000000000000000000, 0.000000000000000000 ) ) ;
#199468 = CARTESIAN_POINT ( 'NONE',  ( 5.049401038298161559, -19.05341960407611168, 72.70724293864768129 ) ) ;
#199469 = CARTESIAN_POINT ( 'NONE',  ( 8.224510206698953496, -14.34966873604960469, 47.91557627198102409 ) ) ;
#199470 = CARTESIAN_POINT ( 'NONE',  ( -13.89961937509977652, 13.97604488694528158, 100.6239096053143669 ) ) ;
#199471 = CARTESIAN_POINT ( 'NONE',  ( -17.50000000000002842, -5.499999999999952927, 76.28230962303568674 ) ) ;
#199472 = CARTESIAN_POINT ( 'NONE',  ( -13.89961937509957401, -13.97604488694547875, 54.37609039468565442 ) ) ;
#199473 = CARTESIAN_POINT ( 'NONE',  ( -5.823673210054116645, -21.52544592524344225, 92.29057627198103830 ) ) ;
#199474 = CARTESIAN_POINT ( 'NONE',  ( -13.97604488694527625, -13.89961937509977652, 36.87390960531436690 ) ) ;
#199475 = CARTESIAN_POINT ( 'NONE',  ( 16.46253265017160672, -9.564922557960803928, 23.33224293864769194 ) ) ;
#199476 = CARTESIAN_POINT ( 'NONE',  ( -21.52544592524334988, -5.823673210054445271, 48.95942372801902565 ) ) ;
#199477 = CIRCLE ( 'NONE', #170464, 206.0437394197456342 ) ;
#199478 = CARTESIAN_POINT ( 'NONE',  ( 22.44159573604009594, -16.30477369853687364, 147.6750000027311671 ) ) ;
#199479 = CARTESIAN_POINT ( 'NONE',  ( 4.483927247898545687, 16.52544592524342804, 24.79057627198103120 ) ) ;
#199480 = CARTESIAN_POINT ( 'NONE',  ( -0.05219959533909027116, -19.03943276465977164, 47.49890960531435979 ) ) ;
#199481 = CARTESIAN_POINT ( 'NONE',  ( -16.46253265017160317, 9.564922557960807481, 100.8322429386477097 ) ) ;
#199482 = CARTESIAN_POINT ( 'NONE',  ( -15.80617190586745835, -15.72974639402198527, 61.87390960531436690 ) ) ;
#199483 = CARTESIAN_POINT ( 'NONE',  ( 8.571926809382597767, 26.38167802310806209, 146.2750000027311899 ) ) ;
#199484 = CARTESIAN_POINT ( 'NONE',  ( 9.474510206698971260, -16.51473224551069308, 42.91557627198103120 ) ) ;
#199485 = CARTESIAN_POINT ( 'NONE',  ( 21.55341960407610458, 5.719274019375980345, 58.95724293864770971 ) ) ;
#199486 = CARTESIAN_POINT ( 'NONE',  ( -10.81492255796105439, 18.62759615963255655, 87.91775706135234714 ) ) ;
#199489 = CARTESIAN_POINT ( 'NONE',  ( -8.224510206698948167, 14.34966873604960824, 70.41557627198102409 ) ) ;
#199488 = CARTESIAN_POINT ( 'NONE',  ( 4.379528057220092307, 16.55341960407617563, 82.29275706135234714 ) ) ;
#199487 = CARTESIAN_POINT ( 'NONE',  ( 12.38288446667197995, -41.98357824127743498, -20.85955585120671074 ) ) ;
#199490 = CARTESIAN_POINT ( 'NONE',  ( 14.29746914071037800, 8.314922557961029526, 91.66775706135234714 ) ) ;
#199491 = CARTESIAN_POINT ( 'NONE',  ( 5.153800228976335163, 19.02544592524342804, 69.79057627198103830 ) ) ;
#199492 = ORIENTED_EDGE ( 'NONE', *, *, #62108, .T. ) ;
#199493 = CARTESIAN_POINT ( 'NONE',  ( 5.153800228976615827, -19.02544592524334988, 25.20942372801900433 ) ) ;
#199494 = CARTESIAN_POINT ( 'NONE',  ( 12.14591786802327356, -12.06949235617739191, 90.62609039468567573 ) ) ;
#199495 = CARTESIAN_POINT ( 'NONE',  ( -21.55341960407619339, 5.719274019375674811, 108.5427570613523756 ) ) ;
#199496 = CARTESIAN_POINT ( 'NONE',  ( -19.03943276465977164, 0.05219959533909376836, 76.24890960531435269 ) ) ;
#199497 = CARTESIAN_POINT ( 'NONE',  ( 0.05219959533907565091, 21.53943276465977519, 49.99890960531437401 ) ) ;
#199498 = CARTESIAN_POINT ( 'NONE',  ( -16.52544592524335698, -4.483927247898792601, 28.95942372801902209 ) ) ;
#199499 = CARTESIAN_POINT ( 'NONE',  ( 10.72451020669871369, 18.67979575497193778, 77.08442372801901854 ) ) ;
#199500 = CARTESIAN_POINT ( 'NONE',  ( -12.14591786802326823, 12.06949235617739902, 68.12609039468567573 ) ) ;
#199501 = CARTESIAN_POINT ( 'NONE',  ( 5.823673210054444382, -21.52544592524334988, 20.20942372801900788 ) ) ;
#199502 = CARTESIAN_POINT ( 'NONE',  ( 13.89961937509957401, 13.97604488694547697, 106.8760903946856757 ) ) ;
#199503 = CARTESIAN_POINT ( 'NONE',  ( -9.564922557960796823, -16.46253265017161027, 92.08224293864769550 ) ) ;
#199504 = CARTESIAN_POINT ( 'NONE',  ( -4.379528057220086978, -16.55341960407618274, 34.79275706135235424 ) ) ;
#199505 = CARTESIAN_POINT ( 'NONE',  ( -9.474510206698964154, 16.51473224551069663, 45.41557627198103120 ) ) ;
#199506 = CARTESIAN_POINT ( 'NONE',  ( 14.34966873604972726, -8.224510206698740333, 20.83442372801901143 ) ) ;
#199507 = CARTESIAN_POINT ( 'NONE',  ( 14.29746914071049879, -8.314922557960816363, 83.33224293864769550 ) ) ;
#199508 = CARTESIAN_POINT ( 'NONE',  ( 16.52544592524335698, 4.483927247898782831, 81.45942372801900433 ) ) ;
#199510 = CARTESIAN_POINT ( 'NONE',  ( -19.02544592524342804, 5.153800228976336051, 61.04057627198103120 ) ) ;
#199509 = CARTESIAN_POINT ( 'NONE',  ( 18.62759615963255655, 10.81492255796105972, 36.66775706135234714 ) ) ;
#199511 = CARTESIAN_POINT ( 'NONE',  ( 13.89961937509977652, -13.97604488694527269, 73.12390960531436690 ) ) ;
#199512 = CARTESIAN_POINT ( 'NONE',  ( 16.55341960407618274, -4.379528057220086978, 81.04275706135236135 ) ) ;
#199514 = ORIENTED_EDGE ( 'NONE', *, *, #149523, .T. ) ;
#199513 = CARTESIAN_POINT ( 'NONE',  ( -21.84611564451295962, -8.148379233835273183, 169.4346228884814707 ) ) ;
#199515 = VERTEX_POINT ( 'NONE', #69650 ) ;
#199516 = CARTESIAN_POINT ( 'NONE',  ( 19.03943276465977164, 0.05219959533936151252, 31.25109039468566863 ) ) ;
#199517 = CARTESIAN_POINT ( 'NONE',  ( -16.51473224551069308, -9.474510206698971260, 51.66557627198102409 ) ) ;
#199519 = VERTEX_POINT ( 'NONE', #177844 ) ;
#199518 = CARTESIAN_POINT ( 'NONE',  ( -13.97604488694527625, -13.89961937509977652, 111.8739096053143243 ) ) ;
#199520 = CARTESIAN_POINT ( 'NONE',  ( 16.55341960407618274, -4.379528057220086978, 31.04275706135234714 ) ) ;
#199522 = CARTESIAN_POINT ( 'NONE',  ( -16.55341960407617563, 4.379528057220093196, 48.54275706135234714 ) ) ;
#199521 = CARTESIAN_POINT ( 'NONE',  ( -5.049401038297874678, -19.05341960407617918, 54.79275706135234003 ) ) ;
#199523 = CARTESIAN_POINT ( 'NONE',  ( -19.02544592524342804, 5.153800228976336051, 111.0405762719810099 ) ) ;
#199524 = CARTESIAN_POINT ( 'NONE',  ( 13.89961937509977652, -13.97604488694527269, 78.12390960531433848 ) ) ;
#199525 = CARTESIAN_POINT ( 'NONE',  ( 10.72451020669898902, -18.67979575497178502, 97.91557627198103830 ) ) ;
#199526 = CARTESIAN_POINT ( 'NONE',  ( 0.05219959533936267826, -19.03943276465977164, 70.00109039468566152 ) ) ;
#199528 = CARTESIAN_POINT ( 'NONE',  ( 9.564922557960805705, 16.46253265017160317, 24.58224293864769194 ) ) ;
#199527 = CARTESIAN_POINT ( 'NONE',  ( 19.05341960407611168, 5.049401038298154454, 93.95724293864769550 ) ) ;
#199529 = CARTESIAN_POINT ( 'NONE',  ( 19.03943276465977164, -0.05219959533909143690, 58.74890960531435979 ) ) ;
#199530 = CARTESIAN_POINT ( 'NONE',  ( -12.14591786802309592, -12.06949235617757132, 21.87390960531436690 ) ) ;
#199531 = CARTESIAN_POINT ( 'NONE',  ( 16.51473224551083163, -9.474510206698727899, 35.83442372801899722 ) ) ;
#199532 = CARTESIAN_POINT ( 'NONE',  ( 16.55341960407611168, 4.379528057220329451, 73.95724293864769550 ) ) ;
#199533 = CARTESIAN_POINT ( 'NONE',  ( 15.72974639402176855, 15.80617190586768217, 101.8760903946857042 ) ) ;
#199534 = CARTESIAN_POINT ( 'NONE',  ( 16.51473224551069308, 9.474510206698969483, 39.16557627198103120 ) ) ;
#199535 = CARTESIAN_POINT ( 'NONE',  ( 16.52544592524335698, 4.483927247898782831, 51.45942372801901854 ) ) ;
#199537 = CARTESIAN_POINT ( 'NONE',  ( -5.823673210054431948, 21.52544592524334988, 92.70942372801901854 ) ) ;
#199536 = CARTESIAN_POINT ( 'NONE',  ( -16.55341960407611168, -4.379528057220339221, 41.45724293864769550 ) ) ;
#199538 = CARTESIAN_POINT ( 'NONE',  ( -19.03943276465977164, 0.05219959533909376836, 96.24890960531436690 ) ) ;
#199539 = CARTESIAN_POINT ( 'NONE',  ( -5.153800228976328057, -19.02544592524343514, 97.29057627198099567 ) ) ;
#199540 = CARTESIAN_POINT ( 'NONE',  ( 14.29746914071049879, -8.314922557960816363, 113.3322429386476955 ) ) ;
#199541 = CARTESIAN_POINT ( 'NONE',  ( 8.224510206698953496, -14.34966873604960469, 67.91557627198102409 ) ) ;
#199542 = CARTESIAN_POINT ( 'NONE',  ( -0.05219959533907301413, -21.53943276465977519, 77.49890960531433848 ) ) ;
#199543 = CARTESIAN_POINT ( 'NONE',  ( 13.89961937509977652, -13.97604488694527269, 88.12390960531438111 ) ) ;
#199544 = CARTESIAN_POINT ( 'NONE',  ( -21.55341960407610458, -5.719274019375992779, 96.45724293864770971 ) ) ;
#199545 = CARTESIAN_POINT ( 'NONE',  ( -13.89961937509957401, -13.97604488694547875, 79.37609039468567573 ) ) ;
#199547 = CARTESIAN_POINT ( 'NONE',  ( 14.29746914071049879, -8.314922557960816363, 83.33224293864769550 ) ) ;
#199546 = CARTESIAN_POINT ( 'NONE',  ( -19.49671883438226416, -5.500000000000080824, 89.89279849105683695 ) ) ;
#199548 = CARTESIAN_POINT ( 'NONE',  ( 13.89961937509977652, -13.97604488694527269, 53.12390960531434558 ) ) ;
#199549 = CARTESIAN_POINT ( 'NONE',  ( -10.81492255796078084, -18.62759615963271287, 72.08224293864769550 ) ) ;
#199550 = CARTESIAN_POINT ( 'NONE',  ( 17.44279575226823198, -5.990770900252459619, 28.33557567514318620 ) ) ;
#199552 = CARTESIAN_POINT ( 'NONE',  ( 0.000000000000000000, 0.000000000000000000, -20.00000000000000000 ) ) ;
#199551 = CARTESIAN_POINT ( 'NONE',  ( 12.06949235617757843, -12.14591786802309237, 23.12390960531436335 ) ) ;
#199553 = CARTESIAN_POINT ( 'NONE',  ( -4.379528057220086978, -16.55341960407618274, 19.79275706135235069 ) ) ;
#199554 = EDGE_CURVE ( 'NONE', #110784, #89826, #39312, .T. ) ;
#199555 = CARTESIAN_POINT ( 'NONE',  ( -8.224510206698948167, 14.34966873604960824, 80.41557627198103830 ) ) ;
#199556 = DIRECTION ( 'NONE',  ( 0.000000000000000000, 0.000000000000000000, 1.000000000000000000 ) ) ;
#199557 = CARTESIAN_POINT ( 'NONE',  ( 9.564922557960805705, 16.46253265017160317, 69.58224293864770971 ) ) ;
#199558 = CARTESIAN_POINT ( 'NONE',  ( 19.05341960407611168, 5.049401038298154454, 33.95724293864769550 ) ) ;
#199559 = CARTESIAN_POINT ( 'NONE',  ( 16.52544592524342804, -4.483927247898539470, 63.54057627198103830 ) ) ;
#199560 = CARTESIAN_POINT ( 'NONE',  ( -15.80617190586745835, -15.72974639402198527, 21.87390960531436690 ) ) ;
#199561 = CARTESIAN_POINT ( 'NONE',  ( -16.51473224551082808, 9.474510206698731452, 83.33442372801899012 ) ) ;
#199562 = CARTESIAN_POINT ( 'NONE',  ( -19.05341960407611168, -5.049401038298163336, 101.4572429386476955 ) ) ;
#199563 = CARTESIAN_POINT ( 'NONE',  ( -18.67979575497178146, -10.72451020669898902, 71.66557627198100988 ) ) ;
#199564 = CARTESIAN_POINT ( 'NONE',  ( 4.483927247898790824, -16.52544592524335698, 75.20942372801901854 ) ) ;
#199565 = CARTESIAN_POINT ( 'NONE',  ( 16.46253265017146816, 9.564922557961045513, 106.6677570613523471 ) ) ;
#199566 = CARTESIAN_POINT ( 'NONE',  ( -19.03943276465977164, 0.05219959533909376836, 66.24890960531436690 ) ) ;
#199567 = CARTESIAN_POINT ( 'NONE',  ( -21.52544592524343514, 5.823673210054127303, 71.04057627198103830 ) ) ;
#199568 = CARTESIAN_POINT ( 'NONE',  ( -19.05341960407617563, 5.049401038297882671, 113.5427570613523471 ) ) ;
#199570 = CARTESIAN_POINT ( 'NONE',  ( -18.62759615963255300, -10.81492255796106328, 59.16775706135234714 ) ) ;
#199569 = CARTESIAN_POINT ( 'NONE',  ( 14.34966873604960469, 8.224510206698951720, 34.16557627198102409 ) ) ;
#199571 = DIRECTION ( 'NONE',  ( 0.000000000000000000, 1.000000000000000000, 0.000000000000000000 ) ) ;
#199573 = CARTESIAN_POINT ( 'NONE',  ( 16.46253265017160672, -9.564922557960803928, 108.3322429386476955 ) ) ;
#199572 = CARTESIAN_POINT ( 'NONE',  ( 12.06949235617739724, 12.14591786802326823, 76.87609039468567573 ) ) ;
#199574 = CARTESIAN_POINT ( 'NONE',  ( 19.03943276465977164, -0.05219959533909143690, 103.7489096053143669 ) ) ;
#199575 = CARTESIAN_POINT ( 'NONE',  ( 1.280994563191180546, 31.20196472458911785, -49.99722732359649058 ) ) ;
#199576 = B_SPLINE_CURVE_WITH_KNOTS ( 'NONE', 3,
 ( #19732, #4536, #78405, #66229, #35888, #188600, #16757, #96554 ),
 .UNSPECIFIED., .F., .F.,
 ( 4, 2, 2, 4 ),
 ( 0.03534151991400943243, 0.03926041079282514140, 0.04121985623223303058, 0.04317930167164092670 ),
 .UNSPECIFIED. ) ;
#199577 = CARTESIAN_POINT ( 'NONE',  ( -0.05219959533934338120, 16.53943276465976808, 97.50109039468567573 ) ) ;
#199578 = CARTESIAN_POINT ( 'NONE',  ( 8.314922557961029526, -14.29746914071037800, 40.41775706135234714 ) ) ;
#199579 = CARTESIAN_POINT ( 'NONE',  ( -9.474510206698964154, 16.51473224551069663, 65.41557627198102409 ) ) ;
#199580 = CARTESIAN_POINT ( 'NONE',  ( 5.153800228976335163, 19.02544592524342804, 79.79057627198102409 ) ) ;
#199581 = CARTESIAN_POINT ( 'NONE',  ( -5.823673210054431948, 21.52544592524334988, 62.70942372801902565 ) ) ;
#199582 = CARTESIAN_POINT ( 'NONE',  ( -14.29746914071037622, -8.314922557961029526, 59.16775706135234714 ) ) ;
#199583 = CARTESIAN_POINT ( 'NONE',  ( 8.314922557960818139, 14.29746914071049879, 29.58224293864769905 ) ) ;
#199584 = CARTESIAN_POINT ( 'NONE',  ( 19.02544592524343514, -5.153800228976328945, 38.54057627198103120 ) ) ;
#199585 = CARTESIAN_POINT ( 'NONE',  ( -16.51473224551069308, -9.474510206698971260, 36.66557627198102409 ) ) ;
#199587 = ORIENTED_EDGE ( 'NONE', *, *, #8537, .F. ) ;
#199586 = CARTESIAN_POINT ( 'NONE',  ( 12.14591786802327356, -12.06949235617739191, 25.62609039468567929 ) ) ;
#199588 = CARTESIAN_POINT ( 'NONE',  ( -16.46253265017146816, -9.564922557961047289, 79.16775706135234714 ) ) ;
#199589 = CARTESIAN_POINT ( 'NONE',  ( -16.52544592524342804, 4.483927247898546575, 96.04057627198102409 ) ) ;
#199590 = CARTESIAN_POINT ( 'NONE',  ( 9.564922557960805705, 16.46253265017160317, 49.58224293864770260 ) ) ;
#199592 = CARTESIAN_POINT ( 'NONE',  ( 28.79475375365586132, 2.781246896534039337E-14, 148.9843446568999923 ) ) ;
#199591 = CARTESIAN_POINT ( 'NONE',  ( -16.51473224551082808, 9.474510206698731452, 83.33442372801899012 ) ) ;
#199593 = CARTESIAN_POINT ( 'NONE',  ( -21.53943276465977519, -0.05219959533937600094, 88.75109039468567573 ) ) ;
#199594 = CARTESIAN_POINT ( 'NONE',  ( -12.06949235617739369, -12.14591786802326823, 59.37609039468568284 ) ) ;
#199595 = FACE_OUTER_BOUND ( 'NONE', #25973, .T. ) ;
#199596 = CARTESIAN_POINT ( 'NONE',  ( 21.52544592524344225, -5.823673210054117533, 43.54057627198103830 ) ) ;
#199597 = CARTESIAN_POINT ( 'NONE',  ( 8.314922557961029526, -14.29746914071037800, 35.41775706135234003 ) ) ;
#199598 = CARTESIAN_POINT ( 'NONE',  ( -16.51473224551069308, -9.474510206698971260, 36.66557627198102409 ) ) ;
#199599 = CARTESIAN_POINT ( 'NONE',  ( -13.97604488694547697, 13.89961937509957934, 38.12609039468566152 ) ) ;
#199600 = CARTESIAN_POINT ( 'NONE',  ( -5.049401038298153566, 19.05341960407611168, 90.20724293864766707 ) ) ;
#199601 = CARTESIAN_POINT ( 'NONE',  ( 16.46253265017160672, -9.564922557960803928, 53.33224293864768839 ) ) ;
#199602 = AXIS2_PLACEMENT_3D ( 'NONE', #55659, #39488, #54657 ) ;
#199603 = CARTESIAN_POINT ( 'NONE',  ( -22.24618122112613960, -22.80753876826822690, -49.18602036547672185 ) ) ;
#199604 = CARTESIAN_POINT ( 'NONE',  ( -15.72974639402176322, -15.80617190586768395, 74.37609039468568994 ) ) ;
#199605 = CARTESIAN_POINT ( 'NONE',  ( 22.94331271462294097, 3.784814030245898575, 190.0000000000000000 ) ) ;
#199606 = CARTESIAN_POINT ( 'NONE',  ( 9.474510206698729675, 16.51473224551082808, 27.08442372801900433 ) ) ;
#199607 = CARTESIAN_POINT ( 'NONE',  ( -15.80617190586768217, 15.72974639402176855, 113.1260903946856899 ) ) ;
#199608 = CARTESIAN_POINT ( 'NONE',  ( 8.224510206698953496, -14.34966873604960469, 52.91557627198103830 ) ) ;
#199609 = CARTESIAN_POINT ( 'NONE',  ( 16.46253265017160672, -9.564922557960803928, 53.33224293864768839 ) ) ;
#199610 = CARTESIAN_POINT ( 'NONE',  ( 0.05219959533909260263, 19.03943276465977164, 109.9989096053143669 ) ) ;
#199611 = CARTESIAN_POINT ( 'NONE',  ( -18.67979575497193778, 10.72451020669871902, 83.33442372801903275 ) ) ;
#199612 = CARTESIAN_POINT ( 'NONE',  ( -16.46253265017160317, 9.564922557960807481, 65.83224293864769550 ) ) ;
#199613 = CARTESIAN_POINT ( 'NONE',  ( -15.80617190586768217, 15.72974639402176855, 83.12609039468568994 ) ) ;
#199614 = CARTESIAN_POINT ( 'NONE',  ( -18.67979575497178146, -10.72451020669898902, 41.66557627198103120 ) ) ;
#199615 = CARTESIAN_POINT ( 'NONE',  ( 21.52544592524334988, 5.823673210054432836, 31.45942372801901854 ) ) ;
#199616 = CARTESIAN_POINT ( 'NONE',  ( 9.564922557961047289, -16.46253265017146816, 65.41775706135233293 ) ) ;
#199617 = CARTESIAN_POINT ( 'NONE',  ( -5.153800228976328057, -19.02544592524343514, 32.29057627198102409 ) ) ;
#199618 = CARTESIAN_POINT ( 'NONE',  ( -9.474510206698964154, 16.51473224551069663, 70.41557627198102409 ) ) ;
#199619 = CARTESIAN_POINT ( 'NONE',  ( 16.55341960407618274, -4.379528057220086978, 36.04275706135234714 ) ) ;
#199620 = CARTESIAN_POINT ( 'NONE',  ( -12.06949235617756955, 12.14591786802309770, 85.62390960531436690 ) ) ;
#199621 = CARTESIAN_POINT ( 'NONE',  ( 9.564922557960805705, 16.46253265017160317, 59.58224293864769550 ) ) ;
#199622 = CARTESIAN_POINT ( 'NONE',  ( -0.05219959533907301413, -21.53943276465977519, 37.49890960531436690 ) ) ;
#199623 = CARTESIAN_POINT ( 'NONE',  ( -0.05219959533936034679, 19.03943276465977164, 107.5010903946856615 ) ) ;
#199624 = CARTESIAN_POINT ( 'NONE',  ( 18.67979575497194134, -10.72451020669871369, 25.83442372801901499 ) ) ;
#199625 = CARTESIAN_POINT ( 'NONE',  ( -21.53943276465977519, -0.05219959533937600094, 73.75109039468567573 ) ) ;
#199626 = CARTESIAN_POINT ( 'NONE',  ( -16.52544592524335698, -4.483927247898792601, 68.95942372801901854 ) ) ;
#199627 = CARTESIAN_POINT ( 'NONE',  ( 12.06949235617739724, 12.14591786802326823, 66.87609039468568994 ) ) ;
#199628 = CARTESIAN_POINT ( 'NONE',  ( -13.97604488694527625, -13.89961937509977652, 61.87390960531435979 ) ) ;
#199629 = CARTESIAN_POINT ( 'NONE',  ( -14.29746914071037622, -8.314922557961029526, 84.16775706135234714 ) ) ;
#199630 = CARTESIAN_POINT ( 'NONE',  ( 13.97604488694548053, -13.89961937509957401, 40.62609039468564731 ) ) ;
#199631 = CARTESIAN_POINT ( 'NONE',  ( -18.67979575497193778, 10.72451020669871902, 23.33442372801901499 ) ) ;
#199632 = CARTESIAN_POINT ( 'NONE',  ( 16.52544592524342804, -4.483927247898539470, 68.54057627198103830 ) ) ;
#199633 = CARTESIAN_POINT ( 'NONE',  ( -13.97604488694527625, -13.89961937509977652, 86.87390960531436690 ) ) ;
#199634 = CARTESIAN_POINT ( 'NONE',  ( 12.14591786802327356, -12.06949235617739191, 95.62609039468568994 ) ) ;
#199635 = CARTESIAN_POINT ( 'NONE',  ( 15.72974639402176855, 15.80617190586768217, 56.87609039468568994 ) ) ;
#199636 = CARTESIAN_POINT ( 'NONE',  ( -12.06949235617739369, -12.14591786802326823, 24.37609039468567573 ) ) ;
#199637 = AXIS2_PLACEMENT_3D ( 'NONE', #135790, #197461, #71118 ) ;
#199638 = CARTESIAN_POINT ( 'NONE',  ( 10.72451020669898902, -18.67979575497178502, 107.9155762719810241 ) ) ;
#199639 = CARTESIAN_POINT ( 'NONE',  ( 14.34966873604960469, 8.224510206698951720, 54.16557627198103120 ) ) ;
#199640 = EDGE_LOOP ( 'NONE', ( #115007, #47043, #20579, #43271 ) ) ;
#199641 = CARTESIAN_POINT ( 'NONE',  ( 15.80617190586746368, 15.72974639402197994, 94.37390960531436690 ) ) ;
#199642 = CARTESIAN_POINT ( 'NONE',  ( -14.29746914071049879, 8.314922557960819915, 35.83224293864768839 ) ) ;
#199643 = ORIENTED_EDGE ( 'NONE', *, *, #173518, .T. ) ;
#199644 = CARTESIAN_POINT ( 'NONE',  ( -3.573655867282028392E-15, 2.428612866367529932E-14, 2.000000000000000000 ) ) ;
#199645 = CARTESIAN_POINT ( 'NONE',  ( -10.72451020669870658, -18.67979575497194134, 19.58442372801901143 ) ) ;
#199646 = CARTESIAN_POINT ( 'NONE',  ( -9.474510206698964154, 16.51473224551069663, 105.4155762719810383 ) ) ;
#199647 = CARTESIAN_POINT ( 'NONE',  ( 21.52544592524334988, 5.823673210054432836, 36.45942372801901143 ) ) ;
#199648 = CARTESIAN_POINT ( 'NONE',  ( 16.52544592524342804, -4.483927247898539470, 48.54057627198103120 ) ) ;
#199649 = CARTESIAN_POINT ( 'NONE',  ( -19.02544592524342804, 5.153800228976336051, 56.04057627198100988 ) ) ;
#199650 = CARTESIAN_POINT ( 'NONE',  ( -19.02544592524334988, -5.153800228976617603, 63.95942372801899012 ) ) ;
#199651 = CARTESIAN_POINT ( 'NONE',  ( 5.153800228976335163, 19.02544592524342804, 99.79057627198102409 ) ) ;
#199652 = CARTESIAN_POINT ( 'NONE',  ( 21.55341960407610458, 5.719274019375980345, 43.95724293864769550 ) ) ;
#199653 = CARTESIAN_POINT ( 'NONE',  ( -15.59283147534494063, -34.52683219101068346, -28.07673947521500324 ) ) ;
#199654 = CARTESIAN_POINT ( 'NONE',  ( 0.05219959533909260263, 19.03943276465977164, 59.99890960531436690 ) ) ;
#199655 = CARTESIAN_POINT ( 'NONE',  ( -12.14591786802326823, 12.06949235617739902, 33.12609039468569705 ) ) ;
#199656 = CARTESIAN_POINT ( 'NONE',  ( -16.51473224551082808, 9.474510206698731452, 63.33442372801900433 ) ) ;
#199657 = CARTESIAN_POINT ( 'NONE',  ( -10.81492255796105439, 18.62759615963255655, 22.91775706135235069 ) ) ;
#199658 = CARTESIAN_POINT ( 'NONE',  ( 16.53943276465976808, -0.05219959533910856209, 48.74890960531435979 ) ) ;
#199659 = ORIENTED_EDGE ( 'NONE', *, *, #194281, .T. ) ;
#199660 = CARTESIAN_POINT ( 'NONE',  ( 19.03943276465977164, -0.05219959533909143690, 88.74890960531436690 ) ) ;
#199661 = CARTESIAN_POINT ( 'NONE',  ( -10.81492255796078084, -18.62759615963271287, 72.08224293864769550 ) ) ;
#199663 = CARTESIAN_POINT ( 'NONE',  ( -16.55341960407617563, 4.379528057220093196, 33.54275706135234714 ) ) ;
#199662 = CARTESIAN_POINT ( 'NONE',  ( 21.52544592524344225, -5.823673210054117533, 103.5405762719810383 ) ) ;
#199664 = EDGE_CURVE ( 'NONE', #44725, #50285, #150851, .T. ) ;
#199665 = CARTESIAN_POINT ( 'NONE',  ( -21.52544592524343514, 5.823673210054127303, 31.04057627198102409 ) ) ;
#199666 = CARTESIAN_POINT ( 'NONE',  ( -15.80617190586768217, 15.72974639402176855, 98.12609039468570415 ) ) ;
#199667 = CARTESIAN_POINT ( 'NONE',  ( 19.02544592524343514, -5.153800228976328945, 88.54057627198102409 ) ) ;
#199668 = CARTESIAN_POINT ( 'NONE',  ( -5.153800228976328057, -19.02544592524343514, 37.29057627198102409 ) ) ;
#199669 = CARTESIAN_POINT ( 'NONE',  ( 19.02544592524343514, -5.153800228976328945, 98.54057627198100988 ) ) ;
#199670 = CARTESIAN_POINT ( 'NONE',  ( -19.03943276465977164, 0.05219959533909376836, 71.24890960531435269 ) ) ;
#199671 = CARTESIAN_POINT ( 'NONE',  ( -16.53943276465976808, -0.05219959533934237506, 18.75109039468568639 ) ) ;
#199672 = DIRECTION ( 'NONE',  ( 1.000000000000000000, 0.000000000000000000, 0.000000000000000000 ) ) ;
#199673 = CARTESIAN_POINT ( 'NONE',  ( -16.51473224551082808, 9.474510206698731452, 53.33442372801900433 ) ) ;
#199675 = CARTESIAN_POINT ( 'NONE',  ( -5.719274019375978568, 21.55341960407610458, 30.20724293864769550 ) ) ;
#199674 = CARTESIAN_POINT ( 'NONE',  ( -10.72451020669870658, -18.67979575497194134, 104.5844237280190185 ) ) ;
#199677 = ADVANCED_FACE ( 'NONE', ( #15953 ), #181391, .F. ) ;
#199676 = CARTESIAN_POINT ( 'NONE',  ( 12.14591786802327356, -12.06949235617739191, 100.6260903946857184 ) ) ;
#199678 = CARTESIAN_POINT ( 'NONE',  ( 1.300000000000000044, 1.082531754730548856, 0.6250000000000006661 ) ) ;
#199679 = CARTESIAN_POINT ( 'NONE',  ( -19.02544592524334988, -5.153800228976617603, 68.95942372801896170 ) ) ;
#199680 = CARTESIAN_POINT ( 'NONE',  ( 16.46253265017146816, 9.564922557961045513, 26.66775706135234003 ) ) ;
#199681 = CARTESIAN_POINT ( 'NONE',  ( 22.06725540229016502, -16.90544345524162395, 140.0000000000001421 ) ) ;
#199682 = CARTESIAN_POINT ( 'NONE',  ( -13.97604488694527625, -13.89961937509977652, 36.87390960531436690 ) ) ;
#199683 = CARTESIAN_POINT ( 'NONE',  ( 16.53943276465976808, -0.05219959533910856209, 38.74890960531435979 ) ) ;
#199684 = CARTESIAN_POINT ( 'NONE',  ( -16.52216118717206328, -7.221426719304512964, 111.0759902104699108 ) ) ;
#199685 = CARTESIAN_POINT ( 'NONE',  ( -4.483927247898539470, -16.52544592524342804, 32.29057627198102409 ) ) ;
#199686 = CARTESIAN_POINT ( 'NONE',  ( 8.388830574159379737E-16, 13.70000000000001528, -60.44446360152740283 ) ) ;
#199687 = CARTESIAN_POINT ( 'NONE',  ( -0.05219959533934338120, 16.53943276465976808, 92.50109039468567573 ) ) ;
#199688 = CARTESIAN_POINT ( 'NONE',  ( 19.05341960407611168, 5.049401038298154454, 38.95724293864767418 ) ) ;
#199689 = CARTESIAN_POINT ( 'NONE',  ( 21.55341960407619695, -5.719274019375665929, 106.0427570613523471 ) ) ;
#199690 = CARTESIAN_POINT ( 'NONE',  ( 8.314922557961029526, -14.29746914071037800, 25.41775706135235779 ) ) ;
#199692 = ORIENTED_EDGE ( 'NONE', *, *, #27064, .T. ) ;
#199691 = CARTESIAN_POINT ( 'NONE',  ( -21.52544592524334988, -5.823673210054445271, 73.95942372801901854 ) ) ;
#199693 = CARTESIAN_POINT ( 'NONE',  ( -16.46253265017146816, -9.564922557961047289, 54.16775706135234003 ) ) ;
#199694 = CARTESIAN_POINT ( 'NONE',  ( 19.05341960407611168, 5.049401038298154454, 93.95724293864769550 ) ) ;
#199695 = CARTESIAN_POINT ( 'NONE',  ( 5.153800228976335163, 19.02544592524342804, 84.79057627198099567 ) ) ;
#199696 = CARTESIAN_POINT ( 'NONE',  ( 22.81625015709509441, 31.40387420917330275, -9.324999997268813345 ) ) ;
#199697 = CARTESIAN_POINT ( 'NONE',  ( -21.52544592524343514, 5.823673210054127303, 106.0405762719810525 ) ) ;
#199698 = CARTESIAN_POINT ( 'NONE',  ( -4.379528057220328563, 16.55341960407611168, 65.20724293864768129 ) ) ;
#199699 = CARTESIAN_POINT ( 'NONE',  ( 0.05219959533907565091, 21.53943276465977519, 64.99890960531435269 ) ) ;
#199700 = CARTESIAN_POINT ( 'NONE',  ( -19.05341960407611168, -5.049401038298163336, 61.45724293864769550 ) ) ;
#199702 = CARTESIAN_POINT ( 'NONE',  ( 0.05219959533934541429, -16.53943276465976808, 95.00109039468568994 ) ) ;
#199701 = CARTESIAN_POINT ( 'NONE',  ( 21.53943276465977519, -0.05219959533907433946, 103.7489096053143669 ) ) ;
#199703 = VERTEX_POINT ( 'NONE', #186310 ) ;
#199704 = CARTESIAN_POINT ( 'NONE',  ( 13.89961937509977652, -13.97604488694527269, 58.12390960531436690 ) ) ;
#199705 = EDGE_CURVE ( 'NONE', #144934, #93307, #192011, .T. ) ;
#199707 = DIRECTION ( 'NONE',  ( 1.000000000000000000, 0.000000000000000000, 0.000000000000000000 ) ) ;
#199706 = CARTESIAN_POINT ( 'NONE',  ( 14.34966873604960469, 8.224510206698951720, 94.16557627198103830 ) ) ;
#199708 = CARTESIAN_POINT ( 'NONE',  ( 13.97604488694527802, 13.89961937509977652, 54.37390960531435979 ) ) ;
#199709 = CARTESIAN_POINT ( 'NONE',  ( -9.474510206698720793, -16.51473224551083518, 79.58442372801899012 ) ) ;
#199710 = CARTESIAN_POINT ( 'NONE',  ( 12.06949235617757843, -12.14591786802309237, 78.12390960531436690 ) ) ;
#199711 = CARTESIAN_POINT ( 'NONE',  ( 5.823673210054444382, -21.52544592524334988, 55.20942372801902565 ) ) ;
#199713 = CARTESIAN_POINT ( 'NONE',  ( 21.55341960407610458, 5.719274019375980345, 103.9572429386476813 ) ) ;
#199712 = CARTESIAN_POINT ( 'NONE',  ( -5.049401038298153566, 19.05341960407611168, 30.20724293864768839 ) ) ;
#199714 = CARTESIAN_POINT ( 'NONE',  ( -16.52544592524342804, 4.483927247898546575, 86.04057627198102409 ) ) ;
#199715 = CARTESIAN_POINT ( 'NONE',  ( 13.89961937509977652, -13.97604488694527269, 58.12390960531436690 ) ) ;
#199716 = CARTESIAN_POINT ( 'NONE',  ( 18.56101223717332260, 5.499999999999943157, 48.94978406935677384 ) ) ;
#199718 = CARTESIAN_POINT ( 'NONE',  ( -16.46253265017160317, 9.564922557960807481, 110.8322429386476955 ) ) ;
#199717 = CARTESIAN_POINT ( 'NONE',  ( -9.564922557961040184, 16.46253265017147172, 92.91775706135233293 ) ) ;
#199719 = CARTESIAN_POINT ( 'NONE',  ( 15.72974639402176855, 15.80617190586768217, 41.87609039468568284 ) ) ;
#199720 = CARTESIAN_POINT ( 'NONE',  ( -0.05219959533909027116, -19.03943276465977164, 82.49890960531436690 ) ) ;
#199721 = CARTESIAN_POINT ( 'NONE',  ( 5.153800228976615827, -19.02544592524334988, 65.20942372801900433 ) ) ;
#199722 = CARTESIAN_POINT ( 'NONE',  ( -19.05341960407611168, -5.049401038298163336, 61.45724293864769550 ) ) ;
#199723 = CARTESIAN_POINT ( 'NONE',  ( -12.06949235617756955, 12.14591786802309770, 80.62390960531438111 ) ) ;
#199724 = CARTESIAN_POINT ( 'NONE',  ( -16.55341960407611168, -4.379528057220339221, 66.45724293864768129 ) ) ;
#199725 = CARTESIAN_POINT ( 'NONE',  ( 19.05341960407611168, 5.049401038298154454, 93.95724293864769550 ) ) ;
#199726 = CARTESIAN_POINT ( 'NONE',  ( -21.52544592524343514, 5.823673210054127303, 106.0405762719810525 ) ) ;
#199727 = CARTESIAN_POINT ( 'NONE',  ( -19.05341960407611168, -5.049401038298163336, 86.45724293864769550 ) ) ;
#199728 = CARTESIAN_POINT ( 'NONE',  ( -9.564922557961040184, 16.46253265017147172, 32.91775706135233293 ) ) ;
#199731 = CARTESIAN_POINT ( 'NONE',  ( -4.379528057220328563, 16.55341960407611168, 105.2072429386477097 ) ) ;
#199730 = CARTESIAN_POINT ( 'NONE',  ( 12.06949235617757843, -12.14591786802309237, 28.12390960531435979 ) ) ;
#199729 = CARTESIAN_POINT ( 'NONE',  ( 0.05219959533909260263, 19.03943276465977164, 39.99890960531436690 ) ) ;
#199732 = VERTEX_POINT ( 'NONE', #96254 ) ;
#199733 = CARTESIAN_POINT ( 'NONE',  ( -21.52544592524334988, -5.823673210054445271, 43.95942372801902565 ) ) ;
#199734 = CARTESIAN_POINT ( 'NONE',  ( -5.049401038297874678, -19.05341960407617918, 69.79275706135233293 ) ) ;
#199735 = CARTESIAN_POINT ( 'NONE',  ( 4.483927247898545687, 16.52544592524342804, 39.79057627198103830 ) ) ;
#199736 = CARTESIAN_POINT ( 'NONE',  ( -10.81492255796078084, -18.62759615963271287, 87.08224293864769550 ) ) ;
#199737 = CARTESIAN_POINT ( 'NONE',  ( 0.05219959533907565091, 21.53943276465977519, 24.99890960531435624 ) ) ;
#199738 = CARTESIAN_POINT ( 'NONE',  ( 16.53943276465976808, -0.05219959533910856209, 68.74890960531435269 ) ) ;
#199739 = CARTESIAN_POINT ( 'NONE',  ( -19.05341960407611168, -5.049401038298163336, 31.45724293864769550 ) ) ;
#199740 = CARTESIAN_POINT ( 'NONE',  ( 9.474510206698729675, 16.51473224551082808, 27.08442372801900433 ) ) ;
#199741 = CARTESIAN_POINT ( 'NONE',  ( 16.52544592524335698, 4.483927247898782831, 106.4594237280190328 ) ) ;
#199742 = CARTESIAN_POINT ( 'NONE',  ( 16.55341960407618274, -4.379528057220086978, 61.04275706135234714 ) ) ;
#199743 = CARTESIAN_POINT ( 'NONE',  ( -5.823673210054116645, -21.52544592524344225, 32.29057627198102409 ) ) ;
#199744 = CARTESIAN_POINT ( 'NONE',  ( 21.53943276465977519, 0.05219959533937863772, 106.2510903946856757 ) ) ;
#199745 = CARTESIAN_POINT ( 'NONE',  ( -16.51473224551069308, -9.474510206698971260, 76.66557627198103830 ) ) ;
#199746 = CARTESIAN_POINT ( 'NONE',  ( -4.379528057220086978, -16.55341960407618274, 79.79275706135236135 ) ) ;
#199747 = CARTESIAN_POINT ( 'NONE',  ( 19.02544592524343514, -5.153800228976328945, 23.54057627198102054 ) ) ;
#199748 = CARTESIAN_POINT ( 'NONE',  ( 4.379528057220339221, -16.55341960407611168, 32.70724293864770260 ) ) ;
#199750 = CARTESIAN_POINT ( 'NONE',  ( 9.564922557960805705, 16.46253265017160317, 89.58224293864769550 ) ) ;
#199749 = CARTESIAN_POINT ( 'NONE',  ( -19.02544592524342804, 5.153800228976336051, 106.0405762719810241 ) ) ;
#199751 = CARTESIAN_POINT ( 'NONE',  ( 9.474510206698971260, -16.51473224551069308, 102.9155762719810241 ) ) ;
#199752 = CARTESIAN_POINT ( 'NONE',  ( -0.05219959533910754901, -16.53943276465976808, 62.49890960531436690 ) ) ;
#199753 = CARTESIAN_POINT ( 'NONE',  ( -16.52544592524342804, 4.483927247898546575, 31.04057627198102409 ) ) ;
#199754 = ORIENTED_EDGE ( 'NONE', *, *, #125272, .T. ) ;
#199755 = CARTESIAN_POINT ( 'NONE',  ( -8.314922557960811034, -14.29746914071050412, 52.08224293864768839 ) ) ;
#199757 = CARTESIAN_POINT ( 'NONE',  ( 13.97604488694548053, -13.89961937509957401, 60.62609039468566152 ) ) ;
#199756 = CARTESIAN_POINT ( 'NONE',  ( 12.06949235617739724, 12.14591786802326823, 41.87609039468568284 ) ) ;
#199758 = CARTESIAN_POINT ( 'NONE',  ( 19.02544592524334988, 5.153800228976608722, 46.45942372801899012 ) ) ;
#199759 = CARTESIAN_POINT ( 'NONE',  ( 16.46253265017160672, -9.564922557960803928, 88.33224293864769550 ) ) ;
#199760 = CARTESIAN_POINT ( 'NONE',  ( 5.153800228976615827, -19.02544592524334988, 60.20942372801899012 ) ) ;
#199761 = CARTESIAN_POINT ( 'NONE',  ( 17.14385361876520264, -23.59649016807271238, 144.0750000027311444 ) ) ;
#199762 = CARTESIAN_POINT ( 'NONE',  ( -5.049401038297874678, -19.05341960407617918, 59.79275706135231871 ) ) ;
#199764 = CARTESIAN_POINT ( 'NONE',  ( 0.05219959533934541429, -16.53943276465976808, 80.00109039468568994 ) ) ;
#199763 = CARTESIAN_POINT ( 'NONE',  ( 5.049401038297881783, 19.05341960407617563, 92.29275706135234714 ) ) ;
#199765 = CARTESIAN_POINT ( 'NONE',  ( 27.73933785331498214, 9.013057229001095294, 148.4750000027311785 ) ) ;
#199766 = CARTESIAN_POINT ( 'NONE',  ( -13.97604488694527625, -13.89961937509977652, 21.87390960531435979 ) ) ;
#199767 = CARTESIAN_POINT ( 'NONE',  ( -5.153800228976328057, -19.02544592524343514, 112.2905762719810099 ) ) ;
#199768 = CARTESIAN_POINT ( 'NONE',  ( 21.52544592524334988, 5.823673210054432836, 36.45942372801901143 ) ) ;
#199769 = CARTESIAN_POINT ( 'NONE',  ( 0.05219959533936267826, -19.03943276465977164, 110.0010903946856757 ) ) ;
#199771 = CARTESIAN_POINT ( 'NONE',  ( -9.564922557960796823, -16.46253265017161027, 57.08224293864769550 ) ) ;
#199770 = CARTESIAN_POINT ( 'NONE',  ( 17.50000000000000000, -3.471454075611694723, 106.9833258114436347 ) ) ;
#199772 = CARTESIAN_POINT ( 'NONE',  ( 5.153800228976335163, 19.02544592524342804, 109.7905762719810099 ) ) ;
#199774 = CARTESIAN_POINT ( 'NONE',  ( 19.02544592524343514, -5.153800228976328945, 58.54057627198102409 ) ) ;
#199773 = CARTESIAN_POINT ( 'NONE',  ( -12.06949235617756955, 12.14591786802309770, 55.62390960531436690 ) ) ;
#199775 = CARTESIAN_POINT ( 'NONE',  ( 16.46253265017160672, -9.564922557960803928, 73.33224293864769550 ) ) ;
#199776 = CARTESIAN_POINT ( 'NONE',  ( 19.03943276465977164, 0.05219959533936151252, 76.25109039468566152 ) ) ;
#199777 = CARTESIAN_POINT ( 'NONE',  ( -15.80617190586745835, -15.72974639402198527, 56.87390960531436690 ) ) ;
#199778 = CARTESIAN_POINT ( 'NONE',  ( -4.483927247898539470, -16.52544592524342804, 107.2905762719810525 ) ) ;
#199779 = CARTESIAN_POINT ( 'NONE',  ( -19.05341960407617563, 5.049401038297882671, 48.54275706135233293 ) ) ;
#199780 = CARTESIAN_POINT ( 'NONE',  ( 19.02544592524343514, -5.153800228976328945, 83.54057627198100988 ) ) ;
#199781 = CARTESIAN_POINT ( 'NONE',  ( -18.62759615963270932, 10.81492255796079327, 70.83224293864770971 ) ) ;
#199783 = CARTESIAN_POINT ( 'NONE',  ( -9.474510206698720793, -16.51473224551083518, 29.58442372801900433 ) ) ;
#199782 = CARTESIAN_POINT ( 'NONE',  ( -16.53943276465976808, 0.05219959533911058130, 86.24890960531436690 ) ) ;
#199784 = CARTESIAN_POINT ( 'NONE',  ( -18.67979575497178146, -10.72451020669898902, 71.66557627198100988 ) ) ;
#199785 = CARTESIAN_POINT ( 'NONE',  ( -15.80617190586745835, -15.72974639402198527, 61.87390960531436690 ) ) ;
#199786 = CARTESIAN_POINT ( 'NONE',  ( 5.719274019375991003, -21.55341960407610458, 37.70724293864769550 ) ) ;
#199787 = CARTESIAN_POINT ( 'NONE',  ( -0.05219959533937732626, 21.53943276465977519, 92.50109039468567573 ) ) ;
#199788 = CARTESIAN_POINT ( 'NONE',  ( -13.89961937509977652, 13.97604488694528158, 65.62390960531436690 ) ) ;
#199789 = CARTESIAN_POINT ( 'NONE',  ( -5.049401038298153566, 19.05341960407611168, 25.20724293864768484 ) ) ;
#199790 = CARTESIAN_POINT ( 'NONE',  ( 21.52544592524334988, 5.823673210054432836, 26.45942372801901854 ) ) ;
#199792 = EDGE_CURVE ( 'NONE', #128521, #59885, #68811, .T. ) ;
#199791 = CARTESIAN_POINT ( 'NONE',  ( 1.322848289251850051, 15.93242547297147738, -61.66673749439198104 ) ) ;
#199793 = CARTESIAN_POINT ( 'NONE',  ( 18.62759615963255655, 10.81492255796105972, 41.66775706135235424 ) ) ;
#199794 = CARTESIAN_POINT ( 'NONE',  ( 13.97604488694527802, 13.89961937509977652, 39.37390960531435269 ) ) ;
#199795 = CARTESIAN_POINT ( 'NONE',  ( -21.55341960407610458, -5.719274019375992779, 106.4572429386477097 ) ) ;
#199796 = CARTESIAN_POINT ( 'NONE',  ( -16.51473224551082808, 9.474510206698731452, 53.33442372801900433 ) ) ;
#199797 = CARTESIAN_POINT ( 'NONE',  ( 16.51473224551069308, 9.474510206698969483, 39.16557627198103120 ) ) ;
#199798 = CARTESIAN_POINT ( 'NONE',  ( -19.05341960407611168, -5.049401038298163336, 21.45724293864768839 ) ) ;
#199799 = CARTESIAN_POINT ( 'NONE',  ( 16.79442582748877655, -6.866825916363270110, 21.31585826573617126 ) ) ;
#199800 = CARTESIAN_POINT ( 'NONE',  ( -14.34966873604972548, 8.224510206698743886, 58.33442372801901143 ) ) ;
#199801 = CARTESIAN_POINT ( 'NONE',  ( 0.05219959533909260263, 19.03943276465977164, 24.99890960531435269 ) ) ;
#199802 = CARTESIAN_POINT ( 'NONE',  ( -25.47140278216090081, -9.703455644540127878, 170.7619267275368600 ) ) ;
#199803 = CARTESIAN_POINT ( 'NONE',  ( 16.46253265017160672, -9.564922557960803928, 88.33224293864769550 ) ) ;
#199804 = CARTESIAN_POINT ( 'NONE',  ( 14.29746914071049879, -8.314922557960816363, 103.3322429386476955 ) ) ;
#199805 = CARTESIAN_POINT ( 'NONE',  ( -5.823673210054116645, -21.52544592524344225, 62.29057627198102409 ) ) ;
#199806 = CARTESIAN_POINT ( 'NONE',  ( 16.52544592524335698, 4.483927247898782831, 51.45942372801901854 ) ) ;
#199807 = CARTESIAN_POINT ( 'NONE',  ( 21.55341960407619695, -5.719274019375665929, 96.04275706135236135 ) ) ;
#199808 = CARTESIAN_POINT ( 'NONE',  ( 16.51473224551069308, 9.474510206698969483, 29.16557627198103475 ) ) ;
#199809 = CARTESIAN_POINT ( 'NONE',  ( -12.06949235617739369, -12.14591786802326823, 109.3760903946857042 ) ) ;
#199810 = CARTESIAN_POINT ( 'NONE',  ( 16.53943276465976808, -0.05219959533910856209, 53.74890960531437401 ) ) ;
#199811 = CARTESIAN_POINT ( 'NONE',  ( 19.05341960407611168, 5.049401038298154454, 53.95724293864770260 ) ) ;
#199812 = CARTESIAN_POINT ( 'NONE',  ( 10.72451020669871369, 18.67979575497193778, 107.0844237280190043 ) ) ;
#199813 = CARTESIAN_POINT ( 'NONE',  ( -21.52544592524334988, -5.823673210054445271, 28.95942372801902209 ) ) ;
#199814 = CARTESIAN_POINT ( 'NONE',  ( 5.719274019375673035, 21.55341960407619339, 77.29275706135234714 ) ) ;
#199815 = CARTESIAN_POINT ( 'NONE',  ( 16.53943276465976808, 0.05219959533934440121, 56.25109039468568284 ) ) ;
#199816 = CARTESIAN_POINT ( 'NONE',  ( -8.224510206698735004, -14.34966873604973081, 29.58442372801901854 ) ) ;
#199818 = CARTESIAN_POINT ( 'NONE',  ( -10.81492255796105439, 18.62759615963255655, 92.91775706135236135 ) ) ;
#199817 = CARTESIAN_POINT ( 'NONE',  ( -8.224510206698948167, 14.34966873604960824, 80.41557627198103830 ) ) ;
#199819 = CARTESIAN_POINT ( 'NONE',  ( -12.14591786802309592, -12.06949235617757132, 21.87390960531436690 ) ) ;
#199820 = FACE_OUTER_BOUND ( 'NONE', #121027, .T. ) ;
#199821 = CARTESIAN_POINT ( 'NONE',  ( -12.06949235617739369, -12.14591786802326823, 34.37609039468568284 ) ) ;
#199822 = CARTESIAN_POINT ( 'NONE',  ( 16.55341960407611168, 4.379528057220329451, 38.95724293864768839 ) ) ;
#199823 = CARTESIAN_POINT ( 'NONE',  ( -0.05219959533934338120, 16.53943276465976808, 87.50109039468568994 ) ) ;
#199824 = CARTESIAN_POINT ( 'NONE',  ( -9.564922557960796823, -16.46253265017161027, 97.08224293864769550 ) ) ;
#199825 = CARTESIAN_POINT ( 'NONE',  ( 15.72974639402199770, -15.80617190586745480, 23.12390960531436335 ) ) ;
#199826 = CARTESIAN_POINT ( 'NONE',  ( -10.72451020669870658, -18.67979575497194134, 94.58442372801901854 ) ) ;
#199827 = EDGE_CURVE ( 'NONE', #40357, #142969, #191780, .T. ) ;
#199828 = CARTESIAN_POINT ( 'NONE',  ( -16.55341960407617563, 4.379528057220093196, 103.5427570613523613 ) ) ;
#199829 = CARTESIAN_POINT ( 'NONE',  ( -16.52544592524342804, 4.483927247898546575, 71.04057627198103830 ) ) ;
#199830 = CARTESIAN_POINT ( 'NONE',  ( 13.89961937509977652, -13.97604488694527269, 83.12390960531436690 ) ) ;
#199831 = VERTEX_POINT ( 'NONE', #171125 ) ;
#199832 = CARTESIAN_POINT ( 'NONE',  ( 8.224510206698742110, 14.34966873604972548, 37.08442372801901143 ) ) ;
#199833 = CARTESIAN_POINT ( 'NONE',  ( -19.03943276465977164, 0.05219959533909376836, 41.24890960531435269 ) ) ;
#199834 = CARTESIAN_POINT ( 'NONE',  ( 16.46253265017160672, -9.564922557960803928, 98.33224293864769550 ) ) ;
#199836 = CARTESIAN_POINT ( 'NONE',  ( 22.81625015709509441, 31.40387420917330275, -3.324999997268812901 ) ) ;
#199835 = CARTESIAN_POINT ( 'NONE',  ( -0.05219959533934338120, 16.53943276465976808, 32.50109039468568284 ) ) ;
#199837 = CARTESIAN_POINT ( 'NONE',  ( 19.05341960407617918, -5.049401038297876454, 31.04275706135232227 ) ) ;
#199838 = CARTESIAN_POINT ( 'NONE',  ( 14.29746914071037800, 8.314922557961029526, 91.66775706135234714 ) ) ;
#199839 = CARTESIAN_POINT ( 'NONE',  ( -16.51473224551069308, -9.474510206698971260, 36.66557627198102409 ) ) ;
#199840 = CARTESIAN_POINT ( 'NONE',  ( -8.314922557961024197, 14.29746914071037800, 82.91775706135234714 ) ) ;
#199841 = CARTESIAN_POINT ( 'NONE',  ( 4.379528057220092307, 16.55341960407617563, 72.29275706135236135 ) ) ;
#199842 = CARTESIAN_POINT ( 'NONE',  ( -19.05341960407617563, 5.049401038297882671, 88.54275706135230450 ) ) ;
#199843 = CARTESIAN_POINT ( 'NONE',  ( -19.03943276465977164, -0.05219959533935918106, 28.75109039468566507 ) ) ;
#199844 = CARTESIAN_POINT ( 'NONE',  ( 13.97604488694527802, 13.89961937509977652, 54.37390960531435979 ) ) ;
#199845 = EDGE_CURVE ( 'NONE', #161202, #93070, #44381, .T. ) ;
#199846 = CARTESIAN_POINT ( 'NONE',  ( 4.483927247898545687, 16.52544592524342804, 79.79057627198102409 ) ) ;
#199847 = CARTESIAN_POINT ( 'NONE',  ( -13.89961937509957401, -13.97604488694547875, 59.37609039468566863 ) ) ;
#199848 = CARTESIAN_POINT ( 'NONE',  ( -18.62759615963270932, 10.81492255796079327, 50.83224293864770971 ) ) ;
#199849 = CARTESIAN_POINT ( 'NONE',  ( 19.05341960407617918, -5.049401038297876454, 31.04275706135232227 ) ) ;
#199850 = CARTESIAN_POINT ( 'NONE',  ( -19.02544592524342804, 5.153800228976336051, 106.0405762719810241 ) ) ;
#199851 = CARTESIAN_POINT ( 'NONE',  ( -21.55341960407610458, -5.719274019375992779, 81.45724293864769550 ) ) ;
#199852 = CARTESIAN_POINT ( 'NONE',  ( 19.03943276465977164, -0.05219959533909143690, 103.7489096053143669 ) ) ;
#199853 = CARTESIAN_POINT ( 'NONE',  ( -9.564922557961040184, 16.46253265017147172, 97.91775706135233293 ) ) ;
#199854 = CARTESIAN_POINT ( 'NONE',  ( 5.153800228976335163, 19.02544592524342804, 114.7905762719810241 ) ) ;
#199855 = CARTESIAN_POINT ( 'NONE',  ( 4.483927247898790824, -16.52544592524335698, 20.20942372801900788 ) ) ;
#199856 = CARTESIAN_POINT ( 'NONE',  ( -0.05219959533909027116, -19.03943276465977164, 37.49890960531436690 ) ) ;
#199857 = CARTESIAN_POINT ( 'NONE',  ( -5.153800228976328057, -19.02544592524343514, 97.29057627198099567 ) ) ;
#199858 = CARTESIAN_POINT ( 'NONE',  ( 21.55341960407610458, 5.719274019375980345, 78.95724293864769550 ) ) ;
#199859 = CIRCLE ( 'NONE', #148191, 2.500000000000002220 ) ;
#199860 = CARTESIAN_POINT ( 'NONE',  ( 8.314922557961029526, -14.29746914071037800, 60.41775706135235424 ) ) ;
#199861 = CARTESIAN_POINT ( 'NONE',  ( 18.67979575497194134, -10.72451020669871369, 60.83442372801901854 ) ) ;
#199863 = CARTESIAN_POINT ( 'NONE',  ( 21.55341960407619695, -5.719274019375665929, 106.0427570613523471 ) ) ;
#199862 = CARTESIAN_POINT ( 'NONE',  ( -5.049401038297874678, -19.05341960407617918, 109.7927570613523187 ) ) ;
#199865 = CARTESIAN_POINT ( 'NONE',  ( -0.05219959533934338120, 16.53943276465976808, 112.5010903946857042 ) ) ;
#199864 = B_SPLINE_CURVE_WITH_KNOTS ( 'NONE', 3,
 ( #144440, #159606, #35280, #116110, #96935, #38275, #129262, #20107, #177798, #190957, #143438, #99929, #4925, #66607, #128271, #147454, #161614, #39268, #145436, #65615 ),
 .UNSPECIFIED., .F., .F.,
 ( 4, 2, 2, 2, 2, 2, 2, 2, 2, 4 ),
 ( 3.469446951953614189E-18, 0.0004987090165372576323, 0.0009974180330745117951, 0.001246772541343138660, 0.001496127049611765741, 0.001994836066149053514, 0.002493545082686341070, 0.002742899590954985499, 0.002992254099223629060, 0.003989672132298176417 ),
 .UNSPECIFIED. ) ;
#199866 = CARTESIAN_POINT ( 'NONE',  ( -5.719274019375978568, 21.55341960407610458, 100.2072429386476955 ) ) ;
#199867 = CARTESIAN_POINT ( 'NONE',  ( -8.224510206698948167, 14.34966873604960824, 35.41557627198102409 ) ) ;
#199868 = CARTESIAN_POINT ( 'NONE',  ( 19.02544592524334988, 5.153800228976608722, 76.45942372801897591 ) ) ;
#199869 = CARTESIAN_POINT ( 'NONE',  ( -21.55341960407619339, 5.719274019375674811, 53.54275706135234714 ) ) ;
#199870 = CARTESIAN_POINT ( 'NONE',  ( -19.02544592524334988, -5.153800228976617603, 33.95942372801897591 ) ) ;
#199871 = CARTESIAN_POINT ( 'NONE',  ( -8.224510206698948167, 14.34966873604960824, 110.4155762719810383 ) ) ;
#199872 = CARTESIAN_POINT ( 'NONE',  ( -10.72451020669898014, 18.67979575497178502, 25.41557627198103120 ) ) ;
#199873 = CARTESIAN_POINT ( 'NONE',  ( 8.224510206698953496, -14.34966873604960469, 32.91557627198102409 ) ) ;
#199874 = CARTESIAN_POINT ( 'NONE',  ( -21.53943276465977519, -0.05219959533937600094, 98.75109039468568994 ) ) ;
#199875 = CARTESIAN_POINT ( 'NONE',  ( 16.55341960407618274, -4.379528057220086978, 66.04275706135236135 ) ) ;
#199876 = CARTESIAN_POINT ( 'NONE',  ( -8.224510206698948167, 14.34966873604960824, 25.41557627198103120 ) ) ;
#199877 = CARTESIAN_POINT ( 'NONE',  ( -5.719274019375665041, -21.55341960407619695, 59.79275706135234714 ) ) ;
#199878 = CARTESIAN_POINT ( 'NONE',  ( 10.81492255796106328, -18.62759615963255655, 55.41775706135234714 ) ) ;
#199879 = VERTEX_POINT ( 'NONE', #114408 ) ;
#199880 = CARTESIAN_POINT ( 'NONE',  ( 5.153800228976335163, 19.02544592524342804, 24.79057627198102765 ) ) ;
#199881 = CARTESIAN_POINT ( 'NONE',  ( -10.72451020669870658, -18.67979575497194134, 44.58442372801901854 ) ) ;
#199882 = CARTESIAN_POINT ( 'NONE',  ( -16.53943276465976808, 0.05219959533911058130, 111.2489096053143669 ) ) ;
#199883 = CARTESIAN_POINT ( 'NONE',  ( -19.03943276465977164, 0.05219959533909376836, 36.24890960531436690 ) ) ;
#199884 = CARTESIAN_POINT ( 'NONE',  ( 4.379528057220339221, -16.55341960407611168, 77.70724293864770971 ) ) ;
#199885 = CARTESIAN_POINT ( 'NONE',  ( -5.153800228976328057, -19.02544592524343514, 72.29057627198102409 ) ) ;
#199886 = CARTESIAN_POINT ( 'NONE',  ( -4.379528057220328563, 16.55341960407611168, 25.20724293864769550 ) ) ;
#199887 = CARTESIAN_POINT ( 'NONE',  ( 21.52544592524344225, -5.823673210054117533, 53.54057627198103120 ) ) ;
#199888 = CARTESIAN_POINT ( 'NONE',  ( -4.483927247898539470, -16.52544592524342804, 97.29057627198105251 ) ) ;
#199889 = CARTESIAN_POINT ( 'NONE',  ( 21.52544592524344225, -5.823673210054117533, 103.5405762719810383 ) ) ;
#199890 = CARTESIAN_POINT ( 'NONE',  ( -19.03943276465977164, 0.05219959533909376836, 106.2489096053143669 ) ) ;
#199892 = CARTESIAN_POINT ( 'NONE',  ( -16.46253265017146816, -9.564922557961047289, 99.16775706135233293 ) ) ;
#199891 = CARTESIAN_POINT ( 'NONE',  ( -16.46253265017160317, 9.564922557960807481, 70.83224293864770971 ) ) ;
#199893 = CARTESIAN_POINT ( 'NONE',  ( 15.80617190586746368, 15.72974639402197994, 54.37390960531435979 ) ) ;
#199894 = CARTESIAN_POINT ( 'NONE',  ( -18.62759615963255300, -10.81492255796106328, 84.16775706135234714 ) ) ;
#199895 = CARTESIAN_POINT ( 'NONE',  ( -0.05219959533909027116, -19.03943276465977164, 72.49890960531435269 ) ) ;
#199896 = CARTESIAN_POINT ( 'NONE',  ( 16.46253265017160672, -9.564922557960803928, 103.3322429386476955 ) ) ;
#199897 = CARTESIAN_POINT ( 'NONE',  ( 4.379528057220092307, 16.55341960407617563, 72.29275706135236135 ) ) ;
#199898 = CARTESIAN_POINT ( 'NONE',  ( 5.719274019375673035, 21.55341960407619339, 62.29275706135236845 ) ) ;
#199899 = CARTESIAN_POINT ( 'NONE',  ( -15.72974639402176322, -15.80617190586768395, 89.37609039468568994 ) ) ;
#199900 = CARTESIAN_POINT ( 'NONE',  ( -10.81492255796078084, -18.62759615963271287, 107.0822429386476955 ) ) ;
#199901 = CARTESIAN_POINT ( 'NONE',  ( 12.06949235617739724, 12.14591786802326823, 71.87609039468568994 ) ) ;
#199902 = CARTESIAN_POINT ( 'NONE',  ( -15.80617190586745835, -15.72974639402198527, 71.87390960531438111 ) ) ;
#199903 = CARTESIAN_POINT ( 'NONE',  ( -19.05341960407617563, 5.049401038297882671, 48.54275706135233293 ) ) ;
#199904 = CARTESIAN_POINT ( 'NONE',  ( -5.719274019375978568, 21.55341960407610458, 40.20724293864769550 ) ) ;
#199906 = CARTESIAN_POINT ( 'NONE',  ( -8.224510206698948167, 14.34966873604960824, 25.41557627198103120 ) ) ;
#199905 = CARTESIAN_POINT ( 'NONE',  ( 9.564922557960805705, 16.46253265017160317, 84.58224293864769550 ) ) ;
#199907 = CYLINDRICAL_SURFACE ( 'NONE', #20852, 2.649999999999999911 ) ;
#199908 = CARTESIAN_POINT ( 'NONE',  ( 9.474510206698971260, -16.51473224551069308, 112.9155762719810383 ) ) ;
#199909 = CARTESIAN_POINT ( 'NONE',  ( -19.25176906914648356, -5.499999999999850786, 80.99927264242278113 ) ) ;
#199910 = CARTESIAN_POINT ( 'NONE',  ( -19.02544592524334988, -5.153800228976617603, 88.95942372801897591 ) ) ;
#199911 = CARTESIAN_POINT ( 'NONE',  ( -15.80617190586745835, -15.72974639402198527, 76.87390960531439532 ) ) ;
#199912 = CARTESIAN_POINT ( 'NONE',  ( 14.34966873604960469, 8.224510206698951720, 49.16557627198102409 ) ) ;
#199913 = CARTESIAN_POINT ( 'NONE',  ( 19.03943276465977164, 0.05219959533936151252, 106.2510903946856615 ) ) ;
#199914 = CARTESIAN_POINT ( 'NONE',  ( -0.05219959533909027116, -19.03943276465977164, 27.49890960531435624 ) ) ;
#199915 = CARTESIAN_POINT ( 'NONE',  ( 13.97604488694548053, -13.89961937509957401, 110.6260903946856615 ) ) ;
#199917 = CARTESIAN_POINT ( 'NONE',  ( -9.474510206698720793, -16.51473224551083518, 69.58442372801901854 ) ) ;
#199916 = CARTESIAN_POINT ( 'NONE',  ( -15.80617190586745835, -15.72974639402198527, 106.8739096053143811 ) ) ;
#199918 = CARTESIAN_POINT ( 'NONE',  ( -16.51473224551069308, -9.474510206698971260, 86.66557627198102409 ) ) ;
#199919 = CARTESIAN_POINT ( 'NONE',  ( -14.34966873604960291, -8.224510206698953496, 81.66557627198103830 ) ) ;
#199920 =( BOUNDED_CURVE ( )  B_SPLINE_CURVE ( 2, ( #106972, #171641, #108967, #148773, #167672, #87087, #183832, #138316, #169649, #31145, #45322 ),
 .UNSPECIFIED., .F., .T. ) 
 B_SPLINE_CURVE_WITH_KNOTS ( ( 3, 2, 2, 2, 2, 3 ),
 ( 0.5000000000000001110, 0.5200000000000001288, 0.5400000000000001465, 0.5600000000000001643, 0.5800000000000000711, 0.6000000000000000888 ),
 .UNSPECIFIED. ) 
 CURVE ( )  GEOMETRIC_REPRESENTATION_ITEM ( )  RATIONAL_B_SPLINE_CURVE ( ( 0.9999999999999997780, 0.9510565162951537532, 1.000000000000000000, 0.9510565162951535312, 1.000000000000000000, 0.9510565162951535312, 1.000000000000000000, 0.9510565162951535312, 1.000000000000000000, 0.9510565162951533091, 1.000000000000000222 ) ) 
 REPRESENTATION_ITEM ( '' )  );
#199921 = CARTESIAN_POINT ( 'NONE',  ( -9.564922557960796823, -16.46253265017161027, 57.08224293864769550 ) ) ;
#199922 = CARTESIAN_POINT ( 'NONE',  ( 4.483927247898545687, 16.52544592524342804, 69.79057627198102409 ) ) ;
#199923 = CARTESIAN_POINT ( 'NONE',  ( -5.153800228976328057, -19.02544592524343514, 27.29057627198103120 ) ) ;
#199924 = CARTESIAN_POINT ( 'NONE',  ( -36.78376627615639904, -4.378768456387976293, 48.34741972342521166 ) ) ;
#199925 = CARTESIAN_POINT ( 'NONE',  ( 12.14591786802309770, 12.06949235617756955, 39.37390960531436690 ) ) ;
#199926 = CARTESIAN_POINT ( 'NONE',  ( 5.153800228976335163, 19.02544592524342804, 94.79057627198103830 ) ) ;
#199927 = FACE_BOUND ( 'NONE', #10749, .T. ) ;
#199928 = CARTESIAN_POINT ( 'NONE',  ( -0.05219959533936034679, 19.03943276465977164, 47.50109039468566863 ) ) ;
#199929 = CARTESIAN_POINT ( 'NONE',  ( -16.55341960407617563, 4.379528057220093196, 63.54275706135234003 ) ) ;
#199930 = CARTESIAN_POINT ( 'NONE',  ( 5.823673210054125526, 21.52544592524343514, 59.79057627198103120 ) ) ;
#199931 = CARTESIAN_POINT ( 'NONE',  ( -13.97604488694547697, 13.89961937509957934, 23.12609039468565442 ) ) ;
#199932 = CARTESIAN_POINT ( 'NONE',  ( -5.153800228976328057, -19.02544592524343514, 82.29057627198103830 ) ) ;
#199933 = CARTESIAN_POINT ( 'NONE',  ( -22.39645207350164924, -22.70003318984301188, -45.66685071139480812 ) ) ;
#199934 = CARTESIAN_POINT ( 'NONE',  ( -5.719274019375978568, 21.55341960407610458, 35.20724293864768839 ) ) ;
#199935 = CARTESIAN_POINT ( 'NONE',  ( -9.564922557960796823, -16.46253265017161027, 57.08224293864769550 ) ) ;
#199936 = CARTESIAN_POINT ( 'NONE',  ( -15.80617190586768217, 15.72974639402176855, 58.12609039468568994 ) ) ;
#199937 = CARTESIAN_POINT ( 'NONE',  ( 16.52544592524342804, -4.483927247898539470, 108.5405762719810241 ) ) ;
#199940 = VERTEX_POINT ( 'NONE', #130579 ) ;
#199939 = CARTESIAN_POINT ( 'NONE',  ( -16.51473224551069308, -9.474510206698971260, 101.6655762719810241 ) ) ;
#199938 = CARTESIAN_POINT ( 'NONE',  ( 18.62759615963271287, -10.81492255796078972, 98.33224293864769550 ) ) ;
#199941 = CARTESIAN_POINT ( 'NONE',  ( 5.719274019375673035, 21.55341960407619339, 42.29275706135235424 ) ) ;
#199942 = VERTEX_POINT ( 'NONE', #39580 ) ;
#199943 = CARTESIAN_POINT ( 'NONE',  ( 5.153800228976335163, 19.02544592524342804, 94.79057627198103830 ) ) ;
#199944 = CARTESIAN_POINT ( 'NONE',  ( -13.89961937509977830, 13.97604488694528158, 90.62390960531433848 ) ) ;
#199945 = CARTESIAN_POINT ( 'NONE',  ( -5.823673210054116645, -21.52544592524344225, 92.29057627198103830 ) ) ;
#199946 = CARTESIAN_POINT ( 'NONE',  ( -5.153800228976328057, -19.02544592524343514, 47.29057627198102409 ) ) ;
#199947 = CARTESIAN_POINT ( 'NONE',  ( 8.314922557961029526, -14.29746914071037800, 20.41775706135234714 ) ) ;
#199948 = CARTESIAN_POINT ( 'NONE',  ( -36.91746825000001309, -11.99521256947794789, -5.024999997268813523 ) ) ;
#199949 = CARTESIAN_POINT ( 'NONE',  ( -13.97604488694527625, -13.89961937509977652, 31.87390960531435979 ) ) ;
#199950 = CARTESIAN_POINT ( 'NONE',  ( 21.55341960407619695, -5.719274019375665929, 101.0427570613523756 ) ) ;
#199952 = CARTESIAN_POINT ( 'NONE',  ( 5.823673210054444382, -21.52544592524334988, 50.20942372801901854 ) ) ;
#199951 = CARTESIAN_POINT ( 'NONE',  ( -0.05219959533909027116, -19.03943276465977164, 77.49890960531435269 ) ) ;
#199953 = CARTESIAN_POINT ( 'NONE',  ( 27.73933785331498925, -9.013057229001033122, 144.2750000027311899 ) ) ;
#199954 = CARTESIAN_POINT ( 'NONE',  ( -19.05341960407611168, -5.049401038298163336, 101.4572429386476955 ) ) ;
#199955 = CARTESIAN_POINT ( 'NONE',  ( 18.39639308325436318, 5.500000000000037303, 63.98252246182197212 ) ) ;
#199958 = CARTESIAN_POINT ( 'NONE',  ( 21.55341960407619695, -5.719274019375665929, 61.04275706135234714 ) ) ;
#199957 = CARTESIAN_POINT ( 'NONE',  ( 0.05219959533934541429, -16.53943276465976808, 65.00109039468568994 ) ) ;
#199956 = CARTESIAN_POINT ( 'NONE',  ( 12.14591786802327356, -12.06949235617739191, 35.62609039468568994 ) ) ;
#199959 = CARTESIAN_POINT ( 'NONE',  ( 18.67979575497194134, -10.72451020669871369, 75.83442372801900433 ) ) ;
#199960 = CARTESIAN_POINT ( 'NONE',  ( 12.06208868505712672, -11.49801227349071731, -59.15175176635164433 ) ) ;
#199961 = CARTESIAN_POINT ( 'NONE',  ( -19.02544592524334988, -5.153800228976617603, 103.9594237280190043 ) ) ;
#199962 = CARTESIAN_POINT ( 'NONE',  ( -19.03943276465977164, 0.05219959533909376836, 76.24890960531435269 ) ) ;
#199963 = CARTESIAN_POINT ( 'NONE',  ( -9.564922557960796823, -16.46253265017161027, 102.0822429386477097 ) ) ;
#199964 = CARTESIAN_POINT ( 'NONE',  ( -14.29746914071049879, 8.314922557960819915, 110.8322429386476955 ) ) ;
#199965 = CARTESIAN_POINT ( 'NONE',  ( -5.823673210054116645, -21.52544592524344225, 27.29057627198103120 ) ) ;
#199966 = CARTESIAN_POINT ( 'NONE',  ( 8.224510206698742110, 14.34966873604972548, 92.08442372801901854 ) ) ;
#199968 = CARTESIAN_POINT ( 'NONE',  ( -19.05341960407611168, -5.049401038298163336, 51.45724293864770260 ) ) ;
#199967 = CARTESIAN_POINT ( 'NONE',  ( 12.06949235617757843, -12.14591786802309237, 73.12390960531436690 ) ) ;
#199969 = CARTESIAN_POINT ( 'NONE',  ( -10.72451020669870658, -18.67979575497194134, 74.58442372801901854 ) ) ;
#199970 = CARTESIAN_POINT ( 'NONE',  ( 4.500000000000000888, -140.0000000000000000, 22.27940468532398910 ) ) ;
#199971 = CARTESIAN_POINT ( 'NONE',  ( 5.153800228976615827, -19.02544592524334988, 100.2094237280190043 ) ) ;
#199972 = CARTESIAN_POINT ( 'NONE',  ( -0.05219959533910754901, -16.53943276465976808, 77.49890960531433848 ) ) ;
#199973 = CARTESIAN_POINT ( 'NONE',  ( -15.72974639402176322, -15.80617190586768395, 29.37609039468568284 ) ) ;
#199974 = CARTESIAN_POINT ( 'NONE',  ( -10.81492255796078084, -18.62759615963271287, 57.08224293864769550 ) ) ;
#199975 = CARTESIAN_POINT ( 'NONE',  ( -28.82186960331499392, -9.364793116373526516, 140.0999999999999943 ) ) ;
#199976 = CARTESIAN_POINT ( 'NONE',  ( -5.429308488886486681E-15, 30.30510711980690175, 145.7500000054623115 ) ) ;
#199977 = CARTESIAN_POINT ( 'NONE',  ( 19.03943276465977164, -0.05219959533909143690, 88.74890960531436690 ) ) ;
#199978 = CARTESIAN_POINT ( 'NONE',  ( 16.55341960407611168, 4.379528057220329451, 48.95724293864770971 ) ) ;
#199979 = CARTESIAN_POINT ( 'NONE',  ( -16.55341960407611168, -4.379528057220339221, 41.45724293864769550 ) ) ;
#199980 = CARTESIAN_POINT ( 'NONE',  ( -14.34966873604972548, 8.224510206698743886, 98.33442372801901854 ) ) ;
#199981 = CARTESIAN_POINT ( 'NONE',  ( 13.97604488694548053, -13.89961937509957401, 55.62609039468566863 ) ) ;
#199982 = CARTESIAN_POINT ( 'NONE',  ( 17.26058549869088665, 6.457015423128624754, 48.87745837476069966 ) ) ;
#199983 = CARTESIAN_POINT ( 'NONE',  ( 13.89961937509977652, -13.97604488694527269, 108.1239096053143669 ) ) ;
#199984 = CARTESIAN_POINT ( 'NONE',  ( 12.14591786802309770, 12.06949235617756955, 79.37390960531436690 ) ) ;
#199985 = CARTESIAN_POINT ( 'NONE',  ( -5.153800228976607833, 19.02544592524334988, 37.70942372801899722 ) ) ;
#199987 = CARTESIAN_POINT ( 'NONE',  ( 10.72451020669898902, -18.67979575497178502, 32.91557627198102409 ) ) ;
#199986 = CARTESIAN_POINT ( 'NONE',  ( -16.51473224551069308, -9.474510206698971260, 31.66557627198102054 ) ) ;
#199988 = CARTESIAN_POINT ( 'NONE',  ( -18.62759615963270932, 10.81492255796079327, 70.83224293864770971 ) ) ;
#199989 = CARTESIAN_POINT ( 'NONE',  ( 8.314922557960818139, 14.29746914071049879, 99.58224293864770971 ) ) ;
#199990 = CARTESIAN_POINT ( 'NONE',  ( -4.483927247898782831, 16.52544592524335698, 47.70942372801902565 ) ) ;
#199991 = CARTESIAN_POINT ( 'NONE',  ( 18.62759615963255655, 10.81492255796105972, 46.66775706135234714 ) ) ;
#199992 = CARTESIAN_POINT ( 'NONE',  ( 8.314922557960818139, 14.29746914071049879, 89.58224293864768129 ) ) ;
#199993 = FACE_OUTER_BOUND ( 'NONE', #31159, .T. ) ;
#199994 = CARTESIAN_POINT ( 'NONE',  ( -17.26172910966779384, 6.454744622555852018, 50.80646908649227100 ) ) ;
#199995 = CARTESIAN_POINT ( 'NONE',  ( -18.67979575497178146, -10.72451020669898902, 36.66557627198103120 ) ) ;
#199996 = DIRECTION ( 'NONE',  ( -1.000000000000000000, 0.000000000000000000, 0.000000000000000000 ) ) ;
#199997 = CARTESIAN_POINT ( 'NONE',  ( -17.97182807773875268, 5.499999999999872990, 43.53038844047289047 ) ) ;
#199998 = CIRCLE ( 'NONE', #64459, 4.500000000000000000 ) ;
#200000 = CARTESIAN_POINT ( 'NONE',  ( 12.14591786802309770, 12.06949235617756955, 34.37390960531435979 ) ) ;
#199999 = CARTESIAN_POINT ( 'NONE',  ( -0.05219959533934338120, 16.53943276465976808, 37.50109039468568284 ) ) ;
#200001 = CARTESIAN_POINT ( 'NONE',  ( 0.05219959533907565091, 21.53943276465977519, 64.99890960531435269 ) ) ;
#200002 = CARTESIAN_POINT ( 'NONE',  ( -5.153800228976607833, 19.02544592524334988, 82.70942372801897591 ) ) ;
#200003 = CARTESIAN_POINT ( 'NONE',  ( -0.05219959533907301413, -21.53943276465977519, 67.49890960531436690 ) ) ;
#200004 = CARTESIAN_POINT ( 'NONE',  ( -21.16427095311448880, 10.71512246325695372, 170.2843762835011319 ) ) ;
#200005 = CARTESIAN_POINT ( 'NONE',  ( -14.29746914071037622, -8.314922557961029526, 54.16775706135235424 ) ) ;
#200007 = CARTESIAN_POINT ( 'NONE',  ( -9.474510206698964154, 16.51473224551069663, 95.41557627198102409 ) ) ;
#200006 = CARTESIAN_POINT ( 'NONE',  ( -13.89961937509977652, 13.97604488694528158, 35.62390960531435269 ) ) ;
#200008 = CARTESIAN_POINT ( 'NONE',  ( -13.89961937509977652, 13.97604488694528158, 40.62390960531435979 ) ) ;
#200009 = CARTESIAN_POINT ( 'NONE',  ( 12.14591786802309770, 12.06949235617756955, 114.3739096053143527 ) ) ;
#200010 = CARTESIAN_POINT ( 'NONE',  ( 36.99999999999933920, 1.011436372600181938E-12, 95.00000000000025580 ) ) ;
#200011 = CARTESIAN_POINT ( 'NONE',  ( 9.564922557960805705, 16.46253265017160317, 114.5822429386476955 ) ) ;
#200012 = CARTESIAN_POINT ( 'NONE',  ( -12.06949235617739369, -12.14591786802326823, 69.37609039468567573 ) ) ;
#200013 = CARTESIAN_POINT ( 'NONE',  ( -5.719274019375978568, 21.55341960407610458, 95.20724293864769550 ) ) ;
#200014 = CARTESIAN_POINT ( 'NONE',  ( -13.89961937509977652, 13.97604488694528158, 55.62390960531434558 ) ) ;
#200015 = CARTESIAN_POINT ( 'NONE',  ( 5.719274019375673035, 21.55341960407619339, 27.29275706135234358 ) ) ;
#200016 = CARTESIAN_POINT ( 'NONE',  ( -19.03943276465977164, 0.05219959533909376836, 81.24890960531436690 ) ) ;
#200017 = FACE_BOUND ( 'NONE', #135372, .T. ) ;
#200018 = VERTEX_POINT ( 'NONE', #37579 ) ;
#200019 = CARTESIAN_POINT ( 'NONE',  ( -10.72451020669898014, 18.67979575497178502, 115.4155762719810241 ) ) ;
#200022 = CARTESIAN_POINT ( 'NONE',  ( -0.05219959533936034679, 19.03943276465977164, 92.50109039468566152 ) ) ;
#200021 = CARTESIAN_POINT ( 'NONE',  ( 19.02544592524343514, -5.153800228976328945, 113.5405762719810241 ) ) ;
#200020 = CARTESIAN_POINT ( 'NONE',  ( 0.05219959533909260263, 19.03943276465977164, 24.99890960531435269 ) ) ;
#200023 = CARTESIAN_POINT ( 'NONE',  ( 19.05341960407617918, -5.049401038297876454, 31.04275706135232227 ) ) ;
#200024 = CARTESIAN_POINT ( 'NONE',  ( 10.81492255796078972, 18.62759615963270932, 99.58224293864770971 ) ) ;
#200025 = CARTESIAN_POINT ( 'NONE',  ( -13.89961937509957401, -13.97604488694547875, 29.37609039468565797 ) ) ;
#200026 = CARTESIAN_POINT ( 'NONE',  ( 4.483927247898790824, -16.52544592524335698, 80.20942372801901854 ) ) ;
#200027 = CARTESIAN_POINT ( 'NONE',  ( -5.153800228976328057, -19.02544592524343514, 102.2905762719810383 ) ) ;
#200028 = CARTESIAN_POINT ( 'NONE',  ( 19.02544592524343514, -5.153800228976328945, 53.54057627198102409 ) ) ;
#200029 = CIRCLE ( 'NONE', #158005, 61.99999999999998579 ) ;
#200030 = CARTESIAN_POINT ( 'NONE',  ( 21.52544592524334988, 5.823673210054432836, 61.45942372801901854 ) ) ;
#200031 = CARTESIAN_POINT ( 'NONE',  ( 10.72451020669871369, 18.67979575497193778, 87.08442372801901854 ) ) ;
#200032 = CARTESIAN_POINT ( 'NONE',  ( 19.03943276465977164, -0.05219959533909143690, 113.7489096053143669 ) ) ;
#200033 = CARTESIAN_POINT ( 'NONE',  ( 19.02544592524343514, -5.153800228976328945, 78.54057627198099567 ) ) ;
#200034 = CARTESIAN_POINT ( 'NONE',  ( 10.81492255796106328, -18.62759615963255655, 45.41775706135234003 ) ) ;
#200035 = CARTESIAN_POINT ( 'NONE',  ( -19.02544592524334988, -5.153800228976617603, 93.95942372801900433 ) ) ;
#200036 = CARTESIAN_POINT ( 'NONE',  ( -9.564922557960796823, -16.46253265017161027, 52.08224293864768839 ) ) ;
#200037 = CARTESIAN_POINT ( 'NONE',  ( 9.564922557960805705, 16.46253265017160317, 94.58224293864769550 ) ) ;
#200038 = CARTESIAN_POINT ( 'NONE',  ( -16.46253265017160317, 9.564922557960807481, 65.83224293864769550 ) ) ;
#200039 = CARTESIAN_POINT ( 'NONE',  ( 16.46253265017160672, -9.564922557960803928, 48.33224293864769550 ) ) ;
#200040 = CARTESIAN_POINT ( 'NONE',  ( 21.52544592524344225, -5.823673210054117533, 98.54057627198105251 ) ) ;
#200041 = CARTESIAN_POINT ( 'NONE',  ( 8.314922557961029526, -14.29746914071037800, 90.41775706135236135 ) ) ;
#200042 = CARTESIAN_POINT ( 'NONE',  ( -21.56952297831560372, 5.557039098534931831, 173.4609804364286276 ) ) ;
#200043 = CARTESIAN_POINT ( 'NONE',  ( -16.51473224551082808, 9.474510206698731452, 43.33442372801900433 ) ) ;
#200044 = CARTESIAN_POINT ( 'NONE',  ( 5.049401038298161559, -19.05341960407611168, 62.70724293864769550 ) ) ;
#200045 = CARTESIAN_POINT ( 'NONE',  ( -12.06949235617756955, 12.14591786802309770, 55.62390960531436690 ) ) ;
#200046 = CARTESIAN_POINT ( 'NONE',  ( 4.379528057220339221, -16.55341960407611168, 92.70724293864770971 ) ) ;
#200047 = CARTESIAN_POINT ( 'NONE',  ( 21.52544592524344225, -5.823673210054117533, 23.54057627198102765 ) ) ;
#200048 = CARTESIAN_POINT ( 'NONE',  ( -16.51473224551069308, -9.474510206698971260, 86.66557627198102409 ) ) ;
#200049 = CARTESIAN_POINT ( 'NONE',  ( -9.474510206698964154, 16.51473224551069663, 105.4155762719810383 ) ) ;
#200050 = CARTESIAN_POINT ( 'NONE',  ( -18.67979575497193778, 10.72451020669871902, 108.3344237280190185 ) ) ;
#200051 = CARTESIAN_POINT ( 'NONE',  ( 16.53943276465976808, 0.05219959533934440121, 96.25109039468568994 ) ) ;
#200052 = CARTESIAN_POINT ( 'NONE',  ( 5.049401038298161559, -19.05341960407611168, 77.70724293864765286 ) ) ;
#200053 = CARTESIAN_POINT ( 'NONE',  ( -5.823673210054431948, 21.52544592524334988, 42.70942372801901854 ) ) ;
#200054 = CARTESIAN_POINT ( 'NONE',  ( -21.55341960407610458, -5.719274019375992779, 36.45724293864768839 ) ) ;
#200055 = CARTESIAN_POINT ( 'NONE',  ( -21.55341960407619339, 5.719274019375674811, 23.54275706135235424 ) ) ;
#200056 = CARTESIAN_POINT ( 'NONE',  ( 10.81492255796078972, 18.62759615963270932, 64.58224293864769550 ) ) ;
#200057 = CARTESIAN_POINT ( 'NONE',  ( 14.29746914071049879, -8.314922557960816363, 83.33224293864769550 ) ) ;
#200058 = CARTESIAN_POINT ( 'NONE',  ( -9.564922557961040184, 16.46253265017147172, 37.91775706135233293 ) ) ;
#200059 = EDGE_CURVE ( 'NONE', #99831, #17478, #5234, .T. ) ;
#200060 = CARTESIAN_POINT ( 'NONE',  ( 0.05219959533909260263, 19.03943276465977164, 34.99890960531435979 ) ) ;
#200061 = CARTESIAN_POINT ( 'NONE',  ( 13.89961937509977652, -13.97604488694527269, 83.12390960531436690 ) ) ;
#200062 = CARTESIAN_POINT ( 'NONE',  ( -19.02544592524342804, 5.153800228976336051, 76.04057627198102409 ) ) ;
#200063 = CARTESIAN_POINT ( 'NONE',  ( -27.73933785331498925, 9.013057229001088189, 146.7750000027311899 ) ) ;
#200064 = CARTESIAN_POINT ( 'NONE',  ( 8.224510206698953496, -14.34966873604960469, 97.91557627198103830 ) ) ;
#200065 = EDGE_LOOP ( 'NONE', ( #62673, #149828 ) ) ;
#200066 = CARTESIAN_POINT ( 'NONE',  ( 4.379528057220092307, 16.55341960407617563, 107.2927570613523471 ) ) ;
#200067 = CARTESIAN_POINT ( 'NONE',  ( 4.379528057220092307, 16.55341960407617563, 32.29275706135235424 ) ) ;
#200068 = CARTESIAN_POINT ( 'NONE',  ( -21.52544592524334988, -5.823673210054445271, 88.95942372801901854 ) ) ;
#200069 = CARTESIAN_POINT ( 'NONE',  ( -19.03943276465977164, 0.05219959533909376836, 101.2489096053143669 ) ) ;
#200070 = CARTESIAN_POINT ( 'NONE',  ( -5.719274019375665041, -21.55341960407619695, 24.79275706135235779 ) ) ;
#200071 = CARTESIAN_POINT ( 'NONE',  ( -0.05219959533909027116, -19.03943276465977164, 27.49890960531435624 ) ) ;
#200072 = CARTESIAN_POINT ( 'NONE',  ( -14.34966873604972548, 8.224510206698743886, 33.33442372801900433 ) ) ;
#200073 = CARTESIAN_POINT ( 'NONE',  ( -9.564922557961040184, 16.46253265017147172, 102.9177570613523329 ) ) ;
#200074 = CARTESIAN_POINT ( 'NONE',  ( 0.05219959533907565091, 21.53943276465977519, 109.9989096053143527 ) ) ;
#200075 = CARTESIAN_POINT ( 'NONE',  ( 9.474510206698729675, 16.51473224551082808, 72.08442372801900433 ) ) ;
#200076 = CARTESIAN_POINT ( 'NONE',  ( 5.049401038298161559, -19.05341960407611168, 22.70724293864769194 ) ) ;
#200077 = CARTESIAN_POINT ( 'NONE',  ( 21.52544592524334988, 5.823673210054432836, 21.45942372801901499 ) ) ;
#200078 = CARTESIAN_POINT ( 'NONE',  ( 37.99626262588768810, 12.34573411038912027, -4.647842220587803830 ) ) ;
#200079 = CARTESIAN_POINT ( 'NONE',  ( -19.02544592524342804, 5.153800228976336051, 91.04057627198100988 ) ) ;
#200080 = CARTESIAN_POINT ( 'NONE',  ( -6.019987952026120409E-15, 39.95163481335720235, -6.502157773949823749 ) ) ;
#200081 = CARTESIAN_POINT ( 'NONE',  ( 0.05219959533909260263, 19.03943276465977164, 84.99890960531436690 ) ) ;
#200083 = CARTESIAN_POINT ( 'NONE',  ( 16.52544592524342804, -4.483927247898539470, 78.54057627198103830 ) ) ;
#200082 = CARTESIAN_POINT ( 'NONE',  ( -5.823673210054431948, 21.52544592524334988, 22.70942372801901499 ) ) ;
#200084 = CARTESIAN_POINT ( 'NONE',  ( 9.564922557960805705, 16.46253265017160317, 79.58224293864769550 ) ) ;
#200086 = CARTESIAN_POINT ( 'NONE',  ( -19.02544592524334988, -5.153800228976617603, 53.95942372801898301 ) ) ;
#200085 = CARTESIAN_POINT ( 'NONE',  ( 8.224510206698742110, 14.34966873604972548, 57.08442372801901854 ) ) ;
#200087 = CARTESIAN_POINT ( 'NONE',  ( -21.52544592524334988, -5.823673210054445271, 68.95942372801901854 ) ) ;
#200088 = CARTESIAN_POINT ( 'NONE',  ( -12.14591786802326823, 12.06949235617739902, 33.12609039468569705 ) ) ;
#200089 = CARTESIAN_POINT ( 'NONE',  ( 5.049401038298161559, -19.05341960407611168, 62.70724293864769550 ) ) ;
#200090 = CARTESIAN_POINT ( 'NONE',  ( 19.02544592524334988, 5.153800228976608722, 91.45942372801900433 ) ) ;
#200091 = CARTESIAN_POINT ( 'NONE',  ( -4.379528057220086978, -16.55341960407618274, 54.79275706135235424 ) ) ;
#200092 = CARTESIAN_POINT ( 'NONE',  ( 5.719274019375673035, 21.55341960407619339, 92.29275706135236135 ) ) ;
#200093 = CARTESIAN_POINT ( 'NONE',  ( 9.474510206698729675, 16.51473224551082808, 77.08442372801900433 ) ) ;
#200094 = CARTESIAN_POINT ( 'NONE',  ( 13.97604488694527802, 13.89961937509977652, 49.37390960531434558 ) ) ;
#200095 = CARTESIAN_POINT ( 'NONE',  ( 10.81492255796078972, 18.62759615963270932, 69.58224293864769550 ) ) ;
#200097 = CARTESIAN_POINT ( 'NONE',  ( -16.46253265017146816, -9.564922557961047289, 79.16775706135234714 ) ) ;
#200096 = CARTESIAN_POINT ( 'NONE',  ( 16.52544592524342804, -4.483927247898539470, 73.54057627198102409 ) ) ;
#200098 = CARTESIAN_POINT ( 'NONE',  ( 17.31747979337943022, -6.344076630961145824, 61.12055131934815932 ) ) ;
#200099 = CARTESIAN_POINT ( 'NONE',  ( -5.049401038297874678, -19.05341960407617918, 44.79275706135232582 ) ) ;
#200100 = CARTESIAN_POINT ( 'NONE',  ( 12.14591786802327356, -12.06949235617739191, 110.6260903946857042 ) ) ;
#200101 = CARTESIAN_POINT ( 'NONE',  ( 4.379528057220339221, -16.55341960407611168, 62.70724293864769550 ) ) ;
#200103 = CARTESIAN_POINT ( 'NONE',  ( 22.44159573604009594, -16.30477369853687364, 147.6750000027311671 ) ) ;
#200102 = CARTESIAN_POINT ( 'NONE',  ( -18.67979575497193778, 10.72451020669871902, 103.3344237280190043 ) ) ;
#200104 = CARTESIAN_POINT ( 'NONE',  ( -0.05219959533907301413, -21.53943276465977519, 112.4989096053143669 ) ) ;
#200105 = CARTESIAN_POINT ( 'NONE',  ( -19.02544592524342804, 5.153800228976336051, 61.04057627198103120 ) ) ;
#200106 = CARTESIAN_POINT ( 'NONE',  ( 21.52544592524334988, 5.823673210054432836, 81.45942372801900433 ) ) ;
#200107 = CARTESIAN_POINT ( 'NONE',  ( 9.474510206698971260, -16.51473224551069308, 62.91557627198102409 ) ) ;
#200108 = ORIENTED_EDGE ( 'NONE', *, *, #139548, .F. ) ;
#200109 = CARTESIAN_POINT ( 'NONE',  ( 19.05341960407611168, 5.049401038298154454, 28.95724293864769550 ) ) ;
#200110 = CARTESIAN_POINT ( 'NONE',  ( -5.049401038298153566, 19.05341960407611168, 115.2072429386477097 ) ) ;
#200111 = CARTESIAN_POINT ( 'NONE',  ( 12.06949235617757843, -12.14591786802309237, 68.12390960531436690 ) ) ;
#200112 = CARTESIAN_POINT ( 'NONE',  ( -9.474510206698964154, 16.51473224551069663, 25.41557627198103120 ) ) ;
#200113 = CARTESIAN_POINT ( 'NONE',  ( 12.06949235617757843, -12.14591786802309237, 83.12390960531436690 ) ) ;
#200114 = CARTESIAN_POINT ( 'NONE',  ( -18.62759615963270932, 10.81492255796079327, 100.8322429386477097 ) ) ;
#200115 = CARTESIAN_POINT ( 'NONE',  ( 21.53943276465977519, 0.05219959533937863772, 46.25109039468567573 ) ) ;
#200116 = CARTESIAN_POINT ( 'NONE',  ( 28.82186960331500813, 9.364793116373537174, 149.0999999999999943 ) ) ;
#200117 = CARTESIAN_POINT ( 'NONE',  ( 8.224510206698742110, 14.34966873604972548, 52.08442372801901854 ) ) ;
#200118 = CARTESIAN_POINT ( 'NONE',  ( 21.55341960407610458, 5.719274019375980345, 98.95724293864770971 ) ) ;
#200119 = CARTESIAN_POINT ( 'NONE',  ( -0.05219959533936034679, 19.03943276465977164, 32.50109039468566863 ) ) ;
#200120 = CARTESIAN_POINT ( 'NONE',  ( 5.153800228976335163, 19.02544592524342804, 104.7905762719809957 ) ) ;
#200121 = CARTESIAN_POINT ( 'NONE',  ( 5.719274019375673035, 21.55341960407619339, 57.29275706135234714 ) ) ;
#200122 = CARTESIAN_POINT ( 'NONE',  ( 18.67979575497178502, 10.72451020669898547, 39.16557627198102409 ) ) ;
#200123 = CARTESIAN_POINT ( 'NONE',  ( 14.29746914071049879, -8.314922557960816363, 23.33224293864769194 ) ) ;
#200125 = CARTESIAN_POINT ( 'NONE',  ( -10.81492255796105439, 18.62759615963255655, 92.91775706135236135 ) ) ;
#200124 = CARTESIAN_POINT ( 'NONE',  ( 5.719274019375673035, 21.55341960407619339, 62.29275706135236845 ) ) ;
#200126 = CARTESIAN_POINT ( 'NONE',  ( -19.03943276465977164, -0.05219959533935918106, 33.75109039468566863 ) ) ;
#200127 = CARTESIAN_POINT ( 'NONE',  ( -16.52544592524335698, -4.483927247898792601, 88.95942372801901854 ) ) ;
#200128 = CARTESIAN_POINT ( 'NONE',  ( -15.80617190586768217, 15.72974639402176855, 58.12609039468568994 ) ) ;
#200129 = CARTESIAN_POINT ( 'NONE',  ( 19.02544592524343514, -5.153800228976328945, 48.54057627198103120 ) ) ;
#200130 = CARTESIAN_POINT ( 'NONE',  ( -19.02544592524334988, -5.153800228976617603, 23.95942372801900078 ) ) ;
#200131 = CARTESIAN_POINT ( 'NONE',  ( -21.55341960407610458, -5.719274019375992779, 31.45724293864769550 ) ) ;
#200132 = CARTESIAN_POINT ( 'NONE',  ( -21.53943276465977519, -0.05219959533937600094, 23.75109039468567929 ) ) ;
#200133 = CARTESIAN_POINT ( 'NONE',  ( -15.80617190586745835, -15.72974639402198527, 76.87390960531439532 ) ) ;
#200134 = CARTESIAN_POINT ( 'NONE',  ( 4.483927247898790824, -16.52544592524335698, 35.20942372801901854 ) ) ;
#200136 = CARTESIAN_POINT ( 'NONE',  ( -5.719274019375978568, 21.55341960407610458, 80.20724293864769550 ) ) ;
#200135 = DIRECTION ( 'NONE',  ( -1.000000000000000000, 6.391086490440865492E-16, 0.000000000000000000 ) ) ;
#200138 = CARTESIAN_POINT ( 'NONE',  ( 8.314922557960818139, 14.29746914071049879, 69.58224293864769550 ) ) ;
#200137 = CARTESIAN_POINT ( 'NONE',  ( 0.05219959533934541429, -16.53943276465976808, 65.00109039468568994 ) ) ;
#200139 = CARTESIAN_POINT ( 'NONE',  ( -22.99905646750782751, 21.51934928555102289, -46.25979504214461713 ) ) ;
#200140 = CARTESIAN_POINT ( 'NONE',  ( 19.03943276465977164, 0.05219959533936151252, 106.2510903946856615 ) ) ;
#200141 = CARTESIAN_POINT ( 'NONE',  ( -21.55341960407610458, -5.719274019375992779, 41.45724293864769550 ) ) ;
#200142 = CARTESIAN_POINT ( 'NONE',  ( 22.55659503568693580, -29.32441354047577065, -8.000000000000001776 ) ) ;
#200143 = CARTESIAN_POINT ( 'NONE',  ( -14.34966873604972548, 8.224510206698743886, 33.33442372801900433 ) ) ;
#200144 = CARTESIAN_POINT ( 'NONE',  ( 10.81492255796106328, -18.62759615963255655, 20.41775706135234714 ) ) ;
#200145 = CARTESIAN_POINT ( 'NONE',  ( -5.719274019375978568, 21.55341960407610458, 30.20724293864769550 ) ) ;
#200146 = CARTESIAN_POINT ( 'NONE',  ( -16.52544592524335698, -4.483927247898792601, 53.95942372801900433 ) ) ;
#200147 = CARTESIAN_POINT ( 'NONE',  ( 5.153800228976335163, 19.02544592524342804, 89.79057627198102409 ) ) ;
#200149 = CARTESIAN_POINT ( 'NONE',  ( -9.564922557961040184, 16.46253265017147172, 107.9177570613523471 ) ) ;
#200148 = CARTESIAN_POINT ( 'NONE',  ( 5.719274019375673035, 21.55341960407619339, 37.29275706135235424 ) ) ;
#200150 = CARTESIAN_POINT ( 'NONE',  ( 15.72974639402199770, -15.80617190586745480, 33.12390960531435979 ) ) ;
#200151 = ORIENTED_EDGE ( 'NONE', *, *, #182855, .F. ) ;
#200152 = CARTESIAN_POINT ( 'NONE',  ( -5.049401038297874678, -19.05341960407617918, 24.79275706135233648 ) ) ;
#200153 = CARTESIAN_POINT ( 'NONE',  ( -14.29746914071037622, -8.314922557961029526, 39.16775706135235424 ) ) ;
#200154 = CARTESIAN_POINT ( 'NONE',  ( 19.02544592524343514, -5.153800228976328945, 103.5405762719809957 ) ) ;
#200155 = CARTESIAN_POINT ( 'NONE',  ( -18.67979575497178146, -10.72451020669898902, 106.6655762719810383 ) ) ;
#200156 = CARTESIAN_POINT ( 'NONE',  ( -16.51473224551069308, -9.474510206698971260, 71.66557627198102409 ) ) ;
#200157 = DIRECTION ( 'NONE',  ( 0.000000000000000000, 0.000000000000000000, 1.000000000000000000 ) ) ;
#200158 = CARTESIAN_POINT ( 'NONE',  ( -0.05219959533910754901, -16.53943276465976808, 87.49890960531436690 ) ) ;
#200159 = CARTESIAN_POINT ( 'NONE',  ( 10.72451020669898902, -18.67979575497178502, 37.91557627198102409 ) ) ;
#200160 = CARTESIAN_POINT ( 'NONE',  ( -19.05341960407611168, -5.049401038298163336, 21.45724293864768839 ) ) ;
#200161 = CARTESIAN_POINT ( 'NONE',  ( 12.14591786802327356, -12.06949235617739191, 70.62609039468567573 ) ) ;
#200162 = CARTESIAN_POINT ( 'NONE',  ( 10.81492255796078972, 18.62759615963270932, 104.5822429386477097 ) ) ;
#200163 = CARTESIAN_POINT ( 'NONE',  ( 16.46253265017146816, 9.564922557961045513, 76.66775706135234714 ) ) ;
#200164 = CARTESIAN_POINT ( 'NONE',  ( -19.03943276465977164, 0.05219959533909376836, 31.24890960531435979 ) ) ;
#200165 = CARTESIAN_POINT ( 'NONE',  ( 21.52544592524344225, -5.823673210054117533, 63.54057627198103830 ) ) ;
#200166 = VECTOR ( 'NONE', #47631, 1000.000000000000000 ) ;
#200167 = CARTESIAN_POINT ( 'NONE',  ( -5.049401038298153566, 19.05341960407611168, 95.20724293864770971 ) ) ;
#200168 = CARTESIAN_POINT ( 'NONE',  ( 15.80617190586769283, -15.72974639402175789, 90.62609039468567573 ) ) ;
#200169 = CARTESIAN_POINT ( 'NONE',  ( 5.153800228976335163, 19.02544592524342804, 64.79057627198100988 ) ) ;
#200170 = CARTESIAN_POINT ( 'NONE',  ( 16.52544592524335698, 4.483927247898782831, 46.45942372801901854 ) ) ;
#200171 = CARTESIAN_POINT ( 'NONE',  ( 9.474510206698971260, -16.51473224551069308, 52.91557627198102409 ) ) ;
#200172 = CARTESIAN_POINT ( 'NONE',  ( 15.80617190586769283, -15.72974639402175789, 75.62609039468567573 ) ) ;
#200173 = EDGE_LOOP ( 'NONE', ( #163171, #30976 ) ) ;
#200174 = CARTESIAN_POINT ( 'NONE',  ( -5.153800228976607833, 19.02544592524334988, 32.70942372801899722 ) ) ;
#200175 = CARTESIAN_POINT ( 'NONE',  ( 5.153800228976615827, -19.02544592524334988, 55.20942372801899722 ) ) ;
#200176 = CARTESIAN_POINT ( 'NONE',  ( 5.823673210054444382, -21.52544592524334988, 55.20942372801902565 ) ) ;
#200177 = CARTESIAN_POINT ( 'NONE',  ( -6.941592873960384935, 1.351304681146122233, -62.33628431810819137 ) ) ;
#200178 = CARTESIAN_POINT ( 'NONE',  ( -19.05341960407617563, 5.049401038297882671, 43.54275706135232582 ) ) ;
#200179 = CARTESIAN_POINT ( 'NONE',  ( -5.153800228976328057, -19.02544592524343514, 92.29057627198099567 ) ) ;
#200180 = CARTESIAN_POINT ( 'NONE',  ( 16.51473224551069308, 9.474510206698969483, 74.16557627198103830 ) ) ;
#200181 = CARTESIAN_POINT ( 'NONE',  ( 14.29746914071037800, 8.314922557961029526, 111.6677570613523613 ) ) ;
#200183 = CARTESIAN_POINT ( 'NONE',  ( 18.62759615963255655, 10.81492255796105972, 91.66775706135234714 ) ) ;
#200182 = CARTESIAN_POINT ( 'NONE',  ( -15.80617190586745835, -15.72974639402198527, 21.87390960531436690 ) ) ;
#200184 = CARTESIAN_POINT ( 'NONE',  ( -29.86685920354755552, 21.69954338932564397, -9.324999997268813345 ) ) ;
#200185 = CARTESIAN_POINT ( 'NONE',  ( 17.26172910966777607, 6.454744622555867117, 56.69353091350777873 ) ) ;
#200186 = CARTESIAN_POINT ( 'NONE',  ( 18.62759615963255655, 10.81492255796105972, 96.66775706135234714 ) ) ;
#200187 = CARTESIAN_POINT ( 'NONE',  ( 23.88070017481517837, -1.044764468832730664, -57.07230391339720654 ) ) ;
#200188 = CARTESIAN_POINT ( 'NONE',  ( 16.53943276465976808, -0.05219959533910856209, 113.7489096053143527 ) ) ;
#200189 = CARTESIAN_POINT ( 'NONE',  ( 19.02544592524343514, -5.153800228976328945, 113.5405762719810241 ) ) ;
#200190 = EDGE_CURVE ( 'NONE', #24501, #163173, #175184, .T. ) ;
#200191 = CARTESIAN_POINT ( 'NONE',  ( -26.47570757000579533, -8.223507928023325420, 167.6031463996532977 ) ) ;
#200192 = CARTESIAN_POINT ( 'NONE',  ( 19.05341960407617918, -5.049401038297876454, 61.04275706135232582 ) ) ;
#200193 = NEXT_ASSEMBLY_USAGE_OCCURRENCE ( 'NAUO1', ' ', ' ', #25201, #180876, $ ) ;
#200194 = NEXT_ASSEMBLY_USAGE_OCCURRENCE ( 'NAUO2', ' ', ' ', #25201, #115338, $ ) ;
#200195 = NEXT_ASSEMBLY_USAGE_OCCURRENCE ( 'NAUO3', ' ', ' ', #25201, #117858, $ ) ;
#200196 = NEXT_ASSEMBLY_USAGE_OCCURRENCE ( 'NAUO4', ' ', ' ', #25201, #48691, $ ) ;
#200197 = NEXT_ASSEMBLY_USAGE_OCCURRENCE ( 'NAUO5', ' ', ' ', #25201, #75840, $ ) ;
#200198 = NEXT_ASSEMBLY_USAGE_OCCURRENCE ( 'NAUO6', ' ', ' ', #25201, #183372, $ ) ;
#200199 = NEXT_ASSEMBLY_USAGE_OCCURRENCE ( 'NAUO7', ' ', ' ', #25201, #52321, $ ) ;
#200200 = NEXT_ASSEMBLY_USAGE_OCCURRENCE ( 'NAUO8', ' ', ' ', #25201, #189524, $ ) ;
#200201 = NEXT_ASSEMBLY_USAGE_OCCURRENCE ( 'NAUO9', ' ', ' ', #25201, #189524, $ ) ;
#200202 = NEXT_ASSEMBLY_USAGE_OCCURRENCE ( 'NAUO10', ' ', ' ', #25201, #189524, $ ) ;
#200203 = NEXT_ASSEMBLY_USAGE_OCCURRENCE ( 'NAUO11', ' ', ' ', #25201, #189524, $ ) ;
#200204 = NEXT_ASSEMBLY_USAGE_OCCURRENCE ( 'NAUO12', ' ', ' ', #25201, #103014, $ ) ;
#200205 = NEXT_ASSEMBLY_USAGE_OCCURRENCE ( 'NAUO13', ' ', ' ', #25201, #103014, $ ) ;
ENDSEC;
END-ISO-10303-21;
